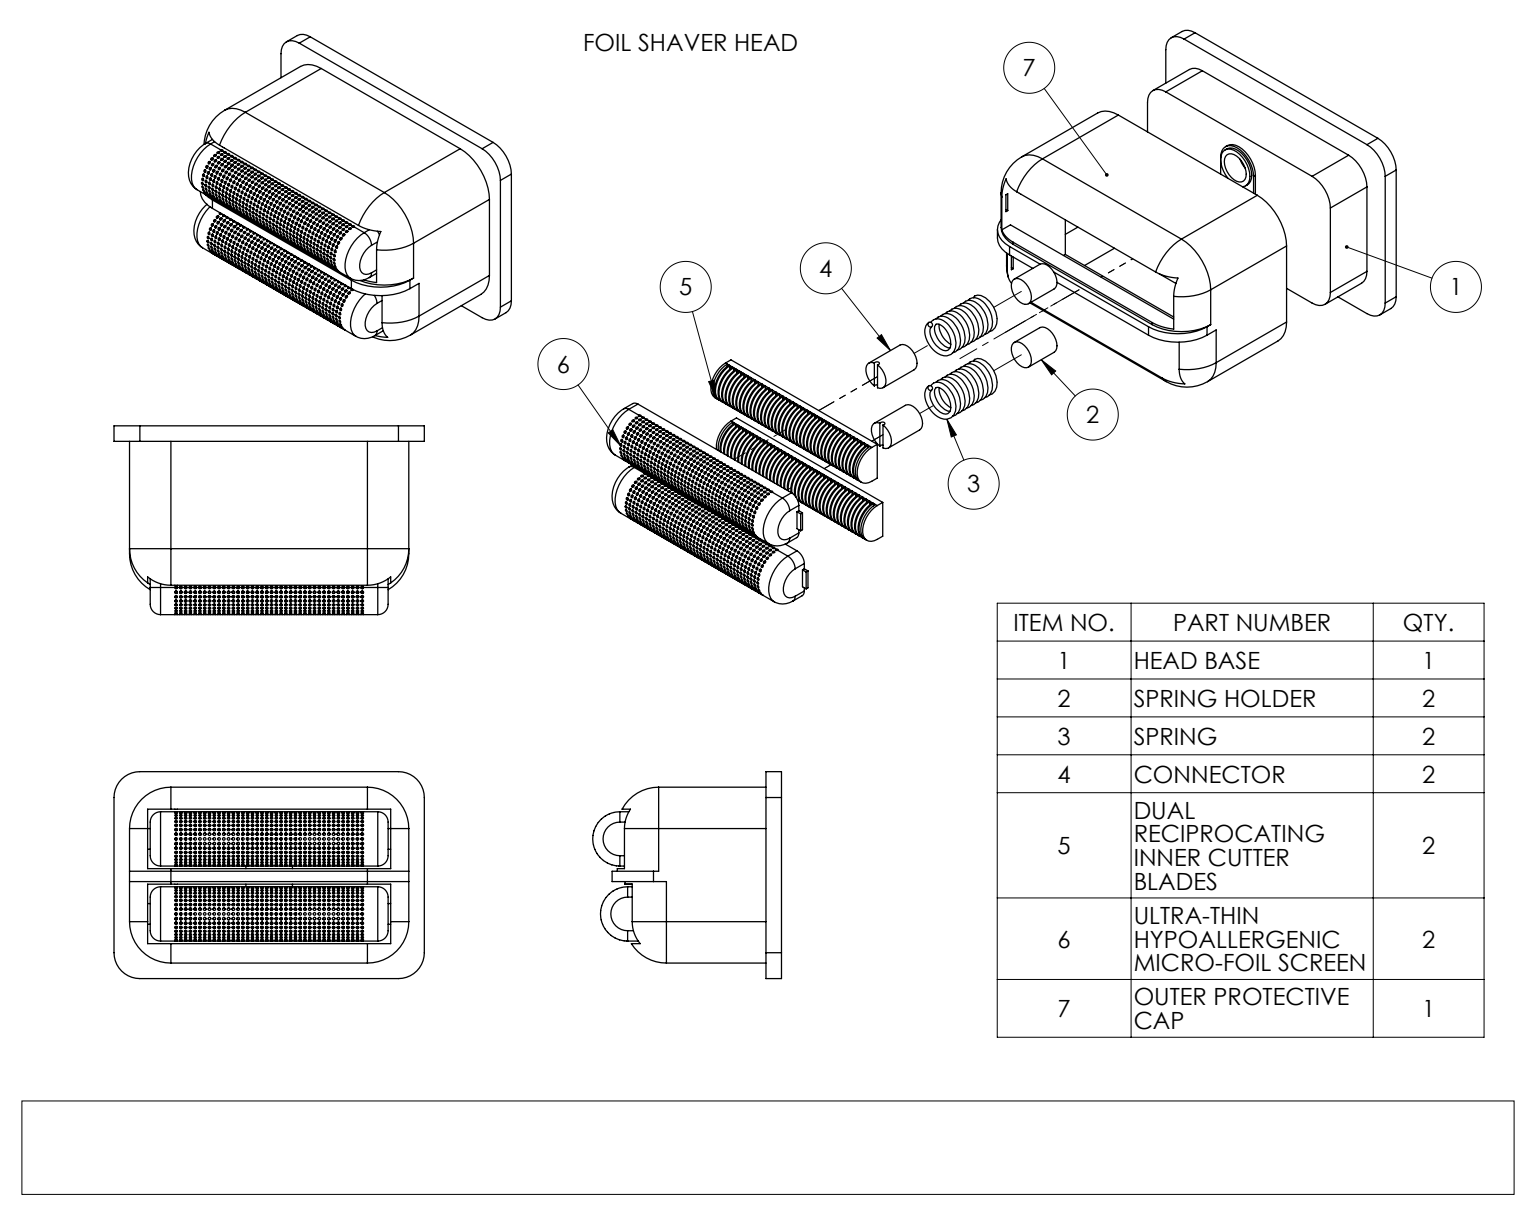
ISO-10303-21;
HEADER;
FILE_DESCRIPTION (('STEP AP214'),
    '1' );
FILE_NAME ('BR-833',
    '2026-10-05T05:16:24',
    ( '' ),
    ( '' ),
    'SwSTEP 2.0',
    'SolidWorks 2026',
    '' );
FILE_SCHEMA (( 'AUTOMOTIVE_DESIGN' ));
ENDSEC;

DATA;
#1 = ORIENTED_EDGE ( 'NONE', *, *, #60678, .F. ) ;
#3 = VERTEX_POINT ( 'NONE', #26210 ) ;
#2 = CARTESIAN_POINT ( 'NONE',  ( 7.173131342990376247, -12.65882529074907126, 30.72640787790839312 ) ) ;
#4 = CARTESIAN_POINT ( 'NONE',  ( -5.143005456283213483, -4.661471528628507777, 34.16647553114621871 ) ) ;
#5 = CARTESIAN_POINT ( 'NONE',  ( -13.13461538461396394, -7.500000000000154543, 35.00000000000007105 ) ) ;
#6 = CARTESIAN_POINT ( 'NONE',  ( 9.561616225640134914, -4.809359713505814149, 33.96456829005828837 ) ) ;
#7 = EDGE_LOOP ( 'NONE', ( #52254, #76310 ) ) ;
#8 = CARTESIAN_POINT ( 'NONE',  ( -3.230769230769352962, -3.643525952248796163, 33.31231777344771672 ) ) ;
#9 = MANIFOLD_SOLID_BREP ( 'Cavity1', #19917 ) ;
#10 = VERTEX_POINT ( 'NONE', #55017 ) ;
#11 = CARTESIAN_POINT ( 'NONE',  ( 8.096099255531889582, -12.68172785388650681, 30.59649109432439218 ) ) ;
#12 = ORIENTED_EDGE ( 'NONE', *, *, #66253, .T. ) ;
#13 = CARTESIAN_POINT ( 'NONE',  ( -14.17690186672535901, -11.93129842949671726, 32.56571108434900452 ) ) ;
#14 = ORIENTED_EDGE ( 'NONE', *, *, #40073, .T. ) ;
#15 = CARTESIAN_POINT ( 'NONE',  ( 1.634669696253701288, -6.567000820036038355, 34.66262288849541306 ) ) ;
#16 = AXIS2_PLACEMENT_3D ( 'NONE', #36065, #63514, #64832 ) ;
#17 = CARTESIAN_POINT ( 'NONE',  ( 12.46153846153846168, -2.292212530054420494, 30.41441678777542634 ) ) ;
#18 = FACE_BOUND ( 'NONE', #68088, .T. ) ;
#19 = CARTESIAN_POINT ( 'NONE',  ( -17.93480601821664777, -2.506253911140446711, 29.99999999999985434 ) ) ;
#20 = CARTESIAN_POINT ( 'NONE',  ( 16.08776377448601735, -3.322132147404559976, 32.92929555188719348 ) ) ;
#21 = CARTESIAN_POINT ( 'NONE',  ( 9.562159722575998444, -2.373036134822904319, 30.88089517874952250 ) ) ;
#22 = CARTESIAN_POINT ( 'NONE',  ( 10.36540787133602493, -10.06842814019191401, 34.32929386961144758 ) ) ;
#23 = CARTESIAN_POINT ( 'NONE',  ( -3.230769230769351186, -3.300289026999228881, 32.46337939537708905 ) ) ;
#24 = CARTESIAN_POINT ( 'NONE',  ( -8.096177070375302876, -9.356822207818506598, 34.66110646841856635 ) ) ;
#25 = DIRECTION ( 'NONE',  ( -0.000000000000000000, 1.000000000000000000, 3.491481338843133355E-15 ) ) ;
#26 = ORIENTED_EDGE ( 'NONE', *, *, #20674, .T. ) ;
#27 = ORIENTED_EDGE ( 'NONE', *, *, #74196, .T. ) ;
#29 = CYLINDRICAL_SURFACE ( 'NONE', #7462, 0.2499999999999994726 ) ;
#28 = CARTESIAN_POINT ( 'NONE',  ( -17.07692307692307665, -9.780366693483667717, 34.19971097300155094 ) ) ;
#30 = FACE_OUTER_BOUND ( 'NONE', #56324, .T. ) ;
#31 = CARTESIAN_POINT ( 'NONE',  ( 3.453548772037640990, -10.81320215134717344, 33.49497208177562868 ) ) ;
#32 = CARTESIAN_POINT ( 'NONE',  ( 9.019230769230707878, -7.565270000091922853, 34.99999999999999289 ) ) ;
#33 = CARTESIAN_POINT ( 'NONE',  ( 11.53846153846153832, -12.09954503811598769, 35.62045528018868623 ) ) ;
#34 = ORIENTED_EDGE ( 'NONE', *, *, #66033, .T. ) ;
#35 = CARTESIAN_POINT ( 'NONE',  ( 2.057669070399343436, -9.271318131107980420, 34.42618302367067429 ) ) ;
#36 = CARTESIAN_POINT ( 'NONE',  ( 3.453548772037639214, -11.41317474335729187, 32.86274602512330034 ) ) ;
#37 = CARTESIAN_POINT ( 'NONE',  ( -14.08491263871424160, -12.47679350104403007, 31.42216943046555855 ) ) ;
#38 = CARTESIAN_POINT ( 'NONE',  ( -7.053224892808619195, -6.809168938359898782, 34.95455904226513866 ) ) ;
#39 = VERTEX_POINT ( 'NONE', #74855 ) ;
#40 = EDGE_LOOP ( 'NONE', ( #88640, #57937, #33954, #2221 ) ) ;
#41 = VECTOR ( 'NONE', #83929, 1000.000000000000000 ) ;
#42 = VECTOR ( 'NONE', #62583, 1000.000000000000114 ) ;
#43 = ORIENTED_EDGE ( 'NONE', *, *, #10350, .F. ) ;
#44 = CARTESIAN_POINT ( 'NONE',  ( -4.153846153846274980, -8.656820664282941280, 34.87096338111179961 ) ) ;
#45 = VERTEX_POINT ( 'NONE', #81605 ) ;
#46 = DIRECTION ( 'NONE',  ( -0.000000000000000000, 1.000000000000000000, 3.491481338843133355E-15 ) ) ;
#47 = CARTESIAN_POINT ( 'NONE',  ( 15.45378207486262667, -4.026326845037962343, 33.68677907613344047 ) ) ;
#48 = CARTESIAN_POINT ( 'NONE',  ( 4.946775867484856093, -6.852621066184267029, 34.70813303252209181 ) ) ;
#49 = CARTESIAN_POINT ( 'NONE',  ( 1.553300858899129944, -11.24999999999998934, 14.70312500000000355 ) ) ;
#50 = CIRCLE ( 'NONE', #37444, 0.2500000000000002220 ) ;
#51 = CIRCLE ( 'NONE', #79120, 0.2500000000000002220 ) ;
#52 = DIRECTION ( 'NONE',  ( 0.000000000000000000, 0.9848077530122072432, 0.1736481776669354937 ) ) ;
#53 = VERTEX_POINT ( 'NONE', #13143 ) ;
#55 = CARTESIAN_POINT ( 'NONE',  ( -15.23076923076922995, -2.486705287966279876, 31.30864560766543647 ) ) ;
#54 = PRESENTATION_LAYER_ASSIGNMENT (  '', '', ( #59002 ) ) ;
#57 = VERTEX_POINT ( 'NONE', #40625 ) ;
#56 = CARTESIAN_POINT ( 'NONE',  ( -0.5276208408985970655, -5.471508081941601986, 34.59228464037088457 ) ) ;
#58 = CARTESIAN_POINT ( 'NONE',  ( -6.923076923076922462, -2.499999999999998668, 29.50000000000001066 ) ) ;
#59 = CYLINDRICAL_SURFACE ( 'NONE', #2416, 0.2500000000000002220 ) ;
#60 = CARTESIAN_POINT ( 'NONE',  ( -13.60754160213153163, -4.887634598454295265, 34.01352882383564946 ) ) ;
#61 = CARTESIAN_POINT ( 'NONE',  ( 11.53846153846153832, -9.905515769479276145, 34.41647553114623292 ) ) ;
#62 = CARTESIAN_POINT ( 'NONE',  ( 2.438482748659261290, -2.494656445102013453, 31.33466734024120015 ) ) ;
#63 = CARTESIAN_POINT ( 'NONE',  ( -10.28846153846153832, -7.500000000000000000, 29.75000000000000355 ) ) ;
#64 = CARTESIAN_POINT ( 'NONE',  ( -3.454254174493178287, -6.760086850603068243, 34.69517049084099369 ) ) ;
#65 = CARTESIAN_POINT ( 'NONE',  ( 1.200186371490529202, -4.775308065498752974, 18.23624329374151642 ) ) ;
#66 = ORIENTED_EDGE ( 'NONE', *, *, #42296, .F. ) ;
#67 = CARTESIAN_POINT ( 'NONE',  ( 15.00784301325308157, -8.239355502252617924, 34.69524867566427417 ) ) ;
#68 = CARTESIAN_POINT ( 'NONE',  ( -14.17716686945866122, -3.625058011473228703, 33.29252011169590020 ) ) ;
#69 = EDGE_CURVE ( 'NONE', #39109, #41438, #13798, .T. ) ;
#70 = CARTESIAN_POINT ( 'NONE',  ( 9.692307692307695177, -10.67929555188718282, 33.92786785259544047 ) ) ;
#71 = ORIENTED_EDGE ( 'NONE', *, *, #84593, .F. ) ;
#72 = ORIENTED_EDGE ( 'NONE', *, *, #88944, .T. ) ;
#73 = CARTESIAN_POINT ( 'NONE',  ( 20.74999999999998224, -2.499999999999999556, 27.25000000000000000 ) ) ;
#74 = CARTESIAN_POINT ( 'NONE',  ( -3.100243529005668019, -6.001044277235011215, 34.52024696741798948 ) ) ;
#75 = CARTESIAN_POINT ( 'NONE',  ( -16.15384615384627409, -3.835265460704628815, 33.15142922262033665 ) ) ;
#76 = CARTESIAN_POINT ( 'NONE',  ( 8.769230769230768274, -1.466349020453238561, 30.81389545987213907 ) ) ;
#77 = CARTESIAN_POINT ( 'NONE',  ( 17.86985203026830504, -2.647304123082329763, 31.75400227202886683 ) ) ;
#78 = ORIENTED_EDGE ( 'NONE', *, *, #41184, .T. ) ;
#79 = DIRECTION ( 'NONE',  ( 0.000000000000000000, 0.000000000000000000, 1.000000000000000000 ) ) ;
#80 = EDGE_CURVE ( 'NONE', #19996, #25471, #12251, .T. ) ;
#81 = CARTESIAN_POINT ( 'NONE',  ( -14.53117725141625094, -2.847400154188067578, 31.58180166144859058 ) ) ;
#82 = LINE ( 'NONE', #529, #19231 ) ;
#84 = ORIENTED_EDGE ( 'NONE', *, *, #75949, .F. ) ;
#83 = AXIS2_PLACEMENT_3D ( 'NONE', #55221, #39954, #48454 ) ;
#85 = CARTESIAN_POINT ( 'NONE',  ( -6.416666666666667851, -7.500000000000000000, 33.75000000000000000 ) ) ;
#86 = EDGE_LOOP ( 'NONE', ( #15345, #5769, #84477, #70207 ) ) ;
#87 = CARTESIAN_POINT ( 'NONE',  ( -16.28453762051371712, -5.582088688514999397, 34.36776431015576350 ) ) ;
#88 = CYLINDRICAL_SURFACE ( 'NONE', #13871, 0.2499999999999997502 ) ;
#89 = ORIENTED_EDGE ( 'NONE', *, *, #31781, .F. ) ;
#90 = B_SPLINE_CURVE_WITH_KNOTS ( 'NONE', 3,
 ( #88183, #40422, #6186, #26896, #54800, #20574, #33653, #54355, #75089, #55682 ),
 .UNSPECIFIED., .F., .F.,
 ( 4, 2, 2, 2, 4 ),
 ( 0.000000000000000000, 0.0001954311564186868202, 0.0003908623128373736404, 0.0005862934692560604335, 0.0007817246256747472808 ),
 .UNSPECIFIED. ) ;
#91 = CARTESIAN_POINT ( 'NONE',  ( 10.74591005361826035, -11.66157788607254098, 32.95092075102925833 ) ) ;
#92 = CYLINDRICAL_SURFACE ( 'NONE', #79519, 0.2499999999999986955 ) ;
#93 = CARTESIAN_POINT ( 'NONE',  ( 1.319344938654610333, -4.481592998940161721, 33.73612834413957984 ) ) ;
#94 = CARTESIAN_POINT ( 'NONE',  ( -8.096177070375304652, -4.931416488878822335, 34.32920672191015399 ) ) ;
#95 = DIRECTION ( 'NONE',  ( -0.000000000000000000, -0.7660444431189791237, -0.6427876096865379196 ) ) ;
#96 = EDGE_CURVE ( 'NONE', #40194, #70315, #60434, .T. ) ;
#97 = ORIENTED_EDGE ( 'NONE', *, *, #11144, .F. ) ;
#98 = AXIS2_PLACEMENT_3D ( 'NONE', #21974, #77793, #7575 ) ;
#99 = FACE_BOUND ( 'NONE', #31817, .T. ) ;
#100 = ORIENTED_EDGE ( 'NONE', *, *, #35787, .T. ) ;
#102 = VECTOR ( 'NONE', #77496, 999.9999999999998863 ) ;
#101 = CYLINDRICAL_SURFACE ( 'NONE', #51513, 0.2499999999999973355 ) ;
#103 = EDGE_CURVE ( 'NONE', #84442, #3259, #72212, .T. ) ;
#104 = VECTOR ( 'NONE', #2101, 1000.000000000000000 ) ;
#105 = EDGE_CURVE ( 'NONE', #4412, #9551, #46022, .T. ) ;
#106 = CARTESIAN_POINT ( 'NONE',  ( 4.853996859406928266, -11.76352882383564769, 32.36236540154569497 ) ) ;
#107 = CARTESIAN_POINT ( 'NONE',  ( 5.999999999999878320, -5.941354392335915335, 34.76329471203413846 ) ) ;
#108 = CARTESIAN_POINT ( 'NONE',  ( 7.145856464345329506, -10.11255958852956027, 34.01340905677048454 ) ) ;
#109 = VECTOR ( 'NONE', #52522, 1000.000000000000227 ) ;
#110 = EDGE_LOOP ( 'NONE', ( #30011, #23876 ) ) ;
#111 = EDGE_LOOP ( 'NONE', ( #30455, #63884, #82521, #35885, #30536 ) ) ;
#112 = EDGE_LOOP ( 'NONE', ( #70272, #77319 ) ) ;
#113 = FACE_OUTER_BOUND ( 'NONE', #58827, .T. ) ;
#114 = ORIENTED_EDGE ( 'NONE', *, *, #66071, .T. ) ;
#115 = CARTESIAN_POINT ( 'NONE',  ( 4.219913487196229163, -9.905515769479277921, 34.41647553114623292 ) ) ;
#116 = B_SPLINE_CURVE_WITH_KNOTS ( 'NONE', 3,
 ( #3209, #77983, #15855, #1446, #43753, #43319, #9097, #77545, #29810, #58146 ),
 .UNSPECIFIED., .F., .F.,
 ( 4, 2, 2, 2, 4 ),
 ( 0.000000000000000000, 0.0001954311564186862239, 0.0003908623128373724478, 0.0005862934692560586988, 0.0007817246256747448956 ),
 .UNSPECIFIED. ) ;
#117 = CARTESIAN_POINT ( 'NONE',  ( -11.76138849736838488, -5.582147617184174848, 34.63737895849758530 ) ) ;
#118 = DIRECTION ( 'NONE',  ( 0.000000000000000000, 0.8660254037844377084, 0.5000000000000015543 ) ) ;
#119 = B_SPLINE_CURVE_WITH_KNOTS ( 'NONE', 3,
 ( #65439, #64982, #64535, #3731, #23563, #51451, #79408, #16806, #85720, #17710 ),
 .UNSPECIFIED., .F., .F.,
 ( 4, 2, 2, 2, 4 ),
 ( 0.000000000000000000, 0.0001954311564186878773, 0.0003908623128373757546, 0.0005862934692560635777, 0.0007817246256747515092 ),
 .UNSPECIFIED. ) ;
#120 = CARTESIAN_POINT ( 'NONE',  ( 3.361294669002876656, -9.503571793651733657, 34.60286762892837942 ) ) ;
#121 = CARTESIAN_POINT ( 'NONE',  ( 2.651650429449539104, -4.848349570550432475, 24.31250000000000000 ) ) ;
#122 = CARTESIAN_POINT ( 'NONE',  ( 5.207448778686637247, -11.46989282347013095, 32.79007818306219946 ) ) ;
#123 = FACE_OUTER_BOUND ( 'NONE', #61461, .T. ) ;
#124 = CARTESIAN_POINT ( 'NONE',  ( 17.29970261819148902, -2.600157965045223563, 30.74683119005207033 ) ) ;
#125 = ORIENTED_EDGE ( 'NONE', *, *, #59924, .F. ) ;
#126 = VERTEX_POINT ( 'NONE', #50456 ) ;
#127 = ORIENTED_EDGE ( 'NONE', *, *, #9186, .F. ) ;
#128 = CARTESIAN_POINT ( 'NONE',  ( -11.76194648218548622, -12.44517049084099725, 30.48991314939691932 ) ) ;
#130 = DIRECTION ( 'NONE',  ( -0.000000000000000000, 1.000000000000000000, -0.000000000000000000 ) ) ;
#129 = DIRECTION ( 'NONE',  ( -0.000000000000000000, -0.1736481776669307198, -0.9848077530122080203 ) ) ;
#131 = VECTOR ( 'NONE', #1295, 1000.000000000000000 ) ;
#132 = CARTESIAN_POINT ( 'NONE',  ( -9.692307692307691624, -13.75783147151868846, 33.36296068462461051 ) ) ;
#133 = FACE_OUTER_BOUND ( 'NONE', #80352, .T. ) ;
#134 = FACE_BOUND ( 'NONE', #49727, .T. ) ;
#135 = CARTESIAN_POINT ( 'NONE',  ( 7.976679547917409963, -11.46989282347013095, 32.79007818306219946 ) ) ;
#136 = ORIENTED_EDGE ( 'NONE', *, *, #30561, .F. ) ;
#137 = LINE ( 'NONE', #38123, #5695 ) ;
#138 = LINE ( 'NONE', #88449, #37538 ) ;
#139 = CARTESIAN_POINT ( 'NONE',  ( -1.515305987725692694, -3.338472653186242756, 32.95098750199972670 ) ) ;
#140 = CIRCLE ( 'NONE', #14540, 4.000000000000000000 ) ;
#141 = EDGE_LOOP ( 'NONE', ( #49067, #42517 ) ) ;
#142 = DIRECTION ( 'NONE',  ( -1.000000000000000000, 0.000000000000000000, 0.000000000000000000 ) ) ;
#143 = ORIENTED_EDGE ( 'NONE', *, *, #6318, .F. ) ;
#144 = FACE_BOUND ( 'NONE', #88806, .T. ) ;
#145 = CARTESIAN_POINT ( 'NONE',  ( -17.14219307747939425, -4.320704448112772766, 33.92786785259540494 ) ) ;
#146 = CARTESIAN_POINT ( 'NONE',  ( -6.249999999999997335, -7.433931650972300353, 34.75000000000000711 ) ) ;
#147 = CARTESIAN_POINT ( 'NONE',  ( -12.46153846153846168, -11.91647553114624181, 32.58852847137148245 ) ) ;
#148 = VERTEX_POINT ( 'NONE', #49138 ) ;
#149 = CARTESIAN_POINT ( 'NONE',  ( -1.384615384615383471, -12.29105614889573062, 35.45975837776705220 ) ) ;
#150 = CARTESIAN_POINT ( 'NONE',  ( 4.153846153846154188, -1.367168528481310208, 33.57946703557072254 ) ) ;
#151 = DIRECTION ( 'NONE',  ( -0.000000000000000000, -0.7660444431189791237, -0.6427876096865379196 ) ) ;
#152 = CYLINDRICAL_SURFACE ( 'NONE', #86329, 0.2499999999999979738 ) ;
#153 = ORIENTED_EDGE ( 'NONE', *, *, #56606, .F. ) ;
#154 = ADVANCED_FACE ( 'NONE', ( #8609 ), #21669, .F. ) ;
#155 = CARTESIAN_POINT ( 'NONE',  ( 17.99999999999987566, -5.219633306517616589, 34.19971097300220464 ) ) ;
#156 = CARTESIAN_POINT ( 'NONE',  ( 0.000000000000000000, -4.000000000000000000, 29.65000000000000213 ) ) ;
#158 = EDGE_LOOP ( 'NONE', ( #23871, #73123 ) ) ;
#157 = CYLINDRICAL_SURFACE ( 'NONE', #25456, 0.2499999999999997502 ) ;
#159 = DIRECTION ( 'NONE',  ( -0.000000000000000000, -0.000000000000000000, -1.000000000000000000 ) ) ;
#160 = CARTESIAN_POINT ( 'NONE',  ( 0.7114838709165050012, -10.92531984108285670, 33.72920026020278073 ) ) ;
#161 = CARTESIAN_POINT ( 'NONE',  ( -4.946397375159514276, -8.586989748646452369, 34.63063291749215011 ) ) ;
#162 = CARTESIAN_POINT ( 'NONE',  ( -13.16183584334697265, -3.755027918224367323, 33.06320215134714857 ) ) ;
#163 = LINE ( 'NONE', #28079, #50987 ) ;
#165 = CARTESIAN_POINT ( 'NONE',  ( 6.923076923076802558, -6.026961402154118908, 34.52809138561165270 ) ) ;
#164 = CARTESIAN_POINT ( 'NONE',  ( 9.019230769230768274, -2.249999999999998668, 29.75000000000000355 ) ) ;
#166 = B_SPLINE_CURVE_WITH_KNOTS ( 'NONE', 3,
 ( #17891, #45348, #37256, #46689, #46249, #54325, #5263, #80940, #74167, #26867 ),
 .UNSPECIFIED., .F., .F.,
 ( 4, 2, 2, 2, 4 ),
 ( 0.0007817359430256306564, 0.0009771253907249969738, 0.001172514838424363291, 0.001367904286123729826, 0.001563293733823096143 ),
 .UNSPECIFIED. ) ;
#167 = CARTESIAN_POINT ( 'NONE',  ( 7.976945653978636308, -4.118422570099831148, 33.43335022499816489 ) ) ;
#168 = CARTESIAN_POINT ( 'NONE',  ( -2.749999999999998224, -7.500000000000015987, 20.09375000000000000 ) ) ;
#169 = ORIENTED_EDGE ( 'NONE', *, *, #57936, .F. ) ;
#170 = B_SPLINE_CURVE_WITH_KNOTS ( 'NONE', 3,
 ( #23736, #63848, #16993, #84585, #2145, #85454, #30936, #70611, #58864, #78697 ),
 .UNSPECIFIED., .F., .F.,
 ( 4, 2, 2, 2, 4 ),
 ( 0.000000000000000000, 0.0001954339857564080165, 0.0003908679715128160329, 0.0005863019572692240765, 0.0007817359430256320659 ),
 .UNSPECIFIED. ) ;
#171 = CARTESIAN_POINT ( 'NONE',  ( -17.86947429823644029, -9.417988943895561960, 34.36773134775778260 ) ) ;
#172 = ORIENTED_EDGE ( 'NONE', *, *, #13053, .F. ) ;
#173 = AXIS2_PLACEMENT_3D ( 'NONE', #50512, #36570, #71672 ) ;
#174 = EDGE_CURVE ( 'NONE', #81993, #52360, #48073, .T. ) ;
#175 = ORIENTED_EDGE ( 'NONE', *, *, #79367, .F. ) ;
#176 = DIRECTION ( 'NONE',  ( -1.000000000000000000, 1.799314243699348838E-16, 0.000000000000000000 ) ) ;
#177 = VERTEX_POINT ( 'NONE', #56344 ) ;
#178 = CARTESIAN_POINT ( 'NONE',  ( -5.326946301144536378, -11.56360843649121861, 33.07473185843129926 ) ) ;
#179 = CARTESIAN_POINT ( 'NONE',  ( 2.750000000000001776, -7.499999999999984013, 18.21875000000000000 ) ) ;
#180 = CARTESIAN_POINT ( 'NONE',  ( 14.37376065869474751, -11.16473453929635440, 33.15142922261926373 ) ) ;
#181 = ADVANCED_FACE ( 'NONE', ( #62640 ), #1839, .F. ) ;
#182 = CARTESIAN_POINT ( 'NONE',  ( 16.15384615384603251, -12.46129190930018460, 30.37095296980731973 ) ) ;
#183 = CYLINDRICAL_SURFACE ( 'NONE', #47613, 0.2499999999999986955 ) ;
#184 = AXIS2_PLACEMENT_3D ( 'NONE', #19967, #48769, #88028 ) ;
#185 = DIRECTION ( 'NONE',  ( -0.000000000000000000, 0.1736481776669307198, -0.9848077530122080203 ) ) ;
#186 = CARTESIAN_POINT ( 'NONE',  ( -1.384615384615383471, -4.098570777380720287, 33.41473453929634729 ) ) ;
#187 = DIRECTION ( 'NONE',  ( -1.000000000000000000, -0.000000000000000000, -0.000000000000000000 ) ) ;
#188 = CARTESIAN_POINT ( 'NONE',  ( -2.651650429449565305, -4.848349570550461785, 26.50000000000000355 ) ) ;
#189 = CARTESIAN_POINT ( 'NONE',  ( 10.55011416942384272, -2.625532179533445198, 30.86335684631481513 ) ) ;
#190 = CARTESIAN_POINT ( 'NONE',  ( -16.94613263595612906, -10.70102852606553157, 33.91149625220312913 ) ) ;
#191 = EDGE_CURVE ( 'NONE', #15565, #57014, #22554, .T. ) ;
#192 = FACE_OUTER_BOUND ( 'NONE', #7478, .T. ) ;
#193 = CARTESIAN_POINT ( 'NONE',  ( 11.53846153846141753, -5.219633306517616589, 34.19971097300220464 ) ) ;
#194 = EDGE_CURVE ( 'NONE', #29769, #50046, #28803, .T. ) ;
#195 = ORIENTED_EDGE ( 'NONE', *, *, #5496, .T. ) ;
#196 = ORIENTED_EDGE ( 'NONE', *, *, #14784, .T. ) ;
#197 = CARTESIAN_POINT ( 'NONE',  ( -7.173076923076921574, -2.249999999999998668, 29.75000000000000355 ) ) ;
#198 = CARTESIAN_POINT ( 'NONE',  ( 1.515140822849032176, -3.625058011473228259, 33.29252011169590020 ) ) ;
#199 = CARTESIAN_POINT ( 'NONE',  ( -6.792286482109973988, -11.93129842949671726, 32.56571108434900452 ) ) ;
#200 = CARTESIAN_POINT ( 'NONE',  ( 0.3954560821783253965, -9.905515769479277921, 34.41647553114623292 ) ) ;
#201 = EDGE_CURVE ( 'NONE', #75095, #37056, #56777, .T. ) ;
#202 = CARTESIAN_POINT ( 'NONE',  ( 9.823098133274644539, -11.37503395064541678, 33.29242100308974273 ) ) ;
#203 = FACE_OUTER_BOUND ( 'NONE', #61905, .T. ) ;
#204 = AXIS2_PLACEMENT_3D ( 'NONE', #81774, #26380, #5659 ) ;
#205 = CARTESIAN_POINT ( 'NONE',  ( -12.46153846153858247, -10.90142922262034020, 33.41473453929536674 ) ) ;
#206 = B_SPLINE_CURVE_WITH_KNOTS ( 'NONE', 3,
 ( #5381, #32848, #40069, #18451, #4487, #53554, #45461, #67081, #59870, #45907 ),
 .UNSPECIFIED., .F., .F.,
 ( 4, 2, 2, 2, 4 ),
 ( 0.000000000000000000, 0.0001954311564186865763, 0.0003908623128373731525, 0.0005862934692560596746, 0.0007817246256747463051 ),
 .UNSPECIFIED. ) ;
#207 = EDGE_CURVE ( 'NONE', #60261, #51867, #35183, .T. ) ;
#208 = ORIENTED_EDGE ( 'NONE', *, *, #85819, .F. ) ;
#209 = FACE_OUTER_BOUND ( 'NONE', #38454, .T. ) ;
#210 = EDGE_CURVE ( 'NONE', #70883, #82406, #15810, .T. ) ;
#211 = ORIENTED_EDGE ( 'NONE', *, *, #69069, .F. ) ;
#212 = CARTESIAN_POINT ( 'NONE',  ( 16.15384615384603251, -9.528491918059723176, 34.59228464037033035 ) ) ;
#213 = CARTESIAN_POINT ( 'NONE',  ( 8.769230769230645706, -9.528491918059723176, 34.59228464037033035 ) ) ;
#214 = EDGE_CURVE ( 'NONE', #41163, #3816, #38532, .T. ) ;
#215 = CARTESIAN_POINT ( 'NONE',  ( 14.05771557674995442, -4.943428324936578910, 34.04746400365624481 ) ) ;
#216 = EDGE_CURVE ( 'NONE', #29227, #38893, #56032, .T. ) ;
#217 = CARTESIAN_POINT ( 'NONE',  ( 16.15384615384615330, -13.63283147151868846, 33.57946703557072254 ) ) ;
#218 = CYLINDRICAL_SURFACE ( 'NONE', #17781, 4.999999999999997335 ) ;
#219 = VERTEX_POINT ( 'NONE', #73411 ) ;
#220 = ORIENTED_EDGE ( 'NONE', *, *, #40538, .F. ) ;
#221 = VERTEX_POINT ( 'NONE', #52233 ) ;
#222 = ORIENTED_EDGE ( 'NONE', *, *, #80830, .F. ) ;
#223 = CARTESIAN_POINT ( 'NONE',  ( -10.68065461594093257, -12.51329471203370325, 31.30864560766548976 ) ) ;
#224 = CARTESIAN_POINT ( 'NONE',  ( 7.596130608860882205, -3.711651800289232916, 33.01384336483936011 ) ) ;
#225 = CARTESIAN_POINT ( 'NONE',  ( 4.153846153846030731, -12.16647553114689728, 32.15551576947799362 ) ) ;
#226 = AXIS2_PLACEMENT_3D ( 'NONE', #60512, #52858, #32161 ) ;
#227 = DIRECTION ( 'NONE',  ( 1.000000000000000000, 0.000000000000000000, 0.000000000000000000 ) ) ;
#228 = CARTESIAN_POINT ( 'NONE',  ( -7.846153846153844924, -4.786620604624113540, 33.94971097300155094 ) ) ;
#229 = CARTESIAN_POINT ( 'NONE',  ( -15.23076923076922995, -2.486705287966279876, 31.30864560766543647 ) ) ;
#230 = ORIENTED_EDGE ( 'NONE', *, *, #73529, .T. ) ;
#231 = ORIENTED_EDGE ( 'NONE', *, *, #20585, .T. ) ;
#232 = AXIS2_PLACEMENT_3D ( 'NONE', #57713, #64451, #65352 ) ;
#233 = ORIENTED_EDGE ( 'NONE', *, *, #46432, .F. ) ;
#235 = VERTEX_POINT ( 'NONE', #52679 ) ;
#234 = CARTESIAN_POINT ( 'NONE',  ( 8.769230769230647482, -9.442884908241554243, 34.35708131394783038 ) ) ;
#236 = CARTESIAN_POINT ( 'NONE',  ( 17.29970274590113632, -10.97394488606063589, 33.68653795673696294 ) ) ;
#237 = CARTESIAN_POINT ( 'NONE',  ( -5.010854725920638408, -11.16473453929635440, 33.15142922261926373 ) ) ;
#238 = EDGE_CURVE ( 'NONE', #50121, #11896, #56698, .T. ) ;
#239 = CARTESIAN_POINT ( 'NONE',  ( -2.651650429449535551, -10.15165042944956753, 18.68750000000000000 ) ) ;
#240 = ORIENTED_EDGE ( 'NONE', *, *, #48332, .T. ) ;
#241 = EDGE_CURVE ( 'NONE', #37535, #9541, #20178, .T. ) ;
#242 = ORIENTED_EDGE ( 'NONE', *, *, #19023, .F. ) ;
#243 = ADVANCED_FACE ( 'NONE', ( #11714 ), #66194, .F. ) ;
#244 = CARTESIAN_POINT ( 'NONE',  ( 7.846153846153846700, -12.10708131394839349, 31.69288490824020244 ) ) ;
#245 = FACE_BOUND ( 'NONE', #29215, .T. ) ;
#246 = CARTESIAN_POINT ( 'NONE',  ( 5.076923076922953193, -5.094484230521993062, 34.41647553114689373 ) ) ;
#247 = EDGE_CURVE ( 'NONE', #52855, #6141, #63243, .T. ) ;
#248 = CARTESIAN_POINT ( 'NONE',  ( -4.376773112753002515, -10.01117774369187252, 34.36070679894347535 ) ) ;
#249 = ORIENTED_EDGE ( 'NONE', *, *, #43935, .F. ) ;
#250 = CARTESIAN_POINT ( 'NONE',  ( 8.769230769230768274, -11.91647553114624181, 32.58852847137148245 ) ) ;
#251 = CARTESIAN_POINT ( 'NONE',  ( 6.923076923076800782, -12.16647553114689728, 32.15551576947799362 ) ) ;
#252 = CARTESIAN_POINT ( 'NONE',  ( 16.37685750545900376, -2.554770724473668597, 30.48948780036025852 ) ) ;
#253 = CARTESIAN_POINT ( 'NONE',  ( 1.384615384615386802, -10.51840700105979565, 33.73612834413961536 ) ) ;
#254 = ORIENTED_EDGE ( 'NONE', *, *, #43401, .T. ) ;
#255 = EDGE_CURVE ( 'NONE', #87291, #13888, #15871, .T. ) ;
#256 = VECTOR ( 'NONE', #26612, 1000.000000000000227 ) ;
#257 = CARTESIAN_POINT ( 'NONE',  ( -0.5268613770306369570, -7.749976743299138882, 34.99404534957040624 ) ) ;
#258 = CARTESIAN_POINT ( 'NONE',  ( 1.634560902963528184, -8.433404298154336232, 34.66254593164985920 ) ) ;
#259 = CARTESIAN_POINT ( 'NONE',  ( -12.68446467905460473, -12.15238873228292071, 31.58232369045353849 ) ) ;
#260 = CARTESIAN_POINT ( 'NONE',  ( -2.557715544985271094, -10.76384336483936011, 33.53834819971076087 ) ) ;
#261 = LINE ( 'NONE', #27723, #60185 ) ;
#262 = FACE_BOUND ( 'NONE', #7058, .T. ) ;
#264 = CARTESIAN_POINT ( 'NONE',  ( 16.82694633287448838, -2.920706130388546651, 32.31842814019191223 ) ) ;
#263 = CARTESIAN_POINT ( 'NONE',  ( 17.07692307692295586, -3.835265460704628815, 33.15142922262033665 ) ) ;
#265 = CARTESIAN_POINT ( 'NONE',  ( 5.326868486301119532, -9.357781135181031829, 34.66075350412533851 ) ) ;
#267 = CARTESIAN_POINT ( 'NONE',  ( -11.47239420511146513, -10.67929555188718282, 33.92786785259544757 ) ) ;
#266 = DIRECTION ( 'NONE',  ( 0.000000000000000000, 0.9848077530122072432, 0.1736481776669354937 ) ) ;
#268 = AXIS2_PLACEMENT_3D ( 'NONE', #2934, #72732, #79505 ) ;
#269 = CARTESIAN_POINT ( 'NONE',  ( -10.86540783960607115, -6.652501968072648708, 34.93155406624980941 ) ) ;
#270 = CARTESIAN_POINT ( 'NONE',  ( -1.987747218494660295, -5.598659921968651254, 17.49813170625848713 ) ) ;
#271 = ORIENTED_EDGE ( 'NONE', *, *, #6399, .T. ) ;
#272 = DIRECTION ( 'NONE',  ( -0.000000000000000000, -0.7660444431189791237, -0.6427876096865379196 ) ) ;
#273 = VERTEX_POINT ( 'NONE', #30632 ) ;
#274 = CARTESIAN_POINT ( 'NONE',  ( 0.5915836243732391919, -2.504778602574659896, 29.97347330155780298 ) ) ;
#275 = VERTEX_POINT ( 'NONE', #24313 ) ;
#276 = CARTESIAN_POINT ( 'NONE',  ( -11.28840722682322451, -2.779044189368095275, 31.39831045268885745 ) ) ;
#277 = CARTESIAN_POINT ( 'NONE',  ( -7.846153846153844924, -9.780366693483667717, 34.19971097300155094 ) ) ;
#279 = EDGE_LOOP ( 'NONE', ( #7724, #29052, #33264, #45854 ) ) ;
#278 = CARTESIAN_POINT ( 'NONE',  ( 5.999999999999878320, -8.656820664282941280, 34.87096338111179961 ) ) ;
#280 = CARTESIAN_POINT ( 'NONE',  ( 5.299935921016470708, -11.98016756924215009, 32.48728574198911190 ) ) ;
#281 = CARTESIAN_POINT ( 'NONE',  ( 1.200186371490561621, -10.22469193450123193, 19.45125670625849068 ) ) ;
#282 = EDGE_CURVE ( 'NONE', #18719, #16151, #10625, .T. ) ;
#283 = CARTESIAN_POINT ( 'NONE',  ( 3.903822916553188804, -9.271318131107980420, 34.42618302367067429 ) ) ;
#284 = CARTESIAN_POINT ( 'NONE',  ( -19.50000000000000000, -3.499999999999999556, 29.75000000000000355 ) ) ;
#285 = CARTESIAN_POINT ( 'NONE',  ( 12.21156173059611127, -2.779195860258146578, 31.39871582349836032 ) ) ;
#286 = CARTESIAN_POINT ( 'NONE',  ( 20.00000000000000000, -4.000000000000000000, 29.75000000000000355 ) ) ;
#287 = CARTESIAN_POINT ( 'NONE',  ( -0.2114841499001467451, -4.235687564193446164, 33.53795663066793509 ) ) ;
#288 = CARTESIAN_POINT ( 'NONE',  ( 11.60452988946397745, -3.513871655860379306, 32.76840700105978499 ) ) ;
#289 = CARTESIAN_POINT ( 'NONE',  ( 1.492201783934598236, -11.27530806549875031, 21.20499329374151998 ) ) ;
#290 = DIRECTION ( 'NONE',  ( 0.000000000000000000, 0.9396926207859126468, 0.3420201433256571111 ) ) ;
#291 = CARTESIAN_POINT ( 'NONE',  ( -1.384615384615383471, -12.78798330534102945, 29.74999999999997868 ) ) ;
#292 = VERTEX_POINT ( 'NONE', #79277 ) ;
#293 = DIRECTION ( 'NONE',  ( 0.000000000000000000, 0.000000000000000000, -1.000000000000000000 ) ) ;
#294 = CARTESIAN_POINT ( 'NONE',  ( 2.608446859217924629, -10.19485399968118422, 24.87686829374151642 ) ) ;
#295 = AXIS2_PLACEMENT_3D ( 'NONE', #58758, #37145, #86253 ) ;
#296 = LINE ( 'NONE', #12484, #72000 ) ;
#297 = CARTESIAN_POINT ( 'NONE',  ( -8.769230769230892619, -3.643525952248795718, 33.31231777344771672 ) ) ;
#298 = VECTOR ( 'NONE', #58906, 1000.000000000000000 ) ;
#299 = ORIENTED_EDGE ( 'NONE', *, *, #31219, .F. ) ;
#300 = CARTESIAN_POINT ( 'NONE',  ( 17.07692307692307665, -12.78798330534102767, 29.49999999999997868 ) ) ;
#301 = CARTESIAN_POINT ( 'NONE',  ( 16.15384615384603251, -2.657715359629662544, 31.77849191805970364 ) ) ;
#303 = ORIENTED_EDGE ( 'NONE', *, *, #59543, .T. ) ;
#302 = CARTESIAN_POINT ( 'NONE',  ( 4.023698184114458343, -9.504002272028875709, 34.60269587691767867 ) ) ;
#304 = CYLINDRICAL_SURFACE ( 'NONE', #8160, 0.2500000000000009437 ) ;
#305 = CARTESIAN_POINT ( 'NONE',  ( -11.53846153846153655, -2.517432740324522911, 35.29906147534542527 ) ) ;
#306 = VECTOR ( 'NONE', #74624, 1000.000000000000000 ) ;
#307 = MANIFOLD_SOLID_BREP ( 'Mirror3', #61571 ) ;
#308 = CARTESIAN_POINT ( 'NONE',  ( 7.053867364043872712, -11.93129842949671726, 32.56571108434900452 ) ) ;
#309 = CARTESIAN_POINT ( 'NONE',  ( -11.53846153846153655, -9.905515769479276145, 34.41647553114623292 ) ) ;
#310 = CARTESIAN_POINT ( 'NONE',  ( -13.38461538461550582, -11.94971097300221174, 32.03036669348237098 ) ) ;
#311 = ADVANCED_FACE ( 'NONE', ( #54905 ), #17579, .F. ) ;
#312 = EDGE_CURVE ( 'NONE', #18504, #32170, #73011, .T. ) ;
#313 = VERTEX_POINT ( 'NONE', #40952 ) ;
#314 = VERTEX_POINT ( 'NONE', #12156 ) ;
#315 = EDGE_CURVE ( 'NONE', #65909, #14846, #33750, .T. ) ;
#316 = ORIENTED_EDGE ( 'NONE', *, *, #59548, .F. ) ;
#317 = CARTESIAN_POINT ( 'NONE',  ( -16.40382289789474513, -3.436278759898155677, 33.07459398097509506 ) ) ;
#318 = CARTESIAN_POINT ( 'NONE',  ( 6.673100192134572950, -2.779195860258147022, 31.39871582349836743 ) ) ;
#319 = ADVANCED_FACE ( 'NONE', ( #87382 ), #67987, .F. ) ;
#320 = CARTESIAN_POINT ( 'NONE',  ( -16.15384615384615330, -11.11383981884818262, 36.00935417666054406 ) ) ;
#321 = CARTESIAN_POINT ( 'NONE',  ( -17.29980259366066520, -7.630690623152299956, 34.99857592706774057 ) ) ;
#322 = ORIENTED_EDGE ( 'NONE', *, *, #43206, .F. ) ;
#323 = ADVANCED_FACE ( 'NONE', ( #5837 ), #60772, .F. ) ;
#324 = CARTESIAN_POINT ( 'NONE',  ( -18.13047670811646483, -7.276988635370451597, 34.74523720219453793 ) ) ;
#325 = VECTOR ( 'NONE', #40257, 1000.000000000000000 ) ;
#326 = ORIENTED_EDGE ( 'NONE', *, *, #40277, .T. ) ;
#327 = VERTEX_POINT ( 'NONE', #68417 ) ;
#328 = VERTEX_POINT ( 'NONE', #87839 ) ;
#330 = ORIENTED_EDGE ( 'NONE', *, *, #1788, .T. ) ;
#329 = DIRECTION ( 'NONE',  ( 0.000000000000000000, 0.9396926207859126468, -0.3420201433256571111 ) ) ;
#331 = CARTESIAN_POINT ( 'NONE',  ( 4.403900465484468008, -5.728107161865375829, 34.42597550085002922 ) ) ;
#332 = VECTOR ( 'NONE', #25563, 1000.000000000000000 ) ;
#333 = ADVANCED_FACE ( 'NONE', ( #53570 ), #13914, .F. ) ;
#334 = B_SPLINE_CURVE_WITH_KNOTS ( 'NONE', 3,
 ( #64908, #72563, #59048, #79330, #31581, #86548, #17176, #4555, #18076, #87001 ),
 .UNSPECIFIED., .F., .F.,
 ( 4, 2, 2, 2, 4 ),
 ( 0.000000000000000000, 0.0001954339857564099680, 0.0003908679715128199361, 0.0005863019572692299312, 0.0007817359430256398721 ),
 .UNSPECIFIED. ) ;
#335 = B_SPLINE_CURVE_WITH_KNOTS ( 'NONE', 3,
 ( #13254, #76272, #55557, #69520, #33961, #81720, #26766, #20005, #48800, #61867 ),
 .UNSPECIFIED., .F., .F.,
 ( 4, 2, 2, 2, 4 ),
 ( 0.0007817246256747453293, 0.0009771112852218889842, 0.001172497944769032531, 0.001367884604316176294, 0.001563271263863319840 ),
 .UNSPECIFIED. ) ;
#336 = LINE ( 'NONE', #27798, #62504 ) ;
#337 = ADVANCED_FACE ( 'NONE', ( #33314 ), #46817, .F. ) ;
#338 = CARTESIAN_POINT ( 'NONE',  ( -12.39628289026243557, -12.27809138561124591, 31.22303859784720359 ) ) ;
#339 = CARTESIAN_POINT ( 'NONE',  ( 1.653273178848927064E-15, -7.500000000000000000, 0.000000000000000000 ) ) ;
#340 = ORIENTED_EDGE ( 'NONE', *, *, #84982, .F. ) ;
#341 = EDGE_LOOP ( 'NONE', ( #3510, #61163, #15292, #57174 ) ) ;
#342 = ORIENTED_EDGE ( 'NONE', *, *, #84967, .F. ) ;
#343 = CARTESIAN_POINT ( 'NONE',  ( -2.242437168179467477, -3.643525952247864463, 33.31231777344670064 ) ) ;
#345 = VERTEX_POINT ( 'NONE', #74747 ) ;
#344 = DIRECTION ( 'NONE',  ( -0.000000000000000000, -0.000000000000000000, -1.000000000000000000 ) ) ;
#346 = CARTESIAN_POINT ( 'NONE',  ( 6.792385456409367528, -6.413092428213692742, 34.63065189839063152 ) ) ;
#347 = ADVANCED_FACE ( 'NONE', ( #13036 ), #40520, .F. ) ;
#348 = DIRECTION ( 'NONE',  ( -0.000000000000000000, 0.9848077530122085754, -0.1736481776669273613 ) ) ;
#349 = EDGE_LOOP ( 'NONE', ( #49195, #32576, #79895, #88984 ) ) ;
#350 = DIRECTION ( 'NONE',  ( -0.000000000000000000, -0.000000000000000000, -1.000000000000000000 ) ) ;
#351 = DIRECTION ( 'NONE',  ( -1.000000000000000000, -0.000000000000000000, -0.000000000000000000 ) ) ;
#352 = ORIENTED_EDGE ( 'NONE', *, *, #65664, .F. ) ;
#353 = FACE_BOUND ( 'NONE', #30448, .T. ) ;
#354 = EDGE_CURVE ( 'NONE', #24770, #59241, #83681, .T. ) ;
#355 = CARTESIAN_POINT ( 'NONE',  ( -19.00000000000000355, 12.75000000000000888, 23.75000000000000000 ) ) ;
#356 = CARTESIAN_POINT ( 'NONE',  ( 16.02369818411445834, -2.647304123082329763, 31.75400227202886683 ) ) ;
#357 = FACE_OUTER_BOUND ( 'NONE', #7317, .T. ) ;
#359 = CARTESIAN_POINT ( 'NONE',  ( -0.4615384615384611200, -3.050289026998446396, 32.03036669348365706 ) ) ;
#358 = CARTESIAN_POINT ( 'NONE',  ( 7.912221179503920787, -10.67929555188718282, 33.92786785259544757 ) ) ;
#360 = AXIS2_PLACEMENT_3D ( 'NONE', #65343, #45520, #72546 ) ;
#361 = FACE_OUTER_BOUND ( 'NONE', #8504, .T. ) ;
#362 = CARTESIAN_POINT ( 'NONE',  ( 5.198717948717946236, -4.000000000000000000, 29.75000000000000355 ) ) ;
#363 = VERTEX_POINT ( 'NONE', #29220 ) ;
#364 = CARTESIAN_POINT ( 'NONE',  ( 11.53846153846153832, -5.415277668671390821, 36.20867863119892149 ) ) ;
#365 = CARTESIAN_POINT ( 'NONE',  ( -19.99999999999996803, 12.00000000000000711, 13.00000000000000178 ) ) ;
#366 = EDGE_LOOP ( 'NONE', ( #41568, #20899 ) ) ;
#367 = AXIS2_PLACEMENT_3D ( 'NONE', #88511, #80411, #5626 ) ;
#368 = B_SPLINE_CURVE_WITH_KNOTS ( 'NONE', 3,
 ( #9005, #62598, #77017, #71569, #35588, #35137, #64363, #36035, #36472, #2659 ),
 .UNSPECIFIED., .F., .F.,
 ( 4, 2, 2, 2, 4 ),
 ( 0.0007817246256747503166, 0.0009771112852218944052, 0.001172497944769038602, 0.001367884604316182799, 0.001563271263863326996 ),
 .UNSPECIFIED. ) ;
#369 = EDGE_CURVE ( 'NONE', #87698, #17125, #35522, .T. ) ;
#370 = CARTESIAN_POINT ( 'NONE',  ( -14.30769230769242917, -9.528491918059723176, 34.59228464037033035 ) ) ;
#371 = CARTESIAN_POINT ( 'NONE',  ( 9.692307692307695177, -2.721908614388771852, 31.22303859784724978 ) ) ;
#373 = VERTEX_POINT ( 'NONE', #845 ) ;
#372 = B_SPLINE_CURVE_WITH_KNOTS ( 'NONE', 3,
 ( #22654, #8712, #16776, #20977, #9578, #2369, #77603, #30301, #37488, #70855 ),
 .UNSPECIFIED., .F., .F.,
 ( 4, 2, 2, 2, 4 ),
 ( 0.0007817246336856289524, 0.0009771112958940101571, 0.001172497958102391253, 0.001367884620310772350, 0.001563271282519153446 ),
 .UNSPECIFIED. ) ;
#374 = CARTESIAN_POINT ( 'NONE',  ( -16.15384615384615330, -11.16473453929635440, 33.15142922261926373 ) ) ;
#375 = CYLINDRICAL_SURFACE ( 'NONE', #76000, 0.2499999999999998890 ) ;
#376 = FACE_BOUND ( 'NONE', #11299, .T. ) ;
#377 = ADVANCED_FACE ( 'NONE', ( #29653 ), #76057, .T. ) ;
#379 = CARTESIAN_POINT ( 'NONE',  ( -4.087777802843714170, -8.120952969808772792, 34.71129190929999453 ) ) ;
#378 = CYLINDRICAL_SURFACE ( 'NONE', #27428, 0.2500000000000002220 ) ;
#380 = CARTESIAN_POINT ( 'NONE',  ( 7.912222197156284054, -8.973038597847271092, 34.52809138561121216 ) ) ;
#381 = CARTESIAN_POINT ( 'NONE',  ( 1.450682717965462443, -12.62096338111211757, 30.90682066428152908 ) ) ;
#382 = CARTESIAN_POINT ( 'NONE',  ( 0.2386122440223126528, -5.667676309546436642, 34.40238873228292249 ) ) ;
#383 = FACE_OUTER_BOUND ( 'NONE', #27024, .T. ) ;
#384 = CARTESIAN_POINT ( 'NONE',  ( -1.614399933863656544, -3.775308065498769405, 16.32625670625849068 ) ) ;
#385 = ORIENTED_EDGE ( 'NONE', *, *, #9056, .F. ) ;
#386 = ORIENTED_EDGE ( 'NONE', *, *, #4189, .F. ) ;
#387 = CARTESIAN_POINT ( 'NONE',  ( -9.757577692864012775, -2.379036618887870436, 30.90682066428147934 ) ) ;
#388 = CARTESIAN_POINT ( 'NONE',  ( 14.37294744720514572, -12.70778746994558439, 30.41441678777536595 ) ) ;
#389 = CARTESIAN_POINT ( 'NONE',  ( -12.46153846153846168, -1.466349020453238561, 30.81389545987213907 ) ) ;
#390 = CARTESIAN_POINT ( 'NONE',  ( -9.019207513279361876, -8.347322224742351082, 34.93158281831414058 ) ) ;
#391 = CARTESIAN_POINT ( 'NONE',  ( 2.980745993476266342, -11.37209801155882971, 32.91403422569032955 ) ) ;
#392 = CARTESIAN_POINT ( 'NONE',  ( -2.608446859217889546, -10.19485399968121264, 18.43563170625848713 ) ) ;
#393 = EDGE_CURVE ( 'NONE', #23382, #20924, #8053, .T. ) ;
#394 = CARTESIAN_POINT ( 'NONE',  ( -11.78846153846154010, -7.566082377512564960, 35.00000000000000711 ) ) ;
#395 = CARTESIAN_POINT ( 'NONE',  ( -3.480769230769229061, -7.500000000000001776, 34.75000000000000000 ) ) ;
#396 = EDGE_CURVE ( 'NONE', #70653, #65231, #6317, .T. ) ;
#397 = CARTESIAN_POINT ( 'NONE',  ( 16.15384615384603251, -2.379036618888197729, 30.90682066428292885 ) ) ;
#398 = CARTESIAN_POINT ( 'NONE',  ( 4.403846153847589484, -7.500000000000155431, 34.75000000000007105 ) ) ;
#399 = CARTESIAN_POINT ( 'NONE',  ( -15.00798968950082291, -11.41317474335729543, 32.86274602512330034 ) ) ;
#400 = CARTESIAN_POINT ( 'NONE',  ( -5.076923076923199218, -6.835583212225970762, 34.95778746994575670 ) ) ;
#401 = CARTESIAN_POINT ( 'NONE',  ( 5.933916589044121004, -12.10708131394839349, 31.69288490824020244 ) ) ;
#402 = CARTESIAN_POINT ( 'NONE',  ( 14.53047184896071897, -11.89424750095246175, 32.13594075562310337 ) ) ;
#403 = LINE ( 'NONE', #13907, #87417 ) ;
#404 = ORIENTED_EDGE ( 'NONE', *, *, #80528, .F. ) ;
#405 = CARTESIAN_POINT ( 'NONE',  ( -0.2387589202700510504, -3.755027918224367767, 33.06320215134714857 ) ) ;
#406 = CARTESIAN_POINT ( 'NONE',  ( 7.622668921589514923, -4.988325925672468131, 34.36044203135681130 ) ) ;
#407 = CARTESIAN_POINT ( 'NONE',  ( -2.724691934501246582, -6.299813628509474128, 20.42374329374152353 ) ) ;
#408 = LINE ( 'NONE', #82831, #54785 ) ;
#409 = DIRECTION ( 'NONE',  ( -0.000000000000000000, -0.3420201433256694901, -0.9396926207859082059 ) ) ;
#410 = ORIENTED_EDGE ( 'NONE', *, *, #80404, .T. ) ;
#411 = DIRECTION ( 'NONE',  ( -0.000000000000000000, 1.000000000000000000, 3.491481338843133355E-15 ) ) ;
#413 = ORIENTED_EDGE ( 'NONE', *, *, #39036, .T. ) ;
#412 = DIRECTION ( 'NONE',  ( 1.000000000000000000, 0.000000000000000000, 0.000000000000000000 ) ) ;
#414 = CARTESIAN_POINT ( 'NONE',  ( 13.38461538461538680, -13.20930481340135110, 34.54067556320372745 ) ) ;
#415 = DIRECTION ( 'NONE',  ( 0.000000000000000000, 0.000000000000000000, 1.000000000000000000 ) ) ;
#416 = ORIENTED_EDGE ( 'NONE', *, *, #77856, .F. ) ;
#417 = DIRECTION ( 'NONE',  ( 1.000000000000000000, 0.000000000000000000, 0.000000000000000000 ) ) ;
#418 = CARTESIAN_POINT ( 'NONE',  ( -16.81410256410256565, -11.50000000000000000, 29.75000000000000355 ) ) ;
#419 = ORIENTED_EDGE ( 'NONE', *, *, #191, .T. ) ;
#420 = CARTESIAN_POINT ( 'NONE',  ( 16.94677586748485609, -11.47017969459903952, 32.78971311882035167 ) ) ;
#421 = CARTESIAN_POINT ( 'NONE',  ( 8.096153846155281997, -7.500000000000155431, 34.75000000000007105 ) ) ;
#422 = CARTESIAN_POINT ( 'NONE',  ( -15.09997742294444478, -12.38066358083363738, 30.83685684665853444 ) ) ;
#423 = VERTEX_POINT ( 'NONE', #22006 ) ;
#424 = ORIENTED_EDGE ( 'NONE', *, *, #87981, .T. ) ;
#425 = CARTESIAN_POINT ( 'NONE',  ( -10.36533019547115941, -2.318338780012835443, 30.59689888758630261 ) ) ;
#426 = COLOUR_RGB ( '', 0.72549020, 0.75294118, 0.79215686) ;
#427 = VERTEX_POINT ( 'NONE', #8497 ) ;
#428 = CARTESIAN_POINT ( 'NONE',  ( -14.98071481085577972, -4.074993327901527351, 33.72946981652012255 ) ) ;
#429 = CARTESIAN_POINT ( 'NONE',  ( -1.161604033002534786, -2.554770724473667709, 30.48948780036025852 ) ) ;
#430 = CARTESIAN_POINT ( 'NONE',  ( -1.384615384615506484, -11.67786785259630911, 32.92929555188603530 ) ) ;
#431 = EDGE_CURVE ( 'NONE', #11896, #58120, #76950, .T. ) ;
#432 = CARTESIAN_POINT ( 'NONE',  ( 0.4615384615384611200, -9.819645486525091727, 36.12317359536749706 ) ) ;
#433 = CARTESIAN_POINT ( 'NONE',  ( -0.4615384615385840772, -5.941354392335915335, 34.76329471203413846 ) ) ;
#434 = FACE_OUTER_BOUND ( 'NONE', #71808, .T. ) ;
#435 = VECTOR ( 'NONE', #75425, 1000.000000000000000 ) ;
#436 = EDGE_CURVE ( 'NONE', #46513, #56514, #28312, .T. ) ;
#437 = CARTESIAN_POINT ( 'NONE',  ( 15.90382292962469180, -12.68155406624981119, 30.59749803192733708 ) ) ;
#438 = ORIENTED_EDGE ( 'NONE', *, *, #56597, .F. ) ;
#439 = ORIENTED_EDGE ( 'NONE', *, *, #3601, .F. ) ;
#441 = VERTEX_POINT ( 'NONE', #70189 ) ;
#440 = CARTESIAN_POINT ( 'NONE',  ( -0.3954701105360236002, -12.10708131394839704, 31.69288490824020954 ) ) ;
#442 = EDGE_CURVE ( 'NONE', #68729, #70011, #35447, .T. ) ;
#443 = CARTESIAN_POINT ( 'NONE',  ( -5.142193077479396912, -5.094484230520674117, 34.41647553114621161 ) ) ;
#444 = ORIENTED_EDGE ( 'NONE', *, *, #26257, .F. ) ;
#445 = CARTESIAN_POINT ( 'NONE',  ( 11.66925197942849302, -3.338503747796866872, 32.95102852606553512 ) ) ;
#446 = CARTESIAN_POINT ( 'NONE',  ( 5.076923076922954969, -3.835265460704628371, 33.15142922262033665 ) ) ;
#447 = ORIENTED_EDGE ( 'NONE', *, *, #84542, .F. ) ;
#448 = DIRECTION ( 'NONE',  ( 0.000000000000000000, 0.000000000000000000, 1.000000000000000000 ) ) ;
#449 = EDGE_CURVE ( 'NONE', #49542, #26693, #14245, .T. ) ;
#450 = AXIS2_PLACEMENT_3D ( 'NONE', #84938, #2938, #44359 ) ;
#451 = ORIENTED_EDGE ( 'NONE', *, *, #81392, .T. ) ;
#452 = CARTESIAN_POINT ( 'NONE',  ( 7.846153846153723244, -12.70778746994576025, 30.41441678777401236 ) ) ;
#453 = ORIENTED_EDGE ( 'NONE', *, *, #29446, .F. ) ;
#454 = CIRCLE ( 'NONE', #72316, 0.4999999999999994449 ) ;
#455 = LINE ( 'NONE', #48625, #11505 ) ;
#456 = VERTEX_POINT ( 'NONE', #21105 ) ;
#457 = CARTESIAN_POINT ( 'NONE',  ( 18.00000000000000000, -6.343179335718451384, 34.87096338111211935 ) ) ;
#458 = CARTESIAN_POINT ( 'NONE',  ( -4.284536756956461190, -6.369640206132550553, 34.87707690430378449 ) ) ;
#459 = B_SPLINE_CURVE_WITH_KNOTS ( 'NONE', 3,
 ( #38721, #52670, #86941, #51764, #3145, #31061, #37374, #10807, #11251, #64844 ),
 .UNSPECIFIED., .F., .F.,
 ( 4, 2, 2, 2, 4 ),
 ( 0.000000000000000000, 0.0001954339857564073659, 0.0003908679715128147319, 0.0005863019572692221250, 0.0007817359430256294638 ),
 .UNSPECIFIED. ) ;
#460 = FACE_BOUND ( 'NONE', #10409, .T. ) ;
#461 = EDGE_CURVE ( 'NONE', #35423, #73834, #49030, .T. ) ;
#462 = CARTESIAN_POINT ( 'NONE',  ( 5.749976775778542937, -2.341070481393820124, 30.72580821765574299 ) ) ;
#463 = CYLINDRICAL_SURFACE ( 'NONE', #51418, 0.2500000000000004996 ) ;
#464 = CARTESIAN_POINT ( 'NONE',  ( 9.442330948259105128, -11.47974371597207899, 33.17467449705390692 ) ) ;
#465 = CARTESIAN_POINT ( 'NONE',  ( -17.07692307692307665, -12.34228464037088635, 31.77849191805839268 ) ) ;
#466 = CARTESIAN_POINT ( 'NONE',  ( -17.32689982097166492, -8.347322224742351082, 34.93158281831414058 ) ) ;
#467 = CARTESIAN_POINT ( 'NONE',  ( -4.219116599806928214, -11.48612834413959582, 32.76840700105983473 ) ) ;
#468 = EDGE_CURVE ( 'NONE', #6055, #84853, #21558, .T. ) ;
#469 = CARTESIAN_POINT ( 'NONE',  ( 8.102564102564102200, -11.00000000000000000, 29.75000000000000355 ) ) ;
#470 = EDGE_LOOP ( 'NONE', ( #48935, #2508, #11631, #61677 ) ) ;
#471 = ORIENTED_EDGE ( 'NONE', *, *, #28570, .F. ) ;
#473 = CARTESIAN_POINT ( 'NONE',  ( 15.00728428704528561, -12.24155766932282496, 31.33739205006857986 ) ) ;
#472 = CARTESIAN_POINT ( 'NONE',  ( -19.99999999999996447, -15.00000000000000533, 13.00000000000000178 ) ) ;
#474 = CARTESIAN_POINT ( 'NONE',  ( -11.66915300512909859, -11.71456829005830080, 32.44064028649416542 ) ) ;
#475 = DIRECTION ( 'NONE',  ( -0.000000000000000000, 0.5000000000000011102, -0.8660254037844380415 ) ) ;
#476 = CARTESIAN_POINT ( 'NONE',  ( -14.30769230769230660, -3.513871655860378418, 32.76840700105978499 ) ) ;
#477 = CYLINDRICAL_SURFACE ( 'NONE', #63424, 0.2499999999999997502 ) ;
#478 = EDGE_LOOP ( 'NONE', ( #50034, #54764 ) ) ;
#479 = CARTESIAN_POINT ( 'NONE',  ( 13.31853197365950692, -4.786620604624113540, 33.94971097300155805 ) ) ;
#480 = EDGE_CURVE ( 'NONE', #74721, #66781, #42289, .T. ) ;
#481 = LINE ( 'NONE', #56306, #79055 ) ;
#482 = DIRECTION ( 'NONE',  ( 0.000000000000000000, 0.000000000000000000, 1.000000000000000000 ) ) ;
#483 = DIRECTION ( 'NONE',  ( -1.845450506358306311E-16, 1.000000000000000000, -5.102127870520021228E-17 ) ) ;
#484 = EDGE_LOOP ( 'NONE', ( #60123, #67289, #74118, #28070 ) ) ;
#485 = VERTEX_POINT ( 'NONE', #68858 ) ;
#486 = AXIS2_PLACEMENT_3D ( 'NONE', #32374, #72456, #59839 ) ;
#487 = EDGE_LOOP ( 'NONE', ( #82911, #37209, #13825, #34035 ) ) ;
#488 = CARTESIAN_POINT ( 'NONE',  ( -9.442362173959550020, -12.43552623307873972, 30.55307653245132826 ) ) ;
#489 = ORIENTED_EDGE ( 'NONE', *, *, #55931, .T. ) ;
#490 = CARTESIAN_POINT ( 'NONE',  ( -9.561517251340744039, -9.929761469519743144, 34.40412654351204225 ) ) ;
#491 = CYLINDRICAL_SURFACE ( 'NONE', #21511, 0.2500000000000009437 ) ;
#492 = CARTESIAN_POINT ( 'NONE',  ( 14.30769230769231015, -5.180354513474913603, 36.12317359536750416 ) ) ;
#493 = CARTESIAN_POINT ( 'NONE',  ( 1.553300858899087311, -3.749999999999992006, 14.23437500000000355 ) ) ;
#494 = ADVANCED_FACE ( 'NONE', ( #69745 ), #7164, .F. ) ;
#495 = CYLINDRICAL_SURFACE ( 'NONE', #2877, 0.2499999999999986955 ) ;
#496 = VERTEX_POINT ( 'NONE', #69311 ) ;
#497 = CARTESIAN_POINT ( 'NONE',  ( 4.403791672194295792, -4.336752205174647656, 33.62275283266504289 ) ) ;
#499 = EDGE_LOOP ( 'NONE', ( #8065, #69891, #54153, #58268 ) ) ;
#498 = FACE_OUTER_BOUND ( 'NONE', #59189, .T. ) ;
#500 = CARTESIAN_POINT ( 'NONE',  ( -9.561781990544126586, -4.459921816937791661, 33.71989282347011851 ) ) ;
#501 = CARTESIAN_POINT ( 'NONE',  ( -8.992110285968356820, -7.630690623152299956, 34.99857592706774057 ) ) ;
#503 = B_SPLINE_CURVE_WITH_KNOTS ( 'NONE', 3,
 ( #55324, #55765, #21540, #35953, #49893, #76935, #63408, #77371, #42272, #34617 ),
 .UNSPECIFIED., .F., .F.,
 ( 4, 2, 2, 2, 4 ),
 ( 0.0007817359527651090859, 0.0009771254036996478414, 0.001172514854634186489, 0.001367904305568725136, 0.001563293756503263783 ),
 .UNSPECIFIED. ) ;
#502 = CYLINDRICAL_SURFACE ( 'NONE', #24257, 0.2500000000000002220 ) ;
#504 = EDGE_CURVE ( 'NONE', #73834, #24183, #58251, .T. ) ;
#505 = ADVANCED_FACE ( 'NONE', ( #65191 ), #59330, .F. ) ;
#506 = CARTESIAN_POINT ( 'NONE',  ( 9.822833394071261992, -10.88167719472716399, 33.43325721877153711 ) ) ;
#507 = CARTESIAN_POINT ( 'NONE',  ( -9.822455662039391910, -12.50552854090298993, 31.33409797877408920 ) ) ;
#508 = CARTESIAN_POINT ( 'NONE',  ( 17.32692307692451195, -7.500000000000155431, 34.75000000000007105 ) ) ;
#509 = B_SPLINE_CURVE_WITH_KNOTS ( 'NONE', 3,
 ( #53464, #32756, #11153, #32322, #19251, #59784, #88619, #20134, #12059, #47600 ),
 .UNSPECIFIED., .F., .F.,
 ( 4, 2, 2, 2, 4 ),
 ( 0.000000000000000000, 0.0001954311584214071026, 0.0003908623168428142051, 0.0005862934752642213077, 0.0007817246336856284103 ),
 .UNSPECIFIED. ) ;
#510 = CARTESIAN_POINT ( 'NONE',  ( -3.296852641725110722, -6.386643153685125363, 34.62446782046654903 ) ) ;
#511 = CARTESIAN_POINT ( 'NONE',  ( 1.901340078031373171, -9.487747218494639867, 23.62686829374151287 ) ) ;
#512 = ORIENTED_EDGE ( 'NONE', *, *, #29886, .T. ) ;
#513 = B_SPLINE_CURVE_WITH_KNOTS ( 'NONE', 3,
 ( #47860, #40679, #88875, #68140, #13632, #69020, #14520, #28035, #82556, #69465 ),
 .UNSPECIFIED., .F., .F.,
 ( 4, 2, 2, 2, 4 ),
 ( 0.000000000000000000, 0.0001954339857564093175, 0.0003908679715128186350, 0.0005863019572692279796, 0.0007817359430256372700 ),
 .UNSPECIFIED. ) ;
#514 = EDGE_CURVE ( 'NONE', #25678, #10982, #60501, .T. ) ;
#515 = CARTESIAN_POINT ( 'NONE',  ( -16.94613126909828793, -10.54018710029568595, 33.71981072465678864 ) ) ;
#516 = FACE_OUTER_BOUND ( 'NONE', #38907, .T. ) ;
#517 = CARTESIAN_POINT ( 'NONE',  ( 8.899756207464411872, -11.04252011169590020, 33.62494198852677130 ) ) ;
#518 = PRESENTATION_STYLE_ASSIGNMENT (( #82052 ) ) ;
#519 = VERTEX_POINT ( 'NONE', #78265 ) ;
#520 = CARTESIAN_POINT ( 'NONE',  ( -4.153846153846152411, -4.661471528628507777, 34.16647553114623292 ) ) ;
#521 = CARTESIAN_POINT ( 'NONE',  ( 11.28848479441295005, -4.075325502946081535, 33.72974371597206300 ) ) ;
#522 = CARTESIAN_POINT ( 'NONE',  ( 1.161689167099238862, -9.086856451489515152, 34.49173150075333183 ) ) ;
#523 = VECTOR ( 'NONE', #26290, 1000.000000000000000 ) ;
#524 = CARTESIAN_POINT ( 'NONE',  ( -6.000000000000119904, -6.879047030192662504, 34.71129190930017927 ) ) ;
#525 = AXIS2_PLACEMENT_3D ( 'NONE', #7311, #6858, #76199 ) ;
#526 = ORIENTED_EDGE ( 'NONE', *, *, #76556, .F. ) ;
#527 = CARTESIAN_POINT ( 'NONE',  ( 16.94623161025551639, -3.062553014421049991, 32.05460306192773601 ) ) ;
#528 = CARTESIAN_POINT ( 'NONE',  ( -3.262820512820514107, -7.500000000000000000, 29.75000000000000355 ) ) ;
#529 = CARTESIAN_POINT ( 'NONE',  ( 12.46153846153846168, -1.629998284177014645, 34.34916445242399163 ) ) ;
#530 = VERTEX_POINT ( 'NONE', #79611 ) ;
#531 = CARTESIAN_POINT ( 'NONE',  ( -2.557692307692305267, -7.500000000000001776, 34.75000000000000000 ) ) ;
#532 = ORIENTED_EDGE ( 'NONE', *, *, #45439, .F. ) ;
#533 = CARTESIAN_POINT ( 'NONE',  ( -2.373775718648186928, -12.10708131394839349, 31.69288490824020244 ) ) ;
#534 = CARTESIAN_POINT ( 'NONE',  ( 1.653273178848927064E-15, -7.500000000000000000, 11.00000000000000178 ) ) ;
#535 = VERTEX_POINT ( 'NONE', #30960 ) ;
#536 = DIRECTION ( 'NONE',  ( 0.000000000000000000, 0.4999999999999960032, -0.8660254037844410391 ) ) ;
#537 = LINE ( 'NONE', #63557, #72302 ) ;
#538 = CARTESIAN_POINT ( 'NONE',  ( -11.78843826940389583, -6.567427716900048118, 34.66269422305636283 ) ) ;
#539 = B_SPLINE_CURVE_WITH_KNOTS ( 'NONE', 3,
 ( #46049, #67220, #52352, #73535, #39310, #24434, #66766, #5067, #60006, #5518 ),
 .UNSPECIFIED., .F., .F.,
 ( 4, 2, 2, 2, 4 ),
 ( 0.0007817359430256372700, 0.0009771253907250054306, 0.001172514838424373483, 0.001367904286123741535, 0.001563293733823109804 ),
 .UNSPECIFIED. ) ;
#540 = B_SPLINE_CURVE_WITH_KNOTS ( 'NONE', 3,
 ( #44835, #25469, #38544, #3854, #5198, #87634, #25913, #52038, #30880, #10621 ),
 .UNSPECIFIED., .F., .F.,
 ( 4, 2, 2, 2, 4 ),
 ( 0.0007817359430256392216, 0.0009771253907250073822, 0.001172514838424375651, 0.001367904286123743920, 0.001563293733823112189 ),
 .UNSPECIFIED. ) ;
#541 = CARTESIAN_POINT ( 'NONE',  ( -0.7115384615384606759, -7.500000000000001776, 35.04278698407183867 ) ) ;
#542 = CARTESIAN_POINT ( 'NONE',  ( -6.923076923076922462, -1.367168528481310208, 33.57946703557072254 ) ) ;
#543 = B_SPLINE_CURVE_WITH_KNOTS ( 'NONE', 3,
 ( #64384, #38707, #65281, #4016, #4480, #31504, #58970, #2684, #57642, #86473 ),
 .UNSPECIFIED., .F., .F.,
 ( 4, 2, 2, 2, 4 ),
 ( 0.000000000000000000, 0.0001954311564186865221, 0.0003908623128373730441, 0.0005862934692560595662, 0.0007817246256747460882 ),
 .UNSPECIFIED. ) ;
#544 = CIRCLE ( 'NONE', #45150, 4.000000000000000000 ) ;
#545 = VERTEX_POINT ( 'NONE', #25105 ) ;
#546 = FACE_BOUND ( 'NONE', #34527, .T. ) ;
#547 = ORIENTED_EDGE ( 'NONE', *, *, #30603, .T. ) ;
#548 = DIRECTION ( 'NONE',  ( -0.000000000000000000, 1.000000000000000000, -0.000000000000000000 ) ) ;
#549 = VECTOR ( 'NONE', #26235, 1000.000000000000227 ) ;
#550 = VECTOR ( 'NONE', #21356, 1000.000000000000000 ) ;
#551 = CARTESIAN_POINT ( 'NONE',  ( 4.826899839630111266, -11.86270091957321249, 32.19358267280087915 ) ) ;
#552 = DIRECTION ( 'NONE',  ( -0.000000000000000000, -0.8660254037844397068, -0.4999999999999978906 ) ) ;
#553 = CARTESIAN_POINT ( 'NONE',  ( 14.37375964104238513, -8.164416787775445883, 34.95778746994558617 ) ) ;
#554 = ORIENTED_EDGE ( 'NONE', *, *, #61196, .F. ) ;
#555 = ORIENTED_EDGE ( 'NONE', *, *, #60770, .T. ) ;
#556 = ORIENTED_EDGE ( 'NONE', *, *, #27457, .T. ) ;
#557 = DIRECTION ( 'NONE',  ( -0.000000000000000000, -0.000000000000000000, 1.000000000000000000 ) ) ;
#558 = VERTEX_POINT ( 'NONE', #38171 ) ;
#559 = CARTESIAN_POINT ( 'NONE',  ( 4.403900573759606196, -10.06805714834173848, 34.32951233291982618 ) ) ;
#560 = CARTESIAN_POINT ( 'NONE',  ( -16.82692307692307665, -2.499999999999998668, 29.75000000000000355 ) ) ;
#561 = CARTESIAN_POINT ( 'NONE',  ( -18.06527000055631760, -6.835583212224500826, 34.95778746994557906 ) ) ;
#563 = ADVANCED_FACE ( 'NONE', ( #72839 ), #85923, .F. ) ;
#562 = CARTESIAN_POINT ( 'NONE',  ( -5.076923076923197442, -10.90142922262034020, 33.41473453929536674 ) ) ;
#564 = B_SPLINE_CURVE_WITH_KNOTS ( 'NONE', 3,
 ( #69872, #41076, #87, #61323, #27112, #74871, #49153, #76634, #75736, #54575 ),
 .UNSPECIFIED., .F., .F.,
 ( 4, 2, 2, 2, 4 ),
 ( 0.000000000000000000, 0.0001954339857564075015, 0.0003908679715128150029, 0.0005863019572692224502, 0.0007817359430256300059 ),
 .UNSPECIFIED. ) ;
#565 = CARTESIAN_POINT ( 'NONE',  ( 17.07692307692295586, -4.481592998941358097, 33.73612834414048933 ) ) ;
#566 = CARTESIAN_POINT ( 'NONE',  ( 15.36156103859402222, -8.999086150933475636, 34.52020707165672775 ) ) ;
#567 = FACE_OUTER_BOUND ( 'NONE', #79244, .T. ) ;
#569 = CARTESIAN_POINT ( 'NONE',  ( -8.769230769230768274, -2.833524468853757305, 32.15551576947925838 ) ) ;
#568 = B_SPLINE_CURVE_WITH_KNOTS ( 'NONE', 3,
 ( #50304, #64261, #58842, #19201, #52528, #86350, #31835, #17873, #30920, #12009 ),
 .UNSPECIFIED., .F., .F.,
 ( 4, 2, 2, 2, 4 ),
 ( 0.0007817246256747451124, 0.0009771112852218881168, 0.001172497944769031230, 0.001367884604316174126, 0.001563271263863317238 ),
 .UNSPECIFIED. ) ;
#570 = ORIENTED_EDGE ( 'NONE', *, *, #5698, .T. ) ;
#571 = EDGE_LOOP ( 'NONE', ( #21663, #30842, #13535, #23130 ) ) ;
#572 = VERTEX_POINT ( 'NONE', #44919 ) ;
#573 = CARTESIAN_POINT ( 'NONE',  ( 20.00000000000000000, -4.000000000000000000, 29.75000000000000355 ) ) ;
#574 = VECTOR ( 'NONE', #40145, 1000.000000000000114 ) ;
#576 = CARTESIAN_POINT ( 'NONE',  ( 10.61538461538461675, -13.63283147151868846, 33.57946703557072254 ) ) ;
#575 = DIRECTION ( 'NONE',  ( 0.000000000000000000, 0.000000000000000000, 1.000000000000000000 ) ) ;
#577 = CARTESIAN_POINT ( 'NONE',  ( 1.515405825582335497, -12.35292014791297710, 31.75344720912887198 ) ) ;
#578 = CARTESIAN_POINT ( 'NONE',  ( -6.673022611438608642, -3.627508038966690496, 32.91356715214248396 ) ) ;
#579 = FACE_BOUND ( 'NONE', #10836, .T. ) ;
#580 = CARTESIAN_POINT ( 'NONE',  ( 16.15384615384615330, -3.050289026998446396, 32.03036669348365706 ) ) ;
#581 = ORIENTED_EDGE ( 'NONE', *, *, #27829, .T. ) ;
#582 = LINE ( 'NONE', #53856, #58701 ) ;
#583 = EDGE_CURVE ( 'NONE', #87491, #41440, #57996, .T. ) ;
#584 = DIRECTION ( 'NONE',  ( -1.000000000000000000, -0.000000000000000000, 0.000000000000000000 ) ) ;
#585 = CARTESIAN_POINT ( 'NONE',  ( 16.82689983963011926, -6.695914987888146541, 34.68535235679833306 ) ) ;
#586 = CARTESIAN_POINT ( 'NONE',  ( 7.146089767170319185, -9.172514111537584114, 34.72667873470787470 ) ) ;
#587 = ORIENTED_EDGE ( 'NONE', *, *, #4080, .T. ) ;
#588 = CARTESIAN_POINT ( 'NONE',  ( 18.22301135161285046, -12.39991518177334129, 30.74647679643404530 ) ) ;
#589 = EDGE_LOOP ( 'NONE', ( #40662, #68267, #42370, #16279 ) ) ;
#590 = FACE_BOUND ( 'NONE', #13874, .T. ) ;
#591 = CARTESIAN_POINT ( 'NONE',  ( -17.07692307692319744, -4.320704448113951379, 33.92786785259630022 ) ) ;
#592 = CARTESIAN_POINT ( 'NONE',  ( -12.33101275977490197, -8.586989748646452369, 34.63063291749215011 ) ) ;
#593 = CARTESIAN_POINT ( 'NONE',  ( -0.4615384615384611200, -9.584722331328613620, 36.20867863119891439 ) ) ;
#594 = ORIENTED_EDGE ( 'NONE', *, *, #40606, .F. ) ;
#595 = CARTESIAN_POINT ( 'NONE',  ( 0.2386122440223146512, -10.61292498521070549, 33.66303323003028680 ) ) ;
#596 = CARTESIAN_POINT ( 'NONE',  ( 5.326923076924511946, -7.500000000000155431, 34.75000000000007105 ) ) ;
#597 = CARTESIAN_POINT ( 'NONE',  ( 18.13052543823364360, -11.04252011169589842, 33.62494198852677840 ) ) ;
#598 = DIRECTION ( 'NONE',  ( 0.000000000000000000, -0.000000000000000000, 1.000000000000000000 ) ) ;
#599 = ORIENTED_EDGE ( 'NONE', *, *, #70850, .F. ) ;
#600 = CARTESIAN_POINT ( 'NONE',  ( 16.28463796167093847, -10.54018710029568595, 33.71981072465678864 ) ) ;
#601 = ORIENTED_EDGE ( 'NONE', *, *, #47247, .T. ) ;
#603 = VERTEX_POINT ( 'NONE', #44032 ) ;
#602 = CARTESIAN_POINT ( 'NONE',  ( -39.05038313613820122, -12.50000000000000000, 29.75000000000000355 ) ) ;
#604 = CARTESIAN_POINT ( 'NONE',  ( 15.93036122928181975, -4.225889041578354544, 33.85425143139329407 ) ) ;
#605 = CARTESIAN_POINT ( 'NONE',  ( -6.792551221313358312, -11.93748526763465279, 32.05452791011430946 ) ) ;
#606 = CARTESIAN_POINT ( 'NONE',  ( 13.13463865367303463, -9.148715823498378086, 34.47080413974185120 ) ) ;
#607 = CARTESIAN_POINT ( 'NONE',  ( 14.08476609017615644, -9.086856451489515152, 34.49173150075333183 ) ) ;
#608 = ADVANCED_FACE ( 'NONE', ( #4389 ), #80051, .F. ) ;
#609 = EDGE_CURVE ( 'NONE', #36550, #75687, #65629, .T. ) ;
#610 = CARTESIAN_POINT ( 'NONE',  ( -39.05038313613820122, -2.499999999999999556, 29.75000000000000355 ) ) ;
#612 = LINE ( 'NONE', #14123, #34562 ) ;
#611 = CARTESIAN_POINT ( 'NONE',  ( -15.23076923076935252, -3.083524468854526912, 32.58852847137268327 ) ) ;
#613 = CARTESIAN_POINT ( 'NONE',  ( 8.096208157792162297, -4.235687564193446164, 33.53795663066793509 ) ) ;
#614 = B_SPLINE_CURVE_WITH_KNOTS ( 'NONE', 3,
 ( #6623, #34090, #7516, #89062, #34972, #75520, #19692, #54356, #26007, #33654 ),
 .UNSPECIFIED., .F., .F.,
 ( 4, 2, 2, 2, 4 ),
 ( 0.000000000000000000, 0.0001954339857564085315, 0.0003908679715128170629, 0.0005863019572692255944, 0.0007817359430256341259 ),
 .UNSPECIFIED. ) ;
#615 = CARTESIAN_POINT ( 'NONE',  ( 1.139087296526029469, -10.24999999999999467, 19.70312500000000355 ) ) ;
#616 = ORIENTED_EDGE ( 'NONE', *, *, #51029, .F. ) ;
#617 = AXIS2_PLACEMENT_3D ( 'NONE', #45736, #44381, #25020 ) ;
#618 = FACE_OUTER_BOUND ( 'NONE', #12115, .T. ) ;
#619 = ORIENTED_EDGE ( 'NONE', *, *, #51470, .F. ) ;
#620 = VECTOR ( 'NONE', #80304, 1000.000000000000000 ) ;
#621 = ADVANCED_FACE ( 'NONE', ( #23757 ), #78718, .F. ) ;
#622 = VERTEX_POINT ( 'NONE', #17015 ) ;
#623 = CARTESIAN_POINT ( 'NONE',  ( 3.164685819813350509, -4.786620604624113540, 33.94971097300155805 ) ) ;
#624 = EDGE_LOOP ( 'NONE', ( #77449, #46209, #13975, #53295 ) ) ;
#625 = CARTESIAN_POINT ( 'NONE',  ( -15.23076923076922995, -2.721908614388771852, 31.22303859784724978 ) ) ;
#626 = CARTESIAN_POINT ( 'NONE',  ( -8.069080805060693251, -8.282780595021769443, 34.94152052738834158 ) ) ;
#627 = FACE_OUTER_BOUND ( 'NONE', #35004, .T. ) ;
#628 = FACE_OUTER_BOUND ( 'NONE', #50378, .T. ) ;
#629 = CARTESIAN_POINT ( 'NONE',  ( 10.83816428436268176, -6.717445702608402236, 34.94155399931962336 ) ) ;
#630 = CARTESIAN_POINT ( 'NONE',  ( -8.769230769230892619, -2.657715359629662544, 31.77849191805970364 ) ) ;
#631 = DIRECTION ( 'NONE',  ( -0.000000000000000000, 0.6427876096865404731, -0.7660444431189771253 ) ) ;
#632 = CARTESIAN_POINT ( 'NONE',  ( 6.857806922520603976, -10.33852847137145048, 34.16647553114627556 ) ) ;
#633 = CARTESIAN_POINT ( 'NONE',  ( -2.176901866725353241, -2.845873456487966635, 32.17976146951972538 ) ) ;
#634 = DIRECTION ( 'NONE',  ( 1.000000000000000000, 0.000000000000000000, 0.000000000000000000 ) ) ;
#635 = LINE ( 'NONE', #42076, #15392 ) ;
#636 = B_SPLINE_CURVE_WITH_KNOTS ( 'NONE', 3,
 ( #21746, #28510, #84351, #50094, #8244, #29406, #50962, #1034, #2345, #42918 ),
 .UNSPECIFIED., .F., .F.,
 ( 4, 2, 2, 2, 4 ),
 ( 0.0007817359430256317406, 0.0009771253907249982749, 0.001172514838424365026, 0.001367904286123731560, 0.001563293733823098094 ),
 .UNSPECIFIED. ) ;
#637 = EDGE_LOOP ( 'NONE', ( #36007, #70907 ) ) ;
#638 = ORIENTED_EDGE ( 'NONE', *, *, #72178, .F. ) ;
#639 = CARTESIAN_POINT ( 'NONE',  ( 12.46153846153833911, -2.657715359629662544, 31.77849191805970364 ) ) ;
#640 = CARTESIAN_POINT ( 'NONE',  ( 0.7114838709165033359, -12.07971442181321997, 32.31769673815850297 ) ) ;
#641 = CARTESIAN_POINT ( 'NONE',  ( 20.00000000000000000, -4.000000000000000000, 29.75000000000000355 ) ) ;
#642 = LINE ( 'NONE', #55575, #34057 ) ;
#643 = CARTESIAN_POINT ( 'NONE',  ( -16.08777882049607655, -8.164416787775445883, 34.95778746994558617 ) ) ;
#644 = CARTESIAN_POINT ( 'NONE',  ( -6.130691466667557599, -8.147922237126337563, 34.70805685702651999 ) ) ;
#645 = AXIS2_PLACEMENT_3D ( 'NONE', #22951, #25062, #80914 ) ;
#646 = DIRECTION ( 'NONE',  ( 0.000000000000000000, 0.000000000000000000, 1.000000000000000000 ) ) ;
#647 = ORIENTED_EDGE ( 'NONE', *, *, #5980, .F. ) ;
#648 = CARTESIAN_POINT ( 'NONE',  ( 6.923076923076924238, -4.945431358278436385, 36.03766855953609394 ) ) ;
#649 = ORIENTED_EDGE ( 'NONE', *, *, #54191, .F. ) ;
#650 = CYLINDRICAL_SURFACE ( 'NONE', #59244, 0.2500000000000002220 ) ;
#651 = LINE ( 'NONE', #55589, #47066 ) ;
#652 = CARTESIAN_POINT ( 'NONE',  ( -0.3307466537136748430, -6.413143153341451352, 34.63066358083362672 ) ) ;
#653 = DIRECTION ( 'NONE',  ( -0.000000000000000000, -0.5000000000000009992, -0.8660254037844380415 ) ) ;
#654 = CARTESIAN_POINT ( 'NONE',  ( 5.869852790561782996, -2.882441371585227063, 31.66841991370171527 ) ) ;
#655 = EDGE_CURVE ( 'NONE', #29143, #16341, #58885, .T. ) ;
#656 = EDGE_LOOP ( 'NONE', ( #72252, #17241 ) ) ;
#657 = EDGE_LOOP ( 'NONE', ( #24562, #75991 ) ) ;
#658 = EDGE_CURVE ( 'NONE', #7553, #4867, #48697, .T. ) ;
#659 = ORIENTED_EDGE ( 'NONE', *, *, #57921, .F. ) ;
#660 = ORIENTED_EDGE ( 'NONE', *, *, #52723, .T. ) ;
#661 = CARTESIAN_POINT ( 'NONE',  ( -5.999999999999998224, -1.629998284177014645, 34.34916445242399163 ) ) ;
#662 = CARTESIAN_POINT ( 'NONE',  ( -12.71151520558705350, -12.65889640711025521, 30.72598325615533454 ) ) ;
#663 = CARTESIAN_POINT ( 'NONE',  ( 4.403900573759607084, -12.01375889529407281, 32.43194544308182969 ) ) ;
#664 = VECTOR ( 'NONE', #76082, 1000.000000000000114 ) ;
#665 = VECTOR ( 'NONE', #5935, 1000.000000000000000 ) ;
#667 = EDGE_CURVE ( 'NONE', #82157, #47301, #84125, .T. ) ;
#666 = CARTESIAN_POINT ( 'NONE',  ( 14.37283708841194318, -7.750023224968867197, 34.99404313364389907 ) ) ;
#668 = CARTESIAN_POINT ( 'NONE',  ( 17.77651507543566822, -3.019605429927187501, 32.48692288466676814 ) ) ;
#669 = DIRECTION ( 'NONE',  ( -0.000000000000000000, -0.9848077530122085754, -0.1736481776669273613 ) ) ;
#670 = ORIENTED_EDGE ( 'NONE', *, *, #69279, .T. ) ;
#671 = EDGE_CURVE ( 'NONE', #32456, #13048, #12924, .T. ) ;
#672 = ORIENTED_EDGE ( 'NONE', *, *, #46655, .T. ) ;
#673 = VERTEX_POINT ( 'NONE', #5723 ) ;
#675 = ORIENTED_EDGE ( 'NONE', *, *, #8517, .T. ) ;
#674 = CARTESIAN_POINT ( 'NONE',  ( 4.023698944407934519, -2.882441371585227063, 31.66841991370171527 ) ) ;
#676 = CARTESIAN_POINT ( 'NONE',  ( 10.39245839786846837, -12.39988816332205701, 30.74660775122750778 ) ) ;
#677 = DIRECTION ( 'NONE',  ( 0.000000000000000000, 1.000000000000000000, 0.000000000000000000 ) ) ;
#678 = CARTESIAN_POINT ( 'NONE',  ( -3.749999999999997335, -7.500000000000021316, 22.59375000000000355 ) ) ;
#679 = ORIENTED_EDGE ( 'NONE', *, *, #61599, .T. ) ;
#680 = EDGE_CURVE ( 'NONE', #18725, #44707, #22528, .T. ) ;
#681 = ORIENTED_EDGE ( 'NONE', *, *, #24672, .T. ) ;
#682 = CARTESIAN_POINT ( 'NONE',  ( 5.142067857642707018, -7.750023224968867197, 34.99404313364389907 ) ) ;
#683 = VERTEX_POINT ( 'NONE', #12485 ) ;
#684 = FACE_BOUND ( 'NONE', #47971, .T. ) ;
#685 = CARTESIAN_POINT ( 'NONE',  ( 3.230769230769108269, -2.657715359629662544, 31.77849191805970364 ) ) ;
#686 = DIRECTION ( 'NONE',  ( -0.000000000000000000, 1.000000000000000000, -0.000000000000000000 ) ) ;
#687 = ORIENTED_EDGE ( 'NONE', *, *, #60462, .T. ) ;
#688 = CARTESIAN_POINT ( 'NONE',  ( -6.700297381808512753, -5.114059244376869984, 34.14424750095245287 ) ) ;
#689 = CARTESIAN_POINT ( 'NONE',  ( -16.02332071561251325, -12.70449254468099198, 30.44128974285582956 ) ) ;
#690 = CARTESIAN_POINT ( 'NONE',  ( 8.899756207464417201, -8.630441415882550871, 34.87705825610312615 ) ) ;
#691 = PLANE ( 'NONE',  #60122 ) ;
#692 = CARTESIAN_POINT ( 'NONE',  ( -3.453696189676080053, -9.172386477786396597, 34.72672124145550043 ) ) ;
#693 = ORIENTED_EDGE ( 'NONE', *, *, #28396, .T. ) ;
#694 = B_SPLINE_CURVE_WITH_KNOTS ( 'NONE', 3,
 ( #37095, #16831, #71325, #9629, #64555, #46532, #25818, #73575, #37996, #12301 ),
 .UNSPECIFIED., .F., .F.,
 ( 4, 2, 2, 2, 4 ),
 ( 0.000000000000000000, 0.0001954311564186864949, 0.0003908623128373729899, 0.0005862934692560594577, 0.0007817246256747459798 ),
 .UNSPECIFIED. ) ;
#695 = VECTOR ( 'NONE', #44680, 1000.000000000000000 ) ;
#696 = CARTESIAN_POINT ( 'NONE',  ( 15.90384615384615330, -7.500000000000001776, 34.75000000000000000 ) ) ;
#697 = CARTESIAN_POINT ( 'NONE',  ( -5.933932666649925025, -3.937682226553329556, 33.60647404775216529 ) ) ;
#698 = CARTESIAN_POINT ( 'NONE',  ( 0.2115617305961062233, -11.79746400365624659, 32.30657167506340954 ) ) ;
#699 = CYLINDRICAL_SURFACE ( 'NONE', #86069, 0.2499999999999979738 ) ;
#700 = FACE_OUTER_BOUND ( 'NONE', #21142, .T. ) ;
#701 = EDGE_CURVE ( 'NONE', #47506, #74563, #43282, .T. ) ;
#702 = FACE_BOUND ( 'NONE', #7070, .T. ) ;
#704 = CARTESIAN_POINT ( 'NONE',  ( 16.40384615384757439, -7.500000000000154543, 35.00000000000007105 ) ) ;
#703 = CARTESIAN_POINT ( 'NONE',  ( 8.769230769230768274, -1.629998284177014645, 34.34916445242399163 ) ) ;
#705 = CARTESIAN_POINT ( 'NONE',  ( 5.326977496836529546, -9.233818618650603938, 34.70587769442853698 ) ) ;
#707 = CARTESIAN_POINT ( 'NONE',  ( -6.222926217516146608, -4.887634598454295265, 34.01352882383564946 ) ) ;
#706 = CARTESIAN_POINT ( 'NONE',  ( 3.512820512820510555, -3.499999999999999556, 29.75000000000000355 ) ) ;
#708 = ADVANCED_FACE ( 'NONE', ( #88171 ), #40412, .F. ) ;
#709 = LINE ( 'NONE', #20095, #66392 ) ;
#710 = CARTESIAN_POINT ( 'NONE',  ( -1.901340078031346525, -9.487747218494661183, 19.68563170625849068 ) ) ;
#711 = EDGE_LOOP ( 'NONE', ( #17027, #50438 ) ) ;
#712 = CARTESIAN_POINT ( 'NONE',  ( 1.254468175177162914, -12.27039167877662251, 31.24851455888617835 ) ) ;
#713 = EDGE_LOOP ( 'NONE', ( #36866, #45226, #35384, #85177 ) ) ;
#714 = CARTESIAN_POINT ( 'NONE',  ( -13.25408994638174320, -11.04252011169590020, 33.62494198852677130 ) ) ;
#715 = EDGE_CURVE ( 'NONE', #45738, #29450, #27327, .T. ) ;
#716 = ORIENTED_EDGE ( 'NONE', *, *, #29790, .F. ) ;
#717 = ADVANCED_FACE ( 'NONE', ( #61106 ), #88613, .F. ) ;
#718 = CARTESIAN_POINT ( 'NONE',  ( -11.28851612908349722, -6.653508905675592722, 34.93172785388651391 ) ) ;
#719 = LINE ( 'NONE', #86139, #25829 ) ;
#720 = VERTEX_POINT ( 'NONE', #73297 ) ;
#721 = CARTESIAN_POINT ( 'NONE',  ( -15.45425417449318317, -5.113361153441934093, 34.14387501736622710 ) ) ;
#722 = CARTESIAN_POINT ( 'NONE',  ( 1.987747218494664292, -9.401340078031346081, 19.37313170625848713 ) ) ;
#723 = DIRECTION ( 'NONE',  ( 1.000000000000000000, 0.000000000000000000, 0.000000000000000000 ) ) ;
#724 = DIRECTION ( 'NONE',  ( -0.000000000000000000, 0.5000000000000011102, -0.8660254037844381525 ) ) ;
#725 = CARTESIAN_POINT ( 'NONE',  ( 12.46153846153846168, -2.721908614388771852, 31.22303859784724978 ) ) ;
#726 = LINE ( 'NONE', #39956, #60282 ) ;
#727 = DIRECTION ( 'NONE',  ( -0.000000000000000000, -0.9848077530122085754, -0.1736481776669273613 ) ) ;
#728 = DIRECTION ( 'NONE',  ( -1.000000000000000000, -0.000000000000000000, -0.000000000000000000 ) ) ;
#729 = CARTESIAN_POINT ( 'NONE',  ( -0.06109907496450878162, -11.25000000000000000, 23.78311829374151998 ) ) ;
#730 = AXIS2_PLACEMENT_3D ( 'NONE', #16205, #11228, #78786 ) ;
#731 = CARTESIAN_POINT ( 'NONE',  ( -9.822454901745913958, -3.817052484675422797, 33.13202310037935661 ) ) ;
#732 = CARTESIAN_POINT ( 'NONE',  ( -14.30769230769230660, -12.48256725967547354, 35.29906147534542527 ) ) ;
#733 = EDGE_LOOP ( 'NONE', ( #34474, #45884, #50430, #8739 ) ) ;
#734 = CARTESIAN_POINT ( 'NONE',  ( -18.00000000000012079, -6.879047030192663392, 34.71129190930017927 ) ) ;
#735 = CARTESIAN_POINT ( 'NONE',  ( 2.694853999681185108, -4.891553140782077591, 23.31436829374150932 ) ) ;
#736 = AXIS2_PLACEMENT_3D ( 'NONE', #62957, #67314, #32632 ) ;
#738 = CARTESIAN_POINT ( 'NONE',  ( -16.15384615384627409, -12.51329471203414379, 31.30864560766407578 ) ) ;
#737 = B_SPLINE_CURVE_WITH_KNOTS ( 'NONE', 3,
 ( #7790, #54628, #21744, #13218, #6896, #62715 ),
 .UNSPECIFIED., .F., .F.,
 ( 4, 2, 4 ),
 ( 0.0003909569690057828153, 0.0005862646681846093912, 0.0007815723673634359129 ),
 .UNSPECIFIED. ) ;
#739 = CARTESIAN_POINT ( 'NONE',  ( -15.23076923076922995, -1.367168528481310208, 33.57946703557072254 ) ) ;
#740 = ORIENTED_EDGE ( 'NONE', *, *, #36232, .T. ) ;
#741 = CARTESIAN_POINT ( 'NONE',  ( 14.30769230769231015, -2.538708090699994813, 30.37095296980875503 ) ) ;
#742 = CARTESIAN_POINT ( 'NONE',  ( 16.40379156322419973, -2.589246495874658827, 31.60778113518102828 ) ) ;
#744 = ORIENTED_EDGE ( 'NONE', *, *, #2317, .F. ) ;
#743 = CARTESIAN_POINT ( 'NONE',  ( 4.023155550735845409, -9.084618155246140248, 34.75535874321725771 ) ) ;
#745 = CARTESIAN_POINT ( 'NONE',  ( -39.05038313613820122, -12.75000000000000178, 29.75000000000000355 ) ) ;
#746 = AXIS2_PLACEMENT_3D ( 'NONE', #34224, #7204, #34678 ) ;
#747 = CARTESIAN_POINT ( 'NONE',  ( 13.51540719244017374, -2.541949514083464479, 30.39797389878540557 ) ) ;
#748 = FACE_OUTER_BOUND ( 'NONE', #30218, .T. ) ;
#749 = CARTESIAN_POINT ( 'NONE',  ( 4.946231610255519051, -4.118384482072085184, 33.43331474514187107 ) ) ;
#750 = EDGE_CURVE ( 'NONE', #66274, #83278, #76626, .T. ) ;
#751 = CARTESIAN_POINT ( 'NONE',  ( 10.36540788444226102, -3.627789207965226748, 32.91389620160131102 ) ) ;
#752 = ORIENTED_EDGE ( 'NONE', *, *, #194, .T. ) ;
#753 = ORIENTED_EDGE ( 'NONE', *, *, #12775, .F. ) ;
#754 = ORIENTED_EDGE ( 'NONE', *, *, #69554, .T. ) ;
#755 = CARTESIAN_POINT ( 'NONE',  ( -9.561781990544128362, -3.285477652293413264, 32.44071101563363158 ) ) ;
#756 = LINE ( 'NONE', #28222, #84616 ) ;
#757 = CARTESIAN_POINT ( 'NONE',  ( -2.307692307692428724, -6.835583212225970762, 34.95778746994575670 ) ) ;
#758 = CARTESIAN_POINT ( 'NONE',  ( -6.923076923076922462, -10.51840700105979565, 33.73612834413961536 ) ) ;
#759 = EDGE_CURVE ( 'NONE', #21493, #48689, #46710, .T. ) ;
#760 = EDGE_CURVE ( 'NONE', #41806, #15172, #56192, .T. ) ;
#761 = ORIENTED_EDGE ( 'NONE', *, *, #66448, .F. ) ;
#762 = CARTESIAN_POINT ( 'NONE',  ( -17.20707028636129721, -4.460286881179643004, 33.72017969459903242 ) ) ;
#763 = VERTEX_POINT ( 'NONE', #78492 ) ;
#764 = ORIENTED_EDGE ( 'NONE', *, *, #17336, .F. ) ;
#765 = VERTEX_POINT ( 'NONE', #50578 ) ;
#767 = EDGE_LOOP ( 'NONE', ( #7918, #41144, #11280, #63000 ) ) ;
#766 = LINE ( 'NONE', #35889, #12781 ) ;
#768 = B_SPLINE_CURVE_WITH_KNOTS ( 'NONE', 3,
 ( #36697, #64149, #2452, #84894, #23180, #71354, #17764, #72247, #80360, #18658 ),
 .UNSPECIFIED., .F., .F.,
 ( 4, 2, 2, 2, 4 ),
 ( 0.000000000000000000, 0.0001954311564186861426, 0.0003908623128373722852, 0.0005862934692560583735, 0.0007817246256747445703 ),
 .UNSPECIFIED. ) ;
#769 = LINE ( 'NONE', #20160, #80481 ) ;
#770 = CARTESIAN_POINT ( 'NONE',  ( 6.065255139512839122, -2.657715359629131857, 31.77849191805844242 ) ) ;
#771 = EDGE_CURVE ( 'NONE', #85264, #19690, #69198, .T. ) ;
#772 = CARTESIAN_POINT ( 'NONE',  ( -3.230769230769351186, -4.481592998941358097, 33.73612834414048933 ) ) ;
#773 = FACE_OUTER_BOUND ( 'NONE', #14188, .T. ) ;
#774 = ORIENTED_EDGE ( 'NONE', *, *, #775, .F. ) ;
#775 = EDGE_CURVE ( 'NONE', #46484, #84195, #71288, .T. ) ;
#776 = ORIENTED_EDGE ( 'NONE', *, *, #15608, .T. ) ;
#777 = ORIENTED_EDGE ( 'NONE', *, *, #70790, .T. ) ;
#778 = CARTESIAN_POINT ( 'NONE',  ( -6.673022503163469565, -2.920487667080175154, 32.31805714834170828 ) ) ;
#780 = ORIENTED_EDGE ( 'NONE', *, *, #80659, .F. ) ;
#779 = CARTESIAN_POINT ( 'NONE',  ( -2.307692307692427391, -2.892918686052166066, 31.69288490824153470 ) ) ;
#781 = DIRECTION ( 'NONE',  ( -0.000000000000000000, -0.8660254037844397068, -0.4999999999999978906 ) ) ;
#782 = VECTOR ( 'NONE', #87590, 1000.000000000000114 ) ;
#783 = CARTESIAN_POINT ( 'NONE',  ( -2.307692307692305711, -4.945431358278436385, 36.03766855953609394 ) ) ;
#784 = ORIENTED_EDGE ( 'NONE', *, *, #41224, .F. ) ;
#785 = EDGE_CURVE ( 'NONE', #34790, #49709, #15373, .T. ) ;
#786 = CARTESIAN_POINT ( 'NONE',  ( -18.00000000000012079, -5.941354392335914447, 34.76329471203413846 ) ) ;
#787 = CARTESIAN_POINT ( 'NONE',  ( -39.05038313613820122, -2.249999999999998668, 29.75000000000000355 ) ) ;
#788 = ORIENTED_EDGE ( 'NONE', *, *, #10295, .T. ) ;
#789 = FACE_BOUND ( 'NONE', #47609, .T. ) ;
#791 = B_SPLINE_CURVE_WITH_KNOTS ( 'NONE', 3,
 ( #20855, #88459, #592, #54189, #81685, #19966, #34810, #40701, #68163, #62277 ),
 .UNSPECIFIED., .F., .F.,
 ( 4, 2, 2, 2, 4 ),
 ( 0.0007817359430256315238, 0.0009771253907249980580, 0.001172514838424364592, 0.001367904286123730910, 0.001563293733823097444 ),
 .UNSPECIFIED. ) ;
#790 = CARTESIAN_POINT ( 'NONE',  ( -11.78843828251013015, -11.47974371597208076, 33.17467449705390692 ) ) ;
#792 = CARTESIAN_POINT ( 'NONE',  ( -18.75000000000000000, -4.000000000000000000, 29.75000000000000355 ) ) ;
#793 = CARTESIAN_POINT ( 'NONE',  ( -9.692307692307691624, -10.67929555188718282, 33.92786785259544047 ) ) ;
#795 = CARTESIAN_POINT ( 'NONE',  ( 4.853996859406926490, -9.886141570436013382, 34.14413921362392301 ) ) ;
#794 = DIRECTION ( 'NONE',  ( -0.000000000000000000, 0.6427876096865404731, -0.7660444431189770143 ) ) ;
#796 = CARTESIAN_POINT ( 'NONE',  ( -3.165514091256391271, -3.643525952247864463, 33.31231777344670064 ) ) ;
#797 = CARTESIAN_POINT ( 'NONE',  ( -4.219928533206287469, -10.67929555188718460, 33.92786785259543336 ) ) ;
#798 = VERTEX_POINT ( 'NONE', #3277 ) ;
#799 = CARTESIAN_POINT ( 'NONE',  ( 14.53047184896071542, -12.44528174975671853, 30.48912976160716681 ) ) ;
#800 = VECTOR ( 'NONE', #28708, 1000.000000000000114 ) ;
#801 = DIRECTION ( 'NONE',  ( -0.000000000000000000, -0.000000000000000000, -1.000000000000000000 ) ) ;
#802 = ORIENTED_EDGE ( 'NONE', *, *, #42651, .F. ) ;
#803 = CYLINDRICAL_SURFACE ( 'NONE', #41598, 0.2499999999999994726 ) ;
#804 = CARTESIAN_POINT ( 'NONE',  ( -7.623374177175779032, -2.353885683473779800, 30.79025554430704403 ) ) ;
#805 = EDGE_LOOP ( 'NONE', ( #48407, #3484, #58265, #43843 ) ) ;
#806 = CYLINDRICAL_SURFACE ( 'NONE', #26995, 0.2499999999999994726 ) ;
#807 = CARTESIAN_POINT ( 'NONE',  ( -10.61538461538461320, -1.790695186598648903, 34.54067556320373455 ) ) ;
#808 = ADVANCED_FACE ( 'NONE', ( #44245 ), #41733, .F. ) ;
#809 = FACE_BOUND ( 'NONE', #1125, .T. ) ;
#811 = DIRECTION ( 'NONE',  ( 1.000000000000000000, 0.000000000000000000, 0.000000000000000000 ) ) ;
#810 = CYLINDRICAL_SURFACE ( 'NONE', #50418, 0.2500000000000009437 ) ;
#812 = CARTESIAN_POINT ( 'NONE',  ( 3.480714749117371998, -8.433404298154334455, 34.66254593164985920 ) ) ;
#813 = CARTESIAN_POINT ( 'NONE',  ( -16.15384615384627409, -2.625532179533778709, 30.86335684631627174 ) ) ;
#815 = CARTESIAN_POINT ( 'NONE',  ( 6.989145274079363368, -12.37446782046654192, 30.86335684631486842 ) ) ;
#814 = CARTESIAN_POINT ( 'NONE',  ( 0.000000000000000000, 14.50000000000000533, 1.499999999999997780 ) ) ;
#816 = CARTESIAN_POINT ( 'NONE',  ( -2.307692307692305711, -2.538708090699994813, 30.37095296980875503 ) ) ;
#817 = CARTESIAN_POINT ( 'NONE',  ( -3.749999999999996447, -7.561099074964554134, 17.34188170625849068 ) ) ;
#818 = EDGE_LOOP ( 'NONE', ( #13516, #54259, #65486, #44692 ) ) ;
#819 = EDGE_CURVE ( 'NONE', #85855, #5133, #61991, .T. ) ;
#820 = VERTEX_POINT ( 'NONE', #30316 ) ;
#821 = CARTESIAN_POINT ( 'NONE',  ( -9.692307692307691624, -2.292212530054420494, 30.41441678777542634 ) ) ;
#822 = VECTOR ( 'NONE', #47003, 1000.000000000000000 ) ;
#823 = EDGE_CURVE ( 'NONE', #22055, #5633, #71733, .T. ) ;
#824 = CARTESIAN_POINT ( 'NONE',  ( 14.55774672760575861, -12.65882529074907126, 30.72640787790839312 ) ) ;
#825 = CARTESIAN_POINT ( 'NONE',  ( 14.55763771707035303, -9.357781135181031829, 34.66075350412533851 ) ) ;
#826 = CARTESIAN_POINT ( 'NONE',  ( 8.519230769230768274, -2.249999999999998668, 29.75000000000000355 ) ) ;
#827 = CARTESIAN_POINT ( 'NONE',  ( -13.31936024510254590, -2.657715359629131857, 31.77849191805844242 ) ) ;
#828 = CARTESIAN_POINT ( 'NONE',  ( 0.06109907496455496689, -11.24999999999999822, 15.77938170625848890 ) ) ;
#829 = CARTESIAN_POINT ( 'NONE',  ( 6.856994543716785628, -2.292212530054419606, 30.41441678777542634 ) ) ;
#830 = CYLINDRICAL_SURFACE ( 'NONE', #73375, 0.2499999999999973355 ) ;
#831 = VECTOR ( 'NONE', #8380, 999.9999999999998863 ) ;
#832 = CARTESIAN_POINT ( 'NONE',  ( 16.81410256410256565, -3.499999999999999556, 29.75000000000000355 ) ) ;
#833 = CARTESIAN_POINT ( 'NONE',  ( -0.4615384615384611200, -10.51840700105979565, 33.73612834413961536 ) ) ;
#834 = DIRECTION ( 'NONE',  ( 0.000000000000000000, -1.000000000000000000, -0.000000000000000000 ) ) ;
#835 = LINE ( 'NONE', #62090, #39737 ) ;
#836 = CARTESIAN_POINT ( 'NONE',  ( -9.757577692864012775, -12.70778746994557551, 30.41441678777548319 ) ) ;
#837 = CARTESIAN_POINT ( 'NONE',  ( -14.05774678934416499, -3.202959910592335646, 32.30730279482227019 ) ) ;
#838 = CARTESIAN_POINT ( 'NONE',  ( -17.78205128205128105, -3.499999999999999556, 29.75000000000000355 ) ) ;
#839 = EDGE_CURVE ( 'NONE', #4529, #49069, #7942, .T. ) ;
#840 = ORIENTED_EDGE ( 'NONE', *, *, #396, .T. ) ;
#841 = LINE ( 'NONE', #21553, #59983 ) ;
#842 = CARTESIAN_POINT ( 'NONE',  ( -0.4615384615384611200, -3.886160181151819604, 36.00935417666054406 ) ) ;
#843 = CARTESIAN_POINT ( 'NONE',  ( -2.749999999999999112, -7.438900925035484057, 22.84561829374151642 ) ) ;
#844 = CARTESIAN_POINT ( 'NONE',  ( -5.749945580086545327, -12.41089969410671223, 31.60739465890703670 ) ) ;
#845 = CARTESIAN_POINT ( 'NONE',  ( -11.53846153846165912, -4.481592998941358097, 33.73612834414048933 ) ) ;
#846 = ORIENTED_EDGE ( 'NONE', *, *, #33882, .T. ) ;
#847 = EDGE_CURVE ( 'NONE', #31771, #32696, #72861, .T. ) ;
#848 = CARTESIAN_POINT ( 'NONE',  ( 10.61538461538492406, -2.506253911140615021, 30.00000000000323297 ) ) ;
#850 = ORIENTED_EDGE ( 'NONE', *, *, #41234, .F. ) ;
#849 = CARTESIAN_POINT ( 'NONE',  ( -1.161835843346973984, -4.387253974876678342, 33.66317474335728832 ) ) ;
#851 = CARTESIAN_POINT ( 'NONE',  ( 20.00000000000000000, -3.499999999999999556, 29.75000000000000355 ) ) ;
#852 = CARTESIAN_POINT ( 'NONE',  ( -9.442362282929648742, -5.766571408460171355, 34.70601412856602508 ) ) ;
#853 = ORIENTED_EDGE ( 'NONE', *, *, #48241, .F. ) ;
#854 = CARTESIAN_POINT ( 'NONE',  ( -13.25408968285182176, -2.619367082507849442, 30.83698974864643461 ) ) ;
#855 = FACE_OUTER_BOUND ( 'NONE', #52842, .T. ) ;
#856 = VERTEX_POINT ( 'NONE', #42182 ) ;
#857 = LINE ( 'NONE', #49041, #17570 ) ;
#858 = EDGE_CURVE ( 'NONE', #40515, #5216, #48469, .T. ) ;
#859 = LINE ( 'NONE', #33327, #83953 ) ;
#860 = LINE ( 'NONE', #69327, #48492 ) ;
#861 = VERTEX_POINT ( 'NONE', #2824 ) ;
#862 = ORIENTED_EDGE ( 'NONE', *, *, #13935, .F. ) ;
#863 = CARTESIAN_POINT ( 'NONE',  ( -6.673131513698878692, -8.476813868363244353, 34.90874843262270133 ) ) ;
#864 = EDGE_CURVE ( 'NONE', #87613, #38306, #6742, .T. ) ;
#865 = ORIENTED_EDGE ( 'NONE', *, *, #66693, .F. ) ;
#866 = EDGE_CURVE ( 'NONE', #87922, #72293, #29882, .T. ) ;
#867 = CARTESIAN_POINT ( 'NONE',  ( 4.153846153846032507, -6.879047030192662504, 34.71129190930017927 ) ) ;
#868 = CARTESIAN_POINT ( 'NONE',  ( -7.173100147298380413, -2.341070481393820124, 30.72580821765574299 ) ) ;
#869 = CARTESIAN_POINT ( 'NONE',  ( -5.869209559033048862, -5.496552790871117367, 34.60292014791297532 ) ) ;
#870 = DIRECTION ( 'NONE',  ( -0.000000000000000000, -0.1736481776669307198, -0.9848077530122080203 ) ) ;
#871 = CARTESIAN_POINT ( 'NONE',  ( 8.769230769230768274, -13.75783147151868846, 33.36296068462461051 ) ) ;
#872 = B_SPLINE_CURVE_WITH_KNOTS ( 'NONE', 3,
 ( #45408, #38215, #52164, #73342, #87320, #11646, #25597, #32799, #79654, #17954 ),
 .UNSPECIFIED., .F., .F.,
 ( 4, 2, 2, 2, 4 ),
 ( 0.0007817246256747469556, 0.0009771112852218896347, 0.001172497944769032531, 0.001367884604316175427, 0.001563271263863318106 ),
 .UNSPECIFIED. ) ;
#873 = CARTESIAN_POINT ( 'NONE',  ( 0.6845015958051353655, -7.369474539155827841, 34.99858011523955525 ) ) ;
#874 = EDGE_CURVE ( 'NONE', #18726, #10877, #86197, .T. ) ;
#875 = CARTESIAN_POINT ( 'NONE',  ( 3.165499230212911019, -10.33852847137145048, 34.16647553114627556 ) ) ;
#876 = ORIENTED_EDGE ( 'NONE', *, *, #18715, .F. ) ;
#877 = ORIENTED_EDGE ( 'NONE', *, *, #70211, .T. ) ;
#879 = VERTEX_POINT ( 'NONE', #51895 ) ;
#878 = CARTESIAN_POINT ( 'NONE',  ( 4.153846153846154188, -8.164416787775445883, 34.95778746994557906 ) ) ;
#880 = CARTESIAN_POINT ( 'NONE',  ( 7.780071466793709867, -2.486705287966279432, 31.30864560766542937 ) ) ;
#881 = ORIENTED_EDGE ( 'NONE', *, *, #4862, .F. ) ;
#882 = VECTOR ( 'NONE', #7598, 1000.000000000000000 ) ;
#883 = CARTESIAN_POINT ( 'NONE',  ( -4.153846153846152411, -7.500000000000001776, 35.04278698407183867 ) ) ;
#884 = CARTESIAN_POINT ( 'NONE',  ( 6.700149964170072359, -9.172386477786396597, 34.72672124145550043 ) ) ;
#885 = ORIENTED_EDGE ( 'NONE', *, *, #13025, .T. ) ;
#886 = EDGE_CURVE ( 'NONE', #67642, #25620, #63682, .T. ) ;
#887 = DIRECTION ( 'NONE',  ( 0.000000000000000000, 0.3420201433256641055, -0.9396926207859100932 ) ) ;
#888 = VECTOR ( 'NONE', #63429, 1000.000000000000000 ) ;
#889 = ORIENTED_EDGE ( 'NONE', *, *, #12602, .F. ) ;
#891 = ORIENTED_EDGE ( 'NONE', *, *, #87975, .T. ) ;
#890 = CARTESIAN_POINT ( 'NONE',  ( -16.40386939113911779, -3.711651800289232916, 33.01384336483936011 ) ) ;
#892 = DIRECTION ( 'NONE',  ( 0.000000000000000000, -6.938893903907222067E-15, 1.000000000000000000 ) ) ;
#893 = EDGE_LOOP ( 'NONE', ( #12164, #44683, #39104, #42360 ) ) ;
#894 = CARTESIAN_POINT ( 'NONE',  ( 14.98074600654777377, -2.341070481393819236, 30.72580821765574299 ) ) ;
#895 = CARTESIAN_POINT ( 'NONE',  ( -4.403869378067608586, -6.652501968072646932, 34.93155406624980941 ) ) ;
#896 = FACE_BOUND ( 'NONE', #56374, .T. ) ;
#897 = B_SPLINE_CURVE_WITH_KNOTS ( 'NONE', 3,
 ( #11961, #39439, #33563, #60574, #74102, #68664, #12395, #60128, #5634, #88091 ),
 .UNSPECIFIED., .F., .F.,
 ( 4, 2, 2, 2, 4 ),
 ( 0.0007817359430256319575, 0.0009771253907249984917, 0.001172514838424365026, 0.001367904286123731343, 0.001563293733823097878 ),
 .UNSPECIFIED. ) ;
#898 = CYLINDRICAL_SURFACE ( 'NONE', #57135, 0.2499999999999993616 ) ;
#899 = DIRECTION ( 'NONE',  ( -0.000000000000000000, -0.8660254037844399289, -0.4999999999999980016 ) ) ;
#900 = CARTESIAN_POINT ( 'NONE',  ( 4.153846153846032507, -12.46129190930018460, 30.37095296980731973 ) ) ;
#901 = B_SPLINE_CURVE_WITH_KNOTS ( 'NONE', 3,
 ( #47578, #67414, #60646, #88158, #38609, #59318, #86825, #25091, #49794, #1167 ),
 .UNSPECIFIED., .F., .F.,
 ( 4, 2, 2, 2, 4 ),
 ( 0.0007817359430256390048, 0.0009771253907250075990, 0.001172514838424376085, 0.001367904286123744571, 0.001563293733823113056 ),
 .UNSPECIFIED. ) ;
#902 = CARTESIAN_POINT ( 'NONE',  ( 0.7115384615384748868, -2.249999999999999112, 29.81603969181031033 ) ) ;
#903 = CARTESIAN_POINT ( 'NONE',  ( -17.14300545628321260, -8.164416787775445883, 34.95778746994557906 ) ) ;
#904 = DIRECTION ( 'NONE',  ( -0.000000000000000000, 0.5000000000000011102, -0.8660254037844380415 ) ) ;
#905 = EDGE_LOOP ( 'NONE', ( #32769, #30107, #48312, #37232 ) ) ;
#906 = CARTESIAN_POINT ( 'NONE',  ( -14.17716660592874334, -3.816742781228458004, 33.13167719472716044 ) ) ;
#907 = ORIENTED_EDGE ( 'NONE', *, *, #15104, .T. ) ;
#908 = ORIENTED_EDGE ( 'NONE', *, *, #77155, .T. ) ;
#910 = DIRECTION ( 'NONE',  ( 0.000000000000000000, 0.4999999999999960032, -0.8660254037844410391 ) ) ;
#909 = CARTESIAN_POINT ( 'NONE',  ( -5.198717948717948012, -7.500000000000000000, 33.75000000000000000 ) ) ;
#911 = LINE ( 'NONE', #28379, #24043 ) ;
#912 = CARTESIAN_POINT ( 'NONE',  ( -16.94613263595612906, -9.929761469519743144, 34.40412654351204225 ) ) ;
#913 = CARTESIAN_POINT ( 'NONE',  ( 19.99999999999997513, -14.99999999999999467, 3.000000000000000888 ) ) ;
#914 = CARTESIAN_POINT ( 'NONE',  ( -12.21148404162500967, -4.818054556918156983, 34.26375889529406749 ) ) ;
#915 = ORIENTED_EDGE ( 'NONE', *, *, #33523, .T. ) ;
#916 = AXIS2_PLACEMENT_3D ( 'NONE', #41610, #74963, #69079 ) ;
#917 = CYLINDRICAL_SURFACE ( 'NONE', #15586, 0.2500000000000002220 ) ;
#918 = CARTESIAN_POINT ( 'NONE',  ( 3.230769230769231726, -11.16473453929635440, 33.15142922261926373 ) ) ;
#919 = CARTESIAN_POINT ( 'NONE',  ( 16.82689985270161870, -4.175268141568689195, 33.81360843649122216 ) ) ;
#920 = DIRECTION ( 'NONE',  ( -0.000000000000000000, 0.6427876096865404731, -0.7660444431189770143 ) ) ;
#921 = DIRECTION ( 'NONE',  ( 0.000000000000000000, 0.3420201433256641055, -0.9396926207859100932 ) ) ;
#922 = VERTEX_POINT ( 'NONE', #31648 ) ;
#923 = ADVANCED_BREP_SHAPE_REPRESENTATION ( '', ( #28293, #83448 ), #70522 ) ;
#924 = ORIENTED_EDGE ( 'NONE', *, *, #46404, .T. ) ;
#925 = EDGE_CURVE ( 'NONE', #39506, #47746, #87062, .T. ) ;
#926 = ORIENTED_EDGE ( 'NONE', *, *, #25814, .T. ) ;
#927 = CARTESIAN_POINT ( 'NONE',  ( -6.989160334032802346, -8.120952969808774569, 34.71129190930000163 ) ) ;
#929 = ORIENTED_EDGE ( 'NONE', *, *, #6810, .F. ) ;
#928 = ADVANCED_FACE ( 'NONE', ( #44697 ), #65861, .F. ) ;
#930 = CARTESIAN_POINT ( 'NONE',  ( -6.923076923076922462, -4.786620604624113540, 33.94971097300155094 ) ) ;
#931 = CARTESIAN_POINT ( 'NONE',  ( -11.53846153846153655, -2.249999999999998668, 29.75000000000001776 ) ) ;
#932 = DIRECTION ( 'NONE',  ( -0.000000000000000000, 0.9396926207859093161, -0.3420201433256662704 ) ) ;
#933 = CARTESIAN_POINT ( 'NONE',  ( -2.651650429449565305, -4.848349570550461785, 14.00000000000000000 ) ) ;
#934 = CARTESIAN_POINT ( 'NONE',  ( 9.823099500132483897, -5.582136614379148654, 34.36778462344220486 ) ) ;
#935 = ORIENTED_EDGE ( 'NONE', *, *, #44196, .T. ) ;
#936 = EDGE_CURVE ( 'NONE', #4757, #82729, #32582, .T. ) ;
#937 = CARTESIAN_POINT ( 'NONE',  ( 4.377221639618572802, -2.251407671071270489, 29.88021292934942252 ) ) ;
#939 = ORIENTED_EDGE ( 'NONE', *, *, #22476, .F. ) ;
#938 = DIRECTION ( 'NONE',  ( 0.000000000000000000, 0.000000000000000000, -1.000000000000000000 ) ) ;
#940 = CYLINDRICAL_SURFACE ( 'NONE', #5295, 4.000000000000000000 ) ;
#941 = CARTESIAN_POINT ( 'NONE',  ( 3.100077764101673239, -12.38065189839062263, 30.83690757178629482 ) ) ;
#942 = CARTESIAN_POINT ( 'NONE',  ( 16.82689983963011926, -3.711651800289232916, 33.01384336483936011 ) ) ;
#943 = CARTESIAN_POINT ( 'NONE',  ( -2.557715531913763218, -12.68155406624981119, 30.59749803192733708 ) ) ;
#944 = CARTESIAN_POINT ( 'NONE',  ( -9.692307692307691624, -12.34228464037088635, 31.77849191805839268 ) ) ;
#945 = CARTESIAN_POINT ( 'NONE',  ( -3.453696189676077832, -10.77366814457252175, 33.85459836347579454 ) ) ;
#946 = FACE_OUTER_BOUND ( 'NONE', #27174, .T. ) ;
#947 = ADVANCED_FACE ( 'NONE', ( #86160 ), #59111, .F. ) ;
#948 = CARTESIAN_POINT ( 'NONE',  ( 1.492201783934598236, -11.27530806549875031, 14.95499329374151642 ) ) ;
#949 = VERTEX_POINT ( 'NONE', #24881 ) ;
#950 = CARTESIAN_POINT ( 'NONE',  ( -4.826923076923015365, -7.434744860731433924, 35.00000000000000711 ) ) ;
#951 = CARTESIAN_POINT ( 'NONE',  ( -1.319360245102545681, -3.643525952247864463, 33.31231777344670064 ) ) ;
#952 = CARTESIAN_POINT ( 'NONE',  ( 8.096099364501988305, -2.587454068350147907, 30.68340429815432202 ) ) ;
#954 = CARTESIAN_POINT ( 'NONE',  ( -7.780898706641007578, -3.083524468853784839, 32.58852847137153930 ) ) ;
#953 = VECTOR ( 'NONE', #29326, 1000.000000000000114 ) ;
#955 = VERTEX_POINT ( 'NONE', #59557 ) ;
#956 = CARTESIAN_POINT ( 'NONE',  ( 1.799775606325937360E-14, -10.25000000000000000, 14.78125000000000178 ) ) ;
#957 = CARTESIAN_POINT ( 'NONE',  ( -3.230769230769229949, -10.51840700105979565, 33.73612834413961536 ) ) ;
#958 = B_SPLINE_CURVE_WITH_KNOTS ( 'NONE', 3,
 ( #11696, #32846, #18003, #72041, #52661, #10351, #45458, #65284, #31508, #26090 ),
 .UNSPECIFIED., .F., .F.,
 ( 4, 2, 2, 2, 4 ),
 ( 0.000000000000000000, 0.0001954339857564078809, 0.0003908679715128157619, 0.0005863019572692236428, 0.0007817359430256315238 ),
 .UNSPECIFIED. ) ;
#959 = AXIS2_PLACEMENT_3D ( 'NONE', #1082, #49271, #73543 ) ;
#960 = CARTESIAN_POINT ( 'NONE',  ( 8.769230769230768274, -13.37000171582298513, 34.34916445242398453 ) ) ;
#961 = DIRECTION ( 'NONE',  ( 0.000000000000000000, 0.9396926207859126468, -0.3420201433256571111 ) ) ;
#962 = ORIENTED_EDGE ( 'NONE', *, *, #41239, .F. ) ;
#963 = PRODUCT ( 'Ultra-Thin Hypoallergenic Micro-Foil Screen', 'Ultra-Thin Hypoallergenic Micro-Foil Screen', '', ( #87462 ) ) ;
#964 = DIRECTION ( 'NONE',  ( -0.000000000000000000, 1.000000000000000000, 3.491481338843133355E-15 ) ) ;
#965 = VECTOR ( 'NONE', #65719, 1000.000000000000000 ) ;
#966 = CARTESIAN_POINT ( 'NONE',  ( 7.846153846153725020, -6.026961402154118019, 34.52809138561165270 ) ) ;
#967 = LINE ( 'NONE', #54571, #72315 ) ;
#968 = ORIENTED_EDGE ( 'NONE', *, *, #4573, .F. ) ;
#969 = CARTESIAN_POINT ( 'NONE',  ( -6.673022503163470454, -6.523592122091591783, 34.90882529074906415 ) ) ;
#970 = EDGE_CURVE ( 'NONE', #1945, #59177, #85244, .T. ) ;
#971 = EDGE_LOOP ( 'NONE', ( #65571, #72867 ) ) ;
#972 = DIRECTION ( 'NONE',  ( -0.000000000000000000, 1.000000000000000000, -0.000000000000000000 ) ) ;
#973 = CARTESIAN_POINT ( 'NONE',  ( -3.930883250284669117, -7.369474270740069777, 34.74850911626239736 ) ) ;
#974 = ORIENTED_EDGE ( 'NONE', *, *, #27473, .F. ) ;
#975 = CARTESIAN_POINT ( 'NONE',  ( -17.77722033102192967, -10.23759521482555535, 34.22997729860117033 ) ) ;
#976 = CARTESIAN_POINT ( 'NONE',  ( -24.00000000000000000, 5.000000000000023093, 29.24999999999999645 ) ) ;
#977 = CARTESIAN_POINT ( 'NONE',  ( -11.66860874789976066, -6.852621066184266141, 34.70813303252209181 ) ) ;
#978 = ADVANCED_FACE ( 'NONE', ( #52797 ), #80287, .F. ) ;
#979 = B_SPLINE_CURVE_WITH_KNOTS ( 'NONE', 3,
 ( #36155, #56847, #63605, #84343, #22618, #70821, #15880, #43342, #64040, #2337 ),
 .UNSPECIFIED., .F., .F.,
 ( 4, 2, 2, 2, 4 ),
 ( 0.0007817359430256369448, 0.0009771253907250049969, 0.001172514838424373049, 0.001367904286123741101, 0.001563293733823109153 ),
 .UNSPECIFIED. ) ;
#980 = DIRECTION ( 'NONE',  ( -0.000000000000000000, 0.6427876096865404731, -0.7660444431189770143 ) ) ;
#981 = CARTESIAN_POINT ( 'NONE',  ( -10.03846153846153832, -4.000000000000000000, 29.25000000000000000 ) ) ;
#982 = B_SPLINE_CURVE_WITH_KNOTS ( 'NONE', 3,
 ( #17469, #52571, #25998, #19248, #5727, #12489, #26450, #59334, #38175, #3935 ),
 .UNSPECIFIED., .F., .F.,
 ( 4, 2, 2, 2, 4 ),
 ( 0.0007817246256747445703, 0.0009771112852218872494, 0.001172497944769030145, 0.001367884604316172825, 0.001563271263863315504 ),
 .UNSPECIFIED. ) ;
#983 = VECTOR ( 'NONE', #76955, 1000.000000000000114 ) ;
#984 = EDGE_CURVE ( 'NONE', #16925, #51011, #66763, .T. ) ;
#985 = ORIENTED_EDGE ( 'NONE', *, *, #59724, .T. ) ;
#987 = EDGE_LOOP ( 'NONE', ( #37352, #22515, #57564, #42926 ) ) ;
#986 = EDGE_CURVE ( 'NONE', #67360, #34311, #25781, .T. ) ;
#988 = FACE_BOUND ( 'NONE', #42867, .T. ) ;
#989 = EDGE_LOOP ( 'NONE', ( #83458, #29915 ) ) ;
#990 = DIRECTION ( 'NONE',  ( -0.000000000000000000, 0.8660254037844397068, -0.4999999999999978906 ) ) ;
#991 = CARTESIAN_POINT ( 'NONE',  ( 4.403791672194296680, -11.86320923018887541, 32.19269448109604781 ) ) ;
#992 = VECTOR ( 'NONE', #4402, 1000.000000000000000 ) ;
#993 = FACE_OUTER_BOUND ( 'NONE', #69056, .T. ) ;
#994 = CARTESIAN_POINT ( 'NONE',  ( -16.15384615384615330, -2.708943851104267164, 35.45975837776705220 ) ) ;
#995 = EDGE_CURVE ( 'NONE', #22351, #45196, #30345, .T. ) ;
#996 = ORIENTED_EDGE ( 'NONE', *, *, #82380, .F. ) ;
#997 = EDGE_LOOP ( 'NONE', ( #81985, #73221, #79489, #65801 ) ) ;
#998 = VERTEX_POINT ( 'NONE', #41961 ) ;
#999 = CYLINDRICAL_SURFACE ( 'NONE', #7439, 0.2499999999999998890 ) ;
#1000 = ADVANCED_FACE ( 'NONE', ( #68534 ), #20790, .F. ) ;
#1002 = VERTEX_POINT ( 'NONE', #13154 ) ;
#1001 = EDGE_CURVE ( 'NONE', #61364, #13048, #34667, .T. ) ;
#1003 = DIRECTION ( 'NONE',  ( -0.000000000000000000, 0.3420201433256694901, -0.9396926207859082059 ) ) ;
#1004 = CARTESIAN_POINT ( 'NONE',  ( -11.78848476268299628, -5.765609946408404518, 34.70566812827425451 ) ) ;
#1005 = EDGE_CURVE ( 'NONE', #29769, #31113, #19901, .T. ) ;
#1006 = CARTESIAN_POINT ( 'NONE',  ( -4.480769230769229061, -4.000000000000000000, 29.75000000000000355 ) ) ;
#1007 = DIRECTION ( 'NONE',  ( -0.000000000000000000, 0.8660254037844399289, -0.4999999999999980016 ) ) ;
#1008 = CARTESIAN_POINT ( 'NONE',  ( -15.23076923076935252, -3.643525952248795718, 33.31231777344771672 ) ) ;
#1009 = CARTESIAN_POINT ( 'NONE',  ( 2.307692307692309264, -2.249999999999998668, 29.75000000000001776 ) ) ;
#1010 = CARTESIAN_POINT ( 'NONE',  ( 11.66925334628632527, -8.147973898785416225, 34.70805048591653730 ) ) ;
#1011 = ORIENTED_EDGE ( 'NONE', *, *, #79161, .T. ) ;
#1012 = VERTEX_POINT ( 'NONE', #48701 ) ;
#1013 = EDGE_LOOP ( 'NONE', ( #6290, #11618, #80010, #73134 ) ) ;
#1014 = DIRECTION ( 'NONE',  ( -0.000000000000000000, -0.1736481776669307198, -0.9848077530122080203 ) ) ;
#1016 = CARTESIAN_POINT ( 'NONE',  ( 10.68064018666064285, -6.879047030191282275, 34.71129190930002295 ) ) ;
#1015 = CARTESIAN_POINT ( 'NONE',  ( -3.007989561791163613, -10.23759521482555357, 34.22997729860117033 ) ) ;
#1017 = CARTESIAN_POINT ( 'NONE',  ( -18.00000000000000000, -5.471508081941599322, 34.59228464037088457 ) ) ;
#1018 = CARTESIAN_POINT ( 'NONE',  ( -3.360916440207448286, -11.47017969459903952, 32.78971311882034456 ) ) ;
#1019 = FACE_BOUND ( 'NONE', #24352, .T. ) ;
#1020 = CARTESIAN_POINT ( 'NONE',  ( 8.545745844666436497, -10.97335522853832579, 33.68706563782419749 ) ) ;
#1021 = ORIENTED_EDGE ( 'NONE', *, *, #63505, .T. ) ;
#1022 = CARTESIAN_POINT ( 'NONE',  ( 17.07692307692295586, -10.90142922262034020, 33.41473453929536674 ) ) ;
#1023 = CIRCLE ( 'NONE', #35556, 4.755951259987792668 ) ;
#1024 = DIRECTION ( 'NONE',  ( -0.000000000000000000, -0.000000000000000000, -1.000000000000000000 ) ) ;
#1025 = LINE ( 'NONE', #61828, #73513 ) ;
#1026 = CARTESIAN_POINT ( 'NONE',  ( 3.361559671736183752, -11.37503395064541678, 33.29242100308974983 ) ) ;
#1027 = ORIENTED_EDGE ( 'NONE', *, *, #76304, .F. ) ;
#1028 = CARTESIAN_POINT ( 'NONE',  ( 6.223012844093395834, -10.77377354290276301, 33.85451476688484718 ) ) ;
#1029 = ORIENTED_EDGE ( 'NONE', *, *, #8831, .T. ) ;
#1030 = FACE_BOUND ( 'NONE', #47160, .T. ) ;
#1031 = ADVANCED_FACE ( 'NONE', ( #5959 ), #53690, .T. ) ;
#1032 = DIRECTION ( 'NONE',  ( -0.000000000000000000, -0.7660444431189791237, -0.6427876096865379196 ) ) ;
#1033 = DIRECTION ( 'NONE',  ( -0.000000000000000000, -0.1736481776669307198, -0.9848077530122080203 ) ) ;
#1034 = CARTESIAN_POINT ( 'NONE',  ( -3.099977422944443894, -8.147973898785416225, 34.70805048591653730 ) ) ;
#1035 = ORIENTED_EDGE ( 'NONE', *, *, #39496, .T. ) ;
#1036 = DIRECTION ( 'NONE',  ( 0.000000000000000000, 0.000000000000000000, -1.000000000000000000 ) ) ;
#1037 = CARTESIAN_POINT ( 'NONE',  ( -5.749945580086545327, -9.233818618650603938, 34.70587769442853698 ) ) ;
#1038 = CARTESIAN_POINT ( 'NONE',  ( -9.692307692307691624, -3.050289026998446396, 32.03036669348365706 ) ) ;
#1039 = CARTESIAN_POINT ( 'NONE',  ( -4.826977667545033768, -5.766571408460171355, 34.70601412856602508 ) ) ;
#1040 = EDGE_LOOP ( 'NONE', ( #39631, #21106 ) ) ;
#1041 = B_SPLINE_CURVE_WITH_KNOTS ( 'NONE', 3,
 ( #44749, #72230, #85313, #10539, #65477, #59160, #51950, #86215, #86667, #24931 ),
 .UNSPECIFIED., .F., .F.,
 ( 4, 2, 2, 2, 4 ),
 ( 0.000000000000000000, 0.0001954311564186863323, 0.0003908623128373726646, 0.0005862934692560590241, 0.0007817246256747453293 ),
 .UNSPECIFIED. ) ;
#1042 = CARTESIAN_POINT ( 'NONE',  ( 16.40379167219429490, -10.76462480002816413, 33.53768742498949962 ) ) ;
#1043 = ORIENTED_EDGE ( 'NONE', *, *, #60668, .F. ) ;
#1044 = ADVANCED_FACE ( 'NONE', ( #6406 ), #74411, .F. ) ;
#1046 = VERTEX_POINT ( 'NONE', #41070 ) ;
#1045 = CARTESIAN_POINT ( 'NONE',  ( -7.846153846153844924, -13.20930481340135110, 34.54067556320372745 ) ) ;
#1047 = CARTESIAN_POINT ( 'NONE',  ( 7.715462379486291766, -10.54014554554150607, 33.71984207302941883 ) ) ;
#1048 = CARTESIAN_POINT ( 'NONE',  ( -6.700297381808511865, -11.89424750095246175, 32.13594075562311758 ) ) ;
#1049 = DIRECTION ( 'NONE',  ( -0.000000000000000000, 1.000000000000000000, 3.491481338843133355E-15 ) ) ;
#1050 = CARTESIAN_POINT ( 'NONE',  ( 23.49999999999999645, 1.250000000000003775, 28.00000000000000000 ) ) ;
#1051 = VECTOR ( 'NONE', #75352, 1000.000000000000000 ) ;
#1052 = CARTESIAN_POINT ( 'NONE',  ( 9.692307692307572609, -9.442884908241554243, 34.35708131394783038 ) ) ;
#1054 = CARTESIAN_POINT ( 'NONE',  ( 16.40390046548447245, -5.728107161865375829, 34.42597550085002922 ) ) ;
#1053 = CARTESIAN_POINT ( 'NONE',  ( -5.869209559033047974, -6.369690395747422684, 34.87708834333098196 ) ) ;
#1055 = CARTESIAN_POINT ( 'NONE',  ( 14.08476609017615644, -3.586966769969701208, 32.86292498521069660 ) ) ;
#1056 = CARTESIAN_POINT ( 'NONE',  ( 2.749999999999995115, -6.360912703473971419, 21.89062500000000355 ) ) ;
#1057 = EDGE_LOOP ( 'NONE', ( #1568, #37917, #18646, #65919 ) ) ;
#1058 = CARTESIAN_POINT ( 'NONE',  ( 14.55769230769231015, -2.499999999999998668, 29.75000000000000355 ) ) ;
#1059 = ORIENTED_EDGE ( 'NONE', *, *, #26331, .T. ) ;
#1060 = ORIENTED_EDGE ( 'NONE', *, *, #64186, .T. ) ;
#1061 = DIRECTION ( 'NONE',  ( 1.000000000000000000, -0.000000000000000000, -0.000000000000000000 ) ) ;
#1063 = ORIENTED_EDGE ( 'NONE', *, *, #7601, .F. ) ;
#1062 = VECTOR ( 'NONE', #67531, 1000.000000000000000 ) ;
#1064 = DIRECTION ( 'NONE',  ( -0.000000000000000000, 0.9848077530122085754, -0.1736481776669273613 ) ) ;
#1065 = LINE ( 'NONE', #41612, #19384 ) ;
#1066 = DIRECTION ( 'NONE',  ( -0.000000000000000000, 0.5000000000000011102, -0.8660254037844381525 ) ) ;
#1067 = CARTESIAN_POINT ( 'NONE',  ( -7.146561847641254239, -9.417330523894424488, 34.63758898049880486 ) ) ;
#1068 = CYLINDRICAL_SURFACE ( 'NONE', #27243, 0.2499999999999995559 ) ;
#1070 = EDGE_CURVE ( 'NONE', #51469, #4867, #82066, .T. ) ;
#1069 = CARTESIAN_POINT ( 'NONE',  ( -16.37733109757010652, -3.236172620538810385, 32.36188796281389557 ) ) ;
#1071 = CARTESIAN_POINT ( 'NONE',  ( 15.90382291655318880, -11.86270091957321071, 32.19358267280088626 ) ) ;
#1072 = CARTESIAN_POINT ( 'NONE',  ( 3.749999999999992006, -5.946699141100872943, 24.39062500000000000 ) ) ;
#1073 = DIRECTION ( 'NONE',  ( 0.000000000000000000, 0.9848077530122072432, -0.1736481776669354937 ) ) ;
#1074 = LINE ( 'NONE', #83501, #7513 ) ;
#1075 = CARTESIAN_POINT ( 'NONE',  ( 14.37288628947566593, -2.506253911140448043, 29.99999999999988631 ) ) ;
#1076 = DIRECTION ( 'NONE',  ( -0.000000000000000000, 0.6427876096865404731, -0.7660444431189771253 ) ) ;
#1077 = ORIENTED_EDGE ( 'NONE', *, *, #57096, .F. ) ;
#1078 = EDGE_LOOP ( 'NONE', ( #31275, #76014, #59362, #29560 ) ) ;
#1079 = AXIS2_PLACEMENT_3D ( 'NONE', #20945, #39913, #48415 ) ;
#1080 = CARTESIAN_POINT ( 'NONE',  ( -15.00798968950081758, -8.496831190052096971, 34.64984203495476578 ) ) ;
#1081 = CARTESIAN_POINT ( 'NONE',  ( -15.90384615384615330, -2.249999999999998668, 29.75000000000000355 ) ) ;
#1082 = CARTESIAN_POINT ( 'NONE',  ( -16.81410256410256565, -7.500000000000000000, 29.75000000000000355 ) ) ;
#1083 = CARTESIAN_POINT ( 'NONE',  ( 9.942253101685738059, -12.07971442181322352, 32.31769673815850297 ) ) ;
#1084 = ORIENTED_EDGE ( 'NONE', *, *, #14407, .T. ) ;
#1085 = ADVANCED_FACE ( 'NONE', ( #26664 ), #48258, .F. ) ;
#1086 = EDGE_CURVE ( 'NONE', #31481, #54731, #6721, .T. ) ;
#1087 = CARTESIAN_POINT ( 'NONE',  ( 9.915087361285756629, -11.60474049983371003, 33.02348890104160262 ) ) ;
#1088 = DIRECTION ( 'NONE',  ( -0.000000000000000000, 0.8660254037844399289, -0.4999999999999980016 ) ) ;
#1089 = CARTESIAN_POINT ( 'NONE',  ( -3.230769230769351186, -12.27809138561165270, 31.22303859784587132 ) ) ;
#1090 = EDGE_CURVE ( 'NONE', #14619, #43616, #79819, .T. ) ;
#1091 = AXIS2_PLACEMENT_3D ( 'NONE', #46818, #39638, #67988 ) ;
#1092 = ORIENTED_EDGE ( 'NONE', *, *, #823, .F. ) ;
#1093 = CARTESIAN_POINT ( 'NONE',  ( -13.38461538461550582, -10.21337939537710326, 33.94971097300076224 ) ) ;
#1094 = ORIENTED_EDGE ( 'NONE', *, *, #49611, .F. ) ;
#1095 = CARTESIAN_POINT ( 'NONE',  ( 0.4615384615384611200, -10.51840700105979565, 33.73612834413961536 ) ) ;
#1096 = CARTESIAN_POINT ( 'NONE',  ( -18.00000000000000711, -12.74702886152665471, 29.99985851721553587 ) ) ;
#1097 = CARTESIAN_POINT ( 'NONE',  ( 12.33139125210024112, -8.587444163452046197, 34.63053765926554206 ) ) ;
#1098 = DIRECTION ( 'NONE',  ( 0.000000000000000000, -1.084202172485503448E-16, 1.000000000000000000 ) ) ;
#1099 = FACE_OUTER_BOUND ( 'NONE', #19965, .T. ) ;
#1100 = EDGE_LOOP ( 'NONE', ( #57674, #76067 ) ) ;
#1101 = ORIENTED_EDGE ( 'NONE', *, *, #72965, .F. ) ;
#1102 = AXIS2_PLACEMENT_3D ( 'NONE', #32167, #59628, #87129 ) ;
#1103 = EDGE_CURVE ( 'NONE', #81224, #48029, #68558, .T. ) ;
#1104 = VERTEX_POINT ( 'NONE', #49597 ) ;
#1105 = ORIENTED_EDGE ( 'NONE', *, *, #51314, .T. ) ;
#1106 = CARTESIAN_POINT ( 'NONE',  ( 13.38461538461526601, -3.300289026999228881, 32.46337939537708905 ) ) ;
#1107 = CARTESIAN_POINT ( 'NONE',  ( -2.557669051740897537, -10.06842814019191401, 34.32929386961144758 ) ) ;
#1108 = VECTOR ( 'NONE', #67592, 1000.000000000000000 ) ;
#1109 = B_SPLINE_CURVE_WITH_KNOTS ( 'NONE', 3,
 ( #52985, #73735, #66520, #39503, #66964, #69615, #42162, #89028, #47567, #20105 ),
 .UNSPECIFIED., .F., .F.,
 ( 4, 2, 2, 2, 4 ),
 ( 0.0007817359430256326080, 0.0009771253907250047801, 0.001172514838424369796, 0.001367904286123735030, 0.001563293733823100263 ),
 .UNSPECIFIED. ) ;
#1110 = CARTESIAN_POINT ( 'NONE',  ( -4.376773112753000738, -12.38737895849757820, 31.66785238281580206 ) ) ;
#1111 = CARTESIAN_POINT ( 'NONE',  ( -2.084679463598911209, -11.43677907613345113, 33.22367315496201456 ) ) ;
#1112 = CARTESIAN_POINT ( 'NONE',  ( -7.596208436775802930, -4.176053281294515251, 33.81426240980091791 ) ) ;
#1113 = CARTESIAN_POINT ( 'NONE',  ( 6.923076923076924238, -10.67929555188718282, 33.92786785259544047 ) ) ;
#1114 = AXIS2_PLACEMENT_3D ( 'NONE', #36527, #65751, #65313 ) ;
#1115 = EDGE_LOOP ( 'NONE', ( #10565, #19181, #33919, #82141 ) ) ;
#1116 = ORIENTED_EDGE ( 'NONE', *, *, #74661, .T. ) ;
#1117 = ORIENTED_EDGE ( 'NONE', *, *, #87020, .T. ) ;
#1119 = ORIENTED_EDGE ( 'NONE', *, *, #83593, .T. ) ;
#1118 = CARTESIAN_POINT ( 'NONE',  ( 3.930919936330007136, -2.758268499246657957, 31.33685645148949561 ) ) ;
#1121 = CARTESIAN_POINT ( 'NONE',  ( 13.63466980452883881, -4.074993327901527351, 33.72946981652012255 ) ) ;
#1120 = CARTESIAN_POINT ( 'NONE',  ( -17.01085472592063752, -8.973038597847269315, 34.52809138561122637 ) ) ;
#1122 = CARTESIAN_POINT ( 'NONE',  ( -17.07692307692307665, -12.37446782046654192, 30.86335684631486131 ) ) ;
#1123 = CARTESIAN_POINT ( 'NONE',  ( 13.45068373561782593, -8.120952969808772792, 34.71129190929999453 ) ) ;
#1124 = ORIENTED_EDGE ( 'NONE', *, *, #12894, .T. ) ;
#1125 = EDGE_LOOP ( 'NONE', ( #67403, #51145 ) ) ;
#1126 = DIRECTION ( 'NONE',  ( -0.000000000000000000, 1.000000000000000000, 3.491481338843133355E-15 ) ) ;
#1127 = EDGE_LOOP ( 'NONE', ( #66624, #58900 ) ) ;
#1128 = FACE_BOUND ( 'NONE', #14400, .T. ) ;
#1129 = CARTESIAN_POINT ( 'NONE',  ( -1.384615384615076605, -2.506253911140615021, 30.00000000000323297 ) ) ;
#1130 = AXIS2_PLACEMENT_3D ( 'NONE', #6250, #89121, #33712 ) ;
#1131 = CARTESIAN_POINT ( 'NONE',  ( 7.846153846153723244, -5.941354392335915335, 34.76329471203413846 ) ) ;
#1132 = ORIENTED_EDGE ( 'NONE', *, *, #59762, .F. ) ;
#1133 = DIRECTION ( 'NONE',  ( 0.000000000000000000, 0.000000000000000000, 1.000000000000000000 ) ) ;
#1134 = DIRECTION ( 'NONE',  ( -0.000000000000000000, 1.000000000000000000, 3.491481338843133355E-15 ) ) ;
#1135 = LINE ( 'NONE', #35819, #16238 ) ;
#1136 = CARTESIAN_POINT ( 'NONE',  ( 4.153846153846154188, -11.16473453929635440, 33.15142922261926373 ) ) ;
#1137 = CARTESIAN_POINT ( 'NONE',  ( 4.284371855609720114, -3.285477652293412820, 32.44071101563363158 ) ) ;
#1138 = ORIENTED_EDGE ( 'NONE', *, *, #84705, .T. ) ;
#1139 = VECTOR ( 'NONE', #24290, 1000.000000000000000 ) ;
#1140 = CARTESIAN_POINT ( 'NONE',  ( 6.130525701763564150, -8.586989748646452369, 34.63063291749215011 ) ) ;
#1141 = CARTESIAN_POINT ( 'NONE',  ( -6.923076923076922462, -9.780366693483667717, 34.19971097300155094 ) ) ;
#1142 = CARTESIAN_POINT ( 'NONE',  ( -0.4615384615384611200, -1.790695186598648903, 34.54067556320373455 ) ) ;
#1143 = CARTESIAN_POINT ( 'NONE',  ( -0.7115152055870532788, -4.818429247618089661, 34.26397095200675125 ) ) ;
#1144 = CARTESIAN_POINT ( 'NONE',  ( -15.23076923076935074, -11.94971097300221174, 32.03036669348237098 ) ) ;
#1145 = FACE_BOUND ( 'NONE', #3062, .T. ) ;
#1147 = CARTESIAN_POINT ( 'NONE',  ( 17.07692307692295586, -3.083524468854526912, 32.58852847137268327 ) ) ;
#1146 = CARTESIAN_POINT ( 'NONE',  ( 13.25392391794783009, -11.71456829005830080, 32.44064028649416542 ) ) ;
#1148 = VECTOR ( 'NONE', #38524, 1000.000000000000000 ) ;
#1149 = CARTESIAN_POINT ( 'NONE',  ( -7.173100160369889622, -12.22074536777954989, 31.39888409691088356 ) ) ;
#1151 = CARTESIAN_POINT ( 'NONE',  ( -18.22348492456433178, -3.019605429927188833, 32.48692288466676104 ) ) ;
#1150 = CARTESIAN_POINT ( 'NONE',  ( -11.28840722682322628, -11.28795663066794575, 33.01431243580653785 ) ) ;
#1152 = CARTESIAN_POINT ( 'NONE',  ( -18.22292621751614305, -9.886141570436018711, 34.14413921362392301 ) ) ;
#1153 = CARTESIAN_POINT ( 'NONE',  ( -0.06109907496454585613, -4.750000000000000000, 23.90438170625849068 ) ) ;
#1154 = ORIENTED_EDGE ( 'NONE', *, *, #4618, .F. ) ;
#1155 = CARTESIAN_POINT ( 'NONE',  ( 12.46153846153846168, -2.538708090699994813, 30.37095296980875503 ) ) ;
#1156 = ORIENTED_EDGE ( 'NONE', *, *, #36963, .F. ) ;
#1157 = CARTESIAN_POINT ( 'NONE',  ( 8.769230769230647482, -6.026961402154118019, 34.52809138561165270 ) ) ;
#1158 = VERTEX_POINT ( 'NONE', #56355 ) ;
#1159 = CARTESIAN_POINT ( 'NONE',  ( -11.47239318745909920, -2.721908614388772296, 31.22303859784725333 ) ) ;
#1160 = CARTESIAN_POINT ( 'NONE',  ( -18.22292621751614305, -2.554751324335734264, 30.48935550225260727 ) ) ;
#1161 = VERTEX_POINT ( 'NONE', #83844 ) ;
#1162 = CARTESIAN_POINT ( 'NONE',  ( -15.36146069743678844, -4.809359713505814149, 33.96456829005828837 ) ) ;
#1163 = CARTESIAN_POINT ( 'NONE',  ( -1.077988221561460236, -10.27530806549876452, 19.60750670625849068 ) ) ;
#1164 = CARTESIAN_POINT ( 'NONE',  ( 2.307692307692186251, -5.941354392335915335, 34.76329471203413846 ) ) ;
#1165 = CARTESIAN_POINT ( 'NONE',  ( -15.23076923076935252, -9.528491918059723176, 34.59228464037033035 ) ) ;
#1166 = CARTESIAN_POINT ( 'NONE',  ( 16.02369818411445834, -8.630895178749536711, 34.87696386517710323 ) ) ;
#1167 = CARTESIAN_POINT ( 'NONE',  ( 7.846153846153846700, -11.69971097300155272, 32.46337939537588113 ) ) ;
#1168 = CARTESIAN_POINT ( 'NONE',  ( 11.31497659473759398, -2.847400154188068022, 31.58180166144859058 ) ) ;
#1169 = DIRECTION ( 'NONE',  ( -0.000000000000000000, 0.3420201433256694901, -0.9396926207859082059 ) ) ;
#1170 = CARTESIAN_POINT ( 'NONE',  ( -2.694853999681181556, -10.10844685921792241, 22.68936829374151287 ) ) ;
#1171 = CARTESIAN_POINT ( 'NONE',  ( -3.230769230769229949, -9.819645486525091727, 36.12317359536749706 ) ) ;
#1172 = CARTESIAN_POINT ( 'NONE',  ( -11.53846153846165912, -11.94971097300221174, 32.03036669348237098 ) ) ;
#1173 = LINE ( 'NONE', #61539, #40183 ) ;
#1174 = CARTESIAN_POINT ( 'NONE',  ( 3.724691934501251023, -9.114399933863618131, 23.54874329374151642 ) ) ;
#1175 = EDGE_CURVE ( 'NONE', #60227, #41430, #46471, .T. ) ;
#1176 = CARTESIAN_POINT ( 'NONE',  ( -20.00000000000000355, 10.00000000000000711, 0.000000000000000000 ) ) ;
#1177 = ORIENTED_EDGE ( 'NONE', *, *, #22871, .T. ) ;
#1178 = CARTESIAN_POINT ( 'NONE',  ( 14.53047184896071897, -2.600157965045224895, 30.74683119005207743 ) ) ;
#1179 = CARTESIAN_POINT ( 'NONE',  ( 16.21910129335899597, -2.657715359629131857, 31.77849191805844242 ) ) ;
#1180 = CARTESIAN_POINT ( 'NONE',  ( -16.85396017336159247, -7.369474270740072441, 34.74850911626239736 ) ) ;
#1181 = DIRECTION ( 'NONE',  ( 0.000000000000000000, 0.4999999999999960032, -0.8660254037844410391 ) ) ;
#1182 = EDGE_CURVE ( 'NONE', #21592, #31771, #29736, .T. ) ;
#1183 = CARTESIAN_POINT ( 'NONE',  ( -16.37677237136229991, -10.61292498521070549, 33.66303323003028680 ) ) ;
#1184 = CARTESIAN_POINT ( 'NONE',  ( 6.989144256427000990, -11.91647553114624358, 32.58852847137148245 ) ) ;
#1185 = FACE_OUTER_BOUND ( 'NONE', #27868, .T. ) ;
#1186 = CARTESIAN_POINT ( 'NONE',  ( 2.307692307692309264, -3.886160181151819604, 36.00935417666054406 ) ) ;
#1187 = EDGE_CURVE ( 'NONE', #82311, #58008, #62561, .T. ) ;
#1188 = ORIENTED_EDGE ( 'NONE', *, *, #40388, .F. ) ;
#1189 = ORIENTED_EDGE ( 'NONE', *, *, #2614, .F. ) ;
#1190 = ORIENTED_EDGE ( 'NONE', *, *, #44498, .T. ) ;
#1191 = CARTESIAN_POINT ( 'NONE',  ( -16.15384615384627409, -3.643525952248796163, 33.31231777344771672 ) ) ;
#1192 = CARTESIAN_POINT ( 'NONE',  ( -4.153846153846152411, -13.87047571288749737, 32.06866353760679544 ) ) ;
#1193 = LINE ( 'NONE', #21916, #2914 ) ;
#1194 = CARTESIAN_POINT ( 'NONE',  ( -13.13456107297707121, -12.17597550085003633, 31.52189283813461884 ) ) ;
#1195 = CARTESIAN_POINT ( 'NONE',  ( 18.00000000000000000, -9.058645607665452459, 34.76329471203371924 ) ) ;
#1196 = VECTOR ( 'NONE', #82084, 1000.000000000000114 ) ;
#1197 = EDGE_LOOP ( 'NONE', ( #72989, #17926 ) ) ;
#1198 = CARTESIAN_POINT ( 'NONE',  ( 23.49999999999998934, 12.75000000000000711, 13.00000000000000178 ) ) ;
#1199 = ORIENTED_EDGE ( 'NONE', *, *, #32116, .T. ) ;
#1200 = ADVANCED_FACE ( 'NONE', ( #42410 ), #83395, .F. ) ;
#1201 = EDGE_LOOP ( 'NONE', ( #63869, #3784 ) ) ;
#1202 = AXIS2_PLACEMENT_3D ( 'NONE', #5534, #46941, #53707 ) ;
#1203 = EDGE_LOOP ( 'NONE', ( #39780, #41369 ) ) ;
#1206 = ORIENTED_EDGE ( 'NONE', *, *, #30331, .F. ) ;
#1205 = EDGE_CURVE ( 'NONE', #18616, #63332, #75754, .T. ) ;
#1204 = CARTESIAN_POINT ( 'NONE',  ( 13.25392478150507891, -4.684245665217972032, 34.18127051446801090 ) ) ;
#1207 = LINE ( 'NONE', #62023, #64637 ) ;
#1208 = EDGE_CURVE ( 'NONE', #76314, #62928, #62650, .T. ) ;
#1209 = CARTESIAN_POINT ( 'NONE',  ( -3.453696189676077832, -11.98009711892699691, 32.48740034544075428 ) ) ;
#1210 = EDGE_CURVE ( 'NONE', #41958, #22384, #59220, .T. ) ;
#1211 = CARTESIAN_POINT ( 'NONE',  ( -9.915233909823838232, -8.239355502252617924, 34.69524867566427417 ) ) ;
#1212 = CARTESIAN_POINT ( 'NONE',  ( 14.53065544195898440, -7.369474539155828730, 34.99858011523957657 ) ) ;
#1213 = EDGE_LOOP ( 'NONE', ( #27297, #63065, #59456, #32063, #63736, #10968 ) ) ;
#1214 = ORIENTED_EDGE ( 'NONE', *, *, #71167, .T. ) ;
#1215 = ORIENTED_EDGE ( 'NONE', *, *, #66533, .F. ) ;
#1216 = CARTESIAN_POINT ( 'NONE',  ( -6.792551484843280640, -3.068774925481847937, 32.56582465632704526 ) ) ;
#1218 = ORIENTED_EDGE ( 'NONE', *, *, #85820, .T. ) ;
#1217 = CARTESIAN_POINT ( 'NONE',  ( 4.376857505459002873, -11.24521262558773671, 33.06293181088029343 ) ) ;
#1219 = LINE ( 'NONE', #77325, #70914 ) ;
#1220 = CARTESIAN_POINT ( 'NONE',  ( -2.084680956079457026, -8.239487800360276282, 34.69522927552633718 ) ) ;
#1221 = CARTESIAN_POINT ( 'NONE',  ( -0.2114840416250089172, -9.233818618650603938, 34.70587769442853698 ) ) ;
#1222 = EDGE_LOOP ( 'NONE', ( #64618, #77801, #78282, #649 ) ) ;
#1223 = FACE_OUTER_BOUND ( 'NONE', #27080, .T. ) ;
#1224 = CARTESIAN_POINT ( 'NONE',  ( -1.384615384615383471, -2.708943851104267164, 35.45975837776705220 ) ) ;
#1225 = B_SPLINE_CURVE_WITH_KNOTS ( 'NONE', 3,
 ( #80204, #18943, #39223, #58138, #58578, #86985, #25252, #72547, #31565, #52714 ),
 .UNSPECIFIED., .F., .F.,
 ( 4, 2, 2, 2, 4 ),
 ( 0.000000000000000000, 0.0001954311564186862510, 0.0003908623128373725020, 0.0005862934692560588072, 0.0007817246256747450040 ),
 .UNSPECIFIED. ) ;
#1226 = AXIS2_PLACEMENT_3D ( 'NONE', #35034, #1696, #8462 ) ;
#1227 = ORIENTED_EDGE ( 'NONE', *, *, #63659, .T. ) ;
#1228 = FACE_BOUND ( 'NONE', #18967, .T. ) ;
#1229 = CARTESIAN_POINT ( 'NONE',  ( -11.66860950819323328, -11.66186481527757302, 32.95055677023626117 ) ) ;
#1230 = CARTESIAN_POINT ( 'NONE',  ( 20.00000000000000711, -9.999999999999994671, 13.00000000000000178 ) ) ;
#1231 = DIRECTION ( 'NONE',  ( 0.000000000000000000, 0.000000000000000000, -1.000000000000000000 ) ) ;
#1233 = CARTESIAN_POINT ( 'NONE',  ( 13.38461538461538680, -4.945431358278436385, 36.03766855953609394 ) ) ;
#1232 = CARTESIAN_POINT ( 'NONE',  ( 18.13079044096695469, -2.845873456487966635, 32.17976146951972538 ) ) ;
#1234 = CARTESIAN_POINT ( 'NONE',  ( -30.00000000000000000, -15.00000000000000000, 0.000000000000000000 ) ) ;
#1235 = CARTESIAN_POINT ( 'NONE',  ( 18.06525557127602610, -2.892918686051626498, 31.69288490824026638 ) ) ;
#1236 = ORIENTED_EDGE ( 'NONE', *, *, #29058, .T. ) ;
#1237 = CARTESIAN_POINT ( 'NONE',  ( -2.307692307692428724, -4.320704448113951379, 33.92786785259630022 ) ) ;
#1238 = CARTESIAN_POINT ( 'NONE',  ( -6.065270000556319374, -11.67786785259541027, 32.92929555188721480 ) ) ;
#1239 = ORIENTED_EDGE ( 'NONE', *, *, #43935, .T. ) ;
#1240 = CARTESIAN_POINT ( 'NONE',  ( 8.519254038288416098, -3.137211980971221781, 32.19342716148376837 ) ) ;
#1241 = CARTESIAN_POINT ( 'NONE',  ( 9.469381474791543241, -2.758268499246657068, 31.33685645148948140 ) ) ;
#1242 = ORIENTED_EDGE ( 'NONE', *, *, #61678, .F. ) ;
#1243 = EDGE_CURVE ( 'NONE', #12426, #74753, #36094, .T. ) ;
#1244 = CARTESIAN_POINT ( 'NONE',  ( -13.16183571563731647, -11.60474049983371003, 33.02348890104160262 ) ) ;
#1245 = CARTESIAN_POINT ( 'NONE',  ( 4.403900465484469784, -9.943054286541403997, 34.11300777759954883 ) ) ;
#1246 = FACE_BOUND ( 'NONE', #48721, .T. ) ;
#1248 = CARTESIAN_POINT ( 'NONE',  ( 3.930919194939304973, -12.38737895849757820, 31.66785238281580206 ) ) ;
#1247 = CARTESIAN_POINT ( 'NONE',  ( 8.769230769230768274, -13.53365097954675988, 30.81389545987213552 ) ) ;
#1249 = LINE ( 'NONE', #48104, #79871 ) ;
#1251 = CARTESIAN_POINT ( 'NONE',  ( -14.05769230769088729, -7.500000000000154543, 35.00000000000007105 ) ) ;
#1250 = CARTESIAN_POINT ( 'NONE',  ( 20.00000000000000000, -4.000000000000000000, 29.75000000000000355 ) ) ;
#1252 = LINE ( 'NONE', #22415, #73550 ) ;
#1253 = CARTESIAN_POINT ( 'NONE',  ( -1.929879867024197893E-14, -3.750000000000000000, 25.40625000000000000 ) ) ;
#1254 = ORIENTED_EDGE ( 'NONE', *, *, #37154, .F. ) ;
#1255 = EDGE_LOOP ( 'NONE', ( #1876, #5321, #78832, #65229 ) ) ;
#1256 = VECTOR ( 'NONE', #85243, 1000.000000000000227 ) ;
#1257 = CARTESIAN_POINT ( 'NONE',  ( 16.15384615384615330, -9.058645607665452459, 34.76329471203371924 ) ) ;
#1258 = CARTESIAN_POINT ( 'NONE',  ( -15.23076923076922995, -5.471508081941601098, 34.59228464037088457 ) ) ;
#1259 = CARTESIAN_POINT ( 'NONE',  ( 5.999999999999880096, -10.21337939537710326, 33.94971097300076224 ) ) ;
#1260 = FACE_OUTER_BOUND ( 'NONE', #59587, .T. ) ;
#1261 = CARTESIAN_POINT ( 'NONE',  ( -13.16160254052199008, -2.523321265292115534, 31.42251411153756990 ) ) ;
#1262 = CARTESIAN_POINT ( 'NONE',  ( 3.775308065498768517, -8.992201783934554271, 15.54500670625849246 ) ) ;
#1263 = EDGE_CURVE ( 'NONE', #72081, #77897, #57141, .T. ) ;
#1264 = DIRECTION ( 'NONE',  ( 0.000000000000000000, 8.131516293641283255E-17, 1.000000000000000000 ) ) ;
#1265 = CARTESIAN_POINT ( 'NONE',  ( 3.903869409797562806, -12.01397095200673881, 32.43157075238190146 ) ) ;
#1266 = CARTESIAN_POINT ( 'NONE',  ( -17.07692307692319744, -5.219633306517616589, 34.19971097300220464 ) ) ;
#1267 = CARTESIAN_POINT ( 'NONE',  ( 17.93474900983875386, -2.506253911140460477, 30.00000000000013856 ) ) ;
#1268 = CARTESIAN_POINT ( 'NONE',  ( 6.416666666666664298, -11.50000000000000000, 29.75000000000000355 ) ) ;
#1269 = CARTESIAN_POINT ( 'NONE',  ( 16.15384615384603251, -5.219633306517616589, 34.19971097300220464 ) ) ;
#1270 = VECTOR ( 'NONE', #7494, 999.9999999999998863 ) ;
#1271 = CARTESIAN_POINT ( 'NONE',  ( 9.942362003946008997, -11.28795663066794575, 33.01431243580653785 ) ) ;
#1272 = DIRECTION ( 'NONE',  ( -0.000000000000000000, -0.3420201433256694901, -0.9396926207859082059 ) ) ;
#1273 = VECTOR ( 'NONE', #84236, 1000.000000000000000 ) ;
#1274 = B_SPLINE_CURVE_WITH_KNOTS ( 'NONE', 3,
 ( #40226, #60926, #54158, #26259, #53728, #67694, #88428, #6869, #54601, #40673 ),
 .UNSPECIFIED., .F., .F.,
 ( 4, 2, 2, 2, 4 ),
 ( 0.000000000000000000, 0.0001954311564186858715, 0.0003908623128373717431, 0.0005862934692560576146, 0.0007817246256747434861 ),
 .UNSPECIFIED. ) ;
#1275 = FACE_OUTER_BOUND ( 'NONE', #59675, .T. ) ;
#1276 = ORIENTED_EDGE ( 'NONE', *, *, #29973, .F. ) ;
#1277 = CARTESIAN_POINT ( 'NONE',  ( 4.153846153846154188, -4.786620604624113540, 33.94971097300155094 ) ) ;
#1278 = CARTESIAN_POINT ( 'NONE',  ( 7.715463243043537034, -4.684245665217972032, 34.18127051446801090 ) ) ;
#1279 = CARTESIAN_POINT ( 'NONE',  ( 2.724691934501250135, -8.700186371490531201, 22.29874329374151642 ) ) ;
#1280 = B_SPLINE_CURVE_WITH_KNOTS ( 'NONE', 3,
 ( #37925, #51399, #4125, #65388, #32058, #17201, #78020, #44657, #72143, #2787 ),
 .UNSPECIFIED., .F., .F.,
 ( 4, 2, 2, 2, 4 ),
 ( 0.000000000000000000, 0.0001954339857564082062, 0.0003908679715128164124, 0.0005863019572692246186, 0.0007817359430256328248 ),
 .UNSPECIFIED. ) ;
#1281 = EDGE_CURVE ( 'NONE', #88074, #55385, #19492, .T. ) ;
#1282 = DIRECTION ( 'NONE',  ( 0.000000000000000000, 0.3420201433256641055, -0.9396926207859100932 ) ) ;
#1283 = CARTESIAN_POINT ( 'NONE',  ( 16.85399611801622655, -11.43668979543635089, 33.22377378376089752 ) ) ;
#1284 = ORIENTED_EDGE ( 'NONE', *, *, #40773, .F. ) ;
#1285 = CARTESIAN_POINT ( 'NONE',  ( 10.36538461538461320, -2.499999999999999556, 29.81609845454691765 ) ) ;
#1287 = VERTEX_POINT ( 'NONE', #66661 ) ;
#1286 = CARTESIAN_POINT ( 'NONE',  ( -14.43783951713053249, -12.27039167877662251, 31.24851455888617835 ) ) ;
#1288 = CARTESIAN_POINT ( 'NONE',  ( 6.988332494352950341, -3.835265460703683349, 33.15142922261929925 ) ) ;
#1289 = CARTESIAN_POINT ( 'NONE',  ( -2.557669051740896649, -10.82459398097509684, 33.81372124010185587 ) ) ;
#1290 = EDGE_CURVE ( 'NONE', #40661, #65909, #31310, .T. ) ;
#1291 = ORIENTED_EDGE ( 'NONE', *, *, #48742, .T. ) ;
#1292 = CARTESIAN_POINT ( 'NONE',  ( -5.326946314216042033, -11.37209801155882971, 32.91403422569032955 ) ) ;
#1293 = CARTESIAN_POINT ( 'NONE',  ( 13.13459216039392885, -9.356822207818506598, 34.66110646841856635 ) ) ;
#1294 = ORIENTED_EDGE ( 'NONE', *, *, #33309, .T. ) ;
#1295 = DIRECTION ( 'NONE',  ( -0.000000000000000000, 1.000000000000000000, 3.491481338843133355E-15 ) ) ;
#1296 = CARTESIAN_POINT ( 'NONE',  ( -11.78843828251013015, -12.41104346484419452, 31.60698883733904196 ) ) ;
#1297 = CARTESIAN_POINT ( 'NONE',  ( -9.627113710524334067, -2.506253911140448487, 29.99999999999988631 ) ) ;
#1298 = EDGE_CURVE ( 'NONE', #29793, #8757, #25230, .T. ) ;
#1299 = ORIENTED_EDGE ( 'NONE', *, *, #42085, .F. ) ;
#1300 = ORIENTED_EDGE ( 'NONE', *, *, #66318, .F. ) ;
#1301 = CARTESIAN_POINT ( 'NONE',  ( -10.39237177129122003, -2.308499170217967134, 30.53291367094873721 ) ) ;
#1302 = ORIENTED_EDGE ( 'NONE', *, *, #36299, .T. ) ;
#1303 = EDGE_CURVE ( 'NONE', #18982, #31195, #9931, .T. ) ;
#1304 = CARTESIAN_POINT ( 'NONE',  ( -1.134561072977069651, -2.564540009722895419, 30.55348353981670684 ) ) ;
#1305 = DIRECTION ( 'NONE',  ( 0.000000000000000000, -1.835858764360062270E-15, -1.000000000000000000 ) ) ;
#1306 = EDGE_CURVE ( 'NONE', #63487, #26549, #52692, .T. ) ;
#1307 = CARTESIAN_POINT ( 'NONE',  ( -4.153846153846273204, -6.879047030192662504, 34.71129190930017927 ) ) ;
#1308 = CARTESIAN_POINT ( 'NONE',  ( -3.903791733932699515, -12.65882529074907126, 30.72640787790839312 ) ) ;
#1309 = B_SPLINE_CURVE_WITH_KNOTS ( 'NONE', 3,
 ( #63041, #54975, #49548, #7681, #21180, #1353, #28842, #15322, #82899, #34706 ),
 .UNSPECIFIED., .F., .F.,
 ( 4, 2, 2, 2, 4 ),
 ( 0.0007817359430256390048, 0.0009771253907250078159, 0.001172514838424376735, 0.001367904286123745655, 0.001563293733823114574 ),
 .UNSPECIFIED. ) ;
#1310 = CARTESIAN_POINT ( 'NONE',  ( 3.100078627658922947, -9.929715669179220328, 34.40415004197138416 ) ) ;
#1311 = B_SPLINE_CURVE_WITH_KNOTS ( 'NONE', 3,
 ( #45122, #64944, #30722, #31161, #58188, #29416, #56865, #51406, #78912, #58634 ),
 .UNSPECIFIED., .F., .F.,
 ( 4, 2, 2, 2, 4 ),
 ( 0.000000000000000000, 0.0001954339857564055499, 0.0003908679715128110998, 0.0005863019572692165955, 0.0007817359430256221996 ),
 .UNSPECIFIED. ) ;
#1312 = EDGE_CURVE ( 'NONE', #74314, #10085, #59898, .T. ) ;
#1313 = ORIENTED_EDGE ( 'NONE', *, *, #22945, .T. ) ;
#1314 = ORIENTED_EDGE ( 'NONE', *, *, #41131, .F. ) ;
#1316 = VERTEX_POINT ( 'NONE', #37852 ) ;
#1315 = CARTESIAN_POINT ( 'NONE',  ( 9.561616225640136690, -4.118384482072086072, 33.43331474514187107 ) ) ;
#1317 = CARTESIAN_POINT ( 'NONE',  ( -5.300408001487407539, -4.988325925672468131, 34.36044203135681130 ) ) ;
#1318 = EDGE_LOOP ( 'NONE', ( #8769, #9636 ) ) ;
#1319 = AXIS2_PLACEMENT_3D ( 'NONE', #27859, #8927, #49896 ) ;
#1320 = CIRCLE ( 'NONE', #45869, 0.2500000000000002220 ) ;
#1321 = ADVANCED_FACE ( 'NONE', ( #85598 ), #37400, .F. ) ;
#1322 = EDGE_CURVE ( 'NONE', #60496, #33135, #52828, .T. ) ;
#1323 = DIRECTION ( 'NONE',  ( -0.000000000000000000, -0.000000000000000000, -1.000000000000000000 ) ) ;
#1324 = CARTESIAN_POINT ( 'NONE',  ( 6.699591998512593349, -9.417330523894424488, 34.63758898049880486 ) ) ;
#1325 = ORIENTED_EDGE ( 'NONE', *, *, #58150, .T. ) ;
#1326 = CARTESIAN_POINT ( 'NONE',  ( -12.21148414990014786, -5.728107161865378494, 34.42597550085002922 ) ) ;
#1327 = AXIS2_PLACEMENT_3D ( 'NONE', #67691, #28352, #40223 ) ;
#1328 = EDGE_LOOP ( 'NONE', ( #27351, #18473, #24324, #5513 ) ) ;
#1330 = EDGE_LOOP ( 'NONE', ( #65690, #41436, #43338, #58463 ) ) ;
#1329 = CARTESIAN_POINT ( 'NONE',  ( -6.923076923076922462, -11.16473453929635440, 33.15142922261926373 ) ) ;
#1331 = AXIS2_PLACEMENT_3D ( 'NONE', #28757, #51198, #49466 ) ;
#1332 = DIRECTION ( 'NONE',  ( 0.000000000000000000, 1.000000000000000000, 0.000000000000000000 ) ) ;
#1333 = VERTEX_POINT ( 'NONE', #30644 ) ;
#1334 = CARTESIAN_POINT ( 'NONE',  ( 16.15384615384615330, -12.37446782046654192, 30.86335684631486131 ) ) ;
#1335 = CARTESIAN_POINT ( 'NONE',  ( -15.23076923076922995, -2.900454961884010974, 35.62045528018868623 ) ) ;
#1336 = FACE_BOUND ( 'NONE', #67379, .T. ) ;
#1337 = CARTESIAN_POINT ( 'NONE',  ( -11.60373198442231413, -2.625532179533444754, 30.86335684631481513 ) ) ;
#1338 = CARTESIAN_POINT ( 'NONE',  ( -17.86947429823643674, -12.27024696741798770, 31.24895572276497901 ) ) ;
#1339 = CARTESIAN_POINT ( 'NONE',  ( -16.15384615384627409, -5.094484230521993062, 34.41647553114689373 ) ) ;
#1340 = CARTESIAN_POINT ( 'NONE',  ( 3.230769230769231726, -4.661471528628507777, 34.16647553114623292 ) ) ;
#1341 = EDGE_CURVE ( 'NONE', #39, #63016, #10830, .T. ) ;
#1342 = DIRECTION ( 'NONE',  ( -0.000000000000000000, 0.3420201433256694901, -0.9396926207859082059 ) ) ;
#1343 = CARTESIAN_POINT ( 'NONE',  ( 10.48469401227430886, -10.70098750199973203, 33.91152734681376302 ) ) ;
#1344 = VERTEX_POINT ( 'NONE', #38745 ) ;
#1345 = CARTESIAN_POINT ( 'NONE',  ( -5.999999999999690914, -2.506253911140614576, 30.00000000000323297 ) ) ;
#1346 = ORIENTED_EDGE ( 'NONE', *, *, #76373, .F. ) ;
#1347 = ORIENTED_EDGE ( 'NONE', *, *, #86412, .F. ) ;
#1349 = CARTESIAN_POINT ( 'NONE',  ( 15.00784301325307979, -12.15238873228292071, 31.58232369045353849 ) ) ;
#1348 = CARTESIAN_POINT ( 'NONE',  ( -8.769230769230768274, -13.75783147151868846, 33.36296068462461051 ) ) ;
#1350 = CARTESIAN_POINT ( 'NONE',  ( -11.78848477575450282, -11.86270091957321249, 32.19358267280087915 ) ) ;
#1351 = DIRECTION ( 'NONE',  ( 1.000000000000000000, 0.000000000000000000, -0.000000000000000000 ) ) ;
#1352 = CARTESIAN_POINT ( 'NONE',  ( -12.33101302330482341, -2.647132371071621471, 31.75357179365171589 ) ) ;
#1353 = CARTESIAN_POINT ( 'NONE',  ( 9.942362003946010773, -2.564540009722896752, 30.55348353981670684 ) ) ;
#1354 = ORIENTED_EDGE ( 'NONE', *, *, #69690, .F. ) ;
#1355 = ADVANCED_FACE ( 'NONE', ( #66208 ), #78831, .F. ) ;
#1356 = CARTESIAN_POINT ( 'NONE',  ( 13.31934493865461278, -5.219633306516282545, 34.19971097300152962 ) ) ;
#1357 = CARTESIAN_POINT ( 'NONE',  ( -6.223484943723947893, -6.760086850603068243, 34.69517049084099369 ) ) ;
#1358 = CARTESIAN_POINT ( 'NONE',  ( -10.39237326377176451, -9.886259254753566594, 34.14407573483972413 ) ) ;
#1359 = CARTESIAN_POINT ( 'NONE',  ( -3.230769230769352962, -3.083524468854526912, 32.58852847137268327 ) ) ;
#1360 = CYLINDRICAL_SURFACE ( 'NONE', #50617, 0.2500000000000012212 ) ;
#1361 = ORIENTED_EDGE ( 'NONE', *, *, #87825, .F. ) ;
#1362 = AXIS2_PLACEMENT_3D ( 'NONE', #81252, #32171, #38483 ) ;
#1363 = EDGE_CURVE ( 'NONE', #62783, #21910, #30186, .T. ) ;
#1364 = CARTESIAN_POINT ( 'NONE',  ( -0.7115616857599191825, -2.341070481393820124, 30.72580821765574299 ) ) ;
#1365 = ORIENTED_EDGE ( 'NONE', *, *, #57441, .T. ) ;
#1367 = ADVANCED_FACE ( 'NONE', ( #32877 ), #46389, .F. ) ;
#1366 = ORIENTED_EDGE ( 'NONE', *, *, #74010, .T. ) ;
#1368 = CARTESIAN_POINT ( 'NONE',  ( -6.065270000556318486, -4.320704448112771878, 33.92786785259540494 ) ) ;
#1369 = VERTEX_POINT ( 'NONE', #40966 ) ;
#1370 = DIRECTION ( 'NONE',  ( -8.673617379884044347E-16, 1.000000000000000000, -5.102127870520020612E-17 ) ) ;
#1371 = CARTESIAN_POINT ( 'NONE',  ( 17.07692307692307665, -13.75783147151868846, 33.36296068462461051 ) ) ;
#1372 = CARTESIAN_POINT ( 'NONE',  ( 14.30769230769231015, -9.905515769479276145, 34.41647553114623292 ) ) ;
#1373 = CARTESIAN_POINT ( 'NONE',  ( 2.557746727605761272, -10.06805714834173848, 34.32951233291982618 ) ) ;
#1374 = FACE_OUTER_BOUND ( 'NONE', #33214, .T. ) ;
#1375 = ADVANCED_FACE ( 'NONE', ( #33764 ), #13928, .F. ) ;
#1376 = CYLINDRICAL_SURFACE ( 'NONE', #15842, 0.2499999999999979738 ) ;
#1377 = ORIENTED_EDGE ( 'NONE', *, *, #68097, .T. ) ;
#1378 = CARTESIAN_POINT ( 'NONE',  ( 4.403900465484468008, -4.235687564193446164, 33.53795663066793509 ) ) ;
#1380 = ORIENTED_EDGE ( 'NONE', *, *, #80549, .T. ) ;
#1379 = CARTESIAN_POINT ( 'NONE',  ( -0.4615384615384611200, -5.471508081941601098, 34.59228464037088457 ) ) ;
#1381 = CARTESIAN_POINT ( 'NONE',  ( -9.442362173959551797, -4.336752205174649433, 33.62275283266504289 ) ) ;
#1382 = FACE_OUTER_BOUND ( 'NONE', #53496, .T. ) ;
#1383 = CARTESIAN_POINT ( 'NONE',  ( -0.7115152055870537229, -4.075325502946086864, 33.72974371597207721 ) ) ;
#1384 = CARTESIAN_POINT ( 'NONE',  ( -3.454254174493178731, -5.113361153441932316, 34.14387501736621999 ) ) ;
#1385 = CARTESIAN_POINT ( 'NONE',  ( -2.177166869458661669, -2.372941743896878286, 30.88044141588254377 ) ) ;
#1386 = PLANE ( 'NONE',  #17654 ) ;
#1387 = DIRECTION ( 'NONE',  ( -0.000000000000000000, -0.1736481776669307198, -0.9848077530122080203 ) ) ;
#1388 = CARTESIAN_POINT ( 'NONE',  ( 1.200186371490529202, -4.775308065498752974, 23.23624329374151642 ) ) ;
#1389 = ORIENTED_EDGE ( 'NONE', *, *, #33394, .T. ) ;
#1390 = CARTESIAN_POINT ( 'NONE',  ( -1.384615384615383471, -11.16473453929635440, 33.15142922261926373 ) ) ;
#1391 = CARTESIAN_POINT ( 'NONE',  ( -1.384615384615383471, -3.322132147404559976, 32.92929555188717927 ) ) ;
#1392 = VECTOR ( 'NONE', #70371, 1000.000000000000114 ) ;
#1393 = AXIS2_PLACEMENT_3D ( 'NONE', #18730, #59256, #59702 ) ;
#1394 = CARTESIAN_POINT ( 'NONE',  ( 9.692307692307695177, -12.29105614889573062, 35.45975837776705220 ) ) ;
#1395 = DIRECTION ( 'NONE',  ( 1.000000000000000000, 0.000000000000000000, 0.000000000000000000 ) ) ;
#1396 = ORIENTED_EDGE ( 'NONE', *, *, #48193, .T. ) ;
#1397 = DIRECTION ( 'NONE',  ( -1.000000000000000000, -0.000000000000000000, 0.000000000000000000 ) ) ;
#1398 = CARTESIAN_POINT ( 'NONE',  ( -16.08777780284372128, -12.10708131394839882, 31.69288490824020954 ) ) ;
#1399 = ADVANCED_FACE ( 'NONE', ( #5854 ), #67554, .F. ) ;
#1400 = AXIS2_PLACEMENT_3D ( 'NONE', #83248, #42268, #48554 ) ;
#1401 = VECTOR ( 'NONE', #24481, 1000.000000000000000 ) ;
#1402 = CARTESIAN_POINT ( 'NONE',  ( 1.134592147322421418, -9.271318131107980420, 34.42618302367067429 ) ) ;
#1403 = ADVANCED_FACE ( 'NONE', ( #73870 ), #3864, .F. ) ;
#1404 = CARTESIAN_POINT ( 'NONE',  ( -0.5276208408985972875, -10.67929555188718460, 33.92786785259543336 ) ) ;
#1405 = AXIS2_PLACEMENT_3D ( 'NONE', #11950, #31322, #53361 ) ;
#1406 = ORIENTED_EDGE ( 'NONE', *, *, #78616, .F. ) ;
#1407 = CARTESIAN_POINT ( 'NONE',  ( -15.48074596171158213, -2.779195860258146578, 31.39871582349836032 ) ) ;
#1408 = CARTESIAN_POINT ( 'NONE',  ( -17.14300545628321260, -2.292212530054420050, 30.41441678777542634 ) ) ;
#1409 = CARTESIAN_POINT ( 'NONE',  ( 1.653273178848927064E-15, -7.500000000000000000, 10.00000000000000178 ) ) ;
#1410 = FACE_OUTER_BOUND ( 'NONE', #39229, .T. ) ;
#1411 = ORIENTED_EDGE ( 'NONE', *, *, #7656, .F. ) ;
#1412 = CARTESIAN_POINT ( 'NONE',  ( -6.923076923076922462, -6.343179335718451384, 34.87096338111211935 ) ) ;
#1413 = B_SPLINE_CURVE_WITH_KNOTS ( 'NONE', 3,
 ( #19596, #45281, #74107, #4306, #66900, #39442, #88095, #86750, #59247, #52486 ),
 .UNSPECIFIED., .F., .F.,
 ( 4, 2, 2, 2, 4 ),
 ( 0.0007817246256747505334, 0.0009771112852218954894, 0.001172497944769040554, 0.001367884604316185618, 0.001563271263863330682 ),
 .UNSPECIFIED. ) ;
#1414 = ORIENTED_EDGE ( 'NONE', *, *, #59284, .T. ) ;
#1415 = CARTESIAN_POINT ( 'NONE',  ( -0.6089743589743593644, -3.499999999999999556, 29.75000000000000355 ) ) ;
#1416 = CYLINDRICAL_SURFACE ( 'NONE', #3843, 0.2499999999999995559 ) ;
#1417 = ORIENTED_EDGE ( 'NONE', *, *, #17439, .T. ) ;
#1418 = FACE_OUTER_BOUND ( 'NONE', #24802, .T. ) ;
#1419 = CARTESIAN_POINT ( 'NONE',  ( 4.153846153846154188, -9.058645607665452459, 34.76329471203371924 ) ) ;
#1420 = CARTESIAN_POINT ( 'NONE',  ( 0.2386122440223140684, -4.186968288167447483, 33.49512374952580984 ) ) ;
#1421 = CARTESIAN_POINT ( 'NONE',  ( 13.38461538461526423, -12.16647553114689728, 32.15551576947799362 ) ) ;
#1422 = CARTESIAN_POINT ( 'NONE',  ( -18.22292621751614305, -4.186968288167451036, 33.49512374952581695 ) ) ;
#1423 = EDGE_CURVE ( 'NONE', #25798, #52031, #74311, .T. ) ;
#1425 = ORIENTED_EDGE ( 'NONE', *, *, #59426, .F. ) ;
#1424 = EDGE_CURVE ( 'NONE', #81511, #81196, #74355, .T. ) ;
#1426 = EDGE_LOOP ( 'NONE', ( #11958, #3521 ) ) ;
#1427 = FACE_BOUND ( 'NONE', #5912, .T. ) ;
#1428 = ORIENTED_EDGE ( 'NONE', *, *, #57736, .F. ) ;
#1429 = CARTESIAN_POINT ( 'NONE',  ( -7.912236225513979981, -5.471508081941602875, 34.59228464037088457 ) ) ;
#1430 = VECTOR ( 'NONE', #86578, 1000.000000000000000 ) ;
#1431 = B_SPLINE_CURVE_WITH_KNOTS ( 'NONE', 3,
 ( #54758, #26411, #82245, #81362, #55201, #12887, #13773, #41258, #48890, #43025 ),
 .UNSPECIFIED., .F., .F.,
 ( 4, 2, 2, 2, 4 ),
 ( 0.000000000000000000, 0.0001954339881912774070, 0.0003908679763825548140, 0.0005863019645738322752, 0.0007817359527651096280 ),
 .UNSPECIFIED. ) ;
#1432 = EDGE_CURVE ( 'NONE', #22613, #47954, #51688, .T. ) ;
#1433 = CARTESIAN_POINT ( 'NONE',  ( -14.08491263871423982, -11.60474049983371003, 33.02348890104160262 ) ) ;
#1434 = EDGE_CURVE ( 'NONE', #50542, #83291, #88729, .T. ) ;
#1435 = CARTESIAN_POINT ( 'NONE',  ( 9.442284455014730682, -12.22074536777954989, 31.39888409691088356 ) ) ;
#1436 = CARTESIAN_POINT ( 'NONE',  ( 0.7114838709165044461, -12.68172785388650681, 30.59649109432439573 ) ) ;
#1437 = VERTEX_POINT ( 'NONE', #81079 ) ;
#1439 = EDGE_CURVE ( 'NONE', #28677, #64411, #73254, .T. ) ;
#1438 = ORIENTED_EDGE ( 'NONE', *, *, #64153, .T. ) ;
#1440 = ORIENTED_EDGE ( 'NONE', *, *, #81732, .T. ) ;
#1441 = CARTESIAN_POINT ( 'NONE',  ( 13.25400502499085675, -7.722926236386453702, 34.74524107206102030 ) ) ;
#1442 = ORIENTED_EDGE ( 'NONE', *, *, #71141, .T. ) ;
#1443 = VECTOR ( 'NONE', #79777, 999.9999999999998863 ) ;
#1444 = CARTESIAN_POINT ( 'NONE',  ( 19.00000000000000000, 1.250000000000002220, 23.75000000000000000 ) ) ;
#1445 = EDGE_CURVE ( 'NONE', #17692, #1987, #20253, .T. ) ;
#1446 = CARTESIAN_POINT ( 'NONE',  ( 14.08476534878545827, -11.98009711892699514, 32.48740034544076138 ) ) ;
#1447 = CARTESIAN_POINT ( 'NONE',  ( 13.60739505359345181, -11.60474049983371003, 33.02348890104160262 ) ) ;
#1448 = ORIENTED_EDGE ( 'NONE', *, *, #31385, .F. ) ;
#1449 = CARTESIAN_POINT ( 'NONE',  ( -8.703975629717932705, -4.320704448112861584, 33.92786785259548310 ) ) ;
#1450 = AXIS2_PLACEMENT_3D ( 'NONE', #52880, #24518, #79482 ) ;
#1451 = DIRECTION ( 'NONE',  ( -0.000000000000000000, 0.1736481776669307198, -0.9848077530122080203 ) ) ;
#1452 = EDGE_CURVE ( 'NONE', #74112, #56593, #80776, .T. ) ;
#1453 = CARTESIAN_POINT ( 'NONE',  ( -18.00000000000000000, -3.679149656540967150, 35.86790692298802696 ) ) ;
#1454 = CARTESIAN_POINT ( 'NONE',  ( -11.53846153846165912, -3.300289026999228881, 32.46337939537708905 ) ) ;
#1455 = ORIENTED_EDGE ( 'NONE', *, *, #59844, .F. ) ;
#1456 = ORIENTED_EDGE ( 'NONE', *, *, #88867, .T. ) ;
#1457 = VECTOR ( 'NONE', #23969, 1000.000000000000000 ) ;
#1458 = ORIENTED_EDGE ( 'NONE', *, *, #42077, .F. ) ;
#1459 = VECTOR ( 'NONE', #50275, 1000.000000000000227 ) ;
#1460 = CARTESIAN_POINT ( 'NONE',  ( 3.454195629684017277, -7.630147987733843173, 34.99859428049665411 ) ) ;
#1462 = CARTESIAN_POINT ( 'NONE',  ( 1.450682717965462887, -11.35647404775217595, 33.31231777344667222 ) ) ;
#1461 = CARTESIAN_POINT ( 'NONE',  ( -8.069080063669991532, -6.503392248772476236, 34.64988816332204635 ) ) ;
#1463 = VECTOR ( 'NONE', #18706, 1000.000000000000227 ) ;
#1464 = CARTESIAN_POINT ( 'NONE',  ( -17.74994558008654622, -5.642605341092954419, 34.66089969410670335 ) ) ;
#1465 = CARTESIAN_POINT ( 'NONE',  ( 12.46153846153846168, -12.62096338111211580, 30.90682066428153263 ) ) ;
#1466 = FACE_BOUND ( 'NONE', #28995, .T. ) ;
#1467 = CARTESIAN_POINT ( 'NONE',  ( 8.639082799499069765, -11.04286588640298561, 33.62463336215343901 ) ) ;
#1468 = EDGE_LOOP ( 'NONE', ( #13731, #4681 ) ) ;
#1469 = CARTESIAN_POINT ( 'NONE',  ( 17.32686859527121470, -10.76462480002816413, 33.53768742498949962 ) ) ;
#1470 = CARTESIAN_POINT ( 'NONE',  ( 9.562159722576005549, -12.15440758774515473, 32.17923288041532004 ) ) ;
#1471 = CARTESIAN_POINT ( 'NONE',  ( 11.40798483034507527, -7.276988635370452485, 34.74523720219453793 ) ) ;
#1472 = CARTESIAN_POINT ( 'NONE',  ( 7.053602361310569613, -9.503571793651733657, 34.60286762892837942 ) ) ;
#1473 = ORIENTED_EDGE ( 'NONE', *, *, #63442, .F. ) ;
#1474 = CARTESIAN_POINT ( 'NONE',  ( -18.06527044596078113, -8.613356846314824011, 34.62446782046655613 ) ) ;
#1475 = EDGE_CURVE ( 'NONE', #48420, #40198, #13133, .T. ) ;
#1476 = ORIENTED_EDGE ( 'NONE', *, *, #76162, .F. ) ;
#1477 = FACE_BOUND ( 'NONE', #64109, .T. ) ;
#1478 = CARTESIAN_POINT ( 'NONE',  ( 6.000000000000001776, -12.62096338111211580, 30.90682066428153263 ) ) ;
#1479 = DIRECTION ( 'NONE',  ( 0.000000000000000000, 0.3420201433256610524, 0.9396926207859113145 ) ) ;
#1480 = CARTESIAN_POINT ( 'NONE',  ( -17.76215049426127024, 12.75000000000001599, 30.81664701255127881 ) ) ;
#1481 = ORIENTED_EDGE ( 'NONE', *, *, #32747, .T. ) ;
#1482 = CARTESIAN_POINT ( 'NONE',  ( 0.3313912521002408962, -10.88202310037936194, 33.43294751532457099 ) ) ;
#1483 = CARTESIAN_POINT ( 'NONE',  ( -3.453696189676078276, -2.308479472611653094, 30.53278059502174457 ) ) ;
#1484 = CARTESIAN_POINT ( 'NONE',  ( 8.769230769230768274, -8.164416787775445883, 34.95778746994557906 ) ) ;
#1485 = CARTESIAN_POINT ( 'NONE',  ( -16.15384615384615330, -6.435427911321262684, 35.78748833219616898 ) ) ;
#1486 = VERTEX_POINT ( 'NONE', #30102 ) ;
#1487 = B_SPLINE_CURVE_WITH_KNOTS ( 'NONE', 3,
 ( #50518, #16738, #43334, #70812, #72125, #30265, #71680, #3223, #30697, #9115 ),
 .UNSPECIFIED., .F., .F.,
 ( 4, 2, 2, 2, 4 ),
 ( 0.000000000000000000, 0.0001954339857564074202, 0.0003908679715128148403, 0.0005863019572692222334, 0.0007817359430256296806 ),
 .UNSPECIFIED. ) ;
#1488 = B_SPLINE_CURVE_WITH_KNOTS ( 'NONE', 3,
 ( #57728, #2327, #83891, #16736, #37447, #71678 ),
 .UNSPECIFIED., .F., .F.,
 ( 4, 2, 4 ),
 ( 0.4999999999999957812, 0.7499999999999978906, 1.000000000000000000 ),
 .UNSPECIFIED. ) ;
#1489 = EDGE_CURVE ( 'NONE', #37467, #53160, #71084, .T. ) ;
#1490 = CARTESIAN_POINT ( 'NONE',  ( -18.03205128205128105, -3.499999999999999556, 29.75000000000000355 ) ) ;
#1491 = EDGE_LOOP ( 'NONE', ( #25827, #67846, #4888, #4081 ) ) ;
#1493 = VERTEX_POINT ( 'NONE', #21123 ) ;
#1492 = CARTESIAN_POINT ( 'NONE',  ( 4.219913487196228274, -2.833524468853757750, 32.15551576947925838 ) ) ;
#1494 = CARTESIAN_POINT ( 'NONE',  ( 11.66898724022510159, -6.852161475712352789, 34.70806712695775786 ) ) ;
#1495 = DIRECTION ( 'NONE',  ( -1.000000000000000000, -0.000000000000000000, -0.000000000000000000 ) ) ;
#1496 = LINE ( 'NONE', #28982, #40056 ) ;
#1497 = B_SPLINE_CURVE_WITH_KNOTS ( 'NONE', 3,
 ( #50986, #61969, #64501, #9157, #34506, #2809, #57326, #84822, #64956, #278 ),
 .UNSPECIFIED., .F., .F.,
 ( 4, 2, 2, 2, 4 ),
 ( 0.000000000000000000, 0.0001954311564186872810, 0.0003908623128373745620, 0.0005862934692560618430, 0.0007817246256747491240 ),
 .UNSPECIFIED. ) ;
#1498 = CARTESIAN_POINT ( 'NONE',  ( -12.68502338610279345, -10.97335522853832579, 33.68706563782419749 ) ) ;
#1500 = CARTESIAN_POINT ( 'NONE',  ( 8.639082799499073317, -4.299443229763728169, 33.91186481527756058 ) ) ;
#1499 = CARTESIAN_POINT ( 'NONE',  ( -5.869474561766354626, -6.808710257144159783, 34.95449254468098843 ) ) ;
#1501 = ADVANCED_FACE ( 'NONE', ( #63440 ), #77841, .F. ) ;
#1502 = CARTESIAN_POINT ( 'NONE',  ( 8.068933387422255521, -4.387253974876678342, 33.66317474335728832 ) ) ;
#1503 = VECTOR ( 'NONE', #30513, 1000.000000000000000 ) ;
#1504 = CARTESIAN_POINT ( 'NONE',  ( -2.749999999999991562, -8.639087296526025028, 26.26562500000000000 ) ) ;
#1505 = ORIENTED_EDGE ( 'NONE', *, *, #84173, .T. ) ;
#1506 = FACE_OUTER_BOUND ( 'NONE', #62728, .T. ) ;
#1507 = ORIENTED_EDGE ( 'NONE', *, *, #80002, .T. ) ;
#1508 = ORIENTED_EDGE ( 'NONE', *, *, #431, .F. ) ;
#1509 = CARTESIAN_POINT ( 'NONE',  ( 4.153846153846154188, -12.34228464037088635, 31.77849191805839268 ) ) ;
#1510 = VERTEX_POINT ( 'NONE', #22020 ) ;
#1511 = CARTESIAN_POINT ( 'NONE',  ( 16.94623161025552704, -4.809359713505814149, 33.96456829005828837 ) ) ;
#1512 = EDGE_CURVE ( 'NONE', #50046, #70330, #62546, .T. ) ;
#1513 = CARTESIAN_POINT ( 'NONE',  ( -5.076923076923075762, -12.62096338111211580, 30.90682066428153263 ) ) ;
#1514 = CARTESIAN_POINT ( 'NONE',  ( 18.00000000000031264, -2.255955759149395501, 30.00000000000324363 ) ) ;
#1515 = LINE ( 'NONE', #29000, #34445 ) ;
#1516 = CARTESIAN_POINT ( 'NONE',  ( 12.46153846153833911, -10.90142922262034020, 33.41473453929536674 ) ) ;
#1517 = EDGE_CURVE ( 'NONE', #55049, #67618, #860, .T. ) ;
#1518 = CARTESIAN_POINT ( 'NONE',  ( 16.15384615384615330, -11.69971097300155272, 32.46337939537588113 ) ) ;
#1519 = CARTESIAN_POINT ( 'NONE',  ( -15.16551409125639260, -8.656820664281605460, 34.87096338111211224 ) ) ;
#1520 = EDGE_CURVE ( 'NONE', #50046, #29769, #88292, .T. ) ;
#1521 = CARTESIAN_POINT ( 'NONE',  ( -18.00000000000012079, -8.613356846316285953, 34.62446782046622218 ) ) ;
#1522 = CARTESIAN_POINT ( 'NONE',  ( -2.307692307692305711, -2.833524468853757305, 32.15551576947925838 ) ) ;
#1523 = DIRECTION ( 'NONE',  ( -1.000000000000000000, 5.997714145664496128E-17, -5.202187765341190574E-33 ) ) ;
#1524 = CARTESIAN_POINT ( 'NONE',  ( 7.846153846153846700, -2.292212530054420494, 30.41441678777542634 ) ) ;
#1525 = AXIS2_PLACEMENT_3D ( 'NONE', #68477, #60388, #68918 ) ;
#1526 = ORIENTED_EDGE ( 'NONE', *, *, #34553, .F. ) ;
#1527 = ORIENTED_EDGE ( 'NONE', *, *, #47274, .F. ) ;
#1528 = CARTESIAN_POINT ( 'NONE',  ( 12.52679360105129724, -2.657715359629132301, 31.77849191805844242 ) ) ;
#1529 = CARTESIAN_POINT ( 'NONE',  ( 3.480823650682683734, -10.82426656108011720, 33.81400080652039009 ) ) ;
#1530 = CARTESIAN_POINT ( 'NONE',  ( -2.373449110206616641, -7.249945686854185389, 34.74374336980224598 ) ) ;
#1531 = VERTEX_POINT ( 'NONE', #22460 ) ;
#1532 = VECTOR ( 'NONE', #28097, 1000.000000000000000 ) ;
#1533 = CARTESIAN_POINT ( 'NONE',  ( 12.21151522424549896, -9.271318131107980420, 34.42618302367067429 ) ) ;
#1534 = AXIS2_PLACEMENT_3D ( 'NONE', #68702, #89001, #40360 ) ;
#1535 = CARTESIAN_POINT ( 'NONE',  ( -10.61538461538473577, -12.70778746994576025, 30.41441678777401236 ) ) ;
#1536 = AXIS2_PLACEMENT_3D ( 'NONE', #48543, #26525, #89128 ) ;
#1537 = CARTESIAN_POINT ( 'NONE',  ( -12.23875892027004753, -10.81320215134717344, 33.49497208177562868 ) ) ;
#1538 = VERTEX_POINT ( 'NONE', #49922 ) ;
#1539 = CYLINDRICAL_SURFACE ( 'NONE', #87522, 0.2499999999999993616 ) ;
#1540 = EDGE_LOOP ( 'NONE', ( #24940, #19961, #33858, #62612 ) ) ;
#1541 = CARTESIAN_POINT ( 'NONE',  ( 10.83816415665302380, -8.496831190052093419, 34.64984203495476578 ) ) ;
#1542 = CARTESIAN_POINT ( 'NONE',  ( 8.900021210197715860, -9.084667340241226796, 34.75534355489798344 ) ) ;
#1543 = CYLINDRICAL_SURFACE ( 'NONE', #7052, 0.2500000000000012212 ) ;
#1544 = CARTESIAN_POINT ( 'NONE',  ( -9.822455662039388358, -8.630895178749533159, 34.87696386517710323 ) ) ;
#1545 = CARTESIAN_POINT ( 'NONE',  ( -17.86947456176635640, -12.50538340440932394, 31.33453814440721885 ) ) ;
#1546 = ORIENTED_EDGE ( 'NONE', *, *, #44070, .T. ) ;
#1547 = EDGE_CURVE ( 'NONE', #76633, #31437, #38415, .T. ) ;
#1548 = ORIENTED_EDGE ( 'NONE', *, *, #24604, .T. ) ;
#1549 = ORIENTED_EDGE ( 'NONE', *, *, #14770, .F. ) ;
#1550 = CARTESIAN_POINT ( 'NONE',  ( 13.38461538461538680, -3.050289026998446396, 32.03036669348365706 ) ) ;
#1551 = CARTESIAN_POINT ( 'NONE',  ( 13.60762673622823726, -9.886259254753566594, 34.14407573483972413 ) ) ;
#1552 = CIRCLE ( 'NONE', #4433, 0.2500000000000002220 ) ;
#1553 = EDGE_CURVE ( 'NONE', #78266, #17849, #49497, .T. ) ;
#1554 = DIRECTION ( 'NONE',  ( 0.000000000000000000, 0.8660254037844377084, 0.5000000000000015543 ) ) ;
#1555 = CARTESIAN_POINT ( 'NONE',  ( 0.3954560821783242308, -12.34228464037088280, 31.77849191805838558 ) ) ;
#1556 = CARTESIAN_POINT ( 'NONE',  ( -7.846153846153844924, -3.937682226553329556, 33.60647404775216529 ) ) ;
#1557 = LINE ( 'NONE', #29045, #38017 ) ;
#1558 = EDGE_LOOP ( 'NONE', ( #33756, #39218 ) ) ;
#1559 = ORIENTED_EDGE ( 'NONE', *, *, #71272, .T. ) ;
#1560 = ORIENTED_EDGE ( 'NONE', *, *, #74064, .F. ) ;
#1561 = EDGE_CURVE ( 'NONE', #27440, #31586, #35624, .T. ) ;
#1563 = ORIENTED_EDGE ( 'NONE', *, *, #50794, .F. ) ;
#1562 = LINE ( 'NONE', #56940, #28726 ) ;
#1565 = DIRECTION ( 'NONE',  ( 0.000000000000000000, 0.000000000000000000, -1.000000000000000000 ) ) ;
#1564 = CARTESIAN_POINT ( 'NONE',  ( -9.822999158975250111, -8.999036380462717588, 34.52022231692819076 ) ) ;
#1566 = CARTESIAN_POINT ( 'NONE',  ( -10.61538461538461320, -5.180354513474913603, 36.12317359536750416 ) ) ;
#1567 = CARTESIAN_POINT ( 'NONE',  ( -10.83886955910856464, -11.89387501736622710, 32.13663884655806413 ) ) ;
#1568 = ORIENTED_EDGE ( 'NONE', *, *, #54155, .F. ) ;
#1569 = VECTOR ( 'NONE', #41135, 1000.000000000000000 ) ;
#1570 = EDGE_LOOP ( 'NONE', ( #71156, #18996, #23444, #80993 ) ) ;
#1571 = CARTESIAN_POINT ( 'NONE',  ( 13.63456079399343146, -10.92531984108285670, 33.72920026020278073 ) ) ;
#1572 = EDGE_CURVE ( 'NONE', #20924, #27696, #5306, .T. ) ;
#1573 = ORIENTED_EDGE ( 'NONE', *, *, #85018, .T. ) ;
#1574 = FACE_BOUND ( 'NONE', #53527, .T. ) ;
#1576 = VECTOR ( 'NONE', #71122, 1000.000000000000000 ) ;
#1575 = CARTESIAN_POINT ( 'NONE',  ( 6.700150705560777631, -4.186968288167446595, 33.49512374952580274 ) ) ;
#1577 = VECTOR ( 'NONE', #24271, 1000.000000000000114 ) ;
#1578 = CARTESIAN_POINT ( 'NONE',  ( -4.284536756956462966, -9.929715669179216775, 34.40415004197138416 ) ) ;
#1579 = ORIENTED_EDGE ( 'NONE', *, *, #36750, .F. ) ;
#1580 = CARTESIAN_POINT ( 'NONE',  ( -14.24162497434223162, -8.164416787775445883, 34.95778746994558617 ) ) ;
#1581 = ADVANCED_FACE ( 'NONE', ( #36425 ), #42744, .F. ) ;
#1582 = DIRECTION ( 'NONE',  ( -1.000000000000000000, -0.000000000000000000, -0.000000000000000000 ) ) ;
#1583 = DIRECTION ( 'NONE',  ( 0.000000000000000000, 0.000000000000000000, -1.000000000000000000 ) ) ;
#1584 = DIRECTION ( 'NONE',  ( -0.000000000000000000, 0.000000000000000000, 1.000000000000000000 ) ) ;
#1585 = CARTESIAN_POINT ( 'NONE',  ( -17.07692307692319744, -2.625532179533778709, 30.86335684631627174 ) ) ;
#1586 = VERTEX_POINT ( 'NONE', #29669 ) ;
#1587 = VECTOR ( 'NONE', #24500, 1000.000000000000000 ) ;
#1588 = CARTESIAN_POINT ( 'NONE',  ( 16.37680905740764103, -7.369474270740072441, 34.74850911626239736 ) ) ;
#1589 = CARTESIAN_POINT ( 'NONE',  ( -8.069638770718174925, -12.11044203135681840, 32.26167407432752299 ) ) ;
#1590 = DIRECTION ( 'NONE',  ( -0.000000000000000000, -0.7660444431189791237, -0.6427876096865379196 ) ) ;
#1591 = CARTESIAN_POINT ( 'NONE',  ( 13.51540582558233794, -2.295524264805589354, 30.44142389570982488 ) ) ;
#1592 = CARTESIAN_POINT ( 'NONE',  ( -15.00798968950081758, -11.89424750095246175, 32.13594075562311758 ) ) ;
#1593 = CARTESIAN_POINT ( 'NONE',  ( 8.992010438208833278, -4.226511098958373402, 33.85474049983370293 ) ) ;
#1595 = CARTESIAN_POINT ( 'NONE',  ( 11.40798635338582123, -7.276987145209184327, 34.99546412871779211 ) ) ;
#1594 = CARTESIAN_POINT ( 'NONE',  ( 5.076923076922954969, -11.48612834414049644, 32.76840700105863391 ) ) ;
#1596 = EDGE_CURVE ( 'NONE', #3333, #49885, #76447, .T. ) ;
#1597 = CARTESIAN_POINT ( 'NONE',  ( -0.4615384615384611200, -2.900454961884010974, 35.62045528018868623 ) ) ;
#1599 = CARTESIAN_POINT ( 'NONE',  ( 2.307692307692186251, -6.835583212225970762, 34.95778746994575670 ) ) ;
#1598 = DIRECTION ( 'NONE',  ( -0.000000000000000000, -0.1736481776669307198, -0.9848077530122080203 ) ) ;
#1600 = CARTESIAN_POINT ( 'NONE',  ( -2.307692307692428724, -5.941354392335915335, 34.76329471203413846 ) ) ;
#1601 = CARTESIAN_POINT ( 'NONE',  ( 2.775308065498768517, -8.577988221561467341, 20.54500670625849068 ) ) ;
#1602 = VERTEX_POINT ( 'NONE', #72854 ) ;
#1603 = B_SPLINE_CURVE_WITH_KNOTS ( 'NONE', 3,
 ( #75818, #21762, #54650, #49240, #6915, #63185, #1937, #48342, #76714, #68621 ),
 .UNSPECIFIED., .F., .F.,
 ( 4, 2, 2, 2, 4 ),
 ( 0.000000000000000000, 0.0001954339857564054144, 0.0003908679715128108288, 0.0005863019572692162703, 0.0007817359430256216575 ),
 .UNSPECIFIED. ) ;
#1604 = CARTESIAN_POINT ( 'NONE',  ( 12.68431800280687050, -2.600157965045224895, 30.74683119005207743 ) ) ;
#1605 = ORIENTED_EDGE ( 'NONE', *, *, #8664, .F. ) ;
#1606 = CARTESIAN_POINT ( 'NONE',  ( -13.38461538461538325, -9.058645607665452459, 34.76329471203371924 ) ) ;
#1607 = ORIENTED_EDGE ( 'NONE', *, *, #49753, .T. ) ;
#1608 = CARTESIAN_POINT ( 'NONE',  ( -13.16160254052199008, -2.308499170217967134, 30.53291367094873721 ) ) ;
#1609 = CARTESIAN_POINT ( 'NONE',  ( 6.000000000000001776, -2.900454961884010974, 35.62045528018868623 ) ) ;
#1610 = ORIENTED_EDGE ( 'NONE', *, *, #74543, .F. ) ;
#1611 = CARTESIAN_POINT ( 'NONE',  ( -7.976301055592065481, -6.001485441113819874, 34.52039167877662607 ) ) ;
#1612 = CARTESIAN_POINT ( 'NONE',  ( -0.06109907496454585613, -4.750000000000000000, 25.15438170625849068 ) ) ;
#1613 = FACE_OUTER_BOUND ( 'NONE', #38638, .T. ) ;
#1614 = EDGE_CURVE ( 'NONE', #32479, #19139, #52139, .T. ) ;
#1615 = CARTESIAN_POINT ( 'NONE',  ( -4.153846153845837108, -2.255955759149395501, 30.00000000000324363 ) ) ;
#1616 = CARTESIAN_POINT ( 'NONE',  ( 17.07692307692295586, -9.528491918059723176, 34.59228464037033035 ) ) ;
#1617 = CARTESIAN_POINT ( 'NONE',  ( 16.94623161025552704, -12.38065189839062263, 30.83690757178629482 ) ) ;
#1618 = CARTESIAN_POINT ( 'NONE',  ( 15.16544521796492262, -7.749976730030849303, 34.74374725381503737 ) ) ;
#1619 = CARTESIAN_POINT ( 'NONE',  ( -39.05038313613820122, -2.499999999999999556, 29.75000000000000355 ) ) ;
#1620 = AXIS2_PLACEMENT_3D ( 'NONE', #26129, #39662, #54032 ) ;
#1621 = CARTESIAN_POINT ( 'NONE',  ( -1.553300858899125059, -3.750000000000009326, 15.32812500000000355 ) ) ;
#1622 = EDGE_CURVE ( 'NONE', #5191, #15410, #45829, .T. ) ;
#1623 = EDGE_CURVE ( 'NONE', #39944, #28593, #65207, .T. ) ;
#1624 = B_SPLINE_CURVE_WITH_KNOTS ( 'NONE', 3,
 ( #85308, #86659, #71329, #78096, #3319, #51482, #79879, #58707, #17284, #57825 ),
 .UNSPECIFIED., .F., .F.,
 ( 4, 2, 2, 2, 4 ),
 ( 0.000000000000000000, 0.0001954339857564097512, 0.0003908679715128195024, 0.0005863019572692292807, 0.0007817359430256390048 ),
 .UNSPECIFIED. ) ;
#1625 = CARTESIAN_POINT ( 'NONE',  ( 11.31497661389721010, -5.827078755546623690, 34.72654668319379567 ) ) ;
#1626 = CARTESIAN_POINT ( 'NONE',  ( 14.53047184896071897, -10.81320215134717344, 33.49497208177562868 ) ) ;
#1627 = VECTOR ( 'NONE', #61858, 1000.000000000000000 ) ;
#1628 = EDGE_CURVE ( 'NONE', #21791, #14730, #87164, .T. ) ;
#1629 = DIRECTION ( 'NONE',  ( 0.000000000000000000, 0.8660254037844377084, -0.5000000000000015543 ) ) ;
#1630 = CARTESIAN_POINT ( 'NONE',  ( -2.651650429449535551, -10.15165042944956753, 17.43750000000000000 ) ) ;
#1631 = EDGE_CURVE ( 'NONE', #69859, #18936, #78279, .T. ) ;
#1632 = B_SPLINE_CURVE_WITH_KNOTS ( 'NONE', 3,
 ( #47902, #83029, #21761, #48787, #6485, #47452, #41155, #68620, #34387, #21313 ),
 .UNSPECIFIED., .F., .F.,
 ( 4, 2, 2, 2, 4 ),
 ( 0.0007817246256747434861, 0.0009771112852218859484, 0.001172497944769028411, 0.001367884604316171090, 0.001563271263863313552 ),
 .UNSPECIFIED. ) ;
#1633 = LINE ( 'NONE', #43054, #36096 ) ;
#1634 = ORIENTED_EDGE ( 'NONE', *, *, #88902, .T. ) ;
#1635 = FACE_OUTER_BOUND ( 'NONE', #22221, .T. ) ;
#1636 = CARTESIAN_POINT ( 'NONE',  ( 16.15384615384603251, -12.27809138561165270, 31.22303859784587132 ) ) ;
#1637 = CARTESIAN_POINT ( 'NONE',  ( -8.899922235898330314, -11.18331474514187995, 33.13161551792790505 ) ) ;
#1638 = CARTESIAN_POINT ( 'NONE',  ( 8.769230769230645706, -5.941354392335915335, 34.76329471203413846 ) ) ;
#1639 = CARTESIAN_POINT ( 'NONE',  ( -16.40386939113911779, -10.76384336483936011, 33.53834819971076087 ) ) ;
#1640 = CARTESIAN_POINT ( 'NONE',  ( -3.164701897419154975, -5.471508081941601098, 34.59228464037088457 ) ) ;
#1641 = CYLINDRICAL_SURFACE ( 'NONE', #77982, 0.2499999999999995559 ) ;
#1642 = VECTOR ( 'NONE', #82692, 1000.000000000000114 ) ;
#1643 = ORIENTED_EDGE ( 'NONE', *, *, #71969, .F. ) ;
#1644 = ORIENTED_EDGE ( 'NONE', *, *, #35630, .T. ) ;
#1645 = VERTEX_POINT ( 'NONE', #64756 ) ;
#1646 = VECTOR ( 'NONE', #7114, 1000.000000000000227 ) ;
#1647 = DIRECTION ( 'NONE',  ( -0.000000000000000000, -0.6427876096865404731, -0.7660444431189770143 ) ) ;
#1648 = DIRECTION ( 'NONE',  ( 0.000000000000000000, 0.3420201433256610524, 0.9396926207859113145 ) ) ;
#1649 = CARTESIAN_POINT ( 'NONE',  ( 6.699591998512590685, -3.019605429927184836, 32.48692288466676814 ) ) ;
#1650 = DIRECTION ( 'NONE',  ( -0.000000000000000000, 0.3420201433256694901, -0.9396926207859082059 ) ) ;
#1651 = CARTESIAN_POINT ( 'NONE',  ( 17.86930939688969033, -9.084618155246140248, 34.75535874321725771 ) ) ;
#1652 = VERTEX_POINT ( 'NONE', #78732 ) ;
#1653 = DIRECTION ( 'NONE',  ( -0.000000000000000000, -0.6427876096865404731, -0.7660444431189771253 ) ) ;
#1654 = ORIENTED_EDGE ( 'NONE', *, *, #27147, .T. ) ;
#1655 = ORIENTED_EDGE ( 'NONE', *, *, #17163, .F. ) ;
#1656 = ORIENTED_EDGE ( 'NONE', *, *, #23547, .T. ) ;
#1658 = ORIENTED_EDGE ( 'NONE', *, *, #86170, .F. ) ;
#1657 = CARTESIAN_POINT ( 'NONE',  ( 8.703148389870630552, -12.34228464037088280, 31.77849191805838558 ) ) ;
#1659 = DIRECTION ( 'NONE',  ( -0.000000000000000000, -0.9848077530122085754, -0.1736481776669273613 ) ) ;
#1660 = CARTESIAN_POINT ( 'NONE',  ( -10.61538461538461320, -4.786620604624113540, 33.94971097300155094 ) ) ;
#1661 = CARTESIAN_POINT ( 'NONE',  ( -9.915792636031639518, -8.496056993536548418, 34.65000542017679663 ) ) ;
#1662 = ORIENTED_EDGE ( 'NONE', *, *, #56806, .T. ) ;
#1663 = EDGE_LOOP ( 'NONE', ( #25110, #61996, #65349, #45435 ) ) ;
#1664 = ORIENTED_EDGE ( 'NONE', *, *, #70919, .F. ) ;
#1665 = CARTESIAN_POINT ( 'NONE',  ( -14.08426534583073675, -7.630147231320743018, 34.74852402298682819 ) ) ;
#1667 = ORIENTED_EDGE ( 'NONE', *, *, #53635, .T. ) ;
#1666 = DIRECTION ( 'NONE',  ( -0.000000000000000000, 0.6427876096865404731, -0.7660444431189770143 ) ) ;
#1668 = CARTESIAN_POINT ( 'NONE',  ( -0.4615384615384611200, -1.367168528481310208, 33.57946703557072254 ) ) ;
#1669 = DIRECTION ( 'NONE',  ( 1.000000000000000000, 0.000000000000000000, 0.000000000000000000 ) ) ;
#1670 = CARTESIAN_POINT ( 'NONE',  ( -2.980714919130914353, -9.943054286541407549, 34.11300777759954883 ) ) ;
#1671 = EDGE_LOOP ( 'NONE', ( #37476, #13300, #1227, #9317 ) ) ;
#1672 = VECTOR ( 'NONE', #82272, 999.9999999999998863 ) ;
#1673 = CARTESIAN_POINT ( 'NONE',  ( -11.40793583669797684, -5.195472089885680766, 34.18748526763464923 ) ) ;
#1674 = CARTESIAN_POINT ( 'NONE',  ( -5.999999999999998224, -2.833524468853757305, 32.15551576947925838 ) ) ;
#1675 = VERTEX_POINT ( 'NONE', #16580 ) ;
#1676 = FACE_BOUND ( 'NONE', #75859, .T. ) ;
#1677 = CARTESIAN_POINT ( 'NONE',  ( -10.74553258511630993, -5.070767119584671079, 34.40440758774516183 ) ) ;
#1678 = CARTESIAN_POINT ( 'NONE',  ( -17.07692307692307665, -3.050289026998446396, 32.03036669348365706 ) ) ;
#1679 = EDGE_CURVE ( 'NONE', #34673, #24943, #58899, .T. ) ;
#1680 = CYLINDRICAL_SURFACE ( 'NONE', #72480, 0.2500000000000008882 ) ;
#1681 = B_SPLINE_CURVE_WITH_KNOTS ( 'NONE', 3,
 ( #73432, #31089, #24332, #45942, #18042, #11278, #45499, #87402, #66668, #38752 ),
 .UNSPECIFIED., .F., .F.,
 ( 4, 2, 2, 2, 4 ),
 ( 0.000000000000000000, 0.0001954311564186867931, 0.0003908623128373735862, 0.0005862934692560603251, 0.0007817246256747471724 ),
 .UNSPECIFIED. ) ;
#1683 = CARTESIAN_POINT ( 'NONE',  ( 14.98076923076923173, -2.249999999999998668, 29.75000000000000355 ) ) ;
#1682 = CARTESIAN_POINT ( 'NONE',  ( -2.294871794871794712, -11.00000000000000000, 29.75000000000000355 ) ) ;
#1684 = CARTESIAN_POINT ( 'NONE',  ( 6.923076923076924238, -2.249999999999998668, 29.50000000000001421 ) ) ;
#1685 = CARTESIAN_POINT ( 'NONE',  ( 18.13052570176355971, -2.882268652242222728, 31.66798894389554064 ) ) ;
#1686 = VERTEX_POINT ( 'NONE', #44482 ) ;
#1687 = CARTESIAN_POINT ( 'NONE',  ( -11.28851602011339494, -12.22109172314383052, 31.39792113162168263 ) ) ;
#1688 = DIRECTION ( 'NONE',  ( 0.000000000000000000, 0.4999999999999960032, -0.8660254037844410391 ) ) ;
#1689 = B_SPLINE_CURVE_WITH_KNOTS ( 'NONE', 3,
 ( #61294, #52771, #87937, #88811, #46902, #80261, #18558, #12240, #54544, #47797 ),
 .UNSPECIFIED., .F., .F.,
 ( 4, 2, 2, 2, 4 ),
 ( 0.0007817246256747455461, 0.0009771112852218883336, 0.001172497944769031230, 0.001367884604316174126, 0.001563271263863317022 ),
 .UNSPECIFIED. ) ;
#1690 = VERTEX_POINT ( 'NONE', #11615 ) ;
#1691 = CARTESIAN_POINT ( 'NONE',  ( -16.28399412357785536, -12.70455904226513866, 30.44083106164009322 ) ) ;
#1692 = CARTESIAN_POINT ( 'NONE',  ( -14.17690186672535901, -9.084667340241226796, 34.75534355489798344 ) ) ;
#1693 = CARTESIAN_POINT ( 'NONE',  ( 2.980769230769232614, -7.433931650972300353, 34.75000000000000711 ) ) ;
#1694 = CARTESIAN_POINT ( 'NONE',  ( 2.177001704582000485, -5.496505350115500121, 34.60290016733514307 ) ) ;
#1695 = CARTESIAN_POINT ( 'NONE',  ( -0.2385271099256124072, -12.39991518177334129, 30.74647679643404530 ) ) ;
#1696 = DIRECTION ( 'NONE',  ( -0.000000000000000000, 1.000000000000000000, 3.491481338843133355E-15 ) ) ;
#1697 = FACE_BOUND ( 'NONE', #74741, .T. ) ;
#1699 = CARTESIAN_POINT ( 'NONE',  ( 15.36129493253279499, -12.27024696741798770, 31.24895572276497546 ) ) ;
#1698 = CARTESIAN_POINT ( 'NONE',  ( 13.25392478150507891, -2.295517848115769421, 30.44137282052137294 ) ) ;
#1700 = EDGE_CURVE ( 'NONE', #10997, #441, #68954, .T. ) ;
#1701 = CARTESIAN_POINT ( 'NONE',  ( -16.15384615384615330, -2.538708090699994813, 30.37095296980875503 ) ) ;
#1703 = CARTESIAN_POINT ( 'NONE',  ( -12.68446467905460828, -4.186968288167449259, 33.49512374952580274 ) ) ;
#1702 = CARTESIAN_POINT ( 'NONE',  ( -6.700064078983529292, -10.77377354290276301, 33.85451476688484718 ) ) ;
#1704 = FACE_OUTER_BOUND ( 'NONE', #66995, .T. ) ;
#1705 = CARTESIAN_POINT ( 'NONE',  ( 0.06109907496455496689, -11.24999999999999822, 22.02938170625849068 ) ) ;
#1706 = VERTEX_POINT ( 'NONE', #4864 ) ;
#1707 = VECTOR ( 'NONE', #20948, 1000.000000000000114 ) ;
#1708 = ORIENTED_EDGE ( 'NONE', *, *, #14428, .T. ) ;
#1709 = CARTESIAN_POINT ( 'NONE',  ( -9.692307692307812417, -11.94971097300221174, 32.03036669348237098 ) ) ;
#1710 = CARTESIAN_POINT ( 'NONE',  ( -0.4615384615385826339, -2.892918686052166066, 31.69288490824153470 ) ) ;
#1711 = CARTESIAN_POINT ( 'NONE',  ( -9.442362173959551797, -9.272278438253398036, 34.42582936511637115 ) ) ;
#1712 = LINE ( 'NONE', #82812, #61063 ) ;
#1713 = CARTESIAN_POINT ( 'NONE',  ( -17.07692307692307665, -6.386643153685126251, 34.62446782046654192 ) ) ;
#1714 = CARTESIAN_POINT ( 'NONE',  ( 1.614399933863660985, -11.22469193450123193, 20.70125670625849423 ) ) ;
#1715 = VECTOR ( 'NONE', #28103, 1000.000000000000227 ) ;
#1716 = CARTESIAN_POINT ( 'NONE',  ( 0.5276057948885357618, -3.937682226553329556, 33.60647404775216529 ) ) ;
#1717 = CARTESIAN_POINT ( 'NONE',  ( 3.930919194939304973, -11.98009711892699691, 32.48740034544075428 ) ) ;
#1718 = CARTESIAN_POINT ( 'NONE',  ( 15.48071474911737333, -11.86320923018887719, 32.19269448109604070 ) ) ;
#1719 = CARTESIAN_POINT ( 'NONE',  ( 17.86930939688969033, -8.191372820521381826, 34.95448215188423546 ) ) ;
#1720 = CARTESIAN_POINT ( 'NONE',  ( -3.361459833879539616, -3.957541250942359756, 33.62499894934981626 ) ) ;
#1721 = DIRECTION ( 'NONE',  ( -0.000000000000000000, -0.9848077530122086864, -0.1736481776669273613 ) ) ;
#1722 = ADVANCED_FACE ( 'NONE', ( #66096 ), #85492, .F. ) ;
#1723 = ADVANCED_FACE ( 'NONE', ( #71972 ), #59347, .F. ) ;
#1724 = CARTESIAN_POINT ( 'NONE',  ( 12.59206389977210705, -2.372941743896879174, 30.88044141588253666 ) ) ;
#1725 = DIRECTION ( 'NONE',  ( 0.000000000000000000, 0.000000000000000000, 1.000000000000000000 ) ) ;
#1726 = VERTEX_POINT ( 'NONE', #86402 ) ;
#1727 = CARTESIAN_POINT ( 'NONE',  ( 2.177544337960614751, -3.625366637846545448, 33.29286588640298561 ) ) ;
#1728 = CARTESIAN_POINT ( 'NONE',  ( 10.68145194873469173, -5.471508081941601098, 34.59228464037088457 ) ) ;
#1729 = CARTESIAN_POINT ( 'NONE',  ( 1.200186371490529202, -4.775308065498752974, 21.98624329374151642 ) ) ;
#1730 = CARTESIAN_POINT ( 'NONE',  ( 4.023698184114456566, -5.070767119584671079, 34.40440758774516183 ) ) ;
#1731 = CARTESIAN_POINT ( 'NONE',  ( 14.16025641025641235, -3.499999999999999556, 29.75000000000000355 ) ) ;
#1732 = EDGE_LOOP ( 'NONE', ( #67383, #34344 ) ) ;
#1733 = DIRECTION ( 'NONE',  ( 0.000000000000000000, 0.000000000000000000, -1.000000000000000000 ) ) ;
#1735 = ORIENTED_EDGE ( 'NONE', *, *, #61774, .F. ) ;
#1734 = FACE_OUTER_BOUND ( 'NONE', #71110, .T. ) ;
#1736 = DIRECTION ( 'NONE',  ( 0.000000000000000000, 0.6427876096865368094, 0.7660444431189802339 ) ) ;
#1737 = CARTESIAN_POINT ( 'NONE',  ( -2.307692307692305711, -2.499999999999998668, 29.50000000000001066 ) ) ;
#1738 = ADVANCED_FACE ( 'NONE', ( #45379 ), #86854, .F. ) ;
#1739 = ORIENTED_EDGE ( 'NONE', *, *, #13994, .F. ) ;
#1740 = DIRECTION ( 'NONE',  ( 0.000000000000000000, 0.6427876096865373645, -0.7660444431189797898 ) ) ;
#1741 = DIRECTION ( 'NONE',  ( -0.000000000000000000, -0.9396926207859092051, -0.3420201433256662704 ) ) ;
#1742 = ORIENTED_EDGE ( 'NONE', *, *, #3228, .T. ) ;
#1743 = VECTOR ( 'NONE', #59624, 1000.000000000000000 ) ;
#1744 = CARTESIAN_POINT ( 'NONE',  ( 9.019176178608812933, -2.341251567377310217, 30.72681386836322659 ) ) ;
#1745 = CARTESIAN_POINT ( 'NONE',  ( -11.60454391782167605, -12.34228464037088280, 31.77849191805838558 ) ) ;
#1746 = CARTESIAN_POINT ( 'NONE',  ( -15.16470087976679437, -12.37446782046654192, 30.86335684631486842 ) ) ;
#1747 = ORIENTED_EDGE ( 'NONE', *, *, #24136, .F. ) ;
#1749 = ORIENTED_EDGE ( 'NONE', *, *, #53727, .T. ) ;
#1748 = VECTOR ( 'NONE', #2612, 1000.000000000000227 ) ;
#1750 = VERTEX_POINT ( 'NONE', #88187 ) ;
#1751 = CARTESIAN_POINT ( 'NONE',  ( 15.29602437028206907, -12.70778746994558439, 30.41441678777536595 ) ) ;
#1752 = PLANE ( 'NONE',  #35748 ) ;
#1753 = CARTESIAN_POINT ( 'NONE',  ( -3.100243792535585907, -8.630441415882550871, 34.87705825610312615 ) ) ;
#1754 = CARTESIAN_POINT ( 'NONE',  ( -17.29984929443922681, -6.503392248772476236, 34.64988816332204635 ) ) ;
#1755 = ORIENTED_EDGE ( 'NONE', *, *, #16817, .F. ) ;
#1756 = EDGE_LOOP ( 'NONE', ( #66255, #3639 ) ) ;
#1758 = EDGE_LOOP ( 'NONE', ( #66722, #50817 ) ) ;
#1757 = CARTESIAN_POINT ( 'NONE',  ( -2.557692307692305711, -7.433932668274255029, 35.00000000000000711 ) ) ;
#1759 = CARTESIAN_POINT ( 'NONE',  ( 18.75000000000000000, -4.000000000000000000, 29.75000000000000355 ) ) ;
#1760 = AXIS2_PLACEMENT_3D ( 'NONE', #26968, #48544, #74267 ) ;
#1761 = ORIENTED_EDGE ( 'NONE', *, *, #17169, .F. ) ;
#1762 = AXIS2_PLACEMENT_3D ( 'NONE', #5424, #67570, #87866 ) ;
#1763 = CYLINDRICAL_SURFACE ( 'NONE', #47856, 0.2499999999999994726 ) ;
#1764 = CARTESIAN_POINT ( 'NONE',  ( 6.923076923076924238, -9.058645607665452459, 34.76329471203371924 ) ) ;
#1765 = ORIENTED_EDGE ( 'NONE', *, *, #75906, .T. ) ;
#1766 = CARTESIAN_POINT ( 'NONE',  ( 7.976945653978629203, -8.147973898785416225, 34.70805048591653730 ) ) ;
#1767 = VECTOR ( 'NONE', #11156, 1000.000000000000114 ) ;
#1768 = EDGE_CURVE ( 'NONE', #63242, #45204, #39547, .T. ) ;
#1769 = ORIENTED_EDGE ( 'NONE', *, *, #79116, .T. ) ;
#1771 = VERTEX_POINT ( 'NONE', #19696 ) ;
#1770 = FACE_OUTER_BOUND ( 'NONE', #23896, .T. ) ;
#1772 = CARTESIAN_POINT ( 'NONE',  ( -5.776988648387149539, -8.239487800360276282, 34.69522927552633718 ) ) ;
#1773 = B_SPLINE_CURVE_WITH_KNOTS ( 'NONE', 3,
 ( #52051, #9740, #86313, #17843, #71431, #85852, #37206, #58357, #24135, #31801 ),
 .UNSPECIFIED., .F., .F.,
 ( 4, 2, 2, 2, 4 ),
 ( 0.000000000000000000, 0.0001954311564186862781, 0.0003908623128373725562, 0.0005862934692560588072, 0.0007817246256747451124 ),
 .UNSPECIFIED. ) ;
#1774 = PLANE ( 'NONE',  #72639 ) ;
#1775 = ORIENTED_EDGE ( 'NONE', *, *, #3712, .T. ) ;
#1776 = CARTESIAN_POINT ( 'NONE',  ( 15.48082354240754555, -3.136992222400443175, 32.19305428654138979 ) ) ;
#1777 = CARTESIAN_POINT ( 'NONE',  ( 6.673100179028331524, -5.643011162660950042, 34.66104346484419096 ) ) ;
#1778 = FACE_BOUND ( 'NONE', #27909, .T. ) ;
#1779 = CARTESIAN_POINT ( 'NONE',  ( -9.626240358957616650, -3.937682226553329556, 33.60647404775216529 ) ) ;
#1780 = FACE_OUTER_BOUND ( 'NONE', #5751, .T. ) ;
#1781 = EDGE_CURVE ( 'NONE', #18284, #20058, #26459, .T. ) ;
#1782 = CARTESIAN_POINT ( 'NONE',  ( 15.36129466900287177, -2.647132371071621471, 31.75357179365171589 ) ) ;
#1783 = DIRECTION ( 'NONE',  ( -0.000000000000000000, -0.9396926207859093161, -0.3420201433256663259 ) ) ;
#1784 = CARTESIAN_POINT ( 'NONE',  ( -11.47320596718551045, -3.300289026998473041, 32.46337939537591666 ) ) ;
#1785 = CARTESIAN_POINT ( 'NONE',  ( 10.36540787133602670, -10.82459398097509329, 33.81372124010185587 ) ) ;
#1786 = ORIENTED_EDGE ( 'NONE', *, *, #69158, .F. ) ;
#1787 = CARTESIAN_POINT ( 'NONE',  ( 14.43848274865925774, -6.369690395747422684, 34.87708834333098196 ) ) ;
#1788 = EDGE_CURVE ( 'NONE', #86079, #14268, #87289, .T. ) ;
#1789 = EDGE_LOOP ( 'NONE', ( #33863, #68262, #3065, #56633 ) ) ;
#1790 = VERTEX_POINT ( 'NONE', #25566 ) ;
#1792 = CYLINDRICAL_SURFACE ( 'NONE', #37614, 0.2500000000000008882 ) ;
#1791 = CARTESIAN_POINT ( 'NONE',  ( 7.780070435197965928, -6.386643153685125363, 34.62446782046654903 ) ) ;
#1793 = VECTOR ( 'NONE', #32508, 1000.000000000000114 ) ;
#1794 = CARTESIAN_POINT ( 'NONE',  ( -11.78843826940389405, -11.79746400365624659, 32.30657167506340954 ) ) ;
#1795 = CARTESIAN_POINT ( 'NONE',  ( 8.068933515131911705, -3.563462043263030399, 33.22394488606062879 ) ) ;
#1796 = CARTESIAN_POINT ( 'NONE',  ( -13.38461538461538325, -7.500000000000001776, 35.04278698407183867 ) ) ;
#1797 = CARTESIAN_POINT ( 'NONE',  ( -0.3962828902624368488, -11.94971097300157403, 32.03036669348361443 ) ) ;
#1798 = EDGE_LOOP ( 'NONE', ( #62360, #54900, #10023, #7450 ) ) ;
#1799 = DIRECTION ( 'NONE',  ( -0.000000000000000000, 1.000000000000000000, 3.491481338843133355E-15 ) ) ;
#1800 = CARTESIAN_POINT ( 'NONE',  ( -6.222926217516143055, -6.503392248772476236, 34.64988816332204635 ) ) ;
#1801 = CARTESIAN_POINT ( 'NONE',  ( -10.55012904410859242, -10.21337939537593620, 33.94971097300152252 ) ) ;
#1802 = EDGE_CURVE ( 'NONE', #18545, #32170, #34092, .T. ) ;
#1803 = CYLINDRICAL_SURFACE ( 'NONE', #35245, 0.2499999999999979738 ) ;
#1804 = CARTESIAN_POINT ( 'NONE',  ( 13.44987052412822237, -5.941354392334607049, 34.76329471203374055 ) ) ;
#1805 = CARTESIAN_POINT ( 'NONE',  ( -3.749999999999997335, -7.500000000000021316, 15.09375000000000000 ) ) ;
#1806 = ORIENTED_EDGE ( 'NONE', *, *, #680, .T. ) ;
#1808 = EDGE_CURVE ( 'NONE', #85122, #71718, #29245, .T. ) ;
#1807 = ORIENTED_EDGE ( 'NONE', *, *, #77572, .T. ) ;
#1809 = CARTESIAN_POINT ( 'NONE',  ( -9.627052121031665521, -12.46129190930001052, 30.37095296980870174 ) ) ;
#1810 = ORIENTED_EDGE ( 'NONE', *, *, #17759, .T. ) ;
#1811 = CARTESIAN_POINT ( 'NONE',  ( -9.758391103263571509, -12.37446782046654192, 30.86335684631486487 ) ) ;
#1812 = CARTESIAN_POINT ( 'NONE',  ( -1.254089946381739651, -10.31582465632705237, 34.18122507451815295 ) ) ;
#1813 = DIRECTION ( 'NONE',  ( -0.000000000000000000, 1.000000000000000000, -0.000000000000000000 ) ) ;
#1814 = CARTESIAN_POINT ( 'NONE',  ( 2.530705151785703322, -10.01129605718032778, 34.36064277460058491 ) ) ;
#1815 = CARTESIAN_POINT ( 'NONE',  ( 2.651650429449569302, -10.15165042944953733, 14.62500000000000000 ) ) ;
#1816 = B_SPLINE_CURVE_WITH_KNOTS ( 'NONE', 3,
 ( #35621, #78701, #71487, #16997, #57977, #63069 ),
 .UNSPECIFIED., .F., .F.,
 ( 4, 2, 4 ),
 ( 0.000000000000000000, 0.0001954784845028921395, 0.0003909569690057842790 ),
 .UNSPECIFIED. ) ;
#1817 = CYLINDRICAL_SURFACE ( 'NONE', #60375, 0.2499999999999973355 ) ;
#1818 = EDGE_LOOP ( 'NONE', ( #71715, #13718 ) ) ;
#1819 = CARTESIAN_POINT ( 'NONE',  ( -12.52680890749923570, -10.90142922261923886, 33.41473453929638993 ) ) ;
#1821 = ORIENTED_EDGE ( 'NONE', *, *, #64204, .F. ) ;
#1820 = CARTESIAN_POINT ( 'NONE',  ( -16.37733109757010297, -11.89387501736623420, 32.13663884655804992 ) ) ;
#1822 = DIRECTION ( 'NONE',  ( -0.000000000000000000, 0.9396926207859092051, -0.3420201433256662704 ) ) ;
#1823 = CARTESIAN_POINT ( 'NONE',  ( -0.7115616857599181833, -4.175268141568689195, 33.81360843649122216 ) ) ;
#1824 = B_SPLINE_CURVE_WITH_KNOTS ( 'NONE', 3,
 ( #47501, #47943, #63232, #48832, #20481, #76760, #40763, #42097, #76306, #14612 ),
 .UNSPECIFIED., .F., .F.,
 ( 4, 2, 2, 2, 4 ),
 ( 0.0007817246256747434861, 0.0009771112852218861652, 0.001172497944769028844, 0.001367884604316171740, 0.001563271263863314419 ),
 .UNSPECIFIED. ) ;
#1825 = CARTESIAN_POINT ( 'NONE',  ( -17.86947429823643674, -11.93748526763465279, 32.05452791011430946 ) ) ;
#1826 = CARTESIAN_POINT ( 'NONE',  ( -16.15384615384615330, -2.292212530054420494, 30.41441678777542634 ) ) ;
#1827 = EDGE_CURVE ( 'NONE', #50611, #13813, #56027, .T. ) ;
#1828 = FACE_OUTER_BOUND ( 'NONE', #30091, .T. ) ;
#1829 = EDGE_CURVE ( 'NONE', #64127, #48416, #12500, .T. ) ;
#1830 = CARTESIAN_POINT ( 'NONE',  ( -1.492201783934593573, -3.724691934501250135, 13.07999329374151642 ) ) ;
#1831 = VERTEX_POINT ( 'NONE', #6188 ) ;
#1832 = DIRECTION ( 'NONE',  ( -1.000000000000000000, -0.000000000000000000, -0.000000000000000000 ) ) ;
#1833 = DIRECTION ( 'NONE',  ( -0.000000000000000000, 1.000000000000000000, 3.491481338843133355E-15 ) ) ;
#1834 = CARTESIAN_POINT ( 'NONE',  ( 2.749999999999995115, -6.360912703473971419, 18.14062500000000711 ) ) ;
#1835 =( GEOMETRIC_REPRESENTATION_CONTEXT ( 3 ) GLOBAL_UNCERTAINTY_ASSIGNED_CONTEXT ( ( #35290 ) ) GLOBAL_UNIT_ASSIGNED_CONTEXT ( ( #39286, #45578, #18562 ) ) REPRESENTATION_CONTEXT ( 'NONE', 'WORKASPACE' ) );
#1836 = AXIS2_PLACEMENT_3D ( 'NONE', #49620, #77094, #64004 ) ;
#1837 = EDGE_CURVE ( 'NONE', #20157, #51126, #54917, .T. ) ;
#1838 = CARTESIAN_POINT ( 'NONE',  ( -13.51476259405360203, -12.45813303252208648, 30.39737893381572675 ) ) ;
#1839 = PLANE ( 'NONE',  #51896 ) ;
#1840 = EDGE_CURVE ( 'NONE', #36102, #52068, #59942, .T. ) ;
#1841 = ORIENTED_EDGE ( 'NONE', *, *, #10731, .F. ) ;
#1842 = CARTESIAN_POINT ( 'NONE',  ( 2.749999999999995115, -6.360912703473971419, 14.39062500000000000 ) ) ;
#1843 = CARTESIAN_POINT ( 'NONE',  ( -16.15384615384615330, -4.945431358278436385, 36.03766855953609394 ) ) ;
#1844 = AXIS2_PLACEMENT_3D ( 'NONE', #65328, #85609, #43296 ) ;
#1845 = ORIENTED_EDGE ( 'NONE', *, *, #82568, .T. ) ;
#1846 = CARTESIAN_POINT ( 'NONE',  ( 6.923076923076924238, -2.499999999999998668, 29.50000000000001066 ) ) ;
#1847 = FACE_OUTER_BOUND ( 'NONE', #20720, .T. ) ;
#1848 = ORIENTED_EDGE ( 'NONE', *, *, #4862, .T. ) ;
#1849 = DIRECTION ( 'NONE',  ( 0.000000000000000000, 0.9848077530122072432, 0.1736481776669354937 ) ) ;
#1850 = CARTESIAN_POINT ( 'NONE',  ( -5.869954837165220596, -2.504778602574660340, 29.97347330155780298 ) ) ;
#1851 = CARTESIAN_POINT ( 'NONE',  ( -12.59222906464877134, -9.929715669179220328, 34.40415004197138416 ) ) ;
#1852 = CARTESIAN_POINT ( 'NONE',  ( -13.25382494364843389, -12.62708834333097663, 30.88030960425257021 ) ) ;
#1853 = ORIENTED_EDGE ( 'NONE', *, *, #14845, .F. ) ;
#1854 = CARTESIAN_POINT ( 'NONE',  ( -8.899790682844132661, -2.254533558242299396, 29.97296025877828285 ) ) ;
#1855 = EDGE_LOOP ( 'NONE', ( #17903, #9416, #24823, #13466 ) ) ;
#1856 = LINE ( 'NONE', #63987, #27063 ) ;
#1857 = CARTESIAN_POINT ( 'NONE',  ( -10.68065506134539078, -2.892918686051582977, 31.69288490824015980 ) ) ;
#1858 = ORIENTED_EDGE ( 'NONE', *, *, #32430, .F. ) ;
#1859 = B_SPLINE_CURVE_WITH_KNOTS ( 'NONE', 3,
 ( #73875, #12173, #32884, #87859, #26125, #81084, #12618, #73265, #65162, #79134 ),
 .UNSPECIFIED., .F., .F.,
 ( 4, 2, 2, 2, 4 ),
 ( 0.000000000000000000, 0.0001954339857564081249, 0.0003908679715128162498, 0.0005863019572692244018, 0.0007817359430256324996 ),
 .UNSPECIFIED. ) ;
#1860 = CARTESIAN_POINT ( 'NONE',  ( -6.066082379360134169, -10.67929555188718460, 33.92786785259543336 ) ) ;
#1861 = DIRECTION ( 'NONE',  ( -0.000000000000000000, 1.000000000000000000, -0.000000000000000000 ) ) ;
#1862 = CARTESIAN_POINT ( 'NONE',  ( 0.2115152242454955700, -4.335965774309649134, 33.62209801155880484 ) ) ;
#1863 = VECTOR ( 'NONE', #23258, 1000.000000000000000 ) ;
#1864 = DIRECTION ( 'NONE',  ( 0.000000000000000000, 0.7660444431189807890, 0.6427876096865361433 ) ) ;
#1865 = CARTESIAN_POINT ( 'NONE',  ( -13.91025641025641058, -11.50000000000000000, 29.75000000000000355 ) ) ;
#1866 = ADVANCED_FACE ( 'NONE', ( #31277 ), #73617, .F. ) ;
#1867 = VERTEX_POINT ( 'NONE', #4701 ) ;
#1868 = VERTEX_POINT ( 'NONE', #59188 ) ;
#1869 = FACE_BOUND ( 'NONE', #86958, .T. ) ;
#1870 = VERTEX_POINT ( 'NONE', #3351 ) ;
#1871 = CARTESIAN_POINT ( 'NONE',  ( 8.703147358274884837, -3.513871655860377086, 32.76840700105978499 ) ) ;
#1872 = EDGE_CURVE ( 'NONE', #31746, #72998, #36661, .T. ) ;
#1873 = CARTESIAN_POINT ( 'NONE',  ( 17.07692307692295586, -12.51329471203414379, 31.30864560766407578 ) ) ;
#1874 = CARTESIAN_POINT ( 'NONE',  ( 6.250054419913455561, -2.920487667080175154, 32.31805714834170828 ) ) ;
#1875 = CARTESIAN_POINT ( 'NONE',  ( -14.08468095607945614, -9.086983370893049639, 34.49168942202179267 ) ) ;
#1876 = ORIENTED_EDGE ( 'NONE', *, *, #17283, .T. ) ;
#1877 = ADVANCED_FACE ( 'NONE', ( #25410 ), #51976, .F. ) ;
#1878 = VERTEX_POINT ( 'NONE', #66841 ) ;
#1879 = VERTEX_POINT ( 'NONE', #4247 ) ;
#1880 = CARTESIAN_POINT ( 'NONE',  ( -9.692307692307691624, -12.09954503811598769, 35.62045528018868623 ) ) ;
#1881 = ORIENTED_EDGE ( 'NONE', *, *, #87497, .T. ) ;
#1882 = CARTESIAN_POINT ( 'NONE',  ( 13.31934493865461278, -2.892918686051582533, 31.69288490824015980 ) ) ;
#1883 = CARTESIAN_POINT ( 'NONE',  ( -2.307692307692305711, -12.34228464037088635, 31.77849191805839268 ) ) ;
#1884 = B_SPLINE_CURVE_WITH_KNOTS ( 'NONE', 3,
 ( #85158, #23443, #50897, #30646, #36533, #84289, #9933, #36095, #30217, #23008 ),
 .UNSPECIFIED., .F., .F.,
 ( 4, 2, 2, 2, 4 ),
 ( 0.0007817246256747453293, 0.0009771112852218889842, 0.001172497944769032531, 0.001367884604316176294, 0.001563271263863319840 ),
 .UNSPECIFIED. ) ;
#1885 = CARTESIAN_POINT ( 'NONE',  ( -17.07692307692319744, -3.083524468854526912, 32.58852847137268327 ) ) ;
#1886 = ORIENTED_EDGE ( 'NONE', *, *, #25312, .F. ) ;
#1887 = CARTESIAN_POINT ( 'NONE',  ( -8.769230769230768274, -3.937682226553329556, 33.60647404775216529 ) ) ;
#1888 = MECHANICAL_DESIGN_GEOMETRIC_PRESENTATION_REPRESENTATION (  '', ( #79567 ), #65141 ) ;
#1889 = EDGE_CURVE ( 'NONE', #12525, #14877, #53795, .T. ) ;
#1890 = CARTESIAN_POINT ( 'NONE',  ( 2.557692307692308376, -2.499999999999998668, 29.75000000000000355 ) ) ;
#1891 = CARTESIAN_POINT ( 'NONE',  ( -17.75000000000000355, -7.500000000000000000, 35.00000000000000000 ) ) ;
#1892 = DIRECTION ( 'NONE',  ( -1.000000000000000000, 0.000000000000000000, -0.000000000000000000 ) ) ;
#1893 = EDGE_LOOP ( 'NONE', ( #21618, #11266 ) ) ;
#1894 = EDGE_CURVE ( 'NONE', #16582, #12053, #65499, .T. ) ;
#1895 = EDGE_LOOP ( 'NONE', ( #86192, #47505, #21474, #23869 ) ) ;
#1896 = ORIENTED_EDGE ( 'NONE', *, *, #35482, .F. ) ;
#1897 = CARTESIAN_POINT ( 'NONE',  ( -3.903791842207835483, -9.943054286541407549, 34.11300777759954883 ) ) ;
#1899 = CARTESIAN_POINT ( 'NONE',  ( 10.36536139116315880, -2.341070481393819236, 30.72580821765574299 ) ) ;
#1898 = CARTESIAN_POINT ( 'NONE',  ( -3.262820512820514107, -7.500000000000000000, 33.75000000000000000 ) ) ;
#1900 = DIRECTION ( 'NONE',  ( -0.000000000000000000, -0.3420201433256694901, -0.9396926207859082059 ) ) ;
#1901 = CARTESIAN_POINT ( 'NONE',  ( -2.241624974342231624, -2.486705287966280320, 31.30864560766543647 ) ) ;
#1902 = FACE_BOUND ( 'NONE', #3198, .T. ) ;
#1903 = CARTESIAN_POINT ( 'NONE',  ( 16.21910172512217585, -3.300289026998473929, 32.46337939537591666 ) ) ;
#1904 = EDGE_LOOP ( 'NONE', ( #76502, #22251 ) ) ;
#1905 = CARTESIAN_POINT ( 'NONE',  ( -18.00000000000012079, -12.46129190930018460, 30.37095296980731973 ) ) ;
#1906 = CYLINDRICAL_SURFACE ( 'NONE', #2779, 0.2499999999999997502 ) ;
#1907 = DIRECTION ( 'NONE',  ( -0.000000000000000000, -0.3420201433256694346, -0.9396926207859080948 ) ) ;
#1908 = ADVANCED_FACE ( 'NONE', ( #60074 ), #86239, .F. ) ;
#1909 = CARTESIAN_POINT ( 'NONE',  ( 3.230769230769231726, -11.35647404775217417, 33.31231777344666511 ) ) ;
#1910 = ORIENTED_EDGE ( 'NONE', *, *, #27758, .F. ) ;
#1911 = CARTESIAN_POINT ( 'NONE',  ( 6.130525438233645374, -11.04252011169590020, 33.62494198852677130 ) ) ;
#1912 = B_SPLINE_CURVE_WITH_KNOTS ( 'NONE', 3,
 ( #25401, #38926, #65032, #3343, #72245, #18656, #10556, #24949, #32163, #79902 ),
 .UNSPECIFIED., .F., .F.,
 ( 4, 2, 2, 2, 4 ),
 ( 0.000000000000000000, 0.0001954339857564086670, 0.0003908679715128173340, 0.0005863019572692260281, 0.0007817359430256346680 ),
 .UNSPECIFIED. ) ;
#1913 = VERTEX_POINT ( 'NONE', #65040 ) ;
#1914 = FACE_BOUND ( 'NONE', #68021, .T. ) ;
#1915 = CARTESIAN_POINT ( 'NONE',  ( 4.853438133199126980, -5.912607949931405038, 34.49155766932282319 ) ) ;
#1916 = B_SPLINE_CURVE_WITH_KNOTS ( 'NONE', 3,
 ( #48411, #55613, #75019, #13747, #33586, #61924, #53848, #81335, #237, #76332 ),
 .UNSPECIFIED., .F., .F.,
 ( 4, 2, 2, 2, 4 ),
 ( 0.0007817359430256257775, 0.0009771253907249911191, 0.001172514838424356352, 0.001367904286123721586, 0.001563293733823086819 ),
 .UNSPECIFIED. ) ;
#1917 = CARTESIAN_POINT ( 'NONE',  ( 4.376858997939548246, -2.523321265292115090, 31.42251411153756280 ) ) ;
#1918 = CARTESIAN_POINT ( 'NONE',  ( 14.17700084102475699, -11.71456829005830080, 32.44064028649416542 ) ) ;
#1919 = ORIENTED_EDGE ( 'NONE', *, *, #26185, .T. ) ;
#1920 = FACE_OUTER_BOUND ( 'NONE', #21485, .T. ) ;
#1921 = CARTESIAN_POINT ( 'NONE',  ( -18.00000000000012079, -2.892918686052166066, 31.69288490824153470 ) ) ;
#1922 = LINE ( 'NONE', #43789, #4961 ) ;
#1923 = CARTESIAN_POINT ( 'NONE',  ( -5.011667937410237528, -5.941354392334606160, 34.76329471203374055 ) ) ;
#1924 = ORIENTED_EDGE ( 'NONE', *, *, #49393, .T. ) ;
#1925 = CARTESIAN_POINT ( 'NONE',  ( -7.846153846153965716, -10.90142922262034020, 33.41473453929536674 ) ) ;
#1927 = ORIENTED_EDGE ( 'NONE', *, *, #17655, .T. ) ;
#1926 = VECTOR ( 'NONE', #72975, 1000.000000000000000 ) ;
#1928 = B_SPLINE_CURVE_WITH_KNOTS ( 'NONE', 3,
 ( #77028, #48655, #42807, #84242, #29291, #56747, #9016, #36484, #76131, #63937 ),
 .UNSPECIFIED., .F., .F.,
 ( 4, 2, 2, 2, 4 ),
 ( 0.0007817246256747524850, 0.0009771112852218972241, 0.001172497944769042072, 0.001367884604316186702, 0.001563271263863331550 ),
 .UNSPECIFIED. ) ;
#1931 = EDGE_LOOP ( 'NONE', ( #9396, #65765, #83074, #80289 ) ) ;
#1930 = VECTOR ( 'NONE', #5639, 999.9999999999998863 ) ;
#1929 = CARTESIAN_POINT ( 'NONE',  ( 13.51514108637895184, -12.27024696741798770, 31.24895572276497546 ) ) ;
#1932 = CARTESIAN_POINT ( 'NONE',  ( 7.623227628637700093, -10.61292498521070549, 33.66303323003028680 ) ) ;
#1933 = CARTESIAN_POINT ( 'NONE',  ( -10.61538461538473399, -12.46129190930018460, 30.37095296980731973 ) ) ;
#1934 = B_SPLINE_CURVE_WITH_KNOTS ( 'NONE', 3,
 ( #45267, #12385, #24556, #39866, #66885, #31774, #11501, #5182, #72298, #72739 ),
 .UNSPECIFIED., .F., .F.,
 ( 4, 2, 2, 2, 4 ),
 ( 0.0007817246256747521597, 0.0009771112852218961399, 0.001172497944769040337, 0.001367884604316184534, 0.001563271263863328514 ),
 .UNSPECIFIED. ) ;
#1935 = CARTESIAN_POINT ( 'NONE',  ( 4.153846153846154188, -11.11383981884818262, 36.00935417666054406 ) ) ;
#1936 = CARTESIAN_POINT ( 'NONE',  ( -12.23852710992561477, -2.758310577978207778, 31.33698337089302299 ) ) ;
#1938 = CARTESIAN_POINT ( 'NONE',  ( -11.60454391782167427, -9.058645607665454236, 34.76329471203372634 ) ) ;
#1937 = CARTESIAN_POINT ( 'NONE',  ( -8.069638789877792817, -10.81261337010820256, 33.49550067578627477 ) ) ;
#1939 = ADVANCED_FACE ( 'NONE', ( #85784 ), #24958, .F. ) ;
#1940 = DIRECTION ( 'NONE',  ( -0.000000000000000000, 0.9396926207859092051, -0.3420201433256662704 ) ) ;
#1941 = CARTESIAN_POINT ( 'NONE',  ( -2.749999999999998224, -7.500000000000015987, 23.84375000000000000 ) ) ;
#1942 = EDGE_LOOP ( 'NONE', ( #7971, #37007, #50893, #53738 ) ) ;
#1943 = FACE_OUTER_BOUND ( 'NONE', #30824, .T. ) ;
#1944 = DIRECTION ( 'NONE',  ( -1.000000000000000000, 0.000000000000000000, -0.000000000000000000 ) ) ;
#1945 = VERTEX_POINT ( 'NONE', #79016 ) ;
#1946 = EDGE_CURVE ( 'NONE', #68769, #43616, #52426, .T. ) ;
#1947 = VERTEX_POINT ( 'NONE', #17771 ) ;
#1948 = EDGE_CURVE ( 'NONE', #49139, #78712, #8756, .T. ) ;
#1949 = ORIENTED_EDGE ( 'NONE', *, *, #22741, .T. ) ;
#1950 = CARTESIAN_POINT ( 'NONE',  ( 10.74591005361826390, -8.630441415882550871, 34.87705825610312615 ) ) ;
#1951 = CARTESIAN_POINT ( 'NONE',  ( -17.14300648787895653, -8.973038597847269315, 34.52809138561120506 ) ) ;
#1952 = LINE ( 'NONE', #29437, #39934 ) ;
#1953 = CARTESIAN_POINT ( 'NONE',  ( -5.076923076923197442, -3.835265460704628371, 33.15142922262033665 ) ) ;
#1954 = CARTESIAN_POINT ( 'NONE',  ( -8.899378738962468560, -2.647304123082328875, 31.75400227202885972 ) ) ;
#1955 = CARTESIAN_POINT ( 'NONE',  ( -8.899921372341079717, -2.845849958028613624, 32.17971566917920967 ) ) ;
#1956 = FACE_OUTER_BOUND ( 'NONE', #49288, .T. ) ;
#1957 = CARTESIAN_POINT ( 'NONE',  ( 7.384615384615385025, -3.499999999999999556, 29.75000000000000355 ) ) ;
#1958 = DIRECTION ( 'NONE',  ( 0.000000000000000000, 0.1736481776669267785, -0.9848077530122087975 ) ) ;
#1959 = B_SPLINE_CURVE_WITH_KNOTS ( 'NONE', 3,
 ( #14843, #15279, #8522, #1754, #29244, #56697, #63889, #52146, #66104, #30114 ),
 .UNSPECIFIED., .F., .F.,
 ( 4, 2, 2, 2, 4 ),
 ( 0.000000000000000000, 0.0001954339857564075286, 0.0003908679715128150572, 0.0005863019572692225586, 0.0007817359430256301143 ),
 .UNSPECIFIED. ) ;
#1960 = VECTOR ( 'NONE', #27474, 1000.000000000000000 ) ;
#1961 = EDGE_CURVE ( 'NONE', #20256, #73637, #73203, .T. ) ;
#1962 = CARTESIAN_POINT ( 'NONE',  ( 7.846153846153725020, -2.892918686052165622, 31.69288490824153470 ) ) ;
#1963 = CARTESIAN_POINT ( 'NONE',  ( -5.076923076923075762, -1.422936976036506707, 30.56769352161908415 ) ) ;
#1964 = CIRCLE ( 'NONE', #52285, 4.000000000000000000 ) ;
#1965 = VECTOR ( 'NONE', #10753, 1000.000000000000000 ) ;
#1966 = ORIENTED_EDGE ( 'NONE', *, *, #12521, .T. ) ;
#1967 = CARTESIAN_POINT ( 'NONE',  ( -17.07692307692307665, -2.486705287966279876, 31.30864560766543647 ) ) ;
#1968 = CARTESIAN_POINT ( 'NONE',  ( 1.384615384615386802, -3.322132147404559976, 32.92929555188717927 ) ) ;
#1969 = CARTESIAN_POINT ( 'NONE',  ( 3.361294669002873992, -11.04252011169590020, 33.62494198852677130 ) ) ;
#1970 = EDGE_CURVE ( 'NONE', #30104, #87793, #20865, .T. ) ;
#1971 = CYLINDRICAL_SURFACE ( 'NONE', #11049, 0.2499999999999994726 ) ;
#1972 = EDGE_LOOP ( 'NONE', ( #51803, #60788, #41402, #7362 ) ) ;
#1973 = CARTESIAN_POINT ( 'NONE',  ( 12.23861224402230974, -9.086856451489515152, 34.49173150075333183 ) ) ;
#1974 = DIRECTION ( 'NONE',  ( 0.000000000000000000, 1.000000000000000000, 0.000000000000000000 ) ) ;
#1975 = CARTESIAN_POINT ( 'NONE',  ( -3.007989689500819352, -12.24180327182771855, 31.33663988360758168 ) ) ;
#1976 = EDGE_CURVE ( 'NONE', #30954, #40782, #4423, .T. ) ;
#1977 = ORIENTED_EDGE ( 'NONE', *, *, #13682, .T. ) ;
#1978 = CARTESIAN_POINT ( 'NONE',  ( 0.6845498131513104711, -5.667800583137508674, 34.40243808032445827 ) ) ;
#1979 = ORIENTED_EDGE ( 'NONE', *, *, #72545, .F. ) ;
#1980 = EDGE_CURVE ( 'NONE', #55785, #38648, #82590, .T. ) ;
#1981 = CARTESIAN_POINT ( 'NONE',  ( 9.692307692307695177, -11.69971097300155272, 32.46337939537588113 ) ) ;
#1982 = DIRECTION ( 'NONE',  ( -0.000000000000000000, 0.3420201433256694346, -0.9396926207859080948 ) ) ;
#1983 = CARTESIAN_POINT ( 'NONE',  ( -6.249976730942354841, -2.564618984488975961, 30.55390908950641915 ) ) ;
#1984 = B_SPLINE_CURVE_WITH_KNOTS ( 'NONE', 3,
 ( #56943, #77218, #15085, #14636, #42121, #8328, #29488, #76331, #77659, #15529 ),
 .UNSPECIFIED., .F., .F.,
 ( 4, 2, 2, 2, 4 ),
 ( 0.0007817246256747484735, 0.0009771112852218931041, 0.001172497944769037735, 0.001367884604316182365, 0.001563271263863326996 ),
 .UNSPECIFIED. ) ;
#1985 = CARTESIAN_POINT ( 'NONE',  ( 12.46153846153846168, -1.466349020453238561, 30.81389545987213907 ) ) ;
#1986 = DIRECTION ( 'NONE',  ( -0.000000000000000000, 0.9848077530122086864, -0.1736481776669273891 ) ) ;
#1987 = VERTEX_POINT ( 'NONE', #88912 ) ;
#1988 = EDGE_CURVE ( 'NONE', #62210, #30670, #7364, .T. ) ;
#1989 = B_SPLINE_CURVE_WITH_KNOTS ( 'NONE', 3,
 ( #85951, #58027, #73326, #78743, #17045, #37755 ),
 .UNSPECIFIED., .F., .F.,
 ( 4, 2, 4 ),
 ( 0.0003909512603273880690, 0.0005862562993132132720, 0.0007815613382990384750 ),
 .UNSPECIFIED. ) ;
#1990 = VECTOR ( 'NONE', #41020, 1000.000000000000227 ) ;
#1991 = ORIENTED_EDGE ( 'NONE', *, *, #54747, .T. ) ;
#1992 = ORIENTED_EDGE ( 'NONE', *, *, #87731, .T. ) ;
#1993 = EDGE_CURVE ( 'NONE', #27467, #75394, #77501, .T. ) ;
#1994 = DIRECTION ( 'NONE',  ( -0.000000000000000000, 0.3420201433256694901, -0.9396926207859082059 ) ) ;
#1995 = CYLINDRICAL_SURFACE ( 'NONE', #44502, 0.2499999999999994726 ) ;
#1996 = CARTESIAN_POINT ( 'NONE',  ( 0.5267936010512989098, -6.835583212224609184, 34.95778746994559327 ) ) ;
#1997 = CARTESIAN_POINT ( 'NONE',  ( -2.057746898314263273, -11.56426240980093567, 33.07394671870546432 ) ) ;
#1998 = CARTESIAN_POINT ( 'NONE',  ( 7.623325748518968936, -7.369209533119140509, 34.99857337881830688 ) ) ;
#1999 = CARTESIAN_POINT ( 'NONE',  ( -6.923076923077045919, -10.33852847137269571, 34.16647553114546554 ) ) ;
#2000 = ORIENTED_EDGE ( 'NONE', *, *, #23568, .F. ) ;
#2001 = EDGE_CURVE ( 'NONE', #45061, #56939, #12783, .T. ) ;
#2002 = EDGE_LOOP ( 'NONE', ( #69498, #76017 ) ) ;
#2003 = ORIENTED_EDGE ( 'NONE', *, *, #18087, .F. ) ;
#2005 = VERTEX_POINT ( 'NONE', #81253 ) ;
#2004 = CARTESIAN_POINT ( 'NONE',  ( -16.15384615384627409, -6.026961402154118908, 34.52809138561165270 ) ) ;
#2006 = EDGE_CURVE ( 'NONE', #35616, #13977, #81696, .T. ) ;
#2008 = CARTESIAN_POINT ( 'NONE',  ( -8.519176457592454454, -11.28795663066794575, 33.01431243580653785 ) ) ;
#2007 = CARTESIAN_POINT ( 'NONE',  ( 8.834486340506792601, -8.613356846314928816, 34.62446782046653482 ) ) ;
#2009 = CARTESIAN_POINT ( 'NONE',  ( -1.553300858899125059, -3.750000000000009326, 25.32812500000000355 ) ) ;
#2010 = ORIENTED_EDGE ( 'NONE', *, *, #58469, .F. ) ;
#2011 = ORIENTED_EDGE ( 'NONE', *, *, #85768, .T. ) ;
#2012 = CARTESIAN_POINT ( 'NONE',  ( 5.011600161430901146, -7.749976743299137993, 34.99404534957040624 ) ) ;
#2013 = VECTOR ( 'NONE', #80302, 1000.000000000000114 ) ;
#2014 = ORIENTED_EDGE ( 'NONE', *, *, #10859, .F. ) ;
#2015 = FACE_BOUND ( 'NONE', #70340, .T. ) ;
#2016 = CARTESIAN_POINT ( 'NONE',  ( 3.480714640147272831, -2.589246495874657938, 31.60778113518102828 ) ) ;
#2017 = CARTESIAN_POINT ( 'NONE',  ( -14.55769230769230660, -7.500000000000001776, 35.00000000000000000 ) ) ;
#2018 = ORIENTED_EDGE ( 'NONE', *, *, #45523, .F. ) ;
#2019 = CARTESIAN_POINT ( 'NONE',  ( 2.177000841024750777, -8.147922237126337563, 34.70805685702651999 ) ) ;
#2020 = CARTESIAN_POINT ( 'NONE',  ( 3.480714749117372886, -3.202959910592335202, 32.30730279482227019 ) ) ;
#2021 = CARTESIAN_POINT ( 'NONE',  ( -8.769230769230768274, -2.721908614388771852, 31.22303859784724978 ) ) ;
#2022 = CARTESIAN_POINT ( 'NONE',  ( -11.60454494941741999, -5.557115091759785130, 34.35708131394839171 ) ) ;
#2023 = CARTESIAN_POINT ( 'NONE',  ( -1.384615384615383471, -2.499999999999998668, 29.50000000000001066 ) ) ;
#2024 = CARTESIAN_POINT ( 'NONE',  ( -7.053768389744480949, -11.18331474514187995, 33.13161551792790505 ) ) ;
#2025 = CARTESIAN_POINT ( 'NONE',  ( -1.384615384615506484, -2.379036618888197285, 30.90682066428292885 ) ) ;
#2026 = CARTESIAN_POINT ( 'NONE',  ( 0.3308469948709038544, -11.71456829005830080, 32.44064028649416542 ) ) ;
#2027 = CARTESIAN_POINT ( 'NONE',  ( -5.198717948717948012, -7.500000000000000000, 33.75000000000000000 ) ) ;
#2028 = DIRECTION ( 'NONE',  ( -0.000000000000000000, -0.7660444431189791237, -0.6427876096865379196 ) ) ;
#2029 = FACE_OUTER_BOUND ( 'NONE', #23695, .T. ) ;
#2031 = CARTESIAN_POINT ( 'NONE',  ( 11.66925334628632882, -4.118422570099828484, 33.43335022499816489 ) ) ;
#2030 = DIRECTION ( 'NONE',  ( 0.000000000000000000, 0.1736481776669267785, -0.9848077530122087975 ) ) ;
#2032 = CARTESIAN_POINT ( 'NONE',  ( -1.318548051265308274, -9.058645607665452459, 34.76329471203371924 ) ) ;
#2034 = CARTESIAN_POINT ( 'NONE',  ( 2.372947447205147053, -6.835583212224609184, 34.95778746994559327 ) ) ;
#2033 = CARTESIAN_POINT ( 'NONE',  ( 12.46153846153846168, -12.37446782046654192, 30.86335684631486131 ) ) ;
#2035 = CARTESIAN_POINT ( 'NONE',  ( 13.25400572941130584, -7.722926974430166069, 34.99546784045485737 ) ) ;
#2036 = CARTESIAN_POINT ( 'NONE',  ( -1.200186371490556958, -4.775308065498765409, 21.32625670625849423 ) ) ;
#2037 = ORIENTED_EDGE ( 'NONE', *, *, #32084, .T. ) ;
#2038 = B_SPLINE_CURVE_WITH_KNOTS ( 'NONE', 3,
 ( #28665, #37177, #63764, #16032, #57006, #70975, #84499, #78171, #76851, #57894 ),
 .UNSPECIFIED., .F., .F.,
 ( 4, 2, 2, 2, 4 ),
 ( 0.000000000000000000, 0.0001954311564186870913, 0.0003908623128373741825, 0.0005862934692560613009, 0.0007817246256747483650 ),
 .UNSPECIFIED. ) ;
#2039 = CARTESIAN_POINT ( 'NONE',  ( 3.155571303690441365, -7.975156536449540035, 14.00000000000001066 ) ) ;
#2040 = ORIENTED_EDGE ( 'NONE', *, *, #30730, .T. ) ;
#2041 = ADVANCED_FACE ( 'NONE', ( #14114 ), #67291, .F. ) ;
#2042 = CARTESIAN_POINT ( 'NONE',  ( -2.557669051740897537, -2.920706130388546651, 32.31842814019191223 ) ) ;
#2043 = ORIENTED_EDGE ( 'NONE', *, *, #39798, .T. ) ;
#2044 = CARTESIAN_POINT ( 'NONE',  ( -10.61538461538461320, -10.89733346790207413, 36.13435417666054406 ) ) ;
#2045 = EDGE_CURVE ( 'NONE', #23088, #78524, #40872, .T. ) ;
#2046 = CARTESIAN_POINT ( 'NONE',  ( 14.30769230769231015, -2.292212530054420494, 30.41441678777542634 ) ) ;
#2047 = ORIENTED_EDGE ( 'NONE', *, *, #16725, .F. ) ;
#2048 = CARTESIAN_POINT ( 'NONE',  ( -6.222926217516144831, -11.76352882383564769, 32.36236540154569497 ) ) ;
#2049 = CARTESIAN_POINT ( 'NONE',  ( -1.077988221561460236, -10.27530806549876452, 22.10750670625849068 ) ) ;
#2050 = CARTESIAN_POINT ( 'NONE',  ( -17.93474486048716088, -9.528491918058456633, 34.59228464037085615 ) ) ;
#2051 = CARTESIAN_POINT ( 'NONE',  ( -5.869474298236434961, -9.417988943895561960, 34.36773134775778260 ) ) ;
#2052 = CARTESIAN_POINT ( 'NONE',  ( 15.90382292962469535, -8.475808217655753651, 34.90892951860618609 ) ) ;
#2053 = AXIS2_PLACEMENT_3D ( 'NONE', #11556, #43662, #73710 ) ;
#2054 = CARTESIAN_POINT ( 'NONE',  ( 15.23076923076910916, -8.656820664282941280, 34.87096338111179961 ) ) ;
#2055 = CARTESIAN_POINT ( 'NONE',  ( -7.846153846153844924, -4.098570777380720287, 33.41473453929634729 ) ) ;
#2056 = LINE ( 'NONE', #43928, #71280 ) ;
#2057 = EDGE_CURVE ( 'NONE', #10922, #33240, #61362, .T. ) ;
#2058 = CARTESIAN_POINT ( 'NONE',  ( 1.553300858899087311, -3.749999999999992006, 15.48437500000000178 ) ) ;
#2059 = CARTESIAN_POINT ( 'NONE',  ( -9.942330929600656120, -3.711651800289232028, 33.01384336483936011 ) ) ;
#2060 = DIRECTION ( 'NONE',  ( 0.000000000000000000, 0.9396926207859126468, 0.3420201433256571111 ) ) ;
#2061 = EDGE_CURVE ( 'NONE', #39874, #45094, #39182, .T. ) ;
#2062 = CARTESIAN_POINT ( 'NONE',  ( 14.43821800945587341, -3.285477652293413264, 32.44071101563363158 ) ) ;
#2063 = CARTESIAN_POINT ( 'NONE',  ( -3.749999999999997335, -7.500000000000021316, 15.09375000000000000 ) ) ;
#2064 = CARTESIAN_POINT ( 'NONE',  ( -13.38461538461538325, -2.499999999999998668, 29.75000000000001421 ) ) ;
#2065 = ORIENTED_EDGE ( 'NONE', *, *, #24111, .T. ) ;
#2066 = CARTESIAN_POINT ( 'NONE',  ( -17.75005448165185484, -2.824170634883621744, 31.52227843825337317 ) ) ;
#2067 = CARTESIAN_POINT ( 'NONE',  ( 11.76147289007438701, -5.667800583137506010, 34.40243808032445827 ) ) ;
#2068 = CARTESIAN_POINT ( 'NONE',  ( 1.254468175177166689, -12.45813303252208648, 30.39737893381572675 ) ) ;
#2069 = CARTESIAN_POINT ( 'NONE',  ( 5.299702618191483694, -2.847695495035524882, 31.58253572463339509 ) ) ;
#2070 = CARTESIAN_POINT ( 'NONE',  ( -19.50000000000000000, -3.499999999999999556, 29.75000000000000355 ) ) ;
#2071 = CARTESIAN_POINT ( 'NONE',  ( -9.019254006523732770, -8.432397168068783699, 34.66272746175022945 ) ) ;
#2072 = DIRECTION ( 'NONE',  ( -0.000000000000000000, -0.8660254037844397068, -0.4999999999999978906 ) ) ;
#2073 = VERTEX_POINT ( 'NONE', #45913 ) ;
#2074 = EDGE_LOOP ( 'NONE', ( #21777, #5506, #55375, #74626, #78628, #49482, #5060, #5658 ) ) ;
#2075 = EDGE_CURVE ( 'NONE', #42909, #68446, #37764, .T. ) ;
#2076 = ORIENTED_EDGE ( 'NONE', *, *, #48961, .T. ) ;
#2077 = CARTESIAN_POINT ( 'NONE',  ( 6.250000000000063949, -7.434744429011176159, 34.75000000000000711 ) ) ;
#2078 = CARTESIAN_POINT ( 'NONE',  ( 6.856993512121045242, -2.721908614388772740, 31.22303859784724622 ) ) ;
#2079 = CARTESIAN_POINT ( 'NONE',  ( 16.15384615384603251, -2.892918686052165622, 31.69288490824153470 ) ) ;
#2080 = CARTESIAN_POINT ( 'NONE',  ( 2.057669070399342992, -5.851115903089112003, 34.47074536777953568 ) ) ;
#2081 = CARTESIAN_POINT ( 'NONE',  ( 17.93472955403921887, -9.442884908240170461, 34.35708131394840592 ) ) ;
#2082 = ORIENTED_EDGE ( 'NONE', *, *, #21168, .T. ) ;
#2083 = EDGE_CURVE ( 'NONE', #7867, #68565, #82969, .T. ) ;
#2084 = CARTESIAN_POINT ( 'NONE',  ( -17.86916158198723181, -7.277220443632451463, 34.74524770363009196 ) ) ;
#2085 = VERTEX_POINT ( 'NONE', #74740 ) ;
#2086 = ORIENTED_EDGE ( 'NONE', *, *, #40449, .T. ) ;
#2087 = EDGE_CURVE ( 'NONE', #19865, #25459, #46367, .T. ) ;
#2088 = EDGE_CURVE ( 'NONE', #25490, #52597, #69994, .T. ) ;
#2090 = VERTEX_POINT ( 'NONE', #18014 ) ;
#2089 = CARTESIAN_POINT ( 'NONE',  ( -15.48074596171158213, -12.17611988154120972, 31.52148481390971213 ) ) ;
#2091 = CARTESIAN_POINT ( 'NONE',  ( 8.519254038288416098, -2.779195860258146578, 31.39871582349836032 ) ) ;
#2092 = CARTESIAN_POINT ( 'NONE',  ( -19.00000000000000000, -7.500000000000000000, 29.75000000000000355 ) ) ;
#2093 = FACE_OUTER_BOUND ( 'NONE', #61524, .T. ) ;
#2094 = DIRECTION ( 'NONE',  ( 0.000000000000000000, 0.6427876096865373645, -0.7660444431189797898 ) ) ;
#2095 = ORIENTED_EDGE ( 'NONE', *, *, #39042, .F. ) ;
#2096 = EDGE_CURVE ( 'NONE', #52736, #41563, #78509, .T. ) ;
#2097 = VERTEX_POINT ( 'NONE', #18899 ) ;
#2098 = CARTESIAN_POINT ( 'NONE',  ( -1.553300858899081538, -11.25000000000000711, 19.85937500000000355 ) ) ;
#2099 = AXIS2_PLACEMENT_3D ( 'NONE', #8921, #49011, #22424 ) ;
#2100 = EDGE_LOOP ( 'NONE', ( #46921, #81866 ) ) ;
#2101 = DIRECTION ( 'NONE',  ( -1.000000000000000000, -0.000000000000000000, 0.000000000000000000 ) ) ;
#2103 = EDGE_LOOP ( 'NONE', ( #22284, #27746, #22039, #53223 ) ) ;
#2102 = FACE_OUTER_BOUND ( 'NONE', #80839, .T. ) ;
#2104 = CARTESIAN_POINT ( 'NONE',  ( 11.47319109250076430, -6.879047030191174805, 34.71129190930000163 ) ) ;
#2105 = CARTESIAN_POINT ( 'NONE',  ( 13.38461538461569411, -2.506253911140615021, 30.00000000000323297 ) ) ;
#2106 = EDGE_CURVE ( 'NONE', #22650, #19302, #52763, .T. ) ;
#2107 = EDGE_CURVE ( 'NONE', #51215, #32941, #66641, .T. ) ;
#2108 = CARTESIAN_POINT ( 'NONE',  ( -0.4615384615385840772, -9.528491918059723176, 34.59228464037033035 ) ) ;
#2109 = ORIENTED_EDGE ( 'NONE', *, *, #5296, .T. ) ;
#2110 = FACE_OUTER_BOUND ( 'NONE', #73589, .T. ) ;
#2111 = CARTESIAN_POINT ( 'NONE',  ( 15.00728430620489995, -2.612411019501189369, 31.66733052389439962 ) ) ;
#2112 = VERTEX_POINT ( 'NONE', #62960 ) ;
#2113 = FACE_BOUND ( 'NONE', #58635, .T. ) ;
#2114 = EDGE_CURVE ( 'NONE', #20560, #13624, #16245, .T. ) ;
#2115 = CARTESIAN_POINT ( 'NONE',  ( -11.76138849736838488, -11.43668979543635089, 33.22377378376089752 ) ) ;
#2116 = CARTESIAN_POINT ( 'NONE',  ( 0.3589743589743582541, -7.500000000000000000, 29.75000000000000355 ) ) ;
#2117 = CARTESIAN_POINT ( 'NONE',  ( -15.00775638667583678, -2.889357225399414197, 32.26129605718031002 ) ) ;
#2119 = CARTESIAN_POINT ( 'NONE',  ( 4.853438133199126980, -3.236172620538810385, 32.36188796281390267 ) ) ;
#2118 = CARTESIAN_POINT ( 'NONE',  ( 8.069166690247241647, -10.77377354290276124, 33.85451476688484718 ) ) ;
#2120 = CARTESIAN_POINT ( 'NONE',  ( 8.546304551714618114, -5.667676309546437530, 34.40238873228292249 ) ) ;
#2121 = CARTESIAN_POINT ( 'NONE',  ( 20.00000000000000000, -4.000000000000000000, 29.75000000000000355 ) ) ;
#2122 = VERTEX_POINT ( 'NONE', #76944 ) ;
#2123 = CARTESIAN_POINT ( 'NONE',  ( 10.61538461538461675, -1.790695186598648903, 34.54067556320373455 ) ) ;
#2124 = CARTESIAN_POINT ( 'NONE',  ( -16.82697766754503377, -6.653508905675593610, 34.93172785388651391 ) ) ;
#2125 = ORIENTED_EDGE ( 'NONE', *, *, #16712, .F. ) ;
#2126 = CARTESIAN_POINT ( 'NONE',  ( -12.21159305216042057, -3.520799739797214389, 33.17531984108286025 ) ) ;
#2127 = CARTESIAN_POINT ( 'NONE',  ( 15.45378058238208219, -4.187068189119697692, 33.49521262558774026 ) ) ;
#2128 = CARTESIAN_POINT ( 'NONE',  ( 3.165012428254921240, -7.249945686854185389, 34.74374336980224598 ) ) ;
#2129 = CARTESIAN_POINT ( 'NONE',  ( 16.82692307692307665, -7.500000000000001776, 35.00000000000000000 ) ) ;
#2130 = DIRECTION ( 'NONE',  ( -0.000000000000000000, -0.7660444431189791237, -0.6427876096865379196 ) ) ;
#2131 = FACE_OUTER_BOUND ( 'NONE', #32724, .T. ) ;
#2132 = FACE_BOUND ( 'NONE', #17620, .T. ) ;
#2134 = CARTESIAN_POINT ( 'NONE',  ( 1.515141086378949398, -2.619367082507848998, 30.83698974864644171 ) ) ;
#2133 = CARTESIAN_POINT ( 'NONE',  ( -1.608100309179714804, -6.716662450894490100, 34.94144148231605840 ) ) ;
#2135 = CARTESIAN_POINT ( 'NONE',  ( -18.00000000000000000, -8.164416787775447659, 34.95778746994557906 ) ) ;
#2137 = CARTESIAN_POINT ( 'NONE',  ( 7.596153846153846700, -2.499999999999998668, 29.75000000000000355 ) ) ;
#2136 = CARTESIAN_POINT ( 'NONE',  ( -7.596208436775802930, -12.68172785388650681, 30.59649109432439218 ) ) ;
#2138 = CYLINDRICAL_SURFACE ( 'NONE', #50494, 0.2499999999999994726 ) ;
#2139 = CARTESIAN_POINT ( 'NONE',  ( 3.749999999999999556, -7.438900925035446754, 19.21688170625848358 ) ) ;
#2140 = EDGE_LOOP ( 'NONE', ( #72686, #39670, #86380, #88421 ) ) ;
#2141 = ADVANCED_FACE ( 'NONE', ( #28304 ), #7155, .F. ) ;
#2142 = ORIENTED_EDGE ( 'NONE', *, *, #37566, .T. ) ;
#2143 = AXIS2_PLACEMENT_3D ( 'NONE', #55120, #69080, #48357 ) ;
#2144 = FACE_OUTER_BOUND ( 'NONE', #19220, .T. ) ;
#2145 = CARTESIAN_POINT ( 'NONE',  ( -4.403822884788507253, -3.137211980971221781, 32.19342716148376837 ) ) ;
#2146 = FACE_OUTER_BOUND ( 'NONE', #5200, .T. ) ;
#2147 = B_SPLINE_CURVE_WITH_KNOTS ( 'NONE', 3,
 ( #73769, #12064, #39543, #60229, #87734, #26006 ),
 .UNSPECIFIED., .F., .F.,
 ( 4, 2, 4 ),
 ( 0.0003909512603273878522, 0.0005862562993132138141, 0.0007815613382990396676 ),
 .UNSPECIFIED. ) ;
#2149 = VECTOR ( 'NONE', #54384, 1000.000000000000114 ) ;
#2148 = CARTESIAN_POINT ( 'NONE',  ( -0.7115616857599186273, -2.985938066672154445, 32.43141759479405550 ) ) ;
#2150 = CARTESIAN_POINT ( 'NONE',  ( -16.15384615384627409, -12.27809138561165270, 31.22303859784587132 ) ) ;
#2151 = CARTESIAN_POINT ( 'NONE',  ( -2.608446859217889546, -10.19485399968121264, 23.43563170625848713 ) ) ;
#2152 = CARTESIAN_POINT ( 'NONE',  ( -1.253777054128622614, -7.277220318596959281, 34.99547417642776992 ) ) ;
#2153 = DIRECTION ( 'NONE',  ( -0.000000000000000000, -0.8660254037844397068, -0.4999999999999978906 ) ) ;
#2154 = CARTESIAN_POINT ( 'NONE',  ( -8.096177070375302876, -2.985938066672154445, 32.43141759479405550 ) ) ;
#2155 = CARTESIAN_POINT ( 'NONE',  ( -1.449885830576159496, -12.46129190929999986, 30.37095296980880832 ) ) ;
#2156 = CARTESIAN_POINT ( 'NONE',  ( -3.454254155333561727, -4.225889041578354544, 33.85425143139329407 ) ) ;
#2157 = DIRECTION ( 'NONE',  ( 0.000000000000000000, 0.6427876096865373645, -0.7660444431189797898 ) ) ;
#2158 = CARTESIAN_POINT ( 'NONE',  ( 14.37376065869474751, -11.69971097300155272, 32.46337939537588113 ) ) ;
#2159 = DIRECTION ( 'NONE',  ( -0.000000000000000000, 0.3420201433256694901, -0.9396926207859082059 ) ) ;
#2160 = ORIENTED_EDGE ( 'NONE', *, *, #26803, .T. ) ;
#2161 = CARTESIAN_POINT ( 'NONE',  ( 15.00784227186238162, -11.43668979543634734, 33.22377378376089752 ) ) ;
#2162 = CARTESIAN_POINT ( 'NONE',  ( -17.20761454359063691, -2.729777683071817229, 31.24903638046269450 ) ) ;
#2163 = CARTESIAN_POINT ( 'NONE',  ( 1.492201783934598236, -11.27530806549875031, 13.70499329374151287 ) ) ;
#2164 = CARTESIAN_POINT ( 'NONE',  ( 0.5923289025054120360, -3.338503747796865984, 32.95102852606553512 ) ) ;
#2165 = CARTESIAN_POINT ( 'NONE',  ( 24.00000000000000000, 9.000000000000024869, 28.74999999999999645 ) ) ;
#2166 = VERTEX_POINT ( 'NONE', #13465 ) ;
#2167 = CARTESIAN_POINT ( 'NONE',  ( 10.55013362522337239, -2.506253911140460922, 30.00000000000013856 ) ) ;
#2169 = VERTEX_POINT ( 'NONE', #27429 ) ;
#2168 = DIRECTION ( 'NONE',  ( -0.000000000000000000, -0.3420201433256694346, -0.9396926207859080948 ) ) ;
#2170 = CARTESIAN_POINT ( 'NONE',  ( 7.976679547917411739, -3.816742781228458892, 33.13167719472716044 ) ) ;
#2171 = DIRECTION ( 'NONE',  ( 0.000000000000000000, 0.8660254037844377084, -0.5000000000000015543 ) ) ;
#2172 = EDGE_LOOP ( 'NONE', ( #70945, #66750, #87537, #2367 ) ) ;
#2173 = CARTESIAN_POINT ( 'NONE',  ( -5.143006487878955646, -11.16473453929635440, 33.15142922261925662 ) ) ;
#2174 = VECTOR ( 'NONE', #49018, 1000.000000000000000 ) ;
#2176 = EDGE_CURVE ( 'NONE', #63712, #74006, #46292, .T. ) ;
#2175 = CARTESIAN_POINT ( 'NONE',  ( 8.992242120843618736, -4.887748414852792322, 34.01359900205216746 ) ) ;
#2177 = ORIENTED_EDGE ( 'NONE', *, *, #59364, .T. ) ;
#2178 = CARTESIAN_POINT ( 'NONE',  ( -12.52762084089859940, -2.292212530054419606, 30.41441678777542634 ) ) ;
#2179 = FILL_AREA_STYLE ('',( #15712 ) ) ;
#2180 = DIRECTION ( 'NONE',  ( 0.000000000000000000, 0.9848077530122072432, 0.1736481776669354937 ) ) ;
#2181 = ORIENTED_EDGE ( 'NONE', *, *, #84922, .T. ) ;
#2182 = VERTEX_POINT ( 'NONE', #7603 ) ;
#2183 = ORIENTED_EDGE ( 'NONE', *, *, #14015, .F. ) ;
#2184 = CARTESIAN_POINT ( 'NONE',  ( 3.230769230769108269, -2.379036618888197285, 30.90682066428292885 ) ) ;
#2185 = CARTESIAN_POINT ( 'NONE',  ( 2.530471976670372936, -11.60474049983370648, 33.02348890104160262 ) ) ;
#2186 = EDGE_CURVE ( 'NONE', #10414, #5178, #33471, .T. ) ;
#2187 = CARTESIAN_POINT ( 'NONE',  ( -8.096153846153844924, -7.500000000000001776, 34.75000000000000000 ) ) ;
#2188 = CARTESIAN_POINT ( 'NONE',  ( 2.980746006547774218, -10.18141759479407327, 34.26406193332782379 ) ) ;
#2189 = VECTOR ( 'NONE', #24278, 1000.000000000000114 ) ;
#2190 = ORIENTED_EDGE ( 'NONE', *, *, #70727, .F. ) ;
#2191 = ADVANCED_FACE ( 'NONE', ( #48569 ), #76050, .F. ) ;
#2192 = VERTEX_POINT ( 'NONE', #15248 ) ;
#2194 = ORIENTED_EDGE ( 'NONE', *, *, #21005, .T. ) ;
#2193 = CARTESIAN_POINT ( 'NONE',  ( 9.692307692307572609, -4.481592998941358097, 33.73612834414048933 ) ) ;
#2195 = CARTESIAN_POINT ( 'NONE',  ( 17.07692307692295586, -5.219633306517616589, 34.19971097300220464 ) ) ;
#2196 = VERTEX_POINT ( 'NONE', #35514 ) ;
#2197 = DIRECTION ( 'NONE',  ( -0.000000000000000000, 0.3420201433256694901, -0.9396926207859082059 ) ) ;
#2198 = CARTESIAN_POINT ( 'NONE',  ( -8.519176349317316266, -12.65882529074907126, 30.72640787790839312 ) ) ;
#2199 = AXIS2_PLACEMENT_3D ( 'NONE', #14959, #44167, #77095 ) ;
#2200 = ORIENTED_EDGE ( 'NONE', *, *, #64434, .F. ) ;
#2201 = ORIENTED_EDGE ( 'NONE', *, *, #69425, .F. ) ;
#2203 = ORIENTED_EDGE ( 'NONE', *, *, #24683, .F. ) ;
#2202 = DIRECTION ( 'NONE',  ( -1.000000000000000000, 0.000000000000000000, 0.000000000000000000 ) ) ;
#2204 = CARTESIAN_POINT ( 'NONE',  ( 4.403900465484468008, -4.943051570960392382, 34.04725096376909477 ) ) ;
#2205 = ADVANCED_FACE ( 'NONE', ( #1275 ), #42721, .F. ) ;
#2206 = CARTESIAN_POINT ( 'NONE',  ( 14.08476534878545827, -5.582147617184174848, 34.63737895849758530 ) ) ;
#2207 = EDGE_LOOP ( 'NONE', ( #10098, #41399 ) ) ;
#2208 = CARTESIAN_POINT ( 'NONE',  ( 15.45378058238208041, -3.105924265160262543, 32.13625925475356127 ) ) ;
#2209 = LINE ( 'NONE', #65680, #52288 ) ;
#2210 = CARTESIAN_POINT ( 'NONE',  ( 17.93391762063986050, -12.34228464037088280, 31.77849191805838558 ) ) ;
#2211 = FACE_BOUND ( 'NONE', #10306, .T. ) ;
#2212 = CARTESIAN_POINT ( 'NONE',  ( -18.75000000000000000, -11.50000000000000000, 29.75000000000000355 ) ) ;
#2213 = CARTESIAN_POINT ( 'NONE',  ( -11.53846153846166089, -6.835583212225970762, 34.95778746994575670 ) ) ;
#2214 = CARTESIAN_POINT ( 'NONE',  ( -13.38461538461538325, -1.509761064869970415, 31.06009739812519044 ) ) ;
#2216 = CARTESIAN_POINT ( 'NONE',  ( -16.02332071561251681, -3.068774925481847937, 32.56582465632704526 ) ) ;
#2215 = CARTESIAN_POINT ( 'NONE',  ( 0.5915835174582330103, -2.254550872974306674, 29.97347326024527447 ) ) ;
#2217 = CARTESIAN_POINT ( 'NONE',  ( -7.976301055592065481, -3.285722584762969856, 32.44110544564090759 ) ) ;
#2218 = CARTESIAN_POINT ( 'NONE',  ( -9.942307692307691624, -2.249999999999998668, 29.75000000000000355 ) ) ;
#2219 = ORIENTED_EDGE ( 'NONE', *, *, #22671, .F. ) ;
#2220 = CARTESIAN_POINT ( 'NONE',  ( -15.90379173393269596, -3.435999193479609026, 33.07426656108011542 ) ) ;
#2221 = ORIENTED_EDGE ( 'NONE', *, *, #54401, .F. ) ;
#2222 = ORIENTED_EDGE ( 'NONE', *, *, #70191, .T. ) ;
#2223 = VECTOR ( 'NONE', #1169, 999.9999999999998863 ) ;
#2225 = LINE ( 'NONE', #55849, #67827 ) ;
#2224 = CARTESIAN_POINT ( 'NONE',  ( -3.230769230769229949, -3.886160181151819604, 36.00935417666054406 ) ) ;
#2226 = DIRECTION ( 'NONE',  ( -0.000000000000000000, -0.1736481776669307198, -0.9848077530122080203 ) ) ;
#2227 = DIRECTION ( 'NONE',  ( -0.000000000000000000, 0.9396926207859093161, -0.3420201433256663259 ) ) ;
#2228 = CARTESIAN_POINT ( 'NONE',  ( -10.39237177129122003, -12.38742843783360748, 31.66772728687926985 ) ) ;
#2229 = CARTESIAN_POINT ( 'NONE',  ( -0.2385271099256119354, -11.76359900205217457, 32.36225158514719880 ) ) ;
#2230 = ORIENTED_EDGE ( 'NONE', *, *, #43221, .T. ) ;
#2231 = CYLINDRICAL_SURFACE ( 'NONE', #37096, 0.2499999999999998890 ) ;
#2232 = CARTESIAN_POINT ( 'NONE',  ( 14.17700170458200581, -12.62707690430377383, 30.88035979386743435 ) ) ;
#2233 = CARTESIAN_POINT ( 'NONE',  ( -2.057692307690886846, -7.500000000000154543, 35.00000000000007105 ) ) ;
#2234 = FACE_OUTER_BOUND ( 'NONE', #22715, .T. ) ;
#2235 = CARTESIAN_POINT ( 'NONE',  ( 20.00000000000000000, -4.000000000000000000, 29.75000000000000355 ) ) ;
#2236 = CARTESIAN_POINT ( 'NONE',  ( 2.320192649118979489E-14, -11.25000000000000000, 16.03125000000000000 ) ) ;
#2237 = EDGE_LOOP ( 'NONE', ( #84036, #26205, #82453, #32891, #73664 ) ) ;
#2238 = ORIENTED_EDGE ( 'NONE', *, *, #56649, .F. ) ;
#2239 = CARTESIAN_POINT ( 'NONE',  ( -7.596099426240391139, -12.01375889529407281, 32.43194544308182969 ) ) ;
#2240 = ORIENTED_EDGE ( 'NONE', *, *, #29973, .T. ) ;
#2241 = CYLINDRICAL_SURFACE ( 'NONE', #25393, 0.2500000000000012212 ) ;
#2242 = CARTESIAN_POINT ( 'NONE',  ( 17.99999999999987566, -6.026961402154118908, 34.52809138561165270 ) ) ;
#2243 = CARTESIAN_POINT ( 'NONE',  ( -6.923076923076922462, -1.242168528481310874, 33.36296068462461051 ) ) ;
#2244 = CARTESIAN_POINT ( 'NONE',  ( -5.010855743573002563, -3.322132147404559976, 32.92929555188717927 ) ) ;
#2245 = CARTESIAN_POINT ( 'NONE',  ( -2.651650429449565305, -4.848349570550461785, 16.50000000000000000 ) ) ;
#2246 = CARTESIAN_POINT ( 'NONE',  ( 8.519254038288414321, -6.567427716900048118, 34.66269422305636283 ) ) ;
#2247 = ORIENTED_EDGE ( 'NONE', *, *, #64813, .T. ) ;
#2249 = B_SPLINE_CURVE_WITH_KNOTS ( 'NONE', 3,
 ( #65012, #3320, #11419, #3766, #31697, #59155, #30792, #86661, #38904, #13631 ),
 .UNSPECIFIED., .F., .F.,
 ( 4, 2, 2, 2, 4 ),
 ( 0.0007817359430256322827, 0.0009771253907249989254, 0.001172514838424365460, 0.001367904286123731994, 0.001563293733823098745 ),
 .UNSPECIFIED. ) ;
#2248 = CARTESIAN_POINT ( 'NONE',  ( 1.326923076923075762, -11.00000000000000000, 29.75000000000000355 ) ) ;
#2251 = VERTEX_POINT ( 'NONE', #62523 ) ;
#2250 = CARTESIAN_POINT ( 'NONE',  ( -2.241623956689869246, -10.51840700105979565, 33.73612834413962247 ) ) ;
#2252 = CARTESIAN_POINT ( 'NONE',  ( 3.100078627658924280, -12.35290016733513951, 31.75349464988449455 ) ) ;
#2253 = CARTESIAN_POINT ( 'NONE',  ( -0.5276208408985965104, -3.937682226553329556, 33.60647404775217240 ) ) ;
#2254 = CARTESIAN_POINT ( 'NONE',  ( -3.361460697436789324, -4.809359713505814149, 33.96456829005828837 ) ) ;
#2256 = AXIS2_PLACEMENT_3D ( 'NONE', #9773, #56636, #71466 ) ;
#2255 = CARTESIAN_POINT ( 'NONE',  ( -12.46153846153846168, -9.780366693483667717, 34.19971097300155094 ) ) ;
#2257 = CARTESIAN_POINT ( 'NONE',  ( 1.384615384615386802, -4.098570777380720287, 33.41473453929634729 ) ) ;
#2258 = FACE_OUTER_BOUND ( 'NONE', #13603, .T. ) ;
#2259 = CARTESIAN_POINT ( 'NONE',  ( -0.06109907496450878162, -11.25000000000000000, 15.03311829374151287 ) ) ;
#2260 = ORIENTED_EDGE ( 'NONE', *, *, #66486, .F. ) ;
#2261 = CARTESIAN_POINT ( 'NONE',  ( -17.01166750564705055, -10.90142922261932057, 33.41473453929631887 ) ) ;
#2262 = DIRECTION ( 'NONE',  ( 0.000000000000000000, 0.7660444431189822323, -0.6427876096865344779 ) ) ;
#2263 = CARTESIAN_POINT ( 'NONE',  ( -2.749999999999991562, -8.639087296526025028, 23.76562499999999645 ) ) ;
#2264 = CARTESIAN_POINT ( 'NONE',  ( -15.93083330975275658, -11.43677907613345113, 33.22367315496201456 ) ) ;
#2265 = CARTESIAN_POINT ( 'NONE',  ( 2.307692307692186251, -12.16647553114689728, 32.15551576947799362 ) ) ;
#2266 = VERTEX_POINT ( 'NONE', #82381 ) ;
#2267 = CARTESIAN_POINT ( 'NONE',  ( -1.139087296525992388, -10.25000000000000711, 16.10937500000000355 ) ) ;
#2268 = CYLINDRICAL_SURFACE ( 'NONE', #74318, 0.2500000000000012212 ) ;
#2269 = CIRCLE ( 'NONE', #6595, 4.000000000000000000 ) ;
#2270 = ORIENTED_EDGE ( 'NONE', *, *, #86880, .F. ) ;
#2271 = DIRECTION ( 'NONE',  ( -0.000000000000000000, 0.7660444431189791237, -0.6427876096865379196 ) ) ;
#2272 = UNCERTAINTY_MEASURE_WITH_UNIT (LENGTH_MEASURE( 1.000000000000000082E-05 ), #31200, 'distance_accuracy_value', 'NONE');
#2273 = EDGE_CURVE ( 'NONE', #37486, #51137, #75601, .T. ) ;
#2274 = EDGE_LOOP ( 'NONE', ( #42968, #75217 ) ) ;
#2275 = CARTESIAN_POINT ( 'NONE',  ( 17.77651505627605033, -6.760086850603066466, 34.69517049084099369 ) ) ;
#2276 = CARTESIAN_POINT ( 'NONE',  ( -17.20707104665477161, -2.373036134822905208, 30.88089517874952250 ) ) ;
#2277 = DIRECTION ( 'NONE',  ( -0.000000000000000000, -0.9848077530122085754, -0.1736481776669273613 ) ) ;
#2278 = CARTESIAN_POINT ( 'NONE',  ( -16.15384615384615330, -5.415277668671390821, 36.20867863119892149 ) ) ;
#2279 = ORIENTED_EDGE ( 'NONE', *, *, #42735, .T. ) ;
#2280 = DIRECTION ( 'NONE',  ( -0.000000000000000000, -5.102127870520021228E-17, -1.000000000000000000 ) ) ;
#2281 = EDGE_CURVE ( 'NONE', #62668, #32981, #403, .T. ) ;
#2282 = EDGE_LOOP ( 'NONE', ( #39969, #10820 ) ) ;
#2283 = CARTESIAN_POINT ( 'NONE',  ( -6.673076923076923350, -2.499999999999998668, 29.75000000000000355 ) ) ;
#2284 = DIRECTION ( 'NONE',  ( -0.000000000000000000, 0.7660444431189791237, -0.6427876096865379196 ) ) ;
#2285 = AXIS2_PLACEMENT_3D ( 'NONE', #3586, #86481, #24753 ) ;
#2286 = ORIENTED_EDGE ( 'NONE', *, *, #77754, .T. ) ;
#2287 = EDGE_CURVE ( 'NONE', #23070, #235, #14045, .T. ) ;
#2288 = CARTESIAN_POINT ( 'NONE',  ( 11.78851595837499211, -12.65882529074907126, 30.72640787790839312 ) ) ;
#2289 = DIRECTION ( 'NONE',  ( 0.000000000000000000, 0.9848077530122072432, 0.1736481776669354937 ) ) ;
#2290 = CARTESIAN_POINT ( 'NONE',  ( 0.4615384615383396616, -4.481592998941358097, 33.73612834414048933 ) ) ;
#2291 = VECTOR ( 'NONE', #33549, 1000.000000000000000 ) ;
#2292 = CARTESIAN_POINT ( 'NONE',  ( 27.00000000000000000, 1.250000000000004663, 31.75000000000000000 ) ) ;
#2293 = LINE ( 'NONE', #22141, #25357 ) ;
#2294 = B_SPLINE_CURVE_WITH_KNOTS ( 'NONE', 3,
 ( #3009, #2564, #65154, #23721, #16979, #22844, #44428, #43561, #58390, #50747 ),
 .UNSPECIFIED., .F., .F.,
 ( 4, 2, 2, 2, 4 ),
 ( 0.0007817246336856293861, 0.0009771112958940108076, 0.001172497958102392121, 0.001367884620310773434, 0.001563271282519154747 ),
 .UNSPECIFIED. ) ;
#2295 = VERTEX_POINT ( 'NONE', #6278 ) ;
#2296 = ORIENTED_EDGE ( 'NONE', *, *, #49343, .F. ) ;
#2297 = EDGE_CURVE ( 'NONE', #69664, #33072, #42283, .T. ) ;
#2298 = FACE_BOUND ( 'NONE', #32128, .T. ) ;
#2299 = ORIENTED_EDGE ( 'NONE', *, *, #85061, .F. ) ;
#2300 = CARTESIAN_POINT ( 'NONE',  ( 8.769230769230768274, -3.513871655860378418, 32.76840700105978499 ) ) ;
#2301 = CARTESIAN_POINT ( 'NONE',  ( -18.06527000055631760, -11.06231777344663136, 33.60647404775220082 ) ) ;
#2302 = CARTESIAN_POINT ( 'NONE',  ( 19.00000000000000000, 17.00000000000000000, 2.999999999999999112 ) ) ;
#2303 = CARTESIAN_POINT ( 'NONE',  ( 5.299934428535925335, -4.187068189119697692, 33.49521262558774026 ) ) ;
#2304 = VERTEX_POINT ( 'NONE', #33743 ) ;
#2305 = EDGE_LOOP ( 'NONE', ( #53271, #45181 ) ) ;
#2306 = CARTESIAN_POINT ( 'NONE',  ( 8.769230769230768274, -4.945431358278436385, 36.03766855953609394 ) ) ;
#2307 = ORIENTED_EDGE ( 'NONE', *, *, #76762, .T. ) ;
#2308 = CARTESIAN_POINT ( 'NONE',  ( -10.68065461594093435, -8.656820664281498878, 34.87096338111211935 ) ) ;
#2309 = AXIS2_PLACEMENT_3D ( 'NONE', #9147, #50105, #76708 ) ;
#2310 = EDGE_CURVE ( 'NONE', #42810, #46099, #9751, .T. ) ;
#2311 = DIRECTION ( 'NONE',  ( -0.000000000000000000, 1.000000000000000000, -0.000000000000000000 ) ) ;
#2312 = EDGE_CURVE ( 'NONE', #74382, #19612, #71948, .T. ) ;
#2313 = CARTESIAN_POINT ( 'NONE',  ( 12.46153846153846168, -2.538708090699994813, 30.37095296980875503 ) ) ;
#2314 = CARTESIAN_POINT ( 'NONE',  ( -18.24997673094235751, -11.28823185664189310, 33.01397839955799896 ) ) ;
#2315 = VERTEX_POINT ( 'NONE', #64292 ) ;
#2316 = CARTESIAN_POINT ( 'NONE',  ( 16.40390057375960708, -2.318338780012835443, 30.59689888758630616 ) ) ;
#2317 = EDGE_CURVE ( 'NONE', #37303, #13779, #85916, .T. ) ;
#2318 = CARTESIAN_POINT ( 'NONE',  ( -6.223484924564330001, -6.716662450894490100, 34.94144148231605840 ) ) ;
#2319 = ADVANCED_FACE ( 'NONE', ( #77380 ), #23751, .F. ) ;
#2320 = CARTESIAN_POINT ( 'NONE',  ( -7.846153846153844924, -1.466349020453238561, 30.81389545987213907 ) ) ;
#2321 = CARTESIAN_POINT ( 'NONE',  ( 8.992243613324164997, -6.460100341425560444, 34.89618726649961644 ) ) ;
#2322 = ORIENTED_EDGE ( 'NONE', *, *, #44361, .F. ) ;
#2323 = VECTOR ( 'NONE', #15206, 1000.000000000000114 ) ;
#2324 = PRODUCT_DEFINITION_CONTEXT ( 'detailed design', #14719, 'design' ) ;
#2325 = ORIENTED_EDGE ( 'NONE', *, *, #62800, .F. ) ;
#2326 = EDGE_LOOP ( 'NONE', ( #24112, #73313, #27769, #48180 ) ) ;
#2328 = CARTESIAN_POINT ( 'NONE',  ( -9.469528023329624844, -8.540255544307065350, 34.89611431652622286 ) ) ;
#2327 = CARTESIAN_POINT ( 'NONE',  ( -18.06870381900330713, -2.255952184585098053, 29.99992509483742609 ) ) ;
#2329 = CARTESIAN_POINT ( 'NONE',  ( -18.00000000000000000, -2.249999999999989786, 29.74999999999998579 ) ) ;
#2330 = CARTESIAN_POINT ( 'NONE',  ( -2.084912638714241595, -2.612705202774697533, 31.66806509827799943 ) ) ;
#2331 = LINE ( 'NONE', #21733, #24220 ) ;
#2332 = DIRECTION ( 'NONE',  ( -0.000000000000000000, -0.6427876096865404731, -0.7660444431189771253 ) ) ;
#2333 = ORIENTED_EDGE ( 'NONE', *, *, #66591, .F. ) ;
#2334 = CARTESIAN_POINT ( 'NONE',  ( -3.230769230769351186, -2.625532179533779154, 30.86335684631627174 ) ) ;
#2335 = CARTESIAN_POINT ( 'NONE',  ( 9.692307692307570832, -12.16647553114689728, 32.15551576947799362 ) ) ;
#2336 = CARTESIAN_POINT ( 'NONE',  ( -9.692307692307691624, -9.819645486525091727, 36.12317359536749706 ) ) ;
#2337 = CARTESIAN_POINT ( 'NONE',  ( -11.53846153846153655, -3.513871655860378418, 32.76840700105978499 ) ) ;
#2338 = ORIENTED_EDGE ( 'NONE', *, *, #31520, .F. ) ;
#2339 = CARTESIAN_POINT ( 'NONE',  ( 14.43848411551709887, -8.999086150933475636, 34.52020707165672775 ) ) ;
#2340 = ORIENTED_EDGE ( 'NONE', *, *, #76448, .T. ) ;
#2341 = FACE_BOUND ( 'NONE', #44611, .T. ) ;
#2342 = B_SPLINE_CURVE_WITH_KNOTS ( 'NONE', 3,
 ( #50353, #70644, #854, #42738, #55791, #15262, #22014, #84615, #77397, #22452 ),
 .UNSPECIFIED., .F., .F.,
 ( 4, 2, 2, 2, 4 ),
 ( 0.0007817359430256392216, 0.0009771253907250080327, 0.001172514838424376952, 0.001367904286123745872, 0.001563293733823114791 ),
 .UNSPECIFIED. ) ;
#2343 = CARTESIAN_POINT ( 'NONE',  ( -0.4615384615384611200, -13.75783147151868846, 33.36296068462461051 ) ) ;
#2344 = DIRECTION ( 'NONE',  ( -0.000000000000000000, -0.8660254037844399289, -0.4999999999999980016 ) ) ;
#2345 = CARTESIAN_POINT ( 'NONE',  ( -3.164700879766791708, -8.120952969808772792, 34.71129190929999453 ) ) ;
#2346 = VERTEX_POINT ( 'NONE', #79155 ) ;
#2347 = CARTESIAN_POINT ( 'NONE',  ( -14.53061852520844965, -12.39988816332205701, 30.74660775122750778 ) ) ;
#2348 = CARTESIAN_POINT ( 'NONE',  ( 15.29602437028206907, -2.379036618887895305, 30.90682066428158592 ) ) ;
#2349 = CARTESIAN_POINT ( 'NONE',  ( 8.703148389870634105, -8.164416787775445883, 34.95778746994557906 ) ) ;
#2350 = CARTESIAN_POINT ( 'NONE',  ( -18.00000000000012079, -3.835265460704626150, 33.15142922262032954 ) ) ;
#2351 = EDGE_LOOP ( 'NONE', ( #79932, #72056, #42009, #57754 ) ) ;
#2352 = AXIS2_PLACEMENT_3D ( 'NONE', #51446, #87512, #17246 ) ;
#2353 = CARTESIAN_POINT ( 'NONE',  ( 14.30769230769218581, -5.094484230521993062, 34.41647553114689373 ) ) ;
#2354 = ORIENTED_EDGE ( 'NONE', *, *, #15042, .F. ) ;
#2356 = ORIENTED_EDGE ( 'NONE', *, *, #33390, .F. ) ;
#2355 = CARTESIAN_POINT ( 'NONE',  ( 13.44987052412822237, -8.656820664281605460, 34.87096338111211224 ) ) ;
#2357 = CARTESIAN_POINT ( 'NONE',  ( 9.626224281351809964, -3.513871655860377086, 32.76840700105978499 ) ) ;
#2358 = CARTESIAN_POINT ( 'NONE',  ( -1.634638608836841644, -12.45566812827425096, 31.48439005359158926 ) ) ;
#2359 = CARTESIAN_POINT ( 'NONE',  ( 7.623226887246994821, -10.01117774369187252, 34.36070679894347535 ) ) ;
#2360 = EDGE_CURVE ( 'NONE', #29827, #86419, #51204, .T. ) ;
#2361 = CARTESIAN_POINT ( 'NONE',  ( -15.36137888597331091, -7.722926974430166069, 34.99546784045485737 ) ) ;
#2363 = CARTESIAN_POINT ( 'NONE',  ( 8.546303810323918171, -4.026226216239094491, 33.68668979543634379 ) ) ;
#2362 = CYLINDRICAL_SURFACE ( 'NONE', #36184, 4.000000000000000000 ) ;
#2364 = VECTOR ( 'NONE', #29528, 1000.000000000000114 ) ;
#2365 = CARTESIAN_POINT ( 'NONE',  ( -9.822998295417995962, -11.93127051446799847, 32.56575433478202797 ) ) ;
#2366 = CARTESIAN_POINT ( 'NONE',  ( -2.749999999999998224, -7.500000000000015987, 25.09374999999999645 ) ) ;
#2367 = ORIENTED_EDGE ( 'NONE', *, *, #77511, .F. ) ;
#2368 = CARTESIAN_POINT ( 'NONE',  ( -0.4615384615385826339, -6.026961402154118908, 34.52809138561165270 ) ) ;
#2369 = CARTESIAN_POINT ( 'NONE',  ( 13.31886195630205805, -7.249945578846651806, 34.99404164642496795 ) ) ;
#2370 = ORIENTED_EDGE ( 'NONE', *, *, #26120, .T. ) ;
#2371 = EDGE_LOOP ( 'NONE', ( #8849, #30221, #25616, #7528 ) ) ;
#2372 = EDGE_LOOP ( 'NONE', ( #81677, #11518 ) ) ;
#2373 = CARTESIAN_POINT ( 'NONE',  ( 4.087762742890273415, -12.10708131394839349, 31.69288490824020244 ) ) ;
#2374 = CARTESIAN_POINT ( 'NONE',  ( -19.99999999999996803, 15.00000000000000711, 3.000000000000000000 ) ) ;
#2375 = CARTESIAN_POINT ( 'NONE',  ( -17.32689980786543060, -9.148715823498378086, 34.47080413974185120 ) ) ;
#2376 = EDGE_CURVE ( 'NONE', #63608, #72717, #64359, .T. ) ;
#2377 = LINE ( 'NONE', #22225, #38519 ) ;
#2378 = DIRECTION ( 'NONE',  ( -1.000000000000000000, -0.000000000000000000, -0.000000000000000000 ) ) ;
#2379 = CARTESIAN_POINT ( 'NONE',  ( 7.053602624840487501, -11.46989282347013095, 32.79007818306219946 ) ) ;
#2380 = CARTESIAN_POINT ( 'NONE',  ( 5.750000000000003553, -7.566082377512563184, 35.00000000000000711 ) ) ;
#2381 = VERTEX_POINT ( 'NONE', #36404 ) ;
#2382 = CIRCLE ( 'NONE', #15324, 4.000000000000000000 ) ;
#2383 = CARTESIAN_POINT ( 'NONE',  ( -6.923076923076922462, -5.415277668671390821, 36.20867863119892149 ) ) ;
#2384 = CARTESIAN_POINT ( 'NONE',  ( -5.076923076923075762, -8.973038597847269315, 34.52809138561121927 ) ) ;
#2385 = CARTESIAN_POINT ( 'NONE',  ( -9.626239341305254271, -11.16473453929635440, 33.15142922261926373 ) ) ;
#2386 = CARTESIAN_POINT ( 'NONE',  ( 5.076923076922954969, -3.300289026999228881, 32.46337939537708905 ) ) ;
#2387 = B_SPLINE_CURVE_WITH_KNOTS ( 'NONE', 3,
 ( #46987, #80356, #39372, #87568, #33493, #54187, #26284, #60952, #88457, #60063 ),
 .UNSPECIFIED., .F., .F.,
 ( 4, 2, 2, 2, 4 ),
 ( 0.0007817359430256285964, 0.0009771253907249948054, 0.001172514838424360906, 0.001367904286123727223, 0.001563293733823093324 ),
 .UNSPECIFIED. ) ;
#2388 = ORIENTED_EDGE ( 'NONE', *, *, #75261, .T. ) ;
#2389 = DIRECTION ( 'NONE',  ( 0.000000000000000000, 0.7660444431189822323, -0.6427876096865344779 ) ) ;
#2390 = B_SPLINE_CURVE_WITH_KNOTS ( 'NONE', 3,
 ( #30173, #57201, #79696, #71587, #77910, #9457, #64382, #23403, #9896, #37358 ),
 .UNSPECIFIED., .F., .F.,
 ( 4, 2, 2, 2, 4 ),
 ( 0.000000000000000000, 0.0001954339857564099951, 0.0003908679715128199903, 0.0005863019572692300396, 0.0007817359430256399806 ),
 .UNSPECIFIED. ) ;
#2391 = EDGE_CURVE ( 'NONE', #59690, #29899, #8490, .T. ) ;
#2392 = VERTEX_POINT ( 'NONE', #78711 ) ;
#2393 = CARTESIAN_POINT ( 'NONE',  ( 12.33084785842815378, -9.084618155246140248, 34.75535874321725771 ) ) ;
#2394 = CARTESIAN_POINT ( 'NONE',  ( -15.90384615384614264, -2.249999999999999112, 29.81603969181033165 ) ) ;
#2395 = CARTESIAN_POINT ( 'NONE',  ( 3.296836564119306701, -10.67929555188718282, 33.92786785259544757 ) ) ;
#2396 = CARTESIAN_POINT ( 'NONE',  ( -14.30769230769230660, -11.11383981884818262, 36.00935417666054406 ) ) ;
#2397 = ORIENTED_EDGE ( 'NONE', *, *, #22673, .F. ) ;
#2398 = VECTOR ( 'NONE', #12052, 1000.000000000000114 ) ;
#2399 = ADVANCED_FACE ( 'NONE', ( #9805 ), #30953, .F. ) ;
#2400 = CARTESIAN_POINT ( 'NONE',  ( 12.71148387091650278, -10.92531984108285670, 33.72920026020278073 ) ) ;
#2401 = CARTESIAN_POINT ( 'NONE',  ( -13.38461538461550759, -11.06231777344772027, 33.60647404775119895 ) ) ;
#2402 = CARTESIAN_POINT ( 'NONE',  ( 8.992010310499175318, -4.387253974876679230, 33.66317474335728832 ) ) ;
#2403 = EDGE_LOOP ( 'NONE', ( #48266, #24806, #24783, #35003 ) ) ;
#2404 = EDGE_CURVE ( 'NONE', #30706, #45661, #63862, .T. ) ;
#2405 = CARTESIAN_POINT ( 'NONE',  ( 7.780071466793708979, -11.35647404775217595, 33.31231777344666511 ) ) ;
#2406 = VERTEX_POINT ( 'NONE', #17007 ) ;
#2407 = CARTESIAN_POINT ( 'NONE',  ( 9.757563263583715951, -11.94971097300157403, 32.03036669348361443 ) ) ;
#2408 = EDGE_CURVE ( 'NONE', #292, #19083, #84998, .T. ) ;
#2409 = CARTESIAN_POINT ( 'NONE',  ( 6.923076923076924238, -2.833524468853757305, 32.15551576947925838 ) ) ;
#2410 = CIRCLE ( 'NONE', #57062, 0.2500000000000002220 ) ;
#2411 = CARTESIAN_POINT ( 'NONE',  ( -7.976301815885547875, -2.647304123082328875, 31.75400227202885972 ) ) ;
#2412 = EDGE_CURVE ( 'NONE', #54986, #54522, #37667, .T. ) ;
#2413 = CARTESIAN_POINT ( 'NONE',  ( -14.24243673641628227, -10.21337939537593620, 33.94971097300152252 ) ) ;
#2414 = CARTESIAN_POINT ( 'NONE',  ( 18.25005441991345378, -8.346898887586322147, 34.93166121998716278 ) ) ;
#2415 = B_SPLINE_CURVE_WITH_KNOTS ( 'NONE', 3,
 ( #75033, #24728, #11670, #66612, #4913, #54743 ),
 .UNSPECIFIED., .F., .F.,
 ( 4, 2, 4 ),
 ( 3.252606517456513302E-19, 0.0001954784845028939284, 0.0003909569690057875316 ),
 .UNSPECIFIED. ) ;
#2416 = AXIS2_PLACEMENT_3D ( 'NONE', #22539, #75706, #54998 ) ;
#2417 = ORIENTED_EDGE ( 'NONE', *, *, #41255, .T. ) ;
#2418 = ORIENTED_EDGE ( 'NONE', *, *, #24350, .F. ) ;
#2419 = VERTEX_POINT ( 'NONE', #3038 ) ;
#2420 = EDGE_CURVE ( 'NONE', #38559, #21246, #24756, .T. ) ;
#2421 = VECTOR ( 'NONE', #3040, 1000.000000000000000 ) ;
#2422 = CARTESIAN_POINT ( 'NONE',  ( 8.769230769230768274, -2.900454961884010974, 35.62045528018868623 ) ) ;
#2423 = CARTESIAN_POINT ( 'NONE',  ( -17.01085472592063397, -3.513871655860379306, 32.76840700105978499 ) ) ;
#2424 = CARTESIAN_POINT ( 'NONE',  ( 14.30769230769231015, -2.486705287966279876, 31.30864560766543647 ) ) ;
#2425 = EDGE_CURVE ( 'NONE', #48052, #5633, #24651, .T. ) ;
#2426 = FACE_OUTER_BOUND ( 'NONE', #52785, .T. ) ;
#2427 = CARTESIAN_POINT ( 'NONE',  ( 11.53846153846153832, -1.129524287112498415, 32.06866353760679544 ) ) ;
#2428 = EDGE_CURVE ( 'NONE', #80371, #39612, #58183, .T. ) ;
#2429 = CARTESIAN_POINT ( 'NONE',  ( 5.326977388561390470, -9.943054286541403997, 34.11300777759954883 ) ) ;
#2430 = EDGE_LOOP ( 'NONE', ( #58554, #86194, #30591, #25383 ) ) ;
#2431 = ORIENTED_EDGE ( 'NONE', *, *, #77572, .F. ) ;
#2432 = ORIENTED_EDGE ( 'NONE', *, *, #24288, .T. ) ;
#2434 = ORIENTED_EDGE ( 'NONE', *, *, #22837, .T. ) ;
#2433 = CARTESIAN_POINT ( 'NONE',  ( 4.153846153846154188, -3.937682226553329556, 33.60647404775216529 ) ) ;
#2436 = CARTESIAN_POINT ( 'NONE',  ( -5.142193077479396024, -12.70778746994557551, 30.41441678777548319 ) ) ;
#2435 = CARTESIAN_POINT ( 'NONE',  ( 0.5920641633020248262, -8.586989748646450593, 34.63063291749215011 ) ) ;
#2437 = VECTOR ( 'NONE', #87966, 1000.000000000000000 ) ;
#2438 = CARTESIAN_POINT ( 'NONE',  ( -3.750000000000007550, -5.946699141100917352, 25.17187500000000000 ) ) ;
#2439 = VERTEX_POINT ( 'NONE', #11138 ) ;
#2440 = ADVANCED_FACE ( 'NONE', ( #25986 ), #31865, .F. ) ;
#2441 = ORIENTED_EDGE ( 'NONE', *, *, #7391, .T. ) ;
#2442 = CARTESIAN_POINT ( 'NONE',  ( 5.326923076923011813, -7.565270000091922853, 34.99999999999999289 ) ) ;
#2443 = ORIENTED_EDGE ( 'NONE', *, *, #1263, .T. ) ;
#2444 = FACE_BOUND ( 'NONE', #1100, .T. ) ;
#2445 = CARTESIAN_POINT ( 'NONE',  ( 3.480823650682684622, -2.544122305571458575, 31.48381861865057729 ) ) ;
#2446 = CYLINDRICAL_SURFACE ( 'NONE', #13219, 0.2499999999999994726 ) ;
#2447 = ORIENTED_EDGE ( 'NONE', *, *, #6766, .T. ) ;
#2448 = EDGE_CURVE ( 'NONE', #6548, #11602, #73751, .T. ) ;
#2449 = CARTESIAN_POINT ( 'NONE',  ( 16.15384615384615330, -11.16473453929635440, 33.15142922261926373 ) ) ;
#2450 = CARTESIAN_POINT ( 'NONE',  ( -10.61538461538461320, -3.886160181151819604, 36.00935417666054406 ) ) ;
#2451 = AXIS2_PLACEMENT_3D ( 'NONE', #65757, #79734, #87396 ) ;
#2452 = CARTESIAN_POINT ( 'NONE',  ( 1.253924781505077801, -3.338472653186242756, 32.95098750199972670 ) ) ;
#2453 = CARTESIAN_POINT ( 'NONE',  ( -11.60373198442231590, -6.026961402152685388, 34.52809138561120506 ) ) ;
#2454 = CYLINDRICAL_SURFACE ( 'NONE', #75419, 0.2500000000000004996 ) ;
#2455 = CARTESIAN_POINT ( 'NONE',  ( 7.846153846153723244, -11.67786785259630911, 32.92929555188603530 ) ) ;
#2456 = FACE_OUTER_BOUND ( 'NONE', #34698, .T. ) ;
#2457 = CARTESIAN_POINT ( 'NONE',  ( -7.976301815885538105, -12.15440758774515473, 32.17923288041532004 ) ) ;
#2458 = CARTESIAN_POINT ( 'NONE',  ( -6.222926217516146608, -5.667676309546437530, 34.40238873228292249 ) ) ;
#2459 = CARTESIAN_POINT ( 'NONE',  ( 16.15384615384615330, -10.67929555188718282, 33.92786785259544047 ) ) ;
#2460 = CYLINDRICAL_SURFACE ( 'NONE', #84762, 0.2499999999999995559 ) ;
#2461 = ADVANCED_FACE ( 'NONE', ( #39519 ), #3924, .F. ) ;
#2462 = CARTESIAN_POINT ( 'NONE',  ( -13.31854805126531005, -12.34228464037088813, 31.77849191805839268 ) ) ;
#2464 = CARTESIAN_POINT ( 'NONE',  ( 2.372947878968333146, -10.21337939537593797, 33.94971097300152252 ) ) ;
#2463 = CARTESIAN_POINT ( 'NONE',  ( 5.011652630962300847, -12.46129190929999986, 30.37095296980880832 ) ) ;
#2465 = CARTESIAN_POINT ( 'NONE',  ( -0.4615384615384611200, -8.164416787775445883, 34.95778746994557906 ) ) ;
#2467 = DIRECTION ( 'NONE',  ( 1.000000000000000000, 0.000000000000000000, 0.000000000000000000 ) ) ;
#2466 = CARTESIAN_POINT ( 'NONE',  ( 12.46153846153846168, -12.29105614889573062, 35.45975837776705220 ) ) ;
#2468 = CARTESIAN_POINT ( 'NONE',  ( -5.749945688361683516, -12.41262288849542017, 30.68299917996395010 ) ) ;
#2469 = CARTESIAN_POINT ( 'NONE',  ( 2.750000000000001332, -7.438900925035452083, 24.21688170625849068 ) ) ;
#2471 = EDGE_CURVE ( 'NONE', #11784, #5488, #12045, .T. ) ;
#2470 = ORIENTED_EDGE ( 'NONE', *, *, #2001, .T. ) ;
#2472 = LINE ( 'NONE', #65061, #49003 ) ;
#2473 = ORIENTED_EDGE ( 'NONE', *, *, #80206, .T. ) ;
#2474 = EDGE_CURVE ( 'NONE', #45845, #16480, #75885, .T. ) ;
#2475 = LINE ( 'NONE', #80266, #50704 ) ;
#2476 = CIRCLE ( 'NONE', #28394, 7.066647012551277918 ) ;
#2477 = VERTEX_POINT ( 'NONE', #33190 ) ;
#2478 = CYLINDRICAL_SURFACE ( 'NONE', #28280, 0.2499999999999994726 ) ;
#2479 = VERTEX_POINT ( 'NONE', #79605 ) ;
#2480 = CARTESIAN_POINT ( 'NONE',  ( -6.130691466667556710, -11.71456829005830080, 32.44064028649416542 ) ) ;
#2481 = CARTESIAN_POINT ( 'NONE',  ( 1.901340078031349856, -5.512252781505337929, 22.81063170625848713 ) ) ;
#2483 = B_SPLINE_CURVE_WITH_KNOTS ( 'NONE', 3,
 ( #28884, #36517, #35634, #23425, #36940, #77059, #63966, #15805, #56341, #43270 ),
 .UNSPECIFIED., .F., .F.,
 ( 4, 2, 2, 2, 4 ),
 ( 0.000000000000000000, 0.0001954339857564058210, 0.0003908679715128116419, 0.0005863019572692174629, 0.0007817359430256232838 ),
 .UNSPECIFIED. ) ;
#2482 = CARTESIAN_POINT ( 'NONE',  ( 6.065255139512838234, -6.835583212224609184, 34.95778746994559327 ) ) ;
#2484 = CARTESIAN_POINT ( 'NONE',  ( -5.777220458731589403, -9.332535724633407526, 34.40230450496446224 ) ) ;
#2485 = CARTESIAN_POINT ( 'NONE',  ( -11.53846153846122391, -2.255955759149395501, 30.00000000000324363 ) ) ;
#2486 = EDGE_CURVE ( 'NONE', #7349, #76616, #3305, .T. ) ;
#2487 = CARTESIAN_POINT ( 'NONE',  ( -17.07692307692307665, -12.62096338111211580, 30.90682066428153263 ) ) ;
#2488 = CARTESIAN_POINT ( 'NONE',  ( -13.51530598772569292, -8.191372820521381826, 34.95448215188424967 ) ) ;
#2489 = CARTESIAN_POINT ( 'NONE',  ( -13.38461538461550759, -12.16647553114689728, 32.15551576947799362 ) ) ;
#2490 = CARTESIAN_POINT ( 'NONE',  ( 2.320192649118979489E-14, -11.25000000000000000, 17.28125000000000000 ) ) ;
#2491 = FACE_OUTER_BOUND ( 'NONE', #51838, .T. ) ;
#2492 = CARTESIAN_POINT ( 'NONE',  ( -15.23076923076935074, -2.625532179533778709, 30.86335684631627174 ) ) ;
#2493 = VECTOR ( 'NONE', #28205, 1000.000000000000000 ) ;
#2494 = CARTESIAN_POINT ( 'NONE',  ( 14.55774661933062397, -3.136992222400443175, 32.19305428654138979 ) ) ;
#2495 = CARTESIAN_POINT ( 'NONE',  ( 1.553300858899129944, -11.24999999999998934, 15.95312500000000000 ) ) ;
#2496 = CARTESIAN_POINT ( 'NONE',  ( -10.48459417441766206, -5.496552790871120031, 34.60292014791297532 ) ) ;
#2497 = VERTEX_POINT ( 'NONE', #32307 ) ;
#2498 = CARTESIAN_POINT ( 'NONE',  ( 17.32697738856139225, -12.17597550085003633, 31.52189283813461884 ) ) ;
#2499 = CARTESIAN_POINT ( 'NONE',  ( 11.66925334628632882, -5.582136614379148654, 34.36778462344220486 ) ) ;
#2500 = CARTESIAN_POINT ( 'NONE',  ( 9.942253210655836781, -6.696923467548660192, 34.68552623307873972 ) ) ;
#2501 = CARTESIAN_POINT ( 'NONE',  ( 5.326868595271218254, -2.824170634883622188, 31.52227843825338738 ) ) ;
#2502 = EDGE_CURVE ( 'NONE', #24740, #74652, #52560, .T. ) ;
#2503 = CARTESIAN_POINT ( 'NONE',  ( 4.087763774486019130, -3.322132147404559976, 32.92929555188719348 ) ) ;
#2504 = CARTESIAN_POINT ( 'NONE',  ( 9.561616225640134914, -11.18331474514187995, 33.13161551792790505 ) ) ;
#2505 = CARTESIAN_POINT ( 'NONE',  ( 8.519254038288414321, -10.66389620160130036, 33.62221079203477103 ) ) ;
#2506 = EDGE_LOOP ( 'NONE', ( #86542, #44118, #22143, #15946, #48903, #37980, #41332, #20143 ) ) ;
#2507 = CARTESIAN_POINT ( 'NONE',  ( 17.86930853333243974, -12.38065189839062263, 30.83690757178629482 ) ) ;
#2508 = ORIENTED_EDGE ( 'NONE', *, *, #42310, .T. ) ;
#2509 = VECTOR ( 'NONE', #35018, 1000.000000000000000 ) ;
#2510 = ORIENTED_EDGE ( 'NONE', *, *, #84358, .T. ) ;
#2511 = CARTESIAN_POINT ( 'NONE',  ( -6.130690603110307890, -12.62707690430377383, 30.88035979386743435 ) ) ;
#2512 = CARTESIAN_POINT ( 'NONE',  ( -13.91025641025641058, -3.499999999999999556, 29.75000000000000355 ) ) ;
#2513 = AXIS2_PLACEMENT_3D ( 'NONE', #838, #35064, #62095 ) ;
#2514 = CYLINDRICAL_SURFACE ( 'NONE', #76706, 0.2499999999999995559 ) ;
#2515 = CYLINDRICAL_SURFACE ( 'NONE', #82657, 0.2500000000000002220 ) ;
#2516 = ORIENTED_EDGE ( 'NONE', *, *, #79009, .T. ) ;
#2517 = CARTESIAN_POINT ( 'NONE',  ( 27.00000000000000355, -1.749999999999999778, 30.25000000000000000 ) ) ;
#2518 = ORIENTED_EDGE ( 'NONE', *, *, #19738, .F. ) ;
#2519 = ORIENTED_EDGE ( 'NONE', *, *, #20527, .F. ) ;
#2520 = EDGE_CURVE ( 'NONE', #84646, #4955, #55947, .T. ) ;
#2521 = CYLINDRICAL_SURFACE ( 'NONE', #58800, 0.2500000000000008882 ) ;
#2522 = FACE_OUTER_BOUND ( 'NONE', #16135, .T. ) ;
#2523 = CARTESIAN_POINT ( 'NONE',  ( -2.307692307692305711, -1.117168528481311540, 33.14645433367849847 ) ) ;
#2524 = EDGE_CURVE ( 'NONE', #37993, #5737, #83944, .T. ) ;
#2525 = AXIS2_PLACEMENT_3D ( 'NONE', #15439, #15882, #9127 ) ;
#2526 = CARTESIAN_POINT ( 'NONE',  ( 6.923076923076924238, -13.37000171582298513, 34.34916445242398453 ) ) ;
#2527 = EDGE_CURVE ( 'NONE', #88852, #39806, #37607, .T. ) ;
#2528 = DIRECTION ( 'NONE',  ( 0.000000000000000000, 0.000000000000000000, 1.000000000000000000 ) ) ;
#2529 = VERTEX_POINT ( 'NONE', #21338 ) ;
#2530 = ORIENTED_EDGE ( 'NONE', *, *, #33972, .F. ) ;
#2531 = CARTESIAN_POINT ( 'NONE',  ( -3.749999999999988454, -9.053300858899127945, 20.01562500000000355 ) ) ;
#2532 = ORIENTED_EDGE ( 'NONE', *, *, #18031, .T. ) ;
#2533 = AXIS2_PLACEMENT_3D ( 'NONE', #32136, #10977, #59152 ) ;
#2535 = EDGE_LOOP ( 'NONE', ( #71781, #25472 ) ) ;
#2534 = CARTESIAN_POINT ( 'NONE',  ( 24.99999999999999645, -19.99999999999999645, 3.000000000000000000 ) ) ;
#2536 = EDGE_CURVE ( 'NONE', #74452, #36240, #19433, .T. ) ;
#2537 = CARTESIAN_POINT ( 'NONE',  ( 1.449870955891410906, -9.442884908240271713, 34.35708131394835618 ) ) ;
#2538 = CARTESIAN_POINT ( 'NONE',  ( -19.50000000000000000, -11.50000000000000000, 29.75000000000000355 ) ) ;
#2539 = B_SPLINE_CURVE_WITH_KNOTS ( 'NONE', 3,
 ( #38395, #73068, #58654, #65416, #59102, #86149, #11366, #31183, #79835, #24420 ),
 .UNSPECIFIED., .F., .F.,
 ( 4, 2, 2, 2, 4 ),
 ( 0.0007817246256747450040, 0.0009771112852218872494, 0.001172497944769029278, 0.001367884604316171523, 0.001563271263863313769 ),
 .UNSPECIFIED. ) ;
#2540 = CARTESIAN_POINT ( 'NONE',  ( 7.146088274689773812, -11.76359900205217457, 32.36225158514719880 ) ) ;
#2541 = VERTEX_POINT ( 'NONE', #15034 ) ;
#2542 = AXIS2_PLACEMENT_3D ( 'NONE', #17138, #23447, #84293 ) ;
#2543 = EDGE_CURVE ( 'NONE', #3325, #1645, #76278, .T. ) ;
#2544 = CARTESIAN_POINT ( 'NONE',  ( -14.98082382139119062, -12.45601412856602686, 31.48342859153981621 ) ) ;
#2545 = ORIENTED_EDGE ( 'NONE', *, *, #27219, .F. ) ;
#2546 = FACE_BOUND ( 'NONE', #81293, .T. ) ;
#2547 = CARTESIAN_POINT ( 'NONE',  ( 15.36129466900287532, -11.66157788607254098, 32.95092075102925833 ) ) ;
#2548 = CARTESIAN_POINT ( 'NONE',  ( 10.68145296638705410, -8.973038597847271092, 34.52809138561121216 ) ) ;
#2549 = B_SPLINE_CURVE_WITH_KNOTS ( 'NONE', 3,
 ( #33079, #31756, #88493, #59213, #67756, #88062, #4271, #81279, #19562, #52451 ),
 .UNSPECIFIED., .F., .F.,
 ( 4, 2, 2, 2, 4 ),
 ( 0.000000000000000000, 0.0001954339857564080707, 0.0003908679715128161414, 0.0005863019572692241849, 0.0007817359430256322827 ),
 .UNSPECIFIED. ) ;
#2550 = DIRECTION ( 'NONE',  ( 0.000000000000000000, 0.6427876096865368094, 0.7660444431189802339 ) ) ;
#2552 = DIRECTION ( 'NONE',  ( 0.000000000000000000, 0.8660254037844377084, 0.5000000000000015543 ) ) ;
#2551 = CYLINDRICAL_SURFACE ( 'NONE', #79179, 0.2499999999999973355 ) ;
#2553 = CARTESIAN_POINT ( 'NONE',  ( -1.384615384615506484, -8.656820664282941280, 34.87096338111179961 ) ) ;
#2554 = CARTESIAN_POINT ( 'NONE',  ( -10.68146802634049486, -10.51840700105979387, 33.73612834413961536 ) ) ;
#2555 = EDGE_LOOP ( 'NONE', ( #62347, #89031 ) ) ;
#2556 = CARTESIAN_POINT ( 'NONE',  ( -11.40766973063675316, -4.118422570099827595, 33.43335022499816489 ) ) ;
#2557 = CYLINDRICAL_SURFACE ( 'NONE', #47928, 0.2500000000000004996 ) ;
#2558 = VERTEX_POINT ( 'NONE', #42950 ) ;
#2559 = CARTESIAN_POINT ( 'NONE',  ( -12.39628332202562433, -3.643525952247864463, 33.31231777344670064 ) ) ;
#2560 = CARTESIAN_POINT ( 'NONE',  ( 15.23076923076911093, -4.481592998941358097, 33.73612834414048933 ) ) ;
#2561 = CARTESIAN_POINT ( 'NONE',  ( -2.939152317953646711E-15, 7.500000000000000000, 14.00000000000000178 ) ) ;
#2562 = CARTESIAN_POINT ( 'NONE',  ( -7.715363405186894674, -10.70102852606553157, 33.91149625220312913 ) ) ;
#2563 = DIRECTION ( 'NONE',  ( 0.000000000000000000, 0.6427876096865373645, -0.7660444431189797898 ) ) ;
#2564 = CARTESIAN_POINT ( 'NONE',  ( -7.596153846153782752, -7.434744860731433924, 35.00000000000000711 ) ) ;
#2565 = FACE_BOUND ( 'NONE', #84441, .T. ) ;
#2567 = CYLINDRICAL_SURFACE ( 'NONE', #24453, 0.2499999999999995559 ) ;
#2566 = CARTESIAN_POINT ( 'NONE',  ( 12.39626801557768587, -3.300289026998414865, 32.46337939537583139 ) ) ;
#2568 = CARTESIAN_POINT ( 'NONE',  ( 15.90386942290380290, -3.137211980971220893, 32.19342716148376837 ) ) ;
#2570 = CARTESIAN_POINT ( 'NONE',  ( -12.46153846153858247, -4.481592998941358097, 33.73612834414048933 ) ) ;
#2569 = CARTESIAN_POINT ( 'NONE',  ( -7.780086512803769949, -12.62096338111211757, 30.90682066428152908 ) ) ;
#2571 = LINE ( 'NONE', #30063, #7312 ) ;
#2572 = CARTESIAN_POINT ( 'NONE',  ( -2.694853999681210865, -4.891553140782108677, 22.49813170625848713 ) ) ;
#2573 = EDGE_CURVE ( 'NONE', #6905, #67687, #74625, .T. ) ;
#2574 = VERTEX_POINT ( 'NONE', #14584 ) ;
#2575 = CYLINDRICAL_SURFACE ( 'NONE', #69438, 0.2500000000000002220 ) ;
#2576 = ADVANCED_FACE ( 'NONE', ( #36202 ), #69525, .F. ) ;
#2577 = AXIS2_PLACEMENT_3D ( 'NONE', #76, #55458, #42841 ) ;
#2578 = CYLINDRICAL_SURFACE ( 'NONE', #19672, 0.2499999999999997502 ) ;
#2579 = CARTESIAN_POINT ( 'NONE',  ( 12.94230769230769340, -3.499999999999999556, 29.75000000000000355 ) ) ;
#2580 = CARTESIAN_POINT ( 'NONE',  ( 16.85399611801622655, -8.282780595021769443, 34.94152052738834868 ) ) ;
#2581 = CARTESIAN_POINT ( 'NONE',  ( 10.68145296638705588, -12.10708131394839704, 31.69288490824020954 ) ) ;
#2582 = CARTESIAN_POINT ( 'NONE',  ( 1.492201783934554493, -3.724691934501233703, 22.73250670625849068 ) ) ;
#2583 = CARTESIAN_POINT ( 'NONE',  ( -11.53846153846153655, -3.513871655860378418, 32.76840700105978499 ) ) ;
#2585 = LINE ( 'NONE', #16552, #25870 ) ;
#2584 = B_SPLINE_CURVE_WITH_KNOTS ( 'NONE', 3,
 ( #49743, #63700, #1564, #56509, #43873, #16847, #70912, #78991, #29487, #22279 ),
 .UNSPECIFIED., .F., .F.,
 ( 4, 2, 2, 2, 4 ),
 ( 0.000000000000000000, 0.0001954339857564073659, 0.0003908679715128147319, 0.0005863019572692221250, 0.0007817359430256294638 ),
 .UNSPECIFIED. ) ;
#2586 = EDGE_CURVE ( 'NONE', #40289, #76427, #56889, .T. ) ;
#2587 = CARTESIAN_POINT ( 'NONE',  ( 3.453548899747297618, -4.226511098958374291, 33.85474049983370293 ) ) ;
#2588 = CARTESIAN_POINT ( 'NONE',  ( -3.007756386675836335, -11.98016756924214832, 32.48728574198911190 ) ) ;
#2589 = CARTESIAN_POINT ( 'NONE',  ( -16.82686865700962286, -4.818054556918155207, 34.26375889529406749 ) ) ;
#2590 = CARTESIAN_POINT ( 'NONE',  ( 12.33139049180676672, -12.70455904226513866, 30.44083106164009322 ) ) ;
#2591 = B_SPLINE_CURVE_WITH_KNOTS ( 'NONE', 3,
 ( #39787, #81215, #40675, #19500, #60927, #81656, #49633, #84766, #36566, #562 ),
 .UNSPECIFIED., .F., .F.,
 ( 4, 2, 2, 2, 4 ),
 ( 0.000000000000000000, 0.0001954339857564053873, 0.0003908679715128107746, 0.0005863019572692161618, 0.0007817359430256215491 ),
 .UNSPECIFIED. ) ;
#2592 = CARTESIAN_POINT ( 'NONE',  ( -14.30769230769230660, -3.886160181151819604, 36.00935417666054406 ) ) ;
#2593 = ADVANCED_FACE ( 'NONE', ( #36631 ), #40405, .F. ) ;
#2594 = CARTESIAN_POINT ( 'NONE',  ( 17.32697749683652688, -2.544122305571458575, 31.48381861865057729 ) ) ;
#2595 = EDGE_LOOP ( 'NONE', ( #64131, #30840, #58349, #12862 ) ) ;
#2596 = CARTESIAN_POINT ( 'NONE',  ( 3.480714640147273720, -12.45601412856602686, 31.48342859153981621 ) ) ;
#2597 = DIRECTION ( 'NONE',  ( -0.000000000000000000, 0.9396926207859093161, -0.3420201433256663259 ) ) ;
#2598 = CARTESIAN_POINT ( 'NONE',  ( -2.694853999681181556, -10.10844685921792241, 15.18936829374151465 ) ) ;
#2599 = CARTESIAN_POINT ( 'NONE',  ( 8.769230769231075584, -2.506253911140615021, 30.00000000000323297 ) ) ;
#2601 = CARTESIAN_POINT ( 'NONE',  ( -17.07692307692307665, -5.471508081941601098, 34.59228464037088457 ) ) ;
#2600 = VECTOR ( 'NONE', #70934, 1000.000000000000114 ) ;
#2602 = VERTEX_POINT ( 'NONE', #35297 ) ;
#2603 = CARTESIAN_POINT ( 'NONE',  ( -16.21911615440247090, -4.320704448112772766, 33.92786785259540494 ) ) ;
#2605 = ORIENTED_EDGE ( 'NONE', *, *, #45005, .F. ) ;
#2604 = CARTESIAN_POINT ( 'NONE',  ( 12.39626801557768587, -6.026961402152685388, 34.52809138561120506 ) ) ;
#2606 = CARTESIAN_POINT ( 'NONE',  ( 11.76124120743959978, -4.989023458446560255, 34.36081565061822118 ) ) ;
#2607 = CARTESIAN_POINT ( 'NONE',  ( -13.31854703361294590, -9.780366693483667717, 34.19971097300155805 ) ) ;
#2608 = EDGE_CURVE ( 'NONE', #80662, #81634, #61100, .T. ) ;
#2609 = DIRECTION ( 'NONE',  ( -0.000000000000000000, -0.3420201433256694346, -0.9396926207859080948 ) ) ;
#2610 = CARTESIAN_POINT ( 'NONE',  ( -0.4615384615384611200, -2.538708090699994813, 30.37095296980875503 ) ) ;
#2611 = ORIENTED_EDGE ( 'NONE', *, *, #6377, .T. ) ;
#2612 = DIRECTION ( 'NONE',  ( -0.000000000000000000, 0.6427876096865404731, -0.7660444431189771253 ) ) ;
#2613 = EDGE_CURVE ( 'NONE', #74655, #67341, #23714, .T. ) ;
#2614 = EDGE_CURVE ( 'NONE', #84921, #11924, #49411, .T. ) ;
#2615 = DIRECTION ( 'NONE',  ( -0.000000000000000000, 0.9848077530122085754, -0.1736481776669273613 ) ) ;
#2616 = CIRCLE ( 'NONE', #27123, 4.000000000000000000 ) ;
#2617 = CARTESIAN_POINT ( 'NONE',  ( 12.46153846153833911, -12.16647553114689728, 32.15551576947799362 ) ) ;
#2618 = VERTEX_POINT ( 'NONE', #78050 ) ;
#2619 = ORIENTED_EDGE ( 'NONE', *, *, #44342, .T. ) ;
#2620 = ADVANCED_FACE ( 'NONE', ( #9587 ), #58213, .F. ) ;
#2621 = EDGE_LOOP ( 'NONE', ( #26570, #72888 ) ) ;
#2622 = FACE_OUTER_BOUND ( 'NONE', #85958, .T. ) ;
#2623 = FACE_OUTER_BOUND ( 'NONE', #72608, .T. ) ;
#2624 = CARTESIAN_POINT ( 'NONE',  ( -7.976630554270308870, -7.276988635370452485, 34.74523720219453793 ) ) ;
#2625 = CARTESIAN_POINT ( 'NONE',  ( -19.99999999999996447, -15.00000000000000533, 3.000000000000000000 ) ) ;
#2626 = EDGE_LOOP ( 'NONE', ( #14256, #1573, #31480, #28064 ) ) ;
#2627 = ORIENTED_EDGE ( 'NONE', *, *, #66914, .T. ) ;
#2629 = EDGE_LOOP ( 'NONE', ( #45771, #11641, #56818, #22527 ) ) ;
#2628 = CARTESIAN_POINT ( 'NONE',  ( 9.469381474791545017, -4.186968288167450147, 33.49512374952580274 ) ) ;
#2630 = CIRCLE ( 'NONE', #81807, 4.999999999999997335 ) ;
#2631 = EDGE_CURVE ( 'NONE', #35283, #64127, #30743, .T. ) ;
#2632 = CARTESIAN_POINT ( 'NONE',  ( -15.23076923076922995, -3.050289026998446396, 32.03036669348365706 ) ) ;
#2633 = CARTESIAN_POINT ( 'NONE',  ( 15.23076923076923173, -1.129524287112498415, 32.06866353760679544 ) ) ;
#2634 = CARTESIAN_POINT ( 'NONE',  ( -8.546217925137375104, -12.64618726649961289, 30.78989965857442712 ) ) ;
#2635 = ORIENTED_EDGE ( 'NONE', *, *, #88523, .T. ) ;
#2636 = EDGE_LOOP ( 'NONE', ( #55609, #79230, #54953, #31412 ) ) ;
#2638 = ORIENTED_EDGE ( 'NONE', *, *, #61565, .F. ) ;
#2637 = CARTESIAN_POINT ( 'NONE',  ( -8.769230769230890843, -8.613356846316285953, 34.62446782046622218 ) ) ;
#2639 = EDGE_CURVE ( 'NONE', #38598, #75373, #12873, .T. ) ;
#2640 = CARTESIAN_POINT ( 'NONE',  ( -5.999999999999998224, -8.120952969808772792, 34.71129190930000163 ) ) ;
#2641 = CARTESIAN_POINT ( 'NONE',  ( -10.68065461594093435, -9.528491918058357157, 34.59228464037090589 ) ) ;
#2642 = ORIENTED_EDGE ( 'NONE', *, *, #72584, .F. ) ;
#2643 = CARTESIAN_POINT ( 'NONE',  ( -6.700297254098856570, -4.989023458446560255, 34.36081565061822118 ) ) ;
#2644 = CARTESIAN_POINT ( 'NONE',  ( 5.326977388561388693, -11.28795663066794219, 33.01431243580653785 ) ) ;
#2645 = EDGE_CURVE ( 'NONE', #63578, #81582, #76378, .T. ) ;
#2646 = CARTESIAN_POINT ( 'NONE',  ( 17.77651507543566112, -12.47654668319379567, 31.42292124445336654 ) ) ;
#2647 = FACE_BOUND ( 'NONE', #52747, .T. ) ;
#2648 = CARTESIAN_POINT ( 'NONE',  ( -8.519176349317316266, -2.318338780012835443, 30.59689888758630261 ) ) ;
#2649 = CARTESIAN_POINT ( 'NONE',  ( 4.023155550735845409, -2.295517848115769421, 30.44137282052136939 ) ) ;
#2650 = CARTESIAN_POINT ( 'NONE',  ( -12.46153846153846168, -4.661471528628507777, 34.16647553114623292 ) ) ;
#2652 = FACE_OUTER_BOUND ( 'NONE', #80909, .T. ) ;
#2651 = LINE ( 'NONE', #79222, #14432 ) ;
#2653 = DIRECTION ( 'NONE',  ( 0.000000000000000000, 1.000000000000000000, 0.000000000000000000 ) ) ;
#2654 = CARTESIAN_POINT ( 'NONE',  ( -16.15384615384615330, -8.564572088678739092, 35.78748833219616898 ) ) ;
#2655 = ORIENTED_EDGE ( 'NONE', *, *, #11058, .F. ) ;
#2656 = CARTESIAN_POINT ( 'NONE',  ( 14.05769230769230838, -7.566083408709835645, 34.74999999999999289 ) ) ;
#2657 = ORIENTED_EDGE ( 'NONE', *, *, #2937, .T. ) ;
#2658 = ORIENTED_EDGE ( 'NONE', *, *, #76196, .T. ) ;
#2660 = CARTESIAN_POINT ( 'NONE',  ( 10.74617505635156789, -12.62708834333097663, 30.88030960425257021 ) ) ;
#2659 = CARTESIAN_POINT ( 'NONE',  ( -1.384615384615383471, -4.661471528628507777, 34.16647553114623292 ) ) ;
#2661 = ADVANCED_FACE ( 'NONE', ( #24423 ), #30310, .F. ) ;
#2662 = AXIS2_PLACEMENT_3D ( 'NONE', #67394, #47108, #27293 ) ;
#2663 = CARTESIAN_POINT ( 'NONE',  ( 13.31934538405906565, -11.67786785259540849, 32.92929555188721480 ) ) ;
#2664 = FACE_OUTER_BOUND ( 'NONE', #68760, .T. ) ;
#2665 = CARTESIAN_POINT ( 'NONE',  ( 2.307692307692309264, -2.292212530054420494, 30.41441678777542634 ) ) ;
#2666 = CARTESIAN_POINT ( 'NONE',  ( -3.930833309752757021, -3.395485233115139057, 33.02377354290275946 ) ) ;
#2667 = ORIENTED_EDGE ( 'NONE', *, *, #61590, .F. ) ;
#2668 = DIRECTION ( 'NONE',  ( 0.000000000000000000, 1.000000000000000000, 0.000000000000000000 ) ) ;
#2669 = DIRECTION ( 'NONE',  ( -0.000000000000000000, -0.5000000000000009992, -0.8660254037844380415 ) ) ;
#2670 = CARTESIAN_POINT ( 'NONE',  ( 17.14217864819909920, -6.879047030191284051, 34.71129190930002295 ) ) ;
#2671 = CARTESIAN_POINT ( 'NONE',  ( 12.46153846153846168, -10.89733346790207413, 36.13435417666054406 ) ) ;
#2672 = LINE ( 'NONE', #2235, #40622 ) ;
#2673 = B_SPLINE_CURVE_WITH_KNOTS ( 'NONE', 3,
 ( #54549, #5499, #81161, #61300, #5939, #55005, #33411, #81600, #48238, #13573 ),
 .UNSPECIFIED., .F., .F.,
 ( 4, 2, 2, 2, 4 ),
 ( 0.0007817359430256253438, 0.0009771253907249898181, 0.001172514838424354401, 0.001367904286123718983, 0.001563293733823083566 ),
 .UNSPECIFIED. ) ;
#2674 = CARTESIAN_POINT ( 'NONE',  ( 2.651650429449569302, -10.15165042944953733, 15.87500000000000000 ) ) ;
#2675 = ORIENTED_EDGE ( 'NONE', *, *, #66910, .T. ) ;
#2676 = ADVANCED_FACE ( 'NONE', ( #72621 ), #10929, .F. ) ;
#2677 = B_SPLINE_CURVE_WITH_KNOTS ( 'NONE', 3,
 ( #60763, #27425, #19783, #53108, #53560, #54898, #20230, #89148, #41386, #26098 ),
 .UNSPECIFIED., .F., .F.,
 ( 4, 2, 2, 2, 4 ),
 ( 0.0007817246256747444619, 0.0009771112852218868158, 0.001172497944769029061, 0.001367884604316171523, 0.001563271263863313769 ),
 .UNSPECIFIED. ) ;
#2678 = ORIENTED_EDGE ( 'NONE', *, *, #36115, .T. ) ;
#2679 = CARTESIAN_POINT ( 'NONE',  ( 14.30769230769231015, -12.34228464037088635, 31.77849191805839268 ) ) ;
#2680 = EDGE_CURVE ( 'NONE', #74021, #13621, #37497, .T. ) ;
#2681 = ORIENTED_EDGE ( 'NONE', *, *, #20197, .T. ) ;
#2682 = CARTESIAN_POINT ( 'NONE',  ( -18.24999999999999645, -7.566083408709835645, 34.74999999999999289 ) ) ;
#2683 = FACE_OUTER_BOUND ( 'NONE', #70992, .T. ) ;
#2684 = CARTESIAN_POINT ( 'NONE',  ( 4.023698184114455678, -11.04286588640298561, 33.62463336215343901 ) ) ;
#2685 = CARTESIAN_POINT ( 'NONE',  ( 17.32692307692449418, -7.500000000000154543, 35.00000000000007105 ) ) ;
#2686 = CARTESIAN_POINT ( 'NONE',  ( 2.651650429449539104, -4.848349570550432475, 16.81250000000000000 ) ) ;
#2687 = FACE_OUTER_BOUND ( 'NONE', #22273, .T. ) ;
#2688 = ORIENTED_EDGE ( 'NONE', *, *, #11664, .T. ) ;
#2689 = DIRECTION ( 'NONE',  ( -0.000000000000000000, -0.3420201433256694346, -0.9396926207859080948 ) ) ;
#2691 = ORIENTED_EDGE ( 'NONE', *, *, #69342, .T. ) ;
#2690 = CYLINDRICAL_SURFACE ( 'NONE', #46803, 0.2500000000000012212 ) ;
#2692 = CARTESIAN_POINT ( 'NONE',  ( 7.846153846153846700, -12.78798330534102767, 29.49999999999997868 ) ) ;
#2693 = CYLINDRICAL_SURFACE ( 'NONE', #8473, 0.2499999999999995559 ) ;
#2694 = CARTESIAN_POINT ( 'NONE',  ( 11.28848480751918437, -4.236021600441997492, 33.53823185664189310 ) ) ;
#2695 = CARTESIAN_POINT ( 'NONE',  ( 13.38461538461526423, -5.094484230521993062, 34.41647553114689373 ) ) ;
#2696 = EDGE_CURVE ( 'NONE', #75758, #57723, #22604, .T. ) ;
#2697 = CARTESIAN_POINT ( 'NONE',  ( -12.46153846153858247, -12.46129190930018460, 30.37095296980731973 ) ) ;
#2698 = CARTESIAN_POINT ( 'NONE',  ( -8.096130577096200653, -12.41269422305637171, 30.68257228309993323 ) ) ;
#2699 = CARTESIAN_POINT ( 'NONE',  ( 3.775308065498752086, -6.007798216065404873, 19.64249329374151642 ) ) ;
#2700 = ORIENTED_EDGE ( 'NONE', *, *, #82394, .F. ) ;
#2701 = CARTESIAN_POINT ( 'NONE',  ( 1.254468175177166245, -6.001485441113818986, 34.52039167877662607 ) ) ;
#2702 = CARTESIAN_POINT ( 'NONE',  ( -13.45069879557126136, -8.973038597847271092, 34.52809138561120506 ) ) ;
#2703 = CARTESIAN_POINT ( 'NONE',  ( 1.799775606325937360E-14, -10.25000000000000000, 24.78125000000000000 ) ) ;
#2704 = CARTESIAN_POINT ( 'NONE',  ( -3.480745961711583902, -9.148715823498378086, 34.47080413974185120 ) ) ;
#2705 = CARTESIAN_POINT ( 'NONE',  ( -0.4615384615384611200, -8.810774026931790459, 35.74407628777942847 ) ) ;
#2706 = ORIENTED_EDGE ( 'NONE', *, *, #48885, .F. ) ;
#2707 = CARTESIAN_POINT ( 'NONE',  ( 7.846153846153846700, -11.91647553114624181, 32.58852847137148245 ) ) ;
#2708 = CARTESIAN_POINT ( 'NONE',  ( -1.384615384615505151, -10.21337939537710326, 33.94971097300076224 ) ) ;
#2709 = EDGE_CURVE ( 'NONE', #24126, #59899, #50573, .T. ) ;
#2710 = EDGE_LOOP ( 'NONE', ( #44549, #61475 ) ) ;
#2711 = CARTESIAN_POINT ( 'NONE',  ( -4.087778820496077437, -2.486705287966279876, 31.30864560766543647 ) ) ;
#2712 = ORIENTED_EDGE ( 'NONE', *, *, #58714, .F. ) ;
#2713 = B_SPLINE_CURVE_WITH_KNOTS ( 'NONE', 3,
 ( #5377, #47686, #39172, #75171, #40937, #21088, #84151, #28754, #41378, #14796 ),
 .UNSPECIFIED., .F., .F.,
 ( 4, 2, 2, 2, 4 ),
 ( 0.000000000000000000, 0.0001954311564186866305, 0.0003908623128373732609, 0.0005862934692560598914, 0.0007817246256747465219 ),
 .UNSPECIFIED. ) ;
#2714 = CARTESIAN_POINT ( 'NONE',  ( 14.53047184896071720, -12.24180327182771855, 31.33663988360758879 ) ) ;
#2715 = ADVANCED_FACE ( 'NONE', ( #59551 ), #68098, .F. ) ;
#2716 = EDGE_CURVE ( 'NONE', #53841, #77088, #5511, .T. ) ;
#2717 = CARTESIAN_POINT ( 'NONE',  ( 3.903822916553188360, -3.711651800289232028, 33.01384336483936011 ) ) ;
#2718 = CARTESIAN_POINT ( 'NONE',  ( -6.923076923076922462, -3.669653830205710676, 35.88435417666054406 ) ) ;
#2719 = CARTESIAN_POINT ( 'NONE',  ( -4.403869378067612139, -11.56360843649121861, 33.07473185843129926 ) ) ;
#2720 = ORIENTED_EDGE ( 'NONE', *, *, #37888, .T. ) ;
#2721 = DIRECTION ( 'NONE',  ( 0.000000000000000000, 0.1736481776669275834, 0.9848077530122086864 ) ) ;
#2722 = B_SPLINE_CURVE_WITH_KNOTS ( 'NONE', 3,
 ( #41589, #47448, #6910, #88916, #46571, #60968, #34383, #54645, #88041, #39825 ),
 .UNSPECIFIED., .F., .F.,
 ( 4, 2, 2, 2, 4 ),
 ( 0.000000000000000000, 0.0001954339857564099951, 0.0003908679715128199903, 0.0005863019572692300396, 0.0007817359430256399806 ),
 .UNSPECIFIED. ) ;
#2723 = B_SPLINE_CURVE_WITH_KNOTS ( 'NONE', 3,
 ( #81048, #47241, #13021, #74735, #12582, #61193, #54442, #67082, #72942, #11699 ),
 .UNSPECIFIED., .F., .F.,
 ( 4, 2, 2, 2, 4 ),
 ( 0.0007817359430256294638, 0.0009771253907249941549, 0.001172514838424358954, 0.001367904286123723754, 0.001563293733823095492 ),
 .UNSPECIFIED. ) ;
#2724 = ORIENTED_EDGE ( 'NONE', *, *, #51536, .T. ) ;
#2725 = VECTOR ( 'NONE', #47467, 1000.000000000000000 ) ;
#2726 = FACE_OUTER_BOUND ( 'NONE', #35318, .T. ) ;
#2727 = CARTESIAN_POINT ( 'NONE',  ( -10.61538461538461320, -2.721908614388771852, 31.22303859784724978 ) ) ;
#2728 = ORIENTED_EDGE ( 'NONE', *, *, #2297, .T. ) ;
#2729 = CARTESIAN_POINT ( 'NONE',  ( 11.76147438255493149, -12.64618726649961289, 30.78989965857442712 ) ) ;
#2730 = LINE ( 'NONE', #51339, #60800 ) ;
#2731 = CARTESIAN_POINT ( 'NONE',  ( -11.76138849736838488, -2.889293201056495786, 32.26117774369186009 ) ) ;
#2732 = DIRECTION ( 'NONE',  ( -1.000000000000000000, 5.997714145664496128E-17, 0.000000000000000000 ) ) ;
#2733 = CARTESIAN_POINT ( 'NONE',  ( -39.05038313613820122, -2.499999999999999556, 29.75000000000000355 ) ) ;
#2734 = AXIS2_PLACEMENT_3D ( 'NONE', #8121, #83342, #7234 ) ;
#2735 = EDGE_LOOP ( 'NONE', ( #63554, #63257 ) ) ;
#2736 = ORIENTED_EDGE ( 'NONE', *, *, #87918, .T. ) ;
#2737 = FACE_BOUND ( 'NONE', #6199, .T. ) ;
#2738 = VERTEX_POINT ( 'NONE', #87056 ) ;
#2739 = CARTESIAN_POINT ( 'NONE',  ( -8.638438961405979555, -4.118422570099831148, 33.43335022499816489 ) ) ;
#2740 = FACE_OUTER_BOUND ( 'NONE', #35708, .T. ) ;
#2741 = CARTESIAN_POINT ( 'NONE',  ( -14.30769230769230660, -8.973038597847269315, 34.52809138561121927 ) ) ;
#2742 = ORIENTED_EDGE ( 'NONE', *, *, #79560, .T. ) ;
#2743 = ORIENTED_EDGE ( 'NONE', *, *, #84313, .T. ) ;
#2744 = B_SPLINE_CURVE_WITH_KNOTS ( 'NONE', 3,
 ( #66752, #80732, #11363, #17683, #38393, #31638, #4150, #18573, #59546, #52338 ),
 .UNSPECIFIED., .F., .F.,
 ( 4, 2, 2, 2, 4 ),
 ( 0.000000000000000000, 0.0001954311564186862781, 0.0003908623128373725562, 0.0005862934692560588072, 0.0007817246256747451124 ),
 .UNSPECIFIED. ) ;
#2745 = ORIENTED_EDGE ( 'NONE', *, *, #43114, .T. ) ;
#2746 = CARTESIAN_POINT ( 'NONE',  ( 0.3308478584281538404, -8.191372820521381826, 34.95448215188423546 ) ) ;
#2747 = EDGE_LOOP ( 'NONE', ( #44824, #22707 ) ) ;
#2748 = B_SPLINE_CURVE_WITH_KNOTS ( 'NONE', 3,
 ( #48164, #34661, #62131, #35551, #27903, #62995, #14386, #47730, #54932, #54034 ),
 .UNSPECIFIED., .F., .F.,
 ( 4, 2, 2, 2, 4 ),
 ( 0.000000000000000000, 0.0001954311564186878773, 0.0003908623128373757546, 0.0005862934692560635777, 0.0007817246256747515092 ),
 .UNSPECIFIED. ) ;
#2749 = CARTESIAN_POINT ( 'NONE',  ( -10.61538461538473577, -8.656820664282941280, 34.87096338111179961 ) ) ;
#2750 = B_SPLINE_CURVE_WITH_KNOTS ( 'NONE', 3,
 ( #76419, #34979, #21015, #29130, #70095, #14721, #69655, #68331, #54812, #75971 ),
 .UNSPECIFIED., .F., .F.,
 ( 4, 2, 2, 2, 4 ),
 ( 0.000000000000000000, 0.0001954339857564092362, 0.0003908679715128184724, 0.0005863019572692276544, 0.0007817359430256369448 ),
 .UNSPECIFIED. ) ;
#2751 = CARTESIAN_POINT ( 'NONE',  ( 2.980745993476266342, -2.823816976329320827, 31.52131813110797154 ) ) ;
#2752 = VECTOR ( 'NONE', #29953, 1000.000000000000114 ) ;
#2753 = CARTESIAN_POINT ( 'NONE',  ( 17.01165307636676260, -3.643525952247789856, 33.31231777344662959 ) ) ;
#2754 = FACE_BOUND ( 'NONE', #11158, .T. ) ;
#2755 = ORIENTED_EDGE ( 'NONE', *, *, #33766, .F. ) ;
#2756 = CARTESIAN_POINT ( 'NONE',  ( 13.38461538461538680, -10.67929555188718282, 33.92786785259544047 ) ) ;
#2757 = CARTESIAN_POINT ( 'NONE',  ( -15.00775638667583500, -3.395485233115139057, 33.02377354290275946 ) ) ;
#2758 = DIRECTION ( 'NONE',  ( 0.000000000000000000, 0.9396926207859126468, -0.3420201433256571111 ) ) ;
#2759 = CARTESIAN_POINT ( 'NONE',  ( 8.769230769230768274, -6.343179335718451384, 34.87096338111211935 ) ) ;
#2760 = ORIENTED_EDGE ( 'NONE', *, *, #10928, .T. ) ;
#2761 = EDGE_LOOP ( 'NONE', ( #60057, #78188, #11316, #9953 ) ) ;
#2762 = ORIENTED_EDGE ( 'NONE', *, *, #79178, .F. ) ;
#2764 = CARTESIAN_POINT ( 'NONE',  ( 6.923076923076924238, -5.180354513474913603, 36.12317359536750416 ) ) ;
#2763 = DIRECTION ( 'NONE',  ( -1.000000000000000000, -0.000000000000000000, -0.000000000000000000 ) ) ;
#2765 = CARTESIAN_POINT ( 'NONE',  ( -8.769230769230768274, -12.34228464037088635, 31.77849191805839268 ) ) ;
#2766 = CARTESIAN_POINT ( 'NONE',  ( -13.38461538461550759, -3.083524468854526912, 32.58852847137268327 ) ) ;
#2767 = CARTESIAN_POINT ( 'NONE',  ( 7.846153846153725020, -12.46129190930018460, 30.37095296980731973 ) ) ;
#2768 = CARTESIAN_POINT ( 'NONE',  ( -6.988346923633241836, -3.643525952247789412, 33.31231777344662959 ) ) ;
#2769 = ORIENTED_EDGE ( 'NONE', *, *, #52930, .T. ) ;
#2770 = DIRECTION ( 'NONE',  ( 1.000000000000000000, 0.000000000000000000, 0.000000000000000000 ) ) ;
#2771 = CARTESIAN_POINT ( 'NONE',  ( -4.153846153846152411, -8.164416787775445883, 34.95778746994557906 ) ) ;
#2772 = DIRECTION ( 'NONE',  ( -0.000000000000000000, -0.7660444431189791237, -0.6427876096865379196 ) ) ;
#2773 = CARTESIAN_POINT ( 'NONE',  ( -3.930834802233303282, -3.587049720035815792, 32.86302985866382897 ) ) ;
#2774 = EDGE_LOOP ( 'NONE', ( #81169, #56402, #25840, #28505 ) ) ;
#2775 = ORIENTED_EDGE ( 'NONE', *, *, #6683, .F. ) ;
#2776 = FACE_BOUND ( 'NONE', #49924, .T. ) ;
#2777 = ADVANCED_FACE ( 'NONE', ( #66757 ), #33425, .F. ) ;
#2778 = B_SPLINE_CURVE_WITH_KNOTS ( 'NONE', 3,
 ( #40848, #42622, #21899, #7945, #2066, #48030, #69637, #48471, #7506, #41735 ),
 .UNSPECIFIED., .F., .F.,
 ( 4, 2, 2, 2, 4 ),
 ( 0.0007817359430256319575, 0.0009771253907250002264, 0.001172514838424368495, 0.001367904286123736764, 0.001563293733823097878 ),
 .UNSPECIFIED. ) ;
#2779 = AXIS2_PLACEMENT_3D ( 'NONE', #42906, #41565, #69038 ) ;
#2780 = B_SPLINE_CURVE_WITH_KNOTS ( 'NONE', 3,
 ( #55747, #35937, #84134, #22410, #43132, #84573, #64266, #27841, #76475, #14777 ),
 .UNSPECIFIED., .F., .F.,
 ( 4, 2, 2, 2, 4 ),
 ( 0.000000000000000000, 0.0001954339857564076641, 0.0003908679715128153282, 0.0005863019572692229923, 0.0007817359430256306564 ),
 .UNSPECIFIED. ) ;
#2781 = VECTOR ( 'NONE', #43857, 1000.000000000000000 ) ;
#2782 = CARTESIAN_POINT ( 'NONE',  ( -7.146561847641254239, -10.23692288466677880, 34.23039457007281072 ) ) ;
#2783 = CARTESIAN_POINT ( 'NONE',  ( 12.39626801557768943, -12.27809138561121394, 31.22303859784730307 ) ) ;
#2784 = B_SPLINE_CURVE_WITH_KNOTS ( 'NONE', 3,
 ( #65951, #37427, #70791, #37882, #36981, #43748, #64010, #51814, #23468, #58583 ),
 .UNSPECIFIED., .F., .F.,
 ( 4, 2, 2, 2, 4 ),
 ( 0.000000000000000000, 0.0001954339857564078538, 0.0003908679715128157077, 0.0005863019572692235344, 0.0007817359430256314154 ),
 .UNSPECIFIED. ) ;
#2785 = ORIENTED_EDGE ( 'NONE', *, *, #6461, .T. ) ;
#2787 = CARTESIAN_POINT ( 'NONE',  ( -3.230769230769351186, -12.46129190930018460, 30.37095296980731973 ) ) ;
#2786 = B_SPLINE_CURVE_WITH_KNOTS ( 'NONE', 3,
 ( #61848, #46132, #40718, #11912, #39388, #40273, #66845, #39826, #33512, #5589 ),
 .UNSPECIFIED., .F., .F.,
 ( 4, 2, 2, 2, 4 ),
 ( 0.000000000000000000, 0.0001954311564186861697, 0.0003908623128373723394, 0.0005862934692560584820, 0.0007817246256747446788 ),
 .UNSPECIFIED. ) ;
#2788 = CARTESIAN_POINT ( 'NONE',  ( 6.856993512121043466, -10.51840700105979387, 33.73612834413961536 ) ) ;
#2789 = CARTESIAN_POINT ( 'NONE',  ( 8.545745844666436497, -2.353723527008296568, 30.78948104536958752 ) ) ;
#2790 = DIRECTION ( 'NONE',  ( 0.000000000000000000, 0.9848077530122072432, 0.1736481776669354937 ) ) ;
#2791 = VERTEX_POINT ( 'NONE', #87496 ) ;
#2792 = VECTOR ( 'NONE', #5260, 1000.000000000000000 ) ;
#2793 = AXIS2_PLACEMENT_3D ( 'NONE', #16606, #50821, #77431 ) ;
#2794 = CARTESIAN_POINT ( 'NONE',  ( -7.596208327805704208, -10.76462480002816235, 33.53768742498949962 ) ) ;
#2795 = ORIENTED_EDGE ( 'NONE', *, *, #80548, .T. ) ;
#2796 = AXIS2_PLACEMENT_3D ( 'NONE', #85379, #21900, #44364 ) ;
#2798 = ORIENTED_EDGE ( 'NONE', *, *, #32188, .F. ) ;
#2797 = CARTESIAN_POINT ( 'NONE',  ( -19.99999999999996803, 15.00000000000000711, 13.00000000000000178 ) ) ;
#2799 = CARTESIAN_POINT ( 'NONE',  ( -8.519230769230832223, -7.565270445406050648, 34.75000000000000000 ) ) ;
#2800 = CARTESIAN_POINT ( 'NONE',  ( 15.10062202133100939, -2.882441371585227508, 31.66841991370172238 ) ) ;
#2801 = FACE_OUTER_BOUND ( 'NONE', #26415, .T. ) ;
#2802 = CARTESIAN_POINT ( 'NONE',  ( -14.30769230769230660, -1.790695186598648903, 34.54067556320373455 ) ) ;
#2803 = LINE ( 'NONE', #58194, #86523 ) ;
#2804 = EDGE_CURVE ( 'NONE', #84823, #52632, #35549, .T. ) ;
#2805 = CARTESIAN_POINT ( 'NONE',  ( 6.250054311638318261, -2.779044189368096163, 31.39831045268886456 ) ) ;
#2806 = CARTESIAN_POINT ( 'NONE',  ( -1.901340078031369618, -5.512252781505359245, 13.00186829374151465 ) ) ;
#2807 = ORIENTED_EDGE ( 'NONE', *, *, #6581, .T. ) ;
#2808 = CARTESIAN_POINT ( 'NONE',  ( 13.38461538461538680, -12.62096338111211580, 30.90682066428153263 ) ) ;
#2809 = CARTESIAN_POINT ( 'NONE',  ( 5.749976775778544713, -8.475808217655753651, 34.90892951860618609 ) ) ;
#2810 = VERTEX_POINT ( 'NONE', #18579 ) ;
#2811 = ORIENTED_EDGE ( 'NONE', *, *, #67110, .F. ) ;
#2812 = ORIENTED_EDGE ( 'NONE', *, *, #12957, .F. ) ;
#2813 = CARTESIAN_POINT ( 'NONE',  ( 5.076923076923075762, -13.88283147151868846, 33.14645433367849847 ) ) ;
#2814 = CARTESIAN_POINT ( 'NONE',  ( 12.46153846153833911, -4.320704448113951379, 33.92786785259630022 ) ) ;
#2815 = CARTESIAN_POINT ( 'NONE',  ( -1.384615384615505151, -9.442884908241554243, 34.35708131394783038 ) ) ;
#2816 = CARTESIAN_POINT ( 'NONE',  ( 9.469381474791545017, -12.39988816332205701, 30.74660775122750778 ) ) ;
#2817 = CYLINDRICAL_SURFACE ( 'NONE', #76173, 0.2499999999999998890 ) ;
#2818 = CARTESIAN_POINT ( 'NONE',  ( -8.899922235898328537, -11.71456829005830080, 32.44064028649416542 ) ) ;
#2819 = ORIENTED_EDGE ( 'NONE', *, *, #30073, .F. ) ;
#2820 = CARTESIAN_POINT ( 'NONE',  ( -12.46153846153846168, -1.044019251281081972, 31.83374038241031911 ) ) ;
#2822 = EDGE_CURVE ( 'NONE', #23412, #71441, #83887, .T. ) ;
#2821 = CARTESIAN_POINT ( 'NONE',  ( -0.3962828902624374594, -8.613356846314930593, 34.62446782046653482 ) ) ;
#2823 = B_SPLINE_CURVE_WITH_KNOTS ( 'NONE', 3,
 ( #67906, #41318, #34994, #49404, #7974, #35441, #61133, #81871, #34559, #68345 ),
 .UNSPECIFIED., .F., .F.,
 ( 4, 2, 2, 2, 4 ),
 ( 0.0007817246256747519429, 0.0009771112852218970073, 0.001172497944769042288, 0.001367884604316187353, 0.001563271263863332417 ),
 .UNSPECIFIED. ) ;
#2824 = CARTESIAN_POINT ( 'NONE',  ( 9.019230769230768274, -2.499999999999998668, 29.75000000000000355 ) ) ;
#2825 = B_SPLINE_CURVE_WITH_KNOTS ( 'NONE', 3,
 ( #73146, #11445, #4694, #32165, #59626, #87126, #40703, #60516, #39813, #49107 ),
 .UNSPECIFIED., .F., .F.,
 ( 4, 2, 2, 2, 4 ),
 ( 0.000000000000000000, 0.0001954311584214072923, 0.0003908623168428145846, 0.0005862934752642218498, 0.0007817246336856291692 ),
 .UNSPECIFIED. ) ;
#2826 = CARTESIAN_POINT ( 'NONE',  ( 7.911409417429871027, -2.892918686051624722, 31.69288490824025928 ) ) ;
#2828 = ORIENTED_EDGE ( 'NONE', *, *, #53808, .F. ) ;
#2827 = VECTOR ( 'NONE', #8252, 1000.000000000000000 ) ;
#2829 = CARTESIAN_POINT ( 'NONE',  ( 9.692307692307695177, -13.04860791097971706, 34.73218667398347037 ) ) ;
#2831 = EDGE_CURVE ( 'NONE', #67219, #84018, #82059, .T. ) ;
#2830 = ORIENTED_EDGE ( 'NONE', *, *, #48090, .T. ) ;
#2832 = CARTESIAN_POINT ( 'NONE',  ( 12.23805353697413167, -9.417330523894424488, 34.63758898049880486 ) ) ;
#2833 = DIRECTION ( 'NONE',  ( -0.000000000000000000, 0.9396926207859092051, -0.3420201433256662704 ) ) ;
#2834 = CARTESIAN_POINT ( 'NONE',  ( 6.130790440966952026, -12.62708834333097663, 30.88030960425257021 ) ) ;
#2835 = VERTEX_POINT ( 'NONE', #88385 ) ;
#2836 = LINE ( 'NONE', #37071, #56430 ) ;
#2837 = LINE ( 'NONE', #57795, #85406 ) ;
#2838 = CYLINDRICAL_SURFACE ( 'NONE', #21101, 0.2499999999999997502 ) ;
#2839 = CARTESIAN_POINT ( 'NONE',  ( -12.21148414990014786, -10.66356715214248396, 33.62249196103329751 ) ) ;
#2840 = ORIENTED_EDGE ( 'NONE', *, *, #874, .F. ) ;
#2841 = AXIS2_PLACEMENT_3D ( 'NONE', #69835, #8142, #63062 ) ;
#2842 = CARTESIAN_POINT ( 'NONE',  ( -0.5276218724943421146, -8.120952969808774569, 34.71129190930000163 ) ) ;
#2843 = VERTEX_POINT ( 'NONE', #20356 ) ;
#2844 = DIRECTION ( 'NONE',  ( -0.000000000000000000, 0.3420201433256694346, -0.9396926207859080948 ) ) ;
#2845 = B_SPLINE_CURVE_WITH_KNOTS ( 'NONE', 3,
 ( #70032, #43451, #71800, #30816, #16423, #44310, #29502, #78120, #10104, #84451 ),
 .UNSPECIFIED., .F., .F.,
 ( 4, 2, 2, 2, 4 ),
 ( 0.0007817359430256314154, 0.0009771253907249980580, 0.001172514838424364592, 0.001367904286123731127, 0.001563293733823097661 ),
 .UNSPECIFIED. ) ;
#2846 = AXIS2_PLACEMENT_3D ( 'NONE', #87239, #18319, #88136 ) ;
#2847 = AXIS2_PLACEMENT_3D ( 'NONE', #8327, #35803, #63258 ) ;
#2848 = CARTESIAN_POINT ( 'NONE',  ( -16.82697766754503377, -3.520799739797214389, 33.17531984108286025 ) ) ;
#2849 = CARTESIAN_POINT ( 'NONE',  ( -1.450697763975518972, -9.058645607665454236, 34.76329471203372634 ) ) ;
#2850 = CARTESIAN_POINT ( 'NONE',  ( -9.942330916529147800, -8.475808217655753651, 34.90892951860618609 ) ) ;
#2851 = CARTESIAN_POINT ( 'NONE',  ( 15.10007776410167679, -11.71456829005830080, 32.44064028649416542 ) ) ;
#2852 = VECTOR ( 'NONE', #1832, 1000.000000000000000 ) ;
#2853 = CIRCLE ( 'NONE', #11558, 4.000000000000000000 ) ;
#2854 = VERTEX_POINT ( 'NONE', #54118 ) ;
#2855 = ORIENTED_EDGE ( 'NONE', *, *, #6324, .T. ) ;
#2856 = VERTEX_POINT ( 'NONE', #75296 ) ;
#2857 = CARTESIAN_POINT ( 'NONE',  ( -10.48459280755982981, -8.147973898785416225, 34.70805048591653730 ) ) ;
#2858 = CARTESIAN_POINT ( 'NONE',  ( 16.15384615384615330, -5.471508081941601098, 34.59228464037088457 ) ) ;
#2859 = CARTESIAN_POINT ( 'NONE',  ( -4.023320715612507925, -6.808710257144159783, 34.95449254468098843 ) ) ;
#2860 = CARTESIAN_POINT ( 'NONE',  ( -0.4615384615385840772, -4.320704448113951379, 33.92786785259630022 ) ) ;
#2861 = CARTESIAN_POINT ( 'NONE',  ( 7.846153846153846700, -12.62096338111211580, 30.90682066428153263 ) ) ;
#2862 = CARTESIAN_POINT ( 'NONE',  ( 11.47319109250076608, -12.27809138561121394, 31.22303859784730307 ) ) ;
#2863 = CARTESIAN_POINT ( 'NONE',  ( -8.769230769230768274, -2.499999999999998668, 29.75000000000001421 ) ) ;
#2864 = CARTESIAN_POINT ( 'NONE',  ( -4.087777802843715946, -10.51840700105979565, 33.73612834413962247 ) ) ;
#2865 = ORIENTED_EDGE ( 'NONE', *, *, #67406, .F. ) ;
#2866 = ORIENTED_EDGE ( 'NONE', *, *, #19475, .T. ) ;
#2867 = EDGE_CURVE ( 'NONE', #38648, #58158, #59998, .T. ) ;
#2868 = ORIENTED_EDGE ( 'NONE', *, *, #61951, .T. ) ;
#2870 = ORIENTED_EDGE ( 'NONE', *, *, #10012, .F. ) ;
#2869 = CARTESIAN_POINT ( 'NONE',  ( 17.78205128205128105, -3.499999999999999556, 29.75000000000000355 ) ) ;
#2872 = CARTESIAN_POINT ( 'NONE',  ( 10.39189967166066708, -9.331801661448606566, 34.40259984581193464 ) ) ;
#2871 = CARTESIAN_POINT ( 'NONE',  ( -11.53846153846153655, -3.937682226553329556, 33.60647404775216529 ) ) ;
#2873 = CARTESIAN_POINT ( 'NONE',  ( 1.634669804528839476, -4.818054556918156983, 34.26375889529406749 ) ) ;
#2874 = CARTESIAN_POINT ( 'NONE',  ( -1.553300858899081760, -11.25000000000000888, 23.60937500000000711 ) ) ;
#2875 = VERTEX_POINT ( 'NONE', #53684 ) ;
#2876 = B_SPLINE_CURVE_WITH_KNOTS ( 'NONE', 3,
 ( #34488, #62826, #8801, #20962, #69165, #7470, #28169, #36272, #63284, #1594 ),
 .UNSPECIFIED., .F., .F.,
 ( 4, 2, 2, 2, 4 ),
 ( 0.000000000000000000, 0.0001954339857564064444, 0.0003908679715128128888, 0.0005863019572692193060, 0.0007817359430256257775 ),
 .UNSPECIFIED. ) ;
#2877 = AXIS2_PLACEMENT_3D ( 'NONE', #82482, #82034, #13124 ) ;
#2878 = ORIENTED_EDGE ( 'NONE', *, *, #4475, .T. ) ;
#2879 = CARTESIAN_POINT ( 'NONE',  ( -11.60373153901785948, -12.16647553114622049, 32.15551576947930812 ) ) ;
#2880 = ORIENTED_EDGE ( 'NONE', *, *, #32246, .T. ) ;
#2881 = FACE_BOUND ( 'NONE', #12925, .T. ) ;
#2882 = CARTESIAN_POINT ( 'NONE',  ( 3.453782074862625784, -2.523321265292116422, 31.42251411153756990 ) ) ;
#2883 = ADVANCED_FACE ( 'NONE', ( #25775 ), #11824, .F. ) ;
#2884 = CARTESIAN_POINT ( 'NONE',  ( 8.769230769230645706, -8.656820664282941280, 34.87096338111179961 ) ) ;
#2885 = VERTEX_POINT ( 'NONE', #13586 ) ;
#2886 = CARTESIAN_POINT ( 'NONE',  ( 16.40390046548447245, -11.28795663066794575, 33.01431243580653785 ) ) ;
#2887 = DIRECTION ( 'NONE',  ( -0.000000000000000000, 0.1736481776669307198, -0.9848077530122080203 ) ) ;
#2888 = LINE ( 'NONE', #77675, #65136 ) ;
#2889 = ORIENTED_EDGE ( 'NONE', *, *, #40562, .T. ) ;
#2890 = EDGE_CURVE ( 'NONE', #10355, #2843, #41066, .T. ) ;
#2891 = CARTESIAN_POINT ( 'NONE',  ( 17.74999999999999645, -7.566082377512564960, 35.00000000000000711 ) ) ;
#2892 = LINE ( 'NONE', #35821, #25065 ) ;
#2893 = VERTEX_POINT ( 'NONE', #80737 ) ;
#2894 = CARTESIAN_POINT ( 'NONE',  ( 3.453780582382080411, -8.239487800360276282, 34.69522927552633718 ) ) ;
#2895 = DIRECTION ( 'NONE',  ( -0.000000000000000000, 1.000000000000000000, 3.491481338843133355E-15 ) ) ;
#2896 = CYLINDRICAL_SURFACE ( 'NONE', #31059, 0.2500000000000002220 ) ;
#2897 = CARTESIAN_POINT ( 'NONE',  ( -2.437839517130525824, -2.619462340734462380, 30.83744416345203021 ) ) ;
#2898 = CARTESIAN_POINT ( 'NONE',  ( 5.869852790561781219, -5.195881422630167279, 34.18770438780618548 ) ) ;
#2899 = DIRECTION ( 'NONE',  ( 0.000000000000000000, -6.938893903907222067E-15, 1.000000000000000000 ) ) ;
#2900 = CARTESIAN_POINT ( 'NONE',  ( 8.096099255531889582, -2.986452184633680673, 32.43230066228895225 ) ) ;
#2902 = DIRECTION ( 'NONE',  ( -0.000000000000000000, 0.6427876096865404731, -0.7660444431189770143 ) ) ;
#2901 = CARTESIAN_POINT ( 'NONE',  ( 4.219101725122178514, -12.27809138561124591, 31.22303859784720359 ) ) ;
#2903 = AXIS2_PLACEMENT_3D ( 'NONE', #6235, #19298, #81009 ) ;
#2904 = EDGE_CURVE ( 'NONE', #35531, #86970, #68527, .T. ) ;
#2905 = CARTESIAN_POINT ( 'NONE',  ( 18.00000000000000000, -1.629998284177014645, 34.34916445242399163 ) ) ;
#2907 = DIRECTION ( 'NONE',  ( 0.000000000000000000, 0.000000000000000000, 1.000000000000000000 ) ) ;
#2906 = CARTESIAN_POINT ( 'NONE',  ( 12.21153846153846168, -7.500000000000001776, 35.00000000000000000 ) ) ;
#2908 = DIRECTION ( 'NONE',  ( 0.000000000000000000, 0.000000000000000000, -1.000000000000000000 ) ) ;
#2909 = CARTESIAN_POINT ( 'NONE',  ( 2.775308065498768517, -8.577988221561467341, 21.79500670625849068 ) ) ;
#2910 = ORIENTED_EDGE ( 'NONE', *, *, #31657, .T. ) ;
#2911 = DIRECTION ( 'NONE',  ( -0.000000000000000000, -0.3420201433256694346, -0.9396926207859080948 ) ) ;
#2912 = ORIENTED_EDGE ( 'NONE', *, *, #70528, .T. ) ;
#2913 = VECTOR ( 'NONE', #79043, 1000.000000000000000 ) ;
#2914 = VECTOR ( 'NONE', #77739, 1000.000000000000114 ) ;
#2915 = ADVANCED_FACE ( 'NONE', ( #46489 ), #73967, .F. ) ;
#2916 = CARTESIAN_POINT ( 'NONE',  ( 9.627037246346919375, -6.879047030191174805, 34.71129190930000163 ) ) ;
#2917 = VERTEX_POINT ( 'NONE', #60440 ) ;
#2918 = CARTESIAN_POINT ( 'NONE',  ( 17.86985279056177589, -12.27039167877662251, 31.24851455888617835 ) ) ;
#2919 = B_SPLINE_CURVE_WITH_KNOTS ( 'NONE', 3,
 ( #59947, #75248, #40143, #33810, #61264, #39250, #80231, #19409, #46876, #27498 ),
 .UNSPECIFIED., .F., .F.,
 ( 4, 2, 2, 2, 4 ),
 ( 0.0007817359430256219828, 0.0009771253907249863487, 0.001172514838424350498, 0.001367904286123714647, 0.001563293733823079013 ),
 .UNSPECIFIED. ) ;
#2920 = EDGE_LOOP ( 'NONE', ( #70504, #51298, #18508, #75672 ) ) ;
#2921 = CARTESIAN_POINT ( 'NONE',  ( -8.069080063669989755, -5.667676309546437530, 34.40238873228292249 ) ) ;
#2922 = CARTESIAN_POINT ( 'NONE',  ( -2.724691934501232371, -8.700186371490559623, 23.51375670625848713 ) ) ;
#2923 = CARTESIAN_POINT ( 'NONE',  ( 7.780883845597525550, -8.656820664281498878, 34.87096338111211935 ) ) ;
#2924 = VECTOR ( 'NONE', #62953, 1000.000000000000227 ) ;
#2925 = CARTESIAN_POINT ( 'NONE',  ( 6.699591979352976345, -11.41268669641500466, 32.86336882939237825 ) ) ;
#2926 = CARTESIAN_POINT ( 'NONE',  ( 7.145856592054988354, -10.23759521482555357, 34.22997729860117033 ) ) ;
#2927 = CARTESIAN_POINT ( 'NONE',  ( -8.769230769230768274, -3.886160181151819604, 36.00935417666054406 ) ) ;
#2928 = AXIS2_PLACEMENT_3D ( 'NONE', #34029, #20950, #48421 ) ;
#2929 = B_SPLINE_CURVE_WITH_KNOTS ( 'NONE', 3,
 ( #55591, #83080, #16380, #15948, #9197, #57364, #8753, #1097, #49284, #50151 ),
 .UNSPECIFIED., .F., .F.,
 ( 4, 2, 2, 2, 4 ),
 ( 0.000000000000000000, 0.0001954339857564079623, 0.0003908679715128159245, 0.0005863019572692238597, 0.0007817359430256318490 ),
 .UNSPECIFIED. ) ;
#2930 = CARTESIAN_POINT ( 'NONE',  ( 15.16468685140909578, -8.164416787775445883, 34.95778746994557906 ) ) ;
#2931 = CARTESIAN_POINT ( 'NONE',  ( -13.38461538461550759, -8.656820664282941280, 34.87096338111179961 ) ) ;
#2932 = CARTESIAN_POINT ( 'NONE',  ( -2.307692307692427391, -5.219633306517616589, 34.19971097300220464 ) ) ;
#2933 = CARTESIAN_POINT ( 'NONE',  ( -1.929879867024197893E-14, -3.750000000000000000, 16.65625000000000000 ) ) ;
#2934 = CARTESIAN_POINT ( 'NONE',  ( -16.15384615384615330, -13.87047571288749737, 32.06866353760679544 ) ) ;
#2936 = EDGE_CURVE ( 'NONE', #32904, #66010, #47339, .T. ) ;
#2935 = DIRECTION ( 'NONE',  ( -0.000000000000000000, 0.9848077530122086864, -0.1736481776669273891 ) ) ;
#2937 = EDGE_CURVE ( 'NONE', #62741, #43377, #7279, .T. ) ;
#2938 = DIRECTION ( 'NONE',  ( -0.000000000000000000, -0.9396926207859093161, -0.3420201433256663259 ) ) ;
#2939 = CARTESIAN_POINT ( 'NONE',  ( 1.553300858899129944, -11.24999999999998934, 17.20312500000000000 ) ) ;
#2940 = ORIENTED_EDGE ( 'NONE', *, *, #74648, .T. ) ;
#2941 = EDGE_CURVE ( 'NONE', #9090, #7426, #31222, .T. ) ;
#2942 = CARTESIAN_POINT ( 'NONE',  ( -13.51530598772569469, -6.369640206132551441, 34.87707690430378449 ) ) ;
#2943 = FACE_OUTER_BOUND ( 'NONE', #39032, .T. ) ;
#2944 = CARTESIAN_POINT ( 'NONE',  ( 1.253924781505078689, -5.496505350115500121, 34.60290016733514307 ) ) ;
#2945 = CARTESIAN_POINT ( 'NONE',  ( 18.22301135161285046, -10.61302985866384141, 33.66295027996417843 ) ) ;
#2946 = ADVANCED_FACE ( 'NONE', ( #1847 ), #63540, .F. ) ;
#2947 = CARTESIAN_POINT ( 'NONE',  ( 15.48076923077066702, -7.500000000000155431, 34.75000000000007105 ) ) ;
#2948 = CARTESIAN_POINT ( 'NONE',  ( -8.835314180186648159, -8.120952969808774569, 34.71129190930000163 ) ) ;
#2949 = ORIENTED_EDGE ( 'NONE', *, *, #30482, .T. ) ;
#2950 = CYLINDRICAL_SURFACE ( 'NONE', #55857, 0.2500000000000004996 ) ;
#2951 = VERTEX_POINT ( 'NONE', #524 ) ;
#2952 = B_SPLINE_CURVE_WITH_KNOTS ( 'NONE', 3,
 ( #22080, #49551, #15328, #7238, #36044, #34709, #22518, #41916, #56745, #29289 ),
 .UNSPECIFIED., .F., .F.,
 ( 4, 2, 2, 2, 4 ),
 ( 0.0007817359430256232838, 0.0009771253907249928539, 0.001172514838424355485, 0.001367904286123718116, 0.001563293733823080747 ),
 .UNSPECIFIED. ) ;
#2953 = VECTOR ( 'NONE', #7163, 1000.000000000000000 ) ;
#2954 = ORIENTED_EDGE ( 'NONE', *, *, #25673, .F. ) ;
#2955 = CARTESIAN_POINT ( 'NONE',  ( -8.769230769230768274, -1.242168528481310874, 33.36296068462461051 ) ) ;
#2956 = CARTESIAN_POINT ( 'NONE',  ( -16.15384615384627409, -12.51329471203414379, 31.30864560766407578 ) ) ;
#2957 = CARTESIAN_POINT ( 'NONE',  ( -8.992157728137616601, -2.308479472611653094, 30.53278059502174457 ) ) ;
#2958 = B_SPLINE_CURVE_WITH_KNOTS ( 'NONE', 3,
 ( #18821, #38643, #80073, #87294, #39989, #60238, #46287, #88632, #6194, #53479 ),
 .UNSPECIFIED., .F., .F.,
 ( 4, 2, 2, 2, 4 ),
 ( 0.000000000000000000, 0.0001954339857564080165, 0.0003908679715128160329, 0.0005863019572692240765, 0.0007817359430256320659 ),
 .UNSPECIFIED. ) ;
#2959 = CARTESIAN_POINT ( 'NONE',  ( -6.000000000000119904, -3.300289026999228881, 32.46337939537708905 ) ) ;
#2960 = LINE ( 'NONE', #30443, #61035 ) ;
#2961 = ORIENTED_EDGE ( 'NONE', *, *, #9294, .F. ) ;
#2962 = CARTESIAN_POINT ( 'NONE',  ( -5.999999999999998224, -5.180354513474913603, 36.12317359536750416 ) ) ;
#2963 = VERTEX_POINT ( 'NONE', #28432 ) ;
#2964 = ADVANCED_FACE ( 'NONE', ( #83390 ), #15371, .F. ) ;
#2965 = ORIENTED_EDGE ( 'NONE', *, *, #31612, .F. ) ;
#2966 = VECTOR ( 'NONE', #38248, 1000.000000000000000 ) ;
#2967 = CARTESIAN_POINT ( 'NONE',  ( -6.988346923633243613, -12.16647553114622049, 32.15551576947930812 ) ) ;
#2968 = CARTESIAN_POINT ( 'NONE',  ( -4.153846153846152411, -7.500000000000001776, 35.04278698407183867 ) ) ;
#2969 = EDGE_CURVE ( 'NONE', #38795, #49416, #67773, .T. ) ;
#2970 = FACE_OUTER_BOUND ( 'NONE', #88818, .T. ) ;
#2971 = AXIS2_PLACEMENT_3D ( 'NONE', #88227, #19741, #47202 ) ;
#2972 = AXIS2_PLACEMENT_3D ( 'NONE', #41805, #26956, #54413 ) ;
#2973 = EDGE_CURVE ( 'NONE', #71975, #46832, #35641, .T. ) ;
#2974 = CARTESIAN_POINT ( 'NONE',  ( -11.76138849736838488, -8.282780595021769443, 34.94152052738834158 ) ) ;
#2975 = CARTESIAN_POINT ( 'NONE',  ( -12.46153846153858424, -5.941354392335915335, 34.76329471203413846 ) ) ;
#2976 = VERTEX_POINT ( 'NONE', #76172 ) ;
#2977 = EDGE_LOOP ( 'NONE', ( #77447, #33383 ) ) ;
#2978 = CARTESIAN_POINT ( 'NONE',  ( -1.553300858899081538, -11.25000000000000711, 23.60937500000000711 ) ) ;
#2979 = VECTOR ( 'NONE', #40702, 1000.000000000000000 ) ;
#2980 = EDGE_CURVE ( 'NONE', #66580, #66677, #10823, .T. ) ;
#2981 = EDGE_LOOP ( 'NONE', ( #73358, #79094, #78240, #84210 ) ) ;
#2983 = VERTEX_POINT ( 'NONE', #41956 ) ;
#2982 = CARTESIAN_POINT ( 'NONE',  ( 15.23076923076910916, -10.33852847137269571, 34.16647553114546554 ) ) ;
#2984 = PRODUCT_DEFINITION_FORMATION_WITH_SPECIFIED_SOURCE ( 'ANY', '', #6674, .NOT_KNOWN. ) ;
#2985 = DIRECTION ( 'NONE',  ( -0.000000000000000000, -0.000000000000000000, -1.000000000000000000 ) ) ;
#2986 = DIRECTION ( 'NONE',  ( -0.000000000000000000, 0.6427876096865404731, -0.7660444431189771253 ) ) ;
#2987 = DIRECTION ( 'NONE',  ( -0.000000000000000000, -0.000000000000000000, -1.000000000000000000 ) ) ;
#2988 = ORIENTED_EDGE ( 'NONE', *, *, #38854, .T. ) ;
#2989 = CARTESIAN_POINT ( 'NONE',  ( 10.61538461538449418, -2.379036618888197729, 30.90682066428292885 ) ) ;
#2990 = ORIENTED_EDGE ( 'NONE', *, *, #9445, .F. ) ;
#2991 = CARTESIAN_POINT ( 'NONE',  ( -3.230769230769229949, -1.367168528481310208, 33.57946703557072254 ) ) ;
#2992 = CARTESIAN_POINT ( 'NONE',  ( 6.923076923076924238, -5.471508081941601098, 34.59228464037088457 ) ) ;
#2993 = DIRECTION ( 'NONE',  ( -0.000000000000000000, -0.9848077530122085754, -0.1736481776669273613 ) ) ;
#2995 = CARTESIAN_POINT ( 'NONE',  ( 5.076923076922954969, -3.300289026999228881, 32.46337939537708905 ) ) ;
#2994 = CARTESIAN_POINT ( 'NONE',  ( 14.98076923076923173, -7.500000000000001776, 34.75000000000000000 ) ) ;
#2996 = CARTESIAN_POINT ( 'NONE',  ( -0.6850233861027943405, -12.47654668319379567, 31.42292124445336654 ) ) ;
#2997 = DIRECTION ( 'NONE',  ( -0.000000000000000000, -0.000000000000000000, -1.000000000000000000 ) ) ;
#2998 = ORIENTED_EDGE ( 'NONE', *, *, #80490, .F. ) ;
#2999 = CARTESIAN_POINT ( 'NONE',  ( -11.53846153846165912, -12.27809138561165270, 31.22303859784587132 ) ) ;
#3000 = LINE ( 'NONE', #16972, #69460 ) ;
#3001 = B_SPLINE_CURVE_WITH_KNOTS ( 'NONE', 3,
 ( #20656, #75593, #13898, #34618, #62514, #27858 ),
 .UNSPECIFIED., .F., .F.,
 ( 4, 2, 4 ),
 ( 4.220987180333913997E-17, 0.0001954756301637161793, 0.0003909512603273901832 ),
 .UNSPECIFIED. ) ;
#3002 = ADVANCED_FACE ( 'NONE', ( #20785 ), #48253, .F. ) ;
#3003 = EDGE_LOOP ( 'NONE', ( #83634, #75850, #22090, #9340 ) ) ;
#3004 = CARTESIAN_POINT ( 'NONE',  ( 5.448717948717947124, -7.500000000000000000, 29.75000000000000355 ) ) ;
#3005 = CARTESIAN_POINT ( 'NONE',  ( 10.54930120442873687, -6.386643153685125363, 34.62446782046654903 ) ) ;
#3006 = CARTESIAN_POINT ( 'NONE',  ( -15.90390063549801347, -10.76462480002816413, 33.53768742498949962 ) ) ;
#3007 = CARTESIAN_POINT ( 'NONE',  ( 2.307692307692186251, -5.941354392335915335, 34.76329471203413846 ) ) ;
#3008 = DIRECTION ( 'NONE',  ( -0.000000000000000000, 0.9848077530122085754, -0.1736481776669273613 ) ) ;
#3009 = CARTESIAN_POINT ( 'NONE',  ( -7.596153846152425615, -7.500000000000154543, 35.00000000000007105 ) ) ;
#3010 = FACE_BOUND ( 'NONE', #2372, .T. ) ;
#3012 = CARTESIAN_POINT ( 'NONE',  ( 18.00000000000000000, -10.67929555188718282, 33.92786785259544047 ) ) ;
#3011 = CARTESIAN_POINT ( 'NONE',  ( 5.076923076923075762, -5.471508081941601098, 34.59228464037088457 ) ) ;
#3013 = CARTESIAN_POINT ( 'NONE',  ( 4.153846153846154188, -13.53365097954675988, 30.81389545987213552 ) ) ;
#3015 = CARTESIAN_POINT ( 'NONE',  ( 14.17700170458200581, -10.70098750199973203, 33.91152734681376302 ) ) ;
#3014 = CARTESIAN_POINT ( 'NONE',  ( -6.857009589726848375, -10.67929555188718282, 33.92786785259544757 ) ) ;
#3016 = CIRCLE ( 'NONE', #41878, 8.000000000000000000 ) ;
#3017 = CARTESIAN_POINT ( 'NONE',  ( 8.769230769230647482, -10.90142922262034020, 33.41473453929536674 ) ) ;
#3018 = CARTESIAN_POINT ( 'NONE',  ( -3.724691934501229262, -9.114399933863657211, 18.51375670625849068 ) ) ;
#3019 = EDGE_LOOP ( 'NONE', ( #83513, #66737 ) ) ;
#3020 = DIRECTION ( 'NONE',  ( 0.000000000000000000, 0.1736481776669275834, 0.9848077530122086864 ) ) ;
#3021 = CARTESIAN_POINT ( 'NONE',  ( -5.076923076923197442, -3.300289026999228881, 32.46337939537708905 ) ) ;
#3022 = CARTESIAN_POINT ( 'NONE',  ( -18.00000000000012079, -9.442884908241554243, 34.35708131394783038 ) ) ;
#3023 = DIRECTION ( 'NONE',  ( -0.000000000000000000, 0.5000000000000011102, -0.8660254037844380415 ) ) ;
#3024 = CARTESIAN_POINT ( 'NONE',  ( 10.83839596699746721, -12.15243808032445827, 31.58219941686247978 ) ) ;
#3025 = LINE ( 'NONE', #76147, #16719 ) ;
#3026 = CARTESIAN_POINT ( 'NONE',  ( -3.749999999999996447, -7.561099074964554134, 22.34188170625849068 ) ) ;
#3027 = CARTESIAN_POINT ( 'NONE',  ( -8.638438961405986660, -2.729792928343269587, 31.24908615093345077 ) ) ;
#3028 = DIRECTION ( 'NONE',  ( 1.000000000000000000, 0.000000000000000000, 0.000000000000000000 ) ) ;
#3029 = CARTESIAN_POINT ( 'NONE',  ( 18.03205128205128105, -11.00000000000000000, 29.75000000000000355 ) ) ;
#3031 = B_SPLINE_CURVE_WITH_KNOTS ( 'NONE', 3,
 ( #18980, #66721, #87458, #60398, #75686, #87916, #82468, #68059, #75257, #54526 ),
 .UNSPECIFIED., .F., .F.,
 ( 4, 2, 2, 2, 4 ),
 ( 0.0007817246256747480398, 0.0009771112852218900684, 0.001172497944769032314, 0.001367884604316174559, 0.001563271263863316588 ),
 .UNSPECIFIED. ) ;
#3030 = CARTESIAN_POINT ( 'NONE',  ( 17.86943940825807076, -2.504760397472873823, 29.97295953869789997 ) ) ;
#3032 = CARTESIAN_POINT ( 'NONE',  ( -17.07692307692319744, -5.094484230521993062, 34.41647553114689373 ) ) ;
#3033 = CARTESIAN_POINT ( 'NONE',  ( 10.74542977821939260, -2.504778602574659896, 29.97347330155780654 ) ) ;
#3034 = B_SPLINE_CURVE_WITH_KNOTS ( 'NONE', 3,
 ( #76400, #88617, #55676, #34530, #61110, #83167, #82728, #26889, #48927, #61995 ),
 .UNSPECIFIED., .F., .F.,
 ( 4, 2, 2, 2, 4 ),
 ( 0.000000000000000000, 0.0001954339857564126514, 0.0003908679715128183098, 0.0005863019572692239681, 0.0007817359430256294638 ),
 .UNSPECIFIED. ) ;
#3036 = EDGE_CURVE ( 'NONE', #82729, #4757, #74139, .T. ) ;
#3035 = CYLINDRICAL_SURFACE ( 'NONE', #60594, 2.000000000000001776 ) ;
#3037 = ADVANCED_FACE ( 'NONE', ( #17126 ), #59001, .F. ) ;
#3038 = CARTESIAN_POINT ( 'NONE',  ( -4.153846153846152411, -3.513871655860378418, 32.76840700105978499 ) ) ;
#3039 = ORIENTED_EDGE ( 'NONE', *, *, #49867, .T. ) ;
#3040 = DIRECTION ( 'NONE',  ( -1.000000000000000000, -0.000000000000000000, -0.000000000000000000 ) ) ;
#3041 = CARTESIAN_POINT ( 'NONE',  ( 7.053602624840485724, -5.195472089885680766, 34.18748526763464923 ) ) ;
#3042 = CARTESIAN_POINT ( 'NONE',  ( 1.987747218494642309, -5.598659921968629050, 24.56436829374151287 ) ) ;
#3043 = EDGE_CURVE ( 'NONE', #43765, #49073, #43042, .T. ) ;
#3044 = VECTOR ( 'NONE', #84328, 1000.000000000000000 ) ;
#3045 = DIRECTION ( 'NONE',  ( -0.000000000000000000, -0.7660444431189791237, -0.6427876096865379196 ) ) ;
#3046 = CARTESIAN_POINT ( 'NONE',  ( -16.94613263595612551, -5.496552790871120031, 34.60292014791297532 ) ) ;
#3047 = ORIENTED_EDGE ( 'NONE', *, *, #34476, .F. ) ;
#3048 = DIRECTION ( 'NONE',  ( 1.000000000000000000, 0.000000000000000000, 0.000000000000000000 ) ) ;
#3050 = EDGE_LOOP ( 'NONE', ( #74419, #33768, #65001, #74676 ) ) ;
#3049 = FACE_OUTER_BOUND ( 'NONE', #71413, .T. ) ;
#3051 = CARTESIAN_POINT ( 'NONE',  ( -11.47326755667818077, -2.506253911140448487, 29.99999999999988631 ) ) ;
#3052 = CARTESIAN_POINT ( 'NONE',  ( 17.20697051217352680, -7.723484941389743952, 34.99544897038808955 ) ) ;
#3053 = EDGE_CURVE ( 'NONE', #22156, #16798, #60255, .T. ) ;
#3054 = CARTESIAN_POINT ( 'NONE',  ( -6.923076923076922462, -4.945431358278436385, 36.03766855953609394 ) ) ;
#3055 = VECTOR ( 'NONE', #65184, 999.9999999999998863 ) ;
#3056 = FACE_OUTER_BOUND ( 'NONE', #7180, .T. ) ;
#3057 = VERTEX_POINT ( 'NONE', #58111 ) ;
#3059 = CARTESIAN_POINT ( 'NONE',  ( -13.38461538461538325, -12.29105614889573062, 35.45975837776705220 ) ) ;
#3058 = B_SPLINE_CURVE_WITH_KNOTS ( 'NONE', 3,
 ( #66267, #85218, #44647, #51387, #38358, #23498, #31141, #9545, #50954, #78444 ),
 .UNSPECIFIED., .F., .F.,
 ( 4, 2, 2, 2, 4 ),
 ( 0.000000000000000000, 0.0001954311564186862510, 0.0003908623128373725020, 0.0005862934692560588072, 0.0007817246256747450040 ),
 .UNSPECIFIED. ) ;
#3060 = CARTESIAN_POINT ( 'NONE',  ( -19.50000000000000000, -3.499999999999999556, 29.75000000000000355 ) ) ;
#3061 = CARTESIAN_POINT ( 'NONE',  ( 4.023154687178593925, -9.804603061927743113, 34.18744698557895845 ) ) ;
#3062 = EDGE_LOOP ( 'NONE', ( #62395, #37464 ) ) ;
#3063 = VERTEX_POINT ( 'NONE', #51324 ) ;
#3064 = EDGE_CURVE ( 'NONE', #65231, #2602, #79730, .T. ) ;
#3065 = ORIENTED_EDGE ( 'NONE', *, *, #78363, .F. ) ;
#3066 = CARTESIAN_POINT ( 'NONE',  ( -18.06527044596078113, -3.835265460703606522, 33.15142922261924241 ) ) ;
#3067 = CARTESIAN_POINT ( 'NONE',  ( -3.164701897419154530, -2.833524468853757750, 32.15551576947925838 ) ) ;
#3068 = EDGE_CURVE ( 'NONE', #78512, #17646, #30111, .T. ) ;
#3069 = FACE_OUTER_BOUND ( 'NONE', #47658, .T. ) ;
#3070 = CARTESIAN_POINT ( 'NONE',  ( -17.75000000000000000, -7.500000000000001776, 35.00000000000000000 ) ) ;
#3071 = VECTOR ( 'NONE', #44190, 1000.000000000000114 ) ;
#3072 = ADVANCED_FACE ( 'NONE', ( #64412 ), #51781, .F. ) ;
#3073 = ORIENTED_EDGE ( 'NONE', *, *, #9713, .T. ) ;
#3074 = ORIENTED_EDGE ( 'NONE', *, *, #10327, .F. ) ;
#3076 = ORIENTED_EDGE ( 'NONE', *, *, #247, .T. ) ;
#3075 = CARTESIAN_POINT ( 'NONE',  ( 15.23076923076911093, -5.219633306517616589, 34.19971097300220464 ) ) ;
#3077 = AXIS2_PLACEMENT_3D ( 'NONE', #88927, #42055, #49246 ) ;
#3078 = ADVANCED_FACE ( 'NONE', ( #71181 ), #23000, .F. ) ;
#3079 = DIRECTION ( 'NONE',  ( 0.000000000000000000, 0.1736481776669275834, 0.9848077530122086864 ) ) ;
#3080 = CARTESIAN_POINT ( 'NONE',  ( 2.372947878968333146, -3.835265460703683349, 33.15142922261929925 ) ) ;
#3081 = DIRECTION ( 'NONE',  ( 0.000000000000000000, 0.000000000000000000, -1.000000000000000000 ) ) ;
#3082 = ORIENTED_EDGE ( 'NONE', *, *, #34856, .T. ) ;
#3083 = B_SPLINE_CURVE_WITH_KNOTS ( 'NONE', 3,
 ( #77215, #42992, #62361, #7879, #77656, #70910, #9215, #48853, #36680, #2433 ),
 .UNSPECIFIED., .F., .F.,
 ( 4, 2, 2, 2, 4 ),
 ( 0.0007817246256747473893, 0.0009771112852218905021, 0.001172497944769033615, 0.001367884604316176944, 0.001563271263863320057 ),
 .UNSPECIFIED. ) ;
#3084 = EDGE_CURVE ( 'NONE', #22055, #74851, #83095, .T. ) ;
#3085 = B_SPLINE_CURVE_WITH_KNOTS ( 'NONE', 3,
 ( #84963, #70107, #21479, #75982, #2089, #8418, #48950, #14281, #70997, #29577 ),
 .UNSPECIFIED., .F., .F.,
 ( 4, 2, 2, 2, 4 ),
 ( 0.000000000000000000, 0.0001954339857564083417, 0.0003908679715128166835, 0.0005863019572692250523, 0.0007817359430256333669 ),
 .UNSPECIFIED. ) ;
#3086 = ORIENTED_EDGE ( 'NONE', *, *, #86630, .F. ) ;
#3088 = ORIENTED_EDGE ( 'NONE', *, *, #36649, .F. ) ;
#3087 = CARTESIAN_POINT ( 'NONE',  ( -6.923076923077044142, -11.48612834414049644, 32.76840700105863391 ) ) ;
#3089 = CARTESIAN_POINT ( 'NONE',  ( -10.03846153846153832, -3.499999999999999556, 29.75000000000000355 ) ) ;
#3090 = DIRECTION ( 'NONE',  ( -0.000000000000000000, 1.000000000000000000, -0.000000000000000000 ) ) ;
#3091 = ORIENTED_EDGE ( 'NONE', *, *, #14653, .T. ) ;
#3092 = EDGE_CURVE ( 'NONE', #55585, #60558, #72966, .T. ) ;
#3093 = CARTESIAN_POINT ( 'NONE',  ( -8.102564102564102200, -7.500000000000000000, 29.75000000000000355 ) ) ;
#3094 = CARTESIAN_POINT ( 'NONE',  ( -14.08467946359890988, -12.64618726649961289, 30.78989965857442712 ) ) ;
#3095 = CARTESIAN_POINT ( 'NONE',  ( 16.09615384615384670, -3.499999999999999556, 29.75000000000000355 ) ) ;
#3096 = FACE_BOUND ( 'NONE', #78501, .T. ) ;
#3097 = CARTESIAN_POINT ( 'NONE',  ( -11.53846153846153655, -2.538708090699994813, 30.37095296980875503 ) ) ;
#3098 = CARTESIAN_POINT ( 'NONE',  ( -6.857009589726848375, -9.058645607665452459, 34.76329471203371924 ) ) ;
#3099 = VECTOR ( 'NONE', #55182, 1000.000000000000000 ) ;
#3100 = CARTESIAN_POINT ( 'NONE',  ( -10.61538461538461320, -6.435427911321262684, 35.78748833219616898 ) ) ;
#3102 = LINE ( 'NONE', #10760, #1576 ) ;
#3101 = CARTESIAN_POINT ( 'NONE',  ( 3.230769230769231726, -3.322132147404559976, 32.92929555188717927 ) ) ;
#3103 = CARTESIAN_POINT ( 'NONE',  ( -1.384615384615383471, -2.499999999999998668, 29.75000000000001421 ) ) ;
#3104 = CARTESIAN_POINT ( 'NONE',  ( 5.326868595271218254, -2.587454068350147462, 30.68340429815432202 ) ) ;
#3105 = ORIENTED_EDGE ( 'NONE', *, *, #72228, .F. ) ;
#3106 = CARTESIAN_POINT ( 'NONE',  ( -5.869474298236434073, -11.93748526763465279, 32.05452791011430946 ) ) ;
#3107 = ORIENTED_EDGE ( 'NONE', *, *, #61059, .F. ) ;
#3108 = EDGE_CURVE ( 'NONE', #83058, #40235, #5404, .T. ) ;
#3109 = ORIENTED_EDGE ( 'NONE', *, *, #59134, .F. ) ;
#3111 = CARTESIAN_POINT ( 'NONE',  ( 1.449870524128225258, -5.941354392334606160, 34.76329471203374055 ) ) ;
#3110 = LINE ( 'NONE', #10770, #87836 ) ;
#3112 = EDGE_CURVE ( 'NONE', #44980, #72129, #11267, .T. ) ;
#3113 = CARTESIAN_POINT ( 'NONE',  ( 2.438484115517094875, -2.541949514083463590, 30.39797389878540557 ) ) ;
#3114 = DIRECTION ( 'NONE',  ( -0.000000000000000000, 0.9848077530122086864, -0.1736481776669273891 ) ) ;
#3115 = DIRECTION ( 'NONE',  ( 0.000000000000000000, 0.7660444431189807890, 0.6427876096865361433 ) ) ;
#3116 = CARTESIAN_POINT ( 'NONE',  ( 14.55774672760576394, -11.47946981652013498, 33.17500667209847620 ) ) ;
#3117 = ORIENTED_EDGE ( 'NONE', *, *, #10410, .F. ) ;
#3118 = CARTESIAN_POINT ( 'NONE',  ( -11.97435897435897267, -7.500000000000000000, 29.75000000000000355 ) ) ;
#3119 = CARTESIAN_POINT ( 'NONE',  ( 0.4615384615384611200, -12.62096338111211580, 30.90682066428153263 ) ) ;
#3120 = CARTESIAN_POINT ( 'NONE',  ( -12.46153846153858247, -5.219633306517616589, 34.19971097300220464 ) ) ;
#3121 = CARTESIAN_POINT ( 'NONE',  ( 14.30769230769218581, -3.643525952248795718, 33.31231777344771672 ) ) ;
#3122 = DIRECTION ( 'NONE',  ( 0.000000000000000000, 0.000000000000000000, -1.000000000000000000 ) ) ;
#3123 = B_SPLINE_CURVE_WITH_KNOTS ( 'NONE', 3,
 ( #31922, #38668, #66131, #4435, #59383, #40465, #27380, #81449, #7552, #6229 ),
 .UNSPECIFIED., .F., .F.,
 ( 4, 2, 2, 2, 4 ),
 ( 0.0007817359430256294638, 0.0009771253907249974075, 0.001172514838424365460, 0.001367904286123733295, 0.001563293733823094191 ),
 .UNSPECIFIED. ) ;
#3124 = CARTESIAN_POINT ( 'NONE',  ( -3.749999999999997335, -7.500000000000021316, 18.84375000000000000 ) ) ;
#3125 = ORIENTED_EDGE ( 'NONE', *, *, #60449, .T. ) ;
#3126 = ORIENTED_EDGE ( 'NONE', *, *, #24364, .T. ) ;
#3127 = DIRECTION ( 'NONE',  ( -0.000000000000000000, 0.6427876096865404731, -0.7660444431189771253 ) ) ;
#3128 = ORIENTED_EDGE ( 'NONE', *, *, #73177, .F. ) ;
#3129 = CARTESIAN_POINT ( 'NONE',  ( 17.29970274590113632, -4.226511098958373402, 33.85474049983370293 ) ) ;
#3130 = CARTESIAN_POINT ( 'NONE',  ( 18.13052570176355971, -6.001044277235009439, 34.52024696741798948 ) ) ;
#3131 = CYLINDRICAL_SURFACE ( 'NONE', #63952, 0.2500000000000009437 ) ;
#3132 = LINE ( 'NONE', #58081, #1139 ) ;
#3133 = CARTESIAN_POINT ( 'NONE',  ( 3.749999999999992006, -5.946699141100872943, 18.14062500000000711 ) ) ;
#3134 = CARTESIAN_POINT ( 'NONE',  ( 14.24160992833217065, -6.343179335718451384, 34.87096338111212646 ) ) ;
#3135 = ORIENTED_EDGE ( 'NONE', *, *, #46165, .F. ) ;
#3136 = FACE_OUTER_BOUND ( 'NONE', #20499, .T. ) ;
#3138 = ORIENTED_EDGE ( 'NONE', *, *, #86303, .T. ) ;
#3137 = CARTESIAN_POINT ( 'NONE',  ( -1.161604033002533454, -9.086983370893047862, 34.49168942202179267 ) ) ;
#3139 = DIRECTION ( 'NONE',  ( -0.000000000000000000, 1.000000000000000000, -0.000000000000000000 ) ) ;
#3140 = CARTESIAN_POINT ( 'NONE',  ( 3.480714749117372442, -2.824170634883621744, 31.52227843825338738 ) ) ;
#3141 = AXIS2_PLACEMENT_3D ( 'NONE', #53306, #32596, #73605 ) ;
#3142 = CARTESIAN_POINT ( 'NONE',  ( 2.242421861731533017, -3.300289026998414865, 32.46337939537583139 ) ) ;
#3143 = CARTESIAN_POINT ( 'NONE',  ( -8.769230769230768274, -2.249999999999998668, 29.75000000000001776 ) ) ;
#3144 = FACE_OUTER_BOUND ( 'NONE', #55607, .T. ) ;
#3145 = CARTESIAN_POINT ( 'NONE',  ( -4.403822884788507253, -9.148715823498378086, 34.47080413974185120 ) ) ;
#3146 = CARTESIAN_POINT ( 'NONE',  ( -7.173053654019278191, -4.943428324936578910, 34.04746400365624481 ) ) ;
#3147 = VECTOR ( 'NONE', #77172, 1000.000000000000114 ) ;
#3148 = CARTESIAN_POINT ( 'NONE',  ( 2.608446859217924629, -10.19485399968118422, 16.12686829374151287 ) ) ;
#3149 = EDGE_LOOP ( 'NONE', ( #52160, #54596, #79589, #55688 ) ) ;
#3150 = CARTESIAN_POINT ( 'NONE',  ( -16.15384615384615330, -9.058645607665452459, 34.76329471203371924 ) ) ;
#3151 = CARTESIAN_POINT ( 'NONE',  ( -13.38461538461550759, -10.33852847137269571, 34.16647553114546554 ) ) ;
#3152 = FACE_OUTER_BOUND ( 'NONE', #73334, .T. ) ;
#3153 = CARTESIAN_POINT ( 'NONE',  ( 1.139087296525997273, -4.749999999999992895, 22.98437500000000000 ) ) ;
#3154 = EDGE_CURVE ( 'NONE', #43102, #76951, #87849, .T. ) ;
#3155 = CARTESIAN_POINT ( 'NONE',  ( -6.923076923076922462, -1.117168528481311540, 33.14645433367849847 ) ) ;
#3156 = CARTESIAN_POINT ( 'NONE',  ( 15.90386940979756858, -4.818429247618089661, 34.26397095200675125 ) ) ;
#3157 = ORIENTED_EDGE ( 'NONE', *, *, #17944, .F. ) ;
#3158 = CARTESIAN_POINT ( 'NONE',  ( -1.944543648263014957, -5.555456351737005249, 19.00000000000000000 ) ) ;
#3159 = CARTESIAN_POINT ( 'NONE',  ( -1.384615384615506484, -12.51329471203414379, 31.30864560766407578 ) ) ;
#3160 = EDGE_CURVE ( 'NONE', #47174, #67701, #53718, .T. ) ;
#3161 = EDGE_LOOP ( 'NONE', ( #12682, #65661, #23637, #63398 ) ) ;
#3162 = CARTESIAN_POINT ( 'NONE',  ( -4.283994123577847368, -8.630895178749536711, 34.87696386517710323 ) ) ;
#3163 = EDGE_CURVE ( 'NONE', #58504, #53160, #9512, .T. ) ;
#3164 = VERTEX_POINT ( 'NONE', #88289 ) ;
#3165 = CARTESIAN_POINT ( 'NONE',  ( 6.923076923076924238, -3.937682226553329556, 33.60647404775216529 ) ) ;
#3166 = CARTESIAN_POINT ( 'NONE',  ( 4.023154687178593036, -3.530157926970578508, 32.79014554554150607 ) ) ;
#3167 = B_SPLINE_CURVE_WITH_KNOTS ( 'NONE', 3,
 ( #65046, #31733, #87139, #25415, #16874, #38040, #65504, #31282, #10118, #44323 ),
 .UNSPECIFIED., .F., .F.,
 ( 4, 2, 2, 2, 4 ),
 ( 0.0007817359527651089775, 0.0009771254036996502267, 0.001172514854634191693, 0.001367904305568727955, 0.001563293756503264216 ),
 .UNSPECIFIED. ) ;
#3168 = CARTESIAN_POINT ( 'NONE',  ( 16.82694633287449193, -6.524016743844656574, 34.90889640711025521 ) ) ;
#3169 = ORIENTED_EDGE ( 'NONE', *, *, #12308, .F. ) ;
#3170 = CARTESIAN_POINT ( 'NONE',  ( -14.55769230769230660, -7.500000000000001776, 35.00000000000000000 ) ) ;
#3171 = B_SPLINE_CURVE_WITH_KNOTS ( 'NONE', 3,
 ( #20875, #36185, #63634, #22212, #41600, #49679, #84369, #69508, #7815, #7377 ),
 .UNSPECIFIED., .F., .F.,
 ( 4, 2, 2, 2, 4 ),
 ( 0.000000000000000000, 0.0001954339881912775425, 0.0003908679763825550850, 0.0005863019645738326005, 0.0007817359527651101701 ),
 .UNSPECIFIED. ) ;
#3172 = ORIENTED_EDGE ( 'NONE', *, *, #77886, .F. ) ;
#3173 = EDGE_CURVE ( 'NONE', #29450, #36333, #27884, .T. ) ;
#3174 = CARTESIAN_POINT ( 'NONE',  ( -5.749945580086545327, -2.318338780012835443, 30.59689888758630261 ) ) ;
#3175 = B_SPLINE_CURVE_WITH_KNOTS ( 'NONE', 3,
 ( #72834, #58423, #16562, #2161, #85918, #31414, #57992, #37721, #45360, #85037 ),
 .UNSPECIFIED., .F., .F.,
 ( 4, 2, 2, 2, 4 ),
 ( 0.000000000000000000, 0.0001954311564186865763, 0.0003908623128373731525, 0.0005862934692560596746, 0.0007817246256747463051 ),
 .UNSPECIFIED. ) ;
#3176 = AXIS2_PLACEMENT_3D ( 'NONE', #38592, #66048, #79133 ) ;
#3177 = ORIENTED_EDGE ( 'NONE', *, *, #74398, .F. ) ;
#3179 = CARTESIAN_POINT ( 'NONE',  ( -18.00000000000000000, -11.91647553114624358, 32.58852847137147535 ) ) ;
#3178 = VECTOR ( 'NONE', #42643, 1000.000000000000000 ) ;
#3180 = CARTESIAN_POINT ( 'NONE',  ( 12.59206416330202849, -12.27024696741798770, 31.24895572276497546 ) ) ;
#3181 = ORIENTED_EDGE ( 'NONE', *, *, #60176, .T. ) ;
#3182 = CARTESIAN_POINT ( 'NONE',  ( 8.519207545009313876, -4.931416488878822335, 34.32920672191015399 ) ) ;
#3183 = CARTESIAN_POINT ( 'NONE',  ( -12.68502340526241312, -5.912607949931405926, 34.49155766932282319 ) ) ;
#3184 = CARTESIAN_POINT ( 'NONE',  ( -4.000000000000002665, 7.500000000000000000, 14.00000000000000178 ) ) ;
#3185 = CIRCLE ( 'NONE', #19071, 4.000000000000000000 ) ;
#3186 = ADVANCED_FACE ( 'NONE', ( #80175 ), #39196, .F. ) ;
#3187 = CARTESIAN_POINT ( 'NONE',  ( -14.17690186672535901, -9.929761469519743144, 34.40412654351204225 ) ) ;
#3188 = LINE ( 'NONE', #65770, #78107 ) ;
#3189 = EDGE_LOOP ( 'NONE', ( #70282, #29367 ) ) ;
#3190 = ORIENTED_EDGE ( 'NONE', *, *, #858, .T. ) ;
#3191 = VERTEX_POINT ( 'NONE', #18475 ) ;
#3193 = ORIENTED_EDGE ( 'NONE', *, *, #45330, .F. ) ;
#3192 = CARTESIAN_POINT ( 'NONE',  ( -7.911423846710166075, -5.941354392334499579, 34.76329471203369792 ) ) ;
#3194 = EDGE_CURVE ( 'NONE', #16561, #39467, #55788, .T. ) ;
#3195 = ADVANCED_FACE ( 'NONE', ( #14824 ), #68425, .F. ) ;
#3196 = CARTESIAN_POINT ( 'NONE',  ( 13.38461538461538680, -10.51840700105979565, 33.73612834413961536 ) ) ;
#3197 = CARTESIAN_POINT ( 'NONE',  ( -14.05763799605399278, -9.148310452688876993, 34.47095581063188519 ) ) ;
#3198 = EDGE_LOOP ( 'NONE', ( #48782, #56070 ) ) ;
#3199 = ORIENTED_EDGE ( 'NONE', *, *, #33265, .T. ) ;
#3200 = ORIENTED_EDGE ( 'NONE', *, *, #34878, .F. ) ;
#3201 = DIRECTION ( 'NONE',  ( -0.000000000000000000, -0.3420201433256694346, -0.9396926207859080948 ) ) ;
#3202 = ORIENTED_EDGE ( 'NONE', *, *, #59874, .F. ) ;
#3203 = VECTOR ( 'NONE', #28287, 1000.000000000000227 ) ;
#3204 = B_SPLINE_CURVE_WITH_KNOTS ( 'NONE', 3,
 ( #84488, #85369, #63754, #84051, #71392, #28651, #22763, #36730, #64184, #2489 ),
 .UNSPECIFIED., .F., .F.,
 ( 4, 2, 2, 2, 4 ),
 ( 0.000000000000000000, 0.0001954311564186861968, 0.0003908623128373723936, 0.0005862934692560585904, 0.0007817246256747447872 ),
 .UNSPECIFIED. ) ;
#3205 = CARTESIAN_POINT ( 'NONE',  ( 11.76147289007438701, -11.24521262558773493, 33.06293181088029343 ) ) ;
#3206 = EDGE_CURVE ( 'NONE', #79207, #29486, #51450, .T. ) ;
#3207 = CARTESIAN_POINT ( 'NONE',  ( 4.153846153846030731, -12.70778746994576025, 30.41441678777401236 ) ) ;
#3208 = VECTOR ( 'NONE', #88293, 1000.000000000000000 ) ;
#3209 = CARTESIAN_POINT ( 'NONE',  ( 14.30769230769231015, -11.91647553114624181, 32.58852847137148245 ) ) ;
#3210 = FACE_BOUND ( 'NONE', #54456, .T. ) ;
#3211 = EDGE_LOOP ( 'NONE', ( #80246, #65990, #20775, #64687 ) ) ;
#3212 = CARTESIAN_POINT ( 'NONE',  ( -11.25641025641025550, -3.499999999999999556, 29.75000000000000355 ) ) ;
#3213 = FACE_OUTER_BOUND ( 'NONE', #51443, .T. ) ;
#3214 = CARTESIAN_POINT ( 'NONE',  ( 9.019285080869083870, -3.136992222400443175, 32.19305428654138979 ) ) ;
#3215 = CARTESIAN_POINT ( 'NONE',  ( -19.50000000000000000, -3.499999999999999556, 29.75000000000000355 ) ) ;
#3216 = ORIENTED_EDGE ( 'NONE', *, *, #65232, .F. ) ;
#3217 = CARTESIAN_POINT ( 'NONE',  ( 2.307692307692187583, -10.90142922262034020, 33.41473453929536674 ) ) ;
#3218 = ORIENTED_EDGE ( 'NONE', *, *, #514, .F. ) ;
#3219 = EDGE_CURVE ( 'NONE', #20214, #18112, #50351, .T. ) ;
#3220 = ORIENTED_EDGE ( 'NONE', *, *, #87400, .T. ) ;
#3222 = DIRECTION ( 'NONE',  ( -0.000000000000000000, 1.000000000000000000, 3.491481338843133355E-15 ) ) ;
#3221 = CARTESIAN_POINT ( 'NONE',  ( 8.769230769230768274, -13.87047571288749737, 32.06866353760679544 ) ) ;
#3223 = CARTESIAN_POINT ( 'NONE',  ( 16.02369894440793630, -6.001485441113818986, 34.52039167877662607 ) ) ;
#3224 = CARTESIAN_POINT ( 'NONE',  ( -6.923076923077045919, -4.320704448113951379, 33.92786785259630022 ) ) ;
#3225 = EDGE_CURVE ( 'NONE', #25408, #21841, #34246, .T. ) ;
#3226 = CARTESIAN_POINT ( 'NONE',  ( -18.06608237936013950, -5.471508081941600210, 34.59228464037088457 ) ) ;
#3227 = CARTESIAN_POINT ( 'NONE',  ( -12.46153846153858247, -4.481592998941358097, 33.73612834414048933 ) ) ;
#3228 = EDGE_CURVE ( 'NONE', #61593, #37663, #89166, .T. ) ;
#3229 = ORIENTED_EDGE ( 'NONE', *, *, #65466, .F. ) ;
#3230 = CARTESIAN_POINT ( 'NONE',  ( -5.326899820971668476, -6.524016743844655686, 34.90889640711025521 ) ) ;
#3231 = CARTESIAN_POINT ( 'NONE',  ( -11.66860874789975888, -10.19110544564092002, 33.96427741523702792 ) ) ;
#3232 = CARTESIAN_POINT ( 'NONE',  ( 11.66929995647430118, -7.277220443632450575, 34.74524770363009196 ) ) ;
#3233 = CARTESIAN_POINT ( 'NONE',  ( -23.50000000000000000, 9.000000000000024869, 28.74999999999999645 ) ) ;
#3234 = ORIENTED_EDGE ( 'NONE', *, *, #86325, .T. ) ;
#3235 = ADVANCED_FACE ( 'NONE', ( #56246 ), #62541, .F. ) ;
#3236 = ORIENTED_EDGE ( 'NONE', *, *, #16268, .T. ) ;
#3237 = FACE_BOUND ( 'NONE', #74474, .T. ) ;
#3238 = VECTOR ( 'NONE', #34391, 1000.000000000000000 ) ;
#3239 = ORIENTED_EDGE ( 'NONE', *, *, #89142, .T. ) ;
#3240 = CARTESIAN_POINT ( 'NONE',  ( 18.00000000000000000, -12.62096338111211580, 30.90682066428153263 ) ) ;
#3241 = CARTESIAN_POINT ( 'NONE',  ( -1.134669975237340367, -2.341251567377310217, 30.72681386836322659 ) ) ;
#3242 = EDGE_LOOP ( 'NONE', ( #68213, #74958 ) ) ;
#3243 = DIRECTION ( 'NONE',  ( -0.000000000000000000, 0.5000000000000011102, -0.8660254037844381525 ) ) ;
#3244 = CARTESIAN_POINT ( 'NONE',  ( -2.057637996053991447, -4.235687564193446164, 33.53795663066793509 ) ) ;
#3245 = CARTESIAN_POINT ( 'NONE',  ( -8.638705067467205012, -6.852161475712352789, 34.70806712695775786 ) ) ;
#3246 = DIRECTION ( 'NONE',  ( 0.000000000000000000, 0.4999999999999960032, -0.8660254037844410391 ) ) ;
#3247 = ORIENTED_EDGE ( 'NONE', *, *, #45459, .T. ) ;
#3248 = DIRECTION ( 'NONE',  ( -0.000000000000000000, 0.6427876096865404731, -0.7660444431189770143 ) ) ;
#3249 = ORIENTED_EDGE ( 'NONE', *, *, #67110, .T. ) ;
#3251 = ORIENTED_EDGE ( 'NONE', *, *, #79029, .T. ) ;
#3250 = CARTESIAN_POINT ( 'NONE',  ( 10.61538461538461675, -4.661471528628507777, 34.16647553114623292 ) ) ;
#3252 = CARTESIAN_POINT ( 'NONE',  ( -7.715628144390283438, -9.417988943895561960, 34.36773134775777550 ) ) ;
#3253 = CARTESIAN_POINT ( 'NONE',  ( -12.71156168575991785, -2.985938066672154445, 32.43141759479405550 ) ) ;
#3254 = DIRECTION ( 'NONE',  ( -0.000000000000000000, 0.7660444431189791237, -0.6427876096865379196 ) ) ;
#3255 = CARTESIAN_POINT ( 'NONE',  ( 5.750000000000002665, -7.500000000000001776, 35.00000000000000000 ) ) ;
#3256 = CARTESIAN_POINT ( 'NONE',  ( 17.07692307692307665, -2.900454961884010974, 35.62045528018868623 ) ) ;
#3257 = CARTESIAN_POINT ( 'NONE',  ( 5.142178648199100977, -12.46129190930001052, 30.37095296980870174 ) ) ;
#3258 = CARTESIAN_POINT ( 'NONE',  ( -2.749999999999999112, -7.438900925035484057, 15.34561829374151465 ) ) ;
#3259 = VERTEX_POINT ( 'NONE', #7619 ) ;
#3260 = CARTESIAN_POINT ( 'NONE',  ( 13.63456079399343146, -12.68172785388650681, 30.59649109432439218 ) ) ;
#3261 = CARTESIAN_POINT ( 'NONE',  ( 6.065193981783355781, -2.506253911140448487, 29.99999999999988631 ) ) ;
#3262 = VERTEX_POINT ( 'NONE', #418 ) ;
#3263 = EDGE_LOOP ( 'NONE', ( #12497, #81130 ) ) ;
#3264 = CARTESIAN_POINT ( 'NONE',  ( 9.942253101685738059, -3.520799739797214389, 33.17531984108286025 ) ) ;
#3265 = CARTESIAN_POINT ( 'NONE',  ( -14.05774689831426727, -2.589246495874658383, 31.60778113518102828 ) ) ;
#3266 = B_SPLINE_CURVE_WITH_KNOTS ( 'NONE', 3,
 ( #51594, #79095, #20501, #81331, #34012, #74566, #61043, #41225, #46645, #33583 ),
 .UNSPECIFIED., .F., .F.,
 ( 4, 2, 2, 2, 4 ),
 ( 0.0007817359430256388964, 0.0009771253907250075990, 0.001172514838424376085, 0.001367904286123744571, 0.001563293733823113273 ),
 .UNSPECIFIED. ) ;
#3267 = CARTESIAN_POINT ( 'NONE',  ( -5.076923076923199218, -12.70778746994576025, 30.41441678777401236 ) ) ;
#3268 = DIRECTION ( 'NONE',  ( -1.000000000000000000, 0.000000000000000000, 0.000000000000000000 ) ) ;
#3269 = CARTESIAN_POINT ( 'NONE',  ( 13.16168842570853492, -2.889293201056495786, 32.26117774369186009 ) ) ;
#3270 = AXIS2_PLACEMENT_3D ( 'NONE', #14250, #42179, #1629 ) ;
#3271 = CARTESIAN_POINT ( 'NONE',  ( 16.28437159207980045, -3.625058011473227815, 33.29252011169590020 ) ) ;
#3272 = VECTOR ( 'NONE', #61182, 1000.000000000000227 ) ;
#3273 = CARTESIAN_POINT ( 'NONE',  ( -6.923076923077044142, -11.94971097300221174, 32.03036669348237098 ) ) ;
#3274 = EDGE_LOOP ( 'NONE', ( #55570, #68131 ) ) ;
#3275 = DIRECTION ( 'NONE',  ( 0.000000000000000000, 0.000000000000000000, -1.000000000000000000 ) ) ;
#3276 = CARTESIAN_POINT ( 'NONE',  ( -17.32689980786543060, -12.17611988154120795, 31.52148481390971213 ) ) ;
#3277 = CARTESIAN_POINT ( 'NONE',  ( 13.38461538461538680, -12.37446782046654192, 30.86335684631486131 ) ) ;
#3278 = CARTESIAN_POINT ( 'NONE',  ( 2.242421861731532573, -3.835265460703609186, 33.15142922261924241 ) ) ;
#3279 = EDGE_LOOP ( 'NONE', ( #82038, #71886 ) ) ;
#3280 = CARTESIAN_POINT ( 'NONE',  ( -17.32692307692307665, -2.249999999999998668, 29.75000000000000355 ) ) ;
#3281 = VERTEX_POINT ( 'NONE', #42299 ) ;
#3282 = CARTESIAN_POINT ( 'NONE',  ( 8.834485908743600291, -3.083524468853784839, 32.58852847137153930 ) ) ;
#3283 = CARTESIAN_POINT ( 'NONE',  ( -1.514762594053604916, -9.418419913701741919, 34.36755862841477693 ) ) ;
#3284 = CARTESIAN_POINT ( 'NONE',  ( -2.057692307692242650, -7.434744429011176159, 34.75000000000000711 ) ) ;
#3285 = ORIENTED_EDGE ( 'NONE', *, *, #46933, .T. ) ;
#3286 = CARTESIAN_POINT ( 'NONE',  ( 7.846153846153846700, -5.415277668671390821, 36.20867863119892149 ) ) ;
#3287 = CARTESIAN_POINT ( 'NONE',  ( 10.55011416942384272, -3.835265460703609186, 33.15142922261924241 ) ) ;
#3288 = CARTESIAN_POINT ( 'NONE',  ( -17.30040802064702987, -3.754499324213721234, 33.06261337010820256 ) ) ;
#3289 = ADVANCED_FACE ( 'NONE', ( #855 ), #21118, .F. ) ;
#3290 = CARTESIAN_POINT ( 'NONE',  ( 8.899278375486456838, -7.723484964179501588, 34.74522123443823318 ) ) ;
#3291 = CARTESIAN_POINT ( 'NONE',  ( -4.854143407945009869, -8.540255544307065350, 34.89611431652622286 ) ) ;
#3292 = VERTEX_POINT ( 'NONE', #27887 ) ;
#3293 = CARTESIAN_POINT ( 'NONE',  ( 7.846153846153723244, -11.67786785259630911, 32.92929555188603530 ) ) ;
#3294 = ORIENTED_EDGE ( 'NONE', *, *, #55497, .F. ) ;
#3295 = B_SPLINE_CURVE_WITH_KNOTS ( 'NONE', 3,
 ( #45530, #4089, #26154, #72110, #72556, #60376, #37890, #53623, #32461, #87887 ),
 .UNSPECIFIED., .F., .F.,
 ( 4, 2, 2, 2, 4 ),
 ( 0.0007817246256747481482, 0.0009771112852218911526, 0.001172497944769034265, 0.001367884604316177161, 0.001563271263863320274 ),
 .UNSPECIFIED. ) ;
#3296 = CIRCLE ( 'NONE', #66576, 4.000000000000000000 ) ;
#3297 = SPHERICAL_SURFACE ( 'NONE', #10520, 8.000000000000000000 ) ;
#3298 = VECTOR ( 'NONE', #9210, 1000.000000000000000 ) ;
#3299 = CARTESIAN_POINT ( 'NONE',  ( -3.230769230769229949, -12.10708131394839349, 31.69288490824020244 ) ) ;
#3300 = B_SPLINE_CURVE_WITH_KNOTS ( 'NONE', 3,
 ( #24187, #29633, #16546, #64722, #31397, #44013, #85020, #77367, #84586, #3470 ),
 .UNSPECIFIED., .F., .F.,
 ( 4, 2, 2, 2, 4 ),
 ( 0.000000000000000000, 0.0001954311564186860884, 0.0003908623128373721767, 0.0005862934692560582651, 0.0007817246256747443535 ),
 .UNSPECIFIED. ) ;
#3301 = CARTESIAN_POINT ( 'NONE',  ( 9.942362112221147186, -2.544122305571458575, 31.48381861865057729 ) ) ;
#3302 = EDGE_CURVE ( 'NONE', #5633, #496, #34222, .T. ) ;
#3303 = FACE_OUTER_BOUND ( 'NONE', #83869, .T. ) ;
#3304 = CARTESIAN_POINT ( 'NONE',  ( 12.71159277317677549, -9.943054286541403997, 34.11300777759954883 ) ) ;
#3305 = B_SPLINE_CURVE_WITH_KNOTS ( 'NONE', 3,
 ( #60210, #52117, #53450, #73291, #58879, #87716, #26440, #72387, #12479, #80953 ),
 .UNSPECIFIED., .F., .F.,
 ( 4, 2, 2, 2, 4 ),
 ( 0.0007817246256747455461, 0.0009771112852218885505, 0.001172497944769031663, 0.001367884604316174559, 0.001563271263863317672 ),
 .UNSPECIFIED. ) ;
#3306 = AXIS2_PLACEMENT_3D ( 'NONE', #72090, #58565, #59017 ) ;
#3307 = ORIENTED_EDGE ( 'NONE', *, *, #7182, .T. ) ;
#3308 = VERTEX_POINT ( 'NONE', #84178 ) ;
#3309 = VERTEX_POINT ( 'NONE', #82399 ) ;
#3310 = EDGE_LOOP ( 'NONE', ( #83643, #82972, #52409, #33244, #73566 ) ) ;
#3311 = EDGE_CURVE ( 'NONE', #27279, #61816, #47711, .T. ) ;
#3312 = CARTESIAN_POINT ( 'NONE',  ( 12.52760681254089903, -11.69971097300155272, 32.46337939537588113 ) ) ;
#3313 = CYLINDRICAL_SURFACE ( 'NONE', #79056, 0.2499999999999998890 ) ;
#3314 = CARTESIAN_POINT ( 'NONE',  ( -3.931066484868086075, -6.717445702608402236, 34.94155399931962336 ) ) ;
#3315 = CARTESIAN_POINT ( 'NONE',  ( -12.46153846153846168, -12.34228464037088635, 31.77849191805839268 ) ) ;
#3316 = B_SPLINE_CURVE_WITH_KNOTS ( 'NONE', 3,
 ( #20890, #40296, #41174, #5613, #19129, #47029, #82621, #46600, #53348, #27651 ),
 .UNSPECIFIED., .F., .F.,
 ( 4, 2, 2, 2, 4 ),
 ( 0.000000000000000000, 0.0001954311564186871184, 0.0003908623128373742367, 0.0005862934692560614093, 0.0007817246256747484735 ),
 .UNSPECIFIED. ) ;
#3317 = CARTESIAN_POINT ( 'NONE',  ( -13.25382357679059986, -5.582136614379148654, 34.36778462344220486 ) ) ;
#3318 = CARTESIAN_POINT ( 'NONE',  ( 8.639083559792549494, -9.418419913701741919, 34.36755862841477693 ) ) ;
#3319 = CARTESIAN_POINT ( 'NONE',  ( 5.750023269057646935, -11.79746400365624659, 32.30657167506340954 ) ) ;
#3320 = CARTESIAN_POINT ( 'NONE',  ( -7.780898274877821486, -3.300289026998474817, 32.46337939537591666 ) ) ;
#3321 = EDGE_LOOP ( 'NONE', ( #51330, #45872, #49558, #18736 ) ) ;
#3322 = VERTEX_POINT ( 'NONE', #13485 ) ;
#3323 = ORIENTED_EDGE ( 'NONE', *, *, #83178, .F. ) ;
#3325 = VERTEX_POINT ( 'NONE', #40962 ) ;
#3324 = DIRECTION ( 'NONE',  ( 0.000000000000000000, 0.3420201433256641055, -0.9396926207859100932 ) ) ;
#3326 = AXIS2_PLACEMENT_3D ( 'NONE', #84353, #69491, #7797 ) ;
#3328 = CARTESIAN_POINT ( 'NONE',  ( 10.39245839786846659, -9.086856451489515152, 34.49173150075333183 ) ) ;
#3327 = CARTESIAN_POINT ( 'NONE',  ( 16.37662569511456567, -11.89424750095246175, 32.13594075562311758 ) ) ;
#3329 = CARTESIAN_POINT ( 'NONE',  ( 8.519230769230768274, -7.500000000000001776, 34.75000000000000000 ) ) ;
#3330 = ADVANCED_FACE ( 'NONE', ( #3056 ), #23767, .F. ) ;
#3331 = DIRECTION ( 'NONE',  ( -0.000000000000000000, 0.7660444431189791237, -0.6427876096865379196 ) ) ;
#3332 = EDGE_CURVE ( 'NONE', #37853, #58001, #85933, .T. ) ;
#3333 = VERTEX_POINT ( 'NONE', #8948 ) ;
#3334 = B_SPLINE_CURVE_WITH_KNOTS ( 'NONE', 3,
 ( #21528, #29625, #57526, #8909, #62939, #7580, #76922, #36380, #815, #43567 ),
 .UNSPECIFIED., .F., .F.,
 ( 4, 2, 2, 2, 4 ),
 ( 0.0007817359430256322827, 0.0009771253907249989254, 0.001172514838424365676, 0.001367904286123732428, 0.001563293733823098962 ),
 .UNSPECIFIED. ) ;
#3335 = VERTEX_POINT ( 'NONE', #36848 ) ;
#3336 = CARTESIAN_POINT ( 'NONE',  ( -6.923076923077045919, -6.835583212225970762, 34.95778746994575670 ) ) ;
#3337 = B_SPLINE_CURVE_WITH_KNOTS ( 'NONE', 3,
 ( #83491, #74961, #74506, #14574, #75393, #48352, #42059, #41607, #27643, #12802 ),
 .UNSPECIFIED., .F., .F.,
 ( 4, 2, 2, 2, 4 ),
 ( 0.0007817246256747474977, 0.0009771112852218911526, 0.001172497944769034699, 0.001367884604316178462, 0.001563271263863322009 ),
 .UNSPECIFIED. ) ;
#3338 = EDGE_LOOP ( 'NONE', ( #76233, #47912 ) ) ;
#3339 = FACE_BOUND ( 'NONE', #711, .T. ) ;
#3340 = DIRECTION ( 'NONE',  ( 0.000000000000000000, 0.000000000000000000, 1.000000000000000000 ) ) ;
#3341 = CARTESIAN_POINT ( 'NONE',  ( -14.30769230769230660, -6.343179335718451384, 34.87096338111211935 ) ) ;
#3342 = ORIENTED_EDGE ( 'NONE', *, *, #24027, .F. ) ;
#3343 = CARTESIAN_POINT ( 'NONE',  ( 17.77707378248385339, -2.758268499246657068, 31.33685645148948851 ) ) ;
#3344 = CARTESIAN_POINT ( 'NONE',  ( 9.692307692307695177, -2.900454961884010974, 35.62045528018868623 ) ) ;
#3345 = CARTESIAN_POINT ( 'NONE',  ( 2.242422307135989001, -11.67786785259541027, 32.92929555188721480 ) ) ;
#3346 = ORIENTED_EDGE ( 'NONE', *, *, #27533, .F. ) ;
#3347 = CARTESIAN_POINT ( 'NONE',  ( -11.76194646302587010, -4.988325925672468131, 34.36044203135681130 ) ) ;
#3348 = CARTESIAN_POINT ( 'NONE',  ( -18.24997673094235751, -4.943428324936578910, 34.04746400365624481 ) ) ;
#3349 = VERTEX_POINT ( 'NONE', #31430 ) ;
#3350 = CARTESIAN_POINT ( 'NONE',  ( 6.250000000001421085, -7.500000000000154543, 35.00000000000007105 ) ) ;
#3351 = CARTESIAN_POINT ( 'NONE',  ( -9.692307692307814193, -2.379036618888197729, 30.90682066428292885 ) ) ;
#3352 = ORIENTED_EDGE ( 'NONE', *, *, #71775, .T. ) ;
#3353 = CARTESIAN_POINT ( 'NONE',  ( 8.519207545009310323, -11.56360843649121861, 33.07473185843129926 ) ) ;
#3354 = CARTESIAN_POINT ( 'NONE',  ( 13.31853197365950514, -2.538708090699994813, 30.37095296980875148 ) ) ;
#3355 = CARTESIAN_POINT ( 'NONE',  ( -8.769230769230890843, -12.46129190930018460, 30.37095296980731973 ) ) ;
#3356 = CARTESIAN_POINT ( 'NONE',  ( 9.070512820512819374, -3.499999999999999556, 29.75000000000000355 ) ) ;
#3357 = CARTESIAN_POINT ( 'NONE',  ( 9.442330948259103351, -12.41104346484419452, 31.60698883733904196 ) ) ;
#3358 = FACE_BOUND ( 'NONE', #81878, .T. ) ;
#3360 = CARTESIAN_POINT ( 'NONE',  ( 7.173131234715237170, -3.136992222400443175, 32.19305428654138979 ) ) ;
#3359 = CARTESIAN_POINT ( 'NONE',  ( 27.00000000000000000, 8.999999999999996447, 23.75000000000000000 ) ) ;
#3361 = DIRECTION ( 'NONE',  ( -0.000000000000000000, -0.7660444431189791237, -0.6427876096865379196 ) ) ;
#3363 = CARTESIAN_POINT ( 'NONE',  ( 12.21156171748986985, -4.818429247618089661, 34.26397095200675125 ) ) ;
#3362 = CARTESIAN_POINT ( 'NONE',  ( 3.007902967706132191, -2.251424796025575770, 29.88072029997477586 ) ) ;
#3364 = CARTESIAN_POINT ( 'NONE',  ( -5.999999999999998224, -12.37446782046654192, 30.86335684631486131 ) ) ;
#3365 = CARTESIAN_POINT ( 'NONE',  ( 2.750000000000008438, -8.639087296525996607, 14.54687500000000178 ) ) ;
#3366 = VERTEX_POINT ( 'NONE', #22890 ) ;
#3367 = CARTESIAN_POINT ( 'NONE',  ( -15.23076923076922995, -12.34228464037088635, 31.77849191805839268 ) ) ;
#3368 = VERTEX_POINT ( 'NONE', #78728 ) ;
#3369 = AXIS2_PLACEMENT_3D ( 'NONE', #86885, #65241, #17512 ) ;
#3370 = CARTESIAN_POINT ( 'NONE',  ( 11.53846153846153832, -11.11383981884818262, 36.00935417666054406 ) ) ;
#3371 = ORIENTED_EDGE ( 'NONE', *, *, #83505, .T. ) ;
#3372 = LINE ( 'NONE', #72275, #49878 ) ;
#3373 = ORIENTED_EDGE ( 'NONE', *, *, #78418, .F. ) ;
#3374 = CARTESIAN_POINT ( 'NONE',  ( -6.000000000000119904, -11.94971097300221174, 32.03036669348237098 ) ) ;
#3375 = CARTESIAN_POINT ( 'NONE',  ( 2.750000000000001332, -7.438900925035452083, 24.21688170625849068 ) ) ;
#3376 = CARTESIAN_POINT ( 'NONE',  ( -17.86920819217521483, -5.582136614379148654, 34.36778462344220486 ) ) ;
#3377 = CARTESIAN_POINT ( 'NONE',  ( -5.750054590621957118, -11.56426240980093745, 33.07394671870546432 ) ) ;
#3378 = CARTESIAN_POINT ( 'NONE',  ( 13.38461538461526423, -3.083524468854526912, 32.58852847137268327 ) ) ;
#3380 = CARTESIAN_POINT ( 'NONE',  ( -6.066082379360134169, -2.486705287966279432, 31.30864560766542937 ) ) ;
#3379 = B_SPLINE_CURVE_WITH_KNOTS ( 'NONE', 3,
 ( #3999, #60732, #86906, #11672, #31487, #19309, #25619, #52191, #46781, #88240 ),
 .UNSPECIFIED., .F., .F.,
 ( 4, 2, 2, 2, 4 ),
 ( 0.0007817359527651104954, 0.0009771254036996493593, 0.001172514854634188440, 0.001367904305568727304, 0.001563293756503266168 ),
 .UNSPECIFIED. ) ;
#3381 = CARTESIAN_POINT ( 'NONE',  ( 15.10007862765892739, -8.191372820521381826, 34.95448215188423546 ) ) ;
#3382 = CARTESIAN_POINT ( 'NONE',  ( -7.623374304885436104, -2.847695495035523994, 31.58253572463339509 ) ) ;
#3383 = CARTESIAN_POINT ( 'NONE',  ( 14.98076923076923173, -7.500000000000001776, 35.00000000000000000 ) ) ;
#3384 = B_SPLINE_CURVE_WITH_KNOTS ( 'NONE', 3,
 ( #19609, #61917, #88981, #54270, #13739, #67803, #60591, #82207, #20496, #33579 ),
 .UNSPECIFIED., .F., .F.,
 ( 4, 2, 2, 2, 4 ),
 ( 0.000000000000000000, 0.0001954311564186860071, 0.0003908623128373720141, 0.0005862934692560580483, 0.0007817246256747440282 ),
 .UNSPECIFIED. ) ;
#3385 = CARTESIAN_POINT ( 'NONE',  ( 1.553300858899129944, -11.24999999999998934, 14.70312500000000355 ) ) ;
#3386 = CARTESIAN_POINT ( 'NONE',  ( 1.384615384615265343, -3.300289026999228881, 32.46337939537708905 ) ) ;
#3387 = DIRECTION ( 'NONE',  ( 0.000000000000000000, -2.546383084002652634E-16, -1.000000000000000000 ) ) ;
#3388 = CYLINDRICAL_SURFACE ( 'NONE', #33506, 0.2500000000000009437 ) ;
#3389 = CARTESIAN_POINT ( 'NONE',  ( -3.750000000000008438, -5.946699141100917352, 15.17187500000000000 ) ) ;
#3390 = VERTEX_POINT ( 'NONE', #43606 ) ;
#3391 = CARTESIAN_POINT ( 'NONE',  ( -13.60810030917971858, -6.716662450894489211, 34.94144148231605840 ) ) ;
#3392 = CARTESIAN_POINT ( 'NONE',  ( 17.07692307692307665, -1.242168528481310874, 33.36296068462461051 ) ) ;
#3393 = LINE ( 'NONE', #38526, #85756 ) ;
#3394 = CARTESIAN_POINT ( 'NONE',  ( 18.06606835100243558, -10.51840700105979565, 33.73612834413962247 ) ) ;
#3395 = CARTESIAN_POINT ( 'NONE',  ( 17.20771351789002424, -12.35292014791297710, 31.75344720912887198 ) ) ;
#3396 = ADVANCED_FACE ( 'NONE', ( #64310 ), #10716, .F. ) ;
#3397 = CARTESIAN_POINT ( 'NONE',  ( -3.230769230769229949, -11.35647404775217417, 33.31231777344666511 ) ) ;
#3398 = EDGE_CURVE ( 'NONE', #3876, #58816, #16576, .T. ) ;
#3399 = ORIENTED_EDGE ( 'NONE', *, *, #32573, .T. ) ;
#3400 = CARTESIAN_POINT ( 'NONE',  ( 7.846153846153723244, -3.083524468854526912, 32.58852847137268327 ) ) ;
#3401 = VERTEX_POINT ( 'NONE', #57124 ) ;
#3402 = ORIENTED_EDGE ( 'NONE', *, *, #51805, .F. ) ;
#3403 = CARTESIAN_POINT ( 'NONE',  ( 10.61538461538461675, -1.044019251281081972, 31.83374038241031911 ) ) ;
#3404 = EDGE_CURVE ( 'NONE', #23906, #22078, #46057, .T. ) ;
#3405 = CARTESIAN_POINT ( 'NONE',  ( 3.361294932532794100, -6.001044277235011215, 34.52024696741798948 ) ) ;
#3406 = CARTESIAN_POINT ( 'NONE',  ( -0.2385753272717870410, -7.369474539155827841, 34.99858011523955525 ) ) ;
#3407 = EDGE_CURVE ( 'NONE', #87412, #1287, #86928, .T. ) ;
#3408 = CARTESIAN_POINT ( 'NONE',  ( -13.38461538461538325, -8.973038597847269315, 34.52809138561121927 ) ) ;
#3409 = CARTESIAN_POINT ( 'NONE',  ( -5.076923076923075762, -8.164416787775445883, 34.95778746994557906 ) ) ;
#3410 = VERTEX_POINT ( 'NONE', #2610 ) ;
#3411 = EDGE_LOOP ( 'NONE', ( #7730, #87088 ) ) ;
#3413 = VERTEX_POINT ( 'NONE', #30098 ) ;
#3412 = AXIS2_PLACEMENT_3D ( 'NONE', #23863, #24768, #31979 ) ;
#3414 = VECTOR ( 'NONE', #68678, 1000.000000000000000 ) ;
#3415 = EDGE_CURVE ( 'NONE', #14630, #80116, #66472, .T. ) ;
#3416 = CARTESIAN_POINT ( 'NONE',  ( 1.319344938654611887, -11.48612834413959582, 32.76840700105983473 ) ) ;
#3417 = CARTESIAN_POINT ( 'NONE',  ( 16.28463796167094557, -12.38066358083363738, 30.83685684665853444 ) ) ;
#3418 = DIRECTION ( 'NONE',  ( -0.000000000000000000, -0.8660254037844397068, -0.4999999999999980016 ) ) ;
#3419 = COLOUR_RGB ( '', 0.09019608, 0.27058824, 0.51372549) ;
#3420 = VECTOR ( 'NONE', #31207, 1000.000000000000000 ) ;
#3421 = CARTESIAN_POINT ( 'NONE',  ( -15.23076923076935074, -3.300289026999228881, 32.46337939537708905 ) ) ;
#3422 = CARTESIAN_POINT ( 'NONE',  ( -4.153846153846152411, -8.120952969808772792, 34.71129190930000163 ) ) ;
#3423 = CARTESIAN_POINT ( 'NONE',  ( 17.86985279056177944, -8.587444163452046197, 34.63053765926554206 ) ) ;
#3424 = ORIENTED_EDGE ( 'NONE', *, *, #26826, .T. ) ;
#3425 = ORIENTED_EDGE ( 'NONE', *, *, #17387, .F. ) ;
#3426 = B_SPLINE_CURVE_WITH_KNOTS ( 'NONE', 3,
 ( #16830, #72211, #84865, #3757, #36668, #59146, #65896, #85302, #24469, #44279 ),
 .UNSPECIFIED., .F., .F.,
 ( 4, 2, 2, 2, 4 ),
 ( 0.0007817359430256324996, 0.0009771253907249991422, 0.001172514838424365676, 0.001367904286123732428, 0.001563293733823098962 ),
 .UNSPECIFIED. ) ;
#3427 = CARTESIAN_POINT ( 'NONE',  ( 2.651650429449539104, -4.848349570550432475, 20.56250000000000000 ) ) ;
#3428 = ORIENTED_EDGE ( 'NONE', *, *, #51871, .F. ) ;
#3430 = ORIENTED_EDGE ( 'NONE', *, *, #69548, .T. ) ;
#3429 = CARTESIAN_POINT ( 'NONE',  ( -5.869208192175213945, -3.062576670634119758, 32.05464942895959979 ) ) ;
#3431 = CARTESIAN_POINT ( 'NONE',  ( -10.39260494640654464, -4.226511098958373402, 33.85474049983370293 ) ) ;
#3432 = CARTESIAN_POINT ( 'NONE',  ( 6.250054311638314708, -12.41262288849542017, 30.68299917996395010 ) ) ;
#3433 = CARTESIAN_POINT ( 'NONE',  ( 3.749999999999992006, -5.946699141100872943, 15.64062500000000178 ) ) ;
#3434 = ADVANCED_FACE ( 'NONE', ( #50788 ), #10275, .F. ) ;
#3435 = ORIENTED_EDGE ( 'NONE', *, *, #19569, .F. ) ;
#3436 = EDGE_CURVE ( 'NONE', #53046, #51788, #42874, .T. ) ;
#3437 = CARTESIAN_POINT ( 'NONE',  ( -14.30769230769230660, -12.34228464037088635, 31.77849191805839268 ) ) ;
#3438 = ORIENTED_EDGE ( 'NONE', *, *, #30030, .T. ) ;
#3439 = CARTESIAN_POINT ( 'NONE',  ( -8.992715693795101828, -4.988325925672468131, 34.36044203135681130 ) ) ;
#3440 = CARTESIAN_POINT ( 'NONE',  ( 17.07692307692307665, -13.88283147151868846, 33.14645433367849847 ) ) ;
#3441 = CARTESIAN_POINT ( 'NONE',  ( 2.177001704582003150, -12.35290016733513951, 31.75349464988449455 ) ) ;
#3443 = LINE ( 'NONE', #37677, #56986 ) ;
#3442 = CARTESIAN_POINT ( 'NONE',  ( 5.750023255951411727, -12.41104346484419452, 31.60698883733904196 ) ) ;
#3444 = EDGE_CURVE ( 'NONE', #50148, #24402, #75102, .T. ) ;
#3445 = CARTESIAN_POINT ( 'NONE',  ( 8.519254038288416098, -5.728515186090277211, 34.42611988154120439 ) ) ;
#3446 = LINE ( 'NONE', #58380, #53455 ) ;
#3447 = EDGE_LOOP ( 'NONE', ( #37992, #2627, #21349, #15975 ) ) ;
#3448 = EDGE_CURVE ( 'NONE', #76927, #73366, #25114, .T. ) ;
#3449 = CYLINDRICAL_SURFACE ( 'NONE', #56164, 0.2499999999999998890 ) ;
#3450 = DIRECTION ( 'NONE',  ( -0.000000000000000000, 1.000000000000000000, -0.000000000000000000 ) ) ;
#3451 = ORIENTED_EDGE ( 'NONE', *, *, #5763, .F. ) ;
#3452 = DIRECTION ( 'NONE',  ( 0.000000000000000000, 0.4999999999999960032, -0.8660254037844410391 ) ) ;
#3453 = CARTESIAN_POINT ( 'NONE',  ( -4.826977558574935045, -5.852078868378311149, 34.47109172314383585 ) ) ;
#3454 = CARTESIAN_POINT ( 'NONE',  ( 10.48469401227430886, -8.191372820521381826, 34.95448215188423546 ) ) ;
#3455 = FACE_OUTER_BOUND ( 'NONE', #34753, .T. ) ;
#3456 = CARTESIAN_POINT ( 'NONE',  ( -24.99999999999999645, 20.00000000000000355, 3.000000000000000000 ) ) ;
#3457 = FACE_BOUND ( 'NONE', #21369, .T. ) ;
#3459 = CARTESIAN_POINT ( 'NONE',  ( 1.607626736228235487, -2.554770724473667709, 30.48948780036025852 ) ) ;
#3458 = CARTESIAN_POINT ( 'NONE',  ( 12.39545608217832395, -9.905515769479276145, 34.41647553114623292 ) ) ;
#3460 = CYLINDRICAL_SURFACE ( 'NONE', #20960, 0.2499999999999993616 ) ;
#3462 = CARTESIAN_POINT ( 'NONE',  ( 9.915319043920545639, -4.187068189119697692, 33.49521262558774026 ) ) ;
#3461 = CARTESIAN_POINT ( 'NONE',  ( 3.007284287045282500, -4.386631170607603991, 33.66268669641500111 ) ) ;
#3463 = CYLINDRICAL_SURFACE ( 'NONE', #48393, 0.2500000000000004996 ) ;
#3464 = CARTESIAN_POINT ( 'NONE',  ( 17.07692307692307665, -1.509761064869970415, 31.06009739812519044 ) ) ;
#3465 = CARTESIAN_POINT ( 'NONE',  ( -2.608446859217889546, -10.19485399968121264, 20.93563170625849068 ) ) ;
#3466 = EDGE_LOOP ( 'NONE', ( #67477, #25046, #38237, #39668, #79080, #56446 ) ) ;
#3467 = CARTESIAN_POINT ( 'NONE',  ( -9.692307692307814193, -3.083524468854526912, 32.58852847137268327 ) ) ;
#3468 = B_SPLINE_CURVE_WITH_KNOTS ( 'NONE', 3,
 ( #40600, #25300, #6797, #27073, #81146, #13120, #87468, #33827, #61285, #39718 ),
 .UNSPECIFIED., .F., .F.,
 ( 4, 2, 2, 2, 4 ),
 ( 0.000000000000000000, 0.0001954339857564073659, 0.0003908679715128147319, 0.0005863019572692221250, 0.0007817359430256294638 ),
 .UNSPECIFIED. ) ;
#3469 = CARTESIAN_POINT ( 'NONE',  ( -14.43838377435986864, -6.413092428213692742, 34.63065189839063152 ) ) ;
#3470 = CARTESIAN_POINT ( 'NONE',  ( -0.4615384615385840772, -3.643525952248795718, 33.31231777344771672 ) ) ;
#3471 = CARTESIAN_POINT ( 'NONE',  ( 2.557692307692308376, -2.249999999999998668, 29.75000000000000355 ) ) ;
#3472 = CARTESIAN_POINT ( 'NONE',  ( 6.792928953345226617, -12.70455904226513866, 30.44083106164009322 ) ) ;
#3473 = DIRECTION ( 'NONE',  ( -0.000000000000000000, 0.5000000000000011102, -0.8660254037844381525 ) ) ;
#3474 = CARTESIAN_POINT ( 'NONE',  ( 0.06109907496455496689, -11.24999999999999822, 22.02938170625849068 ) ) ;
#3475 = CARTESIAN_POINT ( 'NONE',  ( -1.134615384613964384, -7.500000000000154543, 35.00000000000007105 ) ) ;
#3476 = CARTESIAN_POINT ( 'NONE',  ( 0.4615384615384611200, -3.513871655860378418, 32.76840700105978499 ) ) ;
#3477 = CARTESIAN_POINT ( 'NONE',  ( 11.28846153846154188, -7.566082377512564960, 35.00000000000000711 ) ) ;
#3478 = DIRECTION ( 'NONE',  ( 0.000000000000000000, -6.938893903907222067E-15, 1.000000000000000000 ) ) ;
#3479 = CARTESIAN_POINT ( 'NONE',  ( 0.3962680155776860391, -11.48612834413959582, 32.76840700105983473 ) ) ;
#3480 = CARTESIAN_POINT ( 'NONE',  ( 15.23076923076923173, -11.11383981884818262, 36.00935417666054406 ) ) ;
#3481 = EDGE_CURVE ( 'NONE', #46107, #77857, #82617, .T. ) ;
#3482 = FACE_OUTER_BOUND ( 'NONE', #38746, .T. ) ;
#3483 = CARTESIAN_POINT ( 'NONE',  ( 17.07692307692295586, -2.657715359629662544, 31.77849191805970364 ) ) ;
#3484 = ORIENTED_EDGE ( 'NONE', *, *, #73546, .F. ) ;
#3485 = CARTESIAN_POINT ( 'NONE',  ( 3.230769230769108269, -12.51329471203414379, 31.30864560766407578 ) ) ;
#3486 = CARTESIAN_POINT ( 'NONE',  ( 3.230769230769231726, -13.87047571288749737, 32.06866353760679544 ) ) ;
#3487 = CARTESIAN_POINT ( 'NONE',  ( 2.608446859217924629, -10.19485399968118422, 16.12686829374151287 ) ) ;
#3488 = AXIS2_PLACEMENT_3D ( 'NONE', #63887, #16156, #15722 ) ;
#3489 = VECTOR ( 'NONE', #65292, 1000.000000000000000 ) ;
#3490 = CARTESIAN_POINT ( 'NONE',  ( 2.084766090176161324, -4.186968288167446595, 33.49512374952580274 ) ) ;
#3491 = CARTESIAN_POINT ( 'NONE',  ( -16.82686865700962642, -5.642605341092955307, 34.66089969410670335 ) ) ;
#3492 = ORIENTED_EDGE ( 'NONE', *, *, #69496, .F. ) ;
#3493 = CARTESIAN_POINT ( 'NONE',  ( -18.13014720943822056, -9.418419913701741919, 34.36755862841476272 ) ) ;
#3494 = CARTESIAN_POINT ( 'NONE',  ( 2.307692307692309264, -10.67929555188718282, 33.92786785259544047 ) ) ;
#3496 = EDGE_LOOP ( 'NONE', ( #69343, #672 ) ) ;
#3495 = DIRECTION ( 'NONE',  ( 0.000000000000000000, 0.000000000000000000, -1.000000000000000000 ) ) ;
#3497 = CARTESIAN_POINT ( 'NONE',  ( -3.262820512820514107, -7.500000000000000000, 29.75000000000000355 ) ) ;
#3498 = CARTESIAN_POINT ( 'NONE',  ( -17.07692307692307665, -2.486705287966279876, 31.30864560766543647 ) ) ;
#3499 = DIRECTION ( 'NONE',  ( -0.000000000000000000, 0.7660444431189791237, -0.6427876096865379196 ) ) ;
#3500 = EDGE_CURVE ( 'NONE', #62030, #70013, #60673, .T. ) ;
#3501 = CARTESIAN_POINT ( 'NONE',  ( -14.08491276642389955, -11.41317474335729543, 32.86274602512330034 ) ) ;
#3502 = ORIENTED_EDGE ( 'NONE', *, *, #75844, .T. ) ;
#3503 = CARTESIAN_POINT ( 'NONE',  ( 3.230769230769231726, -2.486705287966279876, 31.30864560766543647 ) ) ;
#3504 =( NAMED_UNIT ( * ) SI_UNIT ( $, .STERADIAN. ) SOLID_ANGLE_UNIT ( ) );
#3505 = B_SPLINE_CURVE_WITH_KNOTS ( 'NONE', 3,
 ( #72936, #4481, #11238, #31958, #59422, #78797, #64386, #3578, #79253, #86929 ),
 .UNSPECIFIED., .F., .F.,
 ( 4, 2, 2, 2, 4 ),
 ( 0.0007817359527651096280, 0.0009771254036996484919, 0.001172514854634187573, 0.001367904305568726653, 0.001563293756503265517 ),
 .UNSPECIFIED. ) ;
#3506 = CARTESIAN_POINT ( 'NONE',  ( 15.10062126103753499, -10.31621877034669588, 34.18098118002070152 ) ) ;
#3507 = ORIENTED_EDGE ( 'NONE', *, *, #68893, .T. ) ;
#3508 = ORIENTED_EDGE ( 'NONE', *, *, #3043, .T. ) ;
#3509 = B_SPLINE_CURVE_WITH_KNOTS ( 'NONE', 3,
 ( #87434, #11761, #67149, #59936, #53173, #36027 ),
 .UNSPECIFIED., .F., .F.,
 ( 4, 2, 4 ),
 ( 0.000000000000000000, 0.0001954784845028934947, 0.0003909569690057869895 ),
 .UNSPECIFIED. ) ;
#3510 = ORIENTED_EDGE ( 'NONE', *, *, #50763, .T. ) ;
#3511 = ADVANCED_FACE ( 'NONE', ( #87732 ), #12495, .F. ) ;
#3512 = DIRECTION ( 'NONE',  ( 0.000000000000000000, 0.9848077530122072432, -0.1736481776669354937 ) ) ;
#3513 = CARTESIAN_POINT ( 'NONE',  ( -7.846153846153844924, -13.75783147151868846, 33.36296068462461051 ) ) ;
#3514 = EDGE_CURVE ( 'NONE', #7867, #87048, #88180, .T. ) ;
#3515 = CARTESIAN_POINT ( 'NONE',  ( 13.25392391794782654, -11.18331474514187995, 33.13161551792790505 ) ) ;
#3516 = CARTESIAN_POINT ( 'NONE',  ( 7.846153846153846700, -8.120952969808772792, 34.71129190930000163 ) ) ;
#3517 = VERTEX_POINT ( 'NONE', #47153 ) ;
#3519 = ORIENTED_EDGE ( 'NONE', *, *, #19505, .T. ) ;
#3518 = EDGE_CURVE ( 'NONE', #44526, #16365, #12061, .T. ) ;
#3521 = ORIENTED_EDGE ( 'NONE', *, *, #76748, .T. ) ;
#3520 = CARTESIAN_POINT ( 'NONE',  ( -11.53846153846153655, -2.538708090699994813, 30.37095296980875503 ) ) ;
#3522 = LINE ( 'NONE', #64334, #19383 ) ;
#3523 = EDGE_CURVE ( 'NONE', #59454, #38026, #68704, .T. ) ;
#3524 = CARTESIAN_POINT ( 'NONE',  ( 10.48523740594639442, -11.47017969459903952, 32.78971311882035167 ) ) ;
#3525 = FACE_OUTER_BOUND ( 'NONE', #75446, .T. ) ;
#3526 = EDGE_CURVE ( 'NONE', #60787, #58112, #6351, .T. ) ;
#3527 = EDGE_LOOP ( 'NONE', ( #70212, #78672 ) ) ;
#3528 = ORIENTED_EDGE ( 'NONE', *, *, #25050, .F. ) ;
#3529 = VERTEX_POINT ( 'NONE', #52133 ) ;
#3531 = ORIENTED_EDGE ( 'NONE', *, *, #8095, .F. ) ;
#3530 = CARTESIAN_POINT ( 'NONE',  ( 9.019176287578909879, -2.587454068350148351, 30.68340429815432202 ) ) ;
#3532 = CARTESIAN_POINT ( 'NONE',  ( -0.5916856709766812328, -10.88202310037936194, 33.43294751532457099 ) ) ;
#3533 = B_SPLINE_CURVE_WITH_KNOTS ( 'NONE', 3,
 ( #1379, #56, #20764, #62626, #6803, #83816, #69401, #54995, #40608, #7708 ),
 .UNSPECIFIED., .F., .F.,
 ( 4, 2, 2, 2, 4 ),
 ( 0.000000000000000000, 0.0001954311564186865221, 0.0003908623128373730441, 0.0005862934692560595662, 0.0007817246256747460882 ),
 .UNSPECIFIED. ) ;
#3534 = VECTOR ( 'NONE', #27048, 1000.000000000000227 ) ;
#3535 = CARTESIAN_POINT ( 'NONE',  ( -10.86536135943320502, -9.234221910056348293, 34.70572697212741531 ) ) ;
#3537 = ORIENTED_EDGE ( 'NONE', *, *, #16422, .T. ) ;
#3536 = EDGE_CURVE ( 'NONE', #87771, #4656, #47150, .T. ) ;
#3538 = CARTESIAN_POINT ( 'NONE',  ( 6.923076923077231548, -2.506253911140614576, 30.00000000000323297 ) ) ;
#3539 = CARTESIAN_POINT ( 'NONE',  ( -17.07692307692307665, -4.786620604624113540, 33.94971097300155094 ) ) ;
#3540 = CARTESIAN_POINT ( 'NONE',  ( -5.750054590621955342, -3.520799739797213501, 33.17531984108286025 ) ) ;
#3541 = FACE_BOUND ( 'NONE', #33905, .T. ) ;
#3542 = AXIS2_PLACEMENT_3D ( 'NONE', #21368, #42537, #23139 ) ;
#3543 = CARTESIAN_POINT ( 'NONE',  ( 15.16549878480845770, -6.026961402152685388, 34.52809138561120506 ) ) ;
#3545 = EDGE_CURVE ( 'NONE', #148, #38452, #20572, .T. ) ;
#3544 = CARTESIAN_POINT ( 'NONE',  ( 11.28848480751918437, -8.303909089506435137, 34.68538101551103381 ) ) ;
#3546 = VECTOR ( 'NONE', #50538, 1000.000000000000114 ) ;
#3547 = DIRECTION ( 'NONE',  ( 0.000000000000000000, 0.9848077530122072432, -0.1736481776669354937 ) ) ;
#3549 = CARTESIAN_POINT ( 'NONE',  ( -5.999999999999998224, -10.51840700105979565, 33.73612834413961536 ) ) ;
#3548 = CARTESIAN_POINT ( 'NONE',  ( -12.46153846153858247, -4.481592998941358097, 33.73612834414048933 ) ) ;
#3550 = CARTESIAN_POINT ( 'NONE',  ( -7.911424292114620727, -3.300289026998414865, 32.46337939537583139 ) ) ;
#3551 = CARTESIAN_POINT ( 'NONE',  ( 1.449870524128225036, -2.379036618887895305, 30.90682066428159303 ) ) ;
#3552 = ORIENTED_EDGE ( 'NONE', *, *, #82172, .F. ) ;
#3553 = EDGE_CURVE ( 'NONE', #81210, #35763, #61114, .T. ) ;
#3554 = CARTESIAN_POINT ( 'NONE',  ( 10.39189967166066708, -10.81261337010820256, 33.49550067578627477 ) ) ;
#3555 = EDGE_LOOP ( 'NONE', ( #25277, #67546, #29792, #69570 ) ) ;
#3556 = EDGE_LOOP ( 'NONE', ( #16356, #50702, #32472, #87338 ) ) ;
#3558 = CARTESIAN_POINT ( 'NONE',  ( 1.161689167099240194, -10.61292498521070549, 33.66303323003028680 ) ) ;
#3557 = CARTESIAN_POINT ( 'NONE',  ( -6.857821351800899023, -8.613356846314928816, 34.62446782046653482 ) ) ;
#3559 = CARTESIAN_POINT ( 'NONE',  ( 11.31497661389720832, -8.539481045369596401, 34.89627647299170832 ) ) ;
#3560 = CYLINDRICAL_SURFACE ( 'NONE', #84747, 0.2499999999999998890 ) ;
#3561 = CARTESIAN_POINT ( 'NONE',  ( -2.530619266599154038, -11.43668979543635089, 33.22377378376089752 ) ) ;
#3562 = ORIENTED_EDGE ( 'NONE', *, *, #35933, .T. ) ;
#3563 = DIRECTION ( 'NONE',  ( 0.000000000000000000, 0.000000000000000000, -1.000000000000000000 ) ) ;
#3564 = CARTESIAN_POINT ( 'NONE',  ( 6.856993512121043466, -3.513871655860377086, 32.76840700105978499 ) ) ;
#3565 = CARTESIAN_POINT ( 'NONE',  ( -12.59168567097668401, -5.195881422630166391, 34.18770438780619259 ) ) ;
#3566 = CARTESIAN_POINT ( 'NONE',  ( 5.076923076923075762, -2.499999999999998668, 29.75000000000001421 ) ) ;
#3567 = CARTESIAN_POINT ( 'NONE',  ( 4.153846153846154188, -13.87047571288749737, 32.06866353760679544 ) ) ;
#3568 = ADVANCED_FACE ( 'NONE', ( #56134 ), #48931, .F. ) ;
#3569 = CARTESIAN_POINT ( 'NONE',  ( 3.749999999999992006, -5.946699141100872943, 14.39062500000000178 ) ) ;
#3570 = ORIENTED_EDGE ( 'NONE', *, *, #76304, .T. ) ;
#3571 = ORIENTED_EDGE ( 'NONE', *, *, #23831, .F. ) ;
#3572 = CARTESIAN_POINT ( 'NONE',  ( -5.076923076923075762, -2.499999999999998668, 29.75000000000001421 ) ) ;
#3573 = EDGE_CURVE ( 'NONE', #32448, #64799, #80532, .T. ) ;
#3574 = ORIENTED_EDGE ( 'NONE', *, *, #36519, .T. ) ;
#3575 = CARTESIAN_POINT ( 'NONE',  ( -0.4615384615385840772, -12.16647553114689728, 32.15551576947799362 ) ) ;
#3576 = CARTESIAN_POINT ( 'NONE',  ( -12.39628289026243557, -10.21337939537593620, 33.94971097300152252 ) ) ;
#3577 = LINE ( 'NONE', #17552, #29459 ) ;
#3578 = CARTESIAN_POINT ( 'NONE',  ( 2.084865615213304491, -7.369208160676173236, 34.74850200257122879 ) ) ;
#3579 = CARTESIAN_POINT ( 'NONE',  ( 3.750000000000009770, -9.053300858899081760, 17.04687500000000000 ) ) ;
#3580 = DIRECTION ( 'NONE',  ( -0.000000000000000000, 0.9396926207859093161, -0.3420201433256663259 ) ) ;
#3582 = EDGE_LOOP ( 'NONE', ( #8943, #44814, #13659, #18476 ) ) ;
#3581 = AXIS2_PLACEMENT_3D ( 'NONE', #55321, #76932, #63404 ) ;
#3583 = CARTESIAN_POINT ( 'NONE',  ( -1.384615384615383471, -1.129524287112498415, 32.06866353760679544 ) ) ;
#3585 = EDGE_LOOP ( 'NONE', ( #22965, #230 ) ) ;
#3584 = CARTESIAN_POINT ( 'NONE',  ( -1.384615384615383471, -8.973038597847269315, 34.52809138561121927 ) ) ;
#3586 = CARTESIAN_POINT ( 'NONE',  ( 8.769230769230768274, -13.75783147151868846, 33.36296068462461051 ) ) ;
#3587 = CARTESIAN_POINT ( 'NONE',  ( 18.00000000000000000, -13.04860791097971706, 34.73218667398347037 ) ) ;
#3588 = CARTESIAN_POINT ( 'NONE',  ( -12.59222906464877134, -8.191372820521381826, 34.95448215188424967 ) ) ;
#3589 = EDGE_CURVE ( 'NONE', #88590, #78118, #24681, .T. ) ;
#3590 = CYLINDRICAL_SURFACE ( 'NONE', #6993, 0.2500000000000009437 ) ;
#3591 = LINE ( 'NONE', #17566, #8917 ) ;
#3592 = DIRECTION ( 'NONE',  ( 0.000000000000000000, 0.9848077530122072432, 0.1736481776669354937 ) ) ;
#3593 = DIRECTION ( 'NONE',  ( 0.000000000000000000, 0.000000000000000000, 1.000000000000000000 ) ) ;
#3594 = CARTESIAN_POINT ( 'NONE',  ( 0.06109907496451268821, -3.749999999999999556, 16.90811829374151287 ) ) ;
#3595 = ORIENTED_EDGE ( 'NONE', *, *, #77455, .T. ) ;
#3596 = CARTESIAN_POINT ( 'NONE',  ( -4.376772371362299907, -4.887634598454295265, 34.01352882383564946 ) ) ;
#3597 = ADVANCED_FACE ( 'NONE', ( #41300 ), #13373, .F. ) ;
#3598 = CARTESIAN_POINT ( 'NONE',  ( -13.25382494364843389, -9.929761469519743144, 34.40412654351204225 ) ) ;
#3599 = LINE ( 'NONE', #72503, #8832 ) ;
#3600 = CARTESIAN_POINT ( 'NONE',  ( 1.799775606325937360E-14, -10.25000000000000000, 26.03125000000000000 ) ) ;
#3601 = EDGE_CURVE ( 'NONE', #21923, #31481, #62869, .T. ) ;
#3602 = CARTESIAN_POINT ( 'NONE',  ( -3.361460697436788436, -8.999036380462717588, 34.52022231692819076 ) ) ;
#3603 = CARTESIAN_POINT ( 'NONE',  ( -17.30040802064702987, -2.599994579823202923, 30.74605699353653776 ) ) ;
#3605 = ORIENTED_EDGE ( 'NONE', *, *, #64105, .F. ) ;
#3604 = CARTESIAN_POINT ( 'NONE',  ( 8.519207531937805555, -11.37209801155882793, 32.91403422569033665 ) ) ;
#3606 = CARTESIAN_POINT ( 'NONE',  ( 1.944543648262996083, -5.555456351736983045, 19.31250000000000000 ) ) ;
#3607 = CARTESIAN_POINT ( 'NONE',  ( -1.514762594053607581, -10.19110544564091825, 33.96427741523702792 ) ) ;
#3608 = EDGE_LOOP ( 'NONE', ( #22359, #1291, #31792, #24930 ) ) ;
#3609 = EDGE_CURVE ( 'NONE', #12402, #39715, #52591, .T. ) ;
#3610 = CARTESIAN_POINT ( 'NONE',  ( -4.023055712879203938, -2.494656445102013453, 31.33466734024120015 ) ) ;
#3611 = ORIENTED_EDGE ( 'NONE', *, *, #82733, .T. ) ;
#3612 = CARTESIAN_POINT ( 'NONE',  ( 14.53070365930516061, -12.15243808032445827, 31.58219941686247978 ) ) ;
#3613 = CARTESIAN_POINT ( 'NONE',  ( -7.846153846153844924, -11.69971097300155272, 32.46337939537588113 ) ) ;
#3614 = VECTOR ( 'NONE', #80699, 1000.000000000000000 ) ;
#3615 = CARTESIAN_POINT ( 'NONE',  ( -1.634638621908348632, -4.335965774309649134, 33.62209801155881905 ) ) ;
#3616 = VERTEX_POINT ( 'NONE', #62431 ) ;
#3617 = CARTESIAN_POINT ( 'NONE',  ( 0.2380535369741292595, -4.988325925672468131, 34.36044203135681130 ) ) ;
#3618 = ORIENTED_EDGE ( 'NONE', *, *, #4431, .F. ) ;
#3619 = DIRECTION ( 'NONE',  ( -0.000000000000000000, 0.7660444431189791237, -0.6427876096865379196 ) ) ;
#3620 = EDGE_LOOP ( 'NONE', ( #78325, #40008 ) ) ;
#3621 = CARTESIAN_POINT ( 'NONE',  ( -6.673076923076920686, -2.499999999999999112, 29.81604066197450109 ) ) ;
#3622 = CARTESIAN_POINT ( 'NONE',  ( 12.46153846153833911, -12.27809138561165270, 31.22303859784587132 ) ) ;
#3623 = ORIENTED_EDGE ( 'NONE', *, *, #22161, .T. ) ;
#3624 = VECTOR ( 'NONE', #69672, 1000.000000000000000 ) ;
#3625 = CARTESIAN_POINT ( 'NONE',  ( -5.750054481651856619, -11.37275283266503756, 32.91324779482534524 ) ) ;
#3627 = ADVANCED_FACE ( 'NONE', ( #748 ), #14710, .F. ) ;
#3626 = CARTESIAN_POINT ( 'NONE',  ( -12.46153846153846168, -5.557115091759785130, 34.35708131394839171 ) ) ;
#3628 = CARTESIAN_POINT ( 'NONE',  ( 11.97435897435897623, -11.50000000000000000, 29.75000000000000355 ) ) ;
#3629 = CARTESIAN_POINT ( 'NONE',  ( 20.00000000000000000, -4.000000000000000000, 29.75000000000000355 ) ) ;
#3630 = CARTESIAN_POINT ( 'NONE',  ( -13.31936024510254590, -12.16647553114626490, 32.15551576947920864 ) ) ;
#3631 = ORIENTED_EDGE ( 'NONE', *, *, #64025, .F. ) ;
#3632 = ORIENTED_EDGE ( 'NONE', *, *, #85186, .T. ) ;
#3633 = VERTEX_POINT ( 'NONE', #7952 ) ;
#3635 = ORIENTED_EDGE ( 'NONE', *, *, #64166, .F. ) ;
#3634 = CARTESIAN_POINT ( 'NONE',  ( -19.50000000000000000, -7.500000000000000000, 33.75000000000000000 ) ) ;
#3636 = CARTESIAN_POINT ( 'NONE',  ( -8.992156986746914882, -9.886141570436013382, 34.14413921362392301 ) ) ;
#3637 = CARTESIAN_POINT ( 'NONE',  ( 1.449870955891410906, -2.892918686051626498, 31.69288490824025928 ) ) ;
#3638 = ORIENTED_EDGE ( 'NONE', *, *, #21291, .T. ) ;
#3639 = ORIENTED_EDGE ( 'NONE', *, *, #30452, .T. ) ;
#3640 = EDGE_LOOP ( 'NONE', ( #61494, #14865 ) ) ;
#3641 = CARTESIAN_POINT ( 'NONE',  ( -18.00000000000000000, -11.91647553114624358, 32.58852847137147535 ) ) ;
#3642 = VERTEX_POINT ( 'NONE', #83173 ) ;
#3643 = CARTESIAN_POINT ( 'NONE',  ( 2.557746619330623528, -4.235687564193446164, 33.53795663066793509 ) ) ;
#3644 = FACE_OUTER_BOUND ( 'NONE', #80112, .T. ) ;
#3645 = CARTESIAN_POINT ( 'NONE',  ( -9.822782877383410494, -7.276987145209185215, 34.99546412871779211 ) ) ;
#3646 = FACE_BOUND ( 'NONE', #42577, .T. ) ;
#3647 = EDGE_LOOP ( 'NONE', ( #62792, #87525, #25905, #75128, #60301 ) ) ;
#3648 = CARTESIAN_POINT ( 'NONE',  ( 2.177081948067780104, -7.722926236386453702, 34.74524107206102030 ) ) ;
#3650 = ADVANCED_FACE ( 'NONE', ( #20136 ), #6621, .F. ) ;
#3649 = CARTESIAN_POINT ( 'NONE',  ( 12.52760681254089903, -5.557115091759786019, 34.35708131394839882 ) ) ;
#3651 = DIRECTION ( 'NONE',  ( 0.000000000000000000, 0.9848077530122072432, 0.1736481776669354937 ) ) ;
#3652 = CARTESIAN_POINT ( 'NONE',  ( 8.992242120843616959, -3.105924265160262543, 32.13625925475356127 ) ) ;
#3653 = CARTESIAN_POINT ( 'NONE',  ( 17.20771488474786892, -8.999086150933472084, 34.52020707165672064 ) ) ;
#3654 = EDGE_LOOP ( 'NONE', ( #47561, #62986, #5738, #74868 ) ) ;
#3655 = EDGE_CURVE ( 'NONE', #32155, #88566, #56903, .T. ) ;
#3656 = CARTESIAN_POINT ( 'NONE',  ( -7.053768389744480949, -6.413092428213692742, 34.63065189839063152 ) ) ;
#3657 = VERTEX_POINT ( 'NONE', #9712 ) ;
#3658 = ORIENTED_EDGE ( 'NONE', *, *, #34878, .T. ) ;
#3660 = CARTESIAN_POINT ( 'NONE',  ( -9.626240358957616650, -8.164416787775445883, 34.95778746994558617 ) ) ;
#3659 = CARTESIAN_POINT ( 'NONE',  ( 2.307692307692309264, -6.681629849574314051, 35.83090037661290239 ) ) ;
#3661 = EDGE_CURVE ( 'NONE', #68446, #72207, #77728, .T. ) ;
#3662 = CARTESIAN_POINT ( 'NONE',  ( -10.74553182482283908, -12.27039167877662251, 31.24851455888617835 ) ) ;
#3663 = CARTESIAN_POINT ( 'NONE',  ( 12.46153846153846168, -13.75783147151868846, 33.36296068462461051 ) ) ;
#3664 = CARTESIAN_POINT ( 'NONE',  ( -1.326923076923076872, -3.499999999999999556, 29.75000000000000355 ) ) ;
#3665 = FACE_OUTER_BOUND ( 'NONE', #20317, .T. ) ;
#3666 = ORIENTED_EDGE ( 'NONE', *, *, #70394, .T. ) ;
#3667 = B_SPLINE_CURVE_WITH_KNOTS ( 'NONE', 3,
 ( #35911, #63366, #1673, #70128, #29595, #29161, #64239, #15197, #28252, #84105 ),
 .UNSPECIFIED., .F., .F.,
 ( 4, 2, 2, 2, 4 ),
 ( 0.0007817359430256287049, 0.0009771253907249945886, 0.001172514838424360255, 0.001367904286123725922, 0.001563293733823091806 ),
 .UNSPECIFIED. ) ;
#3668 = VECTOR ( 'NONE', #4082, 1000.000000000000000 ) ;
#3669 = CARTESIAN_POINT ( 'NONE',  ( 6.857806922520603976, -2.657715359629089225, 31.77849191805834295 ) ) ;
#3670 = CARTESIAN_POINT ( 'NONE',  ( -5.999999999999998224, -2.249999999999998668, 29.75000000000001776 ) ) ;
#3671 = CARTESIAN_POINT ( 'NONE',  ( 4.153846153846468603, -2.255955759149395501, 30.00000000000324363 ) ) ;
#3672 = CARTESIAN_POINT ( 'NONE',  ( -3.903791842207838148, -3.627508038966689607, 32.91356715214248396 ) ) ;
#3673 = VERTEX_POINT ( 'NONE', #50244 ) ;
#3674 = EDGE_CURVE ( 'NONE', #63787, #17157, #7458, .T. ) ;
#3675 = VERTEX_POINT ( 'NONE', #70536 ) ;
#3676 = FACE_BOUND ( 'NONE', #83568, .T. ) ;
#3677 = ORIENTED_EDGE ( 'NONE', *, *, #71444, .F. ) ;
#3678 = CARTESIAN_POINT ( 'NONE',  ( 11.60371667797437922, -12.51329471203373345, 31.30864560766537963 ) ) ;
#3679 = DIRECTION ( 'NONE',  ( -0.000000000000000000, -0.3420201433256694346, -0.9396926207859080948 ) ) ;
#3680 = VERTEX_POINT ( 'NONE', #37182 ) ;
#3681 = AXIS2_PLACEMENT_3D ( 'NONE', #35574, #49529, #56280 ) ;
#3682 = CARTESIAN_POINT ( 'NONE',  ( -16.37677311275299985, -11.43668979543635089, 33.22377378376089752 ) ) ;
#3683 = CARTESIAN_POINT ( 'NONE',  ( -10.74553182482283198, -6.852621066184266141, 34.70813303252209181 ) ) ;
#3684 = CARTESIAN_POINT ( 'NONE',  ( 16.08857570788537572, -8.613356846314824011, 34.62446782046655613 ) ) ;
#3685 = CARTESIAN_POINT ( 'NONE',  ( -6.792285115252136407, -3.062576670634119758, 32.05464942895959979 ) ) ;
#3686 = EDGE_LOOP ( 'NONE', ( #46969, #18682, #79831, #72227, #6479, #3837 ) ) ;
#3687 = CARTESIAN_POINT ( 'NONE',  ( -3.903791842207838148, -6.567000820036038355, 34.66262288849541306 ) ) ;
#3688 = VERTEX_POINT ( 'NONE', #56578 ) ;
#3690 = VERTEX_POINT ( 'NONE', #3397 ) ;
#3689 = DIRECTION ( 'NONE',  ( 1.000000000000000000, 0.000000000000000000, 0.000000000000000000 ) ) ;
#3691 = DIRECTION ( 'NONE',  ( 0.000000000000000000, 0.9396926207859126468, -0.3420201433256571111 ) ) ;
#3692 = DIRECTION ( 'NONE',  ( 0.000000000000000000, 0.000000000000000000, -1.000000000000000000 ) ) ;
#3693 = DIRECTION ( 'NONE',  ( -0.000000000000000000, -0.8660254037844397068, -0.4999999999999978906 ) ) ;
#3694 = CARTESIAN_POINT ( 'NONE',  ( 15.29683758177167086, -12.37446782046654192, 30.86335684631486842 ) ) ;
#3695 = CARTESIAN_POINT ( 'NONE',  ( -14.37377468705243899, -8.164416787775445883, 34.95778746994557906 ) ) ;
#3696 = DIRECTION ( 'NONE',  ( -0.000000000000000000, -0.9848077530122086864, -0.1736481776669273613 ) ) ;
#3697 = CARTESIAN_POINT ( 'NONE',  ( -2.749999999999999112, -7.438900925035484057, 14.09561829374151642 ) ) ;
#3698 = ORIENTED_EDGE ( 'NONE', *, *, #27739, .F. ) ;
#3699 = EDGE_CURVE ( 'NONE', #62418, #41186, #32201, .T. ) ;
#3700 = CARTESIAN_POINT ( 'NONE',  ( 4.946232473812769648, -11.93127051446800024, 32.56575433478200665 ) ) ;
#3701 = CARTESIAN_POINT ( 'NONE',  ( 8.102564102564102200, -7.500000000000000000, 29.75000000000000355 ) ) ;
#3702 = CARTESIAN_POINT ( 'NONE',  ( 7.846153846153846700, -2.249999999999998668, 29.50000000000001421 ) ) ;
#3704 = EDGE_LOOP ( 'NONE', ( #35032, #33615, #14508, #211 ) ) ;
#3703 = VECTOR ( 'NONE', #30517, 1000.000000000000114 ) ;
#3705 = ORIENTED_EDGE ( 'NONE', *, *, #12894, .F. ) ;
#3706 = CARTESIAN_POINT ( 'NONE',  ( -1.449866374776626055, -2.506253911140460922, 30.00000000000013856 ) ) ;
#3707 = CARTESIAN_POINT ( 'NONE',  ( -7.715628407920200438, -5.915461855592780260, 34.75538340440931506 ) ) ;
#3708 = CARTESIAN_POINT ( 'NONE',  ( -0.6850233861027920090, -9.417330523894424488, 34.63758898049880486 ) ) ;
#3709 = B_SPLINE_CURVE_WITH_KNOTS ( 'NONE', 3,
 ( #45821, #3051, #4395, #17471, #36845, #44925 ),
 .UNSPECIFIED., .F., .F.,
 ( 4, 2, 4 ),
 ( 0.0003909569690057817311, 0.0005862646681846062470, 0.0007815723673634307088 ),
 .UNSPECIFIED. ) ;
#3710 = CARTESIAN_POINT ( 'NONE',  ( 10.48523740594639619, -6.001485441113819874, 34.52039167877662607 ) ) ;
#3711 = CARTESIAN_POINT ( 'NONE',  ( 16.08776377448601735, -9.905515769479276145, 34.41647553114623292 ) ) ;
#3712 = EDGE_CURVE ( 'NONE', #48041, #62888, #16477, .T. ) ;
#3713 = CARTESIAN_POINT ( 'NONE',  ( -8.834501215191545853, -11.94971097300153140, 32.03036669348370680 ) ) ;
#3714 = B_SPLINE_CURVE_WITH_KNOTS ( 'NONE', 3,
 ( #70659, #71090, #1753, #77850, #8965, #71979, #22031, #36864, #85066, #29677 ),
 .UNSPECIFIED., .F., .F.,
 ( 4, 2, 2, 2, 4 ),
 ( 0.0007817246256747494492, 0.0009771112852218935378, 0.001172497944769037518, 0.001367884604316181498, 0.001563271263863325695 ),
 .UNSPECIFIED. ) ;
#3715 = DIRECTION ( 'NONE',  ( 0.000000000000000000, 0.6427876096865368094, 0.7660444431189802339 ) ) ;
#3716 = EDGE_LOOP ( 'NONE', ( #58715, #36906, #26630, #962 ) ) ;
#3717 = B_SPLINE_CURVE_WITH_KNOTS ( 'NONE', 3,
 ( #3763, #59153, #23590, #10531, #51941, #51481, #38902, #66360, #65903, #18626 ),
 .UNSPECIFIED., .F., .F.,
 ( 4, 2, 2, 2, 4 ),
 ( 0.000000000000000000, 0.0001954311564186882568, 0.0003908623128373765136, 0.0005862934692560647703, 0.0007817246256747530271 ),
 .UNSPECIFIED. ) ;
#3718 = B_SPLINE_CURVE_WITH_KNOTS ( 'NONE', 3,
 ( #73044, #85672, #17663, #23949, #72593, #10901, #59524, #11340, #59078, #87028 ),
 .UNSPECIFIED., .F., .F.,
 ( 4, 2, 2, 2, 4 ),
 ( 0.000000000000000000, 0.0001954339857564126514, 0.0003908679715128183098, 0.0005863019572692239681, 0.0007817359430256294638 ),
 .UNSPECIFIED. ) ;
#3719 = CARTESIAN_POINT ( 'NONE',  ( 6.066068351002440018, -10.51840700105979565, 33.73612834413962247 ) ) ;
#3720 = CARTESIAN_POINT ( 'NONE',  ( 16.15384615384615330, -1.466349020453238561, 30.81389545987213907 ) ) ;
#3721 = EDGE_CURVE ( 'NONE', #10587, #59888, #23562, .T. ) ;
#3722 = CARTESIAN_POINT ( 'NONE',  ( 6.923076923076924238, -6.343179335718451384, 34.87096338111211935 ) ) ;
#3723 = CARTESIAN_POINT ( 'NONE',  ( 9.561617089197389063, -2.494641256782728966, 31.33461815524612959 ) ) ;
#3724 = ORIENTED_EDGE ( 'NONE', *, *, #22949, .T. ) ;
#3725 = CARTESIAN_POINT ( 'NONE',  ( 13.63466969625370062, -6.567000820036036579, 34.66262288849541306 ) ) ;
#3726 = VERTEX_POINT ( 'NONE', #29556 ) ;
#3727 = CARTESIAN_POINT ( 'NONE',  ( 12.46153846153833911, -9.528491918059723176, 34.59228464037033035 ) ) ;
#3728 = CARTESIAN_POINT ( 'NONE',  ( 10.36536139116316058, -3.520140089381495585, 33.17453946501458262 ) ) ;
#3729 = FACE_OUTER_BOUND ( 'NONE', #37395, .T. ) ;
#3730 = VERTEX_POINT ( 'NONE', #57456 ) ;
#3732 = EDGE_CURVE ( 'NONE', #68579, #66377, #30432, .T. ) ;
#3731 = CARTESIAN_POINT ( 'NONE',  ( -1.607542343522232686, -12.64616026154729411, 30.79003144601913533 ) ) ;
#3733 = DIRECTION ( 'NONE',  ( 0.000000000000000000, 0.1736481776669267785, -0.9848077530122087975 ) ) ;
#3734 = CARTESIAN_POINT ( 'NONE',  ( 9.019230769232203571, -7.500000000000155431, 34.75000000000007105 ) ) ;
#3735 = CARTESIAN_POINT ( 'NONE',  ( -4.826868657009623753, -10.82426656108011720, 33.81400080652039009 ) ) ;
#3736 = EDGE_CURVE ( 'NONE', #88905, #54183, #64385, .T. ) ;
#3737 = EDGE_CURVE ( 'NONE', #52906, #5237, #35362, .T. ) ;
#3738 = VECTOR ( 'NONE', #79914, 1000.000000000000114 ) ;
#3739 = ORIENTED_EDGE ( 'NONE', *, *, #70719, .T. ) ;
#3740 = PLANE ( 'NONE',  #67370 ) ;
#3741 = ORIENTED_EDGE ( 'NONE', *, *, #1512, .T. ) ;
#3742 = CARTESIAN_POINT ( 'NONE',  ( -2.557715531913765439, -2.588893531581426544, 31.60682220781847818 ) ) ;
#3743 = ADVANCED_FACE ( 'NONE', ( #52912 ), #38077, .F. ) ;
#3744 = CARTESIAN_POINT ( 'NONE',  ( 4.853438133199126092, -12.24155766932282496, 31.33739205006857986 ) ) ;
#3745 = B_SPLINE_CURVE_WITH_KNOTS ( 'NONE', 3,
 ( #75209, #68876, #27459, #6306, #82413, #47276, #34206, #83292, #75630, #35091 ),
 .UNSPECIFIED., .F., .F.,
 ( 4, 2, 2, 2, 4 ),
 ( 0.000000000000000000, 0.0001954311564186866034, 0.0003908623128373732067, 0.0005862934692560597830, 0.0007817246256747464135 ),
 .UNSPECIFIED. ) ;
#3746 = CARTESIAN_POINT ( 'NONE',  ( -3.480769230769229061, -7.566083408709834757, 34.74999999999999289 ) ) ;
#3747 = CARTESIAN_POINT ( 'NONE',  ( 7.846153846153846700, -13.20930481340135110, 34.54067556320372745 ) ) ;
#3748 = B_SPLINE_CURVE_WITH_KNOTS ( 'NONE', 3,
 ( #26844, #81353, #34038, #61502, #20956, #40807, #67385, #27720, #33155, #19638 ),
 .UNSPECIFIED., .F., .F.,
 ( 4, 2, 2, 2, 4 ),
 ( 0.0007817359430256252354, 0.0009771253907249898181, 0.001172514838424354618, 0.001367904286123719200, 0.001563293733823083783 ),
 .UNSPECIFIED. ) ;
#3749 = AXIS2_PLACEMENT_3D ( 'NONE', #5078, #73991, #18600 ) ;
#3750 = LINE ( 'NONE', #73105, #68099 ) ;
#3751 = CARTESIAN_POINT ( 'NONE',  ( 14.98074599347626368, -11.86270091957321249, 32.19358267280087915 ) ) ;
#3752 = EDGE_LOOP ( 'NONE', ( #12490, #71544, #35024, #451, #52192 ) ) ;
#3753 = ORIENTED_EDGE ( 'NONE', *, *, #10731, .T. ) ;
#3754 = ORIENTED_EDGE ( 'NONE', *, *, #50268, .T. ) ;
#3755 = ORIENTED_EDGE ( 'NONE', *, *, #62683, .T. ) ;
#3756 = VERTEX_POINT ( 'NONE', #79520 ) ;
#3757 = CARTESIAN_POINT ( 'NONE',  ( -1.161835843346973096, -3.236590943229498585, 32.36255958852954251 ) ) ;
#3758 = CARTESIAN_POINT ( 'NONE',  ( -1.253823576790598304, -12.38066358083363738, 30.83685684665853444 ) ) ;
#3759 = CARTESIAN_POINT ( 'NONE',  ( -6.988327913238165934, -2.506253911140460477, 30.00000000000013856 ) ) ;
#3760 = DIRECTION ( 'NONE',  ( 0.000000000000000000, 0.1736481776669267785, -0.9848077530122087975 ) ) ;
#3761 = CARTESIAN_POINT ( 'NONE',  ( -13.63459212866397685, -3.436278759898153901, 33.07459398097509506 ) ) ;
#3762 = EDGE_CURVE ( 'NONE', #14846, #32458, #14960, .T. ) ;
#3763 = CARTESIAN_POINT ( 'NONE',  ( -12.46153846153846168, -12.34228464037088635, 31.77849191805839268 ) ) ;
#3764 = VECTOR ( 'NONE', #64961, 1000.000000000000000 ) ;
#3765 = CARTESIAN_POINT ( 'NONE',  ( -24.00000000000000000, -9.499999999999982236, 27.74999999999999645 ) ) ;
#3766 = CARTESIAN_POINT ( 'NONE',  ( -7.623374304885432551, -3.236590943229497253, 32.36255958852954251 ) ) ;
#3767 = CARTESIAN_POINT ( 'NONE',  ( -4.376772371362299907, -9.886141570436013382, 34.14413921362392301 ) ) ;
#3768 = EDGE_LOOP ( 'NONE', ( #32033, #51337, #64941, #21875 ) ) ;
#3769 = ORIENTED_EDGE ( 'NONE', *, *, #42615, .T. ) ;
#3770 = EDGE_CURVE ( 'NONE', #2392, #2085, #58787, .T. ) ;
#3771 = AXIS2_PLACEMENT_3D ( 'NONE', #57117, #30530, #3495 ) ;
#3772 = EDGE_LOOP ( 'NONE', ( #75303, #84039, #61919, #19823 ) ) ;
#3774 = EDGE_LOOP ( 'NONE', ( #10199, #84548, #42447, #64543 ) ) ;
#3773 = DIRECTION ( 'NONE',  ( -0.000000000000000000, 1.000000000000000000, -0.000000000000000000 ) ) ;
#3776 = CARTESIAN_POINT ( 'NONE',  ( 10.48523740594639619, -9.418419913701741919, 34.36755862841477693 ) ) ;
#3775 = CARTESIAN_POINT ( 'NONE',  ( 6.673053698855464511, -11.56360843649121861, 33.07473185843129926 ) ) ;
#3777 = ADVANCED_FACE ( 'NONE', ( #65986 ), #45270, .F. ) ;
#3778 = DIRECTION ( 'NONE',  ( 1.000000000000000000, 0.000000000000000000, 0.000000000000000000 ) ) ;
#3779 = CARTESIAN_POINT ( 'NONE',  ( -14.43838377435986864, -9.804603061927743113, 34.18744698557895845 ) ) ;
#3780 = ORIENTED_EDGE ( 'NONE', *, *, #63579, .F. ) ;
#3781 = ORIENTED_EDGE ( 'NONE', *, *, #80505, .F. ) ;
#3782 = ADVANCED_FACE ( 'NONE', ( #25457 ), #46177, .F. ) ;
#3783 = CARTESIAN_POINT ( 'NONE',  ( -2.372962753653082402, -12.46129190929999986, 30.37095296980880832 ) ) ;
#3784 = ORIENTED_EDGE ( 'NONE', *, *, #20149, .T. ) ;
#3785 = FACE_BOUND ( 'NONE', #28868, .T. ) ;
#3786 = CARTESIAN_POINT ( 'NONE',  ( 15.00784301325308157, -9.886141570436013382, 34.14413921362392301 ) ) ;
#3787 = CARTESIAN_POINT ( 'NONE',  ( -3.930834802233303282, -11.76359900205217457, 32.36225158514719880 ) ) ;
#3788 = ORIENTED_EDGE ( 'NONE', *, *, #26692, .T. ) ;
#3789 = CARTESIAN_POINT ( 'NONE',  ( 0.000000000000000000, -11.00000000000000000, 29.75000000000000355 ) ) ;
#3790 = CARTESIAN_POINT ( 'NONE',  ( -6.923076923076922462, -2.292212530054420494, 30.41441678777542634 ) ) ;
#3791 = CARTESIAN_POINT ( 'NONE',  ( 2.177544337960611642, -11.66186481527757479, 32.95055677023626117 ) ) ;
#3792 = VERTEX_POINT ( 'NONE', #72743 ) ;
#3793 = LINE ( 'NONE', #59183, #35643 ) ;
#3794 = DIRECTION ( 'NONE',  ( 0.000000000000000000, -6.938893903907222067E-15, 1.000000000000000000 ) ) ;
#3795 = ORIENTED_EDGE ( 'NONE', *, *, #26653, .T. ) ;
#3796 = ADVANCED_FACE ( 'NONE', ( #5187 ), #52027, .F. ) ;
#3797 = CARTESIAN_POINT ( 'NONE',  ( -5.076923076923075762, -13.75783147151868846, 33.36296068462461051 ) ) ;
#3798 = DIRECTION ( 'NONE',  ( 0.000000000000000000, 0.000000000000000000, -1.000000000000000000 ) ) ;
#3799 = ORIENTED_EDGE ( 'NONE', *, *, #51457, .F. ) ;
#3800 = CARTESIAN_POINT ( 'NONE',  ( 7.146089767170318297, -2.523321265292115090, 31.42251411153756280 ) ) ;
#3801 = CARTESIAN_POINT ( 'NONE',  ( -12.39547011053602432, -2.538708090699994813, 30.37095296980875503 ) ) ;
#3802 = CYLINDRICAL_SURFACE ( 'NONE', #28339, 0.2499999999999979738 ) ;
#3803 = CARTESIAN_POINT ( 'NONE',  ( -8.519285250882628446, -9.272278438253398036, 34.42582936511637115 ) ) ;
#3804 = CARTESIAN_POINT ( 'NONE',  ( -18.25002323729296450, -6.695914987888146541, 34.68535235679833306 ) ) ;
#3805 = VECTOR ( 'NONE', #55218, 1000.000000000000000 ) ;
#3806 = CARTESIAN_POINT ( 'NONE',  ( -0.2115384615384616196, -2.249999999999998668, 29.75000000000000355 ) ) ;
#3808 = CARTESIAN_POINT ( 'NONE',  ( 9.915087361285756629, -4.989023458446560255, 34.36081565061822118 ) ) ;
#3807 = CARTESIAN_POINT ( 'NONE',  ( -1.384615384615505151, -2.892918686052166066, 31.69288490824153470 ) ) ;
#3809 = DIRECTION ( 'NONE',  ( 0.000000000000000000, 0.9848077530122072432, 0.1736481776669354937 ) ) ;
#3811 = CARTESIAN_POINT ( 'NONE',  ( -5.076923076923199218, -2.657715359629662988, 31.77849191805970364 ) ) ;
#3810 = CARTESIAN_POINT ( 'NONE',  ( 2.980769230769232170, -2.249999999999998668, 29.75000000000000355 ) ) ;
#3812 = CARTESIAN_POINT ( 'NONE',  ( 1.139087296525997273, -4.749999999999992895, 15.48437500000000178 ) ) ;
#3813 = ORIENTED_EDGE ( 'NONE', *, *, #74543, .T. ) ;
#3814 = CARTESIAN_POINT ( 'NONE',  ( 0.3308469948709023556, -12.38065189839062263, 30.83690757178629482 ) ) ;
#3815 = ORIENTED_EDGE ( 'NONE', *, *, #58445, .F. ) ;
#3816 = VERTEX_POINT ( 'NONE', #4293 ) ;
#3817 = EDGE_CURVE ( 'NONE', #44275, #69035, #53547, .T. ) ;
#3818 = FACE_OUTER_BOUND ( 'NONE', #11087, .T. ) ;
#3820 = ORIENTED_EDGE ( 'NONE', *, *, #78843, .F. ) ;
#3819 = VECTOR ( 'NONE', #9595, 1000.000000000000000 ) ;
#3821 = CARTESIAN_POINT ( 'NONE',  ( 3.453548772037639214, -10.11255958852955850, 34.01340905677048454 ) ) ;
#3822 = CARTESIAN_POINT ( 'NONE',  ( 1.944543648263018731, -9.444543648262994751, 17.12500000000000000 ) ) ;
#3823 = CARTESIAN_POINT ( 'NONE',  ( -11.53846153846153655, -1.242168528481310874, 33.36296068462461051 ) ) ;
#3824 = EDGE_CURVE ( 'NONE', #48826, #63003, #39538, .T. ) ;
#3825 = CARTESIAN_POINT ( 'NONE',  ( -4.826868765284761942, -2.779044189368096163, 31.39831045268886456 ) ) ;
#3826 = CARTESIAN_POINT ( 'NONE',  ( -3.512820512820513663, -3.499999999999999556, 29.75000000000000355 ) ) ;
#3827 = CARTESIAN_POINT ( 'NONE',  ( 17.93472999944368240, -2.379036618887870436, 30.90682066428148644 ) ) ;
#3828 = CARTESIAN_POINT ( 'NONE',  ( -8.638705067467206788, -5.195472089885680766, 34.18748526763464923 ) ) ;
#3829 = DIRECTION ( 'NONE',  ( 0.000000000000000000, 0.7660444431189807890, 0.6427876096865361433 ) ) ;
#3830 = CARTESIAN_POINT ( 'NONE',  ( -7.846153846153844924, -12.10708131394839349, 31.69288490824020244 ) ) ;
#3831 = CARTESIAN_POINT ( 'NONE',  ( -1.553300858899081538, -11.25000000000000711, 19.85937500000000355 ) ) ;
#3832 = CARTESIAN_POINT ( 'NONE',  ( 1.607394925883797177, -3.236590943229498585, 32.36255958852954251 ) ) ;
#3833 = CARTESIAN_POINT ( 'NONE',  ( 13.13459216039393240, -3.520140089381495585, 33.17453946501458262 ) ) ;
#3834 = EDGE_CURVE ( 'NONE', #29630, #74179, #48822, .T. ) ;
#3835 = CARTESIAN_POINT ( 'NONE',  ( 14.43848411551709177, -3.062576670634119758, 32.05464942895959979 ) ) ;
#3836 = ORIENTED_EDGE ( 'NONE', *, *, #73095, .T. ) ;
#3837 = ORIENTED_EDGE ( 'NONE', *, *, #29448, .T. ) ;
#3838 = CARTESIAN_POINT ( 'NONE',  ( -6.673076923076923350, -7.500000000000001776, 35.04278698407183867 ) ) ;
#3839 = LINE ( 'NONE', #12384, #43124 ) ;
#3840 = CARTESIAN_POINT ( 'NONE',  ( -17.07692307692307665, -8.810774026931790459, 35.74407628777942847 ) ) ;
#3841 = FACE_OUTER_BOUND ( 'NONE', #46348, .T. ) ;
#3842 = CARTESIAN_POINT ( 'NONE',  ( 14.08476534878545827, -3.395401636524185474, 33.02366814457250399 ) ) ;
#3843 = AXIS2_PLACEMENT_3D ( 'NONE', #83402, #21684, #28908 ) ;
#3844 = CARTESIAN_POINT ( 'NONE',  ( -16.15384615384615330, -8.973038597847269315, 34.52809138561121927 ) ) ;
#3845 = EDGE_CURVE ( 'NONE', #12325, #44606, #81486, .T. ) ;
#3846 = ORIENTED_EDGE ( 'NONE', *, *, #42171, .F. ) ;
#3847 = CARTESIAN_POINT ( 'NONE',  ( -1.384615384615383471, -9.780366693483667717, 34.19971097300155094 ) ) ;
#3848 = EDGE_LOOP ( 'NONE', ( #9958, #53180 ) ) ;
#3849 = ORIENTED_EDGE ( 'NONE', *, *, #73890, .F. ) ;
#3850 = CARTESIAN_POINT ( 'NONE',  ( -5.776988648387149539, -5.667800583137508674, 34.40243808032445827 ) ) ;
#3851 = CARTESIAN_POINT ( 'NONE',  ( 12.46153846153846168, -2.249999999999998668, 29.50000000000001421 ) ) ;
#3852 = CARTESIAN_POINT ( 'NONE',  ( -4.219116154402472674, -12.70778746994557551, 30.41441678777548319 ) ) ;
#3853 = LINE ( 'NONE', #67347, #86829 ) ;
#3854 = CARTESIAN_POINT ( 'NONE',  ( -2.084912766423895558, -11.89424750095246175, 32.13594075562311758 ) ) ;
#3855 = ORIENTED_EDGE ( 'NONE', *, *, #77944, .T. ) ;
#3856 = VERTEX_POINT ( 'NONE', #13713 ) ;
#3857 = ORIENTED_EDGE ( 'NONE', *, *, #30161, .T. ) ;
#3858 = CARTESIAN_POINT ( 'NONE',  ( -6.923076923077045919, -12.16647553114689728, 32.15551576947799362 ) ) ;
#3859 = CARTESIAN_POINT ( 'NONE',  ( -6.000000000000121680, -9.528491918059723176, 34.59228464037033035 ) ) ;
#3860 = DIRECTION ( 'NONE',  ( 0.000000000000000000, -8.673617379884028076E-17, -1.000000000000000000 ) ) ;
#3861 = CARTESIAN_POINT ( 'NONE',  ( 10.36540787133602493, -4.818429247618089661, 34.26397095200675125 ) ) ;
#3862 = CARTESIAN_POINT ( 'NONE',  ( -4.377331097570101193, -8.496056993536548418, 34.65000542017679663 ) ) ;
#3863 = CARTESIAN_POINT ( 'NONE',  ( -15.90390063549801347, -2.824170634883621744, 31.52227843825337317 ) ) ;
#3864 = TOROIDAL_SURFACE ( 'NONE', #28319, 3.000000000000000888, 2.000000000000000000 ) ;
#3865 = ORIENTED_EDGE ( 'NONE', *, *, #23777, .F. ) ;
#3866 = ORIENTED_EDGE ( 'NONE', *, *, #468, .T. ) ;
#3867 = CARTESIAN_POINT ( 'NONE',  ( -3.750000000000008438, -5.946699141100917352, 22.67187500000000355 ) ) ;
#3868 = B_SPLINE_CURVE_WITH_KNOTS ( 'NONE', 3,
 ( #46035, #73066, #37491, #44684, #52787, #11819, #38845, #58207, #5053, #32517 ),
 .UNSPECIFIED., .F., .F.,
 ( 4, 2, 2, 2, 4 ),
 ( 0.000000000000000000, 0.0001954339857564054144, 0.0003908679715128108288, 0.0005863019572692162703, 0.0007817359430256216575 ),
 .UNSPECIFIED. ) ;
#3869 = ORIENTED_EDGE ( 'NONE', *, *, #38115, .F. ) ;
#3871 = EDGE_LOOP ( 'NONE', ( #60480, #5811, #3957, #27026 ) ) ;
#3870 = CARTESIAN_POINT ( 'NONE',  ( 15.48071474911737333, -5.852078868378309373, 34.47109172314383585 ) ) ;
#3872 = CARTESIAN_POINT ( 'NONE',  ( 7.911409417429871027, -12.46129190930001052, 30.37095296980870174 ) ) ;
#3873 = DIRECTION ( 'NONE',  ( 0.000000000000000000, 0.6427876096865368094, 0.7660444431189802339 ) ) ;
#3874 = B_SPLINE_CURVE_WITH_KNOTS ( 'NONE', 3,
 ( #3299, #22691, #83973, #15947, #72201, #77194, #64545, #70447, #10516, #29904 ),
 .UNSPECIFIED., .F., .F.,
 ( 4, 2, 2, 2, 4 ),
 ( 0.000000000000000000, 0.0001954339857564083146, 0.0003908679715128166293, 0.0005863019572692249439, 0.0007817359430256332585 ),
 .UNSPECIFIED. ) ;
#3875 = CARTESIAN_POINT ( 'NONE',  ( 1.553300858899086867, -3.749999999999992006, 16.73437500000000000 ) ) ;
#3876 = VERTEX_POINT ( 'NONE', #42087 ) ;
#3877 = CARTESIAN_POINT ( 'NONE',  ( -1.254089946381741871, -2.647132371071621471, 31.75357179365173010 ) ) ;
#3878 = ORIENTED_EDGE ( 'NONE', *, *, #69519, .F. ) ;
#3879 = DIRECTION ( 'NONE',  ( 0.000000000000000000, 0.1736481776669275834, 0.9848077530122086864 ) ) ;
#3880 = CYLINDRICAL_SURFACE ( 'NONE', #68751, 0.2500000000000009437 ) ;
#3881 = FACE_BOUND ( 'NONE', #28778, .T. ) ;
#3883 = DIRECTION ( 'NONE',  ( -0.000000000000000000, -0.5000000000000009992, -0.8660254037844380415 ) ) ;
#3882 = CARTESIAN_POINT ( 'NONE',  ( -16.15384615384615330, -12.29105614889573062, 35.45975837776705220 ) ) ;
#3884 = AXIS2_PLACEMENT_3D ( 'NONE', #41339, #8443, #62915 ) ;
#3885 = CARTESIAN_POINT ( 'NONE',  ( -13.19230769230769162, -11.50000000000000000, 29.75000000000000355 ) ) ;
#3886 = PLANE ( 'NONE',  #83698 ) ;
#3887 = ORIENTED_EDGE ( 'NONE', *, *, #79981, .F. ) ;
#3888 = FACE_OUTER_BOUND ( 'NONE', #46997, .T. ) ;
#3889 = CARTESIAN_POINT ( 'NONE',  ( 1.269044939587668397, -4.511073634464840332, 13.80223852175840626 ) ) ;
#3890 = ORIENTED_EDGE ( 'NONE', *, *, #17597, .F. ) ;
#3891 = CARTESIAN_POINT ( 'NONE',  ( -8.638705330997124676, -3.625058011473228703, 33.29252011169590020 ) ) ;
#3892 = CARTESIAN_POINT ( 'NONE',  ( -5.011667505647053211, -6.026961402152789304, 34.52809138561124769 ) ) ;
#3893 = CARTESIAN_POINT ( 'NONE',  ( 10.36536139116316235, -8.475808217655753651, 34.90892951860618609 ) ) ;
#3894 = DIRECTION ( 'NONE',  ( 1.000000000000000000, 0.000000000000000000, 0.000000000000000000 ) ) ;
#3895 = CARTESIAN_POINT ( 'NONE',  ( -22.75000000000000000, -10.50000000000000000, 29.75000000000000355 ) ) ;
#3896 = FACE_BOUND ( 'NONE', #17016, .T. ) ;
#3898 = DIRECTION ( 'NONE',  ( -1.000000000000000000, -0.000000000000000000, -0.000000000000000000 ) ) ;
#3897 = CARTESIAN_POINT ( 'NONE',  ( -2.557692307692305267, -2.499999999999998668, 29.75000000000000355 ) ) ;
#3899 = AXIS2_PLACEMENT_3D ( 'NONE', #7605, #49903, #68854 ) ;
#3900 = CYLINDRICAL_SURFACE ( 'NONE', #75550, 0.2499999999999997502 ) ;
#3902 = CARTESIAN_POINT ( 'NONE',  ( 0.5923289025054107038, -2.845873456487965747, 32.17976146951972538 ) ) ;
#3901 = CARTESIAN_POINT ( 'NONE',  ( 18.00000000000000000, -11.16473453929635440, 33.15142922261926373 ) ) ;
#3903 = CARTESIAN_POINT ( 'NONE',  ( -4.153846153846274980, -11.06231777344772027, 33.60647404775119895 ) ) ;
#3904 = CARTESIAN_POINT ( 'NONE',  ( 8.834486340506792601, -10.90142922261932057, 33.41473453929631887 ) ) ;
#3905 = CARTESIAN_POINT ( 'NONE',  ( -2.608446859217889546, -10.19485399968121264, 23.43563170625848713 ) ) ;
#3906 = ORIENTED_EDGE ( 'NONE', *, *, #40114, .T. ) ;
#3907 = EDGE_CURVE ( 'NONE', #77663, #76807, #19095, .T. ) ;
#3908 = B_SPLINE_CURVE_WITH_KNOTS ( 'NONE', 3,
 ( #9131, #10779, #66155, #66618, #58956, #59409, #84348, #42916, #4920, #32385 ),
 .UNSPECIFIED., .F., .F.,
 ( 4, 2, 2, 2, 4 ),
 ( 0.0007817359430256374869, 0.0009771253907250054306, 0.001172514838424373266, 0.001367904286123741101, 0.001563293733823109153 ),
 .UNSPECIFIED. ) ;
#3909 = CARTESIAN_POINT ( 'NONE',  ( -8.096130577096200653, -11.28823185664190376, 33.01397839955799896 ) ) ;
#3910 = CARTESIAN_POINT ( 'NONE',  ( 5.076923076923075762, -13.20930481340135110, 34.54067556320372745 ) ) ;
#3911 = CARTESIAN_POINT ( 'NONE',  ( 5.869309396889694774, -5.496505350115500121, 34.60290016733514307 ) ) ;
#3912 = CARTESIAN_POINT ( 'NONE',  ( 0.4769952865663710795, -10.20868217879685425, 29.42381992869616880 ) ) ;
#3913 = CARTESIAN_POINT ( 'NONE',  ( 2.307692307692309264, -13.87047571288749737, 32.06866353760679544 ) ) ;
#3914 = CARTESIAN_POINT ( 'NONE',  ( -12.46153846153858424, -6.835583212225970762, 34.95778746994575670 ) ) ;
#3915 = CARTESIAN_POINT ( 'NONE',  ( -2.694853999681210865, -4.891553140782108677, 23.74813170625849068 ) ) ;
#3916 = CARTESIAN_POINT ( 'NONE',  ( -15.29685161012936767, -12.62096338111211580, 30.90682066428152908 ) ) ;
#3917 = DIRECTION ( 'NONE',  ( 0.000000000000000000, 0.6427876096865368094, 0.7660444431189802339 ) ) ;
#3918 = CARTESIAN_POINT ( 'NONE',  ( -7.715363405186896451, -9.929761469519743144, 34.40412654351204225 ) ) ;
#3919 = FACE_OUTER_BOUND ( 'NONE', #55815, .T. ) ;
#3920 = CARTESIAN_POINT ( 'NONE',  ( -6.989160334032802346, -4.098570777380720287, 33.41473453929634729 ) ) ;
#3921 = CARTESIAN_POINT ( 'NONE',  ( 5.207713517890025123, -8.191423895709842640, 34.95447573519442130 ) ) ;
#3922 = LINE ( 'NONE', #72385, #16048 ) ;
#3923 = ADVANCED_FACE ( 'NONE', ( #47936 ), #28113, .F. ) ;
#3924 = CYLINDRICAL_SURFACE ( 'NONE', #78726, 0.2499999999999994726 ) ;
#3925 = ORIENTED_EDGE ( 'NONE', *, *, #49061, .T. ) ;
#3926 = DIRECTION ( 'NONE',  ( -0.000000000000000000, 0.7660444431189791237, -0.6427876096865379196 ) ) ;
#3927 = CARTESIAN_POINT ( 'NONE',  ( -5.750054590621957118, -2.589246495874657938, 31.60778113518102828 ) ) ;
#3928 = VECTOR ( 'NONE', #10062, 1000.000000000000000 ) ;
#3929 = CARTESIAN_POINT ( 'NONE',  ( -2.749999999999999112, -7.438900925035484057, 25.34561829374151642 ) ) ;
#3930 = CARTESIAN_POINT ( 'NONE',  ( -10.86536135943320502, -2.544273027872575366, 31.48422191005632342 ) ) ;
#3931 = CARTESIAN_POINT ( 'NONE',  ( -39.05038313613820122, -2.249999999999998668, 29.75000000000000355 ) ) ;
#3932 = ORIENTED_EDGE ( 'NONE', *, *, #27797, .T. ) ;
#3933 = CARTESIAN_POINT ( 'NONE',  ( 10.61538461538461675, -6.386643153685126251, 34.62446782046654192 ) ) ;
#3934 = CYLINDRICAL_SURFACE ( 'NONE', #28728, 0.2500000000000012212 ) ;
#3936 = VERTEX_POINT ( 'NONE', #68220 ) ;
#3935 = CARTESIAN_POINT ( 'NONE',  ( 8.769230769230768274, -2.486705287966279876, 31.30864560766543647 ) ) ;
#3937 = CARTESIAN_POINT ( 'NONE',  ( -13.63459212866397685, -10.06842814019191401, 34.32929386961144758 ) ) ;
#3938 = CARTESIAN_POINT ( 'NONE',  ( 15.23076923076923173, -6.435427911321262684, 35.78748833219616898 ) ) ;
#3939 = VECTOR ( 'NONE', #25329, 1000.000000000000000 ) ;
#3940 = DIRECTION ( 'NONE',  ( -0.000000000000000000, -0.3420201433256694346, -0.9396926207859080948 ) ) ;
#3941 = CARTESIAN_POINT ( 'NONE',  ( -13.38461538461538325, -3.050289026998446396, 32.03036669348365706 ) ) ;
#3942 = EDGE_LOOP ( 'NONE', ( #35822, #28676, #75035, #62032 ) ) ;
#3943 = DIRECTION ( 'NONE',  ( -0.000000000000000000, 0.3420201433256694346, -0.9396926207859080948 ) ) ;
#3944 = DIRECTION ( 'NONE',  ( -1.000000000000000000, -0.000000000000000000, -0.000000000000000000 ) ) ;
#3945 = EDGE_CURVE ( 'NONE', #34461, #49704, #58502, .T. ) ;
#3946 = DIRECTION ( 'NONE',  ( -0.000000000000000000, 0.8660254037844397068, -0.4999999999999978906 ) ) ;
#3947 = ORIENTED_EDGE ( 'NONE', *, *, #60976, .F. ) ;
#3948 = ORIENTED_EDGE ( 'NONE', *, *, #34547, .F. ) ;
#3949 = EDGE_CURVE ( 'NONE', #43000, #60966, #41755, .T. ) ;
#3950 = ORIENTED_EDGE ( 'NONE', *, *, #9686, .T. ) ;
#3951 = ADVANCED_FACE ( 'NONE', ( #203 ), #83069, .F. ) ;
#3952 = VECTOR ( 'NONE', #74260, 1000.000000000000000 ) ;
#3953 = FACE_OUTER_BOUND ( 'NONE', #65208, .T. ) ;
#3954 = CARTESIAN_POINT ( 'NONE',  ( 6.130525438233648039, -2.372941743896878286, 30.88044141588254377 ) ) ;
#3955 = CARTESIAN_POINT ( 'NONE',  ( -9.469294848214296678, -12.64618726649961289, 30.78989965857442712 ) ) ;
#3956 = FACE_OUTER_BOUND ( 'NONE', #54120, .T. ) ;
#3957 = ORIENTED_EDGE ( 'NONE', *, *, #5157, .T. ) ;
#3958 = AXIS2_PLACEMENT_3D ( 'NONE', #26557, #26996, #54011 ) ;
#3959 = ORIENTED_EDGE ( 'NONE', *, *, #37262, .T. ) ;
#3961 = VERTEX_POINT ( 'NONE', #6522 ) ;
#3960 = CARTESIAN_POINT ( 'NONE',  ( 15.36129493253279499, -5.195472089885680766, 34.18748526763464923 ) ) ;
#3962 = CARTESIAN_POINT ( 'NONE',  ( -5.207613680033381875, -2.494641256782728966, 31.33461815524612959 ) ) ;
#3963 = B_SPLINE_CURVE_WITH_KNOTS ( 'NONE', 3,
 ( #63054, #77471, #69392, #63944, #83354, #21639, #22089, #69829, #1368, #8136 ),
 .UNSPECIFIED., .F., .F.,
 ( 4, 2, 2, 2, 4 ),
 ( 0.000000000000000000, 0.0001954311564186868473, 0.0003908623128373736946, 0.0005862934692560605419, 0.0007817246256747473893 ),
 .UNSPECIFIED. ) ;
#3964 = CARTESIAN_POINT ( 'NONE',  ( 12.46153846153846168, -11.35647404775217417, 33.31231777344666511 ) ) ;
#3965 = CARTESIAN_POINT ( 'NONE',  ( 2.530703659305158393, -3.587049720035815348, 32.86302985866382897 ) ) ;
#3966 = CARTESIAN_POINT ( 'NONE',  ( -1.134669975237340367, -12.68172785388650681, 30.59649109432439573 ) ) ;
#3967 = ORIENTED_EDGE ( 'NONE', *, *, #75764, .F. ) ;
#3968 = ORIENTED_EDGE ( 'NONE', *, *, #34909, .F. ) ;
#3969 = ORIENTED_EDGE ( 'NONE', *, *, #48301, .F. ) ;
#3971 = ORIENTED_EDGE ( 'NONE', *, *, #76726, .T. ) ;
#3970 = CARTESIAN_POINT ( 'NONE',  ( 5.326977388561390470, -4.943051570960391494, 34.04725096376909477 ) ) ;
#3972 = DIRECTION ( 'NONE',  ( 0.000000000000000000, 0.000000000000000000, -1.000000000000000000 ) ) ;
#3973 = ADVANCED_FACE ( 'NONE', ( #67775 ), #83519, .F. ) ;
#3974 = VECTOR ( 'NONE', #64826, 1000.000000000000000 ) ;
#3975 = CARTESIAN_POINT ( 'NONE',  ( -13.51530685128294351, -6.413092428213692742, 34.63065189839063152 ) ) ;
#3976 = ORIENTED_EDGE ( 'NONE', *, *, #4874, .T. ) ;
#3977 = CARTESIAN_POINT ( 'NONE',  ( 12.46153846153833911, -6.835583212225970762, 34.95778746994575670 ) ) ;
#3978 = CARTESIAN_POINT ( 'NONE',  ( -2.307692307692305711, -12.29105614889573062, 35.45975837776705220 ) ) ;
#3979 = DIRECTION ( 'NONE',  ( 1.000000000000000000, 0.000000000000000000, 0.000000000000000000 ) ) ;
#3980 = VECTOR ( 'NONE', #70242, 1000.000000000000000 ) ;
#3981 = FACE_BOUND ( 'NONE', #25485, .T. ) ;
#3982 = CARTESIAN_POINT ( 'NONE',  ( -0.6844646790546080606, -4.186968288167446595, 33.49512374952580274 ) ) ;
#3983 = CARTESIAN_POINT ( 'NONE',  ( 9.469480999828689960, -7.369208160676172348, 34.74850200257122879 ) ) ;
#3984 = LINE ( 'NONE', #2214, #62440 ) ;
#3986 = CARTESIAN_POINT ( 'NONE',  ( -5.869474298236436738, -2.882268652242224505, 31.66798894389554064 ) ) ;
#3985 = DIRECTION ( 'NONE',  ( -0.000000000000000000, 0.6427876096865404731, -0.7660444431189770143 ) ) ;
#3987 = CARTESIAN_POINT ( 'NONE',  ( -11.47239318745910097, -3.050289026998446840, 32.03036669348366416 ) ) ;
#3988 = CARTESIAN_POINT ( 'NONE',  ( 2.294871794871793380, -7.500000000000000000, 29.75000000000000355 ) ) ;
#3989 = ORIENTED_EDGE ( 'NONE', *, *, #57321, .T. ) ;
#3990 = CARTESIAN_POINT ( 'NONE',  ( -16.15384615384627409, -3.643525952248796163, 33.31231777344771672 ) ) ;
#3991 = CARTESIAN_POINT ( 'NONE',  ( -7.596208327805703320, -2.587454068350147462, 30.68340429815432202 ) ) ;
#3992 = ORIENTED_EDGE ( 'NONE', *, *, #52615, .T. ) ;
#3993 = ORIENTED_EDGE ( 'NONE', *, *, #44371, .F. ) ;
#3994 = EDGE_CURVE ( 'NONE', #78946, #64675, #15916, .T. ) ;
#3996 = CARTESIAN_POINT ( 'NONE',  ( -5.869208192175212169, -12.11778462344220841, 31.66786338562085135 ) ) ;
#3995 = CARTESIAN_POINT ( 'NONE',  ( -11.60454391782167605, -12.62096338111211580, 30.90682066428152908 ) ) ;
#3997 = CARTESIAN_POINT ( 'NONE',  ( -6.857821351800898135, -6.879047030191282275, 34.71129190930002295 ) ) ;
#3998 = CARTESIAN_POINT ( 'NONE',  ( -5.198717948717948012, -7.500000000000000000, 29.75000000000000355 ) ) ;
#3999 = CARTESIAN_POINT ( 'NONE',  ( -14.98076923076779465, -7.500000000000155431, 34.75000000000007105 ) ) ;
#4000 = EDGE_LOOP ( 'NONE', ( #72568, #88952 ) ) ;
#4001 = CARTESIAN_POINT ( 'NONE',  ( 5.326923076923075762, -7.500000000000001776, 35.04278698407183867 ) ) ;
#4002 = CARTESIAN_POINT ( 'NONE',  ( -1.384615384615506484, -12.16647553114689728, 32.15551576947799362 ) ) ;
#4004 = CYLINDRICAL_SURFACE ( 'NONE', #61751, 0.2499999999999998890 ) ;
#4003 = CARTESIAN_POINT ( 'NONE',  ( 19.99999999999996803, 15.00000000000000711, 3.000000000000000000 ) ) ;
#4005 = CARTESIAN_POINT ( 'NONE',  ( -1.634638608836840756, -10.18141759479407327, 34.26406193332782379 ) ) ;
#4006 = CARTESIAN_POINT ( 'NONE',  ( 0.2115152373170040290, -3.520140089381497361, 33.17453946501458262 ) ) ;
#4007 = CARTESIAN_POINT ( 'NONE',  ( -17.01166793741023042, -2.657715359629131857, 31.77849191805844242 ) ) ;
#4008 = CARTESIAN_POINT ( 'NONE',  ( 2.651650429449569302, -10.15165042944953733, 23.37500000000000000 ) ) ;
#4009 = ORIENTED_EDGE ( 'NONE', *, *, #36789, .T. ) ;
#4010 = VERTEX_POINT ( 'NONE', #57796 ) ;
#4011 = EDGE_CURVE ( 'NONE', #64127, #17254, #64104, .T. ) ;
#4012 = AXIS2_PLACEMENT_3D ( 'NONE', #47900, #19109, #88476 ) ;
#4013 = LINE ( 'NONE', #31954, #31966 ) ;
#4014 = CARTESIAN_POINT ( 'NONE',  ( 17.07692307692295586, -4.320704448113951379, 33.92786785259630022 ) ) ;
#4015 = DIRECTION ( 'NONE',  ( -0.000000000000000000, -0.5000000000000009992, -0.8660254037844380415 ) ) ;
#4016 = CARTESIAN_POINT ( 'NONE',  ( 3.930919194939304973, -10.77366814457252175, 33.85459836347579454 ) ) ;
#4017 = EDGE_CURVE ( 'NONE', #65065, #26721, #85722, .T. ) ;
#4018 = CYLINDRICAL_SURFACE ( 'NONE', #57208, 0.2500000000000008882 ) ;
#4019 = CARTESIAN_POINT ( 'NONE',  ( -3.749999999999997335, -7.500000000000021316, 17.59375000000000000 ) ) ;
#4020 = CARTESIAN_POINT ( 'NONE',  ( -11.76194646302586655, -9.417330523894424488, 34.63758898049880486 ) ) ;
#4021 = LINE ( 'NONE', #32402, #50337 ) ;
#4022 = CIRCLE ( 'NONE', #22682, 4.000000000000000000 ) ;
#4023 = CYLINDRICAL_SURFACE ( 'NONE', #44457, 0.2500000000000009437 ) ;
#4024 = DIRECTION ( 'NONE',  ( -0.000000000000000000, -0.7660444431189791237, -0.6427876096865379196 ) ) ;
#4025 = CARTESIAN_POINT ( 'NONE',  ( -24.00000000000000000, 5.000000000000023093, 28.74999999999999645 ) ) ;
#4026 = CARTESIAN_POINT ( 'NONE',  ( 3.361294932532794100, -2.882268652242222284, 31.66798894389554064 ) ) ;
#4027 = CARTESIAN_POINT ( 'NONE',  ( -18.00000000000000000, -5.184797716151534175, 36.11096599634342397 ) ) ;
#4028 = CARTESIAN_POINT ( 'NONE',  ( 17.32692307692307665, -2.499999999999998668, 29.75000000000000355 ) ) ;
#4029 = CARTESIAN_POINT ( 'NONE',  ( 10.83839596699746366, -2.758310577978208666, 31.33698337089302299 ) ) ;
#4030 = ADVANCED_FACE ( 'NONE', ( #35772 ), #2838, .F. ) ;
#4031 = CARTESIAN_POINT ( 'NONE',  ( 7.780071466793711643, -3.322132147404559532, 32.92929555188719348 ) ) ;
#4032 = CARTESIAN_POINT ( 'NONE',  ( -15.23076923076935074, -3.300289026999228881, 32.46337939537708905 ) ) ;
#4033 = ORIENTED_EDGE ( 'NONE', *, *, #88681, .F. ) ;
#4034 = FACE_OUTER_BOUND ( 'NONE', #28136, .T. ) ;
#4035 = CARTESIAN_POINT ( 'NONE',  ( -5.326923076923075762, -7.500000000000001776, 35.00000000000000000 ) ) ;
#4036 = DIRECTION ( 'NONE',  ( -1.000000000000000000, -0.000000000000000000, -0.000000000000000000 ) ) ;
#4037 = CARTESIAN_POINT ( 'NONE',  ( 1.944543648262996083, -5.555456351736983045, 25.56250000000000355 ) ) ;
#4038 = EDGE_CURVE ( 'NONE', #56240, #51377, #5212, .T. ) ;
#4039 = CARTESIAN_POINT ( 'NONE',  ( -14.24162395668986747, -4.786620604624113540, 33.94971097300155805 ) ) ;
#4040 = CARTESIAN_POINT ( 'NONE',  ( 2.530705151785703322, -11.98016756924214832, 32.48728574198911190 ) ) ;
#4042 = ORIENTED_EDGE ( 'NONE', *, *, #13960, .T. ) ;
#4041 = CARTESIAN_POINT ( 'NONE',  ( 10.39255651774974076, -7.369209533119137845, 34.99857337881830688 ) ) ;
#4043 = CARTESIAN_POINT ( 'NONE',  ( -2.749999999999998224, -7.500000000000015987, 18.84375000000000000 ) ) ;
#4044 = DIRECTION ( 'NONE',  ( -0.000000000000000000, 0.5000000000000011102, -0.8660254037844381525 ) ) ;
#4045 = EDGE_CURVE ( 'NONE', #41861, #52419, #8406, .T. ) ;
#4046 = B_SPLINE_CURVE_WITH_KNOTS ( 'NONE', 3,
 ( #60153, #38564, #66018, #73236, #25492, #66479 ),
 .UNSPECIFIED., .F., .F.,
 ( 4, 2, 4 ),
 ( 4.220987180333913997E-17, 0.0001954756301637156914, 0.0003909512603273892074 ),
 .UNSPECIFIED. ) ;
#4047 = VERTEX_POINT ( 'NONE', #8743 ) ;
#4048 = CARTESIAN_POINT ( 'NONE',  ( 6.673053698855467175, -6.652501968072646932, 34.93155406624980941 ) ) ;
#4049 = EDGE_LOOP ( 'NONE', ( #71534, #10954, #36982, #59686 ) ) ;
#4050 = CARTESIAN_POINT ( 'NONE',  ( 3.230769230769231726, -1.466349020453238561, 30.81389545987213907 ) ) ;
#4051 = CARTESIAN_POINT ( 'NONE',  ( -1.515305987725691361, -11.93127051446800024, 32.56575433478200665 ) ) ;
#4052 = EDGE_CURVE ( 'NONE', #15474, #19611, #80362, .T. ) ;
#4053 = CARTESIAN_POINT ( 'NONE',  ( 17.07692307692295586, -6.835583212225970762, 34.95778746994575670 ) ) ;
#4054 = VERTEX_POINT ( 'NONE', #37520 ) ;
#4055 = CARTESIAN_POINT ( 'NONE',  ( -10.48459280755982981, -12.38066358083363738, 30.83685684665853444 ) ) ;
#4056 = ORIENTED_EDGE ( 'NONE', *, *, #50291, .T. ) ;
#4057 = CARTESIAN_POINT ( 'NONE',  ( -6.000000000000121680, -2.379036618888197729, 30.90682066428292885 ) ) ;
#4058 = AXIS2_PLACEMENT_3D ( 'NONE', #29828, #76228, #28497 ) ;
#4059 = EDGE_LOOP ( 'NONE', ( #64446, #17971, #7795, #35113 ) ) ;
#4060 = CARTESIAN_POINT ( 'NONE',  ( -0.4615384615385826339, -3.300289026999228881, 32.46337939537708905 ) ) ;
#4061 = FACE_OUTER_BOUND ( 'NONE', #78141, .T. ) ;
#4062 = EDGE_CURVE ( 'NONE', #63180, #2976, #24504, .T. ) ;
#4063 = EDGE_LOOP ( 'NONE', ( #83005, #56493, #12614, #77672 ) ) ;
#4064 = EDGE_CURVE ( 'NONE', #85264, #74870, #71429, .T. ) ;
#4065 = LINE ( 'NONE', #45945, #46226 ) ;
#4066 = CARTESIAN_POINT ( 'NONE',  ( 10.61538461538461675, -12.78798330534103123, 29.99999999999997868 ) ) ;
#4067 = DIRECTION ( 'NONE',  ( -0.000000000000000000, -0.1736481776669307198, -0.9848077530122080203 ) ) ;
#4068 = DIRECTION ( 'NONE',  ( 0.000000000000000000, 0.4999999999999985567, 0.8660254037844395958 ) ) ;
#4069 = CARTESIAN_POINT ( 'NONE',  ( -18.00000000000000000, -5.557115091759784242, 34.35708131394839171 ) ) ;
#4070 = ORIENTED_EDGE ( 'NONE', *, *, #77427, .T. ) ;
#4071 = ORIENTED_EDGE ( 'NONE', *, *, #18028, .T. ) ;
#4072 = EDGE_LOOP ( 'NONE', ( #78909, #62436, #43868, #71226 ) ) ;
#4074 = ORIENTED_EDGE ( 'NONE', *, *, #75691, .T. ) ;
#4073 = CARTESIAN_POINT ( 'NONE',  ( 15.23076923076923173, -2.538708090699994813, 30.37095296980875503 ) ) ;
#4075 = B_SPLINE_CURVE_WITH_KNOTS ( 'NONE', 3,
 ( #75609, #1285, #14358, #22882, #2167, #848 ),
 .UNSPECIFIED., .F., .F.,
 ( 4, 2, 4 ),
 ( 0.000000000000000000, 0.0001954784845028902692, 0.0003909569690057805385 ),
 .UNSPECIFIED. ) ;
#4076 = CARTESIAN_POINT ( 'NONE',  ( -6.923076923076922462, -8.120952969808772792, 34.71129190930000163 ) ) ;
#4077 = CARTESIAN_POINT ( 'NONE',  ( 6.250054419913455561, -10.06805714834173848, 34.32951233291982618 ) ) ;
#4078 = B_SPLINE_CURVE_WITH_KNOTS ( 'NONE', 3,
 ( #30981, #31440, #36859, #30548, #64321, #24225, #57576, #79632, #79185, #17486 ),
 .UNSPECIFIED., .F., .F.,
 ( 4, 2, 2, 2, 4 ),
 ( 0.000000000000000000, 0.0001954339857564090194, 0.0003908679715128180387, 0.0005863019572692270039, 0.0007817359430256360774 ),
 .UNSPECIFIED. ) ;
#4079 = ORIENTED_EDGE ( 'NONE', *, *, #62537, .T. ) ;
#4080 = EDGE_CURVE ( 'NONE', #62746, #27408, #42707, .T. ) ;
#4081 = ORIENTED_EDGE ( 'NONE', *, *, #16703, .F. ) ;
#4082 = DIRECTION ( 'NONE',  ( -0.000000000000000000, -0.5000000000000009992, -0.8660254037844380415 ) ) ;
#4083 = ORIENTED_EDGE ( 'NONE', *, *, #3436, .F. ) ;
#4084 = VECTOR ( 'NONE', #85447, 1000.000000000000000 ) ;
#4085 = CARTESIAN_POINT ( 'NONE',  ( 11.60452988946397745, -11.16473453929635440, 33.15142922261926373 ) ) ;
#4086 = ADVANCED_FACE ( 'NONE', ( #88735 ), #67121, .F. ) ;
#4087 = CARTESIAN_POINT ( 'NONE',  ( 17.01084069756293715, -12.34228464037088280, 31.77849191805838558 ) ) ;
#4088 = ADVANCED_FACE ( 'NONE', ( #19368 ), #12174, .F. ) ;
#4089 = CARTESIAN_POINT ( 'NONE',  ( -16.08859101433330707, -11.06231777344670775, 33.60647404775212266 ) ) ;
#4090 = ADVANCED_FACE ( 'NONE', ( #12619 ), #59906, .F. ) ;
#4091 = FACE_BOUND ( 'NONE', #82233, .T. ) ;
#4092 = EDGE_LOOP ( 'NONE', ( #69559, #18044 ) ) ;
#4093 = CARTESIAN_POINT ( 'NONE',  ( -7.846153846153844924, -2.499999999999998668, 29.75000000000001421 ) ) ;
#4094 = DIRECTION ( 'NONE',  ( 0.000000000000000000, 0.7660444431189807890, 0.6427876096865361433 ) ) ;
#4095 = EDGE_CURVE ( 'NONE', #56825, #33571, #11733, .T. ) ;
#4096 = CARTESIAN_POINT ( 'NONE',  ( -13.38461538461538325, -12.62096338111211580, 30.90682066428153263 ) ) ;
#4097 = CARTESIAN_POINT ( 'NONE',  ( -14.37296275365308418, -9.442884908240170461, 34.35708131394840592 ) ) ;
#4098 = CARTESIAN_POINT ( 'NONE',  ( 19.00000000000000000, -13.24999999999999822, 22.25000000000000000 ) ) ;
#4099 = ORIENTED_EDGE ( 'NONE', *, *, #75056, .F. ) ;
#4100 = CARTESIAN_POINT ( 'NONE',  ( -7.146561866800870355, -6.760086850603068243, 34.69517049084099369 ) ) ;
#4101 = ORIENTED_EDGE ( 'NONE', *, *, #50813, .F. ) ;
#4102 = ORIENTED_EDGE ( 'NONE', *, *, #37745, .F. ) ;
#4103 = EDGE_CURVE ( 'NONE', #9873, #48052, #5861, .T. ) ;
#4105 = CARTESIAN_POINT ( 'NONE',  ( -1.449885385171703289, -5.941354392334500467, 34.76329471203369792 ) ) ;
#4104 = CARTESIAN_POINT ( 'NONE',  ( -7.146561847641255127, -4.225889041578354544, 33.85425143139329407 ) ) ;
#4106 = CARTESIAN_POINT ( 'NONE',  ( -8.519285359852727169, -12.45601412856602686, 31.48342859153981621 ) ) ;
#4107 = LINE ( 'NONE', #51381, #45120 ) ;
#4108 = CARTESIAN_POINT ( 'NONE',  ( 1.515407192440173301, -9.804649428959606894, 34.18742332936588468 ) ) ;
#4109 = CARTESIAN_POINT ( 'NONE',  ( -11.60454391782167427, -2.292212530054419606, 30.41441678777542634 ) ) ;
#4110 = ORIENTED_EDGE ( 'NONE', *, *, #23019, .T. ) ;
#4111 = CARTESIAN_POINT ( 'NONE',  ( 6.699591998512590685, -2.612411019501189813, 31.66733052389439962 ) ) ;
#4112 = DIRECTION ( 'NONE',  ( -0.000000000000000000, -0.5000000000000009992, -0.8660254037844380415 ) ) ;
#4113 = CARTESIAN_POINT ( 'NONE',  ( 2.307692307692186251, -12.70778746994576025, 30.41441678777401236 ) ) ;
#4114 = CARTESIAN_POINT ( 'NONE',  ( 10.86533013373275836, -11.86320923018887719, 32.19269448109604070 ) ) ;
#4115 = VERTEX_POINT ( 'NONE', #13058 ) ;
#4116 = VECTOR ( 'NONE', #46671, 1000.000000000000000 ) ;
#4117 = B_SPLINE_CURVE_WITH_KNOTS ( 'NONE', 3,
 ( #88072, #25892, #81291, #74522, #12817, #73651 ),
 .UNSPECIFIED., .F., .F.,
 ( 4, 2, 4 ),
 ( 0.0003909569690057827069, 0.0005862646681846092828, 0.0007815723673634358045 ),
 .UNSPECIFIED. ) ;
#4118 = ORIENTED_EDGE ( 'NONE', *, *, #24235, .F. ) ;
#4119 = FACE_BOUND ( 'NONE', #73231, .T. ) ;
#4120 = CONTEXT_DEPENDENT_SHAPE_REPRESENTATION ( #63636, #72208 ) ;
#4121 = VERTEX_POINT ( 'NONE', #20260 ) ;
#4122 = CARTESIAN_POINT ( 'NONE',  ( 18.24994540937804643, -12.68172785388650681, 30.59649109432439573 ) ) ;
#4123 = CARTESIAN_POINT ( 'NONE',  ( 6.923076923076924238, -12.10708131394839349, 31.69288490824020244 ) ) ;
#4124 = ORIENTED_EDGE ( 'NONE', *, *, #20014, .T. ) ;
#4125 = CARTESIAN_POINT ( 'NONE',  ( -3.361460697436789324, -12.38065189839062263, 30.83690757178629482 ) ) ;
#4126 = FACE_OUTER_BOUND ( 'NONE', #733, .T. ) ;
#4127 = CYLINDRICAL_SURFACE ( 'NONE', #16458, 0.2499999999999997502 ) ;
#4128 = EDGE_CURVE ( 'NONE', #31550, #87883, #51453, .T. ) ;
#4129 = CARTESIAN_POINT ( 'NONE',  ( -1.384615384615383471, -3.937682226553329556, 33.60647404775216529 ) ) ;
#4130 = EDGE_CURVE ( 'NONE', #20820, #6804, #87878, .T. ) ;
#4131 = CARTESIAN_POINT ( 'NONE',  ( -0.4615384615384611200, -1.629998284177014645, 34.34916445242399163 ) ) ;
#4132 = ORIENTED_EDGE ( 'NONE', *, *, #13927, .T. ) ;
#4134 = ORIENTED_EDGE ( 'NONE', *, *, #49668, .F. ) ;
#4133 = CARTESIAN_POINT ( 'NONE',  ( -15.10024379253558635, -2.372941743896879174, 30.88044141588253666 ) ) ;
#4135 = CARTESIAN_POINT ( 'NONE',  ( -16.15384615384615330, -2.499999999999998668, 29.75000000000001421 ) ) ;
#4136 = CARTESIAN_POINT ( 'NONE',  ( 15.23076923076910916, -5.094484230521993062, 34.41647553114689373 ) ) ;
#4137 = LINE ( 'NONE', #37479, #81837 ) ;
#4138 = CARTESIAN_POINT ( 'NONE',  ( 18.25005431163831204, -8.303483539816726378, 34.68545999027711702 ) ) ;
#4139 = CARTESIAN_POINT ( 'NONE',  ( -5.999999999999683808, -2.255955759149395501, 30.00000000000324363 ) ) ;
#4140 = CARTESIAN_POINT ( 'NONE',  ( 5.326977388561390470, -12.41262288849542017, 30.68299917996395010 ) ) ;
#4141 = CARTESIAN_POINT ( 'NONE',  ( -2.724691934501246582, -6.299813628509474128, 14.17374329374151287 ) ) ;
#4142 = ORIENTED_EDGE ( 'NONE', *, *, #16662, .F. ) ;
#4143 = DIRECTION ( 'NONE',  ( -0.000000000000000000, 0.3420201433256694346, -0.9396926207859080948 ) ) ;
#4144 = LINE ( 'NONE', #39735, #21807 ) ;
#4145 = FACE_OUTER_BOUND ( 'NONE', #47836, .T. ) ;
#4146 = B_SPLINE_CURVE_WITH_KNOTS ( 'NONE', 3,
 ( #59943, #75244, #13974, #77013, #69805, #83779, #63485, #48199, #56293, #41904 ),
 .UNSPECIFIED., .F., .F.,
 ( 4, 2, 2, 2, 4 ),
 ( 0.000000000000000000, 0.0001954339857564091007, 0.0003908679715128182013, 0.0005863019572692273291, 0.0007817359430256364027 ),
 .UNSPECIFIED. ) ;
#4147 = AXIS2_PLACEMENT_3D ( 'NONE', #88267, #13459, #32850 ) ;
#4148 = ORIENTED_EDGE ( 'NONE', *, *, #48127, .F. ) ;
#4149 = VERTEX_POINT ( 'NONE', #66670 ) ;
#4150 = CARTESIAN_POINT ( 'NONE',  ( -8.992715693795100051, -5.827078755546623690, 34.72654668319379567 ) ) ;
#4151 = CARTESIAN_POINT ( 'NONE',  ( -7.846153846153967493, -5.941354392335915335, 34.76329471203413846 ) ) ;
#4152 = CARTESIAN_POINT ( 'NONE',  ( -0.7115152055870527237, -9.234221910056348293, 34.70572697212741531 ) ) ;
#4153 = B_SPLINE_CURVE_WITH_KNOTS ( 'NONE', 3,
 ( #81455, #75138, #87783, #26500, #19740, #26056, #53963, #27386, #87331, #74693 ),
 .UNSPECIFIED., .F., .F.,
 ( 4, 2, 2, 2, 4 ),
 ( 0.000000000000000000, 0.0001954311564186868202, 0.0003908623128373735320, 0.0005862934692560603251, 0.0007817246256747470640 ),
 .UNSPECIFIED. ) ;
#4154 = VECTOR ( 'NONE', #80200, 1000.000000000000000 ) ;
#4155 = CARTESIAN_POINT ( 'NONE',  ( 13.31853300525525086, -2.833524468853757305, 32.15551576947924417 ) ) ;
#4156 = B_SPLINE_CURVE_WITH_KNOTS ( 'NONE', 3,
 ( #32813, #81457, #74696, #12986, #28718, #7562, #62052, #70138, #8449, #35921 ),
 .UNSPECIFIED., .F., .F.,
 ( 4, 2, 2, 2, 4 ),
 ( 0.0007817359430256215491, 0.0009771253907249856981, 0.001172514838424349847, 0.001367904286123713779, 0.001563293733823077928 ),
 .UNSPECIFIED. ) ;
#4157 = DIRECTION ( 'NONE',  ( -0.000000000000000000, 1.000000000000000000, -0.000000000000000000 ) ) ;
#4158 = AXIS2_PLACEMENT_3D ( 'NONE', #66634, #18450, #74282 ) ;
#4159 = CARTESIAN_POINT ( 'NONE',  ( -7.146003140593069958, -11.76352882383564769, 32.36236540154569497 ) ) ;
#4160 = B_SPLINE_CURVE_WITH_KNOTS ( 'NONE', 3,
 ( #55784, #82835, #22009, #75610, #35075, #14359, #76953, #20676, #40523, #7167 ),
 .UNSPECIFIED., .F., .F.,
 ( 4, 2, 2, 2, 4 ),
 ( 0.000000000000000000, 0.0001954311584214072923, 0.0003908623168428145846, 0.0005862934752642218498, 0.0007817246336856291692 ),
 .UNSPECIFIED. ) ;
#4161 = ORIENTED_EDGE ( 'NONE', *, *, #42753, .F. ) ;
#4162 = CARTESIAN_POINT ( 'NONE',  ( -3.230769230769352962, -12.70778746994576025, 30.41441678777401236 ) ) ;
#4163 = DIRECTION ( 'NONE',  ( -1.000000000000000000, -1.734723475976813504E-16, 0.000000000000000000 ) ) ;
#4164 = EDGE_CURVE ( 'NONE', #22486, #11909, #49253, .T. ) ;
#4165 = VECTOR ( 'NONE', #4349, 1000.000000000000000 ) ;
#4166 = EDGE_CURVE ( 'NONE', #40441, #40827, #64213, .T. ) ;
#4167 = CARTESIAN_POINT ( 'NONE',  ( 7.053602361310569613, -6.808710257144159783, 34.95449254468098843 ) ) ;
#4168 = CARTESIAN_POINT ( 'NONE',  ( 17.07692307692339284, -2.255955759149395501, 30.00000000000324363 ) ) ;
#4169 = ORIENTED_EDGE ( 'NONE', *, *, #50814, .F. ) ;
#4170 = CARTESIAN_POINT ( 'NONE',  ( 23.49999999999998934, -9.499999999999982236, 32.75000000000000000 ) ) ;
#4171 = ADVANCED_FACE ( 'NONE', ( #18928 ), #46397, .F. ) ;
#4172 = EDGE_LOOP ( 'NONE', ( #11667, #17271 ) ) ;
#4173 = CARTESIAN_POINT ( 'NONE',  ( 1.634615384615450084, -7.434744429011176159, 34.75000000000000711 ) ) ;
#4174 =( LENGTH_UNIT ( ) NAMED_UNIT ( * ) SI_UNIT ( .MILLI., .METRE. ) );
#4175 = CARTESIAN_POINT ( 'NONE',  ( 16.40384615384617462, -2.249999999999997780, 29.81603969181029257 ) ) ;
#4176 = CARTESIAN_POINT ( 'NONE',  ( -0.4615384615384611200, -4.661471528628507777, 34.16647553114623292 ) ) ;
#4177 = ORIENTED_EDGE ( 'NONE', *, *, #5225, .F. ) ;
#4178 = ADVANCED_FACE ( 'NONE', ( #8518 ), #7634, .F. ) ;
#4179 = DIRECTION ( 'NONE',  ( 0.000000000000000000, 0.000000000000000000, -1.000000000000000000 ) ) ;
#4180 = CARTESIAN_POINT ( 'NONE',  ( 5.869308533332442401, -9.804603061927743113, 34.18744698557895845 ) ) ;
#4181 = CARTESIAN_POINT ( 'NONE',  ( -6.792551484843277976, -12.50538340440932217, 31.33453814440721885 ) ) ;
#4182 = EDGE_CURVE ( 'NONE', #29819, #65895, #7294, .T. ) ;
#4183 = LINE ( 'NONE', #79854, #35127 ) ;
#4184 = CARTESIAN_POINT ( 'NONE',  ( -11.00641025641025550, -11.00000000000000000, 29.75000000000000355 ) ) ;
#4185 = ORIENTED_EDGE ( 'NONE', *, *, #52252, .F. ) ;
#4186 = CARTESIAN_POINT ( 'NONE',  ( 7.596177102105255763, -11.47974371597207899, 33.17467449705390692 ) ) ;
#4187 = ORIENTED_EDGE ( 'NONE', *, *, #69668, .F. ) ;
#4189 = EDGE_CURVE ( 'NONE', #4777, #84330, #21330, .T. ) ;
#4188 = CARTESIAN_POINT ( 'NONE',  ( 5.207713517890026900, -11.37503395064541678, 33.29242100308974983 ) ) ;
#4190 = AXIS2_PLACEMENT_3D ( 'NONE', #16875, #79022, #17322 ) ;
#4191 = FACE_OUTER_BOUND ( 'NONE', #38214, .T. ) ;
#4192 = CARTESIAN_POINT ( 'NONE',  ( -0.3310130233048198534, -2.647132371071621915, 31.75357179365173010 ) ) ;
#4193 = CARTESIAN_POINT ( 'NONE',  ( 7.715463243043540587, -12.35290016733513951, 31.75349464988449455 ) ) ;
#4194 = EDGE_CURVE ( 'NONE', #25778, #5919, #83546, .T. ) ;
#4195 = CARTESIAN_POINT ( 'NONE',  ( -5.999999999999998224, -4.098570777380720287, 33.41473453929634729 ) ) ;
#4196 = CARTESIAN_POINT ( 'NONE',  ( -2.294871794871794712, -7.500000000000000000, 29.75000000000000355 ) ) ;
#4197 = ORIENTED_EDGE ( 'NONE', *, *, #16463, .T. ) ;
#4198 = VERTEX_POINT ( 'NONE', #22027 ) ;
#4199 = ORIENTED_EDGE ( 'NONE', *, *, #46404, .F. ) ;
#4200 = B_SPLINE_CURVE_WITH_KNOTS ( 'NONE', 3,
 ( #62067, #60294, #81917, #74265, #89126, #14327, #6255, #34601, #21073, #53533 ),
 .UNSPECIFIED., .F., .F.,
 ( 4, 2, 2, 2, 4 ),
 ( 0.000000000000000000, 0.0001954339857564074473, 0.0003908679715128148945, 0.0005863019572692223418, 0.0007817359430256297891 ),
 .UNSPECIFIED. ) ;
#4201 = ORIENTED_EDGE ( 'NONE', *, *, #73939, .T. ) ;
#4203 = VERTEX_POINT ( 'NONE', #28333 ) ;
#4202 = EDGE_CURVE ( 'NONE', #79454, #65351, #52420, .T. ) ;
#4204 = DIRECTION ( 'NONE',  ( -1.000000000000000000, -2.602085213965214586E-16, 0.000000000000000000 ) ) ;
#4205 = CYLINDRICAL_SURFACE ( 'NONE', #54603, 0.2500000000000004996 ) ;
#4206 = CARTESIAN_POINT ( 'NONE',  ( -10.39260494640654819, -4.989023458446560255, 34.36081565061822118 ) ) ;
#4207 = EDGE_CURVE ( 'NONE', #80539, #64011, #78272, .T. ) ;
#4208 = CARTESIAN_POINT ( 'NONE',  ( -7.053768389744483613, -3.062553014421049546, 32.05460306192773601 ) ) ;
#4209 = CARTESIAN_POINT ( 'NONE',  ( 13.31853197365950692, -8.120952969808774569, 34.71129190930000163 ) ) ;
#4210 = CARTESIAN_POINT ( 'NONE',  ( 0.6843180028068696075, -5.114059244376869984, 34.14424750095245287 ) ) ;
#4211 = VECTOR ( 'NONE', #14778, 1000.000000000000000 ) ;
#4212 = DIRECTION ( 'NONE',  ( 1.000000000000000000, -0.000000000000000000, -0.000000000000000000 ) ) ;
#4213 = LINE ( 'NONE', #71778, #7812 ) ;
#4214 = LINE ( 'NONE', #66811, #56233 ) ;
#4215 = EDGE_LOOP ( 'NONE', ( #60600, #50026 ) ) ;
#4216 = ORIENTED_EDGE ( 'NONE', *, *, #61033, .F. ) ;
#4217 = B_SPLINE_CURVE_WITH_KNOTS ( 'NONE', 3,
 ( #69911, #49198, #56403, #14977, #20837, #83890, #82562, #7772, #76677, #28486 ),
 .UNSPECIFIED., .F., .F.,
 ( 4, 2, 2, 2, 4 ),
 ( 0.000000000000000000, 0.0001954311564186862239, 0.0003908623128373724478, 0.0005862934692560586988, 0.0007817246256747448956 ),
 .UNSPECIFIED. ) ;
#4218 = EDGE_LOOP ( 'NONE', ( #49024, #33790, #37115, #25724 ) ) ;
#4219 = CIRCLE ( 'NONE', #9944, 2.000000000000001776 ) ;
#4222 = ORIENTED_EDGE ( 'NONE', *, *, #28490, .T. ) ;
#4221 = EDGE_CURVE ( 'NONE', #65186, #28534, #36325, .T. ) ;
#4220 = CARTESIAN_POINT ( 'NONE',  ( 0.3962684609821406356, -12.16647553114622049, 32.15551576947930812 ) ) ;
#4224 = CARTESIAN_POINT ( 'NONE',  ( -0.4615384615384611200, -1.215029322943914858, 32.30358669280327177 ) ) ;
#4223 = CARTESIAN_POINT ( 'NONE',  ( -16.15384615384627409, -6.879047030192662504, 34.71129190930017927 ) ) ;
#4225 = DIRECTION ( 'NONE',  ( -0.000000000000000000, 0.3420201433256694346, -0.9396926207859080948 ) ) ;
#4226 = CARTESIAN_POINT ( 'NONE',  ( -10.61538461538473399, -11.94971097300221174, 32.03036669348237098 ) ) ;
#4227 = FACE_BOUND ( 'NONE', #25106, .T. ) ;
#4228 = ORIENTED_EDGE ( 'NONE', *, *, #72896, .T. ) ;
#4229 = EDGE_CURVE ( 'NONE', #18188, #20537, #68544, .T. ) ;
#4230 = ORIENTED_EDGE ( 'NONE', *, *, #52347, .T. ) ;
#4231 = CARTESIAN_POINT ( 'NONE',  ( -6.923076923077045919, -5.094484230521993062, 34.41647553114689373 ) ) ;
#4232 = ORIENTED_EDGE ( 'NONE', *, *, #30406, .F. ) ;
#4233 = FACE_BOUND ( 'NONE', #70260, .T. ) ;
#4234 = CARTESIAN_POINT ( 'NONE',  ( -9.561517251340744039, -2.295524264805589354, 30.44142389570982488 ) ) ;
#4235 = FACE_OUTER_BOUND ( 'NONE', #14357, .T. ) ;
#4236 = ORIENTED_EDGE ( 'NONE', *, *, #43509, .T. ) ;
#4237 = LINE ( 'NONE', #11443, #1743 ) ;
#4238 = CYLINDRICAL_SURFACE ( 'NONE', #82165, 0.2500000000000004996 ) ;
#4239 = CARTESIAN_POINT ( 'NONE',  ( 2.307692307692309264, -11.35647404775217417, 33.31231777344666511 ) ) ;
#4240 = EDGE_LOOP ( 'NONE', ( #29342, #74023, #19363, #82436 ) ) ;
#4241 = CARTESIAN_POINT ( 'NONE',  ( 12.39545505058258179, -4.786620604624113540, 33.94971097300155805 ) ) ;
#4242 = CARTESIAN_POINT ( 'NONE',  ( 3.165498784808456367, -12.27809138561121394, 31.22303859784730307 ) ) ;
#4243 = EDGE_CURVE ( 'NONE', #40235, #83058, #10484, .T. ) ;
#4244 = ORIENTED_EDGE ( 'NONE', *, *, #41762, .T. ) ;
#4245 = ADVANCED_FACE ( 'NONE', ( #30108 ), #10283, .F. ) ;
#4246 = FACE_OUTER_BOUND ( 'NONE', #51472, .T. ) ;
#4247 = CARTESIAN_POINT ( 'NONE',  ( 13.38461538461538680, -9.780366693483667717, 34.19971097300155094 ) ) ;
#4248 = ORIENTED_EDGE ( 'NONE', *, *, #80438, .T. ) ;
#4249 = CARTESIAN_POINT ( 'NONE',  ( -12.59168643127016196, -5.915902021225889484, 34.75552854090298638 ) ) ;
#4250 = CARTESIAN_POINT ( 'NONE',  ( -12.21148414990014963, -2.564540009722895419, 30.55348353981670684 ) ) ;
#4251 = CARTESIAN_POINT ( 'NONE',  ( -15.90390063549801347, -8.433404298154332679, 34.66254593164985920 ) ) ;
#4252 = CARTESIAN_POINT ( 'NONE',  ( -10.39260507411620260, -5.913360116392397892, 34.49180327182771322 ) ) ;
#4253 = CARTESIAN_POINT ( 'NONE',  ( 0.2115617174898712927, -2.544273027872575366, 31.48422191005632342 ) ) ;
#4254 = DIRECTION ( 'NONE',  ( 0.000000000000000000, 0.000000000000000000, 1.000000000000000000 ) ) ;
#4256 = DIRECTION ( 'NONE',  ( -0.000000000000000000, -0.1736481776669307198, -0.9848077530122080203 ) ) ;
#4255 = CARTESIAN_POINT ( 'NONE',  ( -13.45069776397551564, -3.937682226553330445, 33.60647404775217240 ) ) ;
#4257 = CARTESIAN_POINT ( 'NONE',  ( 10.83816428436268176, -9.418065098278013636, 34.63729479722530158 ) ) ;
#4259 = CARTESIAN_POINT ( 'NONE',  ( -6.673076923075486278, -7.500000000000155431, 34.75000000000007105 ) ) ;
#4258 = CARTESIAN_POINT ( 'NONE',  ( 12.23865894480087846, -7.630690623152299956, 34.99857592706774057 ) ) ;
#4260 = VECTOR ( 'NONE', #42806, 1000.000000000000000 ) ;
#4261 = CARTESIAN_POINT ( 'NONE',  ( 2.749999999999995115, -6.360912703473971419, 15.64062500000000178 ) ) ;
#4262 = VERTEX_POINT ( 'NONE', #77847 ) ;
#4263 = CARTESIAN_POINT ( 'NONE',  ( -4.023055712879203938, -5.496552790871117367, 34.60292014791297532 ) ) ;
#4264 = ORIENTED_EDGE ( 'NONE', *, *, #18566, .F. ) ;
#4265 = ORIENTED_EDGE ( 'NONE', *, *, #77504, .F. ) ;
#4266 = CARTESIAN_POINT ( 'NONE',  ( -7.623141002060450866, -2.523321265292116422, 31.42251411153756990 ) ) ;
#4267 = VERTEX_POINT ( 'NONE', #44048 ) ;
#4268 = CARTESIAN_POINT ( 'NONE',  ( -39.05038313613820122, -2.499999999999999556, 29.75000000000000355 ) ) ;
#4269 = CARTESIAN_POINT ( 'NONE',  ( 1.139087296526029469, -10.24999999999999467, 17.20312500000000000 ) ) ;
#4270 = CARTESIAN_POINT ( 'NONE',  ( -13.31854805126531005, -5.471508081941601098, 34.59228464037088457 ) ) ;
#4271 = CARTESIAN_POINT ( 'NONE',  ( -8.992715712954719720, -3.236172620538810385, 32.36188796281390267 ) ) ;
#4272 = CARTESIAN_POINT ( 'NONE',  ( 19.00000000000000000, -9.000000000000001776, 3.000000000000000444 ) ) ;
#4273 = DIRECTION ( 'NONE',  ( -0.000000000000000000, -0.5000000000000009992, -0.8660254037844380415 ) ) ;
#4274 = CARTESIAN_POINT ( 'NONE',  ( -4.853910232829681703, -2.523321265292115090, 31.42251411153756280 ) ) ;
#4275 = CYLINDRICAL_SURFACE ( 'NONE', #87637, 0.2499999999999973355 ) ;
#4276 = CARTESIAN_POINT ( 'NONE',  ( 5.749976762707035505, -4.335965774309649134, 33.62209801155881905 ) ) ;
#4277 = CARTESIAN_POINT ( 'NONE',  ( -3.749999999999988454, -9.053300858899127945, 21.26562500000000000 ) ) ;
#4278 = CARTESIAN_POINT ( 'NONE',  ( 1.450683735617824821, -3.050289026998446840, 32.03036669348366416 ) ) ;
#4279 = DIRECTION ( 'NONE',  ( 0.000000000000000000, 0.8660254037844377084, -0.5000000000000015543 ) ) ;
#4280 = VECTOR ( 'NONE', #42004, 1000.000000000000227 ) ;
#4281 = FACE_OUTER_BOUND ( 'NONE', #57087, .T. ) ;
#4282 = AXIS2_PLACEMENT_3D ( 'NONE', #37203, #1659, #70557 ) ;
#4283 = ORIENTED_EDGE ( 'NONE', *, *, #55584, .T. ) ;
#4284 = EDGE_LOOP ( 'NONE', ( #69640, #81347 ) ) ;
#4285 = CARTESIAN_POINT ( 'NONE',  ( 0.000000000000000000, -11.00000000000000000, 29.75000000000000355 ) ) ;
#4286 = CARTESIAN_POINT ( 'NONE',  ( -17.07692307692319744, -8.613356846316285953, 34.62446782046622218 ) ) ;
#4287 = DIRECTION ( 'NONE',  ( 0.000000000000000000, 0.000000000000000000, 1.000000000000000000 ) ) ;
#4288 = CARTESIAN_POINT ( 'NONE',  ( -6.988346923633241836, -5.941354392334500467, 34.76329471203369792 ) ) ;
#4289 = ADVANCED_FACE ( 'NONE', ( #24679 ), #51228, .F. ) ;
#4290 = AXIS2_PLACEMENT_3D ( 'NONE', #16216, #30174, #45001 ) ;
#4291 = LINE ( 'NONE', #65088, #73741 ) ;
#4292 = AXIS2_PLACEMENT_3D ( 'NONE', #78754, #24243, #36017 ) ;
#4293 = CARTESIAN_POINT ( 'NONE',  ( 2.307692307692309264, -11.91647553114624181, 32.58852847137148245 ) ) ;
#4294 = ADVANCED_FACE ( 'NONE', ( #3953 ), #71088, .F. ) ;
#4295 = AXIS2_PLACEMENT_3D ( 'NONE', #3392, #60117, #86737 ) ;
#4296 = B_SPLINE_CURVE_WITH_KNOTS ( 'NONE', 3,
 ( #57961, #85441, #62932, #1244, #56197, #21971, #32275, #86797, #58843, #4351 ),
 .UNSPECIFIED., .F., .F.,
 ( 4, 2, 2, 2, 4 ),
 ( 0.0007817246256747463051, 0.0009771112852218896347, 0.001172497944769032747, 0.001367884604316176077, 0.001563271263863319407 ),
 .UNSPECIFIED. ) ;
#4297 = ORIENTED_EDGE ( 'NONE', *, *, #15295, .F. ) ;
#4298 = CARTESIAN_POINT ( 'NONE',  ( 7.596177102105254875, -2.920706130388546651, 32.31842814019191223 ) ) ;
#4299 = VERTEX_POINT ( 'NONE', #9833 ) ;
#4300 = B_SPLINE_CURVE_WITH_KNOTS ( 'NONE', 3,
 ( #47224, #75580, #68387, #88690, #82360, #46791, #81919, #27405, #26077, #61624 ),
 .UNSPECIFIED., .F., .F.,
 ( 4, 2, 2, 2, 4 ),
 ( 0.000000000000000000, 0.0001954311564186864949, 0.0003908623128373729899, 0.0005862934692560594577, 0.0007817246256747459798 ),
 .UNSPECIFIED. ) ;
#4301 = ADVANCED_FACE ( 'NONE', ( #2622 ), #51682, .F. ) ;
#4302 = VERTEX_POINT ( 'NONE', #9399 ) ;
#4303 = CARTESIAN_POINT ( 'NONE',  ( -9.561782254074051579, -3.068774925481847493, 32.56582465632704526 ) ) ;
#4304 = CARTESIAN_POINT ( 'NONE',  ( 5.869523291883536054, -7.276988635370452485, 34.74523720219453793 ) ) ;
#4305 = CARTESIAN_POINT ( 'NONE',  ( -0.5272918898517936492, -7.249945578846653582, 34.99404164642496795 ) ) ;
#4306 = CARTESIAN_POINT ( 'NONE',  ( 11.76124120743960333, -2.353885683473779800, 30.79025554430704403 ) ) ;
#4307 = PLANE ( 'NONE',  #4987 ) ;
#4309 = EDGE_CURVE ( 'NONE', #6804, #20820, #4078, .T. ) ;
#4308 = ORIENTED_EDGE ( 'NONE', *, *, #85512, .F. ) ;
#4310 = VERTEX_POINT ( 'NONE', #44938 ) ;
#4311 = ORIENTED_EDGE ( 'NONE', *, *, #31894, .F. ) ;
#4312 = CARTESIAN_POINT ( 'NONE',  ( -4.023320715612509701, -12.15418822224088657, 32.17964115625579069 ) ) ;
#4313 = CARTESIAN_POINT ( 'NONE',  ( -1.384615384615506484, -5.094484230521993062, 34.41647553114689373 ) ) ;
#4314 = EDGE_CURVE ( 'NONE', #81411, #2917, #72416, .T. ) ;
#4315 = DIRECTION ( 'NONE',  ( 0.000000000000000000, 0.4999999999999985567, 0.8660254037844395958 ) ) ;
#4316 = CARTESIAN_POINT ( 'NONE',  ( 2.307692307692309264, -11.16473453929635440, 33.15142922261926373 ) ) ;
#4317 = CARTESIAN_POINT ( 'NONE',  ( -11.66860950819323328, -8.630895178749533159, 34.87696386517710323 ) ) ;
#4318 = EDGE_CURVE ( 'NONE', #1947, #21625, #27695, .T. ) ;
#4319 = CARTESIAN_POINT ( 'NONE',  ( 9.692307692307695177, -8.564572088678739092, 35.78748833219616898 ) ) ;
#4320 = ORIENTED_EDGE ( 'NONE', *, *, #28448, .F. ) ;
#4321 = ORIENTED_EDGE ( 'NONE', *, *, #25774, .F. ) ;
#4322 = DIRECTION ( 'NONE',  ( 0.000000000000000000, 0.9396926207859126468, 0.3420201433256571111 ) ) ;
#4323 = EDGE_LOOP ( 'NONE', ( #39501, #2728, #18523, #49780 ) ) ;
#4325 = VERTEX_POINT ( 'NONE', #12504 ) ;
#4324 = CARTESIAN_POINT ( 'NONE',  ( -5.749945688361685292, -3.136992222400443175, 32.19305428654138979 ) ) ;
#4326 = CARTESIAN_POINT ( 'NONE',  ( -10.54931728203453822, -3.937682226553329556, 33.60647404775216529 ) ) ;
#4327 = CARTESIAN_POINT ( 'NONE',  ( 8.096153846153846700, -2.499999999999998668, 29.75000000000000355 ) ) ;
#4328 = CARTESIAN_POINT ( 'NONE',  ( -2.651650429449565305, -4.848349570550461785, 16.50000000000000000 ) ) ;
#4329 = ORIENTED_EDGE ( 'NONE', *, *, #31031, .T. ) ;
#4330 = EDGE_CURVE ( 'NONE', #31749, #31146, #2958, .T. ) ;
#4331 = AXIS2_PLACEMENT_3D ( 'NONE', #67044, #88667, #26947 ) ;
#4332 = CARTESIAN_POINT ( 'NONE',  ( -13.60810032833933292, -12.24155766932282496, 31.33739205006857986 ) ) ;
#4333 = VERTEX_POINT ( 'NONE', #46730 ) ;
#4334 = CARTESIAN_POINT ( 'NONE',  ( 11.53846153846141753, -2.892918686052165622, 31.69288490824153470 ) ) ;
#4335 = CARTESIAN_POINT ( 'NONE',  ( 14.43821774592595197, -12.50538340440932394, 31.33453814440721885 ) ) ;
#4336 = FACE_BOUND ( 'NONE', #39804, .T. ) ;
#4338 = DIRECTION ( 'NONE',  ( -0.000000000000000000, 0.1736481776669307198, -0.9848077530122080203 ) ) ;
#4337 = CARTESIAN_POINT ( 'NONE',  ( -6.923076923076922462, -5.471508081941601098, 34.59228464037088457 ) ) ;
#4339 = VECTOR ( 'NONE', #88764, 1000.000000000000000 ) ;
#4340 = CARTESIAN_POINT ( 'NONE',  ( -1.514763354347077540, -3.625366637846545448, 33.29286588640298561 ) ) ;
#4341 = FACE_OUTER_BOUND ( 'NONE', #61544, .T. ) ;
#4342 = EDGE_LOOP ( 'NONE', ( #33568, #63033 ) ) ;
#4343 = CYLINDRICAL_SURFACE ( 'NONE', #67685, 0.2500000000000004996 ) ;
#4344 = CARTESIAN_POINT ( 'NONE',  ( 15.00728428704528561, -4.386631170607603991, 33.66268669641500111 ) ) ;
#4346 = VERTEX_POINT ( 'NONE', #32334 ) ;
#4345 = ADVANCED_FACE ( 'NONE', ( #19702 ), #67450, .F. ) ;
#4347 = AXIS2_PLACEMENT_3D ( 'NONE', #14329, #5805, #46790 ) ;
#4348 = CARTESIAN_POINT ( 'NONE',  ( -8.638440328263817136, -3.338503747796866872, 32.95102852606553512 ) ) ;
#4349 = DIRECTION ( 'NONE',  ( -1.000000000000000000, -0.000000000000000000, -0.000000000000000000 ) ) ;
#4350 = CARTESIAN_POINT ( 'NONE',  ( 14.53047197667037516, -10.23759521482555357, 34.22997729860117033 ) ) ;
#4351 = CARTESIAN_POINT ( 'NONE',  ( -13.38461538461538325, -11.35647404775217417, 33.31231777344666511 ) ) ;
#4352 = ADVANCED_FACE ( 'NONE', ( #59352 ), #18375, .F. ) ;
#4354 = EDGE_CURVE ( 'NONE', #21191, #52651, #15398, .T. ) ;
#4353 = CARTESIAN_POINT ( 'NONE',  ( 12.46153846153833911, -4.320704448113951379, 33.92786785259630022 ) ) ;
#4355 = FACE_BOUND ( 'NONE', #88030, .T. ) ;
#4357 = DIRECTION ( 'NONE',  ( -1.000000000000000000, -0.000000000000000000, 0.000000000000000000 ) ) ;
#4356 = DIRECTION ( 'NONE',  ( -1.000000000000000000, 0.000000000000000000, 0.000000000000000000 ) ) ;
#4358 = LINE ( 'NONE', #59296, #82768 ) ;
#4360 = CARTESIAN_POINT ( 'NONE',  ( 9.822833394071258439, -4.459921816937791661, 33.71989282347011851 ) ) ;
#4359 = CARTESIAN_POINT ( 'NONE',  ( 18.25005431163831204, -11.28795663066794575, 33.01431243580653785 ) ) ;
#4361 = DIRECTION ( 'NONE',  ( -0.000000000000000000, -0.8660254037844399289, -0.4999999999999980016 ) ) ;
#4362 = EDGE_CURVE ( 'NONE', #33850, #61846, #12719, .T. ) ;
#4363 = CARTESIAN_POINT ( 'NONE',  ( 0.000000000000000000, -11.00000000000000000, 29.75000000000000355 ) ) ;
#4364 = CARTESIAN_POINT ( 'NONE',  ( 3.775308065498768517, -8.992201783934554271, 23.04500670625849068 ) ) ;
#4365 = EDGE_CURVE ( 'NONE', #82116, #24019, #22274, .T. ) ;
#4366 = CARTESIAN_POINT ( 'NONE',  ( -12.71153846153846168, -7.500000000000001776, 35.00000000000000000 ) ) ;
#4367 = EDGE_LOOP ( 'NONE', ( #49499, #6334, #67461, #28804 ) ) ;
#4368 = CARTESIAN_POINT ( 'NONE',  ( -4.219929564802034072, -11.69971097300155272, 32.46337939537587403 ) ) ;
#4369 = CARTESIAN_POINT ( 'NONE',  ( -3.230769230769229949, -1.242168528481310874, 33.36296068462461051 ) ) ;
#4370 = CARTESIAN_POINT ( 'NONE',  ( -1.161835843346973762, -10.81320215134717344, 33.49497208177562868 ) ) ;
#4371 = CARTESIAN_POINT ( 'NONE',  ( -9.822999158975248335, -10.54014554554150607, 33.71984207302941883 ) ) ;
#4372 = CARTESIAN_POINT ( 'NONE',  ( 6.673100179028333301, -12.65889640711025521, 30.72598325615533454 ) ) ;
#4373 = CARTESIAN_POINT ( 'NONE',  ( -10.61538461538461320, -1.129524287112498415, 32.06866353760679544 ) ) ;
#4374 = CARTESIAN_POINT ( 'NONE',  ( -0.06109907496455085213, -3.750000000000000888, 23.90438170625849068 ) ) ;
#4375 = DIRECTION ( 'NONE',  ( -0.000000000000000000, 0.9396926207859093161, -0.3420201433256663259 ) ) ;
#4376 = LINE ( 'NONE', #17895, #8707 ) ;
#4377 = CARTESIAN_POINT ( 'NONE',  ( -0.1741240272142571821, -4.754468449490619086, 28.77324492963870028 ) ) ;
#4378 = CARTESIAN_POINT ( 'NONE',  ( 8.769230769230768274, -12.78798330534102945, 29.74999999999997868 ) ) ;
#4379 = CARTESIAN_POINT ( 'NONE',  ( 14.30769230769218581, -3.083524468854526912, 32.58852847137268327 ) ) ;
#4380 = CARTESIAN_POINT ( 'NONE',  ( 1.515405825582336163, -9.929761469519744921, 34.40412654351204225 ) ) ;
#4381 = CARTESIAN_POINT ( 'NONE',  ( -12.46153846153846168, -12.29105614889573062, 35.45975837776705220 ) ) ;
#4382 = CARTESIAN_POINT ( 'NONE',  ( 0.3589743589743582541, -3.499999999999999556, 29.75000000000000355 ) ) ;
#4383 = ORIENTED_EDGE ( 'NONE', *, *, #85167, .F. ) ;
#4384 = AXIS2_PLACEMENT_3D ( 'NONE', #83254, #31858, #78704 ) ;
#4385 = CARTESIAN_POINT ( 'NONE',  ( 16.21991348719623360, -4.661471528628508665, 34.16647553114624003 ) ) ;
#4386 = CARTESIAN_POINT ( 'NONE',  ( -12.46153846153846168, -1.242168528481310874, 33.36296068462461051 ) ) ;
#4387 = CARTESIAN_POINT ( 'NONE',  ( 2.694853999681185108, -4.891553140782077591, 19.56436829374151287 ) ) ;
#4388 = DIRECTION ( 'NONE',  ( -0.000000000000000000, 0.9848077530122085754, -0.1736481776669273613 ) ) ;
#4389 = FACE_OUTER_BOUND ( 'NONE', #33317, .T. ) ;
#4390 = VERTEX_POINT ( 'NONE', #12073 ) ;
#4391 = CARTESIAN_POINT ( 'NONE',  ( 1.384615384615386802, -4.098570777380720287, 33.41473453929634729 ) ) ;
#4392 = CARTESIAN_POINT ( 'NONE',  ( -17.07692307692319744, -9.528491918059723176, 34.59228464037033035 ) ) ;
#4394 = ORIENTED_EDGE ( 'NONE', *, *, #86524, .T. ) ;
#4393 = CARTESIAN_POINT ( 'NONE',  ( 4.826946332874485712, -12.41104346484419452, 31.60698883733904196 ) ) ;
#4395 = CARTESIAN_POINT ( 'NONE',  ( -11.40841637562676070, -2.504778602574660340, 29.97347330155780654 ) ) ;
#4396 = CARTESIAN_POINT ( 'NONE',  ( -3.007989689500820241, -3.755027918224367767, 33.06320215134714857 ) ) ;
#4397 = CARTESIAN_POINT ( 'NONE',  ( -12.46153846153846168, -8.564572088678739092, 35.78748833219616898 ) ) ;
#4398 = CARTESIAN_POINT ( 'NONE',  ( -11.66860950819324039, -2.647304123082328875, 31.75400227202885972 ) ) ;
#4399 = ORIENTED_EDGE ( 'NONE', *, *, #46738, .F. ) ;
#4400 = CARTESIAN_POINT ( 'NONE',  ( -11.53846153846153655, -8.120952969808772792, 34.71129190930000163 ) ) ;
#4401 = LINE ( 'NONE', #25117, #46585 ) ;
#4402 = DIRECTION ( 'NONE',  ( -1.000000000000000000, -0.000000000000000000, 0.000000000000000000 ) ) ;
#4403 = ORIENTED_EDGE ( 'NONE', *, *, #35968, .F. ) ;
#4404 = EDGE_LOOP ( 'NONE', ( #84042, #53048, #56399, #85782 ) ) ;
#4405 = ORIENTED_EDGE ( 'NONE', *, *, #53561, .T. ) ;
#4406 = AXIS2_PLACEMENT_3D ( 'NONE', #15425, #30695, #58160 ) ;
#4407 = DIRECTION ( 'NONE',  ( -0.000000000000000000, 0.7660444431189791237, -0.6427876096865379196 ) ) ;
#4408 = FACE_OUTER_BOUND ( 'NONE', #79355, .T. ) ;
#4409 = CARTESIAN_POINT ( 'NONE',  ( 2.530703659305158837, -5.667800583137508674, 34.40243808032445827 ) ) ;
#4410 = EDGE_CURVE ( 'NONE', #13301, #6878, #35382, .T. ) ;
#4411 = LINE ( 'NONE', #64770, #26209 ) ;
#4412 = VERTEX_POINT ( 'NONE', #39551 ) ;
#4413 = ORIENTED_EDGE ( 'NONE', *, *, #43709, .T. ) ;
#4415 = ORIENTED_EDGE ( 'NONE', *, *, #43726, .F. ) ;
#4414 = DIRECTION ( 'NONE',  ( -0.000000000000000000, 1.000000000000000000, -0.000000000000000000 ) ) ;
#4416 = CARTESIAN_POINT ( 'NONE',  ( -6.673131513698878692, -4.176053281294514363, 33.81426240980091791 ) ) ;
#4417 = B_SPLINE_CURVE_WITH_KNOTS ( 'NONE', 3,
 ( #62459, #70114, #14739, #65005, #42218, #7979, #58257, #57819, #17279, #42655 ),
 .UNSPECIFIED., .F., .F.,
 ( 4, 2, 2, 2, 4 ),
 ( 0.0007817359527651090859, 0.0009771254036996478414, 0.001172514854634186489, 0.001367904305568725136, 0.001563293756503263783 ),
 .UNSPECIFIED. ) ;
#4418 = CARTESIAN_POINT ( 'NONE',  ( 15.23076923076911093, -3.300289026999228881, 32.46337939537708905 ) ) ;
#4419 = EDGE_CURVE ( 'NONE', #52360, #49441, #4868, .T. ) ;
#4420 = CARTESIAN_POINT ( 'NONE',  ( 6.000000000000001776, -3.937682226553329556, 33.60647404775216529 ) ) ;
#4421 = CARTESIAN_POINT ( 'NONE',  ( -1.318548051265307830, -12.62096338111211757, 30.90682066428152908 ) ) ;
#4422 = EDGE_LOOP ( 'NONE', ( #14875, #83873, #69204, #25680 ) ) ;
#4423 = B_SPLINE_CURVE_WITH_KNOTS ( 'NONE', 3,
 ( #74052, #48334, #33056, #88038, #41585, #82139, #13233, #6477, #27626, #19978 ),
 .UNSPECIFIED., .F., .F.,
 ( 4, 2, 2, 2, 4 ),
 ( 0.000000000000000000, 0.0001954311564186865221, 0.0003908623128373730441, 0.0005862934692560595662, 0.0007817246256747460882 ),
 .UNSPECIFIED. ) ;
#4424 = ORIENTED_EDGE ( 'NONE', *, *, #31815, .F. ) ;
#4425 = VERTEX_POINT ( 'NONE', #40434 ) ;
#4427 = EDGE_LOOP ( 'NONE', ( #53587, #66227 ) ) ;
#4426 = CARTESIAN_POINT ( 'NONE',  ( 9.692307692307572609, -11.94971097300221174, 32.03036669348237098 ) ) ;
#4428 = CARTESIAN_POINT ( 'NONE',  ( 16.82689985270161870, -5.765609946408405406, 34.70566812827424741 ) ) ;
#4429 = CARTESIAN_POINT ( 'NONE',  ( -0.2115930521604186265, -4.932303261841488151, 34.32971442181322885 ) ) ;
#4430 = VERTEX_POINT ( 'NONE', #52588 ) ;
#4431 = EDGE_CURVE ( 'NONE', #59397, #30893, #54491, .T. ) ;
#4432 = DIRECTION ( 'NONE',  ( 1.000000000000000000, 0.000000000000000000, 0.000000000000000000 ) ) ;
#4433 = AXIS2_PLACEMENT_3D ( 'NONE', #2064, #84060, #29548 ) ;
#4434 = DIRECTION ( 'NONE',  ( 0.000000000000000000, 0.000000000000000000, -1.000000000000000000 ) ) ;
#4435 = CARTESIAN_POINT ( 'NONE',  ( 4.376625695114563008, -2.847695495035524882, 31.58253572463339509 ) ) ;
#4436 = FACE_BOUND ( 'NONE', #41964, .T. ) ;
#4437 = B_SPLINE_CURVE_WITH_KNOTS ( 'NONE', 3,
 ( #45803, #65181, #72382, #73285, #58415, #66530, #59766, #87261, #25541, #52994 ),
 .UNSPECIFIED., .F., .F.,
 ( 4, 2, 2, 2, 4 ),
 ( 0.000000000000000000, 0.0001954311564186868202, 0.0003908623128373736404, 0.0005862934692560604335, 0.0007817246256747472808 ),
 .UNSPECIFIED. ) ;
#4438 = CARTESIAN_POINT ( 'NONE',  ( -0.7115151924808161832, -4.236021600441998380, 33.53823185664189310 ) ) ;
#4439 = CARTESIAN_POINT ( 'NONE',  ( 11.53846153846141753, -8.613356846316285953, 34.62446782046622218 ) ) ;
#4440 = DIRECTION ( 'NONE',  ( 0.000000000000000000, 0.7660444431189822323, -0.6427876096865344779 ) ) ;
#4442 = CARTESIAN_POINT ( 'NONE',  ( 6.792928953345223064, -11.04286588640298561, 33.62463336215343901 ) ) ;
#4441 = CARTESIAN_POINT ( 'NONE',  ( 16.94677510719138169, -9.504002272028873932, 34.60269587691767867 ) ) ;
#4443 = CARTESIAN_POINT ( 'NONE',  ( 5.076923076923075762, -13.53365097954675988, 30.81389545987213552 ) ) ;
#4444 = CARTESIAN_POINT ( 'NONE',  ( 1.607628228708780638, -2.308499170217967134, 30.53291367094873721 ) ) ;
#4445 = EDGE_LOOP ( 'NONE', ( #50104, #31752 ) ) ;
#4446 = CARTESIAN_POINT ( 'NONE',  ( -15.90384615384471800, -7.500000000000155431, 34.75000000000007105 ) ) ;
#4447 = CYLINDRICAL_SURFACE ( 'NONE', #11997, 0.2499999999999995559 ) ;
#4448 = ORIENTED_EDGE ( 'NONE', *, *, #36636, .F. ) ;
#4449 = EDGE_LOOP ( 'NONE', ( #5427, #34764, #48947, #61517 ) ) ;
#4451 = CARTESIAN_POINT ( 'NONE',  ( 0.4615384615383382183, -8.656820664282941280, 34.87096338111179961 ) ) ;
#4450 = CARTESIAN_POINT ( 'NONE',  ( 16.15384615384615330, -2.708943851104267164, 35.45975837776705220 ) ) ;
#4452 = CARTESIAN_POINT ( 'NONE',  ( 16.21991450484859953, -2.538708090699994813, 30.37095296980875503 ) ) ;
#4453 = CARTESIAN_POINT ( 'NONE',  ( 2.530471976670374268, -2.353885683473778023, 30.79025554430704759 ) ) ;
#4454 = DIRECTION ( 'NONE',  ( -0.000000000000000000, -0.3420201433256694346, -0.9396926207859080948 ) ) ;
#4455 = ORIENTED_EDGE ( 'NONE', *, *, #14588, .F. ) ;
#4457 = EDGE_CURVE ( 'NONE', #28781, #69896, #74933, .T. ) ;
#4456 = PLANE ( 'NONE',  #9739 ) ;
#4458 = EDGE_CURVE ( 'NONE', #63745, #58726, #7071, .T. ) ;
#4459 = CARTESIAN_POINT ( 'NONE',  ( 18.22301284409340028, -2.523321265292116866, 31.42251411153756990 ) ) ;
#4460 = B_SPLINE_CURVE_WITH_KNOTS ( 'NONE', 3,
 ( #75589, #76037, #7590, #41376, #55322, #391, #35051, #63851, #22859, #15236 ),
 .UNSPECIFIED., .F., .F.,
 ( 4, 2, 2, 2, 4 ),
 ( 0.000000000000000000, 0.0001954339857564065528, 0.0003908679715128131056, 0.0005863019572692196313, 0.0007817359430256262112 ),
 .UNSPECIFIED. ) ;
#4462 = DIRECTION ( 'NONE',  ( -0.000000000000000000, -0.6427876096865404731, -0.7660444431189770143 ) ) ;
#4461 = CARTESIAN_POINT ( 'NONE',  ( 11.53846153846141576, -3.083524468854526912, 32.58852847137268327 ) ) ;
#4464 = CARTESIAN_POINT ( 'NONE',  ( 7.846153846153725020, -6.026961402154118019, 34.52809138561165270 ) ) ;
#4463 = B_SPLINE_CURVE_WITH_KNOTS ( 'NONE', 3,
 ( #8683, #35709, #55081, #22620, #48319, #43346, #22189, #69042, #1474, #36158 ),
 .UNSPECIFIED., .F., .F.,
 ( 4, 2, 2, 2, 4 ),
 ( 0.000000000000000000, 0.0001954339857564082062, 0.0003908679715128164124, 0.0005863019572692246186, 0.0007817359430256328248 ),
 .UNSPECIFIED. ) ;
#4465 = VECTOR ( 'NONE', #62632, 1000.000000000000000 ) ;
#4466 = CARTESIAN_POINT ( 'NONE',  ( -1.384615384615383471, -13.04860791097971706, 34.73218667398347037 ) ) ;
#4467 = CARTESIAN_POINT ( 'NONE',  ( -15.16551409125639260, -11.06231777344671130, 33.60647404775212976 ) ) ;
#4468 = B_SPLINE_CURVE_WITH_KNOTS ( 'NONE', 3,
 ( #1131, #21403, #84448, #34473, #21846, #8339, #14649, #63269, #7453, #42132 ),
 .UNSPECIFIED., .F., .F.,
 ( 4, 2, 2, 2, 4 ),
 ( 0.0007817246256747453293, 0.0009771112852218885505, 0.001172497944769031663, 0.001367884604316174993, 0.001563271263863318106 ),
 .UNSPECIFIED. ) ;
#4469 = CARTESIAN_POINT ( 'NONE',  ( -3.749999999999997335, -7.500000000000021316, 20.09375000000000000 ) ) ;
#4470 = EDGE_LOOP ( 'NONE', ( #55949, #42737, #52267, #78416 ) ) ;
#4471 = B_SPLINE_CURVE_WITH_KNOTS ( 'NONE', 3,
 ( #14900, #22529, #28859, #75695, #35609, #56318, #20755, #69831, #49561, #77037 ),
 .UNSPECIFIED., .F., .F.,
 ( 4, 2, 2, 2, 4 ),
 ( 0.0007817359430256318490, 0.0009771253907249984917, 0.001172514838424365026, 0.001367904286123731560, 0.001563293733823098311 ),
 .UNSPECIFIED. ) ;
#4472 = VECTOR ( 'NONE', #37440, 1000.000000000000227 ) ;
#4473 = VECTOR ( 'NONE', #74483, 1000.000000000000000 ) ;
#4474 = ORIENTED_EDGE ( 'NONE', *, *, #28725, .T. ) ;
#4475 = EDGE_CURVE ( 'NONE', #85765, #3642, #49820, .T. ) ;
#4476 = CARTESIAN_POINT ( 'NONE',  ( 19.50000000000000000, -3.499999999999999556, 28.25000000000000000 ) ) ;
#4477 = CYLINDRICAL_SURFACE ( 'NONE', #29701, 0.2500000000000008882 ) ;
#4478 = CARTESIAN_POINT ( 'NONE',  ( 4.403846153846153300, -2.499999999999998668, 29.75000000000000355 ) ) ;
#4479 = EDGE_CURVE ( 'NONE', #80242, #45697, #48490, .T. ) ;
#4480 = CARTESIAN_POINT ( 'NONE',  ( 3.903869409797563250, -10.82459398097509684, 33.81372124010185587 ) ) ;
#4481 = CARTESIAN_POINT ( 'NONE',  ( 2.557692307692372768, -7.434744429011176159, 34.75000000000000711 ) ) ;
#4482 = CARTESIAN_POINT ( 'NONE',  ( 1.553300858899129944, -11.24999999999998934, 23.45312500000000000 ) ) ;
#4483 = AXIS2_PLACEMENT_3D ( 'NONE', #46990, #40258, #13658 ) ;
#4484 = CARTESIAN_POINT ( 'NONE',  ( 13.38461538461538680, -1.629998284177014645, 34.34916445242399163 ) ) ;
#4485 = CARTESIAN_POINT ( 'NONE',  ( -13.38461538461538325, -12.10708131394839349, 31.69288490824020244 ) ) ;
#4486 = CARTESIAN_POINT ( 'NONE',  ( -8.899378738962466784, -12.70455904226513866, 30.44083106164009322 ) ) ;
#4487 = CARTESIAN_POINT ( 'NONE',  ( 12.21156171748987163, -11.47974371597207899, 33.17467449705390692 ) ) ;
#4488 = DIRECTION ( 'NONE',  ( 1.000000000000000000, 0.000000000000000000, 0.000000000000000000 ) ) ;
#4489 = CARTESIAN_POINT ( 'NONE',  ( 14.17754509825408604, -12.27039167877662251, 31.24851455888617835 ) ) ;
#4490 = CYLINDRICAL_SURFACE ( 'NONE', #81182, 0.2500000000000012212 ) ;
#4491 = CARTESIAN_POINT ( 'NONE',  ( 8.069166690247241647, -8.282913670948747864, 34.94150082978203642 ) ) ;
#4492 = CARTESIAN_POINT ( 'NONE',  ( -5.869209559033049750, -4.684288915650984819, 34.18129842949671371 ) ) ;
#4493 = CARTESIAN_POINT ( 'NONE',  ( 9.627037691751372250, -5.094484230520674117, 34.41647553114621161 ) ) ;
#4494 = CARTESIAN_POINT ( 'NONE',  ( -15.45369544828537656, -8.239355502252617924, 34.69524867566427417 ) ) ;
#4495 = ORIENTED_EDGE ( 'NONE', *, *, #45969, .T. ) ;
#4496 = CARTESIAN_POINT ( 'NONE',  ( -16.40382289789473802, -9.234221910056350069, 34.70572697212741531 ) ) ;
#4497 = CARTESIAN_POINT ( 'NONE',  ( 1.318531973659506029, -5.557115091759785130, 34.35708131394839171 ) ) ;
#4498 = CARTESIAN_POINT ( 'NONE',  ( -4.376773112752999850, -5.582147617184174848, 34.63737895849758530 ) ) ;
#4499 = CARTESIAN_POINT ( 'NONE',  ( -2.775308065498752086, -8.577988221561495763, 17.76749329374151287 ) ) ;
#4500 = CARTESIAN_POINT ( 'NONE',  ( 17.07692307692307665, -6.386643153685126251, 34.62446782046654192 ) ) ;
#4501 = DIRECTION ( 'NONE',  ( 0.000000000000000000, 1.000000000000000000, 0.000000000000000000 ) ) ;
#4503 = ORIENTED_EDGE ( 'NONE', *, *, #19598, .F. ) ;
#4502 = CARTESIAN_POINT ( 'NONE',  ( 10.86538461538603606, -7.500000000000154543, 35.00000000000007105 ) ) ;
#4504 = CARTESIAN_POINT ( 'NONE',  ( 1.944543648263018731, -9.444543648262994751, 18.37500000000000355 ) ) ;
#4505 = CARTESIAN_POINT ( 'NONE',  ( -1.515306851282943734, -9.804603061927743113, 34.18744698557895845 ) ) ;
#4506 = ORIENTED_EDGE ( 'NONE', *, *, #64092, .F. ) ;
#4507 = B_SPLINE_CURVE_WITH_KNOTS ( 'NONE', 3,
 ( #69380, #83791, #22077, #42801, #55853, #83343, #33814, #76578, #54521, #82014 ),
 .UNSPECIFIED., .F., .F.,
 ( 4, 2, 2, 2, 4 ),
 ( 0.0007817359430256253438, 0.0009771253907249898181, 0.001172514838424354401, 0.001367904286123718983, 0.001563293733823083566 ),
 .UNSPECIFIED. ) ;
#4508 = CARTESIAN_POINT ( 'NONE',  ( -17.77722045873158763, -3.755027918224366879, 33.06320215134716278 ) ) ;
#4509 = ORIENTED_EDGE ( 'NONE', *, *, #16269, .T. ) ;
#4510 = AXIS2_PLACEMENT_3D ( 'NONE', #432, #6736, #14838 ) ;
#4511 = B_SPLINE_CURVE_WITH_KNOTS ( 'NONE', 3,
 ( #50003, #77918, #15347, #23844, #31053, #37366, #43689, #9465, #64835, #78802 ),
 .UNSPECIFIED., .F., .F.,
 ( 4, 2, 2, 2, 4 ),
 ( 0.0007817246256747511840, 0.0009771112852218952725, 0.001172497944769039470, 0.001367884604316183667, 0.001563271263863327864 ),
 .UNSPECIFIED. ) ;
#4512 = CYLINDRICAL_SURFACE ( 'NONE', #46369, 0.2499999999999998890 ) ;
#4513 = LINE ( 'NONE', #87394, #83999 ) ;
#4514 = CARTESIAN_POINT ( 'NONE',  ( -18.00000000000000000, -12.75000000000001066, 29.99999999999997868 ) ) ;
#4515 = ORIENTED_EDGE ( 'NONE', *, *, #36042, .T. ) ;
#4516 = CARTESIAN_POINT ( 'NONE',  ( -10.61538461538473399, -12.46129190930018460, 30.37095296980731973 ) ) ;
#4518 = ORIENTED_EDGE ( 'NONE', *, *, #29798, .F. ) ;
#4517 = AXIS2_PLACEMENT_3D ( 'NONE', #59989, #80272, #32967 ) ;
#4519 = CARTESIAN_POINT ( 'NONE',  ( -5.933932666649922361, -2.292212530054420494, 30.41441678777542990 ) ) ;
#4520 = EDGE_LOOP ( 'NONE', ( #13365, #70301 ) ) ;
#4521 = CARTESIAN_POINT ( 'NONE',  ( 11.53846153846153832, -3.937682226553329556, 33.60647404775216529 ) ) ;
#4522 = CARTESIAN_POINT ( 'NONE',  ( -16.15384615384627409, -9.528491918059723176, 34.59228464037033035 ) ) ;
#4523 = CARTESIAN_POINT ( 'NONE',  ( -10.83886953994894320, -12.11044203135681840, 32.26167407432752299 ) ) ;
#4524 = CARTESIAN_POINT ( 'NONE',  ( -3.165514091256391715, -5.094484230520773593, 34.41647553114626845 ) ) ;
#4525 = CARTESIAN_POINT ( 'NONE',  ( 11.47319109250076075, -11.94971097300153140, 32.03036669348370680 ) ) ;
#4526 = EDGE_CURVE ( 'NONE', #64401, #65515, #8403, .T. ) ;
#4527 = CARTESIAN_POINT ( 'NONE',  ( 13.38461538461538680, -13.75783147151868846, 33.36296068462461051 ) ) ;
#4528 = ORIENTED_EDGE ( 'NONE', *, *, #82243, .F. ) ;
#4529 = VERTEX_POINT ( 'NONE', #27346 ) ;
#4530 = ORIENTED_EDGE ( 'NONE', *, *, #87060, .T. ) ;
#4532 = VERTEX_POINT ( 'NONE', #83183 ) ;
#4531 = CARTESIAN_POINT ( 'NONE',  ( 3.361294669002873547, -12.70449254468099198, 30.44128974285582956 ) ) ;
#4533 = VECTOR ( 'NONE', #81786, 1000.000000000000000 ) ;
#4534 = ADVANCED_FACE ( 'NONE', ( #48939 ), #35878, .F. ) ;
#4535 = CARTESIAN_POINT ( 'NONE',  ( 4.153846153846154188, -8.810774026931790459, 35.74407628777942847 ) ) ;
#4536 = CARTESIAN_POINT ( 'NONE',  ( -10.86540785267757947, -9.271318131107980420, 34.42618302367067429 ) ) ;
#4538 = EDGE_LOOP ( 'NONE', ( #25366, #23644 ) ) ;
#4537 = EDGE_CURVE ( 'NONE', #54993, #2251, #2750, .T. ) ;
#4539 = CARTESIAN_POINT ( 'NONE',  ( -17.07692307692307665, -8.318370150425687726, 35.83090037661290239 ) ) ;
#4540 = VECTOR ( 'NONE', #9373, 1000.000000000000000 ) ;
#4541 = ORIENTED_EDGE ( 'NONE', *, *, #79517, .T. ) ;
#4542 = CARTESIAN_POINT ( 'NONE',  ( -10.68065506134539078, -3.300289026998414865, 32.46337939537583139 ) ) ;
#4543 = VERTEX_POINT ( 'NONE', #82299 ) ;
#4544 = CARTESIAN_POINT ( 'NONE',  ( -12.71153846153846168, -7.500000000000001776, 35.00000000000000000 ) ) ;
#4545 = EDGE_CURVE ( 'NONE', #83475, #66483, #49905, .T. ) ;
#4546 = LINE ( 'NONE', #59487, #5762 ) ;
#4547 = DIRECTION ( 'NONE',  ( -0.000000000000000000, -1.000000000000000000, -0.000000000000000000 ) ) ;
#4548 = FACE_BOUND ( 'NONE', #49176, .T. ) ;
#4549 = DIRECTION ( 'NONE',  ( -1.000000000000000000, 0.000000000000000000, 0.000000000000000000 ) ) ;
#4550 = CARTESIAN_POINT ( 'NONE',  ( 12.59206416330202671, -6.001044277235009439, 34.52024696741798948 ) ) ;
#4551 = EDGE_CURVE ( 'NONE', #87881, #31043, #62441, .T. ) ;
#4552 = CARTESIAN_POINT ( 'NONE',  ( 13.63456079399342791, -4.932303261841489928, 34.32971442181322885 ) ) ;
#4553 = LINE ( 'NONE', #44629, #17255 ) ;
#4554 = LINE ( 'NONE', #24818, #45205 ) ;
#4555 = CARTESIAN_POINT ( 'NONE',  ( -1.514762594053604250, -2.619462340734462380, 30.83744416345203021 ) ) ;
#4556 = ORIENTED_EDGE ( 'NONE', *, *, #80069, .T. ) ;
#4557 = CARTESIAN_POINT ( 'NONE',  ( 8.769230769230768274, -1.466349020453238561, 30.81389545987213907 ) ) ;
#4558 = B_SPLINE_CURVE_WITH_KNOTS ( 'NONE', 3,
 ( #59667, #54232, #25445, #52901, #32639, #45709, #79946, #26332, #53798, #18247 ),
 .UNSPECIFIED., .F., .F.,
 ( 4, 2, 2, 2, 4 ),
 ( 0.0007817246256747447872, 0.0009771112852218874663, 0.001172497944769030362, 0.001367884604316173258, 0.001563271263863315937 ),
 .UNSPECIFIED. ) ;
#4559 = ORIENTED_EDGE ( 'NONE', *, *, #44696, .T. ) ;
#4560 = B_SPLINE_CURVE_WITH_KNOTS ( 'NONE', 3,
 ( #53511, #25158, #40469, #26055, #73350, #58936, #81008, #88225, #25606, #40026 ),
 .UNSPECIFIED., .F., .F.,
 ( 4, 2, 2, 2, 4 ),
 ( 0.0007817246256747453293, 0.0009771112852218889842, 0.001172497944769032531, 0.001367884604316176294, 0.001563271263863319840 ),
 .UNSPECIFIED. ) ;
#4561 = ORIENTED_EDGE ( 'NONE', *, *, #201, .F. ) ;
#4563 = CYLINDRICAL_SURFACE ( 'NONE', #50593, 0.2499999999999986955 ) ;
#4562 = CARTESIAN_POINT ( 'NONE',  ( 5.999999999999878320, -12.16647553114689728, 32.15551576947799362 ) ) ;
#4564 = CARTESIAN_POINT ( 'NONE',  ( 16.37662582282421653, -11.60474049983370648, 33.02348890104160262 ) ) ;
#4565 = CARTESIAN_POINT ( 'NONE',  ( -4.153846153846273204, -4.481592998941358097, 33.73612834414048933 ) ) ;
#4566 = FACE_OUTER_BOUND ( 'NONE', #29098, .T. ) ;
#4567 = CARTESIAN_POINT ( 'NONE',  ( -15.36146069743679199, -3.530157926970578952, 32.79014554554150607 ) ) ;
#4568 = ORIENTED_EDGE ( 'NONE', *, *, #76269, .T. ) ;
#4569 = ADVANCED_FACE ( 'NONE', ( #28679 ), #7961, .F. ) ;
#4570 = CARTESIAN_POINT ( 'NONE',  ( 16.85343813319912698, -5.912607949931405038, 34.49155766932282319 ) ) ;
#4571 = CARTESIAN_POINT ( 'NONE',  ( -11.78843826940389583, -9.943427161483782584, 34.11278801902876978 ) ) ;
#4572 = CARTESIAN_POINT ( 'NONE',  ( 2.557746727605760384, -12.65882529074907126, 30.72640787790839312 ) ) ;
#4573 = EDGE_CURVE ( 'NONE', #31319, #26024, #65127, .T. ) ;
#4574 = CARTESIAN_POINT ( 'NONE',  ( 4.946312717298547490, -7.722926236386453702, 34.74524107206102030 ) ) ;
#4575 = VECTOR ( 'NONE', #84387, 1000.000000000000000 ) ;
#4576 = VERTEX_POINT ( 'NONE', #84953 ) ;
#4577 = ORIENTED_EDGE ( 'NONE', *, *, #61961, .T. ) ;
#4578 = SHAPE_DEFINITION_REPRESENTATION ( #68530, #14956 ) ;
#4579 = VERTEX_POINT ( 'NONE', #36753 ) ;
#4580 = EDGE_CURVE ( 'NONE', #48470, #58457, #30440, .T. ) ;
#4581 = CARTESIAN_POINT ( 'NONE',  ( 17.93424319748568507, -7.249945686854186278, 34.74374336980224598 ) ) ;
#4583 = EDGE_CURVE ( 'NONE', #36979, #84371, #55411, .T. ) ;
#4582 = CARTESIAN_POINT ( 'NONE',  ( -7.780085495151405794, -4.786620604624114428, 33.94971097300155805 ) ) ;
#4584 = VERTEX_POINT ( 'NONE', #70544 ) ;
#4585 = CARTESIAN_POINT ( 'NONE',  ( 8.769230769230768274, -2.721908614388771852, 31.22303859784724978 ) ) ;
#4586 = CARTESIAN_POINT ( 'NONE',  ( 6.065255139512839122, -11.67786785259547777, 32.92929555188713664 ) ) ;
#4587 = CARTESIAN_POINT ( 'NONE',  ( 0.4615384615384611200, -12.10708131394839349, 31.69288490824020244 ) ) ;
#4588 = CARTESIAN_POINT ( 'NONE',  ( 14.08486561521330493, -7.369208160676172348, 34.74850200257122879 ) ) ;
#4589 = CARTESIAN_POINT ( 'NONE',  ( -2.307692307692305711, -1.129524287112498415, 32.06866353760679544 ) ) ;
#4590 = ORIENTED_EDGE ( 'NONE', *, *, #50857, .T. ) ;
#4592 = EDGE_LOOP ( 'NONE', ( #10183, #18232, #36716, #50559 ) ) ;
#4591 = CARTESIAN_POINT ( 'NONE',  ( -15.23076923076935252, -12.16647553114689728, 32.15551576947799362 ) ) ;
#4593 = DIRECTION ( 'NONE',  ( 0.000000000000000000, 0.8660254037844377084, -0.5000000000000015543 ) ) ;
#4594 = LINE ( 'NONE', #78915, #51129 ) ;
#4595 = CARTESIAN_POINT ( 'NONE',  ( -7.846153846153967493, -3.643525952248795718, 33.31231777344771672 ) ) ;
#4596 = CARTESIAN_POINT ( 'NONE',  ( -4.087777802843713282, -12.37446782046654192, 30.86335684631486842 ) ) ;
#4597 = CARTESIAN_POINT ( 'NONE',  ( 13.25446741488368829, -4.299443229763728169, 33.91186481527756058 ) ) ;
#4598 = CARTESIAN_POINT ( 'NONE',  ( 18.00000000000000000, -2.538708090699994813, 30.37095296980875503 ) ) ;
#4599 = CARTESIAN_POINT ( 'NONE',  ( -2.775308065498752086, -8.577988221561495763, 17.76749329374151287 ) ) ;
#4600 = ORIENTED_EDGE ( 'NONE', *, *, #85508, .T. ) ;
#4601 = B_SPLINE_CURVE_WITH_KNOTS ( 'NONE', 3,
 ( #4195, #79863, #31220, #58691, #18164, #80317, #72203, #25808, #18613, #11401 ),
 .UNSPECIFIED., .F., .F.,
 ( 4, 2, 2, 2, 4 ),
 ( 0.000000000000000000, 0.0001954339857564075828, 0.0003908679715128151656, 0.0005863019572692227755, 0.0007817359430256303312 ),
 .UNSPECIFIED. ) ;
#4602 = CARTESIAN_POINT ( 'NONE',  ( 17.20744851515671670, -3.068774925481847937, 32.56582465632704526 ) ) ;
#4603 = FACE_OUTER_BOUND ( 'NONE', #4716, .T. ) ;
#4604 = CARTESIAN_POINT ( 'NONE',  ( 1.653273178848927064E-15, -7.500000000000000000, 14.00000000000000178 ) ) ;
#4605 = B_SPLINE_CURVE_WITH_KNOTS ( 'NONE', 3,
 ( #36420, #14364, #35080, #7618, #63434, #23329, #76959, #70198, #83279, #35532 ),
 .UNSPECIFIED., .F., .F.,
 ( 4, 2, 2, 2, 4 ),
 ( 0.000000000000000000, 0.0001954339857564081520, 0.0003908679715128163040, 0.0005863019572692244018, 0.0007817359430256326080 ),
 .UNSPECIFIED. ) ;
#4606 = AXIS2_PLACEMENT_3D ( 'NONE', #9450, #30166, #63938 ) ;
#4607 = VECTOR ( 'NONE', #22252, 1000.000000000000000 ) ;
#4608 = ORIENTED_EDGE ( 'NONE', *, *, #75949, .T. ) ;
#4609 = VERTEX_POINT ( 'NONE', #78624 ) ;
#4610 = CARTESIAN_POINT ( 'NONE',  ( 8.769230769230768274, -8.564572088678739092, 35.78748833219616898 ) ) ;
#4611 = CARTESIAN_POINT ( 'NONE',  ( 12.59232890250541281, -3.957578996910242619, 33.62503395064540257 ) ) ;
#4612 = CARTESIAN_POINT ( 'NONE',  ( -4.153846153846273204, -9.442884908241554243, 34.35708131394783038 ) ) ;
#4613 = AXIS2_PLACEMENT_3D ( 'NONE', #74305, #4163, #7172 ) ;
#4614 = CARTESIAN_POINT ( 'NONE',  ( 9.019230769230768274, -2.249999999999998668, 29.75000000000000355 ) ) ;
#4615 = CARTESIAN_POINT ( 'NONE',  ( -8.992156986746916658, -11.76352882383564769, 32.36236540154569497 ) ) ;
#4616 = CARTESIAN_POINT ( 'NONE',  ( -15.23076923076922995, -8.164416787775445883, 34.95778746994557906 ) ) ;
#4617 = EDGE_LOOP ( 'NONE', ( #3754, #23959, #69110, #80274 ) ) ;
#4618 = EDGE_CURVE ( 'NONE', #24436, #80960, #53352, .T. ) ;
#4619 = CARTESIAN_POINT ( 'NONE',  ( -3.165514091256391271, -12.70778746994558439, 30.41441678777536595 ) ) ;
#4620 = CARTESIAN_POINT ( 'NONE',  ( -2.084680956079456582, -9.886259254753566594, 34.14407573483972413 ) ) ;
#4621 = CARTESIAN_POINT ( 'NONE',  ( 9.442284468086237226, -2.588893531581426988, 31.60682220781847818 ) ) ;
#4622 = ORIENTED_EDGE ( 'NONE', *, *, #23777, .T. ) ;
#4623 = CARTESIAN_POINT ( 'NONE',  ( 10.36540787133602670, -9.234221910056348293, 34.70572697212741531 ) ) ;
#4624 = EDGE_LOOP ( 'NONE', ( #41223, #51347, #56237, #68123 ) ) ;
#4625 = CARTESIAN_POINT ( 'NONE',  ( 1.318858582101077204, -7.249945686854186278, 34.74374336980224598 ) ) ;
#4626 = CARTESIAN_POINT ( 'NONE',  ( 6.923076923076924238, -5.557115091759785130, 34.35708131394839171 ) ) ;
#4627 = CARTESIAN_POINT ( 'NONE',  ( 3.100078627658922503, -2.845849958028613624, 32.17971566917920967 ) ) ;
#4628 = EDGE_LOOP ( 'NONE', ( #32446, #19660, #65413, #36113 ) ) ;
#4629 = FACE_OUTER_BOUND ( 'NONE', #4063, .T. ) ;
#4631 = EDGE_CURVE ( 'NONE', #11542, #66197, #56532, .T. ) ;
#4630 = CARTESIAN_POINT ( 'NONE',  ( 17.07692307692307665, -9.819645486525091727, 36.12317359536749706 ) ) ;
#4632 = DIRECTION ( 'NONE',  ( -0.000000000000000000, -0.6427876096865404731, -0.7660444431189771253 ) ) ;
#4633 = ADVANCED_FACE ( 'NONE', ( #24569 ), #63778, .T. ) ;
#4634 = AXIS2_PLACEMENT_3D ( 'NONE', #3572, #52653, #31042 ) ;
#4635 = CARTESIAN_POINT ( 'NONE',  ( -7.846153846153967493, -5.094484230521993062, 34.41647553114689373 ) ) ;
#4636 = CARTESIAN_POINT ( 'NONE',  ( -2.057637887778853703, -10.82426656108011720, 33.81400080652039009 ) ) ;
#4637 = ORIENTED_EDGE ( 'NONE', *, *, #32326, .T. ) ;
#4638 = B_SPLINE_CURVE_WITH_KNOTS ( 'NONE', 3,
 ( #29740, #33942, #27186, #84253, #54644, #1373, #1814, #57204, #29304, #49117 ),
 .UNSPECIFIED., .F., .F.,
 ( 4, 2, 2, 2, 4 ),
 ( 0.0007817246256747461966, 0.0009771112852218892010, 0.001172497944769032314, 0.001367884604316175427, 0.001563271263863318323 ),
 .UNSPECIFIED. ) ;
#4639 = CYLINDRICAL_SURFACE ( 'NONE', #78865, 0.2500000000000008882 ) ;
#4640 = ORIENTED_EDGE ( 'NONE', *, *, #9256, .T. ) ;
#4641 = AXIS2_PLACEMENT_3D ( 'NONE', #83628, #62870, #29558 ) ;
#4642 = CARTESIAN_POINT ( 'NONE',  ( 7.596153846153846700, -2.499999999999998668, 29.75000000000000355 ) ) ;
#4643 = B_SPLINE_CURVE_WITH_KNOTS ( 'NONE', 3,
 ( #67973, #401, #67084, #54897, #89147, #48126, #26544, #82821, #47692, #60315 ),
 .UNSPECIFIED., .F., .F.,
 ( 4, 2, 2, 2, 4 ),
 ( 0.000000000000000000, 0.0001954339857564081520, 0.0003908679715128163040, 0.0005863019572692244018, 0.0007817359430256326080 ),
 .UNSPECIFIED. ) ;
#4644 = CARTESIAN_POINT ( 'NONE',  ( -9.469528151039279251, -12.24180327182772388, 31.33663988360758168 ) ) ;
#4646 = EDGE_CURVE ( 'NONE', #69108, #65429, #73780, .T. ) ;
#4645 = CARTESIAN_POINT ( 'NONE',  ( -0.3962833220256236078, -2.657715359629131857, 31.77849191805844242 ) ) ;
#4647 = DIRECTION ( 'NONE',  ( 1.000000000000000000, 0.000000000000000000, 0.000000000000000000 ) ) ;
#4648 = CARTESIAN_POINT ( 'NONE',  ( 9.019285080869083870, -3.627508038966690496, 32.91356715214248396 ) ) ;
#4649 = LINE ( 'NONE', #53267, #36451 ) ;
#4650 = CARTESIAN_POINT ( 'NONE',  ( 16.02315555073584008, -11.93127051446800380, 32.56575433478200665 ) ) ;
#4651 = EDGE_CURVE ( 'NONE', #28571, #16403, #9297, .T. ) ;
#4652 = ORIENTED_EDGE ( 'NONE', *, *, #30004, .F. ) ;
#4653 = ORIENTED_EDGE ( 'NONE', *, *, #14276, .F. ) ;
#4654 = VERTEX_POINT ( 'NONE', #2956 ) ;
#4655 = EDGE_LOOP ( 'NONE', ( #57573, #71400 ) ) ;
#4656 = VERTEX_POINT ( 'NONE', #3851 ) ;
#4657 = CARTESIAN_POINT ( 'NONE',  ( -4.403846153846151523, -2.499999999999998668, 29.75000000000000355 ) ) ;
#4658 = EDGE_CURVE ( 'NONE', #13650, #84346, #86728, .T. ) ;
#4659 = CARTESIAN_POINT ( 'NONE',  ( -2.084680956079457914, -3.105924265160262543, 32.13625925475356127 ) ) ;
#4660 = LINE ( 'NONE', #52834, #76990 ) ;
#4661 = CARTESIAN_POINT ( 'NONE',  ( -6.923076923077044142, -3.300289026999228881, 32.46337939537708905 ) ) ;
#4662 = CARTESIAN_POINT ( 'NONE',  ( 7.622668921589514923, -12.69144148231606017, 30.53333754910549303 ) ) ;
#4663 = AXIS2_PLACEMENT_3D ( 'NONE', #31170, #84818, #58196 ) ;
#4664 = CARTESIAN_POINT ( 'NONE',  ( 3.164685819813350509, -5.557115091759785130, 34.35708131394839171 ) ) ;
#4665 = DIRECTION ( 'NONE',  ( 1.000000000000000000, 0.000000000000000000, 0.000000000000000000 ) ) ;
#4666 = CARTESIAN_POINT ( 'NONE',  ( 17.07692307692295586, -6.835583212225970762, 34.95778746994575670 ) ) ;
#4667 = CARTESIAN_POINT ( 'NONE',  ( 8.069166690247241647, -4.762714258010882773, 34.23016756924214832 ) ) ;
#4668 = VERTEX_POINT ( 'NONE', #39440 ) ;
#4669 = ORIENTED_EDGE ( 'NONE', *, *, #82770, .F. ) ;
#4670 = AXIS2_PLACEMENT_3D ( 'NONE', #7512, #21903, #77287 ) ;
#4671 = B_SPLINE_CURVE_WITH_KNOTS ( 'NONE', 3,
 ( #45430, #3995, #52184, #59399, #25169, #78775, #72908, #11214, #39146, #86901 ),
 .UNSPECIFIED., .F., .F.,
 ( 4, 2, 2, 2, 4 ),
 ( 0.000000000000000000, 0.0001954311564186876876, 0.0003908623128373753751, 0.0005862934692560630356, 0.0007817246256747507503 ),
 .UNSPECIFIED. ) ;
#4672 = VERTEX_POINT ( 'NONE', #46186 ) ;
#4674 = ORIENTED_EDGE ( 'NONE', *, *, #55465, .T. ) ;
#4673 = CARTESIAN_POINT ( 'NONE',  ( 0.3308478584281537849, -11.93127051446800024, 32.56575433478200665 ) ) ;
#4676 = CARTESIAN_POINT ( 'NONE',  ( -17.93474486048716088, -11.67786785259547777, 32.92929555188713664 ) ) ;
#4675 = DIRECTION ( 'NONE',  ( 0.000000000000000000, 1.000000000000000000, 0.000000000000000000 ) ) ;
#4677 = B_SPLINE_CURVE_WITH_KNOTS ( 'NONE', 3,
 ( #42764, #63458, #71099, #70224, #8528, #30557 ),
 .UNSPECIFIED., .F., .F.,
 ( 4, 2, 4 ),
 ( 0.0003909569690057827069, 0.0005862646681846092828, 0.0007815723673634358045 ),
 .UNSPECIFIED. ) ;
#4678 = CYLINDRICAL_SURFACE ( 'NONE', #34147, 0.2500000000000012212 ) ;
#4679 = CARTESIAN_POINT ( 'NONE',  ( -14.53117725141625627, -10.11188796281391511, 34.01382737946119050 ) ) ;
#4680 = FACE_BOUND ( 'NONE', #38021, .T. ) ;
#4681 = ORIENTED_EDGE ( 'NONE', *, *, #42842, .T. ) ;
#4682 = EDGE_CURVE ( 'NONE', #20422, #68899, #44713, .T. ) ;
#4683 = ORIENTED_EDGE ( 'NONE', *, *, #5175, .T. ) ;
#4684 = CARTESIAN_POINT ( 'NONE',  ( -11.53846153846153655, -11.91647553114624181, 32.58852847137148245 ) ) ;
#4686 = ADVANCED_FACE ( 'NONE', ( #25910 ), #17827, .F. ) ;
#4685 = EDGE_LOOP ( 'NONE', ( #33890, #60463 ) ) ;
#4687 = FACE_BOUND ( 'NONE', #32223, .T. ) ;
#4688 = CARTESIAN_POINT ( 'NONE',  ( -9.692307692307814193, -2.379036618888197729, 30.90682066428292885 ) ) ;
#4689 = FACE_OUTER_BOUND ( 'NONE', #67138, .T. ) ;
#4690 = VERTEX_POINT ( 'NONE', #66897 ) ;
#4691 = CARTESIAN_POINT ( 'NONE',  ( 12.46153846153846168, -9.780366693483667717, 34.19971097300155094 ) ) ;
#4693 = ADVANCED_FACE ( 'NONE', ( #18268 ), #12836, .F. ) ;
#4692 = CARTESIAN_POINT ( 'NONE',  ( -1.514763354347078872, -8.630895178749536711, 34.87696386517710323 ) ) ;
#4694 = CARTESIAN_POINT ( 'NONE',  ( -5.299802593660662531, -7.630690623152302621, 34.99857592706774057 ) ) ;
#4695 = VERTEX_POINT ( 'NONE', #59692 ) ;
#4696 = FACE_OUTER_BOUND ( 'NONE', #16049, .T. ) ;
#4697 = CARTESIAN_POINT ( 'NONE',  ( 3.230769230769231726, -12.10708131394839349, 31.69288490824020244 ) ) ;
#4698 = CARTESIAN_POINT ( 'NONE',  ( -0.4615384615384611200, -2.517432740324522911, 35.29906147534542527 ) ) ;
#4699 = VERTEX_POINT ( 'NONE', #5194 ) ;
#4700 = CARTESIAN_POINT ( 'NONE',  ( -1.608100328339332030, -5.912607949931405038, 34.49155766932282319 ) ) ;
#4701 = CARTESIAN_POINT ( 'NONE',  ( -9.692307692307691624, -11.35647404775217417, 33.31231777344666511 ) ) ;
#4703 = ORIENTED_EDGE ( 'NONE', *, *, #12062, .T. ) ;
#4702 = CIRCLE ( 'NONE', #86692, 0.2500000000000002220 ) ;
#4704 = FACE_OUTER_BOUND ( 'NONE', #40079, .T. ) ;
#4705 = CARTESIAN_POINT ( 'NONE',  ( -10.61538461538473399, -5.219633306517616589, 34.19971097300220464 ) ) ;
#4706 = CARTESIAN_POINT ( 'NONE',  ( 21.00000000000000355, -7.500000000000000000, 29.75000000000000355 ) ) ;
#4707 = DIRECTION ( 'NONE',  ( 1.000000000000000000, 0.000000000000000000, 0.000000000000000000 ) ) ;
#4708 = CYLINDRICAL_SURFACE ( 'NONE', #51604, 0.2500000000000002220 ) ;
#4709 = CARTESIAN_POINT ( 'NONE',  ( 17.29970274590113632, -4.989023458446561143, 34.36081565061822118 ) ) ;
#4711 = CARTESIAN_POINT ( 'NONE',  ( -17.01166750564705055, -8.613356846314930593, 34.62446782046653482 ) ) ;
#4710 = DIRECTION ( 'NONE',  ( -0.000000000000000000, 0.6427876096865404731, -0.7660444431189770143 ) ) ;
#4712 = CARTESIAN_POINT ( 'NONE',  ( 10.74617505635156789, -9.084667340241226796, 34.75534355489798344 ) ) ;
#4713 = LINE ( 'NONE', #41159, #37759 ) ;
#4714 = EDGE_CURVE ( 'NONE', #50483, #65254, #57654, .T. ) ;
#4715 = CARTESIAN_POINT ( 'NONE',  ( -1.139087296526025916, -4.750000000000006217, 14.07812500000000178 ) ) ;
#4716 = EDGE_LOOP ( 'NONE', ( #63443, #14466, #29500, #67780 ) ) ;
#4717 = DIRECTION ( 'NONE',  ( -1.000000000000000000, 0.000000000000000000, -0.000000000000000000 ) ) ;
#4718 = EDGE_LOOP ( 'NONE', ( #4907, #42635, #22946, #57955 ) ) ;
#4719 = B_SPLINE_CURVE_WITH_KNOTS ( 'NONE', 3,
 ( #74987, #12831, #53815, #88517, #59687, #73663, #87184, #80415, #12392, #5190 ),
 .UNSPECIFIED., .F., .F.,
 ( 4, 2, 2, 2, 4 ),
 ( 0.0007817359430256322827, 0.0009771253907249989254, 0.001172514838424365676, 0.001367904286123732428, 0.001563293733823098962 ),
 .UNSPECIFIED. ) ;
#4720 = EDGE_CURVE ( 'NONE', #43004, #66583, #25016, .T. ) ;
#4721 = EDGE_LOOP ( 'NONE', ( #4265, #20171, #85178, #4177 ) ) ;
#4722 = DIRECTION ( 'NONE',  ( -0.000000000000000000, -0.9848077530122085754, -0.1736481776669273613 ) ) ;
#4723 = ORIENTED_EDGE ( 'NONE', *, *, #24111, .F. ) ;
#4724 = CARTESIAN_POINT ( 'NONE',  ( 11.53846153846141576, -2.657715359629662544, 31.77849191805970364 ) ) ;
#4725 = CARTESIAN_POINT ( 'NONE',  ( 1.987747218494664292, -9.401340078031346081, 26.87313170625849423 ) ) ;
#4726 = CARTESIAN_POINT ( 'NONE',  ( 2.307692307692309264, -4.661471528628507777, 34.16647553114623292 ) ) ;
#4727 = CARTESIAN_POINT ( 'NONE',  ( -15.45425415533356528, -12.47654668319379567, 31.42292124445336654 ) ) ;
#4728 = CARTESIAN_POINT ( 'NONE',  ( -0.3307466537136744544, -5.582136614379148654, 34.36778462344220486 ) ) ;
#4729 = CARTESIAN_POINT ( 'NONE',  ( -14.43838291080261449, -10.70098750199973203, 33.91152734681376302 ) ) ;
#4730 = CARTESIAN_POINT ( 'NONE',  ( -10.61538461538461320, -3.322132147404559976, 32.92929555188717927 ) ) ;
#4731 = CARTESIAN_POINT ( 'NONE',  ( -10.74607608205217346, -4.118384482072085184, 33.43331474514187107 ) ) ;
#4732 = FACE_OUTER_BOUND ( 'NONE', #13536, .T. ) ;
#4733 = CARTESIAN_POINT ( 'NONE',  ( -1.929879867024197893E-14, -3.750000000000000000, 21.65625000000000355 ) ) ;
#4734 = B_SPLINE_CURVE_WITH_KNOTS ( 'NONE', 3,
 ( #42398, #76613, #60877, #19890, #27540, #6394, #62638, #75288, #14920, #33849 ),
 .UNSPECIFIED., .F., .F.,
 ( 4, 2, 2, 2, 4 ),
 ( 0.0007817246256747484735, 0.0009771112852218931041, 0.001172497944769037735, 0.001367884604316182365, 0.001563271263863326996 ),
 .UNSPECIFIED. ) ;
#4735 = EDGE_CURVE ( 'NONE', #88166, #19996, #32622, .T. ) ;
#4736 = CARTESIAN_POINT ( 'NONE',  ( -7.173053667125516064, -4.818429247618089661, 34.26397095200675125 ) ) ;
#4737 = DIRECTION ( 'NONE',  ( 0.000000000000000000, 0.000000000000000000, 1.000000000000000000 ) ) ;
#4738 = CARTESIAN_POINT ( 'NONE',  ( 5.869852030268307708, -3.625366637846544560, 33.29286588640298561 ) ) ;
#4739 = EDGE_CURVE ( 'NONE', #87539, #46286, #32931, .T. ) ;
#4740 = AXIS2_PLACEMENT_3D ( 'NONE', #57764, #43803, #31628 ) ;
#4741 = EDGE_CURVE ( 'NONE', #22687, #56815, #74542, .T. ) ;
#4742 = CIRCLE ( 'NONE', #88146, 0.2500000000000002220 ) ;
#4743 = VERTEX_POINT ( 'NONE', #33564 ) ;
#4744 = ORIENTED_EDGE ( 'NONE', *, *, #27598, .T. ) ;
#4745 = CARTESIAN_POINT ( 'NONE',  ( 6.673100192134568509, -2.564618984488975961, 30.55390908950641915 ) ) ;
#4746 = CARTESIAN_POINT ( 'NONE',  ( -14.05774678934416499, -8.433404298154334455, 34.66254593164985920 ) ) ;
#4747 = LINE ( 'NONE', #53362, #31095 ) ;
#4748 = CARTESIAN_POINT ( 'NONE',  ( 2.307692307692309264, -2.292212530054420494, 30.41441678777542634 ) ) ;
#4749 = CARTESIAN_POINT ( 'NONE',  ( -0.3589743589743593088, -7.500000000000000000, 33.75000000000000000 ) ) ;
#4750 = VECTOR ( 'NONE', #41521, 1000.000000000000114 ) ;
#4751 = CARTESIAN_POINT ( 'NONE',  ( -16.28453762051371712, -8.999036380462719364, 34.52022231692819076 ) ) ;
#4752 = ADVANCED_FACE ( 'NONE', ( #52035 ), #72752, .F. ) ;
#4753 = EDGE_CURVE ( 'NONE', #70987, #76146, #41643, .T. ) ;
#4754 = ORIENTED_EDGE ( 'NONE', *, *, #35336, .F. ) ;
#4755 = LINE ( 'NONE', #19150, #73167 ) ;
#4756 = ORIENTED_EDGE ( 'NONE', *, *, #14798, .F. ) ;
#4757 = VERTEX_POINT ( 'NONE', #62340 ) ;
#4758 = CARTESIAN_POINT ( 'NONE',  ( 7.716005876422148191, -11.04286588640298561, 33.62463336215343901 ) ) ;
#4759 = CARTESIAN_POINT ( 'NONE',  ( -2.307692307692428724, -9.528491918059723176, 34.59228464037033035 ) ) ;
#4760 = CARTESIAN_POINT ( 'NONE',  ( -4.153846153846152411, -12.62096338111211580, 30.90682066428153263 ) ) ;
#4761 = CARTESIAN_POINT ( 'NONE',  ( -4.153846153846152411, -6.435427911321262684, 35.78748833219616898 ) ) ;
#4762 = CARTESIAN_POINT ( 'NONE',  ( 13.31934538405906565, -5.941354392334499579, 34.76329471203369792 ) ) ;
#4763 = ADVANCED_FACE ( 'NONE', ( #15060 ), #42533, .F. ) ;
#4764 = ORIENTED_EDGE ( 'NONE', *, *, #40650, .T. ) ;
#4765 = CIRCLE ( 'NONE', #76641, 3.249999999999999556 ) ;
#4766 = AXIS2_PLACEMENT_3D ( 'NONE', #70291, #8598, #63525 ) ;
#4767 = EDGE_LOOP ( 'NONE', ( #78259, #70125, #69660, #69925 ) ) ;
#4768 = VERTEX_POINT ( 'NONE', #21364 ) ;
#4769 = CARTESIAN_POINT ( 'NONE',  ( 17.07692307692307665, -2.499999999999998668, 29.75000000000001421 ) ) ;
#4770 = CARTESIAN_POINT ( 'NONE',  ( -0.2387587925603949501, -10.23759521482555357, 34.22997729860117033 ) ) ;
#4771 = B_SPLINE_CURVE_WITH_KNOTS ( 'NONE', 3,
 ( #42664, #2537, #57489, #56612, #70122, #43097, #84978, #8430, #50720, #22380 ),
 .UNSPECIFIED., .F., .F.,
 ( 4, 2, 2, 2, 4 ),
 ( 0.0007817359430256293554, 0.0009771253907249950223, 0.001172514838424360906, 0.001367904286123726790, 0.001563293733823092457 ),
 .UNSPECIFIED. ) ;
#4772 = DIRECTION ( 'NONE',  ( 0.000000000000000000, 0.7660444431189822323, -0.6427876096865344779 ) ) ;
#4773 = DIRECTION ( 'NONE',  ( 0.000000000000000000, 0.8660254037844377084, -0.5000000000000015543 ) ) ;
#4774 = CARTESIAN_POINT ( 'NONE',  ( -4.283993363284373856, -8.587444163452046197, 34.63053765926554206 ) ) ;
#4775 = CARTESIAN_POINT ( 'NONE',  ( 5.999999999999880096, -12.46129190930018460, 30.37095296980731973 ) ) ;
#4776 = EDGE_LOOP ( 'NONE', ( #22085, #4916 ) ) ;
#4777 = VERTEX_POINT ( 'NONE', #54254 ) ;
#4778 = CARTESIAN_POINT ( 'NONE',  ( 0.5267940328144856688, -11.94971097300157403, 32.03036669348361443 ) ) ;
#4780 = EDGE_LOOP ( 'NONE', ( #63878, #80858, #78523, #73454 ) ) ;
#4779 = CARTESIAN_POINT ( 'NONE',  ( -5.999999999999998224, -3.050289026998446396, 32.03036669348365706 ) ) ;
#4781 = CARTESIAN_POINT ( 'NONE',  ( -39.05038313613820122, -2.249999999999998668, 29.75000000000000355 ) ) ;
#4782 = CARTESIAN_POINT ( 'NONE',  ( -9.758391103263571509, -11.69971097300155272, 32.46337939537587403 ) ) ;
#4783 = CARTESIAN_POINT ( 'NONE',  ( -3.749999999999997335, -7.500000000000021316, 16.34375000000000000 ) ) ;
#4784 = VERTEX_POINT ( 'NONE', #28120 ) ;
#4785 = DIRECTION ( 'NONE',  ( 1.000000000000000000, 0.000000000000000000, 0.000000000000000000 ) ) ;
#4786 = ORIENTED_EDGE ( 'NONE', *, *, #34339, .T. ) ;
#4787 = FACE_OUTER_BOUND ( 'NONE', #88658, .T. ) ;
#4788 = CARTESIAN_POINT ( 'NONE',  ( -5.076923076923075762, -6.386643153685126251, 34.62446782046654192 ) ) ;
#4789 =( GEOMETRIC_REPRESENTATION_CONTEXT ( 3 ) GLOBAL_UNCERTAINTY_ASSIGNED_CONTEXT ( ( #48799 ) ) GLOBAL_UNIT_ASSIGNED_CONTEXT ( ( #88673, #50737, #78670 ) ) REPRESENTATION_CONTEXT ( 'NONE', 'WORKASPACE' ) );
#4790 = ADVANCED_FACE ( 'NONE', ( #6966 ), #69112, .F. ) ;
#4791 = FACE_BOUND ( 'NONE', #4092, .T. ) ;
#4793 = CARTESIAN_POINT ( 'NONE',  ( 7.976944287120795174, -2.295524264805589354, 30.44142389570982488 ) ) ;
#4792 = CARTESIAN_POINT ( 'NONE',  ( 11.53846153846153832, -12.29105614889573062, 35.45975837776705220 ) ) ;
#4794 = CIRCLE ( 'NONE', #86786, 0.2500000000000002220 ) ;
#4795 = DIRECTION ( 'NONE',  ( -0.000000000000000000, 0.5000000000000011102, -0.8660254037844381525 ) ) ;
#4796 = EDGE_LOOP ( 'NONE', ( #59463, #14742 ) ) ;
#4798 = EDGE_CURVE ( 'NONE', #59654, #76676, #651, .T. ) ;
#4797 = CARTESIAN_POINT ( 'NONE',  ( -11.53846153846166089, -8.656820664282941280, 34.87096338111179961 ) ) ;
#4799 = CARTESIAN_POINT ( 'NONE',  ( 11.53846153846185274, -2.255955759149395501, 30.00000000000324363 ) ) ;
#4800 = CARTESIAN_POINT ( 'NONE',  ( 16.15384615384603251, -5.941354392335915335, 34.76329471203413846 ) ) ;
#4801 = VERTEX_POINT ( 'NONE', #35780 ) ;
#4802 = EDGE_CURVE ( 'NONE', #12672, #87474, #1824, .T. ) ;
#4803 = B_SPLINE_CURVE_WITH_KNOTS ( 'NONE', 3,
 ( #3378, #57880, #24538, #29974, #10146, #23650, #56991, #8820, #84484, #43485 ),
 .UNSPECIFIED., .F., .F.,
 ( 4, 2, 2, 2, 4 ),
 ( 0.0007817246256747440282, 0.0009771112852218863821, 0.001172497944769028844, 0.001367884604316171307, 0.001563271263863313769 ),
 .UNSPECIFIED. ) ;
#4804 = LINE ( 'NONE', #18761, #54503 ) ;
#4805 = CARTESIAN_POINT ( 'NONE',  ( -8.769230769230892619, -3.083524468854526912, 32.58852847137268327 ) ) ;
#4806 = CARTESIAN_POINT ( 'NONE',  ( -16.21992853320628925, -11.91647553114624181, 32.58852847137148245 ) ) ;
#4807 = CARTESIAN_POINT ( 'NONE',  ( 7.976679547917411739, -3.285477652293412820, 32.44071101563363158 ) ) ;
#4808 = FACE_BOUND ( 'NONE', #13389, .T. ) ;
#4810 = DIRECTION ( 'NONE',  ( -0.000000000000000000, 0.8660254037844397068, -0.4999999999999978906 ) ) ;
#4809 = DIRECTION ( 'NONE',  ( 1.000000000000000000, 2.891205793294679312E-16, -0.000000000000000000 ) ) ;
#4811 = CARTESIAN_POINT ( 'NONE',  ( 4.153846153846032507, -2.892918686052165622, 31.69288490824153470 ) ) ;
#4812 = CARTESIAN_POINT ( 'NONE',  ( 17.99999999999987566, -11.48612834414049644, 32.76840700105863391 ) ) ;
#4813 = CARTESIAN_POINT ( 'NONE',  ( -4.087778820496076548, -10.67929555188718282, 33.92786785259544757 ) ) ;
#4814 = EDGE_CURVE ( 'NONE', #33014, #88650, #15467, .T. ) ;
#4815 = CARTESIAN_POINT ( 'NONE',  ( 13.38461538461526423, -2.657715359629662544, 31.77849191805970364 ) ) ;
#4816 = CARTESIAN_POINT ( 'NONE',  ( 2.608446859217893099, -4.805146000318787358, 26.56063170625849068 ) ) ;
#4817 = B_SPLINE_CURVE_WITH_KNOTS ( 'NONE', 3,
 ( #54102, #81596, #19883, #47349, #74845, #943, #77051, #23415, #35626, #69847 ),
 .UNSPECIFIED., .F., .F.,
 ( 4, 2, 2, 2, 4 ),
 ( 0.000000000000000000, 0.0001954311564186877960, 0.0003908623128373755920, 0.0005862934692560633609, 0.0007817246256747511840 ),
 .UNSPECIFIED. ) ;
#4818 = DIRECTION ( 'NONE',  ( -0.000000000000000000, -0.7660444431189791237, -0.6427876096865379196 ) ) ;
#4819 = ORIENTED_EDGE ( 'NONE', *, *, #6488, .F. ) ;
#4820 = CARTESIAN_POINT ( 'NONE',  ( -4.153846153846273204, -11.94971097300221174, 32.03036669348237098 ) ) ;
#4821 = CARTESIAN_POINT ( 'NONE',  ( 2.057669083470851756, -2.341070481393819236, 30.72580821765574299 ) ) ;
#4822 = CARTESIAN_POINT ( 'NONE',  ( -1.134561072977068985, -10.66356715214248396, 33.62249196103329751 ) ) ;
#4823 = DIRECTION ( 'NONE',  ( 0.000000000000000000, 0.4999999999999960032, -0.8660254037844410391 ) ) ;
#4824 = CARTESIAN_POINT ( 'NONE',  ( -10.48485917715097315, -12.15418822224088835, 32.17964115625579069 ) ) ;
#4825 = CARTESIAN_POINT ( 'NONE',  ( -12.59222906464877134, -6.369640206132551441, 34.87707690430378449 ) ) ;
#4826 = CARTESIAN_POINT ( 'NONE',  ( -1.614399933863656544, -3.775308065498769405, 26.32625670625849068 ) ) ;
#4827 = CARTESIAN_POINT ( 'NONE',  ( 14.17754509825408960, -10.88202310037935661, 33.43294751532457099 ) ) ;
#4828 = LINE ( 'NONE', #46253, #87807 ) ;
#4829 = VECTOR ( 'NONE', #63096, 1000.000000000000227 ) ;
#4830 = CARTESIAN_POINT ( 'NONE',  ( -4.946132635956128176, -11.93129842949671726, 32.56571108434900452 ) ) ;
#4831 = CARTESIAN_POINT ( 'NONE',  ( 9.442284468086237226, -4.175268141568685643, 33.81360843649122216 ) ) ;
#4832 = LINE ( 'NONE', #31406, #62664 ) ;
#4833 = DIRECTION ( 'NONE',  ( -0.000000000000000000, 0.3420201433256694346, -0.9396926207859080948 ) ) ;
#4834 = CARTESIAN_POINT ( 'NONE',  ( 14.17754509825408960, -6.001485441113819874, 34.52039167877662607 ) ) ;
#4835 = CARTESIAN_POINT ( 'NONE',  ( -11.40793583669797506, -10.88167719472716399, 33.43325721877153711 ) ) ;
#4836 = ORIENTED_EDGE ( 'NONE', *, *, #71660, .T. ) ;
#4837 = CARTESIAN_POINT ( 'NONE',  ( 17.07692307692307665, -2.721908614388771852, 31.22303859784724978 ) ) ;
#4838 = FACE_OUTER_BOUND ( 'NONE', #34839, .T. ) ;
#4839 = CARTESIAN_POINT ( 'NONE',  ( -3.724691934501248802, -5.885600066136383646, 17.92374329374151287 ) ) ;
#4840 = EDGE_CURVE ( 'NONE', #28639, #43192, #82192, .T. ) ;
#4841 = LINE ( 'NONE', #60215, #74920 ) ;
#4842 = CARTESIAN_POINT ( 'NONE',  ( 5.076923076922953193, -6.835583212225970762, 34.95778746994575670 ) ) ;
#4843 = ORIENTED_EDGE ( 'NONE', *, *, #1547, .F. ) ;
#4844 = CARTESIAN_POINT ( 'NONE',  ( 6.923076923076924238, -8.120952969808772792, 34.71129190930000163 ) ) ;
#4845 = CARTESIAN_POINT ( 'NONE',  ( 5.999999999999880096, -11.48612834414049644, 32.76840700105863391 ) ) ;
#4847 = ORIENTED_EDGE ( 'NONE', *, *, #6096, .T. ) ;
#4846 = CARTESIAN_POINT ( 'NONE',  ( 11.78846153846154010, -2.249999999999998668, 29.75000000000000355 ) ) ;
#4848 = CARTESIAN_POINT ( 'NONE',  ( 11.78851585009985570, -4.943051570960394159, 34.04725096376909477 ) ) ;
#4849 = CARTESIAN_POINT ( 'NONE',  ( -3.230769230769351186, -3.835265460704628371, 33.15142922262033665 ) ) ;
#4850 = DIRECTION ( 'NONE',  ( 0.000000000000000000, 0.8660254037844377084, 0.5000000000000015543 ) ) ;
#4851 = B_SPLINE_CURVE_WITH_KNOTS ( 'NONE', 3,
 ( #3280, #64527, #23552, #35761, #83951, #51005 ),
 .UNSPECIFIED., .F., .F.,
 ( 4, 2, 4 ),
 ( 1.769077770938648657E-17, 0.0001954756301636913782, 0.0003909512603273650297 ),
 .UNSPECIFIED. ) ;
#4852 = CARTESIAN_POINT ( 'NONE',  ( -16.37667425148103106, -7.369209533119136069, 34.99857337881830688 ) ) ;
#4853 = EDGE_CURVE ( 'NONE', #5644, #53642, #69989, .T. ) ;
#4854 = ORIENTED_EDGE ( 'NONE', *, *, #36509, .F. ) ;
#4855 = B_SPLINE_CURVE_WITH_KNOTS ( 'NONE', 3,
 ( #69659, #7965, #35428, #56146, #70100, #8409, #35882, #72757, #32231, #86301 ),
 .UNSPECIFIED., .F., .F.,
 ( 4, 2, 2, 2, 4 ),
 ( 0.000000000000000000, 0.0001954311564186870913, 0.0003908623128373741825, 0.0005862934692560613009, 0.0007817246256747483650 ),
 .UNSPECIFIED. ) ;
#4856 = CYLINDRICAL_SURFACE ( 'NONE', #61980, 0.2499999999999986955 ) ;
#4857 = B_SPLINE_CURVE_WITH_KNOTS ( 'NONE', 3,
 ( #64845, #31062, #44125, #58529, #3146, #10364, #9472, #65735, #63962, #71166 ),
 .UNSPECIFIED., .F., .F.,
 ( 4, 2, 2, 2, 4 ),
 ( 0.000000000000000000, 0.0001954339857564070678, 0.0003908679715128141356, 0.0005863019572692211492, 0.0007817359430256282712 ),
 .UNSPECIFIED. ) ;
#4858 = B_SPLINE_CURVE_WITH_KNOTS ( 'NONE', 3,
 ( #73499, #86576, #38822, #32496, #10459, #44213, #66282, #25301, #37927, #4587 ),
 .UNSPECIFIED., .F., .F.,
 ( 4, 2, 2, 2, 4 ),
 ( 0.0007817359430256235007, 0.0009771253907249932875, 0.001172514838424355919, 0.001367904286123718983, 0.001563293733823081615 ),
 .UNSPECIFIED. ) ;
#4859 = LINE ( 'NONE', #32329, #22149 ) ;
#4860 = PRESENTATION_LAYER_ASSIGNMENT (  '', '', ( #29349 ) ) ;
#4861 = VECTOR ( 'NONE', #24583, 1000.000000000000000 ) ;
#4862 = EDGE_CURVE ( 'NONE', #10877, #18726, #8205, .T. ) ;
#4863 = EDGE_CURVE ( 'NONE', #63786, #29793, #64013, .T. ) ;
#4864 = CARTESIAN_POINT ( 'NONE',  ( -15.23076923076922995, -6.343179335718451384, 34.87096338111211935 ) ) ;
#4865 = VERTEX_POINT ( 'NONE', #34437 ) ;
#4866 = ORIENTED_EDGE ( 'NONE', *, *, #51633, .F. ) ;
#4867 = VERTEX_POINT ( 'NONE', #61900 ) ;
#4868 = LINE ( 'NONE', #67009, #23991 ) ;
#4869 = FACE_OUTER_BOUND ( 'NONE', #47292, .T. ) ;
#4870 = CARTESIAN_POINT ( 'NONE',  ( -9.692307692307691624, -5.180354513474913603, 36.12317359536750416 ) ) ;
#4871 = EDGE_CURVE ( 'NONE', #64358, #47735, #18894, .T. ) ;
#4872 = CARTESIAN_POINT ( 'NONE',  ( -18.12834546406995528, -7.274827144381421640, 34.99539338292708379 ) ) ;
#4873 = EDGE_LOOP ( 'NONE', ( #21431, #65058, #63052, #41099 ) ) ;
#4874 = EDGE_CURVE ( 'NONE', #11165, #85470, #9196, .T. ) ;
#4875 = ADVANCED_FACE ( 'NONE', ( #49720 ), #77637, .F. ) ;
#4876 = ORIENTED_EDGE ( 'NONE', *, *, #85167, .T. ) ;
#4877 = ORIENTED_EDGE ( 'NONE', *, *, #6370, .F. ) ;
#4879 = ORIENTED_EDGE ( 'NONE', *, *, #17863, .T. ) ;
#4878 = CARTESIAN_POINT ( 'NONE',  ( 11.66925197942848946, -11.37503395064541678, 33.29242100308974273 ) ) ;
#4880 = DIRECTION ( 'NONE',  ( -0.000000000000000000, -0.9848077530122085754, -0.1736481776669273891 ) ) ;
#4881 = EDGE_CURVE ( 'NONE', #64027, #72207, #3874, .T. ) ;
#4882 = CARTESIAN_POINT ( 'NONE',  ( -3.480792454990687457, -4.931416488878823223, 34.32920672191015399 ) ) ;
#4883 = B_SPLINE_CURVE_WITH_KNOTS ( 'NONE', 3,
 ( #44825, #44373, #2507, #79071, #25010, #72306, #79523, #38536, #52478, #79962 ),
 .UNSPECIFIED., .F., .F.,
 ( 4, 2, 2, 2, 4 ),
 ( 0.000000000000000000, 0.0001954339857564080978, 0.0003908679715128161956, 0.0005863019572692242934, 0.0007817359430256323911 ),
 .UNSPECIFIED. ) ;
#4884 = CARTESIAN_POINT ( 'NONE',  ( 10.55011416942384095, -11.48612834413959582, 32.76840700105983473 ) ) ;
#4885 = CARTESIAN_POINT ( 'NONE',  ( -1.134560964701931463, -12.65882529074907126, 30.72640787790839312 ) ) ;
#4886 = EDGE_LOOP ( 'NONE', ( #16594, #13139, #67745, #50693, #20912, #63814, #12403, #82588, #60363, #32892 ) ) ;
#4887 = B_SPLINE_CURVE_WITH_KNOTS ( 'NONE', 3,
 ( #38941, #23626, #24513, #79915, #45229, #71362, #66398, #2897, #59638, #65942 ),
 .UNSPECIFIED., .F., .F.,
 ( 4, 2, 2, 2, 4 ),
 ( 0.000000000000000000, 0.0001954339857564100222, 0.0003908679715128200445, 0.0005863019572692300396, 0.0007817359430256400890 ),
 .UNSPECIFIED. ) ;
#4888 = ORIENTED_EDGE ( 'NONE', *, *, #15569, .T. ) ;
#4889 = ORIENTED_EDGE ( 'NONE', *, *, #36115, .F. ) ;
#4890 = CARTESIAN_POINT ( 'NONE',  ( 14.30769230769231015, -10.67929555188718282, 33.92786785259544047 ) ) ;
#4892 = ORIENTED_EDGE ( 'NONE', *, *, #701, .T. ) ;
#4891 = CARTESIAN_POINT ( 'NONE',  ( 14.16025641025641235, -11.50000000000000000, 29.75000000000000355 ) ) ;
#4893 = CARTESIAN_POINT ( 'NONE',  ( 3.007843013253083786, -11.76352882383564769, 32.36236540154569497 ) ) ;
#4894 = CARTESIAN_POINT ( 'NONE',  ( -13.38461538461538325, -6.386643153685126251, 34.62446782046654192 ) ) ;
#4895 = CARTESIAN_POINT ( 'NONE',  ( 12.68431813051652846, -6.717445702608402236, 34.94155399931962336 ) ) ;
#4896 = CARTESIAN_POINT ( 'NONE',  ( -1.384615384615383471, -8.120952969808772792, 34.71129190930000163 ) ) ;
#4897 = CARTESIAN_POINT ( 'NONE',  ( -2.176900499867519212, -11.18335022499818621, 33.13157742990016885 ) ) ;
#4898 = FACE_BOUND ( 'NONE', #84623, .T. ) ;
#4899 = CARTESIAN_POINT ( 'NONE',  ( 18.00000000000000000, -11.91647553114624181, 32.58852847137148245 ) ) ;
#4900 = CARTESIAN_POINT ( 'NONE',  ( 10.61538461538461675, -1.367168528481310208, 33.57946703557072254 ) ) ;
#4901 = EDGE_CURVE ( 'NONE', #20256, #69595, #8752, .T. ) ;
#4902 = CARTESIAN_POINT ( 'NONE',  ( -8.992156986746914882, -4.186968288167449259, 33.49512374952580274 ) ) ;
#4904 = CARTESIAN_POINT ( 'NONE',  ( 6.856994543716785628, -10.67929555188718460, 33.92786785259543336 ) ) ;
#4903 = CARTESIAN_POINT ( 'NONE',  ( 9.561616225640133138, -3.062553014421049546, 32.05460306192773601 ) ) ;
#4905 = CARTESIAN_POINT ( 'NONE',  ( 0.2115152242454951537, -12.22074536777954989, 31.39888409691088356 ) ) ;
#4906 = CARTESIAN_POINT ( 'NONE',  ( 7.846153846153725020, -11.48612834414049644, 32.76840700105863391 ) ) ;
#4907 = ORIENTED_EDGE ( 'NONE', *, *, #2075, .T. ) ;
#4908 = DIRECTION ( 'NONE',  ( -0.000000000000000000, -0.6427876096865404731, -0.7660444431189770143 ) ) ;
#4909 = CARTESIAN_POINT ( 'NONE',  ( 12.46153846153846168, -3.322132147404559976, 32.92929555188717927 ) ) ;
#4910 = ORIENTED_EDGE ( 'NONE', *, *, #42355, .F. ) ;
#4911 = EDGE_LOOP ( 'NONE', ( #28871, #3047 ) ) ;
#4912 = CARTESIAN_POINT ( 'NONE',  ( 8.769230769230645706, -11.67786785259630911, 32.92929555188603530 ) ) ;
#4913 = CARTESIAN_POINT ( 'NONE',  ( -0.5267894516997033705, -2.506253911140460922, 30.00000000000013856 ) ) ;
#4914 = DIRECTION ( 'NONE',  ( -0.000000000000000000, 0.5000000000000011102, -0.8660254037844380415 ) ) ;
#4915 = CARTESIAN_POINT ( 'NONE',  ( 12.21156171748987163, -10.82459398097509329, 33.81372124010185587 ) ) ;
#4916 = ORIENTED_EDGE ( 'NONE', *, *, #4362, .T. ) ;
#4917 = CARTESIAN_POINT ( 'NONE',  ( 14.53047184896071542, -9.332535724633409302, 34.40230450496446934 ) ) ;
#4918 = CARTESIAN_POINT ( 'NONE',  ( -4.376773112753001627, -9.172386477786396597, 34.72672124145550043 ) ) ;
#4919 = AXIS2_PLACEMENT_3D ( 'NONE', #2320, #10872, #23048 ) ;
#4921 = CARTESIAN_POINT ( 'NONE',  ( 5.777073041093150785, -6.459968553980839800, 34.89616026154728701 ) ) ;
#4920 = CARTESIAN_POINT ( 'NONE',  ( 18.06606835100244268, -3.513871655860379306, 32.76840700105978499 ) ) ;
#4922 = CARTESIAN_POINT ( 'NONE',  ( 9.692307692307695177, -1.367168528481310208, 33.57946703557072254 ) ) ;
#4923 = CARTESIAN_POINT ( 'NONE',  ( -5.076923076923075762, -8.973038597847269315, 34.52809138561121927 ) ) ;
#4924 = CARTESIAN_POINT ( 'NONE',  ( -19.50000000000000000, -7.500000000000000000, 29.75000000000000355 ) ) ;
#4925 = B_SPLINE_CURVE_WITH_KNOTS ( 'NONE', 3,
 ( #32040, #23932, #64919, #51843, #37907, #18086, #79339, #80233, #17184, #2766 ),
 .UNSPECIFIED., .F., .F.,
 ( 4, 2, 2, 2, 4 ),
 ( 0.000000000000000000, 0.0001954311564186860613, 0.0003908623128373721225, 0.0005862934692560581567, 0.0007817246256747442451 ),
 .UNSPECIFIED. ) ;
#4926 = CARTESIAN_POINT ( 'NONE',  ( 2.651650429449569302, -10.15165042944953733, 19.62500000000000000 ) ) ;
#4927 = EDGE_LOOP ( 'NONE', ( #16053, #57932, #79017, #52065 ) ) ;
#4928 = AXIS2_PLACEMENT_3D ( 'NONE', #12936, #39980, #20576 ) ;
#4929 = EDGE_LOOP ( 'NONE', ( #67408, #77553 ) ) ;
#4930 = LINE ( 'NONE', #53991, #75177 ) ;
#4931 = CARTESIAN_POINT ( 'NONE',  ( 12.39578165902414852, -7.249945686854186278, 34.74374336980224598 ) ) ;
#4932 = CARTESIAN_POINT ( 'NONE',  ( -19.50000000000000000, -3.499999999999999556, 29.75000000000000355 ) ) ;
#4933 = CARTESIAN_POINT ( 'NONE',  ( 20.99999999999998934, -2.249999999999998668, 29.75000000000000355 ) ) ;
#4934 = DIRECTION ( 'NONE',  ( -0.000000000000000000, 0.7660444431189791237, -0.6427876096865379196 ) ) ;
#4935 = CARTESIAN_POINT ( 'NONE',  ( 2.320192649118979489E-14, -11.25000000000000000, 23.53125000000000000 ) ) ;
#4936 = DIRECTION ( 'NONE',  ( -0.000000000000000000, 1.000000000000000000, -0.000000000000000000 ) ) ;
#4937 = CARTESIAN_POINT ( 'NONE',  ( -12.46153846153846168, -6.386643153685126251, 34.62446782046654192 ) ) ;
#4938 = EDGE_CURVE ( 'NONE', #39482, #83084, #36126, .T. ) ;
#4939 = CARTESIAN_POINT ( 'NONE',  ( 17.01083966596719321, -12.10708131394839349, 31.69288490824020244 ) ) ;
#4940 = CARTESIAN_POINT ( 'NONE',  ( 6.000000000000001776, -9.905515769479276145, 34.41647553114623292 ) ) ;
#4941 = CARTESIAN_POINT ( 'NONE',  ( 4.153846153846154188, -13.78497067705608181, 32.30358669280327177 ) ) ;
#4942 = CARTESIAN_POINT ( 'NONE',  ( 8.545745825506822158, -12.24155766932282496, 31.33739205006857986 ) ) ;
#4943 = CARTESIAN_POINT ( 'NONE',  ( 2.952004793765244717, -6.965521097154411478, 14.00000000000000178 ) ) ;
#4944 = CARTESIAN_POINT ( 'NONE',  ( 3.903822916553188804, -12.43535235679832596, 30.55408501211184813 ) ) ;
#4945 = CARTESIAN_POINT ( 'NONE',  ( 10.68064018666064285, -2.892918686051625166, 31.69288490824026638 ) ) ;
#4946 = CARTESIAN_POINT ( 'NONE',  ( 8.519230769230768274, -7.500000000000001776, 35.04278698407183867 ) ) ;
#4947 = ORIENTED_EDGE ( 'NONE', *, *, #68117, .F. ) ;
#4948 = CARTESIAN_POINT ( 'NONE',  ( -1.384615384615383471, -2.538708090699994813, 30.37095296980875503 ) ) ;
#4949 = DIRECTION ( 'NONE',  ( -0.000000000000000000, -0.3420201433256694901, -0.9396926207859082059 ) ) ;
#4950 = DIRECTION ( 'NONE',  ( 0.000000000000000000, 0.3420201433256641055, -0.9396926207859100932 ) ) ;
#4951 = CARTESIAN_POINT ( 'NONE',  ( 1.987747218494642309, -5.598659921968629050, 15.81436829374151465 ) ) ;
#4952 = CARTESIAN_POINT ( 'NONE',  ( 5.326868486301119532, -10.18230066228895758, 34.26354781536631577 ) ) ;
#4953 = CARTESIAN_POINT ( 'NONE',  ( -0.4615384615384611200, -6.189225973068211317, 35.74407628777942847 ) ) ;
#4955 = VERTEX_POINT ( 'NONE', #23136 ) ;
#4954 = CARTESIAN_POINT ( 'NONE',  ( 11.53846153846153832, -2.249999999999998668, 29.75000000000001776 ) ) ;
#4956 = CARTESIAN_POINT ( 'NONE',  ( 1.944543648262996083, -5.555456351736983045, 16.81250000000000000 ) ) ;
#4957 = EDGE_CURVE ( 'NONE', #27791, #58249, #60838, .T. ) ;
#4958 = CYLINDRICAL_SURFACE ( 'NONE', #44058, 4.000000000000000000 ) ;
#4959 = EDGE_CURVE ( 'NONE', #88786, #21236, #50603, .T. ) ;
#4960 = VERTEX_POINT ( 'NONE', #85290 ) ;
#4961 = VECTOR ( 'NONE', #42035, 1000.000000000000227 ) ;
#4962 = CARTESIAN_POINT ( 'NONE',  ( 18.22301135161285046, -9.086983370893049639, 34.49168942202179267 ) ) ;
#4963 = ORIENTED_EDGE ( 'NONE', *, *, #16281, .T. ) ;
#4964 = CARTESIAN_POINT ( 'NONE',  ( -7.596099426240392027, -6.523592122091590895, 34.90882529074906415 ) ) ;
#4965 = CARTESIAN_POINT ( 'NONE',  ( 13.25392391794783187, -9.804603061927743113, 34.18744698557895845 ) ) ;
#4966 = EDGE_CURVE ( 'NONE', #49902, #86068, #51022, .T. ) ;
#4967 = CARTESIAN_POINT ( 'NONE',  ( -1.384615384615505151, -4.481592998941358097, 33.73612834414048933 ) ) ;
#4968 = EDGE_LOOP ( 'NONE', ( #31152, #88726 ) ) ;
#4969 = CARTESIAN_POINT ( 'NONE',  ( -10.39237326377176451, -12.39991518177334129, 30.74647679643404530 ) ) ;
#4970 = EDGE_LOOP ( 'NONE', ( #62096, #9225, #36111, #48053 ) ) ;
#4971 = ORIENTED_EDGE ( 'NONE', *, *, #63299, .F. ) ;
#4972 = CARTESIAN_POINT ( 'NONE',  ( 19.00000000000000000, 0.7500000000000051070, 32.75000000000000000 ) ) ;
#4973 = CARTESIAN_POINT ( 'NONE',  ( -0.4615384615385826339, -10.90142922262034020, 33.41473453929536674 ) ) ;
#4974 = CARTESIAN_POINT ( 'NONE',  ( -10.54931626438217585, -6.386643153685127139, 34.62446782046654192 ) ) ;
#4975 = CARTESIAN_POINT ( 'NONE',  ( 9.561616225640136690, -8.999036380462717588, 34.52022231692819076 ) ) ;
#4976 = CARTESIAN_POINT ( 'NONE',  ( -3.100243792535585907, -5.070358843744209310, 34.40418822224088302 ) ) ;
#4977 = LINE ( 'NONE', #45947, #71069 ) ;
#4978 = DIRECTION ( 'NONE',  ( 0.000000000000000000, 0.000000000000000000, 1.000000000000000000 ) ) ;
#4979 = B_SPLINE_CURVE_WITH_KNOTS ( 'NONE', 3,
 ( #75592, #829, #8925, #28294, #7146, #21989, #43147, #56657, #83253, #49462 ),
 .UNSPECIFIED., .F., .F.,
 ( 4, 2, 2, 2, 4 ),
 ( 0.000000000000000000, 0.0001954311564186879044, 0.0003908623128373758088, 0.0005862934692560636861, 0.0007817246256747516176 ),
 .UNSPECIFIED. ) ;
#4980 = EDGE_CURVE ( 'NONE', #31594, #15866, #17937, .T. ) ;
#4981 = VECTOR ( 'NONE', #68913, 1000.000000000000000 ) ;
#4982 = ORIENTED_EDGE ( 'NONE', *, *, #6426, .F. ) ;
#4983 = VERTEX_POINT ( 'NONE', #72649 ) ;
#4984 = VERTEX_POINT ( 'NONE', #73998 ) ;
#4986 = VERTEX_POINT ( 'NONE', #65885 ) ;
#4985 = DIRECTION ( 'NONE',  ( -1.000000000000000000, 0.000000000000000000, 0.000000000000000000 ) ) ;
#4987 = AXIS2_PLACEMENT_3D ( 'NONE', #31788, #79533, #38092 ) ;
#4988 = B_SPLINE_CURVE_WITH_KNOTS ( 'NONE', 3,
 ( #76045, #68848, #75598, #41383, #9803, #79153, #17454, #3921, #71494, #23311 ),
 .UNSPECIFIED., .F., .F.,
 ( 4, 2, 2, 2, 4 ),
 ( 0.0007817246256747491240, 0.0009771112852218931041, 0.001172497944769036867, 0.001367884604316180631, 0.001563271263863324611 ),
 .UNSPECIFIED. ) ;
#4989 = VECTOR ( 'NONE', #41050, 1000.000000000000114 ) ;
#4990 = CARTESIAN_POINT ( 'NONE',  ( -8.769230769230768274, -9.780366693483667717, 34.19971097300155094 ) ) ;
#4991 = CARTESIAN_POINT ( 'NONE',  ( -10.86536134632696715, -9.148715823498378086, 34.47080413974185120 ) ) ;
#4992 = ORIENTED_EDGE ( 'NONE', *, *, #58669, .T. ) ;
#4993 = DIRECTION ( 'NONE',  ( 0.000000000000000000, 0.000000000000000000, -1.000000000000000000 ) ) ;
#4994 = VERTEX_POINT ( 'NONE', #52817 ) ;
#4995 = CARTESIAN_POINT ( 'NONE',  ( 16.15384615384615330, -13.37000171582298513, 34.34916445242398453 ) ) ;
#4996 = ORIENTED_EDGE ( 'NONE', *, *, #28211, .F. ) ;
#4997 = CARTESIAN_POINT ( 'NONE',  ( -18.06608237936013595, -9.058645607665454236, 34.76329471203372634 ) ) ;
#4998 = CARTESIAN_POINT ( 'NONE',  ( -11.60454494941741999, -3.513871655860377086, 32.76840700105978499 ) ) ;
#4999 = CARTESIAN_POINT ( 'NONE',  ( -11.28851612908349722, -12.07971442181322175, 32.31769673815850297 ) ) ;
#5000 = FACE_BOUND ( 'NONE', #16448, .T. ) ;
#5001 = CARTESIAN_POINT ( 'NONE',  ( 17.07692307692307665, -6.343179335718451384, 34.87096338111211935 ) ) ;
#5002 = DIRECTION ( 'NONE',  ( 0.000000000000000000, 0.8660254037844377084, 0.5000000000000015543 ) ) ;
#5003 = CARTESIAN_POINT ( 'NONE',  ( 13.60739505359345181, -4.989023458446560255, 34.36081565061822118 ) ) ;
#5004 = FACE_OUTER_BOUND ( 'NONE', #51269, .T. ) ;
#5005 = DIRECTION ( 'NONE',  ( -1.000000000000000000, -0.000000000000000000, -0.000000000000000000 ) ) ;
#5006 = CARTESIAN_POINT ( 'NONE',  ( 2.307692307692309264, -1.790695186598648903, 34.54067556320373455 ) ) ;
#5007 = ORIENTED_EDGE ( 'NONE', *, *, #83665, .F. ) ;
#5008 = CARTESIAN_POINT ( 'NONE',  ( 2.307692307692309264, -12.48256725967547354, 35.29906147534542527 ) ) ;
#5009 = ORIENTED_EDGE ( 'NONE', *, *, #64284, .T. ) ;
#5010 = VERTEX_POINT ( 'NONE', #5538 ) ;
#5012 = CARTESIAN_POINT ( 'NONE',  ( -14.17690049986752143, -12.38066358083363738, 30.83685684665853444 ) ) ;
#5011 = CARTESIAN_POINT ( 'NONE',  ( -6.923076923076922462, -3.937682226553329556, 33.60647404775216529 ) ) ;
#5013 = DIRECTION ( 'NONE',  ( -0.000000000000000000, -0.3420201433256694901, -0.9396926207859082059 ) ) ;
#5014 = CARTESIAN_POINT ( 'NONE',  ( -14.55766905174089665, -12.01397095200674059, 32.43157075238190146 ) ) ;
#5015 = LINE ( 'NONE', #75251, #25653 ) ;
#5016 = CARTESIAN_POINT ( 'NONE',  ( 4.480769230769229061, -7.500000000000000000, 33.75000000000000000 ) ) ;
#5017 = ORIENTED_EDGE ( 'NONE', *, *, #40433, .T. ) ;
#5018 = LINE ( 'NONE', #32481, #8385 ) ;
#5019 = DIRECTION ( 'NONE',  ( 0.000000000000000000, 0.000000000000000000, 1.000000000000000000 ) ) ;
#5020 = CARTESIAN_POINT ( 'NONE',  ( 10.36536137809165403, -3.202444869320336451, 32.30641848906366675 ) ) ;
#5021 = CARTESIAN_POINT ( 'NONE',  ( -3.296851610129365451, -12.62096338111211580, 30.90682066428152197 ) ) ;
#5022 = ORIENTED_EDGE ( 'NONE', *, *, #32219, .F. ) ;
#5023 = ORIENTED_EDGE ( 'NONE', *, *, #80249, .T. ) ;
#5024 = VERTEX_POINT ( 'NONE', #24905 ) ;
#5025 = CARTESIAN_POINT ( 'NONE',  ( 0.000000000000000000, -11.00000000000000000, 29.75000000000000355 ) ) ;
#5026 = CARTESIAN_POINT ( 'NONE',  ( 4.826946332874483936, -2.920706130388546651, 32.31842814019191223 ) ) ;
#5027 = ORIENTED_EDGE ( 'NONE', *, *, #61538, .T. ) ;
#5028 = CARTESIAN_POINT ( 'NONE',  ( 3.007842271862382066, -12.64616026154729411, 30.79003144601913533 ) ) ;
#5029 = DIRECTION ( 'NONE',  ( 0.000000000000000000, 0.000000000000000000, 1.000000000000000000 ) ) ;
#5030 = CARTESIAN_POINT ( 'NONE',  ( -7.911424292114622503, -11.94971097300153140, 32.03036669348370680 ) ) ;
#5031 = LINE ( 'NONE', #5485, #21571 ) ;
#5032 = CARTESIAN_POINT ( 'NONE',  ( -11.53846153846165912, -9.442884908241554243, 34.35708131394783038 ) ) ;
#5033 = EDGE_LOOP ( 'NONE', ( #80228, #50565 ) ) ;
#5035 = VERTEX_POINT ( 'NONE', #53264 ) ;
#5034 = CARTESIAN_POINT ( 'NONE',  ( -15.23076923076922995, -2.292212530054420494, 30.41441678777542634 ) ) ;
#5036 = CARTESIAN_POINT ( 'NONE',  ( -11.97435897435897267, -3.499999999999999556, 29.75000000000000355 ) ) ;
#5037 = CARTESIAN_POINT ( 'NONE',  ( 8.519230769230768274, -2.499999999999998668, 29.75000000000000355 ) ) ;
#5038 = CARTESIAN_POINT ( 'NONE',  ( -11.78843828251013015, -10.82459398097509329, 33.81372124010185587 ) ) ;
#5039 = LINE ( 'NONE', #10471, #48112 ) ;
#5041 = VECTOR ( 'NONE', #66159, 1000.000000000000000 ) ;
#5040 = CARTESIAN_POINT ( 'NONE',  ( -3.903900744468109529, -4.932303261841489039, 34.32971442181322885 ) ) ;
#5042 = CARTESIAN_POINT ( 'NONE',  ( 5.076923076923075762, -8.564572088678739092, 35.78748833219616898 ) ) ;
#5043 = CARTESIAN_POINT ( 'NONE',  ( 1.200186371490529202, -4.775308065498752974, 15.73624329374151998 ) ) ;
#5044 = ORIENTED_EDGE ( 'NONE', *, *, #6399, .F. ) ;
#5045 = CARTESIAN_POINT ( 'NONE',  ( 11.66898724022509981, -2.882268652242222284, 31.66798894389554064 ) ) ;
#5046 = LINE ( 'NONE', #19450, #64928 ) ;
#5047 = CARTESIAN_POINT ( 'NONE',  ( -8.769230769230768274, -9.819645486525091727, 36.12317359536749706 ) ) ;
#5048 = VECTOR ( 'NONE', #59966, 1000.000000000000227 ) ;
#5049 = EDGE_CURVE ( 'NONE', #87441, #39364, #15710, .T. ) ;
#5050 = B_SPLINE_CURVE_WITH_KNOTS ( 'NONE', 3,
 ( #73704, #60163, #81785, #20075, #68260, #87667, #53406, #19190, #46660, #74133 ),
 .UNSPECIFIED., .F., .F.,
 ( 4, 2, 2, 2, 4 ),
 ( 0.0007817359430256326080, 0.0009771253907250047801, 0.001172514838424369796, 0.001367904286123735030, 0.001563293733823100046 ),
 .UNSPECIFIED. ) ;
#5051 = ORIENTED_EDGE ( 'NONE', *, *, #3404, .F. ) ;
#5052 = EDGE_LOOP ( 'NONE', ( #56781, #1021, #42484, #31637 ) ) ;
#5053 = CARTESIAN_POINT ( 'NONE',  ( -11.60373198442231590, -10.90142922261923886, 33.41473453929638993 ) ) ;
#5054 = CYLINDRICAL_SURFACE ( 'NONE', #54110, 0.2500000000000002220 ) ;
#5055 = ADVANCED_FACE ( 'NONE', ( #46072 ), #86638, .T. ) ;
#5056 = FACE_OUTER_BOUND ( 'NONE', #64063, .T. ) ;
#5057 = CARTESIAN_POINT ( 'NONE',  ( 10.61538461538449418, -5.094484230521993062, 34.41647553114689373 ) ) ;
#5058 = DIRECTION ( 'NONE',  ( -1.000000000000000000, -0.000000000000000000, -0.000000000000000000 ) ) ;
#5059 = CARTESIAN_POINT ( 'NONE',  ( -7.173053654019277303, -11.79746400365624659, 32.30657167506340954 ) ) ;
#5060 = ORIENTED_EDGE ( 'NONE', *, *, #65557, .F. ) ;
#5061 = B_SPLINE_CURVE_WITH_KNOTS ( 'NONE', 3,
 ( #76614, #8159, #517, #55891, #83380, #83830, #28886, #7722, #5167, #46158 ),
 .UNSPECIFIED., .F., .F.,
 ( 4, 2, 2, 2, 4 ),
 ( 0.0007817246256747451124, 0.0009771112852218885505, 0.001172497944769032097, 0.001367884604316175427, 0.001563271263863318973 ),
 .UNSPECIFIED. ) ;
#5062 = CYLINDRICAL_SURFACE ( 'NONE', #86565, 0.2500000000000009437 ) ;
#5063 = EDGE_CURVE ( 'NONE', #33483, #66604, #75842, .T. ) ;
#5064 = CARTESIAN_POINT ( 'NONE',  ( -2.176900499867519212, -9.804649428959608670, 34.18742332936588468 ) ) ;
#5065 = LINE ( 'NONE', #60004, #57982 ) ;
#5066 = ORIENTED_EDGE ( 'NONE', *, *, #12826, .F. ) ;
#5067 = CARTESIAN_POINT ( 'NONE',  ( 12.59233026936324684, -3.530189275343204702, 32.79018710029569661 ) ) ;
#5068 = VERTEX_POINT ( 'NONE', #11857 ) ;
#5069 = CARTESIAN_POINT ( 'NONE',  ( -0.3307466537136773965, -2.729792928343270031, 31.24908615093345432 ) ) ;
#5070 = CARTESIAN_POINT ( 'NONE',  ( -13.63461538461538147, -7.566082377512564960, 35.00000000000000711 ) ) ;
#5071 = CYLINDRICAL_SURFACE ( 'NONE', #62838, 0.2500000000000012212 ) ;
#5072 = ORIENTED_EDGE ( 'NONE', *, *, #52468, .T. ) ;
#5073 = CARTESIAN_POINT ( 'NONE',  ( -13.25382494364843389, -4.684288915650983043, 34.18129842949671371 ) ) ;
#5074 = CARTESIAN_POINT ( 'NONE',  ( -11.47320596718551045, -12.46129190930001052, 30.37095296980870174 ) ) ;
#5075 = CARTESIAN_POINT ( 'NONE',  ( 19.00000000000000000, -7.500000000000000000, 33.75000000000000000 ) ) ;
#5076 = AXIS2_PLACEMENT_3D ( 'NONE', #22433, #43585, #29209 ) ;
#5077 = CARTESIAN_POINT ( 'NONE',  ( 11.78846153846154010, -2.249999999999998668, 29.75000000000000355 ) ) ;
#5078 = CARTESIAN_POINT ( 'NONE',  ( -0.4615384615384611200, -13.87047571288749737, 32.06866353760679544 ) ) ;
#5079 = ADVANCED_FACE ( 'NONE', ( #38882 ), #32117, .F. ) ;
#5080 = B_SPLINE_CURVE_WITH_KNOTS ( 'NONE', 3,
 ( #74966, #53789, #41169, #74510, #40292, #6932, #25017, #45280, #11066, #44832 ),
 .UNSPECIFIED., .F., .F.,
 ( 4, 2, 2, 2, 4 ),
 ( 0.0007817246256747442451, 0.0009771112852218865989, 0.001172497944769029061, 0.001367884604316171523, 0.001563271263863313986 ),
 .UNSPECIFIED. ) ;
#5081 = ORIENTED_EDGE ( 'NONE', *, *, #82787, .F. ) ;
#5082 = LINE ( 'NONE', #73098, #30014 ) ;
#5083 = ADVANCED_FACE ( 'NONE', ( #11398 ), #59580, .F. ) ;
#5084 = VERTEX_POINT ( 'NONE', #66788 ) ;
#5085 = CARTESIAN_POINT ( 'NONE',  ( 5.326977496836529546, -11.47946981652013498, 33.17500667209846910 ) ) ;
#5086 = B_SPLINE_CURVE_WITH_KNOTS ( 'NONE', 3,
 ( #30918, #2559, #58386, #17422, #2126, #43125, #30050, #85881, #50302, #70592 ),
 .UNSPECIFIED., .F., .F.,
 ( 4, 2, 2, 2, 4 ),
 ( 0.0007817246256747434861, 0.0009771112852218859484, 0.001172497944769028411, 0.001367884604316171090, 0.001563271263863313552 ),
 .UNSPECIFIED. ) ;
#5087 = DIRECTION ( 'NONE',  ( 0.000000000000000000, 0.000000000000000000, -1.000000000000000000 ) ) ;
#5088 = CARTESIAN_POINT ( 'NONE',  ( -3.480769230769229061, -7.500000000000001776, 34.75000000000000000 ) ) ;
#5089 = EDGE_CURVE ( 'NONE', #10170, #67262, #80155, .T. ) ;
#5090 = CARTESIAN_POINT ( 'NONE',  ( 11.53846153846153832, -4.786620604624113540, 33.94971097300155094 ) ) ;
#5091 = ADVANCED_FACE ( 'NONE', ( #2258 ), #37827, .F. ) ;
#5092 = CARTESIAN_POINT ( 'NONE',  ( -14.30769230769230660, -12.10708131394839349, 31.69288490824020244 ) ) ;
#5093 = CARTESIAN_POINT ( 'NONE',  ( 3.230769230769231726, -13.04860791097971706, 34.73218667398347037 ) ) ;
#5094 = DIRECTION ( 'NONE',  ( 0.000000000000000000, 0.000000000000000000, -1.000000000000000000 ) ) ;
#5095 = ORIENTED_EDGE ( 'NONE', *, *, #63450, .T. ) ;
#5096 = ORIENTED_EDGE ( 'NONE', *, *, #14503, .F. ) ;
#5097 = EDGE_LOOP ( 'NONE', ( #57875, #7750 ) ) ;
#5098 = EDGE_LOOP ( 'NONE', ( #10810, #53051, #45393, #64566 ) ) ;
#5099 = AXIS2_PLACEMENT_3D ( 'NONE', #24175, #65159, #36810 ) ;
#5100 = CARTESIAN_POINT ( 'NONE',  ( -5.207613680033385428, -3.957541250942359756, 33.62499894934981626 ) ) ;
#5101 = LINE ( 'NONE', #66801, #28717 ) ;
#5102 = CARTESIAN_POINT ( 'NONE',  ( -2.557692307692304823, -7.566083408709834757, 34.74999999999999289 ) ) ;
#5103 = CARTESIAN_POINT ( 'NONE',  ( 6.250054311638317373, -12.17597550085003633, 31.52189283813461884 ) ) ;
#5104 = CARTESIAN_POINT ( 'NONE',  ( 11.31497659473759043, -2.599994579823202923, 30.74605699353653776 ) ) ;
#5105 = B_SPLINE_CURVE_WITH_KNOTS ( 'NONE', 3,
 ( #40801, #13757, #69151, #28613, #68263, #27713, #41240, #7456, #61495, #21849 ),
 .UNSPECIFIED., .F., .F.,
 ( 4, 2, 2, 2, 4 ),
 ( 0.000000000000000000, 0.0001954311564186871184, 0.0003908623128373742367, 0.0005862934692560614093, 0.0007817246256747484735 ),
 .UNSPECIFIED. ) ;
#5106 = DIRECTION ( 'NONE',  ( -0.000000000000000000, 0.9396926207859092051, -0.3420201433256662704 ) ) ;
#5107 = CARTESIAN_POINT ( 'NONE',  ( -4.854143535654664277, -4.387253974876676565, 33.66317474335728832 ) ) ;
#5108 = CARTESIAN_POINT ( 'NONE',  ( 10.61538461538461675, -13.88283147151868846, 33.14645433367849847 ) ) ;
#5109 = ORIENTED_EDGE ( 'NONE', *, *, #21698, .F. ) ;
#5110 = VECTOR ( 'NONE', #83323, 1000.000000000000000 ) ;
#5111 = ORIENTED_EDGE ( 'NONE', *, *, #65230, .T. ) ;
#5112 = ORIENTED_EDGE ( 'NONE', *, *, #11291, .F. ) ;
#5114 = EDGE_LOOP ( 'NONE', ( #51373, #19888, #35046, #71300 ) ) ;
#5113 = CARTESIAN_POINT ( 'NONE',  ( 5.076923076923075762, -6.681629849574314051, 35.83090037661290239 ) ) ;
#5116 = CARTESIAN_POINT ( 'NONE',  ( 17.07692307692307665, -11.33034616979429110, 35.88435417666054406 ) ) ;
#5115 = CARTESIAN_POINT ( 'NONE',  ( -16.15384615384615330, -6.386643153685126251, 34.62446782046654192 ) ) ;
#5117 = EDGE_CURVE ( 'NONE', #52597, #25490, #61948, .T. ) ;
#5118 = CARTESIAN_POINT ( 'NONE',  ( -0.2115930521604179326, -2.341251567377309772, 30.72681386836322659 ) ) ;
#5119 = CARTESIAN_POINT ( 'NONE',  ( 4.219914504848593317, -2.538708090699994813, 30.37095296980875503 ) ) ;
#5120 = FACE_BOUND ( 'NONE', #37417, .T. ) ;
#5121 = EDGE_LOOP ( 'NONE', ( #8371, #25842 ) ) ;
#5122 = ORIENTED_EDGE ( 'NONE', *, *, #80185, .F. ) ;
#5123 = CARTESIAN_POINT ( 'NONE',  ( 4.946775107191380805, -2.373036134822904319, 30.88089517874952250 ) ) ;
#5124 = ORIENTED_EDGE ( 'NONE', *, *, #84379, .F. ) ;
#5125 = FACE_BOUND ( 'NONE', #4342, .T. ) ;
#5126 = LINE ( 'NONE', #38472, #13082 ) ;
#5127 = LINE ( 'NONE', #73142, #82204 ) ;
#5128 = ORIENTED_EDGE ( 'NONE', *, *, #26771, .T. ) ;
#5129 = AXIS2_PLACEMENT_3D ( 'NONE', #50549, #10909, #38379 ) ;
#5130 = CARTESIAN_POINT ( 'NONE',  ( 10.61538461538461675, -11.69971097300155272, 32.46337939537588113 ) ) ;
#5131 = CARTESIAN_POINT ( 'NONE',  ( -15.23076923076922995, -2.249999999999998668, 29.50000000000001421 ) ) ;
#5132 = CARTESIAN_POINT ( 'NONE',  ( -18.24997674404858827, -4.075325502946086864, 33.72974371597207721 ) ) ;
#5133 = VERTEX_POINT ( 'NONE', #4032 ) ;
#5134 = LINE ( 'NONE', #33500, #19821 ) ;
#5135 = CARTESIAN_POINT ( 'NONE',  ( -18.22348494372394967, -5.113361153441933205, 34.14387501736621999 ) ) ;
#5136 = CARTESIAN_POINT ( 'NONE',  ( -9.442362173959550020, -2.587454068350147018, 30.68340429815432202 ) ) ;
#5137 = ORIENTED_EDGE ( 'NONE', *, *, #13606, .F. ) ;
#5138 = EDGE_CURVE ( 'NONE', #2097, #33427, #59718, .T. ) ;
#5139 = VECTOR ( 'NONE', #74516, 1000.000000000000000 ) ;
#5140 = CARTESIAN_POINT ( 'NONE',  ( -1.449885830576159274, -6.026961402152685388, 34.52809138561120506 ) ) ;
#5141 = CARTESIAN_POINT ( 'NONE',  ( 12.46153846153846168, -1.367168528481310208, 33.57946703557072254 ) ) ;
#5142 = ORIENTED_EDGE ( 'NONE', *, *, #78791, .F. ) ;
#5143 = CARTESIAN_POINT ( 'NONE',  ( 0.3962680155776848734, -9.442884908240170461, 34.35708131394840592 ) ) ;
#5144 = LINE ( 'NONE', #10116, #39705 ) ;
#5145 = CARTESIAN_POINT ( 'NONE',  ( -7.976844449264153702, -12.35290016733513951, 31.75349464988449455 ) ) ;
#5146 = CARTESIAN_POINT ( 'NONE',  ( -0.4615384615385826339, -9.442884908241554243, 34.35708131394783038 ) ) ;
#5147 = CARTESIAN_POINT ( 'NONE',  ( -9.692307692307691624, -6.386643153685126251, 34.62446782046654192 ) ) ;
#5148 = FACE_OUTER_BOUND ( 'NONE', #54609, .T. ) ;
#5150 = CARTESIAN_POINT ( 'NONE',  ( -15.36091644020745051, -12.45813303252208648, 30.39737893381572675 ) ) ;
#5149 = CARTESIAN_POINT ( 'NONE',  ( 14.08482688548867223, -2.501496062324912284, 29.88072118266895671 ) ) ;
#5151 = DIRECTION ( 'NONE',  ( 1.000000000000000000, 0.000000000000000000, 0.000000000000000000 ) ) ;
#5152 = CARTESIAN_POINT ( 'NONE',  ( 0.6089743589743582541, -3.499999999999999556, 29.75000000000000355 ) ) ;
#5153 = CARTESIAN_POINT ( 'NONE',  ( 2.750000000000001332, -7.438900925035452083, 25.46688170625849423 ) ) ;
#5154 = VERTEX_POINT ( 'NONE', #15800 ) ;
#5155 = DIRECTION ( 'NONE',  ( 0.000000000000000000, 0.000000000000000000, -1.000000000000000000 ) ) ;
#5156 = ORIENTED_EDGE ( 'NONE', *, *, #26506, .T. ) ;
#5157 = EDGE_CURVE ( 'NONE', #24285, #64772, #13965, .T. ) ;
#5158 = ORIENTED_EDGE ( 'NONE', *, *, #49477, .F. ) ;
#5159 = CARTESIAN_POINT ( 'NONE',  ( -7.780898706641008467, -2.657715359629131857, 31.77849191805844242 ) ) ;
#5160 = EDGE_LOOP ( 'NONE', ( #49037, #87439, #51459, #27698 ) ) ;
#5161 = CARTESIAN_POINT ( 'NONE',  ( 3.296837581771670411, -9.780366693483667717, 34.19971097300155805 ) ) ;
#5162 = CARTESIAN_POINT ( 'NONE',  ( 1.077988221561464899, -4.724691934501233703, 26.48250670625848713 ) ) ;
#5163 = CARTESIAN_POINT ( 'NONE',  ( -13.13456096470193124, -5.642605341092957971, 34.66089969410670335 ) ) ;
#5164 = EDGE_CURVE ( 'NONE', #62928, #27137, #4857, .T. ) ;
#5165 = CARTESIAN_POINT ( 'NONE',  ( -15.48079245499068612, -12.45566812827425451, 31.48439005359158926 ) ) ;
#5166 = CARTESIAN_POINT ( 'NONE',  ( -9.942307692307691624, -7.500000000000001776, 35.04278698407183867 ) ) ;
#5167 = CARTESIAN_POINT ( 'NONE',  ( 8.835298102580845025, -10.67929555188718282, 33.92786785259544757 ) ) ;
#5168 = CARTESIAN_POINT ( 'NONE',  ( -8.703162418228330921, -4.786620604624113540, 33.94971097300155805 ) ) ;
#5169 = DIRECTION ( 'NONE',  ( -0.000000000000000000, 0.8660254037844397068, -0.4999999999999978906 ) ) ;
#5170 = CARTESIAN_POINT ( 'NONE',  ( -7.623374304885432551, -12.24180327182771855, 31.33663988360758168 ) ) ;
#5171 = CARTESIAN_POINT ( 'NONE',  ( 3.750000000000009770, -9.053300858899081760, 22.04687500000000000 ) ) ;
#5172 = VECTOR ( 'NONE', #59290, 1000.000000000000000 ) ;
#5173 = DIRECTION ( 'NONE',  ( -0.000000000000000000, 0.1736481776669307198, -0.9848077530122080203 ) ) ;
#5174 = CARTESIAN_POINT ( 'NONE',  ( -13.31935981333935537, -6.879047030191282275, 34.71129190930002295 ) ) ;
#5175 = EDGE_CURVE ( 'NONE', #46048, #75057, #45020, .T. ) ;
#5176 = CARTESIAN_POINT ( 'NONE',  ( -2.557715544985271094, -4.335965774309649134, 33.62209801155881905 ) ) ;
#5177 = EDGE_CURVE ( 'NONE', #79680, #87031, #5977, .T. ) ;
#5178 = VERTEX_POINT ( 'NONE', #16231 ) ;
#5179 = ORIENTED_EDGE ( 'NONE', *, *, #24235, .T. ) ;
#5180 = CARTESIAN_POINT ( 'NONE',  ( 14.05771556364371655, -8.347322224742351082, 34.93158281831414769 ) ) ;
#5181 = CARTESIAN_POINT ( 'NONE',  ( 6.000000000000001776, -4.945431358278436385, 36.03766855953609394 ) ) ;
#5182 = CARTESIAN_POINT ( 'NONE',  ( 16.28463659481310444, -12.35292014791297710, 31.75344720912887198 ) ) ;
#5183 = CARTESIAN_POINT ( 'NONE',  ( -16.15384615384627409, -12.46129190930018460, 30.37095296980731973 ) ) ;
#5184 = ADVANCED_FACE ( 'NONE', ( #85139 ), #50448, .F. ) ;
#5185 = CIRCLE ( 'NONE', #64636, 4.000000000000000000 ) ;
#5186 = CARTESIAN_POINT ( 'NONE',  ( 8.519207531937803779, -4.335965774309649134, 33.62209801155881905 ) ) ;
#5187 = FACE_OUTER_BOUND ( 'NONE', #24799, .T. ) ;
#5188 = ADVANCED_FACE ( 'NONE', ( #85579 ), #50878, .F. ) ;
#5189 = EDGE_LOOP ( 'NONE', ( #37507, #59341 ) ) ;
#5190 = CARTESIAN_POINT ( 'NONE',  ( -5.076923076923075762, -12.37446782046654192, 30.86335684631486131 ) ) ;
#5191 = VERTEX_POINT ( 'NONE', #40995 ) ;
#5192 = ORIENTED_EDGE ( 'NONE', *, *, #53688, .T. ) ;
#5193 = CARTESIAN_POINT ( 'NONE',  ( -14.55769230769230660, -7.500000000000001776, 34.75000000000000000 ) ) ;
#5194 = CARTESIAN_POINT ( 'NONE',  ( -7.846153846153965716, -10.90142922262034020, 33.41473453929536674 ) ) ;
#5195 = CARTESIAN_POINT ( 'NONE',  ( -9.692307692307691624, -6.386643153685126251, 34.62446782046654192 ) ) ;
#5196 = EDGE_CURVE ( 'NONE', #8026, #57991, #12349, .T. ) ;
#5197 = DIRECTION ( 'NONE',  ( -0.000000000000000000, -0.000000000000000000, 1.000000000000000000 ) ) ;
#5198 = CARTESIAN_POINT ( 'NONE',  ( -2.057746789344163219, -11.86320923018887719, 32.19269448109604781 ) ) ;
#5199 = VECTOR ( 'NONE', #60118, 1000.000000000000000 ) ;
#5200 = EDGE_LOOP ( 'NONE', ( #9204, #61459, #36948, #14172 ) ) ;
#5201 = VERTEX_POINT ( 'NONE', #76549 ) ;
#5202 = VERTEX_POINT ( 'NONE', #8 ) ;
#5203 = DIRECTION ( 'NONE',  ( -0.000000000000000000, 1.000000000000000000, -0.000000000000000000 ) ) ;
#5204 = CARTESIAN_POINT ( 'NONE',  ( 10.39245765647776842, -11.43668979543634734, 33.22377378376089752 ) ) ;
#5205 = EDGE_CURVE ( 'NONE', #81424, #20877, #55827, .T. ) ;
#5206 = CARTESIAN_POINT ( 'NONE',  ( 16.37662582282421653, -5.827830569534415694, 34.72679350104403539 ) ) ;
#5207 = CARTESIAN_POINT ( 'NONE',  ( -8.519285359852727169, -10.18230066228895758, 34.26354781536631577 ) ) ;
#5208 = EDGE_CURVE ( 'NONE', #41231, #30159, #28813, .T. ) ;
#5209 = CARTESIAN_POINT ( 'NONE',  ( 17.77707378248385339, -4.887634598454295265, 34.01352882383564946 ) ) ;
#5210 = DIRECTION ( 'NONE',  ( 0.000000000000000000, 0.9848077530122072432, 0.1736481776669354937 ) ) ;
#5211 = ORIENTED_EDGE ( 'NONE', *, *, #73596, .T. ) ;
#5212 = B_SPLINE_CURVE_WITH_KNOTS ( 'NONE', 3,
 ( #8296, #9610, #23566, #30330, #9188, #22244 ),
 .UNSPECIFIED., .F., .F.,
 ( 4, 2, 4 ),
 ( 0.000000000000000000, 0.0001954784845028914076, 0.0003909569690057828153 ),
 .UNSPECIFIED. ) ;
#5213 = EDGE_LOOP ( 'NONE', ( #2736, #63189, #16064, #60573 ) ) ;
#5214 = CARTESIAN_POINT ( 'NONE',  ( 3.750000000000000888, -7.499999999999978684, 25.71875000000000000 ) ) ;
#5216 = VERTEX_POINT ( 'NONE', #27478 ) ;
#5215 = CARTESIAN_POINT ( 'NONE',  ( -11.53846153846153655, -13.20930481340135110, 34.54067556320372745 ) ) ;
#5217 = CARTESIAN_POINT ( 'NONE',  ( 1.384615384615386802, -3.886160181151819604, 36.00935417666054406 ) ) ;
#5218 = CARTESIAN_POINT ( 'NONE',  ( 12.71159288145191013, -8.346898887586323923, 34.93166121998716278 ) ) ;
#5219 = ADVANCED_FACE ( 'NONE', ( #76095 ), #23689, .F. ) ;
#5220 = AXIS2_PLACEMENT_3D ( 'NONE', #4373, #26427, #59760 ) ;
#5221 = CARTESIAN_POINT ( 'NONE',  ( 13.13461538461538680, -7.500000000000001776, 35.04278698407183867 ) ) ;
#5222 = ORIENTED_EDGE ( 'NONE', *, *, #18541, .T. ) ;
#5223 = CARTESIAN_POINT ( 'NONE',  ( 23.00000000000000000, -2.249999999999999556, 27.25000000000000000 ) ) ;
#5224 = VERTEX_POINT ( 'NONE', #29257 ) ;
#5225 = EDGE_CURVE ( 'NONE', #15004, #25632, #67234, .T. ) ;
#5226 = DIRECTION ( 'NONE',  ( -0.000000000000000000, 1.000000000000000000, -0.000000000000000000 ) ) ;
#5227 = PLANE ( 'NONE',  #65899 ) ;
#5228 = DIRECTION ( 'NONE',  ( 1.000000000000000000, 0.000000000000000000, 0.000000000000000000 ) ) ;
#5230 = CARTESIAN_POINT ( 'NONE',  ( 8.096099255531889582, -2.341251567377310217, 30.72681386836322659 ) ) ;
#5229 = CARTESIAN_POINT ( 'NONE',  ( -7.173053654019278191, -3.627789207965226748, 32.91389620160131102 ) ) ;
#5231 = ADVANCED_FACE ( 'NONE', ( #28350 ), #15293, .F. ) ;
#5232 = DIRECTION ( 'NONE',  ( 0.000000000000000000, 0.000000000000000000, 1.000000000000000000 ) ) ;
#5233 = EDGE_LOOP ( 'NONE', ( #25318, #57800, #17857, #64875 ) ) ;
#5234 = CARTESIAN_POINT ( 'NONE',  ( -11.40793610022789650, -8.630441415882550871, 34.87705825610312615 ) ) ;
#5235 = CARTESIAN_POINT ( 'NONE',  ( 8.900022577055556994, -6.413143153341454017, 34.63066358083362672 ) ) ;
#5236 = CARTESIAN_POINT ( 'NONE',  ( -14.17716660592874867, -2.882268652242222284, 31.66798894389554064 ) ) ;
#5237 = VERTEX_POINT ( 'NONE', #42769 ) ;
#5238 = ADVANCED_FACE ( 'NONE', ( #62144 ), #82434, .F. ) ;
#5239 = CARTESIAN_POINT ( 'NONE',  ( -9.627052552794857831, -5.094484230520773593, 34.41647553114626845 ) ) ;
#5240 = DIRECTION ( 'NONE',  ( 0.000000000000000000, 0.8660254037844377084, 0.5000000000000015543 ) ) ;
#5241 = DIRECTION ( 'NONE',  ( -0.000000000000000000, 0.6427876096865404731, -0.7660444431189771253 ) ) ;
#5242 = CARTESIAN_POINT ( 'NONE',  ( 4.153846153846030731, -8.656820664282941280, 34.87096338111179961 ) ) ;
#5243 = DIRECTION ( 'NONE',  ( -0.000000000000000000, 0.5000000000000011102, -0.8660254037844381525 ) ) ;
#5244 = FACE_BOUND ( 'NONE', #86644, .T. ) ;
#5246 = CARTESIAN_POINT ( 'NONE',  ( -20.00000000000000355, -10.00000000000000533, 3.000000000000000000 ) ) ;
#5245 = DIRECTION ( 'NONE',  ( -1.000000000000000000, 0.000000000000000000, -0.000000000000000000 ) ) ;
#5247 = DIRECTION ( 'NONE',  ( -0.000000000000000000, -0.8660254037844397068, -0.4999999999999978906 ) ) ;
#5249 = CARTESIAN_POINT ( 'NONE',  ( 14.30769230769231015, -1.466349020453238561, 30.81389545987213907 ) ) ;
#5248 = CARTESIAN_POINT ( 'NONE',  ( -17.93393164899756087, -11.16473453929635440, 33.15142922261927083 ) ) ;
#5250 = B_SPLINE_CURVE_WITH_KNOTS ( 'NONE', 3,
 ( #81707, #20443, #69951, #1055, #83930, #48344, #55993, #14124, #29426, #55548 ),
 .UNSPECIFIED., .F., .F.,
 ( 4, 2, 2, 2, 4 ),
 ( 0.000000000000000000, 0.0001954339857564093175, 0.0003908679715128186350, 0.0005863019572692279796, 0.0007817359430256372700 ),
 .UNSPECIFIED. ) ;
#5251 = DIRECTION ( 'NONE',  ( -0.000000000000000000, -0.8660254037844397068, -0.4999999999999978906 ) ) ;
#5252 = CARTESIAN_POINT ( 'NONE',  ( -1.987747218494660295, -5.598659921968651254, 14.99813170625848713 ) ) ;
#5253 = ORIENTED_EDGE ( 'NONE', *, *, #61708, .F. ) ;
#5254 = DIRECTION ( 'NONE',  ( -0.000000000000000000, 0.000000000000000000, 1.000000000000000000 ) ) ;
#5255 = ORIENTED_EDGE ( 'NONE', *, *, #39907, .F. ) ;
#5256 = DIRECTION ( 'NONE',  ( 1.000000000000000000, 0.000000000000000000, 0.000000000000000000 ) ) ;
#5257 = VECTOR ( 'NONE', #18911, 1000.000000000000000 ) ;
#5258 = EDGE_LOOP ( 'NONE', ( #63900, #27367 ) ) ;
#5259 = CARTESIAN_POINT ( 'NONE',  ( 7.622668902429897919, -9.331801661448606566, 34.40259984581193464 ) ) ;
#5260 = DIRECTION ( 'NONE',  ( -1.000000000000000000, -0.000000000000000000, -0.000000000000000000 ) ) ;
#5262 = ORIENTED_EDGE ( 'NONE', *, *, #42796, .T. ) ;
#5261 = FACE_OUTER_BOUND ( 'NONE', #1972, .T. ) ;
#5263 = CARTESIAN_POINT ( 'NONE',  ( 3.453780582382080855, -6.503523203565942268, 34.64991518177335195 ) ) ;
#5264 = CARTESIAN_POINT ( 'NONE',  ( 6.000000000000001776, -3.322132147404559976, 32.92929555188717927 ) ) ;
#5265 = CARTESIAN_POINT ( 'NONE',  ( 1.614399933863660985, -11.22469193450123193, 24.45125670625849423 ) ) ;
#5266 = EDGE_CURVE ( 'NONE', #54936, #19690, #64296, .T. ) ;
#5267 = CARTESIAN_POINT ( 'NONE',  ( 4.153846153846032507, -10.90142922262034020, 33.41473453929536674 ) ) ;
#5268 = CARTESIAN_POINT ( 'NONE',  ( -14.55766905174089665, -11.47974371597208076, 33.17467449705390692 ) ) ;
#5269 = AXIS2_PLACEMENT_3D ( 'NONE', #43724, #49154, #42417 ) ;
#5270 = DIRECTION ( 'NONE',  ( -0.000000000000000000, -0.8660254037844397068, -0.4999999999999978906 ) ) ;
#5271 = DIRECTION ( 'NONE',  ( 0.000000000000000000, 0.000000000000000000, 1.000000000000000000 ) ) ;
#5272 = CARTESIAN_POINT ( 'NONE',  ( 0.3313912521002431166, -11.47017969459903952, 32.78971311882034456 ) ) ;
#5273 = CARTESIAN_POINT ( 'NONE',  ( 1.515140822849031066, -10.31582465632705237, 34.18122507451815295 ) ) ;
#5274 = CARTESIAN_POINT ( 'NONE',  ( -1.614399933863613468, -11.22469193450124969, 20.11124329374151642 ) ) ;
#5275 = DIRECTION ( 'NONE',  ( 0.000000000000000000, 0.1736481776669267785, -0.9848077530122087975 ) ) ;
#5276 = CARTESIAN_POINT ( 'NONE',  ( 3.230769230769231726, -11.11383981884818262, 36.00935417666054406 ) ) ;
#5277 = ORIENTED_EDGE ( 'NONE', *, *, #44723, .F. ) ;
#5278 = CARTESIAN_POINT ( 'NONE',  ( 6.000000000000001776, -12.29105614889573062, 35.45975837776705220 ) ) ;
#5279 = LINE ( 'NONE', #52563, #73335 ) ;
#5280 = CARTESIAN_POINT ( 'NONE',  ( 3.724691934501251023, -9.114399933863618131, 18.54874329374151642 ) ) ;
#5281 = CARTESIAN_POINT ( 'NONE',  ( 2.177545098254088707, -4.460286881179643004, 33.72017969459903242 ) ) ;
#5282 = DIRECTION ( 'NONE',  ( 0.000000000000000000, 1.000000000000000000, 0.000000000000000000 ) ) ;
#5283 = VERTEX_POINT ( 'NONE', #84207 ) ;
#5284 = CARTESIAN_POINT ( 'NONE',  ( -2.307692307692305711, -6.435427911321262684, 35.78748833219616898 ) ) ;
#5285 = CARTESIAN_POINT ( 'NONE',  ( -6.923076923077045919, -12.16647553114689728, 32.15551576947799362 ) ) ;
#5287 = ORIENTED_EDGE ( 'NONE', *, *, #60360, .F. ) ;
#5286 = CARTESIAN_POINT ( 'NONE',  ( 11.47237915910140771, -2.833524468853757305, 32.15551576947924417 ) ) ;
#5288 = LINE ( 'NONE', #32755, #48480 ) ;
#5289 = CARTESIAN_POINT ( 'NONE',  ( -8.769230769230768274, -2.833524468853757305, 32.15551576947925838 ) ) ;
#5290 = B_SPLINE_CURVE_WITH_KNOTS ( 'NONE', 3,
 ( #56758, #35159, #76141, #77041, #62622, #29305, #47790, #84254, #68500, #41039 ),
 .UNSPECIFIED., .F., .F.,
 ( 4, 2, 2, 2, 4 ),
 ( 0.0007817359430256283796, 0.0009771253907249943717, 0.001172514838424360255, 0.001367904286123726356, 0.001563293733823092240 ),
 .UNSPECIFIED. ) ;
#5291 = CYLINDRICAL_SURFACE ( 'NONE', #36316, 0.2499999999999995559 ) ;
#5292 = CARTESIAN_POINT ( 'NONE',  ( -16.40384615384615330, -7.433932668274255917, 35.00000000000000711 ) ) ;
#5293 = ORIENTED_EDGE ( 'NONE', *, *, #80713, .T. ) ;
#5294 = CARTESIAN_POINT ( 'NONE',  ( 1.326923076923076206, -11.50000000000000000, 29.75000000000000355 ) ) ;
#5295 = AXIS2_PLACEMENT_3D ( 'NONE', #28407, #24190, #22101 ) ;
#5296 = EDGE_CURVE ( 'NONE', #36772, #54237, #51141, .T. ) ;
#5297 = CARTESIAN_POINT ( 'NONE',  ( 1.134638640566794754, -2.920706130388546651, 32.31842814019191223 ) ) ;
#5298 = VERTEX_POINT ( 'NONE', #20714 ) ;
#5299 = VERTEX_POINT ( 'NONE', #41434 ) ;
#5300 = AXIS2_PLACEMENT_3D ( 'NONE', #20580, #48046, #41307 ) ;
#5301 = EDGE_CURVE ( 'NONE', #29766, #27440, #22075, .T. ) ;
#5302 = ORIENTED_EDGE ( 'NONE', *, *, #41534, .T. ) ;
#5303 = DIRECTION ( 'NONE',  ( -0.000000000000000000, 0.6427876096865404731, -0.7660444431189771253 ) ) ;
#5304 = CARTESIAN_POINT ( 'NONE',  ( -6.923076923077044142, -4.481592998941358097, 33.73612834414048933 ) ) ;
#5305 = ADVANCED_FACE ( 'NONE', ( #11977 ), #32244, .F. ) ;
#5306 = CIRCLE ( 'NONE', #35530, 4.000000000000000000 ) ;
#5307 = CARTESIAN_POINT ( 'NONE',  ( 9.692307692307695177, -12.78798330534103123, 29.99999999999997868 ) ) ;
#5308 = EDGE_CURVE ( 'NONE', #12209, #19490, #62887, .T. ) ;
#5309 = CARTESIAN_POINT ( 'NONE',  ( -17.77451305701315221, -7.371803252071508439, 34.99865873832523278 ) ) ;
#5310 = VERTEX_POINT ( 'NONE', #18733 ) ;
#5311 = ORIENTED_EDGE ( 'NONE', *, *, #4739, .T. ) ;
#5312 = VERTEX_POINT ( 'NONE', #32674 ) ;
#5314 = ORIENTED_EDGE ( 'NONE', *, *, #30408, .T. ) ;
#5313 = CARTESIAN_POINT ( 'NONE',  ( -7.846153846153844924, -4.786620604624113540, 33.94971097300155094 ) ) ;
#5315 = CARTESIAN_POINT ( 'NONE',  ( -6.792286482109971324, -3.957578996910242619, 33.62503395064540257 ) ) ;
#5316 = EDGE_CURVE ( 'NONE', #76174, #11728, #59705, .T. ) ;
#5317 = CYLINDRICAL_SURFACE ( 'NONE', #52279, 0.2500000000000009437 ) ;
#5318 = AXIS2_PLACEMENT_3D ( 'NONE', #11306, #25715, #26156 ) ;
#5319 = CARTESIAN_POINT ( 'NONE',  ( 5.750023255951409951, -4.075325502946086864, 33.72974371597207721 ) ) ;
#5320 = CARTESIAN_POINT ( 'NONE',  ( 3.230769230769110045, -8.613356846316285953, 34.62446782046622218 ) ) ;
#5321 = ORIENTED_EDGE ( 'NONE', *, *, #10065, .T. ) ;
#5322 = ORIENTED_EDGE ( 'NONE', *, *, #38640, .F. ) ;
#5323 = AXIS2_PLACEMENT_3D ( 'NONE', #16986, #44435, #10238 ) ;
#5324 = VERTEX_POINT ( 'NONE', #79543 ) ;
#5325 = CARTESIAN_POINT ( 'NONE',  ( 10.68145296638705410, -10.51840700105979565, 33.73612834413962247 ) ) ;
#5327 = ORIENTED_EDGE ( 'NONE', *, *, #62910, .T. ) ;
#5326 = CARTESIAN_POINT ( 'NONE',  ( 8.992242120843616959, -2.554770724473668153, 30.48948780036025852 ) ) ;
#5328 = B_SPLINE_CURVE_WITH_KNOTS ( 'NONE', 3,
 ( #48654, #46885, #68487, #60845, #75685, #919, #54525, #82903, #69384, #74368 ),
 .UNSPECIFIED., .F., .F.,
 ( 4, 2, 2, 2, 4 ),
 ( 0.000000000000000000, 0.0001954311564186869015, 0.0003908623128373738030, 0.0005862934692560607588, 0.0007817246256747476061 ),
 .UNSPECIFIED. ) ;
#5329 = CARTESIAN_POINT ( 'NONE',  ( 17.01165307636676260, -5.941354392334501355, 34.76329471203369792 ) ) ;
#5330 = FACE_OUTER_BOUND ( 'NONE', #68814, .T. ) ;
#5331 = AXIS2_PLACEMENT_3D ( 'NONE', #20450, #41165, #176 ) ;
#5332 = CARTESIAN_POINT ( 'NONE',  ( 16.28463796167094557, -8.147973898785416225, 34.70805048591653730 ) ) ;
#5333 = CARTESIAN_POINT ( 'NONE',  ( -24.00000000000000000, -9.499999999999982236, 27.74999999999999645 ) ) ;
#5334 = CARTESIAN_POINT ( 'NONE',  ( 8.835299120233207404, -5.557115091759786019, 34.35708131394839882 ) ) ;
#5335 = FACE_BOUND ( 'NONE', #64145, .T. ) ;
#5336 = EDGE_CURVE ( 'NONE', #88472, #5216, #57472, .T. ) ;
#5337 = CARTESIAN_POINT ( 'NONE',  ( -0.5268089074992376997, -4.481592998940161721, 33.73612834413957984 ) ) ;
#5338 = DIRECTION ( 'NONE',  ( -0.000000000000000000, -1.000000000000000000, 3.491481338843133355E-15 ) ) ;
#5339 = CARTESIAN_POINT ( 'NONE',  ( 11.78851585009985214, -12.41262288849542017, 30.68299917996395010 ) ) ;
#5341 = CARTESIAN_POINT ( 'NONE',  ( -5.143006487878955646, -3.050289026998445951, 32.03036669348365706 ) ) ;
#5340 = CARTESIAN_POINT ( 'NONE',  ( 9.468822748583747284, -3.236172620538810385, 32.36188796281390267 ) ) ;
#5342 = ADVANCED_FACE ( 'NONE', ( #24133 ), #71881, .F. ) ;
#5343 = CARTESIAN_POINT ( 'NONE',  ( 0.3954550505825807361, -12.10708131394839349, 31.69288490824020244 ) ) ;
#5344 = CARTESIAN_POINT ( 'NONE',  ( 12.71159288145191368, -2.920487667080175598, 32.31805714834170828 ) ) ;
#5345 = ORIENTED_EDGE ( 'NONE', *, *, #64657, .T. ) ;
#5346 = CARTESIAN_POINT ( 'NONE',  ( -17.14300545628320904, -5.471508081941601986, 34.59228464037088457 ) ) ;
#5347 = DIRECTION ( 'NONE',  ( 0.000000000000000000, 0.9848077530122072432, -0.1736481776669354937 ) ) ;
#5348 = ORIENTED_EDGE ( 'NONE', *, *, #54458, .T. ) ;
#5349 = ORIENTED_EDGE ( 'NONE', *, *, #61432, .F. ) ;
#5350 = CARTESIAN_POINT ( 'NONE',  ( -17.20707028636130076, -11.47017969459903952, 32.78971311882035167 ) ) ;
#5351 = EDGE_CURVE ( 'NONE', #68924, #33447, #33877, .T. ) ;
#5352 = CARTESIAN_POINT ( 'NONE',  ( 15.90382291655318880, -3.711651800289232916, 33.01384336483936011 ) ) ;
#5353 = CARTESIAN_POINT ( 'NONE',  ( 20.00000000000000000, -4.000000000000000000, 29.75000000000000355 ) ) ;
#5354 = VERTEX_POINT ( 'NONE', #25922 ) ;
#5355 = AXIS2_PLACEMENT_3D ( 'NONE', #78495, #22233, #16796 ) ;
#5356 = CARTESIAN_POINT ( 'NONE',  ( -2.544871794871794268, -3.499999999999999556, 29.75000000000000355 ) ) ;
#5357 = DIRECTION ( 'NONE',  ( -1.000000000000000000, 0.000000000000000000, 0.000000000000000000 ) ) ;
#5358 = EDGE_CURVE ( 'NONE', #5133, #31652, #73624, .T. ) ;
#5360 = CARTESIAN_POINT ( 'NONE',  ( -16.85354759115065448, -2.251407671071268712, 29.88021292934942963 ) ) ;
#5359 = CARTESIAN_POINT ( 'NONE',  ( -14.37296230824862775, -4.320704448112771878, 33.92786785259540494 ) ) ;
#5361 = DIRECTION ( 'NONE',  ( 0.000000000000000000, 0.000000000000000000, 1.000000000000000000 ) ) ;
#5362 = CARTESIAN_POINT ( 'NONE',  ( -8.102564102564102200, -7.500000000000000000, 29.75000000000000355 ) ) ;
#5364 = CARTESIAN_POINT ( 'NONE',  ( -10.48485917715097138, -11.66157788607254098, 32.95092075102925833 ) ) ;
#5363 =( NAMED_UNIT ( * ) SI_UNIT ( $, .STERADIAN. ) SOLID_ANGLE_UNIT ( ) );
#5365 = AXIS2_PLACEMENT_3D ( 'NONE', #34227, #21152, #887 ) ;
#5366 = CARTESIAN_POINT ( 'NONE',  ( -1.929879867024197893E-14, -3.750000000000000000, 20.40625000000000000 ) ) ;
#5367 = ORIENTED_EDGE ( 'NONE', *, *, #53165, .F. ) ;
#5368 = ORIENTED_EDGE ( 'NONE', *, *, #25211, .F. ) ;
#5369 = CARTESIAN_POINT ( 'NONE',  ( -9.757577692864012775, -2.657715359629089225, 31.77849191805832874 ) ) ;
#5370 = VECTOR ( 'NONE', #81390, 1000.000000000000000 ) ;
#5371 = FACE_OUTER_BOUND ( 'NONE', #47563, .T. ) ;
#5372 = DIRECTION ( 'NONE',  ( -0.000000000000000000, 0.3420201433256694346, -0.9396926207859080948 ) ) ;
#5373 = CARTESIAN_POINT ( 'NONE',  ( -0.2385755579769766321, -7.369474270740072441, 34.74850911626239736 ) ) ;
#5374 = CARTESIAN_POINT ( 'NONE',  ( -3.296039676730006196, -6.026961402152685388, 34.52809138561120506 ) ) ;
#5375 = CARTESIAN_POINT ( 'NONE',  ( -3.749999999999988454, -9.053300858899127945, 25.01562500000000000 ) ) ;
#5376 = EDGE_CURVE ( 'NONE', #23382, #4960, #58809, .T. ) ;
#5377 = CARTESIAN_POINT ( 'NONE',  ( -12.46153846153846168, -3.937682226553329556, 33.60647404775216529 ) ) ;
#5378 = DIRECTION ( 'NONE',  ( 0.000000000000000000, 0.3420201433256641055, -0.9396926207859100932 ) ) ;
#5379 = EDGE_CURVE ( 'NONE', #12293, #81839, #14586, .T. ) ;
#5380 = CARTESIAN_POINT ( 'NONE',  ( -13.13461538461394973, -7.500000000000155431, 34.75000000000007105 ) ) ;
#5381 = CARTESIAN_POINT ( 'NONE',  ( 12.46153846153846168, -11.35647404775217417, 33.31231777344666511 ) ) ;
#5382 = CYLINDRICAL_SURFACE ( 'NONE', #79967, 0.2499999999999986955 ) ;
#5383 = CYLINDRICAL_SURFACE ( 'NONE', #4147, 0.2500000000000008882 ) ;
#5384 = EDGE_CURVE ( 'NONE', #38268, #62375, #61914, .T. ) ;
#5385 = EDGE_CURVE ( 'NONE', #82638, #50277, #85920, .T. ) ;
#5386 = CARTESIAN_POINT ( 'NONE',  ( 7.053867364043878929, -3.338503747796866872, 32.95102852606553512 ) ) ;
#5387 = CARTESIAN_POINT ( 'NONE',  ( 3.930361210122206295, -12.44517049084099725, 30.48991314939691932 ) ) ;
#5388 = CARTESIAN_POINT ( 'NONE',  ( -8.703975629717932705, -11.67786785259547777, 32.92929555188713664 ) ) ;
#5389 = CARTESIAN_POINT ( 'NONE',  ( -7.623142494540996239, -12.39991518177334129, 30.74647679643404530 ) ) ;
#5390 = ORIENTED_EDGE ( 'NONE', *, *, #72138, .F. ) ;
#5391 = EDGE_CURVE ( 'NONE', #41035, #83912, #24127, .T. ) ;
#5392 = CARTESIAN_POINT ( 'NONE',  ( -4.853911725310226188, -11.76359900205217457, 32.36225158514719880 ) ) ;
#5393 = CARTESIAN_POINT ( 'NONE',  ( -17.14219307747939425, -6.835583212224499938, 34.95778746994557906 ) ) ;
#5394 = CARTESIAN_POINT ( 'NONE',  ( 5.750023255951412615, -2.544273027872574922, 31.48422191005632342 ) ) ;
#5395 = CARTESIAN_POINT ( 'NONE',  ( 1.901340078031373171, -9.487747218494639867, 18.62686829374151642 ) ) ;
#5396 = CARTESIAN_POINT ( 'NONE',  ( -17.99999999999969447, -2.506253911140613244, 30.00000000000320455 ) ) ;
#5398 = DIRECTION ( 'NONE',  ( 0.000000000000000000, 0.9848077530122072432, -0.1736481776669354937 ) ) ;
#5397 = CIRCLE ( 'NONE', #65743, 0.2500000000000002220 ) ;
#5399 = CARTESIAN_POINT ( 'NONE',  ( -11.31568186948346977, -4.989023458446560255, 34.36081565061822118 ) ) ;
#5401 = ORIENTED_EDGE ( 'NONE', *, *, #72516, .T. ) ;
#5400 = CYLINDRICAL_SURFACE ( 'NONE', #55474, 0.2499999999999994726 ) ;
#5402 = CARTESIAN_POINT ( 'NONE',  ( -1.139087296525992388, -10.25000000000000711, 24.85937500000000711 ) ) ;
#5403 = CARTESIAN_POINT ( 'NONE',  ( -14.43838291080261627, -5.496505350115501010, 34.60290016733514307 ) ) ;
#5404 = B_SPLINE_CURVE_WITH_KNOTS ( 'NONE', 3,
 ( #60333, #66657, #40092, #4508, #54019, #32872, #20248, #19358, #46825, #66203 ),
 .UNSPECIFIED., .F., .F.,
 ( 4, 2, 2, 2, 4 ),
 ( 0.0007817359430256385711, 0.0009771253907250075990, 0.001172514838424376735, 0.001367904286123745872, 0.001563293733823115008 ),
 .UNSPECIFIED. ) ;
#5405 = VERTEX_POINT ( 'NONE', #33124 ) ;
#5406 = CARTESIAN_POINT ( 'NONE',  ( 0.2386122440223136243, -2.758268499246656180, 31.33685645148946719 ) ) ;
#5407 = ORIENTED_EDGE ( 'NONE', *, *, #42903, .T. ) ;
#5408 = CARTESIAN_POINT ( 'NONE',  ( 3.165499230212912352, -5.094484230520674117, 34.41647553114621161 ) ) ;
#5409 = CARTESIAN_POINT ( 'NONE',  ( -9.442362173959551797, -2.824170634883621744, 31.52227843825338738 ) ) ;
#5410 = VECTOR ( 'NONE', #25554, 1000.000000000000000 ) ;
#5411 = CARTESIAN_POINT ( 'NONE',  ( -7.912237257109728361, -3.513871655860377086, 32.76840700105978499 ) ) ;
#5412 = ORIENTED_EDGE ( 'NONE', *, *, #51691, .T. ) ;
#5413 = EDGE_LOOP ( 'NONE', ( #8614, #19727 ) ) ;
#5414 = B_SPLINE_CURVE_WITH_KNOTS ( 'NONE', 3,
 ( #55897, #28893, #58430, #522, #77067, #1402, #24209, #57999, #14474, #41506 ),
 .UNSPECIFIED., .F., .F.,
 ( 4, 2, 2, 2, 4 ),
 ( 0.000000000000000000, 0.0001954339857564073388, 0.0003908679715128146777, 0.0005863019572692220165, 0.0007817359430256293554 ),
 .UNSPECIFIED. ) ;
#5415 = EDGE_LOOP ( 'NONE', ( #81856, #81074 ) ) ;
#5416 = CARTESIAN_POINT ( 'NONE',  ( -16.08777882049607655, -2.292212530054420494, 30.41441678777542990 ) ) ;
#5417 = CARTESIAN_POINT ( 'NONE',  ( -2.307692307692427391, -9.442884908241554243, 34.35708131394783038 ) ) ;
#5418 = CARTESIAN_POINT ( 'NONE',  ( -9.469528151039281028, -10.11255958852956027, 34.01340905677048454 ) ) ;
#5419 = CARTESIAN_POINT ( 'NONE',  ( 0.6089743589743582541, -11.00000000000000000, 29.75000000000000355 ) ) ;
#5420 = CARTESIAN_POINT ( 'NONE',  ( 9.442284455014730682, -9.271318131107980420, 34.42618302367067429 ) ) ;
#5421 = CARTESIAN_POINT ( 'NONE',  ( 24.00000000000000000, -5.499999999999981348, 27.75000000000000000 ) ) ;
#5422 = CARTESIAN_POINT ( 'NONE',  ( -12.46153846153846168, -4.098570777380720287, 33.41473453929634729 ) ) ;
#5423 = EDGE_CURVE ( 'NONE', #13394, #88674, #27691, .T. ) ;
#5424 = CARTESIAN_POINT ( 'NONE',  ( -17.07692307692307665, -7.500000000000001776, 35.04278698407183867 ) ) ;
#5425 = CIRCLE ( 'NONE', #47060, 4.000000000000000000 ) ;
#5426 = EDGE_LOOP ( 'NONE', ( #41313, #37789, #11722, #54633 ) ) ;
#5427 = ORIENTED_EDGE ( 'NONE', *, *, #55798, .F. ) ;
#5428 = VERTEX_POINT ( 'NONE', #13297 ) ;
#5430 = ORIENTED_EDGE ( 'NONE', *, *, #82470, .F. ) ;
#5429 = CARTESIAN_POINT ( 'NONE',  ( -4.087778820496076548, -8.164416787775445883, 34.95778746994558617 ) ) ;
#5431 = EDGE_CURVE ( 'NONE', #22911, #17317, #28456, .T. ) ;
#5432 = CIRCLE ( 'NONE', #45730, 2.000000000000001776 ) ;
#5433 = B_SPLINE_CURVE_WITH_KNOTS ( 'NONE', 3,
 ( #33074, #38054, #87153, #59653, #26318, #17794, #45246, #18685, #79933, #87598 ),
 .UNSPECIFIED., .F., .F.,
 ( 4, 2, 2, 2, 4 ),
 ( 0.0007817246256747480398, 0.0009771112852218900684, 0.001172497944769032314, 0.001367884604316174559, 0.001563271263863316588 ),
 .UNSPECIFIED. ) ;
#5434 = AXIS2_PLACEMENT_3D ( 'NONE', #17025, #44040, #84617 ) ;
#5435 = CARTESIAN_POINT ( 'NONE',  ( 10.36538461538461675, -2.249999999999998668, 29.75000000000000355 ) ) ;
#5436 = CARTESIAN_POINT ( 'NONE',  ( 12.52679403281448600, -3.300289026998473041, 32.46337939537591666 ) ) ;
#5437 = ORIENTED_EDGE ( 'NONE', *, *, #61784, .F. ) ;
#5438 = LINE ( 'NONE', #32901, #44408 ) ;
#5439 = EDGE_CURVE ( 'NONE', #54976, #84095, #85398, .T. ) ;
#5440 = ORIENTED_EDGE ( 'NONE', *, *, #72392, .F. ) ;
#5441 = CARTESIAN_POINT ( 'NONE',  ( 0.4615384615384611200, -5.180354513474913603, 36.12317359536750416 ) ) ;
#5442 = ORIENTED_EDGE ( 'NONE', *, *, #56930, .T. ) ;
#5443 = CARTESIAN_POINT ( 'NONE',  ( -12.21153846153704237, -7.500000000000154543, 35.00000000000007105 ) ) ;
#5444 = CARTESIAN_POINT ( 'NONE',  ( -2.307692307692305711, -11.33034616979429110, 35.88435417666054406 ) ) ;
#5445 = CARTESIAN_POINT ( 'NONE',  ( -14.30769230769242917, -12.16647553114689728, 32.15551576947799362 ) ) ;
#5446 = FACE_BOUND ( 'NONE', #34330, .T. ) ;
#5447 = ADVANCED_FACE ( 'NONE', ( #41659 ), #33577, .F. ) ;
#5448 = CARTESIAN_POINT ( 'NONE',  ( 2.057692307692309708, -7.500000000000001776, 34.75000000000000000 ) ) ;
#5449 = CARTESIAN_POINT ( 'NONE',  ( 12.46153846153846168, -8.564572088678739092, 35.78748833219616898 ) ) ;
#5450 = FACE_OUTER_BOUND ( 'NONE', #47522, .T. ) ;
#5451 = CARTESIAN_POINT ( 'NONE',  ( 3.230769230769108269, -5.094484230521993062, 34.41647553114689373 ) ) ;
#5452 = AXIS2_PLACEMENT_3D ( 'NONE', #47666, #75151, #34596 ) ;
#5453 = DIRECTION ( 'NONE',  ( 0.000000000000000000, 0.9848077530122072432, 0.1736481776669354937 ) ) ;
#5454 = CARTESIAN_POINT ( 'NONE',  ( 16.08857570788537572, -4.481592998940161721, 33.73612834413957984 ) ) ;
#5455 = VERTEX_POINT ( 'NONE', #82659 ) ;
#5456 = EDGE_CURVE ( 'NONE', #86258, #65223, #56371, .T. ) ;
#5457 = DIRECTION ( 'NONE',  ( 0.000000000000000000, 0.3420201433256641055, -0.9396926207859100932 ) ) ;
#5458 = VERTEX_POINT ( 'NONE', #47514 ) ;
#5459 = B_SPLINE_CURVE_WITH_KNOTS ( 'NONE', 3,
 ( #19752, #40480, #12995, #804, #27836, #61613, #7124, #33710, #28272, #55299 ),
 .UNSPECIFIED., .F., .F.,
 ( 4, 2, 2, 2, 4 ),
 ( 0.0007817246256747504250, 0.0009771112852218954894, 0.001172497944769040554, 0.001367884604316185401, 0.001563271263863330466 ),
 .UNSPECIFIED. ) ;
#5460 = ORIENTED_EDGE ( 'NONE', *, *, #83293, .T. ) ;
#5461 = VECTOR ( 'NONE', #79594, 1000.000000000000000 ) ;
#5463 = DIRECTION ( 'NONE',  ( -0.000000000000000000, 0.1736481776669307198, -0.9848077530122080203 ) ) ;
#5462 = CYLINDRICAL_SURFACE ( 'NONE', #73408, 0.2499999999999994726 ) ;
#5464 = B_SPLINE_CURVE_WITH_KNOTS ( 'NONE', 3,
 ( #81217, #53282, #47859, #5107, #25825, #74450, #19067, #33468, #60930, #12747 ),
 .UNSPECIFIED., .F., .F.,
 ( 4, 2, 2, 2, 4 ),
 ( 0.0007817359430256303312, 0.0009771253907249965402, 0.001172514838424362641, 0.001367904286123728958, 0.001563293733823095059 ),
 .UNSPECIFIED. ) ;
#5465 = B_SPLINE_CURVE_WITH_KNOTS ( 'NONE', 3,
 ( #55769, #26541, #54000, #13456, #27422, #40940, #83258, #81492, #47689, #68847 ),
 .UNSPECIFIED., .F., .F.,
 ( 4, 2, 2, 2, 4 ),
 ( 0.0007817246256747434861, 0.0009771112852218861652, 0.001172497944769028844, 0.001367884604316171740, 0.001563271263863314419 ),
 .UNSPECIFIED. ) ;
#5466 = FACE_OUTER_BOUND ( 'NONE', #6093, .T. ) ;
#5467 = CARTESIAN_POINT ( 'NONE',  ( 3.453780582382079523, -10.61302985866383963, 33.66295027996417843 ) ) ;
#5468 = DIRECTION ( 'NONE',  ( -1.000000000000000000, -0.000000000000000000, 0.000000000000000000 ) ) ;
#5469 = DIRECTION ( 'NONE',  ( -0.000000000000000000, 0.9396926207859092051, -0.3420201433256662704 ) ) ;
#5470 = ORIENTED_EDGE ( 'NONE', *, *, #48090, .F. ) ;
#5471 = CARTESIAN_POINT ( 'NONE',  ( 2.177000841024750777, -8.999036380462717588, 34.52022231692819076 ) ) ;
#5472 = EDGE_CURVE ( 'NONE', #69315, #83335, #44535, .T. ) ;
#5473 = CARTESIAN_POINT ( 'NONE',  ( 15.16549923021291058, -4.320704448112771878, 33.92786785259540494 ) ) ;
#5474 = DIRECTION ( 'NONE',  ( 0.000000000000000000, 0.000000000000000000, -1.000000000000000000 ) ) ;
#5475 = CARTESIAN_POINT ( 'NONE',  ( -3.230769230769351186, -11.94971097300221174, 32.03036669348237098 ) ) ;
#5476 = ORIENTED_EDGE ( 'NONE', *, *, #60288, .F. ) ;
#5477 = VERTEX_POINT ( 'NONE', #62789 ) ;
#5478 = ORIENTED_EDGE ( 'NONE', *, *, #67436, .F. ) ;
#5479 = FACE_OUTER_BOUND ( 'NONE', #37572, .T. ) ;
#5480 = CARTESIAN_POINT ( 'NONE',  ( 1.653273178848927064E-15, -7.500000000000000000, 29.50000000000000355 ) ) ;
#5481 = EDGE_LOOP ( 'NONE', ( #44732, #24211 ) ) ;
#5482 = CARTESIAN_POINT ( 'NONE',  ( 9.692307692307695177, -2.833524468853757305, 32.15551576947925838 ) ) ;
#5483 = CARTESIAN_POINT ( 'NONE',  ( 14.37375964104238335, -5.471508081941601098, 34.59228464037088457 ) ) ;
#5484 = CARTESIAN_POINT ( 'NONE',  ( 6.416666666666664298, -3.499999999999999556, 29.75000000000000355 ) ) ;
#5485 = CARTESIAN_POINT ( 'NONE',  ( 17.07692307692307665, -1.951392089020283160, 34.73218667398347748 ) ) ;
#5486 = EDGE_CURVE ( 'NONE', #30238, #88839, #84428, .T. ) ;
#5487 = CARTESIAN_POINT ( 'NONE',  ( -0.5268089074992364784, -11.48612834413959582, 32.76840700105983473 ) ) ;
#5488 = VERTEX_POINT ( 'NONE', #55604 ) ;
#5490 = EDGE_LOOP ( 'NONE', ( #68024, #52183, #40695, #29887, #49586 ) ) ;
#5489 = CARTESIAN_POINT ( 'NONE',  ( -5.076923076923075762, -2.833524468853757305, 32.15551576947925838 ) ) ;
#5491 = CARTESIAN_POINT ( 'NONE',  ( 20.00000000000000000, -4.000000000000000000, 29.75000000000000355 ) ) ;
#5492 = FACE_OUTER_BOUND ( 'NONE', #50613, .T. ) ;
#5493 = CARTESIAN_POINT ( 'NONE',  ( 11.53846153846153832, -9.905515769479276145, 34.41647553114623292 ) ) ;
#5494 = AXIS2_PLACEMENT_3D ( 'NONE', #62378, #63274, #16425 ) ;
#5495 = EDGE_CURVE ( 'NONE', #74234, #82533, #8041, .T. ) ;
#5496 = EDGE_CURVE ( 'NONE', #18616, #70011, #21378, .T. ) ;
#5497 = CARTESIAN_POINT ( 'NONE',  ( 15.48071474911737333, -12.43552623307873972, 30.55307653245132826 ) ) ;
#5498 = CARTESIAN_POINT ( 'NONE',  ( 2.530471976670372936, -2.612705202774697533, 31.66806509827799943 ) ) ;
#5499 = CARTESIAN_POINT ( 'NONE',  ( 12.52679403281448245, -11.48612834413965977, 32.76840700105972815 ) ) ;
#5500 = CARTESIAN_POINT ( 'NONE',  ( 1.901340078031373171, -9.487747218494639867, 21.12686829374151287 ) ) ;
#5501 = VERTEX_POINT ( 'NONE', #42546 ) ;
#5502 = CARTESIAN_POINT ( 'NONE',  ( -6.923076923076922462, -10.67929555188718282, 33.92786785259544047 ) ) ;
#5503 = CARTESIAN_POINT ( 'NONE',  ( 2.373759641042384239, -3.937682226553329556, 33.60647404775216529 ) ) ;
#5504 = DIRECTION ( 'NONE',  ( -1.000000000000000000, -0.000000000000000000, -0.000000000000000000 ) ) ;
#5506 = ORIENTED_EDGE ( 'NONE', *, *, #58155, .F. ) ;
#5505 = VECTOR ( 'NONE', #27782, 1000.000000000000114 ) ;
#5507 = CARTESIAN_POINT ( 'NONE',  ( 2.438530638179069232, -7.277220318596959281, 34.99547417642776992 ) ) ;
#5508 = CARTESIAN_POINT ( 'NONE',  ( -12.59168567097668401, -3.285722584762969856, 32.44110544564090759 ) ) ;
#5509 = CARTESIAN_POINT ( 'NONE',  ( -0.5922290646487698984, -9.084618155246140248, 34.75535874321725771 ) ) ;
#5510 = DIRECTION ( 'NONE',  ( -0.000000000000000000, 0.1736481776669307198, -0.9848077530122080203 ) ) ;
#5511 = LINE ( 'NONE', #52791, #60013 ) ;
#5512 = CARTESIAN_POINT ( 'NONE',  ( -14.43838291080261627, -2.845849958028613624, 32.17971566917920967 ) ) ;
#5513 = ORIENTED_EDGE ( 'NONE', *, *, #26133, .F. ) ;
#5514 = CARTESIAN_POINT ( 'NONE',  ( -3.007989561791164945, -12.69155399931963046, 30.53255429739157734 ) ) ;
#5515 = CARTESIAN_POINT ( 'NONE',  ( -2.307692307692427391, -10.21337939537710326, 33.94971097300076224 ) ) ;
#5516 = DIRECTION ( 'NONE',  ( -0.000000000000000000, 0.5000000000000011102, -0.8660254037844380415 ) ) ;
#5517 = ORIENTED_EDGE ( 'NONE', *, *, #21257, .T. ) ;
#5518 = CARTESIAN_POINT ( 'NONE',  ( 12.46153846153846168, -3.513871655860378418, 32.76840700105978499 ) ) ;
#5519 = ORIENTED_EDGE ( 'NONE', *, *, #46958, .F. ) ;
#5520 = VECTOR ( 'NONE', #87585, 1000.000000000000227 ) ;
#5521 = DIRECTION ( 'NONE',  ( 0.000000000000000000, 0.000000000000000000, -1.000000000000000000 ) ) ;
#5522 = FILL_AREA_STYLE ('',( #67224 ) ) ;
#5523 = CARTESIAN_POINT ( 'NONE',  ( 5.750000000000002665, -7.500000000000001776, 34.75000000000000000 ) ) ;
#5524 = ORIENTED_EDGE ( 'NONE', *, *, #8488, .T. ) ;
#5525 = B_SPLINE_CURVE_WITH_KNOTS ( 'NONE', 3,
 ( #68102, #27103, #527, #21228, #74863, #6404, #75729, #13152, #28434, #48699 ),
 .UNSPECIFIED., .F., .F.,
 ( 4, 2, 2, 2, 4 ),
 ( 0.000000000000000000, 0.0001954339857564079352, 0.0003908679715128158703, 0.0005863019572692237513, 0.0007817359430256317406 ),
 .UNSPECIFIED. ) ;
#5526 = CARTESIAN_POINT ( 'NONE',  ( -13.13466997523734214, -4.932303261841489928, 34.32971442181322885 ) ) ;
#5527 = CARTESIAN_POINT ( 'NONE',  ( 5.776515056276053883, -10.11188796281391511, 34.01382737946119050 ) ) ;
#5528 = B_SPLINE_CURVE_WITH_KNOTS ( 'NONE', 3,
 ( #62786, #8314, #49293, #15512, #15958, #55601, #42982, #70002, #9205, #48399 ),
 .UNSPECIFIED., .F., .F.,
 ( 4, 2, 2, 2, 4 ),
 ( 0.000000000000000000, 0.0001954339857564064444, 0.0003908679715128128888, 0.0005863019572692193060, 0.0007817359430256257775 ),
 .UNSPECIFIED. ) ;
#5529 = DIRECTION ( 'NONE',  ( 0.000000000000000000, 0.4999999999999960032, -0.8660254037844410391 ) ) ;
#5530 = CARTESIAN_POINT ( 'NONE',  ( 6.989144256427000990, -12.34228464037088813, 31.77849191805839268 ) ) ;
#5531 = CARTESIAN_POINT ( 'NONE',  ( 16.15384615384615330, -4.098570777380720287, 33.41473453929634729 ) ) ;
#5532 = AXIS2_PLACEMENT_3D ( 'NONE', #3664, #37452, #37909 ) ;
#5533 = ORIENTED_EDGE ( 'NONE', *, *, #41239, .T. ) ;
#5534 = CARTESIAN_POINT ( 'NONE',  ( 4.153846153846154188, -1.790695186598648903, 34.54067556320373455 ) ) ;
#5535 = VERTEX_POINT ( 'NONE', #14627 ) ;
#5536 = CARTESIAN_POINT ( 'NONE',  ( 8.769230769230768274, -12.37446782046654192, 30.86335684631486131 ) ) ;
#5537 = FACE_OUTER_BOUND ( 'NONE', #88731, .T. ) ;
#5538 = CARTESIAN_POINT ( 'NONE',  ( 2.307692307692187583, -4.481592998941358097, 33.73612834414048933 ) ) ;
#5539 = DIRECTION ( 'NONE',  ( -0.000000000000000000, -0.6427876096865404731, -0.7660444431189770143 ) ) ;
#5540 = CARTESIAN_POINT ( 'NONE',  ( -14.24243673641627872, -12.27809138561124591, 31.22303859784720359 ) ) ;
#5541 = CARTESIAN_POINT ( 'NONE',  ( -10.61538461538473399, -9.442884908241554243, 34.35708131394783038 ) ) ;
#5542 = ORIENTED_EDGE ( 'NONE', *, *, #42232, .F. ) ;
#5543 = ORIENTED_EDGE ( 'NONE', *, *, #50372, .T. ) ;
#5544 = EDGE_LOOP ( 'NONE', ( #73729, #82208, #42243, #74709 ) ) ;
#5545 = ORIENTED_EDGE ( 'NONE', *, *, #12553, .F. ) ;
#5546 = CARTESIAN_POINT ( 'NONE',  ( 2.084207363968360038, -5.113361153441932316, 34.14387501736621999 ) ) ;
#5547 = CARTESIAN_POINT ( 'NONE',  ( 4.403791563224197070, -10.18230066228895758, 34.26354781536631577 ) ) ;
#5548 = CARTESIAN_POINT ( 'NONE',  ( -2.530570990120954100, -7.630691491037286056, 34.74850469731152458 ) ) ;
#5549 = LINE ( 'NONE', #80333, #86014 ) ;
#5551 = EDGE_CURVE ( 'NONE', #30008, #45585, #26382, .T. ) ;
#5550 = LINE ( 'NONE', #61804, #70093 ) ;
#5552 = CARTESIAN_POINT ( 'NONE',  ( 5.076923076923075762, -2.499999999999998668, 29.75000000000001421 ) ) ;
#5553 = CARTESIAN_POINT ( 'NONE',  ( -2.307692307692427391, -3.835265460704628371, 33.15142922262033665 ) ) ;
#5554 = PLANE ( 'NONE',  #79245 ) ;
#5555 = VERTEX_POINT ( 'NONE', #56931 ) ;
#5556 = EDGE_LOOP ( 'NONE', ( #38375, #63616, #22591, #39013 ) ) ;
#5557 = EDGE_LOOP ( 'NONE', ( #670, #43528, #17289, #50294 ) ) ;
#5559 = ORIENTED_EDGE ( 'NONE', *, *, #55685, .F. ) ;
#5558 = CARTESIAN_POINT ( 'NONE',  ( 2.084766090176160436, -2.554751324335734264, 30.48935550225260727 ) ) ;
#5561 = CARTESIAN_POINT ( 'NONE',  ( -7.912237257109724808, -4.098570777380719399, 33.41473453929634729 ) ) ;
#5560 = CARTESIAN_POINT ( 'NONE',  ( 16.15384615384615330, -11.69971097300155272, 32.46337939537588113 ) ) ;
#5562 = CARTESIAN_POINT ( 'NONE',  ( 16.37727311570772670, -7.630147231320743018, 34.74852402298682819 ) ) ;
#5563 = CARTESIAN_POINT ( 'NONE',  ( -9.942284423250047354, -6.567427716900048118, 34.66269422305636283 ) ) ;
#5564 = FACE_BOUND ( 'NONE', #6462, .T. ) ;
#5565 = VERTEX_POINT ( 'NONE', #69565 ) ;
#5566 = EDGE_CURVE ( 'NONE', #3333, #58130, #35793, .T. ) ;
#5567 = EDGE_LOOP ( 'NONE', ( #82605, #51474, #60399, #9534 ) ) ;
#5568 = CARTESIAN_POINT ( 'NONE',  ( -1.384615384615383471, -11.91647553114624181, 32.58852847137148245 ) ) ;
#5569 = ORIENTED_EDGE ( 'NONE', *, *, #18028, .F. ) ;
#5570 = FACE_BOUND ( 'NONE', #38233, .T. ) ;
#5571 = CARTESIAN_POINT ( 'NONE',  ( 9.915320536401090123, -5.582272713120729257, 34.63742843783360570 ) ) ;
#5572 = VECTOR ( 'NONE', #63305, 1000.000000000000227 ) ;
#5573 = CARTESIAN_POINT ( 'NONE',  ( 15.10062126103753855, -6.809168938359901446, 34.95455904226513866 ) ) ;
#5574 = VERTEX_POINT ( 'NONE', #23152 ) ;
#5575 = CARTESIAN_POINT ( 'NONE',  ( -5.933830859037342975, -7.250054483168843156, 34.74374881642865631 ) ) ;
#5576 = CARTESIAN_POINT ( 'NONE',  ( 4.153846153846154188, -1.242168528481310874, 33.36296068462461051 ) ) ;
#5577 = CARTESIAN_POINT ( 'NONE',  ( 17.07692307692307665, -12.29105614889573062, 35.45975837776705220 ) ) ;
#5578 = ORIENTED_EDGE ( 'NONE', *, *, #84632, .F. ) ;
#5579 = CYLINDRICAL_SURFACE ( 'NONE', #74461, 0.2500000000000008882 ) ;
#5580 = CARTESIAN_POINT ( 'NONE',  ( 6.700150705560775855, -12.39988816332205701, 30.74660775122750778 ) ) ;
#5581 = CARTESIAN_POINT ( 'NONE',  ( -39.05038313613820122, -2.249999999999999556, 27.25000000000000000 ) ) ;
#5582 = ORIENTED_EDGE ( 'NONE', *, *, #86968, .T. ) ;
#5583 = CARTESIAN_POINT ( 'NONE',  ( 18.00000000000000000, -10.51840700105979565, 33.73612834413961536 ) ) ;
#5584 = CARTESIAN_POINT ( 'NONE',  ( 2.557746727605761272, -3.435999193479609470, 33.07426656108011542 ) ) ;
#5585 = AXIS2_PLACEMENT_3D ( 'NONE', #3143, #58092, #36073 ) ;
#5586 = ORIENTED_EDGE ( 'NONE', *, *, #25752, .T. ) ;
#5587 = CARTESIAN_POINT ( 'NONE',  ( 3.480823650682684178, -6.523592122091589118, 34.90882529074906415 ) ) ;
#5588 = DIRECTION ( 'NONE',  ( -0.000000000000000000, 1.000000000000000000, -0.000000000000000000 ) ) ;
#5589 = CARTESIAN_POINT ( 'NONE',  ( -14.30769230769242917, -2.657715359629662544, 31.77849191805970364 ) ) ;
#5590 = CARTESIAN_POINT ( 'NONE',  ( -11.66860874789975888, -8.587444163452046197, 34.63053765926554206 ) ) ;
#5591 = CARTESIAN_POINT ( 'NONE',  ( 0.4615384615383382183, -2.657715359629662544, 31.77849191805970364 ) ) ;
#5592 = EDGE_CURVE ( 'NONE', #29939, #63009, #13460, .T. ) ;
#5593 = ADVANCED_FACE ( 'NONE', ( #2426 ), #29919, .F. ) ;
#5594 = CARTESIAN_POINT ( 'NONE',  ( 17.14217821643591932, -5.094484230520771817, 34.41647553114626845 ) ) ;
#5596 = CARTESIAN_POINT ( 'NONE',  ( -15.29603967673000575, -12.46129190929999986, 30.37095296980880832 ) ) ;
#5595 = CARTESIAN_POINT ( 'NONE',  ( 14.05769230769230838, -2.499999999999998668, 29.75000000000000355 ) ) ;
#5597 = CARTESIAN_POINT ( 'NONE',  ( -3.230769230769351186, -2.625532179533779154, 30.86335684631627174 ) ) ;
#5598 = CARTESIAN_POINT ( 'NONE',  ( -6.673022611438607754, -2.779044189368096163, 31.39831045268886456 ) ) ;
#5599 = CARTESIAN_POINT ( 'NONE',  ( 2.749999999999995115, -6.360912703473971419, 19.39062500000000711 ) ) ;
#5600 = EDGE_LOOP ( 'NONE', ( #35797, #28180, #48878, #80964 ) ) ;
#5601 = CARTESIAN_POINT ( 'NONE',  ( 6.923076923076924238, -7.500000000000001776, 35.04278698407183867 ) ) ;
#5602 = ORIENTED_EDGE ( 'NONE', *, *, #20892, .T. ) ;
#5603 = ADVANCED_FACE ( 'NONE', ( #43862 ), #71328, .F. ) ;
#5604 = ORIENTED_EDGE ( 'NONE', *, *, #60963, .T. ) ;
#5605 = CARTESIAN_POINT ( 'NONE',  ( 11.53846153846153832, -4.661471528628507777, 34.16647553114623292 ) ) ;
#5606 = VERTEX_POINT ( 'NONE', #58261 ) ;
#5607 = CARTESIAN_POINT ( 'NONE',  ( -5.933932666649923249, -9.905515769479277921, 34.41647553114623292 ) ) ;
#5608 = CARTESIAN_POINT ( 'NONE',  ( -1.077988221561460236, -10.27530806549876452, 27.10750670625849423 ) ) ;
#5609 = CARTESIAN_POINT ( 'NONE',  ( 14.53047184896071542, -11.41317474335729543, 32.86274602512330034 ) ) ;
#5610 = CARTESIAN_POINT ( 'NONE',  ( -18.00000000000000000, -11.91647553114624358, 32.58852847137147535 ) ) ;
#5611 = CARTESIAN_POINT ( 'NONE',  ( -7.780898274877820597, -6.026961402152789304, 34.52809138561124769 ) ) ;
#5612 = CARTESIAN_POINT ( 'NONE',  ( -12.46153846153846168, -11.91647553114624181, 32.58852847137148245 ) ) ;
#5613 = CARTESIAN_POINT ( 'NONE',  ( -15.45369618967607828, -4.762599654559228846, 34.23009711892697737 ) ) ;
#5614 = CARTESIAN_POINT ( 'NONE',  ( 2.057715576749954867, -9.943427161483782584, 34.11278801902876978 ) ) ;
#5615 = CARTESIAN_POINT ( 'NONE',  ( 2.320192649118979489E-14, -11.25000000000000000, 23.53125000000000000 ) ) ;
#5616 = CARTESIAN_POINT ( 'NONE',  ( -7.146003881983771677, -4.762599654559228846, 34.23009711892697737 ) ) ;
#5617 = CARTESIAN_POINT ( 'NONE',  ( -17.77722033102193322, -2.353885683473780244, 30.79025554430704759 ) ) ;
#5618 = CYLINDRICAL_SURFACE ( 'NONE', #6183, 0.2500000000000009437 ) ;
#5619 = VECTOR ( 'NONE', #37011, 1000.000000000000000 ) ;
#5620 = EDGE_LOOP ( 'NONE', ( #14694, #50528 ) ) ;
#5621 = ORIENTED_EDGE ( 'NONE', *, *, #87981, .F. ) ;
#5622 = CYLINDRICAL_SURFACE ( 'NONE', #42882, 0.2500000000000009437 ) ;
#5623 = CARTESIAN_POINT ( 'NONE',  ( -3.230769230769229949, -13.75783147151868846, 33.36296068462461051 ) ) ;
#5624 = CARTESIAN_POINT ( 'NONE',  ( 2.307692307692309264, -12.78798330534102945, 29.74999999999997868 ) ) ;
#5625 = CARTESIAN_POINT ( 'NONE',  ( -7.146561847641253351, -5.827078755546623690, 34.72654668319379567 ) ) ;
#5626 = DIRECTION ( 'NONE',  ( 0.000000000000000000, 0.1736481776669275834, 0.9848077530122086864 ) ) ;
#5627 = B_SPLINE_CURVE_WITH_KNOTS ( 'NONE', 3,
 ( #25405, #4241, #71356, #66388, #58736, #72250, #11007, #58287, #24061, #51971 ),
 .UNSPECIFIED., .F., .F.,
 ( 4, 2, 2, 2, 4 ),
 ( 0.000000000000000000, 0.0001954339857564072033, 0.0003908679715128144066, 0.0005863019572692215828, 0.0007817359430256288133 ),
 .UNSPECIFIED. ) ;
#5628 = CARTESIAN_POINT ( 'NONE',  ( -0.5276218724943421146, -6.386643153685125363, 34.62446782046654903 ) ) ;
#5629 = B_SPLINE_CURVE_WITH_KNOTS ( 'NONE', 3,
 ( #23363, #36882, #78756, #17058, #3535, #71109, #22927, #30567, #2641, #31006 ),
 .UNSPECIFIED., .F., .F.,
 ( 4, 2, 2, 2, 4 ),
 ( 0.000000000000000000, 0.0001954311564186865221, 0.0003908623128373730441, 0.0005862934692560595662, 0.0007817246256747460882 ),
 .UNSPECIFIED. ) ;
#5630 = ORIENTED_EDGE ( 'NONE', *, *, #51166, .F. ) ;
#5631 = LINE ( 'NONE', #25460, #9828 ) ;
#5632 = VERTEX_POINT ( 'NONE', #32137 ) ;
#5633 = VERTEX_POINT ( 'NONE', #65469 ) ;
#5634 = CARTESIAN_POINT ( 'NONE',  ( 5.142991427925513115, -8.120952969808772792, 34.71129190929999453 ) ) ;
#5635 = AXIS2_PLACEMENT_3D ( 'NONE', #15136, #20553, #7493 ) ;
#5636 = VECTOR ( 'NONE', #83417, 1000.000000000000000 ) ;
#5637 = CARTESIAN_POINT ( 'NONE',  ( -2.372962308248625085, -9.528491918058357157, 34.59228464037090589 ) ) ;
#5638 = CARTESIAN_POINT ( 'NONE',  ( -4.283993363284373856, -4.460286881179643004, 33.72017969459903242 ) ) ;
#5639 = DIRECTION ( 'NONE',  ( -0.000000000000000000, 0.3420201433256694901, -0.9396926207859082059 ) ) ;
#5640 = CARTESIAN_POINT ( 'NONE',  ( -13.51476335434708709, -2.647304123082328875, 31.75400227202885972 ) ) ;
#5641 = EDGE_CURVE ( 'NONE', #66197, #11542, #66093, .T. ) ;
#5642 = VERTEX_POINT ( 'NONE', #24030 ) ;
#5643 = VECTOR ( 'NONE', #45009, 1000.000000000000000 ) ;
#5644 = VERTEX_POINT ( 'NONE', #44740 ) ;
#5645 = ORIENTED_EDGE ( 'NONE', *, *, #3053, .F. ) ;
#5646 = VERTEX_POINT ( 'NONE', #59598 ) ;
#5647 = DIRECTION ( 'NONE',  ( 0.000000000000000000, 0.7660444431189822323, -0.6427876096865344779 ) ) ;
#5648 = CARTESIAN_POINT ( 'NONE',  ( 10.48523664565292002, -11.66186481527757302, 32.95055677023626117 ) ) ;
#5649 = LINE ( 'NONE', #12849, #3414 ) ;
#5651 = EDGE_CURVE ( 'NONE', #18982, #558, #3717, .T. ) ;
#5650 = CARTESIAN_POINT ( 'NONE',  ( -15.36146069743678844, -11.18331474514187995, 33.13161551792790505 ) ) ;
#5652 = CARTESIAN_POINT ( 'NONE',  ( 17.75002326905764605, -4.943428324936578910, 34.04746400365624481 ) ) ;
#5653 = CARTESIAN_POINT ( 'NONE',  ( -10.36543909703647337, -12.22109172314383052, 31.39792113162168263 ) ) ;
#5654 = VERTEX_POINT ( 'NONE', #85307 ) ;
#5655 = EDGE_CURVE ( 'NONE', #21025, #26289, #71520, .T. ) ;
#5656 = ORIENTED_EDGE ( 'NONE', *, *, #11400, .T. ) ;
#5658 = ORIENTED_EDGE ( 'NONE', *, *, #36655, .F. ) ;
#5657 = CARTESIAN_POINT ( 'NONE',  ( 17.14217864819910275, -12.46129190930001052, 30.37095296980869819 ) ) ;
#5659 = DIRECTION ( 'NONE',  ( 0.000000000000000000, 0.000000000000000000, 1.000000000000000000 ) ) ;
#5660 = CARTESIAN_POINT ( 'NONE',  ( 12.71148387091650278, -8.476813868363244353, 34.90874843262270133 ) ) ;
#5661 = CARTESIAN_POINT ( 'NONE',  ( 3.750000000000009770, -9.053300858899081760, 19.54687500000000000 ) ) ;
#5662 = VERTEX_POINT ( 'NONE', #11872 ) ;
#5663 = EDGE_CURVE ( 'NONE', #86404, #60435, #24924, .T. ) ;
#5664 = CARTESIAN_POINT ( 'NONE',  ( -1.134669975237341921, -2.589246495874657938, 31.60778113518102828 ) ) ;
#5665 = ORIENTED_EDGE ( 'NONE', *, *, #4431, .T. ) ;
#5666 = CARTESIAN_POINT ( 'NONE',  ( -5.999999999999998224, -12.29105614889573062, 35.45975837776705220 ) ) ;
#5667 = DIRECTION ( 'NONE',  ( 1.000000000000000000, 0.000000000000000000, 0.000000000000000000 ) ) ;
#5668 = CARTESIAN_POINT ( 'NONE',  ( -19.50000000000000000, -3.499999999999999556, 29.75000000000000355 ) ) ;
#5669 = CARTESIAN_POINT ( 'NONE',  ( -5.934744860487159990, -3.083524468853784839, 32.58852847137153930 ) ) ;
#5670 = EDGE_CURVE ( 'NONE', #32572, #67440, #61781, .T. ) ;
#5671 = CARTESIAN_POINT ( 'NONE',  ( 8.519254038288414321, -4.943428324936578910, 34.04746400365624481 ) ) ;
#5672 = ORIENTED_EDGE ( 'NONE', *, *, #5914, .T. ) ;
#5673 = DIRECTION ( 'NONE',  ( 0.000000000000000000, 0.3420201433256610524, 0.9396926207859113145 ) ) ;
#5674 =( NAMED_UNIT ( * ) PLANE_ANGLE_UNIT ( ) SI_UNIT ( $, .RADIAN. ) );
#5675 = CARTESIAN_POINT ( 'NONE',  ( -14.08468095607945969, -2.758310577978207778, 31.33698337089302299 ) ) ;
#5676 = ORIENTED_EDGE ( 'NONE', *, *, #60848, .F. ) ;
#5677 = CARTESIAN_POINT ( 'NONE',  ( -9.442253272394237840, -4.818054556918156983, 34.26375889529406749 ) ) ;
#5678 = CARTESIAN_POINT ( 'NONE',  ( -4.023320715612507925, -10.31582465632705237, 34.18122507451815295 ) ) ;
#5679 = CARTESIAN_POINT ( 'NONE',  ( -16.40384615384616041, -2.250000000000000000, 29.81609741502490607 ) ) ;
#5680 = CARTESIAN_POINT ( 'NONE',  ( -9.692307692307691624, -1.790695186598648903, 34.54067556320373455 ) ) ;
#5681 = CARTESIAN_POINT ( 'NONE',  ( 8.899756207464413649, -10.31582465632705237, 34.18122507451815295 ) ) ;
#5682 = EDGE_CURVE ( 'NONE', #13118, #48938, #51040, .T. ) ;
#5683 = FACE_BOUND ( 'NONE', #62574, .T. ) ;
#5685 = DIRECTION ( 'NONE',  ( -1.000000000000000000, -0.000000000000000000, -0.000000000000000000 ) ) ;
#5684 = CARTESIAN_POINT ( 'NONE',  ( 1.319292469123210854, -7.749976743299137993, 34.99404534957040624 ) ) ;
#5686 = CARTESIAN_POINT ( 'NONE',  ( 2.084765348785458272, -10.01117774369187252, 34.36070679894347535 ) ) ;
#5688 = CARTESIAN_POINT ( 'NONE',  ( -2.057692307692306599, -2.499999999999998668, 29.75000000000000355 ) ) ;
#5687 = CARTESIAN_POINT ( 'NONE',  ( -7.134615384615385025, -7.500000000000000000, 33.75000000000000000 ) ) ;
#5689 = EDGE_CURVE ( 'NONE', #66615, #50015, #42509, .T. ) ;
#5690 = CARTESIAN_POINT ( 'NONE',  ( 6.130790440966950250, -4.684288915650984819, 34.18129842949671371 ) ) ;
#5691 = CARTESIAN_POINT ( 'NONE',  ( 0.06109907496455496689, -11.24999999999999822, 23.27938170625849068 ) ) ;
#5692 = ORIENTED_EDGE ( 'NONE', *, *, #3407, .T. ) ;
#5693 = CARTESIAN_POINT ( 'NONE',  ( 10.48523664565292357, -12.15440758774515473, 32.17923288041532004 ) ) ;
#5694 = ORIENTED_EDGE ( 'NONE', *, *, #18098, .T. ) ;
#5695 = VECTOR ( 'NONE', #68592, 1000.000000000000000 ) ;
#5696 = VECTOR ( 'NONE', #83649, 1000.000000000000000 ) ;
#5697 = DIRECTION ( 'NONE',  ( 0.000000000000000000, 0.3420201433256641055, -0.9396926207859100932 ) ) ;
#5698 = EDGE_CURVE ( 'NONE', #72772, #12820, #25263, .T. ) ;
#5699 = ORIENTED_EDGE ( 'NONE', *, *, #76759, .F. ) ;
#5700 = ADVANCED_FACE ( 'NONE', ( #74902 ), #54160, .F. ) ;
#5701 = CARTESIAN_POINT ( 'NONE',  ( 7.846153846153725020, -9.442884908241554243, 34.35708131394783038 ) ) ;
#5702 = DIRECTION ( 'NONE',  ( -1.000000000000000000, 0.000000000000000000, -0.000000000000000000 ) ) ;
#5704 = ORIENTED_EDGE ( 'NONE', *, *, #42159, .T. ) ;
#5703 = CARTESIAN_POINT ( 'NONE',  ( -10.68065461594093435, -11.67786785259540849, 32.92929555188721480 ) ) ;
#5705 = CARTESIAN_POINT ( 'NONE',  ( 7.846153846153725020, -9.442884908241554243, 34.35708131394783038 ) ) ;
#5706 = DIRECTION ( 'NONE',  ( -0.000000000000000000, 0.9396926207859092051, -0.3420201433256662704 ) ) ;
#5707 = CARTESIAN_POINT ( 'NONE',  ( -2.608446859217889546, -10.19485399968121264, 25.93563170625849423 ) ) ;
#5708 = CARTESIAN_POINT ( 'NONE',  ( 4.219101725122178514, -10.90142922261932057, 33.41473453929631887 ) ) ;
#5709 = CARTESIAN_POINT ( 'NONE',  ( 8.639082799499067988, -2.647304123082328875, 31.75400227202885972 ) ) ;
#5710 = CARTESIAN_POINT ( 'NONE',  ( -0.4998584449498338911, -4.795810369898659609, 29.16127627612525330 ) ) ;
#5711 = CARTESIAN_POINT ( 'NONE',  ( 4.023698944407932743, -11.93770438780619259, 32.05411857736982029 ) ) ;
#5712 = CARTESIAN_POINT ( 'NONE',  ( -1.134560964701931018, -6.523592122091591783, 34.90882529074906415 ) ) ;
#5713 = CARTESIAN_POINT ( 'NONE',  ( 1.450682717965462221, -9.905515769479277921, 34.41647553114623292 ) ) ;
#5714 = VECTOR ( 'NONE', #63324, 1000.000000000000000 ) ;
#5715 = CARTESIAN_POINT ( 'NONE',  ( 2.608446859217924629, -10.19485399968118422, 17.37686829374151287 ) ) ;
#5716 = CARTESIAN_POINT ( 'NONE',  ( -4.219928533206289245, -2.833524468853757305, 32.15551576947924417 ) ) ;
#5717 = CARTESIAN_POINT ( 'NONE',  ( -11.53846153846165912, -10.90142922262034020, 33.41473453929536674 ) ) ;
#5718 = EDGE_LOOP ( 'NONE', ( #35076, #3105 ) ) ;
#5719 = DIRECTION ( 'NONE',  ( 1.000000000000000000, 0.000000000000000000, 0.000000000000000000 ) ) ;
#5720 = DIRECTION ( 'NONE',  ( 0.000000000000000000, 0.4999999999999960032, -0.8660254037844410391 ) ) ;
#5721 = CARTESIAN_POINT ( 'NONE',  ( 0.06109907496451268821, -3.749999999999999556, 18.15811829374151642 ) ) ;
#5722 = CARTESIAN_POINT ( 'NONE',  ( 2.177544337960612086, -5.070767119584671967, 34.40440758774516183 ) ) ;
#5723 = CARTESIAN_POINT ( 'NONE',  ( 6.923076923077231548, -2.506253911140614576, 30.00000000000323297 ) ) ;
#5724 = ORIENTED_EDGE ( 'NONE', *, *, #78900, .T. ) ;
#5725 = DIRECTION ( 'NONE',  ( -0.000000000000000000, -0.1736481776669307198, -0.9848077530122080203 ) ) ;
#5726 = DIRECTION ( 'NONE',  ( -0.000000000000000000, -0.3420201433256694346, -0.9396926207859080948 ) ) ;
#5728 = ORIENTED_EDGE ( 'NONE', *, *, #44247, .F. ) ;
#5727 = CARTESIAN_POINT ( 'NONE',  ( 9.019176178608811156, -2.589246495874658383, 31.60778113518102828 ) ) ;
#5729 = FACE_OUTER_BOUND ( 'NONE', #80632, .T. ) ;
#5730 = CARTESIAN_POINT ( 'NONE',  ( -15.00775638667583678, -11.98016756924215009, 32.48728574198911190 ) ) ;
#5731 = CARTESIAN_POINT ( 'NONE',  ( -23.50000000000000000, -4.999999999999999112, 28.00000000000000000 ) ) ;
#5732 = ORIENTED_EDGE ( 'NONE', *, *, #5813, .F. ) ;
#5733 = CARTESIAN_POINT ( 'NONE',  ( 5.011652630962299959, -4.481592998940161721, 33.73612834413957984 ) ) ;
#5734 = EDGE_CURVE ( 'NONE', #31351, #1868, #5550, .T. ) ;
#5735 = CARTESIAN_POINT ( 'NONE',  ( 19.00000000000000000, -8.999999999999996447, 22.25000000000000000 ) ) ;
#5736 = CARTESIAN_POINT ( 'NONE',  ( 1.384615384615386802, -2.833524468853757305, 32.15551576947925838 ) ) ;
#5737 = VERTEX_POINT ( 'NONE', #46535 ) ;
#5738 = ORIENTED_EDGE ( 'NONE', *, *, #4753, .T. ) ;
#5739 = ORIENTED_EDGE ( 'NONE', *, *, #57543, .F. ) ;
#5740 = EDGE_CURVE ( 'NONE', #72102, #87523, #45511, .T. ) ;
#5741 = VECTOR ( 'NONE', #58632, 1000.000000000000114 ) ;
#5742 = ORIENTED_EDGE ( 'NONE', *, *, #88799, .T. ) ;
#5743 = ADVANCED_FACE ( 'NONE', ( #53280 ), #68572, .F. ) ;
#5744 = CARTESIAN_POINT ( 'NONE',  ( 5.326868595271218254, -12.22109172314383052, 31.39792113162168263 ) ) ;
#5745 = CARTESIAN_POINT ( 'NONE',  ( -2.307692307692427391, -6.026961402154118908, 34.52809138561165270 ) ) ;
#5746 = DIRECTION ( 'NONE',  ( -0.000000000000000000, 1.000000000000000000, -0.000000000000000000 ) ) ;
#5747 = FACE_OUTER_BOUND ( 'NONE', #42025, .T. ) ;
#5748 = EDGE_CURVE ( 'NONE', #18634, #26348, #21908, .T. ) ;
#5749 = DIRECTION ( 'NONE',  ( -1.000000000000000000, -0.000000000000000000, -0.000000000000000000 ) ) ;
#5750 = ORIENTED_EDGE ( 'NONE', *, *, #34917, .F. ) ;
#5751 = EDGE_LOOP ( 'NONE', ( #41470, #31607, #88440, #45608 ) ) ;
#5752 = B_SPLINE_CURVE_WITH_KNOTS ( 'NONE', 3,
 ( #47989, #5679, #26845, #60618, #61503, #34484 ),
 .UNSPECIFIED., .F., .F.,
 ( 4, 2, 4 ),
 ( 1.769077770938648657E-17, 0.0001954756301636913782, 0.0003909512603273650297 ),
 .UNSPECIFIED. ) ;
#5753 = VECTOR ( 'NONE', #41479, 1000.000000000000000 ) ;
#5754 = ORIENTED_EDGE ( 'NONE', *, *, #21698, .T. ) ;
#5756 = ORIENTED_EDGE ( 'NONE', *, *, #71480, .F. ) ;
#5755 = CARTESIAN_POINT ( 'NONE',  ( -2.980769230769230393, -2.499999999999998668, 29.75000000000000355 ) ) ;
#5757 = CARTESIAN_POINT ( 'NONE',  ( -16.37677311275299985, -12.38737895849757820, 31.66785238281580206 ) ) ;
#5758 = B_SPLINE_CURVE_WITH_KNOTS ( 'NONE', 3,
 ( #46772, #39590, #33702, #33263, #34587, #12111, #88670, #75142, #53966, #13425 ),
 .UNSPECIFIED., .F., .F.,
 ( 4, 2, 2, 2, 4 ),
 ( 0.000000000000000000, 0.0001954339857564092904, 0.0003908679715128185808, 0.0005863019572692278712, 0.0007817359430256371616 ),
 .UNSPECIFIED. ) ;
#5759 = B_SPLINE_CURVE_WITH_KNOTS ( 'NONE', 3,
 ( #59495, #39690, #25717, #88332, #46867, #47308, #74800, #13091, #73470, #86998 ),
 .UNSPECIFIED., .F., .F.,
 ( 4, 2, 2, 2, 4 ),
 ( 0.000000000000000000, 0.0001954311564186878773, 0.0003908623128373757546, 0.0005862934692560635777, 0.0007817246256747515092 ),
 .UNSPECIFIED. ) ;
#5760 = DIRECTION ( 'NONE',  ( 0.000000000000000000, 0.7660444431189807890, 0.6427876096865361433 ) ) ;
#5761 = VECTOR ( 'NONE', #25421, 1000.000000000000000 ) ;
#5762 = VECTOR ( 'NONE', #80214, 1000.000000000000227 ) ;
#5763 = EDGE_CURVE ( 'NONE', #10580, #58351, #13290, .T. ) ;
#5764 = CARTESIAN_POINT ( 'NONE',  ( 13.19230769230769340, -4.000000000000000000, 29.75000000000000355 ) ) ;
#5765 = CARTESIAN_POINT ( 'NONE',  ( 4.000000000000001776, -7.499999999999999112, 14.00000000000000178 ) ) ;
#5766 = VERTEX_POINT ( 'NONE', #88001 ) ;
#5767 = ADVANCED_FACE ( 'NONE', ( #60039 ), #87546, .F. ) ;
#5768 = ORIENTED_EDGE ( 'NONE', *, *, #63089, .F. ) ;
#5769 = ORIENTED_EDGE ( 'NONE', *, *, #39546, .T. ) ;
#5770 = CARTESIAN_POINT ( 'NONE',  ( 10.68064018666063930, -10.90142922261932057, 33.41473453929631887 ) ) ;
#5772 = EDGE_LOOP ( 'NONE', ( #62273, #26038, #23597, #37806 ) ) ;
#5771 = CYLINDRICAL_SURFACE ( 'NONE', #61688, 0.2499999999999995559 ) ;
#5773 = DIRECTION ( 'NONE',  ( -0.000000000000000000, -0.3420201433256694901, -0.9396926207859082059 ) ) ;
#5774 = DIRECTION ( 'NONE',  ( -1.000000000000000000, -0.000000000000000000, 0.000000000000000000 ) ) ;
#5775 = ORIENTED_EDGE ( 'NONE', *, *, #9846, .T. ) ;
#5776 = FACE_OUTER_BOUND ( 'NONE', #2140, .T. ) ;
#5777 = DIRECTION ( 'NONE',  ( -1.000000000000000000, 0.000000000000000000, 0.000000000000000000 ) ) ;
#5778 = FACE_OUTER_BOUND ( 'NONE', #8619, .T. ) ;
#5779 = FACE_BOUND ( 'NONE', #66797, .T. ) ;
#5780 = CARTESIAN_POINT ( 'NONE',  ( -15.23076923076935252, -8.656820664282941280, 34.87096338111179961 ) ) ;
#5781 = CARTESIAN_POINT ( 'NONE',  ( -1.318547033612944563, -11.69971097300155272, 32.46337939537588113 ) ) ;
#5782 = DIRECTION ( 'NONE',  ( -0.000000000000000000, -0.3420201433256694901, -0.9396926207859082059 ) ) ;
#5784 = CARTESIAN_POINT ( 'NONE',  ( 15.36155967173618286, -9.929761469519743144, 34.40412654351204225 ) ) ;
#5783 = DIRECTION ( 'NONE',  ( -0.000000000000000000, -0.1736481776669307198, -0.9848077530122080203 ) ) ;
#5785 = CYLINDRICAL_SURFACE ( 'NONE', #50979, 0.2499999999999995559 ) ;
#5786 = CARTESIAN_POINT ( 'NONE',  ( 12.46153846153833911, -3.083524468854526912, 32.58852847137268327 ) ) ;
#5787 = ORIENTED_EDGE ( 'NONE', *, *, #83805, .T. ) ;
#5788 = CARTESIAN_POINT ( 'NONE',  ( -17.20761368003338276, -5.496505350115500121, 34.60290016733514307 ) ) ;
#5789 = CARTESIAN_POINT ( 'NONE',  ( 10.61538461538449596, -3.835265460704628371, 33.15142922262033665 ) ) ;
#5790 = ORIENTED_EDGE ( 'NONE', *, *, #37887, .F. ) ;
#5791 = ORIENTED_EDGE ( 'NONE', *, *, #1572, .T. ) ;
#5792 = CARTESIAN_POINT ( 'NONE',  ( -17.14219352288385423, -11.48612834413959582, 32.76840700105983473 ) ) ;
#5793 = CARTESIAN_POINT ( 'NONE',  ( -15.45425417449317784, -2.599994579823203367, 30.74605699353653776 ) ) ;
#5794 = CARTESIAN_POINT ( 'NONE',  ( -11.76194646302586655, -10.23692288466677880, 34.23039457007281072 ) ) ;
#5795 = ORIENTED_EDGE ( 'NONE', *, *, #43074, .F. ) ;
#5796 = CARTESIAN_POINT ( 'NONE',  ( -16.15384615384627409, -11.48612834414049644, 32.76840700105863391 ) ) ;
#5797 = CARTESIAN_POINT ( 'NONE',  ( -4.284536756956460302, -9.084618155246140248, 34.75535874321725771 ) ) ;
#5798 = EDGE_CURVE ( 'NONE', #42433, #17811, #2591, .T. ) ;
#5799 = EDGE_CURVE ( 'NONE', #60703, #10963, #14405, .T. ) ;
#5800 = FACE_BOUND ( 'NONE', #9323, .T. ) ;
#5802 = CARTESIAN_POINT ( 'NONE',  ( -9.915792636031639518, -4.386631170607603991, 33.66268669641500111 ) ) ;
#5801 = DIRECTION ( 'NONE',  ( -0.000000000000000000, 0.9848077530122085754, -0.1736481776669273613 ) ) ;
#5803 = CARTESIAN_POINT ( 'NONE',  ( -13.51530598772569292, -2.295517848115769421, 30.44137282052137294 ) ) ;
#5804 = DIRECTION ( 'NONE',  ( -1.000000000000000000, -0.000000000000000000, -0.000000000000000000 ) ) ;
#5806 = DIRECTION ( 'NONE',  ( -0.000000000000000000, -0.7660444431189791237, -0.6427876096865379196 ) ) ;
#5805 = DIRECTION ( 'NONE',  ( 0.000000000000000000, 0.000000000000000000, 1.000000000000000000 ) ) ;
#5807 = AXIS2_PLACEMENT_3D ( 'NONE', #14922, #54557, #75716 ) ;
#5808 = CARTESIAN_POINT ( 'NONE',  ( -3.750000000000008438, -5.946699141100917352, 21.42187500000000000 ) ) ;
#5809 = VERTEX_POINT ( 'NONE', #76667 ) ;
#5810 = ADVANCED_FACE ( 'NONE', ( #9102 ), #50508, .F. ) ;
#5811 = ORIENTED_EDGE ( 'NONE', *, *, #30990, .T. ) ;
#5812 = CARTESIAN_POINT ( 'NONE',  ( -12.39547112818838670, -5.471508081941601098, 34.59228464037088457 ) ) ;
#5813 = EDGE_CURVE ( 'NONE', #50015, #66615, #59554, .T. ) ;
#5814 = CARTESIAN_POINT ( 'NONE',  ( -4.153846153846273204, -12.46129190930018460, 30.37095296980731973 ) ) ;
#5815 = CARTESIAN_POINT ( 'NONE',  ( -10.61538461538461320, -2.292212530054420494, 30.41441678777542634 ) ) ;
#5816 = DIRECTION ( 'NONE',  ( -1.000000000000000000, -0.000000000000000000, 0.000000000000000000 ) ) ;
#5817 = CARTESIAN_POINT ( 'NONE',  ( -7.716108790234073034, -2.254550872974305342, 29.97347326024527447 ) ) ;
#5818 = CARTESIAN_POINT ( 'NONE',  ( 3.749999999999992006, -5.946699141100872943, 23.14062500000000000 ) ) ;
#5819 = CARTESIAN_POINT ( 'NONE',  ( -8.899378738962465007, -10.31621877034669588, 34.18098118002070152 ) ) ;
#5820 = CARTESIAN_POINT ( 'NONE',  ( 5.869309396889694774, -2.845849958028613624, 32.17971566917920967 ) ) ;
#5821 = CARTESIAN_POINT ( 'NONE',  ( 23.49999999999998934, 1.674711738930281374E-15, 32.75000000000000000 ) ) ;
#5822 = CARTESIAN_POINT ( 'NONE',  ( 13.25392478150507891, -9.929715669179220328, 34.40415004197138416 ) ) ;
#5823 = DIRECTION ( 'NONE',  ( -0.000000000000000000, -0.3420201433256694901, -0.9396926207859082059 ) ) ;
#5824 = CARTESIAN_POINT ( 'NONE',  ( 13.31853197365950514, -4.098570777380720287, 33.41473453929634729 ) ) ;
#5825 = DIRECTION ( 'NONE',  ( -0.000000000000000000, -0.000000000000000000, -1.000000000000000000 ) ) ;
#5826 = CARTESIAN_POINT ( 'NONE',  ( 12.94230769230769340, -4.000000000000000000, 29.75000000000000355 ) ) ;
#5827 = AXIS2_PLACEMENT_3D ( 'NONE', #12108, #39134, #39587 ) ;
#5828 = CARTESIAN_POINT ( 'NONE',  ( -15.23076923076935074, -10.21337939537710326, 33.94971097300076224 ) ) ;
#5829 = ADVANCED_FACE ( 'NONE', ( #69902 ), #56826, .F. ) ;
#5830 = VERTEX_POINT ( 'NONE', #42887 ) ;
#5831 = CARTESIAN_POINT ( 'NONE',  ( -7.846153846153844924, -12.78798330534102767, 29.49999999999997868 ) ) ;
#5832 = CARTESIAN_POINT ( 'NONE',  ( 18.22301284409339672, -4.762714258010882773, 34.23016756924214832 ) ) ;
#5833 = CARTESIAN_POINT ( 'NONE',  ( -1.200186371490524317, -10.22469193450124791, 15.11124329374151287 ) ) ;
#5834 = AXIS2_PLACEMENT_3D ( 'NONE', #56873, #84368, #72487 ) ;
#5835 = AXIS2_PLACEMENT_3D ( 'NONE', #84338, #84781, #85215 ) ;
#5836 = CARTESIAN_POINT ( 'NONE',  ( -18.25000000000000000, -2.499999999999999556, 29.75000000000000355 ) ) ;
#5837 = FACE_OUTER_BOUND ( 'NONE', #87459, .T. ) ;
#5838 = EDGE_CURVE ( 'NONE', #23792, #13144, #35689, .T. ) ;
#5839 = CARTESIAN_POINT ( 'NONE',  ( -1.384615384615383471, -13.88283147151868846, 33.14645433367849847 ) ) ;
#5841 = ORIENTED_EDGE ( 'NONE', *, *, #66428, .T. ) ;
#5840 = CARTESIAN_POINT ( 'NONE',  ( 10.68155122197626028, -7.250054591869670162, 34.99404684341514127 ) ) ;
#5842 = CARTESIAN_POINT ( 'NONE',  ( -1.139087296526025250, -4.750000000000006217, 22.82812500000000355 ) ) ;
#5843 = CARTESIAN_POINT ( 'NONE',  ( 17.07692307692307665, -8.810774026931790459, 35.74407628777942847 ) ) ;
#5844 = CIRCLE ( 'NONE', #71980, 0.2500000000000002220 ) ;
#5845 = EDGE_LOOP ( 'NONE', ( #59574, #30913, #65334, #72865 ) ) ;
#5846 = CARTESIAN_POINT ( 'NONE',  ( -5.076923076923197442, -11.94971097300221174, 32.03036669348237098 ) ) ;
#5847 = AXIS2_PLACEMENT_3D ( 'NONE', #71910, #10220, #36364 ) ;
#5848 = CARTESIAN_POINT ( 'NONE',  ( 18.13079180782478872, -8.999086150933472084, 34.52020707165672064 ) ) ;
#5849 = AXIS2_PLACEMENT_3D ( 'NONE', #41814, #68386, #62069 ) ;
#5850 = ORIENTED_EDGE ( 'NONE', *, *, #87416, .F. ) ;
#5851 = CARTESIAN_POINT ( 'NONE',  ( 3.007842271862381622, -4.762599654559228846, 34.23009711892697737 ) ) ;
#5852 = EDGE_CURVE ( 'NONE', #8365, #47121, #67056, .T. ) ;
#5853 = CARTESIAN_POINT ( 'NONE',  ( -16.21917016665046418, -7.749976730030849303, 34.74374725381503737 ) ) ;
#5854 = FACE_OUTER_BOUND ( 'NONE', #63365, .T. ) ;
#5855 = ORIENTED_EDGE ( 'NONE', *, *, #84982, .T. ) ;
#5856 = VERTEX_POINT ( 'NONE', #56394 ) ;
#5857 = EDGE_CURVE ( 'NONE', #42328, #65392, #69119, .T. ) ;
#5858 = ORIENTED_EDGE ( 'NONE', *, *, #46650, .T. ) ;
#5859 = DIRECTION ( 'NONE',  ( -0.000000000000000000, 0.8660254037844399289, -0.4999999999999980016 ) ) ;
#5860 = CARTESIAN_POINT ( 'NONE',  ( 15.90384615384615330, -2.499999999999998668, 29.75000000000000355 ) ) ;
#5861 = LINE ( 'NONE', #25683, #8194 ) ;
#5862 = CARTESIAN_POINT ( 'NONE',  ( -15.45369618967607828, -2.308479472611653094, 30.53278059502174457 ) ) ;
#5863 = DIRECTION ( 'NONE',  ( 1.000000000000000000, 0.000000000000000000, 0.000000000000000000 ) ) ;
#5864 = LINE ( 'NONE', #38758, #24848 ) ;
#5865 = CARTESIAN_POINT ( 'NONE',  ( 12.46153846153833911, -5.219633306517616589, 34.19971097300220464 ) ) ;
#5866 = EDGE_CURVE ( 'NONE', #314, #32867, #23022, .T. ) ;
#5867 = CARTESIAN_POINT ( 'NONE',  ( 16.02315555073584363, -12.62707690430377383, 30.88035979386743435 ) ) ;
#5868 = ORIENTED_EDGE ( 'NONE', *, *, #48932, .T. ) ;
#5870 = EDGE_CURVE ( 'NONE', #40595, #7366, #10870, .T. ) ;
#5869 = EDGE_LOOP ( 'NONE', ( #49224, #63503 ) ) ;
#5871 = VERTEX_POINT ( 'NONE', #44180 ) ;
#5873 = ORIENTED_EDGE ( 'NONE', *, *, #22145, .T. ) ;
#5872 = DIRECTION ( 'NONE',  ( 0.000000000000000000, 1.000000000000000000, 0.000000000000000000 ) ) ;
#5874 = AXIS2_PLACEMENT_3D ( 'NONE', #8938, #3045, #70634 ) ;
#5875 = DIRECTION ( 'NONE',  ( 0.000000000000000000, -6.938893903907222067E-15, 1.000000000000000000 ) ) ;
#5876 = CARTESIAN_POINT ( 'NONE',  ( 11.78840705680967993, -12.22109172314383052, 31.39792113162168263 ) ) ;
#5877 = VERTEX_POINT ( 'NONE', #18072 ) ;
#5878 = EDGE_CURVE ( 'NONE', #70194, #48033, #55245, .T. ) ;
#5879 = CARTESIAN_POINT ( 'NONE',  ( -12.46153846153858424, -11.67786785259630911, 32.92929555188603530 ) ) ;
#5880 = ADVANCED_FACE ( 'NONE', ( #86997 ), #85640, .F. ) ;
#5881 = ORIENTED_EDGE ( 'NONE', *, *, #69342, .F. ) ;
#5882 = CARTESIAN_POINT ( 'NONE',  ( 16.94623161025551639, -9.804603061927743113, 34.18744698557895845 ) ) ;
#5883 = EDGE_LOOP ( 'NONE', ( #61223, #1848, #48991, #19306 ) ) ;
#5884 = LINE ( 'NONE', #67141, #17206 ) ;
#5885 = CARTESIAN_POINT ( 'NONE',  ( 1.607626736228236819, -6.503523203565942268, 34.64991518177335195 ) ) ;
#5886 = CARTESIAN_POINT ( 'NONE',  ( 16.94677586748486320, -2.882441371585227508, 31.66841991370172238 ) ) ;
#5887 = B_SPLINE_CURVE_WITH_KNOTS ( 'NONE', 3,
 ( #65572, #31358, #65125, #3431, #58819, #52507, #44402, #11536, #4326, #86322 ),
 .UNSPECIFIED., .F., .F.,
 ( 4, 2, 2, 2, 4 ),
 ( 0.0007817246256747465219, 0.0009771112852218900684, 0.001172497944769033615, 0.001367884604316177378, 0.001563271263863320925 ),
 .UNSPECIFIED. ) ;
#5888 = FACE_BOUND ( 'NONE', #82907, .T. ) ;
#5889 = CARTESIAN_POINT ( 'NONE',  ( -14.43784027742400156, -9.504002272028875709, 34.60269587691767867 ) ) ;
#5890 = CARTESIAN_POINT ( 'NONE',  ( 8.769230769230645706, -5.941354392335915335, 34.76329471203413846 ) ) ;
#5891 = VECTOR ( 'NONE', #53283, 1000.000000000000227 ) ;
#5892 = VECTOR ( 'NONE', #53076, 1000.000000000000000 ) ;
#5893 = DIRECTION ( 'NONE',  ( 1.000000000000000000, 0.000000000000000000, 0.000000000000000000 ) ) ;
#5894 = CARTESIAN_POINT ( 'NONE',  ( 0.000000000000000000, -11.00000000000000000, 29.75000000000000355 ) ) ;
#5895 = CYLINDRICAL_SURFACE ( 'NONE', #36611, 4.000000000000000000 ) ;
#5896 = CYLINDRICAL_SURFACE ( 'NONE', #13159, 0.2500000000000012212 ) ;
#5897 = CYLINDRICAL_SURFACE ( 'NONE', #87767, 0.2499999999999979738 ) ;
#5898 = EDGE_LOOP ( 'NONE', ( #50989, #37839, #11867, #56311 ) ) ;
#5899 = EDGE_LOOP ( 'NONE', ( #67957, #38556 ) ) ;
#5900 = VECTOR ( 'NONE', #55086, 1000.000000000000000 ) ;
#5902 = DIRECTION ( 'NONE',  ( 0.000000000000000000, 0.8660254037844377084, -0.5000000000000015543 ) ) ;
#5901 = CARTESIAN_POINT ( 'NONE',  ( -3.230769230769229949, -2.538708090699994813, 30.37095296980875503 ) ) ;
#5903 = FACE_OUTER_BOUND ( 'NONE', #86304, .T. ) ;
#5904 = CARTESIAN_POINT ( 'NONE',  ( -13.38461538461538325, -13.57706302396349152, 30.56769352161908060 ) ) ;
#5905 = CYLINDRICAL_SURFACE ( 'NONE', #8415, 8.000000000000000000 ) ;
#5906 = CARTESIAN_POINT ( 'NONE',  ( -2.242436736416282717, -2.892918686051626498, 31.69288490824026638 ) ) ;
#5907 = ORIENTED_EDGE ( 'NONE', *, *, #78893, .F. ) ;
#5908 = CARTESIAN_POINT ( 'NONE',  ( -5.076923076923075762, -5.471508081941601098, 34.59228464037088457 ) ) ;
#5909 = CARTESIAN_POINT ( 'NONE',  ( 14.08476609017615644, -11.24512374952581872, 33.06303171183252942 ) ) ;
#5910 = FACE_OUTER_BOUND ( 'NONE', #87078, .T. ) ;
#5911 = CARTESIAN_POINT ( 'NONE',  ( 6.923076923076924238, -2.499999999999998668, 29.75000000000001421 ) ) ;
#5912 = EDGE_LOOP ( 'NONE', ( #17761, #34670 ) ) ;
#5913 = ORIENTED_EDGE ( 'NONE', *, *, #36418, .F. ) ;
#5914 = EDGE_CURVE ( 'NONE', #34591, #52302, #64905, .T. ) ;
#5915 = PRODUCT_CONTEXT ( 'NONE', #31413, 'mechanical' ) ;
#5916 = ORIENTED_EDGE ( 'NONE', *, *, #58604, .T. ) ;
#5917 = CARTESIAN_POINT ( 'NONE',  ( 0.3310617534219970626, -7.276988635370452485, 34.74523720219453793 ) ) ;
#5919 = VERTEX_POINT ( 'NONE', #45533 ) ;
#5918 = ADVANCED_FACE ( 'NONE', ( #52287 ), #85201, .F. ) ;
#5920 = LINE ( 'NONE', #88358, #39585 ) ;
#5921 = CARTESIAN_POINT ( 'NONE',  ( 14.43821774592595553, -5.915461855592780260, 34.75538340440931506 ) ) ;
#5922 = CARTESIAN_POINT ( 'NONE',  ( 3.230769230769108269, -10.33852847137269571, 34.16647553114546554 ) ) ;
#5923 = DIRECTION ( 'NONE',  ( -0.000000000000000000, -0.7660444431189791237, -0.6427876096865379196 ) ) ;
#5924 = CARTESIAN_POINT ( 'NONE',  ( 8.546304551714619890, -6.503392248772476236, 34.64988816332204635 ) ) ;
#5925 = ORIENTED_EDGE ( 'NONE', *, *, #55195, .F. ) ;
#5926 = EDGE_CURVE ( 'NONE', #74684, #52843, #75658, .T. ) ;
#5927 = CARTESIAN_POINT ( 'NONE',  ( -15.00775638667583500, -2.523321265292115534, 31.42251411153756990 ) ) ;
#5929 = VERTEX_POINT ( 'NONE', #52728 ) ;
#5928 = CARTESIAN_POINT ( 'NONE',  ( -15.48079245499068435, -12.07920672191015221, 32.31858351112116168 ) ) ;
#5930 = DIRECTION ( 'NONE',  ( -0.000000000000000000, -0.8660254037844399289, -0.4999999999999980016 ) ) ;
#5931 = CARTESIAN_POINT ( 'NONE',  ( -2.531177251416254936, -9.331801661448606566, 34.40259984581193464 ) ) ;
#5933 = B_SPLINE_CURVE_WITH_KNOTS ( 'NONE', 3,
 ( #5267, #5708, #6155, #12906, #67854, #88156, #19229, #75065, #80491, #60644 ),
 .UNSPECIFIED., .F., .F.,
 ( 4, 2, 2, 2, 4 ),
 ( 0.0007817359430256215491, 0.0009771253907249856981, 0.001172514838424349847, 0.001367904286123713779, 0.001563293733823077928 ),
 .UNSPECIFIED. ) ;
#5932 = CARTESIAN_POINT ( 'NONE',  ( -11.53846153846166089, -11.06231777344772027, 33.60647404775119895 ) ) ;
#5934 = AXIS2_PLACEMENT_3D ( 'NONE', #51338, #37863, #45051 ) ;
#5935 = DIRECTION ( 'NONE',  ( -0.000000000000000000, 1.000000000000000000, 3.491481338843133355E-15 ) ) ;
#5936 = FACE_OUTER_BOUND ( 'NONE', #18233, .T. ) ;
#5937 = CARTESIAN_POINT ( 'NONE',  ( -8.519285359852727169, -9.357781135181031829, 34.66075350412533851 ) ) ;
#5938 = B_SPLINE_CURVE_WITH_KNOTS ( 'NONE', 3,
 ( #12825, #33097, #79956, #40310, #67772, #45268 ),
 .UNSPECIFIED., .F., .F.,
 ( 4, 2, 4 ),
 ( 0.0003909512603273932732, 0.0005862562993132219456, 0.0007815613382990506180 ),
 .UNSPECIFIED. ) ;
#5939 = CARTESIAN_POINT ( 'NONE',  ( 12.71148397988660328, -11.37275283266504111, 32.91324779482534524 ) ) ;
#5940 = AXIS2_PLACEMENT_3D ( 'NONE', #42833, #9476, #2262 ) ;
#5941 = EDGE_CURVE ( 'NONE', #50855, #66461, #31123, .T. ) ;
#5942 = CARTESIAN_POINT ( 'NONE',  ( -2.749999999999999112, -7.438900925035484057, 20.34561829374151287 ) ) ;
#5943 = ORIENTED_EDGE ( 'NONE', *, *, #37165, .F. ) ;
#5944 = B_SPLINE_CURVE_WITH_KNOTS ( 'NONE', 3,
 ( #29509, #76809, #8796, #36267, #84459, #49764, #1589, #2457, #22734, #51076 ),
 .UNSPECIFIED., .F., .F.,
 ( 4, 2, 2, 2, 4 ),
 ( 0.000000000000000000, 0.0001954311564186861968, 0.0003908623128373723936, 0.0005862934692560585904, 0.0007817246256747447872 ),
 .UNSPECIFIED. ) ;
#5945 = CARTESIAN_POINT ( 'NONE',  ( -6.989159302437059296, -10.67929555188718460, 33.92786785259543336 ) ) ;
#5946 = CARTESIAN_POINT ( 'NONE',  ( -1.161835715637316913, -3.563462043263030399, 33.22394488606062879 ) ) ;
#5947 = B_SPLINE_CURVE_WITH_KNOTS ( 'NONE', 3,
 ( #55882, #83369, #15353, #16659, #63072, #8151, #84263, #15796, #71600, #84706 ),
 .UNSPECIFIED., .F., .F.,
 ( 4, 2, 2, 2, 4 ),
 ( 0.0007817246256747440282, 0.0009771112852218863821, 0.001172497944769028844, 0.001367884604316171307, 0.001563271263863313769 ),
 .UNSPECIFIED. ) ;
#5948 = EDGE_CURVE ( 'NONE', #59502, #20820, #9525, .T. ) ;
#5949 = ORIENTED_EDGE ( 'NONE', *, *, #3036, .F. ) ;
#5950 = CARTESIAN_POINT ( 'NONE',  ( -1.384615384615383471, -11.69971097300155272, 32.46337939537588113 ) ) ;
#5951 = CARTESIAN_POINT ( 'NONE',  ( -3.230769230769229949, -5.557115091759785130, 34.35708131394839171 ) ) ;
#5952 = LINE ( 'NONE', #26658, #24339 ) ;
#5953 = EDGE_CURVE ( 'NONE', #8955, #37810, #11217, .T. ) ;
#5954 = CARTESIAN_POINT ( 'NONE',  ( 6.923076923076924238, -5.557115091759785130, 34.35708131394839171 ) ) ;
#5955 = CARTESIAN_POINT ( 'NONE',  ( 17.93391762063986761, -2.486705287966279432, 31.30864560766543647 ) ) ;
#5956 = ORIENTED_EDGE ( 'NONE', *, *, #81788, .F. ) ;
#5957 = CYLINDRICAL_SURFACE ( 'NONE', #64990, 0.2499999999999995559 ) ;
#5958 = AXIS2_PLACEMENT_3D ( 'NONE', #65402, #51413, #65837 ) ;
#5959 = FACE_OUTER_BOUND ( 'NONE', #2351, .T. ) ;
#5960 = CARTESIAN_POINT ( 'NONE',  ( 18.13079044096694759, -12.35292014791297710, 31.75344720912887198 ) ) ;
#5961 = VERTEX_POINT ( 'NONE', #72560 ) ;
#5962 = CARTESIAN_POINT ( 'NONE',  ( -17.01166793741023042, -12.16647553114626490, 32.15551576947920864 ) ) ;
#5963 = EDGE_CURVE ( 'NONE', #44313, #87990, #31577, .T. ) ;
#5964 = ORIENTED_EDGE ( 'NONE', *, *, #13142, .T. ) ;
#5965 = CARTESIAN_POINT ( 'NONE',  ( 13.60762673622823549, -3.587049720035815348, 32.86302985866382897 ) ) ;
#5966 = CARTESIAN_POINT ( 'NONE',  ( 15.23076923076923173, -1.790695186598648903, 34.54067556320373455 ) ) ;
#5967 = VERTEX_POINT ( 'NONE', #75239 ) ;
#5968 = ADVANCED_FACE ( 'NONE', ( #39238 ), #46424, .F. ) ;
#5969 = DIRECTION ( 'NONE',  ( -1.000000000000000000, 0.000000000000000000, 0.000000000000000000 ) ) ;
#5970 = CARTESIAN_POINT ( 'NONE',  ( -6.130147969731694069, -2.373036134822904319, 30.88089517874952250 ) ) ;
#5971 = CARTESIAN_POINT ( 'NONE',  ( -9.942284423250045577, -2.564618984488975073, 30.55390908950641915 ) ) ;
#5972 = VECTOR ( 'NONE', #50658, 1000.000000000000000 ) ;
#5973 = B_SPLINE_CURVE_WITH_KNOTS ( 'NONE', 3,
 ( #69316, #1288, #63873, #63431, #57119, #8058, #84172, #15259, #71077, #76512 ),
 .UNSPECIFIED., .F., .F.,
 ( 4, 2, 2, 2, 4 ),
 ( 0.0007817359430256372700, 0.0009771253907250052138, 0.001172514838424373266, 0.001367904286123741101, 0.001563293733823109153 ),
 .UNSPECIFIED. ) ;
#5974 = B_SPLINE_CURVE_WITH_KNOTS ( 'NONE', 3,
 ( #6335, #61697, #54054, #75235, #61250, #47303, #26152, #60820, #74793, #34686 ),
 .UNSPECIFIED., .F., .F.,
 ( 4, 2, 2, 2, 4 ),
 ( 0.0007817246256747453293, 0.0009771112852218889842, 0.001172497944769032531, 0.001367884604316176294, 0.001563271263863319840 ),
 .UNSPECIFIED. ) ;
#5975 = CARTESIAN_POINT ( 'NONE',  ( -14.30769230769230660, -4.786620604624113540, 33.94971097300155094 ) ) ;
#5976 = CARTESIAN_POINT ( 'NONE',  ( -1.514763354347082647, -11.04286588640298561, 33.62463336215343901 ) ) ;
#5977 = B_SPLINE_CURVE_WITH_KNOTS ( 'NONE', 3,
 ( #86025, #72499, #58095, #78812, #70739, #57220, #10808, #17112, #44567, #56769 ),
 .UNSPECIFIED., .F., .F.,
 ( 4, 2, 2, 2, 4 ),
 ( 0.0007817359430256253438, 0.0009771253907249898181, 0.001172514838424354401, 0.001367904286123718983, 0.001563293733823083566 ),
 .UNSPECIFIED. ) ;
#5978 = EDGE_CURVE ( 'NONE', #67015, #76205, #39689, .T. ) ;
#5979 = ORIENTED_EDGE ( 'NONE', *, *, #25373, .F. ) ;
#5980 = EDGE_CURVE ( 'NONE', #81438, #38465, #26157, .T. ) ;
#5981 = FACE_BOUND ( 'NONE', #40325, .T. ) ;
#5982 = ORIENTED_EDGE ( 'NONE', *, *, #36049, .T. ) ;
#5983 = CARTESIAN_POINT ( 'NONE',  ( -9.692307692307691624, -2.499999999999998668, 29.75000000000001421 ) ) ;
#5984 = DIRECTION ( 'NONE',  ( 0.000000000000000000, 0.000000000000000000, 1.000000000000000000 ) ) ;
#5985 = CARTESIAN_POINT ( 'NONE',  ( -13.38461538461538325, -13.88283147151868846, 33.14645433367849847 ) ) ;
#5986 = LINE ( 'NONE', #40217, #62207 ) ;
#5987 = CARTESIAN_POINT ( 'NONE',  ( -11.28851602011339672, -2.587454068350147018, 30.68340429815432202 ) ) ;
#5988 = EDGE_CURVE ( 'NONE', #68238, #35285, #74469, .T. ) ;
#5989 = ORIENTED_EDGE ( 'NONE', *, *, #22457, .T. ) ;
#5990 = VERTEX_POINT ( 'NONE', #18959 ) ;
#5991 = VERTEX_POINT ( 'NONE', #87433 ) ;
#5992 = VECTOR ( 'NONE', #26273, 1000.000000000000227 ) ;
#5993 = EDGE_CURVE ( 'NONE', #88630, #88864, #8984, .T. ) ;
#5995 = EDGE_LOOP ( 'NONE', ( #73917, #38811 ) ) ;
#5994 = EDGE_CURVE ( 'NONE', #11924, #84921, #61611, .T. ) ;
#5996 = CARTESIAN_POINT ( 'NONE',  ( 2.241608896736428047, -4.786620604624113540, 33.94971097300155805 ) ) ;
#5997 = CARTESIAN_POINT ( 'NONE',  ( -6.130147209438218781, -12.45813303252208648, 30.39737893381572675 ) ) ;
#5998 = VECTOR ( 'NONE', #76844, 1000.000000000000000 ) ;
#5999 = CARTESIAN_POINT ( 'NONE',  ( 15.23076923076911093, -5.219633306517616589, 34.19971097300220464 ) ) ;
#6000 = ADVANCED_FACE ( 'NONE', ( #18517 ), #40133, .F. ) ;
#6001 = CARTESIAN_POINT ( 'NONE',  ( 6.222779541268411485, -12.24180327182771855, 31.33663988360758168 ) ) ;
#6002 = CARTESIAN_POINT ( 'NONE',  ( 1.384615384615386802, -8.564572088678739092, 35.78748833219616898 ) ) ;
#6003 = CYLINDRICAL_SURFACE ( 'NONE', #69535, 0.2499999999999997502 ) ;
#6004 = CYLINDRICAL_SURFACE ( 'NONE', #72537, 0.2499999999999979738 ) ;
#6005 = CARTESIAN_POINT ( 'NONE',  ( -4.854143407945010757, -11.60474049983371003, 33.02348890104160262 ) ) ;
#6006 = ORIENTED_EDGE ( 'NONE', *, *, #69682, .T. ) ;
#6007 = VERTEX_POINT ( 'NONE', #5890 ) ;
#6008 = EDGE_LOOP ( 'NONE', ( #11268, #77406 ) ) ;
#6010 = VERTEX_POINT ( 'NONE', #26600 ) ;
#6009 = CARTESIAN_POINT ( 'NONE',  ( -11.78848477575450282, -12.43535235679832596, 30.55408501211184813 ) ) ;
#6012 = CARTESIAN_POINT ( 'NONE',  ( -5.776988648387149539, -3.587049720035815348, 32.86302985866382897 ) ) ;
#6011 = CARTESIAN_POINT ( 'NONE',  ( -3.100243792535585907, -10.31582465632705237, 34.18122507451815295 ) ) ;
#6013 = CARTESIAN_POINT ( 'NONE',  ( -13.38461538461550582, -8.613356846316285953, 34.62446782046622218 ) ) ;
#6014 = CARTESIAN_POINT ( 'NONE',  ( 27.00000000000000000, -1.249999999999999112, 32.75000000000000000 ) ) ;
#6015 = FACE_BOUND ( 'NONE', #82561, .T. ) ;
#6016 = VERTEX_POINT ( 'NONE', #41007 ) ;
#6017 = CYLINDRICAL_SURFACE ( 'NONE', #63395, 0.2500000000000009437 ) ;
#6018 = CARTESIAN_POINT ( 'NONE',  ( -3.296039231325550212, -3.643525952247789412, 33.31231777344662959 ) ) ;
#6019 = EDGE_LOOP ( 'NONE', ( #27780, #74664, #15185, #9682 ) ) ;
#6020 = CARTESIAN_POINT ( 'NONE',  ( 17.32697749683652688, -5.642605341092955307, 34.66089969410670335 ) ) ;
#6021 = ORIENTED_EDGE ( 'NONE', *, *, #44175, .T. ) ;
#6022 = FACE_BOUND ( 'NONE', #13822, .T. ) ;
#6024 = VECTOR ( 'NONE', #83112, 1000.000000000000000 ) ;
#6023 = CARTESIAN_POINT ( 'NONE',  ( -10.61538461538461320, -2.833524468853757305, 32.15551576947925838 ) ) ;
#6025 = CARTESIAN_POINT ( 'NONE',  ( -24.00000000000000000, 9.000000000000024869, 29.25000000000000000 ) ) ;
#6026 = EDGE_LOOP ( 'NONE', ( #81850, #78827 ) ) ;
#6027 = LINE ( 'NONE', #61835, #57855 ) ;
#6028 = CARTESIAN_POINT ( 'NONE',  ( -12.52762084089859584, -11.91647553114624181, 32.58852847137148245 ) ) ;
#6029 = CYLINDRICAL_SURFACE ( 'NONE', #52230, 0.2500000000000008882 ) ;
#6030 = ORIENTED_EDGE ( 'NONE', *, *, #46375, .T. ) ;
#6031 = CARTESIAN_POINT ( 'NONE',  ( 6.673100192134570285, -9.943427161483782584, 34.11278801902876978 ) ) ;
#6032 = CARTESIAN_POINT ( 'NONE',  ( -7.715363405186894674, -8.191423895709840863, 34.95447573519442130 ) ) ;
#6033 = CARTESIAN_POINT ( 'NONE',  ( 12.59233026936325039, -6.413143153341454017, 34.63066358083362672 ) ) ;
#6034 = CARTESIAN_POINT ( 'NONE',  ( -8.096130577096197101, -2.779195860258146578, 31.39871582349836032 ) ) ;
#6035 = ORIENTED_EDGE ( 'NONE', *, *, #74689, .T. ) ;
#6036 = AXIS2_PLACEMENT_3D ( 'NONE', #16575, #79619, #58435 ) ;
#6037 = CARTESIAN_POINT ( 'NONE',  ( 4.826923076923076650, -7.500000000000001776, 35.04278698407183867 ) ) ;
#6038 = CARTESIAN_POINT ( 'NONE',  ( 5.076923076923075762, -1.242168528481310874, 33.36296068462461051 ) ) ;
#6039 = EDGE_LOOP ( 'NONE', ( #23897, #26384, #32819, #20124, #6320 ) ) ;
#6040 = CARTESIAN_POINT ( 'NONE',  ( 18.24994551834813805, -6.696923467548659303, 34.68552623307873972 ) ) ;
#6041 = CARTESIAN_POINT ( 'NONE',  ( 22.00000000000000711, 9.999999999999971578, 10.00000000000000178 ) ) ;
#6042 = CARTESIAN_POINT ( 'NONE',  ( 0.5267936010512995759, -11.06231777344671130, 33.60647404775212976 ) ) ;
#6043 = FACE_OUTER_BOUND ( 'NONE', #22470, .T. ) ;
#6044 = CARTESIAN_POINT ( 'NONE',  ( -15.90390063549801347, -4.336752205174650321, 33.62275283266504289 ) ) ;
#6045 = CARTESIAN_POINT ( 'NONE',  ( 15.10007862765892206, -5.496505350115501010, 34.60290016733514307 ) ) ;
#6047 = CARTESIAN_POINT ( 'NONE',  ( -2.307692307691999289, -2.506253911140615021, 30.00000000000323297 ) ) ;
#6046 = CARTESIAN_POINT ( 'NONE',  ( 0.7114838709165038910, -11.56426240980093567, 33.07394671870546432 ) ) ;
#6048 = CARTESIAN_POINT ( 'NONE',  ( 27.00000000000000000, -9.000000000000001776, 2.291744775602387568E-15 ) ) ;
#6049 = CARTESIAN_POINT ( 'NONE',  ( 1.944543648263018731, -9.444543648262994751, 20.87500000000000000 ) ) ;
#6050 = VERTEX_POINT ( 'NONE', #81556 ) ;
#6051 = CARTESIAN_POINT ( 'NONE',  ( 4.853996118016224770, -6.459968553980839800, 34.89616026154728701 ) ) ;
#6052 = VERTEX_POINT ( 'NONE', #13088 ) ;
#6053 = ORIENTED_EDGE ( 'NONE', *, *, #22052, .F. ) ;
#6054 = CARTESIAN_POINT ( 'NONE',  ( 3.230769230769231726, -2.708943851104267164, 35.45975837776705220 ) ) ;
#6055 = VERTEX_POINT ( 'NONE', #19842 ) ;
#6056 = CARTESIAN_POINT ( 'NONE',  ( -1.384615384615506484, -2.657715359629662544, 31.77849191805970364 ) ) ;
#6057 = CARTESIAN_POINT ( 'NONE',  ( 1.139087296525997273, -4.749999999999992895, 19.23437500000000355 ) ) ;
#6058 = CARTESIAN_POINT ( 'NONE',  ( -7.384615384615385025, -3.499999999999999556, 29.75000000000000355 ) ) ;
#6059 = CARTESIAN_POINT ( 'NONE',  ( 5.869308533332445066, -11.18331474514187995, 33.13161551792790505 ) ) ;
#6060 = CARTESIAN_POINT ( 'NONE',  ( -3.099977422944443006, -8.999086150933472084, 34.52020707165672064 ) ) ;
#6061 = DIRECTION ( 'NONE',  ( -0.000000000000000000, -0.6427876096865404731, -0.7660444431189770143 ) ) ;
#6062 = LINE ( 'NONE', #88065, #81908 ) ;
#6064 = ADVANCED_FACE ( 'NONE', ( #45974 ), #47307, .T. ) ;
#6063 = CARTESIAN_POINT ( 'NONE',  ( -11.60454494941741999, -4.786620604624113540, 33.94971097300155805 ) ) ;
#6065 = CIRCLE ( 'NONE', #33378, 5.000000000000000888 ) ;
#6066 = CARTESIAN_POINT ( 'NONE',  ( -1.553300858899125059, -3.750000000000009326, 24.07812500000000355 ) ) ;
#6067 = LINE ( 'NONE', #68207, #37670 ) ;
#6068 = LINE ( 'NONE', #88069, #1715 ) ;
#6069 = CIRCLE ( 'NONE', #42074, 8.000000000000000000 ) ;
#6070 = CARTESIAN_POINT ( 'NONE',  ( 5.933917620639865831, -3.322132147404559976, 32.92929555188719348 ) ) ;
#6071 = ORIENTED_EDGE ( 'NONE', *, *, #67894, .T. ) ;
#6072 = VERTEX_POINT ( 'NONE', #13526 ) ;
#6073 = CARTESIAN_POINT ( 'NONE',  ( -9.692307692307691624, -3.513871655860378418, 32.76840700105978499 ) ) ;
#6074 = CARTESIAN_POINT ( 'NONE',  ( 15.29602437028206907, -12.16647553114626490, 32.15551576947920864 ) ) ;
#6075 = CARTESIAN_POINT ( 'NONE',  ( -6.792551484843279752, -12.15418822224088657, 32.17964115625579069 ) ) ;
#6076 = CARTESIAN_POINT ( 'NONE',  ( -15.90379184220783948, -12.41262288849542017, 30.68299917996395010 ) ) ;
#6077 = ADVANCED_FACE ( 'NONE', ( #32464 ), #25716, .F. ) ;
#6078 = CARTESIAN_POINT ( 'NONE',  ( -24.00000000000000000, -5.499999999999981348, 27.25000000000000000 ) ) ;
#6079 = CARTESIAN_POINT ( 'NONE',  ( 24.00000000000000000, -9.499999999999982236, 27.74999999999999645 ) ) ;
#6080 = DIRECTION ( 'NONE',  ( 1.000000000000000000, 0.000000000000000000, 0.000000000000000000 ) ) ;
#6081 = ADVANCED_FACE ( 'NONE', ( #82000 ), #20293, .F. ) ;
#6082 = ORIENTED_EDGE ( 'NONE', *, *, #88861, .F. ) ;
#6083 = CARTESIAN_POINT ( 'NONE',  ( 17.07692307692295586, -3.835265460704628815, 33.15142922262033665 ) ) ;
#6084 = ORIENTED_EDGE ( 'NONE', *, *, #66703, .T. ) ;
#6085 = ORIENTED_EDGE ( 'NONE', *, *, #46754, .F. ) ;
#6086 = AXIS2_PLACEMENT_3D ( 'NONE', #32389, #59414, #73374 ) ;
#6087 = CARTESIAN_POINT ( 'NONE',  ( 7.846153846153846700, -13.57706302396349152, 30.56769352161908060 ) ) ;
#6088 = DIRECTION ( 'NONE',  ( -0.000000000000000000, 0.6427876096865404731, -0.7660444431189771253 ) ) ;
#6089 = CARTESIAN_POINT ( 'NONE',  ( 11.66925334628632527, -10.54018710029568595, 33.71981072465678864 ) ) ;
#6090 = CARTESIAN_POINT ( 'NONE',  ( 4.087763774486018242, -6.343179335718451384, 34.87096338111212646 ) ) ;
#6091 = CARTESIAN_POINT ( 'NONE',  ( 11.53846153846153832, -13.75783147151868846, 33.36296068462461051 ) ) ;
#6092 = AXIS2_PLACEMENT_3D ( 'NONE', #84847, #51012, #50589 ) ;
#6093 = EDGE_LOOP ( 'NONE', ( #1858, #68731, #53604, #13435 ) ) ;
#6094 = EDGE_LOOP ( 'NONE', ( #72840, #31198 ) ) ;
#6095 = B_SPLINE_CURVE_WITH_KNOTS ( 'NONE', 3,
 ( #40375, #19209, #39047, #80018, #33161, #52091, #45333, #53875, #32710, #67391 ),
 .UNSPECIFIED., .F., .F.,
 ( 4, 2, 2, 2, 4 ),
 ( 0.0007817246256747517261, 0.0009771112852218961399, 0.001172497944769040771, 0.001367884604316185401, 0.001563271263863329815 ),
 .UNSPECIFIED. ) ;
#6096 = EDGE_CURVE ( 'NONE', #12296, #43958, #55397, .T. ) ;
#6097 = EDGE_CURVE ( 'NONE', #58471, #7620, #5432, .T. ) ;
#6098 = ORIENTED_EDGE ( 'NONE', *, *, #39397, .F. ) ;
#6099 = ORIENTED_EDGE ( 'NONE', *, *, #77450, .T. ) ;
#6100 = LINE ( 'NONE', #26809, #6987 ) ;
#6101 = CARTESIAN_POINT ( 'NONE',  ( -17.06410256410256565, -7.500000000000000000, 33.75000000000000000 ) ) ;
#6102 = CARTESIAN_POINT ( 'NONE',  ( 14.24242230713598723, -2.657715359629088780, 31.77849191805832874 ) ) ;
#6103 = CARTESIAN_POINT ( 'NONE',  ( 16.28437185560971656, -10.19071101563364401, 33.96452234770658407 ) ) ;
#6104 = CARTESIAN_POINT ( 'NONE',  ( -16.15384615384615330, -3.322132147404559976, 32.92929555188717927 ) ) ;
#6105 = CARTESIAN_POINT ( 'NONE',  ( 14.30769230769231015, -12.37446782046654192, 30.86335684631486131 ) ) ;
#6106 = ORIENTED_EDGE ( 'NONE', *, *, #20185, .T. ) ;
#6107 = ORIENTED_EDGE ( 'NONE', *, *, #34999, .F. ) ;
#6108 = EDGE_LOOP ( 'NONE', ( #82918, #3739, #85509, #73785 ) ) ;
#6110 = EDGE_LOOP ( 'NONE', ( #57144, #47599, #41354, #18356 ) ) ;
#6109 = CARTESIAN_POINT ( 'NONE',  ( 17.14299142792551578, -12.37446782046654192, 30.86335684631486842 ) ) ;
#6111 = DIRECTION ( 'NONE',  ( 0.000000000000000000, 0.8660254037844377084, 0.5000000000000015543 ) ) ;
#6112 = PLANE ( 'NONE',  #43188 ) ;
#6113 = AXIS2_PLACEMENT_3D ( 'NONE', #20540, #35840, #75932 ) ;
#6114 = CARTESIAN_POINT ( 'NONE',  ( 3.750000000000000888, -7.499999999999978684, 21.96875000000000355 ) ) ;
#6115 = VERTEX_POINT ( 'NONE', #8550 ) ;
#6116 = CARTESIAN_POINT ( 'NONE',  ( -2.980823712421087901, -12.43552623307873972, 30.55307653245132826 ) ) ;
#6117 = ORIENTED_EDGE ( 'NONE', *, *, #74086, .F. ) ;
#6118 = CYLINDRICAL_SURFACE ( 'NONE', #41320, 0.2499999999999973355 ) ;
#6119 = FACE_BOUND ( 'NONE', #67032, .T. ) ;
#6120 = CYLINDRICAL_SURFACE ( 'NONE', #66181, 0.2499999999999979738 ) ;
#6121 = CARTESIAN_POINT ( 'NONE',  ( 6.416666666666664298, -7.500000000000000000, 33.75000000000000000 ) ) ;
#6122 = EDGE_LOOP ( 'NONE', ( #15540, #30793, #86613, #83352 ) ) ;
#6123 = CARTESIAN_POINT ( 'NONE',  ( 5.076923076923075762, -13.75783147151868846, 33.36296068462461051 ) ) ;
#6124 = B_SPLINE_CURVE_WITH_KNOTS ( 'NONE', 3,
 ( #4451, #26510, #66609, #53524, #67500, #28156, #59400, #86902, #48872, #53973 ),
 .UNSPECIFIED., .F., .F.,
 ( 4, 2, 2, 2, 4 ),
 ( 0.0007817246256747495577, 0.0009771112852218935378, 0.001172497944769037518, 0.001367884604316181715, 0.001563271263863325695 ),
 .UNSPECIFIED. ) ;
#6125 = CARTESIAN_POINT ( 'NONE',  ( 15.23076923076923173, -6.343179335718451384, 34.87096338111211935 ) ) ;
#6126 = EDGE_LOOP ( 'NONE', ( #69156, #87071, #7183, #82131 ) ) ;
#6127 = B_SPLINE_CURVE_WITH_KNOTS ( 'NONE', 3,
 ( #67250, #31691, #58256, #65464, #38443, #79433, #74011, #32132, #59594, #53276 ),
 .UNSPECIFIED., .F., .F.,
 ( 4, 2, 2, 2, 4 ),
 ( 0.000000000000000000, 0.0001954311564186867389, 0.0003908623128373734778, 0.0005862934692560602167, 0.0007817246256747469556 ),
 .UNSPECIFIED. ) ;
#6128 = LINE ( 'NONE', #73713, #57389 ) ;
#6129 = CARTESIAN_POINT ( 'NONE',  ( 1.384615384615386802, -8.120952969808772792, 34.71129190930000163 ) ) ;
#6130 = CARTESIAN_POINT ( 'NONE',  ( -6.923076923076922462, -6.343179335718451384, 34.87096338111211935 ) ) ;
#6131 = DIRECTION ( 'NONE',  ( -0.000000000000000000, -0.7660444431189791237, -0.6427876096865379196 ) ) ;
#6132 = DIRECTION ( 'NONE',  ( -0.000000000000000000, -0.5000000000000009992, -0.8660254037844380415 ) ) ;
#6133 = FACE_BOUND ( 'NONE', #13512, .T. ) ;
#6135 = LINE ( 'NONE', #66044, #12959 ) ;
#6134 = CARTESIAN_POINT ( 'NONE',  ( -10.03846153846153832, -1.926643599941765039, 29.65000000000000213 ) ) ;
#6136 = DIRECTION ( 'NONE',  ( -0.000000000000000000, -0.5000000000000009992, -0.8660254037844380415 ) ) ;
#6138 = CARTESIAN_POINT ( 'NONE',  ( -2.176901866725356349, -8.191423895709840863, 34.95447573519442130 ) ) ;
#6137 = CARTESIAN_POINT ( 'NONE',  ( -5.999999999999998224, -9.780366693483667717, 34.19971097300155094 ) ) ;
#6139 = CARTESIAN_POINT ( 'NONE',  ( 9.019176178608812933, -12.68172785388650681, 30.59649109432439218 ) ) ;
#6140 = CARTESIAN_POINT ( 'NONE',  ( 1.200186371490561621, -10.22469193450123193, 16.95125670625848713 ) ) ;
#6141 = VERTEX_POINT ( 'NONE', #77440 ) ;
#6142 = AXIS2_PLACEMENT_3D ( 'NONE', #69408, #49129, #28415 ) ;
#6143 = CARTESIAN_POINT ( 'NONE',  ( -8.519176457592452678, -5.728107161865378494, 34.42597550085002922 ) ) ;
#6144 = ORIENTED_EDGE ( 'NONE', *, *, #74043, .F. ) ;
#6145 = VECTOR ( 'NONE', #64443, 1000.000000000000227 ) ;
#6146 = CARTESIAN_POINT ( 'NONE',  ( 1.319364394454144440, -2.506253911140460922, 30.00000000000013856 ) ) ;
#6147 = ORIENTED_EDGE ( 'NONE', *, *, #52746, .T. ) ;
#6148 = CARTESIAN_POINT ( 'NONE',  ( 11.97435897435897267, -3.499999999999999556, 29.75000000000000355 ) ) ;
#6149 = CARTESIAN_POINT ( 'NONE',  ( -2.057692307692306599, -7.500000000000001776, 35.04278698407183867 ) ) ;
#6151 = ORIENTED_EDGE ( 'NONE', *, *, #64435, .T. ) ;
#6150 = CARTESIAN_POINT ( 'NONE',  ( -9.692307692307691624, -12.37446782046654192, 30.86335684631486131 ) ) ;
#6152 = CARTESIAN_POINT ( 'NONE',  ( -11.53846153846153655, -2.721908614388771852, 31.22303859784724978 ) ) ;
#6153 = CARTESIAN_POINT ( 'NONE',  ( 0.4615384615384611200, -12.62096338111211580, 30.90682066428153263 ) ) ;
#6154 = CARTESIAN_POINT ( 'NONE',  ( -2.775308065498764964, -6.422011778438537988, 16.17000670625848713 ) ) ;
#6155 = CARTESIAN_POINT ( 'NONE',  ( 4.284371855609718338, -10.88167719472716399, 33.43325721877153711 ) ) ;
#6156 = CARTESIAN_POINT ( 'NONE',  ( 4.946231610255517275, -4.809359713505814149, 33.96456829005828837 ) ) ;
#6157 = CARTESIAN_POINT ( 'NONE',  ( 2.307692307692309264, -2.486705287966279876, 31.30864560766543647 ) ) ;
#6158 = CARTESIAN_POINT ( 'NONE',  ( 1.253924781505077801, -4.684245665217972032, 34.18127051446801090 ) ) ;
#6159 = CYLINDRICAL_SURFACE ( 'NONE', #38239, 0.2500000000000008882 ) ;
#6160 = ADVANCED_FACE ( 'NONE', ( #14412 ), #463, .F. ) ;
#6161 = CARTESIAN_POINT ( 'NONE',  ( 9.561617089197383734, -3.338472653186243644, 32.95098750199972670 ) ) ;
#6162 = EDGE_CURVE ( 'NONE', #59859, #33344, #50909, .T. ) ;
#6163 = CARTESIAN_POINT ( 'NONE',  ( 3.775308065498752086, -6.007798216065404873, 23.39249329374151642 ) ) ;
#6164 = CARTESIAN_POINT ( 'NONE',  ( 9.442307692307693401, -7.566083408709835645, 34.74999999999999289 ) ) ;
#6165 = DIRECTION ( 'NONE',  ( 0.000000000000000000, 0.8660254037844377084, 0.5000000000000015543 ) ) ;
#6166 = ORIENTED_EDGE ( 'NONE', *, *, #15177, .T. ) ;
#6167 = CARTESIAN_POINT ( 'NONE',  ( 7.146503321991712454, -7.630147987733840509, 34.99859428049665411 ) ) ;
#6168 = CARTESIAN_POINT ( 'NONE',  ( -2.608446859217920633, -4.805146000318815780, 19.25186829374151287 ) ) ;
#6169 = ADVANCED_FACE ( 'NONE', ( #43213 ), #36026, .T. ) ;
#6170 = B_SPLINE_CURVE_WITH_KNOTS ( 'NONE', 3,
 ( #16570, #44034, #71074, #10267, #58887, #9382, #71507, #64302, #2603, #51212 ),
 .UNSPECIFIED., .F., .F.,
 ( 4, 2, 2, 2, 4 ),
 ( 0.000000000000000000, 0.0001954311564186870099, 0.0003908623128373740199, 0.0005862934692560609756, 0.0007817246256747480398 ),
 .UNSPECIFIED. ) ;
#6171 = DIRECTION ( 'NONE',  ( -0.000000000000000000, -0.1736481776669307198, -0.9848077530122080203 ) ) ;
#6172 = CARTESIAN_POINT ( 'NONE',  ( 17.29993442853592711, -11.76359900205217457, 32.36225158514719880 ) ) ;
#6173 = VERTEX_POINT ( 'NONE', #84220 ) ;
#6174 = CYLINDRICAL_SURFACE ( 'NONE', #85949, 0.2500000000000002220 ) ;
#6175 = CARTESIAN_POINT ( 'NONE',  ( -17.01085574357299990, -9.058645607665452459, 34.76329471203371924 ) ) ;
#6177 = EDGE_LOOP ( 'NONE', ( #79473, #64330 ) ) ;
#6176 = CARTESIAN_POINT ( 'NONE',  ( 10.36538461538461675, -7.500000000000001776, 35.00000000000000000 ) ) ;
#6178 = FACE_OUTER_BOUND ( 'NONE', #49006, .T. ) ;
#6179 = ADVANCED_FACE ( 'NONE', ( #62587 ), #35578, .F. ) ;
#6180 = B_SPLINE_CURVE_WITH_KNOTS ( 'NONE', 3,
 ( #2727, #84738, #83850, #63553, #23014, #62658, #35654, #8629, #1857, #29341 ),
 .UNSPECIFIED., .F., .F.,
 ( 4, 2, 2, 2, 4 ),
 ( 0.000000000000000000, 0.0001954339857564073388, 0.0003908679715128146777, 0.0005863019572692220165, 0.0007817359430256293554 ),
 .UNSPECIFIED. ) ;
#6181 = CARTESIAN_POINT ( 'NONE',  ( 5.011169648609741678, -7.249945578846651806, 34.99404164642496795 ) ) ;
#6182 = CARTESIAN_POINT ( 'NONE',  ( -12.68502338610279523, -4.988325925672468131, 34.36044203135681130 ) ) ;
#6183 = AXIS2_PLACEMENT_3D ( 'NONE', #60113, #46168, #80856 ) ;
#6184 = ORIENTED_EDGE ( 'NONE', *, *, #63808, .T. ) ;
#6185 = VECTOR ( 'NONE', #83185, 1000.000000000000000 ) ;
#6186 = CARTESIAN_POINT ( 'NONE',  ( 2.177001704581999153, -3.957541250942359756, 33.62499894934981626 ) ) ;
#6187 = CARTESIAN_POINT ( 'NONE',  ( -13.38461538461538325, -11.69971097300155272, 32.46337939537588113 ) ) ;
#6188 = CARTESIAN_POINT ( 'NONE',  ( 2.307692307692309264, -8.164416787775445883, 34.95778746994557906 ) ) ;
#6189 = ADVANCED_FACE ( 'NONE', ( #1780 ), #55837, .F. ) ;
#6190 = EDGE_LOOP ( 'NONE', ( #65881, #37152 ) ) ;
#6191 = ORIENTED_EDGE ( 'NONE', *, *, #10250, .F. ) ;
#6192 = ORIENTED_EDGE ( 'NONE', *, *, #17038, .F. ) ;
#6193 = ORIENTED_EDGE ( 'NONE', *, *, #59556, .F. ) ;
#6194 = CARTESIAN_POINT ( 'NONE',  ( 0.3962680155776852065, -8.613356846314824011, 34.62446782046655613 ) ) ;
#6195 = CARTESIAN_POINT ( 'NONE',  ( 14.24160889673642849, -4.098570777380720287, 33.41473453929634729 ) ) ;
#6196 = CARTESIAN_POINT ( 'NONE',  ( -16.37733107841048508, -3.019605429927187501, 32.48692288466676814 ) ) ;
#6197 = CARTESIAN_POINT ( 'NONE',  ( -19.50000000000000000, -4.000000000000000000, 28.25000000000000000 ) ) ;
#6198 = CARTESIAN_POINT ( 'NONE',  ( -18.25000000000000355, -7.500000000000000000, 35.00000000000000000 ) ) ;
#6199 = EDGE_LOOP ( 'NONE', ( #31704, #58187 ) ) ;
#6200 = EDGE_CURVE ( 'NONE', #3325, #1602, #52997, .T. ) ;
#6201 = EDGE_LOOP ( 'NONE', ( #68130, #39645, #7697, #46448 ) ) ;
#6202 = B_SPLINE_CURVE_WITH_KNOTS ( 'NONE', 3,
 ( #60314, #47243, #20228, #67971, #81049, #39626, #4942, #67083, #40072, #26094 ),
 .UNSPECIFIED., .F., .F.,
 ( 4, 2, 2, 2, 4 ),
 ( 0.000000000000000000, 0.0001954339857564083688, 0.0003908679715128167377, 0.0005863019572692250523, 0.0007817359430256334753 ),
 .UNSPECIFIED. ) ;
#6203 = ORIENTED_EDGE ( 'NONE', *, *, #53113, .F. ) ;
#6206 = ORIENTED_EDGE ( 'NONE', *, *, #22249, .T. ) ;
#6205 = EDGE_CURVE ( 'NONE', #30718, #38938, #16478, .T. ) ;
#6204 = CYLINDRICAL_SURFACE ( 'NONE', #19976, 0.2500000000000008882 ) ;
#6207 = B_SPLINE_CURVE_WITH_KNOTS ( 'NONE', 3,
 ( #68958, #35628, #35175, #945, #34284, #62633, #55443, #82928, #21659, #7266 ),
 .UNSPECIFIED., .F., .F.,
 ( 4, 2, 2, 2, 4 ),
 ( 0.000000000000000000, 0.0001954311564186864949, 0.0003908623128373729899, 0.0005862934692560594577, 0.0007817246256747459798 ),
 .UNSPECIFIED. ) ;
#6208 = CARTESIAN_POINT ( 'NONE',  ( 4.219914504848592429, -5.557115091759786019, 34.35708131394839882 ) ) ;
#6209 = B_SPLINE_CURVE_WITH_KNOTS ( 'NONE', 3,
 ( #28248, #14297, #21492, #6225, #27376, #55280, #54842, #82769, #21044, #53953 ),
 .UNSPECIFIED., .F., .F.,
 ( 4, 2, 2, 2, 4 ),
 ( 0.000000000000000000, 0.0001954311564186867660, 0.0003908623128373735320, 0.0005862934692560603251, 0.0007817246256747470640 ),
 .UNSPECIFIED. ) ;
#6210 = DIRECTION ( 'NONE',  ( 0.000000000000000000, 1.000000000000000000, 0.000000000000000000 ) ) ;
#6211 = AXIS2_PLACEMENT_3D ( 'NONE', #29179, #84561, #8007 ) ;
#6212 = VECTOR ( 'NONE', #16061, 1000.000000000000000 ) ;
#6213 = EDGE_CURVE ( 'NONE', #7402, #39647, #18727, .T. ) ;
#6214 = EDGE_CURVE ( 'NONE', #7653, #37364, #52042, .T. ) ;
#6215 = DIRECTION ( 'NONE',  ( 1.000000000000000000, 0.000000000000000000, 0.000000000000000000 ) ) ;
#6216 = CARTESIAN_POINT ( 'NONE',  ( 0.000000000000000000, -11.00000000000000000, 29.75000000000000355 ) ) ;
#6217 = ORIENTED_EDGE ( 'NONE', *, *, #7602, .T. ) ;
#6218 = VECTOR ( 'NONE', #33444, 1000.000000000000000 ) ;
#6219 = ORIENTED_EDGE ( 'NONE', *, *, #31118, .F. ) ;
#6220 = ORIENTED_EDGE ( 'NONE', *, *, #1802, .T. ) ;
#6221 = LINE ( 'NONE', #25594, #20237 ) ;
#6223 = ORIENTED_EDGE ( 'NONE', *, *, #72660, .F. ) ;
#6222 = DIRECTION ( 'NONE',  ( -0.000000000000000000, 0.8660254037844399289, -0.4999999999999980016 ) ) ;
#6224 = CARTESIAN_POINT ( 'NONE',  ( 9.627037246346915822, -11.94971097300153140, 32.03036669348370680 ) ) ;
#6225 = CARTESIAN_POINT ( 'NONE',  ( -0.6844654204453101132, -6.459968553980839800, 34.89616026154728701 ) ) ;
#6226 = ORIENTED_EDGE ( 'NONE', *, *, #64141, .F. ) ;
#6227 = CYLINDRICAL_SURFACE ( 'NONE', #79111, 0.2499999999999995559 ) ;
#6228 = CARTESIAN_POINT ( 'NONE',  ( 16.40390046548447245, -3.627508038966690496, 32.91356715214248396 ) ) ;
#6229 = CARTESIAN_POINT ( 'NONE',  ( 4.153846153846154188, -2.721908614388771852, 31.22303859784724978 ) ) ;
#6230 = FACE_BOUND ( 'NONE', #4445, .T. ) ;
#6232 = B_SPLINE_CURVE_WITH_KNOTS ( 'NONE', 3,
 ( #63713, #28612, #56075, #83569, #76802, #42571, #56521, #70031, #43009, #8341 ),
 .UNSPECIFIED., .F., .F.,
 ( 4, 2, 2, 2, 4 ),
 ( 0.0007817246336856289524, 0.0009771112958940101571, 0.001172497958102391253, 0.001367884620310772350, 0.001563271282519153446 ),
 .UNSPECIFIED. ) ;
#6231 = CARTESIAN_POINT ( 'NONE',  ( -17.74994568836168440, -8.303483539816726378, 34.68545999027711702 ) ) ;
#6233 = CARTESIAN_POINT ( 'NONE',  ( -1.161604033002534120, -11.76359900205217457, 32.36225158514719880 ) ) ;
#6234 = CARTESIAN_POINT ( 'NONE',  ( 12.23861150263161157, -6.459968553980841577, 34.89616026154728701 ) ) ;
#6236 = CARTESIAN_POINT ( 'NONE',  ( -0.5922299282060162762, -12.11776431015575994, 31.66791131148498906 ) ) ;
#6235 = CARTESIAN_POINT ( 'NONE',  ( -23.00000000000000000, -7.500000000000000000, 29.75000000000000355 ) ) ;
#6237 = CARTESIAN_POINT ( 'NONE',  ( 7.384615384615385025, -11.50000000000000000, 29.75000000000000355 ) ) ;
#6238 = CARTESIAN_POINT ( 'NONE',  ( -4.153846153846274980, -11.67786785259630911, 32.92929555188603530 ) ) ;
#6239 = EDGE_LOOP ( 'NONE', ( #53272, #79400, #16735, #4877 ) ) ;
#6240 = CARTESIAN_POINT ( 'NONE',  ( 2.307692307692187583, -6.879047030192662504, 34.71129190930017927 ) ) ;
#6241 = CARTESIAN_POINT ( 'NONE',  ( -7.846153846153537614, -2.506253911140614576, 30.00000000000323297 ) ) ;
#6242 = ORIENTED_EDGE ( 'NONE', *, *, #72877, .F. ) ;
#6243 = CARTESIAN_POINT ( 'NONE',  ( -6.792285115252136407, -4.809403383903225304, 33.96459661697924304 ) ) ;
#6244 = VECTOR ( 'NONE', #37854, 1000.000000000000000 ) ;
#6245 = VECTOR ( 'NONE', #1098, 1000.000000000000000 ) ;
#6246 = CARTESIAN_POINT ( 'NONE',  ( -13.63463860883683942, -4.931416488878822335, 34.32920672191015399 ) ) ;
#6247 = DIRECTION ( 'NONE',  ( 0.000000000000000000, 0.3420201433256641055, -0.9396926207859100932 ) ) ;
#6248 = VERTEX_POINT ( 'NONE', #57168 ) ;
#6249 = ADVANCED_FACE ( 'NONE', ( #57608 ), #72895, .F. ) ;
#6250 = CARTESIAN_POINT ( 'NONE',  ( -11.53846153846153655, -12.29105614889573062, 35.45975837776705220 ) ) ;
#6251 = CARTESIAN_POINT ( 'NONE',  ( 6.923076923076800782, -8.656820664282941280, 34.87096338111179961 ) ) ;
#6252 = FACE_BOUND ( 'NONE', #38843, .T. ) ;
#6254 = CARTESIAN_POINT ( 'NONE',  ( -16.82692307692307665, -2.249999999999998668, 29.75000000000000355 ) ) ;
#6253 = CARTESIAN_POINT ( 'NONE',  ( 11.53846153846184563, -2.506253911140615021, 30.00000000000323297 ) ) ;
#6255 = CARTESIAN_POINT ( 'NONE',  ( -8.992715712954719720, -6.760086850603066466, 34.69517049084099369 ) ) ;
#6256 = CARTESIAN_POINT ( 'NONE',  ( -5.143006487878955646, -8.973038597847269315, 34.52809138561120506 ) ) ;
#6258 = CARTESIAN_POINT ( 'NONE',  ( -8.546219417617917813, -12.15243808032446005, 31.58219941686247978 ) ) ;
#6257 = DIRECTION ( 'NONE',  ( 0.000000000000000000, 0.000000000000000000, 1.000000000000000000 ) ) ;
#6259 = CARTESIAN_POINT ( 'NONE',  ( -3.749999999999996447, -7.561099074964554134, 16.09188170625848713 ) ) ;
#6260 = ORIENTED_EDGE ( 'NONE', *, *, #59532, .F. ) ;
#6261 = ORIENTED_EDGE ( 'NONE', *, *, #30593, .T. ) ;
#6262 = CARTESIAN_POINT ( 'NONE',  ( 25.00000000000000711, -9.999999999999957367, 3.000000000000000000 ) ) ;
#6263 = CARTESIAN_POINT ( 'NONE',  ( -4.219116599806928214, -12.46129190929999986, 30.37095296980880832 ) ) ;
#6264 = CARTESIAN_POINT ( 'NONE',  ( 16.40379156322419973, -2.986452184633680229, 32.43230066228895225 ) ) ;
#6265 = CARTESIAN_POINT ( 'NONE',  ( -0.5272952640527707180, -7.249945686854186278, 34.74374336980224598 ) ) ;
#6266 = CARTESIAN_POINT ( 'NONE',  ( -3.360916440207450506, -6.001485441113818986, 34.52039167877662607 ) ) ;
#6267 = CARTESIAN_POINT ( 'NONE',  ( -1.553300858899081538, -11.25000000000000711, 21.10937500000000711 ) ) ;
#6268 = EDGE_CURVE ( 'NONE', #28219, #23488, #34828, .T. ) ;
#6269 = CARTESIAN_POINT ( 'NONE',  ( 16.81410256410256565, -4.000000000000000000, 29.75000000000000355 ) ) ;
#6270 = CARTESIAN_POINT ( 'NONE',  ( 8.769230769230768274, -2.833524468853757305, 32.15551576947925838 ) ) ;
#6271 = CARTESIAN_POINT ( 'NONE',  ( 17.93391762063986405, -3.937682226553330445, 33.60647404775217240 ) ) ;
#6272 = CARTESIAN_POINT ( 'NONE',  ( -15.09997742294444301, -11.18335022499818621, 33.13157742990016885 ) ) ;
#6273 = DIRECTION ( 'NONE',  ( -0.000000000000000000, 0.9396926207859092051, -0.3420201433256662704 ) ) ;
#6274 = CARTESIAN_POINT ( 'NONE',  ( 13.38461538461526601, -4.481592998941358097, 33.73612834414048933 ) ) ;
#6275 = LINE ( 'NONE', #54445, #45213 ) ;
#6276 = B_SPLINE_CURVE_WITH_KNOTS ( 'NONE', 3,
 ( #80980, #39556, #88196, #53933, #74662, #12948, #40440, #13388, #67898, #48051 ),
 .UNSPECIFIED., .F., .F.,
 ( 4, 2, 2, 2, 4 ),
 ( 0.0007817359430256282712, 0.0009771253907249941549, 0.001172514838424359822, 0.001367904286123725489, 0.001563293733823091372 ),
 .UNSPECIFIED. ) ;
#6277 = CARTESIAN_POINT ( 'NONE',  ( -8.769230769230768274, -13.95598074871891292, 31.83374038241031911 ) ) ;
#6278 = CARTESIAN_POINT ( 'NONE',  ( 4.403846153846153300, -2.249999999999998668, 29.75000000000000355 ) ) ;
#6279 = ORIENTED_EDGE ( 'NONE', *, *, #33882, .F. ) ;
#6280 = CARTESIAN_POINT ( 'NONE',  ( 1.134592147322422084, -2.587272538249755449, 30.68239716806877837 ) ) ;
#6281 = LINE ( 'NONE', #81501, #58998 ) ;
#6282 = CARTESIAN_POINT ( 'NONE',  ( 0.06109907496451789238, -4.749999999999998224, 16.90811829374151287 ) ) ;
#6283 = AXIS2_PLACEMENT_3D ( 'NONE', #19019, #46491, #86154 ) ;
#6284 = VECTOR ( 'NONE', #36456, 1000.000000000000000 ) ;
#6285 = EDGE_CURVE ( 'NONE', #9213, #27850, #87501, .T. ) ;
#6286 = CARTESIAN_POINT ( 'NONE',  ( 3.930361229281821966, -4.988325925672468131, 34.36044203135681130 ) ) ;
#6287 = CARTESIAN_POINT ( 'NONE',  ( -12.46153846153846168, -11.11383981884818262, 36.00935417666054406 ) ) ;
#6288 = CYLINDRICAL_SURFACE ( 'NONE', #3958, 0.2500000000000008882 ) ;
#6290 = ORIENTED_EDGE ( 'NONE', *, *, #82822, .T. ) ;
#6289 = CARTESIAN_POINT ( 'NONE',  ( -1.134669866267242311, -4.336752205174647656, 33.62275283266504289 ) ) ;
#6291 = CARTESIAN_POINT ( 'NONE',  ( 1.799775606325937360E-14, -10.25000000000000000, 22.28125000000000355 ) ) ;
#6292 = CARTESIAN_POINT ( 'NONE',  ( -1.384615384615383471, -9.819645486525091727, 36.12317359536749706 ) ) ;
#6293 = EDGE_CURVE ( 'NONE', #66691, #54559, #26222, .T. ) ;
#6294 = ORIENTED_EDGE ( 'NONE', *, *, #81115, .T. ) ;
#6295 = CARTESIAN_POINT ( 'NONE',  ( -15.90379184220783948, -9.943054286541403997, 34.11300777759954883 ) ) ;
#6296 = CARTESIAN_POINT ( 'NONE',  ( -2.307692307692427391, -2.625532179533779154, 30.86335684631627174 ) ) ;
#6297 = ORIENTED_EDGE ( 'NONE', *, *, #14711, .T. ) ;
#6298 = CARTESIAN_POINT ( 'NONE',  ( 7.715462379486291766, -4.118384482072085184, 33.43331474514187107 ) ) ;
#6299 = CARTESIAN_POINT ( 'NONE',  ( -15.09993090028246954, -7.277220318596961057, 34.99547417642776992 ) ) ;
#6300 = CARTESIAN_POINT ( 'NONE',  ( -8.069638789877796370, -3.754499324213721234, 33.06261337010820256 ) ) ;
#6301 = EDGE_CURVE ( 'NONE', #19438, #79333, #46632, .T. ) ;
#6302 = ORIENTED_EDGE ( 'NONE', *, *, #68492, .T. ) ;
#6303 = VERTEX_POINT ( 'NONE', #24712 ) ;
#6304 = ORIENTED_EDGE ( 'NONE', *, *, #81061, .F. ) ;
#6305 = EDGE_CURVE ( 'NONE', #56065, #57354, #11655, .T. ) ;
#6306 = CARTESIAN_POINT ( 'NONE',  ( 7.623226887246995709, -9.172386477786396597, 34.72672124145550043 ) ) ;
#6307 = CARTESIAN_POINT ( 'NONE',  ( 7.145856592054987466, -11.60474049983371003, 33.02348890104160262 ) ) ;
#6308 = CARTESIAN_POINT ( 'NONE',  ( 0.4615384615384611200, -13.87047571288749737, 32.06866353760679544 ) ) ;
#6309 = CARTESIAN_POINT ( 'NONE',  ( -12.46153846153858247, -3.300289026999228881, 32.46337939537708905 ) ) ;
#6310 = ADVANCED_FACE ( 'NONE', ( #25156 ), #67486, .F. ) ;
#6311 = CARTESIAN_POINT ( 'NONE',  ( -2.307692307692305711, -4.098570777380720287, 33.41473453929634729 ) ) ;
#6312 = CYLINDRICAL_SURFACE ( 'NONE', #16247, 0.2499999999999973355 ) ;
#6313 = CARTESIAN_POINT ( 'NONE',  ( 13.38461538461526601, -3.300289026999228881, 32.46337939537708905 ) ) ;
#6314 = B_SPLINE_CURVE_WITH_KNOTS ( 'NONE', 3,
 ( #19825, #26137, #53606, #68885, #81096, #19381, #46849, #7199, #74780, #68020 ),
 .UNSPECIFIED., .F., .F.,
 ( 4, 2, 2, 2, 4 ),
 ( 0.0007817246256747484735, 0.0009771112852218915863, 0.001172497944769034916, 0.001367884604316178029, 0.001563271263863321141 ),
 .UNSPECIFIED. ) ;
#6315 = VECTOR ( 'NONE', #34704, 999.9999999999998863 ) ;
#6316 = CARTESIAN_POINT ( 'NONE',  ( -0.3310130233048143023, -12.50538340440932217, 31.33453814440721885 ) ) ;
#6317 = B_SPLINE_CURVE_WITH_KNOTS ( 'NONE', 3,
 ( #50343, #14814, #41844, #1283, #28771, #76507, #56236, #83721, #34635, #22880 ),
 .UNSPECIFIED., .F., .F.,
 ( 4, 2, 2, 2, 4 ),
 ( 0.000000000000000000, 0.0001954311564186872268, 0.0003908623128373744536, 0.0005862934692560616261, 0.0007817246256747489071 ),
 .UNSPECIFIED. ) ;
#6318 = EDGE_CURVE ( 'NONE', #7411, #38055, #78846, .T. ) ;
#6319 = ORIENTED_EDGE ( 'NONE', *, *, #18918, .F. ) ;
#6320 = ORIENTED_EDGE ( 'NONE', *, *, #17694, .F. ) ;
#6322 = VERTEX_POINT ( 'NONE', #33697 ) ;
#6321 = CARTESIAN_POINT ( 'NONE',  ( -1.634615384615383027, -7.500000000000001776, 34.75000000000000000 ) ) ;
#6323 = ADVANCED_FACE ( 'NONE', ( #53961 ), #81453, .T. ) ;
#6324 = EDGE_CURVE ( 'NONE', #79249, #2843, #60269, .T. ) ;
#6325 = LINE ( 'NONE', #68891, #21959 ) ;
#6326 = CARTESIAN_POINT ( 'NONE',  ( 11.60452988946398101, -12.10708131394839704, 31.69288490824020954 ) ) ;
#6327 = ORIENTED_EDGE ( 'NONE', *, *, #64020, .T. ) ;
#6328 = CARTESIAN_POINT ( 'NONE',  ( 15.29683656411930848, -9.058645607665452459, 34.76329471203371924 ) ) ;
#6329 = ORIENTED_EDGE ( 'NONE', *, *, #46955, .F. ) ;
#6330 = CARTESIAN_POINT ( 'NONE',  ( 17.20744851515672025, -9.503571793651730104, 34.60286762892837942 ) ) ;
#6331 = ORIENTED_EDGE ( 'NONE', *, *, #74672, .F. ) ;
#6332 = CARTESIAN_POINT ( 'NONE',  ( -6.923076923076922462, -2.833524468853757305, 32.15551576947925838 ) ) ;
#6333 = AXIS2_PLACEMENT_3D ( 'NONE', #9309, #16941, #16058 ) ;
#6334 = ORIENTED_EDGE ( 'NONE', *, *, #66448, .T. ) ;
#6335 = CARTESIAN_POINT ( 'NONE',  ( -12.46153846153858424, -10.33852847137269571, 34.16647553114546554 ) ) ;
#6336 = EDGE_CURVE ( 'NONE', #43656, #27369, #8316, .T. ) ;
#6337 = B_SPLINE_CURVE_WITH_KNOTS ( 'NONE', 3,
 ( #16180, #43645, #57605, #23368, #50826, #78311, #16611, #32361, #10754, #17961 ),
 .UNSPECIFIED., .F., .F.,
 ( 4, 2, 2, 2, 4 ),
 ( 0.0007817359430256372700, 0.0009771253907250054306, 0.001172514838424373483, 0.001367904286123741535, 0.001563293733823109804 ),
 .UNSPECIFIED. ) ;
#6338 = CARTESIAN_POINT ( 'NONE',  ( 12.23805353697412812, -2.353723527008296568, 30.78948104536958752 ) ) ;
#6339 = FACE_BOUND ( 'NONE', #60342, .T. ) ;
#6340 = B_SPLINE_CURVE_WITH_KNOTS ( 'NONE', 3,
 ( #31969, #16663, #51763, #58981, #44565, #59433, #24759, #10806, #52221, #80158 ),
 .UNSPECIFIED., .F., .F.,
 ( 4, 2, 2, 2, 4 ),
 ( 0.0007817359430256257775, 0.0009771253907249906855, 0.001172514838424355485, 0.001367904286123720285, 0.001563293733823085301 ),
 .UNSPECIFIED. ) ;
#6341 = VECTOR ( 'NONE', #57691, 1000.000000000000000 ) ;
#6342 = CARTESIAN_POINT ( 'NONE',  ( 5.869309396889694774, -2.295517848115769421, 30.44137282052136939 ) ) ;
#6343 = DIRECTION ( 'NONE',  ( -0.000000000000000000, -0.6427876096865404731, -0.7660444431189771253 ) ) ;
#6344 = AXIS2_PLACEMENT_3D ( 'NONE', #18151, #51914, #51455 ) ;
#6345 = DIRECTION ( 'NONE',  ( -1.000000000000000000, -0.000000000000000000, -0.000000000000000000 ) ) ;
#6346 = CARTESIAN_POINT ( 'NONE',  ( 10.48523664565292179, -10.31621877034669588, 34.18098118002070152 ) ) ;
#6347 = EDGE_CURVE ( 'NONE', #68662, #84581, #66924, .T. ) ;
#6348 = DIRECTION ( 'NONE',  ( -0.000000000000000000, 0.1736481776669307198, -0.9848077530122080203 ) ) ;
#6349 = CARTESIAN_POINT ( 'NONE',  ( -9.070512820512819374, -7.500000000000000000, 29.75000000000000355 ) ) ;
#6350 = CARTESIAN_POINT ( 'NONE',  ( -11.76138849736838488, -3.395401636524185474, 33.02366814457250399 ) ) ;
#6351 = B_SPLINE_CURVE_WITH_KNOTS ( 'NONE', 3,
 ( #32325, #53917, #40420, #81405, #19688, #67880, #6182, #24668, #33651, #86396 ),
 .UNSPECIFIED., .F., .F.,
 ( 4, 2, 2, 2, 4 ),
 ( 0.000000000000000000, 0.0001954311564186871184, 0.0003908623128373742367, 0.0005862934692560614093, 0.0007817246256747484735 ),
 .UNSPECIFIED. ) ;
#6352 = VERTEX_POINT ( 'NONE', #52622 ) ;
#6353 = EDGE_LOOP ( 'NONE', ( #24009, #63196, #2003, #1314 ) ) ;
#6355 = CARTESIAN_POINT ( 'NONE',  ( 10.61538461538461675, -5.557115091759785130, 34.35708131394839171 ) ) ;
#6354 = CARTESIAN_POINT ( 'NONE',  ( -17.01085472592063397, -9.780366693483667717, 34.19971097300155805 ) ) ;
#6356 = CARTESIAN_POINT ( 'NONE',  ( 16.40390057375960708, -11.47946981652013498, 33.17500667209846910 ) ) ;
#6357 = CARTESIAN_POINT ( 'NONE',  ( -3.931066484868084299, -9.418065098278011860, 34.63729479722530158 ) ) ;
#6358 = CARTESIAN_POINT ( 'NONE',  ( -17.32689982097166492, -12.41104346484419452, 31.60698883733904196 ) ) ;
#6359 = CARTESIAN_POINT ( 'NONE',  ( -12.22435897435897267, -11.50000000000000000, 29.75000000000000355 ) ) ;
#6360 = EDGE_LOOP ( 'NONE', ( #254, #44849, #64413, #29279 ) ) ;
#6361 = EDGE_CURVE ( 'NONE', #45648, #53485, #81895, .T. ) ;
#6362 = CARTESIAN_POINT ( 'NONE',  ( -5.777220331021931443, -8.540255544307065350, 34.89611431652622286 ) ) ;
#6363 = CARTESIAN_POINT ( 'NONE',  ( 14.05766907039934210, -11.37209801155882793, 32.91403422569033665 ) ) ;
#6364 = CARTESIAN_POINT ( 'NONE',  ( -3.480745974817820887, -11.47974371597207899, 33.17467449705390692 ) ) ;
#6365 = FACE_OUTER_BOUND ( 'NONE', #50860, .T. ) ;
#6366 = EDGE_LOOP ( 'NONE', ( #3618, #3428 ) ) ;
#6367 = EDGE_CURVE ( 'NONE', #76991, #72654, #40025, .T. ) ;
#6368 = ORIENTED_EDGE ( 'NONE', *, *, #17546, .T. ) ;
#6370 = EDGE_CURVE ( 'NONE', #50376, #23593, #19296, .T. ) ;
#6369 = ORIENTED_EDGE ( 'NONE', *, *, #27784, .F. ) ;
#6371 = CARTESIAN_POINT ( 'NONE',  ( 10.61538461538449418, -4.320704448113951379, 33.92786785259630022 ) ) ;
#6372 = ORIENTED_EDGE ( 'NONE', *, *, #31261, .T. ) ;
#6373 = CARTESIAN_POINT ( 'NONE',  ( 17.07692307692307665, -12.78798330534102945, 29.74999999999997868 ) ) ;
#6374 = CARTESIAN_POINT ( 'NONE',  ( -6.923076923077044142, -2.625532179533778709, 30.86335684631627174 ) ) ;
#6375 = CARTESIAN_POINT ( 'NONE',  ( 3.453782074862625784, -5.582272713120728369, 34.63742843783360570 ) ) ;
#6376 = CARTESIAN_POINT ( 'NONE',  ( 20.00000000000000000, -4.000000000000000000, 29.75000000000000355 ) ) ;
#6377 = EDGE_CURVE ( 'NONE', #219, #62136, #15408, .T. ) ;
#6378 = CARTESIAN_POINT ( 'NONE',  ( -11.40766973063675316, -6.413143153341454017, 34.63066358083362672 ) ) ;
#6380 = VERTEX_POINT ( 'NONE', #73805 ) ;
#6379 = VECTOR ( 'NONE', #1813, 1000.000000000000000 ) ;
#6381 = CARTESIAN_POINT ( 'NONE',  ( -11.66893672353726075, -7.276987145209185215, 34.99546412871779211 ) ) ;
#6383 = EDGE_LOOP ( 'NONE', ( #48624, #12280 ) ) ;
#6382 = CARTESIAN_POINT ( 'NONE',  ( -12.46153846153846168, -11.69971097300155272, 32.46337939537588113 ) ) ;
#6384 = CARTESIAN_POINT ( 'NONE',  ( 17.06410256410256565, -7.500000000000000000, 29.75000000000000355 ) ) ;
#6385 = DIRECTION ( 'NONE',  ( -0.000000000000000000, -0.9848077530122086864, -0.1736481776669273613 ) ) ;
#6386 = FACE_OUTER_BOUND ( 'NONE', #28320, .T. ) ;
#6387 = CARTESIAN_POINT ( 'NONE',  ( 11.60371667797437567, -10.33852847137154107, 34.16647553114620450 ) ) ;
#6388 = CARTESIAN_POINT ( 'NONE',  ( -9.692307692307814193, -12.51329471203414379, 31.30864560766407578 ) ) ;
#6389 = B_SPLINE_CURVE_WITH_KNOTS ( 'NONE', 3,
 ( #72494, #72943, #4026, #17107, #3140, #30185, #30617, #65291, #51300, #86019 ),
 .UNSPECIFIED., .F., .F.,
 ( 4, 2, 2, 2, 4 ),
 ( 0.0007817359430256294638, 0.0009771253907249937212, 0.001172514838424358087, 0.001367904286123722453, 0.001563293733823093758 ),
 .UNSPECIFIED. ) ;
#6390 = DIRECTION ( 'NONE',  ( 0.000000000000000000, 0.000000000000000000, 1.000000000000000000 ) ) ;
#6391 = CARTESIAN_POINT ( 'NONE',  ( -0.06109907496451398579, -10.25000000000000178, 22.53311829374151642 ) ) ;
#6392 = ORIENTED_EDGE ( 'NONE', *, *, #62889, .T. ) ;
#6393 = CARTESIAN_POINT ( 'NONE',  ( -16.40384615384615330, -7.500000000000001776, 35.04278698407183867 ) ) ;
#6394 = CARTESIAN_POINT ( 'NONE',  ( 12.71159288145191368, -4.818054556918156983, 34.26375889529406749 ) ) ;
#6395 = SURFACE_STYLE_FILL_AREA ( #48245 ) ;
#6396 = ORIENTED_EDGE ( 'NONE', *, *, #28478, .F. ) ;
#6397 = CARTESIAN_POINT ( 'NONE',  ( 2.557692307693728129, -7.500000000000154543, 35.00000000000007105 ) ) ;
#6398 = CARTESIAN_POINT ( 'NONE',  ( -5.143006487878956534, -6.386643153685125363, 34.62446782046654903 ) ) ;
#6399 = EDGE_CURVE ( 'NONE', #81961, #24104, #53033, .T. ) ;
#6400 = CARTESIAN_POINT ( 'NONE',  ( -10.61538461538461320, -2.292212530054420494, 30.41441678777542634 ) ) ;
#6401 = CARTESIAN_POINT ( 'NONE',  ( -4.853547136224893421, -2.501478030877322567, 29.88021232661720816 ) ) ;
#6402 = DIRECTION ( 'NONE',  ( -0.000000000000000000, 1.000000000000000000, -0.000000000000000000 ) ) ;
#6403 = ORIENTED_EDGE ( 'NONE', *, *, #25235, .F. ) ;
#6404 = CARTESIAN_POINT ( 'NONE',  ( 16.82689983963010860, -3.202444869320336451, 32.30641848906366675 ) ) ;
#6405 = VECTOR ( 'NONE', #55502, 1000.000000000000000 ) ;
#6406 = FACE_OUTER_BOUND ( 'NONE', #65035, .T. ) ;
#6407 = CARTESIAN_POINT ( 'NONE',  ( 18.24994540937804643, -12.45601412856602686, 31.48342859153981621 ) ) ;
#6408 = ORIENTED_EDGE ( 'NONE', *, *, #25530, .F. ) ;
#6409 = CARTESIAN_POINT ( 'NONE',  ( -16.82686865700962286, -12.01375889529407992, 32.43194544308182969 ) ) ;
#6410 = VECTOR ( 'NONE', #82418, 1000.000000000000227 ) ;
#6411 = EDGE_LOOP ( 'NONE', ( #81329, #29247 ) ) ;
#6412 = DIRECTION ( 'NONE',  ( 0.000000000000000000, 0.000000000000000000, -1.000000000000000000 ) ) ;
#6413 = FACE_OUTER_BOUND ( 'NONE', #58921, .T. ) ;
#6414 = ORIENTED_EDGE ( 'NONE', *, *, #17597, .T. ) ;
#6415 = CARTESIAN_POINT ( 'NONE',  ( 12.46153846153846168, -3.513871655860378418, 32.76840700105978499 ) ) ;
#6416 = CARTESIAN_POINT ( 'NONE',  ( 5.869852790561781219, -10.19110544564092002, 33.96427741523702792 ) ) ;
#6417 = CARTESIAN_POINT ( 'NONE',  ( -11.76138775597768138, -6.503392248772476236, 34.64988816332204635 ) ) ;
#6418 = CARTESIAN_POINT ( 'NONE',  ( 2.307692307692309264, -3.050289026998446396, 32.03036669348365706 ) ) ;
#6419 = DIRECTION ( 'NONE',  ( -1.000000000000000000, 0.000000000000000000, 0.000000000000000000 ) ) ;
#6421 = VERTEX_POINT ( 'NONE', #14757 ) ;
#6420 = EDGE_CURVE ( 'NONE', #80799, #72564, #49855, .T. ) ;
#6422 = FACE_OUTER_BOUND ( 'NONE', #7079, .T. ) ;
#6423 = EDGE_LOOP ( 'NONE', ( #70553, #59602, #31130, #64987 ) ) ;
#6424 = CARTESIAN_POINT ( 'NONE',  ( 5.999999999999880096, -2.892918686052165622, 31.69288490824153470 ) ) ;
#6425 = DIRECTION ( 'NONE',  ( -1.000000000000000000, -0.000000000000000000, -0.000000000000000000 ) ) ;
#6426 = EDGE_CURVE ( 'NONE', #14948, #87491, #22893, .T. ) ;
#6427 = CARTESIAN_POINT ( 'NONE',  ( 18.25005431163831915, -12.17597550085003633, 31.52189283813461884 ) ) ;
#6428 = EDGE_CURVE ( 'NONE', #1675, #87698, #55728, .T. ) ;
#6429 = LINE ( 'NONE', #33453, #7561 ) ;
#6430 = CARTESIAN_POINT ( 'NONE',  ( 7.053868730901709405, -9.804649428959608670, 34.18742332936588468 ) ) ;
#6431 = ORIENTED_EDGE ( 'NONE', *, *, #81941, .F. ) ;
#6433 = ADVANCED_FACE ( 'NONE', ( #43109 ), #82334, .T. ) ;
#6432 = VERTEX_POINT ( 'NONE', #1678 ) ;
#6434 = VERTEX_POINT ( 'NONE', #61601 ) ;
#6435 = VERTEX_POINT ( 'NONE', #34132 ) ;
#6436 = CARTESIAN_POINT ( 'NONE',  ( -5.076923076923197442, -5.219633306517616589, 34.19971097300220464 ) ) ;
#6437 = EDGE_CURVE ( 'NONE', #26337, #67575, #82779, .T. ) ;
#6438 = CARTESIAN_POINT ( 'NONE',  ( -9.626138551345036376, -7.250054483168843156, 34.74374881642865631 ) ) ;
#6439 = LINE ( 'NONE', #13194, #81723 ) ;
#6440 = ORIENTED_EDGE ( 'NONE', *, *, #67406, .T. ) ;
#6441 = CARTESIAN_POINT ( 'NONE',  ( 11.31553532094538994, -2.554751324335735152, 30.48935550225260727 ) ) ;
#6442 = CARTESIAN_POINT ( 'NONE',  ( -2.438383774359865974, -4.809359713505814149, 33.96456829005828837 ) ) ;
#6443 = CARTESIAN_POINT ( 'NONE',  ( -2.242436736416281384, -3.835265460703683349, 33.15142922261929925 ) ) ;
#6444 = CARTESIAN_POINT ( 'NONE',  ( -4.946397638689434828, -11.66157788607254275, 32.95092075102925833 ) ) ;
#6445 = VERTEX_POINT ( 'NONE', #22391 ) ;
#6446 = ORIENTED_EDGE ( 'NONE', *, *, #86777, .F. ) ;
#6447 = ORIENTED_EDGE ( 'NONE', *, *, #468, .F. ) ;
#6448 = DIRECTION ( 'NONE',  ( -0.000000000000000000, 0.1736481776669307198, -0.9848077530122080203 ) ) ;
#6450 = CARTESIAN_POINT ( 'NONE',  ( -7.715628407920200438, -9.503571793651731880, 34.60286762892837942 ) ) ;
#6449 = CARTESIAN_POINT ( 'NONE',  ( 1.634669696253701288, -5.728107161865378494, 34.42597550085002922 ) ) ;
#6451 = B_SPLINE_CURVE_WITH_KNOTS ( 'NONE', 3,
 ( #47325, #27952, #34710, #37, #21186, #81133, #76129, #40589, #54980, #14431 ),
 .UNSPECIFIED., .F., .F.,
 ( 4, 2, 2, 2, 4 ),
 ( 0.0007817246256747530271, 0.0009771112852218978746, 0.001172497944769042939, 0.001367884604316188003, 0.001563271263863332851 ),
 .UNSPECIFIED. ) ;
#6452 = LINE ( 'NONE', #33911, #78709 ) ;
#6453 = CARTESIAN_POINT ( 'NONE',  ( -10.83831083290076158, -3.586966769969701208, 32.86292498521069660 ) ) ;
#6454 = FACE_BOUND ( 'NONE', #70472, .T. ) ;
#6455 = ORIENTED_EDGE ( 'NONE', *, *, #11182, .T. ) ;
#6456 = VECTOR ( 'NONE', #40249, 1000.000000000000227 ) ;
#6457 = CARTESIAN_POINT ( 'NONE',  ( -1.253823576790599637, -2.729792928343270031, 31.24908615093345432 ) ) ;
#6458 = CARTESIAN_POINT ( 'NONE',  ( 3.100077764101675459, -10.54014554554150607, 33.71984207302941883 ) ) ;
#6459 = ORIENTED_EDGE ( 'NONE', *, *, #78541, .F. ) ;
#6460 = CARTESIAN_POINT ( 'NONE',  ( 5.076923076923075762, -2.292212530054420494, 30.41441678777542634 ) ) ;
#6461 = EDGE_CURVE ( 'NONE', #24326, #60483, #18351, .T. ) ;
#6462 = EDGE_LOOP ( 'NONE', ( #32561, #67551 ) ) ;
#6463 = FACE_BOUND ( 'NONE', #34588, .T. ) ;
#6464 = CARTESIAN_POINT ( 'NONE',  ( -6.166666666666667851, -11.50000000000000000, 29.75000000000000355 ) ) ;
#6465 = ORIENTED_EDGE ( 'NONE', *, *, #8401, .F. ) ;
#6466 = CARTESIAN_POINT ( 'NONE',  ( -2.307692307692305711, -2.249999999999998668, 29.50000000000001421 ) ) ;
#6467 = DIRECTION ( 'NONE',  ( 1.000000000000000000, 0.000000000000000000, 0.000000000000000000 ) ) ;
#6468 = CARTESIAN_POINT ( 'NONE',  ( 1.384615384615386802, -3.050289026998446396, 32.03036669348365706 ) ) ;
#6469 = ORIENTED_EDGE ( 'NONE', *, *, #81443, .F. ) ;
#6470 = CARTESIAN_POINT ( 'NONE',  ( 6.856993512121041690, -9.780366693483667717, 34.19971097300155805 ) ) ;
#6471 = CARTESIAN_POINT ( 'NONE',  ( 14.55774672760576394, -3.435999193479609914, 33.07426656108010832 ) ) ;
#6472 = CARTESIAN_POINT ( 'NONE',  ( -16.28453762051371356, -12.38065189839062263, 30.83690757178629482 ) ) ;
#6473 = CYLINDRICAL_SURFACE ( 'NONE', #21700, 0.2499999999999995559 ) ;
#6474 = ORIENTED_EDGE ( 'NONE', *, *, #52098, .F. ) ;
#6475 = EDGE_CURVE ( 'NONE', #6435, #2497, #9963, .T. ) ;
#6476 = CARTESIAN_POINT ( 'NONE',  ( -12.23875892027004930, -3.236590943229499029, 32.36255958852954251 ) ) ;
#6477 = CARTESIAN_POINT ( 'NONE',  ( 4.023698184114458343, -10.31621877034669588, 34.18098118002070152 ) ) ;
#6479 = ORIENTED_EDGE ( 'NONE', *, *, #71103, .T. ) ;
#6478 = CARTESIAN_POINT ( 'NONE',  ( 1.515405825582336607, -2.845873456487965747, 32.17976146951972538 ) ) ;
#6480 = CARTESIAN_POINT ( 'NONE',  ( -8.769230769230890843, -10.90142922262034020, 33.41473453929536674 ) ) ;
#6481 = CARTESIAN_POINT ( 'NONE',  ( 0.3589743589743582541, -3.499999999999999556, 29.75000000000000355 ) ) ;
#6482 = CARTESIAN_POINT ( 'NONE',  ( -13.16160403300253279, -4.887748414852792322, 34.01359900205216746 ) ) ;
#6483 = CYLINDRICAL_SURFACE ( 'NONE', #4012, 4.755951259987790891 ) ;
#6484 = CARTESIAN_POINT ( 'NONE',  ( -10.36533030374629938, -2.564540009722895419, 30.55348353981670684 ) ) ;
#6485 = CARTESIAN_POINT ( 'NONE',  ( -13.13466997523734037, -3.520799739797214389, 33.17531984108286025 ) ) ;
#6487 = CARTESIAN_POINT ( 'NONE',  ( -5.198717948717948012, -7.500000000000000000, 29.75000000000000355 ) ) ;
#6486 = PLANE ( 'NONE',  #23167 ) ;
#6488 = EDGE_CURVE ( 'NONE', #62563, #80983, #41793, .T. ) ;
#6489 = CARTESIAN_POINT ( 'NONE',  ( -12.33101275977490197, -11.46989282347013095, 32.79007818306219946 ) ) ;
#6490 = CARTESIAN_POINT ( 'NONE',  ( -2.749999999999991562, -8.639087296526025028, 18.76562500000000000 ) ) ;
#6491 = ORIENTED_EDGE ( 'NONE', *, *, #46945, .F. ) ;
#6492 = CARTESIAN_POINT ( 'NONE',  ( 14.30769230769231015, -1.790695186598648903, 34.54067556320373455 ) ) ;
#6493 = EDGE_LOOP ( 'NONE', ( #87279, #33703, #64868, #42133 ) ) ;
#6494 = ORIENTED_EDGE ( 'NONE', *, *, #2391, .F. ) ;
#6495 = PLANE ( 'NONE',  #5331 ) ;
#6496 = VERTEX_POINT ( 'NONE', #792 ) ;
#6497 = CARTESIAN_POINT ( 'NONE',  ( 14.16025641025641235, -7.500000000000000000, 29.75000000000000355 ) ) ;
#6498 = CARTESIAN_POINT ( 'NONE',  ( -1.409462824231155764E-14, -4.749999999999999112, 17.90625000000000000 ) ) ;
#6499 = CARTESIAN_POINT ( 'NONE',  ( 17.93472999944368240, -5.094484230520675894, 34.41647553114621161 ) ) ;
#6500 = ADVANCED_FACE ( 'NONE', ( #28257 ), #83217, .F. ) ;
#6501 = DIRECTION ( 'NONE',  ( 0.000000000000000000, 0.000000000000000000, -1.000000000000000000 ) ) ;
#6502 = CARTESIAN_POINT ( 'NONE',  ( -1.384615384615383471, -9.819645486525091727, 36.12317359536749706 ) ) ;
#6503 = CIRCLE ( 'NONE', #79853, 8.000000000000000000 ) ;
#6504 = CARTESIAN_POINT ( 'NONE',  ( 13.38461538461538680, -2.499999999999998668, 29.75000000000001421 ) ) ;
#6505 = CYLINDRICAL_SURFACE ( 'NONE', #73288, 0.2499999999999998890 ) ;
#6506 = CARTESIAN_POINT ( 'NONE',  ( 10.61538461538461675, -2.517432740324522911, 35.29906147534542527 ) ) ;
#6507 = CARTESIAN_POINT ( 'NONE',  ( 2.651650429449539104, -4.848349570550432475, 24.31250000000000000 ) ) ;
#6508 = EDGE_CURVE ( 'NONE', #54081, #56507, #21954, .T. ) ;
#6509 = EDGE_CURVE ( 'NONE', #13749, #83195, #15203, .T. ) ;
#6510 = CARTESIAN_POINT ( 'NONE',  ( -7.053224892808620083, -5.070767119584671079, 34.40440758774516183 ) ) ;
#6511 = CARTESIAN_POINT ( 'NONE',  ( -13.13456107297706943, -6.567000820036036579, 34.66262288849541306 ) ) ;
#6512 = CARTESIAN_POINT ( 'NONE',  ( 5.934729999443681514, -11.67786785259541027, 32.92929555188721480 ) ) ;
#6513 = B_SPLINE_CURVE_WITH_KNOTS ( 'NONE', 3,
 ( #46302, #73789, #19721, #47179, #74674, #12963, #37097, #10077, #30351, #78528 ),
 .UNSPECIFIED., .F., .F.,
 ( 4, 2, 2, 2, 4 ),
 ( 0.0007817359430256294638, 0.0009771253907249948054, 0.001172514838424360255, 0.001367904286123725489, 0.001563293733823090939 ),
 .UNSPECIFIED. ) ;
#6514 = ADVANCED_FACE ( 'NONE', ( #43982 ), #3880, .F. ) ;
#6515 = ORIENTED_EDGE ( 'NONE', *, *, #7975, .T. ) ;
#6516 = EDGE_LOOP ( 'NONE', ( #55360, #30269, #63798, #1254 ) ) ;
#6517 = CARTESIAN_POINT ( 'NONE',  ( 2.980792486720641232, -10.82459398097509684, 33.81372124010185587 ) ) ;
#6518 = CARTESIAN_POINT ( 'NONE',  ( 0.4615384615383382183, -12.16647553114689728, 32.15551576947799362 ) ) ;
#6519 = CARTESIAN_POINT ( 'NONE',  ( 10.61538461538461675, -1.509761064869970415, 31.06009739812519044 ) ) ;
#6520 = CARTESIAN_POINT ( 'NONE',  ( 9.823098133274644539, -11.93129842949671726, 32.56571108434900452 ) ) ;
#6521 = CARTESIAN_POINT ( 'NONE',  ( 6.250054311638316484, -4.943051570960391494, 34.04725096376909477 ) ) ;
#6522 = CARTESIAN_POINT ( 'NONE',  ( -3.230769230769352962, -11.67786785259630911, 32.92929555188603530 ) ) ;
#6523 = CARTESIAN_POINT ( 'NONE',  ( 19.99999999999999289, -11.99999999999999467, 0.000000000000000000 ) ) ;
#6524 = AXIS2_PLACEMENT_3D ( 'NONE', #26178, #27510, #32484 ) ;
#6525 = ORIENTED_EDGE ( 'NONE', *, *, #27829, .F. ) ;
#6526 = DIRECTION ( 'NONE',  ( -0.000000000000000000, -0.5000000000000009992, -0.8660254037844380415 ) ) ;
#6527 = ORIENTED_EDGE ( 'NONE', *, *, #34266, .T. ) ;
#6528 = B_SPLINE_CURVE_WITH_KNOTS ( 'NONE', 3,
 ( #73069, #11367, #20784, #48251, #67209, #32977, #33423, #68096, #34297, #53682 ),
 .UNSPECIFIED., .F., .F.,
 ( 4, 2, 2, 2, 4 ),
 ( 0.000000000000000000, 0.0001954311564186863323, 0.0003908623128373726646, 0.0005862934692560590241, 0.0007817246256747453293 ),
 .UNSPECIFIED. ) ;
#6529 = EDGE_CURVE ( 'NONE', #52479, #73448, #71629, .T. ) ;
#6530 = CARTESIAN_POINT ( 'NONE',  ( -8.703975629717932705, -5.094484230520773593, 34.41647553114626845 ) ) ;
#6531 = DIRECTION ( 'NONE',  ( 0.000000000000000000, 0.000000000000000000, -1.000000000000000000 ) ) ;
#6532 = CARTESIAN_POINT ( 'NONE',  ( -7.145956439814507455, -7.630690623152302621, 34.99857592706774057 ) ) ;
#6533 = AXIS2_PLACEMENT_3D ( 'NONE', #20167, #67910, #34116 ) ;
#6534 = CARTESIAN_POINT ( 'NONE',  ( 2.980746006547773774, -8.475808217655753651, 34.90892951860618609 ) ) ;
#6535 = DIRECTION ( 'NONE',  ( -0.000000000000000000, 0.8660254037844399289, -0.4999999999999980016 ) ) ;
#6536 = ORIENTED_EDGE ( 'NONE', *, *, #69796, .T. ) ;
#6537 = EDGE_CURVE ( 'NONE', #2738, #76676, #26095, .T. ) ;
#6538 = ORIENTED_EDGE ( 'NONE', *, *, #41649, .T. ) ;
#6539 = EDGE_LOOP ( 'NONE', ( #20938, #55997, #49401, #4683, #29417, #46971 ) ) ;
#6540 = ORIENTED_EDGE ( 'NONE', *, *, #53299, .F. ) ;
#6541 = CARTESIAN_POINT ( 'NONE',  ( -6.130147969731695845, -5.070767119584671079, 34.40440758774516183 ) ) ;
#6542 = CARTESIAN_POINT ( 'NONE',  ( 4.826899839630110378, -10.76384336483936011, 33.53834819971076087 ) ) ;
#6543 = EDGE_CURVE ( 'NONE', #79083, #69664, #46508, .T. ) ;
#6544 = CARTESIAN_POINT ( 'NONE',  ( 16.02328624023278891, -2.254533558242299396, 29.97296025877828640 ) ) ;
#6545 = CARTESIAN_POINT ( 'NONE',  ( 14.55769230769224798, -7.565270000091922853, 34.99999999999999289 ) ) ;
#6546 = DIRECTION ( 'NONE',  ( -0.000000000000000000, 1.000000000000000000, -0.000000000000000000 ) ) ;
#6547 = CARTESIAN_POINT ( 'NONE',  ( 1.576923076923075762, -11.00000000000000000, 29.75000000000000355 ) ) ;
#6548 = VERTEX_POINT ( 'NONE', #10212 ) ;
#6549 = EDGE_LOOP ( 'NONE', ( #29578, #77211 ) ) ;
#6550 = EDGE_LOOP ( 'NONE', ( #71703, #86951, #74443, #40159 ) ) ;
#6551 = ADVANCED_FACE ( 'NONE', ( #65135 ), #51159, .F. ) ;
#6553 = ORIENTED_EDGE ( 'NONE', *, *, #1976, .T. ) ;
#6552 = DIRECTION ( 'NONE',  ( 0.000000000000000000, 0.7660444431189807890, 0.6427876096865361433 ) ) ;
#6554 = CARTESIAN_POINT ( 'NONE',  ( 8.769230769230768274, -9.819645486525091727, 36.12317359536749706 ) ) ;
#6555 = CARTESIAN_POINT ( 'NONE',  ( 6.923076923076924238, -11.11383981884818262, 36.00935417666054406 ) ) ;
#6556 = CARTESIAN_POINT ( 'NONE',  ( -1.553300858899081760, -11.25000000000000888, 22.35937500000000355 ) ) ;
#6557 = ORIENTED_EDGE ( 'NONE', *, *, #36159, .F. ) ;
#6558 = CARTESIAN_POINT ( 'NONE',  ( -5.999999999999998224, -9.058645607665452459, 34.76329471203371924 ) ) ;
#6559 = ORIENTED_EDGE ( 'NONE', *, *, #18862, .T. ) ;
#6560 = CARTESIAN_POINT ( 'NONE',  ( 2.057669070399342992, -6.695914987888143877, 34.68535235679833306 ) ) ;
#6561 = FACE_BOUND ( 'NONE', #5620, .T. ) ;
#6562 = CARTESIAN_POINT ( 'NONE',  ( 14.87820512820512953, -3.499999999999999556, 29.75000000000000355 ) ) ;
#6563 = CARTESIAN_POINT ( 'NONE',  ( 5.999999999999878320, -3.083524468854526912, 32.58852847137268327 ) ) ;
#6564 = VERTEX_POINT ( 'NONE', #2992 ) ;
#6565 = EDGE_CURVE ( 'NONE', #37401, #85779, #78661, .T. ) ;
#6566 = FACE_OUTER_BOUND ( 'NONE', #15968, .T. ) ;
#6567 = CARTESIAN_POINT ( 'NONE',  ( 8.992243613324164997, -8.282913670948747864, 34.94150082978203642 ) ) ;
#6568 = CARTESIAN_POINT ( 'NONE',  ( 16.21910172512217585, -2.625532179533470512, 30.86335684631491105 ) ) ;
#6569 = LINE ( 'NONE', #21410, #7852 ) ;
#6570 = ORIENTED_EDGE ( 'NONE', *, *, #88271, .T. ) ;
#6571 = CARTESIAN_POINT ( 'NONE',  ( 11.60371710973756620, -3.300289026998473041, 32.46337939537591666 ) ) ;
#6572 = CARTESIAN_POINT ( 'NONE',  ( -6.000000000000121680, -4.320704448113951379, 33.92786785259630022 ) ) ;
#6573 = CARTESIAN_POINT ( 'NONE',  ( 17.29970261819148192, -10.11255958852955672, 34.01340905677048454 ) ) ;
#6574 = LINE ( 'NONE', #33605, #21325 ) ;
#6575 = CARTESIAN_POINT ( 'NONE',  ( -13.38461538461550582, -10.90142922262034020, 33.41473453929536674 ) ) ;
#6576 = AXIS2_PLACEMENT_3D ( 'NONE', #65152, #37235, #15656 ) ;
#6577 = FACE_BOUND ( 'NONE', #2305, .T. ) ;
#6579 = CARTESIAN_POINT ( 'NONE',  ( 11.28843830116857383, -12.43535235679832596, 30.55408501211184813 ) ) ;
#6578 = CARTESIAN_POINT ( 'NONE',  ( -3.230769230769229949, -11.91647553114624181, 32.58852847137148245 ) ) ;
#6580 = EDGE_CURVE ( 'NONE', #54838, #3756, #72342, .T. ) ;
#6581 = EDGE_CURVE ( 'NONE', #49750, #47506, #30472, .T. ) ;
#6582 = DIRECTION ( 'NONE',  ( 0.000000000000000000, 0.4999999999999960032, -0.8660254037844410391 ) ) ;
#6584 = CARTESIAN_POINT ( 'NONE',  ( -2.084912638714241595, -12.47679350104403007, 31.42216943046555855 ) ) ;
#6583 = CARTESIAN_POINT ( 'NONE',  ( -8.638705067467203236, -11.93748526763465279, 32.05452791011430946 ) ) ;
#6585 = CARTESIAN_POINT ( 'NONE',  ( -5.326946301144534601, -12.45566812827425096, 31.48439005359158926 ) ) ;
#6586 = CARTESIAN_POINT ( 'NONE',  ( 0.06109907496454976272, -10.25000000000000000, 18.27938170625849068 ) ) ;
#6587 = ORIENTED_EDGE ( 'NONE', *, *, #63531, .F. ) ;
#6588 = CARTESIAN_POINT ( 'NONE',  ( -8.519230769230704325, -7.434744429011176159, 34.75000000000000711 ) ) ;
#6589 = ORIENTED_EDGE ( 'NONE', *, *, #17057, .F. ) ;
#6590 = CARTESIAN_POINT ( 'NONE',  ( -18.13014796973169851, -3.625366637846541007, 33.29286588640297850 ) ) ;
#6591 = ORIENTED_EDGE ( 'NONE', *, *, #9553, .F. ) ;
#6592 = DIRECTION ( 'NONE',  ( 0.000000000000000000, 1.000000000000000000, 0.000000000000000000 ) ) ;
#6593 = CARTESIAN_POINT ( 'NONE',  ( -16.02332071561251325, -12.15418822224088657, 32.17964115625579069 ) ) ;
#6596 = ORIENTED_EDGE ( 'NONE', *, *, #50969, .T. ) ;
#6595 = AXIS2_PLACEMENT_3D ( 'NONE', #54505, #33360, #41893 ) ;
#6594 = DIRECTION ( 'NONE',  ( -0.000000000000000000, -0.5000000000000009992, -0.8660254037844380415 ) ) ;
#6597 = CARTESIAN_POINT ( 'NONE',  ( -15.29603967673000575, -5.219633306516282545, 34.19971097300152962 ) ) ;
#6598 = CARTESIAN_POINT ( 'NONE',  ( -1.901340078031346525, -9.487747218494661183, 17.18563170625848713 ) ) ;
#6599 = DIRECTION ( 'NONE',  ( 0.000000000000000000, 1.000000000000000000, 0.000000000000000000 ) ) ;
#6600 = DIRECTION ( 'NONE',  ( -0.000000000000000000, -0.000000000000000000, 1.000000000000000000 ) ) ;
#6601 = CARTESIAN_POINT ( 'NONE',  ( -9.692307692307812417, -10.90142922262034020, 33.41473453929536674 ) ) ;
#6602 = LINE ( 'NONE', #12909, #78993 ) ;
#6603 = FACE_OUTER_BOUND ( 'NONE', #73604, .T. ) ;
#6604 = CARTESIAN_POINT ( 'NONE',  ( -2.121320343559653487, -5.378679656440369605, 14.00000000000000178 ) ) ;
#6605 = CARTESIAN_POINT ( 'NONE',  ( -2.608446859217920633, -4.805146000318815780, 24.25186829374150932 ) ) ;
#6606 = EDGE_CURVE ( 'NONE', #20850, #78839, #85868, .T. ) ;
#6607 = CARTESIAN_POINT ( 'NONE',  ( 3.100294045693512857, -7.276987145209184327, 34.99546412871779211 ) ) ;
#6608 = ORIENTED_EDGE ( 'NONE', *, *, #10778, .T. ) ;
#6609 = DIRECTION ( 'NONE',  ( 1.000000000000000000, 0.000000000000000000, 0.000000000000000000 ) ) ;
#6610 = CARTESIAN_POINT ( 'NONE',  ( -3.749999999999997780, -7.438900925035489387, 25.34561829374151642 ) ) ;
#6611 = CARTESIAN_POINT ( 'NONE',  ( 14.16025641025641235, -3.499999999999999556, 29.75000000000000355 ) ) ;
#6612 = CARTESIAN_POINT ( 'NONE',  ( -20.99999999999999645, -12.75000000000000178, 27.25000000000000000 ) ) ;
#6613 = ORIENTED_EDGE ( 'NONE', *, *, #18377, .T. ) ;
#6614 = CARTESIAN_POINT ( 'NONE',  ( 6.673076923076925127, -7.500000000000001776, 35.04278698407183867 ) ) ;
#6615 = CARTESIAN_POINT ( 'NONE',  ( -0.3310127597748996342, -10.19071101563364401, 33.96452234770657697 ) ) ;
#6617 = ORIENTED_EDGE ( 'NONE', *, *, #72018, .F. ) ;
#6616 = CARTESIAN_POINT ( 'NONE',  ( -20.74999999999999645, -10.50000000000000000, 27.25000000000000000 ) ) ;
#6618 = CARTESIAN_POINT ( 'NONE',  ( 0.4615384615384611200, -1.129524287112498415, 32.06866353760679544 ) ) ;
#6619 = CARTESIAN_POINT ( 'NONE',  ( -16.82692307692165556, -7.500000000000154543, 35.00000000000007105 ) ) ;
#6620 = VECTOR ( 'NONE', #30863, 1000.000000000000000 ) ;
#6621 = CYLINDRICAL_SURFACE ( 'NONE', #35656, 0.2500000000000002220 ) ;
#6622 = CARTESIAN_POINT ( 'NONE',  ( 3.165499230212911463, -2.657715359629089225, 31.77849191805834295 ) ) ;
#6623 = CARTESIAN_POINT ( 'NONE',  ( -18.00000000000000000, -12.10708131394839349, 31.69288490824020244 ) ) ;
#6624 = DIRECTION ( 'NONE',  ( 0.000000000000000000, 0.000000000000000000, 1.000000000000000000 ) ) ;
#6625 = ORIENTED_EDGE ( 'NONE', *, *, #70339, .F. ) ;
#6626 = EDGE_LOOP ( 'NONE', ( #78773, #26281, #23100, #22709 ) ) ;
#6627 = ORIENTED_EDGE ( 'NONE', *, *, #42062, .F. ) ;
#6628 = VERTEX_POINT ( 'NONE', #52070 ) ;
#6629 = CARTESIAN_POINT ( 'NONE',  ( 0.4615384615384611755, -11.33034616979429110, 35.88435417666054406 ) ) ;
#6630 = CARTESIAN_POINT ( 'NONE',  ( 14.05771557674995442, -4.236021600441997492, 33.53823185664189310 ) ) ;
#6631 = B_SPLINE_CURVE_WITH_KNOTS ( 'NONE', 3,
 ( #36530, #23439, #56786, #16686, #36951, #9060, #22562, #43283, #78829, #3165 ),
 .UNSPECIFIED., .F., .F.,
 ( 4, 2, 2, 2, 4 ),
 ( 0.0007817246256747473893, 0.0009771112852218905021, 0.001172497944769033615, 0.001367884604316176944, 0.001563271263863320057 ),
 .UNSPECIFIED. ) ;
#6632 = CARTESIAN_POINT ( 'NONE',  ( -25.00000000000000355, 9.999999999999971578, 3.000000000000000000 ) ) ;
#6633 = CARTESIAN_POINT ( 'NONE',  ( -17.20753273212715939, -7.722926974430166069, 34.99546784045485737 ) ) ;
#6634 = B_SPLINE_CURVE_WITH_KNOTS ( 'NONE', 3,
 ( #35439, #62891, #1204, #30449, #17384, #65559, #32238, #44841, #37648, #78194 ),
 .UNSPECIFIED., .F., .F.,
 ( 4, 2, 2, 2, 4 ),
 ( 0.000000000000000000, 0.0001954311564186871184, 0.0003908623128373742367, 0.0005862934692560614093, 0.0007817246256747484735 ),
 .UNSPECIFIED. ) ;
#6635 = CARTESIAN_POINT ( 'NONE',  ( 17.99999999999987566, -11.94971097300221174, 32.03036669348237098 ) ) ;
#6636 = ORIENTED_EDGE ( 'NONE', *, *, #33792, .T. ) ;
#6637 = VECTOR ( 'NONE', #33943, 1000.000000000000000 ) ;
#6638 = ORIENTED_EDGE ( 'NONE', *, *, #46515, .F. ) ;
#6639 = ORIENTED_EDGE ( 'NONE', *, *, #30742, .F. ) ;
#6641 = ORIENTED_EDGE ( 'NONE', *, *, #16725, .T. ) ;
#6640 = CARTESIAN_POINT ( 'NONE',  ( -6.923076923077045919, -8.656820664282941280, 34.87096338111179961 ) ) ;
#6642 = CARTESIAN_POINT ( 'NONE',  ( -0.7115151924808164052, -4.943428324936578910, 34.04746400365624481 ) ) ;
#6643 = CARTESIAN_POINT ( 'NONE',  ( 5.749976775778542937, -12.68155406624981119, 30.59749803192733708 ) ) ;
#6644 = DIRECTION ( 'NONE',  ( -0.000000000000000000, 0.5000000000000011102, -0.8660254037844380415 ) ) ;
#6645 = CARTESIAN_POINT ( 'NONE',  ( 10.03846153846153832, -1.926643599941765039, 29.65000000000000213 ) ) ;
#6646 = AXIS2_PLACEMENT_3D ( 'NONE', #7560, #21054, #48982 ) ;
#6647 = ORIENTED_EDGE ( 'NONE', *, *, #51633, .T. ) ;
#6648 = VERTEX_POINT ( 'NONE', #24603 ) ;
#6649 = ORIENTED_EDGE ( 'NONE', *, *, #86961, .F. ) ;
#6650 = CARTESIAN_POINT ( 'NONE',  ( -5.142247089727384868, -7.749976730030849303, 34.74374725381503737 ) ) ;
#6652 = ORIENTED_EDGE ( 'NONE', *, *, #18647, .T. ) ;
#6651 = CARTESIAN_POINT ( 'NONE',  ( -10.39237177129122003, -2.523321265292115534, 31.42251411153756990 ) ) ;
#6653 = CARTESIAN_POINT ( 'NONE',  ( -11.53846153846153655, -12.62096338111211580, 30.90682066428153263 ) ) ;
#6654 = CYLINDRICAL_SURFACE ( 'NONE', #14858, 0.2500000000000014988 ) ;
#6655 = ORIENTED_EDGE ( 'NONE', *, *, #65346, .F. ) ;
#6656 = CARTESIAN_POINT ( 'NONE',  ( 16.37662569511456567, -3.755027918224367767, 33.06320215134714857 ) ) ;
#6657 = DIRECTION ( 'NONE',  ( -0.000000000000000000, 0.5000000000000011102, -0.8660254037844381525 ) ) ;
#6658 = FACE_BOUND ( 'NONE', #30601, .T. ) ;
#6659 = CARTESIAN_POINT ( 'NONE',  ( 10.83816415665302380, -10.11255958852956027, 34.01340905677048454 ) ) ;
#6660 = CARTESIAN_POINT ( 'NONE',  ( 13.63456079399342791, -6.653508905675592722, 34.93172785388651391 ) ) ;
#6661 = EDGE_CURVE ( 'NONE', #72951, #35434, #9331, .T. ) ;
#6662 = CARTESIAN_POINT ( 'NONE',  ( 15.23076923076923173, -8.318370150425687726, 35.83090037661290239 ) ) ;
#6664 = CARTESIAN_POINT ( 'NONE',  ( -0.5268089074992368115, -12.27809138561121394, 31.22303859784730307 ) ) ;
#6663 = CARTESIAN_POINT ( 'NONE',  ( -10.61538461538461320, -9.584722331328613620, 36.20867863119891439 ) ) ;
#6665 = CIRCLE ( 'NONE', #57004, 5.000000000000000888 ) ;
#6666 = CARTESIAN_POINT ( 'NONE',  ( -4.087777802843714170, -2.721908614388772296, 31.22303859784725333 ) ) ;
#6667 = CARTESIAN_POINT ( 'NONE',  ( -3.903900744468110418, -11.56426240980093745, 33.07394671870546432 ) ) ;
#6668 = ORIENTED_EDGE ( 'NONE', *, *, #86809, .F. ) ;
#6669 = CARTESIAN_POINT ( 'NONE',  ( -7.976844449264153702, -6.369640206132551441, 34.87707690430378449 ) ) ;
#6670 = CARTESIAN_POINT ( 'NONE',  ( -7.976714437895769727, -2.504760397472875155, 29.97295953869789997 ) ) ;
#6671 = VERTEX_POINT ( 'NONE', #17411 ) ;
#6672 = AXIS2_PLACEMENT_3D ( 'NONE', #53142, #80646, #46836 ) ;
#6673 = LINE ( 'NONE', #18864, #41528 ) ;
#6674 = PRODUCT ( 'connector', 'connector', '', ( #46889 ) ) ;
#6675 = CARTESIAN_POINT ( 'NONE',  ( -4.376773112753001627, -3.395401636524186362, 33.02366814457250399 ) ) ;
#6676 = EDGE_LOOP ( 'NONE', ( #15043, #40540 ) ) ;
#6677 = DIRECTION ( 'NONE',  ( 0.000000000000000000, 0.8660254037844377084, -0.5000000000000015543 ) ) ;
#6678 = DIRECTION ( 'NONE',  ( 0.000000000000000000, -6.938893903907222067E-15, 1.000000000000000000 ) ) ;
#6679 = FACE_BOUND ( 'NONE', #80386, .T. ) ;
#6681 = CARTESIAN_POINT ( 'NONE',  ( 15.45354877203763877, -12.24180327182771855, 31.33663988360758879 ) ) ;
#6680 = FACE_OUTER_BOUND ( 'NONE', #20603, .T. ) ;
#6682 = CARTESIAN_POINT ( 'NONE',  ( 7.976679547917409963, -9.417988943895561960, 34.36773134775777550 ) ) ;
#6683 = EDGE_CURVE ( 'NONE', #9491, #40013, #42206, .T. ) ;
#6684 = VECTOR ( 'NONE', #54321, 1000.000000000000000 ) ;
#6685 = CARTESIAN_POINT ( 'NONE',  ( 2.372947878968333590, -5.219633306516380244, 34.19971097300157936 ) ) ;
#6687 = CARTESIAN_POINT ( 'NONE',  ( -0.4615384615384611200, -1.951392089020283160, 34.73218667398347748 ) ) ;
#6686 = CARTESIAN_POINT ( 'NONE',  ( 0.000000000000000000, 0.000000000000000000, 0.000000000000000000 ) ) ;
#6688 = CARTESIAN_POINT ( 'NONE',  ( -1.553300858899081538, -11.25000000000000711, 24.85937500000001421 ) ) ;
#6689 = ORIENTED_EDGE ( 'NONE', *, *, #58662, .T. ) ;
#6690 = ORIENTED_EDGE ( 'NONE', *, *, #44095, .T. ) ;
#6691 = CARTESIAN_POINT ( 'NONE',  ( -15.23076923076922995, -11.69971097300155272, 32.46337939537588113 ) ) ;
#6692 = CARTESIAN_POINT ( 'NONE',  ( -10.36533019547115941, -8.346898887586323923, 34.93166121998716278 ) ) ;
#6693 = DIRECTION ( 'NONE',  ( -0.000000000000000000, -0.6427876096865404731, -0.7660444431189770143 ) ) ;
#6694 = CARTESIAN_POINT ( 'NONE',  ( 6.857806477116148436, -12.27809138561121394, 31.22303859784730307 ) ) ;
#6695 = CARTESIAN_POINT ( 'NONE',  ( 5.207713517890028676, -3.338503747796866872, 32.95102852606553512 ) ) ;
#6696 = CARTESIAN_POINT ( 'NONE',  ( 3.749999999999999556, -7.438900925035446754, 17.96688170625848713 ) ) ;
#6697 = CARTESIAN_POINT ( 'NONE',  ( 0.5915860677941437995, -7.723484964179500700, 34.74522123443823318 ) ) ;
#6698 = CARTESIAN_POINT ( 'NONE',  ( 1.161130460051056357, -10.23692288466677880, 34.23039457007281072 ) ) ;
#6699 = CARTESIAN_POINT ( 'NONE',  ( 17.75002325595140817, -4.075325502946085976, 33.72974371597207721 ) ) ;
#6700 = DIRECTION ( 'NONE',  ( -1.000000000000000000, -0.000000000000000000, -0.000000000000000000 ) ) ;
#6701 = CARTESIAN_POINT ( 'NONE',  ( 18.25005431163831204, -9.943054286541403997, 34.11300777759954883 ) ) ;
#6702 = CARTESIAN_POINT ( 'NONE',  ( 6.250054419913455561, -6.523592122091591783, 34.90882529074906415 ) ) ;
#6703 = CARTESIAN_POINT ( 'NONE',  ( 6.988332062589760696, -3.643525952247864463, 33.31231777344670064 ) ) ;
#6704 = ADVANCED_FACE ( 'NONE', ( #57058 ), #32690, .F. ) ;
#6705 = DIRECTION ( 'NONE',  ( 0.000000000000000000, 0.3420201433256610524, 0.9396926207859113145 ) ) ;
#6706 = CARTESIAN_POINT ( 'NONE',  ( -12.59209905328038026, -2.504760397472875155, 29.97295953869789997 ) ) ;
#6707 = ORIENTED_EDGE ( 'NONE', *, *, #44492, .T. ) ;
#6708 = B_SPLINE_CURVE_WITH_KNOTS ( 'NONE', 3,
 ( #16728, #44184, #28481, #83437, #21720, #69905, #49191, #8215, #63139, #1454 ),
 .UNSPECIFIED., .F., .F.,
 ( 4, 2, 2, 2, 4 ),
 ( 0.000000000000000000, 0.0001954339857564080707, 0.0003908679715128161414, 0.0005863019572692241849, 0.0007817359430256322827 ),
 .UNSPECIFIED. ) ;
#6709 = CARTESIAN_POINT ( 'NONE',  ( 0.4615384615384611200, -8.564572088678739092, 35.78748833219616898 ) ) ;
#6710 = CARTESIAN_POINT ( 'NONE',  ( -17.30040800148741198, -6.716662450894490100, 34.94144148231605840 ) ) ;
#6711 = CARTESIAN_POINT ( 'NONE',  ( -2.724691934501246582, -6.299813628509474128, 21.67374329374151287 ) ) ;
#6712 = ADVANCED_FACE ( 'NONE', ( #66489 ), #86781, .F. ) ;
#6713 = EDGE_CURVE ( 'NONE', #84305, #59182, #63722, .T. ) ;
#6714 = LINE ( 'NONE', #48575, #2953 ) ;
#6715 = DIRECTION ( 'NONE',  ( 0.000000000000000000, 0.9396926207859126468, 0.3420201433256571111 ) ) ;
#6716 = CARTESIAN_POINT ( 'NONE',  ( -11.53846153846153655, -4.661471528628507777, 34.16647553114623292 ) ) ;
#6718 = EDGE_LOOP ( 'NONE', ( #71439, #24664, #38934, #23582 ) ) ;
#6717 = DIRECTION ( 'NONE',  ( -0.000000000000000000, -0.9848077530122086864, -0.1736481776669273613 ) ) ;
#6719 = CARTESIAN_POINT ( 'NONE',  ( 1.944543648262996083, -5.555456351736983045, 25.56250000000000355 ) ) ;
#6720 = CARTESIAN_POINT ( 'NONE',  ( -14.30769230769242917, -5.941354392335915335, 34.76329471203413846 ) ) ;
#6721 = CIRCLE ( 'NONE', #57038, 7.066647012551277918 ) ;
#6722 = VERTEX_POINT ( 'NONE', #4788 ) ;
#6723 = CARTESIAN_POINT ( 'NONE',  ( 11.66925197942848769, -9.084667340241226796, 34.75534355489798344 ) ) ;
#6724 = CARTESIAN_POINT ( 'NONE',  ( 10.83839745947800992, -10.77377354290276124, 33.85451476688484718 ) ) ;
#6725 = ORIENTED_EDGE ( 'NONE', *, *, #29681, .T. ) ;
#6726 = CARTESIAN_POINT ( 'NONE',  ( 16.82689983963011215, -11.37209801155882793, 32.91403422569033665 ) ) ;
#6727 = LINE ( 'NONE', #34200, #7691 ) ;
#6728 = CARTESIAN_POINT ( 'NONE',  ( 2.177001704582001818, -12.62707690430377383, 30.88035979386743435 ) ) ;
#6729 = EDGE_LOOP ( 'NONE', ( #27355, #62874 ) ) ;
#6730 = VERTEX_POINT ( 'NONE', #32263 ) ;
#6731 = CARTESIAN_POINT ( 'NONE',  ( 15.45378207486262667, -4.762714258010881885, 34.23016756924214832 ) ) ;
#6732 = EDGE_LOOP ( 'NONE', ( #22007, #12714, #55571, #82893, #84727, #32780, #29589, #11892, #20486, #69305, #45069, #41570, #8770, #19516, #76424, #88197, #86066, #77163, #13618, #60068, #66458, #56708, #17357, #40141, #77014, #86223, #6974, #14962, #58072, #65817, #48595, #69662, #76166, #49047, #7948, #45831, #8960, #29724, #48770, #78647, #11151, #80574, #43607, #4541, #80061, #17587, #65323, #24272, #34896, #23065, #26972, #74702, #84230, #24839, #30342, #61277, #20497, #29129, #47612, #44170, #50715, #77781, #14043, #14906, #39795, #47545, #49913, #87314, #87688, #88531, #22922, #85957, #1526, #18470, #10522, #19414, #23812, #10562, #89167, #28977, #73570, #4132, #86573, #37817, #8363, #6647 ) ) ;
#6733 = CARTESIAN_POINT ( 'NONE',  ( 3.296836564119306701, -11.91647553114624358, 32.58852847137148245 ) ) ;
#6734 = CARTESIAN_POINT ( 'NONE',  ( -9.469296340694841163, -9.886259254753566594, 34.14407573483972413 ) ) ;
#6735 = CARTESIAN_POINT ( 'NONE',  ( 9.692307692307695177, -9.058645607665452459, 34.76329471203371924 ) ) ;
#6736 = DIRECTION ( 'NONE',  ( -0.000000000000000000, 0.3420201433256694346, -0.9396926207859080948 ) ) ;
#6737 = CARTESIAN_POINT ( 'NONE',  ( 1.384615384615265343, -4.481592998941358097, 33.73612834414048933 ) ) ;
#6738 = CARTESIAN_POINT ( 'NONE',  ( -2.438252221305670542, -2.254533558242299396, 29.97296025877828285 ) ) ;
#6739 = AXIS2_PLACEMENT_3D ( 'NONE', #13130, #82040, #54100 ) ;
#6740 = B_SPLINE_CURVE_WITH_KNOTS ( 'NONE', 3,
 ( #22564, #1408, #57240, #29333, #36531, #63978, #15376, #2276, #64416, #56787 ),
 .UNSPECIFIED., .F., .F.,
 ( 4, 2, 2, 2, 4 ),
 ( 0.000000000000000000, 0.0001954311564186882026, 0.0003908623128373764051, 0.0005862934692560646619, 0.0007817246256747528103 ),
 .UNSPECIFIED. ) ;
#6741 = CARTESIAN_POINT ( 'NONE',  ( -12.68502340526241312, -6.760086850603066466, 34.69517049084099369 ) ) ;
#6742 = B_SPLINE_CURVE_WITH_KNOTS ( 'NONE', 3,
 ( #35407, #23115, #57784, #16359, #83163, #21454, #48923, #85267, #2385, #23548 ),
 .UNSPECIFIED., .F., .F.,
 ( 4, 2, 2, 2, 4 ),
 ( 0.0007817359430256252354, 0.0009771253907249898181, 0.001172514838424354401, 0.001367904286123718983, 0.001563293733823083566 ),
 .UNSPECIFIED. ) ;
#6743 = ADVANCED_FACE ( 'NONE', ( #18299 ), #66025, .F. ) ;
#6744 = ORIENTED_EDGE ( 'NONE', *, *, #63330, .T. ) ;
#6745 = ORIENTED_EDGE ( 'NONE', *, *, #14433, .F. ) ;
#6747 = ORIENTED_EDGE ( 'NONE', *, *, #86116, .T. ) ;
#6746 = CARTESIAN_POINT ( 'NONE',  ( 6.988332062589761584, -12.70778746994558439, 30.41441678777537305 ) ) ;
#6748 = CARTESIAN_POINT ( 'NONE',  ( 2.307692307692309264, -13.37000171582298513, 34.34916445242398453 ) ) ;
#6749 = CARTESIAN_POINT ( 'NONE',  ( -13.63461538461538503, -7.433932668274256805, 35.00000000000000711 ) ) ;
#6750 = CARTESIAN_POINT ( 'NONE',  ( 11.66925334628632704, -12.11778462344221019, 31.66786338562085135 ) ) ;
#6751 = VERTEX_POINT ( 'NONE', #69037 ) ;
#6752 = CARTESIAN_POINT ( 'NONE',  ( -12.46153846153846168, -5.557115091759785130, 34.35708131394839171 ) ) ;
#6753 = ADVANCED_FACE ( 'NONE', ( #34799 ), #62267, .F. ) ;
#6754 = ORIENTED_EDGE ( 'NONE', *, *, #75629, .T. ) ;
#6755 = CARTESIAN_POINT ( 'NONE',  ( -9.692307692307691624, -7.500000000000001776, 35.04278698407183867 ) ) ;
#6756 = ORIENTED_EDGE ( 'NONE', *, *, #4583, .F. ) ;
#6757 = LINE ( 'NONE', #7210, #21513 ) ;
#6758 = VECTOR ( 'NONE', #42515, 1000.000000000000000 ) ;
#6759 = ORIENTED_EDGE ( 'NONE', *, *, #22364, .T. ) ;
#6760 = CARTESIAN_POINT ( 'NONE',  ( 12.46153846153833911, -2.379036618888197729, 30.90682066428292885 ) ) ;
#6761 = CARTESIAN_POINT ( 'NONE',  ( 3.230769230769231726, -2.292212530054420494, 30.41441678777542634 ) ) ;
#6762 = FACE_BOUND ( 'NONE', #39766, .T. ) ;
#6763 = CARTESIAN_POINT ( 'NONE',  ( 14.30769230769231015, -1.129524287112498415, 32.06866353760679544 ) ) ;
#6764 = CARTESIAN_POINT ( 'NONE',  ( 12.22435897435897267, -7.500000000000000000, 29.75000000000000355 ) ) ;
#6765 = B_SPLINE_CURVE_WITH_KNOTS ( 'NONE', 3,
 ( #2560, #44425, #51620, #58387, #51172, #8898, #2127, #23717, #30051, #50743 ),
 .UNSPECIFIED., .F., .F.,
 ( 4, 2, 2, 2, 4 ),
 ( 0.0007817359430256315238, 0.0009771253907249976244, 0.001172514838424363508, 0.001367904286123729392, 0.001563293733823095492 ),
 .UNSPECIFIED. ) ;
#6766 = EDGE_CURVE ( 'NONE', #50121, #70789, #582, .T. ) ;
#6767 = CARTESIAN_POINT ( 'NONE',  ( -24.00000000000000000, -5.499999999999981348, 27.25000000000000000 ) ) ;
#6768 = CARTESIAN_POINT ( 'NONE',  ( 4.403900465484468896, -8.303483539816728154, 34.68545999027711702 ) ) ;
#6769 = CARTESIAN_POINT ( 'NONE',  ( -4.946397638689432164, -4.299079248970732792, 33.91157788607253565 ) ) ;
#6770 = FACE_OUTER_BOUND ( 'NONE', #47897, .T. ) ;
#6771 = AXIS2_PLACEMENT_3D ( 'NONE', #16870, #44319, #3798 ) ;
#6772 = CARTESIAN_POINT ( 'NONE',  ( 14.37294744720514572, -6.835583212224610072, 34.95778746994559327 ) ) ;
#6773 = EDGE_CURVE ( 'NONE', #48865, #4543, #11996, .T. ) ;
#6774 = EDGE_LOOP ( 'NONE', ( #17258, #68046, #58584, #42297, #2432 ) ) ;
#6775 = VERTEX_POINT ( 'NONE', #55516 ) ;
#6777 = DIRECTION ( 'NONE',  ( -0.000000000000000000, -0.9848077530122085754, -0.1736481776669273613 ) ) ;
#6776 = CARTESIAN_POINT ( 'NONE',  ( -16.94613126909828793, -9.804649428959608670, 34.18742332936588468 ) ) ;
#6778 = CARTESIAN_POINT ( 'NONE',  ( -9.692307692307814193, -12.51329471203414379, 31.30864560766407578 ) ) ;
#6779 = CARTESIAN_POINT ( 'NONE',  ( -14.30769230769230660, -11.91647553114624181, 32.58852847137148245 ) ) ;
#6780 = CARTESIAN_POINT ( 'NONE',  ( -17.20707104665477516, -12.50552854090298638, 31.33409797877408920 ) ) ;
#6781 = CARTESIAN_POINT ( 'NONE',  ( -12.21159305216042057, -4.932303261841489928, 34.32971442181322885 ) ) ;
#6782 = EDGE_LOOP ( 'NONE', ( #51489, #20979, #54498, #61337 ) ) ;
#6783 = DIRECTION ( 'NONE',  ( -0.000000000000000000, 1.000000000000000000, -0.000000000000000000 ) ) ;
#6784 = CARTESIAN_POINT ( 'NONE',  ( 14.16025641025641235, -11.50000000000000000, 29.75000000000000355 ) ) ;
#6785 = CARTESIAN_POINT ( 'NONE',  ( -3.296851610129365895, -11.35647404775217595, 33.31231777344666511 ) ) ;
#6786 = EDGE_CURVE ( 'NONE', #70777, #48900, #73243, .T. ) ;
#6787 = DIRECTION ( 'NONE',  ( 1.000000000000000000, 0.000000000000000000, 0.000000000000000000 ) ) ;
#6788 = VERTEX_POINT ( 'NONE', #75786 ) ;
#6789 = ORIENTED_EDGE ( 'NONE', *, *, #30004, .T. ) ;
#6791 = EDGE_CURVE ( 'NONE', #84846, #34142, #44404, .T. ) ;
#6790 = ORIENTED_EDGE ( 'NONE', *, *, #8197, .F. ) ;
#6792 = VECTOR ( 'NONE', #55177, 1000.000000000000000 ) ;
#6793 = FACE_OUTER_BOUND ( 'NONE', #60416, .T. ) ;
#6794 = ORIENTED_EDGE ( 'NONE', *, *, #62694, .T. ) ;
#6795 = ADVANCED_FACE ( 'NONE', ( #39027, #31822 ), #5227, .F. ) ;
#6796 = DIRECTION ( 'NONE',  ( 0.000000000000000000, -6.938893903907222067E-15, 1.000000000000000000 ) ) ;
#6797 = CARTESIAN_POINT ( 'NONE',  ( 15.10007776410167679, -8.999036380462717588, 34.52022231692819076 ) ) ;
#6798 = CARTESIAN_POINT ( 'NONE',  ( 18.00000000000000000, -8.120952969808772792, 34.71129190930000163 ) ) ;
#6799 = CARTESIAN_POINT ( 'NONE',  ( -17.20707104665477161, -9.504002272028873932, 34.60269587691767867 ) ) ;
#6800 = CARTESIAN_POINT ( 'NONE',  ( 9.915319043920545639, -5.667800583137506010, 34.40243808032445827 ) ) ;
#6801 = VERTEX_POINT ( 'NONE', #60161 ) ;
#6802 = CARTESIAN_POINT ( 'NONE',  ( -15.16470189741915320, -2.486705287966280320, 31.30864560766543647 ) ) ;
#6804 = VERTEX_POINT ( 'NONE', #26388 ) ;
#6803 = CARTESIAN_POINT ( 'NONE',  ( -0.7115152055870527237, -5.643011162660950042, 34.66104346484419096 ) ) ;
#6805 = CYLINDRICAL_SURFACE ( 'NONE', #18222, 0.2499999999999986955 ) ;
#6806 = CARTESIAN_POINT ( 'NONE',  ( -3.230769230769229949, -2.708943851104267164, 35.45975837776705220 ) ) ;
#6807 = DIRECTION ( 'NONE',  ( -1.000000000000000000, 0.000000000000000000, 0.000000000000000000 ) ) ;
#6808 = DIRECTION ( 'NONE',  ( -1.000000000000000000, 0.000000000000000000, 0.000000000000000000 ) ) ;
#6809 = CARTESIAN_POINT ( 'NONE',  ( 6.000000000000001776, -1.242168528481310874, 33.36296068462461051 ) ) ;
#6810 = EDGE_CURVE ( 'NONE', #49750, #33268, #48732, .T. ) ;
#6811 = LINE ( 'NONE', #41941, #40674 ) ;
#6812 = CARTESIAN_POINT ( 'NONE',  ( -11.00641025641025550, -3.499999999999999556, 29.75000000000000355 ) ) ;
#6813 = CARTESIAN_POINT ( 'NONE',  ( -2.749999999999999112, -7.438900925035484057, 22.84561829374151642 ) ) ;
#6814 = ORIENTED_EDGE ( 'NONE', *, *, #74797, .T. ) ;
#6815 = PLANE ( 'NONE',  #64702 ) ;
#6816 = CARTESIAN_POINT ( 'NONE',  ( 0.6845498131513094719, -3.105924265160262543, 32.13625925475356127 ) ) ;
#6817 = EDGE_CURVE ( 'NONE', #60898, #30751, #77567, .T. ) ;
#6818 = CARTESIAN_POINT ( 'NONE',  ( 9.758375025657770152, -10.67929555188718282, 33.92786785259544757 ) ) ;
#6819 = ORIENTED_EDGE ( 'NONE', *, *, #82316, .T. ) ;
#6820 = EDGE_CURVE ( 'NONE', #41209, #57354, #76657, .T. ) ;
#6821 = ORIENTED_EDGE ( 'NONE', *, *, #43391, .F. ) ;
#6822 = CARTESIAN_POINT ( 'NONE',  ( -5.869208192175211281, -2.541949514083464479, 30.39797389878540557 ) ) ;
#6823 = CARTESIAN_POINT ( 'NONE',  ( -3.230769230769352962, -5.094484230521993062, 34.41647553114689373 ) ) ;
#6824 = CARTESIAN_POINT ( 'NONE',  ( 10.74591005361826035, -5.070358843744210198, 34.40418822224088302 ) ) ;
#6825 = CARTESIAN_POINT ( 'NONE',  ( 6.989145274079363368, -5.557115091759786019, 34.35708131394839882 ) ) ;
#6826 = CARTESIAN_POINT ( 'NONE',  ( 18.00000000000000000, -2.486705287966279876, 31.30864560766543647 ) ) ;
#6827 = ORIENTED_EDGE ( 'NONE', *, *, #32526, .F. ) ;
#6828 = AXIS2_PLACEMENT_3D ( 'NONE', #2329, #59056, #86556 ) ;
#6829 = CARTESIAN_POINT ( 'NONE',  ( 6.250054311638314708, -5.728107161865375829, 34.42597550085002922 ) ) ;
#6830 = CARTESIAN_POINT ( 'NONE',  ( 3.296024802045256052, -12.27809138561124591, 31.22303859784720359 ) ) ;
#6831 = CARTESIAN_POINT ( 'NONE',  ( 5.142178216435913107, -12.51329471203373700, 31.30864560766537963 ) ) ;
#6832 = ORIENTED_EDGE ( 'NONE', *, *, #62487, .T. ) ;
#6833 = CARTESIAN_POINT ( 'NONE',  ( 7.846153846153846700, -1.790695186598648903, 34.54067556320373455 ) ) ;
#6834 = B_SPLINE_CURVE_WITH_KNOTS ( 'NONE', 3,
 ( #88968, #49285, #67788, #68233, #76763, #6534, #27238, #48834, #54704, #14615 ),
 .UNSPECIFIED., .F., .F.,
 ( 4, 2, 2, 2, 4 ),
 ( 0.000000000000000000, 0.0001954311564186873623, 0.0003908623128373747246, 0.0005862934692560620598, 0.0007817246256747494492 ),
 .UNSPECIFIED. ) ;
#6835 = VECTOR ( 'NONE', #62575, 1000.000000000000227 ) ;
#6836 = ORIENTED_EDGE ( 'NONE', *, *, #71965, .F. ) ;
#6837 = CARTESIAN_POINT ( 'NONE',  ( 1.161788692136382695, -7.369208160676172348, 34.74850200257122879 ) ) ;
#6838 = CARTESIAN_POINT ( 'NONE',  ( 11.28843831424007860, -2.588893531581426988, 31.60682220781847818 ) ) ;
#6839 = EDGE_LOOP ( 'NONE', ( #60946, #27921, #43809, #23205 ) ) ;
#6840 = VECTOR ( 'NONE', #49258, 1000.000000000000000 ) ;
#6841 = CARTESIAN_POINT ( 'NONE',  ( -17.77698715590660328, -10.01129605718032956, 34.36064277460058491 ) ) ;
#6842 = CARTESIAN_POINT ( 'NONE',  ( 4.376625822824220080, -9.418065098278011860, 34.63729479722530158 ) ) ;
#6843 = FACE_OUTER_BOUND ( 'NONE', #15745, .T. ) ;
#6844 = CARTESIAN_POINT ( 'NONE',  ( 11.53846153846141576, -12.51329471203414379, 31.30864560766407578 ) ) ;
#6845 = CARTESIAN_POINT ( 'NONE',  ( 3.480714749117373330, -12.43552623307873972, 30.55307653245132826 ) ) ;
#6846 = EDGE_CURVE ( 'NONE', #66812, #61417, #24180, .T. ) ;
#6847 = ORIENTED_EDGE ( 'NONE', *, *, #22304, .T. ) ;
#6848 = FACE_BOUND ( 'NONE', #17152, .T. ) ;
#6849 = ORIENTED_EDGE ( 'NONE', *, *, #59724, .F. ) ;
#6850 = DIRECTION ( 'NONE',  ( -0.000000000000000000, -0.9848077530122086864, -0.1736481776669273613 ) ) ;
#6851 = EDGE_CURVE ( 'NONE', #7007, #31488, #34702, .T. ) ;
#6852 = EDGE_CURVE ( 'NONE', #11900, #77704, #83899, .T. ) ;
#6853 = AXIS2_PLACEMENT_3D ( 'NONE', #39637, #81949, #32864 ) ;
#6854 = EDGE_CURVE ( 'NONE', #79445, #81564, #36932, .T. ) ;
#6855 = VECTOR ( 'NONE', #3008, 1000.000000000000114 ) ;
#6856 = FACE_OUTER_BOUND ( 'NONE', #79271, .T. ) ;
#6857 = CARTESIAN_POINT ( 'NONE',  ( 2.980746006547773330, -11.56360843649121861, 33.07473185843129926 ) ) ;
#6858 = DIRECTION ( 'NONE',  ( 1.000000000000000000, 0.000000000000000000, 0.000000000000000000 ) ) ;
#6859 = ORIENTED_EDGE ( 'NONE', *, *, #50072, .F. ) ;
#6860 = EDGE_CURVE ( 'NONE', #61382, #66664, #9543, .T. ) ;
#6861 = VECTOR ( 'NONE', #36062, 1000.000000000000000 ) ;
#6862 = ORIENTED_EDGE ( 'NONE', *, *, #1298, .F. ) ;
#6863 = ORIENTED_EDGE ( 'NONE', *, *, #79994, .F. ) ;
#6864 = CARTESIAN_POINT ( 'NONE',  ( -3.007989561791164945, -11.60474049983370648, 33.02348890104160262 ) ) ;
#6865 = EDGE_LOOP ( 'NONE', ( #18169, #87912 ) ) ;
#6866 = VECTOR ( 'NONE', #88282, 1000.000000000000227 ) ;
#6867 = CARTESIAN_POINT ( 'NONE',  ( 15.10007862765892206, -3.338472653186243644, 32.95098750199972670 ) ) ;
#6868 = DIRECTION ( 'NONE',  ( -0.000000000000000000, 0.3420201433256694346, -0.9396926207859080948 ) ) ;
#6869 = CARTESIAN_POINT ( 'NONE',  ( -7.976301815885543434, -3.625366637846544116, 33.29286588640298561 ) ) ;
#6870 = CARTESIAN_POINT ( 'NONE',  ( 3.903846153846154632, -2.499999999999998668, 29.75000000000000355 ) ) ;
#6871 = CARTESIAN_POINT ( 'NONE',  ( 3.750000000000000888, -7.499999999999978684, 24.46875000000000000 ) ) ;
#6872 = CARTESIAN_POINT ( 'NONE',  ( -2.531177251416254936, -5.113361153441932316, 34.14387501736621999 ) ) ;
#6873 = CARTESIAN_POINT ( 'NONE',  ( -6.923076923076922462, -12.29105614889573062, 35.45975837776705220 ) ) ;
#6874 = CARTESIAN_POINT ( 'NONE',  ( -8.519285359852727169, -2.986452184633680229, 32.43230066228895225 ) ) ;
#6875 = VERTEX_POINT ( 'NONE', #1905 ) ;
#6876 = ADVANCED_FACE ( 'NONE', ( #16310 ), #57290, .F. ) ;
#6877 = ORIENTED_EDGE ( 'NONE', *, *, #35665, .T. ) ;
#6878 = VERTEX_POINT ( 'NONE', #23066 ) ;
#6879 = CARTESIAN_POINT ( 'NONE',  ( -11.53846153846165912, -12.46129190930018460, 30.37095296980731973 ) ) ;
#6881 = CARTESIAN_POINT ( 'NONE',  ( -0.4615384615385840772, -8.656820664282941280, 34.87096338111179961 ) ) ;
#6880 = CARTESIAN_POINT ( 'NONE',  ( 1.515407192440173745, -5.582136614379148654, 34.36778462344220486 ) ) ;
#6882 = CARTESIAN_POINT ( 'NONE',  ( 11.53846153846153832, -2.292212530054420494, 30.41441678777542634 ) ) ;
#6883 = AXIS2_PLACEMENT_3D ( 'NONE', #86575, #24845, #18107 ) ;
#6884 = CARTESIAN_POINT ( 'NONE',  ( -10.86540785267757947, -3.711651800289232028, 33.01384336483936011 ) ) ;
#6885 = FACE_BOUND ( 'NONE', #9734, .T. ) ;
#6886 = CARTESIAN_POINT ( 'NONE',  ( -7.173100147298380413, -3.520140089381497361, 33.17453946501458262 ) ) ;
#6887 = VERTEX_POINT ( 'NONE', #50523 ) ;
#6888 = CARTESIAN_POINT ( 'NONE',  ( 7.911408985666682270, -2.379036618887895305, 30.90682066428158592 ) ) ;
#6889 = CARTESIAN_POINT ( 'NONE',  ( -1.254089682851821541, -2.882268652242222728, 31.66798894389554064 ) ) ;
#6890 = CARTESIAN_POINT ( 'NONE',  ( -17.07692307692307665, -3.886160181151819604, 36.00935417666054406 ) ) ;
#6891 = ORIENTED_EDGE ( 'NONE', *, *, #29407, .T. ) ;
#6892 = CARTESIAN_POINT ( 'NONE',  ( -13.38461538461538325, -4.786620604624113540, 33.94971097300155094 ) ) ;
#6893 = VECTOR ( 'NONE', #6343, 1000.000000000000227 ) ;
#6894 = ORIENTED_EDGE ( 'NONE', *, *, #65779, .T. ) ;
#6895 = FACE_BOUND ( 'NONE', #41773, .T. ) ;
#6896 = CARTESIAN_POINT ( 'NONE',  ( -15.90384615384615330, -2.499999999999999112, 29.81604066197449754 ) ) ;
#6897 = CARTESIAN_POINT ( 'NONE',  ( 15.23076923076923173, -13.49023893513002648, 31.06009739812518688 ) ) ;
#6898 = DIRECTION ( 'NONE',  ( 0.000000000000000000, 1.000000000000000000, 0.000000000000000000 ) ) ;
#6899 = VECTOR ( 'NONE', #1741, 1000.000000000000114 ) ;
#6900 = ORIENTED_EDGE ( 'NONE', *, *, #80438, .F. ) ;
#6901 = DIRECTION ( 'NONE',  ( -0.000000000000000000, 0.9396926207859093161, -0.3420201433256663259 ) ) ;
#6902 = LINE ( 'NONE', #66836, #8310 ) ;
#6903 = CARTESIAN_POINT ( 'NONE',  ( 12.46153846153846168, -6.386643153685126251, 34.62446782046654192 ) ) ;
#6904 = CARTESIAN_POINT ( 'NONE',  ( 1.384615384615265343, -6.879047030192662504, 34.71129190930017927 ) ) ;
#6905 = VERTEX_POINT ( 'NONE', #78005 ) ;
#6906 = DIRECTION ( 'NONE',  ( 1.734723475976812518E-16, -1.000000000000000000, 0.000000000000000000 ) ) ;
#6907 = CARTESIAN_POINT ( 'NONE',  ( -16.08859101433330707, -10.33852847137154107, 34.16647553114620450 ) ) ;
#6909 = ORIENTED_EDGE ( 'NONE', *, *, #29491, .T. ) ;
#6908 = DIRECTION ( 'NONE',  ( 0.000000000000000000, 0.000000000000000000, -1.000000000000000000 ) ) ;
#6910 = CARTESIAN_POINT ( 'NONE',  ( -4.284537620513712675, -2.541943142973490666, 30.39792223712631980 ) ) ;
#6911 = CARTESIAN_POINT ( 'NONE',  ( 16.81410256410256565, -3.499999999999999556, 29.75000000000000355 ) ) ;
#6912 = DIRECTION ( 'NONE',  ( -1.000000000000000000, -0.000000000000000000, -0.000000000000000000 ) ) ;
#6913 = CARTESIAN_POINT ( 'NONE',  ( 14.17700084102475522, -8.999036380462717588, 34.52022231692819076 ) ) ;
#6914 = CARTESIAN_POINT ( 'NONE',  ( 18.75000000000000000, -7.500000000000000000, 33.75000000000000000 ) ) ;
#6916 = CARTESIAN_POINT ( 'NONE',  ( 10.03846153846153832, -1.926643599941765039, 29.65000000000000213 ) ) ;
#6915 = CARTESIAN_POINT ( 'NONE',  ( -8.096130577096200653, -10.66389620160130036, 33.62221079203477103 ) ) ;
#6917 = EDGE_CURVE ( 'NONE', #68189, #15487, #37008, .T. ) ;
#6918 = ADVANCED_FACE ( 'NONE', ( #30270 ), #57738, .T. ) ;
#6919 = CARTESIAN_POINT ( 'NONE',  ( 9.692307692307695177, -8.973038597847269315, 34.52809138561121927 ) ) ;
#6920 = CARTESIAN_POINT ( 'NONE',  ( -2.749999999999991562, -8.639087296526025028, 17.51562500000000000 ) ) ;
#6921 = ORIENTED_EDGE ( 'NONE', *, *, #29572, .F. ) ;
#6922 = DIRECTION ( 'NONE',  ( -0.000000000000000000, -0.9848077530122086864, -0.1736481776669273613 ) ) ;
#6923 = ORIENTED_EDGE ( 'NONE', *, *, #13682, .F. ) ;
#6924 = EDGE_CURVE ( 'NONE', #20735, #50090, #31595, .T. ) ;
#6925 = AXIS2_PLACEMENT_3D ( 'NONE', #59193, #4707, #79478 ) ;
#6926 = ORIENTED_EDGE ( 'NONE', *, *, #47745, .T. ) ;
#6927 = CARTESIAN_POINT ( 'NONE',  ( 20.00000000000000355, 10.00000000000000533, 13.00000000000000178 ) ) ;
#6928 = EDGE_CURVE ( 'NONE', #85149, #35421, #44646, .T. ) ;
#6929 = ORIENTED_EDGE ( 'NONE', *, *, #2543, .F. ) ;
#6930 = CARTESIAN_POINT ( 'NONE',  ( -12.46153846153846168, -4.102666532097928531, 36.13435417666054406 ) ) ;
#6931 = CARTESIAN_POINT ( 'NONE',  ( -2.749999999999991562, -8.639087296526025028, 22.51562500000000000 ) ) ;
#6932 = CARTESIAN_POINT ( 'NONE',  ( -14.05763788777885637, -2.920487667080175598, 32.31805714834170828 ) ) ;
#6933 = DIRECTION ( 'NONE',  ( -0.000000000000000000, 0.3420201433256694901, -0.9396926207859082059 ) ) ;
#6934 = DIRECTION ( 'NONE',  ( 0.000000000000000000, 0.9396926207859126468, 0.3420201433256571111 ) ) ;
#6936 = CARTESIAN_POINT ( 'NONE',  ( -6.988346923633242724, -9.528491918058357157, 34.59228464037090589 ) ) ;
#6935 = AXIS2_PLACEMENT_3D ( 'NONE', #14383, #15274, #16154 ) ;
#6937 = CARTESIAN_POINT ( 'NONE',  ( 16.09615384615384670, -7.500000000000000000, 33.75000000000000000 ) ) ;
#6938 = DIRECTION ( 'NONE',  ( 0.000000000000000000, -6.938893903907222067E-15, 1.000000000000000000 ) ) ;
#6939 = ADVANCED_FACE ( 'NONE', ( #86561 ), #59062, .F. ) ;
#6940 = DIRECTION ( 'NONE',  ( -0.000000000000000000, -0.9848077530122086864, -0.1736481776669273613 ) ) ;
#6941 = CARTESIAN_POINT ( 'NONE',  ( 6.673100179028332413, -10.06842814019191401, 34.32929386961144758 ) ) ;
#6942 = CARTESIAN_POINT ( 'NONE',  ( 15.23076923076910916, -9.528491918059723176, 34.59228464037033035 ) ) ;
#6943 = AXIS2_PLACEMENT_3D ( 'NONE', #84942, #24554, #52021 ) ;
#6944 = EDGE_CURVE ( 'NONE', #4960, #30751, #85658, .T. ) ;
#6945 = DIRECTION ( 'NONE',  ( -0.000000000000000000, -0.3420201433256694901, -0.9396926207859082059 ) ) ;
#6946 = CARTESIAN_POINT ( 'NONE',  ( -9.942330916529147800, -3.520140089381495585, 33.17453946501458262 ) ) ;
#6947 = B_SPLINE_CURVE_WITH_KNOTS ( 'NONE', 3,
 ( #23232, #18263, #52030, #64207, #72747, #8074, #16921, #38082, #71862, #78619 ),
 .UNSPECIFIED., .F., .F.,
 ( 4, 2, 2, 2, 4 ),
 ( 0.000000000000000000, 0.0001954311584214072923, 0.0003908623168428145846, 0.0005862934752642218498, 0.0007817246336856291692 ),
 .UNSPECIFIED. ) ;
#6948 = ORIENTED_EDGE ( 'NONE', *, *, #25515, .T. ) ;
#6949 = EDGE_LOOP ( 'NONE', ( #61040, #37601, #63641, #78757, #20835, #88190, #51917, #53034, #28989, #28438 ) ) ;
#6950 = LINE ( 'NONE', #44704, #68720 ) ;
#6951 = CARTESIAN_POINT ( 'NONE',  ( 5.299934428535925335, -9.086983370893049639, 34.49168942202179267 ) ) ;
#6952 = CARTESIAN_POINT ( 'NONE',  ( -0.4615384615384611200, -6.681629849574314051, 35.83090037661290239 ) ) ;
#6953 = ADVANCED_FACE ( 'NONE', ( #78890 ), #16743, .F. ) ;
#6954 = CARTESIAN_POINT ( 'NONE',  ( 9.942362112221147186, -12.01375889529407281, 32.43194544308182969 ) ) ;
#6955 = B_SPLINE_CURVE_WITH_KNOTS ( 'NONE', 3,
 ( #4705, #32175, #86695, #18218, #25861, #79019, #31731, #59191, #10567, #45228 ),
 .UNSPECIFIED., .F., .F.,
 ( 4, 2, 2, 2, 4 ),
 ( 0.0007817359430256287049, 0.0009771253907249945886, 0.001172514838424360255, 0.001367904286123725922, 0.001563293733823091806 ),
 .UNSPECIFIED. ) ;
#6956 = CARTESIAN_POINT ( 'NONE',  ( 9.692307692307570832, -11.67786785259630911, 32.92929555188603530 ) ) ;
#6957 = CARTESIAN_POINT ( 'NONE',  ( -10.03846153846153832, -7.500000000000000000, 29.75000000000000355 ) ) ;
#6958 = CARTESIAN_POINT ( 'NONE',  ( 20.00000000000000000, -4.000000000000000000, 29.75000000000000355 ) ) ;
#6959 = ADVANCED_FACE ( 'NONE', ( #73486 ), #17188, .F. ) ;
#6960 = ORIENTED_EDGE ( 'NONE', *, *, #37205, .F. ) ;
#6961 = CARTESIAN_POINT ( 'NONE',  ( -14.53117723225664015, -12.69144148231606017, 30.53333754910549303 ) ) ;
#6962 = ORIENTED_EDGE ( 'NONE', *, *, #55480, .F. ) ;
#6963 = VECTOR ( 'NONE', #16964, 1000.000000000000000 ) ;
#6964 = EDGE_CURVE ( 'NONE', #64638, #27377, #31513, .T. ) ;
#6965 = CARTESIAN_POINT ( 'NONE',  ( 0.4615384615383382183, -5.094484230521993062, 34.41647553114689373 ) ) ;
#6966 = FACE_OUTER_BOUND ( 'NONE', #25400, .T. ) ;
#6967 = CARTESIAN_POINT ( 'NONE',  ( -7.173076923076921574, -7.500000000000001776, 35.00000000000000000 ) ) ;
#6968 = CARTESIAN_POINT ( 'NONE',  ( -15.48079246806219267, -3.202444869320336451, 32.30641848906366675 ) ) ;
#6969 = DIRECTION ( 'NONE',  ( -1.000000000000000000, -0.000000000000000000, -0.000000000000000000 ) ) ;
#6970 = VERTEX_POINT ( 'NONE', #11778 ) ;
#6971 = ADVANCED_FACE ( 'NONE', ( #79343 ), #86105, .F. ) ;
#6972 = ORIENTED_EDGE ( 'NONE', *, *, #63381, .F. ) ;
#6973 = EDGE_LOOP ( 'NONE', ( #85060, #43370 ) ) ;
#6974 = ORIENTED_EDGE ( 'NONE', *, *, #88867, .F. ) ;
#6975 = EDGE_CURVE ( 'NONE', #45215, #47964, #47624, .T. ) ;
#6976 = CARTESIAN_POINT ( 'NONE',  ( 17.07692307692307665, -9.905515769479276145, 34.41647553114623292 ) ) ;
#6977 = CARTESIAN_POINT ( 'NONE',  ( -12.52762084089859584, -12.62096338111211580, 30.90682066428152908 ) ) ;
#6978 = CARTESIAN_POINT ( 'NONE',  ( -3.480745961711584346, -9.943427161483782584, 34.11278801902876978 ) ) ;
#6979 = CARTESIAN_POINT ( 'NONE',  ( 16.28463796167094202, -9.804649428959608670, 34.18742332936588468 ) ) ;
#6980 = VECTOR ( 'NONE', #12241, 1000.000000000000227 ) ;
#6981 = CARTESIAN_POINT ( 'NONE',  ( -7.715363405186896451, -3.957578996910242619, 33.62503395064540257 ) ) ;
#6982 = CARTESIAN_POINT ( 'NONE',  ( -10.48485891362104816, -12.27024696741798948, 31.24895572276497546 ) ) ;
#6983 = ORIENTED_EDGE ( 'NONE', *, *, #23229, .T. ) ;
#6984 = EDGE_CURVE ( 'NONE', #13048, #61364, #51916, .T. ) ;
#6985 = EDGE_LOOP ( 'NONE', ( #87739, #6986, #36817, #66625 ) ) ;
#6986 = ORIENTED_EDGE ( 'NONE', *, *, #52585, .F. ) ;
#6987 = VECTOR ( 'NONE', #73678, 1000.000000000000227 ) ;
#6989 = ORIENTED_EDGE ( 'NONE', *, *, #785, .F. ) ;
#6988 = CARTESIAN_POINT ( 'NONE',  ( 9.692307692307570832, -6.835583212225970762, 34.95778746994575670 ) ) ;
#6990 = EDGE_CURVE ( 'NONE', #1652, #27448, #5018, .T. ) ;
#6991 = CARTESIAN_POINT ( 'NONE',  ( 17.14299041027315695, -10.67929555188718282, 33.92786785259544757 ) ) ;
#6992 = CARTESIAN_POINT ( 'NONE',  ( -12.39547112818838492, -11.91647553114624358, 32.58852847137148245 ) ) ;
#6993 = AXIS2_PLACEMENT_3D ( 'NONE', #58525, #42828, #86021 ) ;
#6994 = CARTESIAN_POINT ( 'NONE',  ( 1.553300858899129722, -11.24999999999999112, 18.45312499999999645 ) ) ;
#6995 = ORIENTED_EDGE ( 'NONE', *, *, #82028, .F. ) ;
#6996 = VECTOR ( 'NONE', #75423, 1000.000000000000000 ) ;
#6997 = ORIENTED_EDGE ( 'NONE', *, *, #38899, .T. ) ;
#6998 = CARTESIAN_POINT ( 'NONE',  ( 10.03846153846153832, -3.499999999999999556, 29.75000000000000355 ) ) ;
#6999 = FACE_BOUND ( 'NONE', #66921, .T. ) ;
#7000 = CARTESIAN_POINT ( 'NONE',  ( 4.826946332874483936, -4.818429247618089661, 34.26397095200675125 ) ) ;
#7001 = CARTESIAN_POINT ( 'NONE',  ( 4.153846153846154188, -2.249999999999998668, 29.50000000000001421 ) ) ;
#7002 = ORIENTED_EDGE ( 'NONE', *, *, #60808, .F. ) ;
#7003 = CARTESIAN_POINT ( 'NONE',  ( 3.230769230769231726, -12.78798330534102767, 29.49999999999997868 ) ) ;
#7004 = CARTESIAN_POINT ( 'NONE',  ( 6.673053698855464511, -12.07920672191015221, 32.31858351112116168 ) ) ;
#7005 = DIRECTION ( 'NONE',  ( -0.000000000000000000, -0.9848077530122085754, -0.1736481776669273613 ) ) ;
#7006 = LINE ( 'NONE', #69594, #82636 ) ;
#7007 = VERTEX_POINT ( 'NONE', #67165 ) ;
#7008 = CARTESIAN_POINT ( 'NONE',  ( 6.065255571276024327, -8.613356846314928816, 34.62446782046653482 ) ) ;
#7009 = CARTESIAN_POINT ( 'NONE',  ( -4.088591014333315066, -10.33852847137154107, 34.16647553114620450 ) ) ;
#7010 = LINE ( 'NONE', #12441, #31149 ) ;
#7011 = DIRECTION ( 'NONE',  ( -0.000000000000000000, 0.5000000000000011102, -0.8660254037844381525 ) ) ;
#7012 = DIRECTION ( 'NONE',  ( 0.000000000000000000, 1.000000000000000000, 0.000000000000000000 ) ) ;
#7013 = FACE_BOUND ( 'NONE', #15182, .T. ) ;
#7015 = CARTESIAN_POINT ( 'NONE',  ( -17.20707104665477516, -11.04286588640298561, 33.62463336215343901 ) ) ;
#7014 = CARTESIAN_POINT ( 'NONE',  ( -9.019230769230768274, -2.499999999999998668, 29.75000000000000355 ) ) ;
#7016 = FACE_OUTER_BOUND ( 'NONE', #84005, .T. ) ;
#7018 = CARTESIAN_POINT ( 'NONE',  ( 15.48071474911737333, -10.05730279482229683, 34.04704008940765902 ) ) ;
#7017 = CARTESIAN_POINT ( 'NONE',  ( -18.24997674404858827, -2.318417181685855422, 30.59732222474233865 ) ) ;
#7019 = CARTESIAN_POINT ( 'NONE',  ( -1.384615384615383471, -13.53365097954675988, 30.81389545987213552 ) ) ;
#7020 = CIRCLE ( 'NONE', #47273, 4.000000000000000000 ) ;
#7021 = CARTESIAN_POINT ( 'NONE',  ( -2.724691934501232371, -8.700186371490559623, 17.26375670625849068 ) ) ;
#7022 = ORIENTED_EDGE ( 'NONE', *, *, #8986, .F. ) ;
#7023 = CARTESIAN_POINT ( 'NONE',  ( -5.869474561766357290, -11.04252011169590020, 33.62494198852677130 ) ) ;
#7024 = ORIENTED_EDGE ( 'NONE', *, *, #49260, .T. ) ;
#7025 = DIRECTION ( 'NONE',  ( -0.000000000000000000, 0.6427876096865404731, -0.7660444431189771253 ) ) ;
#7026 = ORIENTED_EDGE ( 'NONE', *, *, #15358, .F. ) ;
#7027 = DIRECTION ( 'NONE',  ( 0.000000000000000000, 0.000000000000000000, 1.000000000000000000 ) ) ;
#7028 = ADVANCED_FACE ( 'NONE', ( #25732 ), #19859, .F. ) ;
#7029 = LINE ( 'NONE', #88592, #15737 ) ;
#7031 = ORIENTED_EDGE ( 'NONE', *, *, #38234, .T. ) ;
#7030 = CARTESIAN_POINT ( 'NONE',  ( -9.561782254074051579, -11.66157788607254098, 32.95092075102925833 ) ) ;
#7032 = CARTESIAN_POINT ( 'NONE',  ( 17.77717190236512224, -7.369209533119136069, 34.99857337881830688 ) ) ;
#7033 = CARTESIAN_POINT ( 'NONE',  ( -1.200186371490556958, -4.775308065498765409, 18.82625670625848713 ) ) ;
#7034 = DIRECTION ( 'NONE',  ( -0.000000000000000000, -0.6427876096865404731, -0.7660444431189770143 ) ) ;
#7035 = FACE_OUTER_BOUND ( 'NONE', #25856, .T. ) ;
#7036 = DIRECTION ( 'NONE',  ( 1.000000000000000000, 0.000000000000000000, 0.000000000000000000 ) ) ;
#7037 = CARTESIAN_POINT ( 'NONE',  ( 19.00000000000000000, -7.500000000000000000, 29.75000000000000355 ) ) ;
#7038 = CARTESIAN_POINT ( 'NONE',  ( 6.923076923076924238, -4.098570777380720287, 33.41473453929634729 ) ) ;
#7039 = CARTESIAN_POINT ( 'NONE',  ( 7.846153846153846700, -6.343179335718451384, 34.87096338111211935 ) ) ;
#7040 = EDGE_CURVE ( 'NONE', #42225, #2251, #81131, .T. ) ;
#7041 = B_SPLINE_CURVE_WITH_KNOTS ( 'NONE', 3,
 ( #34169, #13453, #87364, #80604, #32845, #18888, #53551, #19334, #46356, #25196 ),
 .UNSPECIFIED., .F., .F.,
 ( 4, 2, 2, 2, 4 ),
 ( 0.0007817359430256315238, 0.0009771253907249980580, 0.001172514838424364592, 0.001367904286123730910, 0.001563293733823097444 ),
 .UNSPECIFIED. ) ;
#7042 = CARTESIAN_POINT ( 'NONE',  ( 3.724691934501251023, -9.114399933863618131, 24.79874329374151998 ) ) ;
#7043 = CARTESIAN_POINT ( 'NONE',  ( -18.00000000000012079, -11.67786785259630733, 32.92929555188604240 ) ) ;
#7044 = DIRECTION ( 'NONE',  ( -0.000000000000000000, 1.000000000000000000, -0.000000000000000000 ) ) ;
#7045 = B_SPLINE_CURVE_WITH_KNOTS ( 'NONE', 3,
 ( #42625, #68761, #7059, #28209, #83169, #21460, #13370, #21004, #56575, #13814 ),
 .UNSPECIFIED., .F., .F.,
 ( 4, 2, 2, 2, 4 ),
 ( 0.000000000000000000, 0.0001954339881912763499, 0.0003908679763825526998, 0.0005863019645738316247, 0.0007817359527651106038 ),
 .UNSPECIFIED. ) ;
#7046 = EDGE_LOOP ( 'NONE', ( #36217, #44593, #5072, #64822, #89091, #69780 ) ) ;
#7047 = EDGE_CURVE ( 'NONE', #535, #10551, #71215, .T. ) ;
#7048 = CARTESIAN_POINT ( 'NONE',  ( 9.019176287578908102, -10.05730279482229683, 34.04704008940765902 ) ) ;
#7049 = B_SPLINE_CURVE_WITH_KNOTS ( 'NONE', 3,
 ( #62821, #56529, #37134, #23625, #70932, #8350, #43017, #84021, #9242, #85339 ),
 .UNSPECIFIED., .F., .F.,
 ( 4, 2, 2, 2, 4 ),
 ( 0.0007817359430256304396, 0.0009771253907249963233, 0.001172514838424362424, 0.001367904286123728524, 0.001563293733823094408 ),
 .UNSPECIFIED. ) ;
#7050 = CARTESIAN_POINT ( 'NONE',  ( 3.775308065498752086, -6.007798216065404873, 23.39249329374151642 ) ) ;
#7051 = CARTESIAN_POINT ( 'NONE',  ( 2.307692307692309264, -4.661471528628507777, 34.16647553114623292 ) ) ;
#7053 = CARTESIAN_POINT ( 'NONE',  ( 4.088523238353977796, -7.749976743299137993, 34.99404534957040624 ) ) ;
#7052 = AXIS2_PLACEMENT_3D ( 'NONE', #49722, #56486, #85291 ) ;
#7054 = EDGE_LOOP ( 'NONE', ( #33026, #20969, #20577, #49044 ) ) ;
#7055 = CARTESIAN_POINT ( 'NONE',  ( -4.153846153846274980, -2.657715359629662988, 31.77849191805970364 ) ) ;
#7056 = CARTESIAN_POINT ( 'NONE',  ( -14.53061852520844965, -11.24512374952581872, 33.06303171183252942 ) ) ;
#7058 = EDGE_LOOP ( 'NONE', ( #32320, #9191 ) ) ;
#7057 = CARTESIAN_POINT ( 'NONE',  ( 8.769230769230768274, -1.215029322943914858, 32.30358669280327177 ) ) ;
#7059 = CARTESIAN_POINT ( 'NONE',  ( -8.069032528582491537, -7.630691491037285168, 34.74850469731151748 ) ) ;
#7060 = CARTESIAN_POINT ( 'NONE',  ( -17.14267650523641251, -7.249945578846654470, 34.99404164642496795 ) ) ;
#7061 = VECTOR ( 'NONE', #54276, 1000.000000000000227 ) ;
#7063 = ADVANCED_FACE ( 'NONE', ( #75683 ), #88348, .F. ) ;
#7062 = CARTESIAN_POINT ( 'NONE',  ( -10.54931728203453822, -9.058645607665452459, 34.76329471203371924 ) ) ;
#7064 = VECTOR ( 'NONE', #82267, 1000.000000000000227 ) ;
#7065 = CARTESIAN_POINT ( 'NONE',  ( 5.010839665967194989, -4.098570777380720287, 33.41473453929634729 ) ) ;
#7066 = CARTESIAN_POINT ( 'NONE',  ( -13.51476259405360203, -11.93770438780619259, 32.05411857736982029 ) ) ;
#7067 = ORIENTED_EDGE ( 'NONE', *, *, #36613, .F. ) ;
#7068 = ORIENTED_EDGE ( 'NONE', *, *, #75334, .T. ) ;
#7069 = EDGE_CURVE ( 'NONE', #75335, #83859, #64663, .T. ) ;
#7070 = EDGE_LOOP ( 'NONE', ( #54166, #66474 ) ) ;
#7071 = LINE ( 'NONE', #89070, #77224 ) ;
#7072 = PLANE ( 'NONE',  #81771 ) ;
#7073 = EDGE_CURVE ( 'NONE', #11434, #5312, #13171, .T. ) ;
#7074 = DIRECTION ( 'NONE',  ( -0.000000000000000000, 1.000000000000000000, -0.000000000000000000 ) ) ;
#7075 = CARTESIAN_POINT ( 'NONE',  ( -17.32692307692308020, -7.566082377512564960, 35.00000000000000711 ) ) ;
#7076 = CARTESIAN_POINT ( 'NONE',  ( 17.20744851515671670, -11.66157788607254275, 32.95092075102925833 ) ) ;
#7077 = B_SPLINE_CURVE_WITH_KNOTS ( 'NONE', 3,
 ( #86059, #50906, #84299, #2731, #22576, #37865, #57253, #10398, #30227, #24337 ),
 .UNSPECIFIED., .F., .F.,
 ( 4, 2, 2, 2, 4 ),
 ( 0.000000000000000000, 0.0001954311564186860613, 0.0003908623128373721225, 0.0005862934692560581567, 0.0007817246256747442451 ),
 .UNSPECIFIED. ) ;
#7078 = ORIENTED_EDGE ( 'NONE', *, *, #4318, .F. ) ;
#7079 = EDGE_LOOP ( 'NONE', ( #35890, #9296, #56081, #20142 ) ) ;
#7080 = EDGE_CURVE ( 'NONE', #29264, #39978, #24963, .T. ) ;
#7081 = ORIENTED_EDGE ( 'NONE', *, *, #44105, .T. ) ;
#7083 = VERTEX_POINT ( 'NONE', #74366 ) ;
#7082 = CARTESIAN_POINT ( 'NONE',  ( -7.146561847641254239, -8.539481045369598178, 34.89627647299170832 ) ) ;
#7084 = CARTESIAN_POINT ( 'NONE',  ( -14.30769230769230660, -8.810774026931790459, 35.74407628777942847 ) ) ;
#7085 = VECTOR ( 'NONE', #67739, 1000.000000000000114 ) ;
#7086 = CARTESIAN_POINT ( 'NONE',  ( -2.307692307692305711, -2.486705287966279876, 31.30864560766543647 ) ) ;
#7087 = CARTESIAN_POINT ( 'NONE',  ( 6.988332062589761584, -5.094484230520773593, 34.41647553114626845 ) ) ;
#7088 = DIRECTION ( 'NONE',  ( -0.000000000000000000, 0.8660254037844397068, -0.4999999999999978906 ) ) ;
#7089 = ORIENTED_EDGE ( 'NONE', *, *, #10205, .T. ) ;
#7090 = EDGE_CURVE ( 'NONE', #4584, #45693, #57182, .T. ) ;
#7091 = ORIENTED_EDGE ( 'NONE', *, *, #28640, .F. ) ;
#7092 = ORIENTED_EDGE ( 'NONE', *, *, #85130, .T. ) ;
#7093 = DIRECTION ( 'NONE',  ( -0.000000000000000000, 1.000000000000000000, -0.000000000000000000 ) ) ;
#7095 = ORIENTED_EDGE ( 'NONE', *, *, #38218, .F. ) ;
#7094 = LINE ( 'NONE', #12527, #34376 ) ;
#7096 = CARTESIAN_POINT ( 'NONE',  ( -11.31544869436814338, -12.64618726649961289, 30.78989965857442712 ) ) ;
#7097 = ADVANCED_FACE ( 'NONE', ( #70261 ), #917, .F. ) ;
#7098 = EDGE_CURVE ( 'NONE', #7083, #44733, #55416, .T. ) ;
#7099 = FACE_OUTER_BOUND ( 'NONE', #54374, .T. ) ;
#7100 = VERTEX_POINT ( 'NONE', #28844 ) ;
#7101 = CARTESIAN_POINT ( 'NONE',  ( 16.28437185560972011, -3.816742781228458448, 33.13167719472716044 ) ) ;
#7102 = CARTESIAN_POINT ( 'NONE',  ( 12.52760579488853665, -9.058645607665452459, 34.76329471203371924 ) ) ;
#7103 = ORIENTED_EDGE ( 'NONE', *, *, #44196, .F. ) ;
#7104 = FACE_BOUND ( 'NONE', #40317, .T. ) ;
#7105 = EDGE_CURVE ( 'NONE', #35739, #24943, #82901, .T. ) ;
#7106 = DIRECTION ( 'NONE',  ( -0.000000000000000000, 1.000000000000000000, 3.491481338843133355E-15 ) ) ;
#7107 = CARTESIAN_POINT ( 'NONE',  ( 13.63466980452883881, -6.523592122091592671, 34.90882529074906415 ) ) ;
#7108 = CYLINDRICAL_SURFACE ( 'NONE', #27931, 0.2499999999999994726 ) ;
#7111 = CARTESIAN_POINT ( 'NONE',  ( 4.826899839630108602, -10.05641848906368097, 34.04755513067966177 ) ) ;
#7110 = VECTOR ( 'NONE', #52517, 1000.000000000000114 ) ;
#7109 = CARTESIAN_POINT ( 'NONE',  ( 18.06606733335007675, -2.833524468853757750, 32.15551576947925838 ) ) ;
#7112 = VECTOR ( 'NONE', #45288, 1000.000000000000000 ) ;
#7113 = CYLINDRICAL_SURFACE ( 'NONE', #29474, 0.2500000000000002220 ) ;
#7114 = DIRECTION ( 'NONE',  ( -0.000000000000000000, 0.6427876096865404731, -0.7660444431189771253 ) ) ;
#7115 = EDGE_LOOP ( 'NONE', ( #80553, #1662 ) ) ;
#7116 = CARTESIAN_POINT ( 'NONE',  ( 14.55774661933062042, -12.41262288849542017, 30.68299917996395010 ) ) ;
#7117 = CARTESIAN_POINT ( 'NONE',  ( -15.84615384615384670, -3.499999999999999556, 29.75000000000000355 ) ) ;
#7118 = B_SPLINE_CURVE_WITH_KNOTS ( 'NONE', 3,
 ( #33060, #12788, #5145, #60527, #53770, #60969, #26744, #54204, #32610, #81257 ),
 .UNSPECIFIED., .F., .F.,
 ( 4, 2, 2, 2, 4 ),
 ( 0.000000000000000000, 0.0001954311564186879044, 0.0003908623128373758088, 0.0005862934692560636861, 0.0007817246256747516176 ),
 .UNSPECIFIED. ) ;
#7119 = AXIS2_PLACEMENT_3D ( 'NONE', #389, #13449, #55760 ) ;
#7120 = EDGE_LOOP ( 'NONE', ( #75564, #24034 ) ) ;
#7121 = CIRCLE ( 'NONE', #43123, 0.2500000000000002220 ) ;
#7122 = VECTOR ( 'NONE', #46272, 1000.000000000000000 ) ;
#7123 = LINE ( 'NONE', #35477, #25711 ) ;
#7124 = CARTESIAN_POINT ( 'NONE',  ( -7.623141002060451754, -2.308499170217967134, 30.53291367094873721 ) ) ;
#7125 = B_SPLINE_CURVE_WITH_KNOTS ( 'NONE', 3,
 ( #26719, #54179, #54622, #41566, #60944, #585, #55078, #20412, #47424, #61377 ),
 .UNSPECIFIED., .F., .F.,
 ( 4, 2, 2, 2, 4 ),
 ( 0.000000000000000000, 0.0001954339857564075286, 0.0003908679715128150572, 0.0005863019572692225586, 0.0007817359430256301143 ),
 .UNSPECIFIED. ) ;
#7126 = ORIENTED_EDGE ( 'NONE', *, *, #1679, .T. ) ;
#7127 = CARTESIAN_POINT ( 'NONE',  ( -19.99999999999996803, 15.00000000000000711, 13.00000000000000178 ) ) ;
#7128 = CARTESIAN_POINT ( 'NONE',  ( -9.019254006523732770, -5.851115903089112003, 34.47074536777953568 ) ) ;
#7129 = FACE_BOUND ( 'NONE', #24342, .T. ) ;
#7131 = CARTESIAN_POINT ( 'NONE',  ( 15.29683758177167441, -12.10708131394839704, 31.69288490824020954 ) ) ;
#7130 = CARTESIAN_POINT ( 'NONE',  ( -18.00000000000012079, -3.300289026999231545, 32.46337939537709616 ) ) ;
#7132 = CARTESIAN_POINT ( 'NONE',  ( -13.51476335434707821, -2.373036134822904319, 30.88089517874952250 ) ) ;
#7133 = CARTESIAN_POINT ( 'NONE',  ( 1.449870524128224814, -12.70778746994558439, 30.41441678777537305 ) ) ;
#7135 = CARTESIAN_POINT ( 'NONE',  ( 2.307692307692187583, -3.300289026999228881, 32.46337939537708905 ) ) ;
#7134 = CARTESIAN_POINT ( 'NONE',  ( 0.000000000000000000, 0.000000000000000000, 0.000000000000000000 ) ) ;
#7136 = DIRECTION ( 'NONE',  ( 0.000000000000000000, 1.000000000000000000, 8.673617379884033500E-16 ) ) ;
#7137 = CARTESIAN_POINT ( 'NONE',  ( 2.694853999681214862, -10.10844685921789043, 15.62313170625848890 ) ) ;
#7138 = ORIENTED_EDGE ( 'NONE', *, *, #64704, .F. ) ;
#7139 = VERTEX_POINT ( 'NONE', #16202 ) ;
#7140 = CARTESIAN_POINT ( 'NONE',  ( 5.142991427925513115, -6.386643153685127139, 34.62446782046654192 ) ) ;
#7141 = CARTESIAN_POINT ( 'NONE',  ( -15.48079245499068612, -5.765609946408404518, 34.70566812827425451 ) ) ;
#7142 = CARTESIAN_POINT ( 'NONE',  ( 16.21991348719623360, -2.833524468853757750, 32.15551576947925838 ) ) ;
#7143 = CARTESIAN_POINT ( 'NONE',  ( -8.835313148590902443, -8.164416787775445883, 34.95778746994557906 ) ) ;
#7144 = CARTESIAN_POINT ( 'NONE',  ( -16.37733109757011007, -12.24155766932282496, 31.33739205006857986 ) ) ;
#7145 = CARTESIAN_POINT ( 'NONE',  ( 3.775308065498768517, -8.992201783934554271, 16.79500670625849068 ) ) ;
#7146 = CARTESIAN_POINT ( 'NONE',  ( 6.673100179028331524, -2.318417181685854978, 30.59732222474233865 ) ) ;
#7147 = DIRECTION ( 'NONE',  ( 0.000000000000000000, -0.000000000000000000, 1.000000000000000000 ) ) ;
#7148 = CARTESIAN_POINT ( 'NONE',  ( 3.230769230769108269, -4.320704448113951379, 33.92786785259630022 ) ) ;
#7149 = CARTESIAN_POINT ( 'NONE',  ( 1.384615384615386802, -5.557115091759785130, 34.35708131394839171 ) ) ;
#7150 = CARTESIAN_POINT ( 'NONE',  ( -15.16551365949320562, -11.48612834413965977, 32.76840700105972815 ) ) ;
#7151 = CARTESIAN_POINT ( 'NONE',  ( 16.15384615384615330, -4.786620604624113540, 33.94971097300155094 ) ) ;
#7152 = CARTESIAN_POINT ( 'NONE',  ( -3.480792454990687013, -10.18141759479407327, 34.26406193332782379 ) ) ;
#7153 = B_SPLINE_CURVE_WITH_KNOTS ( 'NONE', 3,
 ( #67679, #60913, #26688, #61343, #54145, #88858, #38203, #77093, #2301, #36116 ),
 .UNSPECIFIED., .F., .F.,
 ( 4, 2, 2, 2, 4 ),
 ( 0.000000000000000000, 0.0001954311564186854107, 0.0003908623128373708215, 0.0005862934692560562051, 0.0007817246256747416430 ),
 .UNSPECIFIED. ) ;
#7154 = LINE ( 'NONE', #80613, #57776 ) ;
#7155 = CYLINDRICAL_SURFACE ( 'NONE', #52862, 0.2500000000000008882 ) ;
#7156 = B_SPLINE_CURVE_WITH_KNOTS ( 'NONE', 3,
 ( #11825, #39303, #12259, #4159, #5059, #32523, #65423, #23980, #31644, #3273 ),
 .UNSPECIFIED., .F., .F.,
 ( 4, 2, 2, 2, 4 ),
 ( 0.000000000000000000, 0.0001954339857564097512, 0.0003908679715128195024, 0.0005863019572692292807, 0.0007817359430256390048 ),
 .UNSPECIFIED. ) ;
#7157 = ORIENTED_EDGE ( 'NONE', *, *, #86706, .T. ) ;
#7158 = AXIS2_PLACEMENT_3D ( 'NONE', #11010, #72700, #33055 ) ;
#7160 = CARTESIAN_POINT ( 'NONE',  ( -0.3310127597748955264, -3.816742781228458448, 33.13167719472716044 ) ) ;
#7159 = B_SPLINE_CURVE_WITH_KNOTS ( 'NONE', 3,
 ( #10991, #66820, #85320, #10546, #73132, #18643, #65482, #51495, #23602, #58719 ),
 .UNSPECIFIED., .F., .F.,
 ( 4, 2, 2, 2, 4 ),
 ( 0.0007817246256747460882, 0.0009771112852218900684, 0.001172497944769033832, 0.001367884604316177595, 0.001563271263863321575 ),
 .UNSPECIFIED. ) ;
#7161 = CARTESIAN_POINT ( 'NONE',  ( 7.623226887246995709, -4.762599654559228846, 34.23009711892697737 ) ) ;
#7162 = CARTESIAN_POINT ( 'NONE',  ( -1.987747218494638313, -9.401340078031370950, 23.93936829374151642 ) ) ;
#7163 = DIRECTION ( 'NONE',  ( -0.000000000000000000, -5.102127870520021228E-17, -1.000000000000000000 ) ) ;
#7164 = CYLINDRICAL_SURFACE ( 'NONE', #80075, 0.2499999999999986955 ) ;
#7165 = VERTEX_POINT ( 'NONE', #55856 ) ;
#7166 = CARTESIAN_POINT ( 'NONE',  ( -9.692307692307691624, -5.471508081941601098, 34.59228464037088457 ) ) ;
#7168 = ORIENTED_EDGE ( 'NONE', *, *, #86757, .T. ) ;
#7167 = CARTESIAN_POINT ( 'NONE',  ( -5.749999999998578915, -7.500000000000154543, 35.00000000000007105 ) ) ;
#7169 = CARTESIAN_POINT ( 'NONE',  ( -2.749999999999991562, -8.639087296526026805, 22.51562500000000000 ) ) ;
#7170 = CARTESIAN_POINT ( 'NONE',  ( -5.011667505647053211, -10.21337939537593620, 33.94971097300152252 ) ) ;
#7171 = VERTEX_POINT ( 'NONE', #49550 ) ;
#7172 = DIRECTION ( 'NONE',  ( 1.734723475976813504E-16, -1.000000000000000000, 0.000000000000000000 ) ) ;
#7173 = DIRECTION ( 'NONE',  ( -0.000000000000000000, -0.000000000000000000, 1.000000000000000000 ) ) ;
#7174 = ORIENTED_EDGE ( 'NONE', *, *, #88331, .T. ) ;
#7175 = CARTESIAN_POINT ( 'NONE',  ( 6.923076923076924238, -1.951392089020283160, 34.73218667398347748 ) ) ;
#7176 = CARTESIAN_POINT ( 'NONE',  ( 2.530705151785704210, -8.282913670948747864, 34.94150082978203642 ) ) ;
#7178 = CARTESIAN_POINT ( 'NONE',  ( 2.057715563643717882, -12.65889640711025521, 30.72598325615533454 ) ) ;
#7177 = AXIS2_PLACEMENT_3D ( 'NONE', #70355, #36135, #63587 ) ;
#7179 = ORIENTED_EDGE ( 'NONE', *, *, #39305, .T. ) ;
#7180 = EDGE_LOOP ( 'NONE', ( #43433, #77292, #3193, #88759 ) ) ;
#7181 = CARTESIAN_POINT ( 'NONE',  ( -6.857009589726848375, -8.164416787775445883, 34.95778746994558617 ) ) ;
#7182 = EDGE_CURVE ( 'NONE', #68002, #14815, #50414, .T. ) ;
#7183 = ORIENTED_EDGE ( 'NONE', *, *, #62280, .T. ) ;
#7184 = CIRCLE ( 'NONE', #40303, 5.000000000000000888 ) ;
#7185 = AXIS2_PLACEMENT_3D ( 'NONE', #85524, #86436, #17959 ) ;
#7186 = DIRECTION ( 'NONE',  ( -0.000000000000000000, 0.6427876096865404731, -0.7660444431189771253 ) ) ;
#7187 = CARTESIAN_POINT ( 'NONE',  ( 12.52679403281448600, -9.442884908240273489, 34.35708131394835618 ) ) ;
#7188 = CARTESIAN_POINT ( 'NONE',  ( -1.607542343522232464, -11.43668979543635089, 33.22377378376089752 ) ) ;
#7189 = LINE ( 'NONE', #27018, #85069 ) ;
#7190 = FACE_OUTER_BOUND ( 'NONE', #50073, .T. ) ;
#7191 = CARTESIAN_POINT ( 'NONE',  ( -2.307692307691991296, -2.255955759149395501, 30.00000000000324363 ) ) ;
#7192 = VECTOR ( 'NONE', #52780, 1000.000000000000227 ) ;
#7193 = VECTOR ( 'NONE', #16509, 1000.000000000000000 ) ;
#7194 = AXIS2_PLACEMENT_3D ( 'NONE', #5623, #12823, #20901 ) ;
#7195 = CARTESIAN_POINT ( 'NONE',  ( 10.39245839786846659, -12.15238873228292071, 31.58232369045353849 ) ) ;
#7196 = ORIENTED_EDGE ( 'NONE', *, *, #12757, .F. ) ;
#7197 = EDGE_CURVE ( 'NONE', #49278, #78341, #42361, .T. ) ;
#7198 = VERTEX_POINT ( 'NONE', #29726 ) ;
#7200 = ORIENTED_EDGE ( 'NONE', *, *, #8617, .F. ) ;
#7199 = CARTESIAN_POINT ( 'NONE',  ( 18.13079044096694759, -9.084667340241228572, 34.75534355489798344 ) ) ;
#7201 = CARTESIAN_POINT ( 'NONE',  ( -5.076923076923075762, -4.661471528628507777, 34.16647553114623292 ) ) ;
#7202 = ORIENTED_EDGE ( 'NONE', *, *, #15942, .T. ) ;
#7203 = CARTESIAN_POINT ( 'NONE',  ( -13.25377705412862106, -7.277220318596961057, 34.99547417642776992 ) ) ;
#7204 = DIRECTION ( 'NONE',  ( -0.000000000000000000, 0.8660254037844399289, -0.4999999999999980016 ) ) ;
#7205 = ORIENTED_EDGE ( 'NONE', *, *, #69818, .T. ) ;
#7206 = CARTESIAN_POINT ( 'NONE',  ( -9.942307692307691624, -2.499999999999998668, 29.75000000000000355 ) ) ;
#7207 = ORIENTED_EDGE ( 'NONE', *, *, #80705, .T. ) ;
#7208 = CARTESIAN_POINT ( 'NONE',  ( -16.08859101433330707, -5.941354392334603496, 34.76329471203374055 ) ) ;
#7209 = EDGE_LOOP ( 'NONE', ( #36281, #17636, #10798, #64824 ) ) ;
#7210 = CARTESIAN_POINT ( 'NONE',  ( -22.75000000000000000, -2.249999999999999556, 27.25000000000000000 ) ) ;
#7211 = B_SPLINE_CURVE_WITH_KNOTS ( 'NONE', 3,
 ( #3012, #85009, #10233, #15663, #57965, #30925, #23290, #23725, #58393, #85889 ),
 .UNSPECIFIED., .F., .F.,
 ( 4, 2, 2, 2, 4 ),
 ( 0.000000000000000000, 0.0001954311564186871455, 0.0003908623128373742909, 0.0005862934692560614093, 0.0007817246256747485819 ),
 .UNSPECIFIED. ) ;
#7212 = EDGE_CURVE ( 'NONE', #18418, #51867, #48565, .T. ) ;
#7213 = EDGE_CURVE ( 'NONE', #60134, #54717, #27036, .T. ) ;
#7214 = ORIENTED_EDGE ( 'NONE', *, *, #52463, .T. ) ;
#7215 = CARTESIAN_POINT ( 'NONE',  ( -6.857821783564084228, -5.094484230520773593, 34.41647553114626845 ) ) ;
#7216 = B_SPLINE_CURVE_WITH_KNOTS ( 'NONE', 3,
 ( #18766, #20090, #75044, #88577, #12883, #13770, #40374, #89014, #67390, #33160 ),
 .UNSPECIFIED., .F., .F.,
 ( 4, 2, 2, 2, 4 ),
 ( 0.000000000000000000, 0.0001954311564186875792, 0.0003908623128373751583, 0.0005862934692560627103, 0.0007817246256747503166 ),
 .UNSPECIFIED. ) ;
#7217 = VECTOR ( 'NONE', #57206, 1000.000000000000000 ) ;
#7218 = CARTESIAN_POINT ( 'NONE',  ( 16.85399685940693004, -2.758268499246657068, 31.33685645148948851 ) ) ;
#7219 = FACE_BOUND ( 'NONE', #83397, .T. ) ;
#7220 = CARTESIAN_POINT ( 'NONE',  ( -3.230769230769229949, -7.500000000000001776, 35.04278698407183867 ) ) ;
#7221 = DIRECTION ( 'NONE',  ( 0.000000000000000000, 0.8660254037844377084, -0.5000000000000015543 ) ) ;
#7222 = CARTESIAN_POINT ( 'NONE',  ( -15.93106648486808119, -4.989023458446560255, 34.36081565061822118 ) ) ;
#7224 = EDGE_CURVE ( 'NONE', #48794, #53001, #68992, .T. ) ;
#7223 = CARTESIAN_POINT ( 'NONE',  ( 10.61538461538461675, -9.905515769479276145, 34.41647553114623292 ) ) ;
#7225 = CARTESIAN_POINT ( 'NONE',  ( 18.00000000000000000, -6.386643153685126251, 34.62446782046654192 ) ) ;
#7226 = FACE_OUTER_BOUND ( 'NONE', #77540, .T. ) ;
#7227 = CYLINDRICAL_SURFACE ( 'NONE', #74890, 0.2499999999999997502 ) ;
#7228 = ORIENTED_EDGE ( 'NONE', *, *, #72529, .T. ) ;
#7229 = ORIENTED_EDGE ( 'NONE', *, *, #44604, .T. ) ;
#7231 = DIRECTION ( 'NONE',  ( -0.000000000000000000, 1.000000000000000000, -0.000000000000000000 ) ) ;
#7230 = CARTESIAN_POINT ( 'NONE',  ( -17.07692307692319744, -10.21337939537710326, 33.94971097300076224 ) ) ;
#7232 = CARTESIAN_POINT ( 'NONE',  ( -11.60454494941741999, -11.69971097300155272, 32.46337939537587403 ) ) ;
#7233 = FACE_OUTER_BOUND ( 'NONE', #4059, .T. ) ;
#7234 = DIRECTION ( 'NONE',  ( 0.000000000000000000, 0.9396926207859126468, -0.3420201433256571111 ) ) ;
#7235 = LINE ( 'NONE', #14885, #30321 ) ;
#7236 = EDGE_LOOP ( 'NONE', ( #23234, #40364, #3451, #87851 ) ) ;
#7237 = CARTESIAN_POINT ( 'NONE',  ( -5.300408001487404874, -5.827078755546623690, 34.72654668319379567 ) ) ;
#7238 = CARTESIAN_POINT ( 'NONE',  ( 1.607394925883796510, -12.24180327182771855, 31.33663988360758168 ) ) ;
#7239 = CARTESIAN_POINT ( 'NONE',  ( -8.834501215191544077, -12.27809138561121394, 31.22303859784730307 ) ) ;
#7240 = VECTOR ( 'NONE', #63373, 1000.000000000000114 ) ;
#7241 = CARTESIAN_POINT ( 'NONE',  ( 3.100622021331011169, -3.285722584762969856, 32.44110544564090759 ) ) ;
#7242 = VERTEX_POINT ( 'NONE', #9013 ) ;
#7243 = ORIENTED_EDGE ( 'NONE', *, *, #4840, .T. ) ;
#7244 = CIRCLE ( 'NONE', #57574, 4.000000000000000000 ) ;
#7245 = VERTEX_POINT ( 'NONE', #49980 ) ;
#7246 = CARTESIAN_POINT ( 'NONE',  ( -9.692307692307691624, -12.37446782046654192, 30.86335684631486131 ) ) ;
#7247 = ORIENTED_EDGE ( 'NONE', *, *, #50545, .T. ) ;
#7248 = B_SPLINE_CURVE_WITH_KNOTS ( 'NONE', 3,
 ( #26167, #33375, #66712, #25726, #60835, #81567, #18529, #5012, #74360, #18971 ),
 .UNSPECIFIED., .F., .F.,
 ( 4, 2, 2, 2, 4 ),
 ( 0.0007817359430256326080, 0.0009771253907249993591, 0.001172514838424366327, 0.001367904286123733078, 0.001563293733823099829 ),
 .UNSPECIFIED. ) ;
#7249 = CARTESIAN_POINT ( 'NONE',  ( -9.822999158975250111, -12.38065189839062263, 30.83690757178629482 ) ) ;
#7250 = CARTESIAN_POINT ( 'NONE',  ( 15.36155967173618286, -3.957578996910242619, 33.62503395064540257 ) ) ;
#7251 = DIRECTION ( 'NONE',  ( -0.000000000000000000, -0.9848077530122085754, -0.1736481776669273613 ) ) ;
#7252 = CARTESIAN_POINT ( 'NONE',  ( 3.750000000000000888, -7.499999999999978684, 14.46875000000000000 ) ) ;
#7253 = VECTOR ( 'NONE', #38968, 1000.000000000000000 ) ;
#7254 = VECTOR ( 'NONE', #55735, 1000.000000000000227 ) ;
#7255 = CARTESIAN_POINT ( 'NONE',  ( 9.692307692307695177, -5.557115091759785130, 34.35708131394839171 ) ) ;
#7256 = ORIENTED_EDGE ( 'NONE', *, *, #66349, .F. ) ;
#7258 = CARTESIAN_POINT ( 'NONE',  ( 4.283891209765926966, -2.254550872974306674, 29.97347326024527447 ) ) ;
#7257 = AXIS2_PLACEMENT_3D ( 'NONE', #54875, #54423, #69277 ) ;
#7260 = ORIENTED_EDGE ( 'NONE', *, *, #27981, .F. ) ;
#7259 = CARTESIAN_POINT ( 'NONE',  ( -11.53846153846166089, -11.67786785259630911, 32.92929555188603530 ) ) ;
#7261 = CARTESIAN_POINT ( 'NONE',  ( -17.01085574357300345, -8.164416787775445883, 34.95778746994558617 ) ) ;
#7262 = CYLINDRICAL_SURFACE ( 'NONE', #9622, 0.2499999999999995559 ) ;
#7263 = DIRECTION ( 'NONE',  ( 0.000000000000000000, 0.000000000000000000, -1.000000000000000000 ) ) ;
#7264 = CARTESIAN_POINT ( 'NONE',  ( -6.923076923076922462, -12.78798330534102767, 29.49999999999997868 ) ) ;
#7265 = CARTESIAN_POINT ( 'NONE',  ( 2.307692307692309264, -2.486705287966279876, 31.30864560766543647 ) ) ;
#7266 = CARTESIAN_POINT ( 'NONE',  ( -3.230769230769352962, -11.06231777344772027, 33.60647404775119895 ) ) ;
#7267 = CARTESIAN_POINT ( 'NONE',  ( -0.6850233861027952287, -2.612411019501189369, 31.66733052389439962 ) ) ;
#7268 = CARTESIAN_POINT ( 'NONE',  ( -1.901340078031369618, -5.512252781505359245, 19.25186829374151287 ) ) ;
#7269 = ORIENTED_EDGE ( 'NONE', *, *, #54079, .F. ) ;
#7270 = CARTESIAN_POINT ( 'NONE',  ( -3.164701897419154975, -6.343179335718452272, 34.87096338111212646 ) ) ;
#7271 = DIRECTION ( 'NONE',  ( 0.000000000000000000, 0.000000000000000000, 1.000000000000000000 ) ) ;
#7272 = CARTESIAN_POINT ( 'NONE',  ( 8.068933387422251968, -2.600157965045225783, 30.74683119005207743 ) ) ;
#7273 = CARTESIAN_POINT ( 'NONE',  ( -13.31854703361294767, -8.120952969808772792, 34.71129190929999453 ) ) ;
#7274 = ORIENTED_EDGE ( 'NONE', *, *, #45958, .F. ) ;
#7275 = CARTESIAN_POINT ( 'NONE',  ( 2.373858914283949240, -7.250054591869667497, 34.99404684341514127 ) ) ;
#7276 = CARTESIAN_POINT ( 'NONE',  ( 11.47237915910140771, -3.937682226553330445, 33.60647404775217240 ) ) ;
#7277 = ADVANCED_FACE ( 'NONE', ( #15768 ), #62172, .F. ) ;
#7278 = CARTESIAN_POINT ( 'NONE',  ( -1.161604033002533454, -6.503523203565942268, 34.64991518177335195 ) ) ;
#7279 = LINE ( 'NONE', #49143, #84516 ) ;
#7280 = CARTESIAN_POINT ( 'NONE',  ( -14.30769230769230660, -2.833524468853757305, 32.15551576947925838 ) ) ;
#7281 = ORIENTED_EDGE ( 'NONE', *, *, #39271, .F. ) ;
#7282 = CARTESIAN_POINT ( 'NONE',  ( -12.23852710992561121, -9.086983370893049639, 34.49168942202179267 ) ) ;
#7283 = CARTESIAN_POINT ( 'NONE',  ( 3.361561038594018669, -12.11778462344221019, 31.66786338562085135 ) ) ;
#7284 = CYLINDRICAL_SURFACE ( 'NONE', #30659, 0.2499999999999994726 ) ;
#7286 = EDGE_LOOP ( 'NONE', ( #59348, #15601, #28024, #83746 ) ) ;
#7285 = AXIS2_PLACEMENT_3D ( 'NONE', #284, #32733, #25978 ) ;
#7287 = LINE ( 'NONE', #13158, #2437 ) ;
#7288 = ADVANCED_FACE ( 'NONE', ( #63934 ), #2231, .F. ) ;
#7289 = ORIENTED_EDGE ( 'NONE', *, *, #38087, .T. ) ;
#7290 = B_SPLINE_CURVE_WITH_KNOTS ( 'NONE', 3,
 ( #67759, #80396, #39414, #18693, #60106, #88064, #4274, #86724, #40295, #17802 ),
 .UNSPECIFIED., .F., .F.,
 ( 4, 2, 2, 2, 4 ),
 ( 0.0007817246256747457630, 0.0009771112852218887673, 0.001172497944769031880, 0.001367884604316174993, 0.001563271263863318106 ),
 .UNSPECIFIED. ) ;
#7291 = CARTESIAN_POINT ( 'NONE',  ( -2.307692307692305711, -12.10708131394839349, 31.69288490824020244 ) ) ;
#7292 = CARTESIAN_POINT ( 'NONE',  ( 11.60371667797437567, -6.835583212224610072, 34.95778746994559327 ) ) ;
#7293 = VERTEX_POINT ( 'NONE', #31032 ) ;
#7294 = B_SPLINE_CURVE_WITH_KNOTS ( 'NONE', 3,
 ( #55805, #1751, #13936, #42751, #41865, #15720, #83294, #28794, #69333, #87907 ),
 .UNSPECIFIED., .F., .F.,
 ( 4, 2, 2, 2, 4 ),
 ( 0.0007817246256747507503, 0.0009771112852218959231, 0.001172497944769040987, 0.001367884604316186052, 0.001563271263863331116 ),
 .UNSPECIFIED. ) ;
#7295 = ADVANCED_FACE ( 'NONE', ( #85549 ), #58955, .F. ) ;
#7296 = CARTESIAN_POINT ( 'NONE',  ( 7.622668902429896143, -12.24155766932282496, 31.33739205006857986 ) ) ;
#7297 = CARTESIAN_POINT ( 'NONE',  ( 4.403791563224197070, -9.357781135181031829, 34.66075350412533851 ) ) ;
#7298 = CARTESIAN_POINT ( 'NONE',  ( 13.31853197365950692, -6.386643153685125363, 34.62446782046654903 ) ) ;
#7299 = CARTESIAN_POINT ( 'NONE',  ( 4.826923076923076650, -2.499999999999998668, 29.75000000000000355 ) ) ;
#7300 = CARTESIAN_POINT ( 'NONE',  ( 3.361561038594017781, -12.38066358083363738, 30.83685684665853444 ) ) ;
#7301 = EDGE_LOOP ( 'NONE', ( #88865, #12964, #41411, #27718 ) ) ;
#7302 = VECTOR ( 'NONE', #32279, 1000.000000000000000 ) ;
#7303 = EDGE_CURVE ( 'NONE', #16925, #38200, #58064, .T. ) ;
#7304 = FACE_BOUND ( 'NONE', #4685, .T. ) ;
#7305 = ORIENTED_EDGE ( 'NONE', *, *, #41393, .T. ) ;
#7306 = CARTESIAN_POINT ( 'NONE',  ( -8.769230769230768274, -12.34228464037088635, 31.77849191805839268 ) ) ;
#7307 = VECTOR ( 'NONE', #27504, 1000.000000000000227 ) ;
#7308 = EDGE_CURVE ( 'NONE', #53380, #12502, #85104, .T. ) ;
#7309 = CARTESIAN_POINT ( 'NONE',  ( 18.22301135161285046, -12.15243808032446005, 31.58219941686247978 ) ) ;
#7310 = LINE ( 'NONE', #41987, #10453 ) ;
#7311 = CARTESIAN_POINT ( 'NONE',  ( -7.134615384615385025, -7.500000000000000000, 29.75000000000000355 ) ) ;
#7312 = VECTOR ( 'NONE', #71477, 1000.000000000000000 ) ;
#7313 = ORIENTED_EDGE ( 'NONE', *, *, #17589, .F. ) ;
#7314 = ORIENTED_EDGE ( 'NONE', *, *, #4130, .F. ) ;
#7315 = VERTEX_POINT ( 'NONE', #9882 ) ;
#7316 = CARTESIAN_POINT ( 'NONE',  ( -10.83886953994894675, -8.539481045369596401, 34.89627647299170832 ) ) ;
#7317 = EDGE_LOOP ( 'NONE', ( #51929, #19614, #55066, #88928 ) ) ;
#7318 = EDGE_CURVE ( 'NONE', #64772, #24285, #29985, .T. ) ;
#7319 = B_SPLINE_CURVE_WITH_KNOTS ( 'NONE', 3,
 ( #17342, #53342, #46154, #52450, #31302, #39410, #65070, #3376, #86266, #11035 ),
 .UNSPECIFIED., .F., .F.,
 ( 4, 2, 2, 2, 4 ),
 ( 0.0007817359430256278375, 0.0009771253907249935044, 0.001172514838424359171, 0.001367904286123724838, 0.001563293733823090505 ),
 .UNSPECIFIED. ) ;
#7320 = CARTESIAN_POINT ( 'NONE',  ( 15.23076923076923173, -3.322132147404559976, 32.92929555188717927 ) ) ;
#7321 = EDGE_CURVE ( 'NONE', #76030, #46479, #65704, .T. ) ;
#7322 = CARTESIAN_POINT ( 'NONE',  ( -6.857883934782265989, -2.255955759149235629, 29.99999999999988631 ) ) ;
#7323 = CARTESIAN_POINT ( 'NONE',  ( -1.384615384615383471, -9.905515769479276145, 34.41647553114623292 ) ) ;
#7324 = CARTESIAN_POINT ( 'NONE',  ( 16.37685899793955357, -2.308499170217968022, 30.53291367094874076 ) ) ;
#7325 = ADVANCED_FACE ( 'NONE', ( #51277 ), #24275, .F. ) ;
#7326 = CARTESIAN_POINT ( 'NONE',  ( 2.320192649118979489E-14, -11.25000000000000000, 24.78125000000000000 ) ) ;
#7327 = CARTESIAN_POINT ( 'NONE',  ( -14.17716686945866655, -12.70449254468099198, 30.44128974285582956 ) ) ;
#7328 = EDGE_CURVE ( 'NONE', #63430, #31770, #67882, .T. ) ;
#7329 = CARTESIAN_POINT ( 'NONE',  ( 4.023698184114453014, -2.647304123082328875, 31.75400227202885262 ) ) ;
#7330 = CARTESIAN_POINT ( 'NONE',  ( 17.29993442853592711, -2.554770724473668597, 30.48948780036025852 ) ) ;
#7331 = ORIENTED_EDGE ( 'NONE', *, *, #54372, .F. ) ;
#7332 = B_SPLINE_CURVE_WITH_KNOTS ( 'NONE', 3,
 ( #67523, #74731, #88263, #12579, #33298, #13454, #53998, #48121, #40065, #54437 ),
 .UNSPECIFIED., .F., .F.,
 ( 4, 2, 2, 2, 4 ),
 ( 0.000000000000000000, 0.0001954311564186872810, 0.0003908623128373745620, 0.0005862934692560618430, 0.0007817246256747491240 ),
 .UNSPECIFIED. ) ;
#7333 = ORIENTED_EDGE ( 'NONE', *, *, #49393, .F. ) ;
#7334 = ORIENTED_EDGE ( 'NONE', *, *, #88402, .F. ) ;
#7335 = CYLINDRICAL_SURFACE ( 'NONE', #56041, 0.2499999999999997502 ) ;
#7337 = CARTESIAN_POINT ( 'NONE',  ( -13.44988583057615905, -6.026961402152685388, 34.52809138561120506 ) ) ;
#7336 = LINE ( 'NONE', #82108, #69095 ) ;
#7338 = AXIS2_PLACEMENT_3D ( 'NONE', #12274, #12720, #39759 ) ;
#7339 = FACE_OUTER_BOUND ( 'NONE', #40458, .T. ) ;
#7340 = DIRECTION ( 'NONE',  ( -0.000000000000000000, -0.9396926207859092051, -0.3420201433256662704 ) ) ;
#7341 = LINE ( 'NONE', #70814, #81779 ) ;
#7342 = LINE ( 'NONE', #82115, #24528 ) ;
#7343 = EDGE_LOOP ( 'NONE', ( #69651, #78962, #11450, #67844 ) ) ;
#7344 = DIRECTION ( 'NONE',  ( 0.000000000000000000, 0.6427876096865373645, -0.7660444431189797898 ) ) ;
#7345 = CARTESIAN_POINT ( 'NONE',  ( -15.84615384615384670, -3.499999999999999556, 29.75000000000000355 ) ) ;
#7346 = FACE_OUTER_BOUND ( 'NONE', #50999, .T. ) ;
#7347 = CARTESIAN_POINT ( 'NONE',  ( -3.230769230769352962, -3.643525952248796163, 33.31231777344771672 ) ) ;
#7348 = VECTOR ( 'NONE', #75930, 1000.000000000000000 ) ;
#7349 = VERTEX_POINT ( 'NONE', #4002 ) ;
#7350 = CARTESIAN_POINT ( 'NONE',  ( 18.13052570176356326, -12.45806712695776319, 30.39783852428763566 ) ) ;
#7351 = ORIENTED_EDGE ( 'NONE', *, *, #10327, .T. ) ;
#7352 = FACE_BOUND ( 'NONE', #45153, .T. ) ;
#7353 = CARTESIAN_POINT ( 'NONE',  ( 20.00000000000000000, -4.000000000000000000, 29.75000000000000355 ) ) ;
#7354 = B_SPLINE_CURVE_WITH_KNOTS ( 'NONE', 3,
 ( #1122, #35805, #85646, #52293, #23925, #57724, #51835, #71674, #18078, #79782 ),
 .UNSPECIFIED., .F., .F.,
 ( 4, 2, 2, 2, 4 ),
 ( 0.000000000000000000, 0.0001954339857564082062, 0.0003908679715128164124, 0.0005863019572692246186, 0.0007817359430256328248 ),
 .UNSPECIFIED. ) ;
#7355 = LINE ( 'NONE', #55085, #14659 ) ;
#7356 = CARTESIAN_POINT ( 'NONE',  ( 17.01165307636676260, -12.16647553114622049, 32.15551576947930812 ) ) ;
#7357 = ORIENTED_EDGE ( 'NONE', *, *, #63784, .T. ) ;
#7358 = CARTESIAN_POINT ( 'NONE',  ( 13.91025641025641235, -7.500000000000000000, 29.75000000000000355 ) ) ;
#7359 = CARTESIAN_POINT ( 'NONE',  ( -17.86947456176635640, -4.299079248970731904, 33.91157788607253565 ) ) ;
#7360 = CARTESIAN_POINT ( 'NONE',  ( 6.792385456409367528, -12.38065189839062263, 30.83690757178629482 ) ) ;
#7361 = CYLINDRICAL_SURFACE ( 'NONE', #67614, 0.2499999999999998890 ) ;
#7362 = ORIENTED_EDGE ( 'NONE', *, *, #45497, .T. ) ;
#7363 = CARTESIAN_POINT ( 'NONE',  ( -12.33074665371367651, -3.062576670634119758, 32.05464942895959979 ) ) ;
#7364 = LINE ( 'NONE', #34822, #54220 ) ;
#7366 = VERTEX_POINT ( 'NONE', #72023 ) ;
#7365 = DIRECTION ( 'NONE',  ( 0.000000000000000000, 0.6427876096865368094, 0.7660444431189802339 ) ) ;
#7367 = CARTESIAN_POINT ( 'NONE',  ( -6.166666666666667851, -3.499999999999999556, 29.75000000000000355 ) ) ;
#7368 = DIRECTION ( 'NONE',  ( 0.000000000000000000, 0.4999999999999985567, 0.8660254037844395958 ) ) ;
#7369 = B_SPLINE_CURVE_WITH_KNOTS ( 'NONE', 3,
 ( #76060, #88719, #42292, #83274, #62973, #75190, #69748, #21108, #13478, #8056 ),
 .UNSPECIFIED., .F., .F.,
 ( 4, 2, 2, 2, 4 ),
 ( 0.0007817359430256287049, 0.0009771253907249945886, 0.001172514838424360255, 0.001367904286123725922, 0.001563293733823091806 ),
 .UNSPECIFIED. ) ;
#7370 = CARTESIAN_POINT ( 'NONE',  ( 4.826899852701616034, -2.588893531581426544, 31.60682220781847818 ) ) ;
#7371 = CARTESIAN_POINT ( 'NONE',  ( -13.13456107297707121, -3.627508038966690496, 32.91356715214248396 ) ) ;
#7372 = EDGE_CURVE ( 'NONE', #7245, #45245, #17538, .T. ) ;
#7373 = CARTESIAN_POINT ( 'NONE',  ( 16.85399611801622655, -4.762599654559227069, 34.23009711892697737 ) ) ;
#7375 = CARTESIAN_POINT ( 'NONE',  ( -16.82686876528476105, -8.303483539816726378, 34.68545999027711702 ) ) ;
#7374 = CARTESIAN_POINT ( 'NONE',  ( -2.980714810855777053, -4.074993327901525575, 33.72946981652012255 ) ) ;
#7376 = CIRCLE ( 'NONE', #5585, 0.2500000000000002220 ) ;
#7377 = CARTESIAN_POINT ( 'NONE',  ( 12.71153846153989697, -7.500000000000155431, 34.75000000000007105 ) ) ;
#7378 = CARTESIAN_POINT ( 'NONE',  ( -1.944543648262992530, -9.444543648263016067, 18.68750000000000000 ) ) ;
#7379 = ORIENTED_EDGE ( 'NONE', *, *, #13473, .F. ) ;
#7380 = CARTESIAN_POINT ( 'NONE',  ( 17.99999999999987566, -4.481592998941358097, 33.73612834414048933 ) ) ;
#7381 = ORIENTED_EDGE ( 'NONE', *, *, #62694, .F. ) ;
#7382 = VECTOR ( 'NONE', #7670, 1000.000000000000000 ) ;
#7383 = ORIENTED_EDGE ( 'NONE', *, *, #11988, .T. ) ;
#7384 = DIRECTION ( 'NONE',  ( -0.000000000000000000, -0.6427876096865404731, -0.7660444431189770143 ) ) ;
#7385 = ORIENTED_EDGE ( 'NONE', *, *, #61279, .T. ) ;
#7386 = CARTESIAN_POINT ( 'NONE',  ( -5.142193077479396912, -11.67786785259541027, 32.92929555188721480 ) ) ;
#7387 = EDGE_CURVE ( 'NONE', #86865, #75988, #59253, .T. ) ;
#7388 = LINE ( 'NONE', #13692, #55380 ) ;
#7389 = CARTESIAN_POINT ( 'NONE',  ( 6.066068351002440906, -3.050289026998446840, 32.03036669348366416 ) ) ;
#7390 = AXIS2_PLACEMENT_3D ( 'NONE', #57083, #16540, #50754 ) ;
#7391 = EDGE_CURVE ( 'NONE', #83716, #50957, #37799, .T. ) ;
#7392 = CYLINDRICAL_SURFACE ( 'NONE', #55968, 0.2499999999999998890 ) ;
#7393 = LINE ( 'NONE', #20459, #83318 ) ;
#7394 = CARTESIAN_POINT ( 'NONE',  ( 1.384615384615386802, -8.564572088678739092, 35.78748833219616898 ) ) ;
#7395 = CARTESIAN_POINT ( 'NONE',  ( -1.553300858899125059, -3.750000000000009326, 25.32812500000000711 ) ) ;
#7396 = CARTESIAN_POINT ( 'NONE',  ( -12.46153846153846168, -6.435427911321262684, 35.78748833219616898 ) ) ;
#7397 = CARTESIAN_POINT ( 'NONE',  ( 15.16468685140909400, -9.058645607665454236, 34.76329471203372634 ) ) ;
#7398 = CARTESIAN_POINT ( 'NONE',  ( 5.326868486301119532, -10.92531984108285670, 33.72920026020278073 ) ) ;
#7399 = CARTESIAN_POINT ( 'NONE',  ( -7.976301055592065481, -8.587444163452046197, 34.63053765926554206 ) ) ;
#7401 = EDGE_LOOP ( 'NONE', ( #39382, #63078 ) ) ;
#7400 = EDGE_CURVE ( 'NONE', #67446, #54682, #11330, .T. ) ;
#7402 = VERTEX_POINT ( 'NONE', #40044 ) ;
#7403 = CARTESIAN_POINT ( 'NONE',  ( -15.09997742294444478, -8.147973898785416225, 34.70805048591653730 ) ) ;
#7404 = CARTESIAN_POINT ( 'NONE',  ( 5.326977388561390470, -9.148310452688871663, 34.47095581063188519 ) ) ;
#7405 = LINE ( 'NONE', #40751, #88621 ) ;
#7406 = CARTESIAN_POINT ( 'NONE',  ( 9.692307692307695177, -11.91647553114624181, 32.58852847137148245 ) ) ;
#7407 = EDGE_CURVE ( 'NONE', #43255, #47148, #73308, .T. ) ;
#7408 = CARTESIAN_POINT ( 'NONE',  ( -8.102564102564102200, -3.499999999999999556, 29.75000000000000355 ) ) ;
#7409 = CARTESIAN_POINT ( 'NONE',  ( 11.78840694783958298, -4.176053281294518804, 33.81426240980091791 ) ) ;
#7410 = LINE ( 'NONE', #13273, #39455 ) ;
#7411 = VERTEX_POINT ( 'NONE', #53079 ) ;
#7412 = ADVANCED_FACE ( 'NONE', ( #89122 ), #53529, .F. ) ;
#7413 = DIRECTION ( 'NONE',  ( -0.000000000000000000, -0.3420201433256694346, -0.9396926207859080948 ) ) ;
#7414 = ORIENTED_EDGE ( 'NONE', *, *, #86184, .F. ) ;
#7415 = AXIS2_PLACEMENT_3D ( 'NONE', #77933, #71171, #77493 ) ;
#7416 = CARTESIAN_POINT ( 'NONE',  ( 13.31934538405906565, -12.51329471203370325, 31.30864560766548976 ) ) ;
#7417 = CARTESIAN_POINT ( 'NONE',  ( 1.653273178848927064E-15, -7.500000000000000000, 29.50000000000000355 ) ) ;
#7418 = DIRECTION ( 'NONE',  ( -1.000000000000000000, 0.000000000000000000, 0.000000000000000000 ) ) ;
#7419 = B_SPLINE_CURVE_WITH_KNOTS ( 'NONE', 3,
 ( #36964, #16697, #63991, #31092, #36540, #2288, #2729, #50041, #56799, #30655 ),
 .UNSPECIFIED., .F., .F.,
 ( 4, 2, 2, 2, 4 ),
 ( 0.0007817246256747507503, 0.0009771112852218959231, 0.001172497944769040987, 0.001367884604316186052, 0.001563271263863331116 ),
 .UNSPECIFIED. ) ;
#7420 = CARTESIAN_POINT ( 'NONE',  ( -15.29603967673000575, -3.300289026998414865, 32.46337939537583139 ) ) ;
#7421 = CARTESIAN_POINT ( 'NONE',  ( -18.00000000000012079, -12.51329471203414379, 31.30864560766407578 ) ) ;
#7422 = VERTEX_POINT ( 'NONE', #19314 ) ;
#7423 = EDGE_LOOP ( 'NONE', ( #42089, #34458, #9044, #97 ) ) ;
#7424 = PRODUCT ( 'Outer Protective Cap', 'Outer Protective Cap', '', ( #53651 ) ) ;
#7425 = ORIENTED_EDGE ( 'NONE', *, *, #74183, .T. ) ;
#7426 = VERTEX_POINT ( 'NONE', #80585 ) ;
#7427 = EDGE_CURVE ( 'NONE', #33889, #53025, #20202, .T. ) ;
#7428 = CARTESIAN_POINT ( 'NONE',  ( -10.86540783960607115, -12.45566812827425451, 31.48439005359158926 ) ) ;
#7429 = CARTESIAN_POINT ( 'NONE',  ( -12.46153846153846168, -12.62096338111211580, 30.90682066428153263 ) ) ;
#7430 = CARTESIAN_POINT ( 'NONE',  ( 14.05771556364371833, -2.544273027872575366, 31.48422191005632342 ) ) ;
#7431 = ADVANCED_FACE ( 'NONE', ( #87347 ), #68380, .F. ) ;
#7432 = CIRCLE ( 'NONE', #54881, 0.2500000000000002220 ) ;
#7433 = DIRECTION ( 'NONE',  ( 0.000000000000000000, 0.6427876096865368094, 0.7660444431189802339 ) ) ;
#7434 = CARTESIAN_POINT ( 'NONE',  ( 4.403900465484468008, -6.567000820036038355, 34.66262288849541306 ) ) ;
#7435 = EDGE_CURVE ( 'NONE', #79431, #62505, #2630, .T. ) ;
#7436 = CYLINDRICAL_SURFACE ( 'NONE', #55248, 0.2499999999999995559 ) ;
#7437 = EDGE_LOOP ( 'NONE', ( #68832, #81407, #41481, #25142 ) ) ;
#7438 = VERTEX_POINT ( 'NONE', #33276 ) ;
#7439 = AXIS2_PLACEMENT_3D ( 'NONE', #27581, #76658, #13623 ) ;
#7440 = EDGE_LOOP ( 'NONE', ( #71409, #11511, #30035, #24478 ) ) ;
#7442 = ORIENTED_EDGE ( 'NONE', *, *, #18711, .F. ) ;
#7441 = CARTESIAN_POINT ( 'NONE',  ( 12.68431800280687050, -8.496831190052093419, 34.64984203495476578 ) ) ;
#7443 = CARTESIAN_POINT ( 'NONE',  ( 10.54930120442873331, -12.37446782046654192, 30.86335684631486487 ) ) ;
#7444 = CARTESIAN_POINT ( 'NONE',  ( -12.46153846153858424, -12.16647553114689728, 32.15551576947799362 ) ) ;
#7445 = CARTESIAN_POINT ( 'NONE',  ( 2.320192649118979489E-14, -11.25000000000000000, 21.03125000000000000 ) ) ;
#7446 = VERTEX_POINT ( 'NONE', #60736 ) ;
#7447 = EDGE_CURVE ( 'NONE', #36450, #81317, #61484, .T. ) ;
#7448 = EDGE_LOOP ( 'NONE', ( #31981, #7843, #8982, #37425 ) ) ;
#7449 = CYLINDRICAL_SURFACE ( 'NONE', #49990, 0.2500000000000004996 ) ;
#7450 = ORIENTED_EDGE ( 'NONE', *, *, #32378, .F. ) ;
#7451 = FACE_BOUND ( 'NONE', #42332, .T. ) ;
#7452 = CARTESIAN_POINT ( 'NONE',  ( -2.057637887778852814, -4.818054556918156983, 34.26375889529406749 ) ) ;
#7453 = CARTESIAN_POINT ( 'NONE',  ( 7.912221179503920787, -5.471508081941601098, 34.59228464037088457 ) ) ;
#7454 = EDGE_LOOP ( 'NONE', ( #21254, #47428, #8860, #67117 ) ) ;
#7455 = EDGE_CURVE ( 'NONE', #86041, #59263, #37884, .T. ) ;
#7456 = CARTESIAN_POINT ( 'NONE',  ( -9.822455662039388358, -5.070767119584671079, 34.40440758774516183 ) ) ;
#7457 = CARTESIAN_POINT ( 'NONE',  ( 8.769230769230645706, -8.656820664282941280, 34.87096338111179961 ) ) ;
#7458 = B_SPLINE_CURVE_WITH_KNOTS ( 'NONE', 3,
 ( #44369, #35871, #71859, #51122, #71407, #49812, #57012, #16918, #65090, #36746 ),
 .UNSPECIFIED., .F., .F.,
 ( 4, 2, 2, 2, 4 ),
 ( 0.000000000000000000, 0.0001954339857564083146, 0.0003908679715128166293, 0.0005863019572692249439, 0.0007817359430256332585 ),
 .UNSPECIFIED. ) ;
#7459 = CARTESIAN_POINT ( 'NONE',  ( 0.5920641633020244932, -6.852161475712352789, 34.70806712695775786 ) ) ;
#7460 = CARTESIAN_POINT ( 'NONE',  ( 15.36129466900287532, -6.808710257144161559, 34.95449254468098843 ) ) ;
#7461 = EDGE_LOOP ( 'NONE', ( #39097, #38410 ) ) ;
#7462 = AXIS2_PLACEMENT_3D ( 'NONE', #11772, #73480, #45985 ) ;
#7463 = CARTESIAN_POINT ( 'NONE',  ( -0.7115384615384606759, -7.566082377512564960, 35.00000000000000711 ) ) ;
#7464 = CARTESIAN_POINT ( 'NONE',  ( -5.777220331021931443, -4.226511098958374291, 33.85474049983370293 ) ) ;
#7465 = DIRECTION ( 'NONE',  ( 1.000000000000000000, 0.000000000000000000, 0.000000000000000000 ) ) ;
#7466 = FACE_OUTER_BOUND ( 'NONE', #80389, .T. ) ;
#7467 = CYLINDRICAL_SURFACE ( 'NONE', #87543, 0.2499999999999995559 ) ;
#7468 = EDGE_CURVE ( 'NONE', #41734, #62713, #86244, .T. ) ;
#7469 = FACE_BOUND ( 'NONE', #14445, .T. ) ;
#7471 = CARTESIAN_POINT ( 'NONE',  ( 11.31497659473759043, -12.44517049084099725, 30.48991314939691932 ) ) ;
#7470 = CARTESIAN_POINT ( 'NONE',  ( 4.826899839630110378, -11.37209801155882971, 32.91403422569032955 ) ) ;
#7472 = CARTESIAN_POINT ( 'NONE',  ( -6.923076923076922462, -12.10708131394839349, 31.69288490824020244 ) ) ;
#7474 = CARTESIAN_POINT ( 'NONE',  ( 2.307692307692309264, -6.343179335718451384, 34.87096338111211935 ) ) ;
#7473 = CARTESIAN_POINT ( 'NONE',  ( -18.00000000000012079, -2.379036618888197285, 30.90682066428292885 ) ) ;
#7475 = AXIS2_PLACEMENT_3D ( 'NONE', #56460, #55566, #68642 ) ;
#7476 = CARTESIAN_POINT ( 'NONE',  ( -18.25002323729296450, -10.05641848906368629, 34.04755513067964756 ) ) ;
#7477 = CARTESIAN_POINT ( 'NONE',  ( -1.200186371490556958, -4.775308065498765409, 17.57625670625849068 ) ) ;
#7479 = EDGE_CURVE ( 'NONE', #62888, #53841, #84714, .T. ) ;
#7478 = EDGE_LOOP ( 'NONE', ( #42084, #46511, #70092, #34398 ) ) ;
#7480 = CARTESIAN_POINT ( 'NONE',  ( 1.134638653673032627, -12.17611988154120972, 31.52148481390971213 ) ) ;
#7481 = ORIENTED_EDGE ( 'NONE', *, *, #3154, .T. ) ;
#7482 = ADVANCED_FACE ( 'NONE', ( #41808 ), #375, .F. ) ;
#7483 = CYLINDRICAL_SURFACE ( 'NONE', #6113, 0.2500000000000002220 ) ;
#7484 = ORIENTED_EDGE ( 'NONE', *, *, #42372, .T. ) ;
#7485 = DIRECTION ( 'NONE',  ( 1.000000000000000000, 0.000000000000000000, -0.000000000000000000 ) ) ;
#7486 = CARTESIAN_POINT ( 'NONE',  ( 14.05771556364371833, -4.075325502946081535, 33.72974371597206300 ) ) ;
#7487 = ORIENTED_EDGE ( 'NONE', *, *, #5385, .F. ) ;
#7488 = DIRECTION ( 'NONE',  ( 0.000000000000000000, 0.1736481776669267785, -0.9848077530122087975 ) ) ;
#7489 = CARTESIAN_POINT ( 'NONE',  ( 1.077988221561464899, -4.724691934501233703, 16.48250670625849423 ) ) ;
#7490 = CARTESIAN_POINT ( 'NONE',  ( 4.153846153846154188, -8.973038597847269315, 34.52809138561121927 ) ) ;
#7491 = CARTESIAN_POINT ( 'NONE',  ( 16.02315555073584363, -8.191372820521381826, 34.95448215188423546 ) ) ;
#7492 = EDGE_CURVE ( 'NONE', #27260, #78559, #83996, .T. ) ;
#7493 = DIRECTION ( 'NONE',  ( 0.000000000000000000, 0.7660444431189807890, 0.6427876096865361433 ) ) ;
#7494 = DIRECTION ( 'NONE',  ( -0.000000000000000000, 0.3420201433256694901, -0.9396926207859082059 ) ) ;
#7495 = CARTESIAN_POINT ( 'NONE',  ( 2.557746619330623972, -2.779044189368095719, 31.39831045268885745 ) ) ;
#7496 = CARTESIAN_POINT ( 'NONE',  ( -23.50000000000000000, 12.75000000000000533, 32.75000000000000000 ) ) ;
#7497 = CARTESIAN_POINT ( 'NONE',  ( -1.614399933863613468, -11.22469193450124969, 21.36124329374151642 ) ) ;
#7498 = DIRECTION ( 'NONE',  ( -0.000000000000000000, -0.6427876096865404731, -0.7660444431189771253 ) ) ;
#7499 = CARTESIAN_POINT ( 'NONE',  ( -14.30769230769230660, -9.819645486525091727, 36.12317359536749706 ) ) ;
#7500 = ORIENTED_EDGE ( 'NONE', *, *, #77421, .T. ) ;
#7501 = DIRECTION ( 'NONE',  ( -0.000000000000000000, 1.000000000000000000, -0.000000000000000000 ) ) ;
#7502 = CARTESIAN_POINT ( 'NONE',  ( -2.694853999681181556, -10.10844685921792241, 22.68936829374151287 ) ) ;
#7503 = CARTESIAN_POINT ( 'NONE',  ( 2.241609928332172874, -4.661471528628506888, 34.16647553114621871 ) ) ;
#7504 = DIRECTION ( 'NONE',  ( 1.000000000000000000, 0.000000000000000000, 0.000000000000000000 ) ) ;
#7505 = EDGE_LOOP ( 'NONE', ( #32192, #50257 ) ) ;
#7506 = CARTESIAN_POINT ( 'NONE',  ( -17.93393164899756442, -2.721908614388772296, 31.22303859784725333 ) ) ;
#7507 = CARTESIAN_POINT ( 'NONE',  ( -0.4615384615385826339, -10.21337939537710326, 33.94971097300076224 ) ) ;
#7509 = ORIENTED_EDGE ( 'NONE', *, *, #30019, .T. ) ;
#7508 = PLANE ( 'NONE',  #35416 ) ;
#7510 = CARTESIAN_POINT ( 'NONE',  ( 8.638540166120458608, -5.496505350115501010, 34.60290016733514307 ) ) ;
#7511 = EDGE_CURVE ( 'NONE', #45323, #52135, #77615, .T. ) ;
#7512 = CARTESIAN_POINT ( 'NONE',  ( 1.653273178848927064E-15, -7.500000000000000000, 21.00000000000000000 ) ) ;
#7513 = VECTOR ( 'NONE', #20895, 1000.000000000000114 ) ;
#7514 = CARTESIAN_POINT ( 'NONE',  ( -10.36543920600657209, -9.357781135181031829, 34.66075350412533851 ) ) ;
#7515 = CARTESIAN_POINT ( 'NONE',  ( -9.561517251340742263, -2.494656445102012565, 31.33466734024120015 ) ) ;
#7516 = CARTESIAN_POINT ( 'NONE',  ( -18.13069146666756382, -12.11776431015576172, 31.66791131148498906 ) ) ;
#7517 = ORIENTED_EDGE ( 'NONE', *, *, #54217, .T. ) ;
#7518 = ORIENTED_EDGE ( 'NONE', *, *, #67285, .T. ) ;
#7519 = EDGE_LOOP ( 'NONE', ( #24928, #18571 ) ) ;
#7520 = DIRECTION ( 'NONE',  ( 0.000000000000000000, 0.7660444431189822323, -0.6427876096865344779 ) ) ;
#7521 = FACE_OUTER_BOUND ( 'NONE', #13956, .T. ) ;
#7522 = CARTESIAN_POINT ( 'NONE',  ( -13.13466986626724164, -12.22109172314383052, 31.39792113162168263 ) ) ;
#7523 = CARTESIAN_POINT ( 'NONE',  ( -5.076923076923075762, -13.75783147151868846, 33.36296068462461051 ) ) ;
#7524 = ORIENTED_EDGE ( 'NONE', *, *, #69729, .F. ) ;
#7525 = B_SPLINE_CURVE_WITH_KNOTS ( 'NONE', 3,
 ( #43652, #24258, #45422, #84664, #57613, #72900, #85535, #51264, #71562, #10761 ),
 .UNSPECIFIED., .F., .F.,
 ( 4, 2, 2, 2, 4 ),
 ( 0.000000000000000000, 0.0001954311564186864949, 0.0003908623128373729899, 0.0005862934692560594577, 0.0007817246256747459798 ),
 .UNSPECIFIED. ) ;
#7526 = CARTESIAN_POINT ( 'NONE',  ( -17.06410256410256565, -4.000000000000000000, 29.75000000000000355 ) ) ;
#7527 = AXIS2_PLACEMENT_3D ( 'NONE', #33271, #18421, #46333 ) ;
#7528 = ORIENTED_EDGE ( 'NONE', *, *, #37619, .F. ) ;
#7529 = ORIENTED_EDGE ( 'NONE', *, *, #11272, .F. ) ;
#7530 = ORIENTED_EDGE ( 'NONE', *, *, #67351, .F. ) ;
#7532 = ORIENTED_EDGE ( 'NONE', *, *, #56827, .T. ) ;
#7531 = DIRECTION ( 'NONE',  ( -0.000000000000000000, -0.8660254037844397068, -0.4999999999999978906 ) ) ;
#7533 = CARTESIAN_POINT ( 'NONE',  ( -0.5916856709766811218, -5.195881422630166391, 34.18770438780619259 ) ) ;
#7534 = CIRCLE ( 'NONE', #53563, 4.000000000000000000 ) ;
#7535 = CARTESIAN_POINT ( 'NONE',  ( -3.296039231325550656, -12.16647553114622049, 32.15551576947930812 ) ) ;
#7536 = ADVANCED_FACE ( 'NONE', ( #76473 ), #68823, .F. ) ;
#7537 = CARTESIAN_POINT ( 'NONE',  ( -3.100243529005666687, -4.459921816937789885, 33.71989282347011851 ) ) ;
#7538 = CARTESIAN_POINT ( 'NONE',  ( 8.769230769230647482, -2.625532179533778709, 30.86335684631627174 ) ) ;
#7539 = ADVANCED_FACE ( 'NONE', ( #29619 ), #77353, .F. ) ;
#7540 = ORIENTED_EDGE ( 'NONE', *, *, #86846, .F. ) ;
#7541 = ORIENTED_EDGE ( 'NONE', *, *, #82198, .F. ) ;
#7542 = ORIENTED_EDGE ( 'NONE', *, *, #63795, .T. ) ;
#7543 = DIRECTION ( 'NONE',  ( -1.000000000000000000, -0.000000000000000000, -0.000000000000000000 ) ) ;
#7545 = ORIENTED_EDGE ( 'NONE', *, *, #22235, .F. ) ;
#7544 = DIRECTION ( 'NONE',  ( 0.000000000000000000, 0.4999999999999985567, 0.8660254037844395958 ) ) ;
#7546 = EDGE_CURVE ( 'NONE', #441, #10997, #41086, .T. ) ;
#7547 = CARTESIAN_POINT ( 'NONE',  ( -2.084912766423896446, -8.496831190052096971, 34.64984203495476578 ) ) ;
#7548 = CARTESIAN_POINT ( 'NONE',  ( 7.846153846153846700, -8.564572088678739092, 35.78748833219616898 ) ) ;
#7549 = EDGE_LOOP ( 'NONE', ( #59106, #80811 ) ) ;
#7550 = CARTESIAN_POINT ( 'NONE',  ( -4.153846153846152411, -4.786620604624113540, 33.94971097300155094 ) ) ;
#7551 = EDGE_CURVE ( 'NONE', #86305, #34265, #49873, .T. ) ;
#7552 = CARTESIAN_POINT ( 'NONE',  ( 4.219914504848593317, -2.721908614388772296, 31.22303859784725333 ) ) ;
#7553 = VERTEX_POINT ( 'NONE', #63836 ) ;
#7554 = FACE_BOUND ( 'NONE', #3848, .T. ) ;
#7555 = DIRECTION ( 'NONE',  ( -1.000000000000000000, -9.819216796286635314E-16, -2.454804199071659026E-15 ) ) ;
#7556 = DIRECTION ( 'NONE',  ( 1.000000000000000000, 0.000000000000000000, 0.000000000000000000 ) ) ;
#7557 = AXIS2_PLACEMENT_3D ( 'NONE', #73630, #19549, #39396 ) ;
#7558 = CARTESIAN_POINT ( 'NONE',  ( -19.50000000000000000, -3.499999999999999556, 29.75000000000000355 ) ) ;
#7560 = CARTESIAN_POINT ( 'NONE',  ( -5.076923076923075762, -12.29105614889573062, 35.45975837776705220 ) ) ;
#7559 = CARTESIAN_POINT ( 'NONE',  ( -6.673076923075486278, -7.500000000000155431, 34.75000000000007105 ) ) ;
#7561 = VECTOR ( 'NONE', #20381, 1000.000000000000114 ) ;
#7562 = CARTESIAN_POINT ( 'NONE',  ( -4.826868765284761942, -10.66356715214248396, 33.62249196103329751 ) ) ;
#7563 = CARTESIAN_POINT ( 'NONE',  ( -2.557669038634660996, -3.627789207965226748, 32.91389620160131102 ) ) ;
#7564 = ORIENTED_EDGE ( 'NONE', *, *, #9056, .T. ) ;
#7565 = CARTESIAN_POINT ( 'NONE',  ( -7.846153846153844924, -6.343179335718451384, 34.87096338111211935 ) ) ;
#7566 = CARTESIAN_POINT ( 'NONE',  ( 13.13461538461538680, -7.433931650972300353, 34.75000000000000711 ) ) ;
#7567 = ORIENTED_EDGE ( 'NONE', *, *, #63726, .T. ) ;
#7568 = AXIS2_PLACEMENT_3D ( 'NONE', #37517, #16371, #65873 ) ;
#7569 = CARTESIAN_POINT ( 'NONE',  ( 8.769230769230768274, -3.050289026998446396, 32.03036669348365706 ) ) ;
#7570 = CARTESIAN_POINT ( 'NONE',  ( 9.468822748583749060, -2.847400154188068022, 31.58180166144859058 ) ) ;
#7571 = EDGE_LOOP ( 'NONE', ( #65774, #12763, #56591, #14116 ) ) ;
#7572 = CARTESIAN_POINT ( 'NONE',  ( 17.75002326905764960, -5.728515186090277211, 34.42611988154120439 ) ) ;
#7573 = CARTESIAN_POINT ( 'NONE',  ( -4.376773112752999850, -2.308479472611653094, 30.53278059502174457 ) ) ;
#7574 = FACE_BOUND ( 'NONE', #72500, .T. ) ;
#7576 = LINE ( 'NONE', #35038, #34435 ) ;
#7575 = DIRECTION ( 'NONE',  ( 0.000000000000000000, 0.6427876096865373645, -0.7660444431189797898 ) ) ;
#7577 = CARTESIAN_POINT ( 'NONE',  ( 10.55011416942384095, -8.613356846314824011, 34.62446782046655613 ) ) ;
#7578 = CARTESIAN_POINT ( 'NONE',  ( -15.48074596171158213, -9.148715823498378086, 34.47080413974185120 ) ) ;
#7580 = CARTESIAN_POINT ( 'NONE',  ( 7.173131234715237170, -12.41262288849542017, 30.68299917996395010 ) ) ;
#7579 = PRESENTATION_STYLE_ASSIGNMENT (( #34156 ) ) ;
#7581 = CARTESIAN_POINT ( 'NONE',  ( -2.939152317953646711E-15, 7.500000000000000000, 10.00000000000000178 ) ) ;
#7582 = CARTESIAN_POINT ( 'NONE',  ( -3.724691934501229262, -9.114399933863657211, 17.26375670625849068 ) ) ;
#7583 = ORIENTED_EDGE ( 'NONE', *, *, #52444, .F. ) ;
#7584 = EDGE_CURVE ( 'NONE', #21400, #53945, #48537, .T. ) ;
#7585 = EDGE_LOOP ( 'NONE', ( #10787, #24479, #49614, #27170 ) ) ;
#7586 = CARTESIAN_POINT ( 'NONE',  ( 8.102564102564102200, -7.500000000000000000, 29.75000000000000355 ) ) ;
#7587 = CARTESIAN_POINT ( 'NONE',  ( -24.00000000000000000, -9.499999999999982236, 27.74999999999999645 ) ) ;
#7588 = CARTESIAN_POINT ( 'NONE',  ( 6.792601738001206257, -7.276987145209185215, 34.99546412871779211 ) ) ;
#7589 = FACE_OUTER_BOUND ( 'NONE', #54038, .T. ) ;
#7590 = CARTESIAN_POINT ( 'NONE',  ( 3.100077764101674127, -11.18331474514187995, 33.13161551792790505 ) ) ;
#7591 = CARTESIAN_POINT ( 'NONE',  ( 1.492201783934554493, -3.724691934501233703, 15.23250670625848713 ) ) ;
#7592 = PLANE ( 'NONE',  #58990 ) ;
#7593 = DIRECTION ( 'NONE',  ( -0.000000000000000000, 0.7660444431189791237, -0.6427876096865379196 ) ) ;
#7594 = ADVANCED_FACE ( 'NONE', ( #2131 ), #76019, .F. ) ;
#7595 = CARTESIAN_POINT ( 'NONE',  ( -3.230769230769351186, -6.026961402154118908, 34.52809138561165270 ) ) ;
#7596 = CARTESIAN_POINT ( 'NONE',  ( -5.076923076923075762, -2.292212530054420494, 30.41441678777542634 ) ) ;
#7597 = CARTESIAN_POINT ( 'NONE',  ( 4.153846153846154188, -1.117168528481311540, 33.14645433367849847 ) ) ;
#7598 = DIRECTION ( 'NONE',  ( -1.000000000000000000, -0.000000000000000000, 0.000000000000000000 ) ) ;
#7599 = CARTESIAN_POINT ( 'NONE',  ( -4.826977558574936822, -2.824170634883622188, 31.52227843825338738 ) ) ;
#7601 = EDGE_CURVE ( 'NONE', #47075, #28663, #36761, .T. ) ;
#7600 = CARTESIAN_POINT ( 'NONE',  ( 14.30769230769218758, -11.94971097300221174, 32.03036669348237098 ) ) ;
#7602 = EDGE_CURVE ( 'NONE', #31488, #7007, #2294, .T. ) ;
#7603 = CARTESIAN_POINT ( 'NONE',  ( -13.38461538461550759, -6.835583212225970762, 34.95778746994575670 ) ) ;
#7604 = ORIENTED_EDGE ( 'NONE', *, *, #48463, .T. ) ;
#7605 = CARTESIAN_POINT ( 'NONE',  ( 8.769230769230768274, -6.435427911321262684, 35.78748833219616898 ) ) ;
#7606 = CARTESIAN_POINT ( 'NONE',  ( 0.4615384615384611200, -2.538708090699994813, 30.37095296980875503 ) ) ;
#7607 = CARTESIAN_POINT ( 'NONE',  ( 1.987747218494642309, -5.598659921968629050, 20.81436829374151287 ) ) ;
#7608 = CARTESIAN_POINT ( 'NONE',  ( -5.869474561766353737, -12.50538340440932217, 31.33453814440721885 ) ) ;
#7609 = CARTESIAN_POINT ( 'NONE',  ( -15.93083330975275658, -2.523321265292116866, 31.42251411153756990 ) ) ;
#7610 = ORIENTED_EDGE ( 'NONE', *, *, #62332, .T. ) ;
#7611 = CARTESIAN_POINT ( 'NONE',  ( -9.692307692307814193, -5.941354392335915335, 34.76329471203413846 ) ) ;
#7613 = EDGE_LOOP ( 'NONE', ( #85569, #33522, #7981, #87550 ) ) ;
#7612 = LINE ( 'NONE', #20242, #18059 ) ;
#7614 = CARTESIAN_POINT ( 'NONE',  ( -1.944543648263015179, -5.555456351737005249, 26.50000000000000355 ) ) ;
#7615 = DIRECTION ( 'NONE',  ( -0.000000000000000000, 0.9848077530122085754, -0.1736481776669273613 ) ) ;
#7616 = EDGE_CURVE ( 'NONE', #10070, #62944, #49697, .T. ) ;
#7617 = EDGE_LOOP ( 'NONE', ( #1667, #5858, #26804, #65192 ) ) ;
#7618 = CARTESIAN_POINT ( 'NONE',  ( -5.299849294439222369, -12.15238873228292071, 31.58232369045353849 ) ) ;
#7619 = CARTESIAN_POINT ( 'NONE',  ( 14.87820512820512953, -7.500000000000000000, 33.75000000000000000 ) ) ;
#7620 = VERTEX_POINT ( 'NONE', #3895 ) ;
#7621 = CARTESIAN_POINT ( 'NONE',  ( -10.68065461594093435, -4.320704448112771878, 33.92786785259540494 ) ) ;
#7622 = EDGE_CURVE ( 'NONE', #57991, #8026, #31342, .T. ) ;
#7623 = EDGE_CURVE ( 'NONE', #64470, #19590, #58845, .T. ) ;
#7624 = CARTESIAN_POINT ( 'NONE',  ( -15.16460262417758820, -7.250054591869670162, 34.99404684341514127 ) ) ;
#7625 = CARTESIAN_POINT ( 'NONE',  ( 9.692307692307695177, -6.681629849574314051, 35.83090037661290239 ) ) ;
#7626 = VERTEX_POINT ( 'NONE', #72360 ) ;
#7627 = ORIENTED_EDGE ( 'NONE', *, *, #67473, .T. ) ;
#7628 = CARTESIAN_POINT ( 'NONE',  ( 15.29683758177167086, -10.51840700105979565, 33.73612834413962247 ) ) ;
#7629 = ADVANCED_FACE ( 'NONE', ( #30490 ), #35778, .T. ) ;
#7630 = B_SPLINE_CURVE_WITH_KNOTS ( 'NONE', 3,
 ( #37973, #36645, #51911, #64103, #2400, #23126, #85280, #31205, #24001, #10048 ),
 .UNSPECIFIED., .F., .F.,
 ( 4, 2, 2, 2, 4 ),
 ( 0.0007817246256747451124, 0.0009771112852218885505, 0.001172497944769032097, 0.001367884604316175427, 0.001563271263863318973 ),
 .UNSPECIFIED. ) ;
#7631 = PRESENTATION_LAYER_ASSIGNMENT (  '', '', ( #49347 ) ) ;
#7632 = EDGE_LOOP ( 'NONE', ( #65336, #75891, #43852, #62695 ) ) ;
#7633 = CARTESIAN_POINT ( 'NONE',  ( 3.361559671736180199, -11.93129842949671726, 32.56571108434900452 ) ) ;
#7634 = CYLINDRICAL_SURFACE ( 'NONE', #62807, 0.2499999999999997502 ) ;
#7635 = CARTESIAN_POINT ( 'NONE',  ( 13.51540582558234149, -3.338503747796866872, 32.95102852606553512 ) ) ;
#7636 = CARTESIAN_POINT ( 'NONE',  ( -6.792286482109970436, -11.37503395064541678, 33.29242100308974983 ) ) ;
#7637 = FACE_OUTER_BOUND ( 'NONE', #54344, .T. ) ;
#7638 = CARTESIAN_POINT ( 'NONE',  ( -2.530558570755406134, -2.251424796025575770, 29.88072029997477586 ) ) ;
#7639 = VECTOR ( 'NONE', #65098, 1000.000000000000000 ) ;
#7640 = CYLINDRICAL_SURFACE ( 'NONE', #27614, 0.2500000000000008882 ) ;
#7641 = ORIENTED_EDGE ( 'NONE', *, *, #13372, .F. ) ;
#7642 = ORIENTED_EDGE ( 'NONE', *, *, #32646, .T. ) ;
#7644 = VERTEX_POINT ( 'NONE', #9347 ) ;
#7643 = CARTESIAN_POINT ( 'NONE',  ( -0.3307466537136750095, -12.11778462344221019, 31.66786338562085135 ) ) ;
#7645 = EDGE_CURVE ( 'NONE', #69999, #32213, #86111, .T. ) ;
#7646 = CARTESIAN_POINT ( 'NONE',  ( 16.94623247381277054, -2.295517848115769421, 30.44137282052136939 ) ) ;
#7647 = EDGE_LOOP ( 'NONE', ( #51745, #86403, #38735, #36858 ) ) ;
#7648 = CARTESIAN_POINT ( 'NONE',  ( -24.00000000000000000, 9.000000000000024869, 28.74999999999999645 ) ) ;
#7649 = CARTESIAN_POINT ( 'NONE',  ( -8.069080805060693251, -10.01117774369187252, 34.36070679894347535 ) ) ;
#7650 = ORIENTED_EDGE ( 'NONE', *, *, #80851, .T. ) ;
#7651 = CARTESIAN_POINT ( 'NONE',  ( -15.23076923076922995, -1.951392089020283160, 34.73218667398347748 ) ) ;
#7652 = CIRCLE ( 'NONE', #63699, 4.000000000000000000 ) ;
#7653 = VERTEX_POINT ( 'NONE', #16531 ) ;
#7655 = ORIENTED_EDGE ( 'NONE', *, *, #63111, .T. ) ;
#7654 = CARTESIAN_POINT ( 'NONE',  ( -16.28453762051371712, -3.530157926970578508, 32.79014554554150607 ) ) ;
#7656 = EDGE_CURVE ( 'NONE', #85495, #74960, #38137, .T. ) ;
#7657 = AXIS2_PLACEMENT_3D ( 'NONE', #55885, #36510, #63961 ) ;
#7658 = CARTESIAN_POINT ( 'NONE',  ( 17.99999999999987566, -9.528491918059723176, 34.59228464037033035 ) ) ;
#7659 = VERTEX_POINT ( 'NONE', #9777 ) ;
#7660 = B_SPLINE_CURVE_WITH_KNOTS ( 'NONE', 3,
 ( #67409, #81378, #4824, #52988, #18333, #11581, #67851, #18782, #26426, #33178 ),
 .UNSPECIFIED., .F., .F.,
 ( 4, 2, 2, 2, 4 ),
 ( 0.0007817246256747447872, 0.0009771112852218876831, 0.001172497944769030579, 0.001367884604316173475, 0.001563271263863316371 ),
 .UNSPECIFIED. ) ;
#7661 = CARTESIAN_POINT ( 'NONE',  ( 17.77651505627605033, -10.81261337010820256, 33.49550067578627477 ) ) ;
#7662 = CARTESIAN_POINT ( 'NONE',  ( -8.992715712954716167, -2.847400154188067578, 31.58180166144859058 ) ) ;
#7663 = FACE_BOUND ( 'NONE', #21652, .T. ) ;
#7664 = B_SPLINE_CURVE_WITH_KNOTS ( 'NONE', 3,
 ( #60986, #33528, #82612, #88932, #62306, #7823, #27203, #55115, #19999, #75828 ),
 .UNSPECIFIED., .F., .F.,
 ( 4, 2, 2, 2, 4 ),
 ( 0.0007817246256747504250, 0.0009771112852218954894, 0.001172497944769040554, 0.001367884604316185401, 0.001563271263863330466 ),
 .UNSPECIFIED. ) ;
#7665 = CARTESIAN_POINT ( 'NONE',  ( -14.30769230769230660, -9.058645607665452459, 34.76329471203371924 ) ) ;
#7666 = DIRECTION ( 'NONE',  ( 0.000000000000000000, 0.000000000000000000, 1.000000000000000000 ) ) ;
#7667 = CARTESIAN_POINT ( 'NONE',  ( 4.153846153846154188, -12.37446782046654192, 30.86335684631486131 ) ) ;
#7668 = DIRECTION ( 'NONE',  ( -1.000000000000000000, -0.000000000000000000, -0.000000000000000000 ) ) ;
#7669 = CARTESIAN_POINT ( 'NONE',  ( 5.142178648199100088, -10.90142922261932057, 33.41473453929631887 ) ) ;
#7670 = DIRECTION ( 'NONE',  ( 1.000000000000000000, 0.000000000000000000, 0.000000000000000000 ) ) ;
#7671 = EDGE_LOOP ( 'NONE', ( #19042, #25972 ) ) ;
#7672 = CARTESIAN_POINT ( 'NONE',  ( -14.05774678934416499, -3.712312575010499049, 33.01462480002815170 ) ) ;
#7673 = EDGE_LOOP ( 'NONE', ( #59250, #10074 ) ) ;
#7674 = EDGE_LOOP ( 'NONE', ( #8253, #50348 ) ) ;
#7676 = DIRECTION ( 'NONE',  ( -0.000000000000000000, -0.8660254037844399289, -0.4999999999999980016 ) ) ;
#7675 = CARTESIAN_POINT ( 'NONE',  ( 2.242421861731532573, -10.90142922261923886, 33.41473453929638993 ) ) ;
#7677 = EDGE_CURVE ( 'NONE', #63997, #5154, #37238, .T. ) ;
#7678 = CARTESIAN_POINT ( 'NONE',  ( -12.59222992820602194, -2.541943142973491554, 30.39792223712631980 ) ) ;
#7679 = CARTESIAN_POINT ( 'NONE',  ( -16.85414340794500276, -10.23759521482555357, 34.22997729860117033 ) ) ;
#7680 = CYLINDRICAL_SURFACE ( 'NONE', #14195, 0.2499999999999998890 ) ;
#7681 = CARTESIAN_POINT ( 'NONE',  ( 9.915087233576102221, -2.600157965045224895, 30.74683119005207743 ) ) ;
#7682 = ORIENTED_EDGE ( 'NONE', *, *, #1322, .F. ) ;
#7683 = CARTESIAN_POINT ( 'NONE',  ( 11.53846153846153832, -3.322132147404559976, 32.92929555188717927 ) ) ;
#7684 = VECTOR ( 'NONE', #15729, 1000.000000000000114 ) ;
#7685 = CARTESIAN_POINT ( 'NONE',  ( -14.53061926659915315, -10.01117774369187252, 34.36070679894347535 ) ) ;
#7686 = CARTESIAN_POINT ( 'NONE',  ( -3.230769230769229949, -11.35647404775217417, 33.31231777344666511 ) ) ;
#7687 = CARTESIAN_POINT ( 'NONE',  ( -13.91025641025641058, -3.499999999999999556, 29.75000000000000355 ) ) ;
#7688 = CARTESIAN_POINT ( 'NONE',  ( -13.60754160213152808, -10.61292498521070549, 33.66303323003028680 ) ) ;
#7689 = VERTEX_POINT ( 'NONE', #4353 ) ;
#7690 = ORIENTED_EDGE ( 'NONE', *, *, #64805, .F. ) ;
#7691 = VECTOR ( 'NONE', #54919, 1000.000000000000227 ) ;
#7692 = ITEM_DEFINED_TRANSFORMATION ( 'NONE', 'NONE', #56169,  #83448 ) ;
#7693 = ORIENTED_EDGE ( 'NONE', *, *, #16052, .F. ) ;
#7694 = AXIS2_PLACEMENT_3D ( 'NONE', #60929, #88430, #53730 ) ;
#7695 = LINE ( 'NONE', #42371, #86626 ) ;
#7696 = ADVANCED_FACE ( 'NONE', ( #85442 ), #65595, .F. ) ;
#7697 = ORIENTED_EDGE ( 'NONE', *, *, #17808, .T. ) ;
#7698 = CARTESIAN_POINT ( 'NONE',  ( -9.469528023329623068, -10.23759521482555357, 34.22997729860117033 ) ) ;
#7699 = CARTESIAN_POINT ( 'NONE',  ( -12.46153846153858247, -6.879047030192662504, 34.71129190930017927 ) ) ;
#7700 = CYLINDRICAL_SURFACE ( 'NONE', #72569, 0.2500000000000004996 ) ;
#7701 = CARTESIAN_POINT ( 'NONE',  ( -2.651650429449565305, -4.848349570550461785, 15.25000000000000000 ) ) ;
#7702 = ADVANCED_FACE ( 'NONE', ( #31837 ), #59292, .F. ) ;
#7703 = B_SPLINE_CURVE_WITH_KNOTS ( 'NONE', 3,
 ( #21734, #22182, #77122, #41124, #68588, #6886, #34354, #61825, #2768, #44644 ),
 .UNSPECIFIED., .F., .F.,
 ( 4, 2, 2, 2, 4 ),
 ( 0.000000000000000000, 0.0001954311564186861155, 0.0003908623128373722310, 0.0005862934692560583735, 0.0007817246256747444619 ),
 .UNSPECIFIED. ) ;
#7704 = CARTESIAN_POINT ( 'NONE',  ( 12.39626801557768587, -10.21337939537584383, 33.94971097300158647 ) ) ;
#7705 = ORIENTED_EDGE ( 'NONE', *, *, #84527, .F. ) ;
#7707 = B_SPLINE_CURVE_WITH_KNOTS ( 'NONE', 3,
 ( #24476, #87100, #25376, #9635, #86208, #66362, #23592, #78984, #18181, #37103 ),
 .UNSPECIFIED., .F., .F.,
 ( 4, 2, 2, 2, 4 ),
 ( 0.000000000000000000, 0.0001954311564186863052, 0.0003908623128373726104, 0.0005862934692560589156, 0.0007817246256747452209 ),
 .UNSPECIFIED. ) ;
#7706 = CARTESIAN_POINT ( 'NONE',  ( 8.519230769230768274, -2.249999999999998668, 29.75000000000000355 ) ) ;
#7709 = ORIENTED_EDGE ( 'NONE', *, *, #17869, .F. ) ;
#7708 = CARTESIAN_POINT ( 'NONE',  ( -0.4615384615385840772, -5.941354392335915335, 34.76329471203413846 ) ) ;
#7710 = CARTESIAN_POINT ( 'NONE',  ( -3.361329822511150311, -2.504760397472875155, 29.97295953869789997 ) ) ;
#7711 = CARTESIAN_POINT ( 'NONE',  ( 3.230769230769231726, -12.37446782046654192, 30.86335684631486131 ) ) ;
#7712 = CARTESIAN_POINT ( 'NONE',  ( 17.20771488474786892, -11.18335022499818621, 33.13157742990016885 ) ) ;
#7713 = LINE ( 'NONE', #13569, #4989 ) ;
#7714 = CARTESIAN_POINT ( 'NONE',  ( -17.93474486048716088, -11.06231777344670952, 33.60647404775212266 ) ) ;
#7715 = EDGE_CURVE ( 'NONE', #81881, #26475, #7020, .T. ) ;
#7716 = FACE_OUTER_BOUND ( 'NONE', #35899, .T. ) ;
#7717 = CARTESIAN_POINT ( 'NONE',  ( 6.923076923076800782, -11.67786785259630911, 32.92929555188603530 ) ) ;
#7718 = CARTESIAN_POINT ( 'NONE',  ( 2.608446859217924629, -10.19485399968118422, 14.87686829374151465 ) ) ;
#7719 = ORIENTED_EDGE ( 'NONE', *, *, #15620, .T. ) ;
#7720 = CARTESIAN_POINT ( 'NONE',  ( -4.826923076921656452, -7.500000000000154543, 35.00000000000007105 ) ) ;
#7721 = CARTESIAN_POINT ( 'NONE',  ( -14.05774689831426372, -3.520799739797214389, 33.17531984108286025 ) ) ;
#7722 = CARTESIAN_POINT ( 'NONE',  ( 8.900021210197715860, -10.70102852606553157, 33.91149625220312913 ) ) ;
#7723 = CARTESIAN_POINT ( 'NONE',  ( 9.692307692307570832, -6.835583212225970762, 34.95778746994575670 ) ) ;
#7724 = ORIENTED_EDGE ( 'NONE', *, *, #4901, .F. ) ;
#7725 = CARTESIAN_POINT ( 'NONE',  ( -1.139087296525992388, -10.25000000000000711, 14.85937500000000355 ) ) ;
#7726 = CARTESIAN_POINT ( 'NONE',  ( 23.49999999999998934, -9.499999999999982236, 27.24999999999999645 ) ) ;
#7727 = CARTESIAN_POINT ( 'NONE',  ( -1.318547033612945452, -6.386643153685127139, 34.62446782046654192 ) ) ;
#7728 = VECTOR ( 'NONE', #23716, 1000.000000000000000 ) ;
#7729 = CARTESIAN_POINT ( 'NONE',  ( 14.17754509825408960, -3.285722584762969856, 32.44110544564090759 ) ) ;
#7730 = ORIENTED_EDGE ( 'NONE', *, *, #30780, .T. ) ;
#7731 = CARTESIAN_POINT ( 'NONE',  ( 15.23076923076911093, -4.481592998941358097, 33.73612834414048933 ) ) ;
#7732 = EDGE_CURVE ( 'NONE', #31209, #65326, #52875, .T. ) ;
#7733 = CARTESIAN_POINT ( 'NONE',  ( -0.5268084620947813823, -10.33852847137145048, 34.16647553114627556 ) ) ;
#7734 = CARTESIAN_POINT ( 'NONE',  ( -14.08472917342563591, -7.369474539155828730, 34.99858011523957657 ) ) ;
#7735 = VERTEX_POINT ( 'NONE', #87236 ) ;
#7736 = DIRECTION ( 'NONE',  ( -0.000000000000000000, 0.3420201433256694346, -0.9396926207859080948 ) ) ;
#7737 = ORIENTED_EDGE ( 'NONE', *, *, #51029, .T. ) ;
#7738 = CARTESIAN_POINT ( 'NONE',  ( -2.530618525208453651, -12.15238873228292071, 31.58232369045353849 ) ) ;
#7739 = CARTESIAN_POINT ( 'NONE',  ( 4.853438152358745761, -5.827078755546623690, 34.72654668319379567 ) ) ;
#7740 = EDGE_LOOP ( 'NONE', ( #55686, #47275, #8190, #46826, #38658, #51031, #61137, #86767 ) ) ;
#7741 = DIRECTION ( 'NONE',  ( -0.000000000000000000, -0.8660254037844399289, -0.4999999999999980016 ) ) ;
#7742 = CARTESIAN_POINT ( 'NONE',  ( 7.846153846153846700, -3.886160181151819604, 36.00935417666054406 ) ) ;
#7743 = CARTESIAN_POINT ( 'NONE',  ( 10.61538461538461675, -1.422936976036506707, 30.56769352161908415 ) ) ;
#7744 = CARTESIAN_POINT ( 'NONE',  ( -11.47320639894870276, -5.941354392334607049, 34.76329471203374055 ) ) ;
#7745 = CARTESIAN_POINT ( 'NONE',  ( -0.4615384615384611200, -1.466349020453238561, 30.81389545987213907 ) ) ;
#7746 = AXIS2_PLACEMENT_3D ( 'NONE', #88977, #53834, #14625 ) ;
#7747 = ORIENTED_EDGE ( 'NONE', *, *, #79413, .F. ) ;
#7748 = EDGE_LOOP ( 'NONE', ( #57149, #6414 ) ) ;
#7749 = FACE_BOUND ( 'NONE', #69583, .T. ) ;
#7750 = ORIENTED_EDGE ( 'NONE', *, *, #4229, .F. ) ;
#7751 = CARTESIAN_POINT ( 'NONE',  ( -5.076923076923075762, -8.318370150425687726, 35.83090037661290239 ) ) ;
#7752 = VECTOR ( 'NONE', #80972, 1000.000000000000000 ) ;
#7753 = PLANE ( 'NONE',  #58862 ) ;
#7754 = CARTESIAN_POINT ( 'NONE',  ( 6.222779668978068557, -5.827830569534416583, 34.72679350104403539 ) ) ;
#7755 = CARTESIAN_POINT ( 'NONE',  ( 14.53070515178570332, -8.282913670948747864, 34.94150082978203642 ) ) ;
#7756 = B_SPLINE_CURVE_WITH_KNOTS ( 'NONE', 3,
 ( #27655, #29004, #15037, #28551, #54672, #82170, #61874, #8281, #189, #76281 ),
 .UNSPECIFIED., .F., .F.,
 ( 4, 2, 2, 2, 4 ),
 ( 0.000000000000000000, 0.0001954339857564097512, 0.0003908679715128195024, 0.0005863019572692292807, 0.0007817359430256390048 ),
 .UNSPECIFIED. ) ;
#7757 = ORIENTED_EDGE ( 'NONE', *, *, #56503, .T. ) ;
#7758 = ORIENTED_EDGE ( 'NONE', *, *, #70785, .F. ) ;
#7759 = VERTEX_POINT ( 'NONE', #12012 ) ;
#7760 = FACE_OUTER_BOUND ( 'NONE', #35788, .T. ) ;
#7761 = EDGE_LOOP ( 'NONE', ( #59539, #13844 ) ) ;
#7762 = DIRECTION ( 'NONE',  ( 5.997714145664496128E-17, 1.000000000000000000, -5.102127870520021228E-17 ) ) ;
#7763 = CARTESIAN_POINT ( 'NONE',  ( -11.66860950819323328, -5.915902021225889484, 34.75552854090298638 ) ) ;
#7764 = CARTESIAN_POINT ( 'NONE',  ( -18.06527044596078113, -11.48612834413959405, 32.76840700105983473 ) ) ;
#7765 = CARTESIAN_POINT ( 'NONE',  ( -1.253776966602621057, -7.277220443632450575, 34.74524770363009196 ) ) ;
#7766 = DIRECTION ( 'NONE',  ( 0.000000000000000000, 0.000000000000000000, 1.000000000000000000 ) ) ;
#7767 = CARTESIAN_POINT ( 'NONE',  ( -17.75000000000000711, -12.75000000000000178, 29.75000000000000355 ) ) ;
#7768 = CARTESIAN_POINT ( 'NONE',  ( 17.20771488474786537, -2.541949514083464479, 30.39797389878540557 ) ) ;
#7769 = ORIENTED_EDGE ( 'NONE', *, *, #8010, .F. ) ;
#7770 = ORIENTED_EDGE ( 'NONE', *, *, #28128, .F. ) ;
#7771 = ORIENTED_EDGE ( 'NONE', *, *, #62359, .F. ) ;
#7772 = CARTESIAN_POINT ( 'NONE',  ( 4.023698184114455678, -3.069018819979302926, 32.56621877034667278 ) ) ;
#7773 = VECTOR ( 'NONE', #48648, 1000.000000000000114 ) ;
#7775 = CARTESIAN_POINT ( 'NONE',  ( -13.60810032833933469, -5.912607949931405926, 34.49155766932282319 ) ) ;
#7774 = PLANE ( 'NONE',  #14439 ) ;
#7776 = CARTESIAN_POINT ( 'NONE',  ( 11.40777093535123221, -2.295517848115769421, 30.44137282052137294 ) ) ;
#7777 = DIRECTION ( 'NONE',  ( -0.000000000000000000, 0.3420201433256694901, -0.9396926207859082059 ) ) ;
#7778 = FACE_BOUND ( 'NONE', #23111, .T. ) ;
#7779 = DIRECTION ( 'NONE',  ( -0.000000000000000000, -0.3420201433256694901, -0.9396926207859082059 ) ) ;
#7780 = ORIENTED_EDGE ( 'NONE', *, *, #7492, .F. ) ;
#7781 = CARTESIAN_POINT ( 'NONE',  ( 17.32697749683652688, -12.01375889529407992, 32.43194544308182969 ) ) ;
#7782 = LINE ( 'NONE', #36153, #1392 ) ;
#7783 = CARTESIAN_POINT ( 'NONE',  ( -10.61538461538473577, -3.083524468854526912, 32.58852847137268327 ) ) ;
#7784 = DIRECTION ( 'NONE',  ( 0.000000000000000000, 0.000000000000000000, -1.000000000000000000 ) ) ;
#7785 = VERTEX_POINT ( 'NONE', #52530 ) ;
#7786 = CARTESIAN_POINT ( 'NONE',  ( 8.769230769230768274, -12.62096338111211580, 30.90682066428153263 ) ) ;
#7787 = ORIENTED_EDGE ( 'NONE', *, *, #8596, .F. ) ;
#7788 = FACE_BOUND ( 'NONE', #30256, .T. ) ;
#7789 = B_SPLINE_CURVE_WITH_KNOTS ( 'NONE', 3,
 ( #6619, #82289, #13815, #74193, #68763, #7060, #53014, #12494, #39976, #82732 ),
 .UNSPECIFIED., .F., .F.,
 ( 4, 2, 2, 2, 4 ),
 ( 0.0007817246336856291692, 0.0009771112958940103739, 0.001172497958102391470, 0.001367884620310772566, 0.001563271282519153663 ),
 .UNSPECIFIED. ) ;
#7790 = CARTESIAN_POINT ( 'NONE',  ( -16.15384615384584777, -2.506253911140615021, 30.00000000000323297 ) ) ;
#7791 = EDGE_CURVE ( 'NONE', #6141, #52855, #71059, .T. ) ;
#7792 = B_SPLINE_CURVE_WITH_KNOTS ( 'NONE', 3,
 ( #18991, #12232, #5921, #88359, #54091, #67180, #81584, #19872, #5483, #82031 ),
 .UNSPECIFIED., .F., .F.,
 ( 4, 2, 2, 2, 4 ),
 ( 0.0007817246256747450040, 0.0009771112852218881168, 0.001172497944769031230, 0.001367884604316174342, 0.001563271263863317455 ),
 .UNSPECIFIED. ) ;
#7793 = CARTESIAN_POINT ( 'NONE',  ( 17.01083966596718611, -11.69971097300155272, 32.46337939537587403 ) ) ;
#7794 = CARTESIAN_POINT ( 'NONE',  ( 0.000000000000000000, -11.00000000000000000, 29.75000000000000355 ) ) ;
#7795 = ORIENTED_EDGE ( 'NONE', *, *, #37270, .T. ) ;
#7796 = EDGE_CURVE ( 'NONE', #16308, #1913, #82875, .T. ) ;
#7797 = DIRECTION ( 'NONE',  ( 0.000000000000000000, 0.7660444431189807890, 0.6427876096865361433 ) ) ;
#7798 = CARTESIAN_POINT ( 'NONE',  ( -5.776987155906603277, -9.172514111537584114, 34.72667873470787470 ) ) ;
#7799 = CARTESIAN_POINT ( 'NONE',  ( 8.703960768674447124, -8.656820664281498878, 34.87096338111211935 ) ) ;
#7800 = CARTESIAN_POINT ( 'NONE',  ( 6.222779541268413261, -3.755027918224367767, 33.06320215134714857 ) ) ;
#7801 = ORIENTED_EDGE ( 'NONE', *, *, #60754, .F. ) ;
#7802 = CARTESIAN_POINT ( 'NONE',  ( 16.40390046548447245, -10.66356715214248574, 33.62249196103329751 ) ) ;
#7803 = VERTEX_POINT ( 'NONE', #60175 ) ;
#7805 = ORIENTED_EDGE ( 'NONE', *, *, #54149, .F. ) ;
#7804 = CARTESIAN_POINT ( 'NONE',  ( 4.284636594813106214, -2.845873456487966635, 32.17976146951972538 ) ) ;
#7806 = CARTESIAN_POINT ( 'NONE',  ( 7.596130608860880429, -10.76384336483936011, 33.53834819971076087 ) ) ;
#7807 = CARTESIAN_POINT ( 'NONE',  ( -4.377331097570098528, -2.847400154188068022, 31.58180166144859058 ) ) ;
#7808 = LINE ( 'NONE', #62734, #78854 ) ;
#7809 = LINE ( 'NONE', #35275, #28633 ) ;
#7810 = CARTESIAN_POINT ( 'NONE',  ( -8.769230769230768274, -12.78798330534102767, 29.49999999999997868 ) ) ;
#7813 = CARTESIAN_POINT ( 'NONE',  ( 16.28437185560972011, -6.001044277235009439, 34.52024696741798948 ) ) ;
#7812 = VECTOR ( 'NONE', #44744, 1000.000000000000000 ) ;
#7811 = CARTESIAN_POINT ( 'NONE',  ( -3.230769230769352962, -4.320704448113951379, 33.92786785259630022 ) ) ;
#7814 = EDGE_CURVE ( 'NONE', #78459, #28559, #40810, .T. ) ;
#7815 = CARTESIAN_POINT ( 'NONE',  ( 12.71153846153839950, -7.565270445406050648, 34.75000000000000000 ) ) ;
#7816 = CARTESIAN_POINT ( 'NONE',  ( 1.944543648263018731, -9.444543648262994751, 23.37500000000000000 ) ) ;
#7817 = VERTEX_POINT ( 'NONE', #53418 ) ;
#7818 = CIRCLE ( 'NONE', #38020, 0.2500000000000002220 ) ;
#7819 = CARTESIAN_POINT ( 'NONE',  ( 5.076923076923075762, -1.422936976036506707, 30.56769352161908415 ) ) ;
#7820 = VERTEX_POINT ( 'NONE', #81356 ) ;
#7821 = VECTOR ( 'NONE', #46135, 1000.000000000000227 ) ;
#7822 = ORIENTED_EDGE ( 'NONE', *, *, #9348, .F. ) ;
#7823 = CARTESIAN_POINT ( 'NONE',  ( -11.28840711854808632, -2.318338780012835443, 30.59689888758630261 ) ) ;
#7824 = ORIENTED_EDGE ( 'NONE', *, *, #55980, .F. ) ;
#7825 = CARTESIAN_POINT ( 'NONE',  ( 4.088575707885377497, -12.27809138561121394, 31.22303859784730307 ) ) ;
#7826 = CARTESIAN_POINT ( 'NONE',  ( -7.976301815885541657, -8.630895178749533159, 34.87696386517710323 ) ) ;
#7827 = CYLINDRICAL_SURFACE ( 'NONE', #33218, 0.2499999999999994726 ) ;
#7828 = CARTESIAN_POINT ( 'NONE',  ( 1.161688425708538031, -2.523278758544489353, 31.42238647778637528 ) ) ;
#7829 = CARTESIAN_POINT ( 'NONE',  ( 10.83839745947800992, -6.460100341425560444, 34.89618726649961644 ) ) ;
#7830 = CARTESIAN_POINT ( 'NONE',  ( 12.39626801557768587, -10.90142922261923886, 33.41473453929638993 ) ) ;
#7831 = CARTESIAN_POINT ( 'NONE',  ( 17.07692307692307665, -8.164416787775445883, 34.95778746994557906 ) ) ;
#7832 = CARTESIAN_POINT ( 'NONE',  ( 2.651650429449569302, -10.15165042944953733, 25.87500000000000355 ) ) ;
#7833 = CYLINDRICAL_SURFACE ( 'NONE', #7475, 0.2500000000000009437 ) ;
#7835 = EDGE_CURVE ( 'NONE', #88017, #89081, #47101, .T. ) ;
#7834 = CARTESIAN_POINT ( 'NONE',  ( 18.00000000000000000, -11.69971097300155272, 32.46337939537588113 ) ) ;
#7836 = EDGE_CURVE ( 'NONE', #16729, #66445, #19205, .T. ) ;
#7837 = LINE ( 'NONE', #63208, #86753 ) ;
#7838 = B_SPLINE_CURVE_WITH_KNOTS ( 'NONE', 3,
 ( #72453, #31931, #23811, #24720, #3104, #78770, #17071, #17970, #30579, #52178 ),
 .UNSPECIFIED., .F., .F.,
 ( 4, 2, 2, 2, 4 ),
 ( 0.0007817359430256399806, 0.0009771253907250089001, 0.001172514838424378036, 0.001367904286123746956, 0.001563293733823115875 ),
 .UNSPECIFIED. ) ;
#7839 = CARTESIAN_POINT ( 'NONE',  ( 11.66925334628632882, -4.809403383903225304, 33.96459661697924304 ) ) ;
#7841 = EDGE_CURVE ( 'NONE', #67170, #38356, #73195, .T. ) ;
#7840 = B_SPLINE_CURVE_WITH_KNOTS ( 'NONE', 3,
 ( #46597, #24986, #87158, #53790, #59659, #25436, #53343, #19126, #80844, #74076 ),
 .UNSPECIFIED., .F., .F.,
 ( 4, 2, 2, 2, 4 ),
 ( 0.0007817246256747445703, 0.0009771112852218872494, 0.001172497944769030145, 0.001367884604316172825, 0.001563271263863315504 ),
 .UNSPECIFIED. ) ;
#7842 = EDGE_LOOP ( 'NONE', ( #76539, #32485, #86213, #29033 ) ) ;
#7844 = EDGE_CURVE ( 'NONE', #72978, #82350, #39043, .T. ) ;
#7843 = ORIENTED_EDGE ( 'NONE', *, *, #8207, .T. ) ;
#7845 = DIRECTION ( 'NONE',  ( 1.000000000000000000, 0.000000000000000000, 0.000000000000000000 ) ) ;
#7846 = LINE ( 'NONE', #15046, #20121 ) ;
#7847 = CARTESIAN_POINT ( 'NONE',  ( 3.230769230769231726, -10.67929555188718282, 33.92786785259544047 ) ) ;
#7848 = DIRECTION ( 'NONE',  ( -0.000000000000000000, 0.6427876096865404731, -0.7660444431189771253 ) ) ;
#7849 = EDGE_LOOP ( 'NONE', ( #58330, #72961, #23904, #18650 ) ) ;
#7850 = DIRECTION ( 'NONE',  ( 0.000000000000000000, 0.000000000000000000, -1.000000000000000000 ) ) ;
#7851 = CARTESIAN_POINT ( 'NONE',  ( 11.53846153846141576, -4.320704448113951379, 33.92786785259630022 ) ) ;
#7852 = VECTOR ( 'NONE', #74586, 1000.000000000000227 ) ;
#7853 = FACE_OUTER_BOUND ( 'NONE', #1895, .T. ) ;
#7854 = ORIENTED_EDGE ( 'NONE', *, *, #6336, .F. ) ;
#7855 = CARTESIAN_POINT ( 'NONE',  ( -14.53061926659915315, -12.64616026154729411, 30.79003144601914244 ) ) ;
#7856 = ORIENTED_EDGE ( 'NONE', *, *, #23569, .T. ) ;
#7857 = CARTESIAN_POINT ( 'NONE',  ( -8.769230769230768274, -7.500000000000001776, 35.04278698407183867 ) ) ;
#7858 = CARTESIAN_POINT ( 'NONE',  ( 4.403846153847572609, -7.500000000000154543, 35.00000000000007105 ) ) ;
#7859 = CARTESIAN_POINT ( 'NONE',  ( -1.608100309179714360, -9.417330523894424488, 34.63758898049880486 ) ) ;
#7860 = CARTESIAN_POINT ( 'NONE',  ( -2.307692307692305711, -11.69971097300155272, 32.46337939537588113 ) ) ;
#7861 = CARTESIAN_POINT ( 'NONE',  ( -2.980769230767811084, -7.500000000000154543, 35.00000000000007105 ) ) ;
#7862 = ORIENTED_EDGE ( 'NONE', *, *, #85061, .T. ) ;
#7863 = VERTEX_POINT ( 'NONE', #6575 ) ;
#7864 = B_SPLINE_CURVE_WITH_KNOTS ( 'NONE', 3,
 ( #47120, #67407, #47570, #32727, #34061, #19223, #68291, #12029, #87697, #40391 ),
 .UNSPECIFIED., .F., .F.,
 ( 4, 2, 2, 2, 4 ),
 ( 0.0007817246256747472808, 0.0009771112852218907189, 0.001172497944769034265, 0.001367884604316177595, 0.001563271263863321141 ),
 .UNSPECIFIED. ) ;
#7865 = EDGE_CURVE ( 'NONE', #43710, #77653, #86062, .T. ) ;
#7866 = ORIENTED_EDGE ( 'NONE', *, *, #13576, .F. ) ;
#7867 = VERTEX_POINT ( 'NONE', #13767 ) ;
#7868 = CARTESIAN_POINT ( 'NONE',  ( 13.16168916709923664, -3.105860786376062332, 32.13614157043599562 ) ) ;
#7869 = CARTESIAN_POINT ( 'NONE',  ( -12.71156168575991785, -12.68155406624981119, 30.59749803192733708 ) ) ;
#7870 = CARTESIAN_POINT ( 'NONE',  ( -4.219116154402471786, -12.51329471203370325, 31.30864560766548976 ) ) ;
#7871 = AXIS2_PLACEMENT_3D ( 'NONE', #9847, #64776, #3079 ) ;
#7872 = CARTESIAN_POINT ( 'NONE',  ( 16.85399611801622299, -10.01117774369187252, 34.36070679894347535 ) ) ;
#7873 = FACE_OUTER_BOUND ( 'NONE', #28467, .T. ) ;
#7874 = CARTESIAN_POINT ( 'NONE',  ( 14.43821800945587341, -10.19071101563364756, 33.96452234770658407 ) ) ;
#7875 = VERTEX_POINT ( 'NONE', #7906 ) ;
#7876 = ORIENTED_EDGE ( 'NONE', *, *, #34261, .F. ) ;
#7877 = ADVANCED_FACE ( 'NONE', ( #69163 ), #7467, .F. ) ;
#7878 = EDGE_LOOP ( 'NONE', ( #31110, #78542, #65387, #46441 ) ) ;
#7880 = VERTEX_POINT ( 'NONE', #20526 ) ;
#7879 = CARTESIAN_POINT ( 'NONE',  ( 4.376625822824220080, -4.226511098958374291, 33.85474049983370293 ) ) ;
#7882 = CARTESIAN_POINT ( 'NONE',  ( 13.44987052412822237, -4.320704448112861584, 33.92786785259548310 ) ) ;
#7881 = CARTESIAN_POINT ( 'NONE',  ( -16.94639737515951339, -9.417988943895561960, 34.36773134775778260 ) ) ;
#7883 = CARTESIAN_POINT ( 'NONE',  ( 0.000000000000000000, -11.00000000000000000, 29.75000000000000355 ) ) ;
#7884 = CARTESIAN_POINT ( 'NONE',  ( 13.51514108637895006, -8.586989748646452369, 34.63063291749215011 ) ) ;
#7885 = ORIENTED_EDGE ( 'NONE', *, *, #34867, .T. ) ;
#7886 = ORIENTED_EDGE ( 'NONE', *, *, #75416, .T. ) ;
#7887 = CARTESIAN_POINT ( 'NONE',  ( 3.930919194939302308, -4.026226216239095379, 33.68668979543632958 ) ) ;
#7888 = ORIENTED_EDGE ( 'NONE', *, *, #59827, .T. ) ;
#7889 = FACE_BOUND ( 'NONE', #48450, .T. ) ;
#7890 = CARTESIAN_POINT ( 'NONE',  ( 6.673053685783957967, -4.335965774309649134, 33.62209801155881905 ) ) ;
#7891 = ADVANCED_FACE ( 'NONE', ( #700 ), #69601, .F. ) ;
#7892 = LINE ( 'NONE', #83567, #34752 ) ;
#7893 = ORIENTED_EDGE ( 'NONE', *, *, #21803, .F. ) ;
#7894 = DIRECTION ( 'NONE',  ( -1.000000000000000000, -0.000000000000000000, -0.000000000000000000 ) ) ;
#7895 = CARTESIAN_POINT ( 'NONE',  ( -16.15384615384615330, -12.62096338111211580, 30.90682066428153263 ) ) ;
#7896 = DIRECTION ( 'NONE',  ( 0.000000000000000000, 1.000000000000000000, 0.000000000000000000 ) ) ;
#7897 = EDGE_CURVE ( 'NONE', #80982, #4310, #15110, .T. ) ;
#7898 = CARTESIAN_POINT ( 'NONE',  ( 0.5276068125408991394, -6.386643153685127139, 34.62446782046654192 ) ) ;
#7899 = CARTESIAN_POINT ( 'NONE',  ( 15.48071464014727283, -6.653508905675592722, 34.93172785388651391 ) ) ;
#7900 = ORIENTED_EDGE ( 'NONE', *, *, #4457, .F. ) ;
#7901 = AXIS2_PLACEMENT_3D ( 'NONE', #17225, #51880, #38842 ) ;
#7902 = CARTESIAN_POINT ( 'NONE',  ( -11.28851612908349722, -12.45601412856602686, 31.48342859153981621 ) ) ;
#7903 = LINE ( 'NONE', #83577, #12377 ) ;
#7904 = DIRECTION ( 'NONE',  ( -0.000000000000000000, 0.000000000000000000, 1.000000000000000000 ) ) ;
#7905 = CARTESIAN_POINT ( 'NONE',  ( 6.000000000000001776, -4.786620604624113540, 33.94971097300155094 ) ) ;
#7906 = CARTESIAN_POINT ( 'NONE',  ( -8.769230769230890843, -2.625532179533778709, 30.86335684631627174 ) ) ;
#7907 = FACE_BOUND ( 'NONE', #19903, .T. ) ;
#7909 = DIRECTION ( 'NONE',  ( -1.000000000000000000, 0.000000000000000000, 0.000000000000000000 ) ) ;
#7908 = CARTESIAN_POINT ( 'NONE',  ( -6.923076923076922462, -12.62096338111211580, 30.90682066428153263 ) ) ;
#7910 = EDGE_CURVE ( 'NONE', #16403, #59207, #12742, .T. ) ;
#7911 = CARTESIAN_POINT ( 'NONE',  ( -14.43838291080261627, -3.338472653186243644, 32.95098750199972670 ) ) ;
#7913 = CARTESIAN_POINT ( 'NONE',  ( 5.999999999999880096, -10.90142922262034020, 33.41473453929536674 ) ) ;
#7912 = CARTESIAN_POINT ( 'NONE',  ( -11.31545018684868964, -11.24521262558773493, 33.06293181088029343 ) ) ;
#7914 = DIRECTION ( 'NONE',  ( 0.000000000000000000, 0.8660254037844377084, -0.5000000000000015543 ) ) ;
#7915 = CARTESIAN_POINT ( 'NONE',  ( -2.749999999999997780, -7.561099074964547917, 18.59188170625849068 ) ) ;
#7916 = ORIENTED_EDGE ( 'NONE', *, *, #5049, .T. ) ;
#7917 = CARTESIAN_POINT ( 'NONE',  ( -8.899707477347234885, -7.276988635370452485, 34.74523720219453793 ) ) ;
#7918 = ORIENTED_EDGE ( 'NONE', *, *, #58239, .F. ) ;
#7919 = ADVANCED_FACE ( 'NONE', ( #49335 ), #61949, .F. ) ;
#7920 = CARTESIAN_POINT ( 'NONE',  ( -18.00000000000000000, -6.386643153685127139, 34.62446782046654192 ) ) ;
#7921 = ORIENTED_EDGE ( 'NONE', *, *, #14548, .T. ) ;
#7922 = CARTESIAN_POINT ( 'NONE',  ( -11.28840711854808632, -6.523592122091592671, 34.90882529074906415 ) ) ;
#7924 = EDGE_CURVE ( 'NONE', #27570, #17114, #11885, .T. ) ;
#7923 = CARTESIAN_POINT ( 'NONE',  ( 14.05766908347084865, -4.175268141568685643, 33.81360843649122216 ) ) ;
#7925 = VERTEX_POINT ( 'NONE', #34922 ) ;
#7926 = CARTESIAN_POINT ( 'NONE',  ( -9.942307692307691624, -7.566083408709835645, 34.74999999999999289 ) ) ;
#7927 = CARTESIAN_POINT ( 'NONE',  ( -1.901340078031346525, -9.487747218494661183, 18.43563170625848713 ) ) ;
#7928 = CARTESIAN_POINT ( 'NONE',  ( -10.36533019547115941, -12.65882529074907126, 30.72640787790839312 ) ) ;
#7929 = CARTESIAN_POINT ( 'NONE',  ( 6.989145274079363368, -8.973038597847269315, 34.52809138561122637 ) ) ;
#7930 = CARTESIAN_POINT ( 'NONE',  ( 5.076923076922954969, -6.879047030192662504, 34.71129190930017927 ) ) ;
#7931 = DIRECTION ( 'NONE',  ( -1.000000000000000000, 0.000000000000000000, 0.000000000000000000 ) ) ;
#7932 = LINE ( 'NONE', #14689, #79909 ) ;
#7933 = CARTESIAN_POINT ( 'NONE',  ( -6.000000000000119904, -10.90142922262034020, 33.41473453929536674 ) ) ;
#7934 = CARTESIAN_POINT ( 'NONE',  ( 2.608446859217924629, -10.19485399968118422, 23.62686829374151287 ) ) ;
#7935 = VECTOR ( 'NONE', #43237, 1000.000000000000114 ) ;
#7936 = DIRECTION ( 'NONE',  ( -0.000000000000000000, 0.7660444431189791237, -0.6427876096865379196 ) ) ;
#7938 = EDGE_CURVE ( 'NONE', #14112, #37020, #18542, .T. ) ;
#7937 = CARTESIAN_POINT ( 'NONE',  ( 10.86533013373275658, -11.37275283266504111, 32.91324779482534524 ) ) ;
#7939 = DIRECTION ( 'NONE',  ( -1.000000000000000000, -0.000000000000000000, -0.000000000000000000 ) ) ;
#7940 = CARTESIAN_POINT ( 'NONE',  ( -3.749999999999997780, -7.438900925035489387, 21.59561829374151287 ) ) ;
#7941 = CARTESIAN_POINT ( 'NONE',  ( -17.32692307692307665, -7.500000000000001776, 34.75000000000000000 ) ) ;
#7942 = LINE ( 'NONE', #75956, #39776 ) ;
#7943 = ORIENTED_EDGE ( 'NONE', *, *, #17262, .T. ) ;
#7944 = ADVANCED_FACE ( 'NONE', ( #42582 ), #34486, .F. ) ;
#7945 = CARTESIAN_POINT ( 'NONE',  ( -17.77722045873158763, -2.847695495035523106, 31.58253572463339154 ) ) ;
#7946 = CARTESIAN_POINT ( 'NONE',  ( 16.21991348719623360, -2.486705287966280320, 31.30864560766543647 ) ) ;
#7948 = ORIENTED_EDGE ( 'NONE', *, *, #77177, .F. ) ;
#7947 = CARTESIAN_POINT ( 'NONE',  ( -0.4615384615384611200, -4.102666532097928531, 36.13435417666054406 ) ) ;
#7949 = CARTESIAN_POINT ( 'NONE',  ( -14.53061852520845498, -11.76352882383564769, 32.36236540154569497 ) ) ;
#7950 = EDGE_CURVE ( 'NONE', #62974, #19083, #28166, .T. ) ;
#7951 = CARTESIAN_POINT ( 'NONE',  ( -1.449885830576159940, -10.90142922261923886, 33.41473453929638993 ) ) ;
#7952 = CARTESIAN_POINT ( 'NONE',  ( -12.94230769230769162, -7.500000000000000000, 33.75000000000000000 ) ) ;
#7953 = CARTESIAN_POINT ( 'NONE',  ( -39.05038313613820122, -2.499999999999999556, 29.75000000000000355 ) ) ;
#7954 = CARTESIAN_POINT ( 'NONE',  ( -10.39260507411620260, -10.81320215134717344, 33.49497208177562868 ) ) ;
#7955 = ORIENTED_EDGE ( 'NONE', *, *, #88303, .T. ) ;
#7956 = CARTESIAN_POINT ( 'NONE',  ( 7.053602361310566948, -11.66157788607254275, 32.95092075102925833 ) ) ;
#7957 = VERTEX_POINT ( 'NONE', #8799 ) ;
#7958 = B_SPLINE_CURVE_WITH_KNOTS ( 'NONE', 3,
 ( #45510, #37869, #65332, #74208, #12507, #58568, #86061, #24341, #60685, #81419 ),
 .UNSPECIFIED., .F., .F.,
 ( 4, 2, 2, 2, 4 ),
 ( 0.000000000000000000, 0.0001954311564186877418, 0.0003908623128373754836, 0.0005862934692560632524, 0.0007817246256747509671 ),
 .UNSPECIFIED. ) ;
#7960 = EDGE_LOOP ( 'NONE', ( #80731, #3323 ) ) ;
#7959 = B_SPLINE_CURVE_WITH_KNOTS ( 'NONE', 3,
 ( #7834, #69970, #77173, #54673, #48808, #20464, #83054, #22231, #70424, #56013 ),
 .UNSPECIFIED., .F., .F.,
 ( 4, 2, 2, 2, 4 ),
 ( 0.000000000000000000, 0.0001954339857564096699, 0.0003908679715128193398, 0.0005863019572692289554, 0.0007817359430256386795 ),
 .UNSPECIFIED. ) ;
#7961 = CYLINDRICAL_SURFACE ( 'NONE', #34096, 0.2499999999999979738 ) ;
#7962 = CARTESIAN_POINT ( 'NONE',  ( 6.857806477116149324, -2.892918686051582089, 31.69288490824015270 ) ) ;
#7963 = EDGE_CURVE ( 'NONE', #23024, #87173, #261, .T. ) ;
#7964 = CARTESIAN_POINT ( 'NONE',  ( 9.942362003946010773, -4.943051570960394159, 34.04725096376909477 ) ) ;
#7965 = CARTESIAN_POINT ( 'NONE',  ( 13.31853300525524908, -8.164416787775445883, 34.95778746994557906 ) ) ;
#7966 = ORIENTED_EDGE ( 'NONE', *, *, #14932, .F. ) ;
#7967 = CARTESIAN_POINT ( 'NONE',  ( -17.29984929443921970, -4.186968288167451036, 33.49512374952580274 ) ) ;
#7968 = EDGE_LOOP ( 'NONE', ( #38906, #47783, #15264, #4169 ) ) ;
#7969 = ADVANCED_FACE ( 'NONE', ( #70042 ), #48431, .T. ) ;
#7970 = EDGE_LOOP ( 'NONE', ( #62182, #86002, #35987, #14720 ) ) ;
#7971 = ORIENTED_EDGE ( 'NONE', *, *, #65140, .T. ) ;
#7973 = VERTEX_POINT ( 'NONE', #15551 ) ;
#7972 = DIRECTION ( 'NONE',  ( -1.000000000000000000, -0.000000000000000000, 0.000000000000000000 ) ) ;
#7974 = CARTESIAN_POINT ( 'NONE',  ( -4.826977667545032880, -12.45601412856602863, 31.48342859153981621 ) ) ;
#7975 = EDGE_CURVE ( 'NONE', #42322, #16211, #70491, .T. ) ;
#7976 = CARTESIAN_POINT ( 'NONE',  ( -3.230769230769352962, -12.16647553114689728, 32.15551576947799362 ) ) ;
#7977 = ADVANCED_FACE ( 'NONE', ( #41690 ), #77683, .F. ) ;
#7978 = DIRECTION ( 'NONE',  ( 0.000000000000000000, 0.9396926207859126468, -0.3420201433256571111 ) ) ;
#7979 = CARTESIAN_POINT ( 'NONE',  ( -5.142679879437387136, -7.249945686854186278, 34.74374336980224598 ) ) ;
#7980 = ORIENTED_EDGE ( 'NONE', *, *, #74850, .T. ) ;
#7981 = ORIENTED_EDGE ( 'NONE', *, *, #62093, .T. ) ;
#7982 = EDGE_CURVE ( 'NONE', #41734, #74112, #44324, .T. ) ;
#7983 = ORIENTED_EDGE ( 'NONE', *, *, #56884, .F. ) ;
#7984 = CARTESIAN_POINT ( 'NONE',  ( -2.084679463598910765, -3.395485233115138168, 33.02377354290276656 ) ) ;
#7986 = ORIENTED_EDGE ( 'NONE', *, *, #61460, .T. ) ;
#7985 = CARTESIAN_POINT ( 'NONE',  ( 4.403900465484468008, -11.28795663066794219, 33.01431243580653785 ) ) ;
#7987 = LINE ( 'NONE', #1668, #19163 ) ;
#7988 = DIRECTION ( 'NONE',  ( -1.000000000000000000, 1.681660752236433198E-16, 0.000000000000000000 ) ) ;
#7989 = B_SPLINE_CURVE_WITH_KNOTS ( 'NONE', 3,
 ( #42711, #394, #70617, #43580, #37710, #58411, #85024, #71053, #37259, #10251 ),
 .UNSPECIFIED., .F., .F.,
 ( 4, 2, 2, 2, 4 ),
 ( 0.000000000000000000, 0.0001954311584214072923, 0.0003908623168428145846, 0.0005862934752642218498, 0.0007817246336856291692 ),
 .UNSPECIFIED. ) ;
#7990 = VECTOR ( 'NONE', #5151, 1000.000000000000000 ) ;
#7991 = CARTESIAN_POINT ( 'NONE',  ( -0.3307480205715107036, -9.084667340241226796, 34.75534355489798344 ) ) ;
#7992 = ORIENTED_EDGE ( 'NONE', *, *, #61695, .F. ) ;
#7993 = DIRECTION ( 'NONE',  ( 0.000000000000000000, 0.6427876096865368094, 0.7660444431189802339 ) ) ;
#7994 = CARTESIAN_POINT ( 'NONE',  ( 15.16468685140909400, -2.486705287966279432, 31.30864560766542937 ) ) ;
#7995 = VERTEX_POINT ( 'NONE', #43901 ) ;
#7996 = FACE_BOUND ( 'NONE', #11816, .T. ) ;
#7997 = CARTESIAN_POINT ( 'NONE',  ( -18.00000000000000000, -12.50000000000000000, 29.74999999999997868 ) ) ;
#7998 = CARTESIAN_POINT ( 'NONE',  ( 13.38461538461526423, -6.835583212225970762, 34.95778746994575670 ) ) ;
#7999 = B_SPLINE_CURVE_WITH_KNOTS ( 'NONE', 3,
 ( #49676, #77152, #71262, #85245, #64495, #43365, #70847, #64950, #15461, #76713 ),
 .UNSPECIFIED., .F., .F.,
 ( 4, 2, 2, 2, 4 ),
 ( 0.0007817359430256315238, 0.0009771253907249976244, 0.001172514838424363508, 0.001367904286123729392, 0.001563293733823095492 ),
 .UNSPECIFIED. ) ;
#8000 = CYLINDRICAL_SURFACE ( 'NONE', #52354, 2.000000000000001776 ) ;
#8002 = CARTESIAN_POINT ( 'NONE',  ( 18.22301135161285046, -4.187068189119696804, 33.49521262558774026 ) ) ;
#8001 = DIRECTION ( 'NONE',  ( -0.000000000000000000, -0.000000000000000000, -1.000000000000000000 ) ) ;
#8003 = CARTESIAN_POINT ( 'NONE',  ( -11.53846153846166089, -10.33852847137269571, 34.16647553114546554 ) ) ;
#8004 = CARTESIAN_POINT ( 'NONE',  ( -2.372962753653082402, -3.835265460703609186, 33.15142922261924241 ) ) ;
#8005 = EDGE_LOOP ( 'NONE', ( #10524, #88073, #64116, #46392 ) ) ;
#8006 = DIRECTION ( 'NONE',  ( 0.000000000000000000, 0.6427876096865368094, 0.7660444431189802339 ) ) ;
#8007 = DIRECTION ( 'NONE',  ( 0.000000000000000000, 0.3420201433256610524, 0.9396926207859113145 ) ) ;
#8008 = EDGE_CURVE ( 'NONE', #17545, #64477, #74256, .T. ) ;
#8009 = ORIENTED_EDGE ( 'NONE', *, *, #19204, .T. ) ;
#8010 = EDGE_CURVE ( 'NONE', #5191, #47721, #52706, .T. ) ;
#8011 = DIRECTION ( 'NONE',  ( 0.000000000000000000, -1.000000000000000000, 0.000000000000000000 ) ) ;
#8012 = CARTESIAN_POINT ( 'NONE',  ( 9.562160482869474620, -2.882441371585227508, 31.66841991370172238 ) ) ;
#8013 = VERTEX_POINT ( 'NONE', #57860 ) ;
#8014 = CARTESIAN_POINT ( 'NONE',  ( -0.2387589202700529378, -12.44528174975671853, 30.48912976160716681 ) ) ;
#8015 = DIRECTION ( 'NONE',  ( -0.000000000000000000, -0.7660444431189791237, -0.6427876096865379196 ) ) ;
#8016 = FACE_BOUND ( 'NONE', #31257, .T. ) ;
#8018 = CARTESIAN_POINT ( 'NONE',  ( 15.23076923076923173, -12.10708131394839349, 31.69288490824020244 ) ) ;
#8017 = CARTESIAN_POINT ( 'NONE',  ( -5.076923076923197442, -2.892918686052165622, 31.69288490824153470 ) ) ;
#8019 = CARTESIAN_POINT ( 'NONE',  ( 5.198717948717946236, -7.500000000000000000, 29.75000000000000355 ) ) ;
#8020 = CARTESIAN_POINT ( 'NONE',  ( 12.21156171748987163, -12.41104346484419452, 31.60698883733904196 ) ) ;
#8022 = CARTESIAN_POINT ( 'NONE',  ( 7.780902855992604117, -2.506253911140460922, 30.00000000000013856 ) ) ;
#8021 = CARTESIAN_POINT ( 'NONE',  ( -3.099977422944444783, -11.71459661697925903, 32.44059661609676937 ) ) ;
#8023 = CARTESIAN_POINT ( 'NONE',  ( -14.17690186672535901, -5.496552790871120031, 34.60292014791297532 ) ) ;
#8024 = CARTESIAN_POINT ( 'NONE',  ( 2.320192649118979489E-14, -11.25000000000000000, 26.03125000000000000 ) ) ;
#8025 = ORIENTED_EDGE ( 'NONE', *, *, #44155, .F. ) ;
#8026 = VERTEX_POINT ( 'NONE', #58299 ) ;
#8027 = PLANE ( 'NONE',  #52136 ) ;
#8028 = VECTOR ( 'NONE', #69628, 1000.000000000000227 ) ;
#8029 = CARTESIAN_POINT ( 'NONE',  ( -10.48485917715096782, -8.630441415882550871, 34.87705825610312615 ) ) ;
#8030 = CARTESIAN_POINT ( 'NONE',  ( 1.607395053593452694, -9.418065098278011860, 34.63729479722530158 ) ) ;
#8031 = CARTESIAN_POINT ( 'NONE',  ( -0.4615384615385840772, -3.083524468854526912, 32.58852847137268327 ) ) ;
#8032 = CARTESIAN_POINT ( 'NONE',  ( -13.38461538461550759, -2.657715359629662544, 31.77849191805970364 ) ) ;
#8033 = CARTESIAN_POINT ( 'NONE',  ( -1.929879867024197893E-14, -3.750000000000000000, 25.40625000000000000 ) ) ;
#8034 = CARTESIAN_POINT ( 'NONE',  ( -19.00000000000000000, -1.249999999999997558, 22.25000000000000000 ) ) ;
#8035 = DIRECTION ( 'NONE',  ( -1.000000000000000000, 0.000000000000000000, 0.000000000000000000 ) ) ;
#8036 = VECTOR ( 'NONE', #60996, 1000.000000000000000 ) ;
#8037 = CYLINDRICAL_SURFACE ( 'NONE', #1319, 0.2499999999999997502 ) ;
#8038 = CARTESIAN_POINT ( 'NONE',  ( 7.623226887246997485, -5.582147617184174848, 34.63737895849758530 ) ) ;
#8039 = DIRECTION ( 'NONE',  ( -0.000000000000000000, 1.000000000000000000, 3.491481338843133355E-15 ) ) ;
#8040 = CARTESIAN_POINT ( 'NONE',  ( -17.07692307692307665, -2.249999999999998668, 29.75000000000001776 ) ) ;
#8041 = B_SPLINE_CURVE_WITH_KNOTS ( 'NONE', 3,
 ( #28589, #70461, #43429, #83092, #1997, #77207, #1111, #42985, #70005, #22703 ),
 .UNSPECIFIED., .F., .F.,
 ( 4, 2, 2, 2, 4 ),
 ( 0.0007817246256747478229, 0.0009771112852218913694, 0.001172497944769034916, 0.001367884604316178679, 0.001563271263863322226 ),
 .UNSPECIFIED. ) ;
#8042 = CARTESIAN_POINT ( 'NONE',  ( -9.692307692307814193, -12.70778746994576025, 30.41441678777401236 ) ) ;
#8044 = ADVANCED_FACE ( 'NONE', ( #45231 ), #64158, .F. ) ;
#8043 = DIRECTION ( 'NONE',  ( -0.000000000000000000, 0.9396926207859092051, -0.3420201433256662704 ) ) ;
#8045 = ADVANCED_FACE ( 'NONE', ( #65505 ), #43461, .F. ) ;
#8046 = CARTESIAN_POINT ( 'NONE',  ( -12.71153846153846168, -2.499999999999998668, 29.75000000000000355 ) ) ;
#8047 = EDGE_LOOP ( 'NONE', ( #555, #12318, #44257, #88757 ) ) ;
#8048 = CARTESIAN_POINT ( 'NONE',  ( -14.37377571864818293, -3.513871655860377086, 32.76840700105978499 ) ) ;
#8049 = CARTESIAN_POINT ( 'NONE',  ( 7.846153846153846700, -4.661471528628507777, 34.16647553114623292 ) ) ;
#8050 = CARTESIAN_POINT ( 'NONE',  ( 0.06109907496451789238, -4.749999999999998224, 20.65811829374151287 ) ) ;
#8051 = ADVANCED_FACE ( 'NONE', ( #72260 ), #2460, .F. ) ;
#8052 = DIRECTION ( 'NONE',  ( -0.000000000000000000, 0.7660444431189791237, -0.6427876096865379196 ) ) ;
#8053 = LINE ( 'NONE', #1731, #26952 ) ;
#8054 = ORIENTED_EDGE ( 'NONE', *, *, #54675, .F. ) ;
#8055 = CARTESIAN_POINT ( 'NONE',  ( -9.758390071667825794, -5.471508081941602875, 34.59228464037088457 ) ) ;
#8057 = VERTEX_POINT ( 'NONE', #57410 ) ;
#8056 = CARTESIAN_POINT ( 'NONE',  ( -9.692307692307691624, -4.786620604624113540, 33.94971097300155094 ) ) ;
#8058 = CARTESIAN_POINT ( 'NONE',  ( 7.173131234715237170, -3.627508038966690496, 32.91356715214248396 ) ) ;
#8059 = CARTESIAN_POINT ( 'NONE',  ( -2.438382910802613157, -10.70098750199973203, 33.91152734681376302 ) ) ;
#8060 = EDGE_CURVE ( 'NONE', #24465, #37632, #85790, .T. ) ;
#8061 = EDGE_LOOP ( 'NONE', ( #80915, #38701, #80256, #24488 ) ) ;
#8062 = DIRECTION ( 'NONE',  ( 0.000000000000000000, -1.000000000000000000, 0.000000000000000000 ) ) ;
#8063 = CARTESIAN_POINT ( 'NONE',  ( 13.38461538461538680, -9.058645607665452459, 34.76329471203371924 ) ) ;
#8064 = EDGE_CURVE ( 'NONE', #23956, #32626, #76075, .T. ) ;
#8065 = ORIENTED_EDGE ( 'NONE', *, *, #33339, .F. ) ;
#8066 = CARTESIAN_POINT ( 'NONE',  ( 17.01165263096230262, -11.48612834413959582, 32.76840700105983473 ) ) ;
#8067 = DIRECTION ( 'NONE',  ( 1.000000000000000000, 0.000000000000000000, 0.000000000000000000 ) ) ;
#8068 = DIRECTION ( 'NONE',  ( -0.000000000000000000, 1.000000000000000000, -0.000000000000000000 ) ) ;
#8069 = VERTEX_POINT ( 'NONE', #72707 ) ;
#8070 = EDGE_LOOP ( 'NONE', ( #71863, #42234 ) ) ;
#8071 = ADVANCED_FACE ( 'NONE', ( #10570 ), #37137, .F. ) ;
#8072 = CARTESIAN_POINT ( 'NONE',  ( -10.55012947587177941, -2.379036618887895305, 30.90682066428158592 ) ) ;
#8073 = ORIENTED_EDGE ( 'NONE', *, *, #79413, .T. ) ;
#8074 = CARTESIAN_POINT ( 'NONE',  ( -10.55023983466498017, -7.750023224968867197, 34.99404313364389907 ) ) ;
#8075 = CARTESIAN_POINT ( 'NONE',  ( 5.326977496836529546, -4.818054556918156095, 34.26375889529406749 ) ) ;
#8076 = CARTESIAN_POINT ( 'NONE',  ( -14.37377571864818293, -3.050289026998445951, 32.03036669348365706 ) ) ;
#8077 = ADVANCED_FACE ( 'NONE', ( #23628 ), #78572, .F. ) ;
#8078 = AXIS2_PLACEMENT_3D ( 'NONE', #21958, #42676, #88668 ) ;
#8079 = CARTESIAN_POINT ( 'NONE',  ( -5.076923076923197442, -12.27809138561165270, 31.22303859784587132 ) ) ;
#8080 = CARTESIAN_POINT ( 'NONE',  ( 11.53846153846153832, -1.629998284177014645, 34.34916445242399163 ) ) ;
#8081 = CARTESIAN_POINT ( 'NONE',  ( 15.48076923076923705, -2.499999999999999556, 29.81604066197449754 ) ) ;
#8082 = ORIENTED_EDGE ( 'NONE', *, *, #10857, .F. ) ;
#8083 = ORIENTED_EDGE ( 'NONE', *, *, #30057, .F. ) ;
#8085 = ORIENTED_EDGE ( 'NONE', *, *, #65230, .F. ) ;
#8084 = DIRECTION ( 'NONE',  ( -0.000000000000000000, 0.5000000000000011102, -0.8660254037844381525 ) ) ;
#8086 = EDGE_CURVE ( 'NONE', #8684, #60639, #53111, .T. ) ;
#8087 = CARTESIAN_POINT ( 'NONE',  ( 7.622668921589513147, -2.612411019501189369, 31.66733052389439962 ) ) ;
#8088 = ORIENTED_EDGE ( 'NONE', *, *, #59355, .F. ) ;
#8089 = AXIS2_PLACEMENT_3D ( 'NONE', #20353, #54114, #80733 ) ;
#8090 = CARTESIAN_POINT ( 'NONE',  ( 9.692307692307695177, -12.48256725967547354, 35.29906147534542527 ) ) ;
#8091 = CARTESIAN_POINT ( 'NONE',  ( 8.096208157792160520, -4.943051570960394159, 34.04725096376909477 ) ) ;
#8092 = ORIENTED_EDGE ( 'NONE', *, *, #86036, .F. ) ;
#8093 = CARTESIAN_POINT ( 'NONE',  ( -12.46153846153858247, -6.026961402154118019, 34.52809138561165270 ) ) ;
#8094 = AXIS2_PLACEMENT_3D ( 'NONE', #49374, #78611, #70084 ) ;
#8095 = EDGE_CURVE ( 'NONE', #62614, #4262, #87196, .T. ) ;
#8096 = ORIENTED_EDGE ( 'NONE', *, *, #45232, .F. ) ;
#8098 = ORIENTED_EDGE ( 'NONE', *, *, #38884, .T. ) ;
#8097 = CARTESIAN_POINT ( 'NONE',  ( -8.546451227962359454, -8.496831190052096971, 34.64984203495476578 ) ) ;
#8099 = CARTESIAN_POINT ( 'NONE',  ( -14.24243716817946925, -12.16647553114626490, 32.15551576947920864 ) ) ;
#8100 = VERTEX_POINT ( 'NONE', #26746 ) ;
#8101 = EDGE_CURVE ( 'NONE', #45738, #41484, #66759, .T. ) ;
#8102 = CARTESIAN_POINT ( 'NONE',  ( 14.30769230769231015, -2.499999999999998668, 29.75000000000001421 ) ) ;
#8103 = CARTESIAN_POINT ( 'NONE',  ( 17.93472999944368240, -12.51329471203370325, 31.30864560766548976 ) ) ;
#8104 = FACE_BOUND ( 'NONE', #85866, .T. ) ;
#8105 = CARTESIAN_POINT ( 'NONE',  ( 1.634560902963529072, -12.43552623307873972, 30.55307653245132826 ) ) ;
#8106 = CARTESIAN_POINT ( 'NONE',  ( -18.00000000000000000, -12.10708131394839349, 31.69288490824020244 ) ) ;
#8107 = CARTESIAN_POINT ( 'NONE',  ( 9.469380733400843297, -11.43668979543634734, 33.22377378376089752 ) ) ;
#8108 = CARTESIAN_POINT ( 'NONE',  ( 12.39626846098214230, -3.643525952247789412, 33.31231777344662959 ) ) ;
#8109 = CARTESIAN_POINT ( 'NONE',  ( 6.000000000000001776, -12.37446782046654192, 30.86335684631486131 ) ) ;
#8110 = CARTESIAN_POINT ( 'NONE',  ( -16.28453762051371356, -8.147922237126337563, 34.70805685702651999 ) ) ;
#8111 = ORIENTED_EDGE ( 'NONE', *, *, #69050, .T. ) ;
#8112 = CYLINDRICAL_SURFACE ( 'NONE', #33152, 0.2500000000000002220 ) ;
#8113 = ORIENTED_EDGE ( 'NONE', *, *, #2474, .T. ) ;
#8114 = EDGE_CURVE ( 'NONE', #32882, #3366, #81702, .T. ) ;
#8115 = ORIENTED_EDGE ( 'NONE', *, *, #42048, .T. ) ;
#8117 = DIRECTION ( 'NONE',  ( 0.000000000000000000, 0.3420201433256610524, 0.9396926207859113145 ) ) ;
#8116 = CARTESIAN_POINT ( 'NONE',  ( 9.692307692308007816, -2.255955759149395501, 30.00000000000324363 ) ) ;
#8118 = EDGE_CURVE ( 'NONE', #21774, #75150, #12350, .T. ) ;
#8119 = DIRECTION ( 'NONE',  ( -0.000000000000000000, -0.8660254037844399289, -0.4999999999999980016 ) ) ;
#8120 = CARTESIAN_POINT ( 'NONE',  ( -16.82697766754503377, -10.18230066228895758, 34.26354781536631577 ) ) ;
#8121 = CARTESIAN_POINT ( 'NONE',  ( 5.076923076923075762, -5.180354513474913603, 36.12317359536750416 ) ) ;
#8122 = CARTESIAN_POINT ( 'NONE',  ( -12.39547112818838492, -4.661471528628508665, 34.16647553114624003 ) ) ;
#8123 = ADVANCED_FACE ( 'NONE', ( #60080 ), #4708, .F. ) ;
#8124 = EDGE_LOOP ( 'NONE', ( #72308, #87766, #31778, #65672 ) ) ;
#8125 = VECTOR ( 'NONE', #1064, 1000.000000000000114 ) ;
#8126 = CARTESIAN_POINT ( 'NONE',  ( 11.53846153846141576, -3.643525952248795718, 33.31231777344771672 ) ) ;
#8127 = CARTESIAN_POINT ( 'NONE',  ( -6.065270445960775803, -6.879047030191174805, 34.71129190930000163 ) ) ;
#8128 = LINE ( 'NONE', #8570, #54588 ) ;
#8129 = CARTESIAN_POINT ( 'NONE',  ( 10.61538461538461675, -8.120952969808772792, 34.71129190930000163 ) ) ;
#8130 = CARTESIAN_POINT ( 'NONE',  ( 2.372947447205147942, -5.941354392334606160, 34.76329471203374055 ) ) ;
#8131 = VERTEX_POINT ( 'NONE', #53322 ) ;
#8132 = CARTESIAN_POINT ( 'NONE',  ( -0.5276208408985981757, -2.292212530054419606, 30.41441678777542634 ) ) ;
#8133 = VERTEX_POINT ( 'NONE', #5147 ) ;
#8134 = ITEM_DEFINED_TRANSFORMATION ( 'NONE', 'NONE', #15870,  #83448 ) ;
#8135 = ORIENTED_EDGE ( 'NONE', *, *, #69016, .T. ) ;
#8136 = CARTESIAN_POINT ( 'NONE',  ( -6.000000000000121680, -4.320704448113951379, 33.92786785259630022 ) ) ;
#8137 = EDGE_LOOP ( 'NONE', ( #55390, #48515 ) ) ;
#8138 = PLANE ( 'NONE',  #17965 ) ;
#8139 = CARTESIAN_POINT ( 'NONE',  ( -8.352564102564102200, -7.500000000000000000, 29.75000000000000355 ) ) ;
#8140 = CARTESIAN_POINT ( 'NONE',  ( -17.76215049426128445, -1.749999999999992450, 28.00000000000000000 ) ) ;
#8141 = CARTESIAN_POINT ( 'NONE',  ( -17.14219307747939069, -12.70778746994557551, 30.41441678777548319 ) ) ;
#8142 = DIRECTION ( 'NONE',  ( -0.000000000000000000, 1.000000000000000000, 3.491481338843133355E-15 ) ) ;
#8143 = CARTESIAN_POINT ( 'NONE',  ( 8.703960323269994248, -6.879047030191174805, 34.71129190930000163 ) ) ;
#8144 = EDGE_LOOP ( 'NONE', ( #16860, #78803, #52814, #32722 ) ) ;
#8145 = CARTESIAN_POINT ( 'NONE',  ( -11.40762320797477614, -7.277220318596961057, 34.99547417642776992 ) ) ;
#8147 = ORIENTED_EDGE ( 'NONE', *, *, #57036, .T. ) ;
#8146 = CARTESIAN_POINT ( 'NONE',  ( -17.07692307692319744, -4.481592998941358097, 33.73612834414048933 ) ) ;
#8148 = CARTESIAN_POINT ( 'NONE',  ( -6.000000000000121680, -3.643525952248796163, 33.31231777344771672 ) ) ;
#8149 = LINE ( 'NONE', #63070, #71463 ) ;
#8150 = CARTESIAN_POINT ( 'NONE',  ( -17.32689982097166492, -12.01397095200673881, 32.43157075238190146 ) ) ;
#8151 = CARTESIAN_POINT ( 'NONE',  ( 15.48082365068267841, -2.920487667080175598, 32.31805714834170828 ) ) ;
#8152 = CARTESIAN_POINT ( 'NONE',  ( -9.915234651214539952, -12.38737895849757820, 31.66785238281580206 ) ) ;
#8153 = FACE_OUTER_BOUND ( 'NONE', #15511, .T. ) ;
#8154 = DIRECTION ( 'NONE',  ( 0.000000000000000000, 0.6427876096865368094, 0.7660444431189802339 ) ) ;
#8155 = CARTESIAN_POINT ( 'NONE',  ( -1.614399933863613468, -11.22469193450124969, 13.86124329374151820 ) ) ;
#8156 = ORIENTED_EDGE ( 'NONE', *, *, #39642, .T. ) ;
#8157 = CARTESIAN_POINT ( 'NONE',  ( -16.94639737515951339, -10.88167719472716399, 33.43325721877153711 ) ) ;
#8158 = CARTESIAN_POINT ( 'NONE',  ( -13.51476259405360203, -9.418419913701741919, 34.36755862841477693 ) ) ;
#8159 = CARTESIAN_POINT ( 'NONE',  ( 8.834485908743605620, -11.06231777344671130, 33.60647404775212976 ) ) ;
#8161 = CARTESIAN_POINT ( 'NONE',  ( 9.626225312947559232, -6.343179335718451384, 34.87096338111212646 ) ) ;
#8160 = AXIS2_PLACEMENT_3D ( 'NONE', #14261, #48475, #70085 ) ;
#8162 = EDGE_LOOP ( 'NONE', ( #5322, #67100 ) ) ;
#8163 = DIRECTION ( 'NONE',  ( -0.000000000000000000, 0.9848077530122085754, -0.1736481776669273613 ) ) ;
#8164 = CARTESIAN_POINT ( 'NONE',  ( -15.90379184220783948, -12.17597550085003633, 31.52189283813461884 ) ) ;
#8165 = AXIS2_PLACEMENT_3D ( 'NONE', #19814, #47277, #40542 ) ;
#8166 = CARTESIAN_POINT ( 'NONE',  ( 14.05769230769230838, -2.249999999999998668, 29.75000000000000355 ) ) ;
#8167 = DIRECTION ( 'NONE',  ( -0.000000000000000000, -0.3420201433256694901, -0.9396926207859082059 ) ) ;
#8168 = EDGE_CURVE ( 'NONE', #15450, #38452, #9915, .T. ) ;
#8169 = VERTEX_POINT ( 'NONE', #45682 ) ;
#8170 = B_SPLINE_CURVE_WITH_KNOTS ( 'NONE', 3,
 ( #11241, #36182, #72938, #2363, #49241, #42934, #79703, #1500, #70403, #29425 ),
 .UNSPECIFIED., .F., .F.,
 ( 4, 2, 2, 2, 4 ),
 ( 0.000000000000000000, 0.0001954311564186866034, 0.0003908623128373732067, 0.0005862934692560597830, 0.0007817246256747464135 ),
 .UNSPECIFIED. ) ;
#8171 = CARTESIAN_POINT ( 'NONE',  ( -12.21148414990014963, -9.148310452688876993, 34.47095581063188519 ) ) ;
#8172 = B_SPLINE_CURVE_WITH_KNOTS ( 'NONE', 3,
 ( #12413, #41219, #88106, #34007, #32245, #75443, #54269, #88538, #33578, #11978 ),
 .UNSPECIFIED., .F., .F.,
 ( 4, 2, 2, 2, 4 ),
 ( 0.0007817246256747460882, 0.0009771112852218900684, 0.001172497944769033832, 0.001367884604316177595, 0.001563271263863321575 ),
 .UNSPECIFIED. ) ;
#8173 = AXIS2_PLACEMENT_3D ( 'NONE', #81816, #21432, #76372 ) ;
#8174 = CARTESIAN_POINT ( 'NONE',  ( -0.6850233861027921201, -10.23692288466677880, 34.23039457007281072 ) ) ;
#8175 = CARTESIAN_POINT ( 'NONE',  ( -13.25408994638174320, -12.70449254468099198, 30.44128974285582956 ) ) ;
#8176 = VERTEX_POINT ( 'NONE', #88044 ) ;
#8177 = ADVANCED_FACE ( 'NONE', ( #59194 ), #47451, .F. ) ;
#8178 = CARTESIAN_POINT ( 'NONE',  ( 9.692307692307695177, -12.09954503811598769, 35.62045528018868623 ) ) ;
#8179 = VERTEX_POINT ( 'NONE', #32178 ) ;
#8180 = CARTESIAN_POINT ( 'NONE',  ( -2.531177251416256713, -12.24155766932282496, 31.33739205006857986 ) ) ;
#8181 = CARTESIAN_POINT ( 'NONE',  ( 6.223426961861570739, -7.630147231320743018, 34.74852402298682819 ) ) ;
#8182 = ORIENTED_EDGE ( 'NONE', *, *, #44950, .F. ) ;
#8183 = CARTESIAN_POINT ( 'NONE',  ( -19.50000000000000000, -11.50000000000000000, 29.75000000000000355 ) ) ;
#8184 = CARTESIAN_POINT ( 'NONE',  ( -8.992715712954716167, -2.599994579823203367, 30.74605699353653776 ) ) ;
#8185 = CARTESIAN_POINT ( 'NONE',  ( 1.161130440891438687, -4.386631170607604879, 33.66268669641500111 ) ) ;
#8186 = EDGE_CURVE ( 'NONE', #57379, #66205, #17295, .T. ) ;
#8187 = DIRECTION ( 'NONE',  ( -0.000000000000000000, -0.9848077530122085754, -0.1736481776669273613 ) ) ;
#8188 = FACE_OUTER_BOUND ( 'NONE', #73969, .T. ) ;
#8189 = ORIENTED_EDGE ( 'NONE', *, *, #22291, .F. ) ;
#8190 = ORIENTED_EDGE ( 'NONE', *, *, #7435, .F. ) ;
#8191 = FACE_BOUND ( 'NONE', #53229, .T. ) ;
#8192 = ORIENTED_EDGE ( 'NONE', *, *, #73661, .T. ) ;
#8193 = DIRECTION ( 'NONE',  ( 0.000000000000000000, 0.000000000000000000, 1.000000000000000000 ) ) ;
#8194 = VECTOR ( 'NONE', #53595, 1000.000000000000000 ) ;
#8195 = ADVANCED_FACE ( 'NONE', ( #59640 ), #87140, .F. ) ;
#8196 = CARTESIAN_POINT ( 'NONE',  ( 23.49999999999999645, -4.999999999999999112, 28.00000000000000000 ) ) ;
#8197 = EDGE_CURVE ( 'NONE', #28285, #14918, #42045, .T. ) ;
#8198 = CYLINDRICAL_SURFACE ( 'NONE', #73733, 0.2500000000000004996 ) ;
#8199 = CARTESIAN_POINT ( 'NONE',  ( -13.91025641025641058, -3.499999999999999556, 29.75000000000000355 ) ) ;
#8200 = VERTEX_POINT ( 'NONE', #83479 ) ;
#8201 = B_SPLINE_CURVE_WITH_KNOTS ( 'NONE', 3,
 ( #65850, #10482, #65414, #72616, #3706, #59098 ),
 .UNSPECIFIED., .F., .F.,
 ( 4, 2, 4 ),
 ( 0.000000000000000000, 0.0001954784845028911366, 0.0003909569690057822732 ),
 .UNSPECIFIED. ) ;
#8202 = ORIENTED_EDGE ( 'NONE', *, *, #70714, .F. ) ;
#8203 = ORIENTED_EDGE ( 'NONE', *, *, #34977, .F. ) ;
#8204 = CARTESIAN_POINT ( 'NONE',  ( -0.2385271099256131566, -3.105924265160262543, 32.13625925475356127 ) ) ;
#8205 = B_SPLINE_CURVE_WITH_KNOTS ( 'NONE', 3,
 ( #7858, #81749, #35320, #62776, #28577, #13726, #74993, #41200, #13281, #33991 ),
 .UNSPECIFIED., .F., .F.,
 ( 4, 2, 2, 2, 4 ),
 ( 0.0007817246336856291692, 0.0009771112958940103739, 0.001172497958102391470, 0.001367884620310772566, 0.001563271282519153879 ),
 .UNSPECIFIED. ) ;
#8206 = VERTEX_POINT ( 'NONE', #27190 ) ;
#8207 = EDGE_CURVE ( 'NONE', #42366, #55800, #54648, .T. ) ;
#8208 = CARTESIAN_POINT ( 'NONE',  ( -14.30769230769242739, -3.300289026999228881, 32.46337939537708905 ) ) ;
#8209 = CARTESIAN_POINT ( 'NONE',  ( 1.384615384615264011, -6.835583212225970762, 34.95778746994575670 ) ) ;
#8210 = CARTESIAN_POINT ( 'NONE',  ( 13.38461538461538680, -11.35647404775217417, 33.31231777344666511 ) ) ;
#8211 = DIRECTION ( 'NONE',  ( 0.000000000000000000, 0.4999999999999960032, -0.8660254037844410391 ) ) ;
#8212 = CARTESIAN_POINT ( 'NONE',  ( -6.130690603110307002, -6.369640206132550553, 34.87707690430378449 ) ) ;
#8213 = AXIS2_PLACEMENT_3D ( 'NONE', #11952, #39867, #60563 ) ;
#8214 = LINE ( 'NONE', #28942, #15016 ) ;
#8215 = CARTESIAN_POINT ( 'NONE',  ( -11.66860874789975888, -3.285722584762969856, 32.44110544564090759 ) ) ;
#8216 = ORIENTED_EDGE ( 'NONE', *, *, #51280, .F. ) ;
#8217 = ORIENTED_EDGE ( 'NONE', *, *, #86095, .F. ) ;
#8218 = EDGE_CURVE ( 'NONE', #36898, #60372, #20437, .T. ) ;
#8219 = VERTEX_POINT ( 'NONE', #1050 ) ;
#8220 = CARTESIAN_POINT ( 'NONE',  ( -4.023320452082591814, -10.19071101563364756, 33.96452234770658407 ) ) ;
#8222 = CARTESIAN_POINT ( 'NONE',  ( 10.36540787133602670, -2.318417181685855422, 30.59732222474233865 ) ) ;
#8221 = DIRECTION ( 'NONE',  ( -1.000000000000000000, -0.000000000000000000, -0.000000000000000000 ) ) ;
#8223 = CARTESIAN_POINT ( 'NONE',  ( 1.607628228708780860, -12.38742843783360748, 31.66772728687926985 ) ) ;
#8224 = CARTESIAN_POINT ( 'NONE',  ( 12.46153846153833911, -12.70778746994576025, 30.41441678777401236 ) ) ;
#8225 = ADVANCED_FACE ( 'NONE', ( #55102 ), #68618, .F. ) ;
#8226 = FACE_BOUND ( 'NONE', #38844, .T. ) ;
#8227 = CARTESIAN_POINT ( 'NONE',  ( 7.912222197156282277, -11.16473453929635440, 33.15142922261926373 ) ) ;
#8228 = EDGE_CURVE ( 'NONE', #2251, #54993, #60207, .T. ) ;
#8229 = VERTEX_POINT ( 'NONE', #48786 ) ;
#8230 = DIRECTION ( 'NONE',  ( -0.000000000000000000, 1.000000000000000000, -0.000000000000000000 ) ) ;
#8231 = VECTOR ( 'NONE', #32857, 1000.000000000000227 ) ;
#8232 = DIRECTION ( 'NONE',  ( 0.000000000000000000, 0.000000000000000000, -1.000000000000000000 ) ) ;
#8233 = CARTESIAN_POINT ( 'NONE',  ( -17.29984929443922681, -11.76352882383564769, 32.36236540154569497 ) ) ;
#8234 = CYLINDRICAL_SURFACE ( 'NONE', #28050, 0.2499999999999995559 ) ;
#8235 = VERTEX_POINT ( 'NONE', #76711 ) ;
#8236 = CARTESIAN_POINT ( 'NONE',  ( 2.530471848960718084, -11.89424750095246175, 32.13594075562311758 ) ) ;
#8237 = EDGE_CURVE ( 'NONE', #81196, #16341, #66022, .T. ) ;
#8238 = ORIENTED_EDGE ( 'NONE', *, *, #52947, .F. ) ;
#8239 = FACE_BOUND ( 'NONE', #70342, .T. ) ;
#8240 = CARTESIAN_POINT ( 'NONE',  ( 24.00000000000000000, 5.000000000000023093, 29.24999999999999645 ) ) ;
#8241 = B_SPLINE_CURVE_WITH_KNOTS ( 'NONE', 3,
 ( #35410, #62863, #28664, #61993, #76398, #56129, #55236, #77282, #70531, #83165 ),
 .UNSPECIFIED., .F., .F.,
 ( 4, 2, 2, 2, 4 ),
 ( 0.000000000000000000, 0.0001954339881912772715, 0.0003908679763825545429, 0.0005863019645738318415, 0.0007817359527651090859 ),
 .UNSPECIFIED. ) ;
#8242 = B_SPLINE_CURVE_WITH_KNOTS ( 'NONE', 3,
 ( #83127, #48433, #1146, #21860, #75919, #29082, #22306, #56970, #84464, #50200 ),
 .UNSPECIFIED., .F., .F.,
 ( 4, 2, 2, 2, 4 ),
 ( 0.000000000000000000, 0.0001954339857564097241, 0.0003908679715128194482, 0.0005863019572692291723, 0.0007817359430256388964 ),
 .UNSPECIFIED. ) ;
#8243 = CARTESIAN_POINT ( 'NONE',  ( 4.219101293358989757, -2.657715359629131857, 31.77849191805844242 ) ) ;
#8244 = CARTESIAN_POINT ( 'NONE',  ( -2.980823712421088789, -8.433404298154334455, 34.66254593164985920 ) ) ;
#8245 = B_SPLINE_CURVE_WITH_KNOTS ( 'NONE', 3,
 ( #11022, #88048, #46580, #4257, #53327, #32618, #18226, #4712, #38949, #60086 ),
 .UNSPECIFIED., .F., .F.,
 ( 4, 2, 2, 2, 4 ),
 ( 0.0007817246256747459798, 0.0009771112852218896347, 0.001172497944769033398, 0.001367884604316177161, 0.001563271263863320708 ),
 .UNSPECIFIED. ) ;
#8246 = EDGE_LOOP ( 'NONE', ( #16076, #72558 ) ) ;
#8247 = CARTESIAN_POINT ( 'NONE',  ( 0.3308469948709041319, -10.54014554554150607, 33.71984207302941883 ) ) ;
#8248 = CARTESIAN_POINT ( 'NONE',  ( -18.00000000000012079, -4.320704448113953156, 33.92786785259630022 ) ) ;
#8249 = CARTESIAN_POINT ( 'NONE',  ( 8.639082799499073317, -2.373036134822904319, 30.88089517874952250 ) ) ;
#8250 = CARTESIAN_POINT ( 'NONE',  ( -6.923076923077044142, -10.90142922262034020, 33.41473453929536674 ) ) ;
#8251 = ORIENTED_EDGE ( 'NONE', *, *, #43621, .T. ) ;
#8252 = DIRECTION ( 'NONE',  ( -0.000000000000000000, 1.000000000000000000, -0.000000000000000000 ) ) ;
#8253 = ORIENTED_EDGE ( 'NONE', *, *, #42719, .T. ) ;
#8255 = VERTEX_POINT ( 'NONE', #47901 ) ;
#8254 = CARTESIAN_POINT ( 'NONE',  ( -8.835314180186649935, -3.513871655860377086, 32.76840700105978499 ) ) ;
#8256 = CARTESIAN_POINT ( 'NONE',  ( -8.519230769229334754, -7.500000000000155431, 34.75000000000007105 ) ) ;
#8257 = LINE ( 'NONE', #82594, #66991 ) ;
#8258 = CARTESIAN_POINT ( 'NONE',  ( 7.716005876422150855, -10.31621877034669588, 34.18098118002070152 ) ) ;
#8259 = B_SPLINE_CURVE_WITH_KNOTS ( 'NONE', 3,
 ( #52005, #24539, #79500, #44803, #24988, #17801, #30850, #79940, #37610, #58321 ),
 .UNSPECIFIED., .F., .F.,
 ( 4, 2, 2, 2, 4 ),
 ( 0.0007817246256747465219, 0.0009771112852218900684, 0.001172497944769033615, 0.001367884604316177378, 0.001563271263863320925 ),
 .UNSPECIFIED. ) ;
#8260 = VECTOR ( 'NONE', #9877, 1000.000000000000000 ) ;
#8261 = CARTESIAN_POINT ( 'NONE',  ( -12.21159294319032362, -2.824170634883621744, 31.52227843825338738 ) ) ;
#8263 = CARTESIAN_POINT ( 'NONE',  ( 2.307692307692309264, -10.05456864172156806, 36.03766855953608683 ) ) ;
#8262 = CARTESIAN_POINT ( 'NONE',  ( 8.834423757525421195, -2.255955759149236073, 29.99999999999988631 ) ) ;
#8264 = CARTESIAN_POINT ( 'NONE',  ( 7.846153846153725020, -4.481592998941358097, 33.73612834414048933 ) ) ;
#8265 = CARTESIAN_POINT ( 'NONE',  ( -1.139087296526025916, -4.750000000000006217, 24.07812500000000355 ) ) ;
#8266 = ORIENTED_EDGE ( 'NONE', *, *, #26687, .F. ) ;
#8267 = VECTOR ( 'NONE', #45746, 1000.000000000000000 ) ;
#8268 = CARTESIAN_POINT ( 'NONE',  ( -16.40386937806761125, -4.931416488878823223, 34.32920672191015399 ) ) ;
#8269 = ORIENTED_EDGE ( 'NONE', *, *, #79918, .F. ) ;
#8270 = ORIENTED_EDGE ( 'NONE', *, *, #15736, .T. ) ;
#8271 = CARTESIAN_POINT ( 'NONE',  ( -15.93083330975275658, -6.460100341425561332, 34.89618726649961644 ) ) ;
#8273 = ORIENTED_EDGE ( 'NONE', *, *, #29370, .T. ) ;
#8272 = VECTOR ( 'NONE', #71064, 1000.000000000000114 ) ;
#8274 = CARTESIAN_POINT ( 'NONE',  ( 10.83816428436267820, -8.540255544307065350, 34.89611431652622286 ) ) ;
#8275 = CARTESIAN_POINT ( 'NONE',  ( 2.980792499826876440, -8.303909089506435137, 34.68538101551103381 ) ) ;
#8276 = CARTESIAN_POINT ( 'NONE',  ( -11.76194648218548267, -11.41268669641500466, 32.86336882939237825 ) ) ;
#8277 = LINE ( 'NONE', #56887, #35872 ) ;
#8278 = CARTESIAN_POINT ( 'NONE',  ( 13.38461538461526423, -2.657715359629662544, 31.77849191805970364 ) ) ;
#8279 = CARTESIAN_POINT ( 'NONE',  ( 6.988332494352946789, -11.48612834413965977, 32.76840700105972815 ) ) ;
#8280 = CARTESIAN_POINT ( 'NONE',  ( 13.38461538461538680, -8.318370150425687726, 35.83090037661290239 ) ) ;
#8281 = CARTESIAN_POINT ( 'NONE',  ( 10.48523740594639442, -2.619462340734462380, 30.83744416345203021 ) ) ;
#8282 = CARTESIAN_POINT ( 'NONE',  ( 15.10007862765892206, -9.084618155246140248, 34.75535874321725771 ) ) ;
#8283 = B_SPLINE_CURVE_WITH_KNOTS ( 'NONE', 3,
 ( #7280, #26661, #5512, #47818, #41067, #67654, #68528, #33857, #61315, #61762 ),
 .UNSPECIFIED., .F., .F.,
 ( 4, 2, 2, 2, 4 ),
 ( 0.000000000000000000, 0.0001954311564186860613, 0.0003908623128373721225, 0.0005862934692560581567, 0.0007817246256747442451 ),
 .UNSPECIFIED. ) ;
#8284 = CARTESIAN_POINT ( 'NONE',  ( 14.55769230769231370, -2.499999999999999556, 29.81604066197449754 ) ) ;
#8285 = PLANE ( 'NONE',  #5355 ) ;
#8286 = B_SPLINE_CURVE_WITH_KNOTS ( 'NONE', 3,
 ( #62281, #36597, #21748, #57305, #15000, #50096, #75802, #64055, #42920, #42033 ),
 .UNSPECIFIED., .F., .F.,
 ( 4, 2, 2, 2, 4 ),
 ( 0.0007817359430256320659, 0.0009771253907249987086, 0.001172514838424365460, 0.001367904286123731994, 0.001563293733823098745 ),
 .UNSPECIFIED. ) ;
#8287 = VERTEX_POINT ( 'NONE', #62295 ) ;
#8288 = VERTEX_POINT ( 'NONE', #82596 ) ;
#8289 = VECTOR ( 'NONE', #30906, 1000.000000000000000 ) ;
#8290 = CARTESIAN_POINT ( 'NONE',  ( -15.23076923076935074, -8.613356846316285953, 34.62446782046622218 ) ) ;
#8291 = DIRECTION ( 'NONE',  ( 0.000000000000000000, 1.000000000000000000, 0.000000000000000000 ) ) ;
#8292 = CARTESIAN_POINT ( 'NONE',  ( -2.980823712421089233, -2.824170634883621744, 31.52227843825338738 ) ) ;
#8293 = CARTESIAN_POINT ( 'NONE',  ( 0.2380535369741302587, -10.23692288466677702, 34.23039457007281072 ) ) ;
#8294 = ORIENTED_EDGE ( 'NONE', *, *, #87040, .F. ) ;
#8295 = CARTESIAN_POINT ( 'NONE',  ( 6.000000000000001776, -4.786620604624113540, 33.94971097300155094 ) ) ;
#8296 = CARTESIAN_POINT ( 'NONE',  ( -17.32692307692307665, -2.499999999999998668, 29.75000000000000355 ) ) ;
#8297 = CARTESIAN_POINT ( 'NONE',  ( -3.099977422944442562, -12.11778462344221019, 31.66786338562085135 ) ) ;
#8298 = VECTOR ( 'NONE', #83941, 1000.000000000000000 ) ;
#8299 = ORIENTED_EDGE ( 'NONE', *, *, #49583, .F. ) ;
#8300 = CARTESIAN_POINT ( 'NONE',  ( 18.22277966897806678, -3.563462043263029955, 33.22394488606062879 ) ) ;
#8301 = ORIENTED_EDGE ( 'NONE', *, *, #50058, .F. ) ;
#8302 = DIRECTION ( 'NONE',  ( 0.000000000000000000, 0.000000000000000000, -1.000000000000000000 ) ) ;
#8303 = EDGE_CURVE ( 'NONE', #83509, #60361, #27989, .T. ) ;
#8304 = DIRECTION ( 'NONE',  ( -0.000000000000000000, -0.9848077530122085754, -0.1736481776669273613 ) ) ;
#8305 = CARTESIAN_POINT ( 'NONE',  ( -6.130691466667558487, -2.541943142973490666, 30.39792223712631980 ) ) ;
#8306 = CARTESIAN_POINT ( 'NONE',  ( -14.24162395668986747, -11.69971097300155272, 32.46337939537588113 ) ) ;
#8307 = CARTESIAN_POINT ( 'NONE',  ( 18.13052543823364360, -8.630441415882549094, 34.87705825610312615 ) ) ;
#8308 = ORIENTED_EDGE ( 'NONE', *, *, #46456, .T. ) ;
#8309 = VERTEX_POINT ( 'NONE', #69504 ) ;
#8310 = VECTOR ( 'NONE', #53759, 1000.000000000000000 ) ;
#8311 = ORIENTED_EDGE ( 'NONE', *, *, #27265, .F. ) ;
#8312 = ORIENTED_EDGE ( 'NONE', *, *, #59850, .F. ) ;
#8313 = EDGE_CURVE ( 'NONE', #861, #60596, #7809, .T. ) ;
#8314 = CARTESIAN_POINT ( 'NONE',  ( -6.066083410955878996, -11.16473453929635440, 33.15142922261925662 ) ) ;
#8315 = FACE_OUTER_BOUND ( 'NONE', #87004, .T. ) ;
#8316 = CIRCLE ( 'NONE', #19827, 0.2500000000000002220 ) ;
#8317 = DIRECTION ( 'NONE',  ( -0.000000000000000000, 0.5000000000000011102, -0.8660254037844381525 ) ) ;
#8318 = CARTESIAN_POINT ( 'NONE',  ( 16.94677510719138169, -10.31621877034669588, 34.18098118002070152 ) ) ;
#8319 = CARTESIAN_POINT ( 'NONE',  ( 4.284637961670941131, -6.413143153341454017, 34.63066358083362672 ) ) ;
#8320 = DIRECTION ( 'NONE',  ( -0.000000000000000000, -0.000000000000000000, -1.000000000000000000 ) ) ;
#8321 = AXIS2_PLACEMENT_3D ( 'NONE', #88622, #48477, #42629 ) ;
#8322 = ORIENTED_EDGE ( 'NONE', *, *, #33933, .F. ) ;
#8323 = ORIENTED_EDGE ( 'NONE', *, *, #7372, .F. ) ;
#8324 = VERTEX_POINT ( 'NONE', #25254 ) ;
#8326 = ORIENTED_EDGE ( 'NONE', *, *, #26310, .F. ) ;
#8325 = CARTESIAN_POINT ( 'NONE',  ( -3.007757879156381264, -10.61302985866383963, 33.66295027996417843 ) ) ;
#8328 = CARTESIAN_POINT ( 'NONE',  ( 14.55774672760575861, -4.818054556918156983, 34.26375889529406749 ) ) ;
#8327 = CARTESIAN_POINT ( 'NONE',  ( -13.38461538461538325, -13.75783147151868846, 33.36296068462461051 ) ) ;
#8329 = CYLINDRICAL_SURFACE ( 'NONE', #46013, 0.2499999999999973355 ) ;
#8330 = ADVANCED_FACE ( 'NONE', ( #60368 ), #33352, .T. ) ;
#8331 = CARTESIAN_POINT ( 'NONE',  ( 13.44987095589141113, -8.613356846314928816, 34.62446782046653482 ) ) ;
#8332 = EDGE_CURVE ( 'NONE', #79011, #30706, #44066, .T. ) ;
#8333 = VERTEX_POINT ( 'NONE', #26590 ) ;
#8334 = ORIENTED_EDGE ( 'NONE', *, *, #78010, .F. ) ;
#8335 = CARTESIAN_POINT ( 'NONE',  ( 4.023155550735844521, -3.957541250942359756, 33.62499894934981626 ) ) ;
#8336 = ORIENTED_EDGE ( 'NONE', *, *, #103, .T. ) ;
#8337 = FACE_BOUND ( 'NONE', #40593, .T. ) ;
#8338 = DIRECTION ( 'NONE',  ( 0.000000000000000000, 0.3420201433256610524, 0.9396926207859113145 ) ) ;
#8339 = CARTESIAN_POINT ( 'NONE',  ( 8.096208266067300485, -5.642605341092957971, 34.66089969410670335 ) ) ;
#8340 = ORIENTED_EDGE ( 'NONE', *, *, #46518, .F. ) ;
#8341 = CARTESIAN_POINT ( 'NONE',  ( 14.98076923076923173, -7.500000000000001776, 35.00000000000000000 ) ) ;
#8342 = CARTESIAN_POINT ( 'NONE',  ( 11.31497661389720832, -6.716662450894489211, 34.94144148231605840 ) ) ;
#8343 = DIRECTION ( 'NONE',  ( -0.000000000000000000, -0.5000000000000009992, -0.8660254037844380415 ) ) ;
#8344 = EDGE_CURVE ( 'NONE', #18328, #37947, #19376, .T. ) ;
#8345 = CARTESIAN_POINT ( 'NONE',  ( 0.6845498131513110263, -6.503523203565942268, 34.64991518177335195 ) ) ;
#8346 = DIRECTION ( 'NONE',  ( -1.000000000000000000, -0.000000000000000000, -0.000000000000000000 ) ) ;
#8347 = ORIENTED_EDGE ( 'NONE', *, *, #67920, .F. ) ;
#8348 = VECTOR ( 'NONE', #20433, 1000.000000000000227 ) ;
#8349 = CARTESIAN_POINT ( 'NONE',  ( 11.78851585009985570, -3.136992222400443175, 32.19305428654138979 ) ) ;
#8350 = CARTESIAN_POINT ( 'NONE',  ( 3.480823542407545546, -4.235687564193446164, 33.53795663066793509 ) ) ;
#8351 = CARTESIAN_POINT ( 'NONE',  ( 16.28437185560972011, -9.417988943895561960, 34.36773134775778260 ) ) ;
#8352 = DIRECTION ( 'NONE',  ( -1.000000000000000000, -0.000000000000000000, -0.000000000000000000 ) ) ;
#8353 = CARTESIAN_POINT ( 'NONE',  ( -5.999999999999998224, -1.129524287112498415, 32.06866353760679544 ) ) ;
#8354 = FACE_BOUND ( 'NONE', #52019, .T. ) ;
#8356 = CARTESIAN_POINT ( 'NONE',  ( -8.769230769230892619, -9.528491918059723176, 34.59228464037033035 ) ) ;
#8355 = CARTESIAN_POINT ( 'NONE',  ( -6.673131513698879580, -12.68172785388650681, 30.59649109432439573 ) ) ;
#8357 = AXIS2_PLACEMENT_3D ( 'NONE', #11380, #5521, #60895 ) ;
#8358 = LINE ( 'NONE', #1597, #19494 ) ;
#8360 = CARTESIAN_POINT ( 'NONE',  ( -18.24997674404859183, -2.920706130388549759, 32.31842814019191223 ) ) ;
#8359 = CARTESIAN_POINT ( 'NONE',  ( -3.296039231325550212, -3.083524468853724443, 32.58852847137143272 ) ) ;
#8361 = FACE_OUTER_BOUND ( 'NONE', #59475, .T. ) ;
#8362 = CARTESIAN_POINT ( 'NONE',  ( 2.724691934501235036, -6.299813628509441266, 24.13875670625849068 ) ) ;
#8363 = ORIENTED_EDGE ( 'NONE', *, *, #63023, .F. ) ;
#8364 = CARTESIAN_POINT ( 'NONE',  ( -1.790671178605550695, -4.201618623452029411, 14.00000000000000711 ) ) ;
#8365 = VERTEX_POINT ( 'NONE', #81544 ) ;
#8366 = CARTESIAN_POINT ( 'NONE',  ( -11.53846153846166089, -12.51329471203414379, 31.30864560766407578 ) ) ;
#8367 = ORIENTED_EDGE ( 'NONE', *, *, #5384, .F. ) ;
#8368 = CARTESIAN_POINT ( 'NONE',  ( -11.31545018684869142, -2.758310577978207778, 31.33698337089302299 ) ) ;
#8369 = CARTESIAN_POINT ( 'NONE',  ( -18.25002323729296450, -2.587272538249755005, 30.68239716806877837 ) ) ;
#8370 = B_SPLINE_CURVE_WITH_KNOTS ( 'NONE', 3,
 ( #70701, #9006, #22071, #63491, #29281, #62599, #55407, #36473, #49544, #36036 ),
 .UNSPECIFIED., .F., .F.,
 ( 4, 2, 2, 2, 4 ),
 ( 0.0007817359430256339090, 0.0009771253907250065148, 0.001172514838424371965, 0.001367904286123737632, 0.001563293733823103299 ),
 .UNSPECIFIED. ) ;
#8371 = ORIENTED_EDGE ( 'NONE', *, *, #47317, .F. ) ;
#8372 = CARTESIAN_POINT ( 'NONE',  ( -18.13069146666755671, -12.38065189839062263, 30.83690757178629482 ) ) ;
#8373 = CARTESIAN_POINT ( 'NONE',  ( -1.200186371490556958, -4.775308065498765409, 25.07625670625849423 ) ) ;
#8374 = LINE ( 'NONE', #35847, #5572 ) ;
#8375 = CARTESIAN_POINT ( 'NONE',  ( -15.29603923132555110, -9.528491918058357157, 34.59228464037090589 ) ) ;
#8376 = CARTESIAN_POINT ( 'NONE',  ( 16.15384615384615330, -8.164416787775445883, 34.95778746994557906 ) ) ;
#8377 = B_SPLINE_CURVE_WITH_KNOTS ( 'NONE', 3,
 ( #42321, #56264, #1315, #2628, #16593, #78294, #84636, #62565, #8526, #2193 ),
 .UNSPECIFIED., .F., .F.,
 ( 4, 2, 2, 2, 4 ),
 ( 0.000000000000000000, 0.0001954339857564078809, 0.0003908679715128157619, 0.0005863019572692236428, 0.0007817359430256315238 ),
 .UNSPECIFIED. ) ;
#8378 = CARTESIAN_POINT ( 'NONE',  ( -3.007393744996809115, -2.251407671071270489, 29.88021292934942252 ) ) ;
#8379 = CYLINDRICAL_SURFACE ( 'NONE', #12784, 0.2499999999999993616 ) ;
#8380 = DIRECTION ( 'NONE',  ( -0.000000000000000000, -0.9848077530122086864, -0.1736481776669273613 ) ) ;
#8381 = CARTESIAN_POINT ( 'NONE',  ( 2.320192649118979489E-14, -11.25000000000000000, 14.78125000000000178 ) ) ;
#8382 = CARTESIAN_POINT ( 'NONE',  ( -18.25002322422145440, -11.56360843649121861, 33.07473185843129926 ) ) ;
#8383 = DIRECTION ( 'NONE',  ( 0.000000000000000000, 0.7660444431189807890, 0.6427876096865361433 ) ) ;
#8384 = DIRECTION ( 'NONE',  ( 0.000000000000000000, 0.000000000000000000, -1.000000000000000000 ) ) ;
#8385 = VECTOR ( 'NONE', #6783, 1000.000000000000000 ) ;
#8386 = CARTESIAN_POINT ( 'NONE',  ( 3.775308065498752086, -6.007798216065404873, 22.14249329374151998 ) ) ;
#8387 = CARTESIAN_POINT ( 'NONE',  ( -14.08468095607945791, -10.61302985866383963, 33.66295027996417843 ) ) ;
#8388 = VERTEX_POINT ( 'NONE', #52716 ) ;
#8389 = CYLINDRICAL_SURFACE ( 'NONE', #71603, 0.2499999999999995559 ) ;
#8390 = CARTESIAN_POINT ( 'NONE',  ( 20.00000000000000000, -4.000000000000000000, 29.75000000000000355 ) ) ;
#8391 = CARTESIAN_POINT ( 'NONE',  ( 1.384615384615386802, -12.37446782046654192, 30.86335684631486131 ) ) ;
#8392 = CARTESIAN_POINT ( 'NONE',  ( -5.142193522883852452, -6.026961402152685388, 34.52809138561120506 ) ) ;
#8393 = PLANE ( 'NONE',  #37709 ) ;
#8394 = EDGE_CURVE ( 'NONE', #22482, #72792, #40560, .T. ) ;
#8395 = DIRECTION ( 'NONE',  ( -0.000000000000000000, 1.000000000000000000, 3.491481338843133355E-15 ) ) ;
#8396 = CARTESIAN_POINT ( 'NONE',  ( -5.999999999999998224, -2.499999999999998668, 29.50000000000001066 ) ) ;
#8397 = ORIENTED_EDGE ( 'NONE', *, *, #50545, .F. ) ;
#8398 = ORIENTED_EDGE ( 'NONE', *, *, #41539, .T. ) ;
#8399 = APPLICATION_CONTEXT ( 'automotive_design' ) ;
#8400 = ORIENTED_EDGE ( 'NONE', *, *, #57473, .T. ) ;
#8401 = EDGE_CURVE ( 'NONE', #11121, #17125, #86987, .T. ) ;
#8402 = VECTOR ( 'NONE', #71363, 1000.000000000000000 ) ;
#8403 = LINE ( 'NONE', #61563, #88766 ) ;
#8404 = CARTESIAN_POINT ( 'NONE',  ( -6.792285115252135519, -4.118422570099827595, 33.43335022499816489 ) ) ;
#8405 = CARTESIAN_POINT ( 'NONE',  ( -15.36091720050093024, -11.04286588640298561, 33.62463336215343901 ) ) ;
#8406 = B_SPLINE_CURVE_WITH_KNOTS ( 'NONE', 3,
 ( #43838, #71303, #70881, #56906, #77187, #50591, #43402, #76750, #49711, #64537 ),
 .UNSPECIFIED., .F., .F.,
 ( 4, 2, 2, 2, 4 ),
 ( 0.0007817359527651104954, 0.0009771254036996493593, 0.001172514854634188223, 0.001367904305568727087, 0.001563293756503265951 ),
 .UNSPECIFIED. ) ;
#8407 = EDGE_CURVE ( 'NONE', #52040, #82649, #35476, .T. ) ;
#8408 = DIRECTION ( 'NONE',  ( 1.000000000000000000, 0.000000000000000000, 0.000000000000000000 ) ) ;
#8409 = CARTESIAN_POINT ( 'NONE',  ( 13.13459216039393240, -8.475808217655753651, 34.90892951860618609 ) ) ;
#8410 = VECTOR ( 'NONE', #6850, 999.9999999999998863 ) ;
#8411 = EDGE_LOOP ( 'NONE', ( #70986, #57155, #45065, #52294, #13962 ) ) ;
#8412 = CYLINDRICAL_SURFACE ( 'NONE', #56421, 0.2500000000000004996 ) ;
#8413 = ORIENTED_EDGE ( 'NONE', *, *, #63582, .T. ) ;
#8414 = ORIENTED_EDGE ( 'NONE', *, *, #84070, .T. ) ;
#8415 = AXIS2_PLACEMENT_3D ( 'NONE', #33381, #60839, #33813 ) ;
#8417 = ORIENTED_EDGE ( 'NONE', *, *, #57440, .T. ) ;
#8416 = EDGE_CURVE ( 'NONE', #64954, #4054, #50629, .T. ) ;
#8419 = ORIENTED_EDGE ( 'NONE', *, *, #89077, .T. ) ;
#8418 = CARTESIAN_POINT ( 'NONE',  ( -15.48079246806219800, -12.22074536777954989, 31.39888409691088356 ) ) ;
#8420 = DIRECTION ( 'NONE',  ( -0.000000000000000000, -0.8660254037844397068, -0.4999999999999978906 ) ) ;
#8421 = LINE ( 'NONE', #37651, #65263 ) ;
#8422 = ADVANCED_FACE ( 'NONE', ( #66232 ), #32454, .F. ) ;
#8423 = CARTESIAN_POINT ( 'NONE',  ( -9.942284423250047354, -8.303909089506435137, 34.68538101551103381 ) ) ;
#8424 = VERTEX_POINT ( 'NONE', #12192 ) ;
#8425 = ORIENTED_EDGE ( 'NONE', *, *, #37773, .F. ) ;
#8426 = EDGE_LOOP ( 'NONE', ( #32679, #30335, #71228, #4033 ) ) ;
#8427 = CARTESIAN_POINT ( 'NONE',  ( 14.30769230769231015, -8.810774026931790459, 35.74407628777942847 ) ) ;
#8429 = VERTEX_POINT ( 'NONE', #39677 ) ;
#8428 = CARTESIAN_POINT ( 'NONE',  ( 10.61538461538461675, -1.629998284177014645, 34.34916445242399163 ) ) ;
#8430 = CARTESIAN_POINT ( 'NONE',  ( 1.515407192440174189, -8.999086150933472084, 34.52020707165672064 ) ) ;
#8431 = CARTESIAN_POINT ( 'NONE',  ( 6.923076923076800782, -12.51329471203414379, 31.30864560766407578 ) ) ;
#8432 = CARTESIAN_POINT ( 'NONE',  ( -2.980823712421090121, -10.05730279482229683, 34.04704008940765902 ) ) ;
#8433 = EDGE_CURVE ( 'NONE', #70653, #80357, #5438, .T. ) ;
#8434 = ORIENTED_EDGE ( 'NONE', *, *, #37084, .F. ) ;
#8435 = EDGE_CURVE ( 'NONE', #126, #24282, #23499, .T. ) ;
#8436 = B_SPLINE_CURVE_WITH_KNOTS ( 'NONE', 3,
 ( #87229, #25508, #80461, #30915, #46222, #73709, #58384, #51617, #79117, #17420 ),
 .UNSPECIFIED., .F., .F.,
 ( 4, 2, 2, 2, 4 ),
 ( 0.000000000000000000, 0.0001954311564186866305, 0.0003908623128373732609, 0.0005862934692560598914, 0.0007817246256747465219 ),
 .UNSPECIFIED. ) ;
#8437 = CARTESIAN_POINT ( 'NONE',  ( 14.98079249982687777, -10.66389620160130036, 33.62221079203477103 ) ) ;
#8438 = CYLINDRICAL_SURFACE ( 'NONE', #52605, 0.2499999999999979738 ) ;
#8439 = VECTOR ( 'NONE', #57628, 1000.000000000000114 ) ;
#8440 = ORIENTED_EDGE ( 'NONE', *, *, #32237, .T. ) ;
#8441 = FACE_BOUND ( 'NONE', #74790, .T. ) ;
#8442 = B_SPLINE_CURVE_WITH_KNOTS ( 'NONE', 3,
 ( #86612, #24882, #52798, #11830, #46045, #52350, #80288, #73533, #39308, #66764 ),
 .UNSPECIFIED., .F., .F.,
 ( 4, 2, 2, 2, 4 ),
 ( 0.000000000000000000, 0.0001954311564186872810, 0.0003908623128373745620, 0.0005862934692560618430, 0.0007817246256747491240 ),
 .UNSPECIFIED. ) ;
#8443 = DIRECTION ( 'NONE',  ( -0.000000000000000000, -0.000000000000000000, -1.000000000000000000 ) ) ;
#8444 = CARTESIAN_POINT ( 'NONE',  ( -18.22348492456433178, -12.47654668319379567, 31.42292124445336654 ) ) ;
#8445 = CARTESIAN_POINT ( 'NONE',  ( 9.692307692307695177, -1.466349020453238561, 30.81389545987213907 ) ) ;
#8447 = DIRECTION ( 'NONE',  ( -0.000000000000000000, -0.5000000000000009992, -0.8660254037844380415 ) ) ;
#8446 = CARTESIAN_POINT ( 'NONE',  ( -7.846153846153844924, -10.89733346790207413, 36.13435417666054406 ) ) ;
#8448 = EDGE_CURVE ( 'NONE', #85898, #17034, #44200, .T. ) ;
#8449 = CARTESIAN_POINT ( 'NONE',  ( -5.010854725920639297, -10.51840700105979565, 33.73612834413962247 ) ) ;
#8450 = CARTESIAN_POINT ( 'NONE',  ( -4.219116154402473562, -11.06231777344662781, 33.60647404775220082 ) ) ;
#8451 = ORIENTED_EDGE ( 'NONE', *, *, #49791, .F. ) ;
#8452 = EDGE_CURVE ( 'NONE', #78712, #49139, #81755, .T. ) ;
#8453 = CARTESIAN_POINT ( 'NONE',  ( 14.53070365930516239, -12.39991518177334129, 30.74647679643404530 ) ) ;
#8454 = CARTESIAN_POINT ( 'NONE',  ( -17.07692307692307665, -6.343179335718451384, 34.87096338111211935 ) ) ;
#8455 = B_SPLINE_CURVE_WITH_KNOTS ( 'NONE', 3,
 ( #69731, #9798, #23307, #1717, #1265, #16118, #84592, #28755, #49015, #21990 ),
 .UNSPECIFIED., .F., .F.,
 ( 4, 2, 2, 2, 4 ),
 ( 0.000000000000000000, 0.0001954311564186861697, 0.0003908623128373723394, 0.0005862934692560584820, 0.0007817246256747446788 ),
 .UNSPECIFIED. ) ;
#8456 = EDGE_LOOP ( 'NONE', ( #33582, #63134 ) ) ;
#8457 = FACE_OUTER_BOUND ( 'NONE', #24417, .T. ) ;
#8458 = CARTESIAN_POINT ( 'NONE',  ( -14.08467946359890988, -9.172514111537584114, 34.72667873470787470 ) ) ;
#8459 = CARTESIAN_POINT ( 'NONE',  ( -3.903900635498010807, -2.587454068350147462, 30.68340429815432202 ) ) ;
#8460 = CARTESIAN_POINT ( 'NONE',  ( -5.207614543590634248, -11.71456829005830080, 32.44064028649416542 ) ) ;
#8461 = CARTESIAN_POINT ( 'NONE',  ( 8.068933515131908152, -6.717445702608402236, 34.94155399931962336 ) ) ;
#8462 = DIRECTION ( 'NONE',  ( 0.000000000000000000, -6.938893903907222067E-15, 1.000000000000000000 ) ) ;
#8463 = FACE_BOUND ( 'NONE', #4284, .T. ) ;
#8465 = LINE ( 'NONE', #40919, #66054 ) ;
#8464 = CARTESIAN_POINT ( 'NONE',  ( -1.449885385171703289, -6.835583212224499938, 34.95778746994557906 ) ) ;
#8466 = CYLINDRICAL_SURFACE ( 'NONE', #33842, 0.2500000000000009437 ) ;
#8468 = CARTESIAN_POINT ( 'NONE',  ( -14.30769230769230660, -2.708943851104267164, 35.45975837776705220 ) ) ;
#8467 = LINE ( 'NONE', #1250, #25708 ) ;
#8469 = DIRECTION ( 'NONE',  ( -1.000000000000000000, 0.000000000000000000, 0.000000000000000000 ) ) ;
#8470 = CARTESIAN_POINT ( 'NONE',  ( 3.775308065498768517, -8.992201783934554271, 21.79500670625849068 ) ) ;
#8471 = ORIENTED_EDGE ( 'NONE', *, *, #47507, .T. ) ;
#8472 = EDGE_LOOP ( 'NONE', ( #68867, #48581 ) ) ;
#8473 = AXIS2_PLACEMENT_3D ( 'NONE', #57213, #23847, #44120 ) ;
#8474 = CARTESIAN_POINT ( 'NONE',  ( 5.207714884747862705, -6.413143153341454017, 34.63066358083362672 ) ) ;
#8475 = CARTESIAN_POINT ( 'NONE',  ( -12.23875879256039489, -6.717445702608402236, 34.94155399931962336 ) ) ;
#8476 = CARTESIAN_POINT ( 'NONE',  ( 16.28463659481310799, -2.845873456487966635, 32.17976146951972538 ) ) ;
#8477 = CYLINDRICAL_SURFACE ( 'NONE', #3581, 0.2500000000000009437 ) ;
#8478 = CARTESIAN_POINT ( 'NONE',  ( -16.21911659980693088, -12.27809138561121394, 31.22303859784730307 ) ) ;
#8479 = CARTESIAN_POINT ( 'NONE',  ( -3.724691934501229262, -9.114399933863657211, 17.26375670625849068 ) ) ;
#8480 = B_SPLINE_CURVE_WITH_KNOTS ( 'NONE', 3,
 ( #1008, #77549, #14971, #21718, #23047, #9105, #2757, #63137, #15416, #70802 ),
 .UNSPECIFIED., .F., .F.,
 ( 4, 2, 2, 2, 4 ),
 ( 0.0007817246256747434861, 0.0009771112852218859484, 0.001172497944769028411, 0.001367884604316171090, 0.001563271263863313552 ),
 .UNSPECIFIED. ) ;
#8481 = CARTESIAN_POINT ( 'NONE',  ( 0.5923289025054119250, -3.957578996910242619, 33.62503395064540257 ) ) ;
#8482 = LINE ( 'NONE', #49463, #40282 ) ;
#8483 = AXIS2_PLACEMENT_3D ( 'NONE', #74554, #32670, #53831 ) ;
#8484 = CARTESIAN_POINT ( 'NONE',  ( -17.20707028636129721, -5.195881422630167279, 34.18770438780618548 ) ) ;
#8485 = CARTESIAN_POINT ( 'NONE',  ( -3.164701897419154530, -11.91647553114624358, 32.58852847137148245 ) ) ;
#8486 = LINE ( 'NONE', #23310, #31024 ) ;
#8487 = CARTESIAN_POINT ( 'NONE',  ( -5.011667937410237528, -6.835583212224609184, 34.95778746994559327 ) ) ;
#8488 = EDGE_CURVE ( 'NONE', #36228, #86632, #43341, .T. ) ;
#8489 = CARTESIAN_POINT ( 'NONE',  ( 14.30769230769231015, -11.69971097300155272, 32.46337939537588113 ) ) ;
#8490 = LINE ( 'NONE', #35961, #70098 ) ;
#8491 = ORIENTED_EDGE ( 'NONE', *, *, #40453, .T. ) ;
#8492 = CARTESIAN_POINT ( 'NONE',  ( -4.230769230769230838, -11.00000000000000000, 29.75000000000000355 ) ) ;
#8493 = CARTESIAN_POINT ( 'NONE',  ( 10.68063975489745232, -5.941354392334607049, 34.76329471203374055 ) ) ;
#8494 = CARTESIAN_POINT ( 'NONE',  ( -1.200186371490524317, -10.22469193450124791, 22.61124329374151287 ) ) ;
#8495 = EDGE_CURVE ( 'NONE', #15822, #82638, #9546, .T. ) ;
#8496 = CARTESIAN_POINT ( 'NONE',  ( -2.373774687052441656, -4.661471528628506888, 34.16647553114621871 ) ) ;
#8497 = CARTESIAN_POINT ( 'NONE',  ( -12.22435897435897267, -7.500000000000000000, 33.75000000000000000 ) ) ;
#8498 = ORIENTED_EDGE ( 'NONE', *, *, #86823, .F. ) ;
#8499 = CARTESIAN_POINT ( 'NONE',  ( -9.822998295418001291, -5.496505350115501010, 34.60290016733514307 ) ) ;
#8501 = EDGE_LOOP ( 'NONE', ( #39216, #29158, #58541, #53017 ) ) ;
#8500 = CARTESIAN_POINT ( 'NONE',  ( 3.903822916553187028, -5.851115903089112003, 34.47074536777953568 ) ) ;
#8502 = DIRECTION ( 'NONE',  ( 1.000000000000000000, 0.000000000000000000, 0.000000000000000000 ) ) ;
#8503 = CARTESIAN_POINT ( 'NONE',  ( 17.01084069756293715, -2.486705287966279432, 31.30864560766543647 ) ) ;
#8504 = EDGE_LOOP ( 'NONE', ( #88100, #11085, #12876, #83969 ) ) ;
#8505 = CYLINDRICAL_SURFACE ( 'NONE', #21831, 0.2499999999999998890 ) ;
#8506 = EDGE_CURVE ( 'NONE', #56881, #50988, #8523, .T. ) ;
#8507 = CARTESIAN_POINT ( 'NONE',  ( 10.83816428436268176, -10.97394488606064122, 33.68653795673694873 ) ) ;
#8508 = ORIENTED_EDGE ( 'NONE', *, *, #21935, .T. ) ;
#8509 = DIRECTION ( 'NONE',  ( 0.000000000000000000, 0.9396926207859126468, -0.3420201433256571111 ) ) ;
#8510 = CARTESIAN_POINT ( 'NONE',  ( -11.76194646302587010, -12.47654668319379567, 31.42292124445336654 ) ) ;
#8511 = CARTESIAN_POINT ( 'NONE',  ( 12.46153846153846168, -11.91647553114624181, 32.58852847137148245 ) ) ;
#8512 = ORIENTED_EDGE ( 'NONE', *, *, #14215, .F. ) ;
#8513 = ORIENTED_EDGE ( 'NONE', *, *, #63450, .F. ) ;
#8514 = CARTESIAN_POINT ( 'NONE',  ( 15.29602480204525605, -10.90142922261932057, 33.41473453929631887 ) ) ;
#8515 = VECTOR ( 'NONE', #30273, 1000.000000000000227 ) ;
#8516 = ORIENTED_EDGE ( 'NONE', *, *, #84912, .T. ) ;
#8517 = EDGE_CURVE ( 'NONE', #32626, #65460, #36154, .T. ) ;
#8518 = FACE_OUTER_BOUND ( 'NONE', #75318, .T. ) ;
#8519 = CARTESIAN_POINT ( 'NONE',  ( -15.36091720050093024, -2.373036134822904319, 30.88089517874952250 ) ) ;
#8520 = EDGE_CURVE ( 'NONE', #55273, #7366, #71687, .T. ) ;
#8521 = DIRECTION ( 'NONE',  ( -0.000000000000000000, -0.9848077530122086864, -0.1736481776669273613 ) ) ;
#8522 = CARTESIAN_POINT ( 'NONE',  ( -17.20761454359063691, -6.413092428213692742, 34.63065189839063152 ) ) ;
#8523 = B_SPLINE_CURVE_WITH_KNOTS ( 'NONE', 3,
 ( #69923, #37457, #85219, #29830, #30704, #29397, #57292, #50955, #56846, #64473 ),
 .UNSPECIFIED., .F., .F.,
 ( 4, 2, 2, 2, 4 ),
 ( 0.0007817359430256294638, 0.0009771253907249952391, 0.001172514838424361123, 0.001367904286123726790, 0.001563293733823092673 ),
 .UNSPECIFIED. ) ;
#8524 = EDGE_LOOP ( 'NONE', ( #36740, #25811 ) ) ;
#8525 = EDGE_LOOP ( 'NONE', ( #32011, #9530, #20385, #1505, #19589, #71220 ) ) ;
#8527 = EDGE_LOOP ( 'NONE', ( #38016, #40563 ) ) ;
#8526 = CARTESIAN_POINT ( 'NONE',  ( 9.627037246346919375, -4.481592998940162609, 33.73612834413957984 ) ) ;
#8528 = CARTESIAN_POINT ( 'NONE',  ( 16.40384615384615685, -2.499999999999999556, 29.81604066197449754 ) ) ;
#8529 = VERTEX_POINT ( 'NONE', #84342 ) ;
#8530 = AXIS2_PLACEMENT_3D ( 'NONE', #3670, #57739, #72580 ) ;
#8531 = VECTOR ( 'NONE', #83529, 1000.000000000000000 ) ;
#8532 = DIRECTION ( 'NONE',  ( 0.000000000000000000, 0.8660254037844377084, -0.5000000000000015543 ) ) ;
#8533 = CARTESIAN_POINT ( 'NONE',  ( 7.976945653978634532, -4.809403383903225304, 33.96459661697924304 ) ) ;
#8534 = ORIENTED_EDGE ( 'NONE', *, *, #89064, .T. ) ;
#8535 = DIRECTION ( 'NONE',  ( 0.000000000000000000, 1.000000000000000000, 0.000000000000000000 ) ) ;
#8536 = B_SPLINE_CURVE_WITH_KNOTS ( 'NONE', 3,
 ( #39794, #67261, #60935, #5558, #88438, #33031, #88009, #26270, #53736, #81223 ),
 .UNSPECIFIED., .F., .F.,
 ( 4, 2, 2, 2, 4 ),
 ( 0.000000000000000000, 0.0001954339857564100222, 0.0003908679715128200445, 0.0005863019572692300396, 0.0007817359430256400890 ),
 .UNSPECIFIED. ) ;
#8537 = AXIS2_PLACEMENT_3D ( 'NONE', #23795, #69789, #2202 ) ;
#8538 = B_SPLINE_CURVE_WITH_KNOTS ( 'NONE', 3,
 ( #37299, #85500, #78287, #25125, #52589, #11622, #23779, #44049, #39101, #10284 ),
 .UNSPECIFIED., .F., .F.,
 ( 4, 2, 2, 2, 4 ),
 ( 0.0007817359430256322827, 0.0009771253907249989254, 0.001172514838424365676, 0.001367904286123732428, 0.001563293733823098962 ),
 .UNSPECIFIED. ) ;
#8539 = ORIENTED_EDGE ( 'NONE', *, *, #78866, .F. ) ;
#8541 = VERTEX_POINT ( 'NONE', #23938 ) ;
#8540 = DIRECTION ( 'NONE',  ( 1.000000000000000000, 0.000000000000000000, 0.000000000000000000 ) ) ;
#8542 = CARTESIAN_POINT ( 'NONE',  ( -0.5276218724943410043, -10.51840700105979387, 33.73612834413961536 ) ) ;
#8543 = DIRECTION ( 'NONE',  ( -1.000000000000000000, -0.000000000000000000, -0.000000000000000000 ) ) ;
#8545 = ORIENTED_EDGE ( 'NONE', *, *, #44605, .T. ) ;
#8544 = EDGE_CURVE ( 'NONE', #64424, #47910, #33245, .T. ) ;
#8546 = CARTESIAN_POINT ( 'NONE',  ( 15.16468685140909045, -2.292212530054419606, 30.41441678777542634 ) ) ;
#8547 = CARTESIAN_POINT ( 'NONE',  ( 6.856994543716788293, -5.471508081941601986, 34.59228464037088457 ) ) ;
#8548 = FACE_BOUND ( 'NONE', #77843, .T. ) ;
#8549 = CARTESIAN_POINT ( 'NONE',  ( 1.607394925883794068, -12.44528174975671853, 30.48912976160716681 ) ) ;
#8551 = ADVANCED_FACE ( 'NONE', ( #51388 ), #9123, .F. ) ;
#8550 = CARTESIAN_POINT ( 'NONE',  ( -0.3589743589743593088, -11.00000000000000000, 29.75000000000000355 ) ) ;
#8552 = CARTESIAN_POINT ( 'NONE',  ( 4.376857505459002873, -12.39991518177334129, 30.74647679643404530 ) ) ;
#8553 = CARTESIAN_POINT ( 'NONE',  ( 16.15384615384603251, -4.320704448113951379, 33.92786785259630022 ) ) ;
#8554 = CARTESIAN_POINT ( 'NONE',  ( 14.16025641025641235, -3.499999999999999556, 29.75000000000000355 ) ) ;
#8555 = DIRECTION ( 'NONE',  ( 0.000000000000000000, 0.8660254037844377084, 0.5000000000000015543 ) ) ;
#8556 = ORIENTED_EDGE ( 'NONE', *, *, #33561, .T. ) ;
#8557 = EDGE_CURVE ( 'NONE', #61557, #84346, #84786, .T. ) ;
#8558 = LINE ( 'NONE', #27493, #67628 ) ;
#8559 = ORIENTED_EDGE ( 'NONE', *, *, #41284, .F. ) ;
#8560 = ORIENTED_EDGE ( 'NONE', *, *, #50296, .F. ) ;
#8562 = FACE_OUTER_BOUND ( 'NONE', #3608, .T. ) ;
#8561 = CYLINDRICAL_SURFACE ( 'NONE', #54737, 0.2499999999999994726 ) ;
#8563 = CARTESIAN_POINT ( 'NONE',  ( -9.692307692307691624, -2.833524468853757305, 32.15551576947925838 ) ) ;
#8564 = CARTESIAN_POINT ( 'NONE',  ( 7.846153846153723244, -3.643525952248796163, 33.31231777344771672 ) ) ;
#8565 = CARTESIAN_POINT ( 'NONE',  ( 17.07692307692295586, -10.33852847137269571, 34.16647553114546554 ) ) ;
#8566 = CARTESIAN_POINT ( 'NONE',  ( 14.43848274865926129, -11.37503395064541678, 33.29242100308974273 ) ) ;
#8567 = ORIENTED_EDGE ( 'NONE', *, *, #84000, .T. ) ;
#8568 = CARTESIAN_POINT ( 'NONE',  ( 13.38461538461538680, -4.786620604624113540, 33.94971097300155094 ) ) ;
#8569 = CARTESIAN_POINT ( 'NONE',  ( -6.000000000000119904, -6.879047030192662504, 34.71129190930017927 ) ) ;
#8570 = CARTESIAN_POINT ( 'NONE',  ( 23.49999999999998579, -13.25000000000000000, 32.75000000000000000 ) ) ;
#8571 = CARTESIAN_POINT ( 'NONE',  ( 3.164685819813350509, -3.050289026998445951, 32.03036669348365706 ) ) ;
#8572 = CARTESIAN_POINT ( 'NONE',  ( 2.557746727605761716, -5.642605341092957083, 34.66089969410670335 ) ) ;
#8573 = EDGE_CURVE ( 'NONE', #7973, #76696, #18607, .T. ) ;
#8574 = B_SPLINE_CURVE_WITH_KNOTS ( 'NONE', 3,
 ( #16512, #7994, #56619, #70578, #43979, #9327, #2111, #22823, #15198, #29596 ),
 .UNSPECIFIED., .F., .F.,
 ( 4, 2, 2, 2, 4 ),
 ( 0.000000000000000000, 0.0001954311564186861426, 0.0003908623128373722852, 0.0005862934692560583735, 0.0007817246256747445703 ),
 .UNSPECIFIED. ) ;
#8575 = AXIS2_PLACEMENT_3D ( 'NONE', #78910, #3248, #22634 ) ;
#8576 = CARTESIAN_POINT ( 'NONE',  ( 2.980746006547773774, -12.07920672191015221, 32.31858351112116168 ) ) ;
#8577 = EDGE_LOOP ( 'NONE', ( #42958, #40337 ) ) ;
#8578 = ORIENTED_EDGE ( 'NONE', *, *, #83886, .T. ) ;
#8579 = B_SPLINE_CURVE_WITH_KNOTS ( 'NONE', 3,
 ( #51207, #9808, #45361, #64295, #16127, #65188 ),
 .UNSPECIFIED., .F., .F.,
 ( 4, 2, 4 ),
 ( 4.220987180333913997E-17, 0.0001954756301637146886, 0.0003909512603273872016 ),
 .UNSPECIFIED. ) ;
#8580 = CARTESIAN_POINT ( 'NONE',  ( -19.50000000000000000, -3.499999999999999556, 29.75000000000000355 ) ) ;
#8581 = EDGE_CURVE ( 'NONE', #50385, #67353, #51561, .T. ) ;
#8582 = ORIENTED_EDGE ( 'NONE', *, *, #71164, .F. ) ;
#8583 = DIRECTION ( 'NONE',  ( -0.000000000000000000, 0.9396926207859093161, -0.3420201433256663259 ) ) ;
#8584 = CARTESIAN_POINT ( 'NONE',  ( 3.230769230769231726, -13.63283147151868846, 33.57946703557072254 ) ) ;
#8585 = DIRECTION ( 'NONE',  ( -0.000000000000000000, 0.1736481776669307198, -0.9848077530122080203 ) ) ;
#8586 = LINE ( 'NONE', #88473, #6861 ) ;
#8587 = CARTESIAN_POINT ( 'NONE',  ( -17.07692307692307665, -12.10708131394839349, 31.69288490824020244 ) ) ;
#8588 = FACE_OUTER_BOUND ( 'NONE', #45657, .T. ) ;
#8589 = ORIENTED_EDGE ( 'NONE', *, *, #83067, .F. ) ;
#8590 = DIRECTION ( 'NONE',  ( -1.000000000000000000, 0.000000000000000000, -0.000000000000000000 ) ) ;
#8592 = ORIENTED_EDGE ( 'NONE', *, *, #80126, .F. ) ;
#8591 = CARTESIAN_POINT ( 'NONE',  ( 17.86944008638663206, -2.254533558242299396, 29.97296025877827930 ) ) ;
#8593 = CARTESIAN_POINT ( 'NONE',  ( -10.36543909703647159, -3.712312575010499049, 33.01462480002815170 ) ) ;
#8594 = CARTESIAN_POINT ( 'NONE',  ( -17.30040800148741198, -12.11044203135681840, 32.26167407432752299 ) ) ;
#8595 = CARTESIAN_POINT ( 'NONE',  ( 11.53846153846153832, -4.098570777380720287, 33.41473453929634729 ) ) ;
#8596 = EDGE_CURVE ( 'NONE', #59070, #70481, #15068, .T. ) ;
#8597 = CARTESIAN_POINT ( 'NONE',  ( 0.5923302693632450655, -2.729792928343270031, 31.24908615093345432 ) ) ;
#8598 = DIRECTION ( 'NONE',  ( 0.000000000000000000, -5.102127870520020612E-17, -1.000000000000000000 ) ) ;
#8599 = CARTESIAN_POINT ( 'NONE',  ( -1.077988221561493543, -4.724691934501247914, 23.07999329374151998 ) ) ;
#8600 = ORIENTED_EDGE ( 'NONE', *, *, #89007, .F. ) ;
#8601 = EDGE_CURVE ( 'NONE', #37486, #45648, #89096, .T. ) ;
#8602 = CARTESIAN_POINT ( 'NONE',  ( -15.29603923132555110, -6.835583212224499938, 34.95778746994557906 ) ) ;
#8603 = B_SPLINE_CURVE_WITH_KNOTS ( 'NONE', 3,
 ( #50127, #15919, #43382, #29873, #78048, #59103, #16785, #38396, #31642, #50995 ),
 .UNSPECIFIED., .F., .F.,
 ( 4, 2, 2, 2, 4 ),
 ( 0.0007817246256747463051, 0.0009771112852218896347, 0.001172497944769033181, 0.001367884604316176728, 0.001563271263863320057 ),
 .UNSPECIFIED. ) ;
#8604 = CARTESIAN_POINT ( 'NONE',  ( -17.32694630114453105, -4.931416488878823223, 34.32920672191015399 ) ) ;
#8605 = CARTESIAN_POINT ( 'NONE',  ( -2.750000000000007105, -6.360912703474006946, 21.42187500000000000 ) ) ;
#8606 = CIRCLE ( 'NONE', #58914, 4.500000000000001776 ) ;
#8607 = VECTOR ( 'NONE', #16720, 1000.000000000000227 ) ;
#8608 = DIRECTION ( 'NONE',  ( -0.000000000000000000, -0.8660254037844397068, -0.4999999999999978906 ) ) ;
#8609 = FACE_OUTER_BOUND ( 'NONE', #14018, .T. ) ;
#8610 = ORIENTED_EDGE ( 'NONE', *, *, #19797, .T. ) ;
#8611 = FACE_OUTER_BOUND ( 'NONE', #22313, .T. ) ;
#8612 = CARTESIAN_POINT ( 'NONE',  ( -3.230769230769351186, -10.90142922262034020, 33.41473453929536674 ) ) ;
#8613 = CIRCLE ( 'NONE', #74774, 4.000000000000000000 ) ;
#8614 = ORIENTED_EDGE ( 'NONE', *, *, #76421, .F. ) ;
#8615 = CIRCLE ( 'NONE', #58922, 0.2500000000000002220 ) ;
#8616 = CARTESIAN_POINT ( 'NONE',  ( 0.000000000000000000, -4.000000000000000000, 29.65000000000000213 ) ) ;
#8617 = EDGE_CURVE ( 'NONE', #8229, #63457, #68932, .T. ) ;
#8618 = CARTESIAN_POINT ( 'NONE',  ( 9.561698037103610659, -7.722926974430166069, 34.99546784045485737 ) ) ;
#8619 = EDGE_LOOP ( 'NONE', ( #50496, #73110, #74874, #30023 ) ) ;
#8620 = DIRECTION ( 'NONE',  ( -0.000000000000000000, 1.000000000000000000, -0.000000000000000000 ) ) ;
#8621 = CARTESIAN_POINT ( 'NONE',  ( 2.307692307692309264, -8.564572088678739092, 35.78748833219616898 ) ) ;
#8622 = EDGE_CURVE ( 'NONE', #51137, #53485, #81594, .T. ) ;
#8623 = DIRECTION ( 'NONE',  ( 1.000000000000000000, 0.000000000000000000, 0.000000000000000000 ) ) ;
#8624 = FACE_OUTER_BOUND ( 'NONE', #85714, .T. ) ;
#8625 = ORIENTED_EDGE ( 'NONE', *, *, #81418, .T. ) ;
#8626 = LINE ( 'NONE', #36535, #16851 ) ;
#8627 = ORIENTED_EDGE ( 'NONE', *, *, #8118, .F. ) ;
#8628 = CARTESIAN_POINT ( 'NONE',  ( -17.77698715590659972, -11.98016756924215187, 32.48728574198910479 ) ) ;
#8629 = CARTESIAN_POINT ( 'NONE',  ( -10.74553182482283198, -2.882441371585227508, 31.66841991370172238 ) ) ;
#8630 = ORIENTED_EDGE ( 'NONE', *, *, #49330, .T. ) ;
#8631 = DIRECTION ( 'NONE',  ( 0.000000000000000000, 0.6427876096865373645, -0.7660444431189797898 ) ) ;
#8633 = ADVANCED_FACE ( 'NONE', ( #65813 ), #58615, .T. ) ;
#8632 = CYLINDRICAL_SURFACE ( 'NONE', #42167, 0.2499999999999994726 ) ;
#8634 = CARTESIAN_POINT ( 'NONE',  ( 3.230769230769231726, -8.318370150425687726, 35.83090037661290239 ) ) ;
#8635 = EDGE_CURVE ( 'NONE', #71093, #62448, #11395, .T. ) ;
#8636 = LINE ( 'NONE', #2292, #13220 ) ;
#8637 = CARTESIAN_POINT ( 'NONE',  ( -4.088591014333315066, -4.320704448112861584, 33.92786785259548310 ) ) ;
#8638 = ORIENTED_EDGE ( 'NONE', *, *, #63673, .F. ) ;
#8639 = EDGE_LOOP ( 'NONE', ( #56017, #6297, #72657, #28269 ) ) ;
#8640 = FACE_BOUND ( 'NONE', #8162, .T. ) ;
#8641 = VERTEX_POINT ( 'NONE', #3671 ) ;
#8642 = CARTESIAN_POINT ( 'NONE',  ( 15.48082354240754555, -2.564540009722896752, 30.55348353981670684 ) ) ;
#8643 = CYLINDRICAL_SURFACE ( 'NONE', #78982, 2.000000000000001776 ) ;
#8644 = CARTESIAN_POINT ( 'NONE',  ( 9.469381474791543241, -12.15238873228292071, 31.58232369045353849 ) ) ;
#8645 = CARTESIAN_POINT ( 'NONE',  ( -2.057637887778853703, -10.06805714834173848, 34.32951233291982618 ) ) ;
#8646 = B_SPLINE_CURVE_WITH_KNOTS ( 'NONE', 3,
 ( #45565, #72146, #31616, #64940, #78023, #71700, #10460, #85673, #37928, #4129 ),
 .UNSPECIFIED., .F., .F.,
 ( 4, 2, 2, 2, 4 ),
 ( 0.0007817246256747478229, 0.0009771112852218911526, 0.001172497944769034482, 0.001367884604316177595, 0.001563271263863320925 ),
 .UNSPECIFIED. ) ;
#8647 = EDGE_LOOP ( 'NONE', ( #46101, #6106, #1807, #44948, #17020, #65251 ) ) ;
#8648 = ORIENTED_EDGE ( 'NONE', *, *, #33223, .F. ) ;
#8649 = ORIENTED_EDGE ( 'NONE', *, *, #36816, .F. ) ;
#8650 = CARTESIAN_POINT ( 'NONE',  ( -0.2387589202700509394, -3.236590943229497697, 32.36255958852954251 ) ) ;
#8651 = ORIENTED_EDGE ( 'NONE', *, *, #53689, .T. ) ;
#8652 = FACE_OUTER_BOUND ( 'NONE', #76883, .T. ) ;
#8653 = CARTESIAN_POINT ( 'NONE',  ( -12.21153846153846168, -2.249999999999998668, 29.75000000000000355 ) ) ;
#8654 = CARTESIAN_POINT ( 'NONE',  ( -18.06608341095587633, -11.16473453929635440, 33.15142922261927083 ) ) ;
#8655 = ORIENTED_EDGE ( 'NONE', *, *, #28948, .F. ) ;
#8657 = EDGE_CURVE ( 'NONE', #47954, #22613, #37532, .T. ) ;
#8656 = CARTESIAN_POINT ( 'NONE',  ( 13.31934493865461278, -10.90142922261923886, 33.41473453929638993 ) ) ;
#8658 = VECTOR ( 'NONE', #20222, 1000.000000000000227 ) ;
#8659 = AXIS2_PLACEMENT_3D ( 'NONE', #54172, #81667, #19948 ) ;
#8660 = FACE_OUTER_BOUND ( 'NONE', #64758, .T. ) ;
#8661 = LINE ( 'NONE', #1453, #30804 ) ;
#8662 = CARTESIAN_POINT ( 'NONE',  ( 8.835298102580843249, -6.343179335718452272, 34.87096338111212646 ) ) ;
#8663 = ORIENTED_EDGE ( 'NONE', *, *, #79002, .T. ) ;
#8664 = EDGE_CURVE ( 'NONE', #48302, #1690, #67706, .T. ) ;
#8665 = ORIENTED_EDGE ( 'NONE', *, *, #78746, .T. ) ;
#8666 = ORIENTED_EDGE ( 'NONE', *, *, #24551, .F. ) ;
#8667 = AXIS2_PLACEMENT_3D ( 'NONE', #53950, #5773, #26489 ) ;
#8668 = FACE_OUTER_BOUND ( 'NONE', #77864, .T. ) ;
#8670 = DIRECTION ( 'NONE',  ( 0.000000000000000000, 1.084202172485504434E-16, -1.000000000000000000 ) ) ;
#8669 = FACE_OUTER_BOUND ( 'NONE', #86734, .T. ) ;
#8671 = EDGE_CURVE ( 'NONE', #23103, #60060, #5328, .T. ) ;
#8672 = DIRECTION ( 'NONE',  ( 0.000000000000000000, 0.000000000000000000, 1.000000000000000000 ) ) ;
#8673 = CARTESIAN_POINT ( 'NONE',  ( -8.899378738962466784, -6.809168938359901446, 34.95455904226513866 ) ) ;
#8674 = FACE_BOUND ( 'NONE', #49397, .T. ) ;
#8675 = CARTESIAN_POINT ( 'NONE',  ( 8.096208157792160520, -11.28795663066794575, 33.01431243580653785 ) ) ;
#8676 = VERTEX_POINT ( 'NONE', #27509 ) ;
#8677 = CARTESIAN_POINT ( 'NONE',  ( -3.007757879156381264, -2.554770724473667709, 30.48948780036025852 ) ) ;
#8678 = FACE_OUTER_BOUND ( 'NONE', #33432, .T. ) ;
#8679 = CARTESIAN_POINT ( 'NONE',  ( 11.31563484598253311, -7.369208160676172348, 34.74850200257122879 ) ) ;
#8680 = CARTESIAN_POINT ( 'NONE',  ( 4.153846153846154188, -6.435427911321262684, 35.78748833219616898 ) ) ;
#8681 = ORIENTED_EDGE ( 'NONE', *, *, #19206, .T. ) ;
#8682 = EDGE_CURVE ( 'NONE', #38328, #45741, #22900, .T. ) ;
#8683 = CARTESIAN_POINT ( 'NONE',  ( -18.00000000000000000, -8.120952969808772792, 34.71129190930000163 ) ) ;
#8684 = VERTEX_POINT ( 'NONE', #13111 ) ;
#8685 = FACE_BOUND ( 'NONE', #31543, .T. ) ;
#8686 = CARTESIAN_POINT ( 'NONE',  ( -17.01166750564705055, -4.481592998940251427, 33.73612834413965089 ) ) ;
#8687 = ADVANCED_FACE ( 'NONE', ( #61720 ), #41027, .F. ) ;
#8688 = FACE_OUTER_BOUND ( 'NONE', #49817, .T. ) ;
#8689 = CARTESIAN_POINT ( 'NONE',  ( 12.23861224402230619, -12.15238873228292071, 31.58232369045353849 ) ) ;
#8690 = ORIENTED_EDGE ( 'NONE', *, *, #35351, .F. ) ;
#8691 = DIRECTION ( 'NONE',  ( 0.000000000000000000, 0.000000000000000000, 1.000000000000000000 ) ) ;
#8692 = CARTESIAN_POINT ( 'NONE',  ( -14.43838377435986864, -4.118384482072085184, 33.43331474514187107 ) ) ;
#8693 = LINE ( 'NONE', #63619, #55274 ) ;
#8694 = CARTESIAN_POINT ( 'NONE',  ( -7.053224132515142131, -10.88202310037935661, 33.43294751532457099 ) ) ;
#8695 = ORIENTED_EDGE ( 'NONE', *, *, #70896, .F. ) ;
#8696 = CARTESIAN_POINT ( 'NONE',  ( -9.822455662039393687, -3.069018819979302926, 32.56621877034667278 ) ) ;
#8697 = EDGE_LOOP ( 'NONE', ( #6053, #69356 ) ) ;
#8699 = EDGE_LOOP ( 'NONE', ( #52953, #19507 ) ) ;
#8698 = DIRECTION ( 'NONE',  ( 1.000000000000000000, 0.000000000000000000, 0.000000000000000000 ) ) ;
#8700 = CARTESIAN_POINT ( 'NONE',  ( 11.78851585009985214, -6.567000820036036579, 34.66262288849541306 ) ) ;
#8701 = CARTESIAN_POINT ( 'NONE',  ( -10.86536134632696715, -12.41269422305637171, 30.68257228309993323 ) ) ;
#8702 = CARTESIAN_POINT ( 'NONE',  ( 7.780071466793709867, -9.905515769479276145, 34.41647553114623292 ) ) ;
#8703 = CARTESIAN_POINT ( 'NONE',  ( -3.931066612577741370, -12.44528174975671853, 30.48912976160716681 ) ) ;
#8705 = CYLINDRICAL_SURFACE ( 'NONE', #20163, 0.2499999999999986955 ) ;
#8704 = CARTESIAN_POINT ( 'NONE',  ( -3.164701897419155863, -3.937682226553329556, 33.60647404775216529 ) ) ;
#8706 = LINE ( 'NONE', #49242, #73730 ) ;
#8707 = VECTOR ( 'NONE', #71940, 1000.000000000000000 ) ;
#8708 = CARTESIAN_POINT ( 'NONE',  ( 1.799775606325937360E-14, -10.25000000000000000, 24.78125000000000000 ) ) ;
#8709 = VERTEX_POINT ( 'NONE', #13547 ) ;
#8710 = ADVANCED_FACE ( 'NONE', ( #74818 ), #20745, .F. ) ;
#8711 = FACE_OUTER_BOUND ( 'NONE', #83800, .T. ) ;
#8712 = CARTESIAN_POINT ( 'NONE',  ( 13.63461538461544897, -7.434744860731433924, 35.00000000000000711 ) ) ;
#8713 = ORIENTED_EDGE ( 'NONE', *, *, #9611, .T. ) ;
#8714 = ORIENTED_EDGE ( 'NONE', *, *, #3500, .T. ) ;
#8715 = ORIENTED_EDGE ( 'NONE', *, *, #40494, .F. ) ;
#8716 = CARTESIAN_POINT ( 'NONE',  ( 10.86543903529806876, -8.346898887586323923, 34.93166121998716278 ) ) ;
#8717 = B_SPLINE_CURVE_WITH_KNOTS ( 'NONE', 3,
 ( #77506, #70756, #72073, #30641, #44141, #63977, #2275, #29770, #85595, #57237 ),
 .UNSPECIFIED., .F., .F.,
 ( 4, 2, 2, 2, 4 ),
 ( 0.000000000000000000, 0.0001954339857564075286, 0.0003908679715128150572, 0.0005863019572692225586, 0.0007817359430256301143 ),
 .UNSPECIFIED. ) ;
#8718 = B_SPLINE_CURVE_WITH_KNOTS ( 'NONE', 3,
 ( #2637, #58034, #42331, #8097, #30128, #35568, #49522, #76995, #70232, #43202 ),
 .UNSPECIFIED., .F., .F.,
 ( 4, 2, 2, 2, 4 ),
 ( 0.0007817359430256315238, 0.0009771253907249980580, 0.001172514838424364592, 0.001367904286123730910, 0.001563293733823097444 ),
 .UNSPECIFIED. ) ;
#8719 = DIRECTION ( 'NONE',  ( 0.000000000000000000, 0.000000000000000000, 1.000000000000000000 ) ) ;
#8720 = DIRECTION ( 'NONE',  ( -0.000000000000000000, 1.000000000000000000, 0.000000000000000000 ) ) ;
#8721 = DIRECTION ( 'NONE',  ( 0.000000000000000000, 0.9848077530122072432, 0.1736481776669354937 ) ) ;
#8722 = CARTESIAN_POINT ( 'NONE',  ( 8.639083559792547717, -11.47017969459903952, 32.78971311882035167 ) ) ;
#8723 = EDGE_CURVE ( 'NONE', #21125, #29522, #6451, .T. ) ;
#8724 = CARTESIAN_POINT ( 'NONE',  ( -9.019253993452222673, -2.985938066672154445, 32.43141759479405550 ) ) ;
#8725 = FACE_OUTER_BOUND ( 'NONE', #14849, .T. ) ;
#8726 = CARTESIAN_POINT ( 'NONE',  ( 3.007843013253084230, -6.503392248772476236, 34.64988816332204635 ) ) ;
#8727 = CARTESIAN_POINT ( 'NONE',  ( 14.98079248672064345, -9.234221910056348293, 34.70572697212741531 ) ) ;
#8728 = EDGE_CURVE ( 'NONE', #35073, #12236, #66588, .T. ) ;
#8729 = ADVANCED_FACE ( 'NONE', ( #5910 ), #61273, .F. ) ;
#8730 = VECTOR ( 'NONE', #11999, 1000.000000000000000 ) ;
#8731 = CARTESIAN_POINT ( 'NONE',  ( -1.384615384615069056, -2.255955759149395501, 30.00000000000324363 ) ) ;
#8732 = CARTESIAN_POINT ( 'NONE',  ( 3.230769230769231726, -6.189225973068211317, 35.74407628777942847 ) ) ;
#8733 = VECTOR ( 'NONE', #29711, 1000.000000000000000 ) ;
#8734 = ORIENTED_EDGE ( 'NONE', *, *, #59573, .T. ) ;
#8735 = CARTESIAN_POINT ( 'NONE',  ( 0.6845498131513112483, -9.086983370893047862, 34.49168942202179267 ) ) ;
#8736 = CARTESIAN_POINT ( 'NONE',  ( -15.93047066807373469, -2.251407671071268712, 29.88021292934942963 ) ) ;
#8737 = FACE_OUTER_BOUND ( 'NONE', #12896, .T. ) ;
#8738 = CARTESIAN_POINT ( 'NONE',  ( -2.241523166729649574, -7.250054483168843156, 34.74374881642865631 ) ) ;
#8739 = ORIENTED_EDGE ( 'NONE', *, *, #39774, .F. ) ;
#8740 = VECTOR ( 'NONE', #33630, 999.9999999999998863 ) ;
#8742 = EDGE_CURVE ( 'NONE', #3690, #3961, #20333, .T. ) ;
#8741 = CARTESIAN_POINT ( 'NONE',  ( -15.84615384615384670, -7.500000000000000000, 29.75000000000000355 ) ) ;
#8743 = CARTESIAN_POINT ( 'NONE',  ( 4.153846153846030731, -3.643525952248796163, 33.31231777344771672 ) ) ;
#8744 = CARTESIAN_POINT ( 'NONE',  ( 8.769230769230647482, -4.481592998941358097, 33.73612834414048933 ) ) ;
#8745 = EDGE_CURVE ( 'NONE', #15980, #19105, #75256, .T. ) ;
#8746 = ADVANCED_FACE ( 'NONE', ( #30164 ), #49552, .F. ) ;
#8747 = EDGE_LOOP ( 'NONE', ( #36110, #40984, #75532, #17105 ) ) ;
#8748 = CARTESIAN_POINT ( 'NONE',  ( 4.153846153846154188, -13.88283147151868846, 33.14645433367849847 ) ) ;
#8749 = EDGE_LOOP ( 'NONE', ( #50171, #88542, #74373, #14419 ) ) ;
#8750 = EDGE_CURVE ( 'NONE', #87698, #26806, #49101, .T. ) ;
#8751 = CARTESIAN_POINT ( 'NONE',  ( -14.87820512820512953, -11.50000000000000000, 29.75000000000000355 ) ) ;
#8752 = LINE ( 'NONE', #64993, #88838 ) ;
#8753 = CARTESIAN_POINT ( 'NONE',  ( 12.23805351781451201, -8.496056993536548418, 34.65000542017679663 ) ) ;
#8754 = DIRECTION ( 'NONE',  ( -0.000000000000000000, 0.8660254037844397068, -0.4999999999999978906 ) ) ;
#8755 = CARTESIAN_POINT ( 'NONE',  ( 18.06606733335007675, -8.164416787775445883, 34.95778746994558617 ) ) ;
#8756 = B_SPLINE_CURVE_WITH_KNOTS ( 'NONE', 3,
 ( #73156, #38937, #66394, #59634, #52870, #80369, #18666, #46128, #11907, #39384 ),
 .UNSPECIFIED., .F., .F.,
 ( 4, 2, 2, 2, 4 ),
 ( 0.0007817359430256384627, 0.0009771253907250067317, 0.001172514838424375001, 0.001367904286123743270, 0.001563293733823111539 ),
 .UNSPECIFIED. ) ;
#8757 = VERTEX_POINT ( 'NONE', #71140 ) ;
#8758 = ORIENTED_EDGE ( 'NONE', *, *, #66269, .T. ) ;
#8759 = ORIENTED_EDGE ( 'NONE', *, *, #47438, .T. ) ;
#8760 = CARTESIAN_POINT ( 'NONE',  ( -3.480769230769229061, -2.249999999999998668, 29.75000000000000355 ) ) ;
#8761 = CARTESIAN_POINT ( 'NONE',  ( -12.52680846209478460, -12.70778746994557551, 30.41441678777548319 ) ) ;
#8762 = VECTOR ( 'NONE', #73268, 1000.000000000000000 ) ;
#8763 = CARTESIAN_POINT ( 'NONE',  ( -3.230769230769351186, -10.21337939537710326, 33.94971097300076224 ) ) ;
#8764 = EDGE_CURVE ( 'NONE', #68166, #63712, #36910, .T. ) ;
#8765 = CARTESIAN_POINT ( 'NONE',  ( 0.3308478584281538404, -12.35290016733513951, 31.75349464988449455 ) ) ;
#8766 = DIRECTION ( 'NONE',  ( -0.000000000000000000, -0.8660254037844397068, -0.4999999999999978906 ) ) ;
#8767 = DIRECTION ( 'NONE',  ( 0.000000000000000000, -1.000000000000000000, 0.000000000000000000 ) ) ;
#8768 = ORIENTED_EDGE ( 'NONE', *, *, #80913, .F. ) ;
#8769 = ORIENTED_EDGE ( 'NONE', *, *, #77727, .F. ) ;
#8770 = ORIENTED_EDGE ( 'NONE', *, *, #18098, .F. ) ;
#8772 = ORIENTED_EDGE ( 'NONE', *, *, #56400, .T. ) ;
#8771 = CARTESIAN_POINT ( 'NONE',  ( -3.165513659493205623, -10.90142922261932057, 33.41473453929631887 ) ) ;
#8774 = CARTESIAN_POINT ( 'NONE',  ( 13.63456079399342791, -4.176053281294518804, 33.81426240980091791 ) ) ;
#8773 = CARTESIAN_POINT ( 'NONE',  ( 8.769230769230647482, -8.613356846316285953, 34.62446782046622218 ) ) ;
#8775 = CARTESIAN_POINT ( 'NONE',  ( -2.651650429449565305, -4.848349570550461785, 25.25000000000000000 ) ) ;
#8776 = ORIENTED_EDGE ( 'NONE', *, *, #75153, .F. ) ;
#8777 = B_SPLINE_CURVE_WITH_KNOTS ( 'NONE', 3,
 ( #69581, #50634, #63265, #77666, #76337, #41675, #42128, #15979, #21842, #70918 ),
 .UNSPECIFIED., .F., .F.,
 ( 4, 2, 2, 2, 4 ),
 ( 0.0007817246256747473893, 0.0009771112852218902852, 0.001172497944769033181, 0.001367884604316176294, 0.001563271263863319190 ),
 .UNSPECIFIED. ) ;
#8778 = VECTOR ( 'NONE', #44002, 1000.000000000000114 ) ;
#8779 = ORIENTED_EDGE ( 'NONE', *, *, #29078, .T. ) ;
#8780 = DIRECTION ( 'NONE',  ( -0.000000000000000000, -0.8660254037844399289, -0.4999999999999980016 ) ) ;
#8781 = ORIENTED_EDGE ( 'NONE', *, *, #40063, .F. ) ;
#8782 = FACE_BOUND ( 'NONE', #6865, .T. ) ;
#8784 = AXIS2_PLACEMENT_3D ( 'NONE', #14973, #29817, #43326 ) ;
#8783 = CARTESIAN_POINT ( 'NONE',  ( -5.869474561766359066, -3.068774925481847937, 32.56582465632704526 ) ) ;
#8785 = VECTOR ( 'NONE', #73028, 1000.000000000000000 ) ;
#8786 = DIRECTION ( 'NONE',  ( -0.000000000000000000, 0.5000000000000011102, -0.8660254037844380415 ) ) ;
#8787 = ORIENTED_EDGE ( 'NONE', *, *, #56126, .F. ) ;
#8788 = CARTESIAN_POINT ( 'NONE',  ( -4.284406745588072774, -2.504760397472873823, 29.97295953869789997 ) ) ;
#8789 = CARTESIAN_POINT ( 'NONE',  ( 5.010840697562939816, -8.164416787775445883, 34.95778746994557906 ) ) ;
#8790 = CARTESIAN_POINT ( 'NONE',  ( 9.692307692307695177, -11.69971097300155272, 32.46337939537588113 ) ) ;
#8791 = DIRECTION ( 'NONE',  ( -0.000000000000000000, -1.000000000000000000, -8.673617379884033500E-16 ) ) ;
#8792 = CARTESIAN_POINT ( 'NONE',  ( -13.13466986626723987, -11.86320923018887541, 32.19269448109604781 ) ) ;
#8793 = AXIS2_PLACEMENT_3D ( 'NONE', #28742, #56206, #42260 ) ;
#8794 = EDGE_CURVE ( 'NONE', #51157, #84431, #83839, .T. ) ;
#8795 = DIRECTION ( 'NONE',  ( -0.000000000000000000, -0.6427876096865404731, -0.7660444431189770143 ) ) ;
#8796 = CARTESIAN_POINT ( 'NONE',  ( -7.976844449264150150, -11.93127051446799847, 32.56575433478202797 ) ) ;
#8797 = CARTESIAN_POINT ( 'NONE',  ( -5.076923076923075762, -11.16473453929635440, 33.15142922261926373 ) ) ;
#8798 = CARTESIAN_POINT ( 'NONE',  ( -0.4615384615385840772, -5.094484230521993062, 34.41647553114689373 ) ) ;
#8799 = CARTESIAN_POINT ( 'NONE',  ( -6.923076923076922462, -2.486705287966279876, 31.30864560766543647 ) ) ;
#8800 = CARTESIAN_POINT ( 'NONE',  ( 8.835298102580843249, -3.937682226553329556, 33.60647404775216529 ) ) ;
#8802 = CARTESIAN_POINT ( 'NONE',  ( 2.307692307692187583, -10.21337939537710326, 33.94971097300076224 ) ) ;
#8801 = CARTESIAN_POINT ( 'NONE',  ( 4.946231610255518163, -11.18331474514187995, 33.13161551792790505 ) ) ;
#8803 = CARTESIAN_POINT ( 'NONE',  ( 1.515407192440174189, -11.18335022499818621, 33.13157742990016885 ) ) ;
#8805 = CARTESIAN_POINT ( 'NONE',  ( 8.769230769230647482, -2.892918686052165622, 31.69288490824153470 ) ) ;
#8804 = CARTESIAN_POINT ( 'NONE',  ( 3.903869409797562806, -5.643011162660950042, 34.66104346484419096 ) ) ;
#8806 = CARTESIAN_POINT ( 'NONE',  ( -2.373774687052442545, -5.471508081941601986, 34.59228464037088457 ) ) ;
#8807 = CARTESIAN_POINT ( 'NONE',  ( 1.200186371490561621, -10.22469193450123193, 20.70125670625849423 ) ) ;
#8808 = VERTEX_POINT ( 'NONE', #2233 ) ;
#8809 = CARTESIAN_POINT ( 'NONE',  ( 3.432150206517289082, -7.475741165495100482, 14.00000000000201794 ) ) ;
#8810 = ORIENTED_EDGE ( 'NONE', *, *, #81121, .T. ) ;
#8811 = CARTESIAN_POINT ( 'NONE',  ( 2.294871794871793380, -7.500000000000000000, 29.75000000000000355 ) ) ;
#8812 = VERTEX_POINT ( 'NONE', #16204 ) ;
#8813 = EDGE_CURVE ( 'NONE', #22240, #42959, #9448, .T. ) ;
#8814 = CARTESIAN_POINT ( 'NONE',  ( 0.4615384615384611755, -4.102666532097928531, 36.13435417666054406 ) ) ;
#8815 = CARTESIAN_POINT ( 'NONE',  ( -3.454254174493179619, -3.236172620538810385, 32.36188796281390267 ) ) ;
#8816 = VERTEX_POINT ( 'NONE', #71578 ) ;
#8817 = DIRECTION ( 'NONE',  ( 0.000000000000000000, 0.3420201433256641055, -0.9396926207859100932 ) ) ;
#8818 = CARTESIAN_POINT ( 'NONE',  ( -0.06109907496454585613, -4.750000000000000000, 21.40438170625849068 ) ) ;
#8819 = CARTESIAN_POINT ( 'NONE',  ( 17.14217864819909920, -8.613356846314930593, 34.62446782046653482 ) ) ;
#8820 = CARTESIAN_POINT ( 'NONE',  ( 13.51540582558234149, -2.845873456487966635, 32.17976146951972538 ) ) ;
#8822 = CARTESIAN_POINT ( 'NONE',  ( -5.300408020647024543, -5.113361153441932316, 34.14387501736621999 ) ) ;
#8821 = B_SPLINE_CURVE_WITH_KNOTS ( 'NONE', 3,
 ( #22612, #64033, #37006, #86103, #29826, #43774, #58610, #58166, #51383, #10441 ),
 .UNSPECIFIED., .F., .F.,
 ( 4, 2, 2, 2, 4 ),
 ( 0.000000000000000000, 0.0001954311564186858715, 0.0003908623128373717431, 0.0005862934692560576146, 0.0007817246256747434861 ),
 .UNSPECIFIED. ) ;
#8823 = CARTESIAN_POINT ( 'NONE',  ( -16.28399412357784826, -10.31621877034669588, 34.18098118002070152 ) ) ;
#8824 = LINE ( 'NONE', #21886, #25776 ) ;
#8825 = LINE ( 'NONE', #36297, #831 ) ;
#8826 = B_SPLINE_CURVE_WITH_KNOTS ( 'NONE', 3,
 ( #20052, #61469, #41658, #21377, #6978, #13296, #27250, #34453, #61912, #8763 ),
 .UNSPECIFIED., .F., .F.,
 ( 4, 2, 2, 2, 4 ),
 ( 0.000000000000000000, 0.0001954339857564090465, 0.0003908679715128180929, 0.0005863019572692271123, 0.0007817359430256361858 ),
 .UNSPECIFIED. ) ;
#8827 = AXIS2_PLACEMENT_3D ( 'NONE', #10945, #31660, #42193 ) ;
#8828 = CARTESIAN_POINT ( 'NONE',  ( -2.651650429449565305, -4.848349570550461785, 16.50000000000000000 ) ) ;
#8829 = CARTESIAN_POINT ( 'NONE',  ( 11.53846153846153832, -5.471508081941601098, 34.59228464037088457 ) ) ;
#8830 = DIRECTION ( 'NONE',  ( -0.000000000000000000, 0.3420201433256694346, -0.9396926207859080948 ) ) ;
#8831 = EDGE_CURVE ( 'NONE', #53391, #4984, #50850, .T. ) ;
#8832 = VECTOR ( 'NONE', #10813, 1000.000000000000227 ) ;
#8833 = CARTESIAN_POINT ( 'NONE',  ( -27.00000000000000000, 0.7500000000000059952, 24.75000000000000000 ) ) ;
#8834 = CARTESIAN_POINT ( 'NONE',  ( -2.651650429449535551, -10.15165042944956753, 18.68750000000000000 ) ) ;
#8835 = LINE ( 'NONE', #15588, #61986 ) ;
#8836 = ORIENTED_EDGE ( 'NONE', *, *, #87240, .T. ) ;
#8837 = CARTESIAN_POINT ( 'NONE',  ( 1.607628228708781526, -8.282913670948747864, 34.94150082978203642 ) ) ;
#8838 = CARTESIAN_POINT ( 'NONE',  ( 11.76124107972994537, -5.913360116392397892, 34.49180327182771322 ) ) ;
#8839 = DIRECTION ( 'NONE',  ( 0.000000000000000000, 0.7660444431189822323, -0.6427876096865344779 ) ) ;
#8840 = DIRECTION ( 'NONE',  ( -0.000000000000000000, -0.000000000000000000, -1.000000000000000000 ) ) ;
#8841 = CARTESIAN_POINT ( 'NONE',  ( -16.40382288478850725, -10.66389620160130036, 33.62221079203477103 ) ) ;
#8842 = CARTESIAN_POINT ( 'NONE',  ( 9.562160482869471068, -11.47017969459903952, 32.78971311882035167 ) ) ;
#8843 = CARTESIAN_POINT ( 'NONE',  ( 8.639083559792549494, -10.88202310037935661, 33.43294751532457099 ) ) ;
#8844 = EDGE_CURVE ( 'NONE', #79547, #52311, #8128, .T. ) ;
#8845 = EDGE_CURVE ( 'NONE', #37947, #18328, #69773, .T. ) ;
#8846 = VECTOR ( 'NONE', #54547, 1000.000000000000000 ) ;
#8847 = VERTEX_POINT ( 'NONE', #85113 ) ;
#8848 = VERTEX_POINT ( 'NONE', #83796 ) ;
#8849 = ORIENTED_EDGE ( 'NONE', *, *, #72762, .F. ) ;
#8850 = B_SPLINE_CURVE_WITH_KNOTS ( 'NONE', 3,
 ( #25173, #81909, #87795, #67944, #68376, #80580, #5793, #47213, #26511, #40040 ),
 .UNSPECIFIED., .F., .F.,
 ( 4, 2, 2, 2, 4 ),
 ( 0.000000000000000000, 0.0001954339857564098054, 0.0003908679715128196108, 0.0005863019572692293891, 0.0007817359430256392216 ),
 .UNSPECIFIED. ) ;
#8851 = VECTOR ( 'NONE', #12312, 1000.000000000000000 ) ;
#8852 = CARTESIAN_POINT ( 'NONE',  ( 3.480714749117373330, -5.852078868378310261, 34.47109172314383585 ) ) ;
#8853 = CARTESIAN_POINT ( 'NONE',  ( -6.923076923076922462, -4.098570777380720287, 33.41473453929634729 ) ) ;
#8854 = CARTESIAN_POINT ( 'NONE',  ( 6.923076923076924238, -2.833524468853757305, 32.15551576947925838 ) ) ;
#8855 = CARTESIAN_POINT ( 'NONE',  ( 4.403900465484468008, -3.627508038966689607, 32.91356715214248396 ) ) ;
#8856 = LINE ( 'NONE', #76868, #20795 ) ;
#8857 = VECTOR ( 'NONE', #77251, 1000.000000000000227 ) ;
#8858 = ORIENTED_EDGE ( 'NONE', *, *, #27806, .T. ) ;
#8859 = CARTESIAN_POINT ( 'NONE',  ( -1.384615384615383471, -2.486705287966279876, 31.30864560766543647 ) ) ;
#8860 = ORIENTED_EDGE ( 'NONE', *, *, #5431, .F. ) ;
#8861 = EDGE_LOOP ( 'NONE', ( #71509, #54945, #40186, #29010 ) ) ;
#8863 = ORIENTED_EDGE ( 'NONE', *, *, #8401, .T. ) ;
#8862 = CARTESIAN_POINT ( 'NONE',  ( -30.00000000000000000, -15.00000000000000000, 3.000000000000000000 ) ) ;
#8864 = CARTESIAN_POINT ( 'NONE',  ( 16.40379167219429846, -12.43552623307873972, 30.55307653245132826 ) ) ;
#8865 = DIRECTION ( 'NONE',  ( -1.000000000000000000, -0.000000000000000000, -0.000000000000000000 ) ) ;
#8866 = CARTESIAN_POINT ( 'NONE',  ( 4.153846153846032507, -4.481592998941358097, 33.73612834414048933 ) ) ;
#8867 = CYLINDRICAL_SURFACE ( 'NONE', #38197, 0.2499999999999998890 ) ;
#8868 = EDGE_LOOP ( 'NONE', ( #23998, #58084 ) ) ;
#8869 = B_SPLINE_CURVE_WITH_KNOTS ( 'NONE', 3,
 ( #24546, #58326, #23657, #77716, #29980, #37616, #57438, #65975, #43931, #71395 ),
 .UNSPECIFIED., .F., .F.,
 ( 4, 2, 2, 2, 4 ),
 ( 0.000000000000000000, 0.0001954339857564125972, 0.0003908679715128181471, 0.0005863019572692237513, 0.0007817359430256293554 ),
 .UNSPECIFIED. ) ;
#8870 = EDGE_LOOP ( 'NONE', ( #55065, #59083 ) ) ;
#8871 = CARTESIAN_POINT ( 'NONE',  ( -2.651650429449565305, -4.848349570550461785, 20.25000000000000000 ) ) ;
#8872 = ORIENTED_EDGE ( 'NONE', *, *, #62029, .F. ) ;
#8873 = CARTESIAN_POINT ( 'NONE',  ( -6.792286482109968659, -2.845873456487966635, 32.17976146951972538 ) ) ;
#8875 = ORIENTED_EDGE ( 'NONE', *, *, #54892, .F. ) ;
#8874 = CARTESIAN_POINT ( 'NONE',  ( 8.769230769230768274, -12.29105614889573062, 35.45975837776705220 ) ) ;
#8876 = LINE ( 'NONE', #57047, #1863 ) ;
#8877 = CARTESIAN_POINT ( 'NONE',  ( 4.853438133199125204, -3.754499324213721234, 33.06261337010820256 ) ) ;
#8878 = CYLINDRICAL_SURFACE ( 'NONE', #45056, 0.2499999999999986955 ) ;
#8879 = ORIENTED_EDGE ( 'NONE', *, *, #74087, .F. ) ;
#8880 = VECTOR ( 'NONE', #33968, 1000.000000000000000 ) ;
#8881 = FACE_OUTER_BOUND ( 'NONE', #73444, .T. ) ;
#8882 = CARTESIAN_POINT ( 'NONE',  ( -9.692307692307691624, -4.098570777380720287, 33.41473453929634729 ) ) ;
#8883 = ORIENTED_EDGE ( 'NONE', *, *, #864, .F. ) ;
#8884 = FACE_BOUND ( 'NONE', #52182, .T. ) ;
#8885 = LINE ( 'NONE', #78213, #15417 ) ;
#8886 = CARTESIAN_POINT ( 'NONE',  ( -7.146561866800869467, -2.847400154188068022, 31.58180166144859058 ) ) ;
#8887 = DIRECTION ( 'NONE',  ( 1.000000000000000000, 0.000000000000000000, 0.000000000000000000 ) ) ;
#8889 = CARTESIAN_POINT ( 'NONE',  ( -5.076923076923075762, -11.11383981884818262, 36.00935417666054406 ) ) ;
#8888 = CARTESIAN_POINT ( 'NONE',  ( -6.699649961215353500, -7.630147231320743018, 34.74852402298682819 ) ) ;
#8890 = CARTESIAN_POINT ( 'NONE',  ( 8.703147358274886614, -5.557115091759785130, 34.35708131394839171 ) ) ;
#8891 = CARTESIAN_POINT ( 'NONE',  ( 12.71153846153989697, -7.500000000000155431, 34.75000000000007105 ) ) ;
#8892 = ORIENTED_EDGE ( 'NONE', *, *, #22887, .F. ) ;
#8893 = CARTESIAN_POINT ( 'NONE',  ( -11.31568199719312773, -4.387253974876679230, 33.66317474335728832 ) ) ;
#8894 = ORIENTED_EDGE ( 'NONE', *, *, #59168, .T. ) ;
#8895 = EDGE_CURVE ( 'NONE', #66929, #42644, #29290, .T. ) ;
#8896 = ADVANCED_FACE ( 'NONE', ( #22081 ), #22519, .F. ) ;
#8897 = CARTESIAN_POINT ( 'NONE',  ( 11.28843831424008215, -12.07920672191015221, 32.31858351112116168 ) ) ;
#8898 = CARTESIAN_POINT ( 'NONE',  ( 15.48082354240754555, -4.235687564193448829, 33.53795663066793509 ) ) ;
#8900 = CARTESIAN_POINT ( 'NONE',  ( -16.15384615384615330, -10.51840700105979565, 33.73612834413961536 ) ) ;
#8899 = PRODUCT ( 'BR-833', 'BR-833', '', ( #79801 ) ) ;
#8901 = CARTESIAN_POINT ( 'NONE',  ( 2.241609928332173762, -5.471508081941601986, 34.59228464037088457 ) ) ;
#8902 = CARTESIAN_POINT ( 'NONE',  ( -0.3954701105360228230, -12.37446782046654192, 30.86335684631486842 ) ) ;
#8903 = CARTESIAN_POINT ( 'NONE',  ( 4.284637961670942907, -9.804649428959608670, 34.18742332936588468 ) ) ;
#8904 = FACE_BOUND ( 'NONE', #57727, .T. ) ;
#8906 = CYLINDRICAL_SURFACE ( 'NONE', #48898, 0.2499999999999979738 ) ;
#8905 = CARTESIAN_POINT ( 'NONE',  ( 6.700149964170072359, -4.026226216239095379, 33.68668979543632958 ) ) ;
#8907 = CARTESIAN_POINT ( 'NONE',  ( -15.36146069743679021, -8.999036380462717588, 34.52022231692819076 ) ) ;
#8909 = CARTESIAN_POINT ( 'NONE',  ( 7.145856464345331283, -12.44528174975671853, 30.48912976160716681 ) ) ;
#8908 = CARTESIAN_POINT ( 'NONE',  ( -3.230769230769229949, -11.69971097300155272, 32.46337939537588113 ) ) ;
#8910 = CARTESIAN_POINT ( 'NONE',  ( 8.769230769230768274, -10.51840700105979565, 33.73612834413961536 ) ) ;
#8911 = B_SPLINE_CURVE_WITH_KNOTS ( 'NONE', 3,
 ( #15505, #9619, #85736, #51467, #78968, #42536, #69992, #70892, #8306, #9199 ),
 .UNSPECIFIED., .F., .F.,
 ( 4, 2, 2, 2, 4 ),
 ( 0.0007817359430256388964, 0.0009771253907250075990, 0.001172514838424376085, 0.001367904286123744571, 0.001563293733823113273 ),
 .UNSPECIFIED. ) ;
#8912 = CARTESIAN_POINT ( 'NONE',  ( 1.614399933863660985, -11.22469193450123193, 20.70125670625849423 ) ) ;
#8913 = ORIENTED_EDGE ( 'NONE', *, *, #22016, .F. ) ;
#8914 = AXIS2_PLACEMENT_3D ( 'NONE', #61935, #35357, #70480 ) ;
#8915 = ORIENTED_EDGE ( 'NONE', *, *, #23750, .F. ) ;
#8916 = EDGE_CURVE ( 'NONE', #40550, #10987, #24616, .T. ) ;
#8917 = VECTOR ( 'NONE', #23418, 1000.000000000000114 ) ;
#8918 = DIRECTION ( 'NONE',  ( -0.000000000000000000, -0.9396926207859093161, -0.3420201433256663259 ) ) ;
#8919 = CARTESIAN_POINT ( 'NONE',  ( -14.37296275365308418, -6.879047030191174805, 34.71129190930000163 ) ) ;
#8920 = CARTESIAN_POINT ( 'NONE',  ( -7.715363405186893786, -11.37503395064541678, 33.29242100308974983 ) ) ;
#8921 = CARTESIAN_POINT ( 'NONE',  ( 12.46153846153846168, -1.129524287112498415, 32.06866353760679544 ) ) ;
#8922 = EDGE_CURVE ( 'NONE', #47411, #41231, #54780, .T. ) ;
#8923 = CARTESIAN_POINT ( 'NONE',  ( -13.13456096470192769, -2.544122305571458575, 31.48381861865057729 ) ) ;
#8924 = CARTESIAN_POINT ( 'NONE',  ( 2.694853999681214862, -10.10844685921789043, 19.37313170625848713 ) ) ;
#8925 = CARTESIAN_POINT ( 'NONE',  ( 6.792386319966616348, -2.295517848115769421, 30.44137282052136939 ) ) ;
#8926 = CARTESIAN_POINT ( 'NONE',  ( 3.230769230769231726, -3.513871655860378418, 32.76840700105978499 ) ) ;
#8927 = DIRECTION ( 'NONE',  ( -0.000000000000000000, 0.7660444431189791237, -0.6427876096865379196 ) ) ;
#8928 = CARTESIAN_POINT ( 'NONE',  ( 10.61538461538449418, -6.835583212225970762, 34.95778746994575670 ) ) ;
#8929 = DIRECTION ( 'NONE',  ( 0.000000000000000000, 0.9396926207859126468, 0.3420201433256571111 ) ) ;
#8930 = CARTESIAN_POINT ( 'NONE',  ( 13.63461538461680611, -7.500000000000154543, 35.00000000000007105 ) ) ;
#8931 = CARTESIAN_POINT ( 'NONE',  ( 14.53070365930516061, -11.76359900205217635, 32.36225158514719880 ) ) ;
#8932 = EDGE_CURVE ( 'NONE', #43893, #4302, #73371, .T. ) ;
#8933 = DIRECTION ( 'NONE',  ( -0.000000000000000000, -0.5000000000000009992, -0.8660254037844380415 ) ) ;
#8934 = VERTEX_POINT ( 'NONE', #39606 ) ;
#8935 = DIRECTION ( 'NONE',  ( 0.000000000000000000, 0.000000000000000000, -1.000000000000000000 ) ) ;
#8936 = CARTESIAN_POINT ( 'NONE',  ( -8.769230769230768274, -12.62096338111211580, 30.90682066428153263 ) ) ;
#8937 = CARTESIAN_POINT ( 'NONE',  ( -2.775308065498752086, -8.577988221561495763, 25.26749329374151642 ) ) ;
#8938 = CARTESIAN_POINT ( 'NONE',  ( 7.846153846153846700, -1.790695186598648903, 34.54067556320373455 ) ) ;
#8939 = CARTESIAN_POINT ( 'NONE',  ( -10.61538461538461320, -13.63283147151868846, 33.57946703557072254 ) ) ;
#8940 = EDGE_LOOP ( 'NONE', ( #66011, #64024, #70456, #87506 ) ) ;
#8941 = DIRECTION ( 'NONE',  ( 0.000000000000000000, 0.9396926207859126468, -0.3420201433256571111 ) ) ;
#8943 = ORIENTED_EDGE ( 'NONE', *, *, #54144, .F. ) ;
#8942 = CARTESIAN_POINT ( 'NONE',  ( 7.622668902429898807, -2.599994579823202923, 30.74605699353653776 ) ) ;
#8944 = CARTESIAN_POINT ( 'NONE',  ( 9.469442270104055481, -2.501496062324912284, 29.88072118266895671 ) ) ;
#8945 = CARTESIAN_POINT ( 'NONE',  ( 12.59206389977210705, -5.915461855592780260, 34.75538340440931506 ) ) ;
#8946 = EDGE_LOOP ( 'NONE', ( #34097, #5578, #55629, #61111 ) ) ;
#8947 = DIRECTION ( 'NONE',  ( 0.000000000000000000, 0.6427876096865368094, 0.7660444431189802339 ) ) ;
#8948 = CARTESIAN_POINT ( 'NONE',  ( 15.23076923076923173, -9.905515769479276145, 34.41647553114623292 ) ) ;
#8949 = ORIENTED_EDGE ( 'NONE', *, *, #54889, .T. ) ;
#8950 = DIRECTION ( 'NONE',  ( 0.000000000000000000, 0.1736481776669267785, -0.9848077530122087975 ) ) ;
#8951 = CARTESIAN_POINT ( 'NONE',  ( 5.448717948717947124, -7.500000000000000000, 33.75000000000000000 ) ) ;
#8952 = ADVANCED_FACE ( 'NONE', ( #25181 ), #59411, .F. ) ;
#8953 = B_SPLINE_CURVE_WITH_KNOTS ( 'NONE', 3,
 ( #63477, #78314, #77876, #71116, #30141, #50828, #71557, #84219, #1779, #49959 ),
 .UNSPECIFIED., .F., .F.,
 ( 4, 2, 2, 2, 4 ),
 ( 0.0007817246256747465219, 0.0009771112852218900684, 0.001172497944769033615, 0.001367884604316177378, 0.001563271263863320925 ),
 .UNSPECIFIED. ) ;
#8954 = CARTESIAN_POINT ( 'NONE',  ( -9.468931751609508396, -2.501478030877323455, 29.88021232661721172 ) ) ;
#8955 = VERTEX_POINT ( 'NONE', #31494 ) ;
#8956 = EDGE_CURVE ( 'NONE', #55506, #1287, #65708, .T. ) ;
#8958 = ORIENTED_EDGE ( 'NONE', *, *, #65458, .F. ) ;
#8957 = VECTOR ( 'NONE', #27006, 1000.000000000000000 ) ;
#8959 = B_SPLINE_CURVE_WITH_KNOTS ( 'NONE', 3,
 ( #17564, #87370, #3588, #86020, #58979, #72944, #46363, #25205, #66177, #24300 ),
 .UNSPECIFIED., .F., .F.,
 ( 4, 2, 2, 2, 4 ),
 ( 0.000000000000000000, 0.0001954311564186871184, 0.0003908623128373742367, 0.0005862934692560614093, 0.0007817246256747484735 ),
 .UNSPECIFIED. ) ;
#8960 = ORIENTED_EDGE ( 'NONE', *, *, #26750, .F. ) ;
#8961 = ADVANCED_FACE ( 'NONE', ( #58067 ), #86913, .F. ) ;
#8962 = DIRECTION ( 'NONE',  ( 0.000000000000000000, 0.6427876096865373645, -0.7660444431189797898 ) ) ;
#8963 = CARTESIAN_POINT ( 'NONE',  ( -15.23076923076935252, -2.379036618888197729, 30.90682066428292885 ) ) ;
#8964 = EDGE_CURVE ( 'NONE', #8309, #60949, #86462, .T. ) ;
#8965 = CARTESIAN_POINT ( 'NONE',  ( -2.980823821391187067, -8.476813868363244353, 34.90874843262270133 ) ) ;
#8966 = CARTESIAN_POINT ( 'NONE',  ( 14.30769230769218581, -4.320704448113951379, 33.92786785259630022 ) ) ;
#8967 = ORIENTED_EDGE ( 'NONE', *, *, #73884, .T. ) ;
#8968 = ORIENTED_EDGE ( 'NONE', *, *, #71436, .F. ) ;
#8970 = ORIENTED_EDGE ( 'NONE', *, *, #77003, .T. ) ;
#8969 = CARTESIAN_POINT ( 'NONE',  ( -1.134615384615447420, -7.565270445406050648, 34.75000000000000000 ) ) ;
#8971 = CARTESIAN_POINT ( 'NONE',  ( 12.59206389977210705, -11.66157788607254098, 32.95092075102925833 ) ) ;
#8972 = ORIENTED_EDGE ( 'NONE', *, *, #63331, .T. ) ;
#8973 = AXIS2_PLACEMENT_3D ( 'NONE', #36865, #55811, #28802 ) ;
#8974 = CARTESIAN_POINT ( 'NONE',  ( 11.78846153846154010, -2.499999999999998668, 29.75000000000000355 ) ) ;
#8975 = CARTESIAN_POINT ( 'NONE',  ( 1.653273178848927064E-15, -7.500000000000000000, 11.00000000000000178 ) ) ;
#8976 = ORIENTED_EDGE ( 'NONE', *, *, #84507, .T. ) ;
#8977 = VECTOR ( 'NONE', #55579, 1000.000000000000227 ) ;
#8978 = B_SPLINE_CURVE_WITH_KNOTS ( 'NONE', 3,
 ( #6882, #76680, #7776, #56406, #69915, #55511, #35240, #49203, #77560, #77119 ),
 .UNSPECIFIED., .F., .F.,
 ( 4, 2, 2, 2, 4 ),
 ( 0.000000000000000000, 0.0001954311564186876334, 0.0003908623128373752667, 0.0005862934692560629272, 0.0007817246256747505334 ),
 .UNSPECIFIED. ) ;
#8979 = B_SPLINE_CURVE_WITH_KNOTS ( 'NONE', 3,
 ( #40580, #47765, #75247, #13537, #76120, #46875, #34249, #41017, #7675, #41457 ),
 .UNSPECIFIED., .F., .F.,
 ( 4, 2, 2, 2, 4 ),
 ( 0.000000000000000000, 0.0001954339857564054957, 0.0003908679715128109914, 0.0005863019572692164871, 0.0007817359430256219828 ),
 .UNSPECIFIED. ) ;
#8980 = ORIENTED_EDGE ( 'NONE', *, *, #60693, .F. ) ;
#8982 = ORIENTED_EDGE ( 'NONE', *, *, #56462, .F. ) ;
#8981 = CARTESIAN_POINT ( 'NONE',  ( -12.23875892027004753, -5.114059244376869984, 34.14424750095245287 ) ) ;
#8983 = CARTESIAN_POINT ( 'NONE',  ( 4.219101725122176738, -5.219633306516380244, 34.19971097300157936 ) ) ;
#8984 = B_SPLINE_CURVE_WITH_KNOTS ( 'NONE', 3,
 ( #53626, #54059, #73908, #34239, #73465, #27045, #88330, #66700, #81114, #27488 ),
 .UNSPECIFIED., .F., .F.,
 ( 4, 2, 2, 2, 4 ),
 ( 0.0007817246336856293861, 0.0009771112958940105907, 0.001172497958102391904, 0.001367884620310773217, 0.001563271282519154530 ),
 .UNSPECIFIED. ) ;
#8985 = B_SPLINE_CURVE_WITH_KNOTS ( 'NONE', 3,
 ( #61632, #19331, #5373, #39169, #26535, #6265, #59863, #19772, #74725, #47233 ),
 .UNSPECIFIED., .F., .F.,
 ( 4, 2, 2, 2, 4 ),
 ( 0.0007817359527651099533, 0.0009771254036996487088, 0.001172514854634187573, 0.001367904305568726220, 0.001563293756503265084 ),
 .UNSPECIFIED. ) ;
#8986 = EDGE_CURVE ( 'NONE', #39878, #13065, #79240, .T. ) ;
#8987 = CARTESIAN_POINT ( 'NONE',  ( 14.17700170458200404, -5.496505350115501010, 34.60290016733514307 ) ) ;
#8988 = ORIENTED_EDGE ( 'NONE', *, *, #66143, .F. ) ;
#8989 = CARTESIAN_POINT ( 'NONE',  ( 15.10062126103753855, -2.373036134822904319, 30.88089517874952250 ) ) ;
#8990 = CARTESIAN_POINT ( 'NONE',  ( -14.17690186672535901, -12.62708834333097663, 30.88030960425257021 ) ) ;
#8991 = CARTESIAN_POINT ( 'NONE',  ( 6.923076923076800782, -5.941354392335915335, 34.76329471203413846 ) ) ;
#8992 = FACE_BOUND ( 'NONE', #85133, .T. ) ;
#8993 = CARTESIAN_POINT ( 'NONE',  ( -8.769230769230892619, -2.379036618888197729, 30.90682066428292885 ) ) ;
#8994 = DIRECTION ( 'NONE',  ( 0.000000000000000000, 0.1736481776669275834, 0.9848077530122086864 ) ) ;
#8995 = CARTESIAN_POINT ( 'NONE',  ( 8.519207531937803779, -2.587272538249754117, 30.68239716806877837 ) ) ;
#8997 = CARTESIAN_POINT ( 'NONE',  ( -15.90390074446811042, -2.986452184633680229, 32.43230066228895225 ) ) ;
#8996 = CARTESIAN_POINT ( 'NONE',  ( -5.999999999999998224, -8.164416787775445883, 34.95778746994557906 ) ) ;
#8998 = CARTESIAN_POINT ( 'NONE',  ( -4.826868657009622865, -4.074993327901525575, 33.72946981652012255 ) ) ;
#8999 = FACE_OUTER_BOUND ( 'NONE', #45170, .T. ) ;
#9000 = EDGE_LOOP ( 'NONE', ( #59965, #48043 ) ) ;
#9001 = CARTESIAN_POINT ( 'NONE',  ( 10.36540788444226280, -10.66389620160130036, 33.62221079203477103 ) ) ;
#9002 = ORIENTED_EDGE ( 'NONE', *, *, #86075, .F. ) ;
#9003 = ORIENTED_EDGE ( 'NONE', *, *, #77748, .T. ) ;
#9004 = EDGE_CURVE ( 'NONE', #27408, #18603, #66620, .T. ) ;
#9006 = CARTESIAN_POINT ( 'NONE',  ( 16.21910172512217585, -12.27809138561124591, 31.22303859784720359 ) ) ;
#9005 = CARTESIAN_POINT ( 'NONE',  ( -1.384615384615506484, -5.094484230521993062, 34.41647553114689373 ) ) ;
#9007 = AXIS2_PLACEMENT_3D ( 'NONE', #8811, #84474, #10134 ) ;
#9008 = DIRECTION ( 'NONE',  ( 0.000000000000000000, 0.000000000000000000, -1.000000000000000000 ) ) ;
#9009 = CARTESIAN_POINT ( 'NONE',  ( -11.53846153846153655, -13.87047571288749737, 32.06866353760679544 ) ) ;
#9010 = DIRECTION ( 'NONE',  ( -0.000000000000000000, -0.000000000000000000, -1.000000000000000000 ) ) ;
#9011 = CARTESIAN_POINT ( 'NONE',  ( -2.373774687052441656, -11.35647404775217595, 33.31231777344666511 ) ) ;
#9012 = ORIENTED_EDGE ( 'NONE', *, *, #45343, .T. ) ;
#9013 = CARTESIAN_POINT ( 'NONE',  ( 14.05769230769230838, -2.249999999999998668, 29.75000000000000355 ) ) ;
#9014 = CARTESIAN_POINT ( 'NONE',  ( 14.30769230769231015, -12.62096338111211580, 30.90682066428153263 ) ) ;
#9015 = DIRECTION ( 'NONE',  ( 1.000000000000000000, 0.000000000000000000, 0.000000000000000000 ) ) ;
#9016 = CARTESIAN_POINT ( 'NONE',  ( 15.45378207486262667, -12.38742843783360748, 31.66772728687926985 ) ) ;
#9017 = CARTESIAN_POINT ( 'NONE',  ( 13.60762822870878530, -5.582272713120729257, 34.63742843783360570 ) ) ;
#9018 = CARTESIAN_POINT ( 'NONE',  ( -3.749999999999997335, -7.500000000000021316, 17.59375000000000000 ) ) ;
#9019 = ORIENTED_EDGE ( 'NONE', *, *, #21243, .F. ) ;
#9020 = B_SPLINE_CURVE_WITH_KNOTS ( 'NONE', 3,
 ( #60124, #82189, #80867, #54249, #73210, #74537, #11509, #66446, #38989, #33105 ),
 .UNSPECIFIED., .F., .F.,
 ( 4, 2, 2, 2, 4 ),
 ( 0.000000000000000000, 0.0001954311564186867389, 0.0003908623128373734778, 0.0005862934692560602167, 0.0007817246256747469556 ),
 .UNSPECIFIED. ) ;
#9021 = EDGE_LOOP ( 'NONE', ( #65119, #19753, #26900, #32776 ) ) ;
#9022 = EDGE_CURVE ( 'NONE', #82557, #54935, #41871, .T. ) ;
#9023 = CARTESIAN_POINT ( 'NONE',  ( -7.623374177175780808, -12.11081565061823717, 32.26097654155341843 ) ) ;
#9024 = ORIENTED_EDGE ( 'NONE', *, *, #1298, .T. ) ;
#9025 = CYLINDRICAL_SURFACE ( 'NONE', #11059, 0.2499999999999994726 ) ;
#9026 = CARTESIAN_POINT ( 'NONE',  ( 17.77707304109314634, -11.43668979543635089, 33.22377378376089752 ) ) ;
#9027 = LINE ( 'NONE', #36497, #72514 ) ;
#9028 = ADVANCED_FACE ( 'NONE', ( #85551 ), #23825, .F. ) ;
#9029 = CARTESIAN_POINT ( 'NONE',  ( -0.5276208408985973985, -11.91647553114624181, 32.58852847137148245 ) ) ;
#9030 = CARTESIAN_POINT ( 'NONE',  ( -3.749999999999997335, -7.500000000000021316, 16.34375000000000000 ) ) ;
#9031 = CARTESIAN_POINT ( 'NONE',  ( 14.30769230769231015, -2.708943851104267164, 35.45975837776705220 ) ) ;
#9032 = ORIENTED_EDGE ( 'NONE', *, *, #45241, .F. ) ;
#9033 = CARTESIAN_POINT ( 'NONE',  ( -2.294871794871794712, -3.499999999999999556, 29.75000000000000355 ) ) ;
#9035 = ORIENTED_EDGE ( 'NONE', *, *, #16167, .T. ) ;
#9034 = CARTESIAN_POINT ( 'NONE',  ( 18.00000000000031264, -2.255955759149395501, 30.00000000000324363 ) ) ;
#9036 = CARTESIAN_POINT ( 'NONE',  ( -13.38461538461550582, -11.48612834414049644, 32.76840700105863391 ) ) ;
#9037 = CARTESIAN_POINT ( 'NONE',  ( 20.00000000000000000, -3.499999999999999556, 29.75000000000000355 ) ) ;
#9038 = CARTESIAN_POINT ( 'NONE',  ( 6.000000000000001776, -9.058645607665452459, 34.76329471203371924 ) ) ;
#9039 = CARTESIAN_POINT ( 'NONE',  ( 0.7115927731767757169, -2.779044189368096607, 31.39831045268885035 ) ) ;
#9040 = EDGE_CURVE ( 'NONE', #58008, #82311, #38661, .T. ) ;
#9041 = CARTESIAN_POINT ( 'NONE',  ( -9.692307692307691624, -1.629998284177014645, 34.34916445242399163 ) ) ;
#9042 = CARTESIAN_POINT ( 'NONE',  ( -11.28840711854808632, -2.920487667080175598, 32.31805714834170828 ) ) ;
#9043 = CARTESIAN_POINT ( 'NONE',  ( 0.06109907496451268821, -3.749999999999999556, 13.15811829374151642 ) ) ;
#9044 = ORIENTED_EDGE ( 'NONE', *, *, #36731, .F. ) ;
#9045 = CARTESIAN_POINT ( 'NONE',  ( -17.07692307692319744, -10.90142922262034020, 33.41473453929536674 ) ) ;
#9046 = CARTESIAN_POINT ( 'NONE',  ( 4.153846153846030731, -11.06231777344772027, 33.60647404775119895 ) ) ;
#9047 = CARTESIAN_POINT ( 'NONE',  ( 1.799775606325937360E-14, -10.25000000000000000, 21.03125000000000000 ) ) ;
#9048 = CIRCLE ( 'NONE', #4663, 4.000000000000000000 ) ;
#9049 = ADVANCED_FACE ( 'NONE', ( #26074 ), #20207, .F. ) ;
#9050 = AXIS2_PLACEMENT_3D ( 'NONE', #75325, #14501, #62676 ) ;
#9051 = CARTESIAN_POINT ( 'NONE',  ( -13.38461538461538325, -12.37446782046654192, 30.86335684631486131 ) ) ;
#9052 = DIRECTION ( 'NONE',  ( -0.000000000000000000, 0.9396926207859092051, -0.3420201433256662704 ) ) ;
#9053 = VERTEX_POINT ( 'NONE', #47221 ) ;
#9054 = CARTESIAN_POINT ( 'NONE',  ( 0.000000000000000000, -11.00000000000000000, 29.75000000000000355 ) ) ;
#9055 = CARTESIAN_POINT ( 'NONE',  ( -5.142193522883852452, -6.879047030191174805, 34.71129190930000163 ) ) ;
#9056 = EDGE_CURVE ( 'NONE', #83747, #16683, #9624, .T. ) ;
#9057 = ORIENTED_EDGE ( 'NONE', *, *, #63446, .F. ) ;
#9058 = CARTESIAN_POINT ( 'NONE',  ( -18.24997674404859183, -4.818429247618089661, 34.26397095200675125 ) ) ;
#9059 = ORIENTED_EDGE ( 'NONE', *, *, #6924, .T. ) ;
#9060 = CARTESIAN_POINT ( 'NONE',  ( 7.173131342990376247, -4.074993327901525575, 33.72946981652012255 ) ) ;
#9061 = CARTESIAN_POINT ( 'NONE',  ( -12.46153846153846168, -2.499999999999998668, 29.50000000000001066 ) ) ;
#9062 = EDGE_CURVE ( 'NONE', #61963, #18170, #67952, .T. ) ;
#9063 = DIRECTION ( 'NONE',  ( 0.000000000000000000, 0.000000000000000000, 1.000000000000000000 ) ) ;
#9064 = DIRECTION ( 'NONE',  ( -0.000000000000000000, -0.3420201433256694346, -0.9396926207859080948 ) ) ;
#9065 = EDGE_LOOP ( 'NONE', ( #69141, #36454, #49626, #49654 ) ) ;
#9066 = CARTESIAN_POINT ( 'NONE',  ( -3.007756386675836335, -2.308499170217967134, 30.53291367094873721 ) ) ;
#9067 = EDGE_CURVE ( 'NONE', #10320, #82155, #4200, .T. ) ;
#9068 = ORIENTED_EDGE ( 'NONE', *, *, #46916, .T. ) ;
#9069 = CARTESIAN_POINT ( 'NONE',  ( 12.46153846153833911, -12.16647553114689728, 32.15551576947799362 ) ) ;
#9070 = CARTESIAN_POINT ( 'NONE',  ( 0.5923289025054103707, -9.929761469519744921, 34.40412654351204225 ) ) ;
#9071 = ORIENTED_EDGE ( 'NONE', *, *, #20346, .T. ) ;
#9072 = EDGE_CURVE ( 'NONE', #56712, #56271, #46788, .T. ) ;
#9073 = DIRECTION ( 'NONE',  ( -0.000000000000000000, 0.8660254037844397068, -0.4999999999999978906 ) ) ;
#9074 = FACE_OUTER_BOUND ( 'NONE', #45275, .T. ) ;
#9075 = LINE ( 'NONE', #8634, #10632 ) ;
#9076 = AXIS2_PLACEMENT_3D ( 'NONE', #58222, #44698, #23116 ) ;
#9077 = VECTOR ( 'NONE', #84540, 1000.000000000000227 ) ;
#9078 = DIRECTION ( 'NONE',  ( -0.000000000000000000, 0.9396926207859093161, -0.3420201433256663259 ) ) ;
#9079 = CARTESIAN_POINT ( 'NONE',  ( -3.930833309752757909, -4.026326845037961455, 33.68677907613344047 ) ) ;
#9080 = ORIENTED_EDGE ( 'NONE', *, *, #88924, .T. ) ;
#9081 = ORIENTED_EDGE ( 'NONE', *, *, #61418, .F. ) ;
#9082 = FACE_BOUND ( 'NONE', #50798, .T. ) ;
#9083 = ORIENTED_EDGE ( 'NONE', *, *, #8932, .F. ) ;
#9085 = EDGE_CURVE ( 'NONE', #37091, #14199, #72967, .T. ) ;
#9084 = FACE_OUTER_BOUND ( 'NONE', #84669, .T. ) ;
#9086 = CARTESIAN_POINT ( 'NONE',  ( 0.000000000000000000, -3.499999999999999556, 29.25000000000000000 ) ) ;
#9087 = EDGE_CURVE ( 'NONE', #37061, #67514, #79030, .T. ) ;
#9088 = CYLINDRICAL_SURFACE ( 'NONE', #1836, 0.2500000000000004996 ) ;
#9089 = PLANE ( 'NONE',  #43867 ) ;
#9090 = VERTEX_POINT ( 'NONE', #40049 ) ;
#9091 = EDGE_LOOP ( 'NONE', ( #77364, #9625 ) ) ;
#9092 = DIRECTION ( 'NONE',  ( -0.000000000000000000, -0.3420201433256694346, -0.9396926207859080948 ) ) ;
#9093 = ORIENTED_EDGE ( 'NONE', *, *, #45927, .T. ) ;
#9094 = CYLINDRICAL_SURFACE ( 'NONE', #232, 0.2499999999999986955 ) ;
#9095 = EDGE_CURVE ( 'NONE', #47058, #75513, #55718, .T. ) ;
#9096 = LINE ( 'NONE', #69457, #50235 ) ;
#9097 = CARTESIAN_POINT ( 'NONE',  ( 14.08420738312798015, -12.11044203135681840, 32.26167407432752299 ) ) ;
#9098 = EDGE_CURVE ( 'NONE', #34676, #34885, #45986, .T. ) ;
#9099 = CARTESIAN_POINT ( 'NONE',  ( -18.06608237936013239, -6.343179335718451384, 34.87096338111212646 ) ) ;
#9100 = EDGE_LOOP ( 'NONE', ( #65822, #78103 ) ) ;
#9101 = B_SPLINE_CURVE_WITH_KNOTS ( 'NONE', 3,
 ( #5595, #79920, #5149, #67299, #88921, #60084 ),
 .UNSPECIFIED., .F., .F.,
 ( 4, 2, 4 ),
 ( 0.000000000000000000, 0.0001954784845028915703, 0.0003909569690057831406 ),
 .UNSPECIFIED. ) ;
#9102 = FACE_OUTER_BOUND ( 'NONE', #75969, .T. ) ;
#9103 = ADVANCED_FACE ( 'NONE', ( #42256 ), #21524, .F. ) ;
#9104 = AXIS2_PLACEMENT_3D ( 'NONE', #63794, #35000, #43525 ) ;
#9105 = CARTESIAN_POINT ( 'NONE',  ( -14.98071481085577972, -3.435999193479609914, 33.07426656108010832 ) ) ;
#9106 = CARTESIAN_POINT ( 'NONE',  ( -17.93129618099654010, -7.749508974024934105, 34.99406763069168846 ) ) ;
#9107 = CARTESIAN_POINT ( 'NONE',  ( -9.692307692307691624, -13.37000171582298513, 34.34916445242398453 ) ) ;
#9108 = ORIENTED_EDGE ( 'NONE', *, *, #84957, .T. ) ;
#9109 = EDGE_LOOP ( 'NONE', ( #65669, #69428 ) ) ;
#9110 = VECTOR ( 'NONE', #88413, 999.9999999999998863 ) ;
#9111 = EDGE_LOOP ( 'NONE', ( #71627, #58649 ) ) ;
#9112 = ADVANCED_FACE ( 'NONE', ( #69274 ), #16869, .F. ) ;
#9114 = CARTESIAN_POINT ( 'NONE',  ( 10.86533013373275836, -6.696923467548660192, 34.68552623307873972 ) ) ;
#9113 = CARTESIAN_POINT ( 'NONE',  ( -5.999999999999998224, -2.900454961884010974, 35.62045528018868623 ) ) ;
#9115 = CARTESIAN_POINT ( 'NONE',  ( 16.15384615384603251, -6.026961402154118908, 34.52809138561165270 ) ) ;
#9116 = CARTESIAN_POINT ( 'NONE',  ( -14.30769230769230660, -12.62096338111211580, 30.90682066428153263 ) ) ;
#9117 = FACE_BOUND ( 'NONE', #55522, .T. ) ;
#9118 = CARTESIAN_POINT ( 'NONE',  ( -2.307692307692305711, -9.780366693483667717, 34.19971097300155094 ) ) ;
#9119 = EDGE_LOOP ( 'NONE', ( #51356, #83465, #3967, #15486 ) ) ;
#9120 = CARTESIAN_POINT ( 'NONE',  ( 17.29993442853592711, -10.61302985866384141, 33.66295027996417843 ) ) ;
#9121 = DIRECTION ( 'NONE',  ( -0.000000000000000000, -0.9396926207859093161, -0.3420201433256663259 ) ) ;
#9123 = CYLINDRICAL_SURFACE ( 'NONE', #63130, 0.2499999999999986955 ) ;
#9122 = B_SPLINE_CURVE_WITH_KNOTS ( 'NONE', 3,
 ( #27225, #20903, #54686, #28111, #1083, #6954, #21796, #6520, #48375, #7406 ),
 .UNSPECIFIED., .F., .F.,
 ( 4, 2, 2, 2, 4 ),
 ( 0.0007817246256747448956, 0.0009771112852218876831, 0.001172497944769030579, 0.001367884604316173475, 0.001563271263863316371 ),
 .UNSPECIFIED. ) ;
#9124 = CARTESIAN_POINT ( 'NONE',  ( 10.36538461538461675, -7.500000000000001776, 34.75000000000000000 ) ) ;
#9125 = ORIENTED_EDGE ( 'NONE', *, *, #61260, .F. ) ;
#9126 = B_SPLINE_CURVE_WITH_KNOTS ( 'NONE', 3,
 ( #18839, #5770, #81439, #19725, #82323, #74678, #20604, #61140, #5325, #46750 ),
 .UNSPECIFIED., .F., .F.,
 ( 4, 2, 2, 2, 4 ),
 ( 0.0007817359430256216575, 0.0009771253907249856981, 0.001172514838424349630, 0.001367904286123713779, 0.001563293733823077711 ),
 .UNSPECIFIED. ) ;
#9127 = DIRECTION ( 'NONE',  ( 0.000000000000000000, 0.9396926207859126468, 0.3420201433256571111 ) ) ;
#9128 = EDGE_LOOP ( 'NONE', ( #79849, #16010, #34978, #1077 ) ) ;
#9130 = FACE_BOUND ( 'NONE', #24148, .T. ) ;
#9129 = B_SPLINE_CURVE_WITH_KNOTS ( 'NONE', 3,
 ( #58193, #85684, #49239, #8703, #36180, #32960, #87479, #24858, #4596, #25758 ),
 .UNSPECIFIED., .F., .F.,
 ( 4, 2, 2, 2, 4 ),
 ( 0.0007817359430256322827, 0.0009771253907249989254, 0.001172514838424365676, 0.001367904286123732428, 0.001563293733823098962 ),
 .UNSPECIFIED. ) ;
#9131 = CARTESIAN_POINT ( 'NONE',  ( 17.99999999999987566, -3.835265460704628815, 33.15142922262033665 ) ) ;
#9132 = CARTESIAN_POINT ( 'NONE',  ( -18.00000000000000000, -2.292212530054419606, 30.41441678777542990 ) ) ;
#9133 = CARTESIAN_POINT ( 'NONE',  ( -11.53846153846153655, -8.973038597847269315, 34.52809138561121927 ) ) ;
#9134 = VERTEX_POINT ( 'NONE', #79470 ) ;
#9135 = CARTESIAN_POINT ( 'NONE',  ( 11.76147438255493149, -10.77377354290276124, 33.85451476688484718 ) ) ;
#9136 = CARTESIAN_POINT ( 'NONE',  ( -14.55771554498526932, -4.335965774309648246, 33.62209801155881905 ) ) ;
#9137 = CARTESIAN_POINT ( 'NONE',  ( -9.757578138268467427, -3.300289026998414865, 32.46337939537583139 ) ) ;
#9138 = EDGE_CURVE ( 'NONE', #19850, #81242, #82544, .T. ) ;
#9139 = LINE ( 'NONE', #23083, #74819 ) ;
#9140 = ORIENTED_EDGE ( 'NONE', *, *, #26398, .T. ) ;
#9141 = CARTESIAN_POINT ( 'NONE',  ( -9.757577692864012775, -3.083524468853724443, 32.58852847137143272 ) ) ;
#9143 = ORIENTED_EDGE ( 'NONE', *, *, #25495, .T. ) ;
#9142 = AXIS2_PLACEMENT_3D ( 'NONE', #7358, #43353, #1036 ) ;
#9146 = ORIENTED_EDGE ( 'NONE', *, *, #37247, .T. ) ;
#9145 = VECTOR ( 'NONE', #87989, 1000.000000000000227 ) ;
#9144 = DIRECTION ( 'NONE',  ( 1.000000000000000000, 0.000000000000000000, 0.000000000000000000 ) ) ;
#9147 = CARTESIAN_POINT ( 'NONE',  ( 13.38461538461538680, -9.819645486525091727, 36.12317359536749706 ) ) ;
#9148 = DIRECTION ( 'NONE',  ( -0.000000000000000000, -0.000000000000000000, -1.000000000000000000 ) ) ;
#9149 = CARTESIAN_POINT ( 'NONE',  ( 4.853438152358743096, -2.612411019501189813, 31.66733052389439962 ) ) ;
#9150 = CARTESIAN_POINT ( 'NONE',  ( -15.45364874750681849, -7.630690623152299956, 34.99857592706774057 ) ) ;
#9152 = CARTESIAN_POINT ( 'NONE',  ( 15.23076923076923173, -5.180354513474913603, 36.12317359536750416 ) ) ;
#9151 = DIRECTION ( 'NONE',  ( -1.000000000000000000, -0.000000000000000000, -0.000000000000000000 ) ) ;
#9153 = CARTESIAN_POINT ( 'NONE',  ( 6.130525701763565039, -2.882268652242224505, 31.66798894389554064 ) ) ;
#9154 = CARTESIAN_POINT ( 'NONE',  ( -1.944543648262992530, -9.444543648263016067, 22.43750000000000000 ) ) ;
#9155 = ORIENTED_EDGE ( 'NONE', *, *, #24435, .F. ) ;
#9156 = DIRECTION ( 'NONE',  ( -0.000000000000000000, -0.1736481776669307198, -0.9848077530122080203 ) ) ;
#9157 = CARTESIAN_POINT ( 'NONE',  ( 5.777073041093150785, -8.282780595021769443, 34.94152052738834868 ) ) ;
#9158 = ORIENTED_EDGE ( 'NONE', *, *, #17243, .T. ) ;
#9159 = VERTEX_POINT ( 'NONE', #76477 ) ;
#9160 = ORIENTED_EDGE ( 'NONE', *, *, #10972, .T. ) ;
#9161 = CARTESIAN_POINT ( 'NONE',  ( 4.023154687178592148, -12.11776431015576172, 31.66791131148498906 ) ) ;
#9162 = CARTESIAN_POINT ( 'NONE',  ( -17.07692307692307665, -8.973038597847269315, 34.52809138561121927 ) ) ;
#9163 = B_SPLINE_CURVE_WITH_KNOTS ( 'NONE', 3,
 ( #30219, #85160, #36957, #1854, #14936, #42413 ),
 .UNSPECIFIED., .F., .F.,
 ( 4, 2, 4 ),
 ( 3.879202041849147211E-17, 0.0001954756301637101891, 0.0003909512603273816180 ),
 .UNSPECIFIED. ) ;
#9164 = FACE_OUTER_BOUND ( 'NONE', #78650, .T. ) ;
#9165 = CARTESIAN_POINT ( 'NONE',  ( 6.000000000000001776, -2.538708090699994813, 30.37095296980875503 ) ) ;
#9166 = CARTESIAN_POINT ( 'NONE',  ( -13.38461538461538325, -6.343179335718451384, 34.87096338111211935 ) ) ;
#9167 = DIRECTION ( 'NONE',  ( -0.000000000000000000, -0.7660444431189791237, -0.6427876096865379196 ) ) ;
#9168 = CARTESIAN_POINT ( 'NONE',  ( 0.3962885297643758964, -2.255955759149247619, 30.00000000000013856 ) ) ;
#9169 = ORIENTED_EDGE ( 'NONE', *, *, #63015, .F. ) ;
#9170 = B_SPLINE_CURVE_WITH_KNOTS ( 'NONE', 3,
 ( #80711, #26634, #82032, #46459, #81585, #61286, #6375, #60412, #40601, #67625 ),
 .UNSPECIFIED., .F., .F.,
 ( 4, 2, 2, 2, 4 ),
 ( 0.0007817246256747458714, 0.0009771112852218889842, 0.001172497944769032097, 0.001367884604316175210, 0.001563271263863318323 ),
 .UNSPECIFIED. ) ;
#9171 = CARTESIAN_POINT ( 'NONE',  ( 0.000000000000000000, -11.00000000000000000, 29.75000000000000355 ) ) ;
#9172 = CARTESIAN_POINT ( 'NONE',  ( -16.82692307692164135, -7.500000000000155431, 34.75000000000007105 ) ) ;
#9173 = VECTOR ( 'NONE', #78196, 1000.000000000000000 ) ;
#9174 = ADVANCED_FACE ( 'NONE', ( #28279 ), #58742, .F. ) ;
#9175 = CARTESIAN_POINT ( 'NONE',  ( -3.230769230769229949, -5.180354513474913603, 36.12317359536750416 ) ) ;
#9176 = DIRECTION ( 'NONE',  ( -0.000000000000000000, -0.1736481776669307198, -0.9848077530122080203 ) ) ;
#9177 = CIRCLE ( 'NONE', #20670, 4.000000000000000000 ) ;
#9178 = EDGE_CURVE ( 'NONE', #67715, #56424, #34197, .T. ) ;
#9179 = AXIS2_PLACEMENT_3D ( 'NONE', #72001, #44516, #51254 ) ;
#9180 = EDGE_LOOP ( 'NONE', ( #7202, #7955, #6085, #32079 ) ) ;
#9181 = CARTESIAN_POINT ( 'NONE',  ( -17.29985003582992320, -2.523278758544490685, 31.42238647778638239 ) ) ;
#9182 = PRESENTATION_STYLE_ASSIGNMENT (( #42961 ) ) ;
#9183 = LINE ( 'NONE', #42522, #42685 ) ;
#9184 = CARTESIAN_POINT ( 'NONE',  ( 6.130525438233648927, -12.70449254468099198, 30.44128974285582956 ) ) ;
#9185 = ORIENTED_EDGE ( 'NONE', *, *, #10972, .F. ) ;
#9186 = EDGE_CURVE ( 'NONE', #85950, #4986, #27811, .T. ) ;
#9187 = CARTESIAN_POINT ( 'NONE',  ( -2.372962308248625085, -6.835583212224499938, 34.95778746994557906 ) ) ;
#9188 = CARTESIAN_POINT ( 'NONE',  ( -17.14217406708431923, -2.506253911140460477, 30.00000000000013856 ) ) ;
#9189 = ADVANCED_FACE ( 'NONE', ( #10112 ), #50645, .F. ) ;
#9190 = CARTESIAN_POINT ( 'NONE',  ( 6.923076923076924238, -12.78798330534102767, 29.49999999999997868 ) ) ;
#9191 = ORIENTED_EDGE ( 'NONE', *, *, #54470, .T. ) ;
#9192 = CARTESIAN_POINT ( 'NONE',  ( -0.5268089074992371446, -8.613356846314824011, 34.62446782046655613 ) ) ;
#9193 = ORIENTED_EDGE ( 'NONE', *, *, #4314, .F. ) ;
#9194 = EDGE_CURVE ( 'NONE', #48093, #61557, #19199, .T. ) ;
#9195 = CARTESIAN_POINT ( 'NONE',  ( 13.38461538461538680, -12.34228464037088635, 31.77849191805839268 ) ) ;
#9196 = LINE ( 'NONE', #71314, #3928 ) ;
#9197 = CARTESIAN_POINT ( 'NONE',  ( 12.21156173059610772, -8.303909089506435137, 34.68538101551103381 ) ) ;
#9198 = B_SPLINE_CURVE_WITH_KNOTS ( 'NONE', 3,
 ( #30454, #7208, #29582, #9312, #15622, #84094, #22809, #43089, #70564, #57037 ),
 .UNSPECIFIED., .F., .F.,
 ( 4, 2, 2, 2, 4 ),
 ( 0.0007817246256747470640, 0.0009771112852218896347, 0.001172497944769032314, 0.001367884604316174993, 0.001563271263863317455 ),
 .UNSPECIFIED. ) ;
#9199 = CARTESIAN_POINT ( 'NONE',  ( -14.30769230769230660, -11.69971097300155272, 32.46337939537588113 ) ) ;
#9200 = CARTESIAN_POINT ( 'NONE',  ( -3.361378885973311359, -7.722926974430166069, 34.99546784045485737 ) ) ;
#9201 = EDGE_LOOP ( 'NONE', ( #47443, #43947 ) ) ;
#9202 = VECTOR ( 'NONE', #21280, 1000.000000000000000 ) ;
#9203 = ORIENTED_EDGE ( 'NONE', *, *, #57163, .T. ) ;
#9204 = ORIENTED_EDGE ( 'NONE', *, *, #11183, .T. ) ;
#9205 = CARTESIAN_POINT ( 'NONE',  ( -6.065270445960774914, -11.48612834413959582, 32.76840700105983473 ) ) ;
#9206 = CARTESIAN_POINT ( 'NONE',  ( -16.85391172531022619, -3.587049720035815348, 32.86302985866382897 ) ) ;
#9207 = ADVANCED_FACE ( 'NONE', ( #66840 ), #31727, .F. ) ;
#9208 = CARTESIAN_POINT ( 'NONE',  ( 0.7114838709165038910, -6.653508905675592722, 34.93172785388651391 ) ) ;
#9209 = CARTESIAN_POINT ( 'NONE',  ( 0.2380535369741280383, -12.47654668319379567, 31.42292124445336654 ) ) ;
#9210 = DIRECTION ( 'NONE',  ( -0.000000000000000000, -0.5000000000000009992, -0.8660254037844380415 ) ) ;
#9211 = CARTESIAN_POINT ( 'NONE',  ( -24.99999999999999645, -15.00000000000000000, 3.000000000000000000 ) ) ;
#9212 = ORIENTED_EDGE ( 'NONE', *, *, #34213, .F. ) ;
#9213 = VERTEX_POINT ( 'NONE', #52869 ) ;
#9214 = EDGE_LOOP ( 'NONE', ( #47397, #35475, #51473, #6587 ) ) ;
#9217 = ORIENTED_EDGE ( 'NONE', *, *, #74705, .T. ) ;
#9216 = EDGE_CURVE ( 'NONE', #14730, #21791, #29895, .T. ) ;
#9215 = CARTESIAN_POINT ( 'NONE',  ( 4.376858997939548246, -4.026326845037961455, 33.68677907613344047 ) ) ;
#9219 = CARTESIAN_POINT ( 'NONE',  ( -5.207613680033385428, -12.62707690430377383, 30.88035979386743435 ) ) ;
#9218 = CARTESIAN_POINT ( 'NONE',  ( 9.019176287578908102, -8.433404298154334455, 34.66254593164985920 ) ) ;
#9220 = CARTESIAN_POINT ( 'NONE',  ( -2.651650429449565305, -4.848349570550461785, 26.50000000000000355 ) ) ;
#9221 = ORIENTED_EDGE ( 'NONE', *, *, #34560, .T. ) ;
#9222 = AXIS2_PLACEMENT_3D ( 'NONE', #77108, #49190, #76671 ) ;
#9223 = EDGE_CURVE ( 'NONE', #74234, #26718, #19102, .T. ) ;
#9224 = B_SPLINE_CURVE_WITH_KNOTS ( 'NONE', 3,
 ( #86449, #25614, #53070, #40035, #17528, #39593, #60278, #87791, #51725, #19304 ),
 .UNSPECIFIED., .F., .F.,
 ( 4, 2, 2, 2, 4 ),
 ( 0.0007817246256747465219, 0.0009771112852218900684, 0.001172497944769033615, 0.001367884604316177378, 0.001563271263863320925 ),
 .UNSPECIFIED. ) ;
#9225 = ORIENTED_EDGE ( 'NONE', *, *, #5495, .T. ) ;
#9226 = B_SPLINE_CURVE_WITH_KNOTS ( 'NONE', 3,
 ( #74462, #55072, #25838, #39800, #88015, #48309, #47871, #40244, #81671, #40688 ),
 .UNSPECIFIED., .F., .F.,
 ( 4, 2, 2, 2, 4 ),
 ( 0.000000000000000000, 0.0001954311564186863323, 0.0003908623128373726646, 0.0005862934692560590241, 0.0007817246256747453293 ),
 .UNSPECIFIED. ) ;
#9227 = CARTESIAN_POINT ( 'NONE',  ( -7.846153846153967493, -12.16647553114689728, 32.15551576947799362 ) ) ;
#9228 = AXIS2_PLACEMENT_3D ( 'NONE', #71638, #23453, #50043 ) ;
#9229 = ORIENTED_EDGE ( 'NONE', *, *, #62889, .F. ) ;
#9230 = FACE_BOUND ( 'NONE', #59012, .T. ) ;
#9231 = CARTESIAN_POINT ( 'NONE',  ( 3.361559671736182864, -2.494656445102013453, 31.33466734024120015 ) ) ;
#9232 = VECTOR ( 'NONE', #85093, 1000.000000000000227 ) ;
#9233 = FACE_OUTER_BOUND ( 'NONE', #83023, .T. ) ;
#9234 = VERTEX_POINT ( 'NONE', #79910 ) ;
#9235 = CARTESIAN_POINT ( 'NONE',  ( 16.21991450484859598, -11.16473453929635440, 33.15142922261926373 ) ) ;
#9236 = CARTESIAN_POINT ( 'NONE',  ( 5.076923076923075762, -8.164416787775445883, 34.95778746994557906 ) ) ;
#9237 = CARTESIAN_POINT ( 'NONE',  ( -20.74999999999999645, -4.499999999999999112, 27.25000000000000000 ) ) ;
#9238 = CARTESIAN_POINT ( 'NONE',  ( -24.00000000000000000, 9.000000000000024869, 29.25000000000000000 ) ) ;
#9239 = CARTESIAN_POINT ( 'NONE',  ( 1.450682717965461999, -2.486705287966280320, 31.30864560766543647 ) ) ;
#9240 = ADVANCED_FACE ( 'NONE', ( #74486 ), #88037, .F. ) ;
#9241 = CARTESIAN_POINT ( 'NONE',  ( 8.519254025182180001, -11.47974371597207899, 33.17467449705390692 ) ) ;
#9242 = CARTESIAN_POINT ( 'NONE',  ( 3.296837581771669523, -4.098570777380720287, 33.41473453929635440 ) ) ;
#9243 = CARTESIAN_POINT ( 'NONE',  ( 0.3962680155776844848, -11.94971097300153140, 32.03036669348370680 ) ) ;
#9244 = CARTESIAN_POINT ( 'NONE',  ( 19.50000000000000000, -4.000000000000000000, 28.25000000000000000 ) ) ;
#9245 = ADVANCED_FACE ( 'NONE', ( #4246 ), #32605, .F. ) ;
#9247 = ADVANCED_FACE ( 'NONE', ( #46127 ), #18213, .F. ) ;
#9246 = CARTESIAN_POINT ( 'NONE',  ( -18.24997673094235751, -6.567427716900049006, 34.66269422305636283 ) ) ;
#9248 = CARTESIAN_POINT ( 'NONE',  ( 8.899756207464413649, -4.299079248970732792, 33.91157788607253565 ) ) ;
#9250 = CARTESIAN_POINT ( 'NONE',  ( -7.384615384615385025, -7.500000000000000000, 29.75000000000000355 ) ) ;
#9249 = CARTESIAN_POINT ( 'NONE',  ( 4.284637961670940243, -12.11778462344220841, 31.66786338562085135 ) ) ;
#9251 = CARTESIAN_POINT ( 'NONE',  ( -0.2385256174450666455, -8.282913670948747864, 34.94150082978203642 ) ) ;
#9253 = PLANE ( 'NONE',  #47808 ) ;
#9252 = CARTESIAN_POINT ( 'NONE',  ( -11.40766973063674961, -11.18335022499818621, 33.13157742990016885 ) ) ;
#9254 = CARTESIAN_POINT ( 'NONE',  ( 0.4615384615384611200, -12.37446782046654192, 30.86335684631486131 ) ) ;
#9255 = CARTESIAN_POINT ( 'NONE',  ( 2.724691934501235036, -6.299813628509441266, 20.38875670625849068 ) ) ;
#9256 = EDGE_CURVE ( 'NONE', #10196, #26718, #87993, .T. ) ;
#9257 = ORIENTED_EDGE ( 'NONE', *, *, #51248, .T. ) ;
#9258 = CARTESIAN_POINT ( 'NONE',  ( 3.271582784339720273, -7.991356743646568006, 14.00000000000000533 ) ) ;
#9259 = EDGE_LOOP ( 'NONE', ( #42412, #73949 ) ) ;
#9260 = DIRECTION ( 'NONE',  ( -0.000000000000000000, 0.1736481776669307198, -0.9848077530122080203 ) ) ;
#9261 = ORIENTED_EDGE ( 'NONE', *, *, #58675, .T. ) ;
#9262 = DIRECTION ( 'NONE',  ( -0.000000000000000000, 1.000000000000000000, -0.000000000000000000 ) ) ;
#9263 = ORIENTED_EDGE ( 'NONE', *, *, #8452, .F. ) ;
#9264 = CARTESIAN_POINT ( 'NONE',  ( -16.15384615384615330, -1.367168528481310208, 33.57946703557072254 ) ) ;
#9265 = CARTESIAN_POINT ( 'NONE',  ( 1.987747218494664292, -9.401340078031346081, 25.62313170625849068 ) ) ;
#9266 = CARTESIAN_POINT ( 'NONE',  ( 7.846153846153723244, -8.656820664282941280, 34.87096338111179961 ) ) ;
#9267 = CARTESIAN_POINT ( 'NONE',  ( -3.165514091256390827, -12.51329471203373700, 31.30864560766537963 ) ) ;
#9268 = CARTESIAN_POINT ( 'NONE',  ( 17.74997677577853850, -2.341070481393820124, 30.72580821765574299 ) ) ;
#9269 = VECTOR ( 'NONE', #55187, 1000.000000000000000 ) ;
#9270 = DIRECTION ( 'NONE',  ( -0.000000000000000000, -1.000000000000000000, -8.673617379884033500E-16 ) ) ;
#9271 = CARTESIAN_POINT ( 'NONE',  ( 1.161130460051055024, -4.988325925672468131, 34.36044203135681130 ) ) ;
#9272 = DIRECTION ( 'NONE',  ( 0.000000000000000000, 0.3420201433256610524, 0.9396926207859113145 ) ) ;
#9273 = CARTESIAN_POINT ( 'NONE',  ( -3.749999999999988454, -9.053300858899127945, 16.26562500000000000 ) ) ;
#9274 = CARTESIAN_POINT ( 'NONE',  ( 18.06525513951283202, -11.67786785259547777, 32.92929555188713664 ) ) ;
#9275 = LINE ( 'NONE', #79051, #76492 ) ;
#9276 = CARTESIAN_POINT ( 'NONE',  ( 13.60739492588379562, -4.387253974876679230, 33.66317474335728832 ) ) ;
#9277 = CARTESIAN_POINT ( 'NONE',  ( -1.929879867024197893E-14, -3.750000000000000000, 16.65625000000000000 ) ) ;
#9278 = EDGE_CURVE ( 'NONE', #9598, #57919, #11906, .T. ) ;
#9279 = CARTESIAN_POINT ( 'NONE',  ( -14.05763799605399278, -10.66356715214248396, 33.62249196103329751 ) ) ;
#9280 = ORIENTED_EDGE ( 'NONE', *, *, #43658, .T. ) ;
#9281 = CYLINDRICAL_SURFACE ( 'NONE', #34258, 0.2499999999999995559 ) ;
#9282 = CYLINDRICAL_SURFACE ( 'NONE', #44511, 0.2499999999999986955 ) ;
#9283 = DIRECTION ( 'NONE',  ( -0.000000000000000000, 0.9848077530122086864, -0.1736481776669273891 ) ) ;
#9284 = LINE ( 'NONE', #44819, #15362 ) ;
#9285 = CARTESIAN_POINT ( 'NONE',  ( -1.608100328339332474, -10.81261337010820256, 33.49550067578627477 ) ) ;
#9286 = DIRECTION ( 'NONE',  ( -1.000000000000000000, -0.000000000000000000, -0.000000000000000000 ) ) ;
#9287 = EDGE_CURVE ( 'NONE', #52855, #86735, #59633, .T. ) ;
#9289 = DIRECTION ( 'NONE',  ( -0.000000000000000000, -0.1736481776669307198, -0.9848077530122080203 ) ) ;
#9288 = B_SPLINE_CURVE_WITH_KNOTS ( 'NONE', 3,
 ( #40723, #27635, #55107, #82600, #55991, #6047 ),
 .UNSPECIFIED., .F., .F.,
 ( 4, 2, 4 ),
 ( 4.336808689942017736E-19, 0.0001954784845028939555, 0.0003909569690057874774 ),
 .UNSPECIFIED. ) ;
#9290 = B_SPLINE_CURVE_WITH_KNOTS ( 'NONE', 3,
 ( #50712, #51142, #86763, #2974, #11528, #11079, #72767, #4317, #51587, #30453 ),
 .UNSPECIFIED., .F., .F.,
 ( 4, 2, 2, 2, 4 ),
 ( 0.000000000000000000, 0.0001954311564186871184, 0.0003908623128373742367, 0.0005862934692560614093, 0.0007817246256747484735 ),
 .UNSPECIFIED. ) ;
#9291 = VECTOR ( 'NONE', #89110, 1000.000000000000000 ) ;
#9292 = ORIENTED_EDGE ( 'NONE', *, *, #46342, .T. ) ;
#9293 = EDGE_LOOP ( 'NONE', ( #82227, #30318 ) ) ;
#9294 = EDGE_CURVE ( 'NONE', #63541, #69885, #63221, .T. ) ;
#9295 = AXIS2_PLACEMENT_3D ( 'NONE', #48942, #39993, #61567 ) ;
#9296 = ORIENTED_EDGE ( 'NONE', *, *, #65655, .T. ) ;
#9297 = LINE ( 'NONE', #38088, #67346 ) ;
#9298 = CARTESIAN_POINT ( 'NONE',  ( 16.40384615384759215, -7.500000000000155431, 34.75000000000007105 ) ) ;
#9299 = CARTESIAN_POINT ( 'NONE',  ( 1.515407192440173079, -11.71459661697925903, 32.44059661609676937 ) ) ;
#9300 = CARTESIAN_POINT ( 'NONE',  ( 17.93391762063986050, -9.058645607665454236, 34.76329471203372634 ) ) ;
#9302 = EDGE_CURVE ( 'NONE', #54584, #87771, #71843, .T. ) ;
#9301 = VERTEX_POINT ( 'NONE', #5583 ) ;
#9303 = FACE_OUTER_BOUND ( 'NONE', #22132, .T. ) ;
#9304 = VERTEX_POINT ( 'NONE', #155 ) ;
#9305 = ORIENTED_EDGE ( 'NONE', *, *, #53256, .F. ) ;
#9306 = DIRECTION ( 'NONE',  ( -0.000000000000000000, 0.8660254037844397068, -0.4999999999999978906 ) ) ;
#9307 = CARTESIAN_POINT ( 'NONE',  ( 8.638539302563215116, -2.729777683071817229, 31.24903638046269450 ) ) ;
#9308 = EDGE_CURVE ( 'NONE', #28968, #20065, #73920, .T. ) ;
#9309 = CARTESIAN_POINT ( 'NONE',  ( -14.30769230769230660, -7.500000000000001776, 35.04278698407183867 ) ) ;
#9310 = CARTESIAN_POINT ( 'NONE',  ( -3.165513659493205623, -4.481592998940250538, 33.73612834413965089 ) ) ;
#9311 = ADVANCED_FACE ( 'NONE', ( #75374 ), #69939, .F. ) ;
#9312 = CARTESIAN_POINT ( 'NONE',  ( -15.93106648486808119, -5.827830569534415694, 34.72679350104403539 ) ) ;
#9313 = ORIENTED_EDGE ( 'NONE', *, *, #56372, .F. ) ;
#9314 = ORIENTED_EDGE ( 'NONE', *, *, #48626, .F. ) ;
#9315 = CARTESIAN_POINT ( 'NONE',  ( 3.749999999999992006, -5.946699141100872943, 21.89062500000000355 ) ) ;
#9316 = B_SPLINE_CURVE_WITH_KNOTS ( 'NONE', 3,
 ( #44797, #38056, #80390, #3821, #80840, #18687, #32629, #11930, #5161, #25878 ),
 .UNSPECIFIED., .F., .F.,
 ( 4, 2, 2, 2, 4 ),
 ( 0.0007817359430256361858, 0.0009771253907250041296, 0.001172514838424372182, 0.001367904286123740234, 0.001563293733823108286 ),
 .UNSPECIFIED. ) ;
#9317 = ORIENTED_EDGE ( 'NONE', *, *, #8794, .F. ) ;
#9319 = ORIENTED_EDGE ( 'NONE', *, *, #18067, .F. ) ;
#9318 = CARTESIAN_POINT ( 'NONE',  ( 4.284637961670941131, -11.18335022499818621, 33.13157742990016885 ) ) ;
#9320 = CARTESIAN_POINT ( 'NONE',  ( -7.146561866800870355, -12.44517049084099725, 30.48991314939691932 ) ) ;
#9321 = LINE ( 'NONE', #49845, #66202 ) ;
#9322 = CARTESIAN_POINT ( 'NONE',  ( 7.173022441425066731, -11.86320923018887541, 32.19269448109604781 ) ) ;
#9323 = EDGE_LOOP ( 'NONE', ( #79209, #45554 ) ) ;
#9324 = EDGE_CURVE ( 'NONE', #38200, #69999, #20864, .T. ) ;
#9325 = EDGE_CURVE ( 'NONE', #61773, #20358, #69497, .T. ) ;
#9326 = CARTESIAN_POINT ( 'NONE',  ( 15.23076923076911093, -10.90142922262034020, 33.41473453929536674 ) ) ;
#9327 = CARTESIAN_POINT ( 'NONE',  ( 14.98074600654777200, -2.588893531581426988, 31.60682220781847818 ) ) ;
#9328 = EDGE_LOOP ( 'NONE', ( #60045, #3948, #71017, #78144 ) ) ;
#9329 = FACE_BOUND ( 'NONE', #17510, .T. ) ;
#9330 = CARTESIAN_POINT ( 'NONE',  ( -11.53846153846166089, -11.67786785259630911, 32.92929555188603530 ) ) ;
#9331 = LINE ( 'NONE', #64244, #34289 ) ;
#9332 = CARTESIAN_POINT ( 'NONE',  ( 5.448717948717947124, -7.500000000000000000, 33.75000000000000000 ) ) ;
#9334 = CARTESIAN_POINT ( 'NONE',  ( -1.384615384615505151, -6.026961402154118908, 34.52809138561165270 ) ) ;
#9333 = CARTESIAN_POINT ( 'NONE',  ( -16.09615384615384670, -11.50000000000000000, 29.75000000000000355 ) ) ;
#9335 = CARTESIAN_POINT ( 'NONE',  ( 4.853438133199127869, -2.599994579823202923, 30.74605699353653776 ) ) ;
#9336 = CARTESIAN_POINT ( 'NONE',  ( -15.90379184220783948, -9.148310452688871663, 34.47095581063188519 ) ) ;
#9337 = VERTEX_POINT ( 'NONE', #62286 ) ;
#9338 = CARTESIAN_POINT ( 'NONE',  ( -11.28851602011339672, -4.336752205174649433, 33.62275283266504289 ) ) ;
#9340 = ORIENTED_EDGE ( 'NONE', *, *, #53723, .F. ) ;
#9339 = EDGE_CURVE ( 'NONE', #47459, #60558, #35313, .T. ) ;
#9341 = CARTESIAN_POINT ( 'NONE',  ( 6.988332494352946789, -2.892918686051625166, 31.69288490824025928 ) ) ;
#9342 = CARTESIAN_POINT ( 'NONE',  ( 17.01165307636676260, -11.06231777344662959, 33.60647404775220082 ) ) ;
#9343 = CYLINDRICAL_SURFACE ( 'NONE', #6576, 0.2500000000000002220 ) ;
#9344 = CARTESIAN_POINT ( 'NONE',  ( -7.623141002060451754, -10.77377354290276301, 33.85451476688484718 ) ) ;
#9345 = CARTESIAN_POINT ( 'NONE',  ( 18.00000000000000000, -1.117168528481311540, 33.14645433367849847 ) ) ;
#9346 = EDGE_CURVE ( 'NONE', #5967, #60430, #80464, .T. ) ;
#9348 = EDGE_CURVE ( 'NONE', #80176, #84519, #54597, .T. ) ;
#9347 = CARTESIAN_POINT ( 'NONE',  ( -2.544871794871794268, -7.500000000000000000, 33.75000000000000000 ) ) ;
#9349 = VECTOR ( 'NONE', #27491, 1000.000000000000000 ) ;
#9350 = FACE_BOUND ( 'NONE', #23606, .T. ) ;
#9352 = CYLINDRICAL_SURFACE ( 'NONE', #74764, 0.2499999999999995559 ) ;
#9351 = CARTESIAN_POINT ( 'NONE',  ( -1.607542343522232464, -6.459968553980839800, 34.89616026154728701 ) ) ;
#9353 = CARTESIAN_POINT ( 'NONE',  ( -18.24997674404858827, -8.347322224742352859, 34.93158281831414058 ) ) ;
#9355 = CARTESIAN_POINT ( 'NONE',  ( 20.00000000000000000, -4.000000000000000000, 29.75000000000000355 ) ) ;
#9354 = CARTESIAN_POINT ( 'NONE',  ( -3.230769230769229949, -1.466349020453238561, 30.81389545987213907 ) ) ;
#9356 = CARTESIAN_POINT ( 'NONE',  ( -3.230769230769229949, -11.11383981884818262, 36.00935417666054406 ) ) ;
#9357 = CARTESIAN_POINT ( 'NONE',  ( -2.694853999681210865, -4.891553140782108677, 21.24813170625848713 ) ) ;
#9358 = EDGE_LOOP ( 'NONE', ( #23435, #40477 ) ) ;
#9359 = AXIS2_PLACEMENT_3D ( 'NONE', #6373, #12231, #6796 ) ;
#9360 = CARTESIAN_POINT ( 'NONE',  ( -4.219116599806927326, -11.94971097300153140, 32.03036669348370680 ) ) ;
#9361 = B_SPLINE_CURVE_WITH_KNOTS ( 'NONE', 3,
 ( #75923, #41257, #62828, #56093, #41695, #27292, #42588, #70047, #82694, #21422 ),
 .UNSPECIFIED., .F., .F.,
 ( 4, 2, 2, 2, 4 ),
 ( 0.0007817246256747448956, 0.0009771112852218876831, 0.001172497944769030579, 0.001367884604316173475, 0.001563271263863316371 ),
 .UNSPECIFIED. ) ;
#9362 = CYLINDRICAL_SURFACE ( 'NONE', #45516, 0.2500000000000008882 ) ;
#9363 = CARTESIAN_POINT ( 'NONE',  ( -9.626239341305254271, -8.973038597847271092, 34.52809138561121216 ) ) ;
#9364 = CARTESIAN_POINT ( 'NONE',  ( -0.08744816603778379771, -10.24999508951804650, 28.75002700765198327 ) ) ;
#9365 = CARTESIAN_POINT ( 'NONE',  ( -4.376773112753001627, -4.762599654559228846, 34.23009711892697737 ) ) ;
#9366 = CARTESIAN_POINT ( 'NONE',  ( -3.749999999999996447, -7.561099074964554134, 21.09188170625849068 ) ) ;
#9367 = CARTESIAN_POINT ( 'NONE',  ( -2.307692307692305711, -3.322132147404559976, 32.92929555188717927 ) ) ;
#9368 = CARTESIAN_POINT ( 'NONE',  ( -8.769230769230768274, -6.386643153685126251, 34.62446782046654192 ) ) ;
#9369 = CARTESIAN_POINT ( 'NONE',  ( -16.85414353565466072, -5.913360116392398780, 34.49180327182771322 ) ) ;
#9370 = CARTESIAN_POINT ( 'NONE',  ( -11.53846153846153655, -9.584722331328613620, 36.20867863119891439 ) ) ;
#9371 = CARTESIAN_POINT ( 'NONE',  ( 2.557692307692308376, -2.249999999999998668, 29.75000000000000355 ) ) ;
#9372 = CARTESIAN_POINT ( 'NONE',  ( 4.023698944407932743, -10.88202310037935661, 33.43294751532457099 ) ) ;
#9373 = DIRECTION ( 'NONE',  ( -0.000000000000000000, 1.000000000000000000, -0.000000000000000000 ) ) ;
#9374 = CARTESIAN_POINT ( 'NONE',  ( 8.068933387422251968, -6.760870238392817200, 34.69528174975672385 ) ) ;
#9375 = VERTEX_POINT ( 'NONE', #63176 ) ;
#9376 = CARTESIAN_POINT ( 'NONE',  ( 7.846153846153846700, -13.04860791097971706, 34.73218667398347037 ) ) ;
#9377 = CARTESIAN_POINT ( 'NONE',  ( 7.145856464345331283, -5.114059244376869984, 34.14424750095245287 ) ) ;
#9378 = CARTESIAN_POINT ( 'NONE',  ( 3.750000000000001776, -7.561099074964511502, 14.72061829374151465 ) ) ;
#9379 = CYLINDRICAL_SURFACE ( 'NONE', #70605, 0.2500000000000012212 ) ;
#9380 = DIRECTION ( 'NONE',  ( -0.000000000000000000, 0.3420201433256694346, -0.9396926207859080948 ) ) ;
#9381 = ORIENTED_EDGE ( 'NONE', *, *, #7602, .F. ) ;
#9382 = CARTESIAN_POINT ( 'NONE',  ( -16.40386937806761125, -4.175268141568689195, 33.81360843649122216 ) ) ;
#9384 = EDGE_LOOP ( 'NONE', ( #169, #86856, #59499, #76673 ) ) ;
#9383 = CARTESIAN_POINT ( 'NONE',  ( 7.596177115211490083, -2.564618984488975961, 30.55390908950641915 ) ) ;
#9385 = DIRECTION ( 'NONE',  ( -0.000000000000000000, 0.8660254037844399289, -0.4999999999999980016 ) ) ;
#9386 = CARTESIAN_POINT ( 'NONE',  ( 3.930919936330006248, -8.239355502252617924, 34.69524867566427417 ) ) ;
#9387 = FACE_OUTER_BOUND ( 'NONE', #19600, .T. ) ;
#9388 = AXIS2_PLACEMENT_3D ( 'NONE', #60419, #19437, #26196 ) ;
#9389 = CARTESIAN_POINT ( 'NONE',  ( -15.29601916254331329, -2.255955759149247619, 30.00000000000013856 ) ) ;
#9390 = ORIENTED_EDGE ( 'NONE', *, *, #12535, .F. ) ;
#9391 = LINE ( 'NONE', #44479, #86633 ) ;
#9392 = CARTESIAN_POINT ( 'NONE',  ( 5.142116065217731347, -2.255955759149235629, 29.99999999999988631 ) ) ;
#9393 = B_SPLINE_CURVE_WITH_KNOTS ( 'NONE', 3,
 ( #80842, #10142, #37606, #79041, #52002, #11932, #44799, #58768, #73640, #73182 ),
 .UNSPECIFIED., .F., .F.,
 ( 4, 2, 2, 2, 4 ),
 ( 0.000000000000000000, 0.0001954311564186879044, 0.0003908623128373758088, 0.0005862934692560636861, 0.0007817246256747516176 ),
 .UNSPECIFIED. ) ;
#9394 = CARTESIAN_POINT ( 'NONE',  ( 12.59232890250541281, -11.93129842949671726, 32.56571108434900452 ) ) ;
#9395 = EDGE_LOOP ( 'NONE', ( #75224, #42056, #47172, #55235, #42415 ) ) ;
#9396 = ORIENTED_EDGE ( 'NONE', *, *, #65193, .F. ) ;
#9397 = B_SPLINE_CURVE_WITH_KNOTS ( 'NONE', 3,
 ( #16254, #43719, #56356, #64419, #22128, #2719, #77074, #15379, #10832, #18037 ),
 .UNSPECIFIED., .F., .F.,
 ( 4, 2, 2, 2, 4 ),
 ( 0.000000000000000000, 0.0001954311564186868744, 0.0003908623128373737488, 0.0005862934692560606504, 0.0007817246256747474977 ),
 .UNSPECIFIED. ) ;
#9398 = ORIENTED_EDGE ( 'NONE', *, *, #18684, .T. ) ;
#9399 = CARTESIAN_POINT ( 'NONE',  ( -17.07692307692307665, -8.973038597847269315, 34.52809138561121927 ) ) ;
#9400 = PLANE ( 'NONE',  #74565 ) ;
#9401 = CARTESIAN_POINT ( 'NONE',  ( -7.715315428141081178, -7.277220443632450575, 34.74524770363008486 ) ) ;
#9402 = CARTESIAN_POINT ( 'NONE',  ( 15.48076923076923173, -2.499999999999998668, 29.75000000000000355 ) ) ;
#9403 = AXIS2_PLACEMENT_3D ( 'NONE', #3566, #31035, #25182 ) ;
#9404 = ORIENTED_EDGE ( 'NONE', *, *, #21500, .T. ) ;
#9405 = EDGE_LOOP ( 'NONE', ( #51700, #32936 ) ) ;
#9407 = ORIENTED_EDGE ( 'NONE', *, *, #42263, .T. ) ;
#9406 = CARTESIAN_POINT ( 'NONE',  ( 12.46153846153846168, -1.117168528481311540, 33.14645433367849847 ) ) ;
#9408 = CARTESIAN_POINT ( 'NONE',  ( 17.20744877868664346, -5.195472089885680766, 34.18748526763464923 ) ) ;
#9409 = EDGE_CURVE ( 'NONE', #72081, #86292, #54640, .T. ) ;
#9410 = CARTESIAN_POINT ( 'NONE',  ( -17.77698864838715309, -3.105924265160264319, 32.13625925475356127 ) ) ;
#9411 = CARTESIAN_POINT ( 'NONE',  ( -7.976844449264155479, -9.929715669179220328, 34.40415004197138416 ) ) ;
#9413 = EDGE_LOOP ( 'NONE', ( #37798, #35222, #86346, #41951, #17194 ) ) ;
#9412 = PRODUCT_RELATED_PRODUCT_CATEGORY ( 'part', '', ( #7424 ) ) ;
#9414 = ORIENTED_EDGE ( 'NONE', *, *, #57036, .F. ) ;
#9416 = ORIENTED_EDGE ( 'NONE', *, *, #20713, .T. ) ;
#9415 = CARTESIAN_POINT ( 'NONE',  ( -6.673131404728780858, -11.37275283266503756, 32.91324779482534524 ) ) ;
#9417 = CARTESIAN_POINT ( 'NONE',  ( -0.5922299282060183856, -10.54014554554150607, 33.71984207302941883 ) ) ;
#9418 = CARTESIAN_POINT ( 'NONE',  ( -5.299849294439224145, -9.886141570436013382, 34.14413921362392301 ) ) ;
#9419 = ORIENTED_EDGE ( 'NONE', *, *, #14407, .F. ) ;
#9420 = ADVANCED_FACE ( 'NONE', ( #49231 ), #13668, .F. ) ;
#9421 = CARTESIAN_POINT ( 'NONE',  ( 15.16549923021291058, -2.379036618887870436, 30.90682066428147934 ) ) ;
#9422 = PLANE ( 'NONE',  #46519 ) ;
#9423 = DIRECTION ( 'NONE',  ( -0.000000000000000000, 0.6427876096865404731, -0.7660444431189771253 ) ) ;
#9424 = FACE_BOUND ( 'NONE', #21190, .T. ) ;
#9425 = CARTESIAN_POINT ( 'NONE',  ( 1.384615384615265343, -12.46129190930018460, 30.37095296980731973 ) ) ;
#9426 = CARTESIAN_POINT ( 'NONE',  ( -4.403869391139119571, -12.22074536777954989, 31.39888409691088356 ) ) ;
#9427 = CARTESIAN_POINT ( 'NONE',  ( 8.638539302563209787, -2.541943142973491554, 30.39792223712631980 ) ) ;
#9429 = CARTESIAN_POINT ( 'NONE',  ( -13.91025641025641058, -3.499999999999999556, 29.75000000000000355 ) ) ;
#9428 = CARTESIAN_POINT ( 'NONE',  ( -0.2385256174450665345, -2.889357225399415086, 32.26129605718031712 ) ) ;
#9430 = AXIS2_PLACEMENT_3D ( 'NONE', #14458, #36070, #68952 ) ;
#9431 = DIRECTION ( 'NONE',  ( 1.000000000000000000, 0.000000000000000000, 0.000000000000000000 ) ) ;
#9432 = CARTESIAN_POINT ( 'NONE',  ( -16.28453675695646652, -2.494641256782729855, 31.33461815524612959 ) ) ;
#9433 = VERTEX_POINT ( 'NONE', #10006 ) ;
#9434 = CARTESIAN_POINT ( 'NONE',  ( -16.08777882049607655, -3.322132147404559532, 32.92929555188717927 ) ) ;
#9435 = ORIENTED_EDGE ( 'NONE', *, *, #24038, .F. ) ;
#9436 = ORIENTED_EDGE ( 'NONE', *, *, #71167, .F. ) ;
#9437 = VECTOR ( 'NONE', #74971, 1000.000000000000000 ) ;
#9439 = DIRECTION ( 'NONE',  ( -0.000000000000000000, -0.5000000000000009992, -0.8660254037844380415 ) ) ;
#9438 = DIRECTION ( 'NONE',  ( 0.000000000000000000, 0.000000000000000000, 1.000000000000000000 ) ) ;
#9440 = CARTESIAN_POINT ( 'NONE',  ( 13.16113046005105858, -11.60425143139329940, 33.02411095842164457 ) ) ;
#9441 = CARTESIAN_POINT ( 'NONE',  ( 20.74999999999999645, -10.50000000000000000, 27.25000000000000000 ) ) ;
#9442 = DIRECTION ( 'NONE',  ( -0.000000000000000000, -0.000000000000000000, -1.000000000000000000 ) ) ;
#9443 = CARTESIAN_POINT ( 'NONE',  ( 14.30769230769218581, -11.67786785259630911, 32.92929555188603530 ) ) ;
#9444 = ORIENTED_EDGE ( 'NONE', *, *, #7212, .F. ) ;
#9445 = EDGE_CURVE ( 'NONE', #39542, #17339, #67550, .T. ) ;
#9446 = DIRECTION ( 'NONE',  ( 0.000000000000000000, 0.000000000000000000, 1.000000000000000000 ) ) ;
#9447 = CARTESIAN_POINT ( 'NONE',  ( 6.923076923076924238, -3.513871655860378418, 32.76840700105978499 ) ) ;
#9448 = LINE ( 'NONE', #42363, #40214 ) ;
#9449 = CARTESIAN_POINT ( 'NONE',  ( -17.07692307692307665, -10.51840700105979565, 33.73612834413961536 ) ) ;
#9450 = CARTESIAN_POINT ( 'NONE',  ( 12.46153846153846168, -12.78798330534102945, 29.74999999999997868 ) ) ;
#9451 = CARTESIAN_POINT ( 'NONE',  ( 2.651650429449569302, -10.15165042944953733, 14.62500000000000000 ) ) ;
#9452 = ORIENTED_EDGE ( 'NONE', *, *, #85914, .F. ) ;
#9453 = EDGE_LOOP ( 'NONE', ( #58901, #45691 ) ) ;
#9454 = EDGE_CURVE ( 'NONE', #81222, #85470, #45970, .T. ) ;
#9455 = CARTESIAN_POINT ( 'NONE',  ( 14.08420738312797482, -12.47654668319379567, 31.42292124445336654 ) ) ;
#9456 = EDGE_LOOP ( 'NONE', ( #8894, #28406, #50049, #88518, #36283 ) ) ;
#9457 = CARTESIAN_POINT ( 'NONE',  ( -7.173100160369888734, -2.587272538249754117, 30.68239716806877837 ) ) ;
#9458 = CARTESIAN_POINT ( 'NONE',  ( 18.00000000000000000, -5.557115091759785130, 34.35708131394839171 ) ) ;
#9459 = CARTESIAN_POINT ( 'NONE',  ( 5.198717948717946236, -3.499999999999999556, 29.75000000000000355 ) ) ;
#9460 = CARTESIAN_POINT ( 'NONE',  ( -8.638705067467205012, -10.88167719472716399, 33.43325721877153711 ) ) ;
#9461 = CARTESIAN_POINT ( 'NONE',  ( 2.651650429449539104, -4.848349570550432475, 15.56250000000000000 ) ) ;
#9462 = CARTESIAN_POINT ( 'NONE',  ( 0.7114838709165042241, -9.357781135181031829, 34.66075350412533851 ) ) ;
#9463 = EDGE_LOOP ( 'NONE', ( #83758, #87340, #11262, #51150 ) ) ;
#9464 = CARTESIAN_POINT ( 'NONE',  ( 4.377273115707725815, -7.630147231320743018, 34.74852402298682819 ) ) ;
#9466 = ORIENTED_EDGE ( 'NONE', *, *, #20584, .F. ) ;
#9465 = CARTESIAN_POINT ( 'NONE',  ( -2.176901866725356349, -12.62708834333097663, 30.88030960425257021 ) ) ;
#9467 = DIRECTION ( 'NONE',  ( 0.000000000000000000, 0.000000000000000000, 1.000000000000000000 ) ) ;
#9468 = DIRECTION ( 'NONE',  ( 0.000000000000000000, 0.6427876096865368094, 0.7660444431189802339 ) ) ;
#9469 = CARTESIAN_POINT ( 'NONE',  ( -3.453695448285377001, -4.887634598454295265, 34.01352882383564946 ) ) ;
#9470 = CARTESIAN_POINT ( 'NONE',  ( 11.78840694783958298, -8.476813868363244353, 34.90874843262270133 ) ) ;
#9471 = CARTESIAN_POINT ( 'NONE',  ( -3.361244415844949263, -7.276987145209184327, 34.99546412871779211 ) ) ;
#9472 = CARTESIAN_POINT ( 'NONE',  ( -7.146561866800870355, -5.113361153441932316, 34.14387501736621999 ) ) ;
#9473 = CARTESIAN_POINT ( 'NONE',  ( -1.987747218494638313, -9.401340078031370950, 23.93936829374151642 ) ) ;
#9474 = ORIENTED_EDGE ( 'NONE', *, *, #29009, .T. ) ;
#9475 = CARTESIAN_POINT ( 'NONE',  ( -12.52686247434276900, -7.749976730030849303, 34.74374725381503737 ) ) ;
#9476 = DIRECTION ( 'NONE',  ( -0.000000000000000000, -0.6427876096865404731, -0.7660444431189770143 ) ) ;
#9477 = CARTESIAN_POINT ( 'NONE',  ( -2.749999999999998224, -7.500000000000015987, 26.34375000000000000 ) ) ;
#9478 = CARTESIAN_POINT ( 'NONE',  ( 0.4615384615383396616, -3.835265460704628371, 33.15142922262033665 ) ) ;
#9479 = CARTESIAN_POINT ( 'NONE',  ( 9.692307692307695177, -6.343179335718451384, 34.87096338111211935 ) ) ;
#9480 = EDGE_LOOP ( 'NONE', ( #36003, #61646, #82215, #45761 ) ) ;
#9481 = DIRECTION ( 'NONE',  ( 0.000000000000000000, 0.6427876096865373645, -0.7660444431189797898 ) ) ;
#9482 = CARTESIAN_POINT ( 'NONE',  ( 3.100622021331010725, -9.418419913701741919, 34.36755862841477693 ) ) ;
#9483 = VECTOR ( 'NONE', #20190, 1000.000000000000000 ) ;
#9484 = ORIENTED_EDGE ( 'NONE', *, *, #40138, .F. ) ;
#9485 = CARTESIAN_POINT ( 'NONE',  ( -4.219116154402471786, -8.656820664281497102, 34.87096338111211935 ) ) ;
#9486 = VERTEX_POINT ( 'NONE', #51404 ) ;
#9487 = CARTESIAN_POINT ( 'NONE',  ( -5.198717948717946236, -4.000000000000000000, 29.75000000000000355 ) ) ;
#9488 = CARTESIAN_POINT ( 'NONE',  ( 4.023698944407931855, -3.817052484675422797, 33.13202310037935661 ) ) ;
#9489 = CARTESIAN_POINT ( 'NONE',  ( -12.52762084089859407, -9.905515769479276145, 34.41647553114623292 ) ) ;
#9490 = DIRECTION ( 'NONE',  ( 1.000000000000000000, 0.000000000000000000, 0.000000000000000000 ) ) ;
#9491 = VERTEX_POINT ( 'NONE', #44663 ) ;
#9492 = CARTESIAN_POINT ( 'NONE',  ( -6.857009589726848375, -6.343179335718452272, 34.87096338111212646 ) ) ;
#9493 = ORIENTED_EDGE ( 'NONE', *, *, #84815, .T. ) ;
#9494 = CARTESIAN_POINT ( 'NONE',  ( -1.384615384615506484, -11.67786785259630911, 32.92929555188603530 ) ) ;
#9495 = CARTESIAN_POINT ( 'NONE',  ( -4.219602956360462009, -7.249945686854186278, 34.74374336980224598 ) ) ;
#9496 = EDGE_LOOP ( 'NONE', ( #55832, #16505 ) ) ;
#9497 = CARTESIAN_POINT ( 'NONE',  ( -5.869208192175211281, -11.18335022499818621, 33.13157742990016885 ) ) ;
#9498 = CARTESIAN_POINT ( 'NONE',  ( 10.61538461538461675, -3.050289026998446396, 32.03036669348365706 ) ) ;
#9499 = CARTESIAN_POINT ( 'NONE',  ( -3.903846153846152855, -2.499999999999998668, 29.75000000000000355 ) ) ;
#9500 = ADVANCED_FACE ( 'NONE', ( #30286 ), #29846, .F. ) ;
#9501 = CARTESIAN_POINT ( 'NONE',  ( -11.31544869436814160, -5.582272713120729257, 34.63742843783360570 ) ) ;
#9502 = DIRECTION ( 'NONE',  ( 0.000000000000000000, -6.938893903907222067E-15, 1.000000000000000000 ) ) ;
#9503 = ORIENTED_EDGE ( 'NONE', *, *, #88754, .T. ) ;
#9504 = ORIENTED_EDGE ( 'NONE', *, *, #23915, .T. ) ;
#9505 = FACE_BOUND ( 'NONE', #45109, .T. ) ;
#9506 = ORIENTED_EDGE ( 'NONE', *, *, #18954, .T. ) ;
#9507 = CARTESIAN_POINT ( 'NONE',  ( -7.846153846153844924, -5.471508081941601098, 34.59228464037088457 ) ) ;
#9508 = B_SPLINE_CURVE_WITH_KNOTS ( 'NONE', 3,
 ( #83220, #48085, #6236, #49429, #48525, #21504, #76903, #82782, #6664, #62051 ),
 .UNSPECIFIED., .F., .F.,
 ( 4, 2, 2, 2, 4 ),
 ( 0.000000000000000000, 0.0001954339857564058210, 0.0003908679715128116419, 0.0005863019572692174629, 0.0007817359430256232838 ),
 .UNSPECIFIED. ) ;
#9509 = ADVANCED_FACE ( 'NONE', ( #36172 ), #44216, .F. ) ;
#9510 = CARTESIAN_POINT ( 'NONE',  ( 13.60739492588379385, -10.81320215134717344, 33.49497208177562868 ) ) ;
#9511 = CARTESIAN_POINT ( 'NONE',  ( -14.08491276642389423, -9.332535724633409302, 34.40230450496446934 ) ) ;
#9512 = B_SPLINE_CURVE_WITH_KNOTS ( 'NONE', 3,
 ( #6296, #12163, #73419, #39646, #13045, #73866, #32425, #33323, #74306, #60781 ),
 .UNSPECIFIED., .F., .F.,
 ( 4, 2, 2, 2, 4 ),
 ( 0.0007817359430256400890, 0.0009771253907250091169, 0.001172514838424378253, 0.001367904286123747173, 0.001563293733823116309 ),
 .UNSPECIFIED. ) ;
#9513 = EDGE_CURVE ( 'NONE', #73448, #24740, #68997, .T. ) ;
#9514 = ORIENTED_EDGE ( 'NONE', *, *, #38418, .F. ) ;
#9515 = ORIENTED_EDGE ( 'NONE', *, *, #19062, .T. ) ;
#9516 = CARTESIAN_POINT ( 'NONE',  ( 0.2115152373170033073, -8.475808217655753651, 34.90892951860618609 ) ) ;
#9517 = ORIENTED_EDGE ( 'NONE', *, *, #38313, .F. ) ;
#9518 = CARTESIAN_POINT ( 'NONE',  ( 2.530703659305157949, -4.187068189119697692, 33.49521262558774026 ) ) ;
#9519 = VECTOR ( 'NONE', #81699, 1000.000000000000000 ) ;
#9520 = ADVANCED_FACE ( 'NONE', ( #63624 ), #50970, .F. ) ;
#9521 = CARTESIAN_POINT ( 'NONE',  ( -6.923076923076922462, -1.790695186598648903, 34.54067556320373455 ) ) ;
#9522 = CARTESIAN_POINT ( 'NONE',  ( 16.82689985270161870, -3.520140089381496473, 33.17453946501458262 ) ) ;
#9523 = FACE_BOUND ( 'NONE', #57756, .T. ) ;
#9524 = ORIENTED_EDGE ( 'NONE', *, *, #87657, .T. ) ;
#9525 = LINE ( 'NONE', #36991, #77361 ) ;
#9526 = ADVANCED_FACE ( 'NONE', ( #64060 ), #43793, .F. ) ;
#9527 = DIRECTION ( 'NONE',  ( 0.000000000000000000, 0.000000000000000000, 1.000000000000000000 ) ) ;
#9528 = CARTESIAN_POINT ( 'NONE',  ( 2.084207383127978375, -8.539481045369598178, 34.89627647299170832 ) ) ;
#9529 = FACE_OUTER_BOUND ( 'NONE', #29127, .T. ) ;
#9530 = ORIENTED_EDGE ( 'NONE', *, *, #10202, .F. ) ;
#9531 = VECTOR ( 'NONE', #85157, 1000.000000000000000 ) ;
#9532 = PRODUCT_DEFINITION_CONTEXT ( 'detailed design', #39452, 'design' ) ;
#9533 = VERTEX_POINT ( 'NONE', #37473 ) ;
#9534 = ORIENTED_EDGE ( 'NONE', *, *, #47043, .F. ) ;
#9536 = CARTESIAN_POINT ( 'NONE',  ( 5.749976762707036393, -3.202444869320336451, 32.30641848906366675 ) ) ;
#9535 = CARTESIAN_POINT ( 'NONE',  ( 12.39626801557768943, -6.879047030191174805, 34.71129190930000163 ) ) ;
#9537 = FACE_OUTER_BOUND ( 'NONE', #50183, .T. ) ;
#9538 = DIRECTION ( 'NONE',  ( -0.000000000000000000, -0.6427876096865404731, -0.7660444431189771253 ) ) ;
#9539 = CARTESIAN_POINT ( 'NONE',  ( 7.622668902429898807, -12.44517049084099725, 30.48991314939691932 ) ) ;
#9540 = CARTESIAN_POINT ( 'NONE',  ( -11.53846153846166089, -2.379036618888197729, 30.90682066428292885 ) ) ;
#9541 = VERTEX_POINT ( 'NONE', #2353 ) ;
#9542 = EDGE_CURVE ( 'NONE', #4699, #73779, #85723, .T. ) ;
#9543 = LINE ( 'NONE', #63602, #18485 ) ;
#9544 = B_SPLINE_CURVE_WITH_KNOTS ( 'NONE', 3,
 ( #46573, #68180, #61402, #80824, #60970, #74057, #33945, #41591, #54205, #68617 ),
 .UNSPECIFIED., .F., .F.,
 ( 4, 2, 2, 2, 4 ),
 ( 0.0007817359430256324996, 0.0009771253907249993591, 0.001172514838424366110, 0.001367904286123732861, 0.001563293733823099829 ),
 .UNSPECIFIED. ) ;
#9545 = CARTESIAN_POINT ( 'NONE',  ( 17.86985203026830504, -3.625366637846545448, 33.29286588640298561 ) ) ;
#9546 = LINE ( 'NONE', #63156, #38725 ) ;
#9547 = EDGE_CURVE ( 'NONE', #55800, #68993, #84777, .T. ) ;
#9548 = CARTESIAN_POINT ( 'NONE',  ( 3.296836564119307589, -11.35647404775217595, 33.31231777344667222 ) ) ;
#9549 = EDGE_LOOP ( 'NONE', ( #86115, #45046 ) ) ;
#9550 = CARTESIAN_POINT ( 'NONE',  ( 4.480769230769229061, -3.499999999999999556, 29.75000000000000355 ) ) ;
#9551 = VERTEX_POINT ( 'NONE', #77588 ) ;
#9552 = FACE_BOUND ( 'NONE', #73019, .T. ) ;
#9553 = EDGE_CURVE ( 'NONE', #83933, #73212, #9966, .T. ) ;
#9554 = CARTESIAN_POINT ( 'NONE',  ( -17.07692307692307665, -1.242168528481310874, 33.36296068462461051 ) ) ;
#9556 = EDGE_CURVE ( 'NONE', #18984, #30445, #38374, .T. ) ;
#9555 = CARTESIAN_POINT ( 'NONE',  ( 14.08420736396836226, -11.89387501736622710, 32.13663884655806413 ) ) ;
#9557 = ORIENTED_EDGE ( 'NONE', *, *, #22267, .F. ) ;
#9558 = CARTESIAN_POINT ( 'NONE',  ( -16.15384615384627409, -11.67786785259630911, 32.92929555188603530 ) ) ;
#9559 = CARTESIAN_POINT ( 'NONE',  ( -16.15384615384615330, -12.48256725967547354, 35.29906147534542527 ) ) ;
#9560 = CARTESIAN_POINT ( 'NONE',  ( -11.97435897435897267, -7.500000000000000000, 33.75000000000000000 ) ) ;
#9561 = DIRECTION ( 'NONE',  ( -0.000000000000000000, 0.9848077530122085754, -0.1736481776669273613 ) ) ;
#9562 = ORIENTED_EDGE ( 'NONE', *, *, #69703, .T. ) ;
#9563 = VECTOR ( 'NONE', #86806, 1000.000000000000227 ) ;
#9564 = CARTESIAN_POINT ( 'NONE',  ( -7.715628144390283438, -10.88167719472716399, 33.43325721877153711 ) ) ;
#9565 = VERTEX_POINT ( 'NONE', #66733 ) ;
#9567 = EDGE_LOOP ( 'NONE', ( #84097, #52609, #81694, #30604 ) ) ;
#9566 = CARTESIAN_POINT ( 'NONE',  ( 13.63466969625370595, -12.17597550085003810, 31.52189283813460463 ) ) ;
#9568 = CARTESIAN_POINT ( 'NONE',  ( -18.25000000000000000, -12.75000000000000888, 29.74999999999997868 ) ) ;
#9569 = CARTESIAN_POINT ( 'NONE',  ( -12.46153846153858424, -3.083524468854526912, 32.58852847137268327 ) ) ;
#9570 = DIRECTION ( 'NONE',  ( -0.000000000000000000, -0.7660444431189791237, -0.6427876096865379196 ) ) ;
#9571 = CARTESIAN_POINT ( 'NONE',  ( -15.00734283185444440, -7.630147987733840509, 34.99859428049665411 ) ) ;
#9572 = DIRECTION ( 'NONE',  ( -0.000000000000000000, 1.000000000000000000, 3.491481338843133355E-15 ) ) ;
#9573 = VECTOR ( 'NONE', #51746, 1000.000000000000000 ) ;
#9574 = CARTESIAN_POINT ( 'NONE',  ( 12.23805353697412990, -5.827078755546623690, 34.72654668319379567 ) ) ;
#9575 = CARTESIAN_POINT ( 'NONE',  ( -1.944543648262992530, -9.444543648263016067, 23.68750000000000000 ) ) ;
#9576 = VERTEX_POINT ( 'NONE', #11798 ) ;
#9577 = CARTESIAN_POINT ( 'NONE',  ( 13.44987052412822059, -12.70778746994558439, 30.41441678777536595 ) ) ;
#9578 = CARTESIAN_POINT ( 'NONE',  ( 13.45078199120703033, -7.250054591869670162, 34.99404684341514127 ) ) ;
#9579 = VERTEX_POINT ( 'NONE', #52319 ) ;
#9580 = EDGE_LOOP ( 'NONE', ( #56855, #52321 ) ) ;
#9581 = ORIENTED_EDGE ( 'NONE', *, *, #11760, .T. ) ;
#9582 = CARTESIAN_POINT ( 'NONE',  ( 13.38461538461526423, -11.06231777344772027, 33.60647404775119895 ) ) ;
#9583 = CARTESIAN_POINT ( 'NONE',  ( 11.40831356872984514, -5.070767119584671079, 34.40440758774516183 ) ) ;
#9584 = CARTESIAN_POINT ( 'NONE',  ( -17.14219352288385778, -9.442884908240170461, 34.35708131394840592 ) ) ;
#9585 = CARTESIAN_POINT ( 'NONE',  ( -3.230769230769229949, -7.500000000000001776, 35.04278698407183867 ) ) ;
#9586 = CARTESIAN_POINT ( 'NONE',  ( 8.769230769230768274, -2.292212530054420494, 30.41441678777542634 ) ) ;
#9587 = FACE_OUTER_BOUND ( 'NONE', #10376, .T. ) ;
#9588 = CARTESIAN_POINT ( 'NONE',  ( 5.777120483262417672, -7.630690623152302621, 34.99857592706774057 ) ) ;
#9589 = B_SPLINE_CURVE_WITH_KNOTS ( 'NONE', 3,
 ( #27439, #13916, #41398, #68860, #9383, #71958, #8942, #36414, #30093, #23324 ),
 .UNSPECIFIED., .F., .F.,
 ( 4, 2, 2, 2, 4 ),
 ( 0.000000000000000000, 0.0001954339857564100765, 0.0003908679715128201529, 0.0005863019572692302565, 0.0007817359430256403058 ),
 .UNSPECIFIED. ) ;
#9590 = ORIENTED_EDGE ( 'NONE', *, *, #48894, .F. ) ;
#9591 = EDGE_CURVE ( 'NONE', #68628, #52889, #18084, .T. ) ;
#9592 = AXIS2_PLACEMENT_3D ( 'NONE', #37707, #3473, #44447 ) ;
#9593 = CARTESIAN_POINT ( 'NONE',  ( -4.153846153846152411, -5.557115091759785130, 34.35708131394839171 ) ) ;
#9594 = CARTESIAN_POINT ( 'NONE',  ( -1.384615384615505151, -6.879047030192662504, 34.71129190930017927 ) ) ;
#9595 = DIRECTION ( 'NONE',  ( -1.000000000000000000, -0.000000000000000000, -0.000000000000000000 ) ) ;
#9596 = CARTESIAN_POINT ( 'NONE',  ( 7.912222197156285830, -2.721908614388772740, 31.22303859784725333 ) ) ;
#9597 = ADVANCED_FACE ( 'NONE', ( #32498 ), #24849, .F. ) ;
#9598 = VERTEX_POINT ( 'NONE', #24401 ) ;
#9599 = CARTESIAN_POINT ( 'NONE',  ( 7.622668921589514035, -2.353723527008296124, 30.78948104536958397 ) ) ;
#9600 = EDGE_CURVE ( 'NONE', #23257, #20836, #42825, .T. ) ;
#9601 = EDGE_LOOP ( 'NONE', ( #4474, #3190, #71046, #5881 ) ) ;
#9602 = CARTESIAN_POINT ( 'NONE',  ( -17.75005459062195712, -8.476813868363244353, 34.90874843262270133 ) ) ;
#9603 = DIRECTION ( 'NONE',  ( -0.000000000000000000, 0.7660444431189791237, -0.6427876096865379196 ) ) ;
#9604 = CARTESIAN_POINT ( 'NONE',  ( 11.53846153846153832, -9.780366693483667717, 34.19971097300155094 ) ) ;
#9605 = CARTESIAN_POINT ( 'NONE',  ( 12.46153846153846168, -10.51840700105979565, 33.73612834413961536 ) ) ;
#9606 = ORIENTED_EDGE ( 'NONE', *, *, #32741, .T. ) ;
#9607 = AXIS2_PLACEMENT_3D ( 'NONE', #72077, #31991, #10384 ) ;
#9608 = CARTESIAN_POINT ( 'NONE',  ( 15.23076923076923173, -2.499999999999998668, 29.50000000000001066 ) ) ;
#9609 = DIRECTION ( 'NONE',  ( 0.000000000000000000, 0.8660254037844377084, -0.5000000000000015543 ) ) ;
#9610 = CARTESIAN_POINT ( 'NONE',  ( -17.32692307692308376, -2.499999999999999556, 29.81609845454691765 ) ) ;
#9611 = EDGE_CURVE ( 'NONE', #75299, #63322, #32953, .T. ) ;
#9612 = FACE_OUTER_BOUND ( 'NONE', #818, .T. ) ;
#9613 = EDGE_LOOP ( 'NONE', ( #23989, #1927, #40536, #47332 ) ) ;
#9614 = CARTESIAN_POINT ( 'NONE',  ( 7.622668921589515811, -11.60425143139329940, 33.02411095842164457 ) ) ;
#9615 = ORIENTED_EDGE ( 'NONE', *, *, #83641, .T. ) ;
#9616 = CARTESIAN_POINT ( 'NONE',  ( 12.46153846153846168, -9.819645486525091727, 36.12317359536749706 ) ) ;
#9617 = DIRECTION ( 'NONE',  ( -0.000000000000000000, 0.1736481776669307198, -0.9848077530122080203 ) ) ;
#9618 = CARTESIAN_POINT ( 'NONE',  ( -13.38461538461538325, -10.67929555188718282, 33.92786785259544047 ) ) ;
#9619 = CARTESIAN_POINT ( 'NONE',  ( -14.24243673641628050, -11.94971097300157403, 32.03036669348361443 ) ) ;
#9620 = DIRECTION ( 'NONE',  ( 0.000000000000000000, 0.000000000000000000, 1.000000000000000000 ) ) ;
#9621 = ADVANCED_FACE ( 'NONE', ( #25304 ), #67629, .F. ) ;
#9622 = AXIS2_PLACEMENT_3D ( 'NONE', #35622, #70287, #76148 ) ;
#9623 = VERTEX_POINT ( 'NONE', #26194 ) ;
#9624 = B_SPLINE_CURVE_WITH_KNOTS ( 'NONE', 3,
 ( #87802, #13441, #5803, #13002, #54421, #48541, #32830, #7132, #88247, #20638 ),
 .UNSPECIFIED., .F., .F.,
 ( 4, 2, 2, 2, 4 ),
 ( 0.000000000000000000, 0.0001954311564186876063, 0.0003908623128373752125, 0.0005862934692560628188, 0.0007817246256747504250 ),
 .UNSPECIFIED. ) ;
#9625 = ORIENTED_EDGE ( 'NONE', *, *, #18792, .F. ) ;
#9626 = EDGE_LOOP ( 'NONE', ( #60849, #76752, #77419, #67362 ) ) ;
#9627 = VECTOR ( 'NONE', #25212, 1000.000000000000227 ) ;
#9628 = CARTESIAN_POINT ( 'NONE',  ( -10.39237326377176451, -8.239487800360276282, 34.69522927552633718 ) ) ;
#9629 = CARTESIAN_POINT ( 'NONE',  ( 11.31553457955468645, -9.172386477786396597, 34.72672124145550043 ) ) ;
#9630 = DIRECTION ( 'NONE',  ( -0.000000000000000000, 0.6427876096865404731, -0.7660444431189771253 ) ) ;
#9631 = CARTESIAN_POINT ( 'NONE',  ( -12.21148404162501144, -12.41089969410671223, 31.60739465890703670 ) ) ;
#9632 = CARTESIAN_POINT ( 'NONE',  ( 3.262820512820510999, -7.500000000000000000, 29.75000000000000355 ) ) ;
#9633 = CARTESIAN_POINT ( 'NONE',  ( 11.53846153846153832, -1.466349020453238561, 30.81389545987213907 ) ) ;
#9634 = CYLINDRICAL_SURFACE ( 'NONE', #22026, 0.2500000000000002220 ) ;
#9635 = CARTESIAN_POINT ( 'NONE',  ( 9.469380733400843297, -10.01117774369187252, 34.36070679894347535 ) ) ;
#9636 = ORIENTED_EDGE ( 'NONE', *, *, #54217, .F. ) ;
#9637 = ORIENTED_EDGE ( 'NONE', *, *, #37123, .F. ) ;
#9638 = ORIENTED_EDGE ( 'NONE', *, *, #38910, .T. ) ;
#9640 = EDGE_LOOP ( 'NONE', ( #52202, #50522, #72406, #78322 ) ) ;
#9639 = CARTESIAN_POINT ( 'NONE',  ( 11.66925197942849302, -2.494656445102012565, 31.33466734024120015 ) ) ;
#9642 = CARTESIAN_POINT ( 'NONE',  ( -10.48459417441766561, -6.369690395747422684, 34.87708834333098196 ) ) ;
#9641 = CARTESIAN_POINT ( 'NONE',  ( 0.000000000000000000, -11.00000000000000000, 29.75000000000000355 ) ) ;
#9643 = DIRECTION ( 'NONE',  ( -0.000000000000000000, 1.000000000000000000, -0.000000000000000000 ) ) ;
#9644 = VECTOR ( 'NONE', #27997, 1000.000000000000227 ) ;
#9645 = CARTESIAN_POINT ( 'NONE',  ( -10.68146802634049486, -11.69971097300155272, 32.46337939537587403 ) ) ;
#9646 = ORIENTED_EDGE ( 'NONE', *, *, #76130, .T. ) ;
#9647 = ADVANCED_FACE ( 'NONE', ( #87471 ), #80255, .F. ) ;
#9648 = EDGE_CURVE ( 'NONE', #42418, #70591, #51864, .T. ) ;
#9649 = ORIENTED_EDGE ( 'NONE', *, *, #18162, .F. ) ;
#9650 = CARTESIAN_POINT ( 'NONE',  ( -11.78843828251013015, -12.01397095200674059, 32.43157075238190146 ) ) ;
#9651 = VECTOR ( 'NONE', #77650, 1000.000000000000000 ) ;
#9653 = EDGE_CURVE ( 'NONE', #36678, #33529, #87030, .T. ) ;
#9652 = ORIENTED_EDGE ( 'NONE', *, *, #1001, .T. ) ;
#9654 = FACE_BOUND ( 'NONE', #82022, .T. ) ;
#9655 = FACE_OUTER_BOUND ( 'NONE', #58028, .T. ) ;
#9656 = CARTESIAN_POINT ( 'NONE',  ( 16.08776274289027342, -6.386643153685125363, 34.62446782046654903 ) ) ;
#9657 = ORIENTED_EDGE ( 'NONE', *, *, #80772, .F. ) ;
#9658 = CARTESIAN_POINT ( 'NONE',  ( -14.30769230769230660, -8.164416787775445883, 34.95778746994557906 ) ) ;
#9660 = EDGE_CURVE ( 'NONE', #30359, #38114, #86309, .T. ) ;
#9659 = FACE_OUTER_BOUND ( 'NONE', #60021, .T. ) ;
#9661 = AXIS2_PLACEMENT_3D ( 'NONE', #88828, #27100, #74860 ) ;
#9662 = CARTESIAN_POINT ( 'NONE',  ( -23.00000000000000000, -5.499999999999981348, 27.25000000000000000 ) ) ;
#9663 = ORIENTED_EDGE ( 'NONE', *, *, #41092, .T. ) ;
#9664 = CARTESIAN_POINT ( 'NONE',  ( -11.76138849736838488, -4.762599654559228846, 34.23009711892697737 ) ) ;
#9665 = LINE ( 'NONE', #23618, #33684 ) ;
#9666 = EDGE_LOOP ( 'NONE', ( #89, #41043, #9723, #58789, #79308 ) ) ;
#9667 = CARTESIAN_POINT ( 'NONE',  ( -1.384615384615383471, -13.53365097954675988, 30.81389545987213552 ) ) ;
#9668 = DIRECTION ( 'NONE',  ( 0.000000000000000000, -0.000000000000000000, -1.000000000000000000 ) ) ;
#9669 = CARTESIAN_POINT ( 'NONE',  ( 2.242422307135988557, -12.16647553114622049, 32.15551576947930812 ) ) ;
#9670 = CYLINDRICAL_SURFACE ( 'NONE', #72881, 0.2499999999999998890 ) ;
#9671 = CARTESIAN_POINT ( 'NONE',  ( -0.5916864312701582973, -5.070767119584671967, 34.40440758774516183 ) ) ;
#9672 = CARTESIAN_POINT ( 'NONE',  ( -4.153846153846152411, -8.564572088678739092, 35.78748833219616898 ) ) ;
#9673 = CARTESIAN_POINT ( 'NONE',  ( -13.13466997523734214, -12.45601412856602686, 31.48342859153981621 ) ) ;
#9675 = CARTESIAN_POINT ( 'NONE',  ( 11.78851585009985570, -4.235687564193448829, 33.53795663066793509 ) ) ;
#9674 = CARTESIAN_POINT ( 'NONE',  ( -1.608100328339330254, -2.847400154188068022, 31.58180166144859058 ) ) ;
#9676 = CARTESIAN_POINT ( 'NONE',  ( -1.319360245102545681, -9.528491918058460186, 34.59228464037085615 ) ) ;
#9678 = CARTESIAN_POINT ( 'NONE',  ( -10.61538461538473399, -8.613356846316285953, 34.62446782046622218 ) ) ;
#9677 = CARTESIAN_POINT ( 'NONE',  ( -18.00000000000000000, -2.249999999999990674, 29.49999999999998579 ) ) ;
#9679 = EDGE_CURVE ( 'NONE', #76954, #66225, #76195, .T. ) ;
#9680 = CARTESIAN_POINT ( 'NONE',  ( -0.4615384615384611200, -13.88283147151868846, 33.14645433367849847 ) ) ;
#9681 = CARTESIAN_POINT ( 'NONE',  ( -2.749999999999997780, -7.561099074964547917, 21.09188170625849068 ) ) ;
#9682 = ORIENTED_EDGE ( 'NONE', *, *, #60650, .F. ) ;
#9683 = CARTESIAN_POINT ( 'NONE',  ( 9.692307692307695177, -5.415277668671390821, 36.20867863119892149 ) ) ;
#9684 = ORIENTED_EDGE ( 'NONE', *, *, #25027, .F. ) ;
#9685 = CARTESIAN_POINT ( 'NONE',  ( -9.757578138268467427, -6.026961402152685388, 34.52809138561120506 ) ) ;
#9686 = EDGE_CURVE ( 'NONE', #25656, #50820, #11343, .T. ) ;
#9687 = ORIENTED_EDGE ( 'NONE', *, *, #70774, .F. ) ;
#9688 = CARTESIAN_POINT ( 'NONE',  ( 16.08776274289027342, -11.16473453929635440, 33.15142922261925662 ) ) ;
#9689 = ORIENTED_EDGE ( 'NONE', *, *, #15832, .F. ) ;
#9690 = CARTESIAN_POINT ( 'NONE',  ( -7.976845312821408740, -5.582088688514999397, 34.36776431015576350 ) ) ;
#9691 = CARTESIAN_POINT ( 'NONE',  ( -2.775308065498764964, -6.422011778438537988, 24.92000670625849068 ) ) ;
#9692 = CARTESIAN_POINT ( 'NONE',  ( 17.07692307692295586, -8.613356846316285953, 34.62446782046622218 ) ) ;
#9693 = CARTESIAN_POINT ( 'NONE',  ( 6.792929713638706346, -11.47017969459903952, 32.78971311882034456 ) ) ;
#9694 = CARTESIAN_POINT ( 'NONE',  ( 6.416666666666664298, -3.499999999999999556, 29.75000000000000355 ) ) ;
#9695 = CYLINDRICAL_SURFACE ( 'NONE', #36021, 0.2499999999999994726 ) ;
#9696 = CYLINDRICAL_SURFACE ( 'NONE', #44635, 0.2499999999999993616 ) ;
#9697 = CARTESIAN_POINT ( 'NONE',  ( 11.40777007179398339, -2.729777683071817229, 31.24903638046269450 ) ) ;
#9698 = CARTESIAN_POINT ( 'NONE',  ( -14.30769230769242917, -5.094484230521993062, 34.41647553114689373 ) ) ;
#9699 = CARTESIAN_POINT ( 'NONE',  ( -1.929879867024197893E-14, -3.750000000000000000, 15.40625000000000000 ) ) ;
#9700 = ADVANCED_FACE ( 'NONE', ( #20326 ), #495, .F. ) ;
#9701 = CARTESIAN_POINT ( 'NONE',  ( -11.31544869436814160, -2.523321265292115534, 31.42251411153756990 ) ) ;
#9702 = DIRECTION ( 'NONE',  ( -0.000000000000000000, -0.5000000000000009992, -0.8660254037844380415 ) ) ;
#9703 = CARTESIAN_POINT ( 'NONE',  ( 10.61538461538449418, -5.941354392335915335, 34.76329471203413846 ) ) ;
#9704 = CARTESIAN_POINT ( 'NONE',  ( -2.651650429449535551, -10.15165042944956753, 14.93750000000000000 ) ) ;
#9705 = ADVANCED_FACE ( 'NONE', ( #33400 ), #74835, .F. ) ;
#9706 = ORIENTED_EDGE ( 'NONE', *, *, #20494, .F. ) ;
#9707 = LINE ( 'NONE', #79513, #50062 ) ;
#9708 = FACE_OUTER_BOUND ( 'NONE', #67246, .T. ) ;
#9709 = CARTESIAN_POINT ( 'NONE',  ( -8.835314180186648159, -11.16473453929635440, 33.15142922261925662 ) ) ;
#9710 = CARTESIAN_POINT ( 'NONE',  ( 18.06525557127601900, -10.90142922261932057, 33.41473453929631887 ) ) ;
#9711 = CARTESIAN_POINT ( 'NONE',  ( 15.48076923076929212, -7.434744429011176159, 34.75000000000000711 ) ) ;
#9712 = CARTESIAN_POINT ( 'NONE',  ( -10.61538461538473577, -11.06231777344772027, 33.60647404775119895 ) ) ;
#9713 = EDGE_CURVE ( 'NONE', #57265, #29932, #33084, .T. ) ;
#9714 = AXIS2_PLACEMENT_3D ( 'NONE', #16304, #58163, #17183 ) ;
#9715 = EDGE_CURVE ( 'NONE', #54361, #1645, #13762, .T. ) ;
#9716 = B_SPLINE_CURVE_WITH_KNOTS ( 'NONE', 3,
 ( #77546, #9099, #83431, #49185, #21714, #63133, #36132, #69012, #561, #43320 ),
 .UNSPECIFIED., .F., .F.,
 ( 4, 2, 2, 2, 4 ),
 ( 0.000000000000000000, 0.0001954311564186868473, 0.0003908623128373736946, 0.0005862934692560605419, 0.0007817246256747473893 ),
 .UNSPECIFIED. ) ;
#9717 = B_SPLINE_CURVE_WITH_KNOTS ( 'NONE', 3,
 ( #2459, #84903, #23188, #14663, #69600, #49334, #76811, #58749, #46133, #79021 ),
 .UNSPECIFIED., .F., .F.,
 ( 4, 2, 2, 2, 4 ),
 ( 0.000000000000000000, 0.0001954311564186871455, 0.0003908623128373742909, 0.0005862934692560614093, 0.0007817246256747485819 ),
 .UNSPECIFIED. ) ;
#9718 = ORIENTED_EDGE ( 'NONE', *, *, #10720, .F. ) ;
#9719 = CARTESIAN_POINT ( 'NONE',  ( 20.00000000000000000, -4.000000000000000000, 29.75000000000000355 ) ) ;
#9720 = EDGE_LOOP ( 'NONE', ( #35564, #24836 ) ) ;
#9721 = VECTOR ( 'NONE', #29167, 1000.000000000000000 ) ;
#9722 = B_SPLINE_CURVE_WITH_KNOTS ( 'NONE', 3,
 ( #71380, #57874, #78588, #37157, #77703, #50665, #49784, #16891, #78148, #85359 ),
 .UNSPECIFIED., .F., .F.,
 ( 4, 2, 2, 2, 4 ),
 ( 0.0007817359430256257775, 0.0009771253907249909023, 0.001172514838424356136, 0.001367904286123721369, 0.001563293733823086602 ),
 .UNSPECIFIED. ) ;
#9723 = ORIENTED_EDGE ( 'NONE', *, *, #42881, .F. ) ;
#9724 = CARTESIAN_POINT ( 'NONE',  ( -24.00000000000000000, -9.499999999999982236, 27.25000000000000000 ) ) ;
#9725 = CARTESIAN_POINT ( 'NONE',  ( -6.923076923077045919, -5.941354392335915335, 34.76329471203413846 ) ) ;
#9726 = CARTESIAN_POINT ( 'NONE',  ( 6.856994543716787405, -2.833524468853757305, 32.15551576947924417 ) ) ;
#9727 = AXIS2_PLACEMENT_3D ( 'NONE', #84384, #43385, #42507 ) ;
#9728 = CARTESIAN_POINT ( 'NONE',  ( -8.769230769230768274, -13.04860791097971706, 34.73218667398347037 ) ) ;
#9729 = CARTESIAN_POINT ( 'NONE',  ( 17.75002325595141173, -9.234221910056350069, 34.70572697212741531 ) ) ;
#9730 = ADVANCED_FACE ( 'NONE', ( #75271 ), #40604, .F. ) ;
#9731 = ORIENTED_EDGE ( 'NONE', *, *, #35752, .T. ) ;
#9732 = ADVANCED_FACE ( 'NONE', ( #88805 ), #34721, .F. ) ;
#9733 = CARTESIAN_POINT ( 'NONE',  ( 15.90384615384615330, -7.500000000000001776, 35.04278698407183867 ) ) ;
#9734 = EDGE_LOOP ( 'NONE', ( #55932, #24020 ) ) ;
#9735 = ORIENTED_EDGE ( 'NONE', *, *, #43717, .T. ) ;
#9736 = CARTESIAN_POINT ( 'NONE',  ( 0.4615384615383396616, -11.94971097300221174, 32.03036669348237098 ) ) ;
#9737 = DIRECTION ( 'NONE',  ( -1.000000000000000000, 0.000000000000000000, -0.000000000000000000 ) ) ;
#9738 = CYLINDRICAL_SURFACE ( 'NONE', #50848, 4.000000000000000000 ) ;
#9739 = AXIS2_PLACEMENT_3D ( 'NONE', #80124, #18426, #45886 ) ;
#9740 = CARTESIAN_POINT ( 'NONE',  ( 11.47237915910140416, -10.67929555188718460, 33.92786785259543336 ) ) ;
#9741 = CARTESIAN_POINT ( 'NONE',  ( 8.068933515131908152, -12.69155399931963046, 30.53255429739157734 ) ) ;
#9742 = ORIENTED_EDGE ( 'NONE', *, *, #81166, .F. ) ;
#9743 = ORIENTED_EDGE ( 'NONE', *, *, #68543, .F. ) ;
#9744 = CARTESIAN_POINT ( 'NONE',  ( 2.651650429449569302, -10.15165042944953733, 23.37500000000000000 ) ) ;
#9745 = B_SPLINE_CURVE_WITH_KNOTS ( 'NONE', 3,
 ( #68608, #87576, #61393, #67288, #27178, #88909, #12339, #39818, #25855, #53312 ),
 .UNSPECIFIED., .F., .F.,
 ( 4, 2, 2, 2, 4 ),
 ( 0.0007817246256747446788, 0.0009771112852218872494, 0.001172497944769029929, 0.001367884604316172391, 0.001563271263863315070 ),
 .UNSPECIFIED. ) ;
#9746 = ORIENTED_EDGE ( 'NONE', *, *, #22256, .T. ) ;
#9748 = ORIENTED_EDGE ( 'NONE', *, *, #64096, .T. ) ;
#9747 = CARTESIAN_POINT ( 'NONE',  ( 11.60452887181161508, -5.471508081941601098, 34.59228464037088457 ) ) ;
#9749 = CARTESIAN_POINT ( 'NONE',  ( 3.230769230769108269, -2.379036618888197285, 30.90682066428292885 ) ) ;
#9750 = CARTESIAN_POINT ( 'NONE',  ( 11.53846153846153832, -5.557115091759785130, 34.35708131394839171 ) ) ;
#9751 = B_SPLINE_CURVE_WITH_KNOTS ( 'NONE', 3,
 ( #22437, #65185, #44459, #63417, #15689, #17457, #43155, #56666, #49901, #10259 ),
 .UNSPECIFIED., .F., .F.,
 ( 4, 2, 2, 2, 4 ),
 ( 0.000000000000000000, 0.0001954339857564074473, 0.0003908679715128148945, 0.0005863019572692223418, 0.0007817359430256297891 ),
 .UNSPECIFIED. ) ;
#9752 = B_SPLINE_CURVE_WITH_KNOTS ( 'NONE', 3,
 ( #18789, #3920, #79602, #46696, #73286, #85910, #39514, #80496, #60205, #10695 ),
 .UNSPECIFIED., .F., .F.,
 ( 4, 2, 2, 2, 4 ),
 ( 0.000000000000000000, 0.0001954339857564075828, 0.0003908679715128151656, 0.0005863019572692227755, 0.0007817359430256303312 ),
 .UNSPECIFIED. ) ;
#9753 = CARTESIAN_POINT ( 'NONE',  ( -2.307692307692305711, -1.367168528481310208, 33.57946703557072254 ) ) ;
#9754 = ORIENTED_EDGE ( 'NONE', *, *, #1263, .F. ) ;
#9755 = VECTOR ( 'NONE', #52255, 1000.000000000000227 ) ;
#9756 = CYLINDRICAL_SURFACE ( 'NONE', #33981, 0.2500000000000009437 ) ;
#9757 = ORIENTED_EDGE ( 'NONE', *, *, #30561, .T. ) ;
#9758 = CARTESIAN_POINT ( 'NONE',  ( -10.83831157429146330, -4.762599654559228846, 34.23009711892697737 ) ) ;
#9759 = CARTESIAN_POINT ( 'NONE',  ( -13.38461538461538325, -9.819645486525091727, 36.12317359536749706 ) ) ;
#9760 = DIRECTION ( 'NONE',  ( -0.000000000000000000, -0.000000000000000000, -1.000000000000000000 ) ) ;
#9762 = CARTESIAN_POINT ( 'NONE',  ( -14.30769230769230660, -8.973038597847269315, 34.52809138561121927 ) ) ;
#9761 = CARTESIAN_POINT ( 'NONE',  ( -0.3954711281883854790, -11.35647404775217595, 33.31231777344667222 ) ) ;
#9763 = CARTESIAN_POINT ( 'NONE',  ( -1.134560964701930796, -8.346898887586323923, 34.93166121998716278 ) ) ;
#9764 = CARTESIAN_POINT ( 'NONE',  ( -15.12820512820512953, -11.50000000000000000, 29.75000000000000355 ) ) ;
#9765 = ORIENTED_EDGE ( 'NONE', *, *, #11046, .F. ) ;
#9767 = EDGE_CURVE ( 'NONE', #55252, #52031, #62112, .T. ) ;
#9766 = CARTESIAN_POINT ( 'NONE',  ( -18.06527044596078113, -10.90142922261924063, 33.41473453929638993 ) ) ;
#9768 = CARTESIAN_POINT ( 'NONE',  ( 4.853438152358743984, -4.225889041578354544, 33.85425143139329407 ) ) ;
#9769 = ORIENTED_EDGE ( 'NONE', *, *, #61583, .T. ) ;
#9770 = EDGE_CURVE ( 'NONE', #16297, #61213, #32127, .T. ) ;
#9771 = CARTESIAN_POINT ( 'NONE',  ( -16.37733107841048863, -12.69144148231606017, 30.53333754910549303 ) ) ;
#9772 = CARTESIAN_POINT ( 'NONE',  ( -4.826868765284762830, -5.728107161865375829, 34.42597550085002922 ) ) ;
#9773 = CARTESIAN_POINT ( 'NONE',  ( -19.00000000000000000, -7.500000000000000000, 29.75000000000000355 ) ) ;
#9774 = LINE ( 'NONE', #30488, #20294 ) ;
#9775 = CIRCLE ( 'NONE', #21279, 0.2500000000000002220 ) ;
#9776 = CARTESIAN_POINT ( 'NONE',  ( -10.54931728203453822, -2.833524468853757305, 32.15551576947925838 ) ) ;
#9777 = CARTESIAN_POINT ( 'NONE',  ( -14.30769230769242917, -2.657715359629662544, 31.77849191805970364 ) ) ;
#9778 = FACE_BOUND ( 'NONE', #5899, .T. ) ;
#9780 = DIRECTION ( 'NONE',  ( 0.000000000000000000, 0.9848077530122072432, -0.1736481776669354937 ) ) ;
#9779 = CARTESIAN_POINT ( 'NONE',  ( 12.23861150263161157, -10.01117774369187252, 34.36070679894347535 ) ) ;
#9781 = CARTESIAN_POINT ( 'NONE',  ( 15.93036121012220541, -3.236172620538810385, 32.36188796281390267 ) ) ;
#9783 = CARTESIAN_POINT ( 'NONE',  ( 0.6843181305165246808, -3.020022701398813236, 32.48759521482552515 ) ) ;
#9782 = FACE_OUTER_BOUND ( 'NONE', #46587, .T. ) ;
#9784 = EDGE_CURVE ( 'NONE', #45204, #59880, #57797, .T. ) ;
#9785 = CARTESIAN_POINT ( 'NONE',  ( -6.000000000000119904, -10.90142922262034020, 33.41473453929536674 ) ) ;
#9786 = VECTOR ( 'NONE', #62607, 1000.000000000000000 ) ;
#9787 = CARTESIAN_POINT ( 'NONE',  ( -1.614399933863656544, -3.775308065498769405, 18.82625670625848713 ) ) ;
#9788 = ORIENTED_EDGE ( 'NONE', *, *, #61810, .F. ) ;
#9789 = FACE_OUTER_BOUND ( 'NONE', #21188, .T. ) ;
#9790 = VECTOR ( 'NONE', #9286, 1000.000000000000000 ) ;
#9791 = CARTESIAN_POINT ( 'NONE',  ( 4.153846153846154188, -13.57706302396349152, 30.56769352161908060 ) ) ;
#9792 = CARTESIAN_POINT ( 'NONE',  ( 6.000000000000001776, -5.471508081941601098, 34.59228464037088457 ) ) ;
#9793 = CARTESIAN_POINT ( 'NONE',  ( 0.08713905105068281420, -10.25000490179539980, 28.74997304012405408 ) ) ;
#9794 = LINE ( 'NONE', #24640, #45704 ) ;
#9795 = LINE ( 'NONE', #35168, #32613 ) ;
#9796 = CARTESIAN_POINT ( 'NONE',  ( 3.724691934501232815, -5.885600066136343678, 20.38875670625849068 ) ) ;
#9797 = CARTESIAN_POINT ( 'NONE',  ( -16.28399412357784826, -5.915902021225892149, 34.75552854090298638 ) ) ;
#9798 = CARTESIAN_POINT ( 'NONE',  ( 4.087763774486017354, -11.91647553114624181, 32.58852847137148245 ) ) ;
#9799 = EDGE_CURVE ( 'NONE', #22144, #53138, #69701, .T. ) ;
#9800 = CARTESIAN_POINT ( 'NONE',  ( -7.846153846153967493, -3.083524468854526912, 32.58852847137268327 ) ) ;
#9801 = CARTESIAN_POINT ( 'NONE',  ( 18.00000000000030553, -2.506253911140615021, 30.00000000000323297 ) ) ;
#9802 = CARTESIAN_POINT ( 'NONE',  ( -16.85391023282967993, -4.762714258010882773, 34.23016756924214832 ) ) ;
#9803 = CARTESIAN_POINT ( 'NONE',  ( 5.326868486301119532, -8.476813868363244353, 34.90874843262270133 ) ) ;
#9804 = CARTESIAN_POINT ( 'NONE',  ( -6.249976744048589161, -12.01397095200673881, 32.43157075238190146 ) ) ;
#9805 = FACE_OUTER_BOUND ( 'NONE', #52983, .T. ) ;
#9806 = EDGE_LOOP ( 'NONE', ( #3117, #82029, #13039, #81646 ) ) ;
#9807 = CARTESIAN_POINT ( 'NONE',  ( 17.20771351789002424, -12.62708834333097663, 30.88030960425256310 ) ) ;
#9808 = CARTESIAN_POINT ( 'NONE',  ( -1.634615384615400124, -2.249999999999999112, 29.81609741502488120 ) ) ;
#9809 = CARTESIAN_POINT ( 'NONE',  ( 3.750000000000001776, -7.561099074964511502, 15.97061829374151287 ) ) ;
#9810 = EDGE_CURVE ( 'NONE', #27448, #14834, #37363, .T. ) ;
#9811 = CARTESIAN_POINT ( 'NONE',  ( 7.173131342990376247, -10.82426656108011720, 33.81400080652039009 ) ) ;
#9813 = CARTESIAN_POINT ( 'NONE',  ( -5.299849294439222369, -2.554751324335733820, 30.48935550225260727 ) ) ;
#9812 = CIRCLE ( 'NONE', #41449, 0.2500000000000002220 ) ;
#9814 = ORIENTED_EDGE ( 'NONE', *, *, #81201, .F. ) ;
#9815 = CARTESIAN_POINT ( 'NONE',  ( 1.515407192440173745, -4.118422570099827595, 33.43335022499816489 ) ) ;
#9817 = VERTEX_POINT ( 'NONE', #16221 ) ;
#9816 = CYLINDRICAL_SURFACE ( 'NONE', #81464, 0.2500000000000002220 ) ;
#9818 = CARTESIAN_POINT ( 'NONE',  ( -12.68502338610279168, -9.417330523894424488, 34.63758898049880486 ) ) ;
#9819 = EDGE_CURVE ( 'NONE', #68727, #71459, #36925, .T. ) ;
#9820 = CARTESIAN_POINT ( 'NONE',  ( 17.32692307692301270, -7.565270000091922853, 34.99999999999999289 ) ) ;
#9821 = DIRECTION ( 'NONE',  ( 1.000000000000000000, 0.000000000000000000, 0.000000000000000000 ) ) ;
#9822 = VECTOR ( 'NONE', #30982, 1000.000000000000000 ) ;
#9823 = CARTESIAN_POINT ( 'NONE',  ( -13.51476259405360203, -3.285722584762969856, 32.44110544564090759 ) ) ;
#9824 = ORIENTED_EDGE ( 'NONE', *, *, #81387, .F. ) ;
#9825 = CARTESIAN_POINT ( 'NONE',  ( 8.992010438208831502, -2.353885683473779800, 30.79025554430704403 ) ) ;
#9826 = DIRECTION ( 'NONE',  ( -1.000000000000000000, 0.000000000000000000, -0.000000000000000000 ) ) ;
#9827 = ADVANCED_FACE ( 'NONE', ( #51294 ), #1376, .F. ) ;
#9828 = VECTOR ( 'NONE', #53370, 1000.000000000000000 ) ;
#9829 = CARTESIAN_POINT ( 'NONE',  ( 4.153846153846154188, -9.780366693483667717, 34.19971097300155094 ) ) ;
#9830 = ORIENTED_EDGE ( 'NONE', *, *, #68117, .T. ) ;
#9831 = EDGE_LOOP ( 'NONE', ( #82464, #43035 ) ) ;
#9832 = ORIENTED_EDGE ( 'NONE', *, *, #74425, .T. ) ;
#9833 = CARTESIAN_POINT ( 'NONE',  ( 18.00000000000000000, -2.833524468853757305, 32.15551576947925838 ) ) ;
#9834 = CARTESIAN_POINT ( 'NONE',  ( -7.846153846153844924, -12.62096338111211580, 30.90682066428153263 ) ) ;
#9835 = CARTESIAN_POINT ( 'NONE',  ( -8.068980538632848365, -7.369208160676172348, 34.74850200257123589 ) ) ;
#9836 = EDGE_CURVE ( 'NONE', #21723, #49031, #43686, .T. ) ;
#9837 = CARTESIAN_POINT ( 'NONE',  ( -10.48459280755982981, -3.062576670634119758, 32.05464942895959979 ) ) ;
#9838 = ADVANCED_FACE ( 'NONE', ( #43254 ), #64388, .F. ) ;
#9839 = ADVANCED_FACE ( 'NONE', ( #2687, #15344 ), #42819, .T. ) ;
#9840 = ORIENTED_EDGE ( 'NONE', *, *, #26247, .F. ) ;
#9841 = ORIENTED_EDGE ( 'NONE', *, *, #31867, .F. ) ;
#9843 = ORIENTED_EDGE ( 'NONE', *, *, #82230, .T. ) ;
#9842 = CARTESIAN_POINT ( 'NONE',  ( 3.230769230769110045, -11.48612834414049644, 32.76840700105863391 ) ) ;
#9844 = B_SPLINE_CURVE_WITH_KNOTS ( 'NONE', 3,
 ( #446, #27915, #55383, #82869, #48620, #76093, #14399, #76547, #29692, #63006 ),
 .UNSPECIFIED., .F., .F.,
 ( 4, 2, 2, 2, 4 ),
 ( 0.0007817359430256372700, 0.0009771253907250052138, 0.001172514838424373266, 0.001367904286123741101, 0.001563293733823109153 ),
 .UNSPECIFIED. ) ;
#9845 = AXIS2_PLACEMENT_3D ( 'NONE', #63282, #76356, #61505 ) ;
#9846 = EDGE_CURVE ( 'NONE', #27810, #16174, #17101, .T. ) ;
#9847 = CARTESIAN_POINT ( 'NONE',  ( -10.61538461538461320, -13.53365097954675988, 30.81389545987213552 ) ) ;
#9848 = B_SPLINE_CURVE_WITH_KNOTS ( 'NONE', 3,
 ( #48116, #70169, #63403, #62509, #825, #76488, #14792, #62947, #54885, #20651 ),
 .UNSPECIFIED., .F., .F.,
 ( 4, 2, 2, 2, 4 ),
 ( 0.0007817246256747459798, 0.0009771112852218896347, 0.001172497944769033398, 0.001367884604316177161, 0.001563271263863320708 ),
 .UNSPECIFIED. ) ;
#9849 = CARTESIAN_POINT ( 'NONE',  ( 2.307692307692187583, -3.835265460704628371, 33.15142922262033665 ) ) ;
#9850 = CARTESIAN_POINT ( 'NONE',  ( 13.60739505359345181, -10.23759521482555357, 34.22997729860117033 ) ) ;
#9851 = ORIENTED_EDGE ( 'NONE', *, *, #9715, .F. ) ;
#9852 = ORIENTED_EDGE ( 'NONE', *, *, #87956, .T. ) ;
#9854 = ORIENTED_EDGE ( 'NONE', *, *, #36587, .F. ) ;
#9853 = CYLINDRICAL_SURFACE ( 'NONE', #40189, 0.2499999999999994726 ) ;
#9855 = CYLINDRICAL_SURFACE ( 'NONE', #4292, 0.2499999999999986955 ) ;
#9856 = CARTESIAN_POINT ( 'NONE',  ( -16.02305434602136458, -3.530189275343204702, 32.79018710029569661 ) ) ;
#9857 = ORIENTED_EDGE ( 'NONE', *, *, #655, .F. ) ;
#9858 = CARTESIAN_POINT ( 'NONE',  ( -8.899377978668987055, -10.88202310037935661, 33.43294751532457099 ) ) ;
#9859 = CARTESIAN_POINT ( 'NONE',  ( -2.437839517130527156, -5.195881422630167279, 34.18770438780618548 ) ) ;
#9860 = DIRECTION ( 'NONE',  ( -0.000000000000000000, -0.1736481776669307198, -0.9848077530122080203 ) ) ;
#9861 = FACE_BOUND ( 'NONE', #69453, .T. ) ;
#9862 = CARTESIAN_POINT ( 'NONE',  ( 2.294871794871793380, -7.500000000000000000, 33.75000000000000000 ) ) ;
#9863 = CARTESIAN_POINT ( 'NONE',  ( -4.153846153846273204, -12.27809138561165270, 31.22303859784587132 ) ) ;
#9864 = DIRECTION ( 'NONE',  ( -0.000000000000000000, -0.6427876096865404731, -0.7660444431189770143 ) ) ;
#9866 = CARTESIAN_POINT ( 'NONE',  ( 6.792929713638702793, -11.93770438780619259, 32.05411857736982029 ) ) ;
#9865 = CARTESIAN_POINT ( 'NONE',  ( 3.453548899747298062, -3.563462043263030399, 33.22394488606062879 ) ) ;
#9867 = AXIS2_PLACEMENT_3D ( 'NONE', #56556, #84045, #22325 ) ;
#9868 = CARTESIAN_POINT ( 'NONE',  ( 18.00000000000000000, -6.343179335718451384, 34.87096338111211935 ) ) ;
#9869 = CARTESIAN_POINT ( 'NONE',  ( -16.21911659980693443, -8.613356846314824011, 34.62446782046655613 ) ) ;
#9870 = ORIENTED_EDGE ( 'NONE', *, *, #36108, .T. ) ;
#9871 = FACE_OUTER_BOUND ( 'NONE', #31619, .T. ) ;
#9872 = ORIENTED_EDGE ( 'NONE', *, *, #32996, .F. ) ;
#9873 = VERTEX_POINT ( 'NONE', #71592 ) ;
#9875 = CARTESIAN_POINT ( 'NONE',  ( 1.161130440891438242, -10.81261337010820256, 33.49550067578627477 ) ) ;
#9874 = CARTESIAN_POINT ( 'NONE',  ( 5.934729554039225974, -6.879047030191174805, 34.71129190930000163 ) ) ;
#9876 = AXIS2_PLACEMENT_3D ( 'NONE', #51296, #84699, #85131 ) ;
#9877 = DIRECTION ( 'NONE',  ( -0.000000000000000000, -0.000000000000000000, -1.000000000000000000 ) ) ;
#9878 = CARTESIAN_POINT ( 'NONE',  ( -13.38461538461550759, -11.67786785259630911, 32.92929555188603530 ) ) ;
#9879 = CARTESIAN_POINT ( 'NONE',  ( 14.43773736361208293, -2.254550872974306230, 29.97347326024527092 ) ) ;
#9880 = DIRECTION ( 'NONE',  ( 1.000000000000000000, -0.000000000000000000, -0.000000000000000000 ) ) ;
#9881 = ORIENTED_EDGE ( 'NONE', *, *, #31408, .F. ) ;
#9882 = CARTESIAN_POINT ( 'NONE',  ( -13.63461538461538325, -2.499999999999998668, 29.75000000000000355 ) ) ;
#9883 = VECTOR ( 'NONE', #46227, 1000.000000000000000 ) ;
#9884 = CARTESIAN_POINT ( 'NONE',  ( -15.00798968950081758, -10.11255958852956027, 34.01340905677048454 ) ) ;
#9886 = CARTESIAN_POINT ( 'NONE',  ( -10.36543909703647337, -10.05730279482229683, 34.04704008940765902 ) ) ;
#9885 = B_SPLINE_CURVE_WITH_KNOTS ( 'NONE', 3,
 ( #9425, #43212, #76562, #8549, #8105, #42343, #23370, #36459, #77006, #36889 ),
 .UNSPECIFIED., .F., .F.,
 ( 4, 2, 2, 2, 4 ),
 ( 0.0007817359430256330417, 0.0009771253907250000096, 0.001172514838424367194, 0.001367904286123734162, 0.001563293733823101130 ),
 .UNSPECIFIED. ) ;
#9887 = CARTESIAN_POINT ( 'NONE',  ( 10.61538461538461675, -3.669653830205710676, 35.88435417666054406 ) ) ;
#9888 = CARTESIAN_POINT ( 'NONE',  ( 6.000000000000001776, -13.95598074871891292, 31.83374038241031911 ) ) ;
#9889 = B_SPLINE_CURVE_WITH_KNOTS ( 'NONE', 3,
 ( #41237, #68700, #1578, #248, #29064, #27711, #76799, #28154, #41679, #56519 ),
 .UNSPECIFIED., .F., .F.,
 ( 4, 2, 2, 2, 4 ),
 ( 0.000000000000000000, 0.0001954311564186865221, 0.0003908623128373730441, 0.0005862934692560595662, 0.0007817246256747460882 ),
 .UNSPECIFIED. ) ;
#9890 = CARTESIAN_POINT ( 'NONE',  ( 1.553300858899087311, -3.749999999999992006, 15.48437500000000178 ) ) ;
#9891 = VERTEX_POINT ( 'NONE', #85128 ) ;
#9892 = B_SPLINE_CURVE_WITH_KNOTS ( 'NONE', 3,
 ( #32396, #74272, #46350, #88695, #60304, #59861, #53094, #80597, #18882, #67073 ),
 .UNSPECIFIED., .F., .F.,
 ( 4, 2, 2, 2, 4 ),
 ( 0.0007817359430256326080, 0.0009771253907250047801, 0.001172514838424369796, 0.001367904286123735030, 0.001563293733823100046 ),
 .UNSPECIFIED. ) ;
#9893 = ORIENTED_EDGE ( 'NONE', *, *, #62074, .F. ) ;
#9894 = CARTESIAN_POINT ( 'NONE',  ( -7.976844449264153702, -11.37499894934982692, 33.29245874905763003 ) ) ;
#9895 = EDGE_LOOP ( 'NONE', ( #35199, #80636, #31357, #13832 ) ) ;
#9896 = CARTESIAN_POINT ( 'NONE',  ( -6.988347369037698265, -2.625532179533445198, 30.86335684631481513 ) ) ;
#9897 = CARTESIAN_POINT ( 'NONE',  ( -12.33101275977490197, -10.19071101563364756, 33.96452234770658407 ) ) ;
#9898 = CARTESIAN_POINT ( 'NONE',  ( -16.40382288478850725, -2.779195860258148798, 31.39871582349836743 ) ) ;
#9899 = DIRECTION ( 'NONE',  ( -0.000000000000000000, -0.1736481776669307198, -0.9848077530122080203 ) ) ;
#9900 = CARTESIAN_POINT ( 'NONE',  ( -3.749999999999997335, -7.500000000000021316, 20.09375000000000000 ) ) ;
#9901 = DIRECTION ( 'NONE',  ( -0.000000000000000000, -0.000000000000000000, -1.000000000000000000 ) ) ;
#9902 = EDGE_LOOP ( 'NONE', ( #44486, #12934, #46200, #87148, #46539 ) ) ;
#9903 = CARTESIAN_POINT ( 'NONE',  ( 3.903846153846154632, -7.500000000000001776, 34.75000000000000000 ) ) ;
#9905 = ORIENTED_EDGE ( 'NONE', *, *, #16269, .F. ) ;
#9904 = CARTESIAN_POINT ( 'NONE',  ( -1.161835843346973984, -9.332535724633405749, 34.40230450496446224 ) ) ;
#9906 = CARTESIAN_POINT ( 'NONE',  ( 4.153846153846154188, -13.04860791097971706, 34.73218667398347037 ) ) ;
#9907 = DIRECTION ( 'NONE',  ( -0.000000000000000000, 1.000000000000000000, 3.491481338843133355E-15 ) ) ;
#9908 = CARTESIAN_POINT ( 'NONE',  ( -18.00000000000012079, -6.835583212225971650, 34.95778746994575670 ) ) ;
#9909 = LINE ( 'NONE', #30191, #11679 ) ;
#9910 = CARTESIAN_POINT ( 'NONE',  ( -5.999999999999998224, -9.780366693483667717, 34.19971097300155094 ) ) ;
#9911 = CARTESIAN_POINT ( 'NONE',  ( 11.28843830116857383, -6.695914987888146541, 34.68535235679833306 ) ) ;
#9912 = DIRECTION ( 'NONE',  ( 0.000000000000000000, 0.000000000000000000, -1.000000000000000000 ) ) ;
#9913 = CARTESIAN_POINT ( 'NONE',  ( -0.06109907496450878162, -11.25000000000000000, 20.03311829374151287 ) ) ;
#9914 = ORIENTED_EDGE ( 'NONE', *, *, #12070, .F. ) ;
#9915 = CIRCLE ( 'NONE', #54528, 0.2500000000000002220 ) ;
#9916 = CARTESIAN_POINT ( 'NONE',  ( -9.070512820512819374, -4.000000000000000000, 29.75000000000000355 ) ) ;
#9917 = CARTESIAN_POINT ( 'NONE',  ( 1.384615384615265343, -6.026961402154118908, 34.52809138561165270 ) ) ;
#9918 = CARTESIAN_POINT ( 'NONE',  ( -17.29985003582992320, -4.762599654559227957, 34.23009711892697737 ) ) ;
#9919 = CARTESIAN_POINT ( 'NONE',  ( -0.06109907496451398579, -10.25000000000000178, 13.78311829374151287 ) ) ;
#9920 = CARTESIAN_POINT ( 'NONE',  ( -3.453695448285377445, -9.086856451489515152, 34.49173150075333183 ) ) ;
#9921 = CARTESIAN_POINT ( 'NONE',  ( -17.07692307692319744, -2.625532179533778709, 30.86335684631627174 ) ) ;
#9922 = VERTEX_POINT ( 'NONE', #15788 ) ;
#9923 = CARTESIAN_POINT ( 'NONE',  ( 1.799775606325937360E-14, -10.25000000000000000, 19.78125000000000000 ) ) ;
#9924 = FACE_OUTER_BOUND ( 'NONE', #12091, .T. ) ;
#9925 = EDGE_LOOP ( 'NONE', ( #21512, #56941, #37531, #39255 ) ) ;
#9926 = CARTESIAN_POINT ( 'NONE',  ( -3.903900744468110862, -2.589246495874657938, 31.60778113518102828 ) ) ;
#9927 = EDGE_LOOP ( 'NONE', ( #3857, #18015 ) ) ;
#9928 = CARTESIAN_POINT ( 'NONE',  ( 14.30769230769231015, -12.10708131394839349, 31.69288490824020244 ) ) ;
#9929 = CYLINDRICAL_SURFACE ( 'NONE', #49470, 0.2499999999999995559 ) ;
#9930 = ADVANCED_FACE ( 'NONE', ( #8588 ), #50867, .F. ) ;
#9931 = LINE ( 'NONE', #24780, #71382 ) ;
#9932 = ORIENTED_EDGE ( 'NONE', *, *, #70896, .T. ) ;
#9933 = CARTESIAN_POINT ( 'NONE',  ( -12.23852561744506851, -10.77377354290276124, 33.85451476688484718 ) ) ;
#9934 = VERTEX_POINT ( 'NONE', #69837 ) ;
#9935 = CARTESIAN_POINT ( 'NONE',  ( -2.531177232256634824, -12.11044203135681840, 32.26167407432752299 ) ) ;
#9936 = ORIENTED_EDGE ( 'NONE', *, *, #49343, .T. ) ;
#9937 = VECTOR ( 'NONE', #73104, 999.9999999999998863 ) ;
#9938 = CARTESIAN_POINT ( 'NONE',  ( 12.33139049180676849, -12.15440758774515473, 32.17923288041532004 ) ) ;
#9939 = CARTESIAN_POINT ( 'NONE',  ( -0.4615384615385826339, -4.481592998941358097, 33.73612834414048933 ) ) ;
#9940 = ORIENTED_EDGE ( 'NONE', *, *, #24872, .F. ) ;
#9941 = CARTESIAN_POINT ( 'NONE',  ( -5.933931648997561759, -11.16473453929635440, 33.15142922261926373 ) ) ;
#9942 = CYLINDRICAL_SURFACE ( 'NONE', #66582, 0.2499999999999998890 ) ;
#9943 = CARTESIAN_POINT ( 'NONE',  ( -11.76194648218548267, -2.847400154188067578, 31.58180166144859058 ) ) ;
#9944 = AXIS2_PLACEMENT_3D ( 'NONE', #70571, #83659, #76887 ) ;
#9945 = VECTOR ( 'NONE', #66875, 1000.000000000000000 ) ;
#9946 = CARTESIAN_POINT ( 'NONE',  ( 4.153846153846154188, -2.708943851104267164, 35.45975837776705220 ) ) ;
#9947 = CARTESIAN_POINT ( 'NONE',  ( -13.31854805126531005, -11.91647553114624358, 32.58852847137148245 ) ) ;
#9948 = ADVANCED_FACE ( 'NONE', ( #78352 ), #1817, .F. ) ;
#9949 = EDGE_CURVE ( 'NONE', #11048, #19576, #81529, .T. ) ;
#9950 = ORIENTED_EDGE ( 'NONE', *, *, #67195, .T. ) ;
#9951 = EDGE_LOOP ( 'NONE', ( #59721, #44233, #57671, #86222 ) ) ;
#9952 = FACE_BOUND ( 'NONE', #20310, .T. ) ;
#9953 = ORIENTED_EDGE ( 'NONE', *, *, #19460, .F. ) ;
#9955 = ORIENTED_EDGE ( 'NONE', *, *, #57563, .F. ) ;
#9954 = DIRECTION ( 'NONE',  ( -1.000000000000000000, -0.000000000000000000, -0.000000000000000000 ) ) ;
#9956 = DIRECTION ( 'NONE',  ( -0.000000000000000000, -0.7660444431189791237, -0.6427876096865379196 ) ) ;
#9957 = CARTESIAN_POINT ( 'NONE',  ( 7.846153846153725020, -11.94971097300221174, 32.03036669348237098 ) ) ;
#9958 = ORIENTED_EDGE ( 'NONE', *, *, #57238, .F. ) ;
#9959 = ORIENTED_EDGE ( 'NONE', *, *, #10586, .T. ) ;
#9960 = ORIENTED_EDGE ( 'NONE', *, *, #64405, .F. ) ;
#9961 = CARTESIAN_POINT ( 'NONE',  ( -1.514762594053605360, -11.93770438780619259, 32.05411857736982029 ) ) ;
#9962 = ORIENTED_EDGE ( 'NONE', *, *, #43391, .T. ) ;
#9963 = B_SPLINE_CURVE_WITH_KNOTS ( 'NONE', 3,
 ( #54852, #55288, #13859, #41340, #21051, #68808, #76004, #356, #14305, #28712 ),
 .UNSPECIFIED., .F., .F.,
 ( 4, 2, 2, 2, 4 ),
 ( 0.000000000000000000, 0.0001954311564186867389, 0.0003908623128373734778, 0.0005862934692560602167, 0.0007817246256747469556 ),
 .UNSPECIFIED. ) ;
#9964 = CARTESIAN_POINT ( 'NONE',  ( 2.307692307692309264, -4.098570777380720287, 33.41473453929634729 ) ) ;
#9965 = CARTESIAN_POINT ( 'NONE',  ( 3.930919194939304084, -12.64616026154729411, 30.79003144601913533 ) ) ;
#9966 = CIRCLE ( 'NONE', #86254, 0.2500000000000002220 ) ;
#9967 = CYLINDRICAL_SURFACE ( 'NONE', #41115, 4.000000000000000000 ) ;
#9968 = FACE_BOUND ( 'NONE', #15268, .T. ) ;
#9969 = ORIENTED_EDGE ( 'NONE', *, *, #88741, .F. ) ;
#9970 = CARTESIAN_POINT ( 'NONE',  ( 13.38461538461526601, -9.442884908241554243, 34.35708131394783038 ) ) ;
#9971 = CYLINDRICAL_SURFACE ( 'NONE', #69008, 0.2499999999999994726 ) ;
#9972 = CARTESIAN_POINT ( 'NONE',  ( 6.000000000000001776, -2.538708090699994813, 30.37095296980875503 ) ) ;
#9973 = CARTESIAN_POINT ( 'NONE',  ( 11.60371710973756443, -8.613356846314928816, 34.62446782046653482 ) ) ;
#9974 = ORIENTED_EDGE ( 'NONE', *, *, #65701, .F. ) ;
#9975 = CARTESIAN_POINT ( 'NONE',  ( 10.03846153846153832, -1.926643599941765039, 29.65000000000000213 ) ) ;
#9976 = ORIENTED_EDGE ( 'NONE', *, *, #50449, .F. ) ;
#9977 = B_SPLINE_CURVE_WITH_KNOTS ( 'NONE', 3,
 ( #30830, #29513, #77244, #56969, #29954, #58300, #85792, #15553, #57411, #43021 ),
 .UNSPECIFIED., .F., .F.,
 ( 4, 2, 2, 2, 4 ),
 ( 0.0007817359430256365111, 0.0009771253907250043464, 0.001172514838424372399, 0.001367904286123740234, 0.001563293733823108069 ),
 .UNSPECIFIED. ) ;
#9978 = ORIENTED_EDGE ( 'NONE', *, *, #47230, .T. ) ;
#9980 = CARTESIAN_POINT ( 'NONE',  ( 5.933916589044121004, -3.050289026998445951, 32.03036669348365706 ) ) ;
#9979 = CYLINDRICAL_SURFACE ( 'NONE', #11620, 0.2500000000000008882 ) ;
#9981 = FACE_OUTER_BOUND ( 'NONE', #43949, .T. ) ;
#9982 = FACE_OUTER_BOUND ( 'NONE', #9214, .T. ) ;
#9983 = CARTESIAN_POINT ( 'NONE',  ( 16.82692307692307665, -7.433931650972299465, 34.75000000000000711 ) ) ;
#9984 = CARTESIAN_POINT ( 'NONE',  ( -2.531177251416254936, -10.11188796281391511, 34.01382737946119050 ) ) ;
#9985 = VERTEX_POINT ( 'NONE', #4485 ) ;
#9986 = DIRECTION ( 'NONE',  ( 0.000000000000000000, 0.000000000000000000, 1.000000000000000000 ) ) ;
#9987 = CARTESIAN_POINT ( 'NONE',  ( -0.3310130233048161896, -3.625058011473227815, 33.29252011169590020 ) ) ;
#9988 = CARTESIAN_POINT ( 'NONE',  ( 11.78846153846297362, -7.500000000000155431, 34.75000000000007105 ) ) ;
#9989 = CARTESIAN_POINT ( 'NONE',  ( -13.45069776397551742, -12.62096338111211580, 30.90682066428152908 ) ) ;
#9990 = EDGE_LOOP ( 'NONE', ( #5081, #33228, #44372, #84536, #51679, #5873 ) ) ;
#9991 = ORIENTED_EDGE ( 'NONE', *, *, #43239, .F. ) ;
#9992 = FACE_BOUND ( 'NONE', #46430, .T. ) ;
#9993 = AXIS2_PLACEMENT_3D ( 'NONE', #19318, #53983, #19758 ) ;
#9994 = AXIS2_PLACEMENT_3D ( 'NONE', #56497, #42983, #57818 ) ;
#9995 = EDGE_LOOP ( 'NONE', ( #58558, #84278, #85540, #81521 ) ) ;
#9996 = CARTESIAN_POINT ( 'NONE',  ( -1.384615384615506484, -5.941354392335915335, 34.76329471203413846 ) ) ;
#9997 = CARTESIAN_POINT ( 'NONE',  ( -6.988833725591232060, -7.249945686854186278, 34.74374336980224598 ) ) ;
#9998 = VERTEX_POINT ( 'NONE', #65726 ) ;
#9999 = CARTESIAN_POINT ( 'NONE',  ( -7.623374304885436104, -4.387253974876677454, 33.66317474335728832 ) ) ;
#10000 = CARTESIAN_POINT ( 'NONE',  ( 6.857806477116147548, -10.90142922261923886, 33.41473453929638993 ) ) ;
#10001 = CARTESIAN_POINT ( 'NONE',  ( 1.384615384615265343, -2.625532179533778709, 30.86335684631627174 ) ) ;
#10002 = CARTESIAN_POINT ( 'NONE',  ( 4.153846153846154188, -6.343179335718451384, 34.87096338111211935 ) ) ;
#10003 = ORIENTED_EDGE ( 'NONE', *, *, #60963, .F. ) ;
#10004 = EDGE_CURVE ( 'NONE', #17825, #69315, #86012, .T. ) ;
#10005 = VECTOR ( 'NONE', #3773, 1000.000000000000000 ) ;
#10006 = CARTESIAN_POINT ( 'NONE',  ( 3.262820512820510999, -11.00000000000000000, 29.75000000000000355 ) ) ;
#10007 = EDGE_LOOP ( 'NONE', ( #26592, #30001 ) ) ;
#10008 = AXIS2_PLACEMENT_3D ( 'NONE', #13367, #12927, #82727 ) ;
#10010 = ORIENTED_EDGE ( 'NONE', *, *, #56011, .T. ) ;
#10009 = LINE ( 'NONE', #2797, #85627 ) ;
#10011 = DIRECTION ( 'NONE',  ( 0.000000000000000000, 0.000000000000000000, 1.000000000000000000 ) ) ;
#10012 = EDGE_CURVE ( 'NONE', #74750, #5929, #4021, .T. ) ;
#10013 = CARTESIAN_POINT ( 'NONE',  ( 4.153846153846154188, -6.386643153685126251, 34.62446782046654192 ) ) ;
#10014 = CARTESIAN_POINT ( 'NONE',  ( -12.46153846153858424, -10.33852847137269571, 34.16647553114546554 ) ) ;
#10015 = DIRECTION ( 'NONE',  ( -0.000000000000000000, -0.7660444431189791237, -0.6427876096865379196 ) ) ;
#10016 = DIRECTION ( 'NONE',  ( -0.000000000000000000, 0.3420201433256694346, -0.9396926207859080948 ) ) ;
#10017 = CARTESIAN_POINT ( 'NONE',  ( 12.46153846153833911, -5.941354392335915335, 34.76329471203413846 ) ) ;
#10018 = CARTESIAN_POINT ( 'NONE',  ( 2.724691934501250135, -8.700186371490531201, 16.04874329374151287 ) ) ;
#10019 = VERTEX_POINT ( 'NONE', #37816 ) ;
#10020 = CARTESIAN_POINT ( 'NONE',  ( -14.98071491913091791, -3.627508038966690496, 32.91356715214248396 ) ) ;
#10021 = CARTESIAN_POINT ( 'NONE',  ( -14.30769230769230660, -1.509761064869970415, 31.06009739812519044 ) ) ;
#10022 = ADVANCED_FACE ( 'NONE', ( #18448 ), #53100, .F. ) ;
#10023 = ORIENTED_EDGE ( 'NONE', *, *, #29186, .T. ) ;
#10024 = ORIENTED_EDGE ( 'NONE', *, *, #56308, .F. ) ;
#10025 = CARTESIAN_POINT ( 'NONE',  ( 12.46153846153846168, -12.78798330534102767, 29.49999999999997868 ) ) ;
#10026 = CARTESIAN_POINT ( 'NONE',  ( -14.30769230769242917, -2.657715359629662544, 31.77849191805970364 ) ) ;
#10027 = EDGE_CURVE ( 'NONE', #41438, #39109, #958, .T. ) ;
#10028 = CARTESIAN_POINT ( 'NONE',  ( 3.100622021331010281, -10.19110544564092002, 33.96427741523702792 ) ) ;
#10029 = CARTESIAN_POINT ( 'NONE',  ( 0.4615384615383382183, -5.941354392335915335, 34.76329471203413846 ) ) ;
#10030 = CARTESIAN_POINT ( 'NONE',  ( 13.25392478150507891, -2.845849958028613624, 32.17971566917920967 ) ) ;
#10031 = CARTESIAN_POINT ( 'NONE',  ( 16.15384615384615330, -3.322132147404559976, 32.92929555188717927 ) ) ;
#10032 = FACE_OUTER_BOUND ( 'NONE', #51511, .T. ) ;
#10033 = ORIENTED_EDGE ( 'NONE', *, *, #30398, .T. ) ;
#10034 = CARTESIAN_POINT ( 'NONE',  ( -4.087777802843714170, -5.557115091759786019, 34.35708131394839882 ) ) ;
#10035 = CARTESIAN_POINT ( 'NONE',  ( -16.15384615384615330, -2.249999999999998668, 29.75000000000001776 ) ) ;
#10036 = ADVANCED_FACE ( 'NONE', ( #73843 ), #72939, .F. ) ;
#10037 = CARTESIAN_POINT ( 'NONE',  ( -9.019207513279360100, -11.47974371597208076, 33.17467449705390692 ) ) ;
#10038 = CYLINDRICAL_SURFACE ( 'NONE', #47893, 0.2499999999999994726 ) ;
#10040 = ORIENTED_EDGE ( 'NONE', *, *, #23491, .T. ) ;
#10039 = VECTOR ( 'NONE', #38712, 1000.000000000000114 ) ;
#10041 = CARTESIAN_POINT ( 'NONE',  ( -19.50000000000000000, -3.499999999999999556, 29.75000000000000355 ) ) ;
#10042 = B_SPLINE_CURVE_WITH_KNOTS ( 'NONE', 3,
 ( #39049, #58851, #86357, #31842, #80020, #11570, #66508, #73723, #12017, #39494 ),
 .UNSPECIFIED., .F., .F.,
 ( 4, 2, 2, 2, 4 ),
 ( 0.000000000000000000, 0.0001954311564186878773, 0.0003908623128373757546, 0.0005862934692560635777, 0.0007817246256747515092 ),
 .UNSPECIFIED. ) ;
#10043 = VERTEX_POINT ( 'NONE', #38267 ) ;
#10044 = CARTESIAN_POINT ( 'NONE',  ( -17.86920955903304886, -8.191423895709844416, 34.95447573519442130 ) ) ;
#10045 = CARTESIAN_POINT ( 'NONE',  ( -12.94230769230769340, -4.000000000000000000, 29.75000000000000355 ) ) ;
#10046 = CARTESIAN_POINT ( 'NONE',  ( 12.71148397988660328, -10.76462480002816235, 33.53768742498949962 ) ) ;
#10047 = ORIENTED_EDGE ( 'NONE', *, *, #42146, .T. ) ;
#10048 = CARTESIAN_POINT ( 'NONE',  ( 12.46153846153846168, -10.67929555188718282, 33.92786785259544047 ) ) ;
#10049 = CARTESIAN_POINT ( 'NONE',  ( 10.48523740594639087, -3.817052484675422797, 33.13202310037935661 ) ) ;
#10050 = CARTESIAN_POINT ( 'NONE',  ( -17.14300648787895653, -3.513871655860377086, 32.76840700105978499 ) ) ;
#10051 = DIRECTION ( 'NONE',  ( 0.000000000000000000, 0.000000000000000000, 1.000000000000000000 ) ) ;
#10052 = EDGE_CURVE ( 'NONE', #78478, #17849, #59425, .T. ) ;
#10053 = EDGE_LOOP ( 'NONE', ( #13055, #72477 ) ) ;
#10054 = AXIS2_PLACEMENT_3D ( 'NONE', #69903, #77107, #76212 ) ;
#10055 = CARTESIAN_POINT ( 'NONE',  ( -17.07692307692319744, -2.892918686052165622, 31.69288490824153470 ) ) ;
#10056 = EDGE_CURVE ( 'NONE', #1686, #20644, #58974, .T. ) ;
#10057 = ORIENTED_EDGE ( 'NONE', *, *, #1837, .F. ) ;
#10058 = B_SPLINE_CURVE_WITH_KNOTS ( 'NONE', 3,
 ( #30848, #78594, #62519, #24092, #41833, #1271, #16897, #44349, #24537, #10145 ),
 .UNSPECIFIED., .F., .F.,
 ( 4, 2, 2, 2, 4 ),
 ( 0.0007817359430256253438, 0.0009771253907249898181, 0.001172514838424354401, 0.001367904286123718983, 0.001563293733823083566 ),
 .UNSPECIFIED. ) ;
#10059 = DIRECTION ( 'NONE',  ( 0.000000000000000000, 0.1736481776669267785, -0.9848077530122087975 ) ) ;
#10060 = CIRCLE ( 'NONE', #76211, 0.2500000000000002220 ) ;
#10061 = AXIS2_PLACEMENT_3D ( 'NONE', #79322, #52281, #38332 ) ;
#10062 = DIRECTION ( 'NONE',  ( -0.000000000000000000, 1.000000000000000000, -0.000000000000000000 ) ) ;
#10063 = EDGE_CURVE ( 'NONE', #63601, #20057, #84724, .T. ) ;
#10064 = DIRECTION ( 'NONE',  ( 0.000000000000000000, 0.000000000000000000, 1.000000000000000000 ) ) ;
#10065 = EDGE_CURVE ( 'NONE', #32856, #39715, #51754, .T. ) ;
#10066 = DIRECTION ( 'NONE',  ( -0.000000000000000000, -0.9848077530122085754, -0.1736481776669273613 ) ) ;
#10067 = CARTESIAN_POINT ( 'NONE',  ( 9.468822748583747284, -8.496056993536548418, 34.65000542017679663 ) ) ;
#10068 = VECTOR ( 'NONE', #29097, 1000.000000000000000 ) ;
#10069 = AXIS2_PLACEMENT_3D ( 'NONE', #4557, #60385, #26163 ) ;
#10070 = VERTEX_POINT ( 'NONE', #79257 ) ;
#10071 = EDGE_LOOP ( 'NONE', ( #25690, #61515 ) ) ;
#10072 = AXIS2_PLACEMENT_3D ( 'NONE', #57790, #8291, #51008 ) ;
#10073 = EDGE_LOOP ( 'NONE', ( #1124, #24464, #29061, #70869 ) ) ;
#10074 = ORIENTED_EDGE ( 'NONE', *, *, #43323, .F. ) ;
#10075 = DIRECTION ( 'NONE',  ( -0.000000000000000000, -0.6427876096865404731, -0.7660444431189771253 ) ) ;
#10076 = DIRECTION ( 'NONE',  ( -0.000000000000000000, 0.5000000000000011102, -0.8660254037844381525 ) ) ;
#10077 = CARTESIAN_POINT ( 'NONE',  ( -15.09997742294444301, -8.999086150933475636, 34.52020707165672775 ) ) ;
#10078 = DIRECTION ( 'NONE',  ( -0.000000000000000000, 1.000000000000000000, -0.000000000000000000 ) ) ;
#10079 = CARTESIAN_POINT ( 'NONE',  ( -8.769230769230768274, -3.937682226553329556, 33.60647404775216529 ) ) ;
#10080 = CARTESIAN_POINT ( 'NONE',  ( 0.7114839798866023912, -5.057305518903949526, 34.11320923018887896 ) ) ;
#10081 = DIRECTION ( 'NONE',  ( -0.000000000000000000, 0.5000000000000011102, -0.8660254037844380415 ) ) ;
#10082 = CARTESIAN_POINT ( 'NONE',  ( -18.00000000000000000, -6.386643153685127139, 34.62446782046654192 ) ) ;
#10083 = ORIENTED_EDGE ( 'NONE', *, *, #39056, .F. ) ;
#10084 = VERTEX_POINT ( 'NONE', #66633 ) ;
#10085 = VERTEX_POINT ( 'NONE', #4937 ) ;
#10087 = ORIENTED_EDGE ( 'NONE', *, *, #88235, .F. ) ;
#10086 = FACE_OUTER_BOUND ( 'NONE', #29914, .T. ) ;
#10089 = CARTESIAN_POINT ( 'NONE',  ( -16.37677237136229991, -9.886141570436013382, 34.14413921362392301 ) ) ;
#10088 = CARTESIAN_POINT ( 'NONE',  ( 16.15384615384603251, -11.94971097300221174, 32.03036669348237098 ) ) ;
#10090 = B_SPLINE_CURVE_WITH_KNOTS ( 'NONE', 3,
 ( #1660, #22368, #84092, #77314, #16497, #84528, #71430, #63351, #29145, #63791 ),
 .UNSPECIFIED., .F., .F.,
 ( 4, 2, 2, 2, 4 ),
 ( 0.000000000000000000, 0.0001954339857564071762, 0.0003908679715128143524, 0.0005863019572692215828, 0.0007817359430256287049 ),
 .UNSPECIFIED. ) ;
#10091 = ADVANCED_FACE ( 'NONE', ( #17556 ), #18889, .F. ) ;
#10092 = DIRECTION ( 'NONE',  ( 0.000000000000000000, 0.000000000000000000, -1.000000000000000000 ) ) ;
#10093 = CARTESIAN_POINT ( 'NONE',  ( -16.15384615384615330, -4.098570777380720287, 33.41473453929634729 ) ) ;
#10094 = ORIENTED_EDGE ( 'NONE', *, *, #27779, .F. ) ;
#10095 = VECTOR ( 'NONE', #54775, 1000.000000000000000 ) ;
#10096 = ORIENTED_EDGE ( 'NONE', *, *, #86397, .F. ) ;
#10097 = CARTESIAN_POINT ( 'NONE',  ( -6.923076923076922462, -1.951392089020283160, 34.73218667398347748 ) ) ;
#10098 = ORIENTED_EDGE ( 'NONE', *, *, #11331, .T. ) ;
#10099 = FACE_BOUND ( 'NONE', #86598, .T. ) ;
#10100 = CARTESIAN_POINT ( 'NONE',  ( 3.230769230769231726, -2.486705287966279876, 31.30864560766543647 ) ) ;
#10101 = CARTESIAN_POINT ( 'NONE',  ( 15.90382291655318880, -6.695914987888146541, 34.68535235679833306 ) ) ;
#10102 = EDGE_LOOP ( 'NONE', ( #57749, #17846, #10785, #28814 ) ) ;
#10103 = CARTESIAN_POINT ( 'NONE',  ( -1.161602540521988969, -5.582272713120728369, 34.63742843783360570 ) ) ;
#10104 = CARTESIAN_POINT ( 'NONE',  ( 16.21991450484859598, -4.098570777380720287, 33.41473453929635440 ) ) ;
#10105 = CARTESIAN_POINT ( 'NONE',  ( 5.076923076922954969, -2.625532179533778709, 30.86335684631627174 ) ) ;
#10106 = EDGE_LOOP ( 'NONE', ( #15957, #53429, #62234, #11666 ) ) ;
#10107 = CYLINDRICAL_SURFACE ( 'NONE', #88884, 0.2500000000000002220 ) ;
#10108 = CARTESIAN_POINT ( 'NONE',  ( 1.384615384615264011, -2.657715359629662544, 31.77849191805970364 ) ) ;
#10109 = EDGE_CURVE ( 'NONE', #88311, #16692, #87365, .T. ) ;
#10110 = ORIENTED_EDGE ( 'NONE', *, *, #22267, .T. ) ;
#10111 = ADVANCED_FACE ( 'NONE', ( #33735 ), #61189, .F. ) ;
#10112 = FACE_OUTER_BOUND ( 'NONE', #33230, .T. ) ;
#10113 = DIRECTION ( 'NONE',  ( -0.000000000000000000, -0.8660254037844397068, -0.4999999999999978906 ) ) ;
#10114 = ORIENTED_EDGE ( 'NONE', *, *, #17333, .T. ) ;
#10115 = CYLINDRICAL_SURFACE ( 'NONE', #67444, 0.2500000000000002220 ) ;
#10116 = CARTESIAN_POINT ( 'NONE',  ( -2.307692307692305711, -13.57706302396349152, 30.56769352161908060 ) ) ;
#10117 = DIRECTION ( 'NONE',  ( -0.000000000000000000, 0.9848077530122085754, -0.1736481776669273613 ) ) ;
#10118 = CARTESIAN_POINT ( 'NONE',  ( 7.596153846153847589, -7.433931650972299465, 34.75000000000000000 ) ) ;
#10119 = CARTESIAN_POINT ( 'NONE',  ( -18.00000000000012079, -6.879047030192663392, 34.71129190930017927 ) ) ;
#10120 = CARTESIAN_POINT ( 'NONE',  ( 17.07692307692295586, -5.094484230521993062, 34.41647553114689373 ) ) ;
#10122 = CARTESIAN_POINT ( 'NONE',  ( 2.557746619330623972, -9.943054286541407549, 34.11300777759954883 ) ) ;
#10121 = DIRECTION ( 'NONE',  ( 0.000000000000000000, 0.7660444431189807890, 0.6427876096865361433 ) ) ;
#10123 = VECTOR ( 'NONE', #7668, 1000.000000000000000 ) ;
#10124 = CARTESIAN_POINT ( 'NONE',  ( -15.93106661257773915, -11.89424750095246175, 32.13594075562311758 ) ) ;
#10126 = CARTESIAN_POINT ( 'NONE',  ( -10.83886955910856464, -8.496056993536548418, 34.65000542017679663 ) ) ;
#10125 = CARTESIAN_POINT ( 'NONE',  ( -12.71153846153846168, -2.249999999999998668, 29.75000000000000355 ) ) ;
#10127 = CARTESIAN_POINT ( 'NONE',  ( -5.777220458731586739, -12.44528174975671853, 30.48912976160716681 ) ) ;
#10128 = CARTESIAN_POINT ( 'NONE',  ( 1.901340078031349856, -5.512252781505337929, 20.31063170625848713 ) ) ;
#10129 = ORIENTED_EDGE ( 'NONE', *, *, #18407, .T. ) ;
#10130 = CARTESIAN_POINT ( 'NONE',  ( 18.13079180782478872, -11.71459661697925903, 32.44059661609676937 ) ) ;
#10131 = ORIENTED_EDGE ( 'NONE', *, *, #71669, .T. ) ;
#10132 = VECTOR ( 'NONE', #10795, 1000.000000000000227 ) ;
#10133 = VECTOR ( 'NONE', #50699, 1000.000000000000114 ) ;
#10134 = DIRECTION ( 'NONE',  ( 0.000000000000000000, 0.000000000000000000, -1.000000000000000000 ) ) ;
#10135 = ADVANCED_FACE ( 'NONE', ( #60756 ), #68843, .F. ) ;
#10136 = VERTEX_POINT ( 'NONE', #6270 ) ;
#10137 = B_SPLINE_CURVE_WITH_KNOTS ( 'NONE', 3,
 ( #65941, #51518, #66844, #38038, #18669, #4250, #25413, #17774, #3801, #52873 ),
 .UNSPECIFIED., .F., .F.,
 ( 4, 2, 2, 2, 4 ),
 ( 0.0007817359430256392216, 0.0009771253907250080327, 0.001172514838424376952, 0.001367904286123745872, 0.001563293733823114791 ),
 .UNSPECIFIED. ) ;
#10138 = CARTESIAN_POINT ( 'NONE',  ( 15.93036121012220185, -11.41268669641499756, 32.86336882939238535 ) ) ;
#10139 = ORIENTED_EDGE ( 'NONE', *, *, #53594, .F. ) ;
#10140 = CARTESIAN_POINT ( 'NONE',  ( -7.911424292114620727, -6.026961402152685388, 34.52809138561120506 ) ) ;
#10141 = CARTESIAN_POINT ( 'NONE',  ( -1.901340078031346525, -9.487747218494661183, 25.93563170625849423 ) ) ;
#10142 = CARTESIAN_POINT ( 'NONE',  ( 3.164686851409094004, -2.292212530054419606, 30.41441678777542634 ) ) ;
#10143 = ADVANCED_FACE ( 'NONE', ( #26539 ), #47687, .F. ) ;
#10144 = AXIS2_PLACEMENT_3D ( 'NONE', #24645, #51197, #44021 ) ;
#10145 = CARTESIAN_POINT ( 'NONE',  ( 9.692307692307695177, -11.16473453929635440, 33.15142922261926373 ) ) ;
#10146 = CARTESIAN_POINT ( 'NONE',  ( 13.63456079399342791, -2.986452184633680673, 32.43230066228895225 ) ) ;
#10147 = FACE_OUTER_BOUND ( 'NONE', #88297, .T. ) ;
#10148 = AXIS2_PLACEMENT_3D ( 'NONE', #25944, #53409, #5673 ) ;
#10149 = CARTESIAN_POINT ( 'NONE',  ( 12.46153846153833911, -11.06231777344772027, 33.60647404775119895 ) ) ;
#10150 = DIRECTION ( 'NONE',  ( -0.000000000000000000, 0.7660444431189791237, -0.6427876096865379196 ) ) ;
#10151 = DIRECTION ( 'NONE',  ( -0.000000000000000000, -0.000000000000000000, -1.000000000000000000 ) ) ;
#10152 =( GEOMETRIC_REPRESENTATION_CONTEXT ( 3 ) GLOBAL_UNCERTAINTY_ASSIGNED_CONTEXT ( ( #28487 ) ) GLOBAL_UNIT_ASSIGNED_CONTEXT ( ( #73982, #12270, #74417 ) ) REPRESENTATION_CONTEXT ( 'NONE', 'WORKASPACE' ) );
#10153 = CARTESIAN_POINT ( 'NONE',  ( -2.651650429449535551, -10.15165042944956753, 14.93750000000000000 ) ) ;
#10154 = CARTESIAN_POINT ( 'NONE',  ( -6.416666666666667851, -3.499999999999999556, 29.75000000000000355 ) ) ;
#10155 = DIRECTION ( 'NONE',  ( -0.000000000000000000, -0.1736481776669307198, -0.9848077530122080203 ) ) ;
#10156 = EDGE_CURVE ( 'NONE', #83859, #75335, #7332, .T. ) ;
#10157 = DIRECTION ( 'NONE',  ( 0.000000000000000000, 0.8660254037844377084, 0.5000000000000015543 ) ) ;
#10158 = CARTESIAN_POINT ( 'NONE',  ( 2.651650429449569302, -10.15165042944953733, 18.37500000000000355 ) ) ;
#10159 = ORIENTED_EDGE ( 'NONE', *, *, #74577, .F. ) ;
#10160 = DIRECTION ( 'NONE',  ( -1.000000000000000000, 0.000000000000000000, -0.000000000000000000 ) ) ;
#10161 = CARTESIAN_POINT ( 'NONE',  ( 16.08776274289027342, -12.10708131394839349, 31.69288490824020244 ) ) ;
#10162 = CYLINDRICAL_SURFACE ( 'NONE', #36827, 0.2500000000000009437 ) ;
#10163 = CARTESIAN_POINT ( 'NONE',  ( -3.230769230769229949, -2.249999999999998668, 29.75000000000001776 ) ) ;
#10164 = EDGE_CURVE ( 'NONE', #23513, #26351, #44856, .T. ) ;
#10165 = CARTESIAN_POINT ( 'NONE',  ( 17.14299041027315695, -12.34228464037088813, 31.77849191805839268 ) ) ;
#10166 = CARTESIAN_POINT ( 'NONE',  ( -14.30769230769230660, -3.937682226553329556, 33.60647404775216529 ) ) ;
#10167 = EDGE_CURVE ( 'NONE', #10019, #64009, #11639, .T. ) ;
#10168 = EDGE_LOOP ( 'NONE', ( #46737, #80657 ) ) ;
#10169 = CARTESIAN_POINT ( 'NONE',  ( 7.623226887246995709, -2.889293201056495786, 32.26117774369186009 ) ) ;
#10170 = VERTEX_POINT ( 'NONE', #395 ) ;
#10171 = VECTOR ( 'NONE', #53782, 1000.000000000000227 ) ;
#10172 = EDGE_CURVE ( 'NONE', #13065, #38188, #3001, .T. ) ;
#10173 = ORIENTED_EDGE ( 'NONE', *, *, #52088, .F. ) ;
#10174 = CARTESIAN_POINT ( 'NONE',  ( -9.442253272394237840, -2.920487667080175598, 32.31805714834170828 ) ) ;
#10175 = CARTESIAN_POINT ( 'NONE',  ( -6.923076923076922462, -5.471508081941601098, 34.59228464037088457 ) ) ;
#10176 = CARTESIAN_POINT ( 'NONE',  ( -15.48074597481782178, -10.82459398097509329, 33.81372124010185587 ) ) ;
#10177 = ADVANCED_FACE ( 'NONE', ( #46802 ), #55325, .F. ) ;
#10178 = CARTESIAN_POINT ( 'NONE',  ( 11.53846153846153832, -9.058645607665452459, 34.76329471203371924 ) ) ;
#10179 = CARTESIAN_POINT ( 'NONE',  ( 13.16168842570853492, -5.582147617184174848, 34.63737895849758530 ) ) ;
#10180 = ORIENTED_EDGE ( 'NONE', *, *, #16276, .T. ) ;
#10181 = CARTESIAN_POINT ( 'NONE',  ( -14.05774678934416499, -12.22109172314383052, 31.39792113162168263 ) ) ;
#10182 = ORIENTED_EDGE ( 'NONE', *, *, #6214, .T. ) ;
#10183 = ORIENTED_EDGE ( 'NONE', *, *, #38518, .T. ) ;
#10184 = VECTOR ( 'NONE', #42027, 1000.000000000000000 ) ;
#10185 = CARTESIAN_POINT ( 'NONE',  ( 18.25005441991345378, -2.318338780012835443, 30.59689888758630616 ) ) ;
#10186 = LINE ( 'NONE', #16496, #37308 ) ;
#10187 = ADVANCED_FACE ( 'NONE', ( #76040 ), #830, .F. ) ;
#10188 = B_SPLINE_CURVE_WITH_KNOTS ( 'NONE', 3,
 ( #25042, #3872, #87654, #85861, #11088, #39464, #73235, #25930, #10203, #37664 ),
 .UNSPECIFIED., .F., .F.,
 ( 4, 2, 2, 2, 4 ),
 ( 0.0007817359430256323911, 0.0009771253907249991422, 0.001172514838424365893, 0.001367904286123732861, 0.001563293733823099612 ),
 .UNSPECIFIED. ) ;
#10189 = CARTESIAN_POINT ( 'NONE',  ( -16.21992956480203318, -4.098570777380720287, 33.41473453929634729 ) ) ;
#10190 = VECTOR ( 'NONE', #56637, 1000.000000000000000 ) ;
#10191 = CARTESIAN_POINT ( 'NONE',  ( -24.00000000000000000, -5.499999999999981348, 27.75000000000000000 ) ) ;
#10192 = ADVANCED_FACE ( 'NONE', ( #15681 ), #57095, .F. ) ;
#10193 = CARTESIAN_POINT ( 'NONE',  ( -17.01166750564705410, -3.300289026998475261, 32.46337939537591666 ) ) ;
#10194 = CARTESIAN_POINT ( 'NONE',  ( 17.75002326905764605, -8.303909089506435137, 34.68538101551103381 ) ) ;
#10195 = ORIENTED_EDGE ( 'NONE', *, *, #82259, .T. ) ;
#10196 = VERTEX_POINT ( 'NONE', #36826 ) ;
#10197 = CARTESIAN_POINT ( 'NONE',  ( -3.750000000000008438, -5.946699141100917352, 21.42187500000000000 ) ) ;
#10198 = AXIS2_PLACEMENT_3D ( 'NONE', #51631, #79136, #17437 ) ;
#10199 = ORIENTED_EDGE ( 'NONE', *, *, #54161, .T. ) ;
#10201 = VERTEX_POINT ( 'NONE', #49894 ) ;
#10200 = CARTESIAN_POINT ( 'NONE',  ( -13.63463860883683942, -5.765609946408404518, 34.70566812827425451 ) ) ;
#10202 = EDGE_CURVE ( 'NONE', #64231, #11769, #86291, .T. ) ;
#10203 = CARTESIAN_POINT ( 'NONE',  ( 7.912222197156284054, -12.37446782046654192, 30.86335684631486842 ) ) ;
#10204 = CARTESIAN_POINT ( 'NONE',  ( 6.223011351612852238, -12.39991518177334129, 30.74647679643404530 ) ) ;
#10205 = EDGE_CURVE ( 'NONE', #76909, #21625, #63854, .T. ) ;
#10206 = LINE ( 'NONE', #5221, #68146 ) ;
#10207 = ORIENTED_EDGE ( 'NONE', *, *, #40990, .F. ) ;
#10208 = FACE_OUTER_BOUND ( 'NONE', #83814, .T. ) ;
#10209 = ORIENTED_EDGE ( 'NONE', *, *, #50931, .F. ) ;
#10210 = EDGE_CURVE ( 'NONE', #62470, #26559, #62952, .T. ) ;
#10211 = DIRECTION ( 'NONE',  ( 1.000000000000000000, 0.000000000000000000, 0.000000000000000000 ) ) ;
#10212 = CARTESIAN_POINT ( 'NONE',  ( 19.00000000000000000, -11.50000000000000000, 29.75000000000000355 ) ) ;
#10213 = LINE ( 'NONE', #16081, #45156 ) ;
#10215 = CARTESIAN_POINT ( 'NONE',  ( -14.87820512820512953, -7.500000000000000000, 33.75000000000000000 ) ) ;
#10214 = LINE ( 'NONE', #44868, #15853 ) ;
#10216 = ADVANCED_FACE ( 'NONE', ( #56658 ), #71490, .F. ) ;
#10217 = CARTESIAN_POINT ( 'NONE',  ( 11.25641025641025550, -11.50000000000000000, 29.75000000000000355 ) ) ;
#10218 = CARTESIAN_POINT ( 'NONE',  ( -3.230769230769229949, -8.164416787775445883, 34.95778746994557906 ) ) ;
#10219 = VERTEX_POINT ( 'NONE', #64283 ) ;
#10220 = DIRECTION ( 'NONE',  ( -0.000000000000000000, 0.9396926207859093161, -0.3420201433256663259 ) ) ;
#10221 = CARTESIAN_POINT ( 'NONE',  ( 2.787413173340201222, -6.056457615119054338, 13.93844569653987087 ) ) ;
#10222 = ORIENTED_EDGE ( 'NONE', *, *, #62108, .T. ) ;
#10223 = ADVANCED_FACE ( 'NONE', ( #85025 ), #70174, .F. ) ;
#10224 = CYLINDRICAL_SURFACE ( 'NONE', #32148, 0.2500000000000004996 ) ;
#10225 = VECTOR ( 'NONE', #11385, 1000.000000000000000 ) ;
#10226 = CARTESIAN_POINT ( 'NONE',  ( 17.07692307692307665, -10.67929555188718282, 33.92786785259544047 ) ) ;
#10227 = CARTESIAN_POINT ( 'NONE',  ( 16.02369818411445834, -6.809168938359901446, 34.95455904226513866 ) ) ;
#10228 = CARTESIAN_POINT ( 'NONE',  ( -16.28399412357784826, -12.15440758774515473, 32.17923288041532004 ) ) ;
#10229 = CARTESIAN_POINT ( 'NONE',  ( 7.780883400193070898, -8.613356846314824011, 34.62446782046655613 ) ) ;
#10230 = B_SPLINE_CURVE_WITH_KNOTS ( 'NONE', 3,
 ( #4896, #46313, #38221, #78760, #73801, #31009, #12102, #58474, #85970, #58931 ),
 .UNSPECIFIED., .F., .F.,
 ( 4, 2, 2, 2, 4 ),
 ( 0.000000000000000000, 0.0001954339857564079623, 0.0003908679715128159245, 0.0005863019572692238597, 0.0007817359430256318490 ),
 .UNSPECIFIED. ) ;
#10231 = FACE_BOUND ( 'NONE', #40413, .T. ) ;
#10233 = CARTESIAN_POINT ( 'NONE',  ( 17.86930939688969033, -10.70098750199973203, 33.91152734681376302 ) ) ;
#10232 = CARTESIAN_POINT ( 'NONE',  ( 17.07692307692307665, -13.78497067705608181, 32.30358669280327177 ) ) ;
#10234 = B_SPLINE_CURVE_WITH_KNOTS ( 'NONE', 3,
 ( #83277, #21564, #8059, #35529, #1289, #56242, #83727, #22012, #49488, #76956 ),
 .UNSPECIFIED., .F., .F.,
 ( 4, 2, 2, 2, 4 ),
 ( 0.000000000000000000, 0.0001954311564186864949, 0.0003908623128373729899, 0.0005862934692560594577, 0.0007817246256747459798 ),
 .UNSPECIFIED. ) ;
#10235 = CARTESIAN_POINT ( 'NONE',  ( 15.93091993633000492, -3.105860786376062332, 32.13614157043599562 ) ) ;
#10237 = CARTESIAN_POINT ( 'NONE',  ( -11.28840711854808632, -10.82426656108012075, 33.81400080652039009 ) ) ;
#10236 = CARTESIAN_POINT ( 'NONE',  ( 3.007843013253084230, -4.186968288167446595, 33.49512374952580274 ) ) ;
#10238 = DIRECTION ( 'NONE',  ( 0.000000000000000000, 0.9848077530122072432, 0.1736481776669354937 ) ) ;
#10239 = VECTOR ( 'NONE', #272, 1000.000000000000227 ) ;
#10240 = CARTESIAN_POINT ( 'NONE',  ( 11.53846153846185274, -2.255955759149395501, 30.00000000000324363 ) ) ;
#10241 = CARTESIAN_POINT ( 'NONE',  ( -1.614399933863656544, -3.775308065498769405, 20.07625670625849068 ) ) ;
#10242 = ORIENTED_EDGE ( 'NONE', *, *, #15057, .F. ) ;
#10243 = CARTESIAN_POINT ( 'NONE',  ( -1.384615384615383471, -12.78798330534102945, 29.74999999999997868 ) ) ;
#10244 = CARTESIAN_POINT ( 'NONE',  ( -4.946131269098291483, -3.062576670634119758, 32.05464942895959979 ) ) ;
#10245 = DIRECTION ( 'NONE',  ( -0.000000000000000000, 1.000000000000000000, 3.491481338843133355E-15 ) ) ;
#10246 = CARTESIAN_POINT ( 'NONE',  ( 0.3253212748352863892, -10.23174463298371073, 28.86040964833806299 ) ) ;
#10247 = CARTESIAN_POINT ( 'NONE',  ( -4.284536756956462078, -4.684245665217972032, 34.18127051446801090 ) ) ;
#10248 = CARTESIAN_POINT ( 'NONE',  ( -16.82697766754503377, -8.476813868363244353, 34.90874843262270133 ) ) ;
#10249 = CARTESIAN_POINT ( 'NONE',  ( 3.749999999999999556, -7.438900925035446754, 19.21688170625848358 ) ) ;
#10250 = EDGE_CURVE ( 'NONE', #45495, #38893, #2585, .T. ) ;
#10251 = CARTESIAN_POINT ( 'NONE',  ( -11.28846153846011902, -7.500000000000154543, 35.00000000000007105 ) ) ;
#10252 = CARTESIAN_POINT ( 'NONE',  ( -19.50000000000000000, -3.499999999999999556, 29.75000000000000355 ) ) ;
#10253 = DIRECTION ( 'NONE',  ( 0.000000000000000000, -1.000000000000000000, -8.673617379884033500E-16 ) ) ;
#10254 = CARTESIAN_POINT ( 'NONE',  ( 17.86985203026830504, -8.630895178749536711, 34.87696386517710323 ) ) ;
#10255 = DIRECTION ( 'NONE',  ( -0.000000000000000000, 0.3420201433256694901, -0.9396926207859082059 ) ) ;
#10256 = DIRECTION ( 'NONE',  ( 0.000000000000000000, 0.3420201433256610524, 0.9396926207859113145 ) ) ;
#10257 = CARTESIAN_POINT ( 'NONE',  ( -9.692307692307691624, -1.422936976036506707, 30.56769352161908415 ) ) ;
#10258 = AXIS2_PLACEMENT_3D ( 'NONE', #42148, #35829, #49770 ) ;
#10259 = CARTESIAN_POINT ( 'NONE',  ( 14.30769230769218758, -6.879047030192662504, 34.71129190930017927 ) ) ;
#10260 = VERTEX_POINT ( 'NONE', #22862 ) ;
#10261 = CARTESIAN_POINT ( 'NONE',  ( -11.53846153846153655, -11.11383981884818262, 36.00935417666054406 ) ) ;
#10262 = CARTESIAN_POINT ( 'NONE',  ( -3.230769230769229949, -6.386643153685126251, 34.62446782046654192 ) ) ;
#10263 = CARTESIAN_POINT ( 'NONE',  ( 1.492201783934598236, -11.27530806549875031, 14.95499329374151642 ) ) ;
#10264 = CARTESIAN_POINT ( 'NONE',  ( 6.249945518348143381, -4.336752205174647656, 33.62275283266504289 ) ) ;
#10265 = CARTESIAN_POINT ( 'NONE',  ( 3.361561038594017337, -11.71459661697925903, 32.44059661609676937 ) ) ;
#10266 = ORIENTED_EDGE ( 'NONE', *, *, #29790, .T. ) ;
#10267 = CARTESIAN_POINT ( 'NONE',  ( -16.37677311275300340, -4.026226216239093603, 33.68668979543632958 ) ) ;
#10268 = LINE ( 'NONE', #8616, #50245 ) ;
#10270 = ORIENTED_EDGE ( 'NONE', *, *, #78671, .T. ) ;
#10269 = CARTESIAN_POINT ( 'NONE',  ( 4.023154687178594813, -5.582088688514999397, 34.36776431015576350 ) ) ;
#10271 = CARTESIAN_POINT ( 'NONE',  ( 2.307692307692309264, -13.75783147151868846, 33.36296068462461051 ) ) ;
#10272 = CARTESIAN_POINT ( 'NONE',  ( -13.25408968285182532, -10.19071101563364756, 33.96452234770658407 ) ) ;
#10273 = CYLINDRICAL_SURFACE ( 'NONE', #42101, 0.2499999999999997502 ) ;
#10274 = VECTOR ( 'NONE', #87686, 1000.000000000000000 ) ;
#10275 = CYLINDRICAL_SURFACE ( 'NONE', #80275, 0.2499999999999994726 ) ;
#10276 = EDGE_LOOP ( 'NONE', ( #51440, #38812, #86210, #83993 ) ) ;
#10277 = CARTESIAN_POINT ( 'NONE',  ( -12.46153846153846168, -13.57706302396349152, 30.56769352161908060 ) ) ;
#10278 = CARTESIAN_POINT ( 'NONE',  ( 15.16549923021291058, -10.33852847137145048, 34.16647553114627556 ) ) ;
#10279 = ORIENTED_EDGE ( 'NONE', *, *, #41502, .T. ) ;
#10280 = EDGE_LOOP ( 'NONE', ( #88879, #83982, #85742, #32925, #69482 ) ) ;
#10281 = EDGE_CURVE ( 'NONE', #62019, #35285, #8482, .T. ) ;
#10282 = ORIENTED_EDGE ( 'NONE', *, *, #41002, .T. ) ;
#10283 = CYLINDRICAL_SURFACE ( 'NONE', #32816, 0.2500000000000004996 ) ;
#10284 = CARTESIAN_POINT ( 'NONE',  ( -8.769230769230768274, -3.050289026998446396, 32.03036669348365706 ) ) ;
#10285 = EDGE_CURVE ( 'NONE', #80414, #16715, #8455, .T. ) ;
#10286 = CARTESIAN_POINT ( 'NONE',  ( 0.2115384615384615641, -7.500000000000001776, 35.00000000000000000 ) ) ;
#10287 = EDGE_CURVE ( 'NONE', #16973, #64228, #31712, .T. ) ;
#10288 = CARTESIAN_POINT ( 'NONE',  ( 15.00784301325307979, -3.586966769969701208, 32.86292498521069660 ) ) ;
#10289 = VECTOR ( 'NONE', #83892, 1000.000000000000227 ) ;
#10290 = VERTEX_POINT ( 'NONE', #76936 ) ;
#10291 = ORIENTED_EDGE ( 'NONE', *, *, #78257, .F. ) ;
#10293 = ORIENTED_EDGE ( 'NONE', *, *, #33937, .F. ) ;
#10292 = CARTESIAN_POINT ( 'NONE',  ( 15.29602480204525605, -5.219633306516380244, 34.19971097300157936 ) ) ;
#10294 = VECTOR ( 'NONE', #24865, 1000.000000000000114 ) ;
#10295 = EDGE_CURVE ( 'NONE', #10290, #33013, #41802, .T. ) ;
#10296 = CARTESIAN_POINT ( 'NONE',  ( 17.20771488474786892, -4.809403383903225304, 33.96459661697925014 ) ) ;
#10297 = CARTESIAN_POINT ( 'NONE',  ( -8.546219417617921366, -12.39991518177334129, 30.74647679643404530 ) ) ;
#10298 = CARTESIAN_POINT ( 'NONE',  ( -13.16183584334697443, -12.44528174975671853, 30.48912976160716681 ) ) ;
#10299 = VERTEX_POINT ( 'NONE', #8926 ) ;
#10300 = ORIENTED_EDGE ( 'NONE', *, *, #33109, .F. ) ;
#10301 = ORIENTED_EDGE ( 'NONE', *, *, #42106, .F. ) ;
#10303 = ORIENTED_EDGE ( 'NONE', *, *, #76518, .T. ) ;
#10302 = CARTESIAN_POINT ( 'NONE',  ( 3.230769230769231726, -1.466349020453238561, 30.81389545987213907 ) ) ;
#10304 = CARTESIAN_POINT ( 'NONE',  ( 5.076923076923075762, -5.471508081941601098, 34.59228464037088457 ) ) ;
#10305 = DIRECTION ( 'NONE',  ( 0.000000000000000000, 0.000000000000000000, 1.000000000000000000 ) ) ;
#10306 = EDGE_LOOP ( 'NONE', ( #75024, #34935 ) ) ;
#10307 = CARTESIAN_POINT ( 'NONE',  ( 6.857825932915681655, -2.506253911140460477, 30.00000000000013856 ) ) ;
#10308 = LINE ( 'NONE', #87325, #10585 ) ;
#10309 = FACE_OUTER_BOUND ( 'NONE', #7849, .T. ) ;
#10310 = FACE_BOUND ( 'NONE', #12952, .T. ) ;
#10311 = EDGE_CURVE ( 'NONE', #22055, #54542, #36393, .T. ) ;
#10312 = DIRECTION ( 'NONE',  ( -1.000000000000000000, -0.000000000000000000, 0.000000000000000000 ) ) ;
#10313 = CARTESIAN_POINT ( 'NONE',  ( 9.626550889793387356, -7.249945686854186278, 34.74374336980224598 ) ) ;
#10314 = AXIS2_PLACEMENT_3D ( 'NONE', #47090, #18754, #12870 ) ;
#10315 = CARTESIAN_POINT ( 'NONE',  ( 13.25392478150508069, -12.62707690430377383, 30.88035979386743435 ) ) ;
#10317 = CARTESIAN_POINT ( 'NONE',  ( -16.08777882049607655, -2.833524468853757750, 32.15551576947925838 ) ) ;
#10316 = CARTESIAN_POINT ( 'NONE',  ( 14.55769230769372946, -7.500000000000154543, 35.00000000000007105 ) ) ;
#10318 = CARTESIAN_POINT ( 'NONE',  ( 18.00000000000000000, -13.95598074871891292, 31.83374038241031911 ) ) ;
#10319 = LINE ( 'NONE', #51722, #15983 ) ;
#10320 = VERTEX_POINT ( 'NONE', #9368 ) ;
#10321 = CARTESIAN_POINT ( 'NONE',  ( -5.869208192175213945, -11.71459661697925903, 32.44059661609676937 ) ) ;
#10322 = ORIENTED_EDGE ( 'NONE', *, *, #80431, .F. ) ;
#10323 = ORIENTED_EDGE ( 'NONE', *, *, #86756, .T. ) ;
#10324 = VECTOR ( 'NONE', #69753, 1000.000000000000000 ) ;
#10326 = CARTESIAN_POINT ( 'NONE',  ( -6.000000000000119904, -12.27809138561165270, 31.22303859784587132 ) ) ;
#10325 = CARTESIAN_POINT ( 'NONE',  ( 5.749976762707036393, -6.695914987888143877, 34.68535235679833306 ) ) ;
#10327 = EDGE_CURVE ( 'NONE', #66664, #30312, #50765, .T. ) ;
#10328 = CARTESIAN_POINT ( 'NONE',  ( -6.673131404728780858, -6.696923467548660192, 34.68552623307873972 ) ) ;
#10329 = CARTESIAN_POINT ( 'NONE',  ( 15.23076923076923173, -8.973038597847269315, 34.52809138561121927 ) ) ;
#10330 = CARTESIAN_POINT ( 'NONE',  ( -3.931066484868084299, -3.563462043263029067, 33.22394488606062879 ) ) ;
#10331 = EDGE_LOOP ( 'NONE', ( #21817, #83851 ) ) ;
#10332 = CARTESIAN_POINT ( 'NONE',  ( 4.153846153846030731, -5.094484230521993062, 34.41647553114689373 ) ) ;
#10333 = EDGE_CURVE ( 'NONE', #4609, #68238, #66228, .T. ) ;
#10334 = EDGE_CURVE ( 'NONE', #80428, #33744, #4376, .T. ) ;
#10335 = CARTESIAN_POINT ( 'NONE',  ( -15.16470087976679082, -9.780366693483667717, 34.19971097300155805 ) ) ;
#10336 = DIRECTION ( 'NONE',  ( -0.000000000000000000, 0.1736481776669307198, -0.9848077530122080203 ) ) ;
#10337 = CARTESIAN_POINT ( 'NONE',  ( 0.2380535369741302032, -3.562934362175799841, 33.22335522853832401 ) ) ;
#10338 = DIRECTION ( 'NONE',  ( -0.000000000000000000, -0.1736481776669307198, -0.9848077530122080203 ) ) ;
#10339 = B_SPLINE_CURVE_WITH_KNOTS ( 'NONE', 3,
 ( #60053, #87558, #88885, #53293, #80796, #74027, #28953, #8673, #16305, #55954 ),
 .UNSPECIFIED., .F., .F.,
 ( 4, 2, 2, 2, 4 ),
 ( 0.000000000000000000, 0.0001954311564186868744, 0.0003908623128373737488, 0.0005862934692560606504, 0.0007817246256747474977 ),
 .UNSPECIFIED. ) ;
#10340 = CARTESIAN_POINT ( 'NONE',  ( 1.553300858899087311, -3.749999999999992006, 19.23437500000000355 ) ) ;
#10341 = EDGE_LOOP ( 'NONE', ( #73695, #18486, #19239, #8336 ) ) ;
#10342 = ORIENTED_EDGE ( 'NONE', *, *, #38744, .F. ) ;
#10343 = CARTESIAN_POINT ( 'NONE',  ( -14.55771553191376277, -4.931416488878822335, 34.32920672191015399 ) ) ;
#10344 = ORIENTED_EDGE ( 'NONE', *, *, #30504, .T. ) ;
#10345 = CARTESIAN_POINT ( 'NONE',  ( -19.50000000000000000, -11.50000000000000000, 29.75000000000000355 ) ) ;
#10346 = CARTESIAN_POINT ( 'NONE',  ( -12.46153846153846168, -9.780366693483667717, 34.19971097300155094 ) ) ;
#10347 = DIRECTION ( 'NONE',  ( 0.000000000000000000, 0.3420201433256610524, 0.9396926207859113145 ) ) ;
#10348 = DIRECTION ( 'NONE',  ( 0.000000000000000000, 0.7660444431189807890, 0.6427876096865361433 ) ) ;
#10349 = CARTESIAN_POINT ( 'NONE',  ( -2.651650429449535551, -10.15165042944956753, 17.43750000000000000 ) ) ;
#10350 = EDGE_CURVE ( 'NONE', #21924, #27341, #52109, .T. ) ;
#10351 = CARTESIAN_POINT ( 'NONE',  ( -13.63463862190834952, -8.432397168068783699, 34.66272746175022945 ) ) ;
#10352 = ORIENTED_EDGE ( 'NONE', *, *, #86756, .F. ) ;
#10353 = CARTESIAN_POINT ( 'NONE',  ( 27.00000000000000000, -16.99999999999999289, 30.25000000000000000 ) ) ;
#10355 = VERTEX_POINT ( 'NONE', #32298 ) ;
#10354 = DIRECTION ( 'NONE',  ( -0.000000000000000000, 0.9396926207859092051, -0.3420201433256662704 ) ) ;
#10356 = DIRECTION ( 'NONE',  ( 0.000000000000000000, 0.000000000000000000, -1.000000000000000000 ) ) ;
#10357 = FACE_OUTER_BOUND ( 'NONE', #9626, .T. ) ;
#10358 = EDGE_CURVE ( 'NONE', #18795, #11372, #72879, .T. ) ;
#10359 = EDGE_CURVE ( 'NONE', #24353, #57187, #67471, .T. ) ;
#10360 = CARTESIAN_POINT ( 'NONE',  ( -2.980769230769166445, -7.434744429011176159, 34.75000000000000711 ) ) ;
#10361 = CARTESIAN_POINT ( 'NONE',  ( 11.60452887181161508, -8.164416787775445883, 34.95778746994558617 ) ) ;
#10362 = CARTESIAN_POINT ( 'NONE',  ( -14.30769230769242917, -11.67786785259630911, 32.92929555188603530 ) ) ;
#10363 = DIRECTION ( 'NONE',  ( -0.000000000000000000, -0.000000000000000000, -1.000000000000000000 ) ) ;
#10364 = CARTESIAN_POINT ( 'NONE',  ( -7.173100160369889622, -5.056417327199099532, 34.11270091957320716 ) ) ;
#10365 = VECTOR ( 'NONE', #17806, 1000.000000000000000 ) ;
#10366 = CARTESIAN_POINT ( 'NONE',  ( -0.06109907496450878162, -11.25000000000000000, 16.28311829374151287 ) ) ;
#10367 = EDGE_LOOP ( 'NONE', ( #84539, #15281, #67349, #10969 ) ) ;
#10368 = EDGE_CURVE ( 'NONE', #23052, #81809, #52553, .T. ) ;
#10369 = CARTESIAN_POINT ( 'NONE',  ( -16.08859101433330707, -6.835583212224605631, 34.95778746994559327 ) ) ;
#10370 = CARTESIAN_POINT ( 'NONE',  ( -13.16160254052199008, -10.01129605718032600, 34.36064277460058491 ) ) ;
#10372 = CARTESIAN_POINT ( 'NONE',  ( -4.219928533206288357, -5.471508081941601986, 34.59228464037088457 ) ) ;
#10371 = B_SPLINE_CURVE_WITH_KNOTS ( 'NONE', 3,
 ( #39166, #40497, #60748, #32394, #60302, #67960, #73381, #81925, #53092, #18881 ),
 .UNSPECIFIED., .F., .F.,
 ( 4, 2, 2, 2, 4 ),
 ( 0.000000000000000000, 0.0001954311564186865492, 0.0003908623128373730983, 0.0005862934692560596746, 0.0007817246256747461966 ),
 .UNSPECIFIED. ) ;
#10373 = CARTESIAN_POINT ( 'NONE',  ( -2.749999999999998224, -7.500000000000015987, 25.09374999999999645 ) ) ;
#10374 = CARTESIAN_POINT ( 'NONE',  ( 0.2115152242454959863, -3.711651800289232916, 33.01384336483936011 ) ) ;
#10375 = CARTESIAN_POINT ( 'NONE',  ( 8.519207545009313876, -10.18141759479407327, 34.26406193332782379 ) ) ;
#10376 = EDGE_LOOP ( 'NONE', ( #23159, #28106, #44586, #21061 ) ) ;
#10377 = CARTESIAN_POINT ( 'NONE',  ( 1.799775606325937360E-14, -10.25000000000000000, 17.28125000000000000 ) ) ;
#10378 = CARTESIAN_POINT ( 'NONE',  ( 3.100077764101673239, -8.999036380462717588, 34.52022231692819076 ) ) ;
#10379 = ORIENTED_EDGE ( 'NONE', *, *, #45373, .F. ) ;
#10380 = CARTESIAN_POINT ( 'NONE',  ( -4.153846153846152411, -8.164416787775445883, 34.95778746994557906 ) ) ;
#10381 = ORIENTED_EDGE ( 'NONE', *, *, #60976, .T. ) ;
#10382 = LINE ( 'NONE', #15818, #27584 ) ;
#10383 = CARTESIAN_POINT ( 'NONE',  ( 13.31934493865461278, -10.21337939537584383, 33.94971097300158647 ) ) ;
#10384 = DIRECTION ( 'NONE',  ( 0.000000000000000000, 0.4999999999999985567, 0.8660254037844395958 ) ) ;
#10385 = ORIENTED_EDGE ( 'NONE', *, *, #26761, .F. ) ;
#10386 = DIRECTION ( 'NONE',  ( -0.000000000000000000, -0.7660444431189791237, -0.6427876096865379196 ) ) ;
#10387 = ORIENTED_EDGE ( 'NONE', *, *, #49931, .F. ) ;
#10388 = DIRECTION ( 'NONE',  ( 0.000000000000000000, 0.000000000000000000, -1.000000000000000000 ) ) ;
#10389 = EDGE_CURVE ( 'NONE', #18498, #3281, #49178, .T. ) ;
#10390 = VECTOR ( 'NONE', #82803, 1000.000000000000227 ) ;
#10391 = ORIENTED_EDGE ( 'NONE', *, *, #77994, .F. ) ;
#10393 = CARTESIAN_POINT ( 'NONE',  ( 12.23805353697413167, -12.11044203135681840, 32.26167407432752299 ) ) ;
#10392 = VECTOR ( 'NONE', #38196, 1000.000000000000000 ) ;
#10394 = CARTESIAN_POINT ( 'NONE',  ( -17.07692307692307665, -13.87047571288749737, 32.06866353760679544 ) ) ;
#10395 = ORIENTED_EDGE ( 'NONE', *, *, #5878, .F. ) ;
#10396 = CARTESIAN_POINT ( 'NONE',  ( -6.000000000000119904, -11.48612834414049644, 32.76840700105863391 ) ) ;
#10397 = CARTESIAN_POINT ( 'NONE',  ( -14.53061852520844610, -10.61292498521070549, 33.66303323003028680 ) ) ;
#10398 = CARTESIAN_POINT ( 'NONE',  ( -11.66860950819323861, -3.069018819979302926, 32.56621877034667278 ) ) ;
#10399 = VECTOR ( 'NONE', #22780, 1000.000000000000000 ) ;
#10400 = ADVANCED_FACE ( 'NONE', ( #38158 ), #45801, .F. ) ;
#10401 = DIRECTION ( 'NONE',  ( -0.000000000000000000, 0.6427876096865404731, -0.7660444431189770143 ) ) ;
#10402 = CARTESIAN_POINT ( 'NONE',  ( 18.00000000000000000, -2.292212530054420494, 30.41441678777542634 ) ) ;
#10403 = B_SPLINE_CURVE_WITH_KNOTS ( 'NONE', 3,
 ( #9447, #3564, #44098, #36909, #64814, #64371, #51278, #72024, #72472, #31033 ),
 .UNSPECIFIED., .F., .F.,
 ( 4, 2, 2, 2, 4 ),
 ( 0.000000000000000000, 0.0001954339857564093175, 0.0003908679715128186350, 0.0005863019572692279796, 0.0007817359430256372700 ),
 .UNSPECIFIED. ) ;
#10404 = B_SPLINE_CURVE_WITH_KNOTS ( 'NONE', 3,
 ( #10740, #45399, #78747, #38654, #17049, #51698, #10297, #37761, #65227, #85955 ),
 .UNSPECIFIED., .F., .F.,
 ( 4, 2, 2, 2, 4 ),
 ( 0.0007817359430256326080, 0.0009771253907249993591, 0.001172514838424366327, 0.001367904286123733078, 0.001563293733823099829 ),
 .UNSPECIFIED. ) ;
#10405 = ORIENTED_EDGE ( 'NONE', *, *, #55576, .T. ) ;
#10406 = ORIENTED_EDGE ( 'NONE', *, *, #52347, .F. ) ;
#10407 = ORIENTED_EDGE ( 'NONE', *, *, #32430, .T. ) ;
#10409 = EDGE_LOOP ( 'NONE', ( #39309, #7281 ) ) ;
#10408 = CARTESIAN_POINT ( 'NONE',  ( 2.980792486720639900, -5.643011162660950042, 34.66104346484419096 ) ) ;
#10410 = EDGE_CURVE ( 'NONE', #59263, #78986, #4828, .T. ) ;
#10411 = CARTESIAN_POINT ( 'NONE',  ( 10.39245839786846837, -4.887634598454295265, 34.01352882383564946 ) ) ;
#10412 = CARTESIAN_POINT ( 'NONE',  ( -19.50000000000000000, -11.50000000000000000, 29.75000000000000355 ) ) ;
#10413 = ORIENTED_EDGE ( 'NONE', *, *, #10004, .T. ) ;
#10414 = VERTEX_POINT ( 'NONE', #31403 ) ;
#10415 = ADVANCED_FACE ( 'NONE', ( #86372 ), #66528, .F. ) ;
#10416 = VERTEX_POINT ( 'NONE', #57981 ) ;
#10417 = CARTESIAN_POINT ( 'NONE',  ( 0.3962684609821412463, -8.656820664281497102, 34.87096338111211935 ) ) ;
#10418 = EDGE_LOOP ( 'NONE', ( #44227, #9652 ) ) ;
#10419 = AXIS2_PLACEMENT_3D ( 'NONE', #33289, #87811, #39613 ) ;
#10420 = CARTESIAN_POINT ( 'NONE',  ( -10.36533030374629760, -9.148310452688876993, 34.47095581063188519 ) ) ;
#10421 = CARTESIAN_POINT ( 'NONE',  ( 17.01165307636676260, -12.51329471203370325, 31.30864560766548976 ) ) ;
#10422 = CARTESIAN_POINT ( 'NONE',  ( 12.39626801557768943, -2.625532179533445198, 30.86335684631481513 ) ) ;
#10423 = FACE_BOUND ( 'NONE', #78723, .T. ) ;
#10424 = ORIENTED_EDGE ( 'NONE', *, *, #51993, .F. ) ;
#10425 = CARTESIAN_POINT ( 'NONE',  ( 12.46153846153846168, -6.681629849574314051, 35.83090037661290239 ) ) ;
#10426 = CARTESIAN_POINT ( 'NONE',  ( 1.384615384615386802, -12.62096338111211580, 30.90682066428153263 ) ) ;
#10427 = CARTESIAN_POINT ( 'NONE',  ( 8.835299120233207404, -3.050289026998446840, 32.03036669348366416 ) ) ;
#10428 = CARTESIAN_POINT ( 'NONE',  ( 17.14299142792551578, -8.973038597847269315, 34.52809138561122637 ) ) ;
#10429 = ORIENTED_EDGE ( 'NONE', *, *, #11533, .F. ) ;
#10430 = EDGE_CURVE ( 'NONE', #35664, #22972, #21367, .T. ) ;
#10431 = B_SPLINE_CURVE_WITH_KNOTS ( 'NONE', 3,
 ( #10326, #17077, #79675, #24267, #57180, #36901, #44533, #3996, #71570, #58491 ),
 .UNSPECIFIED., .F., .F.,
 ( 4, 2, 2, 2, 4 ),
 ( 0.0007817359430256326080, 0.0009771253907250047801, 0.001172514838424369796, 0.001367904286123735030, 0.001563293733823100046 ),
 .UNSPECIFIED. ) ;
#10432 = CARTESIAN_POINT ( 'NONE',  ( 9.562160482869472844, -2.619462340734462380, 30.83744416345203021 ) ) ;
#10433 = VERTEX_POINT ( 'NONE', #53442 ) ;
#10434 = ADVANCED_FACE ( 'NONE', ( #20984 ), #88600, .F. ) ;
#10435 = ORIENTED_EDGE ( 'NONE', *, *, #12690, .T. ) ;
#10437 = CARTESIAN_POINT ( 'NONE',  ( -1.634592128663975075, -5.643011162660950042, 34.66104346484419096 ) ) ;
#10436 = CARTESIAN_POINT ( 'NONE',  ( -7.846153846153967493, -5.094484230521993062, 34.41647553114689373 ) ) ;
#10438 = CARTESIAN_POINT ( 'NONE',  ( -10.83831083290076158, -12.15238873228292071, 31.58232369045353849 ) ) ;
#10439 = CARTESIAN_POINT ( 'NONE',  ( -3.903846153844716671, -7.500000000000155431, 34.75000000000007105 ) ) ;
#10440 = CARTESIAN_POINT ( 'NONE',  ( 16.85409638444407321, -7.369208160676171460, 34.74850200257122879 ) ) ;
#10441 = CARTESIAN_POINT ( 'NONE',  ( -15.23076923076935252, -3.643525952248795718, 33.31231777344771672 ) ) ;
#10442 = VERTEX_POINT ( 'NONE', #53895 ) ;
#10443 = DIRECTION ( 'NONE',  ( -0.000000000000000000, 0.3420201433256694346, -0.9396926207859080948 ) ) ;
#10444 = ADVANCED_FACE ( 'NONE', ( #47126 ), #74617, .F. ) ;
#10445 = DIRECTION ( 'NONE',  ( -0.000000000000000000, -0.3420201433256694346, -0.9396926207859080948 ) ) ;
#10446 = CARTESIAN_POINT ( 'NONE',  ( 10.48523664565292002, -3.069018819979302926, 32.56621877034667278 ) ) ;
#10447 = CARTESIAN_POINT ( 'NONE',  ( -13.51530598772569114, -12.62707690430377383, 30.88035979386743435 ) ) ;
#10448 = ORIENTED_EDGE ( 'NONE', *, *, #72403, .F. ) ;
#10449 = ORIENTED_EDGE ( 'NONE', *, *, #76096, .T. ) ;
#10450 = FACE_BOUND ( 'NONE', #44497, .T. ) ;
#10451 = VECTOR ( 'NONE', #52776, 1000.000000000000000 ) ;
#10452 = ORIENTED_EDGE ( 'NONE', *, *, #37766, .F. ) ;
#10453 = VECTOR ( 'NONE', #41095, 1000.000000000000114 ) ;
#10454 = CARTESIAN_POINT ( 'NONE',  ( 18.22301284409339672, -12.64618726649961289, 30.78989965857442712 ) ) ;
#10455 = CARTESIAN_POINT ( 'NONE',  ( -13.38461538461550582, -10.90142922262034020, 33.41473453929536674 ) ) ;
#10456 = ORIENTED_EDGE ( 'NONE', *, *, #27115, .F. ) ;
#10457 = DIRECTION ( 'NONE',  ( 0.000000000000000000, 0.8660254037844377084, 0.5000000000000015543 ) ) ;
#10458 = CARTESIAN_POINT ( 'NONE',  ( 6.000000000000001776, -3.937682226553329556, 33.60647404775216529 ) ) ;
#10459 = CARTESIAN_POINT ( 'NONE',  ( 0.7114839798866031684, -12.22109172314383052, 31.39792113162168263 ) ) ;
#10460 = CARTESIAN_POINT ( 'NONE',  ( -1.161602540521988969, -4.026326845037962343, 33.68677907613344047 ) ) ;
#10461 = ORIENTED_EDGE ( 'NONE', *, *, #62958, .F. ) ;
#10462 = VECTOR ( 'NONE', #73879, 1000.000000000000227 ) ;
#10463 = CARTESIAN_POINT ( 'NONE',  ( -3.931066612577742259, -6.760870238392817200, 34.69528174975672385 ) ) ;
#10464 = EDGE_LOOP ( 'NONE', ( #57468, #25844, #77721, #42103 ) ) ;
#10466 = ORIENTED_EDGE ( 'NONE', *, *, #5175, .F. ) ;
#10465 = CARTESIAN_POINT ( 'NONE',  ( -2.307692307692428724, -9.528491918059723176, 34.59228464037033035 ) ) ;
#10467 = CARTESIAN_POINT ( 'NONE',  ( -8.546451227962359454, -10.11255958852956027, 34.01340905677048454 ) ) ;
#10468 = DIRECTION ( 'NONE',  ( -0.000000000000000000, -0.9848077530122086864, -0.1736481776669273613 ) ) ;
#10469 = CARTESIAN_POINT ( 'NONE',  ( -0.4615384615384611200, -1.117168528481311540, 33.14645433367849847 ) ) ;
#10470 = EDGE_CURVE ( 'NONE', #62031, #62397, #26871, .T. ) ;
#10471 = CARTESIAN_POINT ( 'NONE',  ( 17.07692307692307665, -10.05456864172156806, 36.03766855953608683 ) ) ;
#10472 = CARTESIAN_POINT ( 'NONE',  ( -14.43838291080261449, -8.191372820521381826, 34.95448215188424967 ) ) ;
#10473 = LINE ( 'NONE', #85247, #43497 ) ;
#10474 = CARTESIAN_POINT ( 'NONE',  ( 1.200186371490529202, -4.775308065498752974, 16.98624329374151287 ) ) ;
#10475 = ORIENTED_EDGE ( 'NONE', *, *, #8831, .F. ) ;
#10476 = CARTESIAN_POINT ( 'NONE',  ( 14.17700170458200226, -2.295517848115769421, 30.44137282052137294 ) ) ;
#10477 = DIRECTION ( 'NONE',  ( 0.000000000000000000, 0.000000000000000000, -1.000000000000000000 ) ) ;
#10478 = CARTESIAN_POINT ( 'NONE',  ( -0.3310127597748983574, -5.195472089885679878, 34.18748526763464213 ) ) ;
#10479 = B_SPLINE_CURVE_WITH_KNOTS ( 'NONE', 3,
 ( #83048, #69964, #42066, #41173, #63199, #62311, #8276, #26768, #48802, #54227 ),
 .UNSPECIFIED., .F., .F.,
 ( 4, 2, 2, 2, 4 ),
 ( 0.000000000000000000, 0.0001954339857564063089, 0.0003908679715128126177, 0.0005863019572692189808, 0.0007817359430256252354 ),
 .UNSPECIFIED. ) ;
#10480 = ORIENTED_EDGE ( 'NONE', *, *, #79759, .F. ) ;
#10481 = ORIENTED_EDGE ( 'NONE', *, *, #10532, .T. ) ;
#10482 = CARTESIAN_POINT ( 'NONE',  ( -1.634615384615389466, -2.499999999999999556, 29.81609845454691765 ) ) ;
#10483 = CARTESIAN_POINT ( 'NONE',  ( 11.47319153790521717, -5.094484230520674117, 34.41647553114621161 ) ) ;
#10484 = B_SPLINE_CURVE_WITH_KNOTS ( 'NONE', 3,
 ( #85064, #84627, #78286, #45386, #50368, #37747, #16153, #72859, #3066, #23778 ),
 .UNSPECIFIED., .F., .F.,
 ( 4, 2, 2, 2, 4 ),
 ( 0.000000000000000000, 0.0001954339857564096428, 0.0003908679715128192855, 0.0005863019572692289554, 0.0007817359430256385711 ),
 .UNSPECIFIED. ) ;
#10485 = CARTESIAN_POINT ( 'NONE',  ( -4.946397638689432164, -12.70449254468099198, 30.44128974285582956 ) ) ;
#10486 = DIRECTION ( 'NONE',  ( -0.000000000000000000, -0.9848077530122086864, -0.1736481776669273613 ) ) ;
#10487 = LINE ( 'NONE', #37953, #18641 ) ;
#10488 = AXIS2_PLACEMENT_3D ( 'NONE', #65977, #80403, #87611 ) ;
#10489 = CARTESIAN_POINT ( 'NONE',  ( 16.15384615384603251, -11.94971097300221174, 32.03036669348237098 ) ) ;
#10490 = CARTESIAN_POINT ( 'NONE',  ( -5.076923076923075762, -2.249999999999998668, 29.75000000000001776 ) ) ;
#10491 = ORIENTED_EDGE ( 'NONE', *, *, #59941, .T. ) ;
#10492 = CARTESIAN_POINT ( 'NONE',  ( 3.007284287045283389, -6.760086850603068243, 34.69517049084099369 ) ) ;
#10493 = CARTESIAN_POINT ( 'NONE',  ( -16.82692307692314415, -7.565270445406050648, 34.75000000000000000 ) ) ;
#10494 = CARTESIAN_POINT ( 'NONE',  ( 6.923076923076800782, -6.835583212225970762, 34.95778746994575670 ) ) ;
#10495 = DIRECTION ( 'NONE',  ( -1.000000000000000000, -0.000000000000000000, -0.000000000000000000 ) ) ;
#10496 = ORIENTED_EDGE ( 'NONE', *, *, #84014, .F. ) ;
#10497 = CARTESIAN_POINT ( 'NONE',  ( 10.61538461538461675, -9.058645607665452459, 34.76329471203371924 ) ) ;
#10498 = ORIENTED_EDGE ( 'NONE', *, *, #38163, .T. ) ;
#10499 = CARTESIAN_POINT ( 'NONE',  ( 15.00784301325308157, -11.24512374952581872, 33.06303171183252942 ) ) ;
#10500 =( NAMED_UNIT ( * ) SI_UNIT ( $, .STERADIAN. ) SOLID_ANGLE_UNIT ( ) );
#10501 = PLANE ( 'NONE',  #58464 ) ;
#10502 = DIRECTION ( 'NONE',  ( -0.000000000000000000, -0.5000000000000009992, -0.8660254037844380415 ) ) ;
#10503 = ORIENTED_EDGE ( 'NONE', *, *, #48075, .T. ) ;
#10504 = CARTESIAN_POINT ( 'NONE',  ( -2.557669051740897537, -6.524016743844655686, 34.90889640711025521 ) ) ;
#10505 = CARTESIAN_POINT ( 'NONE',  ( -3.230769230769229949, -1.466349020453238561, 30.81389545987213907 ) ) ;
#10506 = CARTESIAN_POINT ( 'NONE',  ( -3.230769230769229949, -8.810774026931790459, 35.74407628777942847 ) ) ;
#10507 = CARTESIAN_POINT ( 'NONE',  ( 3.453782074862629337, -2.889357225399416862, 32.26129605718031002 ) ) ;
#10508 = VERTEX_POINT ( 'NONE', #20552 ) ;
#10509 = CARTESIAN_POINT ( 'NONE',  ( -0.7115151924808160722, -8.303909089506435137, 34.68538101551103381 ) ) ;
#10510 = ORIENTED_EDGE ( 'NONE', *, *, #79259, .T. ) ;
#10511 = DIRECTION ( 'NONE',  ( -0.000000000000000000, 0.3420201433256694901, -0.9396926207859082059 ) ) ;
#10512 = B_SPLINE_CURVE_WITH_KNOTS ( 'NONE', 3,
 ( #4516, #31993, #65759, #66663, #59900, #11274, #4969, #4055, #52694, #65319 ),
 .UNSPECIFIED., .F., .F.,
 ( 4, 2, 2, 2, 4 ),
 ( 0.0007817359430256326080, 0.0009771253907249993591, 0.001172514838424366327, 0.001367904286123733078, 0.001563293733823099829 ),
 .UNSPECIFIED. ) ;
#10513 = MECHANICAL_DESIGN_GEOMETRIC_PRESENTATION_REPRESENTATION (  '', ( #49347 ), #4789 ) ;
#10514 = CYLINDRICAL_SURFACE ( 'NONE', #75079, 0.2499999999999986955 ) ;
#10515 = AXIS2_PLACEMENT_3D ( 'NONE', #86207, #24925, #71776 ) ;
#10516 = CARTESIAN_POINT ( 'NONE',  ( -3.296039676730005752, -12.27809138561121394, 31.22303859784730307 ) ) ;
#10517 = CARTESIAN_POINT ( 'NONE',  ( -17.07692307692307665, -12.78798330534102767, 29.49999999999997868 ) ) ;
#10518 = CARTESIAN_POINT ( 'NONE',  ( 5.076923076923383071, -2.506253911140614576, 30.00000000000323297 ) ) ;
#10519 = CARTESIAN_POINT ( 'NONE',  ( 16.08857615328984281, -12.16647553114622049, 32.15551576947930812 ) ) ;
#10520 = AXIS2_PLACEMENT_3D ( 'NONE', #59132, #37525, #64991 ) ;
#10521 = ORIENTED_EDGE ( 'NONE', *, *, #67361, .T. ) ;
#10522 = ORIENTED_EDGE ( 'NONE', *, *, #37549, .F. ) ;
#10523 = ORIENTED_EDGE ( 'NONE', *, *, #5117, .T. ) ;
#10524 = ORIENTED_EDGE ( 'NONE', *, *, #54773, .F. ) ;
#10525 = EDGE_LOOP ( 'NONE', ( #66337, #46151 ) ) ;
#10526 = CARTESIAN_POINT ( 'NONE',  ( 7.384615384615385025, -3.499999999999999556, 29.75000000000000355 ) ) ;
#10527 = CARTESIAN_POINT ( 'NONE',  ( -1.319359813339359144, -12.46129190930001052, 30.37095296980870174 ) ) ;
#10528 = DIRECTION ( 'NONE',  ( -0.000000000000000000, 0.5000000000000011102, -0.8660254037844380415 ) ) ;
#10529 = DIRECTION ( 'NONE',  ( -0.000000000000000000, -0.6427876096865404731, -0.7660444431189771253 ) ) ;
#10530 = CYLINDRICAL_SURFACE ( 'NONE', #29894, 0.2500000000000002220 ) ;
#10532 = EDGE_CURVE ( 'NONE', #87552, #63347, #74019, .T. ) ;
#10531 = CARTESIAN_POINT ( 'NONE',  ( -12.68446542044531000, -12.38737895849757820, 31.66785238281580206 ) ) ;
#10533 = FACE_OUTER_BOUND ( 'NONE', #61216, .T. ) ;
#10534 = CARTESIAN_POINT ( 'NONE',  ( -18.00000000000012079, -6.879047030192663392, 34.71129190930017927 ) ) ;
#10535 = CARTESIAN_POINT ( 'NONE',  ( 7.846153846153723244, -2.379036618888197729, 30.90682066428292885 ) ) ;
#10536 = EDGE_LOOP ( 'NONE', ( #38546, #69007, #54151, #33815 ) ) ;
#10537 = EDGE_LOOP ( 'NONE', ( #81268, #81094 ) ) ;
#10538 = EDGE_LOOP ( 'NONE', ( #3855, #29671, #36248, #36547 ) ) ;
#10540 = VERTEX_POINT ( 'NONE', #12907 ) ;
#10539 = CARTESIAN_POINT ( 'NONE',  ( 0.2386115026316112386, -2.889293201056495786, 32.26117774369186009 ) ) ;
#10541 = AXIS2_PLACEMENT_3D ( 'NONE', #64258, #71913, #29614 ) ;
#10543 = CARTESIAN_POINT ( 'NONE',  ( 9.692307692307695177, -12.10708131394839349, 31.69288490824020244 ) ) ;
#10542 = LINE ( 'NONE', #18638, #40304 ) ;
#10544 = AXIS2_PLACEMENT_3D ( 'NONE', #1985, #10066, #23577 ) ;
#10545 = DIRECTION ( 'NONE',  ( -0.000000000000000000, 0.6427876096865404731, -0.7660444431189770143 ) ) ;
#10546 = CARTESIAN_POINT ( 'NONE',  ( -11.31568186948346977, -9.418065098278013636, 34.63729479722530158 ) ) ;
#10547 = ORIENTED_EDGE ( 'NONE', *, *, #11925, .T. ) ;
#10548 = ADVANCED_FACE ( 'NONE', ( #12468 ), #40831, .F. ) ;
#10549 = ORIENTED_EDGE ( 'NONE', *, *, #36299, .F. ) ;
#10550 = CARTESIAN_POINT ( 'NONE',  ( -11.78848476268299628, -12.07920672191015221, 32.31858351112116168 ) ) ;
#10551 = VERTEX_POINT ( 'NONE', #40397 ) ;
#10552 = FACE_BOUND ( 'NONE', #49761, .T. ) ;
#10553 = DIRECTION ( 'NONE',  ( 1.000000000000000000, 0.000000000000000000, 0.000000000000000000 ) ) ;
#10554 = CARTESIAN_POINT ( 'NONE',  ( -14.55766905174090020, -6.524016743844655686, 34.90889640711025521 ) ) ;
#10555 = EDGE_LOOP ( 'NONE', ( #9976, #76996 ) ) ;
#10556 = CARTESIAN_POINT ( 'NONE',  ( 17.77651505627605033, -2.847400154188068910, 31.58180166144859768 ) ) ;
#10557 = DIRECTION ( 'NONE',  ( -0.000000000000000000, 1.000000000000000000, -0.000000000000000000 ) ) ;
#10558 = DIRECTION ( 'NONE',  ( -1.000000000000000000, -0.000000000000000000, -0.000000000000000000 ) ) ;
#10559 = EDGE_LOOP ( 'NONE', ( #51227, #43315 ) ) ;
#10560 = FACE_OUTER_BOUND ( 'NONE', #50269, .T. ) ;
#10561 = CYLINDRICAL_SURFACE ( 'NONE', #45178, 0.2500000000000002220 ) ;
#10562 = ORIENTED_EDGE ( 'NONE', *, *, #775, .T. ) ;
#10563 = CARTESIAN_POINT ( 'NONE',  ( 7.911408985666684046, -11.67786785259547777, 32.92929555188713664 ) ) ;
#10564 = CARTESIAN_POINT ( 'NONE',  ( -9.442362282929646966, -9.357781135181031829, 34.66075350412533851 ) ) ;
#10565 = ORIENTED_EDGE ( 'NONE', *, *, #45999, .T. ) ;
#10566 = FACE_OUTER_BOUND ( 'NONE', #75774, .T. ) ;
#10567 = CARTESIAN_POINT ( 'NONE',  ( -10.54931626438217585, -4.786620604624113540, 33.94971097300155805 ) ) ;
#10568 = DIRECTION ( 'NONE',  ( -1.000000000000000000, -0.000000000000000000, -0.000000000000000000 ) ) ;
#10569 = CARTESIAN_POINT ( 'NONE',  ( -10.39237326377176274, -5.667800583137506010, 34.40243808032445827 ) ) ;
#10570 = FACE_OUTER_BOUND ( 'NONE', #8525, .T. ) ;
#10571 = EDGE_CURVE ( 'NONE', #10700, #31320, #75066, .T. ) ;
#10572 = DIRECTION ( 'NONE',  ( 0.000000000000000000, 0.000000000000000000, 1.000000000000000000 ) ) ;
#10574 = CARTESIAN_POINT ( 'NONE',  ( -15.45369544828537656, -12.39988816332205701, 30.74660775122750778 ) ) ;
#10573 = DIRECTION ( 'NONE',  ( 0.000000000000000000, 0.000000000000000000, -1.000000000000000000 ) ) ;
#10575 = CARTESIAN_POINT ( 'NONE',  ( -7.846153846153844924, -13.87047571288749737, 32.06866353760679544 ) ) ;
#10577 = CARTESIAN_POINT ( 'NONE',  ( -10.86536134632696715, -8.303909089506435137, 34.68538101551103381 ) ) ;
#10576 = CARTESIAN_POINT ( 'NONE',  ( 4.153846153846030731, -5.094484230521993062, 34.41647553114689373 ) ) ;
#10578 = EDGE_CURVE ( 'NONE', #71586, #80366, #89034, .T. ) ;
#10579 = CARTESIAN_POINT ( 'NONE',  ( -1.139087296526025916, -4.750000000000006217, 15.32812500000000355 ) ) ;
#10580 = VERTEX_POINT ( 'NONE', #74171 ) ;
#10581 = EDGE_CURVE ( 'NONE', #88786, #31128, #27312, .T. ) ;
#10582 = VECTOR ( 'NONE', #79390, 1000.000000000000000 ) ;
#10583 = CARTESIAN_POINT ( 'NONE',  ( 3.148534467955792948, -7.948670516411742604, 14.00000000000001066 ) ) ;
#10584 = VERTEX_POINT ( 'NONE', #13792 ) ;
#10585 = VECTOR ( 'NONE', #25600, 1000.000000000000000 ) ;
#10586 = EDGE_CURVE ( 'NONE', #83291, #32479, #67413, .T. ) ;
#10587 = VERTEX_POINT ( 'NONE', #75492 ) ;
#10588 = CARTESIAN_POINT ( 'NONE',  ( -2.176900499867520988, -12.38066358083363738, 30.83685684665853444 ) ) ;
#10589 = VERTEX_POINT ( 'NONE', #68739 ) ;
#10590 = CARTESIAN_POINT ( 'NONE',  ( -5.869209559033048862, -9.929761469519744921, 34.40412654351204225 ) ) ;
#10591 = CARTESIAN_POINT ( 'NONE',  ( 2.750000000000001776, -7.499999999999984013, 16.96875000000000000 ) ) ;
#10592 = CYLINDRICAL_SURFACE ( 'NONE', #21379, 0.2500000000000002220 ) ;
#10593 = CARTESIAN_POINT ( 'NONE',  ( -9.942330916529147800, -12.68155406624981119, 30.59749803192733708 ) ) ;
#10594 = CARTESIAN_POINT ( 'NONE',  ( -0.4615384615385826339, -6.026961402154118908, 34.52809138561165270 ) ) ;
#10595 = CARTESIAN_POINT ( 'NONE',  ( -5.999999999999998224, -2.486705287966279876, 31.30864560766543647 ) ) ;
#10596 = CARTESIAN_POINT ( 'NONE',  ( 20.00000000000000711, -9.999999999999994671, 13.00000000000000178 ) ) ;
#10597 = CARTESIAN_POINT ( 'NONE',  ( -7.596099534515531992, -2.779044189368096163, 31.39831045268886456 ) ) ;
#10598 = CARTESIAN_POINT ( 'NONE',  ( 0.5267936010512987988, -2.657715359629131857, 31.77849191805844242 ) ) ;
#10599 = CARTESIAN_POINT ( 'NONE',  ( -3.750000000000008438, -5.946699141100917352, 20.17187500000000000 ) ) ;
#10600 = DIRECTION ( 'NONE',  ( 0.000000000000000000, -6.938893903907222067E-15, 1.000000000000000000 ) ) ;
#10601 = CARTESIAN_POINT ( 'NONE',  ( 5.076923076922954969, -8.613356846316285953, 34.62446782046622218 ) ) ;
#10602 = CARTESIAN_POINT ( 'NONE',  ( 23.49999999999998934, 12.75000000000000888, 32.75000000000000000 ) ) ;
#10603 = EDGE_LOOP ( 'NONE', ( #41531, #61146, #802, #14183 ) ) ;
#10604 = EDGE_LOOP ( 'NONE', ( #59159, #22755, #2203, #69060 ) ) ;
#10605 = CARTESIAN_POINT ( 'NONE',  ( 14.55763782604044998, -5.057305518903948638, 34.11320923018887896 ) ) ;
#10606 = CARTESIAN_POINT ( 'NONE',  ( -17.32694631421604115, -8.432397168068783699, 34.66272746175022945 ) ) ;
#10607 = DIRECTION ( 'NONE',  ( -1.000000000000000000, -0.000000000000000000, -0.000000000000000000 ) ) ;
#10608 = CARTESIAN_POINT ( 'NONE',  ( 5.142178648199100977, -2.892918686051625166, 31.69288490824025928 ) ) ;
#10609 = CARTESIAN_POINT ( 'NONE',  ( 14.98076923076923173, -7.500000000000001776, 34.75000000000000000 ) ) ;
#10610 = CARTESIAN_POINT ( 'NONE',  ( -16.28399336328437386, -9.418419913701741919, 34.36755862841477693 ) ) ;
#10611 = AXIS2_PLACEMENT_3D ( 'NONE', #73251, #16197, #46224 ) ;
#10612 = ADVANCED_FACE ( 'NONE', ( #7035 ), #34512, .F. ) ;
#10613 = VERTEX_POINT ( 'NONE', #56558 ) ;
#10614 = CARTESIAN_POINT ( 'NONE',  ( 7.596130621932389637, -2.985938066672154445, 32.43141759479405550 ) ) ;
#10615 = ORIENTED_EDGE ( 'NONE', *, *, #15278, .T. ) ;
#10616 = VERTEX_POINT ( 'NONE', #15135 ) ;
#10617 = CARTESIAN_POINT ( 'NONE',  ( -9.626240358957616650, -2.833524468853757305, 32.15551576947925838 ) ) ;
#10618 = CARTESIAN_POINT ( 'NONE',  ( -11.47239420511146157, -11.35647404775217595, 33.31231777344666511 ) ) ;
#10619 = CARTESIAN_POINT ( 'NONE',  ( -13.38461538461550759, -2.657715359629662544, 31.77849191805970364 ) ) ;
#10620 = CARTESIAN_POINT ( 'NONE',  ( 2.242421861731533017, -6.026961402152685388, 34.52809138561120506 ) ) ;
#10621 = CARTESIAN_POINT ( 'NONE',  ( -2.307692307692305711, -11.69971097300155272, 32.46337939537588113 ) ) ;
#10622 = EDGE_CURVE ( 'NONE', #53698, #71149, #35234, .T. ) ;
#10623 = EDGE_LOOP ( 'NONE', ( #18195, #86501, #4042, #44837 ) ) ;
#10624 = ORIENTED_EDGE ( 'NONE', *, *, #49933, .F. ) ;
#10626 = VERTEX_POINT ( 'NONE', #2485 ) ;
#10625 = CIRCLE ( 'NONE', #82529, 4.000000000000000000 ) ;
#10627 = VECTOR ( 'NONE', #66466, 1000.000000000000000 ) ;
#10628 = CARTESIAN_POINT ( 'NONE',  ( 12.71153846153846523, -2.499999999999999556, 29.81604066197449754 ) ) ;
#10629 = CARTESIAN_POINT ( 'NONE',  ( 9.757562831820528970, -2.379036618887895305, 30.90682066428158592 ) ) ;
#10630 = B_SPLINE_CURVE_WITH_KNOTS ( 'NONE', 3,
 ( #75662, #68464, #62152, #54055, #61698, #81552, #7662, #33795, #69362, #27485 ),
 .UNSPECIFIED., .F., .F.,
 ( 4, 2, 2, 2, 4 ),
 ( 0.000000000000000000, 0.0001954339857564073388, 0.0003908679715128146777, 0.0005863019572692220165, 0.0007817359430256293554 ),
 .UNSPECIFIED. ) ;
#10631 = DIRECTION ( 'NONE',  ( -1.000000000000000000, -0.000000000000000000, 0.000000000000000000 ) ) ;
#10632 = VECTOR ( 'NONE', #23018, 1000.000000000000000 ) ;
#10633 = VECTOR ( 'NONE', #34133, 1000.000000000000000 ) ;
#10635 = EDGE_CURVE ( 'NONE', #6496, #36253, #23210, .T. ) ;
#10634 = CARTESIAN_POINT ( 'NONE',  ( -15.16470087976679437, -3.050289026998446840, 32.03036669348366416 ) ) ;
#10636 = CARTESIAN_POINT ( 'NONE',  ( -4.403822884788508141, -8.303909089506435137, 34.68538101551103381 ) ) ;
#10637 = DIRECTION ( 'NONE',  ( 0.000000000000000000, 0.9396926207859126468, 0.3420201433256571111 ) ) ;
#10638 = VERTEX_POINT ( 'NONE', #1616 ) ;
#10639 = EDGE_CURVE ( 'NONE', #22873, #86754, #87927, .T. ) ;
#10640 = ORIENTED_EDGE ( 'NONE', *, *, #54380, .F. ) ;
#10641 = CARTESIAN_POINT ( 'NONE',  ( 1.553300858899087311, -3.749999999999992006, 21.73437500000000000 ) ) ;
#10642 = ORIENTED_EDGE ( 'NONE', *, *, #41663, .F. ) ;
#10644 = ORIENTED_EDGE ( 'NONE', *, *, #68694, .F. ) ;
#10643 = CARTESIAN_POINT ( 'NONE',  ( -12.46153846153858247, -11.48612834414049644, 32.76840700105863391 ) ) ;
#10645 = CARTESIAN_POINT ( 'NONE',  ( 1.134592147322421196, -10.05641848906368452, 34.04755513067966177 ) ) ;
#10646 = CARTESIAN_POINT ( 'NONE',  ( -2.242437168179467033, -4.320704448112861584, 33.92786785259548310 ) ) ;
#10647 = CARTESIAN_POINT ( 'NONE',  ( -1.553300858899125059, -3.750000000000009326, 17.82812500000000000 ) ) ;
#10648 = ORIENTED_EDGE ( 'NONE', *, *, #24978, .F. ) ;
#10649 = ADVANCED_FACE ( 'NONE', ( #69622 ), #22327, .F. ) ;
#10650 = DIRECTION ( 'NONE',  ( -0.000000000000000000, 1.000000000000000000, 3.491481338843133355E-15 ) ) ;
#10651 = ORIENTED_EDGE ( 'NONE', *, *, #12299, .T. ) ;
#10652 = CARTESIAN_POINT ( 'NONE',  ( -4.153846153846152411, -13.53365097954675988, 30.81389545987213552 ) ) ;
#10653 = CARTESIAN_POINT ( 'NONE',  ( -7.053768389744479173, -2.729777683071817229, 31.24903638046268739 ) ) ;
#10654 = FACE_BOUND ( 'NONE', #67921, .T. ) ;
#10656 = DIRECTION ( 'NONE',  ( 0.000000000000000000, 0.000000000000000000, -1.000000000000000000 ) ) ;
#10655 = LINE ( 'NONE', #64246, #57567 ) ;
#10657 = ADVANCED_FACE ( 'NONE', ( #29975 ), #63308, .F. ) ;
#10658 = CARTESIAN_POINT ( 'NONE',  ( 8.703960323269994248, -6.026961402152685388, 34.52809138561120506 ) ) ;
#10659 = CARTESIAN_POINT ( 'NONE',  ( -3.480745974817821331, -8.347322224742351082, 34.93158281831414769 ) ) ;
#10660 = EDGE_LOOP ( 'NONE', ( #80879, #42791, #16990, #56690 ) ) ;
#10661 = PLANE ( 'NONE',  #23127 ) ;
#10662 = EDGE_CURVE ( 'NONE', #69035, #44275, #39570, .T. ) ;
#10663 = FILL_AREA_STYLE ('',( #72353 ) ) ;
#10664 = ORIENTED_EDGE ( 'NONE', *, *, #22912, .F. ) ;
#10665 = VECTOR ( 'NONE', #21643, 1000.000000000000114 ) ;
#10666 = DIRECTION ( 'NONE',  ( 0.000000000000000000, 0.000000000000000000, -1.000000000000000000 ) ) ;
#10667 = CARTESIAN_POINT ( 'NONE',  ( 12.33097786979653776, -2.504760397472875155, 29.97295953869789997 ) ) ;
#10668 = CARTESIAN_POINT ( 'NONE',  ( 0.000000000000000000, -11.00000000000000000, 29.75000000000000355 ) ) ;
#10669 = DIRECTION ( 'NONE',  ( -1.000000000000000000, 0.000000000000000000, 0.000000000000000000 ) ) ;
#10670 = CARTESIAN_POINT ( 'NONE',  ( 20.99999999999999645, -7.500000000000000000, 29.75000000000000355 ) ) ;
#10671 = EDGE_CURVE ( 'NONE', #87581, #36938, #30916, .T. ) ;
#10672 = FACE_BOUND ( 'NONE', #64893, .T. ) ;
#10674 = CARTESIAN_POINT ( 'NONE',  ( -10.36538461538455280, -7.434744860731433924, 35.00000000000000711 ) ) ;
#10673 = CARTESIAN_POINT ( 'NONE',  ( 12.21151523731700550, -10.18141759479407327, 34.26406193332782379 ) ) ;
#10675 = LINE ( 'NONE', #50312, #41052 ) ;
#10677 = CYLINDRICAL_SURFACE ( 'NONE', #44893, 0.2499999999999973355 ) ;
#10676 = CARTESIAN_POINT ( 'NONE',  ( -1.161835843346973318, -12.24180327182771855, 31.33663988360758168 ) ) ;
#10678 = CARTESIAN_POINT ( 'NONE',  ( 6.000000000000001776, -13.78497067705608181, 32.30358669280327177 ) ) ;
#10679 = DIRECTION ( 'NONE',  ( 0.000000000000000000, 0.4999999999999960032, -0.8660254037844410391 ) ) ;
#10680 = CARTESIAN_POINT ( 'NONE',  ( 3.749999999999999556, -7.438900925035446754, 26.71688170625849068 ) ) ;
#10681 = ORIENTED_EDGE ( 'NONE', *, *, #1596, .F. ) ;
#10682 = CARTESIAN_POINT ( 'NONE',  ( 16.08857615328984281, -9.528491918058357157, 34.59228464037090589 ) ) ;
#10683 = EDGE_CURVE ( 'NONE', #18413, #63168, #42754, .T. ) ;
#10684 = EDGE_CURVE ( 'NONE', #67703, #44265, #57881, .T. ) ;
#10685 = CARTESIAN_POINT ( 'NONE',  ( -14.30769230769230660, -1.466349020453238561, 30.81389545987213907 ) ) ;
#10686 = DIRECTION ( 'NONE',  ( 0.000000000000000000, -6.938893903907222067E-15, 1.000000000000000000 ) ) ;
#10687 = CARTESIAN_POINT ( 'NONE',  ( -0.4769917816027518520, -10.20868273765699819, 29.42382599947123722 ) ) ;
#10688 = CARTESIAN_POINT ( 'NONE',  ( 4.230769230769229061, -11.50000000000000000, 29.75000000000000355 ) ) ;
#10689 = CARTESIAN_POINT ( 'NONE',  ( 5.326868486301118644, -12.07971442181322352, 32.31769673815850297 ) ) ;
#10690 = CARTESIAN_POINT ( 'NONE',  ( 3.724691934501232815, -5.885600066136343678, 24.13875670625849068 ) ) ;
#10691 = CARTESIAN_POINT ( 'NONE',  ( -1.134615384615321076, -7.434744860731434812, 35.00000000000000711 ) ) ;
#10692 = CARTESIAN_POINT ( 'NONE',  ( -2.242437168179467033, -6.835583212224609184, 34.95778746994559327 ) ) ;
#10693 = CARTESIAN_POINT ( 'NONE',  ( -7.715628407920200438, -10.31582465632705237, 34.18122507451815295 ) ) ;
#10694 = CARTESIAN_POINT ( 'NONE',  ( 5.076923076922953193, -12.70778746994576025, 30.41441678777401236 ) ) ;
#10695 = CARTESIAN_POINT ( 'NONE',  ( -6.923076923077044142, -4.481592998941358097, 33.73612834414048933 ) ) ;
#10696 = LINE ( 'NONE', #16556, #3703 ) ;
#10697 = VECTOR ( 'NONE', #49299, 1000.000000000000000 ) ;
#10698 = CARTESIAN_POINT ( 'NONE',  ( -18.22292621751615016, -2.758268499246660621, 31.33685645148950272 ) ) ;
#10699 = CARTESIAN_POINT ( 'NONE',  ( 8.096208266067295156, -9.233818618650603938, 34.70587769442853698 ) ) ;
#10700 = VERTEX_POINT ( 'NONE', #85366 ) ;
#10701 = CARTESIAN_POINT ( 'NONE',  ( 3.296024370282069516, -12.51329471203373700, 31.30864560766537963 ) ) ;
#10702 = CARTESIAN_POINT ( 'NONE',  ( 0.4615384615383396616, -10.90142922262034020, 33.41473453929536674 ) ) ;
#10703 = CARTESIAN_POINT ( 'NONE',  ( 2.608446859217924629, -10.19485399968118422, 14.87686829374151465 ) ) ;
#10704 = VECTOR ( 'NONE', #60762, 1000.000000000000000 ) ;
#10705 = DIRECTION ( 'NONE',  ( -0.000000000000000000, 0.9848077530122085754, -0.1736481776669273613 ) ) ;
#10706 = DIRECTION ( 'NONE',  ( -0.000000000000000000, 0.000000000000000000, 1.000000000000000000 ) ) ;
#10707 = ORIENTED_EDGE ( 'NONE', *, *, #53737, .T. ) ;
#10708 = ADVANCED_FACE ( 'NONE', ( #65968 ), #9695, .F. ) ;
#10709 = CARTESIAN_POINT ( 'NONE',  ( -18.22292621751614305, -9.086856451489518705, 34.49173150075333183 ) ) ;
#10710 = FACE_OUTER_BOUND ( 'NONE', #26145, .T. ) ;
#10712 = ORIENTED_EDGE ( 'NONE', *, *, #16924, .T. ) ;
#10711 = CARTESIAN_POINT ( 'NONE',  ( 8.096099255531886030, -2.589246495874658383, 31.60778113518102828 ) ) ;
#10713 = CARTESIAN_POINT ( 'NONE',  ( -13.45069776397551564, -9.905515769479276145, 34.41647553114623292 ) ) ;
#10714 = CARTESIAN_POINT ( 'NONE',  ( 17.14206785764270080, -7.750023224968865421, 34.99404313364389907 ) ) ;
#10715 = CARTESIAN_POINT ( 'NONE',  ( -8.519176457592452678, -2.564540009722895419, 30.55348353981670684 ) ) ;
#10716 = CYLINDRICAL_SURFACE ( 'NONE', #5434, 0.2500000000000008882 ) ;
#10717 = ORIENTED_EDGE ( 'NONE', *, *, #26671, .F. ) ;
#10718 = B_SPLINE_CURVE_WITH_KNOTS ( 'NONE', 3,
 ( #68742, #20987, #75069, #13355, #61531, #89039, #88160, #26435, #61978, #40400 ),
 .UNSPECIFIED., .F., .F.,
 ( 4, 2, 2, 2, 4 ),
 ( 0.0007817246256747484735, 0.0009771112852218928873, 0.001172497944769037084, 0.001367884604316181498, 0.001563271263863325912 ),
 .UNSPECIFIED. ) ;
#10719 = CARTESIAN_POINT ( 'NONE',  ( -6.923076923076922462, -5.180354513474913603, 36.12317359536750416 ) ) ;
#10720 = EDGE_CURVE ( 'NONE', #40851, #20364, #63142, .T. ) ;
#10721 = CARTESIAN_POINT ( 'NONE',  ( 20.00000000000000000, -4.000000000000000000, 29.75000000000000355 ) ) ;
#10722 = CARTESIAN_POINT ( 'NONE',  ( -1.254089682851821763, -6.001044277235011215, 34.52024696741798948 ) ) ;
#10723 = ORIENTED_EDGE ( 'NONE', *, *, #35617, .F. ) ;
#10724 = ORIENTED_EDGE ( 'NONE', *, *, #4479, .F. ) ;
#10725 = EDGE_CURVE ( 'NONE', #17506, #3164, #16849, .T. ) ;
#10726 = VERTEX_POINT ( 'NONE', #58771 ) ;
#10727 = ADVANCED_FACE ( 'NONE', ( #52453 ), #38061, .F. ) ;
#10728 = DIRECTION ( 'NONE',  ( -0.000000000000000000, -0.8660254037844397068, -0.4999999999999978906 ) ) ;
#10729 = CARTESIAN_POINT ( 'NONE',  ( 15.23076923076910916, -11.67786785259630911, 32.92929555188603530 ) ) ;
#10730 = CARTESIAN_POINT ( 'NONE',  ( 2.372947878968333146, -6.026961402152789304, 34.52809138561124769 ) ) ;
#10731 = EDGE_CURVE ( 'NONE', #60841, #82469, #59215, .T. ) ;
#10732 = VECTOR ( 'NONE', #79377, 1000.000000000000000 ) ;
#10733 = CARTESIAN_POINT ( 'NONE',  ( -17.06410256410256565, -11.00000000000000000, 29.75000000000000355 ) ) ;
#10734 = EDGE_LOOP ( 'NONE', ( #6754, #32538, #83656, #41931 ) ) ;
#10735 = ORIENTED_EDGE ( 'NONE', *, *, #38234, .F. ) ;
#10737 = VERTEX_POINT ( 'NONE', #71838 ) ;
#10736 = CARTESIAN_POINT ( 'NONE',  ( 11.60452887181161508, -11.35647404775217595, 33.31231777344666511 ) ) ;
#10738 = CARTESIAN_POINT ( 'NONE',  ( 6.792517009463559852, -2.254533558242299396, 29.97296025877828285 ) ) ;
#10739 = CARTESIAN_POINT ( 'NONE',  ( 15.00784301325307979, -3.105860786376062332, 32.13614157043599562 ) ) ;
#10740 = CARTESIAN_POINT ( 'NONE',  ( -8.769230769230890843, -12.46129190930018460, 30.37095296980731973 ) ) ;
#10741 = CARTESIAN_POINT ( 'NONE',  ( -7.976301815885543434, -10.31621877034669588, 34.18098118002070152 ) ) ;
#10742 = ORIENTED_EDGE ( 'NONE', *, *, #73680, .F. ) ;
#10743 = ADVANCED_FACE ( 'NONE', ( #10147 ), #86721, .F. ) ;
#10744 = ORIENTED_EDGE ( 'NONE', *, *, #36401, .T. ) ;
#10745 = EDGE_CURVE ( 'NONE', #11766, #18984, #8259, .T. ) ;
#10746 = ORIENTED_EDGE ( 'NONE', *, *, #42753, .T. ) ;
#10748 = ORIENTED_EDGE ( 'NONE', *, *, #18434, .T. ) ;
#10747 = CARTESIAN_POINT ( 'NONE',  ( 9.019285080869083870, -2.564540009722896752, 30.55348353981670684 ) ) ;
#10749 = CARTESIAN_POINT ( 'NONE',  ( 3.100077764101675015, -11.71456829005830080, 32.44064028649416542 ) ) ;
#10750 = CARTESIAN_POINT ( 'NONE',  ( 18.22277966897806678, -5.827830569534415694, 34.72679350104403539 ) ) ;
#10751 = VERTEX_POINT ( 'NONE', #18242 ) ;
#10752 = CARTESIAN_POINT ( 'NONE',  ( 9.692307692307695177, -1.790695186598648903, 34.54067556320373455 ) ) ;
#10753 = DIRECTION ( 'NONE',  ( -0.000000000000000000, -0.5000000000000009992, -0.8660254037844380415 ) ) ;
#10754 = CARTESIAN_POINT ( 'NONE',  ( 10.68145296638705410, -3.513871655860379306, 32.76840700105978499 ) ) ;
#10755 = FACE_BOUND ( 'NONE', #31138, .T. ) ;
#10756 = DIRECTION ( 'NONE',  ( 0.000000000000000000, 0.000000000000000000, -1.000000000000000000 ) ) ;
#10757 = CARTESIAN_POINT ( 'NONE',  ( 9.942307692309128697, -7.500000000000155431, 34.75000000000007105 ) ) ;
#10758 = CARTESIAN_POINT ( 'NONE',  ( 1.384615384615386802, -1.242168528481310874, 33.36296068462461051 ) ) ;
#10760 = CARTESIAN_POINT ( 'NONE',  ( 20.00000000000000000, -4.000000000000000000, 29.75000000000000355 ) ) ;
#10759 = CARTESIAN_POINT ( 'NONE',  ( 17.07692307692295586, -9.528491918059723176, 34.59228464037033035 ) ) ;
#10761 = CARTESIAN_POINT ( 'NONE',  ( 8.769230769230645706, -9.528491918059723176, 34.59228464037033035 ) ) ;
#10762 = CARTESIAN_POINT ( 'NONE',  ( -1.326923076923076872, -7.500000000000000000, 29.75000000000000355 ) ) ;
#10763 = EDGE_LOOP ( 'NONE', ( #87595, #1507 ) ) ;
#10764 = CARTESIAN_POINT ( 'NONE',  ( -6.000000000000119904, -11.94971097300221174, 32.03036669348237098 ) ) ;
#10765 = B_SPLINE_CURVE_WITH_KNOTS ( 'NONE', 3,
 ( #63879, #2178, #71968, #76964, #15265, #16144, #36423, #36851, #22455, #17028 ),
 .UNSPECIFIED., .F., .F.,
 ( 4, 2, 2, 2, 4 ),
 ( 0.000000000000000000, 0.0001954311564186876063, 0.0003908623128373752125, 0.0005862934692560628188, 0.0007817246256747504250 ),
 .UNSPECIFIED. ) ;
#10766 = LINE ( 'NONE', #59395, #32190 ) ;
#10767 = VERTEX_POINT ( 'NONE', #45703 ) ;
#10768 = B_SPLINE_CURVE_WITH_KNOTS ( 'NONE', 3,
 ( #19726, #13847, #41327, #62466, #81883, #53499, #6651, #27809, #80996, #46751 ),
 .UNSPECIFIED., .F., .F.,
 ( 4, 2, 2, 2, 4 ),
 ( 0.0007817246256747446788, 0.0009771112852218874663, 0.001172497944769030145, 0.001367884604316172825, 0.001563271263863315720 ),
 .UNSPECIFIED. ) ;
#10769 = ORIENTED_EDGE ( 'NONE', *, *, #47227, .F. ) ;
#10771 = CARTESIAN_POINT ( 'NONE',  ( 1.319344938654610555, -10.90142922261923886, 33.41473453929638993 ) ) ;
#10770 = CARTESIAN_POINT ( 'NONE',  ( 14.30769230769231015, -13.88283147151868846, 33.14645433367849847 ) ) ;
#10772 = CARTESIAN_POINT ( 'NONE',  ( 11.40777093535123399, -8.191372820521381826, 34.95448215188423546 ) ) ;
#10773 = CARTESIAN_POINT ( 'NONE',  ( 0.4615384615383396616, -10.21337939537710326, 33.94971097300076224 ) ) ;
#10774 = CARTESIAN_POINT ( 'NONE',  ( -3.480769230769229061, -2.499999999999998668, 29.75000000000000355 ) ) ;
#10775 = VERTEX_POINT ( 'NONE', #24094 ) ;
#10776 = CARTESIAN_POINT ( 'NONE',  ( 0.000000000000000000, -11.00000000000000000, 29.25000000000000000 ) ) ;
#10777 = EDGE_CURVE ( 'NONE', #27408, #62746, #54501, .T. ) ;
#10778 = EDGE_CURVE ( 'NONE', #67178, #49738, #17983, .T. ) ;
#10780 = CARTESIAN_POINT ( 'NONE',  ( -9.758391103263571509, -4.098570777380719399, 33.41473453929634729 ) ) ;
#10779 = CARTESIAN_POINT ( 'NONE',  ( 18.06525557127602610, -3.835265460703683349, 33.15142922261929925 ) ) ;
#10781 = CARTESIAN_POINT ( 'NONE',  ( -1.514763354347079316, -10.31621877034669588, 34.18098118002070152 ) ) ;
#10782 = LINE ( 'NONE', #30165, #5041 ) ;
#10783 = CARTESIAN_POINT ( 'NONE',  ( -16.82697766754503377, -2.589246495874658827, 31.60778113518102828 ) ) ;
#10784 = CARTESIAN_POINT ( 'NONE',  ( 1.553300858899087311, -3.749999999999992006, 21.73437500000000000 ) ) ;
#10785 = ORIENTED_EDGE ( 'NONE', *, *, #3206, .F. ) ;
#10786 = EDGE_CURVE ( 'NONE', #4262, #49317, #27982, .T. ) ;
#10787 = ORIENTED_EDGE ( 'NONE', *, *, #59543, .F. ) ;
#10788 = CARTESIAN_POINT ( 'NONE',  ( 14.30769230769231015, -10.51840700105979565, 33.73612834413961536 ) ) ;
#10789 = ADVANCED_FACE ( 'NONE', ( #39413 ), #48687, .F. ) ;
#10790 = CARTESIAN_POINT ( 'NONE',  ( -17.86995239374431677, -7.723484964179501588, 34.74522123443823318 ) ) ;
#10791 = CARTESIAN_POINT ( 'NONE',  ( 8.769230769230647482, -12.27809138561165270, 31.22303859784587132 ) ) ;
#10792 = CARTESIAN_POINT ( 'NONE',  ( -14.17690049986752321, -6.413143153341454017, 34.63066358083362672 ) ) ;
#10793 = CARTESIAN_POINT ( 'NONE',  ( -0.5268084620947817154, -12.16647553114622049, 32.15551576947930812 ) ) ;
#10794 = CARTESIAN_POINT ( 'NONE',  ( 1.553300858899129944, -11.24999999999998934, 15.95312500000000000 ) ) ;
#10795 = DIRECTION ( 'NONE',  ( -0.000000000000000000, -0.7660444431189791237, -0.6427876096865379196 ) ) ;
#10796 = CARTESIAN_POINT ( 'NONE',  ( 14.24242230713598900, -6.835583212224499938, 34.95778746994557906 ) ) ;
#10798 = ORIENTED_EDGE ( 'NONE', *, *, #71941, .F. ) ;
#10797 = AXIS2_PLACEMENT_3D ( 'NONE', #70842, #9144, #36604 ) ;
#10799 = ADVANCED_FACE ( 'NONE', ( #55451 ), #76163, .F. ) ;
#10800 = CARTESIAN_POINT ( 'NONE',  ( 17.07692307692295586, -12.27809138561165270, 31.22303859784587132 ) ) ;
#10801 = CARTESIAN_POINT ( 'NONE',  ( -18.24999999999999289, -12.50000000000000000, 29.81604066197449043 ) ) ;
#10802 = DIRECTION ( 'NONE',  ( 1.000000000000000000, 0.000000000000000000, 0.000000000000000000 ) ) ;
#10803 = CARTESIAN_POINT ( 'NONE',  ( -15.23076923076922995, -2.538708090699994813, 30.37095296980875503 ) ) ;
#10804 = CARTESIAN_POINT ( 'NONE',  ( -3.007806327207746211, -7.369474270740069777, 34.74850911626239736 ) ) ;
#10805 = CARTESIAN_POINT ( 'NONE',  ( 6.923076923076924238, -2.292212530054420494, 30.41441678777542634 ) ) ;
#10806 = CARTESIAN_POINT ( 'NONE',  ( -0.3307466537136740103, -11.18335022499818621, 33.13157742990016885 ) ) ;
#10807 = CARTESIAN_POINT ( 'NONE',  ( -4.283993363284374745, -9.418419913701741919, 34.36755862841477693 ) ) ;
#10808 = CARTESIAN_POINT ( 'NONE',  ( 15.45378058238208219, -11.24521262558773493, 33.06293181088029343 ) ) ;
#10809 = EDGE_CURVE ( 'NONE', #79867, #5991, #5061, .T. ) ;
#10810 = ORIENTED_EDGE ( 'NONE', *, *, #7910, .F. ) ;
#10811 = CARTESIAN_POINT ( 'NONE',  ( 8.352564102564102200, -7.500000000000000000, 29.75000000000000355 ) ) ;
#10812 = CARTESIAN_POINT ( 'NONE',  ( 9.019285080869083870, -11.79725096376909654, 32.30694842903959341 ) ) ;
#10813 = DIRECTION ( 'NONE',  ( -0.000000000000000000, 0.6427876096865404731, -0.7660444431189771253 ) ) ;
#10814 = CARTESIAN_POINT ( 'NONE',  ( 1.944543648262996083, -5.555456351736983045, 23.06250000000000000 ) ) ;
#10815 = B_SPLINE_CURVE_WITH_KNOTS ( 'NONE', 3,
 ( #20906, #55139, #62333, #1973, #27669, #1533, #48377, #14156, #41632, #28565 ),
 .UNSPECIFIED., .F., .F.,
 ( 4, 2, 2, 2, 4 ),
 ( 0.000000000000000000, 0.0001954339857564073659, 0.0003908679715128147319, 0.0005863019572692221250, 0.0007817359430256294638 ),
 .UNSPECIFIED. ) ;
#10816 = CARTESIAN_POINT ( 'NONE',  ( 0.3962684609821413573, -5.941354392334500467, 34.76329471203369792 ) ) ;
#10817 = CARTESIAN_POINT ( 'NONE',  ( -17.20761454359064047, -2.541943142973489334, 30.39792223712631980 ) ) ;
#10818 = ADVANCED_FACE ( 'NONE', ( #48244 ), #82935, .F. ) ;
#10820 = ORIENTED_EDGE ( 'NONE', *, *, #74310, .T. ) ;
#10819 = PLANE ( 'NONE',  #74194 ) ;
#10821 = CARTESIAN_POINT ( 'NONE',  ( 2.750000000000008438, -8.639087296525996607, 20.79687500000000000 ) ) ;
#10822 = CARTESIAN_POINT ( 'NONE',  ( -15.48079245499068612, -4.175268141568685643, 33.81360843649122216 ) ) ;
#10823 = B_SPLINE_CURVE_WITH_KNOTS ( 'NONE', 3,
 ( #77503, #1404, #82507, #15816, #55023, #70754, #48694, #14475, #14028, #61760 ),
 .UNSPECIFIED., .F., .F.,
 ( 4, 2, 2, 2, 4 ),
 ( 0.000000000000000000, 0.0001954311564186865221, 0.0003908623128373730441, 0.0005862934692560595662, 0.0007817246256747460882 ),
 .UNSPECIFIED. ) ;
#10824 = ORIENTED_EDGE ( 'NONE', *, *, #6213, .F. ) ;
#10825 = CARTESIAN_POINT ( 'NONE',  ( -4.153846153846274980, -2.657715359629662988, 31.77849191805970364 ) ) ;
#10826 = ORIENTED_EDGE ( 'NONE', *, *, #70670, .F. ) ;
#10827 = CARTESIAN_POINT ( 'NONE',  ( 13.38461538461526601, -12.46129190930018460, 30.37095296980731973 ) ) ;
#10828 = ADVANCED_FACE ( 'NONE', ( #88822 ), #13579, .F. ) ;
#10829 = CARTESIAN_POINT ( 'NONE',  ( -7.715628144390281662, -11.93748526763465279, 32.05452791011430946 ) ) ;
#10830 = LINE ( 'NONE', #80639, #41309 ) ;
#10831 = ORIENTED_EDGE ( 'NONE', *, *, #76048, .F. ) ;
#10832 = CARTESIAN_POINT ( 'NONE',  ( -4.219116154402472674, -11.67786785259541027, 32.92929555188721480 ) ) ;
#10833 = ORIENTED_EDGE ( 'NONE', *, *, #57453, .F. ) ;
#10834 = CARTESIAN_POINT ( 'NONE',  ( 20.00000000000000000, -4.000000000000000000, 29.75000000000000355 ) ) ;
#10835 = EDGE_CURVE ( 'NONE', #22135, #519, #32982, .T. ) ;
#10836 = EDGE_LOOP ( 'NONE', ( #62007, #72139 ) ) ;
#10837 = CYLINDRICAL_SURFACE ( 'NONE', #21261, 0.2500000000000009437 ) ;
#10838 = CARTESIAN_POINT ( 'NONE',  ( 2.438484115517093986, -3.062576670634119758, 32.05464942895959979 ) ) ;
#10839 = ORIENTED_EDGE ( 'NONE', *, *, #16040, .T. ) ;
#10840 = AXIS2_PLACEMENT_3D ( 'NONE', #46090, #18175, #39785 ) ;
#10841 = DIRECTION ( 'NONE',  ( -0.000000000000000000, 0.1736481776669307198, -0.9848077530122080203 ) ) ;
#10842 = CARTESIAN_POINT ( 'NONE',  ( 10.74617642320940369, -3.062576670634119758, 32.05464942895959979 ) ) ;
#10843 = CARTESIAN_POINT ( 'NONE',  ( -1.134669975237339701, -10.92531984108285670, 33.72920026020278073 ) ) ;
#10844 = EDGE_CURVE ( 'NONE', #21562, #58964, #27542, .T. ) ;
#10845 = CARTESIAN_POINT ( 'NONE',  ( -14.30769230769230660, -9.905515769479276145, 34.41647553114623292 ) ) ;
#10846 = CARTESIAN_POINT ( 'NONE',  ( -13.25408994638174320, -12.15418822224088835, 32.17964115625579069 ) ) ;
#10847 = ORIENTED_EDGE ( 'NONE', *, *, #38090, .T. ) ;
#10849 = EDGE_CURVE ( 'NONE', #16242, #10922, #20778, .T. ) ;
#10848 = ORIENTED_EDGE ( 'NONE', *, *, #76712, .F. ) ;
#10850 = VERTEX_POINT ( 'NONE', #70299 ) ;
#10852 = ORIENTED_EDGE ( 'NONE', *, *, #55315, .T. ) ;
#10851 = CARTESIAN_POINT ( 'NONE',  ( 3.007842271862382066, -5.582147617184174848, 34.63737895849758530 ) ) ;
#10853 = B_SPLINE_CURVE_WITH_KNOTS ( 'NONE', 3,
 ( #13783, #41707, #20975, #62401, #22320, #51094, #23204, #2918, #30843, #16011 ),
 .UNSPECIFIED., .F., .F.,
 ( 4, 2, 2, 2, 4 ),
 ( 0.000000000000000000, 0.0001954339857564084773, 0.0003908679715128169545, 0.0005863019572692254860, 0.0007817359430256339090 ),
 .UNSPECIFIED. ) ;
#10854 = CARTESIAN_POINT ( 'NONE',  ( -8.992715712954719720, -10.11188796281391511, 34.01382737946119050 ) ) ;
#10855 = CARTESIAN_POINT ( 'NONE',  ( 9.942307692309128697, -7.500000000000155431, 34.75000000000007105 ) ) ;
#10856 = ORIENTED_EDGE ( 'NONE', *, *, #2391, .T. ) ;
#10857 = EDGE_CURVE ( 'NONE', #83807, #80479, #84505, .T. ) ;
#10858 = AXIS2_PLACEMENT_3D ( 'NONE', #34848, #20460, #67761 ) ;
#10859 = EDGE_CURVE ( 'NONE', #11372, #18795, #25473, .T. ) ;
#10860 = ORIENTED_EDGE ( 'NONE', *, *, #24978, .T. ) ;
#10861 = CARTESIAN_POINT ( 'NONE',  ( 0.4615384615383382183, -8.656820664282941280, 34.87096338111179961 ) ) ;
#10862 = ORIENTED_EDGE ( 'NONE', *, *, #75572, .T. ) ;
#10863 = CARTESIAN_POINT ( 'NONE',  ( 11.60371710973756443, -11.48612834413965977, 32.76840700105972815 ) ) ;
#10864 = EDGE_CURVE ( 'NONE', #5477, #55982, #21156, .T. ) ;
#10865 = CARTESIAN_POINT ( 'NONE',  ( -7.976301055592061928, -2.619462340734462380, 30.83744416345203021 ) ) ;
#10866 = CARTESIAN_POINT ( 'NONE',  ( -9.942307692307691624, -7.500000000000001776, 35.00000000000000000 ) ) ;
#10867 = FACE_BOUND ( 'NONE', #78060, .T. ) ;
#10868 = EDGE_LOOP ( 'NONE', ( #15970, #33705 ) ) ;
#10869 = CYLINDRICAL_SURFACE ( 'NONE', #70112, 0.2499999999999995837 ) ;
#10870 = LINE ( 'NONE', #3212, #71555 ) ;
#10871 = CARTESIAN_POINT ( 'NONE',  ( 4.853996118016225658, -3.395401636524186362, 33.02366814457250399 ) ) ;
#10872 = DIRECTION ( 'NONE',  ( -0.000000000000000000, -0.9848077530122085754, -0.1736481776669273613 ) ) ;
#10873 = CARTESIAN_POINT ( 'NONE',  ( 10.28846153846153832, -11.50000000000000000, 29.75000000000000355 ) ) ;
#10874 = ORIENTED_EDGE ( 'NONE', *, *, #86920, .T. ) ;
#10875 = DIRECTION ( 'NONE',  ( 0.000000000000000000, 0.9396926207859126468, -0.3420201433256571111 ) ) ;
#10876 = ORIENTED_EDGE ( 'NONE', *, *, #68229, .T. ) ;
#10877 = VERTEX_POINT ( 'NONE', #85147 ) ;
#10879 = DIRECTION ( 'NONE',  ( 0.000000000000000000, 0.9396926207859126468, -0.3420201433256571111 ) ) ;
#10878 = CARTESIAN_POINT ( 'NONE',  ( -15.23076923076935252, -3.643525952248795718, 33.31231777344771672 ) ) ;
#10880 = DIRECTION ( 'NONE',  ( -0.000000000000000000, -0.7660444431189791237, -0.6427876096865379196 ) ) ;
#10881 = CARTESIAN_POINT ( 'NONE',  ( 2.307692307692309264, -2.499999999999998668, 29.50000000000001066 ) ) ;
#10882 = CARTESIAN_POINT ( 'NONE',  ( -4.153846153846152411, -2.292212530054420494, 30.41441678777542634 ) ) ;
#10883 = CARTESIAN_POINT ( 'NONE',  ( 14.05771556364371655, -2.920706130388546651, 32.31842814019191223 ) ) ;
#10884 = EDGE_LOOP ( 'NONE', ( #36133, #10921 ) ) ;
#10885 = VECTOR ( 'NONE', #6136, 1000.000000000000000 ) ;
#10886 = CARTESIAN_POINT ( 'NONE',  ( -5.076923076923199218, -6.835583212225970762, 34.95778746994575670 ) ) ;
#10887 = CYLINDRICAL_SURFACE ( 'NONE', #50233, 0.2499999999999994726 ) ;
#10888 = CARTESIAN_POINT ( 'NONE',  ( -1.607541602131532077, -3.586966769969700763, 32.86292498521069660 ) ) ;
#10889 = CARTESIAN_POINT ( 'NONE',  ( 14.43821774592595375, -2.647132371071621471, 31.75357179365171589 ) ) ;
#10890 = ORIENTED_EDGE ( 'NONE', *, *, #35603, .T. ) ;
#10891 = EDGE_LOOP ( 'NONE', ( #39839, #16856 ) ) ;
#10892 = FACE_BOUND ( 'NONE', #25233, .T. ) ;
#10893 = VERTEX_POINT ( 'NONE', #22552 ) ;
#10894 = CARTESIAN_POINT ( 'NONE',  ( -17.74999999976641973, -2.249999999999989786, 29.74999979494859303 ) ) ;
#10895 = CARTESIAN_POINT ( 'NONE',  ( 5.010840697562940704, -2.833524468853757305, 32.15551576947924417 ) ) ;
#10897 = EDGE_LOOP ( 'NONE', ( #60211, #8273, #85221, #79989 ) ) ;
#10896 = EDGE_CURVE ( 'NONE', #80092, #61727, #78108, .T. ) ;
#10898 = AXIS2_PLACEMENT_3D ( 'NONE', #84983, #14753, #50724 ) ;
#10899 = LINE ( 'NONE', #57750, #65410 ) ;
#10900 = CARTESIAN_POINT ( 'NONE',  ( 6.792929713638703682, -10.88202310037935661, 33.43294751532457099 ) ) ;
#10901 = CARTESIAN_POINT ( 'NONE',  ( 4.826899839630108602, -2.823816976329319495, 31.52131813110795733 ) ) ;
#10902 = DIRECTION ( 'NONE',  ( -0.000000000000000000, 0.1736481776669307198, -0.9848077530122080203 ) ) ;
#10903 = CARTESIAN_POINT ( 'NONE',  ( -0.5276218724943415594, -11.16473453929635440, 33.15142922261925662 ) ) ;
#10904 = ORIENTED_EDGE ( 'NONE', *, *, #12821, .F. ) ;
#10905 = EDGE_CURVE ( 'NONE', #23097, #43624, #50885, .T. ) ;
#10907 = ORIENTED_EDGE ( 'NONE', *, *, #77754, .F. ) ;
#10906 = CARTESIAN_POINT ( 'NONE',  ( -14.30769230769199929, -2.506253911140614576, 30.00000000000323297 ) ) ;
#10908 = CARTESIAN_POINT ( 'NONE',  ( -7.623374304885435215, -9.332535724633405749, 34.40230450496446934 ) ) ;
#10909 = DIRECTION ( 'NONE',  ( -0.000000000000000000, -0.6427876096865404731, -0.7660444431189770143 ) ) ;
#10910 = CARTESIAN_POINT ( 'NONE',  ( 12.46153846153846168, -13.20930481340135110, 34.54067556320372745 ) ) ;
#10911 = CARTESIAN_POINT ( 'NONE',  ( 17.99999999999987566, -8.613356846316285953, 34.62446782046622218 ) ) ;
#10912 = LINE ( 'NONE', #70848, #72096 ) ;
#10913 = CARTESIAN_POINT ( 'NONE',  ( 6.000000000000001776, -2.721908614388771852, 31.22303859784724978 ) ) ;
#10914 = EDGE_CURVE ( 'NONE', #45514, #42058, #16240, .T. ) ;
#10915 = CARTESIAN_POINT ( 'NONE',  ( 2.724691934501250135, -8.700186371490531201, 17.29874329374151642 ) ) ;
#10916 = ORIENTED_EDGE ( 'NONE', *, *, #36409, .F. ) ;
#10917 = DIRECTION ( 'NONE',  ( 0.000000000000000000, -0.000000000000000000, -1.000000000000000000 ) ) ;
#10918 = CARTESIAN_POINT ( 'NONE',  ( -9.442362173959551797, -8.433404298154334455, 34.66254593164985920 ) ) ;
#10919 = FACE_OUTER_BOUND ( 'NONE', #62962, .T. ) ;
#10921 = ORIENTED_EDGE ( 'NONE', *, *, #41668, .T. ) ;
#10920 = VECTOR ( 'NONE', #19780, 1000.000000000000114 ) ;
#10922 = VERTEX_POINT ( 'NONE', #43704 ) ;
#10923 = CARTESIAN_POINT ( 'NONE',  ( 9.823098133274648092, -3.338503747796866872, 32.95102852606553512 ) ) ;
#10924 = CARTESIAN_POINT ( 'NONE',  ( 12.71159288145191724, -4.074993327901527351, 33.72946981652012255 ) ) ;
#10925 = LINE ( 'NONE', #65853, #18818 ) ;
#10926 = CARTESIAN_POINT ( 'NONE',  ( 10.39189967166066708, -5.912607949931405926, 34.49155766932282319 ) ) ;
#10927 = CARTESIAN_POINT ( 'NONE',  ( 15.90386940979756503, -10.06842814019191401, 34.32929386961144758 ) ) ;
#10928 = EDGE_CURVE ( 'NONE', #50664, #60409, #64853, .T. ) ;
#10929 = CYLINDRICAL_SURFACE ( 'NONE', #31270, 0.2499999999999995559 ) ;
#10930 = DIRECTION ( 'NONE',  ( -0.000000000000000000, 0.7660444431189791237, -0.6427876096865379196 ) ) ;
#10931 = ORIENTED_EDGE ( 'NONE', *, *, #84971, .F. ) ;
#10932 = CARTESIAN_POINT ( 'NONE',  ( 9.469381474791546793, -10.61292498521070549, 33.66303323003028680 ) ) ;
#10933 = CARTESIAN_POINT ( 'NONE',  ( -0.4615384615384611200, -8.120952969808772792, 34.71129190930000163 ) ) ;
#10934 = CARTESIAN_POINT ( 'NONE',  ( -6.130610359624526495, -7.722926236386453702, 34.74524107206102030 ) ) ;
#10935 = CARTESIAN_POINT ( 'NONE',  ( 17.01165263096229907, -9.442884908240170461, 34.35708131394840592 ) ) ;
#10936 = ORIENTED_EDGE ( 'NONE', *, *, #40498, .F. ) ;
#10937 = CARTESIAN_POINT ( 'NONE',  ( 12.39545608217832218, -2.486705287966279432, 31.30864560766542937 ) ) ;
#10938 = EDGE_CURVE ( 'NONE', #64231, #9817, #58537, .T. ) ;
#10939 = ORIENTED_EDGE ( 'NONE', *, *, #16316, .T. ) ;
#10940 = CARTESIAN_POINT ( 'NONE',  ( 8.769230769230768274, -5.180354513474913603, 36.12317359536750416 ) ) ;
#10941 = CARTESIAN_POINT ( 'NONE',  ( -1.608100328339332252, -9.331801661448606566, 34.40259984581193464 ) ) ;
#10942 = CARTESIAN_POINT ( 'NONE',  ( 15.23076923076923173, -7.500000000000001776, 35.04278698407183867 ) ) ;
#10943 = ORIENTED_EDGE ( 'NONE', *, *, #30776, .F. ) ;
#10944 = EDGE_CURVE ( 'NONE', #11726, #43122, #76999, .T. ) ;
#10945 = CARTESIAN_POINT ( 'NONE',  ( -10.61538461538461320, -1.466349020453238561, 30.81389545987213907 ) ) ;
#10946 = CARTESIAN_POINT ( 'NONE',  ( 5.933916589044118339, -9.780366693483667717, 34.19971097300155805 ) ) ;
#10947 = B_SPLINE_CURVE_WITH_KNOTS ( 'NONE', 3,
 ( #31795, #43960, #79084, #58805, #10628, #30886 ),
 .UNSPECIFIED., .F., .F.,
 ( 4, 2, 4 ),
 ( 0.0003909569690057805385, 0.0005862646681846044039, 0.0007815723673634283235 ),
 .UNSPECIFIED. ) ;
#10948 = CARTESIAN_POINT ( 'NONE',  ( 10.61538461538449418, -12.70778746994576025, 30.41441678777401236 ) ) ;
#10949 = CARTESIAN_POINT ( 'NONE',  ( -3.230769230769229949, -3.669653830205710676, 35.88435417666054406 ) ) ;
#10950 = DIRECTION ( 'NONE',  ( 0.000000000000000000, 0.3420201433256610524, 0.9396926207859113145 ) ) ;
#10951 = EDGE_CURVE ( 'NONE', #57687, #72142, #86948, .T. ) ;
#10952 = ORIENTED_EDGE ( 'NONE', *, *, #36402, .F. ) ;
#10953 = CARTESIAN_POINT ( 'NONE',  ( 5.076923076923075762, -2.833524468853757305, 32.15551576947925838 ) ) ;
#10954 = ORIENTED_EDGE ( 'NONE', *, *, #43118, .F. ) ;
#10955 = CARTESIAN_POINT ( 'NONE',  ( -15.23076923076922995, -6.343179335718451384, 34.87096338111211935 ) ) ;
#10956 = FACE_OUTER_BOUND ( 'NONE', #36844, .T. ) ;
#10957 = CARTESIAN_POINT ( 'NONE',  ( -0.4615384615384611200, -2.486705287966279876, 31.30864560766543647 ) ) ;
#10958 = DIRECTION ( 'NONE',  ( 0.000000000000000000, 0.000000000000000000, 1.000000000000000000 ) ) ;
#10959 = VECTOR ( 'NONE', #60018, 1000.000000000000000 ) ;
#10960 = CARTESIAN_POINT ( 'NONE',  ( 4.854057654719437842, -2.501496062324911840, 29.88072118266895671 ) ) ;
#10961 = CARTESIAN_POINT ( 'NONE',  ( 15.90382292962469535, -12.07920672191015221, 32.31858351112116168 ) ) ;
#10962 = ADVANCED_FACE ( 'NONE', ( #73410 ), #74294, .F. ) ;
#10963 = VERTEX_POINT ( 'NONE', #32417 ) ;
#10964 = ORIENTED_EDGE ( 'NONE', *, *, #54687, .F. ) ;
#10965 = ORIENTED_EDGE ( 'NONE', *, *, #3817, .F. ) ;
#10966 = EDGE_CURVE ( 'NONE', #86663, #72654, #41592, .T. ) ;
#10968 = ORIENTED_EDGE ( 'NONE', *, *, #71445, .F. ) ;
#10967 = EDGE_CURVE ( 'NONE', #70118, #57312, #11430, .T. ) ;
#10969 = ORIENTED_EDGE ( 'NONE', *, *, #82126, .F. ) ;
#10970 = CARTESIAN_POINT ( 'NONE',  ( -10.39260507411620260, -8.496831190052096971, 34.64984203495476578 ) ) ;
#10971 = CARTESIAN_POINT ( 'NONE',  ( -11.78843826940389405, -9.148715823498378086, 34.47080413974185120 ) ) ;
#10972 = EDGE_CURVE ( 'NONE', #37880, #48499, #24767, .T. ) ;
#10973 = B_SPLINE_CURVE_WITH_KNOTS ( 'NONE', 3,
 ( #45400, #79204, #44954, #17501, #3966, #4885, #17050, #31451, #4421, #66579 ),
 .UNSPECIFIED., .F., .F.,
 ( 4, 2, 2, 2, 4 ),
 ( 0.0007817246256747515092, 0.0009771112852218961399, 0.001172497944769040554, 0.001367884604316184968, 0.001563271263863329598 ),
 .UNSPECIFIED. ) ;
#10974 = CARTESIAN_POINT ( 'NONE',  ( -15.36091644020745051, -10.88202310037935661, 33.43294751532457099 ) ) ;
#10975 = ADVANCED_FACE ( 'NONE', ( #46377 ), #46816, .F. ) ;
#10976 = FACE_OUTER_BOUND ( 'NONE', #69430, .T. ) ;
#10977 = DIRECTION ( 'NONE',  ( -0.000000000000000000, -0.8660254037844399289, -0.4999999999999980016 ) ) ;
#10978 = CARTESIAN_POINT ( 'NONE',  ( -6.250023224221454399, -2.985938066672154445, 32.43141759479405550 ) ) ;
#10979 = LINE ( 'NONE', #44285, #3298 ) ;
#10980 = CARTESIAN_POINT ( 'NONE',  ( -4.153846153846273204, -10.90142922262034020, 33.41473453929536674 ) ) ;
#10981 = CARTESIAN_POINT ( 'NONE',  ( 7.911408985666684046, -5.094484230520773593, 34.41647553114626845 ) ) ;
#10982 = VERTEX_POINT ( 'NONE', #45478 ) ;
#10983 = VERTEX_POINT ( 'NONE', #17578 ) ;
#10984 = AXIS2_PLACEMENT_3D ( 'NONE', #10394, #11279, #18488 ) ;
#10985 = EDGE_LOOP ( 'NONE', ( #80655, #15396, #16377, #88338 ) ) ;
#10987 = VERTEX_POINT ( 'NONE', #4500 ) ;
#10986 = CARTESIAN_POINT ( 'NONE',  ( 6.223012844093394946, -12.38742843783360748, 31.66772728687926985 ) ) ;
#10989 = CARTESIAN_POINT ( 'NONE',  ( -17.86947456176635640, -11.66157788607254098, 32.95092075102925833 ) ) ;
#10988 = CARTESIAN_POINT ( 'NONE',  ( 0.3589743589743582541, -3.499999999999999556, 29.75000000000000355 ) ) ;
#10990 = CARTESIAN_POINT ( 'NONE',  ( 1.515405825582335941, -4.684288915650983043, 34.18129842949671371 ) ) ;
#10991 = CARTESIAN_POINT ( 'NONE',  ( -11.53846153846166089, -9.528491918059723176, 34.59228464037033035 ) ) ;
#10992 = FACE_BOUND ( 'NONE', #59052, .T. ) ;
#10993 = EDGE_LOOP ( 'NONE', ( #73196, #31247 ) ) ;
#10994 = VERTEX_POINT ( 'NONE', #25216 ) ;
#10995 = CARTESIAN_POINT ( 'NONE',  ( -12.46153846153846168, -12.62096338111211580, 30.90682066428153263 ) ) ;
#10996 = B_SPLINE_CURVE_WITH_KNOTS ( 'NONE', 3,
 ( #84155, #22432, #49897, #77374, #15684, #63856, #43150, #70620, #2155, #24646 ),
 .UNSPECIFIED., .F., .F.,
 ( 4, 2, 2, 2, 4 ),
 ( 0.000000000000000000, 0.0001954339857564082604, 0.0003908679715128165208, 0.0005863019572692248355, 0.0007817359430256330417 ),
 .UNSPECIFIED. ) ;
#10997 = VERTEX_POINT ( 'NONE', #52678 ) ;
#10998 = FACE_BOUND ( 'NONE', #53242, .T. ) ;
#10999 = CARTESIAN_POINT ( 'NONE',  ( -17.07692307692307665, -12.78798330534103123, 29.99999999999997868 ) ) ;
#11000 = SHAPE_REPRESENTATION ( 'spring', ( #83448 ), #34517 ) ;
#11001 = DIRECTION ( 'NONE',  ( -0.000000000000000000, 0.7660444431189791237, -0.6427876096865379196 ) ) ;
#11002 = ORIENTED_EDGE ( 'NONE', *, *, #55258, .T. ) ;
#11003 = CARTESIAN_POINT ( 'NONE',  ( -1.384615384615506484, -5.941354392335915335, 34.76329471203413846 ) ) ;
#11004 = DIRECTION ( 'NONE',  ( 0.000000000000000000, 0.000000000000000000, -1.000000000000000000 ) ) ;
#11005 = CARTESIAN_POINT ( 'NONE',  ( -18.25002322422145440, -4.175268141568687419, 33.81360843649122216 ) ) ;
#11006 = ORIENTED_EDGE ( 'NONE', *, *, #66327, .T. ) ;
#11007 = CARTESIAN_POINT ( 'NONE',  ( 12.23805351781451201, -5.113361153441934093, 34.14387501736622710 ) ) ;
#11008 = CARTESIAN_POINT ( 'NONE',  ( 7.146089767170319185, -5.582272713120727481, 34.63742843783360570 ) ) ;
#11009 = EDGE_LOOP ( 'NONE', ( #44288, #30691, #10129, #28482 ) ) ;
#11010 = CARTESIAN_POINT ( 'NONE',  ( -8.769230769230768274, -2.708943851104267164, 35.45975837776705220 ) ) ;
#11011 = CARTESIAN_POINT ( 'NONE',  ( 7.173131234715237170, -10.66356715214248396, 33.62249196103329751 ) ) ;
#11012 = ORIENTED_EDGE ( 'NONE', *, *, #26914, .T. ) ;
#11013 = CARTESIAN_POINT ( 'NONE',  ( -12.59222906464877134, -5.496505350115501010, 34.60290016733514307 ) ) ;
#11014 = CARTESIAN_POINT ( 'NONE',  ( 13.16113044089144068, -2.599994579823202923, 30.74605699353653776 ) ) ;
#11015 = CARTESIAN_POINT ( 'NONE',  ( -16.15384615384615330, -8.120952969808772792, 34.71129190930000163 ) ) ;
#11016 = CARTESIAN_POINT ( 'NONE',  ( -10.36543909703647159, -5.852078868378309373, 34.47109172314383585 ) ) ;
#11017 = CARTESIAN_POINT ( 'NONE',  ( 2.307692307692309264, -4.945431358278436385, 36.03766855953609394 ) ) ;
#11018 = VECTOR ( 'NONE', #62308, 1000.000000000000000 ) ;
#11019 = CYLINDRICAL_SURFACE ( 'NONE', #85475, 0.2499999999999995559 ) ;
#11021 = CARTESIAN_POINT ( 'NONE',  ( 9.757562831820530747, -5.094484230520773593, 34.41647553114626845 ) ) ;
#11020 = FACE_OUTER_BOUND ( 'NONE', #22202, .T. ) ;
#11022 = CARTESIAN_POINT ( 'NONE',  ( 10.61538461538449418, -9.528491918059723176, 34.59228464037033035 ) ) ;
#11024 = DIRECTION ( 'NONE',  ( 0.000000000000000000, 0.000000000000000000, 1.000000000000000000 ) ) ;
#11023 = DIRECTION ( 'NONE',  ( 0.000000000000000000, 0.1736481776669275834, 0.9848077530122086864 ) ) ;
#11025 = CARTESIAN_POINT ( 'NONE',  ( 1.944543648262996083, -5.555456351736983045, 15.56250000000000000 ) ) ;
#11026 = ORIENTED_EDGE ( 'NONE', *, *, #86740, .T. ) ;
#11027 = DIRECTION ( 'NONE',  ( -0.000000000000000000, -5.102127870520021228E-17, -1.000000000000000000 ) ) ;
#11028 = ORIENTED_EDGE ( 'NONE', *, *, #20816, .T. ) ;
#11029 = EDGE_LOOP ( 'NONE', ( #55903, #5368 ) ) ;
#11030 = CARTESIAN_POINT ( 'NONE',  ( -7.715363405186893786, -2.494656445102013453, 31.33466734024120015 ) ) ;
#11032 = EDGE_LOOP ( 'NONE', ( #86077, #43231, #74603, #66163 ) ) ;
#11031 = VECTOR ( 'NONE', #53240, 1000.000000000000227 ) ;
#11033 = CARTESIAN_POINT ( 'NONE',  ( -5.750054590621955342, -10.18230066228895758, 34.26354781536631577 ) ) ;
#11034 = CARTESIAN_POINT ( 'NONE',  ( -1.139087296525992166, -10.25000000000000533, 14.85937500000000355 ) ) ;
#11035 = CARTESIAN_POINT ( 'NONE',  ( -18.00000000000000000, -5.557115091759784242, 34.35708131394839171 ) ) ;
#11036 = CARTESIAN_POINT ( 'NONE',  ( -18.13069060311030611, -11.93127051446800024, 32.56575433478201376 ) ) ;
#11037 = DIRECTION ( 'NONE',  ( -0.000000000000000000, -0.8660254037844399289, -0.4999999999999980016 ) ) ;
#11038 = CARTESIAN_POINT ( 'NONE',  ( -6.065270000556317598, -2.657715359629089225, 31.77849191805834295 ) ) ;
#11039 = DIRECTION ( 'NONE',  ( -1.000000000000000000, -0.000000000000000000, -0.000000000000000000 ) ) ;
#11040 = CARTESIAN_POINT ( 'NONE',  ( -10.86536134632696715, -4.236021600441997492, 33.53823185664189310 ) ) ;
#11041 = CARTESIAN_POINT ( 'NONE',  ( 5.933916589044120116, -4.098570777380720287, 33.41473453929634729 ) ) ;
#11042 = CARTESIAN_POINT ( 'NONE',  ( -3.749999999999997335, -7.500000000000021316, 21.34375000000000000 ) ) ;
#11043 = CARTESIAN_POINT ( 'NONE',  ( -11.47320639894870276, -2.657715359629131857, 31.77849191805844242 ) ) ;
#11044 = CARTESIAN_POINT ( 'NONE',  ( -2.241624974342230292, -11.91647553114624358, 32.58852847137148245 ) ) ;
#11045 = CARTESIAN_POINT ( 'NONE',  ( -2.372962753653082846, -4.481592998940161721, 33.73612834413957984 ) ) ;
#11046 = EDGE_CURVE ( 'NONE', #81511, #72329, #25988, .T. ) ;
#11047 = EDGE_LOOP ( 'NONE', ( #69568, #64526, #28938, #58143 ) ) ;
#11048 = VERTEX_POINT ( 'NONE', #81064 ) ;
#11049 = AXIS2_PLACEMENT_3D ( 'NONE', #2396, #77183, #16803 ) ;
#11050 = CARTESIAN_POINT ( 'NONE',  ( -13.45069776397551564, -6.343179335718451384, 34.87096338111212646 ) ) ;
#11051 = CARTESIAN_POINT ( 'NONE',  ( -17.29984929443922681, -8.239355502252617924, 34.69524867566427417 ) ) ;
#11052 = CARTESIAN_POINT ( 'NONE',  ( -1.384615384615383471, -13.87047571288749737, 32.06866353760679544 ) ) ;
#11053 = CARTESIAN_POINT ( 'NONE',  ( -6.250023237292963607, -3.711651800289232916, 33.01384336483936011 ) ) ;
#11054 = CYLINDRICAL_SURFACE ( 'NONE', #24793, 0.2499999999999995559 ) ;
#11055 = B_SPLINE_CURVE_WITH_KNOTS ( 'NONE', 3,
 ( #43227, #72465, #10772, #71571, #50409, #70702, #3559, #30155, #78777, #57623 ),
 .UNSPECIFIED., .F., .F.,
 ( 4, 2, 2, 2, 4 ),
 ( 0.000000000000000000, 0.0001954311564186870913, 0.0003908623128373741825, 0.0005862934692560613009, 0.0007817246256747483650 ),
 .UNSPECIFIED. ) ;
#11056 = VECTOR ( 'NONE', #28002, 1000.000000000000000 ) ;
#11057 = CARTESIAN_POINT ( 'NONE',  ( 11.53846153846153832, -1.466349020453238561, 30.81389545987213907 ) ) ;
#11058 = EDGE_CURVE ( 'NONE', #54717, #60134, #85613, .T. ) ;
#11059 = AXIS2_PLACEMENT_3D ( 'NONE', #44550, #78346, #71150 ) ;
#11060 = ORIENTED_EDGE ( 'NONE', *, *, #82172, .T. ) ;
#11061 = DIRECTION ( 'NONE',  ( -0.000000000000000000, -0.8660254037844399289, -0.4999999999999980016 ) ) ;
#11062 = ORIENTED_EDGE ( 'NONE', *, *, #24489, .F. ) ;
#11063 = ORIENTED_EDGE ( 'NONE', *, *, #31793, .F. ) ;
#11064 = CARTESIAN_POINT ( 'NONE',  ( -5.934744428723973897, -6.026961402152789304, 34.52809138561124769 ) ) ;
#11065 = DIRECTION ( 'NONE',  ( 1.000000000000000000, 0.000000000000000000, 0.000000000000000000 ) ) ;
#11066 = CARTESIAN_POINT ( 'NONE',  ( -14.24162497434223162, -2.833524468853757305, 32.15551576947925838 ) ) ;
#11067 = CARTESIAN_POINT ( 'NONE',  ( 6.222779668978068557, -8.540255544307065350, 34.89611431652622286 ) ) ;
#11068 = CARTESIAN_POINT ( 'NONE',  ( -13.16183584334697443, -3.236590943229499029, 32.36255958852954251 ) ) ;
#11069 = ORIENTED_EDGE ( 'NONE', *, *, #13412, .T. ) ;
#11070 = VERTEX_POINT ( 'NONE', #86493 ) ;
#11071 = AXIS2_PLACEMENT_3D ( 'NONE', #6833, #82517, #35196 ) ;
#11072 = EDGE_CURVE ( 'NONE', #52884, #30224, #70623, .T. ) ;
#11073 = EDGE_CURVE ( 'NONE', #50622, #47174, #26555, .T. ) ;
#11074 = ORIENTED_EDGE ( 'NONE', *, *, #5941, .T. ) ;
#11075 = CARTESIAN_POINT ( 'NONE',  ( 11.53846153846141576, -9.528491918059723176, 34.59228464037033035 ) ) ;
#11076 = LINE ( 'NONE', #73224, #25823 ) ;
#11077 = FACE_OUTER_BOUND ( 'NONE', #19345, .T. ) ;
#11078 = DIRECTION ( 'NONE',  ( -1.000000000000000000, -0.000000000000000000, -0.000000000000000000 ) ) ;
#11079 = CARTESIAN_POINT ( 'NONE',  ( -11.78848476268299628, -8.475808217655753651, 34.90892951860618609 ) ) ;
#11080 = CARTESIAN_POINT ( 'NONE',  ( -15.93106661257774626, -2.847695495035524438, 31.58253572463339154 ) ) ;
#11081 = EDGE_LOOP ( 'NONE', ( #23055, #38895 ) ) ;
#11082 = EDGE_CURVE ( 'NONE', #65772, #45114, #6714, .T. ) ;
#11083 = ORIENTED_EDGE ( 'NONE', *, *, #71200, .T. ) ;
#11084 = CARTESIAN_POINT ( 'NONE',  ( 11.53846153846184563, -2.506253911140615021, 30.00000000000323297 ) ) ;
#11085 = ORIENTED_EDGE ( 'NONE', *, *, #16962, .T. ) ;
#11087 = EDGE_LOOP ( 'NONE', ( #36165, #21532, #76178, #52157 ) ) ;
#11086 = CARTESIAN_POINT ( 'NONE',  ( 2.372947878968333590, -12.46129190930001052, 30.37095296980870174 ) ) ;
#11088 = CARTESIAN_POINT ( 'NONE',  ( 8.096099364501988305, -12.43552623307873972, 30.55307653245132826 ) ) ;
#11089 = CARTESIAN_POINT ( 'NONE',  ( -2.307692307692305711, -3.937682226553329556, 33.60647404775216529 ) ) ;
#11090 = CARTESIAN_POINT ( 'NONE',  ( -3.749999999999988454, -9.053300858899127945, 15.01562500000000178 ) ) ;
#11091 = ORIENTED_EDGE ( 'NONE', *, *, #11555, .T. ) ;
#11092 = CARTESIAN_POINT ( 'NONE',  ( -13.60754160213153163, -12.15238873228292071, 31.58232369045353849 ) ) ;
#11093 = ORIENTED_EDGE ( 'NONE', *, *, #35952, .F. ) ;
#11094 = CARTESIAN_POINT ( 'NONE',  ( 5.869852030268307708, -9.504002272028875709, 34.60269587691767867 ) ) ;
#11095 = CARTESIAN_POINT ( 'NONE',  ( 0.3308478584281527302, -11.37499894934982159, 33.29245874905763003 ) ) ;
#11096 = FACE_BOUND ( 'NONE', #989, .T. ) ;
#11098 = CARTESIAN_POINT ( 'NONE',  ( 23.00000000000000000, -9.499999999999982236, 27.74999999999999645 ) ) ;
#11097 = CARTESIAN_POINT ( 'NONE',  ( -0.2387587925603965044, -11.60474049983370648, 33.02348890104160262 ) ) ;
#11099 = CARTESIAN_POINT ( 'NONE',  ( -1.634592128663976185, -3.436278759898155233, 33.07459398097509506 ) ) ;
#11100 = CARTESIAN_POINT ( 'NONE',  ( 0.6089743589743582541, -7.500000000000000000, 33.75000000000000000 ) ) ;
#11101 = EDGE_LOOP ( 'NONE', ( #7876, #63098, #13245, #14650 ) ) ;
#11102 = FACE_OUTER_BOUND ( 'NONE', #46034, .T. ) ;
#11103 = CARTESIAN_POINT ( 'NONE',  ( 15.10007776410167502, -4.118384482072086072, 33.43331474514187107 ) ) ;
#11104 = EDGE_LOOP ( 'NONE', ( #41554, #62892 ) ) ;
#11105 = B_SPLINE_CURVE_WITH_KNOTS ( 'NONE', 3,
 ( #30040, #84553, #3441, #77336, #15643, #77775, #30908, #43110, #70583, #57499 ),
 .UNSPECIFIED., .F., .F.,
 ( 4, 2, 2, 2, 4 ),
 ( 0.000000000000000000, 0.0001954311564186882026, 0.0003908623128373764051, 0.0005862934692560646619, 0.0007817246256747528103 ),
 .UNSPECIFIED. ) ;
#11106 = CARTESIAN_POINT ( 'NONE',  ( -8.519176349317319819, -3.435999193479609914, 33.07426656108010832 ) ) ;
#11107 = CARTESIAN_POINT ( 'NONE',  ( -9.561782254074051579, -5.070358843744210198, 34.40418822224088302 ) ) ;
#11108 = CARTESIAN_POINT ( 'NONE',  ( -6.249976730942353953, -10.66389620160130036, 33.62221079203477103 ) ) ;
#11109 = LINE ( 'NONE', #46229, #71650 ) ;
#11110 = DIRECTION ( 'NONE',  ( 0.000000000000000000, 0.000000000000000000, 1.000000000000000000 ) ) ;
#11111 = FACE_BOUND ( 'NONE', #53189, .T. ) ;
#11113 = CARTESIAN_POINT ( 'NONE',  ( -2.939152317953646711E-15, 7.500000000000000000, 13.50000000000000178 ) ) ;
#11112 = CARTESIAN_POINT ( 'NONE',  ( 13.38461538461538680, -12.10708131394839349, 31.69288490824020244 ) ) ;
#11114 = AXIS2_PLACEMENT_3D ( 'NONE', #88609, #11596, #86834 ) ;
#11115 = CARTESIAN_POINT ( 'NONE',  ( -6.673131404728780858, -10.76462480002816235, 33.53768742498949962 ) ) ;
#11117 = PLANE ( 'NONE',  #82335 ) ;
#11116 = CARTESIAN_POINT ( 'NONE',  ( 3.165498784808455035, -4.481592998940161721, 33.73612834413957984 ) ) ;
#11118 = CARTESIAN_POINT ( 'NONE',  ( 16.08857570788537572, -10.90142922261923886, 33.41473453929638993 ) ) ;
#11119 = CARTESIAN_POINT ( 'NONE',  ( 6.000000000000001776, -1.367168528481310208, 33.57946703557072254 ) ) ;
#11120 = CARTESIAN_POINT ( 'NONE',  ( -2.694853999681210865, -4.891553140782108677, 23.74813170625849068 ) ) ;
#11121 = VERTEX_POINT ( 'NONE', #55339 ) ;
#11122 = CYLINDRICAL_SURFACE ( 'NONE', #57918, 0.2500000000000002220 ) ;
#11123 = CARTESIAN_POINT ( 'NONE',  ( -15.10072162451355027, -7.723484964179501588, 34.74522123443823318 ) ) ;
#11124 = LINE ( 'NONE', #79592, #57454 ) ;
#11125 = CARTESIAN_POINT ( 'NONE',  ( 17.07692307692295586, -8.656820664282941280, 34.87096338111179961 ) ) ;
#11126 = CARTESIAN_POINT ( 'NONE',  ( -4.403869378067609475, -4.931416488878822335, 34.32920672191015399 ) ) ;
#11127 = CARTESIAN_POINT ( 'NONE',  ( 6.065255139512837346, -3.643525952247864463, 33.31231777344670064 ) ) ;
#11128 = CARTESIAN_POINT ( 'NONE',  ( 2.775308065498768517, -8.577988221561467341, 15.54500670625849246 ) ) ;
#11129 = EDGE_CURVE ( 'NONE', #60966, #43000, #73821, .T. ) ;
#11130 = CARTESIAN_POINT ( 'NONE',  ( -16.37733107841048508, -5.827078755546626354, 34.72654668319379567 ) ) ;
#11131 = CARTESIAN_POINT ( 'NONE',  ( -7.846153846153844924, -2.708943851104267164, 35.45975837776705220 ) ) ;
#11132 = CARTESIAN_POINT ( 'NONE',  ( 3.361294669002876212, -4.299079248970732792, 33.91157788607253565 ) ) ;
#11133 = CARTESIAN_POINT ( 'NONE',  ( 9.626225312947559232, -3.937682226553330445, 33.60647404775217240 ) ) ;
#11134 = CARTESIAN_POINT ( 'NONE',  ( 8.519254038288414321, -9.943427161483782584, 34.11278801902876978 ) ) ;
#11135 = CARTESIAN_POINT ( 'NONE',  ( -8.769230769230768274, -8.973038597847269315, 34.52809138561121927 ) ) ;
#11136 = VECTOR ( 'NONE', #54069, 999.9999999999998863 ) ;
#11137 = LINE ( 'NONE', #37716, #18946 ) ;
#11138 = CARTESIAN_POINT ( 'NONE',  ( 2.307692307692187583, -10.21337939537710326, 33.94971097300076224 ) ) ;
#11139 = ORIENTED_EDGE ( 'NONE', *, *, #5384, .T. ) ;
#11140 = CYLINDRICAL_SURFACE ( 'NONE', #44143, 0.2499999999999994726 ) ;
#11141 = LINE ( 'NONE', #37722, #33099 ) ;
#11142 = AXIS2_PLACEMENT_3D ( 'NONE', #10191, #52495, #66467 ) ;
#11143 = CARTESIAN_POINT ( 'NONE',  ( 1.614399933863618797, -3.775308065498751198, 16.98624329374151287 ) ) ;
#11144 = EDGE_CURVE ( 'NONE', #86745, #19674, #41394, .T. ) ;
#11145 = LINE ( 'NONE', #80506, #53372 ) ;
#11146 = CARTESIAN_POINT ( 'NONE',  ( 4.480769230769229061, -3.499999999999999556, 29.75000000000000355 ) ) ;
#11147 = ORIENTED_EDGE ( 'NONE', *, *, #31665, .T. ) ;
#11148 = CARTESIAN_POINT ( 'NONE',  ( -18.13069146666756382, -8.999036380462717588, 34.52022231692819076 ) ) ;
#11149 = DIRECTION ( 'NONE',  ( 0.000000000000000000, 0.000000000000000000, 1.000000000000000000 ) ) ;
#11151 = ORIENTED_EDGE ( 'NONE', *, *, #22457, .F. ) ;
#11150 = CARTESIAN_POINT ( 'NONE',  ( -7.623374177175780808, -12.47679350104403007, 31.42216943046557276 ) ) ;
#11152 = CARTESIAN_POINT ( 'NONE',  ( 16.15384615384615330, -2.249999999999998668, 29.75000000000001776 ) ) ;
#11153 = CARTESIAN_POINT ( 'NONE',  ( -2.530571824429892036, -7.630690623152302621, 34.99857592706774057 ) ) ;
#11154 = VECTOR ( 'NONE', #19018, 1000.000000000000000 ) ;
#11155 = ADVANCED_FACE ( 'NONE', ( #54452, #62100, #75186, #28311 ), #89157, .F. ) ;
#11156 = DIRECTION ( 'NONE',  ( -0.000000000000000000, 0.9848077530122085754, -0.1736481776669273613 ) ) ;
#11157 = DIRECTION ( 'NONE',  ( -0.000000000000000000, -0.3420201433256694901, -0.9396926207859082059 ) ) ;
#11158 = EDGE_LOOP ( 'NONE', ( #10480, #83018 ) ) ;
#11159 = CARTESIAN_POINT ( 'NONE',  ( -15.23076923076922995, -2.499999999999998668, 29.50000000000001066 ) ) ;
#11160 = FACE_OUTER_BOUND ( 'NONE', #52351, .T. ) ;
#11161 = DIRECTION ( 'NONE',  ( -0.000000000000000000, 0.8660254037844397068, -0.4999999999999978906 ) ) ;
#11162 = EDGE_CURVE ( 'NONE', #55982, #31594, #27875, .T. ) ;
#11163 = ORIENTED_EDGE ( 'NONE', *, *, #46620, .F. ) ;
#11164 = ORIENTED_EDGE ( 'NONE', *, *, #75215, .F. ) ;
#11165 = VERTEX_POINT ( 'NONE', #60771 ) ;
#11166 = EDGE_CURVE ( 'NONE', #77760, #56699, #408, .T. ) ;
#11167 = VECTOR ( 'NONE', #41356, 1000.000000000000227 ) ;
#11168 = CARTESIAN_POINT ( 'NONE',  ( 17.07692307692307665, -6.435427911321262684, 35.78748833219616898 ) ) ;
#11169 = CARTESIAN_POINT ( 'NONE',  ( -3.007756386675832783, -2.889357225399416862, 32.26129605718031002 ) ) ;
#11170 = CARTESIAN_POINT ( 'NONE',  ( -17.07692307692319744, -12.46129190930018460, 30.37095296980731973 ) ) ;
#11171 = VECTOR ( 'NONE', #56824, 1000.000000000000227 ) ;
#11172 = DIRECTION ( 'NONE',  ( -1.000000000000000000, -0.000000000000000000, -0.000000000000000000 ) ) ;
#11173 = EDGE_CURVE ( 'NONE', #66677, #66580, #62003, .T. ) ;
#11174 = EDGE_LOOP ( 'NONE', ( #49943, #70857 ) ) ;
#11175 = ORIENTED_EDGE ( 'NONE', *, *, #28655, .T. ) ;
#11178 = ORIENTED_EDGE ( 'NONE', *, *, #84873, .T. ) ;
#11177 = EDGE_CURVE ( 'NONE', #62136, #219, #74946, .T. ) ;
#11176 = CARTESIAN_POINT ( 'NONE',  ( -1.253823576790597860, -4.809403383903225304, 33.96459661697924304 ) ) ;
#11179 = DIRECTION ( 'NONE',  ( -0.000000000000000000, 0.1736481776669307198, -0.9848077530122080203 ) ) ;
#11180 = B_SPLINE_CURVE_WITH_KNOTS ( 'NONE', 3,
 ( #84098, #42223, #1216, #22376, #55715, #778, #77322, #8873, #48966, #34570 ),
 .UNSPECIFIED., .F., .F.,
 ( 4, 2, 2, 2, 4 ),
 ( 0.0007817246256747447872, 0.0009771112852218874663, 0.001172497944769030362, 0.001367884604316173258, 0.001563271263863315937 ),
 .UNSPECIFIED. ) ;
#11181 = CYLINDRICAL_SURFACE ( 'NONE', #23472, 0.2500000000000002220 ) ;
#11182 = EDGE_CURVE ( 'NONE', #75988, #86865, #37268, .T. ) ;
#11183 = EDGE_CURVE ( 'NONE', #456, #17855, #72679, .T. ) ;
#11184 = CARTESIAN_POINT ( 'NONE',  ( 6.000000000000001776, -9.584722331328613620, 36.20867863119891439 ) ) ;
#11185 = DIRECTION ( 'NONE',  ( 0.000000000000000000, 0.000000000000000000, 1.000000000000000000 ) ) ;
#11186 = ORIENTED_EDGE ( 'NONE', *, *, #26029, .F. ) ;
#11187 = ORIENTED_EDGE ( 'NONE', *, *, #24631, .F. ) ;
#11188 = ORIENTED_EDGE ( 'NONE', *, *, #41617, .T. ) ;
#11190 = ORIENTED_EDGE ( 'NONE', *, *, #69425, .T. ) ;
#11189 = CYLINDRICAL_SURFACE ( 'NONE', #30076, 0.2500000000000008882 ) ;
#11191 = CARTESIAN_POINT ( 'NONE',  ( 16.85399611801622655, -5.582147617184174848, 34.63737895849758530 ) ) ;
#11192 = VECTOR ( 'NONE', #20424, 1000.000000000000227 ) ;
#11193 = CARTESIAN_POINT ( 'NONE',  ( -13.63459211555773720, -6.567427716900048118, 34.66269422305636283 ) ) ;
#11194 = ORIENTED_EDGE ( 'NONE', *, *, #46588, .F. ) ;
#11195 = FACE_OUTER_BOUND ( 'NONE', #49177, .T. ) ;
#11196 = FACE_OUTER_BOUND ( 'NONE', #36285, .T. ) ;
#11197 = CARTESIAN_POINT ( 'NONE',  ( 8.899756470994335089, -6.001044277235009439, 34.52024696741798948 ) ) ;
#11198 = AXIS2_PLACEMENT_3D ( 'NONE', #47756, #49960, #13968 ) ;
#11199 = FACE_BOUND ( 'NONE', #74650, .T. ) ;
#11200 = CARTESIAN_POINT ( 'NONE',  ( 15.10007776410167324, -5.582088688514999397, 34.36776431015576350 ) ) ;
#11201 = CARTESIAN_POINT ( 'NONE',  ( 2.373760658694747061, -8.120952969808772792, 34.71129190929999453 ) ) ;
#11202 = CARTESIAN_POINT ( 'NONE',  ( -7.846153846153965716, -12.27809138561165270, 31.22303859784587132 ) ) ;
#11204 = CARTESIAN_POINT ( 'NONE',  ( 14.30769230769218581, -3.083524468854526912, 32.58852847137268327 ) ) ;
#11203 = CARTESIAN_POINT ( 'NONE',  ( 16.15384615384615330, -3.937682226553329556, 33.60647404775216529 ) ) ;
#11205 = DIRECTION ( 'NONE',  ( 0.000000000000000000, 0.000000000000000000, -1.000000000000000000 ) ) ;
#11206 = CARTESIAN_POINT ( 'NONE',  ( -0.4615384615384611200, -8.973038597847269315, 34.52809138561121927 ) ) ;
#11207 = EDGE_LOOP ( 'NONE', ( #60888, #19930 ) ) ;
#11208 = AXIS2_PLACEMENT_3D ( 'NONE', #17586, #71620, #45036 ) ;
#11209 = CARTESIAN_POINT ( 'NONE',  ( -17.30040800148741198, -5.827078755546626354, 34.72654668319379567 ) ) ;
#11210 = CARTESIAN_POINT ( 'NONE',  ( 12.59232890250541281, -3.338503747796866872, 32.95102852606553512 ) ) ;
#11211 = ORIENTED_EDGE ( 'NONE', *, *, #19148, .F. ) ;
#11212 = EDGE_LOOP ( 'NONE', ( #14437, #11818 ) ) ;
#11213 = B_SPLINE_CURVE_WITH_KNOTS ( 'NONE', 3,
 ( #193, #27660, #66996, #12491, #62759, #4848, #11607, #7839, #74191, #83057 ),
 .UNSPECIFIED., .F., .F.,
 ( 4, 2, 2, 2, 4 ),
 ( 0.0007817359430256288133, 0.0009771253907249948054, 0.001172514838424360689, 0.001367904286123726573, 0.001563293733823092457 ),
 .UNSPECIFIED. ) ;
#11215 = CARTESIAN_POINT ( 'NONE',  ( 1.450682717965462221, -5.471508081941601098, 34.59228464037088457 ) ) ;
#11214 = CARTESIAN_POINT ( 'NONE',  ( -11.66860950819323328, -12.70455904226513866, 30.44083106164009322 ) ) ;
#11216 = CARTESIAN_POINT ( 'NONE',  ( 16.37662569511456567, -2.600157965045223563, 30.74683119005207033 ) ) ;
#11217 = B_SPLINE_CURVE_WITH_KNOTS ( 'NONE', 3,
 ( #2756, #30251, #86088, #45084, #23478, #50935, #78871, #78426, #72113, #24363 ),
 .UNSPECIFIED., .F., .F.,
 ( 4, 2, 2, 2, 4 ),
 ( 0.000000000000000000, 0.0001954311564186862781, 0.0003908623128373725562, 0.0005862934692560588072, 0.0007817246256747451124 ),
 .UNSPECIFIED. ) ;
#11218 = DIRECTION ( 'NONE',  ( -0.000000000000000000, -0.7660444431189791237, -0.6427876096865379196 ) ) ;
#11219 = CARTESIAN_POINT ( 'NONE',  ( -11.53846153846153655, -9.905515769479276145, 34.41647553114623292 ) ) ;
#11221 = ORIENTED_EDGE ( 'NONE', *, *, #65948, .T. ) ;
#11220 = B_SPLINE_CURVE_WITH_KNOTS ( 'NONE', 3,
 ( #41581, #53760, #69054, #39817, #26292, #74482, #12778, #60960, #88465, #15002 ),
 .UNSPECIFIED., .F., .F.,
 ( 4, 2, 2, 2, 4 ),
 ( 0.000000000000000000, 0.0001954339857564126514, 0.0003908679715128183098, 0.0005863019572692239681, 0.0007817359430256294638 ),
 .UNSPECIFIED. ) ;
#11222 = ADVANCED_FACE ( 'NONE', ( #16130 ), #9379, .F. ) ;
#11223 = DIRECTION ( 'NONE',  ( -1.000000000000000000, 0.000000000000000000, -0.000000000000000000 ) ) ;
#11224 = CARTESIAN_POINT ( 'NONE',  ( 4.403791563224197070, -4.932303261841489039, 34.32971442181322885 ) ) ;
#11226 = CARTESIAN_POINT ( 'NONE',  ( -2.298097038856290464, -5.201902961143733961, 26.50000000000000355 ) ) ;
#11225 = CARTESIAN_POINT ( 'NONE',  ( 11.66898697669518192, -3.068774925481848825, 32.56582465632704526 ) ) ;
#11227 = DIRECTION ( 'NONE',  ( -0.000000000000000000, -0.8660254037844397068, -0.4999999999999978906 ) ) ;
#11228 = DIRECTION ( 'NONE',  ( -0.000000000000000000, 1.000000000000000000, -0.000000000000000000 ) ) ;
#11229 = FACE_OUTER_BOUND ( 'NONE', #49290, .T. ) ;
#11230 = CARTESIAN_POINT ( 'NONE',  ( -1.553300858899125059, -3.750000000000009326, 22.82812500000000355 ) ) ;
#11231 = EDGE_LOOP ( 'NONE', ( #53024, #81535 ) ) ;
#11232 = ORIENTED_EDGE ( 'NONE', *, *, #71061, .T. ) ;
#11233 = VECTOR ( 'NONE', #28165, 1000.000000000000000 ) ;
#11234 = LINE ( 'NONE', #58075, #75107 ) ;
#11235 = CARTESIAN_POINT ( 'NONE',  ( -17.86947456176635640, -3.625058011473225150, 33.29252011169590020 ) ) ;
#11236 = LINE ( 'NONE', #80142, #48836 ) ;
#11237 = FACE_OUTER_BOUND ( 'NONE', #10367, .T. ) ;
#11238 = CARTESIAN_POINT ( 'NONE',  ( 2.530655211253793890, -7.369474270740069777, 34.74850911626239736 ) ) ;
#11239 = CARTESIAN_POINT ( 'NONE',  ( 3.750000000000000888, -7.499999999999978684, 24.46875000000000000 ) ) ;
#11240 = ADVANCED_FACE ( 'NONE', ( #22442 ), #62969, .F. ) ;
#11241 = CARTESIAN_POINT ( 'NONE',  ( 8.769230769230768274, -3.937682226553329556, 33.60647404775216529 ) ) ;
#11242 = DIRECTION ( 'NONE',  ( -0.000000000000000000, -0.9848077530122086864, -0.1736481776669273613 ) ) ;
#11243 = VECTOR ( 'NONE', #47390, 1000.000000000000000 ) ;
#11244 = CARTESIAN_POINT ( 'NONE',  ( -9.019253993452226226, -12.68155406624981119, 30.59749803192733708 ) ) ;
#11245 = CARTESIAN_POINT ( 'NONE',  ( 11.53846153846153832, -12.10708131394839349, 31.69288490824020244 ) ) ;
#11246 = CARTESIAN_POINT ( 'NONE',  ( -6.130147209438215228, -2.882441371585227063, 31.66841991370171527 ) ) ;
#11247 = CARTESIAN_POINT ( 'NONE',  ( 14.17700084102474989, -12.11776431015576172, 31.66791131148498906 ) ) ;
#11248 = FACE_OUTER_BOUND ( 'NONE', #40863, .T. ) ;
#11249 = CARTESIAN_POINT ( 'NONE',  ( 7.846153846153723244, -8.656820664282941280, 34.87096338111179961 ) ) ;
#11250 = CARTESIAN_POINT ( 'NONE',  ( 6.000000000000001776, -3.050289026998446396, 32.03036669348365706 ) ) ;
#11251 = CARTESIAN_POINT ( 'NONE',  ( -4.219116599806927326, -9.442884908240170461, 34.35708131394840592 ) ) ;
#11252 = DIRECTION ( 'NONE',  ( -0.000000000000000000, -0.6427876096865404731, -0.7660444431189771253 ) ) ;
#11253 = ORIENTED_EDGE ( 'NONE', *, *, #23861, .F. ) ;
#11254 = DIRECTION ( 'NONE',  ( -0.000000000000000000, -0.000000000000000000, -1.000000000000000000 ) ) ;
#11255 = CARTESIAN_POINT ( 'NONE',  ( 8.835299120233207404, -11.69971097300155272, 32.46337939537588113 ) ) ;
#11256 = LINE ( 'NONE', #59884, #79293 ) ;
#11257 = CARTESIAN_POINT ( 'NONE',  ( 1.944543648263018731, -9.444543648262994751, 23.37500000000000000 ) ) ;
#11258 = EDGE_CURVE ( 'NONE', #72317, #54354, #42727, .T. ) ;
#11259 = CARTESIAN_POINT ( 'NONE',  ( -14.17716660592874689, -5.195472089885680766, 34.18748526763464923 ) ) ;
#11260 = CARTESIAN_POINT ( 'NONE',  ( 2.557746727605762160, -12.01375889529407637, 32.43194544308182969 ) ) ;
#11262 = ORIENTED_EDGE ( 'NONE', *, *, #60230, .T. ) ;
#11261 = DIRECTION ( 'NONE',  ( 0.000000000000000000, 0.8660254037844377084, -0.5000000000000015543 ) ) ;
#11263 = CARTESIAN_POINT ( 'NONE',  ( 2.749999999999995115, -6.360912703473971419, 19.39062500000000355 ) ) ;
#11264 = CARTESIAN_POINT ( 'NONE',  ( 3.230769230769231726, -8.973038597847269315, 34.52809138561121927 ) ) ;
#11265 = EDGE_CURVE ( 'NONE', #86404, #45405, #57695, .T. ) ;
#11266 = ORIENTED_EDGE ( 'NONE', *, *, #21243, .T. ) ;
#11267 = LINE ( 'NONE', #59894, #44232 ) ;
#11268 = ORIENTED_EDGE ( 'NONE', *, *, #35160, .T. ) ;
#11269 = CARTESIAN_POINT ( 'NONE',  ( 9.692307692307695177, -1.790695186598648903, 34.54067556320373455 ) ) ;
#11270 = CARTESIAN_POINT ( 'NONE',  ( 24.00000000000000000, 9.000000000000024869, 29.25000000000000000 ) ) ;
#11271 = CARTESIAN_POINT ( 'NONE',  ( 16.94623247381277054, -6.369640206132551441, 34.87707690430378449 ) ) ;
#11272 = EDGE_CURVE ( 'NONE', #8235, #43627, #36179, .T. ) ;
#11273 = VERTEX_POINT ( 'NONE', #77824 ) ;
#11274 = CARTESIAN_POINT ( 'NONE',  ( -10.36533030374629938, -12.41262288849542017, 30.68299917996395010 ) ) ;
#11275 = ORIENTED_EDGE ( 'NONE', *, *, #75105, .T. ) ;
#11276 = CARTESIAN_POINT ( 'NONE',  ( 11.28843830116857383, -3.711651800289232028, 33.01384336483936011 ) ) ;
#11277 = ORIENTED_EDGE ( 'NONE', *, *, #45726, .T. ) ;
#11278 = CARTESIAN_POINT ( 'NONE',  ( 2.057669083470851756, -9.356822207818506598, 34.66110646841856635 ) ) ;
#11279 = DIRECTION ( 'NONE',  ( -0.000000000000000000, 0.9396926207859093161, -0.3420201433256663259 ) ) ;
#11280 = ORIENTED_EDGE ( 'NONE', *, *, #2831, .T. ) ;
#11281 = CARTESIAN_POINT ( 'NONE',  ( 9.468822748583747284, -9.331801661448606566, 34.40259984581193464 ) ) ;
#11282 = CYLINDRICAL_SURFACE ( 'NONE', #83835, 0.2499999999999973355 ) ;
#11283 = CARTESIAN_POINT ( 'NONE',  ( 12.68454981315131214, -4.887748414852792322, 34.01359900205216746 ) ) ;
#11284 = DIRECTION ( 'NONE',  ( -0.000000000000000000, -0.7660444431189791237, -0.6427876096865379196 ) ) ;
#11285 = EDGE_CURVE ( 'NONE', #16692, #40474, #43288, .T. ) ;
#11286 = ORIENTED_EDGE ( 'NONE', *, *, #85056, .T. ) ;
#11287 = VERTEX_POINT ( 'NONE', #71071 ) ;
#11288 = ORIENTED_EDGE ( 'NONE', *, *, #36750, .T. ) ;
#11290 = ORIENTED_EDGE ( 'NONE', *, *, #25503, .F. ) ;
#11289 = CARTESIAN_POINT ( 'NONE',  ( 3.453548772037640990, -3.755027918224367767, 33.06320215134714857 ) ) ;
#11291 = EDGE_CURVE ( 'NONE', #12426, #861, #81318, .T. ) ;
#11292 = AXIS2_PLACEMENT_3D ( 'NONE', #46361, #68405, #86936 ) ;
#11293 = EDGE_CURVE ( 'NONE', #41920, #32972, #46844, .T. ) ;
#11294 = DIRECTION ( 'NONE',  ( -0.000000000000000000, 0.1736481776669307198, -0.9848077530122080203 ) ) ;
#11295 = CARTESIAN_POINT ( 'NONE',  ( -10.61538461538461320, -6.681629849574314051, 35.83090037661290239 ) ) ;
#11296 = ORIENTED_EDGE ( 'NONE', *, *, #2486, .T. ) ;
#11297 = ORIENTED_EDGE ( 'NONE', *, *, #58686, .F. ) ;
#11298 = CARTESIAN_POINT ( 'NONE',  ( 17.32686848630112308, -9.357781135181033605, 34.66075350412533851 ) ) ;
#11299 = EDGE_LOOP ( 'NONE', ( #36616, #71525 ) ) ;
#11300 = DIRECTION ( 'NONE',  ( -0.000000000000000000, 0.3420201433256694901, -0.9396926207859082059 ) ) ;
#11301 = AXIS2_PLACEMENT_3D ( 'NONE', #83895, #15429, #62703 ) ;
#11302 = CARTESIAN_POINT ( 'NONE',  ( -8.069080063669993308, -2.554751324335734708, 30.48935550225260727 ) ) ;
#11303 = EDGE_CURVE ( 'NONE', #26164, #73448, #32314, .T. ) ;
#11304 = CARTESIAN_POINT ( 'NONE',  ( -11.40767109749459074, -11.93129842949671726, 32.56571108434900452 ) ) ;
#11305 = FACE_BOUND ( 'NONE', #44375, .T. ) ;
#11306 = CARTESIAN_POINT ( 'NONE',  ( 5.076923076923075762, -6.435427911321262684, 35.78748833219616898 ) ) ;
#11307 = DIRECTION ( 'NONE',  ( -0.000000000000000000, -0.7660444431189791237, -0.6427876096865379196 ) ) ;
#11308 = CARTESIAN_POINT ( 'NONE',  ( -4.480769230769230838, -7.500000000000000000, 33.75000000000000000 ) ) ;
#11309 = CARTESIAN_POINT ( 'NONE',  ( -14.30769230769230660, -5.557115091759785130, 34.35708131394839171 ) ) ;
#11310 = EDGE_CURVE ( 'NONE', #65891, #45448, #4841, .T. ) ;
#11311 = CARTESIAN_POINT ( 'NONE',  ( 9.019176287578909879, -3.202959910592335646, 32.30730279482227019 ) ) ;
#11312 = CARTESIAN_POINT ( 'NONE',  ( 7.912222197156284054, -10.51840700105979565, 33.73612834413962247 ) ) ;
#11313 = ORIENTED_EDGE ( 'NONE', *, *, #35473, .T. ) ;
#11314 = CARTESIAN_POINT ( 'NONE',  ( -11.53846153846166089, -3.643525952248795718, 33.31231777344771672 ) ) ;
#11315 = ORIENTED_EDGE ( 'NONE', *, *, #69854, .F. ) ;
#11316 = ORIENTED_EDGE ( 'NONE', *, *, #65950, .T. ) ;
#11318 = CARTESIAN_POINT ( 'NONE',  ( 10.74617642320940369, -5.582136614379148654, 34.36778462344220486 ) ) ;
#11317 = CARTESIAN_POINT ( 'NONE',  ( 10.86533013373275836, -12.43552623307873972, 30.55307653245132826 ) ) ;
#11319 = CARTESIAN_POINT ( 'NONE',  ( 16.37685899793955357, -11.43677907613345113, 33.22367315496201456 ) ) ;
#11320 = CARTESIAN_POINT ( 'NONE',  ( -13.38461538461550759, -12.16647553114689728, 32.15551576947799362 ) ) ;
#11321 = CARTESIAN_POINT ( 'NONE',  ( -19.50000000000000000, -3.499999999999999556, 29.75000000000000355 ) ) ;
#11322 = CARTESIAN_POINT ( 'NONE',  ( -15.23076923076922995, -3.513871655860378418, 32.76840700105978499 ) ) ;
#11323 = VERTEX_POINT ( 'NONE', #24658 ) ;
#11324 = EDGE_CURVE ( 'NONE', #33070, #19283, #85440, .T. ) ;
#11325 = CARTESIAN_POINT ( 'NONE',  ( 16.94623161025551639, -5.582088688514999397, 34.36776431015576350 ) ) ;
#11326 = CARTESIAN_POINT ( 'NONE',  ( 3.007284306204901281, -9.417330523894424488, 34.63758898049880486 ) ) ;
#11327 = CARTESIAN_POINT ( 'NONE',  ( 10.48469314871705649, -3.062553014421049546, 32.05460306192773601 ) ) ;
#11328 = CARTESIAN_POINT ( 'NONE',  ( -4.153846153846152411, -3.513871655860378418, 32.76840700105978499 ) ) ;
#11329 = ORIENTED_EDGE ( 'NONE', *, *, #61789, .T. ) ;
#11330 = CIRCLE ( 'NONE', #45847, 4.000000000000000000 ) ;
#11331 = EDGE_CURVE ( 'NONE', #28697, #5010, #18935, .T. ) ;
#11332 = ORIENTED_EDGE ( 'NONE', *, *, #35351, .T. ) ;
#11333 = APPLICATION_PROTOCOL_DEFINITION ( 'draft international standard', 'automotive_design', 1998, #42340 ) ;
#11334 = EDGE_LOOP ( 'NONE', ( #35981, #75989, #32268, #85677, #58131 ) ) ;
#11335 = CARTESIAN_POINT ( 'NONE',  ( 18.25000000000006395, -7.434744429011175271, 34.75000000000000711 ) ) ;
#11336 = CARTESIAN_POINT ( 'NONE',  ( -13.25408968285182176, -10.88167719472716399, 33.43325721877153711 ) ) ;
#11337 = VERTEX_POINT ( 'NONE', #72838 ) ;
#11338 = DIRECTION ( 'NONE',  ( 0.000000000000000000, 0.6427876096865373645, -0.7660444431189797898 ) ) ;
#11339 = CYLINDRICAL_SURFACE ( 'NONE', #52913, 0.2499999999999994726 ) ;
#11340 = CARTESIAN_POINT ( 'NONE',  ( 4.946775867484856093, -2.882441371585227063, 31.66841991370171527 ) ) ;
#11341 = CARTESIAN_POINT ( 'NONE',  ( 14.55769230769374367, -7.500000000000155431, 34.75000000000007105 ) ) ;
#11342 = EDGE_CURVE ( 'NONE', #68109, #88418, #65628, .T. ) ;
#11343 = LINE ( 'NONE', #31159, #5741 ) ;
#11344 = EDGE_LOOP ( 'NONE', ( #27919, #79427, #71422, #16865 ) ) ;
#11346 = VERTEX_POINT ( 'NONE', #25551 ) ;
#11345 = CYLINDRICAL_SURFACE ( 'NONE', #9388, 0.2500000000000014988 ) ;
#11347 = CARTESIAN_POINT ( 'NONE',  ( -8.546219417617919589, -9.886259254753566594, 34.14407573483972413 ) ) ;
#11348 = DIRECTION ( 'NONE',  ( -1.000000000000000000, -0.000000000000000000, -0.000000000000000000 ) ) ;
#11349 = DIRECTION ( 'NONE',  ( 0.000000000000000000, 0.6427876096865368094, 0.7660444431189802339 ) ) ;
#11350 = CARTESIAN_POINT ( 'NONE',  ( -10.68065461594093435, -3.643525952247789412, 33.31231777344662959 ) ) ;
#11351 = CARTESIAN_POINT ( 'NONE',  ( 13.38461538461538680, -3.937682226553329556, 33.60647404775216529 ) ) ;
#11352 = EDGE_CURVE ( 'NONE', #29059, #62900, #79068, .T. ) ;
#11353 = CARTESIAN_POINT ( 'NONE',  ( 18.13052570176356681, -2.619367082507847666, 30.83698974864643461 ) ) ;
#11354 = CARTESIAN_POINT ( 'NONE',  ( -1.200186371490524317, -10.22469193450124791, 17.61124329374151642 ) ) ;
#11355 = ORIENTED_EDGE ( 'NONE', *, *, #76532, .T. ) ;
#11356 = DIRECTION ( 'NONE',  ( 0.000000000000000000, 0.9396926207859126468, 0.3420201433256571111 ) ) ;
#11357 = DIRECTION ( 'NONE',  ( -0.000000000000000000, -0.6427876096865404731, -0.7660444431189771253 ) ) ;
#11358 = PLANE ( 'NONE',  #7901 ) ;
#11359 = B_SPLINE_CURVE_WITH_KNOTS ( 'NONE', 3,
 ( #11135, #80948, #19235, #72827, #80497, #25094, #67417, #52557, #18790, #80043 ),
 .UNSPECIFIED., .F., .F.,
 ( 4, 2, 2, 2, 4 ),
 ( 0.000000000000000000, 0.0001954339857564073659, 0.0003908679715128147319, 0.0005863019572692221250, 0.0007817359430256294638 ),
 .UNSPECIFIED. ) ;
#11360 = AXIS2_PLACEMENT_3D ( 'NONE', #32553, #4647, #85733 ) ;
#11361 = ORIENTED_EDGE ( 'NONE', *, *, #22386, .T. ) ;
#11362 = VERTEX_POINT ( 'NONE', #80050 ) ;
#11363 = CARTESIAN_POINT ( 'NONE',  ( -8.899921372341079717, -5.496505350115501010, 34.60290016733514307 ) ) ;
#11364 = CARTESIAN_POINT ( 'NONE',  ( -7.623141002060451754, -5.582272713120728369, 34.63742843783360570 ) ) ;
#11365 = EDGE_CURVE ( 'NONE', #69312, #62369, #11145, .T. ) ;
#11366 = CARTESIAN_POINT ( 'NONE',  ( 17.29993592101647693, -3.395485233115139501, 33.02377354290276656 ) ) ;
#11367 = CARTESIAN_POINT ( 'NONE',  ( -8.835313148590902443, -10.67929555188718460, 33.92786785259543336 ) ) ;
#11368 = EDGE_CURVE ( 'NONE', #11539, #73925, #28491, .T. ) ;
#11369 = CARTESIAN_POINT ( 'NONE',  ( 16.21910129335899597, -3.643525952247864019, 33.31231777344670064 ) ) ;
#11370 = AXIS2_PLACEMENT_3D ( 'NONE', #85909, #51649, #13354 ) ;
#11371 = CARTESIAN_POINT ( 'NONE',  ( -15.00775638667583678, -8.282913670948747864, 34.94150082978203642 ) ) ;
#11372 = VERTEX_POINT ( 'NONE', #45813 ) ;
#11373 = CARTESIAN_POINT ( 'NONE',  ( 5.749976762707037281, -3.711651800289232916, 33.01384336483936011 ) ) ;
#11374 = VECTOR ( 'NONE', #80465, 1000.000000000000114 ) ;
#11375 = CARTESIAN_POINT ( 'NONE',  ( 16.15384615384615330, -1.242168528481310874, 33.36296068462461051 ) ) ;
#11376 = CARTESIAN_POINT ( 'NONE',  ( 16.85343813319912698, -9.331801661448606566, 34.40259984581193464 ) ) ;
#11377 = EDGE_LOOP ( 'NONE', ( #87127, #27031, #23662, #63551 ) ) ;
#11378 = CARTESIAN_POINT ( 'NONE',  ( 10.39189969082028497, -9.417330523894424488, 34.63758898049880486 ) ) ;
#11379 = ORIENTED_EDGE ( 'NONE', *, *, #84483, .T. ) ;
#11380 = CARTESIAN_POINT ( 'NONE',  ( -19.50000000000000000, -3.499999999999999556, 29.75000000000000355 ) ) ;
#11381 =( NAMED_UNIT ( * ) SI_UNIT ( $, .STERADIAN. ) SOLID_ANGLE_UNIT ( ) );
#11382 = FACE_OUTER_BOUND ( 'NONE', #15092, .T. ) ;
#11383 = CARTESIAN_POINT ( 'NONE',  ( 17.99999999999987566, -10.33852847137269571, 34.16647553114546554 ) ) ;
#11384 = ORIENTED_EDGE ( 'NONE', *, *, #11817, .F. ) ;
#11385 = DIRECTION ( 'NONE',  ( 1.000000000000000000, 0.000000000000000000, 0.000000000000000000 ) ) ;
#11386 = LINE ( 'NONE', #88404, #36367 ) ;
#11387 = DIRECTION ( 'NONE',  ( -0.000000000000000000, -0.8660254037844399289, -0.4999999999999980016 ) ) ;
#11388 = B_SPLINE_CURVE_WITH_KNOTS ( 'NONE', 3,
 ( #46957, #75336, #75763, #41105, #5547, #559, #26256, #82977, #115, #74445 ),
 .UNSPECIFIED., .F., .F.,
 ( 4, 2, 2, 2, 4 ),
 ( 0.0007817246256747460882, 0.0009771112852218892010, 0.001172497944769032314, 0.001367884604316175210, 0.001563271263863318323 ),
 .UNSPECIFIED. ) ;
#11389 = CARTESIAN_POINT ( 'NONE',  ( -6.130147969731695845, -5.915902021225892149, 34.75552854090298638 ) ) ;
#11390 = CARTESIAN_POINT ( 'NONE',  ( -3.007757879156381264, -12.39991518177334129, 30.74647679643404530 ) ) ;
#11391 = EDGE_LOOP ( 'NONE', ( #42646, #6891, #60136, #64086 ) ) ;
#11392 = DIRECTION ( 'NONE',  ( 0.000000000000000000, -6.938893903907222067E-15, 1.000000000000000000 ) ) ;
#11393 = EDGE_LOOP ( 'NONE', ( #42293, #4283, #64855, #33209 ) ) ;
#11394 = DIRECTION ( 'NONE',  ( -1.000000000000000000, 0.000000000000000000, 0.000000000000000000 ) ) ;
#11395 = CIRCLE ( 'NONE', #30105, 4.000000000000000000 ) ;
#11396 = CARTESIAN_POINT ( 'NONE',  ( 4.946775867484852540, -12.27039167877662251, 31.24851455888617835 ) ) ;
#11397 = EDGE_CURVE ( 'NONE', #1287, #21191, #86585, .T. ) ;
#11398 = FACE_OUTER_BOUND ( 'NONE', #23203, .T. ) ;
#11399 = CARTESIAN_POINT ( 'NONE',  ( -8.769230769230768274, -13.57706302396349152, 30.56769352161908060 ) ) ;
#11400 = EDGE_CURVE ( 'NONE', #79802, #12929, #67714, .T. ) ;
#11401 = CARTESIAN_POINT ( 'NONE',  ( -6.000000000000119904, -4.481592998941358097, 33.73612834414048933 ) ) ;
#11402 = CARTESIAN_POINT ( 'NONE',  ( 9.692307692307572609, -8.613356846316285953, 34.62446782046622218 ) ) ;
#11403 = ORIENTED_EDGE ( 'NONE', *, *, #67902, .T. ) ;
#11405 = EDGE_CURVE ( 'NONE', #20924, #30751, #33642, .T. ) ;
#11404 = ORIENTED_EDGE ( 'NONE', *, *, #33774, .T. ) ;
#11406 = ORIENTED_EDGE ( 'NONE', *, *, #29559, .T. ) ;
#11407 = ORIENTED_EDGE ( 'NONE', *, *, #73136, .T. ) ;
#11408 = EDGE_LOOP ( 'NONE', ( #59627, #46853, #17136, #1841 ) ) ;
#11409 = CARTESIAN_POINT ( 'NONE',  ( -16.21911659980693443, -3.835265460703609186, 33.15142922261924241 ) ) ;
#11410 = CARTESIAN_POINT ( 'NONE',  ( -11.76138775597768671, -9.086856451489515152, 34.49173150075333183 ) ) ;
#11411 = EDGE_CURVE ( 'NONE', #6875, #38908, #41422, .T. ) ;
#11412 = CARTESIAN_POINT ( 'NONE',  ( -4.153846153846273204, -9.442884908241554243, 34.35708131394783038 ) ) ;
#11413 = CARTESIAN_POINT ( 'NONE',  ( -7.146561866800870355, -3.236172620538810385, 32.36188796281390267 ) ) ;
#11414 = CARTESIAN_POINT ( 'NONE',  ( -13.45069776397551564, -3.322132147404559532, 32.92929555188719348 ) ) ;
#11415 = DIRECTION ( 'NONE',  ( -0.000000000000000000, -0.9848077530122085754, -0.1736481776669273613 ) ) ;
#11416 = VECTOR ( 'NONE', #32266, 1000.000000000000000 ) ;
#11417 = VECTOR ( 'NONE', #35791, 1000.000000000000000 ) ;
#11418 = CARTESIAN_POINT ( 'NONE',  ( -5.299849294439221481, -8.239355502252617924, 34.69524867566427417 ) ) ;
#11419 = CARTESIAN_POINT ( 'NONE',  ( -7.715628144390278997, -3.285477652293413264, 32.44071101563363158 ) ) ;
#11421 = DIRECTION ( 'NONE',  ( -1.000000000000000000, 0.000000000000000000, -0.000000000000000000 ) ) ;
#11420 = B_SPLINE_CURVE_WITH_KNOTS ( 'NONE', 3,
 ( #80019, #12016, #12886, #5686, #40376, #53876, #66953, #47556, #53422, #39048 ),
 .UNSPECIFIED., .F., .F.,
 ( 4, 2, 2, 2, 4 ),
 ( 0.000000000000000000, 0.0001954311564186865492, 0.0003908623128373730983, 0.0005862934692560596746, 0.0007817246256747461966 ),
 .UNSPECIFIED. ) ;
#11422 = ORIENTED_EDGE ( 'NONE', *, *, #80030, .T. ) ;
#11423 = ORIENTED_EDGE ( 'NONE', *, *, #66872, .T. ) ;
#11424 = AXIS2_PLACEMENT_3D ( 'NONE', #52103, #59310, #5702 ) ;
#11425 = ORIENTED_EDGE ( 'NONE', *, *, #10683, .T. ) ;
#11427 = VERTEX_POINT ( 'NONE', #68754 ) ;
#11426 = FACE_OUTER_BOUND ( 'NONE', #17052, .T. ) ;
#11429 = FACE_OUTER_BOUND ( 'NONE', #18079, .T. ) ;
#11428 = CYLINDRICAL_SURFACE ( 'NONE', #38881, 0.2500000000000008882 ) ;
#11430 = B_SPLINE_CURVE_WITH_KNOTS ( 'NONE', 3,
 ( #72506, #65742, #11259, #87380, #79276, #80624, #11713, #72958, #4039, #18022 ),
 .UNSPECIFIED., .F., .F.,
 ( 4, 2, 2, 2, 4 ),
 ( 0.0007817359430256287049, 0.0009771253907249945886, 0.001172514838424360255, 0.001367904286123725922, 0.001563293733823091806 ),
 .UNSPECIFIED. ) ;
#11431 = CARTESIAN_POINT ( 'NONE',  ( -1.634638608836841200, -4.931416488878823223, 34.32920672191015399 ) ) ;
#11432 = CARTESIAN_POINT ( 'NONE',  ( 7.053602624840487501, -2.619367082507848554, 30.83698974864644171 ) ) ;
#11433 = FACE_BOUND ( 'NONE', #62326, .T. ) ;
#11434 = VERTEX_POINT ( 'NONE', #61542 ) ;
#11435 = EDGE_LOOP ( 'NONE', ( #46390, #9398, #11904, #10496 ) ) ;
#11436 = DIRECTION ( 'NONE',  ( 1.000000000000000000, 0.000000000000000000, 0.000000000000000000 ) ) ;
#11437 = EDGE_CURVE ( 'NONE', #78559, #27260, #35031, .T. ) ;
#11438 = ORIENTED_EDGE ( 'NONE', *, *, #37757, .F. ) ;
#11439 = FACE_BOUND ( 'NONE', #56805, .T. ) ;
#11440 = CARTESIAN_POINT ( 'NONE',  ( 23.49999999999998934, -9.499999999999982236, 27.74999999999999645 ) ) ;
#11441 = CARTESIAN_POINT ( 'NONE',  ( -13.51530685128294351, -10.54014554554150607, 33.71984207302941883 ) ) ;
#11442 = ORIENTED_EDGE ( 'NONE', *, *, #36567, .T. ) ;
#11443 = CARTESIAN_POINT ( 'NONE',  ( -18.00000000000000000, -11.32085034345903729, 35.86790692298802696 ) ) ;
#11444 = CARTESIAN_POINT ( 'NONE',  ( -1.607542343522232686, -8.282780595021769443, 34.94152052738834868 ) ) ;
#11445 = CARTESIAN_POINT ( 'NONE',  ( -5.326923076923075762, -7.566082377512563184, 35.00000000000000711 ) ) ;
#11446 = ORIENTED_EDGE ( 'NONE', *, *, #12302, .F. ) ;
#11447 = DIRECTION ( 'NONE',  ( -0.000000000000000000, 0.8660254037844399289, -0.4999999999999980016 ) ) ;
#11448 = CARTESIAN_POINT ( 'NONE',  ( 6.923076923076800782, -5.941354392335915335, 34.76329471203413846 ) ) ;
#11449 = CARTESIAN_POINT ( 'NONE',  ( -5.299849294439221481, -11.76352882383564769, 32.36236540154569497 ) ) ;
#11450 = ORIENTED_EDGE ( 'NONE', *, *, #35770, .F. ) ;
#11451 = EDGE_CURVE ( 'NONE', #71975, #29766, #77798, .T. ) ;
#11452 = CARTESIAN_POINT ( 'NONE',  ( -2.307692307692427391, -11.48612834414049644, 32.76840700105863391 ) ) ;
#11453 = CARTESIAN_POINT ( 'NONE',  ( 6.989145274079362480, -10.51840700105979565, 33.73612834413962247 ) ) ;
#11454 = EDGE_LOOP ( 'NONE', ( #11878, #46848 ) ) ;
#11455 = CARTESIAN_POINT ( 'NONE',  ( -17.14300545628321260, -12.62096338111211580, 30.90682066428152908 ) ) ;
#11456 = CARTESIAN_POINT ( 'NONE',  ( -5.076923076923075762, -9.905515769479276145, 34.41647553114623292 ) ) ;
#11457 = CARTESIAN_POINT ( 'NONE',  ( 15.90386940979756503, -2.920706130388546651, 32.31842814019191223 ) ) ;
#11458 = CARTESIAN_POINT ( 'NONE',  ( -11.53846153846165912, -3.300289026999228881, 32.46337939537708905 ) ) ;
#11459 = CARTESIAN_POINT ( 'NONE',  ( -16.02305434602136103, -4.118422570099827595, 33.43335022499816489 ) ) ;
#11460 = CARTESIAN_POINT ( 'NONE',  ( 17.07692307692295586, -6.026961402154118908, 34.52809138561165270 ) ) ;
#11462 = CARTESIAN_POINT ( 'NONE',  ( -15.29685264172511161, -12.37446782046654192, 30.86335684631486487 ) ) ;
#11461 = CARTESIAN_POINT ( 'NONE',  ( -1.607541602131531633, -4.887634598454295265, 34.01352882383564946 ) ) ;
#11463 = ADVANCED_FACE ( 'NONE', ( #47142 ), #34525, .F. ) ;
#11464 = EDGE_CURVE ( 'NONE', #1706, #66304, #296, .T. ) ;
#11465 = CARTESIAN_POINT ( 'NONE',  ( 18.03205128205128105, -3.499999999999999556, 29.75000000000000355 ) ) ;
#11467 = CARTESIAN_POINT ( 'NONE',  ( 12.23805353697412812, -4.988325925672468131, 34.36044203135681130 ) ) ;
#11466 = CARTESIAN_POINT ( 'NONE',  ( -15.00798956179116317, -2.612705202774698421, 31.66806509827799943 ) ) ;
#11468 = B_SPLINE_CURVE_WITH_KNOTS ( 'NONE', 3,
 ( #82623, #26772, #20893, #69085, #34849, #62314, #28101, #83945, #76731, #50131 ),
 .UNSPECIFIED., .F., .F.,
 ( 4, 2, 2, 2, 4 ),
 ( 0.000000000000000000, 0.0001954339857564093175, 0.0003908679715128186350, 0.0005863019572692279796, 0.0007817359430256372700 ),
 .UNSPECIFIED. ) ;
#11469 = AXIS2_PLACEMENT_3D ( 'NONE', #46341, #11678, #66157 ) ;
#11470 = CARTESIAN_POINT ( 'NONE',  ( 2.750000000000001776, -7.499999999999984013, 15.71875000000000000 ) ) ;
#11471 = ORIENTED_EDGE ( 'NONE', *, *, #21667, .T. ) ;
#11472 = LINE ( 'NONE', #79929, #40463 ) ;
#11473 = VERTEX_POINT ( 'NONE', #74630 ) ;
#11474 = ORIENTED_EDGE ( 'NONE', *, *, #34582, .T. ) ;
#11475 = CARTESIAN_POINT ( 'NONE',  ( -2.241623956689867470, -12.37446782046654192, 30.86335684631486842 ) ) ;
#11476 = ORIENTED_EDGE ( 'NONE', *, *, #37138, .F. ) ;
#11477 = CARTESIAN_POINT ( 'NONE',  ( -14.98071491913091791, -5.728107161865378494, 34.42597550085002922 ) ) ;
#11478 = CARTESIAN_POINT ( 'NONE',  ( -2.749999999999991562, -8.639087296526025028, 17.51562500000000000 ) ) ;
#11479 = CARTESIAN_POINT ( 'NONE',  ( -23.50000000000000000, 1.250000000000005329, 32.75000000000000000 ) ) ;
#11480 = EDGE_CURVE ( 'NONE', #40124, #63956, #54342, .T. ) ;
#11481 = CARTESIAN_POINT ( 'NONE',  ( 12.46153846153846168, -2.292212530054420494, 30.41441678777542634 ) ) ;
#11482 = CARTESIAN_POINT ( 'NONE',  ( 9.942362112221147186, -9.233818618650603938, 34.70587769442853698 ) ) ;
#11483 = CARTESIAN_POINT ( 'NONE',  ( 9.822833130541335223, -3.068774925481848825, 32.56582465632704526 ) ) ;
#11484 = CARTESIAN_POINT ( 'NONE',  ( -10.54931728203453822, -3.322132147404559976, 32.92929555188717927 ) ) ;
#11485 = FACE_OUTER_BOUND ( 'NONE', #32353, .T. ) ;
#11486 = CARTESIAN_POINT ( 'NONE',  ( 0.4615384615383382183, -11.06231777344772027, 33.60647404775119895 ) ) ;
#11487 = CARTESIAN_POINT ( 'NONE',  ( 2.320192649118979489E-14, -11.25000000000000000, 21.03125000000000000 ) ) ;
#11488 = EDGE_CURVE ( 'NONE', #3191, #81167, #27763, .T. ) ;
#11489 = EDGE_CURVE ( 'NONE', #48658, #5961, #140, .T. ) ;
#11490 = CARTESIAN_POINT ( 'NONE',  ( 17.29993592101647693, -2.308499170217968022, 30.53291367094874076 ) ) ;
#11491 = LINE ( 'NONE', #74084, #83706 ) ;
#11492 = VECTOR ( 'NONE', #49536, 1000.000000000000000 ) ;
#11493 = LINE ( 'NONE', #52017, #52187 ) ;
#11494 = EDGE_CURVE ( 'NONE', #4654, #70883, #60709, .T. ) ;
#11495 = CIRCLE ( 'NONE', #53199, 1.999999999999998224 ) ;
#11496 = AXIS2_PLACEMENT_3D ( 'NONE', #73128, #4675, #46545 ) ;
#11497 = EDGE_LOOP ( 'NONE', ( #77654, #61795, #2760, #45957 ) ) ;
#11498 = VERTEX_POINT ( 'NONE', #83162 ) ;
#11499 = CARTESIAN_POINT ( 'NONE',  ( 6.856993512121041690, -2.538708090699994813, 30.37095296980875148 ) ) ;
#11500 = PLANE ( 'NONE',  #50301 ) ;
#11501 = CARTESIAN_POINT ( 'NONE',  ( 16.37685899793954292, -12.38742843783360748, 31.66772728687926985 ) ) ;
#11502 = CARTESIAN_POINT ( 'NONE',  ( -7.053767526187231240, -5.496505350115500121, 34.60290016733514307 ) ) ;
#11503 = VECTOR ( 'NONE', #69412, 1000.000000000000114 ) ;
#11504 = CARTESIAN_POINT ( 'NONE',  ( 8.769230769230647482, -11.94971097300221174, 32.03036669348237098 ) ) ;
#11505 = VECTOR ( 'NONE', #21155, 1000.000000000000000 ) ;
#11506 = DIRECTION ( 'NONE',  ( -0.000000000000000000, 1.000000000000000000, -0.000000000000000000 ) ) ;
#11507 = MECHANICAL_DESIGN_GEOMETRIC_PRESENTATION_REPRESENTATION (  '', ( #14389 ), #21585 ) ;
#11508 = ORIENTED_EDGE ( 'NONE', *, *, #70839, .F. ) ;
#11509 = CARTESIAN_POINT ( 'NONE',  ( 3.007284306204901281, -6.716662450894490100, 34.94144148231605840 ) ) ;
#11510 = VERTEX_POINT ( 'NONE', #21453 ) ;
#11512 = ADVANCED_FACE ( 'NONE', ( #74184 ), #16029, .F. ) ;
#11511 = ORIENTED_EDGE ( 'NONE', *, *, #61274, .T. ) ;
#11513 = DIRECTION ( 'NONE',  ( 1.000000000000000000, 0.000000000000000000, 0.000000000000000000 ) ) ;
#11514 = CARTESIAN_POINT ( 'NONE',  ( 5.934243197485690402, -7.249945686854186278, 34.74374336980224598 ) ) ;
#11515 = CARTESIAN_POINT ( 'NONE',  ( -9.469528151039281028, -6.760870238392817200, 34.69528174975672385 ) ) ;
#11516 = CARTESIAN_POINT ( 'NONE',  ( 6.130525438233648039, -8.630441415882550871, 34.87705825610312615 ) ) ;
#11517 = CARTESIAN_POINT ( 'NONE',  ( 17.07692307692307665, -9.780366693483667717, 34.19971097300155094 ) ) ;
#11518 = ORIENTED_EDGE ( 'NONE', *, *, #56904, .T. ) ;
#11519 = ORIENTED_EDGE ( 'NONE', *, *, #2936, .F. ) ;
#11520 = B_SPLINE_CURVE_WITH_KNOTS ( 'NONE', 3,
 ( #28278, #42255, #1699, #6681, #61620, #62066, #48102, #35938, #7131, #8018 ),
 .UNSPECIFIED., .F., .F.,
 ( 4, 2, 2, 2, 4 ),
 ( 0.0007817359430256334753, 0.0009771253907250058643, 0.001172514838424371098, 0.001367904286123736764, 0.001563293733823101998 ),
 .UNSPECIFIED. ) ;
#11521 = ORIENTED_EDGE ( 'NONE', *, *, #40172, .T. ) ;
#11522 = DIRECTION ( 'NONE',  ( -0.000000000000000000, 1.000000000000000000, -0.000000000000000000 ) ) ;
#11523 = CARTESIAN_POINT ( 'NONE',  ( 10.36540787133602670, -11.47974371597207899, 33.17467449705390692 ) ) ;
#11524 = AXIS2_PLACEMENT_3D ( 'NONE', #31050, #3580, #80148 ) ;
#11525 = CARTESIAN_POINT ( 'NONE',  ( 0.000000000000000000, -11.00000000000000000, 29.75000000000000355 ) ) ;
#11526 = CARTESIAN_POINT ( 'NONE',  ( -4.153846153846152411, -3.886160181151819604, 36.00935417666054406 ) ) ;
#11527 = SHAPE_REPRESENTATION ( 'spring holder', ( #83448 ), #56118 ) ;
#11528 = CARTESIAN_POINT ( 'NONE',  ( -11.78843828251013015, -8.347322224742351082, 34.93158281831414058 ) ) ;
#11529 = DIRECTION ( 'NONE',  ( -0.000000000000000000, -0.6427876096865404731, -0.7660444431189770143 ) ) ;
#11530 = ORIENTED_EDGE ( 'NONE', *, *, #16207, .F. ) ;
#11531 = ORIENTED_EDGE ( 'NONE', *, *, #68224, .F. ) ;
#11532 = CARTESIAN_POINT ( 'NONE',  ( -3.230769230769351186, -3.835265460704628371, 33.15142922262033665 ) ) ;
#11533 = EDGE_CURVE ( 'NONE', #68350, #38200, #11650, .T. ) ;
#11535 = VERTEX_POINT ( 'NONE', #7941 ) ;
#11534 = CARTESIAN_POINT ( 'NONE',  ( 15.36129493253280032, -6.001044277235009439, 34.52024696741798948 ) ) ;
#11536 = CARTESIAN_POINT ( 'NONE',  ( -10.48459417441766206, -3.957578996910242619, 33.62503395064540257 ) ) ;
#11537 = CARTESIAN_POINT ( 'NONE',  ( -9.692307692307812417, -11.94971097300221174, 32.03036669348237098 ) ) ;
#11538 = CARTESIAN_POINT ( 'NONE',  ( 3.750000000000009770, -9.053300858899081760, 14.54687500000000000 ) ) ;
#11539 = VERTEX_POINT ( 'NONE', #62860 ) ;
#11540 = AXIS2_PLACEMENT_3D ( 'NONE', #47977, #55621, #76797 ) ;
#11541 = CARTESIAN_POINT ( 'NONE',  ( 10.68145194873469173, -2.292212530054420494, 30.41441678777542990 ) ) ;
#11542 = VERTEX_POINT ( 'NONE', #70972 ) ;
#11543 = CARTESIAN_POINT ( 'NONE',  ( 5.869309396889694774, -9.084618155246140248, 34.75535874321725771 ) ) ;
#11544 = CARTESIAN_POINT ( 'NONE',  ( 27.00000000000000000, 17.00000000000000000, 2.999999999999999112 ) ) ;
#11545 = CARTESIAN_POINT ( 'NONE',  ( -17.07692307692307665, -11.91647553114624181, 32.58852847137148245 ) ) ;
#11547 = CARTESIAN_POINT ( 'NONE',  ( -15.00739329007105027, -2.501478030877323455, 29.88021232661721172 ) ) ;
#11546 = CARTESIAN_POINT ( 'NONE',  ( -7.146003140593069958, -3.586966769969700763, 32.86292498521069660 ) ) ;
#11548 = VECTOR ( 'NONE', #40017, 1000.000000000000000 ) ;
#11549 = CARTESIAN_POINT ( 'NONE',  ( 18.25005431163831560, -2.779044189368097051, 31.39831045268885745 ) ) ;
#11550 = ORIENTED_EDGE ( 'NONE', *, *, #3160, .F. ) ;
#11551 = ADVANCED_FACE ( 'NONE', ( #77720 ), #29114, .F. ) ;
#11552 = CARTESIAN_POINT ( 'NONE',  ( 12.46153846153833911, -6.879047030192662504, 34.71129190930017927 ) ) ;
#11553 = B_SPLINE_CURVE_WITH_KNOTS ( 'NONE', 3,
 ( #82109, #5561, #13639, #27597, #19949, #47416, #60939, #19512, #39797, #55069 ),
 .UNSPECIFIED., .F., .F.,
 ( 4, 2, 2, 2, 4 ),
 ( 0.000000000000000000, 0.0001954339857564078267, 0.0003908679715128156535, 0.0005863019572692235344, 0.0007817359430256313069 ),
 .UNSPECIFIED. ) ;
#11554 = DIRECTION ( 'NONE',  ( 0.000000000000000000, 0.000000000000000000, -1.000000000000000000 ) ) ;
#11555 = EDGE_CURVE ( 'NONE', #77416, #83736, #8835, .T. ) ;
#11556 = CARTESIAN_POINT ( 'NONE',  ( 5.076923076923075762, -12.29105614889573062, 35.45975837776705220 ) ) ;
#11557 = ORIENTED_EDGE ( 'NONE', *, *, #81387, .T. ) ;
#11558 = AXIS2_PLACEMENT_3D ( 'NONE', #84979, #49418, #21942 ) ;
#11559 = B_SPLINE_CURVE_WITH_KNOTS ( 'NONE', 3,
 ( #58315, #39845, #72277, #81276, #68198, #81717, #47022, #88934, #27205, #75831 ),
 .UNSPECIFIED., .F., .F.,
 ( 4, 2, 2, 2, 4 ),
 ( 0.0007817246256747455461, 0.0009771112852218885505, 0.001172497944769031663, 0.001367884604316174559, 0.001563271263863317672 ),
 .UNSPECIFIED. ) ;
#11560 = PRESENTATION_LAYER_ASSIGNMENT (  '', '', ( #79192 ) ) ;
#11561 = CARTESIAN_POINT ( 'NONE',  ( 8.352564102564102200, -7.500000000000000000, 33.75000000000000000 ) ) ;
#11562 = CARTESIAN_POINT ( 'NONE',  ( -6.222926217516144831, -10.61292498521070549, 33.66303323003028680 ) ) ;
#11563 = CARTESIAN_POINT ( 'NONE',  ( 11.40777007179397984, -5.582088688514999397, 34.36776431015576350 ) ) ;
#11564 = CARTESIAN_POINT ( 'NONE',  ( 7.846153846153725020, -3.300289026999228881, 32.46337939537708905 ) ) ;
#11565 = FACE_BOUND ( 'NONE', #15272, .T. ) ;
#11567 = DIRECTION ( 'NONE',  ( 0.000000000000000000, 0.000000000000000000, 1.000000000000000000 ) ) ;
#11566 = CARTESIAN_POINT ( 'NONE',  ( 12.46153846153833911, -10.33852847137269571, 34.16647553114546554 ) ) ;
#11568 = EDGE_CURVE ( 'NONE', #62713, #56593, #48922, .T. ) ;
#11569 = DIRECTION ( 'NONE',  ( -0.000000000000000000, 0.5000000000000011102, -0.8660254037844380415 ) ) ;
#11571 = DIRECTION ( 'NONE',  ( -0.000000000000000000, -0.6427876096865404731, -0.7660444431189771253 ) ) ;
#11570 = CARTESIAN_POINT ( 'NONE',  ( 1.134592160393928628, -12.68155406624981119, 30.59749803192733708 ) ) ;
#11572 = CARTESIAN_POINT ( 'NONE',  ( 16.02315468717859304, -10.54014554554151140, 33.71984207302941883 ) ) ;
#11573 = CARTESIAN_POINT ( 'NONE',  ( -8.638705067467203236, -3.816742781228458004, 33.13167719472716044 ) ) ;
#11574 = CARTESIAN_POINT ( 'NONE',  ( -3.724691934501229262, -9.114399933863657211, 23.51375670625848713 ) ) ;
#11575 = CARTESIAN_POINT ( 'NONE',  ( -8.519285250882626670, -5.852078868378309373, 34.47109172314383585 ) ) ;
#11576 = EDGE_LOOP ( 'NONE', ( #31568, #31942, #15757, #65307 ) ) ;
#11577 = DIRECTION ( 'NONE',  ( -0.000000000000000000, 0.8660254037844399289, -0.4999999999999980016 ) ) ;
#11578 = DIRECTION ( 'NONE',  ( -0.000000000000000000, 1.000000000000000000, -0.000000000000000000 ) ) ;
#11579 = FACE_OUTER_BOUND ( 'NONE', #57814, .T. ) ;
#11580 = DIRECTION ( 'NONE',  ( 1.000000000000000000, -0.000000000000000000, -0.000000000000000000 ) ) ;
#11581 = CARTESIAN_POINT ( 'NONE',  ( -10.36533019547116119, -12.01375889529407281, 32.43194544308182969 ) ) ;
#11582 = CARTESIAN_POINT ( 'NONE',  ( 1.318533005255250412, -11.91647553114624181, 32.58852847137148245 ) ) ;
#11583 = CARTESIAN_POINT ( 'NONE',  ( 1.614399933863660985, -11.22469193450123193, 26.95125670625849068 ) ) ;
#11584 = CARTESIAN_POINT ( 'NONE',  ( 2.307692307692309264, -11.69971097300155272, 32.46337939537588113 ) ) ;
#11585 = DIRECTION ( 'NONE',  ( -0.000000000000000000, 0.7660444431189791237, -0.6427876096865379196 ) ) ;
#11586 = CARTESIAN_POINT ( 'NONE',  ( -5.076923076923199218, -12.16647553114689728, 32.15551576947799362 ) ) ;
#11587 = CARTESIAN_POINT ( 'NONE',  ( -0.7115616857599187384, -8.475808217655753651, 34.90892951860618609 ) ) ;
#11588 = CARTESIAN_POINT ( 'NONE',  ( 14.37376065869474751, -5.557115091759786019, 34.35708131394839882 ) ) ;
#11589 = CARTESIAN_POINT ( 'NONE',  ( 9.627037691751374027, -3.643525952247789412, 33.31231777344662959 ) ) ;
#11590 = EDGE_CURVE ( 'NONE', #70275, #12547, #87713, .T. ) ;
#11591 = CYLINDRICAL_SURFACE ( 'NONE', #53466, 0.2500000000000008882 ) ;
#11592 = CARTESIAN_POINT ( 'NONE',  ( -11.47239318745910275, -10.51840700105979565, 33.73612834413962247 ) ) ;
#11593 = ORIENTED_EDGE ( 'NONE', *, *, #34870, .T. ) ;
#11594 = B_SPLINE_CURVE_WITH_KNOTS ( 'NONE', 3,
 ( #29348, #49162, #64433, #1422, #36968, #22578, #50908, #83858, #69881, #36544 ),
 .UNSPECIFIED., .F., .F.,
 ( 4, 2, 2, 2, 4 ),
 ( 0.000000000000000000, 0.0001954339857564082062, 0.0003908679715128164124, 0.0005863019572692246186, 0.0007817359430256328248 ),
 .UNSPECIFIED. ) ;
#11595 = AXIS2_PLACEMENT_3D ( 'NONE', #83148, #724, #43044 ) ;
#11596 = DIRECTION ( 'NONE',  ( -0.000000000000000000, 0.9848077530122086864, -0.1736481776669273891 ) ) ;
#11597 = CARTESIAN_POINT ( 'NONE',  ( 15.48071464014727283, -10.92531984108285670, 33.72920026020278073 ) ) ;
#11598 = CARTESIAN_POINT ( 'NONE',  ( -3.775308065498748977, -8.992201783934593351, 19.01749329374151287 ) ) ;
#11599 = B_SPLINE_CURVE_WITH_KNOTS ( 'NONE', 3,
 ( #38063, #17348, #3828, #33535, #45705, #87605, #39851, #19128, #5168, #88496 ),
 .UNSPECIFIED., .F., .F.,
 ( 4, 2, 2, 2, 4 ),
 ( 0.0007817359430256287049, 0.0009771253907249945886, 0.001172514838424360255, 0.001367904286123725922, 0.001563293733823091806 ),
 .UNSPECIFIED. ) ;
#11600 = CARTESIAN_POINT ( 'NONE',  ( -10.68065461594093435, -10.33852847137145048, 34.16647553114627556 ) ) ;
#11601 = DIRECTION ( 'NONE',  ( -0.000000000000000000, -0.5000000000000009992, -0.8660254037844380415 ) ) ;
#11602 = VERTEX_POINT ( 'NONE', #63761 ) ;
#11603 = CARTESIAN_POINT ( 'NONE',  ( 0.4615384615383382183, -3.083524468854526912, 32.58852847137268327 ) ) ;
#11604 = DIRECTION ( 'NONE',  ( -0.000000000000000000, -0.000000000000000000, -1.000000000000000000 ) ) ;
#11606 = ORIENTED_EDGE ( 'NONE', *, *, #8764, .T. ) ;
#11605 = CARTESIAN_POINT ( 'NONE',  ( 4.826899852701617810, -12.45566812827425096, 31.48439005359158926 ) ) ;
#11607 = CARTESIAN_POINT ( 'NONE',  ( 11.76147289007438701, -4.887748414852792322, 34.01359900205216746 ) ) ;
#11608 = DIRECTION ( 'NONE',  ( -0.000000000000000000, -0.1736481776669307198, -0.9848077530122080203 ) ) ;
#11609 = DIRECTION ( 'NONE',  ( -0.000000000000000000, 0.5000000000000011102, -0.8660254037844381525 ) ) ;
#11610 = DIRECTION ( 'NONE',  ( 0.000000000000000000, 1.000000000000000000, -8.673617379884035472E-17 ) ) ;
#11611 = VERTEX_POINT ( 'NONE', #56569 ) ;
#11612 = DIRECTION ( 'NONE',  ( -0.000000000000000000, 0.7660444431189791237, -0.6427876096865379196 ) ) ;
#11613 = LINE ( 'NONE', #39094, #39401 ) ;
#11615 = CARTESIAN_POINT ( 'NONE',  ( -14.30769230769242739, -8.613356846316285953, 34.62446782046622218 ) ) ;
#11614 = VECTOR ( 'NONE', #12329, 1000.000000000000000 ) ;
#11616 = ORIENTED_EDGE ( 'NONE', *, *, #13906, .T. ) ;
#11617 = ORIENTED_EDGE ( 'NONE', *, *, #58091, .F. ) ;
#11618 = ORIENTED_EDGE ( 'NONE', *, *, #88423, .T. ) ;
#11619 = VECTOR ( 'NONE', #39120, 1000.000000000000227 ) ;
#11620 = AXIS2_PLACEMENT_3D ( 'NONE', #3221, #14979, #56404 ) ;
#11621 = CARTESIAN_POINT ( 'NONE',  ( -9.942284423250045577, -2.779195860258146578, 31.39871582349836032 ) ) ;
#11622 = CARTESIAN_POINT ( 'NONE',  ( -8.519176457592452678, -3.136992222400443175, 32.19305428654138979 ) ) ;
#11623 = CARTESIAN_POINT ( 'NONE',  ( 13.13459214732242408, -11.37209801155882793, 32.91403422569033665 ) ) ;
#11624 = AXIS2_PLACEMENT_3D ( 'NONE', #44976, #63923, #50836 ) ;
#11625 = PRODUCT_DEFINITION_FORMATION_WITH_SPECIFIED_SOURCE ( 'ANY', '', #7424, .NOT_KNOWN. ) ;
#11626 = CARTESIAN_POINT ( 'NONE',  ( 14.98079249982687955, -3.627789207965226748, 32.91389620160131102 ) ) ;
#11627 = VERTEX_POINT ( 'NONE', #35861 ) ;
#11628 = B_SPLINE_CURVE_WITH_KNOTS ( 'NONE', 3,
 ( #4760, #52922, #25911, #80421, #19156, #73215, #74104, #12398, #3852, #32229 ),
 .UNSPECIFIED., .F., .F.,
 ( 4, 2, 2, 2, 4 ),
 ( 0.000000000000000000, 0.0001954311564186879315, 0.0003908623128373758630, 0.0005862934692560637946, 0.0007817246256747517261 ),
 .UNSPECIFIED. ) ;
#11629 = EDGE_LOOP ( 'NONE', ( #49623, #62547, #46773, #80321 ) ) ;
#11631 = ORIENTED_EDGE ( 'NONE', *, *, #88013, .F. ) ;
#11630 = CARTESIAN_POINT ( 'NONE',  ( 4.403900573759606196, -5.642605341092957083, 34.66089969410670335 ) ) ;
#11632 = B_SPLINE_CURVE_WITH_KNOTS ( 'NONE', 3,
 ( #26507, #43120, #29611, #49864, #2124, #57067, #49434, #64254, #16088, #8454 ),
 .UNSPECIFIED., .F., .F.,
 ( 4, 2, 2, 2, 4 ),
 ( 0.0007817246256747481482, 0.0009771112852218909357, 0.001172497944769033832, 0.001367884604316176728, 0.001563271263863319407 ),
 .UNSPECIFIED. ) ;
#11633 = CARTESIAN_POINT ( 'NONE',  ( -6.792551484843277976, -4.299079248970732792, 33.91157788607253565 ) ) ;
#11634 = B_SPLINE_CURVE_WITH_KNOTS ( 'NONE', 3,
 ( #42616, #56124, #13804, #68750, #7048, #34522, #61987, #49367, #27760, #83614 ),
 .UNSPECIFIED., .F., .F.,
 ( 4, 2, 2, 2, 4 ),
 ( 0.0007817359430256364027, 0.0009771253907250043464, 0.001172514838424372399, 0.001367904286123740234, 0.001563293733823108286 ),
 .UNSPECIFIED. ) ;
#11635 = FACE_OUTER_BOUND ( 'NONE', #36575, .T. ) ;
#11636 = CARTESIAN_POINT ( 'NONE',  ( 1.449870955891410906, -10.90142922261932057, 33.41473453929631887 ) ) ;
#11637 = CARTESIAN_POINT ( 'NONE',  ( -7.846153846153967493, -10.33852847137269571, 34.16647553114546554 ) ) ;
#11638 = ORIENTED_EDGE ( 'NONE', *, *, #5379, .T. ) ;
#11639 = B_SPLINE_CURVE_WITH_KNOTS ( 'NONE', 3,
 ( #47237, #75172, #67967, #40938, #82372, #68400, #6698, #69295, #34170, #61636 ),
 .UNSPECIFIED., .F., .F.,
 ( 4, 2, 2, 2, 4 ),
 ( 0.000000000000000000, 0.0001954311564186864407, 0.0003908623128373728815, 0.0005862934692560593493, 0.0007817246256747457630 ),
 .UNSPECIFIED. ) ;
#11640 = ORIENTED_EDGE ( 'NONE', *, *, #58514, .F. ) ;
#11641 = ORIENTED_EDGE ( 'NONE', *, *, #80830, .T. ) ;
#11642 = LINE ( 'NONE', #80556, #11619 ) ;
#11644 = ORIENTED_EDGE ( 'NONE', *, *, #59706, .T. ) ;
#11643 = CARTESIAN_POINT ( 'NONE',  ( 5.076923076922954969, -5.219633306517616589, 34.19971097300220464 ) ) ;
#11645 = EDGE_CURVE ( 'NONE', #68166, #78927, #1552, .T. ) ;
#11646 = CARTESIAN_POINT ( 'NONE',  ( 18.25005441991345734, -12.01375889529407992, 32.43194544308182969 ) ) ;
#11647 = CIRCLE ( 'NONE', #66291, 4.000000000000000000 ) ;
#11648 = CARTESIAN_POINT ( 'NONE',  ( 12.39626801557768765, -11.48612834413959582, 32.76840700105983473 ) ) ;
#11649 = CARTESIAN_POINT ( 'NONE',  ( -13.51530685128294529, -4.118384482072085184, 33.43331474514187107 ) ) ;
#11650 = CIRCLE ( 'NONE', #83538, 2.000000000000001776 ) ;
#11651 = CARTESIAN_POINT ( 'NONE',  ( -13.51517597635730539, -2.504760397472875155, 29.97295953869789997 ) ) ;
#11652 = CARTESIAN_POINT ( 'NONE',  ( 8.992242120843620512, -5.667800583137506010, 34.40243808032445827 ) ) ;
#11653 = FACE_BOUND ( 'NONE', #12992, .T. ) ;
#11654 = CARTESIAN_POINT ( 'NONE',  ( -0.4615384615384611200, -4.098570777380720287, 33.41473453929634729 ) ) ;
#11655 = LINE ( 'NONE', #45865, #27027 ) ;
#11656 = EDGE_CURVE ( 'NONE', #16922, #72102, #76395, .T. ) ;
#11657 = CARTESIAN_POINT ( 'NONE',  ( -8.899377978668990608, -4.460286881179643004, 33.72017969459903242 ) ) ;
#11659 = CARTESIAN_POINT ( 'NONE',  ( -5.933931648997560870, -2.721908614388772296, 31.22303859784725333 ) ) ;
#11658 = LINE ( 'NONE', #88226, #23038 ) ;
#11660 = CARTESIAN_POINT ( 'NONE',  ( -3.903846153844733102, -7.500000000000154543, 35.00000000000007105 ) ) ;
#11661 = DIRECTION ( 'NONE',  ( 0.000000000000000000, -1.000000000000000000, 4.336808689942017736E-16 ) ) ;
#11662 = ORIENTED_EDGE ( 'NONE', *, *, #49111, .T. ) ;
#11663 = CARTESIAN_POINT ( 'NONE',  ( 11.40777007179397984, -3.062553014421049546, 32.05460306192773601 ) ) ;
#11664 = EDGE_CURVE ( 'NONE', #70063, #8324, #1633, .T. ) ;
#11665 = CARTESIAN_POINT ( 'NONE',  ( 12.52679360105129547, -3.643525952247864463, 33.31231777344670064 ) ) ;
#11666 = ORIENTED_EDGE ( 'NONE', *, *, #60481, .F. ) ;
#11667 = ORIENTED_EDGE ( 'NONE', *, *, #52951, .T. ) ;
#11669 = CARTESIAN_POINT ( 'NONE',  ( 2.307692307692615685, -2.506253911140615021, 30.00000000000323297 ) ) ;
#11668 = CARTESIAN_POINT ( 'NONE',  ( -6.673131404728781746, -8.433404298154334455, 34.66254593164985920 ) ) ;
#11670 = CARTESIAN_POINT ( 'NONE',  ( -0.6844038837421002608, -2.501496062324912284, 29.88072118266895671 ) ) ;
#11671 = CARTESIAN_POINT ( 'NONE',  ( -13.51476335434707821, -5.070767119584671079, 34.40440758774516183 ) ) ;
#11672 = CARTESIAN_POINT ( 'NONE',  ( -15.09993081275646176, -7.277220443632450575, 34.74524770363009196 ) ) ;
#11673 = ORIENTED_EDGE ( 'NONE', *, *, #63094, .F. ) ;
#11674 = CARTESIAN_POINT ( 'NONE',  ( -13.38461538461550759, -12.51329471203414379, 31.30864560766407578 ) ) ;
#11675 = DIRECTION ( 'NONE',  ( -0.000000000000000000, 0.9848077530122086864, -0.1736481776669273891 ) ) ;
#11677 = FACE_OUTER_BOUND ( 'NONE', #77589, .T. ) ;
#11676 = CARTESIAN_POINT ( 'NONE',  ( 11.76147438255493682, -2.889357225399416418, 32.26129605718031002 ) ) ;
#11678 = DIRECTION ( 'NONE',  ( -0.000000000000000000, 0.5000000000000011102, -0.8660254037844381525 ) ) ;
#11679 = VECTOR ( 'NONE', #37824, 1000.000000000000114 ) ;
#11680 = EDGE_CURVE ( 'NONE', #50951, #13993, #45724, .T. ) ;
#11681 = CARTESIAN_POINT ( 'NONE',  ( -3.512820512820514995, -4.000000000000000000, 29.75000000000000355 ) ) ;
#11682 = CARTESIAN_POINT ( 'NONE',  ( -15.23076923076935252, -11.06231777344772027, 33.60647404775119895 ) ) ;
#11683 = CARTESIAN_POINT ( 'NONE',  ( 3.750000000000000888, -7.499999999999978684, 23.21875000000000000 ) ) ;
#11684 = ORIENTED_EDGE ( 'NONE', *, *, #44990, .F. ) ;
#11685 = AXIS2_PLACEMENT_3D ( 'NONE', #62592, #77011, #8555 ) ;
#11686 = AXIS2_PLACEMENT_3D ( 'NONE', #19099, #12779, #13665 ) ;
#11687 = VERTEX_POINT ( 'NONE', #49370 ) ;
#11688 = CARTESIAN_POINT ( 'NONE',  ( 5.207448778686639024, -6.852161475712352789, 34.70806712695775786 ) ) ;
#11689 = CARTESIAN_POINT ( 'NONE',  ( 12.71153846153852385, -7.434744429011176159, 34.75000000000000711 ) ) ;
#11690 = CYLINDRICAL_SURFACE ( 'NONE', #27240, 0.2499999999999993616 ) ;
#11691 = CARTESIAN_POINT ( 'NONE',  ( -16.37677237136229991, -4.887634598454295265, 34.01352882383564946 ) ) ;
#11692 = CYLINDRICAL_SURFACE ( 'NONE', #34195, 0.2499999999999997502 ) ;
#11693 = CARTESIAN_POINT ( 'NONE',  ( 2.651650429449569302, -10.15165042944953733, 22.12500000000000000 ) ) ;
#11694 = AXIS2_PLACEMENT_3D ( 'NONE', #75800, #6467, #61836 ) ;
#11695 = CARTESIAN_POINT ( 'NONE',  ( 8.769230769230768274, -8.810774026931790459, 35.74407628777942847 ) ) ;
#11696 = CARTESIAN_POINT ( 'NONE',  ( -13.38461538461538325, -8.120952969808772792, 34.71129190930000163 ) ) ;
#11697 = CARTESIAN_POINT ( 'NONE',  ( -5.999999999999998224, -1.044019251281081972, 31.83374038241031911 ) ) ;
#11698 = PLANE ( 'NONE',  #22298 ) ;
#11699 = CARTESIAN_POINT ( 'NONE',  ( 9.692307692307695177, -2.721908614388771852, 31.22303859784724978 ) ) ;
#11700 = CARTESIAN_POINT ( 'NONE',  ( 14.98079248672064345, -12.41104346484419452, 31.60698883733904196 ) ) ;
#11701 = CARTESIAN_POINT ( 'NONE',  ( 15.23076923076923173, -2.249999999999998668, 29.75000000000001776 ) ) ;
#11702 = DIRECTION ( 'NONE',  ( -0.000000000000000000, 1.000000000000000000, -0.000000000000000000 ) ) ;
#11703 = EDGE_CURVE ( 'NONE', #32213, #60372, #13648, .T. ) ;
#11704 = CARTESIAN_POINT ( 'NONE',  ( -5.933932666649923249, -4.661471528628508665, 34.16647553114624003 ) ) ;
#11705 = CARTESIAN_POINT ( 'NONE',  ( -17.01085574357300345, -2.833524468853757750, 32.15551576947925838 ) ) ;
#11706 = ADVANCED_FACE ( 'NONE', ( #28499 ), #6017, .F. ) ;
#11707 = ORIENTED_EDGE ( 'NONE', *, *, #59609, .T. ) ;
#11708 = CARTESIAN_POINT ( 'NONE',  ( 8.992243613324164997, -4.762714258010881885, 34.23016756924214832 ) ) ;
#11709 = CARTESIAN_POINT ( 'NONE',  ( -3.361460697436791545, -3.530157926970578508, 32.79014554554150607 ) ) ;
#11710 = CARTESIAN_POINT ( 'NONE',  ( 13.38461538461538680, -6.343179335718451384, 34.87096338111211935 ) ) ;
#11711 = CARTESIAN_POINT ( 'NONE',  ( -2.749999999999999112, -7.438900925035484057, 14.09561829374151642 ) ) ;
#11712 = ADVANCED_FACE ( 'NONE', ( #82574 ), #14095, .F. ) ;
#11713 = CARTESIAN_POINT ( 'NONE',  ( -14.08468095607945791, -4.887748414852792322, 34.01359900205216746 ) ) ;
#11714 = FACE_OUTER_BOUND ( 'NONE', #41414, .T. ) ;
#11715 = EDGE_CURVE ( 'NONE', #10987, #40550, #7125, .T. ) ;
#11717 = ORIENTED_EDGE ( 'NONE', *, *, #75820, .T. ) ;
#11716 = FACE_OUTER_BOUND ( 'NONE', #64439, .T. ) ;
#11718 = CARTESIAN_POINT ( 'NONE',  ( -1.139087296525992388, -10.25000000000000711, 18.60937500000000355 ) ) ;
#11719 = CARTESIAN_POINT ( 'NONE',  ( -3.230769230769352962, -12.70778746994576025, 30.41441678777401236 ) ) ;
#11720 = VERTEX_POINT ( 'NONE', #13211 ) ;
#11721 = CARTESIAN_POINT ( 'NONE',  ( 0.3308469948709040209, -2.729777683071817229, 31.24903638046269450 ) ) ;
#11722 = ORIENTED_EDGE ( 'NONE', *, *, #27918, .T. ) ;
#11723 = DIRECTION ( 'NONE',  ( -0.000000000000000000, 0.9848077530122086864, -0.1736481776669273891 ) ) ;
#11724 = CARTESIAN_POINT ( 'NONE',  ( -15.29603923132555288, -3.083524468853724443, 32.58852847137143272 ) ) ;
#11725 = CARTESIAN_POINT ( 'NONE',  ( 15.36156103859401867, -2.729792928343269587, 31.24908615093345077 ) ) ;
#11726 = VERTEX_POINT ( 'NONE', #20846 ) ;
#11727 = CARTESIAN_POINT ( 'NONE',  ( 0.2115152373170037237, -4.931416488878823223, 34.32920672191015399 ) ) ;
#11728 = VERTEX_POINT ( 'NONE', #55960 ) ;
#11729 = CARTESIAN_POINT ( 'NONE',  ( -5.999999999999998224, -2.292212530054420494, 30.41441678777542634 ) ) ;
#11730 = ORIENTED_EDGE ( 'NONE', *, *, #77999, .T. ) ;
#11731 = CARTESIAN_POINT ( 'NONE',  ( 13.63466969625370417, -11.79725096376909654, 32.30694842903959341 ) ) ;
#11732 = CARTESIAN_POINT ( 'NONE',  ( 12.71148397988660150, -12.22109172314383052, 31.39792113162168263 ) ) ;
#11733 = LINE ( 'NONE', #87404, #39837 ) ;
#11734 = B_SPLINE_CURVE_WITH_KNOTS ( 'NONE', 3,
 ( #40787, #7443, #34897, #676, #62363, #53396, #74123, #12420, #20061, #47523 ),
 .UNSPECIFIED., .F., .F.,
 ( 4, 2, 2, 2, 4 ),
 ( 0.000000000000000000, 0.0001954339857564081249, 0.0003908679715128162498, 0.0005863019572692244018, 0.0007817359430256324996 ),
 .UNSPECIFIED. ) ;
#11735 = LINE ( 'NONE', #39211, #36145 ) ;
#11736 = CARTESIAN_POINT ( 'NONE',  ( -17.07692307692307665, -9.819645486525091727, 36.12317359536749706 ) ) ;
#11737 = CARTESIAN_POINT ( 'NONE',  ( -1.318548051265308052, -10.67929555188718282, 33.92786785259544757 ) ) ;
#11738 = CARTESIAN_POINT ( 'NONE',  ( 5.076923076922954969, -9.442884908241554243, 34.35708131394783038 ) ) ;
#11739 = EDGE_CURVE ( 'NONE', #83736, #30367, #47877, .T. ) ;
#11740 = EDGE_LOOP ( 'NONE', ( #87564, #58835 ) ) ;
#11741 = ORIENTED_EDGE ( 'NONE', *, *, #32681, .F. ) ;
#11742 = EDGE_LOOP ( 'NONE', ( #50390, #67308, #27814, #11211 ) ) ;
#11744 = EDGE_LOOP ( 'NONE', ( #37988, #51134, #20401, #31272, #45517 ) ) ;
#11743 = CARTESIAN_POINT ( 'NONE',  ( 3.480714749117372886, -3.712312575010499938, 33.01462480002815170 ) ) ;
#11745 = CARTESIAN_POINT ( 'NONE',  ( -14.08491263871423982, -10.97394488606064122, 33.68653795673694873 ) ) ;
#11746 = CARTESIAN_POINT ( 'NONE',  ( -10.68146802634049486, -8.973038597847271092, 34.52809138561120506 ) ) ;
#11747 = ORIENTED_EDGE ( 'NONE', *, *, #78758, .T. ) ;
#11748 = CARTESIAN_POINT ( 'NONE',  ( -12.33074802057151409, -11.37503395064541678, 33.29242100308974273 ) ) ;
#11749 = EDGE_CURVE ( 'NONE', #3675, #40454, #1025, .T. ) ;
#11750 = ORIENTED_EDGE ( 'NONE', *, *, #84771, .F. ) ;
#11751 = LINE ( 'NONE', #25259, #32480 ) ;
#11752 = VERTEX_POINT ( 'NONE', #7783 ) ;
#11753 = CARTESIAN_POINT ( 'NONE',  ( -9.468932206535269458, -2.251407671071268712, 29.88021292934943318 ) ) ;
#11754 = CARTESIAN_POINT ( 'NONE',  ( -2.307692307692305711, -13.87047571288749737, 32.06866353760679544 ) ) ;
#11755 = CARTESIAN_POINT ( 'NONE',  ( 3.930979890783055097, -2.251424796025575770, 29.88072029997477586 ) ) ;
#11756 = FACE_BOUND ( 'NONE', #19867, .T. ) ;
#11757 = B_SPLINE_CURVE_WITH_KNOTS ( 'NONE', 3,
 ( #46841, #4524, #4976, #47281, #59908, #53145, #46400, #67567, #39663, #74772 ),
 .UNSPECIFIED., .F., .F.,
 ( 4, 2, 2, 2, 4 ),
 ( 0.0007817246256747499913, 0.0009771112852218944052, 0.001172497944769038819, 0.001367884604316183016, 0.001563271263863327430 ),
 .UNSPECIFIED. ) ;
#11758 = CARTESIAN_POINT ( 'NONE',  ( -7.846153846153844924, -10.05456864172156806, 36.03766855953608683 ) ) ;
#11759 = DIRECTION ( 'NONE',  ( 0.000000000000000000, 0.000000000000000000, -1.000000000000000000 ) ) ;
#11760 = EDGE_CURVE ( 'NONE', #45538, #16403, #138, .T. ) ;
#11761 = CARTESIAN_POINT ( 'NONE',  ( 5.749999999999988454, -2.499999999999999556, 29.81609845454692120 ) ) ;
#11762 = B_SPLINE_CURVE_WITH_KNOTS ( 'NONE', 3,
 ( #76612, #42397, #69855, #63528, #29319, #56340, #15359, #84716, #48685, #1390 ),
 .UNSPECIFIED., .F., .F.,
 ( 4, 2, 2, 2, 4 ),
 ( 0.0007817359430256258859, 0.0009771253907249909023, 0.001172514838424355919, 0.001367904286123720935, 0.001563293733823085951 ),
 .UNSPECIFIED. ) ;
#11763 = CARTESIAN_POINT ( 'NONE',  ( -13.38461538461538325, -5.180354513474913603, 36.12317359536750416 ) ) ;
#11764 = LINE ( 'NONE', #59938, #75436 ) ;
#11765 = CARTESIAN_POINT ( 'NONE',  ( 17.07692307692307665, -8.973038597847269315, 34.52809138561121927 ) ) ;
#11766 = VERTEX_POINT ( 'NONE', #48315 ) ;
#11767 = CARTESIAN_POINT ( 'NONE',  ( -10.39260507411620260, -4.387253974876679230, 33.66317474335728832 ) ) ;
#11768 = EDGE_CURVE ( 'NONE', #59129, #17957, #87943, .T. ) ;
#11769 = VERTEX_POINT ( 'NONE', #81675 ) ;
#11770 = ORIENTED_EDGE ( 'NONE', *, *, #12521, .F. ) ;
#11772 = CARTESIAN_POINT ( 'NONE',  ( -5.076923076923075762, -3.886160181151819604, 36.00935417666054406 ) ) ;
#11771 = CARTESIAN_POINT ( 'NONE',  ( -0.6844646790546091708, -9.086856451489515152, 34.49173150075333183 ) ) ;
#11773 = CARTESIAN_POINT ( 'NONE',  ( 3.230769230769231726, -3.322132147404559976, 32.92929555188717927 ) ) ;
#11774 = CARTESIAN_POINT ( 'NONE',  ( -11.53846153846153655, -1.129524287112498415, 32.06866353760679544 ) ) ;
#11775 = CARTESIAN_POINT ( 'NONE',  ( 16.82689983963011926, -8.432397168068783699, 34.66272746175022945 ) ) ;
#11776 = CARTESIAN_POINT ( 'NONE',  ( -15.36091644020745584, -3.817052484675422797, 33.13202310037935661 ) ) ;
#11777 = ORIENTED_EDGE ( 'NONE', *, *, #68590, .T. ) ;
#11778 = CARTESIAN_POINT ( 'NONE',  ( -6.166666666666667851, -4.000000000000000000, 29.75000000000000355 ) ) ;
#11779 = CARTESIAN_POINT ( 'NONE',  ( -4.946131269098290595, -2.541949514083464479, 30.39797389878540557 ) ) ;
#11780 = CARTESIAN_POINT ( 'NONE',  ( 10.61538461538461675, -3.050289026998446396, 32.03036669348365706 ) ) ;
#11781 = ADVANCED_FACE ( 'NONE', ( #7346 ), #41127, .F. ) ;
#11782 = CARTESIAN_POINT ( 'NONE',  ( 8.769230769230647482, -11.94971097300221174, 32.03036669348237098 ) ) ;
#11783 = VECTOR ( 'NONE', #40299, 1000.000000000000000 ) ;
#11784 = VERTEX_POINT ( 'NONE', #74918 ) ;
#11785 = B_SPLINE_CURVE_WITH_KNOTS ( 'NONE', 3,
 ( #25328, #3711, #24874, #11823, #10927, #87054, #65419, #31185, #51430, #24422 ),
 .UNSPECIFIED., .F., .F.,
 ( 4, 2, 2, 2, 4 ),
 ( 0.000000000000000000, 0.0001954311564186867660, 0.0003908623128373735320, 0.0005862934692560603251, 0.0007817246256747470640 ),
 .UNSPECIFIED. ) ;
#11786 = EDGE_LOOP ( 'NONE', ( #81747, #58600, #21146, #2279, #78024, #81684, #26917, #22752, #44699, #28036, #1092, #54484, #46566, #85352, #75983, #46149, #40359, #76800, #30647, #15158, #85073, #84949, #37862, #86317, #10406, #11139, #40252, #25292, #61926, #2434, #53309, #35326, #58106, #67871, #83489, #18129, #75727, #53301, #36157, #50719, #79728, #63123, #17530, #86073, #41626, #30701, #30650, #78169, #21478, #1992, #30205, #57152, #32586, #42760, #45603, #38976, #44053, #77305, #59553, #75258, #47396, #45939, #35971, #33373, #3993, #80361, #53610, #46528, #26508, #35802, #12841, #35703, #15423, #60400, #39197, #74072, #73796, #86199, #3492, #35711, #69423, #45285, #59915, #61486, #74999, #50583 ) ) ;
#11787 = CONTEXT_DEPENDENT_SHAPE_REPRESENTATION ( #11833, #54300 ) ;
#11789 = EDGE_CURVE ( 'NONE', #16668, #41132, #38216, .T. ) ;
#11788 = ORIENTED_EDGE ( 'NONE', *, *, #32787, .T. ) ;
#11790 = CARTESIAN_POINT ( 'NONE',  ( -1.384615384615505151, -2.892918686052166066, 31.69288490824153470 ) ) ;
#11791 = CARTESIAN_POINT ( 'NONE',  ( -5.869161669513237811, -7.277220318596959281, 34.99547417642776992 ) ) ;
#11792 = ORIENTED_EDGE ( 'NONE', *, *, #72403, .T. ) ;
#11793 = ADVANCED_FACE ( 'NONE', ( #76231 ), #14538, .F. ) ;
#11794 = DIRECTION ( 'NONE',  ( -1.000000000000000000, -0.000000000000000000, -0.000000000000000000 ) ) ;
#11795 = CARTESIAN_POINT ( 'NONE',  ( -5.207614543590633360, -2.729777683071817229, 31.24903638046268739 ) ) ;
#11796 = CARTESIAN_POINT ( 'NONE',  ( 15.93091993633000847, -8.239355502252617924, 34.69524867566427417 ) ) ;
#11797 = CARTESIAN_POINT ( 'NONE',  ( 8.992243613324164997, -3.395485233115139057, 33.02377354290275946 ) ) ;
#11798 = CARTESIAN_POINT ( 'NONE',  ( 18.00000000000000000, -2.538708090699994813, 30.37095296980875503 ) ) ;
#11799 = ORIENTED_EDGE ( 'NONE', *, *, #62043, .F. ) ;
#11801 = ORIENTED_EDGE ( 'NONE', *, *, #55924, .T. ) ;
#11800 = CARTESIAN_POINT ( 'NONE',  ( -15.16551409125639260, -2.379036618887895305, 30.90682066428158592 ) ) ;
#11802 = CARTESIAN_POINT ( 'NONE',  ( -8.519285250882630223, -10.05730279482229683, 34.04704008940765902 ) ) ;
#11803 = CARTESIAN_POINT ( 'NONE',  ( -2.373775718648186484, -8.973038597847271092, 34.52809138561120506 ) ) ;
#11804 = CARTESIAN_POINT ( 'NONE',  ( -13.51476259405360203, -5.195881422630166391, 34.18770438780619259 ) ) ;
#11805 = CARTESIAN_POINT ( 'NONE',  ( 15.36156103859401867, -12.38066358083363738, 30.83685684665853444 ) ) ;
#11806 = CARTESIAN_POINT ( 'NONE',  ( -4.088591014333314178, -5.094484230520773593, 34.41647553114626845 ) ) ;
#11807 = ADVANCED_FACE ( 'NONE', ( #40248 ), #67712, .F. ) ;
#11808 = FACE_OUTER_BOUND ( 'NONE', #77762, .T. ) ;
#11809 = CARTESIAN_POINT ( 'NONE',  ( 9.562160482869472844, -6.852621066184266141, 34.70813303252209181 ) ) ;
#11810 = CARTESIAN_POINT ( 'NONE',  ( 2.775308065498755195, -6.422011778438505125, 13.39249329374151642 ) ) ;
#11811 = ORIENTED_EDGE ( 'NONE', *, *, #83550, .T. ) ;
#11812 = B_SPLINE_CURVE_WITH_KNOTS ( 'NONE', 3,
 ( #3150, #63195, #23857, #66186, #4496, #78368, #16669, #65737, #24763, #58986 ),
 .UNSPECIFIED., .F., .F.,
 ( 4, 2, 2, 2, 4 ),
 ( 0.000000000000000000, 0.0001954311564186870371, 0.0003908623128373740741, 0.0005862934692560610840, 0.0007817246256747481482 ),
 .UNSPECIFIED. ) ;
#11813 = DIRECTION ( 'NONE',  ( -0.000000000000000000, 0.9848077530122085754, -0.1736481776669273613 ) ) ;
#11814 = CARTESIAN_POINT ( 'NONE',  ( -9.561515884482908234, -8.147973898785416225, 34.70805048591653730 ) ) ;
#11815 = DIRECTION ( 'NONE',  ( 0.000000000000000000, -1.734723475976807094E-15, 1.000000000000000000 ) ) ;
#11816 = EDGE_LOOP ( 'NONE', ( #70466, #9381 ) ) ;
#11817 = EDGE_CURVE ( 'NONE', #40406, #11287, #88143, .T. ) ;
#11818 = ORIENTED_EDGE ( 'NONE', *, *, #7924, .T. ) ;
#11819 = CARTESIAN_POINT ( 'NONE',  ( -11.78848477575450282, -10.76384336483936011, 33.53834819971076087 ) ) ;
#11820 = CARTESIAN_POINT ( 'NONE',  ( 0.000000000000000000, -11.00000000000000000, 29.75000000000000355 ) ) ;
#11821 = LINE ( 'NONE', #17685, #38956 ) ;
#11822 = VECTOR ( 'NONE', #48917, 1000.000000000000000 ) ;
#11823 = CARTESIAN_POINT ( 'NONE',  ( 15.93091919493929964, -10.01117774369187252, 34.36070679894347535 ) ) ;
#11824 = CYLINDRICAL_SURFACE ( 'NONE', #88844, 0.2500000000000009437 ) ;
#11825 = CARTESIAN_POINT ( 'NONE',  ( -6.923076923076922462, -11.69971097300155272, 32.46337939537588113 ) ) ;
#11826 = ORIENTED_EDGE ( 'NONE', *, *, #63941, .T. ) ;
#11827 = DIRECTION ( 'NONE',  ( -0.000000000000000000, -0.1736481776669307198, -0.9848077530122080203 ) ) ;
#11828 = CARTESIAN_POINT ( 'NONE',  ( 4.153846153846154188, -13.53365097954675988, 30.81389545987213552 ) ) ;
#11829 = EDGE_CURVE ( 'NONE', #28663, #47075, #66126, .T. ) ;
#11830 = CARTESIAN_POINT ( 'NONE',  ( 3.930919194939304973, -8.282780595021769443, 34.94152052738834868 ) ) ;
#11831 = ORIENTED_EDGE ( 'NONE', *, *, #82010, .F. ) ;
#11832 = CARTESIAN_POINT ( 'NONE',  ( 12.46153846153833911, -2.657715359629662544, 31.77849191805970364 ) ) ;
#11833 =( REPRESENTATION_RELATIONSHIP ('NONE','NONE', #51743, #85713 ) REPRESENTATION_RELATIONSHIP_WITH_TRANSFORMATION ( #73492 )SHAPE_REPRESENTATION_RELATIONSHIP( ) );
#11834 = ORIENTED_EDGE ( 'NONE', *, *, #49289, .T. ) ;
#11835 = DIRECTION ( 'NONE',  ( 1.000000000000000000, 0.000000000000000000, 0.000000000000000000 ) ) ;
#11836 = FILL_AREA_STYLE ('',( #72187 ) ) ;
#11837 = DIRECTION ( 'NONE',  ( 0.000000000000000000, 0.000000000000000000, -1.000000000000000000 ) ) ;
#11838 = EDGE_CURVE ( 'NONE', #83826, #76411, #86811, .T. ) ;
#11839 = CARTESIAN_POINT ( 'NONE',  ( 15.36129466900287532, -5.070358843744210198, 34.40418822224088302 ) ) ;
#11840 = EDGE_LOOP ( 'NONE', ( #46590, #53298 ) ) ;
#11841 = CARTESIAN_POINT ( 'NONE',  ( 0.5920641633020244932, -4.459921816937788996, 33.71989282347011851 ) ) ;
#11842 = CARTESIAN_POINT ( 'NONE',  ( 15.23076923076923173, -9.819645486525091727, 36.12317359536749706 ) ) ;
#11843 = DIRECTION ( 'NONE',  ( -1.000000000000000000, -0.000000000000000000, -0.000000000000000000 ) ) ;
#11844 = B_SPLINE_CURVE_WITH_KNOTS ( 'NONE', 3,
 ( #65797, #30689, #23482, #45087, #72562, #85643, #9528, #52290, #79778, #64907 ),
 .UNSPECIFIED., .F., .F.,
 ( 4, 2, 2, 2, 4 ),
 ( 0.000000000000000000, 0.0001954311564186873623, 0.0003908623128373747246, 0.0005862934692560620598, 0.0007817246256747494492 ),
 .UNSPECIFIED. ) ;
#11845 = AXIS2_PLACEMENT_3D ( 'NONE', #51062, #7894, #1133 ) ;
#11846 = CARTESIAN_POINT ( 'NONE',  ( -7.780898706641007578, -5.094484230520773593, 34.41647553114626845 ) ) ;
#11847 = CARTESIAN_POINT ( 'NONE',  ( -5.076923076923075762, -10.67929555188718282, 33.92786785259544047 ) ) ;
#11848 = B_SPLINE_CURVE_WITH_KNOTS ( 'NONE', 3,
 ( #48458, #27316, #53898, #81385, #20119, #287, #34950, #54778, #67858, #19668 ),
 .UNSPECIFIED., .F., .F.,
 ( 4, 2, 2, 2, 4 ),
 ( 0.0007817359430256302227, 0.0009771253907249963233, 0.001172514838424362424, 0.001367904286123728524, 0.001563293733823094625 ),
 .UNSPECIFIED. ) ;
#11849 = ADVANCED_FACE ( 'NONE', ( #25079 ), #40820, .F. ) ;
#11850 = ORIENTED_EDGE ( 'NONE', *, *, #38124, .T. ) ;
#11851 = FACE_BOUND ( 'NONE', #71276, .T. ) ;
#11852 = ORIENTED_EDGE ( 'NONE', *, *, #64696, .F. ) ;
#11853 = CARTESIAN_POINT ( 'NONE',  ( 8.703960323269994248, -12.46129190929999986, 30.37095296980880832 ) ) ;
#11854 = EDGE_CURVE ( 'NONE', #56424, #67715, #70454, .T. ) ;
#11855 = DIRECTION ( 'NONE',  ( 0.000000000000000000, 0.6427876096865373645, -0.7660444431189797898 ) ) ;
#11856 = ADVANCED_FACE ( 'NONE', ( #25527 ), #39500, .T. ) ;
#11857 = CARTESIAN_POINT ( 'NONE',  ( 3.512820512820510555, -3.499999999999999556, 29.75000000000000355 ) ) ;
#11858 = CARTESIAN_POINT ( 'NONE',  ( -3.230769230769229949, -4.098570777380720287, 33.41473453929634729 ) ) ;
#11859 = CARTESIAN_POINT ( 'NONE',  ( -14.30769230769242739, -12.27809138561165270, 31.22303859784587132 ) ) ;
#11860 = CARTESIAN_POINT ( 'NONE',  ( -9.442362282929648742, -6.653508905675592722, 34.93172785388651391 ) ) ;
#11861 = CARTESIAN_POINT ( 'NONE',  ( 9.561616225640134914, -8.147922237126337563, 34.70805685702651999 ) ) ;
#11862 = ORIENTED_EDGE ( 'NONE', *, *, #39023, .F. ) ;
#11863 = EDGE_CURVE ( 'NONE', #74976, #27257, #13505, .T. ) ;
#11864 = VERTEX_POINT ( 'NONE', #19652 ) ;
#11865 = ORIENTED_EDGE ( 'NONE', *, *, #33322, .T. ) ;
#11866 = ORIENTED_EDGE ( 'NONE', *, *, #46432, .T. ) ;
#11867 = ORIENTED_EDGE ( 'NONE', *, *, #37717, .F. ) ;
#11868 = CARTESIAN_POINT ( 'NONE',  ( -5.076923076923199218, -4.320704448113951379, 33.92786785259630022 ) ) ;
#11869 = CARTESIAN_POINT ( 'NONE',  ( -11.66860874789975888, -9.418419913701741919, 34.36755862841477693 ) ) ;
#11870 = CARTESIAN_POINT ( 'NONE',  ( -10.48485917715097138, -5.070358843744210198, 34.40418822224088302 ) ) ;
#11871 = CARTESIAN_POINT ( 'NONE',  ( 4.853438152358744873, -11.60425143139329940, 33.02411095842164457 ) ) ;
#11872 = CARTESIAN_POINT ( 'NONE',  ( 14.55769230769374367, -7.500000000000155431, 34.75000000000007105 ) ) ;
#11873 = FACE_OUTER_BOUND ( 'NONE', #4970, .T. ) ;
#11874 = CARTESIAN_POINT ( 'NONE',  ( 17.93391658904411656, -2.538708090699995257, 30.37095296980875148 ) ) ;
#11875 = CARTESIAN_POINT ( 'NONE',  ( 0.3954550505825804030, -3.050289026998445951, 32.03036669348365706 ) ) ;
#11876 = EDGE_LOOP ( 'NONE', ( #56262, #29776 ) ) ;
#11877 = EDGE_CURVE ( 'NONE', #70675, #61992, #82271, .T. ) ;
#11878 = ORIENTED_EDGE ( 'NONE', *, *, #11715, .T. ) ;
#11879 = AXIS2_PLACEMENT_3D ( 'NONE', #15050, #29019, #56474 ) ;
#11880 = VERTEX_POINT ( 'NONE', #12892 ) ;
#11882 = ORIENTED_EDGE ( 'NONE', *, *, #32747, .F. ) ;
#11881 = CARTESIAN_POINT ( 'NONE',  ( -1.384615384615505151, -11.48612834414049644, 32.76840700105863391 ) ) ;
#11884 = CARTESIAN_POINT ( 'NONE',  ( 10.61538461538461675, -8.973038597847269315, 34.52809138561121927 ) ) ;
#11883 = CARTESIAN_POINT ( 'NONE',  ( 6.923076923076800782, -11.67786785259630911, 32.92929555188603530 ) ) ;
#11885 = B_SPLINE_CURVE_WITH_KNOTS ( 'NONE', 3,
 ( #1144, #62824, #41251, #1592, #29079, #49767, #14664, #83125, #68715, #76812 ),
 .UNSPECIFIED., .F., .F.,
 ( 4, 2, 2, 2, 4 ),
 ( 0.0007817359430256388964, 0.0009771253907250075990, 0.001172514838424376085, 0.001367904286123744571, 0.001563293733823113273 ),
 .UNSPECIFIED. ) ;
#11886 = CARTESIAN_POINT ( 'NONE',  ( 15.90384615384615330, -7.500000000000001776, 34.75000000000000000 ) ) ;
#11887 = CARTESIAN_POINT ( 'NONE',  ( 4.284637961670941131, -2.541949514083464479, 30.39797389878540557 ) ) ;
#11888 = FACE_BOUND ( 'NONE', #13848, .T. ) ;
#11889 = ORIENTED_EDGE ( 'NONE', *, *, #9660, .T. ) ;
#11890 = ORIENTED_EDGE ( 'NONE', *, *, #76838, .T. ) ;
#11891 = CARTESIAN_POINT ( 'NONE',  ( 1.384615384615701439, -2.255955759149395501, 30.00000000000324363 ) ) ;
#11892 = ORIENTED_EDGE ( 'NONE', *, *, #20072, .T. ) ;
#11893 = FACE_BOUND ( 'NONE', #29847, .T. ) ;
#11894 = CARTESIAN_POINT ( 'NONE',  ( 7.846153846153725020, -11.94971097300221174, 32.03036669348237098 ) ) ;
#11895 = CARTESIAN_POINT ( 'NONE',  ( -13.44988583057615905, -10.90142922261923886, 33.41473453929638993 ) ) ;
#11896 = VERTEX_POINT ( 'NONE', #31848 ) ;
#11897 = CARTESIAN_POINT ( 'NONE',  ( -15.23076923076922995, -12.10708131394839349, 31.69288490824020244 ) ) ;
#11898 = CARTESIAN_POINT ( 'NONE',  ( -24.00000000000000000, -5.499999999999981348, 27.25000000000000000 ) ) ;
#11899 = CARTESIAN_POINT ( 'NONE',  ( 2.177001704582000929, -11.37499894934982514, 33.29245874905763003 ) ) ;
#11900 = VERTEX_POINT ( 'NONE', #40383 ) ;
#11901 = DIRECTION ( 'NONE',  ( 0.000000000000000000, 0.9848077530122072432, 0.1736481776669354937 ) ) ;
#11902 = CARTESIAN_POINT ( 'NONE',  ( -14.37296275365308418, -6.026961402152685388, 34.52809138561120506 ) ) ;
#11903 = CARTESIAN_POINT ( 'NONE',  ( -1.384615384615383471, -11.11383981884818262, 36.00935417666054406 ) ) ;
#11904 = ORIENTED_EDGE ( 'NONE', *, *, #19419, .F. ) ;
#11905 = B_SPLINE_CURVE_WITH_KNOTS ( 'NONE', 3,
 ( #71009, #16506, #83205, #49842, #21489, #77323, #43972, #71440, #57044, #84976 ),
 .UNSPECIFIED., .F., .F.,
 ( 4, 2, 2, 2, 4 ),
 ( 0.0007817246256747504250, 0.0009771112852218954894, 0.001172497944769040554, 0.001367884604316185401, 0.001563271263863330466 ),
 .UNSPECIFIED. ) ;
#11906 = LINE ( 'NONE', #6037, #34467 ) ;
#11907 = CARTESIAN_POINT ( 'NONE',  ( -17.01085472592063397, -11.69971097300155272, 32.46337939537588113 ) ) ;
#11909 = VERTEX_POINT ( 'NONE', #67843 ) ;
#11908 = AXIS2_PLACEMENT_3D ( 'NONE', #5042, #9260, #80724 ) ;
#11910 = CARTESIAN_POINT ( 'NONE',  ( -12.46153846153846168, -5.471508081941601098, 34.59228464037088457 ) ) ;
#11911 = CARTESIAN_POINT ( 'NONE',  ( -5.076923076923075762, -1.790695186598648903, 34.54067556320373455 ) ) ;
#11912 = CARTESIAN_POINT ( 'NONE',  ( -14.53061926659915315, -2.523278758544489797, 31.42238647778637528 ) ) ;
#11913 = CARTESIAN_POINT ( 'NONE',  ( -8.546219417617917813, -9.086983370893049639, 34.49168942202179267 ) ) ;
#11914 = CARTESIAN_POINT ( 'NONE',  ( 1.384615384615386802, -8.810774026931790459, 35.74407628777942847 ) ) ;
#11915 = DIRECTION ( 'NONE',  ( -0.000000000000000000, -0.9848077530122086864, -0.1736481776669273613 ) ) ;
#11917 = DIRECTION ( 'NONE',  ( 0.000000000000000000, -0.000000000000000000, -1.000000000000000000 ) ) ;
#11916 = CARTESIAN_POINT ( 'NONE',  ( 6.065255571276024327, -11.94971097300157403, 32.03036669348361443 ) ) ;
#11918 = EDGE_CURVE ( 'NONE', #59335, #13064, #61821, .T. ) ;
#11919 = LINE ( 'NONE', #45236, #782 ) ;
#11920 = DIRECTION ( 'NONE',  ( 0.000000000000000000, 0.000000000000000000, -1.000000000000000000 ) ) ;
#11921 = CARTESIAN_POINT ( 'NONE',  ( -1.944543648263014957, -5.555456351737005249, 16.50000000000000000 ) ) ;
#11922 = EDGE_LOOP ( 'NONE', ( #1924, #60635 ) ) ;
#11923 = CARTESIAN_POINT ( 'NONE',  ( -7.846153846153844924, -2.249999999999998668, 29.75000000000001776 ) ) ;
#11924 = VERTEX_POINT ( 'NONE', #63294 ) ;
#11925 = EDGE_CURVE ( 'NONE', #57743, #76336, #37089, .T. ) ;
#11926 = EDGE_LOOP ( 'NONE', ( #52166, #34725, #25260, #37870 ) ) ;
#11927 = CARTESIAN_POINT ( 'NONE',  ( -7.846153846153844924, -3.886160181151819604, 36.00935417666054406 ) ) ;
#11928 = EDGE_CURVE ( 'NONE', #43735, #71459, #84035, .T. ) ;
#11929 = ORIENTED_EDGE ( 'NONE', *, *, #88659, .F. ) ;
#11930 = CARTESIAN_POINT ( 'NONE',  ( 3.361561038594018225, -9.804649428959608670, 34.18742332936588468 ) ) ;
#11931 = CARTESIAN_POINT ( 'NONE',  ( 2.750000000000001776, -7.499999999999984013, 14.46875000000000000 ) ) ;
#11932 = CARTESIAN_POINT ( 'NONE',  ( 2.980746006547774218, -2.341070481393819236, 30.72580821765574299 ) ) ;
#11933 = CARTESIAN_POINT ( 'NONE',  ( 11.53846153846141576, -11.06231777344772027, 33.60647404775119895 ) ) ;
#11934 = CARTESIAN_POINT ( 'NONE',  ( -7.623142494540996239, -5.667800583137508674, 34.40243808032445827 ) ) ;
#11935 = CARTESIAN_POINT ( 'NONE',  ( 7.846153846153846700, -2.538708090699994813, 30.37095296980875503 ) ) ;
#11936 = CARTESIAN_POINT ( 'NONE',  ( -5.142193077479396024, -3.643525952247789412, 33.31231777344662959 ) ) ;
#11937 = CARTESIAN_POINT ( 'NONE',  ( -7.623142494540997127, -2.758310577978208222, 31.33698337089303010 ) ) ;
#11938 = CARTESIAN_POINT ( 'NONE',  ( 5.869308533332445066, -4.118384482072085184, 33.43331474514187107 ) ) ;
#11939 = EDGE_CURVE ( 'NONE', #18184, #19674, #32800, .T. ) ;
#11940 = CARTESIAN_POINT ( 'NONE',  ( 1.553300858899087311, -3.749999999999992006, 19.23437500000000355 ) ) ;
#11941 = CARTESIAN_POINT ( 'NONE',  ( -7.173100147298380413, -4.931416488878822335, 34.32920672191015399 ) ) ;
#11942 = CARTESIAN_POINT ( 'NONE',  ( -17.93474486048716088, -2.379036618887894416, 30.90682066428159303 ) ) ;
#11943 = EDGE_CURVE ( 'NONE', #86110, #40731, #68222, .T. ) ;
#11944 = LINE ( 'NONE', #66880, #79535 ) ;
#11945 = AXIS2_PLACEMENT_3D ( 'NONE', #69700, #82790, #60727 ) ;
#11946 = VECTOR ( 'NONE', #83093, 1000.000000000000227 ) ;
#11947 = ORIENTED_EDGE ( 'NONE', *, *, #75227, .F. ) ;
#11948 = ORIENTED_EDGE ( 'NONE', *, *, #37842, .T. ) ;
#11949 = CARTESIAN_POINT ( 'NONE',  ( -9.692307692307812417, -3.835265460704628371, 33.15142922262033665 ) ) ;
#11950 = CARTESIAN_POINT ( 'NONE',  ( -19.50000000000000000, -3.499999999999999556, 29.75000000000000355 ) ) ;
#11951 = CARTESIAN_POINT ( 'NONE',  ( 12.46153846153846168, -11.35647404775217417, 33.31231777344666511 ) ) ;
#11952 = CARTESIAN_POINT ( 'NONE',  ( 9.692307692307695177, -1.466349020453238561, 30.81389545987213907 ) ) ;
#11953 = CARTESIAN_POINT ( 'NONE',  ( 14.05766908347085575, -3.520140089381495585, 33.17453946501458262 ) ) ;
#11954 = AXIS2_PLACEMENT_3D ( 'NONE', #68443, #41868, #14839 ) ;
#11955 = CARTESIAN_POINT ( 'NONE',  ( -4.826868657009622865, -2.920487667080175154, 32.31805714834170828 ) ) ;
#11956 = ORIENTED_EDGE ( 'NONE', *, *, #73989, .F. ) ;
#11957 = CARTESIAN_POINT ( 'NONE',  ( -6.673131404728783522, -10.05730279482229683, 34.04704008940765902 ) ) ;
#11958 = ORIENTED_EDGE ( 'NONE', *, *, #44810, .T. ) ;
#11959 = EDGE_CURVE ( 'NONE', #66553, #84339, #62835, .T. ) ;
#11960 = ORIENTED_EDGE ( 'NONE', *, *, #56342, .F. ) ;
#11961 = CARTESIAN_POINT ( 'NONE',  ( 5.076923076922954969, -8.613356846316285953, 34.62446782046622218 ) ) ;
#11962 = CARTESIAN_POINT ( 'NONE',  ( -2.557715531913763218, -9.356822207818506598, 34.66110646841856635 ) ) ;
#11963 = EDGE_CURVE ( 'NONE', #5202, #83400, #55208, .T. ) ;
#11964 = CARTESIAN_POINT ( 'NONE',  ( 9.942362003946010773, -12.17597550085003810, 31.52189283813460463 ) ) ;
#11965 = CARTESIAN_POINT ( 'NONE',  ( 23.00000000000000000, -5.499999999999981348, 27.75000000000000000 ) ) ;
#11966 = CARTESIAN_POINT ( 'NONE',  ( -13.16160403300253634, -3.105924265160262543, 32.13625925475356127 ) ) ;
#11967 = EDGE_LOOP ( 'NONE', ( #82432, #5179 ) ) ;
#11968 = EDGE_CURVE ( 'NONE', #58506, #69466, #3016, .T. ) ;
#11969 = VECTOR ( 'NONE', #61877, 1000.000000000000227 ) ;
#11970 = AXIS2_PLACEMENT_3D ( 'NONE', #40436, #48049, #8408 ) ;
#11971 = EDGE_LOOP ( 'NONE', ( #37426, #23692 ) ) ;
#11972 = ORIENTED_EDGE ( 'NONE', *, *, #40878, .T. ) ;
#11973 = EDGE_CURVE ( 'NONE', #25338, #61929, #82093, .T. ) ;
#11974 = CARTESIAN_POINT ( 'NONE',  ( 3.230769230769110045, -12.46129190930018460, 30.37095296980731973 ) ) ;
#11975 = CARTESIAN_POINT ( 'NONE',  ( 9.758375025657770152, -2.292212530054420494, 30.41441678777542990 ) ) ;
#11976 = DIRECTION ( 'NONE',  ( 1.000000000000000000, 0.000000000000000000, 0.000000000000000000 ) ) ;
#11977 = FACE_OUTER_BOUND ( 'NONE', #85062, .T. ) ;
#11978 = CARTESIAN_POINT ( 'NONE',  ( -15.23076923076922995, -9.058645607665452459, 34.76329471203371924 ) ) ;
#11979 = CARTESIAN_POINT ( 'NONE',  ( 3.230769230769108269, -2.657715359629662544, 31.77849191805970364 ) ) ;
#11980 = ORIENTED_EDGE ( 'NONE', *, *, #43333, .T. ) ;
#11981 = EDGE_CURVE ( 'NONE', #35784, #57265, #51531, .T. ) ;
#11982 = VERTEX_POINT ( 'NONE', #23638 ) ;
#11983 = CARTESIAN_POINT ( 'NONE',  ( 4.826946332874483936, -10.06842814019191401, 34.32929386961144758 ) ) ;
#11985 = ORIENTED_EDGE ( 'NONE', *, *, #11405, .T. ) ;
#11984 = CARTESIAN_POINT ( 'NONE',  ( 2.373760658694747505, -12.37446782046654192, 30.86335684631486842 ) ) ;
#11986 = FACE_OUTER_BOUND ( 'NONE', #5557, .T. ) ;
#11987 = DIRECTION ( 'NONE',  ( 0.000000000000000000, 0.000000000000000000, -1.000000000000000000 ) ) ;
#11988 = EDGE_CURVE ( 'NONE', #58055, #74098, #29461, .T. ) ;
#11989 = EDGE_CURVE ( 'NONE', #34824, #77581, #2472, .T. ) ;
#11990 = CARTESIAN_POINT ( 'NONE',  ( -1.553300858899125059, -3.750000000000009326, 14.07812500000000178 ) ) ;
#11991 = ORIENTED_EDGE ( 'NONE', *, *, #58006, .F. ) ;
#11992 = CARTESIAN_POINT ( 'NONE',  ( -1.384615384615383471, -11.35647404775217417, 33.31231777344666511 ) ) ;
#11993 = VERTEX_POINT ( 'NONE', #3367 ) ;
#11994 = EDGE_CURVE ( 'NONE', #53679, #14267, #42389, .T. ) ;
#11995 = CARTESIAN_POINT ( 'NONE',  ( -8.992157728137618378, -4.762599654559228846, 34.23009711892697737 ) ) ;
#11996 = LINE ( 'NONE', #45766, #47195 ) ;
#11997 = AXIS2_PLACEMENT_3D ( 'NONE', #45874, #66144, #5347 ) ;
#11998 = CARTESIAN_POINT ( 'NONE',  ( 7.715463243043537034, -3.957541250942359756, 33.62499894934981626 ) ) ;
#12000 = DIRECTION ( 'NONE',  ( 0.000000000000000000, -6.938893903907222067E-15, 1.000000000000000000 ) ) ;
#11999 = DIRECTION ( 'NONE',  ( 1.000000000000000000, 0.000000000000000000, 0.000000000000000000 ) ) ;
#12001 = VECTOR ( 'NONE', #6546, 1000.000000000000000 ) ;
#12002 = LINE ( 'NONE', #46661, #62075 ) ;
#12003 = ORIENTED_EDGE ( 'NONE', *, *, #58507, .F. ) ;
#12004 = CARTESIAN_POINT ( 'NONE',  ( 6.923076923076802558, -8.613356846316285953, 34.62446782046622218 ) ) ;
#12005 = CARTESIAN_POINT ( 'NONE',  ( 8.992010310499175318, -6.760870238392817200, 34.69528174975672385 ) ) ;
#12006 = LINE ( 'NONE', #80462, #65312 ) ;
#12007 = EDGE_LOOP ( 'NONE', ( #20243, #33580, #51334, #48177 ) ) ;
#12008 = DIRECTION ( 'NONE',  ( -0.000000000000000000, -0.6427876096865404731, -0.7660444431189771253 ) ) ;
#12009 = CARTESIAN_POINT ( 'NONE',  ( -15.23076923076922995, -5.471508081941601098, 34.59228464037088457 ) ) ;
#12010 = B_SPLINE_CURVE_WITH_KNOTS ( 'NONE', 3,
 ( #29310, #50441, #57210, #56762, #84258, #22537, #36503, #63955, #2250, #29746 ),
 .UNSPECIFIED., .F., .F.,
 ( 4, 2, 2, 2, 4 ),
 ( 0.0007817359430256219828, 0.0009771253907249863487, 0.001172514838424350498, 0.001367904286123714647, 0.001563293733823079013 ),
 .UNSPECIFIED. ) ;
#12011 = CARTESIAN_POINT ( 'NONE',  ( -16.40382289789474157, -12.01397095200673881, 32.43157075238190146 ) ) ;
#12012 = CARTESIAN_POINT ( 'NONE',  ( 9.692307692307572609, -4.481592998941358097, 33.73612834414048933 ) ) ;
#12013 = FACE_BOUND ( 'NONE', #32426, .T. ) ;
#12015 = CARTESIAN_POINT ( 'NONE',  ( -2.980769230769230393, -2.499999999999998668, 29.75000000000000355 ) ) ;
#12014 = CARTESIAN_POINT ( 'NONE',  ( 13.38461538461526423, -12.51329471203414379, 31.30864560766407578 ) ) ;
#12016 = CARTESIAN_POINT ( 'NONE',  ( 2.241609928332172874, -9.905515769479276145, 34.41647553114623292 ) ) ;
#12018 = CARTESIAN_POINT ( 'NONE',  ( -2.242437168179467477, -8.656820664281605460, 34.87096338111211224 ) ) ;
#12017 = CARTESIAN_POINT ( 'NONE',  ( 1.319345384059067428, -12.70778746994557551, 30.41441678777548319 ) ) ;
#12019 = CARTESIAN_POINT ( 'NONE',  ( 1.607395053593450029, -3.020022701398814124, 32.48759521482552515 ) ) ;
#12020 = CARTESIAN_POINT ( 'NONE',  ( 6.066067333350078528, -4.661471528628508665, 34.16647553114624003 ) ) ;
#12021 = CARTESIAN_POINT ( 'NONE',  ( -2.694853999681210865, -4.891553140782108677, 27.49813170625849068 ) ) ;
#12022 = ORIENTED_EDGE ( 'NONE', *, *, #12273, .F. ) ;
#12023 = EDGE_CURVE ( 'NONE', #45139, #59816, #83208, .T. ) ;
#12024 = CARTESIAN_POINT ( 'NONE',  ( -9.692307692307691624, -4.102666532097928531, 36.13435417666054406 ) ) ;
#12025 = ORIENTED_EDGE ( 'NONE', *, *, #4840, .F. ) ;
#12026 = DIRECTION ( 'NONE',  ( 0.000000000000000000, 0.000000000000000000, -1.000000000000000000 ) ) ;
#12027 = CARTESIAN_POINT ( 'NONE',  ( 7.846153846153846700, -8.973038597847269315, 34.52809138561121927 ) ) ;
#12028 = DIRECTION ( 'NONE',  ( -0.000000000000000000, -0.000000000000000000, -1.000000000000000000 ) ) ;
#12030 = ORIENTED_EDGE ( 'NONE', *, *, #65948, .F. ) ;
#12029 = CARTESIAN_POINT ( 'NONE',  ( -4.946132635956126400, -9.084667340241226796, 34.75534355489798344 ) ) ;
#12031 = DIRECTION ( 'NONE',  ( -0.000000000000000000, -0.6427876096865404731, -0.7660444431189771253 ) ) ;
#12032 = CARTESIAN_POINT ( 'NONE',  ( 6.249945409378045547, -3.520799739797213501, 33.17531984108286025 ) ) ;
#12033 = CARTESIAN_POINT ( 'NONE',  ( 2.608446859217893099, -4.805146000318787358, 25.31063170625848713 ) ) ;
#12034 = CARTESIAN_POINT ( 'NONE',  ( 15.00728430620490350, -12.11044203135681840, 32.26167407432752299 ) ) ;
#12035 = CARTESIAN_POINT ( 'NONE',  ( 8.519207545009310323, -2.588893531581426988, 31.60682220781847818 ) ) ;
#12036 = VECTOR ( 'NONE', #17871, 1000.000000000000000 ) ;
#12037 = LINE ( 'NONE', #66975, #47543 ) ;
#12038 = CARTESIAN_POINT ( 'NONE',  ( -12.46153846153858247, -8.613356846316285953, 34.62446782046622218 ) ) ;
#12039 = CARTESIAN_POINT ( 'NONE',  ( 0.2115617305961066397, -11.28823185664190376, 33.01397839955799896 ) ) ;
#12040 = CYLINDRICAL_SURFACE ( 'NONE', #26728, 0.2499999999999973355 ) ;
#12041 = EDGE_CURVE ( 'NONE', #67890, #28697, #74501, .T. ) ;
#12042 = VECTOR ( 'NONE', #1650, 999.9999999999998863 ) ;
#12043 = CARTESIAN_POINT ( 'NONE',  ( -2.608446859217920633, -4.805146000318815780, 15.50186829374151287 ) ) ;
#12044 = CARTESIAN_POINT ( 'NONE',  ( 14.05766907039934210, -5.851115903089112003, 34.47074536777953568 ) ) ;
#12045 = LINE ( 'NONE', #66982, #85931 ) ;
#12046 = ORIENTED_EDGE ( 'NONE', *, *, #54849, .F. ) ;
#12047 = ADVANCED_FACE ( 'NONE', ( #33524 ), #72716, .F. ) ;
#12048 = CARTESIAN_POINT ( 'NONE',  ( 6.857754007584749623, -7.749976743299137993, 34.99404534957040624 ) ) ;
#12049 = CARTESIAN_POINT ( 'NONE',  ( -19.50000000000000000, -3.499999999999999556, 29.75000000000000355 ) ) ;
#12050 = CARTESIAN_POINT ( 'NONE',  ( -1.614399933863613468, -11.22469193450124969, 17.61124329374151642 ) ) ;
#12051 = CARTESIAN_POINT ( 'NONE',  ( -15.00739374499680778, -2.251407671071270489, 29.88021292934942963 ) ) ;
#12052 = DIRECTION ( 'NONE',  ( -0.000000000000000000, -0.3420201433256694346, -0.9396926207859080948 ) ) ;
#12053 = VERTEX_POINT ( 'NONE', #86710 ) ;
#12054 = FACE_OUTER_BOUND ( 'NONE', #72107, .T. ) ;
#12055 = CARTESIAN_POINT ( 'NONE',  ( -12.21159305216042057, -12.68172785388650681, 30.59649109432439218 ) ) ;
#12057 = EDGE_LOOP ( 'NONE', ( #70026, #88451 ) ) ;
#12056 = CARTESIAN_POINT ( 'NONE',  ( 8.069166690247243423, -2.523321265292118198, 31.42251411153756990 ) ) ;
#12058 = CARTESIAN_POINT ( 'NONE',  ( -9.915792616872023402, -11.60425143139329940, 33.02411095842164457 ) ) ;
#12059 = CARTESIAN_POINT ( 'NONE',  ( -2.057692307692368772, -7.565270000091922853, 34.99999999999999289 ) ) ;
#12060 = CARTESIAN_POINT ( 'NONE',  ( 15.29683656411930848, -5.471508081941601098, 34.59228464037088457 ) ) ;
#12062 = EDGE_CURVE ( 'NONE', #64228, #6730, #37620, .T. ) ;
#12061 = LINE ( 'NONE', #5731, #21237 ) ;
#12063 = EDGE_LOOP ( 'NONE', ( #64275, #79826, #50427, #42765 ) ) ;
#12064 = CARTESIAN_POINT ( 'NONE',  ( 6.988269911371578047, -2.255955759149235629, 29.99999999999988631 ) ) ;
#12065 = CARTESIAN_POINT ( 'NONE',  ( -15.36145983387954139, -11.37499894934982692, 33.29245874905763003 ) ) ;
#12066 = AXIS2_PLACEMENT_3D ( 'NONE', #71879, #59704, #4315 ) ;
#12067 = CARTESIAN_POINT ( 'NONE',  ( 1.253924781505076913, -2.845849958028613624, 32.17971566917920967 ) ) ;
#12068 = ORIENTED_EDGE ( 'NONE', *, *, #72018, .T. ) ;
#12069 = ORIENTED_EDGE ( 'NONE', *, *, #42323, .T. ) ;
#12070 = EDGE_CURVE ( 'NONE', #64945, #68629, #11472, .T. ) ;
#12071 = EDGE_LOOP ( 'NONE', ( #19629, #61689, #89120, #56208, #13405 ) ) ;
#12072 = CIRCLE ( 'NONE', #79631, 0.2500000000000002220 ) ;
#12073 = CARTESIAN_POINT ( 'NONE',  ( -13.38461538461538325, -12.34228464037088635, 31.77849191805839268 ) ) ;
#12074 = DIRECTION ( 'NONE',  ( 0.000000000000000000, 0.9848077530122072432, 0.1736481776669354937 ) ) ;
#12075 = EDGE_CURVE ( 'NONE', #83278, #66274, #52085, .T. ) ;
#12076 = CARTESIAN_POINT ( 'NONE',  ( -12.52680890749923748, -3.835265460703609186, 33.15142922261924241 ) ) ;
#12077 = B_SPLINE_CURVE_WITH_KNOTS ( 'NONE', 3,
 ( #61031, #61466, #87199, #67354, #88975, #46194, #54710, #39450, #47956, #6976 ),
 .UNSPECIFIED., .F., .F.,
 ( 4, 2, 2, 2, 4 ),
 ( 0.0007817246256747470640, 0.0009771112852218898515, 0.001172497944769032747, 0.001367884604316175643, 0.001563271263863318539 ),
 .UNSPECIFIED. ) ;
#12078 = CARTESIAN_POINT ( 'NONE',  ( -16.82686876528476105, -4.943051570960395047, 34.04725096376909477 ) ) ;
#12079 = EDGE_LOOP ( 'NONE', ( #72673, #84952 ) ) ;
#12080 = ORIENTED_EDGE ( 'NONE', *, *, #48877, .F. ) ;
#12081 = ADVANCED_FACE ( 'NONE', ( #87149 ), #66860, .F. ) ;
#12082 = EDGE_LOOP ( 'NONE', ( #11831, #48186 ) ) ;
#12084 = VERTEX_POINT ( 'NONE', #38499 ) ;
#12083 = DIRECTION ( 'NONE',  ( -0.000000000000000000, 0.7660444431189792347, -0.6427876096865379196 ) ) ;
#12085 = CARTESIAN_POINT ( 'NONE',  ( -5.076923076923075762, -2.486705287966279876, 31.30864560766543647 ) ) ;
#12086 = CARTESIAN_POINT ( 'NONE',  ( 15.10062202133100939, -3.285722584762969856, 32.44110544564090759 ) ) ;
#12087 = CARTESIAN_POINT ( 'NONE',  ( -1.384615384615383471, -2.249999999999998668, 29.75000000000001776 ) ) ;
#12088 = CARTESIAN_POINT ( 'NONE',  ( 14.30769230769231015, -13.63283147151868846, 33.57946703557072254 ) ) ;
#12089 = ORIENTED_EDGE ( 'NONE', *, *, #79684, .T. ) ;
#12090 = ADVANCED_FACE ( 'NONE', ( #38954 ), #32623, .F. ) ;
#12091 = EDGE_LOOP ( 'NONE', ( #9390, #73108, #41023, #25285 ) ) ;
#12092 = VECTOR ( 'NONE', #49094, 1000.000000000000114 ) ;
#12093 = EDGE_LOOP ( 'NONE', ( #35540, #62139, #69676, #3635 ) ) ;
#12094 = CARTESIAN_POINT ( 'NONE',  ( -10.86540783960607293, -10.92453946501458795, 33.72985991061850086 ) ) ;
#12096 = ORIENTED_EDGE ( 'NONE', *, *, #13938, .T. ) ;
#12095 = CARTESIAN_POINT ( 'NONE',  ( -13.31942239632073210, -2.255955759149234741, 29.99999999999988631 ) ) ;
#12097 = CARTESIAN_POINT ( 'NONE',  ( 5.076923076922954969, -4.481592998941358097, 33.73612834414048933 ) ) ;
#12098 = ADVANCED_FACE ( 'NONE', ( #46145 ), #73633, .F. ) ;
#12099 = EDGE_CURVE ( 'NONE', #19612, #87599, #78883, .T. ) ;
#12100 = CARTESIAN_POINT ( 'NONE',  ( 12.33084699487090319, -11.18331474514187995, 33.13161551792790505 ) ) ;
#12101 = CARTESIAN_POINT ( 'NONE',  ( -11.28851612908349544, -4.176053281294518804, 33.81426240980091791 ) ) ;
#12102 = CARTESIAN_POINT ( 'NONE',  ( -1.608100328339332696, -8.496056993536548418, 34.65000542017679663 ) ) ;
#12103 = CARTESIAN_POINT ( 'NONE',  ( -2.084680956079457470, -11.24521262558773671, 33.06293181088029343 ) ) ;
#12104 = FACE_BOUND ( 'NONE', #68075, .T. ) ;
#12105 = CARTESIAN_POINT ( 'NONE',  ( -15.23076923076922995, -10.67929555188718282, 33.92786785259544047 ) ) ;
#12106 = CARTESIAN_POINT ( 'NONE',  ( -18.00000000000000000, -12.34228464037088635, 31.77849191805839268 ) ) ;
#12107 = CARTESIAN_POINT ( 'NONE',  ( 12.46153846153846168, -5.180354513474913603, 36.12317359536750416 ) ) ;
#12109 = CARTESIAN_POINT ( 'NONE',  ( 15.23076923076923173, -9.905515769479276145, 34.41647553114623292 ) ) ;
#12108 = CARTESIAN_POINT ( 'NONE',  ( 0.4615384615384611200, -1.466349020453238561, 30.81389545987213907 ) ) ;
#12110 = CARTESIAN_POINT ( 'NONE',  ( -16.15384615384615330, -6.435427911321262684, 35.78748833219616898 ) ) ;
#12111 = CARTESIAN_POINT ( 'NONE',  ( -0.7115616988314261704, -3.711651800289232028, 33.01384336483936011 ) ) ;
#12112 = ORIENTED_EDGE ( 'NONE', *, *, #40665, .T. ) ;
#12113 = CARTESIAN_POINT ( 'NONE',  ( -15.93088325028466734, -7.369474270740072441, 34.74850911626239736 ) ) ;
#12114 = FACE_OUTER_BOUND ( 'NONE', #39569, .T. ) ;
#12115 = EDGE_LOOP ( 'NONE', ( #40087, #31030, #65202, #7900 ) ) ;
#12116 = ORIENTED_EDGE ( 'NONE', *, *, #43323, .T. ) ;
#12117 = FACE_OUTER_BOUND ( 'NONE', #57303, .T. ) ;
#12118 = CARTESIAN_POINT ( 'NONE',  ( 27.00000000000000000, 16.99999999999999289, 31.75000000000000000 ) ) ;
#12119 = CARTESIAN_POINT ( 'NONE',  ( -11.76138849736838488, -10.01117774369187252, 34.36070679894347535 ) ) ;
#12120 = EDGE_LOOP ( 'NONE', ( #67307, #45407, #22975, #20992 ) ) ;
#12121 = FACE_OUTER_BOUND ( 'NONE', #27381, .T. ) ;
#12122 = CARTESIAN_POINT ( 'NONE',  ( -4.403869378067609475, -9.356822207818506598, 34.66110646841856635 ) ) ;
#12123 = AXIS2_PLACEMENT_3D ( 'NONE', #70905, #669, #83094 ) ;
#12125 = CARTESIAN_POINT ( 'NONE',  ( 5.999999999999878320, -6.835583212225970762, 34.95778746994575670 ) ) ;
#12124 = CARTESIAN_POINT ( 'NONE',  ( -14.37377468705243722, -3.937682226553330445, 33.60647404775217240 ) ) ;
#12126 = CARTESIAN_POINT ( 'NONE',  ( -12.52680890749923570, -5.219633306516282545, 34.19971097300152962 ) ) ;
#12127 = CARTESIAN_POINT ( 'NONE',  ( 0.7115928814519140166, -4.818054556918156983, 34.26375889529406749 ) ) ;
#12128 = LINE ( 'NONE', #39609, #65008 ) ;
#12129 = CARTESIAN_POINT ( 'NONE',  ( 3.749999999999992006, -5.946699141100872943, 21.89062500000000355 ) ) ;
#12130 = ORIENTED_EDGE ( 'NONE', *, *, #69022, .F. ) ;
#12131 = B_SPLINE_CURVE_WITH_KNOTS ( 'NONE', 3,
 ( #19778, #6271, #35058, #62088, #6699, #67968, #34171, #88702, #54440, #81934 ),
 .UNSPECIFIED., .F., .F.,
 ( 4, 2, 2, 2, 4 ),
 ( 0.000000000000000000, 0.0001954311564186869015, 0.0003908623128373738030, 0.0005862934692560607588, 0.0007817246256747476061 ),
 .UNSPECIFIED. ) ;
#12132 = EDGE_LOOP ( 'NONE', ( #40428, #59501, #85620, #21590 ) ) ;
#12133 = AXIS2_PLACEMENT_3D ( 'NONE', #47495, #34430, #34866 ) ;
#12134 = CYLINDRICAL_SURFACE ( 'NONE', #10419, 0.2500000000000009437 ) ;
#12135 = CARTESIAN_POINT ( 'NONE',  ( -4.284537620513710010, -12.38065189839062263, 30.83690757178629482 ) ) ;
#12136 = FACE_OUTER_BOUND ( 'NONE', #74962, .T. ) ;
#12137 = DIRECTION ( 'NONE',  ( -0.000000000000000000, 0.8660254037844399289, -0.4999999999999980016 ) ) ;
#12138 = DIRECTION ( 'NONE',  ( -0.000000000000000000, -0.3420201433256694901, -0.9396926207859082059 ) ) ;
#12139 = CARTESIAN_POINT ( 'NONE',  ( -3.749999999999997335, -7.500000000000021316, 23.84375000000000000 ) ) ;
#12140 = CARTESIAN_POINT ( 'NONE',  ( -8.992157728137618378, -10.01117774369187252, 34.36070679894347535 ) ) ;
#12141 = CARTESIAN_POINT ( 'NONE',  ( -0.4330127018922180770, -4.750000000000000000, 29.50000000000000355 ) ) ;
#12142 = CARTESIAN_POINT ( 'NONE',  ( 16.85399685940691938, -12.15238873228291716, 31.58232369045353849 ) ) ;
#12143 = CARTESIAN_POINT ( 'NONE',  ( 5.749976775778544713, -10.18141759479407327, 34.26406193332782379 ) ) ;
#12144 = CARTESIAN_POINT ( 'NONE',  ( 18.06525557127602610, -10.21337939537593797, 33.94971097300152252 ) ) ;
#12145 = DIRECTION ( 'NONE',  ( 0.000000000000000000, 0.000000000000000000, 1.000000000000000000 ) ) ;
#12146 = CARTESIAN_POINT ( 'NONE',  ( -0.2387587925603950056, -4.226511098958374291, 33.85474049983370293 ) ) ;
#12147 = FACE_OUTER_BOUND ( 'NONE', #78149, .T. ) ;
#12148 = CARTESIAN_POINT ( 'NONE',  ( 13.38461538461538680, -2.292212530054420494, 30.41441678777542634 ) ) ;
#12149 = CARTESIAN_POINT ( 'NONE',  ( -3.230769230769229949, -12.34228464037088635, 31.77849191805839268 ) ) ;
#12150 = VERTEX_POINT ( 'NONE', #52442 ) ;
#12151 = DIRECTION ( 'NONE',  ( -0.000000000000000000, 1.000000000000000000, 3.491481338843133355E-15 ) ) ;
#12152 = CYLINDRICAL_SURFACE ( 'NONE', #83440, 0.2500000000000002220 ) ;
#12153 = CARTESIAN_POINT ( 'NONE',  ( 0.4615384615383382183, -8.656820664282941280, 34.87096338111179961 ) ) ;
#12154 = CARTESIAN_POINT ( 'NONE',  ( 2.724691934501250135, -8.700186371490531201, 18.54874329374151642 ) ) ;
#12155 = CARTESIAN_POINT ( 'NONE',  ( 13.63466969625370417, -4.943051570960394159, 34.04725096376909477 ) ) ;
#12156 = CARTESIAN_POINT ( 'NONE',  ( -1.134615384613947953, -7.500000000000155431, 34.75000000000007105 ) ) ;
#12158 = ORIENTED_EDGE ( 'NONE', *, *, #19215, .T. ) ;
#12157 = CARTESIAN_POINT ( 'NONE',  ( -15.12820512820512953, -7.500000000000000000, 29.75000000000000355 ) ) ;
#12159 = CARTESIAN_POINT ( 'NONE',  ( -1.139087296525992388, -10.25000000000000711, 22.35937500000000355 ) ) ;
#12160 = FACE_OUTER_BOUND ( 'NONE', #64616, .T. ) ;
#12161 = ORIENTED_EDGE ( 'NONE', *, *, #17333, .F. ) ;
#12162 = VECTOR ( 'NONE', #53311, 1000.000000000000000 ) ;
#12163 = CARTESIAN_POINT ( 'NONE',  ( -2.242436736416281828, -2.625532179533470512, 30.86335684631491105 ) ) ;
#12164 = ORIENTED_EDGE ( 'NONE', *, *, #22696, .T. ) ;
#12165 = CARTESIAN_POINT ( 'NONE',  ( -18.13014720943822056, -11.93770438780619259, 32.05411857736982029 ) ) ;
#12166 = CARTESIAN_POINT ( 'NONE',  ( -9.692307692307812417, -2.892918686052166066, 31.69288490824153470 ) ) ;
#12167 = CARTESIAN_POINT ( 'NONE',  ( 2.177544337960611198, -12.70455904226513866, 30.44083106164009322 ) ) ;
#12168 = ORIENTED_EDGE ( 'NONE', *, *, #3302, .T. ) ;
#12169 = ORIENTED_EDGE ( 'NONE', *, *, #49174, .T. ) ;
#12170 = EDGE_CURVE ( 'NONE', #71930, #54393, #14460, .T. ) ;
#12171 = EDGE_LOOP ( 'NONE', ( #63462, #16522, #44316, #74552 ) ) ;
#12172 = CARTESIAN_POINT ( 'NONE',  ( -15.90390074446811042, -2.341251567377310217, 30.72681386836322659 ) ) ;
#12173 = CARTESIAN_POINT ( 'NONE',  ( 12.39545505058258001, -12.37446782046654192, 30.86335684631486487 ) ) ;
#12174 = CYLINDRICAL_SURFACE ( 'NONE', #31197, 0.2500000000000008882 ) ;
#12175 = CARTESIAN_POINT ( 'NONE',  ( -17.29984929443921970, -5.667676309546437530, 34.40238873228292249 ) ) ;
#12176 = CARTESIAN_POINT ( 'NONE',  ( -19.50000000000000000, -3.499999999999999556, 29.75000000000000355 ) ) ;
#12177 = DIRECTION ( 'NONE',  ( -0.000000000000000000, 0.9396926207859092051, -0.3420201433256662704 ) ) ;
#12178 = CARTESIAN_POINT ( 'NONE',  ( 11.28848480751918437, -11.79746400365624659, 32.30657167506340954 ) ) ;
#12179 = CARTESIAN_POINT ( 'NONE',  ( -12.71156169883143150, -6.695914987888146541, 34.68535235679833306 ) ) ;
#12180 = CIRCLE ( 'NONE', #20789, 7.999999999999998224 ) ;
#12181 = ORIENTED_EDGE ( 'NONE', *, *, #67653, .F. ) ;
#12182 = ORIENTED_EDGE ( 'NONE', *, *, #70162, .F. ) ;
#12183 = ADVANCED_FACE ( 'NONE', ( #68627 ), #20878, .F. ) ;
#12184 = EDGE_LOOP ( 'NONE', ( #16271, #35220, #29818, #51877 ) ) ;
#12186 = EDGE_LOOP ( 'NONE', ( #63254, #26285, #73699, #63562 ) ) ;
#12185 = CARTESIAN_POINT ( 'NONE',  ( 3.453782074862625784, -12.64618726649961289, 30.78989965857442712 ) ) ;
#12187 = AXIS2_PLACEMENT_3D ( 'NONE', #19276, #67466, #5760 ) ;
#12188 = VECTOR ( 'NONE', #46473, 1000.000000000000000 ) ;
#12189 = CARTESIAN_POINT ( 'NONE',  ( 3.230769230769538147, -2.506253911140615021, 30.00000000000323297 ) ) ;
#12190 = LINE ( 'NONE', #85624, #29554 ) ;
#12191 = ORIENTED_EDGE ( 'NONE', *, *, #39771, .T. ) ;
#12192 = CARTESIAN_POINT ( 'NONE',  ( -0.4615384615385840772, -12.70778746994576025, 30.41441678777401236 ) ) ;
#12193 = ORIENTED_EDGE ( 'NONE', *, *, #34538, .T. ) ;
#12194 = FACE_OUTER_BOUND ( 'NONE', #55388, .T. ) ;
#12195 = ORIENTED_EDGE ( 'NONE', *, *, #72553, .T. ) ;
#12196 = CARTESIAN_POINT ( 'NONE',  ( 9.692307692307572609, -8.613356846316285953, 34.62446782046622218 ) ) ;
#12197 = ADVANCED_FACE ( 'NONE', ( #40727 ), #68192, .F. ) ;
#12198 = ADVANCED_FACE ( 'NONE', ( #55551 ), #69511, .F. ) ;
#12199 = CARTESIAN_POINT ( 'NONE',  ( -8.899377978668987055, -5.195881422630166391, 34.18770438780619259 ) ) ;
#12200 = CARTESIAN_POINT ( 'NONE',  ( -11.47320639894870276, -12.16647553114626490, 32.15551576947920864 ) ) ;
#12201 = FACE_BOUND ( 'NONE', #26513, .T. ) ;
#12202 = CARTESIAN_POINT ( 'NONE',  ( -6.000000000000121680, -8.656820664282941280, 34.87096338111179961 ) ) ;
#12203 = CARTESIAN_POINT ( 'NONE',  ( 16.02369818411445834, -3.625366637846545448, 33.29286588640298561 ) ) ;
#12204 = DIRECTION ( 'NONE',  ( -1.000000000000000000, -0.000000000000000000, -0.000000000000000000 ) ) ;
#12205 = ADVANCED_FACE ( 'NONE', ( #618 ), #21322, .F. ) ;
#12206 = CARTESIAN_POINT ( 'NONE',  ( -3.230769230769351186, -4.481592998941358097, 33.73612834414048933 ) ) ;
#12207 = DIRECTION ( 'NONE',  ( 0.000000000000000000, 0.7660444431189807890, 0.6427876096865361433 ) ) ;
#12208 = LINE ( 'NONE', #82889, #14571 ) ;
#12209 = VERTEX_POINT ( 'NONE', #28990 ) ;
#12210 = CARTESIAN_POINT ( 'NONE',  ( 1.607990870387806526, -2.251407671071270489, 29.88021292934942252 ) ) ;
#12211 = ORIENTED_EDGE ( 'NONE', *, *, #31318, .T. ) ;
#12212 = ORIENTED_EDGE ( 'NONE', *, *, #50083, .F. ) ;
#12213 = AXIS2_PLACEMENT_3D ( 'NONE', #40826, #74610, #4823 ) ;
#12215 = LINE ( 'NONE', #67159, #87994 ) ;
#12214 = CARTESIAN_POINT ( 'NONE',  ( -6.988346923633241836, -4.320704448112771878, 33.92786785259540494 ) ) ;
#12216 = CARTESIAN_POINT ( 'NONE',  ( -4.403846153846151523, -7.566082377512563184, 35.00000000000000711 ) ) ;
#12217 = CYLINDRICAL_SURFACE ( 'NONE', #49436, 0.2500000000000012212 ) ;
#12218 = CARTESIAN_POINT ( 'NONE',  ( 9.019230769232187583, -7.500000000000154543, 35.00000000000007105 ) ) ;
#12219 = CARTESIAN_POINT ( 'NONE',  ( -12.33074665371366940, -4.118422570099831148, 33.43335022499816489 ) ) ;
#12220 = ORIENTED_EDGE ( 'NONE', *, *, #71941, .T. ) ;
#12221 = CARTESIAN_POINT ( 'NONE',  ( -11.66860874789976243, -12.27039167877662251, 31.24851455888617835 ) ) ;
#12222 = CARTESIAN_POINT ( 'NONE',  ( 14.08420736396836048, -11.41268669641499756, 32.86336882939238535 ) ) ;
#12223 = DIRECTION ( 'NONE',  ( 0.000000000000000000, 1.000000000000000000, 0.000000000000000000 ) ) ;
#12224 = CYLINDRICAL_SURFACE ( 'NONE', #88515, 0.2499999999999986955 ) ;
#12225 = EDGE_LOOP ( 'NONE', ( #32835, #26253, #70312, #74313 ) ) ;
#12226 = ORIENTED_EDGE ( 'NONE', *, *, #32924, .T. ) ;
#12227 = ORIENTED_EDGE ( 'NONE', *, *, #75849, .F. ) ;
#12228 = CARTESIAN_POINT ( 'NONE',  ( 10.61538461538461675, -3.937682226553329556, 33.60647404775216529 ) ) ;
#12229 = DIRECTION ( 'NONE',  ( -0.000000000000000000, 0.3420201433256694901, -0.9396926207859082059 ) ) ;
#12230 = VERTEX_POINT ( 'NONE', #33953 ) ;
#12231 = DIRECTION ( 'NONE',  ( -0.000000000000000000, 1.000000000000000000, 3.491481338843133355E-15 ) ) ;
#12232 = CARTESIAN_POINT ( 'NONE',  ( 14.37294744720514572, -5.941354392334607049, 34.76329471203374055 ) ) ;
#12233 = DIRECTION ( 'NONE',  ( -0.000000000000000000, 1.000000000000000000, -0.000000000000000000 ) ) ;
#12234 = CARTESIAN_POINT ( 'NONE',  ( 1.384615384615386802, -3.050289026998446396, 32.03036669348365706 ) ) ;
#12235 = CARTESIAN_POINT ( 'NONE',  ( -0.7115151924808155171, -11.28823185664190376, 33.01397839955799896 ) ) ;
#12236 = VERTEX_POINT ( 'NONE', #61416 ) ;
#12238 = ORIENTED_EDGE ( 'NONE', *, *, #25267, .F. ) ;
#12237 = CARTESIAN_POINT ( 'NONE',  ( 0.2386122440223122920, -9.886141570436013382, 34.14413921362392301 ) ) ;
#12239 = CARTESIAN_POINT ( 'NONE',  ( 4.153846153846154188, -13.63283147151868846, 33.57946703557072254 ) ) ;
#12240 = CARTESIAN_POINT ( 'NONE',  ( -3.099978789802278811, -2.494656445102013453, 31.33466734024120015 ) ) ;
#12241 = DIRECTION ( 'NONE',  ( -0.000000000000000000, 0.6427876096865404731, -0.7660444431189771253 ) ) ;
#12242 = CARTESIAN_POINT ( 'NONE',  ( 18.22301135161285046, -8.239487800360276282, 34.69522927552633718 ) ) ;
#12244 = VECTOR ( 'NONE', #58500, 999.9999999999998863 ) ;
#12243 = CARTESIAN_POINT ( 'NONE',  ( 13.25392478150507891, -3.957541250942358424, 33.62499894934981626 ) ) ;
#12245 = CARTESIAN_POINT ( 'NONE',  ( -5.076923076923075762, -10.67929555188718282, 33.92786785259544047 ) ) ;
#12246 = CARTESIAN_POINT ( 'NONE',  ( -3.480745961711583902, -6.567427716900047230, 34.66269422305636283 ) ) ;
#12247 = CARTESIAN_POINT ( 'NONE',  ( 1.987747218494642309, -5.598659921968629050, 20.81436829374151287 ) ) ;
#12248 = ORIENTED_EDGE ( 'NONE', *, *, #255, .T. ) ;
#12249 = DIRECTION ( 'NONE',  ( -1.000000000000000000, 0.000000000000000000, -0.000000000000000000 ) ) ;
#12250 = CARTESIAN_POINT ( 'NONE',  ( 2.530471976670375156, -4.226511098958374291, 33.85474049983370293 ) ) ;
#12251 = LINE ( 'NONE', #67204, #69275 ) ;
#12252 = EDGE_LOOP ( 'NONE', ( #48815, #65931 ) ) ;
#12253 = CARTESIAN_POINT ( 'NONE',  ( -5.750054481651856619, -2.587454068350147462, 30.68340429815432202 ) ) ;
#12254 = CARTESIAN_POINT ( 'NONE',  ( -3.164700879766791708, -5.557115091759786019, 34.35708131394839882 ) ) ;
#12255 = CARTESIAN_POINT ( 'NONE',  ( 13.38461538461526601, -3.835265460704628371, 33.15142922262033665 ) ) ;
#12256 = ADVANCED_FACE ( 'NONE', ( #1506 ), #48793, .T. ) ;
#12257 = CARTESIAN_POINT ( 'NONE',  ( -9.692307692307691624, -8.810774026931790459, 35.74407628777942847 ) ) ;
#12258 = CARTESIAN_POINT ( 'NONE',  ( -19.50000000000000000, -3.499999999999999556, 29.75000000000000355 ) ) ;
#12259 = CARTESIAN_POINT ( 'NONE',  ( -7.053768389744480949, -11.71456829005830080, 32.44064028649416542 ) ) ;
#12260 = ORIENTED_EDGE ( 'NONE', *, *, #16557, .F. ) ;
#12261 = CARTESIAN_POINT ( 'NONE',  ( -2.307692307692305711, -6.435427911321262684, 35.78748833219616898 ) ) ;
#12262 = CARTESIAN_POINT ( 'NONE',  ( -5.750000000000061284, -7.565270445406050648, 34.75000000000000000 ) ) ;
#12263 = CARTESIAN_POINT ( 'NONE',  ( 17.07692307692295586, -9.442884908241554243, 34.35708131394783038 ) ) ;
#12264 = EDGE_LOOP ( 'NONE', ( #72433, #35155 ) ) ;
#12265 = CARTESIAN_POINT ( 'NONE',  ( -9.320512820512821150, -4.000000000000000000, 29.65000000000000213 ) ) ;
#12266 = B_SPLINE_CURVE_WITH_KNOTS ( 'NONE', 3,
 ( #14672, #34495, #62393, #1152, #27732, #7476, #28632, #83133, #69171, #26854 ),
 .UNSPECIFIED., .F., .F.,
 ( 4, 2, 2, 2, 4 ),
 ( 0.000000000000000000, 0.0001954339857564094801, 0.0003908679715128189603, 0.0005863019572692284133, 0.0007817359430256379206 ),
 .UNSPECIFIED. ) ;
#12267 = EDGE_CURVE ( 'NONE', #66483, #40963, #13683, .T. ) ;
#12268 = ORIENTED_EDGE ( 'NONE', *, *, #73075, .T. ) ;
#12269 = DIRECTION ( 'NONE',  ( -0.000000000000000000, -0.6427876096865404731, -0.7660444431189771253 ) ) ;
#12270 =( NAMED_UNIT ( * ) PLANE_ANGLE_UNIT ( ) SI_UNIT ( $, .RADIAN. ) );
#12271 = CARTESIAN_POINT ( 'NONE',  ( 5.750000000000002665, -2.499999999999998668, 29.75000000000000355 ) ) ;
#12272 = ORIENTED_EDGE ( 'NONE', *, *, #64648, .F. ) ;
#12273 = EDGE_CURVE ( 'NONE', #57, #17236, #27199, .T. ) ;
#12274 = CARTESIAN_POINT ( 'NONE',  ( -0.4615384615384611200, -1.129524287112498415, 32.06866353760679544 ) ) ;
#12275 = CARTESIAN_POINT ( 'NONE',  ( -6.130690603110307890, -2.295517848115769421, 30.44137282052136939 ) ) ;
#12276 = FACE_OUTER_BOUND ( 'NONE', #58063, .T. ) ;
#12277 = VECTOR ( 'NONE', #5774, 1000.000000000000000 ) ;
#12278 = CARTESIAN_POINT ( 'NONE',  ( 8.638620409606241779, -7.722926236386453702, 34.74524107206102030 ) ) ;
#12279 = CARTESIAN_POINT ( 'NONE',  ( 3.230769230769231726, -9.819645486525091727, 36.12317359536749706 ) ) ;
#12280 = ORIENTED_EDGE ( 'NONE', *, *, #69232, .T. ) ;
#12281 = EDGE_CURVE ( 'NONE', #61882, #11602, #54656, .T. ) ;
#12282 = LINE ( 'NONE', #32111, #14145 ) ;
#12283 = ORIENTED_EDGE ( 'NONE', *, *, #4064, .T. ) ;
#12284 = FACE_OUTER_BOUND ( 'NONE', #27778, .T. ) ;
#12285 = B_SPLINE_CURVE_WITH_KNOTS ( 'NONE', 3,
 ( #4812, #72365, #46236, #87242, #85893, #4359, #65600, #52537, #52093, #3901 ),
 .UNSPECIFIED., .F., .F.,
 ( 4, 2, 2, 2, 4 ),
 ( 0.0007817359430256252354, 0.0009771253907249902518, 0.001172514838424355051, 0.001367904286123720068, 0.001563293733823085084 ),
 .UNSPECIFIED. ) ;
#12286 = CARTESIAN_POINT ( 'NONE',  ( -10.36533019547115941, -10.06805714834173493, 34.32951233291982618 ) ) ;
#12287 = EDGE_CURVE ( 'NONE', #40972, #67271, #21943, .T. ) ;
#12288 = DIRECTION ( 'NONE',  ( 0.000000000000000000, 0.4999999999999985567, 0.8660254037844395958 ) ) ;
#12289 = CARTESIAN_POINT ( 'NONE',  ( 6.249945518348142492, -9.272278438253401589, 34.42582936511637826 ) ) ;
#12290 = CARTESIAN_POINT ( 'NONE',  ( -6.700297381808513641, -5.913360116392398780, 34.49180327182771322 ) ) ;
#12291 = CARTESIAN_POINT ( 'NONE',  ( -9.442253272394237840, -6.523592122091592671, 34.90882529074906415 ) ) ;
#12292 = CARTESIAN_POINT ( 'NONE',  ( -5.207613680033387205, -4.684245665217972032, 34.18127051446801090 ) ) ;
#12293 = VERTEX_POINT ( 'NONE', #41603 ) ;
#12294 = ORIENTED_EDGE ( 'NONE', *, *, #1423, .F. ) ;
#12295 = VERTEX_POINT ( 'NONE', #62303 ) ;
#12296 = VERTEX_POINT ( 'NONE', #1058 ) ;
#12297 = B_SPLINE_CURVE_WITH_KNOTS ( 'NONE', 3,
 ( #88961, #55583, #47937, #53813, #81742, #83070, #61013, #69544, #69107, #41634 ),
 .UNSPECIFIED., .F., .F.,
 ( 4, 2, 2, 2, 4 ),
 ( 0.000000000000000000, 0.0001954311564186873623, 0.0003908623128373747246, 0.0005862934692560620598, 0.0007817246256747494492 ),
 .UNSPECIFIED. ) ;
#12298 = VECTOR ( 'NONE', #59644, 1000.000000000000000 ) ;
#12299 = EDGE_CURVE ( 'NONE', #80991, #58896, #74592, .T. ) ;
#12300 = CARTESIAN_POINT ( 'NONE',  ( -10.39237326377176451, -11.24521262558773493, 33.06293181088029343 ) ) ;
#12301 = CARTESIAN_POINT ( 'NONE',  ( 11.53846153846141576, -9.528491918059723176, 34.59228464037033035 ) ) ;
#12302 = EDGE_CURVE ( 'NONE', #20877, #63575, #27375, .T. ) ;
#12303 = B_SPLINE_CURVE_WITH_KNOTS ( 'NONE', 3,
 ( #12985, #31473, #58938, #86444, #24717, #52176, #79666, #17968, #73339, #13406 ),
 .UNSPECIFIED., .F., .F.,
 ( 4, 2, 2, 2, 4 ),
 ( 0.0007817246256747447872, 0.0009771112852218876831, 0.001172497944769030579, 0.001367884604316173475, 0.001563271263863316371 ),
 .UNSPECIFIED. ) ;
#12304 = CARTESIAN_POINT ( 'NONE',  ( -10.61538461538473577, -5.094484230521993062, 34.41647553114689373 ) ) ;
#12305 = CARTESIAN_POINT ( 'NONE',  ( 4.023154687178594813, -3.062553014421049546, 32.05460306192773601 ) ) ;
#12306 = B_SPLINE_CURVE_WITH_KNOTS ( 'NONE', 3,
 ( #42932, #70401, #9150, #2361, #30727, #84816, #29855, #9571, #23524, #78467 ),
 .UNSPECIFIED., .F., .F.,
 ( 4, 2, 2, 2, 4 ),
 ( 0.000000000000000000, 0.0001954311584214072923, 0.0003908623168428145846, 0.0005862934752642218498, 0.0007817246336856291692 ),
 .UNSPECIFIED. ) ;
#12307 = DIRECTION ( 'NONE',  ( 0.000000000000000000, 0.9848077530122072432, 0.1736481776669354937 ) ) ;
#12308 = EDGE_CURVE ( 'NONE', #86632, #1486, #43491, .T. ) ;
#12309 = DIRECTION ( 'NONE',  ( -0.000000000000000000, -0.1736481776669307198, -0.9848077530122080203 ) ) ;
#12310 = ADVANCED_FACE ( 'NONE', ( #1943 ), #70408, .F. ) ;
#12311 = DIRECTION ( 'NONE',  ( -0.000000000000000000, 0.7660444431189791237, -0.6427876096865379196 ) ) ;
#12312 = DIRECTION ( 'NONE',  ( -1.000000000000000000, 0.000000000000000000, -0.000000000000000000 ) ) ;
#12313 = ORIENTED_EDGE ( 'NONE', *, *, #7677, .F. ) ;
#12314 = AXIS2_PLACEMENT_3D ( 'NONE', #32564, #53277, #53726 ) ;
#12315 = VERTEX_POINT ( 'NONE', #78039 ) ;
#12316 = ORIENTED_EDGE ( 'NONE', *, *, #13114, .T. ) ;
#12318 = ORIENTED_EDGE ( 'NONE', *, *, #2317, .T. ) ;
#12317 = CARTESIAN_POINT ( 'NONE',  ( -1.607541602131530967, -11.24512374952581872, 33.06303171183252942 ) ) ;
#12320 = CARTESIAN_POINT ( 'NONE',  ( 11.25641025641025550, -7.500000000000000000, 33.75000000000000000 ) ) ;
#12319 = CYLINDRICAL_SURFACE ( 'NONE', #63296, 0.2500000000000008882 ) ;
#12321 = DIRECTION ( 'NONE',  ( 1.000000000000000000, 0.000000000000000000, -0.000000000000000000 ) ) ;
#12322 = CARTESIAN_POINT ( 'NONE',  ( -15.23076923076922995, -6.386643153685126251, 34.62446782046654192 ) ) ;
#12323 = FACE_BOUND ( 'NONE', #67648, .T. ) ;
#12324 = ORIENTED_EDGE ( 'NONE', *, *, #71663, .F. ) ;
#12325 = VERTEX_POINT ( 'NONE', #43372 ) ;
#12326 = DIRECTION ( 'NONE',  ( -0.000000000000000000, 1.000000000000000000, 3.491481338843133355E-15 ) ) ;
#12327 = VERTEX_POINT ( 'NONE', #64500 ) ;
#12328 = FACE_BOUND ( 'NONE', #78904, .T. ) ;
#12329 = DIRECTION ( 'NONE',  ( -0.000000000000000000, 1.000000000000000000, -0.000000000000000000 ) ) ;
#12330 = CYLINDRICAL_SURFACE ( 'NONE', #77879, 0.2500000000000012212 ) ;
#12331 = ORIENTED_EDGE ( 'NONE', *, *, #73572, .F. ) ;
#12332 = VECTOR ( 'NONE', #58522, 1000.000000000000000 ) ;
#12333 = CARTESIAN_POINT ( 'NONE',  ( 10.61538461538461675, -5.415277668671390821, 36.20867863119892149 ) ) ;
#12334 = CARTESIAN_POINT ( 'NONE',  ( -7.846153846153844924, -12.37446782046654192, 30.86335684631486131 ) ) ;
#12335 = CARTESIAN_POINT ( 'NONE',  ( 1.553300858899087311, -3.749999999999992006, 14.23437500000000355 ) ) ;
#12336 = EDGE_LOOP ( 'NONE', ( #26241, #74454 ) ) ;
#12337 = CARTESIAN_POINT ( 'NONE',  ( 14.30769230769218581, -11.67786785259630911, 32.92929555188603530 ) ) ;
#12338 = CARTESIAN_POINT ( 'NONE',  ( -3.230769230769229949, -1.044019251281081972, 31.83374038241031911 ) ) ;
#12339 = CARTESIAN_POINT ( 'NONE',  ( 2.530705151785706430, -2.889357225399416862, 32.26129605718031002 ) ) ;
#12340 = ORIENTED_EDGE ( 'NONE', *, *, #78372, .F. ) ;
#12341 = AXIS2_PLACEMENT_3D ( 'NONE', #80947, #39070, #65182 ) ;
#12342 = DIRECTION ( 'NONE',  ( -0.000000000000000000, 0.7660444431189791237, -0.6427876096865379196 ) ) ;
#12343 = CARTESIAN_POINT ( 'NONE',  ( -15.90390074446811042, -10.18230066228895758, 34.26354781536631577 ) ) ;
#12344 = ORIENTED_EDGE ( 'NONE', *, *, #46004, .F. ) ;
#12345 = CARTESIAN_POINT ( 'NONE',  ( 8.703960768674447124, -11.67786785259540849, 32.92929555188721480 ) ) ;
#12346 = CARTESIAN_POINT ( 'NONE',  ( -5.999999999999998224, -12.48256725967547354, 35.29906147534542527 ) ) ;
#12347 = CARTESIAN_POINT ( 'NONE',  ( 0.5920638997721030528, -11.04252011169590020, 33.62494198852677130 ) ) ;
#12348 = CARTESIAN_POINT ( 'NONE',  ( 20.00000000000000000, -4.000000000000000000, 29.75000000000000355 ) ) ;
#12349 = B_SPLINE_CURVE_WITH_KNOTS ( 'NONE', 3,
 ( #75652, #63008, #36013, #63463, #56709, #34680, #61687, #1766, #35111, #48178 ),
 .UNSPECIFIED., .F., .F.,
 ( 4, 2, 2, 2, 4 ),
 ( 0.0007817359430256319575, 0.0009771253907249987086, 0.001172514838424365460, 0.001367904286123732428, 0.001563293733823099179 ),
 .UNSPECIFIED. ) ;
#12350 = LINE ( 'NONE', #11914, #14225 ) ;
#12351 = B_SPLINE_CURVE_WITH_KNOTS ( 'NONE', 3,
 ( #1038, #22631, #77584, #85231, #28515, #70835, #23511, #84801, #9137, #36599 ),
 .UNSPECIFIED., .F., .F.,
 ( 4, 2, 2, 2, 4 ),
 ( 0.000000000000000000, 0.0001954339857564080707, 0.0003908679715128161414, 0.0005863019572692241849, 0.0007817359430256322827 ),
 .UNSPECIFIED. ) ;
#12352 = EDGE_CURVE ( 'NONE', #37303, #72857, #36000, .T. ) ;
#12353 = CARTESIAN_POINT ( 'NONE',  ( -0.4615384615381466493, -2.255955759149395501, 30.00000000000324363 ) ) ;
#12355 = CARTESIAN_POINT ( 'NONE',  ( 8.769230769230768274, -2.833524468853757305, 32.15551576947925838 ) ) ;
#12354 = PLANE ( 'NONE',  #13153 ) ;
#12356 = CARTESIAN_POINT ( 'NONE',  ( 9.019176287578909879, -12.22109172314383052, 31.39792113162168263 ) ) ;
#12357 = FACE_OUTER_BOUND ( 'NONE', #79621, .T. ) ;
#12358 = ADVANCED_FACE ( 'NONE', ( #8711 ), #85691, .F. ) ;
#12359 = CARTESIAN_POINT ( 'NONE',  ( 1.139087296525997273, -4.749999999999992895, 17.98437500000000000 ) ) ;
#12360 = ORIENTED_EDGE ( 'NONE', *, *, #1452, .F. ) ;
#12361 = CARTESIAN_POINT ( 'NONE',  ( -19.50000000000000000, -3.499999999999999556, 29.75000000000000355 ) ) ;
#12362 = ORIENTED_EDGE ( 'NONE', *, *, #53585, .T. ) ;
#12363 = ADVANCED_FACE ( 'NONE', ( #17224 ), #56877, .F. ) ;
#12364 = EDGE_LOOP ( 'NONE', ( #36639, #57683 ) ) ;
#12365 = CARTESIAN_POINT ( 'NONE',  ( -7.715628407920203990, -2.647132371071621471, 31.75357179365171589 ) ) ;
#12366 = ORIENTED_EDGE ( 'NONE', *, *, #36409, .T. ) ;
#12367 = CARTESIAN_POINT ( 'NONE',  ( 18.22342696186156985, -7.630147231320743018, 34.74852402298682819 ) ) ;
#12368 = CARTESIAN_POINT ( 'NONE',  ( 1.799775606325937360E-14, -10.25000000000000000, 16.03125000000000000 ) ) ;
#12369 = LINE ( 'NONE', #6058, #27235 ) ;
#12370 = CARTESIAN_POINT ( 'NONE',  ( -18.24997674404858827, -12.01397095200674769, 32.43157075238189435 ) ) ;
#12371 = FACE_OUTER_BOUND ( 'NONE', #48443, .T. ) ;
#12372 = EDGE_CURVE ( 'NONE', #1831, #37364, #36188, .T. ) ;
#12373 = FACE_OUTER_BOUND ( 'NONE', #16410, .T. ) ;
#12374 = CARTESIAN_POINT ( 'NONE',  ( -13.38461538461550582, -2.625532179533778709, 30.86335684631627174 ) ) ;
#12375 = CARTESIAN_POINT ( 'NONE',  ( 2.557746619330623528, -11.28795663066794219, 33.01431243580653785 ) ) ;
#12376 = CARTESIAN_POINT ( 'NONE',  ( -1.929879867024197893E-14, -3.750000000000000000, 22.90625000000000355 ) ) ;
#12377 = VECTOR ( 'NONE', #21855, 1000.000000000000227 ) ;
#12378 = CARTESIAN_POINT ( 'NONE',  ( 17.20771351789003489, -2.295524264805589354, 30.44142389570982488 ) ) ;
#12379 = CARTESIAN_POINT ( 'NONE',  ( -4.376773112752998962, -11.98009711892699691, 32.48740034544075428 ) ) ;
#12380 = CARTESIAN_POINT ( 'NONE',  ( 0.000000000000000000, -11.00000000000000000, 28.75000000000000000 ) ) ;
#12381 = ORIENTED_EDGE ( 'NONE', *, *, #17169, .T. ) ;
#12382 = EDGE_LOOP ( 'NONE', ( #64328, #29253 ) ) ;
#12383 = CARTESIAN_POINT ( 'NONE',  ( 6.923076923076924238, -2.538708090699994813, 30.37095296980875503 ) ) ;
#12384 = CARTESIAN_POINT ( 'NONE',  ( -2.294871794871794712, -3.499999999999999556, 29.75000000000000355 ) ) ;
#12385 = CARTESIAN_POINT ( 'NONE',  ( 16.21910129335899597, -12.51329471203373345, 31.30864560766537963 ) ) ;
#12386 = CYLINDRICAL_SURFACE ( 'NONE', #8213, 0.2500000000000008882 ) ;
#12387 = AXIS2_PLACEMENT_3D ( 'NONE', #80450, #51602, #18745 ) ;
#12388 = ADVANCED_FACE ( 'NONE', ( #77602 ), #15910, .F. ) ;
#12389 = CARTESIAN_POINT ( 'NONE',  ( 9.320512820512821150, -7.500000000000000000, 29.75000000000000355 ) ) ;
#12390 = DIRECTION ( 'NONE',  ( 0.000000000000000000, -1.000000000000000000, 0.000000000000000000 ) ) ;
#12391 = VERTEX_POINT ( 'NONE', #71716 ) ;
#12392 = CARTESIAN_POINT ( 'NONE',  ( -5.010854725920637520, -12.37446782046654192, 30.86335684631486842 ) ) ;
#12393 = ORIENTED_EDGE ( 'NONE', *, *, #81414, .F. ) ;
#12394 = VERTEX_POINT ( 'NONE', #30733 ) ;
#12395 = CARTESIAN_POINT ( 'NONE',  ( 5.299934428535925335, -8.239487800360276282, 34.69522927552633718 ) ) ;
#12396 = CARTESIAN_POINT ( 'NONE',  ( -14.08467946359891165, -6.460100341425560444, 34.89618726649961644 ) ) ;
#12397 = VECTOR ( 'NONE', #25543, 1000.000000000000000 ) ;
#12398 = CARTESIAN_POINT ( 'NONE',  ( -4.283994123577849145, -12.70455904226513866, 30.44083106164009322 ) ) ;
#12399 = CARTESIAN_POINT ( 'NONE',  ( 4.153846153846154188, -2.833524468853757305, 32.15551576947925838 ) ) ;
#12400 = DIRECTION ( 'NONE',  ( -0.000000000000000000, -5.102127870520021228E-17, -1.000000000000000000 ) ) ;
#12401 = ORIENTED_EDGE ( 'NONE', *, *, #27038, .F. ) ;
#12402 = VERTEX_POINT ( 'NONE', #70854 ) ;
#12403 = ORIENTED_EDGE ( 'NONE', *, *, #79194, .F. ) ;
#12404 = ORIENTED_EDGE ( 'NONE', *, *, #32652, .F. ) ;
#12405 = EDGE_CURVE ( 'NONE', #80094, #22635, #30423, .T. ) ;
#12406 = EDGE_CURVE ( 'NONE', #30720, #17545, #37945, .T. ) ;
#12407 = CARTESIAN_POINT ( 'NONE',  ( 5.750023269057646047, -2.564618984488975961, 30.55390908950641915 ) ) ;
#12408 = B_SPLINE_CURVE_WITH_KNOTS ( 'NONE', 3,
 ( #76967, #9392, #64313, #22458, #35537, #50791 ),
 .UNSPECIFIED., .F., .F.,
 ( 4, 2, 4 ),
 ( 0.0003909512603273906169, 0.0005862562993132179340, 0.0007815613382990451970 ),
 .UNSPECIFIED. ) ;
#12409 = DIRECTION ( 'NONE',  ( -0.000000000000000000, -0.5000000000000009992, -0.8660254037844380415 ) ) ;
#12410 = LINE ( 'NONE', #11525, #55174 ) ;
#12411 = EDGE_CURVE ( 'NONE', #8100, #14985, #25131, .T. ) ;
#12412 = CARTESIAN_POINT ( 'NONE',  ( -16.40386937806761125, -2.341070481393820124, 30.72580821765574299 ) ) ;
#12413 = CARTESIAN_POINT ( 'NONE',  ( -15.23076923076935252, -9.528491918059723176, 34.59228464037033035 ) ) ;
#12414 = EDGE_CURVE ( 'NONE', #73086, #27850, #18124, .T. ) ;
#12415 = CARTESIAN_POINT ( 'NONE',  ( -10.55012904410858710, -12.27809138561124591, 31.22303859784720359 ) ) ;
#12416 = ORIENTED_EDGE ( 'NONE', *, *, #22159, .F. ) ;
#12417 = ORIENTED_EDGE ( 'NONE', *, *, #84563, .T. ) ;
#12419 = ORIENTED_EDGE ( 'NONE', *, *, #60821, .T. ) ;
#12418 = DIRECTION ( 'NONE',  ( -0.000000000000000000, 0.7660444431189791237, -0.6427876096865379196 ) ) ;
#12420 = CARTESIAN_POINT ( 'NONE',  ( 10.48523740594639619, -12.45813303252208648, 30.39737893381572675 ) ) ;
#12421 = CARTESIAN_POINT ( 'NONE',  ( -3.230769230769229949, -4.945431358278436385, 36.03766855953609394 ) ) ;
#12422 = CARTESIAN_POINT ( 'NONE',  ( -1.929879867024197893E-14, -3.750000000000000000, 21.65625000000000355 ) ) ;
#12423 = VERTEX_POINT ( 'NONE', #24414 ) ;
#12424 = EDGE_CURVE ( 'NONE', #77096, #38831, #5046, .T. ) ;
#12425 = DIRECTION ( 'NONE',  ( 0.000000000000000000, 0.9848077530122072432, -0.1736481776669354937 ) ) ;
#12426 = VERTEX_POINT ( 'NONE', #31632 ) ;
#12427 = CARTESIAN_POINT ( 'NONE',  ( 19.00000000000000000, -17.00000000000000000, 2.999999999999999112 ) ) ;
#12428 = CARTESIAN_POINT ( 'NONE',  ( 0.2380535369741297036, -11.60425143139329762, 33.02411095842163746 ) ) ;
#12429 = FACE_BOUND ( 'NONE', #74053, .T. ) ;
#12430 = CARTESIAN_POINT ( 'NONE',  ( -6.000000000000121680, -3.083524468854526912, 32.58852847137268327 ) ) ;
#12431 = CARTESIAN_POINT ( 'NONE',  ( 8.769230769230768274, -4.786620604624113540, 33.94971097300155094 ) ) ;
#12432 = EDGE_LOOP ( 'NONE', ( #71291, #20200 ) ) ;
#12433 = EDGE_CURVE ( 'NONE', #37311, #20057, #4144, .T. ) ;
#12434 = LINE ( 'NONE', #39478, #109 ) ;
#12435 = VECTOR ( 'NONE', #14255, 1000.000000000000227 ) ;
#12436 = CARTESIAN_POINT ( 'NONE',  ( -24.99999999999999645, 20.00000000000000355, 3.000000000000000000 ) ) ;
#12437 = CARTESIAN_POINT ( 'NONE',  ( -39.05038313613820122, -2.499999999999999556, 29.75000000000000355 ) ) ;
#12438 = ORIENTED_EDGE ( 'NONE', *, *, #7213, .F. ) ;
#12439 = CARTESIAN_POINT ( 'NONE',  ( -39.05038313613820122, -2.249999999999998668, 29.75000000000000355 ) ) ;
#12440 = DIRECTION ( 'NONE',  ( -0.000000000000000000, 1.000000000000000000, -0.000000000000000000 ) ) ;
#12441 = CARTESIAN_POINT ( 'NONE',  ( 9.320512820512821150, -3.499999999999999556, 29.75000000000000355 ) ) ;
#12442 = CARTESIAN_POINT ( 'NONE',  ( -2.307692307692305711, -9.058645607665452459, 34.76329471203371924 ) ) ;
#12443 = CARTESIAN_POINT ( 'NONE',  ( -0.5268624743427701151, -7.749976730030849303, 34.74374725381503737 ) ) ;
#12444 = EDGE_CURVE ( 'NONE', #33663, #6421, #67108, .T. ) ;
#12445 = FACE_BOUND ( 'NONE', #26271, .T. ) ;
#12447 = DIRECTION ( 'NONE',  ( 0.000000000000000000, 0.000000000000000000, -1.000000000000000000 ) ) ;
#12446 = DIRECTION ( 'NONE',  ( 0.000000000000000000, 0.000000000000000000, 1.000000000000000000 ) ) ;
#12448 = CARTESIAN_POINT ( 'NONE',  ( -15.16551409125639260, -5.094484230520773593, 34.41647553114626845 ) ) ;
#12450 = CARTESIAN_POINT ( 'NONE',  ( -9.442362173959551797, -10.76462480002816235, 33.53768742498949962 ) ) ;
#12449 = FACE_OUTER_BOUND ( 'NONE', #70636, .T. ) ;
#12451 = DIRECTION ( 'NONE',  ( -0.000000000000000000, -0.3420201433256694346, -0.9396926207859080948 ) ) ;
#12452 = CARTESIAN_POINT ( 'NONE',  ( -3.749999999999996447, -7.561099074964554134, 24.84188170625848713 ) ) ;
#12454 = EDGE_CURVE ( 'NONE', #57330, #67890, #45544, .T. ) ;
#12453 = ORIENTED_EDGE ( 'NONE', *, *, #29609, .T. ) ;
#12455 = CARTESIAN_POINT ( 'NONE',  ( -7.173100160369890510, -9.271318131107980420, 34.42618302367067429 ) ) ;
#12456 = ORIENTED_EDGE ( 'NONE', *, *, #21815, .T. ) ;
#12457 = CARTESIAN_POINT ( 'NONE',  ( 1.254054792873465995, -2.504760397472875155, 29.97295953869789997 ) ) ;
#12458 = VECTOR ( 'NONE', #19686, 1000.000000000000000 ) ;
#12459 = VERTEX_POINT ( 'NONE', #74397 ) ;
#12460 = CARTESIAN_POINT ( 'NONE',  ( 7.846153846153846700, -9.905515769479276145, 34.41647553114623292 ) ) ;
#12461 = CARTESIAN_POINT ( 'NONE',  ( -13.63461538461538325, -2.249999999999998668, 29.75000000000000355 ) ) ;
#12463 = VERTEX_POINT ( 'NONE', #66300 ) ;
#12462 = CARTESIAN_POINT ( 'NONE',  ( 3.230769230769231726, -2.833524468853757305, 32.15551576947925838 ) ) ;
#12464 = CARTESIAN_POINT ( 'NONE',  ( -16.94613263595612551, -2.295524264805590686, 30.44142389570982488 ) ) ;
#12465 = CARTESIAN_POINT ( 'NONE',  ( 1.254467414883694065, -12.15440758774515473, 32.17923288041532004 ) ) ;
#12466 = CARTESIAN_POINT ( 'NONE',  ( 2.694853999681214862, -10.10844685921789043, 26.87313170625849423 ) ) ;
#12467 = CARTESIAN_POINT ( 'NONE',  ( 14.98074600654777377, -12.07920672191015221, 32.31858351112116168 ) ) ;
#12468 = FACE_OUTER_BOUND ( 'NONE', #17754, .T. ) ;
#12469 = ADVANCED_FACE ( 'NONE', ( #4603 ), #45136, .T. ) ;
#12470 = LINE ( 'NONE', #54330, #71773 ) ;
#12471 = CARTESIAN_POINT ( 'NONE',  ( 3.930919936330006248, -11.76352882383564769, 32.36236540154569497 ) ) ;
#12472 = CARTESIAN_POINT ( 'NONE',  ( -13.38461538461538325, -6.386643153685126251, 34.62446782046654192 ) ) ;
#12473 = CARTESIAN_POINT ( 'NONE',  ( 1.634669804528838810, -10.06805714834173848, 34.32951233291982618 ) ) ;
#12474 = B_SPLINE_CURVE_WITH_KNOTS ( 'NONE', 3,
 ( #87589, #11021, #25867, #3808, #53325, #80828, #18225, #19113, #46578, #74061 ),
 .UNSPECIFIED., .F., .F.,
 ( 4, 2, 2, 2, 4 ),
 ( 0.0007817246256747484735, 0.0009771112852218931041, 0.001172497944769037735, 0.001367884604316182365, 0.001563271263863326996 ),
 .UNSPECIFIED. ) ;
#12475 = CARTESIAN_POINT ( 'NONE',  ( -3.724691934501248802, -5.885600066136383646, 16.67374329374151998 ) ) ;
#12476 = CARTESIAN_POINT ( 'NONE',  ( 9.942307692309128697, -7.500000000000155431, 34.75000000000007105 ) ) ;
#12477 = ADVANCED_FACE ( 'NONE', ( #52782 ), #87487, .F. ) ;
#12478 = AXIS2_PLACEMENT_3D ( 'NONE', #7587, #47680, #14337 ) ;
#12479 = CARTESIAN_POINT ( 'NONE',  ( -1.318548051265307830, -11.91647553114624358, 32.58852847137148245 ) ) ;
#12480 = ORIENTED_EDGE ( 'NONE', *, *, #57321, .F. ) ;
#12481 = CARTESIAN_POINT ( 'NONE',  ( 7.173076923078343548, -7.500000000000154543, 35.00000000000007105 ) ) ;
#12482 = CARTESIAN_POINT ( 'NONE',  ( 15.23076923076923173, -10.67929555188718282, 33.92786785259544047 ) ) ;
#12483 = CARTESIAN_POINT ( 'NONE',  ( -2.694853999681181556, -10.10844685921792241, 17.68936829374151287 ) ) ;
#12484 = CARTESIAN_POINT ( 'NONE',  ( -15.23076923076922995, -6.189225973068211317, 35.74407628777942847 ) ) ;
#12485 = CARTESIAN_POINT ( 'NONE',  ( 14.30769230769231015, -12.10708131394839349, 31.69288490824020244 ) ) ;
#12486 = ORIENTED_EDGE ( 'NONE', *, *, #25503, .T. ) ;
#12487 = CARTESIAN_POINT ( 'NONE',  ( -11.53846153846153655, -13.75783147151868846, 33.36296068462461051 ) ) ;
#12488 = DIRECTION ( 'NONE',  ( 0.000000000000000000, 0.000000000000000000, -1.000000000000000000 ) ) ;
#12490 = ORIENTED_EDGE ( 'NONE', *, *, #75862, .F. ) ;
#12489 = CARTESIAN_POINT ( 'NONE',  ( 9.019285189144223835, -2.544122305571458575, 31.48381861865057729 ) ) ;
#12491 = CARTESIAN_POINT ( 'NONE',  ( 11.76124107972994359, -5.114059244376869984, 34.14424750095245287 ) ) ;
#12492 = CARTESIAN_POINT ( 'NONE',  ( 8.769230769230768274, -4.102666532097928531, 36.13435417666054406 ) ) ;
#12493 = EDGE_CURVE ( 'NONE', #30065, #87319, #60432, .T. ) ;
#12494 = CARTESIAN_POINT ( 'NONE',  ( -17.29975117455795441, -7.369209533119136069, 34.99857337881830688 ) ) ;
#12495 = CYLINDRICAL_SURFACE ( 'NONE', #88903, 0.2499999999999986955 ) ;
#12496 = ADVANCED_FACE ( 'NONE', ( #31174 ), #59541, .F. ) ;
#12497 = ORIENTED_EDGE ( 'NONE', *, *, #72458, .T. ) ;
#12498 = CARTESIAN_POINT ( 'NONE',  ( -9.692307692307814193, -2.657715359629662544, 31.77849191805970364 ) ) ;
#12499 = CARTESIAN_POINT ( 'NONE',  ( -9.070512820512819374, -7.500000000000000000, 33.75000000000000000 ) ) ;
#12500 = LINE ( 'NONE', #47607, #21112 ) ;
#12501 = ORIENTED_EDGE ( 'NONE', *, *, #72612, .F. ) ;
#12502 = VERTEX_POINT ( 'NONE', #87045 ) ;
#12503 = ORIENTED_EDGE ( 'NONE', *, *, #3736, .F. ) ;
#12504 = CARTESIAN_POINT ( 'NONE',  ( 2.750000000000001776, -7.500000000000000000, 11.00000000000000178 ) ) ;
#12505 = CARTESIAN_POINT ( 'NONE',  ( 14.08420736396836226, -4.386631170607603991, 33.66268669641500111 ) ) ;
#12506 = VECTOR ( 'NONE', #11161, 1000.000000000000227 ) ;
#12507 = CARTESIAN_POINT ( 'NONE',  ( -8.096130590202436750, -12.65889640711025521, 30.72598325615533454 ) ) ;
#12508 = CYLINDRICAL_SURFACE ( 'NONE', #79760, 0.2499999999999986955 ) ;
#12509 = CARTESIAN_POINT ( 'NONE',  ( 16.02369894440793630, -5.195881422630167279, 34.18770438780618548 ) ) ;
#12510 = ORIENTED_EDGE ( 'NONE', *, *, #23861, .T. ) ;
#12511 = B_SPLINE_CURVE_WITH_KNOTS ( 'NONE', 3,
 ( #40363, #20520, #47985, #692, #48425, #75910, #28160, #55628, #54296, #81792 ),
 .UNSPECIFIED., .F., .F.,
 ( 4, 2, 2, 2, 4 ),
 ( 0.000000000000000000, 0.0001954311564186867931, 0.0003908623128373735862, 0.0005862934692560603251, 0.0007817246256747471724 ),
 .UNSPECIFIED. ) ;
#12512 = EDGE_LOOP ( 'NONE', ( #31176, #12169, #57461, #52733 ) ) ;
#12513 = ORIENTED_EDGE ( 'NONE', *, *, #5663, .T. ) ;
#12515 = ORIENTED_EDGE ( 'NONE', *, *, #81933, .T. ) ;
#12514 = CARTESIAN_POINT ( 'NONE',  ( -7.912237257109724808, -4.786620604624113540, 33.94971097300155805 ) ) ;
#12516 = CARTESIAN_POINT ( 'NONE',  ( 11.00641025641025550, -3.499999999999999556, 29.75000000000000355 ) ) ;
#12517 = CARTESIAN_POINT ( 'NONE',  ( -3.230769230769352962, -5.094484230521993062, 34.41647553114689373 ) ) ;
#12518 = EDGE_CURVE ( 'NONE', #62711, #69942, #87538, .T. ) ;
#12519 = DIRECTION ( 'NONE',  ( -0.000000000000000000, -0.9396926207859094271, -0.3420201433256663814 ) ) ;
#12520 = LINE ( 'NONE', #6216, #81312 ) ;
#12521 = EDGE_CURVE ( 'NONE', #64358, #50015, #82050, .T. ) ;
#12522 = ORIENTED_EDGE ( 'NONE', *, *, #8008, .F. ) ;
#12523 = VERTEX_POINT ( 'NONE', #14468 ) ;
#12524 = AXIS2_PLACEMENT_3D ( 'NONE', #34826, #41590, #7368 ) ;
#12525 = VERTEX_POINT ( 'NONE', #41058 ) ;
#12526 = CARTESIAN_POINT ( 'NONE',  ( -4.826923076923139710, -7.565270445406050648, 34.75000000000000000 ) ) ;
#12528 = ORIENTED_EDGE ( 'NONE', *, *, #57921, .T. ) ;
#12527 = CARTESIAN_POINT ( 'NONE',  ( -15.23076923076922995, -13.04860791097971706, 34.73218667398347037 ) ) ;
#12529 = EDGE_CURVE ( 'NONE', #43877, #88176, #27980, .T. ) ;
#12530 = CARTESIAN_POINT ( 'NONE',  ( 2.177544337960608534, -2.647304123082328875, 31.75400227202885262 ) ) ;
#12531 = CARTESIAN_POINT ( 'NONE',  ( 20.00000000000000000, -4.000000000000000000, 29.75000000000000355 ) ) ;
#12532 = ORIENTED_EDGE ( 'NONE', *, *, #80413, .F. ) ;
#12533 = CARTESIAN_POINT ( 'NONE',  ( 16.40390046548447245, -8.303483539816726378, 34.68545999027711702 ) ) ;
#12534 = CARTESIAN_POINT ( 'NONE',  ( 8.899756470994333313, -12.45806712695776319, 30.39783852428763922 ) ) ;
#12535 = EDGE_CURVE ( 'NONE', #31022, #56583, #72080, .T. ) ;
#12536 = FACE_OUTER_BOUND ( 'NONE', #16400, .T. ) ;
#12537 = FACE_BOUND ( 'NONE', #63563, .T. ) ;
#12538 = FACE_OUTER_BOUND ( 'NONE', #86129, .T. ) ;
#12539 = CARTESIAN_POINT ( 'NONE',  ( -12.52680890749923570, -9.442884908240170461, 34.35708131394840592 ) ) ;
#12540 = CARTESIAN_POINT ( 'NONE',  ( -7.911424292114618950, -12.27809138561121394, 31.22303859784730307 ) ) ;
#12542 = CARTESIAN_POINT ( 'NONE',  ( 15.45354889974729673, -10.23759521482555357, 34.22997729860117033 ) ) ;
#12541 = CARTESIAN_POINT ( 'NONE',  ( 8.769230769230768274, -12.78798330534102767, 29.49999999999997868 ) ) ;
#12543 = B_SPLINE_CURVE_WITH_KNOTS ( 'NONE', 3,
 ( #263, #77685, #56536, #69603, #42585, #70045, #48887, #21419, #63728, #22739 ),
 .UNSPECIFIED., .F., .F.,
 ( 4, 2, 2, 2, 4 ),
 ( 0.0007817359430256374869, 0.0009771253907250054306, 0.001172514838424373266, 0.001367904286123741101, 0.001563293733823109153 ),
 .UNSPECIFIED. ) ;
#12544 = EDGE_CURVE ( 'NONE', #49278, #57134, #15582, .T. ) ;
#12545 = CARTESIAN_POINT ( 'NONE',  ( -24.99999999999999645, -19.99999999999999645, 0.000000000000000000 ) ) ;
#12546 = DIRECTION ( 'NONE',  ( -0.000000000000000000, 0.5000000000000011102, -0.8660254037844381525 ) ) ;
#12547 = VERTEX_POINT ( 'NONE', #34291 ) ;
#12548 = CARTESIAN_POINT ( 'NONE',  ( -16.28432286196261458, -7.276988635370451597, 34.74523720219453793 ) ) ;
#12549 = CARTESIAN_POINT ( 'NONE',  ( -7.780898274877818821, -2.625532179533470512, 30.86335684631491105 ) ) ;
#12550 = ORIENTED_EDGE ( 'NONE', *, *, #33141, .T. ) ;
#12551 = VERTEX_POINT ( 'NONE', #20777 ) ;
#12552 = CARTESIAN_POINT ( 'NONE',  ( -6.792551221313360088, -5.195472089885680766, 34.18748526763464923 ) ) ;
#12553 = EDGE_CURVE ( 'NONE', #79092, #78459, #4734, .T. ) ;
#12554 = CARTESIAN_POINT ( 'NONE',  ( 16.15384615384603251, -3.835265460704628815, 33.15142922262033665 ) ) ;
#12555 = LINE ( 'NONE', #72467, #26017 ) ;
#12556 = EDGE_LOOP ( 'NONE', ( #28243, #59158 ) ) ;
#12557 = LINE ( 'NONE', #5356, #12650 ) ;
#12558 = CARTESIAN_POINT ( 'NONE',  ( -4.219116154402471786, -9.528491918058357157, 34.59228464037090589 ) ) ;
#12559 = FACE_BOUND ( 'NONE', #68328, .T. ) ;
#12561 = DIRECTION ( 'NONE',  ( -0.7057856980126717694, -0.7057856980126787638, -0.06109907496453172160 ) ) ;
#12560 = CARTESIAN_POINT ( 'NONE',  ( -18.06608341095587988, -3.050289026998447284, 32.03036669348365706 ) ) ;
#12562 = CARTESIAN_POINT ( 'NONE',  ( 7.911409417429871027, -9.442884908240271713, 34.35708131394835618 ) ) ;
#12563 = CYLINDRICAL_SURFACE ( 'NONE', #25229, 0.2499999999999973355 ) ;
#12565 = CARTESIAN_POINT ( 'NONE',  ( 0.4615384615384611200, -5.557115091759785130, 34.35708131394839171 ) ) ;
#12564 = CARTESIAN_POINT ( 'NONE',  ( 0.000000000000000000, 0.000000000000000000, 0.000000000000000000 ) ) ;
#12566 = CARTESIAN_POINT ( 'NONE',  ( 2.651650429449539104, -4.848349570550432475, 24.31250000000000000 ) ) ;
#12567 = ORIENTED_EDGE ( 'NONE', *, *, #37856, .F. ) ;
#12568 = ADVANCED_FACE ( 'NONE', ( #516 ), #81604, .F. ) ;
#12569 = EDGE_LOOP ( 'NONE', ( #43117, #77644 ) ) ;
#12570 = CARTESIAN_POINT ( 'NONE',  ( -9.070512820512819374, -7.500000000000000000, 29.75000000000000355 ) ) ;
#12571 = EDGE_CURVE ( 'NONE', #14333, #24897, #76843, .T. ) ;
#12572 = AXIS2_PLACEMENT_3D ( 'NONE', #5276, #39961, #66535 ) ;
#12573 = DIRECTION ( 'NONE',  ( -0.000000000000000000, 0.9848077530122086864, -0.1736481776669273891 ) ) ;
#12574 = CARTESIAN_POINT ( 'NONE',  ( -17.75000000000000355, -7.500000000000000000, 35.00000000000000000 ) ) ;
#12575 = DIRECTION ( 'NONE',  ( 0.000000000000000000, 0.4999999999999985567, 0.8660254037844395958 ) ) ;
#12576 = DIRECTION ( 'NONE',  ( 0.000000000000000000, 0.3420201433256641055, -0.9396926207859100932 ) ) ;
#12577 = CARTESIAN_POINT ( 'NONE',  ( -1.929879867024197893E-14, -3.750000000000000000, 22.90625000000000355 ) ) ;
#12578 = CARTESIAN_POINT ( 'NONE',  ( 0.6849654234000311925, -7.630147231320743018, 34.74852402298682819 ) ) ;
#12579 = CARTESIAN_POINT ( 'NONE',  ( -6.222926958906846551, -8.282780595021769443, 34.94152052738834868 ) ) ;
#12580 = CARTESIAN_POINT ( 'NONE',  ( 14.30769230769231015, -13.75783147151868846, 33.36296068462461051 ) ) ;
#12581 = DIRECTION ( 'NONE',  ( 0.000000000000000000, 0.3420201433256641055, -0.9396926207859100932 ) ) ;
#12582 = CARTESIAN_POINT ( 'NONE',  ( 9.942253210655838558, -2.824170634883621744, 31.52227843825338738 ) ) ;
#12583 = DIRECTION ( 'NONE',  ( 0.000000000000000000, 0.000000000000000000, 1.000000000000000000 ) ) ;
#12584 = CARTESIAN_POINT ( 'NONE',  ( 7.146089767170320073, -3.395485233115139057, 33.02377354290275946 ) ) ;
#12586 = EDGE_CURVE ( 'NONE', #44505, #54542, #55449, .T. ) ;
#12585 = DIRECTION ( 'NONE',  ( -0.000000000000000000, 1.000000000000000000, -0.000000000000000000 ) ) ;
#12587 = EDGE_CURVE ( 'NONE', #17248, #58442, #84334, .T. ) ;
#12588 = CARTESIAN_POINT ( 'NONE',  ( -15.45425417449318317, -8.496056993536548418, 34.65000542017679663 ) ) ;
#12589 = B_SPLINE_CURVE_WITH_KNOTS ( 'NONE', 3,
 ( #30311, #2380, #9588, #64518, #70422, #29875, #37055, #43819, #29441, #28550 ),
 .UNSPECIFIED., .F., .F.,
 ( 4, 2, 2, 2, 4 ),
 ( 0.000000000000000000, 0.0001954311584214072923, 0.0003908623168428145846, 0.0005862934752642218498, 0.0007817246336856291692 ),
 .UNSPECIFIED. ) ;
#12590 = EDGE_LOOP ( 'NONE', ( #12238, #38535, #82048, #8883 ) ) ;
#12591 = CARTESIAN_POINT ( 'NONE',  ( -5.076923076923197442, -11.94971097300221174, 32.03036669348237098 ) ) ;
#12592 = DIRECTION ( 'NONE',  ( -1.000000000000000000, 0.000000000000000000, 0.000000000000000000 ) ) ;
#12593 = CARTESIAN_POINT ( 'NONE',  ( -2.749999999999999112, -7.438900925035484057, 16.59561829374151287 ) ) ;
#12594 = CARTESIAN_POINT ( 'NONE',  ( -18.06525099016123548, -2.506253911140459145, 30.00000000000011369 ) ) ;
#12596 = DIRECTION ( 'NONE',  ( 0.000000000000000000, 0.3420201433256610524, 0.9396926207859113145 ) ) ;
#12595 = VECTOR ( 'NONE', #25604, 1000.000000000000000 ) ;
#12597 = CARTESIAN_POINT ( 'NONE',  ( 10.54930120442873687, -5.557115091759785130, 34.35708131394839171 ) ) ;
#12599 = ORIENTED_EDGE ( 'NONE', *, *, #64216, .T. ) ;
#12598 = CARTESIAN_POINT ( 'NONE',  ( 5.207448515156721136, -4.299079248970732792, 33.91157788607253565 ) ) ;
#12600 = CARTESIAN_POINT ( 'NONE',  ( 1.944543648263018731, -9.444543648262994751, 22.12500000000000000 ) ) ;
#12601 = CARTESIAN_POINT ( 'NONE',  ( 17.77707378248384629, -3.586966769969702540, 32.86292498521069660 ) ) ;
#12602 = EDGE_CURVE ( 'NONE', #81210, #80449, #73320, .T. ) ;
#12603 = EDGE_LOOP ( 'NONE', ( #58369, #9978, #54127, #1739 ) ) ;
#12604 = CARTESIAN_POINT ( 'NONE',  ( 8.545745825506822158, -8.496056993536548418, 34.65000542017679663 ) ) ;
#12605 = CARTESIAN_POINT ( 'NONE',  ( 0.2380535178145145869, -2.847400154188068022, 31.58180166144859058 ) ) ;
#12606 = EDGE_LOOP ( 'NONE', ( #18866, #81302, #1313, #69869 ) ) ;
#12607 = DIRECTION ( 'NONE',  ( -0.000000000000000000, 0.9396926207859092051, -0.3420201433256662704 ) ) ;
#12608 = ADVANCED_FACE ( 'NONE', ( #3152 ), #16671, .F. ) ;
#12609 = ADVANCED_FACE ( 'NONE', ( #84717 ), #22988, .F. ) ;
#12610 = CARTESIAN_POINT ( 'NONE',  ( 2.372947447205147942, -8.656820664281605460, 34.87096338111211224 ) ) ;
#12611 = AXIS2_PLACEMENT_3D ( 'NONE', #81066, #82389, #48139 ) ;
#12612 = CARTESIAN_POINT ( 'NONE',  ( 14.30769230769231015, -2.517432740324522911, 35.29906147534542527 ) ) ;
#12613 = ORIENTED_EDGE ( 'NONE', *, *, #30019, .F. ) ;
#12614 = ORIENTED_EDGE ( 'NONE', *, *, #23910, .F. ) ;
#12615 = ADVANCED_FACE ( 'NONE', ( #85145 ), #83828, .F. ) ;
#12616 = ORIENTED_EDGE ( 'NONE', *, *, #1070, .F. ) ;
#12617 = FACE_OUTER_BOUND ( 'NONE', #63975, .T. ) ;
#12618 = CARTESIAN_POINT ( 'NONE',  ( 12.23805351781451201, -12.44517049084099725, 30.48991314939691932 ) ) ;
#12619 = FACE_OUTER_BOUND ( 'NONE', #55973, .T. ) ;
#12620 = CARTESIAN_POINT ( 'NONE',  ( -1.326923076923076872, -7.500000000000000000, 33.75000000000000000 ) ) ;
#12621 = CARTESIAN_POINT ( 'NONE',  ( -10.68065461594093435, -12.16647553114622049, 32.15551576947930812 ) ) ;
#12622 = LINE ( 'NONE', #40546, #65089 ) ;
#12623 = CARTESIAN_POINT ( 'NONE',  ( -1.384615384615506484, -11.06231777344772027, 33.60647404775119895 ) ) ;
#12624 = B_SPLINE_CURVE_WITH_KNOTS ( 'NONE', 3,
 ( #82358, #7133, #62068, #42696, #70155, #62937, #28739, #27403, #381, #42257 ),
 .UNSPECIFIED., .F., .F.,
 ( 4, 2, 2, 2, 4 ),
 ( 0.0007817246256747515092, 0.0009771112852218961399, 0.001172497944769040554, 0.001367884604316184968, 0.001563271263863329598 ),
 .UNSPECIFIED. ) ;
#12625 = CARTESIAN_POINT ( 'NONE',  ( -0.2114840416250085564, -12.41089969410671223, 31.60739465890703670 ) ) ;
#12626 = AXIS2_PLACEMENT_3D ( 'NONE', #73149, #11447, #17767 ) ;
#12627 = ORIENTED_EDGE ( 'NONE', *, *, #7427, .F. ) ;
#12628 = ORIENTED_EDGE ( 'NONE', *, *, #42372, .F. ) ;
#12629 = ORIENTED_EDGE ( 'NONE', *, *, #63136, .T. ) ;
#12631 = ORIENTED_EDGE ( 'NONE', *, *, #28904, .F. ) ;
#12630 = PLANE ( 'NONE',  #77521 ) ;
#12632 = VECTOR ( 'NONE', #43172, 1000.000000000000000 ) ;
#12633 = CARTESIAN_POINT ( 'NONE',  ( 14.05769230769230838, -2.499999999999998668, 29.75000000000000355 ) ) ;
#12634 = CARTESIAN_POINT ( 'NONE',  ( 9.627037246346917598, -5.219633306516282545, 34.19971097300152962 ) ) ;
#12635 = ORIENTED_EDGE ( 'NONE', *, *, #71311, .T. ) ;
#12636 = CARTESIAN_POINT ( 'NONE',  ( -12.21148404162501144, -11.47946981652013498, 33.17500667209847620 ) ) ;
#12637 = ORIENTED_EDGE ( 'NONE', *, *, #59833, .F. ) ;
#12638 = CARTESIAN_POINT ( 'NONE',  ( -9.692307692307691624, -3.937682226553329556, 33.60647404775216529 ) ) ;
#12639 = ORIENTED_EDGE ( 'NONE', *, *, #23910, .T. ) ;
#12640 = CARTESIAN_POINT ( 'NONE',  ( -12.59214811674254442, -7.722926974430166069, 34.99546784045485737 ) ) ;
#12641 = B_SPLINE_CURVE_WITH_KNOTS ( 'NONE', 3,
 ( #40487, #26964, #81916, #5360, #67951, #6254 ),
 .UNSPECIFIED., .F., .F.,
 ( 4, 2, 4 ),
 ( 0.0003909512603273650297, 0.0005862562993131907206, 0.0007815613382990164656 ),
 .UNSPECIFIED. ) ;
#12642 = B_SPLINE_CURVE_WITH_KNOTS ( 'NONE', 3,
 ( #71206, #44166, #36118, #9510, #71651, #29360, #64891, #22588, #57705, #3196 ),
 .UNSPECIFIED., .F., .F.,
 ( 4, 2, 2, 2, 4 ),
 ( 0.0007817359430256216575, 0.0009771253907249856981, 0.001172514838424349630, 0.001367904286123713779, 0.001563293733823077711 ),
 .UNSPECIFIED. ) ;
#12643 = CARTESIAN_POINT ( 'NONE',  ( -8.769230769230890843, -5.219633306517616589, 34.19971097300220464 ) ) ;
#12644 = CARTESIAN_POINT ( 'NONE',  ( 10.68064018666064108, -5.219633306516380244, 34.19971097300157936 ) ) ;
#12645 = FACE_BOUND ( 'NONE', #42008, .T. ) ;
#12646 = LINE ( 'NONE', #21164, #24085 ) ;
#12647 = CARTESIAN_POINT ( 'NONE',  ( 18.00000000000000000, -2.249999999999998668, 29.75000000000001776 ) ) ;
#12648 = DIRECTION ( 'NONE',  ( -0.000000000000000000, 0.000000000000000000, 1.000000000000000000 ) ) ;
#12649 = CARTESIAN_POINT ( 'NONE',  ( 4.153846153846154188, -8.120952969808772792, 34.71129190930000163 ) ) ;
#12650 = VECTOR ( 'NONE', #38246, 1000.000000000000000 ) ;
#12651 = DIRECTION ( 'NONE',  ( -0.000000000000000000, 1.000000000000000000, -0.000000000000000000 ) ) ;
#12652 = DIRECTION ( 'NONE',  ( -0.000000000000000000, -0.9396926207859093161, -0.3420201433256663259 ) ) ;
#12653 = DIRECTION ( 'NONE',  ( -0.000000000000000000, -0.6427876096865404731, -0.7660444431189770143 ) ) ;
#12654 = ORIENTED_EDGE ( 'NONE', *, *, #30958, .T. ) ;
#12655 = EDGE_LOOP ( 'NONE', ( #66353, #3218 ) ) ;
#12657 = DIRECTION ( 'NONE',  ( -0.000000000000000000, -0.5000000000000009992, -0.8660254037844380415 ) ) ;
#12656 = CARTESIAN_POINT ( 'NONE',  ( 2.177001704581999597, -2.845849958028613624, 32.17971566917920967 ) ) ;
#12658 = EDGE_CURVE ( 'NONE', #45245, #720, #2483, .T. ) ;
#12659 = CARTESIAN_POINT ( 'NONE',  ( 15.48082365068268018, -8.346898887586323923, 34.93166121998716278 ) ) ;
#12660 = LINE ( 'NONE', #5904, #574 ) ;
#12661 = DIRECTION ( 'NONE',  ( -0.000000000000000000, 0.1736481776669307198, -0.9848077530122080203 ) ) ;
#12662 = CARTESIAN_POINT ( 'NONE',  ( -1.384615384615383471, -10.89733346790207413, 36.13435417666054406 ) ) ;
#12663 = ORIENTED_EDGE ( 'NONE', *, *, #71119, .F. ) ;
#12664 = CARTESIAN_POINT ( 'NONE',  ( -5.749945580086545327, -8.346898887586323923, 34.93166121998716278 ) ) ;
#12665 = VECTOR ( 'NONE', #12269, 1000.000000000000227 ) ;
#12666 = CARTESIAN_POINT ( 'NONE',  ( 15.00728430620490172, -4.225889041578353655, 33.85425143139329407 ) ) ;
#12667 = DIRECTION ( 'NONE',  ( -0.000000000000000000, 1.000000000000000000, -0.000000000000000000 ) ) ;
#12668 = DIRECTION ( 'NONE',  ( 0.000000000000000000, 0.000000000000000000, 1.000000000000000000 ) ) ;
#12669 = ORIENTED_EDGE ( 'NONE', *, *, #47027, .F. ) ;
#12670 = ORIENTED_EDGE ( 'NONE', *, *, #28655, .F. ) ;
#12671 = APPLICATION_PROTOCOL_DEFINITION ( 'draft international standard', 'automotive_design', 1998, #14719 ) ;
#12672 = VERTEX_POINT ( 'NONE', #69856 ) ;
#12673 = CARTESIAN_POINT ( 'NONE',  ( 0.7115384615398965273, -7.500000000000155431, 34.75000000000007105 ) ) ;
#12674 = EDGE_CURVE ( 'NONE', #58928, #56507, #64674, .T. ) ;
#12675 = ORIENTED_EDGE ( 'NONE', *, *, #52809, .F. ) ;
#12676 = DIRECTION ( 'NONE',  ( 0.000000000000000000, 0.000000000000000000, -1.000000000000000000 ) ) ;
#12677 = CARTESIAN_POINT ( 'NONE',  ( -6.249976744048591826, -9.234221910056348293, 34.70572697212741531 ) ) ;
#12678 = CARTESIAN_POINT ( 'NONE',  ( 5.011652630962299959, -6.879047030191174805, 34.71129190930000163 ) ) ;
#12679 = CARTESIAN_POINT ( 'NONE',  ( -2.437839517130528044, -8.587444163452046197, 34.63053765926554206 ) ) ;
#12680 = B_SPLINE_CURVE_WITH_KNOTS ( 'NONE', 3,
 ( #28704, #13409, #35008, #55719, #19728, #40459, #83207, #67918, #6224, #21491 ),
 .UNSPECIFIED., .F., .F.,
 ( 4, 2, 2, 2, 4 ),
 ( 0.000000000000000000, 0.0001954339857564097241, 0.0003908679715128194482, 0.0005863019572692291723, 0.0007817359430256388964 ),
 .UNSPECIFIED. ) ;
#12681 = CARTESIAN_POINT ( 'NONE',  ( -11.28851602011339672, -9.272278438253398036, 34.42582936511637115 ) ) ;
#12682 = ORIENTED_EDGE ( 'NONE', *, *, #70891, .T. ) ;
#12684 = ORIENTED_EDGE ( 'NONE', *, *, #60417, .F. ) ;
#12683 = CARTESIAN_POINT ( 'NONE',  ( -15.36145983387953606, -11.93127051446799847, 32.56575433478202797 ) ) ;
#12685 = DIRECTION ( 'NONE',  ( -0.000000000000000000, 0.3420201433256694901, -0.9396926207859082059 ) ) ;
#12686 = FACE_OUTER_BOUND ( 'NONE', #3871, .T. ) ;
#12687 = LINE ( 'NONE', #19001, #78925 ) ;
#12688 = CARTESIAN_POINT ( 'NONE',  ( 11.76124120743960333, -10.23759521482555357, 34.22997729860117033 ) ) ;
#12689 = CARTESIAN_POINT ( 'NONE',  ( -5.776624514227577833, -2.251407671071270489, 29.88021292934942252 ) ) ;
#12690 = EDGE_CURVE ( 'NONE', #43255, #48795, #30628, .T. ) ;
#12691 = DIRECTION ( 'NONE',  ( -0.000000000000000000, 0.3420201433256694346, -0.9396926207859080948 ) ) ;
#12692 = CARTESIAN_POINT ( 'NONE',  ( -3.453695448285377445, -6.503392248772476236, 34.64988816332204635 ) ) ;
#12693 = CARTESIAN_POINT ( 'NONE',  ( 1.901340078031373171, -9.487747218494639867, 19.87686829374151287 ) ) ;
#12694 = ORIENTED_EDGE ( 'NONE', *, *, #19711, .T. ) ;
#12695 = AXIS2_PLACEMENT_3D ( 'NONE', #28051, #73701, #66931 ) ;
#12696 = CARTESIAN_POINT ( 'NONE',  ( 11.60371710973756620, -2.892918686051625166, 31.69288490824026638 ) ) ;
#12697 = DIRECTION ( 'NONE',  ( 0.000000000000000000, 0.4999999999999985567, 0.8660254037844395958 ) ) ;
#12698 = ORIENTED_EDGE ( 'NONE', *, *, #63673, .T. ) ;
#12700 = EDGE_LOOP ( 'NONE', ( #88862, #16958 ) ) ;
#12699 = VECTOR ( 'NONE', #58234, 1000.000000000000000 ) ;
#12701 = CARTESIAN_POINT ( 'NONE',  ( -4.153846153846152411, -4.786620604624113540, 33.94971097300155094 ) ) ;
#12702 = CARTESIAN_POINT ( 'NONE',  ( 11.53846153846153832, -12.62096338111211580, 30.90682066428153263 ) ) ;
#12703 = CARTESIAN_POINT ( 'NONE',  ( -10.83831157429146330, -2.308479472611653094, 30.53278059502174457 ) ) ;
#12704 = CARTESIAN_POINT ( 'NONE',  ( -9.320512820512821150, -4.000000000000000000, 29.25000000000000000 ) ) ;
#12705 = CARTESIAN_POINT ( 'NONE',  ( 0.6843181305165273454, -2.353885683473779800, 30.79025554430704759 ) ) ;
#12706 = EDGE_LOOP ( 'NONE', ( #32954, #14510, #35927, #85228 ) ) ;
#12708 = EDGE_CURVE ( 'NONE', #10084, #63192, #37900, .T. ) ;
#12707 = CYLINDRICAL_SURFACE ( 'NONE', #13192, 0.2500000000000002220 ) ;
#12709 = EDGE_CURVE ( 'NONE', #59816, #45139, #74437, .T. ) ;
#12710 = CARTESIAN_POINT ( 'NONE',  ( -14.30769230769242739, -2.892918686052166066, 31.69288490824153470 ) ) ;
#12711 = CARTESIAN_POINT ( 'NONE',  ( -3.480792468062194889, -11.86270091957321249, 32.19358267280087915 ) ) ;
#12712 = ORIENTED_EDGE ( 'NONE', *, *, #44209, .F. ) ;
#12713 = DIRECTION ( 'NONE',  ( -0.000000000000000000, 0.9848077530122086864, -0.1736481776669273891 ) ) ;
#12714 = ORIENTED_EDGE ( 'NONE', *, *, #12768, .F. ) ;
#12715 = B_SPLINE_CURVE_WITH_KNOTS ( 'NONE', 3,
 ( #37556, #71342, #84880, #16406, #43875, #78994, #18191, #85319, #79890, #3329 ),
 .UNSPECIFIED., .F., .F.,
 ( 4, 2, 2, 2, 4 ),
 ( 0.0007817359527651101701, 0.0009771254036996489256, 0.001172514854634187790, 0.001367904305568726653, 0.001563293756503265517 ),
 .UNSPECIFIED. ) ;
#12716 = CYLINDRICAL_SURFACE ( 'NONE', #18458, 0.2499999999999995559 ) ;
#12717 = CARTESIAN_POINT ( 'NONE',  ( 11.31497661389720477, -2.612411019501189369, 31.66733052389439962 ) ) ;
#12718 = ORIENTED_EDGE ( 'NONE', *, *, #62653, .F. ) ;
#12719 = B_SPLINE_CURVE_WITH_KNOTS ( 'NONE', 3,
 ( #87744, #73775, #81861, #47615, #5744, #88192, #67892, #31892, #59797, #47164 ),
 .UNSPECIFIED., .F., .F.,
 ( 4, 2, 2, 2, 4 ),
 ( 0.0007817359430256326080, 0.0009771253907250047801, 0.001172514838424369796, 0.001367904286123735030, 0.001563293733823100046 ),
 .UNSPECIFIED. ) ;
#12720 = DIRECTION ( 'NONE',  ( -0.000000000000000000, -0.9396926207859093161, -0.3420201433256663259 ) ) ;
#12721 = CARTESIAN_POINT ( 'NONE',  ( -5.999999999999998224, -2.292212530054420494, 30.41441678777542634 ) ) ;
#12722 = CARTESIAN_POINT ( 'NONE',  ( -9.915792636031637741, -2.599994579823203367, 30.74605699353653776 ) ) ;
#12723 = VECTOR ( 'NONE', #47839, 1000.000000000000227 ) ;
#12724 = VECTOR ( 'NONE', #79923, 999.9999999999998863 ) ;
#12725 = CARTESIAN_POINT ( 'NONE',  ( -4.153846153846152411, -13.63283147151868846, 33.57946703557072254 ) ) ;
#12726 = CARTESIAN_POINT ( 'NONE',  ( -1.515305987725690917, -10.70098750199973203, 33.91152734681376302 ) ) ;
#12727 = AXIS2_PLACEMENT_3D ( 'NONE', #45274, #84950, #50694 ) ;
#12728 = VERTEX_POINT ( 'NONE', #37832 ) ;
#12729 = FACE_BOUND ( 'NONE', #56879, .T. ) ;
#12730 = VERTEX_POINT ( 'NONE', #18464 ) ;
#12731 = CARTESIAN_POINT ( 'NONE',  ( -8.769230769230892619, -12.51329471203414379, 31.30864560766407578 ) ) ;
#12732 = CARTESIAN_POINT ( 'NONE',  ( -12.21148404162501144, -2.920487667080175598, 32.31805714834170828 ) ) ;
#12733 = CARTESIAN_POINT ( 'NONE',  ( 6.065255571276024327, -9.442884908240271713, 34.35708131394835618 ) ) ;
#12734 = CYLINDRICAL_SURFACE ( 'NONE', #9050, 4.000000000000000000 ) ;
#12735 = FACE_OUTER_BOUND ( 'NONE', #62179, .T. ) ;
#12736 = ORIENTED_EDGE ( 'NONE', *, *, #18080, .T. ) ;
#12737 = ORIENTED_EDGE ( 'NONE', *, *, #80670, .F. ) ;
#12738 = ORIENTED_EDGE ( 'NONE', *, *, #24444, .F. ) ;
#12739 = ORIENTED_EDGE ( 'NONE', *, *, #30189, .T. ) ;
#12740 = CARTESIAN_POINT ( 'NONE',  ( -5.142193077479396024, -4.320704448112771878, 33.92786785259540494 ) ) ;
#12741 = CARTESIAN_POINT ( 'NONE',  ( 15.10062126103753499, -3.625366637846545892, 33.29286588640298561 ) ) ;
#12742 = CIRCLE ( 'NONE', #48684, 2.000000000000001776 ) ;
#12743 = CARTESIAN_POINT ( 'NONE',  ( -2.242546528360342073, -7.750023238201980469, 34.74374492549440419 ) ) ;
#12744 = CARTESIAN_POINT ( 'NONE',  ( 6.065255571276026103, -12.27809138561124591, 31.22303859784720359 ) ) ;
#12745 = DIRECTION ( 'NONE',  ( -0.000000000000000000, 0.000000000000000000, 1.000000000000000000 ) ) ;
#12746 = LINE ( 'NONE', #46094, #83955 ) ;
#12747 = CARTESIAN_POINT ( 'NONE',  ( -5.076923076923075762, -4.098570777380720287, 33.41473453929634729 ) ) ;
#12748 = CYLINDRICAL_SURFACE ( 'NONE', #76418, 0.2499999999999986955 ) ;
#12749 = ORIENTED_EDGE ( 'NONE', *, *, #60356, .T. ) ;
#12750 = ORIENTED_EDGE ( 'NONE', *, *, #76965, .T. ) ;
#12751 = ORIENTED_EDGE ( 'NONE', *, *, #79177, .T. ) ;
#12753 = ORIENTED_EDGE ( 'NONE', *, *, #69657, .T. ) ;
#12752 = LINE ( 'NONE', #39356, #61817 ) ;
#12755 = LINE ( 'NONE', #54173, #46291 ) ;
#12754 = CARTESIAN_POINT ( 'NONE',  ( -1.384615384615383471, -2.486705287966279876, 31.30864560766543647 ) ) ;
#12756 = EDGE_CURVE ( 'NONE', #34882, #66105, #72955, .T. ) ;
#12757 = EDGE_CURVE ( 'NONE', #68985, #33215, #11256, .T. ) ;
#12758 = DIRECTION ( 'NONE',  ( -1.000000000000000000, -0.000000000000000000, -0.000000000000000000 ) ) ;
#12759 = DIRECTION ( 'NONE',  ( 0.000000000000000000, 0.7660444431189822323, -0.6427876096865344779 ) ) ;
#12760 = FACE_BOUND ( 'NONE', #33115, .T. ) ;
#12761 = ORIENTED_EDGE ( 'NONE', *, *, #34356, .T. ) ;
#12762 = CARTESIAN_POINT ( 'NONE',  ( -3.480745974817822663, -3.436278759898155233, 33.07459398097509506 ) ) ;
#12763 = ORIENTED_EDGE ( 'NONE', *, *, #33980, .T. ) ;
#12764 = CARTESIAN_POINT ( 'NONE',  ( 17.07692307692295586, -5.941354392335915335, 34.76329471203413846 ) ) ;
#12765 = VERTEX_POINT ( 'NONE', #32415 ) ;
#12766 = FACE_BOUND ( 'NONE', #10168, .T. ) ;
#12767 = CARTESIAN_POINT ( 'NONE',  ( -1.384615384615506484, -11.06231777344772027, 33.60647404775119895 ) ) ;
#12768 = EDGE_CURVE ( 'NONE', #80730, #82878, #25214, .T. ) ;
#12769 = CARTESIAN_POINT ( 'NONE',  ( 15.23076923076910916, -6.835583212225970762, 34.95778746994575670 ) ) ;
#12770 = ORIENTED_EDGE ( 'NONE', *, *, #81609, .F. ) ;
#12771 = DIRECTION ( 'NONE',  ( 0.000000000000000000, -1.000000000000000000, 0.000000000000000000 ) ) ;
#12772 = CARTESIAN_POINT ( 'NONE',  ( -12.21153846153846168, -7.500000000000001776, 35.04278698407183867 ) ) ;
#12773 = CARTESIAN_POINT ( 'NONE',  ( -0.6844654204453102242, -2.308479472611653094, 30.53278059502174457 ) ) ;
#12774 = ORIENTED_EDGE ( 'NONE', *, *, #61801, .T. ) ;
#12775 = EDGE_CURVE ( 'NONE', #13977, #73914, #87377, .T. ) ;
#12776 = DIRECTION ( 'NONE',  ( -0.000000000000000000, -0.7660444431189791237, -0.6427876096865379196 ) ) ;
#12777 = CARTESIAN_POINT ( 'NONE',  ( 14.05771556364371833, -11.47974371597207899, 33.17467449705390692 ) ) ;
#12778 = CARTESIAN_POINT ( 'NONE',  ( -3.454254174493176954, -2.847400154188067578, 31.58180166144859768 ) ) ;
#12779 = DIRECTION ( 'NONE',  ( -0.000000000000000000, -0.6427876096865404731, -0.7660444431189770143 ) ) ;
#12780 = VERTEX_POINT ( 'NONE', #12153 ) ;
#12781 = VECTOR ( 'NONE', #83647, 1000.000000000000227 ) ;
#12782 = CARTESIAN_POINT ( 'NONE',  ( -1.384615384615505151, -6.026961402154118908, 34.52809138561165270 ) ) ;
#12783 = LINE ( 'NONE', #55095, #15401 ) ;
#12784 = AXIS2_PLACEMENT_3D ( 'NONE', #50225, #15579, #7931 ) ;
#12785 = VERTEX_POINT ( 'NONE', #79274 ) ;
#12786 = CARTESIAN_POINT ( 'NONE',  ( -12.71151520558705172, -5.643011162660950042, 34.66104346484419096 ) ) ;
#12787 = CARTESIAN_POINT ( 'NONE',  ( 9.758474298899335153, -7.250054591869670162, 34.99404684341514127 ) ) ;
#12788 = CARTESIAN_POINT ( 'NONE',  ( -7.912236225513981758, -12.34228464037088280, 31.77849191805838558 ) ) ;
#12789 = DIRECTION ( 'NONE',  ( -0.000000000000000000, 0.8660254037844397068, -0.4999999999999978906 ) ) ;
#12790 = CARTESIAN_POINT ( 'NONE',  ( 0.3954560821783256186, -2.486705287966280320, 31.30864560766544002 ) ) ;
#12791 = CARTESIAN_POINT ( 'NONE',  ( 17.01165307636676260, -5.094484230520675894, 34.41647553114621161 ) ) ;
#12793 = CARTESIAN_POINT ( 'NONE',  ( 16.21991450484859598, -5.557115091759786019, 34.35708131394839882 ) ) ;
#12792 = DIRECTION ( 'NONE',  ( 0.000000000000000000, 0.7660444431189807890, 0.6427876096865361433 ) ) ;
#12794 = AXIS2_PLACEMENT_3D ( 'NONE', #3998, #65258, #64808 ) ;
#12795 = EDGE_CURVE ( 'NONE', #87491, #14948, #81955, .T. ) ;
#12796 = CARTESIAN_POINT ( 'NONE',  ( 18.00000000000000000, -1.790695186598648903, 34.54067556320373455 ) ) ;
#12797 = CARTESIAN_POINT ( 'NONE',  ( 2.750000000000008438, -8.639087296525996607, 17.04687500000000000 ) ) ;
#12798 = ORIENTED_EDGE ( 'NONE', *, *, #62528, .T. ) ;
#12799 = CARTESIAN_POINT ( 'NONE',  ( 17.74997676270703550, -4.335965774309648246, 33.62209801155881905 ) ) ;
#12800 = ORIENTED_EDGE ( 'NONE', *, *, #83946, .T. ) ;
#12801 = EDGE_LOOP ( 'NONE', ( #75487, #7024 ) ) ;
#12802 = CARTESIAN_POINT ( 'NONE',  ( -8.769230769230768274, -6.343179335718451384, 34.87096338111211935 ) ) ;
#12803 = EDGE_LOOP ( 'NONE', ( #19364, #86743, #38988, #9081 ) ) ;
#12804 = CARTESIAN_POINT ( 'NONE',  ( -4.403869378067613027, -2.588893531581426544, 31.60682220781847818 ) ) ;
#12805 = CARTESIAN_POINT ( 'NONE',  ( 2.750000000000008438, -8.639087296525996607, 19.54687499999999645 ) ) ;
#12806 = CARTESIAN_POINT ( 'NONE',  ( 12.33106327646274103, -7.276987145209184327, 34.99546412871779211 ) ) ;
#12807 = CARTESIAN_POINT ( 'NONE',  ( -13.38461538461538325, -11.91647553114624181, 32.58852847137148245 ) ) ;
#12808 = CARTESIAN_POINT ( 'NONE',  ( -4.153846153846273204, -3.835265460704628371, 33.15142922262033665 ) ) ;
#12809 = DIRECTION ( 'NONE',  ( -0.000000000000000000, 1.000000000000000000, -0.000000000000000000 ) ) ;
#12810 = CARTESIAN_POINT ( 'NONE',  ( 14.30769230769231015, -11.35647404775217417, 33.31231777344666511 ) ) ;
#12811 = CARTESIAN_POINT ( 'NONE',  ( 2.557637826040450868, -11.37275283266503756, 32.91324779482534524 ) ) ;
#12812 = CARTESIAN_POINT ( 'NONE',  ( -1.553300858899081538, -11.25000000000000711, 24.85937500000001421 ) ) ;
#12813 = CARTESIAN_POINT ( 'NONE',  ( 10.86543903529806876, -12.41089969410671223, 31.60739465890703670 ) ) ;
#12815 = ADVANCED_FACE ( 'NONE', ( #24310 ), #65739, .F. ) ;
#12814 = CARTESIAN_POINT ( 'NONE',  ( -4.219928533206287469, -11.91647553114624181, 32.58852847137148245 ) ) ;
#12816 = EDGE_CURVE ( 'NONE', #42788, #45049, #3599, .T. ) ;
#12817 = CARTESIAN_POINT ( 'NONE',  ( 18.25000000000000000, -2.499999999999999556, 29.81604066197449754 ) ) ;
#12818 = VECTOR ( 'NONE', #1907, 1000.000000000000114 ) ;
#12819 = ORIENTED_EDGE ( 'NONE', *, *, #81031, .T. ) ;
#12821 = EDGE_CURVE ( 'NONE', #73573, #17458, #17488, .T. ) ;
#12820 = VERTEX_POINT ( 'NONE', #86491 ) ;
#12822 = CARTESIAN_POINT ( 'NONE',  ( 6.923076923076802558, -2.625532179533778709, 30.86335684631627174 ) ) ;
#12823 = DIRECTION ( 'NONE',  ( -0.000000000000000000, 0.8660254037844399289, -0.4999999999999980016 ) ) ;
#12824 = DIRECTION ( 'NONE',  ( 1.000000000000000000, 0.000000000000000000, 0.000000000000000000 ) ) ;
#12825 = CARTESIAN_POINT ( 'NONE',  ( 6.000000000000317080, -2.255955759149395501, 30.00000000000324363 ) ) ;
#12826 = EDGE_CURVE ( 'NONE', #7659, #45196, #46373, .T. ) ;
#12827 = LINE ( 'NONE', #4749, #86665 ) ;
#12828 = CARTESIAN_POINT ( 'NONE',  ( -5.999999999999998224, -8.120952969808772792, 34.71129190930000163 ) ) ;
#12829 = FACE_OUTER_BOUND ( 'NONE', #50735, .T. ) ;
#12830 = ORIENTED_EDGE ( 'NONE', *, *, #84164, .F. ) ;
#12831 = CARTESIAN_POINT ( 'NONE',  ( -5.011667505647053211, -12.46129190930001052, 30.37095296980870174 ) ) ;
#12832 = ORIENTED_EDGE ( 'NONE', *, *, #60564, .T. ) ;
#12833 = ORIENTED_EDGE ( 'NONE', *, *, #82525, .T. ) ;
#12834 = CARTESIAN_POINT ( 'NONE',  ( 17.93391658904412012, -3.050289026998445951, 32.03036669348365706 ) ) ;
#12835 = CIRCLE ( 'NONE', #9993, 4.000000000000000000 ) ;
#12836 = PLANE ( 'NONE',  #51485 ) ;
#12837 = CARTESIAN_POINT ( 'NONE',  ( 14.17754509825408960, -5.195881422630166391, 34.18770438780619259 ) ) ;
#12838 = CARTESIAN_POINT ( 'NONE',  ( 5.999999999999878320, -8.656820664282941280, 34.87096338111179961 ) ) ;
#12839 = CARTESIAN_POINT ( 'NONE',  ( -13.38461538461550759, -2.657715359629662544, 31.77849191805970364 ) ) ;
#12840 = AXIS2_PLACEMENT_3D ( 'NONE', #42772, #37314, #36877 ) ;
#12841 = ORIENTED_EDGE ( 'NONE', *, *, #79709, .F. ) ;
#12842 = VECTOR ( 'NONE', #26217, 1000.000000000000227 ) ;
#12843 = ORIENTED_EDGE ( 'NONE', *, *, #60235, .T. ) ;
#12844 = EDGE_CURVE ( 'NONE', #86258, #54572, #89042, .T. ) ;
#12845 = EDGE_LOOP ( 'NONE', ( #9955, #50916, #35208, #49349, #12025, #62804 ) ) ;
#12846 = EDGE_LOOP ( 'NONE', ( #36419, #48731, #84634, #87750 ) ) ;
#12847 = CARTESIAN_POINT ( 'NONE',  ( -17.14300648787895653, -10.51840700105979565, 33.73612834413961536 ) ) ;
#12848 = CARTESIAN_POINT ( 'NONE',  ( 5.010839665967196765, -10.51840700105979387, 33.73612834413961536 ) ) ;
#12849 = CARTESIAN_POINT ( 'NONE',  ( 20.00000000000000000, -4.000000000000000000, 29.75000000000000355 ) ) ;
#12850 = CARTESIAN_POINT ( 'NONE',  ( -16.40382289789473802, -2.318417181685854978, 30.59732222474233865 ) ) ;
#12851 = LINE ( 'NONE', #46640, #16292 ) ;
#12852 = CYLINDRICAL_SURFACE ( 'NONE', #35117, 0.2499999999999997502 ) ;
#12853 = EDGE_LOOP ( 'NONE', ( #55817, #53038, #84820, #32332 ) ) ;
#12854 = ORIENTED_EDGE ( 'NONE', *, *, #42597, .T. ) ;
#12855 = EDGE_CURVE ( 'NONE', #57187, #53046, #44572, .T. ) ;
#12856 = VERTEX_POINT ( 'NONE', #62853 ) ;
#12858 = ORIENTED_EDGE ( 'NONE', *, *, #26788, .T. ) ;
#12857 = CARTESIAN_POINT ( 'NONE',  ( -0.4615384615384611200, -9.819645486525091727, 36.12317359536749706 ) ) ;
#12859 = CARTESIAN_POINT ( 'NONE',  ( 9.692307692307695177, -8.164416787775445883, 34.95778746994557906 ) ) ;
#12860 = CARTESIAN_POINT ( 'NONE',  ( 6.857320120562612864, -7.249945686854186278, 34.74374336980224598 ) ) ;
#12861 = CARTESIAN_POINT ( 'NONE',  ( 1.553300858899086867, -3.749999999999992006, 19.23437500000000000 ) ) ;
#12862 = ORIENTED_EDGE ( 'NONE', *, *, #36567, .F. ) ;
#12863 = CYLINDRICAL_SURFACE ( 'NONE', #55505, 0.2499999999999995559 ) ;
#12864 = AXIS2_PLACEMENT_3D ( 'NONE', #64942, #50543, #37026 ) ;
#12865 = ORIENTED_EDGE ( 'NONE', *, *, #86142, .T. ) ;
#12866 = DIRECTION ( 'NONE',  ( -0.000000000000000000, -0.3420201433256694346, -0.9396926207859080948 ) ) ;
#12867 = FACE_BOUND ( 'NONE', #30426, .T. ) ;
#12868 = CYLINDRICAL_SURFACE ( 'NONE', #74881, 0.2499999999999973355 ) ;
#12869 = ADVANCED_FACE ( 'NONE', ( #83611 ), #15141, .T. ) ;
#12870 = DIRECTION ( 'NONE',  ( 0.000000000000000000, 0.8660254037844377084, 0.5000000000000015543 ) ) ;
#12871 = ORIENTED_EDGE ( 'NONE', *, *, #36613, .T. ) ;
#12872 = DIRECTION ( 'NONE',  ( -0.000000000000000000, 0.7660444431189792347, -0.6427876096865379196 ) ) ;
#12873 = B_SPLINE_CURVE_WITH_KNOTS ( 'NONE', 3,
 ( #16786, #37954, #79389, #65422, #85704, #17234, #84831, #44690, #43818, #58657 ),
 .UNSPECIFIED., .F., .F.,
 ( 4, 2, 2, 2, 4 ),
 ( 0.0007817246256747489071, 0.0009771112852218920199, 0.001172497944769035133, 0.001367884604316178246, 0.001563271263863321358 ),
 .UNSPECIFIED. ) ;
#12874 = ADVANCED_FACE ( 'NONE', ( #56998 ), #35401, .F. ) ;
#12875 = CARTESIAN_POINT ( 'NONE',  ( 5.076923076923075762, -1.509761064869970415, 31.06009739812519044 ) ) ;
#12876 = ORIENTED_EDGE ( 'NONE', *, *, #66341, .F. ) ;
#12877 = CARTESIAN_POINT ( 'NONE',  ( -9.442362282929648742, -4.932303261841489928, 34.32971442181322885 ) ) ;
#12878 = CARTESIAN_POINT ( 'NONE',  ( 1.253924781505077579, -3.957541250942359756, 33.62499894934981626 ) ) ;
#12879 = CARTESIAN_POINT ( 'NONE',  ( -3.930833309752758797, -2.308499170217967134, 30.53291367094873721 ) ) ;
#12880 = DIRECTION ( 'NONE',  ( 0.000000000000000000, 0.8660254037844377084, 0.5000000000000015543 ) ) ;
#12881 = DIRECTION ( 'NONE',  ( -0.000000000000000000, 0.8660254037844397068, -0.4999999999999978906 ) ) ;
#12882 = FACE_BOUND ( 'NONE', #29180, .T. ) ;
#12884 = CARTESIAN_POINT ( 'NONE',  ( -7.846153846153967493, -11.06231777344772027, 33.60647404775119895 ) ) ;
#12883 = CARTESIAN_POINT ( 'NONE',  ( 5.750023255951409951, -4.818429247618089661, 34.26397095200675125 ) ) ;
#12885 = EDGE_CURVE ( 'NONE', #17603, #28930, #83065, .T. ) ;
#12886 = CARTESIAN_POINT ( 'NONE',  ( 2.177001704581999597, -9.929715669179220328, 34.40415004197138416 ) ) ;
#12888 = CARTESIAN_POINT ( 'NONE',  ( -9.626239341305252495, -10.51840700105979565, 33.73612834413962247 ) ) ;
#12887 = CARTESIAN_POINT ( 'NONE',  ( 3.295915010101195364, -7.750023238201980469, 34.74374492549440419 ) ) ;
#12889 = CARTESIAN_POINT ( 'NONE',  ( -8.703975197954742171, -3.835265460703683349, 33.15142922261929925 ) ) ;
#12890 = CARTESIAN_POINT ( 'NONE',  ( -0.06109907496454585613, -4.750000000000000000, 20.15438170625849068 ) ) ;
#12891 = EDGE_LOOP ( 'NONE', ( #55595, #13985, #3249, #84377 ) ) ;
#12892 = CARTESIAN_POINT ( 'NONE',  ( 8.102564102564102200, -4.000000000000000000, 29.75000000000000355 ) ) ;
#12893 = ORIENTED_EDGE ( 'NONE', *, *, #82910, .F. ) ;
#12894 = EDGE_CURVE ( 'NONE', #32391, #79032, #50802, .T. ) ;
#12895 = CARTESIAN_POINT ( 'NONE',  ( -18.00000000000012079, -3.643525952248793498, 33.31231777344770961 ) ) ;
#12896 = EDGE_LOOP ( 'NONE', ( #30436, #24948, #25039, #4556 ) ) ;
#12897 = CARTESIAN_POINT ( 'NONE',  ( 7.780070435197966816, -8.973038597847269315, 34.52809138561120506 ) ) ;
#12899 = EDGE_CURVE ( 'NONE', #38093, #25274, #21798, .T. ) ;
#12898 = DIRECTION ( 'NONE',  ( -0.000000000000000000, -0.1736481776669307198, -0.9848077530122080203 ) ) ;
#12901 = EDGE_LOOP ( 'NONE', ( #50495, #69490, #6948, #7314 ) ) ;
#12900 = CARTESIAN_POINT ( 'NONE',  ( 15.10020863902730959, -2.504760397472875155, 29.97295953869789997 ) ) ;
#12902 = CARTESIAN_POINT ( 'NONE',  ( -11.53846153846153655, -2.249999999999998668, 29.75000000000001776 ) ) ;
#12903 = CARTESIAN_POINT ( 'NONE',  ( 18.13083833048675686, -7.277220318596959281, 34.99547417642776992 ) ) ;
#12904 = CARTESIAN_POINT ( 'NONE',  ( 2.775308065498768517, -8.577988221561467341, 19.29500670625849068 ) ) ;
#12905 = AXIS2_PLACEMENT_3D ( 'NONE', #25639, #53545, #20217 ) ;
#12906 = CARTESIAN_POINT ( 'NONE',  ( 4.376625695114562120, -10.81320215134717344, 33.49497208177562868 ) ) ;
#12907 = CARTESIAN_POINT ( 'NONE',  ( 10.61538461538449418, -9.528491918059723176, 34.59228464037033035 ) ) ;
#12908 = CARTESIAN_POINT ( 'NONE',  ( -4.853910232829680815, -11.98016756924215009, 32.48728574198911190 ) ) ;
#12909 = CARTESIAN_POINT ( 'NONE',  ( 0.000000000000000000, -11.00000000000000000, 29.75000000000000355 ) ) ;
#12910 = DIRECTION ( 'NONE',  ( 0.000000000000000000, 0.7660444431189807890, 0.6427876096865361433 ) ) ;
#12911 = CARTESIAN_POINT ( 'NONE',  ( -11.28851602011339672, -10.05730279482229683, 34.04704008940765902 ) ) ;
#12912 = AXIS2_PLACEMENT_3D ( 'NONE', #69965, #50571, #63200 ) ;
#12913 = CARTESIAN_POINT ( 'NONE',  ( 3.775308065498752086, -6.007798216065404873, 15.89249329374151820 ) ) ;
#12915 = EDGE_CURVE ( 'NONE', #26314, #27369, #27756, .T. ) ;
#12914 = CARTESIAN_POINT ( 'NONE',  ( 3.480769230769293898, -7.434744860731434812, 35.00000000000000711 ) ) ;
#12916 = B_SPLINE_CURVE_WITH_KNOTS ( 'NONE', 3,
 ( #23627, #73623, #85789, #30389, #3803, #86697, #11913, #32177, #66399, #51078 ),
 .UNSPECIFIED., .F., .F.,
 ( 4, 2, 2, 2, 4 ),
 ( 0.0007817359430256294638, 0.0009771253907249948054, 0.001172514838424360255, 0.001367904286123725489, 0.001563293733823090939 ),
 .UNSPECIFIED. ) ;
#12917 = CARTESIAN_POINT ( 'NONE',  ( 6.989145274079363368, -11.16473453929635440, 33.15142922261926373 ) ) ;
#12918 = VERTEX_POINT ( 'NONE', #75950 ) ;
#12919 = CARTESIAN_POINT ( 'NONE',  ( 8.769230769230645706, -9.528491918059723176, 34.59228464037033035 ) ) ;
#12920 = DIRECTION ( 'NONE',  ( -0.000000000000000000, 1.000000000000000000, -0.000000000000000000 ) ) ;
#12921 = CARTESIAN_POINT ( 'NONE',  ( 2.608446859217924629, -10.19485399968118422, 17.37686829374151287 ) ) ;
#12922 = EDGE_CURVE ( 'NONE', #19281, #39535, #55228, .T. ) ;
#12923 = CARTESIAN_POINT ( 'NONE',  ( -17.93474442872397034, -12.46129190930001052, 30.37095296980869819 ) ) ;
#12924 = LINE ( 'NONE', #53006, #2398 ) ;
#12925 = EDGE_LOOP ( 'NONE', ( #63115, #42892 ) ) ;
#12926 = FACE_OUTER_BOUND ( 'NONE', #49168, .T. ) ;
#12927 = DIRECTION ( 'NONE',  ( 1.000000000000000000, 0.000000000000000000, 0.000000000000000000 ) ) ;
#12929 = VERTEX_POINT ( 'NONE', #41726 ) ;
#12928 = DIRECTION ( 'NONE',  ( 0.000000000000000000, 0.9396926207859126468, 0.3420201433256571111 ) ) ;
#12930 = CARTESIAN_POINT ( 'NONE',  ( 12.71148397988660150, -12.43552623307873972, 30.55307653245132826 ) ) ;
#12931 = EDGE_CURVE ( 'NONE', #5154, #46042, #49365, .T. ) ;
#12932 = CARTESIAN_POINT ( 'NONE',  ( 5.326923076923138822, -7.434744860731433924, 35.00000000000000711 ) ) ;
#12933 = CARTESIAN_POINT ( 'NONE',  ( -11.53846153846153655, -2.486705287966279876, 31.30864560766543647 ) ) ;
#12934 = ORIENTED_EDGE ( 'NONE', *, *, #44903, .T. ) ;
#12935 = CARTESIAN_POINT ( 'NONE',  ( -11.53846153846166089, -4.320704448113951379, 33.92786785259630022 ) ) ;
#12936 = CARTESIAN_POINT ( 'NONE',  ( -24.99999999999999645, 15.00000000000000355, 3.000000000000000000 ) ) ;
#12937 = DIRECTION ( 'NONE',  ( -1.000000000000000000, -0.000000000000000000, 0.000000000000000000 ) ) ;
#12938 = EDGE_LOOP ( 'NONE', ( #81441, #2082, #37092, #74916 ) ) ;
#12939 = ORIENTED_EDGE ( 'NONE', *, *, #73718, .T. ) ;
#12940 = EDGE_CURVE ( 'NONE', #79735, #58351, #29543, .T. ) ;
#12941 = ORIENTED_EDGE ( 'NONE', *, *, #69620, .T. ) ;
#12942 = EDGE_LOOP ( 'NONE', ( #64362, #55957, #60394, #54027 ) ) ;
#12943 = CARTESIAN_POINT ( 'NONE',  ( 12.52760579488853665, -9.905515769479276145, 34.41647553114623292 ) ) ;
#12944 = FACE_OUTER_BOUND ( 'NONE', #69698, .T. ) ;
#12945 = EDGE_CURVE ( 'NONE', #27787, #31685, #48584, .T. ) ;
#12946 = CARTESIAN_POINT ( 'NONE',  ( 13.38461538461538680, -3.050289026998446396, 32.03036669348365706 ) ) ;
#12947 = CARTESIAN_POINT ( 'NONE',  ( -16.85349667800829465, -7.630147987733843173, 34.99859428049665411 ) ) ;
#12948 = CARTESIAN_POINT ( 'NONE',  ( 5.326977388561388693, -5.728107161865375829, 34.42597550085002922 ) ) ;
#12949 = ORIENTED_EDGE ( 'NONE', *, *, #4551, .F. ) ;
#12950 = B_SPLINE_CURVE_WITH_KNOTS ( 'NONE', 3,
 ( #34408, #6063, #61872, #26328, #82622, #14141, #69084, #88498, #25885, #80848 ),
 .UNSPECIFIED., .F., .F.,
 ( 4, 2, 2, 2, 4 ),
 ( 0.000000000000000000, 0.0001954339857564071762, 0.0003908679715128143524, 0.0005863019572692215828, 0.0007817359430256287049 ),
 .UNSPECIFIED. ) ;
#12951 = EDGE_CURVE ( 'NONE', #74505, #57294, #36734, .T. ) ;
#12952 = EDGE_LOOP ( 'NONE', ( #1361, #5542 ) ) ;
#12953 = EDGE_LOOP ( 'NONE', ( #40090, #63762 ) ) ;
#12955 = ORIENTED_EDGE ( 'NONE', *, *, #63416, .T. ) ;
#12954 = CARTESIAN_POINT ( 'NONE',  ( -7.146003881983771677, -8.282780595021769443, 34.94152052738834868 ) ) ;
#12956 = CARTESIAN_POINT ( 'NONE',  ( 15.12820512820512953, -3.499999999999999556, 29.75000000000000355 ) ) ;
#12957 = EDGE_CURVE ( 'NONE', #19489, #83181, #55138, .T. ) ;
#12958 = CARTESIAN_POINT ( 'NONE',  ( -10.55023883605264956, -7.750023238201979581, 34.74374492549440419 ) ) ;
#12959 = VECTOR ( 'NONE', #4357, 1000.000000000000000 ) ;
#12960 = VECTOR ( 'NONE', #28041, 999.9999999999998863 ) ;
#12961 = EDGE_CURVE ( 'NONE', #47159, #43004, #52013, .T. ) ;
#12962 = CARTESIAN_POINT ( 'NONE',  ( 5.999999999999878320, -4.320704448113951379, 33.92786785259630022 ) ) ;
#12963 = CARTESIAN_POINT ( 'NONE',  ( -14.98071491913091791, -9.148310452688876993, 34.47095581063188519 ) ) ;
#12964 = ORIENTED_EDGE ( 'NONE', *, *, #67670, .T. ) ;
#12965 = VECTOR ( 'NONE', #76504, 1000.000000000000114 ) ;
#12966 = ORIENTED_EDGE ( 'NONE', *, *, #70824, .T. ) ;
#12967 = AXIS2_PLACEMENT_3D ( 'NONE', #30029, #37665, #76891 ) ;
#12968 = ADVANCED_FACE ( 'NONE', ( #43492 ), #30855, .F. ) ;
#12969 = ORIENTED_EDGE ( 'NONE', *, *, #63442, .T. ) ;
#12970 = CARTESIAN_POINT ( 'NONE',  ( -10.61538461538473577, -11.06231777344772027, 33.60647404775119895 ) ) ;
#12972 = ORIENTED_EDGE ( 'NONE', *, *, #71227, .F. ) ;
#12971 = DIRECTION ( 'NONE',  ( 0.000000000000000000, 0.9848077530122072432, -0.1736481776669354937 ) ) ;
#12973 =( GEOMETRIC_REPRESENTATION_CONTEXT ( 3 ) GLOBAL_UNCERTAINTY_ASSIGNED_CONTEXT ( ( #69912 ) ) GLOBAL_UNIT_ASSIGNED_CONTEXT ( ( #73083, #38862, #32535 ) ) REPRESENTATION_CONTEXT ( 'NONE', 'WORKASPACE' ) );
#12974 = CARTESIAN_POINT ( 'NONE',  ( -11.53846153846166089, -12.70778746994576025, 30.41441678777401236 ) ) ;
#12975 = CARTESIAN_POINT ( 'NONE',  ( -14.43783951713052716, -2.619462340734462380, 30.83744416345203021 ) ) ;
#12976 = ORIENTED_EDGE ( 'NONE', *, *, #81263, .F. ) ;
#12977 = CARTESIAN_POINT ( 'NONE',  ( -17.07692307692319744, -9.442884908241554243, 34.35708131394783038 ) ) ;
#12978 = CARTESIAN_POINT ( 'NONE',  ( 8.834486340506792601, -12.46129190930001052, 30.37095296980870174 ) ) ;
#12979 = CARTESIAN_POINT ( 'NONE',  ( -14.87820512820512953, -7.500000000000000000, 29.75000000000000355 ) ) ;
#12980 = FACE_BOUND ( 'NONE', #27114, .T. ) ;
#12981 = CARTESIAN_POINT ( 'NONE',  ( -17.07692307692307665, -1.509761064869970415, 31.06009739812519044 ) ) ;
#12982 = CARTESIAN_POINT ( 'NONE',  ( -15.23076923076922995, -9.584722331328613620, 36.20867863119891439 ) ) ;
#12983 = CARTESIAN_POINT ( 'NONE',  ( -3.230769230769229949, -8.164416787775445883, 34.95778746994557906 ) ) ;
#12985 = CARTESIAN_POINT ( 'NONE',  ( -8.769230769230892619, -12.16647553114689728, 32.15551576947799362 ) ) ;
#12984 = CARTESIAN_POINT ( 'NONE',  ( -2.307692307692305711, -8.120952969808772792, 34.71129190930000163 ) ) ;
#12986 = CARTESIAN_POINT ( 'NONE',  ( -4.854143535654665165, -10.81320215134717344, 33.49497208177562868 ) ) ;
#12987 = CARTESIAN_POINT ( 'NONE',  ( 12.68455130563185840, -2.889357225399416418, 32.26129605718031002 ) ) ;
#12988 = ORIENTED_EDGE ( 'NONE', *, *, #28431, .F. ) ;
#12989 = CARTESIAN_POINT ( 'NONE',  ( -17.29985003582992320, -5.582147617184174848, 34.63737895849758530 ) ) ;
#12990 = DIRECTION ( 'NONE',  ( -0.000000000000000000, 0.000000000000000000, 1.000000000000000000 ) ) ;
#12991 = ADVANCED_FACE ( 'NONE', ( #2491 ), #64631, .F. ) ;
#12992 = EDGE_LOOP ( 'NONE', ( #38295, #71646 ) ) ;
#12993 = CARTESIAN_POINT ( 'NONE',  ( -6.673022611438607754, -4.943051570960391494, 34.04725096376909477 ) ) ;
#12994 = CARTESIAN_POINT ( 'NONE',  ( -14.55771554498526932, -5.056417327199099532, 34.11270091957321426 ) ) ;
#12995 = CARTESIAN_POINT ( 'NONE',  ( -7.715628407920204879, -2.372941743896878286, 30.88044141588253666 ) ) ;
#12996 = ORIENTED_EDGE ( 'NONE', *, *, #57907, .T. ) ;
#12997 = FACE_OUTER_BOUND ( 'NONE', #9895, .T. ) ;
#12998 = CARTESIAN_POINT ( 'NONE',  ( 6.792386319966617236, -8.191372820521381826, 34.95448215188423546 ) ) ;
#12999 = FACE_BOUND ( 'NONE', #75713, .T. ) ;
#13001 = DIRECTION ( 'NONE',  ( 0.000000000000000000, 0.6427876096865368094, 0.7660444431189802339 ) ) ;
#13000 = DIRECTION ( 'NONE',  ( -0.000000000000000000, -0.8660254037844397068, -0.4999999999999978906 ) ) ;
#13002 = CARTESIAN_POINT ( 'NONE',  ( -13.60754234352223335, -2.308479472611653094, 30.53278059502174457 ) ) ;
#13003 = CARTESIAN_POINT ( 'NONE',  ( -16.15384615384615330, -5.180354513474913603, 36.12317359536750416 ) ) ;
#13005 = CARTESIAN_POINT ( 'NONE',  ( -10.54931728203453822, -11.35647404775217595, 33.31231777344666511 ) ) ;
#13004 = DIRECTION ( 'NONE',  ( 0.000000000000000000, 0.000000000000000000, 1.000000000000000000 ) ) ;
#13006 = VECTOR ( 'NONE', #6600, 1000.000000000000000 ) ;
#13007 = APPLICATION_CONTEXT ( 'automotive_design' ) ;
#13008 = CARTESIAN_POINT ( 'NONE',  ( -2.651650429449535551, -10.15165042944956753, 26.18750000000000355 ) ) ;
#13009 = ORIENTED_EDGE ( 'NONE', *, *, #77213, .T. ) ;
#13010 = ORIENTED_EDGE ( 'NONE', *, *, #82942, .T. ) ;
#13011 = DIRECTION ( 'NONE',  ( -0.000000000000000000, 0.6427876096865404731, -0.7660444431189771253 ) ) ;
#13012 = CARTESIAN_POINT ( 'NONE',  ( 12.21153846153846168, -7.500000000000001776, 34.75000000000000000 ) ) ;
#13013 = CARTESIAN_POINT ( 'NONE',  ( 16.21910129335899242, -3.083524468853783951, 32.58852847137153930 ) ) ;
#13014 = CARTESIAN_POINT ( 'NONE',  ( 10.83816428436267820, -3.020022701398814569, 32.48759521482552515 ) ) ;
#13015 = CARTESIAN_POINT ( 'NONE',  ( 5.142990410273151625, -3.322132147404559976, 32.92929555188717927 ) ) ;
#13016 = CARTESIAN_POINT ( 'NONE',  ( -2.651650429449565305, -4.848349570550461785, 24.00000000000000000 ) ) ;
#13017 = CARTESIAN_POINT ( 'NONE',  ( -1.608100309179715470, -4.225889041578353655, 33.85425143139329407 ) ) ;
#13018 = CARTESIAN_POINT ( 'NONE',  ( 5.934729999443682402, -3.083524468853724443, 32.58852847137143272 ) ) ;
#13019 = CYLINDRICAL_SURFACE ( 'NONE', #50176, 0.2500000000000002220 ) ;
#13020 = CARTESIAN_POINT ( 'NONE',  ( -1.634615384615382805, -7.566082377512563184, 35.00000000000000711 ) ) ;
#13021 = CARTESIAN_POINT ( 'NONE',  ( 9.822833394071254887, -2.882268652242222284, 31.66798894389554064 ) ) ;
#13022 = CARTESIAN_POINT ( 'NONE',  ( 13.25446817517716447, -4.460286881179643004, 33.72017969459903242 ) ) ;
#13023 = CARTESIAN_POINT ( 'NONE',  ( 6.923076923076924238, -11.16473453929635440, 33.15142922261926373 ) ) ;
#13024 = CARTESIAN_POINT ( 'NONE',  ( 10.61538461538461675, -2.538708090699994813, 30.37095296980875503 ) ) ;
#13025 = EDGE_CURVE ( 'NONE', #32479, #80662, #65078, .T. ) ;
#13026 = VECTOR ( 'NONE', #8001, 1000.000000000000000 ) ;
#13027 = CARTESIAN_POINT ( 'NONE',  ( -16.85414340794500987, -3.020022701398814569, 32.48759521482552515 ) ) ;
#13028 = ORIENTED_EDGE ( 'NONE', *, *, #69781, .F. ) ;
#13029 = CARTESIAN_POINT ( 'NONE',  ( 1.318531973659504697, -2.538708090699994813, 30.37095296980875148 ) ) ;
#13030 = FACE_OUTER_BOUND ( 'NONE', #48326, .T. ) ;
#13031 = CARTESIAN_POINT ( 'NONE',  ( -1.200186371490524317, -10.22469193450124791, 17.61124329374151642 ) ) ;
#13032 = EDGE_CURVE ( 'NONE', #81366, #38816, #8869, .T. ) ;
#13033 = CIRCLE ( 'NONE', #31674, 0.2500000000000002220 ) ;
#13034 = CIRCLE ( 'NONE', #79184, 2.750000000000000000 ) ;
#13035 = DIRECTION ( 'NONE',  ( -0.000000000000000000, 0.3420201433256694901, -0.9396926207859082059 ) ) ;
#13036 = FACE_OUTER_BOUND ( 'NONE', #56502, .T. ) ;
#13037 = CARTESIAN_POINT ( 'NONE',  ( -11.28840711854808632, -4.818054556918156983, 34.26375889529406749 ) ) ;
#13039 = ORIENTED_EDGE ( 'NONE', *, *, #28306, .T. ) ;
#13038 = DIRECTION ( 'NONE',  ( -0.000000000000000000, -0.5000000000000009992, -0.8660254037844380415 ) ) ;
#13040 = CARTESIAN_POINT ( 'NONE',  ( -2.750000000000006217, -6.360912703474006946, 25.17187500000000000 ) ) ;
#13041 = CARTESIAN_POINT ( 'NONE',  ( 3.361559671736180643, -8.191423895709840863, 34.95447573519442130 ) ) ;
#13042 = EDGE_CURVE ( 'NONE', #77857, #46107, #66940, .T. ) ;
#13043 = ORIENTED_EDGE ( 'NONE', *, *, #59532, .T. ) ;
#13044 = PLANE ( 'NONE',  #66457 ) ;
#13045 = CARTESIAN_POINT ( 'NONE',  ( -2.057746789344163663, -2.587454068350147907, 30.68340429815432202 ) ) ;
#13046 = EDGE_CURVE ( 'NONE', #33447, #28242, #51110, .T. ) ;
#13047 =( GEOMETRIC_REPRESENTATION_CONTEXT ( 3 ) GLOBAL_UNCERTAINTY_ASSIGNED_CONTEXT ( ( #36572 ) ) GLOBAL_UNIT_ASSIGNED_CONTEXT ( ( #18432, #17991, #38698 ) ) REPRESENTATION_CONTEXT ( 'NONE', 'WORKASPACE' ) );
#13048 = VERTEX_POINT ( 'NONE', #51549 ) ;
#13049 = CARTESIAN_POINT ( 'NONE',  ( 10.86538461538461675, -2.249999999999998668, 29.75000000000000355 ) ) ;
#13050 = CARTESIAN_POINT ( 'NONE',  ( 8.519207545009313876, -6.652501968072648708, 34.93155406624980941 ) ) ;
#13051 = VERTEX_POINT ( 'NONE', #84490 ) ;
#13052 = EDGE_LOOP ( 'NONE', ( #72517, #69997 ) ) ;
#13053 = EDGE_CURVE ( 'NONE', #3349, #11323, #62620, .T. ) ;
#13054 = B_SPLINE_CURVE_WITH_KNOTS ( 'NONE', 3,
 ( #64199, #29121, #27772, #48476, #21006, #76855, #9285, #35415, #7951, #75964 ),
 .UNSPECIFIED., .F., .F.,
 ( 4, 2, 2, 2, 4 ),
 ( 0.000000000000000000, 0.0001954339857564054686, 0.0003908679715128109372, 0.0005863019572692163787, 0.0007817359430256218744 ),
 .UNSPECIFIED. ) ;
#13055 = ORIENTED_EDGE ( 'NONE', *, *, #70274, .F. ) ;
#13056 = CARTESIAN_POINT ( 'NONE',  ( -15.00775638667583500, -4.026326845037962343, 33.68677907613344047 ) ) ;
#13057 = FACE_OUTER_BOUND ( 'NONE', #46542, .T. ) ;
#13058 = CARTESIAN_POINT ( 'NONE',  ( -17.75000000000000711, -12.75000000000000178, 29.75000000000000355 ) ) ;
#13059 = CARTESIAN_POINT ( 'NONE',  ( -1.515305987725692249, -11.37499894934982514, 33.29245874905763003 ) ) ;
#13060 = LINE ( 'NONE', #88737, #54840 ) ;
#13061 = LINE ( 'NONE', #80649, #10462 ) ;
#13062 = DIRECTION ( 'NONE',  ( -0.000000000000000000, 1.000000000000000000, -0.000000000000000000 ) ) ;
#13063 = DIRECTION ( 'NONE',  ( -0.000000000000000000, -0.5000000000000009992, -0.8660254037844380415 ) ) ;
#13064 = VERTEX_POINT ( 'NONE', #67763 ) ;
#13065 = VERTEX_POINT ( 'NONE', #18697 ) ;
#13067 = ORIENTED_EDGE ( 'NONE', *, *, #20037, .F. ) ;
#13066 = CARTESIAN_POINT ( 'NONE',  ( -8.352564102564102200, -7.500000000000000000, 33.75000000000000000 ) ) ;
#13068 = VECTOR ( 'NONE', #82723, 1000.000000000000227 ) ;
#13069 = EDGE_CURVE ( 'NONE', #67310, #36896, #46605, .T. ) ;
#13070 = B_SPLINE_CURVE_WITH_KNOTS ( 'NONE', 3,
 ( #88159, #40834, #53897, #61530, #75068, #83150, #55224, #20554, #20986, #82713 ),
 .UNSPECIFIED., .F., .F.,
 ( 4, 2, 2, 2, 4 ),
 ( 0.000000000000000000, 0.0001954311564186861426, 0.0003908623128373722852, 0.0005862934692560583735, 0.0007817246256747445703 ),
 .UNSPECIFIED. ) ;
#13071 = CARTESIAN_POINT ( 'NONE',  ( -13.31844877802374327, -7.250054591869670162, 34.99404684341514127 ) ) ;
#13072 = LINE ( 'NONE', #75650, #45347 ) ;
#13073 = ORIENTED_EDGE ( 'NONE', *, *, #22371, .T. ) ;
#13074 = CARTESIAN_POINT ( 'NONE',  ( -12.23852561744506495, -11.43677907613344757, 33.22367315496202167 ) ) ;
#13075 = EDGE_CURVE ( 'NONE', #11627, #26195, #78738, .T. ) ;
#13076 = ORIENTED_EDGE ( 'NONE', *, *, #39541, .F. ) ;
#13077 = CARTESIAN_POINT ( 'NONE',  ( 17.07692307692295586, -9.528491918059723176, 34.59228464037033035 ) ) ;
#13078 = ORIENTED_EDGE ( 'NONE', *, *, #28818, .T. ) ;
#13079 = CARTESIAN_POINT ( 'NONE',  ( 9.942253210655836781, -8.433404298154334455, 34.66254593164985920 ) ) ;
#13080 = ORIENTED_EDGE ( 'NONE', *, *, #79676, .F. ) ;
#13081 = EDGE_CURVE ( 'NONE', #4198, #77888, #61497, .T. ) ;
#13082 = VECTOR ( 'NONE', #65924, 1000.000000000000000 ) ;
#13083 = CARTESIAN_POINT ( 'NONE',  ( -8.769230769230768274, -4.786620604624113540, 33.94971097300155094 ) ) ;
#13084 = CARTESIAN_POINT ( 'NONE',  ( 10.74617642320940369, -4.809403383903225304, 33.96459661697924304 ) ) ;
#13085 = FACE_BOUND ( 'NONE', #80664, .T. ) ;
#13086 = B_SPLINE_CURVE_WITH_KNOTS ( 'NONE', 3,
 ( #13998, #1811, #7249, #48221, #29301, #84250, #82477, #54987, #15783, #43248 ),
 .UNSPECIFIED., .F., .F.,
 ( 4, 2, 2, 2, 4 ),
 ( 0.000000000000000000, 0.0001954339857564081520, 0.0003908679715128163040, 0.0005863019572692244018, 0.0007817359430256326080 ),
 .UNSPECIFIED. ) ;
#13087 = CARTESIAN_POINT ( 'NONE',  ( -17.75000000000000355, -2.499999999999999556, 29.81604066197449043 ) ) ;
#13088 = CARTESIAN_POINT ( 'NONE',  ( 1.134615384615387246, -2.249999999999998668, 29.75000000000000355 ) ) ;
#13089 = AXIS2_PLACEMENT_3D ( 'NONE', #53513, #73808, #19299 ) ;
#13090 = AXIS2_PLACEMENT_3D ( 'NONE', #62060, #35478, #6247 ) ;
#13091 = CARTESIAN_POINT ( 'NONE',  ( -1.514763354347080870, -2.373036134822905208, 30.88089517874951540 ) ) ;
#13092 = CARTESIAN_POINT ( 'NONE',  ( 4.219914504848592429, -8.120952969808772792, 34.71129190929999453 ) ) ;
#13093 = CARTESIAN_POINT ( 'NONE',  ( 14.30769230769231015, -2.499999999999998668, 29.50000000000001066 ) ) ;
#13094 = DIRECTION ( 'NONE',  ( -1.000000000000000000, -0.000000000000000000, -0.000000000000000000 ) ) ;
#13095 = CARTESIAN_POINT ( 'NONE',  ( -10.61538461538461320, -4.098570777380720287, 33.41473453929634729 ) ) ;
#13096 = EDGE_LOOP ( 'NONE', ( #21272, #54152, #38084, #89027 ) ) ;
#13097 = EDGE_CURVE ( 'NONE', #76314, #76451, #24984, .T. ) ;
#13098 = VERTEX_POINT ( 'NONE', #86729 ) ;
#13099 = AXIS2_PLACEMENT_3D ( 'NONE', #35259, #6898, #88901 ) ;
#13101 = CARTESIAN_POINT ( 'NONE',  ( -18.06608237936013239, -9.905515769479279697, 34.41647553114623292 ) ) ;
#13100 = DIRECTION ( 'NONE',  ( -0.000000000000000000, 1.000000000000000000, -0.000000000000000000 ) ) ;
#13102 = CARTESIAN_POINT ( 'NONE',  ( 16.21991348719623360, -11.35647404775217595, 33.31231777344667222 ) ) ;
#13103 = CARTESIAN_POINT ( 'NONE',  ( -3.903791733932699515, -9.233818618650603938, 34.70587769442853698 ) ) ;
#13104 = EDGE_CURVE ( 'NONE', #63264, #45061, #4558, .T. ) ;
#13105 = CARTESIAN_POINT ( 'NONE',  ( 5.076923076923075762, -2.249999999999998668, 29.75000000000001776 ) ) ;
#13106 = CARTESIAN_POINT ( 'NONE',  ( -13.31935981333936603, -2.892918686051626498, 31.69288490824026638 ) ) ;
#13107 = ADVANCED_FACE ( 'NONE', ( #47032 ), #19571, .F. ) ;
#13108 = ORIENTED_EDGE ( 'NONE', *, *, #11162, .F. ) ;
#13109 = CARTESIAN_POINT ( 'NONE',  ( -5.934744860487159102, -8.656820664281605460, 34.87096338111211224 ) ) ;
#13110 = DIRECTION ( 'NONE',  ( 0.000000000000000000, 1.000000000000000000, 0.000000000000000000 ) ) ;
#13111 = CARTESIAN_POINT ( 'NONE',  ( 24.99999999999999645, -19.99999999999999645, 0.000000000000000000 ) ) ;
#13112 = CARTESIAN_POINT ( 'NONE',  ( -3.230769230769352962, -12.70778746994576025, 30.41441678777401236 ) ) ;
#13113 = ORIENTED_EDGE ( 'NONE', *, *, #47017, .T. ) ;
#13114 = EDGE_CURVE ( 'NONE', #37535, #8529, #73190, .T. ) ;
#13115 = ORIENTED_EDGE ( 'NONE', *, *, #76428, .F. ) ;
#13116 = ORIENTED_EDGE ( 'NONE', *, *, #9302, .F. ) ;
#13117 = DIRECTION ( 'NONE',  ( -0.000000000000000000, -0.9396926207859093161, -0.3420201433256663259 ) ) ;
#13118 = VERTEX_POINT ( 'NONE', #39419 ) ;
#13119 = CARTESIAN_POINT ( 'NONE',  ( 2.980746006547773330, -12.68155406624981119, 30.59749803192733708 ) ) ;
#13120 = CARTESIAN_POINT ( 'NONE',  ( 14.98074599347626368, -9.271318131107980420, 34.42618302367067429 ) ) ;
#13121 = CARTESIAN_POINT ( 'NONE',  ( -5.142193522883852452, -4.481592998940161721, 33.73612834413957984 ) ) ;
#13122 = CARTESIAN_POINT ( 'NONE',  ( 8.899756207464417201, -3.625058011473228703, 33.29252011169590020 ) ) ;
#13123 = B_SPLINE_CURVE_WITH_KNOTS ( 'NONE', 3,
 ( #9118, #44194, #15875, #43337, #71683, #78887, #9984, #70815, #64921, #36582 ),
 .UNSPECIFIED., .F., .F.,
 ( 4, 2, 2, 2, 4 ),
 ( 0.000000000000000000, 0.0001954339857564090465, 0.0003908679715128180929, 0.0005863019572692271123, 0.0007817359430256361858 ),
 .UNSPECIFIED. ) ;
#13124 = DIRECTION ( 'NONE',  ( 0.000000000000000000, 0.9396926207859126468, -0.3420201433256571111 ) ) ;
#13125 = ORIENTED_EDGE ( 'NONE', *, *, #20823, .F. ) ;
#13126 = CARTESIAN_POINT ( 'NONE',  ( 15.23076923076923173, -11.16473453929635440, 33.15142922261926373 ) ) ;
#13128 = ORIENTED_EDGE ( 'NONE', *, *, #73089, .T. ) ;
#13127 = DIRECTION ( 'NONE',  ( -0.000000000000000000, 0.7660444431189791237, -0.6427876096865379196 ) ) ;
#13129 = CARTESIAN_POINT ( 'NONE',  ( -19.99999999999996803, 15.00000000000000711, 13.00000000000000178 ) ) ;
#13130 = CARTESIAN_POINT ( 'NONE',  ( -4.153846153846152411, -13.20930481340135110, 34.54067556320372745 ) ) ;
#13131 = CARTESIAN_POINT ( 'NONE',  ( 1.514662990871069592, -7.723484964179500700, 34.74522123443823318 ) ) ;
#13133 = B_SPLINE_CURVE_WITH_KNOTS ( 'NONE', 3,
 ( #2617, #29233, #57130, #84622, #48594, #76968, #56688, #9394, #84183, #8511 ),
 .UNSPECIFIED., .F., .F.,
 ( 4, 2, 2, 2, 4 ),
 ( 0.0007817246256747448956, 0.0009771112852218876831, 0.001172497944769030579, 0.001367884604316173475, 0.001563271263863316371 ),
 .UNSPECIFIED. ) ;
#13132 = VECTOR ( 'NONE', #82955, 1000.000000000000000 ) ;
#13134 = CARTESIAN_POINT ( 'NONE',  ( 8.992243613324164997, -11.98016756924215009, 32.48728574198911190 ) ) ;
#13135 = DIRECTION ( 'NONE',  ( 0.000000000000000000, 1.000000000000000000, 0.000000000000000000 ) ) ;
#13136 = CARTESIAN_POINT ( 'NONE',  ( 18.25005431163831204, -2.564540009722896752, 30.55348353981672105 ) ) ;
#13137 = CARTESIAN_POINT ( 'NONE',  ( -9.692307692307812417, -6.026961402154118019, 34.52809138561165270 ) ) ;
#13138 = CARTESIAN_POINT ( 'NONE',  ( 2.750000000000002665, -7.561099074964516831, 22.22061829374151287 ) ) ;
#13139 = ORIENTED_EDGE ( 'NONE', *, *, #87746, .T. ) ;
#13140 = CARTESIAN_POINT ( 'NONE',  ( 11.78851585009985214, -2.779044189368095719, 31.39831045268885745 ) ) ;
#13141 = DIRECTION ( 'NONE',  ( 1.000000000000000000, 0.000000000000000000, 0.000000000000000000 ) ) ;
#13142 = EDGE_CURVE ( 'NONE', #19996, #17369, #6067, .T. ) ;
#13143 = CARTESIAN_POINT ( 'NONE',  ( -6.923076923076922462, -3.322132147404559976, 32.92929555188717927 ) ) ;
#13144 = VERTEX_POINT ( 'NONE', #33539 ) ;
#13145 = CARTESIAN_POINT ( 'NONE',  ( -5.777220458731590291, -2.600157965045225339, 30.74683119005207743 ) ) ;
#13146 = CARTESIAN_POINT ( 'NONE',  ( -12.71156169883143150, -3.202444869320336451, 32.30641848906366675 ) ) ;
#13147 = CARTESIAN_POINT ( 'NONE',  ( -7.053768389744482725, -5.582088688514999397, 34.36776431015576350 ) ) ;
#13148 = CARTESIAN_POINT ( 'NONE',  ( -4.946877914088298134, -2.504778602574660340, 29.97347330155780298 ) ) ;
#13149 = EDGE_CURVE ( 'NONE', #3410, #9565, #16370, .T. ) ;
#13150 = CARTESIAN_POINT ( 'NONE',  ( -15.23076923076935252, -8.656820664282941280, 34.87096338111179961 ) ) ;
#13151 = EDGE_LOOP ( 'NONE', ( #19153, #17053, #34750, #13184 ) ) ;
#13152 = CARTESIAN_POINT ( 'NONE',  ( 16.94677586748485965, -3.285722584762969856, 32.44110544564090759 ) ) ;
#13153 = AXIS2_PLACEMENT_3D ( 'NONE', #59642, #53774, #87142 ) ;
#13154 = CARTESIAN_POINT ( 'NONE',  ( 9.692307692307572609, -3.835265460704628371, 33.15142922262033665 ) ) ;
#13155 = CARTESIAN_POINT ( 'NONE',  ( -14.05769230769088729, -7.500000000000154543, 35.00000000000007105 ) ) ;
#13156 = VERTEX_POINT ( 'NONE', #1521 ) ;
#13157 = ADVANCED_FACE ( 'NONE', ( #20894 ), #7833, .F. ) ;
#13158 = CARTESIAN_POINT ( 'NONE',  ( 20.00000000000000000, -4.000000000000000000, 29.75000000000000355 ) ) ;
#13159 = AXIS2_PLACEMENT_3D ( 'NONE', #20298, #12652, #40137 ) ;
#13160 = VERTEX_POINT ( 'NONE', #27215 ) ;
#13161 = DIRECTION ( 'NONE',  ( 0.000000000000000000, 0.1736481776669275834, 0.9848077530122086864 ) ) ;
#13162 = DIRECTION ( 'NONE',  ( 0.000000000000000000, 0.000000000000000000, 1.000000000000000000 ) ) ;
#13163 = ORIENTED_EDGE ( 'NONE', *, *, #20905, .F. ) ;
#13164 = DIRECTION ( 'NONE',  ( 0.000000000000000000, 0.000000000000000000, 1.000000000000000000 ) ) ;
#13165 = DIRECTION ( 'NONE',  ( -0.000000000000000000, 0.9396926207859092051, -0.3420201433256662704 ) ) ;
#13166 = CARTESIAN_POINT ( 'NONE',  ( -6.792286482109973988, -12.35292014791297710, 31.75344720912887198 ) ) ;
#13167 = VECTOR ( 'NONE', #12585, 1000.000000000000000 ) ;
#13168 = EDGE_CURVE ( 'NONE', #53882, #83423, #7756, .T. ) ;
#13169 = CARTESIAN_POINT ( 'NONE',  ( 9.692307692307572609, -6.026961402154118019, 34.52809138561165270 ) ) ;
#13170 = LINE ( 'NONE', #542, #28183 ) ;
#13171 = B_SPLINE_CURVE_WITH_KNOTS ( 'NONE', 3,
 ( #87913, #47775, #88788, #33816, #61271, #73927, #40149, #12221, #27062, #54523 ),
 .UNSPECIFIED., .F., .F.,
 ( 4, 2, 2, 2, 4 ),
 ( 0.000000000000000000, 0.0001954339857564083417, 0.0003908679715128166835, 0.0005863019572692250523, 0.0007817359430256333669 ),
 .UNSPECIFIED. ) ;
#13172 = VERTEX_POINT ( 'NONE', #14143 ) ;
#13173 = DIRECTION ( 'NONE',  ( 0.000000000000000000, 0.000000000000000000, 1.000000000000000000 ) ) ;
#13174 = VERTEX_POINT ( 'NONE', #75406 ) ;
#13175 = CARTESIAN_POINT ( 'NONE',  ( -8.769230769230890843, -4.481592998941358097, 33.73612834414048933 ) ) ;
#13176 = CARTESIAN_POINT ( 'NONE',  ( -12.39547112818838492, -2.833524468853757305, 32.15551576947925838 ) ) ;
#13177 = CARTESIAN_POINT ( 'NONE',  ( 4.853438133199127869, -11.89387501736622710, 32.13663884655806413 ) ) ;
#13178 = ADVANCED_FACE ( 'NONE', ( #63204 ), #83947, .F. ) ;
#13179 = CARTESIAN_POINT ( 'NONE',  ( 6.065255139512838234, -5.941354392334606160, 34.76329471203374055 ) ) ;
#13180 = CARTESIAN_POINT ( 'NONE',  ( -7.384615384615385025, -4.000000000000000000, 29.75000000000000355 ) ) ;
#13181 = ADVANCED_FACE ( 'NONE', ( #88945 ), #55126, .T. ) ;
#13182 = B_SPLINE_CURVE_WITH_KNOTS ( 'NONE', 3,
 ( #80826, #73626, #18673, #19111, #46575, #38491, #86247, #58752, #65506, #32180 ),
 .UNSPECIFIED., .F., .F.,
 ( 4, 2, 2, 2, 4 ),
 ( 0.000000000000000000, 0.0001954339857564073659, 0.0003908679715128147319, 0.0005863019572692221250, 0.0007817359430256294638 ),
 .UNSPECIFIED. ) ;
#13183 = VERTEX_POINT ( 'NONE', #69527 ) ;
#13184 = ORIENTED_EDGE ( 'NONE', *, *, #48131, .F. ) ;
#13185 = ORIENTED_EDGE ( 'NONE', *, *, #57147, .F. ) ;
#13186 = VECTOR ( 'NONE', #25835, 1000.000000000000114 ) ;
#13187 = EDGE_LOOP ( 'NONE', ( #35600, #68783 ) ) ;
#13188 = ADVANCED_FACE ( 'NONE', ( #41179 ), #22230, .F. ) ;
#13189 = CARTESIAN_POINT ( 'NONE',  ( 2.057715576749953978, -4.943428324936578910, 34.04746400365624481 ) ) ;
#13190 = ADVANCED_FACE ( 'NONE', ( #41619 ), #61434, .F. ) ;
#13191 = CARTESIAN_POINT ( 'NONE',  ( 16.15384615384615330, -10.67929555188718282, 33.92786785259544047 ) ) ;
#13192 = AXIS2_PLACEMENT_3D ( 'NONE', #25332, #88388, #52345 ) ;
#13193 = DIRECTION ( 'NONE',  ( 1.000000000000000000, 0.000000000000000000, 0.000000000000000000 ) ) ;
#13194 = CARTESIAN_POINT ( 'NONE',  ( -12.46153846153846168, -11.33034616979429110, 35.88435417666054406 ) ) ;
#13195 = ORIENTED_EDGE ( 'NONE', *, *, #42470, .T. ) ;
#13196 = CARTESIAN_POINT ( 'NONE',  ( 3.480714640147274164, -9.357781135181031829, 34.66075350412533851 ) ) ;
#13197 = CARTESIAN_POINT ( 'NONE',  ( -2.307692307692305711, -4.786620604624113540, 33.94971097300155094 ) ) ;
#13198 = CARTESIAN_POINT ( 'NONE',  ( 17.99999999999987566, -2.625532179533778709, 30.86335684631627174 ) ) ;
#13199 = CARTESIAN_POINT ( 'NONE',  ( 2.307692307692186251, -9.528491918059723176, 34.59228464037033035 ) ) ;
#13200 = EDGE_LOOP ( 'NONE', ( #49302, #84788, #47595, #16160 ) ) ;
#13201 = ORIENTED_EDGE ( 'NONE', *, *, #58690, .T. ) ;
#13202 = EDGE_LOOP ( 'NONE', ( #5124, #37956, #67610, #59324, #4652 ) ) ;
#13203 = DIRECTION ( 'NONE',  ( 0.000000000000000000, 0.8660254037844377084, 0.5000000000000015543 ) ) ;
#13205 = CARTESIAN_POINT ( 'NONE',  ( -9.915792616872023402, -4.225889041578353655, 33.85425143139329407 ) ) ;
#13204 = CARTESIAN_POINT ( 'NONE',  ( -2.980823821391186623, -10.18230066228895758, 34.26354781536631577 ) ) ;
#13206 = LINE ( 'NONE', #74460, #75874 ) ;
#13207 = DIRECTION ( 'NONE',  ( 0.000000000000000000, 0.9848077530122072432, -0.1736481776669354937 ) ) ;
#13208 = EDGE_CURVE ( 'NONE', #62266, #48201, #59450, .T. ) ;
#13209 = FACE_BOUND ( 'NONE', #85961, .T. ) ;
#13210 = EDGE_LOOP ( 'NONE', ( #17041, #44560, #75203, #61413 ) ) ;
#13211 = CARTESIAN_POINT ( 'NONE',  ( 20.00000000000000000, -3.499999999999999556, 28.25000000000000000 ) ) ;
#13212 = CARTESIAN_POINT ( 'NONE',  ( -3.099977422944443006, -6.413143153341454017, 34.63066358083362672 ) ) ;
#13213 = EDGE_LOOP ( 'NONE', ( #8009, #27095 ) ) ;
#13215 = B_SPLINE_CURVE_WITH_KNOTS ( 'NONE', 3,
 ( #20483, #47946, #75429, #41203, #35323, #6968, #68667, #75868, #7420, #34879 ),
 .UNSPECIFIED., .F., .F.,
 ( 4, 2, 2, 2, 4 ),
 ( 0.000000000000000000, 0.0001954339857564080707, 0.0003908679715128161414, 0.0005863019572692241849, 0.0007817359430256322827 ),
 .UNSPECIFIED. ) ;
#13214 = CARTESIAN_POINT ( 'NONE',  ( 17.07692307692307665, -5.471508081941601098, 34.59228464037088457 ) ) ;
#13216 = EDGE_LOOP ( 'NONE', ( #56546, #47262 ) ) ;
#13217 = FACE_BOUND ( 'NONE', #33620, .T. ) ;
#13219 = AXIS2_PLACEMENT_3D ( 'NONE', #86229, #57845, #51965 ) ;
#13218 = CARTESIAN_POINT ( 'NONE',  ( -15.93047021314797007, -2.501478030877323011, 29.88021232661721172 ) ) ;
#13220 = VECTOR ( 'NONE', #2732, 1000.000000000000000 ) ;
#13221 = ORIENTED_EDGE ( 'NONE', *, *, #10311, .F. ) ;
#13222 = DIRECTION ( 'NONE',  ( 0.000000000000000000, 0.4999999999999985567, 0.8660254037844395958 ) ) ;
#13223 = LINE ( 'NONE', #12772, #26021 ) ;
#13224 = CARTESIAN_POINT ( 'NONE',  ( -19.50000000000000000, -3.499999999999999556, 29.75000000000000355 ) ) ;
#13225 = ORIENTED_EDGE ( 'NONE', *, *, #51944, .F. ) ;
#13226 = LINE ( 'NONE', #20423, #13431 ) ;
#13227 = CARTESIAN_POINT ( 'NONE',  ( 14.17700170458200581, -11.37499894934982692, 33.29245874905763003 ) ) ;
#13228 = CARTESIAN_POINT ( 'NONE',  ( 15.23076923076923173, -11.91647553114624181, 32.58852847137148245 ) ) ;
#13229 = CARTESIAN_POINT ( 'NONE',  ( -9.627052121031661969, -2.625532179533470512, 30.86335684631491105 ) ) ;
#13230 = ORIENTED_EDGE ( 'NONE', *, *, #8435, .F. ) ;
#13231 = VECTOR ( 'NONE', #19133, 1000.000000000000000 ) ;
#13232 = CARTESIAN_POINT ( 'NONE',  ( -12.39628289026243380, -3.300289026998473041, 32.46337939537591666 ) ) ;
#13233 = CARTESIAN_POINT ( 'NONE',  ( 3.930361229281822855, -10.23692288466677880, 34.23039457007281072 ) ) ;
#13234 = ORIENTED_EDGE ( 'NONE', *, *, #2287, .F. ) ;
#13235 = LINE ( 'NONE', #81698, #24142 ) ;
#13236 = CARTESIAN_POINT ( 'NONE',  ( 9.823146022794453813, -7.277220318596961057, 34.99547417642776992 ) ) ;
#13237 = CARTESIAN_POINT ( 'NONE',  ( 5.934729554039226862, -9.442884908240170461, 34.35708131394840592 ) ) ;
#13238 = CARTESIAN_POINT ( 'NONE',  ( -5.076923076923197442, -8.613356846316285953, 34.62446782046622218 ) ) ;
#13239 = CARTESIAN_POINT ( 'NONE',  ( -10.61538461538461320, -2.538708090699994813, 30.37095296980875503 ) ) ;
#13240 = DIRECTION ( 'NONE',  ( -0.000000000000000000, 0.6427876096865404731, -0.7660444431189771253 ) ) ;
#13242 = CARTESIAN_POINT ( 'NONE',  ( -16.15384615384615330, -8.164416787775445883, 34.95778746994557906 ) ) ;
#13241 = CARTESIAN_POINT ( 'NONE',  ( -1.384615384615383471, -4.786620604624113540, 33.94971097300155094 ) ) ;
#13243 = CARTESIAN_POINT ( 'NONE',  ( -9.692307692307691624, -6.681629849574314051, 35.83090037661290239 ) ) ;
#13244 = CARTESIAN_POINT ( 'NONE',  ( -2.749999999999998224, -7.500000000000015987, 17.59375000000000000 ) ) ;
#13245 = ORIENTED_EDGE ( 'NONE', *, *, #13501, .T. ) ;
#13246 = DIRECTION ( 'NONE',  ( 0.000000000000000000, 0.000000000000000000, -1.000000000000000000 ) ) ;
#13247 = ORIENTED_EDGE ( 'NONE', *, *, #65779, .F. ) ;
#13248 = ORIENTED_EDGE ( 'NONE', *, *, #37353, .F. ) ;
#13249 = DIRECTION ( 'NONE',  ( -0.000000000000000000, 0.9848077530122086864, -0.1736481776669273891 ) ) ;
#13250 = ORIENTED_EDGE ( 'NONE', *, *, #81810, .T. ) ;
#13251 = CARTESIAN_POINT ( 'NONE',  ( -5.143005456283213483, -11.35647404775217595, 33.31231777344666511 ) ) ;
#13252 = CARTESIAN_POINT ( 'NONE',  ( 1.944543648263018731, -9.444543648262994751, 20.87500000000000000 ) ) ;
#13253 = CARTESIAN_POINT ( 'NONE',  ( 14.30769230769218758, -11.48612834414049644, 32.76840700105863391 ) ) ;
#13254 = CARTESIAN_POINT ( 'NONE',  ( -11.53846153846166089, -10.33852847137269571, 34.16647553114546554 ) ) ;
#13255 = CARTESIAN_POINT ( 'NONE',  ( -2.307692307692305711, -6.386643153685126251, 34.62446782046654192 ) ) ;
#13256 = DIRECTION ( 'NONE',  ( -0.000000000000000000, -0.8660254037844399289, -0.4999999999999980016 ) ) ;
#13257 = CARTESIAN_POINT ( 'NONE',  ( -13.63459211555773720, -2.564618984488975073, 30.55390908950641915 ) ) ;
#13258 = LINE ( 'NONE', #81726, #8036 ) ;
#13259 = VECTOR ( 'NONE', #78017, 1000.000000000000000 ) ;
#13260 = CARTESIAN_POINT ( 'NONE',  ( -16.15384615384615330, -8.564572088678739092, 35.78748833219616898 ) ) ;
#13261 = CARTESIAN_POINT ( 'NONE',  ( -6.988346923633242724, -5.094484230520674117, 34.41647553114621161 ) ) ;
#13262 = DIRECTION ( 'NONE',  ( -1.000000000000000000, -0.000000000000000000, -0.000000000000000000 ) ) ;
#13263 = B_SPLINE_CURVE_WITH_KNOTS ( 'NONE', 3,
 ( #62383, #43459, #2026, #16431, #698, #28164, #76354, #76810, #9243, #42143 ),
 .UNSPECIFIED., .F., .F.,
 ( 4, 2, 2, 2, 4 ),
 ( 0.000000000000000000, 0.0001954339857564098596, 0.0003908679715128197192, 0.0005863019572692296059, 0.0007817359430256394385 ),
 .UNSPECIFIED. ) ;
#13264 = CARTESIAN_POINT ( 'NONE',  ( 5.776515075435670887, -11.60425143139329940, 33.02411095842164457 ) ) ;
#13265 = ORIENTED_EDGE ( 'NONE', *, *, #45343, .F. ) ;
#13266 = ORIENTED_EDGE ( 'NONE', *, *, #26362, .T. ) ;
#13267 = CARTESIAN_POINT ( 'NONE',  ( -11.40793583669797506, -6.001044277235009439, 34.52024696741798948 ) ) ;
#13268 = DIRECTION ( 'NONE',  ( -0.000000000000000000, -0.5000000000000009992, -0.8660254037844380415 ) ) ;
#13269 = DIRECTION ( 'NONE',  ( -0.000000000000000000, -0.9848077530122086864, -0.1736481776669273613 ) ) ;
#13270 = CARTESIAN_POINT ( 'NONE',  ( 5.869308533332442401, -5.582088688514999397, 34.36776431015576350 ) ) ;
#13271 = CARTESIAN_POINT ( 'NONE',  ( 24.99999999999999645, -19.99999999999999645, 3.000000000000000000 ) ) ;
#13272 = DIRECTION ( 'NONE',  ( 0.000000000000000000, 0.000000000000000000, -1.000000000000000000 ) ) ;
#13273 = CARTESIAN_POINT ( 'NONE',  ( -39.05038313613820122, -2.499999999999999556, 29.75000000000000355 ) ) ;
#13274 = EDGE_LOOP ( 'NONE', ( #71321, #36383, #30231, #80298 ) ) ;
#13275 = FACE_OUTER_BOUND ( 'NONE', #30377, .T. ) ;
#13276 = ORIENTED_EDGE ( 'NONE', *, *, #31567, .F. ) ;
#13277 = VERTEX_POINT ( 'NONE', #69969 ) ;
#13278 = AXIS2_PLACEMENT_3D ( 'NONE', #44543, #3122, #24280 ) ;
#13279 = CARTESIAN_POINT ( 'NONE',  ( 17.77651505627605033, -3.236172620538810385, 32.36188796281390267 ) ) ;
#13280 = EDGE_CURVE ( 'NONE', #27014, #54976, #42953, .T. ) ;
#13281 = CARTESIAN_POINT ( 'NONE',  ( 3.903846153846155520, -7.433932668274256805, 35.00000000000000711 ) ) ;
#13282 = CARTESIAN_POINT ( 'NONE',  ( -4.403869391139117795, -4.335965774309649134, 33.62209801155881905 ) ) ;
#13283 = CARTESIAN_POINT ( 'NONE',  ( -1.384615384615505151, -6.879047030192662504, 34.71129190930017927 ) ) ;
#13284 = CARTESIAN_POINT ( 'NONE',  ( 5.776515056276056548, -2.847400154188068022, 31.58180166144859058 ) ) ;
#13285 = AXIS2_PLACEMENT_3D ( 'NONE', #73659, #75417, #13711 ) ;
#13286 = B_SPLINE_CURVE_WITH_KNOTS ( 'NONE', 3,
 ( #59054, #67158, #17640, #17181, #51378, #87445, #66258, #51840, #45984, #4562 ),
 .UNSPECIFIED., .F., .F.,
 ( 4, 2, 2, 2, 4 ),
 ( 0.000000000000000000, 0.0001954311564186861697, 0.0003908623128373723394, 0.0005862934692560584820, 0.0007817246256747446788 ),
 .UNSPECIFIED. ) ;
#13287 = ORIENTED_EDGE ( 'NONE', *, *, #25012, .T. ) ;
#13288 = B_SPLINE_CURVE_WITH_KNOTS ( 'NONE', 3,
 ( #52375, #72204, #72653, #79426, #17267, #3304, #80318, #51468, #18165, #46077 ),
 .UNSPECIFIED., .F., .F.,
 ( 4, 2, 2, 2, 4 ),
 ( 0.0007817359430256364027, 0.0009771253907250043464, 0.001172514838424372399, 0.001367904286123740234, 0.001563293733823108286 ),
 .UNSPECIFIED. ) ;
#13289 = ORIENTED_EDGE ( 'NONE', *, *, #53178, .T. ) ;
#13290 = B_SPLINE_CURVE_WITH_KNOTS ( 'NONE', 3,
 ( #53729, #47855, #80784, #6441, #41547, #54602, #5104, #67695, #33899, #13628 ),
 .UNSPECIFIED., .F., .F.,
 ( 4, 2, 2, 2, 4 ),
 ( 0.000000000000000000, 0.0001954339857564097512, 0.0003908679715128195024, 0.0005863019572692292807, 0.0007817359430256390048 ),
 .UNSPECIFIED. ) ;
#13291 = ORIENTED_EDGE ( 'NONE', *, *, #51202, .T. ) ;
#13292 = ORIENTED_EDGE ( 'NONE', *, *, #81649, .T. ) ;
#13293 = EDGE_CURVE ( 'NONE', #70102, #33999, #15482, .T. ) ;
#13294 = CARTESIAN_POINT ( 'NONE',  ( 18.06606733335007675, -2.292212530054420050, 30.41441678777542990 ) ) ;
#13295 = CARTESIAN_POINT ( 'NONE',  ( 4.946231610255519051, -10.54014554554150607, 33.71984207302941883 ) ) ;
#13296 = CARTESIAN_POINT ( 'NONE',  ( -3.480792468062195333, -10.05641848906368097, 34.04755513067966177 ) ) ;
#13297 = CARTESIAN_POINT ( 'NONE',  ( 17.99999999999987566, -5.941354392335915335, 34.76329471203413846 ) ) ;
#13298 = CARTESIAN_POINT ( 'NONE',  ( -17.07692307692307665, -6.435427911321262684, 35.78748833219616898 ) ) ;
#13299 = ORIENTED_EDGE ( 'NONE', *, *, #23539, .F. ) ;
#13300 = ORIENTED_EDGE ( 'NONE', *, *, #57086, .T. ) ;
#13301 = VERTEX_POINT ( 'NONE', #86156 ) ;
#13303 = ORIENTED_EDGE ( 'NONE', *, *, #32323, .T. ) ;
#13302 = CARTESIAN_POINT ( 'NONE',  ( -4.153846153846152411, -12.48256725967547354, 35.29906147534542527 ) ) ;
#13304 = CARTESIAN_POINT ( 'NONE',  ( 17.20771351789002424, -10.70102852606553157, 33.91149625220312913 ) ) ;
#13305 = CARTESIAN_POINT ( 'NONE',  ( 7.173076923078359535, -7.500000000000155431, 34.75000000000007105 ) ) ;
#13306 = VECTOR ( 'NONE', #44896, 1000.000000000000227 ) ;
#13307 = CARTESIAN_POINT ( 'NONE',  ( -3.749999999999988454, -9.053300858899127945, 21.26562500000000000 ) ) ;
#13308 = EDGE_CURVE ( 'NONE', #622, #6303, #18443, .T. ) ;
#13309 = ORIENTED_EDGE ( 'NONE', *, *, #53086, .F. ) ;
#13310 = CARTESIAN_POINT ( 'NONE',  ( -1.134560964701929464, -2.544122305571458575, 31.48381861865057729 ) ) ;
#13311 = ORIENTED_EDGE ( 'NONE', *, *, #83911, .T. ) ;
#13312 = LINE ( 'NONE', #19622, #84476 ) ;
#13313 = ADVANCED_FACE ( 'NONE', ( #24428 ), #45148, .F. ) ;
#13314 = FACE_BOUND ( 'NONE', #79606, .T. ) ;
#13315 = DIRECTION ( 'NONE',  ( 0.000000000000000000, 0.7660444431189807890, 0.6427876096865361433 ) ) ;
#13316 = EDGE_CURVE ( 'NONE', #53642, #45062, #57803, .T. ) ;
#13317 = CARTESIAN_POINT ( 'NONE',  ( 8.769230769230647482, -5.219633306517616589, 34.19971097300220464 ) ) ;
#13318 = EDGE_LOOP ( 'NONE', ( #68055, #11750, #35082, #44569 ) ) ;
#13319 = LINE ( 'NONE', #61938, #34645 ) ;
#13320 = CARTESIAN_POINT ( 'NONE',  ( 6.792386319966616348, -11.93127051446800024, 32.56575433478200665 ) ) ;
#13321 = CARTESIAN_POINT ( 'NONE',  ( -13.31946960528342139, -7.750023238201979581, 34.74374492549440419 ) ) ;
#13322 = CARTESIAN_POINT ( 'NONE',  ( 0.7115927731767756059, -12.41262288849542017, 30.68299917996395010 ) ) ;
#13323 = ORIENTED_EDGE ( 'NONE', *, *, #86586, .T. ) ;
#13324 = CARTESIAN_POINT ( 'NONE',  ( -0.2381120626236742921, -7.630147987733843173, 34.99859428049665411 ) ) ;
#13325 = DIRECTION ( 'NONE',  ( -0.000000000000000000, 0.5000000000000011102, -0.8660254037844381525 ) ) ;
#13326 = CARTESIAN_POINT ( 'NONE',  ( 4.403900573759606196, -11.47946981652013498, 33.17500667209846910 ) ) ;
#13327 = CARTESIAN_POINT ( 'NONE',  ( 7.846153846153846700, -13.95598074871891292, 31.83374038241031911 ) ) ;
#13328 = DIRECTION ( 'NONE',  ( 1.000000000000000000, 0.000000000000000000, 0.000000000000000000 ) ) ;
#13329 = FACE_BOUND ( 'NONE', #85216, .T. ) ;
#13331 = CARTESIAN_POINT ( 'NONE',  ( -5.999999999999998224, -9.905515769479276145, 34.41647553114623292 ) ) ;
#13330 = CARTESIAN_POINT ( 'NONE',  ( -6.989159302437059296, -12.34228464037088280, 31.77849191805838558 ) ) ;
#13332 = CARTESIAN_POINT ( 'NONE',  ( -9.442362282929648742, -12.07971442181322175, 32.31769673815850297 ) ) ;
#13334 = CARTESIAN_POINT ( 'NONE',  ( -9.627052121031667298, -10.90142922261932057, 33.41473453929631887 ) ) ;
#13333 = DIRECTION ( 'NONE',  ( 0.000000000000000000, 0.9848077530122072432, -0.1736481776669354937 ) ) ;
#13335 = CARTESIAN_POINT ( 'NONE',  ( -5.076923076923199218, -12.51329471203414379, 31.30864560766407578 ) ) ;
#13336 = CARTESIAN_POINT ( 'NONE',  ( 1.200186371490561621, -10.22469193450123193, 19.45125670625849068 ) ) ;
#13337 = EDGE_LOOP ( 'NONE', ( #81958, #25707 ) ) ;
#13338 = AXIS2_PLACEMENT_3D ( 'NONE', #365, #61609, #40908 ) ;
#13339 = CARTESIAN_POINT ( 'NONE',  ( -12.21153846153704237, -7.500000000000154543, 35.00000000000007105 ) ) ;
#13340 = ORIENTED_EDGE ( 'NONE', *, *, #38918, .F. ) ;
#13341 = VECTOR ( 'NONE', #2197, 999.9999999999998863 ) ;
#13342 = DIRECTION ( 'NONE',  ( -0.000000000000000000, 0.3420201433256694901, -0.9396926207859082059 ) ) ;
#13343 = ORIENTED_EDGE ( 'NONE', *, *, #64136, .F. ) ;
#13344 = CYLINDRICAL_SURFACE ( 'NONE', #75730, 0.2500000000000009437 ) ;
#13345 = DIRECTION ( 'NONE',  ( -0.000000000000000000, -0.7660444431189791237, -0.6427876096865379196 ) ) ;
#13347 = ORIENTED_EDGE ( 'NONE', *, *, #64791, .F. ) ;
#13346 = DIRECTION ( 'NONE',  ( -0.000000000000000000, 0.1736481776669307198, -0.9848077530122080203 ) ) ;
#13348 = CARTESIAN_POINT ( 'NONE',  ( -15.29685264172511161, -4.786620604624113540, 33.94971097300155805 ) ) ;
#13349 = CARTESIAN_POINT ( 'NONE',  ( 2.775308065498768517, -8.577988221561467341, 18.04500670625848713 ) ) ;
#13350 = AXIS2_PLACEMENT_3D ( 'NONE', #83853, #48268, #75740 ) ;
#13351 = CARTESIAN_POINT ( 'NONE',  ( -18.00000000000000000, -2.721908614388771852, 31.22303859784724978 ) ) ;
#13352 = CARTESIAN_POINT ( 'NONE',  ( -6.923076923076922462, -12.62096338111211580, 30.90682066428153263 ) ) ;
#13353 = CARTESIAN_POINT ( 'NONE',  ( -5.142193522883852452, -12.46129190929999986, 30.37095296980880832 ) ) ;
#13354 = DIRECTION ( 'NONE',  ( -1.000000000000000000, 0.000000000000000000, 0.000000000000000000 ) ) ;
#13355 = CARTESIAN_POINT ( 'NONE',  ( -12.23875879256039489, -8.540255544307065350, 34.89611431652622286 ) ) ;
#13356 = CARTESIAN_POINT ( 'NONE',  ( -5.776988648387150427, -10.61302985866383963, 33.66295027996417843 ) ) ;
#13357 = CARTESIAN_POINT ( 'NONE',  ( -1.492201783934593573, -3.724691934501250135, 23.07999329374151998 ) ) ;
#13358 = EDGE_CURVE ( 'NONE', #75410, #63745, #29443, .T. ) ;
#13359 = CARTESIAN_POINT ( 'NONE',  ( 5.207448515156718472, -2.647132371071621471, 31.75357179365173010 ) ) ;
#13360 = VERTEX_POINT ( 'NONE', #30746 ) ;
#13361 = DIRECTION ( 'NONE',  ( -0.000000000000000000, 0.3420201433256694901, -0.9396926207859082059 ) ) ;
#13362 = CARTESIAN_POINT ( 'NONE',  ( -2.694853999681181556, -10.10844685921792241, 25.18936829374151642 ) ) ;
#13363 = CARTESIAN_POINT ( 'NONE',  ( -5.999999999999998224, -13.37000171582298513, 34.34916445242398453 ) ) ;
#13364 = CARTESIAN_POINT ( 'NONE',  ( 5.299935921016470708, -6.460100341425561332, 34.89618726649961644 ) ) ;
#13365 = ORIENTED_EDGE ( 'NONE', *, *, #8664, .T. ) ;
#13366 = CARTESIAN_POINT ( 'NONE',  ( -0.7115384615384606759, -7.500000000000001776, 34.75000000000000000 ) ) ;
#13367 = CARTESIAN_POINT ( 'NONE',  ( 13.19230769230769340, -7.500000000000000000, 29.75000000000000355 ) ) ;
#13369 = ORIENTED_EDGE ( 'NONE', *, *, #49974, .F. ) ;
#13368 = CARTESIAN_POINT ( 'NONE',  ( -23.00000000000000000, -10.75000000000000000, 29.75000000000000355 ) ) ;
#13370 = CARTESIAN_POINT ( 'NONE',  ( -7.716106239898160801, -7.723484964179499812, 34.74522123443822608 ) ) ;
#13371 = DIRECTION ( 'NONE',  ( 0.000000000000000000, 0.9848077530122072432, 0.1736481776669354937 ) ) ;
#13372 = EDGE_CURVE ( 'NONE', #36979, #25874, #85707, .T. ) ;
#13373 = CYLINDRICAL_SURFACE ( 'NONE', #61550, 0.2500000000000004996 ) ;
#13374 = AXIS2_PLACEMENT_3D ( 'NONE', #62320, #634, #61437 ) ;
#13375 = CARTESIAN_POINT ( 'NONE',  ( -17.01166750564705410, -2.892918686051626054, 31.69288490824025928 ) ) ;
#13376 = LINE ( 'NONE', #81853, #7752 ) ;
#13377 = CARTESIAN_POINT ( 'NONE',  ( -13.38461538461538325, -8.164416787775445883, 34.95778746994557906 ) ) ;
#13378 = ORIENTED_EDGE ( 'NONE', *, *, #70926, .F. ) ;
#13379 = VERTEX_POINT ( 'NONE', #51434 ) ;
#13380 = ORIENTED_EDGE ( 'NONE', *, *, #53594, .T. ) ;
#13381 = ORIENTED_EDGE ( 'NONE', *, *, #51107, .T. ) ;
#13382 = EDGE_CURVE ( 'NONE', #17730, #34333, #85265, .T. ) ;
#13383 = CARTESIAN_POINT ( 'NONE',  ( -9.627052121031665521, -3.300289026998473041, 32.46337939537591666 ) ) ;
#13384 = CARTESIAN_POINT ( 'NONE',  ( 14.30769230769231015, -4.098570777380720287, 33.41473453929634729 ) ) ;
#13385 = EDGE_CURVE ( 'NONE', #38776, #33822, #36634, .T. ) ;
#13386 = CARTESIAN_POINT ( 'NONE',  ( -13.38461538461550582, -12.27809138561165270, 31.22303859784587132 ) ) ;
#13387 = CYLINDRICAL_SURFACE ( 'NONE', #35124, 0.2500000000000009437 ) ;
#13388 = CARTESIAN_POINT ( 'NONE',  ( 5.207714884747862705, -5.582136614379148654, 34.36778462344220486 ) ) ;
#13389 = EDGE_LOOP ( 'NONE', ( #42349, #73873 ) ) ;
#13390 = ORIENTED_EDGE ( 'NONE', *, *, #69998, .F. ) ;
#13392 = VERTEX_POINT ( 'NONE', #63651 ) ;
#13391 = EDGE_CURVE ( 'NONE', #36002, #67813, #88337, .T. ) ;
#13394 = VERTEX_POINT ( 'NONE', #1957 ) ;
#13393 = CARTESIAN_POINT ( 'NONE',  ( -7.173100147298381302, -8.475808217655753651, 34.90892951860618609 ) ) ;
#13395 = CARTESIAN_POINT ( 'NONE',  ( -1.634592128663975741, -2.920706130388546651, 32.31842814019191223 ) ) ;
#13396 = CARTESIAN_POINT ( 'NONE',  ( -10.74599497500914325, -7.722926236386453702, 34.74524107206102030 ) ) ;
#13397 = EDGE_CURVE ( 'NONE', #64660, #14886, #58216, .T. ) ;
#13398 = AXIS2_PLACEMENT_3D ( 'NONE', #23250, #79545, #25034 ) ;
#13399 = CARTESIAN_POINT ( 'NONE',  ( 7.053602361310566948, -5.070358843744210198, 34.40418822224088302 ) ) ;
#13400 = LINE ( 'NONE', #41322, #30939 ) ;
#13401 = EDGE_CURVE ( 'NONE', #87539, #86167, #78054, .T. ) ;
#13402 = ORIENTED_EDGE ( 'NONE', *, *, #29009, .F. ) ;
#13403 = AXIS2_PLACEMENT_3D ( 'NONE', #50907, #9078, #63560 ) ;
#13404 = ORIENTED_EDGE ( 'NONE', *, *, #68033, .T. ) ;
#13405 = ORIENTED_EDGE ( 'NONE', *, *, #32911, .T. ) ;
#13406 = CARTESIAN_POINT ( 'NONE',  ( -8.769230769230768274, -11.91647553114624181, 32.58852847137148245 ) ) ;
#13408 = ORIENTED_EDGE ( 'NONE', *, *, #7732, .T. ) ;
#13407 = CARTESIAN_POINT ( 'NONE',  ( 3.262820512820510999, -7.500000000000000000, 33.75000000000000000 ) ) ;
#13409 = CARTESIAN_POINT ( 'NONE',  ( 9.626224281351811740, -11.69971097300155272, 32.46337939537587403 ) ) ;
#13410 = B_SPLINE_CURVE_WITH_KNOTS ( 'NONE', 3,
 ( #11584, #54328, #39953, #60201, #53894, #18336, #80943, #39066, #66063, #52991 ),
 .UNSPECIFIED., .F., .F.,
 ( 4, 2, 2, 2, 4 ),
 ( 0.000000000000000000, 0.0001954339857564098054, 0.0003908679715128196108, 0.0005863019572692293891, 0.0007817359430256392216 ),
 .UNSPECIFIED. ) ;
#13411 = CARTESIAN_POINT ( 'NONE',  ( -2.294871794871794712, -7.500000000000000000, 29.75000000000000355 ) ) ;
#13412 = EDGE_CURVE ( 'NONE', #14506, #85420, #40932, .T. ) ;
#13413 = ORIENTED_EDGE ( 'NONE', *, *, #29791, .T. ) ;
#13414 = CARTESIAN_POINT ( 'NONE',  ( -4.023320452082589149, -5.195472089885680766, 34.18748526763464923 ) ) ;
#13415 = DIRECTION ( 'NONE',  ( 0.000000000000000000, -6.938893903907222067E-15, 1.000000000000000000 ) ) ;
#13416 = B_SPLINE_CURVE_WITH_KNOTS ( 'NONE', 3,
 ( #21309, #14559, #1047, #1932, #15900, #7806, #83476, #50548, #64492, #70844 ),
 .UNSPECIFIED., .F., .F.,
 ( 4, 2, 2, 2, 4 ),
 ( 0.000000000000000000, 0.0001954339857564054144, 0.0003908679715128108288, 0.0005863019572692162703, 0.0007817359430256216575 ),
 .UNSPECIFIED. ) ;
#13417 = FACE_BOUND ( 'NONE', #37156, .T. ) ;
#13418 = CARTESIAN_POINT ( 'NONE',  ( -0.5916856709766825650, -10.19110544564092002, 33.96427741523702792 ) ) ;
#13419 = CARTESIAN_POINT ( 'NONE',  ( -39.05038313613820122, 12.25000000000000711, 28.74999999999999645 ) ) ;
#13420 = CARTESIAN_POINT ( 'NONE',  ( 12.39626846098214230, -6.835583212224499938, 34.95778746994557906 ) ) ;
#13422 = DIRECTION ( 'NONE',  ( 0.000000000000000000, -1.000000000000000000, 0.000000000000000000 ) ) ;
#13421 = CARTESIAN_POINT ( 'NONE',  ( -17.77440776823446100, -12.74866226681162296, 29.87809195722894628 ) ) ;
#13423 = EDGE_CURVE ( 'NONE', #2558, #7803, #64520, .T. ) ;
#13424 = CYLINDRICAL_SURFACE ( 'NONE', #71108, 0.2500000000000004996 ) ;
#13425 = CARTESIAN_POINT ( 'NONE',  ( -0.4615384615385826339, -3.835265460704628371, 33.15142922262033665 ) ) ;
#13426 = ORIENTED_EDGE ( 'NONE', *, *, #17456, .T. ) ;
#13427 = EDGE_CURVE ( 'NONE', #64802, #80981, #51748, .T. ) ;
#13428 = CARTESIAN_POINT ( 'NONE',  ( -2.437840277424002444, -4.299443229763728169, 33.91186481527756058 ) ) ;
#13429 = PLANE ( 'NONE',  #13338 ) ;
#13430 = ORIENTED_EDGE ( 'NONE', *, *, #23135, .T. ) ;
#13431 = VECTOR ( 'NONE', #12776, 1000.000000000000227 ) ;
#13432 = AXIS2_PLACEMENT_3D ( 'NONE', #40766, #48391, #55592 ) ;
#13433 = CARTESIAN_POINT ( 'NONE',  ( -14.55766903863466055, -4.943428324936578910, 34.04746400365624481 ) ) ;
#13434 = CARTESIAN_POINT ( 'NONE',  ( -4.153846153846274980, -3.643525952248796163, 33.31231777344771672 ) ) ;
#13435 = ORIENTED_EDGE ( 'NONE', *, *, #69105, .F. ) ;
#13436 = DIRECTION ( 'NONE',  ( -0.000000000000000000, 0.9848077530122086864, -0.1736481776669273891 ) ) ;
#13437 = CARTESIAN_POINT ( 'NONE',  ( -15.09997878980228059, -12.62708834333097663, 30.88030960425257021 ) ) ;
#13438 = FACE_BOUND ( 'NONE', #2747, .T. ) ;
#13440 = CARTESIAN_POINT ( 'NONE',  ( -16.85414353565466428, -12.44528174975671853, 30.48912976160715615 ) ) ;
#13439 = CARTESIAN_POINT ( 'NONE',  ( -15.45369544828538011, -5.667676309546437530, 34.40238873228292249 ) ) ;
#13441 = CARTESIAN_POINT ( 'NONE',  ( -13.45069776397551742, -2.292212530054419606, 30.41441678777542634 ) ) ;
#13442 = LINE ( 'NONE', #47673, #49649 ) ;
#13443 = CARTESIAN_POINT ( 'NONE',  ( -8.703975197954742171, -12.27809138561124591, 31.22303859784720359 ) ) ;
#13444 = CARTESIAN_POINT ( 'NONE',  ( 2.320192649118979489E-14, -11.25000000000000000, 24.78125000000000000 ) ) ;
#13445 = ORIENTED_EDGE ( 'NONE', *, *, #74326, .F. ) ;
#13446 = EDGE_LOOP ( 'NONE', ( #86883, #59901, #76602, #31099 ) ) ;
#13447 = CARTESIAN_POINT ( 'NONE',  ( -5.076923076923075762, -13.04860791097971706, 34.73218667398347037 ) ) ;
#13448 = PLANE ( 'NONE',  #12478 ) ;
#13449 = DIRECTION ( 'NONE',  ( -0.000000000000000000, -0.9848077530122085754, -0.1736481776669273613 ) ) ;
#13450 = DIRECTION ( 'NONE',  ( 0.000000000000000000, 0.7660444431189807890, 0.6427876096865361433 ) ) ;
#13451 = CARTESIAN_POINT ( 'NONE',  ( -7.846153846153530509, -2.255955759149395501, 30.00000000000324363 ) ) ;
#13452 = CARTESIAN_POINT ( 'NONE',  ( -2.694853999681210865, -4.891553140782108677, 14.99813170625848713 ) ) ;
#13453 = CARTESIAN_POINT ( 'NONE',  ( -7.780898274877820597, -8.613356846314928816, 34.62446782046653482 ) ) ;
#13454 = CARTESIAN_POINT ( 'NONE',  ( -6.250023224221455287, -8.475808217655753651, 34.90892951860618609 ) ) ;
#13455 = CARTESIAN_POINT ( 'NONE',  ( -4.826868657009623753, -2.318338780012835443, 30.59689888758630261 ) ) ;
#13456 = CARTESIAN_POINT ( 'NONE',  ( 10.83816428436267820, -3.563462043263030399, 33.22394488606062879 ) ) ;
#13457 = CARTESIAN_POINT ( 'NONE',  ( -4.946397638689432164, -6.808710257144159783, 34.95449254468098843 ) ) ;
#13458 = B_SPLINE_CURVE_WITH_KNOTS ( 'NONE', 3,
 ( #45837, #30983, #66103, #31895, #39102, #59800, #87298, #25575, #12076, #39553 ),
 .UNSPECIFIED., .F., .F.,
 ( 4, 2, 2, 2, 4 ),
 ( 0.000000000000000000, 0.0001954339857564092362, 0.0003908679715128184724, 0.0005863019572692276544, 0.0007817359430256369448 ),
 .UNSPECIFIED. ) ;
#13459 = DIRECTION ( 'NONE',  ( -0.000000000000000000, 0.9396926207859093161, -0.3420201433256663259 ) ) ;
#13460 = B_SPLINE_CURVE_WITH_KNOTS ( 'NONE', 3,
 ( #63250, #1555, #8765, #29042, #56499, #70903, #9209, #36234, #50618, #36672 ),
 .UNSPECIFIED., .F., .F.,
 ( 4, 2, 2, 2, 4 ),
 ( 0.000000000000000000, 0.0001954311564186880670, 0.0003908623128373761341, 0.0005862934692560642282, 0.0007817246256747522682 ),
 .UNSPECIFIED. ) ;
#13461 = CARTESIAN_POINT ( 'NONE',  ( 17.32692307692307665, -2.249999999999998668, 29.75000000000000355 ) ) ;
#13462 = EDGE_CURVE ( 'NONE', #19422, #27220, #66774, .T. ) ;
#13463 = VECTOR ( 'NONE', #75430, 1000.000000000000114 ) ;
#13464 = CARTESIAN_POINT ( 'NONE',  ( -3.453695448285377445, -8.239355502252617924, 34.69524867566427417 ) ) ;
#13465 = CARTESIAN_POINT ( 'NONE',  ( 6.000000000000001776, -5.557115091759785130, 34.35708131394839171 ) ) ;
#13466 = ORIENTED_EDGE ( 'NONE', *, *, #15508, .F. ) ;
#13467 = ADVANCED_FACE ( 'NONE', ( #67656 ), #5062, .F. ) ;
#13468 = CARTESIAN_POINT ( 'NONE',  ( -5.010854725920637520, -11.69971097300155272, 32.46337939537588113 ) ) ;
#13469 = ADVANCED_FACE ( 'NONE', ( #73971 ), #12707, .F. ) ;
#13470 = CARTESIAN_POINT ( 'NONE',  ( -3.454254174493179619, -3.754499324213721234, 33.06261337010820256 ) ) ;
#13471 = CARTESIAN_POINT ( 'NONE',  ( 0.06109907496451789238, -4.749999999999998224, 19.40811829374151287 ) ) ;
#13472 = AXIS2_PLACEMENT_3D ( 'NONE', #74758, #27007, #74309 ) ;
#13473 = EDGE_CURVE ( 'NONE', #66098, #34205, #33330, .T. ) ;
#13474 = CIRCLE ( 'NONE', #7694, 0.2500000000000002220 ) ;
#13475 = CARTESIAN_POINT ( 'NONE',  ( -16.15384615384615330, -13.04860791097971706, 34.73218667398347037 ) ) ;
#13476 = CARTESIAN_POINT ( 'NONE',  ( -17.77698864838715309, -10.61302985866384141, 33.66295027996417843 ) ) ;
#13477 = CARTESIAN_POINT ( 'NONE',  ( -11.47239420511146513, -4.661471528628508665, 34.16647553114624003 ) ) ;
#13479 = ORIENTED_EDGE ( 'NONE', *, *, #75333, .T. ) ;
#13478 = CARTESIAN_POINT ( 'NONE',  ( -9.626239341305252495, -4.786620604624113540, 33.94971097300155805 ) ) ;
#13480 = CARTESIAN_POINT ( 'NONE',  ( 2.750000000000001776, -7.499999999999984013, 23.21875000000000000 ) ) ;
#13481 = DIRECTION ( 'NONE',  ( -0.000000000000000000, 0.1736481776669307198, -0.9848077530122080203 ) ) ;
#13482 = ORIENTED_EDGE ( 'NONE', *, *, #59609, .F. ) ;
#13483 = FACE_OUTER_BOUND ( 'NONE', #9413, .T. ) ;
#13484 = ADVANCED_FACE ( 'NONE', ( #79840 ), #5957, .F. ) ;
#13485 = CARTESIAN_POINT ( 'NONE',  ( 4.153846153846154188, -6.343179335718451384, 34.87096338111211935 ) ) ;
#13486 = ORIENTED_EDGE ( 'NONE', *, *, #15552, .T. ) ;
#13487 = CARTESIAN_POINT ( 'NONE',  ( -10.86536135943320502, -4.075325502946081535, 33.72974371597206300 ) ) ;
#13488 = CARTESIAN_POINT ( 'NONE',  ( 27.00000000000000000, 0.7500000000000052180, 31.75000000000000000 ) ) ;
#13489 = CARTESIAN_POINT ( 'NONE',  ( 15.29683758177167086, -2.721908614388771852, 31.22303859784725333 ) ) ;
#13490 = ORIENTED_EDGE ( 'NONE', *, *, #64503, .T. ) ;
#13491 = ORIENTED_EDGE ( 'NONE', *, *, #34818, .T. ) ;
#13492 = CARTESIAN_POINT ( 'NONE',  ( 17.93391762063986405, -9.905515769479276145, 34.41647553114623292 ) ) ;
#13493 = ORIENTED_EDGE ( 'NONE', *, *, #9556, .F. ) ;
#13494 = B_SPLINE_CURVE_WITH_KNOTS ( 'NONE', 3,
 ( #69765, #31779, #65988, #10169, #4298, #10614, #29998, #37633, #65095, #3400 ),
 .UNSPECIFIED., .F., .F.,
 ( 4, 2, 2, 2, 4 ),
 ( 0.000000000000000000, 0.0001954311564186859800, 0.0003908623128373719599, 0.0005862934692560579399, 0.0007817246256747439198 ),
 .UNSPECIFIED. ) ;
#13495 = CARTESIAN_POINT ( 'NONE',  ( -17.86920955903305597, -4.684288915650983043, 34.18129842949671371 ) ) ;
#13496 = CARTESIAN_POINT ( 'NONE',  ( -9.442253380669374252, -9.943054286541403997, 34.11300777759954883 ) ) ;
#13497 = CARTESIAN_POINT ( 'NONE',  ( -17.30040802064702987, -5.912607949931405038, 34.49155766932282319 ) ) ;
#13498 = B_SPLINE_CURVE_WITH_KNOTS ( 'NONE', 3,
 ( #452, #40997, #30021, #9741, #11, #27480, #77317, #20716, #41437, #57481 ),
 .UNSPECIFIED., .F., .F.,
 ( 4, 2, 2, 2, 4 ),
 ( 0.0007817246256747506419, 0.0009771112852218957062, 0.001172497944769040771, 0.001367884604316185835, 0.001563271263863330899 ),
 .UNSPECIFIED. ) ;
#13499 = CARTESIAN_POINT ( 'NONE',  ( 3.230769230769231726, -6.435427911321262684, 35.78748833219616898 ) ) ;
#13501 = EDGE_CURVE ( 'NONE', #36898, #71705, #47720, .T. ) ;
#13500 = CARTESIAN_POINT ( 'NONE',  ( 15.00784301325308157, -6.503392248772476236, 34.64988816332204635 ) ) ;
#13502 = CARTESIAN_POINT ( 'NONE',  ( 13.51514108637895006, -3.285477652293413264, 32.44071101563363158 ) ) ;
#13503 = VECTOR ( 'NONE', #36038, 1000.000000000000000 ) ;
#13504 = DIRECTION ( 'NONE',  ( -0.000000000000000000, -0.000000000000000000, -1.000000000000000000 ) ) ;
#13505 = B_SPLINE_CURVE_WITH_KNOTS ( 'NONE', 3,
 ( #46681, #81368, #39941, #66960, #52982, #80478, #75053, #5693, #60188, #52542 ),
 .UNSPECIFIED., .F., .F.,
 ( 4, 2, 2, 2, 4 ),
 ( 0.000000000000000000, 0.0001954311564186862239, 0.0003908623128373724478, 0.0005862934692560586988, 0.0007817246256747448956 ),
 .UNSPECIFIED. ) ;
#13506 = ORIENTED_EDGE ( 'NONE', *, *, #32299, .T. ) ;
#13507 = ORIENTED_EDGE ( 'NONE', *, *, #48820, .T. ) ;
#13509 = VERTEX_POINT ( 'NONE', #53687 ) ;
#13508 = CYLINDRICAL_SURFACE ( 'NONE', #78931, 0.2500000000000002220 ) ;
#13510 = CARTESIAN_POINT ( 'NONE',  ( -39.05038313613820122, -2.249999999999998668, 29.75000000000000355 ) ) ;
#13511 = CARTESIAN_POINT ( 'NONE',  ( 9.692307692307572609, -5.219633306517616589, 34.19971097300220464 ) ) ;
#13512 = EDGE_LOOP ( 'NONE', ( #45247, #49213 ) ) ;
#13513 = CARTESIAN_POINT ( 'NONE',  ( 15.45378207486262667, -9.172514111537584114, 34.72667873470787470 ) ) ;
#13514 = EDGE_LOOP ( 'NONE', ( #599, #37743, #68344, #84511 ) ) ;
#13515 = DIRECTION ( 'NONE',  ( -1.000000000000000000, -0.000000000000000000, -0.000000000000000000 ) ) ;
#13516 = ORIENTED_EDGE ( 'NONE', *, *, #36717, .F. ) ;
#13517 = FACE_OUTER_BOUND ( 'NONE', #80501, .T. ) ;
#13518 = VECTOR ( 'NONE', #17839, 1000.000000000000227 ) ;
#13520 = ORIENTED_EDGE ( 'NONE', *, *, #87265, .T. ) ;
#13519 = EDGE_CURVE ( 'NONE', #74089, #88595, #74274, .T. ) ;
#13521 = EDGE_CURVE ( 'NONE', #27705, #67440, #52795, .T. ) ;
#13522 = CARTESIAN_POINT ( 'NONE',  ( -4.219928533206287469, -3.937682226553329556, 33.60647404775217240 ) ) ;
#13523 = CARTESIAN_POINT ( 'NONE',  ( 5.448717948717947124, -3.499999999999999556, 29.75000000000000355 ) ) ;
#13524 = FACE_BOUND ( 'NONE', #366, .T. ) ;
#13525 = DIRECTION ( 'NONE',  ( -0.000000000000000000, 0.3420201433256694346, -0.9396926207859080948 ) ) ;
#13527 = EDGE_CURVE ( 'NONE', #42531, #60579, #26663, .T. ) ;
#13526 = CARTESIAN_POINT ( 'NONE',  ( -18.25000000000000355, -7.500000000000000000, 35.00000000000000000 ) ) ;
#13528 = VECTOR ( 'NONE', #71559, 1000.000000000000000 ) ;
#13529 = CARTESIAN_POINT ( 'NONE',  ( 3.230769230769231726, -12.78798330534102945, 29.74999999999997868 ) ) ;
#13530 = CARTESIAN_POINT ( 'NONE',  ( 1.318533005255249746, -12.34228464037088280, 31.77849191805838558 ) ) ;
#13531 = CARTESIAN_POINT ( 'NONE',  ( -9.692307692307812417, -8.613356846316285953, 34.62446782046622218 ) ) ;
#13532 = CARTESIAN_POINT ( 'NONE',  ( -10.03846153846153832, -11.00000000000000000, 29.65000000000000213 ) ) ;
#13533 = EDGE_CURVE ( 'NONE', #52054, #57554, #47468, .T. ) ;
#13534 = CARTESIAN_POINT ( 'NONE',  ( -14.08468095607945969, -3.587049720035815348, 32.86302985866382897 ) ) ;
#13535 = ORIENTED_EDGE ( 'NONE', *, *, #81115, .F. ) ;
#13536 = EDGE_LOOP ( 'NONE', ( #29023, #28902, #26791, #68341 ) ) ;
#13538 = CARTESIAN_POINT ( 'NONE',  ( 9.320512820512821150, -7.500000000000000000, 33.75000000000000000 ) ) ;
#13537 = CARTESIAN_POINT ( 'NONE',  ( 2.084766090176162212, -10.61292498521070549, 33.66303323003028680 ) ) ;
#13539 = EDGE_CURVE ( 'NONE', #48169, #54584, #22728, .T. ) ;
#13540 = CARTESIAN_POINT ( 'NONE',  ( 7.146088274689773812, -6.503523203565942268, 34.64991518177335195 ) ) ;
#13541 = CARTESIAN_POINT ( 'NONE',  ( -3.230769230769229949, -5.557115091759785130, 34.35708131394839171 ) ) ;
#13542 = DIRECTION ( 'NONE',  ( 0.000000000000000000, 0.000000000000000000, -1.000000000000000000 ) ) ;
#13543 = CARTESIAN_POINT ( 'NONE',  ( 9.692307692307695177, -13.49023893513002648, 31.06009739812518688 ) ) ;
#13544 = ORIENTED_EDGE ( 'NONE', *, *, #60808, .T. ) ;
#13545 = CARTESIAN_POINT ( 'NONE',  ( 17.20771488474786182, -3.062576670634119758, 32.05464942895959979 ) ) ;
#13546 = CARTESIAN_POINT ( 'NONE',  ( 15.23076923076923173, -3.937682226553329556, 33.60647404775216529 ) ) ;
#13547 = CARTESIAN_POINT ( 'NONE',  ( 5.999999999999880096, -12.27809138561165270, 31.22303859784587132 ) ) ;
#13548 = CARTESIAN_POINT ( 'NONE',  ( -2.307692307692305711, -4.102666532097928531, 36.13435417666054406 ) ) ;
#13549 = EDGE_LOOP ( 'NONE', ( #32447, #55705, #63906, #42308 ) ) ;
#13550 = EDGE_CURVE ( 'NONE', #54586, #13301, #41069, .T. ) ;
#13551 = ORIENTED_EDGE ( 'NONE', *, *, #33119, .T. ) ;
#13552 = ORIENTED_EDGE ( 'NONE', *, *, #74581, .F. ) ;
#13553 = CARTESIAN_POINT ( 'NONE',  ( 15.23076923076911093, -6.879047030192662504, 34.71129190930017927 ) ) ;
#13554 = EDGE_CURVE ( 'NONE', #39978, #29264, #5525, .T. ) ;
#13555 = VERTEX_POINT ( 'NONE', #34746 ) ;
#13556 = CARTESIAN_POINT ( 'NONE',  ( 3.007284306204899504, -12.69144148231606017, 30.53333754910549303 ) ) ;
#13557 = CARTESIAN_POINT ( 'NONE',  ( -9.692307692307812417, -11.94971097300221174, 32.03036669348237098 ) ) ;
#13558 = CARTESIAN_POINT ( 'NONE',  ( -5.326899807865431491, -4.236021600441998380, 33.53823185664189310 ) ) ;
#13559 = CARTESIAN_POINT ( 'NONE',  ( -17.07692307692307665, -9.058645607665452459, 34.76329471203371924 ) ) ;
#13560 = CARTESIAN_POINT ( 'NONE',  ( 14.37376065869474751, -4.098570777380720287, 33.41473453929635440 ) ) ;
#13562 = ORIENTED_EDGE ( 'NONE', *, *, #17908, .T. ) ;
#13561 = AXIS2_PLACEMENT_3D ( 'NONE', #47095, #61061, #88564 ) ;
#13563 = LINE ( 'NONE', #41044, #24217 ) ;
#13565 = ORIENTED_EDGE ( 'NONE', *, *, #10172, .F. ) ;
#13564 = CARTESIAN_POINT ( 'NONE',  ( -16.28453762051371712, -11.71456829005830080, 32.44064028649416542 ) ) ;
#13566 = CARTESIAN_POINT ( 'NONE',  ( 0.4615384615383396616, -6.026961402154118908, 34.52809138561165270 ) ) ;
#13567 = CYLINDRICAL_SURFACE ( 'NONE', #48265, 0.5000000000000004441 ) ;
#13568 = CARTESIAN_POINT ( 'NONE',  ( 1.319291371811078362, -7.749976730030849303, 34.74374725381503737 ) ) ;
#13569 = CARTESIAN_POINT ( 'NONE',  ( -4.153846153846152411, -1.044019251281081972, 31.83374038241031911 ) ) ;
#13570 = EDGE_CURVE ( 'NONE', #57920, #48838, #48256, .T. ) ;
#13571 = CARTESIAN_POINT ( 'NONE',  ( -12.52762187249434156, -2.721908614388770964, 31.22303859784723912 ) ) ;
#13572 = DIRECTION ( 'NONE',  ( -0.000000000000000000, -0.7660444431189791237, -0.6427876096865379196 ) ) ;
#13573 = CARTESIAN_POINT ( 'NONE',  ( 12.46153846153846168, -11.16473453929635440, 33.15142922261926373 ) ) ;
#13574 = CARTESIAN_POINT ( 'NONE',  ( 2.775308065498755195, -6.422011778438505125, 22.14249329374151998 ) ) ;
#13575 = ORIENTED_EDGE ( 'NONE', *, *, #43956, .F. ) ;
#13576 = EDGE_CURVE ( 'NONE', #84581, #68662, #53842, .T. ) ;
#13577 = CARTESIAN_POINT ( 'NONE',  ( 14.98074599347626368, -8.432397168068783699, 34.66272746175022945 ) ) ;
#13578 = DIRECTION ( 'NONE',  ( 0.000000000000000000, 0.3420201433256641055, -0.9396926207859100932 ) ) ;
#13579 = CYLINDRICAL_SURFACE ( 'NONE', #5807, 0.2500000000000009437 ) ;
#13580 = CARTESIAN_POINT ( 'NONE',  ( -13.13456107297706588, -8.303483539816728154, 34.68545999027711702 ) ) ;
#13581 = VERTEX_POINT ( 'NONE', #7731 ) ;
#13582 = CARTESIAN_POINT ( 'NONE',  ( 23.49999999999998934, 4.710477821889702467E-15, 29.24999999999999289 ) ) ;
#13583 = CARTESIAN_POINT ( 'NONE',  ( 11.31497661389720832, -12.69144148231606017, 30.53333754910549303 ) ) ;
#13584 = CARTESIAN_POINT ( 'NONE',  ( 2.557637717070352590, -10.92531984108285670, 33.72920026020278073 ) ) ;
#13585 = EDGE_CURVE ( 'NONE', #28571, #2346, #82945, .T. ) ;
#13586 = CARTESIAN_POINT ( 'NONE',  ( -19.00000000000000000, 17.00000000000000000, 2.999999999999999112 ) ) ;
#13587 = CARTESIAN_POINT ( 'NONE',  ( 16.15384615384615330, -3.886160181151819604, 36.00935417666054406 ) ) ;
#13588 = VERTEX_POINT ( 'NONE', #55460 ) ;
#13589 = B_SPLINE_CURVE_WITH_KNOTS ( 'NONE', 3,
 ( #46801, #33297, #60755, #61635, #26538, #52660, #13017, #73842, #87818, #80147 ),
 .UNSPECIFIED., .F., .F.,
 ( 4, 2, 2, 2, 4 ),
 ( 0.000000000000000000, 0.0001954311564186869557, 0.0003908623128373739115, 0.0005862934692560608672, 0.0007817246256747478229 ),
 .UNSPECIFIED. ) ;
#13590 = CARTESIAN_POINT ( 'NONE',  ( -16.37733107841048508, -6.716662450894490100, 34.94144148231605840 ) ) ;
#13591 = B_SPLINE_CURVE_WITH_KNOTS ( 'NONE', 3,
 ( #42326, #56269, #85076, #35108, #29691, #42766, #9410, #57150, #43631, #62571 ),
 .UNSPECIFIED., .F., .F.,
 ( 4, 2, 2, 2, 4 ),
 ( 0.0007817359430256324996, 0.0009771253907249991422, 0.001172514838424365676, 0.001367904286123732428, 0.001563293733823098962 ),
 .UNSPECIFIED. ) ;
#13592 = EDGE_CURVE ( 'NONE', #65829, #2166, #69961, .T. ) ;
#13593 = DIRECTION ( 'NONE',  ( -0.000000000000000000, -0.7660444431189791237, -0.6427876096865379196 ) ) ;
#13594 = CARTESIAN_POINT ( 'NONE',  ( -14.53052040532718614, -7.369209533119140509, 34.99857337881830688 ) ) ;
#13595 = ORIENTED_EDGE ( 'NONE', *, *, #70142, .F. ) ;
#13596 = CARTESIAN_POINT ( 'NONE',  ( -5.999999999999998224, -13.04860791097971706, 34.73218667398347037 ) ) ;
#13597 = VECTOR ( 'NONE', #8521, 999.9999999999998863 ) ;
#13598 = B_SPLINE_CURVE_WITH_KNOTS ( 'NONE', 3,
 ( #40170, #27082, #67189, #47347, #20332, #67635, #73507, #73951, #25309, #19440 ),
 .UNSPECIFIED., .F., .F.,
 ( 4, 2, 2, 2, 4 ),
 ( 0.0007817246256747524850, 0.0009771112852218972241, 0.001172497944769042072, 0.001367884604316186702, 0.001563271263863331550 ),
 .UNSPECIFIED. ) ;
#13599 = CIRCLE ( 'NONE', #68243, 4.000000000000000000 ) ;
#13600 = ORIENTED_EDGE ( 'NONE', *, *, #81007, .T. ) ;
#13601 = DIRECTION ( 'NONE',  ( -1.000000000000000000, 0.000000000000000000, -0.000000000000000000 ) ) ;
#13602 = PLANE ( 'NONE',  #46970 ) ;
#13603 = EDGE_LOOP ( 'NONE', ( #73712, #25816, #33241, #63253 ) ) ;
#13604 = CARTESIAN_POINT ( 'NONE',  ( 7.596177115211492747, -12.17611988154120972, 31.52148481390971213 ) ) ;
#13606 = EDGE_CURVE ( 'NONE', #37663, #71986, #86072, .T. ) ;
#13605 = CARTESIAN_POINT ( 'NONE',  ( -14.37296230824862775, -2.379036618887870436, 30.90682066428147934 ) ) ;
#13607 = CARTESIAN_POINT ( 'NONE',  ( -10.61538461538461320, -5.557115091759785130, 34.35708131394839171 ) ) ;
#13608 = ADVANCED_FACE ( 'NONE', ( #47369 ), #40634, .F. ) ;
#13609 = CARTESIAN_POINT ( 'NONE',  ( 6.988332062589760696, -12.51329471203373700, 31.30864560766537963 ) ) ;
#13610 = CARTESIAN_POINT ( 'NONE',  ( -0.4615384615384611200, -11.35647404775217417, 33.31231777344666511 ) ) ;
#13611 = ORIENTED_EDGE ( 'NONE', *, *, #29112, .F. ) ;
#13612 = FACE_BOUND ( 'NONE', #75017, .T. ) ;
#13613 = EDGE_LOOP ( 'NONE', ( #62150, #17032, #28522, #14523 ) ) ;
#13614 = CARTESIAN_POINT ( 'NONE',  ( 11.53846153846153832, -2.292212530054420494, 30.41441678777542634 ) ) ;
#13615 = DIRECTION ( 'NONE',  ( 0.000000000000000000, 0.000000000000000000, 1.000000000000000000 ) ) ;
#13616 = CARTESIAN_POINT ( 'NONE',  ( 3.165499230212911019, -11.67786785259541027, 32.92929555188721480 ) ) ;
#13617 = DIRECTION ( 'NONE',  ( -0.000000000000000000, 1.000000000000000000, -0.000000000000000000 ) ) ;
#13618 = ORIENTED_EDGE ( 'NONE', *, *, #41041, .F. ) ;
#13619 = B_SPLINE_CURVE_WITH_KNOTS ( 'NONE', 3,
 ( #52890, #59210, #65962, #32198, #31753, #85808, #66419, #12367, #87155, #39408 ),
 .UNSPECIFIED., .F., .F.,
 ( 4, 2, 2, 2, 4 ),
 ( 0.000000000000000000, 0.0001954339881912783286, 0.0003908679763825566571, 0.0005863019645738349857, 0.0007817359527651133143 ),
 .UNSPECIFIED. ) ;
#13620 = VECTOR ( 'NONE', #53994, 1000.000000000000000 ) ;
#13621 = VERTEX_POINT ( 'NONE', #9487 ) ;
#13622 = EDGE_LOOP ( 'NONE', ( #26211, #46992, #78375, #45198 ) ) ;
#13623 = DIRECTION ( 'NONE',  ( 0.000000000000000000, 0.6427876096865373645, -0.7660444431189797898 ) ) ;
#13624 = VERTEX_POINT ( 'NONE', #64862 ) ;
#13625 = CARTESIAN_POINT ( 'NONE',  ( -3.230769230769229949, -8.973038597847269315, 34.52809138561121927 ) ) ;
#13626 = LINE ( 'NONE', #82097, #71249 ) ;
#13627 = CARTESIAN_POINT ( 'NONE',  ( 4.853996118016225658, -11.43668979543635089, 33.22377378376089752 ) ) ;
#13628 = CARTESIAN_POINT ( 'NONE',  ( 11.53846153846141753, -2.625532179533778709, 30.86335684631627174 ) ) ;
#13629 = FACE_OUTER_BOUND ( 'NONE', #80211, .T. ) ;
#13630 = CARTESIAN_POINT ( 'NONE',  ( -3.230769230769229949, -1.509761064869970415, 31.06009739812519044 ) ) ;
#13631 = CARTESIAN_POINT ( 'NONE',  ( -7.846153846153844924, -3.050289026998446396, 32.03036669348365706 ) ) ;
#13632 = CARTESIAN_POINT ( 'NONE',  ( -5.326899807865431491, -3.627789207965226748, 32.91389620160131102 ) ) ;
#13633 = EDGE_LOOP ( 'NONE', ( #65998, #29434, #46146, #13287 ) ) ;
#13634 = EDGE_CURVE ( 'NONE', #51834, #30410, #85155, .T. ) ;
#13635 = VERTEX_POINT ( 'NONE', #50030 ) ;
#13636 = EDGE_LOOP ( 'NONE', ( #16690, #17624, #66023, #1755 ) ) ;
#13637 = CARTESIAN_POINT ( 'NONE',  ( -11.66915300512910214, -12.38065189839062263, 30.83690757178629482 ) ) ;
#13639 = CARTESIAN_POINT ( 'NONE',  ( -7.976845312821407852, -4.118384482072085184, 33.43331474514187107 ) ) ;
#13638 = CARTESIAN_POINT ( 'NONE',  ( 30.00000000000000000, 15.00000000000000355, 0.000000000000000000 ) ) ;
#13640 = EDGE_CURVE ( 'NONE', #59182, #26485, #10382, .T. ) ;
#13641 = DIRECTION ( 'NONE',  ( 1.000000000000000000, 0.000000000000000000, 0.000000000000000000 ) ) ;
#13642 = CARTESIAN_POINT ( 'NONE',  ( -9.822999158975251888, -6.413092428213692742, 34.63065189839063152 ) ) ;
#13643 = FACE_BOUND ( 'NONE', #85297, .T. ) ;
#13644 = DIRECTION ( 'NONE',  ( -0.000000000000000000, -0.6427876096865404731, -0.7660444431189771253 ) ) ;
#13645 = ORIENTED_EDGE ( 'NONE', *, *, #13702, .T. ) ;
#13646 = AXIS2_PLACEMENT_3D ( 'NONE', #80003, #19958, #59280 ) ;
#13647 = CARTESIAN_POINT ( 'NONE',  ( 18.75000000000000000, -7.500000000000000000, 29.75000000000000355 ) ) ;
#13648 = LINE ( 'NONE', #75789, #23148 ) ;
#13649 = CARTESIAN_POINT ( 'NONE',  ( 3.165498784808455923, -10.90142922261923886, 33.41473453929638993 ) ) ;
#13650 = VERTEX_POINT ( 'NONE', #17128 ) ;
#13651 = EDGE_CURVE ( 'NONE', #25023, #32515, #50464, .T. ) ;
#13652 = CARTESIAN_POINT ( 'NONE',  ( 17.29970274590113632, -5.827830569534415694, 34.72679350104403539 ) ) ;
#13653 = EDGE_LOOP ( 'NONE', ( #33878, #73585, #81815, #39014 ) ) ;
#13654 = FACE_BOUND ( 'NONE', #86055, .T. ) ;
#13655 = CARTESIAN_POINT ( 'NONE',  ( -4.153846153846273204, -11.48612834414049644, 32.76840700105863391 ) ) ;
#13656 = B_SPLINE_CURVE_WITH_KNOTS ( 'NONE', 3,
 ( #24421, #12597, #26106, #79387, #33315, #47256, #10926, #3710, #40953, #61208 ),
 .UNSPECIFIED., .F., .F.,
 ( 4, 2, 2, 2, 4 ),
 ( 0.000000000000000000, 0.0001954339857564074473, 0.0003908679715128148945, 0.0005863019572692223418, 0.0007817359430256297891 ),
 .UNSPECIFIED. ) ;
#13657 = LINE ( 'NONE', #41137, #46362 ) ;
#13658 = DIRECTION ( 'NONE',  ( 0.000000000000000000, 0.8660254037844377084, 0.5000000000000015543 ) ) ;
#13659 = ORIENTED_EDGE ( 'NONE', *, *, #39986, .T. ) ;
#13660 = VECTOR ( 'NONE', #26036, 1000.000000000000000 ) ;
#13662 = CARTESIAN_POINT ( 'NONE',  ( 25.00000000000000355, 9.999999999999971578, 13.00000000000000178 ) ) ;
#13661 = B_SPLINE_CURVE_WITH_KNOTS ( 'NONE', 3,
 ( #38753, #86972, #31549, #37860, #17602, #16694, #25238, #59014, #45943, #65325 ),
 .UNSPECIFIED., .F., .F.,
 ( 4, 2, 2, 2, 4 ),
 ( 0.0007817359430256261028, 0.0009771253907249911191, 0.001172514838424356136, 0.001367904286123721152, 0.001563293733823086168 ),
 .UNSPECIFIED. ) ;
#13663 = CARTESIAN_POINT ( 'NONE',  ( 3.000000000000001776, -7.500000000000000000, 0.000000000000000000 ) ) ;
#13664 = CARTESIAN_POINT ( 'NONE',  ( -16.21911659980693443, -12.46129190929999986, 30.37095296980880832 ) ) ;
#13665 = DIRECTION ( 'NONE',  ( 0.000000000000000000, 0.7660444431189822323, -0.6427876096865344779 ) ) ;
#13666 = VERTEX_POINT ( 'NONE', #58550 ) ;
#13667 = EDGE_CURVE ( 'NONE', #22635, #51776, #84285, .T. ) ;
#13668 = CYLINDRICAL_SURFACE ( 'NONE', #51680, 0.2499999999999994726 ) ;
#13669 = CARTESIAN_POINT ( 'NONE',  ( -15.23076923076935074, -4.481592998941358097, 33.73612834414048933 ) ) ;
#13671 = VERTEX_POINT ( 'NONE', #22125 ) ;
#13670 = CARTESIAN_POINT ( 'NONE',  ( 16.15384615384615330, -3.513871655860378418, 32.76840700105978499 ) ) ;
#13672 = CARTESIAN_POINT ( 'NONE',  ( 16.08857615328984281, -4.320704448112772766, 33.92786785259540494 ) ) ;
#13673 = CARTESIAN_POINT ( 'NONE',  ( 5.776515056276054771, -9.331801661448606566, 34.40259984581193464 ) ) ;
#13674 = CARTESIAN_POINT ( 'NONE',  ( -11.76138775597768138, -8.239355502252617924, 34.69524867566427417 ) ) ;
#13675 = CARTESIAN_POINT ( 'NONE',  ( -10.54931626438217585, -2.538708090699994813, 30.37095296980875503 ) ) ;
#13676 = CARTESIAN_POINT ( 'NONE',  ( 16.15384615384645883, -2.506253911140615021, 30.00000000000323297 ) ) ;
#13678 = CARTESIAN_POINT ( 'NONE',  ( -16.40386937806761125, -8.475808217655753651, 34.90892951860618609 ) ) ;
#13677 = LINE ( 'NONE', #41156, #24650 ) ;
#13679 = DIRECTION ( 'NONE',  ( -0.000000000000000000, 0.8660254037844399289, -0.4999999999999980016 ) ) ;
#13680 = CARTESIAN_POINT ( 'NONE',  ( -1.139087296525992166, -10.25000000000000533, 21.10937500000000711 ) ) ;
#13681 = ORIENTED_EDGE ( 'NONE', *, *, #43828, .T. ) ;
#13682 = EDGE_CURVE ( 'NONE', #12459, #31749, #37850, .T. ) ;
#13683 = LINE ( 'NONE', #34836, #83613 ) ;
#13684 = EDGE_LOOP ( 'NONE', ( #76119, #29988, #14149, #17158 ) ) ;
#13685 = ORIENTED_EDGE ( 'NONE', *, *, #18414, .F. ) ;
#13686 = EDGE_CURVE ( 'NONE', #40474, #88311, #34853, .T. ) ;
#13687 = CARTESIAN_POINT ( 'NONE',  ( -18.25000000000000000, -12.75000000000000888, 29.74999999999997868 ) ) ;
#13688 = ORIENTED_EDGE ( 'NONE', *, *, #41493, .F. ) ;
#13689 = CARTESIAN_POINT ( 'NONE',  ( 14.30769230769231015, -8.120952969808772792, 34.71129190930000163 ) ) ;
#13690 = CARTESIAN_POINT ( 'NONE',  ( 1.799775606325937360E-14, -10.25000000000000000, 22.28125000000000355 ) ) ;
#13691 = CARTESIAN_POINT ( 'NONE',  ( 17.99999999999987566, -5.094484230521993062, 34.41647553114689373 ) ) ;
#13692 = CARTESIAN_POINT ( 'NONE',  ( 0.000000000000000000, -11.00000000000000000, 29.75000000000000355 ) ) ;
#13693 = CARTESIAN_POINT ( 'NONE',  ( -16.15384615384615330, -5.557115091759785130, 34.35708131394839171 ) ) ;
#13694 = VECTOR ( 'NONE', #6700, 1000.000000000000000 ) ;
#13695 = DIRECTION ( 'NONE',  ( 0.000000000000000000, 0.6427876096865373645, -0.7660444431189797898 ) ) ;
#13696 = CYLINDRICAL_SURFACE ( 'NONE', #22925, 0.2500000000000012212 ) ;
#13697 = CARTESIAN_POINT ( 'NONE',  ( 2.177545098254087375, -10.19110544564092002, 33.96427741523702792 ) ) ;
#13698 = CARTESIAN_POINT ( 'NONE',  ( -2.651650429449535551, -10.15165042944956753, 26.18750000000000355 ) ) ;
#13699 = CARTESIAN_POINT ( 'NONE',  ( 6.700149964170072359, -10.01117774369187252, 34.36070679894347535 ) ) ;
#13700 = DIRECTION ( 'NONE',  ( 0.000000000000000000, 0.9396926207859126468, -0.3420201433256571111 ) ) ;
#13701 = B_SPLINE_CURVE_WITH_KNOTS ( 'NONE', 3,
 ( #41644, #14168, #27237, #88967, #20038, #13282, #19595, #5638, #75428, #88094 ),
 .UNSPECIFIED., .F., .F.,
 ( 4, 2, 2, 2, 4 ),
 ( 0.000000000000000000, 0.0001954339857564075828, 0.0003908679715128151656, 0.0005863019572692227755, 0.0007817359430256303312 ),
 .UNSPECIFIED. ) ;
#13702 = EDGE_CURVE ( 'NONE', #530, #72319, #6631, .T. ) ;
#13703 = B_SPLINE_CURVE_WITH_KNOTS ( 'NONE', 3,
 ( #33426, #67211, #68100, #12705, #81174, #60887, #88386, #14029, #20357, #19458 ),
 .UNSPECIFIED., .F., .F.,
 ( 4, 2, 2, 2, 4 ),
 ( 0.0007817246256747514008, 0.0009771112852218961399, 0.001172497944769040771, 0.001367884604316185401, 0.001563271263863330032 ),
 .UNSPECIFIED. ) ;
#13704 = CARTESIAN_POINT ( 'NONE',  ( 5.326977496836529546, -10.82426656108011720, 33.81400080652039009 ) ) ;
#13705 = ORIENTED_EDGE ( 'NONE', *, *, #48185, .F. ) ;
#13706 = VERTEX_POINT ( 'NONE', #44587 ) ;
#13707 = CARTESIAN_POINT ( 'NONE',  ( 12.46153846153846168, -2.486705287966279876, 31.30864560766543647 ) ) ;
#13708 = CARTESIAN_POINT ( 'NONE',  ( 0.6843181305165253470, -12.11081565061823717, 32.26097654155341843 ) ) ;
#13709 = DIRECTION ( 'NONE',  ( 0.000000000000000000, 0.7660444431189807890, 0.6427876096865361433 ) ) ;
#13710 = CARTESIAN_POINT ( 'NONE',  ( 5.934729554039225974, -6.026961402152685388, 34.52809138561120506 ) ) ;
#13712 = EDGE_CURVE ( 'NONE', #33744, #34857, #8717, .T. ) ;
#13711 = DIRECTION ( 'NONE',  ( 1.000000000000000000, 0.000000000000000000, 0.000000000000000000 ) ) ;
#13713 = CARTESIAN_POINT ( 'NONE',  ( 15.84615384615384670, -7.500000000000000000, 33.75000000000000000 ) ) ;
#13714 = CARTESIAN_POINT ( 'NONE',  ( 27.00000000000000000, 0.000000000000000000, 23.75000000000000000 ) ) ;
#13715 = EDGE_CURVE ( 'NONE', #74633, #39901, #65315, .T. ) ;
#13716 = EDGE_CURVE ( 'NONE', #62266, #83312, #23005, .T. ) ;
#13717 = AXIS2_PLACEMENT_3D ( 'NONE', #77901, #72027, #85114 ) ;
#13718 = ORIENTED_EDGE ( 'NONE', *, *, #19717, .F. ) ;
#13719 = DIRECTION ( 'NONE',  ( -0.000000000000000000, 0.8660254037844397068, -0.4999999999999978906 ) ) ;
#13720 = EDGE_LOOP ( 'NONE', ( #29034, #51704 ) ) ;
#13721 = EDGE_CURVE ( 'NONE', #60694, #683, #14135, .T. ) ;
#13722 = ADVANCED_FACE ( 'NONE', ( #53580 ), #79287, .F. ) ;
#13723 = B_SPLINE_CURVE_WITH_KNOTS ( 'NONE', 3,
 ( #71799, #51505, #17308, #44765, #65491, #31267, #58732, #86231, #24499, #51967 ),
 .UNSPECIFIED., .F., .F.,
 ( 4, 2, 2, 2, 4 ),
 ( 0.000000000000000000, 0.0001954339857564073659, 0.0003908679715128147319, 0.0005863019572692221250, 0.0007817359430256294638 ),
 .UNSPECIFIED. ) ;
#13724 = CARTESIAN_POINT ( 'NONE',  ( -14.43816901580877143, -7.276988635370452485, 34.74523720219453793 ) ) ;
#13725 = B_SPLINE_CURVE_WITH_KNOTS ( 'NONE', 3,
 ( #43222, #65252, #30149, #50404, #9001, #79228, #3554, #71566, #77887, #58942 ),
 .UNSPECIFIED., .F., .F.,
 ( 4, 2, 2, 2, 4 ),
 ( 0.000000000000000000, 0.0001954339857564054144, 0.0003908679715128108288, 0.0005863019572692162703, 0.0007817359430256216575 ),
 .UNSPECIFIED. ) ;
#13726 = CARTESIAN_POINT ( 'NONE',  ( 4.088092725532820992, -7.249945578846651806, 34.99404164642496795 ) ) ;
#13727 = FACE_OUTER_BOUND ( 'NONE', #54515, .T. ) ;
#13728 = FACE_OUTER_BOUND ( 'NONE', #35569, .T. ) ;
#13729 = CARTESIAN_POINT ( 'NONE',  ( 17.99999999999987566, -3.083524468854526912, 32.58852847137268327 ) ) ;
#13730 = VERTEX_POINT ( 'NONE', #38742 ) ;
#13731 = ORIENTED_EDGE ( 'NONE', *, *, #80505, .T. ) ;
#13732 = ORIENTED_EDGE ( 'NONE', *, *, #22754, .T. ) ;
#13733 = ORIENTED_EDGE ( 'NONE', *, *, #78326, .T. ) ;
#13734 = DIRECTION ( 'NONE',  ( 0.000000000000000000, 0.4999999999999960032, -0.8660254037844410391 ) ) ;
#13735 = CARTESIAN_POINT ( 'NONE',  ( 7.622668902429896143, -3.754499324213721234, 33.06261337010820256 ) ) ;
#13736 = DIRECTION ( 'NONE',  ( -1.000000000000000000, 0.000000000000000000, -0.000000000000000000 ) ) ;
#13737 = CARTESIAN_POINT ( 'NONE',  ( 16.37662569511456212, -10.11255958852955672, 34.01340905677048454 ) ) ;
#13738 = CARTESIAN_POINT ( 'NONE',  ( -17.01085472592063752, -3.050289026998446840, 32.03036669348366416 ) ) ;
#13739 = CARTESIAN_POINT ( 'NONE',  ( 12.21156171748986985, -2.920706130388546651, 32.31842814019191223 ) ) ;
#13740 = ORIENTED_EDGE ( 'NONE', *, *, #13894, .F. ) ;
#13741 = ORIENTED_EDGE ( 'NONE', *, *, #18584, .F. ) ;
#13742 = AXIS2_PLACEMENT_3D ( 'NONE', #55661, #61094, #47580 ) ;
#13743 = ORIENTED_EDGE ( 'NONE', *, *, #46376, .T. ) ;
#13745 = ORIENTED_EDGE ( 'NONE', *, *, #77768, .T. ) ;
#13744 = CARTESIAN_POINT ( 'NONE',  ( -3.453696189676078276, -2.523278758544489353, 31.42238647778637528 ) ) ;
#13746 = DIRECTION ( 'NONE',  ( -0.000000000000000000, 0.9848077530122086864, -0.1736481776669273891 ) ) ;
#13747 = CARTESIAN_POINT ( 'NONE',  ( -4.854143535654667829, -11.41317474335729187, 32.86274602512330034 ) ) ;
#13748 = CARTESIAN_POINT ( 'NONE',  ( 2.320192649118979489E-14, -11.25000000000000000, 18.53125000000000000 ) ) ;
#13749 = VERTEX_POINT ( 'NONE', #51783 ) ;
#13750 = CARTESIAN_POINT ( 'NONE',  ( -14.98076923076922995, -2.249999999999998668, 29.75000000000000355 ) ) ;
#13751 = EDGE_LOOP ( 'NONE', ( #67052, #7780 ) ) ;
#13752 = LINE ( 'NONE', #53403, #13995 ) ;
#13753 = FACE_BOUND ( 'NONE', #59476, .T. ) ;
#13754 = CARTESIAN_POINT ( 'NONE',  ( 6.923076923076924238, -4.098570777380720287, 33.41473453929634729 ) ) ;
#13755 = DIRECTION ( 'NONE',  ( 0.000000000000000000, 0.000000000000000000, 1.000000000000000000 ) ) ;
#13756 = ORIENTED_EDGE ( 'NONE', *, *, #34973, .F. ) ;
#13757 = CARTESIAN_POINT ( 'NONE',  ( -9.758390071667825794, -4.661471528628507777, 34.16647553114621871 ) ) ;
#13758 = CARTESIAN_POINT ( 'NONE',  ( 6.673100179028334189, -12.01397095200673881, 32.43157075238190146 ) ) ;
#13759 = LINE ( 'NONE', #54295, #81614 ) ;
#13760 = CARTESIAN_POINT ( 'NONE',  ( 14.08476534878545827, -9.172386477786396597, 34.72672124145550043 ) ) ;
#13761 = VERTEX_POINT ( 'NONE', #39648 ) ;
#13762 = B_SPLINE_CURVE_WITH_KNOTS ( 'NONE', 3,
 ( #61288, #83361, #14451, #48225, #82917, #68945, #62188, #6378, #76142, #47791 ),
 .UNSPECIFIED., .F., .F.,
 ( 4, 2, 2, 2, 4 ),
 ( 0.0007817359430256297891, 0.0009771253907249958896, 0.001172514838424361990, 0.001367904286123728091, 0.001563293733823094191 ),
 .UNSPECIFIED. ) ;
#13763 = CARTESIAN_POINT ( 'NONE',  ( 11.78840705680968171, -3.202959910592335646, 32.30730279482227019 ) ) ;
#13764 = CARTESIAN_POINT ( 'NONE',  ( 1.634669696253701732, -8.303483539816728154, 34.68545999027711702 ) ) ;
#13765 = CARTESIAN_POINT ( 'NONE',  ( 4.376858997939548246, -11.43677907613344757, 33.22367315496201456 ) ) ;
#13766 = CARTESIAN_POINT ( 'NONE',  ( -2.084912638714238931, -9.418065098278011860, 34.63729479722530158 ) ) ;
#13767 = CARTESIAN_POINT ( 'NONE',  ( 8.096153846153846700, -2.249999999999998668, 29.75000000000000355 ) ) ;
#13768 = CIRCLE ( 'NONE', #87166, 3.000000000000000444 ) ;
#13769 = FACE_BOUND ( 'NONE', #22628, .T. ) ;
#13771 = CYLINDRICAL_SURFACE ( 'NONE', #64693, 0.2499999999999994726 ) ;
#13770 = CARTESIAN_POINT ( 'NONE',  ( 5.749976775778542937, -4.931416488878822335, 34.32920672191015399 ) ) ;
#13772 = CARTESIAN_POINT ( 'NONE',  ( -14.43784027742400156, -3.625366637846544116, 33.29286588640298561 ) ) ;
#13774 = CARTESIAN_POINT ( 'NONE',  ( -2.057637887778852814, -8.346898887586323923, 34.93166121998716278 ) ) ;
#13773 = CARTESIAN_POINT ( 'NONE',  ( 3.360816837024914960, -7.723484964179500700, 34.74522123443823318 ) ) ;
#13775 = DIRECTION ( 'NONE',  ( 0.000000000000000000, 0.1736481776669275834, 0.9848077530122086864 ) ) ;
#13776 = CARTESIAN_POINT ( 'NONE',  ( 1.987747218494664292, -9.401340078031346081, 18.12313170625849068 ) ) ;
#13777 = ORIENTED_EDGE ( 'NONE', *, *, #54258, .F. ) ;
#13778 = CARTESIAN_POINT ( 'NONE',  ( 12.46153846153833911, -2.625532179533778709, 30.86335684631627174 ) ) ;
#13779 = VERTEX_POINT ( 'NONE', #10827 ) ;
#13780 = EDGE_CURVE ( 'NONE', #3936, #67310, #59262, .T. ) ;
#13781 = CARTESIAN_POINT ( 'NONE',  ( -13.25408994638174320, -9.503571793651731880, 34.60286762892837942 ) ) ;
#13782 = ORIENTED_EDGE ( 'NONE', *, *, #52361, .F. ) ;
#13783 = CARTESIAN_POINT ( 'NONE',  ( 18.00000000000000000, -12.10708131394839349, 31.69288490824020244 ) ) ;
#13784 = CARTESIAN_POINT ( 'NONE',  ( -16.08777882049607655, -11.91647553114624358, 32.58852847137148245 ) ) ;
#13785 = B_SPLINE_CURVE_WITH_KNOTS ( 'NONE', 3,
 ( #77018, #21620, #27942, #28838, #15762, #14880, #54970, #56299, #83784, #43226 ),
 .UNSPECIFIED., .F., .F.,
 ( 4, 2, 2, 2, 4 ),
 ( 0.0007817359430256365111, 0.0009771253907250045632, 0.001172514838424372615, 0.001367904286123740668, 0.001563293733823108720 ),
 .UNSPECIFIED. ) ;
#13788 = ORIENTED_EDGE ( 'NONE', *, *, #16391, .F. ) ;
#13787 = VECTOR ( 'NONE', #72892, 1000.000000000000114 ) ;
#13786 = DIRECTION ( 'NONE',  ( -0.000000000000000000, -0.8660254037844397068, -0.4999999999999978906 ) ) ;
#13789 = CARTESIAN_POINT ( 'NONE',  ( -15.48079246806219267, -5.056417327199099532, 34.11270091957321426 ) ) ;
#13790 = CARTESIAN_POINT ( 'NONE',  ( 0.06109907496454976272, -10.25000000000000000, 17.02938170625848713 ) ) ;
#13791 = CARTESIAN_POINT ( 'NONE',  ( 3.930919936330004472, -9.086856451489516928, 34.49173150075333183 ) ) ;
#13792 = CARTESIAN_POINT ( 'NONE',  ( -14.05769230769230660, -2.499999999999998668, 29.75000000000000355 ) ) ;
#13793 = B_SPLINE_CURVE_WITH_KNOTS ( 'NONE', 3,
 ( #84524, #55703, #29142, #56598, #76430, #84088, #22365, #57030, #49830, #15616 ),
 .UNSPECIFIED., .F., .F.,
 ( 4, 2, 2, 2, 4 ),
 ( 0.0007817246256747518345, 0.0009771112852218970073, 0.001172497944769042072, 0.001367884604316187136, 0.001563271263863332200 ),
 .UNSPECIFIED. ) ;
#13794 = DIRECTION ( 'NONE',  ( -0.000000000000000000, 0.7660444431189791237, -0.6427876096865379196 ) ) ;
#13795 = CARTESIAN_POINT ( 'NONE',  ( 3.930361210122205406, -11.89387501736622710, 32.13663884655806413 ) ) ;
#13796 = CARTESIAN_POINT ( 'NONE',  ( 2.557637826040450424, -2.824170634883621744, 31.52227843825338738 ) ) ;
#13797 = DIRECTION ( 'NONE',  ( 0.000000000000000000, 0.4999999999999960032, -0.8660254037844410391 ) ) ;
#13798 = B_SPLINE_CURVE_WITH_KNOTS ( 'NONE', 3,
 ( #73961, #19011, #47810, #19451, #75290, #13580, #82501, #41501, #7273, #46482 ),
 .UNSPECIFIED., .F., .F.,
 ( 4, 2, 2, 2, 4 ),
 ( 0.0007817359430256315238, 0.0009771253907249980580, 0.001172514838424364592, 0.001367904286123730910, 0.001563293733823097444 ),
 .UNSPECIFIED. ) ;
#13799 = CARTESIAN_POINT ( 'NONE',  ( 1.614399933863618797, -3.775308065498751198, 20.73624329374151287 ) ) ;
#13800 = CARTESIAN_POINT ( 'NONE',  ( -18.22348492456433178, -11.60425143139329940, 33.02411095842164457 ) ) ;
#13801 = CARTESIAN_POINT ( 'NONE',  ( 10.61538461538461675, -11.16473453929635440, 33.15142922261926373 ) ) ;
#13802 = ADVANCED_FACE ( 'NONE', ( #38299 ), #24777, .F. ) ;
#13803 = ORIENTED_EDGE ( 'NONE', *, *, #27140, .F. ) ;
#13804 = CARTESIAN_POINT ( 'NONE',  ( 8.899756470994329760, -10.19071101563364756, 33.96452234770658407 ) ) ;
#13805 = CARTESIAN_POINT ( 'NONE',  ( 0.06109907496451268821, -3.749999999999999556, 24.40811829374151642 ) ) ;
#13806 = CARTESIAN_POINT ( 'NONE',  ( 2.307692307692186251, -5.094484230521993062, 34.41647553114689373 ) ) ;
#13807 = CARTESIAN_POINT ( 'NONE',  ( -8.769230769230892619, -11.67786785259630911, 32.92929555188603530 ) ) ;
#13808 = ORIENTED_EDGE ( 'NONE', *, *, #64688, .T. ) ;
#13809 = VECTOR ( 'NONE', #30184, 1000.000000000000000 ) ;
#13810 = CARTESIAN_POINT ( 'NONE',  ( 15.84615384615384670, -11.00000000000000000, 29.75000000000000355 ) ) ;
#13811 = CARTESIAN_POINT ( 'NONE',  ( -0.2385271099256117411, -9.886259254753566594, 34.14407573483973124 ) ) ;
#13813 = VERTEX_POINT ( 'NONE', #18033 ) ;
#13812 = CARTESIAN_POINT ( 'NONE',  ( 3.930919194939303196, -9.172386477786396597, 34.72672124145550043 ) ) ;
#13814 = CARTESIAN_POINT ( 'NONE',  ( -7.596153846152408740, -7.500000000000155431, 34.75000000000007105 ) ) ;
#13815 = CARTESIAN_POINT ( 'NONE',  ( -16.85395994265639885, -7.369474539155830506, 34.99858011523957657 ) ) ;
#13816 = AXIS2_PLACEMENT_3D ( 'NONE', #47147, #20568, #12928 ) ;
#13817 = CARTESIAN_POINT ( 'NONE',  ( 0.4615384615384611200, -1.242168528481310874, 33.36296068462461051 ) ) ;
#13818 = CARTESIAN_POINT ( 'NONE',  ( 3.100621261037531440, -2.647304123082328875, 31.75400227202885262 ) ) ;
#13819 = CARTESIAN_POINT ( 'NONE',  ( 6.856993512121044354, -4.786620604624113540, 33.94971097300155805 ) ) ;
#13820 = EDGE_CURVE ( 'NONE', #38892, #11165, #6069, .T. ) ;
#13821 = EDGE_CURVE ( 'NONE', #42909, #64027, #65754, .T. ) ;
#13822 = EDGE_LOOP ( 'NONE', ( #64736, #14150 ) ) ;
#13823 = EDGE_LOOP ( 'NONE', ( #43885, #45123, #86981, #59265 ) ) ;
#13824 = B_SPLINE_CURVE_WITH_KNOTS ( 'NONE', 3,
 ( #23702, #58371, #31363, #11092, #79101, #39024, #4332, #86778, #17408, #25048 ),
 .UNSPECIFIED., .F., .F.,
 ( 4, 2, 2, 2, 4 ),
 ( 0.000000000000000000, 0.0001954339857564083417, 0.0003908679715128166835, 0.0005863019572692250523, 0.0007817359430256333669 ),
 .UNSPECIFIED. ) ;
#13825 = ORIENTED_EDGE ( 'NONE', *, *, #80658, .F. ) ;
#13826 = ADVANCED_FACE ( 'NONE', ( #66659 ), #45489, .F. ) ;
#13827 = DIRECTION ( 'NONE',  ( -1.000000000000000000, -0.000000000000000000, -0.000000000000000000 ) ) ;
#13828 = CARTESIAN_POINT ( 'NONE',  ( -2.176900499867519212, -5.582136614379148654, 34.36778462344220486 ) ) ;
#13829 = DIRECTION ( 'NONE',  ( -0.000000000000000000, 1.000000000000000000, 3.491481338843133355E-15 ) ) ;
#13830 = CARTESIAN_POINT ( 'NONE',  ( -8.069080805060693251, -10.77366814457252175, 33.85459836347579454 ) ) ;
#13831 = CARTESIAN_POINT ( 'NONE',  ( 16.08857570788537572, -5.219633306516282545, 34.19971097300152252 ) ) ;
#13832 = ORIENTED_EDGE ( 'NONE', *, *, #26692, .F. ) ;
#13833 = VECTOR ( 'NONE', #51868, 1000.000000000000114 ) ;
#13834 = ORIENTED_EDGE ( 'NONE', *, *, #10905, .F. ) ;
#13835 = ORIENTED_EDGE ( 'NONE', *, *, #38226, .T. ) ;
#13837 = EDGE_LOOP ( 'NONE', ( #35288, #73676 ) ) ;
#13836 = CARTESIAN_POINT ( 'NONE',  ( -21.00000000000000355, -12.75000000000000178, 27.25000000000000000 ) ) ;
#13838 = DIRECTION ( 'NONE',  ( -1.000000000000000000, 0.000000000000000000, -0.000000000000000000 ) ) ;
#13839 = B_SPLINE_CURVE_WITH_KNOTS ( 'NONE', 3,
 ( #51117, #16914, #50686, #22342, #77283, #43502, #15591, #15149, #57450, #35865 ),
 .UNSPECIFIED., .F., .F.,
 ( 4, 2, 2, 2, 4 ),
 ( 0.0007817359430256314154, 0.0009771253907249978412, 0.001172514838424364375, 0.001367904286123730693, 0.001563293733823097227 ),
 .UNSPECIFIED. ) ;
#13840 = CARTESIAN_POINT ( 'NONE',  ( -3.296851610129365895, -11.91647553114624181, 32.58852847137148245 ) ) ;
#13841 = CARTESIAN_POINT ( 'NONE',  ( -4.230769230769230838, -11.50000000000000000, 29.75000000000000355 ) ) ;
#13842 = LINE ( 'NONE', #74224, #2149 ) ;
#13843 = ORIENTED_EDGE ( 'NONE', *, *, #11489, .T. ) ;
#13844 = ORIENTED_EDGE ( 'NONE', *, *, #15956, .F. ) ;
#13845 = VERTEX_POINT ( 'NONE', #72970 ) ;
#13846 = CARTESIAN_POINT ( 'NONE',  ( -13.38461538461538325, -3.937682226553329556, 33.60647404775216529 ) ) ;
#13848 = EDGE_LOOP ( 'NONE', ( #15522, #46621 ) ) ;
#13847 = CARTESIAN_POINT ( 'NONE',  ( -10.55012947587177763, -2.657715359629131857, 31.77849191805844242 ) ) ;
#13849 = DIRECTION ( 'NONE',  ( -0.000000000000000000, -0.1736481776669307198, -0.9848077530122080203 ) ) ;
#13850 = CARTESIAN_POINT ( 'NONE',  ( -2.307692307692305711, -2.517432740324522911, 35.29906147534542527 ) ) ;
#13851 = EDGE_LOOP ( 'NONE', ( #47724, #69389 ) ) ;
#13852 = B_SPLINE_CURVE_WITH_KNOTS ( 'NONE', 3,
 ( #13238, #67296, #161, #40719, #82595, #67738, #48339, #25863, #53321, #33061 ),
 .UNSPECIFIED., .F., .F.,
 ( 4, 2, 2, 2, 4 ),
 ( 0.0007817359430256319575, 0.0009771253907249984917, 0.001172514838424365026, 0.001367904286123731343, 0.001563293733823097878 ),
 .UNSPECIFIED. ) ;
#13853 = B_SPLINE_CURVE_WITH_KNOTS ( 'NONE', 3,
 ( #42590, #48891, #21865, #76819, #8360, #62830, #1151, #15559, #35833, #64165 ),
 .UNSPECIFIED., .F., .F.,
 ( 4, 2, 2, 2, 4 ),
 ( 0.000000000000000000, 0.0001954311564186868473, 0.0003908623128373736946, 0.0005862934692560605419, 0.0007817246256747473893 ),
 .UNSPECIFIED. ) ;
#13854 = CARTESIAN_POINT ( 'NONE',  ( 9.019176287578909879, -12.43552623307873972, 30.55307653245132826 ) ) ;
#13855 = DIRECTION ( 'NONE',  ( -1.000000000000000000, -0.000000000000000000, -0.000000000000000000 ) ) ;
#13856 = ORIENTED_EDGE ( 'NONE', *, *, #70714, .T. ) ;
#13857 = FACE_BOUND ( 'NONE', #65122, .T. ) ;
#13858 = CARTESIAN_POINT ( 'NONE',  ( 10.83839596699746721, -9.886259254753566594, 34.14407573483972413 ) ) ;
#13859 = CARTESIAN_POINT ( 'NONE',  ( 16.02315555073584008, -2.494641256782728966, 31.33461815524612959 ) ) ;
#13860 = CARTESIAN_POINT ( 'NONE',  ( 3.480714749117372442, -9.272278438253398036, 34.42582936511637826 ) ) ;
#13862 = CARTESIAN_POINT ( 'NONE',  ( 18.13079180782478872, -4.118422570099827595, 33.43335022499816489 ) ) ;
#13861 = CARTESIAN_POINT ( 'NONE',  ( 18.06525513951284267, -3.083524468853783951, 32.58852847137153930 ) ) ;
#13863 = AXIS2_PLACEMENT_3D ( 'NONE', #70196, #42734, #415 ) ;
#13864 = CARTESIAN_POINT ( 'NONE',  ( -4.153846153846273204, -2.625532179533778709, 30.86335684631627174 ) ) ;
#13865 = CARTESIAN_POINT ( 'NONE',  ( -4.023055712879200385, -11.37503395064541678, 33.29242100308974983 ) ) ;
#13866 = ORIENTED_EDGE ( 'NONE', *, *, #72574, .T. ) ;
#13867 = CARTESIAN_POINT ( 'NONE',  ( -18.25002323729296450, -10.76384336483936011, 33.53834819971076087 ) ) ;
#13868 = FILL_AREA_STYLE_COLOUR ( '', #426 ) ;
#13869 = ORIENTED_EDGE ( 'NONE', *, *, #52559, .F. ) ;
#13870 = ADVANCED_FACE ( 'NONE', ( #67552 ), #4512, .F. ) ;
#13871 = AXIS2_PLACEMENT_3D ( 'NONE', #60454, #74418, #60897 ) ;
#13872 = FACE_OUTER_BOUND ( 'NONE', #52695, .T. ) ;
#13873 = CARTESIAN_POINT ( 'NONE',  ( -4.219116154402471786, -3.643525952247789412, 33.31231777344662959 ) ) ;
#13874 = EDGE_LOOP ( 'NONE', ( #30779, #78990 ) ) ;
#13875 = CARTESIAN_POINT ( 'NONE',  ( -15.93083480223330817, -11.24521262558773493, 33.06293181088029343 ) ) ;
#13876 = CARTESIAN_POINT ( 'NONE',  ( -9.019207500173124004, -5.728515186090277211, 34.42611988154120439 ) ) ;
#13877 = FACE_BOUND ( 'NONE', #53500, .T. ) ;
#13879 = CARTESIAN_POINT ( 'NONE',  ( -17.07692307692319744, -3.083524468854526912, 32.58852847137268327 ) ) ;
#13878 = CARTESIAN_POINT ( 'NONE',  ( -15.36091644020745051, -6.001485441113819874, 34.52039167877662607 ) ) ;
#13880 = CARTESIAN_POINT ( 'NONE',  ( 2.307692307692186251, -6.835583212225970762, 34.95778746994575670 ) ) ;
#13881 = AXIS2_PLACEMENT_3D ( 'NONE', #88057, #86261, #58764 ) ;
#13882 = CARTESIAN_POINT ( 'NONE',  ( -5.076923076922761346, -2.255955759149395501, 30.00000000000324363 ) ) ;
#13884 = CARTESIAN_POINT ( 'NONE',  ( -8.546451227962361230, -12.24180327182772388, 31.33663988360758168 ) ) ;
#13883 = SURFACE_STYLE_FILL_AREA ( #48105 ) ;
#13885 = CARTESIAN_POINT ( 'NONE',  ( -5.999999999999998224, -13.63283147151868846, 33.57946703557072254 ) ) ;
#13886 = CARTESIAN_POINT ( 'NONE',  ( -3.749999999999988454, -9.053300858899127945, 25.01562500000000000 ) ) ;
#13887 = ORIENTED_EDGE ( 'NONE', *, *, #68228, .T. ) ;
#13888 = VERTEX_POINT ( 'NONE', #25672 ) ;
#13889 = EDGE_CURVE ( 'NONE', #33135, #40550, #31989, .T. ) ;
#13890 = CARTESIAN_POINT ( 'NONE',  ( 5.299702618191483694, -6.760870238392817200, 34.69528174975672385 ) ) ;
#13891 = CARTESIAN_POINT ( 'NONE',  ( -0.5916856709766799005, -2.882441371585227952, 31.66841991370172948 ) ) ;
#13892 = DIRECTION ( 'NONE',  ( -0.000000000000000000, 0.7660444431189791237, -0.6427876096865379196 ) ) ;
#13893 = CARTESIAN_POINT ( 'NONE',  ( -1.384615384615383471, -3.050289026998446396, 32.03036669348365706 ) ) ;
#13894 = EDGE_CURVE ( 'NONE', #32821, #69536, #38867, .T. ) ;
#13895 = CARTESIAN_POINT ( 'NONE',  ( -16.94639737515951339, -6.852161475712351013, 34.70806712695775786 ) ) ;
#13896 = CARTESIAN_POINT ( 'NONE',  ( -2.651650429449565305, -4.848349570550461785, 26.50000000000000355 ) ) ;
#13897 = CARTESIAN_POINT ( 'NONE',  ( -24.00000000000000000, -5.499999999999981348, 27.75000000000000000 ) ) ;
#13898 = CARTESIAN_POINT ( 'NONE',  ( 2.084826044629209729, -2.251424796025575770, 29.88072029997477586 ) ) ;
#13899 = CARTESIAN_POINT ( 'NONE',  ( 9.469380733400843297, -10.77366814457252175, 33.85459836347579454 ) ) ;
#13900 = CARTESIAN_POINT ( 'NONE',  ( 7.846153846153723244, -5.941354392335915335, 34.76329471203413846 ) ) ;
#13901 = LINE ( 'NONE', #88265, #13694 ) ;
#13902 = CARTESIAN_POINT ( 'NONE',  ( 16.21991450484859598, -4.786620604624113540, 33.94971097300155805 ) ) ;
#13903 = CARTESIAN_POINT ( 'NONE',  ( -0.2114840416250090560, -4.074993327901525575, 33.72946981652012255 ) ) ;
#13904 = VECTOR ( 'NONE', #19226, 1000.000000000000114 ) ;
#13905 = CARTESIAN_POINT ( 'NONE',  ( -3.230769230769229949, -13.87047571288749737, 32.06866353760679544 ) ) ;
#13906 = EDGE_CURVE ( 'NONE', #79258, #77968, #35674, .T. ) ;
#13907 = CARTESIAN_POINT ( 'NONE',  ( -2.307692307692305711, -13.95598074871891292, 31.83374038241031911 ) ) ;
#13908 = VERTEX_POINT ( 'NONE', #13049 ) ;
#13909 = CARTESIAN_POINT ( 'NONE',  ( 12.21156171748987163, -4.075325502946081535, 33.72974371597206300 ) ) ;
#13910 = CARTESIAN_POINT ( 'NONE',  ( 0.5920641633020234940, -2.619367082507848998, 30.83698974864644171 ) ) ;
#13911 = CARTESIAN_POINT ( 'NONE',  ( -2.749999999999999112, -7.438900925035484057, 20.34561829374151287 ) ) ;
#13912 = EDGE_CURVE ( 'NONE', #38831, #45094, #74105, .T. ) ;
#13913 = CARTESIAN_POINT ( 'NONE',  ( 18.00000000000000000, -10.05456864172156806, 36.03766855953608683 ) ) ;
#13914 = CYLINDRICAL_SURFACE ( 'NONE', #25359, 0.2500000000000012212 ) ;
#13915 = FACE_OUTER_BOUND ( 'NONE', #4592, .T. ) ;
#13917 = EDGE_LOOP ( 'NONE', ( #66683, #44661 ) ) ;
#13916 = CARTESIAN_POINT ( 'NONE',  ( 7.780070435197965040, -2.538708090699994813, 30.37095296980875148 ) ) ;
#13918 = CARTESIAN_POINT ( 'NONE',  ( -1.944543648262992530, -9.444543648263016067, 26.18750000000000355 ) ) ;
#13919 = CARTESIAN_POINT ( 'NONE',  ( 13.38461538461538680, -12.34228464037088635, 31.77849191805839268 ) ) ;
#13920 = AXIS2_PLACEMENT_3D ( 'NONE', #60216, #26885, #54343 ) ;
#13921 = ORIENTED_EDGE ( 'NONE', *, *, #80490, .T. ) ;
#13922 = CARTESIAN_POINT ( 'NONE',  ( 11.76124120743960333, -9.418065098278013636, 34.63729479722530158 ) ) ;
#13923 = CARTESIAN_POINT ( 'NONE',  ( 10.86543903529806876, -10.82426656108012075, 33.81400080652039009 ) ) ;
#13924 = EDGE_LOOP ( 'NONE', ( #15978, #71675 ) ) ;
#13925 = CARTESIAN_POINT ( 'NONE',  ( 14.30769230769218758, -2.625532179533778709, 30.86335684631627174 ) ) ;
#13926 = CARTESIAN_POINT ( 'NONE',  ( 2.438217745925952862, -8.630441415882550871, 34.87705825610312615 ) ) ;
#13927 = EDGE_CURVE ( 'NONE', #61963, #53841, #75198, .T. ) ;
#13928 = CYLINDRICAL_SURFACE ( 'NONE', #68631, 0.2499999999999986955 ) ;
#13929 = VERTEX_POINT ( 'NONE', #68427 ) ;
#13930 = EDGE_CURVE ( 'NONE', #10, #47709, #34199, .T. ) ;
#13931 = ORIENTED_EDGE ( 'NONE', *, *, #27924, .F. ) ;
#13932 = CARTESIAN_POINT ( 'NONE',  ( 15.45378058238208041, -10.61302985866384141, 33.66295027996417843 ) ) ;
#13933 = VERTEX_POINT ( 'NONE', #75620 ) ;
#13934 = CARTESIAN_POINT ( 'NONE',  ( -7.911423846710166075, -2.379036618887870436, 30.90682066428147934 ) ) ;
#13935 = EDGE_CURVE ( 'NONE', #80357, #2602, #31180, .T. ) ;
#13936 = CARTESIAN_POINT ( 'NONE',  ( 15.36129466900287532, -12.70449254468099198, 30.44128974285582956 ) ) ;
#13937 = CARTESIAN_POINT ( 'NONE',  ( -17.07692307692307665, -5.557115091759785130, 34.35708131394839171 ) ) ;
#13938 = EDGE_CURVE ( 'NONE', #11611, #5488, #87051, .T. ) ;
#13939 = FACE_OUTER_BOUND ( 'NONE', #5567, .T. ) ;
#13940 = CARTESIAN_POINT ( 'NONE',  ( 12.46153846153846168, -13.57706302396349152, 30.56769352161908060 ) ) ;
#13941 = CARTESIAN_POINT ( 'NONE',  ( 16.09615384615384670, -7.500000000000000000, 29.75000000000000355 ) ) ;
#13942 = AXIS2_PLACEMENT_3D ( 'NONE', #71160, #3139, #9467 ) ;
#13943 = FACE_OUTER_BOUND ( 'NONE', #73554, .T. ) ;
#13944 = ORIENTED_EDGE ( 'NONE', *, *, #69513, .F. ) ;
#13945 = VERTEX_POINT ( 'NONE', #33761 ) ;
#13947 = ORIENTED_EDGE ( 'NONE', *, *, #45451, .F. ) ;
#13946 = CARTESIAN_POINT ( 'NONE',  ( -4.480769230769230838, -11.00000000000000000, 29.75000000000000355 ) ) ;
#13948 = CARTESIAN_POINT ( 'NONE',  ( -5.076923076923199218, -5.094484230521993062, 34.41647553114689373 ) ) ;
#13949 = EDGE_LOOP ( 'NONE', ( #28584, #17270 ) ) ;
#13950 = CARTESIAN_POINT ( 'NONE',  ( -8.638705330997128229, -11.04252011169590020, 33.62494198852677130 ) ) ;
#13951 = FACE_OUTER_BOUND ( 'NONE', #62045, .T. ) ;
#13952 = B_SPLINE_CURVE_WITH_KNOTS ( 'NONE', 3,
 ( #59120, #76857, #70537, #49382, #2505, #36747, #57458, #8843, #86173, #24441 ),
 .UNSPECIFIED., .F., .F.,
 ( 4, 2, 2, 2, 4 ),
 ( 0.000000000000000000, 0.0001954339857564054144, 0.0003908679715128108288, 0.0005863019572692162703, 0.0007817359430256216575 ),
 .UNSPECIFIED. ) ;
#13953 = EDGE_LOOP ( 'NONE', ( #74141, #45424, #51358, #23711 ) ) ;
#13954 = CARTESIAN_POINT ( 'NONE',  ( -12.33074665371367651, -5.582136614379148654, 34.36778462344220486 ) ) ;
#13955 = B_SPLINE_CURVE_WITH_KNOTS ( 'NONE', 3,
 ( #4544, #52278, #81548, #12640, #87884, #79769, #40126, #18064, #18950, #5443 ),
 .UNSPECIFIED., .F., .F.,
 ( 4, 2, 2, 2, 4 ),
 ( 0.000000000000000000, 0.0001954311584214072923, 0.0003908623168428145846, 0.0005862934752642218498, 0.0007817246336856291692 ),
 .UNSPECIFIED. ) ;
#13956 = EDGE_LOOP ( 'NONE', ( #89150, #50924, #49613, #9057 ) ) ;
#13957 = CARTESIAN_POINT ( 'NONE',  ( 14.16025641025641235, -7.500000000000000000, 33.75000000000000000 ) ) ;
#13958 = ORIENTED_EDGE ( 'NONE', *, *, #60991, .T. ) ;
#13959 = FACE_OUTER_BOUND ( 'NONE', #83885, .T. ) ;
#13960 = EDGE_CURVE ( 'NONE', #43735, #3876, #83282, .T. ) ;
#13961 = VECTOR ( 'NONE', #24212, 1000.000000000000227 ) ;
#13962 = ORIENTED_EDGE ( 'NONE', *, *, #50612, .T. ) ;
#13963 = CARTESIAN_POINT ( 'NONE',  ( -13.38461538461550582, -12.46129190930018460, 30.37095296980731973 ) ) ;
#13964 = CARTESIAN_POINT ( 'NONE',  ( -4.377331078410484189, -6.716662450894490100, 34.94144148231605840 ) ) ;
#13965 = CIRCLE ( 'NONE', #26970, 0.5000000000000004441 ) ;
#13966 = FACE_BOUND ( 'NONE', #77871, .T. ) ;
#13967 = DIRECTION ( 'NONE',  ( -1.000000000000000000, 0.000000000000000000, 0.000000000000000000 ) ) ;
#13968 = DIRECTION ( 'NONE',  ( 0.000000000000000000, 0.7660444431189822323, -0.6427876096865344779 ) ) ;
#13969 = CARTESIAN_POINT ( 'NONE',  ( 9.626225312947561008, -11.35647404775217595, 33.31231777344666511 ) ) ;
#13970 = CARTESIAN_POINT ( 'NONE',  ( -3.453695448285377001, -4.186968288167446595, 33.49512374952580274 ) ) ;
#13971 = CARTESIAN_POINT ( 'NONE',  ( 5.076923076923391065, -2.255955759149395501, 30.00000000000324363 ) ) ;
#13972 = CARTESIAN_POINT ( 'NONE',  ( 16.08776274289027342, -4.098570777380720287, 33.41473453929634729 ) ) ;
#13973 = VECTOR ( 'NONE', #65644, 1000.000000000000000 ) ;
#13974 = CARTESIAN_POINT ( 'NONE',  ( 10.48469314871706004, -9.804603061927743113, 34.18744698557895845 ) ) ;
#13975 = ORIENTED_EDGE ( 'NONE', *, *, #30391, .F. ) ;
#13976 = EDGE_CURVE ( 'NONE', #62924, #87005, #59100, .T. ) ;
#13977 = VERTEX_POINT ( 'NONE', #62544 ) ;
#13978 = EDGE_CURVE ( 'NONE', #13635, #44538, #857, .T. ) ;
#13980 = CARTESIAN_POINT ( 'NONE',  ( -3.296039231325549324, -5.941354392334500467, 34.76329471203369792 ) ) ;
#13979 = CARTESIAN_POINT ( 'NONE',  ( 11.97435897435897267, -3.499999999999999556, 29.75000000000000355 ) ) ;
#13981 = CARTESIAN_POINT ( 'NONE',  ( 18.00000000000000000, -12.78798330534102945, 29.74999999999997868 ) ) ;
#13982 = DIRECTION ( 'NONE',  ( -0.000000000000000000, 0.9396926207859093161, -0.3420201433256663259 ) ) ;
#13983 = DIRECTION ( 'NONE',  ( -1.000000000000000000, 0.000000000000000000, 0.000000000000000000 ) ) ;
#13984 = LINE ( 'NONE', #13543, #77823 ) ;
#13985 = ORIENTED_EDGE ( 'NONE', *, *, #4164, .T. ) ;
#13986 = CARTESIAN_POINT ( 'NONE',  ( -5.869209559033047974, -8.191423895709842640, 34.95447573519442130 ) ) ;
#13987 = DIRECTION ( 'NONE',  ( 1.000000000000000000, 0.000000000000000000, 0.000000000000000000 ) ) ;
#13988 = DIRECTION ( 'NONE',  ( -0.000000000000000000, 0.6427876096865404731, -0.7660444431189770143 ) ) ;
#13989 = CYLINDRICAL_SURFACE ( 'NONE', #59742, 0.2499999999999973355 ) ;
#13990 = VERTEX_POINT ( 'NONE', #69757 ) ;
#13991 = B_SPLINE_CURVE_WITH_KNOTS ( 'NONE', 3,
 ( #62685, #7322, #21713, #28029, #42440, #49184 ),
 .UNSPECIFIED., .F., .F.,
 ( 4, 2, 4 ),
 ( 0.0003909512603273892074, 0.0005862562993132157656, 0.0007815613382990422697 ),
 .UNSPECIFIED. ) ;
#13992 = VERTEX_POINT ( 'NONE', #26566 ) ;
#13993 = VERTEX_POINT ( 'NONE', #81515 ) ;
#13994 = EDGE_CURVE ( 'NONE', #11726, #80537, #19804, .T. ) ;
#13995 = VECTOR ( 'NONE', #20073, 1000.000000000000000 ) ;
#13996 = DIRECTION ( 'NONE',  ( -1.000000000000000000, -0.000000000000000000, -0.000000000000000000 ) ) ;
#13997 = EDGE_LOOP ( 'NONE', ( #16494, #51032 ) ) ;
#13998 = CARTESIAN_POINT ( 'NONE',  ( -9.692307692307691624, -12.37446782046654192, 30.86335684631486131 ) ) ;
#13999 = DIRECTION ( 'NONE',  ( -0.000000000000000000, 0.8660254037844399289, -0.4999999999999980016 ) ) ;
#14000 = CARTESIAN_POINT ( 'NONE',  ( -5.999999999999998224, -1.466349020453238561, 30.81389545987213907 ) ) ;
#14001 = EDGE_CURVE ( 'NONE', #18284, #88230, #78395, .T. ) ;
#14002 = CARTESIAN_POINT ( 'NONE',  ( -1.553300858899081538, -11.25000000000000711, 14.85937500000000355 ) ) ;
#14003 = DIRECTION ( 'NONE',  ( -1.000000000000000000, 0.000000000000000000, -0.000000000000000000 ) ) ;
#14004 = EDGE_LOOP ( 'NONE', ( #71643, #12068, #46541, #38993 ) ) ;
#14005 = DIRECTION ( 'NONE',  ( 1.000000000000000000, 0.000000000000000000, 0.000000000000000000 ) ) ;
#14007 = EDGE_LOOP ( 'NONE', ( #84562, #18506, #12522, #55415 ) ) ;
#14006 = CARTESIAN_POINT ( 'NONE',  ( -12.21159294319032007, -11.86320923018887541, 32.19269448109604781 ) ) ;
#14008 = CARTESIAN_POINT ( 'NONE',  ( -5.326946301144534601, -2.341070481393820124, 30.72580821765574299 ) ) ;
#14009 = PLANE ( 'NONE',  #9430 ) ;
#14010 = CARTESIAN_POINT ( 'NONE',  ( 18.00000000000000000, -7.500000000000001776, 35.04278698407183867 ) ) ;
#14011 = CARTESIAN_POINT ( 'NONE',  ( 9.757563263583717728, -10.90142922261932057, 33.41473453929631887 ) ) ;
#14012 = CARTESIAN_POINT ( 'NONE',  ( -17.86947456176635640, -11.04252011169590197, 33.62494198852677840 ) ) ;
#14013 = VECTOR ( 'NONE', #70082, 1000.000000000000114 ) ;
#14014 = CARTESIAN_POINT ( 'NONE',  ( 16.82692307692308376, -7.566083408709835645, 34.74999999999999289 ) ) ;
#14015 = EDGE_CURVE ( 'NONE', #51615, #78324, #30538, .T. ) ;
#14016 = CARTESIAN_POINT ( 'NONE',  ( -2.980769230767811084, -7.500000000000154543, 35.00000000000007105 ) ) ;
#14017 = CARTESIAN_POINT ( 'NONE',  ( -0.06109907496451398579, -10.25000000000000178, 18.78311829374151287 ) ) ;
#14018 = EDGE_LOOP ( 'NONE', ( #82282, #55132, #26037, #46834 ) ) ;
#14019 = CARTESIAN_POINT ( 'NONE',  ( -3.099978789802281032, -6.369690395747422684, 34.87708834333098196 ) ) ;
#14020 = B_SPLINE_CURVE_WITH_KNOTS ( 'NONE', 3,
 ( #41955, #83389, #42404, #70305, #14027, #65195, #7278, #36087, #7727, #62645 ),
 .UNSPECIFIED., .F., .F.,
 ( 4, 2, 2, 2, 4 ),
 ( 0.0007817359430256307648, 0.0009771253907249971907, 0.001172514838424363508, 0.001367904286123729826, 0.001563293733823096143 ),
 .UNSPECIFIED. ) ;
#14021 = CARTESIAN_POINT ( 'NONE',  ( 8.769230769230768274, -10.05456864172156806, 36.03766855953608683 ) ) ;
#14022 = CARTESIAN_POINT ( 'NONE',  ( 8.352564102564102200, -3.499999999999999556, 29.75000000000000355 ) ) ;
#14023 = EDGE_LOOP ( 'NONE', ( #52709, #14495, #1276, #55645 ) ) ;
#14024 = ORIENTED_EDGE ( 'NONE', *, *, #40538, .T. ) ;
#14025 = CARTESIAN_POINT ( 'NONE',  ( 2.557692307692372324, -7.434744860731434812, 35.00000000000000711 ) ) ;
#14026 = CARTESIAN_POINT ( 'NONE',  ( 16.15384615384615330, -3.050289026998446396, 32.03036669348365706 ) ) ;
#14027 = CARTESIAN_POINT ( 'NONE',  ( -1.134669866267241645, -6.696923467548660192, 34.68552623307873972 ) ) ;
#14028 = CARTESIAN_POINT ( 'NONE',  ( -0.5268084620947816044, -11.06231777344662781, 33.60647404775220082 ) ) ;
#14029 = CARTESIAN_POINT ( 'NONE',  ( 0.5923289025054093715, -2.295524264805589354, 30.44142389570982488 ) ) ;
#14030 = VERTEX_POINT ( 'NONE', #22018 ) ;
#14031 = AXIS2_PLACEMENT_3D ( 'NONE', #66713, #5013, #87908 ) ;
#14032 = CARTESIAN_POINT ( 'NONE',  ( 6.000000000000001776, -5.557115091759785130, 34.35708131394839171 ) ) ;
#14033 = EDGE_CURVE ( 'NONE', #53401, #77030, #9391, .T. ) ;
#14034 = B_SPLINE_CURVE_WITH_KNOTS ( 'NONE', 3,
 ( #53596, #39659, #87861, #82415, #19369, #20261, #47727, #48160, #19816, #40976 ),
 .UNSPECIFIED., .F., .F.,
 ( 4, 2, 2, 2, 4 ),
 ( 0.000000000000000000, 0.0001954339857564098054, 0.0003908679715128196108, 0.0005863019572692293891, 0.0007817359430256392216 ),
 .UNSPECIFIED. ) ;
#14035 = CARTESIAN_POINT ( 'NONE',  ( 3.361294932532796320, -12.27024696741798770, 31.24895572276497546 ) ) ;
#14036 = CARTESIAN_POINT ( 'NONE',  ( 17.99999999999987566, -12.51329471203414379, 31.30864560766407578 ) ) ;
#14037 = ORIENTED_EDGE ( 'NONE', *, *, #70283, .F. ) ;
#14038 = CARTESIAN_POINT ( 'NONE',  ( -17.07692307692307665, -11.91647553114624181, 32.58852847137148245 ) ) ;
#14039 = EDGE_CURVE ( 'NONE', #25666, #76945, #10765, .T. ) ;
#14040 = ORIENTED_EDGE ( 'NONE', *, *, #47555, .T. ) ;
#14041 = FACE_OUTER_BOUND ( 'NONE', #70911, .T. ) ;
#14042 = CARTESIAN_POINT ( 'NONE',  ( 10.61538461538449418, -2.379036618888197729, 30.90682066428292885 ) ) ;
#14043 = ORIENTED_EDGE ( 'NONE', *, *, #26033, .F. ) ;
#14044 = EDGE_CURVE ( 'NONE', #60933, #373, #39815, .T. ) ;
#14045 = CIRCLE ( 'NONE', #15473, 4.000000000000000000 ) ;
#14046 = CARTESIAN_POINT ( 'NONE',  ( 7.780070435197965928, -12.10708131394839349, 31.69288490824020244 ) ) ;
#14047 = DIRECTION ( 'NONE',  ( -0.000000000000000000, -0.5000000000000009992, -0.8660254037844380415 ) ) ;
#14048 = CARTESIAN_POINT ( 'NONE',  ( -13.38461538461538325, -9.819645486525091727, 36.12317359536749706 ) ) ;
#14049 = CARTESIAN_POINT ( 'NONE',  ( -7.911423846710166075, -5.094484230520674117, 34.41647553114621161 ) ) ;
#14050 = CARTESIAN_POINT ( 'NONE',  ( 3.296024802045255164, -12.46129190930001052, 30.37095296980870174 ) ) ;
#14051 = ORIENTED_EDGE ( 'NONE', *, *, #5980, .T. ) ;
#14052 = FACE_BOUND ( 'NONE', #8699, .T. ) ;
#14053 = ORIENTED_EDGE ( 'NONE', *, *, #55304, .F. ) ;
#14055 = EDGE_CURVE ( 'NONE', #78946, #1158, #70201, .T. ) ;
#14054 = CARTESIAN_POINT ( 'NONE',  ( -9.019253993452224449, -12.45566812827425451, 31.48439005359158926 ) ) ;
#14056 = AXIS2_PLACEMENT_3D ( 'NONE', #86224, #11436, #24048 ) ;
#14057 = CARTESIAN_POINT ( 'NONE',  ( 18.00000000000000000, -12.10708131394839349, 31.69288490824020244 ) ) ;
#14058 = ADVANCED_FACE ( 'NONE', ( #84619 ), #35535, .F. ) ;
#14059 = DIRECTION ( 'NONE',  ( -0.000000000000000000, 0.3420201433256694346, -0.9396926207859080948 ) ) ;
#14060 = CARTESIAN_POINT ( 'NONE',  ( 14.43848274865925774, -8.191423895709840863, 34.95447573519442130 ) ) ;
#14061 = ORIENTED_EDGE ( 'NONE', *, *, #36088, .F. ) ;
#14062 = VECTOR ( 'NONE', #63512, 1000.000000000000114 ) ;
#14063 = ORIENTED_EDGE ( 'NONE', *, *, #34417, .F. ) ;
#14064 = EDGE_LOOP ( 'NONE', ( #31521, #13311, #88795, #68143 ) ) ;
#14065 = B_SPLINE_CURVE_WITH_KNOTS ( 'NONE', 3,
 ( #4940, #31510, #32404, #19337, #59428, #12143, #52215, #18006, #39624, #72491 ),
 .UNSPECIFIED., .F., .F.,
 ( 4, 2, 2, 2, 4 ),
 ( 0.000000000000000000, 0.0001954311564186865221, 0.0003908623128373730441, 0.0005862934692560595662, 0.0007817246256747460882 ),
 .UNSPECIFIED. ) ;
#14066 = CARTESIAN_POINT ( 'NONE',  ( 13.63461538461532285, -7.565270445406050648, 34.75000000000000000 ) ) ;
#14067 = ORIENTED_EDGE ( 'NONE', *, *, #64670, .T. ) ;
#14068 = ADVANCED_FACE ( 'NONE', ( #30100 ), #71519, .F. ) ;
#14069 = FACE_OUTER_BOUND ( 'NONE', #88530, .T. ) ;
#14070 = CARTESIAN_POINT ( 'NONE',  ( -9.561469274294926990, -7.277220443632450575, 34.74524770363009196 ) ) ;
#14071 = EDGE_CURVE ( 'NONE', #78927, #84142, #37288, .T. ) ;
#14072 = CARTESIAN_POINT ( 'NONE',  ( 3.230769230769108269, -8.656820664282941280, 34.87096338111179961 ) ) ;
#14073 = CARTESIAN_POINT ( 'NONE',  ( 3.230769230769231726, -9.058645607665452459, 34.76329471203371924 ) ) ;
#14074 = EDGE_CURVE ( 'NONE', #4690, #42018, #7534, .T. ) ;
#14075 = CARTESIAN_POINT ( 'NONE',  ( 5.076923076923075762, -9.905515769479276145, 34.41647553114623292 ) ) ;
#14076 = CARTESIAN_POINT ( 'NONE',  ( 15.45378058238208219, -9.086983370893049639, 34.49168942202179267 ) ) ;
#14077 = DIRECTION ( 'NONE',  ( -0.000000000000000000, 0.8660254037844397068, -0.4999999999999978906 ) ) ;
#14078 = CARTESIAN_POINT ( 'NONE',  ( 11.28843830116857383, -10.05641848906368097, 34.04755513067966177 ) ) ;
#14079 = EDGE_LOOP ( 'NONE', ( #86488, #40350, #23639, #52871 ) ) ;
#14080 = ORIENTED_EDGE ( 'NONE', *, *, #62198, .F. ) ;
#14081 = ORIENTED_EDGE ( 'NONE', *, *, #54258, .T. ) ;
#14083 = EDGE_CURVE ( 'NONE', #60639, #81205, #64753, .T. ) ;
#14082 = CARTESIAN_POINT ( 'NONE',  ( 4.153846153846154188, -2.538708090699994813, 30.37095296980875503 ) ) ;
#14085 = CARTESIAN_POINT ( 'NONE',  ( -5.933931648997561759, -3.513871655860379306, 32.76840700105978499 ) ) ;
#14084 = CARTESIAN_POINT ( 'NONE',  ( -3.099978789802281032, -9.929761469519744921, 34.40412654351204225 ) ) ;
#14086 = CARTESIAN_POINT ( 'NONE',  ( 1.515140822849027957, -12.50538340440932394, 31.33453814440721885 ) ) ;
#14087 = AXIS2_PLACEMENT_3D ( 'NONE', #33931, #88907, #41141 ) ;
#14088 = LINE ( 'NONE', #47421, #65233 ) ;
#14089 = FACE_BOUND ( 'NONE', #29530, .T. ) ;
#14090 = CARTESIAN_POINT ( 'NONE',  ( 9.822833394071260216, -3.816742781228458448, 33.13167719472716044 ) ) ;
#14091 = ORIENTED_EDGE ( 'NONE', *, *, #17401, .T. ) ;
#14092 = CARTESIAN_POINT ( 'NONE',  ( 14.53070515178570332, -12.38742843783360748, 31.66772728687926985 ) ) ;
#14093 = ADVANCED_FACE ( 'NONE', ( #50356 ), #42742, .F. ) ;
#14094 = CARTESIAN_POINT ( 'NONE',  ( -0.2115929431903201818, -9.272278438253398036, 34.42582936511637826 ) ) ;
#14095 = CYLINDRICAL_SURFACE ( 'NONE', #26049, 0.2499999999999973355 ) ;
#14096 = CARTESIAN_POINT ( 'NONE',  ( 6.000000000000001776, -11.11383981884818262, 36.00935417666054406 ) ) ;
#14097 = VERTEX_POINT ( 'NONE', #4400 ) ;
#14098 = CARTESIAN_POINT ( 'NONE',  ( 2.530703659305157949, -11.76359900205217457, 32.36225158514719880 ) ) ;
#14099 = AXIS2_PLACEMENT_3D ( 'NONE', #2116, #31366, #64690 ) ;
#14100 = ORIENTED_EDGE ( 'NONE', *, *, #49815, .F. ) ;
#14101 = FACE_BOUND ( 'NONE', #29318, .T. ) ;
#14102 = CARTESIAN_POINT ( 'NONE',  ( -17.30040800148741198, -4.225889041578354544, 33.85425143139329407 ) ) ;
#14103 = CARTESIAN_POINT ( 'NONE',  ( 18.00000000000000000, -8.810774026931790459, 35.74407628777942847 ) ) ;
#14104 = LINE ( 'NONE', #14547, #57645 ) ;
#14105 = VECTOR ( 'NONE', #45825, 1000.000000000000227 ) ;
#14106 = EDGE_LOOP ( 'NONE', ( #6995, #85630 ) ) ;
#14107 = CARTESIAN_POINT ( 'NONE',  ( -14.55771554498526932, -12.43535235679832596, 30.55408501211184813 ) ) ;
#14108 = CARTESIAN_POINT ( 'NONE',  ( -5.869474561766354626, -9.503571793651733657, 34.60286762892837942 ) ) ;
#14109 = DIRECTION ( 'NONE',  ( -0.000000000000000000, -0.9396926207859092051, -0.3420201433256662704 ) ) ;
#14110 = EDGE_CURVE ( 'NONE', #58603, #49729, #11647, .T. ) ;
#14111 = CARTESIAN_POINT ( 'NONE',  ( 4.153846153846154188, -2.708943851104267164, 35.45975837776705220 ) ) ;
#14112 = VERTEX_POINT ( 'NONE', #11159 ) ;
#14113 = CARTESIAN_POINT ( 'NONE',  ( 13.25392391794782654, -5.582088688514999397, 34.36776431015576350 ) ) ;
#14114 = FACE_OUTER_BOUND ( 'NONE', #15899, .T. ) ;
#14116 = ORIENTED_EDGE ( 'NONE', *, *, #71737, .F. ) ;
#14115 = CARTESIAN_POINT ( 'NONE',  ( 3.903846153846154632, -2.499999999999998668, 29.75000000000000355 ) ) ;
#14117 = CARTESIAN_POINT ( 'NONE',  ( 16.02315555073584008, -3.957541250942358424, 33.62499894934981626 ) ) ;
#14118 = DIRECTION ( 'NONE',  ( -1.000000000000000000, 0.000000000000000000, 0.000000000000000000 ) ) ;
#14119 = CARTESIAN_POINT ( 'NONE',  ( 16.40390057375961064, -12.01375889529407992, 32.43194544308182969 ) ) ;
#14120 = CARTESIAN_POINT ( 'NONE',  ( -13.38461538461550582, -3.835265460704628371, 33.15142922262033665 ) ) ;
#14121 = CARTESIAN_POINT ( 'NONE',  ( 11.53846153846141576, -8.656820664282941280, 34.87096338111179961 ) ) ;
#14123 = CARTESIAN_POINT ( 'NONE',  ( -1.944543648263014957, -5.555456351737005249, 14.00000000000000178 ) ) ;
#14122 = CARTESIAN_POINT ( 'NONE',  ( -6.000000000000121680, -6.835583212225970762, 34.95778746994575670 ) ) ;
#14124 = CARTESIAN_POINT ( 'NONE',  ( 14.17754509825408604, -3.817052484675422797, 33.13202310037935661 ) ) ;
#14125 = CARTESIAN_POINT ( 'NONE',  ( 1.139087296525997273, -4.749999999999992895, 16.73437500000000000 ) ) ;
#14126 = EDGE_LOOP ( 'NONE', ( #30032, #47464, #76118, #83266 ) ) ;
#14127 = CARTESIAN_POINT ( 'NONE',  ( -17.93393164899756087, -8.973038597847269315, 34.52809138561122637 ) ) ;
#14128 = ORIENTED_EDGE ( 'NONE', *, *, #74646, .T. ) ;
#14129 = VECTOR ( 'NONE', #72259, 1000.000000000000000 ) ;
#14130 = ORIENTED_EDGE ( 'NONE', *, *, #88659, .T. ) ;
#14131 = CYLINDRICAL_SURFACE ( 'NONE', #67196, 0.2499999999999979738 ) ;
#14132 = VERTEX_POINT ( 'NONE', #5294 ) ;
#14133 = CYLINDRICAL_SURFACE ( 'NONE', #916, 0.2499999999999995559 ) ;
#14134 = CARTESIAN_POINT ( 'NONE',  ( -1.139087296525992166, -10.25000000000000533, 18.60937500000000355 ) ) ;
#14135 = B_SPLINE_CURVE_WITH_KNOTS ( 'NONE', 3,
 ( #58113, #31081, #78382, #2714, #50894, #71623, #3612, #51326, #49593, #9928 ),
 .UNSPECIFIED., .F., .F.,
 ( 4, 2, 2, 2, 4 ),
 ( 0.0007817359430256334753, 0.0009771253907250058643, 0.001172514838424371098, 0.001367904286123736764, 0.001563293733823101998 ),
 .UNSPECIFIED. ) ;
#14136 = FACE_OUTER_BOUND ( 'NONE', #51806, .T. ) ;
#14137 = CARTESIAN_POINT ( 'NONE',  ( 2.980745993476266786, -8.432397168068783699, 34.66272746175022945 ) ) ;
#14139 = CARTESIAN_POINT ( 'NONE',  ( -7.146003881983771677, -9.172386477786396597, 34.72672124145550043 ) ) ;
#14138 = VECTOR ( 'NONE', #44163, 1000.000000000000000 ) ;
#14140 = CARTESIAN_POINT ( 'NONE',  ( 9.942253101685738059, -12.45601412856602686, 31.48342859153981621 ) ) ;
#14141 = CARTESIAN_POINT ( 'NONE',  ( -11.78848477575450282, -5.056417327199099532, 34.11270091957321426 ) ) ;
#14142 = CARTESIAN_POINT ( 'NONE',  ( 2.320192649118979489E-14, -11.25000000000000000, 24.78125000000000000 ) ) ;
#14143 = CARTESIAN_POINT ( 'NONE',  ( -7.846153846153844924, -11.69971097300155272, 32.46337939537588113 ) ) ;
#14144 = CARTESIAN_POINT ( 'NONE',  ( 15.00784227186238162, -9.172386477786396597, 34.72672124145550043 ) ) ;
#14145 = VECTOR ( 'NONE', #39767, 1000.000000000000114 ) ;
#14146 = FACE_OUTER_BOUND ( 'NONE', #24820, .T. ) ;
#14147 = CARTESIAN_POINT ( 'NONE',  ( -13.38461538461550582, -11.48612834414049644, 32.76840700105863391 ) ) ;
#14148 = ADVANCED_FACE ( 'NONE', ( #80062 ), #31885, .F. ) ;
#14149 = ORIENTED_EDGE ( 'NONE', *, *, #39338, .T. ) ;
#14150 = ORIENTED_EDGE ( 'NONE', *, *, #66195, .T. ) ;
#14151 = CARTESIAN_POINT ( 'NONE',  ( -39.05038313613820122, -2.249999999999998668, 29.75000000000000355 ) ) ;
#14152 = DIRECTION ( 'NONE',  ( -0.000000000000000000, 0.6427876096865404731, -0.7660444431189771253 ) ) ;
#14153 = CARTESIAN_POINT ( 'NONE',  ( -16.15384615384615330, -11.33034616979429110, 35.88435417666054406 ) ) ;
#14154 = CARTESIAN_POINT ( 'NONE',  ( -11.78846153846154010, -7.433931650972299465, 34.75000000000000711 ) ) ;
#14155 = ADVANCED_FACE ( 'NONE', ( #86851 ), #4856, .F. ) ;
#14156 = CARTESIAN_POINT ( 'NONE',  ( 12.33139125210024112, -9.418419913701741919, 34.36755862841477693 ) ) ;
#14157 = CARTESIAN_POINT ( 'NONE',  ( -9.822455662039388358, -6.809168938359901446, 34.95455904226513866 ) ) ;
#14158 = EDGE_CURVE ( 'NONE', #62900, #27787, #79622, .T. ) ;
#14159 = CYLINDRICAL_SURFACE ( 'NONE', #50858, 0.2499999999999986955 ) ;
#14160 = ORIENTED_EDGE ( 'NONE', *, *, #84483, .F. ) ;
#14161 = CARTESIAN_POINT ( 'NONE',  ( 15.93036121012220541, -2.847400154188068910, 31.58180166144859768 ) ) ;
#14162 = VERTEX_POINT ( 'NONE', #79175 ) ;
#14163 = EDGE_CURVE ( 'NONE', #5477, #15866, #30973, .T. ) ;
#14164 = AXIS2_PLACEMENT_3D ( 'NONE', #36806, #11110, #86352 ) ;
#14165 = B_SPLINE_CURVE_WITH_KNOTS ( 'NONE', 3,
 ( #59338, #66550, #37285, #65639, #64750, #10715, #32324, #59785, #45372, #73305 ),
 .UNSPECIFIED., .F., .F.,
 ( 4, 2, 2, 2, 4 ),
 ( 0.0007817359430256392216, 0.0009771253907250080327, 0.001172514838424376952, 0.001367904286123745872, 0.001563293733823114791 ),
 .UNSPECIFIED. ) ;
#14166 = CARTESIAN_POINT ( 'NONE',  ( 9.822833394071260216, -11.93748526763465279, 32.05452791011430946 ) ) ;
#14167 = CARTESIAN_POINT ( 'NONE',  ( 18.00000000000000000, -12.78798330534103123, 29.99999999999997868 ) ) ;
#14168 = CARTESIAN_POINT ( 'NONE',  ( -4.219929564802033184, -4.098570777380720287, 33.41473453929634729 ) ) ;
#14169 = CARTESIAN_POINT ( 'NONE',  ( 3.930919194939304973, -6.459968553980839800, 34.89616026154728701 ) ) ;
#14170 = CARTESIAN_POINT ( 'NONE',  ( -20.00000000000000355, -10.00000000000000533, 13.00000000000000178 ) ) ;
#14171 = EDGE_LOOP ( 'NONE', ( #33173, #59631, #23338, #31666 ) ) ;
#14172 = ORIENTED_EDGE ( 'NONE', *, *, #35105, .F. ) ;
#14173 = ORIENTED_EDGE ( 'NONE', *, *, #41024, .T. ) ;
#14174 = VERTEX_POINT ( 'NONE', #58897 ) ;
#14175 = DIRECTION ( 'NONE',  ( -0.000000000000000000, 0.9848077530122085754, -0.1736481776669273613 ) ) ;
#14176 = CARTESIAN_POINT ( 'NONE',  ( 7.780070435197965928, -3.513871655860377086, 32.76840700105978499 ) ) ;
#14177 = ADVANCED_FACE ( 'NONE', ( #44931 ), #18367, .F. ) ;
#14178 = PLANE ( 'NONE',  #53775 ) ;
#14179 = CARTESIAN_POINT ( 'NONE',  ( -15.29685264172511161, -11.16473453929635440, 33.15142922261925662 ) ) ;
#14180 = AXIS2_PLACEMENT_3D ( 'NONE', #27083, #68509, #6807 ) ;
#14181 = CARTESIAN_POINT ( 'NONE',  ( 7.780400417840515281, -7.249945578846652694, 34.99404164642496795 ) ) ;
#14182 = LINE ( 'NONE', #75884, #62434 ) ;
#14183 = ORIENTED_EDGE ( 'NONE', *, *, #8895, .F. ) ;
#14184 = ORIENTED_EDGE ( 'NONE', *, *, #58544, .F. ) ;
#14185 = ORIENTED_EDGE ( 'NONE', *, *, #58318, .F. ) ;
#14188 = EDGE_LOOP ( 'NONE', ( #44401, #48071, #38739, #85769 ) ) ;
#14187 = EDGE_CURVE ( 'NONE', #17157, #63787, #73148, .T. ) ;
#14186 = LINE ( 'NONE', #41666, #77641 ) ;
#14189 = CARTESIAN_POINT ( 'NONE',  ( 9.442330948259101575, -8.347322224742351082, 34.93158281831414769 ) ) ;
#14190 = CARTESIAN_POINT ( 'NONE',  ( -12.33074802057151409, -11.93129842949671726, 32.56571108434900452 ) ) ;
#14191 = AXIS2_PLACEMENT_3D ( 'NONE', #30496, #49448, #49001 ) ;
#14192 = CARTESIAN_POINT ( 'NONE',  ( 3.749999999999992006, -5.946699141100872943, 21.89062500000000355 ) ) ;
#14193 = VERTEX_POINT ( 'NONE', #46281 ) ;
#14194 = EDGE_CURVE ( 'NONE', #85648, #21721, #66555, .T. ) ;
#14195 = AXIS2_PLACEMENT_3D ( 'NONE', #36476, #76577, #36039 ) ;
#14196 = ADVANCED_FACE ( 'NONE', ( #72851 ), #32763, .F. ) ;
#14197 = B_SPLINE_CURVE_WITH_KNOTS ( 'NONE', 3,
 ( #38446, #4209, #18177, #45642, #73117, #38901, #25371, #59597, #87097, #46092 ),
 .UNSPECIFIED., .F., .F.,
 ( 4, 2, 2, 2, 4 ),
 ( 0.000000000000000000, 0.0001954339857564079623, 0.0003908679715128159245, 0.0005863019572692238597, 0.0007817359430256318490 ),
 .UNSPECIFIED. ) ;
#14198 = B_SPLINE_CURVE_WITH_KNOTS ( 'NONE', 3,
 ( #3097, #69797, #35577, #22059, #56283, #30573, #29707, #83772, #1337, #49532 ),
 .UNSPECIFIED., .F., .F.,
 ( 4, 2, 2, 2, 4 ),
 ( 0.000000000000000000, 0.0001954339857564098054, 0.0003908679715128196108, 0.0005863019572692293891, 0.0007817359430256392216 ),
 .UNSPECIFIED. ) ;
#14199 = VERTEX_POINT ( 'NONE', #46722 ) ;
#14200 = CARTESIAN_POINT ( 'NONE',  ( 13.38461538461538680, -10.67929555188718282, 33.92786785259544047 ) ) ;
#14201 = EDGE_LOOP ( 'NONE', ( #9940, #23972 ) ) ;
#14202 = FACE_BOUND ( 'NONE', #55167, .T. ) ;
#14203 = DIRECTION ( 'NONE',  ( -0.000000000000000000, 0.9396926207859093161, -0.3420201433256663259 ) ) ;
#14204 = DIRECTION ( 'NONE',  ( -0.000000000000000000, -0.000000000000000000, -1.000000000000000000 ) ) ;
#14205 = VERTEX_POINT ( 'NONE', #59789 ) ;
#14206 = DIRECTION ( 'NONE',  ( -0.000000000000000000, 1.000000000000000000, 3.491481338843133355E-15 ) ) ;
#14207 = DIRECTION ( 'NONE',  ( -0.000000000000000000, -0.5000000000000011102, -0.8660254037844381525 ) ) ;
#14208 = CARTESIAN_POINT ( 'NONE',  ( -13.38461538461550759, -4.320704448113951379, 33.92786785259630022 ) ) ;
#14210 = EDGE_LOOP ( 'NONE', ( #82121, #65484, #54720, #28127 ) ) ;
#14209 = EDGE_CURVE ( 'NONE', #73790, #26695, #31433, .T. ) ;
#14211 = CARTESIAN_POINT ( 'NONE',  ( -12.39547112818838492, -2.292212530054420494, 30.41441678777542990 ) ) ;
#14212 = CARTESIAN_POINT ( 'NONE',  ( -4.023055712879203938, -9.929761469519744921, 34.40412654351204225 ) ) ;
#14213 = CARTESIAN_POINT ( 'NONE',  ( 4.284371592079796010, -11.66157788607254275, 32.95092075102925833 ) ) ;
#14214 = CARTESIAN_POINT ( 'NONE',  ( -2.057746898314262829, -9.357781135181031829, 34.66075350412533851 ) ) ;
#14215 = EDGE_CURVE ( 'NONE', #23399, #9486, #2147, .T. ) ;
#14217 = EDGE_CURVE ( 'NONE', #85803, #69402, #53470, .T. ) ;
#14216 = DIRECTION ( 'NONE',  ( -0.000000000000000000, 0.5000000000000011102, -0.8660254037844380415 ) ) ;
#14218 = FACE_BOUND ( 'NONE', #56292, .T. ) ;
#14220 = CARTESIAN_POINT ( 'NONE',  ( -6.065270000556318486, -10.33852847137145048, 34.16647553114627556 ) ) ;
#14219 = CARTESIAN_POINT ( 'NONE',  ( -6.700064078983528404, -12.64618726649961289, 30.78989965857442712 ) ) ;
#14221 = CARTESIAN_POINT ( 'NONE',  ( -7.146003140593069958, -12.15238873228292071, 31.58232369045353849 ) ) ;
#14223 = CARTESIAN_POINT ( 'NONE',  ( 2.438482748659258625, -6.369690395747422684, 34.87708834333098196 ) ) ;
#14222 = CARTESIAN_POINT ( 'NONE',  ( -5.777220458731591179, -10.11255958852956027, 34.01340905677048454 ) ) ;
#14224 = CARTESIAN_POINT ( 'NONE',  ( -7.911423846710166075, -4.320704448112771878, 33.92786785259540494 ) ) ;
#14225 = VECTOR ( 'NONE', #38943, 1000.000000000000000 ) ;
#14226 = CARTESIAN_POINT ( 'NONE',  ( -2.749999999999997780, -7.561099074964547917, 17.34188170625849068 ) ) ;
#14227 = EDGE_CURVE ( 'NONE', #35007, #32782, #79531, .T. ) ;
#14228 = VERTEX_POINT ( 'NONE', #81852 ) ;
#14229 = CARTESIAN_POINT ( 'NONE',  ( 1.134592147322421196, -12.22074536777954989, 31.39888409691088356 ) ) ;
#14230 = ORIENTED_EDGE ( 'NONE', *, *, #58489, .T. ) ;
#14231 = CARTESIAN_POINT ( 'NONE',  ( -13.31854805126531005, -10.67929555188718282, 33.92786785259544757 ) ) ;
#14232 = ORIENTED_EDGE ( 'NONE', *, *, #54818, .T. ) ;
#14233 = CARTESIAN_POINT ( 'NONE',  ( -11.53846153846166089, -6.835583212225970762, 34.95778746994575670 ) ) ;
#14234 = CARTESIAN_POINT ( 'NONE',  ( 14.17754433796061875, -4.299443229763728169, 33.91186481527756058 ) ) ;
#14235 = EDGE_LOOP ( 'NONE', ( #41700, #89092, #67946, #46715 ) ) ;
#14236 = CARTESIAN_POINT ( 'NONE',  ( 2.307692307692309264, -8.120952969808772792, 34.71129190930000163 ) ) ;
#14237 = CARTESIAN_POINT ( 'NONE',  ( 0.06109907496454976272, -10.25000000000000000, 18.27938170625849068 ) ) ;
#14238 = CARTESIAN_POINT ( 'NONE',  ( 3.930361210122205406, -9.331801661448606566, 34.40259984581193464 ) ) ;
#14240 = CARTESIAN_POINT ( 'NONE',  ( 5.010839665967195877, -4.786620604624113540, 33.94971097300155805 ) ) ;
#14239 = B_SPLINE_CURVE_WITH_KNOTS ( 'NONE', 3,
 ( #83783, #1791, #50407, #23383, #28377, #55848, #69809, #14879, #43659, #49972 ),
 .UNSPECIFIED., .F., .F.,
 ( 4, 2, 2, 2, 4 ),
 ( 0.000000000000000000, 0.0001954339857564076912, 0.0003908679715128153824, 0.0005863019572692231007, 0.0007817359430256307648 ),
 .UNSPECIFIED. ) ;
#14241 = CARTESIAN_POINT ( 'NONE',  ( -3.100724174849458059, -2.254550872974306674, 29.97347326024527447 ) ) ;
#14242 = DIRECTION ( 'NONE',  ( 0.000000000000000000, -1.000000000000000000, 0.000000000000000000 ) ) ;
#14243 = CARTESIAN_POINT ( 'NONE',  ( 2.373760658694747061, -2.721908614388771852, 31.22303859784725333 ) ) ;
#14244 = CARTESIAN_POINT ( 'NONE',  ( -5.749945688361683516, -10.66356715214248396, 33.62249196103329751 ) ) ;
#14245 = B_SPLINE_CURVE_WITH_KNOTS ( 'NONE', 3,
 ( #27876, #63426, #84167, #63868, #22443, #49909, #7609, #14356, #77387, #43162 ),
 .UNSPECIFIED., .F., .F.,
 ( 4, 2, 2, 2, 4 ),
 ( 0.0007817246256747469556, 0.0009771112852218892010, 0.001172497944769031230, 0.001367884604316173258, 0.001563271263863315504 ),
 .UNSPECIFIED. ) ;
#14246 = CARTESIAN_POINT ( 'NONE',  ( 0.06109907496451268821, -3.749999999999999556, 24.40811829374151642 ) ) ;
#14247 = CARTESIAN_POINT ( 'NONE',  ( -18.13069060311031677, -11.37499894934982514, 33.29245874905763003 ) ) ;
#14248 = CARTESIAN_POINT ( 'NONE',  ( 10.61538461538449596, -11.48612834414049644, 32.76840700105863391 ) ) ;
#14249 = VERTEX_POINT ( 'NONE', #20137 ) ;
#14250 = CARTESIAN_POINT ( 'NONE',  ( 17.07692307692307665, -3.886160181151819604, 36.00935417666054406 ) ) ;
#14251 = CARTESIAN_POINT ( 'NONE',  ( 2.651650429449569302, -10.15165042944953733, 14.62500000000000000 ) ) ;
#14252 = EDGE_CURVE ( 'NONE', #76909, #41676, #54796, .T. ) ;
#14253 = CARTESIAN_POINT ( 'NONE',  ( -15.93106648486808119, -12.47679350104403007, 31.42216943046555855 ) ) ;
#14255 = DIRECTION ( 'NONE',  ( -0.000000000000000000, -0.8660254037844397068, -0.4999999999999978906 ) ) ;
#14254 = AXIS2_PLACEMENT_3D ( 'NONE', #27796, #48058, #13838 ) ;
#14256 = ORIENTED_EDGE ( 'NONE', *, *, #62567, .T. ) ;
#14257 = CARTESIAN_POINT ( 'NONE',  ( 14.37376065869474751, -2.538708090699994813, 30.37095296980875503 ) ) ;
#14258 = CARTESIAN_POINT ( 'NONE',  ( -14.55771554498527287, -11.37209801155882971, 32.91403422569032955 ) ) ;
#14260 = ORIENTED_EDGE ( 'NONE', *, *, #27613, .F. ) ;
#14259 = CARTESIAN_POINT ( 'NONE',  ( -2.749999999999998224, -7.500000000000000000, 11.00000000000000178 ) ) ;
#14261 = CARTESIAN_POINT ( 'NONE',  ( 14.30769230769231015, -13.53365097954675988, 30.81389545987213552 ) ) ;
#14262 = CARTESIAN_POINT ( 'NONE',  ( 13.51514108637895184, -2.619367082507849442, 30.83698974864643461 ) ) ;
#14263 = AXIS2_PLACEMENT_3D ( 'NONE', #82665, #61479, #6552 ) ;
#14264 = CARTESIAN_POINT ( 'NONE',  ( 16.15384615384615330, -8.973038597847269315, 34.52809138561121927 ) ) ;
#14265 = CARTESIAN_POINT ( 'NONE',  ( -17.07692307692307665, -2.721908614388771852, 31.22303859784724978 ) ) ;
#14266 = CARTESIAN_POINT ( 'NONE',  ( 6.699591979352975457, -5.113361153441932316, 34.14387501736621999 ) ) ;
#14267 = VERTEX_POINT ( 'NONE', #69209 ) ;
#14268 = VERTEX_POINT ( 'NONE', #68321 ) ;
#14269 = ORIENTED_EDGE ( 'NONE', *, *, #84507, .F. ) ;
#14270 = B_SPLINE_CURVE_WITH_KNOTS ( 'NONE', 3,
 ( #7569, #20629, #69266, #76469, #1240, #42248, #42687, #22404, #89118, #21515 ),
 .UNSPECIFIED., .F., .F.,
 ( 4, 2, 2, 2, 4 ),
 ( 0.000000000000000000, 0.0001954339857564080707, 0.0003908679715128161414, 0.0005863019572692241849, 0.0007817359430256322827 ),
 .UNSPECIFIED. ) ;
#14271 = CARTESIAN_POINT ( 'NONE',  ( 14.87820512820512953, -3.499999999999999556, 29.75000000000000355 ) ) ;
#14272 = LINE ( 'NONE', #35426, #60149 ) ;
#14273 = CYLINDRICAL_SURFACE ( 'NONE', #37794, 0.2499999999999994726 ) ;
#14274 = CARTESIAN_POINT ( 'NONE',  ( -6.923076923076922462, -3.937682226553329556, 33.60647404775216529 ) ) ;
#14276 = EDGE_CURVE ( 'NONE', #23267, #50940, #36626, .T. ) ;
#14275 = ORIENTED_EDGE ( 'NONE', *, *, #29640, .T. ) ;
#14277 = CARTESIAN_POINT ( 'NONE',  ( 17.14217821643591577, -11.67786785259547777, 32.92929555188713664 ) ) ;
#14278 = VERTEX_POINT ( 'NONE', #12935 ) ;
#14279 = ORIENTED_EDGE ( 'NONE', *, *, #35933, .F. ) ;
#14280 = ORIENTED_EDGE ( 'NONE', *, *, #67022, .T. ) ;
#14282 = VERTEX_POINT ( 'NONE', #309 ) ;
#14281 = CARTESIAN_POINT ( 'NONE',  ( -15.36091644020745584, -12.27039167877662251, 31.24851455888617835 ) ) ;
#14283 = CARTESIAN_POINT ( 'NONE',  ( -0.7115616988314262814, -5.056417327199099532, 34.11270091957321426 ) ) ;
#14284 = AXIS2_PLACEMENT_3D ( 'NONE', #71255, #72148, #36602 ) ;
#14285 = CARTESIAN_POINT ( 'NONE',  ( 5.869852030268304155, -12.70455904226513866, 30.44083106164009322 ) ) ;
#14286 = CARTESIAN_POINT ( 'NONE',  ( -10.61538461538461320, -6.343179335718451384, 34.87096338111211935 ) ) ;
#14287 = EDGE_CURVE ( 'NONE', #67890, #57330, #90, .T. ) ;
#14288 = CARTESIAN_POINT ( 'NONE',  ( -6.923076923076922462, -8.564572088678739092, 35.78748833219616898 ) ) ;
#14289 = ORIENTED_EDGE ( 'NONE', *, *, #49496, .F. ) ;
#14290 = EDGE_CURVE ( 'NONE', #2529, #29364, #41301, .T. ) ;
#14291 = ORIENTED_EDGE ( 'NONE', *, *, #26863, .F. ) ;
#14292 = ORIENTED_EDGE ( 'NONE', *, *, #66998, .F. ) ;
#14293 = CARTESIAN_POINT ( 'NONE',  ( -2.307692307692305711, -3.322132147404559976, 32.92929555188717927 ) ) ;
#14295 = ORIENTED_EDGE ( 'NONE', *, *, #2645, .T. ) ;
#14294 = FACE_OUTER_BOUND ( 'NONE', #9328, .T. ) ;
#14296 = LINE ( 'NONE', #75126, #15867 ) ;
#14297 = CARTESIAN_POINT ( 'NONE',  ( -0.5276208408985970655, -6.343179335718451384, 34.87096338111212646 ) ) ;
#14298 = ORIENTED_EDGE ( 'NONE', *, *, #61408, .T. ) ;
#14299 = EDGE_CURVE ( 'NONE', #45063, #56304, #35500, .T. ) ;
#14300 = CYLINDRICAL_SURFACE ( 'NONE', #23554, 0.2500000000000002220 ) ;
#14301 = DIRECTION ( 'NONE',  ( 0.000000000000000000, 0.000000000000000000, 1.000000000000000000 ) ) ;
#14302 = ORIENTED_EDGE ( 'NONE', *, *, #12281, .F. ) ;
#14303 = FACE_BOUND ( 'NONE', #27001, .T. ) ;
#14304 = CARTESIAN_POINT ( 'NONE',  ( -0.4615384615385826339, -10.21337939537710326, 33.94971097300076224 ) ) ;
#14305 = CARTESIAN_POINT ( 'NONE',  ( 16.08857615328984281, -2.657715359629089669, 31.77849191805833584 ) ) ;
#14306 = CARTESIAN_POINT ( 'NONE',  ( 12.21156171748986985, -6.524016743844655686, 34.90889640711025521 ) ) ;
#14309 = CARTESIAN_POINT ( 'NONE',  ( -9.692307692307812417, -2.892918686052166066, 31.69288490824153470 ) ) ;
#14308 = AXIS2_PLACEMENT_3D ( 'NONE', #87349, #32829, #66619 ) ;
#14307 = CARTESIAN_POINT ( 'NONE',  ( 18.13052543823364360, -3.068774925481847937, 32.56582465632704526 ) ) ;
#14310 = DIRECTION ( 'NONE',  ( 0.000000000000000000, 0.6427876096865373645, -0.7660444431189797898 ) ) ;
#14311 = CARTESIAN_POINT ( 'NONE',  ( -2.307692307692427391, -3.835265460704628371, 33.15142922262033665 ) ) ;
#14312 = ORIENTED_EDGE ( 'NONE', *, *, #64096, .F. ) ;
#14313 = DIRECTION ( 'NONE',  ( -0.000000000000000000, -0.3420201433256694346, -0.9396926207859080948 ) ) ;
#14314 = CARTESIAN_POINT ( 'NONE',  ( 13.60757828817687276, -7.369474270740069777, 34.74850911626239736 ) ) ;
#14315 = VERTEX_POINT ( 'NONE', #21464 ) ;
#14316 = VECTOR ( 'NONE', #70235, 1000.000000000000114 ) ;
#14317 = VECTOR ( 'NONE', #82505, 1000.000000000000000 ) ;
#14318 = CARTESIAN_POINT ( 'NONE',  ( 27.00000000000000000, 0.7500000000000061062, 23.75000000000000000 ) ) ;
#14319 = CARTESIAN_POINT ( 'NONE',  ( 16.81410256410256565, -7.500000000000000000, 33.75000000000000000 ) ) ;
#14320 = ORIENTED_EDGE ( 'NONE', *, *, #70443, .F. ) ;
#14321 = CARTESIAN_POINT ( 'NONE',  ( 18.00000000000000000, -5.557115091759785130, 34.35708131394839171 ) ) ;
#14322 = ADVANCED_FACE ( 'NONE', ( #74198 ), #39979, .F. ) ;
#14323 = DIRECTION ( 'NONE',  ( 0.000000000000000000, 0.6427876096865373645, -0.7660444431189797898 ) ) ;
#14324 = FACE_BOUND ( 'NONE', #72014, .T. ) ;
#14326 = CARTESIAN_POINT ( 'NONE',  ( 4.088576153289833925, -12.51329471203370325, 31.30864560766548976 ) ) ;
#14325 = CARTESIAN_POINT ( 'NONE',  ( 6.673053698855467175, -4.175268141568689195, 33.81360843649122216 ) ) ;
#14327 = CARTESIAN_POINT ( 'NONE',  ( -9.019254006523732770, -6.695914987888146541, 34.68535235679833306 ) ) ;
#14328 = CARTESIAN_POINT ( 'NONE',  ( -15.29685264172511161, -8.973038597847271092, 34.52809138561120506 ) ) ;
#14330 = CARTESIAN_POINT ( 'NONE',  ( 0.2115152242454954590, -5.851115903089113779, 34.47074536777953568 ) ) ;
#14329 = CARTESIAN_POINT ( 'NONE',  ( 0.000000000000000000, 0.000000000000000000, 0.000000000000000000 ) ) ;
#14331 = CARTESIAN_POINT ( 'NONE',  ( -17.86920819217521483, -4.809403383903224416, 33.96459661697924304 ) ) ;
#14332 = CARTESIAN_POINT ( 'NONE',  ( 0.06109907496455496689, -11.24999999999999822, 17.02938170625848713 ) ) ;
#14333 = VERTEX_POINT ( 'NONE', #72636 ) ;
#14334 = B_SPLINE_CURVE_WITH_KNOTS ( 'NONE', 3,
 ( #42178, #35402, #63316, #1626, #29109, #36302, #38517, #77717, #51550, #30422 ),
 .UNSPECIFIED., .F., .F.,
 ( 4, 2, 2, 2, 4 ),
 ( 0.0007817359430256216575, 0.0009771253907249856981, 0.001172514838424349630, 0.001367904286123713779, 0.001563293733823077711 ),
 .UNSPECIFIED. ) ;
#14335 = ORIENTED_EDGE ( 'NONE', *, *, #64595, .T. ) ;
#14336 = CARTESIAN_POINT ( 'NONE',  ( -9.758390071667831123, -2.292212530054419606, 30.41441678777542634 ) ) ;
#14337 = DIRECTION ( 'NONE',  ( 0.000000000000000000, 0.000000000000000000, -1.000000000000000000 ) ) ;
#14338 = CARTESIAN_POINT ( 'NONE',  ( 1.515140822849031732, -9.503571793651733657, 34.60286762892837942 ) ) ;
#14339 = CARTESIAN_POINT ( 'NONE',  ( -8.899378738962466784, -8.630895178749533159, 34.87696386517710323 ) ) ;
#14340 = CARTESIAN_POINT ( 'NONE',  ( -16.28399336328438096, -12.27039167877662251, 31.24851455888617835 ) ) ;
#14341 = CARTESIAN_POINT ( 'NONE',  ( 1.492201783934554493, -3.724691934501233703, 17.73250670625848713 ) ) ;
#14342 = CYLINDRICAL_SURFACE ( 'NONE', #18751, 0.2500000000000008882 ) ;
#14343 = CARTESIAN_POINT ( 'NONE',  ( 5.750023255951409951, -2.920706130388546651, 32.31842814019191223 ) ) ;
#14344 = CARTESIAN_POINT ( 'NONE',  ( 6.065255139512838234, -4.320704448112861584, 33.92786785259548310 ) ) ;
#14345 = DIRECTION ( 'NONE',  ( 0.000000000000000000, 0.000000000000000000, 1.000000000000000000 ) ) ;
#14346 = CARTESIAN_POINT ( 'NONE',  ( -15.10024352900566846, -11.46989282347013095, 32.79007818306219946 ) ) ;
#14347 = CARTESIAN_POINT ( 'NONE',  ( 18.24994551834813805, -10.05730279482229683, 34.04704008940765902 ) ) ;
#14348 = CARTESIAN_POINT ( 'NONE',  ( -9.692307692307691624, -12.62096338111211580, 30.90682066428153263 ) ) ;
#14349 = FACE_OUTER_BOUND ( 'NONE', #29933, .T. ) ;
#14350 = CARTESIAN_POINT ( 'NONE',  ( 2.980745993476267675, -2.587272538249755449, 30.68239716806877837 ) ) ;
#14351 = EDGE_LOOP ( 'NONE', ( #71419, #35741, #18136, #34396 ) ) ;
#14352 = CARTESIAN_POINT ( 'NONE',  ( 2.084765348785459160, -3.395401636524185474, 33.02366814457250399 ) ) ;
#14353 = LINE ( 'NONE', #62526, #21583 ) ;
#14354 = CARTESIAN_POINT ( 'NONE',  ( -2.775308065498752086, -8.577988221561495763, 21.51749329374151998 ) ) ;
#14355 = CARTESIAN_POINT ( 'NONE',  ( -0.3307480205715112032, -10.70102852606553157, 33.91149625220312913 ) ) ;
#14356 = CARTESIAN_POINT ( 'NONE',  ( -16.02305571287920216, -2.494656445102014342, 31.33466734024120015 ) ) ;
#14357 = EDGE_LOOP ( 'NONE', ( #11384, #59528, #83362, #32793 ) ) ;
#14358 = CARTESIAN_POINT ( 'NONE',  ( 10.39251919318097883, -2.501496062324912284, 29.88072118266895671 ) ) ;
#14360 = ORIENTED_EDGE ( 'NONE', *, *, #57133, .F. ) ;
#14359 = CARTESIAN_POINT ( 'NONE',  ( -5.934855219280366967, -7.750023224968867197, 34.99404313364389907 ) ) ;
#14361 = CARTESIAN_POINT ( 'NONE',  ( -22.00000000000000711, 9.999999999999971578, 0.000000000000000000 ) ) ;
#14362 = CARTESIAN_POINT ( 'NONE',  ( -9.626240358957616650, -5.471508081941601098, 34.59228464037088457 ) ) ;
#14363 = VERTEX_POINT ( 'NONE', #8396 ) ;
#14364 = CARTESIAN_POINT ( 'NONE',  ( -5.143006487878956534, -12.10708131394839349, 31.69288490824020244 ) ) ;
#14365 = CARTESIAN_POINT ( 'NONE',  ( 7.976201452409529047, -7.723484964179499812, 34.74522123443822608 ) ) ;
#14366 = ORIENTED_EDGE ( 'NONE', *, *, #75165, .T. ) ;
#14367 = B_SPLINE_CURVE_WITH_KNOTS ( 'NONE', 3,
 ( #28095, #35292, #14579, #27649, #8275, #14137, #61428, #82619, #55558, #83494 ),
 .UNSPECIFIED., .F., .F.,
 ( 4, 2, 2, 2, 4 ),
 ( 0.000000000000000000, 0.0001954339857564079352, 0.0003908679715128158703, 0.0005863019572692237513, 0.0007817359430256317406 ),
 .UNSPECIFIED. ) ;
#14368 = CARTESIAN_POINT ( 'NONE',  ( -10.83886953994894675, -4.225889041578353655, 33.85425143139329407 ) ) ;
#14369 = CARTESIAN_POINT ( 'NONE',  ( -16.02379854759047006, -7.723484964179501588, 34.74522123443823318 ) ) ;
#14370 = B_SPLINE_CURVE_WITH_KNOTS ( 'NONE', 3,
 ( #49272, #200, #76294, #21353, #40752, #27667, #8293, #26784, #34862, #83064 ),
 .UNSPECIFIED., .F., .F.,
 ( 4, 2, 2, 2, 4 ),
 ( 0.000000000000000000, 0.0001954311564186865763, 0.0003908623128373730441, 0.0005862934692560595662, 0.0007817246256747460882 ),
 .UNSPECIFIED. ) ;
#14372 = CARTESIAN_POINT ( 'NONE',  ( 9.692307692307570832, -6.835583212225970762, 34.95778746994575670 ) ) ;
#14371 = AXIS2_PLACEMENT_3D ( 'NONE', #11763, #45535, #17174 ) ;
#14373 = ORIENTED_EDGE ( 'NONE', *, *, #59451, .F. ) ;
#14374 = ORIENTED_EDGE ( 'NONE', *, *, #65155, .T. ) ;
#14375 = CARTESIAN_POINT ( 'NONE',  ( -6.923076923076922462, -8.164416787775445883, 34.95778746994557906 ) ) ;
#14376 = B_SPLINE_CURVE_WITH_KNOTS ( 'NONE', 3,
 ( #17739, #10981, #86662, #66363, #22815, #51484, #4667, #78985, #34343, #55503 ),
 .UNSPECIFIED., .F., .F.,
 ( 4, 2, 2, 2, 4 ),
 ( 0.0007817246256747494492, 0.0009771112852218941883, 0.001172497944769039036, 0.001367884604316183883, 0.001563271263863328731 ),
 .UNSPECIFIED. ) ;
#14377 = B_SPLINE_CURVE_WITH_KNOTS ( 'NONE', 3,
 ( #39179, #10360, #10804, #85575, #38273, #45016, #32407, #51301, #31514, #66638 ),
 .UNSPECIFIED., .F., .F.,
 ( 4, 2, 2, 2, 4 ),
 ( 0.0007817359527651096280, 0.0009771254036996484919, 0.001172514854634187573, 0.001367904305568726653, 0.001563293756503265517 ),
 .UNSPECIFIED. ) ;
#14378 = ORIENTED_EDGE ( 'NONE', *, *, #86712, .F. ) ;
#14379 = CIRCLE ( 'NONE', #50288, 4.999999999999997335 ) ;
#14380 = VECTOR ( 'NONE', #80793, 1000.000000000000114 ) ;
#14381 = CARTESIAN_POINT ( 'NONE',  ( -17.93393266664992325, -4.661471528628506888, 34.16647553114624003 ) ) ;
#14382 = CARTESIAN_POINT ( 'NONE',  ( -6.988346923633241836, -2.379036618887870436, 30.90682066428147934 ) ) ;
#14383 = CARTESIAN_POINT ( 'NONE',  ( 3.230769230769231726, -8.564572088678739092, 35.78748833219616898 ) ) ;
#14384 = CARTESIAN_POINT ( 'NONE',  ( 12.46153846153846168, -8.318370150425687726, 35.83090037661290239 ) ) ;
#14385 = CARTESIAN_POINT ( 'NONE',  ( -0.2115930521604186265, -5.766571408460171355, 34.70601412856602508 ) ) ;
#14386 = CARTESIAN_POINT ( 'NONE',  ( 1.161130460051056135, -2.353723527008297012, 30.78948104536958397 ) ) ;
#14387 = AXIS2_PLACEMENT_3D ( 'NONE', #30198, #50882, #38727 ) ;
#14388 = AXIS2_PLACEMENT_3D ( 'NONE', #1566, #28601, #10875 ) ;
#14389 = STYLED_ITEM ( 'NONE', ( #9182 ), #73996 ) ;
#14390 = FACE_OUTER_BOUND ( 'NONE', #83957, .T. ) ;
#14391 = ORIENTED_EDGE ( 'NONE', *, *, #40180, .F. ) ;
#14392 = EDGE_LOOP ( 'NONE', ( #40033, #5672, #51796, #6921 ) ) ;
#14394 = ORIENTED_EDGE ( 'NONE', *, *, #79644, .F. ) ;
#14393 = CARTESIAN_POINT ( 'NONE',  ( -0.3962828902624367933, -12.27809138561124591, 31.22303859784720359 ) ) ;
#14395 = LINE ( 'NONE', #25809, #85529 ) ;
#14396 = ADVANCED_FACE ( 'NONE', ( #1185 ), #22782, .F. ) ;
#14397 = ORIENTED_EDGE ( 'NONE', *, *, #51107, .F. ) ;
#14398 = DIRECTION ( 'NONE',  ( -0.000000000000000000, 1.000000000000000000, 3.491481338843133355E-15 ) ) ;
#14399 = CARTESIAN_POINT ( 'NONE',  ( 5.299934428535925335, -3.587049720035815348, 32.86302985866382897 ) ) ;
#14400 = EDGE_LOOP ( 'NONE', ( #31361, #42561 ) ) ;
#14401 = CARTESIAN_POINT ( 'NONE',  ( -9.942307692307695177, -2.499999999999999556, 29.81609845454691765 ) ) ;
#14402 = ORIENTED_EDGE ( 'NONE', *, *, #88083, .F. ) ;
#14403 = ORIENTED_EDGE ( 'NONE', *, *, #82442, .T. ) ;
#14404 = CARTESIAN_POINT ( 'NONE',  ( -10.48454619737184679, -7.277220443632450575, 34.74524770363009196 ) ) ;
#14405 = B_SPLINE_CURVE_WITH_KNOTS ( 'NONE', 3,
 ( #28477, #21266, #55940, #77106, #70354, #49187, #14970, #50067, #8656, #77548 ),
 .UNSPECIFIED., .F., .F.,
 ( 4, 2, 2, 2, 4 ),
 ( 0.000000000000000000, 0.0001954339857564054144, 0.0003908679715128108288, 0.0005863019572692162703, 0.0007817359430256216575 ),
 .UNSPECIFIED. ) ;
#14406 = ORIENTED_EDGE ( 'NONE', *, *, #79507, .F. ) ;
#14407 = EDGE_CURVE ( 'NONE', #76825, #55297, #36278, .T. ) ;
#14408 = CARTESIAN_POINT ( 'NONE',  ( 17.77707378248384629, -10.61292498521070549, 33.66303323003028680 ) ) ;
#14409 = CARTESIAN_POINT ( 'NONE',  ( 17.07692307692307665, -2.721908614388771852, 31.22303859784724978 ) ) ;
#14410 = FACE_BOUND ( 'NONE', #13720, .T. ) ;
#14411 = DIRECTION ( 'NONE',  ( -0.000000000000000000, 0.9848077530122085754, -0.1736481776669273613 ) ) ;
#14412 = FACE_OUTER_BOUND ( 'NONE', #12225, .T. ) ;
#14413 = CARTESIAN_POINT ( 'NONE',  ( 4.403900465484468008, -12.41262288849542017, 30.68299917996395010 ) ) ;
#14414 = CARTESIAN_POINT ( 'NONE',  ( 3.480823650682683734, -4.818054556918156983, 34.26375889529406749 ) ) ;
#14415 = CARTESIAN_POINT ( 'NONE',  ( 5.076923076923075762, -10.51840700105979565, 33.73612834413961536 ) ) ;
#14416 = CARTESIAN_POINT ( 'NONE',  ( -9.822867605921057788, -2.254533558242300284, 29.97296025877828285 ) ) ;
#14417 = ORIENTED_EDGE ( 'NONE', *, *, #67038, .F. ) ;
#14418 = CARTESIAN_POINT ( 'NONE',  ( 14.53070515178570332, -6.460100341425560444, 34.89618726649961644 ) ) ;
#14419 = ORIENTED_EDGE ( 'NONE', *, *, #1622, .F. ) ;
#14420 = ORIENTED_EDGE ( 'NONE', *, *, #4802, .T. ) ;
#14422 = CYLINDRICAL_SURFACE ( 'NONE', #33325, 0.2500000000000004996 ) ;
#14421 = FACE_OUTER_BOUND ( 'NONE', #44277, .T. ) ;
#14423 = CARTESIAN_POINT ( 'NONE',  ( -9.561517251340744039, -12.35292014791297710, 31.75344720912887198 ) ) ;
#14424 = LINE ( 'NONE', #41460, #7773 ) ;
#14425 = CARTESIAN_POINT ( 'NONE',  ( 1.607628228708781082, -10.77377354290276301, 33.85451476688484718 ) ) ;
#14426 = DIRECTION ( 'NONE',  ( -0.000000000000000000, 0.1736481776669307198, -0.9848077530122080203 ) ) ;
#14427 = VERTEX_POINT ( 'NONE', #45162 ) ;
#14428 = EDGE_CURVE ( 'NONE', #17730, #34055, #49813, .T. ) ;
#14429 = DIRECTION ( 'NONE',  ( -0.000000000000000000, 0.7660444431189791237, -0.6427876096865379196 ) ) ;
#14430 = CARTESIAN_POINT ( 'NONE',  ( -14.55771553191376277, -10.18141759479407327, 34.26406193332782379 ) ) ;
#14431 = CARTESIAN_POINT ( 'NONE',  ( -14.30769230769230660, -12.34228464037088635, 31.77849191805839268 ) ) ;
#14432 = VECTOR ( 'NONE', #60271, 1000.000000000000000 ) ;
#14433 = EDGE_CURVE ( 'NONE', #74452, #21962, #86623, .T. ) ;
#14434 = CYLINDRICAL_SURFACE ( 'NONE', #22333, 0.2500000000000002220 ) ;
#14435 = CARTESIAN_POINT ( 'NONE',  ( 14.30769230769231015, -8.120952969808772792, 34.71129190930000163 ) ) ;
#14436 = ORIENTED_EDGE ( 'NONE', *, *, #70283, .T. ) ;
#14437 = ORIENTED_EDGE ( 'NONE', *, *, #86872, .T. ) ;
#14438 = ADVANCED_FACE ( 'NONE', ( #63329 ), #77290, .T. ) ;
#14439 = AXIS2_PLACEMENT_3D ( 'NONE', #62698, #76678, #28949 ) ;
#14440 = ORIENTED_EDGE ( 'NONE', *, *, #51673, .T. ) ;
#14441 = ADVANCED_FACE ( 'NONE', ( #84504 ), #1641, .F. ) ;
#14442 = DIRECTION ( 'NONE',  ( -0.000000000000000000, 0.5000000000000011102, -0.8660254037844380415 ) ) ;
#14443 = ADVANCED_FACE ( 'NONE', ( #29125 ), #70088, .F. ) ;
#14444 = B_SPLINE_CURVE_WITH_KNOTS ( 'NONE', 3,
 ( #64946, #86582, #3252, #10908, #65832, #59084, #52324, #66288, #58190, #32066 ),
 .UNSPECIFIED., .F., .F.,
 ( 4, 2, 2, 2, 4 ),
 ( 0.0007817359430256294638, 0.0009771253907249948054, 0.001172514838424360255, 0.001367904286123725706, 0.001563293733823091156 ),
 .UNSPECIFIED. ) ;
#14445 = EDGE_LOOP ( 'NONE', ( #87627, #52521 ) ) ;
#14446 = DIRECTION ( 'NONE',  ( -0.000000000000000000, 0.5000000000000011102, -0.8660254037844381525 ) ) ;
#14447 = DIRECTION ( 'NONE',  ( 1.000000000000000000, 0.000000000000000000, 0.000000000000000000 ) ) ;
#14448 = CARTESIAN_POINT ( 'NONE',  ( 14.24242230713598900, -10.33852847137145048, 34.16647553114627556 ) ) ;
#14449 = CARTESIAN_POINT ( 'NONE',  ( -17.32694630114453105, -9.356822207818511927, 34.66110646841856635 ) ) ;
#14450 = CIRCLE ( 'NONE', #63356, 0.2500000000000002220 ) ;
#14451 = CARTESIAN_POINT ( 'NONE',  ( -11.40793583669797506, -6.852161475712352789, 34.70806712695775786 ) ) ;
#14452 = VERTEX_POINT ( 'NONE', #56581 ) ;
#14454 = CARTESIAN_POINT ( 'NONE',  ( -11.28846153846011902, -7.500000000000154543, 35.00000000000007105 ) ) ;
#14453 =( GEOMETRIC_REPRESENTATION_CONTEXT ( 3 ) GLOBAL_UNCERTAINTY_ASSIGNED_CONTEXT ( ( #83445 ) ) GLOBAL_UNIT_ASSIGNED_CONTEXT ( ( #81033, #52199, #58960 ) ) REPRESENTATION_CONTEXT ( 'NONE', 'WORKASPACE' ) );
#14456 = ORIENTED_EDGE ( 'NONE', *, *, #23340, .F. ) ;
#14455 = DIRECTION ( 'NONE',  ( -0.000000000000000000, -0.9396926207859092051, -0.3420201433256662704 ) ) ;
#14457 = DIRECTION ( 'NONE',  ( -0.000000000000000000, 0.9848077530122085754, -0.1736481776669273613 ) ) ;
#14458 = CARTESIAN_POINT ( 'NONE',  ( -7.134615384615385025, -7.500000000000000000, 29.75000000000000355 ) ) ;
#14459 = CARTESIAN_POINT ( 'NONE',  ( 17.29993442853592711, -11.24521262558773493, 33.06293181088029343 ) ) ;
#14460 = B_SPLINE_CURVE_WITH_KNOTS ( 'NONE', 3,
 ( #18681, #18231, #19553, #88053, #47015, #12799, #45692, #69073, #76264, #7380 ),
 .UNSPECIFIED., .F., .F.,
 ( 4, 2, 2, 2, 4 ),
 ( 0.000000000000000000, 0.0001954339857564078538, 0.0003908679715128157077, 0.0005863019572692235344, 0.0007817359430256314154 ),
 .UNSPECIFIED. ) ;
#14461 = CARTESIAN_POINT ( 'NONE',  ( -16.40384615384615330, -7.500000000000001776, 35.00000000000000000 ) ) ;
#14462 = CARTESIAN_POINT ( 'NONE',  ( -18.00000000000012079, -11.06231777344772027, 33.60647404775119895 ) ) ;
#14463 = CARTESIAN_POINT ( 'NONE',  ( 9.627037246346917598, -10.21337939537584383, 33.94971097300158647 ) ) ;
#14464 = CARTESIAN_POINT ( 'NONE',  ( -12.52762187249434156, -12.37446782046654192, 30.86335684631486487 ) ) ;
#14465 = CARTESIAN_POINT ( 'NONE',  ( 2.694853999681185108, -4.891553140782077591, 14.56436829374151287 ) ) ;
#14466 = ORIENTED_EDGE ( 'NONE', *, *, #8495, .T. ) ;
#14467 = LINE ( 'NONE', #41946, #11503 ) ;
#14468 = CARTESIAN_POINT ( 'NONE',  ( -16.15384615384615330, -5.471508081941601098, 34.59228464037088457 ) ) ;
#14469 = CARTESIAN_POINT ( 'NONE',  ( 7.912222197156284054, -2.538708090699994813, 30.37095296980875503 ) ) ;
#14470 = DIRECTION ( 'NONE',  ( -0.000000000000000000, 1.000000000000000000, -0.000000000000000000 ) ) ;
#14471 = EDGE_LOOP ( 'NONE', ( #75584, #20703, #21404, #58134 ) ) ;
#14472 = CARTESIAN_POINT ( 'NONE',  ( 18.00000000000000000, -3.886160181151819604, 36.00935417666054406 ) ) ;
#14473 = CARTESIAN_POINT ( 'NONE',  ( 10.61538461538461675, -1.129524287112498415, 32.06866353760679544 ) ) ;
#14474 = CARTESIAN_POINT ( 'NONE',  ( 1.319344938654610777, -9.442884908240170461, 34.35708131394840592 ) ) ;
#14475 = CARTESIAN_POINT ( 'NONE',  ( -0.5916864312701604067, -11.04286588640298561, 33.62463336215343901 ) ) ;
#14476 = ORIENTED_EDGE ( 'NONE', *, *, #9004, .T. ) ;
#14477 = ADVANCED_FACE ( 'NONE', ( #38416 ), #84069, .F. ) ;
#14478 = CARTESIAN_POINT ( 'NONE',  ( -12.21159294319032362, -9.272278438253398036, 34.42582936511637115 ) ) ;
#14479 = CARTESIAN_POINT ( 'NONE',  ( -14.55766903863466055, -2.779195860258146578, 31.39871582349836032 ) ) ;
#14480 = CARTESIAN_POINT ( 'NONE',  ( 7.596177115211492747, -9.943427161483782584, 34.11278801902876978 ) ) ;
#14481 = EDGE_LOOP ( 'NONE', ( #13248, #43194, #49056, #48719 ) ) ;
#14482 = CARTESIAN_POINT ( 'NONE',  ( -2.307692307692305711, -12.29105614889573062, 35.45975837776705220 ) ) ;
#14483 = ORIENTED_EDGE ( 'NONE', *, *, #30452, .F. ) ;
#14484 = CYLINDRICAL_SURFACE ( 'NONE', #70204, 0.2500000000000009437 ) ;
#14485 = CARTESIAN_POINT ( 'NONE',  ( 5.010840697562940704, -5.471508081941601986, 34.59228464037088457 ) ) ;
#14486 = ORIENTED_EDGE ( 'NONE', *, *, #19290, .T. ) ;
#14487 = CARTESIAN_POINT ( 'NONE',  ( -17.93474486048716088, -10.33852847137154463, 34.16647553114620450 ) ) ;
#14488 = CARTESIAN_POINT ( 'NONE',  ( 17.07692307692307665, -10.67929555188718282, 33.92786785259544047 ) ) ;
#14489 = CARTESIAN_POINT ( 'NONE',  ( -11.78846153846153832, -7.500000000000001776, 34.75000000000000000 ) ) ;
#14490 = EDGE_CURVE ( 'NONE', #62484, #43877, #22349, .T. ) ;
#14491 = CARTESIAN_POINT ( 'NONE',  ( 18.00000000000000000, -12.34228464037088635, 31.77849191805839268 ) ) ;
#14492 = DIRECTION ( 'NONE',  ( 1.000000000000000000, 0.000000000000000000, 0.000000000000000000 ) ) ;
#14493 = EDGE_LOOP ( 'NONE', ( #70951, #75931, #37434, #43302 ) ) ;
#14494 = FACE_BOUND ( 'NONE', #41863, .T. ) ;
#14495 = ORIENTED_EDGE ( 'NONE', *, *, #14290, .T. ) ;
#14496 = CARTESIAN_POINT ( 'NONE',  ( -11.53846153846153655, -13.04860791097971706, 34.73218667398347037 ) ) ;
#14497 = VECTOR ( 'NONE', #24927, 1000.000000000000227 ) ;
#14498 = VECTOR ( 'NONE', #5469, 1000.000000000000114 ) ;
#14499 = EDGE_CURVE ( 'NONE', #86398, #50071, #16039, .T. ) ;
#14500 = CARTESIAN_POINT ( 'NONE',  ( 4.153846153846154188, -11.69971097300155272, 32.46337939537588113 ) ) ;
#14501 = DIRECTION ( 'NONE',  ( -1.000000000000000000, -0.000000000000000000, -0.000000000000000000 ) ) ;
#14502 = CARTESIAN_POINT ( 'NONE',  ( 7.173022441425064066, -10.05730279482229683, 34.04704008940765902 ) ) ;
#14503 = EDGE_CURVE ( 'NONE', #328, #10043, #13952, .T. ) ;
#14504 = VECTOR ( 'NONE', #69280, 1000.000000000000227 ) ;
#14505 = VERTEX_POINT ( 'NONE', #51910 ) ;
#14506 = VERTEX_POINT ( 'NONE', #79407 ) ;
#14507 = CARTESIAN_POINT ( 'NONE',  ( -5.999999999999998224, -13.95598074871891292, 31.83374038241031911 ) ) ;
#14508 = ORIENTED_EDGE ( 'NONE', *, *, #62276, .F. ) ;
#14509 = LINE ( 'NONE', #69455, #57708 ) ;
#14510 = ORIENTED_EDGE ( 'NONE', *, *, #29458, .T. ) ;
#14511 = ADVANCED_FACE ( 'NONE', ( #76406 ), #15155, .F. ) ;
#14512 = CARTESIAN_POINT ( 'NONE',  ( 15.23076923076910916, -3.643525952248795718, 33.31231777344771672 ) ) ;
#14513 = CARTESIAN_POINT ( 'NONE',  ( 1.449870955891411795, -3.835265460703683349, 33.15142922261929925 ) ) ;
#14514 = CARTESIAN_POINT ( 'NONE',  ( 13.38461538461526423, -11.67786785259630911, 32.92929555188603530 ) ) ;
#14515 = B_SPLINE_CURVE_WITH_KNOTS ( 'NONE', 3,
 ( #70290, #51302, #78808, #56767, #30619, #9039, #43694, #8597, #50010, #85576 ),
 .UNSPECIFIED., .F., .F.,
 ( 4, 2, 2, 2, 4 ),
 ( 0.0007817359430256295722, 0.0009771253907249976244, 0.001172514838424365460, 0.001367904286123733729, 0.001563293733823094625 ),
 .UNSPECIFIED. ) ;
#14516 = CARTESIAN_POINT ( 'NONE',  ( -1.134615384615320410, -7.434744429011176159, 34.75000000000000711 ) ) ;
#14517 = EDGE_CURVE ( 'NONE', #83778, #20800, #69644, .T. ) ;
#14518 = DIRECTION ( 'NONE',  ( -0.000000000000000000, -0.6427876096865404731, -0.7660444431189770143 ) ) ;
#14519 = CARTESIAN_POINT ( 'NONE',  ( -6.923076923076922462, -12.10708131394839349, 31.69288490824020244 ) ) ;
#14520 = CARTESIAN_POINT ( 'NONE',  ( -5.300408020647027207, -3.754499324213721234, 33.06261337010820256 ) ) ;
#14521 = ORIENTED_EDGE ( 'NONE', *, *, #30993, .T. ) ;
#14522 = EDGE_CURVE ( 'NONE', #9579, #67514, #46503, .T. ) ;
#14523 = ORIENTED_EDGE ( 'NONE', *, *, #48667, .F. ) ;
#14524 = ORIENTED_EDGE ( 'NONE', *, *, #5651, .T. ) ;
#14525 = CARTESIAN_POINT ( 'NONE',  ( -3.903900635498012139, -10.05730279482229506, 34.04704008940765902 ) ) ;
#14527 = CARTESIAN_POINT ( 'NONE',  ( 1.515405825582338828, -11.37503395064541678, 33.29242100308974983 ) ) ;
#14526 = CARTESIAN_POINT ( 'NONE',  ( 1.450683735617824821, -5.557115091759786019, 34.35708131394839882 ) ) ;
#14528 = B_SPLINE_CURVE_WITH_KNOTS ( 'NONE', 3,
 ( #49359, #55220, #68295, #41275, #69621, #7928, #42607, #21438, #48453, #48908 ),
 .UNSPECIFIED., .F., .F.,
 ( 4, 2, 2, 2, 4 ),
 ( 0.0007817246256747507503, 0.0009771112852218957062, 0.001172497944769040771, 0.001367884604316185835, 0.001563271263863330682 ),
 .UNSPECIFIED. ) ;
#14529 = AXIS2_PLACEMENT_3D ( 'NONE', #57013, #77730, #56135 ) ;
#14530 = CARTESIAN_POINT ( 'NONE',  ( -11.53846153846165912, -2.625532179533778709, 30.86335684631627174 ) ) ;
#14531 = CARTESIAN_POINT ( 'NONE',  ( -6.700297381808511865, -3.755027918224367767, 33.06320215134714857 ) ) ;
#14532 = FACE_BOUND ( 'NONE', #45594, .T. ) ;
#14533 = LINE ( 'NONE', #27602, #48956 ) ;
#14534 = ORIENTED_EDGE ( 'NONE', *, *, #83665, .T. ) ;
#14535 = EDGE_CURVE ( 'NONE', #4865, #49069, #44085, .T. ) ;
#14536 = CARTESIAN_POINT ( 'NONE',  ( 17.14299142792551578, -10.51840700105979565, 33.73612834413962247 ) ) ;
#14537 = DIRECTION ( 'NONE',  ( 0.000000000000000000, 0.3420201433256641055, -0.9396926207859100932 ) ) ;
#14538 = CYLINDRICAL_SURFACE ( 'NONE', #59090, 0.2500000000000009437 ) ;
#14539 = DIRECTION ( 'NONE',  ( -0.000000000000000000, -0.5000000000000009992, -0.8660254037844380415 ) ) ;
#14540 = AXIS2_PLACEMENT_3D ( 'NONE', #39967, #20996, #75955 ) ;
#14541 = ORIENTED_EDGE ( 'NONE', *, *, #69225, .T. ) ;
#14542 = CARTESIAN_POINT ( 'NONE',  ( 6.250054419913455561, -10.82426656108011720, 33.81400080652039009 ) ) ;
#14543 = ORIENTED_EDGE ( 'NONE', *, *, #58469, .T. ) ;
#14544 = FACE_BOUND ( 'NONE', #44483, .T. ) ;
#14545 = CARTESIAN_POINT ( 'NONE',  ( 9.692307692307572609, -6.026961402154118019, 34.52809138561165270 ) ) ;
#14546 = CARTESIAN_POINT ( 'NONE',  ( 15.12820512820512953, -11.50000000000000000, 29.75000000000000355 ) ) ;
#14548 = EDGE_CURVE ( 'NONE', #955, #88209, #74875, .T. ) ;
#14547 = CARTESIAN_POINT ( 'NONE',  ( 0.000000000000000000, -11.00000000000000000, 29.75000000000000355 ) ) ;
#14549 = VERTEX_POINT ( 'NONE', #46058 ) ;
#14550 = CARTESIAN_POINT ( 'NONE',  ( 11.60452887181161508, -10.67929555188718282, 33.92786785259544757 ) ) ;
#14551 = CARTESIAN_POINT ( 'NONE',  ( -5.750054590621955342, -9.357781135181031829, 34.66075350412533851 ) ) ;
#14552 = CARTESIAN_POINT ( 'NONE',  ( 8.703960768674447124, -2.379036618887870436, 30.90682066428147934 ) ) ;
#14553 = CARTESIAN_POINT ( 'NONE',  ( -5.076923076923075762, -5.471508081941601098, 34.59228464037088457 ) ) ;
#14554 = EDGE_LOOP ( 'NONE', ( #5949, #58963 ) ) ;
#14555 = CARTESIAN_POINT ( 'NONE',  ( 13.13459214732242408, -5.851115903089112003, 34.47074536777953568 ) ) ;
#14556 = VERTEX_POINT ( 'NONE', #25344 ) ;
#14558 = ORIENTED_EDGE ( 'NONE', *, *, #49505, .T. ) ;
#14557 = CARTESIAN_POINT ( 'NONE',  ( 16.22001276043779328, -7.250054591869668386, 34.99404684341514127 ) ) ;
#14559 = CARTESIAN_POINT ( 'NONE',  ( 7.780070435197965040, -10.51840700105979387, 33.73612834413961536 ) ) ;
#14560 = CARTESIAN_POINT ( 'NONE',  ( -4.403822884788506364, -2.779195860258147022, 31.39871582349836743 ) ) ;
#14561 = CARTESIAN_POINT ( 'NONE',  ( 11.53846153846153832, -2.900454961884010974, 35.62045528018868623 ) ) ;
#14562 = CARTESIAN_POINT ( 'NONE',  ( 12.46153846153846168, -6.435427911321262684, 35.78748833219616898 ) ) ;
#14563 = LINE ( 'NONE', #42049, #40928 ) ;
#14565 = CARTESIAN_POINT ( 'NONE',  ( 16.15384615384603251, -6.026961402154118908, 34.52809138561165270 ) ) ;
#14564 = CARTESIAN_POINT ( 'NONE',  ( 13.60762673622823726, -5.667800583137506010, 34.40243808032445827 ) ) ;
#14566 = DIRECTION ( 'NONE',  ( 0.000000000000000000, 0.9396926207859126468, -0.3420201433256571111 ) ) ;
#14567 = CARTESIAN_POINT ( 'NONE',  ( -2.749999999999991562, -8.639087296526025028, 25.01562500000000000 ) ) ;
#14568 = ORIENTED_EDGE ( 'NONE', *, *, #53864, .T. ) ;
#14569 = DIRECTION ( 'NONE',  ( 0.000000000000000000, 0.4999999999999960032, -0.8660254037844410391 ) ) ;
#14570 = EDGE_LOOP ( 'NONE', ( #18554, #1138, #14825, #61797 ) ) ;
#14571 = VECTOR ( 'NONE', #13094, 1000.000000000000000 ) ;
#14572 = ADVANCED_FACE ( 'NONE', ( #4629 ), #53249, .F. ) ;
#14573 = EDGE_LOOP ( 'NONE', ( #48585, #21832, #32728, #52759 ) ) ;
#14574 = CARTESIAN_POINT ( 'NONE',  ( -8.546451100252703270, -6.717445702608402236, 34.94155399931962336 ) ) ;
#14575 = ORIENTED_EDGE ( 'NONE', *, *, #28153, .F. ) ;
#14576 = CARTESIAN_POINT ( 'NONE',  ( -13.38461538461538325, -1.466349020453238561, 30.81389545987213907 ) ) ;
#14577 = UNCERTAINTY_MEASURE_WITH_UNIT (LENGTH_MEASURE( 1.000000000000000082E-05 ), #80064, 'distance_accuracy_value', 'NONE');
#14578 = CARTESIAN_POINT ( 'NONE',  ( -8.069638770718176701, -8.539481045369596401, 34.89627647299170832 ) ) ;
#14579 = CARTESIAN_POINT ( 'NONE',  ( 3.100077764101672795, -8.147922237126337563, 34.70805685702651999 ) ) ;
#14580 = VECTOR ( 'NONE', #70943, 1000.000000000000227 ) ;
#14581 = CYLINDRICAL_SURFACE ( 'NONE', #81650, 0.2500000000000004996 ) ;
#14582 = LINE ( 'NONE', #69523, #57457 ) ;
#14583 = CARTESIAN_POINT ( 'NONE',  ( 12.33139125210024112, -10.88202310037935661, 33.43294751532457099 ) ) ;
#14584 = CARTESIAN_POINT ( 'NONE',  ( -7.846153846153844924, -2.292212530054420494, 30.41441678777542634 ) ) ;
#14585 = CARTESIAN_POINT ( 'NONE',  ( 3.749999999999992006, -5.946699141100872943, 25.64062500000000000 ) ) ;
#14586 = B_SPLINE_CURVE_WITH_KNOTS ( 'NONE', 3,
 ( #4316, #31800, #59258, #18280, #67357, #54268, #68244, #62354, #20493, #20929 ),
 .UNSPECIFIED., .F., .F.,
 ( 4, 2, 2, 2, 4 ),
 ( 0.000000000000000000, 0.0001954339857564065528, 0.0003908679715128131056, 0.0005863019572692196313, 0.0007817359430256262112 ),
 .UNSPECIFIED. ) ;
#14587 = B_SPLINE_CURVE_WITH_KNOTS ( 'NONE', 3,
 ( #20081, #47544, #35364, #88127, #75034, #13322, #26399, #75463, #28616, #77237 ),
 .UNSPECIFIED., .F., .F.,
 ( 4, 2, 2, 2, 4 ),
 ( 0.0007817359430256327164, 0.0009771253907249995759, 0.001172514838424366327, 0.001367904286123733078, 0.001563293733823099829 ),
 .UNSPECIFIED. ) ;
#14588 = EDGE_CURVE ( 'NONE', #9053, #68539, #64509, .T. ) ;
#14589 = DIRECTION ( 'NONE',  ( 0.000000000000000000, 0.1736481776669267785, -0.9848077530122087975 ) ) ;
#14590 = CARTESIAN_POINT ( 'NONE',  ( -17.01166793741023042, -11.06231777344670775, 33.60647404775212266 ) ) ;
#14591 = CARTESIAN_POINT ( 'NONE',  ( 24.00000000000000000, 0.000000000000000000, 0.000000000000000000 ) ) ;
#14592 = CARTESIAN_POINT ( 'NONE',  ( -13.51476335434707821, -10.31621877034669588, 34.18098118002070152 ) ) ;
#14593 = EDGE_CURVE ( 'NONE', #31453, #46051, #28004, .T. ) ;
#14594 = EDGE_CURVE ( 'NONE', #28534, #86900, #33438, .T. ) ;
#14595 = ORIENTED_EDGE ( 'NONE', *, *, #3553, .F. ) ;
#14596 = EDGE_LOOP ( 'NONE', ( #28698, #46000 ) ) ;
#14597 = LINE ( 'NONE', #14151, #32779 ) ;
#14598 = CARTESIAN_POINT ( 'NONE',  ( 0.5920638997721040520, -12.15418822224088657, 32.17964115625579069 ) ) ;
#14599 = DIRECTION ( 'NONE',  ( 0.000000000000000000, 0.9848077530122072432, -0.1736481776669354937 ) ) ;
#14600 = CARTESIAN_POINT ( 'NONE',  ( -11.31549863490005237, -7.369474270740069777, 34.74850911626239736 ) ) ;
#14601 = ORIENTED_EDGE ( 'NONE', *, *, #42355, .T. ) ;
#14602 = CARTESIAN_POINT ( 'NONE',  ( -0.4615384615384611200, -13.57706302396349152, 30.56769352161908060 ) ) ;
#14603 = CARTESIAN_POINT ( 'NONE',  ( 10.61538461538461675, -13.75783147151868846, 33.36296068462461051 ) ) ;
#14604 = EDGE_CURVE ( 'NONE', #51011, #17681, #57730, .T. ) ;
#14605 = AXIS2_PLACEMENT_3D ( 'NONE', #19178, #60597, #54723 ) ;
#14606 = LINE ( 'NONE', #13714, #16418 ) ;
#14607 = VERTEX_POINT ( 'NONE', #19035 ) ;
#14608 = CARTESIAN_POINT ( 'NONE',  ( -25.00000000000000355, 9.999999999999971578, 3.000000000000000000 ) ) ;
#14609 = ORIENTED_EDGE ( 'NONE', *, *, #47267, .T. ) ;
#14610 = CARTESIAN_POINT ( 'NONE',  ( 9.823099500132483897, -11.71459661697925903, 32.44059661609676937 ) ) ;
#14611 = B_SPLINE_CURVE_WITH_KNOTS ( 'NONE', 3,
 ( #33716, #12124, #68382, #20205, #48101, #47219, #60738, #73827, #5359, #75155 ),
 .UNSPECIFIED., .F., .F.,
 ( 4, 2, 2, 2, 4 ),
 ( 0.000000000000000000, 0.0001954311564186866305, 0.0003908623128373732609, 0.0005862934692560598914, 0.0007817246256747465219 ),
 .UNSPECIFIED. ) ;
#14612 = CARTESIAN_POINT ( 'NONE',  ( 15.23076923076923173, -3.322132147404559976, 32.92929555188717927 ) ) ;
#14613 = CARTESIAN_POINT ( 'NONE',  ( -18.00000000000001421, 17.49999999999802824, 32.75000000000000000 ) ) ;
#14614 = B_SPLINE_CURVE_WITH_KNOTS ( 'NONE', 3,
 ( #75046, #12448, #52536, #81803, #74598, #18321, #81361, #60625, #80472, #73722 ),
 .UNSPECIFIED., .F., .F.,
 ( 4, 2, 2, 2, 4 ),
 ( 0.0007817246256747484735, 0.0009771112852218922368, 0.001172497944769036217, 0.001367884604316180197, 0.001563271263863323960 ),
 .UNSPECIFIED. ) ;
#14615 = CARTESIAN_POINT ( 'NONE',  ( 3.230769230769108269, -8.656820664282941280, 34.87096338111179961 ) ) ;
#14616 = B_SPLINE_CURVE_WITH_KNOTS ( 'NONE', 3,
 ( #62293, #55542, #48784, #76251, #14560, #69502, #7807, #62733, #24856, #57760 ),
 .UNSPECIFIED., .F., .F.,
 ( 4, 2, 2, 2, 4 ),
 ( 0.000000000000000000, 0.0001954339857564126514, 0.0003908679715128183098, 0.0005863019572692239681, 0.0007817359430256294638 ),
 .UNSPECIFIED. ) ;
#14617 = CARTESIAN_POINT ( 'NONE',  ( 10.61538461538461675, -5.180354513474913603, 36.12317359536750416 ) ) ;
#14618 = ADVANCED_FACE ( 'NONE', ( #74420 ), #68113, .F. ) ;
#14619 = VERTEX_POINT ( 'NONE', #60899 ) ;
#14620 = ORIENTED_EDGE ( 'NONE', *, *, #1872, .T. ) ;
#14621 = EDGE_LOOP ( 'NONE', ( #8892, #26121, #83182, #81793 ) ) ;
#14622 = ORIENTED_EDGE ( 'NONE', *, *, #87665, .T. ) ;
#14623 = CARTESIAN_POINT ( 'NONE',  ( -10.83831157429145975, -12.38737895849757820, 31.66785238281580206 ) ) ;
#14624 = CARTESIAN_POINT ( 'NONE',  ( -15.93083330975275658, -9.172514111537580561, 34.72667873470787470 ) ) ;
#14625 = DIRECTION ( 'NONE',  ( 1.000000000000000000, 0.000000000000000000, -0.000000000000000000 ) ) ;
#14626 = VECTOR ( 'NONE', #52961, 1000.000000000000000 ) ;
#14627 = CARTESIAN_POINT ( 'NONE',  ( 6.923076923076802558, -2.892918686052165622, 31.69288490824153470 ) ) ;
#14628 = DIRECTION ( 'NONE',  ( 0.000000000000000000, 0.000000000000000000, 1.000000000000000000 ) ) ;
#14629 = CARTESIAN_POINT ( 'NONE',  ( -2.307692307692427391, -12.27809138561165270, 31.22303859784587132 ) ) ;
#14630 = VERTEX_POINT ( 'NONE', #88403 ) ;
#14631 = EDGE_LOOP ( 'NONE', ( #27880, #7567, #75202, #15760 ) ) ;
#14632 = ORIENTED_EDGE ( 'NONE', *, *, #62582, .F. ) ;
#14634 = ORIENTED_EDGE ( 'NONE', *, *, #7601, .T. ) ;
#14633 = CYLINDRICAL_SURFACE ( 'NONE', #48837, 0.2499999999999997502 ) ;
#14636 = CARTESIAN_POINT ( 'NONE',  ( 14.53047197667037516, -4.989023458446560255, 34.36081565061822118 ) ) ;
#14635 = CARTESIAN_POINT ( 'NONE',  ( -16.82686876528476105, -9.148310452688871663, 34.47095581063188519 ) ) ;
#14637 = CARTESIAN_POINT ( 'NONE',  ( -10.03846153846153832, -7.500000000000000000, 29.75000000000000355 ) ) ;
#14638 = CARTESIAN_POINT ( 'NONE',  ( -3.749999999999988454, -9.053300858899127945, 23.76562500000000000 ) ) ;
#14639 = EDGE_LOOP ( 'NONE', ( #22944, #891 ) ) ;
#14640 = EDGE_CURVE ( 'NONE', #72902, #70346, #62038, .T. ) ;
#14641 = B_SPLINE_CURVE_WITH_KNOTS ( 'NONE', 3,
 ( #67553, #41408, #21570, #20687, #68869, #13050, #61218, #20251, #55354, #76069 ),
 .UNSPECIFIED., .F., .F.,
 ( 4, 2, 2, 2, 4 ),
 ( 0.000000000000000000, 0.0001954311564186868473, 0.0003908623128373736946, 0.0005862934692560605419, 0.0007817246256747473893 ),
 .UNSPECIFIED. ) ;
#14642 = EDGE_LOOP ( 'NONE', ( #18236, #31004, #48621, #74126 ) ) ;
#14643 = B_SPLINE_CURVE_WITH_KNOTS ( 'NONE', 3,
 ( #75353, #68151, #60941, #6453, #46548, #6884, #33912, #34352, #19953, #41560 ),
 .UNSPECIFIED., .F., .F.,
 ( 4, 2, 2, 2, 4 ),
 ( 0.000000000000000000, 0.0001954339857564092362, 0.0003908679715128184724, 0.0005863019572692276544, 0.0007817359430256369448 ),
 .UNSPECIFIED. ) ;
#14644 = CARTESIAN_POINT ( 'NONE',  ( -6.923076923076922462, -4.661471528628507777, 34.16647553114623292 ) ) ;
#14646 = EDGE_CURVE ( 'NONE', #36124, #11535, #52362, .T. ) ;
#14645 = VERTEX_POINT ( 'NONE', #24891 ) ;
#14647 = FACE_BOUND ( 'NONE', #76795, .T. ) ;
#14648 = CARTESIAN_POINT ( 'NONE',  ( 4.946232473812766983, -4.684245665217972032, 34.18127051446801090 ) ) ;
#14649 = CARTESIAN_POINT ( 'NONE',  ( 8.069166690247241647, -5.582272713120729257, 34.63742843783360570 ) ) ;
#14650 = ORIENTED_EDGE ( 'NONE', *, *, #20454, .T. ) ;
#14651 = CARTESIAN_POINT ( 'NONE',  ( 1.384615384615386802, -5.471508081941601098, 34.59228464037088457 ) ) ;
#14653 = EDGE_CURVE ( 'NONE', #78266, #64241, #48267, .T. ) ;
#14652 = CARTESIAN_POINT ( 'NONE',  ( 8.703960768674448900, -12.16647553114622049, 32.15551576947930812 ) ) ;
#14654 = CARTESIAN_POINT ( 'NONE',  ( 10.36540788444226635, -2.779195860258146578, 31.39871582349836032 ) ) ;
#14655 = CARTESIAN_POINT ( 'NONE',  ( 0.7115927731767752729, -6.567000820036038355, 34.66262288849541306 ) ) ;
#14656 = CARTESIAN_POINT ( 'NONE',  ( -27.00000000000000000, -1.250000000000000000, 22.25000000000000000 ) ) ;
#14657 = ORIENTED_EDGE ( 'NONE', *, *, #51565, .F. ) ;
#14658 = ADVANCED_FACE ( 'NONE', ( #1418 ), #21238, .F. ) ;
#14659 = VECTOR ( 'NONE', #81243, 1000.000000000000227 ) ;
#14660 = CARTESIAN_POINT ( 'NONE',  ( -11.53846153846153655, -12.34228464037088635, 31.77849191805839268 ) ) ;
#14661 = CARTESIAN_POINT ( 'NONE',  ( 1.450683735617824599, -8.120952969808772792, 34.71129190929999453 ) ) ;
#14662 = CARTESIAN_POINT ( 'NONE',  ( 16.28463796167094557, -8.999086150933472084, 34.52020707165672064 ) ) ;
#14663 = CARTESIAN_POINT ( 'NONE',  ( 15.93091919493930675, -10.77366814457252175, 33.85459836347580875 ) ) ;
#14664 = CARTESIAN_POINT ( 'NONE',  ( -15.00775787915638126, -11.76359900205217457, 32.36225158514719880 ) ) ;
#14665 = FACE_BOUND ( 'NONE', #45855, .T. ) ;
#14667 = CARTESIAN_POINT ( 'NONE',  ( 11.28848480751918437, -12.41269422305637171, 30.68257228309993323 ) ) ;
#14666 = CARTESIAN_POINT ( 'NONE',  ( -8.992096191434411523, -2.501496062324912284, 29.88072118266895671 ) ) ;
#14668 = CARTESIAN_POINT ( 'NONE',  ( 5.207448515156721136, -2.372941743896878286, 30.88044141588254377 ) ) ;
#14670 = CARTESIAN_POINT ( 'NONE',  ( 9.692307692307570832, -3.083524468854526912, 32.58852847137268327 ) ) ;
#14669 = DIRECTION ( 'NONE',  ( -0.000000000000000000, -0.9848077530122085754, -0.1736481776669273613 ) ) ;
#14671 = EDGE_CURVE ( 'NONE', #34671, #68238, #69434, .T. ) ;
#14672 = CARTESIAN_POINT ( 'NONE',  ( -18.00000000000000000, -9.780366693483671270, 34.19971097300155094 ) ) ;
#14673 = CARTESIAN_POINT ( 'NONE',  ( -2.775308065498764964, -6.422011778438537988, 16.17000670625848713 ) ) ;
#14674 = EDGE_LOOP ( 'NONE', ( #12248, #9950 ) ) ;
#14675 = CARTESIAN_POINT ( 'NONE',  ( -5.869209559033048862, -10.70102852606553157, 33.91149625220312913 ) ) ;
#14676 = ORIENTED_EDGE ( 'NONE', *, *, #76201, .F. ) ;
#14677 = CARTESIAN_POINT ( 'NONE',  ( -14.98071491913091613, -4.235687564193445276, 33.53795663066793509 ) ) ;
#14678 = EDGE_CURVE ( 'NONE', #21592, #19635, #77081, .T. ) ;
#14679 = EDGE_LOOP ( 'NONE', ( #20146, #39263 ) ) ;
#14680 = CARTESIAN_POINT ( 'NONE',  ( -11.53846153846165912, -2.892918686052166066, 31.69288490824153470 ) ) ;
#14681 = DIRECTION ( 'NONE',  ( -0.000000000000000000, -0.3420201433256694901, -0.9396926207859082059 ) ) ;
#14682 = ORIENTED_EDGE ( 'NONE', *, *, #2696, .F. ) ;
#14683 = CARTESIAN_POINT ( 'NONE',  ( -9.942307692307691624, -7.500000000000001776, 34.75000000000000000 ) ) ;
#14684 = CARTESIAN_POINT ( 'NONE',  ( -2.724691934501232371, -8.700186371490559623, 21.01375670625849068 ) ) ;
#14685 = DIRECTION ( 'NONE',  ( -0.000000000000000000, 1.000000000000000000, 3.491481338843133355E-15 ) ) ;
#14686 = CARTESIAN_POINT ( 'NONE',  ( -5.142193522883853340, -5.219633306516282545, 34.19971097300152252 ) ) ;
#14687 = CARTESIAN_POINT ( 'NONE',  ( -5.207614543590634248, -12.38065189839062263, 30.83690757178629482 ) ) ;
#14688 = CARTESIAN_POINT ( 'NONE',  ( 15.45419619263079802, -7.630147231320743018, 34.74852402298682819 ) ) ;
#14689 = CARTESIAN_POINT ( 'NONE',  ( -19.50000000000000000, -3.499999999999999556, 29.75000000000000355 ) ) ;
#14690 = CARTESIAN_POINT ( 'NONE',  ( -17.07692307692307665, -1.629998284177014645, 34.34916445242399163 ) ) ;
#14691 = CARTESIAN_POINT ( 'NONE',  ( -3.749999999999997780, -7.438900925035489387, 25.34561829374151642 ) ) ;
#14692 = CARTESIAN_POINT ( 'NONE',  ( -9.822999158975251888, -3.530157926970578952, 32.79014554554150607 ) ) ;
#14693 = CARTESIAN_POINT ( 'NONE',  ( 10.74617642320940369, -11.18335022499818621, 33.13157742990016885 ) ) ;
#14694 = ORIENTED_EDGE ( 'NONE', *, *, #30761, .T. ) ;
#14695 = LINE ( 'NONE', #76846, #14799 ) ;
#14696 = CARTESIAN_POINT ( 'NONE',  ( 1.614399933863618797, -3.775308065498751198, 21.98624329374151642 ) ) ;
#14697 = ADVANCED_FACE ( 'NONE', ( #62661 ), #63106, .F. ) ;
#14698 = CARTESIAN_POINT ( 'NONE',  ( -14.24243673641628050, -10.90142922261932057, 33.41473453929631887 ) ) ;
#14699 = CARTESIAN_POINT ( 'NONE',  ( 9.692307692307695177, -13.75783147151868846, 33.36296068462461051 ) ) ;
#14700 = VECTOR ( 'NONE', #11284, 1000.000000000000227 ) ;
#14701 = VERTEX_POINT ( 'NONE', #54578 ) ;
#14702 = ADVANCED_FACE ( 'NONE', ( #34757 ), #41080, .F. ) ;
#14703 = CARTESIAN_POINT ( 'NONE',  ( 14.55763782604045176, -2.587454068350148351, 30.68340429815432202 ) ) ;
#14704 = CARTESIAN_POINT ( 'NONE',  ( 16.40390057375960708, -2.544122305571458575, 31.48381861865057729 ) ) ;
#14706 = ORIENTED_EDGE ( 'NONE', *, *, #53045, .F. ) ;
#14705 = CARTESIAN_POINT ( 'NONE',  ( 12.46153846153846168, -2.900454961884010974, 35.62045528018868623 ) ) ;
#14707 = CARTESIAN_POINT ( 'NONE',  ( 8.703960768674447124, -5.941354392334499579, 34.76329471203369792 ) ) ;
#14708 = DIRECTION ( 'NONE',  ( -0.000000000000000000, -0.000000000000000000, -1.000000000000000000 ) ) ;
#14709 = VECTOR ( 'NONE', #32653, 1000.000000000000227 ) ;
#14710 = CYLINDRICAL_SURFACE ( 'NONE', #18415, 0.2500000000000009437 ) ;
#14711 = EDGE_CURVE ( 'NONE', #70329, #30760, #88006, .T. ) ;
#14712 = DIRECTION ( 'NONE',  ( 0.000000000000000000, 0.9848077530122072432, -0.1736481776669354937 ) ) ;
#14713 = CARTESIAN_POINT ( 'NONE',  ( 10.36536139116315880, -12.68155406624981119, 30.59749803192733708 ) ) ;
#14714 = B_SPLINE_CURVE_WITH_KNOTS ( 'NONE', 3,
 ( #66113, #11636, #38207, #52603, #30558, #79203, #79646, #59812, #87311, #65667 ),
 .UNSPECIFIED., .F., .F.,
 ( 4, 2, 2, 2, 4 ),
 ( 0.0007817359430256218744, 0.0009771253907249861318, 0.001172514838424350498, 0.001367904286123714864, 0.001563293733823079229 ),
 .UNSPECIFIED. ) ;
#14715 = ADVANCED_FACE ( 'NONE', ( #28446 ), #42858, .F. ) ;
#14716 = EDGE_LOOP ( 'NONE', ( #43267, #46097, #3399, #57529 ) ) ;
#14717 = CARTESIAN_POINT ( 'NONE',  ( -0.2385271099256124627, -10.61302985866383963, 33.66295027996417843 ) ) ;
#14718 = ORIENTED_EDGE ( 'NONE', *, *, #75899, .T. ) ;
#14719 = APPLICATION_CONTEXT ( 'automotive_design' ) ;
#14720 = ORIENTED_EDGE ( 'NONE', *, *, #64191, .F. ) ;
#14721 = CARTESIAN_POINT ( 'NONE',  ( -13.63463862190834952, -3.711651800289232028, 33.01384336483936011 ) ) ;
#14722 = DIRECTION ( 'NONE',  ( -0.000000000000000000, 0.6427876096865404731, -0.7660444431189771253 ) ) ;
#14723 = LINE ( 'NONE', #41310, #56580 ) ;
#14724 = CARTESIAN_POINT ( 'NONE',  ( 14.87820512820512953, -4.000000000000000000, 29.75000000000000355 ) ) ;
#14725 = EDGE_CURVE ( 'NONE', #8176, #47629, #49376, .T. ) ;
#14726 = EDGE_LOOP ( 'NONE', ( #27511, #15472, #70161, #82127 ) ) ;
#14727 = EDGE_CURVE ( 'NONE', #45168, #54472, #35657, .T. ) ;
#14728 = LINE ( 'NONE', #43078, #42029 ) ;
#14729 = AXIS2_PLACEMENT_3D ( 'NONE', #52544, #25081, #5697 ) ;
#14730 = VERTEX_POINT ( 'NONE', #82075 ) ;
#14731 = EDGE_CURVE ( 'NONE', #54551, #79352, #61161, .T. ) ;
#14732 = ORIENTED_EDGE ( 'NONE', *, *, #85858, .T. ) ;
#14733 = ORIENTED_EDGE ( 'NONE', *, *, #62181, .T. ) ;
#14735 = ORIENTED_EDGE ( 'NONE', *, *, #28365, .T. ) ;
#14734 = CARTESIAN_POINT ( 'NONE',  ( -16.15384615384615330, -1.466349020453238561, 30.81389545987213907 ) ) ;
#14736 = CARTESIAN_POINT ( 'NONE',  ( -0.4615384615385826339, -5.219633306517616589, 34.19971097300220464 ) ) ;
#14737 = CARTESIAN_POINT ( 'NONE',  ( 6.250054419913457338, -2.544122305571457687, 31.48381861865059150 ) ) ;
#14738 = CARTESIAN_POINT ( 'NONE',  ( -3.099977422944443450, -4.118422570099827595, 33.43335022499816489 ) ) ;
#14739 = CARTESIAN_POINT ( 'NONE',  ( -4.853960173361592467, -7.369474270740069777, 34.74850911626239736 ) ) ;
#14740 = B_SPLINE_CURVE_WITH_KNOTS ( 'NONE', 3,
 ( #28378, #77892, #44089, #58058, #44982, #38686, #85989, #2660, #51272, #65256 ),
 .UNSPECIFIED., .F., .F.,
 ( 4, 2, 2, 2, 4 ),
 ( 0.0007817246256747507503, 0.0009771112852218959231, 0.001172497944769040987, 0.001367884604316186052, 0.001563271263863331116 ),
 .UNSPECIFIED. ) ;
#14741 = VERTEX_POINT ( 'NONE', #79300 ) ;
#14742 = ORIENTED_EDGE ( 'NONE', *, *, #52006, .T. ) ;
#14743 = B_SPLINE_CURVE_WITH_KNOTS ( 'NONE', 3,
 ( #61971, #13348, #1162, #68293, #48904, #13789, #721, #54771, #6597, #28185 ),
 .UNSPECIFIED., .F., .F.,
 ( 4, 2, 2, 2, 4 ),
 ( 0.000000000000000000, 0.0001954339857564071762, 0.0003908679715128143524, 0.0005863019572692215828, 0.0007817359430256287049 ),
 .UNSPECIFIED. ) ;
#14744 = ORIENTED_EDGE ( 'NONE', *, *, #70435, .T. ) ;
#14745 = CARTESIAN_POINT ( 'NONE',  ( -2.176901866725355461, -3.338503747796865984, 32.95102852606552801 ) ) ;
#14747 = EDGE_LOOP ( 'NONE', ( #8582, #41860, #80788, #56384 ) ) ;
#14746 = CARTESIAN_POINT ( 'NONE',  ( -2.531177251416252272, -2.847400154188067578, 31.58180166144859768 ) ) ;
#14748 = CYLINDRICAL_SURFACE ( 'NONE', #85318, 0.2500000000000002220 ) ;
#14749 = CARTESIAN_POINT ( 'NONE',  ( 13.31936439445414422, -2.506253911140460922, 30.00000000000013856 ) ) ;
#14750 = CARTESIAN_POINT ( 'NONE',  ( 5.999999999999880096, -6.026961402154118908, 34.52809138561165270 ) ) ;
#14751 = ORIENTED_EDGE ( 'NONE', *, *, #25311, .F. ) ;
#14752 = DIRECTION ( 'NONE',  ( -0.000000000000000000, -0.3420201433256694901, -0.9396926207859082059 ) ) ;
#14753 = DIRECTION ( 'NONE',  ( -0.000000000000000000, -0.7660444431189791237, -0.6427876096865379196 ) ) ;
#14754 = ORIENTED_EDGE ( 'NONE', *, *, #61565, .T. ) ;
#14755 = FACE_BOUND ( 'NONE', #60244, .T. ) ;
#14756 = CARTESIAN_POINT ( 'NONE',  ( 23.49999999999998934, 5.000000000000023093, 28.74999999999999645 ) ) ;
#14757 = CARTESIAN_POINT ( 'NONE',  ( -9.692307692307691624, -8.120952969808772792, 34.71129190930000163 ) ) ;
#14758 = VECTOR ( 'NONE', #16339, 1000.000000000000000 ) ;
#14759 = DIRECTION ( 'NONE',  ( -1.000000000000000000, 0.000000000000000000, -0.000000000000000000 ) ) ;
#14761 = CYLINDRICAL_SURFACE ( 'NONE', #6646, 0.2499999999999973355 ) ;
#14760 = CARTESIAN_POINT ( 'NONE',  ( 18.22277966897806323, -3.020022701398814569, 32.48759521482552515 ) ) ;
#14762 = AXIS2_PLACEMENT_3D ( 'NONE', #25358, #36759, #78630 ) ;
#14763 = CARTESIAN_POINT ( 'NONE',  ( -17.07692307692307665, -12.78798330534102945, 29.74999999999997868 ) ) ;
#14764 = CARTESIAN_POINT ( 'NONE',  ( 14.37375964104238513, -2.292212530054420494, 30.41441678777542990 ) ) ;
#14765 = ORIENTED_EDGE ( 'NONE', *, *, #62702, .T. ) ;
#14766 = CARTESIAN_POINT ( 'NONE',  ( -9.692307692307691624, -12.29105614889573062, 35.45975837776705220 ) ) ;
#14767 = PLANE ( 'NONE',  #29169 ) ;
#14768 = VERTEX_POINT ( 'NONE', #58124 ) ;
#14769 = AXIS2_PLACEMENT_3D ( 'NONE', #11842, #32540, #74421 ) ;
#14770 = EDGE_CURVE ( 'NONE', #43224, #29911, #44599, .T. ) ;
#14771 = CARTESIAN_POINT ( 'NONE',  ( -9.692307692307691624, -1.242168528481310874, 33.36296068462461051 ) ) ;
#14772 = FACE_OUTER_BOUND ( 'NONE', #79976, .T. ) ;
#14773 = ORIENTED_EDGE ( 'NONE', *, *, #59345, .F. ) ;
#14774 = CARTESIAN_POINT ( 'NONE',  ( 2.307692307692186251, -8.656820664282941280, 34.87096338111179961 ) ) ;
#14775 = CARTESIAN_POINT ( 'NONE',  ( 2.438217745925953750, -5.070358843744209310, 34.40418822224088302 ) ) ;
#14776 = FACE_BOUND ( 'NONE', #56808, .T. ) ;
#14778 = DIRECTION ( 'NONE',  ( 1.000000000000000000, 0.000000000000000000, 0.000000000000000000 ) ) ;
#14777 = CARTESIAN_POINT ( 'NONE',  ( -2.307692307692427391, -6.879047030192662504, 34.71129190930017927 ) ) ;
#14779 = CARTESIAN_POINT ( 'NONE',  ( -6.673131404728782634, -9.272278438253401589, 34.42582936511637826 ) ) ;
#14780 = CARTESIAN_POINT ( 'NONE',  ( -15.48079246806219267, -9.271318131107980420, 34.42618302367067429 ) ) ;
#14782 = DIRECTION ( 'NONE',  ( -0.000000000000000000, 1.000000000000000000, -0.000000000000000000 ) ) ;
#14781 = CARTESIAN_POINT ( 'NONE',  ( -12.46153846153858247, -3.835265460704628371, 33.15142922262033665 ) ) ;
#14783 = B_SPLINE_CURVE_WITH_KNOTS ( 'NONE', 3,
 ( #28385, #30594, #85112, #9884, #78336, #58066, #79239, #36481, #10335, #63935 ),
 .UNSPECIFIED., .F., .F.,
 ( 4, 2, 2, 2, 4 ),
 ( 0.0007817359430256360774, 0.0009771253907250041296, 0.001172514838424371965, 0.001367904286123740017, 0.001563293733823108069 ),
 .UNSPECIFIED. ) ;
#14784 = EDGE_CURVE ( 'NONE', #54531, #64679, #7419, .T. ) ;
#14785 = CARTESIAN_POINT ( 'NONE',  ( -14.30769230769242917, -5.941354392335915335, 34.76329471203413846 ) ) ;
#14786 = CARTESIAN_POINT ( 'NONE',  ( -1.553300858899125059, -3.750000000000009326, 25.32812500000000711 ) ) ;
#14787 = ORIENTED_EDGE ( 'NONE', *, *, #52743, .F. ) ;
#14788 = ORIENTED_EDGE ( 'NONE', *, *, #73192, .T. ) ;
#14789 = B_SPLINE_CURVE_WITH_KNOTS ( 'NONE', 3,
 ( #47883, #61384, #34808, #75797, #76693, #27168, #82125, #28507, #28060, #14545 ),
 .UNSPECIFIED., .F., .F.,
 ( 4, 2, 2, 2, 4 ),
 ( 0.000000000000000000, 0.0001954339857564074473, 0.0003908679715128148945, 0.0005863019572692223418, 0.0007817359430256297891 ),
 .UNSPECIFIED. ) ;
#14790 = CARTESIAN_POINT ( 'NONE',  ( -0.3589743589743593088, -7.500000000000000000, 29.75000000000000355 ) ) ;
#14791 = CARTESIAN_POINT ( 'NONE',  ( -10.48459417441766561, -8.191423895709840863, 34.95447573519442130 ) ) ;
#14792 = CARTESIAN_POINT ( 'NONE',  ( 14.53070515178570332, -9.172514111537584114, 34.72667873470787470 ) ) ;
#14793 = CARTESIAN_POINT ( 'NONE',  ( -1.450698795571264021, -3.050289026998445951, 32.03036669348365706 ) ) ;
#14794 = CARTESIAN_POINT ( 'NONE',  ( -3.903900744468109973, -2.986452184633680229, 32.43230066228895225 ) ) ;
#14795 = CARTESIAN_POINT ( 'NONE',  ( -1.614399933863656544, -3.775308065498769405, 15.07625670625849068 ) ) ;
#14796 = CARTESIAN_POINT ( 'NONE',  ( -12.46153846153858424, -4.320704448113951379, 33.92786785259630022 ) ) ;
#14797 = DIRECTION ( 'NONE',  ( 0.000000000000000000, 0.4999999999999960032, -0.8660254037844410391 ) ) ;
#14798 = EDGE_CURVE ( 'NONE', #40731, #86110, #40765, .T. ) ;
#14799 = VECTOR ( 'NONE', #78164, 1000.000000000000000 ) ;
#14800 = CARTESIAN_POINT ( 'NONE',  ( 6.066067333350076751, -3.937682226553329556, 33.60647404775216529 ) ) ;
#14801 = CARTESIAN_POINT ( 'NONE',  ( 14.30769230769231015, -2.249999999999998668, 29.75000000000001776 ) ) ;
#14802 = CARTESIAN_POINT ( 'NONE',  ( -15.23076923076922995, -11.16473453929635440, 33.15142922261926373 ) ) ;
#14803 = LINE ( 'NONE', #20227, #15232 ) ;
#14804 = CIRCLE ( 'NONE', #56511, 4.000000000000000000 ) ;
#14805 = CARTESIAN_POINT ( 'NONE',  ( -5.869474561766359066, -11.66157788607254275, 32.95092075102925833 ) ) ;
#14806 = CARTESIAN_POINT ( 'NONE',  ( 12.59232890250541281, -2.295524264805589354, 30.44142389570982488 ) ) ;
#14807 = CARTESIAN_POINT ( 'NONE',  ( 12.68454981315130858, -2.758310577978208666, 31.33698337089302299 ) ) ;
#14808 = ORIENTED_EDGE ( 'NONE', *, *, #48958, .T. ) ;
#14809 = CARTESIAN_POINT ( 'NONE',  ( -14.53117725141625627, -3.754499324213721234, 33.06261337010820256 ) ) ;
#14810 = CARTESIAN_POINT ( 'NONE',  ( 5.999999999999878320, -12.16647553114689728, 32.15551576947799362 ) ) ;
#14811 = CARTESIAN_POINT ( 'NONE',  ( -1.077988221561493543, -4.724691934501247914, 20.57999329374151998 ) ) ;
#14812 = EDGE_CURVE ( 'NONE', #20155, #55155, #26705, .T. ) ;
#14813 = CARTESIAN_POINT ( 'NONE',  ( -5.934744860487159102, -12.51329471203373700, 31.30864560766537963 ) ) ;
#14814 = CARTESIAN_POINT ( 'NONE',  ( 17.01084069756293715, -11.35647404775217595, 33.31231777344666511 ) ) ;
#14815 = VERTEX_POINT ( 'NONE', #23450 ) ;
#14816 = CARTESIAN_POINT ( 'NONE',  ( -6.923076923077045919, -3.083524468854526912, 32.58852847137268327 ) ) ;
#14818 = ORIENTED_EDGE ( 'NONE', *, *, #44361, .T. ) ;
#14817 = CARTESIAN_POINT ( 'NONE',  ( -14.55771554498526932, -12.22074536777954989, 31.39888409691088356 ) ) ;
#14819 = CARTESIAN_POINT ( 'NONE',  ( 7.912222197156284054, -3.513871655860379306, 32.76840700105978499 ) ) ;
#14820 = ADVANCED_FACE ( 'NONE', ( #71636 ), #57689, .T. ) ;
#14821 = DIRECTION ( 'NONE',  ( -0.000000000000000000, -0.9848077530122085754, -0.1736481776669273613 ) ) ;
#14822 = ORIENTED_EDGE ( 'NONE', *, *, #56224, .F. ) ;
#14823 = LINE ( 'NONE', #21566, #69291 ) ;
#14824 = FACE_OUTER_BOUND ( 'NONE', #80704, .T. ) ;
#14825 = ORIENTED_EDGE ( 'NONE', *, *, #47187, .F. ) ;
#14826 = DIRECTION ( 'NONE',  ( -1.000000000000000000, -0.000000000000000000, -0.000000000000000000 ) ) ;
#14827 = LINE ( 'NONE', #57566, #27873 ) ;
#14828 = EDGE_CURVE ( 'NONE', #64401, #74021, #58564, .T. ) ;
#14829 = CARTESIAN_POINT ( 'NONE',  ( 9.823098133274644539, -6.369690395747422684, 34.87708834333098196 ) ) ;
#14830 = ORIENTED_EDGE ( 'NONE', *, *, #41284, .T. ) ;
#14831 = VERTEX_POINT ( 'NONE', #23016 ) ;
#14832 = CARTESIAN_POINT ( 'NONE',  ( -6.673022503163470454, -8.346898887586323923, 34.93166121998716278 ) ) ;
#14833 = VECTOR ( 'NONE', #29068, 1000.000000000000114 ) ;
#14834 = VERTEX_POINT ( 'NONE', #78397 ) ;
#14835 = CARTESIAN_POINT ( 'NONE',  ( -7.912236225513983534, -2.292212530054419606, 30.41441678777542634 ) ) ;
#14836 = CARTESIAN_POINT ( 'NONE',  ( -1.384615384615505151, -2.625532179533778709, 30.86335684631627174 ) ) ;
#14837 = CARTESIAN_POINT ( 'NONE',  ( -14.43783951713053249, -3.285722584762969856, 32.44110544564090759 ) ) ;
#14838 = DIRECTION ( 'NONE',  ( 0.000000000000000000, 0.9396926207859126468, 0.3420201433256571111 ) ) ;
#14839 = DIRECTION ( 'NONE',  ( 0.000000000000000000, 0.7660444431189807890, 0.6427876096865361433 ) ) ;
#14840 = CARTESIAN_POINT ( 'NONE',  ( 0.3957850332251287018, -7.249945578846653582, 34.99404164642496795 ) ) ;
#14841 = EDGE_CURVE ( 'NONE', #14278, #373, #51798, .T. ) ;
#14842 = AXIS2_PLACEMENT_3D ( 'NONE', #69439, #43300, #55914 ) ;
#14843 = CARTESIAN_POINT ( 'NONE',  ( -17.07692307692307665, -6.386643153685126251, 34.62446782046654192 ) ) ;
#14844 = EDGE_CURVE ( 'NONE', #81167, #64959, #39660, .T. ) ;
#14845 = EDGE_CURVE ( 'NONE', #37064, #45937, #57251, .T. ) ;
#14846 = VERTEX_POINT ( 'NONE', #84740 ) ;
#14847 = ORIENTED_EDGE ( 'NONE', *, *, #31312, .T. ) ;
#14849 = EDGE_LOOP ( 'NONE', ( #33617, #5704, #67007, #60878 ) ) ;
#14848 = CARTESIAN_POINT ( 'NONE',  ( -2.307692307692428724, -2.379036618888197285, 30.90682066428292885 ) ) ;
#14850 = EDGE_CURVE ( 'NONE', #82495, #71093, #43727, .T. ) ;
#14851 = DIRECTION ( 'NONE',  ( 0.000000000000000000, -1.000000000000000000, 0.000000000000000000 ) ) ;
#14852 = ORIENTED_EDGE ( 'NONE', *, *, #72931, .T. ) ;
#14853 = B_SPLINE_CURVE_WITH_KNOTS ( 'NONE', 3,
 ( #7565, #20194, #6669, #42681, #21509, #21059, #48091, #48986, #68815, #35025 ),
 .UNSPECIFIED., .F., .F.,
 ( 4, 2, 2, 2, 4 ),
 ( 0.000000000000000000, 0.0001954311564186868744, 0.0003908623128373737488, 0.0005862934692560606504, 0.0007817246256747474977 ),
 .UNSPECIFIED. ) ;
#14854 = LINE ( 'NONE', #49517, #13341 ) ;
#14855 = CARTESIAN_POINT ( 'NONE',  ( -8.769230769230892619, -12.70778746994576025, 30.41441678777401236 ) ) ;
#14856 = ORIENTED_EDGE ( 'NONE', *, *, #29572, .T. ) ;
#14857 = CARTESIAN_POINT ( 'NONE',  ( 14.30769230769231015, -13.87047571288749737, 32.06866353760679544 ) ) ;
#14858 = AXIS2_PLACEMENT_3D ( 'NONE', #47189, #34124, #40894 ) ;
#14859 = ORIENTED_EDGE ( 'NONE', *, *, #54658, .T. ) ;
#14860 = B_SPLINE_CURVE_WITH_KNOTS ( 'NONE', 3,
 ( #27388, #796, #20621, #55732, #83221, #21506, #48087, #75562, #48983, #76463 ),
 .UNSPECIFIED., .F., .F.,
 ( 4, 2, 2, 2, 4 ),
 ( 0.0007817246256747442451, 0.0009771112852218870326, 0.001172497944769029929, 0.001367884604316172825, 0.001563271263863315504 ),
 .UNSPECIFIED. ) ;
#14862 = ORIENTED_EDGE ( 'NONE', *, *, #65778, .F. ) ;
#14861 = CYLINDRICAL_SURFACE ( 'NONE', #12840, 0.2500000000000009437 ) ;
#14863 = VECTOR ( 'NONE', #76609, 1000.000000000000227 ) ;
#14864 = LINE ( 'NONE', #20285, #51703 ) ;
#14865 = ORIENTED_EDGE ( 'NONE', *, *, #37749, .F. ) ;
#14866 = CARTESIAN_POINT ( 'NONE',  ( 5.326923076924511946, -7.500000000000155431, 34.75000000000007105 ) ) ;
#14867 = CARTESIAN_POINT ( 'NONE',  ( -8.899378738962463231, -12.15440758774515473, 32.17923288041532004 ) ) ;
#14868 = FACE_BOUND ( 'NONE', #35978, .T. ) ;
#14869 = DIRECTION ( 'NONE',  ( 0.000000000000000000, 0.000000000000000000, -1.000000000000000000 ) ) ;
#14870 = CARTESIAN_POINT ( 'NONE',  ( -17.93393164899756442, -12.10708131394839882, 31.69288490824020954 ) ) ;
#14871 = CARTESIAN_POINT ( 'NONE',  ( 9.692307692307695177, -11.35647404775217417, 33.31231777344666511 ) ) ;
#14872 = LINE ( 'NONE', #42346, #10123 ) ;
#14873 = CARTESIAN_POINT ( 'NONE',  ( -17.20707104665477161, -8.630895178749536711, 34.87696386517710323 ) ) ;
#14874 = CARTESIAN_POINT ( 'NONE',  ( -16.21992956480203318, -8.120952969808774569, 34.71129190930000163 ) ) ;
#14875 = ORIENTED_EDGE ( 'NONE', *, *, #88572, .T. ) ;
#14876 = DIRECTION ( 'NONE',  ( -0.000000000000000000, -0.1736481776669307198, -0.9848077530122080203 ) ) ;
#14877 = VERTEX_POINT ( 'NONE', #53598 ) ;
#14878 = ORIENTED_EDGE ( 'NONE', *, *, #78056, .F. ) ;
#14880 = CARTESIAN_POINT ( 'NONE',  ( 8.096208157792160520, -9.943054286541403997, 34.11300777759954883 ) ) ;
#14879 = CARTESIAN_POINT ( 'NONE',  ( 7.716006636715624367, -6.852621066184267029, 34.70813303252209181 ) ) ;
#14881 = FACE_OUTER_BOUND ( 'NONE', #29484, .T. ) ;
#14882 = B_SPLINE_CURVE_WITH_KNOTS ( 'NONE', 3,
 ( #3119, #45441, #50416, #77899, #78784, #65266, #52196, #57189, #22956, #23392 ),
 .UNSPECIFIED., .F., .F.,
 ( 4, 2, 2, 2, 4 ),
 ( 0.000000000000000000, 0.0001954311564186878502, 0.0003908623128373757004, 0.0005862934692560635777, 0.0007817246256747514008 ),
 .UNSPECIFIED. ) ;
#14883 = FACE_OUTER_BOUND ( 'NONE', #78494, .T. ) ;
#14884 = CARTESIAN_POINT ( 'NONE',  ( -12.39628332202562788, -2.657715359629131857, 31.77849191805844242 ) ) ;
#14885 = CARTESIAN_POINT ( 'NONE',  ( -19.50000000000000000, -3.499999999999999556, 29.75000000000000355 ) ) ;
#14886 = VERTEX_POINT ( 'NONE', #47280 ) ;
#14887 = CARTESIAN_POINT ( 'NONE',  ( 11.40831356872984514, -3.625366637846545892, 33.29286588640298561 ) ) ;
#14888 = AXIS2_PLACEMENT_3D ( 'NONE', #87757, #25138, #17945 ) ;
#14889 = CARTESIAN_POINT ( 'NONE',  ( -13.38461538461538325, -13.20930481340135110, 34.54067556320372745 ) ) ;
#14890 = DIRECTION ( 'NONE',  ( 0.000000000000000000, 0.000000000000000000, -1.000000000000000000 ) ) ;
#14891 = CARTESIAN_POINT ( 'NONE',  ( -8.519285359852730721, -2.589246495874658383, 31.60778113518102828 ) ) ;
#14892 = CARTESIAN_POINT ( 'NONE',  ( 13.51514082284903040, -5.915461855592780260, 34.75538340440931506 ) ) ;
#14893 = ORIENTED_EDGE ( 'NONE', *, *, #58929, .F. ) ;
#14894 = CARTESIAN_POINT ( 'NONE',  ( 1.161130440891438020, -3.236172620538810385, 32.36188796281390267 ) ) ;
#14895 = EDGE_LOOP ( 'NONE', ( #58995, #51491, #45157, #58694 ) ) ;
#14896 = VECTOR ( 'NONE', #71728, 1000.000000000000000 ) ;
#14897 = ORIENTED_EDGE ( 'NONE', *, *, #88519, .T. ) ;
#14898 = CARTESIAN_POINT ( 'NONE',  ( -7.053224132515142131, -8.587444163452046197, 34.63053765926554206 ) ) ;
#14899 = ORIENTED_EDGE ( 'NONE', *, *, #24855, .T. ) ;
#14900 = CARTESIAN_POINT ( 'NONE',  ( -1.384615384615505151, -8.613356846316285953, 34.62446782046622218 ) ) ;
#14901 = CARTESIAN_POINT ( 'NONE',  ( -12.33101275977490019, -6.852161475712352789, 34.70806712695775786 ) ) ;
#14902 = CARTESIAN_POINT ( 'NONE',  ( -13.38461538461538325, -13.04860791097971706, 34.73218667398347037 ) ) ;
#14903 = CARTESIAN_POINT ( 'NONE',  ( -17.30040800148741553, -12.69144148231606017, 30.53333754910549303 ) ) ;
#14904 = CARTESIAN_POINT ( 'NONE',  ( -17.14300545628321260, -9.058645607665454236, 34.76329471203372634 ) ) ;
#14905 = CARTESIAN_POINT ( 'NONE',  ( 12.23805351781451201, -10.11188796281391511, 34.01382737946119050 ) ) ;
#14906 = ORIENTED_EDGE ( 'NONE', *, *, #47763, .T. ) ;
#14907 = DIRECTION ( 'NONE',  ( -0.000000000000000000, -0.7660444431189791237, -0.6427876096865379196 ) ) ;
#14909 = ORIENTED_EDGE ( 'NONE', *, *, #37512, .T. ) ;
#14908 = DIRECTION ( 'NONE',  ( -1.000000000000000000, 0.000000000000000000, 0.000000000000000000 ) ) ;
#14910 = CARTESIAN_POINT ( 'NONE',  ( -3.453634652972869201, -2.501496062324912284, 29.88072118266895671 ) ) ;
#14911 = CARTESIAN_POINT ( 'NONE',  ( -8.704085988511138794, -7.750023224968867197, 34.99404313364389907 ) ) ;
#14912 = CARTESIAN_POINT ( 'NONE',  ( 17.07692307692307665, -11.16473453929635440, 33.15142922261926373 ) ) ;
#14913 = CARTESIAN_POINT ( 'NONE',  ( -18.00000000000012079, -11.94971097300221352, 32.03036669348236387 ) ) ;
#14914 = CARTESIAN_POINT ( 'NONE',  ( -2.307692307692428724, -2.379036618888197285, 30.90682066428292885 ) ) ;
#14915 = CARTESIAN_POINT ( 'NONE',  ( 9.692307692307572609, -10.21337939537710326, 33.94971097300076224 ) ) ;
#14916 = CARTESIAN_POINT ( 'NONE',  ( -3.296522659082562257, -7.249945578846654470, 34.99404164642496795 ) ) ;
#14917 = CARTESIAN_POINT ( 'NONE',  ( -1.901340078031369618, -5.512252781505359245, 25.50186829374151287 ) ) ;
#14918 = VERTEX_POINT ( 'NONE', #66671 ) ;
#14919 = LINE ( 'NONE', #84271, #50298 ) ;
#14920 = CARTESIAN_POINT ( 'NONE',  ( 12.52760579488853665, -4.661471528628508665, 34.16647553114624003 ) ) ;
#14921 = ADVANCED_FACE ( 'NONE', ( #74771 ), #87405, .F. ) ;
#14922 = CARTESIAN_POINT ( 'NONE',  ( 6.923076923076924238, -13.75783147151868846, 33.36296068462461051 ) ) ;
#14923 = CARTESIAN_POINT ( 'NONE',  ( -3.007756386675836335, -10.77377354290276301, 33.85451476688484718 ) ) ;
#14924 = ORIENTED_EDGE ( 'NONE', *, *, #23135, .F. ) ;
#14925 = LINE ( 'NONE', #76617, #44158 ) ;
#14926 = CARTESIAN_POINT ( 'NONE',  ( -5.076923076923075762, -8.810774026931790459, 35.74407628777942847 ) ) ;
#14927 = LINE ( 'NONE', #68972, #70395 ) ;
#14928 = B_SPLINE_CURVE_WITH_KNOTS ( 'NONE', 3,
 ( #79310, #38768, #4531, #86980, #86067, #18939, #12185, #24801, #72992, #52270 ),
 .UNSPECIFIED., .F., .F.,
 ( 4, 2, 2, 2, 4 ),
 ( 0.0007817246256747511840, 0.0009771112852218952725, 0.001172497944769039470, 0.001367884604316183667, 0.001563271263863327864 ),
 .UNSPECIFIED. ) ;
#14929 = CARTESIAN_POINT ( 'NONE',  ( 14.30769230769218758, -3.300289026999228881, 32.46337939537708905 ) ) ;
#14930 = ORIENTED_EDGE ( 'NONE', *, *, #46203, .T. ) ;
#14931 = CARTESIAN_POINT ( 'NONE',  ( -15.36146069743678844, -2.729777683071817229, 31.24903638046269450 ) ) ;
#14932 = EDGE_CURVE ( 'NONE', #27837, #6801, #23508, .T. ) ;
#14933 = CARTESIAN_POINT ( 'NONE',  ( -8.638440328263817136, -5.496552790871120031, 34.60292014791297532 ) ) ;
#14934 = CARTESIAN_POINT ( 'NONE',  ( -6.923076923076922462, -6.681629849574314051, 35.83090037661290239 ) ) ;
#14935 = EDGE_LOOP ( 'NONE', ( #81151, #74893, #53573, #21298 ) ) ;
#14936 = CARTESIAN_POINT ( 'NONE',  ( -8.834480701004853387, -2.255955759149247619, 30.00000000000013856 ) ) ;
#14937 = ORIENTED_EDGE ( 'NONE', *, *, #40107, .F. ) ;
#14938 = CARTESIAN_POINT ( 'NONE',  ( 12.71148387091650278, -12.45601412856602686, 31.48342859153981621 ) ) ;
#14939 = CARTESIAN_POINT ( 'NONE',  ( -4.087677012883497163, -7.250054483168843156, 34.74374881642865631 ) ) ;
#14940 = ORIENTED_EDGE ( 'NONE', *, *, #42281, .T. ) ;
#14941 = CARTESIAN_POINT ( 'NONE',  ( -17.74994558008654622, -10.06805714834173848, 34.32951233291982618 ) ) ;
#14942 = CARTESIAN_POINT ( 'NONE',  ( -8.992156986746916658, -2.554751324335734708, 30.48935550225260727 ) ) ;
#14943 = CARTESIAN_POINT ( 'NONE',  ( -10.86540785267757947, -5.851115903089112003, 34.47074536777953568 ) ) ;
#14944 = CARTESIAN_POINT ( 'NONE',  ( -11.28840711854808632, -5.642605341092957971, 34.66089969410670335 ) ) ;
#14945 = DIRECTION ( 'NONE',  ( -1.000000000000000000, 0.000000000000000000, -0.000000000000000000 ) ) ;
#14946 = EDGE_CURVE ( 'NONE', #36760, #15767, #25240, .T. ) ;
#14947 = EDGE_CURVE ( 'NONE', #76455, #47929, #4065, .T. ) ;
#14948 = VERTEX_POINT ( 'NONE', #33337 ) ;
#14949 = ORIENTED_EDGE ( 'NONE', *, *, #39053, .T. ) ;
#14950 = FACE_BOUND ( 'NONE', #70822, .T. ) ;
#14951 = ORIENTED_EDGE ( 'NONE', *, *, #11749, .T. ) ;
#14952 = CARTESIAN_POINT ( 'NONE',  ( 8.769230769230647482, -3.835265460704628371, 33.15142922262033665 ) ) ;
#14953 = B_SPLINE_CURVE_WITH_KNOTS ( 'NONE', 3,
 ( #65294, #4945, #23851, #32409, #86939, #24302, #4029, #25207, #79713, #65733 ),
 .UNSPECIFIED., .F., .F.,
 ( 4, 2, 2, 2, 4 ),
 ( 0.0007817359430256294638, 0.0009771253907249941549, 0.001172514838424358954, 0.001367904286123723754, 0.001563293733823095492 ),
 .UNSPECIFIED. ) ;
#14954 = VECTOR ( 'NONE', #4632, 1000.000000000000227 ) ;
#14955 = AXIS2_PLACEMENT_3D ( 'NONE', #38872, #87076, #78958 ) ;
#14956 = SHAPE_REPRESENTATION ( 'connector', ( #83448 ), #41778 ) ;
#14957 = CARTESIAN_POINT ( 'NONE',  ( 4.219101725122177626, -11.94971097300157403, 32.03036669348361443 ) ) ;
#14958 = CARTESIAN_POINT ( 'NONE',  ( 17.99999999999987566, -5.941354392335915335, 34.76329471203413846 ) ) ;
#14959 = CARTESIAN_POINT ( 'NONE',  ( 18.03205128205128105, -7.500000000000000000, 29.75000000000000355 ) ) ;
#14960 = B_SPLINE_CURVE_WITH_KNOTS ( 'NONE', 3,
 ( #60121, #5628, #66443, #17821, #88081, #33102, #31326, #18713, #74095, #38984 ),
 .UNSPECIFIED., .F., .F.,
 ( 4, 2, 2, 2, 4 ),
 ( 0.000000000000000000, 0.0001954339857564077183, 0.0003908679715128154366, 0.0005863019572692231007, 0.0007817359430256308733 ),
 .UNSPECIFIED. ) ;
#14961 = ORIENTED_EDGE ( 'NONE', *, *, #68822, .T. ) ;
#14962 = ORIENTED_EDGE ( 'NONE', *, *, #45241, .T. ) ;
#14963 = ORIENTED_EDGE ( 'NONE', *, *, #14194, .F. ) ;
#14964 = DIRECTION ( 'NONE',  ( -0.000000000000000000, 1.000000000000000000, -0.000000000000000000 ) ) ;
#14965 = ORIENTED_EDGE ( 'NONE', *, *, #28232, .T. ) ;
#14966 = CARTESIAN_POINT ( 'NONE',  ( -4.946131269098290595, -4.809403383903225304, 33.96459661697924304 ) ) ;
#14967 = FACE_OUTER_BOUND ( 'NONE', #11744, .T. ) ;
#14968 = CYLINDRICAL_SURFACE ( 'NONE', #58740, 0.2500000000000012212 ) ;
#14969 = ORIENTED_EDGE ( 'NONE', *, *, #56579, .T. ) ;
#14970 = CARTESIAN_POINT ( 'NONE',  ( 13.16113044089144068, -10.81261337010820256, 33.49550067578627477 ) ) ;
#14971 = CARTESIAN_POINT ( 'NONE',  ( -15.10024379253558635, -3.625058011473228703, 33.29252011169590020 ) ) ;
#14972 = CARTESIAN_POINT ( 'NONE',  ( 14.43821800945587519, -6.852161475712352789, 34.70806712695775786 ) ) ;
#14973 = CARTESIAN_POINT ( 'NONE',  ( 1.653273178848927064E-15, -7.500000000000000000, 14.00000000000000178 ) ) ;
#14974 = VERTEX_POINT ( 'NONE', #38757 ) ;
#14975 = VERTEX_POINT ( 'NONE', #31551 ) ;
#14976 = ORIENTED_EDGE ( 'NONE', *, *, #54694, .T. ) ;
#14977 = CARTESIAN_POINT ( 'NONE',  ( 3.930919194939304084, -2.889293201056495786, 32.26117774369186009 ) ) ;
#14978 = UNCERTAINTY_MEASURE_WITH_UNIT (LENGTH_MEASURE( 1.000000000000000082E-05 ), #26230, 'distance_accuracy_value', 'NONE');
#14980 = CARTESIAN_POINT ( 'NONE',  ( 10.39245765647776309, -2.308479472611653094, 30.53278059502174457 ) ) ;
#14979 = DIRECTION ( 'NONE',  ( -0.000000000000000000, 0.9396926207859093161, -0.3420201433256663259 ) ) ;
#14981 = CARTESIAN_POINT ( 'NONE',  ( 1.634560793993430128, -12.45601412856602686, 31.48342859153981621 ) ) ;
#14982 = CARTESIAN_POINT ( 'NONE',  ( -3.454254174493177842, -11.41268669641500466, 32.86336882939237825 ) ) ;
#14983 = FACE_BOUND ( 'NONE', #7505, .T. ) ;
#14984 = FACE_OUTER_BOUND ( 'NONE', #31157, .T. ) ;
#14985 = VERTEX_POINT ( 'NONE', #53144 ) ;
#14986 = CARTESIAN_POINT ( 'NONE',  ( -2.980714919130916130, -2.564540009722895419, 30.55348353981670684 ) ) ;
#14987 = B_SPLINE_CURVE_WITH_KNOTS ( 'NONE', 3,
 ( #87938, #75279, #60423, #53669, #13568, #74842, #13131, #88812, #60869, #81156 ),
 .UNSPECIFIED., .F., .F.,
 ( 4, 2, 2, 2, 4 ),
 ( 0.000000000000000000, 0.0001954339881912774612, 0.0003908679763825549224, 0.0005863019645738323836, 0.0007817359527651098448 ),
 .UNSPECIFIED. ) ;
#14988 = CARTESIAN_POINT ( 'NONE',  ( -0.2387589202700517999, -9.332535724633405749, 34.40230450496446224 ) ) ;
#14989 = DIRECTION ( 'NONE',  ( -0.000000000000000000, -0.000000000000000000, -1.000000000000000000 ) ) ;
#14990 = CARTESIAN_POINT ( 'NONE',  ( 7.173022332454967120, -9.357781135181031829, 34.66075350412533851 ) ) ;
#14991 = B_SPLINE_CURVE_WITH_KNOTS ( 'NONE', 3,
 ( #58642, #23966, #2365, #23526, #86136, #78919, #50555, #29858, #30296, #78035 ),
 .UNSPECIFIED., .F., .F.,
 ( 4, 2, 2, 2, 4 ),
 ( 0.000000000000000000, 0.0001954311564186861968, 0.0003908623128373723936, 0.0005862934692560585904, 0.0007817246256747447872 ),
 .UNSPECIFIED. ) ;
#14992 = EDGE_LOOP ( 'NONE', ( #79168, #62362, #7758, #75762 ) ) ;
#14993 = CARTESIAN_POINT ( 'NONE',  ( 4.946775107191379028, -12.70455904226513866, 30.44083106164009322 ) ) ;
#14994 = ORIENTED_EDGE ( 'NONE', *, *, #87105, .T. ) ;
#14995 = FACE_BOUND ( 'NONE', #2207, .T. ) ;
#14996 = DIRECTION ( 'NONE',  ( -1.000000000000000000, -0.000000000000000000, -0.000000000000000000 ) ) ;
#14997 = CARTESIAN_POINT ( 'NONE',  ( 17.01165263096229907, -11.94971097300153140, 32.03036669348370680 ) ) ;
#14998 = CARTESIAN_POINT ( 'NONE',  ( 14.08476609017615644, -11.76352882383564769, 32.36236540154569497 ) ) ;
#14999 = ORIENTED_EDGE ( 'NONE', *, *, #56784, .T. ) ;
#15000 = CARTESIAN_POINT ( 'NONE',  ( 5.326868595271218254, -3.202959910592335202, 32.30730279482227019 ) ) ;
#15001 = CARTESIAN_POINT ( 'NONE',  ( -3.296851610129365451, -2.292212530054419606, 30.41441678777542634 ) ) ;
#15002 = CARTESIAN_POINT ( 'NONE',  ( -3.230769230769351186, -2.892918686052166066, 31.69288490824153470 ) ) ;
#15003 = CARTESIAN_POINT ( 'NONE',  ( -6.989160334032800570, -10.51840700105979387, 33.73612834413961536 ) ) ;
#15004 = VERTEX_POINT ( 'NONE', #88307 ) ;
#15005 = ADVANCED_FACE ( 'NONE', ( #32887 ), #79747, .F. ) ;
#15006 = CARTESIAN_POINT ( 'NONE',  ( 12.68491394731088029, -2.251407671071270489, 29.88021292934942963 ) ) ;
#15007 = EDGE_LOOP ( 'NONE', ( #41503, #21897 ) ) ;
#15009 = EDGE_LOOP ( 'NONE', ( #2370, #38166, #11519, #34566 ) ) ;
#15008 = CARTESIAN_POINT ( 'NONE',  ( 10.03846153846153832, -7.500000000000000000, 29.75000000000000355 ) ) ;
#15010 = CARTESIAN_POINT ( 'NONE',  ( 9.562160482869471068, -3.817052484675422797, 33.13202310037935661 ) ) ;
#15011 = CARTESIAN_POINT ( 'NONE',  ( -8.769230769230768274, -11.11383981884818262, 36.00935417666054406 ) ) ;
#15012 = CARTESIAN_POINT ( 'NONE',  ( -18.00000000000012079, -4.320704448113953156, 33.92786785259630022 ) ) ;
#15013 = CARTESIAN_POINT ( 'NONE',  ( -20.74999999999999645, -4.499999999999999112, 29.75000000000000355 ) ) ;
#15014 = CARTESIAN_POINT ( 'NONE',  ( -12.71151520558705172, -10.82459398097509329, 33.81372124010185587 ) ) ;
#15017 = LINE ( 'NONE', #4484, #10132 ) ;
#15016 = VECTOR ( 'NONE', #14077, 1000.000000000000227 ) ;
#15015 = CARTESIAN_POINT ( 'NONE',  ( -12.46153846153858424, -12.70778746994576025, 30.41441678777401236 ) ) ;
#15018 = CYLINDRICAL_SURFACE ( 'NONE', #32051, 0.2499999999999986955 ) ;
#15019 = CARTESIAN_POINT ( 'NONE',  ( 1.944543648262996083, -5.555456351736983045, 23.06250000000000000 ) ) ;
#15020 = ORIENTED_EDGE ( 'NONE', *, *, #3404, .T. ) ;
#15021 = CARTESIAN_POINT ( 'NONE',  ( -16.37677311275300340, -4.762599654559227957, 34.23009711892697737 ) ) ;
#15022 = EDGE_LOOP ( 'NONE', ( #17666, #24776 ) ) ;
#15023 = ADVANCED_FACE ( 'NONE', ( #72982 ), #46840, .F. ) ;
#15024 = ORIENTED_EDGE ( 'NONE', *, *, #88565, .F. ) ;
#15025 = CARTESIAN_POINT ( 'NONE',  ( 11.78851585009985570, -11.79725096376909654, 32.30694842903959341 ) ) ;
#15026 = ORIENTED_EDGE ( 'NONE', *, *, #26087, .T. ) ;
#15027 = LINE ( 'NONE', #2813, #38330 ) ;
#15028 = EDGE_CURVE ( 'NONE', #6548, #6628, #46399, .T. ) ;
#15029 = CARTESIAN_POINT ( 'NONE',  ( 7.623287583090747610, -2.251424796025575770, 29.88072029997477586 ) ) ;
#15030 = B_SPLINE_CURVE_WITH_KNOTS ( 'NONE', 3,
 ( #38673, #38228, #31472, #17967, #31015, #50831, #66137, #4441, #58937, #10759 ),
 .UNSPECIFIED., .F., .F.,
 ( 4, 2, 2, 2, 4 ),
 ( 0.000000000000000000, 0.0001954311564186871184, 0.0003908623128373742367, 0.0005862934692560614093, 0.0007817246256747484735 ),
 .UNSPECIFIED. ) ;
#15031 = CYLINDRICAL_SURFACE ( 'NONE', #28659, 0.2499999999999973355 ) ;
#15032 = FACE_OUTER_BOUND ( 'NONE', #43571, .T. ) ;
#15033 = CARTESIAN_POINT ( 'NONE',  ( 8.769230769230647482, -11.48612834414049644, 32.76840700105863391 ) ) ;
#15034 = CARTESIAN_POINT ( 'NONE',  ( -16.15384615384627409, -5.219633306517616589, 34.19971097300220464 ) ) ;
#15035 = DIRECTION ( 'NONE',  ( 0.000000000000000000, 0.9848077530122072432, -0.1736481776669354937 ) ) ;
#15036 = B_SPLINE_CURVE_WITH_KNOTS ( 'NONE', 3,
 ( #83609, #35398, #56561, #77713, #76383, #43489, #57436, #22331, #49796, #77271 ),
 .UNSPECIFIED., .F., .F.,
 ( 4, 2, 2, 2, 4 ),
 ( 0.000000000000000000, 0.0001954339857564079894, 0.0003908679715128159787, 0.0005863019572692239681, 0.0007817359430256319575 ),
 .UNSPECIFIED. ) ;
#15037 = CARTESIAN_POINT ( 'NONE',  ( 10.48469314871705826, -2.541943142973491554, 30.39792223712631980 ) ) ;
#15038 = CARTESIAN_POINT ( 'NONE',  ( 15.16549923021291058, -9.528491918058357157, 34.59228464037090589 ) ) ;
#15039 = EDGE_CURVE ( 'NONE', #74721, #44439, #55736, .T. ) ;
#15040 = CARTESIAN_POINT ( 'NONE',  ( 5.749976775778542049, -11.56360843649121861, 33.07473185843129926 ) ) ;
#15041 = CARTESIAN_POINT ( 'NONE',  ( 7.716005876422148191, -2.373036134822904319, 30.88089517874951540 ) ) ;
#15042 = EDGE_CURVE ( 'NONE', #44439, #82483, #19817, .T. ) ;
#15043 = ORIENTED_EDGE ( 'NONE', *, *, #31470, .T. ) ;
#15044 = EDGE_LOOP ( 'NONE', ( #69875, #29148, #27198, #55212 ) ) ;
#15045 = CARTESIAN_POINT ( 'NONE',  ( 12.71148387091650278, -2.589246495874658383, 31.60778113518102828 ) ) ;
#15046 = CARTESIAN_POINT ( 'NONE',  ( 1.384615384615386802, -13.04860791097971706, 34.73218667398347037 ) ) ;
#15047 = LINE ( 'NONE', #22676, #68525 ) ;
#15048 = LINE ( 'NONE', #42523, #19719 ) ;
#15049 = ORIENTED_EDGE ( 'NONE', *, *, #78326, .F. ) ;
#15050 = CARTESIAN_POINT ( 'NONE',  ( 13.38461538461538680, -13.20930481340135110, 34.54067556320372745 ) ) ;
#15051 = CARTESIAN_POINT ( 'NONE',  ( -10.83831157429145975, -12.64616026154729411, 30.79003144601914244 ) ) ;
#15052 = AXIS2_PLACEMENT_3D ( 'NONE', #80938, #59757, #87253 ) ;
#15053 = CARTESIAN_POINT ( 'NONE',  ( -12.33074665371367651, -10.54018710029568595, 33.71981072465678864 ) ) ;
#15054 = ADVANCED_FACE ( 'NONE', ( #86973 ), #67566, .F. ) ;
#15055 = ORIENTED_EDGE ( 'NONE', *, *, #40666, .T. ) ;
#15056 = DIRECTION ( 'NONE',  ( -0.000000000000000000, -0.000000000000000000, -1.000000000000000000 ) ) ;
#15057 = EDGE_CURVE ( 'NONE', #47954, #39557, #11735, .T. ) ;
#15058 = EDGE_LOOP ( 'NONE', ( #66437, #50891 ) ) ;
#15059 = CARTESIAN_POINT ( 'NONE',  ( 10.61538461538449418, -2.657715359629662544, 31.77849191805970364 ) ) ;
#15060 = FACE_OUTER_BOUND ( 'NONE', #85986, .T. ) ;
#15061 = ADVANCED_FACE ( 'NONE', ( #69336 ), #82416, .F. ) ;
#15062 = DIRECTION ( 'NONE',  ( 0.000000000000000000, 0.000000000000000000, 1.000000000000000000 ) ) ;
#15063 = ADVANCED_FACE ( 'NONE', ( #13939 ), #61673, .F. ) ;
#15064 = CARTESIAN_POINT ( 'NONE',  ( 14.30769230769231015, -8.564572088678739092, 35.78748833219616898 ) ) ;
#15065 = CARTESIAN_POINT ( 'NONE',  ( -17.74994558008654622, -12.41089969410671046, 31.60739465890703670 ) ) ;
#15066 = ORIENTED_EDGE ( 'NONE', *, *, #60476, .F. ) ;
#15067 = EDGE_LOOP ( 'NONE', ( #30794, #47678 ) ) ;
#15068 = B_SPLINE_CURVE_WITH_KNOTS ( 'NONE', 3,
 ( #59064, #73032, #72581, #87457, #59956, #25289 ),
 .UNSPECIFIED., .F., .F.,
 ( 4, 2, 4 ),
 ( 0.0003909512603273637287, 0.0005862562993131885522, 0.0007815613382990133215 ),
 .UNSPECIFIED. ) ;
#15069 = VERTEX_POINT ( 'NONE', #28335 ) ;
#15070 = ORIENTED_EDGE ( 'NONE', *, *, #69016, .F. ) ;
#15071 = CARTESIAN_POINT ( 'NONE',  ( 13.25392391794782654, -3.062553014421049546, 32.05460306192773601 ) ) ;
#15072 = CARTESIAN_POINT ( 'NONE',  ( 8.096153846153846700, -7.500000000000001776, 35.04278698407183867 ) ) ;
#15073 = CYLINDRICAL_SURFACE ( 'NONE', #35062, 0.2499999999999994726 ) ;
#15074 = AXIS2_PLACEMENT_3D ( 'NONE', #6091, #6535, #33567 ) ;
#15075 = CIRCLE ( 'NONE', #61104, 0.2500000000000002220 ) ;
#15076 = DIRECTION ( 'NONE',  ( 1.000000000000000000, -0.000000000000000000, -0.000000000000000000 ) ) ;
#15077 = CARTESIAN_POINT ( 'NONE',  ( 5.076923076922953193, -12.51329471203414379, 31.30864560766407578 ) ) ;
#15078 = CARTESIAN_POINT ( 'NONE',  ( 14.53070365930516061, -9.886259254753566594, 34.14407573483972413 ) ) ;
#15079 = ORIENTED_EDGE ( 'NONE', *, *, #33984, .T. ) ;
#15080 = VERTEX_POINT ( 'NONE', #6311 ) ;
#15081 = VERTEX_POINT ( 'NONE', #55808 ) ;
#15083 = EDGE_LOOP ( 'NONE', ( #77363, #12966, #32102, #67008 ) ) ;
#15082 = CARTESIAN_POINT ( 'NONE',  ( 12.46153846153846168, -8.120952969808772792, 34.71129190930000163 ) ) ;
#15085 = CARTESIAN_POINT ( 'NONE',  ( 14.43821774592595197, -5.070358843744210198, 34.40418822224088302 ) ) ;
#15084 = CARTESIAN_POINT ( 'NONE',  ( -16.94613126909829148, -8.999086150933472084, 34.52020707165672064 ) ) ;
#15086 = PLANE ( 'NONE',  #25902 ) ;
#15087 = EDGE_CURVE ( 'NONE', #43722, #17581, #20698, .T. ) ;
#15088 = CARTESIAN_POINT ( 'NONE',  ( -10.86540785267757947, -11.86270091957321249, 32.19358267280087915 ) ) ;
#15089 = ORIENTED_EDGE ( 'NONE', *, *, #21148, .T. ) ;
#15090 = ORIENTED_EDGE ( 'NONE', *, *, #51389, .T. ) ;
#15091 = DIRECTION ( 'NONE',  ( 0.000000000000000000, 0.4999999999999960032, -0.8660254037844410391 ) ) ;
#15092 = EDGE_LOOP ( 'NONE', ( #24598, #73476, #63875, #42129 ) ) ;
#15093 = FACE_BOUND ( 'NONE', #33832, .T. ) ;
#15094 = CARTESIAN_POINT ( 'NONE',  ( -1.134615384615383915, -2.499999999999998668, 29.75000000000000355 ) ) ;
#15095 = EDGE_CURVE ( 'NONE', #39467, #16561, #56856, .T. ) ;
#15096 = CARTESIAN_POINT ( 'NONE',  ( -3.230769230769352962, -2.379036618888197285, 30.90682066428292885 ) ) ;
#15097 = ORIENTED_EDGE ( 'NONE', *, *, #88574, .T. ) ;
#15098 = CARTESIAN_POINT ( 'NONE',  ( 20.00000000000000000, -4.000000000000000000, 28.25000000000000000 ) ) ;
#15099 = CARTESIAN_POINT ( 'NONE',  ( 3.296837581771669523, -3.050289026998446840, 32.03036669348366416 ) ) ;
#15100 = PLANE ( 'NONE',  #34933 ) ;
#15101 = CARTESIAN_POINT ( 'NONE',  ( -15.36091644020745051, -6.852621066184266141, 34.70813303252209181 ) ) ;
#15102 = CARTESIAN_POINT ( 'NONE',  ( -7.846153846153844924, -9.905515769479276145, 34.41647553114623292 ) ) ;
#15103 = ORIENTED_EDGE ( 'NONE', *, *, #77646, .T. ) ;
#15104 = EDGE_CURVE ( 'NONE', #69549, #32791, #30997, .T. ) ;
#15105 = VECTOR ( 'NONE', #70409, 1000.000000000000000 ) ;
#15106 = CARTESIAN_POINT ( 'NONE',  ( -12.23852561744506851, -2.308499170217967134, 30.53291367094873721 ) ) ;
#15107 = CARTESIAN_POINT ( 'NONE',  ( -7.715362038329057981, -6.413143153341454017, 34.63066358083362672 ) ) ;
#15108 = CARTESIAN_POINT ( 'NONE',  ( 16.15384615384603251, -9.442884908241554243, 34.35708131394783038 ) ) ;
#15109 = CARTESIAN_POINT ( 'NONE',  ( -0.6850233861027930082, -4.988325925672468131, 34.36044203135681130 ) ) ;
#15110 = LINE ( 'NONE', #84024, #57361 ) ;
#15111 = FACE_BOUND ( 'NONE', #75161, .T. ) ;
#15113 = DIRECTION ( 'NONE',  ( 0.000000000000000000, 0.000000000000000000, -1.000000000000000000 ) ) ;
#15112 = FACE_OUTER_BOUND ( 'NONE', #20416, .T. ) ;
#15114 = CARTESIAN_POINT ( 'NONE',  ( 5.142990410273153401, -2.292212530054420494, 30.41441678777542990 ) ) ;
#15116 = DIRECTION ( 'NONE',  ( 0.000000000000000000, 0.000000000000000000, -1.000000000000000000 ) ) ;
#15115 = CARTESIAN_POINT ( 'NONE',  ( -3.361459833879539172, -2.845849958028613624, 32.17971566917920967 ) ) ;
#15117 = CARTESIAN_POINT ( 'NONE',  ( -5.142193077479396912, -12.51329471203370325, 31.30864560766548976 ) ) ;
#15118 = B_SPLINE_CURVE_WITH_KNOTS ( 'NONE', 3,
 ( #39347, #46533, #25369, #32134, #58702, #52385, #79874, #86202, #74012, #5999 ),
 .UNSPECIFIED., .F., .F.,
 ( 4, 2, 2, 2, 4 ),
 ( 0.000000000000000000, 0.0001954339857564072033, 0.0003908679715128144066, 0.0005863019572692215828, 0.0007817359430256288133 ),
 .UNSPECIFIED. ) ;
#15119 = CARTESIAN_POINT ( 'NONE',  ( -2.724691934501232371, -8.700186371490559623, 22.26375670625849068 ) ) ;
#15120 = ORIENTED_EDGE ( 'NONE', *, *, #53473, .F. ) ;
#15121 = CARTESIAN_POINT ( 'NONE',  ( -3.230769230769229949, -1.951392089020283160, 34.73218667398347748 ) ) ;
#15122 = ORIENTED_EDGE ( 'NONE', *, *, #86699, .F. ) ;
#15123 = CARTESIAN_POINT ( 'NONE',  ( -18.00000000000012079, -5.094484230521992174, 34.41647553114689373 ) ) ;
#15124 = ADVANCED_FACE ( 'NONE', ( #42315 ), #41867, .F. ) ;
#15125 = B_SPLINE_CURVE_WITH_KNOTS ( 'NONE', 3,
 ( #17443, #38151, #15676, #43575, #58865, #70612, #22423, #8920, #36387, #39946 ),
 .UNSPECIFIED., .F., .F.,
 ( 4, 2, 2, 2, 4 ),
 ( 0.0007817246256747463051, 0.0009771112852218898515, 0.001172497944769033181, 0.001367884604316176728, 0.001563271263863320274 ),
 .UNSPECIFIED. ) ;
#15126 = ORIENTED_EDGE ( 'NONE', *, *, #18055, .F. ) ;
#15127 = DIRECTION ( 'NONE',  ( -0.000000000000000000, -0.9396926207859092051, -0.3420201433256662704 ) ) ;
#15128 = CARTESIAN_POINT ( 'NONE',  ( -18.00000000000000000, -2.538708090699994813, 30.37095296980875858 ) ) ;
#15129 = ORIENTED_EDGE ( 'NONE', *, *, #27888, .F. ) ;
#15130 = DIRECTION ( 'NONE',  ( -1.000000000000000000, -0.000000000000000000, -0.000000000000000000 ) ) ;
#15131 = CARTESIAN_POINT ( 'NONE',  ( -2.775308065498764964, -6.422011778438537988, 23.67000670625849779 ) ) ;
#15132 = LINE ( 'NONE', #15575, #76032 ) ;
#15133 = EDGE_CURVE ( 'NONE', #25570, #3292, #13060, .T. ) ;
#15134 = CARTESIAN_POINT ( 'NONE',  ( 4.088575707885377497, -9.442884908240170461, 34.35708131394840592 ) ) ;
#15135 = CARTESIAN_POINT ( 'NONE',  ( 4.153846153846030731, -4.320704448113951379, 33.92786785259630022 ) ) ;
#15136 = CARTESIAN_POINT ( 'NONE',  ( -14.30769230769230660, -12.29105614889573062, 35.45975837776705220 ) ) ;
#15137 = FACE_OUTER_BOUND ( 'NONE', #84143, .T. ) ;
#15138 = CARTESIAN_POINT ( 'NONE',  ( -9.692307692307691624, -3.050289026998446396, 32.03036669348365706 ) ) ;
#15139 = CARTESIAN_POINT ( 'NONE',  ( 3.750000000000000888, -7.499999999999978684, 14.46875000000000000 ) ) ;
#15140 = VECTOR ( 'NONE', #55419, 1000.000000000000000 ) ;
#15141 = PLANE ( 'NONE',  #76525 ) ;
#15142 = CYLINDRICAL_SURFACE ( 'NONE', #29048, 0.2499999999999986955 ) ;
#15143 = DIRECTION ( 'NONE',  ( -0.000000000000000000, -0.8660254037844397068, -0.4999999999999978906 ) ) ;
#15144 = CARTESIAN_POINT ( 'NONE',  ( 2.694853999681185108, -4.891553140782077591, 24.56436829374151287 ) ) ;
#15145 = B_SPLINE_CURVE_WITH_KNOTS ( 'NONE', 3,
 ( #88497, #26769, #20009, #61871, #14140, #47920, #47472, #88941, #82167, #74970 ),
 .UNSPECIFIED., .F., .F.,
 ( 4, 2, 2, 2, 4 ),
 ( 0.0007817246256747524850, 0.0009771112852218972241, 0.001172497944769042072, 0.001367884604316186702, 0.001563271263863331550 ),
 .UNSPECIFIED. ) ;
#15146 = DIRECTION ( 'NONE',  ( 0.000000000000000000, 0.000000000000000000, 1.000000000000000000 ) ) ;
#15147 = EDGE_LOOP ( 'NONE', ( #32677, #75757 ) ) ;
#15148 = LINE ( 'NONE', #82283, #14013 ) ;
#15149 = CARTESIAN_POINT ( 'NONE',  ( -11.40766973063675493, -8.147973898785416225, 34.70805048591653730 ) ) ;
#15150 = CARTESIAN_POINT ( 'NONE',  ( 9.915087233576103998, -6.760870238392817200, 34.69528174975672385 ) ) ;
#15151 = CARTESIAN_POINT ( 'NONE',  ( 8.546303810323914618, -5.582147617184174848, 34.63737895849758530 ) ) ;
#15152 = VECTOR ( 'NONE', #86071, 1000.000000000000114 ) ;
#15153 = CARTESIAN_POINT ( 'NONE',  ( -3.165513659493206067, -5.219633306516380244, 34.19971097300157936 ) ) ;
#15154 = CARTESIAN_POINT ( 'NONE',  ( -18.00000000000000000, -13.72934399251292170, 33.34651343095209342 ) ) ;
#15155 = CYLINDRICAL_SURFACE ( 'NONE', #8827, 0.2500000000000008882 ) ;
#15156 = EDGE_CURVE ( 'NONE', #3726, #58506, #7189, .T. ) ;
#15157 = ORIENTED_EDGE ( 'NONE', *, *, #40029, .T. ) ;
#15158 = ORIENTED_EDGE ( 'NONE', *, *, #25373, .T. ) ;
#15159 = B_SPLINE_CURVE_WITH_KNOTS ( 'NONE', 3,
 ( #29730, #56748, #57192, #28388, #29292, #56310 ),
 .UNSPECIFIED., .F., .F.,
 ( 4, 2, 4 ),
 ( 0.000000000000000000, 0.0001954784845028895374, 0.0003909569690057790748 ),
 .UNSPECIFIED. ) ;
#15160 = EDGE_CURVE ( 'NONE', #43765, #83533, #81977, .T. ) ;
#15161 = ORIENTED_EDGE ( 'NONE', *, *, #3228, .F. ) ;
#15162 = CARTESIAN_POINT ( 'NONE',  ( 5.326977388561390470, -11.79725096376909299, 32.30694842903960762 ) ) ;
#15163 = CARTESIAN_POINT ( 'NONE',  ( 3.230769230769231726, -8.164416787775445883, 34.95778746994557906 ) ) ;
#15164 = CARTESIAN_POINT ( 'NONE',  ( -17.07692307692307665, -13.20930481340135110, 34.54067556320372745 ) ) ;
#15165 = EDGE_CURVE ( 'NONE', #82297, #11287, #84798, .T. ) ;
#15166 = DIRECTION ( 'NONE',  ( 0.000000000000000000, 0.9848077530122072432, 0.1736481776669354937 ) ) ;
#15167 = DIRECTION ( 'NONE',  ( -0.000000000000000000, 0.1736481776669307198, -0.9848077530122080203 ) ) ;
#15168 = VECTOR ( 'NONE', #4024, 1000.000000000000227 ) ;
#15169 = ORIENTED_EDGE ( 'NONE', *, *, #79709, .T. ) ;
#15170 = LINE ( 'NONE', #34986, #3178 ) ;
#15171 = ORIENTED_EDGE ( 'NONE', *, *, #62116, .T. ) ;
#15172 = VERTEX_POINT ( 'NONE', #61482 ) ;
#15173 = ORIENTED_EDGE ( 'NONE', *, *, #85750, .F. ) ;
#15175 = ORIENTED_EDGE ( 'NONE', *, *, #86295, .T. ) ;
#15174 = CARTESIAN_POINT ( 'NONE',  ( 8.703960768674448900, -12.51329471203370325, 31.30864560766548976 ) ) ;
#15176 = CARTESIAN_POINT ( 'NONE',  ( 4.284637961670941131, -5.582136614379148654, 34.36778462344220486 ) ) ;
#15177 = EDGE_CURVE ( 'NONE', #4656, #48169, #39038, .T. ) ;
#15178 = CARTESIAN_POINT ( 'NONE',  ( 10.61538461538461675, -12.78798330534102945, 29.74999999999997868 ) ) ;
#15179 = EDGE_CURVE ( 'NONE', #44047, #56065, #48249, .T. ) ;
#15180 = DIRECTION ( 'NONE',  ( -0.000000000000000000, 0.7660444431189791237, -0.6427876096865379196 ) ) ;
#15181 = CARTESIAN_POINT ( 'NONE',  ( -7.173076923076929567, -2.499999999999999556, 29.81609845454692120 ) ) ;
#15182 = EDGE_LOOP ( 'NONE', ( #87064, #6690 ) ) ;
#15183 = ORIENTED_EDGE ( 'NONE', *, *, #41889, .T. ) ;
#15184 = B_SPLINE_CURVE_WITH_KNOTS ( 'NONE', 3,
 ( #23821, #16199, #37343, #85108, #36905, #15766, #50412, #64368, #85992, #29723 ),
 .UNSPECIFIED., .F., .F.,
 ( 4, 2, 2, 2, 4 ),
 ( 0.000000000000000000, 0.0001954339857564097783, 0.0003908679715128195566, 0.0005863019572692293891, 0.0007817359430256391132 ),
 .UNSPECIFIED. ) ;
#15185 = ORIENTED_EDGE ( 'NONE', *, *, #61798, .F. ) ;
#15186 = DIRECTION ( 'NONE',  ( 0.000000000000000000, 0.000000000000000000, 1.000000000000000000 ) ) ;
#15188 = ORIENTED_EDGE ( 'NONE', *, *, #83244, .T. ) ;
#15187 = DIRECTION ( 'NONE',  ( -0.000000000000000000, -0.000000000000000000, -1.000000000000000000 ) ) ;
#15189 = B_SPLINE_CURVE_WITH_KNOTS ( 'NONE', 3,
 ( #58708, #32141, #59600, #31240, #78535, #24033 ),
 .UNSPECIFIED., .F., .F.,
 ( 4, 2, 4 ),
 ( 4.220987180333913997E-17, 0.0001954756301637163962, 0.0003909512603273906169 ),
 .UNSPECIFIED. ) ;
#15190 = CARTESIAN_POINT ( 'NONE',  ( 4.480769230769229061, -3.499999999999999556, 29.75000000000000355 ) ) ;
#15191 = CARTESIAN_POINT ( 'NONE',  ( -13.38461538461538325, -8.164416787775445883, 34.95778746994557906 ) ) ;
#15192 = B_SPLINE_CURVE_WITH_KNOTS ( 'NONE', 3,
 ( #3032, #77375, #16555, #71057, #84596, #2589, #9802, #77812, #23747, #22866 ),
 .UNSPECIFIED., .F., .F.,
 ( 4, 2, 2, 2, 4 ),
 ( 0.0007817246256747514008, 0.0009771112852218952725, 0.001172497944769039253, 0.001367884604316183233, 0.001563271263863327213 ),
 .UNSPECIFIED. ) ;
#15193 = ADVANCED_FACE ( 'NONE', ( #67809 ), #53847, .F. ) ;
#15194 = VECTOR ( 'NONE', #9092, 1000.000000000000114 ) ;
#15195 = CARTESIAN_POINT ( 'NONE',  ( -3.100243529005668019, -10.19071101563364401, 33.96452234770658407 ) ) ;
#15196 = ORIENTED_EDGE ( 'NONE', *, *, #31049, .T. ) ;
#15197 = CARTESIAN_POINT ( 'NONE',  ( -11.40766973063674961, -4.809403383903225304, 33.96459661697924304 ) ) ;
#15198 = CARTESIAN_POINT ( 'NONE',  ( 15.16549923021291235, -2.657715359629088780, 31.77849191805832874 ) ) ;
#15199 = VERTEX_POINT ( 'NONE', #75892 ) ;
#15200 = FACE_BOUND ( 'NONE', #40681, .T. ) ;
#15201 = ADVANCED_FACE ( 'NONE', ( #19615 ), #40343, .F. ) ;
#15202 = LINE ( 'NONE', #23268, #29815 ) ;
#15203 = LINE ( 'NONE', #63371, #9721 ) ;
#15204 = DIRECTION ( 'NONE',  ( 0.000000000000000000, 0.000000000000000000, -1.000000000000000000 ) ) ;
#15206 = DIRECTION ( 'NONE',  ( -0.000000000000000000, -0.3420201433256694346, -0.9396926207859080948 ) ) ;
#15205 = LINE ( 'NONE', #42239, #46064 ) ;
#15207 = CARTESIAN_POINT ( 'NONE',  ( -4.153846153846152411, -2.721908614388771852, 31.22303859784724978 ) ) ;
#15208 = LINE ( 'NONE', #76010, #41967 ) ;
#15209 = ORIENTED_EDGE ( 'NONE', *, *, #5551, .F. ) ;
#15210 = LINE ( 'NONE', #62485, #7254 ) ;
#15211 = AXIS2_PLACEMENT_3D ( 'NONE', #54846, #81003, #19293 ) ;
#15212 = CARTESIAN_POINT ( 'NONE',  ( 4.826899852701619587, -4.175268141568689195, 33.81360843649122216 ) ) ;
#15213 = ORIENTED_EDGE ( 'NONE', *, *, #13397, .T. ) ;
#15214 = ADVANCED_FACE ( 'NONE', ( #27701 ), #68689, .F. ) ;
#15215 = CARTESIAN_POINT ( 'NONE',  ( 19.00000000000000000, 0.000000000000000000, 24.75000000000000000 ) ) ;
#15216 = CARTESIAN_POINT ( 'NONE',  ( -3.903791842207838592, -2.564540009722896752, 30.55348353981670684 ) ) ;
#15217 = LINE ( 'NONE', #70148, #37510 ) ;
#15218 = CARTESIAN_POINT ( 'NONE',  ( 17.74997676270703550, -5.851115903089112003, 34.47074536777953568 ) ) ;
#15219 = CARTESIAN_POINT ( 'NONE',  ( 4.376857505459002873, -9.886259254753566594, 34.14407573483972413 ) ) ;
#15220 = FACE_BOUND ( 'NONE', #56434, .T. ) ;
#15221 = ADVANCED_FACE ( 'NONE', ( #82216 ), #69135, .F. ) ;
#15223 = CARTESIAN_POINT ( 'NONE',  ( 17.07692307692295586, -9.442884908241554243, 34.35708131394783038 ) ) ;
#15222 = CARTESIAN_POINT ( 'NONE',  ( 13.31853300525524908, -2.292212530054419606, 30.41441678777542634 ) ) ;
#15224 = CARTESIAN_POINT ( 'NONE',  ( 12.46153846153833911, -12.51329471203414379, 31.30864560766407578 ) ) ;
#15226 = CARTESIAN_POINT ( 'NONE',  ( -14.08426590877751927, -7.630147987733840509, 34.99859428049665411 ) ) ;
#15225 = CARTESIAN_POINT ( 'NONE',  ( -4.826977667545033768, -10.18230066228895758, 34.26354781536631577 ) ) ;
#15227 = CARTESIAN_POINT ( 'NONE',  ( -18.00000000000000000, -4.786620604624112651, 33.94971097300155094 ) ) ;
#15228 = CARTESIAN_POINT ( 'NONE',  ( 3.749999999999999556, -7.438900925035446754, 20.46688170625848713 ) ) ;
#15229 = ORIENTED_EDGE ( 'NONE', *, *, #69846, .T. ) ;
#15230 = ORIENTED_EDGE ( 'NONE', *, *, #39982, .F. ) ;
#15231 = CARTESIAN_POINT ( 'NONE',  ( 15.93091919493930320, -9.172386477786394821, 34.72672124145550043 ) ) ;
#15232 = VECTOR ( 'NONE', #47690, 1000.000000000000114 ) ;
#15233 = CARTESIAN_POINT ( 'NONE',  ( -0.5268089074992367005, -2.892918686051582977, 31.69288490824016691 ) ) ;
#15234 = CARTESIAN_POINT ( 'NONE',  ( -9.627052121031665521, -9.442884908240273489, 34.35708131394835618 ) ) ;
#15235 = DIRECTION ( 'NONE',  ( 0.000000000000000000, 0.000000000000000000, -1.000000000000000000 ) ) ;
#15236 = CARTESIAN_POINT ( 'NONE',  ( 3.230769230769110045, -11.48612834414049644, 32.76840700105863391 ) ) ;
#15237 = CARTESIAN_POINT ( 'NONE',  ( -2.608446859217889546, -10.19485399968121264, 17.18563170625848713 ) ) ;
#15238 = EDGE_CURVE ( 'NONE', #20998, #1316, #22399, .T. ) ;
#15239 = CARTESIAN_POINT ( 'NONE',  ( 10.61538461538461675, -9.905515769479276145, 34.41647553114623292 ) ) ;
#15240 = DIRECTION ( 'NONE',  ( 0.000000000000000000, 0.000000000000000000, 1.000000000000000000 ) ) ;
#15241 = VECTOR ( 'NONE', #20891, 1000.000000000000227 ) ;
#15242 = EDGE_CURVE ( 'NONE', #2963, #22454, #11734, .T. ) ;
#15243 = CARTESIAN_POINT ( 'NONE',  ( -17.29984929443922681, -4.887634598454295265, 34.01352882383564946 ) ) ;
#15244 = CARTESIAN_POINT ( 'NONE',  ( -3.100243792535587684, -12.15418822224088657, 32.17964115625579069 ) ) ;
#15245 = CARTESIAN_POINT ( 'NONE',  ( 5.206968239757855166, -2.504778602574660340, 29.97347330155780298 ) ) ;
#15246 = LINE ( 'NONE', #21093, #85751 ) ;
#15247 = CYLINDRICAL_SURFACE ( 'NONE', #80754, 0.2499999999999986955 ) ;
#15248 = CARTESIAN_POINT ( 'NONE',  ( 19.99999999999996803, 12.00000000000000711, 10.00000000000000178 ) ) ;
#15249 = ORIENTED_EDGE ( 'NONE', *, *, #80652, .T. ) ;
#15250 = CARTESIAN_POINT ( 'NONE',  ( 12.23805353697412812, -4.225889041578353655, 33.85425143139329407 ) ) ;
#15251 = CYLINDRICAL_SURFACE ( 'NONE', #86345, 0.2499999999999994726 ) ;
#15252 = CARTESIAN_POINT ( 'NONE',  ( -1.901340078031369618, -5.512252781505359245, 20.50186829374151287 ) ) ;
#15253 = DIRECTION ( 'NONE',  ( 1.000000000000000000, 0.000000000000000000, 0.000000000000000000 ) ) ;
#15254 = CARTESIAN_POINT ( 'NONE',  ( 1.384615384615386802, -2.900454961884010974, 35.62045528018868623 ) ) ;
#15255 = ORIENTED_EDGE ( 'NONE', *, *, #83797, .F. ) ;
#15256 = CARTESIAN_POINT ( 'NONE',  ( -1.326923076923076872, -7.500000000000000000, 29.75000000000000355 ) ) ;
#15258 = ORIENTED_EDGE ( 'NONE', *, *, #8557, .T. ) ;
#15257 = PLANE ( 'NONE',  #3771 ) ;
#15259 = CARTESIAN_POINT ( 'NONE',  ( 7.053868730901711182, -3.530189275343204702, 32.79018710029569661 ) ) ;
#15260 = CARTESIAN_POINT ( 'NONE',  ( -5.010854725920637520, -9.780366693483667717, 34.19971097300155805 ) ) ;
#15261 = ORIENTED_EDGE ( 'NONE', *, *, #241, .F. ) ;
#15262 = CARTESIAN_POINT ( 'NONE',  ( -13.13456107297707121, -2.564540009722895419, 30.55348353981670684 ) ) ;
#15263 = CARTESIAN_POINT ( 'NONE',  ( 13.25446741488369362, -9.504002272028875709, 34.60269587691767867 ) ) ;
#15264 = ORIENTED_EDGE ( 'NONE', *, *, #73825, .F. ) ;
#15265 = CARTESIAN_POINT ( 'NONE',  ( -12.71151520558705172, -2.318417181685855422, 30.59732222474233865 ) ) ;
#15266 = LINE ( 'NONE', #49921, #39454 ) ;
#15267 = DIRECTION ( 'NONE',  ( 0.000000000000000000, 0.000000000000000000, -1.000000000000000000 ) ) ;
#15268 = EDGE_LOOP ( 'NONE', ( #39437, #61320 ) ) ;
#15269 = EDGE_LOOP ( 'NONE', ( #11929, #547, #67051, #45816 ) ) ;
#15270 = CARTESIAN_POINT ( 'NONE',  ( 3.007284306204898172, -3.019605429927184836, 32.48692288466676814 ) ) ;
#15271 = EDGE_CURVE ( 'NONE', #14174, #38958, #54916, .T. ) ;
#15272 = EDGE_LOOP ( 'NONE', ( #77203, #57840 ) ) ;
#15273 = CARTESIAN_POINT ( 'NONE',  ( -13.38461538461538325, -13.20930481340135110, 34.54067556320372745 ) ) ;
#15274 = DIRECTION ( 'NONE',  ( -0.000000000000000000, 0.1736481776669307198, -0.9848077530122080203 ) ) ;
#15275 = EDGE_CURVE ( 'NONE', #8288, #34216, #63234, .T. ) ;
#15276 = AXIS2_PLACEMENT_3D ( 'NONE', #75743, #6419, #82079 ) ;
#15277 = CARTESIAN_POINT ( 'NONE',  ( -3.903846153846152855, -2.499999999999998668, 29.75000000000000355 ) ) ;
#15278 = EDGE_CURVE ( 'NONE', #58032, #59229, #38528, .T. ) ;
#15279 = CARTESIAN_POINT ( 'NONE',  ( -17.14300648787895298, -6.386643153685125363, 34.62446782046654903 ) ) ;
#15280 = ORIENTED_EDGE ( 'NONE', *, *, #32219, .T. ) ;
#15281 = ORIENTED_EDGE ( 'NONE', *, *, #46868, .T. ) ;
#15283 = ORIENTED_EDGE ( 'NONE', *, *, #32794, .T. ) ;
#15282 = CARTESIAN_POINT ( 'NONE',  ( -1.161188422753813176, -7.630147231320743018, 34.74852402298682819 ) ) ;
#15284 = EDGE_CURVE ( 'NONE', #9541, #37535, #1984, .T. ) ;
#15285 = B_SPLINE_CURVE_WITH_KNOTS ( 'NONE', 3,
 ( #51810, #11746, #79314, #45068, #4991, #4536, #53156, #79763, #59030, #17619 ),
 .UNSPECIFIED., .F., .F.,
 ( 4, 2, 2, 2, 4 ),
 ( 0.000000000000000000, 0.0001954339857564073659, 0.0003908679715128147319, 0.0005863019572692221250, 0.0007817359430256294638 ),
 .UNSPECIFIED. ) ;
#15286 = B_SPLINE_CURVE_WITH_KNOTS ( 'NONE', 3,
 ( #24429, #51893, #77617, #15925, #3276, #78055, #51435, #86157, #43822, #30747 ),
 .UNSPECIFIED., .F., .F.,
 ( 4, 2, 2, 2, 4 ),
 ( 0.000000000000000000, 0.0001954339857564084502, 0.0003908679715128169003, 0.0005863019572692253776, 0.0007817359430256338006 ),
 .UNSPECIFIED. ) ;
#15287 = CARTESIAN_POINT ( 'NONE',  ( 24.00000000000000000, -9.499999999999982236, 27.74999999999999645 ) ) ;
#15288 = VERTEX_POINT ( 'NONE', #57384 ) ;
#15289 = EDGE_CURVE ( 'NONE', #77161, #37000, #37546, .T. ) ;
#15290 = CARTESIAN_POINT ( 'NONE',  ( 7.780883845597525550, -12.16647553114622049, 32.15551576947930812 ) ) ;
#15291 = CARTESIAN_POINT ( 'NONE',  ( 6.856994543716788293, -9.058645607665454236, 34.76329471203372634 ) ) ;
#15292 = ORIENTED_EDGE ( 'NONE', *, *, #30780, .F. ) ;
#15293 = CYLINDRICAL_SURFACE ( 'NONE', #5365, 0.2500000000000012212 ) ;
#15294 = AXIS2_PLACEMENT_3D ( 'NONE', #16473, #42624, #8839 ) ;
#15295 = EDGE_CURVE ( 'NONE', #33331, #80197, #15973, .T. ) ;
#15296 = ORIENTED_EDGE ( 'NONE', *, *, #14593, .F. ) ;
#15298 = EDGE_LOOP ( 'NONE', ( #72685, #86643, #75432, #58886, #49251 ) ) ;
#15297 = CARTESIAN_POINT ( 'NONE',  ( 9.758375025657770152, -8.164416787775445883, 34.95778746994558617 ) ) ;
#15299 = CARTESIAN_POINT ( 'NONE',  ( -12.46153846153858424, -3.643525952248795718, 33.31231777344771672 ) ) ;
#15300 = CARTESIAN_POINT ( 'NONE',  ( 14.30769230769218581, -5.941354392335915335, 34.76329471203413846 ) ) ;
#15301 = ORIENTED_EDGE ( 'NONE', *, *, #19197, .T. ) ;
#15302 = CARTESIAN_POINT ( 'NONE',  ( 16.15384615384603251, -12.46129190930018460, 30.37095296980731973 ) ) ;
#15303 = LINE ( 'NONE', #1335, #81376 ) ;
#15304 = FACE_BOUND ( 'NONE', #1758, .T. ) ;
#15305 = EDGE_CURVE ( 'NONE', #66929, #27245, #45050, .T. ) ;
#15306 = DIRECTION ( 'NONE',  ( 1.000000000000000000, 0.000000000000000000, 0.000000000000000000 ) ) ;
#15307 = CARTESIAN_POINT ( 'NONE',  ( -6.857821783564084228, -9.528491918058460186, 34.59228464037085615 ) ) ;
#15308 = CARTESIAN_POINT ( 'NONE',  ( 9.442284468086237226, -2.341070481393819236, 30.72580821765574299 ) ) ;
#15309 = CARTESIAN_POINT ( 'NONE',  ( -0.3307480205715113142, -2.845873456487964859, 32.17976146951973249 ) ) ;
#15310 = CARTESIAN_POINT ( 'NONE',  ( -17.07692307692307665, -8.164416787775445883, 34.95778746994557906 ) ) ;
#15311 = CYLINDRICAL_SURFACE ( 'NONE', #85040, 0.2499999999999997502 ) ;
#15312 = ORIENTED_EDGE ( 'NONE', *, *, #29870, .T. ) ;
#15313 = ADVANCED_FACE ( 'NONE', ( #28142 ), #55612, .T. ) ;
#15314 = FACE_OUTER_BOUND ( 'NONE', #14210, .T. ) ;
#15315 = ORIENTED_EDGE ( 'NONE', *, *, #70455, .F. ) ;
#15316 = VERTEX_POINT ( 'NONE', #29928 ) ;
#15318 = CARTESIAN_POINT ( 'NONE',  ( -3.230769230769229949, -5.471508081941601098, 34.59228464037088457 ) ) ;
#15317 = CARTESIAN_POINT ( 'NONE',  ( 14.37376065869474751, -3.513871655860379306, 32.76840700105978499 ) ) ;
#15319 = CARTESIAN_POINT ( 'NONE',  ( 11.53846153846141576, -12.16647553114689728, 32.15551576947799362 ) ) ;
#15320 = CARTESIAN_POINT ( 'NONE',  ( 7.911408985666682270, -3.643525952247864463, 33.31231777344670064 ) ) ;
#15321 = CARTESIAN_POINT ( 'NONE',  ( -12.33074802057151409, -2.494656445102012565, 31.33466734024120015 ) ) ;
#15322 = CARTESIAN_POINT ( 'NONE',  ( 9.823099500132480344, -2.541949514083464479, 30.39797389878540557 ) ) ;
#15323 = ORIENTED_EDGE ( 'NONE', *, *, #2980, .T. ) ;
#15324 = AXIS2_PLACEMENT_3D ( 'NONE', #6497, #61424, #55556 ) ;
#15325 = CARTESIAN_POINT ( 'NONE',  ( 13.16168916709923664, -4.887634598454295265, 34.01352882383564946 ) ) ;
#15326 = ADVANCED_FACE ( 'NONE', ( #29054 ), #22280, .F. ) ;
#15327 = ADVANCED_FACE ( 'NONE', ( #30799 ), #30364, .F. ) ;
#15328 = CARTESIAN_POINT ( 'NONE',  ( 1.515141086378952062, -12.27024696741798770, 31.24895572276497546 ) ) ;
#15329 = CARTESIAN_POINT ( 'NONE',  ( 24.00000000000000000, 14.50000000000000533, 1.499999999999997780 ) ) ;
#15330 = DIRECTION ( 'NONE',  ( -0.000000000000000000, 1.000000000000000000, 3.491481338843133355E-15 ) ) ;
#15331 = CARTESIAN_POINT ( 'NONE',  ( -11.78846153846153832, -2.499999999999998668, 29.75000000000000355 ) ) ;
#15332 = B_SPLINE_CURVE_WITH_KNOTS ( 'NONE', 3,
 ( #61360, #75773, #27149, #35231, #54607, #14078, #74451, #62254, #82103, #41113 ),
 .UNSPECIFIED., .F., .F.,
 ( 4, 2, 2, 2, 4 ),
 ( 0.000000000000000000, 0.0001954339857564091007, 0.0003908679715128182013, 0.0005863019572692273291, 0.0007817359430256364027 ),
 .UNSPECIFIED. ) ;
#15333 = CARTESIAN_POINT ( 'NONE',  ( 3.100078627658924280, -11.93127051446800024, 32.56575433478200665 ) ) ;
#15334 = ORIENTED_EDGE ( 'NONE', *, *, #28251, .T. ) ;
#15335 = EDGE_LOOP ( 'NONE', ( #61115, #66119 ) ) ;
#15336 = FACE_OUTER_BOUND ( 'NONE', #56504, .T. ) ;
#15337 = ORIENTED_EDGE ( 'NONE', *, *, #22899, .F. ) ;
#15338 = CYLINDRICAL_SURFACE ( 'NONE', #63985, 0.2500000000000008882 ) ;
#15339 = CARTESIAN_POINT ( 'NONE',  ( 15.29683656411930848, -3.937682226553329556, 33.60647404775216529 ) ) ;
#15340 = CARTESIAN_POINT ( 'NONE',  ( -14.24243673641627872, -6.879047030191282275, 34.71129190930002295 ) ) ;
#15341 = DIRECTION ( 'NONE',  ( 0.000000000000000000, 0.000000000000000000, -1.000000000000000000 ) ) ;
#15342 = CARTESIAN_POINT ( 'NONE',  ( 12.22435897435897267, -3.499999999999999556, 29.75000000000000355 ) ) ;
#15343 = EDGE_CURVE ( 'NONE', #43192, #4609, #24458, .T. ) ;
#15344 = FACE_BOUND ( 'NONE', #68935, .T. ) ;
#15345 = ORIENTED_EDGE ( 'NONE', *, *, #10662, .T. ) ;
#15346 = CARTESIAN_POINT ( 'NONE',  ( 3.930967471417507131, -7.630691491037286056, 34.74850469731152458 ) ) ;
#15348 = ORIENTED_EDGE ( 'NONE', *, *, #15509, .F. ) ;
#15347 = CARTESIAN_POINT ( 'NONE',  ( -2.177166869458663889, -12.70449254468099198, 30.44128974285582956 ) ) ;
#15349 = CARTESIAN_POINT ( 'NONE',  ( 3.165498784808455479, -12.46129190929999986, 30.37095296980880832 ) ) ;
#15350 = CARTESIAN_POINT ( 'NONE',  ( -17.20761368003338987, -11.93127051446800380, 32.56575433478200665 ) ) ;
#15351 = EDGE_CURVE ( 'NONE', #76215, #87554, #62128, .T. ) ;
#15352 = ADVANCED_FACE ( 'NONE', ( #11429 ), #66371, .F. ) ;
#15353 = CARTESIAN_POINT ( 'NONE',  ( 15.36129466900287177, -3.068774925481848825, 32.56582465632704526 ) ) ;
#15354 = CARTESIAN_POINT ( 'NONE',  ( -9.758390071667831123, -12.34228464037088280, 31.77849191805838558 ) ) ;
#15355 = CARTESIAN_POINT ( 'NONE',  ( -12.68502340526241312, -12.44517049084099725, 30.48991314939691932 ) ) ;
#15356 = CARTESIAN_POINT ( 'NONE',  ( 2.750000000000002665, -7.561099074964516831, 23.47061829374151642 ) ) ;
#15357 = ORIENTED_EDGE ( 'NONE', *, *, #39036, .F. ) ;
#15358 = EDGE_CURVE ( 'NONE', #88209, #81743, #87110, .T. ) ;
#15359 = CARTESIAN_POINT ( 'NONE',  ( -1.161604033002534342, -11.24521262558773671, 33.06293181088029343 ) ) ;
#15360 = CARTESIAN_POINT ( 'NONE',  ( -13.44988583057615905, -9.442884908240170461, 34.35708131394840592 ) ) ;
#15361 = CARTESIAN_POINT ( 'NONE',  ( -3.296852641725108946, -8.973038597847271092, 34.52809138561120506 ) ) ;
#15363 = CARTESIAN_POINT ( 'NONE',  ( -3.007989561791164945, -10.97394488606064122, 33.68653795673694873 ) ) ;
#15362 = VECTOR ( 'NONE', #17362, 1000.000000000000114 ) ;
#15364 = ORIENTED_EDGE ( 'NONE', *, *, #83244, .F. ) ;
#15365 = DIRECTION ( 'NONE',  ( -0.000000000000000000, -0.7660444431189791237, -0.6427876096865379196 ) ) ;
#15366 = CARTESIAN_POINT ( 'NONE',  ( 11.31497661389720477, -4.225889041578353655, 33.85425143139329407 ) ) ;
#15367 = ORIENTED_EDGE ( 'NONE', *, *, #6860, .F. ) ;
#15368 = B_SPLINE_CURVE_WITH_KNOTS ( 'NONE', 3,
 ( #37450, #64918, #57731, #65805, #4106, #17642, #44191, #29823, #84778, #2765 ),
 .UNSPECIFIED., .F., .F.,
 ( 4, 2, 2, 2, 4 ),
 ( 0.0007817246256747530271, 0.0009771112852218978746, 0.001172497944769042939, 0.001367884604316188003, 0.001563271263863332851 ),
 .UNSPECIFIED. ) ;
#15369 = CIRCLE ( 'NONE', #65671, 4.000000000000000000 ) ;
#15370 = DIRECTION ( 'NONE',  ( -0.000000000000000000, 0.1736481776669307198, -0.9848077530122080203 ) ) ;
#15371 = CYLINDRICAL_SURFACE ( 'NONE', #2577, 0.2500000000000008882 ) ;
#15372 = VERTEX_POINT ( 'NONE', #72233 ) ;
#15373 = B_SPLINE_CURVE_WITH_KNOTS ( 'NONE', 3,
 ( #37059, #20564, #34961, #16792, #10037, #51002, #78058, #62422, #43824, #13807 ),
 .UNSPECIFIED., .F., .F.,
 ( 4, 2, 2, 2, 4 ),
 ( 0.000000000000000000, 0.0001954311564186865763, 0.0003908623128373731525, 0.0005862934692560596746, 0.0007817246256747463051 ),
 .UNSPECIFIED. ) ;
#15374 = B_SPLINE_CURVE_WITH_KNOTS ( 'NONE', 3,
 ( #58470, #79211, #44961, #10750, #65676, #31462, #58927, #24704, #84810, #16763 ),
 .UNSPECIFIED., .F., .F.,
 ( 4, 2, 2, 2, 4 ),
 ( 0.0007817246256747473893, 0.0009771112852218900684, 0.001172497944769032747, 0.001367884604316175643, 0.001563271263863318323 ),
 .UNSPECIFIED. ) ;
#15375 = CARTESIAN_POINT ( 'NONE',  ( 0.4615384615384611200, -8.318370150425687726, 35.83090037661290239 ) ) ;
#15376 = CARTESIAN_POINT ( 'NONE',  ( -17.30040800148741198, -2.353723527008297012, 30.78948104536958752 ) ) ;
#15377 = AXIS2_PLACEMENT_3D ( 'NONE', #36820, #85019, #77366 ) ;
#15378 = CARTESIAN_POINT ( 'NONE',  ( 8.096208157792160520, -5.728107161865378494, 34.42597550085002922 ) ) ;
#15379 = CARTESIAN_POINT ( 'NONE',  ( -4.283994123577849145, -11.66186481527757479, 32.95055677023626117 ) ) ;
#15380 = ORIENTED_EDGE ( 'NONE', *, *, #12931, .F. ) ;
#15381 = CARTESIAN_POINT ( 'NONE',  ( -13.38461538461550759, -3.083524468854526912, 32.58852847137268327 ) ) ;
#15382 = EDGE_CURVE ( 'NONE', #28930, #17603, #49194, .T. ) ;
#15383 = ORIENTED_EDGE ( 'NONE', *, *, #72295, .T. ) ;
#15384 = CARTESIAN_POINT ( 'NONE',  ( -6.857882941293567569, -2.506253911140448487, 29.99999999999988631 ) ) ;
#15385 = CARTESIAN_POINT ( 'NONE',  ( 0.6845513056318554002, -10.01129605718032778, 34.36064277460058491 ) ) ;
#15386 = ORIENTED_EDGE ( 'NONE', *, *, #84475, .F. ) ;
#15387 = CARTESIAN_POINT ( 'NONE',  ( -17.86920955903305597, -9.929761469519744921, 34.40412654351204225 ) ) ;
#15388 = CARTESIAN_POINT ( 'NONE',  ( 16.15384615384615330, -13.78497067705608181, 32.30358669280327177 ) ) ;
#15389 = CARTESIAN_POINT ( 'NONE',  ( -3.930470213147969183, -2.501478030877322567, 29.88021232661720816 ) ) ;
#15390 = CYLINDRICAL_SURFACE ( 'NONE', #23298, 0.2499999999999973355 ) ;
#15391 = PLANE ( 'NONE',  #65588 ) ;
#15392 = VECTOR ( 'NONE', #28556, 1000.000000000000000 ) ;
#15393 = ORIENTED_EDGE ( 'NONE', *, *, #19484, .F. ) ;
#15394 = EDGE_LOOP ( 'NONE', ( #27022, #12830, #647, #52526 ) ) ;
#15395 = FACE_BOUND ( 'NONE', #49828, .T. ) ;
#15396 = ORIENTED_EDGE ( 'NONE', *, *, #73469, .T. ) ;
#15397 = CARTESIAN_POINT ( 'NONE',  ( 15.45354877203763877, -2.600157965045224895, 30.74683119005207743 ) ) ;
#15398 = CIRCLE ( 'NONE', #65711, 0.2500000000000002220 ) ;
#15399 = B_SPLINE_CURVE_WITH_KNOTS ( 'NONE', 3,
 ( #70593, #34144, #21063, #55739, #61612, #48533, #76015, #38134, #30919, #44879 ),
 .UNSPECIFIED., .F., .F.,
 ( 4, 2, 2, 2, 4 ),
 ( 0.000000000000000000, 0.0001954339857564091007, 0.0003908679715128182013, 0.0005863019572692273291, 0.0007817359430256364027 ),
 .UNSPECIFIED. ) ;
#15400 = CARTESIAN_POINT ( 'NONE',  ( 13.13461538461538680, -7.500000000000001776, 34.75000000000000000 ) ) ;
#15401 = VECTOR ( 'NONE', #19539, 1000.000000000000227 ) ;
#15402 = CARTESIAN_POINT ( 'NONE',  ( 17.93391762063986761, -5.471508081941601986, 34.59228464037088457 ) ) ;
#15403 = CARTESIAN_POINT ( 'NONE',  ( -14.05774678934416499, -9.272278438253398036, 34.42582936511637115 ) ) ;
#15404 = ORIENTED_EDGE ( 'NONE', *, *, #47334, .T. ) ;
#15405 = EDGE_CURVE ( 'NONE', #76676, #2738, #23343, .T. ) ;
#15406 = ORIENTED_EDGE ( 'NONE', *, *, #32140, .T. ) ;
#15407 = VERTEX_POINT ( 'NONE', #51493 ) ;
#15408 = B_SPLINE_CURVE_WITH_KNOTS ( 'NONE', 3,
 ( #20187, #68362, #47652, #40468, #75135, #74240, #73349, #31925, #39131, #80105 ),
 .UNSPECIFIED., .F., .F.,
 ( 4, 2, 2, 2, 4 ),
 ( 0.000000000000000000, 0.0001954311564186879857, 0.0003908623128373759715, 0.0005862934692560640114, 0.0007817246256747519429 ),
 .UNSPECIFIED. ) ;
#15409 = CARTESIAN_POINT ( 'NONE',  ( -10.83831157429145975, -8.282780595021769443, 34.94152052738834158 ) ) ;
#15410 = VERTEX_POINT ( 'NONE', #10543 ) ;
#15411 = CARTESIAN_POINT ( 'NONE',  ( 13.25392391794783542, -2.729777683071817229, 31.24903638046269450 ) ) ;
#15412 = CARTESIAN_POINT ( 'NONE',  ( -12.23816297576603951, -2.251407671071268712, 29.88021292934943318 ) ) ;
#15413 = CARTESIAN_POINT ( 'NONE',  ( -17.32694630114453105, -2.985938066672154445, 32.43141759479405550 ) ) ;
#15414 = VERTEX_POINT ( 'NONE', #38010 ) ;
#15415 = CARTESIAN_POINT ( 'NONE',  ( 8.900022577055558770, -8.999086150933475636, 34.52020707165672775 ) ) ;
#15416 = CARTESIAN_POINT ( 'NONE',  ( -15.16470189741915320, -3.322132147404559976, 32.92929555188717927 ) ) ;
#15417 = VECTOR ( 'NONE', #71019, 1000.000000000000000 ) ;
#15418 = CARTESIAN_POINT ( 'NONE',  ( 14.55763782604045176, -6.696923467548660192, 34.68552623307873972 ) ) ;
#15419 = FACE_BOUND ( 'NONE', #79429, .T. ) ;
#15420 = VERTEX_POINT ( 'NONE', #58717 ) ;
#15421 = ADVANCED_FACE ( 'NONE', ( #86218 ), #45200, .F. ) ;
#15422 = EDGE_LOOP ( 'NONE', ( #20487, #79612 ) ) ;
#15423 = ORIENTED_EDGE ( 'NONE', *, *, #11405, .F. ) ;
#15424 = DIRECTION ( 'NONE',  ( 0.000000000000000000, 1.000000000000000000, 0.000000000000000000 ) ) ;
#15426 = CARTESIAN_POINT ( 'NONE',  ( -13.60754160213153163, -5.667676309546437530, 34.40238873228292249 ) ) ;
#15425 = CARTESIAN_POINT ( 'NONE',  ( 24.99999999999999645, 15.00000000000000355, 0.000000000000000000 ) ) ;
#15427 = FACE_OUTER_BOUND ( 'NONE', #59893, .T. ) ;
#15428 = CARTESIAN_POINT ( 'NONE',  ( -2.176901866725354573, -2.494656445102013453, 31.33466734024120015 ) ) ;
#15429 = DIRECTION ( 'NONE',  ( 1.000000000000000000, 0.000000000000000000, 0.000000000000000000 ) ) ;
#15430 = CARTESIAN_POINT ( 'NONE',  ( 7.976945653978634532, -11.18335022499818621, 33.13157742990016885 ) ) ;
#15431 = EDGE_LOOP ( 'NONE', ( #76132, #66816 ) ) ;
#15432 = CARTESIAN_POINT ( 'NONE',  ( -7.716106410903393886, -7.723484941389745728, 34.99544897038809665 ) ) ;
#15433 = EDGE_CURVE ( 'NONE', #87441, #88485, #32150, .T. ) ;
#15434 = CIRCLE ( 'NONE', #45577, 4.000000000000000000 ) ;
#15435 = CYLINDRICAL_SURFACE ( 'NONE', #41641, 0.2500000000000012212 ) ;
#15436 = CARTESIAN_POINT ( 'NONE',  ( -17.32689980786543060, -11.79746400365624659, 32.30657167506340954 ) ) ;
#15437 = FACE_OUTER_BOUND ( 'NONE', #64332, .T. ) ;
#15438 = VERTEX_POINT ( 'NONE', #12320 ) ;
#15439 = CARTESIAN_POINT ( 'NONE',  ( 6.000000000000001776, -9.819645486525091727, 36.12317359536749706 ) ) ;
#15440 = ORIENTED_EDGE ( 'NONE', *, *, #58698, .T. ) ;
#15441 = FACE_BOUND ( 'NONE', #8527, .T. ) ;
#15442 = CARTESIAN_POINT ( 'NONE',  ( -17.07692307692319744, -4.481592998941358097, 33.73612834414048933 ) ) ;
#15443 = DIRECTION ( 'NONE',  ( -1.000000000000000000, 0.000000000000000000, 0.000000000000000000 ) ) ;
#15444 = CARTESIAN_POINT ( 'NONE',  ( -16.15384615384615330, -8.973038597847269315, 34.52809138561121927 ) ) ;
#15445 = EDGE_LOOP ( 'NONE', ( #11792, #68946, #5676, #23822 ) ) ;
#15446 = DIRECTION ( 'NONE',  ( -1.000000000000000000, -0.000000000000000000, -0.000000000000000000 ) ) ;
#15447 = CARTESIAN_POINT ( 'NONE',  ( -5.869209559033047974, -9.084667340241226796, 34.75534355489798344 ) ) ;
#15448 = CARTESIAN_POINT ( 'NONE',  ( 8.545745844666436497, -8.539481045369596401, 34.89627647299170832 ) ) ;
#15449 = CARTESIAN_POINT ( 'NONE',  ( -5.010855743573000787, -5.471508081941601098, 34.59228464037088457 ) ) ;
#15450 = VERTEX_POINT ( 'NONE', #41120 ) ;
#15451 = CARTESIAN_POINT ( 'NONE',  ( -4.087777802843714170, -6.386643153685127139, 34.62446782046654192 ) ) ;
#15452 = ORIENTED_EDGE ( 'NONE', *, *, #12273, .T. ) ;
#15454 = ORIENTED_EDGE ( 'NONE', *, *, #71377, .T. ) ;
#15453 = CARTESIAN_POINT ( 'NONE',  ( 16.28468448433291016, -7.277220318596959281, 34.99547417642776992 ) ) ;
#15455 = CARTESIAN_POINT ( 'NONE',  ( 9.469381474791543241, -3.586966769969701208, 32.86292498521069660 ) ) ;
#15456 = CARTESIAN_POINT ( 'NONE',  ( -10.61538461538461320, -12.37446782046654192, 30.86335684631486131 ) ) ;
#15457 = CARTESIAN_POINT ( 'NONE',  ( 13.38461538461526601, -9.442884908241554243, 34.35708131394783038 ) ) ;
#15458 = AXIS2_PLACEMENT_3D ( 'NONE', #81669, #20405, #25387 ) ;
#15459 = EDGE_CURVE ( 'NONE', #49638, #83085, #81227, .T. ) ;
#15460 = EDGE_CURVE ( 'NONE', #78324, #63745, #12755, .T. ) ;
#15461 = CARTESIAN_POINT ( 'NONE',  ( 12.52760681254089725, -4.098570777380720287, 33.41473453929635440 ) ) ;
#15463 = CARTESIAN_POINT ( 'NONE',  ( -11.76138849736838488, -9.172386477786396597, 34.72672124145550043 ) ) ;
#15462 = CARTESIAN_POINT ( 'NONE',  ( -3.007989561791163169, -4.226511098958374291, 33.85474049983370293 ) ) ;
#15464 = CARTESIAN_POINT ( 'NONE',  ( 8.069165197766697162, -4.187068189119699468, 33.49521262558774026 ) ) ;
#15465 = CARTESIAN_POINT ( 'NONE',  ( 2.750000000000008438, -8.639087296525996607, 22.04687500000000000 ) ) ;
#15466 = ORIENTED_EDGE ( 'NONE', *, *, #56002, .T. ) ;
#15467 = CIRCLE ( 'NONE', #29797, 2.750000000000000000 ) ;
#15468 = DIRECTION ( 'NONE',  ( 0.000000000000000000, 0.4999999999999960032, -0.8660254037844410391 ) ) ;
#15469 = CARTESIAN_POINT ( 'NONE',  ( -9.692307692307691624, -11.35647404775217417, 33.31231777344666511 ) ) ;
#15470 = EDGE_LOOP ( 'NONE', ( #70549, #75362, #14298, #32666 ) ) ;
#15471 = B_SPLINE_CURVE_WITH_KNOTS ( 'NONE', 3,
 ( #48567, #21096, #76049, #62520, #837, #28303, #55772, #21549, #71497, #38164 ),
 .UNSPECIFIED., .F., .F.,
 ( 4, 2, 2, 2, 4 ),
 ( 0.0007817359430256322827, 0.0009771253907249989254, 0.001172514838424365676, 0.001367904286123732428, 0.001563293733823098962 ),
 .UNSPECIFIED. ) ;
#15472 = ORIENTED_EDGE ( 'NONE', *, *, #71880, .T. ) ;
#15474 = VERTEX_POINT ( 'NONE', #88012 ) ;
#15473 = AXIS2_PLACEMENT_3D ( 'NONE', #28764, #55773, #40945 ) ;
#15475 = CARTESIAN_POINT ( 'NONE',  ( 10.68145194873469173, -8.164416787775445883, 34.95778746994558617 ) ) ;
#15476 = CARTESIAN_POINT ( 'NONE',  ( -24.99999999999999645, -15.00000000000000000, 0.000000000000000000 ) ) ;
#15477 = CYLINDRICAL_SURFACE ( 'NONE', #70126, 0.2500000000000008882 ) ;
#15478 = DIRECTION ( 'NONE',  ( -0.000000000000000000, -0.3420201433256694346, -0.9396926207859080948 ) ) ;
#15479 = CARTESIAN_POINT ( 'NONE',  ( -16.21911659980693443, -3.300289026998414865, 32.46337939537583850 ) ) ;
#15480 = CARTESIAN_POINT ( 'NONE',  ( -8.769230769230768274, -2.833524468853757305, 32.15551576947925838 ) ) ;
#15481 = CARTESIAN_POINT ( 'NONE',  ( 13.51466044053515958, -2.254550872974306674, 29.97347326024527092 ) ) ;
#15482 = LINE ( 'NONE', #70423, #8880 ) ;
#15483 = CARTESIAN_POINT ( 'NONE',  ( 11.28843830116857383, -10.76384336483936011, 33.53834819971076087 ) ) ;
#15484 = CARTESIAN_POINT ( 'NONE',  ( 12.23861224402230974, -11.76352882383564769, 32.36236540154569497 ) ) ;
#15485 = CARTESIAN_POINT ( 'NONE',  ( -6.923076923076922462, -2.708943851104267164, 35.45975837776705220 ) ) ;
#15486 = ORIENTED_EDGE ( 'NONE', *, *, #82733, .F. ) ;
#15487 = VERTEX_POINT ( 'NONE', #53741 ) ;
#15488 = VECTOR ( 'NONE', #45208, 1000.000000000000227 ) ;
#15489 = CARTESIAN_POINT ( 'NONE',  ( -17.77713457779637807, -12.49850393767509260, 29.88072118266894250 ) ) ;
#15490 = SHAPE_REPRESENTATION_RELATIONSHIP ( 'NONE' , 'NONE' ,  #85713, #73996 ) ;
#15491 = DIRECTION ( 'NONE',  ( 0.000000000000000000, 0.000000000000000000, -1.000000000000000000 ) ) ;
#15492 = CARTESIAN_POINT ( 'NONE',  ( -14.30769230769230660, -9.780366693483667717, 34.19971097300155094 ) ) ;
#15493 = ORIENTED_EDGE ( 'NONE', *, *, #47371, .F. ) ;
#15494 = DIRECTION ( 'NONE',  ( -0.000000000000000000, 1.000000000000000000, -0.000000000000000000 ) ) ;
#15495 = CARTESIAN_POINT ( 'NONE',  ( -10.61538461538461320, -12.62096338111211580, 30.90682066428153263 ) ) ;
#15496 = CARTESIAN_POINT ( 'NONE',  ( 1.653273178848927064E-15, -7.500000000000000000, 10.00000000000000178 ) ) ;
#15497 = VECTOR ( 'NONE', #80961, 1000.000000000000227 ) ;
#15498 = ORIENTED_EDGE ( 'NONE', *, *, #17958, .T. ) ;
#15499 = B_SPLINE_CURVE_WITH_KNOTS ( 'NONE', 3,
 ( #74145, #34039, #14213, #54302, #68712, #13326, #13765, #75468, #33156, #40808 ),
 .UNSPECIFIED., .F., .F.,
 ( 4, 2, 2, 2, 4 ),
 ( 0.0007817246256747477145, 0.0009771112852218911526, 0.001172497944769034699, 0.001367884604316178246, 0.001563271263863321792 ),
 .UNSPECIFIED. ) ;
#15500 = CARTESIAN_POINT ( 'NONE',  ( -13.60754160213153163, -9.886141570436013382, 34.14413921362392301 ) ) ;
#15501 = VERTEX_POINT ( 'NONE', #60051 ) ;
#15502 = CARTESIAN_POINT ( 'NONE',  ( 13.25446741488368829, -12.50552854090298638, 31.33409797877408920 ) ) ;
#15503 = CARTESIAN_POINT ( 'NONE',  ( 6.988332062589762472, -3.083524468853784839, 32.58852847137153930 ) ) ;
#15504 = CARTESIAN_POINT ( 'NONE',  ( 6.923076923076802558, -8.613356846316285953, 34.62446782046622218 ) ) ;
#15505 = CARTESIAN_POINT ( 'NONE',  ( -14.30769230769242739, -11.94971097300221174, 32.03036669348237098 ) ) ;
#15506 = CARTESIAN_POINT ( 'NONE',  ( 18.00000000000000000, -8.164416787775445883, 34.95778746994557906 ) ) ;
#15507 = ORIENTED_EDGE ( 'NONE', *, *, #70785, .T. ) ;
#15508 = EDGE_CURVE ( 'NONE', #86943, #36959, #77111, .T. ) ;
#15509 = EDGE_CURVE ( 'NONE', #26228, #29264, #33910, .T. ) ;
#15510 = ORIENTED_EDGE ( 'NONE', *, *, #10167, .T. ) ;
#15511 = EDGE_LOOP ( 'NONE', ( #84473, #6540, #51977, #21323, #16006 ) ) ;
#15512 = CARTESIAN_POINT ( 'NONE',  ( -6.222926217516143055, -11.24512374952581872, 33.06303171183252942 ) ) ;
#15513 = CARTESIAN_POINT ( 'NONE',  ( 5.076923076923075762, -11.11383981884818262, 36.00935417666054406 ) ) ;
#15514 = CARTESIAN_POINT ( 'NONE',  ( 17.20744877868664346, -4.459921816937789885, 33.71989282347011851 ) ) ;
#15516 = ADVANCED_FACE ( 'NONE', ( #46546 ), #81668, .F. ) ;
#15515 = CARTESIAN_POINT ( 'NONE',  ( 16.85343815235874132, -10.23692288466677880, 34.23039457007281072 ) ) ;
#15517 = CARTESIAN_POINT ( 'NONE',  ( -17.93474442872397034, -4.481592998940253203, 33.73612834413965089 ) ) ;
#15518 = LINE ( 'NONE', #76322, #10697 ) ;
#15519 = AXIS2_PLACEMENT_3D ( 'NONE', #42739, #34646, #20683 ) ;
#15520 = ORIENTED_EDGE ( 'NONE', *, *, #67891, .F. ) ;
#15521 = EDGE_CURVE ( 'NONE', #87868, #59899, #11553, .T. ) ;
#15522 = ORIENTED_EDGE ( 'NONE', *, *, #53764, .F. ) ;
#15523 = B_SPLINE_CURVE_WITH_KNOTS ( 'NONE', 3,
 ( #73976, #86614, #59560, #39754, #24884, #87065, #25336, #86165, #52800, #18588 ),
 .UNSPECIFIED., .F., .F.,
 ( 4, 2, 2, 2, 4 ),
 ( 0.000000000000000000, 0.0001954311564186880399, 0.0003908623128373760799, 0.0005862934692560641198, 0.0007817246256747521597 ),
 .UNSPECIFIED. ) ;
#15524 = B_SPLINE_CURVE_WITH_KNOTS ( 'NONE', 3,
 ( #63146, #64915, #16301, #1461, #84775, #77997, #22177, #50075, #77117, #50516 ),
 .UNSPECIFIED., .F., .F.,
 ( 4, 2, 2, 2, 4 ),
 ( 0.000000000000000000, 0.0001954339857564074473, 0.0003908679715128148945, 0.0005863019572692223418, 0.0007817359430256297891 ),
 .UNSPECIFIED. ) ;
#15525 = ORIENTED_EDGE ( 'NONE', *, *, #88323, .F. ) ;
#15527 = ORIENTED_EDGE ( 'NONE', *, *, #17696, .F. ) ;
#15526 = CARTESIAN_POINT ( 'NONE',  ( 4.023154687178595701, -2.729777683071817229, 31.24903638046268739 ) ) ;
#15529 = CARTESIAN_POINT ( 'NONE',  ( 14.30769230769231015, -4.661471528628507777, 34.16647553114623292 ) ) ;
#15528 = CARTESIAN_POINT ( 'NONE',  ( 9.019285080869085647, -8.303483539816731707, 34.68545999027711702 ) ) ;
#15530 = CARTESIAN_POINT ( 'NONE',  ( 3.749999999999992006, -5.946699141100872943, 23.14062499999999645 ) ) ;
#15531 = ORIENTED_EDGE ( 'NONE', *, *, #66560, .T. ) ;
#15532 = EDGE_CURVE ( 'NONE', #35909, #79975, #88957, .T. ) ;
#15533 = ORIENTED_EDGE ( 'NONE', *, *, #52025, .F. ) ;
#15534 = CARTESIAN_POINT ( 'NONE',  ( 13.63461538461538680, -2.499999999999998668, 29.75000000000000355 ) ) ;
#15535 = ORIENTED_EDGE ( 'NONE', *, *, #30073, .T. ) ;
#15536 = FACE_BOUND ( 'NONE', #31659, .T. ) ;
#15537 = CARTESIAN_POINT ( 'NONE',  ( 4.853996118016225658, -4.762599654559228846, 34.23009711892697737 ) ) ;
#15538 = AXIS2_PLACEMENT_3D ( 'NONE', #20958, #41689, #54752 ) ;
#15539 = CARTESIAN_POINT ( 'NONE',  ( -8.769230769230768274, -1.215029322943914858, 32.30358669280327177 ) ) ;
#15540 = ORIENTED_EDGE ( 'NONE', *, *, #43863, .T. ) ;
#15541 = CARTESIAN_POINT ( 'NONE',  ( -14.08467946359890988, -8.282913670948747864, 34.94150082978203642 ) ) ;
#15542 = DIRECTION ( 'NONE',  ( -1.799314243699348838E-16, -1.000000000000000000, 5.102127870520021228E-17 ) ) ;
#15543 = DIRECTION ( 'NONE',  ( 1.000000000000000000, 0.000000000000000000, 0.000000000000000000 ) ) ;
#15544 = CARTESIAN_POINT ( 'NONE',  ( -15.45369544828537656, -6.503392248772476236, 34.64988816332204635 ) ) ;
#15545 = DIRECTION ( 'NONE',  ( -0.000000000000000000, -0.9848077530122085754, -0.1736481776669273613 ) ) ;
#15546 = ORIENTED_EDGE ( 'NONE', *, *, #21182, .T. ) ;
#15547 = CARTESIAN_POINT ( 'NONE',  ( -7.173053654019277303, -11.28823185664190376, 33.01397839955799896 ) ) ;
#15548 = DIRECTION ( 'NONE',  ( 1.000000000000000000, 0.000000000000000000, 0.000000000000000000 ) ) ;
#15549 = CARTESIAN_POINT ( 'NONE',  ( -19.50000000000000000, -3.499999999999999556, 29.75000000000000355 ) ) ;
#15550 = DIRECTION ( 'NONE',  ( 0.000000000000000000, -0.000000000000000000, 1.000000000000000000 ) ) ;
#15551 = CARTESIAN_POINT ( 'NONE',  ( 15.12820512820512953, -7.500000000000000000, 33.75000000000000000 ) ) ;
#15552 = EDGE_CURVE ( 'NONE', #26886, #68329, #21271, .T. ) ;
#15553 = CARTESIAN_POINT ( 'NONE',  ( 6.130791807824789608, -9.804649428959608670, 34.18742332936588468 ) ) ;
#15555 = CARTESIAN_POINT ( 'NONE',  ( -7.846153846153844924, -12.29105614889573062, 35.45975837776705220 ) ) ;
#15554 = CARTESIAN_POINT ( 'NONE',  ( 5.198717948717946236, -3.499999999999999556, 29.75000000000000355 ) ) ;
#15556 = AXIS2_PLACEMENT_3D ( 'NONE', #57893, #17359, #70974 ) ;
#15557 = CARTESIAN_POINT ( 'NONE',  ( 8.703979779069525691, -2.506253911140460922, 30.00000000000013856 ) ) ;
#15559 = CARTESIAN_POINT ( 'NONE',  ( -18.13014796973169851, -3.069018819979306034, 32.56621877034668699 ) ) ;
#15558 = CARTESIAN_POINT ( 'NONE',  ( -3.453696189676079609, -2.889293201056495786, 32.26117774369186009 ) ) ;
#15560 = EDGE_CURVE ( 'NONE', #45585, #32628, #68584, .T. ) ;
#15561 = CARTESIAN_POINT ( 'NONE',  ( -2.307692307692305711, -5.471508081941601098, 34.59228464037088457 ) ) ;
#15562 = CARTESIAN_POINT ( 'NONE',  ( -2.775308065498764964, -6.422011778438537988, 21.17000670625848713 ) ) ;
#15563 = ORIENTED_EDGE ( 'NONE', *, *, #59556, .T. ) ;
#15564 = CARTESIAN_POINT ( 'NONE',  ( 0.07543784382008528189, -3.752057646953216530, 13.99999999999965894 ) ) ;
#15565 = VERTEX_POINT ( 'NONE', #6881 ) ;
#15566 = CARTESIAN_POINT ( 'NONE',  ( 0.5267324433218166790, -2.506253911140448043, 29.99999999999988631 ) ) ;
#15567 = EDGE_CURVE ( 'NONE', #74976, #16308, #53290, .T. ) ;
#15568 = ORIENTED_EDGE ( 'NONE', *, *, #63439, .T. ) ;
#15569 = EDGE_CURVE ( 'NONE', #48285, #87573, #76221, .T. ) ;
#15570 = CARTESIAN_POINT ( 'NONE',  ( -13.25382494364843389, -2.295524264805589354, 30.44142389570982488 ) ) ;
#15571 = CARTESIAN_POINT ( 'NONE',  ( 17.29993592101647693, -2.889357225399416418, 32.26129605718031002 ) ) ;
#15572 = EDGE_LOOP ( 'NONE', ( #21637, #21797, #67792, #46496 ) ) ;
#15573 = CARTESIAN_POINT ( 'NONE',  ( -18.06527044596078113, -12.46129190929999986, 30.37095296980880832 ) ) ;
#15574 = CARTESIAN_POINT ( 'NONE',  ( -2.724691934501232371, -8.700186371490559623, 22.26375670625849068 ) ) ;
#15575 = CARTESIAN_POINT ( 'NONE',  ( 7.846153846153846700, -1.509761064869970415, 31.06009739812519044 ) ) ;
#15576 = CARTESIAN_POINT ( 'NONE',  ( -3.230769230769352962, -12.51329471203414379, 31.30864560766407578 ) ) ;
#15577 = CARTESIAN_POINT ( 'NONE',  ( 7.173131234715239835, -9.148310452688871663, 34.47095581063188519 ) ) ;
#15578 = CARTESIAN_POINT ( 'NONE',  ( 8.769230769230768274, -3.513871655860378418, 32.76840700105978499 ) ) ;
#15579 = DIRECTION ( 'NONE',  ( -0.000000000000000000, -0.000000000000000000, -1.000000000000000000 ) ) ;
#15580 = CARTESIAN_POINT ( 'NONE',  ( 1.384615384615386802, -2.292212530054420494, 30.41441678777542634 ) ) ;
#15581 = CARTESIAN_POINT ( 'NONE',  ( -2.651650429449565305, -4.848349570550461785, 15.25000000000000000 ) ) ;
#15582 = B_SPLINE_CURVE_WITH_KNOTS ( 'NONE', 3,
 ( #40621, #41948, #49135, #33416, #20348, #35181, #88820, #68091, #55012, #41498 ),
 .UNSPECIFIED., .F., .F.,
 ( 4, 2, 2, 2, 4 ),
 ( 0.000000000000000000, 0.0001954311564186867931, 0.0003908623128373735862, 0.0005862934692560603251, 0.0007817246256747471724 ),
 .UNSPECIFIED. ) ;
#15583 = CARTESIAN_POINT ( 'NONE',  ( 11.47237915910140771, -5.471508081941602875, 34.59228464037088457 ) ) ;
#15584 = CYLINDRICAL_SURFACE ( 'NONE', #40561, 0.2499999999999979738 ) ;
#15585 = DIRECTION ( 'NONE',  ( -0.000000000000000000, -5.102127870520021228E-17, -1.000000000000000000 ) ) ;
#15586 = AXIS2_PLACEMENT_3D ( 'NONE', #83794, #1799, #84679 ) ;
#15587 = CARTESIAN_POINT ( 'NONE',  ( 2.320192649118979489E-14, -11.25000000000000000, 18.53125000000000000 ) ) ;
#15588 = CARTESIAN_POINT ( 'NONE',  ( 20.00000000000000000, -4.000000000000000000, 28.25000000000000000 ) ) ;
#15589 = ORIENTED_EDGE ( 'NONE', *, *, #34738, .T. ) ;
#15590 = CARTESIAN_POINT ( 'NONE',  ( 14.43848411551709709, -2.541949514083464479, 30.39797389878540557 ) ) ;
#15591 = CARTESIAN_POINT ( 'NONE',  ( -11.31545018684868964, -8.239487800360276282, 34.69522927552633718 ) ) ;
#15592 = CARTESIAN_POINT ( 'NONE',  ( 1.384615384615265343, -12.46129190930018460, 30.37095296980731973 ) ) ;
#15593 = CARTESIAN_POINT ( 'NONE',  ( 16.37727255276093530, -7.630147987733843173, 34.99859428049665411 ) ) ;
#15594 = CARTESIAN_POINT ( 'NONE',  ( -2.980823712421089233, -5.057305518903949526, 34.11320923018887896 ) ) ;
#15595 = CARTESIAN_POINT ( 'NONE',  ( -8.992715712954719720, -8.496056993536548418, 34.65000542017679663 ) ) ;
#15596 = CARTESIAN_POINT ( 'NONE',  ( -24.00000000000000000, -9.499999999999982236, 27.74999999999999645 ) ) ;
#15597 = EDGE_CURVE ( 'NONE', #62488, #64833, #36578, .T. ) ;
#15598 = ORIENTED_EDGE ( 'NONE', *, *, #51644, .F. ) ;
#15599 = B_SPLINE_CURVE_WITH_KNOTS ( 'NONE', 3,
 ( #83283, #75200, #40095, #27452, #5853, #67999, #14369, #88294, #27891, #19805 ),
 .UNSPECIFIED., .F., .F.,
 ( 4, 2, 2, 2, 4 ),
 ( 0.000000000000000000, 0.0001954339881912783015, 0.0003908679763825566029, 0.0005863019645738348773, 0.0007817359527651132059 ),
 .UNSPECIFIED. ) ;
#15600 = ORIENTED_EDGE ( 'NONE', *, *, #86325, .F. ) ;
#15601 = ORIENTED_EDGE ( 'NONE', *, *, #84957, .F. ) ;
#15602 = VECTOR ( 'NONE', #45126, 999.9999999999998863 ) ;
#15603 = CARTESIAN_POINT ( 'NONE',  ( 3.296024802045255164, -6.026961402152789304, 34.52809138561124769 ) ) ;
#15604 = CARTESIAN_POINT ( 'NONE',  ( 6.699591979352978122, -2.847400154188068022, 31.58180166144859058 ) ) ;
#15605 = CYLINDRICAL_SURFACE ( 'NONE', #23046, 0.2500000000000009437 ) ;
#15606 = CARTESIAN_POINT ( 'NONE',  ( 1.384615384615265343, -11.94971097300221174, 32.03036669348237098 ) ) ;
#15607 = CARTESIAN_POINT ( 'NONE',  ( 17.77651505627605033, -9.331801661448606566, 34.40259984581193464 ) ) ;
#15608 = EDGE_CURVE ( 'NONE', #74921, #47774, #82558, .T. ) ;
#15609 = VECTOR ( 'NONE', #26684, 1000.000000000000000 ) ;
#15610 = ORIENTED_EDGE ( 'NONE', *, *, #36512, .F. ) ;
#15611 = CARTESIAN_POINT ( 'NONE',  ( -7.846153846153844924, -2.708943851104267164, 35.45975837776705220 ) ) ;
#15612 = AXIS2_PLACEMENT_3D ( 'NONE', #40377, #61511, #13333 ) ;
#15613 = ORIENTED_EDGE ( 'NONE', *, *, #26758, .T. ) ;
#15614 = EDGE_LOOP ( 'NONE', ( #63496, #38183, #28176, #27077 ) ) ;
#15615 = AXIS2_PLACEMENT_3D ( 'NONE', #18717, #6526, #68226 ) ;
#15617 = ORIENTED_EDGE ( 'NONE', *, *, #12915, .T. ) ;
#15616 = CARTESIAN_POINT ( 'NONE',  ( 4.153846153846154188, -12.34228464037088635, 31.77849191805839268 ) ) ;
#15618 = CARTESIAN_POINT ( 'NONE',  ( 16.37662569511456212, -12.44528174975671853, 30.48912976160715615 ) ) ;
#15619 = CARTESIAN_POINT ( 'NONE',  ( -16.40386939113911779, -4.335965774309648246, 33.62209801155881905 ) ) ;
#15620 = EDGE_CURVE ( 'NONE', #80339, #39978, #56837, .T. ) ;
#15621 = DIRECTION ( 'NONE',  ( 0.000000000000000000, 0.000000000000000000, 1.000000000000000000 ) ) ;
#15622 = CARTESIAN_POINT ( 'NONE',  ( -15.90390074446811042, -5.766571408460170467, 34.70601412856602508 ) ) ;
#15623 = ORIENTED_EDGE ( 'NONE', *, *, #20312, .T. ) ;
#15624 = EDGE_CURVE ( 'NONE', #44546, #9922, #69323, .T. ) ;
#15625 = ORIENTED_EDGE ( 'NONE', *, *, #57544, .F. ) ;
#15626 = VERTEX_POINT ( 'NONE', #42013 ) ;
#15627 = CARTESIAN_POINT ( 'NONE',  ( -9.469528151039279251, -5.913360116392397892, 34.49180327182771322 ) ) ;
#15629 = VERTEX_POINT ( 'NONE', #70811 ) ;
#15628 = CARTESIAN_POINT ( 'NONE',  ( 1.318531973659506251, -8.120952969808774569, 34.71129190930000163 ) ) ;
#15630 = LINE ( 'NONE', #15190, #21995 ) ;
#15631 = CARTESIAN_POINT ( 'NONE',  ( 6.130525701763564150, -12.45806712695776319, 30.39783852428763922 ) ) ;
#15632 = LINE ( 'NONE', #78655, #83919 ) ;
#15633 = ORIENTED_EDGE ( 'NONE', *, *, #23028, .F. ) ;
#15634 = EDGE_CURVE ( 'NONE', #86086, #86521, #20168, .T. ) ;
#15635 = CARTESIAN_POINT ( 'NONE',  ( -10.61538461538461320, -1.509761064869970415, 31.06009739812519044 ) ) ;
#15636 = DIRECTION ( 'NONE',  ( -0.000000000000000000, 1.000000000000000000, -0.000000000000000000 ) ) ;
#15637 = VECTOR ( 'NONE', #45329, 1000.000000000000000 ) ;
#15638 = ORIENTED_EDGE ( 'NONE', *, *, #83550, .F. ) ;
#15639 = FACE_BOUND ( 'NONE', #73541, .T. ) ;
#15640 = CARTESIAN_POINT ( 'NONE',  ( 11.28848480751918437, -4.943428324936578910, 34.04746400365624481 ) ) ;
#15641 = DIRECTION ( 'NONE',  ( 0.000000000000000000, 0.000000000000000000, 1.000000000000000000 ) ) ;
#15642 = B_SPLINE_CURVE_WITH_KNOTS ( 'NONE', 3,
 ( #59536, #11806, #80264, #66742, #5040, #32961, #25759, #26645, #53220, #19443 ),
 .UNSPECIFIED., .F., .F.,
 ( 4, 2, 2, 2, 4 ),
 ( 0.0007817246256747503166, 0.0009771112852218946220, 0.001172497944769039036, 0.001367884604316183450, 0.001563271263863327864 ),
 .UNSPECIFIED. ) ;
#15643 = CARTESIAN_POINT ( 'NONE',  ( 2.057715563643718326, -12.41104346484419452, 31.60698883733904196 ) ) ;
#15645 = CARTESIAN_POINT ( 'NONE',  ( -10.86536135943320502, -5.643011162660950042, 34.66104346484419096 ) ) ;
#15644 = CARTESIAN_POINT ( 'NONE',  ( 8.096099255531889582, -10.92531984108285670, 33.72920026020278073 ) ) ;
#15646 = EDGE_CURVE ( 'NONE', #27448, #34293, #48752, .T. ) ;
#15647 = CARTESIAN_POINT ( 'NONE',  ( 15.90382291655318880, -2.587272538249754117, 30.68239716806877837 ) ) ;
#15648 = CARTESIAN_POINT ( 'NONE',  ( -2.438383774359867751, -3.530157926970578508, 32.79014554554150607 ) ) ;
#15649 = VERTEX_POINT ( 'NONE', #21728 ) ;
#15650 = CYLINDRICAL_SURFACE ( 'NONE', #5847, 0.2500000000000008882 ) ;
#15651 = EDGE_CURVE ( 'NONE', #59172, #43517, #25589, .T. ) ;
#15652 = CARTESIAN_POINT ( 'NONE',  ( 5.076923076923075762, -3.937682226553329556, 33.60647404775216529 ) ) ;
#15653 = ORIENTED_EDGE ( 'NONE', *, *, #54841, .F. ) ;
#15654 = CARTESIAN_POINT ( 'NONE',  ( 23.49999999999998579, -8.999999999999996447, 28.86437827766148345 ) ) ;
#15655 = LINE ( 'NONE', #83682, #51581 ) ;
#15656 = DIRECTION ( 'NONE',  ( 0.000000000000000000, -6.938893903907222067E-15, 1.000000000000000000 ) ) ;
#15657 = CARTESIAN_POINT ( 'NONE',  ( 6.923076923076924238, -6.343179335718451384, 34.87096338111211935 ) ) ;
#15658 = CARTESIAN_POINT ( 'NONE',  ( 7.912221179503920787, -6.343179335718452272, 34.87096338111212646 ) ) ;
#15659 = CARTESIAN_POINT ( 'NONE',  ( -4.283994123577848256, -2.373036134822904319, 30.88089517874952250 ) ) ;
#15660 = EDGE_CURVE ( 'NONE', #80250, #71551, #29908, .T. ) ;
#15661 = FACE_BOUND ( 'NONE', #40342, .T. ) ;
#15663 = CARTESIAN_POINT ( 'NONE',  ( 17.77707304109314279, -10.77366814457252175, 33.85459836347580875 ) ) ;
#15662 = CARTESIAN_POINT ( 'NONE',  ( 6.699591998512592461, -4.225889041578354544, 33.85425143139329407 ) ) ;
#15664 = CARTESIAN_POINT ( 'NONE',  ( -15.23076923076935074, -9.442884908241554243, 34.35708131394783038 ) ) ;
#15666 = CARTESIAN_POINT ( 'NONE',  ( -12.71156169883143150, -4.335965774309648246, 33.62209801155881905 ) ) ;
#15665 = CARTESIAN_POINT ( 'NONE',  ( -17.75005448165186195, -11.37275283266504111, 32.91324779482534524 ) ) ;
#15667 = LINE ( 'NONE', #43137, #86476 ) ;
#15668 = CARTESIAN_POINT ( 'NONE',  ( -0.06109907496455085213, -3.750000000000000888, 22.65438170625849068 ) ) ;
#15669 = ORIENTED_EDGE ( 'NONE', *, *, #21776, .F. ) ;
#15670 = EDGE_CURVE ( 'NONE', #68060, #12150, #50297, .T. ) ;
#15671 = B_SPLINE_CURVE_WITH_KNOTS ( 'NONE', 3,
 ( #73846, #12144, #39625, #62956, #14347, #6701, #54896, #55770, #21994, #83712 ),
 .UNSPECIFIED., .F., .F.,
 ( 4, 2, 2, 2, 4 ),
 ( 0.0007817359430256365111, 0.0009771253907250045632, 0.001172514838424372399, 0.001367904286123740451, 0.001563293733823108503 ),
 .UNSPECIFIED. ) ;
#15672 = VERTEX_POINT ( 'NONE', #30264 ) ;
#15673 = CARTESIAN_POINT ( 'NONE',  ( -9.442253380669377805, -11.79725096376909299, 32.30694842903960762 ) ) ;
#15674 = EDGE_CURVE ( 'NONE', #16624, #40595, #57729, .T. ) ;
#15675 = CARTESIAN_POINT ( 'NONE',  ( -4.854143535654665165, -3.236590943229499029, 32.36255958852954251 ) ) ;
#15676 = CARTESIAN_POINT ( 'NONE',  ( -7.715628407920203102, -11.66157788607254098, 32.95092075102925833 ) ) ;
#15677 = CARTESIAN_POINT ( 'NONE',  ( -16.94613126909829148, -11.18335022499818621, 33.13157742990016885 ) ) ;
#15678 = CARTESIAN_POINT ( 'NONE',  ( -4.087778820496077437, -2.833524468853757750, 32.15551576947925838 ) ) ;
#15679 = CARTESIAN_POINT ( 'NONE',  ( 2.608446859217893099, -4.805146000318787358, 19.06063170625849068 ) ) ;
#15680 = CARTESIAN_POINT ( 'NONE',  ( -5.448717948717948012, -7.500000000000000000, 29.75000000000000355 ) ) ;
#15681 = FACE_OUTER_BOUND ( 'NONE', #18815, .T. ) ;
#15682 = AXIS2_PLACEMENT_3D ( 'NONE', #45518, #17153, #18053 ) ;
#15683 = CARTESIAN_POINT ( 'NONE',  ( 15.29602480204525605, -11.94971097300157403, 32.03036669348361443 ) ) ;
#15684 = CARTESIAN_POINT ( 'NONE',  ( -1.634592115557738090, -12.41269422305637171, 30.68257228309993323 ) ) ;
#15685 = DIRECTION ( 'NONE',  ( -0.000000000000000000, 1.000000000000000000, -0.000000000000000000 ) ) ;
#15686 = CARTESIAN_POINT ( 'NONE',  ( 12.23861150263161157, -12.64616026154729411, 30.79003144601914244 ) ) ;
#15687 = CARTESIAN_POINT ( 'NONE',  ( 14.37294787896832915, -11.94971097300157403, 32.03036669348361443 ) ) ;
#15688 = VECTOR ( 'NONE', #17318, 1000.000000000000000 ) ;
#15689 = CARTESIAN_POINT ( 'NONE',  ( 14.05771557674995442, -6.567427716900048118, 34.66269422305636283 ) ) ;
#15690 = EDGE_CURVE ( 'NONE', #17646, #21818, #51841, .T. ) ;
#15691 = EDGE_LOOP ( 'NONE', ( #45875, #58275, #3088, #16051 ) ) ;
#15692 = DIRECTION ( 'NONE',  ( 1.000000000000000000, 0.000000000000000000, 0.000000000000000000 ) ) ;
#15693 = CARTESIAN_POINT ( 'NONE',  ( 7.780883845597524662, -5.094484230520674117, 34.41647553114621161 ) ) ;
#15694 = CARTESIAN_POINT ( 'NONE',  ( 2.694853999681185108, -4.891553140782077591, 14.56436829374151287 ) ) ;
#15695 = CARTESIAN_POINT ( 'NONE',  ( 4.088576153289833037, -5.094484230520674117, 34.41647553114621161 ) ) ;
#15696 = DIRECTION ( 'NONE',  ( 0.000000000000000000, 0.000000000000000000, 1.000000000000000000 ) ) ;
#15697 = ORIENTED_EDGE ( 'NONE', *, *, #34909, .T. ) ;
#15698 = EDGE_CURVE ( 'NONE', #57142, #17177, #59891, .T. ) ;
#15699 = DIRECTION ( 'NONE',  ( -0.000000000000000000, -0.3420201433256694901, -0.9396926207859082059 ) ) ;
#15701 = ORIENTED_EDGE ( 'NONE', *, *, #40386, .T. ) ;
#15700 = CARTESIAN_POINT ( 'NONE',  ( 12.46153846153846168, -5.557115091759785130, 34.35708131394839171 ) ) ;
#15702 = DIRECTION ( 'NONE',  ( 0.000000000000000000, 0.000000000000000000, -1.000000000000000000 ) ) ;
#15703 = CARTESIAN_POINT ( 'NONE',  ( 17.01165307636676260, -2.657715359629089669, 31.77849191805833584 ) ) ;
#15704 = VERTEX_POINT ( 'NONE', #31133 ) ;
#15705 = CYLINDRICAL_SURFACE ( 'NONE', #46332, 0.2499999999999997502 ) ;
#15706 = B_SPLINE_CURVE_WITH_KNOTS ( 'NONE', 3,
 ( #1334, #42338, #36885, #49954, #36020, #77872, #16178, #76105, #63474, #15302 ),
 .UNSPECIFIED., .F., .F.,
 ( 4, 2, 2, 2, 4 ),
 ( 0.000000000000000000, 0.0001954339857564080978, 0.0003908679715128161956, 0.0005863019572692242934, 0.0007817359430256323911 ),
 .UNSPECIFIED. ) ;
#15707 = DIRECTION ( 'NONE',  ( 0.000000000000000000, 0.1736481776669275834, 0.9848077530122086864 ) ) ;
#15708 = ORIENTED_EDGE ( 'NONE', *, *, #75218, .T. ) ;
#15709 = DIRECTION ( 'NONE',  ( -0.000000000000000000, -0.9848077530122085754, -0.1736481776669273613 ) ) ;
#15710 = B_SPLINE_CURVE_WITH_KNOTS ( 'NONE', 3,
 ( #51924, #4645, #4192, #86187, #80313, #18610, #58688, #80763, #59133, #10957 ),
 .UNSPECIFIED., .F., .F.,
 ( 4, 2, 2, 2, 4 ),
 ( 0.0007817246256747455461, 0.0009771112852218881168, 0.001172497944769030796, 0.001367884604316173475, 0.001563271263863316154 ),
 .UNSPECIFIED. ) ;
#15711 = EDGE_CURVE ( 'NONE', #72244, #45222, #72571, .T. ) ;
#15712 = FILL_AREA_STYLE_COLOUR ( '', #3419 ) ;
#15713 = CARTESIAN_POINT ( 'NONE',  ( -9.442307692307691624, -2.499999999999998668, 29.75000000000000355 ) ) ;
#15714 = VERTEX_POINT ( 'NONE', #23490 ) ;
#15715 = ORIENTED_EDGE ( 'NONE', *, *, #43407, .T. ) ;
#15716 = AXIS2_PLACEMENT_3D ( 'NONE', #25864, #73163, #52432 ) ;
#15717 = EDGE_CURVE ( 'NONE', #34093, #59880, #86099, .T. ) ;
#15718 = ORIENTED_EDGE ( 'NONE', *, *, #79367, .T. ) ;
#15719 = ADVANCED_FACE ( 'NONE', ( #85650 ), #16737, .F. ) ;
#15720 = CARTESIAN_POINT ( 'NONE',  ( 15.48082365068268018, -12.65882529074907126, 30.72640787790839312 ) ) ;
#15721 = CARTESIAN_POINT ( 'NONE',  ( -14.53117725141625627, -3.236172620538810385, 32.36188796281390267 ) ) ;
#15722 = DIRECTION ( 'NONE',  ( 0.000000000000000000, 0.000000000000000000, -1.000000000000000000 ) ) ;
#15723 = EDGE_CURVE ( 'NONE', #75481, #51727, #78882, .T. ) ;
#15724 = CYLINDRICAL_SURFACE ( 'NONE', #40623, 0.2499999999999986955 ) ;
#15725 = ORIENTED_EDGE ( 'NONE', *, *, #48854, .F. ) ;
#15726 = EDGE_LOOP ( 'NONE', ( #11770, #46242, #72549, #5732 ) ) ;
#15728 = ORIENTED_EDGE ( 'NONE', *, *, #17567, .T. ) ;
#15727 = CARTESIAN_POINT ( 'NONE',  ( -2.373445736005638462, -7.249945578846654470, 34.99404164642496795 ) ) ;
#15729 = DIRECTION ( 'NONE',  ( -0.000000000000000000, 0.9848077530122085754, -0.1736481776669273613 ) ) ;
#15730 = ORIENTED_EDGE ( 'NONE', *, *, #41973, .F. ) ;
#15731 = VECTOR ( 'NONE', #69713, 1000.000000000000114 ) ;
#15732 = VECTOR ( 'NONE', #28236, 1000.000000000000000 ) ;
#15733 = DIRECTION ( 'NONE',  ( 0.000000000000000000, 0.000000000000000000, 1.000000000000000000 ) ) ;
#15734 = CARTESIAN_POINT ( 'NONE',  ( 8.096099364501986528, -5.057305518903948638, 34.11320923018887896 ) ) ;
#15735 = ORIENTED_EDGE ( 'NONE', *, *, #80063, .F. ) ;
#15736 = EDGE_CURVE ( 'NONE', #61262, #16685, #84630, .T. ) ;
#15737 = VECTOR ( 'NONE', #13345, 1000.000000000000227 ) ;
#15738 = AXIS2_PLACEMENT_3D ( 'NONE', #8874, #1666, #42662 ) ;
#15739 = EDGE_LOOP ( 'NONE', ( #84316, #30961, #67274, #16814 ) ) ;
#15741 = ORIENTED_EDGE ( 'NONE', *, *, #20905, .T. ) ;
#15740 = CARTESIAN_POINT ( 'NONE',  ( 9.692307692307695177, -8.164416787775445883, 34.95778746994557906 ) ) ;
#15742 = AXIS2_PLACEMENT_3D ( 'NONE', #40190, #74859, #54117 ) ;
#15743 = CARTESIAN_POINT ( 'NONE',  ( -0.7115616988314267255, -10.76384336483936011, 33.53834819971076087 ) ) ;
#15744 = CARTESIAN_POINT ( 'NONE',  ( -6.923076923077044142, -3.835265460704628371, 33.15142922262033665 ) ) ;
#15745 = EDGE_LOOP ( 'NONE', ( #23281, #6368, #23815, #84360 ) ) ;
#15746 = CARTESIAN_POINT ( 'NONE',  ( 15.23076923076910916, -2.379036618888197729, 30.90682066428292885 ) ) ;
#15747 = CARTESIAN_POINT ( 'NONE',  ( -2.557715544985270206, -5.056417327199099532, 34.11270091957320716 ) ) ;
#15748 = CARTESIAN_POINT ( 'NONE',  ( 6.857806922520604864, -5.941354392334500467, 34.76329471203369792 ) ) ;
#15749 = FACE_BOUND ( 'NONE', #52914, .T. ) ;
#15750 = DIRECTION ( 'NONE',  ( -0.000000000000000000, -0.1736481776669307198, -0.9848077530122080203 ) ) ;
#15751 = CARTESIAN_POINT ( 'NONE',  ( -6.923076923076922462, -12.10708131394839349, 31.69288490824020244 ) ) ;
#15752 = CARTESIAN_POINT ( 'NONE',  ( -15.23076923076922995, -5.471508081941601098, 34.59228464037088457 ) ) ;
#15754 = CARTESIAN_POINT ( 'NONE',  ( 4.403900573759605308, -2.318338780012835443, 30.59689888758630261 ) ) ;
#15753 = DIRECTION ( 'NONE',  ( -0.000000000000000000, 0.9848077530122085754, -0.1736481776669273613 ) ) ;
#15755 = CARTESIAN_POINT ( 'NONE',  ( -2.980714919130916574, -3.136992222400443175, 32.19305428654138979 ) ) ;
#15756 = LINE ( 'NONE', #57614, #46197 ) ;
#15757 = ORIENTED_EDGE ( 'NONE', *, *, #24031, .F. ) ;
#15758 = DIRECTION ( 'NONE',  ( 0.000000000000000000, 0.8660254037844377084, -0.5000000000000015543 ) ) ;
#15759 = ORIENTED_EDGE ( 'NONE', *, *, #70436, .F. ) ;
#15760 = ORIENTED_EDGE ( 'NONE', *, *, #24182, .F. ) ;
#15762 = CARTESIAN_POINT ( 'NONE',  ( 8.096099364501986528, -10.05730279482229683, 34.04704008940765902 ) ) ;
#15761 = DIRECTION ( 'NONE',  ( 1.000000000000000000, 0.000000000000000000, 0.000000000000000000 ) ) ;
#15763 = CARTESIAN_POINT ( 'NONE',  ( -5.869208192175211281, -6.413143153341454017, 34.63066358083362672 ) ) ;
#15764 = FACE_OUTER_BOUND ( 'NONE', #22505, .T. ) ;
#15765 = CARTESIAN_POINT ( 'NONE',  ( -10.48485917715096960, -12.50538340440932394, 31.33453814440721885 ) ) ;
#15766 = CARTESIAN_POINT ( 'NONE',  ( 1.134592147322421862, -11.86270091957321249, 32.19358267280087915 ) ) ;
#15767 = VERTEX_POINT ( 'NONE', #24373 ) ;
#15768 = FACE_OUTER_BOUND ( 'NONE', #78452, .T. ) ;
#15769 = ADVANCED_FACE ( 'NONE', ( #17641 ), #4563, .F. ) ;
#15770 = CARTESIAN_POINT ( 'NONE',  ( -14.55766905174090020, -10.06842814019191401, 34.32929386961144758 ) ) ;
#15771 = CARTESIAN_POINT ( 'NONE',  ( 24.00000000000000000, 9.000000000000024869, 29.25000000000000000 ) ) ;
#15772 = CARTESIAN_POINT ( 'NONE',  ( -18.00000000000000000, -8.164416787775447659, 34.95778746994557906 ) ) ;
#15774 = FACE_OUTER_BOUND ( 'NONE', #39099, .T. ) ;
#15773 = B_SPLINE_CURVE_WITH_KNOTS ( 'NONE', 3,
 ( #54632, #8132, #60956, #12773, #35601, #1364, #60067, #40259, #56312, #83801 ),
 .UNSPECIFIED., .F., .F.,
 ( 4, 2, 2, 2, 4 ),
 ( 0.000000000000000000, 0.0001954311564186879315, 0.0003908623128373758630, 0.0005862934692560637946, 0.0007817246256747517261 ),
 .UNSPECIFIED. ) ;
#15775 = AXIS2_PLACEMENT_3D ( 'NONE', #84683, #49984, #43235 ) ;
#15776 = CARTESIAN_POINT ( 'NONE',  ( -3.749999999999997335, -7.500000000000021316, 16.34375000000000000 ) ) ;
#15777 = ORIENTED_EDGE ( 'NONE', *, *, #86886, .F. ) ;
#15778 = EDGE_CURVE ( 'NONE', #16542, #37672, #53494, .T. ) ;
#15779 = ORIENTED_EDGE ( 'NONE', *, *, #4938, .T. ) ;
#15780 = CARTESIAN_POINT ( 'NONE',  ( 3.480769230769230838, -2.499999999999998668, 29.75000000000000355 ) ) ;
#15782 = ORIENTED_EDGE ( 'NONE', *, *, #18060, .F. ) ;
#15781 = ADVANCED_FACE ( 'NONE', ( #32474 ), #29, .F. ) ;
#15783 = CARTESIAN_POINT ( 'NONE',  ( -9.757578138268467427, -12.46129190929999986, 30.37095296980880832 ) ) ;
#15784 = CARTESIAN_POINT ( 'NONE',  ( -12.46153846153846168, -6.386643153685126251, 34.62446782046654192 ) ) ;
#15785 = CARTESIAN_POINT ( 'NONE',  ( 14.30769230769218581, -10.33852847137269571, 34.16647553114546554 ) ) ;
#15786 = LINE ( 'NONE', #76596, #60105 ) ;
#15787 = CARTESIAN_POINT ( 'NONE',  ( -1.553300858899125059, -3.750000000000009326, 15.32812500000000355 ) ) ;
#15788 = CARTESIAN_POINT ( 'NONE',  ( 27.00000000000000000, 0.7500000000000059952, 24.75000000000000000 ) ) ;
#15789 = ORIENTED_EDGE ( 'NONE', *, *, #23423, .T. ) ;
#15790 = EDGE_CURVE ( 'NONE', #51461, #65658, #2919, .T. ) ;
#15791 = CARTESIAN_POINT ( 'NONE',  ( 16.15384615384615330, -12.78798330534103123, 29.99999999999997868 ) ) ;
#15793 = VERTEX_POINT ( 'NONE', #53183 ) ;
#15792 = CARTESIAN_POINT ( 'NONE',  ( 17.75000000000000000, -2.249999999999998668, 29.75000000000000355 ) ) ;
#15794 = CARTESIAN_POINT ( 'NONE',  ( -10.48485891362104816, -3.816742781228458004, 33.13167719472716044 ) ) ;
#15795 = CARTESIAN_POINT ( 'NONE',  ( 16.94677586748485965, -3.817052484675422797, 33.13202310037935661 ) ) ;
#15796 = CARTESIAN_POINT ( 'NONE',  ( 15.36155967173618642, -2.845873456487966635, 32.17976146951972538 ) ) ;
#15797 = CARTESIAN_POINT ( 'NONE',  ( -2.057637887778853703, -2.318338780012835443, 30.59689888758630261 ) ) ;
#15798 = AXIS2_PLACEMENT_3D ( 'NONE', #1485, #55091, #41582 ) ;
#15799 = DIRECTION ( 'NONE',  ( 1.000000000000000000, 0.000000000000000000, 0.000000000000000000 ) ) ;
#15800 = CARTESIAN_POINT ( 'NONE',  ( -9.320512820512821150, -4.000000000000000000, 29.75000000000000355 ) ) ;
#15801 = EDGE_CURVE ( 'NONE', #5654, #13172, #80688, .T. ) ;
#15802 = CARTESIAN_POINT ( 'NONE',  ( -3.775308065498748977, -8.992201783934593351, 14.01749329374151642 ) ) ;
#15803 = ORIENTED_EDGE ( 'NONE', *, *, #39418, .F. ) ;
#15804 = CARTESIAN_POINT ( 'NONE',  ( -15.36145983387953962, -6.369640206132551441, 34.87707690430378449 ) ) ;
#15805 = CARTESIAN_POINT ( 'NONE',  ( -1.514762594053607803, -12.27039167877662251, 31.24851455888617835 ) ) ;
#15806 = CARTESIAN_POINT ( 'NONE',  ( -1.139087296526025916, -4.750000000000006217, 21.57812500000000355 ) ) ;
#15807 = B_SPLINE_CURVE_WITH_KNOTS ( 'NONE', 3,
 ( #9236, #8789, #64588, #22726, #84893, #23614, #15987, #23179, #51064, #71353 ),
 .UNSPECIFIED., .F., .F.,
 ( 4, 2, 2, 2, 4 ),
 ( 0.000000000000000000, 0.0001954311564186872810, 0.0003908623128373745620, 0.0005862934692560618430, 0.0007817246256747491240 ),
 .UNSPECIFIED. ) ;
#15808 = AXIS2_PLACEMENT_3D ( 'NONE', #76207, #34779, #69010 ) ;
#15809 = CARTESIAN_POINT ( 'NONE',  ( -13.51530685128294529, -12.38065189839062263, 30.83690757178629482 ) ) ;
#15810 = LINE ( 'NONE', #70747, #50421 ) ;
#15811 = ORIENTED_EDGE ( 'NONE', *, *, #11368, .T. ) ;
#15812 = CARTESIAN_POINT ( 'NONE',  ( -1.409462824231155764E-14, -4.749999999999999112, 15.40625000000000000 ) ) ;
#15813 = CARTESIAN_POINT ( 'NONE',  ( 11.53846153846153832, -3.937682226553329556, 33.60647404775216529 ) ) ;
#15814 = EDGE_LOOP ( 'NONE', ( #33935, #61292, #28085, #44794 ) ) ;
#15815 = AXIS2_PLACEMENT_3D ( 'NONE', #62149, #21601, #56277 ) ;
#15816 = CARTESIAN_POINT ( 'NONE',  ( -0.6844654204453101132, -10.77366814457252175, 33.85459836347579454 ) ) ;
#15817 = ORIENTED_EDGE ( 'NONE', *, *, #86135, .T. ) ;
#15818 = CARTESIAN_POINT ( 'NONE',  ( 0.4615384615384611755, -13.37000171582298513, 34.34916445242398453 ) ) ;
#15819 = CARTESIAN_POINT ( 'NONE',  ( 16.82692307692308020, -2.499999999999999556, 29.81609845454690699 ) ) ;
#15820 = CARTESIAN_POINT ( 'NONE',  ( 7.846153846153846700, -5.557115091759785130, 34.35708131394839171 ) ) ;
#15821 = PLANE ( 'NONE',  #52263 ) ;
#15822 = VERTEX_POINT ( 'NONE', #87446 ) ;
#15823 = CARTESIAN_POINT ( 'NONE',  ( -6.923076923077045919, -6.835583212225970762, 34.95778746994575670 ) ) ;
#15824 = EDGE_CURVE ( 'NONE', #7139, #77956, #54068, .T. ) ;
#15825 = ORIENTED_EDGE ( 'NONE', *, *, #45812, .F. ) ;
#15826 = CARTESIAN_POINT ( 'NONE',  ( -17.86920955903304886, -11.93129842949672437, 32.56571108434900452 ) ) ;
#15827 = CARTESIAN_POINT ( 'NONE',  ( 8.769230769230647482, -3.300289026999228881, 32.46337939537708905 ) ) ;
#15828 = ORIENTED_EDGE ( 'NONE', *, *, #62605, .T. ) ;
#15829 = CARTESIAN_POINT ( 'NONE',  ( 8.546303810323914618, -4.762599654559228846, 34.23009711892697737 ) ) ;
#15830 = FACE_OUTER_BOUND ( 'NONE', #53816, .T. ) ;
#15831 = CARTESIAN_POINT ( 'NONE',  ( 11.53846153846153832, -1.129524287112498415, 32.06866353760679544 ) ) ;
#15832 = EDGE_CURVE ( 'NONE', #55623, #17845, #7248, .T. ) ;
#15833 = CARTESIAN_POINT ( 'NONE',  ( 1.161130460051055913, -6.716662450894490100, 34.94144148231605840 ) ) ;
#15834 = CARTESIAN_POINT ( 'NONE',  ( -4.023320715612507925, -4.299079248970732792, 33.91157788607253565 ) ) ;
#15835 = B_SPLINE_CURVE_WITH_KNOTS ( 'NONE', 3,
 ( #70337, #43744, #16709, #8644, #36553, #1435, #57262, #42431, #69888, #77974 ),
 .UNSPECIFIED., .F., .F.,
 ( 4, 2, 2, 2, 4 ),
 ( 0.000000000000000000, 0.0001954339857564083688, 0.0003908679715128167377, 0.0005863019572692250523, 0.0007817359430256334753 ),
 .UNSPECIFIED. ) ;
#15836 = EDGE_LOOP ( 'NONE', ( #75234, #68112, #3425, #52812 ) ) ;
#15838 = ADVANCED_FACE ( 'NONE', ( #46436 ), #81125, .F. ) ;
#15837 = VERTEX_POINT ( 'NONE', #39699 ) ;
#15839 = FACE_BOUND ( 'NONE', #86560, .T. ) ;
#15840 = ORIENTED_EDGE ( 'NONE', *, *, #34592, .T. ) ;
#15841 = CARTESIAN_POINT ( 'NONE',  ( 8.546304551714618114, -3.586966769969701208, 32.86292498521069660 ) ) ;
#15842 = AXIS2_PLACEMENT_3D ( 'NONE', #9031, #22096, #28867 ) ;
#15843 = DIRECTION ( 'NONE',  ( -0.000000000000000000, 0.1736481776669307198, -0.9848077530122080203 ) ) ;
#15844 = CARTESIAN_POINT ( 'NONE',  ( 6.000000000000001776, -2.833524468853757305, 32.15551576947925838 ) ) ;
#15845 = DIRECTION ( 'NONE',  ( -0.000000000000000000, 0.6427876096865404731, -0.7660444431189771253 ) ) ;
#15846 = EDGE_CURVE ( 'NONE', #83859, #77663, #12215, .T. ) ;
#15847 = EDGE_LOOP ( 'NONE', ( #86532, #74720 ) ) ;
#15848 = ORIENTED_EDGE ( 'NONE', *, *, #57127, .T. ) ;
#15849 = VERTEX_POINT ( 'NONE', #32928 ) ;
#15850 = CARTESIAN_POINT ( 'NONE',  ( 2.557637826040450424, -4.336752205174647656, 33.62275283266504289 ) ) ;
#15851 = ADVANCED_FACE ( 'NONE', ( #61712 ), #67603, .F. ) ;
#15852 = ADVANCED_FACE ( 'NONE', ( #34250 ), #87905, .F. ) ;
#15853 = VECTOR ( 'NONE', #36793, 1000.000000000000227 ) ;
#15854 = DIRECTION ( 'NONE',  ( -0.000000000000000000, -0.7660444431189791237, -0.6427876096865379196 ) ) ;
#15855 = CARTESIAN_POINT ( 'NONE',  ( 14.17700170458200759, -11.93127051446799847, 32.56575433478202797 ) ) ;
#15856 = EDGE_CURVE ( 'NONE', #30760, #70329, #28797, .T. ) ;
#15857 = DIRECTION ( 'NONE',  ( 0.000000000000000000, 0.3420201433256641055, -0.9396926207859100932 ) ) ;
#15858 = EDGE_LOOP ( 'NONE', ( #752, #3741, #15527, #23603 ) ) ;
#15859 = CARTESIAN_POINT ( 'NONE',  ( 8.899756470994333313, -9.417988943895561960, 34.36773134775777550 ) ) ;
#15860 = CARTESIAN_POINT ( 'NONE',  ( -6.000000000000121680, -6.835583212225970762, 34.95778746994575670 ) ) ;
#15861 = CARTESIAN_POINT ( 'NONE',  ( 4.153846153846154188, -10.51840700105979565, 33.73612834413961536 ) ) ;
#15862 = CARTESIAN_POINT ( 'NONE',  ( 11.76147289007438523, -8.239487800360276282, 34.69522927552633718 ) ) ;
#15863 = VERTEX_POINT ( 'NONE', #22508 ) ;
#15864 = VERTEX_POINT ( 'NONE', #49092 ) ;
#15865 = CIRCLE ( 'NONE', #27310, 0.2500000000000002220 ) ;
#15866 = VERTEX_POINT ( 'NONE', #42354 ) ;
#15867 = VECTOR ( 'NONE', #781, 1000.000000000000227 ) ;
#15869 = CARTESIAN_POINT ( 'NONE',  ( -9.561782254074046250, -8.630441415882550871, 34.87705825610312615 ) ) ;
#15868 = CARTESIAN_POINT ( 'NONE',  ( 12.21156173059610772, -6.567427716900048118, 34.66269422305636283 ) ) ;
#15870 = AXIS2_PLACEMENT_3D ( 'NONE', #34603, #13004, #47223 ) ;
#15871 = B_SPLINE_CURVE_WITH_KNOTS ( 'NONE', 3,
 ( #30204, #86949, #10817, #58539, #44134, #59444, #3603, #16676, #71615, #9921 ),
 .UNSPECIFIED., .F., .F.,
 ( 4, 2, 2, 2, 4 ),
 ( 0.000000000000000000, 0.0001954339857564098867, 0.0003908679715128197734, 0.0005863019572692296059, 0.0007817359430256395469 ),
 .UNSPECIFIED. ) ;
#15872 = DIRECTION ( 'NONE',  ( 0.000000000000000000, 0.9396926207859126468, -0.3420201433256571111 ) ) ;
#15873 = CARTESIAN_POINT ( 'NONE',  ( -10.61538461538473399, -10.90142922262034020, 33.41473453929536674 ) ) ;
#15874 = FACE_BOUND ( 'NONE', #30583, .T. ) ;
#15875 = CARTESIAN_POINT ( 'NONE',  ( -2.438383774359865086, -9.804603061927743113, 34.18744698557895845 ) ) ;
#15876 = VERTEX_POINT ( 'NONE', #35138 ) ;
#15877 = DIRECTION ( 'NONE',  ( 1.000000000000000000, 0.000000000000000000, 0.000000000000000000 ) ) ;
#15878 = CARTESIAN_POINT ( 'NONE',  ( 9.692307692307695177, -11.91647553114624181, 32.58852847137148245 ) ) ;
#15879 = CARTESIAN_POINT ( 'NONE',  ( -17.14300648787895653, -11.69971097300155272, 32.46337939537587403 ) ) ;
#15880 = CARTESIAN_POINT ( 'NONE',  ( -11.31545018684868964, -3.587049720035815348, 32.86302985866382897 ) ) ;
#15881 = ORIENTED_EDGE ( 'NONE', *, *, #8313, .F. ) ;
#15882 = DIRECTION ( 'NONE',  ( -0.000000000000000000, 0.3420201433256694346, -0.9396926207859080948 ) ) ;
#15883 = ORIENTED_EDGE ( 'NONE', *, *, #47708, .F. ) ;
#15884 = FACE_BOUND ( 'NONE', #20880, .T. ) ;
#15885 = ADVANCED_FACE ( 'NONE', ( #48646 ), #68919, .F. ) ;
#15886 = CARTESIAN_POINT ( 'NONE',  ( -16.82686876528476105, -4.235687564193445276, 33.53795663066793509 ) ) ;
#15887 = CARTESIAN_POINT ( 'NONE',  ( 12.46153846153833911, -3.083524468854526912, 32.58852847137268327 ) ) ;
#15888 = CARTESIAN_POINT ( 'NONE',  ( 12.23805351781451378, -12.24155766932282496, 31.33739205006857986 ) ) ;
#15889 = ORIENTED_EDGE ( 'NONE', *, *, #54236, .T. ) ;
#15890 = CARTESIAN_POINT ( 'NONE',  ( -12.68502340526241312, -10.11188796281391511, 34.01382737946119050 ) ) ;
#15891 = CARTESIAN_POINT ( 'NONE',  ( 5.011166274408766164, -7.249945686854186278, 34.74374336980224598 ) ) ;
#15892 = CARTESIAN_POINT ( 'NONE',  ( 8.546303810323914618, -2.308479472611653094, 30.53278059502174457 ) ) ;
#15893 = DIRECTION ( 'NONE',  ( -0.000000000000000000, -0.5000000000000009992, -0.8660254037844380415 ) ) ;
#15894 = ORIENTED_EDGE ( 'NONE', *, *, #71839, .F. ) ;
#15895 = DIRECTION ( 'NONE',  ( -0.000000000000000000, 0.5000000000000011102, -0.8660254037844381525 ) ) ;
#15896 = ORIENTED_EDGE ( 'NONE', *, *, #41010, .T. ) ;
#15897 = ADVANCED_FACE ( 'NONE', ( #8562 ), #1792, .F. ) ;
#15899 = EDGE_LOOP ( 'NONE', ( #67247, #65547, #2470, #54107 ) ) ;
#15898 = DIRECTION ( 'NONE',  ( 0.000000000000000000, 0.000000000000000000, -1.000000000000000000 ) ) ;
#15900 = CARTESIAN_POINT ( 'NONE',  ( 7.596177115211490971, -10.66389620160130036, 33.62221079203477103 ) ) ;
#15901 = CARTESIAN_POINT ( 'NONE',  ( -1.634592128663974853, -12.41104346484419452, 31.60698883733904196 ) ) ;
#15902 = LINE ( 'NONE', #78032, #25635 ) ;
#15903 = CARTESIAN_POINT ( 'NONE',  ( -12.39628289026243912, -2.892918686051626498, 31.69288490824026638 ) ) ;
#15905 = CARTESIAN_POINT ( 'NONE',  ( -11.78848476268299628, -9.356822207818506598, 34.66110646841856635 ) ) ;
#15904 = CARTESIAN_POINT ( 'NONE',  ( 13.45068373561782593, -5.557115091759786019, 34.35708131394839882 ) ) ;
#15906 = CARTESIAN_POINT ( 'NONE',  ( -0.4615384615384611200, -1.509761064869970415, 31.06009739812519044 ) ) ;
#15907 = EDGE_CURVE ( 'NONE', #81743, #5154, #2225, .T. ) ;
#15908 = CARTESIAN_POINT ( 'NONE',  ( 2.750000000000008438, -8.639087296525996607, 24.54687500000000000 ) ) ;
#15909 = ORIENTED_EDGE ( 'NONE', *, *, #61449, .F. ) ;
#15910 = CYLINDRICAL_SURFACE ( 'NONE', #49131, 0.2499999999999994726 ) ;
#15911 = CARTESIAN_POINT ( 'NONE',  ( 15.23076923076923173, -12.78798330534102767, 29.49999999999997868 ) ) ;
#15912 = ORIENTED_EDGE ( 'NONE', *, *, #4038, .F. ) ;
#15913 = ORIENTED_EDGE ( 'NONE', *, *, #69996, .T. ) ;
#15914 = ORIENTED_EDGE ( 'NONE', *, *, #28018, .T. ) ;
#15915 = CARTESIAN_POINT ( 'NONE',  ( 17.07692307692295586, -5.219633306517616589, 34.19971097300220464 ) ) ;
#15916 = B_SPLINE_CURVE_WITH_KNOTS ( 'NONE', 3,
 ( #41633, #33554, #26786, #54245, #81741, #20025, #16808, #69981, #42526, #2401 ),
 .UNSPECIFIED., .F., .F.,
 ( 4, 2, 2, 2, 4 ),
 ( 0.000000000000000000, 0.0001954311564186863323, 0.0003908623128373726646, 0.0005862934692560590241, 0.0007817246256747453293 ),
 .UNSPECIFIED. ) ;
#15917 = CARTESIAN_POINT ( 'NONE',  ( 6.223011351612852238, -11.24521262558773671, 33.06293181088029343 ) ) ;
#15918 = CYLINDRICAL_SURFACE ( 'NONE', #24101, 0.2499999999999993616 ) ;
#15919 = CARTESIAN_POINT ( 'NONE',  ( 8.834485908743605620, -11.67786785259547777, 32.92929555188713664 ) ) ;
#15921 = EDGE_CURVE ( 'NONE', #38438, #22548, #80315, .T. ) ;
#15920 = CARTESIAN_POINT ( 'NONE',  ( -13.16183571563731647, -6.717445702608402236, 34.94155399931962336 ) ) ;
#15922 = CARTESIAN_POINT ( 'NONE',  ( 18.00000000000000000, -1.951392089020283160, 34.73218667398347748 ) ) ;
#15923 = CARTESIAN_POINT ( 'NONE',  ( -20.74999999999999645, -7.500000000000000000, 29.75000000000000355 ) ) ;
#15924 = CARTESIAN_POINT ( 'NONE',  ( -3.903900635498010807, -5.852078868378310261, 34.47109172314383585 ) ) ;
#15925 = CARTESIAN_POINT ( 'NONE',  ( -17.29984929443921970, -12.15238873228291716, 31.58232369045353849 ) ) ;
#15926 = CIRCLE ( 'NONE', #49022, 0.2500000000000002220 ) ;
#15927 = CARTESIAN_POINT ( 'NONE',  ( 2.057715576749953978, -3.627789207965226748, 32.91389620160131102 ) ) ;
#15928 = CARTESIAN_POINT ( 'NONE',  ( 15.23076923076923173, -12.10708131394839349, 31.69288490824020244 ) ) ;
#15929 = EDGE_CURVE ( 'NONE', #56147, #50666, #13785, .T. ) ;
#15930 = ORIENTED_EDGE ( 'NONE', *, *, #85067, .F. ) ;
#15931 = CARTESIAN_POINT ( 'NONE',  ( 15.00728428704528561, -11.41268669641499756, 32.86336882939238535 ) ) ;
#15932 = LINE ( 'NONE', #69539, #59842 ) ;
#15933 = CARTESIAN_POINT ( 'NONE',  ( 12.46153846153846168, -2.833524468853757305, 32.15551576947925838 ) ) ;
#15934 = ORIENTED_EDGE ( 'NONE', *, *, #68888, .F. ) ;
#15935 = EDGE_CURVE ( 'NONE', #20644, #80080, #8370, .T. ) ;
#15936 = CARTESIAN_POINT ( 'NONE',  ( -2.307692307692428724, -6.835583212225970762, 34.95778746994575670 ) ) ;
#15937 = AXIS2_PLACEMENT_3D ( 'NONE', #77674, #56956, #30379 ) ;
#15938 = CARTESIAN_POINT ( 'NONE',  ( 9.442284468086239002, -2.985938066672154445, 32.43141759479405550 ) ) ;
#15939 = PRODUCT_DEFINITION_FORMATION_WITH_SPECIFIED_SOURCE ( 'ANY', '', #963, .NOT_KNOWN. ) ;
#15940 = CARTESIAN_POINT ( 'NONE',  ( -8.834500769787091201, -9.528491918058357157, 34.59228464037090589 ) ) ;
#15941 = B_SPLINE_CURVE_WITH_KNOTS ( 'NONE', 3,
 ( #88492, #68200, #61865, #60546, #88061, #54664, #40734, #81719, #6499, #13691 ),
 .UNSPECIFIED., .F., .F.,
 ( 4, 2, 2, 2, 4 ),
 ( 0.000000000000000000, 0.0001954311564186878502, 0.0003908623128373757004, 0.0005862934692560635777, 0.0007817246256747514008 ),
 .UNSPECIFIED. ) ;
#15942 = EDGE_CURVE ( 'NONE', #54183, #88905, #83515, .T. ) ;
#15943 = VERTEX_POINT ( 'NONE', #21176 ) ;
#15945 = ADVANCED_FACE ( 'NONE', ( #76121 ), #14422, .F. ) ;
#15944 = CARTESIAN_POINT ( 'NONE',  ( -1.384615384615383471, -3.513871655860378418, 32.76840700105978499 ) ) ;
#15946 = ORIENTED_EDGE ( 'NONE', *, *, #29149, .T. ) ;
#15947 = CARTESIAN_POINT ( 'NONE',  ( -3.453695448285377445, -12.15238873228292071, 31.58232369045353849 ) ) ;
#15948 = CARTESIAN_POINT ( 'NONE',  ( 12.23861224402231151, -8.239355502252617924, 34.69524867566427417 ) ) ;
#15949 = CARTESIAN_POINT ( 'NONE',  ( 1.319345384059067428, -8.656820664281497102, 34.87096338111211935 ) ) ;
#15950 = CYLINDRICAL_SURFACE ( 'NONE', #30873, 0.2499999999999986955 ) ;
#15951 = EDGE_CURVE ( 'NONE', #55459, #25295, #14740, .T. ) ;
#15952 = ORIENTED_EDGE ( 'NONE', *, *, #21224, .T. ) ;
#15953 = VECTOR ( 'NONE', #78730, 1000.000000000000000 ) ;
#15954 = EDGE_CURVE ( 'NONE', #67048, #56388, #63057, .T. ) ;
#15956 = EDGE_CURVE ( 'NONE', #27257, #74976, #30932, .T. ) ;
#15955 = VERTEX_POINT ( 'NONE', #64364 ) ;
#15957 = ORIENTED_EDGE ( 'NONE', *, *, #49266, .F. ) ;
#15958 = CARTESIAN_POINT ( 'NONE',  ( -6.249976730942353065, -11.28823185664190376, 33.01397839955799896 ) ) ;
#15959 = CARTESIAN_POINT ( 'NONE',  ( -13.38461538461538325, -1.790695186598648903, 34.54067556320373455 ) ) ;
#15960 = VECTOR ( 'NONE', #77279, 1000.000000000000000 ) ;
#15961 = CARTESIAN_POINT ( 'NONE',  ( -4.153846153846274980, -12.51329471203414379, 31.30864560766407578 ) ) ;
#15962 = CARTESIAN_POINT ( 'NONE',  ( 15.23076923076923173, -10.89733346790207413, 36.13435417666054406 ) ) ;
#15963 = CARTESIAN_POINT ( 'NONE',  ( -17.77698864838715309, -4.187068189119697692, 33.49521262558774026 ) ) ;
#15964 = LINE ( 'NONE', #56935, #29424 ) ;
#15965 = EDGE_LOOP ( 'NONE', ( #11741, #80183 ) ) ;
#15966 = ORIENTED_EDGE ( 'NONE', *, *, #58338, .F. ) ;
#15967 = B_SPLINE_CURVE_WITH_KNOTS ( 'NONE', 3,
 ( #76007, #13861, #14307, #14760, #21053, #76461, #21957, #1232, #7109, #21502 ),
 .UNSPECIFIED., .F., .F.,
 ( 4, 2, 2, 2, 4 ),
 ( 0.0007817246256747550871, 0.0009771112852218989588, 0.001172497944769042939, 0.001367884604316186702, 0.001563271263863330682 ),
 .UNSPECIFIED. ) ;
#15968 = EDGE_LOOP ( 'NONE', ( #4528, #58804, #26338, #7351 ) ) ;
#15970 = ORIENTED_EDGE ( 'NONE', *, *, #76926, .F. ) ;
#15969 = CARTESIAN_POINT ( 'NONE',  ( -2.980823712421088345, -10.76462480002816235, 33.53768742498949962 ) ) ;
#15971 = B_SPLINE_CURVE_WITH_KNOTS ( 'NONE', 3,
 ( #2553, #43115, #23709, #30911, #37678, #9763, #49860, #16968, #43548, #22832 ),
 .UNSPECIFIED., .F., .F.,
 ( 4, 2, 2, 2, 4 ),
 ( 0.0007817246256747497745, 0.0009771112852218937547, 0.001172497944769037518, 0.001367884604316181498, 0.001563271263863325478 ),
 .UNSPECIFIED. ) ;
#15973 = LINE ( 'NONE', #84879, #27580 ) ;
#15972 = DIRECTION ( 'NONE',  ( -0.000000000000000000, 0.5000000000000011102, -0.8660254037844380415 ) ) ;
#15974 = CARTESIAN_POINT ( 'NONE',  ( 13.38461538461526601, -8.613356846316285953, 34.62446782046622218 ) ) ;
#15975 = ORIENTED_EDGE ( 'NONE', *, *, #50866, .F. ) ;
#15976 = VECTOR ( 'NONE', #53324, 1000.000000000000000 ) ;
#15977 = VECTOR ( 'NONE', #55452, 1000.000000000000000 ) ;
#15978 = ORIENTED_EDGE ( 'NONE', *, *, #45472, .F. ) ;
#15979 = CARTESIAN_POINT ( 'NONE',  ( -17.86920955903304886, -2.845873456487967079, 32.17976146951973959 ) ) ;
#15980 = VERTEX_POINT ( 'NONE', #66148 ) ;
#15981 = FACE_BOUND ( 'NONE', #67365, .T. ) ;
#15983 = VECTOR ( 'NONE', #65250, 1000.000000000000000 ) ;
#15982 = CARTESIAN_POINT ( 'NONE',  ( 8.769230769230768274, -3.669653830205710676, 35.88435417666054406 ) ) ;
#15984 = CARTESIAN_POINT ( 'NONE',  ( 15.93091993633000847, -6.503392248772476236, 34.64988816332204635 ) ) ;
#15985 = EDGE_LOOP ( 'NONE', ( #23359, #38033, #42032, #3200 ) ) ;
#15986 = CARTESIAN_POINT ( 'NONE',  ( 16.40379167219429846, -11.37275283266504111, 32.91324779482534524 ) ) ;
#15987 = CARTESIAN_POINT ( 'NONE',  ( 4.853438152358744873, -8.539481045369598178, 34.89627647299170832 ) ) ;
#15988 = CARTESIAN_POINT ( 'NONE',  ( 2.307692307692309264, -4.098570777380720287, 33.41473453929634729 ) ) ;
#15989 = LINE ( 'NONE', #9238, #57236 ) ;
#15990 = CARTESIAN_POINT ( 'NONE',  ( 1.515140822849028179, -2.647132371071621471, 31.75357179365173010 ) ) ;
#15991 = AXIS2_PLACEMENT_3D ( 'NONE', #81244, #27172, #33927 ) ;
#15992 = CARTESIAN_POINT ( 'NONE',  ( 8.769230769230768274, -11.35647404775217417, 33.31231777344666511 ) ) ;
#15993 = CARTESIAN_POINT ( 'NONE',  ( 6.416666666666664298, -7.500000000000000000, 29.75000000000000355 ) ) ;
#15994 = CARTESIAN_POINT ( 'NONE',  ( -7.846153846153844924, -13.20930481340135110, 34.54067556320372745 ) ) ;
#15995 = LINE ( 'NONE', #35826, #2600 ) ;
#15996 = CARTESIAN_POINT ( 'NONE',  ( -18.13069146666755671, -6.413092428213692742, 34.63065189839063152 ) ) ;
#15997 = FACE_BOUND ( 'NONE', #50868, .T. ) ;
#15998 = B_SPLINE_CURVE_WITH_KNOTS ( 'NONE', 3,
 ( #40981, #40549, #5867, #62132, #53602, #437, #27465, #54036, #33778, #82420 ),
 .UNSPECIFIED., .F., .F.,
 ( 4, 2, 2, 2, 4 ),
 ( 0.000000000000000000, 0.0001954311564186879857, 0.0003908623128373759715, 0.0005862934692560640114, 0.0007817246256747519429 ),
 .UNSPECIFIED. ) ;
#16000 = CARTESIAN_POINT ( 'NONE',  ( -15.23076923076922995, -4.098570777380720287, 33.41473453929634729 ) ) ;
#15999 = DIRECTION ( 'NONE',  ( 0.000000000000000000, -1.000000000000000000, 4.336808689942017736E-16 ) ) ;
#16001 = DIRECTION ( 'NONE',  ( 0.000000000000000000, 0.9396926207859126468, 0.3420201433256571111 ) ) ;
#16003 = DIRECTION ( 'NONE',  ( 0.000000000000000000, 0.000000000000000000, -1.000000000000000000 ) ) ;
#16002 = CARTESIAN_POINT ( 'NONE',  ( -6.923076923076922462, -1.466349020453238561, 30.81389545987213907 ) ) ;
#16004 = CARTESIAN_POINT ( 'NONE',  ( 8.769230769230647482, -11.48612834414049644, 32.76840700105863391 ) ) ;
#16005 = CARTESIAN_POINT ( 'NONE',  ( -1.077988221561460236, -10.27530806549876452, 24.60750670625849779 ) ) ;
#16006 = ORIENTED_EDGE ( 'NONE', *, *, #52712, .F. ) ;
#16007 = CARTESIAN_POINT ( 'NONE',  ( 3.181675156714246278, -8.024245293229201437, 13.99999999999999289 ) ) ;
#16008 = VERTEX_POINT ( 'NONE', #29719 ) ;
#16009 = CYLINDRICAL_SURFACE ( 'NONE', #20505, 0.2499999999999994726 ) ;
#16010 = ORIENTED_EDGE ( 'NONE', *, *, #62187, .T. ) ;
#16011 = CARTESIAN_POINT ( 'NONE',  ( 17.99999999999987566, -12.27809138561165270, 31.22303859784587132 ) ) ;
#16012 = ORIENTED_EDGE ( 'NONE', *, *, #20299, .F. ) ;
#16013 = DIRECTION ( 'NONE',  ( -0.000000000000000000, -0.9396926207859093161, -0.3420201433256663259 ) ) ;
#16014 = CARTESIAN_POINT ( 'NONE',  ( -1.987747218494660295, -5.598659921968651254, 21.24813170625848713 ) ) ;
#16015 = CARTESIAN_POINT ( 'NONE',  ( 17.20744877868664346, -8.586989748646450593, 34.63063291749215011 ) ) ;
#16016 = CARTESIAN_POINT ( 'NONE',  ( 6.988332062589762472, -10.33852847137154107, 34.16647553114620450 ) ) ;
#16017 = CARTESIAN_POINT ( 'NONE',  ( 20.00000000000000000, -4.000000000000000000, 29.75000000000000355 ) ) ;
#16018 = CARTESIAN_POINT ( 'NONE',  ( -3.903846153846152855, -7.500000000000001776, 35.04278698407183867 ) ) ;
#16019 = CARTESIAN_POINT ( 'NONE',  ( -19.50000000000000000, -3.499999999999999556, 29.75000000000000355 ) ) ;
#16020 = CARTESIAN_POINT ( 'NONE',  ( 6.923076923076924238, -13.87047571288749737, 32.06866353760679544 ) ) ;
#16021 = AXIS2_PLACEMENT_3D ( 'NONE', #13499, #870, #41418 ) ;
#16022 = CARTESIAN_POINT ( 'NONE',  ( 1.553300858899087311, -3.749999999999992006, 16.73437500000000000 ) ) ;
#16023 = CARTESIAN_POINT ( 'NONE',  ( -10.54931626438217407, -2.721908614388772296, 31.22303859784725333 ) ) ;
#16024 = CARTESIAN_POINT ( 'NONE',  ( -2.307692307692305711, -11.91647553114624181, 32.58852847137148245 ) ) ;
#16025 = VECTOR ( 'NONE', #67645, 1000.000000000000114 ) ;
#16026 = CARTESIAN_POINT ( 'NONE',  ( -2.438383774359863310, -4.118384482072085184, 33.43331474514187107 ) ) ;
#16027 = CARTESIAN_POINT ( 'NONE',  ( -3.749999999999997335, -7.500000000000021316, 17.59375000000000000 ) ) ;
#16028 = EDGE_CURVE ( 'NONE', #49403, #70118, #43660, .T. ) ;
#16029 = PLANE ( 'NONE',  #20272 ) ;
#16030 = ORIENTED_EDGE ( 'NONE', *, *, #9542, .T. ) ;
#16031 = CARTESIAN_POINT ( 'NONE',  ( -13.63459212866397685, -6.524016743844655686, 34.90889640711025521 ) ) ;
#16032 = CARTESIAN_POINT ( 'NONE',  ( 12.23861150263161335, -8.282780595021769443, 34.94152052738834868 ) ) ;
#16033 = CARTESIAN_POINT ( 'NONE',  ( 9.692307692307572609, -6.879047030192662504, 34.71129190930017927 ) ) ;
#16034 = CARTESIAN_POINT ( 'NONE',  ( 14.98076923076922995, -7.566082377512564960, 35.00000000000000711 ) ) ;
#16035 = B_SPLINE_CURVE_WITH_KNOTS ( 'NONE', 3,
 ( #40238, #47414, #13637, #46543, #19946, #6009, #128, #46100, #67702, #6879 ),
 .UNSPECIFIED., .F., .F.,
 ( 4, 2, 2, 2, 4 ),
 ( 0.000000000000000000, 0.0001954339857564081520, 0.0003908679715128163040, 0.0005863019572692244018, 0.0007817359430256326080 ),
 .UNSPECIFIED. ) ;
#16036 = CARTESIAN_POINT ( 'NONE',  ( -3.230769230769229949, -2.499999999999998668, 29.75000000000001421 ) ) ;
#16037 = CARTESIAN_POINT ( 'NONE',  ( -14.05763788777885281, -4.074993327901527351, 33.72946981652012255 ) ) ;
#16038 = B_SPLINE_CURVE_WITH_KNOTS ( 'NONE', 3,
 ( #57701, #84752, #50489, #85182, #23462, #49618 ),
 .UNSPECIFIED., .F., .F.,
 ( 4, 2, 4 ),
 ( 0.0003909512603273906169, 0.0005862562993132179340, 0.0007815613382990451970 ),
 .UNSPECIFIED. ) ;
#16039 = LINE ( 'NONE', #21907, #72072 ) ;
#16040 = EDGE_CURVE ( 'NONE', #29682, #81991, #10431, .T. ) ;
#16041 = ORIENTED_EDGE ( 'NONE', *, *, #22123, .T. ) ;
#16042 = ORIENTED_EDGE ( 'NONE', *, *, #771, .T. ) ;
#16043 = ORIENTED_EDGE ( 'NONE', *, *, #41663, .T. ) ;
#16044 = CARTESIAN_POINT ( 'NONE',  ( 3.453780582382080855, -5.667800583137508674, 34.40243808032445827 ) ) ;
#16045 = FACE_OUTER_BOUND ( 'NONE', #10603, .T. ) ;
#16046 = CARTESIAN_POINT ( 'NONE',  ( -13.31854703361294767, -8.973038597847271092, 34.52809138561121216 ) ) ;
#16047 = CARTESIAN_POINT ( 'NONE',  ( 10.74591005361826213, -10.31582465632705237, 34.18122507451815295 ) ) ;
#16048 = VECTOR ( 'NONE', #17006, 1000.000000000000227 ) ;
#16049 = EDGE_LOOP ( 'NONE', ( #30560, #79792, #19359, #35726 ) ) ;
#16050 = FACE_OUTER_BOUND ( 'NONE', #46467, .T. ) ;
#16051 = ORIENTED_EDGE ( 'NONE', *, *, #50996, .F. ) ;
#16052 = EDGE_CURVE ( 'NONE', #85070, #40219, #22241, .T. ) ;
#16053 = ORIENTED_EDGE ( 'NONE', *, *, #42392, .F. ) ;
#16054 = CARTESIAN_POINT ( 'NONE',  ( -7.846153846153965716, -5.219633306517616589, 34.19971097300220464 ) ) ;
#16055 = CARTESIAN_POINT ( 'NONE',  ( -11.53846153846153655, -11.16473453929635440, 33.15142922261926373 ) ) ;
#16056 = EDGE_CURVE ( 'NONE', #48397, #30065, #78166, .T. ) ;
#16057 = B_SPLINE_CURVE_WITH_KNOTS ( 'NONE', 3,
 ( #86747, #45732, #30875, #73213, #85838, #44830, #79074, #80418, #17373, #24117 ),
 .UNSPECIFIED., .F., .F.,
 ( 4, 2, 2, 2, 4 ),
 ( 0.0007817246256747522682, 0.0009771112852218972241, 0.001172497944769042288, 0.001367884604316187353, 0.001563271263863332417 ),
 .UNSPECIFIED. ) ;
#16058 = DIRECTION ( 'NONE',  ( -1.000000000000000000, 0.000000000000000000, 0.000000000000000000 ) ) ;
#16059 = ADVANCED_FACE ( 'NONE', ( #32822 ), #45879, .F. ) ;
#16060 = B_SPLINE_CURVE_WITH_KNOTS ( 'NONE', 3,
 ( #17905, #38168, #72835, #32745, #39076, #59773, #88168, #87719, #39523, #45810 ),
 .UNSPECIFIED., .F., .F.,
 ( 4, 2, 2, 2, 4 ),
 ( 0.0007817359430256253438, 0.0009771253907249898181, 0.001172514838424354401, 0.001367904286123718983, 0.001563293733823083566 ),
 .UNSPECIFIED. ) ;
#16061 = DIRECTION ( 'NONE',  ( -0.000000000000000000, -0.000000000000000000, -1.000000000000000000 ) ) ;
#16062 = FACE_OUTER_BOUND ( 'NONE', #42556, .T. ) ;
#16063 = ORIENTED_EDGE ( 'NONE', *, *, #42110, .F. ) ;
#16064 = ORIENTED_EDGE ( 'NONE', *, *, #10027, .F. ) ;
#16065 = CARTESIAN_POINT ( 'NONE',  ( 3.749999999999992006, -5.946699141100872943, 20.64062500000000000 ) ) ;
#16066 = ORIENTED_EDGE ( 'NONE', *, *, #34838, .F. ) ;
#16068 = EDGE_LOOP ( 'NONE', ( #5327, #48167 ) ) ;
#16067 = CARTESIAN_POINT ( 'NONE',  ( -11.53846153846166089, -12.70778746994576025, 30.41441678777401236 ) ) ;
#16069 = CARTESIAN_POINT ( 'NONE',  ( 18.00000000000000000, -6.435427911321262684, 35.78748833219616898 ) ) ;
#16070 = DIRECTION ( 'NONE',  ( -0.000000000000000000, -0.000000000000000000, -1.000000000000000000 ) ) ;
#16071 = CARTESIAN_POINT ( 'NONE',  ( 6.988332494352947677, -11.94971097300157403, 32.03036669348361443 ) ) ;
#16072 = ORIENTED_EDGE ( 'NONE', *, *, #26942, .F. ) ;
#16073 = VECTOR ( 'NONE', #18583, 1000.000000000000000 ) ;
#16074 = LINE ( 'NONE', #43537, #72415 ) ;
#16075 = PLANE ( 'NONE',  #64053 ) ;
#16076 = ORIENTED_EDGE ( 'NONE', *, *, #17879, .F. ) ;
#16077 = FACE_BOUND ( 'NONE', #64318, .T. ) ;
#16078 = B_SPLINE_CURVE_WITH_KNOTS ( 'NONE', 3,
 ( #89052, #41295, #20567, #7056, #48031, #14258, #40415, #83166, #81400, #34964 ),
 .UNSPECIFIED., .F., .F.,
 ( 4, 2, 2, 2, 4 ),
 ( 0.000000000000000000, 0.0001954339857564063089, 0.0003908679715128126177, 0.0005863019572692189808, 0.0007817359430256252354 ),
 .UNSPECIFIED. ) ;
#16079 = CARTESIAN_POINT ( 'NONE',  ( 11.31553532094539172, -4.887634598454295265, 34.01352882383564946 ) ) ;
#16080 = CARTESIAN_POINT ( 'NONE',  ( -17.07692307692307665, -12.48256725967547354, 35.29906147534542527 ) ) ;
#16081 = CARTESIAN_POINT ( 'NONE',  ( -39.05038313613820122, -12.50000000000000000, 27.25000000000000000 ) ) ;
#16083 = CARTESIAN_POINT ( 'NONE',  ( 5.011652630962299959, -3.300289026998414865, 32.46337939537583139 ) ) ;
#16082 = LINE ( 'NONE', #17413, #60465 ) ;
#16084 = CARTESIAN_POINT ( 'NONE',  ( 4.946231610255516387, -2.541943142973490666, 30.39792223712631980 ) ) ;
#16085 = CARTESIAN_POINT ( 'NONE',  ( 14.30769230769218581, -2.379036618888197729, 30.90682066428292885 ) ) ;
#16086 = EDGE_LOOP ( 'NONE', ( #33866, #10498 ) ) ;
#16087 = CARTESIAN_POINT ( 'NONE',  ( -10.86540785267757947, -10.05641848906368097, 34.04755513067966177 ) ) ;
#16088 = CARTESIAN_POINT ( 'NONE',  ( -17.01085574357299990, -6.343179335718451384, 34.87096338111212646 ) ) ;
#16089 = ORIENTED_EDGE ( 'NONE', *, *, #34225, .F. ) ;
#16090 = CARTESIAN_POINT ( 'NONE',  ( -5.448717948717948012, -11.50000000000000000, 29.75000000000000355 ) ) ;
#16091 = CARTESIAN_POINT ( 'NONE',  ( 16.94623247381277054, -10.70098750199973203, 33.91152734681376302 ) ) ;
#16092 = DIRECTION ( 'NONE',  ( 0.000000000000000000, 0.000000000000000000, 1.000000000000000000 ) ) ;
#16093 = CARTESIAN_POINT ( 'NONE',  ( 2.084207383127978819, -5.827078755546623690, 34.72654668319379567 ) ) ;
#16094 = CARTESIAN_POINT ( 'NONE',  ( -0.4615384615385826339, -12.46129190930018460, 30.37095296980731973 ) ) ;
#16095 = CARTESIAN_POINT ( 'NONE',  ( 12.46153846153846168, -4.098570777380720287, 33.41473453929634729 ) ) ;
#16096 = FACE_BOUND ( 'NONE', #16068, .T. ) ;
#16098 = CARTESIAN_POINT ( 'NONE',  ( 1.634669696253701288, -2.564540009722895419, 30.55348353981670684 ) ) ;
#16097 = DIRECTION ( 'NONE',  ( 0.000000000000000000, 0.9848077530122072432, 0.1736481776669354937 ) ) ;
#16099 = B_SPLINE_CURVE_WITH_KNOTS ( 'NONE', 3,
 ( #16094, #37237, #64709, #8014, #84130, #29185, #1695, #49442, #8902, #50746 ),
 .UNSPECIFIED., .F., .F.,
 ( 4, 2, 2, 2, 4 ),
 ( 0.0007817359430256330417, 0.0009771253907250000096, 0.001172514838424367194, 0.001367904286123734162, 0.001563293733823101130 ),
 .UNSPECIFIED. ) ;
#16100 = FACE_OUTER_BOUND ( 'NONE', #58359, .T. ) ;
#16102 = CARTESIAN_POINT ( 'NONE',  ( 27.00000000000000000, 0.000000000000000000, 22.25000000000000000 ) ) ;
#16101 = CARTESIAN_POINT ( 'NONE',  ( -7.846153846153844924, -12.62096338111211580, 30.90682066428153263 ) ) ;
#16103 = B_SPLINE_CURVE_WITH_KNOTS ( 'NONE', 3,
 ( #1599, #2034, #29086, #56540, #69169, #84030, #77250, #14223, #36277, #7474 ),
 .UNSPECIFIED., .F., .F.,
 ( 4, 2, 2, 2, 4 ),
 ( 0.0007817246256747469556, 0.0009771112852218902852, 0.001172497944769033615, 0.001367884604316176728, 0.001563271263863320057 ),
 .UNSPECIFIED. ) ;
#16104 = LINE ( 'NONE', #3464, #46159 ) ;
#16105 = CARTESIAN_POINT ( 'NONE',  ( 3.775308065498768517, -8.992201783934554271, 20.54500670625849068 ) ) ;
#16106 = VECTOR ( 'NONE', #37349, 1000.000000000000114 ) ;
#16107 = ORIENTED_EDGE ( 'NONE', *, *, #47261, .T. ) ;
#16108 = VECTOR ( 'NONE', #32997, 1000.000000000000227 ) ;
#16109 = DIRECTION ( 'NONE',  ( 0.000000000000000000, -6.938893903907222067E-15, 1.000000000000000000 ) ) ;
#16110 = FACE_OUTER_BOUND ( 'NONE', #82328, .T. ) ;
#16111 = CARTESIAN_POINT ( 'NONE',  ( -9.469296340694841163, -9.086983370893049639, 34.49168942202179267 ) ) ;
#16112 = CARTESIAN_POINT ( 'NONE',  ( 3.230769230769231726, -13.37000171582298513, 34.34916445242398453 ) ) ;
#16113 = CARTESIAN_POINT ( 'NONE',  ( -4.219928533206289245, -4.661471528628507777, 34.16647553114621871 ) ) ;
#16114 = CARTESIAN_POINT ( 'NONE',  ( -0.06109907496455085213, -3.750000000000000888, 22.65438170625849068 ) ) ;
#16115 = AXIS2_PLACEMENT_3D ( 'NONE', #64521, #36635, #64089 ) ;
#16116 = EDGE_CURVE ( 'NONE', #56516, #69466, #81019, .T. ) ;
#16117 = FACE_OUTER_BOUND ( 'NONE', #85547, .T. ) ;
#16118 = CARTESIAN_POINT ( 'NONE',  ( 3.903822929624694904, -12.07920672191015221, 32.31858351112116168 ) ) ;
#16119 = CARTESIAN_POINT ( 'NONE',  ( 3.361559671736181976, -3.957578996910244395, 33.62503395064540257 ) ) ;
#16120 = CARTESIAN_POINT ( 'NONE',  ( 10.55011461482829738, -6.835583212224499938, 34.95778746994557906 ) ) ;
#16121 = CARTESIAN_POINT ( 'NONE',  ( 2.557692307692323475, -2.249999999999999112, 29.81603969181031033 ) ) ;
#16122 = CARTESIAN_POINT ( 'NONE',  ( 12.46153846153846168, -12.62096338111211580, 30.90682066428153263 ) ) ;
#16123 = CARTESIAN_POINT ( 'NONE',  ( 14.55774661933062575, -11.79725096376909654, 32.30694842903959341 ) ) ;
#16124 = CARTESIAN_POINT ( 'NONE',  ( -14.30769230769230660, -12.78798330534102945, 29.74999999999997868 ) ) ;
#16125 = ORIENTED_EDGE ( 'NONE', *, *, #49514, .F. ) ;
#16126 = CARTESIAN_POINT ( 'NONE',  ( 3.262820512820510999, -3.499999999999999556, 29.75000000000000355 ) ) ;
#16127 = CARTESIAN_POINT ( 'NONE',  ( -1.449865316389469028, -2.255955759149247619, 30.00000000000013856 ) ) ;
#16128 = CARTESIAN_POINT ( 'NONE',  ( -0.06109907496450878162, -11.25000000000000000, 13.78311829374151287 ) ) ;
#16129 = ADVANCED_FACE ( 'NONE', ( #40038 ), #60730, .F. ) ;
#16130 = FACE_OUTER_BOUND ( 'NONE', #5052, .T. ) ;
#16131 = CARTESIAN_POINT ( 'NONE',  ( -4.153846153846152411, -13.37000171582298513, 34.34916445242398453 ) ) ;
#16132 = VERTEX_POINT ( 'NONE', #11669 ) ;
#16133 = CARTESIAN_POINT ( 'NONE',  ( -14.30769230769242917, -9.528491918059723176, 34.59228464037033035 ) ) ;
#16135 = EDGE_LOOP ( 'NONE', ( #9305, #74564, #79348, #72255 ) ) ;
#16134 = CARTESIAN_POINT ( 'NONE',  ( -7.780898706641007578, -12.51329471203373700, 31.30864560766537963 ) ) ;
#16136 = CARTESIAN_POINT ( 'NONE',  ( -15.23076923076922995, -12.09954503811598769, 35.62045528018868623 ) ) ;
#16137 = CARTESIAN_POINT ( 'NONE',  ( 4.023154687178594813, -8.147922237126337563, 34.70805685702651999 ) ) ;
#16138 = EDGE_CURVE ( 'NONE', #88830, #56373, #73362, .T. ) ;
#16139 = B_SPLINE_CURVE_WITH_KNOTS ( 'NONE', 3,
 ( #82587, #75805, #50099, #7800, #69055, #84356, #56428, #83470, #76700, #83916 ),
 .UNSPECIFIED., .F., .F.,
 ( 4, 2, 2, 2, 4 ),
 ( 0.0007817359430256372700, 0.0009771253907250052138, 0.001172514838424373266, 0.001367904286123741101, 0.001563293733823109153 ),
 .UNSPECIFIED. ) ;
#16140 = DIRECTION ( 'NONE',  ( -0.000000000000000000, -0.3420201433256694346, -0.9396926207859080948 ) ) ;
#16141 = CARTESIAN_POINT ( 'NONE',  ( 8.769230769230768274, -4.786620604624113540, 33.94971097300155094 ) ) ;
#16142 = VERTEX_POINT ( 'NONE', #26065 ) ;
#16143 = B_SPLINE_CURVE_WITH_KNOTS ( 'NONE', 3,
 ( #62313, #67319, #40739, #41616, #5614, #88942, #75403, #13697, #27213, #68640 ),
 .UNSPECIFIED., .F., .F.,
 ( 4, 2, 2, 2, 4 ),
 ( 0.000000000000000000, 0.0001954339857564090465, 0.0003908679715128180929, 0.0005863019572692271123, 0.0007817359430256361858 ),
 .UNSPECIFIED. ) ;
#16144 = CARTESIAN_POINT ( 'NONE',  ( -12.71156168575991785, -2.341070481393819236, 30.72580821765574299 ) ) ;
#16145 = CARTESIAN_POINT ( 'NONE',  ( -15.90379184220783948, -3.136992222400443175, 32.19305428654138979 ) ) ;
#16146 = DIRECTION ( 'NONE',  ( 1.000000000000000000, 0.000000000000000000, 0.000000000000000000 ) ) ;
#16147 = EDGE_CURVE ( 'NONE', #12780, #12459, #6124, .T. ) ;
#16148 = VERTEX_POINT ( 'NONE', #4912 ) ;
#16150 = ORIENTED_EDGE ( 'NONE', *, *, #36183, .T. ) ;
#16149 = AXIS2_PLACEMENT_3D ( 'NONE', #4050, #26117, #59896 ) ;
#16151 = VERTEX_POINT ( 'NONE', #67943 ) ;
#16152 = EDGE_CURVE ( 'NONE', #62016, #45177, #86810, .T. ) ;
#16153 = CARTESIAN_POINT ( 'NONE',  ( -18.22348494372394612, -3.754499324213722122, 33.06261337010820256 ) ) ;
#16154 = DIRECTION ( 'NONE',  ( 0.000000000000000000, 0.9848077530122072432, 0.1736481776669354937 ) ) ;
#16155 = EDGE_CURVE ( 'NONE', #78547, #44728, #87341, .T. ) ;
#16156 = DIRECTION ( 'NONE',  ( 1.000000000000000000, 0.000000000000000000, 0.000000000000000000 ) ) ;
#16157 = FACE_OUTER_BOUND ( 'NONE', #3716, .T. ) ;
#16158 = ADVANCED_FACE ( 'NONE', ( #73816 ), #80118, .T. ) ;
#16159 = EDGE_LOOP ( 'NONE', ( #77472, #74219, #42494, #22963 ) ) ;
#16160 = ORIENTED_EDGE ( 'NONE', *, *, #29541, .F. ) ;
#16163 = ADVANCED_FACE ( 'NONE', ( #12117 ), #61164, .F. ) ;
#16162 = ORIENTED_EDGE ( 'NONE', *, *, #54939, .F. ) ;
#16161 = CARTESIAN_POINT ( 'NONE',  ( -1.319469605283419389, -7.750023238201980469, 34.74374492549440419 ) ) ;
#16164 = CARTESIAN_POINT ( 'NONE',  ( 16.28463659481310799, -8.191423895709842640, 34.95447573519442130 ) ) ;
#16165 = COLOUR_RGB ( '', 0.40784314, 0.44705882, 0.49803922) ;
#16166 = VECTOR ( 'NONE', #23782, 1000.000000000000227 ) ;
#16167 = EDGE_CURVE ( 'NONE', #27137, #62928, #21217, .T. ) ;
#16168 = EDGE_CURVE ( 'NONE', #88199, #44873, #17932, .T. ) ;
#16169 = LINE ( 'NONE', #36010, #32054 ) ;
#16170 = DIRECTION ( 'NONE',  ( 0.000000000000000000, 0.000000000000000000, 1.000000000000000000 ) ) ;
#16171 = ORIENTED_EDGE ( 'NONE', *, *, #57988, .F. ) ;
#16172 = ORIENTED_EDGE ( 'NONE', *, *, #8520, .T. ) ;
#16174 = VERTEX_POINT ( 'NONE', #22725 ) ;
#16173 = LINE ( 'NONE', #43636, #27241 ) ;
#16175 = DIRECTION ( 'NONE',  ( -0.000000000000000000, -0.8660254037844399289, -0.4999999999999980016 ) ) ;
#16176 = CARTESIAN_POINT ( 'NONE',  ( -15.90379184220783948, -3.627508038966690496, 32.91356715214248396 ) ) ;
#16177 = ORIENTED_EDGE ( 'NONE', *, *, #14770, .T. ) ;
#16178 = CARTESIAN_POINT ( 'NONE',  ( 15.93036121012220541, -12.44517049084099725, 30.48991314939691932 ) ) ;
#16179 = CARTESIAN_POINT ( 'NONE',  ( -2.372962753653081958, -5.219633306516282545, 34.19971097300152252 ) ) ;
#16180 = CARTESIAN_POINT ( 'NONE',  ( 10.61538461538449596, -3.835265460704628371, 33.15142922262033665 ) ) ;
#16181 = FACE_BOUND ( 'NONE', #37295, .T. ) ;
#16182 = CARTESIAN_POINT ( 'NONE',  ( 14.30769230769231015, -5.557115091759785130, 34.35708131394839171 ) ) ;
#16183 = CARTESIAN_POINT ( 'NONE',  ( 11.31553532094539172, -8.239355502252617924, 34.69524867566427417 ) ) ;
#16184 = CARTESIAN_POINT ( 'NONE',  ( -15.16551365949320740, -10.90142922261932057, 33.41473453929631887 ) ) ;
#16186 = CARTESIAN_POINT ( 'NONE',  ( 6.673053685783957967, -11.86270091957321249, 32.19358267280087915 ) ) ;
#16185 = CARTESIAN_POINT ( 'NONE',  ( -16.85391023282967993, -12.38742843783360748, 31.66772728687926985 ) ) ;
#16187 = DIRECTION ( 'NONE',  ( 0.000000000000000000, 0.000000000000000000, 1.000000000000000000 ) ) ;
#16188 = CARTESIAN_POINT ( 'NONE',  ( -9.915173955370791603, -2.251424796025575326, 29.88072029997477586 ) ) ;
#16189 = EDGE_LOOP ( 'NONE', ( #29685, #66395 ) ) ;
#16190 = DIRECTION ( 'NONE',  ( -0.000000000000000000, -0.000000000000000000, -1.000000000000000000 ) ) ;
#16191 = VERTEX_POINT ( 'NONE', #78556 ) ;
#16192 = B_SPLINE_CURVE_WITH_KNOTS ( 'NONE', 3,
 ( #22048, #77429, #49948, #57594, #50386, #22923, #85081, #71546, #15297, #15740 ),
 .UNSPECIFIED., .F., .F.,
 ( 4, 2, 2, 2, 4 ),
 ( 0.0007817246256747483650, 0.0009771112852218926705, 0.001172497944769037084, 0.001367884604316181498, 0.001563271263863325695 ),
 .UNSPECIFIED. ) ;
#16193 = ORIENTED_EDGE ( 'NONE', *, *, #70436, .T. ) ;
#16195 = CARTESIAN_POINT ( 'NONE',  ( 1.318531973659507139, -10.51840700105979387, 33.73612834413961536 ) ) ;
#16194 = CARTESIAN_POINT ( 'NONE',  ( 1.653273178848927064E-15, -7.500000000000000000, 11.00000000000000178 ) ) ;
#16196 = CARTESIAN_POINT ( 'NONE',  ( 2.438218009455871638, -2.619367082507848998, 30.83698974864644171 ) ) ;
#16197 = DIRECTION ( 'NONE',  ( 0.000000000000000000, 0.000000000000000000, 1.000000000000000000 ) ) ;
#16198 = CARTESIAN_POINT ( 'NONE',  ( 2.307692307692186251, -2.379036618888197285, 30.90682066428292885 ) ) ;
#16199 = CARTESIAN_POINT ( 'NONE',  ( 1.318531973659505363, -11.69971097300155272, 32.46337939537587403 ) ) ;
#16200 = ORIENTED_EDGE ( 'NONE', *, *, #65887, .T. ) ;
#16201 = EDGE_CURVE ( 'NONE', #49352, #23024, #58858, .T. ) ;
#16202 = CARTESIAN_POINT ( 'NONE',  ( 9.320512820512821150, -7.500000000000000000, 33.75000000000000000 ) ) ;
#16203 = CARTESIAN_POINT ( 'NONE',  ( 15.10007862765892739, -10.70098750199973203, 33.91152734681376302 ) ) ;
#16204 = CARTESIAN_POINT ( 'NONE',  ( -18.25000000000000711, -2.249999999999998668, 29.75000000000000355 ) ) ;
#16205 = CARTESIAN_POINT ( 'NONE',  ( -6.923076923076922462, -2.249999999999998668, 29.75000000000001776 ) ) ;
#16206 = CARTESIAN_POINT ( 'NONE',  ( 15.23076923076923173, -1.129524287112498415, 32.06866353760679544 ) ) ;
#16207 = EDGE_CURVE ( 'NONE', #20943, #35516, #74990, .T. ) ;
#16208 = EDGE_CURVE ( 'NONE', #88347, #57345, #70482, .T. ) ;
#16209 = CARTESIAN_POINT ( 'NONE',  ( -3.750000000000008438, -5.946699141100917352, 16.42187500000000000 ) ) ;
#16210 = ORIENTED_EDGE ( 'NONE', *, *, #15567, .F. ) ;
#16212 = EDGE_CURVE ( 'NONE', #69974, #46007, #38344, .T. ) ;
#16211 = VERTEX_POINT ( 'NONE', #36695 ) ;
#16213 = CARTESIAN_POINT ( 'NONE',  ( -15.23076923076922995, -8.564572088678739092, 35.78748833219616898 ) ) ;
#16214 = ORIENTED_EDGE ( 'NONE', *, *, #53478, .F. ) ;
#16215 = CARTESIAN_POINT ( 'NONE',  ( 17.20744851515672025, -4.299079248970731015, 33.91157788607253565 ) ) ;
#16216 = CARTESIAN_POINT ( 'NONE',  ( -1.384615384615383471, -5.180354513474913603, 36.12317359536750416 ) ) ;
#16217 = FACE_OUTER_BOUND ( 'NONE', #87561, .T. ) ;
#16218 = CARTESIAN_POINT ( 'NONE',  ( -8.703162418228330921, -10.51840700105979565, 33.73612834413962247 ) ) ;
#16219 = CARTESIAN_POINT ( 'NONE',  ( 1.553300858899087311, -3.749999999999992006, 15.48437500000000178 ) ) ;
#16220 = EDGE_CURVE ( 'NONE', #30874, #58158, #30378, .T. ) ;
#16221 = CARTESIAN_POINT ( 'NONE',  ( -8.096153846153844924, -2.499999999999998668, 29.75000000000000355 ) ) ;
#16222 = ORIENTED_EDGE ( 'NONE', *, *, #62521, .F. ) ;
#16223 = DIRECTION ( 'NONE',  ( -0.000000000000000000, 0.7660444431189791237, -0.6427876096865379196 ) ) ;
#16225 = EDGE_LOOP ( 'NONE', ( #25828, #32559 ) ) ;
#16224 = CARTESIAN_POINT ( 'NONE',  ( -10.61538461538461320, -10.67929555188718282, 33.92786785259544047 ) ) ;
#16226 = CARTESIAN_POINT ( 'NONE',  ( -12.46153846153846168, -5.471508081941601098, 34.59228464037088457 ) ) ;
#16227 = CARTESIAN_POINT ( 'NONE',  ( -9.822999158975251888, -12.11776431015576172, 31.66791131148498906 ) ) ;
#16228 = CYLINDRICAL_SURFACE ( 'NONE', #78316, 0.2499999999999997502 ) ;
#16229 = CARTESIAN_POINT ( 'NONE',  ( 11.76124120743959978, -8.540255544307065350, 34.89611431652622286 ) ) ;
#16230 = CYLINDRICAL_SURFACE ( 'NONE', #7657, 0.2499999999999986955 ) ;
#16231 = CARTESIAN_POINT ( 'NONE',  ( 3.230769230769110045, -2.625532179533779154, 30.86335684631627174 ) ) ;
#16232 = CARTESIAN_POINT ( 'NONE',  ( -3.775308065498748977, -8.992201783934593351, 15.26749329374151465 ) ) ;
#16233 = ORIENTED_EDGE ( 'NONE', *, *, #49145, .T. ) ;
#16234 = B_SPLINE_CURVE_WITH_KNOTS ( 'NONE', 3,
 ( #37539, #75987, #2859, #3314, #35445, #82760, #37997, #64556, #30786, #65465 ),
 .UNSPECIFIED., .F., .F.,
 ( 4, 2, 2, 2, 4 ),
 ( 0.0007817246256747484735, 0.0009771112852218920199, 0.001172497944769035566, 0.001367884604316179113, 0.001563271263863322659 ),
 .UNSPECIFIED. ) ;
#16235 = CARTESIAN_POINT ( 'NONE',  ( -5.142676505236408069, -7.249945578846651806, 34.99404164642496795 ) ) ;
#16236 = CARTESIAN_POINT ( 'NONE',  ( 0.4615384615384611200, -12.78798330534102945, 29.74999999999997868 ) ) ;
#16237 = CARTESIAN_POINT ( 'NONE',  ( -2.750000000000007105, -6.360912703474006946, 25.17187500000000000 ) ) ;
#16238 = VECTOR ( 'NONE', #37126, 1000.000000000000114 ) ;
#16239 = AXIS2_PLACEMENT_3D ( 'NONE', #61239, #14398, #5875 ) ;
#16240 = LINE ( 'NONE', #43272, #86381 ) ;
#16241 = CARTESIAN_POINT ( 'NONE',  ( 2.530471976670373380, -12.11081565061823717, 32.26097654155341843 ) ) ;
#16242 = VERTEX_POINT ( 'NONE', #57399 ) ;
#16243 = CYLINDRICAL_SURFACE ( 'NONE', #26898, 0.2499999999999998890 ) ;
#16244 = CARTESIAN_POINT ( 'NONE',  ( -15.45425415533356350, -4.225889041578353655, 33.85425143139329407 ) ) ;
#16245 = B_SPLINE_CURVE_WITH_KNOTS ( 'NONE', 3,
 ( #61198, #41836, #48129, #68409, #75180, #21097, #14807, #81942, #68852, #82824 ),
 .UNSPECIFIED., .F., .F.,
 ( 4, 2, 2, 2, 4 ),
 ( 0.0007817359430256294638, 0.0009771253907249941549, 0.001172514838424358954, 0.001367904286123723754, 0.001563293733823095492 ),
 .UNSPECIFIED. ) ;
#16246 = ADVANCED_FACE ( 'NONE', ( #84892 ), #29066, .T. ) ;
#16247 = AXIS2_PLACEMENT_3D ( 'NONE', #20264, #20699, #69337 ) ;
#16248 = ORIENTED_EDGE ( 'NONE', *, *, #35443, .F. ) ;
#16249 = CARTESIAN_POINT ( 'NONE',  ( 6.792928953345228393, -6.809168938359898782, 34.95455904226513866 ) ) ;
#16250 = EDGE_LOOP ( 'NONE', ( #78204, #1775, #48519, #50498 ) ) ;
#16251 = DIRECTION ( 'NONE',  ( -0.000000000000000000, 0.1736481776669307198, -0.9848077530122080203 ) ) ;
#16252 = CARTESIAN_POINT ( 'NONE',  ( 3.007842271862381622, -4.026226216239095379, 33.68668979543632958 ) ) ;
#16253 = CARTESIAN_POINT ( 'NONE',  ( -12.46153846153858424, -10.33852847137269571, 34.16647553114546554 ) ) ;
#16254 = CARTESIAN_POINT ( 'NONE',  ( -4.153846153846152411, -11.35647404775217417, 33.31231777344666511 ) ) ;
#16255 = EDGE_LOOP ( 'NONE', ( #61322, #80747 ) ) ;
#16256 = CARTESIAN_POINT ( 'NONE',  ( -2.437840277423998891, -12.15440758774515473, 32.17923288041532004 ) ) ;
#16257 = B_SPLINE_CURVE_WITH_KNOTS ( 'NONE', 3,
 ( #84050, #56560, #9697, #57883, #35852, #62849, #1168, #85368, #63753, #29537 ),
 .UNSPECIFIED., .F., .F.,
 ( 4, 2, 2, 2, 4 ),
 ( 0.000000000000000000, 0.0001954339857564073659, 0.0003908679715128147319, 0.0005863019572692221250, 0.0007817359430256294638 ),
 .UNSPECIFIED. ) ;
#16258 = ORIENTED_EDGE ( 'NONE', *, *, #81015, .F. ) ;
#16259 = CARTESIAN_POINT ( 'NONE',  ( -6.699700982378739234, -2.501478030877322567, 29.88021232661720816 ) ) ;
#16260 = CYLINDRICAL_SURFACE ( 'NONE', #5269, 0.2499999999999994726 ) ;
#16261 = ORIENTED_EDGE ( 'NONE', *, *, #38599, .F. ) ;
#16262 = CARTESIAN_POINT ( 'NONE',  ( 8.769230769230645706, -5.094484230521993062, 34.41647553114689373 ) ) ;
#16263 = CARTESIAN_POINT ( 'NONE',  ( -12.59168567097668401, -6.001485441113819874, 34.52039167877662607 ) ) ;
#16264 = DIRECTION ( 'NONE',  ( 0.000000000000000000, 0.3420201433256641055, -0.9396926207859100932 ) ) ;
#16265 = AXIS2_PLACEMENT_3D ( 'NONE', #5217, #87212, #79097 ) ;
#16266 = CARTESIAN_POINT ( 'NONE',  ( 1.318533005255250856, -6.343179335718451384, 34.87096338111212646 ) ) ;
#16267 = FACE_OUTER_BOUND ( 'NONE', #44988, .T. ) ;
#16268 = EDGE_CURVE ( 'NONE', #88393, #70106, #6232, .T. ) ;
#16270 = ORIENTED_EDGE ( 'NONE', *, *, #26498, .T. ) ;
#16269 = EDGE_CURVE ( 'NONE', #37364, #7653, #22338, .T. ) ;
#16271 = ORIENTED_EDGE ( 'NONE', *, *, #43978, .T. ) ;
#16272 = FACE_BOUND ( 'NONE', #73041, .T. ) ;
#16273 = EDGE_LOOP ( 'NONE', ( #23432, #74376 ) ) ;
#16274 = DIRECTION ( 'NONE',  ( -0.000000000000000000, -0.1736481776669307198, -0.9848077530122080203 ) ) ;
#16275 = EDGE_CURVE ( 'NONE', #72596, #27372, #1912, .T. ) ;
#16276 = EDGE_CURVE ( 'NONE', #16685, #61262, #54460, .T. ) ;
#16277 = DIRECTION ( 'NONE',  ( 0.000000000000000000, 0.4999999999999960032, -0.8660254037844410391 ) ) ;
#16278 = CYLINDRICAL_SURFACE ( 'NONE', #2199, 4.000000000000000000 ) ;
#16279 = ORIENTED_EDGE ( 'NONE', *, *, #41385, .F. ) ;
#16281 = EDGE_CURVE ( 'NONE', #66547, #37408, #70667, .T. ) ;
#16280 = ORIENTED_EDGE ( 'NONE', *, *, #82877, .F. ) ;
#16282 = CARTESIAN_POINT ( 'NONE',  ( 0.2386115026316120158, -8.282780595021769443, 34.94152052738834868 ) ) ;
#16283 = ORIENTED_EDGE ( 'NONE', *, *, #61363, .T. ) ;
#16284 = CARTESIAN_POINT ( 'NONE',  ( 2.057692307692309708, -7.500000000000001776, 35.00000000000000000 ) ) ;
#16285 = DIRECTION ( 'NONE',  ( 0.000000000000000000, 0.6427876096865373645, -0.7660444431189797898 ) ) ;
#16286 = EDGE_CURVE ( 'NONE', #70329, #485, #4237, .T. ) ;
#16287 = CARTESIAN_POINT ( 'NONE',  ( -12.39634547324380520, -2.255955759149235629, 29.99999999999988987 ) ) ;
#16288 = FACE_BOUND ( 'NONE', #22417, .T. ) ;
#16289 = ORIENTED_EDGE ( 'NONE', *, *, #30331, .T. ) ;
#16290 = VECTOR ( 'NONE', #47094, 1000.000000000000227 ) ;
#16291 = CARTESIAN_POINT ( 'NONE',  ( -8.519176349317316266, -4.074993327901527351, 33.72946981652012255 ) ) ;
#16292 = VECTOR ( 'NONE', #67358, 999.9999999999998863 ) ;
#16293 = FACE_OUTER_BOUND ( 'NONE', #56155, .T. ) ;
#16294 = EDGE_CURVE ( 'NONE', #74652, #24285, #66832, .T. ) ;
#16295 = CARTESIAN_POINT ( 'NONE',  ( -14.53117725141625627, -9.331801661448606566, 34.40259984581193464 ) ) ;
#16296 = CARTESIAN_POINT ( 'NONE',  ( 20.00000000000000000, -4.000000000000000000, 29.75000000000000355 ) ) ;
#16297 = VERTEX_POINT ( 'NONE', #4691 ) ;
#16298 = ORIENTED_EDGE ( 'NONE', *, *, #81831, .F. ) ;
#16299 = B_SPLINE_CURVE_WITH_KNOTS ( 'NONE', 3,
 ( #63170, #20860, #14108, #28970, #14551, #1037, #7798, #15447, #83914, #28514 ),
 .UNSPECIFIED., .F., .F.,
 ( 4, 2, 2, 2, 4 ),
 ( 0.0007817246256747472808, 0.0009771112852218907189, 0.001172497944769034265, 0.001367884604316177595, 0.001563271263863321141 ),
 .UNSPECIFIED. ) ;
#16300 = ORIENTED_EDGE ( 'NONE', *, *, #66974, .F. ) ;
#16302 = CARTESIAN_POINT ( 'NONE',  ( 10.68145296638705410, -5.557115091759786019, 34.35708131394839882 ) ) ;
#16301 = CARTESIAN_POINT ( 'NONE',  ( -7.976845312821407852, -6.413092428213692742, 34.63065189839063152 ) ) ;
#16303 = B_SPLINE_CURVE_WITH_KNOTS ( 'NONE', 3,
 ( #45932, #31082, #4051, #46388, #65316, #58551, #73869, #24778, #59458, #52246 ),
 .UNSPECIFIED., .F., .F.,
 ( 4, 2, 2, 2, 4 ),
 ( 0.000000000000000000, 0.0001954311564186863865, 0.0003908623128373727731, 0.0005862934692560591325, 0.0007817246256747455461 ),
 .UNSPECIFIED. ) ;
#16304 = CARTESIAN_POINT ( 'NONE',  ( -5.076923076923075762, -5.180354513474913603, 36.12317359536750416 ) ) ;
#16305 = CARTESIAN_POINT ( 'NONE',  ( -8.834500769787091201, -6.835583212224499938, 34.95778746994557906 ) ) ;
#16306 = FACE_BOUND ( 'NONE', #12655, .T. ) ;
#16307 = CARTESIAN_POINT ( 'NONE',  ( -11.78843828251013015, -2.318417181685855422, 30.59732222474233865 ) ) ;
#16308 = VERTEX_POINT ( 'NONE', #5130 ) ;
#16309 = ADVANCED_FACE ( 'NONE', ( #80358 ), #44309, .F. ) ;
#16310 = FACE_OUTER_BOUND ( 'NONE', #42104, .T. ) ;
#16311 = CARTESIAN_POINT ( 'NONE',  ( 9.692307692307570832, -11.06231777344772027, 33.60647404775119895 ) ) ;
#16312 = CARTESIAN_POINT ( 'NONE',  ( -17.30040802064702632, -11.89387501736623420, 32.13663884655804992 ) ) ;
#16313 = DIRECTION ( 'NONE',  ( -0.000000000000000000, -0.6427876096865404731, -0.7660444431189770143 ) ) ;
#16314 = ORIENTED_EDGE ( 'NONE', *, *, #52590, .F. ) ;
#16315 = DIRECTION ( 'NONE',  ( -0.000000000000000000, 0.1736481776669307198, -0.9848077530122080203 ) ) ;
#16316 = EDGE_CURVE ( 'NONE', #19193, #13671, #13723, .T. ) ;
#16317 = VERTEX_POINT ( 'NONE', #17762 ) ;
#16318 = FACE_BOUND ( 'NONE', #32688, .T. ) ;
#16319 = CARTESIAN_POINT ( 'NONE',  ( 4.284636594813102661, -2.494656445102013453, 31.33466734024120015 ) ) ;
#16320 = CARTESIAN_POINT ( 'NONE',  ( 12.33139125210024112, -12.27039167877662251, 31.24851455888617835 ) ) ;
#16321 = EDGE_LOOP ( 'NONE', ( #56359, #34421 ) ) ;
#16322 = CARTESIAN_POINT ( 'NONE',  ( 4.153846153846154188, -11.35647404775217417, 33.31231777344666511 ) ) ;
#16323 = CARTESIAN_POINT ( 'NONE',  ( -2.242436736416281384, -4.481592998940250538, 33.73612834413965089 ) ) ;
#16324 = CARTESIAN_POINT ( 'NONE',  ( 22.00000000000000711, 9.999999999999991118, 10.00000000000000178 ) ) ;
#16325 = LINE ( 'NONE', #37024, #28785 ) ;
#16326 = EDGE_LOOP ( 'NONE', ( #11730, #54376 ) ) ;
#16327 = ADVANCED_FACE ( 'NONE', ( #45216 ), #31720, .T. ) ;
#16328 = DIRECTION ( 'NONE',  ( 0.000000000000000000, 0.000000000000000000, -1.000000000000000000 ) ) ;
#16329 = VERTEX_POINT ( 'NONE', #6466 ) ;
#16332 = EDGE_LOOP ( 'NONE', ( #11175, #80174, #67997, #43532, #57382 ) ) ;
#16331 = CIRCLE ( 'NONE', #52264, 4.000000000000000000 ) ;
#16330 = CYLINDRICAL_SURFACE ( 'NONE', #69808, 2.000000000000001776 ) ;
#16333 = CARTESIAN_POINT ( 'NONE',  ( -8.834554782035079157, -7.749976730030849303, 34.74374725381503737 ) ) ;
#16334 = CARTESIAN_POINT ( 'NONE',  ( 15.10007776410167857, -2.729777683071817229, 31.24903638046269450 ) ) ;
#16335 = CARTESIAN_POINT ( 'NONE',  ( -15.23076923076935252, -11.06231777344772027, 33.60647404775119895 ) ) ;
#16336 = FACE_OUTER_BOUND ( 'NONE', #37901, .T. ) ;
#16337 = DIRECTION ( 'NONE',  ( -0.000000000000000000, 0.000000000000000000, 1.000000000000000000 ) ) ;
#16338 = EDGE_CURVE ( 'NONE', #12423, #28595, #74475, .T. ) ;
#16339 = DIRECTION ( 'NONE',  ( -0.000000000000000000, 0.1736481776669307198, -0.9848077530122080203 ) ) ;
#16340 = CARTESIAN_POINT ( 'NONE',  ( -1.409462824231155764E-14, -4.749999999999999112, 21.65625000000000355 ) ) ;
#16341 = VERTEX_POINT ( 'NONE', #54630 ) ;
#16342 = CARTESIAN_POINT ( 'NONE',  ( -14.98082371242109012, -3.712312575010499049, 33.01462480002815170 ) ) ;
#16343 = CARTESIAN_POINT ( 'NONE',  ( 5.076923076923075762, -9.584722331328613620, 36.20867863119891439 ) ) ;
#16344 = EDGE_LOOP ( 'NONE', ( #693, #59782 ) ) ;
#16345 = EDGE_LOOP ( 'NONE', ( #49884, #75544, #54084, #55053 ) ) ;
#16346 = EDGE_LOOP ( 'NONE', ( #88747, #13043, #68580, #14632 ) ) ;
#16347 = CARTESIAN_POINT ( 'NONE',  ( -10.68065506134539078, -11.48612834413959582, 32.76840700105983473 ) ) ;
#16348 = CARTESIAN_POINT ( 'NONE',  ( 6.000000000000001776, -12.29105614889573062, 35.45975837776705220 ) ) ;
#16349 = EDGE_CURVE ( 'NONE', #65895, #19974, #53754, .T. ) ;
#16350 = CARTESIAN_POINT ( 'NONE',  ( 6.222779541268408821, -11.41317474335729187, 32.86274602512330034 ) ) ;
#16351 = FACE_OUTER_BOUND ( 'NONE', #7286, .T. ) ;
#16352 = CARTESIAN_POINT ( 'NONE',  ( 5.999999999999880096, -2.625532179533778709, 30.86335684631627174 ) ) ;
#16353 = EDGE_CURVE ( 'NONE', #38648, #3292, #6027, .T. ) ;
#16354 = CARTESIAN_POINT ( 'NONE',  ( 16.37685899793955357, -3.395485233115139501, 33.02377354290276656 ) ) ;
#16355 = CARTESIAN_POINT ( 'NONE',  ( 13.63461538461538680, -2.249999999999998668, 29.75000000000000355 ) ) ;
#16356 = ORIENTED_EDGE ( 'NONE', *, *, #65444, .T. ) ;
#16357 = CARTESIAN_POINT ( 'NONE',  ( -3.903791842207838148, -5.728107161865378494, 34.42597550085002922 ) ) ;
#16358 = CARTESIAN_POINT ( 'NONE',  ( -1.634638621908349077, -6.695914987888143877, 34.68535235679833306 ) ) ;
#16359 = CARTESIAN_POINT ( 'NONE',  ( -9.469528151039282804, -11.41317474335729543, 32.86274602512330034 ) ) ;
#16360 = CARTESIAN_POINT ( 'NONE',  ( 12.23805351781451201, -11.89387501736622710, 32.13663884655806413 ) ) ;
#16361 = ORIENTED_EDGE ( 'NONE', *, *, #38894, .F. ) ;
#16362 = CARTESIAN_POINT ( 'NONE',  ( 18.75000000000000000, -7.500000000000000000, 29.75000000000000355 ) ) ;
#16363 = VECTOR ( 'NONE', #39747, 1000.000000000000114 ) ;
#16364 = AXIS2_PLACEMENT_3D ( 'NONE', #28114, #62770, #26346 ) ;
#16365 = VERTEX_POINT ( 'NONE', #33495 ) ;
#16366 = CARTESIAN_POINT ( 'NONE',  ( -17.32694630114453460, -2.588893531581426544, 31.60682220781847818 ) ) ;
#16367 = CYLINDRICAL_SURFACE ( 'NONE', #959, 4.000000000000000000 ) ;
#16368 = CARTESIAN_POINT ( 'NONE',  ( 9.692307692307695177, -2.499999999999998668, 29.50000000000001066 ) ) ;
#16369 = ORIENTED_EDGE ( 'NONE', *, *, #81297, .F. ) ;
#16370 = B_SPLINE_CURVE_WITH_KNOTS ( 'NONE', 3,
 ( #80853, #61000, #59223, #83053, #56012, #34850, #47925, #42072, #20463, #35300 ),
 .UNSPECIFIED., .F., .F.,
 ( 4, 2, 2, 2, 4 ),
 ( 0.000000000000000000, 0.0001954339857564100493, 0.0003908679715128200987, 0.0005863019572692301480, 0.0007817359430256401974 ),
 .UNSPECIFIED. ) ;
#16371 = DIRECTION ( 'NONE',  ( 0.7057856980126718804, 0.7057856980126787638, 0.06109907496453181874 ) ) ;
#16372 = FACE_OUTER_BOUND ( 'NONE', #86552, .T. ) ;
#16373 = CARTESIAN_POINT ( 'NONE',  ( 9.468822767743361624, -3.019605429927184392, 32.48692288466676814 ) ) ;
#16374 = CARTESIAN_POINT ( 'NONE',  ( -9.019253993452224449, -9.356822207818506598, 34.66110646841856635 ) ) ;
#16375 = ORIENTED_EDGE ( 'NONE', *, *, #41533, .F. ) ;
#16376 = CARTESIAN_POINT ( 'NONE',  ( -0.4615384615385826339, -8.613356846316285953, 34.62446782046622218 ) ) ;
#16377 = ORIENTED_EDGE ( 'NONE', *, *, #88796, .F. ) ;
#16378 = CARTESIAN_POINT ( 'NONE',  ( -8.769230769230768274, -1.466349020453238561, 30.81389545987213907 ) ) ;
#16379 = CARTESIAN_POINT ( 'NONE',  ( -16.15384615384615330, -8.810774026931790459, 35.74407628777942847 ) ) ;
#16380 = CARTESIAN_POINT ( 'NONE',  ( 12.33084699487090319, -8.147922237126337563, 34.70805685702651999 ) ) ;
#16381 = EDGE_CURVE ( 'NONE', #52756, #16542, #34367, .T. ) ;
#16382 = CARTESIAN_POINT ( 'NONE',  ( 15.23076923076911093, -10.90142922262034020, 33.41473453929536674 ) ) ;
#16383 = CYLINDRICAL_SURFACE ( 'NONE', #3542, 0.2500000000000008882 ) ;
#16384 = ORIENTED_EDGE ( 'NONE', *, *, #71516, .T. ) ;
#16385 = AXIS2_PLACEMENT_3D ( 'NONE', #54175, #68586, #13207 ) ;
#16386 = EDGE_CURVE ( 'NONE', #20537, #10414, #39811, .T. ) ;
#16387 = ORIENTED_EDGE ( 'NONE', *, *, #3589, .F. ) ;
#16388 = ORIENTED_EDGE ( 'NONE', *, *, #84313, .F. ) ;
#16389 = PLANE ( 'NONE',  #38761 ) ;
#16390 = CARTESIAN_POINT ( 'NONE',  ( -6.416666666666667851, -3.499999999999999556, 29.75000000000000355 ) ) ;
#16391 = EDGE_CURVE ( 'NONE', #75823, #68357, #27171, .T. ) ;
#16392 = B_SPLINE_CURVE_WITH_KNOTS ( 'NONE', 3,
 ( #37986, #45175, #86189, #108, #14502, #60916, #41988, #6430, #34771, #69451 ),
 .UNSPECIFIED., .F., .F.,
 ( 4, 2, 2, 2, 4 ),
 ( 0.0007817359430256365111, 0.0009771253907250043464, 0.001172514838424372399, 0.001367904286123740234, 0.001563293733823108069 ),
 .UNSPECIFIED. ) ;
#16393 = CARTESIAN_POINT ( 'NONE',  ( 17.07692307692307665, -4.098570777380720287, 33.41473453929634729 ) ) ;
#16394 = CARTESIAN_POINT ( 'NONE',  ( -16.15384615384627409, -2.625532179533778709, 30.86335684631627174 ) ) ;
#16395 = CARTESIAN_POINT ( 'NONE',  ( 11.28848480751918437, -12.17611988154120972, 31.52148481390971213 ) ) ;
#16396 = FACE_OUTER_BOUND ( 'NONE', #893, .T. ) ;
#16397 = LINE ( 'NONE', #34891, #42336 ) ;
#16398 = EDGE_LOOP ( 'NONE', ( #43805, #41552 ) ) ;
#16399 = ORIENTED_EDGE ( 'NONE', *, *, #78408, .F. ) ;
#16400 = EDGE_LOOP ( 'NONE', ( #23675, #75701, #69456, #78793, #71797, #53091 ) ) ;
#16401 = EDGE_CURVE ( 'NONE', #6730, #36558, #47051, .T. ) ;
#16403 = VERTEX_POINT ( 'NONE', #60514 ) ;
#16402 = CARTESIAN_POINT ( 'NONE',  ( 11.78851595837499566, -2.544122305571458575, 31.48381861865057729 ) ) ;
#16405 = CARTESIAN_POINT ( 'NONE',  ( -8.638705067467208565, -11.46989282347013095, 32.79007818306219946 ) ) ;
#16404 = LINE ( 'NONE', #29053, #27361 ) ;
#16406 = CARTESIAN_POINT ( 'NONE',  ( 8.900069187243529356, -7.277220443632450575, 34.74524770363009196 ) ) ;
#16407 = CARTESIAN_POINT ( 'NONE',  ( -2.651650429449535551, -10.15165042944956753, 24.93750000000000000 ) ) ;
#16408 = ORIENTED_EDGE ( 'NONE', *, *, #65534, .T. ) ;
#16409 = VECTOR ( 'NONE', #80786, 1000.000000000000114 ) ;
#16410 = EDGE_LOOP ( 'NONE', ( #18360, #58582, #56743, #19452 ) ) ;
#16411 =( REPRESENTATION_RELATIONSHIP ('NONE','NONE', #51743, #11000 ) REPRESENTATION_RELATIONSHIP_WITH_TRANSFORMATION ( #66724 )SHAPE_REPRESENTATION_RELATIONSHIP( ) );
#16412 = CARTESIAN_POINT ( 'NONE',  ( -11.60454391782167605, -11.91647553114624181, 32.58852847137148245 ) ) ;
#16413 = EDGE_CURVE ( 'NONE', #25620, #67642, #63161, .T. ) ;
#16414 = B_SPLINE_CURVE_WITH_KNOTS ( 'NONE', 3,
 ( #14454, #82484, #20763, #8145, #56325, #41482, #6381, #40607, #74837, #41932 ),
 .UNSPECIFIED., .F., .F.,
 ( 4, 2, 2, 2, 4 ),
 ( 0.0007817246336856291692, 0.0009771112958940105907, 0.001172497958102391904, 0.001367884620310773434, 0.001563271282519154747 ),
 .UNSPECIFIED. ) ;
#16415 = EDGE_LOOP ( 'NONE', ( #48474, #84559, #55470, #30025 ) ) ;
#16416 = FACE_BOUND ( 'NONE', #73107, .T. ) ;
#16417 = CARTESIAN_POINT ( 'NONE',  ( -6.222926217516146608, -9.086856451489516928, 34.49173150075333183 ) ) ;
#16418 = VECTOR ( 'NONE', #41194, 1000.000000000000000 ) ;
#16419 = CARTESIAN_POINT ( 'NONE',  ( 9.692307692307695177, -4.786620604624113540, 33.94971097300155094 ) ) ;
#16420 = ORIENTED_EDGE ( 'NONE', *, *, #74834, .F. ) ;
#16421 = CARTESIAN_POINT ( 'NONE',  ( -15.00798968950081758, -5.114059244376869984, 34.14424750095245287 ) ) ;
#16422 = EDGE_CURVE ( 'NONE', #10508, #63945, #7355, .T. ) ;
#16423 = CARTESIAN_POINT ( 'NONE',  ( 16.40379167219429490, -4.336752205174650321, 33.62275283266504289 ) ) ;
#16424 = FACE_OUTER_BOUND ( 'NONE', #13202, .T. ) ;
#16425 = DIRECTION ( 'NONE',  ( 0.000000000000000000, 0.000000000000000000, -1.000000000000000000 ) ) ;
#16426 = CARTESIAN_POINT ( 'NONE',  ( 1.384615384615386802, -2.486705287966279876, 31.30864560766543647 ) ) ;
#16427 = EDGE_LOOP ( 'NONE', ( #45138, #48937, #69979, #35694 ) ) ;
#16428 = CARTESIAN_POINT ( 'NONE',  ( 10.61538461538449596, -8.613356846316285953, 34.62446782046622218 ) ) ;
#16429 = FACE_OUTER_BOUND ( 'NONE', #77318, .T. ) ;
#16430 = CARTESIAN_POINT ( 'NONE',  ( 2.084207383127980595, -12.11044203135681840, 32.26167407432752299 ) ) ;
#16431 = CARTESIAN_POINT ( 'NONE',  ( 0.2386122440223129304, -11.76352882383564769, 32.36236540154569497 ) ) ;
#16432 = PLANE ( 'NONE',  #54429 ) ;
#16433 = CARTESIAN_POINT ( 'NONE',  ( -18.00000000000000000, -8.563426751879235965, 35.78099280442780383 ) ) ;
#16434 = CARTESIAN_POINT ( 'NONE',  ( -13.13456096470193302, -12.41089969410671223, 31.60739465890703670 ) ) ;
#16436 = CARTESIAN_POINT ( 'NONE',  ( 2.438484115517095763, -9.804649428959608670, 34.18742332936588468 ) ) ;
#16435 = DIRECTION ( 'NONE',  ( 1.000000000000000000, 0.000000000000000000, 0.000000000000000000 ) ) ;
#16437 = EDGE_CURVE ( 'NONE', #40122, #87461, #13657, .T. ) ;
#16438 = LINE ( 'NONE', #43907, #32432 ) ;
#16440 = LINE ( 'NONE', #23634, #36356 ) ;
#16439 = CYLINDRICAL_SURFACE ( 'NONE', #27120, 0.2500000000000008882 ) ;
#16441 = CARTESIAN_POINT ( 'NONE',  ( 13.31929246912321396, -7.749976743299138882, 34.99404534957040624 ) ) ;
#16442 = B_SPLINE_CURVE_WITH_KNOTS ( 'NONE', 3,
 ( #2218, #76114, #16188, #14416, #28831, #76567 ),
 .UNSPECIFIED., .F., .F.,
 ( 4, 2, 4 ),
 ( 3.508529156471553821E-17, 0.0001954756301637064486, 0.0003909512603273778233 ),
 .UNSPECIFIED. ) ;
#16443 = CARTESIAN_POINT ( 'NONE',  ( -0.06109907496454585613, -4.750000000000000000, 25.15438170625849068 ) ) ;
#16444 = ORIENTED_EDGE ( 'NONE', *, *, #41996, .F. ) ;
#16445 = CARTESIAN_POINT ( 'NONE',  ( 3.174020486757124004, -8.011881170783730965, 14.00000000000000888 ) ) ;
#16446 = ORIENTED_EDGE ( 'NONE', *, *, #27668, .F. ) ;
#16447 = CARTESIAN_POINT ( 'NONE',  ( -2.307692307692305711, -2.833524468853757305, 32.15551576947925838 ) ) ;
#16448 = EDGE_LOOP ( 'NONE', ( #35587, #24721 ) ) ;
#16449 = CARTESIAN_POINT ( 'NONE',  ( -15.23076923076922995, -3.513871655860378418, 32.76840700105978499 ) ) ;
#16450 = ORIENTED_EDGE ( 'NONE', *, *, #50493, .F. ) ;
#16451 = CARTESIAN_POINT ( 'NONE',  ( -6.249976730942353953, -11.79746400365624659, 32.30657167506340954 ) ) ;
#16452 = CARTESIAN_POINT ( 'NONE',  ( 2.775308065498768517, -8.577988221561467341, 24.29500670625849423 ) ) ;
#16453 = CARTESIAN_POINT ( 'NONE',  ( 7.596177102105253987, -8.347322224742351082, 34.93158281831414769 ) ) ;
#16454 = ADVANCED_FACE ( 'NONE', ( #74929 ), #60954, .F. ) ;
#16455 = CARTESIAN_POINT ( 'NONE',  ( 6.700150705560775855, -11.24512374952581872, 33.06303171183252942 ) ) ;
#16456 = CARTESIAN_POINT ( 'NONE',  ( -2.980823821391187511, -12.45601412856602686, 31.48342859153981621 ) ) ;
#16457 = CARTESIAN_POINT ( 'NONE',  ( 15.93036122928182330, -8.539481045369598178, 34.89627647299170832 ) ) ;
#16458 = AXIS2_PLACEMENT_3D ( 'NONE', #31615, #87469, #51401 ) ;
#16459 = CARTESIAN_POINT ( 'NONE',  ( -17.87219494718144119, -2.249999999999999556, 29.52383875849255546 ) ) ;
#16460 = CARTESIAN_POINT ( 'NONE',  ( 1.384615384615264011, -5.094484230521993062, 34.41647553114689373 ) ) ;
#16461 = CARTESIAN_POINT ( 'NONE',  ( -14.08491263871423982, -4.989023458446560255, 34.36081565061822118 ) ) ;
#16462 = CARTESIAN_POINT ( 'NONE',  ( -1.553300858899081538, -11.25000000000000711, 16.10937500000000355 ) ) ;
#16463 = EDGE_CURVE ( 'NONE', #87599, #19612, #791, .T. ) ;
#16464 = EDGE_CURVE ( 'NONE', #56650, #33104, #51230, .T. ) ;
#16465 = DIRECTION ( 'NONE',  ( -0.000000000000000000, 1.000000000000000000, -0.000000000000000000 ) ) ;
#16466 = CARTESIAN_POINT ( 'NONE',  ( 17.07692307692307665, -2.486705287966279876, 31.30864560766543647 ) ) ;
#16467 = CARTESIAN_POINT ( 'NONE',  ( 7.134615384615385025, -3.499999999999999556, 29.75000000000000355 ) ) ;
#16468 = CARTESIAN_POINT ( 'NONE',  ( -1.553300858899125059, -3.750000000000009326, 15.32812500000000355 ) ) ;
#16469 = ADVANCED_FACE ( 'NONE', ( #21745 ), #36163, .F. ) ;
#16470 = ORIENTED_EDGE ( 'NONE', *, *, #4354, .T. ) ;
#16471 = CARTESIAN_POINT ( 'NONE',  ( 17.14217864819909920, -12.27809138561124591, 31.22303859784720359 ) ) ;
#16472 = CARTESIAN_POINT ( 'NONE',  ( 11.78840705680968171, -5.852078868378309373, 34.47109172314383585 ) ) ;
#16473 = CARTESIAN_POINT ( 'NONE',  ( 6.923076923076924238, -2.708943851104267164, 35.45975837776705220 ) ) ;
#16474 = CARTESIAN_POINT ( 'NONE',  ( 15.45419562968402261, -7.630147987733840509, 34.99859428049665411 ) ) ;
#16475 = CARTESIAN_POINT ( 'NONE',  ( 3.930361229281823743, -3.562934362175799841, 33.22335522853832401 ) ) ;
#16476 = B_SPLINE_CURVE_WITH_KNOTS ( 'NONE', 3,
 ( #40582, #12216, #54518, #80232, #81568, #47318, #53185, #66260, #68051, #33811 ),
 .UNSPECIFIED., .F., .F.,
 ( 4, 2, 2, 2, 4 ),
 ( 0.000000000000000000, 0.0001954311584214072652, 0.0003908623168428145304, 0.0005862934752642217414, 0.0007817246336856290608 ),
 .UNSPECIFIED. ) ;
#16477 = LINE ( 'NONE', #70979, #9790 ) ;
#16478 = B_SPLINE_CURVE_WITH_KNOTS ( 'NONE', 3,
 ( #29708, #21608, #1338, #49080, #82447, #48192, #75665, #27930, #14870, #8106 ),
 .UNSPECIFIED., .F., .F.,
 ( 4, 2, 2, 2, 4 ),
 ( 0.0007817359430256341259, 0.0009771253907250067317, 0.001172514838424372399, 0.001367904286123738065, 0.001563293733823103732 ),
 .UNSPECIFIED. ) ;
#16479 = AXIS2_PLACEMENT_3D ( 'NONE', #63920, #86445, #37331 ) ;
#16480 = VERTEX_POINT ( 'NONE', #83909 ) ;
#16481 = CARTESIAN_POINT ( 'NONE',  ( 1.326923076923075762, -3.499999999999999556, 29.75000000000000355 ) ) ;
#16482 = EDGE_LOOP ( 'NONE', ( #58013, #40567 ) ) ;
#16483 = AXIS2_PLACEMENT_3D ( 'NONE', #58452, #17489, #73321 ) ;
#16484 = ORIENTED_EDGE ( 'NONE', *, *, #79684, .F. ) ;
#16485 = CARTESIAN_POINT ( 'NONE',  ( -0.2385256174450663957, -5.582272713120728369, 34.63742843783360570 ) ) ;
#16486 = VECTOR ( 'NONE', #81157, 1000.000000000000114 ) ;
#16487 = DIRECTION ( 'NONE',  ( -0.000000000000000000, -0.000000000000000000, -1.000000000000000000 ) ) ;
#16488 = DIRECTION ( 'NONE',  ( -1.000000000000000000, -0.000000000000000000, -0.000000000000000000 ) ) ;
#16489 = CARTESIAN_POINT ( 'NONE',  ( -6.250023237292964495, -3.202444869320336451, 32.30641848906366675 ) ) ;
#16490 = CARTESIAN_POINT ( 'NONE',  ( -3.903846153844733102, -7.500000000000154543, 35.00000000000007105 ) ) ;
#16491 = ORIENTED_EDGE ( 'NONE', *, *, #69732, .T. ) ;
#16492 = FACE_OUTER_BOUND ( 'NONE', #72236, .T. ) ;
#16493 = ORIENTED_EDGE ( 'NONE', *, *, #58312, .F. ) ;
#16494 = ORIENTED_EDGE ( 'NONE', *, *, #12411, .F. ) ;
#16495 = CARTESIAN_POINT ( 'NONE',  ( 1.384615384615386802, -11.16473453929635440, 33.15142922261926373 ) ) ;
#16496 = CARTESIAN_POINT ( 'NONE',  ( 0.4615384615384611200, -1.117168528481311540, 33.14645433367849847 ) ) ;
#16497 = CARTESIAN_POINT ( 'NONE',  ( -10.86536134632696715, -4.943428324936578910, 34.04746400365624481 ) ) ;
#16498 = B_SPLINE_CURVE_WITH_KNOTS ( 'NONE', 3,
 ( #87011, #25283, #80234, #66715, #54520, #11775, #74363, #54071, #46879, #87910 ),
 .UNSPECIFIED., .F., .F.,
 ( 4, 2, 2, 2, 4 ),
 ( 0.000000000000000000, 0.0001954339857564080165, 0.0003908679715128160329, 0.0005863019572692240765, 0.0007817359430256320659 ),
 .UNSPECIFIED. ) ;
#16499 = CARTESIAN_POINT ( 'NONE',  ( -17.07692307692319744, -3.300289026999228437, 32.46337939537709616 ) ) ;
#16500 = DIRECTION ( 'NONE',  ( 0.000000000000000000, -1.000000000000000000, -8.673617379884033500E-16 ) ) ;
#16501 = EDGE_LOOP ( 'NONE', ( #66558, #67766, #80578, #83136 ) ) ;
#16502 = EDGE_LOOP ( 'NONE', ( #86771, #49639, #9484, #5022 ) ) ;
#16503 = CARTESIAN_POINT ( 'NONE',  ( 1.553300858899129944, -11.24999999999998934, 22.20312500000000000 ) ) ;
#16504 = VECTOR ( 'NONE', #50118, 999.9999999999998863 ) ;
#16505 = ORIENTED_EDGE ( 'NONE', *, *, #22369, .T. ) ;
#16507 = ORIENTED_EDGE ( 'NONE', *, *, #31530, .T. ) ;
#16506 = CARTESIAN_POINT ( 'NONE',  ( -14.24243716817946925, -2.379036618887895305, 30.90682066428158592 ) ) ;
#16508 = FACE_OUTER_BOUND ( 'NONE', #14895, .T. ) ;
#16509 = DIRECTION ( 'NONE',  ( 1.000000000000000000, 0.000000000000000000, 0.000000000000000000 ) ) ;
#16510 = LINE ( 'NONE', #28705, #42247 ) ;
#16511 = VERTEX_POINT ( 'NONE', #9132 ) ;
#16512 = CARTESIAN_POINT ( 'NONE',  ( 15.23076923076923173, -2.486705287966279876, 31.30864560766543647 ) ) ;
#16513 = EDGE_LOOP ( 'NONE', ( #46297, #55250 ) ) ;
#16514 = CARTESIAN_POINT ( 'NONE',  ( 15.36155967173617931, -11.37503395064541678, 33.29242100308974273 ) ) ;
#16515 = CARTESIAN_POINT ( 'NONE',  ( 10.74617642320940725, -8.999086150933475636, 34.52020707165672775 ) ) ;
#16516 = EDGE_CURVE ( 'NONE', #81813, #33011, #18983, .T. ) ;
#16517 = CARTESIAN_POINT ( 'NONE',  ( -17.77698715590659972, -2.523321265292116866, 31.42251411153756990 ) ) ;
#16519 = CARTESIAN_POINT ( 'NONE',  ( -10.83886953994894498, -5.827078755546623690, 34.72654668319379567 ) ) ;
#16518 = CARTESIAN_POINT ( 'NONE',  ( 10.36538461538461675, -7.500000000000001776, 34.75000000000000000 ) ) ;
#16520 = CARTESIAN_POINT ( 'NONE',  ( 4.853996859406926490, -2.554751324335733820, 30.48935550225260727 ) ) ;
#16521 = CARTESIAN_POINT ( 'NONE',  ( -0.2114840416250090838, -12.65882529074907126, 30.72640787790839312 ) ) ;
#16522 = ORIENTED_EDGE ( 'NONE', *, *, #11989, .T. ) ;
#16523 = CARTESIAN_POINT ( 'NONE',  ( -11.47239318745910275, -4.098570777380720287, 33.41473453929635440 ) ) ;
#16524 = CARTESIAN_POINT ( 'NONE',  ( -6.222926958906846551, -11.43668979543635089, 33.22377378376089752 ) ) ;
#16525 = ORIENTED_EDGE ( 'NONE', *, *, #38209, .T. ) ;
#16526 = CARTESIAN_POINT ( 'NONE',  ( -16.40386937806761836, -12.68155406624981119, 30.59749803192733708 ) ) ;
#16527 = CARTESIAN_POINT ( 'NONE',  ( -4.853911725310227077, -5.667800583137508674, 34.40243808032445827 ) ) ;
#16528 = DIRECTION ( 'NONE',  ( 1.000000000000000000, 0.000000000000000000, 0.000000000000000000 ) ) ;
#16529 = CARTESIAN_POINT ( 'NONE',  ( -5.207070286361298095, -11.93770438780619259, 32.05411857736982029 ) ) ;
#16530 = CARTESIAN_POINT ( 'NONE',  ( -10.61538461538461320, -2.833524468853757305, 32.15551576947925838 ) ) ;
#16531 = CARTESIAN_POINT ( 'NONE',  ( 2.307692307692187583, -8.613356846316285953, 34.62446782046622218 ) ) ;
#16532 = CIRCLE ( 'NONE', #730, 0.2500000000000002220 ) ;
#16533 = FACE_BOUND ( 'NONE', #14596, .T. ) ;
#16535 = CARTESIAN_POINT ( 'NONE',  ( -10.74585980046033562, -7.276987145209185215, 34.99546412871779211 ) ) ;
#16534 = CARTESIAN_POINT ( 'NONE',  ( 12.33139049180676672, -10.31621877034669588, 34.18098118002070152 ) ) ;
#16536 = ADVANCED_FACE ( 'NONE', ( #64479 ), #22193, .F. ) ;
#16537 = CARTESIAN_POINT ( 'NONE',  ( -12.21153846153846168, -2.249999999999998668, 29.75000000000000355 ) ) ;
#16539 = CARTESIAN_POINT ( 'NONE',  ( 9.692307692307572609, -4.481592998941358097, 33.73612834414048933 ) ) ;
#16538 = CARTESIAN_POINT ( 'NONE',  ( -4.946132635956127288, -9.929761469519744921, 34.40412654351204225 ) ) ;
#16540 = DIRECTION ( 'NONE',  ( -1.000000000000000000, -0.000000000000000000, -0.000000000000000000 ) ) ;
#16541 = CARTESIAN_POINT ( 'NONE',  ( 2.694853999681214862, -10.10844685921789043, 18.12313170625849068 ) ) ;
#16542 = VERTEX_POINT ( 'NONE', #29405 ) ;
#16543 = AXIS2_PLACEMENT_3D ( 'NONE', #68040, #45975, #45534 ) ;
#16544 = LINE ( 'NONE', #44010, #67972 ) ;
#16545 = CARTESIAN_POINT ( 'NONE',  ( -4.826868765284762830, -3.136992222400443175, 32.19305428654138979 ) ) ;
#16546 = CARTESIAN_POINT ( 'NONE',  ( -0.5922290646487706756, -3.338472653186242756, 32.95098750199972670 ) ) ;
#16547 = CARTESIAN_POINT ( 'NONE',  ( 14.30769230769231015, -11.33034616979429110, 35.88435417666054406 ) ) ;
#16548 = CARTESIAN_POINT ( 'NONE',  ( 6.792386319966616348, -12.62707690430377383, 30.88035979386743435 ) ) ;
#16549 = CARTESIAN_POINT ( 'NONE',  ( -9.561515884482904681, -4.118422570099831148, 33.43335022499816489 ) ) ;
#16550 = CARTESIAN_POINT ( 'NONE',  ( 3.749999999999999556, -7.438900925035446754, 21.71688170625848713 ) ) ;
#16551 = CARTESIAN_POINT ( 'NONE',  ( -16.37677311275299985, -5.582147617184174848, 34.63737895849758530 ) ) ;
#16552 = CARTESIAN_POINT ( 'NONE',  ( -39.05038313613820122, -2.499999999999999556, 29.75000000000000355 ) ) ;
#16553 = CARTESIAN_POINT ( 'NONE',  ( -17.07692307692307665, -5.557115091759785130, 34.35708131394839171 ) ) ;
#16554 = DIRECTION ( 'NONE',  ( -0.000000000000000000, 0.3420201433256694901, -0.9396926207859082059 ) ) ;
#16555 = CARTESIAN_POINT ( 'NONE',  ( -16.94639763868943660, -5.070358843744209310, 34.40418822224088302 ) ) ;
#16556 = CARTESIAN_POINT ( 'NONE',  ( 4.153846153846154188, -4.945431358278436385, 36.03766855953609394 ) ) ;
#16557 = EDGE_CURVE ( 'NONE', #32412, #19193, #83011, .T. ) ;
#16558 = EDGE_CURVE ( 'NONE', #74563, #47506, #55498, .T. ) ;
#16559 = DIRECTION ( 'NONE',  ( 0.000000000000000000, 0.7660444431189807890, 0.6427876096865361433 ) ) ;
#16560 = CARTESIAN_POINT ( 'NONE',  ( 17.32686848630112308, -2.589246495874658827, 31.60778113518102828 ) ) ;
#16561 = VERTEX_POINT ( 'NONE', #84350 ) ;
#16562 = CARTESIAN_POINT ( 'NONE',  ( 15.10007862765892739, -11.37499894934982692, 33.29245874905763003 ) ) ;
#16563 = CARTESIAN_POINT ( 'NONE',  ( -17.20707028636129365, -2.882441371585227508, 31.66841991370172238 ) ) ;
#16564 = CARTESIAN_POINT ( 'NONE',  ( -1.492201783934593573, -3.724691934501250135, 15.57999329374151110 ) ) ;
#16565 = B_SPLINE_CURVE_WITH_KNOTS ( 'NONE', 3,
 ( #33741, #5388, #47246, #88708, #81054, #20663, #68851, #54004, #40512, #34625 ),
 .UNSPECIFIED., .F., .F.,
 ( 4, 2, 2, 2, 4 ),
 ( 0.0007817246256747463051, 0.0009771112852218896347, 0.001172497944769032747, 0.001367884604316176077, 0.001563271263863319407 ),
 .UNSPECIFIED. ) ;
#16566 = ADVANCED_FACE ( 'NONE', ( #49659 ), #77135, .F. ) ;
#16567 = CARTESIAN_POINT ( 'NONE',  ( 7.053602361310566948, -11.04252011169590020, 33.62494198852677130 ) ) ;
#16568 = CARTESIAN_POINT ( 'NONE',  ( 3.296024802045256941, -11.94971097300157403, 32.03036669348361443 ) ) ;
#16569 = ORIENTED_EDGE ( 'NONE', *, *, #67934, .F. ) ;
#16570 = CARTESIAN_POINT ( 'NONE',  ( -16.15384615384615330, -3.937682226553329556, 33.60647404775216529 ) ) ;
#16572 = ORIENTED_EDGE ( 'NONE', *, *, #54053, .F. ) ;
#16571 = CARTESIAN_POINT ( 'NONE',  ( 17.07692307692307665, -11.35647404775217417, 33.31231777344666511 ) ) ;
#16573 = CARTESIAN_POINT ( 'NONE',  ( 6.673053685783957967, -3.202444869320336451, 32.30641848906366675 ) ) ;
#16574 = DIRECTION ( 'NONE',  ( -0.000000000000000000, -0.8660254037844397068, -0.4999999999999978906 ) ) ;
#16575 = CARTESIAN_POINT ( 'NONE',  ( -15.84615384615384670, -7.500000000000000000, 29.75000000000000355 ) ) ;
#16576 = LINE ( 'NONE', #17476, #85982 ) ;
#16577 = ORIENTED_EDGE ( 'NONE', *, *, #36764, .T. ) ;
#16578 = DIRECTION ( 'NONE',  ( 0.000000000000000000, 0.000000000000000000, -1.000000000000000000 ) ) ;
#16579 = CARTESIAN_POINT ( 'NONE',  ( -14.30769230769230660, -12.34228464037088635, 31.77849191805839268 ) ) ;
#16580 = CARTESIAN_POINT ( 'NONE',  ( 24.00000000000000000, 5.000000000000023093, 28.74999999999999645 ) ) ;
#16581 = EDGE_LOOP ( 'NONE', ( #3677, #30869 ) ) ;
#16582 = VERTEX_POINT ( 'NONE', #15887 ) ;
#16583 = ORIENTED_EDGE ( 'NONE', *, *, #36300, .T. ) ;
#16584 = DIRECTION ( 'NONE',  ( 0.000000000000000000, 0.4999999999999960032, -0.8660254037844410391 ) ) ;
#16585 = CARTESIAN_POINT ( 'NONE',  ( 5.999999999999878320, -2.379036618888197729, 30.90682066428292885 ) ) ;
#16586 = CARTESIAN_POINT ( 'NONE',  ( -8.096153846153848477, -7.433931650972301242, 34.75000000000000711 ) ) ;
#16587 = CARTESIAN_POINT ( 'NONE',  ( 15.10062202133101295, -3.817052484675422797, 33.13202310037935661 ) ) ;
#16588 = B_SPLINE_CURVE_WITH_KNOTS ( 'NONE', 3,
 ( #28591, #15517, #82660, #42112, #70007, #22704, #15963, #56053, #20931, #84429 ),
 .UNSPECIFIED., .F., .F.,
 ( 4, 2, 2, 2, 4 ),
 ( 0.0007817359430256328248, 0.0009771253907249995759, 0.001172514838424366327, 0.001367904286123732861, 0.001563293733823099612 ),
 .UNSPECIFIED. ) ;
#16589 = AXIS2_PLACEMENT_3D ( 'NONE', #6755, #55389, #68898 ) ;
#16590 = ORIENTED_EDGE ( 'NONE', *, *, #80160, .T. ) ;
#16591 = B_SPLINE_CURVE_WITH_KNOTS ( 'NONE', 3,
 ( #27770, #55240, #75514, #41298, #61997, #48929, #82730, #76853, #8392, #55678 ),
 .UNSPECIFIED., .F., .F.,
 ( 4, 2, 2, 2, 4 ),
 ( 0.000000000000000000, 0.0001954339857564070678, 0.0003908679715128141356, 0.0005863019572692211492, 0.0007817359430256282712 ),
 .UNSPECIFIED. ) ;
#16592 = ORIENTED_EDGE ( 'NONE', *, *, #9799, .F. ) ;
#16594 = ORIENTED_EDGE ( 'NONE', *, *, #64615, .T. ) ;
#16593 = CARTESIAN_POINT ( 'NONE',  ( 9.442330961365339448, -4.236021600441997492, 33.53823185664189310 ) ) ;
#16595 = B_SPLINE_CURVE_WITH_KNOTS ( 'NONE', 3,
 ( #40721, #74494, #28527, #7373, #68182, #83480, #69065, #27192, #12791, #34830 ),
 .UNSPECIFIED., .F., .F.,
 ( 4, 2, 2, 2, 4 ),
 ( 0.000000000000000000, 0.0001954311564186878502, 0.0003908623128373757004, 0.0005862934692560635777, 0.0007817246256747514008 ),
 .UNSPECIFIED. ) ;
#16596 = CARTESIAN_POINT ( 'NONE',  ( 9.823099500132483897, -12.38066358083363738, 30.83685684665853444 ) ) ;
#16597 = CARTESIAN_POINT ( 'NONE',  ( 15.48076923076924949, -2.249999999999997780, 29.81603969181029257 ) ) ;
#16598 = CARTESIAN_POINT ( 'NONE',  ( -7.912236225513983534, -9.905515769479276145, 34.41647553114623292 ) ) ;
#16599 = VECTOR ( 'NONE', #76896, 1000.000000000000227 ) ;
#16600 = ORIENTED_EDGE ( 'NONE', *, *, #30986, .T. ) ;
#16601 = EDGE_CURVE ( 'NONE', #76696, #42959, #43350, .T. ) ;
#16602 = ORIENTED_EDGE ( 'NONE', *, *, #53839, .T. ) ;
#16604 = ORIENTED_EDGE ( 'NONE', *, *, #60883, .F. ) ;
#16603 = CARTESIAN_POINT ( 'NONE',  ( -10.61538461538461320, -11.16473453929635440, 33.15142922261926373 ) ) ;
#16605 = ADVANCED_FACE ( 'NONE', ( #8688 ), #70830, .F. ) ;
#16606 = CARTESIAN_POINT ( 'NONE',  ( 12.46153846153846168, -1.466349020453238561, 30.81389545987213907 ) ) ;
#16607 = CARTESIAN_POINT ( 'NONE',  ( -16.15384615384627409, -3.835265460704628815, 33.15142922262033665 ) ) ;
#16608 = ORIENTED_EDGE ( 'NONE', *, *, #21707, .T. ) ;
#16609 = CARTESIAN_POINT ( 'NONE',  ( 12.71148387091650278, -6.653508905675592722, 34.93172785388651391 ) ) ;
#16610 = CARTESIAN_POINT ( 'NONE',  ( 15.23076923076923173, -8.973038597847269315, 34.52809138561121927 ) ) ;
#16611 = CARTESIAN_POINT ( 'NONE',  ( 10.83839596699746544, -3.587049720035815348, 32.86302985866382897 ) ) ;
#16612 = FACE_BOUND ( 'NONE', #66658, .T. ) ;
#16613 = CARTESIAN_POINT ( 'NONE',  ( 8.096099255531889582, -12.45601412856602863, 31.48342859153981621 ) ) ;
#16614 = CARTESIAN_POINT ( 'NONE',  ( -6.673131513698878692, -9.357781135181031829, 34.66075350412533851 ) ) ;
#16615 = EDGE_CURVE ( 'NONE', #5809, #34461, #29837, .T. ) ;
#16616 = CARTESIAN_POINT ( 'NONE',  ( -14.98071491913091791, -10.66356715214248396, 33.62249196103329751 ) ) ;
#16618 = CARTESIAN_POINT ( 'NONE',  ( -2.294871794871794712, -3.499999999999999556, 29.75000000000000355 ) ) ;
#16617 = CARTESIAN_POINT ( 'NONE',  ( 17.20696823975784895, -2.504778602574659896, 29.97347330155780654 ) ) ;
#16619 = CARTESIAN_POINT ( 'NONE',  ( 11.47319109250076430, -11.48612834413959582, 32.76840700105983473 ) ) ;
#16620 = CARTESIAN_POINT ( 'NONE',  ( -16.28399336328437386, -8.587444163452046197, 34.63053765926554206 ) ) ;
#16621 = ORIENTED_EDGE ( 'NONE', *, *, #13539, .F. ) ;
#16622 = CARTESIAN_POINT ( 'NONE',  ( 9.942307692307695177, -2.249999999999998668, 29.75000000000000355 ) ) ;
#16623 = EDGE_CURVE ( 'NONE', #69664, #79083, #33971, .T. ) ;
#16624 = VERTEX_POINT ( 'NONE', #46005 ) ;
#16625 = ORIENTED_EDGE ( 'NONE', *, *, #24338, .F. ) ;
#16626 = B_SPLINE_CURVE_WITH_KNOTS ( 'NONE', 3,
 ( #29702, #43643, #64346, #14408, #28820, #69361, #7661, #69793, #56279, #83768 ),
 .UNSPECIFIED., .F., .F.,
 ( 4, 2, 2, 2, 4 ),
 ( 0.000000000000000000, 0.0001954339857564055499, 0.0003908679715128110998, 0.0005863019572692165955, 0.0007817359430256221996 ),
 .UNSPECIFIED. ) ;
#16627 = AXIS2_PLACEMENT_3D ( 'NONE', #7394, #61431, #74080 ) ;
#16629 = CARTESIAN_POINT ( 'NONE',  ( 1.634669804528840142, -5.642605341092957083, 34.66089969410670335 ) ) ;
#16628 = DIRECTION ( 'NONE',  ( -0.000000000000000000, -0.5000000000000009992, -0.8660254037844380415 ) ) ;
#16630 = B_SPLINE_CURVE_WITH_KNOTS ( 'NONE', 3,
 ( #46627, #54705, #75870, #62343, #82195, #80877, #53824, #5640, #47948, #12839 ),
 .UNSPECIFIED., .F., .F.,
 ( 4, 2, 2, 2, 4 ),
 ( 0.000000000000000000, 0.0001954311564186861697, 0.0003908623128373723394, 0.0005862934692560584820, 0.0007817246256747446788 ),
 .UNSPECIFIED. ) ;
#16631 = CARTESIAN_POINT ( 'NONE',  ( 13.38461538461526423, -11.67786785259630911, 32.92929555188603530 ) ) ;
#16632 = CARTESIAN_POINT ( 'NONE',  ( 14.43848274865926129, -3.957578996910242619, 33.62503395064540257 ) ) ;
#16633 = CARTESIAN_POINT ( 'NONE',  ( 1.161689167099239084, -6.503392248772476236, 34.64988816332204635 ) ) ;
#16634 = CARTESIAN_POINT ( 'NONE',  ( -10.61538461538461320, -8.120952969808772792, 34.71129190930000163 ) ) ;
#16635 = ORIENTED_EDGE ( 'NONE', *, *, #37876, .F. ) ;
#16636 = CARTESIAN_POINT ( 'NONE',  ( 18.06606733335007320, -3.937682226553329556, 33.60647404775216529 ) ) ;
#16637 = CARTESIAN_POINT ( 'NONE',  ( -0.4615384615385840772, -10.33852847137269571, 34.16647553114546554 ) ) ;
#16638 = CARTESIAN_POINT ( 'NONE',  ( 17.32686859527121470, -6.696923467548659303, 34.68552623307873972 ) ) ;
#16639 = ADVANCED_FACE ( 'NONE', ( #51395 ), #78901, .F. ) ;
#16640 = CARTESIAN_POINT ( 'NONE',  ( 0.4615384615384611200, -10.89733346790207413, 36.13435417666054406 ) ) ;
#16641 = DIRECTION ( 'NONE',  ( 0.000000000000000000, 0.000000000000000000, 1.000000000000000000 ) ) ;
#16642 = CARTESIAN_POINT ( 'NONE',  ( -2.651650429449535551, -10.15165042944956753, 18.68750000000000000 ) ) ;
#16643 = EDGE_LOOP ( 'NONE', ( #58592, #44065, #15533, #50218 ) ) ;
#16644 = ORIENTED_EDGE ( 'NONE', *, *, #45439, .T. ) ;
#16645 = PLANE ( 'NONE',  #63576 ) ;
#16646 = ORIENTED_EDGE ( 'NONE', *, *, #30477, .F. ) ;
#16647 = LINE ( 'NONE', #10345, #9573 ) ;
#16648 = CARTESIAN_POINT ( 'NONE',  ( 17.75002325595141173, -11.47974371597207899, 33.17467449705390692 ) ) ;
#16649 = CARTESIAN_POINT ( 'NONE',  ( -16.28399336328437386, -2.882441371585227508, 31.66841991370172238 ) ) ;
#16650 = DIRECTION ( 'NONE',  ( -0.000000000000000000, 0.6427876096865404731, -0.7660444431189770143 ) ) ;
#16651 = CARTESIAN_POINT ( 'NONE',  ( -1.929879867024197893E-14, -3.750000000000000000, 17.90625000000000000 ) ) ;
#16652 = DIRECTION ( 'NONE',  ( 0.000000000000000000, 0.7660444431189807890, 0.6427876096865361433 ) ) ;
#16653 = ORIENTED_EDGE ( 'NONE', *, *, #19415, .T. ) ;
#16654 = CARTESIAN_POINT ( 'NONE',  ( 13.38461538461538680, -2.486705287966279876, 31.30864560766543647 ) ) ;
#16656 = VERTEX_POINT ( 'NONE', #17198 ) ;
#16655 = CARTESIAN_POINT ( 'NONE',  ( -16.21911659980693443, -11.94971097300153140, 32.03036669348370680 ) ) ;
#16657 = CARTESIAN_POINT ( 'NONE',  ( -13.51530685128294351, -11.18331474514187995, 33.13161551792790505 ) ) ;
#16658 = CARTESIAN_POINT ( 'NONE',  ( 14.24160889673642849, -12.10708131394839349, 31.69288490824020244 ) ) ;
#16659 = CARTESIAN_POINT ( 'NONE',  ( 15.45354889974729318, -3.020022701398814569, 32.48759521482552515 ) ) ;
#16661 = AXIS2_PLACEMENT_3D ( 'NONE', #60526, #80822, #68615 ) ;
#16660 = CARTESIAN_POINT ( 'NONE',  ( 11.60371667797437567, -8.656820664281605460, 34.87096338111211224 ) ) ;
#16662 = EDGE_CURVE ( 'NONE', #77586, #57769, #42594, .T. ) ;
#16663 = CARTESIAN_POINT ( 'NONE',  ( -0.3962828902624371263, -11.48612834413965977, 32.76840700105972815 ) ) ;
#16664 = CARTESIAN_POINT ( 'NONE',  ( 11.40777007179398161, -6.413092428213692742, 34.63065189839063152 ) ) ;
#16665 = CARTESIAN_POINT ( 'NONE',  ( -7.912237257109724808, -12.37446782046654192, 30.86335684631486487 ) ) ;
#16666 = EDGE_CURVE ( 'NONE', #42722, #76991, #65224, .T. ) ;
#16667 = CARTESIAN_POINT ( 'NONE',  ( -3.749999999999997780, -7.438900925035489387, 17.84561829374150932 ) ) ;
#16668 = VERTEX_POINT ( 'NONE', #11790 ) ;
#16669 = CARTESIAN_POINT ( 'NONE',  ( -16.37733107841048508, -9.417330523894424488, 34.63758898049880486 ) ) ;
#16670 = CARTESIAN_POINT ( 'NONE',  ( 8.992242120843618736, -11.76359900205217635, 32.36225158514719880 ) ) ;
#16671 = CYLINDRICAL_SURFACE ( 'NONE', #5940, 0.2499999999999979738 ) ;
#16672 = CARTESIAN_POINT ( 'NONE',  ( -1.944543648263014957, -5.555456351737005249, 25.25000000000000000 ) ) ;
#16673 = B_SPLINE_CURVE_WITH_KNOTS ( 'NONE', 3,
 ( #68540, #21234, #47378, #61771, #14938, #83401, #35653, #40641, #21683, #55032 ),
 .UNSPECIFIED., .F., .F.,
 ( 4, 2, 2, 2, 4 ),
 ( 0.0007817246256747524850, 0.0009771112852218972241, 0.001172497944769042072, 0.001367884604316186702, 0.001563271263863331550 ),
 .UNSPECIFIED. ) ;
#16674 = ADVANCED_FACE ( 'NONE', ( #52312 ), #79803, .F. ) ;
#16675 = DIRECTION ( 'NONE',  ( -0.000000000000000000, 0.1736481776669307198, -0.9848077530122080203 ) ) ;
#16676 = CARTESIAN_POINT ( 'NONE',  ( -17.20707028636129721, -2.619462340734462380, 30.83744416345203021 ) ) ;
#16677 = EDGE_CURVE ( 'NONE', #26012, #17825, #71610, .T. ) ;
#16678 = B_SPLINE_CURVE_WITH_KNOTS ( 'NONE', 3,
 ( #43526, #22372, #34682, #84532, #62147, #47747 ),
 .UNSPECIFIED., .F., .F.,
 ( 4, 2, 4 ),
 ( 0.0003909569690057804843, 0.0005862646681846042955, 0.0007815723673634281067 ),
 .UNSPECIFIED. ) ;
#16679 = ORIENTED_EDGE ( 'NONE', *, *, #70850, .T. ) ;
#16680 = CARTESIAN_POINT ( 'NONE',  ( 1.799775606325937360E-14, -10.25000000000000000, 18.53125000000000000 ) ) ;
#16681 = CARTESIAN_POINT ( 'NONE',  ( -15.29685161012936412, -3.937682226553330445, 33.60647404775217240 ) ) ;
#16682 = VECTOR ( 'NONE', #14945, 1000.000000000000000 ) ;
#16683 = VERTEX_POINT ( 'NONE', #51856 ) ;
#16684 = DIRECTION ( 'NONE',  ( 0.000000000000000000, 0.1736481776669275834, 0.9848077530122086864 ) ) ;
#16685 = VERTEX_POINT ( 'NONE', #9996 ) ;
#16686 = CARTESIAN_POINT ( 'NONE',  ( 7.145856592054988354, -4.226511098958374291, 33.85474049983370293 ) ) ;
#16687 = CARTESIAN_POINT ( 'NONE',  ( 3.165499230212911908, -4.320704448112771878, 33.92786785259540494 ) ) ;
#16688 = CARTESIAN_POINT ( 'NONE',  ( -12.71151520558705528, -10.06842814019191401, 34.32929386961144758 ) ) ;
#16689 = DIRECTION ( 'NONE',  ( -0.000000000000000000, 0.7660444431189791237, -0.6427876096865379196 ) ) ;
#16690 = ORIENTED_EDGE ( 'NONE', *, *, #3112, .F. ) ;
#16691 = DIRECTION ( 'NONE',  ( 0.000000000000000000, 0.3420201433256641055, -0.9396926207859100932 ) ) ;
#16692 = VERTEX_POINT ( 'NONE', #79353 ) ;
#16693 = CARTESIAN_POINT ( 'NONE',  ( -17.86947456176635640, -12.15418822224088835, 32.17964115625579069 ) ) ;
#16694 = CARTESIAN_POINT ( 'NONE',  ( 0.7115927731767747177, -11.28795663066794219, 33.01431243580653785 ) ) ;
#16695 = VECTOR ( 'NONE', #35399, 1000.000000000000000 ) ;
#16696 = ORIENTED_EDGE ( 'NONE', *, *, #82783, .F. ) ;
#16697 = CARTESIAN_POINT ( 'NONE',  ( 11.60371667797437567, -12.70778746994558439, 30.41441678777536595 ) ) ;
#16698 = CARTESIAN_POINT ( 'NONE',  ( -14.43783951713053249, -10.88202310037935661, 33.43294751532457099 ) ) ;
#16699 = CARTESIAN_POINT ( 'NONE',  ( -11.76138775597768316, -2.758268499246657068, 31.33685645148948140 ) ) ;
#16700 = AXIS2_PLACEMENT_3D ( 'NONE', #11052, #17816, #46613 ) ;
#16701 = DIRECTION ( 'NONE',  ( 0.000000000000000000, 0.7660444431189822323, -0.6427876096865344779 ) ) ;
#16702 = CARTESIAN_POINT ( 'NONE',  ( -16.37677311275300340, -2.889293201056495786, 32.26117774369186009 ) ) ;
#16703 = EDGE_CURVE ( 'NONE', #20844, #87573, #22163, .T. ) ;
#16704 = ORIENTED_EDGE ( 'NONE', *, *, #5651, .F. ) ;
#16705 = ORIENTED_EDGE ( 'NONE', *, *, #63030, .F. ) ;
#16706 = FACE_BOUND ( 'NONE', #88777, .T. ) ;
#16707 = VERTEX_POINT ( 'NONE', #52757 ) ;
#16708 = CARTESIAN_POINT ( 'NONE',  ( -8.096177070375304652, -5.765609946408404518, 34.70566812827425451 ) ) ;
#16709 = CARTESIAN_POINT ( 'NONE',  ( 9.561616225640133138, -12.11776431015576172, 31.66791131148498906 ) ) ;
#16710 = CARTESIAN_POINT ( 'NONE',  ( 0.5923289025054110368, -12.62708834333097663, 30.88030960425257021 ) ) ;
#16711 = ORIENTED_EDGE ( 'NONE', *, *, #55538, .T. ) ;
#16712 = EDGE_CURVE ( 'NONE', #13174, #27068, #80247, .T. ) ;
#16713 = VERTEX_POINT ( 'NONE', #18546 ) ;
#16714 = EDGE_CURVE ( 'NONE', #37962, #42538, #81367, .T. ) ;
#16715 = VERTEX_POINT ( 'NONE', #39713 ) ;
#16716 = CARTESIAN_POINT ( 'NONE',  ( -1.450698795571264688, -11.69971097300155272, 32.46337939537587403 ) ) ;
#16717 = ORIENTED_EDGE ( 'NONE', *, *, #63505, .F. ) ;
#16718 = CYLINDRICAL_SURFACE ( 'NONE', #43380, 0.2500000000000008882 ) ;
#16719 = VECTOR ( 'NONE', #14457, 1000.000000000000114 ) ;
#16720 = DIRECTION ( 'NONE',  ( -0.000000000000000000, 0.8660254037844397068, -0.4999999999999978906 ) ) ;
#16721 = CARTESIAN_POINT ( 'NONE',  ( -2.438382910802612713, -12.35290016733513951, 31.75349464988449455 ) ) ;
#16722 = FACE_BOUND ( 'NONE', #31884, .T. ) ;
#16723 = ORIENTED_EDGE ( 'NONE', *, *, #17473, .T. ) ;
#16724 = CARTESIAN_POINT ( 'NONE',  ( -1.515092092731847861, -7.276988635370452485, 34.74523720219453793 ) ) ;
#16725 = EDGE_CURVE ( 'NONE', #31293, #17102, #6065, .T. ) ;
#16726 = DIRECTION ( 'NONE',  ( 0.000000000000000000, 0.9848077530122072432, -0.1736481776669354937 ) ) ;
#16727 = CARTESIAN_POINT ( 'NONE',  ( 14.30769230769231015, -6.681629849574314051, 35.83090037661290239 ) ) ;
#16728 = CARTESIAN_POINT ( 'NONE',  ( -11.53846153846153655, -3.050289026998446396, 32.03036669348365706 ) ) ;
#16729 = VERTEX_POINT ( 'NONE', #61280 ) ;
#16730 = VECTOR ( 'NONE', #34080, 1000.000000000000000 ) ;
#16731 = UNCERTAINTY_MEASURE_WITH_UNIT (LENGTH_MEASURE( 1.000000000000000082E-05 ), #73373, 'distance_accuracy_value', 'NONE');
#16732 = DIRECTION ( 'NONE',  ( 0.000000000000000000, 0.000000000000000000, 1.000000000000000000 ) ) ;
#16733 = ADVANCED_FACE ( 'NONE', ( #5479 ), #20752, .F. ) ;
#16734 = EDGE_LOOP ( 'NONE', ( #72780, #65253 ) ) ;
#16735 = ORIENTED_EDGE ( 'NONE', *, *, #35123, .F. ) ;
#16737 = CYLINDRICAL_SURFACE ( 'NONE', #26116, 0.2500000000000002220 ) ;
#16736 = CARTESIAN_POINT ( 'NONE',  ( -18.22559223176554966, -2.251337733188375267, 29.87809195722895339 ) ) ;
#16738 = CARTESIAN_POINT ( 'NONE',  ( 16.08776274289027342, -5.557115091759785130, 34.35708131394839171 ) ) ;
#16739 = CARTESIAN_POINT ( 'NONE',  ( -4.023054346021365468, -4.118422570099827595, 33.43335022499816489 ) ) ;
#16740 = CARTESIAN_POINT ( 'NONE',  ( 13.38461538461538680, -1.509761064869970415, 31.06009739812519044 ) ) ;
#16741 = DIRECTION ( 'NONE',  ( 0.000000000000000000, 0.7660444431189807890, 0.6427876096865361433 ) ) ;
#16742 = ORIENTED_EDGE ( 'NONE', *, *, #7047, .T. ) ;
#16743 = CYLINDRICAL_SURFACE ( 'NONE', #86051, 0.2499999999999986955 ) ;
#16744 = CARTESIAN_POINT ( 'NONE',  ( 10.61538461538461675, -4.945431358278436385, 36.03766855953609394 ) ) ;
#16745 = DIRECTION ( 'NONE',  ( -1.000000000000000000, -0.000000000000000000, -0.000000000000000000 ) ) ;
#16746 = EDGE_CURVE ( 'NONE', #42102, #56815, #24386, .T. ) ;
#16747 = CARTESIAN_POINT ( 'NONE',  ( 15.48076923077066702, -7.500000000000155431, 34.75000000000007105 ) ) ;
#16748 = ORIENTED_EDGE ( 'NONE', *, *, #29442, .T. ) ;
#16749 = ORIENTED_EDGE ( 'NONE', *, *, #83334, .F. ) ;
#16750 = FACE_BOUND ( 'NONE', #2002, .T. ) ;
#16751 = VECTOR ( 'NONE', #13481, 1000.000000000000000 ) ;
#16752 = CARTESIAN_POINT ( 'NONE',  ( 11.60452887181161508, -12.34228464037088813, 31.77849191805839268 ) ) ;
#16753 = CARTESIAN_POINT ( 'NONE',  ( -6.700114019515439168, -7.369474270740069777, 34.74850911626239736 ) ) ;
#16754 = ORIENTED_EDGE ( 'NONE', *, *, #13423, .F. ) ;
#16755 = CARTESIAN_POINT ( 'NONE',  ( 3.930919194939304084, -11.43668979543635089, 33.22377378376089752 ) ) ;
#16756 = CARTESIAN_POINT ( 'NONE',  ( 6.700150705560777631, -10.61292498521070549, 33.66303323003028680 ) ) ;
#16757 = CARTESIAN_POINT ( 'NONE',  ( 15.93036121012220541, -8.496056993536548418, 34.65000542017679663 ) ) ;
#16758 = CARTESIAN_POINT ( 'NONE',  ( 27.00000000000000000, 0.000000000000000000, 0.000000000000000000 ) ) ;
#16759 = ORIENTED_EDGE ( 'NONE', *, *, #22544, .T. ) ;
#16760 = CIRCLE ( 'NONE', #52704, 8.000000000000000000 ) ;
#16761 = CARTESIAN_POINT ( 'NONE',  ( -7.623142494540996239, -10.61302985866384141, 33.66295027996417843 ) ) ;
#16762 = EDGE_LOOP ( 'NONE', ( #50973, #8967 ) ) ;
#16764 = ORIENTED_EDGE ( 'NONE', *, *, #64435, .F. ) ;
#16763 = CARTESIAN_POINT ( 'NONE',  ( 18.00000000000000000, -5.471508081941601098, 34.59228464037088457 ) ) ;
#16765 = LINE ( 'NONE', #46020, #68484 ) ;
#16766 = LINE ( 'NONE', #79368, #20930 ) ;
#16768 = B_SPLINE_CURVE_WITH_KNOTS ( 'NONE', 3,
 ( #8802, #2464, #64604, #30832, #44328, #10122, #58302, #16436, #72263, #43464 ),
 .UNSPECIFIED., .F., .F.,
 ( 4, 2, 2, 2, 4 ),
 ( 0.0007817359430256361858, 0.0009771253907250041296, 0.001172514838424372182, 0.001367904286123740234, 0.001563293733823108286 ),
 .UNSPECIFIED. ) ;
#16767 = CYLINDRICAL_SURFACE ( 'NONE', #73081, 0.2500000000000009437 ) ;
#16769 = CARTESIAN_POINT ( 'NONE',  ( -12.52762084089859584, -10.67929555188718460, 33.92786785259543336 ) ) ;
#16770 = CARTESIAN_POINT ( 'NONE',  ( -14.55771553191376277, -8.475808217655753651, 34.90892951860618609 ) ) ;
#16771 = EDGE_CURVE ( 'NONE', #35211, #14267, #47784, .T. ) ;
#16772 = CARTESIAN_POINT ( 'NONE',  ( 6.222779541268410597, -2.847695495035524882, 31.58253572463339509 ) ) ;
#16773 = CARTESIAN_POINT ( 'NONE',  ( -2.775308065498752086, -8.577988221561495763, 16.51749329374151642 ) ) ;
#16774 = ORIENTED_EDGE ( 'NONE', *, *, #14499, .T. ) ;
#16775 = DIRECTION ( 'NONE',  ( 0.000000000000000000, 0.8660254037844377084, -0.5000000000000015543 ) ) ;
#16776 = CARTESIAN_POINT ( 'NONE',  ( 13.60757851888206105, -7.369474539155828730, 34.99858011523957657 ) ) ;
#16777 = EDGE_CURVE ( 'NONE', #52397, #85757, #70502, .T. ) ;
#16778 = ORIENTED_EDGE ( 'NONE', *, *, #74903, .F. ) ;
#16779 = EDGE_CURVE ( 'NONE', #33955, #2392, #33393, .T. ) ;
#16780 = ORIENTED_EDGE ( 'NONE', *, *, #36781, .F. ) ;
#16781 = CARTESIAN_POINT ( 'NONE',  ( -10.61538461538461320, -11.16473453929635440, 33.15142922261926373 ) ) ;
#16782 = DIRECTION ( 'NONE',  ( 1.000000000000000000, 0.000000000000000000, 0.000000000000000000 ) ) ;
#16783 = DIRECTION ( 'NONE',  ( -1.000000000000000000, 0.000000000000000000, 0.000000000000000000 ) ) ;
#16784 = CARTESIAN_POINT ( 'NONE',  ( -5.076923076923075762, -2.499999999999998668, 29.50000000000001066 ) ) ;
#16785 = CARTESIAN_POINT ( 'NONE',  ( 8.992243613324164997, -11.43677907613344757, 33.22367315496202167 ) ) ;
#16786 = CARTESIAN_POINT ( 'NONE',  ( -17.07692307692319744, -11.67786785259630911, 32.92929555188603530 ) ) ;
#16787 = DIRECTION ( 'NONE',  ( -0.000000000000000000, -0.9848077530122086864, -0.1736481776669273613 ) ) ;
#16788 = ORIENTED_EDGE ( 'NONE', *, *, #41453, .T. ) ;
#16789 = AXIS2_PLACEMENT_3D ( 'NONE', #414, #55346, #1736 ) ;
#16790 = DIRECTION ( 'NONE',  ( -1.000000000000000000, -0.000000000000000000, 0.000000000000000000 ) ) ;
#16791 = LINE ( 'NONE', #41403, #49159 ) ;
#16792 = CARTESIAN_POINT ( 'NONE',  ( -8.992157728137614825, -11.43668979543635089, 33.22377378376089752 ) ) ;
#16793 = EDGE_CURVE ( 'NONE', #87653, #42680, #86635, .T. ) ;
#16794 = CARTESIAN_POINT ( 'NONE',  ( 7.497142682080633102E-17, 1.250000000000003553, 28.00000000000000000 ) ) ;
#16795 = ORIENTED_EDGE ( 'NONE', *, *, #53839, .F. ) ;
#16796 = DIRECTION ( 'NONE',  ( 0.000000000000000000, 0.000000000000000000, -1.000000000000000000 ) ) ;
#16797 = VECTOR ( 'NONE', #6088, 1000.000000000000227 ) ;
#16798 = VERTEX_POINT ( 'NONE', #44 ) ;
#16799 = CARTESIAN_POINT ( 'NONE',  ( -18.00000000000012079, -8.656820664282943056, 34.87096338111179961 ) ) ;
#16800 = PRESENTATION_STYLE_ASSIGNMENT (( #37969 ) ) ;
#16801 = CARTESIAN_POINT ( 'NONE',  ( 10.54930223602447903, -3.322132147404559532, 32.92929555188719348 ) ) ;
#16802 = ADVANCED_FACE ( 'NONE', ( #26629 ), #54086, .F. ) ;
#16803 = DIRECTION ( 'NONE',  ( 0.000000000000000000, 0.8660254037844377084, 0.5000000000000015543 ) ) ;
#16804 = ORIENTED_EDGE ( 'NONE', *, *, #62280, .F. ) ;
#16805 = VECTOR ( 'NONE', #67005, 1000.000000000000000 ) ;
#16806 = CARTESIAN_POINT ( 'NONE',  ( -1.514763354347081092, -12.70455904226513866, 30.44083106164009322 ) ) ;
#16807 = CARTESIAN_POINT ( 'NONE',  ( 10.48469314871705826, -3.530157926970578952, 32.79014554554150607 ) ) ;
#16808 = CARTESIAN_POINT ( 'NONE',  ( -13.60810030917971680, -10.97335522853832579, 33.68706563782419749 ) ) ;
#16809 = CARTESIAN_POINT ( 'NONE',  ( -9.692307692307691624, -3.322132147404559976, 32.92929555188717927 ) ) ;
#16810 = B_SPLINE_CURVE_WITH_KNOTS ( 'NONE', 3,
 ( #4565, #59506, #87010, #30698, #37004, #45988, #78439, #16739, #44192, #71681 ),
 .UNSPECIFIED., .F., .F.,
 ( 4, 2, 2, 2, 4 ),
 ( 0.0007817359430256303312, 0.0009771253907249965402, 0.001172514838424362641, 0.001367904286123728958, 0.001563293733823095059 ),
 .UNSPECIFIED. ) ;
#16811 = ADVANCED_FACE ( 'NONE', ( #6793 ), #74827, .F. ) ;
#16812 = ORIENTED_EDGE ( 'NONE', *, *, #7105, .T. ) ;
#16813 = CARTESIAN_POINT ( 'NONE',  ( 7.715463243043538810, -11.37499894934982514, 33.29245874905763003 ) ) ;
#16814 = ORIENTED_EDGE ( 'NONE', *, *, #38096, .T. ) ;
#16815 = EDGE_CURVE ( 'NONE', #33014, #76058, #27958, .T. ) ;
#16816 = CARTESIAN_POINT ( 'NONE',  ( -9.627052121031661969, -12.27809138561124591, 31.22303859784720359 ) ) ;
#16817 = EDGE_CURVE ( 'NONE', #72129, #68389, #74822, .T. ) ;
#16818 = CARTESIAN_POINT ( 'NONE',  ( -16.21992956480203318, -11.16473453929635440, 33.15142922261925662 ) ) ;
#16819 = AXIS2_PLACEMENT_3D ( 'NONE', #54473, #54924, #75627 ) ;
#16820 = CARTESIAN_POINT ( 'NONE',  ( 7.596130621932389637, -12.45566812827425096, 31.48439005359158926 ) ) ;
#16821 = DIRECTION ( 'NONE',  ( -0.000000000000000000, -0.7660444431189791237, -0.6427876096865379196 ) ) ;
#16822 = CARTESIAN_POINT ( 'NONE',  ( 9.626224281351815293, -8.120952969808774569, 34.71129190930000163 ) ) ;
#16823 = VECTOR ( 'NONE', #23413, 1000.000000000000000 ) ;
#16824 = ORIENTED_EDGE ( 'NONE', *, *, #18960, .F. ) ;
#16825 = EDGE_CURVE ( 'NONE', #58630, #58791, #87756, .T. ) ;
#16826 = ORIENTED_EDGE ( 'NONE', *, *, #1445, .F. ) ;
#16827 = ORIENTED_EDGE ( 'NONE', *, *, #37390, .T. ) ;
#16828 = ORIENTED_EDGE ( 'NONE', *, *, #30781, .F. ) ;
#16829 = VECTOR ( 'NONE', #30955, 1000.000000000000114 ) ;
#16830 = CARTESIAN_POINT ( 'NONE',  ( -1.384615384615505151, -3.300289026999228881, 32.46337939537708905 ) ) ;
#16831 = CARTESIAN_POINT ( 'NONE',  ( 11.47237915910140771, -9.058645607665454236, 34.76329471203372634 ) ) ;
#16832 = CYLINDRICAL_SURFACE ( 'NONE', #68371, 0.2499999999999995559 ) ;
#16833 = CARTESIAN_POINT ( 'NONE',  ( 17.14299142792551578, -4.098570777380720287, 33.41473453929635440 ) ) ;
#16834 = CARTESIAN_POINT ( 'NONE',  ( -13.25408968285182176, -6.001044277235009439, 34.52024696741798948 ) ) ;
#16835 = CARTESIAN_POINT ( 'NONE',  ( 2.980745993476265898, -5.851115903089112003, 34.47074536777953568 ) ) ;
#16836 = B_SPLINE_CURVE_WITH_KNOTS ( 'NONE', 3,
 ( #8290, #68214, #88953, #1080, #27222, #35764, #34859, #7403, #28561, #82630 ),
 .UNSPECIFIED., .F., .F.,
 ( 4, 2, 2, 2, 4 ),
 ( 0.0007817359430256314154, 0.0009771253907249978412, 0.001172514838424364375, 0.001367904286123730693, 0.001563293733823097227 ),
 .UNSPECIFIED. ) ;
#16837 = CARTESIAN_POINT ( 'NONE',  ( -18.00000000000012079, -10.21337939537710504, 33.94971097300076224 ) ) ;
#16838 = CARTESIAN_POINT ( 'NONE',  ( 17.01167314514899331, -2.255955759149247619, 30.00000000000014566 ) ) ;
#16839 = B_SPLINE_CURVE_WITH_KNOTS ( 'NONE', 3,
 ( #72266, #51084, #56972, #36275, #15557, #64605 ),
 .UNSPECIFIED., .F., .F.,
 ( 4, 2, 4 ),
 ( 0.000000000000000000, 0.0001954784845028888327, 0.0003909569690057776653 ),
 .UNSPECIFIED. ) ;
#16840 = ORIENTED_EDGE ( 'NONE', *, *, #20438, .F. ) ;
#16841 = B_SPLINE_CURVE_WITH_KNOTS ( 'NONE', 3,
 ( #37514, #79404, #45159, #64979, #72633, #38863, #10941, #3283, #31656, #32100 ),
 .UNSPECIFIED., .F., .F.,
 ( 4, 2, 2, 2, 4 ),
 ( 0.000000000000000000, 0.0001954339857564073388, 0.0003908679715128146777, 0.0005863019572692220165, 0.0007817359430256293554 ),
 .UNSPECIFIED. ) ;
#16842 = EDGE_CURVE ( 'NONE', #29464, #54551, #7695, .T. ) ;
#16843 = ORIENTED_EDGE ( 'NONE', *, *, #18400, .T. ) ;
#16844 = ORIENTED_EDGE ( 'NONE', *, *, #49109, .T. ) ;
#16846 = ORIENTED_EDGE ( 'NONE', *, *, #35105, .T. ) ;
#16845 = LINE ( 'NONE', #44291, #63238 ) ;
#16848 = CARTESIAN_POINT ( 'NONE',  ( -17.86920955903304886, -11.37503395064541678, 33.29242100308974983 ) ) ;
#16847 = CARTESIAN_POINT ( 'NONE',  ( -9.942330929600657896, -9.271318131107980420, 34.42618302367067429 ) ) ;
#16849 = B_SPLINE_CURVE_WITH_KNOTS ( 'NONE', 3,
 ( #59661, #65525, #4729, #85814, #87160, #30416, #51102, #32204, #51543, #38966 ),
 .UNSPECIFIED., .F., .F.,
 ( 4, 2, 2, 2, 4 ),
 ( 0.000000000000000000, 0.0001954311564186863323, 0.0003908623128373726646, 0.0005862934692560590241, 0.0007817246256747453293 ),
 .UNSPECIFIED. ) ;
#16850 = CARTESIAN_POINT ( 'NONE',  ( -0.4615384615385840772, -3.643525952248795718, 33.31231777344771672 ) ) ;
#16851 = VECTOR ( 'NONE', #2280, 1000.000000000000000 ) ;
#16852 = CARTESIAN_POINT ( 'NONE',  ( 4.403900465484467119, -2.564540009722896752, 30.55348353981670684 ) ) ;
#16853 = ORIENTED_EDGE ( 'NONE', *, *, #47781, .T. ) ;
#16854 = ORIENTED_EDGE ( 'NONE', *, *, #68012, .T. ) ;
#16855 = CARTESIAN_POINT ( 'NONE',  ( -13.38461538461538325, -2.833524468853757305, 32.15551576947925838 ) ) ;
#16856 = ORIENTED_EDGE ( 'NONE', *, *, #78621, .T. ) ;
#16857 = FACE_BOUND ( 'NONE', #7115, .T. ) ;
#16858 = CARTESIAN_POINT ( 'NONE',  ( 8.769230769230768274, -12.34228464037088635, 31.77849191805839268 ) ) ;
#16859 = CARTESIAN_POINT ( 'NONE',  ( -4.087777802843713282, -11.69971097300155272, 32.46337939537588113 ) ) ;
#16860 = ORIENTED_EDGE ( 'NONE', *, *, #37599, .F. ) ;
#16861 = CARTESIAN_POINT ( 'NONE',  ( -4.153846153845845102, -2.506253911140614576, 30.00000000000323297 ) ) ;
#16862 = CARTESIAN_POINT ( 'NONE',  ( 11.40777093535123043, -6.369640206132551441, 34.87707690430378449 ) ) ;
#16863 = AXIS2_PLACEMENT_3D ( 'NONE', #46811, #39630, #32411 ) ;
#16864 = CARTESIAN_POINT ( 'NONE',  ( -5.076923076923075762, -12.78798330534102945, 29.74999999999997868 ) ) ;
#16865 = ORIENTED_EDGE ( 'NONE', *, *, #78573, .F. ) ;
#16866 = CARTESIAN_POINT ( 'NONE',  ( -18.00000000000000000, -9.580279128651994824, 36.19647103217484130 ) ) ;
#16867 = CARTESIAN_POINT ( 'NONE',  ( -13.25382357679059986, -11.71459661697925903, 32.44059661609676937 ) ) ;
#16868 = EDGE_LOOP ( 'NONE', ( #10964, #2510, #78224, #14360 ) ) ;
#16869 = CYLINDRICAL_SURFACE ( 'NONE', #27267, 0.2499999999999997502 ) ;
#16870 = CARTESIAN_POINT ( 'NONE',  ( 11.00641025641025550, -7.500000000000000000, 29.75000000000000355 ) ) ;
#16871 = CARTESIAN_POINT ( 'NONE',  ( 8.703148389870634105, -11.35647404775217595, 33.31231777344666511 ) ) ;
#16872 = CARTESIAN_POINT ( 'NONE',  ( 13.38461538461526601, -2.625532179533778709, 30.86335684631627174 ) ) ;
#16873 = CARTESIAN_POINT ( 'NONE',  ( 13.38461538461538680, -1.790695186598648903, 34.54067556320373455 ) ) ;
#16874 = CARTESIAN_POINT ( 'NONE',  ( 7.912322987116502837, -7.250054483168843156, 34.74374881642865631 ) ) ;
#16875 = CARTESIAN_POINT ( 'NONE',  ( -10.61538461538461320, -2.708943851104267164, 35.45975837776705220 ) ) ;
#16876 = LINE ( 'NONE', #44326, #79761 ) ;
#16878 = DIRECTION ( 'NONE',  ( -0.000000000000000000, 0.1736481776669307198, -0.9848077530122080203 ) ) ;
#16877 = DIRECTION ( 'NONE',  ( -0.000000000000000000, 0.6427876096865404731, -0.7660444431189770143 ) ) ;
#16879 = CARTESIAN_POINT ( 'NONE',  ( 1.450683735617824821, -11.16473453929635440, 33.15142922261926373 ) ) ;
#16881 = CARTESIAN_POINT ( 'NONE',  ( -0.4615384615384611200, -4.786620604624113540, 33.94971097300155094 ) ) ;
#16880 = CARTESIAN_POINT ( 'NONE',  ( 3.480769230769234834, -2.499999999999999556, 29.81604066197450109 ) ) ;
#16882 = DIRECTION ( 'NONE',  ( 0.000000000000000000, 0.4999999999999985567, 0.8660254037844395958 ) ) ;
#16883 = CARTESIAN_POINT ( 'NONE',  ( -2.724691934501232371, -8.700186371490559623, 23.51375670625848713 ) ) ;
#16884 = ORIENTED_EDGE ( 'NONE', *, *, #12690, .F. ) ;
#16885 = CARTESIAN_POINT ( 'NONE',  ( 3.064640908609403969, -5.597845033694389016, 14.00000000000009059 ) ) ;
#16886 = EDGE_LOOP ( 'NONE', ( #83392, #38682 ) ) ;
#16887 = EDGE_CURVE ( 'NONE', #22384, #53843, #76136, .T. ) ;
#16888 = CARTESIAN_POINT ( 'NONE',  ( -9.692307692307691624, -5.557115091759785130, 34.35708131394839171 ) ) ;
#16889 = VECTOR ( 'NONE', #87328, 1000.000000000000000 ) ;
#16890 = VERTEX_POINT ( 'NONE', #83806 ) ;
#16891 = CARTESIAN_POINT ( 'NONE',  ( -4.023054346021365468, -11.18335022499818621, 33.13157742990016885 ) ) ;
#16892 = EDGE_CURVE ( 'NONE', #17395, #84497, #3963, .T. ) ;
#16893 = ORIENTED_EDGE ( 'NONE', *, *, #27145, .T. ) ;
#16894 = CYLINDRICAL_SURFACE ( 'NONE', #64221, 0.2500000000000012212 ) ;
#16895 = CARTESIAN_POINT ( 'NONE',  ( 1.077988221561464899, -4.724691934501233703, 21.48250670625849068 ) ) ;
#16896 = CARTESIAN_POINT ( 'NONE',  ( 17.07692307692307665, -9.058645607665452459, 34.76329471203371924 ) ) ;
#16897 = CARTESIAN_POINT ( 'NONE',  ( 9.915319043920545639, -11.24521262558773493, 33.06293181088029343 ) ) ;
#16898 = CARTESIAN_POINT ( 'NONE',  ( -3.100243792535588128, -12.50538340440932217, 31.33453814440721885 ) ) ;
#16899 = CARTESIAN_POINT ( 'NONE',  ( -6.222926958906846551, -2.523278758544489797, 31.42238647778637528 ) ) ;
#16900 = DIRECTION ( 'NONE',  ( 1.000000000000000000, 0.000000000000000000, 0.000000000000000000 ) ) ;
#16901 = CARTESIAN_POINT ( 'NONE',  ( -7.596208327805705096, -2.824170634883622633, 31.52227843825338738 ) ) ;
#16902 = CARTESIAN_POINT ( 'NONE',  ( -7.846153846153965716, -12.27809138561165270, 31.22303859784587132 ) ) ;
#16903 = ADVANCED_FACE ( 'NONE', ( #28857 ), #35606, .F. ) ;
#16904 = CARTESIAN_POINT ( 'NONE',  ( 3.749999999999992006, -5.946699141100872943, 16.89062500000000000 ) ) ;
#16905 = CARTESIAN_POINT ( 'NONE',  ( 1.634669696253700621, -3.136992222400443175, 32.19305428654138979 ) ) ;
#16906 = CYLINDRICAL_SURFACE ( 'NONE', #27624, 8.000000000000000000 ) ;
#16907 = VECTOR ( 'NONE', #72172, 1000.000000000000114 ) ;
#16908 = ADVANCED_FACE ( 'NONE', ( #15336 ), #70273, .F. ) ;
#16909 = DIRECTION ( 'NONE',  ( 0.000000000000000000, 0.4999999999999985567, 0.8660254037844395958 ) ) ;
#16910 = CARTESIAN_POINT ( 'NONE',  ( -1.929879867024197893E-14, -3.750000000000000000, 15.40625000000000000 ) ) ;
#16911 = B_SPLINE_CURVE_WITH_KNOTS ( 'NONE', 3,
 ( #79463, #39375, #17763, #11444, #53307, #38927, #66385, #4692, #66833, #32164 ),
 .UNSPECIFIED., .F., .F.,
 ( 4, 2, 2, 2, 4 ),
 ( 0.000000000000000000, 0.0001954311564186874436, 0.0003908623128373748873, 0.0005862934692560622767, 0.0007817246256747497745 ),
 .UNSPECIFIED. ) ;
#16912 = ORIENTED_EDGE ( 'NONE', *, *, #87067, .T. ) ;
#16913 = PLANE ( 'NONE',  #51458 ) ;
#16914 = CARTESIAN_POINT ( 'NONE',  ( -11.47320596718551045, -8.613356846314928816, 34.62446782046653482 ) ) ;
#16915 = CARTESIAN_POINT ( 'NONE',  ( 1.161130460051056579, -5.827078755546626354, 34.72654668319379567 ) ) ;
#16916 = DIRECTION ( 'NONE',  ( -1.000000000000000000, -0.000000000000000000, -0.000000000000000000 ) ) ;
#16917 = CARTESIAN_POINT ( 'NONE',  ( 14.24160992833217065, -3.322132147404559532, 32.92929555188719348 ) ) ;
#16918 = CARTESIAN_POINT ( 'NONE',  ( 2.177545098254085154, -12.27039167877662251, 31.24851455888617835 ) ) ;
#16919 = AXIS2_PLACEMENT_3D ( 'NONE', #53292, #18642, #81228 ) ;
#16920 = ORIENTED_EDGE ( 'NONE', *, *, #85141, .F. ) ;
#16921 = CARTESIAN_POINT ( 'NONE',  ( -10.48533718013415950, -7.723484941389743952, 34.99544897038808955 ) ) ;
#16922 = VERTEX_POINT ( 'NONE', #15780 ) ;
#16923 = AXIS2_PLACEMENT_3D ( 'NONE', #69798, #83326, #7221 ) ;
#16924 = EDGE_CURVE ( 'NONE', #76326, #5654, #38284, .T. ) ;
#16925 = VERTEX_POINT ( 'NONE', #23400 ) ;
#16926 = CARTESIAN_POINT ( 'NONE',  ( -15.23076923076922995, -12.37446782046654192, 30.86335684631486131 ) ) ;
#16927 = CARTESIAN_POINT ( 'NONE',  ( 5.076923076923075762, -11.69971097300155272, 32.46337939537588113 ) ) ;
#16928 = CARTESIAN_POINT ( 'NONE',  ( 6.700149964170072359, -2.889293201056495786, 32.26117774369186009 ) ) ;
#16929 = VECTOR ( 'NONE', #66090, 1000.000000000000000 ) ;
#16930 = CARTESIAN_POINT ( 'NONE',  ( -13.31935981333936425, -9.442884908240273489, 34.35708131394835618 ) ) ;
#16931 = FACE_OUTER_BOUND ( 'NONE', #9395, .T. ) ;
#16932 = VERTEX_POINT ( 'NONE', #17548 ) ;
#16933 = ADVANCED_FACE ( 'NONE', ( #72930 ), #16645, .F. ) ;
#16934 = CARTESIAN_POINT ( 'NONE',  ( 8.769230769230647482, -3.835265460704628371, 33.15142922262033665 ) ) ;
#16935 = VERTEX_POINT ( 'NONE', #23832 ) ;
#16936 = VERTEX_POINT ( 'NONE', #78344 ) ;
#16937 = EDGE_CURVE ( 'NONE', #70729, #77416, #24742, .T. ) ;
#16938 = EDGE_CURVE ( 'NONE', #73980, #35887, #67327, .T. ) ;
#16939 = CARTESIAN_POINT ( 'NONE',  ( 18.22277966897806678, -2.353885683473779800, 30.79025554430704759 ) ) ;
#16940 = CARTESIAN_POINT ( 'NONE',  ( 16.28437185560971656, -12.45806712695776319, 30.39783852428763566 ) ) ;
#16941 = DIRECTION ( 'NONE',  ( -0.000000000000000000, -0.000000000000000000, -1.000000000000000000 ) ) ;
#16942 = CARTESIAN_POINT ( 'NONE',  ( 10.48469401227430708, -4.684245665217972032, 34.18127051446801090 ) ) ;
#16943 = CARTESIAN_POINT ( 'NONE',  ( -4.376724836274800801, -7.630691491037286056, 34.74850469731152458 ) ) ;
#16944 = CARTESIAN_POINT ( 'NONE',  ( 16.15384615384615330, -1.044019251281081972, 31.83374038241031911 ) ) ;
#16945 = ORIENTED_EDGE ( 'NONE', *, *, #51918, .T. ) ;
#16946 = EDGE_CURVE ( 'NONE', #34142, #84846, #83430, .T. ) ;
#16947 = ORIENTED_EDGE ( 'NONE', *, *, #19034, .F. ) ;
#16948 = CARTESIAN_POINT ( 'NONE',  ( -3.750000000000008438, -5.946699141100917352, 20.17187500000000000 ) ) ;
#16949 = ORIENTED_EDGE ( 'NONE', *, *, #15238, .F. ) ;
#16950 = CIRCLE ( 'NONE', #50001, 0.2500000000000002220 ) ;
#16952 = ORIENTED_EDGE ( 'NONE', *, *, #56076, .F. ) ;
#16951 = CARTESIAN_POINT ( 'NONE',  ( 15.45354877203763877, -5.913360116392397892, 34.49180327182771322 ) ) ;
#16953 = CARTESIAN_POINT ( 'NONE',  ( -9.942330916529147800, -10.18141759479407327, 34.26406193332782379 ) ) ;
#16954 = CARTESIAN_POINT ( 'NONE',  ( 5.999999999999880096, -12.46129190930018460, 30.37095296980731973 ) ) ;
#16955 = EDGE_CURVE ( 'NONE', #72548, #35799, #11234, .T. ) ;
#16956 = EDGE_CURVE ( 'NONE', #65236, #34858, #4013, .T. ) ;
#16957 = CARTESIAN_POINT ( 'NONE',  ( -0.3310130233048164672, -9.503571793651733657, 34.60286762892837942 ) ) ;
#16958 = ORIENTED_EDGE ( 'NONE', *, *, #48163, .T. ) ;
#16959 = AXIS2_PLACEMENT_3D ( 'NONE', #33435, #19469, #87068 ) ;
#16960 = CYLINDRICAL_SURFACE ( 'NONE', #62692, 0.2500000000000008882 ) ;
#16961 = ORIENTED_EDGE ( 'NONE', *, *, #1623, .T. ) ;
#16962 = EDGE_CURVE ( 'NONE', #12394, #67447, #38704, .T. ) ;
#16963 = CARTESIAN_POINT ( 'NONE',  ( 2.307692307692187583, -9.442884908241554243, 34.35708131394783038 ) ) ;
#16964 = DIRECTION ( 'NONE',  ( -1.000000000000000000, -0.000000000000000000, -0.000000000000000000 ) ) ;
#16965 = CARTESIAN_POINT ( 'NONE',  ( -17.86920955903304886, -2.494656445102014342, 31.33466734024120015 ) ) ;
#16967 = CARTESIAN_POINT ( 'NONE',  ( 1.384615384615264011, -8.656820664282941280, 34.87096338111179961 ) ) ;
#16966 = CARTESIAN_POINT ( 'NONE',  ( 5.869309396889695662, -12.35290016733513951, 31.75349464988449455 ) ) ;
#16968 = CARTESIAN_POINT ( 'NONE',  ( -1.253824943648433887, -8.191423895709840863, 34.95447573519442130 ) ) ;
#16969 = FACE_OUTER_BOUND ( 'NONE', #42880, .T. ) ;
#16970 = ORIENTED_EDGE ( 'NONE', *, *, #10864, .F. ) ;
#16971 = CARTESIAN_POINT ( 'NONE',  ( -11.40793583669797151, -12.27024696741798948, 31.24895572276497546 ) ) ;
#16972 = CARTESIAN_POINT ( 'NONE',  ( 6.923076923076924238, -8.318370150425687726, 35.83090037661290239 ) ) ;
#16973 = VERTEX_POINT ( 'NONE', #44999 ) ;
#16974 = CARTESIAN_POINT ( 'NONE',  ( 6.923076923076924238, -2.721908614388771852, 31.22303859784724978 ) ) ;
#16975 = CARTESIAN_POINT ( 'NONE',  ( 10.61538461538449596, -6.879047030192662504, 34.71129190930017927 ) ) ;
#16976 = CARTESIAN_POINT ( 'NONE',  ( 15.93091919493930320, -6.459968553980840689, 34.89616026154728701 ) ) ;
#16977 = AXIS2_PLACEMENT_3D ( 'NONE', #931, #70723, #62184 ) ;
#16978 = CARTESIAN_POINT ( 'NONE',  ( -16.37733107841048508, -12.11044203135681840, 32.26167407432752299 ) ) ;
#16979 = CARTESIAN_POINT ( 'NONE',  ( -7.779987239562206724, -7.250054591869668386, 34.99404684341514127 ) ) ;
#16980 = FACE_BOUND ( 'NONE', #6094, .T. ) ;
#16982 = CARTESIAN_POINT ( 'NONE',  ( -15.23076923076922995, -5.180354513474913603, 36.12317359536750416 ) ) ;
#16981 = LINE ( 'NONE', #10232, #8778 ) ;
#16983 = DIRECTION ( 'NONE',  ( -1.000000000000000000, -0.000000000000000000, 0.000000000000000000 ) ) ;
#16985 = CYLINDRICAL_SURFACE ( 'NONE', #3176, 0.2499999999999986955 ) ;
#16984 = CARTESIAN_POINT ( 'NONE',  ( -1.161604033002533898, -12.15243808032445827, 31.58219941686247978 ) ) ;
#16986 = CARTESIAN_POINT ( 'NONE',  ( -10.61538461538461320, -8.564572088678739092, 35.78748833219616898 ) ) ;
#16987 = DIRECTION ( 'NONE',  ( -0.000000000000000000, -0.8660254037844399289, -0.4999999999999980016 ) ) ;
#16988 = CARTESIAN_POINT ( 'NONE',  ( 2.608446859217893099, -4.805146000318787358, 17.81063170625849068 ) ) ;
#16989 = EDGE_CURVE ( 'NONE', #33332, #49403, #80243, .T. ) ;
#16990 = ORIENTED_EDGE ( 'NONE', *, *, #671, .T. ) ;
#16991 = CARTESIAN_POINT ( 'NONE',  ( 16.15384615384603251, -9.528491918059723176, 34.59228464037033035 ) ) ;
#16992 = AXIS2_PLACEMENT_3D ( 'NONE', #55253, #1647, #40867 ) ;
#16993 = CARTESIAN_POINT ( 'NONE',  ( -4.284537620513712675, -3.062553014421049546, 32.05460306192773601 ) ) ;
#16994 = CARTESIAN_POINT ( 'NONE',  ( 5.749976775778542937, -5.765609946408404518, 34.70566812827425451 ) ) ;
#16995 = LINE ( 'NONE', #58406, #58235 ) ;
#16996 = CARTESIAN_POINT ( 'NONE',  ( 7.715462379486287325, -4.809359713505815925, 33.96456829005828837 ) ) ;
#16997 = CARTESIAN_POINT ( 'NONE',  ( -5.207483668664997012, -2.504760397472873823, 29.97295953869789997 ) ) ;
#16998 = CARTESIAN_POINT ( 'NONE',  ( -1.614399933863656544, -3.775308065498769405, 20.07625670625849068 ) ) ;
#16999 = CARTESIAN_POINT ( 'NONE',  ( -1.634615384615383027, -7.500000000000001776, 35.00000000000000000 ) ) ;
#17000 = CARTESIAN_POINT ( 'NONE',  ( 0.6843180028068712728, -3.755027918224367767, 33.06320215134714857 ) ) ;
#17001 = CARTESIAN_POINT ( 'NONE',  ( -7.846153846153967493, -10.33852847137269571, 34.16647553114546554 ) ) ;
#17002 = LINE ( 'NONE', #9370, #34380 ) ;
#17003 = LINE ( 'NONE', #71944, #42553 ) ;
#17004 = DIRECTION ( 'NONE',  ( -0.000000000000000000, 0.9396926207859093161, -0.3420201433256663259 ) ) ;
#17005 = EDGE_CURVE ( 'NONE', #52632, #43220, #43456, .T. ) ;
#17006 = DIRECTION ( 'NONE',  ( -0.000000000000000000, 0.7660444431189791237, -0.6427876096865379196 ) ) ;
#17007 = CARTESIAN_POINT ( 'NONE',  ( -17.07692307692307665, -5.557115091759785130, 34.35708131394839171 ) ) ;
#17008 = ORIENTED_EDGE ( 'NONE', *, *, #73824, .F. ) ;
#17009 = B_SPLINE_CURVE_WITH_KNOTS ( 'NONE', 3,
 ( #86177, #32108, #87077, #79412, #65877, #52811, #10507, #25796, #24446, #51456 ),
 .UNSPECIFIED., .F., .F.,
 ( 4, 2, 2, 2, 4 ),
 ( 0.0007817246256747446788, 0.0009771112852218872494, 0.001172497944769029929, 0.001367884604316172391, 0.001563271263863315070 ),
 .UNSPECIFIED. ) ;
#17010 = FACE_OUTER_BOUND ( 'NONE', #72206, .T. ) ;
#17011 = CYLINDRICAL_SURFACE ( 'NONE', #74833, 0.2500000000000008882 ) ;
#17012 = CARTESIAN_POINT ( 'NONE',  ( 1.614399933863618797, -3.775308065498751198, 15.73624329374151998 ) ) ;
#17013 = CARTESIAN_POINT ( 'NONE',  ( 6.673100179028331524, -4.818429247618089661, 34.26397095200675125 ) ) ;
#17015 = CARTESIAN_POINT ( 'NONE',  ( 5.999999999999880096, -10.90142922262034020, 33.41473453929536674 ) ) ;
#17014 = VECTOR ( 'NONE', #12789, 1000.000000000000227 ) ;
#17016 = EDGE_LOOP ( 'NONE', ( #56794, #27153 ) ) ;
#17017 = CARTESIAN_POINT ( 'NONE',  ( -18.25002323729296450, -9.271318131107980420, 34.42618302367067429 ) ) ;
#17018 = CARTESIAN_POINT ( 'NONE',  ( -6.923076923076922462, -2.499999999999998668, 29.75000000000001421 ) ) ;
#17020 = ORIENTED_EDGE ( 'NONE', *, *, #29687, .F. ) ;
#17019 = CARTESIAN_POINT ( 'NONE',  ( -15.23076923076922995, -4.102666532097928531, 36.13435417666054406 ) ) ;
#17021 = CARTESIAN_POINT ( 'NONE',  ( -12.71156168575991785, -9.356822207818506598, 34.66110646841856635 ) ) ;
#17022 = FACE_OUTER_BOUND ( 'NONE', #81463, .T. ) ;
#17023 = CARTESIAN_POINT ( 'NONE',  ( 4.153846153846154188, -13.49023893513002648, 31.06009739812518688 ) ) ;
#17024 = AXIS2_PLACEMENT_3D ( 'NONE', #27017, #27461, #76351 ) ;
#17026 = ADVANCED_FACE ( 'NONE', ( #58508 ), #24284, .T. ) ;
#17025 = CARTESIAN_POINT ( 'NONE',  ( 1.384615384615386802, -13.87047571288749737, 32.06866353760679544 ) ) ;
#17027 = ORIENTED_EDGE ( 'NONE', *, *, #61851, .T. ) ;
#17028 = CARTESIAN_POINT ( 'NONE',  ( -12.46153846153858424, -2.379036618888197729, 30.90682066428292885 ) ) ;
#17029 = VECTOR ( 'NONE', #20029, 1000.000000000000114 ) ;
#17030 = CARTESIAN_POINT ( 'NONE',  ( -1.384615384615383471, -5.557115091759785130, 34.35708131394839171 ) ) ;
#17031 = VERTEX_POINT ( 'NONE', #72481 ) ;
#17032 = ORIENTED_EDGE ( 'NONE', *, *, #36849, .T. ) ;
#17033 = ADVANCED_BREP_SHAPE_REPRESENTATION ( '', ( #28008, #83448 ), #41778 ) ;
#17034 = VERTEX_POINT ( 'NONE', #10788 ) ;
#17035 = CARTESIAN_POINT ( 'NONE',  ( -19.50000000000000000, -3.499999999999999556, 29.75000000000000355 ) ) ;
#17036 = DIRECTION ( 'NONE',  ( -0.000000000000000000, -0.8660254037844399289, -0.4999999999999980016 ) ) ;
#17037 = ADVANCED_FACE ( 'NONE', ( #71148 ), #36917, .T. ) ;
#17038 = EDGE_CURVE ( 'NONE', #70094, #42102, #4930, .T. ) ;
#17039 = CARTESIAN_POINT ( 'NONE',  ( -5.999999999999998224, -7.500000000000001776, 35.04278698407183867 ) ) ;
#17040 = CARTESIAN_POINT ( 'NONE',  ( -10.61538461538473399, -3.300289026999228881, 32.46337939537708905 ) ) ;
#17041 = ORIENTED_EDGE ( 'NONE', *, *, #71531, .T. ) ;
#17042 = B_SPLINE_CURVE_WITH_KNOTS ( 'NONE', 3,
 ( #36506, #63958, #15350, #76605, #8150, #42826, #8594, #70288, #62630, #35623 ),
 .UNSPECIFIED., .F., .F.,
 ( 4, 2, 2, 2, 4 ),
 ( 0.000000000000000000, 0.0001954311564186867660, 0.0003908623128373735320, 0.0005862934692560603251, 0.0007817246256747470640 ),
 .UNSPECIFIED. ) ;
#17043 = EDGE_CURVE ( 'NONE', #78354, #56712, #10371, .T. ) ;
#17044 = ORIENTED_EDGE ( 'NONE', *, *, #56551, .F. ) ;
#17046 = EDGE_LOOP ( 'NONE', ( #68780, #7916, #76599, #68817 ) ) ;
#17045 = CARTESIAN_POINT ( 'NONE',  ( 10.86538461538463274, -2.249999999999999112, 29.81603969181029967 ) ) ;
#17047 = B_SPLINE_CURVE_WITH_KNOTS ( 'NONE', 3,
 ( #86344, #71911, #52079, #12005, #60168, #65147, #38580, #5235, #53410, #66035 ),
 .UNSPECIFIED., .F., .F.,
 ( 4, 2, 2, 2, 4 ),
 ( 0.0007817359430256297891, 0.0009771253907249958896, 0.001172514838424361990, 0.001367904286123728091, 0.001563293733823094191 ),
 .UNSPECIFIED. ) ;
#17048 = CARTESIAN_POINT ( 'NONE',  ( 9.692307692307572609, -12.27809138561165270, 31.22303859784587132 ) ) ;
#17049 = CARTESIAN_POINT ( 'NONE',  ( -8.519285250882628446, -12.43552623307873972, 30.55307653245132826 ) ) ;
#17050 = CARTESIAN_POINT ( 'NONE',  ( -1.161602540521988525, -12.64618726649961289, 30.78989965857442712 ) ) ;
#17051 = VERTEX_POINT ( 'NONE', #34162 ) ;
#17052 = EDGE_LOOP ( 'NONE', ( #36620, #11379, #48144, #22619 ) ) ;
#17053 = ORIENTED_EDGE ( 'NONE', *, *, #73902, .T. ) ;
#17055 = ORIENTED_EDGE ( 'NONE', *, *, #66336, .T. ) ;
#17054 = CARTESIAN_POINT ( 'NONE',  ( 8.900022577055555217, -2.541949514083464479, 30.39797389878540557 ) ) ;
#17056 = CARTESIAN_POINT ( 'NONE',  ( 15.23076923076923173, -13.57706302396349152, 30.56769352161908060 ) ) ;
#17057 = EDGE_CURVE ( 'NONE', #88830, #13977, #32839, .T. ) ;
#17058 = CARTESIAN_POINT ( 'NONE',  ( -10.83831157429146330, -9.172386477786396597, 34.72672124145550043 ) ) ;
#17059 = ORIENTED_EDGE ( 'NONE', *, *, #48961, .F. ) ;
#17060 = CARTESIAN_POINT ( 'NONE',  ( -13.45069879557126669, -4.098570777380719399, 33.41473453929634729 ) ) ;
#17061 = DIRECTION ( 'NONE',  ( 0.000000000000000000, 1.000000000000000000, 8.673617379884034486E-16 ) ) ;
#17062 = LINE ( 'NONE', #18848, #20918 ) ;
#17063 = FACE_BOUND ( 'NONE', #2621, .T. ) ;
#17064 = CARTESIAN_POINT ( 'NONE',  ( 15.00728428704528561, -5.912607949931405926, 34.49155766932282319 ) ) ;
#17065 = CARTESIAN_POINT ( 'NONE',  ( 9.915270595869179360, -7.369474270740069777, 34.74850911626239736 ) ) ;
#17066 = CARTESIAN_POINT ( 'NONE',  ( 13.31853300525524908, -12.62096338111211580, 30.90682066428152908 ) ) ;
#17067 = B_SPLINE_CURVE_WITH_KNOTS ( 'NONE', 3,
 ( #79991, #25043, #80447, #45305, #5660, #5218, #38111, #72336, #79554, #19179 ),
 .UNSPECIFIED., .F., .F.,
 ( 4, 2, 2, 2, 4 ),
 ( 0.0007817246256747483650, 0.0009771112852218926705, 0.001172497944769037084, 0.001367884604316181498, 0.001563271263863325695 ),
 .UNSPECIFIED. ) ;
#17069 = DIRECTION ( 'NONE',  ( -0.000000000000000000, 1.000000000000000000, -0.000000000000000000 ) ) ;
#17068 = CARTESIAN_POINT ( 'NONE',  ( 3.453782074862626228, -3.395485233115138168, 33.02377354290276656 ) ) ;
#17070 = CARTESIAN_POINT ( 'NONE',  ( 17.93391762063986761, -6.343179335718451384, 34.87096338111212646 ) ) ;
#17071 = CARTESIAN_POINT ( 'NONE',  ( 5.299934428535924447, -2.554770724473668153, 30.48948780036025852 ) ) ;
#17072 = ORIENTED_EDGE ( 'NONE', *, *, #15824, .T. ) ;
#17073 = CYLINDRICAL_SURFACE ( 'NONE', #11624, 0.2500000000000012212 ) ;
#17074 = ORIENTED_EDGE ( 'NONE', *, *, #58271, .F. ) ;
#17075 = ORIENTED_EDGE ( 'NONE', *, *, #56121, .F. ) ;
#17077 = CARTESIAN_POINT ( 'NONE',  ( -5.934744428723974785, -12.27809138561124591, 31.22303859784720359 ) ) ;
#17076 = CARTESIAN_POINT ( 'NONE',  ( -6.792285115252135519, -8.147973898785416225, 34.70805048591653730 ) ) ;
#17078 = B_SPLINE_CURVE_WITH_KNOTS ( 'NONE', 3,
 ( #78218, #77339, #57949, #57505, #71906, #15647, #79112, #71457, #43986, #50733 ),
 .UNSPECIFIED., .F., .F.,
 ( 4, 2, 2, 2, 4 ),
 ( 0.000000000000000000, 0.0001954339857564098054, 0.0003908679715128196108, 0.0005863019572692293891, 0.0007817359430256392216 ),
 .UNSPECIFIED. ) ;
#17079 = AXIS2_PLACEMENT_3D ( 'NONE', #39180, #31968, #73849 ) ;
#17080 = B_SPLINE_CURVE_WITH_KNOTS ( 'NONE', 3,
 ( #62533, #28315, #61653, #849, #6289, #48140, #33752, #26997, #34189, #89159 ),
 .UNSPECIFIED., .F., .F.,
 ( 4, 2, 2, 2, 4 ),
 ( 0.0007817359430256302227, 0.0009771253907249963233, 0.001172514838424362424, 0.001367904286123728524, 0.001563293733823094625 ),
 .UNSPECIFIED. ) ;
#17081 = LINE ( 'NONE', #56739, #8260 ) ;
#17082 = CARTESIAN_POINT ( 'NONE',  ( 15.23076923076910916, -5.094484230521993062, 34.41647553114689373 ) ) ;
#17083 = CARTESIAN_POINT ( 'NONE',  ( 14.55763771707034948, -11.56426240980093745, 33.07394671870546432 ) ) ;
#17084 = ORIENTED_EDGE ( 'NONE', *, *, #78565, .F. ) ;
#17085 = CARTESIAN_POINT ( 'NONE',  ( 18.22277966897806678, -2.612705202774696200, 31.66806509827799943 ) ) ;
#17086 = AXIS2_PLACEMENT_3D ( 'NONE', #12118, #83229, #54863 ) ;
#17087 = LINE ( 'NONE', #58498, #40229 ) ;
#17088 = CARTESIAN_POINT ( 'NONE',  ( -1.608100309179714582, -10.23692288466677880, 34.23039457007281072 ) ) ;
#17089 = CARTESIAN_POINT ( 'NONE',  ( 10.61538461538449596, -8.613356846316285953, 34.62446782046622218 ) ) ;
#17090 = CARTESIAN_POINT ( 'NONE',  ( -15.23076923076922995, -10.67929555188718282, 33.92786785259544047 ) ) ;
#17091 = CARTESIAN_POINT ( 'NONE',  ( -1.929879867024197893E-14, -3.750000000000000000, 19.15625000000000000 ) ) ;
#17092 = EDGE_LOOP ( 'NONE', ( #35816, #67688 ) ) ;
#17093 = EDGE_LOOP ( 'NONE', ( #83307, #21231, #88931, #17741 ) ) ;
#17094 = DIRECTION ( 'NONE',  ( -0.000000000000000000, -0.7660444431189791237, -0.6427876096865379196 ) ) ;
#17095 = ORIENTED_EDGE ( 'NONE', *, *, #4045, .F. ) ;
#17096 = CARTESIAN_POINT ( 'NONE',  ( 17.20771351789003489, -3.957578996910245284, 33.62503395064540257 ) ) ;
#17097 = CARTESIAN_POINT ( 'NONE',  ( -12.46153846153858247, -10.21337939537710326, 33.94971097300076224 ) ) ;
#17098 = CARTESIAN_POINT ( 'NONE',  ( -16.40382288478850725, -4.943428324936578910, 34.04746400365624481 ) ) ;
#17099 = CARTESIAN_POINT ( 'NONE',  ( -15.00798968950081935, -2.847695495035523550, 31.58253572463339154 ) ) ;
#17100 = CARTESIAN_POINT ( 'NONE',  ( 2.320192649118979489E-14, -11.25000000000000000, 16.03125000000000000 ) ) ;
#17101 = LINE ( 'NONE', #22534, #56066 ) ;
#17102 = VERTEX_POINT ( 'NONE', #6262 ) ;
#17103 = CARTESIAN_POINT ( 'NONE',  ( 4.023235794221623252, -7.722926236386453702, 34.74524107206102030 ) ) ;
#17105 = ORIENTED_EDGE ( 'NONE', *, *, #88396, .T. ) ;
#17104 = FACE_OUTER_BOUND ( 'NONE', #77996, .T. ) ;
#17106 = CARTESIAN_POINT ( 'NONE',  ( 3.007284306204899060, -12.47654668319379567, 31.42292124445336654 ) ) ;
#17107 = CARTESIAN_POINT ( 'NONE',  ( 3.453548772037639658, -2.847695495035523550, 31.58253572463339154 ) ) ;
#17108 = DIRECTION ( 'NONE',  ( 0.000000000000000000, 0.4999999999999960032, -0.8660254037844410391 ) ) ;
#17109 = CARTESIAN_POINT ( 'NONE',  ( 6.792928953345230170, -3.625366637846544560, 33.29286588640298561 ) ) ;
#17110 = CARTESIAN_POINT ( 'NONE',  ( 17.07692307692307665, -4.102666532097928531, 36.13435417666054406 ) ) ;
#17111 = CARTESIAN_POINT ( 'NONE',  ( -30.00000000000000000, 15.00000000000000355, 3.000000000000000000 ) ) ;
#17112 = CARTESIAN_POINT ( 'NONE',  ( 15.36156103859402222, -11.18335022499818621, 33.13157742990016885 ) ) ;
#17113 = CARTESIAN_POINT ( 'NONE',  ( -2.608446859217920633, -4.805146000318815780, 16.75186829374151287 ) ) ;
#17114 = VERTEX_POINT ( 'NONE', #6691 ) ;
#17115 = AXIS2_PLACEMENT_3D ( 'NONE', #65377, #79345, #46444 ) ;
#17116 = CARTESIAN_POINT ( 'NONE',  ( -4.219929564802033184, -4.786620604624113540, 33.94971097300155805 ) ) ;
#17117 = CARTESIAN_POINT ( 'NONE',  ( 8.769230769230768274, -11.69971097300155272, 32.46337939537588113 ) ) ;
#17118 = CARTESIAN_POINT ( 'NONE',  ( 4.219101293358991533, -11.06231777344671130, 33.60647404775212266 ) ) ;
#17119 = CARTESIAN_POINT ( 'NONE',  ( 2.749999999999995115, -6.360912703473971419, 23.14062500000000000 ) ) ;
#17120 = CARTESIAN_POINT ( 'NONE',  ( 0.2380535178145108122, -3.754499324213721234, 33.06261337010820256 ) ) ;
#17121 = CARTESIAN_POINT ( 'NONE',  ( 8.703148389870632329, -9.905515769479276145, 34.41647553114623292 ) ) ;
#17122 = ORIENTED_EDGE ( 'NONE', *, *, #1961, .F. ) ;
#17123 = CARTESIAN_POINT ( 'NONE',  ( 1.139087296525997051, -4.749999999999992895, 20.48437500000000000 ) ) ;
#17124 = CARTESIAN_POINT ( 'NONE',  ( -1.134560964701931240, -12.41089969410671223, 31.60739465890703670 ) ) ;
#17125 = VERTEX_POINT ( 'NONE', #33727 ) ;
#17126 = FACE_OUTER_BOUND ( 'NONE', #12853, .T. ) ;
#17127 = VERTEX_POINT ( 'NONE', #46349 ) ;
#17128 = CARTESIAN_POINT ( 'NONE',  ( 6.250000000001437961, -7.500000000000155431, 34.75000000000007105 ) ) ;
#17129 = CARTESIAN_POINT ( 'NONE',  ( -5.776624059301814107, -2.501478030877322567, 29.88021232661720816 ) ) ;
#17130 = CARTESIAN_POINT ( 'NONE',  ( -0.3310130233048171333, -6.808710257144159783, 34.95449254468098843 ) ) ;
#17131 = EDGE_LOOP ( 'NONE', ( #9506, #70627, #17055, #68156, #39911, #67901, #63783, #41654 ) ) ;
#17132 = LINE ( 'NONE', #44592, #6244 ) ;
#17133 = ORIENTED_EDGE ( 'NONE', *, *, #36151, .F. ) ;
#17134 = CARTESIAN_POINT ( 'NONE',  ( -0.4615384615384611200, -3.669653830205710676, 35.88435417666054406 ) ) ;
#17135 = EDGE_CURVE ( 'NONE', #14030, #75330, #75164, .T. ) ;
#17136 = ORIENTED_EDGE ( 'NONE', *, *, #53932, .F. ) ;
#17137 = VECTOR ( 'NONE', #18161, 1000.000000000000000 ) ;
#17138 = CARTESIAN_POINT ( 'NONE',  ( -15.23076923076922995, -9.819645486525091727, 36.12317359536749706 ) ) ;
#17139 = CARTESIAN_POINT ( 'NONE',  ( 12.68431800280686872, -12.24180327182771855, 31.33663988360758879 ) ) ;
#17140 = ORIENTED_EDGE ( 'NONE', *, *, #47661, .F. ) ;
#17141 = ADVANCED_FACE ( 'NONE', ( #26974 ), #12134, .F. ) ;
#17142 = CARTESIAN_POINT ( 'NONE',  ( -6.250023224221457951, -10.92453946501458439, 33.72985991061850086 ) ) ;
#17143 = FACE_OUTER_BOUND ( 'NONE', #57586, .T. ) ;
#17144 = LINE ( 'NONE', #43729, #59561 ) ;
#17145 = AXIS2_PLACEMENT_3D ( 'NONE', #55277, #344, #82765 ) ;
#17146 = B_SPLINE_CURVE_WITH_KNOTS ( 'NONE', 3,
 ( #83184, #2078, #77297, #43072, #318, #42200, #15604, #70545, #7962, #27783 ),
 .UNSPECIFIED., .F., .F.,
 ( 4, 2, 2, 2, 4 ),
 ( 0.000000000000000000, 0.0001954339857564126514, 0.0003908679715128183098, 0.0005863019572692239681, 0.0007817359430256294638 ),
 .UNSPECIFIED. ) ;
#17147 = CARTESIAN_POINT ( 'NONE',  ( -14.08467946359890988, -10.01129605718032600, 34.36064277460058491 ) ) ;
#17148 = CARTESIAN_POINT ( 'NONE',  ( -16.15384615384627409, -3.083524468854526912, 32.58852847137268327 ) ) ;
#17149 = EDGE_LOOP ( 'NONE', ( #59097, #7381, #58226, #21308, #68307 ) ) ;
#17150 = EDGE_LOOP ( 'NONE', ( #29483, #79524, #57031, #49280 ) ) ;
#17151 = EDGE_CURVE ( 'NONE', #41676, #76909, #79104, .T. ) ;
#17152 = EDGE_LOOP ( 'NONE', ( #26026, #31393 ) ) ;
#17154 = ORIENTED_EDGE ( 'NONE', *, *, #5663, .F. ) ;
#17153 = DIRECTION ( 'NONE',  ( -0.000000000000000000, 0.5000000000000011102, -0.8660254037844381525 ) ) ;
#17155 = CARTESIAN_POINT ( 'NONE',  ( 10.61538461538461675, -4.786620604624113540, 33.94971097300155094 ) ) ;
#17156 = CARTESIAN_POINT ( 'NONE',  ( 5.999999999999878320, -10.33852847137269571, 34.16647553114546554 ) ) ;
#17157 = VERTEX_POINT ( 'NONE', #46795 ) ;
#17158 = ORIENTED_EDGE ( 'NONE', *, *, #34466, .F. ) ;
#17159 = ORIENTED_EDGE ( 'NONE', *, *, #44371, .T. ) ;
#17160 = CARTESIAN_POINT ( 'NONE',  ( -1.607541602131531189, -11.76352882383564769, 32.36236540154569497 ) ) ;
#17161 = ORIENTED_EDGE ( 'NONE', *, *, #64682, .T. ) ;
#17162 = CARTESIAN_POINT ( 'NONE',  ( 16.08857570788537572, -10.21337939537584383, 33.94971097300158647 ) ) ;
#17163 = EDGE_CURVE ( 'NONE', #36033, #72869, #75929, .T. ) ;
#17164 = CARTESIAN_POINT ( 'NONE',  ( 16.82694633287449193, -12.41104346484419452, 31.60698883733904196 ) ) ;
#17165 = ADVANCED_FACE ( 'NONE', ( #19328 ), #74271, .T. ) ;
#17166 = AXIS2_PLACEMENT_3D ( 'NONE', #78785, #10336, #65267 ) ;
#17167 = CARTESIAN_POINT ( 'NONE',  ( 12.21156173059610772, -2.564618984488975517, 30.55390908950641915 ) ) ;
#17168 = FACE_BOUND ( 'NONE', #33765, .T. ) ;
#17170 = ORIENTED_EDGE ( 'NONE', *, *, #16937, .F. ) ;
#17169 = EDGE_CURVE ( 'NONE', #41455, #27570, #54883, .T. ) ;
#17171 = B_SPLINE_CURVE_WITH_KNOTS ( 'NONE', 3,
 ( #3626, #23017, #50477, #77962, #84298, #64877, #3183, #16263, #57690, #17605 ),
 .UNSPECIFIED., .F., .F.,
 ( 4, 2, 2, 2, 4 ),
 ( 0.000000000000000000, 0.0001954339857564074473, 0.0003908679715128148945, 0.0005863019572692223418, 0.0007817359430256297891 ),
 .UNSPECIFIED. ) ;
#17172 = CARTESIAN_POINT ( 'NONE',  ( -1.634615384615383027, -7.433931650972300353, 34.75000000000000711 ) ) ;
#17173 = EDGE_CURVE ( 'NONE', #42667, #82873, #48001, .T. ) ;
#17174 = DIRECTION ( 'NONE',  ( 0.000000000000000000, 0.9396926207859126468, -0.3420201433256571111 ) ) ;
#17175 = FACE_OUTER_BOUND ( 'NONE', #38109, .T. ) ;
#17176 = CARTESIAN_POINT ( 'NONE',  ( -1.608100328339331586, -2.599994579823203367, 30.74605699353653776 ) ) ;
#17177 = VERTEX_POINT ( 'NONE', #35496 ) ;
#17178 = CARTESIAN_POINT ( 'NONE',  ( -5.076923076923199218, -2.379036618888197729, 30.90682066428292885 ) ) ;
#17179 = ORIENTED_EDGE ( 'NONE', *, *, #57485, .T. ) ;
#17180 = ORIENTED_EDGE ( 'NONE', *, *, #43740, .T. ) ;
#17182 = CARTESIAN_POINT ( 'NONE',  ( -1.450697763975519416, -5.471508081941601986, 34.59228464037088457 ) ) ;
#17181 = CARTESIAN_POINT ( 'NONE',  ( 5.777073041093152561, -11.98009711892699691, 32.48740034544075428 ) ) ;
#17183 = DIRECTION ( 'NONE',  ( 0.000000000000000000, 0.9396926207859126468, -0.3420201433256571111 ) ) ;
#17184 = CARTESIAN_POINT ( 'NONE',  ( -13.44988538517170795, -3.083524468853724443, 32.58852847137143272 ) ) ;
#17185 = CARTESIAN_POINT ( 'NONE',  ( 7.596177115211490971, -12.41269422305637171, 30.68257228309993323 ) ) ;
#17186 = CARTESIAN_POINT ( 'NONE',  ( -12.23875892027004753, -4.387253974876679230, 33.66317474335728832 ) ) ;
#17187 = ORIENTED_EDGE ( 'NONE', *, *, #26214, .F. ) ;
#17188 = CYLINDRICAL_SURFACE ( 'NONE', #40021, 0.2499999999999998890 ) ;
#17189 = CARTESIAN_POINT ( 'NONE',  ( 0.4615384615383382183, -9.528491918059723176, 34.59228464037033035 ) ) ;
#17190 = CARTESIAN_POINT ( 'NONE',  ( -1.515306851282945511, -3.530157926970578508, 32.79014554554150607 ) ) ;
#17191 = CARTESIAN_POINT ( 'NONE',  ( 13.31934493865461278, -12.46129190929999986, 30.37095296980880832 ) ) ;
#17192 = ORIENTED_EDGE ( 'NONE', *, *, #51259, .F. ) ;
#17193 = B_SPLINE_CURVE_WITH_KNOTS ( 'NONE', 3,
 ( #5057, #60438, #6824, #59996, #75724, #41065, #87495, #87955, #67651, #40630 ),
 .UNSPECIFIED., .F., .F.,
 ( 4, 2, 2, 2, 4 ),
 ( 0.0007817246256747484735, 0.0009771112852218931041, 0.001172497944769037735, 0.001367884604316182365, 0.001563271263863326996 ),
 .UNSPECIFIED. ) ;
#17194 = ORIENTED_EDGE ( 'NONE', *, *, #55161, .F. ) ;
#17195 = FACE_BOUND ( 'NONE', #77332, .T. ) ;
#17196 = AXIS2_PLACEMENT_3D ( 'NONE', #66156, #4462, #31946 ) ;
#17197 = ORIENTED_EDGE ( 'NONE', *, *, #12041, .T. ) ;
#17198 = CARTESIAN_POINT ( 'NONE',  ( -6.000000000000121680, -5.094484230521993062, 34.41647553114689373 ) ) ;
#17199 = CARTESIAN_POINT ( 'NONE',  ( -1.253824943648435442, -2.295524264805589354, 30.44142389570982488 ) ) ;
#17200 = VERTEX_POINT ( 'NONE', #41371 ) ;
#17201 = CARTESIAN_POINT ( 'NONE',  ( -3.480792468062195333, -12.43535235679832596, 30.55408501211184813 ) ) ;
#17202 = CARTESIAN_POINT ( 'NONE',  ( -10.61538461538473399, -6.879047030192662504, 34.71129190930017927 ) ) ;
#17203 = CARTESIAN_POINT ( 'NONE',  ( 14.30769230769231015, -11.69971097300155272, 32.46337939537588113 ) ) ;
#17204 = CYLINDRICAL_SURFACE ( 'NONE', #53193, 0.2499999999999995559 ) ;
#17205 = EDGE_LOOP ( 'NONE', ( #21140, #33171 ) ) ;
#17206 = VECTOR ( 'NONE', #59928, 1000.000000000000000 ) ;
#17207 = CARTESIAN_POINT ( 'NONE',  ( -7.846153846153844924, -10.51840700105979565, 33.73612834413961536 ) ) ;
#17208 = VERTEX_POINT ( 'NONE', #28747 ) ;
#17209 = VECTOR ( 'NONE', #41615, 1000.000000000000000 ) ;
#17211 = ORIENTED_EDGE ( 'NONE', *, *, #56345, .T. ) ;
#17210 = CARTESIAN_POINT ( 'NONE',  ( 13.38461538461526423, -8.656820664282941280, 34.87096338111179961 ) ) ;
#17212 = DIRECTION ( 'NONE',  ( -0.000000000000000000, -0.1736481776669307198, -0.9848077530122080203 ) ) ;
#17213 = FACE_OUTER_BOUND ( 'NONE', #75434, .T. ) ;
#17214 = LINE ( 'NONE', #10469, #63102 ) ;
#17215 = ADVANCED_FACE ( 'NONE', ( #35946 ), #22420, .F. ) ;
#17216 = CARTESIAN_POINT ( 'NONE',  ( 15.45378058238208396, -12.39991518177334129, 30.74647679643404530 ) ) ;
#17217 = CARTESIAN_POINT ( 'NONE',  ( -14.55766905174089842, -8.347322224742351082, 34.93158281831414058 ) ) ;
#17218 = CARTESIAN_POINT ( 'NONE',  ( 5.076923076923075762, -12.37446782046654192, 30.86335684631486131 ) ) ;
#17219 = B_SPLINE_CURVE_WITH_KNOTS ( 'NONE', 3,
 ( #31843, #24177, #17434, #9783, #51629, #65601, #72366, #3902, #31388, #85448 ),
 .UNSPECIFIED., .F., .F.,
 ( 4, 2, 2, 2, 4 ),
 ( 0.0007817246256747453293, 0.0009771112852218881168, 0.001172497944769030796, 0.001367884604316173475, 0.001563271263863316154 ),
 .UNSPECIFIED. ) ;
#17220 = CARTESIAN_POINT ( 'NONE',  ( -0.06109907496451398579, -10.25000000000000178, 13.78311829374151287 ) ) ;
#17221 = EDGE_LOOP ( 'NONE', ( #64897, #3236, #77100, #67826 ) ) ;
#17222 = B_SPLINE_CURVE_WITH_KNOTS ( 'NONE', 3,
 ( #35964, #63420, #55335, #14352, #70628, #62965, #48132, #1727, #29216, #22439 ),
 .UNSPECIFIED., .F., .F.,
 ( 4, 2, 2, 2, 4 ),
 ( 0.000000000000000000, 0.0001954311564186860613, 0.0003908623128373721225, 0.0005862934692560581567, 0.0007817246256747442451 ),
 .UNSPECIFIED. ) ;
#17223 = CARTESIAN_POINT ( 'NONE',  ( 1.653273178848927064E-15, -7.500000000000000000, 14.00000000000000178 ) ) ;
#17224 = FACE_OUTER_BOUND ( 'NONE', #62307, .T. ) ;
#17225 = CARTESIAN_POINT ( 'NONE',  ( 4.499999999999999112, 7.500000000000002665, 13.50000000000000178 ) ) ;
#17226 = VERTEX_POINT ( 'NONE', #68835 ) ;
#17227 = ORIENTED_EDGE ( 'NONE', *, *, #105, .T. ) ;
#17228 = DIRECTION ( 'NONE',  ( 0.000000000000000000, 0.1736481776669275834, 0.9848077530122086864 ) ) ;
#17229 = DIRECTION ( 'NONE',  ( -1.000000000000000000, 0.000000000000000000, 0.000000000000000000 ) ) ;
#17230 = CARTESIAN_POINT ( 'NONE',  ( 2.980745993476265898, -10.05641848906368097, 34.04755513067966177 ) ) ;
#17231 = EDGE_CURVE ( 'NONE', #68982, #36238, #63401, .T. ) ;
#17232 = CARTESIAN_POINT ( 'NONE',  ( 9.692307692307572609, -12.46129190930018460, 30.37095296980731973 ) ) ;
#17233 = CARTESIAN_POINT ( 'NONE',  ( 10.36536137809165403, -4.335965774309649134, 33.62209801155881905 ) ) ;
#17234 = CARTESIAN_POINT ( 'NONE',  ( -16.82686865700962642, -11.47946981652013498, 33.17500667209846910 ) ) ;
#17235 = DIRECTION ( 'NONE',  ( -0.000000000000000000, 0.5000000000000011102, -0.8660254037844381525 ) ) ;
#17236 = VERTEX_POINT ( 'NONE', #55757 ) ;
#17237 = CARTESIAN_POINT ( 'NONE',  ( 3.100077764101673683, -6.413092428213692742, 34.63065189839063152 ) ) ;
#17238 = CARTESIAN_POINT ( 'NONE',  ( -16.85349611506149969, -7.630147231320743018, 34.74852402298682819 ) ) ;
#17239 = CARTESIAN_POINT ( 'NONE',  ( 4.403846153846090239, -7.565270000091922853, 34.99999999999999289 ) ) ;
#17240 = CARTESIAN_POINT ( 'NONE',  ( 7.846153846153846700, -3.886160181151819604, 36.00935417666054406 ) ) ;
#17241 = ORIENTED_EDGE ( 'NONE', *, *, #57086, .F. ) ;
#17242 = CARTESIAN_POINT ( 'NONE',  ( -7.715628144390278997, -3.816742781228458448, 33.13167719472716044 ) ) ;
#17243 = EDGE_CURVE ( 'NONE', #40454, #74101, #44623, .T. ) ;
#17244 = ORIENTED_EDGE ( 'NONE', *, *, #22877, .T. ) ;
#17245 = CARTESIAN_POINT ( 'NONE',  ( -0.4615384615385826339, -2.892918686052166066, 31.69288490824153470 ) ) ;
#17246 = DIRECTION ( 'NONE',  ( -1.000000000000000000, 0.000000000000000000, 0.000000000000000000 ) ) ;
#17247 = CARTESIAN_POINT ( 'NONE',  ( -2.176853889679542853, -7.277220443632450575, 34.74524770363009196 ) ) ;
#17248 = VERTEX_POINT ( 'NONE', #21534 ) ;
#17249 = EDGE_CURVE ( 'NONE', #69237, #1870, #88713, .T. ) ;
#17250 = CYLINDRICAL_SURFACE ( 'NONE', #6092, 0.2500000000000009437 ) ;
#17251 = LINE ( 'NONE', #51912, #58073 ) ;
#17252 = CYLINDRICAL_SURFACE ( 'NONE', #14955, 0.2500000000000004996 ) ;
#17253 = CARTESIAN_POINT ( 'NONE',  ( 7.846153846153846700, -9.058645607665452459, 34.76329471203371924 ) ) ;
#17254 = VERTEX_POINT ( 'NONE', #27851 ) ;
#17255 = VECTOR ( 'NONE', #24817, 1000.000000000000000 ) ;
#17256 = ADVANCED_FACE ( 'NONE', ( #21081 ), #77365, .F. ) ;
#17257 = CARTESIAN_POINT ( 'NONE',  ( -1.134669866267241423, -3.712312575010499938, 33.01462480002815170 ) ) ;
#17258 = ORIENTED_EDGE ( 'NONE', *, *, #14074, .T. ) ;
#17259 = LINE ( 'NONE', #35879, #77398 ) ;
#17260 = CARTESIAN_POINT ( 'NONE',  ( 5.076923076922954969, -12.27809138561165270, 31.22303859784587132 ) ) ;
#17261 = AXIS2_PLACEMENT_3D ( 'NONE', #49183, #53166, #64901 ) ;
#17262 = EDGE_CURVE ( 'NONE', #60982, #47138, #36385, .T. ) ;
#17263 = CARTESIAN_POINT ( 'NONE',  ( -16.37733109757011007, -11.41268669641499756, 32.86336882939238535 ) ) ;
#17264 = CARTESIAN_POINT ( 'NONE',  ( 8.769230769230647482, -2.892918686052165622, 31.69288490824153470 ) ) ;
#17265 = ADVANCED_FACE ( 'NONE', ( #2144 ), #8027, .F. ) ;
#17266 = DIRECTION ( 'NONE',  ( 0.000000000000000000, 0.000000000000000000, 1.000000000000000000 ) ) ;
#17267 = CARTESIAN_POINT ( 'NONE',  ( 12.71148397988660150, -10.05730279482229683, 34.04704008940765902 ) ) ;
#17268 = AXIS2_PLACEMENT_3D ( 'NONE', #30522, #78714, #79159 ) ;
#17269 = AXIS2_PLACEMENT_3D ( 'NONE', #26381, #75893, #67810 ) ;
#17270 = ORIENTED_EDGE ( 'NONE', *, *, #61896, .T. ) ;
#17271 = ORIENTED_EDGE ( 'NONE', *, *, #71855, .T. ) ;
#17272 = COLOUR_RGB ( '', 0.66274510, 0.83137255, 0.94901961) ;
#17273 = ORIENTED_EDGE ( 'NONE', *, *, #49450, .F. ) ;
#17274 = ORIENTED_EDGE ( 'NONE', *, *, #15856, .T. ) ;
#17275 = ORIENTED_EDGE ( 'NONE', *, *, #39736, .T. ) ;
#17276 = EDGE_CURVE ( 'NONE', #74633, #37657, #53557, .T. ) ;
#17277 = CARTESIAN_POINT ( 'NONE',  ( -12.71153846153846168, -2.249999999999998668, 29.75000000000000355 ) ) ;
#17278 = CARTESIAN_POINT ( 'NONE',  ( -11.76194648218548622, -9.331801661448606566, 34.40259984581193464 ) ) ;
#17279 = CARTESIAN_POINT ( 'NONE',  ( -5.326923076923075762, -7.433931650972300353, 34.75000000000000711 ) ) ;
#17280 = CARTESIAN_POINT ( 'NONE',  ( -0.4615384615385826339, -6.879047030192662504, 34.71129190930017927 ) ) ;
#17281 = CARTESIAN_POINT ( 'NONE',  ( -16.40382288478850725, -2.564618984488975517, 30.55390908950641915 ) ) ;
#17282 = CARTESIAN_POINT ( 'NONE',  ( 3.230769230769110045, -6.026961402154118908, 34.52809138561165270 ) ) ;
#17283 = EDGE_CURVE ( 'NONE', #69537, #32856, #36050, .T. ) ;
#17284 = CARTESIAN_POINT ( 'NONE',  ( 5.934729554039226862, -11.94971097300153140, 32.03036669348370680 ) ) ;
#17285 = EDGE_CURVE ( 'NONE', #6434, #58891, #64276, .T. ) ;
#17286 = CARTESIAN_POINT ( 'NONE',  ( 6.923076923076924238, -11.69971097300155272, 32.46337939537588113 ) ) ;
#17287 = DIRECTION ( 'NONE',  ( 0.000000000000000000, 0.7660444431189822323, -0.6427876096865344779 ) ) ;
#17288 = ORIENTED_EDGE ( 'NONE', *, *, #79170, .F. ) ;
#17289 = ORIENTED_EDGE ( 'NONE', *, *, #68792, .F. ) ;
#17290 = ORIENTED_EDGE ( 'NONE', *, *, #45402, .T. ) ;
#17292 = ORIENTED_EDGE ( 'NONE', *, *, #84190, .T. ) ;
#17291 = DIRECTION ( 'NONE',  ( 0.000000000000000000, 0.4999999999999960032, -0.8660254037844410391 ) ) ;
#17294 = DIRECTION ( 'NONE',  ( 0.000000000000000000, 0.000000000000000000, 1.000000000000000000 ) ) ;
#17293 = FACE_OUTER_BOUND ( 'NONE', #80068, .T. ) ;
#17295 = B_SPLINE_CURVE_WITH_KNOTS ( 'NONE', 3,
 ( #19110, #26305, #65944, #86698, #6044, #24965, #74058, #11459, #81259, #80825 ),
 .UNSPECIFIED., .F., .F.,
 ( 4, 2, 2, 2, 4 ),
 ( 0.0007817359430256315238, 0.0009771253907249980580, 0.001172514838424364592, 0.001367904286123731127, 0.001563293733823097661 ),
 .UNSPECIFIED. ) ;
#17296 = CARTESIAN_POINT ( 'NONE',  ( -1.319422396320729440, -2.255955759149235629, 29.99999999999988631 ) ) ;
#17297 = CARTESIAN_POINT ( 'NONE',  ( 6.923076923076924238, -2.538708090699994813, 30.37095296980875503 ) ) ;
#17298 = ORIENTED_EDGE ( 'NONE', *, *, #85975, .T. ) ;
#17299 = VECTOR ( 'NONE', #36080, 1000.000000000000000 ) ;
#17300 = ORIENTED_EDGE ( 'NONE', *, *, #37296, .T. ) ;
#17301 = CARTESIAN_POINT ( 'NONE',  ( -11.66915214157184089, -11.93127051446799847, 32.56575433478202797 ) ) ;
#17302 = ORIENTED_EDGE ( 'NONE', *, *, #27895, .F. ) ;
#17303 = FACE_BOUND ( 'NONE', #70231, .T. ) ;
#17304 = CARTESIAN_POINT ( 'NONE',  ( 3.361294669002873547, -2.647132371071621471, 31.75357179365173010 ) ) ;
#17305 = CARTESIAN_POINT ( 'NONE',  ( 11.53846153846153832, -9.584722331328613620, 36.20867863119891439 ) ) ;
#17306 = VERTEX_POINT ( 'NONE', #17887 ) ;
#17307 = ADVANCED_FACE ( 'NONE', ( #71931 ), #2575, .F. ) ;
#17308 = CARTESIAN_POINT ( 'NONE',  ( 14.17700084102475699, -2.729777683071817229, 31.24903638046269450 ) ) ;
#17309 = CARTESIAN_POINT ( 'NONE',  ( 8.703477340917435967, -7.249945578846651806, 34.99404164642496795 ) ) ;
#17310 = CARTESIAN_POINT ( 'NONE',  ( -5.076923076923197442, -3.835265460704628371, 33.15142922262033665 ) ) ;
#17311 = ORIENTED_EDGE ( 'NONE', *, *, #33265, .F. ) ;
#17312 = DIRECTION ( 'NONE',  ( -1.000000000000000000, 0.000000000000000000, 0.000000000000000000 ) ) ;
#17313 = CARTESIAN_POINT ( 'NONE',  ( -14.55771554498526932, -5.851115903089112003, 34.47074536777953568 ) ) ;
#17314 = ORIENTED_EDGE ( 'NONE', *, *, #57195, .F. ) ;
#17315 = CARTESIAN_POINT ( 'NONE',  ( 5.869524814924282907, -7.276987145209185215, 34.99546412871779211 ) ) ;
#17316 = CARTESIAN_POINT ( 'NONE',  ( 3.230769230769231726, -13.78497067705608181, 32.30358669280327177 ) ) ;
#17317 = VERTEX_POINT ( 'NONE', #37702 ) ;
#17318 = DIRECTION ( 'NONE',  ( -0.000000000000000000, 0.1736481776669307198, -0.9848077530122080203 ) ) ;
#17319 = CARTESIAN_POINT ( 'NONE',  ( 14.43848411551709177, -8.147973898785416225, 34.70805048591653730 ) ) ;
#17320 = FACE_OUTER_BOUND ( 'NONE', #37785, .T. ) ;
#17321 = DIRECTION ( 'NONE',  ( -0.000000000000000000, 0.5000000000000011102, -0.8660254037844380415 ) ) ;
#17322 = DIRECTION ( 'NONE',  ( 0.000000000000000000, 0.7660444431189822323, -0.6427876096865344779 ) ) ;
#17323 = ADVANCED_FACE ( 'NONE', ( #65166 ), #78242, .F. ) ;
#17324 = DIRECTION ( 'NONE',  ( 0.000000000000000000, 0.000000000000000000, -1.000000000000000000 ) ) ;
#17326 = CARTESIAN_POINT ( 'NONE',  ( 7.053868730901709405, -3.062576670634119758, 32.05464942895959979 ) ) ;
#17325 = CARTESIAN_POINT ( 'NONE',  ( -9.692307692307691624, -5.471508081941601098, 34.59228464037088457 ) ) ;
#17327 = CIRCLE ( 'NONE', #4331, 4.000000000000000000 ) ;
#17328 = CARTESIAN_POINT ( 'NONE',  ( -1.384615384615383471, -9.058645607665452459, 34.76329471203371924 ) ) ;
#17330 = CARTESIAN_POINT ( 'NONE',  ( -8.519230769230754063, -2.249999999999998224, 29.81603969181031033 ) ) ;
#17329 = CARTESIAN_POINT ( 'NONE',  ( 12.52668324225809293, -7.750023224968867197, 34.99404313364389907 ) ) ;
#17331 = CARTESIAN_POINT ( 'NONE',  ( -2.750000000000007105, -6.360912703474006946, 15.17187500000000000 ) ) ;
#17333 = EDGE_CURVE ( 'NONE', #30874, #6322, #51637, .T. ) ;
#17332 = ORIENTED_EDGE ( 'NONE', *, *, #12023, .T. ) ;
#17334 = CARTESIAN_POINT ( 'NONE',  ( 0.2380535178145127273, -12.44517049084099725, 30.48991314939691932 ) ) ;
#17335 = ORIENTED_EDGE ( 'NONE', *, *, #58338, .T. ) ;
#17336 = EDGE_CURVE ( 'NONE', #23503, #31091, #16544, .T. ) ;
#17337 = ORIENTED_EDGE ( 'NONE', *, *, #19916, .T. ) ;
#17338 = CARTESIAN_POINT ( 'NONE',  ( 16.02315468717859659, -11.18331474514187995, 33.13161551792790505 ) ) ;
#17339 = VERTEX_POINT ( 'NONE', #3467 ) ;
#17340 = CARTESIAN_POINT ( 'NONE',  ( -15.16470087976679437, -5.557115091759786019, 34.35708131394839882 ) ) ;
#17341 = CARTESIAN_POINT ( 'NONE',  ( -2.750000000000007105, -6.360912703474006946, 16.42187500000000000 ) ) ;
#17342 = CARTESIAN_POINT ( 'NONE',  ( -18.00000000000012079, -6.026961402154117131, 34.52809138561165270 ) ) ;
#17343 = CARTESIAN_POINT ( 'NONE',  ( -4.946397375159514276, -2.882268652242224505, 31.66798894389554064 ) ) ;
#17344 = CARTESIAN_POINT ( 'NONE',  ( -20.00000000000000355, -10.00000000000000533, 13.00000000000000178 ) ) ;
#17345 = CARTESIAN_POINT ( 'NONE',  ( -6.130147969731699398, -2.647304123082328875, 31.75400227202885262 ) ) ;
#17346 = VECTOR ( 'NONE', #50295, 1000.000000000000114 ) ;
#17347 = EDGE_CURVE ( 'NONE', #34740, #15372, #67145, .T. ) ;
#17348 = CARTESIAN_POINT ( 'NONE',  ( -8.703975197954745724, -5.219633306516380244, 34.19971097300157936 ) ) ;
#17349 = DIRECTION ( 'NONE',  ( -0.000000000000000000, 0.6427876096865404731, -0.7660444431189770143 ) ) ;
#17350 = CARTESIAN_POINT ( 'NONE',  ( -7.596099534515532881, -12.17597550085003633, 31.52189283813461884 ) ) ;
#17351 = AXIS2_PLACEMENT_3D ( 'NONE', #61177, #20640, #60742 ) ;
#17352 = CARTESIAN_POINT ( 'NONE',  ( -1.553300858899081538, -11.25000000000000711, 23.60937500000000711 ) ) ;
#17353 = CARTESIAN_POINT ( 'NONE',  ( 18.22277966897806678, -11.60474049983370648, 33.02348890104160262 ) ) ;
#17354 = CARTESIAN_POINT ( 'NONE',  ( -2.057746898314263717, -12.07971442181321997, 32.31769673815850297 ) ) ;
#17355 = CARTESIAN_POINT ( 'NONE',  ( 11.53846153846153832, -12.62096338111211580, 30.90682066428153263 ) ) ;
#17356 = B_SPLINE_CURVE_WITH_KNOTS ( 'NONE', 3,
 ( #26690, #41096, #54148, #55048, #48728, #81644, #28020, #19929, #34327, #68129 ),
 .UNSPECIFIED., .F., .F.,
 ( 4, 2, 2, 2, 4 ),
 ( 0.000000000000000000, 0.0001954339857564098054, 0.0003908679715128196108, 0.0005863019572692293891, 0.0007817359430256392216 ),
 .UNSPECIFIED. ) ;
#17357 = ORIENTED_EDGE ( 'NONE', *, *, #43153, .F. ) ;
#17358 = ORIENTED_EDGE ( 'NONE', *, *, #71061, .F. ) ;
#17359 = DIRECTION ( 'NONE',  ( -0.000000000000000000, -0.000000000000000000, -1.000000000000000000 ) ) ;
#17360 = DIRECTION ( 'NONE',  ( 0.000000000000000000, 0.000000000000000000, -1.000000000000000000 ) ) ;
#17361 = CARTESIAN_POINT ( 'NONE',  ( -2.557715531913763218, -2.341070481393819236, 30.72580821765574299 ) ) ;
#17362 = DIRECTION ( 'NONE',  ( -0.000000000000000000, -0.9396926207859092051, -0.3420201433256662704 ) ) ;
#17363 = ADVANCED_FACE ( 'NONE', ( #9789 ), #85899, .F. ) ;
#17364 = CARTESIAN_POINT ( 'NONE',  ( 10.61538461538449418, -12.70778746994576025, 30.41441678777401236 ) ) ;
#17365 = CARTESIAN_POINT ( 'NONE',  ( -3.007756386675835003, -5.582272713120728369, 34.63742843783360570 ) ) ;
#17366 = EDGE_CURVE ( 'NONE', #32906, #74101, #24184, .T. ) ;
#17367 = ORIENTED_EDGE ( 'NONE', *, *, #36758, .T. ) ;
#17368 = DIRECTION ( 'NONE',  ( 0.000000000000000000, 0.4999999999999960032, -0.8660254037844410391 ) ) ;
#17369 = VERTEX_POINT ( 'NONE', #79590 ) ;
#17370 = AXIS2_PLACEMENT_3D ( 'NONE', #63321, #42181, #22339 ) ;
#17371 = B_SPLINE_CURVE_WITH_KNOTS ( 'NONE', 3,
 ( #42067, #22662, #21782, #629, #35295, #64082, #7829, #42948, #49256, #63646 ),
 .UNSPECIFIED., .F., .F.,
 ( 4, 2, 2, 2, 4 ),
 ( 0.0007817246256747473893, 0.0009771112852218909357, 0.001172497944769034482, 0.001367884604316178246, 0.001563271263863321792 ),
 .UNSPECIFIED. ) ;
#17372 = ORIENTED_EDGE ( 'NONE', *, *, #85591, .F. ) ;
#17373 = CARTESIAN_POINT ( 'NONE',  ( 0.5276057948885374271, -12.34228464037088813, 31.77849191805839268 ) ) ;
#17374 = CARTESIAN_POINT ( 'NONE',  ( -11.53846153846166089, -11.67786785259630911, 32.92929555188603530 ) ) ;
#17375 = CARTESIAN_POINT ( 'NONE',  ( 14.30769230769218758, -10.90142922262034020, 33.41473453929536674 ) ) ;
#17376 = CARTESIAN_POINT ( 'NONE',  ( 2.084207363968360927, -5.912607949931405038, 34.49155766932282319 ) ) ;
#17377 = CARTESIAN_POINT ( 'NONE',  ( -13.31935981333936070, -3.300289026998473041, 32.46337939537591666 ) ) ;
#17378 = ORIENTED_EDGE ( 'NONE', *, *, #58312, .T. ) ;
#17379 = ORIENTED_EDGE ( 'NONE', *, *, #75404, .T. ) ;
#17380 = ORIENTED_EDGE ( 'NONE', *, *, #30220, .F. ) ;
#17381 = ADVANCED_FACE ( 'NONE', ( #85017 ), #72371, .F. ) ;
#17382 = ADVANCED_FACE ( 'NONE', ( #23299 ), #11122, .F. ) ;
#17383 = VECTOR ( 'NONE', #42693, 1000.000000000000000 ) ;
#17384 = CARTESIAN_POINT ( 'NONE',  ( 13.13463864056679498, -4.818429247618089661, 34.26397095200675125 ) ) ;
#17385 = DIRECTION ( 'NONE',  ( -0.000000000000000000, -0.5000000000000009992, -0.8660254037844380415 ) ) ;
#17386 = DIRECTION ( 'NONE',  ( -0.000000000000000000, -0.6427876096865404731, -0.7660444431189770143 ) ) ;
#17387 = EDGE_CURVE ( 'NONE', #2854, #19448, #21030, .T. ) ;
#17388 = CIRCLE ( 'NONE', #46147, 5.000000000000000888 ) ;
#17389 = VECTOR ( 'NONE', #9880, 1000.000000000000000 ) ;
#17390 = CARTESIAN_POINT ( 'NONE',  ( 1.161689167099237974, -3.586966769969700763, 32.86292498521069660 ) ) ;
#17391 = CARTESIAN_POINT ( 'NONE',  ( -2.307692307692305711, -3.886160181151819604, 36.00935417666054406 ) ) ;
#17392 = ADVANCED_FACE ( 'NONE', ( #74161 ), #80027, .F. ) ;
#17393 = CARTESIAN_POINT ( 'NONE',  ( 17.07692307692307665, -2.708943851104267164, 35.45975837776705220 ) ) ;
#17394 = ORIENTED_EDGE ( 'NONE', *, *, #22436, .T. ) ;
#17395 = VERTEX_POINT ( 'NONE', #32290 ) ;
#17396 = CARTESIAN_POINT ( 'NONE',  ( 2.651650429449569302, -10.15165042944953733, 19.62500000000000000 ) ) ;
#17397 = CIRCLE ( 'NONE', #43313, 4.000000000000000000 ) ;
#17398 = EDGE_LOOP ( 'NONE', ( #18099, #35253, #55555, #82309 ) ) ;
#17400 = VERTEX_POINT ( 'NONE', #39943 ) ;
#17399 = CARTESIAN_POINT ( 'NONE',  ( -13.51530598772569469, -5.496505350115501010, 34.60290016733514307 ) ) ;
#17401 = EDGE_CURVE ( 'NONE', #17400, #57207, #47565, .T. ) ;
#17402 = AXIS2_PLACEMENT_3D ( 'NONE', #53805, #55135, #33548 ) ;
#17403 = CARTESIAN_POINT ( 'NONE',  ( -9.692307692307691624, -9.905515769479276145, 34.41647553114623292 ) ) ;
#17404 = CARTESIAN_POINT ( 'NONE',  ( -9.915792636031639518, -11.89387501736622710, 32.13663884655806413 ) ) ;
#17405 = CARTESIAN_POINT ( 'NONE',  ( -2.651650429449535551, -10.15165042944956753, 17.43750000000000000 ) ) ;
#17406 = ORIENTED_EDGE ( 'NONE', *, *, #85504, .F. ) ;
#17407 = EDGE_CURVE ( 'NONE', #24055, #72513, #4702, .T. ) ;
#17408 = CARTESIAN_POINT ( 'NONE',  ( -13.44988583057615728, -12.27809138561121394, 31.22303859784730307 ) ) ;
#17409 = VERTEX_POINT ( 'NONE', #25529 ) ;
#17410 = DIRECTION ( 'NONE',  ( 0.000000000000000000, 0.000000000000000000, -1.000000000000000000 ) ) ;
#17411 = CARTESIAN_POINT ( 'NONE',  ( 4.153846153846154188, -9.058645607665452459, 34.76329471203371924 ) ) ;
#17412 = CARTESIAN_POINT ( 'NONE',  ( -15.09997878980228059, -2.845873456487965747, 32.17976146951972538 ) ) ;
#17414 = CARTESIAN_POINT ( 'NONE',  ( 4.946775867484856093, -3.285722584762969856, 32.44110544564090759 ) ) ;
#17413 = CARTESIAN_POINT ( 'NONE',  ( 11.53846153846153832, -11.33034616979429110, 35.88435417666054406 ) ) ;
#17415 = CARTESIAN_POINT ( 'NONE',  ( 5.011652630962300847, -2.625532179533445198, 30.86335684631481513 ) ) ;
#17416 = LINE ( 'NONE', #80004, #85092 ) ;
#17417 = EDGE_LOOP ( 'NONE', ( #2260, #85181, #55144, #53399 ) ) ;
#17418 = EDGE_CURVE ( 'NONE', #58891, #27959, #60768, .T. ) ;
#17419 = CARTESIAN_POINT ( 'NONE',  ( -11.53846153846153655, -12.10708131394839349, 31.69288490824020244 ) ) ;
#17420 = CARTESIAN_POINT ( 'NONE',  ( -8.769230769230892619, -4.320704448113951379, 33.92786785259630022 ) ) ;
#17421 = EDGE_LOOP ( 'NONE', ( #51948, #51742 ) ) ;
#17422 = CARTESIAN_POINT ( 'NONE',  ( -12.23875879256039489, -3.563462043263030399, 33.22394488606062879 ) ) ;
#17423 = VECTOR ( 'NONE', #56364, 1000.000000000000000 ) ;
#17424 = CARTESIAN_POINT ( 'NONE',  ( 10.61538461538461675, -6.386643153685126251, 34.62446782046654192 ) ) ;
#17425 = CARTESIAN_POINT ( 'NONE',  ( -6.130691466667555822, -10.54014554554150607, 33.71984207302941883 ) ) ;
#17426 = B_SPLINE_CURVE_WITH_KNOTS ( 'NONE', 3,
 ( #24852, #59974, #52322, #53214, #39723, #66286, #19878, #79814, #67186, #73048 ),
 .UNSPECIFIED., .F., .F.,
 ( 4, 2, 2, 2, 4 ),
 ( 0.0007817359430256360774, 0.0009771253907250039127, 0.001172514838424371965, 0.001367904286123739800, 0.001563293733823107635 ),
 .UNSPECIFIED. ) ;
#17427 = PLANE ( 'NONE',  #54289 ) ;
#17428 = CARTESIAN_POINT ( 'NONE',  ( 12.46153846153833911, -4.481592998941358097, 33.73612834414048933 ) ) ;
#17429 = FACE_BOUND ( 'NONE', #21292, .T. ) ;
#17431 = CARTESIAN_POINT ( 'NONE',  ( -10.86538461538461320, -7.500000000000001776, 35.00000000000000000 ) ) ;
#17430 = CARTESIAN_POINT ( 'NONE',  ( 13.16168842570853492, -2.308479472611653094, 30.53278059502174457 ) ) ;
#17432 = CARTESIAN_POINT ( 'NONE',  ( 0.4615384615383382183, -12.70778746994576025, 30.41441678777401236 ) ) ;
#17434 = CARTESIAN_POINT ( 'NONE',  ( 0.5920638997721023866, -3.068774925481847937, 32.56582465632704526 ) ) ;
#17433 = CARTESIAN_POINT ( 'NONE',  ( -11.47331575912957469, -7.750023238201979581, 34.74374492549440419 ) ) ;
#17435 = CARTESIAN_POINT ( 'NONE',  ( -17.07692307692307665, -1.951392089020283160, 34.73218667398347748 ) ) ;
#17436 = AXIS2_PLACEMENT_3D ( 'NONE', #27640, #13246, #76719 ) ;
#17437 = DIRECTION ( 'NONE',  ( 1.000000000000000000, 0.000000000000000000, 0.000000000000000000 ) ) ;
#17438 = CARTESIAN_POINT ( 'NONE',  ( 0.06109907496455496689, -11.24999999999999822, 25.77938170625848713 ) ) ;
#17439 = EDGE_CURVE ( 'NONE', #23926, #64222, #55337, .T. ) ;
#17440 = ORIENTED_EDGE ( 'NONE', *, *, #75629, .F. ) ;
#17441 = DIRECTION ( 'NONE',  ( 0.000000000000000000, 0.7660444431189822323, -0.6427876096865344779 ) ) ;
#17442 = CARTESIAN_POINT ( 'NONE',  ( 7.846153846153723244, -10.33852847137269571, 34.16647553114546554 ) ) ;
#17443 = CARTESIAN_POINT ( 'NONE',  ( -7.846153846153967493, -11.67786785259630911, 32.92929555188603530 ) ) ;
#17444 = LINE ( 'NONE', #64279, #85568 ) ;
#17445 = CARTESIAN_POINT ( 'NONE',  ( -20.00000000000000000, -3.499999999999999556, 29.75000000000000355 ) ) ;
#17446 = CARTESIAN_POINT ( 'NONE',  ( -16.85391023282967637, -8.282913670948747864, 34.94150082978203642 ) ) ;
#17447 = CARTESIAN_POINT ( 'NONE',  ( 2.694853999681214862, -10.10844685921789043, 23.12313170625848713 ) ) ;
#17448 = DIRECTION ( 'NONE',  ( 0.000000000000000000, 0.9396926207859126468, 0.3420201433256571111 ) ) ;
#17449 = CARTESIAN_POINT ( 'NONE',  ( -2.307692307692305711, -6.343179335718451384, 34.87096338111211935 ) ) ;
#17450 = ADVANCED_FACE ( 'NONE', ( #20103 ), #73734, .F. ) ;
#17451 = CARTESIAN_POINT ( 'NONE',  ( -8.096130590202436750, -2.920706130388546651, 32.31842814019191223 ) ) ;
#17452 = CARTESIAN_POINT ( 'NONE',  ( 9.627037691751372250, -4.320704448112771878, 33.92786785259540494 ) ) ;
#17453 = CARTESIAN_POINT ( 'NONE',  ( 7.146088274689773812, -4.187068189119697692, 33.49521262558774026 ) ) ;
#17454 = CARTESIAN_POINT ( 'NONE',  ( 5.299935921016470708, -8.282913670948747864, 34.94150082978203642 ) ) ;
#17455 = DIRECTION ( 'NONE',  ( -0.000000000000000000, 1.000000000000000000, -0.000000000000000000 ) ) ;
#17456 = EDGE_CURVE ( 'NONE', #81637, #64401, #63649, .T. ) ;
#17457 = CARTESIAN_POINT ( 'NONE',  ( 14.05766907039934210, -6.695914987888146541, 34.68535235679833306 ) ) ;
#17458 = VERTEX_POINT ( 'NONE', #75055 ) ;
#17459 = CARTESIAN_POINT ( 'NONE',  ( -5.076923076923075762, -2.900454961884010974, 35.62045528018868623 ) ) ;
#17460 = CARTESIAN_POINT ( 'NONE',  ( -5.933932666649924137, -2.486705287966279876, 31.30864560766543647 ) ) ;
#17461 = CARTESIAN_POINT ( 'NONE',  ( -1.492201783934593573, -3.724691934501250135, 14.32999329374151465 ) ) ;
#17462 = B_SPLINE_CURVE_WITH_KNOTS ( 'NONE', 3,
 ( #10226, #72357, #16091, #64259, #24619, #64706, #37686, #30486, #9342, #31378 ),
 .UNSPECIFIED., .F., .F.,
 ( 4, 2, 2, 2, 4 ),
 ( 0.000000000000000000, 0.0001954311564186871455, 0.0003908623128373742909, 0.0005862934692560614093, 0.0007817246256747485819 ),
 .UNSPECIFIED. ) ;
#17463 = VECTOR ( 'NONE', #76672, 1000.000000000000227 ) ;
#17464 = CARTESIAN_POINT ( 'NONE',  ( -10.61538461538473577, -10.33852847137269571, 34.16647553114546554 ) ) ;
#17465 = DIRECTION ( 'NONE',  ( 0.000000000000000000, 0.3420201433256610524, 0.9396926207859113145 ) ) ;
#17466 = ORIENTED_EDGE ( 'NONE', *, *, #30653, .F. ) ;
#17467 = CARTESIAN_POINT ( 'NONE',  ( 1.515141086378950508, -4.459921816937788996, 33.71989282347011851 ) ) ;
#17468 = DIRECTION ( 'NONE',  ( 0.000000000000000000, 0.3420201433256641055, -0.9396926207859100932 ) ) ;
#17470 = ORIENTED_EDGE ( 'NONE', *, *, #26580, .F. ) ;
#17469 = CARTESIAN_POINT ( 'NONE',  ( 8.769230769230645706, -2.657715359629662544, 31.77849191805970364 ) ) ;
#17471 = CARTESIAN_POINT ( 'NONE',  ( -11.31508559776335510, -2.501478030877323455, 29.88021232661721172 ) ) ;
#17472 = CARTESIAN_POINT ( 'NONE',  ( 16.82692307692308020, -7.566082377512564960, 35.00000000000000711 ) ) ;
#17473 = EDGE_CURVE ( 'NONE', #28852, #24412, #81814, .T. ) ;
#17474 = LINE ( 'NONE', #305, #70838 ) ;
#17475 = VECTOR ( 'NONE', #86081, 1000.000000000000000 ) ;
#17476 = CARTESIAN_POINT ( 'NONE',  ( 0.000000000000000000, -11.00000000000000000, 29.75000000000000355 ) ) ;
#17477 = EDGE_CURVE ( 'NONE', #83475, #41702, #66962, .T. ) ;
#17478 = EDGE_LOOP ( 'NONE', ( #32249, #21158 ) ) ;
#17479 = CARTESIAN_POINT ( 'NONE',  ( 2.438484115517096207, -12.11778462344221019, 31.66786338562085135 ) ) ;
#17480 = EDGE_CURVE ( 'NONE', #17254, #47272, #88147, .T. ) ;
#17481 = LINE ( 'NONE', #10721, #29356 ) ;
#17482 = DIRECTION ( 'NONE',  ( -0.000000000000000000, -0.000000000000000000, -1.000000000000000000 ) ) ;
#17483 = ORIENTED_EDGE ( 'NONE', *, *, #80515, .T. ) ;
#17484 = VERTEX_POINT ( 'NONE', #25967 ) ;
#17485 = ORIENTED_EDGE ( 'NONE', *, *, #68792, .T. ) ;
#17486 = CARTESIAN_POINT ( 'NONE',  ( -9.692307692307812417, -10.21337939537710326, 33.94971097300076224 ) ) ;
#17487 = CYLINDRICAL_SURFACE ( 'NONE', #25645, 0.2500000000000004996 ) ;
#17488 = B_SPLINE_CURVE_WITH_KNOTS ( 'NONE', 3,
 ( #67093, #24765, #80619, #79720, #5394, #25660, #61535, #53115, #18019, #18903 ),
 .UNSPECIFIED., .F., .F.,
 ( 4, 2, 2, 2, 4 ),
 ( 0.000000000000000000, 0.0001954311564186864407, 0.0003908623128373728815, 0.0005862934692560593493, 0.0007817246256747457630 ),
 .UNSPECIFIED. ) ;
#17489 = DIRECTION ( 'NONE',  ( -0.000000000000000000, 1.000000000000000000, 3.491481338843133355E-15 ) ) ;
#17490 = B_SPLINE_CURVE_WITH_KNOTS ( 'NONE', 3,
 ( #39473, #67375, #79999, #73702, #33142, #18300, #81344, #39028, #46658, #44867 ),
 .UNSPECIFIED., .F., .F.,
 ( 4, 2, 2, 2, 4 ),
 ( 0.0007817359430256326080, 0.0009771253907249993591, 0.001172514838424366327, 0.001367904286123733078, 0.001563293733823099829 ),
 .UNSPECIFIED. ) ;
#17491 = LINE ( 'NONE', #3070, #36309 ) ;
#17492 = AXIS2_PLACEMENT_3D ( 'NONE', #19853, #6777, #60389 ) ;
#17493 = ORIENTED_EDGE ( 'NONE', *, *, #13382, .F. ) ;
#17494 = EDGE_LOOP ( 'NONE', ( #71547, #40140 ) ) ;
#17496 = EDGE_LOOP ( 'NONE', ( #12344, #12893 ) ) ;
#17495 = CARTESIAN_POINT ( 'NONE',  ( 10.36538461538461675, -7.500000000000001776, 35.04278698407183867 ) ) ;
#17497 = FACE_OUTER_BOUND ( 'NONE', #58545, .T. ) ;
#17498 = VECTOR ( 'NONE', #7936, 1000.000000000000227 ) ;
#17499 = CARTESIAN_POINT ( 'NONE',  ( -18.03205128205128105, -7.500000000000000000, 29.75000000000000355 ) ) ;
#17500 = CARTESIAN_POINT ( 'NONE',  ( 8.352564102564102200, -11.00000000000000000, 29.75000000000000355 ) ) ;
#17501 = CARTESIAN_POINT ( 'NONE',  ( -1.161835715637316913, -12.69155399931963046, 30.53255429739158444 ) ) ;
#17502 = ORIENTED_EDGE ( 'NONE', *, *, #86250, .F. ) ;
#17503 = ORIENTED_EDGE ( 'NONE', *, *, #65348, .T. ) ;
#17504 = VERTEX_POINT ( 'NONE', #26419 ) ;
#17506 = VERTEX_POINT ( 'NONE', #80934 ) ;
#17505 = CARTESIAN_POINT ( 'NONE',  ( -13.38461538461506883, -2.255955759149395501, 30.00000000000324363 ) ) ;
#17507 = EDGE_CURVE ( 'NONE', #10416, #36685, #77984, .T. ) ;
#17508 = DIRECTION ( 'NONE',  ( -0.000000000000000000, -0.1736481776669307198, -0.9848077530122080203 ) ) ;
#17509 = CARTESIAN_POINT ( 'NONE',  ( -7.846153846153844924, -3.050289026998446396, 32.03036669348365706 ) ) ;
#17510 = EDGE_LOOP ( 'NONE', ( #36321, #6639 ) ) ;
#17511 = LINE ( 'NONE', #51712, #25894 ) ;
#17512 = DIRECTION ( 'NONE',  ( 0.000000000000000000, 0.9848077530122072432, -0.1736481776669354937 ) ) ;
#17513 = EDGE_CURVE ( 'NONE', #17369, #17400, #59308, .T. ) ;
#17514 = DIRECTION ( 'NONE',  ( 0.000000000000000000, -6.938893903907222067E-15, 1.000000000000000000 ) ) ;
#17515 = B_SPLINE_CURVE_WITH_KNOTS ( 'NONE', 3,
 ( #32663, #6090, #33566, #14169, #27680, #76308, #69555, #61902, #56038, #28122 ),
 .UNSPECIFIED., .F., .F.,
 ( 4, 2, 2, 2, 4 ),
 ( 0.000000000000000000, 0.0001954311564186871184, 0.0003908623128373742367, 0.0005862934692560614093, 0.0007817246256747484735 ),
 .UNSPECIFIED. ) ;
#17516 = FACE_BOUND ( 'NONE', #82836, .T. ) ;
#17517 = DIRECTION ( 'NONE',  ( 0.000000000000000000, 1.000000000000000000, 0.000000000000000000 ) ) ;
#17518 = CARTESIAN_POINT ( 'NONE',  ( 11.28843830116857383, -8.432397168068783699, 34.66272746175022945 ) ) ;
#17519 = VECTOR ( 'NONE', #71026, 1000.000000000000000 ) ;
#17520 = CARTESIAN_POINT ( 'NONE',  ( -15.00775787915638304, -10.61302985866383963, 33.66295027996417843 ) ) ;
#17522 = CARTESIAN_POINT ( 'NONE',  ( 9.692307692307695177, -3.050289026998446396, 32.03036669348365706 ) ) ;
#17521 = FACE_OUTER_BOUND ( 'NONE', #80523, .T. ) ;
#17523 = AXIS2_PLACEMENT_3D ( 'NONE', #24011, #44721, #23134 ) ;
#17524 = FACE_BOUND ( 'NONE', #79964, .T. ) ;
#17525 = CARTESIAN_POINT ( 'NONE',  ( 1.634669804528839254, -2.318338780012835443, 30.59689888758630261 ) ) ;
#17526 = VERTEX_POINT ( 'NONE', #69613 ) ;
#17527 = CYLINDRICAL_SURFACE ( 'NONE', #37446, 0.2499999999999994726 ) ;
#17528 = CARTESIAN_POINT ( 'NONE',  ( -13.13466997523734392, -4.176053281294518804, 33.81426240980091791 ) ) ;
#17529 = ORIENTED_EDGE ( 'NONE', *, *, #5870, .F. ) ;
#17530 = ORIENTED_EDGE ( 'NONE', *, *, #13715, .F. ) ;
#17532 = CARTESIAN_POINT ( 'NONE',  ( 1.384615384615386802, -10.51840700105979565, 33.73612834413961536 ) ) ;
#17531 = CARTESIAN_POINT ( 'NONE',  ( -13.38461538461538325, -12.78798330534102945, 29.74999999999997868 ) ) ;
#17533 = ADVANCED_FACE ( 'NONE', ( #48445 ), #7483, .F. ) ;
#17534 = CARTESIAN_POINT ( 'NONE',  ( -5.777220458731586739, -6.760870238392817200, 34.69528174975672385 ) ) ;
#17535 = CARTESIAN_POINT ( 'NONE',  ( 1.319344938654611221, -6.879047030191174805, 34.71129190930000163 ) ) ;
#17536 = CARTESIAN_POINT ( 'NONE',  ( -0.4615384615385826339, -11.94971097300221174, 32.03036669348237098 ) ) ;
#17537 = ORIENTED_EDGE ( 'NONE', *, *, #25203, .T. ) ;
#17538 = LINE ( 'NONE', #78335, #8439 ) ;
#17540 = CARTESIAN_POINT ( 'NONE',  ( 15.23076923076910916, -11.06231777344772027, 33.60647404775119895 ) ) ;
#17539 = CARTESIAN_POINT ( 'NONE',  ( 11.60452887181161685, -2.833524468853757750, 32.15551576947925838 ) ) ;
#17541 = CARTESIAN_POINT ( 'NONE',  ( 7.780070435197966816, -5.557115091759785130, 34.35708131394839171 ) ) ;
#17542 = DIRECTION ( 'NONE',  ( -0.000000000000000000, 1.000000000000000000, -0.000000000000000000 ) ) ;
#17543 = CARTESIAN_POINT ( 'NONE',  ( -7.846153846153967493, -9.528491918059723176, 34.59228464037033035 ) ) ;
#17544 = CARTESIAN_POINT ( 'NONE',  ( 3.749999999999992006, -5.946699141100872943, 15.64062500000000178 ) ) ;
#17545 = VERTEX_POINT ( 'NONE', #7920 ) ;
#17546 = EDGE_CURVE ( 'NONE', #54081, #8200, #37150, .T. ) ;
#17547 = EDGE_LOOP ( 'NONE', ( #22784, #4071, #2238, #48260 ) ) ;
#17548 = CARTESIAN_POINT ( 'NONE',  ( -15.23076923076935252, -4.320704448113951379, 33.92786785259630022 ) ) ;
#17549 = EDGE_CURVE ( 'NONE', #71998, #86919, #48953, .T. ) ;
#17550 = DIRECTION ( 'NONE',  ( -0.000000000000000000, -0.9396926207859093161, -0.3420201433256663259 ) ) ;
#17551 = CYLINDRICAL_SURFACE ( 'NONE', #4290, 0.2499999999999986955 ) ;
#17552 = CARTESIAN_POINT ( 'NONE',  ( 4.499999999999999112, 7.500000000000002665, 13.50000000000000178 ) ) ;
#17553 = CARTESIAN_POINT ( 'NONE',  ( 16.85409497928819533, -7.369209533119136069, 34.99857337881830688 ) ) ;
#17554 = CARTESIAN_POINT ( 'NONE',  ( -3.749999999999988454, -9.053300858899127945, 17.51562500000000000 ) ) ;
#17555 = CARTESIAN_POINT ( 'NONE',  ( -12.46153846153846168, -3.513871655860378418, 32.76840700105978499 ) ) ;
#17556 = FACE_OUTER_BOUND ( 'NONE', #78037, .T. ) ;
#17557 = EDGE_LOOP ( 'NONE', ( #34766, #49684 ) ) ;
#17558 = CARTESIAN_POINT ( 'NONE',  ( -8.835313148590902443, -12.62096338111211580, 30.90682066428152908 ) ) ;
#17560 = ORIENTED_EDGE ( 'NONE', *, *, #61348, .T. ) ;
#17559 = CARTESIAN_POINT ( 'NONE',  ( 1.384615384615386802, -1.629998284177014645, 34.34916445242399163 ) ) ;
#17561 = CARTESIAN_POINT ( 'NONE',  ( -9.915187209045276617, -7.630690623152299956, 34.99857592706774057 ) ) ;
#17562 = CARTESIAN_POINT ( 'NONE',  ( -9.757578138268465651, -12.27809138561121394, 31.22303859784730307 ) ) ;
#17563 = AXIS2_PLACEMENT_3D ( 'NONE', #54532, #54985, #88798 ) ;
#17564 = CARTESIAN_POINT ( 'NONE',  ( -12.46153846153846168, -8.164416787775445883, 34.95778746994557906 ) ) ;
#17565 = LINE ( 'NONE', #73395, #78935 ) ;
#17567 = EDGE_CURVE ( 'NONE', #84690, #47265, #55648, .T. ) ;
#17566 = CARTESIAN_POINT ( 'NONE',  ( 11.53846153846153832, -1.044019251281081972, 31.83374038241031911 ) ) ;
#17568 = CARTESIAN_POINT ( 'NONE',  ( 7.623226887246995709, -3.395401636524185474, 33.02366814457250399 ) ) ;
#17569 = CARTESIAN_POINT ( 'NONE',  ( -8.069080063669991532, -12.39988816332205701, 30.74660775122750778 ) ) ;
#17570 = VECTOR ( 'NONE', #14826, 1000.000000000000000 ) ;
#17571 = CARTESIAN_POINT ( 'NONE',  ( 1.492201783934598236, -11.27530806549875031, 19.95499329374151642 ) ) ;
#17572 = ORIENTED_EDGE ( 'NONE', *, *, #3945, .F. ) ;
#17573 = PLANE ( 'NONE',  #22615 ) ;
#17574 = CARTESIAN_POINT ( 'NONE',  ( 8.769230769230647482, -11.94971097300221174, 32.03036669348237098 ) ) ;
#17575 = CARTESIAN_POINT ( 'NONE',  ( 13.25446741488368829, -6.809168938359901446, 34.95455904226513866 ) ) ;
#17576 = CARTESIAN_POINT ( 'NONE',  ( 1.901340078031373171, -9.487747218494639867, 13.62686829374151642 ) ) ;
#17577 = B_SPLINE_CURVE_WITH_KNOTS ( 'NONE', 3,
 ( #63480, #82448, #1782, #56288, #82886, #62589, #83774, #49082, #35128, #29272 ),
 .UNSPECIFIED., .F., .F.,
 ( 4, 2, 2, 2, 4 ),
 ( 0.0007817246256747445703, 0.0009771112852218872494, 0.001172497944769030145, 0.001367884604316172825, 0.001563271263863315504 ),
 .UNSPECIFIED. ) ;
#17578 = CARTESIAN_POINT ( 'NONE',  ( 3.230769230769231726, -3.937682226553329556, 33.60647404775216529 ) ) ;
#17579 = CYLINDRICAL_SURFACE ( 'NONE', #34184, 0.2500000000000009437 ) ;
#17581 = VERTEX_POINT ( 'NONE', #34502 ) ;
#17580 = CARTESIAN_POINT ( 'NONE',  ( -9.019253993452226226, -2.588893531581426988, 31.60682220781847818 ) ) ;
#17582 = CARTESIAN_POINT ( 'NONE',  ( -1.139087296526025250, -4.750000000000006217, 19.07812500000000000 ) ) ;
#17583 = CARTESIAN_POINT ( 'NONE',  ( 19.50000000000000000, -3.499999999999999556, 29.75000000000000355 ) ) ;
#17584 = EDGE_CURVE ( 'NONE', #64675, #78946, #27433, .T. ) ;
#17585 = ORIENTED_EDGE ( 'NONE', *, *, #86026, .F. ) ;
#17586 = CARTESIAN_POINT ( 'NONE',  ( -15.84615384615384670, -7.500000000000000000, 29.75000000000000355 ) ) ;
#17587 = ORIENTED_EDGE ( 'NONE', *, *, #28048, .T. ) ;
#17588 = CARTESIAN_POINT ( 'NONE',  ( -7.846153846153967493, -6.835583212225970762, 34.95778746994575670 ) ) ;
#17589 = EDGE_CURVE ( 'NONE', #43442, #3517, #77257, .T. ) ;
#17590 = EDGE_CURVE ( 'NONE', #9159, #67813, #62837, .T. ) ;
#17591 = FACE_OUTER_BOUND ( 'NONE', #38414, .T. ) ;
#17592 = CARTESIAN_POINT ( 'NONE',  ( 16.85399611801622655, -6.459968553980840689, 34.89616026154728701 ) ) ;
#17593 = ORIENTED_EDGE ( 'NONE', *, *, #14844, .T. ) ;
#17594 = CARTESIAN_POINT ( 'NONE',  ( -19.50000000000000000, -3.499999999999999556, 29.75000000000000355 ) ) ;
#17595 = ORIENTED_EDGE ( 'NONE', *, *, #64595, .F. ) ;
#17596 = CARTESIAN_POINT ( 'NONE',  ( 13.13461538461537437, -2.249999999999998668, 29.81609741502487410 ) ) ;
#17597 = EDGE_CURVE ( 'NONE', #78524, #23088, #39235, .T. ) ;
#17598 = CIRCLE ( 'NONE', #72219, 4.000000000000000000 ) ;
#17599 = VERTEX_POINT ( 'NONE', #1157 ) ;
#17601 = CARTESIAN_POINT ( 'NONE',  ( -15.93106648486808119, -2.353885683473779356, 30.79025554430704759 ) ) ;
#17600 = AXIS2_PLACEMENT_3D ( 'NONE', #51687, #58023, #31896 ) ;
#17602 = CARTESIAN_POINT ( 'NONE',  ( 0.7114839798866035014, -11.37275283266503756, 32.91324779482534524 ) ) ;
#17603 = VERTEX_POINT ( 'NONE', #28638 ) ;
#17604 = CARTESIAN_POINT ( 'NONE',  ( -6.065270000556320262, -11.06231777344662781, 33.60647404775220082 ) ) ;
#17605 = CARTESIAN_POINT ( 'NONE',  ( -12.46153846153858247, -6.026961402154118019, 34.52809138561165270 ) ) ;
#17606 = CARTESIAN_POINT ( 'NONE',  ( 12.71159277317677549, -4.943051570960394159, 34.04725096376909477 ) ) ;
#17607 = AXIS2_PLACEMENT_3D ( 'NONE', #8741, #69542, #7850 ) ;
#17608 = B_SPLINE_CURVE_WITH_KNOTS ( 'NONE', 3,
 ( #24374, #44641, #78000, #10438, #43771, #37906, #72572, #3662, #71232, #79338 ),
 .UNSPECIFIED., .F., .F.,
 ( 4, 2, 2, 2, 4 ),
 ( 0.000000000000000000, 0.0001954339857564083417, 0.0003908679715128166835, 0.0005863019572692250523, 0.0007817359430256333669 ),
 .UNSPECIFIED. ) ;
#17609 = B_SPLINE_CURVE_WITH_KNOTS ( 'NONE', 3,
 ( #35324, #62780, #28580, #56039, #83531, #21813, #79864, #18614, #59138, #24016 ),
 .UNSPECIFIED., .F., .F.,
 ( 4, 2, 2, 2, 4 ),
 ( 0.0007817246256747457630, 0.0009771112852218887673, 0.001172497944769031880, 0.001367884604316174993, 0.001563271263863318106 ),
 .UNSPECIFIED. ) ;
#17610 = DIRECTION ( 'NONE',  ( -1.000000000000000000, -0.000000000000000000, -0.000000000000000000 ) ) ;
#17611 = DIRECTION ( 'NONE',  ( -0.000000000000000000, 0.5000000000000011102, -0.8660254037844380415 ) ) ;
#17612 = ORIENTED_EDGE ( 'NONE', *, *, #63108, .F. ) ;
#17613 = VERTEX_POINT ( 'NONE', #76827 ) ;
#17614 = ORIENTED_EDGE ( 'NONE', *, *, #33771, .F. ) ;
#17616 = EDGE_LOOP ( 'NONE', ( #77075, #3091, #65989, #68506 ) ) ;
#17615 = CARTESIAN_POINT ( 'NONE',  ( -39.05038313613820122, -2.499999999999999556, 29.75000000000000355 ) ) ;
#17617 =( REPRESENTATION_RELATIONSHIP ('NONE','NONE', #51743, #36256 ) REPRESENTATION_RELATIONSHIP_WITH_TRANSFORMATION ( #74372 )SHAPE_REPRESENTATION_RELATIONSHIP( ) );
#17618 = CARTESIAN_POINT ( 'NONE',  ( 4.153846153846154188, -10.05456864172156806, 36.03766855953608683 ) ) ;
#17619 = CARTESIAN_POINT ( 'NONE',  ( -10.61538461538473399, -9.442884908241554243, 34.35708131394783038 ) ) ;
#17620 = EDGE_LOOP ( 'NONE', ( #14634, #40286 ) ) ;
#17621 = ORIENTED_EDGE ( 'NONE', *, *, #62398, .T. ) ;
#17622 = ORIENTED_EDGE ( 'NONE', *, *, #68801, .F. ) ;
#17623 = CARTESIAN_POINT ( 'NONE',  ( -1.634638621908348410, -11.86270091957321249, 32.19358267280087915 ) ) ;
#17624 = ORIENTED_EDGE ( 'NONE', *, *, #30742, .T. ) ;
#17625 = VECTOR ( 'NONE', #28179, 1000.000000000000000 ) ;
#17626 = CARTESIAN_POINT ( 'NONE',  ( -10.48485891362105171, -9.417988943895561960, 34.36773134775777550 ) ) ;
#17627 = CARTESIAN_POINT ( 'NONE',  ( 16.85399611801622655, -12.38737895849757820, 31.66785238281580206 ) ) ;
#17628 = CARTESIAN_POINT ( 'NONE',  ( 0.4330127018922180770, -4.750000000000000000, 29.50000000000000355 ) ) ;
#17629 = FACE_BOUND ( 'NONE', #5481, .T. ) ;
#17630 = ORIENTED_EDGE ( 'NONE', *, *, #46184, .F. ) ;
#17631 = CARTESIAN_POINT ( 'NONE',  ( -7.846153846153967493, -5.941354392335915335, 34.76329471203413846 ) ) ;
#17632 = CARTESIAN_POINT ( 'NONE',  ( 12.68431800280687050, -5.913360116392397892, 34.49180327182771322 ) ) ;
#17633 = DIRECTION ( 'NONE',  ( 0.000000000000000000, 0.1736481776669275834, 0.9848077530122086864 ) ) ;
#17634 = CARTESIAN_POINT ( 'NONE',  ( -14.55771554498526932, -9.271318131107980420, 34.42618302367067429 ) ) ;
#17635 = CARTESIAN_POINT ( 'NONE',  ( 7.976679547917413515, -10.88167719472716399, 33.43325721877153711 ) ) ;
#17636 = ORIENTED_EDGE ( 'NONE', *, *, #56477, .T. ) ;
#17637 = CARTESIAN_POINT ( 'NONE',  ( -9.692307692307691624, -12.29105614889573062, 35.45975837776705220 ) ) ;
#17638 = EDGE_LOOP ( 'NONE', ( #35913, #88483 ) ) ;
#17639 = VERTEX_POINT ( 'NONE', #84037 ) ;
#17641 = FACE_OUTER_BOUND ( 'NONE', #43321, .T. ) ;
#17640 = CARTESIAN_POINT ( 'NONE',  ( 5.869309396889695662, -11.93127051446800024, 32.56575433478200665 ) ) ;
#17642 = CARTESIAN_POINT ( 'NONE',  ( -8.519176349317316266, -12.41089969410671223, 31.60739465890703670 ) ) ;
#17643 = DIRECTION ( 'NONE',  ( 0.000000000000000000, 0.000000000000000000, 1.000000000000000000 ) ) ;
#17644 = CARTESIAN_POINT ( 'NONE',  ( 1.634560902963527962, -10.05730279482229683, 34.04704008940765902 ) ) ;
#17645 = CARTESIAN_POINT ( 'NONE',  ( -11.78848476268299628, -2.341070481393819236, 30.72580821765574299 ) ) ;
#17646 = VERTEX_POINT ( 'NONE', #15123 ) ;
#17647 = DIRECTION ( 'NONE',  ( -1.000000000000000000, -0.000000000000000000, -0.000000000000000000 ) ) ;
#17648 = CARTESIAN_POINT ( 'NONE',  ( 11.53846153846153832, -2.721908614388771852, 31.22303859784724978 ) ) ;
#17649 = CARTESIAN_POINT ( 'NONE',  ( 10.48469401227430708, -2.845849958028613624, 32.17971566917920967 ) ) ;
#17650 = CARTESIAN_POINT ( 'NONE',  ( 10.74591031714818357, -11.93748526763465279, 32.05452791011430946 ) ) ;
#17651 = EDGE_LOOP ( 'NONE', ( #24260, #89023, #3307, #10301 ) ) ;
#17652 = VERTEX_POINT ( 'NONE', #8366 ) ;
#17653 = FACE_BOUND ( 'NONE', #85329, .T. ) ;
#17654 = AXIS2_PLACEMENT_3D ( 'NONE', #63, #82492, #20771 ) ;
#17655 = EDGE_CURVE ( 'NONE', #44478, #19274, #22318, .T. ) ;
#17656 = ORIENTED_EDGE ( 'NONE', *, *, #38096, .F. ) ;
#17657 = VECTOR ( 'NONE', #15733, 1000.000000000000000 ) ;
#17658 = CARTESIAN_POINT ( 'NONE',  ( 18.25000000000143530, -7.500000000000155431, 34.75000000000007105 ) ) ;
#17659 = CARTESIAN_POINT ( 'NONE',  ( -13.31854703361294767, -10.51840700105979565, 33.73612834413962247 ) ) ;
#17660 = ORIENTED_EDGE ( 'NONE', *, *, #86872, .F. ) ;
#17661 = FACE_OUTER_BOUND ( 'NONE', #15814, .T. ) ;
#17662 = CARTESIAN_POINT ( 'NONE',  ( -30.00000000000000000, 15.00000000000000355, 3.000000000000000000 ) ) ;
#17663 = CARTESIAN_POINT ( 'NONE',  ( 4.946231610255517275, -2.729777683071817229, 31.24903638046268739 ) ) ;
#17664 = DIRECTION ( 'NONE',  ( -0.000000000000000000, -0.1736481776669307198, -0.9848077530122080203 ) ) ;
#17665 = DIRECTION ( 'NONE',  ( -0.000000000000000000, 0.000000000000000000, 1.000000000000000000 ) ) ;
#17666 = ORIENTED_EDGE ( 'NONE', *, *, #17813, .T. ) ;
#17668 = ORIENTED_EDGE ( 'NONE', *, *, #84407, .F. ) ;
#17667 = CARTESIAN_POINT ( 'NONE',  ( 13.51540582558233794, -8.191423895709840863, 34.95447573519442130 ) ) ;
#17669 = CARTESIAN_POINT ( 'NONE',  ( -14.30769230769230660, -5.180354513474913603, 36.12317359536750416 ) ) ;
#17670 = CYLINDRICAL_SURFACE ( 'NONE', #5129, 0.2499999999999979738 ) ;
#17671 = DIRECTION ( 'NONE',  ( -0.000000000000000000, 0.9848077530122086864, -0.1736481776669273891 ) ) ;
#17672 = CARTESIAN_POINT ( 'NONE',  ( -10.03846153846153832, -7.500000000000000000, 29.75000000000000355 ) ) ;
#17673 = CARTESIAN_POINT ( 'NONE',  ( 12.46153846153833911, -12.27809138561165270, 31.22303859784587132 ) ) ;
#17674 = EDGE_CURVE ( 'NONE', #21236, #68727, #43034, .T. ) ;
#17675 = CARTESIAN_POINT ( 'NONE',  ( 12.21156171748987163, -5.643011162660950042, 34.66104346484419096 ) ) ;
#17676 = CARTESIAN_POINT ( 'NONE',  ( 1.987747218494642309, -5.598659921968629050, 15.81436829374151465 ) ) ;
#17677 = ORIENTED_EDGE ( 'NONE', *, *, #46727, .F. ) ;
#17678 = CARTESIAN_POINT ( 'NONE',  ( -3.453695448285378333, -3.105860786376062332, 32.13614157043598851 ) ) ;
#17679 = CARTESIAN_POINT ( 'NONE',  ( 7.976201281404299515, -7.723484941389745728, 34.99544897038809665 ) ) ;
#17680 = CARTESIAN_POINT ( 'NONE',  ( 0.000000000000000000, -11.00000000000000000, 29.75000000000000355 ) ) ;
#17681 = VERTEX_POINT ( 'NONE', #65063 ) ;
#17682 = ORIENTED_EDGE ( 'NONE', *, *, #65991, .F. ) ;
#17683 = CARTESIAN_POINT ( 'NONE',  ( -8.992157728137616601, -5.582147617184174848, 34.63737895849758530 ) ) ;
#17684 = CARTESIAN_POINT ( 'NONE',  ( -14.17690186672535901, -2.494656445102012565, 31.33466734024120015 ) ) ;
#17685 = CARTESIAN_POINT ( 'NONE',  ( 1.576923076923075762, -7.500000000000000000, 33.75000000000000000 ) ) ;
#17686 = CARTESIAN_POINT ( 'NONE',  ( -4.153846153846152411, -9.058645607665452459, 34.76329471203371924 ) ) ;
#17687 = DIRECTION ( 'NONE',  ( -0.000000000000000000, -0.3420201433256694346, -0.9396926207859080948 ) ) ;
#17688 = VECTOR ( 'NONE', #34854, 999.9999999999998863 ) ;
#17689 = CARTESIAN_POINT ( 'NONE',  ( -8.835314180186648159, -11.69971097300155272, 32.46337939537587403 ) ) ;
#17690 = VECTOR ( 'NONE', #63076, 1000.000000000000000 ) ;
#17691 = CARTESIAN_POINT ( 'NONE',  ( 18.03205128205128105, -3.499999999999999556, 29.75000000000000355 ) ) ;
#17692 = VERTEX_POINT ( 'NONE', #18563 ) ;
#17694 = EDGE_CURVE ( 'NONE', #75640, #1333, #29139, .T. ) ;
#17693 = CARTESIAN_POINT ( 'NONE',  ( 6.065255571276024327, -10.90142922261932057, 33.41473453929631887 ) ) ;
#17696 = EDGE_CURVE ( 'NONE', #31113, #70330, #43523, .T. ) ;
#17695 = CARTESIAN_POINT ( 'NONE',  ( -17.32692307692307310, -7.566083408709835645, 34.74999999999999289 ) ) ;
#17697 = DIRECTION ( 'NONE',  ( -0.000000000000000000, -0.8660254037844399289, -0.4999999999999980016 ) ) ;
#17698 = CARTESIAN_POINT ( 'NONE',  ( 16.82694634598072270, -9.148715823498378086, 34.47080413974185120 ) ) ;
#17699 = EDGE_LOOP ( 'NONE', ( #70208, #12003 ) ) ;
#17700 = CARTESIAN_POINT ( 'NONE',  ( 10.54930223602447903, -9.058645607665454236, 34.76329471203372634 ) ) ;
#17701 = B_SPLINE_CURVE_WITH_KNOTS ( 'NONE', 3,
 ( #48733, #35221, #35680, #6864, #55052, #70343, #28025, #41102, #21259, #55491 ),
 .UNSPECIFIED., .F., .F.,
 ( 4, 2, 2, 2, 4 ),
 ( 0.0007817246256747478229, 0.0009771112852218913694, 0.001172497944769034916, 0.001367884604316178679, 0.001563271263863322226 ),
 .UNSPECIFIED. ) ;
#17702 = EDGE_LOOP ( 'NONE', ( #81995, #63846, #72656, #26267 ) ) ;
#17703 = DIRECTION ( 'NONE',  ( 0.000000000000000000, 0.4999999999999960032, -0.8660254037844410391 ) ) ;
#17704 =( NAMED_UNIT ( * ) SI_UNIT ( $, .STERADIAN. ) SOLID_ANGLE_UNIT ( ) );
#17705 = CARTESIAN_POINT ( 'NONE',  ( -13.51522503981946599, -7.722926974430166069, 34.99546784045485737 ) ) ;
#17706 = CARTESIAN_POINT ( 'NONE',  ( 6.249945409378044658, -12.07971442181322352, 32.31769673815850297 ) ) ;
#17707 = ORIENTED_EDGE ( 'NONE', *, *, #11303, .T. ) ;
#17708 = EDGE_CURVE ( 'NONE', #72244, #5990, #58310, .T. ) ;
#17709 = DIRECTION ( 'NONE',  ( 0.7057856980126718804, 0.7057856980126787638, 0.06109907496453181874 ) ) ;
#17710 = CARTESIAN_POINT ( 'NONE',  ( -1.384615384615506484, -12.70778746994576025, 30.41441678777401236 ) ) ;
#17711 = CARTESIAN_POINT ( 'NONE',  ( -10.55012904410859242, -10.90142922261932057, 33.41473453929631887 ) ) ;
#17712 = CARTESIAN_POINT ( 'NONE',  ( -7.715363405186896451, -4.684288915650983043, 34.18129842949671371 ) ) ;
#17713 = CYLINDRICAL_SURFACE ( 'NONE', #3749, 0.2500000000000008882 ) ;
#17714 = ORIENTED_EDGE ( 'NONE', *, *, #65335, .T. ) ;
#17715 = CARTESIAN_POINT ( 'NONE',  ( -10.83825003758825467, -2.501496062324912284, 29.88072118266895671 ) ) ;
#17716 = ORIENTED_EDGE ( 'NONE', *, *, #77748, .F. ) ;
#17717 = CARTESIAN_POINT ( 'NONE',  ( -17.07692307692319744, -5.219633306517616589, 34.19971097300220464 ) ) ;
#17718 = VECTOR ( 'NONE', #86233, 1000.000000000000114 ) ;
#17719 = CARTESIAN_POINT ( 'NONE',  ( -9.561515884482904681, -12.11778462344220841, 31.66786338562085135 ) ) ;
#17720 = VECTOR ( 'NONE', #4212, 1000.000000000000000 ) ;
#17721 = CARTESIAN_POINT ( 'NONE',  ( -13.63459211555773720, -2.779195860258146578, 31.39871582349836032 ) ) ;
#17722 = FACE_OUTER_BOUND ( 'NONE', #78041, .T. ) ;
#17723 = CARTESIAN_POINT ( 'NONE',  ( 15.23076923076923173, -1.629998284177014645, 34.34916445242399163 ) ) ;
#17724 = CARTESIAN_POINT ( 'NONE',  ( 16.02369818411445834, -12.15440758774515473, 32.17923288041532004 ) ) ;
#17725 = AXIS2_PLACEMENT_3D ( 'NONE', #85288, #23574, #51020 ) ;
#17726 = ORIENTED_EDGE ( 'NONE', *, *, #82926, .F. ) ;
#17727 = EDGE_LOOP ( 'NONE', ( #78379, #49234, #1473, #21840 ) ) ;
#17728 = ORIENTED_EDGE ( 'NONE', *, *, #29449, .T. ) ;
#17729 = ORIENTED_EDGE ( 'NONE', *, *, #67033, .F. ) ;
#17730 = VERTEX_POINT ( 'NONE', #78145 ) ;
#17731 = CARTESIAN_POINT ( 'NONE',  ( -10.48485891362105171, -8.586989748646452369, 34.63063291749215011 ) ) ;
#17732 = CARTESIAN_POINT ( 'NONE',  ( -21.00000000000000000, -2.249999999999998668, 29.75000000000000355 ) ) ;
#17733 = DIRECTION ( 'NONE',  ( -0.000000000000000000, 0.7660444431189791237, -0.6427876096865379196 ) ) ;
#17734 = DIRECTION ( 'NONE',  ( -0.000000000000000000, -0.9848077530122085754, -0.1736481776669273613 ) ) ;
#17735 = CARTESIAN_POINT ( 'NONE',  ( -13.51530598772569469, -3.338472653186243644, 32.95098750199972670 ) ) ;
#17736 = CARTESIAN_POINT ( 'NONE',  ( 0.4615384615384611200, -4.786620604624113540, 33.94971097300155094 ) ) ;
#17737 = CARTESIAN_POINT ( 'NONE',  ( -0.4615384615384611200, -11.69971097300155272, 32.46337939537588113 ) ) ;
#17738 = CARTESIAN_POINT ( 'NONE',  ( 4.153846153846030731, -3.083524468854526912, 32.58852847137268327 ) ) ;
#17739 = CARTESIAN_POINT ( 'NONE',  ( 7.846153846153723244, -5.094484230521993062, 34.41647553114689373 ) ) ;
#17740 = ORIENTED_EDGE ( 'NONE', *, *, #73680, .T. ) ;
#17741 = ORIENTED_EDGE ( 'NONE', *, *, #21803, .T. ) ;
#17742 = EDGE_CURVE ( 'NONE', #33011, #78633, #73512, .T. ) ;
#17743 = ORIENTED_EDGE ( 'NONE', *, *, #31077, .F. ) ;
#17745 = EDGE_LOOP ( 'NONE', ( #61627, #29844, #43434, #48166 ) ) ;
#17744 = CARTESIAN_POINT ( 'NONE',  ( 0.4615384615384611200, -11.91647553114624181, 32.58852847137148245 ) ) ;
#17746 = AXIS2_PLACEMENT_3D ( 'NONE', #69868, #29335, #43287 ) ;
#17748 = CARTESIAN_POINT ( 'NONE',  ( -18.00000000000000000, -11.35647404775217240, 33.31231777344666511 ) ) ;
#17747 = LINE ( 'NONE', #65479, #14380 ) ;
#17749 = VECTOR ( 'NONE', #52374, 1000.000000000000227 ) ;
#17750 = CARTESIAN_POINT ( 'NONE',  ( -1.449885385171703511, -5.094484230520674117, 34.41647553114621161 ) ) ;
#17751 = CARTESIAN_POINT ( 'NONE',  ( -13.38461538461538325, -1.215029322943914858, 32.30358669280327177 ) ) ;
#17752 = FACE_BOUND ( 'NONE', #56490, .T. ) ;
#17753 = ORIENTED_EDGE ( 'NONE', *, *, #62487, .F. ) ;
#17754 = EDGE_LOOP ( 'NONE', ( #17314, #12854, #40284, #7866 ) ) ;
#17755 = CARTESIAN_POINT ( 'NONE',  ( 17.99999999999987566, -3.835265460704628815, 33.15142922262033665 ) ) ;
#17756 = VERTEX_POINT ( 'NONE', #77701 ) ;
#17757 = FACE_BOUND ( 'NONE', #47181, .T. ) ;
#17758 = CARTESIAN_POINT ( 'NONE',  ( -16.15384615384615330, -3.669653830205710676, 35.88435417666054406 ) ) ;
#17759 = EDGE_CURVE ( 'NONE', #51881, #84238, #29672, .T. ) ;
#17760 = CARTESIAN_POINT ( 'NONE',  ( -14.30769230769230660, -13.20930481340135110, 34.54067556320372745 ) ) ;
#17761 = ORIENTED_EDGE ( 'NONE', *, *, #54725, .F. ) ;
#17762 = CARTESIAN_POINT ( 'NONE',  ( 12.21153846153846168, -7.500000000000001776, 35.00000000000000000 ) ) ;
#17763 = CARTESIAN_POINT ( 'NONE',  ( -1.515305987725691139, -8.191372820521381826, 34.95448215188423546 ) ) ;
#17764 = CARTESIAN_POINT ( 'NONE',  ( 1.161130460051056357, -3.562934362175799841, 33.22335522853832401 ) ) ;
#17765 = EDGE_LOOP ( 'NONE', ( #71763, #38131 ) ) ;
#17766 = ADVANCED_FACE ( 'NONE', ( #25761 ), #16009, .F. ) ;
#17767 = DIRECTION ( 'NONE',  ( 0.000000000000000000, 0.4999999999999985567, 0.8660254037844395958 ) ) ;
#17768 = CARTESIAN_POINT ( 'NONE',  ( -18.22292621751613950, -4.887634598454294377, 34.01352882383564946 ) ) ;
#17769 = ORIENTED_EDGE ( 'NONE', *, *, #65265, .F. ) ;
#17770 = DIRECTION ( 'NONE',  ( -0.000000000000000000, -0.1736481776669307198, -0.9848077530122080203 ) ) ;
#17771 = CARTESIAN_POINT ( 'NONE',  ( -9.692307692307691624, -2.721908614388771852, 31.22303859784724978 ) ) ;
#17772 = ORIENTED_EDGE ( 'NONE', *, *, #32652, .T. ) ;
#17773 = CARTESIAN_POINT ( 'NONE',  ( 18.22277954126840172, -6.760870238392814535, 34.69528174975672385 ) ) ;
#17774 = CARTESIAN_POINT ( 'NONE',  ( -12.33074665371367828, -2.541949514083464479, 30.39797389878540557 ) ) ;
#17775 = CARTESIAN_POINT ( 'NONE',  ( 16.15384615384603251, -3.083524468854526912, 32.58852847137268327 ) ) ;
#17776 = CARTESIAN_POINT ( 'NONE',  ( 15.00784227186237985, -12.64616026154729411, 30.79003144601914244 ) ) ;
#17777 = DIRECTION ( 'NONE',  ( -0.000000000000000000, 0.9848077530122085754, -0.1736481776669273613 ) ) ;
#17778 = B_SPLINE_CURVE_WITH_KNOTS ( 'NONE', 3,
 ( #46010, #64939, #24398, #18551, #32060, #86123, #45117, #38372, #5030, #52317 ),
 .UNSPECIFIED., .F., .F.,
 ( 4, 2, 2, 2, 4 ),
 ( 0.000000000000000000, 0.0001954339857564097241, 0.0003908679715128194482, 0.0005863019572692291723, 0.0007817359430256388964 ),
 .UNSPECIFIED. ) ;
#17779 = DIRECTION ( 'NONE',  ( -1.000000000000000000, -0.000000000000000000, -0.000000000000000000 ) ) ;
#17782 = CARTESIAN_POINT ( 'NONE',  ( -17.07692307692319744, -8.613356846316285953, 34.62446782046622218 ) ) ;
#17781 = AXIS2_PLACEMENT_3D ( 'NONE', #14170, #41646, #69115 ) ;
#17780 = CARTESIAN_POINT ( 'NONE',  ( 5.076923076923075762, -12.37446782046654192, 30.86335684631486131 ) ) ;
#17783 = EDGE_CURVE ( 'NONE', #80137, #38748, #23385, .T. ) ;
#17784 = CARTESIAN_POINT ( 'NONE',  ( -3.296039676730006640, -2.625532179533444754, 30.86335684631481513 ) ) ;
#17786 = FACE_OUTER_BOUND ( 'NONE', #33355, .T. ) ;
#17785 = CARTESIAN_POINT ( 'NONE',  ( 12.39621554604628706, -7.749976743299138882, 34.99404534957040624 ) ) ;
#17787 = CARTESIAN_POINT ( 'NONE',  ( 2.724691934501235036, -6.299813628509441266, 26.63875670625848713 ) ) ;
#17788 = ORIENTED_EDGE ( 'NONE', *, *, #50706, .F. ) ;
#17789 = AXIS2_PLACEMENT_3D ( 'NONE', #38850, #17235, #66312 ) ;
#17790 = CARTESIAN_POINT ( 'NONE',  ( -12.52762187249433978, -8.120952969808774569, 34.71129190930000163 ) ) ;
#17791 = ORIENTED_EDGE ( 'NONE', *, *, #76801, .T. ) ;
#17792 = ADVANCED_FACE ( 'NONE', ( #52777 ), #70950, .F. ) ;
#17793 = ORIENTED_EDGE ( 'NONE', *, *, #11664, .F. ) ;
#17794 = CARTESIAN_POINT ( 'NONE',  ( -16.82686865700962642, -4.074993327901529128, 33.72946981652012255 ) ) ;
#17795 = EDGE_LOOP ( 'NONE', ( #58488, #1284, #15173, #62216, #72136 ) ) ;
#17796 = CARTESIAN_POINT ( 'NONE',  ( -5.869474561766354626, -10.31582465632705237, 34.18122507451815295 ) ) ;
#17797 = CARTESIAN_POINT ( 'NONE',  ( -1.409462824231155764E-14, -4.749999999999999112, 14.15625000000000000 ) ) ;
#17798 = CARTESIAN_POINT ( 'NONE',  ( 17.06410256410256565, -3.499999999999999556, 29.75000000000000355 ) ) ;
#17799 = CARTESIAN_POINT ( 'NONE',  ( -15.36091720050092846, -12.50552854090298993, 31.33409797877408920 ) ) ;
#17800 = LINE ( 'NONE', #45252, #87892 ) ;
#17801 = CARTESIAN_POINT ( 'NONE',  ( -12.21148404162501144, -4.074993327901527351, 33.72946981652012255 ) ) ;
#17802 = CARTESIAN_POINT ( 'NONE',  ( -5.076923076923075762, -2.486705287966279876, 31.30864560766543647 ) ) ;
#17803 = CARTESIAN_POINT ( 'NONE',  ( -10.86540785267757947, -4.335965774309648246, 33.62209801155881905 ) ) ;
#17804 = CARTESIAN_POINT ( 'NONE',  ( 6.000000000000001776, -4.098570777380720287, 33.41473453929634729 ) ) ;
#17805 = CARTESIAN_POINT ( 'NONE',  ( -1.553300858899081538, -11.25000000000000711, 22.35937500000000711 ) ) ;
#17806 = DIRECTION ( 'NONE',  ( -0.000000000000000000, -0.5000000000000009992, -0.8660254037844380415 ) ) ;
#17808 = EDGE_CURVE ( 'NONE', #43520, #75897, #2475, .T. ) ;
#17807 = CARTESIAN_POINT ( 'NONE',  ( -15.09997742294444478, -2.541949514083464479, 30.39797389878540557 ) ) ;
#17809 = EDGE_CURVE ( 'NONE', #75253, #43597, #53221, .T. ) ;
#17810 = DIRECTION ( 'NONE',  ( -0.000000000000000000, 0.7660444431189791237, -0.6427876096865379196 ) ) ;
#17811 = VERTEX_POINT ( 'NONE', #78586 ) ;
#17813 = EDGE_CURVE ( 'NONE', #45, #52162, #65059, .T. ) ;
#17812 = ORIENTED_EDGE ( 'NONE', *, *, #84199, .F. ) ;
#17814 = CARTESIAN_POINT ( 'NONE',  ( 14.55774661933062575, -4.943051570960394159, 34.04725096376909477 ) ) ;
#17815 = CARTESIAN_POINT ( 'NONE',  ( -17.30040802064702987, -8.496056993536548418, 34.65000542017679663 ) ) ;
#17816 = DIRECTION ( 'NONE',  ( -0.000000000000000000, 0.9396926207859093161, -0.3420201433256663259 ) ) ;
#17817 = DIRECTION ( 'NONE',  ( -0.000000000000000000, -5.102127870520021228E-17, -1.000000000000000000 ) ) ;
#17818 = EDGE_CURVE ( 'NONE', #15876, #27342, #28557, .T. ) ;
#17819 = B_SPLINE_CURVE_WITH_KNOTS ( 'NONE', 3,
 ( #67737, #87584, #88917, #81700, #68179, #19983, #6482, #33944, #27188, #63182 ),
 .UNSPECIFIED., .F., .F.,
 ( 4, 2, 2, 2, 4 ),
 ( 0.0007817359430256287049, 0.0009771253907249945886, 0.001172514838424360255, 0.001367904286123725922, 0.001563293733823091806 ),
 .UNSPECIFIED. ) ;
#17820 = CARTESIAN_POINT ( 'NONE',  ( 3.903869409797561030, -3.436278759898155677, 33.07459398097509506 ) ) ;
#17821 = CARTESIAN_POINT ( 'NONE',  ( -0.6844646790546087267, -6.503392248772476236, 34.64988816332204635 ) ) ;
#17822 = ORIENTED_EDGE ( 'NONE', *, *, #58663, .T. ) ;
#17823 = CARTESIAN_POINT ( 'NONE',  ( -1.254089682851822873, -10.19071101563364756, 33.96452234770658407 ) ) ;
#17824 = EDGE_LOOP ( 'NONE', ( #13808, #75219 ) ) ;
#17825 = VERTEX_POINT ( 'NONE', #34285 ) ;
#17826 = CARTESIAN_POINT ( 'NONE',  ( 7.846153846153846700, -10.67929555188718282, 33.92786785259544047 ) ) ;
#17827 = PLANE ( 'NONE',  #28511 ) ;
#17828 = CARTESIAN_POINT ( 'NONE',  ( -0.5920136466141803222, -7.276987145209185215, 34.99546412871779921 ) ) ;
#17829 = CARTESIAN_POINT ( 'NONE',  ( 1.319345384059066317, -11.67786785259541027, 32.92929555188721480 ) ) ;
#17830 = CARTESIAN_POINT ( 'NONE',  ( 0.4615384615383396616, -8.613356846316285953, 34.62446782046622218 ) ) ;
#17831 = ORIENTED_EDGE ( 'NONE', *, *, #35325, .F. ) ;
#17832 = ORIENTED_EDGE ( 'NONE', *, *, #80007, .F. ) ;
#17833 = ADVANCED_FACE ( 'NONE', ( #54105 ), #21213, .F. ) ;
#17834 = EDGE_LOOP ( 'NONE', ( #23905, #34991 ) ) ;
#17835 = AXIS2_PLACEMENT_3D ( 'NONE', #35645, #56354, #64863 ) ;
#17836 = CARTESIAN_POINT ( 'NONE',  ( -7.173053667125512511, -12.01397095200673881, 32.43157075238190146 ) ) ;
#17837 = CARTESIAN_POINT ( 'NONE',  ( 17.07692307692307665, -3.669653830205710676, 35.88435417666054406 ) ) ;
#17838 = B_SPLINE_CURVE_WITH_KNOTS ( 'NONE', 3,
 ( #72682, #79891, #78546, #45655, #38915, #16852, #73593, #11887, #5119, #32584 ),
 .UNSPECIFIED., .F., .F.,
 ( 4, 2, 2, 2, 4 ),
 ( 0.0007817359430256399806, 0.0009771253907250089001, 0.001172514838424378036, 0.001367904286123746956, 0.001563293733823115875 ),
 .UNSPECIFIED. ) ;
#17839 = DIRECTION ( 'NONE',  ( -0.000000000000000000, -0.6427876096865404731, -0.7660444431189771253 ) ) ;
#17840 = EDGE_CURVE ( 'NONE', #15955, #48246, #14804, .T. ) ;
#17841 = AXIS2_PLACEMENT_3D ( 'NONE', #75858, #75420, #68221 ) ;
#17842 = CARTESIAN_POINT ( 'NONE',  ( -8.519176349317316266, -10.06805714834173493, 34.32951233291982618 ) ) ;
#17843 = CARTESIAN_POINT ( 'NONE',  ( 11.31553457955469000, -10.77366814457252175, 33.85459836347579454 ) ) ;
#17844 = FACE_OUTER_BOUND ( 'NONE', #67573, .T. ) ;
#17845 = VERTEX_POINT ( 'NONE', #53673 ) ;
#17846 = ORIENTED_EDGE ( 'NONE', *, *, #79994, .T. ) ;
#17847 = CARTESIAN_POINT ( 'NONE',  ( 2.651650429449539104, -4.848349570550432475, 21.81250000000000000 ) ) ;
#17848 = EDGE_CURVE ( 'NONE', #46179, #64437, #2673, .T. ) ;
#17849 = VERTEX_POINT ( 'NONE', #20341 ) ;
#17851 = EDGE_LOOP ( 'NONE', ( #89160, #47155 ) ) ;
#17850 = CARTESIAN_POINT ( 'NONE',  ( 2.438484115517093986, -12.38066358083363738, 30.83685684665853444 ) ) ;
#17852 = DIRECTION ( 'NONE',  ( -0.000000000000000000, 0.7660444431189791237, -0.6427876096865379196 ) ) ;
#17853 = DIRECTION ( 'NONE',  ( -1.000000000000000000, 0.000000000000000000, -0.000000000000000000 ) ) ;
#17854 = CARTESIAN_POINT ( 'NONE',  ( 1.553300858899086867, -3.749999999999992006, 14.23437500000000178 ) ) ;
#17855 = VERTEX_POINT ( 'NONE', #41054 ) ;
#17856 = LINE ( 'NONE', #37221, #62644 ) ;
#17857 = ORIENTED_EDGE ( 'NONE', *, *, #47817, .T. ) ;
#17858 = CARTESIAN_POINT ( 'NONE',  ( 2.372947878968333146, -9.442884908240271713, 34.35708131394835618 ) ) ;
#17859 = DIRECTION ( 'NONE',  ( 0.000000000000000000, 0.1736481776669275834, 0.9848077530122086864 ) ) ;
#17860 = FACE_BOUND ( 'NONE', #27644, .T. ) ;
#17862 = CARTESIAN_POINT ( 'NONE',  ( -14.98076923076922995, -2.499999999999998668, 29.75000000000000355 ) ) ;
#17861 = CARTESIAN_POINT ( 'NONE',  ( 10.48490790726815547, -7.276988635370452485, 34.74523720219453793 ) ) ;
#17863 = EDGE_CURVE ( 'NONE', #70222, #78622, #19886, .T. ) ;
#17864 = CYLINDRICAL_SURFACE ( 'NONE', #43802, 0.2499999999999994726 ) ;
#17865 = CARTESIAN_POINT ( 'NONE',  ( -0.4615384615384611200, -12.62096338111211580, 30.90682066428153263 ) ) ;
#17866 = ORIENTED_EDGE ( 'NONE', *, *, #41453, .F. ) ;
#17867 = CARTESIAN_POINT ( 'NONE',  ( -11.31544869436814338, -8.282913670948747864, 34.94150082978203642 ) ) ;
#17868 = DIRECTION ( 'NONE',  ( 0.000000000000000000, 0.000000000000000000, 1.000000000000000000 ) ) ;
#17869 = EDGE_CURVE ( 'NONE', #21320, #86419, #19446, .T. ) ;
#17870 = EDGE_LOOP ( 'NONE', ( #36258, #27106 ) ) ;
#17871 = DIRECTION ( 'NONE',  ( -1.000000000000000000, -0.000000000000000000, -0.000000000000000000 ) ) ;
#17872 = CARTESIAN_POINT ( 'NONE',  ( 12.21153846153845812, -2.499999999999999556, 29.81609845454691765 ) ) ;
#17873 = CARTESIAN_POINT ( 'NONE',  ( -15.09997878980228059, -5.496552790871120031, 34.60292014791297532 ) ) ;
#17874 = CARTESIAN_POINT ( 'NONE',  ( 11.53846153846141753, -6.026961402154118019, 34.52809138561165270 ) ) ;
#17875 = DIRECTION ( 'NONE',  ( 0.000000000000000000, 0.4999999999999985567, 0.8660254037844395958 ) ) ;
#17876 = FACE_BOUND ( 'NONE', #34263, .T. ) ;
#17878 = DIRECTION ( 'NONE',  ( 0.000000000000000000, 0.000000000000000000, 1.000000000000000000 ) ) ;
#17877 = CARTESIAN_POINT ( 'NONE',  ( 13.13459216039392885, -2.341070481393819236, 30.72580821765574299 ) ) ;
#17879 = EDGE_CURVE ( 'NONE', #39364, #87441, #19923, .T. ) ;
#17880 = FACE_OUTER_BOUND ( 'NONE', #75447, .T. ) ;
#17882 = CARTESIAN_POINT ( 'NONE',  ( 14.24242230713598723, -11.06231777344662781, 33.60647404775220082 ) ) ;
#17881 = CARTESIAN_POINT ( 'NONE',  ( -11.28846153846010303, -7.500000000000155431, 34.75000000000007105 ) ) ;
#17883 = CARTESIAN_POINT ( 'NONE',  ( 12.46153846153846168, -1.242168528481310874, 33.36296068462461051 ) ) ;
#17884 = CARTESIAN_POINT ( 'NONE',  ( -1.634615384615383027, -7.500000000000001776, 35.00000000000000000 ) ) ;
#17885 = CARTESIAN_POINT ( 'NONE',  ( -3.775308065498766297, -6.007798216065450170, 26.17000670625849068 ) ) ;
#17886 = ORIENTED_EDGE ( 'NONE', *, *, #23348, .T. ) ;
#17887 = CARTESIAN_POINT ( 'NONE',  ( -3.230769230769352962, -9.528491918059723176, 34.59228464037033035 ) ) ;
#17888 = CARTESIAN_POINT ( 'NONE',  ( 16.21991348719623360, -12.62096338111211757, 30.90682066428152908 ) ) ;
#17889 = DIRECTION ( 'NONE',  ( 0.000000000000000000, 0.000000000000000000, -1.000000000000000000 ) ) ;
#17890 = CARTESIAN_POINT ( 'NONE',  ( 17.01165307636676260, -8.656820664281497102, 34.87096338111211935 ) ) ;
#17891 = CARTESIAN_POINT ( 'NONE',  ( 3.230769230769110045, -6.879047030192662504, 34.71129190930017927 ) ) ;
#17892 = FACE_OUTER_BOUND ( 'NONE', #71526, .T. ) ;
#17893 = CARTESIAN_POINT ( 'NONE',  ( 1.077988221561464899, -4.724691934501233703, 15.23250670625848713 ) ) ;
#17894 = CARTESIAN_POINT ( 'NONE',  ( -15.29603923132555110, -12.70778746994557551, 30.41441678777548319 ) ) ;
#17895 = CARTESIAN_POINT ( 'NONE',  ( 18.00000000000000000, -6.189225973068211317, 35.74407628777942847 ) ) ;
#17896 = CARTESIAN_POINT ( 'NONE',  ( -7.976844449264155479, -2.845849958028613624, 32.17971566917920967 ) ) ;
#17897 = CARTESIAN_POINT ( 'NONE',  ( 15.12820512820512953, -7.500000000000000000, 29.75000000000000355 ) ) ;
#17898 = CARTESIAN_POINT ( 'NONE',  ( 14.37294787896832915, -6.026961402152789304, 34.52809138561124769 ) ) ;
#17899 = CARTESIAN_POINT ( 'NONE',  ( 1.607395053593452694, -10.23759521482555357, 34.22997729860117033 ) ) ;
#17901 = EDGE_CURVE ( 'NONE', #42078, #50903, #36975, .T. ) ;
#17900 = CARTESIAN_POINT ( 'NONE',  ( -18.24997673094235751, -2.779195860258149686, 31.39871582349837453 ) ) ;
#17902 = DIRECTION ( 'NONE',  ( -0.000000000000000000, -0.9848077530122086864, -0.1736481776669273613 ) ) ;
#17903 = ORIENTED_EDGE ( 'NONE', *, *, #34316, .F. ) ;
#17904 = CARTESIAN_POINT ( 'NONE',  ( 17.29970274590113632, -12.69155399931963046, 30.53255429739158444 ) ) ;
#17905 = CARTESIAN_POINT ( 'NONE',  ( 8.769230769230647482, -11.48612834414049644, 32.76840700105863391 ) ) ;
#17906 = CARTESIAN_POINT ( 'NONE',  ( -1.492201783934593573, -3.724691934501250135, 16.82999329374151287 ) ) ;
#17907 = AXIS2_PLACEMENT_3D ( 'NONE', #76976, #50370, #58022 ) ;
#17908 = EDGE_CURVE ( 'NONE', #58446, #77667, #25185, .T. ) ;
#17909 = CARTESIAN_POINT ( 'NONE',  ( -10.61538461538473577, -2.657715359629662544, 31.77849191805970364 ) ) ;
#17910 = DIRECTION ( 'NONE',  ( 0.000000000000000000, 0.1736481776669267785, -0.9848077530122087975 ) ) ;
#17911 = EDGE_LOOP ( 'NONE', ( #4199, #61139, #59113, #25461 ) ) ;
#17912 = CARTESIAN_POINT ( 'NONE',  ( -17.86920955903305597, -6.369690395747425349, 34.87708834333098196 ) ) ;
#17913 = CARTESIAN_POINT ( 'NONE',  ( 9.626225312947559232, -12.62096338111211580, 30.90682066428152908 ) ) ;
#17915 = ORIENTED_EDGE ( 'NONE', *, *, #15832, .T. ) ;
#17914 = DIRECTION ( 'NONE',  ( 1.000000000000000000, 0.000000000000000000, 0.000000000000000000 ) ) ;
#17916 = CARTESIAN_POINT ( 'NONE',  ( -12.71151520558705172, -9.234221910056348293, 34.70572697212741531 ) ) ;
#17917 = CARTESIAN_POINT ( 'NONE',  ( -0.4615384615384611200, -13.75783147151868846, 33.36296068462461051 ) ) ;
#17918 = ADVANCED_FACE ( 'NONE', ( #77055 ), #84266, .F. ) ;
#17919 = CYLINDRICAL_SURFACE ( 'NONE', #40629, 0.2499999999999994726 ) ;
#17920 = CARTESIAN_POINT ( 'NONE',  ( 12.46153846153846168, -2.249999999999998668, 29.75000000000001776 ) ) ;
#17921 = ORIENTED_EDGE ( 'NONE', *, *, #39881, .T. ) ;
#17922 = CARTESIAN_POINT ( 'NONE',  ( 2.438218009455874302, -12.27024696741798770, 31.24895572276497546 ) ) ;
#17923 = CARTESIAN_POINT ( 'NONE',  ( -12.52762084089859584, -2.486705287966279432, 31.30864560766542937 ) ) ;
#17924 = CARTESIAN_POINT ( 'NONE',  ( 4.087762742890270751, -9.780366693483667717, 34.19971097300155805 ) ) ;
#17925 = ORIENTED_EDGE ( 'NONE', *, *, #31578, .F. ) ;
#17926 = ORIENTED_EDGE ( 'NONE', *, *, #65348, .F. ) ;
#17927 = ADVANCED_FACE ( 'NONE', ( #946 ), #36074, .F. ) ;
#17928 = ORIENTED_EDGE ( 'NONE', *, *, #54075, .T. ) ;
#17929 = CARTESIAN_POINT ( 'NONE',  ( -16.15384615384615330, -1.117168528481311540, 33.14645433367849847 ) ) ;
#17930 = DIRECTION ( 'NONE',  ( 0.000000000000000000, 1.000000000000000000, 0.000000000000000000 ) ) ;
#17931 = ADVANCED_FACE ( 'NONE', ( #85138 ), #22545, .F. ) ;
#17932 = B_SPLINE_CURVE_WITH_KNOTS ( 'NONE', 3,
 ( #57847, #77673, #78119, #16421, #49756, #21848, #64587, #29501, #23178, #50640 ),
 .UNSPECIFIED., .F., .F.,
 ( 4, 2, 2, 2, 4 ),
 ( 0.0007817359430256287049, 0.0009771253907249945886, 0.001172514838424360255, 0.001367904286123725922, 0.001563293733823091806 ),
 .UNSPECIFIED. ) ;
#17933 = CARTESIAN_POINT ( 'NONE',  ( -9.692307692307814193, -12.70778746994576025, 30.41441678777401236 ) ) ;
#17934 = B_SPLINE_CURVE_WITH_KNOTS ( 'NONE', 3,
 ( #41657, #81760, #47511, #69563, #1107, #82202, #28586, #88534, #54711, #40777 ),
 .UNSPECIFIED., .F., .F.,
 ( 4, 2, 2, 2, 4 ),
 ( 0.000000000000000000, 0.0001954311564186865492, 0.0003908623128373730983, 0.0005862934692560596746, 0.0007817246256747461966 ),
 .UNSPECIFIED. ) ;
#17935 = AXIS2_PLACEMENT_3D ( 'NONE', #18781, #6594, #80033 ) ;
#17936 = LINE ( 'NONE', #85503, #16166 ) ;
#17937 = B_SPLINE_CURVE_WITH_KNOTS ( 'NONE', 3,
 ( #78517, #16818, #37082, #85732, #51465, #78965, #17263, #44722, #25355, #46520 ),
 .UNSPECIFIED., .F., .F.,
 ( 4, 2, 2, 2, 4 ),
 ( 0.000000000000000000, 0.0001954339857564062817, 0.0003908679715128125635, 0.0005863019572692188723, 0.0007817359430256251270 ),
 .UNSPECIFIED. ) ;
#17938 = EDGE_CURVE ( 'NONE', #29227, #43656, #35629, .T. ) ;
#17939 = ORIENTED_EDGE ( 'NONE', *, *, #75008, .T. ) ;
#17940 = ORIENTED_EDGE ( 'NONE', *, *, #52253, .F. ) ;
#17942 = ORIENTED_EDGE ( 'NONE', *, *, #38343, .T. ) ;
#17941 = DIRECTION ( 'NONE',  ( -0.000000000000000000, -0.000000000000000000, -1.000000000000000000 ) ) ;
#17943 = DIRECTION ( 'NONE',  ( -0.000000000000000000, 0.9848077530122085754, -0.1736481776669273613 ) ) ;
#17944 = EDGE_CURVE ( 'NONE', #86388, #38093, #56335, .T. ) ;
#17945 = DIRECTION ( 'NONE',  ( 0.000000000000000000, 0.8660254037844377084, 0.5000000000000015543 ) ) ;
#17946 = CARTESIAN_POINT ( 'NONE',  ( -14.30769230769230660, -2.538708090699994813, 30.37095296980875503 ) ) ;
#17947 = FACE_OUTER_BOUND ( 'NONE', #81139, .T. ) ;
#17948 = ORIENTED_EDGE ( 'NONE', *, *, #62576, .T. ) ;
#17949 = ORIENTED_EDGE ( 'NONE', *, *, #50505, .F. ) ;
#17950 = ADVANCED_FACE ( 'NONE', ( #50012 ), #28417, .F. ) ;
#17951 = EDGE_LOOP ( 'NONE', ( #78749, #10860, #39904, #17311 ) ) ;
#17953 = EDGE_LOOP ( 'NONE', ( #74100, #62548, #41992, #41745 ) ) ;
#17952 = CARTESIAN_POINT ( 'NONE',  ( 8.834486340506796154, -2.625532179533470512, 30.86335684631491105 ) ) ;
#17954 = CARTESIAN_POINT ( 'NONE',  ( 18.00000000000000000, -11.91647553114624181, 32.58852847137148245 ) ) ;
#17955 = AXIS2_PLACEMENT_3D ( 'NONE', #73353, #26058, #53515 ) ;
#17956 = CYLINDRICAL_SURFACE ( 'NONE', #78413, 0.2499999999999997502 ) ;
#17957 = VERTEX_POINT ( 'NONE', #83824 ) ;
#17958 = EDGE_CURVE ( 'NONE', #57194, #75095, #22983, .T. ) ;
#17959 = DIRECTION ( 'NONE',  ( 0.000000000000000000, 0.000000000000000000, 1.000000000000000000 ) ) ;
#17960 = CYLINDRICAL_SURFACE ( 'NONE', #20671, 0.2499999999999993616 ) ;
#17961 = CARTESIAN_POINT ( 'NONE',  ( 10.61538461538461675, -3.513871655860378418, 32.76840700105978499 ) ) ;
#17962 = FACE_BOUND ( 'NONE', #60979, .T. ) ;
#17963 = PLANE ( 'NONE',  #48504 ) ;
#17964 = DIRECTION ( 'NONE',  ( 0.000000000000000000, 0.3420201433256641055, -0.9396926207859100932 ) ) ;
#17965 = AXIS2_PLACEMENT_3D ( 'NONE', #83808, #1370, #42374 ) ;
#17966 = DIRECTION ( 'NONE',  ( -0.000000000000000000, -0.6427876096865404731, -0.7660444431189770143 ) ) ;
#17968 = CARTESIAN_POINT ( 'NONE',  ( -8.638440328263820689, -11.93129842949671726, 32.56571108434900452 ) ) ;
#17967 = CARTESIAN_POINT ( 'NONE',  ( 16.85399611801622655, -9.172386477786394821, 34.72672124145550043 ) ) ;
#17969 = CARTESIAN_POINT ( 'NONE',  ( -7.846153846153965716, -3.300289026999228881, 32.46337939537708905 ) ) ;
#17970 = CARTESIAN_POINT ( 'NONE',  ( 5.207714884747862705, -2.541949514083464479, 30.39797389878540557 ) ) ;
#17971 = ORIENTED_EDGE ( 'NONE', *, *, #70707, .T. ) ;
#17972 = DIRECTION ( 'NONE',  ( -0.000000000000000000, 0.000000000000000000, 1.000000000000000000 ) ) ;
#17973 = DIRECTION ( 'NONE',  ( -0.000000000000000000, -0.9396926207859092051, -0.3420201433256662704 ) ) ;
#17974 = ORIENTED_EDGE ( 'NONE', *, *, #29448, .F. ) ;
#17975 = EDGE_CURVE ( 'NONE', #72564, #61394, #53617, .T. ) ;
#17976 = ORIENTED_EDGE ( 'NONE', *, *, #44356, .F. ) ;
#17978 = CARTESIAN_POINT ( 'NONE',  ( 1.384615384615264011, -5.941354392335915335, 34.76329471203413846 ) ) ;
#17977 = CYLINDRICAL_SURFACE ( 'NONE', #38957, 0.2499999999999979738 ) ;
#17979 = ADVANCED_FACE ( 'NONE', ( #77926 ), #16230, .F. ) ;
#17980 = CARTESIAN_POINT ( 'NONE',  ( 16.37685899793954292, -6.460100341425561332, 34.89618726649961644 ) ) ;
#17981 = CARTESIAN_POINT ( 'NONE',  ( 14.30769230769262279, -2.255955759149395501, 30.00000000000324363 ) ) ;
#17982 = LINE ( 'NONE', #5353, #47614 ) ;
#17983 = B_SPLINE_CURVE_WITH_KNOTS ( 'NONE', 3,
 ( #42399, #49137, #69857, #7272, #952, #28425, #56343, #63083, #14469, #11935 ),
 .UNSPECIFIED., .F., .F.,
 ( 4, 2, 2, 2, 4 ),
 ( 0.0007817359430256403058, 0.0009771253907250093337, 0.001172514838424378470, 0.001367904286123747606, 0.001563293733823116743 ),
 .UNSPECIFIED. ) ;
#17984 = ORIENTED_EDGE ( 'NONE', *, *, #28924, .F. ) ;
#17985 = CARTESIAN_POINT ( 'NONE',  ( 8.519207545009312099, -12.68155406624981119, 30.59749803192733708 ) ) ;
#17986 = DIRECTION ( 'NONE',  ( -0.000000000000000000, -0.7660444431189791237, -0.6427876096865379196 ) ) ;
#17988 = CARTESIAN_POINT ( 'NONE',  ( 14.05771556364371833, -12.65889640711025521, 30.72598325615533454 ) ) ;
#17987 = DIRECTION ( 'NONE',  ( 0.000000000000000000, 0.1736481776669267785, -0.9848077530122087975 ) ) ;
#17989 = CARTESIAN_POINT ( 'NONE',  ( 7.716006636715626144, -6.001485441113818986, 34.52039167877662607 ) ) ;
#17990 = CARTESIAN_POINT ( 'NONE',  ( 0.2386115026316113497, -3.395401636524185474, 33.02366814457250399 ) ) ;
#17992 = CARTESIAN_POINT ( 'NONE',  ( -15.09997878980228059, -10.70102852606553157, 33.91149625220312913 ) ) ;
#17991 =( NAMED_UNIT ( * ) PLANE_ANGLE_UNIT ( ) SI_UNIT ( $, .RADIAN. ) );
#17993 = CARTESIAN_POINT ( 'NONE',  ( 3.750000000000000888, -7.499999999999978684, 21.96875000000000355 ) ) ;
#17994 = ORIENTED_EDGE ( 'NONE', *, *, #30633, .T. ) ;
#17995 = VERTEX_POINT ( 'NONE', #2257 ) ;
#17996 = CARTESIAN_POINT ( 'NONE',  ( -7.976301815885543434, -11.66186481527757302, 32.95055677023626117 ) ) ;
#17997 = CARTESIAN_POINT ( 'NONE',  ( 17.32697749683652688, -4.074993327901525575, 33.72946981652012255 ) ) ;
#17998 = CARTESIAN_POINT ( 'NONE',  ( 10.68064018666064285, -2.625532179533470512, 30.86335684631491105 ) ) ;
#17999 = DIRECTION ( 'NONE',  ( -0.000000000000000000, 0.9396926207859093161, -0.3420201433256663259 ) ) ;
#18000 = DIRECTION ( 'NONE',  ( -0.000000000000000000, 0.9396926207859093161, -0.3420201433256663259 ) ) ;
#18001 = CARTESIAN_POINT ( 'NONE',  ( 2.651650429449539104, -4.848349570550432475, 20.56250000000000000 ) ) ;
#18002 = DIRECTION ( 'NONE',  ( 0.000000000000000000, 0.9396926207859126468, -0.3420201433256571111 ) ) ;
#18003 = CARTESIAN_POINT ( 'NONE',  ( -13.51530685128294351, -8.147922237126337563, 34.70805685702651999 ) ) ;
#18004 = AXIS2_PLACEMENT_3D ( 'NONE', #28405, #82920, #68949 ) ;
#18005 = CARTESIAN_POINT ( 'NONE',  ( -8.899921372341076165, -12.62707690430377383, 30.88035979386743435 ) ) ;
#18006 = CARTESIAN_POINT ( 'NONE',  ( 5.869852030268307708, -10.31621877034669588, 34.18098118002070152 ) ) ;
#18007 = CARTESIAN_POINT ( 'NONE',  ( -13.38461538461538325, -11.16473453929635440, 33.15142922261926373 ) ) ;
#18008 = CARTESIAN_POINT ( 'NONE',  ( -9.822454901745915734, -12.27039167877662251, 31.24851455888617835 ) ) ;
#18009 = CARTESIAN_POINT ( 'NONE',  ( 2.177000841024749445, -3.062553014421049991, 32.05460306192774311 ) ) ;
#18010 = FACE_OUTER_BOUND ( 'NONE', #13653, .T. ) ;
#18011 = B_SPLINE_CURVE_WITH_KNOTS ( 'NONE', 3,
 ( #25202, #45909, #87823, #59872, #80610, #53556, #88705, #25649, #53104, #46807 ),
 .UNSPECIFIED., .F., .F.,
 ( 4, 2, 2, 2, 4 ),
 ( 0.0007817246256747445703, 0.0009771112852218872494, 0.001172497944769030145, 0.001367884604316172825, 0.001563271263863315504 ),
 .UNSPECIFIED. ) ;
#18012 = CARTESIAN_POINT ( 'NONE',  ( -5.749945580086545327, -4.818054556918156095, 34.26375889529406749 ) ) ;
#18013 = CARTESIAN_POINT ( 'NONE',  ( 11.31553532094539172, -6.503392248772476236, 34.64988816332204635 ) ) ;
#18014 = CARTESIAN_POINT ( 'NONE',  ( -1.384615384615383471, -9.780366693483667717, 34.19971097300155094 ) ) ;
#18015 = ORIENTED_EDGE ( 'NONE', *, *, #38708, .T. ) ;
#18017 = CARTESIAN_POINT ( 'NONE',  ( 11.66898724022510159, -11.93748526763465279, 32.05452791011430946 ) ) ;
#18016 = B_SPLINE_CURVE_WITH_KNOTS ( 'NONE', 3,
 ( #65591, #35720, #70833, #48771, #48327, #35262, #15890, #62720, #28969, #49663 ),
 .UNSPECIFIED., .F., .F.,
 ( 4, 2, 2, 2, 4 ),
 ( 0.000000000000000000, 0.0001954339857564090194, 0.0003908679715128180387, 0.0005863019572692270039, 0.0007817359430256360774 ),
 .UNSPECIFIED. ) ;
#18018 = CARTESIAN_POINT ( 'NONE',  ( 7.497142682080631869E-17, 1.250000000000003775, 32.75000000000000000 ) ) ;
#18019 = CARTESIAN_POINT ( 'NONE',  ( 5.934729999443683290, -2.657715359629089225, 31.77849191805834295 ) ) ;
#18020 = CARTESIAN_POINT ( 'NONE',  ( -1.139087296525992166, -10.25000000000000533, 23.60937500000000711 ) ) ;
#18021 = EDGE_CURVE ( 'NONE', #38647, #69402, #22002, .T. ) ;
#18022 = CARTESIAN_POINT ( 'NONE',  ( -14.30769230769230660, -4.786620604624113540, 33.94971097300155094 ) ) ;
#18023 = CARTESIAN_POINT ( 'NONE',  ( 8.769230769230768274, -9.905515769479276145, 34.41647553114623292 ) ) ;
#18025 = VERTEX_POINT ( 'NONE', #7717 ) ;
#18024 = CARTESIAN_POINT ( 'NONE',  ( 17.07692307692307665, -13.20930481340135110, 34.54067556320372745 ) ) ;
#18026 = CARTESIAN_POINT ( 'NONE',  ( -1.944543648262992530, -9.444543648263016067, 21.18750000000000000 ) ) ;
#18027 = CARTESIAN_POINT ( 'NONE',  ( 2.557692307692308376, -7.500000000000001776, 35.04278698407183867 ) ) ;
#18028 = EDGE_CURVE ( 'NONE', #31229, #10290, #62634, .T. ) ;
#18029 = ORIENTED_EDGE ( 'NONE', *, *, #13280, .T. ) ;
#18030 = CARTESIAN_POINT ( 'NONE',  ( 17.07692307692307665, -13.37000171582298513, 34.34916445242398453 ) ) ;
#18031 = EDGE_CURVE ( 'NONE', #7626, #2885, #82439, .T. ) ;
#18032 = ORIENTED_EDGE ( 'NONE', *, *, #45920, .T. ) ;
#18033 = CARTESIAN_POINT ( 'NONE',  ( 1.384615384615264011, -3.083524468854526912, 32.58852847137268327 ) ) ;
#18034 = DIRECTION ( 'NONE',  ( -0.000000000000000000, -0.6427876096865404731, -0.7660444431189771253 ) ) ;
#18035 = CARTESIAN_POINT ( 'NONE',  ( -0.4615384615384611200, -6.343179335718451384, 34.87096338111211935 ) ) ;
#18036 = ORIENTED_EDGE ( 'NONE', *, *, #22131, .F. ) ;
#18037 = CARTESIAN_POINT ( 'NONE',  ( -4.153846153846274980, -11.67786785259630911, 32.92929555188603530 ) ) ;
#18038 = EDGE_LOOP ( 'NONE', ( #21725, #8776 ) ) ;
#18039 = ADVANCED_FACE ( 'NONE', ( #1828 ), #29316, .F. ) ;
#18040 = CARTESIAN_POINT ( 'NONE',  ( 11.53846153846153832, -3.513871655860378418, 32.76840700105978499 ) ) ;
#18041 = EDGE_LOOP ( 'NONE', ( #62256, #20792, #21039, #38391 ) ) ;
#18042 = CARTESIAN_POINT ( 'NONE',  ( 2.057715563643717438, -9.234221910056348293, 34.70572697212741531 ) ) ;
#18043 = CYLINDRICAL_SURFACE ( 'NONE', #61365, 0.2500000000000009437 ) ;
#18044 = ORIENTED_EDGE ( 'NONE', *, *, #86630, .T. ) ;
#18045 = DIRECTION ( 'NONE',  ( 1.000000000000000000, 0.000000000000000000, 0.000000000000000000 ) ) ;
#18046 = DIRECTION ( 'NONE',  ( -1.000000000000000000, -0.000000000000000000, -0.000000000000000000 ) ) ;
#18047 = CARTESIAN_POINT ( 'NONE',  ( -1.161835715637319133, -10.97394488606064122, 33.68653795673694873 ) ) ;
#18048 = CARTESIAN_POINT ( 'NONE',  ( -14.24243716817946925, -10.33852847137154107, 34.16647553114620450 ) ) ;
#18049 = DIRECTION ( 'NONE',  ( -0.7057856980126717694, -0.7057856980126787638, -0.06109907496453172160 ) ) ;
#18050 = VERTEX_POINT ( 'NONE', #72498 ) ;
#18051 = ORIENTED_EDGE ( 'NONE', *, *, #71995, .T. ) ;
#18052 = EDGE_LOOP ( 'NONE', ( #64594, #21372, #31903, #18058 ) ) ;
#18054 = ORIENTED_EDGE ( 'NONE', *, *, #87422, .F. ) ;
#18053 = DIRECTION ( 'NONE',  ( 0.000000000000000000, 0.8660254037844377084, 0.5000000000000015543 ) ) ;
#18055 = EDGE_CURVE ( 'NONE', #48795, #24566, #459, .T. ) ;
#18056 = CARTESIAN_POINT ( 'NONE',  ( 10.61538461538449596, -5.219633306517616589, 34.19971097300220464 ) ) ;
#18057 = CARTESIAN_POINT ( 'NONE',  ( 6.000000000000001776, -3.513871655860378418, 32.76840700105978499 ) ) ;
#18058 = ORIENTED_EDGE ( 'NONE', *, *, #85750, .T. ) ;
#18059 = VECTOR ( 'NONE', #412, 1000.000000000000000 ) ;
#18060 = EDGE_CURVE ( 'NONE', #75689, #89174, #74653, .T. ) ;
#18061 = VERTEX_POINT ( 'NONE', #78811 ) ;
#18062 = LINE ( 'NONE', #2306, #55442 ) ;
#18063 = ORIENTED_EDGE ( 'NONE', *, *, #70043, .F. ) ;
#18064 = CARTESIAN_POINT ( 'NONE',  ( -12.23811206262367435, -7.630147987733840509, 34.99859428049665411 ) ) ;
#18065 = B_SPLINE_CURVE_WITH_KNOTS ( 'NONE', 3,
 ( #43777, #52304, #79795, #45104, #71238, #79344, #11326, #85659, #30703, #58169 ),
 .UNSPECIFIED., .F., .F.,
 ( 4, 2, 2, 2, 4 ),
 ( 0.000000000000000000, 0.0001954311564186867931, 0.0003908623128373735862, 0.0005862934692560603251, 0.0007817246256747471724 ),
 .UNSPECIFIED. ) ;
#18066 = EDGE_CURVE ( 'NONE', #40270, #61417, #25208, .T. ) ;
#18067 = EDGE_CURVE ( 'NONE', #51804, #87399, #62806, .T. ) ;
#18068 = DIRECTION ( 'NONE',  ( 0.000000000000000000, 0.6427876096865373645, -0.7660444431189797898 ) ) ;
#18069 = CARTESIAN_POINT ( 'NONE',  ( 0.3313912521002405076, -5.195881422630166391, 34.18770438780619259 ) ) ;
#18070 = FACE_BOUND ( 'NONE', #24678, .T. ) ;
#18071 = CARTESIAN_POINT ( 'NONE',  ( -17.99999999999969447, -2.506253911140613244, 30.00000000000320455 ) ) ;
#18072 = CARTESIAN_POINT ( 'NONE',  ( -14.30769230769230660, -12.10708131394839349, 31.69288490824020244 ) ) ;
#18073 = CARTESIAN_POINT ( 'NONE',  ( 20.00000000000000000, -4.000000000000000000, 29.75000000000000355 ) ) ;
#18074 = DIRECTION ( 'NONE',  ( -0.000000000000000000, -0.1736481776669307198, -0.9848077530122080203 ) ) ;
#18075 = CARTESIAN_POINT ( 'NONE',  ( 8.992010310499175318, -3.236590943229499029, 32.36255958852954251 ) ) ;
#18076 = CARTESIAN_POINT ( 'NONE',  ( -1.449885830576159940, -2.625532179533444754, 30.86335684631481513 ) ) ;
#18077 = VERTEX_POINT ( 'NONE', #24760 ) ;
#18078 = CARTESIAN_POINT ( 'NONE',  ( -17.14219352288385778, -12.46129190929999986, 30.37095296980880832 ) ) ;
#18079 = EDGE_LOOP ( 'NONE', ( #12736, #27067, #82989, #36945 ) ) ;
#18080 = EDGE_CURVE ( 'NONE', #39225, #61500, #53087, .T. ) ;
#18081 = ORIENTED_EDGE ( 'NONE', *, *, #60861, .F. ) ;
#18083 = CARTESIAN_POINT ( 'NONE',  ( 10.86533013373275836, -5.852078868378309373, 34.47109172314383585 ) ) ;
#18082 = CARTESIAN_POINT ( 'NONE',  ( -6.923076923077044142, -11.94971097300221174, 32.03036669348237098 ) ) ;
#18084 = B_SPLINE_CURVE_WITH_KNOTS ( 'NONE', 3,
 ( #5032, #59080, #66284, #18553, #12681, #86126, #60415, #79812, #73945, #80714 ),
 .UNSPECIFIED., .F., .F.,
 ( 4, 2, 2, 2, 4 ),
 ( 0.0007817359430256294638, 0.0009771253907249948054, 0.001172514838424360255, 0.001367904286123725489, 0.001563293733823090939 ),
 .UNSPECIFIED. ) ;
#18085 = CARTESIAN_POINT ( 'NONE',  ( 2.980746006547774218, -3.520140089381496473, 33.17453946501458262 ) ) ;
#18086 = CARTESIAN_POINT ( 'NONE',  ( -13.63463860883683942, -2.985938066672154445, 32.43141759479405550 ) ) ;
#18087 = EDGE_CURVE ( 'NONE', #19800, #5458, #73536, .T. ) ;
#18088 = CARTESIAN_POINT ( 'NONE',  ( -18.00000000000012079, -5.941354392335914447, 34.76329471203413846 ) ) ;
#18089 = DIRECTION ( 'NONE',  ( -0.000000000000000000, 0.3420201433256694901, -0.9396926207859082059 ) ) ;
#18090 = EDGE_CURVE ( 'NONE', #87089, #81733, #7987, .T. ) ;
#18091 = ORIENTED_EDGE ( 'NONE', *, *, #55576, .F. ) ;
#18092 = AXIS2_PLACEMENT_3D ( 'NONE', #10575, #86251, #44332 ) ;
#18093 = CARTESIAN_POINT ( 'NONE',  ( -5.300408001487407539, -6.716662450894490100, 34.94144148231605840 ) ) ;
#18094 = CARTESIAN_POINT ( 'NONE',  ( -1.576923076923076872, -11.00000000000000000, 29.75000000000000355 ) ) ;
#18095 = CARTESIAN_POINT ( 'NONE',  ( 10.61538461538461675, -2.833524468853757305, 32.15551576947925838 ) ) ;
#18096 = CARTESIAN_POINT ( 'NONE',  ( -13.51476335434707821, -12.70455904226513866, 30.44083106164009322 ) ) ;
#18097 = ORIENTED_EDGE ( 'NONE', *, *, #16937, .T. ) ;
#18098 = EDGE_CURVE ( 'NONE', #76696, #25471, #64680, .T. ) ;
#18099 = ORIENTED_EDGE ( 'NONE', *, *, #19426, .T. ) ;
#18100 = ITEM_DEFINED_TRANSFORMATION ( 'NONE', 'NONE', #84934,  #83448 ) ;
#18101 = ORIENTED_EDGE ( 'NONE', *, *, #29503, .T. ) ;
#18102 = CARTESIAN_POINT ( 'NONE',  ( 11.53846153846153832, -12.34228464037088635, 31.77849191805839268 ) ) ;
#18103 = CARTESIAN_POINT ( 'NONE',  ( -6.065753428313330531, -7.249945578846651806, 34.99404164642496795 ) ) ;
#18104 = ORIENTED_EDGE ( 'NONE', *, *, #84084, .T. ) ;
#18105 = AXIS2_PLACEMENT_3D ( 'NONE', #26051, #55284, #53506 ) ;
#18106 = CARTESIAN_POINT ( 'NONE',  ( -7.846153846153844924, -4.098570777380720287, 33.41473453929634729 ) ) ;
#18107 = DIRECTION ( 'NONE',  ( 0.000000000000000000, 0.1736481776669267785, -0.9848077530122087975 ) ) ;
#18108 = CARTESIAN_POINT ( 'NONE',  ( -8.519285250882628446, -6.696923467548660192, 34.68552623307873972 ) ) ;
#18109 = DIRECTION ( 'NONE',  ( 0.000000000000000000, 0.000000000000000000, 1.000000000000000000 ) ) ;
#18110 = B_SPLINE_CURVE_WITH_KNOTS ( 'NONE', 3,
 ( #37770, #8542, #9417, #65237, #84211, #15743, #22488, #3532, #31005, #29698 ),
 .UNSPECIFIED., .F., .F.,
 ( 4, 2, 2, 2, 4 ),
 ( 0.000000000000000000, 0.0001954339857564054686, 0.0003908679715128109372, 0.0005863019572692163787, 0.0007817359430256218744 ),
 .UNSPECIFIED. ) ;
#18111 = DIRECTION ( 'NONE',  ( 0.000000000000000000, 0.000000000000000000, 1.000000000000000000 ) ) ;
#18112 = VERTEX_POINT ( 'NONE', #30028 ) ;
#18114 = ORIENTED_EDGE ( 'NONE', *, *, #20016, .F. ) ;
#18113 = CARTESIAN_POINT ( 'NONE',  ( -14.98071481085577972, -2.318338780012835443, 30.59689888758630261 ) ) ;
#18115 = CARTESIAN_POINT ( 'NONE',  ( 19.99999999999999289, -11.99999999999999467, 10.00000000000000178 ) ) ;
#18116 = CARTESIAN_POINT ( 'NONE',  ( -12.59168643127016374, -3.069018819979302926, 32.56621877034667278 ) ) ;
#18117 = DIRECTION ( 'NONE',  ( 0.000000000000000000, 0.6427876096865373645, -0.7660444431189797898 ) ) ;
#18118 = CARTESIAN_POINT ( 'NONE',  ( 15.36129493253279499, -12.45806712695776319, 30.39783852428763922 ) ) ;
#18119 = DIRECTION ( 'NONE',  ( 1.000000000000000000, 0.000000000000000000, 0.000000000000000000 ) ) ;
#18120 = SURFACE_SIDE_STYLE ('',( #54548 ) ) ;
#18121 = CARTESIAN_POINT ( 'NONE',  ( 1.901340078031373171, -9.487747218494639867, 17.37686829374151287 ) ) ;
#18122 = ORIENTED_EDGE ( 'NONE', *, *, #14490, .T. ) ;
#18123 = CARTESIAN_POINT ( 'NONE',  ( -20.74999999999999645, -2.499999999999999556, 27.25000000000000000 ) ) ;
#18124 = LINE ( 'NONE', #73960, #10294 ) ;
#18125 = DIRECTION ( 'NONE',  ( 0.000000000000000000, 0.9396926207859126468, 0.3420201433256571111 ) ) ;
#18126 = ADVANCED_FACE ( 'NONE', ( #70573 ), #14748, .F. ) ;
#18128 = ORIENTED_EDGE ( 'NONE', *, *, #28490, .F. ) ;
#18127 = VECTOR ( 'NONE', #728, 1000.000000000000000 ) ;
#18129 = ORIENTED_EDGE ( 'NONE', *, *, #84407, .T. ) ;
#18130 = DIRECTION ( 'NONE',  ( -0.000000000000000000, 1.000000000000000000, 3.491481338843133355E-15 ) ) ;
#18131 = CARTESIAN_POINT ( 'NONE',  ( 11.53846153846153832, -4.661471528628507777, 34.16647553114623292 ) ) ;
#18132 = CARTESIAN_POINT ( 'NONE',  ( -0.7115616857599190714, -9.356822207818506598, 34.66110646841856635 ) ) ;
#18133 = DIRECTION ( 'NONE',  ( -0.000000000000000000, -0.7660444431189791237, -0.6427876096865379196 ) ) ;
#18134 = CARTESIAN_POINT ( 'NONE',  ( -8.992715712954719720, -11.89387501736622710, 32.13663884655806413 ) ) ;
#18135 = CYLINDRICAL_SURFACE ( 'NONE', #19188, 0.2499999999999995559 ) ;
#18136 = ORIENTED_EDGE ( 'NONE', *, *, #68323, .F. ) ;
#18137 = CARTESIAN_POINT ( 'NONE',  ( 9.562160482869472844, -10.88202310037935661, 33.43294751532457099 ) ) ;
#18138 = CARTESIAN_POINT ( 'NONE',  ( -2.242436736416282272, -10.21337939537593797, 33.94971097300152252 ) ) ;
#18139 = CARTESIAN_POINT ( 'NONE',  ( 9.442330948259105128, -2.544273027872575366, 31.48422191005632342 ) ) ;
#18140 = ORIENTED_EDGE ( 'NONE', *, *, #38331, .F. ) ;
#18141 = CARTESIAN_POINT ( 'NONE',  ( -7.623142494540996239, -3.587049720035815348, 32.86302985866382897 ) ) ;
#18142 = ORIENTED_EDGE ( 'NONE', *, *, #25008, .F. ) ;
#18143 = CARTESIAN_POINT ( 'NONE',  ( 13.51514108637895184, -3.816742781228458448, 33.13167719472716044 ) ) ;
#18144 = CARTESIAN_POINT ( 'NONE',  ( -13.13461538461396394, -7.500000000000154543, 35.00000000000007105 ) ) ;
#18145 = LINE ( 'NONE', #87070, #48446 ) ;
#18146 = ORIENTED_EDGE ( 'NONE', *, *, #61909, .F. ) ;
#18147 = CARTESIAN_POINT ( 'NONE',  ( 12.23861224402230619, -3.586966769969701208, 32.86292498521069660 ) ) ;
#18148 = CARTESIAN_POINT ( 'NONE',  ( 9.692307692307570832, -9.528491918059723176, 34.59228464037033035 ) ) ;
#18149 = CARTESIAN_POINT ( 'NONE',  ( 30.00000000000000000, -15.00000000000000000, 3.000000000000000000 ) ) ;
#18150 = EDGE_CURVE ( 'NONE', #36240, #46929, #56170, .T. ) ;
#18151 = CARTESIAN_POINT ( 'NONE',  ( -5.999999999999998224, -1.129524287112498415, 32.06866353760679544 ) ) ;
#18152 = CARTESIAN_POINT ( 'NONE',  ( -5.010855743573000787, -10.67929555188718282, 33.92786785259544757 ) ) ;
#18153 = AXIS2_PLACEMENT_3D ( 'NONE', #4135, #30724, #10011 ) ;
#18154 = ORIENTED_EDGE ( 'NONE', *, *, #88340, .F. ) ;
#18155 = LINE ( 'NONE', #19920, #40076 ) ;
#18156 = ORIENTED_EDGE ( 'NONE', *, *, #54191, .T. ) ;
#18157 = CARTESIAN_POINT ( 'NONE',  ( -15.23076923076935252, -6.835583212225970762, 34.95778746994575670 ) ) ;
#18158 = B_SPLINE_CURVE_WITH_KNOTS ( 'NONE', 3,
 ( #79514, #46612, #32216, #11051, #58332, #10606, #17815, #72738, #65982, #4286 ),
 .UNSPECIFIED., .F., .F.,
 ( 4, 2, 2, 2, 4 ),
 ( 0.000000000000000000, 0.0001954339857564079080, 0.0003908679715128158161, 0.0005863019572692237513, 0.0007817359430256316322 ),
 .UNSPECIFIED. ) ;
#18159 = DIRECTION ( 'NONE',  ( -0.000000000000000000, -0.8660254037844397068, -0.4999999999999978906 ) ) ;
#18160 = DIRECTION ( 'NONE',  ( -0.000000000000000000, -0.8660254037844399289, -0.4999999999999980016 ) ) ;
#18161 = DIRECTION ( 'NONE',  ( -0.000000000000000000, 1.000000000000000000, -0.000000000000000000 ) ) ;
#18162 = EDGE_CURVE ( 'NONE', #60114, #41758, #84217, .T. ) ;
#18163 = VECTOR ( 'NONE', #62233, 1000.000000000000000 ) ;
#18164 = CARTESIAN_POINT ( 'NONE',  ( -6.249976730942353953, -4.236021600441998380, 33.53823185664189310 ) ) ;
#18165 = CARTESIAN_POINT ( 'NONE',  ( 12.52760681254089903, -9.780366693483667717, 34.19971097300155805 ) ) ;
#18166 = VERTEX_POINT ( 'NONE', #77763 ) ;
#18167 = EDGE_LOOP ( 'NONE', ( #45296, #84808, #754, #43166 ) ) ;
#18168 = VERTEX_POINT ( 'NONE', #49417 ) ;
#18169 = ORIENTED_EDGE ( 'NONE', *, *, #8622, .T. ) ;
#18170 = VERTEX_POINT ( 'NONE', #29155 ) ;
#18171 = EDGE_CURVE ( 'NONE', #62161, #54250, #1219, .T. ) ;
#18172 = CARTESIAN_POINT ( 'NONE',  ( 17.07692307692307665, -1.629998284177014645, 34.34916445242399163 ) ) ;
#18173 = CARTESIAN_POINT ( 'NONE',  ( 6.000000000000001776, -6.435427911321262684, 35.78748833219616898 ) ) ;
#18174 = B_SPLINE_CURVE_WITH_KNOTS ( 'NONE', 3,
 ( #8805, #63732, #34928, #62392, #65054, #51528, #71821, #24080, #79028, #71371 ),
 .UNSPECIFIED., .F., .F.,
 ( 4, 2, 2, 2, 4 ),
 ( 0.0007817359430256294638, 0.0009771253907249941549, 0.001172514838424358954, 0.001367904286123723754, 0.001563293733823095492 ),
 .UNSPECIFIED. ) ;
#18175 = DIRECTION ( 'NONE',  ( 1.000000000000000000, 0.000000000000000000, 0.000000000000000000 ) ) ;
#18176 = CARTESIAN_POINT ( 'NONE',  ( -5.750054481651857508, -5.057305518903949526, 34.11320923018887896 ) ) ;
#18177 = CARTESIAN_POINT ( 'NONE',  ( 13.25392391794782654, -8.147922237126337563, 34.70805685702651999 ) ) ;
#18178 = CARTESIAN_POINT ( 'NONE',  ( 8.703147358274888390, -8.973038597847271092, 34.52809138561120506 ) ) ;
#18179 = VECTOR ( 'NONE', #54795, 1000.000000000000114 ) ;
#18180 = CARTESIAN_POINT ( 'NONE',  ( -17.86920819217521483, -9.804649428959613999, 34.18742332936588468 ) ) ;
#18181 = CARTESIAN_POINT ( 'NONE',  ( 9.627037691751374027, -10.33852847137145048, 34.16647553114627556 ) ) ;
#18182 = CARTESIAN_POINT ( 'NONE',  ( 6.923076923076924238, -5.415277668671390821, 36.20867863119892149 ) ) ;
#18183 = VERTEX_POINT ( 'NONE', #36778 ) ;
#18184 = VERTEX_POINT ( 'NONE', #21941 ) ;
#18185 = VECTOR ( 'NONE', #52539, 1000.000000000000000 ) ;
#18186 = ORIENTED_EDGE ( 'NONE', *, *, #10109, .T. ) ;
#18188 = VERTEX_POINT ( 'NONE', #9749 ) ;
#18187 = DIRECTION ( 'NONE',  ( -0.000000000000000000, -0.9396926207859093161, -0.3420201433256663259 ) ) ;
#18190 = CARTESIAN_POINT ( 'NONE',  ( 1.384615384615386802, -5.180354513474913603, 36.12317359536750416 ) ) ;
#18189 = CARTESIAN_POINT ( 'NONE',  ( -15.93083480223330817, -6.503523203565941380, 34.64991518177335195 ) ) ;
#18191 = CARTESIAN_POINT ( 'NONE',  ( 8.638754061114305216, -7.276988635370452485, 34.74523720219453793 ) ) ;
#18192 = DIRECTION ( 'NONE',  ( 0.000000000000000000, 0.000000000000000000, 1.000000000000000000 ) ) ;
#18193 = EDGE_CURVE ( 'NONE', #63742, #81234, #15630, .T. ) ;
#18194 = FACE_BOUND ( 'NONE', #87871, .T. ) ;
#18195 = ORIENTED_EDGE ( 'NONE', *, *, #62417, .F. ) ;
#18196 = VECTOR ( 'NONE', #45793, 1000.000000000000000 ) ;
#18197 = VERTEX_POINT ( 'NONE', #57933 ) ;
#18198 = CARTESIAN_POINT ( 'NONE',  ( -16.15384615384615330, -1.629998284177014645, 34.34916445242399163 ) ) ;
#18199 = ORIENTED_EDGE ( 'NONE', *, *, #33134, .F. ) ;
#18200 = FACE_BOUND ( 'NONE', #11231, .T. ) ;
#18201 = FACE_OUTER_BOUND ( 'NONE', #25510, .T. ) ;
#18202 = CARTESIAN_POINT ( 'NONE',  ( -19.50000000000000000, -11.50000000000000000, 29.75000000000000355 ) ) ;
#18203 = ORIENTED_EDGE ( 'NONE', *, *, #60428, .T. ) ;
#18204 = CARTESIAN_POINT ( 'NONE',  ( -1.319360245102545015, -5.941354392334606160, 34.76329471203374055 ) ) ;
#18205 = CARTESIAN_POINT ( 'NONE',  ( -6.923076923077045919, -2.379036618888197729, 30.90682066428292885 ) ) ;
#18206 = CARTESIAN_POINT ( 'NONE',  ( 14.30769230769218581, -10.33852847137269571, 34.16647553114546554 ) ) ;
#18207 = ORIENTED_EDGE ( 'NONE', *, *, #67920, .T. ) ;
#18208 = LINE ( 'NONE', #71803, #45725 ) ;
#18209 = CARTESIAN_POINT ( 'NONE',  ( 3.230769230769110045, -12.27809138561165270, 31.22303859784587132 ) ) ;
#18210 = DIRECTION ( 'NONE',  ( 0.000000000000000000, 0.9396926207859126468, 0.3420201433256571111 ) ) ;
#18211 = ORIENTED_EDGE ( 'NONE', *, *, #64092, .T. ) ;
#18212 = B_SPLINE_CURVE_WITH_KNOTS ( 'NONE', 3,
 ( #13559, #14904, #75270, #21644, #70280, #14449, #27520, #6799, #76597, #34273 ),
 .UNSPECIFIED., .F., .F.,
 ( 4, 2, 2, 2, 4 ),
 ( 0.000000000000000000, 0.0001954311564186870371, 0.0003908623128373740741, 0.0005862934692560610840, 0.0007817246256747481482 ),
 .UNSPECIFIED. ) ;
#18213 = CYLINDRICAL_SURFACE ( 'NONE', #1362, 0.2500000000000012212 ) ;
#18214 = CARTESIAN_POINT ( 'NONE',  ( -10.61538461538461320, -12.29105614889573062, 35.45975837776705220 ) ) ;
#18215 = B_SPLINE_CURVE_WITH_KNOTS ( 'NONE', 3,
 ( #11660, #87786, #46324, #81901, #31930, #86894, #67491, #20191, #18411, #67046 ),
 .UNSPECIFIED., .F., .F.,
 ( 4, 2, 2, 2, 4 ),
 ( 0.0007817246336856290608, 0.0009771112958940101571, 0.001172497958102391253, 0.001367884620310772350, 0.001563271282519153446 ),
 .UNSPECIFIED. ) ;
#18216 = EDGE_LOOP ( 'NONE', ( #66859, #9203, #974, #39477 ) ) ;
#18217 = CARTESIAN_POINT ( 'NONE',  ( 18.00000000000000000, -6.386643153685126251, 34.62446782046654192 ) ) ;
#18218 = CARTESIAN_POINT ( 'NONE',  ( -10.39260507411620260, -5.114059244376869984, 34.14424750095245287 ) ) ;
#18219 = CARTESIAN_POINT ( 'NONE',  ( -10.61538461538461320, -2.708943851104267164, 35.45975837776705220 ) ) ;
#18220 = CARTESIAN_POINT ( 'NONE',  ( 15.00728430620490172, -12.69144148231606017, 30.53333754910549303 ) ) ;
#18221 = CARTESIAN_POINT ( 'NONE',  ( -7.053552108152643108, -7.276987145209185215, 34.99546412871779211 ) ) ;
#18222 = AXIS2_PLACEMENT_3D ( 'NONE', #34279, #81592, #47346 ) ;
#18223 = DIRECTION ( 'NONE',  ( 1.000000000000000000, 0.000000000000000000, 0.000000000000000000 ) ) ;
#18225 = CARTESIAN_POINT ( 'NONE',  ( 9.915320536401090123, -4.762714258010881885, 34.23016756924214832 ) ) ;
#18224 = CARTESIAN_POINT ( 'NONE',  ( -1.634638621908348410, -5.056417327199099532, 34.11270091957321426 ) ) ;
#18226 = CARTESIAN_POINT ( 'NONE',  ( 10.83839745947800992, -9.172514111537584114, 34.72667873470787470 ) ) ;
#18228 = CARTESIAN_POINT ( 'NONE',  ( 12.33084785842815378, -4.684245665217972032, 34.18127051446801090 ) ) ;
#18227 = CARTESIAN_POINT ( 'NONE',  ( -15.23076923076935252, -2.657715359629662544, 31.77849191805970364 ) ) ;
#18229 = CARTESIAN_POINT ( 'NONE',  ( -1.139087296525992166, -10.25000000000000533, 16.10937500000000355 ) ) ;
#18230 = ORIENTED_EDGE ( 'NONE', *, *, #88361, .F. ) ;
#18231 = CARTESIAN_POINT ( 'NONE',  ( 17.93391658904412012, -4.098570777380720287, 33.41473453929634729 ) ) ;
#18232 = ORIENTED_EDGE ( 'NONE', *, *, #78435, .T. ) ;
#18233 = EDGE_LOOP ( 'NONE', ( #31160, #71104, #85666, #72042 ) ) ;
#18234 = DIRECTION ( 'NONE',  ( 0.000000000000000000, 0.1736481776669267785, -0.9848077530122087975 ) ) ;
#18236 = ORIENTED_EDGE ( 'NONE', *, *, #17480, .F. ) ;
#18235 = AXIS2_PLACEMENT_3D ( 'NONE', #14699, #34526, #64524 ) ;
#18237 = CARTESIAN_POINT ( 'NONE',  ( -5.777220331021931443, -10.23759521482555357, 34.22997729860117033 ) ) ;
#18238 = CARTESIAN_POINT ( 'NONE',  ( -1.944543648262992530, -9.444543648263016067, 14.93750000000000000 ) ) ;
#18239 = DIRECTION ( 'NONE',  ( 0.000000000000000000, 0.4999999999999985567, 0.8660254037844395958 ) ) ;
#18240 = CARTESIAN_POINT ( 'NONE',  ( 6.000000000000001776, -11.16473453929635440, 33.15142922261926373 ) ) ;
#18241 = CARTESIAN_POINT ( 'NONE',  ( -15.23076923076922995, -1.242168528481310874, 33.36296068462461051 ) ) ;
#18242 = CARTESIAN_POINT ( 'NONE',  ( 2.750000000000001776, -7.500000000000000000, 18.00000000000000355 ) ) ;
#18243 = DIRECTION ( 'NONE',  ( -0.000000000000000000, 0.1736481776669307198, -0.9848077530122080203 ) ) ;
#18244 = CARTESIAN_POINT ( 'NONE',  ( 7.846153846153846700, -2.486705287966279876, 31.30864560766543647 ) ) ;
#18245 = CARTESIAN_POINT ( 'NONE',  ( -7.623142494540995351, -12.15243808032446005, 31.58219941686247978 ) ) ;
#18246 = CARTESIAN_POINT ( 'NONE',  ( 3.749999999999992006, -5.946699141100872943, 23.14062500000000000 ) ) ;
#18247 = CARTESIAN_POINT ( 'NONE',  ( 5.076923076923075762, -2.833524468853757305, 32.15551576947925838 ) ) ;
#18248 = CARTESIAN_POINT ( 'NONE',  ( 12.46153846153833911, -5.219633306517616589, 34.19971097300220464 ) ) ;
#18249 = CARTESIAN_POINT ( 'NONE',  ( 5.777073041093149897, -3.395401636524186362, 33.02366814457250399 ) ) ;
#18250 = VERTEX_POINT ( 'NONE', #64234 ) ;
#18251 = ORIENTED_EDGE ( 'NONE', *, *, #77562, .T. ) ;
#18252 = VECTOR ( 'NONE', #42580, 1000.000000000000227 ) ;
#18253 = CARTESIAN_POINT ( 'NONE',  ( 7.846153846153846700, -13.20930481340135110, 34.54067556320372745 ) ) ;
#18254 = CARTESIAN_POINT ( 'NONE',  ( 7.846153846153846700, -11.16473453929635440, 33.15142922261926373 ) ) ;
#18255 = CARTESIAN_POINT ( 'NONE',  ( 1.318533005255250412, -10.67929555188718460, 33.92786785259543336 ) ) ;
#18256 = CARTESIAN_POINT ( 'NONE',  ( -10.61538461538461320, -11.91647553114624181, 32.58852847137148245 ) ) ;
#18257 = CARTESIAN_POINT ( 'NONE',  ( -17.07692307692319744, -9.442884908241554243, 34.35708131394783038 ) ) ;
#18258 = CARTESIAN_POINT ( 'NONE',  ( -9.758390071667825794, -6.343179335718451384, 34.87096338111212646 ) ) ;
#18259 = ADVANCED_FACE ( 'NONE', ( #16508 ), #43974, .F. ) ;
#18260 = PRESENTATION_LAYER_ASSIGNMENT (  '', '', ( #74701 ) ) ;
#18261 = AXIS2_PLACEMENT_3D ( 'NONE', #5278, #53452, #75074 ) ;
#18262 = ORIENTED_EDGE ( 'NONE', *, *, #78997, .T. ) ;
#18263 = CARTESIAN_POINT ( 'NONE',  ( -10.86538461538461497, -7.566082377512564960, 35.00000000000000711 ) ) ;
#18264 = VERTEX_POINT ( 'NONE', #28703 ) ;
#18265 = ORIENTED_EDGE ( 'NONE', *, *, #48482, .F. ) ;
#18266 = CARTESIAN_POINT ( 'NONE',  ( -9.561517251340744039, -2.845873456487965747, 32.17976146951972538 ) ) ;
#18267 = EDGE_CURVE ( 'NONE', #572, #78341, #4771, .T. ) ;
#18268 = FACE_OUTER_BOUND ( 'NONE', #82250, .T. ) ;
#18269 = CARTESIAN_POINT ( 'NONE',  ( 11.66898724022510514, -10.88167719472716399, 33.43325721877153711 ) ) ;
#18270 = EDGE_CURVE ( 'NONE', #6115, #7880, #8876, .T. ) ;
#18271 = FACE_OUTER_BOUND ( 'NONE', #7613, .T. ) ;
#18272 = CARTESIAN_POINT ( 'NONE',  ( 13.25392478150507891, -5.496505350115501010, 34.60290016733514307 ) ) ;
#18273 = VERTEX_POINT ( 'NONE', #22818 ) ;
#18274 = ORIENTED_EDGE ( 'NONE', *, *, #42232, .T. ) ;
#18275 = EDGE_LOOP ( 'NONE', ( #45008, #72644, #62771, #34774, #58454, #9637 ) ) ;
#18276 = EDGE_CURVE ( 'NONE', #12463, #1012, #43533, .T. ) ;
#18277 = CARTESIAN_POINT ( 'NONE',  ( -5.999999999999998224, -8.973038597847269315, 34.52809138561121927 ) ) ;
#18278 = CARTESIAN_POINT ( 'NONE',  ( -14.30769230769230660, -2.499999999999998668, 29.75000000000001421 ) ) ;
#18279 = CARTESIAN_POINT ( 'NONE',  ( 16.21910129335899597, -5.941354392334603496, 34.76329471203374055 ) ) ;
#18280 = CARTESIAN_POINT ( 'NONE',  ( 2.084766090176162212, -11.24512374952581872, 33.06303171183252942 ) ) ;
#18281 = CARTESIAN_POINT ( 'NONE',  ( -4.284456513470680683, -7.722926236386453702, 34.74524107206102030 ) ) ;
#18282 = CARTESIAN_POINT ( 'NONE',  ( 5.776515056276055660, -12.44517049084099725, 30.48991314939691932 ) ) ;
#18283 = VECTOR ( 'NONE', #11252, 1000.000000000000227 ) ;
#18284 = VERTEX_POINT ( 'NONE', #66017 ) ;
#18285 = ORIENTED_EDGE ( 'NONE', *, *, #71275, .F. ) ;
#18286 = CARTESIAN_POINT ( 'NONE',  ( 1.553300858899087311, -3.749999999999992006, 25.48437500000000000 ) ) ;
#18288 = ORIENTED_EDGE ( 'NONE', *, *, #16771, .T. ) ;
#18287 = LINE ( 'NONE', #52942, #45877 ) ;
#18289 = FACE_OUTER_BOUND ( 'NONE', #37199, .T. ) ;
#18290 = CARTESIAN_POINT ( 'NONE',  ( -9.757578138268469203, -11.94971097300153140, 32.03036669348370680 ) ) ;
#18291 = CARTESIAN_POINT ( 'NONE',  ( -3.749999999999997335, -7.500000000000021316, 17.59375000000000000 ) ) ;
#18292 = ADVANCED_FACE ( 'NONE', ( #11986 ), #71892, .F. ) ;
#18293 = ORIENTED_EDGE ( 'NONE', *, *, #27286, .T. ) ;
#18294 = EDGE_CURVE ( 'NONE', #273, #19105, #10188, .T. ) ;
#18295 = LINE ( 'NONE', #44862, #67026 ) ;
#18296 = B_SPLINE_CURVE_WITH_KNOTS ( 'NONE', 3,
 ( #2313, #23914, #51364, #78868, #17167, #35686, #38333, #65790, #10422, #87430 ),
 .UNSPECIFIED., .F., .F.,
 ( 4, 2, 2, 2, 4 ),
 ( 0.000000000000000000, 0.0001954339857564097512, 0.0003908679715128195024, 0.0005863019572692292807, 0.0007817359430256390048 ),
 .UNSPECIFIED. ) ;
#18297 = ORIENTED_EDGE ( 'NONE', *, *, #48877, .T. ) ;
#18298 = CARTESIAN_POINT ( 'NONE',  ( 2.438218009455872970, -9.417988943895561960, 34.36773134775778260 ) ) ;
#18299 = FACE_OUTER_BOUND ( 'NONE', #64209, .T. ) ;
#18300 = CARTESIAN_POINT ( 'NONE',  ( -12.21148414990014963, -12.41262288849542017, 30.68299917996395010 ) ) ;
#18302 = DIRECTION ( 'NONE',  ( 1.000000000000000000, 0.000000000000000000, 0.000000000000000000 ) ) ;
#18301 = DIRECTION ( 'NONE',  ( -0.000000000000000000, -0.6427876096865404731, -0.7660444431189770143 ) ) ;
#18303 = EDGE_CURVE ( 'NONE', #87005, #62924, #5887, .T. ) ;
#18304 = B_SPLINE_CURVE_WITH_KNOTS ( 'NONE', 3,
 ( #74853, #12696, #5045, #19889, #32511, #13140, #75287, #34290, #59988, #67202 ),
 .UNSPECIFIED., .F., .F.,
 ( 4, 2, 2, 2, 4 ),
 ( 0.0007817359430256294638, 0.0009771253907249941549, 0.001172514838424358954, 0.001367904286123723754, 0.001563293733823095492 ),
 .UNSPECIFIED. ) ;
#18305 = AXIS2_PLACEMENT_3D ( 'NONE', #31012, #17517, #72447 ) ;
#18306 = DIRECTION ( 'NONE',  ( 0.000000000000000000, 0.000000000000000000, -1.000000000000000000 ) ) ;
#18307 = ORIENTED_EDGE ( 'NONE', *, *, #24435, .T. ) ;
#18308 = EDGE_CURVE ( 'NONE', #79391, #59502, #42429, .T. ) ;
#18309 = DIRECTION ( 'NONE',  ( -0.000000000000000000, 0.7660444431189791237, -0.6427876096865379196 ) ) ;
#18310 = CARTESIAN_POINT ( 'NONE',  ( 4.153846153846154188, -8.120952969808772792, 34.71129190930000163 ) ) ;
#18311 = CARTESIAN_POINT ( 'NONE',  ( -11.53846153846153655, -13.53365097954675988, 30.81389545987213552 ) ) ;
#18312 = VERTEX_POINT ( 'NONE', #44855 ) ;
#18313 = DIRECTION ( 'NONE',  ( 0.000000000000000000, 0.000000000000000000, 1.000000000000000000 ) ) ;
#18314 = CARTESIAN_POINT ( 'NONE',  ( -13.19230769230769162, -3.499999999999999556, 29.75000000000000355 ) ) ;
#18315 = FACE_OUTER_BOUND ( 'NONE', #48149, .T. ) ;
#18316 = CARTESIAN_POINT ( 'NONE',  ( 10.36540788444226280, -11.79746400365624659, 32.30657167506340954 ) ) ;
#18317 = FACE_BOUND ( 'NONE', #42741, .T. ) ;
#18319 = DIRECTION ( 'NONE',  ( -0.000000000000000000, -0.7660444431189792347, -0.6427876096865379196 ) ) ;
#18318 = CARTESIAN_POINT ( 'NONE',  ( 12.23805351781451201, -3.236172620538810385, 32.36188796281390267 ) ) ;
#18320 = AXIS2_PLACEMENT_3D ( 'NONE', #31184, #34188, #19793 ) ;
#18321 = CARTESIAN_POINT ( 'NONE',  ( -14.98071481085577972, -4.818054556918156983, 34.26375889529406749 ) ) ;
#18323 = CARTESIAN_POINT ( 'NONE',  ( 14.08476534878546360, -10.77366814457252175, 33.85459836347579454 ) ) ;
#18322 = CARTESIAN_POINT ( 'NONE',  ( 3.164685819813350065, -4.098570777380720287, 33.41473453929634729 ) ) ;
#18324 = CARTESIAN_POINT ( 'NONE',  ( 16.08776274289027342, -10.51840700105979565, 33.73612834413961536 ) ) ;
#18325 = CARTESIAN_POINT ( 'NONE',  ( 13.13463864056679853, -2.544273027872575366, 31.48422191005632342 ) ) ;
#18326 = CARTESIAN_POINT ( 'NONE',  ( -1.492201783934549164, -11.27530806549876807, 24.60750670625849779 ) ) ;
#18327 = DIRECTION ( 'NONE',  ( 1.000000000000000000, 0.000000000000000000, 0.000000000000000000 ) ) ;
#18328 = VERTEX_POINT ( 'NONE', #52944 ) ;
#18329 = CARTESIAN_POINT ( 'NONE',  ( 0.3313912521002404521, -6.852621066184267029, 34.70813303252209181 ) ) ;
#18330 = CARTESIAN_POINT ( 'NONE',  ( 16.28463659481310444, -12.62708834333097663, 30.88030960425256310 ) ) ;
#18331 = CARTESIAN_POINT ( 'NONE',  ( -1.134669866267242089, -10.76462480002816235, 33.53768742498949962 ) ) ;
#18332 = CARTESIAN_POINT ( 'NONE',  ( -2.531177251416254936, -11.89387501736622710, 32.13663884655806413 ) ) ;
#18333 = CARTESIAN_POINT ( 'NONE',  ( -10.36543920600657209, -12.07971442181322175, 32.31769673815850297 ) ) ;
#18334 = CARTESIAN_POINT ( 'NONE',  ( 1.134592160393927740, -12.07920672191015221, 32.31858351112116168 ) ) ;
#18335 = CARTESIAN_POINT ( 'NONE',  ( 0.06109907496454976272, -10.25000000000000000, 15.77938170625848890 ) ) ;
#18336 = CARTESIAN_POINT ( 'NONE',  ( 2.057669070399343880, -11.86270091957321249, 32.19358267280087915 ) ) ;
#18337 = CARTESIAN_POINT ( 'NONE',  ( -2.241624974342230736, -6.343179335718452272, 34.87096338111212646 ) ) ;
#18338 = CARTESIAN_POINT ( 'NONE',  ( -12.46153846153858424, -9.528491918059723176, 34.59228464037033035 ) ) ;
#18339 = CARTESIAN_POINT ( 'NONE',  ( 9.442330948259105128, -4.075325502946081535, 33.72974371597206300 ) ) ;
#18340 = CARTESIAN_POINT ( 'NONE',  ( 0.2115152242454953757, -11.37209801155882971, 32.91403422569032955 ) ) ;
#18341 = CARTESIAN_POINT ( 'NONE',  ( -5.076923076923075762, -9.819645486525091727, 36.12317359536749706 ) ) ;
#18342 = ADVANCED_FACE ( 'NONE', ( #18289 ), #66478, .F. ) ;
#18343 = AXIS2_PLACEMENT_3D ( 'NONE', #48308, #50077, #15872 ) ;
#18344 = CARTESIAN_POINT ( 'NONE',  ( -2.084316821919886209, -2.251407671071270489, 29.88021292934942252 ) ) ;
#18345 = B_SPLINE_CURVE_WITH_KNOTS ( 'NONE', 3,
 ( #20525, #39929, #40809, #48430, #47990, #260, #61947, #40370, #34485, #27722 ),
 .UNSPECIFIED., .F., .F.,
 ( 4, 2, 2, 2, 4 ),
 ( 0.000000000000000000, 0.0001954339857564054957, 0.0003908679715128109914, 0.0005863019572692164871, 0.0007817359430256219828 ),
 .UNSPECIFIED. ) ;
#18346 = DIRECTION ( 'NONE',  ( 1.000000000000000000, 0.000000000000000000, 0.000000000000000000 ) ) ;
#18347 = EDGE_LOOP ( 'NONE', ( #63660, #73135, #26880, #83535 ) ) ;
#18348 = B_SPLINE_CURVE_WITH_KNOTS ( 'NONE', 3,
 ( #16539, #85894, #4360, #52094, #57968, #37244, #3462, #44006, #38143, #23728 ),
 .UNSPECIFIED., .F., .F.,
 ( 4, 2, 2, 2, 4 ),
 ( 0.0007817359430256315238, 0.0009771253907249976244, 0.001172514838424363508, 0.001367904286123729392, 0.001563293733823095492 ),
 .UNSPECIFIED. ) ;
#18349 = CARTESIAN_POINT ( 'NONE',  ( 17.32697738856139580, -2.779044189368097051, 31.39831045268885745 ) ) ;
#18350 = LINE ( 'NONE', #80503, #54688 ) ;
#18351 = CIRCLE ( 'NONE', #68676, 5.000000000000000888 ) ;
#18352 = CARTESIAN_POINT ( 'NONE',  ( 0.06109907496451268821, -3.749999999999999556, 20.65811829374151287 ) ) ;
#18353 = B_SPLINE_CURVE_WITH_KNOTS ( 'NONE', 3,
 ( #17442, #44897, #72372, #38150, #65608, #31396, #25082, #53434, #60636, #12460 ),
 .UNSPECIFIED., .F., .F.,
 ( 4, 2, 2, 2, 4 ),
 ( 0.0007817246256747452209, 0.0009771112852218889842, 0.001172497944769032747, 0.001367884604316176294, 0.001563271263863320057 ),
 .UNSPECIFIED. ) ;
#18354 = CARTESIAN_POINT ( 'NONE',  ( -10.68065461594093435, -2.657715359629089225, 31.77849191805832874 ) ) ;
#18355 = CARTESIAN_POINT ( 'NONE',  ( -16.21992853320628925, -10.67929555188718460, 33.92786785259543336 ) ) ;
#18356 = ORIENTED_EDGE ( 'NONE', *, *, #72984, .F. ) ;
#18357 = LINE ( 'NONE', #45817, #15497 ) ;
#18358 = LINE ( 'NONE', #72398, #7122 ) ;
#18360 = ORIENTED_EDGE ( 'NONE', *, *, #67448, .F. ) ;
#18359 = CARTESIAN_POINT ( 'NONE',  ( -23.50000000000000000, 1.674711738930281374E-15, 13.00000000000000178 ) ) ;
#18361 = CARTESIAN_POINT ( 'NONE',  ( -6.166666666666667851, -7.500000000000000000, 29.75000000000000355 ) ) ;
#18362 = CARTESIAN_POINT ( 'NONE',  ( -4.153846153846152411, -11.11383981884818262, 36.00935417666054406 ) ) ;
#18363 = FACE_OUTER_BOUND ( 'NONE', #39711, .T. ) ;
#18364 = ADVANCED_FACE ( 'NONE', ( #25491 ), #39019, .F. ) ;
#18365 = CARTESIAN_POINT ( 'NONE',  ( -11.78848476268299628, -2.588893531581426988, 31.60682220781847818 ) ) ;
#18366 = ORIENTED_EDGE ( 'NONE', *, *, #65892, .T. ) ;
#18367 = CYLINDRICAL_SURFACE ( 'NONE', #73509, 0.2499999999999997502 ) ;
#18368 = CARTESIAN_POINT ( 'NONE',  ( 10.68063975489745232, -4.320704448112861584, 33.92786785259548310 ) ) ;
#18369 = CARTESIAN_POINT ( 'NONE',  ( 9.692307692307695177, -13.63283147151868846, 33.57946703557072254 ) ) ;
#18370 = VERTEX_POINT ( 'NONE', #38563 ) ;
#18371 = ORIENTED_EDGE ( 'NONE', *, *, #22379, .F. ) ;
#18372 = ORIENTED_EDGE ( 'NONE', *, *, #73270, .F. ) ;
#18373 = EDGE_CURVE ( 'NONE', #1790, #31437, #45758, .T. ) ;
#18374 = AXIS2_PLACEMENT_3D ( 'NONE', #78011, #16315, #43781 ) ;
#18375 = CYLINDRICAL_SURFACE ( 'NONE', #51283, 0.2499999999999995559 ) ;
#18376 = CARTESIAN_POINT ( 'NONE',  ( -3.230769230769352962, -3.083524468854526912, 32.58852847137268327 ) ) ;
#18377 = EDGE_CURVE ( 'NONE', #73835, #32057, #56281, .T. ) ;
#18378 = CARTESIAN_POINT ( 'NONE',  ( -18.00000000000000000, -9.905515769479279697, 34.41647553114623292 ) ) ;
#18379 = VECTOR ( 'NONE', #76933, 1000.000000000000000 ) ;
#18380 = LINE ( 'NONE', #2625, #49219 ) ;
#18381 = ORIENTED_EDGE ( 'NONE', *, *, #31288, .F. ) ;
#18383 = EDGE_LOOP ( 'NONE', ( #11438, #75957, #72623, #27246 ) ) ;
#18382 = EDGE_CURVE ( 'NONE', #10219, #51322, #64889, .T. ) ;
#18385 = ORIENTED_EDGE ( 'NONE', *, *, #43998, .T. ) ;
#18384 = CARTESIAN_POINT ( 'NONE',  ( -1.384615384615383471, -4.786620604624113540, 33.94971097300155094 ) ) ;
#18386 = CARTESIAN_POINT ( 'NONE',  ( -5.143005456283209931, -2.486705287966279432, 31.30864560766542937 ) ) ;
#18387 = CARTESIAN_POINT ( 'NONE',  ( -3.230769230769229949, -4.661471528628507777, 34.16647553114623292 ) ) ;
#18388 = EDGE_CURVE ( 'NONE', #81411, #25475, #28360, .T. ) ;
#18389 = CARTESIAN_POINT ( 'NONE',  ( 7.846153846153846700, -2.708943851104267164, 35.45975837776705220 ) ) ;
#18390 = CARTESIAN_POINT ( 'NONE',  ( 13.60762822870878352, -10.01129605718032600, 34.36064277460058491 ) ) ;
#18391 = EDGE_CURVE ( 'NONE', #66561, #62271, #66004, .T. ) ;
#18392 = ORIENTED_EDGE ( 'NONE', *, *, #14932, .T. ) ;
#18393 = EDGE_LOOP ( 'NONE', ( #65656, #87690 ) ) ;
#18394 = ORIENTED_EDGE ( 'NONE', *, *, #79201, .F. ) ;
#18396 = ORIENTED_EDGE ( 'NONE', *, *, #40494, .T. ) ;
#18395 = CARTESIAN_POINT ( 'NONE',  ( 8.835299120233207404, -2.538708090699994813, 30.37095296980875503 ) ) ;
#18397 = CYLINDRICAL_SURFACE ( 'NONE', #8667, 0.2499999999999986955 ) ;
#18398 = VECTOR ( 'NONE', #42575, 1000.000000000000000 ) ;
#18399 = CARTESIAN_POINT ( 'NONE',  ( 12.21156173059610772, -11.28823185664190376, 33.01397839955799896 ) ) ;
#18400 = EDGE_CURVE ( 'NONE', #26040, #72902, #65107, .T. ) ;
#18401 = LINE ( 'NONE', #38666, #41704 ) ;
#18402 = DIRECTION ( 'NONE',  ( 0.000000000000000000, -1.000000000000000000, -0.000000000000000000 ) ) ;
#18403 = CYLINDRICAL_SURFACE ( 'NONE', #55456, 0.2499999999999979738 ) ;
#18404 = FACE_BOUND ( 'NONE', #27345, .T. ) ;
#18405 = CARTESIAN_POINT ( 'NONE',  ( -0.5916856709766815658, -4.460286881179644780, 33.72017969459903242 ) ) ;
#18407 = EDGE_CURVE ( 'NONE', #63342, #84095, #64881, .T. ) ;
#18406 = CARTESIAN_POINT ( 'NONE',  ( -1.134669866267240979, -11.86320923018887719, 32.19269448109604781 ) ) ;
#18408 = CARTESIAN_POINT ( 'NONE',  ( -8.992715712954719720, -4.386631170607603991, 33.66268669641500111 ) ) ;
#18410 = CARTESIAN_POINT ( 'NONE',  ( 15.29602437028207085, -10.33852847137154107, 34.16647553114620450 ) ) ;
#18409 = CARTESIAN_POINT ( 'NONE',  ( 16.37685899793955002, -4.026326845037969449, 33.68677907613345468 ) ) ;
#18411 = CARTESIAN_POINT ( 'NONE',  ( -4.403846153846151523, -7.433932668274256805, 35.00000000000000711 ) ) ;
#18412 = DIRECTION ( 'NONE',  ( 1.000000000000000000, 0.000000000000000000, 0.000000000000000000 ) ) ;
#18413 = VERTEX_POINT ( 'NONE', #10402 ) ;
#18414 = EDGE_CURVE ( 'NONE', #34255, #87211, #3188, .T. ) ;
#18415 = AXIS2_PLACEMENT_3D ( 'NONE', #15154, #28213, #55681 ) ;
#18416 = CARTESIAN_POINT ( 'NONE',  ( 11.47237812750566022, -3.050289026998445951, 32.03036669348365706 ) ) ;
#18417 = CYLINDRICAL_SURFACE ( 'NONE', #486, 0.2499999999999994726 ) ;
#18418 = VERTEX_POINT ( 'NONE', #4069 ) ;
#18419 = ORIENTED_EDGE ( 'NONE', *, *, #81201, .T. ) ;
#18421 = DIRECTION ( 'NONE',  ( 1.000000000000000000, 0.000000000000000000, 0.000000000000000000 ) ) ;
#18420 = CARTESIAN_POINT ( 'NONE',  ( 23.00000000000000000, -9.499999999999982236, 27.74999999999999645 ) ) ;
#18422 = CARTESIAN_POINT ( 'NONE',  ( 18.00000000000000000, -1.466349020453238561, 30.81389545987213907 ) ) ;
#18423 = CARTESIAN_POINT ( 'NONE',  ( 16.02369894440793630, -3.817052484675422797, 33.13202310037935661 ) ) ;
#18424 = CARTESIAN_POINT ( 'NONE',  ( -11.66915214157184622, -9.929715669179220328, 34.40415004197138416 ) ) ;
#18425 = ORIENTED_EDGE ( 'NONE', *, *, #56684, .T. ) ;
#18426 = DIRECTION ( 'NONE',  ( 0.000000000000000000, 0.000000000000000000, -1.000000000000000000 ) ) ;
#18427 = CARTESIAN_POINT ( 'NONE',  ( 4.284636594813102661, -4.684288915650984819, 34.18129842949671371 ) ) ;
#18429 = CARTESIAN_POINT ( 'NONE',  ( 16.15384615384615330, -13.87047571288749737, 32.06866353760679544 ) ) ;
#18428 = PLANE ( 'NONE',  #20231 ) ;
#18430 = CARTESIAN_POINT ( 'NONE',  ( -17.07692307692307665, -9.584722331328613620, 36.20867863119891439 ) ) ;
#18431 = CARTESIAN_POINT ( 'NONE',  ( -5.207070286361298095, -9.418419913701741919, 34.36755862841477693 ) ) ;
#18433 = CARTESIAN_POINT ( 'NONE',  ( -15.00798956179116317, -10.97394488606064122, 33.68653795673694873 ) ) ;
#18432 =( LENGTH_UNIT ( ) NAMED_UNIT ( * ) SI_UNIT ( .MILLI., .METRE. ) );
#18434 = EDGE_CURVE ( 'NONE', #73496, #15649, #31557, .T. ) ;
#18435 = CARTESIAN_POINT ( 'NONE',  ( -1.929879867024197893E-14, -3.750000000000000000, 22.90625000000000355 ) ) ;
#18436 = VERTEX_POINT ( 'NONE', #12946 ) ;
#18437 = EDGE_LOOP ( 'NONE', ( #87484, #68449, #37320, #81369 ) ) ;
#18438 = AXIS2_PLACEMENT_3D ( 'NONE', #85885, #51622, #79126 ) ;
#18439 = DIRECTION ( 'NONE',  ( 0.000000000000000000, 0.000000000000000000, 1.000000000000000000 ) ) ;
#18440 = EDGE_CURVE ( 'NONE', #28286, #58074, #454, .T. ) ;
#18441 = CARTESIAN_POINT ( 'NONE',  ( -2.307692307692305711, -6.681629849574314051, 35.83090037661290239 ) ) ;
#18442 = CARTESIAN_POINT ( 'NONE',  ( 4.377222094544336528, -2.501478030877322567, 29.88021232661720816 ) ) ;
#18443 = B_SPLINE_CURVE_WITH_KNOTS ( 'NONE', 3,
 ( #23983, #17693, #64971, #70870, #30313, #44243, #31191, #78939, #3719, #78489 ),
 .UNSPECIFIED., .F., .F.,
 ( 4, 2, 2, 2, 4 ),
 ( 0.0007817359430256215491, 0.0009771253907249856981, 0.001172514838424349847, 0.001367904286123713779, 0.001563293733823077928 ),
 .UNSPECIFIED. ) ;
#18444 = CARTESIAN_POINT ( 'NONE',  ( -16.40386939113912135, -2.823816976329320827, 31.52131813110797154 ) ) ;
#18445 = CARTESIAN_POINT ( 'NONE',  ( -0.6850233861027902327, -12.11044203135681840, 32.26167407432752299 ) ) ;
#18446 = CARTESIAN_POINT ( 'NONE',  ( -1.553300858899125059, -3.750000000000009326, 21.57812500000000355 ) ) ;
#18447 = CARTESIAN_POINT ( 'NONE',  ( 22.75000000000000000, -4.499999999999999112, 27.25000000000000000 ) ) ;
#18448 = FACE_OUTER_BOUND ( 'NONE', #2403, .T. ) ;
#18449 = AXIS2_PLACEMENT_3D ( 'NONE', #1192, #42637, #1648 ) ;
#18450 = DIRECTION ( 'NONE',  ( -0.000000000000000000, -0.5000000000000009992, -0.8660254037844380415 ) ) ;
#18451 = CARTESIAN_POINT ( 'NONE',  ( 12.23861150263161157, -11.43668979543634734, 33.22377378376089752 ) ) ;
#18452 = CARTESIAN_POINT ( 'NONE',  ( -9.758391103263569732, -11.16473453929635440, 33.15142922261925662 ) ) ;
#18453 = CARTESIAN_POINT ( 'NONE',  ( 13.38461538461538680, -4.098570777380720287, 33.41473453929634729 ) ) ;
#18454 = CARTESIAN_POINT ( 'NONE',  ( -19.50000000000000000, -3.499999999999999556, 29.75000000000000355 ) ) ;
#18455 = EDGE_CURVE ( 'NONE', #47638, #46856, #7958, .T. ) ;
#18456 = DIRECTION ( 'NONE',  ( -0.000000000000000000, 0.9396926207859092051, -0.3420201433256662704 ) ) ;
#18457 = CARTESIAN_POINT ( 'NONE',  ( -6.222926217516146608, -9.886141570436013382, 34.14413921362392301 ) ) ;
#18458 = AXIS2_PLACEMENT_3D ( 'NONE', #52357, #53696, #81184 ) ;
#18459 = CARTESIAN_POINT ( 'NONE',  ( -15.29603967673000575, -8.613356846314824011, 34.62446782046655613 ) ) ;
#18460 = ORIENTED_EDGE ( 'NONE', *, *, #84199, .T. ) ;
#18461 = CARTESIAN_POINT ( 'NONE',  ( 8.834485908743605620, -5.094484230520773593, 34.41647553114626845 ) ) ;
#18462 = ADVANCED_FACE ( 'NONE', ( #19705 ), #51802, .F. ) ;
#18463 = DIRECTION ( 'NONE',  ( 0.000000000000000000, 0.000000000000000000, -1.000000000000000000 ) ) ;
#18464 = CARTESIAN_POINT ( 'NONE',  ( 5.076923076923075762, -2.721908614388771852, 31.22303859784724978 ) ) ;
#18465 = CARTESIAN_POINT ( 'NONE',  ( 1.200186371490529202, -4.775308065498752974, 18.23624329374151642 ) ) ;
#18466 = EDGE_CURVE ( 'NONE', #59616, #19865, #46490, .T. ) ;
#18467 = CARTESIAN_POINT ( 'NONE',  ( 0.3313904918067658856, -5.915902021225892149, 34.75552854090298638 ) ) ;
#18468 = CARTESIAN_POINT ( 'NONE',  ( 14.24160992833217065, -4.661471528628507777, 34.16647553114621871 ) ) ;
#18470 = ORIENTED_EDGE ( 'NONE', *, *, #56793, .T. ) ;
#18469 = CARTESIAN_POINT ( 'NONE',  ( -17.99999999841483955, -2.249999999999995115, 29.50000000010503953 ) ) ;
#18471 = CARTESIAN_POINT ( 'NONE',  ( -1.139087296525992388, -10.25000000000000711, 17.35937499999999645 ) ) ;
#18472 = CARTESIAN_POINT ( 'NONE',  ( 17.93472955403921887, -3.835265460703609186, 33.15142922261924241 ) ) ;
#18473 = ORIENTED_EDGE ( 'NONE', *, *, #7328, .T. ) ;
#18474 = EDGE_CURVE ( 'NONE', #83657, #9985, #24049, .T. ) ;
#18475 = CARTESIAN_POINT ( 'NONE',  ( -6.000000000000121680, -11.67786785259630911, 32.92929555188603530 ) ) ;
#18476 = ORIENTED_EDGE ( 'NONE', *, *, #12287, .F. ) ;
#18477 = CARTESIAN_POINT ( 'NONE',  ( 3.230769230769231726, -4.661471528628507777, 34.16647553114623292 ) ) ;
#18478 = CARTESIAN_POINT ( 'NONE',  ( -15.48079245499068435, -2.985938066672154445, 32.43141759479405550 ) ) ;
#18479 = DIRECTION ( 'NONE',  ( -0.000000000000000000, 1.000000000000000000, 3.491481338843133355E-15 ) ) ;
#18480 = ORIENTED_EDGE ( 'NONE', *, *, #19694, .T. ) ;
#18481 = CYLINDRICAL_SURFACE ( 'NONE', #19161, 0.2500000000000009437 ) ;
#18482 = EDGE_LOOP ( 'NONE', ( #52711, #64929 ) ) ;
#18483 = CARTESIAN_POINT ( 'NONE',  ( 13.16174912155229038, -2.251424796025574881, 29.88072029997477586 ) ) ;
#18484 = B_SPLINE_CURVE_WITH_KNOTS ( 'NONE', 3,
 ( #49173, #37423, #55928, #76653, #83867, #22153, #2303, #57263, #30669, #44614 ),
 .UNSPECIFIED., .F., .F.,
 ( 4, 2, 2, 2, 4 ),
 ( 0.0007817359430256303312, 0.0009771253907249965402, 0.001172514838424362641, 0.001367904286123728958, 0.001563293733823095059 ),
 .UNSPECIFIED. ) ;
#18485 = VECTOR ( 'NONE', #8230, 1000.000000000000000 ) ;
#18486 = ORIENTED_EDGE ( 'NONE', *, *, #76117, .F. ) ;
#18487 = CARTESIAN_POINT ( 'NONE',  ( -0.5268089074992375886, -3.300289026998414865, 32.46337939537583139 ) ) ;
#18488 = DIRECTION ( 'NONE',  ( 0.000000000000000000, 0.3420201433256610524, 0.9396926207859113145 ) ) ;
#18489 = B_SPLINE_CURVE_WITH_KNOTS ( 'NONE', 3,
 ( #24744, #85562, #79251, #77911, #79697, #23835, #43681, #51290, #58512, #44110 ),
 .UNSPECIFIED., .F., .F.,
 ( 4, 2, 2, 2, 4 ),
 ( 0.0007817359430256364027, 0.0009771253907250043464, 0.001172514838424372399, 0.001367904286123740234, 0.001563293733823108286 ),
 .UNSPECIFIED. ) ;
#18490 = CARTESIAN_POINT ( 'NONE',  ( -10.36543909703647159, -6.696923467548660192, 34.68552623307873972 ) ) ;
#18491 = DIRECTION ( 'NONE',  ( -0.000000000000000000, 1.000000000000000000, 3.491481338843133355E-15 ) ) ;
#18493 = ADVANCED_FACE ( 'NONE', ( #76867 ), #41756, .F. ) ;
#18492 = CARTESIAN_POINT ( 'NONE',  ( 15.16468581981335184, -6.386643153685125363, 34.62446782046654903 ) ) ;
#18494 = CARTESIAN_POINT ( 'NONE',  ( 12.52760681254089903, -4.786620604624113540, 33.94971097300155805 ) ) ;
#18495 = CARTESIAN_POINT ( 'NONE',  ( 5.011652630962299959, -9.442884908240170461, 34.35708131394840592 ) ) ;
#18496 = ORIENTED_EDGE ( 'NONE', *, *, #75516, .F. ) ;
#18497 = VERTEX_POINT ( 'NONE', #56145 ) ;
#18498 = VERTEX_POINT ( 'NONE', #757 ) ;
#18500 = VERTEX_POINT ( 'NONE', #42201 ) ;
#18499 = CARTESIAN_POINT ( 'NONE',  ( -14.30769230769230660, -8.120952969808772792, 34.71129190930000163 ) ) ;
#18501 = VECTOR ( 'NONE', #29313, 1000.000000000000000 ) ;
#18502 = FACE_OUTER_BOUND ( 'NONE', #13684, .T. ) ;
#18503 = CARTESIAN_POINT ( 'NONE',  ( 1.607626736228234599, -2.758310577978207334, 31.33698337089302299 ) ) ;
#18504 = VERTEX_POINT ( 'NONE', #61566 ) ;
#18505 = CARTESIAN_POINT ( 'NONE',  ( -14.05763799605399278, -4.235687564193447052, 33.53795663066793509 ) ) ;
#18506 = ORIENTED_EDGE ( 'NONE', *, *, #32487, .T. ) ;
#18507 = CARTESIAN_POINT ( 'NONE',  ( 16.82694634598072270, -9.943427161483782584, 34.11278801902876978 ) ) ;
#18508 = ORIENTED_EDGE ( 'NONE', *, *, #69513, .T. ) ;
#18509 = VECTOR ( 'NONE', #51527, 1000.000000000000227 ) ;
#18510 = DIRECTION ( 'NONE',  ( -0.000000000000000000, 1.000000000000000000, -0.000000000000000000 ) ) ;
#18511 = ADVANCED_FACE ( 'NONE', ( #27785 ), #14273, .F. ) ;
#18512 = FACE_OUTER_BOUND ( 'NONE', #75826, .T. ) ;
#18513 = CARTESIAN_POINT ( 'NONE',  ( 0.2380535178145123110, -5.113361153441934093, 34.14387501736622710 ) ) ;
#18514 = FACE_BOUND ( 'NONE', #86907, .T. ) ;
#18515 = B_SPLINE_CURVE_WITH_KNOTS ( 'NONE', 3,
 ( #39717, #59522, #33396, #5028, #20321, #13119, #13556, #32494, #80251, #25299 ),
 .UNSPECIFIED., .F., .F.,
 ( 4, 2, 2, 2, 4 ),
 ( 0.000000000000000000, 0.0001954311564186877960, 0.0003908623128373755920, 0.0005862934692560633609, 0.0007817246256747511840 ),
 .UNSPECIFIED. ) ;
#18516 = FACE_OUTER_BOUND ( 'NONE', #48200, .T. ) ;
#18518 = EDGE_CURVE ( 'NONE', #88116, #36558, #28224, .T. ) ;
#18517 = FACE_OUTER_BOUND ( 'NONE', #34226, .T. ) ;
#18519 = CARTESIAN_POINT ( 'NONE',  ( -24.00000000000000000, -9.499999999999982236, 27.74999999999999645 ) ) ;
#18520 = CARTESIAN_POINT ( 'NONE',  ( -10.61538461538461320, -6.435427911321262684, 35.78748833219616898 ) ) ;
#18521 = LINE ( 'NONE', #18963, #39449 ) ;
#18522 = CARTESIAN_POINT ( 'NONE',  ( 17.07692307692295586, -9.442884908241554243, 34.35708131394783038 ) ) ;
#18523 = ORIENTED_EDGE ( 'NONE', *, *, #44810, .F. ) ;
#18524 = ADVANCED_FACE ( 'NONE', ( #42640 ), #69218, .F. ) ;
#18525 = CARTESIAN_POINT ( 'NONE',  ( -11.76194646302586655, -3.562934362175800285, 33.22335522853832401 ) ) ;
#18526 = ORIENTED_EDGE ( 'NONE', *, *, #82740, .T. ) ;
#18527 = EDGE_LOOP ( 'NONE', ( #10385, #72015, #18366, #30599 ) ) ;
#18529 = CARTESIAN_POINT ( 'NONE',  ( -14.08468095607945969, -12.39991518177334129, 30.74647679643404530 ) ) ;
#18528 = DIRECTION ( 'NONE',  ( 0.000000000000000000, 0.8660254037844377084, -0.5000000000000015543 ) ) ;
#18530 = EDGE_CURVE ( 'NONE', #22067, #22580, #49391, .T. ) ;
#18531 = DIRECTION ( 'NONE',  ( 0.000000000000000000, 0.4999999999999985567, 0.8660254037844395958 ) ) ;
#18532 = LINE ( 'NONE', #57732, #63829 ) ;
#18533 = CARTESIAN_POINT ( 'NONE',  ( 7.623227628637698317, -12.39988816332205701, 30.74660775122750778 ) ) ;
#18534 = DIRECTION ( 'NONE',  ( -0.000000000000000000, 0.5000000000000011102, -0.8660254037844380415 ) ) ;
#18535 = ORIENTED_EDGE ( 'NONE', *, *, #3573, .F. ) ;
#18536 = CARTESIAN_POINT ( 'NONE',  ( 0.6089743589743582541, -3.499999999999999556, 29.75000000000000355 ) ) ;
#18537 = CARTESIAN_POINT ( 'NONE',  ( -4.826868765284761942, -2.564540009722896752, 30.55348353981670684 ) ) ;
#18538 = CARTESIAN_POINT ( 'NONE',  ( -14.37377571864818293, -8.120952969808774569, 34.71129190930000163 ) ) ;
#18539 = CARTESIAN_POINT ( 'NONE',  ( 13.38461538461538680, -12.37446782046654192, 30.86335684631486131 ) ) ;
#18540 = ORIENTED_EDGE ( 'NONE', *, *, #7308, .T. ) ;
#18541 = EDGE_CURVE ( 'NONE', #18197, #64611, #68773, .T. ) ;
#18542 = CIRCLE ( 'NONE', #38652, 0.2500000000000002220 ) ;
#18543 = EDGE_LOOP ( 'NONE', ( #70576, #74032, #30881, #71271 ) ) ;
#18544 = APPLICATION_PROTOCOL_DEFINITION ( 'draft international standard', 'automotive_design', 1998, #71649 ) ;
#18545 = VERTEX_POINT ( 'NONE', #48941 ) ;
#18546 = CARTESIAN_POINT ( 'NONE',  ( 16.15384615384603251, -6.026961402154118908, 34.52809138561165270 ) ) ;
#18547 = CARTESIAN_POINT ( 'NONE',  ( -1.384615384615506484, -2.379036618888197285, 30.90682066428292885 ) ) ;
#18548 = ORIENTED_EDGE ( 'NONE', *, *, #40990, .T. ) ;
#18549 = CARTESIAN_POINT ( 'NONE',  ( -16.08777780284371772, -4.786620604624113540, 33.94971097300155805 ) ) ;
#18550 = CARTESIAN_POINT ( 'NONE',  ( -6.065270000556318486, -9.528491918058357157, 34.59228464037090589 ) ) ;
#18551 = CARTESIAN_POINT ( 'NONE',  ( -8.069080063669991532, -11.76352882383564769, 32.36236540154569497 ) ) ;
#18552 = CARTESIAN_POINT ( 'NONE',  ( 14.43853072570506946, -7.277220443632450575, 34.74524770363009196 ) ) ;
#18553 = CARTESIAN_POINT ( 'NONE',  ( -11.31568199719312773, -9.332535724633409302, 34.40230450496446934 ) ) ;
#18554 = ORIENTED_EDGE ( 'NONE', *, *, #31098, .T. ) ;
#18556 = EDGE_LOOP ( 'NONE', ( #17726, #80518, #48651, #20684 ) ) ;
#18555 = CARTESIAN_POINT ( 'NONE',  ( -15.29685161012936945, -11.91647553114624181, 32.58852847137148245 ) ) ;
#18557 = CARTESIAN_POINT ( 'NONE',  ( 15.48071474911737333, -8.433404298154334455, 34.66254593164985920 ) ) ;
#18558 = CARTESIAN_POINT ( 'NONE',  ( -3.007756386675835003, -2.523321265292116422, 31.42251411153756990 ) ) ;
#18559 = CARTESIAN_POINT ( 'NONE',  ( -13.63459211555773720, -4.943428324936578910, 34.04746400365624481 ) ) ;
#18560 = DIRECTION ( 'NONE',  ( 0.000000000000000000, 0.000000000000000000, 1.000000000000000000 ) ) ;
#18561 = CARTESIAN_POINT ( 'NONE',  ( -8.546451100252699717, -8.540255544307065350, 34.89611431652622286 ) ) ;
#18562 =( NAMED_UNIT ( * ) SI_UNIT ( $, .STERADIAN. ) SOLID_ANGLE_UNIT ( ) );
#18563 = CARTESIAN_POINT ( 'NONE',  ( 2.307692307692186251, -2.657715359629662544, 31.77849191805970364 ) ) ;
#18564 = CARTESIAN_POINT ( 'NONE',  ( 1.200186371490529202, -4.775308065498752974, 14.48624329374151465 ) ) ;
#18565 = EDGE_LOOP ( 'NONE', ( #44308, #55909 ) ) ;
#18566 = EDGE_CURVE ( 'NONE', #43445, #68660, #21472, .T. ) ;
#18567 = CARTESIAN_POINT ( 'NONE',  ( 5.076923076922953193, -12.16647553114689728, 32.15551576947799362 ) ) ;
#18568 = CARTESIAN_POINT ( 'NONE',  ( -9.627052121031665521, -8.613356846314928816, 34.62446782046653482 ) ) ;
#18569 = DIRECTION ( 'NONE',  ( -0.000000000000000000, 1.000000000000000000, 3.491481338843133355E-15 ) ) ;
#18570 = AXIS2_PLACEMENT_3D ( 'NONE', #52819, #65886, #10958 ) ;
#18571 = ORIENTED_EDGE ( 'NONE', *, *, #79521, .T. ) ;
#18572 = ORIENTED_EDGE ( 'NONE', *, *, #25655, .F. ) ;
#18573 = CARTESIAN_POINT ( 'NONE',  ( -8.899378738962466784, -5.915902021225889484, 34.75552854090298638 ) ) ;
#18574 = CARTESIAN_POINT ( 'NONE',  ( -7.780086512803769949, -5.471508081941601098, 34.59228464037088457 ) ) ;
#18575 = CARTESIAN_POINT ( 'NONE',  ( -0.5268084620947812713, -9.528491918058357157, 34.59228464037090589 ) ) ;
#18576 = VECTOR ( 'NONE', #88214, 1000.000000000000000 ) ;
#18577 = CARTESIAN_POINT ( 'NONE',  ( -20.99999999999999289, -7.500000000000000000, 29.75000000000000355 ) ) ;
#18578 = EDGE_CURVE ( 'NONE', #26148, #48943, #14723, .T. ) ;
#18579 = CARTESIAN_POINT ( 'NONE',  ( -15.48076923076922995, -7.500000000000001776, 35.00000000000000000 ) ) ;
#18580 = AXIS2_PLACEMENT_3D ( 'NONE', #78252, #57984, #29642 ) ;
#18581 = LINE ( 'NONE', #72622, #16363 ) ;
#18582 = EDGE_LOOP ( 'NONE', ( #69344, #44033, #11028, #60832 ) ) ;
#18583 = DIRECTION ( 'NONE',  ( -1.000000000000000000, -0.000000000000000000, 0.000000000000000000 ) ) ;
#18584 = EDGE_CURVE ( 'NONE', #52830, #26637, #61540, .T. ) ;
#18585 = CARTESIAN_POINT ( 'NONE',  ( -6.249999999999996447, -7.566083408709834757, 34.74999999999999289 ) ) ;
#18586 = DIRECTION ( 'NONE',  ( 0.000000000000000000, 0.3420201433256641055, -0.9396926207859100932 ) ) ;
#18587 = ORIENTED_EDGE ( 'NONE', *, *, #78682, .T. ) ;
#18588 = CARTESIAN_POINT ( 'NONE',  ( 16.15384615384603251, -12.51329471203414379, 31.30864560766407578 ) ) ;
#18589 = VERTEX_POINT ( 'NONE', #68334 ) ;
#18590 = CARTESIAN_POINT ( 'NONE',  ( -0.2115929431903180169, -2.824170634883619524, 31.52227843825337317 ) ) ;
#18591 = SURFACE_STYLE_FILL_AREA ( #23995 ) ;
#18592 = CARTESIAN_POINT ( 'NONE',  ( 10.55011461482829738, -3.643525952247789412, 33.31231777344662959 ) ) ;
#18593 = DIRECTION ( 'NONE',  ( -1.000000000000000000, 0.000000000000000000, 0.000000000000000000 ) ) ;
#18594 = ORIENTED_EDGE ( 'NONE', *, *, #80536, .T. ) ;
#18595 = CARTESIAN_POINT ( 'NONE',  ( 0.7115927731767753839, -4.235687564193446164, 33.53795663066793509 ) ) ;
#18597 = EDGE_CURVE ( 'NONE', #4430, #44526, #27348, .T. ) ;
#18596 = CARTESIAN_POINT ( 'NONE',  ( 13.45068271796546178, -9.058645607665452459, 34.76329471203371924 ) ) ;
#18598 = CARTESIAN_POINT ( 'NONE',  ( -9.915233909823841785, -2.554751324335734708, 30.48935550225260727 ) ) ;
#18599 = CARTESIAN_POINT ( 'NONE',  ( 24.00000000000000000, -9.499999999999982236, 27.74999999999999645 ) ) ;
#18600 = DIRECTION ( 'NONE',  ( 0.000000000000000000, 0.3420201433256610524, 0.9396926207859113145 ) ) ;
#18601 = EDGE_CURVE ( 'NONE', #3366, #21486, #26139, .T. ) ;
#18602 = EDGE_CURVE ( 'NONE', #54354, #67169, #63776, .T. ) ;
#18603 = VERTEX_POINT ( 'NONE', #44834 ) ;
#18604 = CYLINDRICAL_SURFACE ( 'NONE', #51525, 0.2500000000000002220 ) ;
#18605 = ORIENTED_EDGE ( 'NONE', *, *, #18862, .F. ) ;
#18606 = CARTESIAN_POINT ( 'NONE',  ( -15.00775638667583678, -6.460100341425560444, 34.89618726649961644 ) ) ;
#18607 = CIRCLE ( 'NONE', #60250, 4.000000000000000000 ) ;
#18608 = EDGE_CURVE ( 'NONE', #54359, #5224, #83089, .T. ) ;
#18609 = CARTESIAN_POINT ( 'NONE',  ( -12.23852561744506851, -2.889357225399414197, 32.26129605718031002 ) ) ;
#18610 = CARTESIAN_POINT ( 'NONE',  ( -0.2114840416250075017, -2.544122305571458575, 31.48381861865057729 ) ) ;
#18611 = DIRECTION ( 'NONE',  ( 1.000000000000000000, 0.000000000000000000, 0.000000000000000000 ) ) ;
#18612 = CARTESIAN_POINT ( 'NONE',  ( -6.700065571464073777, -5.667800583137508674, 34.40243808032445827 ) ) ;
#18613 = CARTESIAN_POINT ( 'NONE',  ( -6.065270445960775803, -4.481592998940161721, 33.73612834413957984 ) ) ;
#18614 = CARTESIAN_POINT ( 'NONE',  ( -6.792286482109971324, -2.494656445102013453, 31.33466734024120015 ) ) ;
#18615 = ORIENTED_EDGE ( 'NONE', *, *, #17407, .F. ) ;
#18616 = VERTEX_POINT ( 'NONE', #57021 ) ;
#18617 = VERTEX_POINT ( 'NONE', #10178 ) ;
#18618 = ORIENTED_EDGE ( 'NONE', *, *, #33220, .T. ) ;
#18619 = ORIENTED_EDGE ( 'NONE', *, *, #38778, .F. ) ;
#18620 = CARTESIAN_POINT ( 'NONE',  ( -5.300408001487407539, -4.225889041578354544, 33.85425143139329407 ) ) ;
#18621 = LINE ( 'NONE', #24470, #51697 ) ;
#18622 = CARTESIAN_POINT ( 'NONE',  ( -3.903791842207837259, -9.148310452688871663, 34.47095581063188519 ) ) ;
#18623 = CARTESIAN_POINT ( 'NONE',  ( 24.00000000000000000, -5.499999999999981348, 27.25000000000000000 ) ) ;
#18624 = CARTESIAN_POINT ( 'NONE',  ( -13.19230769230769162, -7.500000000000000000, 29.75000000000000355 ) ) ;
#18625 = EDGE_CURVE ( 'NONE', #34790, #34216, #84080, .T. ) ;
#18626 = CARTESIAN_POINT ( 'NONE',  ( -12.46153846153858424, -12.51329471203414379, 31.30864560766407578 ) ) ;
#18627 = AXIS2_PLACEMENT_3D ( 'NONE', #20411, #80457, #12000 ) ;
#18628 = CARTESIAN_POINT ( 'NONE',  ( -5.207070286361298095, -8.587444163452046197, 34.63053765926554206 ) ) ;
#18629 = CARTESIAN_POINT ( 'NONE',  ( -4.023320452082588261, -10.88167719472716399, 33.43325721877153711 ) ) ;
#18630 = DIRECTION ( 'NONE',  ( 1.000000000000000000, 0.000000000000000000, 0.000000000000000000 ) ) ;
#18631 = ORIENTED_EDGE ( 'NONE', *, *, #3053, .T. ) ;
#18632 = VERTEX_POINT ( 'NONE', #49824 ) ;
#18633 = CIRCLE ( 'NONE', #30125, 4.000000000000000000 ) ;
#18634 = VERTEX_POINT ( 'NONE', #77300 ) ;
#18635 = AXIS2_PLACEMENT_3D ( 'NONE', #59605, #78989, #17291 ) ;
#18637 = ORIENTED_EDGE ( 'NONE', *, *, #35053, .T. ) ;
#18636 = CARTESIAN_POINT ( 'NONE',  ( -1.449885830576158607, -11.48612834413959582, 32.76840700105983473 ) ) ;
#18639 = DIRECTION ( 'NONE',  ( -0.000000000000000000, -0.5000000000000009992, -0.8660254037844380415 ) ) ;
#18638 = CARTESIAN_POINT ( 'NONE',  ( 14.30769230769231015, -1.422936976036506707, 30.56769352161908415 ) ) ;
#18640 = EDGE_CURVE ( 'NONE', #40157, #70140, #18649, .T. ) ;
#18641 = VECTOR ( 'NONE', #17687, 1000.000000000000114 ) ;
#18642 = DIRECTION ( 'NONE',  ( 1.000000000000000000, 0.000000000000000000, 0.000000000000000000 ) ) ;
#18643 = CARTESIAN_POINT ( 'NONE',  ( -11.28840711854808632, -9.233818618650603938, 34.70587769442853698 ) ) ;
#18644 = FACE_BOUND ( 'NONE', #36870, .T. ) ;
#18645 = EDGE_LOOP ( 'NONE', ( #38326, #38369 ) ) ;
#18646 = ORIENTED_EDGE ( 'NONE', *, *, #84038, .T. ) ;
#18647 = EDGE_CURVE ( 'NONE', #56507, #58928, #71268, .T. ) ;
#18649 = B_SPLINE_CURVE_WITH_KNOTS ( 'NONE', 3,
 ( #78186, #71868, #84517, #24121, #43075, #8855, #43953, #22790, #37193, #36326 ),
 .UNSPECIFIED., .F., .F.,
 ( 4, 2, 2, 2, 4 ),
 ( 0.0007817359430256370532, 0.0009771253907250049969, 0.001172514838424372832, 0.001367904286123740668, 0.001563293733823108503 ),
 .UNSPECIFIED. ) ;
#18648 = CARTESIAN_POINT ( 'NONE',  ( -4.946131269098287930, -6.413143153341454017, 34.63066358083362672 ) ) ;
#18650 = ORIENTED_EDGE ( 'NONE', *, *, #29186, .F. ) ;
#18651 = FACE_BOUND ( 'NONE', #20933, .T. ) ;
#18652 = B_SPLINE_CURVE_WITH_KNOTS ( 'NONE', 3,
 ( #46606, #12814, #52902, #12379, #18698, #39856, #73650, #39420, #67322, #40300 ),
 .UNSPECIFIED., .F., .F.,
 ( 4, 2, 2, 2, 4 ),
 ( 0.000000000000000000, 0.0001954311564186861697, 0.0003908623128373723394, 0.0005862934692560584820, 0.0007817246256747446788 ),
 .UNSPECIFIED. ) ;
#18653 = LINE ( 'NONE', #59620, #76335 ) ;
#18654 = LINE ( 'NONE', #18202, #43428 ) ;
#18655 = VERTEX_POINT ( 'NONE', #43515 ) ;
#18656 = CARTESIAN_POINT ( 'NONE',  ( 17.74997676270703550, -2.823816976329320827, 31.52131813110797154 ) ) ;
#18657 = CARTESIAN_POINT ( 'NONE',  ( -20.00000000000000000, -3.499999999999999556, 28.25000000000000000 ) ) ;
#18658 = CARTESIAN_POINT ( 'NONE',  ( 1.384615384615264011, -3.643525952248795718, 33.31231777344771672 ) ) ;
#18659 = EDGE_LOOP ( 'NONE', ( #36150, #38320, #85864, #19305 ) ) ;
#18660 = DIRECTION ( 'NONE',  ( -0.000000000000000000, -0.9848077530122085754, -0.1736481776669273613 ) ) ;
#18661 = CARTESIAN_POINT ( 'NONE',  ( -18.13069146666755671, -4.809359713505812373, 33.96456829005828837 ) ) ;
#18662 = FACE_OUTER_BOUND ( 'NONE', #27264, .T. ) ;
#18663 = ORIENTED_EDGE ( 'NONE', *, *, #47639, .T. ) ;
#18664 = ADVANCED_FACE ( 'NONE', ( #70990 ), #2514, .F. ) ;
#18665 = CARTESIAN_POINT ( 'NONE',  ( -1.634592115557737646, -5.728515186090277211, 34.42611988154120439 ) ) ;
#18666 = CARTESIAN_POINT ( 'NONE',  ( -16.85391172531022974, -11.76359900205217457, 32.36225158514719880 ) ) ;
#18667 = ORIENTED_EDGE ( 'NONE', *, *, #64760, .F. ) ;
#18668 = CARTESIAN_POINT ( 'NONE',  ( -12.46153846153858424, -5.941354392335915335, 34.76329471203413846 ) ) ;
#18669 = CARTESIAN_POINT ( 'NONE',  ( -12.21159294319032185, -2.587454068350147018, 30.68340429815432202 ) ) ;
#18670 = DIRECTION ( 'NONE',  ( -0.000000000000000000, 1.000000000000000000, -0.000000000000000000 ) ) ;
#18671 = CARTESIAN_POINT ( 'NONE',  ( 15.10007862765892739, -12.62707690430377383, 30.88035979386743435 ) ) ;
#18672 = CARTESIAN_POINT ( 'NONE',  ( -7.173076923076922462, -7.433932668274256805, 35.00000000000000711 ) ) ;
#18673 = CARTESIAN_POINT ( 'NONE',  ( 6.792385456409367528, -8.999036380462719364, 34.52022231692819076 ) ) ;
#18675 = DIRECTION ( 'NONE',  ( -0.000000000000000000, -0.000000000000000000, -1.000000000000000000 ) ) ;
#18674 = FACE_OUTER_BOUND ( 'NONE', #2074, .T. ) ;
#18676 = CARTESIAN_POINT ( 'NONE',  ( -3.361460697436789768, -2.541943142973489778, 30.39792223712631980 ) ) ;
#18677 = CARTESIAN_POINT ( 'NONE',  ( -14.87820512820512953, -3.499999999999999556, 29.75000000000000355 ) ) ;
#18678 = CARTESIAN_POINT ( 'NONE',  ( -1.944543648262992530, -9.444543648263016067, 16.18750000000000000 ) ) ;
#18679 = ORIENTED_EDGE ( 'NONE', *, *, #43900, .F. ) ;
#18680 = EDGE_CURVE ( 'NONE', #52311, #4149, #64658, .T. ) ;
#18681 = CARTESIAN_POINT ( 'NONE',  ( 18.00000000000000000, -4.098570777380720287, 33.41473453929634729 ) ) ;
#18682 = ORIENTED_EDGE ( 'NONE', *, *, #62994, .F. ) ;
#18683 = VERTEX_POINT ( 'NONE', #31787 ) ;
#18684 = EDGE_CURVE ( 'NONE', #88590, #19138, #66455, .T. ) ;
#18685 = CARTESIAN_POINT ( 'NONE',  ( -16.94613263595612551, -3.957578996910245284, 33.62503395064540257 ) ) ;
#18686 = ORIENTED_EDGE ( 'NONE', *, *, #86622, .F. ) ;
#18687 = CARTESIAN_POINT ( 'NONE',  ( 3.480823542407546434, -9.943054286541407549, 34.11300777759954883 ) ) ;
#18688 = CARTESIAN_POINT ( 'NONE',  ( -2.750000000000007105, -6.360912703474006946, 15.17187500000000000 ) ) ;
#18689 = CARTESIAN_POINT ( 'NONE',  ( -13.38461538461538325, -5.471508081941601098, 34.59228464037088457 ) ) ;
#18690 = CARTESIAN_POINT ( 'NONE',  ( -18.13014796973169851, -12.15440758774515650, 32.17923288041532004 ) ) ;
#18691 = CARTESIAN_POINT ( 'NONE',  ( -7.715628144390279886, -6.001044277235009439, 34.52024696741798948 ) ) ;
#18692 = CARTESIAN_POINT ( 'NONE',  ( 9.915087361285756629, -3.020022701398814569, 32.48759521482552515 ) ) ;
#18693 = CARTESIAN_POINT ( 'NONE',  ( -4.854143407945009869, -2.612705202774697533, 31.66806509827799943 ) ) ;
#18694 = CARTESIAN_POINT ( 'NONE',  ( 0.6843181305165266792, -5.827830569534416583, 34.72679350104403539 ) ) ;
#18695 = CARTESIAN_POINT ( 'NONE',  ( 0.6843181305165249029, -2.612705202774697533, 31.66806509827799943 ) ) ;
#18696 = CARTESIAN_POINT ( 'NONE',  ( -2.651650429449565305, -4.848349570550461785, 19.00000000000000000 ) ) ;
#18697 = CARTESIAN_POINT ( 'NONE',  ( 2.057692307692309708, -2.249999999999998668, 29.75000000000000355 ) ) ;
#18698 = CARTESIAN_POINT ( 'NONE',  ( -4.403822897894742461, -12.01397095200673881, 32.43157075238190146 ) ) ;
#18699 = EDGE_CURVE ( 'NONE', #61882, #70729, #3853, .T. ) ;
#18700 = B_SPLINE_CURVE_WITH_KNOTS ( 'NONE', 3,
 ( #70878, #57353, #9184, #36643, #84845, #85277, #64533, #2834, #23560, #78500 ),
 .UNSPECIFIED., .F., .F.,
 ( 4, 2, 2, 2, 4 ),
 ( 0.0007817246256747517261, 0.0009771112852218961399, 0.001172497944769040771, 0.001367884604316185401, 0.001563271263863329815 ),
 .UNSPECIFIED. ) ;
#18701 = DIRECTION ( 'NONE',  ( -0.000000000000000000, -0.6427876096865404731, -0.7660444431189771253 ) ) ;
#18702 = AXIS2_PLACEMENT_3D ( 'NONE', #59643, #4256, #79921 ) ;
#18703 = ORIENTED_EDGE ( 'NONE', *, *, #70642, .F. ) ;
#18704 = ORIENTED_EDGE ( 'NONE', *, *, #37296, .F. ) ;
#18705 = CARTESIAN_POINT ( 'NONE',  ( -8.769230769230890843, -12.46129190930018460, 30.37095296980731973 ) ) ;
#18706 = DIRECTION ( 'NONE',  ( -0.000000000000000000, -0.8660254037844397068, -0.4999999999999978906 ) ) ;
#18707 = CARTESIAN_POINT ( 'NONE',  ( 1.134592160393928406, -10.92453946501458439, 33.72985991061850086 ) ) ;
#18708 = CARTESIAN_POINT ( 'NONE',  ( -6.249976730942354841, -3.627789207965226748, 32.91389620160131102 ) ) ;
#18709 = AXIS2_PLACEMENT_3D ( 'NONE', #63965, #56773, #22549 ) ;
#18711 = EDGE_CURVE ( 'NONE', #39142, #3390, #25019, .T. ) ;
#18710 = FACE_OUTER_BOUND ( 'NONE', #1671, .T. ) ;
#18712 = AXIS2_PLACEMENT_3D ( 'NONE', #82217, #81775, #20940 ) ;
#18713 = CARTESIAN_POINT ( 'NONE',  ( -0.5916856709766818989, -6.852621066184267029, 34.70813303252209181 ) ) ;
#18714 = EDGE_CURVE ( 'NONE', #39878, #84116, #60886, .T. ) ;
#18715 = EDGE_CURVE ( 'NONE', #19020, #34521, #79969, .T. ) ;
#18716 = ORIENTED_EDGE ( 'NONE', *, *, #75834, .T. ) ;
#18717 = CARTESIAN_POINT ( 'NONE',  ( -12.46153846153846168, -3.886160181151819604, 36.00935417666054406 ) ) ;
#18718 = ORIENTED_EDGE ( 'NONE', *, *, #36252, .F. ) ;
#18719 = VERTEX_POINT ( 'NONE', #53378 ) ;
#18720 = CARTESIAN_POINT ( 'NONE',  ( 17.75002326905764960, -3.137211980971220893, 32.19342716148376837 ) ) ;
#18721 = CARTESIAN_POINT ( 'NONE',  ( -14.05774689831426372, -6.653508905675592722, 34.93172785388651391 ) ) ;
#18722 = DIRECTION ( 'NONE',  ( -0.000000000000000000, -0.000000000000000000, -1.000000000000000000 ) ) ;
#18723 = CARTESIAN_POINT ( 'NONE',  ( 1.384615384615264011, -11.67786785259630911, 32.92929555188603530 ) ) ;
#18724 = CARTESIAN_POINT ( 'NONE',  ( 5.933916589044122780, -2.721908614388772740, 31.22303859784724622 ) ) ;
#18725 = VERTEX_POINT ( 'NONE', #24571 ) ;
#18726 = VERTEX_POINT ( 'NONE', #60131 ) ;
#18727 = B_SPLINE_CURVE_WITH_KNOTS ( 'NONE', 3,
 ( #22060, #15307, #42783, #30142, #16614, #79663, #44520, #85091, #3098, #38225 ),
 .UNSPECIFIED., .F., .F.,
 ( 4, 2, 2, 2, 4 ),
 ( 0.0007817246256747472808, 0.0009771112852218907189, 0.001172497944769034265, 0.001367884604316177595, 0.001563271263863321141 ),
 .UNSPECIFIED. ) ;
#18728 = EDGE_LOOP ( 'NONE', ( #30677, #47952 ) ) ;
#18729 = CARTESIAN_POINT ( 'NONE',  ( -6.130690603110308778, -4.684245665217972032, 34.18127051446801090 ) ) ;
#18730 = CARTESIAN_POINT ( 'NONE',  ( -14.87820512820512953, -3.499999999999999556, 29.75000000000000355 ) ) ;
#18731 = AXIS2_PLACEMENT_3D ( 'NONE', #4589, #39721, #59526 ) ;
#18732 = CARTESIAN_POINT ( 'NONE',  ( 9.019285189144223835, -5.642605341092957971, 34.66089969410670335 ) ) ;
#18733 = CARTESIAN_POINT ( 'NONE',  ( -8.769230769230768274, -2.292212530054420494, 30.41441678777542634 ) ) ;
#18734 = FACE_OUTER_BOUND ( 'NONE', #68411, .T. ) ;
#18735 = ORIENTED_EDGE ( 'NONE', *, *, #86420, .F. ) ;
#18736 = ORIENTED_EDGE ( 'NONE', *, *, #28502, .F. ) ;
#18737 = CARTESIAN_POINT ( 'NONE',  ( 5.010840697562940704, -9.905515769479276145, 34.41647553114623292 ) ) ;
#18739 = VERTEX_POINT ( 'NONE', #12399 ) ;
#18738 = CARTESIAN_POINT ( 'NONE',  ( 2.557637826040450868, -12.43552623307873972, 30.55307653245132826 ) ) ;
#18740 = CARTESIAN_POINT ( 'NONE',  ( 1.253923917947826983, -9.804603061927743113, 34.18744698557895845 ) ) ;
#18741 = CARTESIAN_POINT ( 'NONE',  ( 5.076923076923075762, -8.973038597847269315, 34.52809138561121927 ) ) ;
#18742 = CARTESIAN_POINT ( 'NONE',  ( -3.749999999999997335, -7.500000000000021316, 15.09375000000000000 ) ) ;
#18743 = EDGE_LOOP ( 'NONE', ( #70898, #19812, #72185, #70920 ) ) ;
#18744 = AXIS2_PLACEMENT_3D ( 'NONE', #85094, #73351, #52175 ) ;
#18745 = DIRECTION ( 'NONE',  ( 0.000000000000000000, -6.938893903907222067E-15, 1.000000000000000000 ) ) ;
#18746 = EDGE_LOOP ( 'NONE', ( #78750, #22535 ) ) ;
#18747 = CARTESIAN_POINT ( 'NONE',  ( -13.60754234352223158, -11.43668979543635089, 33.22377378376089752 ) ) ;
#18748 = CARTESIAN_POINT ( 'NONE',  ( 3.230769230769231726, -2.708943851104267164, 35.45975837776705220 ) ) ;
#18749 = CARTESIAN_POINT ( 'NONE',  ( 7.780071466793709867, -3.937682226553329556, 33.60647404775217240 ) ) ;
#18752 = FACE_OUTER_BOUND ( 'NONE', #81860, .T. ) ;
#18751 = AXIS2_PLACEMENT_3D ( 'NONE', #20655, #41826, #29204 ) ;
#18750 = DIRECTION ( 'NONE',  ( -1.000000000000000000, 0.000000000000000000, 0.000000000000000000 ) ) ;
#18753 = VECTOR ( 'NONE', #60834, 1000.000000000000227 ) ;
#18754 = DIRECTION ( 'NONE',  ( -0.000000000000000000, 0.5000000000000011102, -0.8660254037844381525 ) ) ;
#18755 = ORIENTED_EDGE ( 'NONE', *, *, #66486, .T. ) ;
#18756 = FACE_OUTER_BOUND ( 'NONE', #75785, .T. ) ;
#18757 = CARTESIAN_POINT ( 'NONE',  ( 15.16468581981334829, -4.098570777380720287, 33.41473453929634729 ) ) ;
#18758 = VECTOR ( 'NONE', #46694, 1000.000000000000000 ) ;
#18759 = FACE_OUTER_BOUND ( 'NONE', #79866, .T. ) ;
#18760 = ORIENTED_EDGE ( 'NONE', *, *, #16623, .T. ) ;
#18761 = CARTESIAN_POINT ( 'NONE',  ( -18.00000000000000000, -10.88783764156682032, 36.11790692298802696 ) ) ;
#18762 = CARTESIAN_POINT ( 'NONE',  ( 10.61538461538461675, -8.164416787775445883, 34.95778746994557906 ) ) ;
#18763 = FACE_OUTER_BOUND ( 'NONE', #31023, .T. ) ;
#18764 = DIRECTION ( 'NONE',  ( 0.000000000000000000, 0.000000000000000000, -1.000000000000000000 ) ) ;
#18765 = FACE_BOUND ( 'NONE', #3411, .T. ) ;
#18767 = DIRECTION ( 'NONE',  ( 0.000000000000000000, 0.7660444431189822323, -0.6427876096865344779 ) ) ;
#18766 = CARTESIAN_POINT ( 'NONE',  ( 6.000000000000001776, -4.661471528628507777, 34.16647553114623292 ) ) ;
#18768 = CARTESIAN_POINT ( 'NONE',  ( -9.627052552794854279, -12.16647553114626490, 32.15551576947920864 ) ) ;
#18770 = CARTESIAN_POINT ( 'NONE',  ( 17.75002326905764605, -11.28823185664190376, 33.01397839955799896 ) ) ;
#18769 = CARTESIAN_POINT ( 'NONE',  ( -1.318547033612946118, -12.10708131394839704, 31.69288490824020954 ) ) ;
#18771 = CARTESIAN_POINT ( 'NONE',  ( -4.088591014333314178, -11.06231777344671130, 33.60647404775212976 ) ) ;
#18772 = CARTESIAN_POINT ( 'NONE',  ( 15.23076923076923173, -5.557115091759785130, 34.35708131394839171 ) ) ;
#18773 = CARTESIAN_POINT ( 'NONE',  ( -2.608446859217889546, -10.19485399968121264, 27.18563170625849068 ) ) ;
#18774 = EDGE_LOOP ( 'NONE', ( #12030, #44343 ) ) ;
#18775 = CARTESIAN_POINT ( 'NONE',  ( -6.923076923077044142, -9.442884908241554243, 34.35708131394783038 ) ) ;
#18776 = ORIENTED_EDGE ( 'NONE', *, *, #34004, .F. ) ;
#18777 = ADVANCED_FACE ( 'NONE', ( #18271 ), #73216, .F. ) ;
#18778 = CARTESIAN_POINT ( 'NONE',  ( 1.134615384615387246, -2.499999999999998668, 29.75000000000000355 ) ) ;
#18779 = CARTESIAN_POINT ( 'NONE',  ( -14.98076923076779465, -7.500000000000155431, 34.75000000000007105 ) ) ;
#18780 = CARTESIAN_POINT ( 'NONE',  ( 12.94230769230769340, -7.500000000000000000, 29.75000000000000355 ) ) ;
#18781 = CARTESIAN_POINT ( 'NONE',  ( -5.999999999999998224, -3.886160181151819604, 36.00935417666054406 ) ) ;
#18782 = CARTESIAN_POINT ( 'NONE',  ( -10.48459417441766561, -11.93129842949671726, 32.56571108434900452 ) ) ;
#18783 = CARTESIAN_POINT ( 'NONE',  ( -11.76138849736838488, -4.026226216239094491, 33.68668979543634379 ) ) ;
#18784 = CARTESIAN_POINT ( 'NONE',  ( 2.608446859217893099, -4.805146000318787358, 24.06063170625849423 ) ) ;
#18785 = CYLINDRICAL_SURFACE ( 'NONE', #69094, 0.2499999999999995559 ) ;
#18786 = CARTESIAN_POINT ( 'NONE',  ( 8.519254025182180001, -2.544273027872575366, 31.48422191005632342 ) ) ;
#18787 = CARTESIAN_POINT ( 'NONE',  ( -8.769230769230768274, -4.786620604624113540, 33.94971097300155094 ) ) ;
#18788 = CARTESIAN_POINT ( 'NONE',  ( 17.75000000000000000, -7.500000000000001776, 34.75000000000000000 ) ) ;
#18789 = CARTESIAN_POINT ( 'NONE',  ( -6.923076923076922462, -4.098570777380720287, 33.41473453929634729 ) ) ;
#18790 = CARTESIAN_POINT ( 'NONE',  ( -8.834501215191545853, -9.442884908240170461, 34.35708131394840592 ) ) ;
#18791 = CARTESIAN_POINT ( 'NONE',  ( -16.40384615384615330, -2.499999999999998668, 29.75000000000000355 ) ) ;
#18792 = EDGE_CURVE ( 'NONE', #79735, #48079, #1413, .T. ) ;
#18793 = CARTESIAN_POINT ( 'NONE',  ( 7.846153846153846700, -9.058645607665452459, 34.76329471203371924 ) ) ;
#18794 = B_SPLINE_CURVE_WITH_KNOTS ( 'NONE', 3,
 ( #25794, #52808, #60016, #18598, #5971, #60901, #12722, #87976, #46060, #19037 ),
 .UNSPECIFIED., .F., .F.,
 ( 4, 2, 2, 2, 4 ),
 ( 0.000000000000000000, 0.0001954339857564098054, 0.0003908679715128196108, 0.0005863019572692293891, 0.0007817359430256392216 ),
 .UNSPECIFIED. ) ;
#18795 = VERTEX_POINT ( 'NONE', #58798 ) ;
#18796 = CARTESIAN_POINT ( 'NONE',  ( 16.21910129335899597, -5.094484230520771817, 34.41647553114626845 ) ) ;
#18797 = DIRECTION ( 'NONE',  ( -0.000000000000000000, 0.1736481776669307198, -0.9848077530122080203 ) ) ;
#18798 = CARTESIAN_POINT ( 'NONE',  ( -1.614399933863613468, -11.22469193450124969, 18.86124329374151287 ) ) ;
#18799 = CARTESIAN_POINT ( 'NONE',  ( 6.130525701763565927, -4.459921816937789885, 33.71989282347011851 ) ) ;
#18800 = CARTESIAN_POINT ( 'NONE',  ( 17.32697738856138869, -11.79725096376909299, 32.30694842903960762 ) ) ;
#18801 = VERTEX_POINT ( 'NONE', #46626 ) ;
#18802 = CARTESIAN_POINT ( 'NONE',  ( 7.173022441425065843, -8.433404298154334455, 34.66254593164985920 ) ) ;
#18803 = CARTESIAN_POINT ( 'NONE',  ( 9.442330948259103351, -12.65889640711025521, 30.72598325615533454 ) ) ;
#18805 = ORIENTED_EDGE ( 'NONE', *, *, #20534, .F. ) ;
#18804 = CARTESIAN_POINT ( 'NONE',  ( 11.31497661389720477, -3.019605429927184392, 32.48692288466676814 ) ) ;
#18806 = CARTESIAN_POINT ( 'NONE',  ( -9.942284436356285227, -3.436278759898153901, 33.07459398097509506 ) ) ;
#18807 = CARTESIAN_POINT ( 'NONE',  ( 12.46153846153833911, -12.46129190930018460, 30.37095296980731973 ) ) ;
#18808 = CARTESIAN_POINT ( 'NONE',  ( 15.23076923076923173, -5.471508081941601098, 34.59228464037088457 ) ) ;
#18809 = CARTESIAN_POINT ( 'NONE',  ( -3.230769230769229949, -2.900454961884010974, 35.62045528018868623 ) ) ;
#18810 = ORIENTED_EDGE ( 'NONE', *, *, #31700, .F. ) ;
#18811 = DIRECTION ( 'NONE',  ( 0.000000000000000000, 0.000000000000000000, -1.000000000000000000 ) ) ;
#18812 = CARTESIAN_POINT ( 'NONE',  ( 10.68145194873469173, -3.937682226553329556, 33.60647404775216529 ) ) ;
#18813 = EDGE_CURVE ( 'NONE', #53579, #70248, #74468, .T. ) ;
#18814 = CARTESIAN_POINT ( 'NONE',  ( 8.703960768674448900, -3.643525952247789412, 33.31231777344662959 ) ) ;
#18815 = EDGE_LOOP ( 'NONE', ( #11866, #40592, #10024, #67725 ) ) ;
#18816 = ORIENTED_EDGE ( 'NONE', *, *, #1679, .F. ) ;
#18817 = ORIENTED_EDGE ( 'NONE', *, *, #85768, .F. ) ;
#18818 = VECTOR ( 'NONE', #50832, 999.9999999999998863 ) ;
#18819 = VECTOR ( 'NONE', #48775, 1000.000000000000000 ) ;
#18820 = EDGE_CURVE ( 'NONE', #47774, #74921, #37943, .T. ) ;
#18821 = CARTESIAN_POINT ( 'NONE',  ( 0.4615384615384611200, -8.120952969808772792, 34.71129190930000163 ) ) ;
#18822 = CARTESIAN_POINT ( 'NONE',  ( 9.692307692307570832, -12.51329471203414379, 31.30864560766407578 ) ) ;
#18823 = CARTESIAN_POINT ( 'NONE',  ( 13.16113044089143891, -11.41268669641499756, 32.86336882939238535 ) ) ;
#18824 = AXIS2_PLACEMENT_3D ( 'NONE', #24950, #58733, #51968 ) ;
#18825 = CARTESIAN_POINT ( 'NONE',  ( 7.846153846153846700, -5.557115091759785130, 34.35708131394839171 ) ) ;
#18826 = VERTEX_POINT ( 'NONE', #19157 ) ;
#18827 = VERTEX_POINT ( 'NONE', #72756 ) ;
#18828 = ORIENTED_EDGE ( 'NONE', *, *, #79161, .F. ) ;
#18830 = ORIENTED_EDGE ( 'NONE', *, *, #42850, .T. ) ;
#18829 = CARTESIAN_POINT ( 'NONE',  ( 15.29683758177167086, -4.786620604624113540, 33.94971097300155805 ) ) ;
#18831 = CARTESIAN_POINT ( 'NONE',  ( -16.40386937806761836, -12.45566812827425096, 31.48439005359158926 ) ) ;
#18832 = FACE_OUTER_BOUND ( 'NONE', #69467, .T. ) ;
#18833 = B_SPLINE_CURVE_WITH_KNOTS ( 'NONE', 3,
 ( #43366, #3695, #10472, #23964, #17217, #16770, #37939, #44224, #71711, #64496 ),
 .UNSPECIFIED., .F., .F.,
 ( 4, 2, 2, 2, 4 ),
 ( 0.000000000000000000, 0.0001954311564186871184, 0.0003908623128373742367, 0.0005862934692560614093, 0.0007817246256747484735 ),
 .UNSPECIFIED. ) ;
#18834 = DIRECTION ( 'NONE',  ( 0.000000000000000000, 0.000000000000000000, 1.000000000000000000 ) ) ;
#18835 = CARTESIAN_POINT ( 'NONE',  ( -5.776988648387149539, -4.187068189119697692, 33.49521262558774026 ) ) ;
#18836 = ORIENTED_EDGE ( 'NONE', *, *, #31917, .T. ) ;
#18837 = EDGE_LOOP ( 'NONE', ( #87842, #52718, #19069, #86457 ) ) ;
#18838 = ORIENTED_EDGE ( 'NONE', *, *, #54231, .F. ) ;
#18839 = CARTESIAN_POINT ( 'NONE',  ( 10.61538461538449596, -10.90142922262034020, 33.41473453929536674 ) ) ;
#18841 = VERTEX_POINT ( 'NONE', #46188 ) ;
#18840 = CARTESIAN_POINT ( 'NONE',  ( 5.076923076923075762, -2.499999999999998668, 29.50000000000001066 ) ) ;
#18842 = CARTESIAN_POINT ( 'NONE',  ( 3.230769230769110045, -11.94971097300221174, 32.03036669348237098 ) ) ;
#18843 = VECTOR ( 'NONE', #18045, 1000.000000000000000 ) ;
#18844 = DIRECTION ( 'NONE',  ( 0.000000000000000000, 0.000000000000000000, 1.000000000000000000 ) ) ;
#18845 = CARTESIAN_POINT ( 'NONE',  ( -5.076923076923075762, -4.102666532097928531, 36.13435417666054406 ) ) ;
#18846 = AXIS2_PLACEMENT_3D ( 'NONE', #69039, #75358, #88890 ) ;
#18847 = CARTESIAN_POINT ( 'NONE',  ( 8.352564102564102200, -7.500000000000000000, 33.75000000000000000 ) ) ;
#18848 = CARTESIAN_POINT ( 'NONE',  ( -39.05038313613820122, -2.249999999999998668, 29.75000000000000355 ) ) ;
#18849 = FACE_BOUND ( 'NONE', #40421, .T. ) ;
#18850 = DIRECTION ( 'NONE',  ( -1.000000000000000000, -0.000000000000000000, -0.000000000000000000 ) ) ;
#18851 = DIRECTION ( 'NONE',  ( -0.000000000000000000, 1.000000000000000000, -0.000000000000000000 ) ) ;
#18852 = CARTESIAN_POINT ( 'NONE',  ( -7.846153846153844924, -12.10708131394839349, 31.69288490824020244 ) ) ;
#18854 = CARTESIAN_POINT ( 'NONE',  ( 6.700149964170072359, -10.77366814457252175, 33.85459836347579454 ) ) ;
#18853 = CARTESIAN_POINT ( 'NONE',  ( -17.93129618099663958, -12.74404781541490372, 29.99992509483736214 ) ) ;
#18855 = PLANE ( 'NONE',  #26581 ) ;
#18856 = CARTESIAN_POINT ( 'NONE',  ( -4.087778820496075660, -11.35647404775217595, 33.31231777344667222 ) ) ;
#18857 = ORIENTED_EDGE ( 'NONE', *, *, #23019, .F. ) ;
#18858 = CARTESIAN_POINT ( 'NONE',  ( 11.40831432902331954, -3.285722584762969856, 32.44110544564090759 ) ) ;
#18859 = CARTESIAN_POINT ( 'NONE',  ( 12.71148387091650278, -3.520799739797214389, 33.17531984108286025 ) ) ;
#18860 = ORIENTED_EDGE ( 'NONE', *, *, #14844, .F. ) ;
#18861 = ORIENTED_EDGE ( 'NONE', *, *, #15433, .T. ) ;
#18862 = EDGE_CURVE ( 'NONE', #2073, #68833, #73672, .T. ) ;
#18863 = CARTESIAN_POINT ( 'NONE',  ( 27.00000000000000000, -17.00000000000000000, 2.999999999999999112 ) ) ;
#18864 = CARTESIAN_POINT ( 'NONE',  ( -5.999999999999998224, -10.89733346790207413, 36.13435417666054406 ) ) ;
#18865 = CARTESIAN_POINT ( 'NONE',  ( 12.33139049180676139, -11.04286588640298561, 33.62463336215343901 ) ) ;
#18866 = ORIENTED_EDGE ( 'NONE', *, *, #66948, .F. ) ;
#18867 = DIRECTION ( 'NONE',  ( -0.000000000000000000, 0.6427876096865404731, -0.7660444431189771253 ) ) ;
#18868 = CARTESIAN_POINT ( 'NONE',  ( -7.173100160369890510, -10.05641848906368097, 34.04755513067966177 ) ) ;
#18870 = CARTESIAN_POINT ( 'NONE',  ( 2.307692307692309264, -12.62096338111211580, 30.90682066428153263 ) ) ;
#18869 = DIRECTION ( 'NONE',  ( 0.000000000000000000, 0.000000000000000000, 1.000000000000000000 ) ) ;
#18871 = DIRECTION ( 'NONE',  ( -0.000000000000000000, 0.3420201433256694901, -0.9396926207859082059 ) ) ;
#18872 = VECTOR ( 'NONE', #22643, 1000.000000000000000 ) ;
#18873 = CARTESIAN_POINT ( 'NONE',  ( 0.6843181305165257911, -4.989023458446561143, 34.36081565061822118 ) ) ;
#18874 = DIRECTION ( 'NONE',  ( 0.000000000000000000, 0.000000000000000000, 1.000000000000000000 ) ) ;
#18875 = CARTESIAN_POINT ( 'NONE',  ( 1.553300858899087311, -3.749999999999992006, 20.48437500000000000 ) ) ;
#18876 = ORIENTED_EDGE ( 'NONE', *, *, #88857, .T. ) ;
#18877 = VECTOR ( 'NONE', #32468, 1000.000000000000000 ) ;
#18878 = CIRCLE ( 'NONE', #35984, 0.2500000000000002220 ) ;
#18879 = ORIENTED_EDGE ( 'NONE', *, *, #21446, .T. ) ;
#18880 = EDGE_CURVE ( 'NONE', #3322, #7083, #17515, .T. ) ;
#18881 = CARTESIAN_POINT ( 'NONE',  ( 5.076923076922953193, -11.06231777344772027, 33.60647404775119895 ) ) ;
#18882 = CARTESIAN_POINT ( 'NONE',  ( 6.989145274079364256, -12.10708131394839882, 31.69288490824020954 ) ) ;
#18883 = LINE ( 'NONE', #60305, #54611 ) ;
#18884 = CARTESIAN_POINT ( 'NONE',  ( 13.38461538461538680, -2.900454961884010974, 35.62045528018868623 ) ) ;
#18885 = ADVANCED_FACE ( 'NONE', ( #13728 ), #41645, .F. ) ;
#18886 = CARTESIAN_POINT ( 'NONE',  ( -7.780960857859191115, -2.255955759149236073, 29.99999999999988631 ) ) ;
#18887 = CARTESIAN_POINT ( 'NONE',  ( 3.750000000000000888, -7.499999999999978684, 23.21875000000000000 ) ) ;
#18888 = CARTESIAN_POINT ( 'NONE',  ( -7.596099534515528440, -8.303483539816728154, 34.68545999027711702 ) ) ;
#18889 = CYLINDRICAL_SURFACE ( 'NONE', #54653, 0.2500000000000009437 ) ;
#18890 = CARTESIAN_POINT ( 'NONE',  ( -17.07692307692307665, -2.538708090699994813, 30.37095296980875503 ) ) ;
#18891 = CARTESIAN_POINT ( 'NONE',  ( 13.38461538461526423, -10.33852847137269571, 34.16647553114546554 ) ) ;
#18892 = CARTESIAN_POINT ( 'NONE',  ( -6.223484943723945229, -2.847400154188068022, 31.58180166144859058 ) ) ;
#18893 = FACE_OUTER_BOUND ( 'NONE', #33671, .T. ) ;
#18894 = B_SPLINE_CURVE_WITH_KNOTS ( 'NONE', 3,
 ( #213, #27678, #82644, #44269, #29466, #30337, #70889, #1542, #42974, #50150 ),
 .UNSPECIFIED., .F., .F.,
 ( 4, 2, 2, 2, 4 ),
 ( 0.0007817246256747459798, 0.0009771112852218896347, 0.001172497944769033398, 0.001367884604316177161, 0.001563271263863320708 ),
 .UNSPECIFIED. ) ;
#18895 = DIRECTION ( 'NONE',  ( 0.000000000000000000, 0.000000000000000000, 1.000000000000000000 ) ) ;
#18896 = CARTESIAN_POINT ( 'NONE',  ( 4.088575707885377497, -12.46129190929999986, 30.37095296980880832 ) ) ;
#18897 = DIRECTION ( 'NONE',  ( -1.000000000000000000, -0.000000000000000000, -0.000000000000000000 ) ) ;
#18898 = ADVANCED_FACE ( 'NONE', ( #26799 ), #82194, .F. ) ;
#18899 = CARTESIAN_POINT ( 'NONE',  ( -11.53846153846166089, -3.083524468854526912, 32.58852847137268327 ) ) ;
#18900 = ORIENTED_EDGE ( 'NONE', *, *, #9346, .T. ) ;
#18901 = CARTESIAN_POINT ( 'NONE',  ( -4.219116599806927326, -5.219633306516282545, 34.19971097300152252 ) ) ;
#18902 = CARTESIAN_POINT ( 'NONE',  ( -15.23076923076935252, -12.70778746994576025, 30.41441678777401236 ) ) ;
#18903 = CARTESIAN_POINT ( 'NONE',  ( 5.999999999999878320, -2.657715359629662988, 31.77849191805970364 ) ) ;
#18904 = CARTESIAN_POINT ( 'NONE',  ( 1.077988221561497539, -10.27530806549875386, 16.20499329374151642 ) ) ;
#18905 = ADVANCED_FACE ( 'NONE', ( #69114 ), #33994, .T. ) ;
#18906 = CARTESIAN_POINT ( 'NONE',  ( -5.999999999999998224, -9.819645486525091727, 36.12317359536749706 ) ) ;
#18907 =( NAMED_UNIT ( * ) SI_UNIT ( $, .STERADIAN. ) SOLID_ANGLE_UNIT ( ) );
#18909 = ORIENTED_EDGE ( 'NONE', *, *, #19215, .F. ) ;
#18908 = CARTESIAN_POINT ( 'NONE',  ( -18.25000000000000711, -2.250000000000000000, 29.68055622560741114 ) ) ;
#18910 = CARTESIAN_POINT ( 'NONE',  ( -2.750000000000006217, -6.360912703474006946, 22.67187499999999645 ) ) ;
#18911 = DIRECTION ( 'NONE',  ( -0.000000000000000000, -0.1736481776669307198, -0.9848077530122080203 ) ) ;
#18912 = ORIENTED_EDGE ( 'NONE', *, *, #56308, .T. ) ;
#18913 = CARTESIAN_POINT ( 'NONE',  ( 0.2115617305961081662, -2.779195860258146578, 31.39871582349836032 ) ) ;
#18914 = ORIENTED_EDGE ( 'NONE', *, *, #54639, .F. ) ;
#18915 = AXIS2_PLACEMENT_3D ( 'NONE', #73919, #88342, #68478 ) ;
#18916 = DIRECTION ( 'NONE',  ( 0.000000000000000000, -6.938893903907222067E-15, 1.000000000000000000 ) ) ;
#18917 = CARTESIAN_POINT ( 'NONE',  ( -7.623142494540994463, -11.76359900205217635, 32.36225158514719169 ) ) ;
#18918 = EDGE_CURVE ( 'NONE', #87461, #6628, #16331, .T. ) ;
#18919 = DIRECTION ( 'NONE',  ( -2.891205793294678326E-16, 1.000000000000000000, -0.000000000000000000 ) ) ;
#18920 = EDGE_LOOP ( 'NONE', ( #49541, #54216 ) ) ;
#18921 = EDGE_CURVE ( 'NONE', #67903, #45764, #21366, .T. ) ;
#18922 = FACE_OUTER_BOUND ( 'NONE', #5600, .T. ) ;
#18923 = ORIENTED_EDGE ( 'NONE', *, *, #11272, .T. ) ;
#18924 = VERTEX_POINT ( 'NONE', #13283 ) ;
#18925 = CARTESIAN_POINT ( 'NONE',  ( -0.5276218724943418925, -3.050289026998445951, 32.03036669348365706 ) ) ;
#18926 = CARTESIAN_POINT ( 'NONE',  ( 7.846153846153846700, -12.09954503811598769, 35.62045528018868623 ) ) ;
#18927 = ADVANCED_FACE ( 'NONE', ( #21812 ), #20041, .F. ) ;
#18928 = FACE_OUTER_BOUND ( 'NONE', #25579, .T. ) ;
#18929 = CARTESIAN_POINT ( 'NONE',  ( 9.692307692307570832, -9.528491918059723176, 34.59228464037033035 ) ) ;
#18930 = EDGE_CURVE ( 'NONE', #47846, #47342, #6834, .T. ) ;
#18931 = DIRECTION ( 'NONE',  ( 0.000000000000000000, 0.6427876096865373645, -0.7660444431189797898 ) ) ;
#18932 = DIRECTION ( 'NONE',  ( -0.000000000000000000, 0.3420201433256694346, -0.9396926207859080948 ) ) ;
#18933 = CARTESIAN_POINT ( 'NONE',  ( 0.2115152373170033351, -2.341070481393820124, 30.72580821765574299 ) ) ;
#18934 = CARTESIAN_POINT ( 'NONE',  ( -0.3307480205715124799, -12.35292014791297710, 31.75344720912887198 ) ) ;
#18935 = B_SPLINE_CURVE_WITH_KNOTS ( 'NONE', 3,
 ( #87721, #52122, #25993, #3490, #85922, #53456, #79610, #5281, #80958, #24204 ),
 .UNSPECIFIED., .F., .F.,
 ( 4, 2, 2, 2, 4 ),
 ( 0.000000000000000000, 0.0001954339857564076099, 0.0003908679715128152198, 0.0005863019572692228839, 0.0007817359430256304396 ),
 .UNSPECIFIED. ) ;
#18936 = VERTEX_POINT ( 'NONE', #7860 ) ;
#18937 = VERTEX_POINT ( 'NONE', #20919 ) ;
#18938 = ORIENTED_EDGE ( 'NONE', *, *, #11854, .F. ) ;
#18940 = EDGE_LOOP ( 'NONE', ( #77451, #12774, #8534, #51812 ) ) ;
#18939 = CARTESIAN_POINT ( 'NONE',  ( 3.480823650682683734, -12.65882529074907126, 30.72640787790839312 ) ) ;
#18941 = AXIS2_PLACEMENT_3D ( 'NONE', #26835, #82226, #88559 ) ;
#18942 = CARTESIAN_POINT ( 'NONE',  ( -14.17716686945866655, -11.04252011169590020, 33.62494198852677130 ) ) ;
#18943 = CARTESIAN_POINT ( 'NONE',  ( 9.626225312947559232, -5.471508081941602875, 34.59228464037088457 ) ) ;
#18944 = VERTEX_POINT ( 'NONE', #42099 ) ;
#18945 = DIRECTION ( 'NONE',  ( -0.000000000000000000, -0.000000000000000000, -1.000000000000000000 ) ) ;
#18946 = VECTOR ( 'NONE', #17455, 1000.000000000000000 ) ;
#18947 = ORIENTED_EDGE ( 'NONE', *, *, #23837, .T. ) ;
#18948 = CARTESIAN_POINT ( 'NONE',  ( 17.07692307692295586, -10.21337939537710326, 33.94971097300076224 ) ) ;
#18949 = EDGE_LOOP ( 'NONE', ( #53486, #40201, #81068, #62648 ) ) ;
#18950 = CARTESIAN_POINT ( 'NONE',  ( -12.21153846153852385, -7.565270000091922853, 34.99999999999999289 ) ) ;
#18951 = EDGE_CURVE ( 'NONE', #31652, #5133, #13215, .T. ) ;
#18952 = B_SPLINE_CURVE_WITH_KNOTS ( 'NONE', 3,
 ( #21811, #2849, #57806, #42098, #69553, #63233, #7859, #35321, #84414, #83974 ),
 .UNSPECIFIED., .F., .F.,
 ( 4, 2, 2, 2, 4 ),
 ( 0.000000000000000000, 0.0001954311564186867931, 0.0003908623128373735862, 0.0005862934692560603251, 0.0007817246256747471724 ),
 .UNSPECIFIED. ) ;
#18953 = CARTESIAN_POINT ( 'NONE',  ( 24.00000000000000000, -9.499999999999982236, 27.25000000000000000 ) ) ;
#18954 = EDGE_CURVE ( 'NONE', #45845, #9922, #34439, .T. ) ;
#18955 = LINE ( 'NONE', #17628, #42535 ) ;
#18956 = B_SPLINE_CURVE_WITH_KNOTS ( 'NONE', 3,
 ( #37557, #86221, #3779, #66374, #59165, #31708, #4679, #32153, #24044, #71789 ),
 .UNSPECIFIED., .F., .F.,
 ( 4, 2, 2, 2, 4 ),
 ( 0.000000000000000000, 0.0001954339857564090194, 0.0003908679715128180387, 0.0005863019572692270039, 0.0007817359430256360774 ),
 .UNSPECIFIED. ) ;
#18957 = FACE_BOUND ( 'NONE', #60681, .T. ) ;
#18958 = CARTESIAN_POINT ( 'NONE',  ( 17.32697749683652688, -6.523592122091590895, 34.90882529074906415 ) ) ;
#18959 = CARTESIAN_POINT ( 'NONE',  ( -10.03846153846153832, -11.00000000000000000, 29.75000000000000355 ) ) ;
#18960 = EDGE_CURVE ( 'NONE', #33835, #74655, #28579, .T. ) ;
#18961 = DIRECTION ( 'NONE',  ( -0.000000000000000000, -0.8660254037844399289, -0.4999999999999980016 ) ) ;
#18962 = CARTESIAN_POINT ( 'NONE',  ( -3.360916440207450062, -4.460286881179643004, 33.72017969459903242 ) ) ;
#18963 = CARTESIAN_POINT ( 'NONE',  ( -17.06410256410256565, -3.499999999999999556, 29.75000000000000355 ) ) ;
#18964 = CARTESIAN_POINT ( 'NONE',  ( 17.20744877868664346, -9.417988943895561960, 34.36773134775778260 ) ) ;
#18965 = ORIENTED_EDGE ( 'NONE', *, *, #80007, .T. ) ;
#18966 = DIRECTION ( 'NONE',  ( -1.000000000000000000, -0.000000000000000000, -0.000000000000000000 ) ) ;
#18967 = EDGE_LOOP ( 'NONE', ( #35135, #6756 ) ) ;
#18968 = EDGE_LOOP ( 'NONE', ( #6863, #8734, #27594, #80406 ) ) ;
#18969 = EDGE_CURVE ( 'NONE', #23968, #25274, #37085, .T. ) ;
#18971 = CARTESIAN_POINT ( 'NONE',  ( -14.30769230769230660, -12.37446782046654192, 30.86335684631486131 ) ) ;
#18970 = LINE ( 'NONE', #87007, #46071 ) ;
#18972 = CARTESIAN_POINT ( 'NONE',  ( 3.007284306204900837, -3.562934362175799841, 33.22335522853832401 ) ) ;
#18973 = DIRECTION ( 'NONE',  ( -0.000000000000000000, 0.8660254037844397068, -0.4999999999999978906 ) ) ;
#18974 = CARTESIAN_POINT ( 'NONE',  ( 8.519230769230768274, -7.500000000000001776, 35.00000000000000000 ) ) ;
#18975 = CARTESIAN_POINT ( 'NONE',  ( -15.23076923076935074, -3.835265460704628371, 33.15142922262033665 ) ) ;
#18976 = VERTEX_POINT ( 'NONE', #30339 ) ;
#18977 = CARTESIAN_POINT ( 'NONE',  ( 17.14217864819909920, -3.300289026998473929, 32.46337939537591666 ) ) ;
#18978 = CARTESIAN_POINT ( 'NONE',  ( 11.76188850032310995, -7.630147231320743018, 34.74852402298682819 ) ) ;
#18979 = CARTESIAN_POINT ( 'NONE',  ( -14.55771554498526932, -8.432397168068783699, 34.66272746175022945 ) ) ;
#18980 = CARTESIAN_POINT ( 'NONE',  ( -16.15384615384627409, -4.320704448113951379, 33.92786785259630022 ) ) ;
#18981 = VECTOR ( 'NONE', #16465, 1000.000000000000000 ) ;
#18982 = VERTEX_POINT ( 'NONE', #24015 ) ;
#18983 = B_SPLINE_CURVE_WITH_KNOTS ( 'NONE', 3,
 ( #64048, #8243, #84795, #76694, #28509, #42917, #1917, #16319, #62717, #43784 ),
 .UNSPECIFIED., .F., .F.,
 ( 4, 2, 2, 2, 4 ),
 ( 0.0007817246256747457630, 0.0009771112852218887673, 0.001172497944769031880, 0.001367884604316174993, 0.001563271263863318106 ),
 .UNSPECIFIED. ) ;
#18984 = VERTEX_POINT ( 'NONE', #63678 ) ;
#18985 = ITEM_DEFINED_TRANSFORMATION ( 'NONE', 'NONE', #54692,  #83448 ) ;
#18986 = ORIENTED_EDGE ( 'NONE', *, *, #19777, .T. ) ;
#18987 = CARTESIAN_POINT ( 'NONE',  ( 10.39189969082028675, -4.225889041578353655, 33.85425143139329407 ) ) ;
#18988 = CARTESIAN_POINT ( 'NONE',  ( -13.31935981333936070, -10.90142922261932057, 33.41473453929631887 ) ) ;
#18989 = ORIENTED_EDGE ( 'NONE', *, *, #4651, .T. ) ;
#18990 = DIRECTION ( 'NONE',  ( -0.000000000000000000, -0.7660444431189791237, -0.6427876096865379196 ) ) ;
#18991 = CARTESIAN_POINT ( 'NONE',  ( 14.30769230769218581, -5.941354392335915335, 34.76329471203413846 ) ) ;
#18992 = CARTESIAN_POINT ( 'NONE',  ( 5.010839665967195877, -6.386643153685125363, 34.62446782046654903 ) ) ;
#18993 = ADVANCED_FACE ( 'NONE', ( #64113 ), #49725, .F. ) ;
#18994 = CARTESIAN_POINT ( 'NONE',  ( -17.01166750564705055, -12.27809138561124591, 31.22303859784720359 ) ) ;
#18995 = DIRECTION ( 'NONE',  ( -0.000000000000000000, -0.9848077530122086864, -0.1736481776669273613 ) ) ;
#18996 = ORIENTED_EDGE ( 'NONE', *, *, #50810, .T. ) ;
#18998 = VERTEX_POINT ( 'NONE', #29468 ) ;
#18997 = CARTESIAN_POINT ( 'NONE',  ( -15.48074597481782178, -12.01397095200674059, 32.43157075238190146 ) ) ;
#18999 = CARTESIAN_POINT ( 'NONE',  ( 18.25000000000000000, -7.500000000000001776, 35.04278698407183867 ) ) ;
#19000 = DIRECTION ( 'NONE',  ( -0.000000000000000000, 0.6427876096865404731, -0.7660444431189770143 ) ) ;
#19001 = CARTESIAN_POINT ( 'NONE',  ( 15.23076923076923173, -1.422936976036506707, 30.56769352161908415 ) ) ;
#19002 = CARTESIAN_POINT ( 'NONE',  ( -10.68146699474474914, -3.322132147404559532, 32.92929555188719348 ) ) ;
#19003 = CARTESIAN_POINT ( 'NONE',  ( -8.769230769230768274, -8.164416787775445883, 34.95778746994557906 ) ) ;
#19004 = CYLINDRICAL_SURFACE ( 'NONE', #26260, 0.2499999999999986955 ) ;
#19005 = CARTESIAN_POINT ( 'NONE',  ( -6.923076923076922462, -6.189225973068211317, 35.74407628777942847 ) ) ;
#19006 = CARTESIAN_POINT ( 'NONE',  ( -2.775308065498752086, -8.577988221561495763, 20.26749329374151998 ) ) ;
#19007 = ORIENTED_EDGE ( 'NONE', *, *, #56503, .F. ) ;
#19008 = FACE_OUTER_BOUND ( 'NONE', #86047, .T. ) ;
#19009 = CARTESIAN_POINT ( 'NONE',  ( 7.911298626873478845, -7.750023224968868085, 34.99404313364389907 ) ) ;
#19010 = VECTOR ( 'NONE', #20586, 1000.000000000000114 ) ;
#19011 = CARTESIAN_POINT ( 'NONE',  ( -13.31935981333936425, -8.613356846314928816, 34.62446782046653482 ) ) ;
#19012 = ORIENTED_EDGE ( 'NONE', *, *, #103, .F. ) ;
#19013 = LINE ( 'NONE', #10025, #84386 ) ;
#19014 = CYLINDRICAL_SURFACE ( 'NONE', #8089, 0.2499999999999998890 ) ;
#19015 = CARTESIAN_POINT ( 'NONE',  ( 13.13459214732242408, -3.711651800289232028, 33.01384336483936011 ) ) ;
#19016 = CIRCLE ( 'NONE', #20428, 0.2500000000000002220 ) ;
#19017 = CARTESIAN_POINT ( 'NONE',  ( -10.68146699474474914, -2.292212530054419606, 30.41441678777542634 ) ) ;
#19018 = DIRECTION ( 'NONE',  ( -0.000000000000000000, 1.000000000000000000, -0.000000000000000000 ) ) ;
#19019 = CARTESIAN_POINT ( 'NONE',  ( -0.3589743589743593088, -7.500000000000000000, 29.75000000000000355 ) ) ;
#19020 = VERTEX_POINT ( 'NONE', #29909 ) ;
#19021 = B_SPLINE_CURVE_WITH_KNOTS ( 'NONE', 3,
 ( #9014, #30163, #2232, #37346, #17988, #57629, #29727, #37800, #84682, #65706 ),
 .UNSPECIFIED., .F., .F.,
 ( 4, 2, 2, 2, 4 ),
 ( 0.000000000000000000, 0.0001954311564186876876, 0.0003908623128373753751, 0.0005862934692560630356, 0.0007817246256747507503 ),
 .UNSPECIFIED. ) ;
#19022 = CARTESIAN_POINT ( 'NONE',  ( 5.777073782483851616, -3.586966769969700763, 32.86292498521069660 ) ) ;
#19023 = EDGE_CURVE ( 'NONE', #33753, #74977, #22933, .T. ) ;
#19024 = EDGE_CURVE ( 'NONE', #12150, #68060, #29338, .T. ) ;
#19025 = DIRECTION ( 'NONE',  ( 0.000000000000000000, 0.1736481776669275834, 0.9848077530122086864 ) ) ;
#19026 = CARTESIAN_POINT ( 'NONE',  ( -3.296852641725111166, -11.69971097300155272, 32.46337939537587403 ) ) ;
#19027 = ORIENTED_EDGE ( 'NONE', *, *, #52524, .F. ) ;
#19028 = CARTESIAN_POINT ( 'NONE',  ( 10.55011461482829738, -9.528491918058357157, 34.59228464037090589 ) ) ;
#19029 = ADVANCED_FACE ( 'NONE', ( #3303 ), #23138, .F. ) ;
#19030 = VERTEX_POINT ( 'NONE', #16382 ) ;
#19031 = CARTESIAN_POINT ( 'NONE',  ( 13.38461538461538680, -3.513871655860378418, 32.76840700105978499 ) ) ;
#19032 = CARTESIAN_POINT ( 'NONE',  ( 11.66925197942848769, -6.369690395747422684, 34.87708834333098196 ) ) ;
#19033 = EDGE_LOOP ( 'NONE', ( #12628, #52204 ) ) ;
#19034 = EDGE_CURVE ( 'NONE', #44514, #21774, #66986, .T. ) ;
#19035 = CARTESIAN_POINT ( 'NONE',  ( -7.846153846153844924, -3.322132147404559976, 32.92929555188717927 ) ) ;
#19036 = CARTESIAN_POINT ( 'NONE',  ( -14.53055857075540658, -2.251424796025575326, 29.88072029997477586 ) ) ;
#19037 = CARTESIAN_POINT ( 'NONE',  ( -9.692307692307812417, -2.625532179533778709, 30.86335684631627174 ) ) ;
#19038 = CARTESIAN_POINT ( 'NONE',  ( 8.519230769230768274, -7.566083408709835645, 34.74999999999999289 ) ) ;
#19039 = CARTESIAN_POINT ( 'NONE',  ( -4.826977667545033768, -8.476813868363244353, 34.90874843262270133 ) ) ;
#19040 = ORIENTED_EDGE ( 'NONE', *, *, #61465, .T. ) ;
#19041 = CARTESIAN_POINT ( 'NONE',  ( -4.088591014333315066, -12.51329471203373700, 31.30864560766537963 ) ) ;
#19042 = ORIENTED_EDGE ( 'NONE', *, *, #22386, .F. ) ;
#19043 = AXIS2_PLACEMENT_3D ( 'NONE', #53129, #11723, #45038 ) ;
#19045 = EDGE_CURVE ( 'NONE', #20445, #65338, #8911, .T. ) ;
#19044 = CARTESIAN_POINT ( 'NONE',  ( -15.09997878980228059, -6.369690395747422684, 34.87708834333098196 ) ) ;
#19046 = CARTESIAN_POINT ( 'NONE',  ( -12.46153846153846168, -2.833524468853757305, 32.15551576947925838 ) ) ;
#19047 = CARTESIAN_POINT ( 'NONE',  ( -3.100721624513547159, -7.723484964179500700, 34.74522123443823318 ) ) ;
#19048 = DIRECTION ( 'NONE',  ( -0.000000000000000000, -0.9396926207859093161, -0.3420201433256663259 ) ) ;
#19049 = EDGE_CURVE ( 'NONE', #63003, #48826, #21822, .T. ) ;
#19050 = CARTESIAN_POINT ( 'NONE',  ( -4.153846153846274980, -10.33852847137269571, 34.16647553114546554 ) ) ;
#19051 = DIRECTION ( 'NONE',  ( 0.000000000000000000, 0.000000000000000000, 1.000000000000000000 ) ) ;
#19052 = DIRECTION ( 'NONE',  ( 1.000000000000000000, 0.000000000000000000, 0.000000000000000000 ) ) ;
#19053 = ORIENTED_EDGE ( 'NONE', *, *, #66481, .T. ) ;
#19054 = B_SPLINE_CURVE_WITH_KNOTS ( 'NONE', 3,
 ( #85458, #79145, #23741, #71937, #10248, #30941, #17446, #68951, #7261, #34726 ),
 .UNSPECIFIED., .F., .F.,
 ( 4, 2, 2, 2, 4 ),
 ( 0.0007817246256747477145, 0.0009771112852218907189, 0.001172497944769033615, 0.001367884604316176511, 0.001563271263863319407 ),
 .UNSPECIFIED. ) ;
#19055 = ORIENTED_EDGE ( 'NONE', *, *, #11365, .T. ) ;
#19056 = ORIENTED_EDGE ( 'NONE', *, *, #26362, .F. ) ;
#19057 = ORIENTED_EDGE ( 'NONE', *, *, #7584, .F. ) ;
#19058 = EDGE_CURVE ( 'NONE', #72244, #28699, #3750, .T. ) ;
#19059 = CARTESIAN_POINT ( 'NONE',  ( -10.36533030374629938, -11.28795663066794575, 33.01431243580653785 ) ) ;
#19060 = CARTESIAN_POINT ( 'NONE',  ( -2.084912766423894670, -3.236590943229497253, 32.36255958852954251 ) ) ;
#19061 = CARTESIAN_POINT ( 'NONE',  ( -15.29685264172511161, -10.51840700105979387, 33.73612834413961536 ) ) ;
#19062 = EDGE_CURVE ( 'NONE', #71506, #28072, #4649, .T. ) ;
#19063 = DIRECTION ( 'NONE',  ( 1.000000000000000000, 0.000000000000000000, 0.000000000000000000 ) ) ;
#19064 = VECTOR ( 'NONE', #3696, 999.9999999999998863 ) ;
#19065 = DIRECTION ( 'NONE',  ( -0.000000000000000000, 0.1736481776669307198, -0.9848077530122080203 ) ) ;
#19066 = DIRECTION ( 'NONE',  ( -0.000000000000000000, -0.8660254037844397068, -0.4999999999999978906 ) ) ;
#19067 = CARTESIAN_POINT ( 'NONE',  ( -4.853911725310227077, -4.187068189119697692, 33.49521262558774026 ) ) ;
#19068 = CARTESIAN_POINT ( 'NONE',  ( -19.50000000000000000, -3.499999999999999556, 29.75000000000000355 ) ) ;
#19069 = ORIENTED_EDGE ( 'NONE', *, *, #29492, .F. ) ;
#19070 = EDGE_LOOP ( 'NONE', ( #66329, #88051 ) ) ;
#19071 = AXIS2_PLACEMENT_3D ( 'NONE', #38179, #9821, #72404 ) ;
#19072 = ORIENTED_EDGE ( 'NONE', *, *, #32911, .F. ) ;
#19075 = ORIENTED_EDGE ( 'NONE', *, *, #10202, .T. ) ;
#19074 = EDGE_CURVE ( 'NONE', #23084, #67515, #24459, .T. ) ;
#19073 = CARTESIAN_POINT ( 'NONE',  ( -13.45069776397551742, -12.34228464037088280, 31.77849191805838558 ) ) ;
#19077 = CARTESIAN_POINT ( 'NONE',  ( -5.999999999999998224, -3.513871655860378418, 32.76840700105978499 ) ) ;
#19076 = CARTESIAN_POINT ( 'NONE',  ( 7.622668902429897919, -3.236172620538810385, 32.36188796281390267 ) ) ;
#19078 = CARTESIAN_POINT ( 'NONE',  ( 16.02323579422162680, -7.722926236386454590, 34.74524107206102030 ) ) ;
#19079 = CYLINDRICAL_SURFACE ( 'NONE', #86876, 0.2499999999999973355 ) ;
#19080 = FACE_BOUND ( 'NONE', #26655, .T. ) ;
#19081 = ORIENTED_EDGE ( 'NONE', *, *, #18308, .F. ) ;
#19082 = EDGE_CURVE ( 'NONE', #57294, #80708, #45414, .T. ) ;
#19083 = VERTEX_POINT ( 'NONE', #87086 ) ;
#19084 = CARTESIAN_POINT ( 'NONE',  ( 17.32686848630112308, -5.766571408460170467, 34.70601412856602508 ) ) ;
#19085 = EDGE_LOOP ( 'NONE', ( #20370, #1239 ) ) ;
#19086 = FACE_BOUND ( 'NONE', #35534, .T. ) ;
#19087 = DIRECTION ( 'NONE',  ( -0.000000000000000000, -0.7660444431189791237, -0.6427876096865379196 ) ) ;
#19088 = B_SPLINE_CURVE_WITH_KNOTS ( 'NONE', 3,
 ( #65631, #23759, #71956, #37728, #38173, #52125, #31875, #37279, #64745, #30092 ),
 .UNSPECIFIED., .F., .F.,
 ( 4, 2, 2, 2, 4 ),
 ( 0.0007817246256747460882, 0.0009771112852218892010, 0.001172497944769032314, 0.001367884604316175210, 0.001563271263863318323 ),
 .UNSPECIFIED. ) ;
#19089 = CARTESIAN_POINT ( 'NONE',  ( 7.976198902073619479, -2.254550872974306674, 29.97347326024527092 ) ) ;
#19090 = EDGE_LOOP ( 'NONE', ( #32436, #51061 ) ) ;
#19091 = CARTESIAN_POINT ( 'NONE',  ( -7.053767526187233905, -9.929715669179216775, 34.40415004197138416 ) ) ;
#19092 = DIRECTION ( 'NONE',  ( -0.000000000000000000, 1.000000000000000000, -0.000000000000000000 ) ) ;
#19093 = CARTESIAN_POINT ( 'NONE',  ( -2.115085314324983479, -5.372444627205700485, 13.85595217397070478 ) ) ;
#19094 = ORIENTED_EDGE ( 'NONE', *, *, #44420, .F. ) ;
#19095 = B_SPLINE_CURVE_WITH_KNOTS ( 'NONE', 3,
 ( #12828, #88512, #644, #69104, #34865, #62334, #47494, #48379, #40313, #61011 ),
 .UNSPECIFIED., .F., .F.,
 ( 4, 2, 2, 2, 4 ),
 ( 0.000000000000000000, 0.0001954339857564079894, 0.0003908679715128159787, 0.0005863019572692239681, 0.0007817359430256319575 ),
 .UNSPECIFIED. ) ;
#19096 = CARTESIAN_POINT ( 'NONE',  ( -7.780898706641007578, -8.656820664281605460, 34.87096338111211224 ) ) ;
#19097 = CARTESIAN_POINT ( 'NONE',  ( -18.00000000000012079, -5.219633306517615701, 34.19971097300220464 ) ) ;
#19098 = EDGE_CURVE ( 'NONE', #5646, #2479, #65452, .T. ) ;
#19099 = CARTESIAN_POINT ( 'NONE',  ( -3.230769230769229949, -2.708943851104267164, 35.45975837776705220 ) ) ;
#19100 = ORIENTED_EDGE ( 'NONE', *, *, #65978, .T. ) ;
#19101 = EDGE_CURVE ( 'NONE', #78927, #7315, #20628, .T. ) ;
#19102 = LINE ( 'NONE', #40268, #67533 ) ;
#19104 = CARTESIAN_POINT ( 'NONE',  ( -15.45425417449318317, -4.386631170607604879, 33.66268669641500111 ) ) ;
#19103 = VECTOR ( 'NONE', #15143, 1000.000000000000227 ) ;
#19105 = VERTEX_POINT ( 'NONE', #74002 ) ;
#19106 = CYLINDRICAL_SURFACE ( 'NONE', #75912, 0.2500000000000008882 ) ;
#19107 = LINE ( 'NONE', #12346, #33967 ) ;
#19108 = CARTESIAN_POINT ( 'NONE',  ( 0.5923289025054110368, -10.70102852606553157, 33.91149625220312913 ) ) ;
#19109 = DIRECTION ( 'NONE',  ( -0.000000000000000000, -5.102127870520021228E-17, -1.000000000000000000 ) ) ;
#19110 = CARTESIAN_POINT ( 'NONE',  ( -16.15384615384627409, -4.481592998941358097, 33.73612834414048933 ) ) ;
#19111 = CARTESIAN_POINT ( 'NONE',  ( 6.700150705560775855, -9.086856451489516928, 34.49173150075333183 ) ) ;
#19113 = CARTESIAN_POINT ( 'NONE',  ( 9.823098133274644539, -4.684288915650983043, 34.18129842949671371 ) ) ;
#19112 = CARTESIAN_POINT ( 'NONE',  ( 6.250054311638313820, -11.79725096376909299, 32.30694842903960762 ) ) ;
#19114 = LINE ( 'NONE', #66407, #12298 ) ;
#19115 = CARTESIAN_POINT ( 'NONE',  ( -6.700297381808512753, -2.847695495035524882, 31.58253572463339509 ) ) ;
#19116 = CARTESIAN_POINT ( 'NONE',  ( 1.200186371490561621, -10.22469193450123193, 26.95125670625849068 ) ) ;
#19117 = ORIENTED_EDGE ( 'NONE', *, *, #70213, .T. ) ;
#19118 = CARTESIAN_POINT ( 'NONE',  ( -4.087778820496076548, -5.471508081941601098, 34.59228464037088457 ) ) ;
#19119 = EDGE_LOOP ( 'NONE', ( #51920, #56415, #17380, #55887 ) ) ;
#19120 = ORIENTED_EDGE ( 'NONE', *, *, #4631, .F. ) ;
#19121 = LINE ( 'NONE', #47019, #58472 ) ;
#19122 = ORIENTED_EDGE ( 'NONE', *, *, #1086, .F. ) ;
#19123 = CARTESIAN_POINT ( 'NONE',  ( -0.4615384615384611200, -13.04860791097971706, 34.73218667398347037 ) ) ;
#19124 = CARTESIAN_POINT ( 'NONE',  ( 2.750000000000008438, -8.639087296525996607, 14.54687500000000178 ) ) ;
#19125 = DIRECTION ( 'NONE',  ( -0.000000000000000000, -5.102127870520021228E-17, -1.000000000000000000 ) ) ;
#19126 = CARTESIAN_POINT ( 'NONE',  ( 10.74617505635156789, -2.494656445102012565, 31.33466734024120015 ) ) ;
#19127 = CARTESIAN_POINT ( 'NONE',  ( 9.822833130541338775, -9.503571793651731880, 34.60286762892837942 ) ) ;
#19128 = CARTESIAN_POINT ( 'NONE',  ( -8.638438961405983108, -4.809403383903225304, 33.96459661697924304 ) ) ;
#19129 = CARTESIAN_POINT ( 'NONE',  ( -15.48074597481782178, -4.818429247618089661, 34.26397095200675125 ) ) ;
#19130 = FACE_OUTER_BOUND ( 'NONE', #56912, .T. ) ;
#19131 = CARTESIAN_POINT ( 'NONE',  ( -1.553300858899125059, -3.750000000000009326, 22.82812500000000355 ) ) ;
#19132 = CARTESIAN_POINT ( 'NONE',  ( 14.30769230769231015, -3.669653830205710676, 35.88435417666054406 ) ) ;
#19133 = DIRECTION ( 'NONE',  ( -0.000000000000000000, -0.000000000000000000, -1.000000000000000000 ) ) ;
#19134 = CARTESIAN_POINT ( 'NONE',  ( 5.750023255951409951, -3.436278759898155677, 33.07459398097509506 ) ) ;
#19135 = VECTOR ( 'NONE', #40802, 1000.000000000000000 ) ;
#19136 = EDGE_CURVE ( 'NONE', #44956, #9090, #59585, .T. ) ;
#19137 = AXIS2_PLACEMENT_3D ( 'NONE', #48848, #76321, #14628 ) ;
#19138 = VERTEX_POINT ( 'NONE', #5541 ) ;
#19139 = VERTEX_POINT ( 'NONE', #66791 ) ;
#19140 = CARTESIAN_POINT ( 'NONE',  ( -11.28851602011339672, -5.852078868378309373, 34.47109172314383585 ) ) ;
#19141 = FACE_OUTER_BOUND ( 'NONE', #78182, .T. ) ;
#19142 = DIRECTION ( 'NONE',  ( -0.000000000000000000, 0.5000000000000011102, -0.8660254037844380415 ) ) ;
#19143 = CARTESIAN_POINT ( 'NONE',  ( -6.130691466667561151, -3.530157926970578508, 32.79014554554150607 ) ) ;
#19144 = ADVANCED_FACE ( 'NONE', ( #79425, #44726 ), #32556, .F. ) ;
#19145 = CARTESIAN_POINT ( 'NONE',  ( 8.703960323269994248, -4.481592998940162609, 33.73612834413957984 ) ) ;
#19146 = AXIS2_PLACEMENT_3D ( 'NONE', #62556, #62993, #48162 ) ;
#19147 = CARTESIAN_POINT ( 'NONE',  ( -16.40382288478850725, -9.148715823498378086, 34.47080413974185120 ) ) ;
#19148 = EDGE_CURVE ( 'NONE', #87474, #23981, #60028, .T. ) ;
#19149 = ORIENTED_EDGE ( 'NONE', *, *, #3036, .T. ) ;
#19150 = CARTESIAN_POINT ( 'NONE',  ( -18.00000000000000000, -1.546599033411489632, 31.05360187035683239 ) ) ;
#19151 = ORIENTED_EDGE ( 'NONE', *, *, #85914, .T. ) ;
#19152 = EDGE_CURVE ( 'NONE', #29922, #78448, #4601, .T. ) ;
#19153 = ORIENTED_EDGE ( 'NONE', *, *, #31105, .T. ) ;
#19154 = CARTESIAN_POINT ( 'NONE',  ( -8.519285359852727169, -4.932303261841489928, 34.32971442181322885 ) ) ;
#19155 = CARTESIAN_POINT ( 'NONE',  ( -14.08491263871423982, -6.717445702608402236, 34.94155399931962336 ) ) ;
#19156 = CARTESIAN_POINT ( 'NONE',  ( -4.403822897894743349, -12.65889640711025521, 30.72598325615533454 ) ) ;
#19157 = CARTESIAN_POINT ( 'NONE',  ( 30.00000000000000000, -15.00000000000000000, 3.000000000000000000 ) ) ;
#19158 = FACE_OUTER_BOUND ( 'NONE', #67542, .T. ) ;
#19160 = EDGE_CURVE ( 'NONE', #26482, #48447, #46076, .T. ) ;
#19159 = ORIENTED_EDGE ( 'NONE', *, *, #449, .T. ) ;
#19161 = AXIS2_PLACEMENT_3D ( 'NONE', #45936, #73428, #87398 ) ;
#19162 = B_SPLINE_CURVE_WITH_KNOTS ( 'NONE', 3,
 ( #18539, #51390, #30705, #30274, #86564, #45997, #58171, #24834, #17191, #44649 ),
 .UNSPECIFIED., .F., .F.,
 ( 4, 2, 2, 2, 4 ),
 ( 0.000000000000000000, 0.0001954339857564081249, 0.0003908679715128162498, 0.0005863019572692244018, 0.0007817359430256324996 ),
 .UNSPECIFIED. ) ;
#19163 = VECTOR ( 'NONE', #71442, 1000.000000000000227 ) ;
#19164 = ORIENTED_EDGE ( 'NONE', *, *, #39305, .F. ) ;
#19165 = EDGE_LOOP ( 'NONE', ( #19081, #29717 ) ) ;
#19166 = CARTESIAN_POINT ( 'NONE',  ( 5.869308533332442401, -2.541943142973490666, 30.39792223712631980 ) ) ;
#19167 = CARTESIAN_POINT ( 'NONE',  ( -0.3962833220256234412, -10.33852847137154107, 34.16647553114620450 ) ) ;
#19168 = ADVANCED_FACE ( 'NONE', ( #67244 ), #66346, .F. ) ;
#19169 = LINE ( 'NONE', #44844, #4861 ) ;
#19170 = CARTESIAN_POINT ( 'NONE',  ( 4.153846153846154188, -13.20930481340135110, 34.54067556320372745 ) ) ;
#19171 = CARTESIAN_POINT ( 'NONE',  ( 17.93391762063986050, -2.833524468853757305, 32.15551576947924417 ) ) ;
#19172 = EDGE_CURVE ( 'NONE', #4579, #83312, #16392, .T. ) ;
#19173 = DIRECTION ( 'NONE',  ( 0.000000000000000000, 0.9848077530122072432, -0.1736481776669354937 ) ) ;
#19174 = VERTEX_POINT ( 'NONE', #27576 ) ;
#19175 = EDGE_LOOP ( 'NONE', ( #34540, #16399, #80837, #56876 ) ) ;
#19177 = ORIENTED_EDGE ( 'NONE', *, *, #75759, .T. ) ;
#19176 = CARTESIAN_POINT ( 'NONE',  ( 17.29970261819148192, -12.44528174975671853, 30.48912976160715615 ) ) ;
#19178 = CARTESIAN_POINT ( 'NONE',  ( -5.999999999999998224, -1.466349020453238561, 30.81389545987213907 ) ) ;
#19179 = CARTESIAN_POINT ( 'NONE',  ( 12.46153846153846168, -8.164416787775445883, 34.95778746994557906 ) ) ;
#19180 = CARTESIAN_POINT ( 'NONE',  ( -2.651650429449565305, -4.848349570550461785, 15.25000000000000000 ) ) ;
#19181 = ORIENTED_EDGE ( 'NONE', *, *, #81536, .T. ) ;
#19182 = AXIS2_PLACEMENT_3D ( 'NONE', #68668, #6969, #47057 ) ;
#19183 = EDGE_CURVE ( 'NONE', #81991, #29682, #48614, .T. ) ;
#19184 = CARTESIAN_POINT ( 'NONE',  ( -1.161835715637318689, -11.60474049983370648, 33.02348890104160262 ) ) ;
#19185 = EDGE_LOOP ( 'NONE', ( #44579, #60243, #81332, #19164 ) ) ;
#19186 = CARTESIAN_POINT ( 'NONE',  ( 13.51514082284902862, -11.04252011169590020, 33.62494198852677130 ) ) ;
#19187 = CARTESIAN_POINT ( 'NONE',  ( 0.2115617174898700992, -11.47974371597208076, 33.17467449705390692 ) ) ;
#19188 = AXIS2_PLACEMENT_3D ( 'NONE', #78936, #53236, #80738 ) ;
#19189 = FACE_BOUND ( 'NONE', #88005, .T. ) ;
#19190 = CARTESIAN_POINT ( 'NONE',  ( -4.946131269098289707, -12.11778462344220841, 31.66786338562085135 ) ) ;
#19191 = VECTOR ( 'NONE', #17061, 1000.000000000000000 ) ;
#19192 = CARTESIAN_POINT ( 'NONE',  ( -14.05769230769230660, -2.499999999999998668, 29.75000000000000355 ) ) ;
#19193 = VERTEX_POINT ( 'NONE', #68560 ) ;
#19194 = CARTESIAN_POINT ( 'NONE',  ( 11.53846153846153832, -11.35647404775217417, 33.31231777344666511 ) ) ;
#19195 = CARTESIAN_POINT ( 'NONE',  ( -1.216139819124259613, -4.489159616049914980, 13.64598852175840626 ) ) ;
#19196 = FACE_OUTER_BOUND ( 'NONE', #41609, .T. ) ;
#19198 = ORIENTED_EDGE ( 'NONE', *, *, #2543, .T. ) ;
#19197 = EDGE_CURVE ( 'NONE', #34055, #78547, #62677, .T. ) ;
#19199 = B_SPLINE_CURVE_WITH_KNOTS ( 'NONE', 3,
 ( #3350, #30822, #58292, #24066, #51514, #79015, #17315, #72253, #51975, #41812 ),
 .UNSPECIFIED., .F., .F.,
 ( 4, 2, 2, 2, 4 ),
 ( 0.0007817246336856291692, 0.0009771112958940103739, 0.001172497958102391470, 0.001367884620310772566, 0.001563271282519153879 ),
 .UNSPECIFIED. ) ;
#19200 = LINE ( 'NONE', #11561, #44388 ) ;
#19201 = CARTESIAN_POINT ( 'NONE',  ( -15.00798956179115962, -5.827830569534417471, 34.72679350104403539 ) ) ;
#19202 = CARTESIAN_POINT ( 'NONE',  ( -12.71156169883142795, -12.22074536777954989, 31.39888409691088356 ) ) ;
#19203 = CARTESIAN_POINT ( 'NONE',  ( -8.769230769230768274, -8.318370150425687726, 35.83090037661290239 ) ) ;
#19204 = EDGE_CURVE ( 'NONE', #75911, #6016, #17356, .T. ) ;
#19206 = EDGE_CURVE ( 'NONE', #8429, #65065, #78604, .T. ) ;
#19205 = LINE ( 'NONE', #80014, #78896 ) ;
#19207 = FACE_BOUND ( 'NONE', #45401, .T. ) ;
#19209 = CARTESIAN_POINT ( 'NONE',  ( 4.219101293358990645, -12.70778746994558439, 30.41441678777537305 ) ) ;
#19208 = LINE ( 'NONE', #73720, #69140 ) ;
#19210 = CARTESIAN_POINT ( 'NONE',  ( -15.23076923076922995, -1.242168528481310874, 33.36296068462461051 ) ) ;
#19212 = FACE_OUTER_BOUND ( 'NONE', #54201, .T. ) ;
#19211 = DIRECTION ( 'NONE',  ( -0.000000000000000000, 0.1736481776669307198, -0.9848077530122080203 ) ) ;
#19213 = CARTESIAN_POINT ( 'NONE',  ( 8.834485908743603844, -12.70778746994558439, 30.41441678777536595 ) ) ;
#19214 = CARTESIAN_POINT ( 'NONE',  ( -3.724691934501229262, -9.114399933863657211, 24.76375670625848713 ) ) ;
#19215 = EDGE_CURVE ( 'NONE', #81105, #57687, #78177, .T. ) ;
#19216 = ORIENTED_EDGE ( 'NONE', *, *, #41094, .T. ) ;
#19217 = CARTESIAN_POINT ( 'NONE',  ( -12.52729188985179221, -7.249945578846652694, 34.99404164642496795 ) ) ;
#19218 = ORIENTED_EDGE ( 'NONE', *, *, #74713, .F. ) ;
#19219 = CARTESIAN_POINT ( 'NONE',  ( -18.00000000000000000, -3.322132147404558200, 32.92929555188717217 ) ) ;
#19220 = EDGE_LOOP ( 'NONE', ( #51755, #45089, #67399, #54125, #87305 ) ) ;
#19221 = CARTESIAN_POINT ( 'NONE',  ( 2.307692307692309264, -2.292212530054420494, 30.41441678777542634 ) ) ;
#19222 = DIRECTION ( 'NONE',  ( 0.000000000000000000, 0.000000000000000000, -1.000000000000000000 ) ) ;
#19224 = EDGE_LOOP ( 'NONE', ( #69815, #10270, #3989, #81479 ) ) ;
#19223 = CARTESIAN_POINT ( 'NONE',  ( -4.826868657009622865, -9.233818618650603938, 34.70587769442853698 ) ) ;
#19225 = CARTESIAN_POINT ( 'NONE',  ( -16.82697766754503377, -2.341251567377310217, 30.72681386836322659 ) ) ;
#19226 = DIRECTION ( 'NONE',  ( -0.000000000000000000, 0.9396926207859092051, -0.3420201433256662704 ) ) ;
#19227 = CARTESIAN_POINT ( 'NONE',  ( -1.614399933863656544, -3.775308065498769405, 25.07625670625849423 ) ) ;
#19228 = B_SPLINE_CURVE_WITH_KNOTS ( 'NONE', 3,
 ( #83319, #28817, #20718, #14404, #40999, #35116, #61248, #33791, #62580, #49524 ),
 .UNSPECIFIED., .F., .F.,
 ( 4, 2, 2, 2, 4 ),
 ( 0.0007817359527651104954, 0.0009771254036996493593, 0.001172514854634188223, 0.001367904305568727087, 0.001563293756503265951 ),
 .UNSPECIFIED. ) ;
#19229 = CARTESIAN_POINT ( 'NONE',  ( 4.376857505459002873, -10.61302985866383963, 33.66295027996417843 ) ) ;
#19230 = CARTESIAN_POINT ( 'NONE',  ( -7.173053667125515176, -12.65889640711025521, 30.72598325615533454 ) ) ;
#19231 = VECTOR ( 'NONE', #27994, 1000.000000000000227 ) ;
#19232 = CARTESIAN_POINT ( 'NONE',  ( -4.854143407945010757, -12.11081565061823717, 32.26097654155341843 ) ) ;
#19233 = CARTESIAN_POINT ( 'NONE',  ( -0.6844654204453100022, -8.282780595021769443, 34.94152052738834868 ) ) ;
#19234 = CARTESIAN_POINT ( 'NONE',  ( 0.2386122440223135410, -11.24512374952581872, 33.06303171183252942 ) ) ;
#19235 = CARTESIAN_POINT ( 'NONE',  ( -8.899922235898328537, -8.999036380462717588, 34.52022231692819076 ) ) ;
#19236 = CARTESIAN_POINT ( 'NONE',  ( -3.749999999999997780, -7.438900925035489387, 19.09561829374150932 ) ) ;
#19237 = CARTESIAN_POINT ( 'NONE',  ( 5.326868486301116867, -2.589246495874657938, 31.60778113518102828 ) ) ;
#19238 = CARTESIAN_POINT ( 'NONE',  ( 8.096099255531889582, -9.357781135181031829, 34.66075350412533851 ) ) ;
#19239 = ORIENTED_EDGE ( 'NONE', *, *, #23278, .T. ) ;
#19240 = CARTESIAN_POINT ( 'NONE',  ( 16.40390057375961064, -4.818054556918155207, 34.26375889529406749 ) ) ;
#19241 = CARTESIAN_POINT ( 'NONE',  ( -15.23076923076922995, -11.11383981884818262, 36.00935417666054406 ) ) ;
#19242 = CARTESIAN_POINT ( 'NONE',  ( 3.750000000000001776, -7.561099074964511502, 18.47061829374151287 ) ) ;
#19243 = CARTESIAN_POINT ( 'NONE',  ( -10.83886953994894853, -2.612411019501189369, 31.66733052389439962 ) ) ;
#19244 = CARTESIAN_POINT ( 'NONE',  ( 5.076923076923075762, -6.343179335718451384, 34.87096338111211935 ) ) ;
#19245 = EDGE_LOOP ( 'NONE', ( #37499, #47780, #64998, #32145 ) ) ;
#19246 = CARTESIAN_POINT ( 'NONE',  ( -3.262820512820514107, -3.499999999999999556, 29.75000000000000355 ) ) ;
#19247 = CARTESIAN_POINT ( 'NONE',  ( -19.50000000000000000, -3.499999999999999556, 29.75000000000000355 ) ) ;
#19249 = ORIENTED_EDGE ( 'NONE', *, *, #44932, .T. ) ;
#19248 = CARTESIAN_POINT ( 'NONE',  ( 8.992010438208827949, -2.612705202774698421, 31.66806509827799943 ) ) ;
#19250 = CARTESIAN_POINT ( 'NONE',  ( -13.44988538517170440, -10.33852847137145048, 34.16647553114627556 ) ) ;
#19251 = CARTESIAN_POINT ( 'NONE',  ( -2.373015223184481215, -7.749976743299137993, 34.99404534957040624 ) ) ;
#19252 = CARTESIAN_POINT ( 'NONE',  ( 2.241608896736428047, -12.37446782046654192, 30.86335684631486487 ) ) ;
#19253 = CARTESIAN_POINT ( 'NONE',  ( 11.76124107972994359, -9.332535724633409302, 34.40230450496446934 ) ) ;
#19254 = VERTEX_POINT ( 'NONE', #13180 ) ;
#19255 = CARTESIAN_POINT ( 'NONE',  ( 6.923076923076924238, -9.819645486525091727, 36.12317359536749706 ) ) ;
#19256 = DIRECTION ( 'NONE',  ( -0.000000000000000000, 1.000000000000000000, -0.000000000000000000 ) ) ;
#19257 = VECTOR ( 'NONE', #70309, 1000.000000000000000 ) ;
#19258 = CARTESIAN_POINT ( 'NONE',  ( -13.38461538461550759, -8.656820664282941280, 34.87096338111179961 ) ) ;
#19259 = ORIENTED_EDGE ( 'NONE', *, *, #79178, .T. ) ;
#19260 = VERTEX_POINT ( 'NONE', #20815 ) ;
#19261 = B_SPLINE_CURVE_WITH_KNOTS ( 'NONE', 3,
 ( #9195, #76758, #69111, #70887, #77193, #34873, #56483, #15502, #7416, #21809 ),
 .UNSPECIFIED., .F., .F.,
 ( 4, 2, 2, 2, 4 ),
 ( 0.000000000000000000, 0.0001954311564186881213, 0.0003908623128373762425, 0.0005862934692560643367, 0.0007817246256747524850 ),
 .UNSPECIFIED. ) ;
#19262 = AXIS2_PLACEMENT_3D ( 'NONE', #10505, #65440, #3733 ) ;
#19263 = ORIENTED_EDGE ( 'NONE', *, *, #49174, .F. ) ;
#19264 = VECTOR ( 'NONE', #45165, 1000.000000000000227 ) ;
#19265 = CARTESIAN_POINT ( 'NONE',  ( -9.942330929600657896, -2.823816976329319051, 31.52131813110795733 ) ) ;
#19266 = CYLINDRICAL_SURFACE ( 'NONE', #45755, 8.000000000000000000 ) ;
#19267 = DIRECTION ( 'NONE',  ( -0.000000000000000000, -0.3420201433256694901, -0.9396926207859082059 ) ) ;
#19268 = ADVANCED_FACE ( 'NONE', ( #12735 ), #48284, .F. ) ;
#19269 = CARTESIAN_POINT ( 'NONE',  ( -7.846153846153844924, -10.67929555188718282, 33.92786785259544047 ) ) ;
#19270 = VERTEX_POINT ( 'NONE', #67682 ) ;
#19271 = ORIENTED_EDGE ( 'NONE', *, *, #17975, .T. ) ;
#19272 = ORIENTED_EDGE ( 'NONE', *, *, #29559, .F. ) ;
#19274 = VERTEX_POINT ( 'NONE', #40659 ) ;
#19273 = DIRECTION ( 'NONE',  ( -0.000000000000000000, -0.9848077530122085754, -0.1736481776669273613 ) ) ;
#19275 = CARTESIAN_POINT ( 'NONE',  ( 3.230769230769546141, -2.255955759149395501, 30.00000000000324363 ) ) ;
#19276 = CARTESIAN_POINT ( 'NONE',  ( -0.4615384615384611200, -12.29105614889573062, 35.45975837776705220 ) ) ;
#19277 = FACE_OUTER_BOUND ( 'NONE', #1663, .T. ) ;
#19278 = EDGE_CURVE ( 'NONE', #39220, #48663, #71097, .T. ) ;
#19279 = LINE ( 'NONE', #6645, #13660 ) ;
#19280 = ORIENTED_EDGE ( 'NONE', *, *, #62108, .F. ) ;
#19281 = VERTEX_POINT ( 'NONE', #84754 ) ;
#19282 = AXIS2_PLACEMENT_3D ( 'NONE', #27944, #22512, #22074 ) ;
#19283 = VERTEX_POINT ( 'NONE', #57706 ) ;
#19284 = CARTESIAN_POINT ( 'NONE',  ( 14.43848274865925774, -10.70102852606553157, 33.91149625220312913 ) ) ;
#19286 = VERTEX_POINT ( 'NONE', #56812 ) ;
#19285 = CARTESIAN_POINT ( 'NONE',  ( -8.769230769230892619, -11.67786785259630911, 32.92929555188603530 ) ) ;
#19287 = CARTESIAN_POINT ( 'NONE',  ( 17.07692307692295586, -5.941354392335915335, 34.76329471203413846 ) ) ;
#19288 = LINE ( 'NONE', #26047, #12277 ) ;
#19289 = VERTEX_POINT ( 'NONE', #77537 ) ;
#19290 = EDGE_CURVE ( 'NONE', #35211, #37367, #29163, .T. ) ;
#19291 = CARTESIAN_POINT ( 'NONE',  ( 16.21991450484859598, -8.120952969808772792, 34.71129190929999453 ) ) ;
#19292 = CARTESIAN_POINT ( 'NONE',  ( -3.903791842207837259, -4.943051570960391494, 34.04725096376909477 ) ) ;
#19293 = DIRECTION ( 'NONE',  ( 0.000000000000000000, 0.000000000000000000, -1.000000000000000000 ) ) ;
#19294 = FACE_BOUND ( 'NONE', #57557, .T. ) ;
#19295 = CARTESIAN_POINT ( 'NONE',  ( -0.5276218724943426697, -9.780366693483667717, 34.19971097300155805 ) ) ;
#19296 = LINE ( 'NONE', #12982, #81679 ) ;
#19297 = CARTESIAN_POINT ( 'NONE',  ( 15.90384615384615330, -7.500000000000001776, 35.00000000000000000 ) ) ;
#19299 = DIRECTION ( 'NONE',  ( 0.000000000000000000, 0.4999999999999960032, -0.8660254037844410391 ) ) ;
#19298 = DIRECTION ( 'NONE',  ( 1.000000000000000000, 0.000000000000000000, 0.000000000000000000 ) ) ;
#19300 = CARTESIAN_POINT ( 'NONE',  ( 16.15384615384603251, -6.835583212225970762, 34.95778746994575670 ) ) ;
#19301 = CARTESIAN_POINT ( 'NONE',  ( 13.38461538461538680, -2.517432740324522911, 35.29906147534542527 ) ) ;
#19302 = VERTEX_POINT ( 'NONE', #63122 ) ;
#19303 = CARTESIAN_POINT ( 'NONE',  ( -17.07692307692307665, -5.471508081941601098, 34.59228464037088457 ) ) ;
#19304 = CARTESIAN_POINT ( 'NONE',  ( -13.38461538461538325, -3.937682226553329556, 33.60647404775216529 ) ) ;
#19305 = ORIENTED_EDGE ( 'NONE', *, *, #33220, .F. ) ;
#19306 = ORIENTED_EDGE ( 'NONE', *, *, #23798, .F. ) ;
#19307 = DIRECTION ( 'NONE',  ( 0.000000000000000000, 1.000000000000000000, 5.102127870520020612E-17 ) ) ;
#19308 = CARTESIAN_POINT ( 'NONE',  ( 15.93091993633000136, -3.586966769969702540, 32.86292498521069660 ) ) ;
#19309 = CARTESIAN_POINT ( 'NONE',  ( -15.29652603328353955, -7.249945686854186278, 34.74374336980224598 ) ) ;
#19310 = EDGE_LOOP ( 'NONE', ( #28637, #73773, #20944, #49197 ) ) ;
#19312 = EDGE_CURVE ( 'NONE', #69245, #77080, #49621, .T. ) ;
#19311 = CARTESIAN_POINT ( 'NONE',  ( 14.53070365930516061, -9.086983370893049639, 34.49168942202179267 ) ) ;
#19313 = ADVANCED_FACE ( 'NONE', ( #36119 ), #16278, .T. ) ;
#19314 = CARTESIAN_POINT ( 'NONE',  ( -13.38461538461550759, -10.33852847137269571, 34.16647553114546554 ) ) ;
#19315 = AXIS2_PLACEMENT_3D ( 'NONE', #55062, #67255, #27590 ) ;
#19316 = FACE_BOUND ( 'NONE', #6549, .T. ) ;
#19318 = CARTESIAN_POINT ( 'NONE',  ( -11.00641025641025550, -7.500000000000000000, 29.75000000000000355 ) ) ;
#19317 = CARTESIAN_POINT ( 'NONE',  ( -39.05038313613820122, -2.249999999999998668, 29.75000000000000355 ) ) ;
#19319 = CARTESIAN_POINT ( 'NONE',  ( 2.307692307692309264, -6.343179335718451384, 34.87096338111211935 ) ) ;
#19320 = CARTESIAN_POINT ( 'NONE',  ( -8.769230769230768274, -9.819645486525091727, 36.12317359536749706 ) ) ;
#19321 = CARTESIAN_POINT ( 'NONE',  ( -8.703162418228332697, -12.10708131394839882, 31.69288490824020954 ) ) ;
#19322 = APPLICATION_CONTEXT ( 'automotive_design' ) ;
#19323 = CARTESIAN_POINT ( 'NONE',  ( -1.929879867024197893E-14, -3.750000000000000000, 21.65625000000000355 ) ) ;
#19324 = EDGE_LOOP ( 'NONE', ( #13265, #78729, #20761, #67941 ) ) ;
#19325 = CIRCLE ( 'NONE', #66825, 4.000000000000000000 ) ;
#19326 = ORIENTED_EDGE ( 'NONE', *, *, #74241, .F. ) ;
#19327 = AXIS2_PLACEMENT_3D ( 'NONE', #4027, #52219, #73848 ) ;
#19328 = FACE_OUTER_BOUND ( 'NONE', #54263, .T. ) ;
#19329 = CARTESIAN_POINT ( 'NONE',  ( 16.28463796167094557, -6.413143153341454017, 34.63066358083362672 ) ) ;
#19330 = FACE_OUTER_BOUND ( 'NONE', #15044, .T. ) ;
#19331 = CARTESIAN_POINT ( 'NONE',  ( -0.2115384615383979761, -7.434744429011175271, 34.75000000000000711 ) ) ;
#19332 = CARTESIAN_POINT ( 'NONE',  ( -15.16470087976679082, -2.721908614388772296, 31.22303859784725333 ) ) ;
#19333 = CARTESIAN_POINT ( 'NONE',  ( 2.651650429449569302, -10.15165042944953733, 20.87500000000000000 ) ) ;
#19334 = CARTESIAN_POINT ( 'NONE',  ( -7.715362038329059757, -8.147973898785416225, 34.70805048591653730 ) ) ;
#19335 = DIRECTION ( 'NONE',  ( 0.000000000000000000, 0.7660444431189807890, 0.6427876096865361433 ) ) ;
#19336 = FACE_BOUND ( 'NONE', #83331, .T. ) ;
#19337 = CARTESIAN_POINT ( 'NONE',  ( 5.777073041093149897, -10.01117774369187252, 34.36070679894347535 ) ) ;
#19338 = CARTESIAN_POINT ( 'NONE',  ( -9.942330929600657896, -11.37209801155882971, 32.91403422569032955 ) ) ;
#19339 = CARTESIAN_POINT ( 'NONE',  ( 13.25392391794783187, -4.118384482072086072, 33.43331474514187107 ) ) ;
#19340 = B_SPLINE_CURVE_WITH_KNOTS ( 'NONE', 3,
 ( #28548, #83050, #62752, #38290, #56007, #3604, #76729, #8722, #50128, #15033 ),
 .UNSPECIFIED., .F., .F.,
 ( 4, 2, 2, 2, 4 ),
 ( 0.000000000000000000, 0.0001954339857564063360, 0.0003908679715128126719, 0.0005863019572692189808, 0.0007817359430256253438 ),
 .UNSPECIFIED. ) ;
#19341 = CARTESIAN_POINT ( 'NONE',  ( -19.50000000000000000, -3.499999999999999556, 29.75000000000000355 ) ) ;
#19342 = CARTESIAN_POINT ( 'NONE',  ( 4.153846153846154188, -12.37446782046654192, 30.86335684631486131 ) ) ;
#19343 = CARTESIAN_POINT ( 'NONE',  ( -3.296852641725108946, -8.120952969808774569, 34.71129190930000163 ) ) ;
#19344 = CARTESIAN_POINT ( 'NONE',  ( -15.36091644020745051, -10.19110544564092002, 33.96427741523702792 ) ) ;
#19345 = EDGE_LOOP ( 'NONE', ( #6192, #22689, #44127, #64651 ) ) ;
#19346 = CARTESIAN_POINT ( 'NONE',  ( 9.019285189144222059, -4.818054556918156983, 34.26375889529406749 ) ) ;
#19347 = DIRECTION ( 'NONE',  ( -0.000000000000000000, -0.1736481776669307198, -0.9848077530122080203 ) ) ;
#19348 = CARTESIAN_POINT ( 'NONE',  ( -0.06109907496451398579, -10.25000000000000178, 17.53311829374151287 ) ) ;
#19349 = DIRECTION ( 'NONE',  ( -0.000000000000000000, 0.3420201433256694346, -0.9396926207859080948 ) ) ;
#19350 = CARTESIAN_POINT ( 'NONE',  ( -11.40767109749459074, -4.684288915650983043, 34.18129842949671371 ) ) ;
#19352 = ORIENTED_EDGE ( 'NONE', *, *, #85635, .F. ) ;
#19351 = CARTESIAN_POINT ( 'NONE',  ( 10.48490943030889788, -7.276987145209184327, 34.99546412871779211 ) ) ;
#19353 = CARTESIAN_POINT ( 'NONE',  ( -1.409462824231155764E-14, -4.749999999999999112, 22.90625000000000355 ) ) ;
#19354 = CARTESIAN_POINT ( 'NONE',  ( 17.07692307692307665, -2.486705287966279876, 31.30864560766543647 ) ) ;
#19355 = ORIENTED_EDGE ( 'NONE', *, *, #86846, .T. ) ;
#19356 = CARTESIAN_POINT ( 'NONE',  ( -11.31508605268911793, -2.251407671071268712, 29.88021292934943318 ) ) ;
#19357 = VECTOR ( 'NONE', #53659, 1000.000000000000000 ) ;
#19358 = CARTESIAN_POINT ( 'NONE',  ( -17.86920819217521483, -3.530189275343200705, 32.79018710029568240 ) ) ;
#19359 = ORIENTED_EDGE ( 'NONE', *, *, #73893, .F. ) ;
#19360 = CARTESIAN_POINT ( 'NONE',  ( -19.00000000000000000, 0.7500000000000041078, 23.75000000000000000 ) ) ;
#19361 = CARTESIAN_POINT ( 'NONE',  ( -15.36091720050093024, -3.069018819979302926, 32.56621877034667278 ) ) ;
#19362 = DIRECTION ( 'NONE',  ( -0.000000000000000000, -0.6427876096865404731, -0.7660444431189771253 ) ) ;
#19363 = ORIENTED_EDGE ( 'NONE', *, *, #64924, .T. ) ;
#19364 = ORIENTED_EDGE ( 'NONE', *, *, #74843, .F. ) ;
#19365 = ORIENTED_EDGE ( 'NONE', *, *, #60821, .F. ) ;
#19366 = CARTESIAN_POINT ( 'NONE',  ( -16.02332071561251325, -2.372941743896878286, 30.88044141588253311 ) ) ;
#19367 = LINE ( 'NONE', #18926, #57011 ) ;
#19368 = FACE_OUTER_BOUND ( 'NONE', #49953, .T. ) ;
#19369 = CARTESIAN_POINT ( 'NONE',  ( -10.86536134632696715, -2.564618984488975073, 30.55390908950641915 ) ) ;
#19370 = CARTESIAN_POINT ( 'NONE',  ( -5.999999999999998224, -1.242168528481310874, 33.36296068462461051 ) ) ;
#19371 = CARTESIAN_POINT ( 'NONE',  ( 15.23076923076923173, -12.29105614889573062, 35.45975837776705220 ) ) ;
#19372 = CARTESIAN_POINT ( 'NONE',  ( 11.47237812750565666, -11.69971097300155272, 32.46337939537587403 ) ) ;
#19373 = EDGE_CURVE ( 'NONE', #68660, #21721, #49580, .T. ) ;
#19374 = DIRECTION ( 'NONE',  ( 0.000000000000000000, 0.8660254037844377084, -0.5000000000000015543 ) ) ;
#19375 = EDGE_CURVE ( 'NONE', #79832, #57707, #66803, .T. ) ;
#19376 = B_SPLINE_CURVE_WITH_KNOTS ( 'NONE', 3,
 ( #5879, #39226, #19389, #47293, #74337, #12636, #13074, #11748, #54048, #88756 ),
 .UNSPECIFIED., .F., .F.,
 ( 4, 2, 2, 2, 4 ),
 ( 0.0007817246256747463051, 0.0009771112852218896347, 0.001172497944769032747, 0.001367884604316176077, 0.001563271263863319407 ),
 .UNSPECIFIED. ) ;
#19377 = VECTOR ( 'NONE', #69259, 1000.000000000000000 ) ;
#19378 = ORIENTED_EDGE ( 'NONE', *, *, #41998, .T. ) ;
#19379 = ORIENTED_EDGE ( 'NONE', *, *, #86886, .T. ) ;
#19380 = ORIENTED_EDGE ( 'NONE', *, *, #33487, .F. ) ;
#19382 = ORIENTED_EDGE ( 'NONE', *, *, #10662, .F. ) ;
#19381 = CARTESIAN_POINT ( 'NONE',  ( 18.25005441991345734, -9.233818618650598609, 34.70587769442853698 ) ) ;
#19383 = VECTOR ( 'NONE', #22913, 1000.000000000000114 ) ;
#19384 = VECTOR ( 'NONE', #54666, 1000.000000000000000 ) ;
#19385 = ADVANCED_FACE ( 'NONE', ( #85184 ), #50923, .F. ) ;
#19386 = CARTESIAN_POINT ( 'NONE',  ( 11.66898697669518725, -3.625058011473228703, 33.29252011169590020 ) ) ;
#19387 = FACE_OUTER_BOUND ( 'NONE', #61654, .T. ) ;
#19388 = VERTEX_POINT ( 'NONE', #71652 ) ;
#19389 = CARTESIAN_POINT ( 'NONE',  ( -12.33101302330481808, -11.66157788607254098, 32.95092075102925833 ) ) ;
#19390 = ORIENTED_EDGE ( 'NONE', *, *, #82314, .F. ) ;
#19391 = DIRECTION ( 'NONE',  ( 1.000000000000000000, 0.000000000000000000, 0.000000000000000000 ) ) ;
#19392 = VERTEX_POINT ( 'NONE', #56381 ) ;
#19393 = CARTESIAN_POINT ( 'NONE',  ( -24.00000000000000000, -5.499999999999981348, 27.75000000000000000 ) ) ;
#19394 = ADVANCED_FACE ( 'NONE', ( #50055 ), #9089, .F. ) ;
#19395 = CARTESIAN_POINT ( 'NONE',  ( -4.153846153846152411, -3.937682226553329556, 33.60647404775216529 ) ) ;
#19396 = CARTESIAN_POINT ( 'NONE',  ( -9.469344558041020932, -7.369474539155828730, 34.99858011523957657 ) ) ;
#19397 = FACE_BOUND ( 'NONE', #66494, .T. ) ;
#19398 = CARTESIAN_POINT ( 'NONE',  ( -6.000000000000119904, -6.026961402154118908, 34.52809138561165270 ) ) ;
#19399 = CARTESIAN_POINT ( 'NONE',  ( 15.93036122928181975, -3.562934362175799841, 33.22335522853832401 ) ) ;
#19400 = FACE_OUTER_BOUND ( 'NONE', #17795, .T. ) ;
#19401 = LINE ( 'NONE', #68469, #89171 ) ;
#19402 = DIRECTION ( 'NONE',  ( 0.000000000000000000, 0.000000000000000000, 1.000000000000000000 ) ) ;
#19403 = CARTESIAN_POINT ( 'NONE',  ( 10.61538461538461675, -10.67929555188718282, 33.92786785259544047 ) ) ;
#19404 = CARTESIAN_POINT ( 'NONE',  ( -13.16123944391720180, -2.501478030877323455, 29.88021232661721172 ) ) ;
#19405 = VERTEX_POINT ( 'NONE', #9957 ) ;
#19406 = ORIENTED_EDGE ( 'NONE', *, *, #45927, .F. ) ;
#19407 = CIRCLE ( 'NONE', #88419, 3.000000000000000000 ) ;
#19409 = CARTESIAN_POINT ( 'NONE',  ( 2.438484115517093986, -10.54018710029568595, 33.71981072465678864 ) ) ;
#19408 = LINE ( 'NONE', #67602, #31748 ) ;
#19410 = DIRECTION ( 'NONE',  ( -0.000000000000000000, 0.8660254037844399289, -0.4999999999999980016 ) ) ;
#19411 = CARTESIAN_POINT ( 'NONE',  ( -14.37296230824862953, -12.16647553114622049, 32.15551576947930812 ) ) ;
#19412 = CARTESIAN_POINT ( 'NONE',  ( -17.32694630114453460, -12.45566812827425096, 31.48439005359158926 ) ) ;
#19413 = LINE ( 'NONE', #67608, #8785 ) ;
#19414 = ORIENTED_EDGE ( 'NONE', *, *, #24899, .T. ) ;
#19415 = EDGE_CURVE ( 'NONE', #50940, #23267, #18484, .T. ) ;
#19416 = CARTESIAN_POINT ( 'NONE',  ( 2.241608896736428491, -8.973038597847271092, 34.52809138561120506 ) ) ;
#19417 = CARTESIAN_POINT ( 'NONE',  ( 14.30769230769231015, -11.16473453929635440, 33.15142922261926373 ) ) ;
#19418 = DIRECTION ( 'NONE',  ( 0.000000000000000000, 0.7660444431189807890, 0.6427876096865361433 ) ) ;
#19419 = EDGE_CURVE ( 'NONE', #65478, #19138, #15285, .T. ) ;
#19420 = CARTESIAN_POINT ( 'NONE',  ( -6.988346923633241836, -6.835583212224499938, 34.95778746994557906 ) ) ;
#19421 = ORIENTED_EDGE ( 'NONE', *, *, #6437, .F. ) ;
#19422 = VERTEX_POINT ( 'NONE', #18057 ) ;
#19423 = B_SPLINE_CURVE_WITH_KNOTS ( 'NONE', 3,
 ( #56133, #69206, #28669, #1183, #8841, #1639, #63327, #36315, #63767, #55680 ),
 .UNSPECIFIED., .F., .F.,
 ( 4, 2, 2, 2, 4 ),
 ( 0.000000000000000000, 0.0001954339857564055499, 0.0003908679715128110998, 0.0005863019572692165955, 0.0007817359430256221996 ),
 .UNSPECIFIED. ) ;
#19424 = APPLICATION_PROTOCOL_DEFINITION ( 'draft international standard', 'automotive_design', 1998, #82604 ) ;
#19425 = ORIENTED_EDGE ( 'NONE', *, *, #40988, .T. ) ;
#19426 = EDGE_CURVE ( 'NONE', #42127, #35784, #1225, .T. ) ;
#19427 = CARTESIAN_POINT ( 'NONE',  ( 10.36536139116316058, -4.175268141568685643, 33.81360843649122216 ) ) ;
#19428 = ADVANCED_FACE ( 'NONE', ( #45521 ), #65344, .F. ) ;
#19429 = VERTEX_POINT ( 'NONE', #38772 ) ;
#19430 = CYLINDRICAL_SURFACE ( 'NONE', #43861, 4.000000000000000000 ) ;
#19431 = CARTESIAN_POINT ( 'NONE',  ( -5.999999999999998224, -9.058645607665452459, 34.76329471203371924 ) ) ;
#19433 = B_SPLINE_CURVE_WITH_KNOTS ( 'NONE', 3,
 ( #15480, #88607, #1955, #83498, #33637, #8724, #70866, #47137, #77613, #77169 ),
 .UNSPECIFIED., .F., .F.,
 ( 4, 2, 2, 2, 4 ),
 ( 0.000000000000000000, 0.0001954311564186860613, 0.0003908623128373721225, 0.0005862934692560581567, 0.0007817246256747442451 ),
 .UNSPECIFIED. ) ;
#19432 = CYLINDRICAL_SURFACE ( 'NONE', #35163, 0.2500000000000008882 ) ;
#19434 = CARTESIAN_POINT ( 'NONE',  ( 14.24193550517800055, -7.249945686854186278, 34.74374336980224598 ) ) ;
#19435 = CARTESIAN_POINT ( 'NONE',  ( -12.46153846153846168, -2.517432740324522911, 35.29906147534542527 ) ) ;
#19436 = ORIENTED_EDGE ( 'NONE', *, *, #85018, .F. ) ;
#19438 = VERTEX_POINT ( 'NONE', #10855 ) ;
#19437 = DIRECTION ( 'NONE',  ( -0.000000000000000000, 0.9396926207859094271, -0.3420201433256663259 ) ) ;
#19439 = DIRECTION ( 'NONE',  ( -1.000000000000000000, -0.000000000000000000, -0.000000000000000000 ) ) ;
#19440 = CARTESIAN_POINT ( 'NONE',  ( 8.769230769230768274, -12.34228464037088635, 31.77849191805839268 ) ) ;
#19441 = LINE ( 'NONE', #88371, #73141 ) ;
#19442 = CARTESIAN_POINT ( 'NONE',  ( -3.230769230769351186, -9.442884908241554243, 34.35708131394783038 ) ) ;
#19444 = VECTOR ( 'NONE', #43670, 1000.000000000000000 ) ;
#19443 = CARTESIAN_POINT ( 'NONE',  ( -4.153846153846152411, -4.661471528628507777, 34.16647553114623292 ) ) ;
#19445 = SURFACE_STYLE_USAGE ( .BOTH. , #18120 ) ;
#19446 = LINE ( 'NONE', #6812, #59402 ) ;
#19447 = CARTESIAN_POINT ( 'NONE',  ( 1.200186371490529202, -4.775308065498752974, 20.73624329374151287 ) ) ;
#19448 = VERTEX_POINT ( 'NONE', #46412 ) ;
#19449 = CARTESIAN_POINT ( 'NONE',  ( 13.38461538461538680, -6.386643153685126251, 34.62446782046654192 ) ) ;
#19450 = CARTESIAN_POINT ( 'NONE',  ( 7.846153846153846700, -2.517432740324522911, 35.29906147534542527 ) ) ;
#19451 = CARTESIAN_POINT ( 'NONE',  ( -13.16183584334697265, -8.496831190052096971, 34.64984203495476578 ) ) ;
#19452 = ORIENTED_EDGE ( 'NONE', *, *, #19415, .F. ) ;
#19453 = CARTESIAN_POINT ( 'NONE',  ( 10.61538461538461675, -3.937682226553329556, 33.60647404775216529 ) ) ;
#19454 = LINE ( 'NONE', #19894, #33992 ) ;
#19455 = VECTOR ( 'NONE', #36873, 1000.000000000000114 ) ;
#19456 = CARTESIAN_POINT ( 'NONE',  ( -6.988347369037697376, -6.026961402152685388, 34.52809138561120506 ) ) ;
#19457 = CARTESIAN_POINT ( 'NONE',  ( 7.053868730901711182, -5.582136614379148654, 34.36778462344220486 ) ) ;
#19458 = CARTESIAN_POINT ( 'NONE',  ( 0.4615384615384611200, -2.292212530054420494, 30.41441678777542634 ) ) ;
#19459 = ORIENTED_EDGE ( 'NONE', *, *, #15179, .F. ) ;
#19460 = EDGE_CURVE ( 'NONE', #38816, #81366, #72214, .T. ) ;
#19461 = CARTESIAN_POINT ( 'NONE',  ( -3.164701897419154530, -12.62096338111211757, 30.90682066428152908 ) ) ;
#19462 = B_SPLINE_CURVE_WITH_KNOTS ( 'NONE', 3,
 ( #8032, #827, #68839, #48557, #35502, #8923, #1261, #62511, #63405, #49012 ),
 .UNSPECIFIED., .F., .F.,
 ( 4, 2, 2, 2, 4 ),
 ( 0.0007817246256747446788, 0.0009771112852218874663, 0.001172497944769030145, 0.001367884604316172825, 0.001563271263863315720 ),
 .UNSPECIFIED. ) ;
#19463 = CARTESIAN_POINT ( 'NONE',  ( 17.20744877868664346, -6.001044277235009439, 34.52024696741798948 ) ) ;
#19464 = CARTESIAN_POINT ( 'NONE',  ( -2.084679463598910765, -5.582272713120728369, 34.63742843783360570 ) ) ;
#19465 = B_SPLINE_CURVE_WITH_KNOTS ( 'NONE', 3,
 ( #15331, #77029, #64374, #83349, #76585, #22959 ),
 .UNSPECIFIED., .F., .F.,
 ( 4, 2, 4 ),
 ( 0.000000000000000000, 0.0001954784845028908655, 0.0003909569690057817311 ),
 .UNSPECIFIED. ) ;
#19466 = ORIENTED_EDGE ( 'NONE', *, *, #81414, .T. ) ;
#19467 = FACE_OUTER_BOUND ( 'NONE', #33929, .T. ) ;
#19468 = ORIENTED_EDGE ( 'NONE', *, *, #23312, .T. ) ;
#19469 = DIRECTION ( 'NONE',  ( -0.000000000000000000, 0.6427876096865404731, -0.7660444431189770143 ) ) ;
#19470 = SURFACE_STYLE_FILL_AREA ( #74872 ) ;
#19471 = ORIENTED_EDGE ( 'NONE', *, *, #22493, .T. ) ;
#19472 = DIRECTION ( 'NONE',  ( -0.000000000000000000, 0.3420201433256694901, -0.9396926207859082059 ) ) ;
#19473 = CARTESIAN_POINT ( 'NONE',  ( -11.31545018684868964, -12.39991518177334129, 30.74647679643404530 ) ) ;
#19474 = DIRECTION ( 'NONE',  ( -0.000000000000000000, -0.000000000000000000, -1.000000000000000000 ) ) ;
#19475 = EDGE_CURVE ( 'NONE', #58032, #40441, #72997, .T. ) ;
#19476 = AXIS2_PLACEMENT_3D ( 'NONE', #78307, #77869, #23799 ) ;
#19477 = CARTESIAN_POINT ( 'NONE',  ( -7.912236225513983534, -4.661471528628507777, 34.16647553114621871 ) ) ;
#19478 = CARTESIAN_POINT ( 'NONE',  ( -0.4615384615385840772, -11.67786785259630911, 32.92929555188603530 ) ) ;
#19479 = ORIENTED_EDGE ( 'NONE', *, *, #22242, .F. ) ;
#19480 = DIRECTION ( 'NONE',  ( -1.000000000000000000, -0.000000000000000000, -0.000000000000000000 ) ) ;
#19481 = ORIENTED_EDGE ( 'NONE', *, *, #67814, .T. ) ;
#19482 = CARTESIAN_POINT ( 'NONE',  ( -5.076923076923199218, -6.835583212225970762, 34.95778746994575670 ) ) ;
#19483 = CARTESIAN_POINT ( 'NONE',  ( -12.21159305216042057, -2.986452184633680229, 32.43230066228895225 ) ) ;
#19484 = EDGE_CURVE ( 'NONE', #66313, #32743, #66686, .T. ) ;
#19485 = CARTESIAN_POINT ( 'NONE',  ( 4.826946345980720920, -11.79746400365624659, 32.30657167506340954 ) ) ;
#19486 = CARTESIAN_POINT ( 'NONE',  ( 3.230769230769231726, -11.35647404775217417, 33.31231777344666511 ) ) ;
#19487 = CARTESIAN_POINT ( 'NONE',  ( 17.06410256410256565, -3.499999999999999556, 29.75000000000000355 ) ) ;
#19488 = EDGE_CURVE ( 'NONE', #1493, #80799, #12190, .T. ) ;
#19489 = VERTEX_POINT ( 'NONE', #25697 ) ;
#19490 = VERTEX_POINT ( 'NONE', #39675 ) ;
#19491 = EDGE_LOOP ( 'NONE', ( #83193, #43775 ) ) ;
#19492 = B_SPLINE_CURVE_WITH_KNOTS ( 'NONE', 3,
 ( #43718, #71186, #36954, #65317, #45933, #3615, #71625, #51329, #25675, #4967 ),
 .UNSPECIFIED., .F., .F.,
 ( 4, 2, 2, 2, 4 ),
 ( 0.000000000000000000, 0.0001954339857564075557, 0.0003908679715128151114, 0.0005863019572692226671, 0.0007817359430256302227 ),
 .UNSPECIFIED. ) ;
#19493 = ORIENTED_EDGE ( 'NONE', *, *, #81941, .T. ) ;
#19494 = VECTOR ( 'NONE', #55639, 1000.000000000000227 ) ;
#19495 = CARTESIAN_POINT ( 'NONE',  ( -5.326899820971668476, -4.075325502946086864, 33.72974371597207721 ) ) ;
#19496 = EDGE_CURVE ( 'NONE', #30224, #28230, #67135, .T. ) ;
#19497 = CARTESIAN_POINT ( 'NONE',  ( 16.28437159207980045, -11.04252011169589842, 33.62494198852677840 ) ) ;
#19498 = CARTESIAN_POINT ( 'NONE',  ( -10.36543920600657209, -4.932303261841489928, 34.32971442181322885 ) ) ;
#19499 = CARTESIAN_POINT ( 'NONE',  ( 5.999999999999880096, -12.27809138561165270, 31.22303859784587132 ) ) ;
#19500 = CARTESIAN_POINT ( 'NONE',  ( -5.299849294439221481, -10.61292498521070549, 33.66303323003028680 ) ) ;
#19501 = CARTESIAN_POINT ( 'NONE',  ( -5.076923076923197442, -8.613356846316285953, 34.62446782046622218 ) ) ;
#19502 = FACE_OUTER_BOUND ( 'NONE', #32125, .T. ) ;
#19503 = FACE_OUTER_BOUND ( 'NONE', #73049, .T. ) ;
#19504 = EDGE_LOOP ( 'NONE', ( #42197, #924, #80542, #85617 ) ) ;
#19505 = EDGE_CURVE ( 'NONE', #20712, #5961, #51353, .T. ) ;
#19506 = AXIS2_PLACEMENT_3D ( 'NONE', #88426, #6868, #81654 ) ;
#19507 = ORIENTED_EDGE ( 'NONE', *, *, #64324, .F. ) ;
#19508 = ORIENTED_EDGE ( 'NONE', *, *, #78903, .F. ) ;
#19510 = ORIENTED_EDGE ( 'NONE', *, *, #9085, .T. ) ;
#19509 = CARTESIAN_POINT ( 'NONE',  ( -10.61538461538430589, -2.506253911140614576, 30.00000000000323297 ) ) ;
#19512 = CARTESIAN_POINT ( 'NONE',  ( -7.976301055592065481, -4.460286881179644780, 33.72017969459903242 ) ) ;
#19511 = DIRECTION ( 'NONE',  ( 0.000000000000000000, 0.3420201433256610524, 0.9396926207859113145 ) ) ;
#19513 = CARTESIAN_POINT ( 'NONE',  ( 1.653273178848927064E-15, -7.500000000000000000, 11.00000000000000178 ) ) ;
#19514 = CYLINDRICAL_SURFACE ( 'NONE', #53739, 0.2499999999999979738 ) ;
#19515 = FACE_BOUND ( 'NONE', #27990, .T. ) ;
#19516 = ORIENTED_EDGE ( 'NONE', *, *, #16601, .T. ) ;
#19517 = EDGE_CURVE ( 'NONE', #12327, #76524, #55009, .T. ) ;
#19518 = CARTESIAN_POINT ( 'NONE',  ( -2.980714919130916130, -6.567000820036038355, 34.66262288849541306 ) ) ;
#19519 = ORIENTED_EDGE ( 'NONE', *, *, #5953, .F. ) ;
#19520 = CYLINDRICAL_SURFACE ( 'NONE', #60095, 0.2499999999999986955 ) ;
#19522 = EDGE_CURVE ( 'NONE', #12053, #7293, #79739, .T. ) ;
#19521 = ORIENTED_EDGE ( 'NONE', *, *, #50008, .F. ) ;
#19523 = FACE_BOUND ( 'NONE', #27479, .T. ) ;
#19524 = CARTESIAN_POINT ( 'NONE',  ( 9.942253101685738059, -5.766571408460171355, 34.70601412856602508 ) ) ;
#19525 = CYLINDRICAL_SURFACE ( 'NONE', #226, 0.2499999999999995837 ) ;
#19526 = VERTEX_POINT ( 'NONE', #47740 ) ;
#19527 = VECTOR ( 'NONE', #1721, 999.9999999999998863 ) ;
#19528 = DIRECTION ( 'NONE',  ( -1.000000000000000000, -0.000000000000000000, -0.000000000000000000 ) ) ;
#19530 = EDGE_CURVE ( 'NONE', #46303, #52843, #13072, .T. ) ;
#19529 = CARTESIAN_POINT ( 'NONE',  ( 17.01084069756293715, -11.91647553114624181, 32.58852847137148245 ) ) ;
#19531 = LINE ( 'NONE', #42809, #36428 ) ;
#19532 = ORIENTED_EDGE ( 'NONE', *, *, #41772, .T. ) ;
#19533 = CARTESIAN_POINT ( 'NONE',  ( 6.792929713638702793, -10.19110544564092002, 33.96427741523702792 ) ) ;
#19534 = CARTESIAN_POINT ( 'NONE',  ( 14.24160992833217421, -11.35647404775217595, 33.31231777344666511 ) ) ;
#19535 = CARTESIAN_POINT ( 'NONE',  ( 6.673053685783957967, -12.43535235679832596, 30.55408501211184813 ) ) ;
#19536 = CARTESIAN_POINT ( 'NONE',  ( -9.626239341305252495, -2.538708090699994813, 30.37095296980875503 ) ) ;
#19537 = VERTEX_POINT ( 'NONE', #67578 ) ;
#19538 = CARTESIAN_POINT ( 'NONE',  ( 12.46153846153877609, -2.255955759149395501, 30.00000000000324363 ) ) ;
#19539 = DIRECTION ( 'NONE',  ( -0.000000000000000000, -0.8660254037844397068, -0.4999999999999978906 ) ) ;
#19540 = ORIENTED_EDGE ( 'NONE', *, *, #13550, .T. ) ;
#19541 = CARTESIAN_POINT ( 'NONE',  ( -5.999999999999998224, -13.87047571288749737, 32.06866353760679544 ) ) ;
#19542 = LINE ( 'NONE', #20434, #9519 ) ;
#19543 = CARTESIAN_POINT ( 'NONE',  ( 0.7115928814519127954, -10.82426656108011720, 33.81400080652039009 ) ) ;
#19544 = CARTESIAN_POINT ( 'NONE',  ( 16.28463659481310444, -11.93129842949672437, 32.56571108434900452 ) ) ;
#19545 = DIRECTION ( 'NONE',  ( -0.000000000000000000, -0.1736481776669307198, -0.9848077530122080203 ) ) ;
#19546 = FACE_OUTER_BOUND ( 'NONE', #5098, .T. ) ;
#19548 = CARTESIAN_POINT ( 'NONE',  ( 8.519207545009310323, -2.985938066672154445, 32.43141759479405550 ) ) ;
#19547 = CARTESIAN_POINT ( 'NONE',  ( 0.6845513056318561773, -11.43677907613345113, 33.22367315496201456 ) ) ;
#19549 = DIRECTION ( 'NONE',  ( -0.000000000000000000, 0.8660254037844399289, -0.4999999999999980016 ) ) ;
#19550 = ADVANCED_FACE ( 'NONE', ( #82431, #19387 ), #26144, .F. ) ;
#19551 = CARTESIAN_POINT ( 'NONE',  ( 2.750000000000008438, -8.639087296525996607, 20.79687500000000000 ) ) ;
#19552 = EDGE_LOOP ( 'NONE', ( #74470, #24138, #46729, #21283 ) ) ;
#19553 = CARTESIAN_POINT ( 'NONE',  ( 17.86930853333243618, -4.118384482072086072, 33.43331474514187107 ) ) ;
#19554 = EDGE_LOOP ( 'NONE', ( #24128, #36190, #33057, #80903 ) ) ;
#19555 = EDGE_CURVE ( 'NONE', #26637, #52830, #69986, .T. ) ;
#19556 = VERTEX_POINT ( 'NONE', #26587 ) ;
#19557 = FACE_OUTER_BOUND ( 'NONE', #67647, .T. ) ;
#19558 = ORIENTED_EDGE ( 'NONE', *, *, #38282, .T. ) ;
#19559 = CYLINDRICAL_SURFACE ( 'NONE', #55565, 0.2500000000000002220 ) ;
#19560 = CARTESIAN_POINT ( 'NONE',  ( -1.409462824231155764E-14, -4.749999999999999112, 20.40625000000000000 ) ) ;
#19561 = CARTESIAN_POINT ( 'NONE',  ( 14.37294787896833270, -11.48612834413965977, 32.76840700105972815 ) ) ;
#19562 = CARTESIAN_POINT ( 'NONE',  ( -8.834501215191545853, -3.300289026998414865, 32.46337939537583139 ) ) ;
#19563 = B_SPLINE_CURVE_WITH_KNOTS ( 'NONE', 3,
 ( #26367, #12847, #35790, #56048, #22264, #42107, #76770, #20926, #83536, #50158 ),
 .UNSPECIFIED., .F., .F.,
 ( 4, 2, 2, 2, 4 ),
 ( 0.000000000000000000, 0.0001954339857564055499, 0.0003908679715128110998, 0.0005863019572692165955, 0.0007817359430256221996 ),
 .UNSPECIFIED. ) ;
#19564 = DIRECTION ( 'NONE',  ( 0.000000000000000000, -5.102127870520020612E-17, -1.000000000000000000 ) ) ;
#19565 = CARTESIAN_POINT ( 'NONE',  ( -5.076923076923199218, -3.643525952248796163, 33.31231777344771672 ) ) ;
#19566 = DIRECTION ( 'NONE',  ( 0.000000000000000000, 0.000000000000000000, -1.000000000000000000 ) ) ;
#19567 = CARTESIAN_POINT ( 'NONE',  ( 2.372947878968333146, -11.48612834413965977, 32.76840700105972815 ) ) ;
#19568 = CARTESIAN_POINT ( 'NONE',  ( 6.673100179028333301, -12.41104346484419452, 31.60698883733904196 ) ) ;
#19569 = EDGE_CURVE ( 'NONE', #83335, #69315, #31391, .T. ) ;
#19570 = VECTOR ( 'NONE', #26198, 1000.000000000000000 ) ;
#19571 = CYLINDRICAL_SURFACE ( 'NONE', #50601, 0.2499999999999995559 ) ;
#19572 = CARTESIAN_POINT ( 'NONE',  ( -18.00000000000012079, -2.379036618888197285, 30.90682066428292885 ) ) ;
#19573 = FACE_OUTER_BOUND ( 'NONE', #84994, .T. ) ;
#19574 = ADVANCED_FACE ( 'NONE', ( #13951 ), #33785, .F. ) ;
#19575 = ADVANCED_FACE ( 'NONE', ( #27030 ), #81988, .F. ) ;
#19576 = VERTEX_POINT ( 'NONE', #62142 ) ;
#19577 = EDGE_LOOP ( 'NONE', ( #79374, #57904, #22484, #77969 ) ) ;
#19578 = CYLINDRICAL_SURFACE ( 'NONE', #67324, 0.2499999999999997502 ) ;
#19579 = LINE ( 'NONE', #69100, #37394 ) ;
#19580 = CARTESIAN_POINT ( 'NONE',  ( 2.307692307692309264, -6.435427911321262684, 35.78748833219616898 ) ) ;
#19581 = CARTESIAN_POINT ( 'NONE',  ( -16.08777780284371417, -12.37446782046654192, 30.86335684631486842 ) ) ;
#19582 = VECTOR ( 'NONE', #27823, 1000.000000000000000 ) ;
#19583 = FACE_OUTER_BOUND ( 'NONE', #63292, .T. ) ;
#19584 = DIRECTION ( 'NONE',  ( -0.000000000000000000, 0.3420201433256694346, -0.9396926207859080948 ) ) ;
#19585 = EDGE_CURVE ( 'NONE', #48512, #5871, #9844, .T. ) ;
#19586 = CARTESIAN_POINT ( 'NONE',  ( -3.230769230769351186, -5.219633306517616589, 34.19971097300220464 ) ) ;
#19587 = ORIENTED_EDGE ( 'NONE', *, *, #33552, .F. ) ;
#19588 = CARTESIAN_POINT ( 'NONE',  ( -6.857821351800898135, -10.21337939537593620, 33.94971097300152252 ) ) ;
#19589 = ORIENTED_EDGE ( 'NONE', *, *, #27515, .T. ) ;
#19590 = VERTEX_POINT ( 'NONE', #36443 ) ;
#19591 = CARTESIAN_POINT ( 'NONE',  ( 10.61538461538461675, -12.29105614889573062, 35.45975837776705220 ) ) ;
#19592 = CARTESIAN_POINT ( 'NONE',  ( -14.24162497434223162, -6.343179335718452272, 34.87096338111212646 ) ) ;
#19593 = B_SPLINE_CURVE_WITH_KNOTS ( 'NONE', 3,
 ( #19431, #54535, #66730, #46894, #12677, #68497, #74378, #73942, #18550, #59967 ),
 .UNSPECIFIED., .F., .F.,
 ( 4, 2, 2, 2, 4 ),
 ( 0.000000000000000000, 0.0001954311564186868202, 0.0003908623128373736404, 0.0005862934692560604335, 0.0007817246256747472808 ),
 .UNSPECIFIED. ) ;
#19594 = VECTOR ( 'NONE', #7615, 1000.000000000000114 ) ;
#19595 = CARTESIAN_POINT ( 'NONE',  ( -4.377331097570101193, -4.386631170607603991, 33.66268669641500111 ) ) ;
#19596 = CARTESIAN_POINT ( 'NONE',  ( 11.53846153846141576, -2.379036618888197729, 30.90682066428292885 ) ) ;
#19597 = CARTESIAN_POINT ( 'NONE',  ( 7.846153846153725020, -3.300289026999228881, 32.46337939537708905 ) ) ;
#19598 = EDGE_CURVE ( 'NONE', #28403, #2875, #84057, .T. ) ;
#19599 = VECTOR ( 'NONE', #13269, 999.9999999999998863 ) ;
#19600 = EDGE_LOOP ( 'NONE', ( #67579, #19681, #1910, #85163 ) ) ;
#19601 = VERTEX_POINT ( 'NONE', #29255 ) ;
#19602 = ORIENTED_EDGE ( 'NONE', *, *, #63165, .T. ) ;
#19603 = ORIENTED_EDGE ( 'NONE', *, *, #4753, .F. ) ;
#19604 = LINE ( 'NONE', #20490, #73153 ) ;
#19605 = CARTESIAN_POINT ( 'NONE',  ( 5.076923076923075762, -10.51840700105979565, 33.73612834413961536 ) ) ;
#19606 = FACE_OUTER_BOUND ( 'NONE', #49192, .T. ) ;
#19607 = CARTESIAN_POINT ( 'NONE',  ( 7.384615384615385025, -3.499999999999999556, 29.75000000000000355 ) ) ;
#19608 = CARTESIAN_POINT ( 'NONE',  ( 17.74997676270703550, -5.056417327199097755, 34.11270091957320716 ) ) ;
#19609 = CARTESIAN_POINT ( 'NONE',  ( 12.46153846153846168, -2.833524468853757305, 32.15551576947925838 ) ) ;
#19610 = VERTEX_POINT ( 'NONE', #28348 ) ;
#19611 = VERTEX_POINT ( 'NONE', #35563 ) ;
#19612 = VERTEX_POINT ( 'NONE', #21594 ) ;
#19614 = ORIENTED_EDGE ( 'NONE', *, *, #2716, .T. ) ;
#19613 = CARTESIAN_POINT ( 'NONE',  ( -4.153846153846273204, -3.300289026999228881, 32.46337939537708905 ) ) ;
#19615 = FACE_OUTER_BOUND ( 'NONE', #32316, .T. ) ;
#19616 = FACE_OUTER_BOUND ( 'NONE', #24553, .T. ) ;
#19617 = CARTESIAN_POINT ( 'NONE',  ( -1.553300858899081760, -11.25000000000000888, 19.85937500000000711 ) ) ;
#19618 = ORIENTED_EDGE ( 'NONE', *, *, #216, .T. ) ;
#19619 = B_SPLINE_CURVE_WITH_KNOTS ( 'NONE', 3,
 ( #84109, #22390, #36354, #2115, #790, #29599, #48978, #1229, #77773, #9330 ),
 .UNSPECIFIED., .F., .F.,
 ( 4, 2, 2, 2, 4 ),
 ( 0.000000000000000000, 0.0001954311564186865763, 0.0003908623128373731525, 0.0005862934692560596746, 0.0007817246256747463051 ),
 .UNSPECIFIED. ) ;
#19620 = CARTESIAN_POINT ( 'NONE',  ( 3.480769230769245937, -2.249999999999999112, 29.81603969181031033 ) ) ;
#19621 = EDGE_LOOP ( 'NONE', ( #30882, #77409, #6725, #85048 ) ) ;
#19622 = CARTESIAN_POINT ( 'NONE',  ( 3.230769230769231726, -4.945431358278436385, 36.03766855953609394 ) ) ;
#19623 = CARTESIAN_POINT ( 'NONE',  ( 14.37294744720514927, -12.51329471203373345, 31.30864560766537963 ) ) ;
#19624 = B_SPLINE_CURVE_WITH_KNOTS ( 'NONE', 3,
 ( #1258, #70168, #48115, #68836, #84146, #7141, #83701, #35048, #34612, #62078 ),
 .UNSPECIFIED., .F., .F.,
 ( 4, 2, 2, 2, 4 ),
 ( 0.000000000000000000, 0.0001954311564186862781, 0.0003908623128373725562, 0.0005862934692560588072, 0.0007817246256747451124 ),
 .UNSPECIFIED. ) ;
#19625 = ADVANCED_FACE ( 'NONE', ( #49518 ), #22043, .T. ) ;
#19626 = FACE_BOUND ( 'NONE', #84086, .T. ) ;
#19627 = DIRECTION ( 'NONE',  ( -0.000000000000000000, -0.000000000000000000, -1.000000000000000000 ) ) ;
#19628 = CARTESIAN_POINT ( 'NONE',  ( 8.639083559792549494, -5.195881422630166391, 34.18770438780619259 ) ) ;
#19629 = ORIENTED_EDGE ( 'NONE', *, *, #33937, .T. ) ;
#19631 = EDGE_CURVE ( 'NONE', #42943, #41914, #40020, .T. ) ;
#19630 = CARTESIAN_POINT ( 'NONE',  ( 6.792385456409365752, -8.147922237126337563, 34.70805685702651999 ) ) ;
#19632 = VECTOR ( 'NONE', #26224, 1000.000000000000000 ) ;
#19633 = LINE ( 'NONE', #81790, #16290 ) ;
#19634 = CARTESIAN_POINT ( 'NONE',  ( 15.45378207486262667, -6.460100341425560444, 34.89618726649961644 ) ) ;
#19635 = VERTEX_POINT ( 'NONE', #42327 ) ;
#19636 = EDGE_CURVE ( 'NONE', #5555, #13671, #70227, .T. ) ;
#19637 = CARTESIAN_POINT ( 'NONE',  ( -9.469294848214296678, -4.762714258010881885, 34.23016756924214832 ) ) ;
#19638 = CARTESIAN_POINT ( 'NONE',  ( -7.846153846153844924, -11.16473453929635440, 33.15142922261926373 ) ) ;
#19639 = CARTESIAN_POINT ( 'NONE',  ( -3.230769230769229949, -13.63283147151868846, 33.57946703557072254 ) ) ;
#19640 = FACE_OUTER_BOUND ( 'NONE', #62773, .T. ) ;
#19641 = CARTESIAN_POINT ( 'NONE',  ( 8.769230769230768274, -9.905515769479276145, 34.41647553114623292 ) ) ;
#19642 = FACE_BOUND ( 'NONE', #69264, .T. ) ;
#19644 = FACE_OUTER_BOUND ( 'NONE', #54386, .T. ) ;
#19643 = CARTESIAN_POINT ( 'NONE',  ( -27.00000000000000000, 8.999999999999996447, 23.75000000000000000 ) ) ;
#19645 = CARTESIAN_POINT ( 'NONE',  ( 17.75000000000000000, -2.249999999999998668, 29.75000000000000355 ) ) ;
#19647 = CARTESIAN_POINT ( 'NONE',  ( -9.442253380669377805, -10.66356715214248396, 33.62249196103329751 ) ) ;
#19646 = CARTESIAN_POINT ( 'NONE',  ( -18.06608237936013595, -2.292212530054419606, 30.41441678777542634 ) ) ;
#19648 = EDGE_CURVE ( 'NONE', #46336, #43624, #80869, .T. ) ;
#19649 = CARTESIAN_POINT ( 'NONE',  ( -8.638438961405983108, -3.530189275343204702, 32.79018710029569661 ) ) ;
#19650 = CARTESIAN_POINT ( 'NONE',  ( 1.987747218494664292, -9.401340078031346081, 16.87313170625849068 ) ) ;
#19651 = ORIENTED_EDGE ( 'NONE', *, *, #87825, .T. ) ;
#19652 = CARTESIAN_POINT ( 'NONE',  ( -13.13461538461538325, -2.249999999999998668, 29.75000000000000355 ) ) ;
#19653 = ORIENTED_EDGE ( 'NONE', *, *, #73060, .F. ) ;
#19654 = CARTESIAN_POINT ( 'NONE',  ( -18.24997674404859183, -3.436278759898155233, 33.07459398097509506 ) ) ;
#19655 = VECTOR ( 'NONE', #7848, 1000.000000000000227 ) ;
#19656 = EDGE_LOOP ( 'NONE', ( #52512, #63672 ) ) ;
#19657 = CARTESIAN_POINT ( 'NONE',  ( 2.307692307692186251, -2.379036618888197285, 30.90682066428292885 ) ) ;
#19658 = CARTESIAN_POINT ( 'NONE',  ( 7.846153846153846700, -2.833524468853757305, 32.15551576947925838 ) ) ;
#19660 = ORIENTED_EDGE ( 'NONE', *, *, #47569, .T. ) ;
#19659 = CARTESIAN_POINT ( 'NONE',  ( -10.74553258511631171, -11.66186481527757302, 32.95055677023626117 ) ) ;
#19661 = DIRECTION ( 'NONE',  ( 0.000000000000000000, 0.000000000000000000, 1.000000000000000000 ) ) ;
#19662 = CARTESIAN_POINT ( 'NONE',  ( -9.562260086052006613, -7.723484964179501588, 34.74522123443823318 ) ) ;
#19663 = CARTESIAN_POINT ( 'NONE',  ( -3.749999999999996447, -7.561099074964554134, 26.09188170625848358 ) ) ;
#19664 = DIRECTION ( 'NONE',  ( 0.000000000000000000, 1.000000000000000000, 0.000000000000000000 ) ) ;
#19665 = DIRECTION ( 'NONE',  ( 0.000000000000000000, 0.9396926207859126468, -0.3420201433256571111 ) ) ;
#19666 = CARTESIAN_POINT ( 'NONE',  ( -0.4330127018922180770, -4.784304877199946127, 29.50000000000000355 ) ) ;
#19667 = CARTESIAN_POINT ( 'NONE',  ( 1.384615384615386802, -4.661471528628507777, 34.16647553114623292 ) ) ;
#19668 = CARTESIAN_POINT ( 'NONE',  ( -0.4615384615384611200, -4.098570777380720287, 33.41473453929634729 ) ) ;
#19669 = CARTESIAN_POINT ( 'NONE',  ( 9.468822767743363400, -3.562934362175799841, 33.22335522853832401 ) ) ;
#19670 = CARTESIAN_POINT ( 'NONE',  ( -1.492201783934593573, -3.724691934501250135, 19.32999329374151642 ) ) ;
#19671 = CARTESIAN_POINT ( 'NONE',  ( 5.207713517890026012, -2.494656445102013453, 31.33466734024120015 ) ) ;
#19672 = AXIS2_PLACEMENT_3D ( 'NONE', #3910, #71483, #24186 ) ;
#19673 = CARTESIAN_POINT ( 'NONE',  ( 6.923076923076802558, -11.48612834414049644, 32.76840700105863391 ) ) ;
#19674 = VERTEX_POINT ( 'NONE', #50816 ) ;
#19675 = CARTESIAN_POINT ( 'NONE',  ( 6.792467267872841497, -7.722926974430166069, 34.99546784045485737 ) ) ;
#19676 = CARTESIAN_POINT ( 'NONE',  ( 17.07692307692307665, -2.499999999999998668, 29.50000000000001066 ) ) ;
#19677 = CARTESIAN_POINT ( 'NONE',  ( -3.749999999999997780, -7.438900925035489387, 20.34561829374151287 ) ) ;
#19678 = ADVANCED_FACE ( 'NONE', ( #57151 ), #77863, .T. ) ;
#19679 = CARTESIAN_POINT ( 'NONE',  ( -16.08859101433330707, -12.51329471203373700, 31.30864560766537963 ) ) ;
#19680 = CARTESIAN_POINT ( 'NONE',  ( -11.53846153846153655, -2.499999999999998668, 29.75000000000001421 ) ) ;
#19681 = ORIENTED_EDGE ( 'NONE', *, *, #12756, .T. ) ;
#19682 = CARTESIAN_POINT ( 'NONE',  ( 4.153846153846154188, -3.937682226553329556, 33.60647404775216529 ) ) ;
#19683 = CARTESIAN_POINT ( 'NONE',  ( 3.100077764101670574, -3.530157926970578508, 32.79014554554150607 ) ) ;
#19685 = ORIENTED_EDGE ( 'NONE', *, *, #9770, .F. ) ;
#19684 = CARTESIAN_POINT ( 'NONE',  ( 4.087763774486018242, -9.058645607665454236, 34.76329471203372634 ) ) ;
#19686 = DIRECTION ( 'NONE',  ( -0.000000000000000000, -0.5000000000000009992, -0.8660254037844380415 ) ) ;
#19687 = CARTESIAN_POINT ( 'NONE',  ( 2.307692307692187583, -12.46129190930018460, 30.37095296980731973 ) ) ;
#19688 = CARTESIAN_POINT ( 'NONE',  ( -12.71151520558705528, -4.818429247618089661, 34.26397095200675125 ) ) ;
#19689 = EDGE_CURVE ( 'NONE', #73212, #71584, #48176, .T. ) ;
#19690 = VERTEX_POINT ( 'NONE', #63461 ) ;
#19691 = CARTESIAN_POINT ( 'NONE',  ( -9.442362282929652295, -2.589246495874658383, 31.60778113518102828 ) ) ;
#19692 = CARTESIAN_POINT ( 'NONE',  ( -18.22348494372395322, -12.24155766932282496, 31.33739205006857986 ) ) ;
#19693 = VECTOR ( 'NONE', #69750, 1000.000000000000227 ) ;
#19694 = EDGE_CURVE ( 'NONE', #67157, #9337, #62473, .T. ) ;
#19695 = ADVANCED_FACE ( 'NONE', ( #17947 ), #65668, .F. ) ;
#19696 = CARTESIAN_POINT ( 'NONE',  ( 7.173076923078359535, -7.500000000000155431, 34.75000000000007105 ) ) ;
#19697 = ORIENTED_EDGE ( 'NONE', *, *, #42274, .F. ) ;
#19698 = ORIENTED_EDGE ( 'NONE', *, *, #71480, .T. ) ;
#19699 = ORIENTED_EDGE ( 'NONE', *, *, #88636, .F. ) ;
#19700 = AXIS2_PLACEMENT_3D ( 'NONE', #6079, #21800, #74533 ) ;
#19701 = ORIENTED_EDGE ( 'NONE', *, *, #1547, .T. ) ;
#19702 = FACE_OUTER_BOUND ( 'NONE', #71212, .T. ) ;
#19703 = CARTESIAN_POINT ( 'NONE',  ( -19.00000000000000000, 0.7500000000000051070, 24.75000000000000000 ) ) ;
#19704 = VECTOR ( 'NONE', #53922, 999.9999999999998863 ) ;
#19705 = FACE_OUTER_BOUND ( 'NONE', #60817, .T. ) ;
#19706 = CARTESIAN_POINT ( 'NONE',  ( -16.15384615384627409, -3.643525952248796163, 33.31231777344771672 ) ) ;
#19707 = EDGE_CURVE ( 'NONE', #52584, #82252, #66899, .T. ) ;
#19708 = DIRECTION ( 'NONE',  ( -0.000000000000000000, 0.6427876096865404731, -0.7660444431189771253 ) ) ;
#19709 = ORIENTED_EDGE ( 'NONE', *, *, #6370, .T. ) ;
#19710 = EDGE_CURVE ( 'NONE', #18801, #17226, #38655, .T. ) ;
#19711 = EDGE_CURVE ( 'NONE', #4695, #17051, #78748, .T. ) ;
#19712 = ORIENTED_EDGE ( 'NONE', *, *, #87956, .F. ) ;
#19713 = ORIENTED_EDGE ( 'NONE', *, *, #47736, .F. ) ;
#19715 = VERTEX_POINT ( 'NONE', #86871 ) ;
#19714 = CARTESIAN_POINT ( 'NONE',  ( -7.146561847641257792, -2.612411019501189813, 31.66733052389439962 ) ) ;
#19716 = CARTESIAN_POINT ( 'NONE',  ( -6.700064078983528404, -4.026326845037961455, 33.68677907613344047 ) ) ;
#19717 = EDGE_CURVE ( 'NONE', #83441, #13051, #10973, .T. ) ;
#19718 = CARTESIAN_POINT ( 'NONE',  ( 6.000000000000001776, -2.486705287966279876, 31.30864560766543647 ) ) ;
#19719 = VECTOR ( 'NONE', #48819, 1000.000000000000000 ) ;
#19720 = CARTESIAN_POINT ( 'NONE',  ( -15.12820512820512953, -7.500000000000000000, 29.75000000000000355 ) ) ;
#19721 = CARTESIAN_POINT ( 'NONE',  ( -15.10024352900566846, -9.417988943895561960, 34.36773134775777550 ) ) ;
#19722 = EDGE_LOOP ( 'NONE', ( #84891, #9140, #23023, #23685 ) ) ;
#19723 = VERTEX_POINT ( 'NONE', #87312 ) ;
#19724 = ORIENTED_EDGE ( 'NONE', *, *, #31584, .F. ) ;
#19725 = CARTESIAN_POINT ( 'NONE',  ( 10.83816415665302202, -10.81320215134717344, 33.49497208177562868 ) ) ;
#19727 = ORIENTED_EDGE ( 'NONE', *, *, #36136, .F. ) ;
#19726 = CARTESIAN_POINT ( 'NONE',  ( -10.61538461538473577, -2.657715359629662544, 31.77849191805970364 ) ) ;
#19728 = CARTESIAN_POINT ( 'NONE',  ( 9.442330961365341224, -11.79746400365624659, 32.30657167506340954 ) ) ;
#19729 = CARTESIAN_POINT ( 'NONE',  ( -14.37377571864818293, -2.538708090699994813, 30.37095296980875148 ) ) ;
#19730 = VERTEX_POINT ( 'NONE', #44504 ) ;
#19731 = VECTOR ( 'NONE', #12151, 1000.000000000000000 ) ;
#19732 = CARTESIAN_POINT ( 'NONE',  ( 17.07692307692307665, -8.564572088678739092, 35.78748833219616898 ) ) ;
#19733 = DIRECTION ( 'NONE',  ( -0.000000000000000000, 1.000000000000000000, 3.491481338843133355E-15 ) ) ;
#19734 = CYLINDRICAL_SURFACE ( 'NONE', #59758, 0.2500000000000002220 ) ;
#19735 = FACE_BOUND ( 'NONE', #54659, .T. ) ;
#19736 = CARTESIAN_POINT ( 'NONE',  ( -0.5268089074992373666, -10.21337939537584383, 33.94971097300158647 ) ) ;
#19737 = DIRECTION ( 'NONE',  ( 1.000000000000000000, 0.000000000000000000, 0.000000000000000000 ) ) ;
#19738 = EDGE_CURVE ( 'NONE', #80479, #83807, #23880, .T. ) ;
#19739 = FACE_OUTER_BOUND ( 'NONE', #2326, .T. ) ;
#19741 = DIRECTION ( 'NONE',  ( -0.000000000000000000, 1.000000000000000000, 3.491481338843133355E-15 ) ) ;
#19740 = CARTESIAN_POINT ( 'NONE',  ( 0.2115617174898692943, -6.524016743844655686, 34.90889640711025521 ) ) ;
#19742 = DIRECTION ( 'NONE',  ( 1.000000000000000000, 0.000000000000000000, 0.000000000000000000 ) ) ;
#19743 = CARTESIAN_POINT ( 'NONE',  ( 11.53846153846153832, -9.780366693483667717, 34.19971097300155094 ) ) ;
#19744 = ORIENTED_EDGE ( 'NONE', *, *, #21658, .F. ) ;
#19745 = CARTESIAN_POINT ( 'NONE',  ( -17.14219307747939425, -5.941354392334501355, 34.76329471203369792 ) ) ;
#19746 = FILL_AREA_STYLE ('',( #13868 ) ) ;
#19747 = EDGE_LOOP ( 'NONE', ( #85755, #66963, #57016, #37753 ) ) ;
#19748 = ORIENTED_EDGE ( 'NONE', *, *, #71535, .F. ) ;
#19749 = CARTESIAN_POINT ( 'NONE',  ( -6.673131404728781746, -5.057305518903949526, 34.11320923018887896 ) ) ;
#19750 = ADVANCED_FACE ( 'NONE', ( #3525 ), #31908, .F. ) ;
#19751 = CARTESIAN_POINT ( 'NONE',  ( 8.769230769230645706, -12.51329471203414379, 31.30864560766407578 ) ) ;
#19752 = CARTESIAN_POINT ( 'NONE',  ( -7.846153846153967493, -2.379036618888197729, 30.90682066428292885 ) ) ;
#19753 = ORIENTED_EDGE ( 'NONE', *, *, #25287, .T. ) ;
#19754 = CARTESIAN_POINT ( 'NONE',  ( -9.692307692307691624, -9.058645607665452459, 34.76329471203371924 ) ) ;
#19755 = CARTESIAN_POINT ( 'NONE',  ( -4.403822897894744237, -9.234221910056348293, 34.70572697212741531 ) ) ;
#19756 = FACE_BOUND ( 'NONE', #50047, .T. ) ;
#19758 = DIRECTION ( 'NONE',  ( 0.000000000000000000, 0.000000000000000000, -1.000000000000000000 ) ) ;
#19757 = CARTESIAN_POINT ( 'NONE',  ( -24.99999999999999645, -19.99999999999999645, 3.000000000000000000 ) ) ;
#19759 = DIRECTION ( 'NONE',  ( 1.000000000000000000, 0.000000000000000000, 0.000000000000000000 ) ) ;
#19760 = CARTESIAN_POINT ( 'NONE',  ( -5.076923076923197442, -9.442884908241554243, 34.35708131394783038 ) ) ;
#19762 = CARTESIAN_POINT ( 'NONE',  ( -8.519285250882626670, -12.22109172314383052, 31.39792113162168263 ) ) ;
#19761 = DIRECTION ( 'NONE',  ( 1.000000000000000000, 0.000000000000000000, 0.000000000000000000 ) ) ;
#19763 = EDGE_CURVE ( 'NONE', #5737, #40194, #40993, .T. ) ;
#19764 = VECTOR ( 'NONE', #58706, 1000.000000000000000 ) ;
#19765 = CARTESIAN_POINT ( 'NONE',  ( 3.750000000000009770, -9.053300858899081760, 20.79687500000000000 ) ) ;
#19766 = ORIENTED_EDGE ( 'NONE', *, *, #9556, .T. ) ;
#19767 = VERTEX_POINT ( 'NONE', #80087 ) ;
#19768 = CARTESIAN_POINT ( 'NONE',  ( -9.915234651214539952, -2.523278758544489797, 31.42238647778637528 ) ) ;
#19769 = VECTOR ( 'NONE', #76730, 1000.000000000000000 ) ;
#19770 = CARTESIAN_POINT ( 'NONE',  ( 12.52770760250111870, -7.250054483168843156, 34.74374881642865631 ) ) ;
#19771 = DIRECTION ( 'NONE',  ( -1.000000000000000000, 0.000000000000000000, 0.000000000000000000 ) ) ;
#19772 = CARTESIAN_POINT ( 'NONE',  ( -0.6843651540174652270, -7.369208160676172348, 34.74850200257122879 ) ) ;
#19773 = CARTESIAN_POINT ( 'NONE',  ( -3.296852641725110722, -5.557115091759785130, 34.35708131394839171 ) ) ;
#19774 = CARTESIAN_POINT ( 'NONE',  ( -1.553300858899125059, -3.750000000000009326, 22.82812500000000355 ) ) ;
#19775 = CARTESIAN_POINT ( 'NONE',  ( -8.992715693795100051, -10.23692288466677880, 34.23039457007281072 ) ) ;
#19776 = CARTESIAN_POINT ( 'NONE',  ( 5.776515075435669111, -3.019605429927184836, 32.48692288466676814 ) ) ;
#19777 = EDGE_CURVE ( 'NONE', #47021, #86793, #88378, .T. ) ;
#19778 = CARTESIAN_POINT ( 'NONE',  ( 18.00000000000000000, -3.937682226553329556, 33.60647404775216529 ) ) ;
#19779 = FACE_OUTER_BOUND ( 'NONE', #62503, .T. ) ;
#19780 = DIRECTION ( 'NONE',  ( -0.000000000000000000, -0.3420201433256694346, -0.9396926207859080948 ) ) ;
#19781 = CARTESIAN_POINT ( 'NONE',  ( 15.10007862765892739, -12.35290016733513951, 31.75349464988449455 ) ) ;
#19782 = CARTESIAN_POINT ( 'NONE',  ( -3.230769230769352962, -10.33852847137269571, 34.16647553114546554 ) ) ;
#19783 = CARTESIAN_POINT ( 'NONE',  ( -6.792551484843277976, -3.625058011473227815, 33.29252011169590020 ) ) ;
#19784 = CARTESIAN_POINT ( 'NONE',  ( -17.07692307692319744, -3.083524468854526912, 32.58852847137268327 ) ) ;
#19785 = ORIENTED_EDGE ( 'NONE', *, *, #86511, .T. ) ;
#19786 = CARTESIAN_POINT ( 'NONE',  ( -4.826977558574933269, -11.86320923018887541, 32.19269448109604781 ) ) ;
#19787 = DIRECTION ( 'NONE',  ( -0.000000000000000000, -0.1736481776669307198, -0.9848077530122080203 ) ) ;
#19788 = CARTESIAN_POINT ( 'NONE',  ( -1.987747218494638313, -9.401340078031370950, 16.43936829374151287 ) ) ;
#19789 = B_SPLINE_CURVE_WITH_KNOTS ( 'NONE', 3,
 ( #11249, #80612, #60316, #38718, #87371, #66178, #4491, #25651, #53107, #87826 ),
 .UNSPECIFIED., .F., .F.,
 ( 4, 2, 2, 2, 4 ),
 ( 0.0007817246256747482566, 0.0009771112852218926705, 0.001172497944769037084, 0.001367884604316181281, 0.001563271263863325695 ),
 .UNSPECIFIED. ) ;
#19790 = CARTESIAN_POINT ( 'NONE',  ( 4.023155550735844521, -4.684245665217972032, 34.18127051446801090 ) ) ;
#19792 = DIRECTION ( 'NONE',  ( -0.000000000000000000, -0.1736481776669307198, -0.9848077530122080203 ) ) ;
#19791 = AXIS2_PLACEMENT_3D ( 'NONE', #59492, #32463, #60378 ) ;
#19793 = DIRECTION ( 'NONE',  ( 0.000000000000000000, -1.000000000000000000, 8.673617379884035472E-17 ) ) ;
#19795 = ORIENTED_EDGE ( 'NONE', *, *, #22921, .T. ) ;
#19794 = CARTESIAN_POINT ( 'NONE',  ( -0.2387589202700528268, -2.600157965045225783, 30.74683119005207743 ) ) ;
#19796 = CARTESIAN_POINT ( 'NONE',  ( 1.139087296525997051, -4.749999999999992895, 24.23437500000000355 ) ) ;
#19797 = EDGE_CURVE ( 'NONE', #19260, #80757, #51790, .T. ) ;
#19798 = CARTESIAN_POINT ( 'NONE',  ( 3.453548899747296730, -8.540255544307065350, 34.89611431652622286 ) ) ;
#19799 = EDGE_CURVE ( 'NONE', #11510, #58008, #32790, .T. ) ;
#19800 = VERTEX_POINT ( 'NONE', #81875 ) ;
#19801 = CARTESIAN_POINT ( 'NONE',  ( 8.769230769230647482, -8.613356846316285953, 34.62446782046622218 ) ) ;
#19802 = CARTESIAN_POINT ( 'NONE',  ( 18.00000000000000000, -8.973038597847269315, 34.52809138561121927 ) ) ;
#19803 = ORIENTED_EDGE ( 'NONE', *, *, #37081, .T. ) ;
#19804 = LINE ( 'NONE', #47266, #77786 ) ;
#19805 = CARTESIAN_POINT ( 'NONE',  ( -15.90384615384471800, -7.500000000000155431, 34.75000000000007105 ) ) ;
#19806 = EDGE_CURVE ( 'NONE', #84840, #24050, #13400, .T. ) ;
#19807 = VECTOR ( 'NONE', #33199, 1000.000000000000114 ) ;
#19808 = B_SPLINE_CURVE_WITH_KNOTS ( 'NONE', 3,
 ( #42963, #3284, #30759, #17247, #8738, #1530, #37068, #70433, #36212, #22677 ),
 .UNSPECIFIED., .F., .F.,
 ( 4, 2, 2, 2, 4 ),
 ( 0.0007817359527651096280, 0.0009771254036996484919, 0.001172514854634187573, 0.001367904305568726653, 0.001563293756503265517 ),
 .UNSPECIFIED. ) ;
#19809 = CARTESIAN_POINT ( 'NONE',  ( -7.846153846153844924, -3.513871655860378418, 32.76840700105978499 ) ) ;
#19810 = ORIENTED_EDGE ( 'NONE', *, *, #30140, .T. ) ;
#19811 = EDGE_LOOP ( 'NONE', ( #62538, #26931, #22655, #35586 ) ) ;
#19812 = ORIENTED_EDGE ( 'NONE', *, *, #73551, .F. ) ;
#19813 = CARTESIAN_POINT ( 'NONE',  ( -15.16551409125639260, -4.320704448112861584, 33.92786785259548310 ) ) ;
#19814 = CARTESIAN_POINT ( 'NONE',  ( 1.653273178848927064E-15, -7.500000000000000000, 11.00000000000000178 ) ) ;
#19815 = CARTESIAN_POINT ( 'NONE',  ( 18.06525513951284267, -10.33852847137154107, 34.16647553114620450 ) ) ;
#19816 = CARTESIAN_POINT ( 'NONE',  ( -10.68065506134538722, -2.625532179533444754, 30.86335684631481513 ) ) ;
#19817 = LINE ( 'NONE', #59016, #60567 ) ;
#19818 = FACE_OUTER_BOUND ( 'NONE', #49568, .T. ) ;
#19819 = DIRECTION ( 'NONE',  ( -0.000000000000000000, -0.5000000000000009992, -0.8660254037844380415 ) ) ;
#19820 = CARTESIAN_POINT ( 'NONE',  ( 10.61538461538461675, -12.10708131394839349, 31.69288490824020244 ) ) ;
#19821 = VECTOR ( 'NONE', #27620, 1000.000000000000000 ) ;
#19822 = EDGE_CURVE ( 'NONE', #4054, #67556, #68790, .T. ) ;
#19823 = ORIENTED_EDGE ( 'NONE', *, *, #19648, .F. ) ;
#19824 = ORIENTED_EDGE ( 'NONE', *, *, #81922, .F. ) ;
#19826 = VERTEX_POINT ( 'NONE', #55270 ) ;
#19825 = CARTESIAN_POINT ( 'NONE',  ( 17.99999999999987566, -9.528491918059723176, 34.59228464037033035 ) ) ;
#19827 = AXIS2_PLACEMENT_3D ( 'NONE', #26945, #47199, #32809 ) ;
#19828 = LINE ( 'NONE', #43198, #24840 ) ;
#19829 = CARTESIAN_POINT ( 'NONE',  ( 11.76124107972994537, -12.24180327182771855, 31.33663988360758879 ) ) ;
#19830 = ORIENTED_EDGE ( 'NONE', *, *, #29370, .F. ) ;
#19831 = CARTESIAN_POINT ( 'NONE',  ( 14.43848274865925774, -11.93129842949671726, 32.56571108434900452 ) ) ;
#19832 = ORIENTED_EDGE ( 'NONE', *, *, #36064, .T. ) ;
#19833 = CARTESIAN_POINT ( 'NONE',  ( 11.78851585009985570, -2.564540009722896752, 30.55348353981670684 ) ) ;
#19834 = ORIENTED_EDGE ( 'NONE', *, *, #51576, .T. ) ;
#19835 = CARTESIAN_POINT ( 'NONE',  ( 9.822833394071260216, -8.586989748646452369, 34.63063291749215011 ) ) ;
#19836 = B_SPLINE_CURVE_WITH_KNOTS ( 'NONE', 3,
 ( #54536, #18992, #20323, #75269, #34272, #26191, #61732, #48, #12678, #54989 ),
 .UNSPECIFIED., .F., .F.,
 ( 4, 2, 2, 2, 4 ),
 ( 0.000000000000000000, 0.0001954339857564077183, 0.0003908679715128154366, 0.0005863019572692231007, 0.0007817359430256308733 ),
 .UNSPECIFIED. ) ;
#19837 = EDGE_LOOP ( 'NONE', ( #75794, #59793 ) ) ;
#19838 = CARTESIAN_POINT ( 'NONE',  ( -16.15384615384627409, -6.879047030192662504, 34.71129190930017927 ) ) ;
#19839 = CARTESIAN_POINT ( 'NONE',  ( 16.82694634598072625, -2.779195860258148798, 31.39871582349836743 ) ) ;
#19840 = FACE_BOUND ( 'NONE', #64460, .T. ) ;
#19841 = CYLINDRICAL_SURFACE ( 'NONE', #31296, 0.2500000000000009437 ) ;
#19842 = CARTESIAN_POINT ( 'NONE',  ( -4.153846153846274980, -11.67786785259630911, 32.92929555188603530 ) ) ;
#19843 = CYLINDRICAL_SURFACE ( 'NONE', #58204, 4.000000000000000000 ) ;
#19844 = CARTESIAN_POINT ( 'NONE',  ( 1.319345384059066983, -12.51329471203370325, 31.30864560766548976 ) ) ;
#19845 = VECTOR ( 'NONE', #63387, 1000.000000000000000 ) ;
#19846 = FACE_OUTER_BOUND ( 'NONE', #73774, .T. ) ;
#19847 = CARTESIAN_POINT ( 'NONE',  ( 15.90382291655318880, -4.335965774309648246, 33.62209801155881905 ) ) ;
#19848 = CARTESIAN_POINT ( 'NONE',  ( 1.449808372910040388, -2.255955759149235629, 29.99999999999988631 ) ) ;
#19849 = VERTEX_POINT ( 'NONE', #80990 ) ;
#19850 = VERTEX_POINT ( 'NONE', #5320 ) ;
#19851 = AXIS2_PLACEMENT_3D ( 'NONE', #3913, #85022, #72375 ) ;
#19853 = CARTESIAN_POINT ( 'NONE',  ( 1.384615384615386802, -1.466349020453238561, 30.81389545987213907 ) ) ;
#19852 = CARTESIAN_POINT ( 'NONE',  ( -5.207613680033384540, -11.93127051446800024, 32.56575433478200665 ) ) ;
#19854 = CARTESIAN_POINT ( 'NONE',  ( 3.100621261037536769, -3.625366637846545448, 33.29286588640298561 ) ) ;
#19855 = DIRECTION ( 'NONE',  ( -1.000000000000000000, -0.000000000000000000, -0.000000000000000000 ) ) ;
#19856 = CARTESIAN_POINT ( 'NONE',  ( 8.519230769230766498, -7.566082377512564960, 35.00000000000000711 ) ) ;
#19857 = CARTESIAN_POINT ( 'NONE',  ( -13.31854703361294412, -2.721908614388772296, 31.22303859784725333 ) ) ;
#19858 = ORIENTED_EDGE ( 'NONE', *, *, #36984, .T. ) ;
#19859 = CYLINDRICAL_SURFACE ( 'NONE', #80270, 0.2499999999999994726 ) ;
#19860 = AXIS2_PLACEMENT_3D ( 'NONE', #68983, #6412, #13601 ) ;
#19861 = CARTESIAN_POINT ( 'NONE',  ( 15.00784227186238162, -4.026226216239094491, 33.68668979543634379 ) ) ;
#19862 = DIRECTION ( 'NONE',  ( -0.000000000000000000, 0.000000000000000000, 1.000000000000000000 ) ) ;
#19863 = CARTESIAN_POINT ( 'NONE',  ( 12.46153846153833911, -6.835583212225970762, 34.95778746994575670 ) ) ;
#19864 = ORIENTED_EDGE ( 'NONE', *, *, #69441, .F. ) ;
#19865 = VERTEX_POINT ( 'NONE', #5765 ) ;
#19866 = B_SPLINE_CURVE_WITH_KNOTS ( 'NONE', 3,
 ( #79297, #66214, #79743, #45047, #86971, #11731, #65763, #32439, #86053, #67562 ),
 .UNSPECIFIED., .F., .F.,
 ( 4, 2, 2, 2, 4 ),
 ( 0.0007817359430256388964, 0.0009771253907250073822, 0.001172514838424375868, 0.001367904286123744571, 0.001563293733823113056 ),
 .UNSPECIFIED. ) ;
#19867 = EDGE_LOOP ( 'NONE', ( #21109, #51852 ) ) ;
#19868 = CARTESIAN_POINT ( 'NONE',  ( 7.384615384615385025, -11.50000000000000000, 29.75000000000000355 ) ) ;
#19869 = B_SPLINE_CURVE_WITH_KNOTS ( 'NONE', 3,
 ( #48880, #54750, #12878, #89009, #27282, #20523, #75038, #54301, #55191, #47988 ),
 .UNSPECIFIED., .F., .F.,
 ( 4, 2, 2, 2, 4 ),
 ( 0.000000000000000000, 0.0001954311564186869557, 0.0003908623128373739115, 0.0005862934692560608672, 0.0007817246256747478229 ),
 .UNSPECIFIED. ) ;
#19870 = VERTEX_POINT ( 'NONE', #26924 ) ;
#19871 = CARTESIAN_POINT ( 'NONE',  ( 12.46153846153846168, -1.951392089020283160, 34.73218667398347748 ) ) ;
#19872 = CARTESIAN_POINT ( 'NONE',  ( 14.43848274865926129, -5.496552790871120031, 34.60292014791297532 ) ) ;
#19873 = CARTESIAN_POINT ( 'NONE',  ( 9.692307692307570832, -2.379036618888197729, 30.90682066428292885 ) ) ;
#19874 = CARTESIAN_POINT ( 'NONE',  ( -4.153846153846273204, -10.21337939537710326, 33.94971097300076224 ) ) ;
#19875 = DIRECTION ( 'NONE',  ( -0.000000000000000000, 0.1736481776669307198, -0.9848077530122080203 ) ) ;
#19876 = EDGE_LOOP ( 'NONE', ( #61121, #47462, #26080, #17133 ) ) ;
#19877 = CARTESIAN_POINT ( 'NONE',  ( 2.980769230769210409, -2.249999999999999112, 29.81609741502488120 ) ) ;
#19879 = ORIENTED_EDGE ( 'NONE', *, *, #16558, .F. ) ;
#19878 = CARTESIAN_POINT ( 'NONE',  ( -7.623142494540996239, -9.886259254753566594, 34.14407573483972413 ) ) ;
#19880 = DIRECTION ( 'NONE',  ( -0.000000000000000000, 0.8660254037844397068, -0.4999999999999978906 ) ) ;
#19881 = LINE ( 'NONE', #88370, #55658 ) ;
#19882 = CYLINDRICAL_SURFACE ( 'NONE', #65925, 0.2499999999999986955 ) ;
#19883 = CARTESIAN_POINT ( 'NONE',  ( -2.438382910802614045, -12.62707690430377383, 30.88035979386743435 ) ) ;
#19884 = CARTESIAN_POINT ( 'NONE',  ( -23.00000000000000000, -10.75000000000000000, 27.25000000000000000 ) ) ;
#19885 = CARTESIAN_POINT ( 'NONE',  ( 18.24994551834813805, -2.587454068350149239, 30.68340429815432557 ) ) ;
#19886 = LINE ( 'NONE', #68086, #36399 ) ;
#19887 = CARTESIAN_POINT ( 'NONE',  ( -2.724691934501246582, -6.299813628509474128, 19.17374329374151642 ) ) ;
#19888 = ORIENTED_EDGE ( 'NONE', *, *, #81653, .T. ) ;
#19889 = CARTESIAN_POINT ( 'NONE',  ( 11.76124107972994892, -2.847695495035523550, 31.58253572463339154 ) ) ;
#19890 = CARTESIAN_POINT ( 'NONE',  ( 12.68431813051652846, -4.989023458446560255, 34.36081565061822118 ) ) ;
#19891 = ADVANCED_FACE ( 'NONE', ( #40885 ), #27363, .F. ) ;
#19892 = ORIENTED_EDGE ( 'NONE', *, *, #42792, .T. ) ;
#19893 = DIRECTION ( 'NONE',  ( 0.000000000000000000, 0.000000000000000000, -1.000000000000000000 ) ) ;
#19894 = CARTESIAN_POINT ( 'NONE',  ( -19.50000000000000000, -3.499999999999999556, 29.75000000000000355 ) ) ;
#19895 = CARTESIAN_POINT ( 'NONE',  ( -7.146003140593070846, -5.667676309546437530, 34.40238873228292249 ) ) ;
#19896 = CARTESIAN_POINT ( 'NONE',  ( -4.826923076923076650, -2.499999999999998668, 29.75000000000000355 ) ) ;
#19897 = DIRECTION ( 'NONE',  ( -0.000000000000000000, -0.5000000000000009992, -0.8660254037844380415 ) ) ;
#19898 = VERTEX_POINT ( 'NONE', #60253 ) ;
#19899 = CARTESIAN_POINT ( 'NONE',  ( -16.28453675695646652, -6.369640206132551441, 34.87707690430378449 ) ) ;
#19900 = EDGE_CURVE ( 'NONE', #10019, #73835, #13842, .T. ) ;
#19901 = LINE ( 'NONE', #47372, #19632 ) ;
#19902 = CARTESIAN_POINT ( 'NONE',  ( 5.076923076922953193, -12.51329471203414379, 31.30864560766407578 ) ) ;
#19903 = EDGE_LOOP ( 'NONE', ( #20388, #64780 ) ) ;
#19904 = CARTESIAN_POINT ( 'NONE',  ( -9.019230769230768274, -7.500000000000001776, 35.00000000000000000 ) ) ;
#19905 = EDGE_LOOP ( 'NONE', ( #77698, #25737, #64977, #69074 ) ) ;
#19906 = CARTESIAN_POINT ( 'NONE',  ( -2.437839517130529821, -12.27039167877662251, 31.24851455888617835 ) ) ;
#19907 = CYLINDRICAL_SURFACE ( 'NONE', #78614, 0.2499999999999998890 ) ;
#19908 = ORIENTED_EDGE ( 'NONE', *, *, #9542, .F. ) ;
#19909 = CARTESIAN_POINT ( 'NONE',  ( 12.39626801557768943, -3.835265460703609186, 33.15142922261924241 ) ) ;
#19910 = DIRECTION ( 'NONE',  ( 0.000000000000000000, 0.9396926207859126468, 0.3420201433256571111 ) ) ;
#19911 = DIRECTION ( 'NONE',  ( 1.000000000000000000, 0.000000000000000000, 0.000000000000000000 ) ) ;
#19912 = AXIS2_PLACEMENT_3D ( 'NONE', #40103, #68878, #55364 ) ;
#19913 = VECTOR ( 'NONE', #82695, 1000.000000000000000 ) ;
#19914 = CYLINDRICAL_SURFACE ( 'NONE', #66452, 0.2500000000000004996 ) ;
#19915 = CARTESIAN_POINT ( 'NONE',  ( -1.607542343522232242, -10.77366814457252175, 33.85459836347579454 ) ) ;
#19917 = CLOSED_SHELL ( 'NONE', ( #28910, #86761, #83372, #11512, #19975, #1738 ) ) ;
#19916 = EDGE_CURVE ( 'NONE', #9623, #34447, #19279, .T. ) ;
#19918 = VECTOR ( 'NONE', #5468, 1000.000000000000000 ) ;
#19919 = ORIENTED_EDGE ( 'NONE', *, *, #9324, .T. ) ;
#19920 = CARTESIAN_POINT ( 'NONE',  ( 8.352564102564102200, -11.50000000000000000, 29.75000000000000355 ) ) ;
#19921 = ORIENTED_EDGE ( 'NONE', *, *, #37247, .F. ) ;
#19922 = CARTESIAN_POINT ( 'NONE',  ( 1.384615384615386802, -12.78798330534103123, 29.99999999999997868 ) ) ;
#19923 = B_SPLINE_CURVE_WITH_KNOTS ( 'NONE', 3,
 ( #67640, #40616, #73956, #88816, #67199, #41492, #7267, #61746, #46907, #62200 ),
 .UNSPECIFIED., .F., .F.,
 ( 4, 2, 2, 2, 4 ),
 ( 0.000000000000000000, 0.0001954311564186863865, 0.0003908623128373727731, 0.0005862934692560591325, 0.0007817246256747455461 ),
 .UNSPECIFIED. ) ;
#19924 = ADVANCED_FACE ( 'NONE', ( #47636 ), #61581, .F. ) ;
#19925 = DIRECTION ( 'NONE',  ( -0.000000000000000000, -0.5000000000000009992, -0.8660254037844380415 ) ) ;
#19926 = EDGE_CURVE ( 'NONE', #43749, #20735, #12520, .T. ) ;
#19927 = CARTESIAN_POINT ( 'NONE',  ( 18.13052570176356326, -12.27024696741798770, 31.24895572276497546 ) ) ;
#19928 = CARTESIAN_POINT ( 'NONE',  ( -1.384615384615383471, -3.322132147404559976, 32.92929555188717927 ) ) ;
#19929 = CARTESIAN_POINT ( 'NONE',  ( 16.94677586748485965, -2.619462340734461048, 30.83744416345203021 ) ) ;
#19930 = ORIENTED_EDGE ( 'NONE', *, *, #50291, .F. ) ;
#19931 = VERTEX_POINT ( 'NONE', #40007 ) ;
#19932 = ORIENTED_EDGE ( 'NONE', *, *, #49703, .F. ) ;
#19933 = ORIENTED_EDGE ( 'NONE', *, *, #68223, .F. ) ;
#19934 = CARTESIAN_POINT ( 'NONE',  ( -4.219116599806928214, -6.026961402152685388, 34.52809138561120506 ) ) ;
#19935 = CARTESIAN_POINT ( 'NONE',  ( 16.21991348719623360, -10.67929555188718282, 33.92786785259544757 ) ) ;
#19936 = VECTOR ( 'NONE', #47217, 1000.000000000000114 ) ;
#19937 = CARTESIAN_POINT ( 'NONE',  ( 2.307692307692186251, -3.643525952248796163, 33.31231777344771672 ) ) ;
#19938 = CARTESIAN_POINT ( 'NONE',  ( -11.53846153846153655, -13.87047571288749737, 32.06866353760679544 ) ) ;
#19939 = CARTESIAN_POINT ( 'NONE',  ( 3.453548899747297618, -9.418065098278011860, 34.63729479722530158 ) ) ;
#19940 = DIRECTION ( 'NONE',  ( 0.000000000000000000, 2.413528314402514090E-16, -1.000000000000000000 ) ) ;
#19941 = CARTESIAN_POINT ( 'NONE',  ( -1.384615384615383471, -6.343179335718451384, 34.87096338111211935 ) ) ;
#19942 = CARTESIAN_POINT ( 'NONE',  ( -4.853910232829680815, -11.43677907613344757, 33.22367315496201456 ) ) ;
#19943 = ORIENTED_EDGE ( 'NONE', *, *, #79510, .T. ) ;
#19944 = ORIENTED_EDGE ( 'NONE', *, *, #62373, .F. ) ;
#19945 = EDGE_LOOP ( 'NONE', ( #78042, #61335 ) ) ;
#19947 = EDGE_LOOP ( 'NONE', ( #76390, #10648 ) ) ;
#19946 = CARTESIAN_POINT ( 'NONE',  ( -11.78843826940389583, -12.41269422305637171, 30.68257228309993323 ) ) ;
#19949 = CARTESIAN_POINT ( 'NONE',  ( -8.096130577096200653, -4.236021600441997492, 33.53823185664189310 ) ) ;
#19948 = DIRECTION ( 'NONE',  ( 0.000000000000000000, 0.8660254037844377084, -0.5000000000000015543 ) ) ;
#19950 = B_SPLINE_CURVE_WITH_KNOTS ( 'NONE', 3,
 ( #63729, #29956, #84908, #49771, #77246, #9675, #43023, #2031, #50654, #56971 ),
 .UNSPECIFIED., .F., .F.,
 ( 4, 2, 2, 2, 4 ),
 ( 0.0007817359430256315238, 0.0009771253907249976244, 0.001172514838424363508, 0.001367904286123729392, 0.001563293733823095492 ),
 .UNSPECIFIED. ) ;
#19951 = EDGE_CURVE ( 'NONE', #78448, #29922, #51603, .T. ) ;
#19952 = CARTESIAN_POINT ( 'NONE',  ( -0.3307480205715128685, -2.295524264805589354, 30.44142389570982488 ) ) ;
#19953 = CARTESIAN_POINT ( 'NONE',  ( -10.68065506134538722, -3.835265460703609186, 33.15142922261924241 ) ) ;
#19954 = FACE_BOUND ( 'NONE', #52568, .T. ) ;
#19955 = ORIENTED_EDGE ( 'NONE', *, *, #32140, .F. ) ;
#19957 = DIRECTION ( 'NONE',  ( -1.000000000000000000, 0.000000000000000000, 0.000000000000000000 ) ) ;
#19956 = B_SPLINE_CURVE_WITH_KNOTS ( 'NONE', 3,
 ( #20782, #6398, #33853, #61311, #88826, #54561, #84280, #63087, #9055, #76168 ),
 .UNSPECIFIED., .F., .F.,
 ( 4, 2, 2, 2, 4 ),
 ( 0.000000000000000000, 0.0001954339857564077183, 0.0003908679715128154366, 0.0005863019572692231007, 0.0007817359430256308733 ),
 .UNSPECIFIED. ) ;
#19958 = DIRECTION ( 'NONE',  ( -0.000000000000000000, -0.000000000000000000, -1.000000000000000000 ) ) ;
#19959 = ORIENTED_EDGE ( 'NONE', *, *, #53627, .F. ) ;
#19960 = CARTESIAN_POINT ( 'NONE',  ( 5.076923076922953193, -2.379036618888197729, 30.90682066428292885 ) ) ;
#19961 = ORIENTED_EDGE ( 'NONE', *, *, #56981, .T. ) ;
#19962 = FACE_BOUND ( 'NONE', #69023, .T. ) ;
#19963 = CARTESIAN_POINT ( 'NONE',  ( -10.74607521849492464, -2.845849958028613624, 32.17971566917920967 ) ) ;
#19964 = DIRECTION ( 'NONE',  ( 1.000000000000000000, 0.000000000000000000, 0.000000000000000000 ) ) ;
#19965 = EDGE_LOOP ( 'NONE', ( #25098, #79934, #11644, #17074 ) ) ;
#19966 = CARTESIAN_POINT ( 'NONE',  ( -12.21148414990014786, -8.303483539816728154, 34.68545999027711702 ) ) ;
#19967 = CARTESIAN_POINT ( 'NONE',  ( -1.384615384615383471, -2.249999999999998668, 29.75000000000001776 ) ) ;
#19968 = CYLINDRICAL_SURFACE ( 'NONE', #86782, 0.2499999999999973355 ) ;
#19969 = EDGE_LOOP ( 'NONE', ( #8592, #57595 ) ) ;
#19970 = CARTESIAN_POINT ( 'NONE',  ( 6.673053685783957967, -5.851115903089112003, 34.47074536777953568 ) ) ;
#19971 = CARTESIAN_POINT ( 'NONE',  ( 14.08420738312797837, -11.60425143139329940, 33.02411095842164457 ) ) ;
#19972 = CARTESIAN_POINT ( 'NONE',  ( 6.857806477116147548, -12.46129190929999986, 30.37095296980880832 ) ) ;
#19973 = CARTESIAN_POINT ( 'NONE',  ( -17.75005459062195712, -12.68172785388650681, 30.59649109432439573 ) ) ;
#19974 = VERTEX_POINT ( 'NONE', #82318 ) ;
#19975 = ADVANCED_FACE ( 'NONE', ( #20598 ), #48062, .T. ) ;
#19976 = AXIS2_PLACEMENT_3D ( 'NONE', #54377, #19273, #75111 ) ;
#19977 = CARTESIAN_POINT ( 'NONE',  ( 9.692307692307695177, -2.708943851104267164, 35.45975837776705220 ) ) ;
#19978 = CARTESIAN_POINT ( 'NONE',  ( 4.153846153846030731, -10.33852847137269571, 34.16647553114546554 ) ) ;
#19979 = CIRCLE ( 'NONE', #1331, 4.000000000000000000 ) ;
#19980 = EDGE_LOOP ( 'NONE', ( #57853, #54740, #87183, #22319 ) ) ;
#19981 = CARTESIAN_POINT ( 'NONE',  ( -8.519285250882630223, -10.76462480002816235, 33.53768742498949962 ) ) ;
#19982 = CARTESIAN_POINT ( 'NONE',  ( -8.519230769230768274, -7.500000000000001776, 35.04278698407183867 ) ) ;
#19983 = CARTESIAN_POINT ( 'NONE',  ( -13.13456107297706588, -4.943051570960394159, 34.04725096376909477 ) ) ;
#19984 = CARTESIAN_POINT ( 'NONE',  ( -11.53846153846153655, -8.120952969808772792, 34.71129190930000163 ) ) ;
#19985 = DIRECTION ( 'NONE',  ( 0.000000000000000000, 0.000000000000000000, 1.000000000000000000 ) ) ;
#19986 = COLOUR_RGB ( '', 0.66274510, 0.83137255, 0.94901961) ;
#19987 = CARTESIAN_POINT ( 'NONE',  ( 9.822833394071260216, -9.417988943895561960, 34.36773134775777550 ) ) ;
#19989 = CARTESIAN_POINT ( 'NONE',  ( -16.21992853320628925, -8.164416787775445883, 34.95778746994557906 ) ) ;
#19988 = DIRECTION ( 'NONE',  ( -0.000000000000000000, 0.000000000000000000, 1.000000000000000000 ) ) ;
#19990 = AXIS2_PLACEMENT_3D ( 'NONE', #15215, #8011, #49438 ) ;
#19991 = CYLINDRICAL_SURFACE ( 'NONE', #7557, 0.2500000000000009437 ) ;
#19992 = CARTESIAN_POINT ( 'NONE',  ( 1.139087296526029469, -10.24999999999999467, 17.20312500000000000 ) ) ;
#19993 = ORIENTED_EDGE ( 'NONE', *, *, #6565, .T. ) ;
#19994 = CARTESIAN_POINT ( 'NONE',  ( -16.15384615384627409, -5.094484230521993062, 34.41647553114689373 ) ) ;
#19996 = VERTEX_POINT ( 'NONE', #81432 ) ;
#19995 = PRODUCT_DEFINITION ( 'UNKNOWN', '', #54748, #85206 ) ;
#19997 = EDGE_CURVE ( 'NONE', #48855, #23593, #6513, .T. ) ;
#19998 = ORIENTED_EDGE ( 'NONE', *, *, #57726, .T. ) ;
#19999 = CARTESIAN_POINT ( 'NONE',  ( -11.47239420511146513, -2.292212530054420494, 30.41441678777542990 ) ) ;
#20000 = EDGE_LOOP ( 'NONE', ( #20399, #7709, #28855, #21385 ) ) ;
#20001 = DIRECTION ( 'NONE',  ( -0.000000000000000000, -0.000000000000000000, -1.000000000000000000 ) ) ;
#20002 = CARTESIAN_POINT ( 'NONE',  ( -1.139087296526025916, -4.750000000000006217, 20.32812500000000000 ) ) ;
#20003 = CARTESIAN_POINT ( 'NONE',  ( 2.294871794871793380, -3.499999999999999556, 29.75000000000000355 ) ) ;
#20004 = ADVANCED_FACE ( 'NONE', ( #773 ), #16832, .F. ) ;
#20005 = CARTESIAN_POINT ( 'NONE',  ( -11.40767109749459074, -9.929761469519743144, 34.40412654351204225 ) ) ;
#20006 = CARTESIAN_POINT ( 'NONE',  ( -2.176900499867519212, -6.413143153341454017, 34.63066358083362672 ) ) ;
#20007 = B_SPLINE_CURVE_WITH_KNOTS ( 'NONE', 3,
 ( #13689, #21329, #33958, #41167, #54662, #33530, #82160, #68633, #20452, #48798 ),
 .UNSPECIFIED., .F., .F.,
 ( 4, 2, 2, 2, 4 ),
 ( 0.000000000000000000, 0.0001954339857564079623, 0.0003908679715128159245, 0.0005863019572692238597, 0.0007817359430256318490 ),
 .UNSPECIFIED. ) ;
#20008 = CARTESIAN_POINT ( 'NONE',  ( 1.253924781505080688, -2.494641256782728966, 31.33461815524612959 ) ) ;
#20009 = CARTESIAN_POINT ( 'NONE',  ( 9.822833130541336999, -12.50538340440932394, 31.33453814440721885 ) ) ;
#20010 = DIRECTION ( 'NONE',  ( -0.000000000000000000, 1.000000000000000000, 3.491481338843133355E-15 ) ) ;
#20011 = CARTESIAN_POINT ( 'NONE',  ( -0.4615384615384611200, -12.48256725967547354, 35.29906147534542527 ) ) ;
#20012 = CARTESIAN_POINT ( 'NONE',  ( 10.83816428436267820, -12.47679350104403007, 31.42216943046555855 ) ) ;
#20013 = CARTESIAN_POINT ( 'NONE',  ( -13.38461538461550582, -6.879047030192662504, 34.71129190930017927 ) ) ;
#20014 = EDGE_CURVE ( 'NONE', #67514, #64117, #47328, .T. ) ;
#20015 = DIRECTION ( 'NONE',  ( -0.000000000000000000, 0.9396926207859093161, -0.3420201433256663259 ) ) ;
#20016 = EDGE_CURVE ( 'NONE', #21487, #37386, #4417, .T. ) ;
#20017 = ORIENTED_EDGE ( 'NONE', *, *, #52186, .T. ) ;
#20018 = ORIENTED_EDGE ( 'NONE', *, *, #85698, .F. ) ;
#20019 = FACE_OUTER_BOUND ( 'NONE', #7970, .T. ) ;
#20020 = CARTESIAN_POINT ( 'NONE',  ( 5.299702618191484582, -9.332535724633407526, 34.40230450496446224 ) ) ;
#20021 = DIRECTION ( 'NONE',  ( 1.000000000000000000, 0.000000000000000000, 0.000000000000000000 ) ) ;
#20022 = LINE ( 'NONE', #47489, #67174 ) ;
#20023 = EDGE_CURVE ( 'NONE', #41920, #31746, #83653, .T. ) ;
#20024 = CARTESIAN_POINT ( 'NONE',  ( 6.249945518348142492, -5.057305518903949526, 34.11320923018887896 ) ) ;
#20025 = CARTESIAN_POINT ( 'NONE',  ( -13.63463860883684475, -10.92453946501458795, 33.72985991061850086 ) ) ;
#20026 = CARTESIAN_POINT ( 'NONE',  ( -1.384615384615505151, -8.613356846316285953, 34.62446782046622218 ) ) ;
#20027 = EDGE_CURVE ( 'NONE', #20780, #13277, #71769, .T. ) ;
#20028 = EDGE_LOOP ( 'NONE', ( #83556, #71691 ) ) ;
#20029 = DIRECTION ( 'NONE',  ( -0.000000000000000000, -0.3420201433256694346, -0.9396926207859080948 ) ) ;
#20030 = ORIENTED_EDGE ( 'NONE', *, *, #30527, .T. ) ;
#20031 = ORIENTED_EDGE ( 'NONE', *, *, #28322, .F. ) ;
#20032 = CARTESIAN_POINT ( 'NONE',  ( -14.05769230769224087, -7.434744429011176159, 34.75000000000000711 ) ) ;
#20033 = AXIS2_PLACEMENT_3D ( 'NONE', #14889, #35146, #84240 ) ;
#20034 = B_SPLINE_CURVE_WITH_KNOTS ( 'NONE', 3,
 ( #47669, #75576, #67507, #13439, #32828, #39604, #46786, #13878, #60291, #34599 ),
 .UNSPECIFIED., .F., .F.,
 ( 4, 2, 2, 2, 4 ),
 ( 0.000000000000000000, 0.0001954339857564074473, 0.0003908679715128148945, 0.0005863019572692223418, 0.0007817359430256297891 ),
 .UNSPECIFIED. ) ;
#20035 = VECTOR ( 'NONE', #86868, 1000.000000000000000 ) ;
#20036 = DIRECTION ( 'NONE',  ( -1.000000000000000000, 0.000000000000000000, -0.000000000000000000 ) ) ;
#20037 = EDGE_CURVE ( 'NONE', #77909, #63742, #31234, .T. ) ;
#20038 = CARTESIAN_POINT ( 'NONE',  ( -4.403822884788508141, -4.236021600441998380, 33.53823185664189310 ) ) ;
#20039 = EDGE_CURVE ( 'NONE', #42366, #37921, #16234, .T. ) ;
#20040 = B_SPLINE_CURVE_WITH_KNOTS ( 'NONE', 3,
 ( #80831, #74062, #25422, #79483, #12356, #79922, #52437, #72711, #39833, #52881 ),
 .UNSPECIFIED., .F., .F.,
 ( 4, 2, 2, 2, 4 ),
 ( 0.0007817359430256334753, 0.0009771253907250058643, 0.001172514838424371098, 0.001367904286123736764, 0.001563293733823101998 ),
 .UNSPECIFIED. ) ;
#20041 = CYLINDRICAL_SURFACE ( 'NONE', #13432, 0.2500000000000012212 ) ;
#20042 = B_SPLINE_CURVE_WITH_KNOTS ( 'NONE', 3,
 ( #83022, #48781, #21755, #15453, #14557, #82140, #69499, #35269, #76705, #20431 ),
 .UNSPECIFIED., .F., .F.,
 ( 4, 2, 2, 2, 4 ),
 ( 0.0007817246336856289524, 0.0009771112958940099402, 0.001172497958102391036, 0.001367884620310772133, 0.001563271282519153229 ),
 .UNSPECIFIED. ) ;
#20043 = CARTESIAN_POINT ( 'NONE',  ( -23.50000000000000000, -13.25000000000000888, 32.75000000000000000 ) ) ;
#20044 = AXIS2_PLACEMENT_3D ( 'NONE', #66354, #60484, #32131 ) ;
#20045 = EDGE_LOOP ( 'NONE', ( #20614, #39280 ) ) ;
#20046 = CIRCLE ( 'NONE', #64647, 0.2500000000000002220 ) ;
#20047 = EDGE_LOOP ( 'NONE', ( #80798, #24731, #21576, #71517 ) ) ;
#20048 = EDGE_LOOP ( 'NONE', ( #63504, #33597 ) ) ;
#20049 = ORIENTED_EDGE ( 'NONE', *, *, #10430, .F. ) ;
#20050 = CARTESIAN_POINT ( 'NONE',  ( -6.222926958906846551, -4.762599654559228846, 34.23009711892697737 ) ) ;
#20051 = LINE ( 'NONE', #75004, #89178 ) ;
#20052 = CARTESIAN_POINT ( 'NONE',  ( -3.230769230769229949, -9.780366693483667717, 34.19971097300155094 ) ) ;
#20053 = CARTESIAN_POINT ( 'NONE',  ( -16.21911615440247090, -2.379036618887870880, 30.90682066428148644 ) ) ;
#20054 = CARTESIAN_POINT ( 'NONE',  ( 18.00000000000000000, -4.786620604624113540, 33.94971097300155094 ) ) ;
#20055 = DIRECTION ( 'NONE',  ( -0.000000000000000000, 1.000000000000000000, -0.000000000000000000 ) ) ;
#20056 = ORIENTED_EDGE ( 'NONE', *, *, #80127, .F. ) ;
#20057 = VERTEX_POINT ( 'NONE', #69236 ) ;
#20058 = VERTEX_POINT ( 'NONE', #7538 ) ;
#20060 = ORIENTED_EDGE ( 'NONE', *, *, #80695, .T. ) ;
#20059 = DIRECTION ( 'NONE',  ( -0.000000000000000000, -0.9396926207859092051, -0.3420201433256662704 ) ) ;
#20061 = CARTESIAN_POINT ( 'NONE',  ( 10.55011416942384095, -12.46129190929999986, 30.37095296980880832 ) ) ;
#20062 = DIRECTION ( 'NONE',  ( 0.000000000000000000, 0.000000000000000000, -1.000000000000000000 ) ) ;
#20063 = ADVANCED_FACE ( 'NONE', ( #85746 ), #21035, .F. ) ;
#20064 = CARTESIAN_POINT ( 'NONE',  ( -1.553300858899125059, -3.750000000000009326, 20.32812500000000711 ) ) ;
#20065 = VERTEX_POINT ( 'NONE', #85304 ) ;
#20066 = B_SPLINE_CURVE_WITH_KNOTS ( 'NONE', 3,
 ( #61021, #88524, #20917, #62341, #26798, #54255, #81750, #652, #47502, #28121 ),
 .UNSPECIFIED., .F., .F.,
 ( 4, 2, 2, 2, 4 ),
 ( 0.0007817359430256308733, 0.0009771253907249974075, 0.001172514838424363725, 0.001367904286123730259, 0.001563293733823096577 ),
 .UNSPECIFIED. ) ;
#20067 = CARTESIAN_POINT ( 'NONE',  ( 7.846153846153846700, -3.937682226553329556, 33.60647404775216529 ) ) ;
#20068 = EDGE_CURVE ( 'NONE', #83912, #41035, #66643, .T. ) ;
#20069 = VECTOR ( 'NONE', #87932, 1000.000000000000227 ) ;
#20070 = EDGE_LOOP ( 'NONE', ( #80384, #58763, #78879, #36969 ) ) ;
#20071 = B_SPLINE_CURVE_WITH_KNOTS ( 'NONE', 3,
 ( #36166, #41579, #8247, #595, #83014, #69933, #21299, #1482, #77582, #76241 ),
 .UNSPECIFIED., .F., .F.,
 ( 4, 2, 2, 2, 4 ),
 ( 0.000000000000000000, 0.0001954339857564054415, 0.0003908679715128108830, 0.0005863019572692163787, 0.0007817359430256217660 ),
 .UNSPECIFIED. ) ;
#20072 = EDGE_CURVE ( 'NONE', #38958, #85779, #76880, .T. ) ;
#20073 = DIRECTION ( 'NONE',  ( -0.000000000000000000, -0.000000000000000000, -1.000000000000000000 ) ) ;
#20074 = FACE_BOUND ( 'NONE', #67686, .T. ) ;
#20075 = CARTESIAN_POINT ( 'NONE',  ( -4.854143535654666053, -12.24180327182771855, 31.33663988360758168 ) ) ;
#20076 = EDGE_CURVE ( 'NONE', #75373, #62016, #4660, .T. ) ;
#20077 = DIRECTION ( 'NONE',  ( -0.000000000000000000, -0.9396926207859092051, -0.3420201433256662704 ) ) ;
#20078 = ORIENTED_EDGE ( 'NONE', *, *, #42106, .T. ) ;
#20079 = CARTESIAN_POINT ( 'NONE',  ( 4.826923076923076650, -2.249999999999998668, 29.75000000000000355 ) ) ;
#20080 = CARTESIAN_POINT ( 'NONE',  ( -13.25456777835970179, -7.723484964179501588, 34.74522123443823318 ) ) ;
#20081 = CARTESIAN_POINT ( 'NONE',  ( 0.4615384615383396616, -12.46129190930018460, 30.37095296980731973 ) ) ;
#20082 = EDGE_LOOP ( 'NONE', ( #61014, #84984 ) ) ;
#20083 = EDGE_CURVE ( 'NONE', #75897, #31900, #15118, .T. ) ;
#20084 = CARTESIAN_POINT ( 'NONE',  ( -3.230769230769229949, -13.87047571288749737, 32.06866353760679544 ) ) ;
#20085 = CARTESIAN_POINT ( 'NONE',  ( 1.607394925883795622, -8.496831190052093419, 34.64984203495476578 ) ) ;
#20086 = LINE ( 'NONE', #54751, #36943 ) ;
#20087 = CARTESIAN_POINT ( 'NONE',  ( -10.61538461538461320, -13.49023893513002648, 31.06009739812518688 ) ) ;
#20088 = CARTESIAN_POINT ( 'NONE',  ( 8.992010438208833278, -10.23759521482555357, 34.22997729860117033 ) ) ;
#20089 = FACE_BOUND ( 'NONE', #11104, .T. ) ;
#20091 = DIRECTION ( 'NONE',  ( -0.000000000000000000, -0.5000000000000009992, -0.8660254037844380415 ) ) ;
#20090 = CARTESIAN_POINT ( 'NONE',  ( 5.933917620639865831, -4.661471528628507777, 34.16647553114621871 ) ) ;
#20092 = LINE ( 'NONE', #52975, #66949 ) ;
#20094 = CARTESIAN_POINT ( 'NONE',  ( 17.74997676270703550, -11.37209801155882793, 32.91403422569033665 ) ) ;
#20093 = CARTESIAN_POINT ( 'NONE',  ( -18.13069060311030967, -2.295517848115768977, 30.44137282052137650 ) ) ;
#20095 = CARTESIAN_POINT ( 'NONE',  ( -3.230769230769229949, -13.49023893513002648, 31.06009739812518688 ) ) ;
#20096 = CARTESIAN_POINT ( 'NONE',  ( -1.200186371490556958, -4.775308065498765409, 16.32625670625849068 ) ) ;
#20097 = VERTEX_POINT ( 'NONE', #40225 ) ;
#20098 = CARTESIAN_POINT ( 'NONE',  ( -8.769230769230890843, -6.026961402154118019, 34.52809138561165270 ) ) ;
#20099 = VERTEX_POINT ( 'NONE', #45185 ) ;
#20100 = B_SPLINE_CURVE_WITH_KNOTS ( 'NONE', 3,
 ( #85331, #78557, #16862, #85777, #49324, #42572, #8342, #63272, #56522, #49757 ),
 .UNSPECIFIED., .F., .F.,
 ( 4, 2, 2, 2, 4 ),
 ( 0.000000000000000000, 0.0001954311564186868473, 0.0003908623128373736946, 0.0005862934692560605419, 0.0007817246256747473893 ),
 .UNSPECIFIED. ) ;
#20101 = AXIS2_PLACEMENT_3D ( 'NONE', #39492, #79582, #66952 ) ;
#20102 = CIRCLE ( 'NONE', #73272, 0.2500000000000002220 ) ;
#20103 = FACE_OUTER_BOUND ( 'NONE', #86447, .T. ) ;
#20104 = ORIENTED_EDGE ( 'NONE', *, *, #76024, .F. ) ;
#20105 = CARTESIAN_POINT ( 'NONE',  ( -4.153846153846152411, -12.10708131394839349, 31.69288490824020244 ) ) ;
#20106 = CARTESIAN_POINT ( 'NONE',  ( 14.17700170458200404, -3.957541250942358424, 33.62499894934981626 ) ) ;
#20108 = ORIENTED_EDGE ( 'NONE', *, *, #461, .F. ) ;
#20107 = LINE ( 'NONE', #75061, #52454 ) ;
#20109 = CARTESIAN_POINT ( 'NONE',  ( -13.38461538461538325, -1.466349020453238561, 30.81389545987213907 ) ) ;
#20110 = CARTESIAN_POINT ( 'NONE',  ( 1.901340078031349856, -5.512252781505337929, 20.31063170625848713 ) ) ;
#20111 = EDGE_CURVE ( 'NONE', #42018, #59060, #88525, .T. ) ;
#20112 = VECTOR ( 'NONE', #67405, 1000.000000000000114 ) ;
#20113 = DIRECTION ( 'NONE',  ( 0.000000000000000000, 0.4999999999999960032, -0.8660254037844410391 ) ) ;
#20114 = CARTESIAN_POINT ( 'NONE',  ( 9.692307692307695177, -2.517432740324522911, 35.29906147534542527 ) ) ;
#20115 = VECTOR ( 'NONE', #33356, 1000.000000000000000 ) ;
#20116 = EDGE_CURVE ( 'NONE', #11864, #84142, #52485, .T. ) ;
#20117 = DIRECTION ( 'NONE',  ( -0.000000000000000000, 1.000000000000000000, 3.491481338843133355E-15 ) ) ;
#20118 = LINE ( 'NONE', #81384, #30081 ) ;
#20119 = CARTESIAN_POINT ( 'NONE',  ( -0.2115929431903197377, -4.336752205174647656, 33.62275283266504289 ) ) ;
#20120 = CARTESIAN_POINT ( 'NONE',  ( 11.66925334628632527, -3.530189275343204702, 32.79018710029569661 ) ) ;
#20121 = VECTOR ( 'NONE', #9603, 1000.000000000000227 ) ;
#20122 = CARTESIAN_POINT ( 'NONE',  ( -3.749999999999997780, -7.438900925035489387, 21.59561829374151287 ) ) ;
#20123 = CARTESIAN_POINT ( 'NONE',  ( 14.24160889673642849, -5.557115091759785130, 34.35708131394839171 ) ) ;
#20124 = ORIENTED_EDGE ( 'NONE', *, *, #78640, .F. ) ;
#20125 = CARTESIAN_POINT ( 'NONE',  ( 17.14217864819910275, -2.892918686051626498, 31.69288490824026638 ) ) ;
#20126 = CARTESIAN_POINT ( 'NONE',  ( 1.492201783934598236, -11.27530806549875031, 24.95499329374151287 ) ) ;
#20127 = CARTESIAN_POINT ( 'NONE',  ( -14.98076923076922107, -2.249999999999999112, 29.81603969181033165 ) ) ;
#20128 = CARTESIAN_POINT ( 'NONE',  ( 5.207448515156721136, -6.808710257144159783, 34.95449254468098843 ) ) ;
#20129 = ORIENTED_EDGE ( 'NONE', *, *, #5682, .T. ) ;
#20130 = LINE ( 'NONE', #6614, #5410 ) ;
#20131 = CARTESIAN_POINT ( 'NONE',  ( -0.4615384615384611200, -9.780366693483667717, 34.19971097300155094 ) ) ;
#20133 = EDGE_LOOP ( 'NONE', ( #40340, #86363 ) ) ;
#20132 = DIRECTION ( 'NONE',  ( 0.000000000000000000, 2.413528314402514090E-16, -1.000000000000000000 ) ) ;
#20134 = CARTESIAN_POINT ( 'NONE',  ( -2.084265908777518828, -7.630147987733843173, 34.99859428049665411 ) ) ;
#20135 = CARTESIAN_POINT ( 'NONE',  ( 2.084766090176161324, -12.39988816332205701, 30.74660775122750778 ) ) ;
#20136 = FACE_OUTER_BOUND ( 'NONE', #68489, .T. ) ;
#20137 = CARTESIAN_POINT ( 'NONE',  ( -4.153846153846152411, -2.538708090699994813, 30.37095296980875503 ) ) ;
#20138 = CARTESIAN_POINT ( 'NONE',  ( -10.28846153846153832, -4.000000000000000000, 29.75000000000000355 ) ) ;
#20139 = EDGE_CURVE ( 'NONE', #45673, #85149, #57054, .T. ) ;
#20140 = EDGE_CURVE ( 'NONE', #38794, #67806, #62321, .T. ) ;
#20141 = CARTESIAN_POINT ( 'NONE',  ( 8.769230769230768274, -1.509761064869970415, 31.06009739812519044 ) ) ;
#20142 = ORIENTED_EDGE ( 'NONE', *, *, #41184, .F. ) ;
#20143 = ORIENTED_EDGE ( 'NONE', *, *, #57350, .T. ) ;
#20144 = ORIENTED_EDGE ( 'NONE', *, *, #15521, .F. ) ;
#20145 = EDGE_CURVE ( 'NONE', #88347, #30358, #61162, .T. ) ;
#20146 = ORIENTED_EDGE ( 'NONE', *, *, #85558, .T. ) ;
#20147 = DIRECTION ( 'NONE',  ( -0.000000000000000000, 1.000000000000000000, -0.000000000000000000 ) ) ;
#20148 = CARTESIAN_POINT ( 'NONE',  ( 0.2115617305961061678, -2.564618984488975961, 30.55390908950641915 ) ) ;
#20149 = EDGE_CURVE ( 'NONE', #24566, #48795, #55937, .T. ) ;
#20150 = CARTESIAN_POINT ( 'NONE',  ( 9.822833394071260216, -5.195472089885680766, 34.18748526763464923 ) ) ;
#20151 = CARTESIAN_POINT ( 'NONE',  ( -8.096177070375302876, -10.92453946501458795, 33.72985991061850086 ) ) ;
#20152 = EDGE_CURVE ( 'NONE', #62404, #275, #38724, .T. ) ;
#20153 = CARTESIAN_POINT ( 'NONE',  ( -2.651650429449565305, -4.848349570550461785, 26.50000000000000355 ) ) ;
#20154 = ORIENTED_EDGE ( 'NONE', *, *, #61409, .F. ) ;
#20155 = VERTEX_POINT ( 'NONE', #47402 ) ;
#20156 = VECTOR ( 'NONE', #70135, 1000.000000000000000 ) ;
#20157 = VERTEX_POINT ( 'NONE', #48738 ) ;
#20159 = EDGE_LOOP ( 'NONE', ( #70286, #75062 ) ) ;
#20158 = DIRECTION ( 'NONE',  ( -0.000000000000000000, -0.1736481776669307198, -0.9848077530122080203 ) ) ;
#20160 = CARTESIAN_POINT ( 'NONE',  ( 10.61538461538461675, -13.49023893513002648, 31.06009739812518688 ) ) ;
#20161 = ADVANCED_FACE ( 'NONE', ( #14967 ), #75765, .T. ) ;
#20162 = CARTESIAN_POINT ( 'NONE',  ( -10.83826329781326159, -7.630691491037285168, 34.74850469731152458 ) ) ;
#20163 = AXIS2_PLACEMENT_3D ( 'NONE', #9152, #79256, #18002 ) ;
#20164 = AXIS2_PLACEMENT_3D ( 'NONE', #82564, #55509, #21276 ) ;
#20165 = EDGE_CURVE ( 'NONE', #24900, #60879, #78420, .T. ) ;
#20166 = CARTESIAN_POINT ( 'NONE',  ( -12.21148414990014963, -12.17597550085003633, 31.52189283813461884 ) ) ;
#20167 = CARTESIAN_POINT ( 'NONE',  ( -9.692307692307691624, -13.53365097954675988, 30.81389545987213552 ) ) ;
#20168 = B_SPLINE_CURVE_WITH_KNOTS ( 'NONE', 3,
 ( #21277, #77118, #42451, #15426, #83447, #23058, #7775, #62699, #7337, #22608 ),
 .UNSPECIFIED., .F., .F.,
 ( 4, 2, 2, 2, 4 ),
 ( 0.000000000000000000, 0.0001954339857564074473, 0.0003908679715128148945, 0.0005863019572692223418, 0.0007817359430256297891 ),
 .UNSPECIFIED. ) ;
#20169 = VERTEX_POINT ( 'NONE', #54600 ) ;
#20170 = B_SPLINE_CURVE_WITH_KNOTS ( 'NONE', 3,
 ( #45759, #10646, #86774, #46649, #85862, #59716, #59269, #66923, #39020, #11089 ),
 .UNSPECIFIED., .F., .F.,
 ( 4, 2, 2, 2, 4 ),
 ( 0.0007817246256747472808, 0.0009771112852218905021, 0.001172497944769033832, 0.001367884604316177161, 0.001563271263863320274 ),
 .UNSPECIFIED. ) ;
#20171 = ORIENTED_EDGE ( 'NONE', *, *, #17163, .T. ) ;
#20172 = AXIS2_PLACEMENT_3D ( 'NONE', #63363, #16070, #85418 ) ;
#20173 = ORIENTED_EDGE ( 'NONE', *, *, #40958, .F. ) ;
#20174 = CARTESIAN_POINT ( 'NONE',  ( -14.87820512820512953, -11.50000000000000000, 29.75000000000000355 ) ) ;
#20176 = ORIENTED_EDGE ( 'NONE', *, *, #9278, .F. ) ;
#20175 = CARTESIAN_POINT ( 'NONE',  ( 10.61538461538461675, -1.466349020453238561, 30.81389545987213907 ) ) ;
#20178 = B_SPLINE_CURVE_WITH_KNOTS ( 'NONE', 3,
 ( #51317, #18468, #31072, #50886, #72507, #39190, #65744, #38733, #58993, #45922 ),
 .UNSPECIFIED., .F., .F.,
 ( 4, 2, 2, 2, 4 ),
 ( 0.000000000000000000, 0.0001954311564186871184, 0.0003908623128373742367, 0.0005862934692560614093, 0.0007817246256747484735 ),
 .UNSPECIFIED. ) ;
#20177 = CARTESIAN_POINT ( 'NONE',  ( 6.699591979352975457, -6.760086850603068243, 34.69517049084099369 ) ) ;
#20179 = EDGE_CURVE ( 'NONE', #5216, #88472, #80701, .T. ) ;
#20180 = CARTESIAN_POINT ( 'NONE',  ( -14.30769230769230660, -2.538708090699994813, 30.37095296980875503 ) ) ;
#20181 = ORIENTED_EDGE ( 'NONE', *, *, #73173, .T. ) ;
#20182 = CARTESIAN_POINT ( 'NONE',  ( 16.28463796167094202, -3.530189275343204702, 32.79018710029569661 ) ) ;
#20183 = CARTESIAN_POINT ( 'NONE',  ( 0.3954560821783251190, -9.058645607665454236, 34.76329471203372634 ) ) ;
#20184 = FACE_BOUND ( 'NONE', #6026, .T. ) ;
#20185 = EDGE_CURVE ( 'NONE', #43220, #6788, #13626, .T. ) ;
#20186 = DIRECTION ( 'NONE',  ( -0.000000000000000000, -0.6427876096865404731, -0.7660444431189770143 ) ) ;
#20187 = CARTESIAN_POINT ( 'NONE',  ( -5.999999999999998224, -12.34228464037088635, 31.77849191805839268 ) ) ;
#20188 = CARTESIAN_POINT ( 'NONE',  ( -5.999999999999690914, -2.506253911140614576, 30.00000000000323297 ) ) ;
#20190 = DIRECTION ( 'NONE',  ( -0.000000000000000000, 1.000000000000000000, -0.000000000000000000 ) ) ;
#20189 = DIRECTION ( 'NONE',  ( 0.000000000000000000, -1.000000000000000000, 0.000000000000000000 ) ) ;
#20191 = CARTESIAN_POINT ( 'NONE',  ( -4.376674251481031064, -7.369209533119140509, 34.99857337881830688 ) ) ;
#20192 = CYLINDRICAL_SURFACE ( 'NONE', #67800, 0.2499999999999994726 ) ;
#20193 = EDGE_LOOP ( 'NONE', ( #52938, #6035 ) ) ;
#20194 = CARTESIAN_POINT ( 'NONE',  ( -7.912236225513979981, -6.343179335718451384, 34.87096338111212646 ) ) ;
#20195 = CARTESIAN_POINT ( 'NONE',  ( 0.3962684609821406356, -11.06231777344662781, 33.60647404775220082 ) ) ;
#20196 = ORIENTED_EDGE ( 'NONE', *, *, #86616, .T. ) ;
#20197 = EDGE_CURVE ( 'NONE', #44046, #75329, #13991, .T. ) ;
#20198 = CARTESIAN_POINT ( 'NONE',  ( -14.53061852520844965, -4.887634598454295265, 34.01352882383564946 ) ) ;
#20199 = DIRECTION ( 'NONE',  ( 0.000000000000000000, -4.336808689942017736E-16, 1.000000000000000000 ) ) ;
#20200 = ORIENTED_EDGE ( 'NONE', *, *, #74581, .T. ) ;
#20201 = CARTESIAN_POINT ( 'NONE',  ( 11.47237915910140771, -9.905515769479276145, 34.41647553114623292 ) ) ;
#20202 = LINE ( 'NONE', #67061, #19936 ) ;
#20203 = FACE_BOUND ( 'NONE', #6383, .T. ) ;
#20204 = EDGE_CURVE ( 'NONE', #51377, #62161, #31213, .T. ) ;
#20206 = CYLINDRICAL_SURFACE ( 'NONE', #17196, 0.2499999999999979738 ) ;
#20205 = CARTESIAN_POINT ( 'NONE',  ( -14.53061926659915315, -4.026226216239094491, 33.68668979543634379 ) ) ;
#20207 = PLANE ( 'NONE',  #22960 ) ;
#20208 = DIRECTION ( 'NONE',  ( -0.000000000000000000, -0.6427876096865404731, -0.7660444431189771253 ) ) ;
#20209 = CARTESIAN_POINT ( 'NONE',  ( -10.61538461538473577, -11.67786785259630911, 32.92929555188603530 ) ) ;
#20210 = B_SPLINE_CURVE_WITH_KNOTS ( 'NONE', 3,
 ( #26830, #60601, #53853, #88117, #47085, #20509, #46653, #74575, #39468, #20067 ),
 .UNSPECIFIED., .F., .F.,
 ( 4, 2, 2, 2, 4 ),
 ( 0.0007817246256747465219, 0.0009771112852218900684, 0.001172497944769033615, 0.001367884604316176944, 0.001563271263863320491 ),
 .UNSPECIFIED. ) ;
#20211 = VECTOR ( 'NONE', #13035, 999.9999999999998863 ) ;
#20212 = CARTESIAN_POINT ( 'NONE',  ( 2.651650429449569302, -10.15165042944953733, 24.62500000000000000 ) ) ;
#20213 = ORIENTED_EDGE ( 'NONE', *, *, #79416, .T. ) ;
#20214 = VERTEX_POINT ( 'NONE', #62247 ) ;
#20215 = CARTESIAN_POINT ( 'NONE',  ( -12.23875879256039312, -5.827830569534417471, 34.72679350104403539 ) ) ;
#20216 = CARTESIAN_POINT ( 'NONE',  ( -18.00000000000012079, -3.643525952248793498, 33.31231777344770961 ) ) ;
#20217 = DIRECTION ( 'NONE',  ( 0.000000000000000000, 0.000000000000000000, -1.000000000000000000 ) ) ;
#20218 = LINE ( 'NONE', #89137, #45254 ) ;
#20219 = CYLINDRICAL_SURFACE ( 'NONE', #87444, 0.2500000000000008882 ) ;
#20220 = CARTESIAN_POINT ( 'NONE',  ( 2.608446859217893099, -4.805146000318787358, 17.81063170625849068 ) ) ;
#20221 = EDGE_CURVE ( 'NONE', #17526, #18050, #77491, .T. ) ;
#20222 = DIRECTION ( 'NONE',  ( -0.000000000000000000, -0.8660254037844397068, -0.4999999999999978906 ) ) ;
#20223 = CARTESIAN_POINT ( 'NONE',  ( 5.749976775778544713, -2.985938066672154445, 32.43141759479405550 ) ) ;
#20224 = ADVANCED_FACE ( 'NONE', ( #28475 ), #68569, .F. ) ;
#20225 = FACE_OUTER_BOUND ( 'NONE', #36055, .T. ) ;
#20226 = CARTESIAN_POINT ( 'NONE',  ( 19.00000000000000000, 8.999999999999996447, 23.75000000000000000 ) ) ;
#20227 = CARTESIAN_POINT ( 'NONE',  ( 3.230769230769231726, -1.215029322943914858, 32.30358669280327177 ) ) ;
#20228 = CARTESIAN_POINT ( 'NONE',  ( 8.638539302563209787, -12.11776431015576172, 31.66791131148498906 ) ) ;
#20229 = FACE_OUTER_BOUND ( 'NONE', #31456, .T. ) ;
#20230 = CARTESIAN_POINT ( 'NONE',  ( -6.700064078983527516, -3.395485233115139057, 33.02377354290275946 ) ) ;
#20231 = AXIS2_PLACEMENT_3D ( 'NONE', #23076, #31492, #44991 ) ;
#20232 = CARTESIAN_POINT ( 'NONE',  ( 10.61538461538461675, -1.117168528481311540, 33.14645433367849847 ) ) ;
#20233 = ORIENTED_EDGE ( 'NONE', *, *, #17975, .F. ) ;
#20234 = DIRECTION ( 'NONE',  ( -0.000000000000000000, 1.000000000000000000, -0.000000000000000000 ) ) ;
#20235 = FACE_OUTER_BOUND ( 'NONE', #34647, .T. ) ;
#20236 = CARTESIAN_POINT ( 'NONE',  ( -2.724691934501246582, -6.299813628509474128, 14.17374329374151287 ) ) ;
#20237 = VECTOR ( 'NONE', #33686, 1000.000000000000114 ) ;
#20238 = CIRCLE ( 'NONE', #4406, 5.000000000000000888 ) ;
#20239 = CARTESIAN_POINT ( 'NONE',  ( 5.076923076923075762, -9.905515769479276145, 34.41647553114623292 ) ) ;
#20240 = CARTESIAN_POINT ( 'NONE',  ( -17.74994568836168440, -10.66356715214248752, 33.62249196103329751 ) ) ;
#20241 = DIRECTION ( 'NONE',  ( -0.000000000000000000, -0.5000000000000009992, -0.8660254037844380415 ) ) ;
#20243 = ORIENTED_EDGE ( 'NONE', *, *, #36663, .F. ) ;
#20242 = CARTESIAN_POINT ( 'NONE',  ( -39.05038313613820122, -2.499999999999999556, 29.75000000000000355 ) ) ;
#20244 = CARTESIAN_POINT ( 'NONE',  ( -2.749999999999998224, -7.500000000000015987, 21.34375000000000000 ) ) ;
#20245 = CARTESIAN_POINT ( 'NONE',  ( -14.55766905174089665, -5.643011162660950042, 34.66104346484419096 ) ) ;
#20246 = ORIENTED_EDGE ( 'NONE', *, *, #60883, .T. ) ;
#20247 = CARTESIAN_POINT ( 'NONE',  ( 11.78851595837499211, -9.233818618650603938, 34.70587769442853698 ) ) ;
#20248 = CARTESIAN_POINT ( 'NONE',  ( -17.77698864838715664, -3.587049720035813127, 32.86302985866382897 ) ) ;
#20249 = EDGE_LOOP ( 'NONE', ( #8879, #85572, #59035, #32547 ) ) ;
#20250 = CARTESIAN_POINT ( 'NONE',  ( 14.30769230769231015, -2.538708090699994813, 30.37095296980875503 ) ) ;
#20251 = CARTESIAN_POINT ( 'NONE',  ( 8.639082799499073317, -6.809168938359901446, 34.95455904226513866 ) ) ;
#20252 = B_SPLINE_CURVE_WITH_KNOTS ( 'NONE', 3,
 ( #81937, #54002, #19781, #75176, #11700, #31965, #39177, #52665, #66637, #80154 ),
 .UNSPECIFIED., .F., .F.,
 ( 4, 2, 2, 2, 4 ),
 ( 0.000000000000000000, 0.0001954311564186881213, 0.0003908623128373762425, 0.0005862934692560643367, 0.0007817246256747524850 ),
 .UNSPECIFIED. ) ;
#20253 = LINE ( 'NONE', #61663, #75829 ) ;
#20254 = ORIENTED_EDGE ( 'NONE', *, *, #33188, .F. ) ;
#20255 = B_SPLINE_CURVE_WITH_KNOTS ( 'NONE', 3,
 ( #47540, #27276, #13320, #47983, #13758, #7004, #68703, #34477, #61939, #251 ),
 .UNSPECIFIED., .F., .F.,
 ( 4, 2, 2, 2, 4 ),
 ( 0.000000000000000000, 0.0001954311564186861697, 0.0003908623128373723394, 0.0005862934692560584820, 0.0007817246256747446788 ),
 .UNSPECIFIED. ) ;
#20256 = VERTEX_POINT ( 'NONE', #19937 ) ;
#20257 = CARTESIAN_POINT ( 'NONE',  ( 15.45354889974729495, -4.989023458446560255, 34.36081565061822118 ) ) ;
#20258 = VERTEX_POINT ( 'NONE', #34336 ) ;
#20259 = CARTESIAN_POINT ( 'NONE',  ( -8.069080805060693251, -2.308479472611653094, 30.53278059502174457 ) ) ;
#20260 = CARTESIAN_POINT ( 'NONE',  ( -13.38461538461538325, -2.538708090699994813, 30.37095296980875503 ) ) ;
#20261 = CARTESIAN_POINT ( 'NONE',  ( -10.86540785267757592, -2.587272538249755893, 30.68239716806877837 ) ) ;
#20262 = ADVANCED_FACE ( 'NONE', ( #61802 ), #27585, .F. ) ;
#20263 = CARTESIAN_POINT ( 'NONE',  ( -4.153846153846152411, -1.215029322943914858, 32.30358669280327177 ) ) ;
#20264 = CARTESIAN_POINT ( 'NONE',  ( 17.07692307692307665, -12.29105614889573062, 35.45975837776705220 ) ) ;
#20265 = CARTESIAN_POINT ( 'NONE',  ( -2.557692307692305267, -2.249999999999998668, 29.75000000000000355 ) ) ;
#20266 = EDGE_CURVE ( 'NONE', #30501, #60387, #43028, .T. ) ;
#20267 = CARTESIAN_POINT ( 'NONE',  ( 10.36536137809165403, -12.22074536777954989, 31.39888409691088356 ) ) ;
#20268 = VERTEX_POINT ( 'NONE', #30248 ) ;
#20269 = ORIENTED_EDGE ( 'NONE', *, *, #36522, .T. ) ;
#20271 = ORIENTED_EDGE ( 'NONE', *, *, #37201, .F. ) ;
#20270 = CARTESIAN_POINT ( 'NONE',  ( -17.14219352288385778, -10.21337939537584383, 33.94971097300158647 ) ) ;
#20272 = AXIS2_PLACEMENT_3D ( 'NONE', #50234, #78168, #70529 ) ;
#20273 = EDGE_CURVE ( 'NONE', #74021, #50542, #57272, .T. ) ;
#20274 = B_SPLINE_CURVE_WITH_KNOTS ( 'NONE', 3,
 ( #19303, #5346, #5788, #12989, #72904, #73812, #11209, #80575, #19745, #38679 ),
 .UNSPECIFIED., .F., .F.,
 ( 4, 2, 2, 2, 4 ),
 ( 0.000000000000000000, 0.0001954311564186867660, 0.0003908623128373735320, 0.0005862934692560603251, 0.0007817246256747470640 ),
 .UNSPECIFIED. ) ;
#20275 = CARTESIAN_POINT ( 'NONE',  ( -8.769230769230768274, -10.67929555188718282, 33.92786785259544047 ) ) ;
#20276 = CARTESIAN_POINT ( 'NONE',  ( 9.626224281351815293, -4.786620604624113540, 33.94971097300155805 ) ) ;
#20277 = VERTEX_POINT ( 'NONE', #70349 ) ;
#20278 = CARTESIAN_POINT ( 'NONE',  ( 14.53047197667037516, -12.11081565061823717, 32.26097654155341843 ) ) ;
#20279 = B_SPLINE_CURVE_WITH_KNOTS ( 'NONE', 3,
 ( #82781, #78216, #58377, #51611, #79108, #38122, #17861, #31824, #59278, #16518 ),
 .UNSPECIFIED., .F., .F.,
 ( 4, 2, 2, 2, 4 ),
 ( 0.0007817359527651101701, 0.0009771254036996489256, 0.001172514854634187790, 0.001367904305568726653, 0.001563293756503265517 ),
 .UNSPECIFIED. ) ;
#20280 = EDGE_CURVE ( 'NONE', #70987, #62668, #88203, .T. ) ;
#20281 = ORIENTED_EDGE ( 'NONE', *, *, #20291, .T. ) ;
#20282 = CARTESIAN_POINT ( 'NONE',  ( -15.23076923076922995, -2.249999999999998668, 29.75000000000001776 ) ) ;
#20283 = B_SPLINE_CURVE_WITH_KNOTS ( 'NONE', 3,
 ( #73931, #5021, #33819, #39261, #46446, #26623, #81135, #74369, #25736, #13112 ),
 .UNSPECIFIED., .F., .F.,
 ( 4, 2, 2, 2, 4 ),
 ( 0.000000000000000000, 0.0001954311564186877960, 0.0003908623128373755920, 0.0005862934692560633609, 0.0007817246256747511840 ),
 .UNSPECIFIED. ) ;
#20284 = ORIENTED_EDGE ( 'NONE', *, *, #71311, .F. ) ;
#20285 = CARTESIAN_POINT ( 'NONE',  ( 24.00000000000000000, 5.000000000000023093, 28.74999999999999645 ) ) ;
#20286 = ORIENTED_EDGE ( 'NONE', *, *, #26687, .T. ) ;
#20287 = VECTOR ( 'NONE', #54186, 1000.000000000000000 ) ;
#20288 = CARTESIAN_POINT ( 'NONE',  ( -8.899922235898330314, -4.809359713505814149, 33.96456829005828837 ) ) ;
#20289 = DIRECTION ( 'NONE',  ( -0.000000000000000000, -0.9396926207859092051, -0.3420201433256662704 ) ) ;
#20290 = FACE_BOUND ( 'NONE', #60932, .T. ) ;
#20291 = EDGE_CURVE ( 'NONE', #45665, #50666, #44622, .T. ) ;
#20292 = CARTESIAN_POINT ( 'NONE',  ( 14.30769230769231015, -13.95598074871891292, 31.83374038241031911 ) ) ;
#20293 = CYLINDRICAL_SURFACE ( 'NONE', #11198, 0.2499999999999979738 ) ;
#20294 = VECTOR ( 'NONE', #35932, 1000.000000000000000 ) ;
#20295 = CARTESIAN_POINT ( 'NONE',  ( -15.93083330975275658, -4.762714258010882773, 34.23016756924214832 ) ) ;
#20296 = CARTESIAN_POINT ( 'NONE',  ( 20.00000000000000000, -4.000000000000000000, 29.75000000000000355 ) ) ;
#20297 = CYLINDRICAL_SURFACE ( 'NONE', #84132, 0.2499999999999995559 ) ;
#20298 = CARTESIAN_POINT ( 'NONE',  ( -1.384615384615383471, -1.129524287112498415, 32.06866353760679544 ) ) ;
#20299 = EDGE_CURVE ( 'NONE', #4054, #64954, #116, .T. ) ;
#20300 = CARTESIAN_POINT ( 'NONE',  ( 9.692307692307695177, -2.292212530054420494, 30.41441678777542634 ) ) ;
#20301 = EDGE_LOOP ( 'NONE', ( #22603, #48660, #43357, #10833 ) ) ;
#20302 = ORIENTED_EDGE ( 'NONE', *, *, #39056, .T. ) ;
#20303 = VECTOR ( 'NONE', #72589, 1000.000000000000114 ) ;
#20305 = CARTESIAN_POINT ( 'NONE',  ( -18.06527000055631405, -10.33852847137145403, 34.16647553114627556 ) ) ;
#20304 = CARTESIAN_POINT ( 'NONE',  ( -16.82697755857493149, -10.05730279482229683, 34.04704008940765902 ) ) ;
#20306 = DIRECTION ( 'NONE',  ( 0.000000000000000000, -6.938893903907222067E-15, 1.000000000000000000 ) ) ;
#20307 = CARTESIAN_POINT ( 'NONE',  ( 3.230769230769231726, -10.51840700105979565, 33.73612834413961536 ) ) ;
#20308 = CARTESIAN_POINT ( 'NONE',  ( 8.638621114026685532, -7.722926974430166069, 34.99546784045485737 ) ) ;
#20309 = DIRECTION ( 'NONE',  ( 1.000000000000000000, 0.000000000000000000, 0.000000000000000000 ) ) ;
#20310 = EDGE_LOOP ( 'NONE', ( #52579, #62113 ) ) ;
#20311 = CARTESIAN_POINT ( 'NONE',  ( 17.20744877868664346, -3.285477652293413264, 32.44071101563363158 ) ) ;
#20312 = EDGE_CURVE ( 'NONE', #72884, #35268, #60249, .T. ) ;
#20313 = CARTESIAN_POINT ( 'NONE',  ( 0.5920641633020228278, -10.19071101563364401, 33.96452234770658407 ) ) ;
#20314 = CARTESIAN_POINT ( 'NONE',  ( -3.296039231325550656, -11.67786785259541027, 32.92929555188721480 ) ) ;
#20315 = CARTESIAN_POINT ( 'NONE',  ( -6.923076923076922462, -6.343179335718451384, 34.87096338111211935 ) ) ;
#20316 = ORIENTED_EDGE ( 'NONE', *, *, #8416, .F. ) ;
#20317 = EDGE_LOOP ( 'NONE', ( #40654, #14951, #63924, #26609 ) ) ;
#20318 = ORIENTED_EDGE ( 'NONE', *, *, #4330, .T. ) ;
#20319 = CARTESIAN_POINT ( 'NONE',  ( 0.5923302693632472860, -10.54018710029568595, 33.71981072465678864 ) ) ;
#20320 = EDGE_LOOP ( 'NONE', ( #82382, #10096 ) ) ;
#20321 = CARTESIAN_POINT ( 'NONE',  ( 2.980792486720640788, -12.65889640711025521, 30.72598325615533454 ) ) ;
#20322 = CARTESIAN_POINT ( 'NONE',  ( -2.749999999999998224, -7.500000000000000000, 29.50000000000000355 ) ) ;
#20323 = CARTESIAN_POINT ( 'NONE',  ( 4.946231610255518163, -6.413092428213692742, 34.63065189839063152 ) ) ;
#20324 = CARTESIAN_POINT ( 'NONE',  ( -2.307692307692305711, -8.120952969808772792, 34.71129190930000163 ) ) ;
#20325 = ADVANCED_FACE ( 'NONE', ( #85197 ), #85636, .F. ) ;
#20326 = FACE_OUTER_BOUND ( 'NONE', #76611, .T. ) ;
#20327 = VERTEX_POINT ( 'NONE', #8209 ) ;
#20328 = LINE ( 'NONE', #61736, #42951 ) ;
#20330 = ORIENTED_EDGE ( 'NONE', *, *, #72873, .T. ) ;
#20329 = CARTESIAN_POINT ( 'NONE',  ( 6.416666666666664298, -7.500000000000000000, 33.75000000000000000 ) ) ;
#20331 = PLANE ( 'NONE',  #36853 ) ;
#20333 = B_SPLINE_CURVE_WITH_KNOTS ( 'NONE', 3,
 ( #7686, #6785, #62609, #68058, #6364, #33818, #88790, #27065, #20314, #47777 ),
 .UNSPECIFIED., .F., .F.,
 ( 4, 2, 2, 2, 4 ),
 ( 0.000000000000000000, 0.0001954311564186869557, 0.0003908623128373739115, 0.0005862934692560608672, 0.0007817246256747478229 ),
 .UNSPECIFIED. ) ;
#20332 = CARTESIAN_POINT ( 'NONE',  ( 9.019176178608812933, -12.45601412856602686, 31.48342859153981621 ) ) ;
#20334 = DIRECTION ( 'NONE',  ( -0.000000000000000000, -0.3420201433256694901, -0.9396926207859082059 ) ) ;
#20335 = VECTOR ( 'NONE', #36103, 1000.000000000000000 ) ;
#20336 = ADVANCED_FACE ( 'NONE', ( #30682 ), #9967, .T. ) ;
#20337 = EDGE_CURVE ( 'NONE', #76336, #57743, #18296, .T. ) ;
#20338 = CARTESIAN_POINT ( 'NONE',  ( 11.76147438255493149, -10.01129605718032600, 34.36064277460058491 ) ) ;
#20339 = CARTESIAN_POINT ( 'NONE',  ( 9.692307692307695177, -13.88283147151868846, 33.14645433367849847 ) ) ;
#20340 = CARTESIAN_POINT ( 'NONE',  ( 17.01159906411876932, -7.749976730030849303, 34.74374725381503737 ) ) ;
#20341 = CARTESIAN_POINT ( 'NONE',  ( 5.448717948717947124, -11.00000000000000000, 29.75000000000000355 ) ) ;
#20342 = AXIS2_PLACEMENT_3D ( 'NONE', #5601, #46586, #26756 ) ;
#20343 = CARTESIAN_POINT ( 'NONE',  ( -1.987747218494638313, -9.401340078031370950, 21.43936829374151642 ) ) ;
#20344 = EDGE_CURVE ( 'NONE', #88650, #2791, #18955, .T. ) ;
#20345 = EDGE_LOOP ( 'NONE', ( #13303, #62890 ) ) ;
#20346 = EDGE_CURVE ( 'NONE', #67440, #32572, #34414, .T. ) ;
#20347 = CARTESIAN_POINT ( 'NONE',  ( 13.38461538461538680, -5.471508081941601098, 34.59228464037088457 ) ) ;
#20348 = CARTESIAN_POINT ( 'NONE',  ( 1.134638640566795420, -9.234221910056348293, 34.70572697212741531 ) ) ;
#20349 = CARTESIAN_POINT ( 'NONE',  ( 9.942362112221147186, -10.82426656108012075, 33.81400080652039009 ) ) ;
#20350 = CARTESIAN_POINT ( 'NONE',  ( 11.97435897435897267, -7.500000000000000000, 29.75000000000000355 ) ) ;
#20351 = ORIENTED_EDGE ( 'NONE', *, *, #60462, .F. ) ;
#20352 = CARTESIAN_POINT ( 'NONE',  ( -5.749945688361683516, -2.564540009722896752, 30.55348353981670684 ) ) ;
#20353 = CARTESIAN_POINT ( 'NONE',  ( -16.15384615384615330, -1.790695186598648903, 34.54067556320373455 ) ) ;
#20354 = CARTESIAN_POINT ( 'NONE',  ( 2.372947447205147942, -11.06231777344671130, 33.60647404775212976 ) ) ;
#20355 = B_SPLINE_CURVE_WITH_KNOTS ( 'NONE', 3,
 ( #18157, #39328, #73100, #79859, #53261, #46067, #18606, #19044, #46514, #10955 ),
 .UNSPECIFIED., .F., .F.,
 ( 4, 2, 2, 2, 4 ),
 ( 0.0007817246256747474977, 0.0009771112852218911526, 0.001172497944769034699, 0.001367884604316178462, 0.001563271263863322009 ),
 .UNSPECIFIED. ) ;
#20356 = CARTESIAN_POINT ( 'NONE',  ( 10.28846153846153832, -4.000000000000000000, 29.75000000000000355 ) ) ;
#20357 = CARTESIAN_POINT ( 'NONE',  ( 0.5276057948885373161, -2.292212530054420494, 30.41441678777542990 ) ) ;
#20358 = VERTEX_POINT ( 'NONE', #45079 ) ;
#20359 = PRODUCT_DEFINITION_SHAPE ( 'NONE', 'NONE',  #35967 ) ;
#20360 = CARTESIAN_POINT ( 'NONE',  ( 12.21153846153846168, -2.249999999999998668, 29.75000000000000355 ) ) ;
#20361 = VECTOR ( 'NONE', #29514, 1000.000000000000227 ) ;
#20362 = DIRECTION ( 'NONE',  ( -0.000000000000000000, -0.5000000000000009992, -0.8660254037844380415 ) ) ;
#20363 = CARTESIAN_POINT ( 'NONE',  ( 5.142990410273153401, -12.34228464037088813, 31.77849191805839268 ) ) ;
#20364 = VERTEX_POINT ( 'NONE', #39234 ) ;
#20365 = CARTESIAN_POINT ( 'NONE',  ( -16.94639763868943660, -12.15418822224088657, 32.17964115625579069 ) ) ;
#20366 = ORIENTED_EDGE ( 'NONE', *, *, #78889, .F. ) ;
#20367 = CARTESIAN_POINT ( 'NONE',  ( -2.557669038634660552, -12.17611988154120972, 31.52148481390971213 ) ) ;
#20368 = SURFACE_SIDE_STYLE ('',( #19470 ) ) ;
#20369 = CARTESIAN_POINT ( 'NONE',  ( -5.934744860487160878, -12.16647553114626490, 32.15551576947920864 ) ) ;
#20370 = ORIENTED_EDGE ( 'NONE', *, *, #12899, .T. ) ;
#20371 = CARTESIAN_POINT ( 'NONE',  ( 18.00000000000000000, -12.78798330534102767, 29.49999999999997868 ) ) ;
#20372 = CARTESIAN_POINT ( 'NONE',  ( 4.219101293358989757, -9.528491918058460186, 34.59228464037085615 ) ) ;
#20373 = CARTESIAN_POINT ( 'NONE',  ( 13.25392391794782654, -6.413092428213692742, 34.63065189839063152 ) ) ;
#20374 = CARTESIAN_POINT ( 'NONE',  ( 25.00000000000000711, -9.999999999999957367, 3.000000000000000000 ) ) ;
#20375 = CARTESIAN_POINT ( 'NONE',  ( 3.230769230769110045, -12.46129190930018460, 30.37095296980731973 ) ) ;
#20376 = ORIENTED_EDGE ( 'NONE', *, *, #60235, .F. ) ;
#20377 = FACE_BOUND ( 'NONE', #49312, .T. ) ;
#20378 = EDGE_LOOP ( 'NONE', ( #22388, #14403, #5255, #87717 ) ) ;
#20379 = CARTESIAN_POINT ( 'NONE',  ( -8.835313148590904220, -12.34228464037088280, 31.77849191805838558 ) ) ;
#20380 = DIRECTION ( 'NONE',  ( 0.000000000000000000, 0.7660444431189822323, -0.6427876096865344779 ) ) ;
#20381 = DIRECTION ( 'NONE',  ( -0.000000000000000000, 0.9848077530122085754, -0.1736481776669273613 ) ) ;
#20382 = CARTESIAN_POINT ( 'NONE',  ( -6.066083410955878108, -12.10708131394839349, 31.69288490824020244 ) ) ;
#20383 = EDGE_LOOP ( 'NONE', ( #2762, #7414 ) ) ;
#20384 = ORIENTED_EDGE ( 'NONE', *, *, #83805, .F. ) ;
#20385 = ORIENTED_EDGE ( 'NONE', *, *, #76620, .F. ) ;
#20386 = AXIS2_PLACEMENT_3D ( 'NONE', #68252, #34015, #56062 ) ;
#20387 = CARTESIAN_POINT ( 'NONE',  ( -0.3962828902624365157, -3.300289026998475705, 32.46337939537591666 ) ) ;
#20388 = ORIENTED_EDGE ( 'NONE', *, *, #35123, .T. ) ;
#20389 = CARTESIAN_POINT ( 'NONE',  ( -17.32689982097166492, -10.06842814019191401, 34.32929386961144758 ) ) ;
#20390 = VECTOR ( 'NONE', #82063, 1000.000000000000000 ) ;
#20391 = CARTESIAN_POINT ( 'NONE',  ( 1.607626736228235931, -3.587049720035815348, 32.86302985866382897 ) ) ;
#20392 = CYLINDRICAL_SURFACE ( 'NONE', #87640, 0.2500000000000002220 ) ;
#20394 = EDGE_CURVE ( 'NONE', #47301, #82157, #3295, .T. ) ;
#20393 = DIRECTION ( 'NONE',  ( 1.000000000000000000, 0.000000000000000000, 0.000000000000000000 ) ) ;
#20395 = CARTESIAN_POINT ( 'NONE',  ( 3.750000000000009770, -9.053300858899081760, 24.54687500000000000 ) ) ;
#20396 = CARTESIAN_POINT ( 'NONE',  ( -4.376712416909251502, -2.251424796025575770, 29.88072029997477586 ) ) ;
#20397 = CARTESIAN_POINT ( 'NONE',  ( 18.00000000000000000, -2.538708090699994813, 30.37095296980875503 ) ) ;
#20398 = FACE_OUTER_BOUND ( 'NONE', #57869, .T. ) ;
#20399 = ORIENTED_EDGE ( 'NONE', *, *, #50439, .F. ) ;
#20400 = VERTEX_POINT ( 'NONE', #31119 ) ;
#20401 = ORIENTED_EDGE ( 'NONE', *, *, #26310, .T. ) ;
#20402 = FACE_OUTER_BOUND ( 'NONE', #87185, .T. ) ;
#20404 = CARTESIAN_POINT ( 'NONE',  ( -5.869474298236433185, -3.816742781228458448, 33.13167719472716044 ) ) ;
#20403 = CARTESIAN_POINT ( 'NONE',  ( -3.007756386675836779, -10.01129605718032778, 34.36064277460058491 ) ) ;
#20405 = DIRECTION ( 'NONE',  ( -0.000000000000000000, -0.9848077530122085754, -0.1736481776669273613 ) ) ;
#20406 = CARTESIAN_POINT ( 'NONE',  ( 3.230769230769108269, -10.33852847137269571, 34.16647553114546554 ) ) ;
#20407 = FACE_BOUND ( 'NONE', #16273, .T. ) ;
#20408 = CARTESIAN_POINT ( 'NONE',  ( 16.40379167219429490, -3.202959910592336090, 32.30730279482227019 ) ) ;
#20409 = ORIENTED_EDGE ( 'NONE', *, *, #54134, .F. ) ;
#20410 = EDGE_CURVE ( 'NONE', #71524, #47112, #72057, .T. ) ;
#20411 = CARTESIAN_POINT ( 'NONE',  ( 15.23076923076923173, -12.78798330534102945, 29.74999999999997868 ) ) ;
#20412 = CARTESIAN_POINT ( 'NONE',  ( 16.94677586748485965, -6.852621066184266141, 34.70813303252209181 ) ) ;
#20413 = DIRECTION ( 'NONE',  ( 0.000000000000000000, 0.000000000000000000, 1.000000000000000000 ) ) ;
#20414 = EDGE_LOOP ( 'NONE', ( #65148, #50364, #89112, #85109 ) ) ;
#20415 = CARTESIAN_POINT ( 'NONE',  ( 4.853996118016226546, -2.308479472611653094, 30.53278059502174457 ) ) ;
#20416 = EDGE_LOOP ( 'NONE', ( #28107, #1845, #75651, #86899 ) ) ;
#20417 = FACE_BOUND ( 'NONE', #31726, .T. ) ;
#20418 = CARTESIAN_POINT ( 'NONE',  ( -18.00000000000000000, -1.652287802724643262, 34.33046132563154629 ) ) ;
#20419 = VECTOR ( 'NONE', #35319, 1000.000000000000000 ) ;
#20420 = DIRECTION ( 'NONE',  ( -0.000000000000000000, -0.3420201433256694346, -0.9396926207859080948 ) ) ;
#20421 = DIRECTION ( 'NONE',  ( 0.000000000000000000, 0.8660254037844377084, -0.5000000000000015543 ) ) ;
#20422 = VERTEX_POINT ( 'NONE', #86084 ) ;
#20423 = CARTESIAN_POINT ( 'NONE',  ( 4.153846153846154188, -1.951392089020283160, 34.73218667398347748 ) ) ;
#20424 = DIRECTION ( 'NONE',  ( -0.000000000000000000, -0.8660254037844397068, -0.4999999999999978906 ) ) ;
#20425 = CARTESIAN_POINT ( 'NONE',  ( 16.15384615384615330, -1.509761064869970415, 31.06009739812519044 ) ) ;
#20426 = CARTESIAN_POINT ( 'NONE',  ( -8.069638789877792817, -2.847400154188067578, 31.58180166144859058 ) ) ;
#20427 = ORIENTED_EDGE ( 'NONE', *, *, #31459, .F. ) ;
#20428 = AXIS2_PLACEMENT_3D ( 'NONE', #10035, #22667, #31192 ) ;
#20429 = DIRECTION ( 'NONE',  ( -0.000000000000000000, 0.5000000000000011102, -0.8660254037844380415 ) ) ;
#20430 = CARTESIAN_POINT ( 'NONE',  ( -15.45369544828537656, -4.186968288167451036, 33.49512374952580274 ) ) ;
#20432 = ORIENTED_EDGE ( 'NONE', *, *, #49208, .F. ) ;
#20431 = CARTESIAN_POINT ( 'NONE',  ( 15.90384615384615330, -7.500000000000001776, 35.00000000000000000 ) ) ;
#20433 = DIRECTION ( 'NONE',  ( -0.000000000000000000, -0.7660444431189791237, -0.6427876096865379196 ) ) ;
#20434 = CARTESIAN_POINT ( 'NONE',  ( -10.03846153846153832, -7.500000000000000000, 33.75000000000000000 ) ) ;
#20435 = CARTESIAN_POINT ( 'NONE',  ( 15.48076923076923173, -7.500000000000001776, 35.04278698407183867 ) ) ;
#20436 = FACE_OUTER_BOUND ( 'NONE', #17417, .T. ) ;
#20437 = LINE ( 'NONE', #40720, #48737 ) ;
#20438 = EDGE_CURVE ( 'NONE', #36014, #42886, #50503, .T. ) ;
#20439 = ADVANCED_FACE ( 'NONE', ( #25265 ), #52725, .F. ) ;
#20440 = CARTESIAN_POINT ( 'NONE',  ( 9.915087233576098669, -9.332535724633409302, 34.40230450496446934 ) ) ;
#20442 = DIRECTION ( 'NONE',  ( 0.000000000000000000, 0.000000000000000000, 1.000000000000000000 ) ) ;
#20441 = CARTESIAN_POINT ( 'NONE',  ( 12.22435897435897267, -7.500000000000000000, 29.75000000000000355 ) ) ;
#20443 = CARTESIAN_POINT ( 'NONE',  ( 14.24160889673642494, -3.513871655860377086, 32.76840700105978499 ) ) ;
#20444 = CARTESIAN_POINT ( 'NONE',  ( -1.944543648262992530, -9.444543648263016067, 17.43750000000000000 ) ) ;
#20445 = VERTEX_POINT ( 'NONE', #45971 ) ;
#20446 = CARTESIAN_POINT ( 'NONE',  ( -10.61538461538461320, -13.20930481340135110, 34.54067556320372745 ) ) ;
#20447 = ORIENTED_EDGE ( 'NONE', *, *, #29128, .T. ) ;
#20448 = EDGE_CURVE ( 'NONE', #19635, #8641, #80525, .T. ) ;
#20449 = VERTEX_POINT ( 'NONE', #5445 ) ;
#20450 = CARTESIAN_POINT ( 'NONE',  ( -3.148799926473854982E-16, -1.749999999999995559, 32.75000000000000000 ) ) ;
#20451 = VERTEX_POINT ( 'NONE', #88326 ) ;
#20452 = CARTESIAN_POINT ( 'NONE',  ( 14.24242186173153435, -8.613356846314824011, 34.62446782046655613 ) ) ;
#20453 = CARTESIAN_POINT ( 'NONE',  ( 2.750000000000001776, -7.499999999999984013, 21.96875000000000355 ) ) ;
#20454 = EDGE_CURVE ( 'NONE', #71705, #22195, #74345, .T. ) ;
#20455 = CARTESIAN_POINT ( 'NONE',  ( 12.21153846153846345, -7.433932668274256805, 35.00000000000000711 ) ) ;
#20456 = CARTESIAN_POINT ( 'NONE',  ( 3.230769230769231726, -1.129524287112498415, 32.06866353760679544 ) ) ;
#20457 = CARTESIAN_POINT ( 'NONE',  ( -2.084912766423896446, -6.760870238392817200, 34.69528174975672385 ) ) ;
#20458 = CARTESIAN_POINT ( 'NONE',  ( 17.07692307692307665, -8.120952969808772792, 34.71129190930000163 ) ) ;
#20459 = CARTESIAN_POINT ( 'NONE',  ( -17.07692307692307665, -13.78497067705608181, 32.30358669280327177 ) ) ;
#20460 = DIRECTION ( 'NONE',  ( 1.000000000000000000, 0.000000000000000000, 0.000000000000000000 ) ) ;
#20461 = VECTOR ( 'NONE', #57747, 1000.000000000000000 ) ;
#20462 = LINE ( 'NONE', #55564, #59491 ) ;
#20463 = CARTESIAN_POINT ( 'NONE',  ( -0.5268089074992378107, -2.625532179533444754, 30.86335684631481513 ) ) ;
#20464 = CARTESIAN_POINT ( 'NONE',  ( 17.74997676270703550, -11.86270091957321071, 32.19358267280088626 ) ) ;
#20465 = VECTOR ( 'NONE', #12607, 1000.000000000000114 ) ;
#20466 = PLANE ( 'NONE',  #27774 ) ;
#20467 = VERTEX_POINT ( 'NONE', #34687 ) ;
#20468 = ORIENTED_EDGE ( 'NONE', *, *, #29865, .T. ) ;
#20469 = CARTESIAN_POINT ( 'NONE',  ( -18.22292695890684655, -2.523278758544489353, 31.42238647778637528 ) ) ;
#20470 = CARTESIAN_POINT ( 'NONE',  ( 12.46153846153846168, -3.886160181151819604, 36.00935417666054406 ) ) ;
#20471 = DIRECTION ( 'NONE',  ( -0.000000000000000000, 0.6427876096865404731, -0.7660444431189770143 ) ) ;
#20472 = CARTESIAN_POINT ( 'NONE',  ( 5.750023269057647823, -5.728515186090277211, 34.42611988154120439 ) ) ;
#20473 = CARTESIAN_POINT ( 'NONE',  ( -14.30769230769242739, -12.46129190930018460, 30.37095296980731973 ) ) ;
#20474 = CARTESIAN_POINT ( 'NONE',  ( 11.66898697669518548, -4.299079248970732792, 33.91157788607253565 ) ) ;
#20475 = CARTESIAN_POINT ( 'NONE',  ( 8.769230769230647482, -10.21337939537710326, 33.94971097300076224 ) ) ;
#20476 = VERTEX_POINT ( 'NONE', #13523 ) ;
#20477 = CARTESIAN_POINT ( 'NONE',  ( 18.13079044096695469, -3.338503747796866872, 32.95102852606552801 ) ) ;
#20478 = ORIENTED_EDGE ( 'NONE', *, *, #7950, .F. ) ;
#20479 = AXIS2_PLACEMENT_3D ( 'NONE', #29959, #86705, #57417 ) ;
#20480 = CARTESIAN_POINT ( 'NONE',  ( -8.519176349317314489, -4.818054556918156983, 34.26375889529406749 ) ) ;
#20481 = CARTESIAN_POINT ( 'NONE',  ( 15.48071464014727283, -3.520799739797214389, 33.17531984108286025 ) ) ;
#20482 = CARTESIAN_POINT ( 'NONE',  ( -20.74999999999999289, -7.500000000000000000, 29.75000000000000355 ) ) ;
#20483 = CARTESIAN_POINT ( 'NONE',  ( -15.23076923076922995, -3.050289026998446396, 32.03036669348365706 ) ) ;
#20484 = FACE_OUTER_BOUND ( 'NONE', #11032, .T. ) ;
#20485 = EDGE_CURVE ( 'NONE', #26693, #23594, #68907, .T. ) ;
#20486 = ORIENTED_EDGE ( 'NONE', *, *, #6565, .F. ) ;
#20487 = ORIENTED_EDGE ( 'NONE', *, *, #44870, .T. ) ;
#20488 = VERTEX_POINT ( 'NONE', #20722 ) ;
#20489 = ORIENTED_EDGE ( 'NONE', *, *, #82946, .F. ) ;
#20490 = CARTESIAN_POINT ( 'NONE',  ( 6.416666666666664298, -3.499999999999999556, 29.75000000000000355 ) ) ;
#20491 = CARTESIAN_POINT ( 'NONE',  ( 5.999999999999878320, -2.379036618888197729, 30.90682066428292885 ) ) ;
#20492 = PLANE ( 'NONE',  #75384 ) ;
#20494 = EDGE_CURVE ( 'NONE', #62209, #80426, #71878, .T. ) ;
#20493 = CARTESIAN_POINT ( 'NONE',  ( 2.242421861731534349, -11.48612834413959582, 32.76840700105983473 ) ) ;
#20495 = CARTESIAN_POINT ( 'NONE',  ( 17.77707304109313924, -2.889293201056495786, 32.26117774369186009 ) ) ;
#20496 = CARTESIAN_POINT ( 'NONE',  ( 12.39626846098214052, -3.083524468853724443, 32.58852847137143272 ) ) ;
#20497 = ORIENTED_EDGE ( 'NONE', *, *, #39765, .F. ) ;
#20498 = EDGE_CURVE ( 'NONE', #28583, #66822, #10630, .T. ) ;
#20499 = EDGE_LOOP ( 'NONE', ( #32129, #9638, #52720, #46190, #72294, #21600 ) ) ;
#20500 = ORIENTED_EDGE ( 'NONE', *, *, #78873, .T. ) ;
#20502 = EDGE_LOOP ( 'NONE', ( #7289, #22695, #82197, #44290 ) ) ;
#20501 = CARTESIAN_POINT ( 'NONE',  ( -10.48485891362104816, -11.93748526763465279, 32.05452791011430946 ) ) ;
#20503 = CARTESIAN_POINT ( 'NONE',  ( 12.46153846153846168, -13.53365097954675988, 30.81389545987213552 ) ) ;
#20504 = DIRECTION ( 'NONE',  ( 0.000000000000000000, 0.8660254037844377084, 0.5000000000000015543 ) ) ;
#20505 = AXIS2_PLACEMENT_3D ( 'NONE', #3370, #66744, #43475 ) ;
#20506 = CARTESIAN_POINT ( 'NONE',  ( 2.651650429449569302, -10.15165042944953733, 18.37500000000000355 ) ) ;
#20507 = ORIENTED_EDGE ( 'NONE', *, *, #59355, .T. ) ;
#20508 = EDGE_CURVE ( 'NONE', #37921, #42366, #24677, .T. ) ;
#20509 = CARTESIAN_POINT ( 'NONE',  ( 8.096208266067295156, -4.074993327901524687, 33.72946981652012255 ) ) ;
#20510 = EDGE_LOOP ( 'NONE', ( #73505, #71159, #70792, #63789 ) ) ;
#20511 = CARTESIAN_POINT ( 'NONE',  ( 8.068933387422253745, -12.24180327182772210, 31.33663988360758168 ) ) ;
#20512 = FACE_BOUND ( 'NONE', #40690, .T. ) ;
#20513 = CYLINDRICAL_SURFACE ( 'NONE', #11540, 0.2499999999999995559 ) ;
#20514 = EDGE_CURVE ( 'NONE', #62121, #75871, #64375, .T. ) ;
#20515 = CARTESIAN_POINT ( 'NONE',  ( -14.05769230769230482, -2.499999999999999556, 29.81604066197449754 ) ) ;
#20516 = EDGE_LOOP ( 'NONE', ( #36213, #55092 ) ) ;
#20517 = LINE ( 'NONE', #88561, #79190 ) ;
#20518 = CARTESIAN_POINT ( 'NONE',  ( 8.769230769230768274, -8.164416787775445883, 34.95778746994557906 ) ) ;
#20519 = CARTESIAN_POINT ( 'NONE',  ( -16.85414340794500276, -12.69155399931963046, 30.53255429739158444 ) ) ;
#20520 = CARTESIAN_POINT ( 'NONE',  ( -3.296851610129365451, -9.058645607665454236, 34.76329471203372634 ) ) ;
#20521 = EDGE_LOOP ( 'NONE', ( #2638, #51726, #34122, #11290 ) ) ;
#20522 = CARTESIAN_POINT ( 'NONE',  ( 15.90384615384615685, -7.433931650972299465, 34.75000000000000711 ) ) ;
#20523 = CARTESIAN_POINT ( 'NONE',  ( 1.134592160393929960, -4.175268141568689195, 33.81360843649122216 ) ) ;
#20524 = CARTESIAN_POINT ( 'NONE',  ( -12.52762187249433978, -12.10708131394839349, 31.69288490824020244 ) ) ;
#20525 = CARTESIAN_POINT ( 'NONE',  ( -2.307692307692305711, -10.51840700105979565, 33.73612834413961536 ) ) ;
#20526 = CARTESIAN_POINT ( 'NONE',  ( -0.6089743589743593644, -11.00000000000000000, 29.75000000000000355 ) ) ;
#20527 = EDGE_CURVE ( 'NONE', #45384, #30104, #2269, .T. ) ;
#20528 = FACE_BOUND ( 'NONE', #4796, .T. ) ;
#20530 = CARTESIAN_POINT ( 'NONE',  ( 11.47237812750565666, -12.37446782046654192, 30.86335684631486487 ) ) ;
#20529 = CARTESIAN_POINT ( 'NONE',  ( -6.923076923077045919, -12.51329471203414379, 31.30864560766407578 ) ) ;
#20531 = CARTESIAN_POINT ( 'NONE',  ( 5.076923076923075762, -9.058645607665452459, 34.76329471203371924 ) ) ;
#20533 = CARTESIAN_POINT ( 'NONE',  ( -2.241624974342229404, -12.34228464037088813, 31.77849191805839268 ) ) ;
#20532 = CARTESIAN_POINT ( 'NONE',  ( -5.869474298236438514, -10.19071101563364756, 33.96452234770658407 ) ) ;
#20534 = EDGE_CURVE ( 'NONE', #28242, #89067, #85940, .T. ) ;
#20535 = CARTESIAN_POINT ( 'NONE',  ( -7.846153846153967493, -4.320704448113951379, 33.92786785259630022 ) ) ;
#20536 = CARTESIAN_POINT ( 'NONE',  ( 2.724691934501235036, -6.299813628509441266, 15.38875670625848890 ) ) ;
#20537 = VERTEX_POINT ( 'NONE', #6761 ) ;
#20538 = CARTESIAN_POINT ( 'NONE',  ( -6.000000000000121680, -11.06231777344772027, 33.60647404775119895 ) ) ;
#20539 = EDGE_LOOP ( 'NONE', ( #57546, #2516, #70000, #41509, #46447, #15912 ) ) ;
#20540 = CARTESIAN_POINT ( 'NONE',  ( 13.38461538461538680, -7.500000000000001776, 35.04278698407183867 ) ) ;
#20541 = EDGE_CURVE ( 'NONE', #16932, #78524, #15303, .T. ) ;
#20542 = B_SPLINE_CURVE_WITH_KNOTS ( 'NONE', 3,
 ( #88150, #38602, #66058, #4370, #18331, #4822, #32292, #59756, #20546, #75060 ),
 .UNSPECIFIED., .F., .F.,
 ( 4, 2, 2, 2, 4 ),
 ( 0.0007817359430256218744, 0.0009771253907249861318, 0.001172514838424350498, 0.001367904286123714864, 0.001563293733823079229 ),
 .UNSPECIFIED. ) ;
#20543 = ORIENTED_EDGE ( 'NONE', *, *, #8601, .F. ) ;
#20544 = ADVANCED_FACE ( 'NONE', ( #21605 ), #57164, .F. ) ;
#20545 = FACE_OUTER_BOUND ( 'NONE', #49969, .T. ) ;
#20546 = CARTESIAN_POINT ( 'NONE',  ( -1.318547033612946340, -10.51840700105979565, 33.73612834413962247 ) ) ;
#20548 = EDGE_LOOP ( 'NONE', ( #38439, #11297 ) ) ;
#20547 = CARTESIAN_POINT ( 'NONE',  ( -5.076923076923075762, -1.117168528481311540, 33.14645433367849847 ) ) ;
#20549 = CARTESIAN_POINT ( 'NONE',  ( -14.30769230769230660, -13.88283147151868846, 33.14645433367849847 ) ) ;
#20550 = CARTESIAN_POINT ( 'NONE',  ( 2.775308065498768517, -8.577988221561467341, 20.54500670625849068 ) ) ;
#20551 = CARTESIAN_POINT ( 'NONE',  ( -13.38461538461538325, -2.708943851104267164, 35.45975837776705220 ) ) ;
#20552 = CARTESIAN_POINT ( 'NONE',  ( -4.153846153846152411, -11.35647404775217417, 33.31231777344666511 ) ) ;
#20553 = DIRECTION ( 'NONE',  ( -0.000000000000000000, 0.6427876096865404731, -0.7660444431189770143 ) ) ;
#20554 = CARTESIAN_POINT ( 'NONE',  ( 10.48523664565291469, -2.647304123082328875, 31.75400227202885972 ) ) ;
#20555 = DIRECTION ( 'NONE',  ( -0.000000000000000000, -0.3420201433256694346, -0.9396926207859080948 ) ) ;
#20556 = CARTESIAN_POINT ( 'NONE',  ( 6.000000000000001776, -2.486705287966279876, 31.30864560766543647 ) ) ;
#20557 = CARTESIAN_POINT ( 'NONE',  ( 2.694853999681185108, -4.891553140782077591, 23.31436829374150932 ) ) ;
#20558 = CARTESIAN_POINT ( 'NONE',  ( 11.47319153790521717, -5.941354392334499579, 34.76329471203369792 ) ) ;
#20559 = CARTESIAN_POINT ( 'NONE',  ( -4.219116154402471786, -3.083524468853724443, 32.58852847137143272 ) ) ;
#20560 = VERTEX_POINT ( 'NONE', #36887 ) ;
#20561 = CARTESIAN_POINT ( 'NONE',  ( 10.61538461538449418, -6.835583212225970762, 34.95778746994575670 ) ) ;
#20562 = CARTESIAN_POINT ( 'NONE',  ( 2.608446859217924629, -10.19485399968118422, 22.37686829374150932 ) ) ;
#20563 = CARTESIAN_POINT ( 'NONE',  ( -17.77698864838715309, -12.39991518177334129, 30.74647679643404530 ) ) ;
#20564 = CARTESIAN_POINT ( 'NONE',  ( -8.835313148590902443, -11.35647404775217595, 33.31231777344666511 ) ) ;
#20565 = ORIENTED_EDGE ( 'NONE', *, *, #61059, .T. ) ;
#20566 = CARTESIAN_POINT ( 'NONE',  ( -12.94230769230769162, -11.00000000000000000, 29.75000000000000355 ) ) ;
#20567 = CARTESIAN_POINT ( 'NONE',  ( -14.43838377435986864, -11.18331474514187995, 33.13161551792790505 ) ) ;
#20569 = ORIENTED_EDGE ( 'NONE', *, *, #61678, .T. ) ;
#20568 = DIRECTION ( 'NONE',  ( -0.000000000000000000, 0.3420201433256694346, -0.9396926207859080948 ) ) ;
#20570 = DIRECTION ( 'NONE',  ( 0.000000000000000000, 0.3420201433256641055, -0.9396926207859100932 ) ) ;
#20571 = CARTESIAN_POINT ( 'NONE',  ( -15.23076923076935252, -12.16647553114689728, 32.15551576947799362 ) ) ;
#20572 = LINE ( 'NONE', #82291, #52923 ) ;
#20573 = VECTOR ( 'NONE', #48681, 1000.000000000000227 ) ;
#20574 = CARTESIAN_POINT ( 'NONE',  ( 2.057669083470853089, -4.175268141568689195, 33.81360843649122216 ) ) ;
#20575 = EDGE_CURVE ( 'NONE', #11048, #42810, #64789, .T. ) ;
#20576 = DIRECTION ( 'NONE',  ( -1.000000000000000000, 0.000000000000000000, 0.000000000000000000 ) ) ;
#20577 = ORIENTED_EDGE ( 'NONE', *, *, #59173, .T. ) ;
#20578 = EDGE_LOOP ( 'NONE', ( #29286, #74540 ) ) ;
#20579 = ORIENTED_EDGE ( 'NONE', *, *, #31751, .T. ) ;
#20580 = CARTESIAN_POINT ( 'NONE',  ( 2.307692307692309264, -2.499999999999998668, 29.75000000000001421 ) ) ;
#20581 = CARTESIAN_POINT ( 'NONE',  ( 0.2115152242454959586, -2.587272538249754117, 30.68239716806877837 ) ) ;
#20582 = CARTESIAN_POINT ( 'NONE',  ( -13.16183584334697088, -12.24180327182772388, 31.33663988360758168 ) ) ;
#20583 = FACE_OUTER_BOUND ( 'NONE', #79381, .T. ) ;
#20584 = EDGE_CURVE ( 'NONE', #79867, #10043, #63019, .T. ) ;
#20585 = EDGE_CURVE ( 'NONE', #57207, #36536, #42779, .T. ) ;
#20586 = DIRECTION ( 'NONE',  ( -0.000000000000000000, -0.9396926207859092051, -0.3420201433256662704 ) ) ;
#20587 = ORIENTED_EDGE ( 'NONE', *, *, #46958, .T. ) ;
#20588 = ORIENTED_EDGE ( 'NONE', *, *, #16771, .F. ) ;
#20589 = ORIENTED_EDGE ( 'NONE', *, *, #60157, .T. ) ;
#20591 = ORIENTED_EDGE ( 'NONE', *, *, #1005, .T. ) ;
#20590 = CARTESIAN_POINT ( 'NONE',  ( 11.53846153846153832, -13.95598074871891292, 31.83374038241031911 ) ) ;
#20592 = CARTESIAN_POINT ( 'NONE',  ( 15.23076923076923173, -8.810774026931790459, 35.74407628777942847 ) ) ;
#20593 = DIRECTION ( 'NONE',  ( -0.000000000000000000, -0.1736481776669307198, -0.9848077530122080203 ) ) ;
#20594 = AXIS2_PLACEMENT_3D ( 'NONE', #56188, #17868, #39480 ) ;
#20595 = CIRCLE ( 'NONE', #83881, 0.2500000000000002220 ) ;
#20596 = EDGE_CURVE ( 'NONE', #5035, #33753, #44074, .T. ) ;
#20597 = CARTESIAN_POINT ( 'NONE',  ( -12.46153846153858247, -12.27809138561165270, 31.22303859784587132 ) ) ;
#20598 = FACE_OUTER_BOUND ( 'NONE', #71824, .T. ) ;
#20599 = ORIENTED_EDGE ( 'NONE', *, *, #63770, .F. ) ;
#20600 = EDGE_CURVE ( 'NONE', #43223, #26530, #45078, .T. ) ;
#20601 = VECTOR ( 'NONE', #54135, 999.9999999999998863 ) ;
#20602 = EDGE_LOOP ( 'NONE', ( #13292, #51155 ) ) ;
#20603 = EDGE_LOOP ( 'NONE', ( #82306, #64041, #11862, #16493 ) ) ;
#20604 = CARTESIAN_POINT ( 'NONE',  ( 10.83839596699746544, -10.61302985866384141, 33.66295027996417843 ) ) ;
#20606 = ORIENTED_EDGE ( 'NONE', *, *, #84883, .F. ) ;
#20605 = DIRECTION ( 'NONE',  ( -0.000000000000000000, -0.1736481776669307198, -0.9848077530122080203 ) ) ;
#20607 = B_SPLINE_CURVE_WITH_KNOTS ( 'NONE', 3,
 ( #80886, #18279, #73226, #5206, #80436, #60139, #46637, #74115, #47067, #54713 ),
 .UNSPECIFIED., .F., .F.,
 ( 4, 2, 2, 2, 4 ),
 ( 0.0007817246256747473893, 0.0009771112852218900684, 0.001172497944769032747, 0.001367884604316175643, 0.001563271263863318323 ),
 .UNSPECIFIED. ) ;
#20608 = CARTESIAN_POINT ( 'NONE',  ( 13.25405479287346466, -2.504760397472875155, 29.97295953869789997 ) ) ;
#20609 = CARTESIAN_POINT ( 'NONE',  ( 15.23076923076923173, -12.62096338111211580, 30.90682066428153263 ) ) ;
#20610 = EDGE_LOOP ( 'NONE', ( #39655, #80348 ) ) ;
#20611 = EDGE_CURVE ( 'NONE', #57426, #82401, #52586, .T. ) ;
#20612 = CARTESIAN_POINT ( 'NONE',  ( -4.088590582570128973, -5.219633306516380244, 34.19971097300157936 ) ) ;
#20613 = CARTESIAN_POINT ( 'NONE',  ( -9.692307692307812417, -10.21337939537710326, 33.94971097300076224 ) ) ;
#20614 = ORIENTED_EDGE ( 'NONE', *, *, #16275, .T. ) ;
#20615 = FACE_BOUND ( 'NONE', #63773, .T. ) ;
#20616 = CARTESIAN_POINT ( 'NONE',  ( -13.38461538461538325, -11.35647404775217417, 33.31231777344666511 ) ) ;
#20617 = CARTESIAN_POINT ( 'NONE',  ( 19.00000000000000000, -3.499999999999999556, 29.75000000000000355 ) ) ;
#20618 = CARTESIAN_POINT ( 'NONE',  ( 12.46153846153846168, -6.343179335718451384, 34.87096338111211935 ) ) ;
#20620 = CYLINDRICAL_SURFACE ( 'NONE', #88649, 0.2500000000000002220 ) ;
#20619 = LINE ( 'NONE', #46769, #64755 ) ;
#20621 = CARTESIAN_POINT ( 'NONE',  ( -3.100243792535585463, -3.625058011473228259, 33.29252011169590020 ) ) ;
#20622 = CARTESIAN_POINT ( 'NONE',  ( 6.988270904860278243, -2.506253911140448487, 29.99999999999988631 ) ) ;
#20623 = ORIENTED_EDGE ( 'NONE', *, *, #12885, .T. ) ;
#20624 = CARTESIAN_POINT ( 'NONE',  ( -14.30769230769242739, -4.481592998941358097, 33.73612834414048933 ) ) ;
#20625 = DIRECTION ( 'NONE',  ( 1.000000000000000000, 0.000000000000000000, 0.000000000000000000 ) ) ;
#20626 = ORIENTED_EDGE ( 'NONE', *, *, #87460, .F. ) ;
#20627 = VECTOR ( 'NONE', #41962, 1000.000000000000000 ) ;
#20628 = CIRCLE ( 'NONE', #33570, 0.2500000000000002220 ) ;
#20629 = CARTESIAN_POINT ( 'NONE',  ( 8.703147358274886614, -3.050289026998445951, 32.03036669348365706 ) ) ;
#20630 = DIRECTION ( 'NONE',  ( -1.000000000000000000, -0.000000000000000000, -0.000000000000000000 ) ) ;
#20631 = ORIENTED_EDGE ( 'NONE', *, *, #87488, .T. ) ;
#20632 = CARTESIAN_POINT ( 'NONE',  ( -9.758390071667825794, -9.058645607665454236, 34.76329471203372634 ) ) ;
#20633 = CARTESIAN_POINT ( 'NONE',  ( -15.16470189741915675, -12.62096338111211757, 30.90682066428152908 ) ) ;
#20634 = EDGE_CURVE ( 'NONE', #6564, #3308, #63263, .T. ) ;
#20635 = FACE_BOUND ( 'NONE', #25918, .T. ) ;
#20637 = CARTESIAN_POINT ( 'NONE',  ( -39.05038313613820122, -2.249999999999998668, 29.75000000000000355 ) ) ;
#20636 = DIRECTION ( 'NONE',  ( -0.000000000000000000, 1.000000000000000000, -0.000000000000000000 ) ) ;
#20638 = CARTESIAN_POINT ( 'NONE',  ( -13.38461538461550759, -2.379036618888197729, 30.90682066428292885 ) ) ;
#20639 = DIRECTION ( 'NONE',  ( -0.000000000000000000, 0.9848077530122086864, -0.1736481776669273891 ) ) ;
#20641 = CARTESIAN_POINT ( 'NONE',  ( -14.17764487244185290, -7.723484941389743952, 34.99544897038808955 ) ) ;
#20640 = DIRECTION ( 'NONE',  ( 0.000000000000000000, 0.000000000000000000, 1.000000000000000000 ) ) ;
#20642 = CARTESIAN_POINT ( 'NONE',  ( -39.05038313613820122, -2.249999999999998668, 29.75000000000000355 ) ) ;
#20643 = CARTESIAN_POINT ( 'NONE',  ( -3.749999999999988454, -9.053300858899127945, 26.26562500000000000 ) ) ;
#20644 = VERTEX_POINT ( 'NONE', #36457 ) ;
#20645 = ADVANCED_FACE ( 'NONE', ( #84653 ), #71554, .F. ) ;
#20646 = B_SPLINE_CURVE_WITH_KNOTS ( 'NONE', 3,
 ( #20740, #35141, #83790, #62603, #48207, #62169, #27946, #41912, #76124, #22513 ),
 .UNSPECIFIED., .F., .F.,
 ( 4, 2, 2, 2, 4 ),
 ( 0.0007817359430256372700, 0.0009771253907250054306, 0.001172514838424373483, 0.001367904286123741535, 0.001563293733823109804 ),
 .UNSPECIFIED. ) ;
#20647 = ORIENTED_EDGE ( 'NONE', *, *, #6975, .F. ) ;
#20648 = DIRECTION ( 'NONE',  ( 0.000000000000000000, 0.1736481776669267785, -0.9848077530122087975 ) ) ;
#20649 = EDGE_CURVE ( 'NONE', #29364, #61122, #6337, .T. ) ;
#20650 = CARTESIAN_POINT ( 'NONE',  ( -17.07692307692319744, -5.094484230521993062, 34.41647553114689373 ) ) ;
#20651 = CARTESIAN_POINT ( 'NONE',  ( 14.30769230769231015, -9.058645607665452459, 34.76329471203371924 ) ) ;
#20652 = CARTESIAN_POINT ( 'NONE',  ( 17.30029856269549526, -2.251407671071269601, 29.88021292934942252 ) ) ;
#20653 = CARTESIAN_POINT ( 'NONE',  ( -7.596153846153831601, -2.249999999999998224, 29.81603969181031033 ) ) ;
#20654 = CARTESIAN_POINT ( 'NONE',  ( 3.750000000000009770, -9.053300858899081760, 25.79687500000000355 ) ) ;
#20655 = CARTESIAN_POINT ( 'NONE',  ( -16.15384615384615330, -1.466349020453238561, 30.81389545987213907 ) ) ;
#20656 = CARTESIAN_POINT ( 'NONE',  ( 2.057692307692309708, -2.249999999999998668, 29.75000000000000355 ) ) ;
#20657 = CARTESIAN_POINT ( 'NONE',  ( 15.23076923076923173, -11.69971097300155272, 32.46337939537588113 ) ) ;
#20658 = FACE_OUTER_BOUND ( 'NONE', #75718, .T. ) ;
#20659 = CARTESIAN_POINT ( 'NONE',  ( -1.161188985700596366, -7.630147987733843173, 34.99859428049665411 ) ) ;
#20660 = DIRECTION ( 'NONE',  ( -0.000000000000000000, 0.5000000000000011102, -0.8660254037844380415 ) ) ;
#20661 = CARTESIAN_POINT ( 'NONE',  ( 7.173131342990377135, -3.435999193479609914, 33.07426656108010832 ) ) ;
#20662 = VECTOR ( 'NONE', #78979, 1000.000000000000000 ) ;
#20663 = CARTESIAN_POINT ( 'NONE',  ( -8.519176349317316266, -11.47946981652013498, 33.17500667209847620 ) ) ;
#20664 = CARTESIAN_POINT ( 'NONE',  ( 3.164685819813349177, -2.538708090699994813, 30.37095296980875148 ) ) ;
#20665 = EDGE_CURVE ( 'NONE', #26718, #10196, #48279, .T. ) ;
#20666 = ORIENTED_EDGE ( 'NONE', *, *, #28746, .F. ) ;
#20667 = CARTESIAN_POINT ( 'NONE',  ( 3.903869422903798458, -4.943428324936578910, 34.04746400365624481 ) ) ;
#20668 = CARTESIAN_POINT ( 'NONE',  ( 17.07692307692307665, -4.661471528628507777, 34.16647553114623292 ) ) ;
#20669 = CARTESIAN_POINT ( 'NONE',  ( -2.749999999999999112, -7.438900925035484057, 21.59561829374151287 ) ) ;
#20670 = AXIS2_PLACEMENT_3D ( 'NONE', #30540, #63880, #22019 ) ;
#20671 = AXIS2_PLACEMENT_3D ( 'NONE', #45412, #350, #5777 ) ;
#20672 = CARTESIAN_POINT ( 'NONE',  ( -0.3310130233048192983, -11.04252011169590020, 33.62494198852677130 ) ) ;
#20673 = SURFACE_SIDE_STYLE ('',( #88281 ) ) ;
#20674 = EDGE_CURVE ( 'NONE', #80960, #10201, #67039, .T. ) ;
#20675 = FACE_OUTER_BOUND ( 'NONE', #58693, .T. ) ;
#20677 = ORIENTED_EDGE ( 'NONE', *, *, #77500, .T. ) ;
#20676 = CARTESIAN_POINT ( 'NONE',  ( -5.776573601085211784, -7.630147987733840509, 34.99859428049665411 ) ) ;
#20678 = CARTESIAN_POINT ( 'NONE',  ( 1.139087296526029469, -10.24999999999999289, 25.95312500000000000 ) ) ;
#20679 = CARTESIAN_POINT ( 'NONE',  ( -9.692307692307814193, -5.941354392335915335, 34.76329471203413846 ) ) ;
#20681 = ORIENTED_EDGE ( 'NONE', *, *, #42602, .T. ) ;
#20680 = B_SPLINE_CURVE_WITH_KNOTS ( 'NONE', 3,
 ( #70690, #57169, #9427, #58479, #51718, #8995, #30143, #85976, #78317, #84222 ),
 .UNSPECIFIED., .F., .F.,
 ( 4, 2, 2, 2, 4 ),
 ( 0.000000000000000000, 0.0001954339857564097512, 0.0003908679715128195024, 0.0005863019572692292807, 0.0007817359430256390048 ),
 .UNSPECIFIED. ) ;
#20682 = CARTESIAN_POINT ( 'NONE',  ( -15.93083480223330817, -9.886259254753566594, 34.14407573483972413 ) ) ;
#20683 = DIRECTION ( 'NONE',  ( -1.000000000000000000, 0.000000000000000000, -0.000000000000000000 ) ) ;
#20684 = ORIENTED_EDGE ( 'NONE', *, *, #53035, .F. ) ;
#20685 = CARTESIAN_POINT ( 'NONE',  ( 14.08476609017615644, -2.554751324335735152, 30.48935550225260727 ) ) ;
#20686 = ADVANCED_FACE ( 'NONE', ( #85971 ), #73346, .F. ) ;
#20687 = CARTESIAN_POINT ( 'NONE',  ( 8.546303810323914618, -6.459968553980841577, 34.89616026154728701 ) ) ;
#20688 = CARTESIAN_POINT ( 'NONE',  ( -15.00798968950081758, -12.44528174975671853, 30.48912976160716681 ) ) ;
#20689 = EDGE_LOOP ( 'NONE', ( #9319, #56701 ) ) ;
#20690 = EDGE_LOOP ( 'NONE', ( #74413, #78202 ) ) ;
#20691 = DIRECTION ( 'NONE',  ( -0.000000000000000000, -0.5000000000000009992, -0.8660254037844380415 ) ) ;
#20692 = EDGE_CURVE ( 'NONE', #17599, #2983, #39684, .T. ) ;
#20693 = VERTEX_POINT ( 'NONE', #39128 ) ;
#20694 = EDGE_CURVE ( 'NONE', #80088, #8812, #17062, .T. ) ;
#20695 = CARTESIAN_POINT ( 'NONE',  ( -8.069638770718176701, -2.353723527008296568, 30.78948104536958752 ) ) ;
#20696 = CARTESIAN_POINT ( 'NONE',  ( -6.923076923077045919, -2.379036618888197729, 30.90682066428292885 ) ) ;
#20697 = CARTESIAN_POINT ( 'NONE',  ( -17.07692307692319744, -6.026961402154118908, 34.52809138561165270 ) ) ;
#20698 = LINE ( 'NONE', #14384, #21730 ) ;
#20699 = DIRECTION ( 'NONE',  ( -0.000000000000000000, 0.6427876096865404731, -0.7660444431189770143 ) ) ;
#20700 = CARTESIAN_POINT ( 'NONE',  ( 13.63456090296352841, -3.202959910592335646, 32.30730279482227019 ) ) ;
#20701 = EDGE_CURVE ( 'NONE', #82664, #34676, #86887, .T. ) ;
#20702 = FACE_OUTER_BOUND ( 'NONE', #2774, .T. ) ;
#20704 = ADVANCED_FACE ( 'NONE', ( #10309 ), #18403, .F. ) ;
#20703 = ORIENTED_EDGE ( 'NONE', *, *, #37397, .T. ) ;
#20705 = ORIENTED_EDGE ( 'NONE', *, *, #76368, .T. ) ;
#20707 = ORIENTED_EDGE ( 'NONE', *, *, #63760, .T. ) ;
#20706 = CARTESIAN_POINT ( 'NONE',  ( -0.2115929431903189328, -12.22109172314383052, 31.39792113162168263 ) ) ;
#20708 = B_SPLINE_CURVE_WITH_KNOTS ( 'NONE', 3,
 ( #49917, #2173, #62978, #29662, #57123, #1292, #36847, #57561, #77834, #43603 ),
 .UNSPECIFIED., .F., .F.,
 ( 4, 2, 2, 2, 4 ),
 ( 0.000000000000000000, 0.0001954339857564064444, 0.0003908679715128128888, 0.0005863019572692193060, 0.0007817359430256257775 ),
 .UNSPECIFIED. ) ;
#20709 = DIRECTION ( 'NONE',  ( -0.000000000000000000, -0.9396926207859093161, -0.3420201433256663259 ) ) ;
#20710 = CARTESIAN_POINT ( 'NONE',  ( 10.55013468361053164, -2.255955759149247619, 30.00000000000013856 ) ) ;
#20711 = CARTESIAN_POINT ( 'NONE',  ( 12.71159277317677549, -3.136992222400443175, 32.19305428654138979 ) ) ;
#20712 = VERTEX_POINT ( 'NONE', #59825 ) ;
#20713 = EDGE_CURVE ( 'NONE', #37130, #38219, #23550, .T. ) ;
#20714 = CARTESIAN_POINT ( 'NONE',  ( -19.50000000000000000, -4.000000000000000000, 29.75000000000000355 ) ) ;
#20715 = ORIENTED_EDGE ( 'NONE', *, *, #39986, .F. ) ;
#20716 = CARTESIAN_POINT ( 'NONE',  ( 7.976944287120795174, -12.62708834333097663, 30.88030960425257021 ) ) ;
#20717 = EDGE_LOOP ( 'NONE', ( #36748, #81756, #16759, #73793 ) ) ;
#20718 = CARTESIAN_POINT ( 'NONE',  ( -10.39242171182312724, -7.369474270740069777, 34.74850911626239736 ) ) ;
#20719 = AXIS2_PLACEMENT_3D ( 'NONE', #60382, #54511, #12207 ) ;
#20720 = EDGE_LOOP ( 'NONE', ( #88962, #55741, #6098, #4297 ) ) ;
#20721 = LINE ( 'NONE', #5444, #71905 ) ;
#20722 = CARTESIAN_POINT ( 'NONE',  ( 13.38461538461526423, -12.16647553114689728, 32.15551576947799362 ) ) ;
#20723 = FACE_BOUND ( 'NONE', #25580, .T. ) ;
#20725 = AXIS2_PLACEMENT_3D ( 'NONE', #15831, #64878, #16264 ) ;
#20724 = B_SPLINE_CURVE_WITH_KNOTS ( 'NONE', 3,
 ( #9903, #49569, #15346, #17103, #71157, #58519, #43256, #9464, #36927, #42821 ),
 .UNSPECIFIED., .F., .F.,
 ( 4, 2, 2, 2, 4 ),
 ( 0.000000000000000000, 0.0001954339881912772715, 0.0003908679763825545429, 0.0005863019645738318415, 0.0007817359527651090859 ),
 .UNSPECIFIED. ) ;
#20726 = DIRECTION ( 'NONE',  ( -0.000000000000000000, -0.6427876096865404731, -0.7660444431189770143 ) ) ;
#20727 = CARTESIAN_POINT ( 'NONE',  ( -11.66860950819323328, -6.809168938359901446, 34.95455904226513866 ) ) ;
#20728 = VECTOR ( 'NONE', #21501, 999.9999999999998863 ) ;
#20729 = CARTESIAN_POINT ( 'NONE',  ( 4.219101725122176738, -12.46129190930001052, 30.37095296980870174 ) ) ;
#20730 = DIRECTION ( 'NONE',  ( -1.000000000000000000, -0.000000000000000000, 0.000000000000000000 ) ) ;
#20731 = CARTESIAN_POINT ( 'NONE',  ( -3.165513659493203846, -3.300289026998474817, 32.46337939537591666 ) ) ;
#20732 = CARTESIAN_POINT ( 'NONE',  ( -4.284537620513710010, -11.18331474514187995, 33.13161551792790505 ) ) ;
#20733 = CARTESIAN_POINT ( 'NONE',  ( -14.17690049986752143, -3.530189275343204702, 32.79018710029569661 ) ) ;
#20734 = ORIENTED_EDGE ( 'NONE', *, *, #41502, .F. ) ;
#20735 = VERTEX_POINT ( 'NONE', #86438 ) ;
#20737 = CARTESIAN_POINT ( 'NONE',  ( -3.361459833879539172, -5.496505350115500121, 34.60290016733514307 ) ) ;
#20736 = CARTESIAN_POINT ( 'NONE',  ( -20.74999999999999289, -7.500000000000000000, 34.75000000000000000 ) ) ;
#20738 = CARTESIAN_POINT ( 'NONE',  ( -9.627052552794854279, -12.51329471203373700, 31.30864560766537963 ) ) ;
#20739 = CARTESIAN_POINT ( 'NONE',  ( -4.153846153846152411, -9.058645607665452459, 34.76329471203371924 ) ) ;
#20740 = CARTESIAN_POINT ( 'NONE',  ( 15.23076923076911093, -3.835265460704628371, 33.15142922262033665 ) ) ;
#20741 = DIRECTION ( 'NONE',  ( -0.000000000000000000, 0.5000000000000011102, -0.8660254037844380415 ) ) ;
#20742 = ORIENTED_EDGE ( 'NONE', *, *, #49835, .T. ) ;
#20743 = CARTESIAN_POINT ( 'NONE',  ( 2.084207363968360482, -9.331801661448606566, 34.40259984581193464 ) ) ;
#20744 = CARTESIAN_POINT ( 'NONE',  ( 3.480823542407545546, -11.28795663066794219, 33.01431243580653785 ) ) ;
#20745 = CYLINDRICAL_SURFACE ( 'NONE', #58826, 0.2500000000000008882 ) ;
#20746 = CARTESIAN_POINT ( 'NONE',  ( -6.923076923077045919, -6.835583212225970762, 34.95778746994575670 ) ) ;
#20747 = EDGE_LOOP ( 'NONE', ( #86283, #39640 ) ) ;
#20748 = B_SPLINE_CURVE_WITH_KNOTS ( 'NONE', 3,
 ( #51372, #44631, #17635, #58599, #59939, #59498, #72116, #73015, #11312, #87438 ),
 .UNSPECIFIED., .F., .F.,
 ( 4, 2, 2, 2, 4 ),
 ( 0.0007817359430256216575, 0.0009771253907249856981, 0.001172514838424349847, 0.001367904286123713779, 0.001563293733823077928 ),
 .UNSPECIFIED. ) ;
#20749 = VERTEX_POINT ( 'NONE', #52170 ) ;
#20750 = EDGE_CURVE ( 'NONE', #63009, #61570, #79659, .T. ) ;
#20751 = EDGE_LOOP ( 'NONE', ( #2619, #3126 ) ) ;
#20752 = CYLINDRICAL_SURFACE ( 'NONE', #17563, 0.2499999999999997502 ) ;
#20754 = ORIENTED_EDGE ( 'NONE', *, *, #61784, .T. ) ;
#20753 = EDGE_CURVE ( 'NONE', #35413, #78633, #3123, .T. ) ;
#20755 = CARTESIAN_POINT ( 'NONE',  ( -1.161604033002534120, -8.239487800360276282, 34.69522927552633718 ) ) ;
#20756 = CARTESIAN_POINT ( 'NONE',  ( -12.39628289026243380, -6.879047030191282275, 34.71129190930002295 ) ) ;
#20757 = CARTESIAN_POINT ( 'NONE',  ( -5.207614543590632472, -4.118384482072085184, 33.43331474514187107 ) ) ;
#20758 = CARTESIAN_POINT ( 'NONE',  ( -1.929879867024197893E-14, -3.750000000000000000, 14.15625000000000000 ) ) ;
#20759 = CARTESIAN_POINT ( 'NONE',  ( 9.942362003946008997, -5.728107161865378494, 34.42597550085002922 ) ) ;
#20761 = ORIENTED_EDGE ( 'NONE', *, *, #50937, .T. ) ;
#20760 = AXIS2_PLACEMENT_3D ( 'NONE', #78123, #15545, #44315 ) ;
#20762 = ADVANCED_FACE ( 'NONE', ( #5778 ), #33254, .F. ) ;
#20763 = CARTESIAN_POINT ( 'NONE',  ( -11.31549840419486586, -7.369474539155828730, 34.99858011523957657 ) ) ;
#20765 = ORIENTED_EDGE ( 'NONE', *, *, #50501, .F. ) ;
#20764 = CARTESIAN_POINT ( 'NONE',  ( -0.5922290646487697874, -5.496505350115500121, 34.60290016733514307 ) ) ;
#20766 = DIRECTION ( 'NONE',  ( 1.000000000000000000, 0.000000000000000000, 0.000000000000000000 ) ) ;
#20767 = CARTESIAN_POINT ( 'NONE',  ( 13.38461538461538680, -12.62096338111211580, 30.90682066428153263 ) ) ;
#20768 = CARTESIAN_POINT ( 'NONE',  ( 17.14299142792551578, -11.16473453929635440, 33.15142922261926373 ) ) ;
#20769 = CARTESIAN_POINT ( 'NONE',  ( -15.90384615384622258, -7.565270000091922853, 34.99999999999999289 ) ) ;
#20770 = CARTESIAN_POINT ( 'NONE',  ( -18.00000000000000000, -10.67929555188718282, 33.92786785259543336 ) ) ;
#20771 = DIRECTION ( 'NONE',  ( 0.000000000000000000, 0.000000000000000000, -1.000000000000000000 ) ) ;
#20772 = CARTESIAN_POINT ( 'NONE',  ( -3.296039676730006196, -6.879047030191174805, 34.71129190930000163 ) ) ;
#20773 = EDGE_CURVE ( 'NONE', #53138, #22144, #26753, .T. ) ;
#20774 = CARTESIAN_POINT ( 'NONE',  ( 0.06109907496451789238, -4.749999999999998224, 18.15811829374151642 ) ) ;
#20775 = ORIENTED_EDGE ( 'NONE', *, *, #64087, .T. ) ;
#20776 = CARTESIAN_POINT ( 'NONE',  ( 8.769230769230768274, -13.95598074871891292, 31.83374038241031911 ) ) ;
#20777 = CARTESIAN_POINT ( 'NONE',  ( -0.3589743589743586982, -11.50000000000000000, 29.75000000000000355 ) ) ;
#20778 = LINE ( 'NONE', #41500, #24490 ) ;
#20779 = FILL_AREA_STYLE_COLOUR ( '', #19986 ) ;
#20780 = VERTEX_POINT ( 'NONE', #34129 ) ;
#20781 = DIRECTION ( 'NONE',  ( -0.000000000000000000, -0.5000000000000009992, -0.8660254037844380415 ) ) ;
#20782 = CARTESIAN_POINT ( 'NONE',  ( -5.076923076923075762, -6.386643153685126251, 34.62446782046654192 ) ) ;
#20783 = B_SPLINE_CURVE_WITH_KNOTS ( 'NONE', 3,
 ( #15823, #56358, #50035, #71628, #35649, #969, #63099, #77512, #9492, #1412 ),
 .UNSPECIFIED., .F., .F.,
 ( 4, 2, 2, 2, 4 ),
 ( 0.0007817246256747484735, 0.0009771112852218920199, 0.001172497944769035783, 0.001367884604316179330, 0.001563271263863322876 ),
 .UNSPECIFIED. ) ;
#20784 = CARTESIAN_POINT ( 'NONE',  ( -8.899921372341079717, -10.70098750199973203, 33.91152734681376302 ) ) ;
#20785 = FACE_OUTER_BOUND ( 'NONE', #15691, .T. ) ;
#20786 = CARTESIAN_POINT ( 'NONE',  ( -2.307692307692305711, -10.51840700105979565, 33.73612834413961536 ) ) ;
#20787 = ORIENTED_EDGE ( 'NONE', *, *, #44725, .T. ) ;
#20788 = CARTESIAN_POINT ( 'NONE',  ( -15.36091644020745051, -2.882441371585227508, 31.66841991370172238 ) ) ;
#20789 = AXIS2_PLACEMENT_3D ( 'NONE', #87333, #26502, #80572 ) ;
#20790 = CYLINDRICAL_SURFACE ( 'NONE', #46947, 0.2499999999999994726 ) ;
#20791 = CARTESIAN_POINT ( 'NONE',  ( 7.622668902429897919, -10.11188796281391511, 34.01382737946119050 ) ) ;
#20792 = ORIENTED_EDGE ( 'NONE', *, *, #39114, .T. ) ;
#20793 = CARTESIAN_POINT ( 'NONE',  ( -8.899705954306490696, -7.276987145209185215, 34.99546412871779211 ) ) ;
#20794 = ADVANCED_FACE ( 'NONE', ( #82330 ), #48078, .T. ) ;
#20795 = VECTOR ( 'NONE', #49825, 1000.000000000000000 ) ;
#20796 = AXIS2_PLACEMENT_3D ( 'NONE', #84366, #30294, #23092 ) ;
#20797 = EDGE_LOOP ( 'NONE', ( #81982, #11187 ) ) ;
#20798 = LINE ( 'NONE', #1415, #80238 ) ;
#20799 = FACE_OUTER_BOUND ( 'NONE', #72355, .T. ) ;
#20800 = VERTEX_POINT ( 'NONE', #41335 ) ;
#20801 = CARTESIAN_POINT ( 'NONE',  ( 7.716006636715621703, -12.27039167877662251, 31.24851455888617835 ) ) ;
#20802 = CYLINDRICAL_SURFACE ( 'NONE', #13350, 0.2500000000000002220 ) ;
#20803 = CARTESIAN_POINT ( 'NONE',  ( -8.769230769230890843, -9.442884908241554243, 34.35708131394783038 ) ) ;
#20804 = EDGE_CURVE ( 'NONE', #85054, #77909, #22400, .T. ) ;
#20805 = CARTESIAN_POINT ( 'NONE',  ( 6.923076923076800782, -12.51329471203414379, 31.30864560766407578 ) ) ;
#20806 = CYLINDRICAL_SURFACE ( 'NONE', #23868, 0.2499999999999995559 ) ;
#20807 = EDGE_CURVE ( 'NONE', #58206, #41132, #46762, .T. ) ;
#20808 = ORIENTED_EDGE ( 'NONE', *, *, #88186, .T. ) ;
#20809 = EDGE_CURVE ( 'NONE', #6970, #80662, #53958, .T. ) ;
#20810 = FACE_BOUND ( 'NONE', #9201, .T. ) ;
#20811 = EDGE_LOOP ( 'NONE', ( #3632, #62338, #36762, #45133 ) ) ;
#20812 = CARTESIAN_POINT ( 'NONE',  ( 6.250000000001421085, -7.500000000000154543, 35.00000000000007105 ) ) ;
#20813 = CARTESIAN_POINT ( 'NONE',  ( 18.13079044096694759, -6.369690395747422684, 34.87708834333098196 ) ) ;
#20814 = CARTESIAN_POINT ( 'NONE',  ( 6.249945409378045547, -5.766571408460171355, 34.70601412856602508 ) ) ;
#20815 = CARTESIAN_POINT ( 'NONE',  ( 16.15384615384615330, -11.35647404775217417, 33.31231777344666511 ) ) ;
#20816 = EDGE_CURVE ( 'NONE', #44546, #61438, #41787, .T. ) ;
#20817 = ORIENTED_EDGE ( 'NONE', *, *, #27451, .F. ) ;
#20818 = VECTOR ( 'NONE', #13786, 1000.000000000000227 ) ;
#20819 = ORIENTED_EDGE ( 'NONE', *, *, #8064, .T. ) ;
#20820 = VERTEX_POINT ( 'NONE', #20613 ) ;
#20821 = DIRECTION ( 'NONE',  ( -0.000000000000000000, 0.1736481776669307198, -0.9848077530122080203 ) ) ;
#20822 = ADVANCED_FACE ( 'NONE', ( #12536 ), #19734, .F. ) ;
#20824 = ORIENTED_EDGE ( 'NONE', *, *, #83040, .T. ) ;
#20823 = EDGE_CURVE ( 'NONE', #5830, #21769, #51439, .T. ) ;
#20825 = CARTESIAN_POINT ( 'NONE',  ( -17.29985003582992320, -10.01117774369187252, 34.36070679894347535 ) ) ;
#20826 = DIRECTION ( 'NONE',  ( 0.000000000000000000, 0.000000000000000000, -1.000000000000000000 ) ) ;
#20827 = EDGE_CURVE ( 'NONE', #48447, #78324, #77065, .T. ) ;
#20828 = DIRECTION ( 'NONE',  ( -0.000000000000000000, 1.000000000000000000, -0.000000000000000000 ) ) ;
#20829 = CARTESIAN_POINT ( 'NONE',  ( 4.153846153846460609, -2.506253911140614576, 30.00000000000323297 ) ) ;
#20830 = CARTESIAN_POINT ( 'NONE',  ( -3.749999999999997335, -7.500000000000021316, 26.34375000000000000 ) ) ;
#20831 = CARTESIAN_POINT ( 'NONE',  ( 15.48071474911737333, -9.272278438253398036, 34.42582936511637115 ) ) ;
#20832 = CARTESIAN_POINT ( 'NONE',  ( 17.07692307692307665, -11.91647553114624181, 32.58852847137148245 ) ) ;
#20833 = CARTESIAN_POINT ( 'NONE',  ( -8.546451100252703270, -3.020022701398813236, 32.48759521482552515 ) ) ;
#20834 = ORIENTED_EDGE ( 'NONE', *, *, #14731, .F. ) ;
#20835 = ORIENTED_EDGE ( 'NONE', *, *, #80670, .T. ) ;
#20836 = VERTEX_POINT ( 'NONE', #67483 ) ;
#20837 = CARTESIAN_POINT ( 'NONE',  ( 3.903869409797562806, -2.920706130388546651, 32.31842814019191223 ) ) ;
#20839 = CARTESIAN_POINT ( 'NONE',  ( -9.822455662039388358, -4.299443229763728169, 33.91186481527756058 ) ) ;
#20838 = CARTESIAN_POINT ( 'NONE',  ( 1.449870955891410462, -6.026961402152789304, 34.52809138561124769 ) ) ;
#20840 = DIRECTION ( 'NONE',  ( 1.000000000000000000, 0.000000000000000000, 0.000000000000000000 ) ) ;
#20841 = DIRECTION ( 'NONE',  ( -0.000000000000000000, 0.6427876096865404731, -0.7660444431189770143 ) ) ;
#20842 = FACE_BOUND ( 'NONE', #55962, .T. ) ;
#20843 = CARTESIAN_POINT ( 'NONE',  ( 16.40390046548446890, -3.136992222400443175, 32.19305428654138979 ) ) ;
#20844 = VERTEX_POINT ( 'NONE', #26494 ) ;
#20845 = CARTESIAN_POINT ( 'NONE',  ( -0.3962828902624371263, -9.442884908240271713, 34.35708131394835618 ) ) ;
#20846 = CARTESIAN_POINT ( 'NONE',  ( 0.4615384615384611200, -5.471508081941601098, 34.59228464037088457 ) ) ;
#20847 = CARTESIAN_POINT ( 'NONE',  ( -3.480792454990687013, -3.520140089381496473, 33.17453946501458262 ) ) ;
#20848 = ORIENTED_EDGE ( 'NONE', *, *, #82111, .T. ) ;
#20849 = DIRECTION ( 'NONE',  ( -1.000000000000000000, 0.000000000000000000, 0.000000000000000000 ) ) ;
#20850 = VERTEX_POINT ( 'NONE', #61149 ) ;
#20851 = FACE_BOUND ( 'NONE', #14679, .T. ) ;
#20852 = EDGE_CURVE ( 'NONE', #41806, #26379, #88662, .T. ) ;
#20853 = LINE ( 'NONE', #20418, #1569 ) ;
#20854 = AXIS2_PLACEMENT_3D ( 'NONE', #81557, #18961, #81116 ) ;
#20855 = CARTESIAN_POINT ( 'NONE',  ( -12.46153846153858247, -8.613356846316285953, 34.62446782046622218 ) ) ;
#20856 = CARTESIAN_POINT ( 'NONE',  ( -15.23076923076922995, -9.780366693483667717, 34.19971097300155094 ) ) ;
#20857 = VERTEX_POINT ( 'NONE', #8882 ) ;
#20858 = AXIS2_PLACEMENT_3D ( 'NONE', #994, #75756, #40218 ) ;
#20859 = CARTESIAN_POINT ( 'NONE',  ( -14.30769230769242739, -12.46129190930018460, 30.37095296980731973 ) ) ;
#20860 = CARTESIAN_POINT ( 'NONE',  ( -5.934744860487159102, -9.528491918058460186, 34.59228464037085615 ) ) ;
#20861 = CARTESIAN_POINT ( 'NONE',  ( -16.21992956480203318, -12.37446782046654192, 30.86335684631486487 ) ) ;
#20862 = DIRECTION ( 'NONE',  ( -0.000000000000000000, -0.7660444431189791237, -0.6427876096865379196 ) ) ;
#20863 = ORIENTED_EDGE ( 'NONE', *, *, #6537, .F. ) ;
#20864 = LINE ( 'NONE', #34378, #48810 ) ;
#20865 = LINE ( 'NONE', #26298, #31204 ) ;
#20867 = ORIENTED_EDGE ( 'NONE', *, *, #34345, .F. ) ;
#20866 = FACE_OUTER_BOUND ( 'NONE', #74122, .T. ) ;
#20868 = CARTESIAN_POINT ( 'NONE',  ( 16.15384615384615330, -3.937682226553329556, 33.60647404775216529 ) ) ;
#20869 = CARTESIAN_POINT ( 'NONE',  ( 16.15384615384603251, -2.625532179533778709, 30.86335684631627174 ) ) ;
#20870 = CARTESIAN_POINT ( 'NONE',  ( -11.60454494941741999, -8.120952969808774569, 34.71129190930000163 ) ) ;
#20871 = CARTESIAN_POINT ( 'NONE',  ( 14.30769230769231015, -8.973038597847269315, 34.52809138561121927 ) ) ;
#20872 = CARTESIAN_POINT ( 'NONE',  ( 9.692307692307695177, -8.973038597847269315, 34.52809138561121927 ) ) ;
#20874 = CYLINDRICAL_SURFACE ( 'NONE', #63352, 0.2500000000000009437 ) ;
#20873 = DIRECTION ( 'NONE',  ( -1.000000000000000000, -0.000000000000000000, -0.000000000000000000 ) ) ;
#20875 = CARTESIAN_POINT ( 'NONE',  ( 12.21153846153846168, -7.500000000000001776, 34.75000000000000000 ) ) ;
#20876 = CARTESIAN_POINT ( 'NONE',  ( -2.750000000000007105, -6.360912703474006946, 21.42187500000000000 ) ) ;
#20877 = VERTEX_POINT ( 'NONE', #57494 ) ;
#20878 = PLANE ( 'NONE',  #17436 ) ;
#20879 = ORIENTED_EDGE ( 'NONE', *, *, #13820, .T. ) ;
#20880 = EDGE_LOOP ( 'NONE', ( #52652, #17921 ) ) ;
#20881 = CARTESIAN_POINT ( 'NONE',  ( 2.980745993476266342, -5.056417327199099532, 34.11270091957320716 ) ) ;
#20882 = VERTEX_POINT ( 'NONE', #62912 ) ;
#20883 = CARTESIAN_POINT ( 'NONE',  ( -4.377331078410485965, -2.612411019501189813, 31.66733052389439962 ) ) ;
#20884 = CARTESIAN_POINT ( 'NONE',  ( -2.749999999999991562, -8.639087296526025028, 18.76562500000000000 ) ) ;
#20885 = CARTESIAN_POINT ( 'NONE',  ( 13.51514108637894473, -2.882268652242222284, 31.66798894389554064 ) ) ;
#20886 = DIRECTION ( 'NONE',  ( 1.000000000000000000, 0.000000000000000000, 0.000000000000000000 ) ) ;
#20887 = CARTESIAN_POINT ( 'NONE',  ( 7.596153846153846700, -2.249999999999998668, 29.75000000000000355 ) ) ;
#20888 = AXIS2_PLACEMENT_3D ( 'NONE', #45409, #67479, #53053 ) ;
#20889 = CARTESIAN_POINT ( 'NONE',  ( 1.384615384615386802, -2.486705287966279876, 31.30864560766543647 ) ) ;
#20890 = CARTESIAN_POINT ( 'NONE',  ( -15.23076923076922995, -4.661471528628507777, 34.16647553114623292 ) ) ;
#20892 = EDGE_CURVE ( 'NONE', #37401, #17730, #23266, .T. ) ;
#20891 = DIRECTION ( 'NONE',  ( -0.000000000000000000, -0.6427876096865404731, -0.7660444431189771253 ) ) ;
#20893 = CARTESIAN_POINT ( 'NONE',  ( -4.284537620513712675, -3.530157926970578508, 32.79014554554150607 ) ) ;
#20894 = FACE_OUTER_BOUND ( 'NONE', #66760, .T. ) ;
#20895 = DIRECTION ( 'NONE',  ( -0.000000000000000000, 0.9848077530122085754, -0.1736481776669273613 ) ) ;
#20896 = CARTESIAN_POINT ( 'NONE',  ( 5.076923076922953193, -11.06231777344772027, 33.60647404775119895 ) ) ;
#20897 = CARTESIAN_POINT ( 'NONE',  ( -9.822998295418001291, -3.338472653186243644, 32.95098750199972670 ) ) ;
#20898 = ORIENTED_EDGE ( 'NONE', *, *, #69220, .F. ) ;
#20899 = ORIENTED_EDGE ( 'NONE', *, *, #76983, .F. ) ;
#20900 = CARTESIAN_POINT ( 'NONE',  ( 3.007842271862382066, -10.77366814457252175, 33.85459836347579454 ) ) ;
#20901 = DIRECTION ( 'NONE',  ( 0.000000000000000000, 0.4999999999999985567, 0.8660254037844395958 ) ) ;
#20902 = CARTESIAN_POINT ( 'NONE',  ( -6.673022503163469565, -12.01375889529407281, 32.43194544308182969 ) ) ;
#20903 = CARTESIAN_POINT ( 'NONE',  ( 9.757562831820528970, -12.16647553114626490, 32.15551576947920864 ) ) ;
#20904 = ADVANCED_FACE ( 'NONE', ( #22387 ), #43105, .F. ) ;
#20905 = EDGE_CURVE ( 'NONE', #13730, #72856, #8574, .T. ) ;
#20906 = CARTESIAN_POINT ( 'NONE',  ( 12.46153846153846168, -8.973038597847269315, 34.52809138561121927 ) ) ;
#20907 = CARTESIAN_POINT ( 'NONE',  ( 11.60452887181161508, -3.937682226553329556, 33.60647404775216529 ) ) ;
#20908 = B_SPLINE_CURVE_WITH_KNOTS ( 'NONE', 3,
 ( #66527, #59763, #74170, #46252, #73742, #12467, #12034, #39510, #66972, #35849 ),
 .UNSPECIFIED., .F., .F.,
 ( 4, 2, 2, 2, 4 ),
 ( 0.000000000000000000, 0.0001954311564186862239, 0.0003908623128373724478, 0.0005862934692560586988, 0.0007817246256747448956 ),
 .UNSPECIFIED. ) ;
#20909 = DIRECTION ( 'NONE',  ( -0.000000000000000000, -1.000000000000000000, 8.673617379884028076E-17 ) ) ;
#20910 = VECTOR ( 'NONE', #50851, 1000.000000000000114 ) ;
#20911 = EDGE_CURVE ( 'NONE', #27559, #11993, #31037, .T. ) ;
#20912 = ORIENTED_EDGE ( 'NONE', *, *, #41392, .T. ) ;
#20913 = CARTESIAN_POINT ( 'NONE',  ( -14.43838291080261271, -12.62707690430377383, 30.88035979386743435 ) ) ;
#20914 = EDGE_LOOP ( 'NONE', ( #18396, #53695, #10707, #8858, #77225 ) ) ;
#20915 = CARTESIAN_POINT ( 'NONE',  ( 10.74591031714818357, -8.586989748646452369, 34.63063291749215011 ) ) ;
#20916 = DIRECTION ( 'NONE',  ( 1.000000000000000000, 0.000000000000000000, 0.000000000000000000 ) ) ;
#20917 = CARTESIAN_POINT ( 'NONE',  ( -0.3310127597748980244, -6.852161475712351901, 34.70806712695776497 ) ) ;
#20918 = VECTOR ( 'NONE', #3979, 1000.000000000000000 ) ;
#20919 = CARTESIAN_POINT ( 'NONE',  ( 10.61538461538461675, -10.51840700105979565, 33.73612834413961536 ) ) ;
#20920 = DIRECTION ( 'NONE',  ( -1.000000000000000000, 0.000000000000000000, -0.000000000000000000 ) ) ;
#20921 = ORIENTED_EDGE ( 'NONE', *, *, #10928, .F. ) ;
#20922 = VERTEX_POINT ( 'NONE', #42669 ) ;
#20923 = EDGE_CURVE ( 'NONE', #87771, #63694, #83667, .T. ) ;
#20924 = VERTEX_POINT ( 'NONE', #69686 ) ;
#20925 = EDGE_LOOP ( 'NONE', ( #58644, #20104 ) ) ;
#20926 = CARTESIAN_POINT ( 'NONE',  ( -17.20707028636129721, -10.88202310037936194, 33.43294751532457099 ) ) ;
#20927 = CARTESIAN_POINT ( 'NONE',  ( 13.38461538461538680, -1.466349020453238561, 30.81389545987213907 ) ) ;
#20928 = FACE_BOUND ( 'NONE', #69239, .T. ) ;
#20929 = CARTESIAN_POINT ( 'NONE',  ( 2.307692307692187583, -11.48612834414049644, 32.76840700105863391 ) ) ;
#20930 = VECTOR ( 'NONE', #58637, 1000.000000000000000 ) ;
#20931 = CARTESIAN_POINT ( 'NONE',  ( -17.93393164899755732, -4.098570777380720287, 33.41473453929635440 ) ) ;
#20932 = CARTESIAN_POINT ( 'NONE',  ( 14.24242186173153435, -12.46129190929999986, 30.37095296980880832 ) ) ;
#20933 = EDGE_LOOP ( 'NONE', ( #68853, #3932 ) ) ;
#20934 = EDGE_LOOP ( 'NONE', ( #32158, #5982, #48395, #74502 ) ) ;
#20935 = VECTOR ( 'NONE', #70621, 1000.000000000000227 ) ;
#20936 = EDGE_LOOP ( 'NONE', ( #19508, #56553 ) ) ;
#20938 = ORIENTED_EDGE ( 'NONE', *, *, #17938, .F. ) ;
#20937 = CYLINDRICAL_SURFACE ( 'NONE', #14263, 0.2499999999999973355 ) ;
#20939 = CARTESIAN_POINT ( 'NONE',  ( -9.942330929600657896, -5.056417327199099532, 34.11270091957321426 ) ) ;
#20940 = DIRECTION ( 'NONE',  ( 0.000000000000000000, 0.6427876096865368094, 0.7660444431189802339 ) ) ;
#20941 = B_SPLINE_CURVE_WITH_KNOTS ( 'NONE', 3,
 ( #72313, #17377, #59697, #11068, #65552, #73673, #11966, #39443, #58799, #65102 ),
 .UNSPECIFIED., .F., .F.,
 ( 4, 2, 2, 2, 4 ),
 ( 0.0007817359430256322827, 0.0009771253907249989254, 0.001172514838424365676, 0.001367904286123732428, 0.001563293733823098962 ),
 .UNSPECIFIED. ) ;
#20942 = CARTESIAN_POINT ( 'NONE',  ( 2.651650429449569302, -10.15165042944953733, 20.87500000000000000 ) ) ;
#20943 = VERTEX_POINT ( 'NONE', #50281 ) ;
#20944 = ORIENTED_EDGE ( 'NONE', *, *, #45127, .T. ) ;
#20945 = CARTESIAN_POINT ( 'NONE',  ( 6.923076923076924238, -3.886160181151819604, 36.00935417666054406 ) ) ;
#20946 = FACE_BOUND ( 'NONE', #25449, .T. ) ;
#20947 = CARTESIAN_POINT ( 'NONE',  ( -15.23076923076922995, -13.87047571288749737, 32.06866353760679544 ) ) ;
#20948 = DIRECTION ( 'NONE',  ( -0.000000000000000000, -0.9396926207859092051, -0.3420201433256662704 ) ) ;
#20949 = ORIENTED_EDGE ( 'NONE', *, *, #27663, .F. ) ;
#20950 = DIRECTION ( 'NONE',  ( -0.000000000000000000, 0.000000000000000000, 1.000000000000000000 ) ) ;
#20951 = CARTESIAN_POINT ( 'NONE',  ( -1.384615384615383471, -6.189225973068211317, 35.74407628777942847 ) ) ;
#20952 = CARTESIAN_POINT ( 'NONE',  ( -16.85391023282967993, -12.64618726649961289, 30.78989965857442712 ) ) ;
#20953 = CARTESIAN_POINT ( 'NONE',  ( 15.45354889974729495, -6.717445702608402236, 34.94155399931962336 ) ) ;
#20954 = VERTEX_POINT ( 'NONE', #77770 ) ;
#20955 = CARTESIAN_POINT ( 'NONE',  ( -11.47239420511146513, -12.34228464037088813, 31.77849191805839268 ) ) ;
#20956 = CARTESIAN_POINT ( 'NONE',  ( -7.596208327805703320, -11.37275283266504111, 32.91324779482534524 ) ) ;
#20957 = CARTESIAN_POINT ( 'NONE',  ( -4.088591014333315066, -2.379036618887895305, 30.90682066428159303 ) ) ;
#20958 = CARTESIAN_POINT ( 'NONE',  ( -1.384615384615383471, -1.242168528481310874, 33.36296068462461051 ) ) ;
#20959 = CARTESIAN_POINT ( 'NONE',  ( -15.23076923076922995, -7.500000000000001776, 35.04278698407183867 ) ) ;
#20960 = AXIS2_PLACEMENT_3D ( 'NONE', #30926, #58394, #85892 ) ;
#20961 = FACE_BOUND ( 'NONE', #61463, .T. ) ;
#20963 = CARTESIAN_POINT ( 'NONE',  ( -6.066082379360133281, -9.905515769479276145, 34.41647553114623292 ) ) ;
#20962 = CARTESIAN_POINT ( 'NONE',  ( 4.853996859406927378, -11.24512374952581872, 33.06303171183252942 ) ) ;
#20964 = CARTESIAN_POINT ( 'NONE',  ( 5.299702745901139878, -2.353885683473779800, 30.79025554430704759 ) ) ;
#20966 = CARTESIAN_POINT ( 'NONE',  ( -9.692307692307384315, -2.506253911140614576, 30.00000000000323297 ) ) ;
#20965 = CARTESIAN_POINT ( 'NONE',  ( -18.22348492456433178, -2.353723527008296568, 30.78948104536958752 ) ) ;
#20967 = LINE ( 'NONE', #42153, #53393 ) ;
#20968 = CARTESIAN_POINT ( 'NONE',  ( -1.987747218494660295, -5.598659921968651254, 18.74813170625849068 ) ) ;
#20969 = ORIENTED_EDGE ( 'NONE', *, *, #21788, .T. ) ;
#20970 = DIRECTION ( 'NONE',  ( 0.000000000000000000, -5.102127870520020612E-17, -1.000000000000000000 ) ) ;
#20971 = ORIENTED_EDGE ( 'NONE', *, *, #5748, .F. ) ;
#20972 = B_SPLINE_CURVE_WITH_KNOTS ( 'NONE', 3,
 ( #84395, #51445, #78063, #37513, #71295, #57789, #8735, #50137, #23557, #51007 ),
 .UNSPECIFIED., .F., .F.,
 ( 4, 2, 2, 2, 4 ),
 ( 0.0007817359430256295722, 0.0009771253907249954559, 0.001172514838424361123, 0.001367904286123726790, 0.001563293733823092673 ),
 .UNSPECIFIED. ) ;
#20973 = CARTESIAN_POINT ( 'NONE',  ( 0.4615384615387678746, -2.506253911140615021, 30.00000000000323297 ) ) ;
#20974 = ORIENTED_EDGE ( 'NONE', *, *, #43963, .F. ) ;
#20975 = CARTESIAN_POINT ( 'NONE',  ( 17.86930853333243618, -12.11776431015576172, 31.66791131148498906 ) ) ;
#20976 = CARTESIAN_POINT ( 'NONE',  ( -7.976845312821407852, -9.804603061927743113, 34.18744698557895845 ) ) ;
#20979 = ORIENTED_EDGE ( 'NONE', *, *, #40498, .T. ) ;
#20978 = VECTOR ( 'NONE', #24895, 1000.000000000000000 ) ;
#20977 = CARTESIAN_POINT ( 'NONE',  ( 13.51545371510214189, -7.277220318596961057, 34.99547417642776992 ) ) ;
#20980 = CARTESIAN_POINT ( 'NONE',  ( 17.93424657168666059, -7.249945578846654470, 34.99404164642496795 ) ) ;
#20981 = CARTESIAN_POINT ( 'NONE',  ( -0.06109907496454585613, -4.750000000000000000, 18.90438170625848713 ) ) ;
#20982 = B_SPLINE_CURVE_WITH_KNOTS ( 'NONE', 3,
 ( #10013, #72600, #45573, #37478, #23522, #57316, #85682, #24406, #51409, #73051 ),
 .UNSPECIFIED., .F., .F.,
 ( 4, 2, 2, 2, 4 ),
 ( 0.000000000000000000, 0.0001954339857564077183, 0.0003908679715128154366, 0.0005863019572692231007, 0.0007817359430256308733 ),
 .UNSPECIFIED. ) ;
#20983 = CARTESIAN_POINT ( 'NONE',  ( -11.53846153846153655, -12.78798330534103123, 29.99999999999997868 ) ) ;
#20984 = FACE_OUTER_BOUND ( 'NONE', #12603, .T. ) ;
#20985 = FACE_OUTER_BOUND ( 'NONE', #77381, .T. ) ;
#20986 = CARTESIAN_POINT ( 'NONE',  ( 10.55011461482829560, -2.657715359629088780, 31.77849191805832874 ) ) ;
#20987 = CARTESIAN_POINT ( 'NONE',  ( -12.39628332202562433, -8.656820664281605460, 34.87096338111211224 ) ) ;
#20988 = CARTESIAN_POINT ( 'NONE',  ( -3.262820512820514107, -3.499999999999999556, 29.75000000000000355 ) ) ;
#20989 = CARTESIAN_POINT ( 'NONE',  ( -2.694853999681181556, -10.10844685921792241, 21.43936829374151642 ) ) ;
#20990 = CARTESIAN_POINT ( 'NONE',  ( -10.36543909703647515, -2.824170634883621744, 31.52227843825338738 ) ) ;
#20991 = CARTESIAN_POINT ( 'NONE',  ( -1.384615384615383471, -2.900454961884010974, 35.62045528018868623 ) ) ;
#20992 = ORIENTED_EDGE ( 'NONE', *, *, #61560, .F. ) ;
#20993 = FACE_OUTER_BOUND ( 'NONE', #13318, .T. ) ;
#20994 = CARTESIAN_POINT ( 'NONE',  ( 1.492201783934598236, -11.27530806549875031, 22.45499329374151287 ) ) ;
#20995 = ADVANCED_FACE ( 'NONE', ( #55724 ), #8438, .F. ) ;
#20996 = DIRECTION ( 'NONE',  ( 1.000000000000000000, 0.000000000000000000, 0.000000000000000000 ) ) ;
#20997 = DIRECTION ( 'NONE',  ( -0.000000000000000000, 1.000000000000000000, -0.000000000000000000 ) ) ;
#20998 = VERTEX_POINT ( 'NONE', #48975 ) ;
#20999 = VECTOR ( 'NONE', #68300, 1000.000000000000000 ) ;
#21000 = CARTESIAN_POINT ( 'NONE',  ( -13.91025641025641058, -7.500000000000000000, 29.75000000000000355 ) ) ;
#21001 = CARTESIAN_POINT ( 'NONE',  ( -16.82686865700962286, -9.233818618650598609, 34.70587769442853698 ) ) ;
#21003 = ORIENTED_EDGE ( 'NONE', *, *, #14163, .T. ) ;
#21002 = DIRECTION ( 'NONE',  ( -0.000000000000000000, -0.5000000000000009992, -0.8660254037844380415 ) ) ;
#21004 = CARTESIAN_POINT ( 'NONE',  ( -7.622726884292275074, -7.630147231320743018, 34.74852402298682819 ) ) ;
#21005 = EDGE_CURVE ( 'NONE', #83848, #50855, #76454, .T. ) ;
#21006 = CARTESIAN_POINT ( 'NONE',  ( -1.634592115557738090, -10.66389620160130036, 33.62221079203477103 ) ) ;
#21007 = VECTOR ( 'NONE', #69639, 1000.000000000000000 ) ;
#21008 = CARTESIAN_POINT ( 'NONE',  ( -10.61538461538461320, -9.058645607665452459, 34.76329471203371924 ) ) ;
#21009 = CARTESIAN_POINT ( 'NONE',  ( 2.980746006547771554, -2.588893531581426544, 31.60682220781847818 ) ) ;
#21010 = CARTESIAN_POINT ( 'NONE',  ( -11.53846153846153655, -13.78497067705608181, 32.30358669280327177 ) ) ;
#21011 = EDGE_CURVE ( 'NONE', #8206, #14619, #42233, .T. ) ;
#21012 = ORIENTED_EDGE ( 'NONE', *, *, #66591, .T. ) ;
#21013 = ORIENTED_EDGE ( 'NONE', *, *, #75153, .T. ) ;
#21014 = ORIENTED_EDGE ( 'NONE', *, *, #39422, .F. ) ;
#21015 = CARTESIAN_POINT ( 'NONE',  ( -13.51530685128294884, -3.530157926970578952, 32.79014554554150607 ) ) ;
#21016 = CARTESIAN_POINT ( 'NONE',  ( -3.903791842207836815, -3.136992222400443175, 32.19305428654139689 ) ) ;
#21017 = DIRECTION ( 'NONE',  ( -0.000000000000000000, -5.102127870520021228E-17, -1.000000000000000000 ) ) ;
#21018 = CARTESIAN_POINT ( 'NONE',  ( -7.911423846710166075, -11.06231777344662781, 33.60647404775220082 ) ) ;
#21019 = ORIENTED_EDGE ( 'NONE', *, *, #89064, .F. ) ;
#21020 = CARTESIAN_POINT ( 'NONE',  ( -17.30040802064702987, -4.386631170607603991, 33.66268669641500111 ) ) ;
#21021 = ORIENTED_EDGE ( 'NONE', *, *, #14828, .F. ) ;
#21022 = VECTOR ( 'NONE', #19880, 1000.000000000000227 ) ;
#21023 = EDGE_CURVE ( 'NONE', #63925, #19030, #64240, .T. ) ;
#21024 = ORIENTED_EDGE ( 'NONE', *, *, #78582, .F. ) ;
#21025 = VERTEX_POINT ( 'NONE', #1674 ) ;
#21028 = EDGE_LOOP ( 'NONE', ( #31715, #28055, #61276, #11403 ) ) ;
#21027 = ADVANCED_FACE ( 'NONE', ( #29162 ), #16075, .F. ) ;
#21026 = LINE ( 'NONE', #20590, #65997 ) ;
#21029 = CARTESIAN_POINT ( 'NONE',  ( 4.219101725122176738, -6.026961402152789304, 34.52809138561124769 ) ) ;
#21030 = B_SPLINE_CURVE_WITH_KNOTS ( 'NONE', 3,
 ( #66056, #4368, #77802, #57972, #43573, #71047, #51188, #78696, #9360, #4820 ),
 .UNSPECIFIED., .F., .F.,
 ( 4, 2, 2, 2, 4 ),
 ( 0.000000000000000000, 0.0001954339857564097512, 0.0003908679715128195024, 0.0005863019572692292807, 0.0007817359430256390048 ),
 .UNSPECIFIED. ) ;
#21031 = CARTESIAN_POINT ( 'NONE',  ( -2.939152317953646711E-15, 7.500000000000000000, 14.00000000000000178 ) ) ;
#21032 = EDGE_CURVE ( 'NONE', #52380, #33767, #89151, .T. ) ;
#21033 = EDGE_CURVE ( 'NONE', #1104, #28433, #17856, .T. ) ;
#21034 = FACE_OUTER_BOUND ( 'NONE', #79897, .T. ) ;
#21035 = CYLINDRICAL_SURFACE ( 'NONE', #65474, 0.2499999999999997502 ) ;
#21036 = VECTOR ( 'NONE', #64300, 1000.000000000000000 ) ;
#21037 = ORIENTED_EDGE ( 'NONE', *, *, #36130, .T. ) ;
#21038 = VERTEX_POINT ( 'NONE', #31818 ) ;
#21039 = ORIENTED_EDGE ( 'NONE', *, *, #85642, .F. ) ;
#21040 = CARTESIAN_POINT ( 'NONE',  ( -11.53846153846153655, -8.318370150425687726, 35.83090037661290239 ) ) ;
#21042 = ORIENTED_EDGE ( 'NONE', *, *, #17418, .F. ) ;
#21041 = CARTESIAN_POINT ( 'NONE',  ( 13.38461538461538680, -13.75783147151868846, 33.36296068462461051 ) ) ;
#21043 = CARTESIAN_POINT ( 'NONE',  ( 6.673053685783957967, -6.695914987888143877, 34.68535235679833306 ) ) ;
#21044 = CARTESIAN_POINT ( 'NONE',  ( -0.5268084620947809382, -6.835583212224499938, 34.95778746994557906 ) ) ;
#21045 = ORIENTED_EDGE ( 'NONE', *, *, #24394, .T. ) ;
#21046 = CARTESIAN_POINT ( 'NONE',  ( -17.86947429823643674, -2.619367082507847222, 30.83698974864643461 ) ) ;
#21047 = CARTESIAN_POINT ( 'NONE',  ( 0.2380535369741303697, -9.417330523894424488, 34.63758898049880486 ) ) ;
#21048 = ORIENTED_EDGE ( 'NONE', *, *, #35681, .F. ) ;
#21049 = FACE_BOUND ( 'NONE', #28218, .T. ) ;
#21050 = CARTESIAN_POINT ( 'NONE',  ( -15.29603923132555110, -8.656820664281498878, 34.87096338111211935 ) ) ;
#21051 = CARTESIAN_POINT ( 'NONE',  ( 15.90386940979756858, -2.544273027872574477, 31.48422191005632698 ) ) ;
#21052 = FACE_OUTER_BOUND ( 'NONE', #21843, .T. ) ;
#21054 = DIRECTION ( 'NONE',  ( -0.000000000000000000, 0.6427876096865404731, -0.7660444431189770143 ) ) ;
#21053 = CARTESIAN_POINT ( 'NONE',  ( 18.24994540937804288, -2.986452184633680229, 32.43230066228895225 ) ) ;
#21055 = VECTOR ( 'NONE', #57230, 1000.000000000000000 ) ;
#21056 = DIRECTION ( 'NONE',  ( -0.000000000000000000, -0.7660444431189791237, -0.6427876096865379196 ) ) ;
#21057 = CARTESIAN_POINT ( 'NONE',  ( -2.557715544985270206, -3.711651800289232916, 33.01384336483936011 ) ) ;
#21058 = ORIENTED_EDGE ( 'NONE', *, *, #56870, .F. ) ;
#21059 = CARTESIAN_POINT ( 'NONE',  ( -8.096177070375304652, -6.652501968072648708, 34.93155406624980941 ) ) ;
#21060 = CARTESIAN_POINT ( 'NONE',  ( -1.944543648263015179, -5.555456351737005249, 26.50000000000000355 ) ) ;
#21061 = ORIENTED_EDGE ( 'NONE', *, *, #79422, .T. ) ;
#21062 = B_SPLINE_CURVE_WITH_KNOTS ( 'NONE', 3,
 ( #38946, #11462, #31737, #10574, #24969, #67300, #45235, #5150, #5596, #38044 ),
 .UNSPECIFIED., .F., .F.,
 ( 4, 2, 2, 2, 4 ),
 ( 0.000000000000000000, 0.0001954339857564081520, 0.0003908679715128163040, 0.0005863019572692244018, 0.0007817359430256326080 ),
 .UNSPECIFIED. ) ;
#21063 = CARTESIAN_POINT ( 'NONE',  ( 14.17700084102475344, -9.804603061927743113, 34.18744698557895845 ) ) ;
#21064 = LINE ( 'NONE', #56195, #82156 ) ;
#21065 = ORIENTED_EDGE ( 'NONE', *, *, #55333, .F. ) ;
#21066 = EDGE_CURVE ( 'NONE', #29522, #21125, #36486, .T. ) ;
#21067 = CYLINDRICAL_SURFACE ( 'NONE', #1130, 0.2499999999999973355 ) ;
#21068 = CARTESIAN_POINT ( 'NONE',  ( 4.219101725122177626, -10.21337939537593797, 33.94971097300152252 ) ) ;
#21069 = B_SPLINE_CURVE_WITH_KNOTS ( 'NONE', 3,
 ( #35338, #76775, #77651, #42548, #1112, #35795, #42986, #6981, #55605, #1556 ),
 .UNSPECIFIED., .F., .F.,
 ( 4, 2, 2, 2, 4 ),
 ( 0.0007817246256747465219, 0.0009771112852218902852, 0.001172497944769034049, 0.001367884604316177595, 0.001563271263863321358 ),
 .UNSPECIFIED. ) ;
#21070 = FACE_BOUND ( 'NONE', #13851, .T. ) ;
#21072 = CARTESIAN_POINT ( 'NONE',  ( 0.4615384615384611200, -10.67929555188718282, 33.92786785259544047 ) ) ;
#21071 = CARTESIAN_POINT ( 'NONE',  ( 6.923076923076800782, -4.320704448113951379, 33.92786785259630022 ) ) ;
#21073 = CARTESIAN_POINT ( 'NONE',  ( -8.834501215191544077, -6.879047030191174805, 34.71129190930000163 ) ) ;
#21074 = CARTESIAN_POINT ( 'NONE',  ( -15.23076923076922995, -8.973038597847269315, 34.52809138561121927 ) ) ;
#21076 = CARTESIAN_POINT ( 'NONE',  ( -14.16025641025641058, -7.500000000000000000, 29.75000000000000355 ) ) ;
#21075 = DIRECTION ( 'NONE',  ( 0.000000000000000000, 0.000000000000000000, 1.000000000000000000 ) ) ;
#21077 = DIRECTION ( 'NONE',  ( 1.000000000000000000, 0.000000000000000000, 0.000000000000000000 ) ) ;
#21078 = CARTESIAN_POINT ( 'NONE',  ( 2.608446859217893099, -4.805146000318787358, 16.56063170625848713 ) ) ;
#21079 = EDGE_LOOP ( 'NONE', ( #64408, #33490, #24578, #79511 ) ) ;
#21080 = ORIENTED_EDGE ( 'NONE', *, *, #18960, .T. ) ;
#21081 = FACE_OUTER_BOUND ( 'NONE', #67571, .T. ) ;
#21082 = LINE ( 'NONE', #89135, #61375 ) ;
#21083 = CARTESIAN_POINT ( 'NONE',  ( -5.999999999999998224, -2.486705287966279876, 31.30864560766543647 ) ) ;
#21084 = CARTESIAN_POINT ( 'NONE',  ( -8.992715693795101828, -8.539481045369596401, 34.89627647299170832 ) ) ;
#21085 = LINE ( 'NONE', #27855, #52896 ) ;
#21086 = CARTESIAN_POINT ( 'NONE',  ( -3.749999999999996447, -7.561099074964554134, 18.59188170625849068 ) ) ;
#21087 = EDGE_CURVE ( 'NONE', #6010, #15849, #25239, .T. ) ;
#21088 = CARTESIAN_POINT ( 'NONE',  ( -12.71156168575991963, -4.175268141568685643, 33.81360843649122216 ) ) ;
#21089 = DIRECTION ( 'NONE',  ( -0.000000000000000000, -0.1736481776669307198, -0.9848077530122080203 ) ) ;
#21090 = CARTESIAN_POINT ( 'NONE',  ( 6.130790440966953803, -3.957578996910242619, 33.62503395064540257 ) ) ;
#21091 = CARTESIAN_POINT ( 'NONE',  ( -5.076923076923075762, -12.78798330534102945, 29.74999999999997868 ) ) ;
#21092 = CARTESIAN_POINT ( 'NONE',  ( -14.98071491913091613, -11.28795663066794575, 33.01431243580653785 ) ) ;
#21093 = CARTESIAN_POINT ( 'NONE',  ( -15.84615384615384670, -3.499999999999999556, 29.75000000000000355 ) ) ;
#21094 = CARTESIAN_POINT ( 'NONE',  ( -0.3954711281883867002, -3.937682226553329556, 33.60647404775216529 ) ) ;
#21095 = AXIS2_PLACEMENT_3D ( 'NONE', #78150, #15130, #23645 ) ;
#21096 = CARTESIAN_POINT ( 'NONE',  ( -14.24243673641628050, -3.300289026998473041, 32.46337939537591666 ) ) ;
#21097 = CARTESIAN_POINT ( 'NONE',  ( 12.71159277317678082, -2.779044189368095719, 31.39831045268885745 ) ) ;
#21098 = ORIENTED_EDGE ( 'NONE', *, *, #54483, .F. ) ;
#21099 = CARTESIAN_POINT ( 'NONE',  ( -0.3307466537136750095, -3.530189275343204702, 32.79018710029569661 ) ) ;
#21100 = CARTESIAN_POINT ( 'NONE',  ( -2.307692307692427391, -12.46129190930018460, 30.37095296980731973 ) ) ;
#21101 = AXIS2_PLACEMENT_3D ( 'NONE', #49275, #22681, #29893 ) ;
#21102 = CARTESIAN_POINT ( 'NONE',  ( -2.775308065498752086, -8.577988221561495763, 20.26749329374151998 ) ) ;
#21103 = EDGE_CURVE ( 'NONE', #27440, #18632, #66021, .T. ) ;
#21104 = CARTESIAN_POINT ( 'NONE',  ( -0.3962833220256226641, -11.06231777344671130, 33.60647404775212976 ) ) ;
#21105 = CARTESIAN_POINT ( 'NONE',  ( -2.307692307692305711, -4.661471528628507777, 34.16647553114623292 ) ) ;
#21106 = ORIENTED_EDGE ( 'NONE', *, *, #71200, .F. ) ;
#21107 = DIRECTION ( 'NONE',  ( -0.000000000000000000, 0.9848077530122086864, -0.1736481776669273891 ) ) ;
#21109 = ORIENTED_EDGE ( 'NONE', *, *, #69265, .F. ) ;
#21108 = CARTESIAN_POINT ( 'NONE',  ( -9.561515884482904681, -4.809403383903225304, 33.96459661697924304 ) ) ;
#21110 = CARTESIAN_POINT ( 'NONE',  ( 8.069165197766695385, -3.587049720035815348, 32.86302985866382897 ) ) ;
#21111 = CARTESIAN_POINT ( 'NONE',  ( 12.59232890250541281, -5.496552790871120031, 34.60292014791297532 ) ) ;
#21112 = VECTOR ( 'NONE', #12937, 1000.000000000000000 ) ;
#21113 = ADVANCED_FACE ( 'NONE', ( #24600 ), #73239, .F. ) ;
#21114 = EDGE_LOOP ( 'NONE', ( #27877, #76289, #51780, #74611 ) ) ;
#21115 = FACE_OUTER_BOUND ( 'NONE', #87965, .T. ) ;
#21116 = B_SPLINE_CURVE_WITH_KNOTS ( 'NONE', 3,
 ( #84480, #37604, #9690, #2921, #70064, #63303, #36723, #1611, #10140, #22323 ),
 .UNSPECIFIED., .F., .F.,
 ( 4, 2, 2, 2, 4 ),
 ( 0.000000000000000000, 0.0001954339857564074473, 0.0003908679715128148945, 0.0005863019572692223418, 0.0007817359430256297891 ),
 .UNSPECIFIED. ) ;
#21117 = B_SPLINE_CURVE_WITH_KNOTS ( 'NONE', 3,
 ( #7429, #6977, #34887, #34450, #662, #7869, #35333, #63247, #8761, #84425 ),
 .UNSPECIFIED., .F., .F.,
 ( 4, 2, 2, 2, 4 ),
 ( 0.000000000000000000, 0.0001954311564186876876, 0.0003908623128373753751, 0.0005862934692560630356, 0.0007817246256747507503 ),
 .UNSPECIFIED. ) ;
#21118 = CYLINDRICAL_SURFACE ( 'NONE', #68762, 3.000000000000000444 ) ;
#21119 = EDGE_LOOP ( 'NONE', ( #51930, #1035, #10381, #72432 ) ) ;
#21120 = CARTESIAN_POINT ( 'NONE',  ( -10.74607521849492464, -3.957541250942358424, 33.62499894934981626 ) ) ;
#21121 = B_SPLINE_CURVE_WITH_KNOTS ( 'NONE', 3,
 ( #65933, #79013, #59184, #86688, #87575, #17313, #24954, #66837, #11902, #66389 ),
 .UNSPECIFIED., .F., .F.,
 ( 4, 2, 2, 2, 4 ),
 ( 0.000000000000000000, 0.0001954339857564074473, 0.0003908679715128148945, 0.0005863019572692223418, 0.0007817359430256297891 ),
 .UNSPECIFIED. ) ;
#21122 = CARTESIAN_POINT ( 'NONE',  ( -6.416666666666667851, -7.500000000000000000, 29.75000000000000355 ) ) ;
#21123 = CARTESIAN_POINT ( 'NONE',  ( 19.00000000000000000, -4.000000000000000000, 29.75000000000000355 ) ) ;
#21124 = ADVANCED_FACE ( 'NONE', ( #37671 ), #9756, .F. ) ;
#21125 = VERTEX_POINT ( 'NONE', #57940 ) ;
#21126 = ORIENTED_EDGE ( 'NONE', *, *, #30433, .F. ) ;
#21127 = CARTESIAN_POINT ( 'NONE',  ( 6.222779541268409709, -6.760870238392817200, 34.69528174975672385 ) ) ;
#21128 = VERTEX_POINT ( 'NONE', #86330 ) ;
#21129 = ADVANCED_FACE ( 'NONE', ( #10208 ), #16960, .F. ) ;
#21130 = FACE_OUTER_BOUND ( 'NONE', #79317, .T. ) ;
#21131 = CARTESIAN_POINT ( 'NONE',  ( -5.299850035829926753, -9.172386477786396597, 34.72672124145550043 ) ) ;
#21132 = CARTESIAN_POINT ( 'NONE',  ( -5.777220331021931443, -5.827830569534416583, 34.72679350104403539 ) ) ;
#21133 = EDGE_CURVE ( 'NONE', #71551, #80250, #38550, .T. ) ;
#21134 = CARTESIAN_POINT ( 'NONE',  ( -2.557669038634660108, -5.728515186090277211, 34.42611988154120439 ) ) ;
#21135 = CARTESIAN_POINT ( 'NONE',  ( -0.3307480205715112032, -5.496552790871119143, 34.60292014791297532 ) ) ;
#21136 = PLANE ( 'NONE',  #46638 ) ;
#21137 = AXIS2_PLACEMENT_3D ( 'NONE', #22639, #9148, #14118 ) ;
#21138 = CARTESIAN_POINT ( 'NONE',  ( 15.29596321255258928, -2.506253911140448043, 29.99999999999988631 ) ) ;
#21139 = EDGE_CURVE ( 'NONE', #9985, #83657, #13824, .T. ) ;
#21140 = ORIENTED_EDGE ( 'NONE', *, *, #49791, .T. ) ;
#21141 = VECTOR ( 'NONE', #20234, 1000.000000000000000 ) ;
#21142 = EDGE_LOOP ( 'NONE', ( #24999, #60234, #19653, #60467 ) ) ;
#21144 = ORIENTED_EDGE ( 'NONE', *, *, #84869, .F. ) ;
#21143 = CARTESIAN_POINT ( 'NONE',  ( -17.07692307692307665, -9.780366693483667717, 34.19971097300155094 ) ) ;
#21145 = CARTESIAN_POINT ( 'NONE',  ( 16.82689985270161870, -2.341070481393820124, 30.72580821765574299 ) ) ;
#21146 = ORIENTED_EDGE ( 'NONE', *, *, #78074, .F. ) ;
#21147 = B_SPLINE_CURVE_WITH_KNOTS ( 'NONE', 3,
 ( #55967, #35255, #48766, #49658, #76237, #35715, #14102, #41572, #145, #591 ),
 .UNSPECIFIED., .F., .F.,
 ( 4, 2, 2, 2, 4 ),
 ( 0.000000000000000000, 0.0001954311564186870099, 0.0003908623128373740199, 0.0005862934692560609756, 0.0007817246256747480398 ),
 .UNSPECIFIED. ) ;
#21148 = EDGE_CURVE ( 'NONE', #70481, #86621, #18295, .T. ) ;
#21149 = FACE_OUTER_BOUND ( 'NONE', #33413, .T. ) ;
#21150 = CARTESIAN_POINT ( 'NONE',  ( 9.442284455014730682, -5.056417327199099532, 34.11270091957321426 ) ) ;
#21151 = EDGE_LOOP ( 'NONE', ( #41117, #88489 ) ) ;
#21152 = DIRECTION ( 'NONE',  ( -0.000000000000000000, -0.9396926207859093161, -0.3420201433256663259 ) ) ;
#21153 = ORIENTED_EDGE ( 'NONE', *, *, #48661, .F. ) ;
#21154 = ORIENTED_EDGE ( 'NONE', *, *, #12372, .F. ) ;
#21155 = DIRECTION ( 'NONE',  ( -0.000000000000000000, 1.000000000000000000, -0.000000000000000000 ) ) ;
#21156 = B_SPLINE_CURVE_WITH_KNOTS ( 'NONE', 3,
 ( #77060, #57665, #36942, #65304, #64406, #77495, #2264, #57226, #22991, #84276 ),
 .UNSPECIFIED., .F., .F.,
 ( 4, 2, 2, 2, 4 ),
 ( 0.0007817246256747489071, 0.0009771112852218920199, 0.001172497944769035133, 0.001367884604316178246, 0.001563271263863321358 ),
 .UNSPECIFIED. ) ;
#21157 = AXIS2_PLACEMENT_3D ( 'NONE', #10271, #9385, #58892 ) ;
#21158 = ORIENTED_EDGE ( 'NONE', *, *, #64593, .T. ) ;
#21159 = CARTESIAN_POINT ( 'NONE',  ( -6.700064078983529292, -4.762714258010880997, 34.23016756924214832 ) ) ;
#21160 = EDGE_CURVE ( 'NONE', #37680, #58206, #46046, .T. ) ;
#21161 = CARTESIAN_POINT ( 'NONE',  ( 12.39626846098214230, -2.379036618887870436, 30.90682066428147934 ) ) ;
#21162 = AXIS2_PLACEMENT_3D ( 'NONE', #83079, #20916, #6531 ) ;
#21163 = FACE_BOUND ( 'NONE', #56620, .T. ) ;
#21164 = CARTESIAN_POINT ( 'NONE',  ( -14.87820512820512953, -3.499999999999999556, 29.75000000000000355 ) ) ;
#21165 = CARTESIAN_POINT ( 'NONE',  ( -11.60454391782167249, -6.343179335718451384, 34.87096338111212646 ) ) ;
#21166 = CARTESIAN_POINT ( 'NONE',  ( -16.02332071561251325, -5.070358843744209310, 34.40418822224088302 ) ) ;
#21167 = CARTESIAN_POINT ( 'NONE',  ( 1.384615384615386802, -1.129524287112498415, 32.06866353760679544 ) ) ;
#21168 = EDGE_CURVE ( 'NONE', #44468, #57842, #39521, .T. ) ;
#21169 = CARTESIAN_POINT ( 'NONE',  ( -17.07692307692319744, -8.656820664282941280, 34.87096338111179961 ) ) ;
#21170 = DIRECTION ( 'NONE',  ( 0.000000000000000000, 0.6427876096865368094, 0.7660444431189802339 ) ) ;
#21171 = VECTOR ( 'NONE', #28100, 1000.000000000000000 ) ;
#21172 = DIRECTION ( 'NONE',  ( -0.000000000000000000, 0.7660444431189791237, -0.6427876096865379196 ) ) ;
#21173 = VERTEX_POINT ( 'NONE', #75454 ) ;
#21174 = ORIENTED_EDGE ( 'NONE', *, *, #21160, .F. ) ;
#21176 = CARTESIAN_POINT ( 'NONE',  ( -19.00000000000000000, -1.249999999999999334, 30.25000000000000000 ) ) ;
#21175 = CARTESIAN_POINT ( 'NONE',  ( -17.01166750564705055, -10.21337939537593797, 33.94971097300152252 ) ) ;
#21177 = CARTESIAN_POINT ( 'NONE',  ( -5.076923076923075762, -1.367168528481310208, 33.57946703557072254 ) ) ;
#21178 = DIRECTION ( 'NONE',  ( 0.000000000000000000, 0.8660254037844377084, 0.5000000000000015543 ) ) ;
#21179 = CARTESIAN_POINT ( 'NONE',  ( -10.36533019547115941, -12.41089969410671223, 31.60739465890703670 ) ) ;
#21180 = CARTESIAN_POINT ( 'NONE',  ( 9.942253210655836781, -2.587454068350148351, 30.68340429815432202 ) ) ;
#21181 = ORIENTED_EDGE ( 'NONE', *, *, #22122, .T. ) ;
#21182 = EDGE_CURVE ( 'NONE', #62448, #83471, #52685, .T. ) ;
#21183 = CARTESIAN_POINT ( 'NONE',  ( 13.13463865367303285, -4.943428324936578910, 34.04746400365624481 ) ) ;
#21184 = B_SPLINE_CURVE_WITH_KNOTS ( 'NONE', 3,
 ( #77921, #31056, #16227, #85135, #51760, #24299, #24754, #18008, #17562, #23414 ),
 .UNSPECIFIED., .F., .F.,
 ( 4, 2, 2, 2, 4 ),
 ( 0.000000000000000000, 0.0001954339857564083417, 0.0003908679715128166835, 0.0005863019572692250523, 0.0007817359430256333669 ),
 .UNSPECIFIED. ) ;
#21185 = FACE_OUTER_BOUND ( 'NONE', #58123, .T. ) ;
#21186 = CARTESIAN_POINT ( 'NONE',  ( -14.05774689831426372, -12.45601412856602686, 31.48342859153981621 ) ) ;
#21187 = CARTESIAN_POINT ( 'NONE',  ( -7.846153846153844924, -11.16473453929635440, 33.15142922261926373 ) ) ;
#21188 = EDGE_LOOP ( 'NONE', ( #56520, #4600, #65234, #32143 ) ) ;
#21189 = EDGE_CURVE ( 'NONE', #39874, #77096, #20210, .T. ) ;
#21190 = EDGE_LOOP ( 'NONE', ( #47966, #74429 ) ) ;
#21192 = EDGE_CURVE ( 'NONE', #79428, #21592, #72833, .T. ) ;
#21191 = VERTEX_POINT ( 'NONE', #13750 ) ;
#21193 = VECTOR ( 'NONE', #44865, 1000.000000000000227 ) ;
#21194 = CARTESIAN_POINT ( 'NONE',  ( -7.173100160369890510, -8.432397168068783699, 34.66272746175022945 ) ) ;
#21195 = EDGE_LOOP ( 'NONE', ( #5111, #57766 ) ) ;
#21196 = FACE_OUTER_BOUND ( 'NONE', #71129, .T. ) ;
#21197 = DIRECTION ( 'NONE',  ( 0.000000000000000000, 0.000000000000000000, -1.000000000000000000 ) ) ;
#21198 = CARTESIAN_POINT ( 'NONE',  ( 13.38461538461526423, -3.083524468854526912, 32.58852847137268327 ) ) ;
#21199 = CARTESIAN_POINT ( 'NONE',  ( -3.750000000000008438, -5.946699141100917352, 15.17187500000000000 ) ) ;
#21200 = ADVANCED_FACE ( 'NONE', ( #40792 ), #12863, .F. ) ;
#21201 = CARTESIAN_POINT ( 'NONE',  ( 12.39545505058258001, -9.780366693483667717, 34.19971097300155805 ) ) ;
#21202 = VERTEX_POINT ( 'NONE', #6558 ) ;
#21203 = DIRECTION ( 'NONE',  ( -0.000000000000000000, -0.9396926207859092051, -0.3420201433256662704 ) ) ;
#21205 = ORIENTED_EDGE ( 'NONE', *, *, #78966, .T. ) ;
#21204 = CYLINDRICAL_SURFACE ( 'NONE', #59712, 0.2500000000000002220 ) ;
#21206 = CARTESIAN_POINT ( 'NONE',  ( -17.07692307692307665, -1.422936976036506707, 30.56769352161908415 ) ) ;
#21207 = CARTESIAN_POINT ( 'NONE',  ( -6.000000000000121680, -12.16647553114689728, 32.15551576947799362 ) ) ;
#21208 = CARTESIAN_POINT ( 'NONE',  ( -0.5916864312701578532, -4.299443229763728169, 33.91186481527756058 ) ) ;
#21209 = CARTESIAN_POINT ( 'NONE',  ( -16.21916906933833147, -7.749976743299138882, 34.99404534957040624 ) ) ;
#21210 = CARTESIAN_POINT ( 'NONE',  ( -12.71151519248081563, -2.779195860258146578, 31.39871582349836032 ) ) ;
#21211 = VECTOR ( 'NONE', #42730, 1000.000000000000114 ) ;
#21212 = CARTESIAN_POINT ( 'NONE',  ( 9.692307692307695177, -9.780366693483667717, 34.19971097300155094 ) ) ;
#21213 = CYLINDRICAL_SURFACE ( 'NONE', #29211, 0.2500000000000008882 ) ;
#21214 = CARTESIAN_POINT ( 'NONE',  ( 3.775308065498752086, -6.007798216065404873, 13.39249329374151642 ) ) ;
#21215 = ORIENTED_EDGE ( 'NONE', *, *, #45850, .F. ) ;
#21216 = CYLINDRICAL_SURFACE ( 'NONE', #18709, 0.2500000000000008882 ) ;
#21218 = CARTESIAN_POINT ( 'NONE',  ( -14.87820512820512953, -3.499999999999999556, 29.75000000000000355 ) ) ;
#21217 = B_SPLINE_CURVE_WITH_KNOTS ( 'NONE', 3,
 ( #67054, #46779, #12552, #688, #19749, #12993, #40478, #6243, #33708, #55624 ),
 .UNSPECIFIED., .F., .F.,
 ( 4, 2, 2, 2, 4 ),
 ( 0.0007817359430256282712, 0.0009771253907249945886, 0.001172514838424360689, 0.001367904286123726790, 0.001563293733823093107 ),
 .UNSPECIFIED. ) ;
#21219 = CARTESIAN_POINT ( 'NONE',  ( 9.692307692307695177, -2.833524468853757305, 32.15551576947925838 ) ) ;
#21220 = CARTESIAN_POINT ( 'NONE',  ( -7.846153846153967493, -3.083524468854526912, 32.58852847137268327 ) ) ;
#21221 = ORIENTED_EDGE ( 'NONE', *, *, #86306, .T. ) ;
#21222 = CARTESIAN_POINT ( 'NONE',  ( 2.750000000000001776, -7.499999999999984013, 14.46875000000000000 ) ) ;
#21223 = CARTESIAN_POINT ( 'NONE',  ( -3.480792468062196221, -10.76384336483936011, 33.53834819971076087 ) ) ;
#21224 = EDGE_CURVE ( 'NONE', #74312, #15069, #34022, .T. ) ;
#21225 = CARTESIAN_POINT ( 'NONE',  ( -0.7115616857599196265, -12.68155406624981119, 30.59749803192733708 ) ) ;
#21226 = CARTESIAN_POINT ( 'NONE',  ( 9.915734091222482505, -7.630147987733840509, 34.99859428049665411 ) ) ;
#21227 = EDGE_LOOP ( 'NONE', ( #34198, #83201 ) ) ;
#21228 = CARTESIAN_POINT ( 'NONE',  ( 16.85399685940691938, -3.105860786376062332, 32.13614157043599562 ) ) ;
#21229 = CARTESIAN_POINT ( 'NONE',  ( 17.07692307692307665, -5.557115091759785130, 34.35708131394839171 ) ) ;
#21230 = DIRECTION ( 'NONE',  ( 0.000000000000000000, 0.8660254037844377084, -0.5000000000000015543 ) ) ;
#21231 = ORIENTED_EDGE ( 'NONE', *, *, #80069, .F. ) ;
#21232 = FACE_OUTER_BOUND ( 'NONE', #82663, .T. ) ;
#21233 = VERTEX_POINT ( 'NONE', #40349 ) ;
#21234 = CARTESIAN_POINT ( 'NONE',  ( 12.52679360105129902, -12.51329471203373345, 31.30864560766537963 ) ) ;
#21235 = CARTESIAN_POINT ( 'NONE',  ( 0.7115928814519132395, -10.06805714834173848, 34.32951233291982618 ) ) ;
#21236 = VERTEX_POINT ( 'NONE', #39910 ) ;
#21237 = VECTOR ( 'NONE', #11610, 1000.000000000000000 ) ;
#21238 = CYLINDRICAL_SURFACE ( 'NONE', #76386, 0.2499999999999998890 ) ;
#21239 = CARTESIAN_POINT ( 'NONE',  ( 7.846153846153725020, -10.21337939537710326, 33.94971097300076224 ) ) ;
#21240 = CARTESIAN_POINT ( 'NONE',  ( 1.384615384615386802, -4.098570777380720287, 33.41473453929634729 ) ) ;
#21241 = CARTESIAN_POINT ( 'NONE',  ( -12.46153846153846168, -10.05456864172156806, 36.03766855953608683 ) ) ;
#21242 = CARTESIAN_POINT ( 'NONE',  ( 7.846153846153846700, -1.629998284177014645, 34.34916445242399163 ) ) ;
#21244 = EDGE_LOOP ( 'NONE', ( #48814, #31911 ) ) ;
#21243 = EDGE_CURVE ( 'NONE', #41980, #71008, #44914, .T. ) ;
#21245 = FACE_BOUND ( 'NONE', #75952, .T. ) ;
#21246 = VERTEX_POINT ( 'NONE', #17253 ) ;
#21247 = LINE ( 'NONE', #60908, #1196 ) ;
#21248 = EDGE_CURVE ( 'NONE', #4672, #50472, #80349, .T. ) ;
#21249 = VECTOR ( 'NONE', #40251, 1000.000000000000227 ) ;
#21250 = CARTESIAN_POINT ( 'NONE',  ( -14.30769230769242917, -11.67786785259630911, 32.92929555188603530 ) ) ;
#21251 = EDGE_CURVE ( 'NONE', #76288, #67886, #28821, .T. ) ;
#21252 = CARTESIAN_POINT ( 'NONE',  ( 3.100078627658922947, -11.37499894934982514, 33.29245874905763003 ) ) ;
#21253 = CARTESIAN_POINT ( 'NONE',  ( -11.53846153846153655, -2.538708090699994813, 30.37095296980875503 ) ) ;
#21254 = ORIENTED_EDGE ( 'NONE', *, *, #29759, .T. ) ;
#21255 = AXIS2_PLACEMENT_3D ( 'NONE', #88260, #12138, #26536 ) ;
#21257 = EDGE_CURVE ( 'NONE', #27164, #68374, #17009, .T. ) ;
#21256 = ORIENTED_EDGE ( 'NONE', *, *, #52473, .T. ) ;
#21258 = ORIENTED_EDGE ( 'NONE', *, *, #6336, .T. ) ;
#21259 = CARTESIAN_POINT ( 'NONE',  ( -3.164701897419154530, -11.35647404775217595, 33.31231777344667222 ) ) ;
#21260 = ORIENTED_EDGE ( 'NONE', *, *, #73728, .T. ) ;
#21261 = AXIS2_PLACEMENT_3D ( 'NONE', #86513, #5859, #26572 ) ;
#21262 = CARTESIAN_POINT ( 'NONE',  ( -5.999999999999998224, -12.37446782046654192, 30.86335684631486131 ) ) ;
#21263 = ADVANCED_FACE ( 'NONE', ( #80305 ), #17713, .F. ) ;
#21264 = CARTESIAN_POINT ( 'NONE',  ( -9.758064494821999446, -7.249945686854186278, 34.74374336980224598 ) ) ;
#21265 = DIRECTION ( 'NONE',  ( -0.000000000000000000, -0.9396926207859093161, -0.3420201433256663259 ) ) ;
#21266 = CARTESIAN_POINT ( 'NONE',  ( 13.31853197365950514, -10.51840700105979387, 33.73612834413961536 ) ) ;
#21267 = CARTESIAN_POINT ( 'NONE',  ( 2.651650429449569302, -10.15165042944953733, 24.62500000000000000 ) ) ;
#21268 = CARTESIAN_POINT ( 'NONE',  ( 14.53070365930516239, -6.503523203565941380, 34.64991518177335195 ) ) ;
#21269 = DIRECTION ( 'NONE',  ( 1.000000000000000000, 0.000000000000000000, 0.000000000000000000 ) ) ;
#21270 = ORIENTED_EDGE ( 'NONE', *, *, #5870, .T. ) ;
#21271 = B_SPLINE_CURVE_WITH_KNOTS ( 'NONE', 3,
 ( #34350, #68148, #6450, #74025, #33034, #67264, #61370, #54615, #75351, #60500 ),
 .UNSPECIFIED., .F., .F.,
 ( 4, 2, 2, 2, 4 ),
 ( 0.0007817246256747460882, 0.0009771112852218900684, 0.001172497944769034049, 0.001367884604316177812, 0.001563271263863321792 ),
 .UNSPECIFIED. ) ;
#21272 = ORIENTED_EDGE ( 'NONE', *, *, #47833, .F. ) ;
#21273 = B_SPLINE_CURVE_WITH_KNOTS ( 'NONE', 3,
 ( #76445, #68355, #34123, #20608, #14749, #2105 ),
 .UNSPECIFIED., .F., .F.,
 ( 4, 2, 4 ),
 ( 0.000000000000000000, 0.0001954784845028888327, 0.0003909569690057776653 ),
 .UNSPECIFIED. ) ;
#21274 = EDGE_LOOP ( 'NONE', ( #71575, #45446, #12613, #48734 ) ) ;
#21275 = CARTESIAN_POINT ( 'NONE',  ( 3.480769230769168665, -7.565270000091922853, 34.99999999999999289 ) ) ;
#21277 = CARTESIAN_POINT ( 'NONE',  ( -13.38461538461538325, -5.557115091759785130, 34.35708131394839171 ) ) ;
#21276 = DIRECTION ( 'NONE',  ( 0.000000000000000000, 0.000000000000000000, 1.000000000000000000 ) ) ;
#21278 = DIRECTION ( 'NONE',  ( 0.000000000000000000, 0.3420201433256641055, -0.9396926207859100932 ) ) ;
#21279 = AXIS2_PLACEMENT_3D ( 'NONE', #47337, #39274, #5029 ) ;
#21280 = DIRECTION ( 'NONE',  ( -1.000000000000000000, -0.000000000000000000, -0.000000000000000000 ) ) ;
#21281 = CYLINDRICAL_SURFACE ( 'NONE', #11301, 5.250000000000000888 ) ;
#21282 = CARTESIAN_POINT ( 'NONE',  ( 16.37685750545900021, -3.105924265160262099, 32.13625925475356127 ) ) ;
#21283 = ORIENTED_EDGE ( 'NONE', *, *, #54470, .F. ) ;
#21284 = CARTESIAN_POINT ( 'NONE',  ( 19.00000000000000000, -7.500000000000000000, 29.75000000000000355 ) ) ;
#21285 = CARTESIAN_POINT ( 'NONE',  ( 9.469380733400843297, -11.98009711892699514, 32.48740034544076138 ) ) ;
#21286 = CARTESIAN_POINT ( 'NONE',  ( -1.161835843346974650, -2.847695495035523106, 31.58253572463339154 ) ) ;
#21287 = CARTESIAN_POINT ( 'NONE',  ( 3.230769230769108269, -11.67786785259630911, 32.92929555188603530 ) ) ;
#21288 = EDGE_LOOP ( 'NONE', ( #61942, #16583, #76401, #44036 ) ) ;
#21289 = CARTESIAN_POINT ( 'NONE',  ( 18.13079180782478872, -12.38066358083363738, 30.83685684665853444 ) ) ;
#21290 = VECTOR ( 'NONE', #2770, 1000.000000000000000 ) ;
#21291 = EDGE_CURVE ( 'NONE', #12551, #24740, #45166, .T. ) ;
#21292 = EDGE_LOOP ( 'NONE', ( #60583, #1481 ) ) ;
#21293 = FACE_BOUND ( 'NONE', #75122, .T. ) ;
#21294 = LINE ( 'NONE', #69486, #73459 ) ;
#21295 = ADVANCED_FACE ( 'NONE', ( #87521 ), #46507, .F. ) ;
#21296 = CARTESIAN_POINT ( 'NONE',  ( -10.03846153846153832, -3.499999999999999556, 29.75000000000000355 ) ) ;
#21297 = FACE_OUTER_BOUND ( 'NONE', #55489, .T. ) ;
#21298 = ORIENTED_EDGE ( 'NONE', *, *, #25571, .F. ) ;
#21299 = CARTESIAN_POINT ( 'NONE',  ( 0.2380535178145125053, -10.81261337010820256, 33.49550067578627477 ) ) ;
#21300 = CARTESIAN_POINT ( 'NONE',  ( 4.854096384444071433, -7.369208160676172348, 34.74850200257122879 ) ) ;
#21301 = CARTESIAN_POINT ( 'NONE',  ( -16.28399336328437386, -12.45813303252208648, 30.39737893381572675 ) ) ;
#21302 = CARTESIAN_POINT ( 'NONE',  ( -4.853910232829682592, -5.582272713120727481, 34.63742843783360570 ) ) ;
#21303 = ORIENTED_EDGE ( 'NONE', *, *, #80623, .F. ) ;
#21304 = ADVANCED_FACE ( 'NONE', ( #72643 ), #59126, .F. ) ;
#21305 = CARTESIAN_POINT ( 'NONE',  ( -4.826868657009623753, -4.818054556918156095, 34.26375889529406749 ) ) ;
#21306 = ORIENTED_EDGE ( 'NONE', *, *, #17696, .T. ) ;
#21308 = ORIENTED_EDGE ( 'NONE', *, *, #64257, .F. ) ;
#21307 = CARTESIAN_POINT ( 'NONE',  ( -9.692307692307812417, -12.46129190930018460, 30.37095296980731973 ) ) ;
#21309 = CARTESIAN_POINT ( 'NONE',  ( 7.846153846153846700, -10.51840700105979565, 33.73612834413961536 ) ) ;
#21310 = CARTESIAN_POINT ( 'NONE',  ( 12.46153846153846168, -2.499999999999998668, 29.50000000000001066 ) ) ;
#21311 = CARTESIAN_POINT ( 'NONE',  ( 7.596130621932389637, -10.18141759479407327, 34.26406193332782379 ) ) ;
#21312 = DIRECTION ( 'NONE',  ( -0.000000000000000000, -0.1736481776669307198, -0.9848077530122080203 ) ) ;
#21313 = CARTESIAN_POINT ( 'NONE',  ( -13.38461538461538325, -3.322132147404559976, 32.92929555188717927 ) ) ;
#21315 = CARTESIAN_POINT ( 'NONE',  ( -17.01085472592063752, -8.120952969808772792, 34.71129190929999453 ) ) ;
#21314 = CARTESIAN_POINT ( 'NONE',  ( 13.60739492588379385, -5.913360116392397892, 34.49180327182771322 ) ) ;
#21316 = EDGE_CURVE ( 'NONE', #16624, #88786, #38421, .T. ) ;
#21317 = CARTESIAN_POINT ( 'NONE',  ( 8.096099364501986528, -4.336752205174647656, 33.62275283266504289 ) ) ;
#21318 = B_SPLINE_CURVE_WITH_KNOTS ( 'NONE', 3,
 ( #13610, #76188, #88850, #68119, #88407, #39763, #47835, #60461, #67233, #19478 ),
 .UNSPECIFIED., .F., .F.,
 ( 4, 2, 2, 2, 4 ),
 ( 0.000000000000000000, 0.0001954311564186869286, 0.0003908623128373738573, 0.0005862934692560607588, 0.0007817246256747477145 ),
 .UNSPECIFIED. ) ;
#21319 = CARTESIAN_POINT ( 'NONE',  ( 2.750000000000008438, -8.639087296525996607, 18.29687500000000000 ) ) ;
#21320 = VERTEX_POINT ( 'NONE', #4184 ) ;
#21321 = B_SPLINE_CURVE_WITH_KNOTS ( 'NONE', 3,
 ( #80312, #40656, #40215, #46069, #19483, #12732, #18609, #39772, #13176, #19046 ),
 .UNSPECIFIED., .F., .F.,
 ( 4, 2, 2, 2, 4 ),
 ( 0.0007817246256747442451, 0.0009771112852218865989, 0.001172497944769029061, 0.001367884604316171523, 0.001563271263863313986 ),
 .UNSPECIFIED. ) ;
#21322 = CYLINDRICAL_SURFACE ( 'NONE', #87998, 0.2500000000000004996 ) ;
#21323 = ORIENTED_EDGE ( 'NONE', *, *, #88510, .F. ) ;
#21324 = B_SPLINE_CURVE_WITH_KNOTS ( 'NONE', 3,
 ( #77373, #15683, #28296, #76938, #1718, #29207, #56659, #41380, #82817, #20657 ),
 .UNSPECIFIED., .F., .F.,
 ( 4, 2, 2, 2, 4 ),
 ( 0.0007817359430256388964, 0.0009771253907250073822, 0.001172514838424375868, 0.001367904286123744571, 0.001563293733823113056 ),
 .UNSPECIFIED. ) ;
#21325 = VECTOR ( 'NONE', #75916, 1000.000000000000000 ) ;
#21326 = ORIENTED_EDGE ( 'NONE', *, *, #80030, .F. ) ;
#21327 = CARTESIAN_POINT ( 'NONE',  ( 3.100077764101672795, -4.809359713505814149, 33.96456829005828837 ) ) ;
#21328 = ORIENTED_EDGE ( 'NONE', *, *, #21670, .T. ) ;
#21329 = CARTESIAN_POINT ( 'NONE',  ( 14.24160889673642849, -8.120952969808774569, 34.71129190930000163 ) ) ;
#21330 = B_SPLINE_CURVE_WITH_KNOTS ( 'NONE', 3,
 ( #70214, #41416, #36431, #27899, #48159, #8075, #27460, #62991, #56256, #82414 ),
 .UNSPECIFIED., .F., .F.,
 ( 4, 2, 2, 2, 4 ),
 ( 0.0007817246256747503166, 0.0009771112852218946220, 0.001172497944769039036, 0.001367884604316183233, 0.001563271263863327647 ),
 .UNSPECIFIED. ) ;
#21331 = EDGE_CURVE ( 'NONE', #14831, #3309, #52405, .T. ) ;
#21332 = CARTESIAN_POINT ( 'NONE',  ( -8.096177070375304652, -8.475808217655753651, 34.90892951860618609 ) ) ;
#21333 = CARTESIAN_POINT ( 'NONE',  ( -14.30769230769230660, -11.35647404775217417, 33.31231777344666511 ) ) ;
#21334 = CARTESIAN_POINT ( 'NONE',  ( 1.134592160393927296, -2.588893531581426544, 31.60682220781847818 ) ) ;
#21335 = CARTESIAN_POINT ( 'NONE',  ( 6.066068351002442682, -2.538708090699994813, 30.37095296980875503 ) ) ;
#21336 = CARTESIAN_POINT ( 'NONE',  ( -16.28453762051371712, -3.062553014421049991, 32.05460306192773601 ) ) ;
#21337 = EDGE_CURVE ( 'NONE', #23467, #47762, #13170, .T. ) ;
#21338 = CARTESIAN_POINT ( 'NONE',  ( 10.61538461538449418, -3.643525952248795718, 33.31231777344771672 ) ) ;
#21339 = CARTESIAN_POINT ( 'NONE',  ( 2.651650429449569302, -10.15165042944953733, 24.62500000000000000 ) ) ;
#21340 = ADVANCED_FACE ( 'NONE', ( #53704 ), #28011, .F. ) ;
#21341 = EDGE_CURVE ( 'NONE', #8541, #55049, #82961, .T. ) ;
#21342 = CARTESIAN_POINT ( 'NONE',  ( -9.692307692307691624, -1.466349020453238561, 30.81389545987213907 ) ) ;
#21343 = CARTESIAN_POINT ( 'NONE',  ( 11.47319109250076430, -10.90142922261923886, 33.41473453929638993 ) ) ;
#21344 = AXIS2_PLACEMENT_3D ( 'NONE', #13105, #40584, #68053 ) ;
#21345 = LINE ( 'NONE', #34413, #11969 ) ;
#21346 = CARTESIAN_POINT ( 'NONE',  ( -9.692307692307691624, -11.35647404775217417, 33.31231777344666511 ) ) ;
#21347 = EDGE_CURVE ( 'NONE', #51804, #44547, #47386, .T. ) ;
#21348 = EDGE_LOOP ( 'NONE', ( #10664, #7379, #17159, #80582 ) ) ;
#21349 = ORIENTED_EDGE ( 'NONE', *, *, #2096, .F. ) ;
#21350 = CARTESIAN_POINT ( 'NONE',  ( -17.75000000000001066, -12.50000000000000000, 29.81609845454690699 ) ) ;
#21351 = CARTESIAN_POINT ( 'NONE',  ( 1.515405825582337718, -3.338503747796865984, 32.95102852606552801 ) ) ;
#21352 = DIRECTION ( 'NONE',  ( 0.000000000000000000, -6.938893903907222067E-15, 1.000000000000000000 ) ) ;
#21353 = CARTESIAN_POINT ( 'NONE',  ( 0.2386115026316106003, -10.01117774369187252, 34.36070679894347535 ) ) ;
#21354 = CARTESIAN_POINT ( 'NONE',  ( -13.38461538461538325, -8.318370150425687726, 35.83090037661290239 ) ) ;
#21355 = CARTESIAN_POINT ( 'NONE',  ( 11.60371667797437567, -4.320704448112861584, 33.92786785259548310 ) ) ;
#21356 = DIRECTION ( 'NONE',  ( -0.000000000000000000, 1.000000000000000000, -0.000000000000000000 ) ) ;
#21357 = B_SPLINE_CURVE_WITH_KNOTS ( 'NONE', 3,
 ( #4595, #52772, #31165, #72154, #79818, #58638, #25310, #43799, #80262, #64494 ),
 .UNSPECIFIED., .F., .F.,
 ( 4, 2, 2, 2, 4 ),
 ( 0.0007817246256747434861, 0.0009771112852218861652, 0.001172497944769028844, 0.001367884604316171523, 0.001563271263863314203 ),
 .UNSPECIFIED. ) ;
#21358 = ORIENTED_EDGE ( 'NONE', *, *, #54212, .T. ) ;
#21359 = CARTESIAN_POINT ( 'NONE',  ( -13.63463862190834952, -10.05641848906368097, 34.04755513067966177 ) ) ;
#21360 = EDGE_LOOP ( 'NONE', ( #38657, #67689, #32720, #88982 ) ) ;
#21361 = B_SPLINE_CURVE_WITH_KNOTS ( 'NONE', 3,
 ( #61512, #53424, #54759, #89018, #7018, #80927, #28173, #43026, #48437, #63289 ),
 .UNSPECIFIED., .F., .F.,
 ( 4, 2, 2, 2, 4 ),
 ( 0.0007817359430256364027, 0.0009771253907250043464, 0.001172514838424372399, 0.001367904286123740234, 0.001563293733823108286 ),
 .UNSPECIFIED. ) ;
#21362 = AXIS2_PLACEMENT_3D ( 'NONE', #25622, #81026, #6678 ) ;
#21363 = CARTESIAN_POINT ( 'NONE',  ( -19.00000000000000355, 12.75000000000004974, 30.81664701255125394 ) ) ;
#21364 = CARTESIAN_POINT ( 'NONE',  ( -18.00000000000000000, -8.120952969808772792, 34.71129190930000163 ) ) ;
#21365 = CARTESIAN_POINT ( 'NONE',  ( -6.923076923076922462, -12.34228464037088635, 31.77849191805839268 ) ) ;
#21366 = LINE ( 'NONE', #74995, #29261 ) ;
#21367 = B_SPLINE_CURVE_WITH_KNOTS ( 'NONE', 3,
 ( #24644, #66064, #52992, #80492, #18786, #12035, #39511, #5709, #67855, #81382 ),
 .UNSPECIFIED., .F., .F.,
 ( 4, 2, 2, 2, 4 ),
 ( 0.000000000000000000, 0.0001954311564186861426, 0.0003908623128373722852, 0.0005862934692560583735, 0.0007817246256747445703 ),
 .UNSPECIFIED. ) ;
#21368 = CARTESIAN_POINT ( 'NONE',  ( -14.30769230769230660, -13.87047571288749737, 32.06866353760679544 ) ) ;
#21369 = EDGE_LOOP ( 'NONE', ( #83897, #73567 ) ) ;
#21370 = EDGE_CURVE ( 'NONE', #60953, #27674, #21318, .T. ) ;
#21371 = ORIENTED_EDGE ( 'NONE', *, *, #8964, .T. ) ;
#21372 = ORIENTED_EDGE ( 'NONE', *, *, #4959, .F. ) ;
#21373 = VERTEX_POINT ( 'NONE', #5531 ) ;
#21374 = DIRECTION ( 'NONE',  ( 0.000000000000000000, 0.7660444431189822323, -0.6427876096865344779 ) ) ;
#21375 = CARTESIAN_POINT ( 'NONE',  ( 4.826946345980720920, -10.66389620160130036, 33.62221079203477103 ) ) ;
#21376 = ADVANCED_FACE ( 'NONE', ( #87980 ), #81633, .F. ) ;
#21377 = CARTESIAN_POINT ( 'NONE',  ( -3.453695448285378333, -9.886141570436013382, 34.14413921362392301 ) ) ;
#21378 = LINE ( 'NONE', #50161, #9651 ) ;
#21379 = AXIS2_PLACEMENT_3D ( 'NONE', #24535, #38508, #87602 ) ;
#21380 = CARTESIAN_POINT ( 'NONE',  ( 8.069116980420522722, -7.369474539155828730, 34.99858011523957657 ) ) ;
#21381 = FACE_OUTER_BOUND ( 'NONE', #42989, .T. ) ;
#21382 = ORIENTED_EDGE ( 'NONE', *, *, #51533, .T. ) ;
#21383 = EDGE_LOOP ( 'NONE', ( #73327, #85358 ) ) ;
#21384 = B_SPLINE_CURVE_WITH_KNOTS ( 'NONE', 3,
 ( #28368, #22062, #77009, #22938, #50399, #77881, #16185, #42785, #70244, #465 ),
 .UNSPECIFIED., .F., .F.,
 ( 4, 2, 2, 2, 4 ),
 ( 0.0007817246256747525934, 0.0009771112852218970073, 0.001172497944769041204, 0.001367884604316185401, 0.001563271263863329815 ),
 .UNSPECIFIED. ) ;
#21385 = ORIENTED_EDGE ( 'NONE', *, *, #15674, .T. ) ;
#21386 = AXIS2_PLACEMENT_3D ( 'NONE', #8862, #56154, #63348 ) ;
#21387 = EDGE_CURVE ( 'NONE', #28560, #84690, #53537, .T. ) ;
#21389 = ORIENTED_EDGE ( 'NONE', *, *, #49109, .F. ) ;
#21388 = CARTESIAN_POINT ( 'NONE',  ( -2.980714919130914797, -10.66356715214248396, 33.62249196103329751 ) ) ;
#21390 = B_SPLINE_CURVE_WITH_KNOTS ( 'NONE', 3,
 ( #65584, #84557, #68594, #47425, #12762, #20847, #48316, #75790, #6018, #7347 ),
 .UNSPECIFIED., .F., .F.,
 ( 4, 2, 2, 2, 4 ),
 ( 0.000000000000000000, 0.0001954311564186860613, 0.0003908623128373721225, 0.0005862934692560581567, 0.0007817246256747442451 ),
 .UNSPECIFIED. ) ;
#21392 = CARTESIAN_POINT ( 'NONE',  ( -10.36543920600657209, -6.653508905675592722, 34.93172785388651391 ) ) ;
#21391 = LINE ( 'NONE', #18845, #11548 ) ;
#21393 = CARTESIAN_POINT ( 'NONE',  ( 6.673076923076925127, -7.433931650972300353, 34.75000000000000711 ) ) ;
#21394 = CARTESIAN_POINT ( 'NONE',  ( -1.553300858899125059, -3.750000000000009326, 24.07812500000000711 ) ) ;
#21395 = ORIENTED_EDGE ( 'NONE', *, *, #3536, .T. ) ;
#21396 = AXIS2_PLACEMENT_3D ( 'NONE', #58949, #79678, #67057 ) ;
#21397 = ORIENTED_EDGE ( 'NONE', *, *, #40247, .T. ) ;
#21398 = CARTESIAN_POINT ( 'NONE',  ( -2.530618525208453207, -12.39988816332205701, 30.74660775122750778 ) ) ;
#21399 = ADVANCED_FACE ( 'NONE', ( #55041 ), #20806, .F. ) ;
#21400 = VERTEX_POINT ( 'NONE', #74879 ) ;
#21401 = FACE_BOUND ( 'NONE', #37106, .T. ) ;
#21402 = CARTESIAN_POINT ( 'NONE',  ( -1.161239443917200242, -2.501478030877322567, 29.88021232661720816 ) ) ;
#21403 = CARTESIAN_POINT ( 'NONE',  ( 7.911408985666682270, -5.941354392334607049, 34.76329471203374055 ) ) ;
#21404 = ORIENTED_EDGE ( 'NONE', *, *, #50367, .F. ) ;
#21405 = DIRECTION ( 'NONE',  ( -0.000000000000000000, -0.000000000000000000, 1.000000000000000000 ) ) ;
#21406 = ADVANCED_FACE ( 'NONE', ( #40649 ), #48274, .F. ) ;
#21407 = CARTESIAN_POINT ( 'NONE',  ( -15.93083330975275658, -12.64618726649961289, 30.78989965857442712 ) ) ;
#21408 = CARTESIAN_POINT ( 'NONE',  ( 17.06410256410256565, -7.500000000000000000, 29.75000000000000355 ) ) ;
#21409 = CARTESIAN_POINT ( 'NONE',  ( 3.903869422903799347, -11.28823185664190376, 33.01397839955799896 ) ) ;
#21410 = CARTESIAN_POINT ( 'NONE',  ( 15.23076923076923173, -1.367168528481310208, 33.57946703557072254 ) ) ;
#21411 = ORIENTED_EDGE ( 'NONE', *, *, #56441, .T. ) ;
#21412 = CARTESIAN_POINT ( 'NONE',  ( 6.130791807824788719, -8.147973898785416225, 34.70805048591653730 ) ) ;
#21413 = PLANE ( 'NONE',  #26773 ) ;
#21414 = CARTESIAN_POINT ( 'NONE',  ( 16.37685750545900376, -9.086983370893049639, 34.49168942202179267 ) ) ;
#21415 = CARTESIAN_POINT ( 'NONE',  ( -0.6844654204453110014, -4.762599654559228846, 34.23009711892697737 ) ) ;
#21416 = CARTESIAN_POINT ( 'NONE',  ( -0.2381114996768911307, -7.630147231320743018, 34.74852402298682819 ) ) ;
#21417 = FACE_BOUND ( 'NONE', #6729, .T. ) ;
#21418 = B_SPLINE_CURVE_WITH_KNOTS ( 'NONE', 3,
 ( #37080, #16816, #73102, #4644, #65449, #30771, #86636, #17719, #31672, #84855 ),
 .UNSPECIFIED., .F., .F.,
 ( 4, 2, 2, 2, 4 ),
 ( 0.0007817359430256333669, 0.0009771253907250056474, 0.001172514838424370881, 0.001367904286123736331, 0.001563293733823101564 ),
 .UNSPECIFIED. ) ;
#21420 = LINE ( 'NONE', #48888, #57502 ) ;
#21419 = CARTESIAN_POINT ( 'NONE',  ( 17.20771488474786537, -3.530189275343204702, 32.79018710029569661 ) ) ;
#21421 = EDGE_CURVE ( 'NONE', #49108, #85857, #84651, .T. ) ;
#21422 = CARTESIAN_POINT ( 'NONE',  ( 11.53846153846153832, -11.91647553114624181, 32.58852847137148245 ) ) ;
#21424 = CARTESIAN_POINT ( 'NONE',  ( -6.249976730942354841, -4.943428324936578910, 34.04746400365624481 ) ) ;
#21423 = DIRECTION ( 'NONE',  ( -0.000000000000000000, 1.000000000000000000, -0.000000000000000000 ) ) ;
#21425 = CARTESIAN_POINT ( 'NONE',  ( -5.299850035829924089, -12.38737895849757820, 31.66785238281580206 ) ) ;
#21426 = CARTESIAN_POINT ( 'NONE',  ( -2.749999999999997780, -7.561099074964547917, 19.84188170625848713 ) ) ;
#21427 = ORIENTED_EDGE ( 'NONE', *, *, #77554, .F. ) ;
#21428 = CARTESIAN_POINT ( 'NONE',  ( -5.749945580086545327, -10.82426656108011720, 33.81400080652039009 ) ) ;
#21429 = ORIENTED_EDGE ( 'NONE', *, *, #27051, .T. ) ;
#21430 = CARTESIAN_POINT ( 'NONE',  ( -13.38461538461550759, -11.06231777344772027, 33.60647404775119895 ) ) ;
#21431 = ORIENTED_EDGE ( 'NONE', *, *, #39883, .F. ) ;
#21432 = DIRECTION ( 'NONE',  ( -0.000000000000000000, 0.1736481776669307198, -0.9848077530122080203 ) ) ;
#21433 = CARTESIAN_POINT ( 'NONE',  ( 14.08420738312797837, -4.225889041578353655, 33.85425143139329407 ) ) ;
#21434 = VERTEX_POINT ( 'NONE', #1865 ) ;
#21435 = DIRECTION ( 'NONE',  ( 0.000000000000000000, 0.8660254037844377084, 0.5000000000000015543 ) ) ;
#21436 = CARTESIAN_POINT ( 'NONE',  ( -2.775308065498764964, -6.422011778438537988, 17.42000670625848713 ) ) ;
#21437 = EDGE_CURVE ( 'NONE', #66225, #79431, #63561, .T. ) ;
#21438 = CARTESIAN_POINT ( 'NONE',  ( -10.48459417441766561, -12.62708834333097663, 30.88030960425257021 ) ) ;
#21439 = CARTESIAN_POINT ( 'NONE',  ( -5.076923076923075762, -4.786620604624113540, 33.94971097300155094 ) ) ;
#21440 = CARTESIAN_POINT ( 'NONE',  ( -5.076923076923075762, -12.37446782046654192, 30.86335684631486131 ) ) ;
#21441 = CARTESIAN_POINT ( 'NONE',  ( 4.153846153846154188, -11.69971097300155272, 32.46337939537588113 ) ) ;
#21442 = CARTESIAN_POINT ( 'NONE',  ( -16.15384615384615330, -12.29105614889573062, 35.45975837776705220 ) ) ;
#21443 = FACE_OUTER_BOUND ( 'NONE', #75094, .T. ) ;
#21444 = CARTESIAN_POINT ( 'NONE',  ( 3.775308065498752086, -6.007798216065404873, 22.14249329374151998 ) ) ;
#21445 = EDGE_CURVE ( 'NONE', #39535, #56699, #11594, .T. ) ;
#21446 = EDGE_CURVE ( 'NONE', #27135, #71888, #76644, .T. ) ;
#21447 = CARTESIAN_POINT ( 'NONE',  ( -10.48459280755982981, -2.729792928343269587, 31.24908615093345077 ) ) ;
#21448 = CARTESIAN_POINT ( 'NONE',  ( 20.00000000000000000, -4.000000000000000000, 29.75000000000000355 ) ) ;
#21449 = EDGE_LOOP ( 'NONE', ( #66608, #9003, #88284, #27893 ) ) ;
#21450 = DIRECTION ( 'NONE',  ( -0.000000000000000000, 0.6427876096865404731, -0.7660444431189771253 ) ) ;
#21451 = CARTESIAN_POINT ( 'NONE',  ( 3.750000000000001776, -7.561099074964511502, 23.47061829374151642 ) ) ;
#21452 = AXIS2_PLACEMENT_3D ( 'NONE', #59216, #18243, #76274 ) ;
#21453 = CARTESIAN_POINT ( 'NONE',  ( 7.846153846153846700, -5.471508081941601098, 34.59228464037088457 ) ) ;
#21454 = CARTESIAN_POINT ( 'NONE',  ( -9.442253380669377805, -11.28795663066794575, 33.01431243580653785 ) ) ;
#21455 = ORIENTED_EDGE ( 'NONE', *, *, #56918, .F. ) ;
#21456 = CARTESIAN_POINT ( 'NONE',  ( 1.515140822849031066, -8.630441415882550871, 34.87705825610312615 ) ) ;
#21457 = CARTESIAN_POINT ( 'NONE',  ( 2.980792499826876440, -3.627789207965226748, 32.91389620160131102 ) ) ;
#21459 = VERTEX_POINT ( 'NONE', #56370 ) ;
#21458 = CARTESIAN_POINT ( 'NONE',  ( 4.153846153846030731, -9.528491918059723176, 34.59228464037033035 ) ) ;
#21460 = CARTESIAN_POINT ( 'NONE',  ( -7.781008066821878622, -7.750023238201979581, 34.74374492549440419 ) ) ;
#21461 = CARTESIAN_POINT ( 'NONE',  ( -3.007989689500821573, -5.114059244376869984, 34.14424750095245287 ) ) ;
#21462 = DIRECTION ( 'NONE',  ( -0.000000000000000000, 1.000000000000000000, 3.491481338843133355E-15 ) ) ;
#21463 = VECTOR ( 'NONE', #5169, 1000.000000000000227 ) ;
#21464 = CARTESIAN_POINT ( 'NONE',  ( -8.769230769230768274, -9.058645607665452459, 34.76329471203371924 ) ) ;
#21465 = CARTESIAN_POINT ( 'NONE',  ( -10.36533030374629760, -10.66356715214248396, 33.62249196103329751 ) ) ;
#21466 = VERTEX_POINT ( 'NONE', #28915 ) ;
#21467 = DIRECTION ( 'NONE',  ( 0.000000000000000000, 0.8660254037844377084, 0.5000000000000015543 ) ) ;
#21468 = ORIENTED_EDGE ( 'NONE', *, *, #15351, .F. ) ;
#21469 = ORIENTED_EDGE ( 'NONE', *, *, #69339, .T. ) ;
#21470 = CARTESIAN_POINT ( 'NONE',  ( -9.692307692307691624, -3.050289026998446396, 32.03036669348365706 ) ) ;
#21471 = CARTESIAN_POINT ( 'NONE',  ( -19.50000000000000000, -3.499999999999999556, 29.75000000000000355 ) ) ;
#21472 = LINE ( 'NONE', #76422, #12042 ) ;
#21473 = PLANE ( 'NONE',  #9295 ) ;
#21474 = ORIENTED_EDGE ( 'NONE', *, *, #10578, .F. ) ;
#21475 = CARTESIAN_POINT ( 'NONE',  ( -27.00000000000000000, 9.000000000000001776, 2.999999999999995559 ) ) ;
#21476 = ORIENTED_EDGE ( 'NONE', *, *, #21906, .F. ) ;
#21477 = ORIENTED_EDGE ( 'NONE', *, *, #13889, .F. ) ;
#21478 = ORIENTED_EDGE ( 'NONE', *, *, #42861, .F. ) ;
#21480 = ORIENTED_EDGE ( 'NONE', *, *, #12951, .T. ) ;
#21479 = CARTESIAN_POINT ( 'NONE',  ( -15.36146069743679199, -12.11776431015576172, 31.66791131148498906 ) ) ;
#21481 = CARTESIAN_POINT ( 'NONE',  ( 4.376625695114562120, -5.913360116392398780, 34.49180327182771322 ) ) ;
#21482 = CARTESIAN_POINT ( 'NONE',  ( 6.222779668978065004, -2.612705202774697533, 31.66806509827799943 ) ) ;
#21483 = CARTESIAN_POINT ( 'NONE',  ( -2.980714919130915685, -4.235687564193446164, 33.53795663066793509 ) ) ;
#21484 = DIRECTION ( 'NONE',  ( 0.000000000000000000, 0.9848077530122072432, 0.1736481776669354937 ) ) ;
#21485 = EDGE_LOOP ( 'NONE', ( #70010, #42937, #14037, #69722 ) ) ;
#21486 = VERTEX_POINT ( 'NONE', #21690 ) ;
#21487 = VERTEX_POINT ( 'NONE', #63996 ) ;
#21488 = CARTESIAN_POINT ( 'NONE',  ( -14.05769230769087130, -7.500000000000155431, 34.75000000000007105 ) ) ;
#21490 = ORIENTED_EDGE ( 'NONE', *, *, #13554, .F. ) ;
#21489 = CARTESIAN_POINT ( 'NONE',  ( -14.05774689831426372, -2.341251567377310217, 30.72681386836322659 ) ) ;
#21491 = CARTESIAN_POINT ( 'NONE',  ( 9.692307692307572609, -11.94971097300221174, 32.03036669348237098 ) ) ;
#21492 = CARTESIAN_POINT ( 'NONE',  ( -0.5922290646487691212, -6.369640206132550553, 34.87707690430378449 ) ) ;
#21493 = VERTEX_POINT ( 'NONE', #77967 ) ;
#21494 = CARTESIAN_POINT ( 'NONE',  ( 15.16468581981335007, -10.51840700105979387, 33.73612834413961536 ) ) ;
#21495 = DIRECTION ( 'NONE',  ( 0.000000000000000000, 0.7660444431189822323, -0.6427876096865344779 ) ) ;
#21496 = EDGE_LOOP ( 'NONE', ( #6021, #17292, #1458, #28541 ) ) ;
#21497 = FACE_BOUND ( 'NONE', #23784, .T. ) ;
#21498 = CARTESIAN_POINT ( 'NONE',  ( 15.23076923076923173, -11.35647404775217417, 33.31231777344666511 ) ) ;
#21499 = CARTESIAN_POINT ( 'NONE',  ( 13.60739505359345181, -6.717445702608402236, 34.94155399931962336 ) ) ;
#21500 = EDGE_CURVE ( 'NONE', #53616, #19601, #2293, .T. ) ;
#21501 = DIRECTION ( 'NONE',  ( -0.000000000000000000, 0.3420201433256694901, -0.9396926207859082059 ) ) ;
#21504 = CARTESIAN_POINT ( 'NONE',  ( -0.7115616988314271696, -12.22074536777954989, 31.39888409691088356 ) ) ;
#21503 = AXIS2_PLACEMENT_3D ( 'NONE', #11226, #12561, #38695 ) ;
#21502 = CARTESIAN_POINT ( 'NONE',  ( 18.00000000000000000, -2.833524468853757305, 32.15551576947925838 ) ) ;
#21505 = AXIS2_PLACEMENT_3D ( 'NONE', #57476, #22367, #65111 ) ;
#21506 = CARTESIAN_POINT ( 'NONE',  ( -2.980714810855777497, -3.435999193479609470, 33.07426656108011542 ) ) ;
#21507 = CARTESIAN_POINT ( 'NONE',  ( 14.43821774592595197, -2.372941743896879174, 30.88044141588253666 ) ) ;
#21508 = ORIENTED_EDGE ( 'NONE', *, *, #49160, .F. ) ;
#21509 = CARTESIAN_POINT ( 'NONE',  ( -8.096130590202436750, -6.524016743844655686, 34.90889640711025521 ) ) ;
#21510 = CARTESIAN_POINT ( 'NONE',  ( -8.069019268357486396, -2.501496062324912284, 29.88072118266895671 ) ) ;
#21511 = AXIS2_PLACEMENT_3D ( 'NONE', #1371, #13999, #70277 ) ;
#21512 = ORIENTED_EDGE ( 'NONE', *, *, #11959, .F. ) ;
#21513 = VECTOR ( 'NONE', #1332, 1000.000000000000000 ) ;
#21514 = AXIS2_PLACEMENT_3D ( 'NONE', #46039, #66310, #23538 ) ;
#21515 = CARTESIAN_POINT ( 'NONE',  ( 8.769230769230647482, -3.300289026999228881, 32.46337939537708905 ) ) ;
#21516 = LINE ( 'NONE', #62930, #39008 ) ;
#21517 = ORIENTED_EDGE ( 'NONE', *, *, #55578, .F. ) ;
#21518 = CARTESIAN_POINT ( 'NONE',  ( -9.822455662039388358, -9.504002272028875709, 34.60269587691767867 ) ) ;
#21519 = CARTESIAN_POINT ( 'NONE',  ( 12.46153846153846168, -1.790695186598648903, 34.54067556320373455 ) ) ;
#21520 = FACE_BOUND ( 'NONE', #41665, .T. ) ;
#21522 = CARTESIAN_POINT ( 'NONE',  ( -16.94613126909828793, -12.38066358083363738, 30.83685684665853444 ) ) ;
#21521 = DIRECTION ( 'NONE',  ( 0.000000000000000000, 0.7660444431189822323, -0.6427876096865344779 ) ) ;
#21524 = CYLINDRICAL_SURFACE ( 'NONE', #38781, 0.2500000000000009437 ) ;
#21523 = B_SPLINE_CURVE_WITH_KNOTS ( 'NONE', 3,
 ( #14321, #27838, #76018, #41807, #7572, #15218, #23720, #70149, #43997, #49872 ),
 .UNSPECIFIED., .F., .F.,
 ( 4, 2, 2, 2, 4 ),
 ( 0.000000000000000000, 0.0001954339857564074202, 0.0003908679715128148403, 0.0005863019572692222334, 0.0007817359430256296806 ),
 .UNSPECIFIED. ) ;
#21525 = ADVANCED_FACE ( 'NONE', ( #55915 ), #30229, .F. ) ;
#21526 = CARTESIAN_POINT ( 'NONE',  ( -19.50000000000000000, -3.499999999999999556, 29.75000000000000355 ) ) ;
#21528 = CARTESIAN_POINT ( 'NONE',  ( 6.923076923076802558, -12.46129190930018460, 30.37095296980731973 ) ) ;
#21527 = CARTESIAN_POINT ( 'NONE',  ( -4.854143407945009869, -10.23759521482555357, 34.22997729860117033 ) ) ;
#21529 = B_SPLINE_CURVE_WITH_KNOTS ( 'NONE', 3,
 ( #2137, #30062, #85012, #70157, #8022, #29193 ),
 .UNSPECIFIED., .F., .F.,
 ( 4, 2, 4 ),
 ( 0.000000000000000000, 0.0001954784845028912450, 0.0003909569690057824900 ),
 .UNSPECIFIED. ) ;
#21530 = LINE ( 'NONE', #20642, #77835 ) ;
#21531 = CARTESIAN_POINT ( 'NONE',  ( -1.614399933863656544, -3.775308065498769405, 17.57625670625849068 ) ) ;
#21532 = ORIENTED_EDGE ( 'NONE', *, *, #65614, .T. ) ;
#21533 = ORIENTED_EDGE ( 'NONE', *, *, #30408, .F. ) ;
#21534 = CARTESIAN_POINT ( 'NONE',  ( -1.384615384615506484, -3.643525952248795718, 33.31231777344771672 ) ) ;
#21535 = CARTESIAN_POINT ( 'NONE',  ( 14.43848274865925774, -12.62708834333097663, 30.88030960425257021 ) ) ;
#21536 = CYLINDRICAL_SURFACE ( 'NONE', #7119, 0.2500000000000008882 ) ;
#21537 = CARTESIAN_POINT ( 'NONE',  ( -1.607541602131531855, -3.105860786376062332, 32.13614157043599562 ) ) ;
#21538 = CARTESIAN_POINT ( 'NONE',  ( -16.85414353565466072, -6.760870238392814535, 34.69528174975672385 ) ) ;
#21539 = CARTESIAN_POINT ( 'NONE',  ( 3.749999999999999556, -7.438900925035446754, 16.71688170625848713 ) ) ;
#21540 = CARTESIAN_POINT ( 'NONE',  ( 4.376809057407638370, -7.369474270740069777, 34.74850911626239736 ) ) ;
#21541 = CARTESIAN_POINT ( 'NONE',  ( 18.22301135161284336, -3.105924265160262099, 32.13625925475356127 ) ) ;
#21542 = CARTESIAN_POINT ( 'NONE',  ( 5.999999999999878320, -4.320704448113951379, 33.92786785259630022 ) ) ;
#21543 = FACE_OUTER_BOUND ( 'NONE', #38839, .T. ) ;
#21544 = LINE ( 'NONE', #82375, #2174 ) ;
#21545 = CARTESIAN_POINT ( 'NONE',  ( 16.37662569511456567, -5.114059244376869096, 34.14424750095245287 ) ) ;
#21546 = DIRECTION ( 'NONE',  ( -0.000000000000000000, -0.5000000000000009992, -0.8660254037844380415 ) ) ;
#21547 = ADVANCED_FACE ( 'NONE', ( #8188 ), #49610, .F. ) ;
#21548 = EDGE_CURVE ( 'NONE', #19601, #51674, #36107, .T. ) ;
#21549 = CARTESIAN_POINT ( 'NONE',  ( -14.17690049986752143, -3.062576670634119758, 32.05464942895959979 ) ) ;
#21550 = DIRECTION ( 'NONE',  ( -0.000000000000000000, 0.9848077530122085754, -0.1736481776669273613 ) ) ;
#21551 = ORIENTED_EDGE ( 'NONE', *, *, #34369, .F. ) ;
#21552 = AXIS2_PLACEMENT_3D ( 'NONE', #74381, #72595, #46464 ) ;
#21553 = CARTESIAN_POINT ( 'NONE',  ( -23.50000000000000000, 4.710477821889702467E-15, 29.24999999999999289 ) ) ;
#21554 = CARTESIAN_POINT ( 'NONE',  ( 7.596177102105254875, -4.818429247618089661, 34.26397095200675125 ) ) ;
#21555 = CARTESIAN_POINT ( 'NONE',  ( 1.077988221561497539, -10.27530806549875386, 23.70499329374151642 ) ) ;
#21556 = ADVANCED_FACE ( 'NONE', ( #35662 ), #15391, .T. ) ;
#21557 = CARTESIAN_POINT ( 'NONE',  ( -5.933932666649922361, -12.34228464037088813, 31.77849191805839268 ) ) ;
#21558 = LINE ( 'NONE', #16131, #47634 ) ;
#21559 = ORIENTED_EDGE ( 'NONE', *, *, #19172, .T. ) ;
#21560 = CARTESIAN_POINT ( 'NONE',  ( -7.146003881983771677, -2.889293201056495786, 32.26117774369186009 ) ) ;
#21562 = VERTEX_POINT ( 'NONE', #42863 ) ;
#21561 = CARTESIAN_POINT ( 'NONE',  ( -18.00000000000000000, -13.60434399251292170, 33.56301978189820545 ) ) ;
#21563 = FACE_OUTER_BOUND ( 'NONE', #25115, .T. ) ;
#21564 = CARTESIAN_POINT ( 'NONE',  ( -2.373774687052440768, -10.67929555188718460, 33.92786785259543336 ) ) ;
#21565 = ORIENTED_EDGE ( 'NONE', *, *, #13539, .T. ) ;
#21566 = CARTESIAN_POINT ( 'NONE',  ( -12.46153846153846168, -4.945431358278436385, 36.03766855953609394 ) ) ;
#21567 = CARTESIAN_POINT ( 'NONE',  ( 13.16168842570853492, -9.172386477786396597, 34.72672124145550043 ) ) ;
#21568 = ORIENTED_EDGE ( 'NONE', *, *, #77856, .T. ) ;
#21569 = CARTESIAN_POINT ( 'NONE',  ( -10.74553258511630993, -4.299443229763728169, 33.91186481527756058 ) ) ;
#21570 = CARTESIAN_POINT ( 'NONE',  ( 8.638540166120458608, -6.369640206132551441, 34.87707690430378449 ) ) ;
#21572 = CARTESIAN_POINT ( 'NONE',  ( 9.942362112221147186, -6.523592122091592671, 34.90882529074906415 ) ) ;
#21571 = VECTOR ( 'NONE', #5923, 1000.000000000000227 ) ;
#21573 = EDGE_LOOP ( 'NONE', ( #37545, #82611 ) ) ;
#21574 = ORIENTED_EDGE ( 'NONE', *, *, #44436, .F. ) ;
#21575 = CARTESIAN_POINT ( 'NONE',  ( 1.384615384615265343, -8.613356846316285953, 34.62446782046622218 ) ) ;
#21576 = ORIENTED_EDGE ( 'NONE', *, *, #64688, .F. ) ;
#21577 = CARTESIAN_POINT ( 'NONE',  ( 3.453782074862625340, -11.98016756924214832, 32.48728574198911190 ) ) ;
#21578 = CARTESIAN_POINT ( 'NONE',  ( 12.46153846153833911, -9.442884908241554243, 34.35708131394783038 ) ) ;
#21579 = CARTESIAN_POINT ( 'NONE',  ( -5.999999999999998224, -5.471508081941601098, 34.59228464037088457 ) ) ;
#21580 = CARTESIAN_POINT ( 'NONE',  ( -6.923076923076922462, -11.35647404775217417, 33.31231777344666511 ) ) ;
#21581 = CARTESIAN_POINT ( 'NONE',  ( -13.38461538461550582, -9.442884908241554243, 34.35708131394783038 ) ) ;
#21582 = CARTESIAN_POINT ( 'NONE',  ( 0.3310632764627420288, -7.276987145209185215, 34.99546412871779921 ) ) ;
#21583 = VECTOR ( 'NONE', #57993, 1000.000000000000000 ) ;
#21584 = VECTOR ( 'NONE', #65573, 1000.000000000000114 ) ;
#21585 =( GEOMETRIC_REPRESENTATION_CONTEXT ( 3 ) GLOBAL_UNCERTAINTY_ASSIGNED_CONTEXT ( ( #23001 ) ) GLOBAL_UNIT_ASSIGNED_CONTEXT ( ( #49270, #56469, #71296 ) ) REPRESENTATION_CONTEXT ( 'NONE', 'WORKASPACE' ) );
#21586 = DIRECTION ( 'NONE',  ( -0.000000000000000000, 0.9848077530122086864, -0.1736481776669273891 ) ) ;
#21587 = ORIENTED_EDGE ( 'NONE', *, *, #5456, .T. ) ;
#21588 = ORIENTED_EDGE ( 'NONE', *, *, #44164, .T. ) ;
#21590 = ORIENTED_EDGE ( 'NONE', *, *, #31636, .F. ) ;
#21589 = CARTESIAN_POINT ( 'NONE',  ( 5.076923076923075762, -11.35647404775217417, 33.31231777344666511 ) ) ;
#21591 = DIRECTION ( 'NONE',  ( -2.602085213965214586E-16, 1.000000000000000000, 0.000000000000000000 ) ) ;
#21592 = VERTEX_POINT ( 'NONE', #70327 ) ;
#21593 = DIRECTION ( 'NONE',  ( -0.000000000000000000, 0.6427876096865404731, -0.7660444431189771253 ) ) ;
#21594 = CARTESIAN_POINT ( 'NONE',  ( -12.46153846153846168, -8.120952969808772792, 34.71129190930000163 ) ) ;
#21595 = EDGE_LOOP ( 'NONE', ( #45629, #70501, #9068, #36082 ) ) ;
#21596 = CARTESIAN_POINT ( 'NONE',  ( -12.39547011053602432, -5.557115091759786019, 34.35708131394839882 ) ) ;
#21597 = EDGE_CURVE ( 'NONE', #65096, #38767, #27689, .T. ) ;
#21598 = ORIENTED_EDGE ( 'NONE', *, *, #30958, .F. ) ;
#21600 = ORIENTED_EDGE ( 'NONE', *, *, #63620, .T. ) ;
#21599 = CARTESIAN_POINT ( 'NONE',  ( 2.242421861731533017, -5.219633306516282545, 34.19971097300152252 ) ) ;
#21601 = DIRECTION ( 'NONE',  ( -0.000000000000000000, -0.1736481776669307198, -0.9848077530122080203 ) ) ;
#21602 = VERTEX_POINT ( 'NONE', #69440 ) ;
#21603 = CARTESIAN_POINT ( 'NONE',  ( -6.792286482109974877, -4.684288915650984819, 34.18129842949671371 ) ) ;
#21604 = AXIS2_PLACEMENT_3D ( 'NONE', #35395, #56113, #35850 ) ;
#21605 = FACE_OUTER_BOUND ( 'NONE', #84525, .T. ) ;
#21606 = FACE_BOUND ( 'NONE', #66861, .T. ) ;
#21607 = CARTESIAN_POINT ( 'NONE',  ( -17.86995483716523125, -2.504778602574659008, 29.97347330155778167 ) ) ;
#21608 = CARTESIAN_POINT ( 'NONE',  ( -17.93474442872397390, -12.27809138561124591, 31.22303859784719648 ) ) ;
#21609 = ADVANCED_FACE ( 'NONE', ( #16267 ), #35207, .F. ) ;
#21610 = CARTESIAN_POINT ( 'NONE',  ( 4.284371855609715674, -12.45806712695776319, 30.39783852428763922 ) ) ;
#21611 = CYLINDRICAL_SURFACE ( 'NONE', #54674, 0.2500000000000012212 ) ;
#21612 = CARTESIAN_POINT ( 'NONE',  ( -17.32694630114453105, -8.475808217655753651, 34.90892951860618609 ) ) ;
#21613 = LINE ( 'NONE', #63921, #43308 ) ;
#21614 = ORIENTED_EDGE ( 'NONE', *, *, #84475, .T. ) ;
#21615 = DIRECTION ( 'NONE',  ( -0.000000000000000000, -0.9396926207859092051, -0.3420201433256662704 ) ) ;
#21616 = EDGE_CURVE ( 'NONE', #53616, #55785, #62667, .T. ) ;
#21617 = ORIENTED_EDGE ( 'NONE', *, *, #80281, .F. ) ;
#21618 = ORIENTED_EDGE ( 'NONE', *, *, #62647, .T. ) ;
#21620 = CARTESIAN_POINT ( 'NONE',  ( 7.911409417429869251, -10.21337939537593620, 33.94971097300152252 ) ) ;
#21619 = CARTESIAN_POINT ( 'NONE',  ( 9.627057760533610065, -2.255955759149247619, 30.00000000000013856 ) ) ;
#21621 = CYLINDRICAL_SURFACE ( 'NONE', #32739, 0.2500000000000002220 ) ;
#21622 = LINE ( 'NONE', #63493, #6315 ) ;
#21623 = CARTESIAN_POINT ( 'NONE',  ( 1.515140822849028845, -11.04252011169590020, 33.62494198852677130 ) ) ;
#21624 = DIRECTION ( 'NONE',  ( 0.000000000000000000, 0.6427876096865368094, 0.7660444431189802339 ) ) ;
#21625 = VERTEX_POINT ( 'NONE', #14309 ) ;
#21626 = CARTESIAN_POINT ( 'NONE',  ( 4.153846153846154188, -6.681629849574314051, 35.83090037661290239 ) ) ;
#21627 = DIRECTION ( 'NONE',  ( 0.000000000000000000, 0.000000000000000000, -1.000000000000000000 ) ) ;
#21628 = CARTESIAN_POINT ( 'NONE',  ( -10.48485891362105349, -10.19071101563364756, 33.96452234770658407 ) ) ;
#21629 = AXIS2_PLACEMENT_3D ( 'NONE', #29171, #794, #68810 ) ;
#21630 = EDGE_CURVE ( 'NONE', #28230, #41653, #49243, .T. ) ;
#21631 = CARTESIAN_POINT ( 'NONE',  ( 3.007843013253082010, -3.105860786376062332, 32.13614157043598851 ) ) ;
#21632 = DIRECTION ( 'NONE',  ( -0.000000000000000000, -0.9396926207859093161, -0.3420201433256663259 ) ) ;
#21633 = ORIENTED_EDGE ( 'NONE', *, *, #87891, .T. ) ;
#21634 = CARTESIAN_POINT ( 'NONE',  ( 3.164686851409094004, -11.91647553114624181, 32.58852847137148245 ) ) ;
#21635 = ORIENTED_EDGE ( 'NONE', *, *, #17005, .F. ) ;
#21636 = VECTOR ( 'NONE', #2763, 1000.000000000000000 ) ;
#21638 = ADVANCED_FACE ( 'NONE', ( #41796 ), #20620, .F. ) ;
#21637 = ORIENTED_EDGE ( 'NONE', *, *, #22169, .T. ) ;
#21639 = CARTESIAN_POINT ( 'NONE',  ( -6.250023224221455287, -4.175268141568689195, 33.81360843649122216 ) ) ;
#21640 = EDGE_LOOP ( 'NONE', ( #82862, #15466, #14173, #10395 ) ) ;
#21641 = DIRECTION ( 'NONE',  ( -0.000000000000000000, 0.8660254037844397068, -0.4999999999999978906 ) ) ;
#21642 = CARTESIAN_POINT ( 'NONE',  ( -12.33074665371367651, -6.413143153341454017, 34.63066358083362672 ) ) ;
#21643 = DIRECTION ( 'NONE',  ( -0.000000000000000000, -0.9396926207859092051, -0.3420201433256662704 ) ) ;
#21644 = CARTESIAN_POINT ( 'NONE',  ( -17.29985003582992320, -9.172386477786394821, 34.72672124145550043 ) ) ;
#21645 = VECTOR ( 'NONE', #35507, 1000.000000000000000 ) ;
#21646 = VECTOR ( 'NONE', #2887, 1000.000000000000000 ) ;
#21647 = CARTESIAN_POINT ( 'NONE',  ( 12.33139125210024112, -10.19110544564092002, 33.96427741523702792 ) ) ;
#21648 = ORIENTED_EDGE ( 'NONE', *, *, #42159, .F. ) ;
#21650 = FACE_OUTER_BOUND ( 'NONE', #66667, .T. ) ;
#21649 = COLOUR_RGB ( '', 0.09019608, 0.27058824, 0.51372549) ;
#21652 = EDGE_LOOP ( 'NONE', ( #77607, #79082 ) ) ;
#21651 = CARTESIAN_POINT ( 'NONE',  ( -12.46153846153846168, -7.500000000000001776, 35.04278698407183867 ) ) ;
#21653 = DIRECTION ( 'NONE',  ( 1.000000000000000000, 0.000000000000000000, 0.000000000000000000 ) ) ;
#21654 = CARTESIAN_POINT ( 'NONE',  ( -8.834553684722942890, -7.749976743299138882, 34.99404534957040624 ) ) ;
#21655 = CARTESIAN_POINT ( 'NONE',  ( 17.29970261819148192, -11.41317474335729543, 32.86274602512330034 ) ) ;
#21656 = CARTESIAN_POINT ( 'NONE',  ( 5.999999999999878320, -9.528491918059723176, 34.59228464037033035 ) ) ;
#21657 = CARTESIAN_POINT ( 'NONE',  ( -17.86920955903305597, -10.70102852606553157, 33.91149625220312913 ) ) ;
#21658 = EDGE_CURVE ( 'NONE', #28072, #14886, #9508, .T. ) ;
#21659 = CARTESIAN_POINT ( 'NONE',  ( -3.296039231325550656, -11.06231777344662781, 33.60647404775220082 ) ) ;
#21660 = DIRECTION ( 'NONE',  ( -0.000000000000000000, 0.8660254037844399289, -0.4999999999999980016 ) ) ;
#21661 = ADVANCED_FACE ( 'NONE', ( #55731 ), #14761, .F. ) ;
#21662 = CARTESIAN_POINT ( 'NONE',  ( 1.077988221561497539, -10.27530806549875386, 23.70499329374151642 ) ) ;
#21663 = ORIENTED_EDGE ( 'NONE', *, *, #44813, .T. ) ;
#21664 = CARTESIAN_POINT ( 'NONE',  ( -15.45425415533356350, -6.716662450894489211, 34.94144148231605840 ) ) ;
#21665 = CARTESIAN_POINT ( 'NONE',  ( -14.30769230769230660, -3.322132147404559976, 32.92929555188717927 ) ) ;
#21666 = B_SPLINE_CURVE_WITH_KNOTS ( 'NONE', 3,
 ( #2947, #9711, #30431, #51559, #59234, #57455, #57897, #79064, #84946, #10609 ),
 .UNSPECIFIED., .F., .F.,
 ( 4, 2, 2, 2, 4 ),
 ( 0.0007817359527651101701, 0.0009771254036996489256, 0.001172514854634187790, 0.001367904305568726653, 0.001563293756503265517 ),
 .UNSPECIFIED. ) ;
#21667 = EDGE_CURVE ( 'NONE', #85035, #2085, #41344, .T. ) ;
#21668 = DIRECTION ( 'NONE',  ( 0.000000000000000000, 0.6427876096865373645, -0.7660444431189797898 ) ) ;
#21669 = CYLINDRICAL_SURFACE ( 'NONE', #63418, 0.2499999999999995559 ) ;
#21670 = EDGE_CURVE ( 'NONE', #54393, #71930, #75096, .T. ) ;
#21671 = ORIENTED_EDGE ( 'NONE', *, *, #79676, .T. ) ;
#21672 = CARTESIAN_POINT ( 'NONE',  ( -2.750000000000006217, -6.360912703474006946, 15.17187500000000000 ) ) ;
#21673 = DIRECTION ( 'NONE',  ( 0.000000000000000000, 0.3420201433256641055, -0.9396926207859100932 ) ) ;
#21674 = CARTESIAN_POINT ( 'NONE',  ( -0.5922290646487693433, -12.62707690430377383, 30.88035979386743435 ) ) ;
#21675 = CARTESIAN_POINT ( 'NONE',  ( -4.283993363284373856, -10.88202310037935661, 33.43294751532457099 ) ) ;
#21676 = ORIENTED_EDGE ( 'NONE', *, *, #86411, .T. ) ;
#21677 = CARTESIAN_POINT ( 'NONE',  ( 6.222779541268408821, -5.913360116392398780, 34.49180327182771322 ) ) ;
#21678 = CARTESIAN_POINT ( 'NONE',  ( -8.546217925137373328, -5.582272713120729257, 34.63742843783360570 ) ) ;
#21679 = CARTESIAN_POINT ( 'NONE',  ( 7.846153846153846700, -9.780366693483667717, 34.19971097300155094 ) ) ;
#21680 = ORIENTED_EDGE ( 'NONE', *, *, #63055, .F. ) ;
#21681 = CARTESIAN_POINT ( 'NONE',  ( 9.692307692307695177, -1.129524287112498415, 32.06866353760679544 ) ) ;
#21682 = ORIENTED_EDGE ( 'NONE', *, *, #15620, .F. ) ;
#21683 = CARTESIAN_POINT ( 'NONE',  ( 12.52760579488853665, -12.34228464037088813, 31.77849191805839268 ) ) ;
#21684 = DIRECTION ( 'NONE',  ( -0.000000000000000000, 0.1736481776669307198, -0.9848077530122080203 ) ) ;
#21685 = ORIENTED_EDGE ( 'NONE', *, *, #9278, .T. ) ;
#21686 = CARTESIAN_POINT ( 'NONE',  ( 10.83816428436268176, -11.60474049983371003, 33.02348890104160262 ) ) ;
#21687 = DIRECTION ( 'NONE',  ( -0.000000000000000000, -0.3420201433256694901, -0.9396926207859082059 ) ) ;
#21688 = CARTESIAN_POINT ( 'NONE',  ( -6.700064078983529292, -12.38742843783360748, 31.66772728687926985 ) ) ;
#21689 = FACE_OUTER_BOUND ( 'NONE', #87118, .T. ) ;
#21690 = CARTESIAN_POINT ( 'NONE',  ( 2.307692307692187583, -6.026961402154118908, 34.52809138561165270 ) ) ;
#21691 = ADVANCED_FACE ( 'NONE', ( #69695 ), #68811, .T. ) ;
#21692 = ORIENTED_EDGE ( 'NONE', *, *, #84869, .T. ) ;
#21693 = VERTEX_POINT ( 'NONE', #359 ) ;
#21694 = AXIS2_PLACEMENT_3D ( 'NONE', #56951, #10553, #51059 ) ;
#21695 = FACE_BOUND ( 'NONE', #22322, .T. ) ;
#21696 = ORIENTED_EDGE ( 'NONE', *, *, #76754, .F. ) ;
#21697 = CARTESIAN_POINT ( 'NONE',  ( 15.29602480204525783, -2.625532179533470512, 30.86335684631491105 ) ) ;
#21698 = EDGE_CURVE ( 'NONE', #41427, #5967, #62920, .T. ) ;
#21699 = AXIS2_PLACEMENT_3D ( 'NONE', #59601, #18630, #51946 ) ;
#21700 = AXIS2_PLACEMENT_3D ( 'NONE', #52867, #73612, #26293 ) ;
#21701 = ADVANCED_FACE ( 'NONE', ( #61156 ), #28716, .T. ) ;
#21702 = DIRECTION ( 'NONE',  ( -1.000000000000000000, -0.000000000000000000, 0.000000000000000000 ) ) ;
#21703 = CARTESIAN_POINT ( 'NONE',  ( 18.00000000000000000, -5.471508081941601098, 34.59228464037088457 ) ) ;
#21704 = CARTESIAN_POINT ( 'NONE',  ( -2.177166869458661225, -10.31582465632705237, 34.18122507451815295 ) ) ;
#21705 = CIRCLE ( 'NONE', #11694, 4.000000000000000000 ) ;
#21706 = ORIENTED_EDGE ( 'NONE', *, *, #64542, .T. ) ;
#21707 = EDGE_CURVE ( 'NONE', #58726, #62375, #54404, .T. ) ;
#21708 = ORIENTED_EDGE ( 'NONE', *, *, #36136, .T. ) ;
#21709 = ORIENTED_EDGE ( 'NONE', *, *, #25703, .F. ) ;
#21710 = CARTESIAN_POINT ( 'NONE',  ( -0.3954701105360233782, -3.050289026998446840, 32.03036669348366416 ) ) ;
#21711 = EDGE_LOOP ( 'NONE', ( #73109, #39823, #84399, #14963 ) ) ;
#21712 = CARTESIAN_POINT ( 'NONE',  ( -5.010854725920637520, -4.786620604624113540, 33.94971097300155805 ) ) ;
#21713 = CARTESIAN_POINT ( 'NONE',  ( -6.793031867157151460, -2.254550872974306674, 29.97347326024527447 ) ) ;
#21714 = CARTESIAN_POINT ( 'NONE',  ( -18.24997674404858827, -6.524016743844656574, 34.90889640711025521 ) ) ;
#21715 = ORIENTED_EDGE ( 'NONE', *, *, #68415, .F. ) ;
#21716 = CARTESIAN_POINT ( 'NONE',  ( 8.769230769230768274, -8.973038597847269315, 34.52809138561121927 ) ) ;
#21717 = EDGE_CURVE ( 'NONE', #56939, #65067, #70781, .T. ) ;
#21718 = CARTESIAN_POINT ( 'NONE',  ( -15.00798956179115962, -3.563462043263030399, 33.22394488606062879 ) ) ;
#21719 = LINE ( 'NONE', #82983, #69646 ) ;
#21720 = CARTESIAN_POINT ( 'NONE',  ( -11.78843826940389050, -3.137211980971221781, 32.19342716148376837 ) ) ;
#21721 = VERTEX_POINT ( 'NONE', #9762 ) ;
#21722 = EDGE_CURVE ( 'NONE', #40455, #78447, #86917, .T. ) ;
#21723 = VERTEX_POINT ( 'NONE', #50731 ) ;
#21724 = B_SPLINE_CURVE_WITH_KNOTS ( 'NONE', 3,
 ( #31593, #59951, #46880, #59059, #60840, #88346, #52301, #45548, #87451, #32042 ),
 .UNSPECIFIED., .F., .F.,
 ( 4, 2, 2, 2, 4 ),
 ( 0.0007817246256747478229, 0.0009771112852218911526, 0.001172497944769034482, 0.001367884604316177595, 0.001563271263863320925 ),
 .UNSPECIFIED. ) ;
#21725 = ORIENTED_EDGE ( 'NONE', *, *, #48735, .F. ) ;
#21726 = CARTESIAN_POINT ( 'NONE',  ( 2.980769230769232614, -7.566082377512563184, 35.00000000000000711 ) ) ;
#21728 = CARTESIAN_POINT ( 'NONE',  ( 2.999999999999997335, 7.500000000000000000, 14.00000000000000178 ) ) ;
#21727 = CARTESIAN_POINT ( 'NONE',  ( 12.21151522424549896, -6.695914987888146541, 34.68535235679833306 ) ) ;
#21729 = B_SPLINE_CURVE_WITH_KNOTS ( 'NONE', 3,
 ( #77949, #15819, #29771, #43284, #30643, #58114 ),
 .UNSPECIFIED., .F., .F.,
 ( 4, 2, 4 ),
 ( 0.000000000000000000, 0.0001954784845028886158, 0.0003909569690057772317 ),
 .UNSPECIFIED. ) ;
#21730 = VECTOR ( 'NONE', #34209, 1000.000000000000000 ) ;
#21731 = CARTESIAN_POINT ( 'NONE',  ( -0.4615384615384611200, -1.790695186598648903, 34.54067556320373455 ) ) ;
#21732 = DIRECTION ( 'NONE',  ( -0.000000000000000000, -0.5000000000000009992, -0.8660254037844380415 ) ) ;
#21733 = CARTESIAN_POINT ( 'NONE',  ( 24.00000000000000000, -9.499999999999982236, 27.74999999999999645 ) ) ;
#21734 = CARTESIAN_POINT ( 'NONE',  ( -6.923076923076922462, -3.322132147404559976, 32.92929555188717927 ) ) ;
#21735 = ORIENTED_EDGE ( 'NONE', *, *, #7400, .T. ) ;
#21736 = CARTESIAN_POINT ( 'NONE',  ( -7.622727447239059373, -7.630147987733840509, 34.99859428049666121 ) ) ;
#21737 = CARTESIAN_POINT ( 'NONE',  ( -25.00000000000000355, 9.999999999999971578, 3.000000000000000000 ) ) ;
#21738 = DIRECTION ( 'NONE',  ( 0.000000000000000000, 0.4999999999999985567, 0.8660254037844395958 ) ) ;
#21739 = FACE_OUTER_BOUND ( 'NONE', #46081, .T. ) ;
#21740 = ORIENTED_EDGE ( 'NONE', *, *, #33504, .F. ) ;
#21741 = CARTESIAN_POINT ( 'NONE',  ( 5.010840697562939816, -12.62096338111211580, 30.90682066428152197 ) ) ;
#21742 = ORIENTED_EDGE ( 'NONE', *, *, #88254, .F. ) ;
#21743 = FACE_BOUND ( 'NONE', #50507, .T. ) ;
#21744 = CARTESIAN_POINT ( 'NONE',  ( -16.02380099101138455, -2.504778602574659896, 29.97347330155780654 ) ) ;
#21745 = FACE_OUTER_BOUND ( 'NONE', #63486, .T. ) ;
#21746 = CARTESIAN_POINT ( 'NONE',  ( -3.230769230769351186, -8.613356846316285953, 34.62446782046622218 ) ) ;
#21747 = ORIENTED_EDGE ( 'NONE', *, *, #65167, .T. ) ;
#21748 = CARTESIAN_POINT ( 'NONE',  ( 5.207448778686640800, -3.285477652293412820, 32.44071101563363158 ) ) ;
#21749 = CARTESIAN_POINT ( 'NONE',  ( -17.74994558008654622, -4.074993327901529128, 33.72946981652012255 ) ) ;
#21750 = LINE ( 'NONE', #30283, #37989 ) ;
#21751 = PLANE ( 'NONE',  #69148 ) ;
#21752 = ORIENTED_EDGE ( 'NONE', *, *, #52245, .T. ) ;
#21753 = CARTESIAN_POINT ( 'NONE',  ( -4.826977667545033768, -4.932303261841489039, 34.32971442181322885 ) ) ;
#21754 = ORIENTED_EDGE ( 'NONE', *, *, #71723, .T. ) ;
#21756 = EDGE_LOOP ( 'NONE', ( #73690, #49923, #2940, #72065 ) ) ;
#21755 = CARTESIAN_POINT ( 'NONE',  ( 16.37680928811283110, -7.369474539155830506, 34.99858011523957657 ) ) ;
#21757 = CARTESIAN_POINT ( 'NONE',  ( 3.361561038594017337, -2.541949514083463590, 30.39797389878540557 ) ) ;
#21758 = CARTESIAN_POINT ( 'NONE',  ( -1.514763354347082425, -12.50552854090298993, 31.33409797877408920 ) ) ;
#21759 = CYLINDRICAL_SURFACE ( 'NONE', #87509, 0.2500000000000012212 ) ;
#21760 = CARTESIAN_POINT ( 'NONE',  ( 14.24160889673643027, -8.973038597847271092, 34.52809138561120506 ) ) ;
#21761 = CARTESIAN_POINT ( 'NONE',  ( -13.25408994638174143, -3.625058011473228703, 33.29252011169590020 ) ) ;
#21763 = DIRECTION ( 'NONE',  ( -1.000000000000000000, -0.000000000000000000, -0.000000000000000000 ) ) ;
#21762 = CARTESIAN_POINT ( 'NONE',  ( -7.912237257109724808, -10.51840700105979387, 33.73612834413961536 ) ) ;
#21764 = EDGE_CURVE ( 'NONE', #13993, #50951, #82602, .T. ) ;
#21765 = ADVANCED_FACE ( 'NONE', ( #77777 ), #85427, .F. ) ;
#21766 = AXIS2_PLACEMENT_3D ( 'NONE', #20441, #36181, #42050 ) ;
#21767 = LINE ( 'NONE', #76716, #57890 ) ;
#21768 = CARTESIAN_POINT ( 'NONE',  ( -2.750000000000007105, -6.360912703474006946, 23.92187500000000355 ) ) ;
#21769 = VERTEX_POINT ( 'NONE', #30042 ) ;
#21770 = CARTESIAN_POINT ( 'NONE',  ( -16.28453675695646652, -4.684245665217972032, 34.18127051446801090 ) ) ;
#21771 = ORIENTED_EDGE ( 'NONE', *, *, #25515, .F. ) ;
#21772 = EDGE_CURVE ( 'NONE', #12525, #58918, #63374, .T. ) ;
#21773 = AXIS2_PLACEMENT_3D ( 'NONE', #38232, #52628, #24259 ) ;
#21774 = VERTEX_POINT ( 'NONE', #16967 ) ;
#21775 = CARTESIAN_POINT ( 'NONE',  ( 4.480769230769229061, -11.00000000000000000, 29.75000000000000355 ) ) ;
#21776 = EDGE_CURVE ( 'NONE', #61500, #52830, #23273, .T. ) ;
#21777 = ORIENTED_EDGE ( 'NONE', *, *, #13501, .F. ) ;
#21778 = CARTESIAN_POINT ( 'NONE',  ( -10.61538461538473399, -11.48612834414049644, 32.76840700105863391 ) ) ;
#21779 = CARTESIAN_POINT ( 'NONE',  ( -2.242436736416282272, -6.879047030191282275, 34.71129190930002295 ) ) ;
#21780 = AXIS2_PLACEMENT_3D ( 'NONE', #28174, #69608, #7914 ) ;
#21781 = CARTESIAN_POINT ( 'NONE',  ( -9.692307692307814193, -11.06231777344772027, 33.60647404775119895 ) ) ;
#21782 = CARTESIAN_POINT ( 'NONE',  ( 10.74591005361826035, -6.808710257144161559, 34.95449254468098843 ) ) ;
#21783 = CARTESIAN_POINT ( 'NONE',  ( -16.21992956480203318, -3.050289026998445951, 32.03036669348365706 ) ) ;
#21784 = CARTESIAN_POINT ( 'NONE',  ( 16.08857570788537572, -11.94971097300153140, 32.03036669348370680 ) ) ;
#21785 = CARTESIAN_POINT ( 'NONE',  ( -0.4615384615384611200, -8.164416787775445883, 34.95778746994557906 ) ) ;
#21786 = DIRECTION ( 'NONE',  ( 0.000000000000000000, -0.000000000000000000, -1.000000000000000000 ) ) ;
#21787 = CYLINDRICAL_SURFACE ( 'NONE', #79386, 0.2499999999999986955 ) ;
#21788 = EDGE_CURVE ( 'NONE', #32252, #24890, #71455, .T. ) ;
#21789 = DIRECTION ( 'NONE',  ( 0.000000000000000000, 0.9396926207859126468, -0.3420201433256571111 ) ) ;
#21790 = CARTESIAN_POINT ( 'NONE',  ( -9.692307692307814193, -3.643525952248795718, 33.31231777344771672 ) ) ;
#21791 = VERTEX_POINT ( 'NONE', #9334 ) ;
#21792 = ORIENTED_EDGE ( 'NONE', *, *, #81451, .F. ) ;
#21793 = CARTESIAN_POINT ( 'NONE',  ( -18.13014796973169851, -2.647304123082328875, 31.75400227202885262 ) ) ;
#21794 = DIRECTION ( 'NONE',  ( 0.000000000000000000, 0.000000000000000000, -1.000000000000000000 ) ) ;
#21795 = EDGE_CURVE ( 'NONE', #73491, #69353, #3443, .T. ) ;
#21796 = CARTESIAN_POINT ( 'NONE',  ( 9.915320536401090123, -11.98016756924215009, 32.48728574198911190 ) ) ;
#21797 = ORIENTED_EDGE ( 'NONE', *, *, #78069, .T. ) ;
#21798 = B_SPLINE_CURVE_WITH_KNOTS ( 'NONE', 3,
 ( #69190, #55664, #14692, #63756, #34954, #2059, #29108, #731, #21890, #56564 ),
 .UNSPECIFIED., .F., .F.,
 ( 4, 2, 2, 2, 4 ),
 ( 0.000000000000000000, 0.0001954339857564092362, 0.0003908679715128184724, 0.0005863019572692276544, 0.0007817359430256369448 ),
 .UNSPECIFIED. ) ;
#21799 = FACE_OUTER_BOUND ( 'NONE', #36722, .T. ) ;
#21800 = DIRECTION ( 'NONE',  ( -0.000000000000000000, 1.000000000000000000, 0.000000000000000000 ) ) ;
#21801 = AXIS2_PLACEMENT_3D ( 'NONE', #39905, #47079, #6111 ) ;
#21802 = CARTESIAN_POINT ( 'NONE',  ( -9.627052552794856055, -3.643525952247864463, 33.31231777344670064 ) ) ;
#21803 = EDGE_CURVE ( 'NONE', #17681, #32213, #23708, .T. ) ;
#21804 = ORIENTED_EDGE ( 'NONE', *, *, #11789, .T. ) ;
#21805 = CARTESIAN_POINT ( 'NONE',  ( -9.692307692307814193, -12.70778746994576025, 30.41441678777401236 ) ) ;
#21806 = ORIENTED_EDGE ( 'NONE', *, *, #34547, .T. ) ;
#21807 = VECTOR ( 'NONE', #79828, 1000.000000000000000 ) ;
#21808 = ADVANCED_FACE ( 'NONE', ( #64247 ), #57503, .F. ) ;
#21809 = CARTESIAN_POINT ( 'NONE',  ( 13.38461538461526423, -12.51329471203414379, 31.30864560766407578 ) ) ;
#21810 = DIRECTION ( 'NONE',  ( 0.000000000000000000, 0.000000000000000000, 1.000000000000000000 ) ) ;
#21811 = CARTESIAN_POINT ( 'NONE',  ( -1.384615384615383471, -9.058645607665452459, 34.76329471203371924 ) ) ;
#21812 = FACE_OUTER_BOUND ( 'NONE', #48640, .T. ) ;
#21813 = CARTESIAN_POINT ( 'NONE',  ( -6.673022503163468677, -2.544122305571457687, 31.48381861865059150 ) ) ;
#21814 = ORIENTED_EDGE ( 'NONE', *, *, #63567, .F. ) ;
#21815 = EDGE_CURVE ( 'NONE', #53903, #57115, #82528, .T. ) ;
#21816 = ORIENTED_EDGE ( 'NONE', *, *, #22364, .F. ) ;
#21817 = ORIENTED_EDGE ( 'NONE', *, *, #47113, .T. ) ;
#21818 = VERTEX_POINT ( 'NONE', #55077 ) ;
#21819 = ADVANCED_FACE ( 'NONE', ( #34357 ), #73705, .F. ) ;
#21820 = FACE_OUTER_BOUND ( 'NONE', #21847, .T. ) ;
#21821 = LINE ( 'NONE', #51035, #11417 ) ;
#21822 = B_SPLINE_CURVE_WITH_KNOTS ( 'NONE', 3,
 ( #35782, #83975, #42976, #36659, #11860, #12291, #80767, #25360, #72652, #45625 ),
 .UNSPECIFIED., .F., .F.,
 ( 4, 2, 2, 2, 4 ),
 ( 0.0007817246256747474977, 0.0009771112852218911526, 0.001172497944769034699, 0.001367884604316178462, 0.001563271263863322009 ),
 .UNSPECIFIED. ) ;
#21823 = CARTESIAN_POINT ( 'NONE',  ( 11.53846153846153832, -5.471508081941601098, 34.59228464037088457 ) ) ;
#21824 = VECTOR ( 'NONE', #56952, 1000.000000000000000 ) ;
#21825 = CARTESIAN_POINT ( 'NONE',  ( 11.53846153846141753, -12.27809138561165270, 31.22303859784587132 ) ) ;
#21826 = CARTESIAN_POINT ( 'NONE',  ( -9.692307692307814193, -10.33852847137269571, 34.16647553114546554 ) ) ;
#21827 = CYLINDRICAL_SURFACE ( 'NONE', #68239, 5.000000000000000888 ) ;
#21828 = ORIENTED_EDGE ( 'NONE', *, *, #87785, .F. ) ;
#21829 = EDGE_CURVE ( 'NONE', #25168, #24368, #30872, .T. ) ;
#21830 = ORIENTED_EDGE ( 'NONE', *, *, #59924, .T. ) ;
#21831 = AXIS2_PLACEMENT_3D ( 'NONE', #49038, #35979, #1740 ) ;
#21832 = ORIENTED_EDGE ( 'NONE', *, *, #78548, .T. ) ;
#21834 = ORIENTED_EDGE ( 'NONE', *, *, #73315, .F. ) ;
#21833 = CARTESIAN_POINT ( 'NONE',  ( 12.71148397988660150, -8.433404298154334455, 34.66254593164985920 ) ) ;
#21835 = EDGE_CURVE ( 'NONE', #55506, #56098, #22362, .T. ) ;
#21837 = CARTESIAN_POINT ( 'NONE',  ( -12.94230769230769162, -7.500000000000000000, 29.75000000000000355 ) ) ;
#21836 = CARTESIAN_POINT ( 'NONE',  ( -11.31544869436814160, -4.026326845037962343, 33.68677907613344047 ) ) ;
#21838 = CARTESIAN_POINT ( 'NONE',  ( -2.241623956689868358, -8.973038597847269315, 34.52809138561122637 ) ) ;
#21839 = CARTESIAN_POINT ( 'NONE',  ( 3.750000000000009770, -9.053300858899081760, 24.54687500000000000 ) ) ;
#21840 = ORIENTED_EDGE ( 'NONE', *, *, #12768, .T. ) ;
#21841 = VERTEX_POINT ( 'NONE', #52959 ) ;
#21842 = CARTESIAN_POINT ( 'NONE',  ( -17.93393266664992680, -2.833524468853757305, 32.15551576947926549 ) ) ;
#21843 = EDGE_LOOP ( 'NONE', ( #8589, #33456, #45894, #57040 ) ) ;
#21844 = FACE_BOUND ( 'NONE', #80535, .T. ) ;
#21845 = CARTESIAN_POINT ( 'NONE',  ( -2.242437168179467033, -5.094484230520773593, 34.41647553114626845 ) ) ;
#21846 = CARTESIAN_POINT ( 'NONE',  ( 8.096099255531887806, -5.766571408460171355, 34.70601412856602508 ) ) ;
#21847 = EDGE_LOOP ( 'NONE', ( #13347, #19159, #56945, #66798 ) ) ;
#21848 = CARTESIAN_POINT ( 'NONE',  ( -14.98071491913091791, -4.943051570960394159, 34.04725096376909477 ) ) ;
#21849 = CARTESIAN_POINT ( 'NONE',  ( -9.692307692307814193, -5.094484230521993062, 34.41647553114689373 ) ) ;
#21850 = CARTESIAN_POINT ( 'NONE',  ( 0.6089743589743582541, -7.500000000000000000, 29.75000000000000355 ) ) ;
#21851 = CARTESIAN_POINT ( 'NONE',  ( -4.153846153846152411, -4.098570777380720287, 33.41473453929634729 ) ) ;
#21852 = CARTESIAN_POINT ( 'NONE',  ( 16.15384615384603251, -8.613356846316285953, 34.62446782046622218 ) ) ;
#21853 = ORIENTED_EDGE ( 'NONE', *, *, #75849, .T. ) ;
#21854 = CARTESIAN_POINT ( 'NONE',  ( 16.02336944572969202, -7.276988635370451597, 34.74523720219453793 ) ) ;
#21855 = DIRECTION ( 'NONE',  ( -0.000000000000000000, -0.6427876096865404731, -0.7660444431189771253 ) ) ;
#21856 = CARTESIAN_POINT ( 'NONE',  ( -13.38461538461507594, -2.506253911140614576, 30.00000000000323297 ) ) ;
#21857 = CARTESIAN_POINT ( 'NONE',  ( -25.00000000000000355, 9.999999999999971578, 13.00000000000000178 ) ) ;
#21858 = DIRECTION ( 'NONE',  ( -1.000000000000000000, 0.000000000000000000, 0.000000000000000000 ) ) ;
#21859 = FACE_BOUND ( 'NONE', #79318, .T. ) ;
#21861 = CARTESIAN_POINT ( 'NONE',  ( -6.249976744048591826, -10.06842814019191401, 34.32929386961144758 ) ) ;
#21860 = CARTESIAN_POINT ( 'NONE',  ( 13.16168916709923487, -11.76352882383564769, 32.36236540154569497 ) ) ;
#21862 = B_SPLINE_CURVE_WITH_KNOTS ( 'NONE', 3,
 ( #82851, #35088, #42748, #21127, #41862, #49500, #69762, #35541, #56254, #83289 ),
 .UNSPECIFIED., .F., .F.,
 ( 4, 2, 2, 2, 4 ),
 ( 0.0007817359430256308733, 0.0009771253907249971907, 0.001172514838424363725, 0.001367904286123730259, 0.001563293733823096577 ),
 .UNSPECIFIED. ) ;
#21863 = DIRECTION ( 'NONE',  ( -0.000000000000000000, -0.8660254037844399289, -0.4999999999999980016 ) ) ;
#21865 = CARTESIAN_POINT ( 'NONE',  ( -18.13069060311030611, -2.845849958028614957, 32.17971566917920256 ) ) ;
#21864 = FACE_OUTER_BOUND ( 'NONE', #26755, .T. ) ;
#21866 = VECTOR ( 'NONE', #65425, 1000.000000000000000 ) ;
#21867 = DIRECTION ( 'NONE',  ( 1.000000000000000000, 0.000000000000000000, 0.000000000000000000 ) ) ;
#21868 = B_SPLINE_CURVE_WITH_KNOTS ( 'NONE', 3,
 ( #67698, #54165, #6444, #6005, #60931, #47409, #19942, #82984, #48299, #88432 ),
 .UNSPECIFIED., .F., .F.,
 ( 4, 2, 2, 2, 4 ),
 ( 0.0007817246256747474977, 0.0009771112852218909357, 0.001172497944769034482, 0.001367884604316178029, 0.001563271263863321575 ),
 .UNSPECIFIED. ) ;
#21869 = CARTESIAN_POINT ( 'NONE',  ( 2.775308065498768517, -8.577988221561467341, 23.04500670625849068 ) ) ;
#21870 = VERTEX_POINT ( 'NONE', #31825 ) ;
#21871 = CARTESIAN_POINT ( 'NONE',  ( 1.318531973659506251, -12.10708131394839349, 31.69288490824020244 ) ) ;
#21872 = ORIENTED_EDGE ( 'NONE', *, *, #58162, .F. ) ;
#21873 = ADVANCED_FACE ( 'NONE', ( #18752 ), #45769, .F. ) ;
#21874 = CARTESIAN_POINT ( 'NONE',  ( -15.23076923076935074, -4.481592998941358097, 33.73612834414048933 ) ) ;
#21875 = ORIENTED_EDGE ( 'NONE', *, *, #41723, .T. ) ;
#21876 = CARTESIAN_POINT ( 'NONE',  ( -11.40767109749459074, -6.369690395747422684, 34.87708834333098196 ) ) ;
#21877 = EDGE_CURVE ( 'NONE', #54838, #56977, #5185, .T. ) ;
#21878 = CYLINDRICAL_SURFACE ( 'NONE', #76169, 0.2499999999999986955 ) ;
#21879 = VERTEX_POINT ( 'NONE', #11098 ) ;
#21880 = CARTESIAN_POINT ( 'NONE',  ( -6.066083410955879884, -11.69971097300155272, 32.46337939537587403 ) ) ;
#21881 = CARTESIAN_POINT ( 'NONE',  ( 2.724691934501235036, -6.299813628509441266, 17.88875670625848713 ) ) ;
#21882 = CARTESIAN_POINT ( 'NONE',  ( 6.000000000000001776, -6.343179335718451384, 34.87096338111211935 ) ) ;
#21883 = CARTESIAN_POINT ( 'NONE',  ( 4.023154687178596589, -8.999036380462719364, 34.52022231692819076 ) ) ;
#21884 = CARTESIAN_POINT ( 'NONE',  ( -5.326946314216041145, -5.056417327199099532, 34.11270091957320716 ) ) ;
#21885 = CARTESIAN_POINT ( 'NONE',  ( 12.33084699487090674, -2.729777683071817229, 31.24903638046269450 ) ) ;
#21886 = CARTESIAN_POINT ( 'NONE',  ( 23.00000000000000000, -5.499999999999981348, 27.75000000000000000 ) ) ;
#21887 = DIRECTION ( 'NONE',  ( -0.000000000000000000, -0.8660254037844397068, -0.4999999999999978906 ) ) ;
#21888 = EDGE_CURVE ( 'NONE', #39225, #26637, #137, .T. ) ;
#21889 = CARTESIAN_POINT ( 'NONE',  ( 3.775308065498752086, -6.007798216065404873, 24.64249329374151642 ) ) ;
#21890 = CARTESIAN_POINT ( 'NONE',  ( -9.757578138268465651, -3.835265460703609186, 33.15142922261924241 ) ) ;
#21891 = FACE_OUTER_BOUND ( 'NONE', #21711, .T. ) ;
#21892 = ADVANCED_FACE ( 'NONE', ( #24607 ), #66492, .F. ) ;
#21893 = CARTESIAN_POINT ( 'NONE',  ( -11.53846153846153655, -1.117168528481311540, 33.14645433367849847 ) ) ;
#21894 = CARTESIAN_POINT ( 'NONE',  ( -1.614399933863613468, -11.22469193450124969, 22.61124329374151287 ) ) ;
#21895 = CARTESIAN_POINT ( 'NONE',  ( -10.54931728203453822, -5.471508081941601098, 34.59228464037088457 ) ) ;
#21896 = VECTOR ( 'NONE', #19708, 1000.000000000000227 ) ;
#21897 = ORIENTED_EDGE ( 'NONE', *, *, #69200, .F. ) ;
#21898 = EDGE_CURVE ( 'NONE', #5201, #17409, #31369, .T. ) ;
#21899 = CARTESIAN_POINT ( 'NONE',  ( -17.86947429823643674, -2.882268652242223173, 31.66798894389554064 ) ) ;
#21900 = DIRECTION ( 'NONE',  ( 1.000000000000000000, 0.000000000000000000, 0.000000000000000000 ) ) ;
#21901 = CARTESIAN_POINT ( 'NONE',  ( 1.319344938654610999, -12.46129190929999986, 30.37095296980880832 ) ) ;
#21902 = CARTESIAN_POINT ( 'NONE',  ( 17.07692307692307665, -11.69971097300155272, 32.46337939537588113 ) ) ;
#21903 = DIRECTION ( 'NONE',  ( 0.000000000000000000, 0.000000000000000000, 1.000000000000000000 ) ) ;
#21904 = VECTOR ( 'NONE', #42086, 1000.000000000000114 ) ;
#21906 = EDGE_CURVE ( 'NONE', #75988, #78555, #82573, .T. ) ;
#21905 = CARTESIAN_POINT ( 'NONE',  ( -10.48459417441766561, -9.084667340241226796, 34.75534355489798344 ) ) ;
#21907 = CARTESIAN_POINT ( 'NONE',  ( -39.05038313613820122, -2.499999999999999556, 29.75000000000000355 ) ) ;
#21908 = B_SPLINE_CURVE_WITH_KNOTS ( 'NONE', 3,
 ( #74448, #82552, #120, #19939, #13196, #74014, #34338, #60489, #48295, #14073 ),
 .UNSPECIFIED., .F., .F.,
 ( 4, 2, 2, 2, 4 ),
 ( 0.0007817246256747471724, 0.0009771112852218905021, 0.001172497944769033615, 0.001367884604316176944, 0.001563271263863320274 ),
 .UNSPECIFIED. ) ;
#21909 = DIRECTION ( 'NONE',  ( 0.000000000000000000, 0.6427876096865368094, 0.7660444431189802339 ) ) ;
#21910 = VERTEX_POINT ( 'NONE', #61376 ) ;
#21911 = EDGE_LOOP ( 'NONE', ( #13402, #74439 ) ) ;
#21912 = ADVANCED_FACE ( 'NONE', ( #75357 ), #80001, .F. ) ;
#21913 = ORIENTED_EDGE ( 'NONE', *, *, #50439, .T. ) ;
#21914 = CARTESIAN_POINT ( 'NONE',  ( 5.207448778686640800, -11.93748526763465279, 32.05452791011430946 ) ) ;
#21915 = DIRECTION ( 'NONE',  ( 0.000000000000000000, 0.000000000000000000, -1.000000000000000000 ) ) ;
#21916 = CARTESIAN_POINT ( 'NONE',  ( 12.46153846153846168, -1.215029322943914858, 32.30358669280327177 ) ) ;
#21917 = EDGE_CURVE ( 'NONE', #11165, #64684, #86338, .T. ) ;
#21918 = DIRECTION ( 'NONE',  ( 0.000000000000000000, 0.9396926207859126468, 0.3420201433256571111 ) ) ;
#21919 = CARTESIAN_POINT ( 'NONE',  ( -5.999999999999998224, -11.33034616979429110, 35.88435417666054406 ) ) ;
#21920 = EDGE_LOOP ( 'NONE', ( #39184, #77222, #62977, #87933 ) ) ;
#21921 = DIRECTION ( 'NONE',  ( 0.000000000000000000, 0.7660444431189822323, -0.6427876096865344779 ) ) ;
#21922 = AXIS2_PLACEMENT_3D ( 'NONE', #12570, #40057, #26532 ) ;
#21923 = VERTEX_POINT ( 'NONE', #73246 ) ;
#21924 = VERTEX_POINT ( 'NONE', #59729 ) ;
#21925 = ADVANCED_FACE ( 'NONE', ( #54621 ), #87223, .F. ) ;
#21926 = ADVANCED_FACE ( 'NONE', ( #66934 ), #15435, .F. ) ;
#21927 = EDGE_LOOP ( 'NONE', ( #26060, #28141 ) ) ;
#21929 = ORIENTED_EDGE ( 'NONE', *, *, #5994, .F. ) ;
#21928 = CARTESIAN_POINT ( 'NONE',  ( 8.546303810323914618, -12.38737895849757820, 31.66785238281580206 ) ) ;
#21930 = DIRECTION ( 'NONE',  ( -0.000000000000000000, 0.1736481776669307198, -0.9848077530122080203 ) ) ;
#21931 = CARTESIAN_POINT ( 'NONE',  ( -16.37733109757010652, -4.386631170607603991, 33.66268669641500111 ) ) ;
#21932 = CARTESIAN_POINT ( 'NONE',  ( -15.90384615384615330, -2.499999999999998668, 29.75000000000000355 ) ) ;
#21933 = CARTESIAN_POINT ( 'NONE',  ( 14.17721712261659128, -7.276987145209184327, 34.99546412871779211 ) ) ;
#21934 = EDGE_LOOP ( 'NONE', ( #25497, #78587, #20144, #33216 ) ) ;
#21935 = EDGE_CURVE ( 'NONE', #42554, #59805, #7782, .T. ) ;
#21936 = ORIENTED_EDGE ( 'NONE', *, *, #86397, .T. ) ;
#21937 = EDGE_LOOP ( 'NONE', ( #32162, #17939 ) ) ;
#21938 = CARTESIAN_POINT ( 'NONE',  ( -2.177166869458660781, -3.625058011473228259, 33.29252011169590020 ) ) ;
#21940 = ORIENTED_EDGE ( 'NONE', *, *, #72031, .F. ) ;
#21939 = CARTESIAN_POINT ( 'NONE',  ( -2.437839517130524047, -2.882441371585227508, 31.66841991370171527 ) ) ;
#21941 = CARTESIAN_POINT ( 'NONE',  ( -8.519230769229334754, -7.500000000000155431, 34.75000000000007105 ) ) ;
#21942 = DIRECTION ( 'NONE',  ( 0.000000000000000000, 0.000000000000000000, -1.000000000000000000 ) ) ;
#21943 = B_SPLINE_CURVE_WITH_KNOTS ( 'NONE', 3,
 ( #82154, #69955, #171, #48348, #35284, #75825, #55111, #62742, #14127, #47460 ),
 .UNSPECIFIED., .F., .F.,
 ( 4, 2, 2, 2, 4 ),
 ( 0.0007817359430256289217, 0.0009771253907249945886, 0.001172514838424360255, 0.001367904286123725922, 0.001563293733823091589 ),
 .UNSPECIFIED. ) ;
#21944 = EDGE_CURVE ( 'NONE', #5455, #38257, #84341, .T. ) ;
#21945 = ADVANCED_FACE ( 'NONE', ( #8678 ), #1906, .F. ) ;
#21946 = CARTESIAN_POINT ( 'NONE',  ( 6.989145274079363368, -11.69971097300155272, 32.46337939537588113 ) ) ;
#21947 = ORIENTED_EDGE ( 'NONE', *, *, #89019, .T. ) ;
#21948 = LINE ( 'NONE', #62911, #60912 ) ;
#21949 = CARTESIAN_POINT ( 'NONE',  ( 15.23076923076923173, -12.48256725967547354, 35.29906147534542527 ) ) ;
#21950 = ORIENTED_EDGE ( 'NONE', *, *, #22509, .F. ) ;
#21951 = FACE_BOUND ( 'NONE', #57377, .T. ) ;
#21952 = EDGE_CURVE ( 'NONE', #57828, #87883, #45940, .T. ) ;
#21953 = CARTESIAN_POINT ( 'NONE',  ( -10.61538461538473577, -5.094484230521993062, 34.41647553114689373 ) ) ;
#21954 = LINE ( 'NONE', #49426, #64349 ) ;
#21955 = VECTOR ( 'NONE', #76259, 1000.000000000000114 ) ;
#21956 = DIRECTION ( 'NONE',  ( -0.000000000000000000, -0.9848077530122086864, -0.1736481776669273613 ) ) ;
#21958 = CARTESIAN_POINT ( 'NONE',  ( 14.16025641025641235, -7.500000000000000000, 29.75000000000000355 ) ) ;
#21957 = CARTESIAN_POINT ( 'NONE',  ( 18.22301284409340028, -2.889357225399416418, 32.26129605718031002 ) ) ;
#21959 = VECTOR ( 'NONE', #33784, 1000.000000000000227 ) ;
#21960 = CARTESIAN_POINT ( 'NONE',  ( -3.930834802233305059, -2.758310577978207778, 31.33698337089303010 ) ) ;
#21961 = CARTESIAN_POINT ( 'NONE',  ( 14.30769230769231015, -2.292212530054420494, 30.41441678777542634 ) ) ;
#21962 = VERTEX_POINT ( 'NONE', #34800 ) ;
#21963 = CARTESIAN_POINT ( 'NONE',  ( -2.438382910802615378, -3.957541250942359756, 33.62499894934981626 ) ) ;
#21964 = FACE_BOUND ( 'NONE', #79199, .T. ) ;
#21965 = ORIENTED_EDGE ( 'NONE', *, *, #31041, .F. ) ;
#21966 = VECTOR ( 'NONE', #61328, 1000.000000000000227 ) ;
#21967 = DIRECTION ( 'NONE',  ( -0.000000000000000000, 0.5000000000000011102, -0.8660254037844381525 ) ) ;
#21968 = CARTESIAN_POINT ( 'NONE',  ( 15.90386940979756858, -6.524016743844656574, 34.90889640711025521 ) ) ;
#21969 = LINE ( 'NONE', #4698, #23174 ) ;
#21970 = ORIENTED_EDGE ( 'NONE', *, *, #29881, .F. ) ;
#21971 = CARTESIAN_POINT ( 'NONE',  ( -13.13456096470193124, -11.47946981652013498, 33.17500667209847620 ) ) ;
#21972 = DIRECTION ( 'NONE',  ( -1.000000000000000000, -0.000000000000000000, -0.000000000000000000 ) ) ;
#21973 = FACE_BOUND ( 'NONE', #24798, .T. ) ;
#21975 = CARTESIAN_POINT ( 'NONE',  ( 3.903822929624694904, -12.45566812827425096, 31.48439005359158926 ) ) ;
#21974 = CARTESIAN_POINT ( 'NONE',  ( -16.15384615384615330, -1.790695186598648903, 34.54067556320373455 ) ) ;
#21976 = CARTESIAN_POINT ( 'NONE',  ( -15.90379184220783948, -2.564540009722896752, 30.55348353981672105 ) ) ;
#21978 = FACE_OUTER_BOUND ( 'NONE', #14726, .T. ) ;
#21977 = CARTESIAN_POINT ( 'NONE',  ( -4.853910232829682592, -10.01129605718032778, 34.36064277460058491 ) ) ;
#21979 = CARTESIAN_POINT ( 'NONE',  ( -17.93474442872397034, -5.219633306516379356, 34.19971097300157936 ) ) ;
#21980 = CARTESIAN_POINT ( 'NONE',  ( 2.651650429449569302, -10.15165042944953733, 25.87500000000000355 ) ) ;
#21981 = EDGE_LOOP ( 'NONE', ( #15889, #28216 ) ) ;
#21982 = ORIENTED_EDGE ( 'NONE', *, *, #88519, .F. ) ;
#21983 = CARTESIAN_POINT ( 'NONE',  ( 5.076923076923075762, -6.386643153685126251, 34.62446782046654192 ) ) ;
#21984 = CARTESIAN_POINT ( 'NONE',  ( 14.37375964104238513, -12.62096338111211757, 30.90682066428152908 ) ) ;
#21985 = CYLINDRICAL_SURFACE ( 'NONE', #28723, 0.2500000000000008882 ) ;
#21986 = CARTESIAN_POINT ( 'NONE',  ( -17.07692307692307665, -11.16473453929635440, 33.15142922261926373 ) ) ;
#21987 = CARTESIAN_POINT ( 'NONE',  ( -16.28453762051371712, -12.11776431015576172, 31.66791131148498906 ) ) ;
#21988 = CARTESIAN_POINT ( 'NONE',  ( 1.614399933863660985, -11.22469193450123193, 16.95125670625848713 ) ) ;
#21989 = CARTESIAN_POINT ( 'NONE',  ( 6.673053698855467175, -2.341070481393820124, 30.72580821765574299 ) ) ;
#21990 = CARTESIAN_POINT ( 'NONE',  ( 4.153846153846030731, -12.16647553114689728, 32.15551576947799362 ) ) ;
#21991 = CARTESIAN_POINT ( 'NONE',  ( -4.153846153846274980, -6.835583212225970762, 34.95778746994575670 ) ) ;
#21992 = CARTESIAN_POINT ( 'NONE',  ( 17.77713457779636386, -2.501496062324911840, 29.88072118266895671 ) ) ;
#21993 = DIRECTION ( 'NONE',  ( -0.000000000000000000, 0.3420201433256694346, -0.9396926207859080948 ) ) ;
#21994 = CARTESIAN_POINT ( 'NONE',  ( 18.06606835100244268, -9.780366693483667717, 34.19971097300155805 ) ) ;
#21995 = VECTOR ( 'NONE', #63804, 1000.000000000000000 ) ;
#21996 = CARTESIAN_POINT ( 'NONE',  ( -5.010854725920639297, -2.721908614388772296, 31.22303859784725333 ) ) ;
#21997 = CARTESIAN_POINT ( 'NONE',  ( 10.55006169989244214, -7.749976743299138882, 34.99404534957040624 ) ) ;
#21998 = CARTESIAN_POINT ( 'NONE',  ( 3.100622021331011169, -2.619462340734462380, 30.83744416345203021 ) ) ;
#21999 = ORIENTED_EDGE ( 'NONE', *, *, #70860, .F. ) ;
#22000 = CARTESIAN_POINT ( 'NONE',  ( 12.21151523731700372, -4.175268141568685643, 33.81360843649122216 ) ) ;
#22001 = CARTESIAN_POINT ( 'NONE',  ( 14.30769230769231015, -12.62096338111211580, 30.90682066428153263 ) ) ;
#22002 = B_SPLINE_CURVE_WITH_KNOTS ( 'NONE', 3,
 ( #71165, #14464, #41942, #36935, #43696, #64398, #15355, #69409, #42829, #2697 ),
 .UNSPECIFIED., .F., .F.,
 ( 4, 2, 2, 2, 4 ),
 ( 0.000000000000000000, 0.0001954339857564081520, 0.0003908679715128163040, 0.0005863019572692244018, 0.0007817359430256326080 ),
 .UNSPECIFIED. ) ;
#22003 = CARTESIAN_POINT ( 'NONE',  ( 2.724691934501250135, -8.700186371490531201, 21.04874329374151642 ) ) ;
#22004 = B_SPLINE_CURVE_WITH_KNOTS ( 'NONE', 3,
 ( #33166, #88140, #26413, #81364, #18325, #45787, #73266, #39054, #66511, #4815 ),
 .UNSPECIFIED., .F., .F.,
 ( 4, 2, 2, 2, 4 ),
 ( 0.000000000000000000, 0.0001954311564186861426, 0.0003908623128373722852, 0.0005862934692560583735, 0.0007817246256747445703 ),
 .UNSPECIFIED. ) ;
#22005 = CARTESIAN_POINT ( 'NONE',  ( 6.856994543716787405, -4.661471528628507777, 34.16647553114621871 ) ) ;
#22006 = CARTESIAN_POINT ( 'NONE',  ( -23.50000000000000000, 9.000000000000024869, 29.25000000000000000 ) ) ;
#22007 = ORIENTED_EDGE ( 'NONE', *, *, #70919, .T. ) ;
#22008 = DIRECTION ( 'NONE',  ( -0.000000000000000000, -0.1736481776669307198, -0.9848077530122080203 ) ) ;
#22010 = ORIENTED_EDGE ( 'NONE', *, *, #69854, .T. ) ;
#22009 = CARTESIAN_POINT ( 'NONE',  ( -6.222879516737585881, -7.630690623152302621, 34.99857592706774057 ) ) ;
#22011 = CARTESIAN_POINT ( 'NONE',  ( 4.153846153846154188, -11.33034616979429110, 35.88435417666054406 ) ) ;
#22012 = CARTESIAN_POINT ( 'NONE',  ( -2.437840277424004665, -11.04286588640298561, 33.62463336215343901 ) ) ;
#22013 = ORIENTED_EDGE ( 'NONE', *, *, #41630, .F. ) ;
#22014 = CARTESIAN_POINT ( 'NONE',  ( -13.16160403300253634, -2.554770724473667265, 30.48948780036025852 ) ) ;
#22016 = EDGE_CURVE ( 'NONE', #62711, #42060, #28052, .T. ) ;
#22015 = CARTESIAN_POINT ( 'NONE',  ( 7.623275163725200088, -7.630691491037286056, 34.74850469731151748 ) ) ;
#22017 = ORIENTED_EDGE ( 'NONE', *, *, #62198, .T. ) ;
#22018 = CARTESIAN_POINT ( 'NONE',  ( -5.076923076923075762, -11.35647404775217417, 33.31231777344666511 ) ) ;
#22019 = DIRECTION ( 'NONE',  ( 0.000000000000000000, 0.000000000000000000, -1.000000000000000000 ) ) ;
#22020 = CARTESIAN_POINT ( 'NONE',  ( 15.23076923076923173, -11.35647404775217417, 33.31231777344666511 ) ) ;
#22021 = ORIENTED_EDGE ( 'NONE', *, *, #15651, .T. ) ;
#22022 = VERTEX_POINT ( 'NONE', #29396 ) ;
#22023 = CARTESIAN_POINT ( 'NONE',  ( 2.980792486720639900, -2.920706130388546651, 32.31842814019191223 ) ) ;
#22024 = VECTOR ( 'NONE', #30817, 1000.000000000000114 ) ;
#22025 = VERTEX_POINT ( 'NONE', #35248 ) ;
#22026 = AXIS2_PLACEMENT_3D ( 'NONE', #50619, #64562, #36673 ) ;
#22027 = CARTESIAN_POINT ( 'NONE',  ( 10.61538461538449418, -12.51329471203414379, 31.30864560766407578 ) ) ;
#22028 = CARTESIAN_POINT ( 'NONE',  ( 2.557746727605762160, -11.47946981652013498, 33.17500667209846910 ) ) ;
#22029 = EDGE_CURVE ( 'NONE', #79431, #33821, #35705, .T. ) ;
#22030 = FACE_OUTER_BOUND ( 'NONE', #83532, .T. ) ;
#22031 = CARTESIAN_POINT ( 'NONE',  ( -3.007756386675835891, -8.282913670948747864, 34.94150082978203642 ) ) ;
#22032 = CARTESIAN_POINT ( 'NONE',  ( 12.46153846153833911, -2.625532179533778709, 30.86335684631627174 ) ) ;
#22033 = B_SPLINE_CURVE_WITH_KNOTS ( 'NONE', 3,
 ( #69248, #20612, #13414, #47192, #46761, #19292, #68802, #26938, #40896, #7550 ),
 .UNSPECIFIED., .F., .F.,
 ( 4, 2, 2, 2, 4 ),
 ( 0.0007817359430256282712, 0.0009771253907249943717, 0.001172514838424360689, 0.001367904286123726790, 0.001563293733823092890 ),
 .UNSPECIFIED. ) ;
#22034 = EDGE_LOOP ( 'NONE', ( #24440, #28316 ) ) ;
#22035 = EDGE_CURVE ( 'NONE', #48826, #8133, #55517, .T. ) ;
#22036 = B_SPLINE_CURVE_WITH_KNOTS ( 'NONE', 3,
 ( #82181, #75414, #14600, #69102, #41191, #75855, #74981, #42083, #14154, #69540 ),
 .UNSPECIFIED., .F., .F.,
 ( 4, 2, 2, 2, 4 ),
 ( 0.0007817359527651104954, 0.0009771254036996493593, 0.001172514854634188440, 0.001367904305568727304, 0.001563293756503266168 ),
 .UNSPECIFIED. ) ;
#22037 = ORIENTED_EDGE ( 'NONE', *, *, #88552, .F. ) ;
#22039 = ORIENTED_EDGE ( 'NONE', *, *, #3907, .F. ) ;
#22038 = LINE ( 'NONE', #9406, #86150 ) ;
#22040 = DIRECTION ( 'NONE',  ( -1.000000000000000000, -2.602085213965214586E-16, 0.000000000000000000 ) ) ;
#22041 = VERTEX_POINT ( 'NONE', #77125 ) ;
#22042 = CARTESIAN_POINT ( 'NONE',  ( 7.715463243043539698, -11.93127051446800024, 32.56575433478200665 ) ) ;
#22043 = CYLINDRICAL_SURFACE ( 'NONE', #85607, 8.000000000000000000 ) ;
#22044 = ORIENTED_EDGE ( 'NONE', *, *, #7511, .F. ) ;
#22045 = DIRECTION ( 'NONE',  ( 0.000000000000000000, 0.000000000000000000, 1.000000000000000000 ) ) ;
#22046 = AXIS2_PLACEMENT_3D ( 'NONE', #27175, #81247, #67726 ) ;
#22047 = VERTEX_POINT ( 'NONE', #63155 ) ;
#22049 = VERTEX_POINT ( 'NONE', #83455 ) ;
#22048 = CARTESIAN_POINT ( 'NONE',  ( 9.692307692307570832, -8.656820664282941280, 34.87096338111179961 ) ) ;
#22050 = VECTOR ( 'NONE', #5197, 1000.000000000000000 ) ;
#22051 = CYLINDRICAL_SURFACE ( 'NONE', #34443, 0.2500000000000002220 ) ;
#22052 = EDGE_CURVE ( 'NONE', #39944, #55341, #42798, .T. ) ;
#22053 = EDGE_CURVE ( 'NONE', #50855, #69909, #76686, .T. ) ;
#22054 = DIRECTION ( 'NONE',  ( 1.000000000000000000, 0.000000000000000000, 0.000000000000000000 ) ) ;
#22055 = VERTEX_POINT ( 'NONE', #7345 ) ;
#22056 = CARTESIAN_POINT ( 'NONE',  ( -6.857009589726848375, -4.661471528628508665, 34.16647553114624003 ) ) ;
#22057 = CARTESIAN_POINT ( 'NONE',  ( 17.86930939688969033, -12.35290016733513951, 31.75349464988449455 ) ) ;
#22058 = FACE_BOUND ( 'NONE', #13751, .T. ) ;
#22059 = CARTESIAN_POINT ( 'NONE',  ( -11.76138775597768138, -2.554751324335734708, 30.48935550225260727 ) ) ;
#22060 = CARTESIAN_POINT ( 'NONE',  ( -6.923076923077045919, -9.528491918059723176, 34.59228464037033035 ) ) ;
#22061 = CARTESIAN_POINT ( 'NONE',  ( 9.442330948259103351, -2.318417181685855422, 30.59732222474233865 ) ) ;
#22062 = CARTESIAN_POINT ( 'NONE',  ( -17.01166793741023042, -12.51329471203373700, 31.30864560766537963 ) ) ;
#22063 = LINE ( 'NONE', #8554, #78306 ) ;
#22064 = CARTESIAN_POINT ( 'NONE',  ( -6.923076923077044142, -6.879047030192662504, 34.71129190930017927 ) ) ;
#22065 = ORIENTED_EDGE ( 'NONE', *, *, #38287, .F. ) ;
#22066 = CARTESIAN_POINT ( 'NONE',  ( 1.384615384615386802, -12.78798330534102945, 29.74999999999997868 ) ) ;
#22067 = VERTEX_POINT ( 'NONE', #21737 ) ;
#22068 = ORIENTED_EDGE ( 'NONE', *, *, #62218, .F. ) ;
#22069 = B_SPLINE_CURVE_WITH_KNOTS ( 'NONE', 3,
 ( #22448, #82837, #2170, #29658, #28776, #35077, #21110, #43167, #14819, #56241 ),
 .UNSPECIFIED., .F., .F.,
 ( 4, 2, 2, 2, 4 ),
 ( 0.0007817359430256372700, 0.0009771253907250054306, 0.001172514838424373700, 0.001367904286123741969, 0.001563293733823110238 ),
 .UNSPECIFIED. ) ;
#22071 = CARTESIAN_POINT ( 'NONE',  ( 16.28437185560971656, -12.27024696741798770, 31.24895572276497546 ) ) ;
#22070 = CARTESIAN_POINT ( 'NONE',  ( -5.142193077479397800, -12.16647553114622049, 32.15551576947930812 ) ) ;
#22072 = B_SPLINE_CURVE_WITH_KNOTS ( 'NONE', 3,
 ( #5865, #67125, #38759, #45505, #87865, #17606, #11283, #53600, #18494, #80650 ),
 .UNSPECIFIED., .F., .F.,
 ( 4, 2, 2, 2, 4 ),
 ( 0.0007817359430256288133, 0.0009771253907249948054, 0.001172514838424360689, 0.001367904286123726573, 0.001563293733823092457 ),
 .UNSPECIFIED. ) ;
#22073 = CARTESIAN_POINT ( 'NONE',  ( 6.988332494352946789, -6.879047030191282275, 34.71129190930002295 ) ) ;
#22075 = B_SPLINE_CURVE_WITH_KNOTS ( 'NONE', 3,
 ( #7206, #14401, #27917, #55387, #82871, #69354 ),
 .UNSPECIFIED., .F., .F.,
 ( 4, 2, 4 ),
 ( 0.000000000000000000, 0.0001954784845028902421, 0.0003909569690057804843 ),
 .UNSPECIFIED. ) ;
#22074 = DIRECTION ( 'NONE',  ( 0.000000000000000000, 0.6427876096865368094, 0.7660444431189802339 ) ) ;
#22076 = CARTESIAN_POINT ( 'NONE',  ( -12.21159305216042235, -2.589246495874658383, 31.60778113518102828 ) ) ;
#22077 = CARTESIAN_POINT ( 'NONE',  ( 13.51514108637895184, -11.46989282347013095, 32.79007818306219946 ) ) ;
#22078 = VERTEX_POINT ( 'NONE', #56412 ) ;
#22079 = DIRECTION ( 'NONE',  ( -0.000000000000000000, 0.3420201433256694901, -0.9396926207859082059 ) ) ;
#22080 = CARTESIAN_POINT ( 'NONE',  ( 1.384615384615265343, -12.27809138561165270, 31.22303859784587132 ) ) ;
#22081 = FACE_OUTER_BOUND ( 'NONE', #1013, .T. ) ;
#22082 = CARTESIAN_POINT ( 'NONE',  ( -0.4615384615385840772, -9.528491918059723176, 34.59228464037033035 ) ) ;
#22083 = DIRECTION ( 'NONE',  ( 1.000000000000000000, 0.000000000000000000, 0.000000000000000000 ) ) ;
#22084 = ORIENTED_EDGE ( 'NONE', *, *, #2287, .T. ) ;
#22085 = ORIENTED_EDGE ( 'NONE', *, *, #56918, .T. ) ;
#22086 = VECTOR ( 'NONE', #32980, 1000.000000000000227 ) ;
#22087 = ORIENTED_EDGE ( 'NONE', *, *, #42683, .F. ) ;
#22088 = AXIS2_PLACEMENT_3D ( 'NONE', #77330, #14752, #57051 ) ;
#22089 = CARTESIAN_POINT ( 'NONE',  ( -6.223484924564330001, -4.225889041578354544, 33.85425143139329407 ) ) ;
#22090 = ORIENTED_EDGE ( 'NONE', *, *, #68149, .F. ) ;
#22091 = CARTESIAN_POINT ( 'NONE',  ( -18.03205128205128105, -7.500000000000000000, 33.75000000000000000 ) ) ;
#22092 = DIRECTION ( 'NONE',  ( 0.000000000000000000, 0.000000000000000000, -1.000000000000000000 ) ) ;
#22093 = CARTESIAN_POINT ( 'NONE',  ( -18.00000000000000000, -13.75143057439168182, 32.29137909377919868 ) ) ;
#22094 = CARTESIAN_POINT ( 'NONE',  ( -8.769230769230768274, -10.51840700105979565, 33.73612834413961536 ) ) ;
#22095 = CARTESIAN_POINT ( 'NONE',  ( -17.01085472592064107, -12.10708131394839882, 31.69288490824020954 ) ) ;
#22096 = DIRECTION ( 'NONE',  ( -0.000000000000000000, -0.6427876096865404731, -0.7660444431189770143 ) ) ;
#22097 = ORIENTED_EDGE ( 'NONE', *, *, #36491, .T. ) ;
#22098 = CARTESIAN_POINT ( 'NONE',  ( 4.153846153846154188, -4.098570777380720287, 33.41473453929634729 ) ) ;
#22100 = ORIENTED_EDGE ( 'NONE', *, *, #39651, .F. ) ;
#22099 = CARTESIAN_POINT ( 'NONE',  ( -13.16160403300253279, -4.187068189119699468, 33.49521262558774026 ) ) ;
#22101 = DIRECTION ( 'NONE',  ( 0.000000000000000000, 0.000000000000000000, 1.000000000000000000 ) ) ;
#22102 = CARTESIAN_POINT ( 'NONE',  ( 2.980745993476265010, -12.43535235679832596, 30.55408501211184813 ) ) ;
#22103 = CARTESIAN_POINT ( 'NONE',  ( -0.4615384615384611200, -3.937682226553329556, 33.60647404775216529 ) ) ;
#22104 = CARTESIAN_POINT ( 'NONE',  ( 6.223012844093396723, -9.172514111537584114, 34.72667873470787470 ) ) ;
#22105 = CYLINDRICAL_SURFACE ( 'NONE', #43304, 0.2499999999999986955 ) ;
#22106 = CARTESIAN_POINT ( 'NONE',  ( 16.85404439449444070, -7.630691491037286056, 34.74850469731152458 ) ) ;
#22107 = CARTESIAN_POINT ( 'NONE',  ( -19.50000000000000000, -11.50000000000000000, 29.75000000000000355 ) ) ;
#22108 = CARTESIAN_POINT ( 'NONE',  ( 2.608446859217924629, -10.19485399968118422, 13.62686829374151642 ) ) ;
#22109 = VERTEX_POINT ( 'NONE', #62268 ) ;
#22110 = CARTESIAN_POINT ( 'NONE',  ( 1.384615384615265343, -6.026961402154118908, 34.52809138561165270 ) ) ;
#22111 = CARTESIAN_POINT ( 'NONE',  ( 4.284371592079796898, -11.04252011169590020, 33.62494198852677840 ) ) ;
#22112 = B_SPLINE_CURVE_WITH_KNOTS ( 'NONE', 3,
 ( #44596, #36537, #30222, #77958, #56795, #71192 ),
 .UNSPECIFIED., .F., .F.,
 ( 4, 2, 4 ),
 ( 0.0003909569690057848211, 0.0005862646681846116680, 0.0007815723673634385150 ),
 .UNSPECIFIED. ) ;
#22113 = CARTESIAN_POINT ( 'NONE',  ( 0.3308478584281526191, -5.496505350115500121, 34.60290016733514307 ) ) ;
#22114 = CARTESIAN_POINT ( 'NONE',  ( 9.627037691751372250, -6.835583212224499938, 34.95778746994557906 ) ) ;
#22115 = ORIENTED_EDGE ( 'NONE', *, *, #14548, .F. ) ;
#22116 = CARTESIAN_POINT ( 'NONE',  ( -1.139087296526025250, -4.750000000000006217, 15.32812500000000178 ) ) ;
#22117 = CARTESIAN_POINT ( 'NONE',  ( 11.28843831424008215, -4.175268141568685643, 33.81360843649122216 ) ) ;
#22118 = VERTEX_POINT ( 'NONE', #83900 ) ;
#22119 = CARTESIAN_POINT ( 'NONE',  ( -0.4615384615384611200, -12.62096338111211580, 30.90682066428153263 ) ) ;
#22120 = VECTOR ( 'NONE', #18973, 1000.000000000000227 ) ;
#22121 = CARTESIAN_POINT ( 'NONE',  ( 14.05771557674995265, -3.137211980971221781, 32.19342716148376837 ) ) ;
#22122 = EDGE_CURVE ( 'NONE', #81634, #18370, #49210, .T. ) ;
#22123 = EDGE_CURVE ( 'NONE', #77581, #25833, #63097, .T. ) ;
#22124 = VERTEX_POINT ( 'NONE', #78006 ) ;
#22125 = CARTESIAN_POINT ( 'NONE',  ( 14.30769230769218758, -2.892918686052165622, 31.69288490824153470 ) ) ;
#22126 = CARTESIAN_POINT ( 'NONE',  ( -5.934806018216642443, -2.506253911140448487, 29.99999999999988631 ) ) ;
#22127 = CARTESIAN_POINT ( 'NONE',  ( -8.519176349317316266, -5.642605341092957971, 34.66089969410670335 ) ) ;
#22128 = CARTESIAN_POINT ( 'NONE',  ( -4.403822897894743349, -11.47974371597207899, 33.17467449705390692 ) ) ;
#22129 = ORIENTED_EDGE ( 'NONE', *, *, #51942, .T. ) ;
#22130 = CARTESIAN_POINT ( 'NONE',  ( -2.307692307692305711, -11.91647553114624181, 32.58852847137148245 ) ) ;
#22131 = EDGE_CURVE ( 'NONE', #63016, #67027, #31596, .T. ) ;
#22132 = EDGE_LOOP ( 'NONE', ( #24283, #43612, #54464, #81921 ) ) ;
#22133 = DIRECTION ( 'NONE',  ( -1.000000000000000000, 0.000000000000000000, -0.000000000000000000 ) ) ;
#22134 = CARTESIAN_POINT ( 'NONE',  ( -3.903846153844716671, -7.500000000000155431, 34.75000000000007105 ) ) ;
#22135 = VERTEX_POINT ( 'NONE', #16311 ) ;
#22136 = EDGE_CURVE ( 'NONE', #42284, #42418, #87872, .T. ) ;
#22137 = CARTESIAN_POINT ( 'NONE',  ( 10.86543903529806698, -11.47946981652013498, 33.17500667209847620 ) ) ;
#22138 = CARTESIAN_POINT ( 'NONE',  ( -14.30769230769242917, -2.379036618888197729, 30.90682066428292885 ) ) ;
#22139 = CARTESIAN_POINT ( 'NONE',  ( 1.134638653673032183, -4.236021600441998380, 33.53823185664189310 ) ) ;
#22140 = CARTESIAN_POINT ( 'NONE',  ( -16.15384615384627409, -4.481592998941358097, 33.73612834414048933 ) ) ;
#22141 = CARTESIAN_POINT ( 'NONE',  ( -10.03846153846153832, -1.926643599941765039, 28.25000000000000000 ) ) ;
#22142 = VECTOR ( 'NONE', #79090, 1000.000000000000227 ) ;
#22143 = ORIENTED_EDGE ( 'NONE', *, *, #19098, .T. ) ;
#22144 = VERTEX_POINT ( 'NONE', #17189 ) ;
#22145 = EDGE_CURVE ( 'NONE', #22188, #35493, #30121, .T. ) ;
#22146 = FACE_BOUND ( 'NONE', #48797, .T. ) ;
#22147 = ORIENTED_EDGE ( 'NONE', *, *, #73999, .F. ) ;
#22148 = CARTESIAN_POINT ( 'NONE',  ( -7.846153846153967493, -5.941354392335915335, 34.76329471203413846 ) ) ;
#22149 = VECTOR ( 'NONE', #59790, 1000.000000000000000 ) ;
#22150 = VECTOR ( 'NONE', #40314, 1000.000000000000114 ) ;
#22151 = CARTESIAN_POINT ( 'NONE',  ( 4.376625695114563008, -11.89424750095246175, 32.13594075562311758 ) ) ;
#22152 = CARTESIAN_POINT ( 'NONE',  ( 0.4615384615384611200, -1.242168528481310874, 33.36296068462461051 ) ) ;
#22153 = CARTESIAN_POINT ( 'NONE',  ( 5.326977388561388693, -4.235687564193446164, 33.53795663066793509 ) ) ;
#22154 = EDGE_LOOP ( 'NONE', ( #84362, #28961 ) ) ;
#22155 = VERTEX_POINT ( 'NONE', #58614 ) ;
#22156 = VERTEX_POINT ( 'NONE', #2771 ) ;
#22157 = CARTESIAN_POINT ( 'NONE',  ( 6.000000000000001776, -8.973038597847269315, 34.52809138561121927 ) ) ;
#22158 = ORIENTED_EDGE ( 'NONE', *, *, #11994, .T. ) ;
#22159 = EDGE_CURVE ( 'NONE', #4801, #40289, #3058, .T. ) ;
#22160 = CYLINDRICAL_SURFACE ( 'NONE', #24389, 0.2500000000000008882 ) ;
#22161 = EDGE_CURVE ( 'NONE', #60044, #37672, #50524, .T. ) ;
#22162 = CARTESIAN_POINT ( 'NONE',  ( 17.07692307692307665, -3.322132147404559976, 32.92929555188717927 ) ) ;
#22163 = B_SPLINE_CURVE_WITH_KNOTS ( 'NONE', 3,
 ( #17658, #11335, #37465, #72588, #38817, #4581, #85226, #32055, #87023, #25296 ),
 .UNSPECIFIED., .F., .F.,
 ( 4, 2, 2, 2, 4 ),
 ( 0.0007817359527651133143, 0.0009771254036996530456, 0.001172514854634192777, 0.001367904305568732291, 0.001563293756503272023 ),
 .UNSPECIFIED. ) ;
#22164 = CARTESIAN_POINT ( 'NONE',  ( 13.45068271796546533, -11.35647404775217595, 33.31231777344666511 ) ) ;
#22165 = ORIENTED_EDGE ( 'NONE', *, *, #17549, .F. ) ;
#22166 = DIRECTION ( 'NONE',  ( -0.000000000000000000, -0.8660254037844399289, -0.4999999999999980016 ) ) ;
#22167 = EDGE_CURVE ( 'NONE', #35719, #70760, #71713, .T. ) ;
#22168 = FACE_OUTER_BOUND ( 'NONE', #44826, .T. ) ;
#22169 = EDGE_CURVE ( 'NONE', #26348, #18634, #18065, .T. ) ;
#22170 = CARTESIAN_POINT ( 'NONE',  ( 4.023155550735848074, -2.494641256782728966, 31.33461815524612959 ) ) ;
#22171 = CARTESIAN_POINT ( 'NONE',  ( -1.384615384615383471, -2.833524468853757305, 32.15551576947925838 ) ) ;
#22172 = ORIENTED_EDGE ( 'NONE', *, *, #81922, .T. ) ;
#22173 = VERTEX_POINT ( 'NONE', #17648 ) ;
#22174 = EDGE_LOOP ( 'NONE', ( #81183, #49059, #74549, #63466 ) ) ;
#22175 = CARTESIAN_POINT ( 'NONE',  ( 0.4615384615384611200, -11.16473453929635440, 33.15142922261926373 ) ) ;
#22176 = VECTOR ( 'NONE', #8585, 1000.000000000000000 ) ;
#22178 = DIRECTION ( 'NONE',  ( -0.000000000000000000, -0.000000000000000000, -1.000000000000000000 ) ) ;
#22177 = CARTESIAN_POINT ( 'NONE',  ( -8.069638789877792817, -6.760086850603066466, 34.69517049084099369 ) ) ;
#22179 = CARTESIAN_POINT ( 'NONE',  ( -17.86947456176635640, -5.915461855592775819, 34.75538340440931506 ) ) ;
#22180 = CARTESIAN_POINT ( 'NONE',  ( -2.177166869458664777, -2.647132371071621471, 31.75357179365173010 ) ) ;
#22181 = DIRECTION ( 'NONE',  ( -0.000000000000000000, -0.5000000000000009992, -0.8660254037844380415 ) ) ;
#22182 = CARTESIAN_POINT ( 'NONE',  ( -6.989159302437057519, -3.322132147404559976, 32.92929555188719348 ) ) ;
#22183 = EDGE_LOOP ( 'NONE', ( #77526, #11521, #60092, #853 ) ) ;
#22184 = CARTESIAN_POINT ( 'NONE',  ( 17.20771351789002424, -11.93129842949672437, 32.56571108434900452 ) ) ;
#22185 = CARTESIAN_POINT ( 'NONE',  ( -0.2114841499001460789, -9.148310452688873440, 34.47095581063188519 ) ) ;
#22186 = CARTESIAN_POINT ( 'NONE',  ( -11.00641025641025550, -3.499999999999999556, 29.75000000000000355 ) ) ;
#22187 = LINE ( 'NONE', #83457, #36733 ) ;
#22188 = VERTEX_POINT ( 'NONE', #45551 ) ;
#22189 = CARTESIAN_POINT ( 'NONE',  ( -18.22348494372394967, -8.496056993536548418, 34.65000542017679663 ) ) ;
#22190 = ORIENTED_EDGE ( 'NONE', *, *, #27955, .F. ) ;
#22191 = FACE_BOUND ( 'NONE', #32289, .T. ) ;
#22192 = DIRECTION ( 'NONE',  ( -1.000000000000000000, -0.000000000000000000, -0.000000000000000000 ) ) ;
#22193 = CYLINDRICAL_SURFACE ( 'NONE', #83732, 0.2499999999999995559 ) ;
#22194 = CARTESIAN_POINT ( 'NONE',  ( 9.692307692307695177, -13.95598074871891292, 31.83374038241031911 ) ) ;
#22195 = VERTEX_POINT ( 'NONE', #23937 ) ;
#22196 = CARTESIAN_POINT ( 'NONE',  ( 11.53846153846153832, -10.67929555188718282, 33.92786785259544047 ) ) ;
#22197 = CARTESIAN_POINT ( 'NONE',  ( 15.45378207486262667, -2.308499170217967134, 30.53291367094873721 ) ) ;
#22198 = CARTESIAN_POINT ( 'NONE',  ( 8.769230769230645706, -2.379036618888197729, 30.90682066428292885 ) ) ;
#22199 = CARTESIAN_POINT ( 'NONE',  ( -17.93393266664992325, -12.62096338111211757, 30.90682066428152908 ) ) ;
#22200 = ORIENTED_EDGE ( 'NONE', *, *, #85493, .T. ) ;
#22201 = DIRECTION ( 'NONE',  ( -0.000000000000000000, -0.1736481776669307198, -0.9848077530122080203 ) ) ;
#22202 = EDGE_LOOP ( 'NONE', ( #45301, #45243, #25848, #5142 ) ) ;
#22204 = ORIENTED_EDGE ( 'NONE', *, *, #13906, .F. ) ;
#22203 = CARTESIAN_POINT ( 'NONE',  ( -23.50000000000000000, 1.250000000000005329, 30.36437827766147279 ) ) ;
#22205 = CARTESIAN_POINT ( 'NONE',  ( -9.019230769230768274, -7.566083408709835645, 34.74999999999999289 ) ) ;
#22206 = DIRECTION ( 'NONE',  ( -1.000000000000000000, -0.000000000000000000, -0.000000000000000000 ) ) ;
#22207 = CARTESIAN_POINT ( 'NONE',  ( 7.622668921589517588, -10.23692288466677880, 34.23039457007281072 ) ) ;
#22208 = ADVANCED_FACE ( 'NONE', ( #86562 ), #10887, .F. ) ;
#22209 = CARTESIAN_POINT ( 'NONE',  ( -12.52680846209478460, -11.06231777344662781, 33.60647404775220082 ) ) ;
#22211 = CARTESIAN_POINT ( 'NONE',  ( -11.66860950819323328, -9.504002272028875709, 34.60269587691767867 ) ) ;
#22210 = DIRECTION ( 'NONE',  ( -0.000000000000000000, -0.6427876096865404731, -0.7660444431189771253 ) ) ;
#22212 = CARTESIAN_POINT ( 'NONE',  ( 12.33092810191393518, -7.722926236386453702, 34.74524107206102030 ) ) ;
#22213 = CARTESIAN_POINT ( 'NONE',  ( 2.750000000000001776, -7.499999999999984013, 23.21875000000000000 ) ) ;
#22214 = APPLICATION_CONTEXT ( 'automotive_design' ) ;
#22215 = ORIENTED_EDGE ( 'NONE', *, *, #77394, .T. ) ;
#22216 = CIRCLE ( 'NONE', #85474, 0.2500000000000002220 ) ;
#22217 = CARTESIAN_POINT ( 'NONE',  ( -0.7115151924808155171, -5.728515186090277211, 34.42611988154120439 ) ) ;
#22218 = VERTEX_POINT ( 'NONE', #18094 ) ;
#22219 = ORIENTED_EDGE ( 'NONE', *, *, #16353, .F. ) ;
#22220 = CARTESIAN_POINT ( 'NONE',  ( 11.53846153846153832, -11.69971097300155272, 32.46337939537588113 ) ) ;
#22221 = EDGE_LOOP ( 'NONE', ( #24917, #50963, #73975, #87218 ) ) ;
#22222 = DIRECTION ( 'NONE',  ( -1.000000000000000000, 0.000000000000000000, 0.000000000000000000 ) ) ;
#22223 = CARTESIAN_POINT ( 'NONE',  ( -12.46153846153846168, -12.09954503811598769, 35.62045528018868623 ) ) ;
#22224 = ADVANCED_FACE ( 'NONE', ( #23067 ), #53645, .T. ) ;
#22225 = CARTESIAN_POINT ( 'NONE',  ( -7.846153846153844924, -1.509761064869970415, 31.06009739812519044 ) ) ;
#22226 = LINE ( 'NONE', #36629, #61761 ) ;
#22227 = CARTESIAN_POINT ( 'NONE',  ( 6.000000000000001776, -8.164416787775445883, 34.95778746994557906 ) ) ;
#22228 = CARTESIAN_POINT ( 'NONE',  ( 7.173131234715237170, -11.28795663066794219, 33.01431243580653785 ) ) ;
#22229 = CARTESIAN_POINT ( 'NONE',  ( 13.38461538461570122, -2.255955759149395501, 30.00000000000324363 ) ) ;
#22230 = CYLINDRICAL_SURFACE ( 'NONE', #29026, 0.2499999999999995559 ) ;
#22231 = CARTESIAN_POINT ( 'NONE',  ( 17.86985279056177944, -11.93770438780619259, 32.05411857736982029 ) ) ;
#22232 = CARTESIAN_POINT ( 'NONE',  ( 8.068933387422255521, -2.847695495035523994, 31.58253572463339509 ) ) ;
#22233 = DIRECTION ( 'NONE',  ( 1.000000000000000000, 0.000000000000000000, 0.000000000000000000 ) ) ;
#22235 = EDGE_CURVE ( 'NONE', #47910, #64424, #55698, .T. ) ;
#22234 = ORIENTED_EDGE ( 'NONE', *, *, #71855, .F. ) ;
#22236 = VERTEX_POINT ( 'NONE', #33817 ) ;
#22237 = CARTESIAN_POINT ( 'NONE',  ( 3.007284306204898172, -10.97335522853832579, 33.68706563782419749 ) ) ;
#22238 = CARTESIAN_POINT ( 'NONE',  ( -3.099977422944445671, -2.729792928343269587, 31.24908615093345077 ) ) ;
#22239 = CARTESIAN_POINT ( 'NONE',  ( 12.68431800280686694, -10.81320215134717344, 33.49497208177562868 ) ) ;
#22240 = VERTEX_POINT ( 'NONE', #6784 ) ;
#22241 = B_SPLINE_CURVE_WITH_KNOTS ( 'NONE', 3,
 ( #51729, #64804, #85103, #30153, #58947, #31484, #85542, #23384, #78328, #37791 ),
 .UNSPECIFIED., .F., .F.,
 ( 4, 2, 2, 2, 4 ),
 ( 0.000000000000000000, 0.0001954311564186860071, 0.0003908623128373720141, 0.0005862934692560580483, 0.0007817246256747440282 ),
 .UNSPECIFIED. ) ;
#22242 = EDGE_CURVE ( 'NONE', #45697, #22109, #66400, .T. ) ;
#22243 = DIRECTION ( 'NONE',  ( -0.000000000000000000, -0.8660254037844397068, -0.4999999999999978906 ) ) ;
#22244 = CARTESIAN_POINT ( 'NONE',  ( -17.07692307692277112, -2.506253911140615021, 30.00000000000323297 ) ) ;
#22245 = B_SPLINE_CURVE_WITH_KNOTS ( 'NONE', 3,
 ( #65068, #42604, #8372, #35845, #29099, #84043, #49788, #77264, #15573, #79494 ),
 .UNSPECIFIED., .F., .F.,
 ( 4, 2, 2, 2, 4 ),
 ( 0.000000000000000000, 0.0001954339857564081520, 0.0003908679715128163040, 0.0005863019572692244018, 0.0007817359430256326080 ),
 .UNSPECIFIED. ) ;
#22246 = VECTOR ( 'NONE', #46352, 1000.000000000000227 ) ;
#22247 = CARTESIAN_POINT ( 'NONE',  ( 25.00000000000000711, -9.999999999999957367, 13.00000000000000178 ) ) ;
#22248 = EDGE_LOOP ( 'NONE', ( #58696, #86216, #22909, #17075 ) ) ;
#22249 = EDGE_CURVE ( 'NONE', #32170, #79550, #81574, .T. ) ;
#22250 = CARTESIAN_POINT ( 'NONE',  ( 0.4615384615384611200, -5.557115091759785130, 34.35708131394839171 ) ) ;
#22251 = ORIENTED_EDGE ( 'NONE', *, *, #64648, .T. ) ;
#22252 = DIRECTION ( 'NONE',  ( -1.000000000000000000, -0.000000000000000000, -0.000000000000000000 ) ) ;
#22253 = EDGE_CURVE ( 'NONE', #72117, #29336, #34175, .T. ) ;
#22254 = CARTESIAN_POINT ( 'NONE',  ( -17.07692307692319744, -3.643525952248796163, 33.31231777344771672 ) ) ;
#22255 = CARTESIAN_POINT ( 'NONE',  ( -13.38461538461538325, -2.499999999999998668, 29.50000000000001066 ) ) ;
#22256 = EDGE_CURVE ( 'NONE', #53989, #79559, #29877, .T. ) ;
#22257 = CARTESIAN_POINT ( 'NONE',  ( 1.134638640566794976, -8.347322224742351082, 34.93158281831414769 ) ) ;
#22258 = CARTESIAN_POINT ( 'NONE',  ( 18.06525513951284267, -8.656820664281605460, 34.87096338111211224 ) ) ;
#22259 = ORIENTED_EDGE ( 'NONE', *, *, #85512, .T. ) ;
#22260 = EDGE_LOOP ( 'NONE', ( #24263, #11826, #58781, #51664 ) ) ;
#22261 = EDGE_LOOP ( 'NONE', ( #42222, #38678, #18372, #21411, #55351, #88422 ) ) ;
#22262 = VECTOR ( 'NONE', #82450, 1000.000000000000000 ) ;
#22263 = ADVANCED_FACE ( 'NONE', ( #32938 ), #60844, .F. ) ;
#22264 = CARTESIAN_POINT ( 'NONE',  ( -17.32689980786543060, -10.66389620160130036, 33.62221079203477103 ) ) ;
#22265 = CARTESIAN_POINT ( 'NONE',  ( 16.08776377448601735, -5.471508081941601986, 34.59228464037088457 ) ) ;
#22266 = FACE_OUTER_BOUND ( 'NONE', #82543, .T. ) ;
#22267 = EDGE_CURVE ( 'NONE', #4867, #7553, #78191, .T. ) ;
#22268 = CARTESIAN_POINT ( 'NONE',  ( 17.01165307636676260, -10.33852847137145048, 34.16647553114627556 ) ) ;
#22269 = B_SPLINE_CURVE_WITH_KNOTS ( 'NONE', 3,
 ( #49255, #75838, #47919, #14139, #69522, #54668, #1067, #56005, #6936, #83495 ),
 .UNSPECIFIED., .F., .F.,
 ( 4, 2, 2, 2, 4 ),
 ( 0.000000000000000000, 0.0001954311564186868202, 0.0003908623128373736404, 0.0005862934692560604335, 0.0007817246256747472808 ),
 .UNSPECIFIED. ) ;
#22270 = CARTESIAN_POINT ( 'NONE',  ( 17.74997677577853850, -2.985938066672154889, 32.43141759479405550 ) ) ;
#22271 = ADVANCED_FACE ( 'NONE', ( #21185 ), #83346, .F. ) ;
#22272 = CARTESIAN_POINT ( 'NONE',  ( 4.153846153846154188, -2.486705287966279876, 31.30864560766543647 ) ) ;
#22273 = EDGE_LOOP ( 'NONE', ( #11062, #19944, #52099, #21950, #16369, #27894, #86581, #74895 ) ) ;
#22274 = B_SPLINE_CURVE_WITH_KNOTS ( 'NONE', 3,
 ( #26468, #66562, #53927, #86860, #25124, #75100, #74656, #81416, #12943, #26018 ),
 .UNSPECIFIED., .F., .F.,
 ( 4, 2, 2, 2, 4 ),
 ( 0.0007817246256747452209, 0.0009771112852218887673, 0.001172497944769032531, 0.001367884604316176294, 0.001563271263863319840 ),
 .UNSPECIFIED. ) ;
#22275 = VERTEX_POINT ( 'NONE', #28845 ) ;
#22276 = ORIENTED_EDGE ( 'NONE', *, *, #73716, .F. ) ;
#22278 = ORIENTED_EDGE ( 'NONE', *, *, #8956, .T. ) ;
#22277 = CARTESIAN_POINT ( 'NONE',  ( 3.903869422903798903, -2.779195860258149686, 31.39871582349837453 ) ) ;
#22280 = PLANE ( 'NONE',  #24685 ) ;
#22279 = CARTESIAN_POINT ( 'NONE',  ( -9.692307692307812417, -9.442884908241554243, 34.35708131394783038 ) ) ;
#22281 = CARTESIAN_POINT ( 'NONE',  ( 2.320192649118979489E-14, -11.25000000000000000, 24.78125000000000000 ) ) ;
#22282 = EDGE_LOOP ( 'NONE', ( #15669, #66769, #77324, #13741 ) ) ;
#22283 = ADVANCED_FACE ( 'NONE', ( #42805 ), #55858, .F. ) ;
#22284 = ORIENTED_EDGE ( 'NONE', *, *, #10156, .T. ) ;
#22285 = CARTESIAN_POINT ( 'NONE',  ( 14.30769230769231015, -1.242168528481310874, 33.36296068462461051 ) ) ;
#22286 = VERTEX_POINT ( 'NONE', #34259 ) ;
#22287 = FACE_BOUND ( 'NONE', #47845, .T. ) ;
#22288 = CARTESIAN_POINT ( 'NONE',  ( 5.011653076366756387, -5.094484230520674117, 34.41647553114621161 ) ) ;
#22289 = CARTESIAN_POINT ( 'NONE',  ( 0.000000000000000000, -11.00000000000000000, 29.75000000000000355 ) ) ;
#22290 = ORIENTED_EDGE ( 'NONE', *, *, #55272, .F. ) ;
#22291 = EDGE_CURVE ( 'NONE', #66107, #2951, #35299, .T. ) ;
#22292 = CARTESIAN_POINT ( 'NONE',  ( 16.37685750545900376, -11.24521262558773493, 33.06293181088029343 ) ) ;
#22293 = CARTESIAN_POINT ( 'NONE',  ( 16.15384615384615330, -8.318370150425687726, 35.83090037661290239 ) ) ;
#22294 = DIRECTION ( 'NONE',  ( -0.000000000000000000, 0.000000000000000000, 1.000000000000000000 ) ) ;
#22295 = DIRECTION ( 'NONE',  ( 1.000000000000000000, 0.000000000000000000, 0.000000000000000000 ) ) ;
#22296 = CARTESIAN_POINT ( 'NONE',  ( 4.403791672194295792, -3.202959910592335202, 32.30730279482227019 ) ) ;
#22297 = ORIENTED_EDGE ( 'NONE', *, *, #6437, .T. ) ;
#22298 = AXIS2_PLACEMENT_3D ( 'NONE', #66635, #34172, #75597 ) ;
#22299 = CARTESIAN_POINT ( 'NONE',  ( -7.173100160369889622, -11.37209801155882971, 32.91403422569032955 ) ) ;
#22300 = CARTESIAN_POINT ( 'NONE',  ( 2.084765348785460937, -11.98009711892699691, 32.48740034544075428 ) ) ;
#22301 = CARTESIAN_POINT ( 'NONE',  ( -17.07692307692307665, -2.517432740324522911, 35.29906147534542527 ) ) ;
#22302 = CARTESIAN_POINT ( 'NONE',  ( 1.384615384615386802, -13.75783147151868846, 33.36296068462461051 ) ) ;
#22303 = DIRECTION ( 'NONE',  ( 0.000000000000000000, 0.3420201433256641055, -0.9396926207859100932 ) ) ;
#22304 = EDGE_CURVE ( 'NONE', #82752, #34884, #481, .T. ) ;
#22305 = CARTESIAN_POINT ( 'NONE',  ( -13.25408994638174498, -12.50538340440932394, 31.33453814440721885 ) ) ;
#22307 = DIRECTION ( 'NONE',  ( 0.000000000000000000, 0.7660444431189807890, 0.6427876096865361433 ) ) ;
#22306 = CARTESIAN_POINT ( 'NONE',  ( 13.16113044089144068, -11.89387501736622710, 32.13663884655806413 ) ) ;
#22308 = CARTESIAN_POINT ( 'NONE',  ( 5.299935921016470708, -9.172514111537584114, 34.72667873470787470 ) ) ;
#22310 = CARTESIAN_POINT ( 'NONE',  ( -6.130147209438219669, -5.195881422630167279, 34.18770438780618548 ) ) ;
#22309 = CARTESIAN_POINT ( 'NONE',  ( 8.769230769230768274, -9.780366693483667717, 34.19971097300155094 ) ) ;
#22311 = CARTESIAN_POINT ( 'NONE',  ( -5.776988648387149539, -12.39991518177334129, 30.74647679643404530 ) ) ;
#22312 = CARTESIAN_POINT ( 'NONE',  ( 1.901340078031349856, -5.512252781505337929, 24.06063170625849423 ) ) ;
#22314 = EDGE_CURVE ( 'NONE', #9486, #67330, #55417, .T. ) ;
#22313 = EDGE_LOOP ( 'NONE', ( #38502, #12865, #1425, #764 ) ) ;
#22315 = CARTESIAN_POINT ( 'NONE',  ( -1.196977438190478971, -3.948374222870081773, 14.00000000000000000 ) ) ;
#22316 = VERTEX_POINT ( 'NONE', #63498 ) ;
#22317 = EDGE_CURVE ( 'NONE', #55756, #5035, #35194, .T. ) ;
#22318 = LINE ( 'NONE', #49781, #42123 ) ;
#22319 = ORIENTED_EDGE ( 'NONE', *, *, #69620, .F. ) ;
#22320 = CARTESIAN_POINT ( 'NONE',  ( 17.75002326905764960, -12.17611988154120795, 31.52148481390971213 ) ) ;
#22321 = CARTESIAN_POINT ( 'NONE',  ( 17.32697749683652688, -2.920487667080175154, 32.31805714834170828 ) ) ;
#22322 = EDGE_LOOP ( 'NONE', ( #45493, #67329 ) ) ;
#22323 = CARTESIAN_POINT ( 'NONE',  ( -7.846153846153965716, -6.026961402154118019, 34.52809138561165270 ) ) ;
#22324 = CARTESIAN_POINT ( 'NONE',  ( 1.901340078031349856, -5.512252781505337929, 25.31063170625848713 ) ) ;
#22325 = DIRECTION ( 'NONE',  ( 0.000000000000000000, 0.9848077530122072432, -0.1736481776669354937 ) ) ;
#22326 = DIRECTION ( 'NONE',  ( -1.000000000000000000, -0.000000000000000000, -0.000000000000000000 ) ) ;
#22327 = CYLINDRICAL_SURFACE ( 'NONE', #21604, 0.2499999999999993616 ) ;
#22328 = EDGE_CURVE ( 'NONE', #13064, #59335, #2952, .T. ) ;
#22329 = CARTESIAN_POINT ( 'NONE',  ( -5.300408020647024543, -12.44517049084099725, 30.48991314939691932 ) ) ;
#22330 = CARTESIAN_POINT ( 'NONE',  ( 15.48076923077066702, -7.500000000000155431, 34.75000000000007105 ) ) ;
#22331 = CARTESIAN_POINT ( 'NONE',  ( 4.946775867484856093, -8.587444163452046197, 34.63053765926554206 ) ) ;
#22332 = CARTESIAN_POINT ( 'NONE',  ( -3.749999999999988454, -9.053300858899127945, 18.76562500000000000 ) ) ;
#22333 = AXIS2_PLACEMENT_3D ( 'NONE', #57191, #15330, #22520 ) ;
#22334 = CARTESIAN_POINT ( 'NONE',  ( 11.40777093535123043, -5.496505350115501010, 34.60290016733514307 ) ) ;
#22335 = CARTESIAN_POINT ( 'NONE',  ( -6.223484924564328225, -3.562934362175799841, 33.22335522853832401 ) ) ;
#22336 = CARTESIAN_POINT ( 'NONE',  ( -7.846153846153844924, -1.117168528481311540, 33.14645433367849847 ) ) ;
#22337 = CARTESIAN_POINT ( 'NONE',  ( 2.651650429449539104, -4.848349570550432475, 18.06250000000000355 ) ) ;
#22338 = B_SPLINE_CURVE_WITH_KNOTS ( 'NONE', 3,
 ( #84012, #77231, #2019, #58283, #52416, #39374, #72693, #80808, #86683, #65928 ),
 .UNSPECIFIED., .F., .F.,
 ( 4, 2, 2, 2, 4 ),
 ( 0.000000000000000000, 0.0001954339857564079352, 0.0003908679715128158703, 0.0005863019572692237513, 0.0007817359430256317406 ),
 .UNSPECIFIED. ) ;
#22339 = DIRECTION ( 'NONE',  ( 0.000000000000000000, 0.7660444431189822323, -0.6427876096865344779 ) ) ;
#22340 = EDGE_LOOP ( 'NONE', ( #16952, #46080 ) ) ;
#22341 = DIRECTION ( 'NONE',  ( -0.000000000000000000, -0.1736481776669307198, -0.9848077530122080203 ) ) ;
#22342 = CARTESIAN_POINT ( 'NONE',  ( -11.31568199719312773, -8.496831190052096971, 34.64984203495476578 ) ) ;
#22343 = CARTESIAN_POINT ( 'NONE',  ( 23.00000000000000000, -4.249999999999998224, 27.25000000000000000 ) ) ;
#22344 = CARTESIAN_POINT ( 'NONE',  ( -14.30769230769242739, -11.94971097300221174, 32.03036669348237098 ) ) ;
#22345 = EDGE_CURVE ( 'NONE', #31805, #59859, #69383, .T. ) ;
#22346 = CARTESIAN_POINT ( 'NONE',  ( -19.50000000000000000, -3.499999999999999556, 29.75000000000000355 ) ) ;
#22347 = DIRECTION ( 'NONE',  ( -0.000000000000000000, 0.9396926207859092051, -0.3420201433256662704 ) ) ;
#22348 = B_SPLINE_CURVE_WITH_KNOTS ( 'NONE', 3,
 ( #20315, #67168, #82021, #60846, #53647, #34262, #61721, #38, #19420, #20746 ),
 .UNSPECIFIED., .F., .F.,
 ( 4, 2, 2, 2, 4 ),
 ( 0.000000000000000000, 0.0001954311564186871184, 0.0003908623128373742367, 0.0005862934692560614093, 0.0007817246256747484735 ),
 .UNSPECIFIED. ) ;
#22349 = LINE ( 'NONE', #15596, #64861 ) ;
#22350 = EDGE_LOOP ( 'NONE', ( #61326, #16653 ) ) ;
#22351 = VERTEX_POINT ( 'NONE', #82466 ) ;
#22352 = ORIENTED_EDGE ( 'NONE', *, *, #11365, .F. ) ;
#22353 = CARTESIAN_POINT ( 'NONE',  ( -9.626239341305252495, -3.050289026998446840, 32.03036669348366416 ) ) ;
#22354 = CARTESIAN_POINT ( 'NONE',  ( -3.903900635498011695, -3.202959910592335202, 32.30730279482228440 ) ) ;
#22355 = CARTESIAN_POINT ( 'NONE',  ( 6.923076923076800782, -3.083524468854526912, 32.58852847137268327 ) ) ;
#22356 = CARTESIAN_POINT ( 'NONE',  ( 1.449870955891410462, -11.94971097300157403, 32.03036669348361443 ) ) ;
#22357 = CARTESIAN_POINT ( 'NONE',  ( -5.076923076923197442, -6.879047030192662504, 34.71129190930017927 ) ) ;
#22358 = VECTOR ( 'NONE', #59218, 1000.000000000000000 ) ;
#22359 = ORIENTED_EDGE ( 'NONE', *, *, #57218, .T. ) ;
#22360 = DIRECTION ( 'NONE',  ( 0.000000000000000000, 0.4999999999999960032, -0.8660254037844410391 ) ) ;
#22361 = ORIENTED_EDGE ( 'NONE', *, *, #55475, .F. ) ;
#22362 = B_SPLINE_CURVE_WITH_KNOTS ( 'NONE', 3,
 ( #27604, #45315, #39030, #11547, #88889, #17862 ),
 .UNSPECIFIED., .F., .F.,
 ( 4, 2, 4 ),
 ( 0.0003909569690057790748, 0.0005862646681846022355, 0.0007815723673634252877 ),
 .UNSPECIFIED. ) ;
#22363 = EDGE_LOOP ( 'NONE', ( #12663, #76235 ) ) ;
#22364 = EDGE_CURVE ( 'NONE', #48597, #67515, #47081, .T. ) ;
#22366 = ORIENTED_EDGE ( 'NONE', *, *, #68440, .T. ) ;
#22365 = CARTESIAN_POINT ( 'NONE',  ( 4.376858997939547358, -12.38742843783360748, 31.66772728687926985 ) ) ;
#22367 = DIRECTION ( 'NONE',  ( -0.000000000000000000, 0.5000000000000011102, -0.8660254037844381525 ) ) ;
#22368 = CARTESIAN_POINT ( 'NONE',  ( -10.68146802634049308, -4.786620604624113540, 33.94971097300155805 ) ) ;
#22369 = EDGE_CURVE ( 'NONE', #41563, #52736, #14783, .T. ) ;
#22370 = DIRECTION ( 'NONE',  ( 0.000000000000000000, 0.000000000000000000, -1.000000000000000000 ) ) ;
#22371 = EDGE_CURVE ( 'NONE', #37367, #35211, #14882, .T. ) ;
#22372 = CARTESIAN_POINT ( 'NONE',  ( -12.39634447975510412, -2.506253911140448487, 29.99999999999988631 ) ) ;
#22373 = ORIENTED_EDGE ( 'NONE', *, *, #31738, .T. ) ;
#22374 = ORIENTED_EDGE ( 'NONE', *, *, #26438, .F. ) ;
#22375 = ORIENTED_EDGE ( 'NONE', *, *, #73003, .T. ) ;
#22376 = CARTESIAN_POINT ( 'NONE',  ( -6.700297254098856570, -3.020022701398814569, 32.48759521482552515 ) ) ;
#22378 = ORIENTED_EDGE ( 'NONE', *, *, #49714, .T. ) ;
#22377 = CARTESIAN_POINT ( 'NONE',  ( 11.78840694783958298, -5.766571408460171355, 34.70601412856602508 ) ) ;
#22379 = EDGE_CURVE ( 'NONE', #72548, #63925, #77087, .T. ) ;
#22380 = CARTESIAN_POINT ( 'NONE',  ( 1.384615384615386802, -8.973038597847269315, 34.52809138561121927 ) ) ;
#22381 = CARTESIAN_POINT ( 'NONE',  ( 4.480769230769229061, -7.500000000000000000, 29.75000000000000355 ) ) ;
#22382 = VECTOR ( 'NONE', #37687, 1000.000000000000227 ) ;
#22383 = CARTESIAN_POINT ( 'NONE',  ( 2.530705151785704654, -9.172514111537584114, 34.72667873470787470 ) ) ;
#22384 = VERTEX_POINT ( 'NONE', #16637 ) ;
#22385 = CARTESIAN_POINT ( 'NONE',  ( -8.769230769230892619, -5.941354392335915335, 34.76329471203413846 ) ) ;
#22386 = EDGE_CURVE ( 'NONE', #41905, #72231, #19021, .T. ) ;
#22387 = FACE_OUTER_BOUND ( 'NONE', #87508, .T. ) ;
#22388 = ORIENTED_EDGE ( 'NONE', *, *, #20221, .T. ) ;
#22389 = FACE_BOUND ( 'NONE', #7673, .T. ) ;
#22390 = CARTESIAN_POINT ( 'NONE',  ( -11.60454391782167249, -11.35647404775217595, 33.31231777344666511 ) ) ;
#22391 = CARTESIAN_POINT ( 'NONE',  ( 2.307692307692309264, -11.35647404775217417, 33.31231777344666511 ) ) ;
#22392 = CARTESIAN_POINT ( 'NONE',  ( 9.692307692307695177, -2.721908614388771852, 31.22303859784724978 ) ) ;
#22394 = CARTESIAN_POINT ( 'NONE',  ( 15.16551929899514484, -2.255955759149247619, 30.00000000000013856 ) ) ;
#22393 = DIRECTION ( 'NONE',  ( 0.000000000000000000, 0.000000000000000000, 1.000000000000000000 ) ) ;
#22395 = FACE_OUTER_BOUND ( 'NONE', #83525, .T. ) ;
#22396 = CARTESIAN_POINT ( 'NONE',  ( -16.02305434602136103, -8.999086150933472084, 34.52020707165672064 ) ) ;
#22397 = ORIENTED_EDGE ( 'NONE', *, *, #35675, .F. ) ;
#22398 = CYLINDRICAL_SURFACE ( 'NONE', #86415, 0.2499999999999995559 ) ;
#22399 = B_SPLINE_CURVE_WITH_KNOTS ( 'NONE', 3,
 ( #12859, #47967, #61045, #75450, #14189, #88547, #55170, #26824, #82668, #75018 ),
 .UNSPECIFIED., .F., .F.,
 ( 4, 2, 2, 2, 4 ),
 ( 0.000000000000000000, 0.0001954311564186870913, 0.0003908623128373741825, 0.0005862934692560613009, 0.0007817246256747483650 ),
 .UNSPECIFIED. ) ;
#22400 = CIRCLE ( 'NONE', #15211, 4.000000000000000000 ) ;
#22401 = PLANE ( 'NONE',  #59441 ) ;
#22402 = ORIENTED_EDGE ( 'NONE', *, *, #25917, .T. ) ;
#22403 = CARTESIAN_POINT ( 'NONE',  ( 7.053602624840485724, -2.882268652242224505, 31.66798894389554064 ) ) ;
#22404 = CARTESIAN_POINT ( 'NONE',  ( 8.639083559792549494, -3.285722584762969856, 32.44110544564090759 ) ) ;
#22405 = LINE ( 'NONE', #83683, #52595 ) ;
#22406 = CARTESIAN_POINT ( 'NONE',  ( -7.596208436775802930, -10.92531984108285670, 33.72920026020278073 ) ) ;
#22407 = FACE_OUTER_BOUND ( 'NONE', #46193, .T. ) ;
#22408 = CARTESIAN_POINT ( 'NONE',  ( 4.284371855609715674, -10.19071101563364401, 33.96452234770658407 ) ) ;
#22409 = FACE_BOUND ( 'NONE', #64098, .T. ) ;
#22411 = CARTESIAN_POINT ( 'NONE',  ( -19.50000000000000000, -3.499999999999999556, 29.75000000000000355 ) ) ;
#22410 = CARTESIAN_POINT ( 'NONE',  ( -2.530618525208451874, -6.503392248772476236, 34.64988816332204635 ) ) ;
#22412 = DIRECTION ( 'NONE',  ( 0.000000000000000000, 0.000000000000000000, -1.000000000000000000 ) ) ;
#22414 = DIRECTION ( 'NONE',  ( -0.000000000000000000, 0.7660444431189791237, -0.6427876096865379196 ) ) ;
#22413 = CYLINDRICAL_SURFACE ( 'NONE', #50130, 0.2500000000000008882 ) ;
#22415 = CARTESIAN_POINT ( 'NONE',  ( -3.230769230769229949, -13.37000171582298513, 34.34916445242398453 ) ) ;
#22416 = CARTESIAN_POINT ( 'NONE',  ( -3.749999999999996447, -7.561099074964554134, 22.34188170625849068 ) ) ;
#22417 = EDGE_LOOP ( 'NONE', ( #69569, #83697 ) ) ;
#22418 = ADVANCED_FACE ( 'NONE', ( #51735 ), #4004, .F. ) ;
#22419 = ORIENTED_EDGE ( 'NONE', *, *, #78418, .T. ) ;
#22420 = CYLINDRICAL_SURFACE ( 'NONE', #88114, 0.2500000000000012212 ) ;
#22421 = VECTOR ( 'NONE', #6273, 1000.000000000000114 ) ;
#22422 = CARTESIAN_POINT ( 'NONE',  ( -12.39547112818838670, -6.343179335718452272, 34.87096338111212646 ) ) ;
#22423 = CARTESIAN_POINT ( 'NONE',  ( -7.623141002060450866, -11.43677907613345113, 33.22367315496201456 ) ) ;
#22424 = DIRECTION ( 'NONE',  ( 0.000000000000000000, 0.3420201433256641055, -0.9396926207859100932 ) ) ;
#22425 = CARTESIAN_POINT ( 'NONE',  ( -17.07692307692319744, -6.879047030192662504, 34.71129190930017927 ) ) ;
#22426 = CARTESIAN_POINT ( 'NONE',  ( -3.775308065498766297, -6.007798216065450170, 19.92000670625849068 ) ) ;
#22427 = CARTESIAN_POINT ( 'NONE',  ( 11.53846153846153832, -2.486705287966279876, 31.30864560766543647 ) ) ;
#22428 = CARTESIAN_POINT ( 'NONE',  ( 18.06525557127601900, -3.300289026998473929, 32.46337939537591666 ) ) ;
#22429 = VECTOR ( 'NONE', #42731, 1000.000000000000227 ) ;
#22430 = EDGE_CURVE ( 'NONE', #83085, #47709, #10403, .T. ) ;
#22431 = CARTESIAN_POINT ( 'NONE',  ( 6.250054419913453785, -4.074993327901525575, 33.72946981652012255 ) ) ;
#22432 = CARTESIAN_POINT ( 'NONE',  ( -1.450698795571264021, -12.37446782046654192, 30.86335684631486487 ) ) ;
#22433 = CARTESIAN_POINT ( 'NONE',  ( -19.50000000000000000, -3.499999999999999556, 29.75000000000000355 ) ) ;
#22434 = CARTESIAN_POINT ( 'NONE',  ( 3.903822916553187028, -10.76384336483936011, 33.53834819971076087 ) ) ;
#22435 = DIRECTION ( 'NONE',  ( -0.000000000000000000, -0.3420201433256694346, -0.9396926207859080948 ) ) ;
#22436 = EDGE_CURVE ( 'NONE', #22716, #59465, #17087, .T. ) ;
#22437 = CARTESIAN_POINT ( 'NONE',  ( 14.30769230769231015, -6.386643153685126251, 34.62446782046654192 ) ) ;
#22438 = ORIENTED_EDGE ( 'NONE', *, *, #8573, .T. ) ;
#22439 = CARTESIAN_POINT ( 'NONE',  ( 2.307692307692186251, -3.643525952248796163, 33.31231777344771672 ) ) ;
#22440 = CARTESIAN_POINT ( 'NONE',  ( 7.716005876422150855, -5.070767119584671079, 34.40440758774516183 ) ) ;
#22441 = CARTESIAN_POINT ( 'NONE',  ( 1.901340078031373171, -9.487747218494639867, 19.87686829374151287 ) ) ;
#22442 = FACE_OUTER_BOUND ( 'NONE', #28458, .T. ) ;
#22443 = CARTESIAN_POINT ( 'NONE',  ( -15.90390074446811042, -2.589246495874658827, 31.60778113518102828 ) ) ;
#22444 = ORIENTED_EDGE ( 'NONE', *, *, #14227, .T. ) ;
#22445 = CARTESIAN_POINT ( 'NONE',  ( -9.942330916529147800, -5.765609946408404518, 34.70566812827425451 ) ) ;
#22447 = ORIENTED_EDGE ( 'NONE', *, *, #20649, .F. ) ;
#22446 = CARTESIAN_POINT ( 'NONE',  ( 12.33139125210024112, -6.001485441113819874, 34.52039167877662607 ) ) ;
#22448 = CARTESIAN_POINT ( 'NONE',  ( 7.846153846153725020, -3.835265460704628371, 33.15142922262033665 ) ) ;
#22449 = CARTESIAN_POINT ( 'NONE',  ( -9.469528023329626620, -5.827830569534417471, 34.72679350104403539 ) ) ;
#22450 = EDGE_CURVE ( 'NONE', #20857, #55599, #43732, .T. ) ;
#22451 = EDGE_LOOP ( 'NONE', ( #36589, #43977, #80326, #72907 ) ) ;
#22452 = CARTESIAN_POINT ( 'NONE',  ( -13.38461538461538325, -2.538708090699994813, 30.37095296980875503 ) ) ;
#22453 = CARTESIAN_POINT ( 'NONE',  ( -13.60754160213153163, -3.105860786376062332, 32.13614157043599562 ) ) ;
#22454 = VERTEX_POINT ( 'NONE', #73828 ) ;
#22455 = CARTESIAN_POINT ( 'NONE',  ( -12.52680846209478460, -2.379036618887870436, 30.90682066428147934 ) ) ;
#22456 = EDGE_CURVE ( 'NONE', #32510, #5283, #63013, .T. ) ;
#22457 = EDGE_CURVE ( 'NONE', #13929, #1333, #72920, .T. ) ;
#22458 = CARTESIAN_POINT ( 'NONE',  ( 5.300298562695495264, -2.251407671071270489, 29.88021292934942252 ) ) ;
#22459 = AXIS2_PLACEMENT_3D ( 'NONE', #11911, #31280, #32609 ) ;
#22460 = CARTESIAN_POINT ( 'NONE',  ( -1.384615384615505151, -12.46129190930018460, 30.37095296980731973 ) ) ;
#22461 = ORIENTED_EDGE ( 'NONE', *, *, #55685, .T. ) ;
#22462 = ORIENTED_EDGE ( 'NONE', *, *, #27265, .T. ) ;
#22463 = EDGE_CURVE ( 'NONE', #75823, #43796, #12835, .T. ) ;
#22464 = ORIENTED_EDGE ( 'NONE', *, *, #77994, .T. ) ;
#22465 = CARTESIAN_POINT ( 'NONE',  ( -1.384615384615383471, -2.538708090699994813, 30.37095296980875503 ) ) ;
#22466 = CARTESIAN_POINT ( 'NONE',  ( -14.30769230769230660, -3.050289026998446396, 32.03036669348365706 ) ) ;
#22467 = AXIS2_PLACEMENT_3D ( 'NONE', #7745, #77525, #77086 ) ;
#22468 = CARTESIAN_POINT ( 'NONE',  ( -4.023055712879202162, -12.62708834333097663, 30.88030960425257021 ) ) ;
#22469 = CARTESIAN_POINT ( 'NONE',  ( 3.100621261037536769, -10.31621877034669588, 34.18098118002070152 ) ) ;
#22470 = EDGE_LOOP ( 'NONE', ( #51425, #18029, #84315, #42993 ) ) ;
#22471 = EDGE_LOOP ( 'NONE', ( #55650, #60746, #81219, #46721 ) ) ;
#22473 = ORIENTED_EDGE ( 'NONE', *, *, #759, .T. ) ;
#22472 = CARTESIAN_POINT ( 'NONE',  ( -2.557692307692305267, -7.500000000000001776, 35.00000000000000000 ) ) ;
#22474 = B_SPLINE_CURVE_WITH_KNOTS ( 'NONE', 3,
 ( #46677, #74154, #88139, #6584, #67838, #33612, #87685, #26853, #20533, #68723 ),
 .UNSPECIFIED., .F., .F.,
 ( 4, 2, 2, 2, 4 ),
 ( 0.0007817246256747528103, 0.0009771112852218980915, 0.001172497944769043156, 0.001367884604316188437, 0.001563271263863333718 ),
 .UNSPECIFIED. ) ;
#22475 = B_SPLINE_CURVE_WITH_KNOTS ( 'NONE', 3,
 ( #1277, #34629, #28767, #54901, #20667, #55775, #83717, #36406, #62097, #89153 ),
 .UNSPECIFIED., .F., .F.,
 ( 4, 2, 2, 2, 4 ),
 ( 0.000000000000000000, 0.0001954339857564070136, 0.0003908679715128140272, 0.0005863019572692210407, 0.0007817359430256280543 ),
 .UNSPECIFIED. ) ;
#22476 = EDGE_CURVE ( 'NONE', #58074, #28286, #60345, .T. ) ;
#22477 = DIRECTION ( 'NONE',  ( 0.000000000000000000, 0.000000000000000000, 1.000000000000000000 ) ) ;
#22478 = ORIENTED_EDGE ( 'NONE', *, *, #38447, .F. ) ;
#22479 = AXIS2_PLACEMENT_3D ( 'NONE', #72067, #4044, #31534 ) ;
#22480 = CARTESIAN_POINT ( 'NONE',  ( 0.4615384615384611200, -6.386643153685126251, 34.62446782046654192 ) ) ;
#22481 = CARTESIAN_POINT ( 'NONE',  ( 6.792386319966616348, -9.084618155246140248, 34.75535874321725771 ) ) ;
#22482 = VERTEX_POINT ( 'NONE', #26520 ) ;
#22483 = AXIS2_PLACEMENT_3D ( 'NONE', #31090, #78838, #58560 ) ;
#22484 = ORIENTED_EDGE ( 'NONE', *, *, #41256, .F. ) ;
#22486 = VERTEX_POINT ( 'NONE', #25626 ) ;
#22485 = CARTESIAN_POINT ( 'NONE',  ( -12.33101275977490197, -5.195472089885680766, 34.18748526763464923 ) ) ;
#22487 = ADVANCED_FACE ( 'NONE', ( #54420 ), #81473, .F. ) ;
#22488 = CARTESIAN_POINT ( 'NONE',  ( -0.6850234052624101233, -10.81261337010820256, 33.49550067578627477 ) ) ;
#22489 = CARTESIAN_POINT ( 'NONE',  ( -5.076923076923197442, -10.21337939537710326, 33.94971097300076224 ) ) ;
#22490 = EDGE_LOOP ( 'NONE', ( #46201, #35875 ) ) ;
#22491 = CARTESIAN_POINT ( 'NONE',  ( 15.29602480204525605, -3.300289026998473041, 32.46337939537591666 ) ) ;
#22492 = CARTESIAN_POINT ( 'NONE',  ( 5.299702618191482806, -11.41317474335729187, 32.86274602512330034 ) ) ;
#22493 = EDGE_CURVE ( 'NONE', #27221, #9934, #12641, .T. ) ;
#22494 = CARTESIAN_POINT ( 'NONE',  ( 6.699591998512595126, -5.827078755546623690, 34.72654668319379567 ) ) ;
#22495 = FACE_BOUND ( 'NONE', #20159, .T. ) ;
#22496 = CARTESIAN_POINT ( 'NONE',  ( 8.068933515131915257, -12.47679350104403007, 31.42216943046555855 ) ) ;
#22497 = DIRECTION ( 'NONE',  ( -0.000000000000000000, 0.9848077530122086864, -0.1736481776669273891 ) ) ;
#22498 = LINE ( 'NONE', #58047, #13528 ) ;
#22500 = CARTESIAN_POINT ( 'NONE',  ( -5.749945688361684404, -2.779044189368096163, 31.39831045268886456 ) ) ;
#22499 = CARTESIAN_POINT ( 'NONE',  ( 12.33084785842815378, -3.338472653186243644, 32.95098750199972670 ) ) ;
#22501 = CARTESIAN_POINT ( 'NONE',  ( -11.28851602011339672, -3.202959910592335646, 32.30730279482227019 ) ) ;
#22502 = CYLINDRICAL_SURFACE ( 'NONE', #87967, 0.2499999999999995559 ) ;
#22503 = EDGE_LOOP ( 'NONE', ( #8972, #56902 ) ) ;
#22504 = CARTESIAN_POINT ( 'NONE',  ( 17.07692307692307665, -7.500000000000001776, 35.04278698407183867 ) ) ;
#22505 = EDGE_LOOP ( 'NONE', ( #69906, #76969, #67721, #26861 ) ) ;
#22506 = VERTEX_POINT ( 'NONE', #53081 ) ;
#22508 = CARTESIAN_POINT ( 'NONE',  ( -6.923076923076922462, -11.91647553114624181, 32.58852847137148245 ) ) ;
#22507 = LINE ( 'NONE', #63926, #63353 ) ;
#22509 = EDGE_CURVE ( 'NONE', #50943, #66812, #86912, .T. ) ;
#22510 = B_SPLINE_CURVE_WITH_KNOTS ( 'NONE', 3,
 ( #47759, #41011, #6769, #34243, #87000, #8998, #56731, #28369, #70693, #34694 ),
 .UNSPECIFIED., .F., .F.,
 ( 4, 2, 2, 2, 4 ),
 ( 0.0007817246256747473893, 0.0009771112852218905021, 0.001172497944769033615, 0.001367884604316176944, 0.001563271263863320057 ),
 .UNSPECIFIED. ) ;
#22511 = CARTESIAN_POINT ( 'NONE',  ( -6.923076923077044142, -6.879047030192662504, 34.71129190930017927 ) ) ;
#22512 = DIRECTION ( 'NONE',  ( -0.000000000000000000, 0.7660444431189792347, -0.6427876096865379196 ) ) ;
#22513 = CARTESIAN_POINT ( 'NONE',  ( 15.23076923076923173, -3.513871655860378418, 32.76840700105978499 ) ) ;
#22514 = CARTESIAN_POINT ( 'NONE',  ( -3.903791733932699515, -3.435999193479609914, 33.07426656108010832 ) ) ;
#22515 = ORIENTED_EDGE ( 'NONE', *, *, #53126, .F. ) ;
#22516 = VECTOR ( 'NONE', #5706, 1000.000000000000114 ) ;
#22517 = CARTESIAN_POINT ( 'NONE',  ( 11.40777093535123043, -3.338472653186243644, 32.95098750199972670 ) ) ;
#22518 = CARTESIAN_POINT ( 'NONE',  ( 1.607626736228236597, -12.15243808032445827, 31.58219941686247978 ) ) ;
#22519 = CYLINDRICAL_SURFACE ( 'NONE', #15775, 0.2499999999999986955 ) ;
#22520 = DIRECTION ( 'NONE',  ( 0.000000000000000000, -6.938893903907222067E-15, 1.000000000000000000 ) ) ;
#22521 = DIRECTION ( 'NONE',  ( -0.000000000000000000, 1.000000000000000000, -0.000000000000000000 ) ) ;
#22522 = CARTESIAN_POINT ( 'NONE',  ( 2.651650429449539104, -4.848349570550432475, 15.56250000000000000 ) ) ;
#22523 = ORIENTED_EDGE ( 'NONE', *, *, #88970, .F. ) ;
#22524 = ORIENTED_EDGE ( 'NONE', *, *, #9216, .F. ) ;
#22525 = CARTESIAN_POINT ( 'NONE',  ( -7.146003140593069958, -8.239355502252617924, 34.69524867566427417 ) ) ;
#22526 = ADVANCED_FACE ( 'NONE', ( #33717 ), #61173, .F. ) ;
#22527 = ORIENTED_EDGE ( 'NONE', *, *, #53597, .F. ) ;
#22528 = CIRCLE ( 'NONE', #67103, 0.2500000000000002220 ) ;
#22529 = CARTESIAN_POINT ( 'NONE',  ( -1.319359813339359588, -8.613356846314930593, 34.62446782046653482 ) ) ;
#22530 = CARTESIAN_POINT ( 'NONE',  ( -1.161602540521989191, -10.01129605718032778, 34.36064277460058491 ) ) ;
#22531 = DIRECTION ( 'NONE',  ( -0.000000000000000000, 1.000000000000000000, 3.491481338843133355E-15 ) ) ;
#22532 = CARTESIAN_POINT ( 'NONE',  ( -4.946397638689431275, -3.625058011473227815, 33.29252011169590020 ) ) ;
#22533 = CARTESIAN_POINT ( 'NONE',  ( 3.750000000000000888, -7.499999999999978684, 15.71875000000000000 ) ) ;
#22534 = CARTESIAN_POINT ( 'NONE',  ( 6.000000000000001776, -3.669653830205710676, 35.88435417666054406 ) ) ;
#22535 = ORIENTED_EDGE ( 'NONE', *, *, #86640, .T. ) ;
#22536 = CARTESIAN_POINT ( 'NONE',  ( 1.384615384615386802, -13.37000171582298513, 34.34916445242398453 ) ) ;
#22538 = ORIENTED_EDGE ( 'NONE', *, *, #71445, .T. ) ;
#22537 = CARTESIAN_POINT ( 'NONE',  ( -2.057637996053991447, -10.66356715214248396, 33.62249196103329751 ) ) ;
#22539 = CARTESIAN_POINT ( 'NONE',  ( -18.00000000000000000, -12.75000000000000888, 29.74999999999997868 ) ) ;
#22540 = FACE_OUTER_BOUND ( 'NONE', #69956, .T. ) ;
#22541 = CARTESIAN_POINT ( 'NONE',  ( 11.31553532094539172, -4.186968288167450147, 33.49512374952580274 ) ) ;
#22542 = CARTESIAN_POINT ( 'NONE',  ( 9.692307692307695177, -8.564572088678739092, 35.78748833219616898 ) ) ;
#22543 = ADVANCED_FACE ( 'NONE', ( #60292 ), #87801, .F. ) ;
#22544 = EDGE_CURVE ( 'NONE', #5084, #30133, #52645, .T. ) ;
#22545 = CYLINDRICAL_SURFACE ( 'NONE', #79536, 0.2500000000000008882 ) ;
#22546 = CARTESIAN_POINT ( 'NONE',  ( -7.976301055592065481, -12.45813303252208648, 30.39737893381572675 ) ) ;
#22547 = CARTESIAN_POINT ( 'NONE',  ( 2.750000000000002665, -7.561099074964516831, 24.72061829374150932 ) ) ;
#22548 = VERTEX_POINT ( 'NONE', #45889 ) ;
#22549 = DIRECTION ( 'NONE',  ( 0.000000000000000000, 0.3420201433256610524, 0.9396926207859113145 ) ) ;
#22550 = DIRECTION ( 'NONE',  ( 0.000000000000000000, -6.938893903907222067E-15, 1.000000000000000000 ) ) ;
#22551 = CARTESIAN_POINT ( 'NONE',  ( -1.139087296526025916, -4.750000000000006217, 19.07812500000000000 ) ) ;
#22552 = CARTESIAN_POINT ( 'NONE',  ( 13.38461538461526601, -6.879047030192662504, 34.71129190930017927 ) ) ;
#22554 = LINE ( 'NONE', #2705, #15977 ) ;
#22553 = AXIS2_PLACEMENT_3D ( 'NONE', #15549, #55632, #36703 ) ;
#22555 = ORIENTED_EDGE ( 'NONE', *, *, #3732, .T. ) ;
#22556 = CARTESIAN_POINT ( 'NONE',  ( 1.799775606325937360E-14, -10.25000000000000000, 16.03125000000000000 ) ) ;
#22557 = FACE_OUTER_BOUND ( 'NONE', #9128, .T. ) ;
#22558 = ORIENTED_EDGE ( 'NONE', *, *, #10639, .T. ) ;
#22559 = AXIS2_PLACEMENT_3D ( 'NONE', #4706, #10568, #80374 ) ;
#22560 = CARTESIAN_POINT ( 'NONE',  ( 14.08420736396836226, -3.236172620538810385, 32.36188796281390267 ) ) ;
#22561 = EDGE_LOOP ( 'NONE', ( #75368, #10279 ) ) ;
#22562 = CARTESIAN_POINT ( 'NONE',  ( 7.146089767170319185, -4.026326845037961455, 33.68677907613344047 ) ) ;
#22563 = ADVANCED_FACE ( 'NONE', ( #11677 ), #20206, .F. ) ;
#22564 = CARTESIAN_POINT ( 'NONE',  ( -17.07692307692307665, -2.292212530054420494, 30.41441678777542634 ) ) ;
#22565 = CARTESIAN_POINT ( 'NONE',  ( -12.68502338610279168, -10.23692288466677880, 34.23039457007281072 ) ) ;
#22566 = CARTESIAN_POINT ( 'NONE',  ( -13.16183571563731647, -12.69155399931963046, 30.53255429739157734 ) ) ;
#22567 = VERTEX_POINT ( 'NONE', #80587 ) ;
#22568 = CARTESIAN_POINT ( 'NONE',  ( -2.373774687052441212, -11.91647553114624181, 32.58852847137148245 ) ) ;
#22569 = ORIENTED_EDGE ( 'NONE', *, *, #87668, .T. ) ;
#22570 = CARTESIAN_POINT ( 'NONE',  ( 12.23861150263161335, -11.98009711892699514, 32.48740034544076138 ) ) ;
#22571 = CARTESIAN_POINT ( 'NONE',  ( -4.376672846325156740, -7.369208160676172348, 34.74850200257122879 ) ) ;
#22572 = ORIENTED_EDGE ( 'NONE', *, *, #12433, .F. ) ;
#22573 = CARTESIAN_POINT ( 'NONE',  ( 8.545745844666436497, -4.988325925672468131, 34.36044203135681130 ) ) ;
#22574 = CARTESIAN_POINT ( 'NONE',  ( -14.43838377435986686, -10.54014554554150607, 33.71984207302941883 ) ) ;
#22575 = B_SPLINE_CURVE_WITH_KNOTS ( 'NONE', 3,
 ( #17505, #12095, #24701, #66586, #65235, #32797 ),
 .UNSPECIFIED., .F., .F.,
 ( 4, 2, 4 ),
 ( 0.0003909512603273676860, 0.0005862562993131928890, 0.0007815613382990180920 ),
 .UNSPECIFIED. ) ;
#22576 = CARTESIAN_POINT ( 'NONE',  ( -11.78843828251013015, -2.920706130388546651, 32.31842814019191223 ) ) ;
#22577 = CARTESIAN_POINT ( 'NONE',  ( 13.44987052412822059, -12.16647553114626490, 32.15551576947920864 ) ) ;
#22578 = CARTESIAN_POINT ( 'NONE',  ( -18.25002323729296450, -4.335965774309649134, 33.62209801155881905 ) ) ;
#22579 = VECTOR ( 'NONE', #84839, 1000.000000000000000 ) ;
#22580 = VERTEX_POINT ( 'NONE', #39157 ) ;
#22581 = EDGE_LOOP ( 'NONE', ( #73209, #82308, #44962, #34975 ) ) ;
#22582 = FACE_BOUND ( 'NONE', #68791, .T. ) ;
#22583 = ORIENTED_EDGE ( 'NONE', *, *, #56395, .T. ) ;
#22584 = CARTESIAN_POINT ( 'NONE',  ( 14.98074599347626368, -12.43535235679832596, 30.55408501211184813 ) ) ;
#22585 = AXIS2_PLACEMENT_3D ( 'NONE', #14603, #1088, #28567 ) ;
#22586 = DIRECTION ( 'NONE',  ( -1.000000000000000000, 0.000000000000000000, 0.000000000000000000 ) ) ;
#22587 = VECTOR ( 'NONE', #89065, 999.9999999999998863 ) ;
#22588 = CARTESIAN_POINT ( 'NONE',  ( 13.51540719244017374, -10.54018710029568595, 33.71981072465678864 ) ) ;
#22589 = CARTESIAN_POINT ( 'NONE',  ( 13.38461538461538680, -11.11383981884818262, 36.00935417666054406 ) ) ;
#22590 = EDGE_LOOP ( 'NONE', ( #26650, #48300, #52477, #84269 ) ) ;
#22591 = ORIENTED_EDGE ( 'NONE', *, *, #87751, .F. ) ;
#22592 = ORIENTED_EDGE ( 'NONE', *, *, #74131, .T. ) ;
#22593 = CARTESIAN_POINT ( 'NONE',  ( -18.03205128205128105, -11.50000000000000000, 29.75000000000000355 ) ) ;
#22594 = DIRECTION ( 'NONE',  ( 0.000000000000000000, 0.3420201433256610524, 0.9396926207859113145 ) ) ;
#22595 = CARTESIAN_POINT ( 'NONE',  ( 11.25641025641025550, -7.500000000000000000, 29.75000000000000355 ) ) ;
#22596 = CARTESIAN_POINT ( 'NONE',  ( 9.320512820512821150, -3.499999999999999556, 29.75000000000000355 ) ) ;
#22597 = ORIENTED_EDGE ( 'NONE', *, *, #41255, .F. ) ;
#22598 = CARTESIAN_POINT ( 'NONE',  ( 16.21910129335899597, -2.379036618887895305, 30.90682066428158592 ) ) ;
#22599 = CARTESIAN_POINT ( 'NONE',  ( -6.065270000556318486, -6.835583212224499938, 34.95778746994557906 ) ) ;
#22600 = VECTOR ( 'NONE', #41006, 1000.000000000000000 ) ;
#22601 = CARTESIAN_POINT ( 'NONE',  ( -18.12796115882773407, -7.725261176542461250, 34.99539040900690168 ) ) ;
#22602 = CARTESIAN_POINT ( 'NONE',  ( -1.161602540521988747, -2.889357225399415086, 32.26129605718031002 ) ) ;
#22603 = ORIENTED_EDGE ( 'NONE', *, *, #32392, .T. ) ;
#22604 = B_SPLINE_CURVE_WITH_KNOTS ( 'NONE', 3,
 ( #31643, #23109, #59104, #66311, #86605, #24875, #45592, #64967, #73071, #38849 ),
 .UNSPECIFIED., .F., .F.,
 ( 4, 2, 2, 2, 4 ),
 ( 0.000000000000000000, 0.0001954311564186867389, 0.0003908623128373734778, 0.0005862934692560602167, 0.0007817246256747469556 ),
 .UNSPECIFIED. ) ;
#22605 = ORIENTED_EDGE ( 'NONE', *, *, #57181, .F. ) ;
#22606 = VERTEX_POINT ( 'NONE', #32386 ) ;
#22608 = CARTESIAN_POINT ( 'NONE',  ( -13.38461538461550582, -6.026961402154118019, 34.52809138561165270 ) ) ;
#22607 = CARTESIAN_POINT ( 'NONE',  ( 12.23861224402231151, -6.503392248772476236, 34.64988816332204635 ) ) ;
#22609 = CYLINDRICAL_SURFACE ( 'NONE', #18343, 0.2499999999999986955 ) ;
#22610 = DIRECTION ( 'NONE',  ( -0.000000000000000000, -0.1736481776669307198, -0.9848077530122080203 ) ) ;
#22611 = FACE_BOUND ( 'NONE', #73477, .T. ) ;
#22612 = CARTESIAN_POINT ( 'NONE',  ( -15.23076923076922995, -3.322132147404559976, 32.92929555188717927 ) ) ;
#22613 = VERTEX_POINT ( 'NONE', #18870 ) ;
#22614 = CARTESIAN_POINT ( 'NONE',  ( 17.29970261819148902, -10.81320215134717166, 33.49497208177562868 ) ) ;
#22615 = AXIS2_PLACEMENT_3D ( 'NONE', #45474, #30626, #72501 ) ;
#22616 = CARTESIAN_POINT ( 'NONE',  ( 9.626225312947559232, -11.91647553114624181, 32.58852847137148245 ) ) ;
#22617 = CARTESIAN_POINT ( 'NONE',  ( 11.28846153846153832, -7.500000000000001776, 34.75000000000000000 ) ) ;
#22618 = CARTESIAN_POINT ( 'NONE',  ( -11.28851602011339494, -3.712312575010499049, 33.01462480002815170 ) ) ;
#22619 = ORIENTED_EDGE ( 'NONE', *, *, #49941, .F. ) ;
#22620 = CARTESIAN_POINT ( 'NONE',  ( -18.22292621751613950, -8.239355502252617924, 34.69524867566427417 ) ) ;
#22621 = B_SPLINE_CURVE_WITH_KNOTS ( 'NONE', 3,
 ( #8166, #27986, #35187, #35640, #83837, #55457 ),
 .UNSPECIFIED., .F., .F.,
 ( 4, 2, 4 ),
 ( 4.934251614402251635E-17, 0.0001954756301637220611, 0.0003909512603273947911 ),
 .UNSPECIFIED. ) ;
#22622 = ORIENTED_EDGE ( 'NONE', *, *, #38351, .T. ) ;
#22623 = FACE_BOUND ( 'NONE', #83301, .T. ) ;
#22624 = CARTESIAN_POINT ( 'NONE',  ( -16.82697755857493505, -4.336752205174650321, 33.62275283266504289 ) ) ;
#22625 = EDGE_CURVE ( 'NONE', #24594, #28775, #71641, .T. ) ;
#22626 = CARTESIAN_POINT ( 'NONE',  ( -14.30769230769230660, -7.500000000000001776, 35.04278698407183867 ) ) ;
#22627 = DIRECTION ( 'NONE',  ( -0.000000000000000000, 0.9396926207859092051, -0.3420201433256662704 ) ) ;
#22628 = EDGE_LOOP ( 'NONE', ( #27889, #64943 ) ) ;
#22629 = CARTESIAN_POINT ( 'NONE',  ( 11.78840694783958476, -10.92531984108285670, 33.72920026020278073 ) ) ;
#22630 = CARTESIAN_POINT ( 'NONE',  ( -14.43783951713053249, -4.460286881179643004, 33.72017969459903242 ) ) ;
#22631 = CARTESIAN_POINT ( 'NONE',  ( -9.758391103263569732, -3.050289026998445951, 32.03036669348365706 ) ) ;
#22632 = CARTESIAN_POINT ( 'NONE',  ( -18.00000000000000000, -12.62096338111211580, 30.90682066428153263 ) ) ;
#22633 = ORIENTED_EDGE ( 'NONE', *, *, #76005, .F. ) ;
#22634 = DIRECTION ( 'NONE',  ( 0.000000000000000000, 0.7660444431189807890, 0.6427876096865361433 ) ) ;
#22635 = VERTEX_POINT ( 'NONE', #68826 ) ;
#22637 = ORIENTED_EDGE ( 'NONE', *, *, #9553, .T. ) ;
#22636 = CARTESIAN_POINT ( 'NONE',  ( 6.923076923076924238, -13.88283147151868846, 33.14645433367849847 ) ) ;
#22638 = CARTESIAN_POINT ( 'NONE',  ( 9.442284455014732458, -3.711651800289232028, 33.01384336483936011 ) ) ;
#22639 = CARTESIAN_POINT ( 'NONE',  ( 2.307692307692309264, -7.500000000000001776, 35.04278698407183867 ) ) ;
#22640 = CARTESIAN_POINT ( 'NONE',  ( -1.326923076923076872, -11.00000000000000000, 29.75000000000000355 ) ) ;
#22641 = AXIS2_PLACEMENT_3D ( 'NONE', #58557, #44594, #72082 ) ;
#22642 = CARTESIAN_POINT ( 'NONE',  ( 8.769230769230768274, -2.499999999999998668, 29.75000000000001421 ) ) ;
#22644 = CARTESIAN_POINT ( 'NONE',  ( -19.50000000000000000, -11.50000000000000000, 29.75000000000000355 ) ) ;
#22643 = DIRECTION ( 'NONE',  ( -0.000000000000000000, 0.1736481776669307198, -0.9848077530122080203 ) ) ;
#22645 = B_SPLINE_CURVE_WITH_KNOTS ( 'NONE', 3,
 ( #86908, #25176, #46783, #4917, #73367, #81025, #19311, #2339, #39152, #66616 ),
 .UNSPECIFIED., .F., .F.,
 ( 4, 2, 2, 2, 4 ),
 ( 0.0007817359430256294638, 0.0009771253907249950223, 0.001172514838424360472, 0.001367904286123725922, 0.001563293733823091372 ),
 .UNSPECIFIED. ) ;
#22646 = EDGE_CURVE ( 'NONE', #79547, #65630, #22914, .T. ) ;
#22647 = CARTESIAN_POINT ( 'NONE',  ( 7.976679547917409963, -4.459921816937791661, 33.71989282347011851 ) ) ;
#22648 = B_SPLINE_CURVE_WITH_KNOTS ( 'NONE', 3,
 ( #68829, #13443, #48106, #13884, #19762, #41365, #6258, #88250, #19321, #75159 ),
 .UNSPECIFIED., .F., .F.,
 ( 4, 2, 2, 2, 4 ),
 ( 0.0007817359430256333669, 0.0009771253907250056474, 0.001172514838424370881, 0.001367904286123736331, 0.001563293733823101564 ),
 .UNSPECIFIED. ) ;
#22649 = CARTESIAN_POINT ( 'NONE',  ( 1.139087296525997273, -4.749999999999992895, 21.73437500000000000 ) ) ;
#22650 = VERTEX_POINT ( 'NONE', #13879 ) ;
#22651 = VECTOR ( 'NONE', #75426, 1000.000000000000000 ) ;
#22652 = B_SPLINE_CURVE_WITH_KNOTS ( 'NONE', 3,
 ( #29968, #9688, #17338, #56984, #29096, #57427, #10138, #84478, #43918, #51535 ),
 .UNSPECIFIED., .F., .F.,
 ( 4, 2, 2, 2, 4 ),
 ( 0.000000000000000000, 0.0001954339857564063089, 0.0003908679715128126177, 0.0005863019572692189808, 0.0007817359430256252354 ),
 .UNSPECIFIED. ) ;
#22653 = CARTESIAN_POINT ( 'NONE',  ( 13.51514082284903040, -12.70449254468099198, 30.44128974285582956 ) ) ;
#22654 = CARTESIAN_POINT ( 'NONE',  ( 13.63461538461680611, -7.500000000000154543, 35.00000000000007105 ) ) ;
#22655 = ORIENTED_EDGE ( 'NONE', *, *, #11715, .F. ) ;
#22656 = ORIENTED_EDGE ( 'NONE', *, *, #24357, .T. ) ;
#22658 = ORIENTED_EDGE ( 'NONE', *, *, #78889, .T. ) ;
#22657 = VECTOR ( 'NONE', #64516, 1000.000000000000000 ) ;
#22659 = CARTESIAN_POINT ( 'NONE',  ( -10.86536134632696715, -11.28823185664190376, 33.01397839955799896 ) ) ;
#22660 = CARTESIAN_POINT ( 'NONE',  ( -14.30769230769242917, -5.941354392335915335, 34.76329471203413846 ) ) ;
#22661 = CARTESIAN_POINT ( 'NONE',  ( -1.384615384615383471, -1.466349020453238561, 30.81389545987213907 ) ) ;
#22662 = CARTESIAN_POINT ( 'NONE',  ( 10.68063975489745232, -6.835583212224610072, 34.95778746994559327 ) ) ;
#22663 = CARTESIAN_POINT ( 'NONE',  ( -16.28399336328437386, -3.285722584762970744, 32.44110544564090048 ) ) ;
#22664 = CARTESIAN_POINT ( 'NONE',  ( 10.61538461538461675, -11.11383981884818262, 36.00935417666054406 ) ) ;
#22665 = DIRECTION ( 'NONE',  ( 0.000000000000000000, 0.000000000000000000, 1.000000000000000000 ) ) ;
#22666 = CARTESIAN_POINT ( 'NONE',  ( -4.153846153846273204, -6.026961402154118908, 34.52809138561165270 ) ) ;
#22668 = EDGE_CURVE ( 'NONE', #11864, #86922, #41360, .T. ) ;
#22667 = DIRECTION ( 'NONE',  ( -0.000000000000000000, 1.000000000000000000, -0.000000000000000000 ) ) ;
#22669 = DIRECTION ( 'NONE',  ( 0.000000000000000000, 0.000000000000000000, 1.000000000000000000 ) ) ;
#22670 = LINE ( 'NONE', #49702, #22579 ) ;
#22671 = EDGE_CURVE ( 'NONE', #22548, #38438, #11520, .T. ) ;
#22673 = EDGE_CURVE ( 'NONE', #4203, #40013, #27842, .T. ) ;
#22672 = VERTEX_POINT ( 'NONE', #15223 ) ;
#22674 = AXIS2_PLACEMENT_3D ( 'NONE', #77352, #43129, #56638 ) ;
#22675 = CARTESIAN_POINT ( 'NONE',  ( 15.23076923076923173, -11.16473453929635440, 33.15142922261926373 ) ) ;
#22676 = CARTESIAN_POINT ( 'NONE',  ( 12.46153846153846168, -11.33034616979429110, 35.88435417666054406 ) ) ;
#22677 = CARTESIAN_POINT ( 'NONE',  ( -2.557692307692305267, -7.500000000000001776, 34.75000000000000000 ) ) ;
#22678 = ORIENTED_EDGE ( 'NONE', *, *, #20072, .F. ) ;
#22679 = CARTESIAN_POINT ( 'NONE',  ( 6.223011351612851350, -4.887748414852792322, 34.01359900205216746 ) ) ;
#22680 = B_SPLINE_CURVE_WITH_KNOTS ( 'NONE', 3,
 ( #88362, #53661, #25749, #60413, #59525, #26635, #26192, #68072, #52764, #61287 ),
 .UNSPECIFIED., .F., .F.,
 ( 4, 2, 2, 2, 4 ),
 ( 0.0007817246256747471724, 0.0009771112852218905021, 0.001172497944769033615, 0.001367884604316176944, 0.001563271263863320274 ),
 .UNSPECIFIED. ) ;
#22681 = DIRECTION ( 'NONE',  ( -0.000000000000000000, 0.7660444431189791237, -0.6427876096865379196 ) ) ;
#22682 = AXIS2_PLACEMENT_3D ( 'NONE', #77040, #71153, #15341 ) ;
#22683 = B_SPLINE_CURVE_WITH_KNOTS ( 'NONE', 3,
 ( #10534, #38002, #24926, #57826, #37544, #52390, #45191, #65471, #44286, #10082 ),
 .UNSPECIFIED., .F., .F.,
 ( 4, 2, 2, 2, 4 ),
 ( 0.0007817359430256300059, 0.0009771253907249963233, 0.001172514838424362424, 0.001367904286123728741, 0.001563293733823095059 ),
 .UNSPECIFIED. ) ;
#22684 = DIRECTION ( 'NONE',  ( 1.000000000000000000, 0.000000000000000000, 0.000000000000000000 ) ) ;
#22685 = B_SPLINE_CURVE_WITH_KNOTS ( 'NONE', 3,
 ( #87709, #72826, #25542, #65619, #11134, #73746, #51650, #38611, #86827, #32302 ),
 .UNSPECIFIED., .F., .F.,
 ( 4, 2, 2, 2, 4 ),
 ( 0.000000000000000000, 0.0001954339857564091007, 0.0003908679715128182013, 0.0005863019572692273291, 0.0007817359430256364027 ),
 .UNSPECIFIED. ) ;
#22686 = AXIS2_PLACEMENT_3D ( 'NONE', #38623, #3048, #66082 ) ;
#22687 = VERTEX_POINT ( 'NONE', #21072 ) ;
#22688 = CARTESIAN_POINT ( 'NONE',  ( 7.846153846153725020, -4.481592998941358097, 33.73612834414048933 ) ) ;
#22689 = ORIENTED_EDGE ( 'NONE', *, *, #72386, .T. ) ;
#22690 = CARTESIAN_POINT ( 'NONE',  ( 10.86543892702293412, -8.303483539816731707, 34.68545999027711702 ) ) ;
#22691 = CARTESIAN_POINT ( 'NONE',  ( -3.296852641725109834, -12.10708131394839349, 31.69288490824020244 ) ) ;
#22692 = CARTESIAN_POINT ( 'NONE',  ( -7.846153846153844924, -2.486705287966279876, 31.30864560766543647 ) ) ;
#22693 = CARTESIAN_POINT ( 'NONE',  ( -14.30769230769242739, -10.21337939537710326, 33.94971097300076224 ) ) ;
#22694 = CARTESIAN_POINT ( 'NONE',  ( 19.99999999999997158, -14.99999999999999467, 3.000000000000000000 ) ) ;
#22695 = ORIENTED_EDGE ( 'NONE', *, *, #27251, .T. ) ;
#22696 = EDGE_CURVE ( 'NONE', #63890, #87106, #36246, .T. ) ;
#22697 = VECTOR ( 'NONE', #68168, 1000.000000000000000 ) ;
#22698 = ORIENTED_EDGE ( 'NONE', *, *, #80702, .F. ) ;
#22699 = ORIENTED_EDGE ( 'NONE', *, *, #67325, .F. ) ;
#22700 = DIRECTION ( 'NONE',  ( -0.000000000000000000, -0.9396926207859093161, -0.3420201433256663259 ) ) ;
#22701 = CARTESIAN_POINT ( 'NONE',  ( -18.00000000000012079, -12.70778746994576025, 30.41441678777401236 ) ) ;
#22702 = CARTESIAN_POINT ( 'NONE',  ( 5.999999999999880096, -8.613356846316285953, 34.62446782046622218 ) ) ;
#22703 = CARTESIAN_POINT ( 'NONE',  ( -2.307692307692305711, -11.35647404775217417, 33.31231777344666511 ) ) ;
#22704 = CARTESIAN_POINT ( 'NONE',  ( -17.74994568836168440, -4.235687564193448829, 33.53795663066793509 ) ) ;
#22705 = CARTESIAN_POINT ( 'NONE',  ( 5.076923076922954969, -10.21337939537710326, 33.94971097300076224 ) ) ;
#22706 = EDGE_LOOP ( 'NONE', ( #27609, #38999 ) ) ;
#22707 = ORIENTED_EDGE ( 'NONE', *, *, #32527, .T. ) ;
#22708 = EDGE_CURVE ( 'NONE', #17208, #82422, #8465, .T. ) ;
#22709 = ORIENTED_EDGE ( 'NONE', *, *, #41762, .F. ) ;
#22711 = EDGE_LOOP ( 'NONE', ( #56278, #11083, #76367, #50484 ) ) ;
#22710 = CARTESIAN_POINT ( 'NONE',  ( 3.930361210122207183, -2.847400154188068466, 31.58180166144859768 ) ) ;
#22713 = CARTESIAN_POINT ( 'NONE',  ( -10.55012947587177941, -6.835583212224610072, 34.95778746994559327 ) ) ;
#22712 = CARTESIAN_POINT ( 'NONE',  ( 9.692307692307572609, -10.90142922262034020, 33.41473453929536674 ) ) ;
#22714 = CARTESIAN_POINT ( 'NONE',  ( 2.651650429449539104, -4.848349570550432475, 25.56250000000000355 ) ) ;
#22715 = EDGE_LOOP ( 'NONE', ( #81588, #36066, #51702, #37198, #34716, #79465 ) ) ;
#22716 = VERTEX_POINT ( 'NONE', #56642 ) ;
#22717 = CARTESIAN_POINT ( 'NONE',  ( -2.438383774359864642, -12.38065189839062263, 30.83690757178629482 ) ) ;
#22718 = ORIENTED_EDGE ( 'NONE', *, *, #71377, .F. ) ;
#22719 = FACE_BOUND ( 'NONE', #52295, .T. ) ;
#22720 = CARTESIAN_POINT ( 'NONE',  ( 15.16468581981334829, -9.780366693483667717, 34.19971097300155805 ) ) ;
#22721 = EDGE_CURVE ( 'NONE', #75758, #74098, #7576, .T. ) ;
#22722 = AXIS2_PLACEMENT_3D ( 'NONE', #27189, #27631, #54647 ) ;
#22723 = CARTESIAN_POINT ( 'NONE',  ( -19.50000000000000000, -3.499999999999999556, 29.75000000000000355 ) ) ;
#22724 = EDGE_LOOP ( 'NONE', ( #37684, #23079, #19352, #16063 ) ) ;
#22725 = CARTESIAN_POINT ( 'NONE',  ( 6.000000000000001776, -4.786620604624113540, 33.94971097300155094 ) ) ;
#22726 = CARTESIAN_POINT ( 'NONE',  ( 4.853996118016224770, -8.282780595021769443, 34.94152052738834868 ) ) ;
#22727 = CARTESIAN_POINT ( 'NONE',  ( -4.153846153846274980, -3.083524468854526912, 32.58852847137268327 ) ) ;
#22728 = B_SPLINE_CURVE_WITH_KNOTS ( 'NONE', 3,
 ( #20360, #76175, #68977, #34302, #33859, #61317 ),
 .UNSPECIFIED., .F., .F.,
 ( 4, 2, 4 ),
 ( 4.563551064100006665E-17, 0.0001954756301637168570, 0.0003909512603273880690 ),
 .UNSPECIFIED. ) ;
#22729 = EDGE_CURVE ( 'NONE', #18077, #57194, #84793, .T. ) ;
#22730 = CARTESIAN_POINT ( 'NONE',  ( 3.930919936330005360, -11.24512374952581872, 33.06303171183252942 ) ) ;
#22731 = CARTESIAN_POINT ( 'NONE',  ( -7.846153846153965716, -8.613356846316285953, 34.62446782046622218 ) ) ;
#22732 = CIRCLE ( 'NONE', #19912, 5.000000000000000888 ) ;
#22733 = CARTESIAN_POINT ( 'NONE',  ( 7.173131342990377135, -2.544122305571457687, 31.48381861865059150 ) ) ;
#22734 = CARTESIAN_POINT ( 'NONE',  ( -7.911423846710166075, -12.16647553114622049, 32.15551576947930812 ) ) ;
#22735 = CYLINDRICAL_SURFACE ( 'NONE', #39863, 0.2499999999999998890 ) ;
#22736 = CARTESIAN_POINT ( 'NONE',  ( 5.869308533332443290, -4.809359713505814149, 33.96456829005828837 ) ) ;
#22737 = CARTESIAN_POINT ( 'NONE',  ( -14.30769230769230660, -13.87047571288749737, 32.06866353760679544 ) ) ;
#22738 = CARTESIAN_POINT ( 'NONE',  ( 7.846153846153723244, -3.083524468854526912, 32.58852847137268327 ) ) ;
#22740 = CARTESIAN_POINT ( 'NONE',  ( 11.66929986894829696, -7.277220318596961057, 34.99547417642776992 ) ) ;
#22739 = CARTESIAN_POINT ( 'NONE',  ( 17.07692307692307665, -3.513871655860378418, 32.76840700105978499 ) ) ;
#22741 = EDGE_CURVE ( 'NONE', #30710, #51792, #56663, .T. ) ;
#22742 = CARTESIAN_POINT ( 'NONE',  ( -16.08859058257012720, -11.94971097300157403, 32.03036669348361443 ) ) ;
#22744 = LINE ( 'NONE', #50204, #56420 ) ;
#22743 = CARTESIAN_POINT ( 'NONE',  ( -3.480792454990687013, -2.985938066672154445, 32.43141759479405550 ) ) ;
#22745 = CARTESIAN_POINT ( 'NONE',  ( -1.576923076923076428, -3.499999999999999556, 29.75000000000000355 ) ) ;
#22746 = CARTESIAN_POINT ( 'NONE',  ( 1.200186371490561621, -10.22469193450123193, 21.95125670625849068 ) ) ;
#22747 = ORIENTED_EDGE ( 'NONE', *, *, #75939, .T. ) ;
#22748 = CARTESIAN_POINT ( 'NONE',  ( 0.2386122440223129304, -12.39988816332205701, 30.74660775122750778 ) ) ;
#22749 = ORIENTED_EDGE ( 'NONE', *, *, #33446, .T. ) ;
#22750 = EDGE_CURVE ( 'NONE', #78293, #50090, #76919, .T. ) ;
#22751 = DIRECTION ( 'NONE',  ( -0.000000000000000000, 1.000000000000000000, -0.000000000000000000 ) ) ;
#22752 = ORIENTED_EDGE ( 'NONE', *, *, #55497, .T. ) ;
#22753 = CARTESIAN_POINT ( 'NONE',  ( -22.75000000000000000, -10.49999999999999822, 27.25000000000000000 ) ) ;
#22754 = EDGE_CURVE ( 'NONE', #59461, #77977, #53469, .T. ) ;
#22755 = ORIENTED_EDGE ( 'NONE', *, *, #68888, .T. ) ;
#22756 = CARTESIAN_POINT ( 'NONE',  ( -5.999999999999998224, -11.69971097300155272, 32.46337939537588113 ) ) ;
#22757 = CARTESIAN_POINT ( 'NONE',  ( 2.750000000000001332, -7.438900925035452083, 25.46688170625849423 ) ) ;
#22758 = CARTESIAN_POINT ( 'NONE',  ( 17.29993442853592711, -8.239487800360276282, 34.69522927552633718 ) ) ;
#22759 = CARTESIAN_POINT ( 'NONE',  ( 6.923076923076924238, -12.37446782046654192, 30.86335684631486131 ) ) ;
#22760 = CARTESIAN_POINT ( 'NONE',  ( 7.145856464345332171, -9.332535724633407526, 34.40230450496446224 ) ) ;
#22761 = CARTESIAN_POINT ( 'NONE',  ( -39.05038313613820122, -2.249999999999998668, 29.75000000000000355 ) ) ;
#22762 = CARTESIAN_POINT ( 'NONE',  ( -13.45069776397551742, -8.164416787775445883, 34.95778746994557906 ) ) ;
#22763 = CARTESIAN_POINT ( 'NONE',  ( -13.60810030917971503, -12.11044203135681840, 32.26167407432752299 ) ) ;
#22764 = CARTESIAN_POINT ( 'NONE',  ( 3.750000000000000888, -7.499999999999978684, 15.71875000000000000 ) ) ;
#22765 = CARTESIAN_POINT ( 'NONE',  ( -11.28840711854808632, -2.544122305571458575, 31.48381861865057729 ) ) ;
#22767 = ADVANCED_FACE ( 'NONE', ( #44003 ), #9352, .F. ) ;
#22766 = DIRECTION ( 'NONE',  ( -0.000000000000000000, 0.6427876096865404731, -0.7660444431189770143 ) ) ;
#22768 = CARTESIAN_POINT ( 'NONE',  ( -2.307692307692305711, -4.098570777380720287, 33.41473453929634729 ) ) ;
#22769 = VECTOR ( 'NONE', #45437, 1000.000000000000000 ) ;
#22770 = CARTESIAN_POINT ( 'NONE',  ( -2.651650429449535551, -10.15165042944956753, 16.18750000000000000 ) ) ;
#22771 = B_SPLINE_CURVE_WITH_KNOTS ( 'NONE', 3,
 ( #30534, #58005, #51218, #30969, #72847, #86395, #24667, #52576, #79172, #58894 ),
 .UNSPECIFIED., .F., .F.,
 ( 4, 2, 2, 2, 4 ),
 ( 0.0007817359430256294638, 0.0009771253907249952391, 0.001172514838424361123, 0.001367904286123726790, 0.001563293733823092673 ),
 .UNSPECIFIED. ) ;
#22772 = CARTESIAN_POINT ( 'NONE',  ( -10.39260494640654642, -5.827830569534417471, 34.72679350104403539 ) ) ;
#22773 = EDGE_LOOP ( 'NONE', ( #2755, #20271 ) ) ;
#22774 = EDGE_CURVE ( 'NONE', #7402, #67715, #64267, .T. ) ;
#22775 = CARTESIAN_POINT ( 'NONE',  ( 14.30769230769218758, -5.219633306517616589, 34.19971097300220464 ) ) ;
#22776 = DIRECTION ( 'NONE',  ( -0.000000000000000000, 0.3420201433256694346, -0.9396926207859080948 ) ) ;
#22777 = CARTESIAN_POINT ( 'NONE',  ( -20.00000000000000000, -11.50000000000000000, 29.75000000000000355 ) ) ;
#22778 = CARTESIAN_POINT ( 'NONE',  ( 16.40384615384608935, -7.565270000091922853, 34.99999999999999289 ) ) ;
#22779 = ADVANCED_FACE ( 'NONE', ( #71472 ), #2567, .F. ) ;
#22780 = DIRECTION ( 'NONE',  ( 1.000000000000000000, 0.000000000000000000, 0.000000000000000000 ) ) ;
#22781 = CARTESIAN_POINT ( 'NONE',  ( 9.442330961365339448, -11.28823185664190376, 33.01397839955799896 ) ) ;
#22782 = CYLINDRICAL_SURFACE ( 'NONE', #29087, 0.2499999999999997502 ) ;
#22783 = AXIS2_PLACEMENT_3D ( 'NONE', #39475, #72788, #61827 ) ;
#22784 = ORIENTED_EDGE ( 'NONE', *, *, #59459, .T. ) ;
#22785 = ORIENTED_EDGE ( 'NONE', *, *, #11739, .F. ) ;
#22786 = ORIENTED_EDGE ( 'NONE', *, *, #58126, .F. ) ;
#22787 = CARTESIAN_POINT ( 'NONE',  ( -6.857009589726848375, -5.471508081941601098, 34.59228464037088457 ) ) ;
#22788 = CARTESIAN_POINT ( 'NONE',  ( 7.134615384615385025, -7.500000000000000000, 29.75000000000000355 ) ) ;
#22789 = CARTESIAN_POINT ( 'NONE',  ( 16.28437185560971301, -2.882268652242222728, 31.66798894389554064 ) ) ;
#22790 = CARTESIAN_POINT ( 'NONE',  ( 4.284637961670941131, -3.530189275343204702, 32.79018710029569661 ) ) ;
#22791 = CARTESIAN_POINT ( 'NONE',  ( 10.61538461538449418, -10.33852847137269571, 34.16647553114546554 ) ) ;
#22792 = EDGE_LOOP ( 'NONE', ( #71729, #55862 ) ) ;
#22793 = CARTESIAN_POINT ( 'NONE',  ( 17.20771351789003489, -11.37503395064541678, 33.29242100308974983 ) ) ;
#22794 = AXIS2_PLACEMENT_3D ( 'NONE', #28404, #76144, #34276 ) ;
#22795 = EDGE_LOOP ( 'NONE', ( #49670, #69749, #63124, #53664, #38911 ) ) ;
#22796 = EDGE_CURVE ( 'NONE', #67575, #15414, #80285, .T. ) ;
#22797 = ORIENTED_EDGE ( 'NONE', *, *, #84672, .F. ) ;
#22798 = VECTOR ( 'NONE', #37185, 1000.000000000000000 ) ;
#22799 = B_SPLINE_CURVE_WITH_KNOTS ( 'NONE', 3,
 ( #70931, #57856, #2024, #84458, #15547, #22299, #49763, #85338, #50193, #36266 ),
 .UNSPECIFIED., .F., .F.,
 ( 4, 2, 2, 2, 4 ),
 ( 0.000000000000000000, 0.0001954339857564064444, 0.0003908679715128128888, 0.0005863019572692193060, 0.0007817359430256257775 ),
 .UNSPECIFIED. ) ;
#22800 = B_SPLINE_CURVE_WITH_KNOTS ( 'NONE', 3,
 ( #42782, #29270, #50396, #22496, #16613, #37326, #57167, #64792, #77439, #64351 ),
 .UNSPECIFIED., .F., .F.,
 ( 4, 2, 2, 2, 4 ),
 ( 0.0007817246256747528103, 0.0009771112852218978746, 0.001172497944769042722, 0.001367884604316187570, 0.001563271263863332634 ),
 .UNSPECIFIED. ) ;
#22801 = LINE ( 'NONE', #50261, #61637 ) ;
#22802 = DIRECTION ( 'NONE',  ( -1.000000000000000000, -0.000000000000000000, -0.000000000000000000 ) ) ;
#22803 = EDGE_CURVE ( 'NONE', #19870, #48154, #7211, .T. ) ;
#22804 = B_SPLINE_CURVE_WITH_KNOTS ( 'NONE', 3,
 ( #39809, #87122, #19089, #81683, #32594, #33045 ),
 .UNSPECIFIED., .F., .F.,
 ( 4, 2, 4 ),
 ( 0.0003909512603273869848, 0.0005862562993132133804, 0.0007815613382990397760 ),
 .UNSPECIFIED. ) ;
#22805 = ADVANCED_FACE ( 'NONE', ( #29622 ), #24174, .F. ) ;
#22806 = CARTESIAN_POINT ( 'NONE',  ( -12.46153846153846168, -1.422936976036506707, 30.56769352161908415 ) ) ;
#22807 = EDGE_CURVE ( 'NONE', #55920, #43958, #10060, .T. ) ;
#22808 = CARTESIAN_POINT ( 'NONE',  ( 25.00000000000000355, 9.999999999999971578, 13.00000000000000178 ) ) ;
#22809 = CARTESIAN_POINT ( 'NONE',  ( -15.93083330975275658, -5.582272713120730145, 34.63742843783360570 ) ) ;
#22810 = ORIENTED_EDGE ( 'NONE', *, *, #23029, .T. ) ;
#22811 = ORIENTED_EDGE ( 'NONE', *, *, #22912, .T. ) ;
#22812 = CARTESIAN_POINT ( 'NONE',  ( -1.553300858899125059, -3.750000000000009326, 19.07812500000000000 ) ) ;
#22813 = ADVANCED_FACE ( 'NONE', ( #78234 ), #64713, .F. ) ;
#22814 = ORIENTED_EDGE ( 'NONE', *, *, #30868, .F. ) ;
#22815 = CARTESIAN_POINT ( 'NONE',  ( 8.096099255531887806, -4.932303261841489039, 34.32971442181322885 ) ) ;
#22817 = ORIENTED_EDGE ( 'NONE', *, *, #11166, .T. ) ;
#22816 = CARTESIAN_POINT ( 'NONE',  ( 4.376625695114562120, -11.41317474335729187, 32.86274602512330034 ) ) ;
#22818 = CARTESIAN_POINT ( 'NONE',  ( 20.99999999999998224, -12.75000000000000178, 27.25000000000000000 ) ) ;
#22819 = CARTESIAN_POINT ( 'NONE',  ( 5.076923076922954969, -3.835265460704628371, 33.15142922262033665 ) ) ;
#22820 = CARTESIAN_POINT ( 'NONE',  ( 1.384615384615386802, -1.044019251281081972, 31.83374038241031911 ) ) ;
#22821 = ORIENTED_EDGE ( 'NONE', *, *, #40388, .T. ) ;
#22822 = CARTESIAN_POINT ( 'NONE',  ( 15.00784301325308157, -10.61292498521070549, 33.66303323003028680 ) ) ;
#22823 = CARTESIAN_POINT ( 'NONE',  ( 15.10062126103753322, -2.647304123082328875, 31.75400227202885972 ) ) ;
#22824 = VECTOR ( 'NONE', #6132, 1000.000000000000000 ) ;
#22825 = ORIENTED_EDGE ( 'NONE', *, *, #11656, .F. ) ;
#22826 = FACE_BOUND ( 'NONE', #28313, .T. ) ;
#22827 = CARTESIAN_POINT ( 'NONE',  ( -10.61538461538461320, -4.661471528628507777, 34.16647553114623292 ) ) ;
#22828 = DIRECTION ( 'NONE',  ( 1.000000000000000000, 0.000000000000000000, 0.000000000000000000 ) ) ;
#22829 = CYLINDRICAL_SURFACE ( 'NONE', #25031, 0.2500000000000008882 ) ;
#22831 = CARTESIAN_POINT ( 'NONE',  ( -6.857008572074483332, -2.538708090699994813, 30.37095296980875503 ) ) ;
#22830 = CYLINDRICAL_SURFACE ( 'NONE', #21629, 0.2499999999999973355 ) ;
#22832 = CARTESIAN_POINT ( 'NONE',  ( -1.384615384615383471, -8.164416787775445883, 34.95778746994557906 ) ) ;
#22833 = CARTESIAN_POINT ( 'NONE',  ( -4.403822897894743349, -10.82459398097509684, 33.81372124010185587 ) ) ;
#22834 = ORIENTED_EDGE ( 'NONE', *, *, #4980, .F. ) ;
#22835 = CARTESIAN_POINT ( 'NONE',  ( -0.4615384615384611200, -13.49023893513002648, 31.06009739812518688 ) ) ;
#22836 = CARTESIAN_POINT ( 'NONE',  ( -6.130690603110307890, -11.37499894934982514, 33.29245874905763003 ) ) ;
#22837 = EDGE_CURVE ( 'NONE', #18370, #80137, #38140, .T. ) ;
#22838 = ORIENTED_EDGE ( 'NONE', *, *, #74155, .F. ) ;
#22839 = CARTESIAN_POINT ( 'NONE',  ( -16.40382289789473802, -12.65889640711025521, 30.72598325615533454 ) ) ;
#22840 = CARTESIAN_POINT ( 'NONE',  ( 10.48523740594639442, -6.852621066184266141, 34.70813303252209181 ) ) ;
#22841 = CARTESIAN_POINT ( 'NONE',  ( -16.15384615384627409, -10.90142922262034020, 33.41473453929536674 ) ) ;
#22842 = DIRECTION ( 'NONE',  ( -0.000000000000000000, -0.6427876096865404731, -0.7660444431189771253 ) ) ;
#22843 = LINE ( 'NONE', #9345, #51444 ) ;
#22844 = CARTESIAN_POINT ( 'NONE',  ( -7.911907274467175455, -7.249945578846651806, 34.99404164642496795 ) ) ;
#22845 = FACE_BOUND ( 'NONE', #49152, .T. ) ;
#22847 = CARTESIAN_POINT ( 'NONE',  ( -10.36538461538319389, -7.500000000000154543, 35.00000000000007105 ) ) ;
#22846 = DIRECTION ( 'NONE',  ( 1.000000000000000000, 0.000000000000000000, 0.000000000000000000 ) ) ;
#22848 = CARTESIAN_POINT ( 'NONE',  ( 16.08857570788537572, -3.300289026998414865, 32.46337939537583139 ) ) ;
#22850 = DIRECTION ( 'NONE',  ( 0.000000000000000000, -1.000000000000000000, 0.000000000000000000 ) ) ;
#22849 = CARTESIAN_POINT ( 'NONE',  ( -6.700297254098858346, -10.97394488606064122, 33.68653795673694873 ) ) ;
#22851 = DIRECTION ( 'NONE',  ( -0.000000000000000000, -0.9848077530122086864, -0.1736481776669273613 ) ) ;
#22852 = CARTESIAN_POINT ( 'NONE',  ( -0.06109907496455085213, -3.750000000000000888, 18.90438170625848713 ) ) ;
#22853 = ORIENTED_EDGE ( 'NONE', *, *, #59801, .F. ) ;
#22854 = ORIENTED_EDGE ( 'NONE', *, *, #20023, .T. ) ;
#22855 = CARTESIAN_POINT ( 'NONE',  ( 16.02369818411445834, -9.504002272028873932, 34.60269587691767867 ) ) ;
#22856 = CARTESIAN_POINT ( 'NONE',  ( -5.011667505647051435, -3.300289026998475705, 32.46337939537591666 ) ) ;
#22857 = DIRECTION ( 'NONE',  ( 1.000000000000000000, 2.602085213965214586E-16, 0.000000000000000000 ) ) ;
#22858 = CARTESIAN_POINT ( 'NONE',  ( -1.384615384615505151, -3.300289026999228881, 32.46337939537708905 ) ) ;
#22859 = CARTESIAN_POINT ( 'NONE',  ( 3.165498784808456811, -11.48612834413959582, 32.76840700105983473 ) ) ;
#22860 = CARTESIAN_POINT ( 'NONE',  ( 1.614399933863660985, -11.22469193450123193, 19.45125670625849068 ) ) ;
#22861 = CARTESIAN_POINT ( 'NONE',  ( -16.15384615384627409, -5.941354392335915335, 34.76329471203413846 ) ) ;
#22862 = CARTESIAN_POINT ( 'NONE',  ( -18.00000000000012079, -11.48612834414049644, 32.76840700105863391 ) ) ;
#22863 = VECTOR ( 'NONE', #15187, 1000.000000000000000 ) ;
#22864 = CARTESIAN_POINT ( 'NONE',  ( 3.480714640147274608, -4.176053281294514363, 33.81426240980091791 ) ) ;
#22865 = CARTESIAN_POINT ( 'NONE',  ( 10.48523664565292002, -6.809168938359901446, 34.95455904226513866 ) ) ;
#22866 = CARTESIAN_POINT ( 'NONE',  ( -17.07692307692307665, -4.661471528628507777, 34.16647553114623292 ) ) ;
#22867 = CARTESIAN_POINT ( 'NONE',  ( 10.68057859716797431, -2.506253911140448043, 29.99999999999988631 ) ) ;
#22868 = VECTOR ( 'NONE', #43584, 1000.000000000000227 ) ;
#22870 = ADVANCED_FACE ( 'NONE', ( #77356 ), #8906, .F. ) ;
#22869 = LINE ( 'NONE', #62092, #75014 ) ;
#22871 = EDGE_CURVE ( 'NONE', #85628, #8309, #8606, .T. ) ;
#22872 = CARTESIAN_POINT ( 'NONE',  ( 7.976945653978634532, -6.413143153341454017, 34.63066358083362672 ) ) ;
#22873 = VERTEX_POINT ( 'NONE', #46233 ) ;
#22874 = CARTESIAN_POINT ( 'NONE',  ( 6.166666666666664298, -11.50000000000000000, 29.75000000000000355 ) ) ;
#22875 = DIRECTION ( 'NONE',  ( -0.000000000000000000, -0.1736481776669307198, -0.9848077530122080203 ) ) ;
#22876 = CARTESIAN_POINT ( 'NONE',  ( -1.077988221561493543, -4.724691934501247914, 24.32999329374151642 ) ) ;
#22877 = EDGE_CURVE ( 'NONE', #33903, #31532, #67835, .T. ) ;
#22878 = B_SPLINE_CURVE_WITH_KNOTS ( 'NONE', 3,
 ( #88239, #81466, #59845, #20198, #13433, #12994, #33709, #61166, #88676, #26955 ),
 .UNSPECIFIED., .F., .F.,
 ( 4, 2, 2, 2, 4 ),
 ( 0.000000000000000000, 0.0001954339857564071762, 0.0003908679715128143524, 0.0005863019572692215828, 0.0007817359430256287049 ),
 .UNSPECIFIED. ) ;
#22879 = CARTESIAN_POINT ( 'NONE',  ( -2.307692307692305711, -4.661471528628507777, 34.16647553114623292 ) ) ;
#22880 = CARTESIAN_POINT ( 'NONE',  ( 17.07692307692295586, -11.67786785259630911, 32.92929555188603530 ) ) ;
#22881 = ORIENTED_EDGE ( 'NONE', *, *, #53620, .F. ) ;
#22882 = CARTESIAN_POINT ( 'NONE',  ( 10.48482402364269639, -2.504760397472875155, 29.97295953869789997 ) ) ;
#22884 = VERTEX_POINT ( 'NONE', #12015 ) ;
#22883 = DIRECTION ( 'NONE',  ( -0.000000000000000000, 1.000000000000000000, -0.000000000000000000 ) ) ;
#22885 = CARTESIAN_POINT ( 'NONE',  ( 9.442307692307691624, -2.499999999999999556, 29.81609845454691765 ) ) ;
#22886 = CARTESIAN_POINT ( 'NONE',  ( 6.923076923076800782, -12.70778746994576025, 30.41441678777401236 ) ) ;
#22887 = EDGE_CURVE ( 'NONE', #33821, #78112, #14379, .T. ) ;
#22888 = VERTEX_POINT ( 'NONE', #73261 ) ;
#22889 = CARTESIAN_POINT ( 'NONE',  ( -10.36538461538461320, -7.500000000000001776, 35.04278698407183867 ) ) ;
#22890 = CARTESIAN_POINT ( 'NONE',  ( 2.307692307692309264, -5.557115091759785130, 34.35708131394839171 ) ) ;
#22891 = ADVANCED_FACE ( 'NONE', ( #19644 ), #25518, .F. ) ;
#22892 = VERTEX_POINT ( 'NONE', #45782 ) ;
#22893 = B_SPLINE_CURVE_WITH_KNOTS ( 'NONE', 3,
 ( #7998, #69692, #84110, #21499, #6660, #7107, #62477, #62916, #27384, #34581 ),
 .UNSPECIFIED., .F., .F.,
 ( 4, 2, 2, 2, 4 ),
 ( 0.0007817246256747473893, 0.0009771112852218909357, 0.001172497944769034482, 0.001367884604316178246, 0.001563271263863321792 ),
 .UNSPECIFIED. ) ;
#22894 = CARTESIAN_POINT ( 'NONE',  ( 30.00000000000000000, -15.00000000000000000, 0.000000000000000000 ) ) ;
#22895 = LINE ( 'NONE', #85057, #27799 ) ;
#22896 = CARTESIAN_POINT ( 'NONE',  ( 15.23076923076923173, -9.905515769479276145, 34.41647553114623292 ) ) ;
#22897 = VERTEX_POINT ( 'NONE', #12884 ) ;
#22898 = ORIENTED_EDGE ( 'NONE', *, *, #59874, .T. ) ;
#22899 = EDGE_CURVE ( 'NONE', #70106, #84245, #26408, .T. ) ;
#22900 = CIRCLE ( 'NONE', #80451, 0.2500000000000002220 ) ;
#22901 = ORIENTED_EDGE ( 'NONE', *, *, #16779, .F. ) ;
#22902 = CARTESIAN_POINT ( 'NONE',  ( 6.923076923076924238, -1.242168528481310874, 33.36296068462461051 ) ) ;
#22903 = CARTESIAN_POINT ( 'NONE',  ( -5.750054590621955342, -5.766571408460171355, 34.70601412856602508 ) ) ;
#22904 = EDGE_CURVE ( 'NONE', #18589, #51403, #6095, .T. ) ;
#22905 = CARTESIAN_POINT ( 'NONE',  ( -4.153846153846274980, -12.70778746994576025, 30.41441678777401236 ) ) ;
#22906 = DIRECTION ( 'NONE',  ( 0.000000000000000000, 0.9396926207859126468, -0.3420201433256571111 ) ) ;
#22907 = EDGE_CURVE ( 'NONE', #59376, #64075, #66505, .T. ) ;
#22908 = ORIENTED_EDGE ( 'NONE', *, *, #72543, .T. ) ;
#22909 = ORIENTED_EDGE ( 'NONE', *, *, #88902, .F. ) ;
#22911 = VERTEX_POINT ( 'NONE', #52974 ) ;
#22910 = CARTESIAN_POINT ( 'NONE',  ( 4.403791563224197070, -8.476813868363244353, 34.90874843262270133 ) ) ;
#22912 = EDGE_CURVE ( 'NONE', #34205, #856, #52534, .T. ) ;
#22913 = DIRECTION ( 'NONE',  ( -0.000000000000000000, -0.9396926207859092051, -0.3420201433256662704 ) ) ;
#22914 = CIRCLE ( 'NONE', #86206, 6.614378277661484340 ) ;
#22915 = CIRCLE ( 'NONE', #34436, 8.000000000000000000 ) ;
#22916 = CARTESIAN_POINT ( 'NONE',  ( 7.716005876422152632, -12.15440758774515473, 32.17923288041532004 ) ) ;
#22917 = CARTESIAN_POINT ( 'NONE',  ( -8.546451100252703270, -12.69155399931963046, 30.53255429739157734 ) ) ;
#22918 = ORIENTED_EDGE ( 'NONE', *, *, #1208, .F. ) ;
#22919 = AXIS2_PLACEMENT_3D ( 'NONE', #27743, #70062, #34060 ) ;
#22920 = AXIS2_PLACEMENT_3D ( 'NONE', #28597, #79446, #57831 ) ;
#22921 = EDGE_CURVE ( 'NONE', #55647, #32571, #39933, .T. ) ;
#22922 = ORIENTED_EDGE ( 'NONE', *, *, #52688, .F. ) ;
#22924 = EDGE_LOOP ( 'NONE', ( #43139, #51251, #512, #6474 ) ) ;
#22923 = CARTESIAN_POINT ( 'NONE',  ( 9.942362112221147186, -8.346898887586323923, 34.93166121998716278 ) ) ;
#22925 = AXIS2_PLACEMENT_3D ( 'NONE', #34847, #33082, #67318 ) ;
#22926 = CARTESIAN_POINT ( 'NONE',  ( 4.219914504848592429, -4.786620604624113540, 33.94971097300155805 ) ) ;
#22927 = CARTESIAN_POINT ( 'NONE',  ( -10.83886953994894498, -9.417330523894424488, 34.63758898049880486 ) ) ;
#22928 = ORIENTED_EDGE ( 'NONE', *, *, #59581, .T. ) ;
#22929 = ADVANCED_FACE ( 'NONE', ( #73721 ), #86355, .F. ) ;
#22930 = DIRECTION ( 'NONE',  ( -0.000000000000000000, 0.8660254037844399289, -0.4999999999999980016 ) ) ;
#22931 = LINE ( 'NONE', #27589, #47978 ) ;
#22932 = DIRECTION ( 'NONE',  ( -0.000000000000000000, 0.9848077530122086864, -0.1736481776669273891 ) ) ;
#22933 = B_SPLINE_CURVE_WITH_KNOTS ( 'NONE', 3,
 ( #22693, #2413, #51025, #84858, #57807, #78084, #64549, #37528, #44271, #50605 ),
 .UNSPECIFIED., .F., .F.,
 ( 4, 2, 2, 2, 4 ),
 ( 0.0007817359430256360774, 0.0009771253907250041296, 0.001172514838424371965, 0.001367904286123740017, 0.001563293733823108069 ),
 .UNSPECIFIED. ) ;
#22934 = FACE_BOUND ( 'NONE', #3242, .T. ) ;
#22935 = CARTESIAN_POINT ( 'NONE',  ( -8.519285359852727169, -2.341251567377310217, 30.72681386836322659 ) ) ;
#22936 = CARTESIAN_POINT ( 'NONE',  ( 2.557637826040450424, -8.433404298154334455, 34.66254593164985920 ) ) ;
#22937 = CARTESIAN_POINT ( 'NONE',  ( 13.13463864056679675, -12.65889640711025521, 30.72598325615533454 ) ) ;
#22939 = CARTESIAN_POINT ( 'NONE',  ( 4.403791563224197070, -2.341251567377310217, 30.72681386836322659 ) ) ;
#22938 = CARTESIAN_POINT ( 'NONE',  ( -16.85414340794500276, -12.47679350104403007, 31.42216943046555855 ) ) ;
#22940 = CARTESIAN_POINT ( 'NONE',  ( 17.77707304109314634, -6.459968553980840689, 34.89616026154728701 ) ) ;
#22941 = CARTESIAN_POINT ( 'NONE',  ( -7.846153846153967493, -2.657715359629662544, 31.77849191805970364 ) ) ;
#22942 = ORIENTED_EDGE ( 'NONE', *, *, #51259, .T. ) ;
#22943 = FACE_OUTER_BOUND ( 'NONE', #81967, .T. ) ;
#22944 = ORIENTED_EDGE ( 'NONE', *, *, #82877, .T. ) ;
#22945 = EDGE_CURVE ( 'NONE', #40194, #40709, #11495, .T. ) ;
#22946 = ORIENTED_EDGE ( 'NONE', *, *, #4881, .F. ) ;
#22948 = CARTESIAN_POINT ( 'NONE',  ( 10.74591005361826035, -12.15418822224088657, 32.17964115625579069 ) ) ;
#22947 = LINE ( 'NONE', #71130, #86408 ) ;
#22949 = EDGE_CURVE ( 'NONE', #19931, #65515, #31604, .T. ) ;
#22950 = CARTESIAN_POINT ( 'NONE',  ( -5.776988648387149539, -6.503523203565942268, 34.64991518177335195 ) ) ;
#22951 = CARTESIAN_POINT ( 'NONE',  ( -0.4615384615384611200, -12.78798330534102945, 29.74999999999997868 ) ) ;
#22952 = CARTESIAN_POINT ( 'NONE',  ( 14.55769230769231015, -2.249999999999998668, 29.75000000000000355 ) ) ;
#22953 = DIRECTION ( 'NONE',  ( -0.000000000000000000, 0.1736481776669307198, -0.9848077530122080203 ) ) ;
#22954 = ORIENTED_EDGE ( 'NONE', *, *, #89117, .T. ) ;
#22955 = CARTESIAN_POINT ( 'NONE',  ( -12.46153846153846168, -1.790695186598648903, 34.54067556320373455 ) ) ;
#22956 = CARTESIAN_POINT ( 'NONE',  ( 0.3962684609821418014, -12.70778746994557551, 30.41441678777548319 ) ) ;
#22957 = CARTESIAN_POINT ( 'NONE',  ( 17.20744877868664346, -6.852161475712351013, 34.70806712695775786 ) ) ;
#22958 = FACE_OUTER_BOUND ( 'NONE', #25298, .T. ) ;
#22959 = CARTESIAN_POINT ( 'NONE',  ( -11.53846153846123102, -2.506253911140614576, 30.00000000000323297 ) ) ;
#22960 = AXIS2_PLACEMENT_3D ( 'NONE', #54873, #19759, #27402 ) ;
#22961 = CARTESIAN_POINT ( 'NONE',  ( -1.553300858899081538, -11.25000000000000711, 14.85937500000000355 ) ) ;
#22962 = ORIENTED_EDGE ( 'NONE', *, *, #89173, .T. ) ;
#22963 = ORIENTED_EDGE ( 'NONE', *, *, #66799, .F. ) ;
#22964 = CARTESIAN_POINT ( 'NONE',  ( -7.780086512803768173, -11.91647553114624358, 32.58852847137148245 ) ) ;
#22965 = ORIENTED_EDGE ( 'NONE', *, *, #36252, .T. ) ;
#22966 = CARTESIAN_POINT ( 'NONE',  ( 17.07692307692307665, -3.937682226553329556, 33.60647404775216529 ) ) ;
#22967 = CARTESIAN_POINT ( 'NONE',  ( 18.06606835100243913, -5.557115091759786019, 34.35708131394839882 ) ) ;
#22968 = CARTESIAN_POINT ( 'NONE',  ( -5.076923076923075762, -8.164416787775445883, 34.95778746994557906 ) ) ;
#22969 = CARTESIAN_POINT ( 'NONE',  ( -8.703975197954745724, -10.90142922261932057, 33.41473453929631887 ) ) ;
#22970 = CARTESIAN_POINT ( 'NONE',  ( 3.750000000000009770, -9.053300858899081760, 19.54687499999999645 ) ) ;
#22971 = CARTESIAN_POINT ( 'NONE',  ( 17.07692307692307665, -7.500000000000001776, 35.04278698407183867 ) ) ;
#22972 = VERTEX_POINT ( 'NONE', #53421 ) ;
#22973 = DIRECTION ( 'NONE',  ( -0.000000000000000000, 0.6427876096865404731, -0.7660444431189771253 ) ) ;
#22975 = ORIENTED_EDGE ( 'NONE', *, *, #45850, .T. ) ;
#22974 = CARTESIAN_POINT ( 'NONE',  ( -9.692307692307691624, -2.292212530054420494, 30.41441678777542634 ) ) ;
#22976 = CARTESIAN_POINT ( 'NONE',  ( -9.692307692307691624, -11.11383981884818262, 36.00935417666054406 ) ) ;
#22978 = B_SPLINE_CURVE_WITH_KNOTS ( 'NONE', 3,
 ( #75836, #68202, #48801, #34845, #76273, #55121, #41613, #75400, #42064, #13693 ),
 .UNSPECIFIED., .F., .F.,
 ( 4, 2, 2, 2, 4 ),
 ( 0.0007817359430256300059, 0.0009771253907249963233, 0.001172514838424362858, 0.001367904286123729392, 0.001563293733823095709 ),
 .UNSPECIFIED. ) ;
#22977 = CARTESIAN_POINT ( 'NONE',  ( -12.33101275977489841, -3.816742781228458004, 33.13167719472716044 ) ) ;
#22979 = CARTESIAN_POINT ( 'NONE',  ( 11.53846153846141753, -4.481592998941358097, 33.73612834414048933 ) ) ;
#22980 = CARTESIAN_POINT ( 'NONE',  ( 6.792386319966615460, -3.338472653186242756, 32.95098750199972670 ) ) ;
#22981 = B_SPLINE_CURVE_WITH_KNOTS ( 'NONE', 3,
 ( #84460, #77681, #64156, #2458, #84901, #23187, #48881, #73008, #52286, #19398 ),
 .UNSPECIFIED., .F., .F.,
 ( 4, 2, 2, 2, 4 ),
 ( 0.000000000000000000, 0.0001954339857564070678, 0.0003908679715128141356, 0.0005863019572692211492, 0.0007817359430256282712 ),
 .UNSPECIFIED. ) ;
#22982 = VECTOR ( 'NONE', #82449, 1000.000000000000114 ) ;
#22983 = LINE ( 'NONE', #22107, #62290 ) ;
#22984 = CARTESIAN_POINT ( 'NONE',  ( -7.846153846153844924, -12.37446782046654192, 30.86335684631486131 ) ) ;
#22985 = CARTESIAN_POINT ( 'NONE',  ( 1.987747218494642309, -5.598659921968629050, 23.31436829374150932 ) ) ;
#22986 = ORIENTED_EDGE ( 'NONE', *, *, #25820, .T. ) ;
#22987 = CARTESIAN_POINT ( 'NONE',  ( -2.980823821391186623, -6.653508905675590945, 34.93172785388651391 ) ) ;
#22988 = CYLINDRICAL_SURFACE ( 'NONE', #59149, 0.2500000000000002220 ) ;
#22989 = CARTESIAN_POINT ( 'NONE',  ( 1.139087296525997273, -4.749999999999992895, 24.23437500000000355 ) ) ;
#22990 = AXIS2_PLACEMENT_3D ( 'NONE', #74151, #81360, #47105 ) ;
#22991 = CARTESIAN_POINT ( 'NONE',  ( -16.08777882049607655, -11.35647404775217595, 33.31231777344667222 ) ) ;
#22992 = DIRECTION ( 'NONE',  ( -0.000000000000000000, -0.000000000000000000, -1.000000000000000000 ) ) ;
#22993 = ORIENTED_EDGE ( 'NONE', *, *, #17473, .F. ) ;
#22994 = CYLINDRICAL_SURFACE ( 'NONE', #83028, 0.2499999999999994726 ) ;
#22995 = CARTESIAN_POINT ( 'NONE',  ( 3.164685819813350509, -8.973038597847271092, 34.52809138561120506 ) ) ;
#22996 = ADVANCED_FACE ( 'NONE', ( #38589 ), #80923, .F. ) ;
#22997 = AXIS2_PLACEMENT_3D ( 'NONE', #4386, #73294, #5720 ) ;
#22998 = ORIENTED_EDGE ( 'NONE', *, *, #61421, .F. ) ;
#22999 = AXIS2_PLACEMENT_3D ( 'NONE', #52062, #11987, #17853 ) ;
#23000 = CYLINDRICAL_SURFACE ( 'NONE', #42857, 0.2500000000000009437 ) ;
#23001 = UNCERTAINTY_MEASURE_WITH_UNIT (LENGTH_MEASURE( 1.000000000000000082E-05 ), #49270, 'distance_accuracy_value', 'NONE');
#23002 = EDGE_CURVE ( 'NONE', #77088, #24805, #6135, .T. ) ;
#23003 =( GEOMETRIC_REPRESENTATION_CONTEXT ( 3 ) GLOBAL_UNCERTAINTY_ASSIGNED_CONTEXT ( ( #2272 ) ) GLOBAL_UNIT_ASSIGNED_CONTEXT ( ( #31200, #65434, #11381 ) ) REPRESENTATION_CONTEXT ( 'NONE', 'WORKASPACE' ) );
#23004 = ORIENTED_EDGE ( 'NONE', *, *, #47817, .F. ) ;
#23005 = LINE ( 'NONE', #43715, #40591 ) ;
#23006 = DIRECTION ( 'NONE',  ( 0.000000000000000000, 0.9848077530122072432, 0.1736481776669354937 ) ) ;
#23007 = CARTESIAN_POINT ( 'NONE',  ( -12.59168643127015841, -10.31621877034669588, 34.18098118002070152 ) ) ;
#23008 = CARTESIAN_POINT ( 'NONE',  ( -12.46153846153846168, -10.67929555188718282, 33.92786785259544047 ) ) ;
#23009 = VERTEX_POINT ( 'NONE', #8356 ) ;
#23010 = EDGE_CURVE ( 'NONE', #41430, #47075, #88578, .T. ) ;
#23011 = CARTESIAN_POINT ( 'NONE',  ( 13.13461538461538680, -2.249999999999998668, 29.75000000000000355 ) ) ;
#23012 = VERTEX_POINT ( 'NONE', #40813 ) ;
#23013 = DIRECTION ( 'NONE',  ( -0.000000000000000000, 0.6427876096865404731, -0.7660444431189771253 ) ) ;
#23014 = CARTESIAN_POINT ( 'NONE',  ( -10.86536134632696715, -2.779195860258146578, 31.39871582349836032 ) ) ;
#23015 = ORIENTED_EDGE ( 'NONE', *, *, #16381, .F. ) ;
#23016 = CARTESIAN_POINT ( 'NONE',  ( -2.307692307692428724, -11.06231777344772027, 33.60647404775119895 ) ) ;
#23017 = CARTESIAN_POINT ( 'NONE',  ( -12.52762187249433978, -5.557115091759785130, 34.35708131394839171 ) ) ;
#23018 = DIRECTION ( 'NONE',  ( -0.000000000000000000, 0.1736481776669307198, -0.9848077530122080203 ) ) ;
#23019 = EDGE_CURVE ( 'NONE', #80339, #26228, #49163, .T. ) ;
#23020 = FACE_OUTER_BOUND ( 'NONE', #69469, .T. ) ;
#23021 = DIRECTION ( 'NONE',  ( 0.000000000000000000, -1.000000000000000000, 0.000000000000000000 ) ) ;
#23022 = B_SPLINE_CURVE_WITH_KNOTS ( 'NONE', 3,
 ( #76210, #14516, #69461, #7765, #38786, #30686, #16724, #71668, #17172, #86544 ),
 .UNSPECIFIED., .F., .F.,
 ( 4, 2, 2, 2, 4 ),
 ( 0.0007817359527651098448, 0.0009771254036996487088, 0.001172514854634187573, 0.001367904305568726220, 0.001563293756503265084 ),
 .UNSPECIFIED. ) ;
#23023 = ORIENTED_EDGE ( 'NONE', *, *, #58587, .F. ) ;
#23024 = VERTEX_POINT ( 'NONE', #62388 ) ;
#23025 = FACE_BOUND ( 'NONE', #88720, .T. ) ;
#23026 = ORIENTED_EDGE ( 'NONE', *, *, #23071, .T. ) ;
#23027 = LINE ( 'NONE', #56809, #14138 ) ;
#23028 = EDGE_CURVE ( 'NONE', #82752, #20850, #28760, .T. ) ;
#23029 = EDGE_CURVE ( 'NONE', #26488, #59736, #44839, .T. ) ;
#23030 = CARTESIAN_POINT ( 'NONE',  ( 17.77707304109314634, -5.582147617184174848, 34.63737895849758530 ) ) ;
#23031 = CARTESIAN_POINT ( 'NONE',  ( 0.4615384615383382183, -12.70778746994576025, 30.41441678777401236 ) ) ;
#23032 = ORIENTED_EDGE ( 'NONE', *, *, #13385, .T. ) ;
#23033 = ORIENTED_EDGE ( 'NONE', *, *, #55059, .F. ) ;
#23034 = DIRECTION ( 'NONE',  ( -0.000000000000000000, -0.6427876096865404731, -0.7660444431189771253 ) ) ;
#23035 = ORIENTED_EDGE ( 'NONE', *, *, #32205, .F. ) ;
#23036 = CARTESIAN_POINT ( 'NONE',  ( -10.55012904410859065, -9.442884908240273489, 34.35708131394835618 ) ) ;
#23037 = ADVANCED_FACE ( 'NONE', ( #42149 ), #13771, .F. ) ;
#23038 = VECTOR ( 'NONE', #53062, 1000.000000000000000 ) ;
#23039 = CARTESIAN_POINT ( 'NONE',  ( 13.31853197365950336, -2.721908614388770964, 31.22303859784723912 ) ) ;
#23040 = CARTESIAN_POINT ( 'NONE',  ( 0.000000000000000000, -11.00000000000000000, 29.75000000000000355 ) ) ;
#23041 = FACE_BOUND ( 'NONE', #81868, .T. ) ;
#23042 = ORIENTED_EDGE ( 'NONE', *, *, #74672, .T. ) ;
#23043 = CARTESIAN_POINT ( 'NONE',  ( 8.834486340506792601, -9.442884908240273489, 34.35708131394835618 ) ) ;
#23044 = B_SPLINE_CURVE_WITH_KNOTS ( 'NONE', 3,
 ( #29888, #3282, #43830, #42960, #86168, #65433, #50584, #70430, #85275, #29451 ),
 .UNSPECIFIED., .F., .F.,
 ( 4, 2, 2, 2, 4 ),
 ( 0.0007817246256747440282, 0.0009771112852218863821, 0.001172497944769028844, 0.001367884604316171307, 0.001563271263863313769 ),
 .UNSPECIFIED. ) ;
#23045 = VECTOR ( 'NONE', #74279, 1000.000000000000227 ) ;
#23046 = AXIS2_PLACEMENT_3D ( 'NONE', #63780, #78185, #78625 ) ;
#23047 = CARTESIAN_POINT ( 'NONE',  ( -14.98082382139119062, -3.520799739797214389, 33.17531984108286025 ) ) ;
#23048 = DIRECTION ( 'NONE',  ( 0.000000000000000000, 0.1736481776669267785, -0.9848077530122087975 ) ) ;
#23049 = CARTESIAN_POINT ( 'NONE',  ( -19.50000000000000000, -3.499999999999999556, 29.75000000000000355 ) ) ;
#23050 = ORIENTED_EDGE ( 'NONE', *, *, #60191, .F. ) ;
#23051 = PRODUCT_DEFINITION_CONTEXT ( 'detailed design', #88395, 'design' ) ;
#23052 = VERTEX_POINT ( 'NONE', #704 ) ;
#23053 = VECTOR ( 'NONE', #13794, 1000.000000000000227 ) ;
#23054 = ADVANCED_FACE ( 'NONE', ( #34925 ), #82693, .F. ) ;
#23055 = ORIENTED_EDGE ( 'NONE', *, *, #41178, .T. ) ;
#23056 = VECTOR ( 'NONE', #37899, 1000.000000000000000 ) ;
#23058 = CARTESIAN_POINT ( 'NONE',  ( -13.63463862190834952, -5.851115903089112003, 34.47074536777953568 ) ) ;
#23057 = DIRECTION ( 'NONE',  ( 0.000000000000000000, 0.7660444431189822323, -0.6427876096865344779 ) ) ;
#23059 = FACE_OUTER_BOUND ( 'NONE', #44159, .T. ) ;
#23060 = CARTESIAN_POINT ( 'NONE',  ( -6.923076923077044142, -3.835265460704628371, 33.15142922262033665 ) ) ;
#23061 = EDGE_CURVE ( 'NONE', #60707, #14975, #24426, .T. ) ;
#23062 = CYLINDRICAL_SURFACE ( 'NONE', #83192, 0.2499999999999994726 ) ;
#23063 = CARTESIAN_POINT ( 'NONE',  ( 14.17700170458200404, -2.845849958028613624, 32.17971566917920967 ) ) ;
#23064 = EDGE_CURVE ( 'NONE', #21870, #49519, #21420, .T. ) ;
#23065 = ORIENTED_EDGE ( 'NONE', *, *, #61590, .T. ) ;
#23066 = CARTESIAN_POINT ( 'NONE',  ( -15.90384615384615330, -2.249999999999998668, 29.75000000000000355 ) ) ;
#23067 = FACE_OUTER_BOUND ( 'NONE', #64989, .T. ) ;
#23068 = CARTESIAN_POINT ( 'NONE',  ( 5.750000000000002665, -7.500000000000001776, 35.04278698407183867 ) ) ;
#23069 = CARTESIAN_POINT ( 'NONE',  ( 6.988332062589762472, -9.528491918058460186, 34.59228464037085615 ) ) ;
#23070 = VERTEX_POINT ( 'NONE', #62827 ) ;
#23071 = EDGE_CURVE ( 'NONE', #7366, #68357, #46001, .T. ) ;
#23072 = CARTESIAN_POINT ( 'NONE',  ( -2.307692307692305711, -1.790695186598648903, 34.54067556320373455 ) ) ;
#23073 = EDGE_CURVE ( 'NONE', #2893, #55087, #68301, .T. ) ;
#23074 = EDGE_LOOP ( 'NONE', ( #2642, #6997, #80684, #48968 ) ) ;
#23075 = FACE_BOUND ( 'NONE', #79868, .T. ) ;
#23076 = CARTESIAN_POINT ( 'NONE',  ( -16.81410256410256565, -3.499999999999999556, 29.75000000000000355 ) ) ;
#23077 = CARTESIAN_POINT ( 'NONE',  ( 18.06525513951284267, -12.70778746994558439, 30.41441678777537305 ) ) ;
#23078 = CARTESIAN_POINT ( 'NONE',  ( 12.21156173059610772, -12.17611988154120972, 31.52148481390971213 ) ) ;
#23079 = ORIENTED_EDGE ( 'NONE', *, *, #27744, .F. ) ;
#23080 = CARTESIAN_POINT ( 'NONE',  ( -16.28453675695646652, -11.37499894934982514, 33.29245874905763003 ) ) ;
#23081 = CARTESIAN_POINT ( 'NONE',  ( 6.923076923076802558, -10.90142922262034020, 33.41473453929536674 ) ) ;
#23082 = CARTESIAN_POINT ( 'NONE',  ( 0.4615384615384611200, -4.786620604624113540, 33.94971097300155094 ) ) ;
#23083 = CARTESIAN_POINT ( 'NONE',  ( 1.384615384615386802, -13.57706302396349152, 30.56769352161908060 ) ) ;
#23084 = VERTEX_POINT ( 'NONE', #36273 ) ;
#23085 = CARTESIAN_POINT ( 'NONE',  ( -9.915234651214539952, -2.889293201056495786, 32.26117774369186009 ) ) ;
#23086 = ORIENTED_EDGE ( 'NONE', *, *, #64949, .T. ) ;
#23088 = VERTEX_POINT ( 'NONE', #16000 ) ;
#23087 = DIRECTION ( 'NONE',  ( -1.000000000000000000, 0.000000000000000000, -0.000000000000000000 ) ) ;
#23089 = CARTESIAN_POINT ( 'NONE',  ( -5.999999999999998224, -1.215029322943914858, 32.30358669280327177 ) ) ;
#23090 = CARTESIAN_POINT ( 'NONE',  ( 15.16549923021291058, -5.094484230520674117, 34.41647553114621161 ) ) ;
#23091 = CARTESIAN_POINT ( 'NONE',  ( 5.076923076923075762, -2.486705287966279876, 31.30864560766543647 ) ) ;
#23092 = DIRECTION ( 'NONE',  ( 0.000000000000000000, 0.6427876096865368094, 0.7660444431189802339 ) ) ;
#23093 = CARTESIAN_POINT ( 'NONE',  ( -7.911424292114620727, -9.442884908240170461, 34.35708131394840592 ) ) ;
#23094 = FACE_OUTER_BOUND ( 'NONE', #29583, .T. ) ;
#23095 = AXIS2_PLACEMENT_3D ( 'NONE', #25438, #86270, #52895 ) ;
#23096 = CARTESIAN_POINT ( 'NONE',  ( -1.139087296526025916, -4.750000000000006217, 25.32812500000000711 ) ) ;
#23097 = VERTEX_POINT ( 'NONE', #57863 ) ;
#23098 = CARTESIAN_POINT ( 'NONE',  ( -0.6844646790546095039, -5.667676309546437530, 34.40238873228292249 ) ) ;
#23099 = CARTESIAN_POINT ( 'NONE',  ( 16.81410256410256565, -3.499999999999999556, 29.75000000000000355 ) ) ;
#23100 = ORIENTED_EDGE ( 'NONE', *, *, #67661, .F. ) ;
#23101 =( BOUNDED_CURVE ( )  B_SPLINE_CURVE ( 2, ( #73250, #19195, #59734, #3889, #45322, #10221, #72795 ),
 .UNSPECIFIED., .F., .F. ) 
 B_SPLINE_CURVE_WITH_KNOTS ( ( 3, 2, 2, 3 ),
 ( 0.000000000000000000, 0.01250000000000000069, 0.02500000000000000139, 0.03447824448891075727 ),
 .UNSPECIFIED. ) 
 CURVE ( )  GEOMETRIC_REPRESENTATION_ITEM ( )  RATIONAL_B_SPLINE_CURVE ( ( 0.5359370743784122038, 0.4951412937321941765, 0.5359370743784122038, 0.4951412937321941765, 0.5359370743784122038, 0.5050032837319460288, 0.5209811780000378478 ) ) 
 REPRESENTATION_ITEM ( '' )  );
#23102 = EDGE_LOOP ( 'NONE', ( #22158, #52142 ) ) ;
#23103 = VERTEX_POINT ( 'NONE', #78576 ) ;
#23104 = CARTESIAN_POINT ( 'NONE',  ( 16.82689983963011926, -5.056417327199097755, 34.11270091957320716 ) ) ;
#23105 = DIRECTION ( 'NONE',  ( -0.000000000000000000, -5.102127870520021228E-17, -1.000000000000000000 ) ) ;
#23106 = CARTESIAN_POINT ( 'NONE',  ( 3.230769230769110045, -10.21337939537710326, 33.94971097300076224 ) ) ;
#23107 = CARTESIAN_POINT ( 'NONE',  ( 9.692307692307695177, -12.37446782046654192, 30.86335684631486131 ) ) ;
#23108 = CARTESIAN_POINT ( 'NONE',  ( 6.222779541268408821, -2.600157965045225339, 30.74683119005207743 ) ) ;
#23109 = CARTESIAN_POINT ( 'NONE',  ( 17.93391762063986050, -11.91647553114624181, 32.58852847137148245 ) ) ;
#23110 = FACE_OUTER_BOUND ( 'NONE', #33455, .T. ) ;
#23111 = EDGE_LOOP ( 'NONE', ( #40234, #30434 ) ) ;
#23112 = CARTESIAN_POINT ( 'NONE',  ( 3.165498784808455923, -6.879047030191174805, 34.71129190930000163 ) ) ;
#23113 = CARTESIAN_POINT ( 'NONE',  ( -19.00000000000000000, -16.99999999999999645, 22.25000000000000355 ) ) ;
#23114 = AXIS2_PLACEMENT_3D ( 'NONE', #6134, #5245, #39491 ) ;
#23115 = CARTESIAN_POINT ( 'NONE',  ( -9.627052121031667298, -11.48612834413965977, 32.76840700105972815 ) ) ;
#23116 = DIRECTION ( 'NONE',  ( 0.000000000000000000, 0.000000000000000000, -1.000000000000000000 ) ) ;
#23117 = ORIENTED_EDGE ( 'NONE', *, *, #59459, .F. ) ;
#23118 = CARTESIAN_POINT ( 'NONE',  ( 7.780071466793708979, -2.292212530054419606, 30.41441678777542634 ) ) ;
#23119 = VECTOR ( 'NONE', #7093, 1000.000000000000000 ) ;
#23120 = ORIENTED_EDGE ( 'NONE', *, *, #74834, .T. ) ;
#23121 = CARTESIAN_POINT ( 'NONE',  ( 12.23861150263161335, -9.172386477786396597, 34.72672124145550043 ) ) ;
#23122 = CYLINDRICAL_SURFACE ( 'NONE', #47418, 0.2500000000000009437 ) ;
#23123 = LINE ( 'NONE', #28562, #87193 ) ;
#23124 = CARTESIAN_POINT ( 'NONE',  ( 12.71159277317677549, -10.66356715214248752, 33.62249196103329751 ) ) ;
#23125 = ORIENTED_EDGE ( 'NONE', *, *, #34917, .T. ) ;
#23126 = CARTESIAN_POINT ( 'NONE',  ( 12.71159288145191013, -10.82426656108012075, 33.81400080652039009 ) ) ;
#23127 = AXIS2_PLACEMENT_3D ( 'NONE', #31374, #24611, #59733 ) ;
#23128 = CARTESIAN_POINT ( 'NONE',  ( 9.442330948259101575, -2.920706130388546651, 32.31842814019191223 ) ) ;
#23129 = CARTESIAN_POINT ( 'NONE',  ( 8.835299120233205628, -4.098570777380720287, 33.41473453929635440 ) ) ;
#23130 = ORIENTED_EDGE ( 'NONE', *, *, #43878, .F. ) ;
#23131 = CARTESIAN_POINT ( 'NONE',  ( -1.253823576790597638, -3.530189275343204702, 32.79018710029569661 ) ) ;
#23132 = ORIENTED_EDGE ( 'NONE', *, *, #39125, .F. ) ;
#23133 = B_SPLINE_CURVE_WITH_KNOTS ( 'NONE', 3,
 ( #28080, #55546, #83030, #21314, #48788, #76255, #14564, #85685, #15904, #57763 ),
 .UNSPECIFIED., .F., .F.,
 ( 4, 2, 2, 2, 4 ),
 ( 0.0007817359430256297891, 0.0009771253907249958896, 0.001172514838424362207, 0.001367904286123728524, 0.001563293733823094625 ),
 .UNSPECIFIED. ) ;
#23134 = DIRECTION ( 'NONE',  ( 0.000000000000000000, 0.3420201433256610524, 0.9396926207859113145 ) ) ;
#23135 = EDGE_CURVE ( 'NONE', #49385, #71780, #81972, .T. ) ;
#23136 = CARTESIAN_POINT ( 'NONE',  ( 17.07692307692307665, -8.164416787775445883, 34.95778746994557906 ) ) ;
#23137 = CARTESIAN_POINT ( 'NONE',  ( -7.912236225513978205, -2.486705287966279432, 31.30864560766542937 ) ) ;
#23138 = PLANE ( 'NONE',  #59471 ) ;
#23139 = DIRECTION ( 'NONE',  ( 0.000000000000000000, 0.3420201433256610524, 0.9396926207859113145 ) ) ;
#23140 = ORIENTED_EDGE ( 'NONE', *, *, #48187, .T. ) ;
#23141 = VECTOR ( 'NONE', #67003, 1000.000000000000114 ) ;
#23142 = ORIENTED_EDGE ( 'NONE', *, *, #15569, .F. ) ;
#23144 = ORIENTED_EDGE ( 'NONE', *, *, #21087, .F. ) ;
#23143 = B_SPLINE_CURVE_WITH_KNOTS ( 'NONE', 3,
 ( #17737, #45190, #60490, #27146, #53281, #38903, #74015, #80785, #52838, #45644 ),
 .UNSPECIFIED., .F., .F.,
 ( 4, 2, 2, 2, 4 ),
 ( 0.000000000000000000, 0.0001954339857564098325, 0.0003908679715128196650, 0.0005863019572692294975, 0.0007817359430256393300 ),
 .UNSPECIFIED. ) ;
#23145 = EDGE_CURVE ( 'NONE', #89080, #39107, #40402, .T. ) ;
#23146 = CARTESIAN_POINT ( 'NONE',  ( -7.173076923076921574, -7.500000000000001776, 34.75000000000000000 ) ) ;
#23147 = CARTESIAN_POINT ( 'NONE',  ( -9.692307692307814193, -4.320704448113951379, 33.92786785259630022 ) ) ;
#23148 = VECTOR ( 'NONE', #33484, 1000.000000000000000 ) ;
#23149 = B_SPLINE_CURVE_WITH_KNOTS ( 'NONE', 3,
 ( #63720, #56084, #29950, #57407, #50194, #43458, #78569, #15107, #56962, #77680 ),
 .UNSPECIFIED., .F., .F.,
 ( 4, 2, 2, 2, 4 ),
 ( 0.0007817359430256297891, 0.0009771253907249958896, 0.001172514838424361990, 0.001367904286123727874, 0.001563293733823093975 ),
 .UNSPECIFIED. ) ;
#23150 = CARTESIAN_POINT ( 'NONE',  ( -12.23852561744506851, -12.38742843783360748, 31.66772728687926985 ) ) ;
#23151 = B_SPLINE_CURVE_WITH_KNOTS ( 'NONE', 3,
 ( #78045, #81828, #26875, #28192, #27317, #55662, #83152, #20120, #288, #82269 ),
 .UNSPECIFIED., .F., .F.,
 ( 4, 2, 2, 2, 4 ),
 ( 0.0007817359430256372700, 0.0009771253907250054306, 0.001172514838424373483, 0.001367904286123741535, 0.001563293733823109804 ),
 .UNSPECIFIED. ) ;
#23152 = CARTESIAN_POINT ( 'NONE',  ( -8.769230769230892619, -6.835583212225970762, 34.95778746994575670 ) ) ;
#23153 = CARTESIAN_POINT ( 'NONE',  ( -6.923076923076922462, -3.513871655860378418, 32.76840700105978499 ) ) ;
#23154 = CARTESIAN_POINT ( 'NONE',  ( 5.142991427925515779, -9.780366693483667717, 34.19971097300155805 ) ) ;
#23155 = ORIENTED_EDGE ( 'NONE', *, *, #51424, .T. ) ;
#23156 = ORIENTED_EDGE ( 'NONE', *, *, #54675, .T. ) ;
#23157 = EDGE_LOOP ( 'NONE', ( #69740, #15255 ) ) ;
#23159 = ORIENTED_EDGE ( 'NONE', *, *, #88924, .F. ) ;
#23158 = CARTESIAN_POINT ( 'NONE',  ( -3.164700879766792596, -10.51840700105979565, 33.73612834413962247 ) ) ;
#23161 = CARTESIAN_POINT ( 'NONE',  ( -24.00000000000000000, 9.000000000000024869, 29.25000000000000000 ) ) ;
#23160 = CARTESIAN_POINT ( 'NONE',  ( 0.6843180028068700516, -8.496831190052093419, 34.64984203495476578 ) ) ;
#23162 = CARTESIAN_POINT ( 'NONE',  ( 1.449870524128225258, -5.094484230520773593, 34.41647553114626845 ) ) ;
#23163 = EDGE_CURVE ( 'NONE', #44514, #65922, #37588, .T. ) ;
#23164 = CARTESIAN_POINT ( 'NONE',  ( 3.750000000000000888, -7.499999999999978684, 24.46875000000000000 ) ) ;
#23165 = EDGE_CURVE ( 'NONE', #2439, #13277, #16768, .T. ) ;
#23166 = ORIENTED_EDGE ( 'NONE', *, *, #75120, .T. ) ;
#23167 = AXIS2_PLACEMENT_3D ( 'NONE', #81705, #19988, #40722 ) ;
#23168 = EDGE_LOOP ( 'NONE', ( #53484, #50403 ) ) ;
#23169 = CYLINDRICAL_SURFACE ( 'NONE', #37065, 0.2500000000000002220 ) ;
#23170 = ORIENTED_EDGE ( 'NONE', *, *, #35681, .T. ) ;
#23171 = FACE_BOUND ( 'NONE', #40640, .T. ) ;
#23173 = AXIS2_PLACEMENT_3D ( 'NONE', #67152, #74803, #21170 ) ;
#23172 = CARTESIAN_POINT ( 'NONE',  ( -6.130147209438219669, -9.418419913701741919, 34.36755862841477693 ) ) ;
#23174 = VECTOR ( 'NONE', #22842, 1000.000000000000227 ) ;
#23175 = EDGE_CURVE ( 'NONE', #78911, #57769, #70938, .T. ) ;
#23176 = DIRECTION ( 'NONE',  ( -0.000000000000000000, 0.3420201433256694346, -0.9396926207859080948 ) ) ;
#23177 = EDGE_LOOP ( 'NONE', ( #8347, #889 ) ) ;
#23178 = CARTESIAN_POINT ( 'NONE',  ( -15.16470087976679615, -4.786620604624113540, 33.94971097300155805 ) ) ;
#23179 = CARTESIAN_POINT ( 'NONE',  ( 4.946775107191381693, -8.630895178749536711, 34.87696386517710323 ) ) ;
#23180 = CARTESIAN_POINT ( 'NONE',  ( 1.134638640566794310, -3.436278759898155233, 33.07459398097509506 ) ) ;
#23181 = LINE ( 'NONE', #50643, #29913 ) ;
#23182 = CARTESIAN_POINT ( 'NONE',  ( 1.607628228708781970, -2.523321265292116422, 31.42251411153756990 ) ) ;
#23183 = B_SPLINE_CURVE_WITH_KNOTS ( 'NONE', 3,
 ( #58588, #44176, #45968, #11302, #45077, #66695, #71662, #10865, #65788, #66239 ),
 .UNSPECIFIED., .F., .F.,
 ( 4, 2, 2, 2, 4 ),
 ( 0.000000000000000000, 0.0001954339857564098054, 0.0003908679715128196108, 0.0005863019572692293891, 0.0007817359430256392216 ),
 .UNSPECIFIED. ) ;
#23184 = CARTESIAN_POINT ( 'NONE',  ( 8.069166690247241647, -11.43677907613344757, 33.22367315496202167 ) ) ;
#23185 = CARTESIAN_POINT ( 'NONE',  ( -14.05769230769087130, -7.500000000000155431, 34.75000000000007105 ) ) ;
#23186 = CARTESIAN_POINT ( 'NONE',  ( 2.307692307692309264, -11.91647553114624181, 32.58852847137148245 ) ) ;
#23187 = CARTESIAN_POINT ( 'NONE',  ( -6.250023237292964495, -5.851115903089112003, 34.47074536777953568 ) ) ;
#23188 = CARTESIAN_POINT ( 'NONE',  ( 16.02315555073584363, -10.70098750199973203, 33.91152734681376302 ) ) ;
#23189 = DIRECTION ( 'NONE',  ( 0.000000000000000000, 0.9848077530122072432, 0.1736481776669354937 ) ) ;
#23190 = B_SPLINE_CURVE_WITH_KNOTS ( 'NONE', 3,
 ( #11448, #45221, #39380, #60070, #73150, #32602, #11008, #80364, #51510, #87130 ),
 .UNSPECIFIED., .F., .F.,
 ( 4, 2, 2, 2, 4 ),
 ( 0.0007817246256747459798, 0.0009771112852218896347, 0.001172497944769033181, 0.001367884604316176728, 0.001563271263863320491 ),
 .UNSPECIFIED. ) ;
#23191 = CARTESIAN_POINT ( 'NONE',  ( -39.05038313613820122, -7.500000000000000000, 29.75000000000000355 ) ) ;
#23193 = DIRECTION ( 'NONE',  ( -1.000000000000000000, -0.000000000000000000, -0.000000000000000000 ) ) ;
#23192 = CARTESIAN_POINT ( 'NONE',  ( -13.44988538517170440, -4.320704448112771878, 33.92786785259540494 ) ) ;
#23194 = CARTESIAN_POINT ( 'NONE',  ( -1.161835715637316913, -9.418065098278011860, 34.63729479722530158 ) ) ;
#23196 = CARTESIAN_POINT ( 'NONE',  ( 12.23861150263161157, -4.762599654559228846, 34.23009711892697737 ) ) ;
#23195 = CARTESIAN_POINT ( 'NONE',  ( 16.15384615384603251, -8.656820664282941280, 34.87096338111179961 ) ) ;
#23197 = CARTESIAN_POINT ( 'NONE',  ( -5.934744428723973897, -12.46129190930001052, 30.37095296980870174 ) ) ;
#23198 = CARTESIAN_POINT ( 'NONE',  ( 2.750000000000001332, -7.438900925035452083, 22.96688170625849068 ) ) ;
#23199 = ORIENTED_EDGE ( 'NONE', *, *, #18820, .F. ) ;
#23200 = CARTESIAN_POINT ( 'NONE',  ( 3.255975518055617357, -8.015373823202054382, 14.00000000000003553 ) ) ;
#23201 = ORIENTED_EDGE ( 'NONE', *, *, #15935, .F. ) ;
#23202 = CARTESIAN_POINT ( 'NONE',  ( -9.942330929600657896, -5.851115903089112003, 34.47074536777953568 ) ) ;
#23203 = EDGE_LOOP ( 'NONE', ( #34193, #87536, #86989, #42875 ) ) ;
#23204 = CARTESIAN_POINT ( 'NONE',  ( 17.77651505627604678, -12.24155766932282496, 31.33739205006857986 ) ) ;
#23205 = ORIENTED_EDGE ( 'NONE', *, *, #35133, .F. ) ;
#23206 = CARTESIAN_POINT ( 'NONE',  ( 10.61538461538461675, -2.833524468853757305, 32.15551576947925838 ) ) ;
#23207 = CARTESIAN_POINT ( 'NONE',  ( 2.724691934501235036, -6.299813628509441266, 22.88875670625849068 ) ) ;
#23208 = CARTESIAN_POINT ( 'NONE',  ( -17.75005459062195712, -9.357781135181033605, 34.66075350412533851 ) ) ;
#23209 = LINE ( 'NONE', #3826, #41768 ) ;
#23210 = LINE ( 'NONE', #16017, #54712 ) ;
#23211 = CARTESIAN_POINT ( 'NONE',  ( -17.99999999841483955, -2.249999999999995115, 29.50000000010503953 ) ) ;
#23212 = CARTESIAN_POINT ( 'NONE',  ( -13.63463860883683942, -8.475808217655753651, 34.90892951860618609 ) ) ;
#23213 = CARTESIAN_POINT ( 'NONE',  ( 16.15384615384603251, -11.48612834414049644, 32.76840700105863391 ) ) ;
#23214 = CARTESIAN_POINT ( 'NONE',  ( -3.749999999999997335, -7.500000000000021316, 17.59375000000000000 ) ) ;
#23215 = CARTESIAN_POINT ( 'NONE',  ( -11.53846153846153655, -2.486705287966279876, 31.30864560766543647 ) ) ;
#23216 = CARTESIAN_POINT ( 'NONE',  ( 9.692307692307695177, -13.53365097954675988, 30.81389545987213552 ) ) ;
#23217 = AXIS2_PLACEMENT_3D ( 'NONE', #81165, #32076, #12697 ) ;
#23218 = CARTESIAN_POINT ( 'NONE',  ( 10.39245765647776309, -5.582147617184174848, 34.63737895849758530 ) ) ;
#23219 = CARTESIAN_POINT ( 'NONE',  ( -3.749999999999997335, -7.500000000000021316, 18.84375000000000000 ) ) ;
#23220 = B_SPLINE_CURVE_WITH_KNOTS ( 'NONE', 3,
 ( #639, #1528, #76743, #27664, #15045, #42520, #47931, #75411, #63213, #13707 ),
 .UNSPECIFIED., .F., .F.,
 ( 4, 2, 2, 2, 4 ),
 ( 0.0007817246256747445703, 0.0009771112852218872494, 0.001172497944769030145, 0.001367884604316172825, 0.001563271263863315504 ),
 .UNSPECIFIED. ) ;
#23221 = CARTESIAN_POINT ( 'NONE',  ( -14.30769230769242739, -10.90142922262034020, 33.41473453929536674 ) ) ;
#23222 = ORIENTED_EDGE ( 'NONE', *, *, #81657, .T. ) ;
#23223 = CARTESIAN_POINT ( 'NONE',  ( -13.63463860883683942, -6.652501968072648708, 34.93155406624980941 ) ) ;
#23224 = CARTESIAN_POINT ( 'NONE',  ( 11.53846153846141753, -6.026961402154118019, 34.52809138561165270 ) ) ;
#23225 = DIRECTION ( 'NONE',  ( 0.000000000000000000, 0.000000000000000000, -1.000000000000000000 ) ) ;
#23226 = CARTESIAN_POINT ( 'NONE',  ( 5.142991427925514891, -2.721908614388772296, 31.22303859784725333 ) ) ;
#23227 = B_SPLINE_CURVE_WITH_KNOTS ( 'NONE', 3,
 ( #71707, #84813, #44670, #51869, #30725, #38833, #78465, #78031, #23090, #4136 ),
 .UNSPECIFIED., .F., .F.,
 ( 4, 2, 2, 2, 4 ),
 ( 0.000000000000000000, 0.0001954311564186871184, 0.0003908623128373742367, 0.0005862934692560614093, 0.0007817246256747484735 ),
 .UNSPECIFIED. ) ;
#23228 = CARTESIAN_POINT ( 'NONE',  ( -19.50000000000000000, -3.499999999999999556, 29.75000000000000355 ) ) ;
#23229 = EDGE_CURVE ( 'NONE', #58726, #63997, #64162, .T. ) ;
#23230 = CARTESIAN_POINT ( 'NONE',  ( -8.769230769230890843, -8.613356846316285953, 34.62446782046622218 ) ) ;
#23231 = ORIENTED_EDGE ( 'NONE', *, *, #54826, .F. ) ;
#23232 = CARTESIAN_POINT ( 'NONE',  ( -10.86538461538461320, -7.500000000000001776, 35.00000000000000000 ) ) ;
#23233 = ORIENTED_EDGE ( 'NONE', *, *, #62958, .T. ) ;
#23234 = ORIENTED_EDGE ( 'NONE', *, *, #39240, .T. ) ;
#23235 = ADVANCED_FACE ( 'NONE', ( #29083 ), #56537, .F. ) ;
#23236 = CARTESIAN_POINT ( 'NONE',  ( -11.28840711854808632, -11.47946981652013498, 33.17500667209847620 ) ) ;
#23237 = CARTESIAN_POINT ( 'NONE',  ( -15.45369618967607828, -10.77366814457252175, 33.85459836347579454 ) ) ;
#23238 = EDGE_CURVE ( 'NONE', #56029, #31297, #19950, .T. ) ;
#23239 = CARTESIAN_POINT ( 'NONE',  ( 1.607394925883796510, -11.89424750095246175, 32.13594075562311758 ) ) ;
#23240 = CARTESIAN_POINT ( 'NONE',  ( 7.846153846153723244, -8.656820664282941280, 34.87096338111179961 ) ) ;
#23241 = ORIENTED_EDGE ( 'NONE', *, *, #55873, .T. ) ;
#23242 = CYLINDRICAL_SURFACE ( 'NONE', #66577, 0.2500000000000008882 ) ;
#23243 = ORIENTED_EDGE ( 'NONE', *, *, #12267, .T. ) ;
#23244 = ORIENTED_EDGE ( 'NONE', *, *, #19689, .F. ) ;
#23245 = ADVANCED_FACE ( 'NONE', ( #78134 ), #37141, .F. ) ;
#23246 = CARTESIAN_POINT ( 'NONE',  ( -12.71153846153846168, -7.500000000000001776, 35.04278698407183867 ) ) ;
#23247 = CARTESIAN_POINT ( 'NONE',  ( 16.15384615384615330, -12.37446782046654192, 30.86335684631486131 ) ) ;
#23248 = CARTESIAN_POINT ( 'NONE',  ( -16.28399336328437386, -4.460286881179643004, 33.72017969459903242 ) ) ;
#23249 = EDGE_CURVE ( 'NONE', #56593, #74112, #21062, .T. ) ;
#23250 = CARTESIAN_POINT ( 'NONE',  ( -9.070512820512819374, -7.500000000000000000, 29.75000000000000355 ) ) ;
#23251 = LINE ( 'NONE', #50266, #88575 ) ;
#23252 = VERTEX_POINT ( 'NONE', #45686 ) ;
#23253 = ORIENTED_EDGE ( 'NONE', *, *, #30612, .F. ) ;
#23254 = CARTESIAN_POINT ( 'NONE',  ( 1.553300858899087311, -3.749999999999992006, 22.98437500000000000 ) ) ;
#23255 = ORIENTED_EDGE ( 'NONE', *, *, #26323, .F. ) ;
#23257 = VERTEX_POINT ( 'NONE', #72710 ) ;
#23256 = CARTESIAN_POINT ( 'NONE',  ( 11.76124120743959978, -5.827830569534417471, 34.72679350104403539 ) ) ;
#23258 = DIRECTION ( 'NONE',  ( -1.000000000000000000, -0.000000000000000000, 0.000000000000000000 ) ) ;
#23259 = CARTESIAN_POINT ( 'NONE',  ( 5.076923076923075762, -3.513871655860378418, 32.76840700105978499 ) ) ;
#23260 = AXIS2_PLACEMENT_3D ( 'NONE', #38913, #51953, #72678 ) ;
#23261 = CARTESIAN_POINT ( 'NONE',  ( -0.3954711281883859786, -9.058645607665452459, 34.76329471203371924 ) ) ;
#23262 = EDGE_CURVE ( 'NONE', #68032, #33581, #80379, .T. ) ;
#23263 = ORIENTED_EDGE ( 'NONE', *, *, #23071, .F. ) ;
#23264 = ADVANCED_FACE ( 'NONE', ( #66851 ), #52435, .F. ) ;
#23265 = AXIS2_PLACEMENT_3D ( 'NONE', #37057, #29878, #3275 ) ;
#23266 = LINE ( 'NONE', #78211, #49724 ) ;
#23267 = VERTEX_POINT ( 'NONE', #33066 ) ;
#23268 = CARTESIAN_POINT ( 'NONE',  ( 12.46153846153846168, -1.509761064869970415, 31.06009739812519044 ) ) ;
#23269 = CARTESIAN_POINT ( 'NONE',  ( -7.053224132515140354, -2.882441371585227063, 31.66841991370171527 ) ) ;
#23270 = CARTESIAN_POINT ( 'NONE',  ( 4.230769230769229061, -7.500000000000000000, 29.75000000000000355 ) ) ;
#23271 = B_SPLINE_CURVE_WITH_KNOTS ( 'NONE', 3,
 ( #147, #6028, #61387, #33496, #53755, #55528, #41576, #47885, #88460, #69489 ),
 .UNSPECIFIED., .F., .F.,
 ( 4, 2, 2, 2, 4 ),
 ( 0.000000000000000000, 0.0001954311564186861968, 0.0003908623128373723936, 0.0005862934692560585904, 0.0007817246256747447872 ),
 .UNSPECIFIED. ) ;
#23273 = LINE ( 'NONE', #71024, #45485 ) ;
#23272 = CARTESIAN_POINT ( 'NONE',  ( 5.999999999999878320, -12.51329471203414379, 31.30864560766407578 ) ) ;
#23274 = EDGE_CURVE ( 'NONE', #79550, #22067, #7184, .T. ) ;
#23275 = CARTESIAN_POINT ( 'NONE',  ( 4.946775867484856093, -2.619462340734462380, 30.83744416345203021 ) ) ;
#23276 = CARTESIAN_POINT ( 'NONE',  ( -10.68065506134539078, -10.90142922261923886, 33.41473453929638993 ) ) ;
#23277 = ORIENTED_EDGE ( 'NONE', *, *, #27358, .T. ) ;
#23278 = EDGE_CURVE ( 'NONE', #79307, #84442, #87143, .T. ) ;
#23279 = CARTESIAN_POINT ( 'NONE',  ( -10.61538461538461320, -9.780366693483667717, 34.19971097300155094 ) ) ;
#23280 = FACE_OUTER_BOUND ( 'NONE', #589, .T. ) ;
#23281 = ORIENTED_EDGE ( 'NONE', *, *, #6508, .F. ) ;
#23282 = DIRECTION ( 'NONE',  ( -1.000000000000000000, -0.000000000000000000, -0.000000000000000000 ) ) ;
#23283 = CARTESIAN_POINT ( 'NONE',  ( -18.22292695890684655, -12.64616026154729411, 30.79003144601914244 ) ) ;
#23284 = CARTESIAN_POINT ( 'NONE',  ( -3.230769230769229949, -3.322132147404559976, 32.92929555188717927 ) ) ;
#23285 = CARTESIAN_POINT ( 'NONE',  ( -5.076923076923075762, -11.69971097300155272, 32.46337939537588113 ) ) ;
#23286 = CARTESIAN_POINT ( 'NONE',  ( 7.976944287120794286, -6.369690395747422684, 34.87708834333098196 ) ) ;
#23287 = CARTESIAN_POINT ( 'NONE',  ( 12.23861224402231151, -4.186968288167450147, 33.49512374952580274 ) ) ;
#23288 = FACE_BOUND ( 'NONE', #28376, .T. ) ;
#23290 = CARTESIAN_POINT ( 'NONE',  ( 17.77651507543566822, -10.97335522853832934, 33.68706563782419749 ) ) ;
#23289 = FACE_OUTER_BOUND ( 'NONE', #7617, .T. ) ;
#23291 = CYLINDRICAL_SURFACE ( 'NONE', #69849, 0.2500000000000009437 ) ;
#23293 = CARTESIAN_POINT ( 'NONE',  ( -15.23076923076922995, -6.386643153685126251, 34.62446782046654192 ) ) ;
#23292 = CARTESIAN_POINT ( 'NONE',  ( -5.076923076923199218, -10.33852847137269571, 34.16647553114546554 ) ) ;
#23294 = CYLINDRICAL_SURFACE ( 'NONE', #7390, 4.000000000000000000 ) ;
#23295 = CARTESIAN_POINT ( 'NONE',  ( 1.614399933863660985, -11.22469193450123193, 21.95125670625849068 ) ) ;
#23296 = AXIS2_PLACEMENT_3D ( 'NONE', #84911, #24521, #11024 ) ;
#23297 = ORIENTED_EDGE ( 'NONE', *, *, #45308, .T. ) ;
#23298 = AXIS2_PLACEMENT_3D ( 'NONE', #71198, #70326, #1864 ) ;
#23299 = FACE_OUTER_BOUND ( 'NONE', #81843, .T. ) ;
#23300 = CARTESIAN_POINT ( 'NONE',  ( -12.46153846153846168, -6.343179335718451384, 34.87096338111211935 ) ) ;
#23301 = CARTESIAN_POINT ( 'NONE',  ( 5.776515075435673552, -5.827078755546623690, 34.72654668319379567 ) ) ;
#23302 = CARTESIAN_POINT ( 'NONE',  ( -10.61538461538461320, -11.35647404775217417, 33.31231777344666511 ) ) ;
#23303 = CARTESIAN_POINT ( 'NONE',  ( 7.780883400193070898, -5.219633306516282545, 34.19971097300152252 ) ) ;
#23304 = CARTESIAN_POINT ( 'NONE',  ( 2.694853999681214862, -10.10844685921789043, 21.87313170625849068 ) ) ;
#23305 = AXIS2_PLACEMENT_3D ( 'NONE', #62539, #8062, #56682 ) ;
#23306 = CARTESIAN_POINT ( 'NONE',  ( -8.519176457592452678, -2.779044189368095275, 31.39831045268885745 ) ) ;
#23307 = CARTESIAN_POINT ( 'NONE',  ( 4.023155550735847186, -11.93127051446800024, 32.56575433478200665 ) ) ;
#23308 = CARTESIAN_POINT ( 'NONE',  ( 11.60360631918116958, -7.750023224968867197, 34.99404313364389907 ) ) ;
#23309 = CARTESIAN_POINT ( 'NONE',  ( 17.74999999999999289, -2.499999999999999556, 29.81609845454691765 ) ) ;
#23310 = CARTESIAN_POINT ( 'NONE',  ( 9.320512820512821150, -3.499999999999999556, 29.75000000000000355 ) ) ;
#23311 = CARTESIAN_POINT ( 'NONE',  ( 5.076923076923075762, -8.164416787775445883, 34.95778746994557906 ) ) ;
#23312 = EDGE_CURVE ( 'NONE', #48689, #86112, #69014, .T. ) ;
#23313 = B_SPLINE_CURVE_WITH_KNOTS ( 'NONE', 3,
 ( #5435, #33349, #26143, #54943, #20710, #88315 ),
 .UNSPECIFIED., .F., .F.,
 ( 4, 2, 4 ),
 ( 4.563551064100006665E-17, 0.0001954756301637168570, 0.0003909512603273880690 ),
 .UNSPECIFIED. ) ;
#23314 = DIRECTION ( 'NONE',  ( -0.000000000000000000, 0.3420201433256694901, -0.9396926207859082059 ) ) ;
#23315 = CARTESIAN_POINT ( 'NONE',  ( 17.20771351789003489, -2.494656445102014342, 31.33466734024120015 ) ) ;
#23316 = ORIENTED_EDGE ( 'NONE', *, *, #48958, .F. ) ;
#23317 = CARTESIAN_POINT ( 'NONE',  ( 17.32686848630112308, -12.68172785388650681, 30.59649109432439573 ) ) ;
#23318 = CARTESIAN_POINT ( 'NONE',  ( -5.934744860487160878, -2.657715359629131857, 31.77849191805844242 ) ) ;
#23319 = CARTESIAN_POINT ( 'NONE',  ( -2.608446859217920633, -4.805146000318815780, 14.25186829374151465 ) ) ;
#23320 = CARTESIAN_POINT ( 'NONE',  ( 6.923076923076800782, -11.06231777344772027, 33.60647404775119895 ) ) ;
#23321 = CARTESIAN_POINT ( 'NONE',  ( -16.85414340794500276, -5.827830569534415694, 34.72679350104403539 ) ) ;
#23322 = ORIENTED_EDGE ( 'NONE', *, *, #71208, .T. ) ;
#23323 = FACE_OUTER_BOUND ( 'NONE', #68027, .T. ) ;
#23325 = ORIENTED_EDGE ( 'NONE', *, *, #81007, .F. ) ;
#23324 = CARTESIAN_POINT ( 'NONE',  ( 7.846153846153725020, -2.625532179533779154, 30.86335684631627174 ) ) ;
#23326 = CARTESIAN_POINT ( 'NONE',  ( 6.700150705560774966, -3.105860786376062332, 32.13614157043599562 ) ) ;
#23327 = CARTESIAN_POINT ( 'NONE',  ( -13.31935981333936070, -10.21337939537593620, 33.94971097300152252 ) ) ;
#23328 = EDGE_CURVE ( 'NONE', #60613, #74633, #65508, .T. ) ;
#23329 = CARTESIAN_POINT ( 'NONE',  ( -5.326946314216044698, -12.22074536777954989, 31.39888409691088356 ) ) ;
#23330 = EDGE_CURVE ( 'NONE', #61500, #39225, #12474, .T. ) ;
#23331 = CARTESIAN_POINT ( 'NONE',  ( -13.51530685128294529, -3.062553014421049546, 32.05460306192773601 ) ) ;
#23332 = ORIENTED_EDGE ( 'NONE', *, *, #16842, .F. ) ;
#23333 = VECTOR ( 'NONE', #64380, 1000.000000000000000 ) ;
#23334 = CARTESIAN_POINT ( 'NONE',  ( 8.992243613324164997, -2.308499170217967134, 30.53291367094873721 ) ) ;
#23335 = CARTESIAN_POINT ( 'NONE',  ( -5.198717948717948012, -7.500000000000000000, 29.75000000000000355 ) ) ;
#23336 = CARTESIAN_POINT ( 'NONE',  ( -1.319359813339359144, -6.026961402152789304, 34.52809138561124769 ) ) ;
#23337 = ORIENTED_EDGE ( 'NONE', *, *, #60697, .T. ) ;
#23338 = ORIENTED_EDGE ( 'NONE', *, *, #59227, .F. ) ;
#23339 = VERTEX_POINT ( 'NONE', #51986 ) ;
#23340 = EDGE_CURVE ( 'NONE', #10136, #2618, #85520, .T. ) ;
#23341 = CARTESIAN_POINT ( 'NONE',  ( 3.230769230769231726, -2.292212530054420494, 30.41441678777542634 ) ) ;
#23342 = DIRECTION ( 'NONE',  ( -0.000000000000000000, 0.8660254037844399289, -0.4999999999999980016 ) ) ;
#23343 = B_SPLINE_CURVE_WITH_KNOTS ( 'NONE', 3,
 ( #11884, #44752, #39360, #3328, #24041, #44294, #2872, #3776, #38459, #71786 ),
 .UNSPECIFIED., .F., .F.,
 ( 4, 2, 2, 2, 4 ),
 ( 0.000000000000000000, 0.0001954339857564073659, 0.0003908679715128147319, 0.0005863019572692221250, 0.0007817359430256294638 ),
 .UNSPECIFIED. ) ;
#23344 = ADVANCED_FACE ( 'NONE', ( #58754 ), #86249, .F. ) ;
#23345 = CARTESIAN_POINT ( 'NONE',  ( -3.903900744468108641, -12.68172785388650681, 30.59649109432439573 ) ) ;
#23346 = CARTESIAN_POINT ( 'NONE',  ( -10.03846153846153832, -7.500000000000000000, 29.75000000000000355 ) ) ;
#23347 = ORIENTED_EDGE ( 'NONE', *, *, #52468, .F. ) ;
#23349 = ORIENTED_EDGE ( 'NONE', *, *, #81845, .F. ) ;
#23348 = EDGE_CURVE ( 'NONE', #58923, #72792, #36091, .T. ) ;
#23351 = ORIENTED_EDGE ( 'NONE', *, *, #71766, .F. ) ;
#23350 = CARTESIAN_POINT ( 'NONE',  ( -2.241525701100665735, -7.250054591869667497, 34.99404684341514127 ) ) ;
#23352 = FACE_OUTER_BOUND ( 'NONE', #7878, .T. ) ;
#23353 = AXIS2_PLACEMENT_3D ( 'NONE', #33068, #26752, #11920 ) ;
#23354 = VECTOR ( 'NONE', #23683, 1000.000000000000000 ) ;
#23355 = CARTESIAN_POINT ( 'NONE',  ( -6.923076923077044142, -8.613356846316285953, 34.62446782046622218 ) ) ;
#23356 = CARTESIAN_POINT ( 'NONE',  ( 8.069165197766697162, -4.887748414852792322, 34.01359900205216746 ) ) ;
#23357 = ORIENTED_EDGE ( 'NONE', *, *, #43401, .F. ) ;
#23358 = VECTOR ( 'NONE', #75856, 1000.000000000000000 ) ;
#23359 = ORIENTED_EDGE ( 'NONE', *, *, #34020, .T. ) ;
#23361 = VERTEX_POINT ( 'NONE', #27194 ) ;
#23360 = FACE_OUTER_BOUND ( 'NONE', #39902, .T. ) ;
#23362 = CYLINDRICAL_SURFACE ( 'NONE', #2793, 0.2500000000000008882 ) ;
#23363 = CARTESIAN_POINT ( 'NONE',  ( -10.61538461538461320, -9.058645607665452459, 34.76329471203371924 ) ) ;
#23365 = ORIENTED_EDGE ( 'NONE', *, *, #5866, .T. ) ;
#23364 = ADVANCED_FACE ( 'NONE', ( #61854 ), #41596, .T. ) ;
#23366 = CARTESIAN_POINT ( 'NONE',  ( 12.68455130563185662, -6.460100341425560444, 34.89618726649961644 ) ) ;
#23367 = CARTESIAN_POINT ( 'NONE',  ( 15.45354877203763522, -9.332535724633409302, 34.40230450496446934 ) ) ;
#23368 = CARTESIAN_POINT ( 'NONE',  ( 10.83816415665302735, -3.755027918224367767, 33.06320215134714857 ) ) ;
#23369 = FACE_BOUND ( 'NONE', #70475, .T. ) ;
#23370 = CARTESIAN_POINT ( 'NONE',  ( 1.607626736228235709, -12.39991518177334129, 30.74647679643404530 ) ) ;
#23372 = ADVANCED_FACE ( 'NONE', ( #62298 ), #20874, .F. ) ;
#23371 = CARTESIAN_POINT ( 'NONE',  ( 3.930919194939304973, -2.308479472611653094, 30.53278059502174457 ) ) ;
#23373 = LINE ( 'NONE', #65685, #9232 ) ;
#23375 = CARTESIAN_POINT ( 'NONE',  ( 4.284371592079798674, -2.372941743896878286, 30.88044141588254377 ) ) ;
#23374 = CARTESIAN_POINT ( 'NONE',  ( 3.230769230769108269, -3.643525952248796163, 33.31231777344771672 ) ) ;
#23376 = CARTESIAN_POINT ( 'NONE',  ( -8.096177083446811196, -3.202444869320336451, 32.30641848906366675 ) ) ;
#23377 = CARTESIAN_POINT ( 'NONE',  ( 10.39245765647776842, -10.77366814457252175, 33.85459836347579454 ) ) ;
#23378 = ORIENTED_EDGE ( 'NONE', *, *, #33376, .T. ) ;
#23379 = EDGE_CURVE ( 'NONE', #83302, #49902, #50108, .T. ) ;
#23380 = CYLINDRICAL_SURFACE ( 'NONE', #50436, 0.2499999999999979738 ) ;
#23381 = EDGE_LOOP ( 'NONE', ( #37069, #7529 ) ) ;
#23382 = VERTEX_POINT ( 'NONE', #55547 ) ;
#23384 = CARTESIAN_POINT ( 'NONE',  ( 15.10062126103753855, -3.069018819979302926, 32.56621877034667278 ) ) ;
#23383 = CARTESIAN_POINT ( 'NONE',  ( 7.623227628637697428, -6.503392248772476236, 34.64988816332204635 ) ) ;
#23385 = CIRCLE ( 'NONE', #70867, 4.000000000000000000 ) ;
#23386 = DIRECTION ( 'NONE',  ( 0.000000000000000000, 0.9848077530122072432, -0.1736481776669354937 ) ) ;
#23387 = CARTESIAN_POINT ( 'NONE',  ( -14.17690049986752321, -2.729792928343269587, 31.24908615093345077 ) ) ;
#23388 = CARTESIAN_POINT ( 'NONE',  ( 1.384615384615265343, -6.879047030192662504, 34.71129190930017927 ) ) ;
#23389 = CARTESIAN_POINT ( 'NONE',  ( -2.437840277424003332, -11.66186481527757479, 32.95055677023626117 ) ) ;
#23390 = VERTEX_POINT ( 'NONE', #33949 ) ;
#23391 = CARTESIAN_POINT ( 'NONE',  ( 18.22301284409340028, -4.026326845037969449, 33.68677907613345468 ) ) ;
#23392 = CARTESIAN_POINT ( 'NONE',  ( 0.4615384615383382183, -12.70778746994576025, 30.41441678777401236 ) ) ;
#23393 = DIRECTION ( 'NONE',  ( -0.000000000000000000, -0.000000000000000000, 1.000000000000000000 ) ) ;
#23394 = CARTESIAN_POINT ( 'NONE',  ( 0.3313904918067667182, -3.625366637846545448, 33.29286588640298561 ) ) ;
#23395 = CYLINDRICAL_SURFACE ( 'NONE', #86655, 0.2499999999999979738 ) ;
#23396 = ADVANCED_FACE ( 'NONE', ( #54651 ), #83031, .F. ) ;
#23397 = CARTESIAN_POINT ( 'NONE',  ( 3.749999999999992006, -5.946699141100872943, 16.89062500000000000 ) ) ;
#23398 = ORIENTED_EDGE ( 'NONE', *, *, #80331, .F. ) ;
#23399 = VERTEX_POINT ( 'NONE', #26749 ) ;
#23400 = CARTESIAN_POINT ( 'NONE',  ( -22.00000000000000711, 9.999999999999971578, 10.00000000000000178 ) ) ;
#23401 = ADVANCED_FACE ( 'NONE', ( #47454 ), #41157, .T. ) ;
#23402 = ORIENTED_EDGE ( 'NONE', *, *, #39221, .T. ) ;
#23403 = CARTESIAN_POINT ( 'NONE',  ( -7.053224132515141243, -2.619462340734462380, 30.83744416345203021 ) ) ;
#23404 = CARTESIAN_POINT ( 'NONE',  ( -12.23875892027004753, -10.11255958852956027, 34.01340905677048454 ) ) ;
#23405 = CARTESIAN_POINT ( 'NONE',  ( -14.24162395668986747, -6.386643153685127139, 34.62446782046654192 ) ) ;
#23406 = CARTESIAN_POINT ( 'NONE',  ( -15.23076923076935074, -2.892918686052166066, 31.69288490824153470 ) ) ;
#23407 = CARTESIAN_POINT ( 'NONE',  ( 1.553300858899087311, -3.749999999999992006, 19.23437500000000355 ) ) ;
#23408 = CARTESIAN_POINT ( 'NONE',  ( 0.5276057948885365390, -9.058645607665452459, 34.76329471203371924 ) ) ;
#23409 = ORIENTED_EDGE ( 'NONE', *, *, #12674, .F. ) ;
#23410 = CARTESIAN_POINT ( 'NONE',  ( -12.46153846153858247, -10.90142922262034020, 33.41473453929536674 ) ) ;
#23412 = VERTEX_POINT ( 'NONE', #165 ) ;
#23411 = CARTESIAN_POINT ( 'NONE',  ( -16.28399336328437386, -11.93770438780619259, 32.05411857736982029 ) ) ;
#23413 = DIRECTION ( 'NONE',  ( 1.000000000000000000, -0.000000000000000000, -0.000000000000000000 ) ) ;
#23414 = CARTESIAN_POINT ( 'NONE',  ( -9.692307692307812417, -12.27809138561165270, 31.22303859784587132 ) ) ;
#23415 = CARTESIAN_POINT ( 'NONE',  ( -2.437840277424004221, -12.70455904226513866, 30.44083106164009322 ) ) ;
#23416 = EDGE_CURVE ( 'NONE', #85301, #47862, #9288, .T. ) ;
#23417 = PLANE ( 'NONE',  #77816 ) ;
#23418 = DIRECTION ( 'NONE',  ( -0.000000000000000000, -0.9396926207859092051, -0.3420201433256662704 ) ) ;
#23419 = CARTESIAN_POINT ( 'NONE',  ( 9.626225312947559232, -4.661471528628507777, 34.16647553114621871 ) ) ;
#23420 = DIRECTION ( 'NONE',  ( 0.000000000000000000, 0.000000000000000000, -1.000000000000000000 ) ) ;
#23421 = CARTESIAN_POINT ( 'NONE',  ( 2.608446859217924629, -10.19485399968118422, 18.62686829374151642 ) ) ;
#23422 = EDGE_LOOP ( 'NONE', ( #54111, #66231, #82080, #33389, #68688, #8217, #22473 ) ) ;
#23423 = EDGE_CURVE ( 'NONE', #48528, #313, #48789, .T. ) ;
#23424 = CARTESIAN_POINT ( 'NONE',  ( 1.384615384615386802, -5.557115091759785130, 34.35708131394839171 ) ) ;
#23425 = CARTESIAN_POINT ( 'NONE',  ( -1.607541602131528968, -12.15238873228291538, 31.58232369045354915 ) ) ;
#23426 = CARTESIAN_POINT ( 'NONE',  ( 2.750000000000008438, -8.639087296525996607, 24.54687500000000000 ) ) ;
#23427 = MECHANICAL_DESIGN_GEOMETRIC_PRESENTATION_REPRESENTATION (  '', ( #63737 ), #55130 ) ;
#23428 = EDGE_CURVE ( 'NONE', #73515, #25338, #612, .T. ) ;
#23429 = AXIS2_PLACEMENT_3D ( 'NONE', #56159, #36768, #15621 ) ;
#23430 = CARTESIAN_POINT ( 'NONE',  ( -3.360916440207450950, -9.418419913701741919, 34.36755862841477693 ) ) ;
#23431 = CARTESIAN_POINT ( 'NONE',  ( 16.08776377448601735, -4.661471528628507777, 34.16647553114621871 ) ) ;
#23432 = ORIENTED_EDGE ( 'NONE', *, *, #31245, .F. ) ;
#23433 = CARTESIAN_POINT ( 'NONE',  ( -1.944543648262992530, -9.444543648263016067, 19.93750000000000000 ) ) ;
#23434 = CARTESIAN_POINT ( 'NONE',  ( -1.607541602131532077, -9.886141570436013382, 34.14413921362392301 ) ) ;
#23435 = ORIENTED_EDGE ( 'NONE', *, *, #70926, .T. ) ;
#23436 = EDGE_CURVE ( 'NONE', #16713, #80197, #88744, .T. ) ;
#23437 = CARTESIAN_POINT ( 'NONE',  ( -18.22292695890684655, -4.762599654559228846, 34.23009711892697737 ) ) ;
#23438 = EDGE_LOOP ( 'NONE', ( #54762, #36441 ) ) ;
#23439 = CARTESIAN_POINT ( 'NONE',  ( 6.988332062589762472, -4.320704448112861584, 33.92786785259548310 ) ) ;
#23440 = CARTESIAN_POINT ( 'NONE',  ( 2.980792486720639456, -4.075325502946086864, 33.72974371597207721 ) ) ;
#23441 = EDGE_CURVE ( 'NONE', #61249, #1771, #31960, .T. ) ;
#23442 = DIRECTION ( 'NONE',  ( 0.000000000000000000, 0.000000000000000000, -1.000000000000000000 ) ) ;
#23443 = CARTESIAN_POINT ( 'NONE',  ( -12.39628332202562255, -11.06231777344671130, 33.60647404775212976 ) ) ;
#23444 = ORIENTED_EDGE ( 'NONE', *, *, #48187, .F. ) ;
#23445 = CARTESIAN_POINT ( 'NONE',  ( -2.307692307692428724, -12.16647553114689728, 32.15551576947799362 ) ) ;
#23446 = EDGE_LOOP ( 'NONE', ( #7334, #4723 ) ) ;
#23447 = DIRECTION ( 'NONE',  ( -0.000000000000000000, 0.3420201433256694346, -0.9396926207859080948 ) ) ;
#23448 = CARTESIAN_POINT ( 'NONE',  ( 9.692307692307570832, -4.320704448113951379, 33.92786785259630022 ) ) ;
#23449 = ORIENTED_EDGE ( 'NONE', *, *, #15295, .T. ) ;
#23450 = CARTESIAN_POINT ( 'NONE',  ( 8.769230769230768274, -11.16473453929635440, 33.15142922261926373 ) ) ;
#23452 = EDGE_CURVE ( 'NONE', #13160, #21459, #64762, .T. ) ;
#23451 = DIRECTION ( 'NONE',  ( -0.000000000000000000, 0.1736481776669307198, -0.9848077530122080203 ) ) ;
#23453 = DIRECTION ( 'NONE',  ( -0.000000000000000000, -0.5000000000000009992, -0.8660254037844380415 ) ) ;
#23454 = AXIS2_PLACEMENT_3D ( 'NONE', #55128, #6945, #21789 ) ;
#23455 = VECTOR ( 'NONE', #32255, 1000.000000000000000 ) ;
#23456 = CARTESIAN_POINT ( 'NONE',  ( 20.99999999999998934, -12.75000000000000178, 29.75000000000000355 ) ) ;
#23457 = CARTESIAN_POINT ( 'NONE',  ( -4.153846153846274980, -4.320704448113951379, 33.92786785259630022 ) ) ;
#23458 = ORIENTED_EDGE ( 'NONE', *, *, #39622, .F. ) ;
#23459 = VERTEX_POINT ( 'NONE', #43367 ) ;
#23460 = FACE_BOUND ( 'NONE', #63153, .T. ) ;
#23461 = ORIENTED_EDGE ( 'NONE', *, *, #24908, .F. ) ;
#23462 = CARTESIAN_POINT ( 'NONE',  ( -4.826923076923062439, -2.249999999999999112, 29.81603969181031033 ) ) ;
#23463 = CARTESIAN_POINT ( 'NONE',  ( 4.153846153846154188, -1.790695186598648903, 34.54067556320373455 ) ) ;
#23464 = CARTESIAN_POINT ( 'NONE',  ( -2.241624974342230736, -9.905515769479277921, 34.41647553114623292 ) ) ;
#23465 = ORIENTED_EDGE ( 'NONE', *, *, #78074, .T. ) ;
#23466 = EDGE_LOOP ( 'NONE', ( #74035, #52269 ) ) ;
#23467 = VERTEX_POINT ( 'NONE', #52212 ) ;
#23468 = CARTESIAN_POINT ( 'NONE',  ( 17.01165263096229907, -4.481592998940161721, 33.73612834413957984 ) ) ;
#23469 = EDGE_LOOP ( 'NONE', ( #43969, #80975, #13611, #42541 ) ) ;
#23470 = CARTESIAN_POINT ( 'NONE',  ( 15.93036121012220541, -10.11188796281391511, 34.01382737946119050 ) ) ;
#23471 = B_SPLINE_CURVE_WITH_KNOTS ( 'NONE', 3,
 ( #66566, #81421, #39996, #75106, #60687, #12078, #27350, #54819, #53031, #25578 ),
 .UNSPECIFIED., .F., .F.,
 ( 4, 2, 2, 2, 4 ),
 ( 0.0007817359430256285964, 0.0009771253907249945886, 0.001172514838424360472, 0.001367904286123726356, 0.001563293733823092457 ),
 .UNSPECIFIED. ) ;
#23472 = AXIS2_PLACEMENT_3D ( 'NONE', #72872, #26032, #66575 ) ;
#23473 = CARTESIAN_POINT ( 'NONE',  ( 13.38461538461526601, -2.892918686052165622, 31.69288490824153470 ) ) ;
#23474 = DIRECTION ( 'NONE',  ( -1.000000000000000000, -0.000000000000000000, 0.000000000000000000 ) ) ;
#23475 = FACE_BOUND ( 'NONE', #48638, .T. ) ;
#23476 = EDGE_LOOP ( 'NONE', ( #39445, #18274, #45586, #33805 ) ) ;
#23477 = VECTOR ( 'NONE', #25166, 999.9999999999998863 ) ;
#23479 = EDGE_CURVE ( 'NONE', #3262, #84195, #57320, .T. ) ;
#23478 = CARTESIAN_POINT ( 'NONE',  ( 13.13463864056679853, -10.82459398097509329, 33.81372124010185587 ) ) ;
#23480 = AXIS2_PLACEMENT_3D ( 'NONE', #54605, #19940, #87547 ) ;
#23481 = DIRECTION ( 'NONE',  ( -0.000000000000000000, -0.1736481776669307198, -0.9848077530122080203 ) ) ;
#23482 = CARTESIAN_POINT ( 'NONE',  ( 2.177001704582002262, -8.191372820521381826, 34.95448215188423546 ) ) ;
#23483 = CARTESIAN_POINT ( 'NONE',  ( 11.60452988946397745, -8.120952969808772792, 34.71129190929999453 ) ) ;
#23484 = ORIENTED_EDGE ( 'NONE', *, *, #37339, .T. ) ;
#23485 = EDGE_CURVE ( 'NONE', #31340, #37534, #47869, .T. ) ;
#23486 = CARTESIAN_POINT ( 'NONE',  ( 9.626224281351809964, -2.538708090699994813, 30.37095296980875148 ) ) ;
#23487 = EDGE_LOOP ( 'NONE', ( #48656, #34798, #26915, #53745 ) ) ;
#23488 = VERTEX_POINT ( 'NONE', #64069 ) ;
#23490 = CARTESIAN_POINT ( 'NONE',  ( 0.6089743589743589203, -4.000000000000000000, 29.75000000000000355 ) ) ;
#23489 = CARTESIAN_POINT ( 'NONE',  ( 4.480769230769229061, -4.000000000000000000, 29.75000000000000355 ) ) ;
#23491 = EDGE_CURVE ( 'NONE', #58342, #8131, #8170, .T. ) ;
#23492 = DIRECTION ( 'NONE',  ( -0.000000000000000000, 1.000000000000000000, -0.000000000000000000 ) ) ;
#23493 = CARTESIAN_POINT ( 'NONE',  ( -2.307692307692427391, -12.27809138561165270, 31.22303859784587132 ) ) ;
#23494 = LINE ( 'NONE', #16740, #80380 ) ;
#23495 = CARTESIAN_POINT ( 'NONE',  ( -5.999999999999998224, -12.10708131394839349, 31.69288490824020244 ) ) ;
#23496 = ORIENTED_EDGE ( 'NONE', *, *, #29613, .T. ) ;
#23497 = DIRECTION ( 'NONE',  ( 1.000000000000000000, 0.000000000000000000, 0.000000000000000000 ) ) ;
#23498 = CARTESIAN_POINT ( 'NONE',  ( 17.74997677577854560, -3.520140089381496473, 33.17453946501458262 ) ) ;
#23499 = LINE ( 'NONE', #50525, #35835 ) ;
#23500 = CARTESIAN_POINT ( 'NONE',  ( 5.206970683178758108, -7.723484964179500700, 34.74522123443823318 ) ) ;
#23501 = ORIENTED_EDGE ( 'NONE', *, *, #50205, .T. ) ;
#23502 = ADVANCED_FACE ( 'NONE', ( #51753 ), #8705, .F. ) ;
#23503 = VERTEX_POINT ( 'NONE', #63633 ) ;
#23504 = FACE_BOUND ( 'NONE', #1732, .T. ) ;
#23505 = CARTESIAN_POINT ( 'NONE',  ( 18.22277966897806678, -12.69155399931963046, 30.53255429739158444 ) ) ;
#23506 = CARTESIAN_POINT ( 'NONE',  ( -11.40793583669797329, -11.93748526763465279, 32.05452791011430946 ) ) ;
#23507 = ORIENTED_EDGE ( 'NONE', *, *, #80603, .F. ) ;
#23508 = B_SPLINE_CURVE_WITH_KNOTS ( 'NONE', 3,
 ( #86516, #52701, #4975, #81087, #38311, #5420, #11281, #59907, #73878, #60797 ),
 .UNSPECIFIED., .F., .F.,
 ( 4, 2, 2, 2, 4 ),
 ( 0.000000000000000000, 0.0001954339857564073659, 0.0003908679715128147319, 0.0005863019572692221250, 0.0007817359430256294638 ),
 .UNSPECIFIED. ) ;
#23509 = CARTESIAN_POINT ( 'NONE',  ( -16.28399412357785181, -11.66186481527757479, 32.95055677023626117 ) ) ;
#23510 = CARTESIAN_POINT ( 'NONE',  ( -10.83886955910856464, -6.760086850603066466, 34.69517049084099369 ) ) ;
#23511 = CARTESIAN_POINT ( 'NONE',  ( -9.915792636031639518, -3.236172620538810385, 32.36188796281390267 ) ) ;
#23512 = CARTESIAN_POINT ( 'NONE',  ( -6.700065571464075553, -3.105924265160262543, 32.13625925475356127 ) ) ;
#23513 = VERTEX_POINT ( 'NONE', #24292 ) ;
#23514 = B_SPLINE_CURVE_WITH_KNOTS ( 'NONE', 3,
 ( #86535, #73899, #24810, #11753, #66692, #25710 ),
 .UNSPECIFIED., .F., .F.,
 ( 4, 2, 4 ),
 ( 0.0003909512603273778233, 0.0005862562993132030805, 0.0007815613382990282835 ),
 .UNSPECIFIED. ) ;
#23515 = B_SPLINE_CURVE_WITH_KNOTS ( 'NONE', 3,
 ( #84513, #62442, #57019, #69656, #22354, #21016, #77738, #83636, #69217, #62879 ),
 .UNSPECIFIED., .F., .F.,
 ( 4, 2, 2, 2, 4 ),
 ( 0.0007817359430256320659, 0.0009771253907249987086, 0.001172514838424365460, 0.001367904286123731994, 0.001563293733823098745 ),
 .UNSPECIFIED. ) ;
#23516 = DIRECTION ( 'NONE',  ( -0.000000000000000000, -0.7660444431189791237, -0.6427876096865379196 ) ) ;
#23518 = ORIENTED_EDGE ( 'NONE', *, *, #58018, .T. ) ;
#23517 = VECTOR ( 'NONE', #45042, 1000.000000000000000 ) ;
#23520 = VERTEX_POINT ( 'NONE', #45006 ) ;
#23519 = CARTESIAN_POINT ( 'NONE',  ( 13.60739505359345181, -8.540255544307065350, 34.89611431652622286 ) ) ;
#23521 = FACE_OUTER_BOUND ( 'NONE', #25080, .T. ) ;
#23522 = CARTESIAN_POINT ( 'NONE',  ( 3.903869422903799347, -6.567427716900047230, 34.66269422305636283 ) ) ;
#23523 = CARTESIAN_POINT ( 'NONE',  ( 23.00000000000000000, -7.500000000000000000, 29.75000000000000355 ) ) ;
#23524 = CARTESIAN_POINT ( 'NONE',  ( -14.98076923076929390, -7.565270000091922853, 34.99999999999999289 ) ) ;
#23525 = CARTESIAN_POINT ( 'NONE',  ( -5.198717948717948012, -3.499999999999999556, 29.75000000000000355 ) ) ;
#23526 = CARTESIAN_POINT ( 'NONE',  ( -9.915234651214536399, -11.98009711892699514, 32.48740034544076138 ) ) ;
#23527 = CARTESIAN_POINT ( 'NONE',  ( 2.750000000000001776, -7.499999999999984013, 24.46875000000000000 ) ) ;
#23528 = VERTEX_POINT ( 'NONE', #17555 ) ;
#23529 = EDGE_CURVE ( 'NONE', #5501, #13929, #33144, .T. ) ;
#23530 = CARTESIAN_POINT ( 'NONE',  ( 10.61538461538461675, -1.242168528481310874, 33.36296068462461051 ) ) ;
#23531 = CARTESIAN_POINT ( 'NONE',  ( 7.846153846153846700, -1.367168528481310208, 33.57946703557072254 ) ) ;
#23532 = ORIENTED_EDGE ( 'NONE', *, *, #69211, .F. ) ;
#23533 = ORIENTED_EDGE ( 'NONE', *, *, #15133, .F. ) ;
#23534 = CARTESIAN_POINT ( 'NONE',  ( 17.07692307692307665, -4.786620604624113540, 33.94971097300155094 ) ) ;
#23535 = CARTESIAN_POINT ( 'NONE',  ( 11.40777093535123043, -4.684245665217972032, 34.18127051446801090 ) ) ;
#23536 = CARTESIAN_POINT ( 'NONE',  ( -17.20761454359064047, -8.999036380462719364, 34.52022231692819076 ) ) ;
#23537 = CARTESIAN_POINT ( 'NONE',  ( 0.3962155460462854495, -7.749976743299137993, 34.99404534957040624 ) ) ;
#23538 = DIRECTION ( 'NONE',  ( 0.000000000000000000, 1.084202172485504434E-16, -1.000000000000000000 ) ) ;
#23539 = EDGE_CURVE ( 'NONE', #65380, #35523, #15017, .T. ) ;
#23540 = CARTESIAN_POINT ( 'NONE',  ( 16.37662582282421653, -3.563462043263029955, 33.22394488606062879 ) ) ;
#23541 = CARTESIAN_POINT ( 'NONE',  ( -7.846153846153844924, -3.886160181151819604, 36.00935417666054406 ) ) ;
#23542 = VERTEX_POINT ( 'NONE', #58973 ) ;
#23543 = CARTESIAN_POINT ( 'NONE',  ( 3.230769230769110045, -6.879047030192662504, 34.71129190930017927 ) ) ;
#23544 = CARTESIAN_POINT ( 'NONE',  ( -0.4615384615385826339, -8.613356846316285953, 34.62446782046622218 ) ) ;
#23545 = AXIS2_PLACEMENT_3D ( 'NONE', #25028, #73681, #79979 ) ;
#23546 = ADVANCED_FACE ( 'NONE', ( #45457 ), #42490, .F. ) ;
#23547 = EDGE_CURVE ( 'NONE', #77538, #31266, #31507, .T. ) ;
#23548 = CARTESIAN_POINT ( 'NONE',  ( -9.692307692307691624, -11.16473453929635440, 33.15142922261926373 ) ) ;
#23549 = DIRECTION ( 'NONE',  ( 0.000000000000000000, 0.000000000000000000, 1.000000000000000000 ) ) ;
#23550 = B_SPLINE_CURVE_WITH_KNOTS ( 'NONE', 3,
 ( #65242, #51714, #79216, #87326, #3540, #25152, #24709, #31466, #25601, #58932 ),
 .UNSPECIFIED., .F., .F.,
 ( 4, 2, 2, 2, 4 ),
 ( 0.0007817246256747444619, 0.0009771112852218868158, 0.001172497944769029061, 0.001367884604316171523, 0.001563271263863313769 ),
 .UNSPECIFIED. ) ;
#23551 = EDGE_LOOP ( 'NONE', ( #37212, #3508, #72425, #28254 ) ) ;
#23552 = CARTESIAN_POINT ( 'NONE',  ( -17.29978933998617663, -2.251424796025575770, 29.88072029997477586 ) ) ;
#23553 = B_SPLINE_CURVE_WITH_KNOTS ( 'NONE', 3,
 ( #433, #76534, #54480, #68880, #14385, #83743, #16485, #21135, #75213, #34660 ),
 .UNSPECIFIED., .F., .F.,
 ( 4, 2, 2, 2, 4 ),
 ( 0.0007817246256747460882, 0.0009771112852218892010, 0.001172497944769032314, 0.001367884604316175427, 0.001563271263863318539 ),
 .UNSPECIFIED. ) ;
#23554 = AXIS2_PLACEMENT_3D ( 'NONE', #53957, #19733, #74686 ) ;
#23555 = ORIENTED_EDGE ( 'NONE', *, *, #57239, .T. ) ;
#23556 = B_SPLINE_CURVE_WITH_KNOTS ( 'NONE', 3,
 ( #72824, #3477, #44907, #65617, #85026, #23308, #85908, #50767, #31404, #85463 ),
 .UNSPECIFIED., .F., .F.,
 ( 4, 2, 2, 2, 4 ),
 ( 0.000000000000000000, 0.0001954311584214072381, 0.0003908623168428144762, 0.0005862934752642217414, 0.0007817246336856289524 ),
 .UNSPECIFIED. ) ;
#23557 = CARTESIAN_POINT ( 'NONE',  ( 0.5276068125408986953, -8.973038597847269315, 34.52809138561122637 ) ) ;
#23558 = CARTESIAN_POINT ( 'NONE',  ( 1.450682717965460666, -3.322132147404559976, 32.92929555188717927 ) ) ;
#23559 = DIRECTION ( 'NONE',  ( -0.000000000000000000, -0.000000000000000000, -1.000000000000000000 ) ) ;
#23560 = CARTESIAN_POINT ( 'NONE',  ( 6.066067333350077639, -12.62096338111211757, 30.90682066428152908 ) ) ;
#23561 = EDGE_LOOP ( 'NONE', ( #36422, #58633 ) ) ;
#23562 = B_SPLINE_CURVE_WITH_KNOTS ( 'NONE', 3,
 ( #64201, #2948, #84947, #63768, #85833, #2071, #15595, #29994, #43063, #23230 ),
 .UNSPECIFIED., .F., .F.,
 ( 4, 2, 2, 2, 4 ),
 ( 0.000000000000000000, 0.0001954339857564078809, 0.0003908679715128157619, 0.0005863019572692236428, 0.0007817359430256315238 ),
 .UNSPECIFIED. ) ;
#23564 = EDGE_CURVE ( 'NONE', #25175, #10551, #38711, .T. ) ;
#23563 = CARTESIAN_POINT ( 'NONE',  ( -1.634592128663974409, -12.65889640711025521, 30.72598325615533454 ) ) ;
#23565 = CARTESIAN_POINT ( 'NONE',  ( 10.54930223602447903, -12.62096338111211580, 30.90682066428152908 ) ) ;
#23566 = CARTESIAN_POINT ( 'NONE',  ( -17.29978849912671635, -2.501496062324912284, 29.88072118266895671 ) ) ;
#23567 = CARTESIAN_POINT ( 'NONE',  ( -9.692307692307814193, -3.643525952248795718, 33.31231777344771672 ) ) ;
#23568 = EDGE_CURVE ( 'NONE', #85757, #52397, #80096, .T. ) ;
#23569 = EDGE_CURVE ( 'NONE', #67226, #9533, #7041, .T. ) ;
#23570 = ORIENTED_EDGE ( 'NONE', *, *, #16281, .F. ) ;
#23571 = CARTESIAN_POINT ( 'NONE',  ( -1.161604033002534342, -3.587049720035815348, 32.86302985866382897 ) ) ;
#23572 = ORIENTED_EDGE ( 'NONE', *, *, #82150, .F. ) ;
#23573 = EDGE_CURVE ( 'NONE', #69827, #63622, #13589, .T. ) ;
#23574 = DIRECTION ( 'NONE',  ( -0.000000000000000000, 1.000000000000000000, -0.000000000000000000 ) ) ;
#23575 = CARTESIAN_POINT ( 'NONE',  ( 6.923076923076800782, -3.083524468854526912, 32.58852847137268327 ) ) ;
#23576 = CARTESIAN_POINT ( 'NONE',  ( -6.130147209438218781, -2.619462340734462380, 30.83744416345203021 ) ) ;
#23577 = DIRECTION ( 'NONE',  ( 0.000000000000000000, 0.1736481776669267785, -0.9848077530122087975 ) ) ;
#23578 = LINE ( 'NONE', #59586, #39324 ) ;
#23579 = ORIENTED_EDGE ( 'NONE', *, *, #62389, .F. ) ;
#23580 = VECTOR ( 'NONE', #475, 1000.000000000000114 ) ;
#23581 = EDGE_LOOP ( 'NONE', ( #30242, #11026 ) ) ;
#23582 = ORIENTED_EDGE ( 'NONE', *, *, #11988, .F. ) ;
#23583 = ORIENTED_EDGE ( 'NONE', *, *, #79497, .F. ) ;
#23584 = CARTESIAN_POINT ( 'NONE',  ( 5.448717948717947124, -3.499999999999999556, 29.75000000000000355 ) ) ;
#23585 = CARTESIAN_POINT ( 'NONE',  ( 16.08857615328984281, -5.941354392334501355, 34.76329471203369792 ) ) ;
#23586 = CARTESIAN_POINT ( 'NONE',  ( 18.03205128205128105, -11.50000000000000000, 29.75000000000000355 ) ) ;
#23587 = CARTESIAN_POINT ( 'NONE',  ( 17.29993442853592711, -4.187068189119696804, 33.49521262558774026 ) ) ;
#23588 = CARTESIAN_POINT ( 'NONE',  ( -23.50000000000000000, -9.499999999999982236, 27.74999999999999645 ) ) ;
#23589 = EDGE_CURVE ( 'NONE', #41513, #5871, #53997, .T. ) ;
#23590 = CARTESIAN_POINT ( 'NONE',  ( -12.59222906464876957, -12.35290016733513951, 31.75349464988449455 ) ) ;
#23591 = CARTESIAN_POINT ( 'NONE',  ( 13.38461538461538680, -10.89733346790207413, 36.13435417666054406 ) ) ;
#23592 = CARTESIAN_POINT ( 'NONE',  ( 9.468822767743363400, -10.23692288466677880, 34.23039457007281072 ) ) ;
#23593 = VERTEX_POINT ( 'NONE', #40064 ) ;
#23594 = VERTEX_POINT ( 'NONE', #60309 ) ;
#23595 = VERTEX_POINT ( 'NONE', #18447 ) ;
#23597 = ORIENTED_EDGE ( 'NONE', *, *, #62647, .F. ) ;
#23596 = LINE ( 'NONE', #2869, #10005 ) ;
#23599 = CARTESIAN_POINT ( 'NONE',  ( -16.21911659980693443, -10.21337939537584383, 33.94971097300158647 ) ) ;
#23598 = LINE ( 'NONE', #84878, #33091 ) ;
#23600 = EDGE_CURVE ( 'NONE', #19490, #12209, #55370, .T. ) ;
#23601 = CARTESIAN_POINT ( 'NONE',  ( -1.608100309179715470, -4.988325925672468131, 34.36044203135681130 ) ) ;
#23602 = CARTESIAN_POINT ( 'NONE',  ( -11.47239420511146513, -9.058645607665452459, 34.76329471203371924 ) ) ;
#23603 = ORIENTED_EDGE ( 'NONE', *, *, #1005, .F. ) ;
#23604 = ORIENTED_EDGE ( 'NONE', *, *, #4207, .T. ) ;
#23605 = LINE ( 'NONE', #26279, #48576 ) ;
#23606 = EDGE_LOOP ( 'NONE', ( #79447, #67059 ) ) ;
#23607 = FACE_BOUND ( 'NONE', #81231, .T. ) ;
#23608 = CARTESIAN_POINT ( 'NONE',  ( 30.00000000000000000, 15.00000000000000355, 3.000000000000000000 ) ) ;
#23609 = CIRCLE ( 'NONE', #17841, 8.000000000000000000 ) ;
#23610 =( BOUNDED_SURFACE ( )  B_SPLINE_SURFACE ( 3, 2, ( 
 ( #25851, #77031, #80810, #12335, #67283, #3569, #30168, #64818, #9451, #79243, #58071, #22961, #29731, #72029, #1805, #84244, #30598, #44102, #49987, #9890, #22522, #17544, #56749, #65271, #2674, #50422, #2236, #77468, #57633, #31038, #15776, #16209, #44545, #36051, #44996, #37351, #43240, #23397, #70716, #86000, #77904, #58503, #50854, #72476, #57193, #24281, #9018, #36487, #43672, #78340, #71144, #85116, #36913, #51740, #63939, #71582, #85555, #64376, #63502, #29293, #16642, #84686, #3124, #23828, #51284, #78788, #17091, #10340, #37805, #39610, #53988, #67513, #4926, #67067, #73376, #81478, #32834, #86918, #4469, #46792, #65712, #58962, #5366, #18875, #24739, #73833, #86465, #19765, #31498, #40053, #66623, #25186, #66162, #52201, #32390, #5808, #79690, #80134, #19323, #10784, #47225, #12129, #17993, #87354, #45445, #60745, #52650, #33285, #25631, #38256, #31951, #88251, #72927, #11230, #18435, #53088, #45893, #59857, #11683, #26527, #4008, #74268, #26078, #38700, #59415, #39161, #80593, #46346, #60298, #87808, #53538, #81035, #12566, #68831, #56207, #62942, #20212, #40924, #13444, #6688, #41817, #13886, #34159, #74719, #89131, #14786, #1253, #67956, #27407, #69719, #83696, #54878, #21980, #75160, #8024, #28743, #13008, #20643, #42261, #82361, #35492 ),
 ( #76029, #83241, #62502, #75582, #40492, #62072, #47675, #41368, #7137, #27848, #48108, #61625, #35044, #55312, #6259, #34608, #68388, #384, #69281, #82805, #21078, #33722, #48547, #61179, #88691, #26971, #14332, #54426, #81920, #7582, #817, #28284, #55754, #21531, #49005, #76482, #16988, #63844, #78694, #85015, #16541, #63397, #50755, #77800, #43570, #3018, #57084, #49883, #71478, #9787, #22852, #35943, #51186, #44438, #2139, #30064, #77362, #36814, #84580, #30931, #70160, #57528, #44008, #50316, #71927, #10241, #64274, #84141, #49452, #70607, #15228, #16105, #58399, #8912, #85897, #78239, #3465, #37698, #71045, #37246, #9357, #76924, #64718, #36382, #43138, #85451, #42700, #8470, #30499, #23295, #1705, #57970, #29195, #56647, #22416, #65164, #2572, #29628, #15668, #23731, #45789, #80929, #38146, #4364, #32719, #24181, #5691, #87246, #3905, #11574, #58856, #74157, #11120, #46679, #39055, #60630, #79588, #53426, #65604, #86361, #66052, #66512, #38596, #18326, #31846, #19214, #12452, #87687, #39498, #51632, #39939, #79137, #59302, #24633, #67398, #72812, #73727, #33167, #17438, #73267, #44892, #72369, #52097, #17885, #25078, #45339, #86808, #66957, #4816, #52541, #10680, #31392, #80024, #32286, #59751, #25526, #18773, #52981, #80477, #46241, #12021 ),
 ( #5252, #60186, #25962, #26414, #34051, #20536, #40818, #82249, #47999, #40381, #55206, #68725, #88584, #67841, #75927, #14673, #82698, #20096, #35380, #61514, #69172, #55643, #81808, #41699, #19650, #6140, #53880, #47111, #81365, #7021, #14226, #68281, #270, #7477, #34930, #89021, #69609, #75478, #33614, #54761, #13776, #41261, #6586, #47560, #48439, #34496, #7915, #27296, #20968, #61959, #61077, #74602, #75051, #88141, #27733, #26855, #54314, #13336, #62394, #83135, #710, #28175, #21426, #48893, #76364, #42154, #12890, #29961, #10128, #9255, #57419, #1601, #49777, #8807, #43911, #64610, #36713, #71373, #9681, #15562, #37147, #2036, #84033, #76821, #70944, #84470, #78581, #2909, #23636, #22746, #42592, #77252, #70052, #15119, #43470, #63291, #43030, #62832, #77694, #56097, #30400, #57868, #23198, #21869, #84914, #51088, #70500, #36280, #85351, #16883, #64168, #44337, #71823, #63734, #1153, #29521, #22312, #8362, #2469, #50208, #28634, #83592, #49345, #16005, #35836, #56976, #29089, #56542, #50659, #78140, #16443, #74065, #52440, #30837, #5153, #32620, #87147, #85800, #32186, #25871, #38497, #31292, #65512, #80383, #59202, #24523, #60088, #87592, #53329, #17787, #80833, #66858, #59646, #19116, #86707, #72269, #24973, #45690, #73171, #46582, #38952 ),
 ( #58759, #4715, #65954, #86255, #37594, #51991, #65057, #3365, #58306, #79486, #24081, #51529, #45239, #79031, #38048, #17331, #44788, #10579, #72714, #3812, #11025, #4261, #11470, #25424, #31743, #66410, #79925, #18229, #18678, #52883, #46143, #73631, #11921, #39398, #88050, #14125, #41601, #54213, #82152, #12797, #88925, #19992, #83033, #33069, #20444, #6920, #13244, #34834, #69071, #27197, #47012, #12359, #33521, #67304, #74955, #21319, #60978, #48791, #41160, #55549, #7378, #6490, #68624, #40725, #39835, #34393, #88482, #26754, #61856, #5599, #60536, #33951, #26313, #615, #74498, #67744, #40283, #81708, #168, #68188, #47458, #53779, #61412, #62301, #28084, #81267, #54654, #19551, #6049, #47906, #75387, #13680, #27638, #55109, #82603, #20876, #48345, #75822, #16340, #22649, #43369, #1056, #77600, #15465, #70406, #29859, #83932, #76717, #9154, #36615, #49680, #62740, #78036, #43804, #28988, #56875, #15019, #63635, #22213, #57765, #7816, #84370, #70852, #77157, #9575, #71266, #1941, #21768, #76261, #8265, #42053, #42936, #85249, #35738, #23527, #15908, #30298, #37038, #8708, #64071, #36186, #14567, #2366, #63188, #69952, #23096, #69509, #35282, #57323, #50115, #28532, #84819, #55994, #83486, #49244, #64498, #29427, #1504, #42493, #56443, #50558 ),
 ( #2806, #24861, #30731, #38385, #85688, #11810, #37941, #73514, #65840, #87483, #17220, #80268, #64953, #23967, #3697, #4141, #65405, #45132, #31171, #18564, #46028, #25317, #66297, #50982, #39289, #78472, #58643, #51416, #66745, #59091, #3258, #52331, #37485, #32509, #71714, #5043, #17676, #86137, #44676, #10018, #72607, #59986, #58197, #24411, #59538, #16773, #44226, #79825, #78920, #31629, #72160, #10474, #51876, #79373, #86590, #10915, #18121, #45580, #73058, #11354, #38838, #4599, #32073, #87042, #52778, #82494, #20774, #65, #41055, #25763, #55006, #53222, #40178, #26204, #14017, #74394, #75285, #68960, #34734, #19887, #7268, #41494, #60429, #81162, #53674, #46908, #82047, #54106, #12693, #80726, #67641, #48239, #62202, #19006, #5942, #75712, #46478, #33412, #73957, #19447, #12247, #39732, #67200, #60874, #5500, #88376, #32964, #61301, #20343, #87944, #27088, #81601, #47354, #68515, #26649, #74849, #47803, #13574, #13138, #40618, #27537, #68087, #6391, #33845, #88817, #54550, #6813, #34287, #61747, #8599, #84268, #1388, #22985, #57221, #15356, #35177, #511, #21662, #55446, #63077, #9473, #49132, #36937, #29317, #43698, #84712, #83825, #56771, #28880, #71168, #22547, #76610, #83374, #36513, #82930, #48682, #50014, #27977, #35631, #50450, #14917 ),
 ( #42395, #1830, #9043, #77489, #56338, #21214, #77056, #62635, #22108, #49578, #42830, #8155, #69852, #15802, #70293, #76156, #36075, #43266, #63526, #41944, #14465, #70741, #69410, #63963, #7718, #948, #2259, #29754, #77929, #16232, #28418, #55886, #12043, #33187, #78813, #57660, #32738, #12913, #39516, #60208, #3148, #51308, #10366, #46699, #67418, #66979, #74176, #12475, #17113, #39959, #3594, #85580, #78366, #73748, #86027, #81388, #5715, #26437, #24305, #44126, #44568, #71606, #16667, #46258, #64846, #72055, #64400, #79270, #85142, #60651, #88162, #25984, #23421, #87712, #53900, #65298, #58096, #30624, #19236, #51766, #37828, #19670, #47133, #74623, #31063, #2699, #30195, #53447, #50879, #17571, #9913, #5274, #80950, #37376, #23855, #58530, #76842, #28193, #61534, #13799, #67860, #75498, #61981, #82270, #34518, #289, #81829, #7497, #20989, #40839, #20122, #55663, #56119, #34953, #89041, #40403, #41282, #21444, #27319, #54334, #48460, #27755, #83610, #48915, #1170, #55227, #47583, #54781, #75071, #13357, #75946, #68302, #20557, #6163, #82716, #33634, #7934, #35400, #729, #88605, #62414, #28652, #68744, #34072, #6605, #83153, #14246, #48020, #62852, #21889, #49364, #7042, #61096, #69629, #76387, #26877, #41725, #69189, #14691, #42176, #50675 ),
 ( #70523, #43048, #36298, #71394, #43490, #63755, #15139, #29539, #44355, #3385, #8381, #56997, #10153, #85818, #84489, #24098, #15581, #1621, #9699, #2058, #77715, #71844, #22764, #37615, #78160, #37169, #29107, #16462, #70963, #9273, #57885, #50227, #8828, #64630, #2933, #16022, #56563, #16904, #65077, #36732, #84935, #64185, #2490, #29979, #51548, #35854, #23214, #30420, #57437, #30854, #58325, #43929, #49797, #42612, #85370, #70074, #23656, #63314, #51106, #84052, #78600, #22332, #77272, #73189, #18696, #52458, #33085, #11940, #65972, #72730, #25887, #44807, #38066, #73648, #87165, #3831, #52900, #65529, #60554, #10599, #39417, #59666, #88067, #31765, #66877, #25444, #31311, #58775, #38515, #79048, #11487, #86275, #24544, #4277, #11042, #74081, #46163, #52011, #4733, #80399, #46604, #59221, #72286, #5171, #26329, #32638, #60109, #17805, #86727, #24992, #87608, #80850, #53351, #19131, #12376, #79944, #39854, #18246, #45708, #79504, #67320, #38972, #5615, #17352, #45258, #66430, #32209, #68206, #60997, #6066, #34409, #54230, #6507, #1072, #68641, #47031, #21339, #48806, #14142, #12812, #48363, #42071, #54671, #47474, #81727, #7395, #75405, #40741, #76279, #14585, #69526, #33966, #7832, #83052, #75841, #35298, #13698, #88499, #41176, #61873, #188 ) ),
 .UNSPECIFIED., .T., .F., .F. ) 
 B_SPLINE_SURFACE_WITH_KNOTS ( ( 4, 3, 4 ),
 ( 3, 2, 2, 2, 2, 2, 2, 2, 2, 2, 2, 2, 2, 2, 2, 2, 2, 2, 2, 2, 2, 2, 2, 2, 2, 2, 2, 2, 2, 2, 2, 2, 2, 2, 2, 2, 2, 2, 2, 2, 2, 2, 2, 2, 2, 2, 2, 2, 2, 2, 2, 2, 2, 2, 2, 2, 2, 2, 2, 2, 2, 2, 2, 2, 2, 2, 2, 2, 2, 2, 2, 2, 2, 2, 2, 2, 2, 2, 2, 2, 3 ),
 ( 0.000000000000000000, 0.5000000000000000000, 1.000000000000000000 ),
 ( 0.000000000000000000, 0.01250000000000000069, 0.02500000000000000139, 0.03749999999999999861, 0.05000000000000000278, 0.06250000000000000000, 0.07499999999999999722, 0.08749999999999999445, 0.1000000000000000056, 0.1125000000000000028, 0.1250000000000000000, 0.1375000000000000111, 0.1499999999999999944, 0.1625000000000000056, 0.1749999999999999889, 0.1875000000000000000, 0.2000000000000000111, 0.2124999999999999944, 0.2250000000000000056, 0.2374999999999999889, 0.2500000000000000000, 0.2625000000000000111, 0.2750000000000000222, 0.2874999999999999778, 0.2999999999999999889, 0.3125000000000000000, 0.3250000000000000111, 0.3375000000000000222, 0.3499999999999999778, 0.3624999999999999889, 0.3750000000000000000, 0.3875000000000000111, 0.4000000000000000222, 0.4124999999999999778, 0.4249999999999999889, 0.4375000000000000000, 0.4500000000000000111, 0.4625000000000000222, 0.4749999999999999778, 0.4874999999999999889, 0.5000000000000000000, 0.5124999999999999556, 0.5250000000000000222, 0.5374999999999999778, 0.5500000000000000444, 0.5625000000000000000, 0.5749999999999999556, 0.5875000000000000222, 0.5999999999999999778, 0.6125000000000000444, 0.6250000000000000000, 0.6374999999999999556, 0.6500000000000000222, 0.6624999999999999778, 0.6750000000000000444, 0.6875000000000000000, 0.6999999999999999556, 0.7125000000000000222, 0.7249999999999999778, 0.7375000000000000444, 0.7500000000000000000, 0.7624999999999999556, 0.7750000000000000222, 0.7874999999999999778, 0.8000000000000000444, 0.8125000000000000000, 0.8249999999999999556, 0.8375000000000000222, 0.8499999999999999778, 0.8625000000000000444, 0.8750000000000000000, 0.8874999999999999556, 0.9000000000000000222, 0.9124999999999999778, 0.9250000000000000444, 0.9375000000000000000, 0.9499999999999999556, 0.9625000000000000222, 0.9749999999999999778, 0.9875000000000000444, 1.000000000000000000 ),
 .UNSPECIFIED. ) 
 GEOMETRIC_REPRESENTATION_ITEM ( )  RATIONAL_B_SPLINE_SURFACE ( (
 ( 1.000000000000000000, 0.9238795325112867385, 1.000000000000000000, 0.9238795325112867385, 1.000000000000000000, 0.9238795325112867385, 1.000000000000000000, 0.9238795325112867385, 1.000000000000000000, 0.9238795325112867385, 1.000000000000000000, 0.9238795325112867385, 1.000000000000000000, 0.9238795325112867385, 1.000000000000000000, 0.9238795325112867385, 1.000000000000000000, 0.9238795325112867385, 1.000000000000000000, 0.9238795325112867385, 1.000000000000000000, 0.9238795325112867385, 1.000000000000000000, 0.9238795325112867385, 1.000000000000000000, 0.9238795325112867385, 1.000000000000000000, 0.9238795325112867385, 1.000000000000000000, 0.9238795325112867385, 1.000000000000000000, 0.9238795325112867385, 1.000000000000000000, 0.9238795325112867385, 1.000000000000000000, 0.9238795325112867385, 1.000000000000000000, 0.9238795325112867385, 1.000000000000000000, 0.9238795325112867385, 1.000000000000000000, 0.9238795325112867385, 1.000000000000000000, 0.9238795325112867385, 1.000000000000000000, 0.9238795325112867385, 1.000000000000000000, 0.9238795325112867385, 1.000000000000000000, 0.9238795325112867385, 1.000000000000000000, 0.9238795325112867385, 1.000000000000000000, 0.9238795325112867385, 1.000000000000000000, 0.9238795325112867385, 1.000000000000000000, 0.9238795325112867385, 1.000000000000000000, 0.9238795325112867385, 1.000000000000000000, 0.9238795325112867385, 1.000000000000000000, 0.9238795325112867385, 1.000000000000000000, 0.9238795325112867385, 1.000000000000000000, 0.9238795325112867385, 1.000000000000000000, 0.9238795325112867385, 1.000000000000000000, 0.9238795325112867385, 1.000000000000000000, 0.9238795325112867385, 1.000000000000000000, 0.9238795325112867385, 1.000000000000000000, 0.9238795325112867385, 1.000000000000000000, 0.9238795325112867385, 1.000000000000000000, 0.9238795325112867385, 1.000000000000000000, 0.9238795325112867385, 1.000000000000000000, 0.9238795325112867385, 1.000000000000000000, 0.9238795325112867385, 1.000000000000000000, 0.9238795325112867385, 1.000000000000000000, 0.9238795325112867385, 1.000000000000000000, 0.9238795325112867385, 1.000000000000000000, 0.9238795325112867385, 1.000000000000000000, 0.9238795325112867385, 1.000000000000000000, 0.9238795325112867385, 1.000000000000000000, 0.9238795325112867385, 1.000000000000000000, 0.9238795325112867385, 1.000000000000000000, 0.9238795325112867385, 1.000000000000000000, 0.9238795325112867385, 1.000000000000000000, 0.9238795325112867385, 1.000000000000000000, 0.9238795325112867385, 1.000000000000000000, 0.9238795325112867385, 1.000000000000000000, 0.9238795325112867385, 1.000000000000000000, 0.9238795325112867385, 1.000000000000000000, 0.9238795325112867385, 1.000000000000000000, 0.9238795325112867385, 1.000000000000000000, 0.9238795325112867385, 1.000000000000000000, 0.9238795325112867385, 1.000000000000000000, 0.9238795325112867385, 1.000000000000000000, 0.9238795325112867385, 1.000000000000000000, 0.9238795325112867385, 1.000000000000000000, 0.9238795325112867385, 1.000000000000000000, 0.9238795325112867385, 1.000000000000000000, 0.9238795325112867385, 1.000000000000000000, 0.9238795325112867385, 1.000000000000000000, 0.9238795325112867385, 1.000000000000000000, 0.9238795325112867385, 1.000000000000000000, 0.9238795325112867385, 1.000000000000000000, 0.9238795325112867385, 1.000000000000000000, 0.9238795325112867385, 1.000000000000000000, 0.9238795325112867385, 1.000000000000000000, 0.9238795325112867385, 1.000000000000000000, 0.9238795325112867385, 1.000000000000000000, 0.9238795325112867385, 1.000000000000000000, 0.9238795325112867385, 1.000000000000000000),
 ( 0.3333333333333333703, 0.3079598441704289313, 0.3333333333333333703, 0.3079598441704289313, 0.3333333333333333703, 0.3079598441704289313, 0.3333333333333333703, 0.3079598441704289313, 0.3333333333333333703, 0.3079598441704289313, 0.3333333333333333703, 0.3079598441704289313, 0.3333333333333333703, 0.3079598441704289313, 0.3333333333333333703, 0.3079598441704289313, 0.3333333333333333703, 0.3079598441704289313, 0.3333333333333333703, 0.3079598441704289313, 0.3333333333333333703, 0.3079598441704289313, 0.3333333333333333703, 0.3079598441704289313, 0.3333333333333333703, 0.3079598441704289313, 0.3333333333333333703, 0.3079598441704289313, 0.3333333333333333703, 0.3079598441704289313, 0.3333333333333333703, 0.3079598441704289313, 0.3333333333333333703, 0.3079598441704289313, 0.3333333333333333703, 0.3079598441704289313, 0.3333333333333333703, 0.3079598441704289313, 0.3333333333333333703, 0.3079598441704289313, 0.3333333333333333703, 0.3079598441704289313, 0.3333333333333333703, 0.3079598441704289313, 0.3333333333333333703, 0.3079598441704289313, 0.3333333333333333703, 0.3079598441704289313, 0.3333333333333333703, 0.3079598441704289313, 0.3333333333333333703, 0.3079598441704289313, 0.3333333333333333703, 0.3079598441704289313, 0.3333333333333333703, 0.3079598441704289313, 0.3333333333333333703, 0.3079598441704289313, 0.3333333333333333703, 0.3079598441704289313, 0.3333333333333333703, 0.3079598441704289313, 0.3333333333333333703, 0.3079598441704289313, 0.3333333333333333703, 0.3079598441704289313, 0.3333333333333333703, 0.3079598441704289313, 0.3333333333333333703, 0.3079598441704289313, 0.3333333333333333703, 0.3079598441704289313, 0.3333333333333333703, 0.3079598441704289313, 0.3333333333333333703, 0.3079598441704289313, 0.3333333333333333703, 0.3079598441704289313, 0.3333333333333333703, 0.3079598441704289313, 0.3333333333333333703, 0.3079598441704289313, 0.3333333333333333703, 0.3079598441704289313, 0.3333333333333333703, 0.3079598441704289313, 0.3333333333333333703, 0.3079598441704289313, 0.3333333333333333703, 0.3079598441704289313, 0.3333333333333333703, 0.3079598441704289313, 0.3333333333333333703, 0.3079598441704289313, 0.3333333333333333703, 0.3079598441704289313, 0.3333333333333333703, 0.3079598441704289313, 0.3333333333333333703, 0.3079598441704289313, 0.3333333333333333703, 0.3079598441704289313, 0.3333333333333333703, 0.3079598441704289313, 0.3333333333333333703, 0.3079598441704289313, 0.3333333333333333703, 0.3079598441704289313, 0.3333333333333333703, 0.3079598441704289313, 0.3333333333333333703, 0.3079598441704289313, 0.3333333333333333703, 0.3079598441704289313, 0.3333333333333333703, 0.3079598441704289313, 0.3333333333333333703, 0.3079598441704289313, 0.3333333333333333703, 0.3079598441704289313, 0.3333333333333333703, 0.3079598441704289313, 0.3333333333333333703, 0.3079598441704289313, 0.3333333333333333703, 0.3079598441704289313, 0.3333333333333333703, 0.3079598441704289313, 0.3333333333333333703, 0.3079598441704289313, 0.3333333333333333703, 0.3079598441704289313, 0.3333333333333333703, 0.3079598441704289313, 0.3333333333333333703, 0.3079598441704289313, 0.3333333333333333703, 0.3079598441704289313, 0.3333333333333333703, 0.3079598441704289313, 0.3333333333333333703, 0.3079598441704289313, 0.3333333333333333703, 0.3079598441704289313, 0.3333333333333333703, 0.3079598441704289313, 0.3333333333333333703, 0.3079598441704289313, 0.3333333333333333703, 0.3079598441704289313, 0.3333333333333333703, 0.3079598441704289313, 0.3333333333333333703, 0.3079598441704289313, 0.3333333333333333703, 0.3079598441704289313, 0.3333333333333333703, 0.3079598441704289313, 0.3333333333333333703, 0.3079598441704289313, 0.3333333333333333703),
 ( 0.3333333333333333703, 0.3079598441704289313, 0.3333333333333333703, 0.3079598441704289313, 0.3333333333333333703, 0.3079598441704289313, 0.3333333333333333703, 0.3079598441704289313, 0.3333333333333333703, 0.3079598441704289313, 0.3333333333333333703, 0.3079598441704289313, 0.3333333333333333703, 0.3079598441704289313, 0.3333333333333333703, 0.3079598441704289313, 0.3333333333333333703, 0.3079598441704289313, 0.3333333333333333703, 0.3079598441704289313, 0.3333333333333333703, 0.3079598441704289313, 0.3333333333333333703, 0.3079598441704289313, 0.3333333333333333703, 0.3079598441704289313, 0.3333333333333333703, 0.3079598441704289313, 0.3333333333333333703, 0.3079598441704289313, 0.3333333333333333703, 0.3079598441704289313, 0.3333333333333333703, 0.3079598441704289313, 0.3333333333333333703, 0.3079598441704289313, 0.3333333333333333703, 0.3079598441704289313, 0.3333333333333333703, 0.3079598441704289313, 0.3333333333333333703, 0.3079598441704289313, 0.3333333333333333703, 0.3079598441704289313, 0.3333333333333333703, 0.3079598441704289313, 0.3333333333333333703, 0.3079598441704289313, 0.3333333333333333703, 0.3079598441704289313, 0.3333333333333333703, 0.3079598441704289313, 0.3333333333333333703, 0.3079598441704289313, 0.3333333333333333703, 0.3079598441704289313, 0.3333333333333333703, 0.3079598441704289313, 0.3333333333333333703, 0.3079598441704289313, 0.3333333333333333703, 0.3079598441704289313, 0.3333333333333333703, 0.3079598441704289313, 0.3333333333333333703, 0.3079598441704289313, 0.3333333333333333703, 0.3079598441704289313, 0.3333333333333333703, 0.3079598441704289313, 0.3333333333333333703, 0.3079598441704289313, 0.3333333333333333703, 0.3079598441704289313, 0.3333333333333333703, 0.3079598441704289313, 0.3333333333333333703, 0.3079598441704289313, 0.3333333333333333703, 0.3079598441704289313, 0.3333333333333333703, 0.3079598441704289313, 0.3333333333333333703, 0.3079598441704289313, 0.3333333333333333703, 0.3079598441704289313, 0.3333333333333333703, 0.3079598441704289313, 0.3333333333333333703, 0.3079598441704289313, 0.3333333333333333703, 0.3079598441704289313, 0.3333333333333333703, 0.3079598441704289313, 0.3333333333333333703, 0.3079598441704289313, 0.3333333333333333703, 0.3079598441704289313, 0.3333333333333333703, 0.3079598441704289313, 0.3333333333333333703, 0.3079598441704289313, 0.3333333333333333703, 0.3079598441704289313, 0.3333333333333333703, 0.3079598441704289313, 0.3333333333333333703, 0.3079598441704289313, 0.3333333333333333703, 0.3079598441704289313, 0.3333333333333333703, 0.3079598441704289313, 0.3333333333333333703, 0.3079598441704289313, 0.3333333333333333703, 0.3079598441704289313, 0.3333333333333333703, 0.3079598441704289313, 0.3333333333333333703, 0.3079598441704289313, 0.3333333333333333703, 0.3079598441704289313, 0.3333333333333333703, 0.3079598441704289313, 0.3333333333333333703, 0.3079598441704289313, 0.3333333333333333703, 0.3079598441704289313, 0.3333333333333333703, 0.3079598441704289313, 0.3333333333333333703, 0.3079598441704289313, 0.3333333333333333703, 0.3079598441704289313, 0.3333333333333333703, 0.3079598441704289313, 0.3333333333333333703, 0.3079598441704289313, 0.3333333333333333703, 0.3079598441704289313, 0.3333333333333333703, 0.3079598441704289313, 0.3333333333333333703, 0.3079598441704289313, 0.3333333333333333703, 0.3079598441704289313, 0.3333333333333333703, 0.3079598441704289313, 0.3333333333333333703, 0.3079598441704289313, 0.3333333333333333703, 0.3079598441704289313, 0.3333333333333333703, 0.3079598441704289313, 0.3333333333333333703, 0.3079598441704289313, 0.3333333333333333703, 0.3079598441704289313, 0.3333333333333333703, 0.3079598441704289313, 0.3333333333333333703),
 ( 1.000000000000000000, 0.9238795325112867385, 1.000000000000000000, 0.9238795325112867385, 1.000000000000000000, 0.9238795325112867385, 1.000000000000000000, 0.9238795325112867385, 1.000000000000000000, 0.9238795325112867385, 1.000000000000000000, 0.9238795325112867385, 1.000000000000000000, 0.9238795325112867385, 1.000000000000000000, 0.9238795325112867385, 1.000000000000000000, 0.9238795325112867385, 1.000000000000000000, 0.9238795325112867385, 1.000000000000000000, 0.9238795325112867385, 1.000000000000000000, 0.9238795325112867385, 1.000000000000000000, 0.9238795325112867385, 1.000000000000000000, 0.9238795325112867385, 1.000000000000000000, 0.9238795325112867385, 1.000000000000000000, 0.9238795325112867385, 1.000000000000000000, 0.9238795325112867385, 1.000000000000000000, 0.9238795325112867385, 1.000000000000000000, 0.9238795325112867385, 1.000000000000000000, 0.9238795325112867385, 1.000000000000000000, 0.9238795325112867385, 1.000000000000000000, 0.9238795325112867385, 1.000000000000000000, 0.9238795325112867385, 1.000000000000000000, 0.9238795325112867385, 1.000000000000000000, 0.9238795325112867385, 1.000000000000000000, 0.9238795325112867385, 1.000000000000000000, 0.9238795325112867385, 1.000000000000000000, 0.9238795325112867385, 1.000000000000000000, 0.9238795325112867385, 1.000000000000000000, 0.9238795325112867385, 1.000000000000000000, 0.9238795325112867385, 1.000000000000000000, 0.9238795325112867385, 1.000000000000000000, 0.9238795325112867385, 1.000000000000000000, 0.9238795325112867385, 1.000000000000000000, 0.9238795325112867385, 1.000000000000000000, 0.9238795325112867385, 1.000000000000000000, 0.9238795325112867385, 1.000000000000000000, 0.9238795325112867385, 1.000000000000000000, 0.9238795325112867385, 1.000000000000000000, 0.9238795325112867385, 1.000000000000000000, 0.9238795325112867385, 1.000000000000000000, 0.9238795325112867385, 1.000000000000000000, 0.9238795325112867385, 1.000000000000000000, 0.9238795325112867385, 1.000000000000000000, 0.9238795325112867385, 1.000000000000000000, 0.9238795325112867385, 1.000000000000000000, 0.9238795325112867385, 1.000000000000000000, 0.9238795325112867385, 1.000000000000000000, 0.9238795325112867385, 1.000000000000000000, 0.9238795325112867385, 1.000000000000000000, 0.9238795325112867385, 1.000000000000000000, 0.9238795325112867385, 1.000000000000000000, 0.9238795325112867385, 1.000000000000000000, 0.9238795325112867385, 1.000000000000000000, 0.9238795325112867385, 1.000000000000000000, 0.9238795325112867385, 1.000000000000000000, 0.9238795325112867385, 1.000000000000000000, 0.9238795325112867385, 1.000000000000000000, 0.9238795325112867385, 1.000000000000000000, 0.9238795325112867385, 1.000000000000000000, 0.9238795325112867385, 1.000000000000000000, 0.9238795325112867385, 1.000000000000000000, 0.9238795325112867385, 1.000000000000000000, 0.9238795325112867385, 1.000000000000000000, 0.9238795325112867385, 1.000000000000000000, 0.9238795325112867385, 1.000000000000000000, 0.9238795325112867385, 1.000000000000000000, 0.9238795325112867385, 1.000000000000000000, 0.9238795325112867385, 1.000000000000000000, 0.9238795325112867385, 1.000000000000000000, 0.9238795325112867385, 1.000000000000000000, 0.9238795325112867385, 1.000000000000000000, 0.9238795325112867385, 1.000000000000000000, 0.9238795325112867385, 1.000000000000000000, 0.9238795325112867385, 1.000000000000000000, 0.9238795325112867385, 1.000000000000000000, 0.9238795325112867385, 1.000000000000000000, 0.9238795325112867385, 1.000000000000000000, 0.9238795325112867385, 1.000000000000000000, 0.9238795325112867385, 1.000000000000000000),
 ( 0.3333333333333333703, 0.3079598441704289313, 0.3333333333333333703, 0.3079598441704289313, 0.3333333333333333703, 0.3079598441704289313, 0.3333333333333333703, 0.3079598441704289313, 0.3333333333333333703, 0.3079598441704289313, 0.3333333333333333703, 0.3079598441704289313, 0.3333333333333333703, 0.3079598441704289313, 0.3333333333333333703, 0.3079598441704289313, 0.3333333333333333703, 0.3079598441704289313, 0.3333333333333333703, 0.3079598441704289313, 0.3333333333333333703, 0.3079598441704289313, 0.3333333333333333703, 0.3079598441704289313, 0.3333333333333333703, 0.3079598441704289313, 0.3333333333333333703, 0.3079598441704289313, 0.3333333333333333703, 0.3079598441704289313, 0.3333333333333333703, 0.3079598441704289313, 0.3333333333333333703, 0.3079598441704289313, 0.3333333333333333703, 0.3079598441704289313, 0.3333333333333333703, 0.3079598441704289313, 0.3333333333333333703, 0.3079598441704289313, 0.3333333333333333703, 0.3079598441704289313, 0.3333333333333333703, 0.3079598441704289313, 0.3333333333333333703, 0.3079598441704289313, 0.3333333333333333703, 0.3079598441704289313, 0.3333333333333333703, 0.3079598441704289313, 0.3333333333333333703, 0.3079598441704289313, 0.3333333333333333703, 0.3079598441704289313, 0.3333333333333333703, 0.3079598441704289313, 0.3333333333333333703, 0.3079598441704289313, 0.3333333333333333703, 0.3079598441704289313, 0.3333333333333333703, 0.3079598441704289313, 0.3333333333333333703, 0.3079598441704289313, 0.3333333333333333703, 0.3079598441704289313, 0.3333333333333333703, 0.3079598441704289313, 0.3333333333333333703, 0.3079598441704289313, 0.3333333333333333703, 0.3079598441704289313, 0.3333333333333333703, 0.3079598441704289313, 0.3333333333333333703, 0.3079598441704289313, 0.3333333333333333703, 0.3079598441704289313, 0.3333333333333333703, 0.3079598441704289313, 0.3333333333333333703, 0.3079598441704289313, 0.3333333333333333703, 0.3079598441704289313, 0.3333333333333333703, 0.3079598441704289313, 0.3333333333333333703, 0.3079598441704289313, 0.3333333333333333703, 0.3079598441704289313, 0.3333333333333333703, 0.3079598441704289313, 0.3333333333333333703, 0.3079598441704289313, 0.3333333333333333703, 0.3079598441704289313, 0.3333333333333333703, 0.3079598441704289313, 0.3333333333333333703, 0.3079598441704289313, 0.3333333333333333703, 0.3079598441704289313, 0.3333333333333333703, 0.3079598441704289313, 0.3333333333333333703, 0.3079598441704289313, 0.3333333333333333703, 0.3079598441704289313, 0.3333333333333333703, 0.3079598441704289313, 0.3333333333333333703, 0.3079598441704289313, 0.3333333333333333703, 0.3079598441704289313, 0.3333333333333333703, 0.3079598441704289313, 0.3333333333333333703, 0.3079598441704289313, 0.3333333333333333703, 0.3079598441704289313, 0.3333333333333333703, 0.3079598441704289313, 0.3333333333333333703, 0.3079598441704289313, 0.3333333333333333703, 0.3079598441704289313, 0.3333333333333333703, 0.3079598441704289313, 0.3333333333333333703, 0.3079598441704289313, 0.3333333333333333703, 0.3079598441704289313, 0.3333333333333333703, 0.3079598441704289313, 0.3333333333333333703, 0.3079598441704289313, 0.3333333333333333703, 0.3079598441704289313, 0.3333333333333333703, 0.3079598441704289313, 0.3333333333333333703, 0.3079598441704289313, 0.3333333333333333703, 0.3079598441704289313, 0.3333333333333333703, 0.3079598441704289313, 0.3333333333333333703, 0.3079598441704289313, 0.3333333333333333703, 0.3079598441704289313, 0.3333333333333333703, 0.3079598441704289313, 0.3333333333333333703, 0.3079598441704289313, 0.3333333333333333703, 0.3079598441704289313, 0.3333333333333333703, 0.3079598441704289313, 0.3333333333333333703, 0.3079598441704289313, 0.3333333333333333703),
 ( 0.3333333333333333703, 0.3079598441704289313, 0.3333333333333333703, 0.3079598441704289313, 0.3333333333333333703, 0.3079598441704289313, 0.3333333333333333703, 0.3079598441704289313, 0.3333333333333333703, 0.3079598441704289313, 0.3333333333333333703, 0.3079598441704289313, 0.3333333333333333703, 0.3079598441704289313, 0.3333333333333333703, 0.3079598441704289313, 0.3333333333333333703, 0.3079598441704289313, 0.3333333333333333703, 0.3079598441704289313, 0.3333333333333333703, 0.3079598441704289313, 0.3333333333333333703, 0.3079598441704289313, 0.3333333333333333703, 0.3079598441704289313, 0.3333333333333333703, 0.3079598441704289313, 0.3333333333333333703, 0.3079598441704289313, 0.3333333333333333703, 0.3079598441704289313, 0.3333333333333333703, 0.3079598441704289313, 0.3333333333333333703, 0.3079598441704289313, 0.3333333333333333703, 0.3079598441704289313, 0.3333333333333333703, 0.3079598441704289313, 0.3333333333333333703, 0.3079598441704289313, 0.3333333333333333703, 0.3079598441704289313, 0.3333333333333333703, 0.3079598441704289313, 0.3333333333333333703, 0.3079598441704289313, 0.3333333333333333703, 0.3079598441704289313, 0.3333333333333333703, 0.3079598441704289313, 0.3333333333333333703, 0.3079598441704289313, 0.3333333333333333703, 0.3079598441704289313, 0.3333333333333333703, 0.3079598441704289313, 0.3333333333333333703, 0.3079598441704289313, 0.3333333333333333703, 0.3079598441704289313, 0.3333333333333333703, 0.3079598441704289313, 0.3333333333333333703, 0.3079598441704289313, 0.3333333333333333703, 0.3079598441704289313, 0.3333333333333333703, 0.3079598441704289313, 0.3333333333333333703, 0.3079598441704289313, 0.3333333333333333703, 0.3079598441704289313, 0.3333333333333333703, 0.3079598441704289313, 0.3333333333333333703, 0.3079598441704289313, 0.3333333333333333703, 0.3079598441704289313, 0.3333333333333333703, 0.3079598441704289313, 0.3333333333333333703, 0.3079598441704289313, 0.3333333333333333703, 0.3079598441704289313, 0.3333333333333333703, 0.3079598441704289313, 0.3333333333333333703, 0.3079598441704289313, 0.3333333333333333703, 0.3079598441704289313, 0.3333333333333333703, 0.3079598441704289313, 0.3333333333333333703, 0.3079598441704289313, 0.3333333333333333703, 0.3079598441704289313, 0.3333333333333333703, 0.3079598441704289313, 0.3333333333333333703, 0.3079598441704289313, 0.3333333333333333703, 0.3079598441704289313, 0.3333333333333333703, 0.3079598441704289313, 0.3333333333333333703, 0.3079598441704289313, 0.3333333333333333703, 0.3079598441704289313, 0.3333333333333333703, 0.3079598441704289313, 0.3333333333333333703, 0.3079598441704289313, 0.3333333333333333703, 0.3079598441704289313, 0.3333333333333333703, 0.3079598441704289313, 0.3333333333333333703, 0.3079598441704289313, 0.3333333333333333703, 0.3079598441704289313, 0.3333333333333333703, 0.3079598441704289313, 0.3333333333333333703, 0.3079598441704289313, 0.3333333333333333703, 0.3079598441704289313, 0.3333333333333333703, 0.3079598441704289313, 0.3333333333333333703, 0.3079598441704289313, 0.3333333333333333703, 0.3079598441704289313, 0.3333333333333333703, 0.3079598441704289313, 0.3333333333333333703, 0.3079598441704289313, 0.3333333333333333703, 0.3079598441704289313, 0.3333333333333333703, 0.3079598441704289313, 0.3333333333333333703, 0.3079598441704289313, 0.3333333333333333703, 0.3079598441704289313, 0.3333333333333333703, 0.3079598441704289313, 0.3333333333333333703, 0.3079598441704289313, 0.3333333333333333703, 0.3079598441704289313, 0.3333333333333333703, 0.3079598441704289313, 0.3333333333333333703, 0.3079598441704289313, 0.3333333333333333703, 0.3079598441704289313, 0.3333333333333333703, 0.3079598441704289313, 0.3333333333333333703),
 ( 1.000000000000000000, 0.9238795325112867385, 1.000000000000000000, 0.9238795325112867385, 1.000000000000000000, 0.9238795325112867385, 1.000000000000000000, 0.9238795325112867385, 1.000000000000000000, 0.9238795325112867385, 1.000000000000000000, 0.9238795325112867385, 1.000000000000000000, 0.9238795325112867385, 1.000000000000000000, 0.9238795325112867385, 1.000000000000000000, 0.9238795325112867385, 1.000000000000000000, 0.9238795325112867385, 1.000000000000000000, 0.9238795325112867385, 1.000000000000000000, 0.9238795325112867385, 1.000000000000000000, 0.9238795325112867385, 1.000000000000000000, 0.9238795325112867385, 1.000000000000000000, 0.9238795325112867385, 1.000000000000000000, 0.9238795325112867385, 1.000000000000000000, 0.9238795325112867385, 1.000000000000000000, 0.9238795325112867385, 1.000000000000000000, 0.9238795325112867385, 1.000000000000000000, 0.9238795325112867385, 1.000000000000000000, 0.9238795325112867385, 1.000000000000000000, 0.9238795325112867385, 1.000000000000000000, 0.9238795325112867385, 1.000000000000000000, 0.9238795325112867385, 1.000000000000000000, 0.9238795325112867385, 1.000000000000000000, 0.9238795325112867385, 1.000000000000000000, 0.9238795325112867385, 1.000000000000000000, 0.9238795325112867385, 1.000000000000000000, 0.9238795325112867385, 1.000000000000000000, 0.9238795325112867385, 1.000000000000000000, 0.9238795325112867385, 1.000000000000000000, 0.9238795325112867385, 1.000000000000000000, 0.9238795325112867385, 1.000000000000000000, 0.9238795325112867385, 1.000000000000000000, 0.9238795325112867385, 1.000000000000000000, 0.9238795325112867385, 1.000000000000000000, 0.9238795325112867385, 1.000000000000000000, 0.9238795325112867385, 1.000000000000000000, 0.9238795325112867385, 1.000000000000000000, 0.9238795325112867385, 1.000000000000000000, 0.9238795325112867385, 1.000000000000000000, 0.9238795325112867385, 1.000000000000000000, 0.9238795325112867385, 1.000000000000000000, 0.9238795325112867385, 1.000000000000000000, 0.9238795325112867385, 1.000000000000000000, 0.9238795325112867385, 1.000000000000000000, 0.9238795325112867385, 1.000000000000000000, 0.9238795325112867385, 1.000000000000000000, 0.9238795325112867385, 1.000000000000000000, 0.9238795325112867385, 1.000000000000000000, 0.9238795325112867385, 1.000000000000000000, 0.9238795325112867385, 1.000000000000000000, 0.9238795325112867385, 1.000000000000000000, 0.9238795325112867385, 1.000000000000000000, 0.9238795325112867385, 1.000000000000000000, 0.9238795325112867385, 1.000000000000000000, 0.9238795325112867385, 1.000000000000000000, 0.9238795325112867385, 1.000000000000000000, 0.9238795325112867385, 1.000000000000000000, 0.9238795325112867385, 1.000000000000000000, 0.9238795325112867385, 1.000000000000000000, 0.9238795325112867385, 1.000000000000000000, 0.9238795325112867385, 1.000000000000000000, 0.9238795325112867385, 1.000000000000000000, 0.9238795325112867385, 1.000000000000000000, 0.9238795325112867385, 1.000000000000000000, 0.9238795325112867385, 1.000000000000000000, 0.9238795325112867385, 1.000000000000000000, 0.9238795325112867385, 1.000000000000000000, 0.9238795325112867385, 1.000000000000000000, 0.9238795325112867385, 1.000000000000000000, 0.9238795325112867385, 1.000000000000000000, 0.9238795325112867385, 1.000000000000000000, 0.9238795325112867385, 1.000000000000000000, 0.9238795325112867385, 1.000000000000000000, 0.9238795325112867385, 1.000000000000000000, 0.9238795325112867385, 1.000000000000000000, 0.9238795325112867385, 1.000000000000000000, 0.9238795325112867385, 1.000000000000000000, 0.9238795325112867385, 1.000000000000000000) ) ) 
 REPRESENTATION_ITEM ( '' )  SURFACE ( )  );
#23611 = CARTESIAN_POINT ( 'NONE',  ( 15.90386942290380290, -6.567427716900048118, 34.66269422305636283 ) ) ;
#23612 = ORIENTED_EDGE ( 'NONE', *, *, #6428, .T. ) ;
#23613 = CARTESIAN_POINT ( 'NONE',  ( -14.08491263871424160, -8.540255544307065350, 34.89611431652622286 ) ) ;
#23614 = CARTESIAN_POINT ( 'NONE',  ( 4.826899852701619587, -8.475808217655753651, 34.90892951860618609 ) ) ;
#23615 = CARTESIAN_POINT ( 'NONE',  ( -9.692307692307812417, -3.300289026999228881, 32.46337939537708905 ) ) ;
#23616 = ORIENTED_EDGE ( 'NONE', *, *, #18601, .T. ) ;
#23617 = FACE_OUTER_BOUND ( 'NONE', #27603, .T. ) ;
#23618 = CARTESIAN_POINT ( 'NONE',  ( -5.198717948717948012, -3.499999999999999556, 29.75000000000000355 ) ) ;
#23619 = VERTEX_POINT ( 'NONE', #6269 ) ;
#23620 = B_SPLINE_CURVE_WITH_KNOTS ( 'NONE', 3,
 ( #73911, #13530, #27490, #75241, #88771, #87435, #27047, #48195, #19844, #47309 ),
 .UNSPECIFIED., .F., .F.,
 ( 4, 2, 2, 2, 4 ),
 ( 0.000000000000000000, 0.0001954311564186882026, 0.0003908623128373764051, 0.0005862934692560646619, 0.0007817246256747528103 ),
 .UNSPECIFIED. ) ;
#23621 = ADVANCED_FACE ( 'NONE', ( #25643 ), #53099, .F. ) ;
#23622 = CARTESIAN_POINT ( 'NONE',  ( 3.361561038594017337, -8.147973898785416225, 34.70805048591653730 ) ) ;
#23623 = B_SPLINE_CURVE_WITH_KNOTS ( 'NONE', 3,
 ( #9868, #17070, #37783, #22940, #36894, #38231, #65249, #64356, #31018, #51721 ),
 .UNSPECIFIED., .F., .F.,
 ( 4, 2, 2, 2, 4 ),
 ( 0.000000000000000000, 0.0001954311564186871726, 0.0003908623128373743452, 0.0005862934692560615177, 0.0007817246256747486903 ),
 .UNSPECIFIED. ) ;
#23624 = DIRECTION ( 'NONE',  ( 0.000000000000000000, -6.938893903907222067E-15, 1.000000000000000000 ) ) ;
#23625 = CARTESIAN_POINT ( 'NONE',  ( 3.453548772037639214, -4.387253974876676565, 33.66317474335728832 ) ) ;
#23626 = CARTESIAN_POINT ( 'NONE',  ( -2.373775718648187816, -2.538708090699994813, 30.37095296980875148 ) ) ;
#23627 = CARTESIAN_POINT ( 'NONE',  ( -8.769230769230890843, -9.442884908241554243, 34.35708131394783038 ) ) ;
#23628 = FACE_OUTER_BOUND ( 'NONE', #29795, .T. ) ;
#23629 = CARTESIAN_POINT ( 'NONE',  ( 7.976944287120800503, -2.845873456487966635, 32.17976146951972538 ) ) ;
#23631 = CARTESIAN_POINT ( 'NONE',  ( 11.28846153846154010, -7.433932668274256805, 35.00000000000000711 ) ) ;
#23630 = CARTESIAN_POINT ( 'NONE',  ( 4.946231610255517275, -12.38065189839062263, 30.83690757178629482 ) ) ;
#23632 = CARTESIAN_POINT ( 'NONE',  ( 1.607394925883794068, -11.41317474335729187, 32.86274602512330034 ) ) ;
#23634 = CARTESIAN_POINT ( 'NONE',  ( 0.4615384615384611755, -12.78798330534102767, 29.49999999999997868 ) ) ;
#23633 = DIRECTION ( 'NONE',  ( -0.000000000000000000, -1.000000000000000000, 3.491481338843133355E-15 ) ) ;
#23635 = CARTESIAN_POINT ( 'NONE',  ( -6.923076923076922462, -13.75783147151868846, 33.36296068462461051 ) ) ;
#23636 = CARTESIAN_POINT ( 'NONE',  ( 1.987747218494664292, -9.401340078031346081, 21.87313170625849068 ) ) ;
#23637 = ORIENTED_EDGE ( 'NONE', *, *, #41649, .F. ) ;
#23638 = CARTESIAN_POINT ( 'NONE',  ( 14.30769230769218758, -5.219633306517616589, 34.19971097300220464 ) ) ;
#23639 = ORIENTED_EDGE ( 'NONE', *, *, #11162, .T. ) ;
#23640 = CARTESIAN_POINT ( 'NONE',  ( -2.530619266599154926, -2.889293201056495786, 32.26117774369186009 ) ) ;
#23641 = EDGE_LOOP ( 'NONE', ( #27885, #42942 ) ) ;
#23642 = EDGE_CURVE ( 'NONE', #6970, #79996, #88700, .T. ) ;
#23643 = CARTESIAN_POINT ( 'NONE',  ( -13.25408994638174320, -2.372941743896879174, 30.88044141588253666 ) ) ;
#23644 = ORIENTED_EDGE ( 'NONE', *, *, #63207, .F. ) ;
#23645 = DIRECTION ( 'NONE',  ( 0.000000000000000000, 0.000000000000000000, 1.000000000000000000 ) ) ;
#23646 = CARTESIAN_POINT ( 'NONE',  ( -2.775308065498764964, -6.422011778438537988, 22.42000670625849068 ) ) ;
#23647 = CARTESIAN_POINT ( 'NONE',  ( 17.07692307692307665, -8.120952969808772792, 34.71129190930000163 ) ) ;
#23648 = EDGE_CURVE ( 'NONE', #74633, #52479, #26981, .T. ) ;
#23649 = CYLINDRICAL_SURFACE ( 'NONE', #84144, 0.2499999999999994726 ) ;
#23650 = CARTESIAN_POINT ( 'NONE',  ( 13.63466980452883703, -2.920487667080175598, 32.31805714834170828 ) ) ;
#23651 = CARTESIAN_POINT ( 'NONE',  ( -6.250023224221458840, -2.588893531581426544, 31.60682220781847818 ) ) ;
#23652 = VECTOR ( 'NONE', #12233, 1000.000000000000000 ) ;
#23653 = DIRECTION ( 'NONE',  ( -1.000000000000000000, 0.000000000000000000, 0.000000000000000000 ) ) ;
#23654 = CARTESIAN_POINT ( 'NONE',  ( 1.254467414883689624, -5.070767119584671967, 34.40440758774516183 ) ) ;
#23655 = CARTESIAN_POINT ( 'NONE',  ( -22.00000000000000355, -10.00000000000000533, 0.000000000000000000 ) ) ;
#23656 = CARTESIAN_POINT ( 'NONE',  ( 2.651650429449569302, -10.15165042944953733, 18.37500000000000355 ) ) ;
#23657 = CARTESIAN_POINT ( 'NONE',  ( 1.253923917947829869, -2.729777683071817229, 31.24903638046269094 ) ) ;
#23658 = CARTESIAN_POINT ( 'NONE',  ( -15.00775787915638304, -2.554770724473667265, 30.48948780036025852 ) ) ;
#23659 = EDGE_CURVE ( 'NONE', #26583, #73759, #39619, .T. ) ;
#23660 = CARTESIAN_POINT ( 'NONE',  ( 15.23076923076923173, -13.75783147151868846, 33.36296068462461051 ) ) ;
#23661 = CARTESIAN_POINT ( 'NONE',  ( -1.553300858899125059, -3.750000000000009326, 17.82812500000000000 ) ) ;
#23662 = ORIENTED_EDGE ( 'NONE', *, *, #37339, .F. ) ;
#23663 = LINE ( 'NONE', #51116, #1148 ) ;
#23664 = CARTESIAN_POINT ( 'NONE',  ( -2.307692307692305711, -1.466349020453238561, 30.81389545987213907 ) ) ;
#23665 = FACE_OUTER_BOUND ( 'NONE', #54923, .T. ) ;
#23666 = CARTESIAN_POINT ( 'NONE',  ( 15.90384615384615330, -7.500000000000001776, 35.00000000000000000 ) ) ;
#23667 = CARTESIAN_POINT ( 'NONE',  ( 4.023698184114459231, -3.625366637846544560, 33.29286588640298561 ) ) ;
#23668 = CARTESIAN_POINT ( 'NONE',  ( 9.692307692307572609, -11.48612834414049644, 32.76840700105863391 ) ) ;
#23669 = EDGE_CURVE ( 'NONE', #39542, #69896, #81931, .T. ) ;
#23670 = VECTOR ( 'NONE', #46771, 999.9999999999998863 ) ;
#23671 = ORIENTED_EDGE ( 'NONE', *, *, #50931, .T. ) ;
#23672 = CYLINDRICAL_SURFACE ( 'NONE', #31435, 0.2499999999999998890 ) ;
#23673 = ORIENTED_EDGE ( 'NONE', *, *, #39597, .F. ) ;
#23674 = CIRCLE ( 'NONE', #40858, 0.2500000000000002220 ) ;
#23675 = ORIENTED_EDGE ( 'NONE', *, *, #43087, .F. ) ;
#23676 = CARTESIAN_POINT ( 'NONE',  ( 27.00000000000000000, -16.99999999999999645, 22.25000000000000355 ) ) ;
#23677 = AXIS2_PLACEMENT_3D ( 'NONE', #22642, #56871, #44223 ) ;
#23678 = CARTESIAN_POINT ( 'NONE',  ( -6.673131513698878692, -5.766571408460171355, 34.70601412856602508 ) ) ;
#23679 = CARTESIAN_POINT ( 'NONE',  ( 6.792386319966615460, -2.845849958028613624, 32.17971566917920967 ) ) ;
#23680 = CARTESIAN_POINT ( 'NONE',  ( -13.16183584334697265, -9.332535724633409302, 34.40230450496446934 ) ) ;
#23681 = CARTESIAN_POINT ( 'NONE',  ( 10.86533002476265963, -10.18230066228895758, 34.26354781536631577 ) ) ;
#23682 = ORIENTED_EDGE ( 'NONE', *, *, #31899, .T. ) ;
#23683 = DIRECTION ( 'NONE',  ( 1.000000000000000000, -1.799314243699348838E-16, 0.000000000000000000 ) ) ;
#23684 = ORIENTED_EDGE ( 'NONE', *, *, #33807, .F. ) ;
#23685 = ORIENTED_EDGE ( 'NONE', *, *, #66802, .F. ) ;
#23686 = CARTESIAN_POINT ( 'NONE',  ( -4.023055712879203938, -11.93129842949671726, 32.56571108434900452 ) ) ;
#23687 = CARTESIAN_POINT ( 'NONE',  ( 3.230769230769231726, -8.810774026931790459, 35.74407628777942847 ) ) ;
#23688 = CARTESIAN_POINT ( 'NONE',  ( -16.15384615384627409, -4.481592998941358097, 33.73612834414048933 ) ) ;
#23689 = CYLINDRICAL_SURFACE ( 'NONE', #54266, 0.5000000000000004441 ) ;
#23690 = CARTESIAN_POINT ( 'NONE',  ( -4.219116599806928214, -8.613356846314824011, 34.62446782046655613 ) ) ;
#23691 = CARTESIAN_POINT ( 'NONE',  ( -16.15384615384615330, -2.721908614388771852, 31.22303859784724978 ) ) ;
#23692 = ORIENTED_EDGE ( 'NONE', *, *, #71060, .F. ) ;
#23693 = ORIENTED_EDGE ( 'NONE', *, *, #81873, .F. ) ;
#23694 = CARTESIAN_POINT ( 'NONE',  ( -1.929879867024197893E-14, -3.750000000000000000, 19.15625000000000000 ) ) ;
#23695 = EDGE_LOOP ( 'NONE', ( #46066, #67480, #5390, #31376, #48255, #32943, #76519, #30634, #51723, #50102, #25768, #75509, #30461, #82905, #47258, #66350, #9493, #72104, #59483, #32147, #44495, #26277, #53719, #15535, #62679, #48289, #11606, #74479, #44768, #60847, #15613, #76579, #29876, #71568, #53358, #84314, #46983, #68454, #68968, #22259, #28892, #39463, #15334, #18548, #33675, #4124, #25022, #35002, #5412, #56466, #59032, #43872, #52587, #46270, #54020, #64034, #42749, #87764, #79845, #77123, #33806, #2340, #84120, #36529, #8976, #87857, #88234, #1548, #32342, #33169, #68351, #40906, #1417, #56705, #424, #30384, #78780, #63942, #21260, #38792, #65097, #64771, #15055, #21480, #74928, #42891, #39611, #6832, #46098, #2142, #5293, #62839, #32499, #36426, #74583, #38107, #39791, #48850, #49229, #51288, #79843, #16042, #11980, #84096, #78583, #63777, #41885, #15229, #68225, #56526, #46583, #84508, #52257, #44160, #54273, #53151, #4847, #73176, #19998, #18879, #78834, #60733, #18203, #60679, #60851, #16774, #37516, #2247 ) ) ;
#23697 = ORIENTED_EDGE ( 'NONE', *, *, #87144, .T. ) ;
#23696 = CARTESIAN_POINT ( 'NONE',  ( -5.776988648387152203, -3.105924265160262543, 32.13625925475356127 ) ) ;
#23698 = DIRECTION ( 'NONE',  ( 1.000000000000000000, 0.000000000000000000, 0.000000000000000000 ) ) ;
#23699 = DIRECTION ( 'NONE',  ( -0.000000000000000000, 0.9396926207859092051, -0.3420201433256662704 ) ) ;
#23700 = CARTESIAN_POINT ( 'NONE',  ( -4.153846153846273204, -10.90142922262034020, 33.41473453929536674 ) ) ;
#23701 = EDGE_LOOP ( 'NONE', ( #61050, #37903 ) ) ;
#23702 = CARTESIAN_POINT ( 'NONE',  ( -13.38461538461538325, -12.10708131394839349, 31.69288490824020244 ) ) ;
#23703 = ORIENTED_EDGE ( 'NONE', *, *, #45447, .F. ) ;
#23704 = CARTESIAN_POINT ( 'NONE',  ( 2.530703659305159725, -9.086983370893047862, 34.49168942202179267 ) ) ;
#23705 = CARTESIAN_POINT ( 'NONE',  ( 10.86533013373275658, -9.272278438253398036, 34.42582936511637115 ) ) ;
#23706 = CARTESIAN_POINT ( 'NONE',  ( -15.16470189741915675, -2.833524468853757305, 32.15551576947925838 ) ) ;
#23708 = LINE ( 'NONE', #36794, #68495 ) ;
#23707 = CARTESIAN_POINT ( 'NONE',  ( -6.792551221313360088, -12.45806712695776319, 30.39783852428763922 ) ) ;
#23709 = CARTESIAN_POINT ( 'NONE',  ( -1.254089946381740095, -8.630441415882550871, 34.87705825610312615 ) ) ;
#23710 = CARTESIAN_POINT ( 'NONE',  ( -10.61538461538461320, -10.51840700105979565, 33.73612834413961536 ) ) ;
#23711 = ORIENTED_EDGE ( 'NONE', *, *, #72858, .F. ) ;
#23712 = FACE_OUTER_BOUND ( 'NONE', #8861, .T. ) ;
#23713 = CARTESIAN_POINT ( 'NONE',  ( -4.153846153846152411, -12.37446782046654192, 30.86335684631486131 ) ) ;
#23714 = B_SPLINE_CURVE_WITH_KNOTS ( 'NONE', 3,
 ( #1518, #62753, #55563, #83051, #29002, #1071, #28549, #56009, #21784, #10489 ),
 .UNSPECIFIED., .F., .F.,
 ( 4, 2, 2, 2, 4 ),
 ( 0.000000000000000000, 0.0001954339857564096699, 0.0003908679715128193398, 0.0005863019572692289554, 0.0007817359430256386795 ),
 .UNSPECIFIED. ) ;
#23715 = ORIENTED_EDGE ( 'NONE', *, *, #18813, .F. ) ;
#23716 = DIRECTION ( 'NONE',  ( -0.000000000000000000, -0.5000000000000009992, -0.8660254037844380415 ) ) ;
#23717 = CARTESIAN_POINT ( 'NONE',  ( 15.36156103859402222, -4.118422570099828484, 33.43335022499816489 ) ) ;
#23718 = CARTESIAN_POINT ( 'NONE',  ( 15.93036122928182330, -6.716662450894490988, 34.94144148231605840 ) ) ;
#23719 = DIRECTION ( 'NONE',  ( -0.000000000000000000, 0.3420201433256694346, -0.9396926207859080948 ) ) ;
#23720 = CARTESIAN_POINT ( 'NONE',  ( 17.77651505627605033, -5.912607949931405038, 34.49155766932282319 ) ) ;
#23721 = CARTESIAN_POINT ( 'NONE',  ( -7.715315515667081847, -7.277220318596959281, 34.99547417642776992 ) ) ;
#23722 = AXIS2_PLACEMENT_3D ( 'NONE', #54874, #49879, #28281 ) ;
#23723 = FACE_BOUND ( 'NONE', #31987, .T. ) ;
#23725 = CARTESIAN_POINT ( 'NONE',  ( 17.86985203026830504, -11.04286588640298916, 33.62463336215343901 ) ) ;
#23724 = CARTESIAN_POINT ( 'NONE',  ( -19.50000000000000000, -3.499999999999999556, 29.75000000000000355 ) ) ;
#23726 = CARTESIAN_POINT ( 'NONE',  ( -6.700065571464074665, -10.61302985866383963, 33.66295027996417843 ) ) ;
#23728 = CARTESIAN_POINT ( 'NONE',  ( 9.692307692307695177, -4.098570777380720287, 33.41473453929634729 ) ) ;
#23727 = CARTESIAN_POINT ( 'NONE',  ( 3.100077764101675015, -4.118384482072085184, 33.43331474514187107 ) ) ;
#23729 = DIRECTION ( 'NONE',  ( 0.000000000000000000, 0.6427876096865368094, 0.7660444431189802339 ) ) ;
#23730 = DIRECTION ( 'NONE',  ( -0.000000000000000000, -0.7660444431189791237, -0.6427876096865379196 ) ) ;
#23731 = CARTESIAN_POINT ( 'NONE',  ( 1.492201783934554493, -3.724691934501233703, 22.73250670625849068 ) ) ;
#23732 = ORIENTED_EDGE ( 'NONE', *, *, #80, .F. ) ;
#23733 = VECTOR ( 'NONE', #34844, 1000.000000000000000 ) ;
#23734 = EDGE_CURVE ( 'NONE', #18984, #11766, #2713, .T. ) ;
#23735 = DIRECTION ( 'NONE',  ( 0.000000000000000000, -1.000000000000000000, 0.000000000000000000 ) ) ;
#23736 = CARTESIAN_POINT ( 'NONE',  ( -4.153846153846152411, -3.050289026998446396, 32.03036669348365706 ) ) ;
#23737 = DIRECTION ( 'NONE',  ( -0.000000000000000000, -0.5000000000000009992, -0.8660254037844380415 ) ) ;
#23738 = CARTESIAN_POINT ( 'NONE',  ( -9.942284423250047354, -10.66389620160130036, 33.62221079203477103 ) ) ;
#23739 = ADVANCED_FACE ( 'NONE', ( #36392 ), #69293, .F. ) ;
#23740 = CARTESIAN_POINT ( 'NONE',  ( 7.716006636715625255, -5.195881422630167279, 34.18770438780618548 ) ) ;
#23741 = CARTESIAN_POINT ( 'NONE',  ( -16.94639763868943660, -8.630441415882549094, 34.87705825610312615 ) ) ;
#23742 = CARTESIAN_POINT ( 'NONE',  ( -1.614399933863656544, -3.775308065498769405, 21.32625670625849423 ) ) ;
#23743 = FACE_OUTER_BOUND ( 'NONE', #73036, .T. ) ;
#23744 = CARTESIAN_POINT ( 'NONE',  ( 0.6845498131513103601, -3.587049720035815348, 32.86302985866382897 ) ) ;
#23745 = LINE ( 'NONE', #58414, #48962 ) ;
#23746 = CARTESIAN_POINT ( 'NONE',  ( -6.923076923076922462, -2.517432740324522911, 35.29906147534542527 ) ) ;
#23747 = CARTESIAN_POINT ( 'NONE',  ( -17.01085574357299990, -4.661471528628508665, 34.16647553114624003 ) ) ;
#23748 = CARTESIAN_POINT ( 'NONE',  ( 10.86538461538461853, -2.499999999999999556, 29.81604066197449754 ) ) ;
#23749 = DIRECTION ( 'NONE',  ( -1.734723475976813504E-16, 1.000000000000000000, 0.000000000000000000 ) ) ;
#23750 = EDGE_CURVE ( 'NONE', #2835, #4529, #25386, .T. ) ;
#23751 = PLANE ( 'NONE',  #65780 ) ;
#23752 = ORIENTED_EDGE ( 'NONE', *, *, #66981, .F. ) ;
#23753 = CARTESIAN_POINT ( 'NONE',  ( 3.296836564119307589, -12.34228464037088813, 31.77849191805839268 ) ) ;
#23754 = CARTESIAN_POINT ( 'NONE',  ( -5.869474561766359066, -2.647132371071621471, 31.75357179365173010 ) ) ;
#23755 = CARTESIAN_POINT ( 'NONE',  ( -0.06109907496450878162, -11.25000000000000000, 16.28311829374151287 ) ) ;
#23756 = CARTESIAN_POINT ( 'NONE',  ( -2.557715531913763218, -4.931416488878823223, 34.32920672191015399 ) ) ;
#23757 = FACE_OUTER_BOUND ( 'NONE', #56804, .T. ) ;
#23758 = EDGE_LOOP ( 'NONE', ( #36916, #32956 ) ) ;
#23759 = CARTESIAN_POINT ( 'NONE',  ( -6.857821783564084228, -10.33852847137154107, 34.16647553114620450 ) ) ;
#23760 = CARTESIAN_POINT ( 'NONE',  ( -11.53846153846153655, -11.69971097300155272, 32.46337939537588113 ) ) ;
#23762 = VERTEX_POINT ( 'NONE', #54890 ) ;
#23761 = DIRECTION ( 'NONE',  ( -1.000000000000000000, -0.000000000000000000, -0.000000000000000000 ) ) ;
#23763 = CARTESIAN_POINT ( 'NONE',  ( 6.792929713638703682, -3.285722584762969856, 32.44110544564090759 ) ) ;
#23764 = LINE ( 'NONE', #36846, #29690 ) ;
#23765 = CARTESIAN_POINT ( 'NONE',  ( 17.07692307692307665, -6.189225973068211317, 35.74407628777942847 ) ) ;
#23766 = CIRCLE ( 'NONE', #65441, 0.2500000000000002220 ) ;
#23767 = CYLINDRICAL_SURFACE ( 'NONE', #25612, 0.2500000000000009437 ) ;
#23768 = VERTEX_POINT ( 'NONE', #22427 ) ;
#23769 = CARTESIAN_POINT ( 'NONE',  ( -11.66915300512910214, -4.118384482072085184, 33.43331474514187107 ) ) ;
#23770 = ADVANCED_FACE ( 'NONE', ( #76493 ), #7592, .T. ) ;
#23771 = DIRECTION ( 'NONE',  ( -0.000000000000000000, 0.9396926207859093161, -0.3420201433256663259 ) ) ;
#23772 = ORIENTED_EDGE ( 'NONE', *, *, #26671, .T. ) ;
#23773 = EDGE_CURVE ( 'NONE', #67027, #15943, #67678, .T. ) ;
#23774 = EDGE_LOOP ( 'NONE', ( #38578, #62793, #29612, #65634 ) ) ;
#23775 = ADVANCED_FACE ( 'NONE', ( #82371 ), #14342, .F. ) ;
#23776 = VERTEX_POINT ( 'NONE', #48120 ) ;
#23777 = EDGE_CURVE ( 'NONE', #11427, #57709, #4979, .T. ) ;
#23778 = CARTESIAN_POINT ( 'NONE',  ( -18.00000000000012079, -3.835265460704626150, 33.15142922262032954 ) ) ;
#23779 = CARTESIAN_POINT ( 'NONE',  ( -8.546219417617921366, -3.105924265160262543, 32.13625925475356127 ) ) ;
#23780 = CARTESIAN_POINT ( 'NONE',  ( -18.00000000000012079, -3.300289026999231545, 32.46337939537709616 ) ) ;
#23781 = B_SPLINE_CURVE_WITH_KNOTS ( 'NONE', 3,
 ( #51588, #39458, #72768, #11080, #3863, #32247, #44395, #71884, #37655, #23691 ),
 .UNSPECIFIED., .F., .F.,
 ( 4, 2, 2, 2, 4 ),
 ( 0.0007817359430256347764, 0.0009771253907250036959, 0.001172514838424372832, 0.001367904286123741969, 0.001563293733823103949 ),
 .UNSPECIFIED. ) ;
#23782 = DIRECTION ( 'NONE',  ( -0.000000000000000000, 0.6427876096865404731, -0.7660444431189771253 ) ) ;
#23783 = CIRCLE ( 'NONE', #30985, 0.2500000000000002220 ) ;
#23784 = EDGE_LOOP ( 'NONE', ( #64007, #29276 ) ) ;
#23785 = ORIENTED_EDGE ( 'NONE', *, *, #62600, .T. ) ;
#23787 = ORIENTED_EDGE ( 'NONE', *, *, #58690, .F. ) ;
#23786 = LINE ( 'NONE', #17495, #40120 ) ;
#23788 = CARTESIAN_POINT ( 'NONE',  ( -15.23076923076922995, -8.810774026931790459, 35.74407628777942847 ) ) ;
#23789 = DIRECTION ( 'NONE',  ( 0.000000000000000000, 0.000000000000000000, 1.000000000000000000 ) ) ;
#23790 = DIRECTION ( 'NONE',  ( -0.000000000000000000, 0.5000000000000011102, -0.8660254037844381525 ) ) ;
#23791 = VECTOR ( 'NONE', #37776, 1000.000000000000114 ) ;
#23792 = VERTEX_POINT ( 'NONE', #15239 ) ;
#23793 = ORIENTED_EDGE ( 'NONE', *, *, #4537, .F. ) ;
#23794 = ORIENTED_EDGE ( 'NONE', *, *, #14217, .F. ) ;
#23796 = ORIENTED_EDGE ( 'NONE', *, *, #9302, .T. ) ;
#23795 = CARTESIAN_POINT ( 'NONE',  ( -2.939152317953646711E-15, 7.500000000000000000, 14.00000000000000178 ) ) ;
#23797 = CARTESIAN_POINT ( 'NONE',  ( -5.869208192175211281, -8.147973898785416225, 34.70805048591653730 ) ) ;
#23798 = EDGE_CURVE ( 'NONE', #87392, #74998, #503, .T. ) ;
#23799 = DIRECTION ( 'NONE',  ( 0.000000000000000000, 0.9396926207859126468, 0.3420201433256571111 ) ) ;
#23800 = ORIENTED_EDGE ( 'NONE', *, *, #7645, .T. ) ;
#23801 = DIRECTION ( 'NONE',  ( 0.000000000000000000, 0.1736481776669275834, 0.9848077530122086864 ) ) ;
#23802 = CARTESIAN_POINT ( 'NONE',  ( 16.15384615384603251, -4.320704448113951379, 33.92786785259630022 ) ) ;
#23803 = CARTESIAN_POINT ( 'NONE',  ( -2.084912766423897779, -11.41317474335729187, 32.86274602512330034 ) ) ;
#23804 = FACE_BOUND ( 'NONE', #58509, .T. ) ;
#23805 = DIRECTION ( 'NONE',  ( 1.000000000000000000, 0.000000000000000000, 0.000000000000000000 ) ) ;
#23806 = CARTESIAN_POINT ( 'NONE',  ( 4.023698184114458343, -2.373036134822904319, 30.88089517874952250 ) ) ;
#23807 = CARTESIAN_POINT ( 'NONE',  ( 13.16113046005105325, -12.69144148231606017, 30.53333754910549303 ) ) ;
#23809 = CARTESIAN_POINT ( 'NONE',  ( -15.93106648486808652, -3.020022701398814569, 32.48759521482552515 ) ) ;
#23808 = CARTESIAN_POINT ( 'NONE',  ( -2.544871794871794268, -7.500000000000000000, 29.75000000000000355 ) ) ;
#23810 = CARTESIAN_POINT ( 'NONE',  ( -8.069080063669989755, -3.105860786376062332, 32.13614157043599562 ) ) ;
#23811 = CARTESIAN_POINT ( 'NONE',  ( 5.207448778686637247, -2.619367082507848554, 30.83698974864644171 ) ) ;
#23812 = ORIENTED_EDGE ( 'NONE', *, *, #66122, .F. ) ;
#23813 = CARTESIAN_POINT ( 'NONE',  ( -15.90390074446811042, -3.520799739797214389, 33.17531984108286025 ) ) ;
#23814 = VERTEX_POINT ( 'NONE', #82815 ) ;
#23815 = ORIENTED_EDGE ( 'NONE', *, *, #78285, .T. ) ;
#23816 = EDGE_CURVE ( 'NONE', #76951, #19931, #24527, .T. ) ;
#23818 = CARTESIAN_POINT ( 'NONE',  ( 1.607628228708781748, -5.582272713120728369, 34.63742843783360570 ) ) ;
#23817 = CARTESIAN_POINT ( 'NONE',  ( 5.869308533332445066, -6.413092428213692742, 34.63065189839063152 ) ) ;
#23819 = FACE_OUTER_BOUND ( 'NONE', #49300, .T. ) ;
#23820 = CARTESIAN_POINT ( 'NONE',  ( 14.55769230769232614, -2.249999999999997780, 29.81603969181030322 ) ) ;
#23821 = CARTESIAN_POINT ( 'NONE',  ( 1.384615384615386802, -11.69971097300155272, 32.46337939537588113 ) ) ;
#23822 = ORIENTED_EDGE ( 'NONE', *, *, #37270, .F. ) ;
#23823 = CARTESIAN_POINT ( 'NONE',  ( 18.22277966897806678, -4.226511098958373402, 33.85474049983370293 ) ) ;
#23824 = CARTESIAN_POINT ( 'NONE',  ( 15.00784227186238162, -10.77366814457252175, 33.85459836347579454 ) ) ;
#23825 = CYLINDRICAL_SURFACE ( 'NONE', #17166, 0.2499999999999995559 ) ;
#23826 = CARTESIAN_POINT ( 'NONE',  ( 10.61538461538449596, -4.481592998941358097, 33.73612834414048933 ) ) ;
#23827 = CYLINDRICAL_SURFACE ( 'NONE', #39132, 0.2499999999999979738 ) ;
#23828 = CARTESIAN_POINT ( 'NONE',  ( -3.750000000000008438, -5.946699141100917352, 18.92187500000000355 ) ) ;
#23829 = EDGE_LOOP ( 'NONE', ( #44069, #40168 ) ) ;
#23830 = EDGE_LOOP ( 'NONE', ( #76973, #25363, #59895, #40704 ) ) ;
#23831 = EDGE_CURVE ( 'NONE', #5084, #1104, #7989, .T. ) ;
#23832 = CARTESIAN_POINT ( 'NONE',  ( 3.230769230769231726, -8.973038597847269315, 34.52809138561121927 ) ) ;
#23833 = EDGE_LOOP ( 'NONE', ( #31611, #62886 ) ) ;
#23834 = CARTESIAN_POINT ( 'NONE',  ( 1.653273178848927064E-15, -7.500000000000000000, 29.50000000000000355 ) ) ;
#23835 = CARTESIAN_POINT ( 'NONE',  ( 9.942362003946010773, -9.943054286541403997, 34.11300777759954883 ) ) ;
#23836 = CARTESIAN_POINT ( 'NONE',  ( 14.55763782604045353, -2.824170634883621744, 31.52227843825338738 ) ) ;
#23837 = EDGE_CURVE ( 'NONE', #88055, #69004, #49935, .T. ) ;
#23838 = CARTESIAN_POINT ( 'NONE',  ( 5.750000000000002665, -2.249999999999998668, 29.75000000000000355 ) ) ;
#23839 = CARTESIAN_POINT ( 'NONE',  ( 3.749999999999992006, -5.946699141100872943, 16.89062500000000000 ) ) ;
#23840 = B_SPLINE_CURVE_WITH_KNOTS ( 'NONE', 3,
 ( #86307, #86758, #4312, #51138, #85847, #24581, #52046, #23686, #79539, #57922 ),
 .UNSPECIFIED., .F., .F.,
 ( 4, 2, 2, 2, 4 ),
 ( 0.0007817246256747446788, 0.0009771112852218879000, 0.001172497944769031013, 0.001367884604316174126, 0.001563271263863317238 ),
 .UNSPECIFIED. ) ;
#23841 = CARTESIAN_POINT ( 'NONE',  ( 14.08476534878545827, -6.459968553980841577, 34.89616026154728701 ) ) ;
#23842 = ORIENTED_EDGE ( 'NONE', *, *, #35053, .F. ) ;
#23843 = CARTESIAN_POINT ( 'NONE',  ( -4.153846153845837108, -2.255955759149395501, 30.00000000000324363 ) ) ;
#23845 = EDGE_LOOP ( 'NONE', ( #26990, #8491, #56703, #39948 ) ) ;
#23844 = CARTESIAN_POINT ( 'NONE',  ( -2.084912638714240707, -12.69155399931963046, 30.53255429739157734 ) ) ;
#23846 = CARTESIAN_POINT ( 'NONE',  ( -13.63459211555773720, -11.28823185664190376, 33.01397839955799896 ) ) ;
#23847 = DIRECTION ( 'NONE',  ( -0.000000000000000000, 0.1736481776669307198, -0.9848077530122080203 ) ) ;
#23848 = CARTESIAN_POINT ( 'NONE',  ( -8.769230769230768274, -1.129524287112498415, 32.06866353760679544 ) ) ;
#23850 = AXIS2_PLACEMENT_3D ( 'NONE', #68507, #5930, #33405 ) ;
#23849 = CARTESIAN_POINT ( 'NONE',  ( 6.857806922520603976, -3.643525952247789412, 33.31231777344662959 ) ) ;
#23851 = CARTESIAN_POINT ( 'NONE',  ( 10.74591031714817824, -2.882268652242222284, 31.66798894389554064 ) ) ;
#23852 = ADVANCED_FACE ( 'NONE', ( #23743 ), #51645, .F. ) ;
#23853 = CARTESIAN_POINT ( 'NONE',  ( 7.622668921589515811, -3.562934362175799841, 33.22335522853832401 ) ) ;
#23854 = CARTESIAN_POINT ( 'NONE',  ( -7.976845312821407852, -12.38065189839062263, 30.83690757178629482 ) ) ;
#23855 = CARTESIAN_POINT ( 'NONE',  ( -3.749999999999997780, -7.438900925035489387, 20.34561829374151287 ) ) ;
#23856 = VERTEX_POINT ( 'NONE', #2583 ) ;
#23857 = CARTESIAN_POINT ( 'NONE',  ( -16.28453675695646652, -9.084618155246140248, 34.75535874321725771 ) ) ;
#23858 = CARTESIAN_POINT ( 'NONE',  ( 1.319344938654611221, -6.026961402152685388, 34.52809138561120506 ) ) ;
#23859 = CARTESIAN_POINT ( 'NONE',  ( -17.20707104665477516, -5.070767119584671079, 34.40440758774516183 ) ) ;
#23860 = CARTESIAN_POINT ( 'NONE',  ( -1.200186371490524317, -10.22469193450124791, 13.86124329374151820 ) ) ;
#23861 = EDGE_CURVE ( 'NONE', #66822, #28583, #33839, .T. ) ;
#23862 = CARTESIAN_POINT ( 'NONE',  ( -13.45069879557126669, -12.37446782046654192, 30.86335684631486487 ) ) ;
#23863 = CARTESIAN_POINT ( 'NONE',  ( -6.923076923076922462, -1.129524287112498415, 32.06866353760679544 ) ) ;
#23864 = EDGE_LOOP ( 'NONE', ( #86431, #26150 ) ) ;
#23865 = CARTESIAN_POINT ( 'NONE',  ( 1.139087296525997051, -4.749999999999992895, 17.98437500000000000 ) ) ;
#23866 = CARTESIAN_POINT ( 'NONE',  ( -1.608100328339333585, -10.11188796281391333, 34.01382737946119050 ) ) ;
#23867 = EDGE_CURVE ( 'NONE', #12523, #23814, #38133, .T. ) ;
#23868 = AXIS2_PLACEMENT_3D ( 'NONE', #61332, #60903, #54582 ) ;
#23869 = ORIENTED_EDGE ( 'NONE', *, *, #82942, .F. ) ;
#23870 = CARTESIAN_POINT ( 'NONE',  ( -4.153846153846152411, -2.486705287966279876, 31.30864560766543647 ) ) ;
#23871 = ORIENTED_EDGE ( 'NONE', *, *, #42973, .F. ) ;
#23872 = DIRECTION ( 'NONE',  ( -0.000000000000000000, 0.7660444431189791237, -0.6427876096865379196 ) ) ;
#23873 = DIRECTION ( 'NONE',  ( 0.000000000000000000, 0.9848077530122072432, -0.1736481776669354937 ) ) ;
#23874 = EDGE_CURVE ( 'NONE', #67070, #53330, #51030, .T. ) ;
#23875 = CARTESIAN_POINT ( 'NONE',  ( 16.82689985270161870, -6.652501968072647820, 34.93155406624980941 ) ) ;
#23876 = ORIENTED_EDGE ( 'NONE', *, *, #69545, .T. ) ;
#23877 = DIRECTION ( 'NONE',  ( 0.000000000000000000, 0.6427876096865368094, 0.7660444431189802339 ) ) ;
#23878 = ORIENTED_EDGE ( 'NONE', *, *, #58802, .T. ) ;
#23879 = DIRECTION ( 'NONE',  ( 1.000000000000000000, 0.000000000000000000, 0.000000000000000000 ) ) ;
#23880 = B_SPLINE_CURVE_WITH_KNOTS ( 'NONE', 3,
 ( #25140, #71989, #86426, #10298, #32346, #30996, #59813, #24697, #80551, #72431 ),
 .UNSPECIFIED., .F., .F.,
 ( 4, 2, 2, 2, 4 ),
 ( 0.0007817359430256326080, 0.0009771253907249993591, 0.001172514838424366327, 0.001367904286123733078, 0.001563293733823099829 ),
 .UNSPECIFIED. ) ;
#23881 = ORIENTED_EDGE ( 'NONE', *, *, #35660, .F. ) ;
#23882 = DIRECTION ( 'NONE',  ( -1.000000000000000000, -0.000000000000000000, -0.000000000000000000 ) ) ;
#23883 = CARTESIAN_POINT ( 'NONE',  ( 5.011653076366756387, -5.941354392334500467, 34.76329471203369792 ) ) ;
#23884 = EDGE_CURVE ( 'NONE', #62713, #41734, #67191, .T. ) ;
#23885 = B_SPLINE_CURVE_WITH_KNOTS ( 'NONE', 3,
 ( #41477, #28399, #76594, #43249, #55870, #48665, #47, #7250, #15339, #27518 ),
 .UNSPECIFIED., .F., .F.,
 ( 4, 2, 2, 2, 4 ),
 ( 0.0007817246256747464135, 0.0009771112852218900684, 0.001172497944769033615, 0.001367884604316177161, 0.001563271263863320925 ),
 .UNSPECIFIED. ) ;
#23886 = AXIS2_PLACEMENT_3D ( 'NONE', #62851, #47581, #13797 ) ;
#23887 = ORIENTED_EDGE ( 'NONE', *, *, #56400, .F. ) ;
#23888 = ADVANCED_FACE ( 'NONE', ( #16117 ), #32297, .F. ) ;
#23889 = CARTESIAN_POINT ( 'NONE',  ( 8.639082799499073317, -5.070767119584671079, 34.40440758774516183 ) ) ;
#23890 = CARTESIAN_POINT ( 'NONE',  ( -14.55771554498526932, -10.76384336483936011, 33.53834819971076087 ) ) ;
#23891 = CARTESIAN_POINT ( 'NONE',  ( -11.53846153846165912, -2.892918686052166066, 31.69288490824153470 ) ) ;
#23892 = VECTOR ( 'NONE', #53806, 1000.000000000000000 ) ;
#23893 = FACE_OUTER_BOUND ( 'NONE', #86429, .T. ) ;
#23894 = DIRECTION ( 'NONE',  ( -0.7071067811865510144, 0.7071067811865440200, 0.000000000000000000 ) ) ;
#23895 = ORIENTED_EDGE ( 'NONE', *, *, #34041, .T. ) ;
#23896 = EDGE_LOOP ( 'NONE', ( #31891, #88365, #42732, #62617 ) ) ;
#23897 = ORIENTED_EDGE ( 'NONE', *, *, #85198, .F. ) ;
#23899 = ORIENTED_EDGE ( 'NONE', *, *, #3589, .T. ) ;
#23898 = CARTESIAN_POINT ( 'NONE',  ( 3.230769230769231726, -5.471508081941601098, 34.59228464037088457 ) ) ;
#23900 =( REPRESENTATION_RELATIONSHIP ('NONE','NONE', #51743, #14956 ) REPRESENTATION_RELATIONSHIP_WITH_TRANSFORMATION ( #8134 )SHAPE_REPRESENTATION_RELATIONSHIP( ) );
#23901 = ADVANCED_FACE ( 'NONE', ( #47125 ), #81822, .F. ) ;
#23902 = CARTESIAN_POINT ( 'NONE',  ( 10.55011416942384095, -5.219633306516282545, 34.19971097300152962 ) ) ;
#23903 = CARTESIAN_POINT ( 'NONE',  ( 5.076923076923075762, -10.89733346790207413, 36.13435417666054406 ) ) ;
#23904 = ORIENTED_EDGE ( 'NONE', *, *, #35714, .F. ) ;
#23905 = ORIENTED_EDGE ( 'NONE', *, *, #26553, .T. ) ;
#23906 = VERTEX_POINT ( 'NONE', #67412 ) ;
#23907 = CARTESIAN_POINT ( 'NONE',  ( 0.3954560821783248969, -8.164416787775445883, 34.95778746994557906 ) ) ;
#23908 = EDGE_LOOP ( 'NONE', ( #27712, #34, #69612, #57039 ) ) ;
#23909 = CARTESIAN_POINT ( 'NONE',  ( -10.39260507411620260, -9.332535724633409302, 34.40230450496446934 ) ) ;
#23910 = EDGE_CURVE ( 'NONE', #18826, #84614, #40396, .T. ) ;
#23911 = VECTOR ( 'NONE', #56452, 999.9999999999998863 ) ;
#23912 = B_SPLINE_CURVE_WITH_KNOTS ( 'NONE', 3,
 ( #45864, #87780, #11200, #65244, #85973, #78764, #17064, #44519, #3543, #31468 ),
 .UNSPECIFIED., .F., .F.,
 ( 4, 2, 2, 2, 4 ),
 ( 0.000000000000000000, 0.0001954339857564074473, 0.0003908679715128148945, 0.0005863019572692223418, 0.0007817359430256297891 ),
 .UNSPECIFIED. ) ;
#23913 = CARTESIAN_POINT ( 'NONE',  ( 3.903822929624696236, -12.68155406624981119, 30.59749803192733708 ) ) ;
#23914 = CARTESIAN_POINT ( 'NONE',  ( 12.39545505058257824, -2.538708090699994813, 30.37095296980875148 ) ) ;
#23915 = EDGE_CURVE ( 'NONE', #35763, #33353, #5933, .T. ) ;
#23916 = FACE_BOUND ( 'NONE', #85719, .T. ) ;
#23917 = ORIENTED_EDGE ( 'NONE', *, *, #33446, .F. ) ;
#23918 = CARTESIAN_POINT ( 'NONE',  ( 13.63466969625370240, -9.148310452688876993, 34.47095581063188519 ) ) ;
#23919 = EDGE_CURVE ( 'NONE', #17034, #78771, #60614, .T. ) ;
#23920 = CARTESIAN_POINT ( 'NONE',  ( 4.853438152358745761, -3.562934362175799841, 33.22335522853832401 ) ) ;
#23921 = CARTESIAN_POINT ( 'NONE',  ( 8.834486340506794377, -3.300289026998473041, 32.46337939537591666 ) ) ;
#23922 = CARTESIAN_POINT ( 'NONE',  ( 17.14217864819909920, -9.442884908240273489, 34.35708131394835618 ) ) ;
#23923 = ORIENTED_EDGE ( 'NONE', *, *, #22509, .T. ) ;
#23924 = VECTOR ( 'NONE', #87504, 1000.000000000000000 ) ;
#23925 = CARTESIAN_POINT ( 'NONE',  ( -17.32689980786543060, -12.41269422305637171, 30.68257228309993323 ) ) ;
#23926 = VERTEX_POINT ( 'NONE', #26870 ) ;
#23927 = ORIENTED_EDGE ( 'NONE', *, *, #13032, .T. ) ;
#23928 = EDGE_CURVE ( 'NONE', #13509, #83846, #13410, .T. ) ;
#23930 = CARTESIAN_POINT ( 'NONE',  ( 5.869852790561781219, -3.285722584762969856, 32.44110544564090759 ) ) ;
#23929 = CARTESIAN_POINT ( 'NONE',  ( -16.15384615384615330, -3.886160181151819604, 36.00935417666054406 ) ) ;
#23931 = LINE ( 'NONE', #50947, #78755 ) ;
#23932 = CARTESIAN_POINT ( 'NONE',  ( -13.45069776397551564, -2.833524468853757305, 32.15551576947924417 ) ) ;
#23933 = CARTESIAN_POINT ( 'NONE',  ( -18.22348492456433178, -5.827078755546625466, 34.72654668319379567 ) ) ;
#23934 = CARTESIAN_POINT ( 'NONE',  ( 6.923076923076924238, -2.517432740324522911, 35.29906147534542527 ) ) ;
#23935 = ORIENTED_EDGE ( 'NONE', *, *, #75572, .F. ) ;
#23936 = CARTESIAN_POINT ( 'NONE',  ( 6.856994543716787405, -2.486705287966279432, 31.30864560766542937 ) ) ;
#23937 = CARTESIAN_POINT ( 'NONE',  ( 22.00000000000001066, -9.999999999999957367, 0.000000000000000000 ) ) ;
#23938 = CARTESIAN_POINT ( 'NONE',  ( 10.03846153846153832, -11.50000000000000000, 29.75000000000000355 ) ) ;
#23939 = CARTESIAN_POINT ( 'NONE',  ( -13.60754234352223335, -12.64616026154729411, 30.79003144601914244 ) ) ;
#23940 = EDGE_LOOP ( 'NONE', ( #63774, #14130, #2000, #68872 ) ) ;
#23941 = ORIENTED_EDGE ( 'NONE', *, *, #50007, .T. ) ;
#23942 = FACE_BOUND ( 'NONE', #21937, .T. ) ;
#23943 = ORIENTED_EDGE ( 'NONE', *, *, #42540, .T. ) ;
#23944 = CARTESIAN_POINT ( 'NONE',  ( 14.30769230769231015, -5.180354513474913603, 36.12317359536750416 ) ) ;
#23945 = CARTESIAN_POINT ( 'NONE',  ( -7.623374304885435215, -5.114059244376869984, 34.14424750095245287 ) ) ;
#23946 = ORIENTED_EDGE ( 'NONE', *, *, #13960, .F. ) ;
#23947 = CARTESIAN_POINT ( 'NONE',  ( 16.40384615384615330, -2.249999999999998668, 29.75000000000000355 ) ) ;
#23948 = CARTESIAN_POINT ( 'NONE',  ( 17.99999999999987566, -3.643525952248796163, 33.31231777344771672 ) ) ;
#23949 = CARTESIAN_POINT ( 'NONE',  ( 4.853996859406929154, -2.758268499246657957, 31.33685645148948140 ) ) ;
#23950 = EDGE_CURVE ( 'NONE', #73783, #60358, #87704, .T. ) ;
#23951 = CARTESIAN_POINT ( 'NONE',  ( -17.07692307692307665, -3.322132147404559976, 32.92929555188717927 ) ) ;
#23952 = EDGE_LOOP ( 'NONE', ( #11889, #71790 ) ) ;
#23953 = VECTOR ( 'NONE', #23559, 1000.000000000000000 ) ;
#23954 = ADVANCED_FACE ( 'NONE', ( #81381 ), #18785, .F. ) ;
#23955 = CARTESIAN_POINT ( 'NONE',  ( -4.023320452082589149, -6.852161475712352789, 34.70806712695775786 ) ) ;
#23956 = VERTEX_POINT ( 'NONE', #46692 ) ;
#23957 = B_SPLINE_CURVE_WITH_KNOTS ( 'NONE', 3,
 ( #53041, #74222, #31905, #10739, #73787, #53940, #80545, #12086, #45398, #4418 ),
 .UNSPECIFIED., .F., .F.,
 ( 4, 2, 2, 2, 4 ),
 ( 0.000000000000000000, 0.0001954339857564080707, 0.0003908679715128161414, 0.0005863019572692241849, 0.0007817359430256322827 ),
 .UNSPECIFIED. ) ;
#23959 = ORIENTED_EDGE ( 'NONE', *, *, #71750, .T. ) ;
#23958 = CARTESIAN_POINT ( 'NONE',  ( 13.44987095589141468, -12.27809138561124591, 31.22303859784720359 ) ) ;
#23960 = CARTESIAN_POINT ( 'NONE',  ( 15.36129493253279499, -8.586989748646452369, 34.63063291749215011 ) ) ;
#23961 = LINE ( 'NONE', #31164, #28133 ) ;
#23962 = DIRECTION ( 'NONE',  ( -0.000000000000000000, -0.9396926207859092051, -0.3420201433256662704 ) ) ;
#23963 = CARTESIAN_POINT ( 'NONE',  ( 15.23076923076923173, -12.37446782046654192, 30.86335684631486131 ) ) ;
#23964 = CARTESIAN_POINT ( 'NONE',  ( -14.53061926659915315, -8.282780595021769443, 34.94152052738834158 ) ) ;
#23965 = AXIS2_PLACEMENT_3D ( 'NONE', #77260, #36720, #43479 ) ;
#23966 = CARTESIAN_POINT ( 'NONE',  ( -9.758390071667825794, -11.91647553114624181, 32.58852847137148245 ) ) ;
#23967 = CARTESIAN_POINT ( 'NONE',  ( -2.775308065498752086, -8.577988221561495763, 14.01749329374151642 ) ) ;
#23968 = VERTEX_POINT ( 'NONE', #45800 ) ;
#23969 = DIRECTION ( 'NONE',  ( -0.000000000000000000, -0.1736481776669307198, -0.9848077530122080203 ) ) ;
#23970 = DIRECTION ( 'NONE',  ( 1.000000000000000000, 0.000000000000000000, 0.000000000000000000 ) ) ;
#23971 = DIRECTION ( 'NONE',  ( 0.000000000000000000, 0.9396926207859126468, 0.3420201433256571111 ) ) ;
#23972 = ORIENTED_EDGE ( 'NONE', *, *, #60809, .F. ) ;
#23973 = ORIENTED_EDGE ( 'NONE', *, *, #66703, .F. ) ;
#23974 = CYLINDRICAL_SURFACE ( 'NONE', #29725, 0.2500000000000009437 ) ;
#23975 = CARTESIAN_POINT ( 'NONE',  ( 12.68431813051652313, -4.226511098958373402, 33.85474049983370293 ) ) ;
#23976 = DIRECTION ( 'NONE',  ( -0.000000000000000000, 0.6427876096865404731, -0.7660444431189771253 ) ) ;
#23977 = CARTESIAN_POINT ( 'NONE',  ( 9.627037246346917598, -12.46129190929999986, 30.37095296980880832 ) ) ;
#23978 = CARTESIAN_POINT ( 'NONE',  ( 13.13463864056679498, -2.920706130388546651, 32.31842814019191223 ) ) ;
#23979 = CARTESIAN_POINT ( 'NONE',  ( -8.769230769230768274, -11.69971097300155272, 32.46337939537588113 ) ) ;
#23980 = CARTESIAN_POINT ( 'NONE',  ( -7.053224132515143907, -11.93770438780619259, 32.05411857736982029 ) ) ;
#23981 = VERTEX_POINT ( 'NONE', #87257 ) ;
#23982 = AXIS2_PLACEMENT_3D ( 'NONE', #21681, #78388, #16691 ) ;
#23983 = CARTESIAN_POINT ( 'NONE',  ( 5.999999999999880096, -10.90142922262034020, 33.41473453929536674 ) ) ;
#23984 = CARTESIAN_POINT ( 'NONE',  ( -17.14224708972738753, -7.749976730030849303, 34.74374725381503737 ) ) ;
#23985 = EDGE_CURVE ( 'NONE', #67360, #30707, #20908, .T. ) ;
#23986 = EDGE_CURVE ( 'NONE', #34679, #10626, #40830, .T. ) ;
#23987 = DIRECTION ( 'NONE',  ( -0.000000000000000000, 0.8660254037844397068, -0.4999999999999978906 ) ) ;
#23988 = CARTESIAN_POINT ( 'NONE',  ( -4.153846153846274980, -4.320704448113951379, 33.92786785259630022 ) ) ;
#23989 = ORIENTED_EDGE ( 'NONE', *, *, #85408, .T. ) ;
#23990 = DIRECTION ( 'NONE',  ( 0.000000000000000000, 0.000000000000000000, 1.000000000000000000 ) ) ;
#23991 = VECTOR ( 'NONE', #5303, 1000.000000000000227 ) ;
#23992 = EDGE_CURVE ( 'NONE', #19611, #15474, #14528, .T. ) ;
#23993 = ORIENTED_EDGE ( 'NONE', *, *, #58698, .F. ) ;
#23994 = CARTESIAN_POINT ( 'NONE',  ( 15.16549878480845592, -11.48612834413959582, 32.76840700105983473 ) ) ;
#23995 = FILL_AREA_STYLE ('',( #85716 ) ) ;
#23996 = FACE_OUTER_BOUND ( 'NONE', #17616, .T. ) ;
#23997 = FACE_OUTER_BOUND ( 'NONE', #55774, .T. ) ;
#23998 = ORIENTED_EDGE ( 'NONE', *, *, #194, .F. ) ;
#23999 = EDGE_CURVE ( 'NONE', #17208, #15714, #62845, .T. ) ;
#24000 = AXIS2_PLACEMENT_3D ( 'NONE', #33328, #55355, #40535 ) ;
#24001 = CARTESIAN_POINT ( 'NONE',  ( 12.52760579488853665, -10.67929555188718282, 33.92786785259544757 ) ) ;
#24002 = DIRECTION ( 'NONE',  ( -1.000000000000000000, 0.000000000000000000, -0.000000000000000000 ) ) ;
#24003 = CARTESIAN_POINT ( 'NONE',  ( -10.61538461538473399, -6.879047030192662504, 34.71129190930017927 ) ) ;
#24004 = ADVANCED_FACE ( 'NONE', ( #41715 ), #49792, .F. ) ;
#24005 = CARTESIAN_POINT ( 'NONE',  ( 8.992657731092338125, -7.630147231320743018, 34.74852402298682819 ) ) ;
#24006 = CARTESIAN_POINT ( 'NONE',  ( -4.826977667545032880, -10.92531984108285670, 33.72920026020278073 ) ) ;
#24007 = ORIENTED_EDGE ( 'NONE', *, *, #27409, .T. ) ;
#24008 = CARTESIAN_POINT ( 'NONE',  ( 16.28463659481310444, -9.929761469519743144, 34.40412654351204225 ) ) ;
#24009 = ORIENTED_EDGE ( 'NONE', *, *, #52535, .T. ) ;
#24010 = EDGE_CURVE ( 'NONE', #50376, #82473, #35906, .T. ) ;
#24011 = CARTESIAN_POINT ( 'NONE',  ( -17.07692307692307665, -13.87047571288749737, 32.06866353760679544 ) ) ;
#24012 = CARTESIAN_POINT ( 'NONE',  ( -11.97435897435897267, -3.499999999999999556, 29.75000000000000355 ) ) ;
#24013 = CYLINDRICAL_SURFACE ( 'NONE', #18570, 4.000000000000000000 ) ;
#24014 = ADVANCED_FACE ( 'NONE', ( #28647 ), #56112, .F. ) ;
#24015 = CARTESIAN_POINT ( 'NONE',  ( -12.46153846153846168, -12.34228464037088635, 31.77849191805839268 ) ) ;
#24016 = CARTESIAN_POINT ( 'NONE',  ( -6.923076923076922462, -2.486705287966279876, 31.30864560766543647 ) ) ;
#24017 = VECTOR ( 'NONE', #66739, 1000.000000000000000 ) ;
#24018 = ORIENTED_EDGE ( 'NONE', *, *, #18373, .F. ) ;
#24019 = VERTEX_POINT ( 'NONE', #75490 ) ;
#24020 = ORIENTED_EDGE ( 'NONE', *, *, #79781, .F. ) ;
#24021 = ORIENTED_EDGE ( 'NONE', *, *, #28518, .F. ) ;
#24022 = ORIENTED_EDGE ( 'NONE', *, *, #6096, .F. ) ;
#24023 = CIRCLE ( 'NONE', #52775, 2.999999999999999112 ) ;
#24024 = DIRECTION ( 'NONE',  ( -0.000000000000000000, -0.7660444431189791237, -0.6427876096865379196 ) ) ;
#24025 = CARTESIAN_POINT ( 'NONE',  ( -1.134561072977069651, -12.41262288849542017, 30.68299917996395010 ) ) ;
#24026 = CARTESIAN_POINT ( 'NONE',  ( -7.173076923076921574, -2.499999999999998668, 29.75000000000000355 ) ) ;
#24027 = EDGE_CURVE ( 'NONE', #18998, #52344, #13033, .T. ) ;
#24028 = CARTESIAN_POINT ( 'NONE',  ( -6.416666666666667851, -11.00000000000000000, 29.75000000000000355 ) ) ;
#24029 = CARTESIAN_POINT ( 'NONE',  ( -16.40386939113911779, -2.587272538249754117, 30.68239716806877837 ) ) ;
#24030 = CARTESIAN_POINT ( 'NONE',  ( 19.99999999999996803, 15.00000000000000711, 13.00000000000000178 ) ) ;
#24031 = EDGE_CURVE ( 'NONE', #50988, #56881, #87621, .T. ) ;
#24032 = CARTESIAN_POINT ( 'NONE',  ( -3.999999999999998224, -7.500000000000000000, 14.00000000000000178 ) ) ;
#24033 = CARTESIAN_POINT ( 'NONE',  ( -5.076923076922761346, -2.255955759149395501, 30.00000000000324363 ) ) ;
#24034 = ORIENTED_EDGE ( 'NONE', *, *, #46945, .T. ) ;
#24035 = VERTEX_POINT ( 'NONE', #70068 ) ;
#24036 = ORIENTED_EDGE ( 'NONE', *, *, #37918, .F. ) ;
#24039 = ORIENTED_EDGE ( 'NONE', *, *, #39883, .T. ) ;
#24038 = EDGE_CURVE ( 'NONE', #46042, #80082, #37436, .T. ) ;
#24037 = CARTESIAN_POINT ( 'NONE',  ( 6.250054419913455561, -12.41089969410671223, 31.60739465890703670 ) ) ;
#24041 = CARTESIAN_POINT ( 'NONE',  ( 10.36540788444226280, -9.148715823498378086, 34.47080413974185120 ) ) ;
#24040 = LINE ( 'NONE', #36682, #50290 ) ;
#24042 = CARTESIAN_POINT ( 'NONE',  ( 1.384615384615386802, -12.29105614889573062, 35.45975837776705220 ) ) ;
#24043 = VECTOR ( 'NONE', #55850, 1000.000000000000114 ) ;
#24044 = CARTESIAN_POINT ( 'NONE',  ( -14.37296275365308418, -10.21337939537584383, 33.94971097300158647 ) ) ;
#24045 = ORIENTED_EDGE ( 'NONE', *, *, #25623, .T. ) ;
#24046 = EDGE_CURVE ( 'NONE', #87173, #38328, #34952, .T. ) ;
#24047 = EDGE_LOOP ( 'NONE', ( #44716, #85606, #35451, #64072 ) ) ;
#24049 = B_SPLINE_CURVE_WITH_KNOTS ( 'NONE', 3,
 ( #13386, #82302, #28682, #20582, #7522, #1194, #34545, #75527, #35881, #54367 ),
 .UNSPECIFIED., .F., .F.,
 ( 4, 2, 2, 2, 4 ),
 ( 0.0007817359430256333669, 0.0009771253907250056474, 0.001172514838424370881, 0.001367904286123736331, 0.001563293733823101564 ),
 .UNSPECIFIED. ) ;
#24048 = DIRECTION ( 'NONE',  ( 0.000000000000000000, 0.000000000000000000, -1.000000000000000000 ) ) ;
#24050 = VERTEX_POINT ( 'NONE', #13351 ) ;
#24051 = FACE_BOUND ( 'NONE', #63355, .T. ) ;
#24052 = B_SPLINE_CURVE_WITH_KNOTS ( 'NONE', 3,
 ( #19572, #11942, #66879, #5617, #61435, #38974, #87610, #60556, #24994, #79947 ),
 .UNSPECIFIED., .F., .F.,
 ( 4, 2, 2, 2, 4 ),
 ( 0.0007817246256747490156, 0.0009771112852218922368, 0.001172497944769035350, 0.001367884604316178462, 0.001563271263863321575 ),
 .UNSPECIFIED. ) ;
#24053 = CARTESIAN_POINT ( 'NONE',  ( 13.51540582558233794, -12.35292014791297710, 31.75344720912887198 ) ) ;
#24054 = CARTESIAN_POINT ( 'NONE',  ( 7.846153846153725020, -3.835265460704628371, 33.15142922262033665 ) ) ;
#24055 = VERTEX_POINT ( 'NONE', #61527 ) ;
#24056 = CARTESIAN_POINT ( 'NONE',  ( -1.384615384615383471, -5.471508081941601098, 34.59228464037088457 ) ) ;
#24057 = CARTESIAN_POINT ( 'NONE',  ( 8.900069099717528687, -7.277220318596961057, 34.99547417642776992 ) ) ;
#24058 = VECTOR ( 'NONE', #31411, 1000.000000000000000 ) ;
#24059 = CYLINDRICAL_SURFACE ( 'NONE', #56544, 0.2499999999999979738 ) ;
#24060 = VERTEX_POINT ( 'NONE', #89035 ) ;
#24061 = CARTESIAN_POINT ( 'NONE',  ( 12.39626801557768587, -5.219633306516282545, 34.19971097300152962 ) ) ;
#24062 = CARTESIAN_POINT ( 'NONE',  ( 2.980745993476265010, -12.22074536777954989, 31.39888409691088356 ) ) ;
#24063 = EDGE_CURVE ( 'NONE', #81272, #48918, #45631, .T. ) ;
#24064 = ORIENTED_EDGE ( 'NONE', *, *, #50890, .T. ) ;
#24065 = EDGE_CURVE ( 'NONE', #36243, #79961, #66190, .T. ) ;
#24066 = CARTESIAN_POINT ( 'NONE',  ( 6.130838330486762189, -7.277220318596959281, 34.99547417642776992 ) ) ;
#24067 = CARTESIAN_POINT ( 'NONE',  ( -9.561517251340744039, -9.084667340241226796, 34.75534355489798344 ) ) ;
#24068 = ORIENTED_EDGE ( 'NONE', *, *, #26034, .F. ) ;
#24069 = CARTESIAN_POINT ( 'NONE',  ( 2.307692307692186251, -3.083524468854526912, 32.58852847137268327 ) ) ;
#24070 = CARTESIAN_POINT ( 'NONE',  ( 14.30769230769218758, -8.613356846316285953, 34.62446782046622218 ) ) ;
#24071 = FACE_OUTER_BOUND ( 'NONE', #470, .T. ) ;
#24072 = CARTESIAN_POINT ( 'NONE',  ( -10.61538461538473399, -6.026961402154118019, 34.52809138561165270 ) ) ;
#24074 = EDGE_CURVE ( 'NONE', #21038, #33780, #7244, .T. ) ;
#24073 = CARTESIAN_POINT ( 'NONE',  ( -14.30769230769230660, -5.415277668671390821, 36.20867863119892149 ) ) ;
#24075 = FACE_BOUND ( 'NONE', #34595, .T. ) ;
#24077 = DIRECTION ( 'NONE',  ( -0.000000000000000000, -0.9396926207859092051, -0.3420201433256662704 ) ) ;
#24076 = CARTESIAN_POINT ( 'NONE',  ( -1.607541602131530967, -2.758268499246656624, 31.33685645148948140 ) ) ;
#24078 = CARTESIAN_POINT ( 'NONE',  ( -1.254089946381738985, -9.503571793651733657, 34.60286762892837942 ) ) ;
#24080 = CARTESIAN_POINT ( 'NONE',  ( 8.900022577055551665, -2.729792928343269587, 31.24908615093345077 ) ) ;
#24079 = LINE ( 'NONE', #52438, #18509 ) ;
#24081 = CARTESIAN_POINT ( 'NONE',  ( 1.799775606325937360E-14, -10.25000000000000000, 14.78125000000000178 ) ) ;
#24082 = VERTEX_POINT ( 'NONE', #22759 ) ;
#24083 = CARTESIAN_POINT ( 'NONE',  ( 18.00000000000000000, -11.69971097300155272, 32.46337939537588113 ) ) ;
#24084 = ORIENTED_EDGE ( 'NONE', *, *, #51580, .F. ) ;
#24085 = VECTOR ( 'NONE', #54958, 1000.000000000000000 ) ;
#24086 = ORIENTED_EDGE ( 'NONE', *, *, #52712, .T. ) ;
#24087 = LINE ( 'NONE', #70952, #88746 ) ;
#24088 = EDGE_LOOP ( 'NONE', ( #79534, #62236, #84433, #46405 ) ) ;
#24089 = CARTESIAN_POINT ( 'NONE',  ( -9.692307692307691624, -8.973038597847269315, 34.52809138561121927 ) ) ;
#24090 = CARTESIAN_POINT ( 'NONE',  ( 2.724691934501235036, -6.299813628509441266, 26.63875670625848713 ) ) ;
#24091 = DIRECTION ( 'NONE',  ( -0.000000000000000000, -0.8660254037844399289, -0.4999999999999980016 ) ) ;
#24092 = CARTESIAN_POINT ( 'NONE',  ( 9.915087233576100445, -11.41317474335729543, 32.86274602512330034 ) ) ;
#24093 = CARTESIAN_POINT ( 'NONE',  ( -12.46153846153858424, -2.657715359629662544, 31.77849191805970364 ) ) ;
#24094 = CARTESIAN_POINT ( 'NONE',  ( 4.153846153846154188, -8.164416787775445883, 34.95778746994557906 ) ) ;
#24095 = CARTESIAN_POINT ( 'NONE',  ( -17.74984401280907775, -2.249999999999999556, 29.68153322838372787 ) ) ;
#24096 = DIRECTION ( 'NONE',  ( -0.000000000000000000, 0.3420201433256694346, -0.9396926207859080948 ) ) ;
#24097 = CARTESIAN_POINT ( 'NONE',  ( -4.403846153846151523, -7.500000000000001776, 35.04278698407183867 ) ) ;
#24098 = CARTESIAN_POINT ( 'NONE',  ( -3.750000000000008438, -5.946699141100917352, 15.17187500000000000 ) ) ;
#24099 = CARTESIAN_POINT ( 'NONE',  ( 10.61538461538461675, -4.102666532097928531, 36.13435417666054406 ) ) ;
#24100 = CARTESIAN_POINT ( 'NONE',  ( 13.13463864056679498, -3.436278759898153901, 33.07459398097509506 ) ) ;
#24101 = AXIS2_PLACEMENT_3D ( 'NONE', #9585, #43381, #3268 ) ;
#24102 = CARTESIAN_POINT ( 'NONE',  ( 13.60762673622823726, -4.187068189119697692, 33.49521262558774026 ) ) ;
#24103 = B_SPLINE_CURVE_WITH_KNOTS ( 'NONE', 3,
 ( #30577, #57171, #50400, #77882, #51262, #16186, #85534, #9866, #37330, #37782 ),
 .UNSPECIFIED., .F., .F.,
 ( 4, 2, 2, 2, 4 ),
 ( 0.000000000000000000, 0.0001954339857564097512, 0.0003908679715128195024, 0.0005863019572692292807, 0.0007817359430256390048 ),
 .UNSPECIFIED. ) ;
#24104 = VERTEX_POINT ( 'NONE', #64625 ) ;
#24105 = CARTESIAN_POINT ( 'NONE',  ( -13.51476335434707821, -6.809168938359901446, 34.95455904226513866 ) ) ;
#24106 = LINE ( 'NONE', #5181, #87772 ) ;
#24107 = CARTESIAN_POINT ( 'NONE',  ( 1.384615384615264011, -11.06231777344772027, 33.60647404775119895 ) ) ;
#24108 = CARTESIAN_POINT ( 'NONE',  ( 1.607991325313570252, -2.501478030877322567, 29.88021232661720816 ) ) ;
#24109 = CARTESIAN_POINT ( 'NONE',  ( -0.4615384615384611200, -6.435427911321262684, 35.78748833219616898 ) ) ;
#24110 = CARTESIAN_POINT ( 'NONE',  ( -2.980823821391187955, -5.766571408460171355, 34.70601412856602508 ) ) ;
#24111 = EDGE_CURVE ( 'NONE', #67703, #53125, #4803, .T. ) ;
#24112 = ORIENTED_EDGE ( 'NONE', *, *, #27955, .T. ) ;
#24113 = FACE_OUTER_BOUND ( 'NONE', #26759, .T. ) ;
#24114 = VERTEX_POINT ( 'NONE', #24093 ) ;
#24115 = EDGE_CURVE ( 'NONE', #48201, #62266, #25225, .T. ) ;
#24116 = EDGE_LOOP ( 'NONE', ( #27136, #75054, #77113, #31889 ) ) ;
#24117 = CARTESIAN_POINT ( 'NONE',  ( 0.4615384615384611200, -12.34228464037088635, 31.77849191805839268 ) ) ;
#24118 = CARTESIAN_POINT ( 'NONE',  ( 3.480823542407545101, -5.728107161865378494, 34.42597550085002922 ) ) ;
#24119 = CARTESIAN_POINT ( 'NONE',  ( 9.692307692307572609, -12.27809138561165270, 31.22303859784587132 ) ) ;
#24120 = VECTOR ( 'NONE', #39977, 1000.000000000000000 ) ;
#24121 = CARTESIAN_POINT ( 'NONE',  ( 4.376625695114563896, -3.755027918224367767, 33.06320215134714857 ) ) ;
#24122 = CARTESIAN_POINT ( 'NONE',  ( -5.142193077479396024, -8.656820664281497102, 34.87096338111211935 ) ) ;
#24124 = EDGE_CURVE ( 'NONE', #68446, #42909, #28410, .T. ) ;
#24123 = EDGE_LOOP ( 'NONE', ( #43820, #16030 ) ) ;
#24125 = B_SPLINE_CURVE_WITH_KNOTS ( 'NONE', 3,
 ( #43420, #70893, #28123, #9200, #55593, #36660, #83082, #48835, #69556, #7861 ),
 .UNSPECIFIED., .F., .F.,
 ( 4, 2, 2, 2, 4 ),
 ( 0.000000000000000000, 0.0001954311584214071026, 0.0003908623168428142051, 0.0005862934752642213077, 0.0007817246336856284103 ),
 .UNSPECIFIED. ) ;
#24126 = VERTEX_POINT ( 'NONE', #70516 ) ;
#24127 = B_SPLINE_CURVE_WITH_KNOTS ( 'NONE', 3,
 ( #54714, #75007, #34889, #47959, #75882, #666, #81763, #74557, #6545, #88978 ),
 .UNSPECIFIED., .F., .F.,
 ( 4, 2, 2, 2, 4 ),
 ( 0.000000000000000000, 0.0001954311584214072381, 0.0003908623168428144762, 0.0005862934752642217414, 0.0007817246336856289524 ),
 .UNSPECIFIED. ) ;
#24128 = ORIENTED_EDGE ( 'NONE', *, *, #78502, .T. ) ;
#24129 = CARTESIAN_POINT ( 'NONE',  ( 1.161689167099239084, -11.24512374952581872, 33.06303171183252942 ) ) ;
#24130 = CARTESIAN_POINT ( 'NONE',  ( 8.703960323269994248, -2.892918686051582533, 31.69288490824015980 ) ) ;
#24131 = EDGE_CURVE ( 'NONE', #35014, #23070, #23209, .T. ) ;
#24132 = CARTESIAN_POINT ( 'NONE',  ( 8.992010438208831502, -5.827830569534417471, 34.72679350104403539 ) ) ;
#24133 = FACE_OUTER_BOUND ( 'NONE', #25365, .T. ) ;
#24134 = VECTOR ( 'NONE', #53528, 1000.000000000000000 ) ;
#24135 = CARTESIAN_POINT ( 'NONE',  ( 11.47319153790521717, -11.06231777344662781, 33.60647404775220082 ) ) ;
#24136 = EDGE_CURVE ( 'NONE', #11498, #35739, #71388, .T. ) ;
#24137 = CYLINDRICAL_SURFACE ( 'NONE', #36546, 0.2499999999999979738 ) ;
#24138 = ORIENTED_EDGE ( 'NONE', *, *, #69009, .T. ) ;
#24139 = ORIENTED_EDGE ( 'NONE', *, *, #1840, .F. ) ;
#24140 = CARTESIAN_POINT ( 'NONE',  ( -2.651650429449565305, -4.848349570550461785, 24.00000000000000000 ) ) ;
#24141 = VERTEX_POINT ( 'NONE', #44350 ) ;
#24142 = VECTOR ( 'NONE', #50434, 1000.000000000000000 ) ;
#24144 = ORIENTED_EDGE ( 'NONE', *, *, #10896, .T. ) ;
#24143 = DIRECTION ( 'NONE',  ( 0.000000000000000000, 0.8660254037844377084, 0.5000000000000015543 ) ) ;
#24145 = CARTESIAN_POINT ( 'NONE',  ( -9.758390071667825794, -9.905515769479276145, 34.41647553114623292 ) ) ;
#24146 = CARTESIAN_POINT ( 'NONE',  ( -9.822454901745912181, -11.93770438780619259, 32.05411857736982029 ) ) ;
#24147 = CARTESIAN_POINT ( 'NONE',  ( -1.929879867024197893E-14, -3.750000000000000000, 16.65625000000000000 ) ) ;
#24148 = EDGE_LOOP ( 'NONE', ( #8625, #16041 ) ) ;
#24149 = ADVANCED_FACE ( 'NONE', ( #37163 ), #30415, .F. ) ;
#24150 = CIRCLE ( 'NONE', #6943, 0.2500000000000002220 ) ;
#24151 = CARTESIAN_POINT ( 'NONE',  ( -14.43784027742400866, -12.50552854090298993, 31.33409797877408920 ) ) ;
#24152 = ORIENTED_EDGE ( 'NONE', *, *, #64333, .T. ) ;
#24153 = CARTESIAN_POINT ( 'NONE',  ( -13.51530598772569292, -11.37499894934982692, 33.29245874905763003 ) ) ;
#24154 = CARTESIAN_POINT ( 'NONE',  ( 10.61538461538449596, -9.442884908241554243, 34.35708131394783038 ) ) ;
#24155 = CARTESIAN_POINT ( 'NONE',  ( -14.98082382139119062, -2.986452184633680229, 32.43230066228895225 ) ) ;
#24157 = DIRECTION ( 'NONE',  ( -0.000000000000000000, 0.5000000000000011102, -0.8660254037844381525 ) ) ;
#24156 = CARTESIAN_POINT ( 'NONE',  ( 5.777073041093150785, -12.38737895849757820, 31.66785238281580206 ) ) ;
#24158 = CARTESIAN_POINT ( 'NONE',  ( -0.6844654204453104462, -12.38737895849757820, 31.66785238281580206 ) ) ;
#24159 = CARTESIAN_POINT ( 'NONE',  ( -3.296851610129365451, -8.164416787775445883, 34.95778746994557906 ) ) ;
#24160 = EDGE_LOOP ( 'NONE', ( #5645, #61221 ) ) ;
#24161 = CARTESIAN_POINT ( 'NONE',  ( -11.31568199719312773, -12.24180327182772388, 31.33663988360758168 ) ) ;
#24162 = CARTESIAN_POINT ( 'NONE',  ( 11.47321160668745677, -2.255955759149247619, 30.00000000000013856 ) ) ;
#24164 = ORIENTED_EDGE ( 'NONE', *, *, #79750, .T. ) ;
#24163 = EDGE_CURVE ( 'NONE', #1486, #86632, #42452, .T. ) ;
#24165 = CARTESIAN_POINT ( 'NONE',  ( 11.28848479441295005, -12.01397095200674059, 32.43157075238190146 ) ) ;
#24166 = CARTESIAN_POINT ( 'NONE',  ( -5.076923076923075762, -5.557115091759785130, 34.35708131394839171 ) ) ;
#24167 = DIRECTION ( 'NONE',  ( -1.000000000000000000, -0.000000000000000000, 0.000000000000000000 ) ) ;
#24168 = CARTESIAN_POINT ( 'NONE',  ( -16.15384615384615330, -11.91647553114624181, 32.58852847137148245 ) ) ;
#24169 = ADVANCED_FACE ( 'NONE', ( #12371 ), #38965, .F. ) ;
#24171 = ADVANCED_FACE ( 'NONE', ( #31757 ), #40294, .F. ) ;
#24170 = CARTESIAN_POINT ( 'NONE',  ( 7.846153846153846700, -8.120952969808772792, 34.71129190930000163 ) ) ;
#24172 = FACE_BOUND ( 'NONE', #19085, .T. ) ;
#24174 = CYLINDRICAL_SURFACE ( 'NONE', #35919, 0.2500000000000002220 ) ;
#24173 = CARTESIAN_POINT ( 'NONE',  ( 5.142178216435913107, -5.941354392334606160, 34.76329471203374055 ) ) ;
#24175 = CARTESIAN_POINT ( 'NONE',  ( 0.4615384615384611200, -13.53365097954675988, 30.81389545987213552 ) ) ;
#24177 = CARTESIAN_POINT ( 'NONE',  ( 0.5267936010512991318, -3.083524468853784839, 32.58852847137153930 ) ) ;
#24176 = CARTESIAN_POINT ( 'NONE',  ( -18.00000000000000000, -11.16473453929635440, 33.15142922261927083 ) ) ;
#24178 = CARTESIAN_POINT ( 'NONE',  ( 1.634560793993429906, -2.986452184633681117, 32.43230066228895225 ) ) ;
#24179 = PLANE ( 'NONE',  #10198 ) ;
#24180 = CIRCLE ( 'NONE', #4058, 5.000000000000000888 ) ;
#24181 = CARTESIAN_POINT ( 'NONE',  ( 1.614399933863660985, -11.22469193450123193, 23.20125670625849068 ) ) ;
#24182 = EDGE_CURVE ( 'NONE', #61727, #80092, #81075, .T. ) ;
#24183 = VERTEX_POINT ( 'NONE', #46598 ) ;
#24184 = LINE ( 'NONE', #57530, #13306 ) ;
#24185 = AXIS2_PLACEMENT_3D ( 'NONE', #11168, #65215, #3512 ) ;
#24186 = DIRECTION ( 'NONE',  ( 0.000000000000000000, 0.6427876096865368094, 0.7660444431189802339 ) ) ;
#24187 = CARTESIAN_POINT ( 'NONE',  ( -0.4615384615384611200, -3.322132147404559976, 32.92929555188717927 ) ) ;
#24188 = DIRECTION ( 'NONE',  ( -0.000000000000000000, -0.000000000000000000, 1.000000000000000000 ) ) ;
#24189 = CARTESIAN_POINT ( 'NONE',  ( 10.86543892702293235, -12.17597550085003810, 31.52189283813460463 ) ) ;
#24190 = DIRECTION ( 'NONE',  ( -1.000000000000000000, -0.000000000000000000, -0.000000000000000000 ) ) ;
#24191 = CARTESIAN_POINT ( 'NONE',  ( -3.724691934501229262, -9.114399933863657211, 21.01375670625849068 ) ) ;
#24192 = CARTESIAN_POINT ( 'NONE',  ( -8.769230769230890843, -2.892918686052166066, 31.69288490824153470 ) ) ;
#24193 = CARTESIAN_POINT ( 'NONE',  ( 0.7114839798866033904, -3.712312575010499938, 33.01462480002815170 ) ) ;
#24194 = CARTESIAN_POINT ( 'NONE',  ( -7.780898706641007578, -10.33852847137154107, 34.16647553114620450 ) ) ;
#24195 = CARTESIAN_POINT ( 'NONE',  ( -0.7115152055870529457, -8.347322224742351082, 34.93158281831414769 ) ) ;
#24196 = CARTESIAN_POINT ( 'NONE',  ( -10.61538461538461320, -12.10708131394839349, 31.69288490824020244 ) ) ;
#24197 = PLANE ( 'NONE',  #45421 ) ;
#24198 = CARTESIAN_POINT ( 'NONE',  ( -18.13014720943821700, -2.882441371585227508, 31.66841991370171527 ) ) ;
#24199 = CARTESIAN_POINT ( 'NONE',  ( 13.38461538461538680, -13.57706302396349152, 30.56769352161908060 ) ) ;
#24200 = ORIENTED_EDGE ( 'NONE', *, *, #10745, .F. ) ;
#24201 = DIRECTION ( 'NONE',  ( -0.000000000000000000, -0.6427876096865404731, -0.7660444431189771253 ) ) ;
#24202 = CARTESIAN_POINT ( 'NONE',  ( -0.3589743589743593088, -3.499999999999999556, 29.75000000000000355 ) ) ;
#24203 = CARTESIAN_POINT ( 'NONE',  ( 0.06109907496451268821, -3.749999999999999556, 13.15811829374151642 ) ) ;
#24204 = CARTESIAN_POINT ( 'NONE',  ( 2.307692307692187583, -4.481592998941358097, 33.73612834414048933 ) ) ;
#24206 = CARTESIAN_POINT ( 'NONE',  ( 3.480714749117374218, -11.86320923018887719, 32.19269448109604781 ) ) ;
#24205 = VECTOR ( 'NONE', #9570, 1000.000000000000227 ) ;
#24207 = ORIENTED_EDGE ( 'NONE', *, *, #51909, .F. ) ;
#24208 = CARTESIAN_POINT ( 'NONE',  ( 12.46153846153846168, -6.343179335718451384, 34.87096338111211935 ) ) ;
#24209 = CARTESIAN_POINT ( 'NONE',  ( 1.161130440891438464, -9.331801661448606566, 34.40259984581193464 ) ) ;
#24211 = ORIENTED_EDGE ( 'NONE', *, *, #54862, .F. ) ;
#24210 = CARTESIAN_POINT ( 'NONE',  ( 15.84615384615384670, -3.499999999999999556, 29.75000000000000355 ) ) ;
#24212 = DIRECTION ( 'NONE',  ( -0.000000000000000000, -0.6427876096865404731, -0.7660444431189771253 ) ) ;
#24213 = FACE_OUTER_BOUND ( 'NONE', #65475, .T. ) ;
#24214 = CARTESIAN_POINT ( 'NONE',  ( 6.000000000000001776, -12.78798330534102945, 29.74999999999997868 ) ) ;
#24215 = CARTESIAN_POINT ( 'NONE',  ( 8.769230769230647482, -5.219633306517616589, 34.19971097300220464 ) ) ;
#24216 = ORIENTED_EDGE ( 'NONE', *, *, #78684, .T. ) ;
#24217 = VECTOR ( 'NONE', #68504, 1000.000000000000000 ) ;
#24218 = DIRECTION ( 'NONE',  ( 0.000000000000000000, 0.9848077530122072432, 0.1736481776669354937 ) ) ;
#24219 = CLOSED_SHELL ( 'NONE', ( #72577, #75317, #79081, #79121, #70166, #48705, #83284, #35996, #52238, #57899, #59276, #59206, #68998, #65103, #23364, #62457, #24985, #31495, #25791, #48204, #65810, #30859, #59576, #46365, #74433, #65543, #377, #66666, #49380, #16246, #78857, #58243, #7969, #84139, #53251, #87559, #71495, #12469, #43103, #58407, #1031, #83320, #83514, #76791, #87832, #74737, #44335, #83469, #55359, #59873, #51357, #50168, #47850, #68474, #35112, #45383, #22283, #68067, #4294, #31820, #4693, #30976, #49508, #76155, #69576, #25257, #5091, #87322, #88743, #44273, #16908, #74082, #59074, #37290, #64487, #10612, #41087, #29905, #26160, #2576, #35233, #79574, #40672, #9730, #4790, #52684, #27427, #15885, #47970, #2915, #75750, #12090, #32253, #77071, #30491, #68929, #29557, #1501, #12183, #56287, #33442, #3195, #79469, #47541, #76769, #69414, #71425, #44464, #26881, #41982, #85890, #43846, #42189, #71240, #75327, #1877, #2319, #68333, #23344, #89002, #12047, #88950, #60919, #84920, #11155, #77346, #73118, #27298, #86193, #79305, #82959, #21912, #86262, #10135, #25137, #41467, #85758, #33557, #37985, #32097, #55916, #6918, #27450, #21819, #75648, #19313, #16327, #37114, #21027, #77201, #36971, #19029, #11807, #73010, #62317, #10743, #71666, #61305, #35247, #86709, #27910, #21701, #60164, #44382, #62443, #6169, #34650, #31125, #51983, #85796, #6064, #54933, #2620, #20336, #38783, #1908, #3235, #25810, #12256, #55822, #16933, #75745, #65353, #21340, #39868, #63933, #47519, #17265, #75273, #68777, #52131, #43572, #59730, #46082, #16158, #16163, #64775, #45885, #77385, #9174, #505, #5055, #32306, #61072, #44669, #31268, #14438, #30649, #56481, #26309, #11856, #25815, #8729, #70671, #43618, #28569, #6939, #84590, #57029, #4763, #181, #62775, #72318, #60456, #45378, #32029, #38985, #69075, #52436, #37503, #65936, #83966, #73478, #82671, #20161, #62705, #79394, #68687, #52066, #70127, #85913, #37102, #45632, #38534, #87427, #74096, #75497, #29507, #49369, #82643, #72755, #63907, #9647, #34974, #51114, #75661, #75415, #25564, #17165, #42686, #5743, #61573, #51375, #28119, #28452, #66480, #21556, #81220, #36995, #79049, #12869, #62455, #55679, #6433, #15313, #39044, #19394, #81271, #63976, #9049, #79710, #20794, #48378, #5184, #28220, #55104, #68989, #30000, #85006, #71420, #8633, #41499, #2191, #85963, #68654, #28421, #84068, #51464, #67549, #23401, #41780, #42659, #85399 ) ) ;
#24220 = VECTOR ( 'NONE', #29825, 1000.000000000000000 ) ;
#24221 = CARTESIAN_POINT ( 'NONE',  ( 3.930361210122205406, -10.11188796281391511, 34.01382737946119050 ) ) ;
#24222 = EDGE_LOOP ( 'NONE', ( #30470, #63427, #24862, #57055 ) ) ;
#24223 = ORIENTED_EDGE ( 'NONE', *, *, #36445, .T. ) ;
#24224 = ORIENTED_EDGE ( 'NONE', *, *, #70292, .F. ) ;
#24225 = CARTESIAN_POINT ( 'NONE',  ( -9.942330929600657896, -10.05641848906368097, 34.04755513067966177 ) ) ;
#24226 = CARTESIAN_POINT ( 'NONE',  ( -2.980823821391187511, -2.986452184633681117, 32.43230066228895225 ) ) ;
#24227 = CARTESIAN_POINT ( 'NONE',  ( -9.561782254074051579, -12.70449254468099198, 30.44128974285582956 ) ) ;
#24228 = CYLINDRICAL_SURFACE ( 'NONE', #17600, 0.2499999999999986955 ) ;
#24229 = ORIENTED_EDGE ( 'NONE', *, *, #58218, .T. ) ;
#24230 = EDGE_LOOP ( 'NONE', ( #21598, #21065 ) ) ;
#24232 = ORIENTED_EDGE ( 'NONE', *, *, #18530, .T. ) ;
#24231 = CARTESIAN_POINT ( 'NONE',  ( 15.23076923076923173, -6.189225973068211317, 35.74407628777942847 ) ) ;
#24233 = DIRECTION ( 'NONE',  ( -0.000000000000000000, -1.000000000000000000, 8.673617379884035472E-17 ) ) ;
#24234 = CARTESIAN_POINT ( 'NONE',  ( 16.15384615384603251, -8.656820664282941280, 34.87096338111179961 ) ) ;
#24235 = EDGE_CURVE ( 'NONE', #51727, #87990, #58548, .T. ) ;
#24236 = CARTESIAN_POINT ( 'NONE',  ( 5.869309396889692110, -3.957541250942359756, 33.62499894934981626 ) ) ;
#24237 = DIRECTION ( 'NONE',  ( 0.000000000000000000, 0.8660254037844377084, 0.5000000000000015543 ) ) ;
#24238 = ORIENTED_EDGE ( 'NONE', *, *, #12922, .T. ) ;
#24239 = ORIENTED_EDGE ( 'NONE', *, *, #38614, .F. ) ;
#24240 = ORIENTED_EDGE ( 'NONE', *, *, #71896, .F. ) ;
#24242 = ORIENTED_EDGE ( 'NONE', *, *, #76813, .F. ) ;
#24241 = CARTESIAN_POINT ( 'NONE',  ( 15.00728428704528561, -2.599994579823202923, 30.74605699353653776 ) ) ;
#24243 = DIRECTION ( 'NONE',  ( -0.000000000000000000, -0.3420201433256694901, -0.9396926207859082059 ) ) ;
#24244 = DIRECTION ( 'NONE',  ( -0.000000000000000000, 0.7660444431189791237, -0.6427876096865379196 ) ) ;
#24245 = EDGE_LOOP ( 'NONE', ( #66485, #84961 ) ) ;
#24246 = EDGE_CURVE ( 'NONE', #47112, #60879, #66870, .T. ) ;
#24247 = CARTESIAN_POINT ( 'NONE',  ( -13.38461538461550582, -4.481592998941358097, 33.73612834414048933 ) ) ;
#24248 = CYLINDRICAL_SURFACE ( 'NONE', #9179, 0.2500000000000012212 ) ;
#24249 = CARTESIAN_POINT ( 'NONE',  ( -2.307692307692305711, -11.16473453929635440, 33.15142922261926373 ) ) ;
#24250 = FACE_BOUND ( 'NONE', #71481, .T. ) ;
#24251 = FACE_OUTER_BOUND ( 'NONE', #8124, .T. ) ;
#24252 = CARTESIAN_POINT ( 'NONE',  ( -4.219929564802032296, -12.10708131394839349, 31.69288490824020244 ) ) ;
#24253 = B_SPLINE_CURVE_WITH_KNOTS ( 'NONE', 3,
 ( #65183, #22867, #3033, #85466, #23748, #71945 ),
 .UNSPECIFIED., .F., .F.,
 ( 4, 2, 4 ),
 ( 0.0003909569690057805385, 0.0005862646681846044039, 0.0007815723673634283235 ),
 .UNSPECIFIED. ) ;
#24254 = CARTESIAN_POINT ( 'NONE',  ( 14.30769230769231015, -7.500000000000001776, 35.04278698407183867 ) ) ;
#24256 = CARTESIAN_POINT ( 'NONE',  ( 4.284636594813102661, -2.295524264805589354, 30.44142389570982488 ) ) ;
#24255 = CARTESIAN_POINT ( 'NONE',  ( -7.846153846153965716, -3.300289026999228881, 32.46337939537708905 ) ) ;
#24257 = AXIS2_PLACEMENT_3D ( 'NONE', #55439, #9907, #37369 ) ;
#24258 = CARTESIAN_POINT ( 'NONE',  ( 8.703148389870632329, -9.058645607665454236, 34.76329471203372634 ) ) ;
#24259 = DIRECTION ( 'NONE',  ( 0.000000000000000000, 0.000000000000000000, 1.000000000000000000 ) ) ;
#24260 = ORIENTED_EDGE ( 'NONE', *, *, #88539, .F. ) ;
#24261 = CARTESIAN_POINT ( 'NONE',  ( 14.08481362526366354, -7.630691491037285168, 34.74850469731152458 ) ) ;
#24262 = FACE_OUTER_BOUND ( 'NONE', #85397, .T. ) ;
#24263 = ORIENTED_EDGE ( 'NONE', *, *, #60300, .F. ) ;
#24264 = ORIENTED_EDGE ( 'NONE', *, *, #5866, .F. ) ;
#24265 = VECTOR ( 'NONE', #14175, 1000.000000000000114 ) ;
#24267 = CARTESIAN_POINT ( 'NONE',  ( -5.777220458731588515, -12.24180327182771855, 31.33663988360758168 ) ) ;
#24266 = CARTESIAN_POINT ( 'NONE',  ( -6.792551221313360088, -8.586989748646452369, 34.63063291749215011 ) ) ;
#24268 = AXIS2_PLACEMENT_3D ( 'NONE', #40939, #76043, #40507 ) ;
#24269 = CARTESIAN_POINT ( 'NONE',  ( -6.923076923076922462, -6.386643153685126251, 34.62446782046654192 ) ) ;
#24270 = CARTESIAN_POINT ( 'NONE',  ( 2.557746727605760384, -2.318338780012835443, 30.59689888758630261 ) ) ;
#24271 = DIRECTION ( 'NONE',  ( -0.000000000000000000, 0.9396926207859092051, -0.3420201433256662704 ) ) ;
#24272 = ORIENTED_EDGE ( 'NONE', *, *, #35449, .T. ) ;
#24273 = EDGE_CURVE ( 'NONE', #56000, #17031, #77852, .T. ) ;
#24274 = EDGE_CURVE ( 'NONE', #56516, #76174, #66244, .T. ) ;
#24275 = CYLINDRICAL_SURFACE ( 'NONE', #54474, 0.2500000000000002220 ) ;
#24276 = CARTESIAN_POINT ( 'NONE',  ( 15.16468685140909578, -10.67929555188718460, 33.92786785259543336 ) ) ;
#24277 = CARTESIAN_POINT ( 'NONE',  ( 7.715462379486287325, -5.582088688514999397, 34.36776431015576350 ) ) ;
#24278 = DIRECTION ( 'NONE',  ( -0.000000000000000000, 0.5000000000000011102, -0.8660254037844380415 ) ) ;
#24280 = DIRECTION ( 'NONE',  ( -1.000000000000000000, 0.000000000000000000, -0.000000000000000000 ) ) ;
#24279 = SURFACE_SIDE_STYLE ('',( #59413 ) ) ;
#24281 = CARTESIAN_POINT ( 'NONE',  ( -3.749999999999988454, -9.053300858899127945, 17.51562500000000000 ) ) ;
#24282 = VERTEX_POINT ( 'NONE', #12808 ) ;
#24283 = ORIENTED_EDGE ( 'NONE', *, *, #56784, .F. ) ;
#24284 = PLANE ( 'NONE',  #54971 ) ;
#24285 = VERTEX_POINT ( 'NONE', #60993 ) ;
#24286 = CARTESIAN_POINT ( 'NONE',  ( -18.25000000000000000, -7.500000000000001776, 34.75000000000000000 ) ) ;
#24287 = CARTESIAN_POINT ( 'NONE',  ( 18.13079180782478872, -5.582136614379148654, 34.36778462344220486 ) ) ;
#24288 = EDGE_CURVE ( 'NONE', #17254, #4690, #59214, .T. ) ;
#24289 = CARTESIAN_POINT ( 'NONE',  ( -16.37677237136229991, -2.758268499246657068, 31.33685645148948851 ) ) ;
#24290 = DIRECTION ( 'NONE',  ( -0.000000000000000000, -0.000000000000000000, -1.000000000000000000 ) ) ;
#24291 = CARTESIAN_POINT ( 'NONE',  ( 1.553300858899129944, -11.24999999999998934, 18.45312500000000355 ) ) ;
#24292 = CARTESIAN_POINT ( 'NONE',  ( 6.000000000000001776, -2.833524468853757305, 32.15551576947925838 ) ) ;
#24293 = CARTESIAN_POINT ( 'NONE',  ( 11.53846153846153832, -13.78497067705608181, 32.30358669280327177 ) ) ;
#24294 = EDGE_LOOP ( 'NONE', ( #19892, #19177, #52080, #77758, #41495, #12694, #86417, #14051 ) ) ;
#24295 = DIRECTION ( 'NONE',  ( -0.000000000000000000, 0.000000000000000000, -1.000000000000000000 ) ) ;
#24297 = ORIENTED_EDGE ( 'NONE', *, *, #83655, .F. ) ;
#24296 = DIRECTION ( 'NONE',  ( -0.000000000000000000, 0.8660254037844397068, -0.4999999999999978906 ) ) ;
#24298 = CARTESIAN_POINT ( 'NONE',  ( 3.230769230769108269, -12.51329471203414379, 31.30864560766407578 ) ) ;
#24299 = CARTESIAN_POINT ( 'NONE',  ( -9.942330929600657896, -12.22074536777954989, 31.39888409691088356 ) ) ;
#24300 = CARTESIAN_POINT ( 'NONE',  ( -12.46153846153858424, -8.656820664282941280, 34.87096338111179961 ) ) ;
#24301 = CARTESIAN_POINT ( 'NONE',  ( 11.78851595837499211, -8.346898887586323923, 34.93166121998716278 ) ) ;
#24302 = CARTESIAN_POINT ( 'NONE',  ( 10.86543892702293412, -2.779044189368095719, 31.39831045268885745 ) ) ;
#24303 = CARTESIAN_POINT ( 'NONE',  ( 7.846153846153723244, -3.643525952248796163, 33.31231777344771672 ) ) ;
#24304 = CARTESIAN_POINT ( 'NONE',  ( -2.980769230769293898, -7.565270445406050648, 34.75000000000000000 ) ) ;
#24305 = CARTESIAN_POINT ( 'NONE',  ( -0.06109907496450878162, -11.25000000000000000, 17.53311829374151287 ) ) ;
#24306 = ORIENTED_EDGE ( 'NONE', *, *, #66481, .F. ) ;
#24307 = AXIS2_PLACEMENT_3D ( 'NONE', #15013, #28526, #42047 ) ;
#24308 = CARTESIAN_POINT ( 'NONE',  ( -4.153846153846152411, -11.16473453929635440, 33.15142922261926373 ) ) ;
#24309 = CARTESIAN_POINT ( 'NONE',  ( -12.21153846153852562, -7.565270445406050648, 34.75000000000000000 ) ) ;
#24310 = FACE_OUTER_BOUND ( 'NONE', #68785, .T. ) ;
#24311 = CARTESIAN_POINT ( 'NONE',  ( -1.944543648263014957, -5.555456351737005249, 26.50000000000000355 ) ) ;
#24312 = DIRECTION ( 'NONE',  ( -0.000000000000000000, 0.3420201433256694901, -0.9396926207859082059 ) ) ;
#24313 = CARTESIAN_POINT ( 'NONE',  ( -15.23076923076935074, -10.90142922262034020, 33.41473453929536674 ) ) ;
#24315 = EDGE_LOOP ( 'NONE', ( #56161, #3795, #76349, #55854 ) ) ;
#24314 = CARTESIAN_POINT ( 'NONE',  ( -13.31854805126531005, -6.343179335718452272, 34.87096338111212646 ) ) ;
#24316 = CARTESIAN_POINT ( 'NONE',  ( -1.944543648263014957, -5.555456351737005249, 20.25000000000000000 ) ) ;
#24317 = CARTESIAN_POINT ( 'NONE',  ( -1.384615384615383471, -12.34228464037088635, 31.77849191805839268 ) ) ;
#24318 = ORIENTED_EDGE ( 'NONE', *, *, #48823, .T. ) ;
#24319 = CARTESIAN_POINT ( 'NONE',  ( -4.023320715612509701, -2.647132371071621471, 31.75357179365173010 ) ) ;
#24320 = EDGE_LOOP ( 'NONE', ( #64579, #23241, #66903, #69500 ) ) ;
#24321 = CARTESIAN_POINT ( 'NONE',  ( -18.22292621751614305, -11.76352882383565301, 32.36236540154568075 ) ) ;
#24322 = CARTESIAN_POINT ( 'NONE',  ( 13.31853197365950514, -9.780366693483667717, 34.19971097300155805 ) ) ;
#24323 = CARTESIAN_POINT ( 'NONE',  ( 17.07692307692307665, -6.343179335718451384, 34.87096338111211935 ) ) ;
#24324 = ORIENTED_EDGE ( 'NONE', *, *, #86961, .T. ) ;
#24325 = CARTESIAN_POINT ( 'NONE',  ( -0.5920983751518260618, -2.254533558242299396, 29.97296025877828285 ) ) ;
#24326 = VERTEX_POINT ( 'NONE', #79499 ) ;
#24327 = LINE ( 'NONE', #72525, #74342 ) ;
#24328 = EDGE_LOOP ( 'NONE', ( #23973, #1563 ) ) ;
#24329 = B_SPLINE_CURVE_WITH_KNOTS ( 'NONE', 3,
 ( #81294, #52469, #33547, #31772, #5180, #60560, #60116, #53360, #74527, #67332 ),
 .UNSPECIFIED., .F., .F.,
 ( 4, 2, 2, 2, 4 ),
 ( 0.000000000000000000, 0.0001954311564186870913, 0.0003908623128373741825, 0.0005862934692560613009, 0.0007817246256747483650 ),
 .UNSPECIFIED. ) ;
#24330 = AXIS2_PLACEMENT_3D ( 'NONE', #18429, #88686, #59852 ) ;
#24331 = VECTOR ( 'NONE', #79862, 1000.000000000000114 ) ;
#24332 = CARTESIAN_POINT ( 'NONE',  ( 2.177001704582000929, -9.084618155246140248, 34.75535874321725771 ) ) ;
#24333 = CARTESIAN_POINT ( 'NONE',  ( 12.52760681254090258, -12.10708131394839704, 31.69288490824020954 ) ) ;
#24334 = ORIENTED_EDGE ( 'NONE', *, *, #19707, .F. ) ;
#24335 = CARTESIAN_POINT ( 'NONE',  ( -5.777220458731590291, -11.41317474335729187, 32.86274602512330034 ) ) ;
#24336 = CARTESIAN_POINT ( 'NONE',  ( 10.61538461538461675, -8.564572088678739092, 35.78748833219616898 ) ) ;
#24337 = CARTESIAN_POINT ( 'NONE',  ( -11.53846153846166089, -3.083524468854526912, 32.58852847137268327 ) ) ;
#24338 = EDGE_CURVE ( 'NONE', #88630, #64217, #17800, .T. ) ;
#24339 = VECTOR ( 'NONE', #60884, 1000.000000000000000 ) ;
#24340 = CARTESIAN_POINT ( 'NONE',  ( -4.153846153846152411, -8.318370150425687726, 35.83090037661290239 ) ) ;
#24341 = CARTESIAN_POINT ( 'NONE',  ( -7.976301815885541657, -12.70455904226513866, 30.44083106164009322 ) ) ;
#24342 = EDGE_LOOP ( 'NONE', ( #33217, #23155 ) ) ;
#24343 = ORIENTED_EDGE ( 'NONE', *, *, #29120, .F. ) ;
#24344 = EDGE_LOOP ( 'NONE', ( #24929, #22898, #21048, #38189 ) ) ;
#24346 = ORIENTED_EDGE ( 'NONE', *, *, #19916, .F. ) ;
#24345 = CARTESIAN_POINT ( 'NONE',  ( -4.088591014333315066, -8.656820664281605460, 34.87096338111211224 ) ) ;
#24347 = EDGE_CURVE ( 'NONE', #17177, #57142, #88567, .T. ) ;
#24348 = CARTESIAN_POINT ( 'NONE',  ( 9.692307692307695177, -1.422936976036506707, 30.56769352161908415 ) ) ;
#24349 = CARTESIAN_POINT ( 'NONE',  ( 6.249945409378045547, -10.18230066228895758, 34.26354781536631577 ) ) ;
#24351 = ORIENTED_EDGE ( 'NONE', *, *, #43589, .T. ) ;
#24350 = EDGE_CURVE ( 'NONE', #81242, #19850, #14367, .T. ) ;
#24352 = EDGE_LOOP ( 'NONE', ( #86525, #44840 ) ) ;
#24353 = VERTEX_POINT ( 'NONE', #21333 ) ;
#24354 = LINE ( 'NONE', #65785, #15194 ) ;
#24355 = ORIENTED_EDGE ( 'NONE', *, *, #12844, .F. ) ;
#24356 = CARTESIAN_POINT ( 'NONE',  ( 2.307692307692187583, -4.481592998941358097, 33.73612834414048933 ) ) ;
#24357 = EDGE_CURVE ( 'NONE', #67330, #76071, #55189, .T. ) ;
#24358 = CARTESIAN_POINT ( 'NONE',  ( 16.94623247381277054, -12.35290016733513951, 31.75349464988449455 ) ) ;
#24359 = CARTESIAN_POINT ( 'NONE',  ( 0.4615384615384611200, -4.786620604624113540, 33.94971097300155094 ) ) ;
#24360 = FACE_BOUND ( 'NONE', #80512, .T. ) ;
#24361 = ORIENTED_EDGE ( 'NONE', *, *, #81649, .F. ) ;
#24362 = CARTESIAN_POINT ( 'NONE',  ( -8.769230769230768274, -8.973038597847269315, 34.52809138561121927 ) ) ;
#24363 = CARTESIAN_POINT ( 'NONE',  ( 13.38461538461526423, -11.06231777344772027, 33.60647404775119895 ) ) ;
#24364 = EDGE_CURVE ( 'NONE', #50087, #20467, #22978, .T. ) ;
#24365 = DIRECTION ( 'NONE',  ( -0.000000000000000000, 0.9848077530122086864, -0.1736481776669273891 ) ) ;
#24366 = LINE ( 'NONE', #86091, #40916 ) ;
#24367 = DIRECTION ( 'NONE',  ( 0.000000000000000000, 0.4999999999999960032, -0.8660254037844410391 ) ) ;
#24368 = VERTEX_POINT ( 'NONE', #69081 ) ;
#24369 = CARTESIAN_POINT ( 'NONE',  ( 9.561616225640133138, -2.541943142973491554, 30.39792223712631980 ) ) ;
#24370 = ORIENTED_EDGE ( 'NONE', *, *, #17808, .F. ) ;
#24371 = ORIENTED_EDGE ( 'NONE', *, *, #26628, .F. ) ;
#24373 = CARTESIAN_POINT ( 'NONE',  ( 17.32692307692451195, -7.500000000000155431, 34.75000000000007105 ) ) ;
#24372 = DIRECTION ( 'NONE',  ( -0.000000000000000000, 0.5000000000000011102, -0.8660254037844380415 ) ) ;
#24374 = CARTESIAN_POINT ( 'NONE',  ( -10.61538461538461320, -12.10708131394839349, 31.69288490824020244 ) ) ;
#24375 = FACE_OUTER_BOUND ( 'NONE', #85854, .T. ) ;
#24376 = CARTESIAN_POINT ( 'NONE',  ( 1.449870955891409352, -10.21337939537593620, 33.94971097300152252 ) ) ;
#24377 = CARTESIAN_POINT ( 'NONE',  ( 14.08476534878545827, -2.889293201056495786, 32.26117774369186009 ) ) ;
#24378 = ORIENTED_EDGE ( 'NONE', *, *, #46579, .T. ) ;
#24379 = ADVANCED_FACE ( 'NONE', ( #68637 ), #183, .F. ) ;
#24380 = CARTESIAN_POINT ( 'NONE',  ( -5.326946301144534601, -6.652501968072646932, 34.93155406624980941 ) ) ;
#24381 = CARTESIAN_POINT ( 'NONE',  ( -11.53846153846165912, -10.21337939537710326, 33.94971097300076224 ) ) ;
#24382 = CARTESIAN_POINT ( 'NONE',  ( 10.61538461538449596, -3.300289026999228881, 32.46337939537708905 ) ) ;
#24383 = ADVANCED_FACE ( 'NONE', ( #627 ), #26767, .F. ) ;
#24384 = CARTESIAN_POINT ( 'NONE',  ( -13.60810030917971858, -12.69144148231606017, 30.53333754910549303 ) ) ;
#24385 = ORIENTED_EDGE ( 'NONE', *, *, #61521, .T. ) ;
#24386 = B_SPLINE_CURVE_WITH_KNOTS ( 'NONE', 3,
 ( #25742, #60406, #40158, #53203, #82027, #87464, #82475, #20319, #32946, #27070 ),
 .UNSPECIFIED., .F., .F.,
 ( 4, 2, 2, 2, 4 ),
 ( 0.0007817359430256217660, 0.0009771253907249859150, 0.001172514838424349847, 0.001367904286123713779, 0.001563293733823077928 ),
 .UNSPECIFIED. ) ;
#24387 = EDGE_LOOP ( 'NONE', ( #61574, #49910 ) ) ;
#24388 = FACE_BOUND ( 'NONE', #83990, .T. ) ;
#24389 = AXIS2_PLACEMENT_3D ( 'NONE', #56821, #84320, #22594 ) ;
#24390 = ORIENTED_EDGE ( 'NONE', *, *, #31781, .T. ) ;
#24391 = ADVANCED_FACE ( 'NONE', ( #42501 ), #7827, .F. ) ;
#24392 = CARTESIAN_POINT ( 'NONE',  ( 11.66925197942848769, -12.35292014791297710, 31.75344720912887198 ) ) ;
#24394 = EDGE_CURVE ( 'NONE', #56760, #19723, #75619, .T. ) ;
#24393 = DIRECTION ( 'NONE',  ( -0.000000000000000000, -0.000000000000000000, -1.000000000000000000 ) ) ;
#24395 = ORIENTED_EDGE ( 'NONE', *, *, #51909, .T. ) ;
#24396 = CARTESIAN_POINT ( 'NONE',  ( -6.673076923075503153, -7.500000000000154543, 35.00000000000007105 ) ) ;
#24397 = DIRECTION ( 'NONE',  ( -0.000000000000000000, -0.9396926207859093161, -0.3420201433256663259 ) ) ;
#24398 = CARTESIAN_POINT ( 'NONE',  ( -7.976845312821404299, -11.71456829005830080, 32.44064028649416542 ) ) ;
#24399 = CARTESIAN_POINT ( 'NONE',  ( -6.857008572074484221, -3.050289026998446840, 32.03036669348366416 ) ) ;
#24400 = AXIS2_PLACEMENT_3D ( 'NONE', #37704, #50323, #44898 ) ;
#24401 = CARTESIAN_POINT ( 'NONE',  ( 4.826923076923076650, -7.500000000000001776, 35.00000000000000000 ) ) ;
#24402 = VERTEX_POINT ( 'NONE', #40736 ) ;
#24404 = ORIENTED_EDGE ( 'NONE', *, *, #1210, .F. ) ;
#24403 = DIRECTION ( 'NONE',  ( -0.000000000000000000, -0.000000000000000000, -1.000000000000000000 ) ) ;
#24405 = DIRECTION ( 'NONE',  ( -0.000000000000000000, 0.9848077530122086864, -0.1736481776669273891 ) ) ;
#24406 = CARTESIAN_POINT ( 'NONE',  ( 4.023698944407932743, -6.852621066184267029, 34.70813303252209181 ) ) ;
#24407 = DIRECTION ( 'NONE',  ( -0.000000000000000000, -0.7660444431189791237, -0.6427876096865379196 ) ) ;
#24408 = CARTESIAN_POINT ( 'NONE',  ( -10.86536135943320502, -3.436278759898153901, 33.07459398097509506 ) ) ;
#24409 = CARTESIAN_POINT ( 'NONE',  ( -8.096177083446809419, -9.271318131107980420, 34.42618302367067429 ) ) ;
#24410 = CARTESIAN_POINT ( 'NONE',  ( 12.46153846153846168, -5.471508081941601098, 34.59228464037088457 ) ) ;
#24411 = CARTESIAN_POINT ( 'NONE',  ( -1.200186371490524317, -10.22469193450124791, 16.36124329374151642 ) ) ;
#24412 = VERTEX_POINT ( 'NONE', #2815 ) ;
#24413 = CARTESIAN_POINT ( 'NONE',  ( 14.08420738312797837, -2.353723527008296568, 30.78948104536958752 ) ) ;
#24414 = CARTESIAN_POINT ( 'NONE',  ( 17.99999999999987566, -8.656820664282941280, 34.87096338111179961 ) ) ;
#24415 = CYLINDRICAL_SURFACE ( 'NONE', #28022, 0.2499999999999986955 ) ;
#24416 = ORIENTED_EDGE ( 'NONE', *, *, #12826, .T. ) ;
#24417 = EDGE_LOOP ( 'NONE', ( #9960, #79627, #50621, #51237 ) ) ;
#24418 = CARTESIAN_POINT ( 'NONE',  ( 9.758375025657770152, -3.322132147404559976, 32.92929555188717927 ) ) ;
#24419 = FACE_OUTER_BOUND ( 'NONE', #40427, .T. ) ;
#24420 = CARTESIAN_POINT ( 'NONE',  ( 17.07692307692307665, -3.322132147404559976, 32.92929555188717927 ) ) ;
#24421 = CARTESIAN_POINT ( 'NONE',  ( 10.61538461538461675, -5.557115091759785130, 34.35708131394839171 ) ) ;
#24422 = CARTESIAN_POINT ( 'NONE',  ( 16.15384615384603251, -10.33852847137269571, 34.16647553114546554 ) ) ;
#24423 = FACE_OUTER_BOUND ( 'NONE', #47398, .T. ) ;
#24424 = CARTESIAN_POINT ( 'NONE',  ( -22.75000000000000000, -4.499999999999999112, 27.25000000000000000 ) ) ;
#24425 = EDGE_LOOP ( 'NONE', ( #63584, #89044, #44340, #14676 ) ) ;
#24426 = B_SPLINE_CURVE_WITH_KNOTS ( 'NONE', 3,
 ( #13331, #20963, #83585, #76359, #21861, #41254, #34489, #75920, #14220, #83128 ),
 .UNSPECIFIED., .F., .F.,
 ( 4, 2, 2, 2, 4 ),
 ( 0.000000000000000000, 0.0001954311564186865221, 0.0003908623128373730441, 0.0005862934692560595662, 0.0007817246256747460882 ),
 .UNSPECIFIED. ) ;
#24427 = EDGE_CURVE ( 'NONE', #44538, #2392, #47534, .T. ) ;
#24428 = FACE_OUTER_BOUND ( 'NONE', #53382, .T. ) ;
#24429 = CARTESIAN_POINT ( 'NONE',  ( -17.07692307692307665, -12.10708131394839349, 31.69288490824020244 ) ) ;
#24430 = CARTESIAN_POINT ( 'NONE',  ( -13.38461538461538325, -5.180354513474913603, 36.12317359536750416 ) ) ;
#24431 = CARTESIAN_POINT ( 'NONE',  ( 9.692307692307695177, -2.486705287966279876, 31.30864560766543647 ) ) ;
#24433 = ORIENTED_EDGE ( 'NONE', *, *, #56043, .F. ) ;
#24432 = AXIS2_PLACEMENT_3D ( 'NONE', #62085, #7593, #41379 ) ;
#24434 = CARTESIAN_POINT ( 'NONE',  ( 12.71159277317677549, -3.627508038966690496, 32.91356715214248396 ) ) ;
#24435 = EDGE_CURVE ( 'NONE', #73490, #32743, #46603, .T. ) ;
#24436 = VERTEX_POINT ( 'NONE', #50568 ) ;
#24437 = CARTESIAN_POINT ( 'NONE',  ( 12.39626846098214230, -9.528491918058357157, 34.59228464037090589 ) ) ;
#24438 = CARTESIAN_POINT ( 'NONE',  ( -13.25456794936493310, -7.723484941389743952, 34.99544897038808955 ) ) ;
#24439 = CARTESIAN_POINT ( 'NONE',  ( 17.75002325595140817, -10.06842814019191401, 34.32929386961144758 ) ) ;
#24440 = ORIENTED_EDGE ( 'NONE', *, *, #40150, .F. ) ;
#24441 = CARTESIAN_POINT ( 'NONE',  ( 8.769230769230647482, -10.90142922262034020, 33.41473453929536674 ) ) ;
#24442 = DIRECTION ( 'NONE',  ( 1.000000000000000000, 0.000000000000000000, 0.000000000000000000 ) ) ;
#24443 = CARTESIAN_POINT ( 'NONE',  ( 10.61538461538461675, -12.62096338111211580, 30.90682066428153263 ) ) ;
#24444 = EDGE_CURVE ( 'NONE', #4302, #55479, #34775, .T. ) ;
#24445 = CARTESIAN_POINT ( 'NONE',  ( -7.623374177175779920, -4.989023458446560255, 34.36081565061822118 ) ) ;
#24446 = CARTESIAN_POINT ( 'NONE',  ( 3.296836564119307145, -2.833524468853757750, 32.15551576947925838 ) ) ;
#24447 = ORIENTED_EDGE ( 'NONE', *, *, #39597, .T. ) ;
#24448 = AXIS2_PLACEMENT_3D ( 'NONE', #18520, #23481, #16726 ) ;
#24449 = CARTESIAN_POINT ( 'NONE',  ( 7.846153846153846700, -11.35647404775217417, 33.31231777344666511 ) ) ;
#24450 = EDGE_LOOP ( 'NONE', ( #31689, #66460 ) ) ;
#24451 = CARTESIAN_POINT ( 'NONE',  ( 5.076923076923075762, -11.35647404775217417, 33.31231777344666511 ) ) ;
#24452 = CARTESIAN_POINT ( 'NONE',  ( -10.55019063360125742, -2.506253911140448487, 29.99999999999988631 ) ) ;
#24453 = AXIS2_PLACEMENT_3D ( 'NONE', #36809, #84574, #9780 ) ;
#24454 = CIRCLE ( 'NONE', #74825, 0.2500000000000002220 ) ;
#24456 = EDGE_CURVE ( 'NONE', #88631, #71689, #31589, .T. ) ;
#24455 = CARTESIAN_POINT ( 'NONE',  ( -13.45069879557126669, -2.721908614388770964, 31.22303859784723912 ) ) ;
#24457 = CYLINDRICAL_SURFACE ( 'NONE', #37249, 0.2499999999999997502 ) ;
#24458 = B_SPLINE_CURVE_WITH_KNOTS ( 'NONE', 3,
 ( #31249, #85317, #45653, #65913, #86670, #46103 ),
 .UNSPECIFIED., .F., .F.,
 ( 4, 2, 4 ),
 ( 0.0003909512603274038984, 0.0005862562993132300771, 0.0007815613382990563643 ),
 .UNSPECIFIED. ) ;
#24459 = LINE ( 'NONE', #5093, #9145 ) ;
#24460 = CARTESIAN_POINT ( 'NONE',  ( 15.00784301325308157, -11.76352882383564769, 32.36236540154569497 ) ) ;
#24461 = EDGE_CURVE ( 'NONE', #63896, #52314, #51428, .T. ) ;
#24462 = VECTOR ( 'NONE', #71501, 1000.000000000000000 ) ;
#24463 = AXIS2_PLACEMENT_3D ( 'NONE', #31359, #51597, #25931 ) ;
#24464 = ORIENTED_EDGE ( 'NONE', *, *, #52052, .T. ) ;
#24465 = VERTEX_POINT ( 'NONE', #22660 ) ;
#24466 = ORIENTED_EDGE ( 'NONE', *, *, #8101, .F. ) ;
#24467 = ORIENTED_EDGE ( 'NONE', *, *, #66590, .F. ) ;
#24468 = ORIENTED_EDGE ( 'NONE', *, *, #11959, .T. ) ;
#24469 = CARTESIAN_POINT ( 'NONE',  ( -1.318547033612945674, -3.050289026998446840, 32.03036669348366416 ) ) ;
#24470 = CARTESIAN_POINT ( 'NONE',  ( 12.46153846153846168, -10.05456864172156806, 36.03766855953608683 ) ) ;
#24471 = DIRECTION ( 'NONE',  ( -0.000000000000000000, 1.000000000000000000, -0.000000000000000000 ) ) ;
#24472 = DIRECTION ( 'NONE',  ( -0.000000000000000000, -0.3420201433256694346, -0.9396926207859080948 ) ) ;
#24473 = CARTESIAN_POINT ( 'NONE',  ( 7.596177102105255763, -12.65889640711025521, 30.72598325615533454 ) ) ;
#24474 = CARTESIAN_POINT ( 'NONE',  ( 3.100622021331010725, -6.001485441113818986, 34.52039167877662607 ) ) ;
#24475 = DIRECTION ( 'NONE',  ( 0.000000000000000000, 0.000000000000000000, 1.000000000000000000 ) ) ;
#24476 = CARTESIAN_POINT ( 'NONE',  ( 9.692307692307695177, -9.905515769479276145, 34.41647553114623292 ) ) ;
#24477 = CARTESIAN_POINT ( 'NONE',  ( 12.46153846153846168, -10.51840700105979565, 33.73612834413961536 ) ) ;
#24478 = ORIENTED_EDGE ( 'NONE', *, *, #7732, .F. ) ;
#24479 = ORIENTED_EDGE ( 'NONE', *, *, #83898, .T. ) ;
#24480 = ORIENTED_EDGE ( 'NONE', *, *, #19197, .F. ) ;
#24482 = EDGE_LOOP ( 'NONE', ( #10033, #41029, #19713, #82106 ) ) ;
#24481 = DIRECTION ( 'NONE',  ( -0.000000000000000000, 1.000000000000000000, -0.000000000000000000 ) ) ;
#24484 = DIRECTION ( 'NONE',  ( -0.000000000000000000, -0.3420201433256694901, -0.9396926207859082059 ) ) ;
#24483 = CARTESIAN_POINT ( 'NONE',  ( 6.857806922520602200, -11.67786785259541027, 32.92929555188721480 ) ) ;
#24485 = CARTESIAN_POINT ( 'NONE',  ( 1.384615384615386802, -4.661471528628507777, 34.16647553114623292 ) ) ;
#24486 = CARTESIAN_POINT ( 'NONE',  ( -25.00000000000000355, 9.999999999999971578, 13.00000000000000178 ) ) ;
#24487 = FACE_BOUND ( 'NONE', #9259, .T. ) ;
#24488 = ORIENTED_EDGE ( 'NONE', *, *, #27145, .F. ) ;
#24489 = EDGE_CURVE ( 'NONE', #34053, #34010, #17388, .T. ) ;
#24490 = VECTOR ( 'NONE', #16675, 1000.000000000000000 ) ;
#24491 = ORIENTED_EDGE ( 'NONE', *, *, #43371, .F. ) ;
#24492 = CARTESIAN_POINT ( 'NONE',  ( -2.939152317953646711E-15, 7.500000000000000000, 14.00000000000000178 ) ) ;
#24494 = ADVANCED_FACE ( 'NONE', ( #78930 ), #44236, .F. ) ;
#24493 = ORIENTED_EDGE ( 'NONE', *, *, #51099, .F. ) ;
#24495 = FACE_BOUND ( 'NONE', #62669, .T. ) ;
#24496 = DIRECTION ( 'NONE',  ( 0.000000000000000000, 0.000000000000000000, -1.000000000000000000 ) ) ;
#24497 = CARTESIAN_POINT ( 'NONE',  ( -14.43784027742400689, -6.809168938359901446, 34.95455904226513866 ) ) ;
#24498 = ORIENTED_EDGE ( 'NONE', *, *, #26771, .F. ) ;
#24499 = CARTESIAN_POINT ( 'NONE',  ( 14.24242186173153435, -2.892918686051582533, 31.69288490824015980 ) ) ;
#24501 = EDGE_CURVE ( 'NONE', #61262, #14730, #43379, .T. ) ;
#24500 = DIRECTION ( 'NONE',  ( -1.000000000000000000, -0.000000000000000000, -0.000000000000000000 ) ) ;
#24502 = FACE_OUTER_BOUND ( 'NONE', #42203, .T. ) ;
#24503 = EDGE_LOOP ( 'NONE', ( #74358, #19748 ) ) ;
#24504 = B_SPLINE_CURVE_WITH_KNOTS ( 'NONE', 3,
 ( #29020, #10050, #64984, #56475, #83965, #57356, #3288, #30764, #70438, #63667 ),
 .UNSPECIFIED., .F., .F.,
 ( 4, 2, 2, 2, 4 ),
 ( 0.000000000000000000, 0.0001954339857564092904, 0.0003908679715128185808, 0.0005863019572692278712, 0.0007817359430256371616 ),
 .UNSPECIFIED. ) ;
#24505 = CARTESIAN_POINT ( 'NONE',  ( -11.66915214157184622, -4.684245665217972032, 34.18127051446801090 ) ) ;
#24506 = CARTESIAN_POINT ( 'NONE',  ( 2.980792499826877773, -12.17611988154120972, 31.52148481390971213 ) ) ;
#24507 = ORIENTED_EDGE ( 'NONE', *, *, #42568, .T. ) ;
#24508 = CARTESIAN_POINT ( 'NONE',  ( 7.846153846153846700, -11.35647404775217417, 33.31231777344666511 ) ) ;
#24509 = CARTESIAN_POINT ( 'NONE',  ( 11.53846153846153832, -13.75783147151868846, 33.36296068462461051 ) ) ;
#24510 = ORIENTED_EDGE ( 'NONE', *, *, #27140, .T. ) ;
#24511 = CARTESIAN_POINT ( 'NONE',  ( 3.230769230769231726, -6.343179335718451384, 34.87096338111211935 ) ) ;
#24512 = CARTESIAN_POINT ( 'NONE',  ( 14.53070365930516061, -8.239487800360276282, 34.69522927552633718 ) ) ;
#24513 = CARTESIAN_POINT ( 'NONE',  ( -2.438383774359866418, -2.541943142973489778, 30.39792223712631980 ) ) ;
#24514 = DIRECTION ( 'NONE',  ( 0.000000000000000000, 0.1736481776669275834, 0.9848077530122086864 ) ) ;
#24515 = DIRECTION ( 'NONE',  ( 0.000000000000000000, 1.000000000000000000, 0.000000000000000000 ) ) ;
#24516 = FACE_OUTER_BOUND ( 'NONE', #10341, .T. ) ;
#24518 = DIRECTION ( 'NONE',  ( 0.000000000000000000, 0.000000000000000000, -1.000000000000000000 ) ) ;
#24517 = CARTESIAN_POINT ( 'NONE',  ( -1.515306851282940404, -2.729777683071817229, 31.24903638046269094 ) ) ;
#24519 = CARTESIAN_POINT ( 'NONE',  ( -0.2387587925603957550, -8.540255544307065350, 34.89611431652622286 ) ) ;
#24521 = DIRECTION ( 'NONE',  ( -0.000000000000000000, 1.000000000000000000, -0.000000000000000000 ) ) ;
#24520 = LINE ( 'NONE', #64606, #81776 ) ;
#24522 = EDGE_CURVE ( 'NONE', #2843, #66098, #37493, .T. ) ;
#24523 = CARTESIAN_POINT ( 'NONE',  ( -1.200186371490556958, -4.775308065498765409, 26.32625670625849068 ) ) ;
#24524 = ORIENTED_EDGE ( 'NONE', *, *, #36667, .F. ) ;
#24525 = CARTESIAN_POINT ( 'NONE',  ( 0.3313912521002411737, -12.45813303252208648, 30.39737893381572675 ) ) ;
#24526 = ORIENTED_EDGE ( 'NONE', *, *, #74410, .F. ) ;
#24527 = CIRCLE ( 'NONE', #40355, 4.000000000000000000 ) ;
#24528 = VECTOR ( 'NONE', #47874, 1000.000000000000000 ) ;
#24529 = EDGE_CURVE ( 'NONE', #27245, #66929, #27280, .T. ) ;
#24530 = ORIENTED_EDGE ( 'NONE', *, *, #59426, .T. ) ;
#24531 = CARTESIAN_POINT ( 'NONE',  ( -2.084912766423897335, -12.44528174975671853, 30.48912976160716681 ) ) ;
#24532 = VERTEX_POINT ( 'NONE', #57333 ) ;
#24533 = DIRECTION ( 'NONE',  ( -1.000000000000000000, -0.000000000000000000, -0.000000000000000000 ) ) ;
#24534 = CARTESIAN_POINT ( 'NONE',  ( -1.987747218494660295, -5.598659921968651254, 26.24813170625849068 ) ) ;
#24535 = CARTESIAN_POINT ( 'NONE',  ( 18.00000000000000000, -12.78798330534102945, 29.74999999999997868 ) ) ;
#24536 = CIRCLE ( 'NONE', #36063, 4.000000000000000000 ) ;
#24537 = CARTESIAN_POINT ( 'NONE',  ( 9.758376043310132530, -11.16473453929635440, 33.15142922261926373 ) ) ;
#24538 = CARTESIAN_POINT ( 'NONE',  ( 13.51514082284902862, -3.068774925481848825, 32.56582465632704526 ) ) ;
#24539 = CARTESIAN_POINT ( 'NONE',  ( -12.39628332202562433, -4.320704448112861584, 33.92786785259548310 ) ) ;
#24540 = CARTESIAN_POINT ( 'NONE',  ( 15.00784227186238162, -8.282780595021769443, 34.94152052738834868 ) ) ;
#24541 = CARTESIAN_POINT ( 'NONE',  ( -10.68065506134538545, -4.481592998940162609, 33.73612834413957984 ) ) ;
#24542 = CARTESIAN_POINT ( 'NONE',  ( 0.7115928814519150158, -2.544122305571458575, 31.48381861865057729 ) ) ;
#24543 =( GEOMETRIC_REPRESENTATION_CONTEXT ( 3 ) GLOBAL_UNCERTAINTY_ASSIGNED_CONTEXT ( ( #43763 ) ) GLOBAL_UNIT_ASSIGNED_CONTEXT ( ( #43396, #78064, #17704 ) ) REPRESENTATION_CONTEXT ( 'NONE', 'WORKASPACE' ) );
#24544 = CARTESIAN_POINT ( 'NONE',  ( -2.651650429449535551, -10.15165042944956753, 21.18750000000000000 ) ) ;
#24545 = EDGE_CURVE ( 'NONE', #50957, #58964, #86601, .T. ) ;
#24546 = CARTESIAN_POINT ( 'NONE',  ( 1.384615384615386802, -2.721908614388771852, 31.22303859784724978 ) ) ;
#24547 = CARTESIAN_POINT ( 'NONE',  ( 13.31934538405906743, -3.643525952247789412, 33.31231777344662959 ) ) ;
#24548 = B_SPLINE_CURVE_WITH_KNOTS ( 'NONE', 3,
 ( #83368, #29749, #82489, #21655, #49126, #76149, #14459, #7712, #20768, #14912 ),
 .UNSPECIFIED., .F., .F.,
 ( 4, 2, 2, 2, 4 ),
 ( 0.0007817359430256252354, 0.0009771253907249902518, 0.001172514838424355051, 0.001367904286123720068, 0.001563293733823085084 ),
 .UNSPECIFIED. ) ;
#24549 = FACE_OUTER_BOUND ( 'NONE', #11009, .T. ) ;
#24550 = B_SPLINE_CURVE_WITH_KNOTS ( 'NONE', 3,
 ( #21679, #88835, #33431, #34304, #14480, #27105, #20791, #28437, #34749, #81617 ),
 .UNSPECIFIED., .F., .F.,
 ( 4, 2, 2, 2, 4 ),
 ( 0.000000000000000000, 0.0001954339857564091278, 0.0003908679715128182556, 0.0005863019572692274375, 0.0007817359430256365111 ),
 .UNSPECIFIED. ) ;
#24551 = EDGE_CURVE ( 'NONE', #5501, #85209, #11821, .T. ) ;
#24552 = ORIENTED_EDGE ( 'NONE', *, *, #43371, .T. ) ;
#24553 = EDGE_LOOP ( 'NONE', ( #51234, #9503, #9974, #75775 ) ) ;
#24554 = DIRECTION ( 'NONE',  ( -0.000000000000000000, 1.000000000000000000, -0.000000000000000000 ) ) ;
#24555 = CARTESIAN_POINT ( 'NONE',  ( -19.50000000000000000, -3.499999999999999556, 29.75000000000000355 ) ) ;
#24556 = CARTESIAN_POINT ( 'NONE',  ( 16.28437159207980045, -12.50538340440932394, 31.33453814440721885 ) ) ;
#24557 = DIRECTION ( 'NONE',  ( 1.000000000000000000, 0.000000000000000000, 0.000000000000000000 ) ) ;
#24558 = CARTESIAN_POINT ( 'NONE',  ( 8.769230769230768274, -11.69971097300155272, 32.46337939537588113 ) ) ;
#24559 = DIRECTION ( 'NONE',  ( 0.000000000000000000, -0.000000000000000000, -1.000000000000000000 ) ) ;
#24560 = EDGE_CURVE ( 'NONE', #2196, #34824, #43403, .T. ) ;
#24561 = EDGE_CURVE ( 'NONE', #60387, #30501, #2539, .T. ) ;
#24562 = ORIENTED_EDGE ( 'NONE', *, *, #61596, .F. ) ;
#24563 = CARTESIAN_POINT ( 'NONE',  ( 12.46153846153833911, -12.51329471203414379, 31.30864560766407578 ) ) ;
#24564 = ORIENTED_EDGE ( 'NONE', *, *, #28128, .T. ) ;
#24565 = VECTOR ( 'NONE', #79162, 1000.000000000000000 ) ;
#24566 = VERTEX_POINT ( 'NONE', #4612 ) ;
#24567 = CARTESIAN_POINT ( 'NONE',  ( 7.596177102105255763, -10.82459398097509506, 33.81372124010185587 ) ) ;
#24568 = B_SPLINE_CURVE_WITH_KNOTS ( 'NONE', 3,
 ( #80683, #87900, #40139, #19404, #54064, #61259 ),
 .UNSPECIFIED., .F., .F.,
 ( 4, 2, 4 ),
 ( 0.0003909569690057804843, 0.0005862646681846042955, 0.0007815723673634281067 ),
 .UNSPECIFIED. ) ;
#24569 = FACE_OUTER_BOUND ( 'NONE', #74667, .T. ) ;
#24570 = CARTESIAN_POINT ( 'NONE',  ( -0.2115384615370421995, -7.500000000000154543, 35.00000000000007105 ) ) ;
#24571 = CARTESIAN_POINT ( 'NONE',  ( -11.28846153846153655, -2.499999999999998668, 29.75000000000000355 ) ) ;
#24572 = CARTESIAN_POINT ( 'NONE',  ( -5.143005456283213483, -8.164416787775445883, 34.95778746994557906 ) ) ;
#24573 = ADVANCED_FACE ( 'NONE', ( #5056 ), #51885, .F. ) ;
#24574 = B_SPLINE_CURVE_WITH_KNOTS ( 'NONE', 3,
 ( #47654, #18853, #74243, #13421, #54854, #73807 ),
 .UNSPECIFIED., .F., .F.,
 ( 4, 2, 4 ),
 ( 0.5000000000000000000, 0.7500000000000000000, 1.000000000000000000 ),
 .UNSPECIFIED. ) ;
#24575 = EDGE_LOOP ( 'NONE', ( #62876, #56751, #64093, #48985 ) ) ;
#24576 = EDGE_CURVE ( 'NONE', #17369, #43749, #32083, .T. ) ;
#24577 = B_SPLINE_CURVE_WITH_KNOTS ( 'NONE', 3,
 ( #54856, #41797, #41345, #82340, #56184, #40904, #21960, #68367, #6666, #15207 ),
 .UNSPECIFIED., .F., .F.,
 ( 4, 2, 2, 2, 4 ),
 ( 0.0007817359430256294638, 0.0009771253907249976244, 0.001172514838424365676, 0.001367904286123733729, 0.001563293733823094625 ),
 .UNSPECIFIED. ) ;
#24578 = ORIENTED_EDGE ( 'NONE', *, *, #85284, .T. ) ;
#24579 = ORIENTED_EDGE ( 'NONE', *, *, #28553, .F. ) ;
#24580 = VECTOR ( 'NONE', #87800, 1000.000000000000000 ) ;
#24581 = CARTESIAN_POINT ( 'NONE',  ( -3.903791733932698182, -12.01375889529407281, 32.43194544308182969 ) ) ;
#24582 = CARTESIAN_POINT ( 'NONE',  ( 9.822833130541338775, -2.372941743896879174, 30.88044141588253666 ) ) ;
#24583 = DIRECTION ( 'NONE',  ( -0.000000000000000000, 1.000000000000000000, 3.491481338843133355E-15 ) ) ;
#24584 = AXIS2_PLACEMENT_3D ( 'NONE', #35452, #7543, #15186 ) ;
#24585 = AXIS2_PLACEMENT_3D ( 'NONE', #32169, #49871, #85439 ) ;
#24586 = CARTESIAN_POINT ( 'NONE',  ( 10.48523664565292002, -5.070767119584671079, 34.40440758774516183 ) ) ;
#24587 = CARTESIAN_POINT ( 'NONE',  ( -4.403869391139117795, -8.432397168068783699, 34.66272746175022945 ) ) ;
#24588 = CARTESIAN_POINT ( 'NONE',  ( -1.634615384615383027, -7.500000000000001776, 34.75000000000000000 ) ) ;
#24589 = EDGE_LOOP ( 'NONE', ( #54681, #3950, #16280, #82852 ) ) ;
#24590 = ORIENTED_EDGE ( 'NONE', *, *, #63489, .F. ) ;
#24591 = CARTESIAN_POINT ( 'NONE',  ( 1.553300858899087311, -3.749999999999992006, 20.48437500000000000 ) ) ;
#24592 = ORIENTED_EDGE ( 'NONE', *, *, #53689, .F. ) ;
#24594 = VERTEX_POINT ( 'NONE', #46038 ) ;
#24593 = CARTESIAN_POINT ( 'NONE',  ( -13.63459212866397685, -5.643011162660950042, 34.66104346484419096 ) ) ;
#24595 = CARTESIAN_POINT ( 'NONE',  ( -9.822998295418001291, -9.929715669179220328, 34.40415004197138416 ) ) ;
#24596 = PLANE ( 'NONE',  #22999 ) ;
#24597 = DIRECTION ( 'NONE',  ( 1.000000000000000000, 0.000000000000000000, 0.000000000000000000 ) ) ;
#24598 = ORIENTED_EDGE ( 'NONE', *, *, #53851, .T. ) ;
#24599 = B_SPLINE_CURVE_WITH_KNOTS ( 'NONE', 3,
 ( #87748, #26023, #53482, #2084, #29573, #27788, #324, #49396, #55696, #29138 ),
 .UNSPECIFIED., .F., .F.,
 ( 4, 2, 2, 2, 4 ),
 ( 0.0007817359527651132059, 0.0009771254036996528287, 0.001172514854634192560, 0.001367904305568732291, 0.001563293756503272023 ),
 .UNSPECIFIED. ) ;
#24600 = FACE_OUTER_BOUND ( 'NONE', #61748, .T. ) ;
#24601 = ORIENTED_EDGE ( 'NONE', *, *, #41493, .T. ) ;
#24602 = CARTESIAN_POINT ( 'NONE',  ( 5.777073041093150785, -9.172386477786396597, 34.72672124145550043 ) ) ;
#24603 = CARTESIAN_POINT ( 'NONE',  ( 4.153846153846154188, -3.322132147404559976, 32.92929555188717927 ) ) ;
#24604 = EDGE_CURVE ( 'NONE', #46048, #38377, #78806, .T. ) ;
#24605 = CARTESIAN_POINT ( 'NONE',  ( 7.596130621932389637, -4.175268141568689195, 33.81360843649122216 ) ) ;
#24607 = FACE_OUTER_BOUND ( 'NONE', #37461, .T. ) ;
#24606 = CARTESIAN_POINT ( 'NONE',  ( -6.923076923077044142, -4.481592998941358097, 33.73612834414048933 ) ) ;
#24608 = LINE ( 'NONE', #34803, #6456 ) ;
#24609 = CARTESIAN_POINT ( 'NONE',  ( -10.61538461538473399, -10.90142922262034020, 33.41473453929536674 ) ) ;
#24610 = ORIENTED_EDGE ( 'NONE', *, *, #41622, .T. ) ;
#24612 = EDGE_CURVE ( 'NONE', #35523, #42119, #42301, .T. ) ;
#24611 = DIRECTION ( 'NONE',  ( 1.000000000000000000, 1.734723475976812518E-16, -0.000000000000000000 ) ) ;
#24613 = CARTESIAN_POINT ( 'NONE',  ( 15.23076923076923173, -4.098570777380720287, 33.41473453929634729 ) ) ;
#24614 = ORIENTED_EDGE ( 'NONE', *, *, #36763, .T. ) ;
#24615 = EDGE_CURVE ( 'NONE', #65392, #85801, #10925, .T. ) ;
#24616 = B_SPLINE_CURVE_WITH_KNOTS ( 'NONE', 3,
 ( #70711, #2670, #22957, #77900, #16638, #44099, #64815, #28386, #52197, #45890 ),
 .UNSPECIFIED., .F., .F.,
 ( 4, 2, 2, 2, 4 ),
 ( 0.0007817359430256301143, 0.0009771253907249963233, 0.001172514838424362641, 0.001367904286123728958, 0.001563293733823095276 ),
 .UNSPECIFIED. ) ;
#24617 = CARTESIAN_POINT ( 'NONE',  ( 6.923076923076924238, -9.780366693483667717, 34.19971097300155094 ) ) ;
#24618 = VECTOR ( 'NONE', #71195, 1000.000000000000227 ) ;
#24619 = CARTESIAN_POINT ( 'NONE',  ( 16.82694633287448838, -10.82459398097509862, 33.81372124010183455 ) ) ;
#24620 = CARTESIAN_POINT ( 'NONE',  ( 10.36540787133602493, -8.347322224742351082, 34.93158281831414769 ) ) ;
#24621 = CARTESIAN_POINT ( 'NONE',  ( -18.03205128205128105, -11.00000000000000000, 29.75000000000000355 ) ) ;
#24622 = CARTESIAN_POINT ( 'NONE',  ( 12.21156173059610772, -4.236021600441997492, 33.53823185664189310 ) ) ;
#24623 = FACE_BOUND ( 'NONE', #47637, .T. ) ;
#24625 = CARTESIAN_POINT ( 'NONE',  ( 20.75000000000000000, -10.50000000000000000, 29.75000000000000355 ) ) ;
#24624 = CARTESIAN_POINT ( 'NONE',  ( 12.33084699487089964, -3.062553014421049546, 32.05460306192773601 ) ) ;
#24626 = CARTESIAN_POINT ( 'NONE',  ( -19.50000000000000000, -3.499999999999999556, 29.75000000000000355 ) ) ;
#24628 = CARTESIAN_POINT ( 'NONE',  ( -10.61538461538473577, -11.67786785259630911, 32.92929555188603530 ) ) ;
#24627 = CARTESIAN_POINT ( 'NONE',  ( -11.31503457659996847, -7.630147231320743018, 34.74852402298682819 ) ) ;
#24629 = CARTESIAN_POINT ( 'NONE',  ( 3.230769230769231726, -13.20930481340135110, 34.54067556320372745 ) ) ;
#24630 = VECTOR ( 'NONE', #69413, 1000.000000000000000 ) ;
#24631 = EDGE_CURVE ( 'NONE', #25475, #81411, #84262, .T. ) ;
#24632 = DIRECTION ( 'NONE',  ( 0.000000000000000000, 0.8660254037844377084, 0.5000000000000015543 ) ) ;
#24633 = CARTESIAN_POINT ( 'NONE',  ( 3.724691934501232815, -5.885600066136343678, 25.38875670625849423 ) ) ;
#24634 = ORIENTED_EDGE ( 'NONE', *, *, #50599, .F. ) ;
#24635 = CARTESIAN_POINT ( 'NONE',  ( -7.911424292114620727, -11.48612834413959582, 32.76840700105983473 ) ) ;
#24636 = EDGE_CURVE ( 'NONE', #58140, #35531, #3102, .T. ) ;
#24637 = DIRECTION ( 'NONE',  ( 0.000000000000000000, 0.4999999999999960032, -0.8660254037844410391 ) ) ;
#24638 = CARTESIAN_POINT ( 'NONE',  ( -24.00000000000000000, -5.499999999999981348, 27.75000000000000000 ) ) ;
#24639 = CARTESIAN_POINT ( 'NONE',  ( 0.3892027609374598685, -10.22267510014235370, 28.92434864502809688 ) ) ;
#24640 = CARTESIAN_POINT ( 'NONE',  ( 4.499999999999999112, 7.500000000000002665, 13.50000000000000178 ) ) ;
#24641 = CARTESIAN_POINT ( 'NONE',  ( 5.207448515156719360, -12.15418822224088657, 32.17964115625579069 ) ) ;
#24642 = CARTESIAN_POINT ( 'NONE',  ( -3.749999999999996447, -7.561099074964554134, 27.34188170625848713 ) ) ;
#24643 = CARTESIAN_POINT ( 'NONE',  ( -2.372962308248625973, -3.643525952247789412, 33.31231777344662959 ) ) ;
#24644 = CARTESIAN_POINT ( 'NONE',  ( 8.769230769230768274, -2.486705287966279876, 31.30864560766543647 ) ) ;
#24645 = CARTESIAN_POINT ( 'NONE',  ( 17.07692307692307665, -1.466349020453238561, 30.81389545987213907 ) ) ;
#24646 = CARTESIAN_POINT ( 'NONE',  ( -1.384615384615505151, -12.46129190930018460, 30.37095296980731973 ) ) ;
#24647 = CARTESIAN_POINT ( 'NONE',  ( 0.2380535178145138098, -11.41268669641500466, 32.86336882939237825 ) ) ;
#24648 = CARTESIAN_POINT ( 'NONE',  ( -11.40766973063674961, -9.804649428959608670, 34.18742332936588468 ) ) ;
#24649 = LINE ( 'NONE', #10257, #3055 ) ;
#24650 = VECTOR ( 'NONE', #22210, 1000.000000000000227 ) ;
#24651 = LINE ( 'NONE', #53902, #61474 ) ;
#24652 = ORIENTED_EDGE ( 'NONE', *, *, #53337, .T. ) ;
#24653 = CARTESIAN_POINT ( 'NONE',  ( 9.070512820512819374, -4.000000000000000000, 29.75000000000000355 ) ) ;
#24654 = FACE_OUTER_BOUND ( 'NONE', #39143, .T. ) ;
#24655 = CARTESIAN_POINT ( 'NONE',  ( -0.06109907496450878162, -11.25000000000000000, 15.03311829374151287 ) ) ;
#24656 = EDGE_CURVE ( 'NONE', #21434, #58816, #36464, .T. ) ;
#24657 = CIRCLE ( 'NONE', #70631, 4.000000000000000000 ) ;
#24658 = CARTESIAN_POINT ( 'NONE',  ( 18.00000000000000000, -11.35647404775217417, 33.31231777344666511 ) ) ;
#24659 = CARTESIAN_POINT ( 'NONE',  ( -22.75000000000000000, -4.499999999999999112, 29.75000000000000355 ) ) ;
#24660 = ORIENTED_EDGE ( 'NONE', *, *, #52361, .T. ) ;
#24661 = CARTESIAN_POINT ( 'NONE',  ( -18.06527044596078113, -9.442884908240170461, 34.35708131394842013 ) ) ;
#24662 = FACE_OUTER_BOUND ( 'NONE', #63547, .T. ) ;
#24664 = ORIENTED_EDGE ( 'NONE', *, *, #50958, .T. ) ;
#24663 = LINE ( 'NONE', #18359, #28212 ) ;
#24665 = CARTESIAN_POINT ( 'NONE',  ( 11.66925197942848769, -4.684288915650983043, 34.18129842949671371 ) ) ;
#24666 = DIRECTION ( 'NONE',  ( -0.000000000000000000, 0.7660444431189791237, -0.6427876096865379196 ) ) ;
#24667 = CARTESIAN_POINT ( 'NONE',  ( -4.853911725310227077, -9.086983370893049639, 34.49168942202179267 ) ) ;
#24668 = CARTESIAN_POINT ( 'NONE',  ( -12.59168643127016196, -5.070767119584671079, 34.40440758774516183 ) ) ;
#24669 = EDGE_LOOP ( 'NONE', ( #41638, #14765 ) ) ;
#24670 = DIRECTION ( 'NONE',  ( 0.000000000000000000, 0.6427876096865368094, 0.7660444431189802339 ) ) ;
#24671 = CARTESIAN_POINT ( 'NONE',  ( -12.71151520558705172, -2.544273027872575366, 31.48422191005632342 ) ) ;
#24672 = EDGE_CURVE ( 'NONE', #29224, #54838, #44972, .T. ) ;
#24673 = EDGE_CURVE ( 'NONE', #54559, #66691, #39112, .T. ) ;
#24674 = CARTESIAN_POINT ( 'NONE',  ( 14.98074600654777377, -10.18141759479407327, 34.26406193332782379 ) ) ;
#24675 = ORIENTED_EDGE ( 'NONE', *, *, #210, .F. ) ;
#24676 = VERTEX_POINT ( 'NONE', #3549 ) ;
#24677 = B_SPLINE_CURVE_WITH_KNOTS ( 'NONE', 3,
 ( #40129, #82444, #458, #88765, #46863, #895, #13964, #55394, #55834, #41442 ),
 .UNSPECIFIED., .F., .F.,
 ( 4, 2, 2, 2, 4 ),
 ( 0.000000000000000000, 0.0001954311564186871184, 0.0003908623128373742367, 0.0005862934692560614093, 0.0007817246256747484735 ),
 .UNSPECIFIED. ) ;
#24678 = EDGE_LOOP ( 'NONE', ( #30302, #49394 ) ) ;
#24679 = FACE_OUTER_BOUND ( 'NONE', #7440, .T. ) ;
#24680 = CARTESIAN_POINT ( 'NONE',  ( 6.130790440966951138, -2.295524264805589354, 30.44142389570982488 ) ) ;
#24681 = B_SPLINE_CURVE_WITH_KNOTS ( 'NONE', 3,
 ( #55243, #26893, #82734, #81848, #7514, #89057, #75518, #21905, #7062, #21008 ),
 .UNSPECIFIED., .F., .F.,
 ( 4, 2, 2, 2, 4 ),
 ( 0.0007817246256747460882, 0.0009771112852218900684, 0.001172497944769033832, 0.001367884604316177595, 0.001563271263863321575 ),
 .UNSPECIFIED. ) ;
#24682 = CARTESIAN_POINT ( 'NONE',  ( -18.00000000000012079, -12.27809138561165270, 31.22303859784587132 ) ) ;
#24683 = EDGE_CURVE ( 'NONE', #33151, #19849, #24103, .T. ) ;
#24684 = CARTESIAN_POINT ( 'NONE',  ( 15.16468581981334651, -3.513871655860377086, 32.76840700105978499 ) ) ;
#24685 = AXIS2_PLACEMENT_3D ( 'NONE', #23161, #25385, #17294 ) ;
#24686 = ADVANCED_FACE ( 'NONE', ( #2652 ), #30145, .F. ) ;
#24687 = EDGE_CURVE ( 'NONE', #18603, #30988, #53136, .T. ) ;
#24688 = EDGE_LOOP ( 'NONE', ( #67699, #34871, #83534, #60631 ) ) ;
#24689 = ORIENTED_EDGE ( 'NONE', *, *, #52116, .T. ) ;
#24691 = ORIENTED_EDGE ( 'NONE', *, *, #18270, .F. ) ;
#24690 = CARTESIAN_POINT ( 'NONE',  ( -1.134669866267242533, -5.057305518903949526, 34.11320923018887896 ) ) ;
#24692 = CARTESIAN_POINT ( 'NONE',  ( -5.142193077479396024, -2.657715359629089225, 31.77849191805834295 ) ) ;
#24693 = VECTOR ( 'NONE', #16790, 1000.000000000000000 ) ;
#24694 = EDGE_CURVE ( 'NONE', #60609, #55169, #55205, .T. ) ;
#24695 = DIRECTION ( 'NONE',  ( 0.000000000000000000, 0.000000000000000000, -1.000000000000000000 ) ) ;
#24696 = CARTESIAN_POINT ( 'NONE',  ( -15.23076923076922995, -2.499999999999998668, 29.75000000000001421 ) ) ;
#24697 = CARTESIAN_POINT ( 'NONE',  ( -13.25382357679060519, -12.38066358083363738, 30.83685684665853444 ) ) ;
#24698 = ORIENTED_EDGE ( 'NONE', *, *, #34747, .T. ) ;
#24699 = ORIENTED_EDGE ( 'NONE', *, *, #49703, .T. ) ;
#24700 = ORIENTED_EDGE ( 'NONE', *, *, #78758, .F. ) ;
#24702 = ORIENTED_EDGE ( 'NONE', *, *, #19024, .T. ) ;
#24701 = CARTESIAN_POINT ( 'NONE',  ( -13.25457032869561402, -2.254550872974305342, 29.97347326024527092 ) ) ;
#24703 = LINE ( 'NONE', #38662, #86347 ) ;
#24704 = CARTESIAN_POINT ( 'NONE',  ( 18.13079044096695469, -5.496552790871120031, 34.60292014791297532 ) ) ;
#24705 = ORIENTED_EDGE ( 'NONE', *, *, #23423, .F. ) ;
#24706 = MECHANICAL_DESIGN_GEOMETRIC_PRESENTATION_REPRESENTATION (  '', ( #29349 ), #72806 ) ;
#24707 = CARTESIAN_POINT ( 'NONE',  ( -8.769230769230890843, -10.90142922262034020, 33.41473453929536674 ) ) ;
#24708 = DIRECTION ( 'NONE',  ( 0.000000000000000000, 0.7660444431189807890, 0.6427876096865361433 ) ) ;
#24709 = CARTESIAN_POINT ( 'NONE',  ( -5.776987155906603277, -3.395485233115139057, 33.02377354290275946 ) ) ;
#24710 = FACE_BOUND ( 'NONE', #78334, .T. ) ;
#24711 = CARTESIAN_POINT ( 'NONE',  ( 25.00000000000000355, 9.999999999999971578, 13.00000000000000178 ) ) ;
#24712 = CARTESIAN_POINT ( 'NONE',  ( 6.000000000000001776, -10.51840700105979565, 33.73612834413961536 ) ) ;
#24713 = EDGE_CURVE ( 'NONE', #49885, #3333, #63813, .T. ) ;
#24714 = VECTOR ( 'NONE', #85773, 999.9999999999998863 ) ;
#24715 = CARTESIAN_POINT ( 'NONE',  ( -6.923076923076922462, -12.78798330534103123, 29.99999999999997868 ) ) ;
#24717 = CARTESIAN_POINT ( 'NONE',  ( -8.519285359852728945, -12.07971442181322175, 32.31769673815850297 ) ) ;
#24716 = CARTESIAN_POINT ( 'NONE',  ( 17.07692307692338218, -2.506253911140615021, 30.00000000000323297 ) ) ;
#24718 = AXIS2_PLACEMENT_3D ( 'NONE', #29903, #75863, #8302 ) ;
#24719 = CARTESIAN_POINT ( 'NONE',  ( 16.15384615384615330, -11.91647553114624181, 32.58852847137148245 ) ) ;
#24720 = CARTESIAN_POINT ( 'NONE',  ( 5.299702618191482806, -2.600157965045225339, 30.74683119005207743 ) ) ;
#24721 = ORIENTED_EDGE ( 'NONE', *, *, #58489, .F. ) ;
#24722 = CARTESIAN_POINT ( 'NONE',  ( 8.769230769230768274, -2.538708090699994813, 30.37095296980875503 ) ) ;
#24723 = CARTESIAN_POINT ( 'NONE',  ( -7.623142494540995351, -2.554770724473668153, 30.48948780036025852 ) ) ;
#24724 = ORIENTED_EDGE ( 'NONE', *, *, #49596, .F. ) ;
#24725 = EDGE_LOOP ( 'NONE', ( #61101, #24468, #39342, #70009 ) ) ;
#24727 = CARTESIAN_POINT ( 'NONE',  ( 1.515405825582336607, -5.496552790871119143, 34.60292014791297532 ) ) ;
#24726 = DIRECTION ( 'NONE',  ( -0.000000000000000000, 1.000000000000000000, 3.491481338843133355E-15 ) ) ;
#24728 = CARTESIAN_POINT ( 'NONE',  ( -0.7115384615384742206, -2.499999999999999556, 29.81609845454692120 ) ) ;
#24729 = CARTESIAN_POINT ( 'NONE',  ( 3.230769230769231726, -9.905515769479276145, 34.41647553114623292 ) ) ;
#24730 = DIRECTION ( 'NONE',  ( 0.000000000000000000, 0.8660254037844377084, 0.5000000000000015543 ) ) ;
#24731 = ORIENTED_EDGE ( 'NONE', *, *, #38013, .T. ) ;
#24732 = DIRECTION ( 'NONE',  ( -0.000000000000000000, 0.9396926207859093161, -0.3420201433256662704 ) ) ;
#24733 = CARTESIAN_POINT ( 'NONE',  ( 18.24994540937804643, -4.176053281294515251, 33.81426240980091791 ) ) ;
#24735 = CARTESIAN_POINT ( 'NONE',  ( -9.942330929600657896, -4.335965774309648246, 33.62209801155881905 ) ) ;
#24734 = CARTESIAN_POINT ( 'NONE',  ( 11.76124120743959978, -3.020022701398814569, 32.48759521482552515 ) ) ;
#24736 = CARTESIAN_POINT ( 'NONE',  ( 7.622668902429897919, -5.912607949931405038, 34.49155766932282319 ) ) ;
#24737 = LINE ( 'NONE', #9887, #19444 ) ;
#24738 = CARTESIAN_POINT ( 'NONE',  ( 2.373759641042384683, -5.471508081941601098, 34.59228464037088457 ) ) ;
#24739 = CARTESIAN_POINT ( 'NONE',  ( 2.651650429449539104, -4.848349570550432475, 20.56250000000000000 ) ) ;
#24740 = VERTEX_POINT ( 'NONE', #25160 ) ;
#24741 = ORIENTED_EDGE ( 'NONE', *, *, #26252, .T. ) ;
#24742 = LINE ( 'NONE', #4476, #23333 ) ;
#24743 = DIRECTION ( 'NONE',  ( 0.000000000000000000, 0.000000000000000000, 1.000000000000000000 ) ) ;
#24744 = CARTESIAN_POINT ( 'NONE',  ( 9.692307692307572609, -10.21337939537710326, 33.94971097300076224 ) ) ;
#24745 = CARTESIAN_POINT ( 'NONE',  ( -16.28453762051371356, -4.809359713505814149, 33.96456829005828837 ) ) ;
#24746 = CARTESIAN_POINT ( 'NONE',  ( -0.4615384615385840772, -12.16647553114689728, 32.15551576947799362 ) ) ;
#24747 = CARTESIAN_POINT ( 'NONE',  ( 1.553300858899087311, -3.749999999999992006, 20.48437500000000000 ) ) ;
#24748 = DIRECTION ( 'NONE',  ( -0.000000000000000000, 0.9396926207859092051, -0.3420201433256662704 ) ) ;
#24749 = CARTESIAN_POINT ( 'NONE',  ( 1.607626736228235709, -4.887748414852792322, 34.01359900205216746 ) ) ;
#24750 = EDGE_CURVE ( 'NONE', #69684, #44956, #41336, .T. ) ;
#24751 = DIRECTION ( 'NONE',  ( 1.000000000000000000, 0.000000000000000000, -0.000000000000000000 ) ) ;
#24752 = CARTESIAN_POINT ( 'NONE',  ( 13.16168842570853492, -10.01117774369187252, 34.36070679894347535 ) ) ;
#24753 = DIRECTION ( 'NONE',  ( 0.000000000000000000, 0.4999999999999985567, 0.8660254037844395958 ) ) ;
#24754 = CARTESIAN_POINT ( 'NONE',  ( -9.915792636031639518, -12.24155766932282496, 31.33739205006857986 ) ) ;
#24756 = B_SPLINE_CURVE_WITH_KNOTS ( 'NONE', 3,
 ( #39073, #59770, #46261, #80500, #19238, #10699, #38165, #45358, #65622, #18793 ),
 .UNSPECIFIED., .F., .F.,
 ( 4, 2, 2, 2, 4 ),
 ( 0.0007817246256747464135, 0.0009771112852218902852, 0.001172497944769034265, 0.001367884604316178029, 0.001563271263863322009 ),
 .UNSPECIFIED. ) ;
#24755 = VECTOR ( 'NONE', #83463, 1000.000000000000114 ) ;
#24757 = FACE_OUTER_BOUND ( 'NONE', #10464, .T. ) ;
#24758 = CARTESIAN_POINT ( 'NONE',  ( -2.307692307692428724, -5.941354392335915335, 34.76329471203413846 ) ) ;
#24759 = CARTESIAN_POINT ( 'NONE',  ( -0.2385271099256120741, -11.24521262558773671, 33.06293181088029343 ) ) ;
#24760 = CARTESIAN_POINT ( 'NONE',  ( 13.19230769230769340, -7.500000000000000000, 33.75000000000000000 ) ) ;
#24761 = CARTESIAN_POINT ( 'NONE',  ( 4.000000000000001776, -7.499999999999999112, 14.00000000000000178 ) ) ;
#24762 = ORIENTED_EDGE ( 'NONE', *, *, #42048, .F. ) ;
#24763 = CARTESIAN_POINT ( 'NONE',  ( -16.21911615440247090, -9.528491918058357157, 34.59228464037090589 ) ) ;
#24764 = CARTESIAN_POINT ( 'NONE',  ( 18.06525513951284267, -5.094484230520771817, 34.41647553114626845 ) ) ;
#24765 = CARTESIAN_POINT ( 'NONE',  ( 5.933917620639864943, -2.486705287966279432, 31.30864560766542937 ) ) ;
#24766 = CARTESIAN_POINT ( 'NONE',  ( 2.750000000000008438, -8.639087296525996607, 25.79687500000000355 ) ) ;
#24767 = LINE ( 'NONE', #58992, #30297 ) ;
#24768 = DIRECTION ( 'NONE',  ( -0.000000000000000000, -0.9396926207859093161, -0.3420201433256663259 ) ) ;
#24770 = VERTEX_POINT ( 'NONE', #39588 ) ;
#24769 = CARTESIAN_POINT ( 'NONE',  ( -0.3307466537136761198, -2.541949514083463590, 30.39797389878540557 ) ) ;
#24771 = CARTESIAN_POINT ( 'NONE',  ( 1.139087296526029469, -10.24999999999999289, 20.95312500000000000 ) ) ;
#24772 = EDGE_CURVE ( 'NONE', #81618, #2005, #59516, .T. ) ;
#24773 = CARTESIAN_POINT ( 'NONE',  ( -1.449885830576159940, -10.21337939537584205, 33.94971097300158647 ) ) ;
#24774 = ORIENTED_EDGE ( 'NONE', *, *, #75793, .T. ) ;
#24775 = CARTESIAN_POINT ( 'NONE',  ( -4.376773112753000738, -8.282780595021769443, 34.94152052738834868 ) ) ;
#24776 = ORIENTED_EDGE ( 'NONE', *, *, #24936, .T. ) ;
#24777 = CYLINDRICAL_SURFACE ( 'NONE', #16149, 0.2500000000000008882 ) ;
#24778 = CARTESIAN_POINT ( 'NONE',  ( -1.514763354347077096, -12.15440758774515473, 32.17923288041532004 ) ) ;
#24779 = EDGE_CURVE ( 'NONE', #32972, #41920, #52018, .T. ) ;
#24780 = CARTESIAN_POINT ( 'NONE',  ( -12.46153846153846168, -13.78497067705608181, 32.30358669280327177 ) ) ;
#24781 = VERTEX_POINT ( 'NONE', #40471 ) ;
#24782 = CARTESIAN_POINT ( 'NONE',  ( 11.40777093535123576, -11.93127051446799847, 32.56575433478202797 ) ) ;
#24783 = ORIENTED_EDGE ( 'NONE', *, *, #44940, .F. ) ;
#24784 = CYLINDRICAL_SURFACE ( 'NONE', #22641, 0.2500000000000009437 ) ;
#24785 = ORIENTED_EDGE ( 'NONE', *, *, #43695, .F. ) ;
#24787 = CARTESIAN_POINT ( 'NONE',  ( 6.923076923076924238, -2.900454961884010974, 35.62045528018868623 ) ) ;
#24786 = AXIS2_PLACEMENT_3D ( 'NONE', #72092, #65331, #52265 ) ;
#24788 = CARTESIAN_POINT ( 'NONE',  ( 5.076923076922953193, -5.941354392335915335, 34.76329471203413846 ) ) ;
#24789 = ORIENTED_EDGE ( 'NONE', *, *, #47247, .F. ) ;
#24790 = CARTESIAN_POINT ( 'NONE',  ( -10.61538461538461320, -11.91647553114624181, 32.58852847137148245 ) ) ;
#24791 = CARTESIAN_POINT ( 'NONE',  ( 7.173131342990376247, -8.346898887586323923, 34.93166121998716278 ) ) ;
#24792 = DIRECTION ( 'NONE',  ( 0.000000000000000000, 0.000000000000000000, 1.000000000000000000 ) ) ;
#24793 = AXIS2_PLACEMENT_3D ( 'NONE', #24109, #37181, #45722 ) ;
#24794 = LINE ( 'NONE', #3629, #31999 ) ;
#24795 = DIRECTION ( 'NONE',  ( -0.000000000000000000, -0.000000000000000000, 1.000000000000000000 ) ) ;
#24796 = ADVANCED_FACE ( 'NONE', ( #53063 ), #46322, .F. ) ;
#24797 = ADVANCED_FACE ( 'NONE', ( #46770 ), #74244, .F. ) ;
#24798 = EDGE_LOOP ( 'NONE', ( #25875, #52427 ) ) ;
#24799 = EDGE_LOOP ( 'NONE', ( #40968, #73316, #3107, #83917, #77388, #4608, #51931 ) ) ;
#24800 = ORIENTED_EDGE ( 'NONE', *, *, #85079, .F. ) ;
#24802 = EDGE_LOOP ( 'NONE', ( #59623, #77401, #46016, #81648 ) ) ;
#24801 = CARTESIAN_POINT ( 'NONE',  ( 3.361559671736181976, -12.62708834333097663, 30.88030960425257021 ) ) ;
#24803 = CARTESIAN_POINT ( 'NONE',  ( 3.262820512820511443, -3.499999999999999556, 29.75000000000000355 ) ) ;
#24804 = DIRECTION ( 'NONE',  ( -0.000000000000000000, 1.000000000000000000, -0.000000000000000000 ) ) ;
#24805 = VERTEX_POINT ( 'NONE', #74694 ) ;
#24806 = ORIENTED_EDGE ( 'NONE', *, *, #36402, .T. ) ;
#24807 = CARTESIAN_POINT ( 'NONE',  ( -10.86536134632696715, -3.137211980971221781, 32.19342716148376837 ) ) ;
#24808 = ORIENTED_EDGE ( 'NONE', *, *, #55789, .T. ) ;
#24809 = AXIS2_PLACEMENT_3D ( 'NONE', #33172, #66519, #12026 ) ;
#24810 = CARTESIAN_POINT ( 'NONE',  ( -9.562262636387920622, -2.254550872974305342, 29.97347326024527092 ) ) ;
#24811 = CARTESIAN_POINT ( 'NONE',  ( 17.07692307692307665, -12.34228464037088635, 31.77849191805839268 ) ) ;
#24812 = CARTESIAN_POINT ( 'NONE',  ( -9.915135789942574718, -7.369209533119140509, 34.99857337881830688 ) ) ;
#24813 = FACE_BOUND ( 'NONE', #62357, .T. ) ;
#24814 = ORIENTED_EDGE ( 'NONE', *, *, #11182, .F. ) ;
#24815 = DIRECTION ( 'NONE',  ( -0.000000000000000000, -0.000000000000000000, -1.000000000000000000 ) ) ;
#24816 = CARTESIAN_POINT ( 'NONE',  ( 13.44987095589141113, -9.442884908240273489, 34.35708131394835618 ) ) ;
#24817 = DIRECTION ( 'NONE',  ( -0.000000000000000000, -0.000000000000000000, -1.000000000000000000 ) ) ;
#24818 = CARTESIAN_POINT ( 'NONE',  ( 0.4615384615384611200, -13.04860791097971706, 34.73218667398347037 ) ) ;
#24819 = DIRECTION ( 'NONE',  ( -0.000000000000000000, -0.7660444431189791237, -0.6427876096865379196 ) ) ;
#24820 = EDGE_LOOP ( 'NONE', ( #38485, #41788, #81221, #71106 ) ) ;
#24821 = LINE ( 'NONE', #58156, #23056 ) ;
#24822 = EDGE_LOOP ( 'NONE', ( #74332, #73632, #47750, #30756 ) ) ;
#24823 = ORIENTED_EDGE ( 'NONE', *, *, #49182, .T. ) ;
#24825 = CARTESIAN_POINT ( 'NONE',  ( -9.561517251340744039, -8.191423895709840863, 34.95447573519442130 ) ) ;
#24824 = CARTESIAN_POINT ( 'NONE',  ( -0.5268089074992374776, -9.442884908240170461, 34.35708131394840592 ) ) ;
#24826 = LINE ( 'NONE', #64030, #70090 ) ;
#24827 = CARTESIAN_POINT ( 'NONE',  ( -1.326923076923076872, -7.500000000000000000, 29.75000000000000355 ) ) ;
#24828 = PLANE ( 'NONE',  #58755 ) ;
#24829 = CARTESIAN_POINT ( 'NONE',  ( -16.15384615384615330, -10.67929555188718282, 33.92786785259544047 ) ) ;
#24830 = ORIENTED_EDGE ( 'NONE', *, *, #87105, .F. ) ;
#24831 = CARTESIAN_POINT ( 'NONE',  ( -10.61538461538461320, -3.669653830205710676, 35.88435417666054406 ) ) ;
#24832 = DIRECTION ( 'NONE',  ( 0.000000000000000000, 0.8660254037844377084, -0.5000000000000015543 ) ) ;
#24833 = CARTESIAN_POINT ( 'NONE',  ( 2.438217745925951530, -12.70449254468099198, 30.44128974285582956 ) ) ;
#24834 = CARTESIAN_POINT ( 'NONE',  ( 13.25446817517716980, -12.45813303252208648, 30.39737893381572675 ) ) ;
#24835 = ORIENTED_EDGE ( 'NONE', *, *, #84389, .T. ) ;
#24836 = ORIENTED_EDGE ( 'NONE', *, *, #71737, .T. ) ;
#24837 = FACE_BOUND ( 'NONE', #37354, .T. ) ;
#24838 = CONTEXT_DEPENDENT_SHAPE_REPRESENTATION ( #59027, #40664 ) ;
#24839 = ORIENTED_EDGE ( 'NONE', *, *, #32593, .T. ) ;
#24840 = VECTOR ( 'NONE', #28347, 1000.000000000000000 ) ;
#24841 = CARTESIAN_POINT ( 'NONE',  ( -17.77479207347706236, -2.251340707108580919, 29.87818027815299615 ) ) ;
#24842 = CARTESIAN_POINT ( 'NONE',  ( -1.161602540521989857, -2.308499170217967134, 30.53291367094873721 ) ) ;
#24843 = ORIENTED_EDGE ( 'NONE', *, *, #21032, .T. ) ;
#24844 = CYLINDRICAL_SURFACE ( 'NONE', #79830, 0.2499999999999994726 ) ;
#24845 = DIRECTION ( 'NONE',  ( -0.000000000000000000, -0.9848077530122085754, -0.1736481776669273613 ) ) ;
#24846 = DIRECTION ( 'NONE',  ( -0.000000000000000000, 0.000000000000000000, 1.000000000000000000 ) ) ;
#24847 = CARTESIAN_POINT ( 'NONE',  ( 4.219913487196228274, -6.343179335718452272, 34.87096338111212646 ) ) ;
#24848 = VECTOR ( 'NONE', #18046, 1000.000000000000000 ) ;
#24849 = CYLINDRICAL_SURFACE ( 'NONE', #18731, 0.2500000000000012212 ) ;
#24850 = ORIENTED_EDGE ( 'NONE', *, *, #69818, .F. ) ;
#24851 = EDGE_CURVE ( 'NONE', #26530, #43223, #12303, .T. ) ;
#24853 = VERTEX_POINT ( 'NONE', #67915 ) ;
#24852 = CARTESIAN_POINT ( 'NONE',  ( -7.846153846153965716, -10.21337939537710326, 33.94971097300076224 ) ) ;
#24854 = CARTESIAN_POINT ( 'NONE',  ( -8.638438961405983108, -9.804649428959608670, 34.18742332936588468 ) ) ;
#24855 = EDGE_CURVE ( 'NONE', #5324, #18937, #9126, .T. ) ;
#24856 = CARTESIAN_POINT ( 'NONE',  ( -4.219116599806929102, -2.892918686051582089, 31.69288490824015270 ) ) ;
#24857 = DIRECTION ( 'NONE',  ( 0.000000000000000000, 0.1736481776669275834, 0.9848077530122086864 ) ) ;
#24858 = CARTESIAN_POINT ( 'NONE',  ( -4.023054346021368133, -12.38066358083363738, 30.83685684665853444 ) ) ;
#24859 = CARTESIAN_POINT ( 'NONE',  ( 13.13463864056679853, -4.075325502946081535, 33.72974371597206300 ) ) ;
#24860 = CARTESIAN_POINT ( 'NONE',  ( -15.23076923076922995, -12.48256725967547354, 35.29906147534542527 ) ) ;
#24861 = CARTESIAN_POINT ( 'NONE',  ( -1.077988221561493543, -4.724691934501247914, 13.07999329374151642 ) ) ;
#24862 = ORIENTED_EDGE ( 'NONE', *, *, #45752, .F. ) ;
#24863 = CARTESIAN_POINT ( 'NONE',  ( -3.296852641725109834, -3.050289026998445951, 32.03036669348365706 ) ) ;
#24864 = B_SPLINE_CURVE_WITH_KNOTS ( 'NONE', 3,
 ( #44908, #79151, #52555, #19233, #24195, #11587, #25092, #74173, #80495, #72825 ),
 .UNSPECIFIED., .F., .F.,
 ( 4, 2, 2, 2, 4 ),
 ( 0.000000000000000000, 0.0001954311564186873352, 0.0003908623128373746704, 0.0005862934692560620598, 0.0007817246256747493408 ),
 .UNSPECIFIED. ) ;
#24865 = DIRECTION ( 'NONE',  ( -0.000000000000000000, 0.9396926207859092051, -0.3420201433256662704 ) ) ;
#24866 = CARTESIAN_POINT ( 'NONE',  ( -0.2115929431903200153, -5.057305518903948638, 34.11320923018887186 ) ) ;
#24867 = EDGE_CURVE ( 'NONE', #66835, #33483, #6221, .T. ) ;
#24868 = ORIENTED_EDGE ( 'NONE', *, *, #20485, .F. ) ;
#24869 = ORIENTED_EDGE ( 'NONE', *, *, #82547, .F. ) ;
#24870 = CARTESIAN_POINT ( 'NONE',  ( 9.757562831820530747, -3.643525952247864463, 33.31231777344670064 ) ) ;
#24871 = CARTESIAN_POINT ( 'NONE',  ( 25.00000000000000355, 9.999999999999971578, 3.000000000000000000 ) ) ;
#24872 = EDGE_CURVE ( 'NONE', #69245, #3657, #79950, .T. ) ;
#24873 = CARTESIAN_POINT ( 'NONE',  ( -0.3314932987036833256, -2.504778602574660340, 29.97347330155780298 ) ) ;
#24874 = CARTESIAN_POINT ( 'NONE',  ( 16.02315555073584008, -9.929715669179216775, 34.40415004197138416 ) ) ;
#24875 = CARTESIAN_POINT ( 'NONE',  ( 17.74997677577853850, -12.07920672191015221, 32.31858351112116168 ) ) ;
#24876 = VECTOR ( 'NONE', #10363, 1000.000000000000000 ) ;
#24877 = CYLINDRICAL_SURFACE ( 'NONE', #68125, 0.2499999999999997502 ) ;
#24878 = ORIENTED_EDGE ( 'NONE', *, *, #16662, .T. ) ;
#24879 = CARTESIAN_POINT ( 'NONE',  ( 9.692307692307695177, -10.51840700105979565, 33.73612834413961536 ) ) ;
#24880 = EDGE_CURVE ( 'NONE', #66904, #39806, #11642, .T. ) ;
#24881 = CARTESIAN_POINT ( 'NONE',  ( -19.00000000000000000, -7.500000000000000000, 33.75000000000000000 ) ) ;
#24882 = CARTESIAN_POINT ( 'NONE',  ( 4.087763774486018242, -8.164416787775445883, 34.95778746994557906 ) ) ;
#24883 = ORIENTED_EDGE ( 'NONE', *, *, #79490, .T. ) ;
#24884 = CARTESIAN_POINT ( 'NONE',  ( 15.90386940979756858, -12.41104346484419452, 31.60698883733904196 ) ) ;
#24885 = B_SPLINE_CURVE_WITH_KNOTS ( 'NONE', 3,
 ( #900, #20729, #21610, #48194, #41447, #14413, #8552, #68911, #55398, #7667 ),
 .UNSPECIFIED., .F., .F.,
 ( 4, 2, 2, 2, 4 ),
 ( 0.0007817359430256322827, 0.0009771253907249989254, 0.001172514838424365676, 0.001367904286123732428, 0.001563293733823098962 ),
 .UNSPECIFIED. ) ;
#24886 = ORIENTED_EDGE ( 'NONE', *, *, #67818, .F. ) ;
#24887 = CARTESIAN_POINT ( 'NONE',  ( -7.846153846153844924, -2.517432740324522911, 35.29906147534542527 ) ) ;
#24888 = CARTESIAN_POINT ( 'NONE',  ( -9.442307692306272315, -7.500000000000154543, 35.00000000000007105 ) ) ;
#24889 = CARTESIAN_POINT ( 'NONE',  ( 17.86985203026830504, -10.31621877034669588, 34.18098118002070152 ) ) ;
#24890 = VERTEX_POINT ( 'NONE', #60259 ) ;
#24891 = CARTESIAN_POINT ( 'NONE',  ( 8.769230769230768274, -12.10708131394839349, 31.69288490824020244 ) ) ;
#24892 = FACE_OUTER_BOUND ( 'NONE', #71462, .T. ) ;
#24893 = CARTESIAN_POINT ( 'NONE',  ( 1.326923076923075762, -7.500000000000000000, 29.75000000000000355 ) ) ;
#24894 = CARTESIAN_POINT ( 'NONE',  ( -12.46153846153846168, -3.050289026998446396, 32.03036669348365706 ) ) ;
#24895 = DIRECTION ( 'NONE',  ( -1.000000000000000000, -0.000000000000000000, 0.000000000000000000 ) ) ;
#24896 = EDGE_CURVE ( 'NONE', #66653, #85898, #77860, .T. ) ;
#24897 = VERTEX_POINT ( 'NONE', #27370 ) ;
#24898 = CARTESIAN_POINT ( 'NONE',  ( -4.153846153846152411, -12.34228464037088635, 31.77849191805839268 ) ) ;
#24899 = EDGE_CURVE ( 'NONE', #56816, #26148, #81882, .T. ) ;
#24900 = VERTEX_POINT ( 'NONE', #33242 ) ;
#24901 = CARTESIAN_POINT ( 'NONE',  ( 8.546304551714619890, -12.39988816332205701, 30.74660775122750778 ) ) ;
#24902 = AXIS2_PLACEMENT_3D ( 'NONE', #12436, #39921, #74585 ) ;
#24903 = CARTESIAN_POINT ( 'NONE',  ( 5.010839665967195877, -12.10708131394839349, 31.69288490824020244 ) ) ;
#24904 = COLOUR_RGB ( '', 0.66274510, 0.83137255, 0.94901961) ;
#24905 = CARTESIAN_POINT ( 'NONE',  ( -7.596153846152408740, -7.500000000000155431, 34.75000000000007105 ) ) ;
#24906 = ADVANCED_FACE ( 'NONE', ( #87769 ), #75123, .F. ) ;
#24907 = LINE ( 'NONE', #60026, #17137 ) ;
#24908 = EDGE_CURVE ( 'NONE', #37386, #21487, #84270, .T. ) ;
#24909 = CARTESIAN_POINT ( 'NONE',  ( 27.00000000000000000, -1.249999999999999112, 32.75000000000000000 ) ) ;
#24910 = CARTESIAN_POINT ( 'NONE',  ( -10.61538461538473577, -12.51329471203414379, 31.30864560766407578 ) ) ;
#24911 = AXIS2_PLACEMENT_3D ( 'NONE', #81199, #52816, #11855 ) ;
#24912 = B_SPLINE_CURVE_WITH_KNOTS ( 'NONE', 3,
 ( #30590, #70259, #72021, #10330, #84237, #22514, #2666, #70705, #57186, #37797 ),
 .UNSPECIFIED., .F., .F.,
 ( 4, 2, 2, 2, 4 ),
 ( 0.0007817246256747444619, 0.0009771112852218868158, 0.001172497944769029061, 0.001367884604316171523, 0.001563271263863313769 ),
 .UNSPECIFIED. ) ;
#24913 = ORIENTED_EDGE ( 'NONE', *, *, #56571, .T. ) ;
#24914 = ORIENTED_EDGE ( 'NONE', *, *, #88415, .T. ) ;
#24915 = EDGE_LOOP ( 'NONE', ( #86979, #74573, #80577, #24869 ) ) ;
#24916 = B_SPLINE_CURVE_WITH_KNOTS ( 'NONE', 3,
 ( #73948, #18555, #12683, #33403, #18997, #5928, #73504, #87934, #38830, #4591 ),
 .UNSPECIFIED., .F., .F.,
 ( 4, 2, 2, 2, 4 ),
 ( 0.000000000000000000, 0.0001954311564186861968, 0.0003908623128373723936, 0.0005862934692560585904, 0.0007817246256747447872 ),
 .UNSPECIFIED. ) ;
#24917 = ORIENTED_EDGE ( 'NONE', *, *, #80070, .T. ) ;
#24918 = EDGE_LOOP ( 'NONE', ( #56585, #86428 ) ) ;
#24919 = CARTESIAN_POINT ( 'NONE',  ( -14.30769230769230660, -2.499999999999998668, 29.50000000000001066 ) ) ;
#24920 = DIRECTION ( 'NONE',  ( -0.000000000000000000, -0.8660254037844399289, -0.4999999999999980016 ) ) ;
#24921 = DIRECTION ( 'NONE',  ( -1.000000000000000000, -0.000000000000000000, -0.000000000000000000 ) ) ;
#24922 = CARTESIAN_POINT ( 'NONE',  ( -5.776988648387149539, -4.887748414852792322, 34.01359900205216746 ) ) ;
#24923 = DIRECTION ( 'NONE',  ( 1.000000000000000000, 0.000000000000000000, 0.000000000000000000 ) ) ;
#24924 = LINE ( 'NONE', #31237, #19764 ) ;
#24925 = DIRECTION ( 'NONE',  ( -0.000000000000000000, 0.5000000000000011102, -0.8660254037844381525 ) ) ;
#24926 = CARTESIAN_POINT ( 'NONE',  ( -17.86947429823644029, -6.852161475712352789, 34.70806712695775786 ) ) ;
#24927 = DIRECTION ( 'NONE',  ( -0.000000000000000000, -0.6427876096865404731, -0.7660444431189771253 ) ) ;
#24928 = ORIENTED_EDGE ( 'NONE', *, *, #70642, .T. ) ;
#24929 = ORIENTED_EDGE ( 'NONE', *, *, #40150, .T. ) ;
#24930 = ORIENTED_EDGE ( 'NONE', *, *, #10004, .F. ) ;
#24932 = VERTEX_POINT ( 'NONE', #67475 ) ;
#24931 = CARTESIAN_POINT ( 'NONE',  ( 0.4615384615383382183, -3.083524468854526912, 32.58852847137268327 ) ) ;
#24934 = CARTESIAN_POINT ( 'NONE',  ( -16.15384615384615330, -9.780366693483667717, 34.19971097300155094 ) ) ;
#24933 = CARTESIAN_POINT ( 'NONE',  ( 7.715462379486287325, -3.062553014421049546, 32.05460306192773601 ) ) ;
#24935 = VECTOR ( 'NONE', #31338, 1000.000000000000000 ) ;
#24936 = EDGE_CURVE ( 'NONE', #52162, #45, #43413, .T. ) ;
#24937 = CARTESIAN_POINT ( 'NONE',  ( 1.607395053593452028, -4.989023458446560255, 34.36081565061822118 ) ) ;
#24938 = CARTESIAN_POINT ( 'NONE',  ( 7.173131234715237170, -2.564540009722896752, 30.55348353981670684 ) ) ;
#24939 = FACE_BOUND ( 'NONE', #39343, .T. ) ;
#24940 = ORIENTED_EDGE ( 'NONE', *, *, #74221, .F. ) ;
#24941 = ORIENTED_EDGE ( 'NONE', *, *, #24489, .T. ) ;
#24942 = CARTESIAN_POINT ( 'NONE',  ( -2.057692307692306599, -2.499999999999998668, 29.75000000000000355 ) ) ;
#24943 = VERTEX_POINT ( 'NONE', #48069 ) ;
#24944 = FACE_BOUND ( 'NONE', #37756, .T. ) ;
#24945 = B_SPLINE_CURVE_WITH_KNOTS ( 'NONE', 3,
 ( #17424, #3005, #43557, #86349, #57071, #36802, #84565, #22840, #50303, #16975 ),
 .UNSPECIFIED., .F., .F.,
 ( 4, 2, 2, 2, 4 ),
 ( 0.000000000000000000, 0.0001954339857564074473, 0.0003908679715128148945, 0.0005863019572692223418, 0.0007817359430256297891 ),
 .UNSPECIFIED. ) ;
#24946 = CARTESIAN_POINT ( 'NONE',  ( -10.68065461594093435, -3.083524468853724443, 32.58852847137143272 ) ) ;
#24947 = DIRECTION ( 'NONE',  ( 1.000000000000000000, 0.000000000000000000, 0.000000000000000000 ) ) ;
#24948 = ORIENTED_EDGE ( 'NONE', *, *, #7303, .F. ) ;
#24949 = CARTESIAN_POINT ( 'NONE',  ( 17.86985279056178300, -2.882441371585227508, 31.66841991370172238 ) ) ;
#24950 = CARTESIAN_POINT ( 'NONE',  ( -20.00000000000000000, -7.500000000000000000, 29.75000000000000355 ) ) ;
#24951 = DIRECTION ( 'NONE',  ( 0.000000000000000000, 0.1736481776669275834, 0.9848077530122086864 ) ) ;
#24952 = ORIENTED_EDGE ( 'NONE', *, *, #72945, .T. ) ;
#24953 = CARTESIAN_POINT ( 'NONE',  ( -11.53846153846153655, -4.661471528628507777, 34.16647553114623292 ) ) ;
#24954 = CARTESIAN_POINT ( 'NONE',  ( -14.53117725141625627, -5.912607949931405926, 34.49155766932282319 ) ) ;
#24955 = ORIENTED_EDGE ( 'NONE', *, *, #2006, .F. ) ;
#24956 = EDGE_CURVE ( 'NONE', #8429, #40093, #82764, .T. ) ;
#24957 = CARTESIAN_POINT ( 'NONE',  ( -2.557669038634660108, -11.28823185664190376, 33.01397839955799896 ) ) ;
#24958 = CYLINDRICAL_SURFACE ( 'NONE', #81561, 0.2500000000000009437 ) ;
#24959 = ORIENTED_EDGE ( 'NONE', *, *, #3407, .F. ) ;
#24960 = CARTESIAN_POINT ( 'NONE',  ( 18.06525557127601900, -6.879047030191284051, 34.71129190930002295 ) ) ;
#24961 = FACE_OUTER_BOUND ( 'NONE', #84643, .T. ) ;
#24963 = B_SPLINE_CURVE_WITH_KNOTS ( 'NONE', 3,
 ( #82016, #18977, #20311, #26175, #41025, #39706, #75254, #13545, #41464, #60395 ),
 .UNSPECIFIED., .F., .F.,
 ( 4, 2, 2, 2, 4 ),
 ( 0.0007817359430256317406, 0.0009771253907249982749, 0.001172514838424365026, 0.001367904286123731560, 0.001563293733823098094 ),
 .UNSPECIFIED. ) ;
#24962 = CARTESIAN_POINT ( 'NONE',  ( 12.46153846153846168, -13.49023893513002648, 31.06009739812518688 ) ) ;
#24964 = DIRECTION ( 'NONE',  ( -0.000000000000000000, -0.3420201433256694346, -0.9396926207859080948 ) ) ;
#24965 = CARTESIAN_POINT ( 'NONE',  ( -15.90379184220783948, -4.235687564193445276, 33.53795663066793509 ) ) ;
#24966 = LINE ( 'NONE', #87587, #43810 ) ;
#24969 = CARTESIAN_POINT ( 'NONE',  ( -15.48074596171158390, -12.41269422305637171, 30.68257228309993323 ) ) ;
#24968 = VECTOR ( 'NONE', #26812, 1000.000000000000114 ) ;
#24967 = CARTESIAN_POINT ( 'NONE',  ( 5.076923076922954969, -12.46129190930018460, 30.37095296980731973 ) ) ;
#24970 = DIRECTION ( 'NONE',  ( -0.000000000000000000, 1.000000000000000000, -0.000000000000000000 ) ) ;
#24972 = DIRECTION ( 'NONE',  ( -0.000000000000000000, -0.8660254037844397068, -0.4999999999999978906 ) ) ;
#24971 = CARTESIAN_POINT ( 'NONE',  ( 6.923076923076924238, -13.53365097954675988, 30.81389545987213552 ) ) ;
#24973 = CARTESIAN_POINT ( 'NONE',  ( -1.901340078031346525, -9.487747218494661183, 27.18563170625849068 ) ) ;
#24974 = ORIENTED_EDGE ( 'NONE', *, *, #61769, .F. ) ;
#24975 = VECTOR ( 'NONE', #82846, 1000.000000000000227 ) ;
#24976 = DIRECTION ( 'NONE',  ( 0.000000000000000000, 0.3420201433256641055, -0.9396926207859100932 ) ) ;
#24977 = ORIENTED_EDGE ( 'NONE', *, *, #43709, .F. ) ;
#24978 = EDGE_CURVE ( 'NONE', #69004, #88055, #28420, .T. ) ;
#24979 = ORIENTED_EDGE ( 'NONE', *, *, #73193, .F. ) ;
#24980 = CARTESIAN_POINT ( 'NONE',  ( -2.307692307692305711, -12.37446782046654192, 30.86335684631486131 ) ) ;
#24981 = EDGE_LOOP ( 'NONE', ( #5017, #10222 ) ) ;
#24982 = CARTESIAN_POINT ( 'NONE',  ( -15.00798968950081758, -5.913360116392397892, 34.49180327182771322 ) ) ;
#24983 = CARTESIAN_POINT ( 'NONE',  ( -2.775308065498764964, -6.422011778438537988, 27.42000670625849068 ) ) ;
#24984 = B_SPLINE_CURVE_WITH_KNOTS ( 'NONE', 3,
 ( #26774, #46166, #39855, #5616, #4736, #11941, #88068, #6510, #13261, #24993 ),
 .UNSPECIFIED., .F., .F.,
 ( 4, 2, 2, 2, 4 ),
 ( 0.000000000000000000, 0.0001954311564186875792, 0.0003908623128373751583, 0.0005862934692560627103, 0.0007817246256747503166 ),
 .UNSPECIFIED. ) ;
#24985 = ADVANCED_FACE ( 'NONE', ( #75992 ), #76441, .T. ) ;
#24986 = CARTESIAN_POINT ( 'NONE',  ( 10.68063975489745410, -2.657715359629132301, 31.77849191805844242 ) ) ;
#24987 = DIRECTION ( 'NONE',  ( -0.000000000000000000, -0.000000000000000000, -1.000000000000000000 ) ) ;
#24988 = CARTESIAN_POINT ( 'NONE',  ( -12.21159305216042057, -4.176053281294518804, 33.81426240980091791 ) ) ;
#24989 = LINE ( 'NONE', #53347, #57580 ) ;
#24990 = DIRECTION ( 'NONE',  ( -0.000000000000000000, 0.6427876096865404731, -0.7660444431189770143 ) ) ;
#24991 = FACE_OUTER_BOUND ( 'NONE', #88723, .T. ) ;
#24992 = CARTESIAN_POINT ( 'NONE',  ( -3.749999999999988454, -9.053300858899127945, 22.51562500000000000 ) ) ;
#24993 = CARTESIAN_POINT ( 'NONE',  ( -6.923076923077045919, -5.094484230521993062, 34.41647553114689373 ) ) ;
#24994 = CARTESIAN_POINT ( 'NONE',  ( -17.93393266664992680, -2.292212530054420050, 30.41441678777543345 ) ) ;
#24995 = EDGE_CURVE ( 'NONE', #42300, #14097, #41775, .T. ) ;
#24996 = DIRECTION ( 'NONE',  ( -0.000000000000000000, -0.9396926207859092051, -0.3420201433256662704 ) ) ;
#24997 = EDGE_CURVE ( 'NONE', #55965, #46285, #83134, .T. ) ;
#24998 = ORIENTED_EDGE ( 'NONE', *, *, #76662, .T. ) ;
#24999 = ORIENTED_EDGE ( 'NONE', *, *, #10720, .T. ) ;
#25000 = CARTESIAN_POINT ( 'NONE',  ( -11.53846153846153655, -5.557115091759785130, 34.35708131394839171 ) ) ;
#25001 = DIRECTION ( 'NONE',  ( 0.000000000000000000, 0.3420201433256641055, -0.9396926207859100932 ) ) ;
#25002 = CARTESIAN_POINT ( 'NONE',  ( 1.134638640566795642, -10.82459398097509684, 33.81372124010185587 ) ) ;
#25003 = CARTESIAN_POINT ( 'NONE',  ( -15.93083480223330817, -12.39991518177334129, 30.74647679643404530 ) ) ;
#25004 = EDGE_CURVE ( 'NONE', #35065, #65093, #70570, .T. ) ;
#25005 = CARTESIAN_POINT ( 'NONE',  ( 17.07692307692295586, -12.51329471203414379, 31.30864560766407578 ) ) ;
#25006 = CARTESIAN_POINT ( 'NONE',  ( -4.853910232829679039, -2.889357225399416862, 32.26129605718031002 ) ) ;
#25007 = VECTOR ( 'NONE', #19855, 1000.000000000000000 ) ;
#25008 = EDGE_CURVE ( 'NONE', #23467, #50664, #11180, .T. ) ;
#25009 = EDGE_LOOP ( 'NONE', ( #67616, #43959 ) ) ;
#25010 = CARTESIAN_POINT ( 'NONE',  ( 17.75002326905764605, -12.41269422305637171, 30.68257228309993323 ) ) ;
#25011 = ORIENTED_EDGE ( 'NONE', *, *, #39153, .T. ) ;
#25012 = EDGE_CURVE ( 'NONE', #58001, #18170, #36342, .T. ) ;
#25014 = ORIENTED_EDGE ( 'NONE', *, *, #42156, .F. ) ;
#25013 = B_SPLINE_CURVE_WITH_KNOTS ( 'NONE', 3,
 ( #2492, #50677, #85373, #79506, #45260, #84937, #23658, #17807, #71846, #78162 ),
 .UNSPECIFIED., .F., .F.,
 ( 4, 2, 2, 2, 4 ),
 ( 0.0007817359430256392216, 0.0009771253907250080327, 0.001172514838424376952, 0.001367904286123745872, 0.001563293733823114791 ),
 .UNSPECIFIED. ) ;
#25015 = CARTESIAN_POINT ( 'NONE',  ( -5.777220458731590291, -5.913360116392398780, 34.49180327182771322 ) ) ;
#25016 = LINE ( 'NONE', #45733, #86056 ) ;
#25017 = CARTESIAN_POINT ( 'NONE',  ( -14.08467946359890988, -2.889357225399414197, 32.26129605718031002 ) ) ;
#25018 = EDGE_CURVE ( 'NONE', #5565, #79802, #27435, .T. ) ;
#25019 = LINE ( 'NONE', #25912, #24935 ) ;
#25020 = DIRECTION ( 'NONE',  ( 1.000000000000000000, 0.000000000000000000, 0.000000000000000000 ) ) ;
#25021 = ORIENTED_EDGE ( 'NONE', *, *, #21337, .T. ) ;
#25022 = ORIENTED_EDGE ( 'NONE', *, *, #44481, .T. ) ;
#25023 = VERTEX_POINT ( 'NONE', #13846 ) ;
#25024 = AXIS2_PLACEMENT_3D ( 'NONE', #39895, #17386, #4772 ) ;
#25025 = CARTESIAN_POINT ( 'NONE',  ( -7.053767526187231240, -11.93127051446800024, 32.56575433478200665 ) ) ;
#25026 = CARTESIAN_POINT ( 'NONE',  ( 9.915087361285756629, -2.353885683473779800, 30.79025554430704403 ) ) ;
#25027 = EDGE_CURVE ( 'NONE', #43796, #21320, #41326, .T. ) ;
#25028 = CARTESIAN_POINT ( 'NONE',  ( 0.4615384615384611200, -12.29105614889573062, 35.45975837776705220 ) ) ;
#25030 = STYLED_ITEM ( 'NONE', ( #71522 ), #29637 ) ;
#25029 = B_SPLINE_CURVE_WITH_KNOTS ( 'NONE', 3,
 ( #57098, #23309, #21992, #3030, #1267, #9801 ),
 .UNSPECIFIED., .F., .F.,
 ( 4, 2, 4 ),
 ( 0.000000000000000000, 0.0001954784845028913534, 0.0003909569690057827069 ),
 .UNSPECIFIED. ) ;
#25031 = AXIS2_PLACEMENT_3D ( 'NONE', #8445, #2993, #37675 ) ;
#25032 = CARTESIAN_POINT ( 'NONE',  ( 1.384615384615386802, -3.513871655860378418, 32.76840700105978499 ) ) ;
#25033 = EDGE_CURVE ( 'NONE', #10616, #54130, #27808, .T. ) ;
#25034 = DIRECTION ( 'NONE',  ( 0.000000000000000000, 0.000000000000000000, 1.000000000000000000 ) ) ;
#25035 = LINE ( 'NONE', #44848, #22142 ) ;
#25036 = ORIENTED_EDGE ( 'NONE', *, *, #26654, .F. ) ;
#25037 = ORIENTED_EDGE ( 'NONE', *, *, #26323, .T. ) ;
#25038 = CARTESIAN_POINT ( 'NONE',  ( -3.749999999999988454, -9.053300858899127945, 26.26562500000000000 ) ) ;
#25039 = ORIENTED_EDGE ( 'NONE', *, *, #984, .T. ) ;
#25041 = ORIENTED_EDGE ( 'NONE', *, *, #48193, .F. ) ;
#25040 = CARTESIAN_POINT ( 'NONE',  ( 15.29602480204525605, -6.026961402152789304, 34.52809138561124769 ) ) ;
#25042 = CARTESIAN_POINT ( 'NONE',  ( 7.846153846153725020, -12.46129190930018460, 30.37095296980731973 ) ) ;
#25043 = CARTESIAN_POINT ( 'NONE',  ( 12.52679360105129547, -8.656820664281605460, 34.87096338111211224 ) ) ;
#25044 = EDGE_CURVE ( 'NONE', #27257, #1913, #32142, .T. ) ;
#25045 = CARTESIAN_POINT ( 'NONE',  ( -2.651650429449535551, -10.15165042944956753, 14.93750000000000000 ) ) ;
#25046 = ORIENTED_EDGE ( 'NONE', *, *, #74844, .F. ) ;
#25047 = B_SPLINE_CURVE_WITH_KNOTS ( 'NONE', 3,
 ( #15992, #16871, #77239, #29508, #9241, #3353, #36701, #74054, #12345, #66843 ),
 .UNSPECIFIED., .F., .F.,
 ( 4, 2, 2, 2, 4 ),
 ( 0.000000000000000000, 0.0001954311564186865763, 0.0003908623128373731525, 0.0005862934692560596746, 0.0007817246256747463051 ),
 .UNSPECIFIED. ) ;
#25048 = CARTESIAN_POINT ( 'NONE',  ( -13.38461538461550582, -12.27809138561165270, 31.22303859784587132 ) ) ;
#25049 = ORIENTED_EDGE ( 'NONE', *, *, #25303, .T. ) ;
#25050 = EDGE_CURVE ( 'NONE', #3308, #23412, #45646, .T. ) ;
#25051 = DIRECTION ( 'NONE',  ( 0.000000000000000000, 0.000000000000000000, -1.000000000000000000 ) ) ;
#25052 = CARTESIAN_POINT ( 'NONE',  ( 0.2386115026316120158, -11.43668979543635267, 33.22377378376090462 ) ) ;
#25053 = CARTESIAN_POINT ( 'NONE',  ( 0.2115384615384616196, -2.499999999999998668, 29.75000000000000355 ) ) ;
#25055 = CARTESIAN_POINT ( 'NONE',  ( 8.769230769230768274, -13.57706302396349152, 30.56769352161908060 ) ) ;
#25054 = CARTESIAN_POINT ( 'NONE',  ( 27.00000000000000000, -8.999999999999996447, 22.25000000000000000 ) ) ;
#25056 = EDGE_CURVE ( 'NONE', #31713, #72564, #38451, .T. ) ;
#25057 = CARTESIAN_POINT ( 'NONE',  ( -3.007989689500821573, -6.760870238392817200, 34.69528174975672385 ) ) ;
#25058 = CARTESIAN_POINT ( 'NONE',  ( -9.692307692307691624, -13.87047571288749737, 32.06866353760679544 ) ) ;
#25059 = ORIENTED_EDGE ( 'NONE', *, *, #7924, .F. ) ;
#25060 = CARTESIAN_POINT ( 'NONE',  ( 6.673100192134569397, -8.303909089506435137, 34.68538101551103381 ) ) ;
#25061 = CARTESIAN_POINT ( 'NONE',  ( -11.28846153846010303, -7.500000000000155431, 34.75000000000007105 ) ) ;
#25062 = DIRECTION ( 'NONE',  ( -0.000000000000000000, 1.000000000000000000, 3.491481338843133355E-15 ) ) ;
#25063 = ORIENTED_EDGE ( 'NONE', *, *, #42900, .T. ) ;
#25064 = EDGE_CURVE ( 'NONE', #50717, #14174, #60540, .T. ) ;
#25065 = VECTOR ( 'NONE', #83573, 1000.000000000000114 ) ;
#25066 = CYLINDRICAL_SURFACE ( 'NONE', #68903, 3.000000000000000000 ) ;
#25067 = DIRECTION ( 'NONE',  ( -0.000000000000000000, 1.000000000000000000, -0.000000000000000000 ) ) ;
#25068 = CARTESIAN_POINT ( 'NONE',  ( -10.61538461538461320, -10.51840700105979565, 33.73612834413961536 ) ) ;
#25069 = CARTESIAN_POINT ( 'NONE',  ( 10.48469314871705826, -11.71456829005830080, 32.44064028649416542 ) ) ;
#25070 = FACE_BOUND ( 'NONE', #55261, .T. ) ;
#25072 = CARTESIAN_POINT ( 'NONE',  ( -16.15384615384615330, -13.88283147151868846, 33.14645433367849847 ) ) ;
#25071 = CARTESIAN_POINT ( 'NONE',  ( 5.299935921016469820, -5.582272713120727481, 34.63742843783360570 ) ) ;
#25073 = CARTESIAN_POINT ( 'NONE',  ( 9.942307692307695177, -2.499999999999998668, 29.75000000000000355 ) ) ;
#25075 = DIRECTION ( 'NONE',  ( 0.000000000000000000, 0.6427876096865368094, 0.7660444431189802339 ) ) ;
#25074 = CARTESIAN_POINT ( 'NONE',  ( -1.319359813339359144, -12.27809138561124591, 31.22303859784720359 ) ) ;
#25076 = CARTESIAN_POINT ( 'NONE',  ( -3.903791733932700847, -10.82426656108011720, 33.81400080652039009 ) ) ;
#25077 = CARTESIAN_POINT ( 'NONE',  ( 6.249945409378045547, -4.932303261841489039, 34.32971442181322885 ) ) ;
#25078 = CARTESIAN_POINT ( 'NONE',  ( -2.694853999681210865, -4.891553140782108677, 26.24813170625849068 ) ) ;
#25079 = FACE_OUTER_BOUND ( 'NONE', #9601, .T. ) ;
#25080 = EDGE_LOOP ( 'NONE', ( #56467, #43330, #38851, #86512 ) ) ;
#25081 = DIRECTION ( 'NONE',  ( -0.000000000000000000, -0.9396926207859093161, -0.3420201433256663259 ) ) ;
#25082 = CARTESIAN_POINT ( 'NONE',  ( 8.069166690247241647, -10.01129605718032600, 34.36064277460058491 ) ) ;
#25083 = LINE ( 'NONE', #73275, #2792 ) ;
#25084 = CARTESIAN_POINT ( 'NONE',  ( -0.4330127018922180770, -10.21569512280005299, 29.50000000000000355 ) ) ;
#25085 = CARTESIAN_POINT ( 'NONE',  ( -16.85414340794500276, -2.353885683473779356, 30.79025554430704759 ) ) ;
#25086 = CARTESIAN_POINT ( 'NONE',  ( -12.52680846209478460, -6.835583212224499938, 34.95778746994557906 ) ) ;
#25087 = CARTESIAN_POINT ( 'NONE',  ( 1.901340078031349856, -5.512252781505337929, 15.31063170625849068 ) ) ;
#25088 = EDGE_CURVE ( 'NONE', #24897, #14333, #37014, .T. ) ;
#25089 = DIRECTION ( 'NONE',  ( -0.000000000000000000, -0.1736481776669307198, -0.9848077530122080203 ) ) ;
#25090 = CARTESIAN_POINT ( 'NONE',  ( -14.43838291080261449, -11.37499894934982692, 33.29245874905763003 ) ) ;
#25091 = CARTESIAN_POINT ( 'NONE',  ( 7.976945653978634532, -11.71459661697925903, 32.44059661609676937 ) ) ;
#25092 = CARTESIAN_POINT ( 'NONE',  ( -0.6850233861027921201, -8.539481045369598178, 34.89627647299170832 ) ) ;
#25093 = LINE ( 'NONE', #32736, #77084 ) ;
#25094 = CARTESIAN_POINT ( 'NONE',  ( -9.019254006523732770, -9.271318131107980420, 34.42618302367067429 ) ) ;
#25095 = B_SPLINE_CURVE_WITH_KNOTS ( 'NONE', 3,
 ( #57533, #44899, #58866, #2580, #65172, #85021, #78699, #85456, #17890, #11125 ),
 .UNSPECIFIED., .F., .F.,
 ( 4, 2, 2, 2, 4 ),
 ( 0.000000000000000000, 0.0001954311564186869015, 0.0003908623128373738030, 0.0005862934692560607588, 0.0007817246256747476061 ),
 .UNSPECIFIED. ) ;
#25096 = CYLINDRICAL_SURFACE ( 'NONE', #73614, 0.2499999999999994726 ) ;
#25097 = CARTESIAN_POINT ( 'NONE',  ( 17.32686848630112308, -8.476813868363244353, 34.90874843262270133 ) ) ;
#25098 = ORIENTED_EDGE ( 'NONE', *, *, #64097, .F. ) ;
#25099 = CARTESIAN_POINT ( 'NONE',  ( 6.988221703796556383, -7.750023224968867197, 34.99404313364389907 ) ) ;
#25100 = CARTESIAN_POINT ( 'NONE',  ( -4.153846153846152411, -2.249999999999998668, 29.75000000000001776 ) ) ;
#25101 = CARTESIAN_POINT ( 'NONE',  ( 1.614399933863618797, -3.775308065498751198, 19.48624329374152353 ) ) ;
#25102 = CIRCLE ( 'NONE', #65340, 5.000000000000000888 ) ;
#25103 = VECTOR ( 'NONE', #48341, 1000.000000000000000 ) ;
#25104 = CARTESIAN_POINT ( 'NONE',  ( 6.223011351612852238, -4.187068189119697692, 33.49521262558774026 ) ) ;
#25105 = CARTESIAN_POINT ( 'NONE',  ( -23.50000000000000000, 12.75000000000000355, 29.19862367942583603 ) ) ;
#25106 = EDGE_LOOP ( 'NONE', ( #45111, #33147 ) ) ;
#25107 = CARTESIAN_POINT ( 'NONE',  ( 1.607394925883795622, -4.387253974876678342, 33.66317474335728832 ) ) ;
#25108 = CARTESIAN_POINT ( 'NONE',  ( -12.46153846153846168, -12.62096338111211580, 30.90682066428153263 ) ) ;
#25110 = ORIENTED_EDGE ( 'NONE', *, *, #87812, .F. ) ;
#25109 = CARTESIAN_POINT ( 'NONE',  ( 11.28848479441294650, -2.920706130388546651, 32.31842814019191223 ) ) ;
#25111 = CARTESIAN_POINT ( 'NONE',  ( 11.66898697669518192, -5.070358843744210198, 34.40418822224088302 ) ) ;
#25112 = CYLINDRICAL_SURFACE ( 'NONE', #84349, 0.2499999999999986955 ) ;
#25113 = FACE_OUTER_BOUND ( 'NONE', #84259, .T. ) ;
#25114 = LINE ( 'NONE', #59339, #16929 ) ;
#25115 = EDGE_LOOP ( 'NONE', ( #79780, #56104, #21752, #77479 ) ) ;
#25116 = CARTESIAN_POINT ( 'NONE',  ( 2.557746619330623528, -12.17597550085003455, 31.52189283813461884 ) ) ;
#25117 = CARTESIAN_POINT ( 'NONE',  ( 1.384615384615386802, -13.78497067705608181, 32.30358669280327177 ) ) ;
#25118 = EDGE_CURVE ( 'NONE', #17226, #83191, #71310, .T. ) ;
#25119 = CARTESIAN_POINT ( 'NONE',  ( 15.00728430620490350, -10.23692288466677880, 34.23039457007281072 ) ) ;
#25120 = ORIENTED_EDGE ( 'NONE', *, *, #64050, .T. ) ;
#25121 = ORIENTED_EDGE ( 'NONE', *, *, #22807, .T. ) ;
#25122 = EDGE_CURVE ( 'NONE', #5856, #30896, #60492, .T. ) ;
#25123 = ORIENTED_EDGE ( 'NONE', *, *, #24636, .T. ) ;
#25124 = CARTESIAN_POINT ( 'NONE',  ( 12.71148387091650278, -10.18230066228895758, 34.26354781536631577 ) ) ;
#25125 = CARTESIAN_POINT ( 'NONE',  ( -8.546451227962359454, -3.236590943229499029, 32.36255958852954251 ) ) ;
#25126 = EDGE_CURVE ( 'NONE', #11427, #42436, #4214, .T. ) ;
#25127 = DIRECTION ( 'NONE',  ( -0.000000000000000000, 0.9396926207859092051, -0.3420201433256662704 ) ) ;
#25128 = VECTOR ( 'NONE', #86367, 1000.000000000000227 ) ;
#25129 = ADVANCED_FACE ( 'NONE', ( #60043 ), #87549, .F. ) ;
#25130 = CARTESIAN_POINT ( 'NONE',  ( -10.55012904410859065, -3.300289026998473041, 32.46337939537591666 ) ) ;
#25131 = B_SPLINE_CURVE_WITH_KNOTS ( 'NONE', 3,
 ( #73062, #25766, #80729, #86140, #53677, #19009, #17679, #32512, #66748, #52334 ),
 .UNSPECIFIED., .F., .F.,
 ( 4, 2, 2, 2, 4 ),
 ( 0.000000000000000000, 0.0001954311584214085934, 0.0003908623168428171867, 0.0005862934752642231509, 0.0007817246336856291692 ),
 .UNSPECIFIED. ) ;
#25132 = ORIENTED_EDGE ( 'NONE', *, *, #27337, .F. ) ;
#25133 = VERTEX_POINT ( 'NONE', #67256 ) ;
#25135 = ORIENTED_EDGE ( 'NONE', *, *, #87534, .T. ) ;
#25134 = DIRECTION ( 'NONE',  ( -1.000000000000000000, 0.000000000000000000, 0.000000000000000000 ) ) ;
#25136 = LINE ( 'NONE', #60248, #54556 ) ;
#25137 = ADVANCED_FACE ( 'NONE', ( #79881 ), #5554, .F. ) ;
#25138 = DIRECTION ( 'NONE',  ( -0.000000000000000000, 0.5000000000000011102, -0.8660254037844381525 ) ) ;
#25139 = CARTESIAN_POINT ( 'NONE',  ( 10.36538461538461675, -2.249999999999998668, 29.75000000000000355 ) ) ;
#25140 = CARTESIAN_POINT ( 'NONE',  ( -13.38461538461550582, -12.46129190930018460, 30.37095296980731973 ) ) ;
#25141 = ORIENTED_EDGE ( 'NONE', *, *, #73207, .F. ) ;
#25142 = ORIENTED_EDGE ( 'NONE', *, *, #8750, .F. ) ;
#25143 = VERTEX_POINT ( 'NONE', #24477 ) ;
#25145 = ORIENTED_EDGE ( 'NONE', *, *, #69846, .F. ) ;
#25144 = CARTESIAN_POINT ( 'NONE',  ( -19.50000000000000000, -3.499999999999999556, 29.75000000000000355 ) ) ;
#25146 = CARTESIAN_POINT ( 'NONE',  ( -10.83825087844771495, -2.251424796025575326, 29.88072029997477941 ) ) ;
#25147 = VECTOR ( 'NONE', #14539, 1000.000000000000000 ) ;
#25148 = DIRECTION ( 'NONE',  ( 0.000000000000000000, 0.6427876096865368094, 0.7660444431189802339 ) ) ;
#25149 = VERTEX_POINT ( 'NONE', #38905 ) ;
#25150 = CARTESIAN_POINT ( 'NONE',  ( -8.992156986746913105, -10.61292498521070549, 33.66303323003028680 ) ) ;
#25151 = CARTESIAN_POINT ( 'NONE',  ( -13.63461538461538325, -2.499999999999998668, 29.75000000000000355 ) ) ;
#25152 = CARTESIAN_POINT ( 'NONE',  ( -5.749945580086545327, -3.435999193479609914, 33.07426656108010832 ) ) ;
#25153 = FACE_BOUND ( 'NONE', #88586, .T. ) ;
#25154 = EDGE_CURVE ( 'NONE', #53616, #30978, #46538, .T. ) ;
#25155 = CYLINDRICAL_SURFACE ( 'NONE', #35605, 4.000000000000000000 ) ;
#25156 = FACE_OUTER_BOUND ( 'NONE', #35988, .T. ) ;
#25157 = VECTOR ( 'NONE', #83261, 1000.000000000000114 ) ;
#25158 = CARTESIAN_POINT ( 'NONE',  ( -10.55012947587177408, -11.06231777344671130, 33.60647404775212976 ) ) ;
#25160 = CARTESIAN_POINT ( 'NONE',  ( 0.3589743589743586982, -11.50000000000000000, 29.75000000000000355 ) ) ;
#25159 = CARTESIAN_POINT ( 'NONE',  ( 17.14211705870643243, -2.506253911140448043, 29.99999999999988631 ) ) ;
#25161 = DIRECTION ( 'NONE',  ( 1.000000000000000000, 0.000000000000000000, 0.000000000000000000 ) ) ;
#25162 = FACE_OUTER_BOUND ( 'NONE', #21348, .T. ) ;
#25163 = EDGE_LOOP ( 'NONE', ( #13803, #8434, #1029, #24913 ) ) ;
#25164 = CARTESIAN_POINT ( 'NONE',  ( -16.02300773583338867, -7.277220443632451463, 34.74524770363009196 ) ) ;
#25165 = AXIS2_PLACEMENT_3D ( 'NONE', #61240, #88753, #41432 ) ;
#25166 = DIRECTION ( 'NONE',  ( -0.000000000000000000, 0.3420201433256694901, -0.9396926207859082059 ) ) ;
#25167 = ORIENTED_EDGE ( 'NONE', *, *, #20165, .T. ) ;
#25168 = VERTEX_POINT ( 'NONE', #10535 ) ;
#25170 = CARTESIAN_POINT ( 'NONE',  ( -17.07692307692307665, -11.16473453929635440, 33.15142922261926373 ) ) ;
#25169 = CARTESIAN_POINT ( 'NONE',  ( -11.78843828251013015, -12.65889640711025521, 30.72598325615533454 ) ) ;
#25171 = EDGE_CURVE ( 'NONE', #65576, #23097, #14376, .T. ) ;
#25172 = CARTESIAN_POINT ( 'NONE',  ( -13.44993939741969413, -7.749976730030849303, 34.74374725381503737 ) ) ;
#25173 = CARTESIAN_POINT ( 'NONE',  ( -15.23076923076922995, -2.538708090699994813, 30.37095296980875503 ) ) ;
#25174 = CARTESIAN_POINT ( 'NONE',  ( -5.198717948717948012, -3.499999999999999556, 29.75000000000000355 ) ) ;
#25175 = VERTEX_POINT ( 'NONE', #13199 ) ;
#25176 = CARTESIAN_POINT ( 'NONE',  ( 14.37294787896833270, -9.442884908240273489, 34.35708131394835618 ) ) ;
#25177 = CARTESIAN_POINT ( 'NONE',  ( 18.06606733335007675, -2.486705287966280320, 31.30864560766543647 ) ) ;
#25178 = EDGE_CURVE ( 'NONE', #68357, #75345, #24657, .T. ) ;
#25180 = CARTESIAN_POINT ( 'NONE',  ( 5.749976775778542937, -6.652501968072646932, 34.93155406624980941 ) ) ;
#25179 = DIRECTION ( 'NONE',  ( -0.000000000000000000, -0.9848077530122086864, -0.1736481776669273613 ) ) ;
#25181 = FACE_OUTER_BOUND ( 'NONE', #21449, .T. ) ;
#25182 = DIRECTION ( 'NONE',  ( 0.000000000000000000, 0.000000000000000000, 1.000000000000000000 ) ) ;
#25184 = CARTESIAN_POINT ( 'NONE',  ( -16.85414340794500276, -2.612705202774696200, 31.66806509827799943 ) ) ;
#25183 = SURFACE_STYLE_USAGE ( .BOTH. , #24279 ) ;
#25185 = B_SPLINE_CURVE_WITH_KNOTS ( 'NONE', 3,
 ( #14016, #34733, #27976, #55444, #82929, #14916, #9471, #70738, #57219, #76154 ),
 .UNSPECIFIED., .F., .F.,
 ( 4, 2, 2, 2, 4 ),
 ( 0.0007817246336856284103, 0.0009771112958940092897, 0.001172497958102390169, 0.001367884620310771265, 0.001563271282519152145 ),
 .UNSPECIFIED. ) ;
#25186 = CARTESIAN_POINT ( 'NONE',  ( -1.553300858899081538, -11.25000000000000711, 21.10937500000000711 ) ) ;
#25187 = ORIENTED_EDGE ( 'NONE', *, *, #18434, .F. ) ;
#25188 = EDGE_LOOP ( 'NONE', ( #58026, #5841, #81680, #65762 ) ) ;
#25189 = CARTESIAN_POINT ( 'NONE',  ( -14.53117723225663838, -4.988325925672468131, 34.36044203135681130 ) ) ;
#25190 = LINE ( 'NONE', #18441, #35487 ) ;
#25191 = CARTESIAN_POINT ( 'NONE',  ( 10.86533013373275836, -2.587454068350148351, 30.68340429815432202 ) ) ;
#25192 = CARTESIAN_POINT ( 'NONE',  ( 2.307692307692309264, -3.513871655860378418, 32.76840700105978499 ) ) ;
#25193 = DIRECTION ( 'NONE',  ( 0.000000000000000000, 0.3420201433256610524, 0.9396926207859113145 ) ) ;
#25194 = CARTESIAN_POINT ( 'NONE',  ( -2.651650429449535551, -10.15165042944956753, 22.43750000000000000 ) ) ;
#25195 = ADVANCED_FACE ( 'NONE', ( #20398 ), #12748, .F. ) ;
#25196 = CARTESIAN_POINT ( 'NONE',  ( -7.846153846153844924, -8.120952969808772792, 34.71129190930000163 ) ) ;
#25197 = CARTESIAN_POINT ( 'NONE',  ( 14.30769230769218581, -6.835583212225970762, 34.95778746994575670 ) ) ;
#25198 = AXIS2_PLACEMENT_3D ( 'NONE', #72597, #15898, #23087 ) ;
#25199 = CARTESIAN_POINT ( 'NONE',  ( 17.07692307692307665, -12.10708131394839349, 31.69288490824020244 ) ) ;
#25200 = CARTESIAN_POINT ( 'NONE',  ( 13.16113046005105680, -10.23692288466677880, 34.23039457007281072 ) ) ;
#25201 = CARTESIAN_POINT ( 'NONE',  ( -10.61538461538461320, -8.164416787775445883, 34.95778746994557906 ) ) ;
#25202 = CARTESIAN_POINT ( 'NONE',  ( 13.38461538461526423, -2.657715359629662544, 31.77849191805970364 ) ) ;
#25203 = EDGE_CURVE ( 'NONE', #47389, #28787, #513, .T. ) ;
#25204 = EDGE_CURVE ( 'NONE', #36240, #74452, #32718, .T. ) ;
#25205 = CARTESIAN_POINT ( 'NONE',  ( -12.59168643127016196, -8.630895178749533159, 34.87696386517710323 ) ) ;
#25206 = CARTESIAN_POINT ( 'NONE',  ( 3.903869422903798458, -12.41269422305637171, 30.68257228309993323 ) ) ;
#25207 = CARTESIAN_POINT ( 'NONE',  ( 10.74617642320939837, -2.729792928343269587, 31.24908615093345077 ) ) ;
#25208 = LINE ( 'NONE', #17111, #24876 ) ;
#25209 = CARTESIAN_POINT ( 'NONE',  ( -15.23076923076922995, -9.780366693483667717, 34.19971097300155094 ) ) ;
#25210 = EDGE_LOOP ( 'NONE', ( #49992, #76417 ) ) ;
#25211 = EDGE_CURVE ( 'NONE', #72338, #14030, #21868, .T. ) ;
#25212 = DIRECTION ( 'NONE',  ( -0.000000000000000000, -0.6427876096865404731, -0.7660444431189771253 ) ) ;
#25213 = CYLINDRICAL_SURFACE ( 'NONE', #43187, 2.000000000000001776 ) ;
#25214 = LINE ( 'NONE', #65302, #57742 ) ;
#25215 = CARTESIAN_POINT ( 'NONE',  ( -1.077988221561493543, -4.724691934501247914, 18.07999329374151287 ) ) ;
#25216 = CARTESIAN_POINT ( 'NONE',  ( -14.30769230769230660, -5.471508081941601098, 34.59228464037088457 ) ) ;
#25217 = CARTESIAN_POINT ( 'NONE',  ( 16.02369818411445479, -5.070767119584671079, 34.40440758774516183 ) ) ;
#25219 = EDGE_LOOP ( 'NONE', ( #26134, #76689 ) ) ;
#25218 = LINE ( 'NONE', #59887, #85700 ) ;
#25220 = CARTESIAN_POINT ( 'NONE',  ( -1.944543648263014957, -5.555456351737005249, 16.50000000000000000 ) ) ;
#25221 = DIRECTION ( 'NONE',  ( -1.000000000000000000, 0.000000000000000000, -0.000000000000000000 ) ) ;
#25222 = EDGE_LOOP ( 'NONE', ( #58087, #33371 ) ) ;
#25223 = CARTESIAN_POINT ( 'NONE',  ( 18.06606835100243913, -8.973038597847269315, 34.52809138561122637 ) ) ;
#25224 = VERTEX_POINT ( 'NONE', #33902 ) ;
#25225 = B_SPLINE_CURVE_WITH_KNOTS ( 'NONE', 3,
 ( #85365, #16016, #70958, #2926, #84929, #77267, #50222, #78595, #71837, #78155 ),
 .UNSPECIFIED., .F., .F.,
 ( 4, 2, 2, 2, 4 ),
 ( 0.0007817246256747460882, 0.0009771112852218892010, 0.001172497944769032314, 0.001367884604316175210, 0.001563271263863318323 ),
 .UNSPECIFIED. ) ;
#25226 = CARTESIAN_POINT ( 'NONE',  ( -18.00000000000012079, -11.94971097300221352, 32.03036669348236387 ) ) ;
#25227 = B_SPLINE_CURVE_WITH_KNOTS ( 'NONE', 3,
 ( #69566, #83987, #43431, #70462, #62355, #7434, #83543, #8319, #49735, #77208 ),
 .UNSPECIFIED., .F., .F.,
 ( 4, 2, 2, 2, 4 ),
 ( 0.0007817359430256308733, 0.0009771253907249971907, 0.001172514838424363725, 0.001367904286123730259, 0.001563293733823096577 ),
 .UNSPECIFIED. ) ;
#25228 = CARTESIAN_POINT ( 'NONE',  ( -15.48076923076922995, -7.500000000000001776, 35.04278698407183867 ) ) ;
#25229 = AXIS2_PLACEMENT_3D ( 'NONE', #81918, #34155, #40050 ) ;
#25230 = LINE ( 'NONE', #4514, #59892 ) ;
#25231 = VERTEX_POINT ( 'NONE', #81661 ) ;
#25232 = CARTESIAN_POINT ( 'NONE',  ( 0.3954560821783248969, -4.661471528628507777, 34.16647553114621871 ) ) ;
#25233 = EDGE_LOOP ( 'NONE', ( #21747, #21676 ) ) ;
#25234 = FACE_OUTER_BOUND ( 'NONE', #59474, .T. ) ;
#25235 = EDGE_CURVE ( 'NONE', #25963, #87033, #15332, .T. ) ;
#25236 = ORIENTED_EDGE ( 'NONE', *, *, #53715, .F. ) ;
#25237 = CARTESIAN_POINT ( 'NONE',  ( -6.923076923076922462, -11.33034616979429110, 35.88435417666054406 ) ) ;
#25238 = CARTESIAN_POINT ( 'NONE',  ( 0.6845498131513102491, -11.24521262558773671, 33.06293181088029343 ) ) ;
#25239 = CIRCLE ( 'NONE', #75566, 8.000000000000000000 ) ;
#25240 = LINE ( 'NONE', #25684, #33247 ) ;
#25241 = DIRECTION ( 'NONE',  ( -0.000000000000000000, 0.6427876096865404731, -0.7660444431189770143 ) ) ;
#25242 = CARTESIAN_POINT ( 'NONE',  ( -1.319360245102545237, -11.06231777344671130, 33.60647404775212976 ) ) ;
#25243 = EDGE_CURVE ( 'NONE', #6016, #75911, #84091, .T. ) ;
#25244 = DIRECTION ( 'NONE',  ( 0.000000000000000000, 0.7660444431189807890, 0.6427876096865361433 ) ) ;
#25245 = ORIENTED_EDGE ( 'NONE', *, *, #36636, .T. ) ;
#25246 = ORIENTED_EDGE ( 'NONE', *, *, #83434, .T. ) ;
#25247 = ORIENTED_EDGE ( 'NONE', *, *, #67025, .T. ) ;
#25249 = EDGE_LOOP ( 'NONE', ( #5066, #37248, #1749, #40663 ) ) ;
#25248 = CARTESIAN_POINT ( 'NONE',  ( 3.361561038594017781, -3.530189275343204702, 32.79018710029569661 ) ) ;
#25250 = ADVANCED_FACE ( 'NONE', ( #19503, #15419 ), #56831, .T. ) ;
#25251 = CARTESIAN_POINT ( 'NONE',  ( -8.899922235898328537, -9.804603061927743113, 34.18744698557895845 ) ) ;
#25252 = CARTESIAN_POINT ( 'NONE',  ( 9.468822767743365176, -5.827078755546623690, 34.72654668319379567 ) ) ;
#25253 = ORIENTED_EDGE ( 'NONE', *, *, #14039, .T. ) ;
#25254 = CARTESIAN_POINT ( 'NONE',  ( 16.15384615384615330, -6.386643153685126251, 34.62446782046654192 ) ) ;
#25255 = B_SPLINE_CURVE_WITH_KNOTS ( 'NONE', 3,
 ( #19395, #13522, #27041, #54504, #82443, #75660, #53621, #68463, #34234, #62151 ),
 .UNSPECIFIED., .F., .F.,
 ( 4, 2, 2, 2, 4 ),
 ( 0.000000000000000000, 0.0001954311564186868473, 0.0003908623128373736946, 0.0005862934692560605419, 0.0007817246256747473893 ),
 .UNSPECIFIED. ) ;
#25256 = AXIS2_PLACEMENT_3D ( 'NONE', #49257, #58540, #28099 ) ;
#25257 = ADVANCED_FACE ( 'NONE', ( #9529 ), #63589, .F. ) ;
#25258 = EDGE_LOOP ( 'NONE', ( #80079, #35342, #59026, #45954 ) ) ;
#25259 = CARTESIAN_POINT ( 'NONE',  ( -9.320512820512821150, -11.00000000000000000, 29.25000000000000000 ) ) ;
#25260 = ORIENTED_EDGE ( 'NONE', *, *, #86823, .T. ) ;
#25261 = B_SPLINE_CURVE_WITH_KNOTS ( 'NONE', 3,
 ( #36327, #84081, #37194, #64659, #78187, #64215, #15607, #84518, #2081, #43076 ),
 .UNSPECIFIED., .F., .F.,
 ( 4, 2, 2, 2, 4 ),
 ( 0.000000000000000000, 0.0001954339857564073388, 0.0003908679715128146777, 0.0005863019572692220165, 0.0007817359430256293554 ),
 .UNSPECIFIED. ) ;
#25262 = LINE ( 'NONE', #80212, #31617 ) ;
#25263 = B_SPLINE_CURVE_WITH_KNOTS ( 'NONE', 3,
 ( #88871, #27144, #82099, #67253, #47405, #68137, #33465, #46961, #32566, #25822 ),
 .UNSPECIFIED., .F., .F.,
 ( 4, 2, 2, 2, 4 ),
 ( 0.000000000000000000, 0.0001954339857564091278, 0.0003908679715128182556, 0.0005863019572692274375, 0.0007817359430256365111 ),
 .UNSPECIFIED. ) ;
#25264 = DIRECTION ( 'NONE',  ( -0.000000000000000000, 0.9396926207859093161, -0.3420201433256663259 ) ) ;
#25265 = FACE_OUTER_BOUND ( 'NONE', #44747, .T. ) ;
#25266 = FACE_BOUND ( 'NONE', #48485, .T. ) ;
#25267 = EDGE_CURVE ( 'NONE', #57235, #87613, #57278, .T. ) ;
#25268 = PLANE ( 'NONE',  #29761 ) ;
#25269 = DIRECTION ( 'NONE',  ( 0.000000000000000000, 0.6427876096865373645, -0.7660444431189797898 ) ) ;
#25270 = FACE_OUTER_BOUND ( 'NONE', #74088, .T. ) ;
#25271 = CARTESIAN_POINT ( 'NONE',  ( -14.17690049986752321, -5.582136614379148654, 34.36778462344220486 ) ) ;
#25272 = SPHERICAL_SURFACE ( 'NONE', #48040, 8.000000000000000000 ) ;
#25273 = CARTESIAN_POINT ( 'NONE',  ( -2.651650429449565305, -4.848349570550461785, 14.00000000000000178 ) ) ;
#25274 = VERTEX_POINT ( 'NONE', #77109 ) ;
#25275 = EDGE_CURVE ( 'NONE', #69909, #18250, #50070, .T. ) ;
#25276 = CARTESIAN_POINT ( 'NONE',  ( 1.514660440535158692, -2.254550872974306674, 29.97347326024527447 ) ) ;
#25277 = ORIENTED_EDGE ( 'NONE', *, *, #37660, .T. ) ;
#25278 = EDGE_LOOP ( 'NONE', ( #61906, #4099 ) ) ;
#25280 = CARTESIAN_POINT ( 'NONE',  ( 10.86543892702292879, -5.728107161865378494, 34.42597550085002922 ) ) ;
#25279 = LINE ( 'NONE', #3659, #59044 ) ;
#25281 = DIRECTION ( 'NONE',  ( 0.000000000000000000, 0.9848077530122072432, 0.1736481776669354937 ) ) ;
#25282 = CYLINDRICAL_SURFACE ( 'NONE', #79650, 0.2500000000000009437 ) ;
#25283 = CARTESIAN_POINT ( 'NONE',  ( 17.01083966596719677, -8.120952969808774569, 34.71129190930000163 ) ) ;
#25284 = CARTESIAN_POINT ( 'NONE',  ( -15.48079246806219444, -3.711651800289232028, 33.01384336483936011 ) ) ;
#25285 = ORIENTED_EDGE ( 'NONE', *, *, #38205, .T. ) ;
#25286 = CARTESIAN_POINT ( 'NONE',  ( 17.01165263096229907, -6.026961402152685388, 34.52809138561120506 ) ) ;
#25287 = EDGE_CURVE ( 'NONE', #70777, #48470, #74523, .T. ) ;
#25288 = CARTESIAN_POINT ( 'NONE',  ( 14.17754509825408604, -11.47017969459903952, 32.78971311882035167 ) ) ;
#25289 = CARTESIAN_POINT ( 'NONE',  ( -14.05769230769230660, -2.249999999999998668, 29.75000000000000355 ) ) ;
#25290 = ADVANCED_FACE ( 'NONE', ( #84769 ), #64459, .F. ) ;
#25291 = CARTESIAN_POINT ( 'NONE',  ( 5.326923076923011813, -7.565270445406050648, 34.75000000000000000 ) ) ;
#25292 = ORIENTED_EDGE ( 'NONE', *, *, #82278, .T. ) ;
#25293 = ORIENTED_EDGE ( 'NONE', *, *, #79634, .T. ) ;
#25294 = APPLICATION_PROTOCOL_DEFINITION ( 'draft international standard', 'automotive_design', 1998, #8399 ) ;
#25295 = VERTEX_POINT ( 'NONE', #49636 ) ;
#25296 = CARTESIAN_POINT ( 'NONE',  ( 17.75000000000000000, -7.500000000000001776, 34.75000000000000000 ) ) ;
#25297 = CARTESIAN_POINT ( 'NONE',  ( -5.749999999998578915, -7.500000000000154543, 35.00000000000007105 ) ) ;
#25298 = EDGE_LOOP ( 'NONE', ( #40154, #1325, #29035, #8083 ) ) ;
#25299 = CARTESIAN_POINT ( 'NONE',  ( 3.230769230769108269, -12.70778746994576025, 30.41441678777401236 ) ) ;
#25300 = CARTESIAN_POINT ( 'NONE',  ( 15.16468581981335007, -8.973038597847271092, 34.52809138561120506 ) ) ;
#25301 = CARTESIAN_POINT ( 'NONE',  ( 0.5923302693632472860, -12.11778462344221019, 31.66786338562085135 ) ) ;
#25302 = CARTESIAN_POINT ( 'NONE',  ( -13.13461538461394973, -7.500000000000155431, 34.75000000000007105 ) ) ;
#25303 = EDGE_CURVE ( 'NONE', #34093, #63242, #49776, .T. ) ;
#25304 = FACE_OUTER_BOUND ( 'NONE', #53633, .T. ) ;
#25305 = ORIENTED_EDGE ( 'NONE', *, *, #87387, .T. ) ;
#25307 = ORIENTED_EDGE ( 'NONE', *, *, #71535, .T. ) ;
#25306 = CARTESIAN_POINT ( 'NONE',  ( -0.4615384615384611200, -11.91647553114624181, 32.58852847137148245 ) ) ;
#25308 = DIRECTION ( 'NONE',  ( -0.000000000000000000, -0.5000000000000009992, -0.8660254037844380415 ) ) ;
#25309 = CARTESIAN_POINT ( 'NONE',  ( 8.835298102580845025, -12.34228464037088813, 31.77849191805839268 ) ) ;
#25310 = CARTESIAN_POINT ( 'NONE',  ( -7.623141002060449090, -3.395485233115139057, 33.02377354290275946 ) ) ;
#25311 = EDGE_CURVE ( 'NONE', #23488, #28219, #61578, .T. ) ;
#25312 = EDGE_CURVE ( 'NONE', #68692, #77497, #6708, .T. ) ;
#25313 = CARTESIAN_POINT ( 'NONE',  ( 10.61538461538461675, -12.34228464037088635, 31.77849191805839268 ) ) ;
#25314 = CARTESIAN_POINT ( 'NONE',  ( 13.16168842570853670, -4.026226216239094491, 33.68668979543634379 ) ) ;
#25315 = CARTESIAN_POINT ( 'NONE',  ( -39.05038313613820122, -2.249999999999998668, 29.75000000000000355 ) ) ;
#25316 = CARTESIAN_POINT ( 'NONE',  ( 9.626224281351815293, -6.386643153685125363, 34.62446782046654903 ) ) ;
#25317 = CARTESIAN_POINT ( 'NONE',  ( 2.775308065498755195, -6.422011778438505125, 14.64249329374151110 ) ) ;
#25318 = ORIENTED_EDGE ( 'NONE', *, *, #43766, .F. ) ;
#25319 = CARTESIAN_POINT ( 'NONE',  ( 4.853996118016227435, -11.98009711892699691, 32.48740034544075428 ) ) ;
#25320 = CARTESIAN_POINT ( 'NONE',  ( -14.30769230769242917, -3.643525952248795718, 33.31231777344771672 ) ) ;
#25321 = CARTESIAN_POINT ( 'NONE',  ( -0.2387589202700527991, -5.114059244376870872, 34.14424750095245997 ) ) ;
#25323 = ORIENTED_EDGE ( 'NONE', *, *, #29362, .F. ) ;
#25322 = VECTOR ( 'NONE', #37368, 1000.000000000000227 ) ;
#25324 = EDGE_LOOP ( 'NONE', ( #47375, #6465, #52543, #36998 ) ) ;
#25325 = DIRECTION ( 'NONE',  ( 0.000000000000000000, 0.9848077530122072432, 0.1736481776669354937 ) ) ;
#25326 = CARTESIAN_POINT ( 'NONE',  ( 7.623226887246997485, -6.459968553980839800, 34.89616026154728701 ) ) ;
#25327 = CARTESIAN_POINT ( 'NONE',  ( 0.000000000000000000, -11.00000000000000000, 29.75000000000000355 ) ) ;
#25328 = CARTESIAN_POINT ( 'NONE',  ( 16.15384615384615330, -9.905515769479276145, 34.41647553114623292 ) ) ;
#25329 = DIRECTION ( 'NONE',  ( 0.000000000000000000, 0.000000000000000000, -1.000000000000000000 ) ) ;
#25330 = LINE ( 'NONE', #59552, #86857 ) ;
#25331 = VERTEX_POINT ( 'NONE', #56398 ) ;
#25332 = CARTESIAN_POINT ( 'NONE',  ( -0.4615384615384611200, -12.78798330534102945, 29.74999999999997868 ) ) ;
#25333 = CARTESIAN_POINT ( 'NONE',  ( -2.057746789344165439, -10.05730279482229683, 34.04704008940765902 ) ) ;
#25334 = CARTESIAN_POINT ( 'NONE',  ( -3.296039676730006640, -11.94971097300153140, 32.03036669348370680 ) ) ;
#25335 = ORIENTED_EDGE ( 'NONE', *, *, #40276, .T. ) ;
#25336 = CARTESIAN_POINT ( 'NONE',  ( 15.93036122928181975, -12.47654668319379567, 31.42292124445336654 ) ) ;
#25337 = B_SPLINE_CURVE_WITH_KNOTS ( 'NONE', 3,
 ( #23060, #43772, #62701, #14531, #42015, #578, #70365, #62263, #56839, #49204 ),
 .UNSPECIFIED., .F., .F.,
 ( 4, 2, 2, 2, 4 ),
 ( 0.0007817359430256372700, 0.0009771253907250052138, 0.001172514838424373266, 0.001367904286123741101, 0.001563293733823109153 ),
 .UNSPECIFIED. ) ;
#25338 = VERTEX_POINT ( 'NONE', #25273 ) ;
#25339 = CARTESIAN_POINT ( 'NONE',  ( 18.00000000000000000, -3.513871655860378418, 32.76840700105978499 ) ) ;
#25340 =( NAMED_UNIT ( * ) PLANE_ANGLE_UNIT ( ) SI_UNIT ( $, .RADIAN. ) );
#25341 = CARTESIAN_POINT ( 'NONE',  ( 3.262820512820511443, -11.50000000000000000, 29.75000000000000355 ) ) ;
#25342 = CARTESIAN_POINT ( 'NONE',  ( 3.164686851409094448, -2.833524468853757305, 32.15551576947924417 ) ) ;
#25343 = ORIENTED_EDGE ( 'NONE', *, *, #47979, .T. ) ;
#25344 = CARTESIAN_POINT ( 'NONE',  ( -11.53846153846153655, -12.37446782046654192, 30.86335684631486131 ) ) ;
#25345 = CARTESIAN_POINT ( 'NONE',  ( -11.53846153846153655, -12.37446782046654192, 30.86335684631486131 ) ) ;
#25346 = CARTESIAN_POINT ( 'NONE',  ( 13.38461538461538680, -12.48256725967547354, 35.29906147534542527 ) ) ;
#25347 = CARTESIAN_POINT ( 'NONE',  ( -6.000000000000119904, -2.892918686052165622, 31.69288490824153470 ) ) ;
#25348 = CARTESIAN_POINT ( 'NONE',  ( -4.826868657009622865, -8.346898887586323923, 34.93166121998716278 ) ) ;
#25349 = AXIS2_PLACEMENT_3D ( 'NONE', #15993, #36702, #64155 ) ;
#25350 = EDGE_LOOP ( 'NONE', ( #55919, #86977 ) ) ;
#25351 = FACE_OUTER_BOUND ( 'NONE', #38874, .T. ) ;
#25352 = EDGE_LOOP ( 'NONE', ( #24789, #31500, #39548, #68317 ) ) ;
#25353 = LINE ( 'NONE', #32548, #48644 ) ;
#25354 = CARTESIAN_POINT ( 'NONE',  ( -10.48485917715096960, -10.31582465632705237, 34.18122507451815295 ) ) ;
#25355 = CARTESIAN_POINT ( 'NONE',  ( -16.21911659980693088, -11.48612834413959582, 32.76840700105983473 ) ) ;
#25356 = DIRECTION ( 'NONE',  ( -0.000000000000000000, 0.7660444431189791237, -0.6427876096865379196 ) ) ;
#25357 = VECTOR ( 'NONE', #23021, 1000.000000000000000 ) ;
#25359 = AXIS2_PLACEMENT_3D ( 'NONE', #41396, #74295, #81065 ) ;
#25358 = CARTESIAN_POINT ( 'NONE',  ( 11.25641025641025550, -7.500000000000000000, 29.75000000000000355 ) ) ;
#25360 = CARTESIAN_POINT ( 'NONE',  ( -9.561517251340744039, -6.369690395747422684, 34.87708834333098196 ) ) ;
#25361 = CARTESIAN_POINT ( 'NONE',  ( -10.86538461538461320, -2.249999999999998668, 29.75000000000000355 ) ) ;
#25362 = ORIENTED_EDGE ( 'NONE', *, *, #67587, .T. ) ;
#25363 = ORIENTED_EDGE ( 'NONE', *, *, #63468, .T. ) ;
#25364 = ORIENTED_EDGE ( 'NONE', *, *, #40334, .F. ) ;
#25365 = EDGE_LOOP ( 'NONE', ( #41088, #41114, #80654, #40729 ) ) ;
#25366 = ORIENTED_EDGE ( 'NONE', *, *, #37207, .F. ) ;
#25367 = CARTESIAN_POINT ( 'NONE',  ( -4.377331097570101193, -5.912607949931405038, 34.49155766932282319 ) ) ;
#25368 = FACE_OUTER_BOUND ( 'NONE', #4218, .T. ) ;
#25369 = CARTESIAN_POINT ( 'NONE',  ( 15.10007776410167324, -4.809359713505814149, 33.96456829005828837 ) ) ;
#25370 = CARTESIAN_POINT ( 'NONE',  ( 0.4615384615383396616, -5.219633306517616589, 34.19971097300220464 ) ) ;
#25371 = CARTESIAN_POINT ( 'NONE',  ( 13.16113044089144068, -8.496056993536548418, 34.65000542017679663 ) ) ;
#25373 = EDGE_CURVE ( 'NONE', #83780, #7366, #86092, .T. ) ;
#25372 = CARTESIAN_POINT ( 'NONE',  ( -5.999999999999998224, -2.833524468853757305, 32.15551576947925838 ) ) ;
#25374 = VECTOR ( 'NONE', #31427, 999.9999999999998863 ) ;
#25375 = CARTESIAN_POINT ( 'NONE',  ( -12.22435897435897267, -7.500000000000000000, 29.75000000000000355 ) ) ;
#25376 = CARTESIAN_POINT ( 'NONE',  ( 9.561617089197383734, -9.929715669179220328, 34.40415004197138416 ) ) ;
#25377 = CARTESIAN_POINT ( 'NONE',  ( 0.4615384615384611200, -3.050289026998446396, 32.03036669348365706 ) ) ;
#25378 = EDGE_LOOP ( 'NONE', ( #81787, #5739, #20196, #41903 ) ) ;
#25379 = PRODUCT_DEFINITION ( 'UNKNOWN', '', #2984, #30258 ) ;
#25380 = ORIENTED_EDGE ( 'NONE', *, *, #369, .T. ) ;
#25381 = ORIENTED_EDGE ( 'NONE', *, *, #85984, .T. ) ;
#25383 = ORIENTED_EDGE ( 'NONE', *, *, #78507, .F. ) ;
#25382 = CARTESIAN_POINT ( 'NONE',  ( 5.999999999999878320, -12.51329471203414379, 31.30864560766407578 ) ) ;
#25385 = DIRECTION ( 'NONE',  ( 0.000000000000000000, 1.000000000000000000, -0.000000000000000000 ) ) ;
#25384 = CARTESIAN_POINT ( 'NONE',  ( 7.846153846153846700, -1.466349020453238561, 30.81389545987213907 ) ) ;
#25386 = B_SPLINE_CURVE_WITH_KNOTS ( 'NONE', 3,
 ( #56216, #89140, #35505, #83707, #27857, #76039, #35054, #8481, #1716, #62951 ),
 .UNSPECIFIED., .F., .F.,
 ( 4, 2, 2, 2, 4 ),
 ( 0.0007817246256747476061, 0.0009771112852218909357, 0.001172497944769034049, 0.001367884604316177161, 0.001563271263863320491 ),
 .UNSPECIFIED. ) ;
#25387 = DIRECTION ( 'NONE',  ( 0.000000000000000000, 0.1736481776669267785, -0.9848077530122087975 ) ) ;
#25388 = CARTESIAN_POINT ( 'NONE',  ( 6.923076923076802558, -2.625532179533778709, 30.86335684631627174 ) ) ;
#25389 = FACE_BOUND ( 'NONE', #61665, .T. ) ;
#25390 = ORIENTED_EDGE ( 'NONE', *, *, #85118, .F. ) ;
#25391 = B_SPLINE_CURVE_WITH_KNOTS ( 'NONE', 3,
 ( #54715, #19171, #82206, #20495, #56500, #22270, #668, #55162, #27692, #63251 ),
 .UNSPECIFIED., .F., .F.,
 ( 4, 2, 2, 2, 4 ),
 ( 0.000000000000000000, 0.0001954311564186887718, 0.0003908623128373775435, 0.0005862934692560662882, 0.0007817246256747550871 ),
 .UNSPECIFIED. ) ;
#25392 = ADVANCED_FACE ( 'NONE', ( #85644 ), #51833, .F. ) ;
#25393 = AXIS2_PLACEMENT_3D ( 'NONE', #30605, #17550, #57640 ) ;
#25394 = EDGE_LOOP ( 'NONE', ( #79036, #16066 ) ) ;
#25395 = CARTESIAN_POINT ( 'NONE',  ( -5.076923076923075762, -6.681629849574314051, 35.83090037661290239 ) ) ;
#25396 = VERTEX_POINT ( 'NONE', #38791 ) ;
#25397 = FACE_BOUND ( 'NONE', #88188, .T. ) ;
#25398 = CARTESIAN_POINT ( 'NONE',  ( -15.23076923076922995, -6.435427911321262684, 35.78748833219616898 ) ) ;
#25399 = CARTESIAN_POINT ( 'NONE',  ( -13.51476259405360203, -10.88202310037935661, 33.43294751532457099 ) ) ;
#25400 = EDGE_LOOP ( 'NONE', ( #42207, #36019, #79628, #46086 ) ) ;
#25401 = CARTESIAN_POINT ( 'NONE',  ( 18.00000000000000000, -2.721908614388771852, 31.22303859784724978 ) ) ;
#25402 = CARTESIAN_POINT ( 'NONE',  ( 8.992193903497444296, -7.369474539155828730, 34.99858011523957657 ) ) ;
#25403 = CARTESIAN_POINT ( 'NONE',  ( -18.13069060311030611, -3.957541250942359756, 33.62499894934981626 ) ) ;
#25404 = VERTEX_POINT ( 'NONE', #78876 ) ;
#25405 = CARTESIAN_POINT ( 'NONE',  ( 12.46153846153846168, -4.786620604624113540, 33.94971097300155094 ) ) ;
#25406 = DIRECTION ( 'NONE',  ( -1.000000000000000000, 0.000000000000000000, 0.000000000000000000 ) ) ;
#25407 = CARTESIAN_POINT ( 'NONE',  ( -9.469296340694842939, -2.554770724473667265, 30.48948780036025852 ) ) ;
#25408 = VERTEX_POINT ( 'NONE', #66706 ) ;
#25409 = CARTESIAN_POINT ( 'NONE',  ( 2.557637717070352146, -12.45601412856602686, 31.48342859153981621 ) ) ;
#25410 = FACE_OUTER_BOUND ( 'NONE', #8747, .T. ) ;
#25411 = EDGE_LOOP ( 'NONE', ( #76537, #42831 ) ) ;
#25412 = CARTESIAN_POINT ( 'NONE',  ( -2.307692307692427391, -2.892918686052166066, 31.69288490824153470 ) ) ;
#25413 = CARTESIAN_POINT ( 'NONE',  ( -12.23852710992561299, -2.554770724473667265, 30.48948780036025852 ) ) ;
#25414 = CARTESIAN_POINT ( 'NONE',  ( 24.00000000000000000, -5.499999999999981348, 27.75000000000000000 ) ) ;
#25415 = CARTESIAN_POINT ( 'NONE',  ( 7.976992264166607782, -7.277220443632449687, 34.74524770363009907 ) ) ;
#25416 = CARTESIAN_POINT ( 'NONE',  ( -6.700113788810249105, -7.369474539155828730, 34.99858011523957657 ) ) ;
#25417 = VECTOR ( 'NONE', #31300, 1000.000000000000000 ) ;
#25418 = EDGE_CURVE ( 'NONE', #64011, #80539, #334, .T. ) ;
#25419 = CYLINDRICAL_SURFACE ( 'NONE', #39527, 2.000000000000001776 ) ;
#25421 = DIRECTION ( 'NONE',  ( -0.000000000000000000, 1.000000000000000000, -0.000000000000000000 ) ) ;
#25420 = FACE_BOUND ( 'NONE', #77321, .T. ) ;
#25422 = CARTESIAN_POINT ( 'NONE',  ( 8.899756470994333313, -12.27024696741798770, 31.24895572276497546 ) ) ;
#25423 = DIRECTION ( 'NONE',  ( 1.000000000000000000, 0.000000000000000000, 0.000000000000000000 ) ) ;
#25424 = CARTESIAN_POINT ( 'NONE',  ( 2.750000000000008438, -8.639087296525996607, 15.79687500000000178 ) ) ;
#25425 = ORIENTED_EDGE ( 'NONE', *, *, #54694, .F. ) ;
#25426 = CARTESIAN_POINT ( 'NONE',  ( -12.68446467905460828, -8.239355502252617924, 34.69524867566427417 ) ) ;
#25427 = EDGE_LOOP ( 'NONE', ( #41604, #36973, #2657, #6557 ) ) ;
#25428 = ADVANCED_FACE ( 'NONE', ( #65798 ), #80681, .F. ) ;
#25429 = ORIENTED_EDGE ( 'NONE', *, *, #35056, .T. ) ;
#25430 = FACE_OUTER_BOUND ( 'NONE', #45180, .T. ) ;
#25432 = ORIENTED_EDGE ( 'NONE', *, *, #2310, .F. ) ;
#25431 = VECTOR ( 'NONE', #55672, 1000.000000000000227 ) ;
#25433 = CARTESIAN_POINT ( 'NONE',  ( -14.98082371242109012, -5.852078868378309373, 34.47109172314383585 ) ) ;
#25434 = CARTESIAN_POINT ( 'NONE',  ( 1.944543648262996083, -5.555456351736983045, 14.31250000000000000 ) ) ;
#25435 = DIRECTION ( 'NONE',  ( 0.000000000000000000, 1.000000000000000000, 0.000000000000000000 ) ) ;
#25436 = CARTESIAN_POINT ( 'NONE',  ( 10.86543903529806876, -2.544122305571458575, 31.48381861865057729 ) ) ;
#25437 = DIRECTION ( 'NONE',  ( 0.000000000000000000, 0.4999999999999960032, -0.8660254037844410391 ) ) ;
#25438 = CARTESIAN_POINT ( 'NONE',  ( 15.84615384615384670, -7.500000000000000000, 29.75000000000000355 ) ) ;
#25439 = B_SPLINE_CURVE_WITH_KNOTS ( 'NONE', 3,
 ( #48674, #49124, #14910, #7710, #85904, #42386 ),
 .UNSPECIFIED., .F., .F.,
 ( 4, 2, 4 ),
 ( 4.336808689942017736E-19, 0.0001954784845028932508, 0.0003909569690057860679 ),
 .UNSPECIFIED. ) ;
#25440 = B_SPLINE_CURVE_WITH_KNOTS ( 'NONE', 3,
 ( #77205, #70459, #44280, #65004, #56927, #83537, #1551, #29476, #36231, #49294 ),
 .UNSPECIFIED., .F., .F.,
 ( 4, 2, 2, 2, 4 ),
 ( 0.0007817359430256364027, 0.0009771253907250043464, 0.001172514838424372399, 0.001367904286123740234, 0.001563293733823108286 ),
 .UNSPECIFIED. ) ;
#25441 = CARTESIAN_POINT ( 'NONE',  ( -5.326946301144532825, -3.520140089381497361, 33.17453946501458262 ) ) ;
#25442 = LINE ( 'NONE', #46161, #21463 ) ;
#25443 = CARTESIAN_POINT ( 'NONE',  ( -7.715362038329057981, -12.11778462344220841, 31.66786338562085135 ) ) ;
#25444 = CARTESIAN_POINT ( 'NONE',  ( 3.749999999999992006, -5.946699141100872943, 20.64062500000000000 ) ) ;
#25445 = CARTESIAN_POINT ( 'NONE',  ( 5.207448515156718472, -3.068774925481847937, 32.56582465632704526 ) ) ;
#25446 = LINE ( 'NONE', #73191, #13231 ) ;
#25447 = CARTESIAN_POINT ( 'NONE',  ( -9.692307692307691624, -2.517432740324522911, 35.29906147534542527 ) ) ;
#25448 = ORIENTED_EDGE ( 'NONE', *, *, #58126, .T. ) ;
#25449 = EDGE_LOOP ( 'NONE', ( #52943, #13479 ) ) ;
#25450 = VECTOR ( 'NONE', #24557, 1000.000000000000000 ) ;
#25451 = CARTESIAN_POINT ( 'NONE',  ( -8.834501215191545853, -12.46129190929999986, 30.37095296980880832 ) ) ;
#25452 = LINE ( 'NONE', #80408, #1463 ) ;
#25453 = CARTESIAN_POINT ( 'NONE',  ( -2.531177232256636156, -2.353723527008296568, 30.78948104536958752 ) ) ;
#25454 = CARTESIAN_POINT ( 'NONE',  ( -16.15384615384615330, -12.37446782046654192, 30.86335684631486131 ) ) ;
#25455 = LINE ( 'NONE', #6078, #85234 ) ;
#25456 = AXIS2_PLACEMENT_3D ( 'NONE', #1045, #49671, #7365 ) ;
#25457 = FACE_OUTER_BOUND ( 'NONE', #64744, .T. ) ;
#25458 = AXIS2_PLACEMENT_3D ( 'NONE', #73754, #67865, #32309 ) ;
#25459 = VERTEX_POINT ( 'NONE', #52732 ) ;
#25460 = CARTESIAN_POINT ( 'NONE',  ( 20.00000000000000000, -4.000000000000000000, 29.75000000000000355 ) ) ;
#25461 = ORIENTED_EDGE ( 'NONE', *, *, #81900, .F. ) ;
#25462 = VERTEX_POINT ( 'NONE', #10873 ) ;
#25463 = CARTESIAN_POINT ( 'NONE',  ( 7.780883845597524662, -11.06231777344662781, 33.60647404775220082 ) ) ;
#25464 = B_SPLINE_CURVE_WITH_KNOTS ( 'NONE', 3,
 ( #42947, #70862, #36628, #64081, #23537, #78484, #57335, #36198, #71281, #63645 ),
 .UNSPECIFIED., .F., .F.,
 ( 4, 2, 2, 2, 4 ),
 ( 0.000000000000000000, 0.0001954311584214072652, 0.0003908623168428145304, 0.0005862934752642217414, 0.0007817246336856290608 ),
 .UNSPECIFIED. ) ;
#25465 = B_SPLINE_CURVE_WITH_KNOTS ( 'NONE', 3,
 ( #67719, #32592, #47430, #52857, #60062, #25846, #74925, #38923, #88455, #11894 ),
 .UNSPECIFIED., .F., .F.,
 ( 4, 2, 2, 2, 4 ),
 ( 0.000000000000000000, 0.0001954339857564097512, 0.0003908679715128195024, 0.0005863019572692292807, 0.0007817359430256390048 ),
 .UNSPECIFIED. ) ;
#25466 = CARTESIAN_POINT ( 'NONE',  ( -14.24243716817946925, -6.835583212224610072, 34.95778746994559327 ) ) ;
#25467 = CARTESIAN_POINT ( 'NONE',  ( 5.076923076922953193, -12.16647553114689728, 32.15551576947799362 ) ) ;
#25468 = CARTESIAN_POINT ( 'NONE',  ( 1.253924781505078689, -11.37499894934982514, 33.29245874905763003 ) ) ;
#25469 = CARTESIAN_POINT ( 'NONE',  ( -2.242436736416280940, -11.94971097300157403, 32.03036669348361443 ) ) ;
#25470 = EDGE_CURVE ( 'NONE', #47330, #67660, #52291, .T. ) ;
#25471 = VERTEX_POINT ( 'NONE', #79779 ) ;
#25472 = ORIENTED_EDGE ( 'NONE', *, *, #81703, .T. ) ;
#25473 = B_SPLINE_CURVE_WITH_KNOTS ( 'NONE', 3,
 ( #44132, #49584, #84719, #78820, #29760, #10374, #17120, #51315, #37837, #9478 ),
 .UNSPECIFIED., .F., .F.,
 ( 4, 2, 2, 2, 4 ),
 ( 0.000000000000000000, 0.0001954339857564093175, 0.0003908679715128186350, 0.0005863019572692279796, 0.0007817359430256372700 ),
 .UNSPECIFIED. ) ;
#25474 = CIRCLE ( 'NONE', #87345, 3.000000000000000444 ) ;
#25475 = VERTEX_POINT ( 'NONE', #45537 ) ;
#25476 = CARTESIAN_POINT ( 'NONE',  ( 18.00000000000000000, -1.242168528481310874, 33.36296068462461051 ) ) ;
#25477 = CARTESIAN_POINT ( 'NONE',  ( 0.000000000000000000, -11.00000000000000000, 29.75000000000000355 ) ) ;
#25478 = VECTOR ( 'NONE', #227, 1000.000000000000000 ) ;
#25479 = CARTESIAN_POINT ( 'NONE',  ( 4.376625822824220080, -3.563462043263029955, 33.22394488606062879 ) ) ;
#25481 = EDGE_CURVE ( 'NONE', #62418, #52040, #38341, .T. ) ;
#25480 = CARTESIAN_POINT ( 'NONE',  ( 1.161130440891436466, -3.754499324213721234, 33.06261337010820256 ) ) ;
#25482 = LINE ( 'NONE', #40335, #70949 ) ;
#25483 = DIRECTION ( 'NONE',  ( -0.000000000000000000, -0.9396926207859092051, -0.3420201433256662704 ) ) ;
#25484 = AXIS2_PLACEMENT_3D ( 'NONE', #47718, #27892, #54469 ) ;
#25485 = EDGE_LOOP ( 'NONE', ( #75435, #29832 ) ) ;
#25486 = EDGE_CURVE ( 'NONE', #34572, #20451, #20748, .T. ) ;
#25487 = EDGE_LOOP ( 'NONE', ( #29664, #38478 ) ) ;
#25488 = CARTESIAN_POINT ( 'NONE',  ( -1.553300858899081538, -11.25000000000000711, 26.10937500000001066 ) ) ;
#25490 = VERTEX_POINT ( 'NONE', #80224 ) ;
#25489 = DIRECTION ( 'NONE',  ( -0.000000000000000000, 1.000000000000000000, 3.491481338843133355E-15 ) ) ;
#25491 = FACE_OUTER_BOUND ( 'NONE', #23476, .T. ) ;
#25492 = CARTESIAN_POINT ( 'NONE',  ( -6.988326854851008463, -2.255955759149247619, 30.00000000000013856 ) ) ;
#25493 = CARTESIAN_POINT ( 'NONE',  ( 2.651650429449569302, -10.15165042944953733, 15.87500000000000000 ) ) ;
#25494 = ORIENTED_EDGE ( 'NONE', *, *, #25171, .F. ) ;
#25495 = EDGE_CURVE ( 'NONE', #87883, #79547, #75006, .T. ) ;
#25496 = DIRECTION ( 'NONE',  ( -0.000000000000000000, -1.000000000000000000, -0.000000000000000000 ) ) ;
#25497 = ORIENTED_EDGE ( 'NONE', *, *, #53582, .T. ) ;
#25498 = CARTESIAN_POINT ( 'NONE',  ( -13.60810030917971680, -11.60425143139329940, 33.02411095842164457 ) ) ;
#25499 = DIRECTION ( 'NONE',  ( -0.000000000000000000, 5.102127870520020612E-17, 1.000000000000000000 ) ) ;
#25500 = DIRECTION ( 'NONE',  ( -0.000000000000000000, -0.9848077530122085754, -0.1736481776669273613 ) ) ;
#25502 = CARTESIAN_POINT ( 'NONE',  ( -0.4615384615384611200, -8.564572088678739092, 35.78748833219616898 ) ) ;
#25501 = CARTESIAN_POINT ( 'NONE',  ( -7.053224132515143907, -3.817052484675422797, 33.13202310037935661 ) ) ;
#25503 = EDGE_CURVE ( 'NONE', #22672, #24781, #35760, .T. ) ;
#25504 = AXIS2_PLACEMENT_3D ( 'NONE', #6763, #88329, #47306 ) ;
#25505 = CARTESIAN_POINT ( 'NONE',  ( -6.000000000000121680, -3.083524468854526912, 32.58852847137268327 ) ) ;
#25506 = VERTEX_POINT ( 'NONE', #39244 ) ;
#25507 = DIRECTION ( 'NONE',  ( 0.000000000000000000, 0.000000000000000000, 1.000000000000000000 ) ) ;
#25508 = CARTESIAN_POINT ( 'NONE',  ( -8.835313148590904220, -3.937682226553330445, 33.60647404775217240 ) ) ;
#25509 = DIRECTION ( 'NONE',  ( 0.000000000000000000, 0.9396926207859126468, 0.3420201433256571111 ) ) ;
#25510 = EDGE_LOOP ( 'NONE', ( #26866, #57050, #638, #61480 ) ) ;
#25511 = CARTESIAN_POINT ( 'NONE',  ( 12.46153846153833911, -3.835265460704628371, 33.15142922262033665 ) ) ;
#25512 = CARTESIAN_POINT ( 'NONE',  ( -6.250023237292963607, -10.76384336483936011, 33.53834819971076087 ) ) ;
#25513 = CARTESIAN_POINT ( 'NONE',  ( 17.06410256410256565, -7.500000000000000000, 29.75000000000000355 ) ) ;
#25514 = CARTESIAN_POINT ( 'NONE',  ( 7.976945653978629203, -3.062576670634119758, 32.05464942895959979 ) ) ;
#25515 = EDGE_CURVE ( 'NONE', #79391, #6804, #46429, .T. ) ;
#25516 = FACE_BOUND ( 'NONE', #18645, .T. ) ;
#25518 = CYLINDRICAL_SURFACE ( 'NONE', #2846, 0.2499999999999998890 ) ;
#25517 = CARTESIAN_POINT ( 'NONE',  ( 1.161735867877800699, -7.630690623152302621, 34.99857592706774057 ) ) ;
#25519 = VECTOR ( 'NONE', #77610, 1000.000000000000000 ) ;
#25520 = CARTESIAN_POINT ( 'NONE',  ( -3.512820512820513663, -11.00000000000000000, 29.75000000000000355 ) ) ;
#25522 = CARTESIAN_POINT ( 'NONE',  ( -5.076923076923199218, -12.70778746994576025, 30.41441678777401236 ) ) ;
#25521 = CARTESIAN_POINT ( 'NONE',  ( 2.980792499826877329, -4.236021600441998380, 33.53823185664189310 ) ) ;
#25523 = CARTESIAN_POINT ( 'NONE',  ( 1.384615384615264011, -3.083524468854526912, 32.58852847137268327 ) ) ;
#25524 = ADVANCED_FACE ( 'NONE', ( #61258 ), #5896, .F. ) ;
#25525 = LINE ( 'NONE', #53879, #37577 ) ;
#25526 = CARTESIAN_POINT ( 'NONE',  ( -1.492201783934549164, -11.27530806549876807, 27.10750670625849423 ) ) ;
#25527 = FACE_OUTER_BOUND ( 'NONE', #20914, .T. ) ;
#25528 = EDGE_LOOP ( 'NONE', ( #85557, #13195, #49667, #10916 ) ) ;
#25529 = CARTESIAN_POINT ( 'NONE',  ( 8.769230769230647482, -12.46129190930018460, 30.37095296980731973 ) ) ;
#25530 = EDGE_CURVE ( 'NONE', #18328, #21233, #41012, .T. ) ;
#25531 = EDGE_CURVE ( 'NONE', #68329, #26886, #79771, .T. ) ;
#25532 = CARTESIAN_POINT ( 'NONE',  ( 2.177001704582001818, -2.295517848115769421, 30.44137282052137294 ) ) ;
#25533 = DIRECTION ( 'NONE',  ( -0.000000000000000000, 0.3420201433256694901, -0.9396926207859082059 ) ) ;
#25534 = CARTESIAN_POINT ( 'NONE',  ( -19.99999999999998934, 12.00000000000000711, 0.000000000000000000 ) ) ;
#25535 = CARTESIAN_POINT ( 'NONE',  ( 16.85399611801622655, -12.64616026154729411, 30.79003144601914244 ) ) ;
#25536 = CARTESIAN_POINT ( 'NONE',  ( 6.130790440966954691, -3.338503747796866872, 32.95102852606553512 ) ) ;
#25537 = CARTESIAN_POINT ( 'NONE',  ( -1.492201783934549164, -11.27530806549876807, 27.10750670625849423 ) ) ;
#25538 = CARTESIAN_POINT ( 'NONE',  ( 14.08476609017616177, -10.61292498521070549, 33.66303323003028680 ) ) ;
#25539 = CARTESIAN_POINT ( 'NONE',  ( -2.057746898314262829, -6.653508905675590945, 34.93172785388651391 ) ) ;
#25540 = CARTESIAN_POINT ( 'NONE',  ( 0.4765651934480724106, -4.791246328801548771, 29.07531184057632601 ) ) ;
#25541 = CARTESIAN_POINT ( 'NONE',  ( 5.011653076366756387, -9.528491918058357157, 34.59228464037090589 ) ) ;
#25542 = CARTESIAN_POINT ( 'NONE',  ( 8.638539302563209787, -9.804603061927743113, 34.18744698557895845 ) ) ;
#25543 = DIRECTION ( 'NONE',  ( -1.000000000000000000, -0.000000000000000000, -0.000000000000000000 ) ) ;
#25544 = CARTESIAN_POINT ( 'NONE',  ( 9.822355298563376635, -7.723484964179501588, 34.74522123443823318 ) ) ;
#25545 = DIRECTION ( 'NONE',  ( 0.000000000000000000, -1.000000000000000000, -1.084202172485503448E-16 ) ) ;
#25546 = ORIENTED_EDGE ( 'NONE', *, *, #1341, .T. ) ;
#25547 = CARTESIAN_POINT ( 'NONE',  ( 11.78846153846297362, -7.500000000000155431, 34.75000000000007105 ) ) ;
#25548 = CARTESIAN_POINT ( 'NONE',  ( 1.384615384615386802, -1.242168528481310874, 33.36296068462461051 ) ) ;
#25549 = AXIS2_PLACEMENT_3D ( 'NONE', #48979, #56179, #83671 ) ;
#25550 = CARTESIAN_POINT ( 'NONE',  ( 3.750000000000001776, -7.561099074964511502, 17.22061829374151287 ) ) ;
#25551 = CARTESIAN_POINT ( 'NONE',  ( 9.320512820512821150, -4.000000000000000000, 29.65000000000000213 ) ) ;
#25552 = CARTESIAN_POINT ( 'NONE',  ( -5.207070286361294542, -2.619462340734462380, 30.83744416345203021 ) ) ;
#25553 = ORIENTED_EDGE ( 'NONE', *, *, #85111, .F. ) ;
#25554 = DIRECTION ( 'NONE',  ( -0.000000000000000000, -0.000000000000000000, -1.000000000000000000 ) ) ;
#25555 = CARTESIAN_POINT ( 'NONE',  ( -12.39547112818838492, -12.62096338111211757, 30.90682066428152908 ) ) ;
#25557 = ORIENTED_EDGE ( 'NONE', *, *, #3415, .F. ) ;
#25556 = CARTESIAN_POINT ( 'NONE',  ( 11.40777093535123043, -2.845849958028613624, 32.17971566917920967 ) ) ;
#25558 = CARTESIAN_POINT ( 'NONE',  ( -7.912237257109724808, -8.120952969808774569, 34.71129190930000163 ) ) ;
#25559 = CARTESIAN_POINT ( 'NONE',  ( -3.007757879156381264, -3.587049720035815348, 32.86302985866382897 ) ) ;
#25560 = CARTESIAN_POINT ( 'NONE',  ( -5.326923076923075762, -7.500000000000001776, 35.04278698407183867 ) ) ;
#25561 = CARTESIAN_POINT ( 'NONE',  ( 11.60452988946397745, -8.973038597847271092, 34.52809138561121216 ) ) ;
#25562 = EDGE_LOOP ( 'NONE', ( #58309, #62904 ) ) ;
#25563 = DIRECTION ( 'NONE',  ( -1.000000000000000000, -0.000000000000000000, -0.000000000000000000 ) ) ;
#25564 = ADVANCED_FACE ( 'NONE', ( #7226 ), #67597, .T. ) ;
#25565 = CARTESIAN_POINT ( 'NONE',  ( -15.23076923076922995, -11.35647404775217417, 33.31231777344666511 ) ) ;
#25566 = CARTESIAN_POINT ( 'NONE',  ( -11.28846153846153655, -2.249999999999998668, 29.75000000000000355 ) ) ;
#25567 = ORIENTED_EDGE ( 'NONE', *, *, #74004, .F. ) ;
#25568 = ORIENTED_EDGE ( 'NONE', *, *, #20448, .F. ) ;
#25569 = EDGE_CURVE ( 'NONE', #21373, #39792, #54082, .T. ) ;
#25570 = VERTEX_POINT ( 'NONE', #13532 ) ;
#25571 = EDGE_CURVE ( 'NONE', #27642, #82422, #47311, .T. ) ;
#25572 = VECTOR ( 'NONE', #83459, 1000.000000000000000 ) ;
#25573 = CARTESIAN_POINT ( 'NONE',  ( -16.21992853320628925, -3.322132147404559976, 32.92929555188719348 ) ) ;
#25574 = FACE_OUTER_BOUND ( 'NONE', #29296, .T. ) ;
#25575 = CARTESIAN_POINT ( 'NONE',  ( -12.59168567097668756, -3.817052484675422797, 33.13202310037935661 ) ) ;
#25576 = ADVANCED_FACE ( 'NONE', ( #6770 ), #88335, .F. ) ;
#25577 = AXIS2_PLACEMENT_3D ( 'NONE', #70614, #31854, #51192 ) ;
#25578 = CARTESIAN_POINT ( 'NONE',  ( -17.07692307692307665, -4.786620604624113540, 33.94971097300155094 ) ) ;
#25579 = EDGE_LOOP ( 'NONE', ( #7885, #81734, #2014, #31600 ) ) ;
#25580 = EDGE_LOOP ( 'NONE', ( #75641, #79164 ) ) ;
#25581 = AXIS2_PLACEMENT_3D ( 'NONE', #48263, #69431, #27560 ) ;
#25582 = EDGE_LOOP ( 'NONE', ( #58487, #58670 ) ) ;
#25584 = ORIENTED_EDGE ( 'NONE', *, *, #59287, .F. ) ;
#25583 = CARTESIAN_POINT ( 'NONE',  ( -1.384615384615505151, -5.219633306517616589, 34.19971097300220464 ) ) ;
#25585 = DIRECTION ( 'NONE',  ( -0.000000000000000000, 0.000000000000000000, 1.000000000000000000 ) ) ;
#25586 = LINE ( 'NONE', #46300, #72409 ) ;
#25587 = CARTESIAN_POINT ( 'NONE',  ( 2.557637826040450868, -3.712312575010499938, 33.01462480002815170 ) ) ;
#25588 = DIRECTION ( 'NONE',  ( 0.000000000000000000, 0.7660444431189822323, -0.6427876096865344779 ) ) ;
#25589 = B_SPLINE_CURVE_WITH_KNOTS ( 'NONE', 3,
 ( #41558, #1016, #34793, #76679, #9114, #49202, #50076, #28950, #28042, #70363 ),
 .UNSPECIFIED., .F., .F.,
 ( 4, 2, 2, 2, 4 ),
 ( 0.0007817359430256297891, 0.0009771253907249958896, 0.001172514838424361990, 0.001367904286123728091, 0.001563293733823094191 ),
 .UNSPECIFIED. ) ;
#25590 = ORIENTED_EDGE ( 'NONE', *, *, #17848, .F. ) ;
#25591 = EDGE_CURVE ( 'NONE', #23520, #76927, #12208, .T. ) ;
#25592 = ORIENTED_EDGE ( 'NONE', *, *, #3108, .F. ) ;
#25593 = EDGE_LOOP ( 'NONE', ( #65987, #40287, #8216, #59914 ) ) ;
#25594 = CARTESIAN_POINT ( 'NONE',  ( -13.38461538461538325, -1.044019251281081972, 31.83374038241031911 ) ) ;
#25596 = ORIENTED_EDGE ( 'NONE', *, *, #1303, .F. ) ;
#25595 = CARTESIAN_POINT ( 'NONE',  ( 5.142991427925514003, -4.786620604624113540, 33.94971097300155805 ) ) ;
#25597 = CARTESIAN_POINT ( 'NONE',  ( 18.22301284409339672, -11.98016756924215187, 32.48728574198911190 ) ) ;
#25598 = CARTESIAN_POINT ( 'NONE',  ( 15.23076923076923173, -13.20930481340135110, 34.54067556320372745 ) ) ;
#25599 = DIRECTION ( 'NONE',  ( 0.000000000000000000, 0.000000000000000000, 1.000000000000000000 ) ) ;
#25600 = DIRECTION ( 'NONE',  ( 1.000000000000000000, 0.000000000000000000, 0.000000000000000000 ) ) ;
#25601 = CARTESIAN_POINT ( 'NONE',  ( -5.933932666649925025, -3.322132147404559976, 32.92929555188717927 ) ) ;
#25602 = VECTOR ( 'NONE', #22828, 1000.000000000000000 ) ;
#25603 = FACE_BOUND ( 'NONE', #13187, .T. ) ;
#25604 = DIRECTION ( 'NONE',  ( -0.000000000000000000, -1.000000000000000000, -0.000000000000000000 ) ) ;
#25605 = CARTESIAN_POINT ( 'NONE',  ( -12.52762187249433801, -8.973038597847271092, 34.52809138561120506 ) ) ;
#25606 = CARTESIAN_POINT ( 'NONE',  ( -10.54931728203453822, -10.67929555188718282, 33.92786785259544757 ) ) ;
#25608 = CARTESIAN_POINT ( 'NONE',  ( -5.299849294439224145, -3.105860786376062332, 32.13614157043599562 ) ) ;
#25607 = CARTESIAN_POINT ( 'NONE',  ( -17.07692307692319744, -12.70778746994576025, 30.41441678777401236 ) ) ;
#25609 = CARTESIAN_POINT ( 'NONE',  ( 0.4615384615383396616, -12.27809138561165270, 31.22303859784587132 ) ) ;
#25610 = CARTESIAN_POINT ( 'NONE',  ( 7.053122085911702754, -2.504778602574660340, 29.97347330155780298 ) ) ;
#25611 = VERTEX_POINT ( 'NONE', #34244 ) ;
#25612 = AXIS2_PLACEMENT_3D ( 'NONE', #70646, #37286, #15707 ) ;
#25613 = CARTESIAN_POINT ( 'NONE',  ( 2.307692307692309264, -6.386643153685126251, 34.62446782046654192 ) ) ;
#25614 = CARTESIAN_POINT ( 'NONE',  ( -13.31936024510254590, -4.320704448112861584, 33.92786785259548310 ) ) ;
#25615 = ORIENTED_EDGE ( 'NONE', *, *, #46223, .F. ) ;
#25616 = ORIENTED_EDGE ( 'NONE', *, *, #32526, .T. ) ;
#25617 = DIRECTION ( 'NONE',  ( -0.000000000000000000, 0.7660444431189791237, -0.6427876096865379196 ) ) ;
#25618 = CARTESIAN_POINT ( 'NONE',  ( 15.90382292962469535, -2.341070481393820124, 30.72580821765574299 ) ) ;
#25619 = CARTESIAN_POINT ( 'NONE',  ( -15.36124593888569478, -7.276988635370452485, 34.74523720219453793 ) ) ;
#25620 = VERTEX_POINT ( 'NONE', #27492 ) ;
#25621 = DIRECTION ( 'NONE',  ( 0.000000000000000000, 0.6427876096865373645, -0.7660444431189797898 ) ) ;
#25622 = CARTESIAN_POINT ( 'NONE',  ( -9.692307692307691624, -12.78798330534102945, 29.74999999999997868 ) ) ;
#25623 = EDGE_CURVE ( 'NONE', #63945, #84853, #29372, .T. ) ;
#25624 = EDGE_CURVE ( 'NONE', #30118, #80116, #60383, .T. ) ;
#25626 = CARTESIAN_POINT ( 'NONE',  ( 17.99999999999987566, -10.33852847137269571, 34.16647553114546554 ) ) ;
#25625 = CARTESIAN_POINT ( 'NONE',  ( 11.78840694783958298, -2.986452184633680673, 32.43230066228895225 ) ) ;
#25627 = CARTESIAN_POINT ( 'NONE',  ( -12.71151519248081740, -4.943428324936578910, 34.04746400365624481 ) ) ;
#25628 = LINE ( 'NONE', #39607, #74097 ) ;
#25630 = DIRECTION ( 'NONE',  ( -1.000000000000000000, 0.000000000000000000, 0.000000000000000000 ) ) ;
#25629 =( NAMED_UNIT ( * ) PLANE_ANGLE_UNIT ( ) SI_UNIT ( $, .RADIAN. ) );
#25631 = CARTESIAN_POINT ( 'NONE',  ( -2.651650429449535551, -10.15165042944956753, 22.43750000000000000 ) ) ;
#25632 = VERTEX_POINT ( 'NONE', #81119 ) ;
#25633 = EDGE_CURVE ( 'NONE', #21841, #25408, #70210, .T. ) ;
#25634 = ORIENTED_EDGE ( 'NONE', *, *, #37033, .T. ) ;
#25635 = VECTOR ( 'NONE', #76710, 1000.000000000000000 ) ;
#25636 = CARTESIAN_POINT ( 'NONE',  ( -9.942330916529147800, -2.588893531581426988, 31.60682220781847818 ) ) ;
#25637 = ADVANCED_FACE ( 'NONE', ( #85097 ), #15311, .F. ) ;
#25638 = CARTESIAN_POINT ( 'NONE',  ( 16.21910172512217585, -6.879047030191284051, 34.71129190930002295 ) ) ;
#25639 = CARTESIAN_POINT ( 'NONE',  ( 9.320512820512821150, -7.500000000000000000, 29.75000000000000355 ) ) ;
#25640 = CARTESIAN_POINT ( 'NONE',  ( -2.544871794871794268, -7.500000000000000000, 29.75000000000000355 ) ) ;
#25641 = CARTESIAN_POINT ( 'NONE',  ( 15.23076923076910916, -5.941354392335915335, 34.76329471203413846 ) ) ;
#25642 = CARTESIAN_POINT ( 'NONE',  ( -3.750000000000008438, -5.946699141100917352, 21.42187500000000000 ) ) ;
#25643 = FACE_OUTER_BOUND ( 'NONE', #49247, .T. ) ;
#25644 = CARTESIAN_POINT ( 'NONE',  ( 14.08420738312797837, -6.716662450894489211, 34.94144148231605840 ) ) ;
#25645 = AXIS2_PLACEMENT_3D ( 'NONE', #45387, #17036, #72860 ) ;
#25646 = CARTESIAN_POINT ( 'NONE',  ( -13.51509209273184986, -7.276988635370452485, 34.74523720219453793 ) ) ;
#25647 = CARTESIAN_POINT ( 'NONE',  ( 13.25446741488369362, -10.31621877034669588, 34.18098118002070152 ) ) ;
#25648 = DIRECTION ( 'NONE',  ( 1.000000000000000000, 0.000000000000000000, 0.000000000000000000 ) ) ;
#25649 = CARTESIAN_POINT ( 'NONE',  ( 13.51540582558234149, -2.494656445102012565, 31.33466734024120015 ) ) ;
#25650 = LINE ( 'NONE', #58524, #3489 ) ;
#25651 = CARTESIAN_POINT ( 'NONE',  ( 7.976944287120795174, -8.191423895709840863, 34.95447573519442130 ) ) ;
#25652 = DIRECTION ( 'NONE',  ( -0.000000000000000000, 0.9396926207859092051, -0.3420201433256662704 ) ) ;
#25653 = VECTOR ( 'NONE', #88784, 1000.000000000000000 ) ;
#25654 = CARTESIAN_POINT ( 'NONE',  ( -3.361459833879537396, -12.35290016733513951, 31.75349464988449455 ) ) ;
#25655 = EDGE_CURVE ( 'NONE', #59185, #37020, #42348, .T. ) ;
#25656 = VERTEX_POINT ( 'NONE', #22941 ) ;
#25657 = DIRECTION ( 'NONE',  ( 0.000000000000000000, 0.9848077530122072432, 0.1736481776669354937 ) ) ;
#25658 = DIRECTION ( 'NONE',  ( 0.000000000000000000, 0.9848077530122072432, -0.1736481776669354937 ) ) ;
#25659 = B_SPLINE_CURVE_WITH_KNOTS ( 'NONE', 3,
 ( #23224, #71852, #78610, #8838, #16472, #36312, #2067, #2499, #29551, #50238 ),
 .UNSPECIFIED., .F., .F.,
 ( 4, 2, 2, 2, 4 ),
 ( 0.0007817359430256297891, 0.0009771253907249958896, 0.001172514838424362207, 0.001367904286123728524, 0.001563293733823094625 ),
 .UNSPECIFIED. ) ;
#25660 = CARTESIAN_POINT ( 'NONE',  ( 5.749976775778542049, -2.588893531581426544, 31.60682220781847818 ) ) ;
#25661 = CARTESIAN_POINT ( 'NONE',  ( 1.200186371490529202, -4.775308065498752974, 14.48624329374151465 ) ) ;
#25662 = CARTESIAN_POINT ( 'NONE',  ( 13.38461538461526601, -5.219633306517616589, 34.19971097300220464 ) ) ;
#25663 = CARTESIAN_POINT ( 'NONE',  ( -17.86947429823644029, -10.88167719472716577, 33.43325721877153711 ) ) ;
#25664 = EDGE_CURVE ( 'NONE', #48838, #18632, #16442, .T. ) ;
#25666 = VERTEX_POINT ( 'NONE', #41902 ) ;
#25665 = CYLINDRICAL_SURFACE ( 'NONE', #84231, 0.2499999999999997502 ) ;
#25667 = CARTESIAN_POINT ( 'NONE',  ( 1.139087296526029469, -10.24999999999999289, 24.70312500000000000 ) ) ;
#25668 = DIRECTION ( 'NONE',  ( 0.000000000000000000, 0.9396926207859126468, 0.3420201433256571111 ) ) ;
#25669 = ORIENTED_EDGE ( 'NONE', *, *, #73989, .T. ) ;
#25670 = CARTESIAN_POINT ( 'NONE',  ( -7.173100147298381302, -11.56360843649121861, 33.07473185843129926 ) ) ;
#25671 = ORIENTED_EDGE ( 'NONE', *, *, #48750, .F. ) ;
#25672 = CARTESIAN_POINT ( 'NONE',  ( -17.07692307692319744, -2.625532179533778709, 30.86335684631627174 ) ) ;
#25673 = EDGE_CURVE ( 'NONE', #9337, #20097, #21613, .T. ) ;
#25674 = CARTESIAN_POINT ( 'NONE',  ( -7.780898274877822374, -11.94971097300157403, 32.03036669348361443 ) ) ;
#25675 = CARTESIAN_POINT ( 'NONE',  ( -1.449885830576160162, -4.481592998940161721, 33.73612834413957984 ) ) ;
#25676 = VERTEX_POINT ( 'NONE', #22064 ) ;
#25677 = CARTESIAN_POINT ( 'NONE',  ( 0.3313904918067641647, -5.070767119584671967, 34.40440758774516183 ) ) ;
#25678 = VERTEX_POINT ( 'NONE', #56291 ) ;
#25679 = ADVANCED_FACE ( 'NONE', ( #8999 ), #49538, .F. ) ;
#25680 = ORIENTED_EDGE ( 'NONE', *, *, #52186, .F. ) ;
#25681 = CARTESIAN_POINT ( 'NONE',  ( 3.230769230769110045, -2.892918686052166066, 31.69288490824153470 ) ) ;
#25682 = DIRECTION ( 'NONE',  ( -0.000000000000000000, -0.1736481776669307198, -0.9848077530122080203 ) ) ;
#25683 = CARTESIAN_POINT ( 'NONE',  ( -16.81410256410256565, -3.499999999999999556, 29.75000000000000355 ) ) ;
#25684 = CARTESIAN_POINT ( 'NONE',  ( 17.32692307692307665, -7.500000000000001776, 35.04278698407183867 ) ) ;
#25685 = CARTESIAN_POINT ( 'NONE',  ( 9.942362112221147186, -10.06805714834173493, 34.32951233291982618 ) ) ;
#25686 = CARTESIAN_POINT ( 'NONE',  ( -24.00000000000000000, 9.000000000000024869, 28.74999999999999645 ) ) ;
#25687 = EDGE_CURVE ( 'NONE', #26693, #49542, #77693, .T. ) ;
#25688 = DIRECTION ( 'NONE',  ( -0.000000000000000000, -0.6427876096865404731, -0.7660444431189770143 ) ) ;
#25689 = EDGE_LOOP ( 'NONE', ( #42599, #83804, #69649, #82322 ) ) ;
#25691 = ADVANCED_FACE ( 'NONE', ( #70694 ), #50402, .F. ) ;
#25690 = ORIENTED_EDGE ( 'NONE', *, *, #21658, .T. ) ;
#25692 = VERTEX_POINT ( 'NONE', #77884 ) ;
#25694 = ORIENTED_EDGE ( 'NONE', *, *, #43640, .F. ) ;
#25693 = DIRECTION ( 'NONE',  ( 0.000000000000000000, -6.938893903907222067E-15, 1.000000000000000000 ) ) ;
#25695 = CIRCLE ( 'NONE', #77444, 0.2500000000000002220 ) ;
#25696 = DIRECTION ( 'NONE',  ( -0.000000000000000000, 0.8660254037844397068, -0.4999999999999978906 ) ) ;
#25697 = CARTESIAN_POINT ( 'NONE',  ( 1.384615384615265343, -3.300289026999228881, 32.46337939537708905 ) ) ;
#25698 = VERTEX_POINT ( 'NONE', #36895 ) ;
#25699 = ADVANCED_FACE ( 'NONE', ( #64357 ), #22502, .F. ) ;
#25700 = CARTESIAN_POINT ( 'NONE',  ( -7.846153846153844924, -7.500000000000001776, 35.04278698407183867 ) ) ;
#25701 = B_SPLINE_CURVE_WITH_KNOTS ( 'NONE', 3,
 ( #35580, #82887, #76112, #77442, #63025, #43650, #9428, #15309, #62157, #28829 ),
 .UNSPECIFIED., .F., .F.,
 ( 4, 2, 2, 2, 4 ),
 ( 0.0007817246256747453293, 0.0009771112852218881168, 0.001172497944769031013, 0.001367884604316173692, 0.001563271263863316371 ),
 .UNSPECIFIED. ) ;
#25702 = AXIS2_PLACEMENT_3D ( 'NONE', #59025, #32010, #25693 ) ;
#25703 = EDGE_CURVE ( 'NONE', #53001, #89000, #15756, .T. ) ;
#25704 = ORIENTED_EDGE ( 'NONE', *, *, #48823, .F. ) ;
#25705 = DIRECTION ( 'NONE',  ( 0.000000000000000000, 0.000000000000000000, -1.000000000000000000 ) ) ;
#25706 = B_SPLINE_CURVE_WITH_KNOTS ( 'NONE', 3,
 ( #43325, #83883, #22170, #48744, #49635, #42889, #69019, #7329, #70356, #36137 ),
 .UNSPECIFIED., .F., .F.,
 ( 4, 2, 2, 2, 4 ),
 ( 0.000000000000000000, 0.0001954311564186864407, 0.0003908623128373728815, 0.0005862934692560593493, 0.0007817246256747457630 ),
 .UNSPECIFIED. ) ;
#25707 = ORIENTED_EDGE ( 'NONE', *, *, #14001, .F. ) ;
#25708 = VECTOR ( 'NONE', #64270, 1000.000000000000000 ) ;
#25709 = B_SPLINE_CURVE_WITH_KNOTS ( 'NONE', 3,
 ( #15700, #64303, #43165, #44035, #78722, #84610, #37730, #22446, #2604, #78268 ),
 .UNSPECIFIED., .F., .F.,
 ( 4, 2, 2, 2, 4 ),
 ( 0.000000000000000000, 0.0001954339857564074473, 0.0003908679715128148945, 0.0005863019572692223418, 0.0007817359430256297891 ),
 .UNSPECIFIED. ) ;
#25710 = CARTESIAN_POINT ( 'NONE',  ( -9.442307692307691624, -2.249999999999998668, 29.75000000000000355 ) ) ;
#25711 = VECTOR ( 'NONE', #84126, 1000.000000000000114 ) ;
#25712 = CARTESIAN_POINT ( 'NONE',  ( 4.023155550735845409, -12.62707690430377383, 30.88035979386743435 ) ) ;
#25713 = CARTESIAN_POINT ( 'NONE',  ( 4.088596222072069075, -2.255955759149247619, 30.00000000000013856 ) ) ;
#25714 = FACE_BOUND ( 'NONE', #49605, .T. ) ;
#25715 = DIRECTION ( 'NONE',  ( -0.000000000000000000, -0.1736481776669307198, -0.9848077530122080203 ) ) ;
#25716 = CYLINDRICAL_SURFACE ( 'NONE', #29861, 0.2500000000000004996 ) ;
#25717 = CARTESIAN_POINT ( 'NONE',  ( -1.515305987725691805, -2.295517848115769421, 30.44137282052137294 ) ) ;
#25718 = LINE ( 'NONE', #20296, #61799 ) ;
#25719 = CARTESIAN_POINT ( 'NONE',  ( 10.39250593295597014, -7.630691491037285168, 34.74850469731152458 ) ) ;
#25720 = DIRECTION ( 'NONE',  ( -0.000000000000000000, -0.8660254037844399289, -0.4999999999999980016 ) ) ;
#25721 = ORIENTED_EDGE ( 'NONE', *, *, #30154, .F. ) ;
#25722 = CARTESIAN_POINT ( 'NONE',  ( -11.78843828251013015, -3.436278759898153901, 33.07459398097509506 ) ) ;
#25723 = ORIENTED_EDGE ( 'NONE', *, *, #32133, .T. ) ;
#25724 = ORIENTED_EDGE ( 'NONE', *, *, #75129, .F. ) ;
#25726 = CARTESIAN_POINT ( 'NONE',  ( -14.08491276642389423, -12.44528174975671853, 30.48912976160716681 ) ) ;
#25725 = CARTESIAN_POINT ( 'NONE',  ( -10.61538461538461320, -1.044019251281081972, 31.83374038241031911 ) ) ;
#25727 = CARTESIAN_POINT ( 'NONE',  ( 15.45378207486262667, -8.282913670948747864, 34.94150082978203642 ) ) ;
#25728 = CARTESIAN_POINT ( 'NONE',  ( 7.384615384615385025, -7.500000000000000000, 29.75000000000000355 ) ) ;
#25729 = CARTESIAN_POINT ( 'NONE',  ( -1.134615384615383915, -2.499999999999998668, 29.75000000000000355 ) ) ;
#25730 = LINE ( 'NONE', #5016, #87893 ) ;
#25731 = ORIENTED_EDGE ( 'NONE', *, *, #34115, .F. ) ;
#25732 = FACE_OUTER_BOUND ( 'NONE', #63445, .T. ) ;
#25733 = B_SPLINE_CURVE_WITH_KNOTS ( 'NONE', 3,
 ( #76643, #7744, #35206, #56802, #56369, #14944, #9501, #42422, #28454, #69880 ),
 .UNSPECIFIED., .F., .F.,
 ( 4, 2, 2, 2, 4 ),
 ( 0.0007817246256747451124, 0.0009771112852218881168, 0.001172497944769031230, 0.001367884604316174126, 0.001563271263863317238 ),
 .UNSPECIFIED. ) ;
#25734 = CARTESIAN_POINT ( 'NONE',  ( 0.5923302693632473970, -9.804649428959606894, 34.18742332936588468 ) ) ;
#25735 = CARTESIAN_POINT ( 'NONE',  ( -14.30769230769230660, -8.120952969808772792, 34.71129190930000163 ) ) ;
#25736 = CARTESIAN_POINT ( 'NONE',  ( -3.296039231325549768, -12.70778746994557551, 30.41441678777548319 ) ) ;
#25737 = ORIENTED_EDGE ( 'NONE', *, *, #77903, .T. ) ;
#25738 = AXIS2_PLACEMENT_3D ( 'NONE', #78892, #12223, #38359 ) ;
#25739 = ORIENTED_EDGE ( 'NONE', *, *, #72524, .T. ) ;
#25740 = CONTEXT_DEPENDENT_SHAPE_REPRESENTATION ( #16411, #31227 ) ;
#25741 = EDGE_LOOP ( 'NONE', ( #79799, #24351 ) ) ;
#25742 = CARTESIAN_POINT ( 'NONE',  ( 0.4615384615383396616, -10.90142922262034020, 33.41473453929536674 ) ) ;
#25743 = CARTESIAN_POINT ( 'NONE',  ( -1.384615384615383471, -2.292212530054420494, 30.41441678777542634 ) ) ;
#25745 = ORIENTED_EDGE ( 'NONE', *, *, #56477, .F. ) ;
#25744 = EDGE_CURVE ( 'NONE', #24853, #86068, #32549, .T. ) ;
#25746 = CARTESIAN_POINT ( 'NONE',  ( -4.153846153846152411, -2.708943851104267164, 35.45975837776705220 ) ) ;
#25747 = CARTESIAN_POINT ( 'NONE',  ( -9.692307692307814193, -5.094484230521993062, 34.41647553114689373 ) ) ;
#25748 = FACE_OUTER_BOUND ( 'NONE', #11435, .T. ) ;
#25749 = CARTESIAN_POINT ( 'NONE',  ( 1.515140822849030844, -6.808710257144161559, 34.95449254468098843 ) ) ;
#25750 = DIRECTION ( 'NONE',  ( -0.000000000000000000, -0.7660444431189791237, -0.6427876096865379196 ) ) ;
#25751 = ORIENTED_EDGE ( 'NONE', *, *, #37573, .T. ) ;
#25752 = EDGE_CURVE ( 'NONE', #26337, #69932, #48657, .T. ) ;
#25754 = ORIENTED_EDGE ( 'NONE', *, *, #52717, .T. ) ;
#25753 = CARTESIAN_POINT ( 'NONE',  ( 0.2115152242454951537, -10.05641848906368097, 34.04755513067966177 ) ) ;
#25755 = DIRECTION ( 'NONE',  ( 0.000000000000000000, -0.000000000000000000, -1.000000000000000000 ) ) ;
#25756 = CARTESIAN_POINT ( 'NONE',  ( -2.307692307692427391, -9.442884908241554243, 34.35708131394783038 ) ) ;
#25757 = CARTESIAN_POINT ( 'NONE',  ( -2.307692307692305711, -12.48256725967547354, 35.29906147534542527 ) ) ;
#25758 = CARTESIAN_POINT ( 'NONE',  ( -4.153846153846152411, -12.37446782046654192, 30.86335684631486131 ) ) ;
#25759 = CARTESIAN_POINT ( 'NONE',  ( -3.930833309752758797, -4.762714258010880997, 34.23016756924214832 ) ) ;
#25760 = CARTESIAN_POINT ( 'NONE',  ( -5.207613680033383652, -10.70098750199973203, 33.91152734681376302 ) ) ;
#25761 = FACE_OUTER_BOUND ( 'NONE', #60918, .T. ) ;
#25762 = EDGE_CURVE ( 'NONE', #28791, #17236, #7838, .T. ) ;
#25763 = CARTESIAN_POINT ( 'NONE',  ( 2.775308065498755195, -6.422011778438505125, 18.39249329374151642 ) ) ;
#25764 = ORIENTED_EDGE ( 'NONE', *, *, #62187, .F. ) ;
#25765 = CARTESIAN_POINT ( 'NONE',  ( 15.16468581981335184, -8.120952969808774569, 34.71129190930000163 ) ) ;
#25766 = CARTESIAN_POINT ( 'NONE',  ( 7.596153846153845812, -7.566082377512564072, 35.00000000000000711 ) ) ;
#25767 = ORIENTED_EDGE ( 'NONE', *, *, #39897, .T. ) ;
#25768 = ORIENTED_EDGE ( 'NONE', *, *, #75516, .T. ) ;
#25769 = CARTESIAN_POINT ( 'NONE',  ( 5.076923076922953193, -9.528491918059723176, 34.59228464037033035 ) ) ;
#25770 = FACE_OUTER_BOUND ( 'NONE', #62987, .T. ) ;
#25771 = B_SPLINE_CURVE_WITH_KNOTS ( 'NONE', 3,
 ( #80791, #52844, #41118, #12317, #60497, #32577, #74022, #73587, #18636, #11881 ),
 .UNSPECIFIED., .F., .F.,
 ( 4, 2, 2, 2, 4 ),
 ( 0.000000000000000000, 0.0001954339857564064715, 0.0003908679715128129430, 0.0005863019572692194144, 0.0007817359430256258859 ),
 .UNSPECIFIED. ) ;
#25772 = DIRECTION ( 'NONE',  ( -0.000000000000000000, 0.8660254037844399289, -0.4999999999999980016 ) ) ;
#25773 = FACE_OUTER_BOUND ( 'NONE', #9806, .T. ) ;
#25774 = EDGE_CURVE ( 'NONE', #40198, #67006, #79668, .T. ) ;
#25775 = FACE_OUTER_BOUND ( 'NONE', #22711, .T. ) ;
#25776 = VECTOR ( 'NONE', #36296, 1000.000000000000000 ) ;
#25777 = CARTESIAN_POINT ( 'NONE',  ( -3.230769230769229949, -1.629998284177014645, 34.34916445242399163 ) ) ;
#25778 = VERTEX_POINT ( 'NONE', #66603 ) ;
#25779 = CARTESIAN_POINT ( 'NONE',  ( 5.934729554039226862, -3.835265460703609186, 33.15142922261924241 ) ) ;
#25780 = AXIS2_PLACEMENT_3D ( 'NONE', #65282, #16650, #71590 ) ;
#25781 = LINE ( 'NONE', #73973, #11031 ) ;
#25782 = CARTESIAN_POINT ( 'NONE',  ( -2.307692307692428724, -5.941354392335915335, 34.76329471203413846 ) ) ;
#25783 = ORIENTED_EDGE ( 'NONE', *, *, #49926, .F. ) ;
#25784 = CARTESIAN_POINT ( 'NONE',  ( 12.21151523731700372, -2.588893531581426988, 31.60682220781847818 ) ) ;
#25785 = ADVANCED_FACE ( 'NONE', ( #58051 ), #37784, .T. ) ;
#25786 = EDGE_LOOP ( 'NONE', ( #79362, #67559, #58179, #29574 ) ) ;
#25787 = CARTESIAN_POINT ( 'NONE',  ( -0.2387589202700525215, -2.847695495035523550, 31.58253572463339509 ) ) ;
#25788 =( LENGTH_UNIT ( ) NAMED_UNIT ( * ) SI_UNIT ( .MILLI., .METRE. ) );
#25789 = CARTESIAN_POINT ( 'NONE',  ( -13.60749490135297179, -7.630690623152299956, 34.99857592706774057 ) ) ;
#25790 = VERTEX_POINT ( 'NONE', #4906 ) ;
#25791 = ADVANCED_FACE ( 'NONE', ( #87334 ), #79226, .T. ) ;
#25792 = CARTESIAN_POINT ( 'NONE',  ( -20.00000000000000355, -10.00000000000000533, 10.00000000000000178 ) ) ;
#25793 = CARTESIAN_POINT ( 'NONE',  ( -11.47239318745910097, -12.37446782046654192, 30.86335684631486842 ) ) ;
#25794 = CARTESIAN_POINT ( 'NONE',  ( -9.692307692307691624, -2.538708090699994813, 30.37095296980875503 ) ) ;
#25795 = CARTESIAN_POINT ( 'NONE',  ( -0.3589743589743586982, -4.000000000000000000, 29.75000000000000355 ) ) ;
#25796 = CARTESIAN_POINT ( 'NONE',  ( 3.361559671736185528, -2.845873456487966635, 32.17976146951972538 ) ) ;
#25797 = EDGE_CURVE ( 'NONE', #21038, #40946, #10319, .T. ) ;
#25798 = VERTEX_POINT ( 'NONE', #85980 ) ;
#25799 = FACE_BOUND ( 'NONE', #44162, .T. ) ;
#25800 = ORIENTED_EDGE ( 'NONE', *, *, #52045, .F. ) ;
#25801 = CARTESIAN_POINT ( 'NONE',  ( -2.438382910802612269, -2.494641256782728966, 31.33461815524612959 ) ) ;
#25802 = AXIS2_PLACEMENT_3D ( 'NONE', #26296, #53765, #26739 ) ;
#25803 = B_SPLINE_CURVE_WITH_KNOTS ( 'NONE', 3,
 ( #72750, #52919, #4303, #58343, #71865, #10174, #37637, #18266, #10617, #31784 ),
 .UNSPECIFIED., .F., .F.,
 ( 4, 2, 2, 2, 4 ),
 ( 0.0007817246256747442451, 0.0009771112852218865989, 0.001172497944769029061, 0.001367884604316171523, 0.001563271263863313986 ),
 .UNSPECIFIED. ) ;
#25804 = CARTESIAN_POINT ( 'NONE',  ( -10.39260494640654464, -10.23759521482555357, 34.22997729860117033 ) ) ;
#25805 = CARTESIAN_POINT ( 'NONE',  ( -3.165623451437267200, -7.750023238201980469, 34.74374492549440419 ) ) ;
#25806 = CARTESIAN_POINT ( 'NONE',  ( 7.846153846153723244, -12.51329471203414379, 31.30864560766407578 ) ) ;
#25807 = CYLINDRICAL_SURFACE ( 'NONE', #14762, 4.000000000000000000 ) ;
#25808 = CARTESIAN_POINT ( 'NONE',  ( -6.130147209438218781, -4.460286881179643004, 33.72017969459903242 ) ) ;
#25809 = CARTESIAN_POINT ( 'NONE',  ( -19.50000000000000000, -3.499999999999999556, 29.75000000000000355 ) ) ;
#25810 = ADVANCED_FACE ( 'NONE', ( #25162 ), #39138, .T. ) ;
#25811 = ORIENTED_EDGE ( 'NONE', *, *, #59251, .T. ) ;
#25812 = ORIENTED_EDGE ( 'NONE', *, *, #55258, .F. ) ;
#25813 = ORIENTED_EDGE ( 'NONE', *, *, #37876, .T. ) ;
#25814 = EDGE_CURVE ( 'NONE', #62595, #66445, #49081, .T. ) ;
#25816 = ORIENTED_EDGE ( 'NONE', *, *, #31768, .F. ) ;
#25815 = ADVANCED_FACE ( 'NONE', ( #80111 ), #65689, .F. ) ;
#25817 = CARTESIAN_POINT ( 'NONE',  ( -10.39260507411620793, -11.41317474335729543, 32.86274602512330034 ) ) ;
#25818 = CARTESIAN_POINT ( 'NONE',  ( 11.31497661389721010, -9.417330523894424488, 34.63758898049880486 ) ) ;
#25819 = CARTESIAN_POINT ( 'NONE',  ( -4.153846153846152411, -8.973038597847269315, 34.52809138561121927 ) ) ;
#25820 = EDGE_CURVE ( 'NONE', #79559, #13581, #31475, .T. ) ;
#25821 = CARTESIAN_POINT ( 'NONE',  ( 5.076923076923075762, -11.35647404775217417, 33.31231777344666511 ) ) ;
#25822 = CARTESIAN_POINT ( 'NONE',  ( 17.99999999999987566, -10.21337939537710326, 33.94971097300076224 ) ) ;
#25823 = VECTOR ( 'NONE', #73679, 1000.000000000000000 ) ;
#25824 = LINE ( 'NONE', #47407, #73859 ) ;
#25825 = CARTESIAN_POINT ( 'NONE',  ( -4.826977558574935045, -4.336752205174647656, 33.62275283266504289 ) ) ;
#25826 = CARTESIAN_POINT ( 'NONE',  ( 0.3962680155776847624, -3.300289026998414865, 32.46337939537583139 ) ) ;
#25827 = ORIENTED_EDGE ( 'NONE', *, *, #37033, .F. ) ;
#25828 = ORIENTED_EDGE ( 'NONE', *, *, #23928, .T. ) ;
#25829 = VECTOR ( 'NONE', #65407, 1000.000000000000114 ) ;
#25830 = ORIENTED_EDGE ( 'NONE', *, *, #37566, .F. ) ;
#25831 = AXIS2_PLACEMENT_3D ( 'NONE', #71107, #16175, #44512 ) ;
#25833 = VERTEX_POINT ( 'NONE', #11206 ) ;
#25832 = CARTESIAN_POINT ( 'NONE',  ( -13.38461538461550759, -12.51329471203414379, 31.30864560766407578 ) ) ;
#25835 = DIRECTION ( 'NONE',  ( -0.000000000000000000, 0.5000000000000011102, -0.8660254037844380415 ) ) ;
#25834 = FACE_OUTER_BOUND ( 'NONE', #27256, .T. ) ;
#25836 = AXIS2_PLACEMENT_3D ( 'NONE', #18577, #51888, #45590 ) ;
#25837 = CARTESIAN_POINT ( 'NONE',  ( -0.4615384615384611200, -2.292212530054420494, 30.41441678777542634 ) ) ;
#25838 = CARTESIAN_POINT ( 'NONE',  ( -15.36145983387954139, -9.929715669179220328, 34.40415004197138416 ) ) ;
#25839 = FACE_BOUND ( 'NONE', #55018, .T. ) ;
#25840 = ORIENTED_EDGE ( 'NONE', *, *, #78873, .F. ) ;
#25841 = B_SPLINE_CURVE_WITH_KNOTS ( 'NONE', 3,
 ( #14514, #42885, #62686, #1447, #36564, #48740, #28937, #70351, #22164, #8210 ),
 .UNSPECIFIED., .F., .F.,
 ( 4, 2, 2, 2, 4 ),
 ( 0.0007817246256747463051, 0.0009771112852218896347, 0.001172497944769033181, 0.001367884604316176728, 0.001563271263863320057 ),
 .UNSPECIFIED. ) ;
#25842 = ORIENTED_EDGE ( 'NONE', *, *, #43478, .F. ) ;
#25843 = CARTESIAN_POINT ( 'NONE',  ( -8.769230769230460965, -2.506253911140614576, 30.00000000000323297 ) ) ;
#25844 = ORIENTED_EDGE ( 'NONE', *, *, #26545, .T. ) ;
#25845 = FACE_BOUND ( 'NONE', #22503, .T. ) ;
#25846 = CARTESIAN_POINT ( 'NONE',  ( 7.596130608860880429, -11.86270091957321249, 32.19358267280087915 ) ) ;
#25847 = CARTESIAN_POINT ( 'NONE',  ( -13.38461538461550582, -10.90142922262034020, 33.41473453929536674 ) ) ;
#25848 = ORIENTED_EDGE ( 'NONE', *, *, #82307, .T. ) ;
#25849 = CARTESIAN_POINT ( 'NONE',  ( -1.161835715637317801, -5.827830569534415694, 34.72679350104403539 ) ) ;
#25850 = DIRECTION ( 'NONE',  ( 0.000000000000000000, 0.4999999999999960032, -0.8660254037844410391 ) ) ;
#25851 = CARTESIAN_POINT ( 'NONE',  ( -2.651650429449565305, -4.848349570550461785, 14.00000000000000000 ) ) ;
#25852 = VERTEX_POINT ( 'NONE', #38677 ) ;
#25853 = CARTESIAN_POINT ( 'NONE',  ( 14.37294744720514572, -3.643525952247864463, 33.31231777344670064 ) ) ;
#25854 = FACE_OUTER_BOUND ( 'NONE', #30554, .T. ) ;
#25855 = CARTESIAN_POINT ( 'NONE',  ( 2.373759641042384683, -2.833524468853757750, 32.15551576947925838 ) ) ;
#25856 = EDGE_LOOP ( 'NONE', ( #40346, #13340, #35079, #35557 ) ) ;
#25857 = DIRECTION ( 'NONE',  ( 0.000000000000000000, 0.9848077530122072432, -0.1736481776669354937 ) ) ;
#25858 = CARTESIAN_POINT ( 'NONE',  ( 2.373759641042383794, -3.322132147404559976, 32.92929555188717927 ) ) ;
#25859 = ORIENTED_EDGE ( 'NONE', *, *, #11082, .T. ) ;
#25860 = CARTESIAN_POINT ( 'NONE',  ( -12.52680846209478460, -5.941354392334499579, 34.76329471203369792 ) ) ;
#25861 = CARTESIAN_POINT ( 'NONE',  ( -10.36543909703647337, -5.057305518903948638, 34.11320923018887896 ) ) ;
#25862 = CARTESIAN_POINT ( 'NONE',  ( -22.75000000000000000, -7.500000000000000000, 32.75000000000000000 ) ) ;
#25863 = CARTESIAN_POINT ( 'NONE',  ( -4.946131269098287930, -8.147973898785416225, 34.70805048591653730 ) ) ;
#25864 = CARTESIAN_POINT ( 'NONE',  ( 8.769230769230768274, -1.129524287112498415, 32.06866353760679544 ) ) ;
#25865 = LINE ( 'NONE', #53323, #29432 ) ;
#25867 = CARTESIAN_POINT ( 'NONE',  ( 9.822833130541336999, -5.070358843744210198, 34.40418822224088302 ) ) ;
#25866 = CARTESIAN_POINT ( 'NONE',  ( 0.5276057948885370941, -11.35647404775217595, 33.31231777344667222 ) ) ;
#25868 = LINE ( 'NONE', #11465, #35315 ) ;
#25869 = DIRECTION ( 'NONE',  ( 0.000000000000000000, 0.000000000000000000, 1.000000000000000000 ) ) ;
#25870 = VECTOR ( 'NONE', #3028, 1000.000000000000000 ) ;
#25871 = CARTESIAN_POINT ( 'NONE',  ( -1.077988221561460236, -10.27530806549876452, 25.85750670625849068 ) ) ;
#25872 = EDGE_LOOP ( 'NONE', ( #50725, #35743, #53285, #50249 ) ) ;
#25873 = CARTESIAN_POINT ( 'NONE',  ( -3.930833309752757909, -5.582272713120727481, 34.63742843783360570 ) ) ;
#25874 = VERTEX_POINT ( 'NONE', #66140 ) ;
#25875 = ORIENTED_EDGE ( 'NONE', *, *, #18162, .T. ) ;
#25876 = CARTESIAN_POINT ( 'NONE',  ( -7.846153846153844924, -2.486705287966279876, 31.30864560766543647 ) ) ;
#25877 = EDGE_LOOP ( 'NONE', ( #21982, #49947 ) ) ;
#25878 = CARTESIAN_POINT ( 'NONE',  ( 3.230769230769231726, -9.780366693483667717, 34.19971097300155094 ) ) ;
#25879 = CARTESIAN_POINT ( 'NONE',  ( 1.944543648262996083, -5.555456351736983045, 15.56250000000000000 ) ) ;
#25880 = CARTESIAN_POINT ( 'NONE',  ( -13.31936024510254768, -5.941354392334607049, 34.76329471203374055 ) ) ;
#25881 = CARTESIAN_POINT ( 'NONE',  ( -15.45369618967607828, -12.38737895849757820, 31.66785238281580206 ) ) ;
#25882 = CARTESIAN_POINT ( 'NONE',  ( -2.980714919130915685, -9.148310452688873440, 34.47095581063188519 ) ) ;
#25883 = CARTESIAN_POINT ( 'NONE',  ( -10.55012947587177941, -3.643525952247864463, 33.31231777344670064 ) ) ;
#25884 = CARTESIAN_POINT ( 'NONE',  ( -13.45069879557126491, -2.538708090699994813, 30.37095296980875148 ) ) ;
#25885 = CARTESIAN_POINT ( 'NONE',  ( -11.60373198442231590, -5.219633306516282545, 34.19971097300152962 ) ) ;
#25886 = B_SPLINE_CURVE_WITH_KNOTS ( 'NONE', 3,
 ( #47408, #74905, #40678, #29379, #57277, #7767 ),
 .UNSPECIFIED., .F., .F.,
 ( 4, 2, 4 ),
 ( 0.2500000000000000000, 0.3750000652700731796, 0.5000001305401463592 ),
 .UNSPECIFIED. ) ;
#25887 = CARTESIAN_POINT ( 'NONE',  ( 3.750000000000000888, -7.499999999999978684, 19.46875000000000000 ) ) ;
#25888 = B_SPLINE_CURVE_WITH_KNOTS ( 'NONE', 3,
 ( #45010, #52663, #73845, #79261, #58976, #39175 ),
 .UNSPECIFIED., .F., .F.,
 ( 4, 2, 4 ),
 ( 4.220987180333913997E-17, 0.0001954756301637163962, 0.0003909512603273906169 ),
 .UNSPECIFIED. ) ;
#25889 = CARTESIAN_POINT ( 'NONE',  ( 18.00000000000000000, -11.35647404775217417, 33.31231777344666511 ) ) ;
#25890 = CARTESIAN_POINT ( 'NONE',  ( 13.38461538461526423, -3.643525952248795718, 33.31231777344771672 ) ) ;
#25891 = AXIS2_PLACEMENT_3D ( 'NONE', #27963, #83360, #56322 ) ;
#25892 = CARTESIAN_POINT ( 'NONE',  ( 18.06519398178335578, -2.506253911140448043, 29.99999999999988631 ) ) ;
#25893 = AXIS2_PLACEMENT_3D ( 'NONE', #9250, #71368, #51524 ) ;
#25894 = VECTOR ( 'NONE', #30569, 1000.000000000000000 ) ;
#25895 = ORIENTED_EDGE ( 'NONE', *, *, #77054, .T. ) ;
#25896 = ORIENTED_EDGE ( 'NONE', *, *, #49450, .T. ) ;
#25897 = CARTESIAN_POINT ( 'NONE',  ( -9.626239341305252495, -3.513871655860379306, 32.76840700105978499 ) ) ;
#25898 = CARTESIAN_POINT ( 'NONE',  ( -14.30769230769242739, -8.613356846316285953, 34.62446782046622218 ) ) ;
#25899 = CARTESIAN_POINT ( 'NONE',  ( 1.161130460051053914, -10.97335522853832579, 33.68706563782419749 ) ) ;
#25900 = CARTESIAN_POINT ( 'NONE',  ( -6.066083410955879884, -3.513871655860377086, 32.76840700105978499 ) ) ;
#25901 = CARTESIAN_POINT ( 'NONE',  ( 2.307692307692309264, -12.78798330534103123, 29.99999999999997868 ) ) ;
#25902 = AXIS2_PLACEMENT_3D ( 'NONE', #9975, #16732, #79332 ) ;
#25903 = DIRECTION ( 'NONE',  ( -0.000000000000000000, 0.3420201433256694346, -0.9396926207859080948 ) ) ;
#25904 = ADVANCED_FACE ( 'NONE', ( #37332 ), #47657, .F. ) ;
#25905 = ORIENTED_EDGE ( 'NONE', *, *, #4458, .F. ) ;
#25906 = CARTESIAN_POINT ( 'NONE',  ( -6.700065571464073777, -9.886259254753566594, 34.14407573483972413 ) ) ;
#25907 = ORIENTED_EDGE ( 'NONE', *, *, #6661, .T. ) ;
#25908 = ORIENTED_EDGE ( 'NONE', *, *, #34843, .T. ) ;
#25909 = CARTESIAN_POINT ( 'NONE',  ( -14.08472940413082242, -7.369474270740069777, 34.74850911626239736 ) ) ;
#25910 = FACE_OUTER_BOUND ( 'NONE', #14126, .T. ) ;
#25911 = CARTESIAN_POINT ( 'NONE',  ( -4.284536756956459413, -12.62707690430377383, 30.88035979386743435 ) ) ;
#25912 = CARTESIAN_POINT ( 'NONE',  ( 12.46153846153846168, -8.810774026931790459, 35.74407628777942847 ) ) ;
#25913 = CARTESIAN_POINT ( 'NONE',  ( -2.084680956079456582, -11.76359900205217457, 32.36225158514719880 ) ) ;
#25914 = ORIENTED_EDGE ( 'NONE', *, *, #8435, .T. ) ;
#25915 = VERTEX_POINT ( 'NONE', #80573 ) ;
#25916 = ADVANCED_FACE ( 'NONE', ( #73810 ), #20192, .F. ) ;
#25917 = EDGE_CURVE ( 'NONE', #74851, #496, #27389, .T. ) ;
#25918 = EDGE_LOOP ( 'NONE', ( #76511, #10110 ) ) ;
#25919 = CARTESIAN_POINT ( 'NONE',  ( 4.153846153846032507, -6.026961402154118908, 34.52809138561165270 ) ) ;
#25920 = CARTESIAN_POINT ( 'NONE',  ( 11.53846153846141576, -2.379036618888197729, 30.90682066428292885 ) ) ;
#25921 = CARTESIAN_POINT ( 'NONE',  ( 4.284636594813107102, -3.338503747796866872, 32.95102852606553512 ) ) ;
#25922 = CARTESIAN_POINT ( 'NONE',  ( 12.46153846153833911, -2.657715359629662544, 31.77849191805970364 ) ) ;
#25923 = CARTESIAN_POINT ( 'NONE',  ( -19.00000000000000000, -3.499999999999999556, 29.75000000000000355 ) ) ;
#25924 = CARTESIAN_POINT ( 'NONE',  ( -15.23076923076935252, -2.657715359629662544, 31.77849191805970364 ) ) ;
#25925 = ORIENTED_EDGE ( 'NONE', *, *, #3398, .F. ) ;
#25926 = ORIENTED_EDGE ( 'NONE', *, *, #86920, .F. ) ;
#25927 = CARTESIAN_POINT ( 'NONE',  ( 4.853996118016224770, -10.01117774369187252, 34.36070679894347535 ) ) ;
#25929 = ORIENTED_EDGE ( 'NONE', *, *, #19636, .T. ) ;
#25928 = CARTESIAN_POINT ( 'NONE',  ( -3.480792454990688789, -2.588893531581426544, 31.60682220781847818 ) ) ;
#25930 = CARTESIAN_POINT ( 'NONE',  ( 7.976945653978634532, -12.38066358083363738, 30.83685684665853444 ) ) ;
#25931 = DIRECTION ( 'NONE',  ( 0.000000000000000000, 0.000000000000000000, -1.000000000000000000 ) ) ;
#25932 = CARTESIAN_POINT ( 'NONE',  ( 3.750000000000000888, -7.499999999999978684, 14.46875000000000000 ) ) ;
#25933 = ORIENTED_EDGE ( 'NONE', *, *, #26926, .F. ) ;
#25934 = AXIS2_PLACEMENT_3D ( 'NONE', #89107, #20189, #53512 ) ;
#25935 = DIRECTION ( 'NONE',  ( -0.000000000000000000, -0.1736481776669307198, -0.9848077530122080203 ) ) ;
#25936 = VERTEX_POINT ( 'NONE', #62053 ) ;
#25937 = CARTESIAN_POINT ( 'NONE',  ( 2.307692307692309264, -6.386643153685126251, 34.62446782046654192 ) ) ;
#25938 = DIRECTION ( 'NONE',  ( 0.000000000000000000, 0.7660444431189822323, -0.6427876096865344779 ) ) ;
#25939 = CARTESIAN_POINT ( 'NONE',  ( 7.780883845597526438, -4.320704448112771878, 33.92786785259540494 ) ) ;
#25941 = VECTOR ( 'NONE', #76715, 1000.000000000000000 ) ;
#25940 = CARTESIAN_POINT ( 'NONE',  ( -6.923076923076922462, -3.513871655860378418, 32.76840700105978499 ) ) ;
#25942 = DIRECTION ( 'NONE',  ( 0.000000000000000000, 0.000000000000000000, 1.000000000000000000 ) ) ;
#25943 = VERTEX_POINT ( 'NONE', #81012 ) ;
#25944 = CARTESIAN_POINT ( 'NONE',  ( -8.769230769230768274, -13.87047571288749737, 32.06866353760679544 ) ) ;
#25945 = PLANE ( 'NONE',  #70946 ) ;
#25946 = CARTESIAN_POINT ( 'NONE',  ( -14.30769230769230660, -2.721908614388771852, 31.22303859784724978 ) ) ;
#25947 = ORIENTED_EDGE ( 'NONE', *, *, #83557, .F. ) ;
#25948 = AXIS2_PLACEMENT_3D ( 'NONE', #14766, #42244, #69699 ) ;
#25949 = MECHANICAL_DESIGN_GEOMETRIC_PRESENTATION_REPRESENTATION (  '', ( #79192 ), #40366 ) ;
#25950 = LINE ( 'NONE', #53866, #4165 ) ;
#25951 = CARTESIAN_POINT ( 'NONE',  ( 14.37294744720514572, -10.33852847137154107, 34.16647553114620450 ) ) ;
#25952 = DIRECTION ( 'NONE',  ( 1.000000000000000000, -0.000000000000000000, -0.000000000000000000 ) ) ;
#25953 = CARTESIAN_POINT ( 'NONE',  ( 9.692307692307572609, -10.21337939537710326, 33.94971097300076224 ) ) ;
#25954 = CARTESIAN_POINT ( 'NONE',  ( 10.61538461538449596, -11.94971097300221174, 32.03036669348237098 ) ) ;
#25955 = FACE_BOUND ( 'NONE', #68483, .T. ) ;
#25957 = DIRECTION ( 'NONE',  ( 1.000000000000000000, 0.000000000000000000, 0.000000000000000000 ) ) ;
#25956 = CARTESIAN_POINT ( 'NONE',  ( 1.254005729411304060, -7.722926974430166069, 34.99546784045485737 ) ) ;
#25958 = CARTESIAN_POINT ( 'NONE',  ( -3.230769230769351186, -10.90142922262034020, 33.41473453929536674 ) ) ;
#25960 = CARTESIAN_POINT ( 'NONE',  ( -2.241624974342230736, -8.164416787775445883, 34.95778746994558617 ) ) ;
#25959 = CARTESIAN_POINT ( 'NONE',  ( -5.776988648387149539, -9.886259254753566594, 34.14407573483972413 ) ) ;
#25961 = CARTESIAN_POINT ( 'NONE',  ( 8.992243613324164997, -12.64618726649961289, 30.78989965857442712 ) ) ;
#25962 = CARTESIAN_POINT ( 'NONE',  ( -0.06109907496454585613, -4.750000000000000000, 15.15438170625848890 ) ) ;
#25963 = VERTEX_POINT ( 'NONE', #19743 ) ;
#25964 = B_SPLINE_CURVE_WITH_KNOTS ( 'NONE', 3,
 ( #36205, #29005, #83948, #62316, #49699, #15483, #55567, #88946, #21343, #42954 ),
 .UNSPECIFIED., .F., .F.,
 ( 4, 2, 2, 2, 4 ),
 ( 0.000000000000000000, 0.0001954339857564054144, 0.0003908679715128108288, 0.0005863019572692162703, 0.0007817359430256216575 ),
 .UNSPECIFIED. ) ;
#25965 = CARTESIAN_POINT ( 'NONE',  ( -12.59201364661418232, -7.276987145209185215, 34.99546412871779211 ) ) ;
#25966 = EDGE_LOOP ( 'NONE', ( #2990, #438 ) ) ;
#25967 = CARTESIAN_POINT ( 'NONE',  ( 8.769230769230768274, -4.098570777380720287, 33.41473453929634729 ) ) ;
#25968 = ORIENTED_EDGE ( 'NONE', *, *, #2524, .F. ) ;
#25969 = CARTESIAN_POINT ( 'NONE',  ( 2.177544337960613863, -2.373036134822904319, 30.88089517874952250 ) ) ;
#25970 = CARTESIAN_POINT ( 'NONE',  ( -19.99999999999996447, -15.00000000000000533, 13.00000000000000178 ) ) ;
#25972 = ORIENTED_EDGE ( 'NONE', *, *, #63206, .F. ) ;
#25971 = CARTESIAN_POINT ( 'NONE',  ( -2.557669038634660996, -11.79746400365624659, 32.30657167506340954 ) ) ;
#25973 = CARTESIAN_POINT ( 'NONE',  ( -16.85391023282967637, -2.308499170217968466, 30.53291367094874076 ) ) ;
#25974 = CARTESIAN_POINT ( 'NONE',  ( -20.99999999999999645, -10.75000000000000000, 29.75000000000000355 ) ) ;
#25975 = CARTESIAN_POINT ( 'NONE',  ( -0.06109907496455085213, -3.750000000000000888, 26.40438170625848713 ) ) ;
#25976 = EDGE_CURVE ( 'NONE', #16582, #75011, #63657, .T. ) ;
#25977 = CARTESIAN_POINT ( 'NONE',  ( 14.30769230769231015, -10.51840700105979565, 33.73612834413961536 ) ) ;
#25978 = DIRECTION ( 'NONE',  ( -1.000000000000000000, 0.000000000000000000, -0.000000000000000000 ) ) ;
#25979 = CARTESIAN_POINT ( 'NONE',  ( -12.33101302330481808, -9.503571793651731880, 34.60286762892837942 ) ) ;
#25980 = CYLINDRICAL_SURFACE ( 'NONE', #11370, 0.2500000000000002220 ) ;
#25981 = CARTESIAN_POINT ( 'NONE',  ( 7.173022441425065843, -4.336752205174647656, 33.62275283266504289 ) ) ;
#25982 = CARTESIAN_POINT ( 'NONE',  ( -11.31545018684868786, -9.886259254753566594, 34.14407573483972413 ) ) ;
#25983 = EDGE_CURVE ( 'NONE', #37000, #33880, #88229, .T. ) ;
#25984 = CARTESIAN_POINT ( 'NONE',  ( 3.724691934501251023, -9.114399933863618131, 18.54874329374151642 ) ) ;
#25985 = CARTESIAN_POINT ( 'NONE',  ( 14.30769230769231015, -5.557115091759785130, 34.35708131394839171 ) ) ;
#25986 = FACE_OUTER_BOUND ( 'NONE', #59922, .T. ) ;
#25987 = ORIENTED_EDGE ( 'NONE', *, *, #41749, .F. ) ;
#25988 = CIRCLE ( 'NONE', #76318, 2.000000000000001776 ) ;
#25989 = CARTESIAN_POINT ( 'NONE',  ( 17.29993442853592711, -2.758310577978207778, 31.33698337089302299 ) ) ;
#25990 = CARTESIAN_POINT ( 'NONE',  ( 15.45354889974729318, -10.97394488606064122, 33.68653795673694873 ) ) ;
#25991 = CARTESIAN_POINT ( 'NONE',  ( 0.06109907496451268821, -3.749999999999999556, 16.90811829374151287 ) ) ;
#25992 = EDGE_CURVE ( 'NONE', #21493, #81662, #79312, .T. ) ;
#25993 = CARTESIAN_POINT ( 'NONE',  ( 2.177000841024752109, -4.118384482072085184, 33.43331474514187107 ) ) ;
#25994 = CARTESIAN_POINT ( 'NONE',  ( 5.142990410273149848, -6.343179335718452272, 34.87096338111212646 ) ) ;
#25995 = ORIENTED_EDGE ( 'NONE', *, *, #64136, .T. ) ;
#25996 = CARTESIAN_POINT ( 'NONE',  ( 7.053868730901711182, -8.147973898785416225, 34.70805048591653730 ) ) ;
#25997 = CARTESIAN_POINT ( 'NONE',  ( -12.33101302330481808, -12.70449254468099198, 30.44128974285582956 ) ) ;
#25999 = ORIENTED_EDGE ( 'NONE', *, *, #13358, .F. ) ;
#25998 = CARTESIAN_POINT ( 'NONE',  ( 8.899756207464410096, -2.647132371071621471, 31.75357179365171589 ) ) ;
#26000 = CARTESIAN_POINT ( 'NONE',  ( -1.384615384615383471, -6.386643153685126251, 34.62446782046654192 ) ) ;
#26001 = CARTESIAN_POINT ( 'NONE',  ( 4.153846153846032507, -8.613356846316285953, 34.62446782046622218 ) ) ;
#26002 = EDGE_CURVE ( 'NONE', #8955, #60703, #54857, .T. ) ;
#26003 = CARTESIAN_POINT ( 'NONE',  ( -15.00798956179116317, -12.11081565061824250, 32.26097654155340422 ) ) ;
#26004 = CARTESIAN_POINT ( 'NONE',  ( -15.90384615384473399, -7.500000000000154543, 35.00000000000007105 ) ) ;
#26005 = EDGE_LOOP ( 'NONE', ( #78744, #22462 ) ) ;
#26006 = CARTESIAN_POINT ( 'NONE',  ( 7.173076923076923350, -2.249999999999998668, 29.75000000000000355 ) ) ;
#26007 = CARTESIAN_POINT ( 'NONE',  ( -18.06527044596078113, -12.27809138561121394, 31.22303859784730307 ) ) ;
#26008 = B_SPLINE_CURVE_WITH_KNOTS ( 'NONE', 3,
 ( #69926, #50088, #70823, #8236, #69483, #28962, #14098, #36590, #56416, #64042 ),
 .UNSPECIFIED., .F., .F.,
 ( 4, 2, 2, 2, 4 ),
 ( 0.0007817359430256392216, 0.0009771253907250073822, 0.001172514838424375651, 0.001367904286123743920, 0.001563293733823112189 ),
 .UNSPECIFIED. ) ;
#26010 = DIRECTION ( 'NONE',  ( -0.000000000000000000, -0.1736481776669307198, -0.9848077530122080203 ) ) ;
#26009 = CIRCLE ( 'NONE', #37504, 8.000000000000000000 ) ;
#26011 = EDGE_CURVE ( 'NONE', #70591, #22567, #5758, .T. ) ;
#26012 = VERTEX_POINT ( 'NONE', #74247 ) ;
#26013 = ORIENTED_EDGE ( 'NONE', *, *, #77736, .T. ) ;
#26014 = B_SPLINE_CURVE_WITH_KNOTS ( 'NONE', 3,
 ( #3341, #72243, #78554, #31718, #10554, #64585, #71350, #24497, #43448, #36693 ),
 .UNSPECIFIED., .F., .F.,
 ( 4, 2, 2, 2, 4 ),
 ( 0.000000000000000000, 0.0001954311564186868744, 0.0003908623128373737488, 0.0005862934692560606504, 0.0007817246256747474977 ),
 .UNSPECIFIED. ) ;
#26015 = ORIENTED_EDGE ( 'NONE', *, *, #23328, .F. ) ;
#26016 = VECTOR ( 'NONE', #17069, 1000.000000000000000 ) ;
#26017 = VECTOR ( 'NONE', #26512, 1000.000000000000227 ) ;
#26018 = CARTESIAN_POINT ( 'NONE',  ( 12.46153846153846168, -9.905515769479276145, 34.41647553114623292 ) ) ;
#26019 = CARTESIAN_POINT ( 'NONE',  ( 6.923076923076802558, -3.835265460704628371, 33.15142922262033665 ) ) ;
#26020 = DIRECTION ( 'NONE',  ( -1.000000000000000000, 0.000000000000000000, 0.000000000000000000 ) ) ;
#26021 = VECTOR ( 'NONE', #60955, 1000.000000000000000 ) ;
#26022 = VECTOR ( 'NONE', #30131, 1000.000000000000114 ) ;
#26023 = CARTESIAN_POINT ( 'NONE',  ( -17.74999999999992895, -7.434744429011174383, 34.75000000000000711 ) ) ;
#26024 = VERTEX_POINT ( 'NONE', #67492 ) ;
#26025 = EDGE_CURVE ( 'NONE', #673, #76455, #70022, .T. ) ;
#26026 = ORIENTED_EDGE ( 'NONE', *, *, #77535, .F. ) ;
#26027 = ORIENTED_EDGE ( 'NONE', *, *, #67301, .F. ) ;
#26030 = ORIENTED_EDGE ( 'NONE', *, *, #76216, .T. ) ;
#26029 = EDGE_CURVE ( 'NONE', #6055, #10508, #78638, .T. ) ;
#26028 = CARTESIAN_POINT ( 'NONE',  ( -7.053767526187231240, -8.191372820521381826, 34.95448215188423546 ) ) ;
#26031 = CARTESIAN_POINT ( 'NONE',  ( -9.692307692307691624, -9.905515769479276145, 34.41647553114623292 ) ) ;
#26032 = DIRECTION ( 'NONE',  ( -0.000000000000000000, 1.000000000000000000, 3.491481338843133355E-15 ) ) ;
#26033 = EDGE_CURVE ( 'NONE', #955, #78324, #68813, .T. ) ;
#26034 = EDGE_CURVE ( 'NONE', #11784, #20954, #85036, .T. ) ;
#26035 = CARTESIAN_POINT ( 'NONE',  ( 6.989144256427000990, -4.661471528628508665, 34.16647553114624003 ) ) ;
#26036 = DIRECTION ( 'NONE',  ( 0.000000000000000000, -1.000000000000000000, 0.000000000000000000 ) ) ;
#26037 = ORIENTED_EDGE ( 'NONE', *, *, #55742, .T. ) ;
#26038 = ORIENTED_EDGE ( 'NONE', *, *, #63665, .T. ) ;
#26039 = B_SPLINE_CURVE_WITH_KNOTS ( 'NONE', 3,
 ( #67163, #13106, #38804, #39254, #80235, #74813, #32934, #46440, #19857, #47321 ),
 .UNSPECIFIED., .F., .F.,
 ( 4, 2, 2, 2, 4 ),
 ( 0.0007817359430256293554, 0.0009771253907249941549, 0.001172514838424358954, 0.001367904286123723537, 0.001563293733823095276 ),
 .UNSPECIFIED. ) ;
#26040 = VERTEX_POINT ( 'NONE', #69260 ) ;
#26041 = CARTESIAN_POINT ( 'NONE',  ( -18.00000000000000000, -9.815202283848471154, 36.11096599634342397 ) ) ;
#26043 = ORIENTED_EDGE ( 'NONE', *, *, #24182, .T. ) ;
#26042 = CARTESIAN_POINT ( 'NONE',  ( 0.6089743589743582541, -3.499999999999999556, 29.75000000000000355 ) ) ;
#26044 = B_SPLINE_CURVE_WITH_KNOTS ( 'NONE', 3,
 ( #42545, #1996, #29477, #70902, #9208, #29040, #29918, #36670, #35334, #49732 ),
 .UNSPECIFIED., .F., .F.,
 ( 4, 2, 2, 2, 4 ),
 ( 0.0007817246256747470640, 0.0009771112852218902852, 0.001172497944769033398, 0.001367884604316176728, 0.001563271263863319840 ),
 .UNSPECIFIED. ) ;
#26045 = CARTESIAN_POINT ( 'NONE',  ( 3.230769230769231726, -11.69971097300155272, 32.46337939537588113 ) ) ;
#26046 = AXIS2_PLACEMENT_3D ( 'NONE', #79850, #5969, #87973 ) ;
#26047 = CARTESIAN_POINT ( 'NONE',  ( 0.000000000000000000, -11.00000000000000000, 29.75000000000000355 ) ) ;
#26048 = CARTESIAN_POINT ( 'NONE',  ( 19.00000000000000000, -3.499999999999999556, 29.75000000000000355 ) ) ;
#26049 = AXIS2_PLACEMENT_3D ( 'NONE', #33917, #82118, #62269 ) ;
#26050 = DIRECTION ( 'NONE',  ( 0.000000000000000000, 0.000000000000000000, -1.000000000000000000 ) ) ;
#26051 = CARTESIAN_POINT ( 'NONE',  ( -8.352564102564102200, -7.500000000000000000, 29.75000000000000355 ) ) ;
#26052 = FACE_BOUND ( 'NONE', #34161, .T. ) ;
#26053 = CARTESIAN_POINT ( 'NONE',  ( -0.7115616988314271696, -10.05641848906368097, 34.04755513067966177 ) ) ;
#26054 = CARTESIAN_POINT ( 'NONE',  ( -1.319359813339359588, -11.94971097300157403, 32.03036669348361443 ) ) ;
#26055 = CARTESIAN_POINT ( 'NONE',  ( -10.39260494640654819, -10.97394488606064122, 33.68653795673694873 ) ) ;
#26057 = CARTESIAN_POINT ( 'NONE',  ( -5.300408020647025431, -3.236172620538810385, 32.36188796281390267 ) ) ;
#26056 = CARTESIAN_POINT ( 'NONE',  ( 0.2115152373170034461, -6.652501968072650484, 34.93155406624983783 ) ) ;
#26058 = DIRECTION ( 'NONE',  ( 1.000000000000000000, 0.000000000000000000, 0.000000000000000000 ) ) ;
#26059 = CARTESIAN_POINT ( 'NONE',  ( 7.173076923076923350, -2.499999999999998668, 29.75000000000000355 ) ) ;
#26060 = ORIENTED_EDGE ( 'NONE', *, *, #85279, .F. ) ;
#26061 = CARTESIAN_POINT ( 'NONE',  ( 11.31553532094538994, -3.105860786376062332, 32.13614157043599562 ) ) ;
#26062 = CARTESIAN_POINT ( 'NONE',  ( -13.63463860883683942, -9.356822207818506598, 34.66110646841856635 ) ) ;
#26063 = ORIENTED_EDGE ( 'NONE', *, *, #12287, .T. ) ;
#26064 = EDGE_LOOP ( 'NONE', ( #83523, #33941, #5602, #1708, #15301 ) ) ;
#26065 = CARTESIAN_POINT ( 'NONE',  ( 5.076923076923075762, -3.937682226553329556, 33.60647404775216529 ) ) ;
#26066 = CARTESIAN_POINT ( 'NONE',  ( -4.153846153846152411, -2.249999999999998668, 29.50000000000001421 ) ) ;
#26067 = CARTESIAN_POINT ( 'NONE',  ( -15.23076923076935252, -9.528491918059723176, 34.59228464037033035 ) ) ;
#26068 = EDGE_LOOP ( 'NONE', ( #5569, #18104, #82319, #79839 ) ) ;
#26069 = EDGE_CURVE ( 'NONE', #5237, #52906, #60297, .T. ) ;
#26070 = PLANE ( 'NONE',  #39988 ) ;
#26071 = CARTESIAN_POINT ( 'NONE',  ( -7.146561866800873020, -10.11188796281391511, 34.01382737946119050 ) ) ;
#26073 = DIRECTION ( 'NONE',  ( 1.000000000000000000, 0.000000000000000000, 0.000000000000000000 ) ) ;
#26072 = CARTESIAN_POINT ( 'NONE',  ( 15.23076923076923173, -2.833524468853757305, 32.15551576947925838 ) ) ;
#26074 = FACE_OUTER_BOUND ( 'NONE', #77771, .T. ) ;
#26075 = VECTOR ( 'NONE', #43801, 1000.000000000000227 ) ;
#26076 = DIRECTION ( 'NONE',  ( -0.000000000000000000, -0.3420201433256694901, -0.9396926207859082059 ) ) ;
#26077 = CARTESIAN_POINT ( 'NONE',  ( 2.242422307135989001, -11.06231777344662781, 33.60647404775220082 ) ) ;
#26078 = CARTESIAN_POINT ( 'NONE',  ( 2.320192649118979489E-14, -11.25000000000000000, 23.53125000000000000 ) ) ;
#26079 = VERTEX_POINT ( 'NONE', #362 ) ;
#26080 = ORIENTED_EDGE ( 'NONE', *, *, #50996, .T. ) ;
#26081 = CARTESIAN_POINT ( 'NONE',  ( -9.822998295417995962, -2.494641256782728966, 31.33461815524612959 ) ) ;
#26082 = CARTESIAN_POINT ( 'NONE',  ( -17.93393266664992325, -3.322132147404559088, 32.92929555188717217 ) ) ;
#26083 = CYLINDRICAL_SURFACE ( 'NONE', #60354, 0.2499999999999986955 ) ;
#26084 = CARTESIAN_POINT ( 'NONE',  ( -17.07692307692319744, -11.48612834414049644, 32.76840700105863391 ) ) ;
#26085 = CYLINDRICAL_SURFACE ( 'NONE', #32774, 0.2500000000000012212 ) ;
#26086 = CARTESIAN_POINT ( 'NONE',  ( -3.750000000000008438, -5.946699141100917352, 22.67187500000000355 ) ) ;
#26087 = EDGE_CURVE ( 'NONE', #26451, #79311, #81859, .T. ) ;
#26088 = EDGE_CURVE ( 'NONE', #59796, #29766, #83222, .T. ) ;
#26089 = CARTESIAN_POINT ( 'NONE',  ( 0.5266842408704249801, -7.750023238201980469, 34.74374492549440419 ) ) ;
#26090 = CARTESIAN_POINT ( 'NONE',  ( -13.38461538461550582, -8.613356846316285953, 34.62446782046622218 ) ) ;
#26091 = CARTESIAN_POINT ( 'NONE',  ( 17.07692307692307665, -13.57706302396349152, 30.56769352161908060 ) ) ;
#26092 = CARTESIAN_POINT ( 'NONE',  ( 16.15384615384603251, -12.70778746994576025, 30.41441678777401236 ) ) ;
#26093 = CYLINDRICAL_SURFACE ( 'NONE', #52626, 4.000000000000000000 ) ;
#26094 = CARTESIAN_POINT ( 'NONE',  ( 8.769230769230647482, -12.27809138561165270, 31.22303859784587132 ) ) ;
#26095 = B_SPLINE_CURVE_WITH_KNOTS ( 'NONE', 3,
 ( #24154, #78214, #58374, #36791, #23705, #29600, #50285, #16515, #2548, #58829 ),
 .UNSPECIFIED., .F., .F.,
 ( 4, 2, 2, 2, 4 ),
 ( 0.0007817359430256294638, 0.0009771253907249950223, 0.001172514838424360472, 0.001367904286123725922, 0.001563293733823091372 ),
 .UNSPECIFIED. ) ;
#26096 = CARTESIAN_POINT ( 'NONE',  ( -12.71153846153846168, -7.500000000000001776, 35.00000000000000000 ) ) ;
#26097 = CARTESIAN_POINT ( 'NONE',  ( 6.923076923076924238, -4.661471528628507777, 34.16647553114623292 ) ) ;
#26098 = CARTESIAN_POINT ( 'NONE',  ( -6.923076923076922462, -3.322132147404559976, 32.92929555188717927 ) ) ;
#26099 = CARTESIAN_POINT ( 'NONE',  ( -16.82697766754503377, -2.986452184633680229, 32.43230066228895225 ) ) ;
#26100 = EDGE_LOOP ( 'NONE', ( #34362, #65670, #52825, #5437 ) ) ;
#26101 = CARTESIAN_POINT ( 'NONE',  ( -16.15384615384627409, -11.94971097300221174, 32.03036669348237098 ) ) ;
#26102 = CARTESIAN_POINT ( 'NONE',  ( -3.230769230769351186, -3.835265460704628371, 33.15142922262033665 ) ) ;
#26103 = CARTESIAN_POINT ( 'NONE',  ( -1.200186371490524317, -10.22469193450124791, 18.86124329374151287 ) ) ;
#26104 = EDGE_CURVE ( 'NONE', #50090, #31043, #50293, .T. ) ;
#26105 = CARTESIAN_POINT ( 'NONE',  ( 5.207448515156721136, -10.31582465632705237, 34.18122507451815295 ) ) ;
#26106 = CARTESIAN_POINT ( 'NONE',  ( 10.48469314871705649, -5.582088688514999397, 34.36776431015576350 ) ) ;
#26108 = ORIENTED_EDGE ( 'NONE', *, *, #18921, .F. ) ;
#26107 = CARTESIAN_POINT ( 'NONE',  ( 5.299935921016470708, -4.026326845037961455, 33.68677907613344047 ) ) ;
#26109 = CARTESIAN_POINT ( 'NONE',  ( -2.749999999999998224, -7.500000000000015987, 22.59375000000000355 ) ) ;
#26110 = CARTESIAN_POINT ( 'NONE',  ( 18.00000000000000000, -11.69971097300155272, 32.46337939537588113 ) ) ;
#26111 = ADVANCED_FACE ( 'NONE', ( #28719 ), #29605, .F. ) ;
#26112 = EDGE_LOOP ( 'NONE', ( #21517, #6217, #52275, #23253 ) ) ;
#26113 = CARTESIAN_POINT ( 'NONE',  ( 8.639083559792549494, -8.587444163452046197, 34.63053765926554206 ) ) ;
#26114 = DIRECTION ( 'NONE',  ( -0.000000000000000000, 1.000000000000000000, -0.000000000000000000 ) ) ;
#26115 = VERTEX_POINT ( 'NONE', #8891 ) ;
#26116 = AXIS2_PLACEMENT_3D ( 'NONE', #64465, #3222, #79336 ) ;
#26117 = DIRECTION ( 'NONE',  ( -0.000000000000000000, -0.9848077530122085754, -0.1736481776669273613 ) ) ;
#26118 = CARTESIAN_POINT ( 'NONE',  ( -9.692307692307691624, -2.721908614388771852, 31.22303859784724978 ) ) ;
#26119 = CARTESIAN_POINT ( 'NONE',  ( -7.911424292114618950, -3.835265460703609186, 33.15142922261924241 ) ) ;
#26120 = EDGE_CURVE ( 'NONE', #41328, #4532, #36687, .T. ) ;
#26121 = ORIENTED_EDGE ( 'NONE', *, *, #22029, .F. ) ;
#26122 = EDGE_LOOP ( 'NONE', ( #22558, #86043, #35527, #36031 ) ) ;
#26123 = EDGE_LOOP ( 'NONE', ( #27495, #52754, #1656, #22234 ) ) ;
#26124 = CARTESIAN_POINT ( 'NONE',  ( 3.512820512820510555, -3.499999999999999556, 29.75000000000000355 ) ) ;
#26125 = CARTESIAN_POINT ( 'NONE',  ( 12.21156173059610772, -12.41269422305637171, 30.68257228309993323 ) ) ;
#26126 = CARTESIAN_POINT ( 'NONE',  ( -9.627052121031669074, -10.21337939537593620, 33.94971097300152252 ) ) ;
#26127 = CARTESIAN_POINT ( 'NONE',  ( -8.096153846153844924, -7.500000000000001776, 35.04278698407183867 ) ) ;
#26128 = EDGE_CURVE ( 'NONE', #61830, #75640, #15208, .T. ) ;
#26129 = CARTESIAN_POINT ( 'NONE',  ( -15.23076923076922995, -12.29105614889573062, 35.45975837776705220 ) ) ;
#26130 = CARTESIAN_POINT ( 'NONE',  ( 9.692307692307695177, -9.905515769479276145, 34.41647553114623292 ) ) ;
#26131 = CARTESIAN_POINT ( 'NONE',  ( 11.31553532094538994, -11.76352882383564769, 32.36236540154569497 ) ) ;
#26132 = CARTESIAN_POINT ( 'NONE',  ( -7.134615384615385025, -11.50000000000000000, 29.75000000000000355 ) ) ;
#26133 = EDGE_CURVE ( 'NONE', #27372, #72596, #33520, .T. ) ;
#26134 = ORIENTED_EDGE ( 'NONE', *, *, #62462, .F. ) ;
#26135 = EDGE_LOOP ( 'NONE', ( #24144, #26043 ) ) ;
#26136 = ORIENTED_EDGE ( 'NONE', *, *, #25154, .T. ) ;
#26138 = EDGE_LOOP ( 'NONE', ( #47296, #38650 ) ) ;
#26137 = CARTESIAN_POINT ( 'NONE',  ( 18.06525513951284267, -9.528491918058456633, 34.59228464037085615 ) ) ;
#26139 = B_SPLINE_CURVE_WITH_KNOTS ( 'NONE', 3,
 ( #54815, #48493, #62881, #72312, #29133, #2080, #17376, #56589, #10620, #78626 ),
 .UNSPECIFIED., .F., .F.,
 ( 4, 2, 2, 2, 4 ),
 ( 0.000000000000000000, 0.0001954339857564070949, 0.0003908679715128141898, 0.0005863019572692212576, 0.0007817359430256283796 ),
 .UNSPECIFIED. ) ;
#26140 = ADVANCED_FACE ( 'NONE', ( #16969 ), #86788, .F. ) ;
#26141 = AXIS2_PLACEMENT_3D ( 'NONE', #66493, #4795, #59731 ) ;
#26142 = EDGE_CURVE ( 'NONE', #7620, #63664, #3446, .T. ) ;
#26143 = CARTESIAN_POINT ( 'NONE',  ( 10.39251835232151677, -2.251424796025574881, 29.88072029997477230 ) ) ;
#26144 = PLANE ( 'NONE',  #35261 ) ;
#26145 = EDGE_LOOP ( 'NONE', ( #31601, #18861, #50000, #8322 ) ) ;
#26146 = CARTESIAN_POINT ( 'NONE',  ( -14.17716660592874689, -4.459921816937791661, 33.71989282347011851 ) ) ;
#26147 = CIRCLE ( 'NONE', #62145, 0.2500000000000002220 ) ;
#26148 = VERTEX_POINT ( 'NONE', #9764 ) ;
#26149 = CARTESIAN_POINT ( 'NONE',  ( -10.86540785267757947, -3.202444869320336451, 32.30641848906366675 ) ) ;
#26150 = ORIENTED_EDGE ( 'NONE', *, *, #19206, .F. ) ;
#26151 = LINE ( 'NONE', #19393, #41647 ) ;
#26152 = CARTESIAN_POINT ( 'NONE',  ( -12.23852561744506851, -10.01129605718032600, 34.36064277460058491 ) ) ;
#26153 = ADVANCED_FACE ( 'NONE', ( #30912 ), #52075, .F. ) ;
#26154 = CARTESIAN_POINT ( 'NONE',  ( -16.02332071561251325, -11.04252011169590020, 33.62494198852677840 ) ) ;
#26155 = FACE_BOUND ( 'NONE', #20320, .T. ) ;
#26156 = DIRECTION ( 'NONE',  ( 0.000000000000000000, 0.9848077530122072432, -0.1736481776669354937 ) ) ;
#26157 = LINE ( 'NONE', #60379, #1108 ) ;
#26158 = CYLINDRICAL_SURFACE ( 'NONE', #16543, 0.2499999999999986955 ) ;
#26159 = CARTESIAN_POINT ( 'NONE',  ( -11.97435897435897267, -3.499999999999999556, 29.75000000000000355 ) ) ;
#26160 = ADVANCED_FACE ( 'NONE', ( #37229 ), #3886, .F. ) ;
#26161 = CARTESIAN_POINT ( 'NONE',  ( -4.153846153846152411, -8.564572088678739092, 35.78748833219616898 ) ) ;
#26162 = CARTESIAN_POINT ( 'NONE',  ( -7.976301815885543434, -9.504002272028875709, 34.60269587691767867 ) ) ;
#26163 = DIRECTION ( 'NONE',  ( 0.000000000000000000, 0.1736481776669267785, -0.9848077530122087975 ) ) ;
#26164 = VERTEX_POINT ( 'NONE', #11100 ) ;
#26165 = ORIENTED_EDGE ( 'NONE', *, *, #42475, .F. ) ;
#26167 = CARTESIAN_POINT ( 'NONE',  ( -14.30769230769242739, -12.46129190930018460, 30.37095296980731973 ) ) ;
#26166 = CYLINDRICAL_SURFACE ( 'NONE', #51829, 0.2499999999999994726 ) ;
#26168 = AXIS2_PLACEMENT_3D ( 'NONE', #8580, #36057, #63506 ) ;
#26169 = CYLINDRICAL_SURFACE ( 'NONE', #41355, 0.2500000000000009437 ) ;
#26170 = CARTESIAN_POINT ( 'NONE',  ( -0.4615384615384611200, -10.67929555188718282, 33.92786785259544047 ) ) ;
#26171 = CARTESIAN_POINT ( 'NONE',  ( -17.07692307692319744, -12.51329471203414379, 31.30864560766407578 ) ) ;
#26172 = LINE ( 'NONE', #40585, #14498 ) ;
#26173 = ORIENTED_EDGE ( 'NONE', *, *, #34213, .T. ) ;
#26174 = EDGE_CURVE ( 'NONE', #44526, #68629, #17416, .T. ) ;
#26175 = CARTESIAN_POINT ( 'NONE',  ( 17.29970261819148902, -3.236590943229497697, 32.36255958852954251 ) ) ;
#26176 = CARTESIAN_POINT ( 'NONE',  ( -19.00000000000000000, -16.99999999999999289, 22.25000000000000000 ) ) ;
#26177 = CARTESIAN_POINT ( 'NONE',  ( -14.43783951713053249, -8.587444163452046197, 34.63053765926554206 ) ) ;
#26178 = CARTESIAN_POINT ( 'NONE',  ( -13.38461538461538325, -13.87047571288749737, 32.06866353760679544 ) ) ;
#26179 = VECTOR ( 'NONE', #64415, 1000.000000000000227 ) ;
#26180 = ORIENTED_EDGE ( 'NONE', *, *, #53256, .T. ) ;
#26181 = EDGE_CURVE ( 'NONE', #77080, #66348, #66857, .T. ) ;
#26182 = ORIENTED_EDGE ( 'NONE', *, *, #57342, .F. ) ;
#26183 = SHAPE_DEFINITION_REPRESENTATION ( #20359, #60984 ) ;
#26185 = EDGE_CURVE ( 'NONE', #8424, #6380, #76414, .T. ) ;
#26184 = ORIENTED_EDGE ( 'NONE', *, *, #69232, .F. ) ;
#26186 = CARTESIAN_POINT ( 'NONE',  ( 0.2115384615384615918, -7.433931650972300353, 34.75000000000000711 ) ) ;
#26187 = PLANE ( 'NONE',  #51913 ) ;
#26188 = ORIENTED_EDGE ( 'NONE', *, *, #3817, .T. ) ;
#26189 = DIRECTION ( 'NONE',  ( 1.000000000000000000, 0.000000000000000000, 0.000000000000000000 ) ) ;
#26190 = CARTESIAN_POINT ( 'NONE',  ( -5.076923076923075762, -1.951392089020283160, 34.73218667398347748 ) ) ;
#26191 = CARTESIAN_POINT ( 'NONE',  ( 4.826899839630109490, -6.695914987888143877, 34.68535235679833306 ) ) ;
#26192 = CARTESIAN_POINT ( 'NONE',  ( 1.607628228708781748, -6.460100341425561332, 34.89618726649961644 ) ) ;
#26193 = ADVANCED_FACE ( 'NONE', ( #4341 ), #45318, .F. ) ;
#26194 = CARTESIAN_POINT ( 'NONE',  ( 10.03846153846153832, -4.000000000000000000, 29.65000000000000213 ) ) ;
#26195 = VERTEX_POINT ( 'NONE', #78667 ) ;
#26197 = EDGE_LOOP ( 'NONE', ( #63824, #49549, #72030, #26483 ) ) ;
#26196 = DIRECTION ( 'NONE',  ( 0.000000000000000000, 0.3420201433256671586, 0.9396926207859089830 ) ) ;
#26198 = DIRECTION ( 'NONE',  ( -0.000000000000000000, -0.000000000000000000, -1.000000000000000000 ) ) ;
#26199 = DIRECTION ( 'NONE',  ( 0.000000000000000000, 0.7660444431189807890, 0.6427876096865361433 ) ) ;
#26200 = CARTESIAN_POINT ( 'NONE',  ( 17.07692307692307665, -5.180354513474913603, 36.12317359536750416 ) ) ;
#26201 = CARTESIAN_POINT ( 'NONE',  ( 11.66925197942848769, -9.929761469519743144, 34.40412654351204225 ) ) ;
#26202 = CARTESIAN_POINT ( 'NONE',  ( -5.934807011705343527, -2.255955759149235629, 29.99999999999988631 ) ) ;
#26203 = CARTESIAN_POINT ( 'NONE',  ( -0.4615384615384611200, -12.37446782046654192, 30.86335684631486131 ) ) ;
#26204 = CARTESIAN_POINT ( 'NONE',  ( 1.077988221561497539, -10.27530806549875386, 18.70499329374151287 ) ) ;
#26205 = ORIENTED_EDGE ( 'NONE', *, *, #87714, .T. ) ;
#26206 = CARTESIAN_POINT ( 'NONE',  ( -6.923076923077045919, -11.06231777344772027, 33.60647404775119895 ) ) ;
#26207 = CARTESIAN_POINT ( 'NONE',  ( 2.438217745925953750, -4.299079248970732792, 33.91157788607253565 ) ) ;
#26208 = AXIS2_PLACEMENT_3D ( 'NONE', #77467, #22083, #42808 ) ;
#26209 = VECTOR ( 'NONE', #86416, 1000.000000000000227 ) ;
#26210 = CARTESIAN_POINT ( 'NONE',  ( 6.923076923076802558, -6.879047030192662504, 34.71129190930017927 ) ) ;
#26211 = ORIENTED_EDGE ( 'NONE', *, *, #38397, .F. ) ;
#26212 = CARTESIAN_POINT ( 'NONE',  ( 8.069166690247241647, -11.98016756924214832, 32.48728574198911190 ) ) ;
#26213 = CARTESIAN_POINT ( 'NONE',  ( 11.40831356872984514, -12.70455904226513866, 30.44083106164009322 ) ) ;
#26214 = EDGE_CURVE ( 'NONE', #60841, #49648, #58223, .T. ) ;
#26215 = VECTOR ( 'NONE', #53364, 1000.000000000000000 ) ;
#26216 = B_SPLINE_CURVE_WITH_KNOTS ( 'NONE', 3,
 ( #67707, #88444, #39361, #26715, #5118, #54617, #39799, #19952, #32583, #25837 ),
 .UNSPECIFIED., .F., .F.,
 ( 4, 2, 2, 2, 4 ),
 ( 0.0007817246256747517261, 0.0009771112852218963567, 0.001172497944769040987, 0.001367884604316185618, 0.001563271263863330249 ),
 .UNSPECIFIED. ) ;
#26217 = DIRECTION ( 'NONE',  ( -0.000000000000000000, 0.6427876096865404731, -0.7660444431189771253 ) ) ;
#26218 = CARTESIAN_POINT ( 'NONE',  ( -6.923076923076922462, -13.75783147151868846, 33.36296068462461051 ) ) ;
#26219 = B_SPLINE_CURVE_WITH_KNOTS ( 'NONE', 3,
 ( #51928, #52823, #2851, #24460, #37529, #3751, #64997, #78969, #65889, #31221 ),
 .UNSPECIFIED., .F., .F.,
 ( 4, 2, 2, 2, 4 ),
 ( 0.000000000000000000, 0.0001954339857564097241, 0.0003908679715128194482, 0.0005863019572692291723, 0.0007817359430256388964 ),
 .UNSPECIFIED. ) ;
#26220 = DIRECTION ( 'NONE',  ( 0.000000000000000000, 0.8660254037844377084, -0.5000000000000015543 ) ) ;
#26221 = ORIENTED_EDGE ( 'NONE', *, *, #34619, .F. ) ;
#26222 = B_SPLINE_CURVE_WITH_KNOTS ( 'NONE', 3,
 ( #64352, #37327, #2649, #23371, #78315, #64793, #85531, #23806, #51258, #58935 ),
 .UNSPECIFIED., .F., .F.,
 ( 4, 2, 2, 2, 4 ),
 ( 0.000000000000000000, 0.0001954311564186879044, 0.0003908623128373758088, 0.0005862934692560636861, 0.0007817246256747516176 ),
 .UNSPECIFIED. ) ;
#26223 = CARTESIAN_POINT ( 'NONE',  ( 9.626224281351813516, -10.51840700105979387, 33.73612834413961536 ) ) ;
#26224 = DIRECTION ( 'NONE',  ( -0.000000000000000000, -0.1736481776669307198, -0.9848077530122080203 ) ) ;
#26225 = CARTESIAN_POINT ( 'NONE',  ( -3.361460697436787992, -11.71456829005830080, 32.44064028649416542 ) ) ;
#26226 = ORIENTED_EDGE ( 'NONE', *, *, #83157, .F. ) ;
#26227 = DIRECTION ( 'NONE',  ( 0.000000000000000000, 0.000000000000000000, -1.000000000000000000 ) ) ;
#26228 = VERTEX_POINT ( 'NONE', #60165 ) ;
#26229 = DIRECTION ( 'NONE',  ( 0.000000000000000000, 0.9396926207859126468, -0.3420201433256571111 ) ) ;
#26230 =( LENGTH_UNIT ( ) NAMED_UNIT ( * ) SI_UNIT ( .MILLI., .METRE. ) );
#26231 = DIRECTION ( 'NONE',  ( 0.000000000000000000, 1.000000000000000000, -0.000000000000000000 ) ) ;
#26232 = ORIENTED_EDGE ( 'NONE', *, *, #32935, .T. ) ;
#26233 = CARTESIAN_POINT ( 'NONE',  ( 12.21151522424549718, -3.711651800289232028, 33.01384336483936011 ) ) ;
#26234 = CARTESIAN_POINT ( 'NONE',  ( -14.30769230769199218, -2.255955759149395501, 30.00000000000324363 ) ) ;
#26235 = DIRECTION ( 'NONE',  ( -0.000000000000000000, -0.7660444431189791237, -0.6427876096865379196 ) ) ;
#26236 = VECTOR ( 'NONE', #27302, 1000.000000000000000 ) ;
#26237 = CARTESIAN_POINT ( 'NONE',  ( 7.146089767170317408, -12.38742843783360748, 31.66772728687926985 ) ) ;
#26238 = CARTESIAN_POINT ( 'NONE',  ( -5.076923076923075762, -9.819645486525091727, 36.12317359536749706 ) ) ;
#26239 = EDGE_LOOP ( 'NONE', ( #18307, #55051 ) ) ;
#26240 = CARTESIAN_POINT ( 'NONE',  ( -14.30769230769242739, -2.892918686052166066, 31.69288490824153470 ) ) ;
#26241 = ORIENTED_EDGE ( 'NONE', *, *, #75681, .T. ) ;
#26242 = CARTESIAN_POINT ( 'NONE',  ( -2.530619266599153150, -2.523278758544489353, 31.42238647778637528 ) ) ;
#26243 = CARTESIAN_POINT ( 'NONE',  ( -10.54931728203453822, -9.905515769479276145, 34.41647553114623292 ) ) ;
#26244 = EDGE_CURVE ( 'NONE', #88864, #25231, #73706, .T. ) ;
#26245 = B_SPLINE_CURVE_WITH_KNOTS ( 'NONE', 3,
 ( #32546, #19041, #88409, #66338, #46512, #67236, #68122, #73993, #73555, #24898 ),
 .UNSPECIFIED., .F., .F.,
 ( 4, 2, 2, 2, 4 ),
 ( 0.0007817246256747519429, 0.0009771112852218970073, 0.001172497944769042288, 0.001367884604316187353, 0.001563271263863332417 ),
 .UNSPECIFIED. ) ;
#26246 = CARTESIAN_POINT ( 'NONE',  ( 5.011652630962299959, -11.94971097300153140, 32.03036669348370680 ) ) ;
#26247 = EDGE_CURVE ( 'NONE', #61129, #78712, #80458, .T. ) ;
#26248 = DIRECTION ( 'NONE',  ( 0.000000000000000000, -1.000000000000000000, -8.673617379884033500E-16 ) ) ;
#26249 = DIRECTION ( 'NONE',  ( 0.000000000000000000, -6.938893903907222067E-15, 1.000000000000000000 ) ) ;
#26250 = ORIENTED_EDGE ( 'NONE', *, *, #7982, .T. ) ;
#26252 = EDGE_CURVE ( 'NONE', #81813, #35413, #67822, .T. ) ;
#26251 = ORIENTED_EDGE ( 'NONE', *, *, #9085, .F. ) ;
#26253 = ORIENTED_EDGE ( 'NONE', *, *, #1894, .T. ) ;
#26254 = EDGE_LOOP ( 'NONE', ( #69238, #79070, #57196, #59788 ) ) ;
#26255 = CARTESIAN_POINT ( 'NONE',  ( 2.307692307692187583, -5.219633306517616589, 34.19971097300220464 ) ) ;
#26256 = CARTESIAN_POINT ( 'NONE',  ( 4.376858997939548246, -10.01129605718032778, 34.36064277460058491 ) ) ;
#26257 = EDGE_CURVE ( 'NONE', #51846, #38427, #7432, .T. ) ;
#26258 = CARTESIAN_POINT ( 'NONE',  ( -15.45425417449318317, -10.81261337010820256, 33.49550067578627477 ) ) ;
#26259 = CARTESIAN_POINT ( 'NONE',  ( -8.069080805060693251, -3.395401636524185474, 33.02366814457250399 ) ) ;
#26260 = AXIS2_PLACEMENT_3D ( 'NONE', #46476, #12691, #73955 ) ;
#26261 = CARTESIAN_POINT ( 'NONE',  ( -10.03846153846153832, -3.499999999999999556, 29.75000000000000355 ) ) ;
#26262 = VECTOR ( 'NONE', #51809, 999.9999999999998863 ) ;
#26263 = DIRECTION ( 'NONE',  ( 0.000000000000000000, 0.9848077530122072432, -0.1736481776669354937 ) ) ;
#26264 = CARTESIAN_POINT ( 'NONE',  ( -2.176900499867520100, -3.530189275343204702, 32.79018710029569661 ) ) ;
#26265 = CARTESIAN_POINT ( 'NONE',  ( 17.14299142792552288, -2.538708090699994813, 30.37095296980875503 ) ) ;
#26266 = ORIENTED_EDGE ( 'NONE', *, *, #27598, .F. ) ;
#26267 = ORIENTED_EDGE ( 'NONE', *, *, #31657, .F. ) ;
#26268 = VECTOR ( 'NONE', #45277, 1000.000000000000000 ) ;
#26269 = EDGE_LOOP ( 'NONE', ( #47499, #44506, #4201, #51858 ) ) ;
#26271 = EDGE_LOOP ( 'NONE', ( #83870, #73871 ) ) ;
#26270 = CARTESIAN_POINT ( 'NONE',  ( 2.177545098254089151, -2.619462340734462380, 30.83744416345203021 ) ) ;
#26273 = DIRECTION ( 'NONE',  ( -0.000000000000000000, -0.8660254037844397068, -0.4999999999999978906 ) ) ;
#26272 = CARTESIAN_POINT ( 'NONE',  ( 16.40390046548446534, -11.79725096376909299, 32.30694842903960762 ) ) ;
#26274 = CARTESIAN_POINT ( 'NONE',  ( 15.93096747141751379, -7.630691491037286056, 34.74850469731152458 ) ) ;
#26275 = CARTESIAN_POINT ( 'NONE',  ( -9.822454901745910405, -6.852621066184266141, 34.70813303252209181 ) ) ;
#26276 = FACE_BOUND ( 'NONE', #27468, .T. ) ;
#26277 = ORIENTED_EDGE ( 'NONE', *, *, #54639, .T. ) ;
#26278 = ORIENTED_EDGE ( 'NONE', *, *, #22379, .T. ) ;
#26279 = CARTESIAN_POINT ( 'NONE',  ( 15.12820512820512953, -3.499999999999999556, 29.75000000000000355 ) ) ;
#26280 = EDGE_CURVE ( 'NONE', #69003, #10584, #86163, .T. ) ;
#26281 = ORIENTED_EDGE ( 'NONE', *, *, #50318, .T. ) ;
#26282 = FACE_BOUND ( 'NONE', #61078, .T. ) ;
#26283 = CARTESIAN_POINT ( 'NONE',  ( 9.692307692307695177, -5.471508081941601098, 34.59228464037088457 ) ) ;
#26284 = CARTESIAN_POINT ( 'NONE',  ( 18.22301135161285046, -4.887748414852792322, 34.01359900205217457 ) ) ;
#26285 = ORIENTED_EDGE ( 'NONE', *, *, #2061, .T. ) ;
#26286 = DIRECTION ( 'NONE',  ( 1.000000000000000000, 0.000000000000000000, 0.000000000000000000 ) ) ;
#26287 = CARTESIAN_POINT ( 'NONE',  ( 9.692307692307572609, -5.219633306517616589, 34.19971097300220464 ) ) ;
#26288 = CARTESIAN_POINT ( 'NONE',  ( 3.165499230212911019, -12.16647553114622049, 32.15551576947930812 ) ) ;
#26289 = VERTEX_POINT ( 'NONE', #25505 ) ;
#26290 = DIRECTION ( 'NONE',  ( -1.734723475976813750E-16, 1.000000000000000000, -0.000000000000000000 ) ) ;
#26291 = CYLINDRICAL_SURFACE ( 'NONE', #14087, 0.2500000000000012212 ) ;
#26292 = CARTESIAN_POINT ( 'NONE',  ( -3.480745961711585235, -2.779195860258149242, 31.39871582349837453 ) ) ;
#26293 = DIRECTION ( 'NONE',  ( 0.000000000000000000, 0.9848077530122072432, 0.1736481776669354937 ) ) ;
#26294 = ORIENTED_EDGE ( 'NONE', *, *, #7814, .F. ) ;
#26295 = ADVANCED_FACE ( 'NONE', ( #39476 ), #33596, .F. ) ;
#26296 = CARTESIAN_POINT ( 'NONE',  ( 27.00000000000000000, 0.7500000000000052180, 31.75000000000000000 ) ) ;
#26298 = CARTESIAN_POINT ( 'NONE',  ( 5.198717948717946236, -3.499999999999999556, 29.75000000000000355 ) ) ;
#26297 = VECTOR ( 'NONE', #15585, 1000.000000000000000 ) ;
#26300 = ORIENTED_EDGE ( 'NONE', *, *, #22463, .T. ) ;
#26299 = AXIS2_PLACEMENT_3D ( 'NONE', #35176, #15799, #43264 ) ;
#26301 = CARTESIAN_POINT ( 'NONE',  ( 0.4615384615383396616, -9.442884908241554243, 34.35708131394783038 ) ) ;
#26302 = CARTESIAN_POINT ( 'NONE',  ( -4.480769230769230838, -3.499999999999999556, 29.75000000000000355 ) ) ;
#26303 = CARTESIAN_POINT ( 'NONE',  ( 0.5276057948885365390, -10.67929555188718282, 33.92786785259544757 ) ) ;
#26304 = CARTESIAN_POINT ( 'NONE',  ( 12.46153846153846168, -12.34228464037088635, 31.77849191805839268 ) ) ;
#26305 = CARTESIAN_POINT ( 'NONE',  ( -16.08859058257012720, -4.481592998940251427, 33.73612834413965089 ) ) ;
#26306 = CARTESIAN_POINT ( 'NONE',  ( -39.05038313613820122, -2.499999999999999556, 29.75000000000000355 ) ) ;
#26308 = CARTESIAN_POINT ( 'NONE',  ( 8.638540166120458608, -2.845849958028613624, 32.17971566917920967 ) ) ;
#26307 = CARTESIAN_POINT ( 'NONE',  ( -1.514762594053604250, -5.195881422630166391, 34.18770438780619259 ) ) ;
#26309 = ADVANCED_FACE ( 'NONE', ( #46218 ), #74582, .T. ) ;
#26310 = EDGE_CURVE ( 'NONE', #48029, #12230, #12002, .T. ) ;
#26311 = DIRECTION ( 'NONE',  ( -1.000000000000000000, -0.000000000000000000, -0.000000000000000000 ) ) ;
#26312 = LINE ( 'NONE', #18677, #34872 ) ;
#26313 = CARTESIAN_POINT ( 'NONE',  ( 1.944543648263018731, -9.444543648262994751, 19.62500000000000000 ) ) ;
#26314 = VERTEX_POINT ( 'NONE', #33146 ) ;
#26315 = CARTESIAN_POINT ( 'NONE',  ( -4.153846153846152411, -5.471508081941601098, 34.59228464037088457 ) ) ;
#26316 = ORIENTED_EDGE ( 'NONE', *, *, #78163, .F. ) ;
#26317 = ORIENTED_EDGE ( 'NONE', *, *, #37284, .T. ) ;
#26318 = CARTESIAN_POINT ( 'NONE',  ( -16.82697766754503377, -4.176053281294517028, 33.81426240980091791 ) ) ;
#26319 = ORIENTED_EDGE ( 'NONE', *, *, #53367, .F. ) ;
#26320 = CARTESIAN_POINT ( 'NONE',  ( -5.326899820971665811, -11.47974371597207899, 33.17467449705390692 ) ) ;
#26321 = CARTESIAN_POINT ( 'NONE',  ( -2.749999999999998224, -7.500000000000015987, 17.59375000000000000 ) ) ;
#26322 = CARTESIAN_POINT ( 'NONE',  ( 4.153846153846154188, -2.721908614388771852, 31.22303859784724978 ) ) ;
#26323 = EDGE_CURVE ( 'NONE', #69118, #87423, #88123, .T. ) ;
#26324 = LINE ( 'NONE', #38509, #29478 ) ;
#26325 = CARTESIAN_POINT ( 'NONE',  ( 9.942253101685738059, -9.357781135181031829, 34.66075350412533851 ) ) ;
#26326 = CARTESIAN_POINT ( 'NONE',  ( 5.076923076923075762, -2.708943851104267164, 35.45975837776705220 ) ) ;
#26327 = DIRECTION ( 'NONE',  ( -0.000000000000000000, -0.8660254037844397068, -0.4999999999999978906 ) ) ;
#26328 = CARTESIAN_POINT ( 'NONE',  ( -11.76138775597768138, -4.887634598454295265, 34.01352882383564946 ) ) ;
#26329 = CARTESIAN_POINT ( 'NONE',  ( 2.651650429449569302, -10.15165042944953733, 22.12500000000000000 ) ) ;
#26330 = ADVANCED_FACE ( 'NONE', ( #61054 ), #66935, .F. ) ;
#26331 = EDGE_CURVE ( 'NONE', #66483, #22041, #88024, .T. ) ;
#26332 = CARTESIAN_POINT ( 'NONE',  ( 5.207713517890027788, -2.845873456487966635, 32.17976146951972538 ) ) ;
#26333 = DIRECTION ( 'NONE',  ( -0.000000000000000000, 1.000000000000000000, -0.000000000000000000 ) ) ;
#26334 = CARTESIAN_POINT ( 'NONE',  ( 5.749976775778544713, -3.520140089381497361, 33.17453946501458262 ) ) ;
#26335 = EDGE_CURVE ( 'NONE', #22078, #23906, #45289, .T. ) ;
#26336 = AXIS2_PLACEMENT_3D ( 'NONE', #9237, #22294, #48874 ) ;
#26337 = VERTEX_POINT ( 'NONE', #47980 ) ;
#26338 = ORIENTED_EDGE ( 'NONE', *, *, #31627, .T. ) ;
#26339 = CARTESIAN_POINT ( 'NONE',  ( 6.700150705560774966, -2.554751324335733820, 30.48935550225260727 ) ) ;
#26340 = CARTESIAN_POINT ( 'NONE',  ( 20.00000000000000000, -11.50000000000000000, 29.75000000000000355 ) ) ;
#26341 = CARTESIAN_POINT ( 'NONE',  ( 8.769230769230768274, -13.88283147151868846, 33.14645433367849847 ) ) ;
#26342 = CARTESIAN_POINT ( 'NONE',  ( -5.999999999999998224, -3.513871655860378418, 32.76840700105978499 ) ) ;
#26343 = CYLINDRICAL_SURFACE ( 'NONE', #80878, 0.2499999999999994726 ) ;
#26344 = AXIS2_PLACEMENT_3D ( 'NONE', #55476, #76187, #75315 ) ;
#26345 = CARTESIAN_POINT ( 'NONE',  ( -5.010855743573001675, -2.833524468853757750, 32.15551576947925838 ) ) ;
#26346 = DIRECTION ( 'NONE',  ( 0.000000000000000000, 0.8660254037844377084, -0.5000000000000015543 ) ) ;
#26347 = B_SPLINE_CURVE_WITH_KNOTS ( 'NONE', 3,
 ( #70684, #62252, #82554, #23367, #20831, #75771, #14076, #566, #50825, #16610 ),
 .UNSPECIFIED., .F., .F.,
 ( 4, 2, 2, 2, 4 ),
 ( 0.0007817359430256294638, 0.0009771253907249950223, 0.001172514838424360472, 0.001367904286123725922, 0.001563293733823091372 ),
 .UNSPECIFIED. ) ;
#26348 = VERTEX_POINT ( 'NONE', #40799 ) ;
#26349 = B_SPLINE_CURVE_WITH_KNOTS ( 'NONE', 3,
 ( #47042, #86739, #11502, #74530, #53363, #46614, #5625, #73657, #4288, #52472 ),
 .UNSPECIFIED., .F., .F.,
 ( 4, 2, 2, 2, 4 ),
 ( 0.000000000000000000, 0.0001954311564186864949, 0.0003908623128373729899, 0.0005862934692560594577, 0.0007817246256747459798 ),
 .UNSPECIFIED. ) ;
#26350 = CARTESIAN_POINT ( 'NONE',  ( 1.384615384615265343, -5.219633306517616589, 34.19971097300220464 ) ) ;
#26351 = VERTEX_POINT ( 'NONE', #6563 ) ;
#26352 = B_SPLINE_CURVE_WITH_KNOTS ( 'NONE', 3,
 ( #20868, #47898, #14117, #54203, #41151, #61400, #604, #33511, #13672, #27187 ),
 .UNSPECIFIED., .F., .F.,
 ( 4, 2, 2, 2, 4 ),
 ( 0.000000000000000000, 0.0001954311564186869015, 0.0003908623128373738030, 0.0005862934692560607588, 0.0007817246256747476061 ),
 .UNSPECIFIED. ) ;
#26354 = ADVANCED_FACE ( 'NONE', ( #88999 ), #39031, .F. ) ;
#26353 = EDGE_LOOP ( 'NONE', ( #58618, #36209, #22378, #28196 ) ) ;
#26355 = LINE ( 'NONE', #6087, #62257 ) ;
#26356 = DIRECTION ( 'NONE',  ( -1.000000000000000000, 0.000000000000000000, -0.000000000000000000 ) ) ;
#26357 = CARTESIAN_POINT ( 'NONE',  ( -7.173076923076919797, -7.566082377512563184, 35.00000000000000711 ) ) ;
#26358 = CARTESIAN_POINT ( 'NONE',  ( 6.249945409378045547, -8.476813868363244353, 34.90874843262270133 ) ) ;
#26359 = CYLINDRICAL_SURFACE ( 'NONE', #15074, 0.2500000000000009437 ) ;
#26360 = ORIENTED_EDGE ( 'NONE', *, *, #5391, .F. ) ;
#26361 = VECTOR ( 'NONE', #56172, 1000.000000000000114 ) ;
#26362 = EDGE_CURVE ( 'NONE', #40270, #33584, #87225, .T. ) ;
#26363 = VECTOR ( 'NONE', #37640, 1000.000000000000227 ) ;
#26364 = ORIENTED_EDGE ( 'NONE', *, *, #16220, .T. ) ;
#26365 = ORIENTED_EDGE ( 'NONE', *, *, #71227, .T. ) ;
#26366 = ORIENTED_EDGE ( 'NONE', *, *, #72413, .T. ) ;
#26367 = CARTESIAN_POINT ( 'NONE',  ( -17.07692307692307665, -10.51840700105979565, 33.73612834413961536 ) ) ;
#26368 = CYLINDRICAL_SURFACE ( 'NONE', #76161, 0.2499999999999994726 ) ;
#26369 = ADVANCED_FACE ( 'NONE', ( #63711 ), #69149, .F. ) ;
#26370 = CARTESIAN_POINT ( 'NONE',  ( 16.08859622207207707, -2.255955759149247619, 30.00000000000014211 ) ) ;
#26371 = CARTESIAN_POINT ( 'NONE',  ( 16.15384615384603251, -10.21337939537710326, 33.94971097300076224 ) ) ;
#26372 = CARTESIAN_POINT ( 'NONE',  ( -16.15384615384627409, -12.16647553114689728, 32.15551576947799362 ) ) ;
#26373 = DIRECTION ( 'NONE',  ( -0.000000000000000000, 0.7660444431189792347, -0.6427876096865379196 ) ) ;
#26374 = EDGE_LOOP ( 'NONE', ( #24223, #77328, #3925, #37829, #39560 ) ) ;
#26375 = VERTEX_POINT ( 'NONE', #7001 ) ;
#26376 = B_SPLINE_CURVE_WITH_KNOTS ( 'NONE', 3,
 ( #67588, #7215, #26596, #2643, #36455, #83322, #21159, #21603, #22056, #28358 ),
 .UNSPECIFIED., .F., .F.,
 ( 4, 2, 2, 2, 4 ),
 ( 0.0007817246256747503166, 0.0009771112852218946220, 0.001172497944769039036, 0.001367884604316183233, 0.001563271263863327647 ),
 .UNSPECIFIED. ) ;
#26377 = EDGE_CURVE ( 'NONE', #65002, #11510, #4468, .T. ) ;
#26379 = VERTEX_POINT ( 'NONE', #55622 ) ;
#26378 = CARTESIAN_POINT ( 'NONE',  ( 17.75000000000000000, -2.499999999999998668, 29.75000000000000355 ) ) ;
#26380 = DIRECTION ( 'NONE',  ( -0.000000000000000000, 1.000000000000000000, -0.000000000000000000 ) ) ;
#26381 = CARTESIAN_POINT ( 'NONE',  ( 11.53846153846153832, -3.886160181151819604, 36.00935417666054406 ) ) ;
#26382 = B_SPLINE_CURVE_WITH_KNOTS ( 'NONE', 3,
 ( #37100, #42111, #29479, #7872, #48847, #83986, #15515, #8318, #22268, #56052 ),
 .UNSPECIFIED., .F., .F.,
 ( 4, 2, 2, 2, 4 ),
 ( 0.000000000000000000, 0.0001954311564186867660, 0.0003908623128373735320, 0.0005862934692560603251, 0.0007817246256747470640 ),
 .UNSPECIFIED. ) ;
#26383 = CARTESIAN_POINT ( 'NONE',  ( 2.320192649118979489E-14, -11.25000000000000000, 22.28125000000000355 ) ) ;
#26384 = ORIENTED_EDGE ( 'NONE', *, *, #76189, .F. ) ;
#26385 = CARTESIAN_POINT ( 'NONE',  ( -3.007989689500821573, -12.44528174975671853, 30.48912976160716681 ) ) ;
#26386 = VERTEX_POINT ( 'NONE', #2017 ) ;
#26387 = DIRECTION ( 'NONE',  ( 0.000000000000000000, 0.7660444431189807890, 0.6427876096865361433 ) ) ;
#26388 = CARTESIAN_POINT ( 'NONE',  ( -9.692307692307691624, -9.780366693483667717, 34.19971097300155094 ) ) ;
#26389 = TOROIDAL_SURFACE ( 'NONE', #30685, 3.000000000000000888, 2.000000000000000000 ) ;
#26390 = LINE ( 'NONE', #5668, #62506 ) ;
#26391 = DIRECTION ( 'NONE',  ( 0.000000000000000000, 0.000000000000000000, -1.000000000000000000 ) ) ;
#26392 = VECTOR ( 'NONE', #82329, 1000.000000000000000 ) ;
#26393 = DIRECTION ( 'NONE',  ( -0.000000000000000000, 1.000000000000000000, -0.000000000000000000 ) ) ;
#26394 = ORIENTED_EDGE ( 'NONE', *, *, #74787, .F. ) ;
#26395 = EDGE_CURVE ( 'NONE', #54784, #31550, #44829, .T. ) ;
#26396 = CARTESIAN_POINT ( 'NONE',  ( -4.153846153846152411, -3.050289026998446396, 32.03036669348365706 ) ) ;
#26397 = CARTESIAN_POINT ( 'NONE',  ( -14.08468095607945969, -2.554770724473667265, 30.48948780036025852 ) ) ;
#26398 = EDGE_CURVE ( 'NONE', #12209, #4267, #7892, .T. ) ;
#26399 = CARTESIAN_POINT ( 'NONE',  ( 0.6845498131513099160, -12.39991518177334129, 30.74647679643404530 ) ) ;
#26400 = ORIENTED_EDGE ( 'NONE', *, *, #46509, .T. ) ;
#26401 = CARTESIAN_POINT ( 'NONE',  ( 14.30769230769218758, -6.879047030192662504, 34.71129190930017927 ) ) ;
#26402 = CARTESIAN_POINT ( 'NONE',  ( 1.515407192440173079, -8.147973898785416225, 34.70805048591653730 ) ) ;
#26403 = CARTESIAN_POINT ( 'NONE',  ( -23.50000000000000000, 8.999999999999996447, 23.75000000000000000 ) ) ;
#26404 = DIRECTION ( 'NONE',  ( -0.000000000000000000, -0.6427876096865404731, -0.7660444431189770143 ) ) ;
#26405 = CARTESIAN_POINT ( 'NONE',  ( -4.153846153846152411, -11.11383981884818262, 36.00935417666054406 ) ) ;
#26406 = FACE_BOUND ( 'NONE', #55453, .T. ) ;
#26408 = LINE ( 'NONE', #74597, #34500 ) ;
#26407 = CARTESIAN_POINT ( 'NONE',  ( -23.50000000000000000, -16.99999999999999289, 28.86437827766147279 ) ) ;
#26409 = ADVANCED_FACE ( 'NONE', ( #76342 ), #84010, .F. ) ;
#26410 = CARTESIAN_POINT ( 'NONE',  ( -9.561782254074053355, -12.15418822224088835, 32.17964115625579069 ) ) ;
#26412 = CARTESIAN_POINT ( 'NONE',  ( -9.561515884482908234, -10.54018710029568595, 33.71981072465678864 ) ) ;
#26411 = CARTESIAN_POINT ( 'NONE',  ( 2.980769230769232170, -7.566083408709834757, 34.74999999999999289 ) ) ;
#26413 = CARTESIAN_POINT ( 'NONE',  ( 13.25392478150508069, -2.494641256782728966, 31.33461815524612959 ) ) ;
#26414 = CARTESIAN_POINT ( 'NONE',  ( 1.077988221561464899, -4.724691934501233703, 15.23250670625848713 ) ) ;
#26415 = EDGE_LOOP ( 'NONE', ( #69775, #57289, #63872, #20384 ) ) ;
#26416 = CARTESIAN_POINT ( 'NONE',  ( 16.09615384615384670, -3.499999999999999556, 29.75000000000000355 ) ) ;
#26417 = ORIENTED_EDGE ( 'NONE', *, *, #11749, .F. ) ;
#26418 = B_SPLINE_CURVE_WITH_KNOTS ( 'NONE', 3,
 ( #46172, #73654, #42080, #20900, #6517, #76290, #22237, #69538, #49269, #69975 ),
 .UNSPECIFIED., .F., .F.,
 ( 4, 2, 2, 2, 4 ),
 ( 0.000000000000000000, 0.0001954311564186864949, 0.0003908623128373729899, 0.0005862934692560594577, 0.0007817246256747459798 ),
 .UNSPECIFIED. ) ;
#26419 = CARTESIAN_POINT ( 'NONE',  ( 18.25000000000141753, -7.500000000000154543, 35.00000000000007105 ) ) ;
#26420 = ORIENTED_EDGE ( 'NONE', *, *, #14209, .T. ) ;
#26421 = B_SPLINE_CURVE_WITH_KNOTS ( 'NONE', 3,
 ( #31112, #86078, #38327, #86533, #24807, #26149, #52719, #67139, #4542, #54497 ),
 .UNSPECIFIED., .F., .F.,
 ( 4, 2, 2, 2, 4 ),
 ( 0.000000000000000000, 0.0001954339857564080707, 0.0003908679715128161414, 0.0005863019572692241849, 0.0007817359430256322827 ),
 .UNSPECIFIED. ) ;
#26422 = CARTESIAN_POINT ( 'NONE',  ( -15.29609324357353550, -7.749976730030849303, 34.74374725381503737 ) ) ;
#26423 = FACE_OUTER_BOUND ( 'NONE', #43553, .T. ) ;
#26425 = ORIENTED_EDGE ( 'NONE', *, *, #37599, .T. ) ;
#26424 = CARTESIAN_POINT ( 'NONE',  ( -2.530618525208453651, -11.76352882383564769, 32.36236540154569497 ) ) ;
#26426 = CARTESIAN_POINT ( 'NONE',  ( -10.54931728203453822, -11.91647553114624358, 32.58852847137148245 ) ) ;
#26427 = DIRECTION ( 'NONE',  ( -0.000000000000000000, -0.9396926207859093161, -0.3420201433256663259 ) ) ;
#26428 = CARTESIAN_POINT ( 'NONE',  ( 3.775308065498768517, -8.992201783934554271, 26.79500670625849423 ) ) ;
#26429 = B_SPLINE_CURVE_WITH_KNOTS ( 'NONE', 3,
 ( #44322, #30827, #45680, #72705, #4251, #73161, #38039, #30388, #78570, #11015 ),
 .UNSPECIFIED., .F., .F.,
 ( 4, 2, 2, 2, 4 ),
 ( 0.0007817359430256316322, 0.0009771253907249980580, 0.001172514838424364592, 0.001367904286123731127, 0.001563293733823097661 ),
 .UNSPECIFIED. ) ;
#26430 = DIRECTION ( 'NONE',  ( -0.000000000000000000, -0.5000000000000009992, -0.8660254037844380415 ) ) ;
#26431 = CARTESIAN_POINT ( 'NONE',  ( 5.011652630962299959, -5.219633306516282545, 34.19971097300152252 ) ) ;
#26432 = VECTOR ( 'NONE', #21732, 1000.000000000000000 ) ;
#26433 = CARTESIAN_POINT ( 'NONE',  ( -0.08713905105068302237, -4.749995098204598420, 28.74997304012405763 ) ) ;
#26434 = DIRECTION ( 'NONE',  ( 1.000000000000000000, 0.000000000000000000, 0.000000000000000000 ) ) ;
#26435 = CARTESIAN_POINT ( 'NONE',  ( -12.33074802057151409, -8.191423895709840863, 34.95447573519442130 ) ) ;
#26436 = CARTESIAN_POINT ( 'NONE',  ( 13.19230769230769340, -3.499999999999999556, 29.75000000000000355 ) ) ;
#26437 = CARTESIAN_POINT ( 'NONE',  ( 1.492201783934598236, -11.27530806549875031, 17.45499329374151642 ) ) ;
#26438 = EDGE_CURVE ( 'NONE', #64311, #39901, #36257, .T. ) ;
#26439 = CARTESIAN_POINT ( 'NONE',  ( 5.326977496836530435, -2.544122305571457687, 31.48381861865059150 ) ) ;
#26440 = CARTESIAN_POINT ( 'NONE',  ( -1.161602540521989413, -11.98016756924215009, 32.48728574198911190 ) ) ;
#26441 = EDGE_LOOP ( 'NONE', ( #15049, #14852, #41765, #22656, #44775, #2545 ) ) ;
#26442 = CARTESIAN_POINT ( 'NONE',  ( 16.28437159207980045, -5.070358843744208421, 34.40418822224088302 ) ) ;
#26443 = CYLINDRICAL_SURFACE ( 'NONE', #70515, 0.2499999999999994726 ) ;
#26444 = CARTESIAN_POINT ( 'NONE',  ( 3.750000000000001776, -7.561099074964511502, 20.97061829374151642 ) ) ;
#26445 = CARTESIAN_POINT ( 'NONE',  ( -17.07692307692307665, -10.89733346790207413, 36.13435417666054406 ) ) ;
#26446 = CARTESIAN_POINT ( 'NONE',  ( -9.019207513279361876, -3.436278759898153901, 33.07459398097509506 ) ) ;
#26447 = ORIENTED_EDGE ( 'NONE', *, *, #67653, .T. ) ;
#26448 = LINE ( 'NONE', #89051, #31316 ) ;
#26449 = FACE_OUTER_BOUND ( 'NONE', #69433, .T. ) ;
#26451 = VERTEX_POINT ( 'NONE', #35815 ) ;
#26450 = CARTESIAN_POINT ( 'NONE',  ( 8.992243613324164997, -2.523321265292115534, 31.42251411153756990 ) ) ;
#26452 = LINE ( 'NONE', #40418, #12458 ) ;
#26453 = CARTESIAN_POINT ( 'NONE',  ( 5.326923076924495071, -7.500000000000154543, 35.00000000000007105 ) ) ;
#26454 = CARTESIAN_POINT ( 'NONE',  ( -11.76138849736838488, -2.523278758544489797, 31.42238647778637528 ) ) ;
#26455 = ORIENTED_EDGE ( 'NONE', *, *, #3415, .T. ) ;
#26456 = CARTESIAN_POINT ( 'NONE',  ( 3.164686851409095336, -2.486705287966279876, 31.30864560766542937 ) ) ;
#26457 = CARTESIAN_POINT ( 'NONE',  ( 9.692307692307695177, -6.343179335718451384, 34.87096338111211935 ) ) ;
#26458 = VECTOR ( 'NONE', #65006, 1000.000000000000227 ) ;
#26459 = LINE ( 'NONE', #20141, #19704 ) ;
#26460 = ORIENTED_EDGE ( 'NONE', *, *, #13978, .F. ) ;
#26461 = B_SPLINE_CURVE_WITH_KNOTS ( 'NONE', 3,
 ( #33762, #12610, #13926, #28326, #41858, #68428, #7176, #47717, #55796, #34649 ),
 .UNSPECIFIED., .F., .F.,
 ( 4, 2, 2, 2, 4 ),
 ( 0.0007817246256747494492, 0.0009771112852218935378, 0.001172497944769037518, 0.001367884604316181498, 0.001563271263863325695 ),
 .UNSPECIFIED. ) ;
#26462 = EDGE_LOOP ( 'NONE', ( #29924, #87658, #84421, #9814 ) ) ;
#26463 = ORIENTED_EDGE ( 'NONE', *, *, #7400, .F. ) ;
#26464 = B_SPLINE_CURVE_WITH_KNOTS ( 'NONE', 3,
 ( #2108, #29593, #16957, #76892, #83663, #1221, #57049, #7991, #23261, #50722 ),
 .UNSPECIFIED., .F., .F.,
 ( 4, 2, 2, 2, 4 ),
 ( 0.0007817246256747472808, 0.0009771112852218907189, 0.001172497944769034049, 0.001367884604316177595, 0.001563271263863320925 ),
 .UNSPECIFIED. ) ;
#26465 = AXIS2_PLACEMENT_3D ( 'NONE', #24893, #19911, #86625 ) ;
#26466 = ORIENTED_EDGE ( 'NONE', *, *, #86740, .F. ) ;
#26467 = VECTOR ( 'NONE', #21956, 999.9999999999998863 ) ;
#26468 = CARTESIAN_POINT ( 'NONE',  ( 12.46153846153833911, -10.33852847137269571, 34.16647553114546554 ) ) ;
#26469 = CARTESIAN_POINT ( 'NONE',  ( 14.24242186173153435, -4.481592998940162609, 33.73612834413957984 ) ) ;
#26470 = CARTESIAN_POINT ( 'NONE',  ( -13.38461538461550759, -12.16647553114689728, 32.15551576947799362 ) ) ;
#26471 = CARTESIAN_POINT ( 'NONE',  ( -7.976844449264153702, -10.70098750199973203, 33.91152734681376302 ) ) ;
#26472 = LINE ( 'NONE', #89075, #72221 ) ;
#26473 = ORIENTED_EDGE ( 'NONE', *, *, #64542, .F. ) ;
#26474 = EDGE_LOOP ( 'NONE', ( #7067, #17572, #14949, #9407 ) ) ;
#26475 = VERTEX_POINT ( 'NONE', #48870 ) ;
#26477 = ORIENTED_EDGE ( 'NONE', *, *, #2904, .F. ) ;
#26476 = CARTESIAN_POINT ( 'NONE',  ( -7.173053667125512511, -2.544273027872574922, 31.48422191005632342 ) ) ;
#26478 = CARTESIAN_POINT ( 'NONE',  ( -18.00000000000000000, -1.503186988994757778, 30.80739993210377747 ) ) ;
#26479 = CARTESIAN_POINT ( 'NONE',  ( 6.923076923076802558, -10.90142922262034020, 33.41473453929536674 ) ) ;
#26480 = CYLINDRICAL_SURFACE ( 'NONE', #34936, 0.2500000000000012212 ) ;
#26481 = DIRECTION ( 'NONE',  ( -0.000000000000000000, -0.000000000000000000, 1.000000000000000000 ) ) ;
#26482 = VERTEX_POINT ( 'NONE', #62374 ) ;
#26483 = ORIENTED_EDGE ( 'NONE', *, *, #21952, .T. ) ;
#26484 = VECTOR ( 'NONE', #56756, 1000.000000000000000 ) ;
#26485 = VERTEX_POINT ( 'NONE', #70029 ) ;
#26486 = CARTESIAN_POINT ( 'NONE',  ( -9.692307692307812417, -6.026961402154118019, 34.52809138561165270 ) ) ;
#26488 = VERTEX_POINT ( 'NONE', #50186 ) ;
#26487 = CYLINDRICAL_SURFACE ( 'NONE', #77587, 0.2500000000000008882 ) ;
#26489 = DIRECTION ( 'NONE',  ( 0.000000000000000000, 0.9396926207859126468, -0.3420201433256571111 ) ) ;
#26490 = CARTESIAN_POINT ( 'NONE',  ( 5.326923076924495071, -7.500000000000154543, 35.00000000000007105 ) ) ;
#26491 = ORIENTED_EDGE ( 'NONE', *, *, #43427, .F. ) ;
#26492 = LINE ( 'NONE', #67922, #57504 ) ;
#26493 = CARTESIAN_POINT ( 'NONE',  ( 9.942307692307695177, -2.249999999999998668, 29.75000000000000355 ) ) ;
#26494 = CARTESIAN_POINT ( 'NONE',  ( 18.25000000000143530, -7.500000000000155431, 34.75000000000007105 ) ) ;
#26495 = FACE_BOUND ( 'NONE', #11029, .T. ) ;
#26496 = CARTESIAN_POINT ( 'NONE',  ( -0.7115151924808155171, -9.943427161483782584, 34.11278801902876978 ) ) ;
#26497 = CARTESIAN_POINT ( 'NONE',  ( -1.254089682851818877, -11.93748526763465279, 32.05452791011430946 ) ) ;
#26498 = EDGE_CURVE ( 'NONE', #87793, #26079, #56073, .T. ) ;
#26499 = CARTESIAN_POINT ( 'NONE',  ( 11.76147289007438879, -12.39991518177334129, 30.74647679643404530 ) ) ;
#26501 = CARTESIAN_POINT ( 'NONE',  ( 14.43848274865926307, -2.845873456487966635, 32.17976146951972538 ) ) ;
#26500 = CARTESIAN_POINT ( 'NONE',  ( 0.2386115026316120158, -6.459968553980840689, 34.89616026154728701 ) ) ;
#26502 = DIRECTION ( 'NONE',  ( -0.000000000000000000, -4.336808689942017243E-16, -1.000000000000000000 ) ) ;
#26503 = DIRECTION ( 'NONE',  ( -0.000000000000000000, -0.6427876096865404731, -0.7660444431189771253 ) ) ;
#26504 = ORIENTED_EDGE ( 'NONE', *, *, #12023, .F. ) ;
#26505 = CARTESIAN_POINT ( 'NONE',  ( 14.30769230769231015, -12.37446782046654192, 30.86335684631486131 ) ) ;
#26506 = EDGE_CURVE ( 'NONE', #18801, #58277, #9889, .T. ) ;
#26507 = CARTESIAN_POINT ( 'NONE',  ( -17.07692307692319744, -6.835583212225970762, 34.95778746994575670 ) ) ;
#26508 = ORIENTED_EDGE ( 'NONE', *, *, #83353, .F. ) ;
#26509 = VERTEX_POINT ( 'NONE', #15096 ) ;
#26510 = CARTESIAN_POINT ( 'NONE',  ( 0.5267936010512993539, -8.656820664281605460, 34.87096338111211224 ) ) ;
#26511 = CARTESIAN_POINT ( 'NONE',  ( -15.29603967673000575, -2.625532179533444754, 30.86335684631481513 ) ) ;
#26512 = DIRECTION ( 'NONE',  ( -0.000000000000000000, 0.6427876096865404731, -0.7660444431189771253 ) ) ;
#26513 = EDGE_LOOP ( 'NONE', ( #81275, #67917 ) ) ;
#26514 = CARTESIAN_POINT ( 'NONE',  ( -16.02305434602136103, -11.18335022499818621, 33.13157742990016885 ) ) ;
#26515 = CARTESIAN_POINT ( 'NONE',  ( -7.053224132515143907, -10.19110544564092002, 33.96427741523702792 ) ) ;
#26516 = B_SPLINE_CURVE_WITH_KNOTS ( 'NONE', 3,
 ( #83199, #70563, #71002, #29146, #42654, #43088, #29581, #75986, #42217, #8866 ),
 .UNSPECIFIED., .F., .F.,
 ( 4, 2, 2, 2, 4 ),
 ( 0.000000000000000000, 0.0001954339857564075828, 0.0003908679715128151656, 0.0005863019572692227755, 0.0007817359430256303312 ),
 .UNSPECIFIED. ) ;
#26517 = VECTOR ( 'NONE', #54716, 1000.000000000000227 ) ;
#26518 = FACE_BOUND ( 'NONE', #37934, .T. ) ;
#26520 = CARTESIAN_POINT ( 'NONE',  ( -17.07692307692307665, -8.164416787775445883, 34.95778746994557906 ) ) ;
#26519 = CARTESIAN_POINT ( 'NONE',  ( -18.22348494372394967, -3.236172620538811717, 32.36188796281390267 ) ) ;
#26521 = CARTESIAN_POINT ( 'NONE',  ( 7.976945653978636308, -8.999086150933475636, 34.52020707165672775 ) ) ;
#26522 = EDGE_CURVE ( 'NONE', #37056, #53391, #42569, .T. ) ;
#26523 = B_SPLINE_CURVE_WITH_KNOTS ( 'NONE', 3,
 ( #3159, #45484, #50889, #44582, #86040, #17124, #51778, #71618, #37841, #24317 ),
 .UNSPECIFIED., .F., .F.,
 ( 4, 2, 2, 2, 4 ),
 ( 0.0007817246256747528103, 0.0009771112852218978746, 0.001172497944769042939, 0.001367884604316188003, 0.001563271263863333068 ),
 .UNSPECIFIED. ) ;
#26524 = CARTESIAN_POINT ( 'NONE',  ( 0.5923289025054098156, -4.684288915650983043, 34.18129842949671371 ) ) ;
#26526 = CARTESIAN_POINT ( 'NONE',  ( -14.55769230769230660, -7.566082377512564960, 35.00000000000000711 ) ) ;
#26525 = DIRECTION ( 'NONE',  ( 0.000000000000000000, 0.000000000000000000, 1.000000000000000000 ) ) ;
#26527 = CARTESIAN_POINT ( 'NONE',  ( 3.750000000000009770, -9.053300858899081760, 23.29687500000000000 ) ) ;
#26528 = ORIENTED_EDGE ( 'NONE', *, *, #47610, .F. ) ;
#26529 = VECTOR ( 'NONE', #35097, 1000.000000000000000 ) ;
#26530 = VERTEX_POINT ( 'NONE', #49754 ) ;
#26531 = AXIS2_PLACEMENT_3D ( 'NONE', #80156, #31057, #17108 ) ;
#26532 = DIRECTION ( 'NONE',  ( 0.000000000000000000, 0.000000000000000000, -1.000000000000000000 ) ) ;
#26533 = DIRECTION ( 'NONE',  ( -0.000000000000000000, 0.9396926207859093161, -0.3420201433256663259 ) ) ;
#26534 = DIRECTION ( 'NONE',  ( 0.000000000000000000, 0.4999999999999985567, 0.8660254037844395958 ) ) ;
#26535 = CARTESIAN_POINT ( 'NONE',  ( -0.3953693205758047058, -7.250054483168842268, 34.74374881642865631 ) ) ;
#26536 = DIRECTION ( 'NONE',  ( 0.000000000000000000, 0.9396926207859126468, -0.3420201433256571111 ) ) ;
#26537 = CARTESIAN_POINT ( 'NONE',  ( -3.750000000000008438, -5.946699141100917352, 25.17187500000000000 ) ) ;
#26538 = CARTESIAN_POINT ( 'NONE',  ( -1.634592128663975963, -4.075325502946085976, 33.72974371597207721 ) ) ;
#26539 = FACE_OUTER_BOUND ( 'NONE', #29597, .T. ) ;
#26540 = DIRECTION ( 'NONE',  ( -0.000000000000000000, 1.000000000000000000, -0.000000000000000000 ) ) ;
#26541 = CARTESIAN_POINT ( 'NONE',  ( 10.68063975489745232, -3.643525952247864463, 33.31231777344670064 ) ) ;
#26542 = CARTESIAN_POINT ( 'NONE',  ( -6.065270445960774026, -2.892918686051582089, 31.69288490824015270 ) ) ;
#26543 = DIRECTION ( 'NONE',  ( -0.000000000000000000, 0.8660254037844399289, -0.4999999999999980016 ) ) ;
#26544 = CARTESIAN_POINT ( 'NONE',  ( 5.776515056276052107, -12.24155766932282496, 31.33739205006857986 ) ) ;
#26545 = EDGE_CURVE ( 'NONE', #29700, #66822, #77229, .T. ) ;
#26546 = FACE_OUTER_BOUND ( 'NONE', #10536, .T. ) ;
#26547 = CARTESIAN_POINT ( 'NONE',  ( -7.715628144390283438, -12.45806712695776319, 30.39783852428763922 ) ) ;
#26548 = ADVANCED_FACE ( 'NONE', ( #48419 ), #43007, .F. ) ;
#26549 = VERTEX_POINT ( 'NONE', #59176 ) ;
#26550 = CARTESIAN_POINT ( 'NONE',  ( 1.161130440891439131, -2.599994579823203367, 30.74605699353653776 ) ) ;
#26551 = CARTESIAN_POINT ( 'NONE',  ( 18.06606733335007675, -4.661471528628508665, 34.16647553114624003 ) ) ;
#26552 = CARTESIAN_POINT ( 'NONE',  ( -1.987747218494638313, -9.401340078031370950, 15.18936829374151465 ) ) ;
#26553 = EDGE_CURVE ( 'NONE', #8324, #31532, #73225, .T. ) ;
#26554 = EDGE_CURVE ( 'NONE', #18617, #24402, #58281, .T. ) ;
#26555 = LINE ( 'NONE', #13913, #20211 ) ;
#26556 =( NAMED_UNIT ( * ) PLANE_ANGLE_UNIT ( ) SI_UNIT ( $, .RADIAN. ) );
#26557 = CARTESIAN_POINT ( 'NONE',  ( -0.4615384615384611200, -1.466349020453238561, 30.81389545987213907 ) ) ;
#26559 = VERTEX_POINT ( 'NONE', #44763 ) ;
#26558 = CARTESIAN_POINT ( 'NONE',  ( -18.12726022028586925, -2.249999999999999556, 29.52412087102020521 ) ) ;
#26560 = CARTESIAN_POINT ( 'NONE',  ( 1.944543648262996083, -5.555456351736983045, 23.06250000000000000 ) ) ;
#26561 = FACE_OUTER_BOUND ( 'NONE', #31819, .T. ) ;
#26562 = ORIENTED_EDGE ( 'NONE', *, *, #44846, .T. ) ;
#26563 = CARTESIAN_POINT ( 'NONE',  ( -16.08859058257013430, -10.21337939537593797, 33.94971097300152252 ) ) ;
#26564 = CARTESIAN_POINT ( 'NONE',  ( 0.2115152242454939047, -2.823816976329317718, 31.52131813110796443 ) ) ;
#26565 = VERTEX_POINT ( 'NONE', #24054 ) ;
#26566 = CARTESIAN_POINT ( 'NONE',  ( -5.076923076923075762, -11.69971097300155272, 32.46337939537588113 ) ) ;
#26567 = CARTESIAN_POINT ( 'NONE',  ( -14.98076923076916422, -7.434744860731433924, 35.00000000000000711 ) ) ;
#26568 = CARTESIAN_POINT ( 'NONE',  ( 2.084207383127977486, -12.69144148231606017, 30.53333754910549303 ) ) ;
#26569 = ORIENTED_EDGE ( 'NONE', *, *, #431, .T. ) ;
#26570 = ORIENTED_EDGE ( 'NONE', *, *, #24560, .F. ) ;
#26571 = ORIENTED_EDGE ( 'NONE', *, *, #17276, .F. ) ;
#26572 = DIRECTION ( 'NONE',  ( 0.000000000000000000, 0.4999999999999985567, 0.8660254037844395958 ) ) ;
#26573 = FACE_OUTER_BOUND ( 'NONE', #10734, .T. ) ;
#26574 = CARTESIAN_POINT ( 'NONE',  ( 18.22301284409339672, -10.01129605718032423, 34.36064277460058491 ) ) ;
#26575 = CARTESIAN_POINT ( 'NONE',  ( 9.626225312947559232, -9.058645607665454236, 34.76329471203372634 ) ) ;
#26576 = CARTESIAN_POINT ( 'NONE',  ( -10.61538461538473577, -12.16647553114689728, 32.15551576947799362 ) ) ;
#26577 = CARTESIAN_POINT ( 'NONE',  ( 9.757562831820530747, -10.33852847137154107, 34.16647553114620450 ) ) ;
#26578 = DIRECTION ( 'NONE',  ( 0.000000000000000000, 0.000000000000000000, 1.000000000000000000 ) ) ;
#26579 = CARTESIAN_POINT ( 'NONE',  ( -0.4615384615384611200, -12.34228464037088635, 31.77849191805839268 ) ) ;
#26580 = EDGE_CURVE ( 'NONE', #46286, #87539, #26014, .T. ) ;
#26581 = AXIS2_PLACEMENT_3D ( 'NONE', #59835, #60723, #81011 ) ;
#26582 = VERTEX_POINT ( 'NONE', #79005 ) ;
#26583 = VERTEX_POINT ( 'NONE', #2884 ) ;
#26585 = ORIENTED_EDGE ( 'NONE', *, *, #11533, .T. ) ;
#26584 = DIRECTION ( 'NONE',  ( 0.000000000000000000, 0.000000000000000000, -1.000000000000000000 ) ) ;
#26586 = CARTESIAN_POINT ( 'NONE',  ( 11.53846153846141576, -3.643525952248795718, 33.31231777344771672 ) ) ;
#26587 = CARTESIAN_POINT ( 'NONE',  ( 14.16025641025641235, -11.00000000000000000, 29.75000000000000355 ) ) ;
#26588 = ORIENTED_EDGE ( 'NONE', *, *, #65664, .T. ) ;
#26589 = B_SPLINE_CURVE_WITH_KNOTS ( 'NONE', 3,
 ( #43293, #49604, #55468, #82953, #70766, #21235, #15385, #9070, #28443, #76635 ),
 .UNSPECIFIED., .F., .F.,
 ( 4, 2, 2, 2, 4 ),
 ( 0.0007817246256747460882, 0.0009771112852218892010, 0.001172497944769032314, 0.001367884604316175427, 0.001563271263863318539 ),
 .UNSPECIFIED. ) ;
#26590 = CARTESIAN_POINT ( 'NONE',  ( -15.23076923076935252, -2.379036618888197729, 30.90682066428292885 ) ) ;
#26591 = EDGE_CURVE ( 'NONE', #19448, #2854, #68906, .T. ) ;
#26592 = ORIENTED_EDGE ( 'NONE', *, *, #39000, .T. ) ;
#26593 = CARTESIAN_POINT ( 'NONE',  ( 16.82689983963011926, -10.05641848906368097, 34.04755513067966177 ) ) ;
#26594 = ORIENTED_EDGE ( 'NONE', *, *, #39952, .T. ) ;
#26595 = LINE ( 'NONE', #31571, #40237 ) ;
#26596 = CARTESIAN_POINT ( 'NONE',  ( -6.792551484843278864, -5.070358843744210198, 34.40418822224088302 ) ) ;
#26597 = CARTESIAN_POINT ( 'NONE',  ( 12.33084785842815378, -2.295517848115769421, 30.44137282052137294 ) ) ;
#26598 = FACE_BOUND ( 'NONE', #58813, .T. ) ;
#26599 = CARTESIAN_POINT ( 'NONE',  ( 9.692307692307695177, -2.708943851104267164, 35.45975837776705220 ) ) ;
#26600 = CARTESIAN_POINT ( 'NONE',  ( 27.00000000000000000, 8.999999999999996447, 23.75000000000000000 ) ) ;
#26601 = ADVANCED_FACE ( 'NONE', ( #4235 ), #85328, .F. ) ;
#26602 = CARTESIAN_POINT ( 'NONE',  ( 13.60762822870878352, -4.762714258010881885, 34.23016756924214832 ) ) ;
#26603 = CARTESIAN_POINT ( 'NONE',  ( 10.48469401227430708, -9.929715669179220328, 34.40415004197138416 ) ) ;
#26604 = FACE_OUTER_BOUND ( 'NONE', #75656, .T. ) ;
#26605 = CARTESIAN_POINT ( 'NONE',  ( -7.912236225513983534, -9.058645607665454236, 34.76329471203372634 ) ) ;
#26606 = FACE_OUTER_BOUND ( 'NONE', #31729, .T. ) ;
#26607 = ADVANCED_FACE ( 'NONE', ( #51503 ), #2446, .F. ) ;
#26608 = ORIENTED_EDGE ( 'NONE', *, *, #79661, .F. ) ;
#26609 = ORIENTED_EDGE ( 'NONE', *, *, #17366, .F. ) ;
#26610 = AXIS2_PLACEMENT_3D ( 'NONE', #87473, #31620, #26639 ) ;
#26612 = DIRECTION ( 'NONE',  ( -0.000000000000000000, 0.8660254037844397068, -0.4999999999999978906 ) ) ;
#26611 = CARTESIAN_POINT ( 'NONE',  ( -14.30769230769242739, -12.27809138561165270, 31.22303859784587132 ) ) ;
#26613 = CARTESIAN_POINT ( 'NONE',  ( 16.40379156322419973, -11.56426240980093567, 33.07394671870546432 ) ) ;
#26614 = CARTESIAN_POINT ( 'NONE',  ( -0.4615384615385840772, -11.06231777344772027, 33.60647404775119895 ) ) ;
#26615 = LINE ( 'NONE', #53187, #42955 ) ;
#26616 = CARTESIAN_POINT ( 'NONE',  ( -12.39547011053602610, -4.098570777380720287, 33.41473453929635440 ) ) ;
#26617 = ORIENTED_EDGE ( 'NONE', *, *, #31700, .T. ) ;
#26618 = DIRECTION ( 'NONE',  ( 0.000000000000000000, 0.6427876096865373645, -0.7660444431189797898 ) ) ;
#26619 = B_SPLINE_CURVE_WITH_KNOTS ( 'NONE', 3,
 ( #79264, #84703, #22977, #50444, #64394, #78805, #86482, #57653, #71599, #58978 ),
 .UNSPECIFIED., .F., .F.,
 ( 4, 2, 2, 2, 4 ),
 ( 0.0007817359430256369448, 0.0009771253907250049969, 0.001172514838424373049, 0.001367904286123741101, 0.001563293733823109153 ),
 .UNSPECIFIED. ) ;
#26620 = CARTESIAN_POINT ( 'NONE',  ( 14.30769230769218758, -11.48612834414049644, 32.76840700105863391 ) ) ;
#26621 = CARTESIAN_POINT ( 'NONE',  ( 1.576923076923075762, -3.499999999999999556, 29.75000000000000355 ) ) ;
#26622 = ADVANCED_FACE ( 'NONE', ( #44307 ), #79460, .F. ) ;
#26623 = CARTESIAN_POINT ( 'NONE',  ( -3.480792454990687457, -12.68155406624981119, 30.59749803192733708 ) ) ;
#26624 = B_SPLINE_CURVE_WITH_KNOTS ( 'NONE', 3,
 ( #45131, #3257, #85687, #38384, #65839, #4140, #51415, #59089, #72605, #17218 ),
 .UNSPECIFIED., .F., .F.,
 ( 4, 2, 2, 2, 4 ),
 ( 0.0007817359430256322827, 0.0009771253907249989254, 0.001172514838424365676, 0.001367904286123732428, 0.001563293733823098962 ),
 .UNSPECIFIED. ) ;
#26625 = ORIENTED_EDGE ( 'NONE', *, *, #14287, .T. ) ;
#26626 = ORIENTED_EDGE ( 'NONE', *, *, #59236, .F. ) ;
#26628 = EDGE_CURVE ( 'NONE', #3856, #25471, #59242, .T. ) ;
#26627 = EDGE_LOOP ( 'NONE', ( #41454, #22928 ) ) ;
#26629 = FACE_OUTER_BOUND ( 'NONE', #65038, .T. ) ;
#26630 = ORIENTED_EDGE ( 'NONE', *, *, #57587, .F. ) ;
#26631 = ADVANCED_FACE ( 'NONE', ( #9233 ), #57397, .F. ) ;
#26632 = FACE_OUTER_BOUND ( 'NONE', #25258, .T. ) ;
#26633 = CARTESIAN_POINT ( 'NONE',  ( -5.300408020647022767, -2.847400154188068022, 31.58180166144859058 ) ) ;
#26634 = CARTESIAN_POINT ( 'NONE',  ( 3.296024370282069960, -5.941354392334606160, 34.76329471203374055 ) ) ;
#26635 = CARTESIAN_POINT ( 'NONE',  ( 1.634669804528839476, -6.523592122091591783, 34.90882529074906415 ) ) ;
#26636 = CARTESIAN_POINT ( 'NONE',  ( -19.50000000000000000, -3.499999999999999556, 29.75000000000000355 ) ) ;
#26637 = VERTEX_POINT ( 'NONE', #16419 ) ;
#26638 = CARTESIAN_POINT ( 'NONE',  ( -15.29685264172511161, -11.69971097300155272, 32.46337939537587403 ) ) ;
#26640 = EDGE_LOOP ( 'NONE', ( #6989, #72844 ) ) ;
#26639 = DIRECTION ( 'NONE',  ( 0.000000000000000000, 0.000000000000000000, 1.000000000000000000 ) ) ;
#26641 = FACE_OUTER_BOUND ( 'NONE', #69806, .T. ) ;
#26642 = CARTESIAN_POINT ( 'NONE',  ( -17.99999999999969447, -2.506253911140613244, 30.00000000000320455 ) ) ;
#26643 = DIRECTION ( 'NONE',  ( -0.000000000000000000, -0.9396926207859092051, -0.3420201433256662704 ) ) ;
#26644 = LINE ( 'NONE', #48677, #66829 ) ;
#26645 = CARTESIAN_POINT ( 'NONE',  ( -4.023055712879203050, -4.684288915650984819, 34.18129842949671371 ) ) ;
#26646 = EDGE_CURVE ( 'NONE', #4609, #68032, #43884, .T. ) ;
#26647 = CARTESIAN_POINT ( 'NONE',  ( 18.06525557127602610, -2.625532179533470512, 30.86335684631491105 ) ) ;
#26648 = CARTESIAN_POINT ( 'NONE',  ( -0.6850234052624097902, -12.44517049084099725, 30.48991314939691932 ) ) ;
#26649 = CARTESIAN_POINT ( 'NONE',  ( 0.06109907496451789238, -4.749999999999998224, 21.90811829374151642 ) ) ;
#26650 = ORIENTED_EDGE ( 'NONE', *, *, #79530, .T. ) ;
#26651 = CARTESIAN_POINT ( 'NONE',  ( -19.50000000000000000, -3.499999999999999556, 29.75000000000000355 ) ) ;
#26652 = CARTESIAN_POINT ( 'NONE',  ( -1.384615384615506484, -3.643525952248795718, 33.31231777344771672 ) ) ;
#26653 = EDGE_CURVE ( 'NONE', #74762, #85754, #69386, .T. ) ;
#26654 = EDGE_CURVE ( 'NONE', #13908, #49386, #5127, .T. ) ;
#26655 = EDGE_LOOP ( 'NONE', ( #40265, #82137 ) ) ;
#26656 = CARTESIAN_POINT ( 'NONE',  ( -6.000000000000119904, -2.625532179533778709, 30.86335684631627174 ) ) ;
#26657 = CARTESIAN_POINT ( 'NONE',  ( -2.980714919130916130, -5.728107161865378494, 34.42597550085002922 ) ) ;
#26658 = CARTESIAN_POINT ( 'NONE',  ( 24.00000000000000000, 5.000000000000023093, 29.24999999999999645 ) ) ;
#26659 = B_SPLINE_CURVE_WITH_KNOTS ( 'NONE', 3,
 ( #57741, #72582, #10889, #78446, #78894, #85661, #38360, #45106, #71688, #86109 ),
 .UNSPECIFIED., .F., .F.,
 ( 4, 2, 2, 2, 4 ),
 ( 0.0007817246256747445703, 0.0009771112852218872494, 0.001172497944769030145, 0.001367884604316172825, 0.001563271263863315504 ),
 .UNSPECIFIED. ) ;
#26660 = CARTESIAN_POINT ( 'NONE',  ( 7.173022441425066731, -5.852078868378311149, 34.47109172314383585 ) ) ;
#26661 = CARTESIAN_POINT ( 'NONE',  ( -14.37377468705243722, -2.833524468853757305, 32.15551576947924417 ) ) ;
#26662 = ORIENTED_EDGE ( 'NONE', *, *, #44820, .F. ) ;
#26663 = LINE ( 'NONE', #80286, #16073 ) ;
#26664 = FACE_OUTER_BOUND ( 'NONE', #4721, .T. ) ;
#26665 = CARTESIAN_POINT ( 'NONE',  ( 18.25005441991345734, -12.41089969410671223, 31.60739465890703670 ) ) ;
#26666 = ORIENTED_EDGE ( 'NONE', *, *, #25050, .T. ) ;
#26667 = DIRECTION ( 'NONE',  ( -0.000000000000000000, -0.3420201433256694901, -0.9396926207859082059 ) ) ;
#26668 = ORIENTED_EDGE ( 'NONE', *, *, #40228, .F. ) ;
#26669 = CYLINDRICAL_SURFACE ( 'NONE', #16959, 0.2499999999999973355 ) ;
#26670 = CARTESIAN_POINT ( 'NONE',  ( 11.76124120743959978, -6.717445702608402236, 34.94155399931962336 ) ) ;
#26671 = EDGE_CURVE ( 'NONE', #76071, #7867, #22804, .T. ) ;
#26672 = ORIENTED_EDGE ( 'NONE', *, *, #85279, .T. ) ;
#26673 = CARTESIAN_POINT ( 'NONE',  ( -39.05038313613820122, -2.499999999999999556, 29.75000000000000355 ) ) ;
#26674 = CARTESIAN_POINT ( 'NONE',  ( -6.249976744048591826, -2.318417181685854978, 30.59732222474233865 ) ) ;
#26675 = DIRECTION ( 'NONE',  ( -0.000000000000000000, 0.1736481776669307198, -0.9848077530122080203 ) ) ;
#26676 = VECTOR ( 'NONE', #54895, 1000.000000000000227 ) ;
#26677 = CARTESIAN_POINT ( 'NONE',  ( -2.307692307692305711, -1.629998284177014645, 34.34916445242399163 ) ) ;
#26678 = CARTESIAN_POINT ( 'NONE',  ( -2.241624974342230292, -10.67929555188718282, 33.92786785259544757 ) ) ;
#26679 = ADVANCED_FACE ( 'NONE', ( #4689 ), #12330, .F. ) ;
#26680 = B_SPLINE_CURVE_WITH_KNOTS ( 'NONE', 3,
 ( #1421, #22577, #64432, #28914, #57254, #30228, #50044, #77966, #73442, #58567 ),
 .UNSPECIFIED., .F., .F.,
 ( 4, 2, 2, 2, 4 ),
 ( 0.0007817246256747448956, 0.0009771112852218876831, 0.001172497944769030579, 0.001367884604316173475, 0.001563271263863316371 ),
 .UNSPECIFIED. ) ;
#26681 = ORIENTED_EDGE ( 'NONE', *, *, #7622, .F. ) ;
#26682 = DIRECTION ( 'NONE',  ( -0.000000000000000000, 0.9396926207859093161, -0.3420201433256663259 ) ) ;
#26683 = ORIENTED_EDGE ( 'NONE', *, *, #48219, .F. ) ;
#26684 = DIRECTION ( 'NONE',  ( -0.000000000000000000, 0.1736481776669307198, -0.9848077530122080203 ) ) ;
#26685 = ADVANCED_FACE ( 'NONE', ( #41919 ), #19525, .F. ) ;
#26686 = CARTESIAN_POINT ( 'NONE',  ( 18.03205128205128105, -7.500000000000000000, 33.75000000000000000 ) ) ;
#26687 = EDGE_CURVE ( 'NONE', #54790, #18166, #53752, .T. ) ;
#26688 = CARTESIAN_POINT ( 'NONE',  ( -18.13069060311030611, -10.70098750199973203, 33.91152734681374881 ) ) ;
#26689 = CARTESIAN_POINT ( 'NONE',  ( 3.230769230769108269, -11.67786785259630911, 32.92929555188603530 ) ) ;
#26690 = CARTESIAN_POINT ( 'NONE',  ( 17.07692307692307665, -2.538708090699994813, 30.37095296980875503 ) ) ;
#26691 = ORIENTED_EDGE ( 'NONE', *, *, #28535, .T. ) ;
#26692 = EDGE_CURVE ( 'NONE', #9304, #31091, #2387, .T. ) ;
#26693 = VERTEX_POINT ( 'NONE', #45664 ) ;
#26694 = ORIENTED_EDGE ( 'NONE', *, *, #45633, .T. ) ;
#26695 = VERTEX_POINT ( 'NONE', #66382 ) ;
#26696 = CARTESIAN_POINT ( 'NONE',  ( -4.219929564802032296, -5.557115091759785130, 34.35708131394839171 ) ) ;
#26697 = CARTESIAN_POINT ( 'NONE',  ( 16.40379156322419973, -10.92531984108285492, 33.72920026020278073 ) ) ;
#26698 = CARTESIAN_POINT ( 'NONE',  ( -9.822784400424156459, -7.276988635370452485, 34.74523720219453793 ) ) ;
#26699 = DIRECTION ( 'NONE',  ( -0.000000000000000000, 0.5000000000000011102, -0.8660254037844381525 ) ) ;
#26700 = CARTESIAN_POINT ( 'NONE',  ( 4.023285562104232937, -2.504760397472873823, 29.97295953869789997 ) ) ;
#26701 = CYLINDRICAL_SURFACE ( 'NONE', #23480, 8.000000000000000000 ) ;
#26702 = DIRECTION ( 'NONE',  ( -1.000000000000000000, -0.000000000000000000, -0.000000000000000000 ) ) ;
#26703 = CARTESIAN_POINT ( 'NONE',  ( -2.307692307692305711, -9.819645486525091727, 36.12317359536749706 ) ) ;
#26704 = ORIENTED_EDGE ( 'NONE', *, *, #1829, .F. ) ;
#26705 = B_SPLINE_CURVE_WITH_KNOTS ( 'NONE', 3,
 ( #85170, #50476, #77518, #15829, #77961, #3182, #22573, #23889, #50904, #16262 ),
 .UNSPECIFIED., .F., .F.,
 ( 4, 2, 2, 2, 4 ),
 ( 0.000000000000000000, 0.0001954311564186871184, 0.0003908623128373742367, 0.0005862934692560614093, 0.0007817246256747484735 ),
 .UNSPECIFIED. ) ;
#26706 = VECTOR ( 'NONE', #351, 1000.000000000000000 ) ;
#26707 = EDGE_CURVE ( 'NONE', #1158, #7863, #30136, .T. ) ;
#26708 = ORIENTED_EDGE ( 'NONE', *, *, #65444, .F. ) ;
#26709 = ORIENTED_EDGE ( 'NONE', *, *, #38362, .T. ) ;
#26711 = ORIENTED_EDGE ( 'NONE', *, *, #23816, .F. ) ;
#26710 = CARTESIAN_POINT ( 'NONE',  ( -1.384615384615383471, -3.513871655860378418, 32.76840700105978499 ) ) ;
#26712 = EDGE_CURVE ( 'NONE', #58521, #20099, #83931, .T. ) ;
#26714 = CARTESIAN_POINT ( 'NONE',  ( -5.934744428723973897, -3.835265460703683349, 33.15142922261929925 ) ) ;
#26713 = CYLINDRICAL_SURFACE ( 'NONE', #8659, 0.2499999999999994726 ) ;
#26715 = CARTESIAN_POINT ( 'NONE',  ( -0.2387587925603951444, -2.353885683473779356, 30.79025554430704759 ) ) ;
#26716 = FACE_OUTER_BOUND ( 'NONE', #46029, .T. ) ;
#26717 = FACE_BOUND ( 'NONE', #47741, .T. ) ;
#26718 = VERTEX_POINT ( 'NONE', #38924 ) ;
#26719 = CARTESIAN_POINT ( 'NONE',  ( 17.07692307692307665, -6.386643153685126251, 34.62446782046654192 ) ) ;
#26720 = FACE_OUTER_BOUND ( 'NONE', #484, .T. ) ;
#26721 = VERTEX_POINT ( 'NONE', #14435 ) ;
#26722 = CARTESIAN_POINT ( 'NONE',  ( 5.011653076366756387, -2.379036618887870436, 30.90682066428147934 ) ) ;
#26723 = EDGE_LOOP ( 'NONE', ( #81689, #5253 ) ) ;
#26724 = FACE_BOUND ( 'NONE', #22350, .T. ) ;
#26725 = LINE ( 'NONE', #80804, #20287 ) ;
#26726 = CARTESIAN_POINT ( 'NONE',  ( -13.63463862190834952, -10.76384336483936011, 33.53834819971076087 ) ) ;
#26727 = ORIENTED_EDGE ( 'NONE', *, *, #74732, .T. ) ;
#26728 = AXIS2_PLACEMENT_3D ( 'NONE', #16348, #54779, #54333 ) ;
#26729 = CARTESIAN_POINT ( 'NONE',  ( -5.869161581987236254, -7.277220443632450575, 34.74524770363009196 ) ) ;
#26730 = CARTESIAN_POINT ( 'NONE',  ( 17.07692307692307665, -11.91647553114624181, 32.58852847137148245 ) ) ;
#26731 = FACE_OUTER_BOUND ( 'NONE', #68018, .T. ) ;
#26732 = ORIENTED_EDGE ( 'NONE', *, *, #14044, .T. ) ;
#26733 = DIRECTION ( 'NONE',  ( 0.000000000000000000, 0.3420201433256610524, 0.9396926207859113145 ) ) ;
#26734 = CARTESIAN_POINT ( 'NONE',  ( 14.43821774592595553, -3.625058011473228703, 33.29252011169590020 ) ) ;
#26735 = CARTESIAN_POINT ( 'NONE',  ( 6.856993512121044354, -12.37446782046654192, 30.86335684631486487 ) ) ;
#26736 = CARTESIAN_POINT ( 'NONE',  ( -17.77722033102192967, -12.69155399931963046, 30.53255429739158444 ) ) ;
#26737 = ORIENTED_EDGE ( 'NONE', *, *, #35341, .T. ) ;
#26738 = AXIS2_PLACEMENT_3D ( 'NONE', #88066, #187, #54670 ) ;
#26739 = DIRECTION ( 'NONE',  ( 0.000000000000000000, 1.084202172485503448E-16, -1.000000000000000000 ) ) ;
#26740 = CARTESIAN_POINT ( 'NONE',  ( 2.307692307692309264, -3.322132147404559976, 32.92929555188717927 ) ) ;
#26741 = VERTEX_POINT ( 'NONE', #62611 ) ;
#26742 = LINE ( 'NONE', #74942, #14062 ) ;
#26743 = CARTESIAN_POINT ( 'NONE',  ( 9.442307692307695177, -7.433932668274256805, 35.00000000000000711 ) ) ;
#26744 = CARTESIAN_POINT ( 'NONE',  ( -8.069638770718178478, -12.47654668319379567, 31.42292124445336654 ) ) ;
#26745 = CARTESIAN_POINT ( 'NONE',  ( 6.673076923076925127, -7.500000000000001776, 34.75000000000000000 ) ) ;
#26746 = CARTESIAN_POINT ( 'NONE',  ( 7.596153846153846700, -7.500000000000001776, 35.00000000000000000 ) ) ;
#26747 = CARTESIAN_POINT ( 'NONE',  ( 15.23076923076910916, -5.941354392335915335, 34.76329471203413846 ) ) ;
#26749 = CARTESIAN_POINT ( 'NONE',  ( 6.923076923077238654, -2.255955759149395501, 30.00000000000324363 ) ) ;
#26748 = FACE_OUTER_BOUND ( 'NONE', #57997, .T. ) ;
#26750 = EDGE_CURVE ( 'NONE', #45168, #46953, #18654, .T. ) ;
#26751 = EDGE_CURVE ( 'NONE', #86970, #48041, #57822, .T. ) ;
#26752 = DIRECTION ( 'NONE',  ( 1.000000000000000000, 0.000000000000000000, 0.000000000000000000 ) ) ;
#26753 = B_SPLINE_CURVE_WITH_KNOTS ( 'NONE', 3,
 ( #61595, #20183, #75554, #40019, #47649, #60714, #21047, #47194, #48518, #75131 ),
 .UNSPECIFIED., .F., .F.,
 ( 4, 2, 2, 2, 4 ),
 ( 0.000000000000000000, 0.0001954311564186868202, 0.0003908623128373736404, 0.0005862934692560604335, 0.0007817246256747472808 ),
 .UNSPECIFIED. ) ;
#26754 = CARTESIAN_POINT ( 'NONE',  ( 1.139087296525997273, -4.749999999999992895, 19.23437500000000355 ) ) ;
#26755 = EDGE_LOOP ( 'NONE', ( #88368, #53437, #9419, #62148 ) ) ;
#26756 = DIRECTION ( 'NONE',  ( -1.000000000000000000, 0.000000000000000000, 0.000000000000000000 ) ) ;
#26757 = ORIENTED_EDGE ( 'NONE', *, *, #80077, .F. ) ;
#26758 = EDGE_CURVE ( 'NONE', #64904, #34679, #19465, .T. ) ;
#26759 = EDGE_LOOP ( 'NONE', ( #41238, #67805, #1560, #56385 ) ) ;
#26760 = DIRECTION ( 'NONE',  ( 0.000000000000000000, 0.000000000000000000, 1.000000000000000000 ) ) ;
#26761 = EDGE_CURVE ( 'NONE', #46856, #25490, #77902, .T. ) ;
#26762 = ORIENTED_EDGE ( 'NONE', *, *, #30884, .F. ) ;
#26763 = CARTESIAN_POINT ( 'NONE',  ( 10.61538461538461675, -5.557115091759785130, 34.35708131394839171 ) ) ;
#26764 = CARTESIAN_POINT ( 'NONE',  ( -1.944543648262992530, -9.444543648263016067, 21.18750000000000000 ) ) ;
#26765 = CARTESIAN_POINT ( 'NONE',  ( 12.52770506813010343, -7.250054591869670162, 34.99404684341514127 ) ) ;
#26766 = CARTESIAN_POINT ( 'NONE',  ( -11.31544869436814338, -10.01129605718032600, 34.36064277460058491 ) ) ;
#26767 = CYLINDRICAL_SURFACE ( 'NONE', #57635, 0.2499999999999986955 ) ;
#26768 = CARTESIAN_POINT ( 'NONE',  ( -11.66860874789975888, -11.47017969459904130, 32.78971311882034456 ) ) ;
#26769 = CARTESIAN_POINT ( 'NONE',  ( 9.757562831820532523, -12.51329471203373345, 31.30864560766537963 ) ) ;
#26770 = CYLINDRICAL_SURFACE ( 'NONE', #25256, 0.2499999999999998890 ) ;
#26771 = EDGE_CURVE ( 'NONE', #85779, #60579, #49986, .T. ) ;
#26772 = CARTESIAN_POINT ( 'NONE',  ( -4.219929564802033184, -3.513871655860377086, 32.76840700105978499 ) ) ;
#26773 = AXIS2_PLACEMENT_3D ( 'NONE', #84900, #15548, #42142 ) ;
#26774 = CARTESIAN_POINT ( 'NONE',  ( -6.923076923076922462, -4.661471528628507777, 34.16647553114623292 ) ) ;
#26775 = CARTESIAN_POINT ( 'NONE',  ( -13.25382357679059986, -6.413143153341454017, 34.63066358083362672 ) ) ;
#26776 = ADVANCED_FACE ( 'NONE', ( #63048 ), #1360, .F. ) ;
#26777 = CARTESIAN_POINT ( 'NONE',  ( 2.307692307692309264, -9.058645607665452459, 34.76329471203371924 ) ) ;
#26778 = EDGE_LOOP ( 'NONE', ( #58667, #30999 ) ) ;
#26779 = ORIENTED_EDGE ( 'NONE', *, *, #5308, .T. ) ;
#26780 = CARTESIAN_POINT ( 'NONE',  ( 6.673053685783957967, -2.587272538249754117, 30.68239716806877837 ) ) ;
#26781 = LINE ( 'NONE', #48817, #30212 ) ;
#26782 = DIRECTION ( 'NONE',  ( -0.000000000000000000, 1.000000000000000000, -0.000000000000000000 ) ) ;
#26783 = ADVANCED_FACE ( 'NONE', ( #15774 ), #63501, .F. ) ;
#26784 = CARTESIAN_POINT ( 'NONE',  ( 0.3313904918067653860, -10.31621877034669232, 34.18098118002069441 ) ) ;
#26785 = CARTESIAN_POINT ( 'NONE',  ( 15.23076923076910916, -12.51329471203414379, 31.30864560766407578 ) ) ;
#26786 = CARTESIAN_POINT ( 'NONE',  ( -13.51530598772569292, -10.70098750199973203, 33.91152734681376302 ) ) ;
#26787 = CARTESIAN_POINT ( 'NONE',  ( -3.230769230769229949, -2.499999999999998668, 29.75000000000001421 ) ) ;
#26788 = EDGE_CURVE ( 'NONE', #35812, #41427, #41963, .T. ) ;
#26789 = ORIENTED_EDGE ( 'NONE', *, *, #36183, .F. ) ;
#26790 = LINE ( 'NONE', #81744, #17029 ) ;
#26791 = ORIENTED_EDGE ( 'NONE', *, *, #48463, .F. ) ;
#26792 = B_SPLINE_CURVE_WITH_KNOTS ( 'NONE', 3,
 ( #40408, #20125, #39075, #80955, #87718, #18349, #25989, #45809, #66538, #4837 ),
 .UNSPECIFIED., .F., .F.,
 ( 4, 2, 2, 2, 4 ),
 ( 0.0007817359430256346680, 0.0009771253907250002264, 0.001172514838424365893, 0.001367904286123731560, 0.001563293733823104166 ),
 .UNSPECIFIED. ) ;
#26793 = ADVANCED_FACE ( 'NONE', ( #71143 ), #23395, .F. ) ;
#26794 = ORIENTED_EDGE ( 'NONE', *, *, #71323, .T. ) ;
#26795 = CARTESIAN_POINT ( 'NONE',  ( 18.00000000000000000, -3.050289026998446396, 32.03036669348365706 ) ) ;
#26796 = CARTESIAN_POINT ( 'NONE',  ( -1.576923076923076872, -3.499999999999999556, 29.75000000000000355 ) ) ;
#26797 = VECTOR ( 'NONE', #31076, 1000.000000000000114 ) ;
#26798 = CARTESIAN_POINT ( 'NONE',  ( -0.2115929431903193214, -6.696923467548660192, 34.68552623307873972 ) ) ;
#26799 = FACE_OUTER_BOUND ( 'NONE', #5898, .T. ) ;
#26800 = LINE ( 'NONE', #20043, #49400 ) ;
#26801 = VECTOR ( 'NONE', #20021, 1000.000000000000000 ) ;
#26802 = ORIENTED_EDGE ( 'NONE', *, *, #38387, .F. ) ;
#26803 = EDGE_CURVE ( 'NONE', #53825, #40554, #2672, .T. ) ;
#26804 = ORIENTED_EDGE ( 'NONE', *, *, #53761, .F. ) ;
#26805 = PRODUCT_DEFINITION_SHAPE ( 'NONE', 'NONE',  #41349 ) ;
#26806 = VERTEX_POINT ( 'NONE', #78339 ) ;
#26807 = EDGE_LOOP ( 'NONE', ( #21588, #58624 ) ) ;
#26808 = EDGE_CURVE ( 'NONE', #20400, #16925, #69348, .T. ) ;
#26809 = CARTESIAN_POINT ( 'NONE',  ( -14.30769230769230660, -13.04860791097971706, 34.73218667398347037 ) ) ;
#26810 = DIRECTION ( 'NONE',  ( -0.000000000000000000, -0.000000000000000000, -1.000000000000000000 ) ) ;
#26811 = APPLICATION_CONTEXT ( 'automotive_design' ) ;
#26812 = DIRECTION ( 'NONE',  ( -0.000000000000000000, 0.5000000000000011102, -0.8660254037844380415 ) ) ;
#26813 = CARTESIAN_POINT ( 'NONE',  ( -16.28399412357784826, -2.373036134822905208, 30.88089517874952250 ) ) ;
#26814 = SURFACE_STYLE_USAGE ( .BOTH. , #33125 ) ;
#26815 = CARTESIAN_POINT ( 'NONE',  ( -15.29685161012936767, -2.486705287966279432, 31.30864560766542937 ) ) ;
#26816 = ORIENTED_EDGE ( 'NONE', *, *, #26087, .F. ) ;
#26817 = EDGE_CURVE ( 'NONE', #87648, #8709, #70713, .T. ) ;
#26818 = ORIENTED_EDGE ( 'NONE', *, *, #21033, .T. ) ;
#26819 = ORIENTED_EDGE ( 'NONE', *, *, #27521, .F. ) ;
#26821 = ORIENTED_EDGE ( 'NONE', *, *, #24779, .F. ) ;
#26820 = CARTESIAN_POINT ( 'NONE',  ( -3.296039231325550212, -2.657715359629089225, 31.77849191805834295 ) ) ;
#26822 = EDGE_CURVE ( 'NONE', #37020, #55506, #15159, .T. ) ;
#26823 = B_SPLINE_CURVE_WITH_KNOTS ( 'NONE', 3,
 ( #38340, #23921, #36996, #18075, #11311, #3214, #3652, #50938, #10427, #58152 ),
 .UNSPECIFIED., .F., .F.,
 ( 4, 2, 2, 2, 4 ),
 ( 0.0007817359430256322827, 0.0009771253907249989254, 0.001172514838424365676, 0.001367904286123732428, 0.001563293733823099179 ),
 .UNSPECIFIED. ) ;
#26824 = CARTESIAN_POINT ( 'NONE',  ( 9.562159722575998444, -8.630895178749533159, 34.87696386517710323 ) ) ;
#26825 = DIRECTION ( 'NONE',  ( -0.000000000000000000, -0.000000000000000000, -1.000000000000000000 ) ) ;
#26826 = EDGE_CURVE ( 'NONE', #78424, #32882, #47374, .T. ) ;
#26827 = AXIS2_PLACEMENT_3D ( 'NONE', #69618, #47572, #83145 ) ;
#26828 = CARTESIAN_POINT ( 'NONE',  ( -3.750000000000007550, -5.946699141100917352, 20.17187500000000000 ) ) ;
#26829 = ORIENTED_EDGE ( 'NONE', *, *, #15624, .T. ) ;
#26830 = CARTESIAN_POINT ( 'NONE',  ( 7.846153846153723244, -4.320704448113951379, 33.92786785259630022 ) ) ;
#26831 = EDGE_LOOP ( 'NONE', ( #50317, #45161, #77044, #87356 ) ) ;
#26832 = CARTESIAN_POINT ( 'NONE',  ( 2.177000841024751665, -6.413092428213692742, 34.63065189839063152 ) ) ;
#26833 = FACE_BOUND ( 'NONE', #36596, .T. ) ;
#26834 = CARTESIAN_POINT ( 'NONE',  ( -10.61538461538461320, -9.780366693483667717, 34.19971097300155094 ) ) ;
#26835 = CARTESIAN_POINT ( 'NONE',  ( -0.4615384615384611200, -2.708943851104267164, 35.45975837776705220 ) ) ;
#26836 = VERTEX_POINT ( 'NONE', #38254 ) ;
#26837 = CARTESIAN_POINT ( 'NONE',  ( 19.50000000000000000, -4.000000000000000000, 29.75000000000000355 ) ) ;
#26838 = AXIS2_PLACEMENT_3D ( 'NONE', #84836, #20997, #27764 ) ;
#26839 = CARTESIAN_POINT ( 'NONE',  ( 8.834485908743602067, -8.656820664281605460, 34.87096338111211224 ) ) ;
#26840 = CARTESIAN_POINT ( 'NONE',  ( -17.07692307692319744, -12.70778746994576025, 30.41441678777401236 ) ) ;
#26841 = CARTESIAN_POINT ( 'NONE',  ( 14.30769230769218581, -9.528491918059723176, 34.59228464037033035 ) ) ;
#26842 = ORIENTED_EDGE ( 'NONE', *, *, #8488, .F. ) ;
#26843 = CYLINDRICAL_SURFACE ( 'NONE', #55917, 4.000000000000000000 ) ;
#26844 = CARTESIAN_POINT ( 'NONE',  ( -7.846153846153965716, -11.48612834414049644, 32.76840700105863391 ) ) ;
#26845 = CARTESIAN_POINT ( 'NONE',  ( -16.37671241690925683, -2.251424796025575770, 29.88072029997477586 ) ) ;
#26846 = CYLINDRICAL_SURFACE ( 'NONE', #65867, 0.2499999999999994726 ) ;
#26847 = CARTESIAN_POINT ( 'NONE',  ( 8.069165197766695385, -3.105924265160262543, 32.13625925475356127 ) ) ;
#26848 = FACE_BOUND ( 'NONE', #29126, .T. ) ;
#26850 = CARTESIAN_POINT ( 'NONE',  ( -17.07692307692319744, -11.06231777344772027, 33.60647404775119895 ) ) ;
#26849 = CARTESIAN_POINT ( 'NONE',  ( 13.38461538461538680, -11.91647553114624181, 32.58852847137148245 ) ) ;
#26851 = DIRECTION ( 'NONE',  ( 0.000000000000000000, 0.000000000000000000, 1.000000000000000000 ) ) ;
#26853 = CARTESIAN_POINT ( 'NONE',  ( -2.176901866725357682, -12.35292014791297710, 31.75344720912887198 ) ) ;
#26852 = CARTESIAN_POINT ( 'NONE',  ( -5.749945688361683516, -9.943054286541403997, 34.11300777759954883 ) ) ;
#26854 = CARTESIAN_POINT ( 'NONE',  ( -18.00000000000012079, -10.21337939537710504, 33.94971097300076224 ) ) ;
#26855 = CARTESIAN_POINT ( 'NONE',  ( 2.775308065498768517, -8.577988221561467341, 19.29500670625849068 ) ) ;
#26856 = ORIENTED_EDGE ( 'NONE', *, *, #62576, .F. ) ;
#26857 = CARTESIAN_POINT ( 'NONE',  ( -7.146561866800870355, -9.331801661448606566, 34.40259984581193464 ) ) ;
#26858 = ORIENTED_EDGE ( 'NONE', *, *, #77256, .F. ) ;
#26859 = CARTESIAN_POINT ( 'NONE',  ( 16.09615384615384670, -3.499999999999999556, 29.75000000000000355 ) ) ;
#26860 = VECTOR ( 'NONE', #43398, 999.9999999999998863 ) ;
#26861 = ORIENTED_EDGE ( 'NONE', *, *, #29886, .F. ) ;
#26862 = CARTESIAN_POINT ( 'NONE',  ( 7.846153846153846700, -4.102666532097928531, 36.13435417666054406 ) ) ;
#26863 = EDGE_CURVE ( 'NONE', #77695, #75748, #33347, .T. ) ;
#26864 = CYLINDRICAL_SURFACE ( 'NONE', #22919, 0.2499999999999994726 ) ;
#26866 = ORIENTED_EDGE ( 'NONE', *, *, #760, .T. ) ;
#26865 = CARTESIAN_POINT ( 'NONE',  ( -10.83886953994894498, -11.60425143139329940, 33.02411095842164457 ) ) ;
#26867 = CARTESIAN_POINT ( 'NONE',  ( 3.230769230769231726, -6.386643153685126251, 34.62446782046654192 ) ) ;
#26868 = CARTESIAN_POINT ( 'NONE',  ( 5.207713517890025123, -11.93129842949671726, 32.56571108434900452 ) ) ;
#26869 = CARTESIAN_POINT ( 'NONE',  ( 1.901340078031349856, -5.512252781505337929, 16.56063170625848713 ) ) ;
#26870 = CARTESIAN_POINT ( 'NONE',  ( 1.134615384615387246, -2.499999999999998668, 29.75000000000000355 ) ) ;
#26871 = LINE ( 'NONE', #20114, #50392 ) ;
#26872 = CARTESIAN_POINT ( 'NONE',  ( -5.076923076923075762, -11.91647553114624181, 32.58852847137148245 ) ) ;
#26873 = DIRECTION ( 'NONE',  ( 1.000000000000000000, 0.000000000000000000, 0.000000000000000000 ) ) ;
#26874 = DIRECTION ( 'NONE',  ( 0.000000000000000000, 1.000000000000000000, 0.000000000000000000 ) ) ;
#26875 = CARTESIAN_POINT ( 'NONE',  ( 11.66898724022510514, -3.816742781228458448, 33.13167719472716044 ) ) ;
#26876 = EDGE_CURVE ( 'NONE', #7644, #61382, #70828, .T. ) ;
#26877 = CARTESIAN_POINT ( 'NONE',  ( -1.614399933863613468, -11.22469193450124969, 25.11124329374151642 ) ) ;
#26878 = CARTESIAN_POINT ( 'NONE',  ( 9.561697332683166906, -7.722926236386453702, 34.74524107206102030 ) ) ;
#26879 = VECTOR ( 'NONE', #34059, 1000.000000000000000 ) ;
#26880 = ORIENTED_EDGE ( 'NONE', *, *, #34662, .F. ) ;
#26881 = ADVANCED_FACE ( 'NONE', ( #72924 ), #58069, .F. ) ;
#26882 = FACE_OUTER_BOUND ( 'NONE', #66447, .T. ) ;
#26883 = CARTESIAN_POINT ( 'NONE',  ( -2.608446859217920633, -4.805146000318815780, 24.25186829374150932 ) ) ;
#26884 = CARTESIAN_POINT ( 'NONE',  ( -16.02332071561251325, -12.50538340440932394, 31.33453814440721885 ) ) ;
#26885 = DIRECTION ( 'NONE',  ( 1.845450506358306311E-16, -1.000000000000000000, 5.102127870520020612E-17 ) ) ;
#26886 = VERTEX_POINT ( 'NONE', #17543 ) ;
#26887 = DIRECTION ( 'NONE',  ( -0.000000000000000000, 0.9848077530122085754, -0.1736481776669273613 ) ) ;
#26888 = CARTESIAN_POINT ( 'NONE',  ( 3.007284287045282056, -3.754499324213721234, 33.06261337010820256 ) ) ;
#26890 = ORIENTED_EDGE ( 'NONE', *, *, #25154, .F. ) ;
#26889 = CARTESIAN_POINT ( 'NONE',  ( 2.177545098254090927, -2.882441371585227508, 31.66841991370171527 ) ) ;
#26891 = CYLINDRICAL_SURFACE ( 'NONE', #61306, 0.2499999999999995559 ) ;
#26892 = CARTESIAN_POINT ( 'NONE',  ( 15.36129466900288065, -5.915461855592780260, 34.75538340440931506 ) ) ;
#26894 = EDGE_CURVE ( 'NONE', #64220, #34293, #39160, .T. ) ;
#26893 = CARTESIAN_POINT ( 'NONE',  ( -10.55012947587177941, -9.528491918058460186, 34.59228464037086326 ) ) ;
#26895 = ORIENTED_EDGE ( 'NONE', *, *, #67497, .F. ) ;
#26896 = CARTESIAN_POINT ( 'NONE',  ( 2.084765348785459160, -4.026226216239095379, 33.68668979543632958 ) ) ;
#26897 = CARTESIAN_POINT ( 'NONE',  ( 16.81410256410256565, -3.499999999999999556, 29.75000000000000355 ) ) ;
#26898 = AXIS2_PLACEMENT_3D ( 'NONE', #42402, #15365, #9481 ) ;
#26899 = CARTESIAN_POINT ( 'NONE',  ( 8.519207545009313876, -3.520140089381495585, 33.17453946501458262 ) ) ;
#26900 = ORIENTED_EDGE ( 'NONE', *, *, #4580, .T. ) ;
#26901 = EDGE_LOOP ( 'NONE', ( #9146, #75746, #75602, #61027 ) ) ;
#26902 = EDGE_LOOP ( 'NONE', ( #27303, #85412, #27273, #16569 ) ) ;
#26903 = EDGE_CURVE ( 'NONE', #58442, #50385, #44995, .T. ) ;
#26904 = VERTEX_POINT ( 'NONE', #86916 ) ;
#26905 = CARTESIAN_POINT ( 'NONE',  ( -9.915233909823840008, -2.758268499246657068, 31.33685645148948140 ) ) ;
#26906 = CARTESIAN_POINT ( 'NONE',  ( 0.3308469948709010233, -2.541943142973490666, 30.39792223712631980 ) ) ;
#26907 = EDGE_CURVE ( 'NONE', #46529, #292, #45444, .T. ) ;
#26908 = VECTOR ( 'NONE', #35085, 999.9999999999998863 ) ;
#26909 = CARTESIAN_POINT ( 'NONE',  ( -13.25382494364843389, -11.93129842949671726, 32.56571108434900452 ) ) ;
#26910 = DIRECTION ( 'NONE',  ( 0.000000000000000000, 0.000000000000000000, 1.000000000000000000 ) ) ;
#26911 = CARTESIAN_POINT ( 'NONE',  ( -17.75000000000000355, -7.500000000000000000, 35.00000000000000000 ) ) ;
#26912 = ORIENTED_EDGE ( 'NONE', *, *, #11129, .F. ) ;
#26913 = ORIENTED_EDGE ( 'NONE', *, *, #60481, .T. ) ;
#26914 = EDGE_CURVE ( 'NONE', #86693, #57379, #12128, .T. ) ;
#26915 = ORIENTED_EDGE ( 'NONE', *, *, #49145, .F. ) ;
#26917 = ORIENTED_EDGE ( 'NONE', *, *, #66680, .F. ) ;
#26916 = CARTESIAN_POINT ( 'NONE',  ( -6.989159302437059296, -8.164416787775445883, 34.95778746994557906 ) ) ;
#26918 = CARTESIAN_POINT ( 'NONE',  ( -1.384615384615383471, -2.833524468853757305, 32.15551576947925838 ) ) ;
#26919 = B_SPLINE_CURVE_WITH_KNOTS ( 'NONE', 3,
 ( #49378, #15153, #34968, #21461, #15594, #43061, #70535, #28210, #29555, #57010 ),
 .UNSPECIFIED., .F., .F.,
 ( 4, 2, 2, 2, 4 ),
 ( 0.0007817359430256283796, 0.0009771253907249943717, 0.001172514838424360255, 0.001367904286123726356, 0.001563293733823092240 ),
 .UNSPECIFIED. ) ;
#26920 = CARTESIAN_POINT ( 'NONE',  ( -10.86538461538461320, -7.500000000000001776, 34.75000000000000000 ) ) ;
#26921 = B_SPLINE_CURVE_WITH_KNOTS ( 'NONE', 3,
 ( #44462, #44916, #2162, #30087, #50339, #77820, #37274, #16563, #71067, #71951 ),
 .UNSPECIFIED., .F., .F.,
 ( 4, 2, 2, 2, 4 ),
 ( 0.000000000000000000, 0.0001954339857564086941, 0.0003908679715128173882, 0.0005863019572692261365, 0.0007817359430256347764 ),
 .UNSPECIFIED. ) ;
#26922 = AXIS2_PLACEMENT_3D ( 'NONE', #66488, #10211, #17410 ) ;
#26923 = LINE ( 'NONE', #68788, #88206 ) ;
#26924 = CARTESIAN_POINT ( 'NONE',  ( 18.00000000000000000, -10.67929555188718282, 33.92786785259544047 ) ) ;
#26925 = EDGE_LOOP ( 'NONE', ( #2338, #85152 ) ) ;
#26926 = EDGE_CURVE ( 'NONE', #34444, #74304, #46263, .T. ) ;
#26927 = ORIENTED_EDGE ( 'NONE', *, *, #23002, .F. ) ;
#26928 = ORIENTED_EDGE ( 'NONE', *, *, #58401, .F. ) ;
#26929 = CARTESIAN_POINT ( 'NONE',  ( -10.68146699474474914, -10.67929555188718460, 33.92786785259543336 ) ) ;
#26931 = ORIENTED_EDGE ( 'NONE', *, *, #13889, .T. ) ;
#26930 = CARTESIAN_POINT ( 'NONE',  ( -39.05038313613820122, -2.249999999999999556, 27.25000000000000000 ) ) ;
#26932 = CARTESIAN_POINT ( 'NONE',  ( 6.700150705560775855, -6.503392248772476236, 34.64988816332204635 ) ) ;
#26933 = ADVANCED_FACE ( 'NONE', ( #80132 ), #23827, .F. ) ;
#26934 = ADVANCED_FACE ( 'NONE', ( #38699 ), #58961, .F. ) ;
#26935 = CARTESIAN_POINT ( 'NONE',  ( -17.29985003582992320, -3.395401636524186362, 33.02366814457250399 ) ) ;
#26936 = ORIENTED_EDGE ( 'NONE', *, *, #80257, .T. ) ;
#26937 = CYLINDRICAL_SURFACE ( 'NONE', #53201, 0.2500000000000012212 ) ;
#26938 = CARTESIAN_POINT ( 'NONE',  ( -4.023054346021368133, -4.809403383903225304, 33.96459661697924304 ) ) ;
#26939 = CARTESIAN_POINT ( 'NONE',  ( -8.769230769230768274, -1.629998284177014645, 34.34916445242399163 ) ) ;
#26940 = ADVANCED_FACE ( 'NONE', ( #11229 ), #66160, .F. ) ;
#26941 = FACE_BOUND ( 'NONE', #41267, .T. ) ;
#26942 = EDGE_CURVE ( 'NONE', #48246, #85269, #37699, .T. ) ;
#26943 = B_SPLINE_CURVE_WITH_KNOTS ( 'NONE', 3,
 ( #6400, #19017, #74404, #12703, #61313, #88827, #66756, #46488, #27099, #54563 ),
 .UNSPECIFIED., .F., .F.,
 ( 4, 2, 2, 2, 4 ),
 ( 0.000000000000000000, 0.0001954311564186876063, 0.0003908623128373752125, 0.0005862934692560628188, 0.0007817246256747504250 ),
 .UNSPECIFIED. ) ;
#26944 = CARTESIAN_POINT ( 'NONE',  ( 6.000000000000001776, -2.708943851104267164, 35.45975837776705220 ) ) ;
#26945 = CARTESIAN_POINT ( 'NONE',  ( -0.4615384615384611200, -2.249999999999998668, 29.75000000000001776 ) ) ;
#26946 = DIRECTION ( 'NONE',  ( 0.000000000000000000, 0.000000000000000000, -1.000000000000000000 ) ) ;
#26948 = CARTESIAN_POINT ( 'NONE',  ( 18.24994551834813805, -4.336752205174650321, 33.62275283266504289 ) ) ;
#26947 = DIRECTION ( 'NONE',  ( 0.000000000000000000, 0.000000000000000000, -1.000000000000000000 ) ) ;
#26949 = LINE ( 'NONE', #88228, #59614 ) ;
#26950 = CARTESIAN_POINT ( 'NONE',  ( -15.84615384615384670, -7.500000000000000000, 33.75000000000000000 ) ) ;
#26951 = ORIENTED_EDGE ( 'NONE', *, *, #47102, .F. ) ;
#26952 = VECTOR ( 'NONE', #62970, 1000.000000000000000 ) ;
#26953 = FACE_OUTER_BOUND ( 'NONE', #6774, .T. ) ;
#26954 = VERTEX_POINT ( 'NONE', #7135 ) ;
#26955 = CARTESIAN_POINT ( 'NONE',  ( -14.30769230769242739, -5.219633306517616589, 34.19971097300220464 ) ) ;
#26956 = DIRECTION ( 'NONE',  ( -1.000000000000000000, -0.000000000000000000, -0.000000000000000000 ) ) ;
#26957 = ORIENTED_EDGE ( 'NONE', *, *, #42757, .T. ) ;
#26958 = VECTOR ( 'NONE', #57285, 1000.000000000000114 ) ;
#26959 = CARTESIAN_POINT ( 'NONE',  ( 11.28848479441294650, -10.06842814019191401, 34.32929386961144758 ) ) ;
#26960 = CARTESIAN_POINT ( 'NONE',  ( -15.00798956179116317, -12.69155399931963046, 30.53255429739157734 ) ) ;
#26961 = FACE_BOUND ( 'NONE', #13052, .T. ) ;
#26962 = B_SPLINE_CURVE_WITH_KNOTS ( 'NONE', 3,
 ( #75632, #46838, #41417, #5862, #33336, #47279, #74769, #8519, #70657, #8963 ),
 .UNSPECIFIED., .F., .F.,
 ( 4, 2, 2, 2, 4 ),
 ( 0.000000000000000000, 0.0001954311564186876063, 0.0003908623128373752125, 0.0005862934692560628188, 0.0007817246256747504250 ),
 .UNSPECIFIED. ) ;
#26964 = CARTESIAN_POINT ( 'NONE',  ( -17.01173008862841840, -2.255955759149234741, 29.99999999999988276 ) ) ;
#26963 = CARTESIAN_POINT ( 'NONE',  ( -18.06527044596078113, -3.300289026998416642, 32.46337939537583139 ) ) ;
#26965 = CARTESIAN_POINT ( 'NONE',  ( 10.61538461538461675, -8.120952969808772792, 34.71129190930000163 ) ) ;
#26966 = CARTESIAN_POINT ( 'NONE',  ( 15.23076923076923173, -2.517432740324522911, 35.29906147534542527 ) ) ;
#26968 = CARTESIAN_POINT ( 'NONE',  ( -18.00000000000000000, -11.10434399251292881, 35.99290692298802696 ) ) ;
#26967 = DIRECTION ( 'NONE',  ( 1.000000000000000000, 0.000000000000000000, 0.000000000000000000 ) ) ;
#26969 = B_SPLINE_CURVE_WITH_KNOTS ( 'NONE', 3,
 ( #57082, #62500, #49881, #84577, #83694, #43136, #50314, #71043, #42698, #23293 ),
 .UNSPECIFIED., .F., .F.,
 ( 4, 2, 2, 2, 4 ),
 ( 0.0007817359430256297891, 0.0009771253907249958896, 0.001172514838424361990, 0.001367904286123728091, 0.001563293733823094191 ),
 .UNSPECIFIED. ) ;
#26970 = AXIS2_PLACEMENT_3D ( 'NONE', #64399, #72054, #3593 ) ;
#26971 = CARTESIAN_POINT ( 'NONE',  ( 1.614399933863660985, -11.22469193450123193, 16.95125670625848713 ) ) ;
#26972 = ORIENTED_EDGE ( 'NONE', *, *, #59941, .F. ) ;
#26973 = ORIENTED_EDGE ( 'NONE', *, *, #26280, .F. ) ;
#26974 = FACE_OUTER_BOUND ( 'NONE', #51605, .T. ) ;
#26975 = AXIS2_PLACEMENT_3D ( 'NONE', #32088, #57779, #44239 ) ;
#26976 = CARTESIAN_POINT ( 'NONE',  ( -8.769230769230768274, -4.102666532097928531, 36.13435417666054406 ) ) ;
#26977 = CARTESIAN_POINT ( 'NONE',  ( -13.38461538461538325, -13.78497067705608181, 32.30358669280327177 ) ) ;
#26978 = CARTESIAN_POINT ( 'NONE',  ( 6.856993512121043466, -12.10708131394839349, 31.69288490824020244 ) ) ;
#26979 = FACE_OUTER_BOUND ( 'NONE', #79325, .T. ) ;
#26980 = CARTESIAN_POINT ( 'NONE',  ( -3.775308065498766297, -6.007798216065450170, 17.42000670625848713 ) ) ;
#26981 = LINE ( 'NONE', #54436, #35991 ) ;
#26982 = DIRECTION ( 'NONE',  ( 0.000000000000000000, 1.000000000000000000, 0.000000000000000000 ) ) ;
#26983 = FACE_OUTER_BOUND ( 'NONE', #80056, .T. ) ;
#26984 = CARTESIAN_POINT ( 'NONE',  ( -2.307692307692305711, -5.557115091759785130, 34.35708131394839171 ) ) ;
#26985 = CARTESIAN_POINT ( 'NONE',  ( -5.999999999999998224, -2.721908614388771852, 31.22303859784724978 ) ) ;
#26986 = DIRECTION ( 'NONE',  ( 0.000000000000000000, 0.4999999999999985567, 0.8660254037844395958 ) ) ;
#26987 = DIRECTION ( 'NONE',  ( -0.000000000000000000, -0.8660254037844397068, -0.4999999999999978906 ) ) ;
#26988 = CARTESIAN_POINT ( 'NONE',  ( 2.242369392200134204, -7.749976743299137993, 34.99404534957040624 ) ) ;
#26989 = CARTESIAN_POINT ( 'NONE',  ( -12.68440388374210315, -2.501496062324912284, 29.88072118266895671 ) ) ;
#26990 = ORIENTED_EDGE ( 'NONE', *, *, #10914, .F. ) ;
#26991 = CARTESIAN_POINT ( 'NONE',  ( 1.319344938654610333, -2.625532179533444754, 30.86335684631481513 ) ) ;
#26992 = DIRECTION ( 'NONE',  ( 1.000000000000000000, 0.000000000000000000, 0.000000000000000000 ) ) ;
#26993 = CARTESIAN_POINT ( 'NONE',  ( 1.987747218494642309, -5.598659921968629050, 14.56436829374151287 ) ) ;
#26994 = CARTESIAN_POINT ( 'NONE',  ( -9.942330916529149576, -10.92453946501458795, 33.72985991061850086 ) ) ;
#26995 = AXIS2_PLACEMENT_3D ( 'NONE', #76472, #54867, #6677 ) ;
#26996 = DIRECTION ( 'NONE',  ( -0.000000000000000000, -0.9848077530122085754, -0.1736481776669273613 ) ) ;
#26998 = EDGE_LOOP ( 'NONE', ( #6447, #43203, #3537, #77746 ) ) ;
#26997 = CARTESIAN_POINT ( 'NONE',  ( -1.253823576790597194, -4.118422570099827595, 33.43335022499816489 ) ) ;
#26999 = CARTESIAN_POINT ( 'NONE',  ( -1.409462824231155764E-14, -4.749999999999999112, 25.40625000000000000 ) ) ;
#27000 = CARTESIAN_POINT ( 'NONE',  ( -15.23076923076935074, -12.46129190930018460, 30.37095296980731973 ) ) ;
#27001 = EDGE_LOOP ( 'NONE', ( #25800, #22204 ) ) ;
#27002 = B_SPLINE_CURVE_WITH_KNOTS ( 'NONE', 3,
 ( #84128, #43128, #51174, #64708, #22406, #83684, #9344, #2562, #64262, #49440 ),
 .UNSPECIFIED., .F., .F.,
 ( 4, 2, 2, 2, 4 ),
 ( 0.0007817246256747453293, 0.0009771112852218889842, 0.001172497944769032747, 0.001367884604316176294, 0.001563271263863320057 ),
 .UNSPECIFIED. ) ;
#27003 = CARTESIAN_POINT ( 'NONE',  ( -15.90390063549801347, -10.05730279482229683, 34.04704008940765902 ) ) ;
#27004 = CARTESIAN_POINT ( 'NONE',  ( -6.923076923076922462, -11.35647404775217417, 33.31231777344666511 ) ) ;
#27005 = ORIENTED_EDGE ( 'NONE', *, *, #39872, .T. ) ;
#27006 = DIRECTION ( 'NONE',  ( -1.000000000000000000, -0.000000000000000000, -0.000000000000000000 ) ) ;
#27007 = DIRECTION ( 'NONE',  ( 0.000000000000000000, 0.000000000000000000, 1.000000000000000000 ) ) ;
#27008 = VECTOR ( 'NONE', #46712, 1000.000000000000000 ) ;
#27009 = CARTESIAN_POINT ( 'NONE',  ( -7.976301055592065481, -3.817052484675422797, 33.13202310037935661 ) ) ;
#27010 = ORIENTED_EDGE ( 'NONE', *, *, #29496, .F. ) ;
#27011 = ORIENTED_EDGE ( 'NONE', *, *, #55103, .T. ) ;
#27012 = CYLINDRICAL_SURFACE ( 'NONE', #16819, 0.2500000000000002220 ) ;
#27013 = EDGE_CURVE ( 'NONE', #80537, #37045, #39893, .T. ) ;
#27014 = VERTEX_POINT ( 'NONE', #55310 ) ;
#27015 = CARTESIAN_POINT ( 'NONE',  ( -7.846153846153967493, -2.379036618888197729, 30.90682066428292885 ) ) ;
#27016 = DIRECTION ( 'NONE',  ( -0.000000000000000000, 0.9396926207859093161, -0.3420201433256663259 ) ) ;
#27017 = CARTESIAN_POINT ( 'NONE',  ( -5.999999999999998224, -2.708943851104267164, 35.45975837776705220 ) ) ;
#27018 = CARTESIAN_POINT ( 'NONE',  ( 19.00000000000000000, 16.99999999999999289, 31.75000000000000000 ) ) ;
#27019 = CARTESIAN_POINT ( 'NONE',  ( 15.10007776410167324, -6.413092428213692742, 34.63065189839063152 ) ) ;
#27020 = CARTESIAN_POINT ( 'NONE',  ( 4.153846153846154188, -12.37446782046654192, 30.86335684631486131 ) ) ;
#27021 = CARTESIAN_POINT ( 'NONE',  ( -0.3954711281883850904, -12.34228464037088813, 31.77849191805839268 ) ) ;
#27022 = ORIENTED_EDGE ( 'NONE', *, *, #40973, .T. ) ;
#27023 = EDGE_CURVE ( 'NONE', #12236, #35073, #22648, .T. ) ;
#27024 = EDGE_LOOP ( 'NONE', ( #4577, #28228, #62241, #8690 ) ) ;
#27026 = ORIENTED_EDGE ( 'NONE', *, *, #81198, .F. ) ;
#27025 = CARTESIAN_POINT ( 'NONE',  ( -17.20707028636129721, -10.19110544564092002, 33.96427741523702792 ) ) ;
#27027 = VECTOR ( 'NONE', #53060, 1000.000000000000227 ) ;
#27028 = AXIS2_PLACEMENT_3D ( 'NONE', #55793, #54913, #69321 ) ;
#27029 = CARTESIAN_POINT ( 'NONE',  ( -8.703163435880695076, -10.67929555188718282, 33.92786785259544757 ) ) ;
#27030 = FACE_OUTER_BOUND ( 'NONE', #15836, .T. ) ;
#27031 = ORIENTED_EDGE ( 'NONE', *, *, #70670, .T. ) ;
#27032 = CARTESIAN_POINT ( 'NONE',  ( 14.30769230769218581, -12.16647553114689728, 32.15551576947799362 ) ) ;
#27033 = EDGE_LOOP ( 'NONE', ( #65760, #30814 ) ) ;
#27034 = CARTESIAN_POINT ( 'NONE',  ( 0.3962874713772188695, -2.506253911140460922, 30.00000000000013856 ) ) ;
#27035 = EDGE_LOOP ( 'NONE', ( #79294, #8308 ) ) ;
#27036 = B_SPLINE_CURVE_WITH_KNOTS ( 'NONE', 3,
 ( #8568, #479, #56744, #15325, #21183, #63497, #69382, #71137, #1356, #42804 ),
 .UNSPECIFIED., .F., .F.,
 ( 4, 2, 2, 2, 4 ),
 ( 0.000000000000000000, 0.0001954339857564072033, 0.0003908679715128144066, 0.0005863019572692215828, 0.0007817359430256288133 ),
 .UNSPECIFIED. ) ;
#27037 = CARTESIAN_POINT ( 'NONE',  ( -14.05763788777885281, -12.01375889529407281, 32.43194544308182969 ) ) ;
#27038 = EDGE_CURVE ( 'NONE', #58148, #38566, #17598, .T. ) ;
#27039 = EDGE_CURVE ( 'NONE', #64392, #15864, #4300, .T. ) ;
#27040 = ORIENTED_EDGE ( 'NONE', *, *, #87265, .F. ) ;
#27041 = CARTESIAN_POINT ( 'NONE',  ( -4.284536756956462966, -3.957541250942359756, 33.62499894934981626 ) ) ;
#27042 = CARTESIAN_POINT ( 'NONE',  ( 16.85343813319913053, -2.847400154188068910, 31.58180166144859768 ) ) ;
#27043 = FACE_BOUND ( 'NONE', #35567, .T. ) ;
#27044 = CARTESIAN_POINT ( 'NONE',  ( -14.53061926659915315, -9.172386477786396597, 34.72672124145550043 ) ) ;
#27045 = CARTESIAN_POINT ( 'NONE',  ( 1.318861956302054939, -7.249945578846654470, 34.99404164642496795 ) ) ;
#27046 = CARTESIAN_POINT ( 'NONE',  ( 13.38461538461526423, -5.094484230521993062, 34.41647553114689373 ) ) ;
#27047 = CARTESIAN_POINT ( 'NONE',  ( 1.161130460051053692, -12.47654668319379567, 31.42292124445336654 ) ) ;
#27048 = DIRECTION ( 'NONE',  ( -0.000000000000000000, -0.6427876096865404731, -0.7660444431189771253 ) ) ;
#27049 = CARTESIAN_POINT ( 'NONE',  ( 15.93091993633000136, -4.186968288167451036, 33.49512374952580274 ) ) ;
#27050 = FACE_OUTER_BOUND ( 'NONE', #82749, .T. ) ;
#27051 = EDGE_CURVE ( 'NONE', #49709, #8288, #81477, .T. ) ;
#27052 = ORIENTED_EDGE ( 'NONE', *, *, #59031, .T. ) ;
#27053 = ORIENTED_EDGE ( 'NONE', *, *, #72925, .T. ) ;
#27054 = VECTOR ( 'NONE', #55254, 1000.000000000000114 ) ;
#27056 = CARTESIAN_POINT ( 'NONE',  ( -18.25002322422145440, -10.18141759479407327, 34.26406193332782379 ) ) ;
#27055 = CARTESIAN_POINT ( 'NONE',  ( -5.326899820971665811, -12.01397095200673881, 32.43157075238190146 ) ) ;
#27057 = LINE ( 'NONE', #38801, #29854 ) ;
#27058 = CARTESIAN_POINT ( 'NONE',  ( 3.230769230769110045, -10.90142922262034020, 33.41473453929536674 ) ) ;
#27059 = DIRECTION ( 'NONE',  ( -0.000000000000000000, 1.000000000000000000, -0.000000000000000000 ) ) ;
#27060 = CARTESIAN_POINT ( 'NONE',  ( -12.46153846153858424, -5.094484230521993062, 34.41647553114689373 ) ) ;
#27061 = ORIENTED_EDGE ( 'NONE', *, *, #74142, .F. ) ;
#27062 = CARTESIAN_POINT ( 'NONE',  ( -11.60373198442231235, -12.27809138561121394, 31.22303859784730307 ) ) ;
#27063 = VECTOR ( 'NONE', #23882, 1000.000000000000000 ) ;
#27064 = CARTESIAN_POINT ( 'NONE',  ( 0.5276068125408998055, -9.780366693483669494, 34.19971097300155805 ) ) ;
#27065 = CARTESIAN_POINT ( 'NONE',  ( -3.360917200500926239, -11.66186481527757479, 32.95055677023626117 ) ) ;
#27066 = CARTESIAN_POINT ( 'NONE',  ( 7.846153846153725020, -10.90142922262034020, 33.41473453929536674 ) ) ;
#27067 = ORIENTED_EDGE ( 'NONE', *, *, #21776, .T. ) ;
#27068 = VERTEX_POINT ( 'NONE', #62070 ) ;
#27069 = EDGE_LOOP ( 'NONE', ( #32331, #25783, #73355, #81468 ) ) ;
#27070 = CARTESIAN_POINT ( 'NONE',  ( 0.4615384615384611200, -10.51840700105979565, 33.73612834413961536 ) ) ;
#27071 = ORIENTED_EDGE ( 'NONE', *, *, #62570, .F. ) ;
#27072 = DIRECTION ( 'NONE',  ( -0.000000000000000000, 1.000000000000000000, -0.000000000000000000 ) ) ;
#27073 = CARTESIAN_POINT ( 'NONE',  ( 15.00784301325308157, -9.086856451489515152, 34.49173150075333183 ) ) ;
#27074 = CARTESIAN_POINT ( 'NONE',  ( 3.453782074862625340, -10.01129605718032778, 34.36064277460058491 ) ) ;
#27075 = DIRECTION ( 'NONE',  ( -1.000000000000000000, -0.000000000000000000, -0.000000000000000000 ) ) ;
#27076 = CARTESIAN_POINT ( 'NONE',  ( 14.55774661933062575, -4.235687564193448829, 33.53795663066793509 ) ) ;
#27077 = ORIENTED_EDGE ( 'NONE', *, *, #59451, .T. ) ;
#27078 = CARTESIAN_POINT ( 'NONE',  ( 4.376625695114563008, -4.387253974876676565, 33.66317474335728832 ) ) ;
#27080 = EDGE_LOOP ( 'NONE', ( #63627, #32007, #87135, #13595 ) ) ;
#27079 = CARTESIAN_POINT ( 'NONE',  ( -13.25408968285182176, -4.459921816937791661, 33.71989282347011851 ) ) ;
#27081 = CARTESIAN_POINT ( 'NONE',  ( -5.207071046654771607, -2.373036134822904319, 30.88089517874952250 ) ) ;
#27082 = CARTESIAN_POINT ( 'NONE',  ( 8.834485908743607396, -12.51329471203373345, 31.30864560766537963 ) ) ;
#27083 = CARTESIAN_POINT ( 'NONE',  ( -11.53846153846153655, -7.500000000000001776, 35.04278698407183867 ) ) ;
#27084 = CARTESIAN_POINT ( 'NONE',  ( 8.769230769230645706, -12.16647553114689728, 32.15551576947799362 ) ) ;
#27085 = CARTESIAN_POINT ( 'NONE',  ( -12.46153846153846168, -2.721908614388771852, 31.22303859784724978 ) ) ;
#27086 = CARTESIAN_POINT ( 'NONE',  ( -5.300408001487409315, -10.97335522853832579, 33.68706563782419749 ) ) ;
#27087 = CARTESIAN_POINT ( 'NONE',  ( -0.5276218724943422256, -12.37446782046654192, 30.86335684631486487 ) ) ;
#27088 = CARTESIAN_POINT ( 'NONE',  ( -2.749999999999999112, -7.438900925035484057, 21.59561829374151287 ) ) ;
#27089 = ORIENTED_EDGE ( 'NONE', *, *, #88469, .F. ) ;
#27090 = AXIS2_PLACEMENT_3D ( 'NONE', #81343, #48313, #7344 ) ;
#27091 = DIRECTION ( 'NONE',  ( -0.000000000000000000, 0.9848077530122086864, -0.1736481776669273891 ) ) ;
#27092 = DIRECTION ( 'NONE',  ( 1.000000000000000000, -0.000000000000000000, -0.000000000000000000 ) ) ;
#27093 = B_SPLINE_CURVE_WITH_KNOTS ( 'NONE', 3,
 ( #23544, #2821, #37958, #30314, #65426, #58661, #57783, #45149, #72625, #10933 ),
 .UNSPECIFIED., .F., .F.,
 ( 4, 2, 2, 2, 4 ),
 ( 0.0007817359430256318490, 0.0009771253907249984917, 0.001172514838424365026, 0.001367904286123731560, 0.001563293733823098094 ),
 .UNSPECIFIED. ) ;
#27094 = CARTESIAN_POINT ( 'NONE',  ( 9.915087361285756629, -10.97394488606064122, 33.68653795673694873 ) ) ;
#27095 = ORIENTED_EDGE ( 'NONE', *, *, #25243, .T. ) ;
#27096 = CARTESIAN_POINT ( 'NONE',  ( 2.177217122616589950, -7.276987145209184327, 34.99546412871779211 ) ) ;
#27097 = CARTESIAN_POINT ( 'NONE',  ( -3.099977422944443006, -5.582136614379148654, 34.36778462344220486 ) ) ;
#27098 = ADVANCED_FACE ( 'NONE', ( #32833 ), #53536, .F. ) ;
#27099 = CARTESIAN_POINT ( 'NONE',  ( -10.68065461594093435, -2.379036618887870436, 30.90682066428147934 ) ) ;
#27100 = DIRECTION ( 'NONE',  ( -0.000000000000000000, 0.9848077530122086864, -0.1736481776669273891 ) ) ;
#27101 = CARTESIAN_POINT ( 'NONE',  ( 1.384615384615386802, -6.343179335718451384, 34.87096338111211935 ) ) ;
#27102 = ORIENTED_EDGE ( 'NONE', *, *, #65168, .T. ) ;
#27103 = CARTESIAN_POINT ( 'NONE',  ( 17.01083966596719321, -3.050289026998445951, 32.03036669348365706 ) ) ;
#27104 = DIRECTION ( 'NONE',  ( 0.000000000000000000, 0.000000000000000000, 1.000000000000000000 ) ) ;
#27105 = CARTESIAN_POINT ( 'NONE',  ( 7.596130608860880429, -10.05641848906368097, 34.04755513067966177 ) ) ;
#27106 = ORIENTED_EDGE ( 'NONE', *, *, #82211, .T. ) ;
#27107 = DIRECTION ( 'NONE',  ( 1.000000000000000000, 0.000000000000000000, 0.000000000000000000 ) ) ;
#27108 = B_SPLINE_CURVE_WITH_KNOTS ( 'NONE', 3,
 ( #50440, #44116, #36502, #70730, #63954, #58085, #37818, #71595, #1819, #23410 ),
 .UNSPECIFIED., .F., .F.,
 ( 4, 2, 2, 2, 4 ),
 ( 0.000000000000000000, 0.0001954339857564054144, 0.0003908679715128108288, 0.0005863019572692162703, 0.0007817359430256216575 ),
 .UNSPECIFIED. ) ;
#27109 = EDGE_CURVE ( 'NONE', #27279, #80982, #85969, .T. ) ;
#27110 = ORIENTED_EDGE ( 'NONE', *, *, #76555, .T. ) ;
#27111 = AXIS2_PLACEMENT_3D ( 'NONE', #38716, #58089, #66176 ) ;
#27112 = CARTESIAN_POINT ( 'NONE',  ( -16.40382288478850725, -5.728515186090277211, 34.42611988154120439 ) ) ;
#27113 = CARTESIAN_POINT ( 'NONE',  ( -5.933932666649922361, -11.91647553114624358, 32.58852847137148245 ) ) ;
#27114 = EDGE_LOOP ( 'NONE', ( #7747, #83113 ) ) ;
#27115 = EDGE_CURVE ( 'NONE', #42284, #22567, #54876, .T. ) ;
#27116 = CARTESIAN_POINT ( 'NONE',  ( 0.4615384615384611200, -11.11383981884818262, 36.00935417666054406 ) ) ;
#27117 = DIRECTION ( 'NONE',  ( -0.000000000000000000, 1.000000000000000000, 3.491481338843133355E-15 ) ) ;
#27118 = CARTESIAN_POINT ( 'NONE',  ( -6.673131513698879580, -12.45601412856602863, 31.48342859153981621 ) ) ;
#27119 = AXIS2_PLACEMENT_3D ( 'NONE', #80978, #32335, #12074 ) ;
#27120 = AXIS2_PLACEMENT_3D ( 'NONE', #16002, #14669, #43466 ) ;
#27121 = CARTESIAN_POINT ( 'NONE',  ( 15.23076923076911093, -3.835265460704628371, 33.15142922262033665 ) ) ;
#27122 = CARTESIAN_POINT ( 'NONE',  ( -2.176901866725355905, -10.70102852606553157, 33.91149625220312913 ) ) ;
#27123 = AXIS2_PLACEMENT_3D ( 'NONE', #81303, #39436, #67779 ) ;
#27124 = EDGE_LOOP ( 'NONE', ( #56987, #73619, #42729, #46409 ) ) ;
#27125 = B_SPLINE_CURVE_WITH_KNOTS ( 'NONE', 3,
 ( #11910, #39824, #11013, #59190, #12786, #86241, #67293, #4249, #25860, #18668 ),
 .UNSPECIFIED., .F., .F.,
 ( 4, 2, 2, 2, 4 ),
 ( 0.000000000000000000, 0.0001954311564186862781, 0.0003908623128373725562, 0.0005862934692560588072, 0.0007817246256747451124 ),
 .UNSPECIFIED. ) ;
#27126 = EDGE_CURVE ( 'NONE', #26386, #72566, #54877, .T. ) ;
#27127 = FACE_BOUND ( 'NONE', #66656, .T. ) ;
#27128 = EDGE_LOOP ( 'NONE', ( #83722, #60807, #51211, #21551 ) ) ;
#27129 = CARTESIAN_POINT ( 'NONE',  ( -17.78205128205128105, -7.500000000000000000, 33.75000000000000000 ) ) ;
#27130 = ADVANCED_FACE ( 'NONE', ( #77797 ), #76480, .F. ) ;
#27131 = CARTESIAN_POINT ( 'NONE',  ( 18.13052543823364360, -6.808710257144159783, 34.95449254468098843 ) ) ;
#27132 = CARTESIAN_POINT ( 'NONE',  ( 6.223012844093395834, -5.582272713120727481, 34.63742843783360570 ) ) ;
#27133 = CARTESIAN_POINT ( 'NONE',  ( -6.000000000000119904, -12.27809138561165270, 31.22303859784587132 ) ) ;
#27134 = VERTEX_POINT ( 'NONE', #78237 ) ;
#27135 = VERTEX_POINT ( 'NONE', #41815 ) ;
#27136 = ORIENTED_EDGE ( 'NONE', *, *, #29298, .T. ) ;
#27137 = VERTEX_POINT ( 'NONE', #70604 ) ;
#27138 = EDGE_CURVE ( 'NONE', #55802, #79573, #28741, .T. ) ;
#27139 = CARTESIAN_POINT ( 'NONE',  ( -4.854143535654666941, -5.114059244376869984, 34.14424750095245287 ) ) ;
#27140 = EDGE_CURVE ( 'NONE', #59157, #53967, #64271, .T. ) ;
#27141 = AXIS2_PLACEMENT_3D ( 'NONE', #8353, #35827, #22303 ) ;
#27142 = CARTESIAN_POINT ( 'NONE',  ( -15.23076923076935074, -10.90142922262034020, 33.41473453929536674 ) ) ;
#27143 = CARTESIAN_POINT ( 'NONE',  ( -1.384615384615505151, -10.90142922262034020, 33.41473453929536674 ) ) ;
#27144 = CARTESIAN_POINT ( 'NONE',  ( 17.93391658904412012, -9.780366693483667717, 34.19971097300155805 ) ) ;
#27145 = EDGE_CURVE ( 'NONE', #25133, #24082, #3334, .T. ) ;
#27146 = CARTESIAN_POINT ( 'NONE',  ( -0.6844646790546091708, -11.76352882383564769, 32.36236540154569497 ) ) ;
#27147 = EDGE_CURVE ( 'NONE', #22218, #5644, #36812, .T. ) ;
#27148 = DIRECTION ( 'NONE',  ( 0.000000000000000000, 0.6427876096865368094, 0.7660444431189802339 ) ) ;
#27149 = CARTESIAN_POINT ( 'NONE',  ( 11.40777007179398339, -9.804603061927743113, 34.18744698557895845 ) ) ;
#27150 = ORIENTED_EDGE ( 'NONE', *, *, #77421, .F. ) ;
#27151 = ORIENTED_EDGE ( 'NONE', *, *, #42999, .F. ) ;
#27152 = B_SPLINE_CURVE_WITH_KNOTS ( 'NONE', 3,
 ( #63928, #77893, #16196, #44534, #43661, #71132, #37340, #3113, #85543, #30587 ),
 .UNSPECIFIED., .F., .F.,
 ( 4, 2, 2, 2, 4 ),
 ( 0.0007817359430256400890, 0.0009771253907250091169, 0.001172514838424378253, 0.001367904286123747173, 0.001563293733823116309 ),
 .UNSPECIFIED. ) ;
#27153 = ORIENTED_EDGE ( 'NONE', *, *, #52963, .T. ) ;
#27154 = CARTESIAN_POINT ( 'NONE',  ( -13.51476335434708709, -12.50552854090298993, 31.33409797877408920 ) ) ;
#27156 = CARTESIAN_POINT ( 'NONE',  ( -9.757577692864012775, -4.320704448112771878, 33.92786785259540494 ) ) ;
#27155 = LINE ( 'NONE', #74911, #43243 ) ;
#27157 = PLANE ( 'NONE',  #39888 ) ;
#27158 = DIRECTION ( 'NONE',  ( 0.000000000000000000, -8.673617379884028076E-17, -1.000000000000000000 ) ) ;
#27159 = FACE_BOUND ( 'NONE', #28850, .T. ) ;
#27160 = ORIENTED_EDGE ( 'NONE', *, *, #81336, .T. ) ;
#27161 = DIRECTION ( 'NONE',  ( 1.000000000000000000, 0.000000000000000000, 0.000000000000000000 ) ) ;
#27162 = DIRECTION ( 'NONE',  ( 0.000000000000000000, 0.1736481776669275834, 0.9848077530122086864 ) ) ;
#27163 = CARTESIAN_POINT ( 'NONE',  ( 2.980745993476265898, -10.76384336483936011, 33.53834819971076087 ) ) ;
#27164 = VERTEX_POINT ( 'NONE', #28282 ) ;
#27165 = LINE ( 'NONE', #53300, #34186 ) ;
#27166 = ORIENTED_EDGE ( 'NONE', *, *, #57836, .T. ) ;
#27167 = FACE_BOUND ( 'NONE', #2100, .T. ) ;
#27168 = CARTESIAN_POINT ( 'NONE',  ( 9.442284455014730682, -5.851115903089112003, 34.47074536777953568 ) ) ;
#27169 = VECTOR ( 'NONE', #18722, 1000.000000000000000 ) ;
#27170 = ORIENTED_EDGE ( 'NONE', *, *, #52473, .F. ) ;
#27171 = LINE ( 'NONE', #27615, #325 ) ;
#27172 = DIRECTION ( 'NONE',  ( 1.000000000000000000, 0.000000000000000000, 0.000000000000000000 ) ) ;
#27173 = CARTESIAN_POINT ( 'NONE',  ( 1.318531973659506029, -3.050289026998445951, 32.03036669348365706 ) ) ;
#27174 = EDGE_LOOP ( 'NONE', ( #14735, #53305, #20432, #75422 ) ) ;
#27175 = CARTESIAN_POINT ( 'NONE',  ( -2.307692307692305711, -2.249999999999998668, 29.75000000000001776 ) ) ;
#27176 = CARTESIAN_POINT ( 'NONE',  ( -7.623374177175779032, -8.540255544307065350, 34.89611431652622286 ) ) ;
#27177 = CARTESIAN_POINT ( 'NONE',  ( 12.52679403281448600, -6.879047030191282275, 34.71129190930002295 ) ) ;
#27178 = CARTESIAN_POINT ( 'NONE',  ( 2.557637717070351702, -2.986452184633681117, 32.43230066228895225 ) ) ;
#27179 = ORIENTED_EDGE ( 'NONE', *, *, #2428, .T. ) ;
#27180 = VECTOR ( 'NONE', #5872, 1000.000000000000000 ) ;
#27181 = CARTESIAN_POINT ( 'NONE',  ( -5.076923076923075762, -4.661471528628507777, 34.16647553114623292 ) ) ;
#27182 = CARTESIAN_POINT ( 'NONE',  ( -15.29685264172511161, -4.098570777380719399, 33.41473453929634729 ) ) ;
#27183 = VECTOR ( 'NONE', #46358, 1000.000000000000114 ) ;
#27185 = ORIENTED_EDGE ( 'NONE', *, *, #61436, .T. ) ;
#27184 = CARTESIAN_POINT ( 'NONE',  ( -8.769230769230890843, -3.835265460704628371, 33.15142922262033665 ) ) ;
#27186 = CARTESIAN_POINT ( 'NONE',  ( 2.438217745925953750, -10.31582465632705237, 34.18122507451815295 ) ) ;
#27187 = CARTESIAN_POINT ( 'NONE',  ( 16.15384615384603251, -4.320704448113951379, 33.92786785259630022 ) ) ;
#27188 = CARTESIAN_POINT ( 'NONE',  ( -13.31854703361294590, -4.786620604624113540, 33.94971097300155805 ) ) ;
#27189 = CARTESIAN_POINT ( 'NONE',  ( -5.076923076923075762, -2.249999999999998668, 29.75000000000001776 ) ) ;
#27190 = CARTESIAN_POINT ( 'NONE',  ( 3.230769230769108269, -12.51329471203414379, 31.30864560766407578 ) ) ;
#27191 = EDGE_CURVE ( 'NONE', #80196, #66304, #26969, .T. ) ;
#27192 = CARTESIAN_POINT ( 'NONE',  ( 16.94677510719138169, -5.070767119584671079, 34.40440758774516183 ) ) ;
#27194 = CARTESIAN_POINT ( 'NONE',  ( 3.230769230769108269, -11.06231777344772027, 33.60647404775119895 ) ) ;
#27193 = CARTESIAN_POINT ( 'NONE',  ( 0.6843181305165255690, -11.60474049983370648, 33.02348890104160262 ) ) ;
#27195 = VECTOR ( 'NONE', #66944, 999.9999999999998863 ) ;
#27196 = CARTESIAN_POINT ( 'NONE',  ( -6.700065571464075553, -2.758310577978207778, 31.33698337089303010 ) ) ;
#27197 = CARTESIAN_POINT ( 'NONE',  ( -1.139087296526025916, -4.750000000000006217, 17.82812500000000000 ) ) ;
#27198 = ORIENTED_EDGE ( 'NONE', *, *, #80206, .F. ) ;
#27199 = LINE ( 'NONE', #7819, #27536 ) ;
#27200 = EDGE_LOOP ( 'NONE', ( #60517, #60498 ) ) ;
#27201 = B_SPLINE_CURVE_WITH_KNOTS ( 'NONE', 3,
 ( #71134, #64367, #57625, #16633, #50843, #86455, #31940, #85107, #17535, #23388 ),
 .UNSPECIFIED., .F., .F.,
 ( 4, 2, 2, 2, 4 ),
 ( 0.000000000000000000, 0.0001954339857564076912, 0.0003908679715128153824, 0.0005863019572692231007, 0.0007817359430256307648 ),
 .UNSPECIFIED. ) ;
#27202 = VERTEX_POINT ( 'NONE', #83239 ) ;
#27203 = CARTESIAN_POINT ( 'NONE',  ( -11.31544869436814338, -2.308499170217967134, 30.53291367094873721 ) ) ;
#27204 = ORIENTED_EDGE ( 'NONE', *, *, #9072, .T. ) ;
#27205 = CARTESIAN_POINT ( 'NONE',  ( 1.450682717965462665, -11.91647553114624358, 32.58852847137148245 ) ) ;
#27206 = CARTESIAN_POINT ( 'NONE',  ( -2.750000000000007105, -6.360912703474006946, 20.17187500000000000 ) ) ;
#27207 = CARTESIAN_POINT ( 'NONE',  ( 13.60762673622823371, -2.758310577978208666, 31.33698337089302299 ) ) ;
#27208 = CARTESIAN_POINT ( 'NONE',  ( -7.846153846153844924, -8.164416787775445883, 34.95778746994557906 ) ) ;
#27209 = CARTESIAN_POINT ( 'NONE',  ( 7.715593932540479649, -2.254533558242299396, 29.97296025877827930 ) ) ;
#27210 = EDGE_CURVE ( 'NONE', #30445, #83962, #31256, .T. ) ;
#27211 = DIRECTION ( 'NONE',  ( -0.000000000000000000, 0.6427876096865404731, -0.7660444431189770143 ) ) ;
#27212 = CARTESIAN_POINT ( 'NONE',  ( -4.153846153846152411, -1.790695186598648903, 34.54067556320373455 ) ) ;
#27213 = CARTESIAN_POINT ( 'NONE',  ( 2.242421861731533017, -10.21337939537584383, 33.94971097300158647 ) ) ;
#27214 = DIRECTION ( 'NONE',  ( -0.000000000000000000, 0.1736481776669307198, -0.9848077530122080203 ) ) ;
#27215 = CARTESIAN_POINT ( 'NONE',  ( -20.00000000000000000, -7.500000000000000000, 33.75000000000000000 ) ) ;
#27216 = CARTESIAN_POINT ( 'NONE',  ( -17.07692307692319744, -11.06231777344772027, 33.60647404775119895 ) ) ;
#27217 = CARTESIAN_POINT ( 'NONE',  ( 14.55769230769231015, -2.499999999999998668, 29.75000000000000355 ) ) ;
#27218 = VECTOR ( 'NONE', #40119, 1000.000000000000000 ) ;
#27220 = VERTEX_POINT ( 'NONE', #35490 ) ;
#27219 = EDGE_CURVE ( 'NONE', #47929, #33434, #21529, .T. ) ;
#27221 = VERTEX_POINT ( 'NONE', #56205 ) ;
#27222 = CARTESIAN_POINT ( 'NONE',  ( -14.98082371242109012, -8.433404298154334455, 34.66254593164985920 ) ) ;
#27223 = CYLINDRICAL_SURFACE ( 'NONE', #76222, 0.2499999999999994726 ) ;
#27224 = CARTESIAN_POINT ( 'NONE',  ( -6.857009589726848375, -11.91647553114624358, 32.58852847137148245 ) ) ;
#27225 = CARTESIAN_POINT ( 'NONE',  ( 9.692307692307570832, -12.16647553114689728, 32.15551576947799362 ) ) ;
#27226 = ADVANCED_FACE ( 'NONE', ( #21978 ), #49449, .F. ) ;
#27227 = DIRECTION ( 'NONE',  ( 0.000000000000000000, 0.8660254037844377084, 0.5000000000000015543 ) ) ;
#27228 = CARTESIAN_POINT ( 'NONE',  ( 11.66925197942849302, -3.957578996910242619, 33.62503395064540257 ) ) ;
#27229 = DIRECTION ( 'NONE',  ( -0.000000000000000000, 0.6427876096865404731, -0.7660444431189771253 ) ) ;
#27230 = ORIENTED_EDGE ( 'NONE', *, *, #23642, .F. ) ;
#27231 = ADVANCED_FACE ( 'NONE', ( #52977 ), #42028, .T. ) ;
#27232 = CARTESIAN_POINT ( 'NONE',  ( 16.08776274289027342, -2.721908614388770964, 31.22303859784723912 ) ) ;
#27233 = ORIENTED_EDGE ( 'NONE', *, *, #66581, .T. ) ;
#27234 = CARTESIAN_POINT ( 'NONE',  ( -14.55769230769230838, -7.433931650972299465, 34.75000000000000711 ) ) ;
#27235 = VECTOR ( 'NONE', #33078, 1000.000000000000000 ) ;
#27236 = DIRECTION ( 'NONE',  ( -0.000000000000000000, 0.9396926207859092051, -0.3420201433256662704 ) ) ;
#27237 = CARTESIAN_POINT ( 'NONE',  ( -4.284537620513710010, -4.118384482072085184, 33.43331474514187107 ) ) ;
#27238 = CARTESIAN_POINT ( 'NONE',  ( 3.007284306204900837, -8.539481045369598178, 34.89627647299170832 ) ) ;
#27239 = CARTESIAN_POINT ( 'NONE',  ( -7.846153846153844924, -6.681629849574314051, 35.83090037661290239 ) ) ;
#27240 = AXIS2_PLACEMENT_3D ( 'NONE', #47232, #74724, #19771 ) ;
#27241 = VECTOR ( 'NONE', #8540, 1000.000000000000000 ) ;
#27242 = ORIENTED_EDGE ( 'NONE', *, *, #10777, .T. ) ;
#27243 = AXIS2_PLACEMENT_3D ( 'NONE', #76728, #70418, #8721 ) ;
#27244 = ORIENTED_EDGE ( 'NONE', *, *, #86033, .F. ) ;
#27245 = VERTEX_POINT ( 'NONE', #25522 ) ;
#27246 = ORIENTED_EDGE ( 'NONE', *, *, #86706, .F. ) ;
#27247 = ADVANCED_FACE ( 'NONE', ( #51183 ), #16985, .F. ) ;
#27248 = CYLINDRICAL_SURFACE ( 'NONE', #74640, 0.2499999999999979738 ) ;
#27249 = CARTESIAN_POINT ( 'NONE',  ( -16.15384615384615330, -9.058645607665452459, 34.76329471203371924 ) ) ;
#27250 = CARTESIAN_POINT ( 'NONE',  ( -3.454254174493178731, -10.11188796281391511, 34.01382737946119050 ) ) ;
#27251 = EDGE_CURVE ( 'NONE', #2835, #4865, #65161, .T. ) ;
#27252 = CARTESIAN_POINT ( 'NONE',  ( -15.23076923076935074, -11.48612834414049644, 32.76840700105863391 ) ) ;
#27253 = CARTESIAN_POINT ( 'NONE',  ( -7.384615384615385025, -3.499999999999999556, 29.75000000000000355 ) ) ;
#27254 = ADVANCED_FACE ( 'NONE', ( #30497 ), #10677, .F. ) ;
#27255 = CARTESIAN_POINT ( 'NONE',  ( 2.307692307692309264, -1.129524287112498415, 32.06866353760679544 ) ) ;
#27256 = EDGE_LOOP ( 'NONE', ( #14733, #24698, #78190, #49207 ) ) ;
#27257 = VERTEX_POINT ( 'NONE', #58396 ) ;
#27258 = ORIENTED_EDGE ( 'NONE', *, *, #8581, .T. ) ;
#27260 = VERTEX_POINT ( 'NONE', #66509 ) ;
#27259 = CARTESIAN_POINT ( 'NONE',  ( 11.40831432902331954, -9.418419913701741919, 34.36755862841477693 ) ) ;
#27261 = CARTESIAN_POINT ( 'NONE',  ( 17.14217821643591932, -11.06231777344670952, 33.60647404775212266 ) ) ;
#27262 = CARTESIAN_POINT ( 'NONE',  ( -2.177166605928742005, -9.417988943895561960, 34.36773134775778260 ) ) ;
#27263 = CARTESIAN_POINT ( 'NONE',  ( -3.749999999999988454, -9.053300858899127945, 22.51562500000000000 ) ) ;
#27264 = EDGE_LOOP ( 'NONE', ( #64888, #8714, #34499, #78342 ) ) ;
#27265 = EDGE_CURVE ( 'NONE', #7759, #62397, #18348, .T. ) ;
#27266 = CARTESIAN_POINT ( 'NONE',  ( -1.318548051265308274, -2.486705287966280320, 31.30864560766543647 ) ) ;
#27267 = AXIS2_PLACEMENT_3D ( 'NONE', #62498, #35039, #38034 ) ;
#27268 = ORIENTED_EDGE ( 'NONE', *, *, #71332, .F. ) ;
#27269 = CARTESIAN_POINT ( 'NONE',  ( 7.912222197156284054, -12.10708131394839349, 31.69288490824020244 ) ) ;
#27270 = FACE_BOUND ( 'NONE', #60098, .T. ) ;
#27271 = CARTESIAN_POINT ( 'NONE',  ( -2.307692307692428724, -5.094484230521993062, 34.41647553114689373 ) ) ;
#27272 = CARTESIAN_POINT ( 'NONE',  ( -14.30769230769199929, -2.506253911140614576, 30.00000000000323297 ) ) ;
#27273 = ORIENTED_EDGE ( 'NONE', *, *, #16557, .T. ) ;
#27274 = EDGE_CURVE ( 'NONE', #43614, #87443, #17219, .T. ) ;
#27275 = CARTESIAN_POINT ( 'NONE',  ( 8.703148389870630552, -11.91647553114624181, 32.58852847137148245 ) ) ;
#27276 = CARTESIAN_POINT ( 'NONE',  ( 6.856994543716788293, -11.91647553114624181, 32.58852847137148245 ) ) ;
#27277 = CARTESIAN_POINT ( 'NONE',  ( 16.28437159207980045, -6.808710257144159783, 34.95449254468098843 ) ) ;
#27278 = CARTESIAN_POINT ( 'NONE',  ( 15.29602437028206907, -6.835583212224610072, 34.95778746994559327 ) ) ;
#27279 = VERTEX_POINT ( 'NONE', #24628 ) ;
#27280 = B_SPLINE_CURVE_WITH_KNOTS ( 'NONE', 3,
 ( #3267, #44687, #10485, #70861, #29871, #36627, #30739, #72170, #28997, #1513 ),
 .UNSPECIFIED., .F., .F.,
 ( 4, 2, 2, 2, 4 ),
 ( 0.0007817246256747517261, 0.0009771112852218961399, 0.001172497944769040771, 0.001367884604316185401, 0.001563271263863329815 ),
 .UNSPECIFIED. ) ;
#27281 = CARTESIAN_POINT ( 'NONE',  ( 15.93101946136715341, -7.369208160676171460, 34.74850200257122879 ) ) ;
#27282 = CARTESIAN_POINT ( 'NONE',  ( 1.134638640566794310, -4.075325502946085976, 33.72974371597207721 ) ) ;
#27283 = CARTESIAN_POINT ( 'NONE',  ( 11.53846153846141753, -6.026961402154118019, 34.52809138561165270 ) ) ;
#27284 = DIRECTION ( 'NONE',  ( -0.000000000000000000, 0.7660444431189791237, -0.6427876096865379196 ) ) ;
#27285 = DIRECTION ( 'NONE',  ( 0.000000000000000000, 0.9848077530122072432, -0.1736481776669354937 ) ) ;
#27286 = EDGE_CURVE ( 'NONE', #85898, #66653, #50556, .T. ) ;
#27287 = FACE_BOUND ( 'NONE', #59559, .T. ) ;
#27289 = CARTESIAN_POINT ( 'NONE',  ( 16.85399611801622299, -2.889293201056495786, 32.26117774369186009 ) ) ;
#27288 = CARTESIAN_POINT ( 'NONE',  ( 13.25392478150508246, -11.93127051446799847, 32.56575433478202797 ) ) ;
#27290 = B_SPLINE_CURVE_WITH_KNOTS ( 'NONE', 3,
 ( #15108, #70489, #8351, #57408, #83123, #35825, #21414, #14662, #29510, #56963 ),
 .UNSPECIFIED., .F., .F.,
 ( 4, 2, 2, 2, 4 ),
 ( 0.0007817359430256293554, 0.0009771253907249952391, 0.001172514838424361123, 0.001367904286123726790, 0.001563293733823092673 ),
 .UNSPECIFIED. ) ;
#27291 = AXIS2_PLACEMENT_3D ( 'NONE', #80254, #46011, #33830 ) ;
#27292 = CARTESIAN_POINT ( 'NONE',  ( 11.78851595837499211, -12.01375889529407281, 32.43194544308182969 ) ) ;
#27294 = CARTESIAN_POINT ( 'NONE',  ( 17.99999999999987566, -2.892918686052165622, 31.69288490824153470 ) ) ;
#27293 = DIRECTION ( 'NONE',  ( 0.000000000000000000, 0.000000000000000000, -1.000000000000000000 ) ) ;
#27295 = CARTESIAN_POINT ( 'NONE',  ( -8.069080805060693251, -4.026226216239094491, 33.68668979543634379 ) ) ;
#27296 = CARTESIAN_POINT ( 'NONE',  ( -2.775308065498764964, -6.422011778438537988, 18.67000670625849068 ) ) ;
#27298 = ADVANCED_FACE ( 'NONE', ( #64716 ), #11117, .T. ) ;
#27297 = ORIENTED_EDGE ( 'NONE', *, *, #41392, .F. ) ;
#27299 = CARTESIAN_POINT ( 'NONE',  ( -8.546267865669285868, -7.369474270740069777, 34.74850911626239736 ) ) ;
#27300 = EDGE_LOOP ( 'NONE', ( #67401, #30563 ) ) ;
#27301 = VECTOR ( 'NONE', #3898, 1000.000000000000000 ) ;
#27302 = DIRECTION ( 'NONE',  ( -0.000000000000000000, 1.000000000000000000, -0.000000000000000000 ) ) ;
#27303 = ORIENTED_EDGE ( 'NONE', *, *, #19636, .F. ) ;
#27304 = CARTESIAN_POINT ( 'NONE',  ( -11.47239420511146513, -6.343179335718452272, 34.87096338111212646 ) ) ;
#27305 = CARTESIAN_POINT ( 'NONE',  ( -16.02305571287920571, -11.93129842949672437, 32.56571108434900452 ) ) ;
#27307 = ORIENTED_EDGE ( 'NONE', *, *, #74425, .F. ) ;
#27306 = LINE ( 'NONE', #44230, #15105 ) ;
#27308 = CYLINDRICAL_SURFACE ( 'NONE', #41229, 0.2500000000000008882 ) ;
#27309 = CARTESIAN_POINT ( 'NONE',  ( 1.987747218494664292, -9.401340078031346081, 18.12313170625849068 ) ) ;
#27310 = AXIS2_PLACEMENT_3D ( 'NONE', #25100, #12920, #66985 ) ;
#27311 = CARTESIAN_POINT ( 'NONE',  ( -15.48074597481782178, -9.234221910056348293, 34.70572697212741531 ) ) ;
#27312 = LINE ( 'NONE', #46693, #10095 ) ;
#27313 = EDGE_CURVE ( 'NONE', #18683, #28039, #34451, .T. ) ;
#27314 = CARTESIAN_POINT ( 'NONE',  ( 17.07692307692307665, -12.37446782046654192, 30.86335684631486131 ) ) ;
#27315 = CARTESIAN_POINT ( 'NONE',  ( 4.023154687178596589, -11.71456829005830080, 32.44064028649416542 ) ) ;
#27316 = CARTESIAN_POINT ( 'NONE',  ( -0.3962828902624369598, -4.481592998940250538, 33.73612834413965089 ) ) ;
#27317 = CARTESIAN_POINT ( 'NONE',  ( 11.78840705680968171, -3.712312575010499494, 33.01462480002815170 ) ) ;
#27318 = STYLED_ITEM ( 'NONE', ( #72632 ), #37432 ) ;
#27319 = CARTESIAN_POINT ( 'NONE',  ( 3.750000000000001776, -7.561099074964511502, 22.22061829374151287 ) ) ;
#27320 = CARTESIAN_POINT ( 'NONE',  ( 13.13463864056679498, -6.524016743844655686, 34.90889640711025521 ) ) ;
#27321 = CARTESIAN_POINT ( 'NONE',  ( -4.153846153846152411, -2.833524468853757305, 32.15551576947925838 ) ) ;
#27322 = EDGE_CURVE ( 'NONE', #43247, #67219, #78471, .T. ) ;
#27323 = ORIENTED_EDGE ( 'NONE', *, *, #5689, .F. ) ;
#27324 = FACE_OUTER_BOUND ( 'NONE', #56314, .T. ) ;
#27325 = CARTESIAN_POINT ( 'NONE',  ( -1.553300858899125059, -3.750000000000009326, 14.07812500000000178 ) ) ;
#27326 = CARTESIAN_POINT ( 'NONE',  ( -14.98076923076922995, -2.249999999999998668, 29.75000000000000355 ) ) ;
#27327 = LINE ( 'NONE', #33643, #78589 ) ;
#27328 = ORIENTED_EDGE ( 'NONE', *, *, #82885, .F. ) ;
#27329 = CARTESIAN_POINT ( 'NONE',  ( 7.145856464345331283, -8.496831190052096971, 34.64984203495476578 ) ) ;
#27330 = CARTESIAN_POINT ( 'NONE',  ( 16.28463659481310799, -2.494656445102014342, 31.33466734024120015 ) ) ;
#27332 = ORIENTED_EDGE ( 'NONE', *, *, #29946, .T. ) ;
#27331 = FACE_OUTER_BOUND ( 'NONE', #53333, .T. ) ;
#27333 = CARTESIAN_POINT ( 'NONE',  ( -3.230769230769229949, -1.215029322943914858, 32.30358669280327177 ) ) ;
#27334 = EDGE_CURVE ( 'NONE', #19556, #37056, #82246, .T. ) ;
#27335 = CARTESIAN_POINT ( 'NONE',  ( 15.48082365068267841, -5.642605341092957971, 34.66089969410670335 ) ) ;
#27336 = CARTESIAN_POINT ( 'NONE',  ( 15.90382291655318880, -9.271318131107980420, 34.42618302367067429 ) ) ;
#27337 = EDGE_CURVE ( 'NONE', #45031, #79887, #73057, .T. ) ;
#27338 = CARTESIAN_POINT ( 'NONE',  ( 4.946775867484856093, -4.460286881179643004, 33.72017969459903242 ) ) ;
#27339 = B_SPLINE_CURVE_WITH_KNOTS ( 'NONE', 3,
 ( #5922, #32951, #27519, #87930, #68071, #73943, #27074, #33398, #74379, #41478 ),
 .UNSPECIFIED., .F., .F.,
 ( 4, 2, 2, 2, 4 ),
 ( 0.0007817246256747461966, 0.0009771112852218892010, 0.001172497944769032314, 0.001367884604316175427, 0.001563271263863318323 ),
 .UNSPECIFIED. ) ;
#27340 = CARTESIAN_POINT ( 'NONE',  ( 12.46153846153846168, -8.564572088678739092, 35.78748833219616898 ) ) ;
#27341 = VERTEX_POINT ( 'NONE', #41259 ) ;
#27342 = VERTEX_POINT ( 'NONE', #60182 ) ;
#27343 = ORIENTED_EDGE ( 'NONE', *, *, #21347, .F. ) ;
#27344 = AXIS2_PLACEMENT_3D ( 'NONE', #26636, #47341, #14003 ) ;
#27345 = EDGE_LOOP ( 'NONE', ( #46820, #25236 ) ) ;
#27346 = CARTESIAN_POINT ( 'NONE',  ( 0.4615384615384611200, -3.937682226553329556, 33.60647404775216529 ) ) ;
#27347 = CARTESIAN_POINT ( 'NONE',  ( 0.4615384615384611200, -2.538708090699994813, 30.37095296980875503 ) ) ;
#27348 = LINE ( 'NONE', #35427, #37867 ) ;
#27349 = DIRECTION ( 'NONE',  ( -0.000000000000000000, 0.8660254037844399289, -0.4999999999999980016 ) ) ;
#27350 = CARTESIAN_POINT ( 'NONE',  ( -16.85391172531022619, -4.887748414852789658, 34.01359900205216746 ) ) ;
#27351 = ORIENTED_EDGE ( 'NONE', *, *, #45934, .F. ) ;
#27352 = ORIENTED_EDGE ( 'NONE', *, *, #77302, .F. ) ;
#27353 = ORIENTED_EDGE ( 'NONE', *, *, #73458, .T. ) ;
#27355 = ORIENTED_EDGE ( 'NONE', *, *, #8452, .T. ) ;
#27354 = CARTESIAN_POINT ( 'NONE',  ( 5.999999999999878320, -11.67786785259630911, 32.92929555188603530 ) ) ;
#27356 = CARTESIAN_POINT ( 'NONE',  ( -1.449885385171703955, -3.083524468853724443, 32.58852847137143272 ) ) ;
#27357 = DIRECTION ( 'NONE',  ( 0.000000000000000000, 0.000000000000000000, 1.000000000000000000 ) ) ;
#27358 = EDGE_CURVE ( 'NONE', #42649, #13706, #80563, .T. ) ;
#27359 = B_SPLINE_CURVE_WITH_KNOTS ( 'NONE', 3,
 ( #55804, #34656, #81974, #55362, #68436, #81524, #21577, #7633, #6733, #62552 ),
 .UNSPECIFIED., .F., .F.,
 ( 4, 2, 2, 2, 4 ),
 ( 0.0007817246256747451124, 0.0009771112852218879000, 0.001172497944769030796, 0.001367884604316173692, 0.001563271263863316588 ),
 .UNSPECIFIED. ) ;
#27360 = VECTOR ( 'NONE', #14685, 1000.000000000000000 ) ;
#27361 = VECTOR ( 'NONE', #15972, 1000.000000000000114 ) ;
#27362 = CARTESIAN_POINT ( 'NONE',  ( 5.777073041093149897, -4.026226216239095379, 33.68668979543632958 ) ) ;
#27363 = CYLINDRICAL_SURFACE ( 'NONE', #6533, 0.2500000000000009437 ) ;
#27364 = ADVANCED_FACE ( 'NONE', ( #19212 ), #47109, .F. ) ;
#27365 = VERTEX_POINT ( 'NONE', #5688 ) ;
#27366 = AXIS2_PLACEMENT_3D ( 'NONE', #26651, #54552, #12249 ) ;
#27367 = ORIENTED_EDGE ( 'NONE', *, *, #3043, .F. ) ;
#27368 = AXIS2_PLACEMENT_3D ( 'NONE', #61046, #26825, #34898 ) ;
#27369 = VERTEX_POINT ( 'NONE', #54311 ) ;
#27370 = CARTESIAN_POINT ( 'NONE',  ( 0.4615384615384611200, -3.050289026998446396, 32.03036669348365706 ) ) ;
#27372 = VERTEX_POINT ( 'NONE', #27294 ) ;
#27371 = FACE_OUTER_BOUND ( 'NONE', #45525, .T. ) ;
#27373 = EDGE_CURVE ( 'NONE', #62668, #70987, #22474, .T. ) ;
#27374 = LINE ( 'NONE', #41329, #73337 ) ;
#27375 = B_SPLINE_CURVE_WITH_KNOTS ( 'NONE', 3,
 ( #74957, #51420, #58202, #78923, #16342, #10020, #37487, #49682, #56445, #84821 ),
 .UNSPECIFIED., .F., .F.,
 ( 4, 2, 2, 2, 4 ),
 ( 0.0007817359430256369448, 0.0009771253907250049969, 0.001172514838424373049, 0.001367904286123741101, 0.001563293733823109153 ),
 .UNSPECIFIED. ) ;
#27376 = CARTESIAN_POINT ( 'NONE',  ( -0.7115152055870529457, -6.524016743844655686, 34.90889640711025521 ) ) ;
#27377 = VERTEX_POINT ( 'NONE', #34049 ) ;
#27378 = CARTESIAN_POINT ( 'NONE',  ( -17.75005448165186195, -2.587454068350149239, 30.68340429815432557 ) ) ;
#27379 = EDGE_CURVE ( 'NONE', #14228, #58130, #21361, .T. ) ;
#27380 = CARTESIAN_POINT ( 'NONE',  ( 4.376857505459001096, -2.758310577978207778, 31.33698337089303010 ) ) ;
#27381 = EDGE_LOOP ( 'NONE', ( #41222, #55946, #3251, #12195 ) ) ;
#27382 = FACE_BOUND ( 'NONE', #10053, .T. ) ;
#27383 = CARTESIAN_POINT ( 'NONE',  ( 6.923076923076924238, -12.78798330534103123, 29.99999999999997868 ) ) ;
#27384 = CARTESIAN_POINT ( 'NONE',  ( 13.45068271796546178, -6.343179335718452272, 34.87096338111212646 ) ) ;
#27385 = CARTESIAN_POINT ( 'NONE',  ( 3.453548772037640546, -9.332535724633405749, 34.40230450496446224 ) ) ;
#27387 = CARTESIAN_POINT ( 'NONE',  ( 5.076923076922954969, -10.21337939537710326, 33.94971097300076224 ) ) ;
#27386 = CARTESIAN_POINT ( 'NONE',  ( 0.3313904918067649974, -6.809168938359898782, 34.95455904226513866 ) ) ;
#27388 = CARTESIAN_POINT ( 'NONE',  ( -3.230769230769352962, -3.643525952248796163, 33.31231777344771672 ) ) ;
#27389 = LINE ( 'NONE', #26950, #56286 ) ;
#27390 = EDGE_LOOP ( 'NONE', ( #12669, #29256 ) ) ;
#27391 = CARTESIAN_POINT ( 'NONE',  ( -18.13069146666756382, -10.54014554554151140, 33.71984207302941883 ) ) ;
#27392 = CARTESIAN_POINT ( 'NONE',  ( 0.2115152373170027800, -10.92453946501458439, 33.72985991061850086 ) ) ;
#27393 = EDGE_LOOP ( 'NONE', ( #54171, #4394, #326, #27061 ) ) ;
#27394 = DIRECTION ( 'NONE',  ( 0.000000000000000000, 0.000000000000000000, 1.000000000000000000 ) ) ;
#27395 = CYLINDRICAL_SURFACE ( 'NONE', #86468, 4.000000000000000000 ) ;
#27396 = ORIENTED_EDGE ( 'NONE', *, *, #44436, .T. ) ;
#27397 = CARTESIAN_POINT ( 'NONE',  ( -15.93106661257773915, -11.41317474335729543, 32.86274602512330034 ) ) ;
#27398 = CARTESIAN_POINT ( 'NONE',  ( -15.00775638667583678, -12.64618726649961289, 30.78989965857442712 ) ) ;
#27399 = FACE_BOUND ( 'NONE', #33307, .T. ) ;
#27401 = CARTESIAN_POINT ( 'NONE',  ( 4.087763774486016466, -12.34228464037088280, 31.77849191805838558 ) ) ;
#27400 = DIRECTION ( 'NONE',  ( -0.000000000000000000, -0.000000000000000000, -1.000000000000000000 ) ) ;
#27402 = DIRECTION ( 'NONE',  ( 0.000000000000000000, 0.000000000000000000, -1.000000000000000000 ) ) ;
#27403 = CARTESIAN_POINT ( 'NONE',  ( 1.515405825582336607, -12.62708834333097663, 30.88030960425257021 ) ) ;
#27405 = CARTESIAN_POINT ( 'NONE',  ( 2.177544337960610310, -11.04286588640298561, 33.62463336215343901 ) ) ;
#27404 = DIRECTION ( 'NONE',  ( 0.3831982898360153378, -0.9236661034522991587, 0.000000000000000000 ) ) ;
#27406 = AXIS2_PLACEMENT_3D ( 'NONE', #11131, #59764, #87258 ) ;
#27407 = CARTESIAN_POINT ( 'NONE',  ( 2.651650429449539104, -4.848349570550432475, 25.56250000000000355 ) ) ;
#27408 = VERTEX_POINT ( 'NONE', #14670 ) ;
#27409 = EDGE_CURVE ( 'NONE', #2192, #20400, #22744, .T. ) ;
#27410 = EDGE_LOOP ( 'NONE', ( #59618, #2889, #20848, #26662 ) ) ;
#27411 = CARTESIAN_POINT ( 'NONE',  ( -12.33074802057151409, -5.496552790871120031, 34.60292014791297532 ) ) ;
#27412 = CARTESIAN_POINT ( 'NONE',  ( -0.5922299282060184966, -2.729777683071817673, 31.24903638046269094 ) ) ;
#27413 = CARTESIAN_POINT ( 'NONE',  ( 1.384615384615386802, -9.058645607665452459, 34.76329471203371924 ) ) ;
#27414 = CARTESIAN_POINT ( 'NONE',  ( 10.68063975489745410, -3.083524468853784839, 32.58852847137153930 ) ) ;
#27415 = CARTESIAN_POINT ( 'NONE',  ( -3.453695448285377445, -5.667676309546437530, 34.40238873228292249 ) ) ;
#27416 = CARTESIAN_POINT ( 'NONE',  ( 2.694853999681214862, -10.10844685921789043, 15.62313170625848890 ) ) ;
#27417 = DIRECTION ( 'NONE',  ( 0.000000000000000000, 0.9396926207859126468, 0.3420201433256571111 ) ) ;
#27418 = DIRECTION ( 'NONE',  ( 0.000000000000000000, 0.9396926207859126468, 0.3420201433256571111 ) ) ;
#27419 = EDGE_CURVE ( 'NONE', #29899, #33691, #41785, .T. ) ;
#27420 = CARTESIAN_POINT ( 'NONE',  ( 9.692307692307570832, -11.06231777344772027, 33.60647404775119895 ) ) ;
#27421 = DIRECTION ( 'NONE',  ( 0.000000000000000000, 0.7660444431189822323, -0.6427876096865344779 ) ) ;
#27422 = CARTESIAN_POINT ( 'NONE',  ( 10.86533002476265963, -3.520799739797214389, 33.17531984108286025 ) ) ;
#27423 = CARTESIAN_POINT ( 'NONE',  ( -5.010855743573001675, -6.343179335718452272, 34.87096338111212646 ) ) ;
#27424 = CARTESIAN_POINT ( 'NONE',  ( -3.361459833879539172, -9.929715669179220328, 34.40415004197138416 ) ) ;
#27426 = EDGE_CURVE ( 'NONE', #6303, #622, #50379, .T. ) ;
#27425 = CARTESIAN_POINT ( 'NONE',  ( -6.857821783564084228, -3.643525952247864463, 33.31231777344670064 ) ) ;
#27427 = ADVANCED_FACE ( 'NONE', ( #49774 ), #41697, .F. ) ;
#27428 = AXIS2_PLACEMENT_3D ( 'NONE', #74263, #53080, #82354 ) ;
#27429 = CARTESIAN_POINT ( 'NONE',  ( 6.000000000000001776, -6.386643153685126251, 34.62446782046654192 ) ) ;
#27430 = ORIENTED_EDGE ( 'NONE', *, *, #50471, .T. ) ;
#27431 = CARTESIAN_POINT ( 'NONE',  ( -0.4615384615385826339, -3.835265460704628371, 33.15142922262033665 ) ) ;
#27432 = CARTESIAN_POINT ( 'NONE',  ( 10.61538461538461675, -5.471508081941601098, 34.59228464037088457 ) ) ;
#27433 = B_SPLINE_CURVE_WITH_KNOTS ( 'NONE', 3,
 ( #21430, #61965, #714, #55210, #35385, #56548, #82702, #70056, #14231, #76369 ),
 .UNSPECIFIED., .F., .F.,
 ( 4, 2, 2, 2, 4 ),
 ( 0.0007817246256747453293, 0.0009771112852218889842, 0.001172497944769032531, 0.001367884604316176294, 0.001563271263863319840 ),
 .UNSPECIFIED. ) ;
#27434 = CARTESIAN_POINT ( 'NONE',  ( 0.06109907496451789238, -4.749999999999998224, 21.90811829374151642 ) ) ;
#27435 = CIRCLE ( 'NONE', #77752, 4.000000000000000000 ) ;
#27436 = VECTOR ( 'NONE', #51728, 1000.000000000000000 ) ;
#27437 = CARTESIAN_POINT ( 'NONE',  ( 20.00000000000000000, -3.499999999999999556, 28.25000000000000000 ) ) ;
#27438 = CARTESIAN_POINT ( 'NONE',  ( 5.076923076923075762, -8.164416787775445883, 34.95778746994557906 ) ) ;
#27440 = VERTEX_POINT ( 'NONE', #20966 ) ;
#27439 = CARTESIAN_POINT ( 'NONE',  ( 7.846153846153846700, -2.538708090699994813, 30.37095296980875503 ) ) ;
#27441 = CARTESIAN_POINT ( 'NONE',  ( 2.750000000000001776, -7.499999999999984013, 25.71875000000000000 ) ) ;
#27442 = CARTESIAN_POINT ( 'NONE',  ( 12.52760579488853665, -5.471508081941601098, 34.59228464037088457 ) ) ;
#27443 = EDGE_CURVE ( 'NONE', #21602, #44682, #13853, .T. ) ;
#27444 = ORIENTED_EDGE ( 'NONE', *, *, #11854, .T. ) ;
#27445 = CARTESIAN_POINT ( 'NONE',  ( 11.53846153846141576, -9.528491918059723176, 34.59228464037033035 ) ) ;
#27446 = AXIS2_PLACEMENT_3D ( 'NONE', #73249, #39920, #25507 ) ;
#27447 = CARTESIAN_POINT ( 'NONE',  ( -15.23076923076922995, -1.044019251281081972, 31.83374038241031911 ) ) ;
#27448 = VERTEX_POINT ( 'NONE', #28631 ) ;
#27449 = CARTESIAN_POINT ( 'NONE',  ( 14.17700084102474811, -2.541943142973491554, 30.39792223712631980 ) ) ;
#27450 = ADVANCED_FACE ( 'NONE', ( #56095 ), #9253, .T. ) ;
#27451 = EDGE_CURVE ( 'NONE', #14199, #37091, #16103, .T. ) ;
#27452 = CARTESIAN_POINT ( 'NONE',  ( -16.28445651347068335, -7.722926236386454590, 34.74524107206102030 ) ) ;
#27453 = CARTESIAN_POINT ( 'NONE',  ( -15.23076923076935074, -12.46129190930018460, 30.37095296980731973 ) ) ;
#27454 = ORIENTED_EDGE ( 'NONE', *, *, #22317, .F. ) ;
#27455 = ORIENTED_EDGE ( 'NONE', *, *, #45330, .T. ) ;
#27456 = CARTESIAN_POINT ( 'NONE',  ( 15.29683656411930848, -4.661471528628508665, 34.16647553114624003 ) ) ;
#27457 = EDGE_CURVE ( 'NONE', #79057, #62627, #18174, .T. ) ;
#27458 = ORIENTED_EDGE ( 'NONE', *, *, #79281, .T. ) ;
#27459 = CARTESIAN_POINT ( 'NONE',  ( 7.715463243043540587, -9.084618155246140248, 34.75535874321725771 ) ) ;
#27460 = CARTESIAN_POINT ( 'NONE',  ( 5.299935921016468932, -4.762714258010880997, 34.23016756924214832 ) ) ;
#27461 = DIRECTION ( 'NONE',  ( -0.000000000000000000, -0.6427876096865404731, -0.7660444431189770143 ) ) ;
#27462 = CARTESIAN_POINT ( 'NONE',  ( -6.673131513698880468, -11.56426240980093745, 33.07394671870546432 ) ) ;
#27463 = CARTESIAN_POINT ( 'NONE',  ( 15.10062202133101295, -6.852621066184266141, 34.70813303252209181 ) ) ;
#27464 = CARTESIAN_POINT ( 'NONE',  ( -19.50000000000000000, -3.499999999999999556, 29.75000000000000355 ) ) ;
#27465 = CARTESIAN_POINT ( 'NONE',  ( 15.93036122928181975, -12.69144148231606017, 30.53333754910549303 ) ) ;
#27466 = AXIS2_PLACEMENT_3D ( 'NONE', #86399, #85935, #24218 ) ;
#27467 = VERTEX_POINT ( 'NONE', #31291 ) ;
#27468 = EDGE_LOOP ( 'NONE', ( #33786, #88447 ) ) ;
#27470 = ORIENTED_EDGE ( 'NONE', *, *, #50479, .T. ) ;
#27469 = CARTESIAN_POINT ( 'NONE',  ( -0.4615384615385826339, -12.27809138561165270, 31.22303859784587132 ) ) ;
#27471 = B_SPLINE_CURVE_WITH_KNOTS ( 'NONE', 3,
 ( #6572, #67829, #55631, #7464, #61065, #34919, #88569, #62382, #697, #28163 ),
 .UNSPECIFIED., .F., .F.,
 ( 4, 2, 2, 2, 4 ),
 ( 0.0007817246256747473893, 0.0009771112852218905021, 0.001172497944769033615, 0.001367884604316176944, 0.001563271263863320057 ),
 .UNSPECIFIED. ) ;
#27472 = B_SPLINE_CURVE_WITH_KNOTS ( 'NONE', 3,
 ( #67970, #18452, #80609, #87822, #53555, #19338, #88704, #59429, #46806, #74284 ),
 .UNSPECIFIED., .F., .F.,
 ( 4, 2, 2, 2, 4 ),
 ( 0.000000000000000000, 0.0001954339857564063089, 0.0003908679715128126177, 0.0005863019572692189808, 0.0007817359430256252354 ),
 .UNSPECIFIED. ) ;
#27473 = EDGE_CURVE ( 'NONE', #82350, #9234, #34286, .T. ) ;
#27474 = DIRECTION ( 'NONE',  ( -0.000000000000000000, 0.1736481776669307198, -0.9848077530122080203 ) ) ;
#27475 = CARTESIAN_POINT ( 'NONE',  ( -13.60744348225026634, -7.369209533119140509, 34.99857337881830688 ) ) ;
#27476 = CARTESIAN_POINT ( 'NONE',  ( 9.692307692307695177, -4.786620604624113540, 33.94971097300155094 ) ) ;
#27477 = VERTEX_POINT ( 'NONE', #16881 ) ;
#27478 = CARTESIAN_POINT ( 'NONE',  ( 1.384615384615265343, -3.835265460704628371, 33.15142922262033665 ) ) ;
#27479 = EDGE_LOOP ( 'NONE', ( #74453, #78960 ) ) ;
#27480 = CARTESIAN_POINT ( 'NONE',  ( 8.096208266067295156, -12.65882529074907126, 30.72640787790839312 ) ) ;
#27481 = EDGE_LOOP ( 'NONE', ( #44854, #8560, #2724, #12819 ) ) ;
#27482 = CARTESIAN_POINT ( 'NONE',  ( -14.24162497434223162, -11.91647553114624358, 32.58852847137148245 ) ) ;
#27483 = ORIENTED_EDGE ( 'NONE', *, *, #15532, .F. ) ;
#27484 = CARTESIAN_POINT ( 'NONE',  ( 1.515407192440173967, -6.413143153341454017, 34.63066358083362672 ) ) ;
#27485 = CARTESIAN_POINT ( 'NONE',  ( -8.769230769230890843, -2.892918686052166066, 31.69288490824153470 ) ) ;
#27486 = FACE_BOUND ( 'NONE', #16734, .T. ) ;
#27487 = CARTESIAN_POINT ( 'NONE',  ( -13.91025641025641058, -3.499999999999999556, 29.75000000000000355 ) ) ;
#27488 = CARTESIAN_POINT ( 'NONE',  ( 1.134615384615387246, -7.500000000000001776, 35.00000000000000000 ) ) ;
#27489 = CARTESIAN_POINT ( 'NONE',  ( 9.692307692307570832, -2.379036618888197729, 30.90682066428292885 ) ) ;
#27490 = CARTESIAN_POINT ( 'NONE',  ( 1.253924781505079800, -12.35290016733513951, 31.75349464988449455 ) ) ;
#27491 = DIRECTION ( 'NONE',  ( -1.000000000000000000, -0.000000000000000000, 0.000000000000000000 ) ) ;
#27492 = CARTESIAN_POINT ( 'NONE',  ( -5.749999999998562927, -7.500000000000155431, 34.75000000000007105 ) ) ;
#27493 = CARTESIAN_POINT ( 'NONE',  ( -13.38461538461538325, -6.189225973068211317, 35.74407628777942847 ) ) ;
#27494 = VERTEX_POINT ( 'NONE', #3811 ) ;
#27495 = ORIENTED_EDGE ( 'NONE', *, *, #30017, .F. ) ;
#27496 = AXIS2_PLACEMENT_3D ( 'NONE', #7581, #62940, #21077 ) ;
#27498 = CARTESIAN_POINT ( 'NONE',  ( 2.307692307692309264, -10.51840700105979565, 33.73612834413961536 ) ) ;
#27497 = CARTESIAN_POINT ( 'NONE',  ( 2.084765348785459604, -2.889293201056495786, 32.26117774369186009 ) ) ;
#27499 = ADVANCED_FACE ( 'NONE', ( #59200 ), #45238, .F. ) ;
#27500 = B_SPLINE_CURVE_WITH_KNOTS ( 'NONE', 3,
 ( #40207, #67669, #4181, #69878, #27118, #82524, #21688, #13166, #83854, #76186 ),
 .UNSPECIFIED., .F., .F.,
 ( 4, 2, 2, 2, 4 ),
 ( 0.0007817246256747519429, 0.0009771112852218970073, 0.001172497944769042288, 0.001367884604316187353, 0.001563271263863332417 ),
 .UNSPECIFIED. ) ;
#27501 = CARTESIAN_POINT ( 'NONE',  ( 7.053602624840485724, -6.852161475712352789, 34.70806712695775786 ) ) ;
#27502 = CARTESIAN_POINT ( 'NONE',  ( -4.023055712879202162, -9.084667340241226796, 34.75534355489798344 ) ) ;
#27503 = DIRECTION ( 'NONE',  ( -0.000000000000000000, 0.9396926207859092051, -0.3420201433256662704 ) ) ;
#27504 = DIRECTION ( 'NONE',  ( -0.000000000000000000, 0.6427876096865404731, -0.7660444431189771253 ) ) ;
#27506 = ORIENTED_EDGE ( 'NONE', *, *, #54803, .F. ) ;
#27505 = B_SPLINE_CURVE_WITH_KNOTS ( 'NONE', 3,
 ( #41245, #27278, #7460, #20953, #7899, #34033, #19634, #54744, #89005, #6125 ),
 .UNSPECIFIED., .F., .F.,
 ( 4, 2, 2, 2, 4 ),
 ( 0.0007817246256747473893, 0.0009771112852218909357, 0.001172497944769034482, 0.001367884604316178246, 0.001563271263863321792 ),
 .UNSPECIFIED. ) ;
#27507 = CARTESIAN_POINT ( 'NONE',  ( 2.177545098254087819, -9.418419913701741919, 34.36755862841477693 ) ) ;
#27508 = CARTESIAN_POINT ( 'NONE',  ( -6.250023237292964495, -6.695914987888143877, 34.68535235679833306 ) ) ;
#27509 = CARTESIAN_POINT ( 'NONE',  ( -6.923076923077044142, -11.48612834414049644, 32.76840700105863391 ) ) ;
#27510 = DIRECTION ( 'NONE',  ( -0.000000000000000000, 0.9396926207859093161, -0.3420201433256663259 ) ) ;
#27511 = ORIENTED_EDGE ( 'NONE', *, *, #59222, .F. ) ;
#27512 = EDGE_LOOP ( 'NONE', ( #8781, #37967 ) ) ;
#27513 = ORIENTED_EDGE ( 'NONE', *, *, #15921, .F. ) ;
#27514 = DIRECTION ( 'NONE',  ( 0.000000000000000000, 0.000000000000000000, 1.000000000000000000 ) ) ;
#27515 = EDGE_CURVE ( 'NONE', #85639, #36102, #59009, .T. ) ;
#27516 = ORIENTED_EDGE ( 'NONE', *, *, #88872, .T. ) ;
#27517 = CYLINDRICAL_SURFACE ( 'NONE', #52482, 0.2499999999999986955 ) ;
#27518 = CARTESIAN_POINT ( 'NONE',  ( 15.23076923076923173, -3.937682226553329556, 33.60647404775216529 ) ) ;
#27519 = CARTESIAN_POINT ( 'NONE',  ( 3.361294669002876656, -10.31582465632705237, 34.18122507451815295 ) ) ;
#27520 = CARTESIAN_POINT ( 'NONE',  ( -17.30040800148741198, -9.417330523894424488, 34.63758898049880486 ) ) ;
#27521 = EDGE_CURVE ( 'NONE', #21025, #54359, #72713, .T. ) ;
#27522 = CARTESIAN_POINT ( 'NONE',  ( 9.692307692307572609, -6.026961402154118019, 34.52809138561165270 ) ) ;
#27523 = EDGE_LOOP ( 'NONE', ( #47676, #84698, #43550, #75875, #19471, #30611 ) ) ;
#27524 = CARTESIAN_POINT ( 'NONE',  ( 11.40790094671961796, -2.504760397472875155, 29.97295953869789997 ) ) ;
#27526 = ORIENTED_EDGE ( 'NONE', *, *, #61368, .F. ) ;
#27525 = PLANE ( 'NONE',  #30970 ) ;
#27527 = DIRECTION ( 'NONE',  ( -1.000000000000000000, -0.000000000000000000, -0.000000000000000000 ) ) ;
#27528 = FACE_OUTER_BOUND ( 'NONE', #83086, .T. ) ;
#27529 = CARTESIAN_POINT ( 'NONE',  ( -11.60373153901786125, -11.06231777344662781, 33.60647404775220082 ) ) ;
#27530 = AXIS2_PLACEMENT_3D ( 'NONE', #75635, #68010, #62129 ) ;
#27531 = LINE ( 'NONE', #34282, #72544 ) ;
#27532 = FACE_OUTER_BOUND ( 'NONE', #34448, .T. ) ;
#27533 = EDGE_CURVE ( 'NONE', #78459, #79092, #83750, .T. ) ;
#27534 = CARTESIAN_POINT ( 'NONE',  ( 9.469381474791545017, -9.886141570436013382, 34.14413921362392301 ) ) ;
#27535 = CARTESIAN_POINT ( 'NONE',  ( -3.360916440207450506, -6.852621066184267029, 34.70813303252209181 ) ) ;
#27536 = VECTOR ( 'NONE', #6922, 999.9999999999998863 ) ;
#27537 = CARTESIAN_POINT ( 'NONE',  ( 1.901340078031373171, -9.487747218494639867, 22.37686829374150932 ) ) ;
#27538 = ORIENTED_EDGE ( 'NONE', *, *, #11943, .F. ) ;
#27539 = CARTESIAN_POINT ( 'NONE',  ( -7.053767526187229464, -10.70098750199973203, 33.91152734681376302 ) ) ;
#27540 = CARTESIAN_POINT ( 'NONE',  ( 12.71148387091650278, -4.932303261841489928, 34.32971442181322885 ) ) ;
#27541 = B_SPLINE_CURVE_WITH_KNOTS ( 'NONE', 3,
 ( #54683, #48816, #68650, #20469, #56019, #83510, #75852, #21793, #62328, #82178 ),
 .UNSPECIFIED., .F., .F.,
 ( 4, 2, 2, 2, 4 ),
 ( 0.000000000000000000, 0.0001954311564186873352, 0.0003908623128373746704, 0.0005862934692560620598, 0.0007817246256747493408 ),
 .UNSPECIFIED. ) ;
#27542 = LINE ( 'NONE', #14022, #74867 ) ;
#27543 =( NAMED_UNIT ( * ) SI_UNIT ( $, .STERADIAN. ) SOLID_ANGLE_UNIT ( ) );
#27544 = B_SPLINE_CURVE_WITH_KNOTS ( 'NONE', 3,
 ( #38141, #78235, #50751, #85446, #11115, #30060, #23726, #43565, #38590, #79131 ),
 .UNSPECIFIED., .F., .F.,
 ( 4, 2, 2, 2, 4 ),
 ( 0.0007817359430256215491, 0.0009771253907249856981, 0.001172514838424349847, 0.001367904286123713779, 0.001563293733823077928 ),
 .UNSPECIFIED. ) ;
#27545 = VERTEX_POINT ( 'NONE', #57866 ) ;
#27546 = CARTESIAN_POINT ( 'NONE',  ( -12.46153846153846168, -11.69971097300155272, 32.46337939537588113 ) ) ;
#27547 = CARTESIAN_POINT ( 'NONE',  ( -12.59222992820602371, -3.062553014421049546, 32.05460306192773601 ) ) ;
#27548 = B_SPLINE_CURVE_WITH_KNOTS ( 'NONE', 3,
 ( #54129, #47828, #74873, #41518, #33868, #6838, #12717, #68111, #61772, #88400 ),
 .UNSPECIFIED., .F., .F.,
 ( 4, 2, 2, 2, 4 ),
 ( 0.000000000000000000, 0.0001954311564186861426, 0.0003908623128373722852, 0.0005862934692560583735, 0.0007817246256747445703 ),
 .UNSPECIFIED. ) ;
#27549 = LINE ( 'NONE', #55022, #14317 ) ;
#27550 = CARTESIAN_POINT ( 'NONE',  ( 9.442307692307693401, -7.566082377512564960, 35.00000000000000711 ) ) ;
#27551 = FACE_OUTER_BOUND ( 'NONE', #50028, .T. ) ;
#27552 = VERTEX_POINT ( 'NONE', #85799 ) ;
#27553 = CARTESIAN_POINT ( 'NONE',  ( -15.45369544828537656, -2.758268499246657068, 31.33685645148948140 ) ) ;
#27554 = ADVANCED_FACE ( 'NONE', ( #17786 ), #44786, .F. ) ;
#27555 = CARTESIAN_POINT ( 'NONE',  ( 3.480714749117372886, -12.22109172314383052, 31.39792113162168263 ) ) ;
#27556 = CYLINDRICAL_SURFACE ( 'NONE', #57915, 0.2500000000000008882 ) ;
#27557 = ORIENTED_EDGE ( 'NONE', *, *, #53279, .F. ) ;
#27558 = CARTESIAN_POINT ( 'NONE',  ( 17.07692307692307665, -9.819645486525091727, 36.12317359536749706 ) ) ;
#27559 = VERTEX_POINT ( 'NONE', #78138 ) ;
#27560 = DIRECTION ( 'NONE',  ( 0.000000000000000000, 0.000000000000000000, -1.000000000000000000 ) ) ;
#27561 =( NAMED_UNIT ( * ) PLANE_ANGLE_UNIT ( ) SI_UNIT ( $, .RADIAN. ) );
#27562 = CARTESIAN_POINT ( 'NONE',  ( -19.50000000000000000, -4.000000000000000000, 29.75000000000000355 ) ) ;
#27563 = ORIENTED_EDGE ( 'NONE', *, *, #12424, .T. ) ;
#27564 = CARTESIAN_POINT ( 'NONE',  ( 9.692307692307695177, -13.53365097954675988, 30.81389545987213552 ) ) ;
#27565 = DIRECTION ( 'NONE',  ( -0.000000000000000000, -0.000000000000000000, -1.000000000000000000 ) ) ;
#27566 = CYLINDRICAL_SURFACE ( 'NONE', #60980, 0.2499999999999986955 ) ;
#27567 = VECTOR ( 'NONE', #25652, 1000.000000000000114 ) ;
#27568 = LINE ( 'NONE', #21241, #20601 ) ;
#27569 = CARTESIAN_POINT ( 'NONE',  ( -1.608100309179716358, -10.97335522853832579, 33.68706563782419749 ) ) ;
#27570 = VERTEX_POINT ( 'NONE', #85349 ) ;
#27571 = FACE_BOUND ( 'NONE', #51045, .T. ) ;
#27572 = ORIENTED_EDGE ( 'NONE', *, *, #53872, .T. ) ;
#27573 = CARTESIAN_POINT ( 'NONE',  ( 11.53846153846153832, -13.63283147151868846, 33.57946703557072254 ) ) ;
#27574 = CARTESIAN_POINT ( 'NONE',  ( 4.946775867484854317, -11.93770438780619259, 32.05411857736982029 ) ) ;
#27575 = CARTESIAN_POINT ( 'NONE',  ( 3.007842271862382955, -11.43668979543635089, 33.22377378376089752 ) ) ;
#27576 = CARTESIAN_POINT ( 'NONE',  ( 6.923076923076802558, -2.625532179533778709, 30.86335684631627174 ) ) ;
#27577 = EDGE_LOOP ( 'NONE', ( #59351, #38581, #67164, #11673 ) ) ;
#27578 = ORIENTED_EDGE ( 'NONE', *, *, #22161, .F. ) ;
#27579 = ORIENTED_EDGE ( 'NONE', *, *, #44820, .T. ) ;
#27580 = VECTOR ( 'NONE', #43440, 1000.000000000000114 ) ;
#27581 = CARTESIAN_POINT ( 'NONE',  ( 6.000000000000001776, -1.790695186598648903, 34.54067556320373455 ) ) ;
#27582 = VERTEX_POINT ( 'NONE', #64607 ) ;
#27583 = CARTESIAN_POINT ( 'NONE',  ( 15.00728430620490350, -3.562934362175799841, 33.22335522853832401 ) ) ;
#27584 = VECTOR ( 'NONE', #23872, 1000.000000000000227 ) ;
#27585 = CYLINDRICAL_SURFACE ( 'NONE', #69862, 0.2499999999999995559 ) ;
#27586 = CARTESIAN_POINT ( 'NONE',  ( 6.066068351002443571, -12.10708131394839882, 31.69288490824020954 ) ) ;
#27587 = CARTESIAN_POINT ( 'NONE',  ( 8.769230769230647482, -9.442884908241554243, 34.35708131394783038 ) ) ;
#27588 = CARTESIAN_POINT ( 'NONE',  ( -1.553300858899125059, -3.750000000000009326, 24.07812500000000355 ) ) ;
#27589 = CARTESIAN_POINT ( 'NONE',  ( -19.50000000000000000, -3.499999999999999556, 29.75000000000000355 ) ) ;
#27590 = DIRECTION ( 'NONE',  ( 0.000000000000000000, 2.546383084002652634E-16, 1.000000000000000000 ) ) ;
#27591 = CARTESIAN_POINT ( 'NONE',  ( -8.703163435880695076, -2.833524468853757305, 32.15551576947925838 ) ) ;
#27592 = ORIENTED_EDGE ( 'NONE', *, *, #10285, .F. ) ;
#27593 = ORIENTED_EDGE ( 'NONE', *, *, #38191, .F. ) ;
#27594 = ORIENTED_EDGE ( 'NONE', *, *, #82560, .T. ) ;
#27595 = CARTESIAN_POINT ( 'NONE',  ( 3.480769230770650147, -7.500000000000154543, 35.00000000000007105 ) ) ;
#27597 = CARTESIAN_POINT ( 'NONE',  ( -8.069080063669991532, -4.186968288167451036, 33.49512374952580274 ) ) ;
#27596 = CARTESIAN_POINT ( 'NONE',  ( 4.153846153846030731, -11.06231777344772027, 33.60647404775119895 ) ) ;
#27598 = EDGE_CURVE ( 'NONE', #2295, #26375, #77955, .T. ) ;
#27599 = DIRECTION ( 'NONE',  ( -1.000000000000000000, -0.000000000000000000, -0.000000000000000000 ) ) ;
#27600 = CARTESIAN_POINT ( 'NONE',  ( 7.846153846153846700, -8.564572088678739092, 35.78748833219616898 ) ) ;
#27601 = FACE_BOUND ( 'NONE', #28812, .T. ) ;
#27602 = CARTESIAN_POINT ( 'NONE',  ( -1.384615384615383471, -13.95598074871891292, 31.83374038241031911 ) ) ;
#27603 = EDGE_LOOP ( 'NONE', ( #71437, #29962, #69212, #48331 ) ) ;
#27604 = CARTESIAN_POINT ( 'NONE',  ( -15.23076923076892264, -2.506253911140614576, 30.00000000000323297 ) ) ;
#27605 = DIRECTION ( 'NONE',  ( -0.000000000000000000, 0.9848077530122086864, -0.1736481776669273891 ) ) ;
#27606 = DIRECTION ( 'NONE',  ( 0.000000000000000000, 0.8660254037844377084, -0.5000000000000015543 ) ) ;
#27607 = ORIENTED_EDGE ( 'NONE', *, *, #41002, .F. ) ;
#27608 = CARTESIAN_POINT ( 'NONE',  ( 6.000000000000001776, -10.67929555188718282, 33.92786785259544047 ) ) ;
#27609 = ORIENTED_EDGE ( 'NONE', *, *, #59658, .T. ) ;
#27610 = FACE_BOUND ( 'NONE', #40496, .T. ) ;
#27612 = VECTOR ( 'NONE', #22850, 1000.000000000000000 ) ;
#27611 = CARTESIAN_POINT ( 'NONE',  ( 14.30769230769218581, -12.51329471203414379, 31.30864560766407578 ) ) ;
#27613 = EDGE_CURVE ( 'NONE', #8179, #72902, #16440, .T. ) ;
#27614 = AXIS2_PLACEMENT_3D ( 'NONE', #76536, #43623, #27905 ) ;
#27615 = CARTESIAN_POINT ( 'NONE',  ( -11.00641025641025550, -7.500000000000000000, 33.75000000000000000 ) ) ;
#27616 = CYLINDRICAL_SURFACE ( 'NONE', #69157, 0.2499999999999994726 ) ;
#27617 = ORIENTED_EDGE ( 'NONE', *, *, #65855, .T. ) ;
#27618 = EDGE_CURVE ( 'NONE', #49301, #39942, #56482, .T. ) ;
#27619 = DIRECTION ( 'NONE',  ( 0.000000000000000000, 0.7660444431189807890, 0.6427876096865361433 ) ) ;
#27620 = DIRECTION ( 'NONE',  ( -1.000000000000000000, -0.000000000000000000, -0.000000000000000000 ) ) ;
#27621 = CARTESIAN_POINT ( 'NONE',  ( 18.06606733335007675, -10.67929555188718282, 33.92786785259544757 ) ) ;
#27622 = CARTESIAN_POINT ( 'NONE',  ( -4.946397638689432164, -5.915461855592777596, 34.75538340440931506 ) ) ;
#27623 = ORIENTED_EDGE ( 'NONE', *, *, #4814, .T. ) ;
#27624 = AXIS2_PLACEMENT_3D ( 'NONE', #65079, #3387, #38068 ) ;
#27625 = CARTESIAN_POINT ( 'NONE',  ( -12.46153846153858247, -3.300289026999228881, 32.46337939537708905 ) ) ;
#27626 = CARTESIAN_POINT ( 'NONE',  ( 4.088576153289833925, -10.33852847137145048, 34.16647553114627556 ) ) ;
#27628 = VERTEX_POINT ( 'NONE', #4259 ) ;
#27627 = LINE ( 'NONE', #602, #34067 ) ;
#27629 = LINE ( 'NONE', #6041, #84319 ) ;
#27630 = CARTESIAN_POINT ( 'NONE',  ( 0.6845513056318554002, -10.77377354290276301, 33.85451476688484718 ) ) ;
#27631 = DIRECTION ( 'NONE',  ( -0.000000000000000000, 1.000000000000000000, -0.000000000000000000 ) ) ;
#27632 = CARTESIAN_POINT ( 'NONE',  ( -13.25382357679060519, -3.530189275343204702, 32.79018710029569661 ) ) ;
#27633 = CARTESIAN_POINT ( 'NONE',  ( -2.544871794871793824, -11.50000000000000000, 29.75000000000000355 ) ) ;
#27635 = CARTESIAN_POINT ( 'NONE',  ( -2.557692307692319034, -2.499999999999999556, 29.81609845454692120 ) ) ;
#27634 = DIRECTION ( 'NONE',  ( 0.000000000000000000, 0.6427876096865368094, 0.7660444431189802339 ) ) ;
#27636 = ADVANCED_FACE ( 'NONE', ( #31742 ), #54211, .F. ) ;
#27637 = LINE ( 'NONE', #34833, #47854 ) ;
#27638 = CARTESIAN_POINT ( 'NONE',  ( -1.944543648262992530, -9.444543648263016067, 21.18750000000000000 ) ) ;
#27639 = ORIENTED_EDGE ( 'NONE', *, *, #2969, .F. ) ;
#27640 = CARTESIAN_POINT ( 'NONE',  ( -19.50000000000000000, -3.499999999999999556, 29.75000000000000355 ) ) ;
#27641 = EDGE_LOOP ( 'NONE', ( #13788, #41072, #16172, #23026 ) ) ;
#27642 = VERTEX_POINT ( 'NONE', #5152 ) ;
#27643 = CARTESIAN_POINT ( 'NONE',  ( -8.703163435880695076, -6.343179335718452272, 34.87096338111212646 ) ) ;
#27644 = EDGE_LOOP ( 'NONE', ( #42116, #31354 ) ) ;
#27645 = CARTESIAN_POINT ( 'NONE',  ( -5.207613680033385428, -11.37499894934982514, 33.29245874905763003 ) ) ;
#27646 = CARTESIAN_POINT ( 'NONE',  ( 2.749999999999995115, -6.360912703473971419, 19.39062500000000711 ) ) ;
#27647 = CARTESIAN_POINT ( 'NONE',  ( 14.43848411551709887, -11.18335022499818621, 33.13157742990016885 ) ) ;
#27648 = CARTESIAN_POINT ( 'NONE',  ( -30.00000000000000000, -15.00000000000000000, 0.000000000000000000 ) ) ;
#27649 = CARTESIAN_POINT ( 'NONE',  ( 3.007843013253083786, -8.239355502252617924, 34.69524867566427417 ) ) ;
#27650 = CARTESIAN_POINT ( 'NONE',  ( -8.769230769230892619, -12.70778746994576025, 30.41441678777401236 ) ) ;
#27651 = CARTESIAN_POINT ( 'NONE',  ( -15.23076923076935252, -5.094484230521993062, 34.41647553114689373 ) ) ;
#27652 = CARTESIAN_POINT ( 'NONE',  ( 4.153846153846154188, -3.513871655860378418, 32.76840700105978499 ) ) ;
#27653 = VECTOR ( 'NONE', #29940, 1000.000000000000000 ) ;
#27654 = CARTESIAN_POINT ( 'NONE',  ( -18.00000000000012079, -11.67786785259630733, 32.92929555188604240 ) ) ;
#27655 = CARTESIAN_POINT ( 'NONE',  ( 10.61538461538461675, -2.538708090699994813, 30.37095296980875503 ) ) ;
#27657 = EDGE_CURVE ( 'NONE', #56816, #66461, #26312, .T. ) ;
#27656 = CARTESIAN_POINT ( 'NONE',  ( -17.01085574357299990, -10.67929555188718282, 33.92786785259544757 ) ) ;
#27658 = ADVANCED_FACE ( 'NONE', ( #12357 ), #88481, .F. ) ;
#27659 = CARTESIAN_POINT ( 'NONE',  ( -12.46153846153858424, -11.06231777344772027, 33.60647404775119895 ) ) ;
#27660 = CARTESIAN_POINT ( 'NONE',  ( 11.60371710973756443, -5.219633306516380244, 34.19971097300157936 ) ) ;
#27661 = ORIENTED_EDGE ( 'NONE', *, *, #88469, .T. ) ;
#27663 = EDGE_CURVE ( 'NONE', #21233, #34931, #82641, .T. ) ;
#27662 = ORIENTED_EDGE ( 'NONE', *, *, #2936, .T. ) ;
#27664 = CARTESIAN_POINT ( 'NONE',  ( 12.68431813051652313, -2.612705202774698421, 31.66806509827799943 ) ) ;
#27665 = CARTESIAN_POINT ( 'NONE',  ( 0.5267936010512989098, -12.16647553114626490, 32.15551576947920864 ) ) ;
#27666 = CYLINDRICAL_SURFACE ( 'NONE', #74253, 0.2499999999999995559 ) ;
#27667 = CARTESIAN_POINT ( 'NONE',  ( 0.2115152373170036404, -10.18141759479407504, 34.26406193332783801 ) ) ;
#27668 = EDGE_CURVE ( 'NONE', #83905, #8169, #4713, .T. ) ;
#27669 = CARTESIAN_POINT ( 'NONE',  ( 12.21156173059610772, -9.148715823498378086, 34.47080413974185120 ) ) ;
#27670 = CARTESIAN_POINT ( 'NONE',  ( -9.757577692864012775, -6.835583212224499938, 34.95778746994557906 ) ) ;
#27671 = DIRECTION ( 'NONE',  ( 0.000000000000000000, 0.7660444431189822323, -0.6427876096865344779 ) ) ;
#27672 = ORIENTED_EDGE ( 'NONE', *, *, #6846, .T. ) ;
#27673 = CARTESIAN_POINT ( 'NONE',  ( 18.00000000000000000, -3.322132147404559976, 32.92929555188717927 ) ) ;
#27674 = VERTEX_POINT ( 'NONE', #88923 ) ;
#27675 = STYLED_ITEM ( 'NONE', ( #67197 ), #28008 ) ;
#27676 = CARTESIAN_POINT ( 'NONE',  ( 16.40390057375961064, -9.233818618650598609, 34.70587769442853698 ) ) ;
#27677 = VECTOR ( 'NONE', #57025, 1000.000000000000000 ) ;
#27678 = CARTESIAN_POINT ( 'NONE',  ( 8.834485908743603844, -9.528491918058460186, 34.59228464037086326 ) ) ;
#27679 = CARTESIAN_POINT ( 'NONE',  ( 11.78840705680968171, -10.76462480002816235, 33.53768742498949962 ) ) ;
#27680 = CARTESIAN_POINT ( 'NONE',  ( 3.903869409797562806, -6.524016743844655686, 34.90889640711025521 ) ) ;
#27681 = CARTESIAN_POINT ( 'NONE',  ( 5.750023269057650488, -2.779195860258147022, 31.39871582349836743 ) ) ;
#27682 = ORIENTED_EDGE ( 'NONE', *, *, #48574, .T. ) ;
#27683 = ORIENTED_EDGE ( 'NONE', *, *, #36117, .T. ) ;
#27684 = EDGE_CURVE ( 'NONE', #63003, #29891, #47456, .T. ) ;
#27685 = ORIENTED_EDGE ( 'NONE', *, *, #55578, .T. ) ;
#27686 = ORIENTED_EDGE ( 'NONE', *, *, #32996, .T. ) ;
#27687 = CARTESIAN_POINT ( 'NONE',  ( -10.74553258511631348, -12.50552854090298993, 31.33409797877408920 ) ) ;
#27688 = CARTESIAN_POINT ( 'NONE',  ( 22.00000000000000711, 9.999999999999991118, 0.000000000000000000 ) ) ;
#27689 = B_SPLINE_CURVE_WITH_KNOTS ( 'NONE', 3,
 ( #23457, #8637, #15834, #43301, #57255, #70773, #9079, #83409, #29788, #84746 ),
 .UNSPECIFIED., .F., .F.,
 ( 4, 2, 2, 2, 4 ),
 ( 0.0007817246256747473893, 0.0009771112852218905021, 0.001172497944769033615, 0.001367884604316176944, 0.001563271263863320057 ),
 .UNSPECIFIED. ) ;
#27690 = CARTESIAN_POINT ( 'NONE',  ( 14.30769230769231015, -2.486705287966279876, 31.30864560766543647 ) ) ;
#27691 = LINE ( 'NONE', #19607, #75824 ) ;
#27692 = CARTESIAN_POINT ( 'NONE',  ( 17.93472999944368240, -3.083524468853725775, 32.58852847137143272 ) ) ;
#27693 = FACE_OUTER_BOUND ( 'NONE', #66891, .T. ) ;
#27694 = ORIENTED_EDGE ( 'NONE', *, *, #24936, .F. ) ;
#27695 = B_SPLINE_CURVE_WITH_KNOTS ( 'NONE', 3,
 ( #38192, #65650, #74206, #26905, #11621, #19265, #73318, #60683, #33665, #61123 ),
 .UNSPECIFIED., .F., .F.,
 ( 4, 2, 2, 2, 4 ),
 ( 0.000000000000000000, 0.0001954339857564073388, 0.0003908679715128146777, 0.0005863019572692220165, 0.0007817359430256293554 ),
 .UNSPECIFIED. ) ;
#27696 = VERTEX_POINT ( 'NONE', #53328 ) ;
#27697 = ADVANCED_FACE ( 'NONE', ( #32184 ), #19991, .F. ) ;
#27698 = ORIENTED_EDGE ( 'NONE', *, *, #84389, .F. ) ;
#27700 = EDGE_LOOP ( 'NONE', ( #16193, #87472 ) ) ;
#27699 = CARTESIAN_POINT ( 'NONE',  ( 17.29993442853592711, -12.39991518177334129, 30.74647679643404530 ) ) ;
#27701 = FACE_OUTER_BOUND ( 'NONE', #15726, .T. ) ;
#27702 = FACE_OUTER_BOUND ( 'NONE', #10276, .T. ) ;
#27703 = AXIS2_PLACEMENT_3D ( 'NONE', #52101, #65606, #17441 ) ;
#27704 = CARTESIAN_POINT ( 'NONE',  ( -1.929879867024197893E-14, -3.750000000000000000, 19.15625000000000000 ) ) ;
#27705 = VERTEX_POINT ( 'NONE', #40281 ) ;
#27706 = ORIENTED_EDGE ( 'NONE', *, *, #43726, .T. ) ;
#27707 = FACE_OUTER_BOUND ( 'NONE', #59913, .T. ) ;
#27708 = FACE_BOUND ( 'NONE', #16886, .T. ) ;
#27709 = CARTESIAN_POINT ( 'NONE',  ( -2.177166869458661225, -5.070358843744209310, 34.40418822224088302 ) ) ;
#27710 = ADVANCED_FACE ( 'NONE', ( #59645 ), #61411, .F. ) ;
#27711 = CARTESIAN_POINT ( 'NONE',  ( -4.403869378067609475, -10.18141759479407327, 34.26406193332782379 ) ) ;
#27712 = ORIENTED_EDGE ( 'NONE', *, *, #22456, .T. ) ;
#27713 = CARTESIAN_POINT ( 'NONE',  ( -9.942330916529147800, -4.931416488878822335, 34.32920672191015399 ) ) ;
#27714 = FACE_OUTER_BOUND ( 'NONE', #20000, .T. ) ;
#27715 = EDGE_CURVE ( 'NONE', #37043, #5766, #70886, .T. ) ;
#27716 = CARTESIAN_POINT ( 'NONE',  ( -3.230769230769229949, -4.786620604624113540, 33.94971097300155094 ) ) ;
#27717 = DIRECTION ( 'NONE',  ( -0.000000000000000000, -0.9848077530122086864, -0.1736481776669273613 ) ) ;
#27718 = ORIENTED_EDGE ( 'NONE', *, *, #72945, .F. ) ;
#27719 = CARTESIAN_POINT ( 'NONE',  ( -0.3314910262880099157, -7.723484941389743952, 34.99544897038808955 ) ) ;
#27720 = CARTESIAN_POINT ( 'NONE',  ( -7.715362038329057981, -11.18335022499818621, 33.13157742990016885 ) ) ;
#27721 = CARTESIAN_POINT ( 'NONE',  ( -12.71151519248081740, -12.17611988154120972, 31.52148481390971213 ) ) ;
#27722 = CARTESIAN_POINT ( 'NONE',  ( -2.307692307692427391, -10.90142922262034020, 33.41473453929536674 ) ) ;
#27723 = CARTESIAN_POINT ( 'NONE',  ( -4.153846153846152411, -12.78798330534103123, 29.99999999999997868 ) ) ;
#27724 = FACE_BOUND ( 'NONE', #63684, .T. ) ;
#27726 = CARTESIAN_POINT ( 'NONE',  ( 11.31553532094539172, -12.39988816332205701, 30.74660775122750778 ) ) ;
#27725 = CARTESIAN_POINT ( 'NONE',  ( -8.834481759392012634, -2.506253911140460922, 30.00000000000013856 ) ) ;
#27727 = EDGE_CURVE ( 'NONE', #40013, #9491, #62201, .T. ) ;
#27728 = CARTESIAN_POINT ( 'NONE',  ( 5.299702745901139878, -9.418065098278011860, 34.63729479722530158 ) ) ;
#27730 = CARTESIAN_POINT ( 'NONE',  ( 17.86930853333243974, -11.18331474514187995, 33.13161551792790505 ) ) ;
#27729 = PLANE ( 'NONE',  #2662 ) ;
#27731 = B_SPLINE_CURVE_WITH_KNOTS ( 'NONE', 3,
 ( #56334, #14014, #22106, #76153, #20340, #48237, #47801, #55004, #75710, #508 ),
 .UNSPECIFIED., .F., .F.,
 ( 4, 2, 2, 2, 4 ),
 ( 0.000000000000000000, 0.0001954339881912783286, 0.0003908679763825566571, 0.0005863019645738349857, 0.0007817359527651133143 ),
 .UNSPECIFIED. ) ;
#27732 = CARTESIAN_POINT ( 'NONE',  ( -18.24997673094235395, -9.943427161483787913, 34.11278801902876978 ) ) ;
#27733 = CARTESIAN_POINT ( 'NONE',  ( 2.750000000000001332, -7.438900925035452083, 19.21688170625848358 ) ) ;
#27734 = B_SPLINE_CURVE_WITH_KNOTS ( 'NONE', 3,
 ( #36206, #37506, #71734, #56893, #15927, #72182, #37060, #49701, #3278, #44246 ),
 .UNSPECIFIED., .F., .F.,
 ( 4, 2, 2, 2, 4 ),
 ( 0.000000000000000000, 0.0001954339857564093175, 0.0003908679715128186350, 0.0005863019572692279796, 0.0007817359430256372700 ),
 .UNSPECIFIED. ) ;
#27735 = ORIENTED_EDGE ( 'NONE', *, *, #65232, .T. ) ;
#27736 = AXIS2_PLACEMENT_3D ( 'NONE', #78121, #62816, #1583 ) ;
#27737 = CARTESIAN_POINT ( 'NONE',  ( 19.00000000000000000, 9.000000000000001776, 2.999999999999999556 ) ) ;
#27738 = VERTEX_POINT ( 'NONE', #52882 ) ;
#27739 = EDGE_CURVE ( 'NONE', #20476, #29561, #85225, .T. ) ;
#27740 = CARTESIAN_POINT ( 'NONE',  ( 0.6849144022366444595, -2.501478030877322567, 29.88021232661720816 ) ) ;
#27741 = ORIENTED_EDGE ( 'NONE', *, *, #19062, .F. ) ;
#27742 = CARTESIAN_POINT ( 'NONE',  ( -11.40766973063675671, -2.729792928343269587, 31.24908615093345077 ) ) ;
#27744 = EDGE_CURVE ( 'NONE', #79573, #56516, #60535, .T. ) ;
#27743 = CARTESIAN_POINT ( 'NONE',  ( -14.30769230769230660, -3.886160181151819604, 36.00935417666054406 ) ) ;
#27746 = ORIENTED_EDGE ( 'NONE', *, *, #67821, .T. ) ;
#27745 = DIRECTION ( 'NONE',  ( 0.000000000000000000, 0.3420201433256641055, -0.9396926207859100932 ) ) ;
#27747 = FACE_OUTER_BOUND ( 'NONE', #25378, .T. ) ;
#27748 = CARTESIAN_POINT ( 'NONE',  ( -2.724691934501232371, -8.700186371490559623, 19.76375670625849423 ) ) ;
#27749 = CARTESIAN_POINT ( 'NONE',  ( -10.61538461538461320, -2.499999999999998668, 29.75000000000001421 ) ) ;
#27750 = CARTESIAN_POINT ( 'NONE',  ( -7.146003881983769013, -12.64616026154729411, 30.79003144601913533 ) ) ;
#27751 = CARTESIAN_POINT ( 'NONE',  ( 12.21151522424549540, -2.823816976329317274, 31.52131813110795733 ) ) ;
#27752 = CARTESIAN_POINT ( 'NONE',  ( 5.198717948717946236, -11.00000000000000000, 29.75000000000000355 ) ) ;
#27753 = CARTESIAN_POINT ( 'NONE',  ( 2.530471848960717640, -2.847695495035523550, 31.58253572463339154 ) ) ;
#27754 = LINE ( 'NONE', #41281, #55526 ) ;
#27755 = CARTESIAN_POINT ( 'NONE',  ( 1.492201783934598236, -11.27530806549875031, 22.45499329374151287 ) ) ;
#27756 = LINE ( 'NONE', #77273, #52016 ) ;
#27758 = EDGE_CURVE ( 'NONE', #45448, #66105, #5250, .T. ) ;
#27757 = CARTESIAN_POINT ( 'NONE',  ( 10.83839596699746544, -11.24521262558773493, 33.06293181088029343 ) ) ;
#27759 = ORIENTED_EDGE ( 'NONE', *, *, #75225, .T. ) ;
#27760 = CARTESIAN_POINT ( 'NONE',  ( 8.835299120233207404, -9.780366693483667717, 34.19971097300155805 ) ) ;
#27761 = CARTESIAN_POINT ( 'NONE',  ( 3.750000000000000888, -7.499999999999978684, 14.46875000000000000 ) ) ;
#27762 = B_SPLINE_CURVE_WITH_KNOTS ( 'NONE', 3,
 ( #4446, #86897, #12113, #25164, #52630, #60277, #12548, #60726, #87790, #88231 ),
 .UNSPECIFIED., .F., .F.,
 ( 4, 2, 2, 2, 4 ),
 ( 0.0007817359527651132059, 0.0009771254036996528287, 0.001172514854634192560, 0.001367904305568732291, 0.001563293756503272023 ),
 .UNSPECIFIED. ) ;
#27763 = LINE ( 'NONE', #13363, #13068 ) ;
#27764 = DIRECTION ( 'NONE',  ( 0.000000000000000000, 0.000000000000000000, 1.000000000000000000 ) ) ;
#27765 = ORIENTED_EDGE ( 'NONE', *, *, #20809, .F. ) ;
#27766 = CARTESIAN_POINT ( 'NONE',  ( 14.55774661933062397, -2.564540009722896752, 30.55348353981670684 ) ) ;
#27767 = CARTESIAN_POINT ( 'NONE',  ( 3.230769230769231726, -3.513871655860378418, 32.76840700105978499 ) ) ;
#27769 = ORIENTED_EDGE ( 'NONE', *, *, #70616, .F. ) ;
#27768 = LINE ( 'NONE', #13368, #21007 ) ;
#27770 = CARTESIAN_POINT ( 'NONE',  ( -5.076923076923075762, -5.557115091759785130, 34.35708131394839171 ) ) ;
#27771 = EDGE_CURVE ( 'NONE', #7100, #63601, #62300, .T. ) ;
#27772 = CARTESIAN_POINT ( 'NONE',  ( -1.515306851282940848, -10.54014554554150607, 33.71984207302941883 ) ) ;
#27773 = CARTESIAN_POINT ( 'NONE',  ( 6.923076923076800782, -12.16647553114689728, 32.15551576947799362 ) ) ;
#27774 = AXIS2_PLACEMENT_3D ( 'NONE', #14591, #49263, #69531 ) ;
#27775 = VECTOR ( 'NONE', #17611, 1000.000000000000114 ) ;
#27776 = CARTESIAN_POINT ( 'NONE',  ( -16.94639737515952049, -2.882268652242223617, 31.66798894389554064 ) ) ;
#27777 = CARTESIAN_POINT ( 'NONE',  ( 0.4615384615383382183, -2.379036618888197285, 30.90682066428292885 ) ) ;
#27778 = EDGE_LOOP ( 'NONE', ( #10424, #10876, #34468, #50913 ) ) ;
#27779 = EDGE_CURVE ( 'NONE', #31043, #84442, #27637, .T. ) ;
#27780 = ORIENTED_EDGE ( 'NONE', *, *, #31793, .T. ) ;
#27781 = EDGE_LOOP ( 'NONE', ( #60192, #71912 ) ) ;
#27782 = DIRECTION ( 'NONE',  ( -0.000000000000000000, 0.5000000000000011102, -0.8660254037844380415 ) ) ;
#27783 = CARTESIAN_POINT ( 'NONE',  ( 6.923076923076802558, -2.892918686052165622, 31.69288490824153470 ) ) ;
#27784 = EDGE_CURVE ( 'NONE', #75345, #16624, #8706, .T. ) ;
#27785 = FACE_OUTER_BOUND ( 'NONE', #74538, .T. ) ;
#27786 = DIRECTION ( 'NONE',  ( -0.000000000000000000, 0.8660254037844397068, -0.4999999999999978906 ) ) ;
#27787 = VERTEX_POINT ( 'NONE', #82601 ) ;
#27788 = CARTESIAN_POINT ( 'NONE',  ( -18.06575680251431137, -7.249945686854186278, 34.74374336980224598 ) ) ;
#27789 = ORIENTED_EDGE ( 'NONE', *, *, #70891, .F. ) ;
#27790 = EDGE_CURVE ( 'NONE', #37367, #53679, #69068, .T. ) ;
#27791 = VERTEX_POINT ( 'NONE', #28083 ) ;
#27792 = AXIS2_PLACEMENT_3D ( 'NONE', #63679, #1986, #29469 ) ;
#27793 = ORIENTED_EDGE ( 'NONE', *, *, #20185, .F. ) ;
#27795 = ORIENTED_EDGE ( 'NONE', *, *, #33304, .T. ) ;
#27794 = CARTESIAN_POINT ( 'NONE',  ( -7.173053667125516064, -8.347322224742351082, 34.93158281831414769 ) ) ;
#27796 = CARTESIAN_POINT ( 'NONE',  ( -19.50000000000000000, -3.499999999999999556, 29.75000000000000355 ) ) ;
#27797 = EDGE_CURVE ( 'NONE', #45094, #38831, #63318, .T. ) ;
#27798 = CARTESIAN_POINT ( 'NONE',  ( -5.999999999999998224, -6.189225973068211317, 35.74407628777942847 ) ) ;
#27799 = VECTOR ( 'NONE', #42305, 1000.000000000000000 ) ;
#27800 = ADVANCED_FACE ( 'NONE', ( #48790 ), #15018, .F. ) ;
#27801 = AXIS2_PLACEMENT_3D ( 'NONE', #19720, #6215, #22370 ) ;
#27802 = CARTESIAN_POINT ( 'NONE',  ( -12.33101275977489664, -12.27024696741798948, 31.24895572276497546 ) ) ;
#27803 = DIRECTION ( 'NONE',  ( 1.000000000000000000, 0.000000000000000000, 0.000000000000000000 ) ) ;
#27804 = ORIENTED_EDGE ( 'NONE', *, *, #65852, .T. ) ;
#27805 = ORIENTED_EDGE ( 'NONE', *, *, #37842, .F. ) ;
#27806 = EDGE_CURVE ( 'NONE', #13174, #76927, #56442, .T. ) ;
#27807 = ORIENTED_EDGE ( 'NONE', *, *, #1980, .T. ) ;
#27808 = LINE ( 'NONE', #55276, #14497 ) ;
#27810 = VERTEX_POINT ( 'NONE', #75821 ) ;
#27809 = CARTESIAN_POINT ( 'NONE',  ( -10.48459417441766206, -2.494656445102012565, 31.33466734024120015 ) ) ;
#27811 = B_SPLINE_CURVE_WITH_KNOTS ( 'NONE', 3,
 ( #2455, #10563, #83237, #37132, #84898, #71806, #23184, #78125, #85337, #24508 ),
 .UNSPECIFIED., .F., .F.,
 ( 4, 2, 2, 2, 4 ),
 ( 0.0007817246256747466303, 0.0009771112852218900684, 0.001172497944769033398, 0.001367884604316176728, 0.001563271263863320274 ),
 .UNSPECIFIED. ) ;
#27812 = LINE ( 'NONE', #48970, #47493 ) ;
#27813 = CYLINDRICAL_SURFACE ( 'NONE', #33569, 0.2499999999999995559 ) ;
#27814 = ORIENTED_EDGE ( 'NONE', *, *, #57939, .F. ) ;
#27815 = CARTESIAN_POINT ( 'NONE',  ( 9.822352748227467956, -2.254550872974306674, 29.97347326024527092 ) ) ;
#27816 = CARTESIAN_POINT ( 'NONE',  ( 12.46153846153846168, -9.058645607665452459, 34.76329471203371924 ) ) ;
#27817 = ORIENTED_EDGE ( 'NONE', *, *, #57477, .T. ) ;
#27818 = FACE_BOUND ( 'NONE', #62766, .T. ) ;
#27819 = CARTESIAN_POINT ( 'NONE',  ( -15.45369618967607828, -8.282780595021769443, 34.94152052738834158 ) ) ;
#27820 = CARTESIAN_POINT ( 'NONE',  ( 24.00000000000000000, 9.000000000000024869, 28.74999999999999645 ) ) ;
#27821 = CARTESIAN_POINT ( 'NONE',  ( 12.21151523731700550, -6.652501968072648708, 34.93155406624980941 ) ) ;
#27823 = DIRECTION ( 'NONE',  ( 0.000000000000000000, 0.000000000000000000, 1.000000000000000000 ) ) ;
#27822 = CARTESIAN_POINT ( 'NONE',  ( 7.911408985666684046, -11.06231777344671130, 33.60647404775212976 ) ) ;
#27824 = LINE ( 'NONE', #35022, #82652 ) ;
#27825 = CARTESIAN_POINT ( 'NONE',  ( -2.307692307692305711, -3.513871655860378418, 32.76840700105978499 ) ) ;
#27826 = ORIENTED_EDGE ( 'NONE', *, *, #5953, .T. ) ;
#27827 = CARTESIAN_POINT ( 'NONE',  ( -2.373774687052441212, -3.937682226553329556, 33.60647404775217240 ) ) ;
#27828 = FACE_OUTER_BOUND ( 'NONE', #50215, .T. ) ;
#27829 = EDGE_CURVE ( 'NONE', #28684, #26115, #3171, .T. ) ;
#27830 = B_SPLINE_CURVE_WITH_KNOTS ( 'NONE', 3,
 ( #70361, #76219, #8220, #36142, #14525, #1897, #83443, #77115, #29385, #56835 ),
 .UNSPECIFIED., .F., .F.,
 ( 4, 2, 2, 2, 4 ),
 ( 0.0007817359430256365111, 0.0009771253907250043464, 0.001172514838424372399, 0.001367904286123740234, 0.001563293733823108069 ),
 .UNSPECIFIED. ) ;
#27831 = ORIENTED_EDGE ( 'NONE', *, *, #67377, .T. ) ;
#27832 = B_SPLINE_CURVE_WITH_KNOTS ( 'NONE', 3,
 ( #5745, #54366, #75101, #33222, #46288, #60684, #47165, #13828, #41308, #68772 ),
 .UNSPECIFIED., .F., .F.,
 ( 4, 2, 2, 2, 4 ),
 ( 0.0007817359430256283796, 0.0009771253907249941549, 0.001172514838424359822, 0.001367904286123725489, 0.001563293733823091156 ),
 .UNSPECIFIED. ) ;
#27833 = AXIS2_PLACEMENT_3D ( 'NONE', #78833, #10386, #59462 ) ;
#27834 = AXIS2_PLACEMENT_3D ( 'NONE', #33009, #60474, #26249 ) ;
#27835 = DIRECTION ( 'NONE',  ( -0.000000000000000000, 1.000000000000000000, -0.000000000000000000 ) ) ;
#27836 = CARTESIAN_POINT ( 'NONE',  ( -7.596208436775802930, -2.341251567377310217, 30.72681386836322659 ) ) ;
#27837 = VERTEX_POINT ( 'NONE', #6919 ) ;
#27838 = CARTESIAN_POINT ( 'NONE',  ( 17.93391658904412012, -5.557115091759785130, 34.35708131394839171 ) ) ;
#27839 = CARTESIAN_POINT ( 'NONE',  ( 2.530705151785702878, -4.762714258010882773, 34.23016756924214832 ) ) ;
#27840 = FACE_BOUND ( 'NONE', #17638, .T. ) ;
#27842 = LINE ( 'NONE', #55307, #15731 ) ;
#27841 = CARTESIAN_POINT ( 'NONE',  ( -2.437839517130527156, -6.852621066184267029, 34.70813303252209181 ) ) ;
#27843 = CARTESIAN_POINT ( 'NONE',  ( 10.36540788444226102, -8.303909089506435137, 34.68538101551103381 ) ) ;
#27844 = CARTESIAN_POINT ( 'NONE',  ( -8.769230769230768274, -12.10708131394839349, 31.69288490824020244 ) ) ;
#27846 = CARTESIAN_POINT ( 'NONE',  ( 0.3954550505825806250, -5.557115091759785130, 34.35708131394839171 ) ) ;
#27845 = DIRECTION ( 'NONE',  ( 0.000000000000000000, 0.000000000000000000, 0.9999999999999997780 ) ) ;
#27847 = DIRECTION ( 'NONE',  ( -0.000000000000000000, 0.1736481776669307198, -0.9848077530122080203 ) ) ;
#27848 = CARTESIAN_POINT ( 'NONE',  ( 1.614399933863660985, -11.22469193450123193, 15.70125670625848890 ) ) ;
#27849 = ORIENTED_EDGE ( 'NONE', *, *, #24545, .F. ) ;
#27850 = VERTEX_POINT ( 'NONE', #35281 ) ;
#27851 = CARTESIAN_POINT ( 'NONE',  ( -4.230769230769229061, -4.000000000000000000, 29.75000000000000355 ) ) ;
#27852 = CARTESIAN_POINT ( 'NONE',  ( 14.53047197667037338, -12.69155399931963046, 30.53255429739157734 ) ) ;
#27853 = CARTESIAN_POINT ( 'NONE',  ( 6.673076923076925127, -7.500000000000001776, 35.00000000000000000 ) ) ;
#27854 = CARTESIAN_POINT ( 'NONE',  ( -0.7115152055870529457, -2.920706130388546651, 32.31842814019191223 ) ) ;
#27855 = CARTESIAN_POINT ( 'NONE',  ( -6.923076923076922462, -1.422936976036506707, 30.56769352161908415 ) ) ;
#27856 = CARTESIAN_POINT ( 'NONE',  ( 3.749999999999992006, -5.946699141100872943, 25.64062500000000000 ) ) ;
#27857 = CARTESIAN_POINT ( 'NONE',  ( 0.7114838709165043351, -4.176053281294515251, 33.81426240980091791 ) ) ;
#27858 = CARTESIAN_POINT ( 'NONE',  ( 2.307692307692623679, -2.255955759149395501, 30.00000000000324363 ) ) ;
#27859 = CARTESIAN_POINT ( 'NONE',  ( 2.307692307692309264, -13.20930481340135110, 34.54067556320372745 ) ) ;
#27860 = CARTESIAN_POINT ( 'NONE',  ( 10.61538461538461675, -6.343179335718451384, 34.87096338111211935 ) ) ;
#27861 = CARTESIAN_POINT ( 'NONE',  ( -15.00775787915638304, -11.24521262558773493, 33.06293181088029343 ) ) ;
#27862 = CARTESIAN_POINT ( 'NONE',  ( -4.853910232829680815, -6.460100341425561332, 34.89618726649961644 ) ) ;
#27863 = CARTESIAN_POINT ( 'NONE',  ( -0.4615384615385840772, -4.320704448113951379, 33.92786785259630022 ) ) ;
#27864 = VECTOR ( 'NONE', #41319, 1000.000000000000000 ) ;
#27865 = CARTESIAN_POINT ( 'NONE',  ( 14.43821800945587519, -11.93748526763465279, 32.05452791011430946 ) ) ;
#27866 = EDGE_CURVE ( 'NONE', #55482, #1586, #39205, .T. ) ;
#27867 = DIRECTION ( 'NONE',  ( -0.000000000000000000, 0.9396926207859092051, -0.3420201433256662704 ) ) ;
#27868 = EDGE_LOOP ( 'NONE', ( #41662, #88876, #5795, #52769 ) ) ;
#27869 = CARTESIAN_POINT ( 'NONE',  ( -0.2115929431903190994, -3.712312575010499938, 33.01462480002815170 ) ) ;
#27870 = CARTESIAN_POINT ( 'NONE',  ( 10.86543903529806698, -5.642605341092957971, 34.66089969410670335 ) ) ;
#27871 = CARTESIAN_POINT ( 'NONE',  ( -1.200186371490524317, -10.22469193450124791, 23.86124329374151998 ) ) ;
#27872 = B_SPLINE_CURVE_WITH_KNOTS ( 'NONE', 3,
 ( #33338, #26577, #45504, #66672, #54033, #25685, #31552, #59469, #81531, #26130 ),
 .UNSPECIFIED., .F., .F.,
 ( 4, 2, 2, 2, 4 ),
 ( 0.0007817246256747452209, 0.0009771112852218887673, 0.001172497944769032531, 0.001367884604316176294, 0.001563271263863319840 ),
 .UNSPECIFIED. ) ;
#27873 = VECTOR ( 'NONE', #43609, 1000.000000000000000 ) ;
#27874 = EDGE_CURVE ( 'NONE', #59207, #80088, #21767, .T. ) ;
#27875 = LINE ( 'NONE', #13475, #66296 ) ;
#27876 = CARTESIAN_POINT ( 'NONE',  ( -16.15384615384627409, -2.657715359629662988, 31.77849191805970364 ) ) ;
#27877 = ORIENTED_EDGE ( 'NONE', *, *, #53026, .T. ) ;
#27878 = CARTESIAN_POINT ( 'NONE',  ( -8.769230769230768274, -6.681629849574314051, 35.83090037661290239 ) ) ;
#27880 = ORIENTED_EDGE ( 'NONE', *, *, #33792, .F. ) ;
#27879 = CARTESIAN_POINT ( 'NONE',  ( -17.07692307692307665, -13.57706302396349152, 30.56769352161908060 ) ) ;
#27881 = CARTESIAN_POINT ( 'NONE',  ( -6.166666666666667851, -7.500000000000000000, 29.75000000000000355 ) ) ;
#27882 = CARTESIAN_POINT ( 'NONE',  ( 17.07692307692295586, -2.657715359629662544, 31.77849191805970364 ) ) ;
#27883 = EDGE_CURVE ( 'NONE', #60602, #1437, #77156, .T. ) ;
#27884 = B_SPLINE_CURVE_WITH_KNOTS ( 'NONE', 3,
 ( #67106, #33759, #11721, #5406, #18913, #26564, #12605, #61215, #47264, #74755 ),
 .UNSPECIFIED., .F., .F.,
 ( 4, 2, 2, 2, 4 ),
 ( 0.000000000000000000, 0.0001954339857564127327, 0.0003908679715128183640, 0.0005863019572692239681, 0.0007817359430256295722 ),
 .UNSPECIFIED. ) ;
#27885 = ORIENTED_EDGE ( 'NONE', *, *, #83287, .T. ) ;
#27886 = DIRECTION ( 'NONE',  ( -0.000000000000000000, 0.8660254037844399289, -0.4999999999999980016 ) ) ;
#27887 = CARTESIAN_POINT ( 'NONE',  ( -9.320512820512821150, -11.00000000000000000, 29.65000000000000213 ) ) ;
#27888 = EDGE_CURVE ( 'NONE', #18841, #9565, #50114, .T. ) ;
#27889 = ORIENTED_EDGE ( 'NONE', *, *, #23249, .T. ) ;
#27890 = CARTESIAN_POINT ( 'NONE',  ( 14.17754509825408960, -2.619462340734462380, 30.83744416345203021 ) ) ;
#27891 = CARTESIAN_POINT ( 'NONE',  ( -15.90384615384622613, -7.565270445406050648, 34.75000000000000000 ) ) ;
#27892 = DIRECTION ( 'NONE',  ( -0.000000000000000000, -0.9396926207859093161, -0.3420201433256663259 ) ) ;
#27893 = ORIENTED_EDGE ( 'NONE', *, *, #60568, .F. ) ;
#27894 = ORIENTED_EDGE ( 'NONE', *, *, #14083, .F. ) ;
#27895 = EDGE_CURVE ( 'NONE', #48157, #12391, #88087, .T. ) ;
#27896 = CARTESIAN_POINT ( 'NONE',  ( 3.100621261037533216, -3.069018819979302926, 32.56621877034667278 ) ) ;
#27897 = ORIENTED_EDGE ( 'NONE', *, *, #63299, .T. ) ;
#27898 = CARTESIAN_POINT ( 'NONE',  ( -15.23076923076922995, -3.937682226553329556, 33.60647404775216529 ) ) ;
#27899 = CARTESIAN_POINT ( 'NONE',  ( 5.299702745901139878, -4.989023458446560255, 34.36081565061822118 ) ) ;
#27900 = CARTESIAN_POINT ( 'NONE',  ( 9.469380733400845074, -9.172386477786396597, 34.72672124145550043 ) ) ;
#27901 = DIRECTION ( 'NONE',  ( -0.000000000000000000, -0.9396926207859092051, -0.3420201433256662704 ) ) ;
#27902 = CARTESIAN_POINT ( 'NONE',  ( 15.00728428704528561, -6.760086850603066466, 34.69517049084099369 ) ) ;
#27903 = CARTESIAN_POINT ( 'NONE',  ( 1.134638640566795420, -2.318417181685854533, 30.59732222474233865 ) ) ;
#27904 = CIRCLE ( 'NONE', #39433, 4.000000000000000000 ) ;
#27905 = DIRECTION ( 'NONE',  ( 0.000000000000000000, 0.3420201433256610524, 0.9396926207859113145 ) ) ;
#27906 = EDGE_LOOP ( 'NONE', ( #29025, #78291, #50157, #24306 ) ) ;
#27907 = ORIENTED_EDGE ( 'NONE', *, *, #27618, .F. ) ;
#27909 = EDGE_LOOP ( 'NONE', ( #38117, #20971 ) ) ;
#27908 = CARTESIAN_POINT ( 'NONE',  ( -1.607494067044030528, -7.630691491037286056, 34.74850469731152458 ) ) ;
#27910 = ADVANCED_FACE ( 'NONE', ( #23094 ), #70851, .F. ) ;
#27911 = CARTESIAN_POINT ( 'NONE',  ( -12.46153846153846168, -1.129524287112498415, 32.06866353760679544 ) ) ;
#27912 = VERTEX_POINT ( 'NONE', #78470 ) ;
#27913 = EDGE_CURVE ( 'NONE', #48093, #13650, #10473, .T. ) ;
#27914 = CARTESIAN_POINT ( 'NONE',  ( 11.78840694783958298, -3.520799739797214389, 33.17531984108286025 ) ) ;
#27915 = CARTESIAN_POINT ( 'NONE',  ( 5.142178648199100088, -3.835265460703683349, 33.15142922261929925 ) ) ;
#27916 = EDGE_LOOP ( 'NONE', ( #37990, #17072, #85934, #49521 ) ) ;
#27917 = CARTESIAN_POINT ( 'NONE',  ( -9.915173114511331320, -2.501496062324912284, 29.88072118266895671 ) ) ;
#27918 = EDGE_CURVE ( 'NONE', #6671, #50988, #64070, .T. ) ;
#27919 = ORIENTED_EDGE ( 'NONE', *, *, #41033, .F. ) ;
#27920 = CARTESIAN_POINT ( 'NONE',  ( -11.53846153846166089, -12.16647553114689728, 32.15551576947799362 ) ) ;
#27921 = ORIENTED_EDGE ( 'NONE', *, *, #44665, .T. ) ;
#27922 = CARTESIAN_POINT ( 'NONE',  ( -11.53846153846153655, -12.78798330534102945, 29.74999999999997868 ) ) ;
#27923 = ORIENTED_EDGE ( 'NONE', *, *, #369, .F. ) ;
#27924 = EDGE_CURVE ( 'NONE', #16798, #24594, #64952, .T. ) ;
#27925 = CARTESIAN_POINT ( 'NONE',  ( -8.992156986746914882, -4.887634598454295265, 34.01352882383564946 ) ) ;
#27926 = CARTESIAN_POINT ( 'NONE',  ( 12.21151523731700550, -2.341070481393819236, 30.72580821765574299 ) ) ;
#27927 = FACE_BOUND ( 'NONE', #61307, .T. ) ;
#27928 = VECTOR ( 'NONE', #48479, 1000.000000000000114 ) ;
#27929 = CARTESIAN_POINT ( 'NONE',  ( 5.776515075435670887, -2.353723527008295680, 30.78948104536958752 ) ) ;
#27930 = CARTESIAN_POINT ( 'NONE',  ( -17.86920819217521483, -12.11778462344220841, 31.66786338562085135 ) ) ;
#27931 = AXIS2_PLACEMENT_3D ( 'NONE', #62049, #82780, #70134 ) ;
#27932 = CARTESIAN_POINT ( 'NONE',  ( 9.468822767743363400, -2.353723527008296568, 30.78948104536958752 ) ) ;
#27933 = CARTESIAN_POINT ( 'NONE',  ( -12.46153846153846168, -13.49023893513002648, 31.06009739812518688 ) ) ;
#27934 = CARTESIAN_POINT ( 'NONE',  ( -3.100243529005665799, -3.285477652293413264, 32.44071101563363158 ) ) ;
#27935 = CARTESIAN_POINT ( 'NONE',  ( -4.153846153846273204, -11.48612834414049644, 32.76840700105863391 ) ) ;
#27936 = CARTESIAN_POINT ( 'NONE',  ( 8.769230769230768274, -3.050289026998446396, 32.03036669348365706 ) ) ;
#27937 = ORIENTED_EDGE ( 'NONE', *, *, #8228, .F. ) ;
#27938 = EDGE_CURVE ( 'NONE', #48865, #3633, #9048, .T. ) ;
#27939 = B_SPLINE_CURVE_WITH_KNOTS ( 'NONE', 3,
 ( #40708, #68170, #67729, #33053, #6034, #54637, #20426, #80814, #33502, #60961 ),
 .UNSPECIFIED., .F., .F.,
 ( 4, 2, 2, 2, 4 ),
 ( 0.000000000000000000, 0.0001954339857564073388, 0.0003908679715128146777, 0.0005863019572692220165, 0.0007817359430256293554 ),
 .UNSPECIFIED. ) ;
#27940 = ORIENTED_EDGE ( 'NONE', *, *, #84655, .T. ) ;
#27942 = CARTESIAN_POINT ( 'NONE',  ( 7.976679547917406410, -10.19071101563364756, 33.96452234770658407 ) ) ;
#27941 = CARTESIAN_POINT ( 'NONE',  ( 2.057715563643716994, -2.920706130388546651, 32.31842814019191223 ) ) ;
#27943 = CARTESIAN_POINT ( 'NONE',  ( -11.76194648218548622, -11.89387501736622710, 32.13663884655806413 ) ) ;
#27944 = CARTESIAN_POINT ( 'NONE',  ( -18.00000000000000000, -13.18701529485372070, 34.52197243641129631 ) ) ;
#27945 = EDGE_CURVE ( 'NONE', #32906, #3675, #14991, .T. ) ;
#27946 = CARTESIAN_POINT ( 'NONE',  ( 15.45378058238208041, -3.587049720035815348, 32.86302985866382897 ) ) ;
#27947 = DIRECTION ( 'NONE',  ( -0.000000000000000000, 1.000000000000000000, -0.000000000000000000 ) ) ;
#27948 = EDGE_CURVE ( 'NONE', #77695, #275, #79372, .T. ) ;
#27949 = VERTEX_POINT ( 'NONE', #71265 ) ;
#27950 = CARTESIAN_POINT ( 'NONE',  ( 8.769230769230768274, -13.04860791097971706, 34.73218667398347037 ) ) ;
#27951 = CARTESIAN_POINT ( 'NONE',  ( 3.296837581771669079, -11.16473453929635440, 33.15142922261926373 ) ) ;
#27952 = CARTESIAN_POINT ( 'NONE',  ( -14.24243716817946925, -12.51329471203373700, 31.30864560766537963 ) ) ;
#27953 = FACE_OUTER_BOUND ( 'NONE', #62719, .T. ) ;
#27954 = ORIENTED_EDGE ( 'NONE', *, *, #62377, .T. ) ;
#27955 = EDGE_CURVE ( 'NONE', #46303, #60075, #65379, .T. ) ;
#27956 = ORIENTED_EDGE ( 'NONE', *, *, #67448, .T. ) ;
#27957 = ORIENTED_EDGE ( 'NONE', *, *, #4128, .T. ) ;
#27958 = LINE ( 'NONE', #35154, #29073 ) ;
#27959 = VERTEX_POINT ( 'NONE', #37483 ) ;
#27960 = CARTESIAN_POINT ( 'NONE',  ( -9.626240358957616650, -9.905515769479276145, 34.41647553114623292 ) ) ;
#27961 = CARTESIAN_POINT ( 'NONE',  ( 22.75000000000000000, -7.500000000000000000, 29.75000000000000355 ) ) ;
#27962 = CARTESIAN_POINT ( 'NONE',  ( -5.999999999999998224, -12.78798330534102945, 29.74999999999997868 ) ) ;
#27963 = CARTESIAN_POINT ( 'NONE',  ( 20.00000000000000000, -7.500000000000000000, 29.75000000000000355 ) ) ;
#27964 = CARTESIAN_POINT ( 'NONE',  ( 14.30769230769218758, -4.481592998941358097, 33.73612834414048933 ) ) ;
#27966 = ORIENTED_EDGE ( 'NONE', *, *, #73095, .F. ) ;
#27965 = VECTOR ( 'NONE', #151, 1000.000000000000227 ) ;
#27967 = CARTESIAN_POINT ( 'NONE',  ( -1.105886215935217678E-14, 12.75000000000002487, 13.00000000000000178 ) ) ;
#27969 = EDGE_LOOP ( 'NONE', ( #32836, #41056 ) ) ;
#27968 = CARTESIAN_POINT ( 'NONE',  ( -7.846153846153844924, -1.044019251281081972, 31.83374038241031911 ) ) ;
#27970 = CARTESIAN_POINT ( 'NONE',  ( -9.442253380669374252, -4.235687564193447052, 33.53795663066793509 ) ) ;
#27971 = CARTESIAN_POINT ( 'NONE',  ( -8.899840424434849240, -7.722926974430166069, 34.99546784045485737 ) ) ;
#27972 = CARTESIAN_POINT ( 'NONE',  ( 13.38461538461526423, -11.67786785259630911, 32.92929555188603530 ) ) ;
#27973 = CARTESIAN_POINT ( 'NONE',  ( 11.78851595837499211, -10.06805714834173493, 34.32951233291982618 ) ) ;
#27974 = CARTESIAN_POINT ( 'NONE',  ( 2.530705151785704210, -2.523321265292116422, 31.42251411153756990 ) ) ;
#27975 = DIRECTION ( 'NONE',  ( 1.000000000000000000, 0.000000000000000000, 0.000000000000000000 ) ) ;
#27976 = CARTESIAN_POINT ( 'NONE',  ( -3.007806096502555704, -7.369474539155830506, 34.99858011523957657 ) ) ;
#27977 = CARTESIAN_POINT ( 'NONE',  ( -2.775308065498752086, -8.577988221561495763, 25.26749329374151642 ) ) ;
#27978 = ORIENTED_EDGE ( 'NONE', *, *, #55931, .F. ) ;
#27979 = CARTESIAN_POINT ( 'NONE',  ( -1.384615384615383471, -1.509761064869970415, 31.06009739812519044 ) ) ;
#27980 = LINE ( 'NONE', #68963, #60572 ) ;
#27981 = EDGE_CURVE ( 'NONE', #56983, #8169, #26624, .T. ) ;
#27982 = LINE ( 'NONE', #34739, #73449 ) ;
#27983 = ORIENTED_EDGE ( 'NONE', *, *, #44412, .F. ) ;
#27984 = CYLINDRICAL_SURFACE ( 'NONE', #31190, 0.2499999999999994726 ) ;
#27985 = CARTESIAN_POINT ( 'NONE',  ( 11.53846153846141576, -4.320704448113951379, 33.92786785259630022 ) ) ;
#27986 = CARTESIAN_POINT ( 'NONE',  ( 14.05769230769229061, -2.249999999999998668, 29.81609741502487410 ) ) ;
#27987 = CARTESIAN_POINT ( 'NONE',  ( -4.377331097570101193, -10.81261337010820256, 33.49550067578627477 ) ) ;
#27988 = EDGE_CURVE ( 'NONE', #50472, #4672, #35225, .T. ) ;
#27989 = B_SPLINE_CURVE_WITH_KNOTS ( 'NONE', 3,
 ( #20871, #21760, #6913, #607, #76253, #55544, #75381, #34386, #48340, #83027 ),
 .UNSPECIFIED., .F., .F.,
 ( 4, 2, 2, 2, 4 ),
 ( 0.000000000000000000, 0.0001954339857564073659, 0.0003908679715128147319, 0.0005863019572692221250, 0.0007817359430256294638 ),
 .UNSPECIFIED. ) ;
#27990 = EDGE_LOOP ( 'NONE', ( #39378, #53133 ) ) ;
#27991 = CARTESIAN_POINT ( 'NONE',  ( -12.39547011053602610, -8.973038597847271092, 34.52809138561121216 ) ) ;
#27992 = CIRCLE ( 'NONE', #32304, 0.2500000000000002220 ) ;
#27993 = DIRECTION ( 'NONE',  ( 1.000000000000000000, 0.000000000000000000, 0.000000000000000000 ) ) ;
#27994 = DIRECTION ( 'NONE',  ( -0.000000000000000000, -0.7660444431189791237, -0.6427876096865379196 ) ) ;
#27995 = ORIENTED_EDGE ( 'NONE', *, *, #69096, .F. ) ;
#27996 = ADVANCED_FACE ( 'NONE', ( #11808 ), #47352, .F. ) ;
#27997 = DIRECTION ( 'NONE',  ( -0.000000000000000000, 0.7660444431189791237, -0.6427876096865379196 ) ) ;
#27998 = VECTOR ( 'NONE', #25127, 1000.000000000000114 ) ;
#27999 = VECTOR ( 'NONE', #11915, 999.9999999999998863 ) ;
#28000 = ORIENTED_EDGE ( 'NONE', *, *, #72031, .T. ) ;
#28001 = CARTESIAN_POINT ( 'NONE',  ( -2.438383774359869083, -12.11776431015576172, 31.66791131148498906 ) ) ;
#28002 = DIRECTION ( 'NONE',  ( 0.000000000000000000, 0.000000000000000000, 1.000000000000000000 ) ) ;
#28003 = ORIENTED_EDGE ( 'NONE', *, *, #58076, .F. ) ;
#28004 = B_SPLINE_CURVE_WITH_KNOTS ( 'NONE', 3,
 ( #6415, #40644, #32539, #18147, #66330, #26233, #60014, #53700, #19909, #87515 ),
 .UNSPECIFIED., .F., .F.,
 ( 4, 2, 2, 2, 4 ),
 ( 0.000000000000000000, 0.0001954339857564093175, 0.0003908679715128186350, 0.0005863019572692279796, 0.0007817359430256372700 ),
 .UNSPECIFIED. ) ;
#28005 = CARTESIAN_POINT ( 'NONE',  ( 7.846153846153846700, -12.10708131394839349, 31.69288490824020244 ) ) ;
#28006 = CARTESIAN_POINT ( 'NONE',  ( 2.307692307692187583, -6.879047030192662504, 34.71129190930017927 ) ) ;
#28007 = CARTESIAN_POINT ( 'NONE',  ( 13.38461538461526601, -6.879047030192662504, 34.71129190930017927 ) ) ;
#28008 = MANIFOLD_SOLID_BREP ( 'Cut-Extrude2', #84621 ) ;
#28009 = EDGE_CURVE ( 'NONE', #46107, #47096, #46906, .T. ) ;
#28010 = CARTESIAN_POINT ( 'NONE',  ( 11.28843831424008215, -12.45566812827425451, 31.48439005359158926 ) ) ;
#28011 = PLANE ( 'NONE',  #58383 ) ;
#28012 = ORIENTED_EDGE ( 'NONE', *, *, #77522, .T. ) ;
#28013 = FACE_BOUND ( 'NONE', #32750, .T. ) ;
#28014 = ORIENTED_EDGE ( 'NONE', *, *, #63111, .F. ) ;
#28015 = CARTESIAN_POINT ( 'NONE',  ( -2.307692307692428724, -2.657715359629662544, 31.77849191805970364 ) ) ;
#28016 = ADVANCED_FACE ( 'NONE', ( #68085 ), #19004, .F. ) ;
#28017 = CARTESIAN_POINT ( 'NONE',  ( 4.403900465484466231, -11.79725096376909299, 32.30694842903960762 ) ) ;
#28018 = EDGE_CURVE ( 'NONE', #23009, #14315, #71753, .T. ) ;
#28019 = DIRECTION ( 'NONE',  ( -1.000000000000000000, -0.000000000000000000, -0.000000000000000000 ) ) ;
#28020 = CARTESIAN_POINT ( 'NONE',  ( 16.85343813319912698, -2.599994579823202923, 30.74605699353653776 ) ) ;
#28021 = ORIENTED_EDGE ( 'NONE', *, *, #60326, .T. ) ;
#28022 = AXIS2_PLACEMENT_3D ( 'NONE', #5047, #52335, #23971 ) ;
#28023 = ORIENTED_EDGE ( 'NONE', *, *, #54680, .F. ) ;
#28024 = ORIENTED_EDGE ( 'NONE', *, *, #88503, .T. ) ;
#28025 = CARTESIAN_POINT ( 'NONE',  ( -3.007756386675835003, -11.43677907613345113, 33.22367315496201456 ) ) ;
#28026 = ORIENTED_EDGE ( 'NONE', *, *, #59300, .T. ) ;
#28027 = EDGE_CURVE ( 'NONE', #42657, #9576, #56770, .T. ) ;
#28028 = CARTESIAN_POINT ( 'NONE',  ( 15.16468685140909400, -3.322132147404559532, 32.92929555188719348 ) ) ;
#28029 = CARTESIAN_POINT ( 'NONE',  ( -6.699701437304502960, -2.251407671071270489, 29.88021292934942252 ) ) ;
#28030 = CARTESIAN_POINT ( 'NONE',  ( -17.14219307747939425, -3.083524468853725775, 32.58852847137143272 ) ) ;
#28031 = CARTESIAN_POINT ( 'NONE',  ( -8.546451100252701494, -4.226511098958373402, 33.85474049983370293 ) ) ;
#28032 = B_SPLINE_CURVE_WITH_KNOTS ( 'NONE', 3,
 ( #9792, #30069, #3911, #43143, #30506, #16994, #23301, #36821, #85455, #57532 ),
 .UNSPECIFIED., .F., .F.,
 ( 4, 2, 2, 2, 4 ),
 ( 0.000000000000000000, 0.0001954311564186864949, 0.0003908623128373729899, 0.0005862934692560594577, 0.0007817246256747459798 ),
 .UNSPECIFIED. ) ;
#28033 = DIRECTION ( 'NONE',  ( 0.000000000000000000, 0.8660254037844377084, -0.5000000000000015543 ) ) ;
#28034 = LINE ( 'NONE', #83436, #6405 ) ;
#28035 = CARTESIAN_POINT ( 'NONE',  ( -5.207070286361297207, -3.817052484675422797, 33.13202310037935661 ) ) ;
#28036 = ORIENTED_EDGE ( 'NONE', *, *, #2425, .T. ) ;
#28037 = ORIENTED_EDGE ( 'NONE', *, *, #75699, .F. ) ;
#28038 = EDGE_CURVE ( 'NONE', #6878, #87412, #87041, .T. ) ;
#28039 = VERTEX_POINT ( 'NONE', #83823 ) ;
#28040 = DIRECTION ( 'NONE',  ( 0.000000000000000000, 0.6427876096865368094, 0.7660444431189802339 ) ) ;
#28042 = CARTESIAN_POINT ( 'NONE',  ( 10.68145296638705410, -6.386643153685127139, 34.62446782046654192 ) ) ;
#28041 = DIRECTION ( 'NONE',  ( -0.000000000000000000, 0.3420201433256694901, -0.9396926207859082059 ) ) ;
#28043 = CARTESIAN_POINT ( 'NONE',  ( -20.00000000000000355, -10.00000000000000533, 13.00000000000000178 ) ) ;
#28044 = CARTESIAN_POINT ( 'NONE',  ( 16.15384615384615330, -2.249999999999998668, 29.50000000000001421 ) ) ;
#28045 = ADVANCED_FACE ( 'NONE', ( #7716 ), #41491, .F. ) ;
#28046 = FACE_BOUND ( 'NONE', #77062, .T. ) ;
#28047 = CARTESIAN_POINT ( 'NONE',  ( 9.915319043920543862, -3.587049720035815348, 32.86302985866382897 ) ) ;
#28048 = EDGE_CURVE ( 'NONE', #12551, #5961, #82045, .T. ) ;
#28049 = EDGE_LOOP ( 'NONE', ( #14040, #76654 ) ) ;
#28050 = AXIS2_PLACEMENT_3D ( 'NONE', #8680, #63157, #29398 ) ;
#28051 = CARTESIAN_POINT ( 'NONE',  ( -7.846153846153844924, -1.129524287112498415, 32.06866353760679544 ) ) ;
#28052 = LINE ( 'NONE', #36585, #76160 ) ;
#28053 = DIRECTION ( 'NONE',  ( 0.000000000000000000, -1.000000000000000000, 0.000000000000000000 ) ) ;
#28054 = CARTESIAN_POINT ( 'NONE',  ( 3.453548899747295842, -11.60474049983370648, 33.02348890104160262 ) ) ;
#28055 = ORIENTED_EDGE ( 'NONE', *, *, #60734, .F. ) ;
#28056 = CARTESIAN_POINT ( 'NONE',  ( 5.076923076923075762, -12.62096338111211580, 30.90682066428153263 ) ) ;
#28057 = B_SPLINE_CURVE_WITH_KNOTS ( 'NONE', 3,
 ( #59217, #38064, #4731, #86725, #11040, #17803, #32207, #58773, #24541, #72728 ),
 .UNSPECIFIED., .F., .F.,
 ( 4, 2, 2, 2, 4 ),
 ( 0.000000000000000000, 0.0001954339857564078267, 0.0003908679715128156535, 0.0005863019572692235344, 0.0007817359430256313069 ),
 .UNSPECIFIED. ) ;
#28058 = ORIENTED_EDGE ( 'NONE', *, *, #29687, .T. ) ;
#28059 = FACE_BOUND ( 'NONE', #31783, .T. ) ;
#28060 = CARTESIAN_POINT ( 'NONE',  ( 9.627037246346917598, -6.026961402152685388, 34.52809138561120506 ) ) ;
#28061 = VECTOR ( 'NONE', #6345, 1000.000000000000000 ) ;
#28062 = CARTESIAN_POINT ( 'NONE',  ( -6.989159302437059296, -9.905515769479276145, 34.41647553114623292 ) ) ;
#28063 = DIRECTION ( 'NONE',  ( -0.000000000000000000, 0.3420201433256694901, -0.9396926207859082059 ) ) ;
#28064 = ORIENTED_EDGE ( 'NONE', *, *, #58669, .F. ) ;
#28065 = AXIS2_PLACEMENT_3D ( 'NONE', #66114, #58917, #11185 ) ;
#28066 = CARTESIAN_POINT ( 'NONE',  ( -14.37296275365308418, -12.46129190929999986, 30.37095296980880832 ) ) ;
#28067 = CARTESIAN_POINT ( 'NONE',  ( 15.23076923076923173, -2.292212530054420494, 30.41441678777542634 ) ) ;
#28068 = CARTESIAN_POINT ( 'NONE',  ( 12.71159277317677549, -6.567000820036036579, 34.66262288849541306 ) ) ;
#28069 = LINE ( 'NONE', #62284, #57636 ) ;
#28070 = ORIENTED_EDGE ( 'NONE', *, *, #7197, .F. ) ;
#28071 = CARTESIAN_POINT ( 'NONE',  ( 12.59158351745823445, -2.254550872974306674, 29.97347326024527092 ) ) ;
#28072 = VERTEX_POINT ( 'NONE', #41053 ) ;
#28074 = ORIENTED_EDGE ( 'NONE', *, *, #29772, .T. ) ;
#28073 = LINE ( 'NONE', #75376, #41277 ) ;
#28075 = FACE_OUTER_BOUND ( 'NONE', #67778, .T. ) ;
#28076 = CYLINDRICAL_SURFACE ( 'NONE', #59971, 0.2499999999999994726 ) ;
#28077 = CARTESIAN_POINT ( 'NONE',  ( 13.16113044089144068, -9.331801661448606566, 34.40259984581193464 ) ) ;
#28078 = CARTESIAN_POINT ( 'NONE',  ( -13.31935981333935359, -3.835265460703683349, 33.15142922261929925 ) ) ;
#28079 = CARTESIAN_POINT ( 'NONE',  ( 3.230769230769231726, -12.09954503811598769, 35.62045528018868623 ) ) ;
#28081 = CARTESIAN_POINT ( 'NONE',  ( -16.28399412357784826, -8.630895178749536711, 34.87696386517710323 ) ) ;
#28080 = CARTESIAN_POINT ( 'NONE',  ( 13.38461538461526601, -6.026961402154118019, 34.52809138561165270 ) ) ;
#28082 = B_SPLINE_CURVE_WITH_KNOTS ( 'NONE', 3,
 ( #4684, #16412, #17301, #44759, #9650, #10550, #37116, #64580, #2879, #30371 ),
 .UNSPECIFIED., .F., .F.,
 ( 4, 2, 2, 2, 4 ),
 ( 0.000000000000000000, 0.0001954311564186861968, 0.0003908623128373723936, 0.0005862934692560585904, 0.0007817246256747447872 ),
 .UNSPECIFIED. ) ;
#28083 = CARTESIAN_POINT ( 'NONE',  ( 6.923076923076800782, -3.083524468854526912, 32.58852847137268327 ) ) ;
#28084 = CARTESIAN_POINT ( 'NONE',  ( 1.944543648262996083, -5.555456351736983045, 20.56250000000000000 ) ) ;
#28085 = ORIENTED_EDGE ( 'NONE', *, *, #41772, .F. ) ;
#28086 = B_SPLINE_CURVE_WITH_KNOTS ( 'NONE', 3,
 ( #65960, #31750, #59208, #53338, #86714, #39842, #67309, #60542, #40288, #28090 ),
 .UNSPECIFIED., .F., .F.,
 ( 4, 2, 2, 2, 4 ),
 ( 0.0007817246256747471724, 0.0009771112852218905021, 0.001172497944769033615, 0.001367884604316176944, 0.001563271263863320274 ),
 .UNSPECIFIED. ) ;
#28087 = DIRECTION ( 'NONE',  ( 0.000000000000000000, 0.6427876096865373645, -0.7660444431189797898 ) ) ;
#28088 = ORIENTED_EDGE ( 'NONE', *, *, #312, .F. ) ;
#28089 = ORIENTED_EDGE ( 'NONE', *, *, #67908, .F. ) ;
#28090 = CARTESIAN_POINT ( 'NONE',  ( -3.230769230769229949, -9.058645607665452459, 34.76329471203371924 ) ) ;
#28091 = ORIENTED_EDGE ( 'NONE', *, *, #73017, .F. ) ;
#28092 = FACE_OUTER_BOUND ( 'NONE', #60221, .T. ) ;
#28093 = UNCERTAINTY_MEASURE_WITH_UNIT (LENGTH_MEASURE( 1.000000000000000082E-05 ), #47359, 'distance_accuracy_value', 'NONE');
#28094 = LINE ( 'NONE', #27648, #23733 ) ;
#28095 = CARTESIAN_POINT ( 'NONE',  ( 3.230769230769231726, -8.120952969808772792, 34.71129190930000163 ) ) ;
#28096 = VECTOR ( 'NONE', #70731, 1000.000000000000000 ) ;
#28097 = DIRECTION ( 'NONE',  ( -0.000000000000000000, 0.000000000000000000, 1.000000000000000000 ) ) ;
#28098 = CARTESIAN_POINT ( 'NONE',  ( 6.130525701763564150, -2.619367082507848554, 30.83698974864644171 ) ) ;
#28099 = DIRECTION ( 'NONE',  ( 0.000000000000000000, 0.6427876096865373645, -0.7660444431189797898 ) ) ;
#28100 = DIRECTION ( 'NONE',  ( -1.000000000000000000, -0.000000000000000000, -0.000000000000000000 ) ) ;
#28101 = CARTESIAN_POINT ( 'NONE',  ( -4.377331097570102969, -3.754499324213721234, 33.06261337010820256 ) ) ;
#28102 = CARTESIAN_POINT ( 'NONE',  ( 6.923076923076800782, -10.33852847137269571, 34.16647553114546554 ) ) ;
#28103 = DIRECTION ( 'NONE',  ( -0.000000000000000000, 0.7660444431189791237, -0.6427876096865379196 ) ) ;
#28104 = CARTESIAN_POINT ( 'NONE',  ( 11.53846153846141753, -5.219633306517616589, 34.19971097300220464 ) ) ;
#28105 = CARTESIAN_POINT ( 'NONE',  ( -9.692307692307814193, -11.67786785259630911, 32.92929555188603530 ) ) ;
#28106 = ORIENTED_EDGE ( 'NONE', *, *, #68461, .F. ) ;
#28107 = ORIENTED_EDGE ( 'NONE', *, *, #43185, .F. ) ;
#28108 = FACE_OUTER_BOUND ( 'NONE', #35266, .T. ) ;
#28109 = CARTESIAN_POINT ( 'NONE',  ( 1.634669804528839476, -3.435999193479609470, 33.07426656108011542 ) ) ;
#28110 = CARTESIAN_POINT ( 'NONE',  ( -6.700064078983527516, -11.98016756924215009, 32.48728574198911190 ) ) ;
#28111 = CARTESIAN_POINT ( 'NONE',  ( 9.915087361285756629, -12.11081565061823717, 32.26097654155341843 ) ) ;
#28112 = LINE ( 'NONE', #83963, #8977 ) ;
#28113 = CYLINDRICAL_SURFACE ( 'NONE', #55618, 0.2499999999999995559 ) ;
#28114 = CARTESIAN_POINT ( 'NONE',  ( 5.076923076923075762, -3.886160181151819604, 36.00935417666054406 ) ) ;
#28115 = EDGE_LOOP ( 'NONE', ( #83596, #14788, #8085, #39203 ) ) ;
#28116 = CARTESIAN_POINT ( 'NONE',  ( 6.000000000000001776, -7.500000000000001776, 35.04278698407183867 ) ) ;
#28117 = VERTEX_POINT ( 'NONE', #75282 ) ;
#28118 = DIRECTION ( 'NONE',  ( -1.000000000000000000, 0.000000000000000000, 0.000000000000000000 ) ) ;
#28119 = ADVANCED_FACE ( 'NONE', ( #8153 ), #1386, .F. ) ;
#28120 = CARTESIAN_POINT ( 'NONE',  ( 10.61538461538461675, -4.098570777380720287, 33.41473453929634729 ) ) ;
#28121 = CARTESIAN_POINT ( 'NONE',  ( -0.4615384615384611200, -6.386643153685126251, 34.62446782046654192 ) ) ;
#28122 = CARTESIAN_POINT ( 'NONE',  ( 4.153846153846030731, -6.835583212225970762, 34.95778746994575670 ) ) ;
#28123 = CARTESIAN_POINT ( 'NONE',  ( -3.453648747506816719, -7.630690623152302621, 34.99857592706774057 ) ) ;
#28124 = ORIENTED_EDGE ( 'NONE', *, *, #13715, .T. ) ;
#28125 = EDGE_LOOP ( 'NONE', ( #71322, #52707 ) ) ;
#28126 = EDGE_LOOP ( 'NONE', ( #29473, #62971, #51497, #17406 ) ) ;
#28127 = ORIENTED_EDGE ( 'NONE', *, *, #49098, .F. ) ;
#28128 = EDGE_CURVE ( 'NONE', #59563, #88887, #6811, .T. ) ;
#28129 = CARTESIAN_POINT ( 'NONE',  ( 13.13463865367303463, -3.137211980971221781, 32.19342716148376837 ) ) ;
#28130 = CARTESIAN_POINT ( 'NONE',  ( 7.596177115211490083, -3.627789207965226748, 32.91389620160131102 ) ) ;
#28131 = CARTESIAN_POINT ( 'NONE',  ( 1.384615384615386802, -12.48256725967547354, 35.29906147534542527 ) ) ;
#28132 = CARTESIAN_POINT ( 'NONE',  ( -15.23076923076922995, -11.16473453929635440, 33.15142922261926373 ) ) ;
#28133 = VECTOR ( 'NONE', #11348, 1000.000000000000000 ) ;
#28134 = CYLINDRICAL_SURFACE ( 'NONE', #19137, 4.000000000000000000 ) ;
#28135 = CARTESIAN_POINT ( 'NONE',  ( -2.307692307692427391, -3.300289026999228881, 32.46337939537708905 ) ) ;
#28136 = EDGE_LOOP ( 'NONE', ( #65212, #43244, #46892, #72328 ) ) ;
#28137 = EDGE_LOOP ( 'NONE', ( #489, #28598 ) ) ;
#28138 = AXIS2_PLACEMENT_3D ( 'NONE', #16020, #70521, #9272 ) ;
#28139 = ORIENTED_EDGE ( 'NONE', *, *, #52356, .F. ) ;
#28141 = ORIENTED_EDGE ( 'NONE', *, *, #4365, .F. ) ;
#28140 = CARTESIAN_POINT ( 'NONE',  ( 4.153846153846032507, -2.892918686052165622, 31.69288490824153470 ) ) ;
#28142 = FACE_OUTER_BOUND ( 'NONE', #76742, .T. ) ;
#28143 = CARTESIAN_POINT ( 'NONE',  ( -2.084912766423896002, -9.332535724633405749, 34.40230450496446224 ) ) ;
#28144 = EDGE_CURVE ( 'NONE', #52360, #81993, #6207, .T. ) ;
#28145 = CARTESIAN_POINT ( 'NONE',  ( 3.749999999999992006, -5.946699141100872943, 19.39062500000000355 ) ) ;
#28146 = EDGE_CURVE ( 'NONE', #10219, #13098, #63075, .T. ) ;
#28147 = ORIENTED_EDGE ( 'NONE', *, *, #14110, .T. ) ;
#28148 = EDGE_LOOP ( 'NONE', ( #26762, #54706 ) ) ;
#28149 = CARTESIAN_POINT ( 'NONE',  ( 4.087763774486017354, -3.937682226553329556, 33.60647404775217240 ) ) ;
#28150 = ORIENTED_EDGE ( 'NONE', *, *, #68677, .T. ) ;
#28151 = FACE_BOUND ( 'NONE', #42042, .T. ) ;
#28152 = CARTESIAN_POINT ( 'NONE',  ( 6.856993512121043466, -4.098570777380720287, 33.41473453929634729 ) ) ;
#28153 = EDGE_CURVE ( 'NONE', #77091, #15767, #27731, .T. ) ;
#28154 = CARTESIAN_POINT ( 'NONE',  ( -4.283994123577847368, -10.31621877034669588, 34.18098118002070152 ) ) ;
#28155 = ORIENTED_EDGE ( 'NONE', *, *, #32573, .F. ) ;
#28156 = CARTESIAN_POINT ( 'NONE',  ( 0.7115928814519137946, -8.346898887586323923, 34.93166121998716278 ) ) ;
#28157 = CARTESIAN_POINT ( 'NONE',  ( -15.93106648486808119, -12.69155399931963046, 30.53255429739158444 ) ) ;
#28158 = CARTESIAN_POINT ( 'NONE',  ( 9.019285189144222059, -8.346898887586323923, 34.93166121998716278 ) ) ;
#28159 = CARTESIAN_POINT ( 'NONE',  ( 0.5267940328144852247, -6.879047030191282275, 34.71129190930002295 ) ) ;
#28160 = CARTESIAN_POINT ( 'NONE',  ( -3.454254155333561283, -9.417330523894424488, 34.63758898049880486 ) ) ;
#28161 = EDGE_LOOP ( 'NONE', ( #29714, #51578 ) ) ;
#28162 = CARTESIAN_POINT ( 'NONE',  ( -12.33101302330481808, -2.372941743896879174, 30.88044141588253666 ) ) ;
#28163 = CARTESIAN_POINT ( 'NONE',  ( -5.999999999999998224, -3.937682226553329556, 33.60647404775216529 ) ) ;
#28164 = CARTESIAN_POINT ( 'NONE',  ( 0.2115152242454957365, -11.86270091957321071, 32.19358267280088626 ) ) ;
#28165 = DIRECTION ( 'NONE',  ( 1.000000000000000000, 0.000000000000000000, 0.000000000000000000 ) ) ;
#28166 = LINE ( 'NONE', #82690, #68874 ) ;
#28167 = VECTOR ( 'NONE', #53769, 1000.000000000000227 ) ;
#28168 = FACE_BOUND ( 'NONE', #29330, .T. ) ;
#28170 = DIRECTION ( 'NONE',  ( -0.000000000000000000, -0.3420201433256694346, -0.9396926207859080948 ) ) ;
#28169 = CARTESIAN_POINT ( 'NONE',  ( 4.853438133199128757, -11.41268669641500466, 32.86336882939237825 ) ) ;
#28171 = CARTESIAN_POINT ( 'NONE',  ( 5.142990410273152513, -9.058645607665452459, 34.76329471203371924 ) ) ;
#28173 = CARTESIAN_POINT ( 'NONE',  ( 15.45378058238208219, -9.886259254753566594, 34.14407573483972413 ) ) ;
#28172 = CARTESIAN_POINT ( 'NONE',  ( 3.930361229281823743, -5.827078755546623690, 34.72654668319379567 ) ) ;
#28174 = CARTESIAN_POINT ( 'NONE',  ( -15.23076923076922995, -3.886160181151819604, 36.00935417666054406 ) ) ;
#28175 = CARTESIAN_POINT ( 'NONE',  ( -2.724691934501232371, -8.700186371490559623, 19.76375670625849423 ) ) ;
#28176 = ORIENTED_EDGE ( 'NONE', *, *, #35171, .T. ) ;
#28177 = CARTESIAN_POINT ( 'NONE',  ( 12.52679403281448600, -2.625532179533470512, 30.86335684631491105 ) ) ;
#28178 = EDGE_LOOP ( 'NONE', ( #81194, #88098, #61005, #2742 ) ) ;
#28179 = DIRECTION ( 'NONE',  ( -0.000000000000000000, -0.1736481776669307198, -0.9848077530122080203 ) ) ;
#28180 = ORIENTED_EDGE ( 'NONE', *, *, #12587, .T. ) ;
#28181 = DIRECTION ( 'NONE',  ( 0.000000000000000000, 0.000000000000000000, 1.000000000000000000 ) ) ;
#28182 = CYLINDRICAL_SURFACE ( 'NONE', #34442, 0.2500000000000009437 ) ;
#28184 = ORIENTED_EDGE ( 'NONE', *, *, #42226, .F. ) ;
#28183 = VECTOR ( 'NONE', #54136, 1000.000000000000227 ) ;
#28185 = CARTESIAN_POINT ( 'NONE',  ( -15.23076923076935074, -5.219633306517616589, 34.19971097300220464 ) ) ;
#28186 = CARTESIAN_POINT ( 'NONE',  ( 2.775308065498768517, -8.577988221561467341, 16.79500670625849068 ) ) ;
#28187 = DIRECTION ( 'NONE',  ( 0.000000000000000000, 0.000000000000000000, -1.000000000000000000 ) ) ;
#28188 = CARTESIAN_POINT ( 'NONE',  ( -5.142193077479396912, -3.083524468853724443, 32.58852847137143272 ) ) ;
#28189 = CARTESIAN_POINT ( 'NONE',  ( 15.23076923076923173, -6.386643153685126251, 34.62446782046654192 ) ) ;
#28190 = CARTESIAN_POINT ( 'NONE',  ( 23.49999999999998934, 1.674711738930281374E-15, 13.00000000000000178 ) ) ;
#28191 = CARTESIAN_POINT ( 'NONE',  ( 6.989145274079363368, -4.098570777380720287, 33.41473453929635440 ) ) ;
#28192 = CARTESIAN_POINT ( 'NONE',  ( 11.76124107972994537, -3.755027918224367767, 33.06320215134714857 ) ) ;
#28193 = CARTESIAN_POINT ( 'NONE',  ( -1.492201783934593573, -3.724691934501250135, 20.57999329374151998 ) ) ;
#28194 = DIRECTION ( 'NONE',  ( -0.000000000000000000, 0.3420201433256694346, -0.9396926207859080948 ) ) ;
#28195 = DIRECTION ( 'NONE',  ( 0.000000000000000000, -6.938893903907222067E-15, 1.000000000000000000 ) ) ;
#28196 = ORIENTED_EDGE ( 'NONE', *, *, #48596, .F. ) ;
#28197 = DIRECTION ( 'NONE',  ( 0.000000000000000000, 0.000000000000000000, -1.000000000000000000 ) ) ;
#28198 = CARTESIAN_POINT ( 'NONE',  ( -1.492201783934593573, -3.724691934501250135, 21.82999329374151642 ) ) ;
#28199 = B_SPLINE_CURVE_WITH_KNOTS ( 'NONE', 3,
 ( #32759, #19252, #54351, #20135, #46718, #81404, #41299, #80516, #68319, #19687 ),
 .UNSPECIFIED., .F., .F.,
 ( 4, 2, 2, 2, 4 ),
 ( 0.000000000000000000, 0.0001954339857564082062, 0.0003908679715128164124, 0.0005863019572692246186, 0.0007817359430256328248 ),
 .UNSPECIFIED. ) ;
#28200 = CARTESIAN_POINT ( 'NONE',  ( -15.93083330975275658, -12.38742843783360748, 31.66772728687926985 ) ) ;
#28201 = CARTESIAN_POINT ( 'NONE',  ( -39.05038313613820122, -2.499999999999999556, 29.75000000000000355 ) ) ;
#28202 = ORIENTED_EDGE ( 'NONE', *, *, #67690, .T. ) ;
#28203 = B_SPLINE_CURVE_WITH_KNOTS ( 'NONE', 3,
 ( #53207, #40161, #11795, #87929, #75268, #46009, #26633, #73498, #67624, #60411 ),
 .UNSPECIFIED., .F., .F.,
 ( 4, 2, 2, 2, 4 ),
 ( 0.000000000000000000, 0.0001954339857564126514, 0.0003908679715128183098, 0.0005863019572692239681, 0.0007817359430256294638 ),
 .UNSPECIFIED. ) ;
#28204 = CIRCLE ( 'NONE', #49804, 4.000000000000000000 ) ;
#28205 = DIRECTION ( 'NONE',  ( -0.000000000000000000, 1.000000000000000000, 3.491481338843133355E-15 ) ) ;
#28206 = CARTESIAN_POINT ( 'NONE',  ( 16.15384615384615330, -8.564572088678739092, 35.78748833219616898 ) ) ;
#28208 = ORIENTED_EDGE ( 'NONE', *, *, #50505, .T. ) ;
#28207 = CARTESIAN_POINT ( 'NONE',  ( 4.088576153289833925, -9.528491918058357157, 34.59228464037090589 ) ) ;
#28209 = CARTESIAN_POINT ( 'NONE',  ( -7.976764205778374084, -7.722926236386456367, 34.74524107206103452 ) ) ;
#28210 = CARTESIAN_POINT ( 'NONE',  ( -3.099977422944444783, -4.809403383903226192, 33.96459661697924304 ) ) ;
#28211 = EDGE_CURVE ( 'NONE', #54822, #77202, #53586, .T. ) ;
#28212 = VECTOR ( 'NONE', #52127, 1000.000000000000000 ) ;
#28213 = DIRECTION ( 'NONE',  ( -0.000000000000000000, 0.8660254037844399289, -0.4999999999999980016 ) ) ;
#28214 = CARTESIAN_POINT ( 'NONE',  ( 4.826946345980720920, -4.236021600441998380, 33.53823185664189310 ) ) ;
#28215 = FACE_OUTER_BOUND ( 'NONE', #53865, .T. ) ;
#28216 = ORIENTED_EDGE ( 'NONE', *, *, #6301, .T. ) ;
#28217 = CARTESIAN_POINT ( 'NONE',  ( 6.989144256427000101, -11.35647404775217595, 33.31231777344667222 ) ) ;
#28218 = EDGE_LOOP ( 'NONE', ( #1188, #59127 ) ) ;
#28219 = VERTEX_POINT ( 'NONE', #42393 ) ;
#28220 = ADVANCED_FACE ( 'NONE', ( #69850 ), #14767, .F. ) ;
#28221 = CARTESIAN_POINT ( 'NONE',  ( -16.21911615440247090, -3.643525952247790300, 33.31231777344662959 ) ) ;
#28222 = CARTESIAN_POINT ( 'NONE',  ( -18.75000000000000000, -11.50000000000000000, 29.75000000000000355 ) ) ;
#28223 = EDGE_CURVE ( 'NONE', #22687, #70094, #80402, .T. ) ;
#28224 = LINE ( 'NONE', #55255, #42192 ) ;
#28225 = CARTESIAN_POINT ( 'NONE',  ( -17.14224599241525482, -7.749976743299138882, 34.99404534957040624 ) ) ;
#28226 = VERTEX_POINT ( 'NONE', #81461 ) ;
#28227 = CARTESIAN_POINT ( 'NONE',  ( -14.16025641025641058, -3.499999999999999556, 29.75000000000000355 ) ) ;
#28228 = ORIENTED_EDGE ( 'NONE', *, *, #35660, .T. ) ;
#28229 = VECTOR ( 'NONE', #83366, 999.9999999999998863 ) ;
#28230 = VERTEX_POINT ( 'NONE', #48987 ) ;
#28231 = B_SPLINE_CURVE_WITH_KNOTS ( 'NONE', 3,
 ( #70725, #9029, #36498, #84694, #44553, #72485, #18445, #30608, #10793, #24746 ),
 .UNSPECIFIED., .F., .F.,
 ( 4, 2, 2, 2, 4 ),
 ( 0.000000000000000000, 0.0001954311564186863323, 0.0003908623128373726646, 0.0005862934692560590241, 0.0007817246256747453293 ),
 .UNSPECIFIED. ) ;
#28233 = ORIENTED_EDGE ( 'NONE', *, *, #43823, .F. ) ;
#28232 = EDGE_CURVE ( 'NONE', #76954, #31022, #48092, .T. ) ;
#28235 = ORIENTED_EDGE ( 'NONE', *, *, #52746, .F. ) ;
#28234 = CARTESIAN_POINT ( 'NONE',  ( -9.692307692307691624, -6.343179335718451384, 34.87096338111211935 ) ) ;
#28236 = DIRECTION ( 'NONE',  ( -0.000000000000000000, 0.1736481776669307198, -0.9848077530122080203 ) ) ;
#28237 = CARTESIAN_POINT ( 'NONE',  ( 6.130525438233644486, -2.647132371071621471, 31.75357179365173010 ) ) ;
#28238 = EDGE_CURVE ( 'NONE', #41543, #79237, #68568, .T. ) ;
#28239 = CARTESIAN_POINT ( 'NONE',  ( -3.007989689500820241, -4.387253974876676565, 33.66317474335728832 ) ) ;
#28240 = CARTESIAN_POINT ( 'NONE',  ( 4.480769230769229061, -3.499999999999999556, 29.75000000000000355 ) ) ;
#28241 = EDGE_LOOP ( 'NONE', ( #86104, #22373, #46530, #25590 ) ) ;
#28242 = VERTEX_POINT ( 'NONE', #28268 ) ;
#28243 = ORIENTED_EDGE ( 'NONE', *, *, #15351, .T. ) ;
#28244 = CARTESIAN_POINT ( 'NONE',  ( -9.442253380669381357, -5.728107161865378494, 34.42597550085002922 ) ) ;
#28246 = EDGE_LOOP ( 'NONE', ( #25567, #58198 ) ) ;
#28245 = CARTESIAN_POINT ( 'NONE',  ( 1.253923917947828093, -8.147922237126337563, 34.70805685702651999 ) ) ;
#28247 = CARTESIAN_POINT ( 'NONE',  ( 2.307692307692186251, -2.657715359629662544, 31.77849191805970364 ) ) ;
#28248 = CARTESIAN_POINT ( 'NONE',  ( -0.4615384615384611200, -6.343179335718451384, 34.87096338111211935 ) ) ;
#28249 = ADVANCED_FACE ( 'NONE', ( #27828 ), #13429, .T. ) ;
#28250 = EDGE_LOOP ( 'NONE', ( #4622, #73314, #20974, #40113 ) ) ;
#28251 = EDGE_CURVE ( 'NONE', #9817, #88116, #40670, .T. ) ;
#28252 = CARTESIAN_POINT ( 'NONE',  ( -11.47239318745910275, -4.786620604624113540, 33.94971097300155805 ) ) ;
#28253 = CARTESIAN_POINT ( 'NONE',  ( -15.00798956179116317, -12.47679350104403007, 31.42216943046555855 ) ) ;
#28254 = ORIENTED_EDGE ( 'NONE', *, *, #34034, .F. ) ;
#28255 = FACE_BOUND ( 'NONE', #75545, .T. ) ;
#28256 = CARTESIAN_POINT ( 'NONE',  ( -10.86536135943320502, -4.818429247618089661, 34.26397095200675125 ) ) ;
#28257 = FACE_OUTER_BOUND ( 'NONE', #44203, .T. ) ;
#28258 = CARTESIAN_POINT ( 'NONE',  ( 13.19230769230769340, -3.499999999999999556, 29.75000000000000355 ) ) ;
#28260 = CARTESIAN_POINT ( 'NONE',  ( 4.853438133199126980, -10.11188796281391511, 34.01382737946119050 ) ) ;
#28259 = DIRECTION ( 'NONE',  ( -0.000000000000000000, 0.6427876096865404731, -0.7660444431189770143 ) ) ;
#28261 = ADVANCED_FACE ( 'NONE', ( #75567 ), #34141, .F. ) ;
#28262 = AXIS2_PLACEMENT_3D ( 'NONE', #18362, #46276, #73765 ) ;
#28263 = FACE_OUTER_BOUND ( 'NONE', #63255, .T. ) ;
#28264 = CARTESIAN_POINT ( 'NONE',  ( 17.99999999999987566, -2.892918686052165622, 31.69288490824153470 ) ) ;
#28265 = ORIENTED_EDGE ( 'NONE', *, *, #67894, .F. ) ;
#28266 = ADVANCED_FACE ( 'NONE', ( #55296 ), #82344, .F. ) ;
#28267 = CARTESIAN_POINT ( 'NONE',  ( 11.47319109250076430, -3.300289026998414865, 32.46337939537583139 ) ) ;
#28268 = CARTESIAN_POINT ( 'NONE',  ( 10.61538461538449596, -5.219633306517616589, 34.19971097300220464 ) ) ;
#28269 = ORIENTED_EDGE ( 'NONE', *, *, #59581, .F. ) ;
#28270 = B_SPLINE_CURVE_WITH_KNOTS ( 'NONE', 3,
 ( #8854, #9726, #23679, #16928, #42639, #70097, #1649, #29132, #84079, #22355 ),
 .UNSPECIFIED., .F., .F.,
 ( 4, 2, 2, 2, 4 ),
 ( 0.000000000000000000, 0.0001954311564186861968, 0.0003908623128373723936, 0.0005862934692560585904, 0.0007817246256747447872 ),
 .UNSPECIFIED. ) ;
#28271 = CARTESIAN_POINT ( 'NONE',  ( -7.846153846153844924, -12.09954503811598769, 35.62045528018868623 ) ) ;
#28272 = CARTESIAN_POINT ( 'NONE',  ( -7.780086512803768173, -2.292212530054420494, 30.41441678777542990 ) ) ;
#28273 = EDGE_LOOP ( 'NONE', ( #58154, #35775, #25557, #11799 ) ) ;
#28274 = CARTESIAN_POINT ( 'NONE',  ( 2.544871794871793824, -4.000000000000000000, 29.75000000000000355 ) ) ;
#28275 = CARTESIAN_POINT ( 'NONE',  ( 2.438482748659257737, -4.684288915650983043, 34.18129842949671371 ) ) ;
#28276 = FACE_BOUND ( 'NONE', #83640, .T. ) ;
#28278 = CARTESIAN_POINT ( 'NONE',  ( 15.23076923076911093, -12.27809138561165270, 31.22303859784587132 ) ) ;
#28277 = CARTESIAN_POINT ( 'NONE',  ( -1.634592128663975297, -6.524016743844655686, 34.90889640711025521 ) ) ;
#28279 = FACE_OUTER_BOUND ( 'NONE', #55300, .T. ) ;
#28280 = AXIS2_PLACEMENT_3D ( 'NONE', #84923, #64617, #37602 ) ;
#28281 = DIRECTION ( 'NONE',  ( 0.000000000000000000, 0.9848077530122072432, -0.1736481776669354937 ) ) ;
#28282 = CARTESIAN_POINT ( 'NONE',  ( 3.230769230769108269, -3.083524468854526912, 32.58852847137268327 ) ) ;
#28283 = DIRECTION ( 'NONE',  ( -0.000000000000000000, 0.7660444431189791237, -0.6427876096865379196 ) ) ;
#28284 = CARTESIAN_POINT ( 'NONE',  ( -3.775308065498766297, -6.007798216065450170, 17.42000670625848713 ) ) ;
#28285 = VERTEX_POINT ( 'NONE', #88232 ) ;
#28286 = VERTEX_POINT ( 'NONE', #21060 ) ;
#28287 = DIRECTION ( 'NONE',  ( -0.000000000000000000, 0.8660254037844397068, -0.4999999999999978906 ) ) ;
#28288 = CARTESIAN_POINT ( 'NONE',  ( 17.99999999999987566, -2.379036618888197729, 30.90682066428292885 ) ) ;
#28289 = CARTESIAN_POINT ( 'NONE',  ( 1.450682717965462443, -9.058645607665452459, 34.76329471203371924 ) ) ;
#28290 = CARTESIAN_POINT ( 'NONE',  ( -1.515306851282944400, -3.062553014421049546, 32.05460306192773601 ) ) ;
#28291 = CARTESIAN_POINT ( 'NONE',  ( -16.40386939113911779, -12.22074536777955345, 31.39888409691088356 ) ) ;
#28292 = CARTESIAN_POINT ( 'NONE',  ( -1.492201783934549164, -11.27530806549876807, 15.85750670625849068 ) ) ;
#28293 = MANIFOLD_SOLID_BREP ( 'Boss-Extrude6', #24219 ) ;
#28294 = CARTESIAN_POINT ( 'NONE',  ( 6.700149964170073247, -2.308479472611653094, 30.53278059502174457 ) ) ;
#28295 = CARTESIAN_POINT ( 'NONE',  ( 4.153846153846154188, -12.29105614889573062, 35.45975837776705220 ) ) ;
#28296 = CARTESIAN_POINT ( 'NONE',  ( 15.36129493253280032, -11.93748526763465279, 32.05452791011430946 ) ) ;
#28297 = LINE ( 'NONE', #61638, #40192 ) ;
#28298 = CARTESIAN_POINT ( 'NONE',  ( -1.134615384615446976, -7.565270000091922853, 34.99999999999999289 ) ) ;
#28299 = CARTESIAN_POINT ( 'NONE',  ( 16.28437185560972011, -5.195472089885680766, 34.18748526763464923 ) ) ;
#28300 = LINE ( 'NONE', #55771, #25157 ) ;
#28301 = EDGE_CURVE ( 'NONE', #84941, #72951, #11632, .T. ) ;
#28302 = VECTOR ( 'NONE', #37508, 1000.000000000000000 ) ;
#28303 = CARTESIAN_POINT ( 'NONE',  ( -14.05763799605399278, -3.136992222400443175, 32.19305428654138979 ) ) ;
#28304 = FACE_OUTER_BOUND ( 'NONE', #24425, .T. ) ;
#28305 = EDGE_LOOP ( 'NONE', ( #73456, #79417 ) ) ;
#28306 = EDGE_CURVE ( 'NONE', #86041, #69985, #3000, .T. ) ;
#28307 = CARTESIAN_POINT ( 'NONE',  ( 12.39626846098214230, -4.320704448112771878, 33.92786785259540494 ) ) ;
#28308 = DIRECTION ( 'NONE',  ( -0.000000000000000000, 1.000000000000000000, -0.000000000000000000 ) ) ;
#28309 = CARTESIAN_POINT ( 'NONE',  ( -1.077988221561493543, -4.724691934501247914, 23.07999329374151998 ) ) ;
#28310 = ADVANCED_FACE ( 'NONE', ( #83679, #21964 ), #22401, .F. ) ;
#28311 = FACE_BOUND ( 'NONE', #28932, .T. ) ;
#28312 = LINE ( 'NONE', #15254, #57017 ) ;
#28313 = EDGE_LOOP ( 'NONE', ( #16704, #31585 ) ) ;
#28314 = CYLINDRICAL_SURFACE ( 'NONE', #41333, 0.2500000000000009437 ) ;
#28316 = ORIENTED_EDGE ( 'NONE', *, *, #38878, .F. ) ;
#28315 = CARTESIAN_POINT ( 'NONE',  ( -1.319359813339359588, -4.481592998940251427, 33.73612834413965089 ) ) ;
#28317 = DIRECTION ( 'NONE',  ( -1.000000000000000000, -0.000000000000000000, -0.000000000000000000 ) ) ;
#28318 = DIRECTION ( 'NONE',  ( 0.000000000000000000, 0.1736481776669267785, -0.9848077530122087975 ) ) ;
#28319 = AXIS2_PLACEMENT_3D ( 'NONE', #40096, #68430, #67113 ) ;
#28320 = EDGE_LOOP ( 'NONE', ( #81306, #26818, #34203, #63173 ) ) ;
#28321 = CARTESIAN_POINT ( 'NONE',  ( -12.22435897435897267, -7.500000000000000000, 29.75000000000000355 ) ) ;
#28322 = EDGE_CURVE ( 'NONE', #16142, #52128, #76072, .T. ) ;
#28323 = CARTESIAN_POINT ( 'NONE',  ( 10.61538461538449418, -11.06231777344772027, 33.60647404775119895 ) ) ;
#28324 = ORIENTED_EDGE ( 'NONE', *, *, #21224, .F. ) ;
#28325 = CARTESIAN_POINT ( 'NONE',  ( 7.846153846153725020, -4.481592998941358097, 33.73612834414048933 ) ) ;
#28326 = CARTESIAN_POINT ( 'NONE',  ( 2.530471976670374712, -8.540255544307065350, 34.89611431652622286 ) ) ;
#28327 = CARTESIAN_POINT ( 'NONE',  ( 9.757562831820528970, -6.835583212224610072, 34.95778746994559327 ) ) ;
#28328 = ORIENTED_EDGE ( 'NONE', *, *, #46592, .T. ) ;
#28329 = EDGE_LOOP ( 'NONE', ( #35559, #61041, #56617, #60569 ) ) ;
#28330 = CARTESIAN_POINT ( 'NONE',  ( 15.23076923076923173, -10.51840700105979565, 33.73612834413961536 ) ) ;
#28331 = ORIENTED_EDGE ( 'NONE', *, *, #82842, .T. ) ;
#28332 = CARTESIAN_POINT ( 'NONE',  ( -7.976301815885541657, -2.373036134822904319, 30.88089517874952250 ) ) ;
#28333 = CARTESIAN_POINT ( 'NONE',  ( -6.923076923077045919, -2.657715359629662988, 31.77849191805970364 ) ) ;
#28334 = CARTESIAN_POINT ( 'NONE',  ( -5.933932666649923249, -5.471508081941601098, 34.59228464037088457 ) ) ;
#28335 = CARTESIAN_POINT ( 'NONE',  ( 23.00000000000000000, -10.75000000000000000, 27.25000000000000000 ) ) ;
#28337 = ADVANCED_FACE ( 'NONE', ( #63379 ), #2557, .F. ) ;
#28336 = CARTESIAN_POINT ( 'NONE',  ( 14.98074599347626368, -6.695914987888146541, 34.68535235679833306 ) ) ;
#28338 = CARTESIAN_POINT ( 'NONE',  ( 0.5923767920252209773, -7.277220318596960169, 34.99547417642776992 ) ) ;
#28339 = AXIS2_PLACEMENT_3D ( 'NONE', #18219, #51980, #52430 ) ;
#28340 = DIRECTION ( 'NONE',  ( -0.000000000000000000, 1.000000000000000000, -0.000000000000000000 ) ) ;
#28341 = EDGE_LOOP ( 'NONE', ( #9969, #5694, #80227, #60320 ) ) ;
#28342 = VERTEX_POINT ( 'NONE', #23713 ) ;
#28344 = ORIENTED_EDGE ( 'NONE', *, *, #72681, .T. ) ;
#28343 = DIRECTION ( 'NONE',  ( 0.000000000000000000, 0.8660254037844377084, 0.5000000000000015543 ) ) ;
#28345 = CARTESIAN_POINT ( 'NONE',  ( 7.715463243043541475, -2.494641256782728966, 31.33461815524612959 ) ) ;
#28346 = ORIENTED_EDGE ( 'NONE', *, *, #57599, .F. ) ;
#28347 = DIRECTION ( 'NONE',  ( -0.000000000000000000, -0.000000000000000000, -1.000000000000000000 ) ) ;
#28348 = CARTESIAN_POINT ( 'NONE',  ( 2.307692307692187583, -5.219633306517616589, 34.19971097300220464 ) ) ;
#28349 = EDGE_LOOP ( 'NONE', ( #76064, #45955 ) ) ;
#28350 = FACE_OUTER_BOUND ( 'NONE', #43399, .T. ) ;
#28351 = EDGE_LOOP ( 'NONE', ( #44396, #15811 ) ) ;
#28353 = VERTEX_POINT ( 'NONE', #44421 ) ;
#28352 = DIRECTION ( 'NONE',  ( -0.000000000000000000, 0.000000000000000000, 1.000000000000000000 ) ) ;
#28354 = CARTESIAN_POINT ( 'NONE',  ( -12.46153846153846168, -3.322132147404559976, 32.92929555188717927 ) ) ;
#28356 = ORIENTED_EDGE ( 'NONE', *, *, #33763, .F. ) ;
#28355 = ADVANCED_FACE ( 'NONE', ( #23280 ), #63826, .F. ) ;
#28357 = ADVANCED_FACE ( 'NONE', ( #70143 ), #36799, .F. ) ;
#28358 = CARTESIAN_POINT ( 'NONE',  ( -6.923076923076922462, -4.661471528628507777, 34.16647553114623292 ) ) ;
#28359 = CARTESIAN_POINT ( 'NONE',  ( -16.15384615384615330, -1.044019251281081972, 31.83374038241031911 ) ) ;
#28360 = B_SPLINE_CURVE_WITH_KNOTS ( 'NONE', 3,
 ( #78402, #51342, #67895, #16702, #33668, #39992, #6196, #88194, #44157, #17148 ),
 .UNSPECIFIED., .F., .F.,
 ( 4, 2, 2, 2, 4 ),
 ( 0.000000000000000000, 0.0001954311564186888531, 0.0003908623128373777062, 0.0005862934692560666135, 0.0007817246256747554124 ),
 .UNSPECIFIED. ) ;
#28361 = VECTOR ( 'NONE', #52388, 1000.000000000000000 ) ;
#28362 = FACE_BOUND ( 'NONE', #41161, .T. ) ;
#28363 = CARTESIAN_POINT ( 'NONE',  ( 7.846153846153846700, -9.819645486525091727, 36.12317359536749706 ) ) ;
#28365 = EDGE_CURVE ( 'NONE', #59530, #3191, #58824, .T. ) ;
#28364 = CARTESIAN_POINT ( 'NONE',  ( -5.076923076923075762, -13.53365097954675988, 30.81389545987213552 ) ) ;
#28366 = B_SPLINE_CURVE_WITH_KNOTS ( 'NONE', 3,
 ( #84158, #29212, #1724, #41834, #83262, #56665, #49021, #14806, #70179, #70624 ),
 .UNSPECIFIED., .F., .F.,
 ( 4, 2, 2, 2, 4 ),
 ( 0.0007817246256747505334, 0.0009771112852218954894, 0.001172497944769040554, 0.001367884604316185618, 0.001563271263863330682 ),
 .UNSPECIFIED. ) ;
#28367 = CARTESIAN_POINT ( 'NONE',  ( 9.627037691751372250, -2.379036618887870436, 30.90682066428147934 ) ) ;
#28368 = CARTESIAN_POINT ( 'NONE',  ( -17.07692307692319744, -12.51329471203414379, 31.30864560766407578 ) ) ;
#28369 = CARTESIAN_POINT ( 'NONE',  ( -4.946132635956124624, -3.957578996910242619, 33.62503395064540257 ) ) ;
#28370 = CARTESIAN_POINT ( 'NONE',  ( -16.15384615384615330, -2.486705287966279876, 31.30864560766543647 ) ) ;
#28371 = ORIENTED_EDGE ( 'NONE', *, *, #15405, .F. ) ;
#28372 = EDGE_CURVE ( 'NONE', #5766, #37043, #32114, .T. ) ;
#28373 = VECTOR ( 'NONE', #73851, 1000.000000000000000 ) ;
#28374 = CARTESIAN_POINT ( 'NONE',  ( -14.30769230769230660, -11.16473453929635440, 33.15142922261926373 ) ) ;
#28375 = VERTEX_POINT ( 'NONE', #79572 ) ;
#28376 = EDGE_LOOP ( 'NONE', ( #14295, #7157 ) ) ;
#28378 = CARTESIAN_POINT ( 'NONE',  ( 10.61538461538449418, -12.70778746994576025, 30.41441678777401236 ) ) ;
#28377 = CARTESIAN_POINT ( 'NONE',  ( 7.596177115211491859, -6.567427716900047230, 34.66269422305636283 ) ) ;
#28379 = CARTESIAN_POINT ( 'NONE',  ( 15.23076923076923173, -5.415277668671390821, 36.20867863119892149 ) ) ;
#28380 = CARTESIAN_POINT ( 'NONE',  ( 7.912221179503920787, -3.322132147404559976, 32.92929555188717927 ) ) ;
#28381 = CARTESIAN_POINT ( 'NONE',  ( -10.61538461538461320, -12.34228464037088635, 31.77849191805839268 ) ) ;
#28382 = LINE ( 'NONE', #35593, #44702 ) ;
#28383 = VERTEX_POINT ( 'NONE', #18310 ) ;
#28384 = CARTESIAN_POINT ( 'NONE',  ( 6.416666666666664298, -3.499999999999999556, 29.75000000000000355 ) ) ;
#28385 = CARTESIAN_POINT ( 'NONE',  ( -15.23076923076935074, -10.21337939537710326, 33.94971097300076224 ) ) ;
#28386 = CARTESIAN_POINT ( 'NONE',  ( 17.20771488474786892, -6.413143153341454017, 34.63066358083362672 ) ) ;
#28387 = DIRECTION ( 'NONE',  ( 0.000000000000000000, 0.7660444431189807890, 0.6427876096865361433 ) ) ;
#28388 = CARTESIAN_POINT ( 'NONE',  ( -15.36132982251114854, -2.504760397472875155, 29.97295953869789997 ) ) ;
#28389 = VERTEX_POINT ( 'NONE', #66939 ) ;
#28390 = EDGE_CURVE ( 'NONE', #55297, #61929, #23101, .T. ) ;
#28391 = ORIENTED_EDGE ( 'NONE', *, *, #14209, .F. ) ;
#28392 = B_SPLINE_CURVE_WITH_KNOTS ( 'NONE', 3,
 ( #42151, #35376, #15115, #15558, #42589, #22743, #50203, #70048, #8359, #36710 ),
 .UNSPECIFIED., .F., .F.,
 ( 4, 2, 2, 2, 4 ),
 ( 0.000000000000000000, 0.0001954311564186861697, 0.0003908623128373723394, 0.0005862934692560584820, 0.0007817246256747446788 ),
 .UNSPECIFIED. ) ;
#28393 = EDGE_LOOP ( 'NONE', ( #27005, #72760 ) ) ;
#28394 = AXIS2_PLACEMENT_3D ( 'NONE', #355, #34131, #7555 ) ;
#28395 = CARTESIAN_POINT ( 'NONE',  ( -7.146561866800870355, -8.496056993536548418, 34.65000542017679663 ) ) ;
#28396 = EDGE_CURVE ( 'NONE', #56689, #13581, #85823, .T. ) ;
#28397 = ORIENTED_EDGE ( 'NONE', *, *, #4874, .F. ) ;
#28398 = CARTESIAN_POINT ( 'NONE',  ( 12.46153846153833911, -4.481592998941358097, 33.73612834414048933 ) ) ;
#28399 = CARTESIAN_POINT ( 'NONE',  ( 15.29602437028207085, -4.320704448112861584, 33.92786785259548310 ) ) ;
#28400 = CARTESIAN_POINT ( 'NONE',  ( 19.00000000000000000, -1.249999999999999334, 30.25000000000000000 ) ) ;
#28401 = CARTESIAN_POINT ( 'NONE',  ( -16.85391172531022619, -12.15243808032446005, 31.58219941686247978 ) ) ;
#28402 = DIRECTION ( 'NONE',  ( 0.000000000000000000, 0.9396926207859126468, 0.3420201433256571111 ) ) ;
#28403 = VERTEX_POINT ( 'NONE', #58837 ) ;
#28404 = CARTESIAN_POINT ( 'NONE',  ( -14.30769230769230660, -8.564572088678739092, 35.78748833219616898 ) ) ;
#28406 = ORIENTED_EDGE ( 'NONE', *, *, #73070, .T. ) ;
#28405 = CARTESIAN_POINT ( 'NONE',  ( 15.23076923076923173, -9.819645486525091727, 36.12317359536749706 ) ) ;
#28407 = CARTESIAN_POINT ( 'NONE',  ( -5.198717948717948012, -7.500000000000000000, 29.75000000000000355 ) ) ;
#28408 = CARTESIAN_POINT ( 'NONE',  ( 18.00000000000000000, -9.780366693483667717, 34.19971097300155094 ) ) ;
#28410 = B_SPLINE_CURVE_WITH_KNOTS ( 'NONE', 3,
 ( #15576, #9267, #16898, #30849, #16456, #85813, #64180, #43924, #57432, #43043 ),
 .UNSPECIFIED., .F., .F.,
 ( 4, 2, 2, 2, 4 ),
 ( 0.0007817246256747528103, 0.0009771112852218980915, 0.001172497944769043156, 0.001367884604316188437, 0.001563271263863333718 ),
 .UNSPECIFIED. ) ;
#28409 = LINE ( 'NONE', #48232, #41516 ) ;
#28411 = CARTESIAN_POINT ( 'NONE',  ( -3.360916440207450950, -5.195881422630167279, 34.18770438780618548 ) ) ;
#28412 = EDGE_CURVE ( 'NONE', #59880, #45204, #17047, .T. ) ;
#28413 = CARTESIAN_POINT ( 'NONE',  ( -17.74994558008654622, -10.82426656108011720, 33.81400080652039009 ) ) ;
#28414 = AXIS2_PLACEMENT_3D ( 'NONE', #68418, #58655, #45143 ) ;
#28415 = DIRECTION ( 'NONE',  ( 0.000000000000000000, 0.7660444431189807890, 0.6427876096865361433 ) ) ;
#28416 = B_SPLINE_CURVE_WITH_KNOTS ( 'NONE', 3,
 ( #53170, #45973, #79775, #80218, #79326, #18958, #73464, #46423, #38785, #5001 ),
 .UNSPECIFIED., .F., .F.,
 ( 4, 2, 2, 2, 4 ),
 ( 0.0007817246256747486903, 0.0009771112852218918031, 0.001172497944769034699, 0.001367884604316177595, 0.001563271263863320708 ),
 .UNSPECIFIED. ) ;
#28417 = CYLINDRICAL_SURFACE ( 'NONE', #60818, 0.2500000000000009437 ) ;
#28418 = CARTESIAN_POINT ( 'NONE',  ( -3.749999999999997780, -7.438900925035489387, 15.34561829374151465 ) ) ;
#28419 = ORIENTED_EDGE ( 'NONE', *, *, #87760, .T. ) ;
#28420 = B_SPLINE_CURVE_WITH_KNOTS ( 'NONE', 3,
 ( #56166, #343, #21938, #63801, #76886, #49841, #7984, #14745, #35005, #14293 ),
 .UNSPECIFIED., .F., .F.,
 ( 4, 2, 2, 2, 4 ),
 ( 0.0007817246256747442451, 0.0009771112852218870326, 0.001172497944769029929, 0.001367884604316172825, 0.001563271263863315504 ),
 .UNSPECIFIED. ) ;
#28421 = ADVANCED_FACE ( 'NONE', ( #31830 ), #25945, .F. ) ;
#28422 = LINE ( 'NONE', #77058, #2852 ) ;
#28423 = CARTESIAN_POINT ( 'NONE',  ( 0.5267940328144856688, -3.300289026998475705, 32.46337939537591666 ) ) ;
#28424 = B_SPLINE_CURVE_WITH_KNOTS ( 'NONE', 3,
 ( #10911, #44672, #66741, #38381, #65836, #4138, #12242, #39728, #31625, #67192 ),
 .UNSPECIFIED., .F., .F.,
 ( 4, 2, 2, 2, 4 ),
 ( 0.0007817359430256320659, 0.0009771253907249987086, 0.001172514838424365460, 0.001367904286123732211, 0.001563293733823098962 ),
 .UNSPECIFIED. ) ;
#28425 = CARTESIAN_POINT ( 'NONE',  ( 8.096208157792158744, -2.564540009722895419, 30.55348353981670684 ) ) ;
#28426 = CARTESIAN_POINT ( 'NONE',  ( -2.980823821391186623, -10.92531984108285670, 33.72920026020278073 ) ) ;
#28427 = ORIENTED_EDGE ( 'NONE', *, *, #80603, .T. ) ;
#28428 = CARTESIAN_POINT ( 'NONE',  ( -2.749999999999998224, -7.500000000000015987, 15.09375000000000000 ) ) ;
#28429 = CARTESIAN_POINT ( 'NONE',  ( -3.453695448285375669, -10.61292498521070549, 33.66303323003028680 ) ) ;
#28430 = DIRECTION ( 'NONE',  ( -0.000000000000000000, 1.000000000000000000, -0.000000000000000000 ) ) ;
#28431 = EDGE_CURVE ( 'NONE', #38427, #57345, #82472, .T. ) ;
#28432 = CARTESIAN_POINT ( 'NONE',  ( 10.61538461538461675, -12.37446782046654192, 30.86335684631486131 ) ) ;
#28433 = VERTEX_POINT ( 'NONE', #25061 ) ;
#28434 = CARTESIAN_POINT ( 'NONE',  ( 17.01165263096229907, -3.300289026998414865, 32.46337939537583139 ) ) ;
#28435 = EDGE_CURVE ( 'NONE', #49386, #53248, #83590, .T. ) ;
#28436 = CARTESIAN_POINT ( 'NONE',  ( 7.912222197156284054, -5.557115091759786019, 34.35708131394839882 ) ) ;
#28437 = CARTESIAN_POINT ( 'NONE',  ( 7.716006636715624367, -10.19110544564092002, 33.96427741523702792 ) ) ;
#28438 = ORIENTED_EDGE ( 'NONE', *, *, #68324, .T. ) ;
#28439 = CARTESIAN_POINT ( 'NONE',  ( -2.372962308248626417, -12.16647553114622049, 32.15551576947930812 ) ) ;
#28440 = VECTOR ( 'NONE', #18851, 1000.000000000000000 ) ;
#28441 = ORIENTED_EDGE ( 'NONE', *, *, #78966, .F. ) ;
#28442 = CARTESIAN_POINT ( 'NONE',  ( -6.923076923076922462, -8.164416787775445883, 34.95778746994557906 ) ) ;
#28443 = CARTESIAN_POINT ( 'NONE',  ( 0.5276057948885364279, -9.905515769479277921, 34.41647553114623292 ) ) ;
#28444 = ORIENTED_EDGE ( 'NONE', *, *, #8622, .F. ) ;
#28445 = AXIS2_PLACEMENT_3D ( 'NONE', #77068, #8167, #961 ) ;
#28446 = FACE_OUTER_BOUND ( 'NONE', #82640, .T. ) ;
#28448 = EDGE_CURVE ( 'NONE', #47121, #8365, #8436, .T. ) ;
#28447 = CARTESIAN_POINT ( 'NONE',  ( -14.43784027742400689, -2.373036134822904319, 30.88089517874952250 ) ) ;
#28449 = CARTESIAN_POINT ( 'NONE',  ( -11.60373198442231413, -6.879047030191174805, 34.71129190930000163 ) ) ;
#28450 = MANIFOLD_SOLID_BREP ( 'Boss-Extrude3', #78941 ) ;
#28451 = B_SPLINE_CURVE_WITH_KNOTS ( 'NONE', 3,
 ( #58716, #86217, #24933, #52398, #60050, #87555, #19076, #51952, #79448, #45652 ),
 .UNSPECIFIED., .F., .F.,
 ( 4, 2, 2, 2, 4 ),
 ( 0.000000000000000000, 0.0001954339857564080165, 0.0003908679715128160329, 0.0005863019572692240765, 0.0007817359430256320659 ),
 .UNSPECIFIED. ) ;
#28452 = ADVANCED_FACE ( 'NONE', ( #27714 ), #44875, .F. ) ;
#28453 = B_SPLINE_CURVE_WITH_KNOTS ( 'NONE', 3,
 ( #85946, #72419, #3515, #51686, #79187, #11623, #18823, #72863, #66565, #73777 ),
 .UNSPECIFIED., .F., .F.,
 ( 4, 2, 2, 2, 4 ),
 ( 0.000000000000000000, 0.0001954339857564063360, 0.0003908679715128126719, 0.0005863019572692189808, 0.0007817359430256253438 ),
 .UNSPECIFIED. ) ;
#28454 = CARTESIAN_POINT ( 'NONE',  ( -11.47239420511146157, -5.471508081941601098, 34.59228464037088457 ) ) ;
#28455 = CARTESIAN_POINT ( 'NONE',  ( 20.00000000000000000, -11.00000000000000000, 28.25000000000000000 ) ) ;
#28456 = B_SPLINE_CURVE_WITH_KNOTS ( 'NONE', 3,
 ( #28132, #14179, #5650, #61471, #34454, #60590, #80888, #47069, #88105, #27252 ),
 .UNSPECIFIED., .F., .F.,
 ( 4, 2, 2, 2, 4 ),
 ( 0.000000000000000000, 0.0001954339857564063089, 0.0003908679715128126177, 0.0005863019572692189808, 0.0007817359430256252354 ),
 .UNSPECIFIED. ) ;
#28457 = B_SPLINE_CURVE_WITH_KNOTS ( 'NONE', 3,
 ( #46995, #27177, #47441, #33052, #74936, #28068, #83016, #6033, #33501, #6903 ),
 .UNSPECIFIED., .F., .F.,
 ( 4, 2, 2, 2, 4 ),
 ( 0.0007817359430256297891, 0.0009771253907249958896, 0.001172514838424361990, 0.001367904286123728091, 0.001563293733823094191 ),
 .UNSPECIFIED. ) ;
#28458 = EDGE_LOOP ( 'NONE', ( #15625, #32945, #50167, #27593 ) ) ;
#28459 = ORIENTED_EDGE ( 'NONE', *, *, #1948, .F. ) ;
#28460 = FACE_BOUND ( 'NONE', #77130, .T. ) ;
#28461 = ORIENTED_EDGE ( 'NONE', *, *, #65193, .T. ) ;
#28462 = DIRECTION ( 'NONE',  ( 0.000000000000000000, 1.000000000000000000, 0.000000000000000000 ) ) ;
#28463 = AXIS2_PLACEMENT_3D ( 'NONE', #32157, #79456, #58725 ) ;
#28464 = DIRECTION ( 'NONE',  ( 0.000000000000000000, 1.000000000000000000, 0.000000000000000000 ) ) ;
#28465 = CARTESIAN_POINT ( 'NONE',  ( -2.980769230767811084, -7.500000000000154543, 35.00000000000007105 ) ) ;
#28466 = CARTESIAN_POINT ( 'NONE',  ( -6.222926217516146608, -12.15238873228292071, 31.58232369045353849 ) ) ;
#28467 = EDGE_LOOP ( 'NONE', ( #12340, #36058, #35583, #65272 ) ) ;
#28468 = AXIS2_PLACEMENT_3D ( 'NONE', #9632, #24923, #58259 ) ;
#28469 = EDGE_LOOP ( 'NONE', ( #76073, #52887, #40256, #64534 ) ) ;
#28470 = VERTEX_POINT ( 'NONE', #68264 ) ;
#28471 = CYLINDRICAL_SURFACE ( 'NONE', #82210, 0.2499999999999995559 ) ;
#28472 = EDGE_LOOP ( 'NONE', ( #8759, #81697 ) ) ;
#28473 = AXIS2_PLACEMENT_3D ( 'NONE', #55907, #76181, #62657 ) ;
#28474 = FACE_OUTER_BOUND ( 'NONE', #63454, .T. ) ;
#28475 = FACE_OUTER_BOUND ( 'NONE', #74040, .T. ) ;
#28476 = CARTESIAN_POINT ( 'NONE',  ( -17.29985003582992320, -2.889293201056495786, 32.26117774369186009 ) ) ;
#28478 = EDGE_CURVE ( 'NONE', #42959, #87881, #88562, .T. ) ;
#28477 = CARTESIAN_POINT ( 'NONE',  ( 13.38461538461538680, -10.51840700105979565, 33.73612834413961536 ) ) ;
#28479 = CARTESIAN_POINT ( 'NONE',  ( -6.130147969731694069, -6.809168938359898782, 34.95455904226513866 ) ) ;
#28480 = CARTESIAN_POINT ( 'NONE',  ( 14.30769230769231015, -6.386643153685126251, 34.62446782046654192 ) ) ;
#28481 = CARTESIAN_POINT ( 'NONE',  ( -11.66915300512910214, -3.062553014421049546, 32.05460306192773601 ) ) ;
#28482 = ORIENTED_EDGE ( 'NONE', *, *, #5439, .F. ) ;
#28483 = EDGE_CURVE ( 'NONE', #26583, #81768, #67462, .T. ) ;
#28484 = ORIENTED_EDGE ( 'NONE', *, *, #32138, .T. ) ;
#28485 = ORIENTED_EDGE ( 'NONE', *, *, #393, .F. ) ;
#28486 = CARTESIAN_POINT ( 'NONE',  ( 4.153846153846030731, -3.083524468854526912, 32.58852847137268327 ) ) ;
#28487 = UNCERTAINTY_MEASURE_WITH_UNIT (LENGTH_MEASURE( 1.000000000000000082E-05 ), #73982, 'distance_accuracy_value', 'NONE');
#28489 = CARTESIAN_POINT ( 'NONE',  ( 1.634560793993429684, -11.56426240980093567, 33.07394671870546432 ) ) ;
#28488 = CARTESIAN_POINT ( 'NONE',  ( -3.164701897419154975, -9.905515769479277921, 34.41647553114623292 ) ) ;
#28490 = EDGE_CURVE ( 'NONE', #17200, #58944, #52464, .T. ) ;
#28491 = B_SPLINE_CURVE_WITH_KNOTS ( 'NONE', 3,
 ( #59329, #53005, #18799, #30959, #10264, #46268, #25104, #37725, #86837, #52566 ),
 .UNSPECIFIED., .F., .F.,
 ( 4, 2, 2, 2, 4 ),
 ( 0.0007817359430256303312, 0.0009771253907249965402, 0.001172514838424362641, 0.001367904286123728958, 0.001563293733823095059 ),
 .UNSPECIFIED. ) ;
#28492 = CARTESIAN_POINT ( 'NONE',  ( -6.923076923076922462, -5.180354513474913603, 36.12317359536750416 ) ) ;
#28493 = CARTESIAN_POINT ( 'NONE',  ( -2.057746898314264161, -2.589246495874657938, 31.60778113518102828 ) ) ;
#28494 = FACE_BOUND ( 'NONE', #20797, .T. ) ;
#28495 = CARTESIAN_POINT ( 'NONE',  ( 8.769230769230645706, -11.06231777344772027, 33.60647404775119895 ) ) ;
#28496 = ORIENTED_EDGE ( 'NONE', *, *, #58954, .T. ) ;
#28497 = DIRECTION ( 'NONE',  ( -1.000000000000000000, 0.000000000000000000, 0.000000000000000000 ) ) ;
#28498 = CARTESIAN_POINT ( 'NONE',  ( -9.692307692307691624, -6.189225973068211317, 35.74407628777942847 ) ) ;
#28499 = FACE_OUTER_BOUND ( 'NONE', #62569, .T. ) ;
#28500 = DIRECTION ( 'NONE',  ( -0.000000000000000000, 0.6427876096865404731, -0.7660444431189770143 ) ) ;
#28501 = ORIENTED_EDGE ( 'NONE', *, *, #19373, .F. ) ;
#28502 = EDGE_CURVE ( 'NONE', #36501, #31652, #19633, .T. ) ;
#28503 = CARTESIAN_POINT ( 'NONE',  ( 15.12820512820512953, -11.50000000000000000, 29.75000000000000355 ) ) ;
#28504 = VECTOR ( 'NONE', #32044, 1000.000000000000000 ) ;
#28505 = ORIENTED_EDGE ( 'NONE', *, *, #13114, .F. ) ;
#28506 = FACE_BOUND ( 'NONE', #65736, .T. ) ;
#28507 = CARTESIAN_POINT ( 'NONE',  ( 9.562160482869472844, -6.001485441113819874, 34.52039167877662607 ) ) ;
#28508 = ADVANCED_FACE ( 'NONE', ( #55626 ), #83116, .F. ) ;
#28509 = CARTESIAN_POINT ( 'NONE',  ( 4.403791563224195293, -2.589246495874657938, 31.60778113518102828 ) ) ;
#28510 = CARTESIAN_POINT ( 'NONE',  ( -3.165513659493205623, -8.613356846314928816, 34.62446782046653482 ) ) ;
#28511 = AXIS2_PLACEMENT_3D ( 'NONE', #66453, #31785, #32228 ) ;
#28512 = ORIENTED_EDGE ( 'NONE', *, *, #46620, .T. ) ;
#28513 = CARTESIAN_POINT ( 'NONE',  ( -14.55766903863466055, -12.41269422305637171, 30.68257228309993323 ) ) ;
#28514 = CARTESIAN_POINT ( 'NONE',  ( -5.999999999999998224, -9.058645607665452459, 34.76329471203371924 ) ) ;
#28515 = CARTESIAN_POINT ( 'NONE',  ( -9.942284423250045577, -3.137211980971221781, 32.19342716148376837 ) ) ;
#28516 = FACE_OUTER_BOUND ( 'NONE', #14171, .T. ) ;
#28517 = ORIENTED_EDGE ( 'NONE', *, *, #37652, .F. ) ;
#28518 = EDGE_CURVE ( 'NONE', #64799, #32448, #20255, .T. ) ;
#28519 = CARTESIAN_POINT ( 'NONE',  ( -12.21148414990014963, -3.136992222400443175, 32.19305428654138979 ) ) ;
#28520 = ORIENTED_EDGE ( 'NONE', *, *, #62123, .T. ) ;
#28522 = ORIENTED_EDGE ( 'NONE', *, *, #56450, .F. ) ;
#28521 = CARTESIAN_POINT ( 'NONE',  ( -9.019254006523736322, -3.711651800289232028, 33.01384336483936011 ) ) ;
#28523 = CARTESIAN_POINT ( 'NONE',  ( -9.019230769230768274, -7.500000000000001776, 34.75000000000000000 ) ) ;
#28524 = CARTESIAN_POINT ( 'NONE',  ( -10.74553182482283198, -12.45813303252208648, 30.39737893381572675 ) ) ;
#28525 = DIRECTION ( 'NONE',  ( -0.000000000000000000, -0.9396926207859093161, -0.3420201433256663259 ) ) ;
#28526 = DIRECTION ( 'NONE',  ( 0.000000000000000000, -0.000000000000000000, 1.000000000000000000 ) ) ;
#28527 = CARTESIAN_POINT ( 'NONE',  ( 16.94623247381277054, -4.684245665217972032, 34.18127051446801090 ) ) ;
#28529 = CARTESIAN_POINT ( 'NONE',  ( -16.82697755857493505, -8.433404298154332679, 34.66254593164985920 ) ) ;
#28528 = CARTESIAN_POINT ( 'NONE',  ( -3.100243792535585907, -4.299079248970732792, 33.91157788607253565 ) ) ;
#28530 = DIRECTION ( 'NONE',  ( -0.000000000000000000, 1.000000000000000000, -0.000000000000000000 ) ) ;
#28531 = B_SPLINE_CURVE_WITH_KNOTS ( 'NONE', 3,
 ( #31434, #17923, #58898, #86400, #24671, #52138, #46282, #52581, #72852, #66095 ),
 .UNSPECIFIED., .F., .F.,
 ( 4, 2, 2, 2, 4 ),
 ( 0.000000000000000000, 0.0001954311564186861697, 0.0003908623128373723394, 0.0005862934692560584820, 0.0007817246256747446788 ),
 .UNSPECIFIED. ) ;
#28532 = CARTESIAN_POINT ( 'NONE',  ( 2.750000000000001776, -7.499999999999984013, 25.71875000000000000 ) ) ;
#28533 =( REPRESENTATION_RELATIONSHIP ('NONE','NONE', #51743, #36256 ) REPRESENTATION_RELATIONSHIP_WITH_TRANSFORMATION ( #76589 )SHAPE_REPRESENTATION_RELATIONSHIP( ) );
#28534 = VERTEX_POINT ( 'NONE', #55185 ) ;
#28535 = EDGE_CURVE ( 'NONE', #33270, #38366, #82681, .T. ) ;
#28536 = CARTESIAN_POINT ( 'NONE',  ( -16.15384615384615330, -4.661471528628507777, 34.16647553114623292 ) ) ;
#28537 = VERTEX_POINT ( 'NONE', #22727 ) ;
#28538 = ORIENTED_EDGE ( 'NONE', *, *, #64257, .T. ) ;
#28539 = EDGE_CURVE ( 'NONE', #80310, #86521, #1135, .T. ) ;
#28540 = FACE_OUTER_BOUND ( 'NONE', #37305, .T. ) ;
#28541 = ORIENTED_EDGE ( 'NONE', *, *, #73003, .F. ) ;
#28542 = CARTESIAN_POINT ( 'NONE',  ( 17.01083966596719677, -4.786620604624113540, 33.94971097300155805 ) ) ;
#28543 = FACE_OUTER_BOUND ( 'NONE', #81867, .T. ) ;
#28544 = DIRECTION ( 'NONE',  ( 0.000000000000000000, 0.8660254037844377084, 0.5000000000000015543 ) ) ;
#28546 = CARTESIAN_POINT ( 'NONE',  ( 1.319345384059066539, -2.657715359629089225, 31.77849191805834295 ) ) ;
#28545 = VECTOR ( 'NONE', #86861, 1000.000000000000000 ) ;
#28547 = CARTESIAN_POINT ( 'NONE',  ( -4.826868765284762830, -3.627508038966690496, 32.91356715214248396 ) ) ;
#28548 = CARTESIAN_POINT ( 'NONE',  ( 8.769230769230768274, -11.16473453929635440, 33.15142922261926373 ) ) ;
#28549 = CARTESIAN_POINT ( 'NONE',  ( 15.93036121012220541, -11.89387501736623420, 32.13663884655804992 ) ) ;
#28550 = CARTESIAN_POINT ( 'NONE',  ( 6.250000000001421085, -7.500000000000154543, 35.00000000000007105 ) ) ;
#28551 = CARTESIAN_POINT ( 'NONE',  ( 10.39245839786846659, -2.554751324335735152, 30.48935550225260727 ) ) ;
#28552 = CARTESIAN_POINT ( 'NONE',  ( 15.23076923076923173, -9.058645607665452459, 34.76329471203371924 ) ) ;
#28553 = EDGE_CURVE ( 'NONE', #78547, #15822, #3296, .T. ) ;
#28554 = AXIS2_PLACEMENT_3D ( 'NONE', #48600, #69332, #76529 ) ;
#28555 = CARTESIAN_POINT ( 'NONE',  ( 5.076923076922954969, -2.892918686052165622, 31.69288490824153470 ) ) ;
#28556 = DIRECTION ( 'NONE',  ( -0.000000000000000000, -0.1736481776669307198, -0.9848077530122080203 ) ) ;
#28557 = B_SPLINE_CURVE_WITH_KNOTS ( 'NONE', 3,
 ( #26203, #27087, #60873, #88375, #60427, #87942, #26648, #47802, #39731, #68514 ),
 .UNSPECIFIED., .F., .F.,
 ( 4, 2, 2, 2, 4 ),
 ( 0.000000000000000000, 0.0001954339857564082604, 0.0003908679715128165208, 0.0005863019572692248355, 0.0007817359430256330417 ),
 .UNSPECIFIED. ) ;
#28558 = B_SPLINE_CURVE_WITH_KNOTS ( 'NONE', 3,
 ( #53204, #80707, #31610, #23945, #32056, #59964, #87024, #73495, #4582, #51396 ),
 .UNSPECIFIED., .F., .F.,
 ( 4, 2, 2, 2, 4 ),
 ( 0.0007817359430256282712, 0.0009771253907249945886, 0.001172514838424361123, 0.001367904286123727657, 0.001563293733823093975 ),
 .UNSPECIFIED. ) ;
#28559 = VERTEX_POINT ( 'NONE', #56523 ) ;
#28560 = VERTEX_POINT ( 'NONE', #69592 ) ;
#28561 = CARTESIAN_POINT ( 'NONE',  ( -15.16470087976679437, -8.120952969808772792, 34.71129190929999453 ) ) ;
#28562 = CARTESIAN_POINT ( 'NONE',  ( 1.384615384615386802, -2.517432740324522911, 35.29906147534542527 ) ) ;
#28563 = DIRECTION ( 'NONE',  ( -0.000000000000000000, 0.6427876096865404731, -0.7660444431189770143 ) ) ;
#28564 = ORIENTED_EDGE ( 'NONE', *, *, #1889, .T. ) ;
#28566 = EDGE_CURVE ( 'NONE', #45473, #86086, #35361, .T. ) ;
#28565 = CARTESIAN_POINT ( 'NONE',  ( 12.46153846153833911, -9.442884908241554243, 34.35708131394783038 ) ) ;
#28567 = DIRECTION ( 'NONE',  ( 0.000000000000000000, 0.4999999999999985567, 0.8660254037844395958 ) ) ;
#28568 = CARTESIAN_POINT ( 'NONE',  ( 9.019285080869083870, -4.235687564193448829, 33.53795663066793509 ) ) ;
#28569 = ADVANCED_FACE ( 'NONE', ( #16424 ), #43011, .F. ) ;
#28570 = EDGE_CURVE ( 'NONE', #16685, #21791, #63273, .T. ) ;
#28571 = VERTEX_POINT ( 'NONE', #9662 ) ;
#28572 = CARTESIAN_POINT ( 'NONE',  ( -14.43784027742400689, -12.70455904226513866, 30.44083106164009322 ) ) ;
#28573 = ORIENTED_EDGE ( 'NONE', *, *, #41553, .T. ) ;
#28574 = VECTOR ( 'NONE', #71469, 1000.000000000000114 ) ;
#28575 = EDGE_CURVE ( 'NONE', #41328, #32904, #2888, .T. ) ;
#28576 = CARTESIAN_POINT ( 'NONE',  ( 17.78205128205128105, -7.500000000000000000, 29.75000000000000355 ) ) ;
#28577 = CARTESIAN_POINT ( 'NONE',  ( 4.220012760437793276, -7.250054591869668386, 34.99404684341514127 ) ) ;
#28578 = CARTESIAN_POINT ( 'NONE',  ( -39.05038313613820122, -2.499999999999999556, 29.75000000000000355 ) ) ;
#28579 = LINE ( 'NONE', #217, #55153 ) ;
#28580 = CARTESIAN_POINT ( 'NONE',  ( -6.792551484843279752, -2.647132371071621471, 31.75357179365173010 ) ) ;
#28581 = ORIENTED_EDGE ( 'NONE', *, *, #5878, .T. ) ;
#28582 = ORIENTED_EDGE ( 'NONE', *, *, #27147, .F. ) ;
#28583 = VERTEX_POINT ( 'NONE', #2021 ) ;
#28584 = ORIENTED_EDGE ( 'NONE', *, *, #5089, .T. ) ;
#28585 = CARTESIAN_POINT ( 'NONE',  ( -3.453635493832329484, -2.251424796025575770, 29.88072029997477586 ) ) ;
#28586 = CARTESIAN_POINT ( 'NONE',  ( -2.531177232256636156, -10.23692288466677880, 34.23039457007281072 ) ) ;
#28587 = CARTESIAN_POINT ( 'NONE',  ( -12.21159305216042057, -12.45601412856602686, 31.48342859153981621 ) ) ;
#28588 = B_SPLINE_CURVE_WITH_KNOTS ( 'NONE', 3,
 ( #7933, #61095, #55226, #75070, #42175, #14244, #13356, #29869, #40837, #69188 ),
 .UNSPECIFIED., .F., .F.,
 ( 4, 2, 2, 2, 4 ),
 ( 0.0007817359430256215491, 0.0009771253907249856981, 0.001172514838424349847, 0.001367904286123713779, 0.001563293733823077928 ),
 .UNSPECIFIED. ) ;
#28589 = CARTESIAN_POINT ( 'NONE',  ( -2.307692307692428724, -11.67786785259630911, 32.92929555188603530 ) ) ;
#28590 = VECTOR ( 'NONE', #19125, 1000.000000000000000 ) ;
#28591 = CARTESIAN_POINT ( 'NONE',  ( -18.00000000000012079, -4.481592998941359873, 33.73612834414048933 ) ) ;
#28592 = CYLINDRICAL_SURFACE ( 'NONE', #12123, 0.2500000000000008882 ) ;
#28593 = VERTEX_POINT ( 'NONE', #8790 ) ;
#28594 = EDGE_LOOP ( 'NONE', ( #28733, #85647, #14269, #59577, #14940, #72112 ) ) ;
#28595 = VERTEX_POINT ( 'NONE', #57849 ) ;
#28596 = AXIS2_PLACEMENT_3D ( 'NONE', #61575, #40445, #82753 ) ;
#28598 = ORIENTED_EDGE ( 'NONE', *, *, #61260, .T. ) ;
#28597 = CARTESIAN_POINT ( 'NONE',  ( -10.61538461538461320, -2.499999999999998668, 29.75000000000001421 ) ) ;
#28600 = CARTESIAN_POINT ( 'NONE',  ( -5.299850035829924089, -12.64616026154729411, 30.79003144601913533 ) ) ;
#28599 = CARTESIAN_POINT ( 'NONE',  ( -16.82697755857493505, -9.272278438253401589, 34.42582936511637826 ) ) ;
#28601 = DIRECTION ( 'NONE',  ( -0.000000000000000000, -0.3420201433256694901, -0.9396926207859082059 ) ) ;
#28602 = CARTESIAN_POINT ( 'NONE',  ( 2.651650429449539104, -4.848349570550432475, 23.06250000000000000 ) ) ;
#28603 = VERTEX_POINT ( 'NONE', #84015 ) ;
#28604 = VECTOR ( 'NONE', #78677, 1000.000000000000114 ) ;
#28605 = ORIENTED_EDGE ( 'NONE', *, *, #6367, .F. ) ;
#28606 = CARTESIAN_POINT ( 'NONE',  ( 4.088576153289834814, -4.320704448112771878, 33.92786785259540494 ) ) ;
#28607 = ORIENTED_EDGE ( 'NONE', *, *, #26591, .F. ) ;
#28608 = FACE_BOUND ( 'NONE', #81426, .T. ) ;
#28609 = LINE ( 'NONE', #70028, #31667 ) ;
#28610 = CARTESIAN_POINT ( 'NONE',  ( -30.00000000000000000, -15.00000000000000000, 3.000000000000000000 ) ) ;
#28611 = ORIENTED_EDGE ( 'NONE', *, *, #7938, .F. ) ;
#28612 = CARTESIAN_POINT ( 'NONE',  ( 15.48076923076929567, -7.434744860731433924, 35.00000000000000711 ) ) ;
#28613 = CARTESIAN_POINT ( 'NONE',  ( -9.915234651214539952, -4.762599654559228846, 34.23009711892697737 ) ) ;
#28614 = DIRECTION ( 'NONE',  ( 0.000000000000000000, 0.000000000000000000, -1.000000000000000000 ) ) ;
#28615 = CARTESIAN_POINT ( 'NONE',  ( -12.94230769230769162, -7.500000000000000000, 29.75000000000000355 ) ) ;
#28616 = CARTESIAN_POINT ( 'NONE',  ( 0.5276068125408995835, -12.37446782046654192, 30.86335684631486842 ) ) ;
#28617 = ORIENTED_EDGE ( 'NONE', *, *, #36621, .T. ) ;
#28618 = B_SPLINE_CURVE_WITH_KNOTS ( 'NONE', 3,
 ( #26656, #68094, #68969, #13145, #12253, #20352, #81607, #6822, #75292, #33420 ),
 .UNSPECIFIED., .F., .F.,
 ( 4, 2, 2, 2, 4 ),
 ( 0.0007817359430256399806, 0.0009771253907250089001, 0.001172514838424378036, 0.001367904286123746956, 0.001563293733823115875 ),
 .UNSPECIFIED. ) ;
#28619 = B_SPLINE_CURVE_WITH_KNOTS ( 'NONE', 3,
 ( #41766, #21029, #76876, #21481, #34111, #331, #83196, #15176, #6208, #48502 ),
 .UNSPECIFIED., .F., .F.,
 ( 4, 2, 2, 2, 4 ),
 ( 0.0007817359430256282712, 0.0009771253907249939381, 0.001172514838424359822, 0.001367904286123725489, 0.001563293733823091156 ),
 .UNSPECIFIED. ) ;
#28620 = EDGE_CURVE ( 'NONE', #9998, #29143, #75260, .T. ) ;
#28621 = CARTESIAN_POINT ( 'NONE',  ( 6.066068351002440906, -8.120952969808772792, 34.71129190929999453 ) ) ;
#28622 = CARTESIAN_POINT ( 'NONE',  ( 2.241609928332172430, -11.91647553114624181, 32.58852847137148245 ) ) ;
#28623 = DIRECTION ( 'NONE',  ( -0.000000000000000000, 0.8660254037844397068, -0.4999999999999978906 ) ) ;
#28624 = FACE_OUTER_BOUND ( 'NONE', #57462, .T. ) ;
#28625 = CARTESIAN_POINT ( 'NONE',  ( -15.23076923076922995, -2.499999999999998668, 29.75000000000001421 ) ) ;
#28626 = FACE_BOUND ( 'NONE', #9496, .T. ) ;
#28628 = DIRECTION ( 'NONE',  ( -0.000000000000000000, -0.000000000000000000, -1.000000000000000000 ) ) ;
#28627 = CYLINDRICAL_SURFACE ( 'NONE', #49074, 0.2500000000000008882 ) ;
#28629 = CARTESIAN_POINT ( 'NONE',  ( -6.923076923077044142, -12.27809138561165270, 31.22303859784587132 ) ) ;
#28631 = CARTESIAN_POINT ( 'NONE',  ( 8.352564102564102200, -3.499999999999999556, 29.75000000000000355 ) ) ;
#28630 = CARTESIAN_POINT ( 'NONE',  ( -9.019230769230768274, -7.500000000000001776, 35.00000000000000000 ) ) ;
#28632 = CARTESIAN_POINT ( 'NONE',  ( -18.22348494372394967, -10.11188796281392221, 34.01382737946117629 ) ) ;
#28633 = VECTOR ( 'NONE', #62735, 1000.000000000000000 ) ;
#28634 = CARTESIAN_POINT ( 'NONE',  ( 1.987747218494664292, -9.401340078031346081, 24.37313170625848713 ) ) ;
#28635 = ORIENTED_EDGE ( 'NONE', *, *, #63136, .F. ) ;
#28636 = DIRECTION ( 'NONE',  ( -0.000000000000000000, -0.6427876096865404731, -0.7660444431189771253 ) ) ;
#28637 = ORIENTED_EDGE ( 'NONE', *, *, #75606, .F. ) ;
#28638 = CARTESIAN_POINT ( 'NONE',  ( -18.00000000000000000, -11.35647404775217240, 33.31231777344666511 ) ) ;
#28639 = VERTEX_POINT ( 'NONE', #43888 ) ;
#28640 = EDGE_CURVE ( 'NONE', #25404, #33571, #84711, .T. ) ;
#28641 = LINE ( 'NONE', #26862, #6684 ) ;
#28642 = CARTESIAN_POINT ( 'NONE',  ( -18.06527044596078113, -2.625532179533445198, 30.86335684631481513 ) ) ;
#28643 = ORIENTED_EDGE ( 'NONE', *, *, #1187, .T. ) ;
#28644 = CARTESIAN_POINT ( 'NONE',  ( -9.915186374736338237, -7.630691491037285168, 34.74850469731152458 ) ) ;
#28645 = CARTESIAN_POINT ( 'NONE',  ( -1.987747218494660295, -5.598659921968651254, 16.24813170625848713 ) ) ;
#28646 = CARTESIAN_POINT ( 'NONE',  ( -6.923076923076922462, -2.538708090699994813, 30.37095296980875503 ) ) ;
#28647 = FACE_OUTER_BOUND ( 'NONE', #487, .T. ) ;
#28648 = CARTESIAN_POINT ( 'NONE',  ( -5.207613680033387205, -2.845849958028613624, 32.17971566917920967 ) ) ;
#28649 = DIRECTION ( 'NONE',  ( 1.000000000000000000, 0.000000000000000000, 0.000000000000000000 ) ) ;
#28650 = CYLINDRICAL_SURFACE ( 'NONE', #41586, 0.2499999999999986955 ) ;
#28651 = CARTESIAN_POINT ( 'NONE',  ( -13.63463860883684120, -12.07920672191015221, 32.31858351112116168 ) ) ;
#28652 = CARTESIAN_POINT ( 'NONE',  ( -3.775308065498748977, -8.992201783934593351, 24.01749329374151287 ) ) ;
#28653 = CARTESIAN_POINT ( 'NONE',  ( -18.00000000000000000, -11.35647404775217240, 33.31231777344666511 ) ) ;
#28654 = DIRECTION ( 'NONE',  ( 0.000000000000000000, 0.000000000000000000, 1.000000000000000000 ) ) ;
#28655 = EDGE_CURVE ( 'NONE', #27642, #26164, #33543, .T. ) ;
#28656 = CARTESIAN_POINT ( 'NONE',  ( 20.00000000000000000, -4.000000000000000000, 29.75000000000000355 ) ) ;
#28657 = CARTESIAN_POINT ( 'NONE',  ( 2.608446859217924629, -10.19485399968118422, 23.62686829374151287 ) ) ;
#28658 = B_SPLINE_CURVE_WITH_KNOTS ( 'NONE', 3,
 ( #22775, #85378, #29550, #29989, #10605, #17814, #37625, #43501, #50685, #57005 ),
 .UNSPECIFIED., .F., .F.,
 ( 4, 2, 2, 2, 4 ),
 ( 0.0007817359430256288133, 0.0009771253907249948054, 0.001172514838424360689, 0.001367904286123726573, 0.001563293733823092457 ),
 .UNSPECIFIED. ) ;
#28659 = AXIS2_PLACEMENT_3D ( 'NONE', #34846, #27211, #47471 ) ;
#28661 = CARTESIAN_POINT ( 'NONE',  ( -14.05774678934416499, -10.76462480002816235, 33.53768742498949962 ) ) ;
#28660 = B_SPLINE_CURVE_WITH_KNOTS ( 'NONE', 3,
 ( #76815, #56089, #61953, #76358, #8355, #83584, #14219, #41253, #84026, #7908 ),
 .UNSPECIFIED., .F., .F.,
 ( 4, 2, 2, 2, 4 ),
 ( 0.0007817246256747517261, 0.0009771112852218961399, 0.001172497944769040771, 0.001367884604316185401, 0.001563271263863329815 ),
 .UNSPECIFIED. ) ;
#28662 = AXIS2_PLACEMENT_3D ( 'NONE', #44270, #25356, #38433 ) ;
#28663 = VERTEX_POINT ( 'NONE', #29504 ) ;
#28664 = CARTESIAN_POINT ( 'NONE',  ( 6.700198240648278514, -7.630691491037286056, 34.74850469731152458 ) ) ;
#28665 = CARTESIAN_POINT ( 'NONE',  ( 12.46153846153846168, -8.164416787775445883, 34.95778746994557906 ) ) ;
#28666 = CARTESIAN_POINT ( 'NONE',  ( 1.384615384615264011, -5.941354392335915335, 34.76329471203413846 ) ) ;
#28667 = CARTESIAN_POINT ( 'NONE',  ( -14.53117725141625627, -11.89387501736622710, 32.13663884655806413 ) ) ;
#28668 = B_SPLINE_CURVE_WITH_KNOTS ( 'NONE', 3,
 ( #25523, #73725, #31389, #12019, #24178, #40714, #68175, #6478, #33940, #85449 ),
 .UNSPECIFIED., .F., .F.,
 ( 4, 2, 2, 2, 4 ),
 ( 0.0007817246256747450040, 0.0009771112852218876831, 0.001172497944769030579, 0.001367884604316173258, 0.001563271263863315937 ),
 .UNSPECIFIED. ) ;
#28669 = CARTESIAN_POINT ( 'NONE',  ( -16.28453762051371712, -10.54014554554151140, 33.71984207302941883 ) ) ;
#28670 = CARTESIAN_POINT ( 'NONE',  ( 6.923076923076924238, -11.91647553114624181, 32.58852847137148245 ) ) ;
#28671 = CIRCLE ( 'NONE', #65999, 0.2500000000000002220 ) ;
#28672 = DIRECTION ( 'NONE',  ( 0.000000000000000000, 0.7660444431189807890, 0.6427876096865361433 ) ) ;
#28673 = CARTESIAN_POINT ( 'NONE',  ( 10.48523664565292002, -12.70455904226513866, 30.44083106164009322 ) ) ;
#28674 = ADVANCED_FACE ( 'NONE', ( #50190 ), #15100, .F. ) ;
#28675 = EDGE_CURVE ( 'NONE', #79746, #45649, #84453, .T. ) ;
#28676 = ORIENTED_EDGE ( 'NONE', *, *, #18711, .T. ) ;
#28677 = VERTEX_POINT ( 'NONE', #57401 ) ;
#28678 = ORIENTED_EDGE ( 'NONE', *, *, #750, .F. ) ;
#28679 = FACE_OUTER_BOUND ( 'NONE', #11391, .T. ) ;
#28680 = CARTESIAN_POINT ( 'NONE',  ( -6.673131404728781746, -4.336752205174647656, 33.62275283266504289 ) ) ;
#28681 = CARTESIAN_POINT ( 'NONE',  ( -15.48079245499068435, -10.92453946501458795, 33.72985991061850086 ) ) ;
#28682 = CARTESIAN_POINT ( 'NONE',  ( -13.25408968285181999, -12.27024696741798948, 31.24895572276497546 ) ) ;
#28683 = CARTESIAN_POINT ( 'NONE',  ( 17.99999999999987566, -9.528491918059723176, 34.59228464037033035 ) ) ;
#28684 = VERTEX_POINT ( 'NONE', #50642 ) ;
#28685 = CARTESIAN_POINT ( 'NONE',  ( 17.32686848630112308, -11.56426240980093567, 33.07394671870546432 ) ) ;
#28686 = ORIENTED_EDGE ( 'NONE', *, *, #80126, .T. ) ;
#28687 = ORIENTED_EDGE ( 'NONE', *, *, #73060, .T. ) ;
#28688 = B_SPLINE_CURVE_WITH_KNOTS ( 'NONE', 3,
 ( #63120, #43310, #44949, #10738, #82968, #62674 ),
 .UNSPECIFIED., .F., .F.,
 ( 4, 2, 4 ),
 ( 4.220987180333913997E-17, 0.0001954756301637150138, 0.0003909512603273878522 ),
 .UNSPECIFIED. ) ;
#28689 = ORIENTED_EDGE ( 'NONE', *, *, #77924, .F. ) ;
#28691 = EDGE_LOOP ( 'NONE', ( #40318, #46386, #8787, #62171, #75690 ) ) ;
#28690 = CARTESIAN_POINT ( 'NONE',  ( 11.53846153846153832, -3.322132147404559976, 32.92929555188717927 ) ) ;
#28692 = DIRECTION ( 'NONE',  ( -0.000000000000000000, 0.5000000000000011102, -0.8660254037844380415 ) ) ;
#28693 = AXIS2_PLACEMENT_3D ( 'NONE', #19977, #68610, #83472 ) ;
#28694 = CARTESIAN_POINT ( 'NONE',  ( 5.934729999443683290, -12.70778746994557551, 30.41441678777548319 ) ) ;
#28695 = CARTESIAN_POINT ( 'NONE',  ( -9.692307692307691624, -8.120952969808772792, 34.71129190930000163 ) ) ;
#28696 = CARTESIAN_POINT ( 'NONE',  ( 14.24193887937897607, -7.249945578846651806, 34.99404164642496795 ) ) ;
#28697 = VERTEX_POINT ( 'NONE', #15988 ) ;
#28698 = ORIENTED_EDGE ( 'NONE', *, *, #15165, .T. ) ;
#28699 = VERTEX_POINT ( 'NONE', #43452 ) ;
#28700 = DIRECTION ( 'NONE',  ( 1.000000000000000000, 0.000000000000000000, 0.000000000000000000 ) ) ;
#28702 = ORIENTED_EDGE ( 'NONE', *, *, #63735, .F. ) ;
#28701 = CARTESIAN_POINT ( 'NONE',  ( 4.153846153846154188, -11.16473453929635440, 33.15142922261926373 ) ) ;
#28703 = CARTESIAN_POINT ( 'NONE',  ( 3.230769230769108269, -3.643525952248796163, 33.31231777344771672 ) ) ;
#28704 = CARTESIAN_POINT ( 'NONE',  ( 9.692307692307695177, -11.69971097300155272, 32.46337939537588113 ) ) ;
#28705 = CARTESIAN_POINT ( 'NONE',  ( 10.61538461538461675, -10.05456864172156806, 36.03766855953608683 ) ) ;
#28706 = ORIENTED_EDGE ( 'NONE', *, *, #21500, .F. ) ;
#28707 = LINE ( 'NONE', #62471, #29297 ) ;
#28708 = DIRECTION ( 'NONE',  ( -0.000000000000000000, 0.9396926207859092051, -0.3420201433256662704 ) ) ;
#28709 = ORIENTED_EDGE ( 'NONE', *, *, #46650, .F. ) ;
#28710 = FACE_BOUND ( 'NONE', #65841, .T. ) ;
#28711 = CARTESIAN_POINT ( 'NONE',  ( 23.00000000000000000, -2.249999999999999556, 27.25000000000000000 ) ) ;
#28712 = CARTESIAN_POINT ( 'NONE',  ( 16.15384615384603251, -2.657715359629662544, 31.77849191805970364 ) ) ;
#28713 = CARTESIAN_POINT ( 'NONE',  ( 3.296837581771669079, -8.973038597847269315, 34.52809138561122637 ) ) ;
#28716 = CYLINDRICAL_SURFACE ( 'NONE', #8078, 4.000000000000000000 ) ;
#28715 = VECTOR ( 'NONE', #43340, 1000.000000000000227 ) ;
#28714 = CYLINDRICAL_SURFACE ( 'NONE', #76283, 0.2499999999999973355 ) ;
#28717 = VECTOR ( 'NONE', #39784, 1000.000000000000000 ) ;
#28718 = CARTESIAN_POINT ( 'NONE',  ( -4.826977558574934157, -10.76462480002816235, 33.53768742498949962 ) ) ;
#28719 = FACE_OUTER_BOUND ( 'NONE', #55116, .T. ) ;
#28720 = ORIENTED_EDGE ( 'NONE', *, *, #72957, .F. ) ;
#28721 = DIRECTION ( 'NONE',  ( 1.000000000000000000, 0.000000000000000000, 0.000000000000000000 ) ) ;
#28722 = CARTESIAN_POINT ( 'NONE',  ( -6.000000000000121680, -11.67786785259630911, 32.92929555188603530 ) ) ;
#28723 = AXIS2_PLACEMENT_3D ( 'NONE', #41374, #68837, #76931 ) ;
#28724 = ORIENTED_EDGE ( 'NONE', *, *, #77870, .T. ) ;
#28725 = EDGE_CURVE ( 'NONE', #75886, #40515, #768, .T. ) ;
#28726 = VECTOR ( 'NONE', #84434, 1000.000000000000114 ) ;
#28727 = EDGE_CURVE ( 'NONE', #83231, #949, #73607, .T. ) ;
#28728 = AXIS2_PLACEMENT_3D ( 'NONE', #33200, #79166, #17468 ) ;
#28729 = ADVANCED_FACE ( 'NONE', ( #86685 ), #38029, .F. ) ;
#28730 = CYLINDRICAL_SURFACE ( 'NONE', #37200, 4.000000000000000000 ) ;
#28731 = CARTESIAN_POINT ( 'NONE',  ( -15.93083480223330817, -10.61302985866384141, 33.66295027996417843 ) ) ;
#28732 = CARTESIAN_POINT ( 'NONE',  ( 9.627037246346919375, -2.892918686051582533, 31.69288490824015980 ) ) ;
#28733 = ORIENTED_EDGE ( 'NONE', *, *, #49892, .F. ) ;
#28734 = CARTESIAN_POINT ( 'NONE',  ( -10.36533019547115941, -2.920487667080175598, 32.31805714834170828 ) ) ;
#28735 = CARTESIAN_POINT ( 'NONE',  ( 4.219914504848593317, -9.780366693483667717, 34.19971097300155805 ) ) ;
#28736 = FACE_BOUND ( 'NONE', #72097, .T. ) ;
#28738 = CARTESIAN_POINT ( 'NONE',  ( -3.931066612577743147, -8.496831190052096971, 34.64984203495476578 ) ) ;
#28737 = CARTESIAN_POINT ( 'NONE',  ( 6.857806922520604864, -4.320704448112771878, 33.92786785259540494 ) ) ;
#28739 = CARTESIAN_POINT ( 'NONE',  ( 1.607628228708781970, -12.64618726649961289, 30.78989965857442712 ) ) ;
#28741 = LINE ( 'NONE', #16102, #27612 ) ;
#28740 = CARTESIAN_POINT ( 'NONE',  ( -3.007989689500819797, -11.89424750095246175, 32.13594075562311758 ) ) ;
#28742 = CARTESIAN_POINT ( 'NONE',  ( -19.00000000000000000, 1.250000000000004663, 23.75000000000000000 ) ) ;
#28743 = CARTESIAN_POINT ( 'NONE',  ( -1.553300858899081538, -11.25000000000000711, 26.10937500000001066 ) ) ;
#28744 = ORIENTED_EDGE ( 'NONE', *, *, #84632, .T. ) ;
#28745 = ORIENTED_EDGE ( 'NONE', *, *, #13550, .F. ) ;
#28746 = EDGE_CURVE ( 'NONE', #49489, #68389, #66834, .T. ) ;
#28747 = CARTESIAN_POINT ( 'NONE',  ( 1.326923076923076206, -4.000000000000000000, 29.75000000000000355 ) ) ;
#28748 = CARTESIAN_POINT ( 'NONE',  ( -12.33101302330481808, -6.808710257144161559, 34.95449254468098843 ) ) ;
#28749 = FACE_OUTER_BOUND ( 'NONE', #29095, .T. ) ;
#28750 = DIRECTION ( 'NONE',  ( -1.000000000000000000, 0.000000000000000000, -0.000000000000000000 ) ) ;
#28751 = EDGE_CURVE ( 'NONE', #6445, #46418, #29809, .T. ) ;
#28752 = DIRECTION ( 'NONE',  ( -0.000000000000000000, -0.9848077530122086864, -0.1736481776669273613 ) ) ;
#28753 = CARTESIAN_POINT ( 'NONE',  ( 2.651650429449569302, -10.15165042944953733, 25.87500000000000355 ) ) ;
#28754 = CARTESIAN_POINT ( 'NONE',  ( -12.59168643127016196, -4.299443229763728169, 33.91186481527756058 ) ) ;
#28755 = CARTESIAN_POINT ( 'NONE',  ( 4.023698184114460119, -12.15440758774515473, 32.17923288041532004 ) ) ;
#28756 = CARTESIAN_POINT ( 'NONE',  ( 9.562159722575998444, -11.04286588640298561, 33.62463336215343901 ) ) ;
#28757 = CARTESIAN_POINT ( 'NONE',  ( 8.352564102564102200, -7.500000000000000000, 29.75000000000000355 ) ) ;
#28758 = LINE ( 'NONE', #36397, #82746 ) ;
#28759 = FACE_OUTER_BOUND ( 'NONE', #56248, .T. ) ;
#28760 = B_SPLINE_CURVE_WITH_KNOTS ( 'NONE', 3,
 ( #47554, #41693, #54756, #69166, #61508, #89015, #48434, #7015, #42586, #26850 ),
 .UNSPECIFIED., .F., .F.,
 ( 4, 2, 2, 2, 4 ),
 ( 0.000000000000000000, 0.0001954311564186870371, 0.0003908623128373740741, 0.0005862934692560610840, 0.0007817246256747481482 ),
 .UNSPECIFIED. ) ;
#28761 = CARTESIAN_POINT ( 'NONE',  ( -5.869209559033047086, -11.37503395064541678, 33.29242100308974983 ) ) ;
#28762 = FACE_OUTER_BOUND ( 'NONE', #31559, .T. ) ;
#28763 = EDGE_CURVE ( 'NONE', #19281, #77760, #81339, .T. ) ;
#28764 = CARTESIAN_POINT ( 'NONE',  ( -3.512820512820513663, -7.500000000000000000, 29.75000000000000355 ) ) ;
#28765 = ORIENTED_EDGE ( 'NONE', *, *, #40740, .F. ) ;
#28766 = VECTOR ( 'NONE', #72488, 999.9999999999998863 ) ;
#28767 = CARTESIAN_POINT ( 'NONE',  ( 4.023154687178596589, -4.809359713505814149, 33.96456829005828837 ) ) ;
#28768 = CARTESIAN_POINT ( 'NONE',  ( 7.596130621932389637, -4.931416488878822335, 34.32920672191015399 ) ) ;
#28769 = CARTESIAN_POINT ( 'NONE',  ( 2.750000000000002665, -7.561099074964516831, 20.97061829374151642 ) ) ;
#28770 = CARTESIAN_POINT ( 'NONE',  ( 0.4615384615383382183, -3.643525952248795718, 33.31231777344771672 ) ) ;
#28771 = CARTESIAN_POINT ( 'NONE',  ( 16.82694633287449193, -11.47974371597207899, 33.17467449705390692 ) ) ;
#28772 = ORIENTED_EDGE ( 'NONE', *, *, #56596, .F. ) ;
#28773 = CARTESIAN_POINT ( 'NONE',  ( -9.915234651214538175, -5.582147617184174848, 34.63737895849758530 ) ) ;
#28775 = VERTEX_POINT ( 'NONE', #85332 ) ;
#28774 = LINE ( 'NONE', #21561, #56885 ) ;
#28776 = CARTESIAN_POINT ( 'NONE',  ( 8.096099364501988305, -3.712312575010499494, 33.01462480002815170 ) ) ;
#28777 = CARTESIAN_POINT ( 'NONE',  ( 0.4615384615384611200, -1.466349020453238561, 30.81389545987213907 ) ) ;
#28778 = EDGE_LOOP ( 'NONE', ( #24530, #3788 ) ) ;
#28779 = LINE ( 'NONE', #64309, #72171 ) ;
#28780 = CARTESIAN_POINT ( 'NONE',  ( 13.31934538405906743, -9.528491918058357157, 34.59228464037090589 ) ) ;
#28781 = VERTEX_POINT ( 'NONE', #23615 ) ;
#28782 = CARTESIAN_POINT ( 'NONE',  ( -4.230769230769230838, -7.500000000000000000, 29.75000000000000355 ) ) ;
#28783 = CARTESIAN_POINT ( 'NONE',  ( -16.02332045208259004, -3.285477652293413264, 32.44071101563363158 ) ) ;
#28784 = ADVANCED_FACE ( 'NONE', ( #51065 ), #24059, .F. ) ;
#28786 = CARTESIAN_POINT ( 'NONE',  ( -9.562262529472915773, -2.504778602574660340, 29.97347330155780654 ) ) ;
#28785 = VECTOR ( 'NONE', #59079, 1000.000000000000000 ) ;
#28787 = VERTEX_POINT ( 'NONE', #17310 ) ;
#28788 = ADVANCED_FACE ( 'NONE', ( #52863 ), #58734, .F. ) ;
#28789 = ORIENTED_EDGE ( 'NONE', *, *, #20410, .T. ) ;
#28790 = CARTESIAN_POINT ( 'NONE',  ( -10.48459417441766561, -2.295524264805589354, 30.44142389570982488 ) ) ;
#28791 = VERTEX_POINT ( 'NONE', #10105 ) ;
#28792 = AXIS2_PLACEMENT_3D ( 'NONE', #60179, #25957, #12447 ) ;
#28793 = EDGE_CURVE ( 'NONE', #17458, #48157, #44767, .T. ) ;
#28794 = CARTESIAN_POINT ( 'NONE',  ( 15.36155967173618286, -12.62708834333097663, 30.88030960425257021 ) ) ;
#28795 = CARTESIAN_POINT ( 'NONE',  ( -5.934744860487159102, -5.941354392334606160, 34.76329471203374055 ) ) ;
#28796 = ADVANCED_FACE ( 'NONE', ( #24502 ), #51969, .F. ) ;
#28797 = B_SPLINE_CURVE_WITH_KNOTS ( 'NONE', 3,
 ( #47316, #13101, #40581, #68049, #88780, #27056, #54517, #82009, #20305, #47766 ),
 .UNSPECIFIED., .F., .F.,
 ( 4, 2, 2, 2, 4 ),
 ( 0.000000000000000000, 0.0001954311564186870099, 0.0003908623128373740199, 0.0005862934692560609756, 0.0007817246256747480398 ),
 .UNSPECIFIED. ) ;
#28798 = CARTESIAN_POINT ( 'NONE',  ( 17.07692307692307665, -1.242168528481310874, 33.36296068462461051 ) ) ;
#28799 = B_SPLINE_CURVE_WITH_KNOTS ( 'NONE', 3,
 ( #80095, #80560, #72885, #11191, #53052, #4428, #39576, #59377, #5329, #19287 ),
 .UNSPECIFIED., .F., .F.,
 ( 4, 2, 2, 2, 4 ),
 ( 0.000000000000000000, 0.0001954311564186868473, 0.0003908623128373736946, 0.0005862934692560605419, 0.0007817246256747473893 ),
 .UNSPECIFIED. ) ;
#28800 = CARTESIAN_POINT ( 'NONE',  ( -7.596153846152408740, -7.500000000000155431, 34.75000000000007105 ) ) ;
#28801 = VECTOR ( 'NONE', #11813, 1000.000000000000114 ) ;
#28802 = DIRECTION ( 'NONE',  ( 0.000000000000000000, 0.1736481776669275834, 0.9848077530122086864 ) ) ;
#28803 = B_SPLINE_CURVE_WITH_KNOTS ( 'NONE', 3,
 ( #9479, #8161, #48688, #76164, #41950, #36521, #29323, #63969, #22114, #7723 ),
 .UNSPECIFIED., .F., .F.,
 ( 4, 2, 2, 2, 4 ),
 ( 0.000000000000000000, 0.0001954311564186868473, 0.0003908623128373736946, 0.0005862934692560605419, 0.0007817246256747473893 ),
 .UNSPECIFIED. ) ;
#28804 = ORIENTED_EDGE ( 'NONE', *, *, #73089, .F. ) ;
#28805 = ORIENTED_EDGE ( 'NONE', *, *, #13316, .T. ) ;
#28807 = ORIENTED_EDGE ( 'NONE', *, *, #85642, .T. ) ;
#28806 = CARTESIAN_POINT ( 'NONE',  ( 11.00641025641025550, -7.500000000000000000, 33.75000000000000000 ) ) ;
#28808 = CARTESIAN_POINT ( 'NONE',  ( -5.207071046654775159, -5.070767119584671079, 34.40440758774516183 ) ) ;
#28809 = ORIENTED_EDGE ( 'NONE', *, *, #15459, .F. ) ;
#28810 = LINE ( 'NONE', #8090, #56484 ) ;
#28811 = CARTESIAN_POINT ( 'NONE',  ( 6.857806922520603976, -9.528491918058357157, 34.59228464037090589 ) ) ;
#28812 = EDGE_LOOP ( 'NONE', ( #55714, #4754 ) ) ;
#28813 = LINE ( 'NONE', #83759, #45660 ) ;
#28814 = ORIENTED_EDGE ( 'NONE', *, *, #82560, .F. ) ;
#28816 = VERTEX_POINT ( 'NONE', #18206 ) ;
#28815 = CARTESIAN_POINT ( 'NONE',  ( -6.857821351800899023, -11.48612834413965977, 32.76840700105972815 ) ) ;
#28817 = CARTESIAN_POINT ( 'NONE',  ( -10.36538461538455103, -7.434744429011176159, 34.75000000000000711 ) ) ;
#28818 = EDGE_CURVE ( 'NONE', #14974, #84688, #2825, .T. ) ;
#28819 = ORIENTED_EDGE ( 'NONE', *, *, #19797, .F. ) ;
#28820 = CARTESIAN_POINT ( 'NONE',  ( 17.75002326905764960, -10.66389620160130036, 33.62221079203477103 ) ) ;
#28821 = B_SPLINE_CURVE_WITH_KNOTS ( 'NONE', 3,
 ( #64986, #37977, #53254, #3291, #19039, #25348, #80756, #66780, #30766, #58681 ),
 .UNSPECIFIED., .F., .F.,
 ( 4, 2, 2, 2, 4 ),
 ( 0.0007817246256747491240, 0.0009771112852218931041, 0.001172497944769036867, 0.001367884604316180631, 0.001563271263863324611 ),
 .UNSPECIFIED. ) ;
#28822 = VECTOR ( 'NONE', #72379, 1000.000000000000000 ) ;
#28823 = CARTESIAN_POINT ( 'NONE',  ( 17.99999999999987566, -12.51329471203414379, 31.30864560766407578 ) ) ;
#28824 = FACE_BOUND ( 'NONE', #41706, .T. ) ;
#28825 = B_SPLINE_CURVE_WITH_KNOTS ( 'NONE', 3,
 ( #40648, #16266, #85175, #57693, #36543, #70772, #15833, #83408, #35661, #41978 ),
 .UNSPECIFIED., .F., .F.,
 ( 4, 2, 2, 2, 4 ),
 ( 0.000000000000000000, 0.0001954311564186867931, 0.0003908623128373735862, 0.0005862934692560603251, 0.0007817246256747471724 ),
 .UNSPECIFIED. ) ;
#28826 = PLANE ( 'NONE',  #31217 ) ;
#28827 = DIRECTION ( 'NONE',  ( -1.000000000000000000, 0.000000000000000000, 0.000000000000000000 ) ) ;
#28828 = DIRECTION ( 'NONE',  ( -0.000000000000000000, 1.000000000000000000, 3.491481338843133355E-15 ) ) ;
#28829 = CARTESIAN_POINT ( 'NONE',  ( -0.4615384615384611200, -2.833524468853757305, 32.15551576947925838 ) ) ;
#28830 = CARTESIAN_POINT ( 'NONE',  ( 5.299934428535924447, -10.61302985866383963, 33.66295027996417843 ) ) ;
#28831 = CARTESIAN_POINT ( 'NONE',  ( -9.757557624081776737, -2.255955759149247619, 30.00000000000013856 ) ) ;
#28832 = ORIENTED_EDGE ( 'NONE', *, *, #23073, .F. ) ;
#28833 = CARTESIAN_POINT ( 'NONE',  ( 15.23076923076923173, -1.466349020453238561, 30.81389545987213907 ) ) ;
#28834 = ORIENTED_EDGE ( 'NONE', *, *, #29112, .T. ) ;
#28835 = ORIENTED_EDGE ( 'NONE', *, *, #9287, .T. ) ;
#28836 = EDGE_CURVE ( 'NONE', #83181, #19489, #71580, .T. ) ;
#28838 = CARTESIAN_POINT ( 'NONE',  ( 8.068933387422251968, -10.11255958852956027, 34.01340905677048454 ) ) ;
#28837 = DIRECTION ( 'NONE',  ( 0.000000000000000000, 0.4999999999999985567, 0.8660254037844395958 ) ) ;
#28839 = CYLINDRICAL_SURFACE ( 'NONE', #35571, 0.2499999999999995559 ) ;
#28840 = CARTESIAN_POINT ( 'NONE',  ( 17.07692307692307665, -5.415277668671390821, 36.20867863119892149 ) ) ;
#28841 = CYLINDRICAL_SURFACE ( 'NONE', #34390, 0.2500000000000002220 ) ;
#28842 = CARTESIAN_POINT ( 'NONE',  ( 9.915319043920543862, -2.554770724473668153, 30.48948780036025852 ) ) ;
#28843 = ORIENTED_EDGE ( 'NONE', *, *, #14594, .F. ) ;
#28844 = CARTESIAN_POINT ( 'NONE',  ( 1.384615384615264011, -5.094484230521993062, 34.41647553114689373 ) ) ;
#28845 = CARTESIAN_POINT ( 'NONE',  ( 16.40384615384615330, -2.499999999999998668, 29.75000000000000355 ) ) ;
#28846 = CARTESIAN_POINT ( 'NONE',  ( -12.52680846209478460, -11.67786785259540849, 32.92929555188721480 ) ) ;
#28847 = VECTOR ( 'NONE', #15753, 1000.000000000000114 ) ;
#28848 = CARTESIAN_POINT ( 'NONE',  ( -8.546217925137375104, -2.523321265292115534, 31.42251411153756990 ) ) ;
#28849 = CARTESIAN_POINT ( 'NONE',  ( 13.51540582558234149, -5.496552790871120031, 34.60292014791297532 ) ) ;
#28850 = EDGE_LOOP ( 'NONE', ( #17470, #59075 ) ) ;
#28851 = B_SPLINE_CURVE_WITH_KNOTS ( 'NONE', 3,
 ( #301, #1179, #69202, #41736, #742, #14704, #61546, #27330, #7946, #35411 ),
 .UNSPECIFIED., .F., .F.,
 ( 4, 2, 2, 2, 4 ),
 ( 0.0007817246256747469556, 0.0009771112852218889842, 0.001172497944769031013, 0.001367884604316173041, 0.001563271263863315070 ),
 .UNSPECIFIED. ) ;
#28852 = VERTEX_POINT ( 'NONE', #81245 ) ;
#28853 = VECTOR ( 'NONE', #24748, 1000.000000000000114 ) ;
#28854 = VECTOR ( 'NONE', #30263, 1000.000000000000227 ) ;
#28855 = ORIENTED_EDGE ( 'NONE', *, *, #64830, .T. ) ;
#28856 = ADVANCED_FACE ( 'NONE', ( #81688 ), #6029, .F. ) ;
#28857 = FACE_OUTER_BOUND ( 'NONE', #79984, .T. ) ;
#28858 = ORIENTED_EDGE ( 'NONE', *, *, #17944, .T. ) ;
#28859 = CARTESIAN_POINT ( 'NONE',  ( -1.254089682851820431, -8.586989748646450593, 34.63063291749215011 ) ) ;
#28860 = CARTESIAN_POINT ( 'NONE',  ( -12.21148414990014786, -6.567000820036036579, 34.66262288849541306 ) ) ;
#28861 = CARTESIAN_POINT ( 'NONE',  ( 14.05766908347085575, -10.18141759479407327, 34.26406193332782379 ) ) ;
#28862 = ADVANCED_FACE ( 'NONE', ( #69824 ), #19968, .F. ) ;
#28863 = CARTESIAN_POINT ( 'NONE',  ( -12.46153846153858424, -3.083524468854526912, 32.58852847137268327 ) ) ;
#28864 = CARTESIAN_POINT ( 'NONE',  ( -16.85414353565465717, -12.24180327182771855, 31.33663988360758168 ) ) ;
#28865 = VECTOR ( 'NONE', #65969, 1000.000000000000227 ) ;
#28866 = VECTOR ( 'NONE', #18309, 1000.000000000000227 ) ;
#28867 = DIRECTION ( 'NONE',  ( 0.000000000000000000, 0.7660444431189822323, -0.6427876096865344779 ) ) ;
#28868 = EDGE_LOOP ( 'NONE', ( #63705, #35235 ) ) ;
#28869 = CARTESIAN_POINT ( 'NONE',  ( 11.53846153846184563, -2.506253911140615021, 30.00000000000323297 ) ) ;
#28871 = ORIENTED_EDGE ( 'NONE', *, *, #32246, .F. ) ;
#28870 = CARTESIAN_POINT ( 'NONE',  ( -13.16183584334697265, -4.387253974876679230, 33.66317474335728832 ) ) ;
#28872 = CARTESIAN_POINT ( 'NONE',  ( -9.692307692307812417, -4.481592998941358097, 33.73612834414048933 ) ) ;
#28873 = LINE ( 'NONE', #50005, #71273 ) ;
#28874 = CARTESIAN_POINT ( 'NONE',  ( -0.5268084620947807162, -4.320704448112771878, 33.92786785259540494 ) ) ;
#28875 = CARTESIAN_POINT ( 'NONE',  ( -17.77722045873159473, -11.89424750095246175, 32.13594075562311758 ) ) ;
#28876 = CARTESIAN_POINT ( 'NONE',  ( -2.084912638714239375, -2.353885683473778023, 30.79025554430704759 ) ) ;
#28877 = CARTESIAN_POINT ( 'NONE',  ( -11.53846153846153655, -1.951392089020283160, 34.73218667398347748 ) ) ;
#28878 = EDGE_CURVE ( 'NONE', #50472, #42433, #19531, .T. ) ;
#28879 = CARTESIAN_POINT ( 'NONE',  ( -0.4615384615384611200, -12.78798330534102767, 29.49999999999997868 ) ) ;
#28880 = CARTESIAN_POINT ( 'NONE',  ( 1.987747218494642309, -5.598659921968629050, 24.56436829374151287 ) ) ;
#28881 = ORIENTED_EDGE ( 'NONE', *, *, #7546, .T. ) ;
#28882 = B_SPLINE_CURVE_WITH_KNOTS ( 'NONE', 3,
 ( #1962, #2826, #56463, #22232, #50579, #30317, #71290, #29445, #9596, #43392 ),
 .UNSPECIFIED., .F., .F.,
 ( 4, 2, 2, 2, 4 ),
 ( 0.0007817359430256294638, 0.0009771253907249974075, 0.001172514838424365243, 0.001367904286123733078, 0.001563293733823093758 ),
 .UNSPECIFIED. ) ;
#28883 = CARTESIAN_POINT ( 'NONE',  ( -15.45369618967607828, -6.459968553980841577, 34.89616026154728701 ) ) ;
#28884 = CARTESIAN_POINT ( 'NONE',  ( -1.384615384615383471, -12.10708131394839349, 31.69288490824020244 ) ) ;
#28885 = EDGE_CURVE ( 'NONE', #73515, #55297, #39164, .T. ) ;
#28886 = CARTESIAN_POINT ( 'NONE',  ( 8.992243613324164997, -10.77377354290276124, 33.85451476688484718 ) ) ;
#28887 = CARTESIAN_POINT ( 'NONE',  ( -3.230769230769229949, -10.67929555188718282, 33.92786785259544047 ) ) ;
#28888 = ORIENTED_EDGE ( 'NONE', *, *, #9067, .T. ) ;
#28889 = CARTESIAN_POINT ( 'NONE',  ( 0.3962684609821418569, -4.320704448112772766, 33.92786785259541915 ) ) ;
#28890 = CARTESIAN_POINT ( 'NONE',  ( -2.307692307692305711, -3.050289026998446396, 32.03036669348365706 ) ) ;
#28891 = EDGE_CURVE ( 'NONE', #13555, #35423, #52282, .T. ) ;
#28892 = ORIENTED_EDGE ( 'NONE', *, *, #76620, .T. ) ;
#28893 = CARTESIAN_POINT ( 'NONE',  ( 1.318531973659506251, -8.973038597847271092, 34.52809138561120506 ) ) ;
#28894 = CARTESIAN_POINT ( 'NONE',  ( -4.403869391139117795, -10.76384336483936011, 33.53834819971076087 ) ) ;
#28895 = VERTEX_POINT ( 'NONE', #74478 ) ;
#28896 = CARTESIAN_POINT ( 'NONE',  ( -15.48079246806219267, -2.823816976329319051, 31.52131813110795733 ) ) ;
#28897 = CARTESIAN_POINT ( 'NONE',  ( 3.903869422903798458, -3.627789207965226748, 32.91389620160131102 ) ) ;
#28898 = EDGE_CURVE ( 'NONE', #70465, #3756, #76587, .T. ) ;
#28899 = CARTESIAN_POINT ( 'NONE',  ( -0.6844654204453110014, -10.01117774369187252, 34.36070679894347535 ) ) ;
#28900 = CYLINDRICAL_SURFACE ( 'NONE', #39358, 0.2500000000000009437 ) ;
#28902 = ORIENTED_EDGE ( 'NONE', *, *, #46860, .T. ) ;
#28901 = VECTOR ( 'NONE', #57113, 1000.000000000000227 ) ;
#28903 = CARTESIAN_POINT ( 'NONE',  ( -3.007989561791163613, -2.353885683473778023, 30.79025554430704759 ) ) ;
#28904 = EDGE_CURVE ( 'NONE', #52308, #18841, #15773, .T. ) ;
#28906 = ORIENTED_EDGE ( 'NONE', *, *, #84053, .F. ) ;
#28905 = B_SPLINE_CURVE_WITH_KNOTS ( 'NONE', 3,
 ( #34245, #6772, #41013, #55845, #83332, #75671, #14418, #1787, #68472, #76569 ),
 .UNSPECIFIED., .F., .F.,
 ( 4, 2, 2, 2, 4 ),
 ( 0.0007817246256747473893, 0.0009771112852218909357, 0.001172497944769034482, 0.001367884604316178246, 0.001563271263863321792 ),
 .UNSPECIFIED. ) ;
#28907 = DIRECTION ( 'NONE',  ( -0.000000000000000000, 0.9848077530122086864, -0.1736481776669273891 ) ) ;
#28908 = DIRECTION ( 'NONE',  ( 0.000000000000000000, 0.9848077530122072432, 0.1736481776669354937 ) ) ;
#28909 = EDGE_LOOP ( 'NONE', ( #77024, #83685 ) ) ;
#28910 = ADVANCED_FACE ( 'NONE', ( #26731 ), #23610, .T. ) ;
#28911 = DIRECTION ( 'NONE',  ( 0.000000000000000000, 0.8660254037844377084, 0.5000000000000015543 ) ) ;
#28912 = CARTESIAN_POINT ( 'NONE',  ( -8.899377978668987055, -2.619462340734462380, 30.83744416345203021 ) ) ;
#28913 = CARTESIAN_POINT ( 'NONE',  ( 0.2115617305961063344, -4.236021600441995716, 33.53823185664188600 ) ) ;
#28914 = CARTESIAN_POINT ( 'NONE',  ( 13.60739505359345181, -12.11081565061823717, 32.26097654155341843 ) ) ;
#28915 = CARTESIAN_POINT ( 'NONE',  ( -8.096153846153844924, -7.500000000000001776, 34.75000000000000000 ) ) ;
#28916 = EDGE_LOOP ( 'NONE', ( #48130, #23144, #76515, #29524, #51054 ) ) ;
#28917 = ORIENTED_EDGE ( 'NONE', *, *, #7836, .T. ) ;
#28918 = VECTOR ( 'NONE', #71349, 1000.000000000000000 ) ;
#28919 = FACE_BOUND ( 'NONE', #27512, .T. ) ;
#28920 = ORIENTED_EDGE ( 'NONE', *, *, #17507, .F. ) ;
#28922 = EDGE_CURVE ( 'NONE', #11473, #47875, #20462, .T. ) ;
#28921 = CARTESIAN_POINT ( 'NONE',  ( -8.069080805060693251, -5.582147617184174848, 34.63737895849758530 ) ) ;
#28923 = CARTESIAN_POINT ( 'NONE',  ( 4.284371855609720114, -11.93748526763465279, 32.05452791011430946 ) ) ;
#28924 = EDGE_CURVE ( 'NONE', #66677, #63245, #61433, .T. ) ;
#28925 = CARTESIAN_POINT ( 'NONE',  ( -11.53846153846153655, -1.367168528481310208, 33.57946703557072254 ) ) ;
#28926 = CARTESIAN_POINT ( 'NONE',  ( -2.084679463598911653, -10.01129605718032778, 34.36064277460058491 ) ) ;
#28927 = VECTOR ( 'NONE', #24393, 1000.000000000000000 ) ;
#28928 = ORIENTED_EDGE ( 'NONE', *, *, #51658, .F. ) ;
#28929 = VERTEX_POINT ( 'NONE', #53796 ) ;
#28930 = VERTEX_POINT ( 'NONE', #27654 ) ;
#28931 = CARTESIAN_POINT ( 'NONE',  ( 13.31929137181107947, -7.749976730030849303, 34.74374725381503737 ) ) ;
#28932 = EDGE_LOOP ( 'NONE', ( #11091, #31645, #299, #18097 ) ) ;
#28933 = ADVANCED_FACE ( 'NONE', ( #74972 ), #41618, .F. ) ;
#28934 = DIRECTION ( 'NONE',  ( -0.000000000000000000, -0.9396926207859093161, -0.3420201433256663259 ) ) ;
#28935 = CARTESIAN_POINT ( 'NONE',  ( -2.557669051740897093, -12.41104346484419452, 31.60698883733904196 ) ) ;
#28936 = EDGE_CURVE ( 'NONE', #33889, #51136, #85634, .T. ) ;
#28937 = CARTESIAN_POINT ( 'NONE',  ( 13.60762822870878530, -11.43677907613344757, 33.22367315496202167 ) ) ;
#28938 = ORIENTED_EDGE ( 'NONE', *, *, #65778, .T. ) ;
#28939 = CARTESIAN_POINT ( 'NONE',  ( -8.703163435880695076, -3.937682226553329556, 33.60647404775216529 ) ) ;
#28940 = EDGE_CURVE ( 'NONE', #2419, #24282, #11468, .T. ) ;
#28941 = CYLINDRICAL_SURFACE ( 'NONE', #85041, 0.2499999999999995559 ) ;
#28942 = CARTESIAN_POINT ( 'NONE',  ( 6.000000000000001776, -13.88283147151868846, 33.14645433367849847 ) ) ;
#28943 = DIRECTION ( 'NONE',  ( 0.000000000000000000, 0.000000000000000000, -1.000000000000000000 ) ) ;
#28944 = EDGE_LOOP ( 'NONE', ( #31878, #65083 ) ) ;
#28945 = ORIENTED_EDGE ( 'NONE', *, *, #47745, .F. ) ;
#28946 = ORIENTED_EDGE ( 'NONE', *, *, #29295, .T. ) ;
#28948 = EDGE_CURVE ( 'NONE', #70346, #74779, #68410, .T. ) ;
#28947 = LINE ( 'NONE', #55067, #73283 ) ;
#28950 = CARTESIAN_POINT ( 'NONE',  ( 10.74617642320940369, -6.413143153341454017, 34.63066358083362672 ) ) ;
#28949 = DIRECTION ( 'NONE',  ( 0.000000000000000000, 0.000000000000000000, -1.000000000000000000 ) ) ;
#28951 = VECTOR ( 'NONE', #19472, 999.9999999999998863 ) ;
#28952 = CARTESIAN_POINT ( 'NONE',  ( -17.77698715590659972, -5.582272713120728369, 34.63742843783360570 ) ) ;
#28953 = CARTESIAN_POINT ( 'NONE',  ( -8.992715693795101828, -6.716662450894489211, 34.94144148231605840 ) ) ;
#28954 = FACE_BOUND ( 'NONE', #62597, .T. ) ;
#28955 = CARTESIAN_POINT ( 'NONE',  ( 8.703960768674447124, -11.06231777344662781, 33.60647404775220082 ) ) ;
#28956 = ORIENTED_EDGE ( 'NONE', *, *, #25762, .T. ) ;
#28957 = CARTESIAN_POINT ( 'NONE',  ( -8.069033362891428141, -7.630690623152299068, 34.99857592706772635 ) ) ;
#28958 = CARTESIAN_POINT ( 'NONE',  ( -14.16025641025641058, -3.499999999999999556, 29.75000000000000355 ) ) ;
#28959 = DIRECTION ( 'NONE',  ( 0.000000000000000000, 0.000000000000000000, -1.000000000000000000 ) ) ;
#28960 = CARTESIAN_POINT ( 'NONE',  ( -17.07692307692319744, -2.657715359629662988, 31.77849191805970364 ) ) ;
#28961 = ORIENTED_EDGE ( 'NONE', *, *, #40453, .F. ) ;
#28962 = CARTESIAN_POINT ( 'NONE',  ( 2.557746619330622639, -11.79725096376909654, 32.30694842903960762 ) ) ;
#28963 = ORIENTED_EDGE ( 'NONE', *, *, #5993, .F. ) ;
#28964 = FACE_BOUND ( 'NONE', #64107, .T. ) ;
#28965 = CARTESIAN_POINT ( 'NONE',  ( 20.00000000000000000, -7.500000000000000000, 29.75000000000000355 ) ) ;
#28966 = CARTESIAN_POINT ( 'NONE',  ( 16.94623161025552349, -11.71456829005830080, 32.44064028649416542 ) ) ;
#28967 = CARTESIAN_POINT ( 'NONE',  ( -11.47320596718551577, -11.94971097300157403, 32.03036669348361443 ) ) ;
#28968 = VERTEX_POINT ( 'NONE', #56459 ) ;
#28969 = CARTESIAN_POINT ( 'NONE',  ( -12.52680890749923570, -10.21337939537584383, 33.94971097300158647 ) ) ;
#28970 = CARTESIAN_POINT ( 'NONE',  ( -5.777220331021931443, -9.418065098278011860, 34.63729479722530158 ) ) ;
#28971 = CARTESIAN_POINT ( 'NONE',  ( -15.16551409125639260, -10.33852847137154107, 34.16647553114620450 ) ) ;
#28972 = EDGE_CURVE ( 'NONE', #8816, #15450, #87738, .T. ) ;
#28973 = FACE_OUTER_BOUND ( 'NONE', #10985, .T. ) ;
#28974 = ORIENTED_EDGE ( 'NONE', *, *, #32130, .F. ) ;
#28975 = B_SPLINE_CURVE_WITH_KNOTS ( 'NONE', 3,
 ( #13175, #40655, #68124, #33881, #61338, #57260, #69886, #2739, #71205, #70780 ),
 .UNSPECIFIED., .F., .F.,
 ( 4, 2, 2, 2, 4 ),
 ( 0.0007817359430256313069, 0.0009771253907249971907, 0.001172514838424363074, 0.001367904286123728958, 0.001563293733823094842 ),
 .UNSPECIFIED. ) ;
#28976 = CARTESIAN_POINT ( 'NONE',  ( 16.21910172512217585, -10.90142922261932057, 33.41473453929631887 ) ) ;
#28977 = ORIENTED_EDGE ( 'NONE', *, *, #30551, .T. ) ;
#28979 = ORIENTED_EDGE ( 'NONE', *, *, #11645, .F. ) ;
#28978 = CARTESIAN_POINT ( 'NONE',  ( 4.153846153846154188, -2.833524468853757305, 32.15551576947925838 ) ) ;
#28980 = CARTESIAN_POINT ( 'NONE',  ( -8.704084989898801084, -7.750023238201979581, 34.74374492549440419 ) ) ;
#28981 = CARTESIAN_POINT ( 'NONE',  ( -1.384615384615506484, -12.51329471203414379, 31.30864560766407578 ) ) ;
#28982 = CARTESIAN_POINT ( 'NONE',  ( -13.38461538461538325, -13.49023893513002648, 31.06009739812518688 ) ) ;
#28983 = CARTESIAN_POINT ( 'NONE',  ( -12.59222906464877134, -10.70098750199973203, 33.91152734681376302 ) ) ;
#28985 = CARTESIAN_POINT ( 'NONE',  ( 0.3309281019139320157, -7.722926236386453702, 34.74524107206102030 ) ) ;
#28984 = CARTESIAN_POINT ( 'NONE',  ( -5.750054590621955342, -6.653508905675592722, 34.93172785388651391 ) ) ;
#28986 = AXIS2_PLACEMENT_3D ( 'NONE', #65050, #16435, #10573 ) ;
#28987 = CARTESIAN_POINT ( 'NONE',  ( 0.4615384615384611200, -13.49023893513002648, 31.06009739812518688 ) ) ;
#28988 = CARTESIAN_POINT ( 'NONE',  ( -1.409462824231155764E-14, -4.749999999999999112, 22.90625000000000355 ) ) ;
#28989 = ORIENTED_EDGE ( 'NONE', *, *, #85460, .T. ) ;
#28990 = CARTESIAN_POINT ( 'NONE',  ( -8.769230769230892619, -10.33852847137269571, 34.16647553114546554 ) ) ;
#28991 = ORIENTED_EDGE ( 'NONE', *, *, #64087, .F. ) ;
#28992 = VECTOR ( 'NONE', #26503, 1000.000000000000227 ) ;
#28993 = ORIENTED_EDGE ( 'NONE', *, *, #69226, .T. ) ;
#28994 = CARTESIAN_POINT ( 'NONE',  ( 11.76124107972994537, -11.89424750095246175, 32.13594075562310337 ) ) ;
#28995 = EDGE_LOOP ( 'NONE', ( #70767, #88643 ) ) ;
#28996 = CARTESIAN_POINT ( 'NONE',  ( -10.74607608205217346, -11.18331474514187995, 33.13161551792790505 ) ) ;
#28997 = CARTESIAN_POINT ( 'NONE',  ( -5.010855743573001675, -12.62096338111211757, 30.90682066428152908 ) ) ;
#28998 = AXIS2_PLACEMENT_3D ( 'NONE', #7019, #54313, #13775 ) ;
#28999 = LINE ( 'NONE', #49692, #55722 ) ;
#29000 = CARTESIAN_POINT ( 'NONE',  ( -3.230769230769229949, -5.415277668671390821, 36.20867863119892149 ) ) ;
#29001 = DIRECTION ( 'NONE',  ( 0.000000000000000000, 0.000000000000000000, -1.000000000000000000 ) ) ;
#29002 = CARTESIAN_POINT ( 'NONE',  ( 15.90386942290380290, -11.79746400365624659, 32.30657167506340954 ) ) ;
#29003 = CARTESIAN_POINT ( 'NONE',  ( -15.10024379253558635, -8.630441415882550871, 34.87705825610312615 ) ) ;
#29004 = CARTESIAN_POINT ( 'NONE',  ( 10.54930120442873331, -2.538708090699994813, 30.37095296980875148 ) ) ;
#29005 = CARTESIAN_POINT ( 'NONE',  ( 11.47237812750565666, -10.51840700105979387, 33.73612834413961536 ) ) ;
#29006 = ADVANCED_FACE ( 'NONE', ( #10032 ), #77614, .F. ) ;
#29007 = CARTESIAN_POINT ( 'NONE',  ( -5.076923076923075762, -13.20930481340135110, 34.54067556320372745 ) ) ;
#29008 = CARTESIAN_POINT ( 'NONE',  ( 7.780883845597524662, -2.379036618887870436, 30.90682066428147579 ) ) ;
#29009 = EDGE_CURVE ( 'NONE', #61557, #48093, #12589, .T. ) ;
#29010 = ORIENTED_EDGE ( 'NONE', *, *, #77281, .F. ) ;
#29011 = VERTEX_POINT ( 'NONE', #42952 ) ;
#29012 = B_SPLINE_CURVE_WITH_KNOTS ( 'NONE', 3,
 ( #5502, #5945, #27539, #32966, #33848, #60431, #40620, #33415, #87947, #26206 ),
 .UNSPECIFIED., .F., .F.,
 ( 4, 2, 2, 2, 4 ),
 ( 0.000000000000000000, 0.0001954311564186865492, 0.0003908623128373730983, 0.0005862934692560596746, 0.0007817246256747461966 ),
 .UNSPECIFIED. ) ;
#29013 = DIRECTION ( 'NONE',  ( -0.000000000000000000, 0.8660254037844399289, -0.4999999999999980016 ) ) ;
#29014 = DIRECTION ( 'NONE',  ( 0.000000000000000000, -1.000000000000000000, 0.000000000000000000 ) ) ;
#29015 = CARTESIAN_POINT ( 'NONE',  ( 11.53846153846141753, -10.21337939537710326, 33.94971097300076224 ) ) ;
#29016 = DIRECTION ( 'NONE',  ( 0.000000000000000000, 0.8660254037844377084, -0.5000000000000015543 ) ) ;
#29017 = EDGE_LOOP ( 'NONE', ( #74252, #86234, #60031, #78735 ) ) ;
#29018 = ADVANCED_FACE ( 'NONE', ( #8725 ), #63650, .F. ) ;
#29019 = DIRECTION ( 'NONE',  ( -0.000000000000000000, 0.7660444431189791237, -0.6427876096865379196 ) ) ;
#29020 = CARTESIAN_POINT ( 'NONE',  ( -17.07692307692307665, -3.513871655860378418, 32.76840700105978499 ) ) ;
#29021 = ADVANCED_FACE ( 'NONE', ( #71284 ), #26389, .F. ) ;
#29022 = DIRECTION ( 'NONE',  ( 1.000000000000000000, 0.000000000000000000, 0.000000000000000000 ) ) ;
#29023 = ORIENTED_EDGE ( 'NONE', *, *, #69534, .T. ) ;
#29024 = CARTESIAN_POINT ( 'NONE',  ( -14.37296230824862775, -12.70778746994557551, 30.41441678777548319 ) ) ;
#29025 = ORIENTED_EDGE ( 'NONE', *, *, #87416, .T. ) ;
#29026 = AXIS2_PLACEMENT_3D ( 'NONE', #48365, #62756, #1073 ) ;
#29027 = ADVANCED_FACE ( 'NONE', ( #1956 ), #43386, .F. ) ;
#29028 = FACE_OUTER_BOUND ( 'NONE', #3752, .T. ) ;
#29029 = DIRECTION ( 'NONE',  ( 0.000000000000000000, 0.9396926207859126468, 0.3420201433256571111 ) ) ;
#29030 = CARTESIAN_POINT ( 'NONE',  ( 16.82692307692307665, -2.499999999999998668, 29.75000000000000355 ) ) ;
#29031 = DIRECTION ( 'NONE',  ( 1.000000000000000000, 0.000000000000000000, 0.000000000000000000 ) ) ;
#29032 = DIRECTION ( 'NONE',  ( 0.000000000000000000, 0.1736481776669267785, -0.9848077530122087975 ) ) ;
#29033 = ORIENTED_EDGE ( 'NONE', *, *, #33731, .F. ) ;
#29034 = ORIENTED_EDGE ( 'NONE', *, *, #82822, .F. ) ;
#29035 = ORIENTED_EDGE ( 'NONE', *, *, #60852, .F. ) ;
#29036 = B_SPLINE_CURVE_WITH_KNOTS ( 'NONE', 3,
 ( #7905, #56965, #22736, #42144, #84023, #35369, #84461, #2898, #43019, #29952 ),
 .UNSPECIFIED., .F., .F.,
 ( 4, 2, 2, 2, 4 ),
 ( 0.000000000000000000, 0.0001954339857564070678, 0.0003908679715128141356, 0.0005863019572692211492, 0.0007817359430256282712 ),
 .UNSPECIFIED. ) ;
#29037 = CARTESIAN_POINT ( 'NONE',  ( -10.61538461538473577, -12.51329471203414379, 31.30864560766407578 ) ) ;
#29038 = DIRECTION ( 'NONE',  ( 0.000000000000000000, 0.6427876096865373645, -0.7660444431189797898 ) ) ;
#29039 = ADVANCED_FACE ( 'NONE', ( #23110 ), #85263, .F. ) ;
#29040 = CARTESIAN_POINT ( 'NONE',  ( 0.7115928814519136836, -6.523592122091590895, 34.90882529074906415 ) ) ;
#29041 = VECTOR ( 'NONE', #49431, 1000.000000000000000 ) ;
#29042 = CARTESIAN_POINT ( 'NONE',  ( 0.2386115026316116827, -12.38737895849757820, 31.66785238281580206 ) ) ;
#29043 = VECTOR ( 'NONE', #18159, 1000.000000000000227 ) ;
#29044 = LINE ( 'NONE', #62790, #11946 ) ;
#29045 = CARTESIAN_POINT ( 'NONE',  ( 27.00000000000000000, 0.000000000000000000, 24.75000000000000000 ) ) ;
#29046 = ORIENTED_EDGE ( 'NONE', *, *, #48198, .F. ) ;
#29047 = ORIENTED_EDGE ( 'NONE', *, *, #36159, .T. ) ;
#29048 = AXIS2_PLACEMENT_3D ( 'NONE', #7499, #8830, #2060 ) ;
#29049 = VERTEX_POINT ( 'NONE', #56010 ) ;
#29052 = ORIENTED_EDGE ( 'NONE', *, *, #1961, .T. ) ;
#29051 = EDGE_CURVE ( 'NONE', #2574, #30732, #42508, .T. ) ;
#29050 = CARTESIAN_POINT ( 'NONE',  ( 16.15384615384615330, -4.661471528628507777, 34.16647553114623292 ) ) ;
#29054 = FACE_OUTER_BOUND ( 'NONE', #39940, .T. ) ;
#29053 = CARTESIAN_POINT ( 'NONE',  ( -13.38461538461538325, -10.89733346790207413, 36.13435417666054406 ) ) ;
#29055 = CARTESIAN_POINT ( 'NONE',  ( -2.307692307692305711, -8.973038597847269315, 34.52809138561121927 ) ) ;
#29056 = CARTESIAN_POINT ( 'NONE',  ( -2.651650429449535551, -10.15165042944956753, 23.68750000000000000 ) ) ;
#29057 = ORIENTED_EDGE ( 'NONE', *, *, #89162, .F. ) ;
#29058 = EDGE_CURVE ( 'NONE', #58205, #33472, #44240, .T. ) ;
#29059 = VERTEX_POINT ( 'NONE', #83499 ) ;
#29060 = CARTESIAN_POINT ( 'NONE',  ( 13.51540582558233794, -10.70102852606553157, 33.91149625220312913 ) ) ;
#29061 = ORIENTED_EDGE ( 'NONE', *, *, #77155, .F. ) ;
#29062 = FACE_BOUND ( 'NONE', #10007, .T. ) ;
#29063 = CARTESIAN_POINT ( 'NONE',  ( 6.673100192134569397, -4.236021600441998380, 33.53823185664189310 ) ) ;
#29064 = CARTESIAN_POINT ( 'NONE',  ( -4.403822897894744237, -10.06842814019191401, 34.32929386961144758 ) ) ;
#29065 = VERTEX_POINT ( 'NONE', #21785 ) ;
#29066 = CYLINDRICAL_SURFACE ( 'NONE', #11845, 4.000000000000000000 ) ;
#29067 = DIRECTION ( 'NONE',  ( 0.000000000000000000, 0.4999999999999985567, 0.8660254037844395958 ) ) ;
#29068 = DIRECTION ( 'NONE',  ( -0.000000000000000000, -0.3420201433256694346, -0.9396926207859080948 ) ) ;
#29069 = CARTESIAN_POINT ( 'NONE',  ( 4.088575707885378385, -11.48612834413959582, 32.76840700105983473 ) ) ;
#29070 = CARTESIAN_POINT ( 'NONE',  ( -17.01166750564705410, -2.625532179533469623, 30.86335684631491105 ) ) ;
#29072 = ORIENTED_EDGE ( 'NONE', *, *, #57744, .T. ) ;
#29071 = EDGE_CURVE ( 'NONE', #29311, #16242, #41621, .T. ) ;
#29073 = VECTOR ( 'NONE', #62180, 1000.000000000000000 ) ;
#29074 = CARTESIAN_POINT ( 'NONE',  ( 6.250054311638317373, -8.303483539816728154, 34.68545999027711702 ) ) ;
#29075 = LINE ( 'NONE', #70488, #59877 ) ;
#29076 = DIRECTION ( 'NONE',  ( -0.000000000000000000, 0.7660444431189791237, -0.6427876096865379196 ) ) ;
#29077 = CARTESIAN_POINT ( 'NONE',  ( -0.7115616857599184053, -4.931416488878823223, 34.32920672191015399 ) ) ;
#29078 = EDGE_CURVE ( 'NONE', #38958, #42531, #46041, .T. ) ;
#29080 = ADVANCED_FACE ( 'NONE', ( #86606 ), #24877, .F. ) ;
#29079 = CARTESIAN_POINT ( 'NONE',  ( -14.98082371242109012, -11.86320923018887541, 32.19269448109604781 ) ) ;
#29081 = CARTESIAN_POINT ( 'NONE',  ( 15.23076923076910916, -8.656820664282941280, 34.87096338111179961 ) ) ;
#29083 = FACE_OUTER_BOUND ( 'NONE', #58780, .T. ) ;
#29082 = CARTESIAN_POINT ( 'NONE',  ( 13.13459214732242408, -11.86270091957321249, 32.19358267280087915 ) ) ;
#29084 = CARTESIAN_POINT ( 'NONE',  ( -14.37296230824862775, -3.643525952247789412, 33.31231777344662959 ) ) ;
#29086 = CARTESIAN_POINT ( 'NONE',  ( 2.438217745925953750, -6.808710257144159783, 34.95449254468098843 ) ) ;
#29085 = FACE_OUTER_BOUND ( 'NONE', #45991, .T. ) ;
#29087 = AXIS2_PLACEMENT_3D ( 'NONE', #65872, #36318, #43508 ) ;
#29088 = CARTESIAN_POINT ( 'NONE',  ( -5.750054481651856619, -12.43552623307873972, 30.55307653245132826 ) ) ;
#29089 = CARTESIAN_POINT ( 'NONE',  ( -2.749999999999997780, -7.561099074964547917, 24.84188170625848713 ) ) ;
#29090 = ADVANCED_FACE ( 'NONE', ( #73072 ), #87057, .F. ) ;
#29091 = ORIENTED_EDGE ( 'NONE', *, *, #3084, .T. ) ;
#29092 = CARTESIAN_POINT ( 'NONE',  ( 12.71159277317677549, -2.564540009722896752, 30.55348353981670684 ) ) ;
#29093 = ORIENTED_EDGE ( 'NONE', *, *, #35371, .F. ) ;
#29094 = CARTESIAN_POINT ( 'NONE',  ( -13.31936024510254413, -9.528491918058460186, 34.59228464037086326 ) ) ;
#29095 = EDGE_LOOP ( 'NONE', ( #25253, #67430, #47826, #34014 ) ) ;
#29096 = CARTESIAN_POINT ( 'NONE',  ( 15.90386942290380290, -11.28823185664190376, 33.01397839955799896 ) ) ;
#29097 = DIRECTION ( 'NONE',  ( -0.000000000000000000, 1.000000000000000000, -0.000000000000000000 ) ) ;
#29098 = EDGE_LOOP ( 'NONE', ( #88655, #35244, #49215, #1654 ) ) ;
#29099 = CARTESIAN_POINT ( 'NONE',  ( -18.24997673094235751, -12.41269422305637171, 30.68257228309993323 ) ) ;
#29100 = CARTESIAN_POINT ( 'NONE',  ( 1.077988221561464899, -4.724691934501233703, 25.23250670625849068 ) ) ;
#29101 = CYLINDRICAL_SURFACE ( 'NONE', #9867, 0.2499999999999995559 ) ;
#29102 = CARTESIAN_POINT ( 'NONE',  ( -3.930470668073732909, -2.251407671071270489, 29.88021292934942252 ) ) ;
#29103 = CARTESIAN_POINT ( 'NONE',  ( 15.93091919493930320, -8.282780595021769443, 34.94152052738834868 ) ) ;
#29104 = CARTESIAN_POINT ( 'NONE',  ( 17.99999999999987566, -2.625532179533778709, 30.86335684631627174 ) ) ;
#29105 = CARTESIAN_POINT ( 'NONE',  ( 6.000000000000001776, -5.180354513474913603, 36.12317359536750416 ) ) ;
#29106 = LINE ( 'NONE', #30419, #32455 ) ;
#29107 = CARTESIAN_POINT ( 'NONE',  ( 2.320192649118979489E-14, -11.25000000000000000, 16.03125000000000000 ) ) ;
#29108 = CARTESIAN_POINT ( 'NONE',  ( -9.915792636031643070, -3.754499324213721234, 33.06261337010820256 ) ) ;
#29109 = CARTESIAN_POINT ( 'NONE',  ( 14.55763782604045176, -10.76462480002816235, 33.53768742498949962 ) ) ;
#29110 = CARTESIAN_POINT ( 'NONE',  ( -12.46153846153846168, -2.249999999999998668, 29.75000000000001776 ) ) ;
#29111 = CARTESIAN_POINT ( 'NONE',  ( -2.651650429449565305, -4.848349570550461785, 17.75000000000000355 ) ) ;
#29112 = EDGE_CURVE ( 'NONE', #87025, #32375, #44787, .T. ) ;
#29113 = AXIS2_PLACEMENT_3D ( 'NONE', #44101, #16641, #71581 ) ;
#29114 = CYLINDRICAL_SURFACE ( 'NONE', #17370, 0.2499999999999979738 ) ;
#29115 = EDGE_LOOP ( 'NONE', ( #71616, #83473, #18618, #58024 ) ) ;
#29116 = CARTESIAN_POINT ( 'NONE',  ( -3.230769230769229949, -6.435427911321262684, 35.78748833219616898 ) ) ;
#29117 = LINE ( 'NONE', #8390, #5714 ) ;
#29118 = CARTESIAN_POINT ( 'NONE',  ( 9.758376043310132530, -6.386643153685127139, 34.62446782046654192 ) ) ;
#29119 = CARTESIAN_POINT ( 'NONE',  ( -14.30769230769230660, -11.69971097300155272, 32.46337939537588113 ) ) ;
#29120 = EDGE_CURVE ( 'NONE', #25462, #8541, #25330, .T. ) ;
#29121 = CARTESIAN_POINT ( 'NONE',  ( -1.450698795571262689, -10.51840700105979387, 33.73612834413961536 ) ) ;
#29122 = AXIS2_PLACEMENT_3D ( 'NONE', #24214, #80059, #71963 ) ;
#29123 = CARTESIAN_POINT ( 'NONE',  ( -14.08491263871423449, -4.226511098958373402, 33.85474049983370293 ) ) ;
#29124 = EDGE_CURVE ( 'NONE', #36170, #15837, #59999, .T. ) ;
#29125 = FACE_OUTER_BOUND ( 'NONE', #62652, .T. ) ;
#29126 = EDGE_LOOP ( 'NONE', ( #14232, #86708 ) ) ;
#29127 = EDGE_LOOP ( 'NONE', ( #6668, #28391, #76636, #24239 ) ) ;
#29128 = EDGE_CURVE ( 'NONE', #558, #10433, #18581, .T. ) ;
#29129 = ORIENTED_EDGE ( 'NONE', *, *, #68330, .T. ) ;
#29130 = CARTESIAN_POINT ( 'NONE',  ( -13.60754160213153163, -3.586966769969701208, 32.86292498521069660 ) ) ;
#29131 = DIRECTION ( 'NONE',  ( 0.000000000000000000, 0.000000000000000000, -1.000000000000000000 ) ) ;
#29132 = CARTESIAN_POINT ( 'NONE',  ( 6.792928953345224841, -3.069018819979302926, 32.56621877034667278 ) ) ;
#29133 = CARTESIAN_POINT ( 'NONE',  ( 2.057715576749954867, -5.728515186090277211, 34.42611988154120439 ) ) ;
#29134 = CARTESIAN_POINT ( 'NONE',  ( 6.123233995736775897E-17, -2.085786437626902856, 29.75000000000000355 ) ) ;
#29135 = B_SPLINE_CURVE_WITH_KNOTS ( 'NONE', 3,
 ( #38108, #11086, #52058, #86770, #18738, #58363, #31810, #17850, #11984, #57931 ),
 .UNSPECIFIED., .F., .F.,
 ( 4, 2, 2, 2, 4 ),
 ( 0.0007817359430256328248, 0.0009771253907249995759, 0.001172514838424366327, 0.001367904286123733078, 0.001563293733823099829 ),
 .UNSPECIFIED. ) ;
#29137 = EDGE_CURVE ( 'NONE', #49988, #6788, #60909, .T. ) ;
#29136 = ORIENTED_EDGE ( 'NONE', *, *, #69105, .T. ) ;
#29138 = CARTESIAN_POINT ( 'NONE',  ( -18.25000000000000000, -7.500000000000001776, 34.75000000000000000 ) ) ;
#29139 = CIRCLE ( 'NONE', #9007, 4.000000000000000000 ) ;
#29140 = ORIENTED_EDGE ( 'NONE', *, *, #74782, .T. ) ;
#29141 = EDGE_LOOP ( 'NONE', ( #20351, #30640, #35888, #3502, #53926, #53197 ) ) ;
#29143 = VERTEX_POINT ( 'NONE', #24424 ) ;
#29142 = CARTESIAN_POINT ( 'NONE',  ( 4.284371592079798674, -12.50538340440932217, 31.33453814440721885 ) ) ;
#29144 = CARTESIAN_POINT ( 'NONE',  ( -19.50000000000000000, -3.499999999999999556, 29.75000000000000355 ) ) ;
#29145 = CARTESIAN_POINT ( 'NONE',  ( -10.68065506134539078, -5.219633306516282545, 34.19971097300152962 ) ) ;
#29146 = CARTESIAN_POINT ( 'NONE',  ( 3.930919936330006248, -4.186968288167446595, 33.49512374952580274 ) ) ;
#29147 = EDGE_CURVE ( 'NONE', #83740, #81428, #7156, .T. ) ;
#29148 = ORIENTED_EDGE ( 'NONE', *, *, #41033, .T. ) ;
#29149 = EDGE_CURVE ( 'NONE', #2479, #3057, #34997, .T. ) ;
#29150 = ORIENTED_EDGE ( 'NONE', *, *, #36816, .T. ) ;
#29151 = ORIENTED_EDGE ( 'NONE', *, *, #5423, .T. ) ;
#29152 = DIRECTION ( 'NONE',  ( -0.000000000000000000, 1.000000000000000000, 3.491481338843133355E-15 ) ) ;
#29154 = ORIENTED_EDGE ( 'NONE', *, *, #62276, .T. ) ;
#29153 = CYLINDRICAL_SURFACE ( 'NONE', #15738, 0.2499999999999973355 ) ;
#29155 = CARTESIAN_POINT ( 'NONE',  ( -17.78205128205128105, -11.00000000000000000, 29.75000000000000355 ) ) ;
#29156 = FACE_OUTER_BOUND ( 'NONE', #50837, .T. ) ;
#29157 = CARTESIAN_POINT ( 'NONE',  ( -3.007757879156380820, -9.886259254753566594, 34.14407573483972413 ) ) ;
#29158 = ORIENTED_EDGE ( 'NONE', *, *, #25703, .T. ) ;
#29159 = ADVANCED_FACE ( 'NONE', ( #58214 ), #18135, .F. ) ;
#29160 = EDGE_CURVE ( 'NONE', #37657, #12551, #62323, .T. ) ;
#29161 = CARTESIAN_POINT ( 'NONE',  ( -11.28840722682322273, -4.943051570960394159, 34.04725096376909477 ) ) ;
#29162 = FACE_OUTER_BOUND ( 'NONE', #9384, .T. ) ;
#29163 = B_SPLINE_CURVE_WITH_KNOTS ( 'NONE', 3,
 ( #23031, #42873, #84312, #50492, #1436, #36554, #83420, #16710, #77975, #64892 ),
 .UNSPECIFIED., .F., .F.,
 ( 4, 2, 2, 2, 4 ),
 ( 0.0007817246256747514008, 0.0009771112852218959231, 0.001172497944769040337, 0.001367884604316184968, 0.001563271263863329381 ),
 .UNSPECIFIED. ) ;
#29164 = ORIENTED_EDGE ( 'NONE', *, *, #20713, .F. ) ;
#29165 = FACE_BOUND ( 'NONE', #74880, .T. ) ;
#29166 = CARTESIAN_POINT ( 'NONE',  ( 11.53846153846141753, -5.219633306517616589, 34.19971097300220464 ) ) ;
#29167 = DIRECTION ( 'NONE',  ( -0.000000000000000000, -0.000000000000000000, -1.000000000000000000 ) ) ;
#29168 = B_SPLINE_CURVE_WITH_KNOTS ( 'NONE', 3,
 ( #25005, #52026, #38529, #86289, #78174, #30865, #43942, #3395, #10165, #72742 ),
 .UNSPECIFIED., .F., .F.,
 ( 4, 2, 2, 2, 4 ),
 ( 0.0007817246256747521597, 0.0009771112852218961399, 0.001172497944769040337, 0.001367884604316184534, 0.001563271263863328514 ),
 .UNSPECIFIED. ) ;
#29169 = AXIS2_PLACEMENT_3D ( 'NONE', #7117, #12990, #20625 ) ;
#29170 = CARTESIAN_POINT ( 'NONE',  ( 16.15384615384615330, -13.20930481340135110, 34.54067556320372745 ) ) ;
#29172 = CARTESIAN_POINT ( 'NONE',  ( 14.30769230769231015, -6.435427911321262684, 35.78748833219616898 ) ) ;
#29171 = CARTESIAN_POINT ( 'NONE',  ( -11.53846153846153655, -12.29105614889573062, 35.45975837776705220 ) ) ;
#29173 = VECTOR ( 'NONE', #11294, 1000.000000000000000 ) ;
#29174 = B_SPLINE_CURVE_WITH_KNOTS ( 'NONE', 3,
 ( #35049, #82367, #14338, #8030, #76035, #41822, #69287, #35499, #28289, #27413 ),
 .UNSPECIFIED., .F., .F.,
 ( 4, 2, 2, 2, 4 ),
 ( 0.0007817246256747471724, 0.0009771112852218905021, 0.001172497944769033832, 0.001367884604316177161, 0.001563271263863320491 ),
 .UNSPECIFIED. ) ;
#29175 = CARTESIAN_POINT ( 'NONE',  ( 17.06410256410256565, -4.000000000000000000, 29.75000000000000355 ) ) ;
#29176 = CARTESIAN_POINT ( 'NONE',  ( -4.376773112753000738, -10.77366814457252175, 33.85459836347579454 ) ) ;
#29177 = ORIENTED_EDGE ( 'NONE', *, *, #59019, .T. ) ;
#29178 = CARTESIAN_POINT ( 'NONE',  ( -11.47320596718551400, -4.481592998940250538, 33.73612834413965089 ) ) ;
#29179 = CARTESIAN_POINT ( 'NONE',  ( -8.769230769230768274, -13.87047571288749737, 32.06866353760679544 ) ) ;
#29180 = EDGE_LOOP ( 'NONE', ( #36777, #83038 ) ) ;
#29181 = FACE_OUTER_BOUND ( 'NONE', #41195, .T. ) ;
#29182 = CARTESIAN_POINT ( 'NONE',  ( -14.24162497434223162, -9.058645607665452459, 34.76329471203371924 ) ) ;
#29183 = CARTESIAN_POINT ( 'NONE',  ( 3.453732134330715908, -7.369474270740069777, 34.74850911626239736 ) ) ;
#29184 = CARTESIAN_POINT ( 'NONE',  ( -5.326946314216043810, -11.86270091957321249, 32.19358267280087915 ) ) ;
#29185 = CARTESIAN_POINT ( 'NONE',  ( -0.2114841499001468561, -12.41262288849542017, 30.68299917996395010 ) ) ;
#29186 = EDGE_CURVE ( 'NONE', #23103, #34892, #55024, .T. ) ;
#29187 = CARTESIAN_POINT ( 'NONE',  ( 2.372947447205147053, -5.094484230520773593, 34.41647553114626845 ) ) ;
#29188 = FACE_BOUND ( 'NONE', #64613, .T. ) ;
#29190 = CARTESIAN_POINT ( 'NONE',  ( 13.19230769230769340, -7.500000000000000000, 29.75000000000000355 ) ) ;
#29189 = FACE_OUTER_BOUND ( 'NONE', #33449, .T. ) ;
#29191 = FACE_OUTER_BOUND ( 'NONE', #42117, .T. ) ;
#29193 = CARTESIAN_POINT ( 'NONE',  ( 7.846153846154153122, -2.506253911140614576, 30.00000000000323297 ) ) ;
#29192 = CARTESIAN_POINT ( 'NONE',  ( -6.673022503163469565, -10.82426656108011720, 33.81400080652039009 ) ) ;
#29194 = CARTESIAN_POINT ( 'NONE',  ( -14.24243716817947281, -5.941354392334607049, 34.76329471203374055 ) ) ;
#29195 = CARTESIAN_POINT ( 'NONE',  ( -2.608446859217889546, -10.19485399968121264, 22.18563170625848713 ) ) ;
#29196 = EDGE_LOOP ( 'NONE', ( #74426, #28881 ) ) ;
#29197 = EDGE_LOOP ( 'NONE', ( #83889, #27204, #44861, #85324 ) ) ;
#29198 = CARTESIAN_POINT ( 'NONE',  ( -9.627052121031669074, -11.94971097300157403, 32.03036669348361443 ) ) ;
#29199 = CARTESIAN_POINT ( 'NONE',  ( -12.21148404162500967, -6.523592122091592671, 34.90882529074906415 ) ) ;
#29200 = CARTESIAN_POINT ( 'NONE',  ( 6.700248825442047362, -7.369209533119140509, 34.99857337881830688 ) ) ;
#29201 = CARTESIAN_POINT ( 'NONE',  ( 9.692307692307570832, -12.70778746994576025, 30.41441678777401236 ) ) ;
#29202 = LINE ( 'NONE', #69727, #18379 ) ;
#29203 = CARTESIAN_POINT ( 'NONE',  ( 0.06109907496455496689, -11.24999999999999822, 23.27938170625849068 ) ) ;
#29204 = DIRECTION ( 'NONE',  ( 0.000000000000000000, 0.1736481776669267785, -0.9848077530122087975 ) ) ;
#29205 = CARTESIAN_POINT ( 'NONE',  ( -7.846153846153844924, -2.249999999999998668, 29.75000000000001776 ) ) ;
#29206 = AXIS2_PLACEMENT_3D ( 'NONE', #51112, #51552, #10157 ) ;
#29207 = CARTESIAN_POINT ( 'NONE',  ( 15.48082354240754555, -11.79725096376909654, 32.30694842903959341 ) ) ;
#29208 = CARTESIAN_POINT ( 'NONE',  ( -3.230769230769229949, -11.91647553114624181, 32.58852847137148245 ) ) ;
#29209 = DIRECTION ( 'NONE',  ( -1.000000000000000000, 0.000000000000000000, -0.000000000000000000 ) ) ;
#29210 = CARTESIAN_POINT ( 'NONE',  ( -8.769230769230768274, -2.538708090699994813, 30.37095296980875503 ) ) ;
#29211 = AXIS2_PLACEMENT_3D ( 'NONE', #82046, #47353, #68959 ) ;
#29212 = CARTESIAN_POINT ( 'NONE',  ( 12.52679360105129724, -2.379036618887895305, 30.90682066428158592 ) ) ;
#29213 = B_SPLINE_CURVE_WITH_KNOTS ( 'NONE', 3,
 ( #25843, #88020, #88452, #46982, #81678, #88893 ),
 .UNSPECIFIED., .F., .F.,
 ( 4, 2, 4 ),
 ( 0.0003909569690057804843, 0.0005862646681846042955, 0.0007815723673634281067 ),
 .UNSPECIFIED. ) ;
#29214 = CARTESIAN_POINT ( 'NONE',  ( 7.911409417429874580, -6.879047030191282275, 34.71129190930002295 ) ) ;
#29215 = EDGE_LOOP ( 'NONE', ( #20579, #18594 ) ) ;
#29216 = CARTESIAN_POINT ( 'NONE',  ( 2.242422307135989445, -3.643525952247789412, 33.31231777344662959 ) ) ;
#29217 = FACE_OUTER_BOUND ( 'NONE', #61130, .T. ) ;
#29218 = CARTESIAN_POINT ( 'NONE',  ( -1.901340078031369618, -5.512252781505359245, 23.00186829374151287 ) ) ;
#29219 = CARTESIAN_POINT ( 'NONE',  ( 8.899275932065544126, -2.504778602574659896, 29.97347330155780654 ) ) ;
#29220 = CARTESIAN_POINT ( 'NONE',  ( 6.923076923076924238, -4.098570777380720287, 33.41473453929634729 ) ) ;
#29221 = EDGE_LOOP ( 'NONE', ( #761, #83737, #13128, #82931 ) ) ;
#29222 = LINE ( 'NONE', #27878, #77329 ) ;
#29224 = VERTEX_POINT ( 'NONE', #74406 ) ;
#29223 = CARTESIAN_POINT ( 'NONE',  ( 16.15384615384603251, -3.083524468854526912, 32.58852847137268327 ) ) ;
#29225 = CYLINDRICAL_SURFACE ( 'NONE', #16789, 0.2499999999999997502 ) ;
#29226 = CARTESIAN_POINT ( 'NONE',  ( -18.00000000000000000, -13.45340096658850904, 31.05360187035682884 ) ) ;
#29227 = VERTEX_POINT ( 'NONE', #40632 ) ;
#29228 = CARTESIAN_POINT ( 'NONE',  ( 5.999999999999880096, -2.625532179533778709, 30.86335684631627174 ) ) ;
#29229 = CARTESIAN_POINT ( 'NONE',  ( -6.988346923633242724, -11.67786785259541027, 32.92929555188721480 ) ) ;
#29230 = VERTEX_POINT ( 'NONE', #20786 ) ;
#29231 = CARTESIAN_POINT ( 'NONE',  ( 8.769230769230768274, -2.292212530054420494, 30.41441678777542634 ) ) ;
#29232 = CARTESIAN_POINT ( 'NONE',  ( -16.15384615384627409, -3.300289026999228437, 32.46337939537709616 ) ) ;
#29233 = CARTESIAN_POINT ( 'NONE',  ( 12.52679360105129724, -12.16647553114626490, 32.15551576947920864 ) ) ;
#29234 = VERTEX_POINT ( 'NONE', #48254 ) ;
#29235 = ORIENTED_EDGE ( 'NONE', *, *, #24713, .F. ) ;
#29236 = AXIS2_PLACEMENT_3D ( 'NONE', #16864, #44312, #71801 ) ;
#29237 = ORIENTED_EDGE ( 'NONE', *, *, #27981, .T. ) ;
#29238 = AXIS2_PLACEMENT_3D ( 'NONE', #17391, #52496, #44847 ) ;
#29239 = CARTESIAN_POINT ( 'NONE',  ( -6.923076923076922462, -2.292212530054420494, 30.41441678777542634 ) ) ;
#29240 = DIRECTION ( 'NONE',  ( -1.000000000000000000, 0.000000000000000000, -0.000000000000000000 ) ) ;
#29241 = CARTESIAN_POINT ( 'NONE',  ( -20.00000000000000355, 10.00000000000000711, 13.00000000000000178 ) ) ;
#29242 = B_SPLINE_CURVE_WITH_KNOTS ( 'NONE', 3,
 ( #76698, #35721, #8692, #34814, #55531, #9136, #77140, #22630, #50097, #83015 ),
 .UNSPECIFIED., .F., .F.,
 ( 4, 2, 2, 2, 4 ),
 ( 0.000000000000000000, 0.0001954339857564078267, 0.0003908679715128156535, 0.0005863019572692235344, 0.0007817359430256313069 ),
 .UNSPECIFIED. ) ;
#29243 = B_SPLINE_CURVE_WITH_KNOTS ( 'NONE', 3,
 ( #63248, #56498, #15514, #50616, #71326, #56929, #23587, #49295, #16833, #16393 ),
 .UNSPECIFIED., .F., .F.,
 ( 4, 2, 2, 2, 4 ),
 ( 0.0007817359430256314154, 0.0009771253907249980580, 0.001172514838424364592, 0.001367904286123731127, 0.001563293733823097661 ),
 .UNSPECIFIED. ) ;
#29244 = CARTESIAN_POINT ( 'NONE',  ( -17.32689980786543060, -6.567427716900048118, 34.66269422305636283 ) ) ;
#29245 = B_SPLINE_CURVE_WITH_KNOTS ( 'NONE', 3,
 ( #32765, #60232, #53474, #59792, #46283, #26899, #53022, #61118, #18814, #88627 ),
 .UNSPECIFIED., .F., .F.,
 ( 4, 2, 2, 2, 4 ),
 ( 0.000000000000000000, 0.0001954311564186858715, 0.0003908623128373717431, 0.0005862934692560576146, 0.0007817246256747434861 ),
 .UNSPECIFIED. ) ;
#29246 = B_SPLINE_CURVE_WITH_KNOTS ( 'NONE', 3,
 ( #65288, #63517, #50870, #9904, #71596, #57650, #3137, #30614, #58086, #3584 ),
 .UNSPECIFIED., .F., .F.,
 ( 4, 2, 2, 2, 4 ),
 ( 0.0007817359430256293554, 0.0009771253907249950223, 0.001172514838424360906, 0.001367904286123726790, 0.001563293733823092457 ),
 .UNSPECIFIED. ) ;
#29247 = ORIENTED_EDGE ( 'NONE', *, *, #89117, .F. ) ;
#29248 = VERTEX_POINT ( 'NONE', #46920 ) ;
#29250 = EDGE_LOOP ( 'NONE', ( #48286, #15440, #35602, #66498 ) ) ;
#29249 = CARTESIAN_POINT ( 'NONE',  ( -1.134615384613947953, -7.500000000000155431, 34.75000000000007105 ) ) ;
#29251 = CARTESIAN_POINT ( 'NONE',  ( 12.46153846153833911, -11.67786785259630911, 32.92929555188603530 ) ) ;
#29252 = ADVANCED_FACE ( 'NONE', ( #40193 ), #75298, .F. ) ;
#29253 = ORIENTED_EDGE ( 'NONE', *, *, #85045, .T. ) ;
#29254 = DIRECTION ( 'NONE',  ( -1.000000000000000000, 0.000000000000000000, 0.000000000000000000 ) ) ;
#29255 = CARTESIAN_POINT ( 'NONE',  ( -10.03846153846153832, -11.00000000000000000, 28.25000000000000000 ) ) ;
#29256 = ORIENTED_EDGE ( 'NONE', *, *, #48382, .F. ) ;
#29257 = CARTESIAN_POINT ( 'NONE',  ( -6.000000000000119904, -3.300289026999228881, 32.46337939537708905 ) ) ;
#29258 = ORIENTED_EDGE ( 'NONE', *, *, #47068, .F. ) ;
#29260 = ORIENTED_EDGE ( 'NONE', *, *, #14194, .T. ) ;
#29259 = CARTESIAN_POINT ( 'NONE',  ( -12.46153846153858247, -5.219633306517616589, 34.19971097300220464 ) ) ;
#29261 = VECTOR ( 'NONE', #653, 1000.000000000000000 ) ;
#29262 = CARTESIAN_POINT ( 'NONE',  ( -5.933931648997561759, -8.120952969808772792, 34.71129190929999453 ) ) ;
#29263 = CARTESIAN_POINT ( 'NONE',  ( -5.207614543590636913, -9.804603061927743113, 34.18744698557895845 ) ) ;
#29264 = VERTEX_POINT ( 'NONE', #75726 ) ;
#29265 = EDGE_CURVE ( 'NONE', #85537, #45384, #1964, .T. ) ;
#29266 = CARTESIAN_POINT ( 'NONE',  ( 15.23076923076923173, -3.050289026998446396, 32.03036669348365706 ) ) ;
#29267 = CARTESIAN_POINT ( 'NONE',  ( 5.326868595271218254, -11.37275283266503756, 32.91324779482534524 ) ) ;
#29268 = CARTESIAN_POINT ( 'NONE',  ( 6.673053698855467175, -5.765609946408404518, 34.70566812827425451 ) ) ;
#29269 = FACE_BOUND ( 'NONE', #48396, .T. ) ;
#29270 = CARTESIAN_POINT ( 'NONE',  ( 7.911408985666684046, -12.51329471203373700, 31.30864560766537963 ) ) ;
#29271 = CARTESIAN_POINT ( 'NONE',  ( -11.76138849736838488, -6.459968553980841577, 34.89616026154728701 ) ) ;
#29272 = CARTESIAN_POINT ( 'NONE',  ( 15.23076923076923173, -2.486705287966279876, 31.30864560766543647 ) ) ;
#29273 = CARTESIAN_POINT ( 'NONE',  ( 3.361559671736180199, -4.684288915650983043, 34.18129842949671371 ) ) ;
#29274 = CARTESIAN_POINT ( 'NONE',  ( -11.40793583669797506, -3.285477652293413264, 32.44071101563363158 ) ) ;
#29275 = CARTESIAN_POINT ( 'NONE',  ( -13.38461538461538325, -8.564572088678739092, 35.78748833219616898 ) ) ;
#29276 = ORIENTED_EDGE ( 'NONE', *, *, #77814, .F. ) ;
#29277 = LINE ( 'NONE', #42790, #61943 ) ;
#29278 = EDGE_LOOP ( 'NONE', ( #44204, #43527, #30099, #39550 ) ) ;
#29279 = ORIENTED_EDGE ( 'NONE', *, *, #60408, .F. ) ;
#29281 = CARTESIAN_POINT ( 'NONE',  ( 16.40379167219429490, -12.22109172314383052, 31.39792113162168263 ) ) ;
#29280 = CARTESIAN_POINT ( 'NONE',  ( 9.442307692307693401, -2.249999999999998668, 29.75000000000000355 ) ) ;
#29282 = CARTESIAN_POINT ( 'NONE',  ( -12.46153846153846168, -2.538708090699994813, 30.37095296980875503 ) ) ;
#29283 = CARTESIAN_POINT ( 'NONE',  ( 8.096099255531889582, -3.520799739797214389, 33.17531984108286025 ) ) ;
#29284 = LINE ( 'NONE', #56741, #1273 ) ;
#29285 = CARTESIAN_POINT ( 'NONE',  ( -0.3307466537136754536, -11.71459661697925903, 32.44059661609676937 ) ) ;
#29286 = ORIENTED_EDGE ( 'NONE', *, *, #9600, .T. ) ;
#29287 = EDGE_CURVE ( 'NONE', #29866, #52292, #13703, .T. ) ;
#29288 = CARTESIAN_POINT ( 'NONE',  ( -18.13069146666756382, -5.582088688514995845, 34.36776431015576350 ) ) ;
#29289 = CARTESIAN_POINT ( 'NONE',  ( 1.384615384615386802, -12.10708131394839349, 31.69288490824020244 ) ) ;
#29290 = LINE ( 'NONE', #57190, #80526 ) ;
#29291 = CARTESIAN_POINT ( 'NONE',  ( 15.48071464014727461, -12.45601412856602686, 31.48342859153981621 ) ) ;
#29292 = CARTESIAN_POINT ( 'NONE',  ( -15.29602022093047076, -2.506253911140460922, 30.00000000000013856 ) ) ;
#29293 = CARTESIAN_POINT ( 'NONE',  ( -1.553300858899081538, -11.25000000000000711, 18.60937500000000355 ) ) ;
#29294 = ORIENTED_EDGE ( 'NONE', *, *, #48482, .T. ) ;
#29295 = EDGE_CURVE ( 'NONE', #21236, #83780, #68974, .T. ) ;
#29296 = EDGE_LOOP ( 'NONE', ( #18154, #16450, #39448, #34230 ) ) ;
#29297 = VECTOR ( 'NONE', #48974, 1000.000000000000000 ) ;
#29298 = EDGE_CURVE ( 'NONE', #5455, #13666, #8283, .T. ) ;
#29299 = CARTESIAN_POINT ( 'NONE',  ( -7.846153846153967493, -12.16647553114689728, 32.15551576947799362 ) ) ;
#29300 = ORIENTED_EDGE ( 'NONE', *, *, #68789, .F. ) ;
#29301 = CARTESIAN_POINT ( 'NONE',  ( -9.942284423250047354, -12.41269422305637171, 30.68257228309993323 ) ) ;
#29302 = CARTESIAN_POINT ( 'NONE',  ( -1.161835715637317135, -10.23759521482555357, 34.22997729860117033 ) ) ;
#29303 = LINE ( 'NONE', #69833, #10665 ) ;
#29304 = CARTESIAN_POINT ( 'NONE',  ( 2.373759641042384239, -9.905515769479277921, 34.41647553114623292 ) ) ;
#29305 = CARTESIAN_POINT ( 'NONE',  ( -2.057637996053991003, -4.943051570960395047, 34.04725096376909477 ) ) ;
#29306 = B_SPLINE_CURVE_WITH_KNOTS ( 'NONE', 3,
 ( #49961, #16184, #51260, #79221, #43649, #16616, #17520, #38227, #78766, #44970 ),
 .UNSPECIFIED., .F., .F.,
 ( 4, 2, 2, 2, 4 ),
 ( 0.0007817359430256216575, 0.0009771253907249856981, 0.001172514838424349847, 0.001367904286123713779, 0.001563293733823077928 ),
 .UNSPECIFIED. ) ;
#29307 = CARTESIAN_POINT ( 'NONE',  ( 8.769230769230647482, -6.879047030192662504, 34.71129190930017927 ) ) ;
#29308 = ORIENTED_EDGE ( 'NONE', *, *, #75042, .F. ) ;
#29309 = LINE ( 'NONE', #44558, #71727 ) ;
#29311 = VERTEX_POINT ( 'NONE', #13150 ) ;
#29310 = CARTESIAN_POINT ( 'NONE',  ( -2.307692307692427391, -10.90142922262034020, 33.41473453929536674 ) ) ;
#29312 = CARTESIAN_POINT ( 'NONE',  ( 2.980792499826877329, -12.41269422305637171, 30.68257228309993323 ) ) ;
#29313 = DIRECTION ( 'NONE',  ( -1.000000000000000000, -0.000000000000000000, -0.000000000000000000 ) ) ;
#29314 = CARTESIAN_POINT ( 'NONE',  ( 6.130525438233648039, -9.503571793651733657, 34.60286762892837942 ) ) ;
#29315 = CARTESIAN_POINT ( 'NONE',  ( 6.699591998512594238, -3.562934362175799841, 33.22335522853832401 ) ) ;
#29316 = CYLINDRICAL_SURFACE ( 'NONE', #75232, 0.2499999999999995559 ) ;
#29317 = CARTESIAN_POINT ( 'NONE',  ( -2.724691934501246582, -6.299813628509474128, 24.17374329374151642 ) ) ;
#29318 = EDGE_LOOP ( 'NONE', ( #1366, #33558 ) ) ;
#29319 = CARTESIAN_POINT ( 'NONE',  ( -1.134669866267241423, -11.37275283266503756, 32.91324779482534524 ) ) ;
#29320 = CARTESIAN_POINT ( 'NONE',  ( -13.63463862190834952, -9.271318131107980420, 34.42618302367067429 ) ) ;
#29321 = CARTESIAN_POINT ( 'NONE',  ( -1.944543648263014957, -5.555456351737005249, 21.50000000000000000 ) ) ;
#29322 = CARTESIAN_POINT ( 'NONE',  ( 0.2386115026316118215, -5.582147617184174848, 34.63737895849758530 ) ) ;
#29323 = CARTESIAN_POINT ( 'NONE',  ( 9.468822767743363400, -6.716662450894489211, 34.94144148231605840 ) ) ;
#29324 = EDGE_LOOP ( 'NONE', ( #74663, #65027, #10413, #3435 ) ) ;
#29325 = CARTESIAN_POINT ( 'NONE',  ( 0.3313904918067645533, -4.299443229763728169, 33.91186481527756769 ) ) ;
#29326 = DIRECTION ( 'NONE',  ( -0.000000000000000000, -0.3420201433256694346, -0.9396926207859080948 ) ) ;
#29327 = VERTEX_POINT ( 'NONE', #27101 ) ;
#29328 = VECTOR ( 'NONE', #22610, 1000.000000000000000 ) ;
#29329 = CARTESIAN_POINT ( 'NONE',  ( 9.757452473027326434, -7.750023224968867197, 34.99404313364389907 ) ) ;
#29330 = EDGE_LOOP ( 'NONE', ( #36914, #4963 ) ) ;
#29331 = EDGE_CURVE ( 'NONE', #31770, #63430, #60907, .T. ) ;
#29332 = DIRECTION ( 'NONE',  ( 1.000000000000000000, 0.000000000000000000, 0.000000000000000000 ) ) ;
#29333 = CARTESIAN_POINT ( 'NONE',  ( -17.29985003582992320, -2.308479472611653094, 30.53278059502174457 ) ) ;
#29334 = CARTESIAN_POINT ( 'NONE',  ( -12.68446542044531178, -10.01117774369187252, 34.36070679894347535 ) ) ;
#29335 = DIRECTION ( 'NONE',  ( -0.000000000000000000, 0.6427876096865404731, -0.7660444431189770143 ) ) ;
#29336 = VERTEX_POINT ( 'NONE', #74861 ) ;
#29337 = CARTESIAN_POINT ( 'NONE',  ( -13.31936024510254413, -3.083524468853784839, 32.58852847137153930 ) ) ;
#29338 = B_SPLINE_CURVE_WITH_KNOTS ( 'NONE', 3,
 ( #56920, #77197, #84416, #64996, #78520, #2850, #63235, #1544, #70449, #71760 ),
 .UNSPECIFIED., .F., .F.,
 ( 4, 2, 2, 2, 4 ),
 ( 0.000000000000000000, 0.0001954311564186871184, 0.0003908623128373742367, 0.0005862934692560614093, 0.0007817246256747484735 ),
 .UNSPECIFIED. ) ;
#29339 = ORIENTED_EDGE ( 'NONE', *, *, #46342, .F. ) ;
#29340 = CARTESIAN_POINT ( 'NONE',  ( 5.999999999999878320, -5.094484230521993062, 34.41647553114689373 ) ) ;
#29341 = CARTESIAN_POINT ( 'NONE',  ( -10.61538461538473399, -2.892918686052166066, 31.69288490824153470 ) ) ;
#29342 = ORIENTED_EDGE ( 'NONE', *, *, #38128, .F. ) ;
#29343 = CARTESIAN_POINT ( 'NONE',  ( -6.249976744048590049, -10.82459398097509684, 33.81372124010185587 ) ) ;
#29344 = CARTESIAN_POINT ( 'NONE',  ( 10.83816415665302557, -3.236590943229499029, 32.36255958852954251 ) ) ;
#29345 = FACE_OUTER_BOUND ( 'NONE', #43881, .T. ) ;
#29346 = ADVANCED_FACE ( 'NONE', ( #27551 ), #4447, .F. ) ;
#29347 = DIRECTION ( 'NONE',  ( -0.000000000000000000, -0.000000000000000000, -1.000000000000000000 ) ) ;
#29348 = CARTESIAN_POINT ( 'NONE',  ( -18.00000000000000000, -4.098570777380720287, 33.41473453929634729 ) ) ;
#29349 = STYLED_ITEM ( 'NONE', ( #47702 ), #307 ) ;
#29350 = AXIS2_PLACEMENT_3D ( 'NONE', #11270, #38743, #66207 ) ;
#29351 = ORIENTED_EDGE ( 'NONE', *, *, #4814, .F. ) ;
#29352 = ORIENTED_EDGE ( 'NONE', *, *, #40433, .F. ) ;
#29353 = FACE_BOUND ( 'NONE', #52379, .T. ) ;
#29354 = ORIENTED_EDGE ( 'NONE', *, *, #74183, .F. ) ;
#29355 = CARTESIAN_POINT ( 'NONE',  ( 8.639083559792545941, -3.817052484675422797, 33.13202310037935661 ) ) ;
#29356 = VECTOR ( 'NONE', #3944, 1000.000000000000000 ) ;
#29357 = AXIS2_PLACEMENT_3D ( 'NONE', #12107, #5782, #87782 ) ;
#29358 = EDGE_CURVE ( 'NONE', #87090, #58189, #10766, .T. ) ;
#29359 = CYLINDRICAL_SURFACE ( 'NONE', #61683, 0.2499999999999995559 ) ;
#29360 = CARTESIAN_POINT ( 'NONE',  ( 13.63466969625370062, -10.66356715214248752, 33.62249196103329751 ) ) ;
#29361 = CARTESIAN_POINT ( 'NONE',  ( -2.176901866725357237, -9.929761469519744921, 34.40412654351204225 ) ) ;
#29362 = EDGE_CURVE ( 'NONE', #922, #55479, #79229, .T. ) ;
#29363 = EDGE_LOOP ( 'NONE', ( #74550, #37647 ) ) ;
#29364 = VERTEX_POINT ( 'NONE', #5789 ) ;
#29365 = ORIENTED_EDGE ( 'NONE', *, *, #58162, .T. ) ;
#29366 = DIRECTION ( 'NONE',  ( 0.000000000000000000, 0.9848077530122072432, 0.1736481776669354937 ) ) ;
#29367 = ORIENTED_EDGE ( 'NONE', *, *, #20410, .F. ) ;
#29368 = B_SPLINE_CURVE_WITH_KNOTS ( 'NONE', 3,
 ( #47001, #24960, #40271, #17773, #6040, #45227, #72703, #65940, #79913, #18217 ),
 .UNSPECIFIED., .F., .F.,
 ( 4, 2, 2, 2, 4 ),
 ( 0.0007817359430256301143, 0.0009771253907249963233, 0.001172514838424362641, 0.001367904286123728958, 0.001563293733823095276 ),
 .UNSPECIFIED. ) ;
#29369 = B_SPLINE_CURVE_WITH_KNOTS ( 'NONE', 3,
 ( #67386, #81354, #61946, #6573, #82237, #41249, #88570, #80918, #39928, #68271 ),
 .UNSPECIFIED., .F., .F.,
 ( 4, 2, 2, 2, 4 ),
 ( 0.0007817359430256365111, 0.0009771253907250045632, 0.001172514838424372399, 0.001367904286123740451, 0.001563293733823108503 ),
 .UNSPECIFIED. ) ;
#29370 = EDGE_CURVE ( 'NONE', #81013, #25396, #64090, .T. ) ;
#29371 = CYLINDRICAL_SURFACE ( 'NONE', #89109, 0.2499999999999998890 ) ;
#29372 = B_SPLINE_CURVE_WITH_KNOTS ( 'NONE', 3,
 ( #82451, #39693, #20732, #32920, #75670, #55401, #62159, #41451, #467, #27935 ),
 .UNSPECIFIED., .F., .F.,
 ( 4, 2, 2, 2, 4 ),
 ( 0.000000000000000000, 0.0001954339857564064444, 0.0003908679715128128888, 0.0005863019572692193060, 0.0007817359430256257775 ),
 .UNSPECIFIED. ) ;
#29373 = DIRECTION ( 'NONE',  ( -0.000000000000000000, -0.1736481776669307198, -0.9848077530122080203 ) ) ;
#29374 = CARTESIAN_POINT ( 'NONE',  ( 8.769230769230768274, -1.951392089020283160, 34.73218667398347748 ) ) ;
#29375 = ORIENTED_EDGE ( 'NONE', *, *, #43070, .F. ) ;
#29376 = CARTESIAN_POINT ( 'NONE',  ( 16.28437159207980045, -2.372941743896878286, 30.88044141588253311 ) ) ;
#29377 = EDGE_CURVE ( 'NONE', #8200, #54081, #80215, .T. ) ;
#29378 = LINE ( 'NONE', #71223, #4280 ) ;
#29379 = CARTESIAN_POINT ( 'NONE',  ( -17.77694319641476284, -12.75000000000000888, 29.61950345095122827 ) ) ;
#29380 = CARTESIAN_POINT ( 'NONE',  ( -1.254089946381742315, -3.068774925481847493, 32.56582465632704526 ) ) ;
#29381 = ORIENTED_EDGE ( 'NONE', *, *, #19799, .T. ) ;
#29382 = EDGE_CURVE ( 'NONE', #62209, #76336, #85985, .T. ) ;
#29383 = ORIENTED_EDGE ( 'NONE', *, *, #15560, .T. ) ;
#29384 = VERTEX_POINT ( 'NONE', #46329 ) ;
#29385 = CARTESIAN_POINT ( 'NONE',  ( -4.087777802843714170, -9.780366693483667717, 34.19971097300155805 ) ) ;
#29386 = CIRCLE ( 'NONE', #58159, 5.000000000000000888 ) ;
#29388 = CARTESIAN_POINT ( 'NONE',  ( 10.55011461482829738, -2.379036618887870436, 30.90682066428147934 ) ) ;
#29387 = DIRECTION ( 'NONE',  ( -0.000000000000000000, 1.000000000000000000, -0.000000000000000000 ) ) ;
#29389 = FACE_OUTER_BOUND ( 'NONE', #77221, .T. ) ;
#29390 = CARTESIAN_POINT ( 'NONE',  ( -3.361460697436787992, -11.18331474514187995, 33.13161551792790505 ) ) ;
#29391 = FACE_BOUND ( 'NONE', #5121, .T. ) ;
#29392 = CARTESIAN_POINT ( 'NONE',  ( -18.00000000000000000, -12.34228464037088635, 31.77849191805839268 ) ) ;
#29393 = ORIENTED_EDGE ( 'NONE', *, *, #13930, .F. ) ;
#29394 = ADVANCED_FACE ( 'NONE', ( #12114 ), #18417, .F. ) ;
#29395 = CARTESIAN_POINT ( 'NONE',  ( 17.20744877868664346, -10.88167719472716399, 33.43325721877153711 ) ) ;
#29396 = CARTESIAN_POINT ( 'NONE',  ( -14.30769230769242917, -12.70778746994576025, 30.41441678777401236 ) ) ;
#29397 = CARTESIAN_POINT ( 'NONE',  ( 4.403900465484469784, -9.148310452688871663, 34.47095581063188519 ) ) ;
#29398 = DIRECTION ( 'NONE',  ( 0.000000000000000000, 0.9848077530122072432, -0.1736481776669354937 ) ) ;
#29399 = ORIENTED_EDGE ( 'NONE', *, *, #68044, .F. ) ;
#29400 = CARTESIAN_POINT ( 'NONE',  ( 20.00000000000000355, 10.00000000000000533, 13.00000000000000178 ) ) ;
#29401 = EDGE_LOOP ( 'NONE', ( #51471, #75873, #77505, #76051 ) ) ;
#29402 = FACE_BOUND ( 'NONE', #42211, .T. ) ;
#29403 = CARTESIAN_POINT ( 'NONE',  ( 5.010839665967196765, -5.557115091759785130, 34.35708131394839171 ) ) ;
#29404 = ADVANCED_FACE ( 'NONE', ( #24262 ), #81016, .F. ) ;
#29405 = CARTESIAN_POINT ( 'NONE',  ( 10.61538461538449596, -6.026961402154118019, 34.52809138561165270 ) ) ;
#29407 = EDGE_CURVE ( 'NONE', #67015, #25023, #9224, .T. ) ;
#29406 = CARTESIAN_POINT ( 'NONE',  ( -2.980714919130914797, -8.303483539816728154, 34.68545999027711702 ) ) ;
#29408 = ORIENTED_EDGE ( 'NONE', *, *, #50007, .F. ) ;
#29409 = CARTESIAN_POINT ( 'NONE',  ( -14.37377571864818648, -12.37446782046654192, 30.86335684631486487 ) ) ;
#29410 = CARTESIAN_POINT ( 'NONE',  ( -17.77698715590660328, -4.026326845037963231, 33.68677907613344047 ) ) ;
#29411 = CARTESIAN_POINT ( 'NONE',  ( 8.519207545009312099, -2.341070481393819236, 30.72580821765574299 ) ) ;
#29412 = LINE ( 'NONE', #42036, #62010 ) ;
#29413 = ORIENTED_EDGE ( 'NONE', *, *, #41435, .F. ) ;
#29414 = CARTESIAN_POINT ( 'NONE',  ( 0.3589743589743582541, -7.500000000000000000, 29.75000000000000355 ) ) ;
#29415 = ORIENTED_EDGE ( 'NONE', *, *, #33312, .T. ) ;
#29417 = ORIENTED_EDGE ( 'NONE', *, *, #61333, .T. ) ;
#29416 = CARTESIAN_POINT ( 'NONE',  ( 16.82689983963011926, -10.76384336483936011, 33.53834819971076087 ) ) ;
#29418 = CARTESIAN_POINT ( 'NONE',  ( -14.98076923076779465, -7.500000000000155431, 34.75000000000007105 ) ) ;
#29419 = CARTESIAN_POINT ( 'NONE',  ( -1.449885385171703511, -12.51329471203370325, 31.30864560766548976 ) ) ;
#29420 = DIRECTION ( 'NONE',  ( -0.000000000000000000, 0.5000000000000011102, -0.8660254037844381525 ) ) ;
#29421 = B_SPLINE_CURVE_WITH_KNOTS ( 'NONE', 3,
 ( #50863, #31046, #37813, #24289, #9898, #18444, #78348, #16649, #44111, #71589 ),
 .UNSPECIFIED., .F., .F.,
 ( 4, 2, 2, 2, 4 ),
 ( 0.000000000000000000, 0.0001954339857564086941, 0.0003908679715128173882, 0.0005863019572692261365, 0.0007817359430256347764 ),
 .UNSPECIFIED. ) ;
#29422 = CARTESIAN_POINT ( 'NONE',  ( -12.46153846153846168, -2.721908614388771852, 31.22303859784724978 ) ) ;
#29425 = CARTESIAN_POINT ( 'NONE',  ( 8.769230769230645706, -4.320704448113951379, 33.92786785259630022 ) ) ;
#29424 = VECTOR ( 'NONE', #84430, 1000.000000000000000 ) ;
#29423 = FACE_OUTER_BOUND ( 'NONE', #85505, .T. ) ;
#29426 = CARTESIAN_POINT ( 'NONE',  ( 14.24242186173153435, -3.835265460703609186, 33.15142922261924241 ) ) ;
#29427 = CARTESIAN_POINT ( 'NONE',  ( -1.944543648262992530, -9.444543648263016067, 26.18750000000000355 ) ) ;
#29428 = ORIENTED_EDGE ( 'NONE', *, *, #82198, .T. ) ;
#29429 = CARTESIAN_POINT ( 'NONE',  ( 13.38461538461526423, -12.70778746994576025, 30.41441678777401236 ) ) ;
#29430 = CARTESIAN_POINT ( 'NONE',  ( -9.442253272394237840, -11.47946981652013498, 33.17500667209847620 ) ) ;
#29431 = ORIENTED_EDGE ( 'NONE', *, *, #80522, .F. ) ;
#29432 = VECTOR ( 'NONE', #55105, 1000.000000000000114 ) ;
#29433 = VERTEX_POINT ( 'NONE', #46776 ) ;
#29434 = ORIENTED_EDGE ( 'NONE', *, *, #69586, .T. ) ;
#29435 = CARTESIAN_POINT ( 'NONE',  ( -10.83831083290076158, -11.24512374952581872, 33.06303171183252942 ) ) ;
#29436 = CARTESIAN_POINT ( 'NONE',  ( -17.07692307692319744, -9.442884908241554243, 34.35708131394783038 ) ) ;
#29437 = CARTESIAN_POINT ( 'NONE',  ( -14.30769230769230660, -13.63283147151868846, 33.57946703557072254 ) ) ;
#29438 = CARTESIAN_POINT ( 'NONE',  ( -5.010854725920638408, -3.513871655860379306, 32.76840700105978499 ) ) ;
#29439 = CARTESIAN_POINT ( 'NONE',  ( -8.834500769787091201, -2.657715359629089225, 31.77849191805832874 ) ) ;
#29440 = CARTESIAN_POINT ( 'NONE',  ( 19.00000000000000000, -16.99999999999999289, 30.25000000000000000 ) ) ;
#29441 = CARTESIAN_POINT ( 'NONE',  ( 6.249999999999937828, -7.565270000091922853, 34.99999999999999289 ) ) ;
#29442 = EDGE_CURVE ( 'NONE', #23776, #30732, #62961, .T. ) ;
#29443 = LINE ( 'NONE', #9171, #21866 ) ;
#29444 = CARTESIAN_POINT ( 'NONE',  ( -24.00000000000000000, 9.000000000000024869, 28.74999999999999645 ) ) ;
#29445 = CARTESIAN_POINT ( 'NONE',  ( 7.976945653978630979, -2.729792928343270031, 31.24908615093345077 ) ) ;
#29446 = EDGE_CURVE ( 'NONE', #63242, #34093, #14641, .T. ) ;
#29447 = LINE ( 'NONE', #71736, #29789 ) ;
#29448 = EDGE_CURVE ( 'NONE', #9375, #76058, #45082, .T. ) ;
#29449 = EDGE_CURVE ( 'NONE', #76906, #1831, #26461, .T. ) ;
#29450 = VERTEX_POINT ( 'NONE', #40534 ) ;
#29451 = CARTESIAN_POINT ( 'NONE',  ( 8.769230769230768274, -2.833524468853757305, 32.15551576947925838 ) ) ;
#29452 = CARTESIAN_POINT ( 'NONE',  ( -16.15384615384583711, -2.255955759149395501, 30.00000000000324363 ) ) ;
#29453 = CARTESIAN_POINT ( 'NONE',  ( 10.03846153846153832, -11.00000000000000000, 29.25000000000000000 ) ) ;
#29454 = CYLINDRICAL_SURFACE ( 'NONE', #80085, 0.2500000000000008882 ) ;
#29455 = ORIENTED_EDGE ( 'NONE', *, *, #36064, .F. ) ;
#29456 = CARTESIAN_POINT ( 'NONE',  ( 10.03846153846153832, -7.500000000000000000, 29.75000000000000355 ) ) ;
#29457 = DIRECTION ( 'NONE',  ( 0.000000000000000000, 0.000000000000000000, 1.000000000000000000 ) ) ;
#29458 = EDGE_CURVE ( 'NONE', #47437, #45062, #859, .T. ) ;
#29459 = VECTOR ( 'NONE', #79252, 1000.000000000000000 ) ;
#29460 = CARTESIAN_POINT ( 'NONE',  ( -9.019207513279360100, -9.234221910056348293, 34.70572697212741531 ) ) ;
#29461 = B_SPLINE_CURVE_WITH_KNOTS ( 'NONE', 3,
 ( #65514, #58308, #29523, #44339, #71826, #64170, #37151, #10130, #37597, #24083 ),
 .UNSPECIFIED., .F., .F.,
 ( 4, 2, 2, 2, 4 ),
 ( 0.0007817359430256386795, 0.0009771253907250069485, 0.001172514838424375217, 0.001367904286123743486, 0.001563293733823111755 ),
 .UNSPECIFIED. ) ;
#29462 = ORIENTED_EDGE ( 'NONE', *, *, #22921, .F. ) ;
#29463 = CARTESIAN_POINT ( 'NONE',  ( 15.90382291655318880, -2.823816976329320827, 31.52131813110797154 ) ) ;
#29464 = VERTEX_POINT ( 'NONE', #69325 ) ;
#29465 = CARTESIAN_POINT ( 'NONE',  ( -7.846153846153967493, -2.379036618888197729, 30.90682066428292885 ) ) ;
#29466 = CARTESIAN_POINT ( 'NONE',  ( 9.019176178608812933, -9.357781135181031829, 34.66075350412533851 ) ) ;
#29467 = FACE_OUTER_BOUND ( 'NONE', #16868, .T. ) ;
#29468 = CARTESIAN_POINT ( 'NONE',  ( -10.61538461538461320, -2.499999999999998668, 29.50000000000001066 ) ) ;
#29469 = DIRECTION ( 'NONE',  ( 0.000000000000000000, 0.1736481776669275834, 0.9848077530122086864 ) ) ;
#29470 = EDGE_CURVE ( 'NONE', #10613, #2810, #82295, .T. ) ;
#29471 = EDGE_LOOP ( 'NONE', ( #4506, #30806, #10207, #74665, #52118, #76508 ) ) ;
#29472 = ORIENTED_EDGE ( 'NONE', *, *, #64014, .F. ) ;
#29473 = ORIENTED_EDGE ( 'NONE', *, *, #83264, .F. ) ;
#29474 = AXIS2_PLACEMENT_3D ( 'NONE', #14763, #42241, #34586 ) ;
#29475 = CARTESIAN_POINT ( 'NONE',  ( -3.230769230768915534, -2.255955759149395501, 30.00000000000324363 ) ) ;
#29476 = CARTESIAN_POINT ( 'NONE',  ( 13.51540719244017374, -9.804649428959608670, 34.18742332936588468 ) ) ;
#29477 = CARTESIAN_POINT ( 'NONE',  ( 0.5920638997721053842, -6.808710257144159783, 34.95449254468098843 ) ) ;
#29478 = VECTOR ( 'NONE', #60102, 1000.000000000000227 ) ;
#29479 = CARTESIAN_POINT ( 'NONE',  ( 16.94623247381276343, -9.929715669179216775, 34.40415004197138416 ) ) ;
#29480 = CARTESIAN_POINT ( 'NONE',  ( 7.596153846153846700, -7.500000000000001776, 35.00000000000000000 ) ) ;
#29481 = CARTESIAN_POINT ( 'NONE',  ( -7.846153846153844924, -6.386643153685126251, 34.62446782046654192 ) ) ;
#29482 = EDGE_LOOP ( 'NONE', ( #57634, #18540, #19053, #55611 ) ) ;
#29483 = ORIENTED_EDGE ( 'NONE', *, *, #16615, .F. ) ;
#29484 = EDGE_LOOP ( 'NONE', ( #44997, #86850, #66735, #76778 ) ) ;
#29486 = VERTEX_POINT ( 'NONE', #421 ) ;
#29485 = DIRECTION ( 'NONE',  ( -1.000000000000000000, -0.000000000000000000, -0.000000000000000000 ) ) ;
#29488 = CARTESIAN_POINT ( 'NONE',  ( 14.53070515178570332, -4.762714258010881885, 34.23016756924214832 ) ) ;
#29487 = CARTESIAN_POINT ( 'NONE',  ( -9.757578138268467427, -9.442884908240170461, 34.35708131394840592 ) ) ;
#29489 = CARTESIAN_POINT ( 'NONE',  ( -1.929879867024197893E-14, -3.750000000000000000, 25.40625000000000000 ) ) ;
#29490 = ORIENTED_EDGE ( 'NONE', *, *, #32205, .T. ) ;
#29491 = EDGE_CURVE ( 'NONE', #16480, #38892, #81965, .T. ) ;
#29492 = EDGE_CURVE ( 'NONE', #38006, #64208, #15599, .T. ) ;
#29493 = ORIENTED_EDGE ( 'NONE', *, *, #15095, .F. ) ;
#29494 = CYLINDRICAL_SURFACE ( 'NONE', #83111, 0.2500000000000004996 ) ;
#29496 = EDGE_CURVE ( 'NONE', #48420, #25149, #47269, .T. ) ;
#29495 = ORIENTED_EDGE ( 'NONE', *, *, #81425, .F. ) ;
#29497 = FACE_BOUND ( 'NONE', #59141, .T. ) ;
#29498 = CARTESIAN_POINT ( 'NONE',  ( -6.249976730942353953, -9.148715823498378086, 34.47080413974185120 ) ) ;
#29499 = CARTESIAN_POINT ( 'NONE',  ( 27.00000000000000000, -1.249999999999999112, 32.75000000000000000 ) ) ;
#29500 = ORIENTED_EDGE ( 'NONE', *, *, #5385, .T. ) ;
#29501 = CARTESIAN_POINT ( 'NONE',  ( -15.09997742294444478, -4.809403383903225304, 33.96459661697924304 ) ) ;
#29503 = EDGE_CURVE ( 'NONE', #5991, #328, #6727, .T. ) ;
#29502 = CARTESIAN_POINT ( 'NONE',  ( 16.37685750545900376, -4.187068189119696804, 33.49521262558774026 ) ) ;
#29504 = CARTESIAN_POINT ( 'NONE',  ( -8.769230769230890843, -6.026961402154118019, 34.52809138561165270 ) ) ;
#29505 = CARTESIAN_POINT ( 'NONE',  ( -11.66915300512910214, -5.582088688514999397, 34.36776431015576350 ) ) ;
#29506 = CARTESIAN_POINT ( 'NONE',  ( 4.153846153846154188, -3.050289026998446396, 32.03036669348365706 ) ) ;
#29507 = ADVANCED_FACE ( 'NONE', ( #82404 ), #75621, .F. ) ;
#29508 = CARTESIAN_POINT ( 'NONE',  ( 8.546303810323916395, -11.43668979543634734, 33.22377378376089752 ) ) ;
#29509 = CARTESIAN_POINT ( 'NONE',  ( -7.846153846153844924, -11.91647553114624181, 32.58852847137148245 ) ) ;
#29510 = CARTESIAN_POINT ( 'NONE',  ( 16.21991450484859598, -8.973038597847269315, 34.52809138561122637 ) ) ;
#29511 = CARTESIAN_POINT ( 'NONE',  ( 13.44987052412822059, -2.379036618887895305, 30.90682066428158592 ) ) ;
#29512 = CARTESIAN_POINT ( 'NONE',  ( 9.469380733400845074, -12.38737895849757820, 31.66785238281580206 ) ) ;
#29513 = CARTESIAN_POINT ( 'NONE',  ( 6.065255571276025215, -10.21337939537593620, 33.94971097300152252 ) ) ;
#29515 = CARTESIAN_POINT ( 'NONE',  ( 11.60462814505318008, -7.250054591869670162, 34.99404684341514127 ) ) ;
#29514 = DIRECTION ( 'NONE',  ( -0.000000000000000000, -0.7660444431189791237, -0.6427876096865379196 ) ) ;
#29516 = CARTESIAN_POINT ( 'NONE',  ( -14.30769230769230660, -8.164416787775445883, 34.95778746994557906 ) ) ;
#29518 = CARTESIAN_POINT ( 'NONE',  ( 5.933916589044121892, -10.51840700105979387, 33.73612834413961536 ) ) ;
#29517 = CARTESIAN_POINT ( 'NONE',  ( 4.023155550735844521, -5.496505350115500121, 34.60290016733514307 ) ) ;
#29519 = EDGE_CURVE ( 'NONE', #22275, #16729, #49406, .T. ) ;
#29520 = CARTESIAN_POINT ( 'NONE',  ( 2.307692307692309264, -13.78497067705608181, 32.30358669280327177 ) ) ;
#29521 = CARTESIAN_POINT ( 'NONE',  ( 1.077988221561464899, -4.724691934501233703, 23.98250670625849068 ) ) ;
#29522 = VERTEX_POINT ( 'NONE', #16579 ) ;
#29523 = CARTESIAN_POINT ( 'NONE',  ( 18.13052570176355971, -11.93748526763465279, 32.05452791011430946 ) ) ;
#29524 = ORIENTED_EDGE ( 'NONE', *, *, #60367, .T. ) ;
#29525 = DIRECTION ( 'NONE',  ( -1.000000000000000000, -0.000000000000000000, -0.000000000000000000 ) ) ;
#29526 = EDGE_CURVE ( 'NONE', #14701, #17652, #86611, .T. ) ;
#29527 = ORIENTED_EDGE ( 'NONE', *, *, #59358, .T. ) ;
#29528 = DIRECTION ( 'NONE',  ( -0.000000000000000000, 0.5000000000000011102, -0.8660254037844380415 ) ) ;
#29529 = CARTESIAN_POINT ( 'NONE',  ( -3.230769230769351186, -3.300289026999228881, 32.46337939537708905 ) ) ;
#29530 = EDGE_LOOP ( 'NONE', ( #39890, #10057 ) ) ;
#29531 = FACE_OUTER_BOUND ( 'NONE', #11926, .T. ) ;
#29532 = CARTESIAN_POINT ( 'NONE',  ( 2.724691934501235036, -6.299813628509441266, 24.13875670625849068 ) ) ;
#29533 = CARTESIAN_POINT ( 'NONE',  ( 7.596130621932389637, -8.475808217655753651, 34.90892951860618609 ) ) ;
#29534 = CARTESIAN_POINT ( 'NONE',  ( 12.22435897435897267, -7.500000000000000000, 29.75000000000000355 ) ) ;
#29535 = CARTESIAN_POINT ( 'NONE',  ( -5.299849294439222369, -4.887634598454295265, 34.01352882383564946 ) ) ;
#29536 = CARTESIAN_POINT ( 'NONE',  ( -20.00000000000000355, 10.00000000000000711, 13.00000000000000178 ) ) ;
#29537 = CARTESIAN_POINT ( 'NONE',  ( 11.53846153846141753, -2.892918686052165622, 31.69288490824153470 ) ) ;
#29538 = CARTESIAN_POINT ( 'NONE',  ( 6.923076923076924238, -8.120952969808772792, 34.71129190930000163 ) ) ;
#29539 = CARTESIAN_POINT ( 'NONE',  ( 3.750000000000009770, -9.053300858899081760, 14.54687500000000178 ) ) ;
#29541 = EDGE_CURVE ( 'NONE', #37415, #2917, #45743, .T. ) ;
#29540 = B_SPLINE_CURVE_WITH_KNOTS ( 'NONE', 3,
 ( #16837, #72667, #51041, #78534, #85752, #38001, #78983, #18180, #37101, #44743 ),
 .UNSPECIFIED., .F., .F.,
 ( 4, 2, 2, 2, 4 ),
 ( 0.0007817359430256379206, 0.0009771253907250060811, 0.001172514838424374133, 0.001367904286123742185, 0.001563293733823110238 ),
 .UNSPECIFIED. ) ;
#29542 = VECTOR ( 'NONE', #46886, 1000.000000000000000 ) ;
#29543 = LINE ( 'NONE', #48022, #39111 ) ;
#29544 = FACE_OUTER_BOUND ( 'NONE', #48897, .T. ) ;
#29545 = DIRECTION ( 'NONE',  ( -0.000000000000000000, 1.000000000000000000, -0.000000000000000000 ) ) ;
#29546 = CARTESIAN_POINT ( 'NONE',  ( 3.749999999999992006, -5.946699141100872943, 15.64062500000000178 ) ) ;
#29547 = EDGE_CURVE ( 'NONE', #48938, #5501, #9177, .T. ) ;
#29548 = DIRECTION ( 'NONE',  ( 0.000000000000000000, 0.000000000000000000, 1.000000000000000000 ) ) ;
#29549 = ORIENTED_EDGE ( 'NONE', *, *, #16349, .T. ) ;
#29550 = CARTESIAN_POINT ( 'NONE',  ( 14.43821800945587341, -5.195472089885680766, 34.18748526763464923 ) ) ;
#29551 = CARTESIAN_POINT ( 'NONE',  ( 11.60452988946397923, -5.557115091759786019, 34.35708131394839882 ) ) ;
#29552 = CARTESIAN_POINT ( 'NONE',  ( -8.834501215191544077, -11.48612834413959582, 32.76840700105983473 ) ) ;
#29553 = LINE ( 'NONE', #50240, #58538 ) ;
#29554 = VECTOR ( 'NONE', #24804, 1000.000000000000000 ) ;
#29555 = CARTESIAN_POINT ( 'NONE',  ( -3.164700879766792152, -4.786620604624113540, 33.94971097300155805 ) ) ;
#29556 = CARTESIAN_POINT ( 'NONE',  ( 19.00000000000000000, 16.99999999999999645, 23.75000000000000355 ) ) ;
#29557 = ADVANCED_FACE ( 'NONE', ( #63438 ), #70649, .F. ) ;
#29558 = DIRECTION ( 'NONE',  ( 0.000000000000000000, 0.000000000000000000, -1.000000000000000000 ) ) ;
#29559 = EDGE_CURVE ( 'NONE', #83441, #1531, #42743, .T. ) ;
#29560 = ORIENTED_EDGE ( 'NONE', *, *, #81328, .F. ) ;
#29561 = VERTEX_POINT ( 'NONE', #8951 ) ;
#29562 = ORIENTED_EDGE ( 'NONE', *, *, #18400, .F. ) ;
#29563 = CARTESIAN_POINT ( 'NONE',  ( -6.066082379360133281, -12.62096338111211580, 30.90682066428152197 ) ) ;
#29564 = CARTESIAN_POINT ( 'NONE',  ( 4.153846153846032507, -8.613356846316285953, 34.62446782046622218 ) ) ;
#29565 = LINE ( 'NONE', #44379, #64763 ) ;
#29566 = CARTESIAN_POINT ( 'NONE',  ( -6.223484943723947893, -3.236172620538810385, 32.36188796281390267 ) ) ;
#29567 = CARTESIAN_POINT ( 'NONE',  ( 9.692307692307695177, -3.050289026998446396, 32.03036669348365706 ) ) ;
#29568 = EDGE_CURVE ( 'NONE', #33767, #19270, #12408, .T. ) ;
#29569 = B_SPLINE_CURVE_WITH_KNOTS ( 'NONE', 3,
 ( #53243, #32987, #46497, #79844, #51441, #3725, #51899, #79398, #45154, #40199 ),
 .UNSPECIFIED., .F., .F.,
 ( 4, 2, 2, 2, 4 ),
 ( 0.0007817359430256297891, 0.0009771253907249958896, 0.001172514838424361990, 0.001367904286123728091, 0.001563293733823094191 ),
 .UNSPECIFIED. ) ;
#29570 = AXIS2_PLACEMENT_3D ( 'NONE', #50769, #21993, #8929 ) ;
#29571 = VERTEX_POINT ( 'NONE', #76522 ) ;
#29572 = EDGE_CURVE ( 'NONE', #43471, #70228, #14827, .T. ) ;
#29573 = CARTESIAN_POINT ( 'NONE',  ( -17.93383085903734298, -7.250054483168842268, 34.74374881642865631 ) ) ;
#29574 = ORIENTED_EDGE ( 'NONE', *, *, #20027, .F. ) ;
#29575 = B_SPLINE_CURVE_WITH_KNOTS ( 'NONE', 3,
 ( #1372, #82915, #56320, #48666, #49116, #28861, #77475, #76595, #14448, #15785 ),
 .UNSPECIFIED., .F., .F.,
 ( 4, 2, 2, 2, 4 ),
 ( 0.000000000000000000, 0.0001954311564186863052, 0.0003908623128373726104, 0.0005862934692560589156, 0.0007817246256747452209 ),
 .UNSPECIFIED. ) ;
#29576 = EDGE_LOOP ( 'NONE', ( #14374, #12486 ) ) ;
#29578 = ORIENTED_EDGE ( 'NONE', *, *, #59810, .T. ) ;
#29577 = CARTESIAN_POINT ( 'NONE',  ( -15.23076923076935074, -12.27809138561165270, 31.22303859784587132 ) ) ;
#29579 = CARTESIAN_POINT ( 'NONE',  ( 24.00000000000000000, 9.000000000000024869, 29.25000000000000000 ) ) ;
#29580 = DIRECTION ( 'NONE',  ( 1.000000000000000000, 0.000000000000000000, 0.000000000000000000 ) ) ;
#29581 = CARTESIAN_POINT ( 'NONE',  ( 3.930361210122205406, -4.386631170607603991, 33.66268669641500111 ) ) ;
#29582 = CARTESIAN_POINT ( 'NONE',  ( -16.02332071561251325, -5.915461855592777596, 34.75538340440931506 ) ) ;
#29583 = EDGE_LOOP ( 'NONE', ( #50383, #45715, #60543, #35150 ) ) ;
#29584 = ORIENTED_EDGE ( 'NONE', *, *, #77311, .T. ) ;
#29585 = CARTESIAN_POINT ( 'NONE',  ( -1.929879867024197893E-14, -3.750000000000000000, 20.40625000000000000 ) ) ;
#29586 = ORIENTED_EDGE ( 'NONE', *, *, #88513, .T. ) ;
#29587 = DIRECTION ( 'NONE',  ( 0.000000000000000000, 0.000000000000000000, -1.000000000000000000 ) ) ;
#29589 = ORIENTED_EDGE ( 'NONE', *, *, #76670, .F. ) ;
#29588 = CARTESIAN_POINT ( 'NONE',  ( 1.384615384615265343, -8.613356846316285953, 34.62446782046622218 ) ) ;
#29590 = DIRECTION ( 'NONE',  ( 0.000000000000000000, 0.9848077530122072432, -0.1736481776669354937 ) ) ;
#29591 = PLANE ( 'NONE',  #12967 ) ;
#29592 = AXIS2_PLACEMENT_3D ( 'NONE', #61073, #26851, #60180 ) ;
#29593 = CARTESIAN_POINT ( 'NONE',  ( -0.3962833220256229416, -9.528491918058460186, 34.59228464037085615 ) ) ;
#29594 = ORIENTED_EDGE ( 'NONE', *, *, #64006, .T. ) ;
#29595 = CARTESIAN_POINT ( 'NONE',  ( -11.28851602011339672, -5.057305518903948638, 34.11320923018887896 ) ) ;
#29596 = CARTESIAN_POINT ( 'NONE',  ( 15.23076923076910916, -2.657715359629662544, 31.77849191805970364 ) ) ;
#29597 = EDGE_LOOP ( 'NONE', ( #846, #1966, #27323, #81565 ) ) ;
#29598 = FACE_BOUND ( 'NONE', #86666, .T. ) ;
#29599 = CARTESIAN_POINT ( 'NONE',  ( -11.78848476268299628, -11.56360843649121684, 33.07473185843129926 ) ) ;
#29600 = CARTESIAN_POINT ( 'NONE',  ( 10.86543892702293412, -9.148310452688876993, 34.47095581063188519 ) ) ;
#29601 = DIRECTION ( 'NONE',  ( 0.000000000000000000, 0.000000000000000000, -1.000000000000000000 ) ) ;
#29603 = CARTESIAN_POINT ( 'NONE',  ( -10.61538461538461320, -5.471508081941601098, 34.59228464037088457 ) ) ;
#29602 = CARTESIAN_POINT ( 'NONE',  ( 7.976944287120795174, -10.70102852606553157, 33.91149625220312913 ) ) ;
#29604 = DIRECTION ( 'NONE',  ( -1.000000000000000000, 0.000000000000000000, 0.000000000000000000 ) ) ;
#29605 = CYLINDRICAL_SURFACE ( 'NONE', #60658, 0.2500000000000008882 ) ;
#29606 = EDGE_LOOP ( 'NONE', ( #13113, #56057 ) ) ;
#29607 = B_SPLINE_CURVE_WITH_KNOTS ( 'NONE', 3,
 ( #22841, #70594, #85438, #51173, #3006, #77788, #28731, #29616, #35931, #8900 ),
 .UNSPECIFIED., .F., .F.,
 ( 4, 2, 2, 2, 4 ),
 ( 0.0007817359430256221996, 0.0009771253907249863487, 0.001172514838424350498, 0.001367904286123714647, 0.001563293733823078796 ),
 .UNSPECIFIED. ) ;
#29609 = EDGE_CURVE ( 'NONE', #18998, #76633, #22895, .T. ) ;
#29608 = DIRECTION ( 'NONE',  ( -0.000000000000000000, -0.7660444431189791237, -0.6427876096865379196 ) ) ;
#29610 = VECTOR ( 'NONE', #84321, 1000.000000000000114 ) ;
#29611 = CARTESIAN_POINT ( 'NONE',  ( -16.94639763868943660, -6.808710257144159783, 34.95449254468098843 ) ) ;
#29612 = ORIENTED_EDGE ( 'NONE', *, *, #2045, .F. ) ;
#29613 = EDGE_CURVE ( 'NONE', #82495, #81637, #39329, .T. ) ;
#29614 = DIRECTION ( 'NONE',  ( 1.000000000000000000, 0.000000000000000000, 0.000000000000000000 ) ) ;
#29615 = CARTESIAN_POINT ( 'NONE',  ( -3.512820512820514995, -11.50000000000000000, 29.75000000000000355 ) ) ;
#29616 = CARTESIAN_POINT ( 'NONE',  ( -16.02305434602136813, -10.54018710029568595, 33.71981072465678864 ) ) ;
#29617 = CARTESIAN_POINT ( 'NONE',  ( 18.00000000000000000, -9.819645486525091727, 36.12317359536749706 ) ) ;
#29618 = CARTESIAN_POINT ( 'NONE',  ( 8.069166690247241647, -6.460100341425561332, 34.89618726649961644 ) ) ;
#29619 = FACE_OUTER_BOUND ( 'NONE', #51808, .T. ) ;
#29620 = FACE_BOUND ( 'NONE', #38030, .T. ) ;
#29622 = FACE_OUTER_BOUND ( 'NONE', #84432, .T. ) ;
#29621 = CARTESIAN_POINT ( 'NONE',  ( -1.384615384615506484, -6.835583212225970762, 34.95778746994575670 ) ) ;
#29623 = PLANE ( 'NONE',  #71306 ) ;
#29625 = CARTESIAN_POINT ( 'NONE',  ( 6.988332494352946789, -12.46129190930001052, 30.37095296980870174 ) ) ;
#29624 = LINE ( 'NONE', #57081, #40125 ) ;
#29626 = EDGE_CURVE ( 'NONE', #47623, #79680, #15266, .T. ) ;
#29627 = CARTESIAN_POINT ( 'NONE',  ( 1.319365452841301689, -2.255955759149247619, 30.00000000000013856 ) ) ;
#29628 = CARTESIAN_POINT ( 'NONE',  ( -1.614399933863656544, -3.775308065498769405, 22.57625670625848713 ) ) ;
#29629 = ORIENTED_EDGE ( 'NONE', *, *, #39221, .F. ) ;
#29630 = VERTEX_POINT ( 'NONE', #37291 ) ;
#29631 = DIRECTION ( 'NONE',  ( 1.000000000000000000, 0.000000000000000000, 0.000000000000000000 ) ) ;
#29632 = CARTESIAN_POINT ( 'NONE',  ( -14.30769230769242739, -6.879047030192662504, 34.71129190930017927 ) ) ;
#29633 = CARTESIAN_POINT ( 'NONE',  ( -0.5276208408985961773, -3.322132147404559976, 32.92929555188719348 ) ) ;
#29634 = CARTESIAN_POINT ( 'NONE',  ( 8.519230769230757616, -2.249999999999999556, 29.81609741502488120 ) ) ;
#29635 = CARTESIAN_POINT ( 'NONE',  ( -4.153846153846274980, -3.083524468854526912, 32.58852847137268327 ) ) ;
#29636 = CARTESIAN_POINT ( 'NONE',  ( -3.749999999999996447, -7.561099074964554134, 23.59188170625849068 ) ) ;
#29637 = MANIFOLD_SOLID_BREP ( 'Cavity2', #80432 ) ;
#29638 = CARTESIAN_POINT ( 'NONE',  ( -8.546219417617921366, -2.758310577978207778, 31.33698337089302299 ) ) ;
#29639 = CARTESIAN_POINT ( 'NONE',  ( 10.61538461538461675, -1.242168528481310874, 33.36296068462461051 ) ) ;
#29640 = EDGE_CURVE ( 'NONE', #32683, #10626, #79085, .T. ) ;
#29641 = CARTESIAN_POINT ( 'NONE',  ( 24.00000000000000000, 9.000000000000024869, 29.25000000000000000 ) ) ;
#29642 = DIRECTION ( 'NONE',  ( 0.000000000000000000, 0.4999999999999985567, 0.8660254037844395958 ) ) ;
#29643 = CARTESIAN_POINT ( 'NONE',  ( -3.360917200500926683, -4.299443229763728169, 33.91186481527756058 ) ) ;
#29644 = DIRECTION ( 'NONE',  ( 0.000000000000000000, 0.8660254037844377084, 0.5000000000000015543 ) ) ;
#29645 = CARTESIAN_POINT ( 'NONE',  ( -11.53846153846153655, -5.180354513474913603, 36.12317359536750416 ) ) ;
#29646 = CARTESIAN_POINT ( 'NONE',  ( 7.846153846153725020, -6.879047030192662504, 34.71129190930017927 ) ) ;
#29647 = EDGE_LOOP ( 'NONE', ( #57627, #67068 ) ) ;
#29648 = LINE ( 'NONE', #86383, #2421 ) ;
#29649 = CARTESIAN_POINT ( 'NONE',  ( -5.999999999999998224, -2.486705287966279876, 31.30864560766543647 ) ) ;
#29650 = CARTESIAN_POINT ( 'NONE',  ( 0.06109907496451789238, -4.749999999999998224, 24.40811829374151642 ) ) ;
#29651 = ADVANCED_FACE ( 'NONE', ( #11160 ), #80520, .F. ) ;
#29652 = CARTESIAN_POINT ( 'NONE',  ( -2.531177232256637932, -4.988325925672468131, 34.36044203135681130 ) ) ;
#29653 = FACE_OUTER_BOUND ( 'NONE', #32486, .T. ) ;
#29654 = ORIENTED_EDGE ( 'NONE', *, *, #74036, .F. ) ;
#29655 = CARTESIAN_POINT ( 'NONE',  ( -6.989159302437059296, -2.833524468853757305, 32.15551576947924417 ) ) ;
#29657 = EDGE_LOOP ( 'NONE', ( #33601, #67875 ) ) ;
#29656 = CARTESIAN_POINT ( 'NONE',  ( 6.923076923076924238, -1.367168528481310208, 33.57946703557072254 ) ) ;
#29658 = CARTESIAN_POINT ( 'NONE',  ( 8.068933387422253745, -3.755027918224369099, 33.06320215134714857 ) ) ;
#29659 = EDGE_CURVE ( 'NONE', #42538, #37962, #32832, .T. ) ;
#29660 = CARTESIAN_POINT ( 'NONE',  ( -13.13456107297706588, -9.943054286541403997, 34.11300777759954883 ) ) ;
#29661 = ORIENTED_EDGE ( 'NONE', *, *, #79507, .T. ) ;
#29662 = CARTESIAN_POINT ( 'NONE',  ( -5.299849294439222369, -11.24512374952581872, 33.06303171183252942 ) ) ;
#29663 = CARTESIAN_POINT ( 'NONE',  ( 8.835299120233207404, -4.786620604624113540, 33.94971097300155805 ) ) ;
#29664 = ORIENTED_EDGE ( 'NONE', *, *, #27426, .T. ) ;
#29665 = DIRECTION ( 'NONE',  ( 0.000000000000000000, 0.000000000000000000, -1.000000000000000000 ) ) ;
#29666 = SURFACE_SIDE_STYLE ('',( #78277 ) ) ;
#29667 = VECTOR ( 'NONE', #17212, 1000.000000000000000 ) ;
#29668 = EDGE_CURVE ( 'NONE', #55756, #74977, #79176, .T. ) ;
#29669 = CARTESIAN_POINT ( 'NONE',  ( -17.75000000000000355, -12.50000000000000000, 29.75000000000000355 ) ) ;
#29670 = EDGE_LOOP ( 'NONE', ( #47206, #2065, #39206, #61753 ) ) ;
#29671 = ORIENTED_EDGE ( 'NONE', *, *, #74816, .T. ) ;
#29672 = B_SPLINE_CURVE_WITH_KNOTS ( 'NONE', 3,
 ( #16447, #64172, #30841, #23640, #2042, #56982, #37155, #64614, #46477, #50213 ),
 .UNSPECIFIED., .F., .F.,
 ( 4, 2, 2, 2, 4 ),
 ( 0.000000000000000000, 0.0001954311564186861697, 0.0003908623128373723394, 0.0005862934692560584820, 0.0007817246256747446788 ),
 .UNSPECIFIED. ) ;
#29674 = ORIENTED_EDGE ( 'NONE', *, *, #8433, .T. ) ;
#29673 = B_SPLINE_CURVE_WITH_KNOTS ( 'NONE', 3,
 ( #73726, #19213, #80023, #67840, #6139, #39497, #25961, #46678, #74156, #39938 ),
 .UNSPECIFIED., .F., .F.,
 ( 4, 2, 2, 2, 4 ),
 ( 0.0007817246256747507503, 0.0009771112852218959231, 0.001172497944769040987, 0.001367884604316186052, 0.001563271263863331116 ),
 .UNSPECIFIED. ) ;
#29675 = CARTESIAN_POINT ( 'NONE',  ( 3.361294669002876212, -2.372941743896878286, 30.88044141588254377 ) ) ;
#29676 = CARTESIAN_POINT ( 'NONE',  ( 2.530705151785704210, -11.43677907613345113, 33.22367315496201456 ) ) ;
#29677 = CARTESIAN_POINT ( 'NONE',  ( -3.230769230769229949, -8.164416787775445883, 34.95778746994557906 ) ) ;
#29678 = EDGE_CURVE ( 'NONE', #35531, #61773, #17481, .T. ) ;
#29679 = CARTESIAN_POINT ( 'NONE',  ( 20.00000000000000000, -4.000000000000000000, 29.75000000000000355 ) ) ;
#29680 = EDGE_CURVE ( 'NONE', #2558, #24114, #28531, .T. ) ;
#29681 = EDGE_CURVE ( 'NONE', #44409, #59335, #4401, .T. ) ;
#29682 = VERTEX_POINT ( 'NONE', #73310 ) ;
#29683 = ORIENTED_EDGE ( 'NONE', *, *, #55445, .T. ) ;
#29685 = ORIENTED_EDGE ( 'NONE', *, *, #1808, .F. ) ;
#29684 = CARTESIAN_POINT ( 'NONE',  ( 4.376625822824220080, -8.540255544307065350, 34.89611431652622286 ) ) ;
#29686 = EDGE_CURVE ( 'NONE', #27365, #38356, #11613, .T. ) ;
#29687 = EDGE_CURVE ( 'NONE', #84823, #35118, #4859, .T. ) ;
#29688 = CARTESIAN_POINT ( 'NONE',  ( 12.68455130563185840, -11.43677907613344757, 33.22367315496202167 ) ) ;
#29689 = ORIENTED_EDGE ( 'NONE', *, *, #57052, .F. ) ;
#29690 = VECTOR ( 'NONE', #24666, 1000.000000000000227 ) ;
#29691 = CARTESIAN_POINT ( 'NONE',  ( -17.75005448165186195, -3.202959910592339199, 32.30730279482229150 ) ) ;
#29692 = CARTESIAN_POINT ( 'NONE',  ( 5.142991427925513115, -3.513871655860379306, 32.76840700105978499 ) ) ;
#29693 = ORIENTED_EDGE ( 'NONE', *, *, #23919, .F. ) ;
#29694 = AXIS2_PLACEMENT_3D ( 'NONE', #73983, #33436, #81185 ) ;
#29695 = EDGE_LOOP ( 'NONE', ( #55587, #76646 ) ) ;
#29697 = ORIENTED_EDGE ( 'NONE', *, *, #29668, .F. ) ;
#29696 = CYLINDRICAL_SURFACE ( 'NONE', #8537, 4.000000000000000000 ) ;
#29698 = CARTESIAN_POINT ( 'NONE',  ( -0.4615384615385826339, -10.90142922262034020, 33.41473453929536674 ) ) ;
#29699 = CARTESIAN_POINT ( 'NONE',  ( 14.24242230713598900, -5.941354392334499579, 34.76329471203369792 ) ) ;
#29700 = VERTEX_POINT ( 'NONE', #87287 ) ;
#29701 = AXIS2_PLACEMENT_3D ( 'NONE', #88256, #26533, #66627 ) ;
#29702 = CARTESIAN_POINT ( 'NONE',  ( 18.00000000000000000, -10.51840700105979565, 33.73612834413961536 ) ) ;
#29703 = B_SPLINE_CURVE_WITH_KNOTS ( 'NONE', 3,
 ( #957, #62212, #55455, #28429, #43276, #21223, #35186, #70750, #49588, #8612 ),
 .UNSPECIFIED., .F., .F.,
 ( 4, 2, 2, 2, 4 ),
 ( 0.000000000000000000, 0.0001954339857564054957, 0.0003908679715128109914, 0.0005863019572692164871, 0.0007817359430256219828 ),
 .UNSPECIFIED. ) ;
#29704 = CARTESIAN_POINT ( 'NONE',  ( 5.207714884747862705, -11.18335022499818621, 33.13157742990016885 ) ) ;
#29705 = CARTESIAN_POINT ( 'NONE',  ( 17.74997677577854205, -12.45566812827425096, 31.48439005359158926 ) ) ;
#29706 = FACE_BOUND ( 'NONE', #15965, .T. ) ;
#29707 = CARTESIAN_POINT ( 'NONE',  ( -11.76194648218548267, -2.599994579823203367, 30.74605699353653776 ) ) ;
#29708 = CARTESIAN_POINT ( 'NONE',  ( -18.00000000000012079, -12.27809138561165270, 31.22303859784587132 ) ) ;
#29709 = CARTESIAN_POINT ( 'NONE',  ( 14.30769230769218758, -12.27809138561165270, 31.22303859784587132 ) ) ;
#29711 = DIRECTION ( 'NONE',  ( -0.000000000000000000, 1.000000000000000000, -0.000000000000000000 ) ) ;
#29710 = CARTESIAN_POINT ( 'NONE',  ( 12.46153846153833911, -3.643525952248795718, 33.31231777344771672 ) ) ;
#29712 = DIRECTION ( 'NONE',  ( 0.000000000000000000, 0.000000000000000000, -1.000000000000000000 ) ) ;
#29713 = DIRECTION ( 'NONE',  ( -0.000000000000000000, 0.7660444431189791237, -0.6427876096865379196 ) ) ;
#29714 = ORIENTED_EDGE ( 'NONE', *, *, #80070, .F. ) ;
#29715 = CARTESIAN_POINT ( 'NONE',  ( 14.55769230769224620, -7.565270445406050648, 34.75000000000000000 ) ) ;
#29716 = ORIENTED_EDGE ( 'NONE', *, *, #21331, .F. ) ;
#29717 = ORIENTED_EDGE ( 'NONE', *, *, #62921, .F. ) ;
#29719 = CARTESIAN_POINT ( 'NONE',  ( -10.61538461538473577, -2.379036618888197729, 30.90682066428292885 ) ) ;
#29718 = CARTESIAN_POINT ( 'NONE',  ( -23.00000000000000000, -10.75000000000000000, 29.75000000000000355 ) ) ;
#29720 = CARTESIAN_POINT ( 'NONE',  ( 13.16168842570853670, -11.43668979543634734, 33.22377378376089752 ) ) ;
#29721 = FACE_OUTER_BOUND ( 'NONE', #30565, .T. ) ;
#29722 = CARTESIAN_POINT ( 'NONE',  ( 1.634669804528838588, -10.82426656108011720, 33.81400080652039009 ) ) ;
#29723 = CARTESIAN_POINT ( 'NONE',  ( 1.384615384615265343, -11.94971097300221174, 32.03036669348237098 ) ) ;
#29724 = ORIENTED_EDGE ( 'NONE', *, *, #73427, .T. ) ;
#29725 = AXIS2_PLACEMENT_3D ( 'NONE', #51426, #78928, #17228 ) ;
#29726 = CARTESIAN_POINT ( 'NONE',  ( -10.61538461538461320, -12.34228464037088635, 31.77849191805839268 ) ) ;
#29727 = CARTESIAN_POINT ( 'NONE',  ( 14.08420738312797837, -12.69144148231606017, 30.53333754910549303 ) ) ;
#29728 = CARTESIAN_POINT ( 'NONE',  ( -12.59168643127016196, -11.66186481527757302, 32.95055677023626117 ) ) ;
#29729 = CARTESIAN_POINT ( 'NONE',  ( -19.00000000000000000, -13.25000000000000533, 22.25000000000000000 ) ) ;
#29730 = CARTESIAN_POINT ( 'NONE',  ( -15.48076923076922995, -2.499999999999998668, 29.75000000000000355 ) ) ;
#29731 = CARTESIAN_POINT ( 'NONE',  ( -2.651650429449535551, -10.15165042944956753, 14.93750000000000000 ) ) ;
#29732 = ORIENTED_EDGE ( 'NONE', *, *, #4221, .T. ) ;
#29733 = ORIENTED_EDGE ( 'NONE', *, *, #76726, .F. ) ;
#29734 = CARTESIAN_POINT ( 'NONE',  ( -7.623141002060451754, -11.98016756924215009, 32.48728574198911190 ) ) ;
#29735 = ORIENTED_EDGE ( 'NONE', *, *, #49622, .T. ) ;
#29736 = CIRCLE ( 'NONE', #41241, 0.2500000000000002220 ) ;
#29737 = CARTESIAN_POINT ( 'NONE',  ( -17.93485422066803281, -7.750023238201980469, 34.74374492549440419 ) ) ;
#29738 = CARTESIAN_POINT ( 'NONE',  ( 17.86930939688969033, -11.37499894934982514, 33.29245874905763003 ) ) ;
#29739 = CARTESIAN_POINT ( 'NONE',  ( 3.230769230769231726, -6.343179335718451384, 34.87096338111211935 ) ) ;
#29740 = CARTESIAN_POINT ( 'NONE',  ( 2.307692307692186251, -10.33852847137269571, 34.16647553114546554 ) ) ;
#29741 = CARTESIAN_POINT ( 'NONE',  ( -3.750000000000008438, -5.946699141100917352, 18.92187500000000355 ) ) ;
#29743 = CARTESIAN_POINT ( 'NONE',  ( 0.5923289025054114809, -9.084667340241226796, 34.75534355489798344 ) ) ;
#29742 = B_SPLINE_CURVE_WITH_KNOTS ( 'NONE', 3,
 ( #66908, #87643, #53385, #5204, #11523, #67355, #33121, #5648, #60138, #39005 ),
 .UNSPECIFIED., .F., .F.,
 ( 4, 2, 2, 2, 4 ),
 ( 0.000000000000000000, 0.0001954311564186865763, 0.0003908623128373731525, 0.0005862934692560596746, 0.0007817246256747463051 ),
 .UNSPECIFIED. ) ;
#29744 = ORIENTED_EDGE ( 'NONE', *, *, #77988, .F. ) ;
#29745 = DIRECTION ( 'NONE',  ( 0.000000000000000000, 0.000000000000000000, -1.000000000000000000 ) ) ;
#29747 = EDGE_LOOP ( 'NONE', ( #64865, #83275 ) ) ;
#29746 = CARTESIAN_POINT ( 'NONE',  ( -2.307692307692305711, -10.51840700105979565, 33.73612834413961536 ) ) ;
#29748 = CARTESIAN_POINT ( 'NONE',  ( 3.100621261037533216, -12.50552854090298993, 31.33409797877408920 ) ) ;
#29749 = CARTESIAN_POINT ( 'NONE',  ( 17.14217864819910275, -11.48612834413965977, 32.76840700105972815 ) ) ;
#29750 = CARTESIAN_POINT ( 'NONE',  ( 11.31497659473759043, -4.386631170607603991, 33.66268669641500111 ) ) ;
#29751 = CARTESIAN_POINT ( 'NONE',  ( -2.176901866725357682, -2.295524264805589354, 30.44142389570982488 ) ) ;
#29752 = DIRECTION ( 'NONE',  ( -0.000000000000000000, 0.7660444431189791237, -0.6427876096865379196 ) ) ;
#29753 = CARTESIAN_POINT ( 'NONE',  ( -11.40793610022789828, -3.068774925481847493, 32.56582465632704526 ) ) ;
#29754 = CARTESIAN_POINT ( 'NONE',  ( -1.614399933863613468, -11.22469193450124969, 15.11124329374151287 ) ) ;
#29755 = ORIENTED_EDGE ( 'NONE', *, *, #49622, .F. ) ;
#29756 = CARTESIAN_POINT ( 'NONE',  ( -17.07692307692307665, -10.51840700105979565, 33.73612834413961536 ) ) ;
#29757 = CARTESIAN_POINT ( 'NONE',  ( -13.63459211555773720, -9.148715823498378086, 34.47080413974185120 ) ) ;
#29758 = CARTESIAN_POINT ( 'NONE',  ( -1.944543648263014957, -5.555456351737005249, 24.00000000000000000 ) ) ;
#29759 = EDGE_CURVE ( 'NONE', #12856, #20277, #83414, .T. ) ;
#29760 = CARTESIAN_POINT ( 'NONE',  ( 0.2115617305961059735, -3.627789207965226748, 32.91389620160131102 ) ) ;
#29762 = CARTESIAN_POINT ( 'NONE',  ( 2.372947447205147053, -12.16647553114626490, 32.15551576947920864 ) ) ;
#29761 = AXIS2_PLACEMENT_3D ( 'NONE', #52727, #81113, #51827 ) ;
#29763 = ORIENTED_EDGE ( 'NONE', *, *, #8168, .T. ) ;
#29764 = CARTESIAN_POINT ( 'NONE',  ( 7.912221179503920787, -11.91647553114624358, 32.58852847137148245 ) ) ;
#29765 = CARTESIAN_POINT ( 'NONE',  ( -16.15384615384627409, -12.27809138561165270, 31.22303859784587132 ) ) ;
#29766 = VERTEX_POINT ( 'NONE', #61117 ) ;
#29767 = AXIS2_PLACEMENT_3D ( 'NONE', #41486, #62629, #77049 ) ;
#29768 = CARTESIAN_POINT ( 'NONE',  ( -18.00000000000000000, -4.661471528628506000, 34.16647553114623292 ) ) ;
#29769 = VERTEX_POINT ( 'NONE', #26457 ) ;
#29770 = CARTESIAN_POINT ( 'NONE',  ( 17.86985279056177944, -6.852621066184266141, 34.70813303252209181 ) ) ;
#29771 = CARTESIAN_POINT ( 'NONE',  ( 16.85405765471943695, -2.501496062324911840, 29.88072118266895671 ) ) ;
#29772 = EDGE_CURVE ( 'NONE', #23619, #42406, #34537, .T. ) ;
#29773 = CIRCLE ( 'NONE', #70077, 0.2500000000000002220 ) ;
#29774 = DIRECTION ( 'NONE',  ( 0.000000000000000000, 0.000000000000000000, 1.000000000000000000 ) ) ;
#29775 = CARTESIAN_POINT ( 'NONE',  ( -13.38461538461550759, -12.70778746994576025, 30.41441678777401236 ) ) ;
#29776 = ORIENTED_EDGE ( 'NONE', *, *, #83633, .T. ) ;
#29777 = CARTESIAN_POINT ( 'NONE',  ( -19.00000000000000000, 0.7500000000000052180, 31.75000000000000000 ) ) ;
#29778 = ORIENTED_EDGE ( 'NONE', *, *, #34233, .T. ) ;
#29779 = CARTESIAN_POINT ( 'NONE',  ( -10.61538461538473577, -12.16647553114689728, 32.15551576947799362 ) ) ;
#29780 = CARTESIAN_POINT ( 'NONE',  ( 5.777121317571356052, -7.630691491037286056, 34.74850469731152458 ) ) ;
#29781 = ORIENTED_EDGE ( 'NONE', *, *, #73173, .F. ) ;
#29782 = B_SPLINE_CURVE_WITH_KNOTS ( 'NONE', 3,
 ( #7472, #62390, #83587, #14221, #40814, #1149, #34047, #54757, #82244, #28629 ),
 .UNSPECIFIED., .F., .F.,
 ( 4, 2, 2, 2, 4 ),
 ( 0.000000000000000000, 0.0001954339857564081520, 0.0003908679715128163040, 0.0005863019572692244018, 0.0007817359430256326080 ),
 .UNSPECIFIED. ) ;
#29783 = B_SPLINE_CURVE_WITH_KNOTS ( 'NONE', 3,
 ( #3622, #73433, #3180, #17139, #11732, #86514, #39209, #66669, #24333, #44150 ),
 .UNSPECIFIED., .F., .F.,
 ( 4, 2, 2, 2, 4 ),
 ( 0.0007817359430256334753, 0.0009771253907250058643, 0.001172514838424371098, 0.001367904286123736764, 0.001563293733823101998 ),
 .UNSPECIFIED. ) ;
#29784 = CARTESIAN_POINT ( 'NONE',  ( -6.000000000000121680, -11.06231777344772027, 33.60647404775119895 ) ) ;
#29785 = CARTESIAN_POINT ( 'NONE',  ( -14.37377571864818648, -10.51840700105979387, 33.73612834413961536 ) ) ;
#29786 = CARTESIAN_POINT ( 'NONE',  ( -11.66860874789975888, -2.882441371585227508, 31.66841991370172238 ) ) ;
#29787 = CARTESIAN_POINT ( 'NONE',  ( 2.307692307692309264, -1.466349020453238561, 30.81389545987213907 ) ) ;
#29788 = CARTESIAN_POINT ( 'NONE',  ( -4.087778820496078325, -3.937682226553329556, 33.60647404775216529 ) ) ;
#29789 = VECTOR ( 'NONE', #56894, 1000.000000000000000 ) ;
#29790 = EDGE_CURVE ( 'NONE', #38938, #30718, #614, .T. ) ;
#29791 = EDGE_CURVE ( 'NONE', #60435, #81436, #54360, .T. ) ;
#29792 = ORIENTED_EDGE ( 'NONE', *, *, #55076, .F. ) ;
#29793 = VERTEX_POINT ( 'NONE', #40857 ) ;
#29794 = FACE_BOUND ( 'NONE', #80644, .T. ) ;
#29795 = EDGE_LOOP ( 'NONE', ( #34394, #65907, #28993, #15598 ) ) ;
#29796 = CARTESIAN_POINT ( 'NONE',  ( 14.98079249982687777, -12.41269422305637171, 30.68257228309993323 ) ) ;
#29797 = AXIS2_PLACEMENT_3D ( 'NONE', #7417, #21810, #83528 ) ;
#29798 = EDGE_CURVE ( 'NONE', #16317, #28684, #13376, .T. ) ;
#29799 = CARTESIAN_POINT ( 'NONE',  ( -1.634615384615383027, -7.500000000000001776, 35.04278698407183867 ) ) ;
#29800 = AXIS2_PLACEMENT_3D ( 'NONE', #77405, #36855, #64316 ) ;
#29801 = LINE ( 'NONE', #28925, #6145 ) ;
#29802 = CARTESIAN_POINT ( 'NONE',  ( -2.242437168179467033, -10.33852847137154107, 34.16647553114620450 ) ) ;
#29803 = EDGE_LOOP ( 'NONE', ( #33002, #15175, #41606, #14751 ) ) ;
#29804 = EDGE_LOOP ( 'NONE', ( #76328, #75524 ) ) ;
#29805 = CARTESIAN_POINT ( 'NONE',  ( -1.634592115557738312, -11.79746400365624659, 32.30657167506340954 ) ) ;
#29806 = ORIENTED_EDGE ( 'NONE', *, *, #40551, .T. ) ;
#29807 = CARTESIAN_POINT ( 'NONE',  ( 16.08776274289027342, -9.780366693483667717, 34.19971097300155805 ) ) ;
#29808 = CARTESIAN_POINT ( 'NONE',  ( 3.164685819813350953, -2.721908614388772296, 31.22303859784724622 ) ) ;
#29809 = B_SPLINE_CURVE_WITH_KNOTS ( 'NONE', 3,
 ( #4239, #45218, #11899, #66386, #46119, #72695, #65034, #3791, #3345, #37571 ),
 .UNSPECIFIED., .F., .F.,
 ( 4, 2, 2, 2, 4 ),
 ( 0.000000000000000000, 0.0001954311564186869557, 0.0003908623128373739115, 0.0005862934692560608672, 0.0007817246256747478229 ),
 .UNSPECIFIED. ) ;
#29810 = CARTESIAN_POINT ( 'NONE',  ( 14.24242230713599078, -12.16647553114622049, 32.15551576947930812 ) ) ;
#29811 = FACE_BOUND ( 'NONE', #11207, .T. ) ;
#29812 = EDGE_LOOP ( 'NONE', ( #20705, #11890, #83210, #20176 ) ) ;
#29813 = CARTESIAN_POINT ( 'NONE',  ( -8.769230769230892619, -4.320704448113951379, 33.92786785259630022 ) ) ;
#29814 = CARTESIAN_POINT ( 'NONE',  ( 0.6845498131513104711, -11.76359900205217457, 32.36225158514719880 ) ) ;
#29815 = VECTOR ( 'NONE', #55727, 999.9999999999998863 ) ;
#29816 = CYLINDRICAL_SURFACE ( 'NONE', #9222, 0.2500000000000002220 ) ;
#29817 = DIRECTION ( 'NONE',  ( 0.000000000000000000, 0.000000000000000000, 1.000000000000000000 ) ) ;
#29818 = ORIENTED_EDGE ( 'NONE', *, *, #34363, .F. ) ;
#29819 = VERTEX_POINT ( 'NONE', #53920 ) ;
#29820 = ORIENTED_EDGE ( 'NONE', *, *, #36418, .T. ) ;
#29822 = CARTESIAN_POINT ( 'NONE',  ( 17.75000000000000000, -7.500000000000001776, 35.04278698407183867 ) ) ;
#29821 = CARTESIAN_POINT ( 'NONE',  ( 12.46153846153846168, -6.386643153685126251, 34.62446782046654192 ) ) ;
#29823 = CARTESIAN_POINT ( 'NONE',  ( -8.638440328263820689, -12.35292014791297710, 31.75344720912887198 ) ) ;
#29824 = CARTESIAN_POINT ( 'NONE',  ( 18.00000000000000000, -6.681629849574314051, 35.83090037661290239 ) ) ;
#29825 = DIRECTION ( 'NONE',  ( -1.000000000000000000, -0.000000000000000000, -0.000000000000000000 ) ) ;
#29826 = CARTESIAN_POINT ( 'NONE',  ( -15.48074597481782178, -3.436278759898153901, 33.07459398097509506 ) ) ;
#29827 = VERTEX_POINT ( 'NONE', #20138 ) ;
#29828 = CARTESIAN_POINT ( 'NONE',  ( -24.99999999999999645, 15.00000000000000355, 0.000000000000000000 ) ) ;
#29829 = CARTESIAN_POINT ( 'NONE',  ( -10.61538461538461320, -1.129524287112498415, 32.06866353760679544 ) ) ;
#29830 = CARTESIAN_POINT ( 'NONE',  ( 4.376625695114563008, -9.332535724633407526, 34.40230450496446224 ) ) ;
#29831 = CARTESIAN_POINT ( 'NONE',  ( 3.230769230769110045, -10.90142922262034020, 33.41473453929536674 ) ) ;
#29832 = ORIENTED_EDGE ( 'NONE', *, *, #34233, .F. ) ;
#29833 = CARTESIAN_POINT ( 'NONE',  ( 8.546303810323914618, -12.64616026154729411, 30.79003144601914244 ) ) ;
#29834 = ORIENTED_EDGE ( 'NONE', *, *, #33915, .F. ) ;
#29835 = FACE_BOUND ( 'NONE', #41529, .T. ) ;
#29836 = CARTESIAN_POINT ( 'NONE',  ( 5.011652630962299959, -6.026961402152685388, 34.52809138561120506 ) ) ;
#29837 = LINE ( 'NONE', #21296, #36265 ) ;
#29838 = CARTESIAN_POINT ( 'NONE',  ( 8.769230769230768274, -9.905515769479276145, 34.41647553114623292 ) ) ;
#29839 = ORIENTED_EDGE ( 'NONE', *, *, #5472, .T. ) ;
#29840 = CARTESIAN_POINT ( 'NONE',  ( 11.60371667797437567, -11.06231777344671130, 33.60647404775212976 ) ) ;
#29841 = CARTESIAN_POINT ( 'NONE',  ( -3.480745974817821775, -2.318417181685854533, 30.59732222474233865 ) ) ;
#29842 = CARTESIAN_POINT ( 'NONE',  ( 8.769230769230768274, -2.292212530054420494, 30.41441678777542634 ) ) ;
#29843 = CARTESIAN_POINT ( 'NONE',  ( 4.376858997939548246, -6.460100341425561332, 34.89618726649961644 ) ) ;
#29844 = ORIENTED_EDGE ( 'NONE', *, *, #54862, .T. ) ;
#29845 = ADVANCED_FACE ( 'NONE', ( #61555 ), #74199, .F. ) ;
#29846 = CYLINDRICAL_SURFACE ( 'NONE', #12864, 0.2500000000000012212 ) ;
#29847 = EDGE_LOOP ( 'NONE', ( #39405, #65015 ) ) ;
#29848 = B_SPLINE_CURVE_WITH_KNOTS ( 'NONE', 3,
 ( #38697, #58068, #59412, #17990, #44542, #4006, #10337, #23394, #65268, #85998 ),
 .UNSPECIFIED., .F., .F.,
 ( 4, 2, 2, 2, 4 ),
 ( 0.000000000000000000, 0.0001954311564186860884, 0.0003908623128373721767, 0.0005862934692560582651, 0.0007817246256747443535 ),
 .UNSPECIFIED. ) ;
#29850 = ORIENTED_EDGE ( 'NONE', *, *, #77727, .T. ) ;
#29849 = CARTESIAN_POINT ( 'NONE',  ( 13.38461538461538680, -12.10708131394839349, 31.69288490824020244 ) ) ;
#29851 = CARTESIAN_POINT ( 'NONE',  ( 9.561616225640133138, -3.530157926970578952, 32.79014554554150607 ) ) ;
#29852 = CARTESIAN_POINT ( 'NONE',  ( -6.673022611438609530, -11.79725096376909299, 32.30694842903960762 ) ) ;
#29853 = CARTESIAN_POINT ( 'NONE',  ( 7.596177102105253987, -10.06842814019191401, 34.32929386961144758 ) ) ;
#29854 = VECTOR ( 'NONE', #88343, 1000.000000000000227 ) ;
#29855 = CARTESIAN_POINT ( 'NONE',  ( -15.10072179551877802, -7.723484941389743952, 34.99544897038808955 ) ) ;
#29857 = DIRECTION ( 'NONE',  ( -0.000000000000000000, 0.5000000000000011102, -0.8660254037844381525 ) ) ;
#29856 = CARTESIAN_POINT ( 'NONE',  ( 0.4615384615383396616, -9.442884908241554243, 34.35708131394783038 ) ) ;
#29858 = CARTESIAN_POINT ( 'NONE',  ( -9.822455662039384805, -12.15440758774515473, 32.17923288041532004 ) ) ;
#29859 = CARTESIAN_POINT ( 'NONE',  ( 1.139087296526029469, -10.24999999999999467, 22.20312500000000000 ) ) ;
#29860 = ORIENTED_EDGE ( 'NONE', *, *, #73380, .F. ) ;
#29861 = AXIS2_PLACEMENT_3D ( 'NONE', #53171, #88769, #54508 ) ;
#29862 = DIRECTION ( 'NONE',  ( -0.000000000000000000, -0.8660254037844399289, -0.4999999999999980016 ) ) ;
#29863 = LINE ( 'NONE', #20547, #20818 ) ;
#29864 = VERTEX_POINT ( 'NONE', #12499 ) ;
#29865 = EDGE_CURVE ( 'NONE', #19590, #40270, #43741, .T. ) ;
#29866 = VERTEX_POINT ( 'NONE', #27777 ) ;
#29867 = ORIENTED_EDGE ( 'NONE', *, *, #59037, .T. ) ;
#29868 = CARTESIAN_POINT ( 'NONE',  ( 3.930919936330005360, -12.15238873228292071, 31.58232369045353849 ) ) ;
#29869 = CARTESIAN_POINT ( 'NONE',  ( -5.869208192175211281, -10.54018710029568595, 33.71981072465678864 ) ) ;
#29870 = EDGE_CURVE ( 'NONE', #79573, #65630, #68191, .T. ) ;
#29871 = CARTESIAN_POINT ( 'NONE',  ( -4.826977667545032880, -12.68172785388650681, 30.59649109432439573 ) ) ;
#29872 = FACE_OUTER_BOUND ( 'NONE', #76888, .T. ) ;
#29873 = CARTESIAN_POINT ( 'NONE',  ( 8.992010438208831502, -11.60474049983371003, 33.02348890104160262 ) ) ;
#29874 = CARTESIAN_POINT ( 'NONE',  ( -11.53846153846153655, -6.189225973068211317, 35.74407628777942847 ) ) ;
#29875 = CARTESIAN_POINT ( 'NONE',  ( 6.065144780719633921, -7.750023224968867197, 34.99404313364389907 ) ) ;
#29876 = ORIENTED_EDGE ( 'NONE', *, *, #49745, .T. ) ;
#29877 = B_SPLINE_CURVE_WITH_KNOTS ( 'NONE', 3,
 ( #13546, #73928, #80239, #19861, #61272, #39707, #12666, #67166, #5473, #52749 ),
 .UNSPECIFIED., .F., .F.,
 ( 4, 2, 2, 2, 4 ),
 ( 0.000000000000000000, 0.0001954311564186866034, 0.0003908623128373732067, 0.0005862934692560597830, 0.0007817246256747464135 ),
 .UNSPECIFIED. ) ;
#29878 = DIRECTION ( 'NONE',  ( 1.000000000000000000, 0.000000000000000000, 0.000000000000000000 ) ) ;
#29879 = CARTESIAN_POINT ( 'NONE',  ( -2.294871794871794712, -3.499999999999999556, 29.75000000000000355 ) ) ;
#29880 = B_SPLINE_CURVE_WITH_KNOTS ( 'NONE', 3,
 ( #107, #13179, #55047, #7754, #20814, #35214, #27132, #82087, #85183, #76652 ),
 .UNSPECIFIED., .F., .F.,
 ( 4, 2, 2, 2, 4 ),
 ( 0.0007817246256747459798, 0.0009771112852218896347, 0.001172497944769033181, 0.001367884604316176728, 0.001563271263863320491 ),
 .UNSPECIFIED. ) ;
#29881 = EDGE_CURVE ( 'NONE', #48748, #43361, #44609, .T. ) ;
#29882 = LINE ( 'NONE', #57343, #62767 ) ;
#29883 = DIRECTION ( 'NONE',  ( 0.000000000000000000, 0.9396926207859126468, -0.3420201433256571111 ) ) ;
#29884 = EDGE_LOOP ( 'NONE', ( #53317, #16408 ) ) ;
#29885 = LINE ( 'NONE', #57346, #6758 ) ;
#29886 = EDGE_CURVE ( 'NONE', #14701, #11434, #82736, .T. ) ;
#29887 = ORIENTED_EDGE ( 'NONE', *, *, #42090, .T. ) ;
#29888 = CARTESIAN_POINT ( 'NONE',  ( 8.769230769230645706, -3.083524468854526912, 32.58852847137268327 ) ) ;
#29889 = DIRECTION ( 'NONE',  ( 1.000000000000000000, 0.000000000000000000, 0.000000000000000000 ) ) ;
#29890 = FACE_OUTER_BOUND ( 'NONE', #79397, .T. ) ;
#29891 = VERTEX_POINT ( 'NONE', #41744 ) ;
#29892 = PLANE ( 'NONE',  #33422 ) ;
#29893 = DIRECTION ( 'NONE',  ( 0.000000000000000000, 0.6427876096865368094, 0.7660444431189802339 ) ) ;
#29894 = AXIS2_PLACEMENT_3D ( 'NONE', #37541, #65902, #78980 ) ;
#29895 = B_SPLINE_CURVE_WITH_KNOTS ( 'NONE', 3,
 ( #54199, #59187, #86690, #87578, #18665, #80818, #4700, #88470, #5140, #12782 ),
 .UNSPECIFIED., .F., .F.,
 ( 4, 2, 2, 2, 4 ),
 ( 0.000000000000000000, 0.0001954339857564071491, 0.0003908679715128142982, 0.0005863019572692214744, 0.0007817359430256285964 ),
 .UNSPECIFIED. ) ;
#29896 = CARTESIAN_POINT ( 'NONE',  ( -9.626240358957616650, -3.322132147404559976, 32.92929555188717927 ) ) ;
#29897 = ADVANCED_FACE ( 'NONE', ( #69210 ), #62871, .F. ) ;
#29898 = CIRCLE ( 'NONE', #28473, 4.000000000000000000 ) ;
#29899 = VERTEX_POINT ( 'NONE', #51452 ) ;
#29900 = DIRECTION ( 'NONE',  ( 1.799314243699348838E-16, 1.000000000000000000, -5.102127870520020612E-17 ) ) ;
#29901 = ADVANCED_FACE ( 'NONE', ( #16372 ), #85721, .F. ) ;
#29902 = ORIENTED_EDGE ( 'NONE', *, *, #12951, .F. ) ;
#29903 = CARTESIAN_POINT ( 'NONE',  ( 11.25641025641025550, -7.500000000000000000, 29.75000000000000355 ) ) ;
#29904 = CARTESIAN_POINT ( 'NONE',  ( -3.230769230769351186, -12.27809138561165270, 31.22303859784587132 ) ) ;
#29905 = ADVANCED_FACE ( 'NONE', ( #71746 ), #31206, .F. ) ;
#29906 = CARTESIAN_POINT ( 'NONE',  ( -7.846153846153967493, -2.657715359629662544, 31.77849191805970364 ) ) ;
#29907 = EDGE_CURVE ( 'NONE', #83302, #24853, #2837, .T. ) ;
#29908 = B_SPLINE_CURVE_WITH_KNOTS ( 'NONE', 3,
 ( #36144, #55510, #69472, #14980, #8222, #1899, #35698, #64029, #29388, #63147 ),
 .UNSPECIFIED., .F., .F.,
 ( 4, 2, 2, 2, 4 ),
 ( 0.000000000000000000, 0.0001954311564186876334, 0.0003908623128373752667, 0.0005862934692560629272, 0.0007817246256747505334 ),
 .UNSPECIFIED. ) ;
#29909 = CARTESIAN_POINT ( 'NONE',  ( -23.50000000000000000, 5.000000000000023093, 28.74999999999999645 ) ) ;
#29910 = DIRECTION ( 'NONE',  ( -0.000000000000000000, -0.3420201433256694901, -0.9396926207859082059 ) ) ;
#29911 = VERTEX_POINT ( 'NONE', #64983 ) ;
#29912 = B_SPLINE_CURVE_WITH_KNOTS ( 'NONE', 3,
 ( #27469, #14393, #54937, #81538, #20706, #61236, #69345, #7643, #440, #40553 ),
 .UNSPECIFIED., .F., .F.,
 ( 4, 2, 2, 2, 4 ),
 ( 0.0007817359430256232838, 0.0009771253907249930707, 0.001172514838424355702, 0.001367904286123718550, 0.001563293733823081181 ),
 .UNSPECIFIED. ) ;
#29913 = VECTOR ( 'NONE', #64591, 1000.000000000000000 ) ;
#29914 = EDGE_LOOP ( 'NONE', ( #23881, #55420, #11332, #56352 ) ) ;
#29915 = ORIENTED_EDGE ( 'NONE', *, *, #50058, .T. ) ;
#29916 = DIRECTION ( 'NONE',  ( -2.602085213965214586E-16, 1.000000000000000000, 0.000000000000000000 ) ) ;
#29917 = CARTESIAN_POINT ( 'NONE',  ( -17.07692307692307665, -3.513871655860378418, 32.76840700105978499 ) ) ;
#29918 = CARTESIAN_POINT ( 'NONE',  ( 0.6845513056318556222, -6.460100341425561332, 34.89618726649961644 ) ) ;
#29919 = CYLINDRICAL_SURFACE ( 'NONE', #67221, 0.2499999999999979738 ) ;
#29920 = CARTESIAN_POINT ( 'NONE',  ( -20.00000000000000000, -3.499999999999999556, 29.75000000000000355 ) ) ;
#29921 = CARTESIAN_POINT ( 'NONE',  ( 5.299934428535925335, -9.886259254753566594, 34.14407573483972413 ) ) ;
#29922 = VERTEX_POINT ( 'NONE', #78956 ) ;
#29923 = ORIENTED_EDGE ( 'NONE', *, *, #81831, .T. ) ;
#29924 = ORIENTED_EDGE ( 'NONE', *, *, #70651, .F. ) ;
#29926 = EDGE_LOOP ( 'NONE', ( #63970, #73359 ) ) ;
#29925 = FACE_OUTER_BOUND ( 'NONE', #17150, .T. ) ;
#29928 = CARTESIAN_POINT ( 'NONE',  ( -18.00000000000000000, -9.780366693483671270, 34.19971097300155094 ) ) ;
#29927 = CARTESIAN_POINT ( 'NONE',  ( -24.00000000000000000, -5.499999999999981348, 27.75000000000000000 ) ) ;
#29929 = EDGE_CURVE ( 'NONE', #18944, #34055, #76858, .T. ) ;
#29930 = DIRECTION ( 'NONE',  ( -0.000000000000000000, -0.5000000000000009992, -0.8660254037844380415 ) ) ;
#29931 = CARTESIAN_POINT ( 'NONE',  ( 1.553300858899129722, -11.24999999999999112, 23.45312500000000000 ) ) ;
#29932 = VERTEX_POINT ( 'NONE', #43837 ) ;
#29933 = EDGE_LOOP ( 'NONE', ( #84824, #40680, #36384, #68121 ) ) ;
#29934 = CARTESIAN_POINT ( 'NONE',  ( 5.326923076924495071, -7.500000000000154543, 35.00000000000007105 ) ) ;
#29935 = ORIENTED_EDGE ( 'NONE', *, *, #33229, .T. ) ;
#29936 = FACE_BOUND ( 'NONE', #22561, .T. ) ;
#29937 = DIRECTION ( 'NONE',  ( 0.000000000000000000, -1.000000000000000000, 0.000000000000000000 ) ) ;
#29938 = CARTESIAN_POINT ( 'NONE',  ( 16.15384615384603251, -6.879047030192662504, 34.71129190930017927 ) ) ;
#29939 = VERTEX_POINT ( 'NONE', #76407 ) ;
#29940 = DIRECTION ( 'NONE',  ( -1.000000000000000000, 0.000000000000000000, -0.000000000000000000 ) ) ;
#29941 = CARTESIAN_POINT ( 'NONE',  ( 3.480823542407545546, -3.136992222400443175, 32.19305428654138979 ) ) ;
#29942 = DIRECTION ( 'NONE',  ( -0.000000000000000000, -0.3420201433256694346, -0.9396926207859080948 ) ) ;
#29943 = CARTESIAN_POINT ( 'NONE',  ( -11.53846153846165912, -6.026961402154118019, 34.52809138561165270 ) ) ;
#29944 = CARTESIAN_POINT ( 'NONE',  ( 1.515405825582337718, -2.494656445102013453, 31.33466734024120015 ) ) ;
#29945 = EDGE_CURVE ( 'NONE', #38377, #61168, #17251, .T. ) ;
#29946 = EDGE_CURVE ( 'NONE', #25295, #55459, #58665, .T. ) ;
#29947 = AXIS2_PLACEMENT_3D ( 'NONE', #42314, #69767, #1305 ) ;
#29948 = CARTESIAN_POINT ( 'NONE',  ( -6.857821351800898135, -9.442884908240271713, 34.35708131394835618 ) ) ;
#29949 = DIRECTION ( 'NONE',  ( 0.000000000000000000, 0.7660444431189822323, -0.6427876096865344779 ) ) ;
#29950 = CARTESIAN_POINT ( 'NONE',  ( -7.715628144390283438, -6.852161475712352789, 34.70806712695775786 ) ) ;
#29951 = CARTESIAN_POINT ( 'NONE',  ( 7.384615384615385025, -3.499999999999999556, 29.75000000000000355 ) ) ;
#29952 = CARTESIAN_POINT ( 'NONE',  ( 5.999999999999880096, -5.219633306517616589, 34.19971097300220464 ) ) ;
#29953 = DIRECTION ( 'NONE',  ( -0.000000000000000000, -0.3420201433256694346, -0.9396926207859080948 ) ) ;
#29954 = CARTESIAN_POINT ( 'NONE',  ( 6.249945518348141604, -10.05730279482229683, 34.04704008940765902 ) ) ;
#29956 = CARTESIAN_POINT ( 'NONE',  ( 11.60371710973756620, -4.481592998940250538, 33.73612834413965089 ) ) ;
#29955 = CARTESIAN_POINT ( 'NONE',  ( -13.63463860883684120, -4.175268141568685643, 33.81360843649122216 ) ) ;
#29957 = CYLINDRICAL_SURFACE ( 'NONE', #18092, 0.2500000000000008882 ) ;
#29959 = CARTESIAN_POINT ( 'NONE',  ( 7.846153846153846700, -13.87047571288749737, 32.06866353760679544 ) ) ;
#29958 = DIRECTION ( 'NONE',  ( -0.000000000000000000, 0.6427876096865404731, -0.7660444431189770143 ) ) ;
#29960 = CYLINDRICAL_SURFACE ( 'NONE', #40504, 0.2500000000000009437 ) ;
#29961 = CARTESIAN_POINT ( 'NONE',  ( 1.077988221561464899, -4.724691934501233703, 20.23250670625849423 ) ) ;
#29962 = ORIENTED_EDGE ( 'NONE', *, *, #1070, .T. ) ;
#29963 = CARTESIAN_POINT ( 'NONE',  ( -3.931066484868086075, -5.827830569534415694, 34.72679350104403539 ) ) ;
#29964 = EDGE_LOOP ( 'NONE', ( #25754, #10407, #24036, #20606 ) ) ;
#29965 = CARTESIAN_POINT ( 'NONE',  ( -9.758391103263569732, -5.557115091759785130, 34.35708131394839171 ) ) ;
#29966 = EDGE_CURVE ( 'NONE', #66348, #77080, #38253, .T. ) ;
#29967 = ORIENTED_EDGE ( 'NONE', *, *, #50921, .T. ) ;
#29968 = CARTESIAN_POINT ( 'NONE',  ( 16.15384615384615330, -11.16473453929635440, 33.15142922261926373 ) ) ;
#29969 = ORIENTED_EDGE ( 'NONE', *, *, #80281, .T. ) ;
#29970 = CARTESIAN_POINT ( 'NONE',  ( -5.076923076923075762, -1.129524287112498415, 32.06866353760679544 ) ) ;
#29971 = CARTESIAN_POINT ( 'NONE',  ( 1.200186371490561621, -10.22469193450123193, 21.95125670625849068 ) ) ;
#29972 = CARTESIAN_POINT ( 'NONE',  ( -18.00000000000012079, -9.528491918059723176, 34.59228464037033035 ) ) ;
#29973 = EDGE_CURVE ( 'NONE', #61122, #29364, #70473, .T. ) ;
#29974 = CARTESIAN_POINT ( 'NONE',  ( 13.60739505359344825, -3.020022701398814569, 32.48759521482552515 ) ) ;
#29975 = FACE_OUTER_BOUND ( 'NONE', #25352, .T. ) ;
#29976 = CARTESIAN_POINT ( 'NONE',  ( -16.15384615384627409, -10.33852847137269571, 34.16647553114546554 ) ) ;
#29977 = DIRECTION ( 'NONE',  ( -0.000000000000000000, 0.9396926207859092051, -0.3420201433256662704 ) ) ;
#29978 = LINE ( 'NONE', #37168, #68401 ) ;
#29979 = CARTESIAN_POINT ( 'NONE',  ( -1.553300858899081538, -11.25000000000000711, 17.35937500000000000 ) ) ;
#29980 = CARTESIAN_POINT ( 'NONE',  ( 1.134638653673034181, -2.779195860258146134, 31.39871582349836032 ) ) ;
#29981 = CARTESIAN_POINT ( 'NONE',  ( 11.53846153846153832, -3.886160181151819604, 36.00935417666054406 ) ) ;
#29982 = B_SPLINE_CURVE_WITH_KNOTS ( 'NONE', 3,
 ( #24072, #51520, #72706, #4252, #11016, #57859, #10569, #85341, #30828, #78571 ),
 .UNSPECIFIED., .F., .F.,
 ( 4, 2, 2, 2, 4 ),
 ( 0.0007817359430256297891, 0.0009771253907249961065, 0.001172514838424362424, 0.001367904286123728741, 0.001563293733823095059 ),
 .UNSPECIFIED. ) ;
#29983 = ADVANCED_FACE ( 'NONE', ( #28215 ), #55683, .F. ) ;
#29984 = CARTESIAN_POINT ( 'NONE',  ( 14.37376065869474751, -3.050289026998446840, 32.03036669348366416 ) ) ;
#29985 = CIRCLE ( 'NONE', #52917, 0.5000000000000004441 ) ;
#29986 = CARTESIAN_POINT ( 'NONE',  ( -3.749999999999988454, -9.053300858899127945, 16.26562500000000000 ) ) ;
#29987 = CARTESIAN_POINT ( 'NONE',  ( -10.61538461538461320, -5.471508081941601098, 34.59228464037088457 ) ) ;
#29988 = ORIENTED_EDGE ( 'NONE', *, *, #18382, .T. ) ;
#29989 = CARTESIAN_POINT ( 'NONE',  ( 14.53047184896071542, -5.114059244376869984, 34.14424750095245287 ) ) ;
#29990 = LINE ( 'NONE', #43938, #79067 ) ;
#29991 = CARTESIAN_POINT ( 'NONE',  ( 1.134592147322421640, -12.43535235679832596, 30.55408501211184813 ) ) ;
#29992 = CARTESIAN_POINT ( 'NONE',  ( 18.25005431163831204, -10.66356715214248574, 33.62249196103329751 ) ) ;
#29993 = CARTESIAN_POINT ( 'NONE',  ( -24.00000000000000000, -9.499999999999982236, 27.74999999999999645 ) ) ;
#29994 = CARTESIAN_POINT ( 'NONE',  ( -8.899377978668987055, -8.587444163452046197, 34.63053765926554206 ) ) ;
#29995 = DIRECTION ( 'NONE',  ( -0.7071067811865510144, 0.7071067811865440200, 0.000000000000000000 ) ) ;
#29996 = EDGE_CURVE ( 'NONE', #30893, #88462, #83176, .T. ) ;
#29997 = ORIENTED_EDGE ( 'NONE', *, *, #9591, .T. ) ;
#29998 = CARTESIAN_POINT ( 'NONE',  ( 7.622668921589514035, -3.019605429927184836, 32.48692288466676814 ) ) ;
#29999 = ORIENTED_EDGE ( 'NONE', *, *, #3732, .F. ) ;
#30000 = ADVANCED_FACE ( 'NONE', ( #32995 ), #73988, .F. ) ;
#30001 = ORIENTED_EDGE ( 'NONE', *, *, #73558, .T. ) ;
#30002 = CARTESIAN_POINT ( 'NONE',  ( -11.40793610022789828, -11.66157788607254098, 32.95092075102925833 ) ) ;
#30003 = CARTESIAN_POINT ( 'NONE',  ( -8.899921372341079717, -2.295517848115769421, 30.44137282052137294 ) ) ;
#30004 = EDGE_CURVE ( 'NONE', #85209, #14132, #79692, .T. ) ;
#30005 = CARTESIAN_POINT ( 'NONE',  ( 1.607626736228236375, -11.76359900205217457, 32.36225158514719880 ) ) ;
#30006 = CARTESIAN_POINT ( 'NONE',  ( 14.30769230769231015, -12.78798330534102945, 29.74999999999997868 ) ) ;
#30007 = AXIS2_PLACEMENT_3D ( 'NONE', #66682, #39671, #4985 ) ;
#30008 = VERTEX_POINT ( 'NONE', #73090 ) ;
#30009 = DIRECTION ( 'NONE',  ( -0.000000000000000000, -0.9848077530122085754, -0.1736481776669273613 ) ) ;
#30010 = AXIS2_PLACEMENT_3D ( 'NONE', #24971, #38046, #11023 ) ;
#30011 = ORIENTED_EDGE ( 'NONE', *, *, #5431, .T. ) ;
#30012 = B_SPLINE_CURVE_WITH_KNOTS ( 'NONE', 3,
 ( #16033, #43503, #44365, #15150, #2500, #70976, #65086, #71404, #29118, #77724 ),
 .UNSPECIFIED., .F., .F.,
 ( 4, 2, 2, 2, 4 ),
 ( 0.0007817359430256297891, 0.0009771253907249958896, 0.001172514838424361990, 0.001367904286123728091, 0.001563293733823094191 ),
 .UNSPECIFIED. ) ;
#30013 = EDGE_LOOP ( 'NONE', ( #62305, #22854, #41000, #27089 ) ) ;
#30014 = VECTOR ( 'NONE', #19480, 1000.000000000000000 ) ;
#30015 = DIRECTION ( 'NONE',  ( -0.000000000000000000, -0.9848077530122085754, -0.1736481776669273613 ) ) ;
#30016 = DIRECTION ( 'NONE',  ( -1.000000000000000000, 0.000000000000000000, 0.000000000000000000 ) ) ;
#30017 = EDGE_CURVE ( 'NONE', #44792, #85917, #33441, .T. ) ;
#30018 = DIRECTION ( 'NONE',  ( -0.000000000000000000, -0.8660254037844397068, -0.4999999999999978906 ) ) ;
#30019 = EDGE_CURVE ( 'NONE', #85805, #7785, #18794, .T. ) ;
#30020 = CYLINDRICAL_SURFACE ( 'NONE', #80988, 0.2499999999999986955 ) ;
#30021 = CARTESIAN_POINT ( 'NONE',  ( 7.976679284387489410, -12.70449254468099198, 30.44128974285582956 ) ) ;
#30022 = ORIENTED_EDGE ( 'NONE', *, *, #39397, .T. ) ;
#30023 = ORIENTED_EDGE ( 'NONE', *, *, #59300, .F. ) ;
#30024 = CARTESIAN_POINT ( 'NONE',  ( -3.749999999999997335, -7.500000000000021316, 22.59375000000000355 ) ) ;
#30025 = ORIENTED_EDGE ( 'NONE', *, *, #19074, .F. ) ;
#30027 = VERTEX_POINT ( 'NONE', #88405 ) ;
#30026 = CARTESIAN_POINT ( 'NONE',  ( 4.284371855609715674, -11.46989282347013095, 32.79007818306219946 ) ) ;
#30028 = CARTESIAN_POINT ( 'NONE',  ( 13.38461538461526423, -9.528491918059723176, 34.59228464037033035 ) ) ;
#30029 = CARTESIAN_POINT ( 'NONE',  ( -8.102564102564102200, -7.500000000000000000, 29.75000000000000355 ) ) ;
#30030 = EDGE_CURVE ( 'NONE', #20476, #85537, #60459, .T. ) ;
#30031 = CYLINDRICAL_SURFACE ( 'NONE', #88237, 4.999999999999997335 ) ;
#30032 = ORIENTED_EDGE ( 'NONE', *, *, #42626, .T. ) ;
#30033 = CARTESIAN_POINT ( 'NONE',  ( -14.98071481085577972, -12.41089969410671223, 31.60739465890703670 ) ) ;
#30034 = VECTOR ( 'NONE', #9446, 1000.000000000000000 ) ;
#30035 = ORIENTED_EDGE ( 'NONE', *, *, #43878, .T. ) ;
#30036 = FACE_BOUND ( 'NONE', #30304, .T. ) ;
#30037 = EDGE_CURVE ( 'NONE', #37810, #10963, #53702, .T. ) ;
#30038 = CARTESIAN_POINT ( 'NONE',  ( 15.45354889974729495, -11.60474049983371003, 33.02348890104160262 ) ) ;
#30039 = CARTESIAN_POINT ( 'NONE',  ( 11.53846153846153832, -13.53365097954675988, 30.81389545987213552 ) ) ;
#30040 = CARTESIAN_POINT ( 'NONE',  ( 2.307692307692309264, -12.34228464037088635, 31.77849191805839268 ) ) ;
#30042 = CARTESIAN_POINT ( 'NONE',  ( 12.46153846153846168, -9.058645607665452459, 34.76329471203371924 ) ) ;
#30041 = CARTESIAN_POINT ( 'NONE',  ( -39.05038313613820122, -2.249999999999998668, 29.75000000000000355 ) ) ;
#30043 = ADVANCED_FACE ( 'NONE', ( #52364 ), #39319, .F. ) ;
#30044 = CARTESIAN_POINT ( 'NONE',  ( -0.4615384615384611200, -12.34228464037088635, 31.77849191805839268 ) ) ;
#30045 = CARTESIAN_POINT ( 'NONE',  ( -10.86536134632696893, -10.66389620160130036, 33.62221079203477103 ) ) ;
#30046 = ORIENTED_EDGE ( 'NONE', *, *, #83855, .T. ) ;
#30047 = CARTESIAN_POINT ( 'NONE',  ( -18.00000000000012079, -10.90142922262034020, 33.41473453929536674 ) ) ;
#30048 = ORIENTED_EDGE ( 'NONE', *, *, #47370, .T. ) ;
#30049 = EDGE_CURVE ( 'NONE', #30362, #61394, #81190, .T. ) ;
#30050 = CARTESIAN_POINT ( 'NONE',  ( -12.23852561744506495, -3.395485233115139057, 33.02377354290275946 ) ) ;
#30051 = CARTESIAN_POINT ( 'NONE',  ( 15.29683758177166908, -4.098570777380720287, 33.41473453929635440 ) ) ;
#30052 = CARTESIAN_POINT ( 'NONE',  ( -8.519230769230768274, -2.249999999999998668, 29.75000000000000355 ) ) ;
#30053 = LINE ( 'NONE', #78679, #66323 ) ;
#30054 = CARTESIAN_POINT ( 'NONE',  ( 7.846153846153723244, -6.835583212225970762, 34.95778746994575670 ) ) ;
#30055 = CARTESIAN_POINT ( 'NONE',  ( 7.622668902429897919, -8.496056993536548418, 34.65000542017679663 ) ) ;
#30056 = FACE_BOUND ( 'NONE', #68632, .T. ) ;
#30057 = EDGE_CURVE ( 'NONE', #47121, #85711, #87517, .T. ) ;
#30059 = CARTESIAN_POINT ( 'NONE',  ( 1.450683735617826153, -2.538708090699994813, 30.37095296980875503 ) ) ;
#30058 = CARTESIAN_POINT ( 'NONE',  ( 12.33084785842815378, -9.929715669179220328, 34.40415004197138416 ) ) ;
#30060 = CARTESIAN_POINT ( 'NONE',  ( -6.673022611438608642, -10.66356715214248396, 33.62249196103329751 ) ) ;
#30062 = CARTESIAN_POINT ( 'NONE',  ( 7.596153846153840483, -2.499999999999999556, 29.81609845454691765 ) ) ;
#30061 = CARTESIAN_POINT ( 'NONE',  ( -13.38461538461550582, -6.026961402154118019, 34.52809138561165270 ) ) ;
#30063 = CARTESIAN_POINT ( 'NONE',  ( -10.28846153846153832, -3.499999999999999556, 29.75000000000000355 ) ) ;
#30064 = CARTESIAN_POINT ( 'NONE',  ( 3.775308065498768517, -8.992201783934554271, 19.29500670625849068 ) ) ;
#30065 = VERTEX_POINT ( 'NONE', #80753 ) ;
#30066 = VECTOR ( 'NONE', #45397, 1000.000000000000000 ) ;
#30067 = CARTESIAN_POINT ( 'NONE',  ( -8.096177083446809419, -11.37209801155882971, 32.91403422569032955 ) ) ;
#30068 = LINE ( 'NONE', #57089, #32587 ) ;
#30069 = CARTESIAN_POINT ( 'NONE',  ( 5.933917620639865831, -5.471508081941601986, 34.59228464037088457 ) ) ;
#30070 = CARTESIAN_POINT ( 'NONE',  ( 0.4330127018922180770, -10.21569512280005299, 29.50000000000000355 ) ) ;
#30071 = CARTESIAN_POINT ( 'NONE',  ( 7.596130608860880429, -5.056417327199099532, 34.11270091957320716 ) ) ;
#30072 = CARTESIAN_POINT ( 'NONE',  ( -3.749999999999996447, -7.561099074964554134, 19.84188170625848713 ) ) ;
#30073 = EDGE_CURVE ( 'NONE', #10584, #7315, #46505, .T. ) ;
#30074 = CARTESIAN_POINT ( 'NONE',  ( -8.703975197954745724, -2.892918686051626498, 31.69288490824026638 ) ) ;
#30075 = DIRECTION ( 'NONE',  ( -0.000000000000000000, -0.3420201433256694901, -0.9396926207859082059 ) ) ;
#30076 = AXIS2_PLACEMENT_3D ( 'NONE', #10302, #72883, #73795 ) ;
#30077 = CARTESIAN_POINT ( 'NONE',  ( -8.069638770718178478, -3.019605429927184836, 32.48692288466676814 ) ) ;
#30078 = CARTESIAN_POINT ( 'NONE',  ( 10.36540787133602493, -6.524016743844655686, 34.90889640711025521 ) ) ;
#30079 = CARTESIAN_POINT ( 'NONE',  ( 5.326923076923079314, -2.499999999999999112, 29.81604066197450109 ) ) ;
#30080 = CARTESIAN_POINT ( 'NONE',  ( 12.46153846153833911, -12.70778746994576025, 30.41441678777401236 ) ) ;
#30081 = VECTOR ( 'NONE', #47130, 1000.000000000000114 ) ;
#30082 = CARTESIAN_POINT ( 'NONE',  ( -18.22348494372394967, -2.847400154188068022, 31.58180166144859768 ) ) ;
#30083 = AXIS2_PLACEMENT_3D ( 'NONE', #87582, #51978, #88040 ) ;
#30084 = DIRECTION ( 'NONE',  ( -0.000000000000000000, 1.000000000000000000, 3.491481338843133355E-15 ) ) ;
#30085 = EDGE_LOOP ( 'NONE', ( #20409, #57131, #10503, #26466 ) ) ;
#30086 = CARTESIAN_POINT ( 'NONE',  ( 25.00000000000000711, -9.999999999999957367, 13.00000000000000178 ) ) ;
#30087 = CARTESIAN_POINT ( 'NONE',  ( -17.29984929443922681, -2.758268499246657068, 31.33685645148948851 ) ) ;
#30088 = CARTESIAN_POINT ( 'NONE',  ( -3.775308065498748977, -8.992201783934593351, 15.26749329374151465 ) ) ;
#30089 = DIRECTION ( 'NONE',  ( 0.000000000000000000, 0.000000000000000000, 1.000000000000000000 ) ) ;
#30090 = CARTESIAN_POINT ( 'NONE',  ( 3.361294932532797208, -11.93748526763465279, 32.05452791011430946 ) ) ;
#30091 = EDGE_LOOP ( 'NONE', ( #740, #41856, #39679, #59517 ) ) ;
#30092 = CARTESIAN_POINT ( 'NONE',  ( -6.923076923076922462, -9.905515769479276145, 34.41647553114623292 ) ) ;
#30094 = EDGE_LOOP ( 'NONE', ( #40481, #69173 ) ) ;
#30093 = CARTESIAN_POINT ( 'NONE',  ( 7.780883400193072674, -2.625532179533445198, 30.86335684631481513 ) ) ;
#30095 = DIRECTION ( 'NONE',  ( 0.000000000000000000, 0.000000000000000000, -1.000000000000000000 ) ) ;
#30096 = DIRECTION ( 'NONE',  ( -0.000000000000000000, -0.1736481776669307198, -0.9848077530122080203 ) ) ;
#30097 = CARTESIAN_POINT ( 'NONE',  ( 16.15384615384603251, -10.21337939537710326, 33.94971097300076224 ) ) ;
#30098 = CARTESIAN_POINT ( 'NONE',  ( -24.99999999999999645, -19.99999999999999645, 3.000000000000000000 ) ) ;
#30099 = ORIENTED_EDGE ( 'NONE', *, *, #73024, .T. ) ;
#30100 = FACE_OUTER_BOUND ( 'NONE', #56735, .T. ) ;
#30101 = DIRECTION ( 'NONE',  ( 0.000000000000000000, 0.000000000000000000, -1.000000000000000000 ) ) ;
#30102 = CARTESIAN_POINT ( 'NONE',  ( -0.4615384615385826339, -6.026961402154118908, 34.52809138561165270 ) ) ;
#30103 = EDGE_LOOP ( 'NONE', ( #35495, #89175, #23793, #48405 ) ) ;
#30104 = VERTEX_POINT ( 'NONE', #74877 ) ;
#30105 = AXIS2_PLACEMENT_3D ( 'NONE', #32483, #87915, #5474 ) ;
#30106 = ADVANCED_FACE ( 'NONE', ( #12276 ), #38419, .F. ) ;
#30107 = ORIENTED_EDGE ( 'NONE', *, *, #9348, .T. ) ;
#30108 = FACE_OUTER_BOUND ( 'NONE', #3149, .T. ) ;
#30109 = CARTESIAN_POINT ( 'NONE',  ( -19.50000000000000000, -3.499999999999999556, 29.75000000000000355 ) ) ;
#30110 = EDGE_CURVE ( 'NONE', #18826, #60639, #31662, .T. ) ;
#30111 = B_SPLINE_CURVE_WITH_KNOTS ( 'NONE', 3,
 ( #29768, #37847, #36949, #23437, #9058, #44139, #78826, #31079, #86042, #63974 ),
 .UNSPECIFIED., .F., .F.,
 ( 4, 2, 2, 2, 4 ),
 ( 0.000000000000000000, 0.0001954311564186876334, 0.0003908623128373752667, 0.0005862934692560629272, 0.0007817246256747505334 ),
 .UNSPECIFIED. ) ;
#30112 = CARTESIAN_POINT ( 'NONE',  ( -4.023320715612507037, -12.70449254468099198, 30.44128974285582956 ) ) ;
#30113 = ADVANCED_FACE ( 'NONE', ( #39761 ), #67229, .F. ) ;
#30114 = CARTESIAN_POINT ( 'NONE',  ( -17.07692307692319744, -6.879047030192662504, 34.71129190930017927 ) ) ;
#30115 = ORIENTED_EDGE ( 'NONE', *, *, #43751, .F. ) ;
#30116 = ORIENTED_EDGE ( 'NONE', *, *, #33870, .T. ) ;
#30118 = VERTEX_POINT ( 'NONE', #46936 ) ;
#30117 = CYLINDRICAL_SURFACE ( 'NONE', #80367, 0.2499999999999994726 ) ;
#30119 = EDGE_CURVE ( 'NONE', #31805, #78822, #27500, .T. ) ;
#30120 = CARTESIAN_POINT ( 'NONE',  ( 16.40379156322419973, -8.476813868363244353, 34.90874843262270133 ) ) ;
#30121 = CIRCLE ( 'NONE', #8530, 0.2500000000000002220 ) ;
#30122 = DIRECTION ( 'NONE',  ( -0.000000000000000000, -0.9396926207859093161, -0.3420201433256663259 ) ) ;
#30123 = CARTESIAN_POINT ( 'NONE',  ( -8.703975629717932705, -12.70778746994558439, 30.41441678777536595 ) ) ;
#30124 = VERTEX_POINT ( 'NONE', #20803 ) ;
#30125 = AXIS2_PLACEMENT_3D ( 'NONE', #18780, #74609, #17889 ) ;
#30126 = VECTOR ( 'NONE', #11300, 999.9999999999998863 ) ;
#30127 = ORIENTED_EDGE ( 'NONE', *, *, #72331, .T. ) ;
#30129 = ORIENTED_EDGE ( 'NONE', *, *, #68190, .T. ) ;
#30128 = CARTESIAN_POINT ( 'NONE',  ( -8.519285250882628446, -8.433404298154334455, 34.66254593164985920 ) ) ;
#30130 = VECTOR ( 'NONE', #51666, 1000.000000000000227 ) ;
#30131 = DIRECTION ( 'NONE',  ( -0.000000000000000000, 0.9848077530122085754, -0.1736481776669273613 ) ) ;
#30132 = CARTESIAN_POINT ( 'NONE',  ( -5.076923076923075762, -9.780366693483667717, 34.19971097300155094 ) ) ;
#30133 = VERTEX_POINT ( 'NONE', #14489 ) ;
#30134 = B_SPLINE_CURVE_WITH_KNOTS ( 'NONE', 3,
 ( #84628, #28795, #57137, #21132, #22903, #50369, #77848, #869, #28334, #21579 ),
 .UNSPECIFIED., .F., .F.,
 ( 4, 2, 2, 2, 4 ),
 ( 0.0007817246256747459798, 0.0009771112852218896347, 0.001172497944769033181, 0.001367884604316176728, 0.001563271263863320491 ),
 .UNSPECIFIED. ) ;
#30135 = CARTESIAN_POINT ( 'NONE',  ( 15.36129493253279499, -3.285477652293413264, 32.44071101563363158 ) ) ;
#30136 = B_SPLINE_CURVE_WITH_KNOTS ( 'NONE', 3,
 ( #81241, #59622, #11441, #7688, #67278, #26726, #74927, #25399, #11895, #25847 ),
 .UNSPECIFIED., .F., .F.,
 ( 4, 2, 2, 2, 4 ),
 ( 0.000000000000000000, 0.0001954339857564054144, 0.0003908679715128108288, 0.0005863019572692162703, 0.0007817359430256216575 ),
 .UNSPECIFIED. ) ;
#30137 = CARTESIAN_POINT ( 'NONE',  ( 5.142991427925513115, -11.16473453929635440, 33.15142922261926373 ) ) ;
#30138 = CARTESIAN_POINT ( 'NONE',  ( -8.992715693795098275, -12.11044203135681840, 32.26167407432752299 ) ) ;
#30139 = FACE_BOUND ( 'NONE', #74338, .T. ) ;
#30140 = EDGE_CURVE ( 'NONE', #18183, #26741, #83339, .T. ) ;
#30141 = CARTESIAN_POINT ( 'NONE',  ( -9.442362282929650519, -4.176053281294518804, 33.81426240980091791 ) ) ;
#30142 = CARTESIAN_POINT ( 'NONE',  ( -6.700297254098854793, -9.418065098278011860, 34.63729479722530158 ) ) ;
#30143 = CARTESIAN_POINT ( 'NONE',  ( 8.545745825506822158, -2.599994579823202923, 30.74605699353653776 ) ) ;
#30145 = CYLINDRICAL_SURFACE ( 'NONE', #30320, 0.2499999999999994726 ) ;
#30144 = CARTESIAN_POINT ( 'NONE',  ( 3.361559671736182864, -3.338503747796865984, 32.95102852606552801 ) ) ;
#30146 = CARTESIAN_POINT ( 'NONE',  ( 6.416666666666664298, -7.500000000000000000, 29.75000000000000355 ) ) ;
#30147 = DIRECTION ( 'NONE',  ( -0.000000000000000000, 0.1736481776669307198, -0.9848077530122080203 ) ) ;
#30148 = ORIENTED_EDGE ( 'NONE', *, *, #30391, .T. ) ;
#30149 = CARTESIAN_POINT ( 'NONE',  ( 10.48469314871706182, -10.54014554554150607, 33.71984207302941883 ) ) ;
#30150 = VERTEX_POINT ( 'NONE', #56366 ) ;
#30151 = ORIENTED_EDGE ( 'NONE', *, *, #87128, .T. ) ;
#30153 = CARTESIAN_POINT ( 'NONE',  ( 15.00784227186237807, -2.889293201056495786, 32.26117774369186009 ) ) ;
#30152 = CARTESIAN_POINT ( 'NONE',  ( 9.442307692307679190, -2.249999999999998668, 29.81609741502487765 ) ) ;
#30154 = EDGE_CURVE ( 'NONE', #17995, #56514, #52217, .T. ) ;
#30155 = CARTESIAN_POINT ( 'NONE',  ( 11.40831356872984514, -8.630895178749533159, 34.87696386517710323 ) ) ;
#30156 = FACE_OUTER_BOUND ( 'NONE', #29197, .T. ) ;
#30157 = CARTESIAN_POINT ( 'NONE',  ( -19.99999999999996447, -15.00000000000000533, 13.00000000000000178 ) ) ;
#30158 = CARTESIAN_POINT ( 'NONE',  ( -2.307692307692305711, -11.35647404775217417, 33.31231777344666511 ) ) ;
#30159 = VERTEX_POINT ( 'NONE', #48270 ) ;
#30160 = CARTESIAN_POINT ( 'NONE',  ( 4.403900573759605308, -4.818054556918156095, 34.26375889529406749 ) ) ;
#30161 = EDGE_CURVE ( 'NONE', #41440, #10893, #55408, .T. ) ;
#30162 = EDGE_CURVE ( 'NONE', #80250, #53882, #49608, .T. ) ;
#30163 = CARTESIAN_POINT ( 'NONE',  ( 14.24160992833217243, -12.62096338111211580, 30.90682066428152908 ) ) ;
#30164 = FACE_OUTER_BOUND ( 'NONE', #7437, .T. ) ;
#30165 = CARTESIAN_POINT ( 'NONE',  ( -19.00000000000000000, -17.00000000000000000, 2.999999999999997780 ) ) ;
#30166 = DIRECTION ( 'NONE',  ( -0.000000000000000000, 1.000000000000000000, 3.491481338843133355E-15 ) ) ;
#30167 = AXIS2_PLACEMENT_3D ( 'NONE', #37930, #22201, #85676 ) ;
#30168 = CARTESIAN_POINT ( 'NONE',  ( 3.750000000000000888, -7.499999999999978684, 14.46875000000000000 ) ) ;
#30169 = EDGE_LOOP ( 'NONE', ( #17716, #61080, #56401, #37772 ) ) ;
#30170 = ORIENTED_EDGE ( 'NONE', *, *, #21548, .T. ) ;
#30171 = CARTESIAN_POINT ( 'NONE',  ( 14.08476534878545650, -12.38737895849757820, 31.66785238281580206 ) ) ;
#30172 = ORIENTED_EDGE ( 'NONE', *, *, #84530, .F. ) ;
#30173 = CARTESIAN_POINT ( 'NONE',  ( -6.923076923076922462, -2.538708090699994813, 30.37095296980875503 ) ) ;
#30174 = DIRECTION ( 'NONE',  ( -0.000000000000000000, -0.3420201433256694901, -0.9396926207859082059 ) ) ;
#30175 = CARTESIAN_POINT ( 'NONE',  ( 14.53047184896072075, -2.847695495035523550, 31.58253572463339154 ) ) ;
#30176 = DIRECTION ( 'NONE',  ( 0.000000000000000000, 0.6427876096865368094, 0.7660444431189802339 ) ) ;
#30177 = CARTESIAN_POINT ( 'NONE',  ( 1.553300858899129944, -11.24999999999998934, 19.70312500000000355 ) ) ;
#30178 = ADVANCED_FACE ( 'NONE', ( #6843 ), #27566, .F. ) ;
#30179 = DIRECTION ( 'NONE',  ( -0.000000000000000000, 0.000000000000000000, -1.000000000000000000 ) ) ;
#30180 = ORIENTED_EDGE ( 'NONE', *, *, #62429, .F. ) ;
#30181 = CARTESIAN_POINT ( 'NONE',  ( -1.384615384615383471, -9.584722331328613620, 36.20867863119891439 ) ) ;
#30183 = EDGE_LOOP ( 'NONE', ( #63973, #69983 ) ) ;
#30182 = CARTESIAN_POINT ( 'NONE',  ( -16.37677237136229991, -11.76352882383564769, 32.36236540154569497 ) ) ;
#30184 = DIRECTION ( 'NONE',  ( -0.000000000000000000, 1.000000000000000000, 3.491481338843133355E-15 ) ) ;
#30185 = CARTESIAN_POINT ( 'NONE',  ( 3.480823542407545990, -2.779044189368095719, 31.39831045268885745 ) ) ;
#30186 = B_SPLINE_CURVE_WITH_KNOTS ( 'NONE', 3,
 ( #59460, #31540, #86963, #59006, #86504, #80180, #73425, #11725, #13489, #61220 ),
 .UNSPECIFIED., .F., .F.,
 ( 4, 2, 2, 2, 4 ),
 ( 0.0007817359430256294638, 0.0009771253907249941549, 0.001172514838424358954, 0.001367904286123723754, 0.001563293733823095492 ),
 .UNSPECIFIED. ) ;
#30187 = B_SPLINE_CURVE_WITH_KNOTS ( 'NONE', 3,
 ( #44023, #71493, #35958, #50331, #16121, #9371 ),
 .UNSPECIFIED., .F., .F.,
 ( 4, 2, 4 ),
 ( 0.0003909512603273901832, 0.0005862562993132176088, 0.0007815613382990449802 ),
 .UNSPECIFIED. ) ;
#30188 = EDGE_CURVE ( 'NONE', #1645, #54361, #47922, .T. ) ;
#30189 = EDGE_CURVE ( 'NONE', #49069, #4865, #63909, .T. ) ;
#30190 = CARTESIAN_POINT ( 'NONE',  ( 11.47319109250076430, -4.481592998940162609, 33.73612834413957984 ) ) ;
#30191 = CARTESIAN_POINT ( 'NONE',  ( 9.692307692307695177, -11.33034616979429110, 35.88435417666054406 ) ) ;
#30192 = AXIS2_PLACEMENT_3D ( 'NONE', #82982, #72771, #4322 ) ;
#30193 = CARTESIAN_POINT ( 'NONE',  ( 4.153846153846154188, -6.435427911321262684, 35.78748833219616898 ) ) ;
#30194 = CARTESIAN_POINT ( 'NONE',  ( -7.911424292114620727, -12.46129190929999986, 30.37095296980880832 ) ) ;
#30195 = CARTESIAN_POINT ( 'NONE',  ( 3.750000000000001776, -7.561099074964511502, 19.72061829374151287 ) ) ;
#30196 = ORIENTED_EDGE ( 'NONE', *, *, #73424, .F. ) ;
#30197 = EDGE_CURVE ( 'NONE', #14162, #1369, #36542, .T. ) ;
#30198 = CARTESIAN_POINT ( 'NONE',  ( 2.307692307692309264, -2.249999999999998668, 29.75000000000001776 ) ) ;
#30199 = CARTESIAN_POINT ( 'NONE',  ( -13.60754160213153163, -9.086856451489515152, 34.49173150075333183 ) ) ;
#30200 = CARTESIAN_POINT ( 'NONE',  ( -1.944543648262992530, -9.444543648263016067, 23.68750000000000000 ) ) ;
#30201 = VECTOR ( 'NONE', #60532, 1000.000000000000000 ) ;
#30202 = CIRCLE ( 'NONE', #10061, 4.000000000000000000 ) ;
#30203 = CARTESIAN_POINT ( 'NONE',  ( -13.63463862190834952, -12.43535235679832596, 30.55408501211184813 ) ) ;
#30204 = CARTESIAN_POINT ( 'NONE',  ( -17.07692307692307665, -2.538708090699994813, 30.37095296980875503 ) ) ;
#30205 = ORIENTED_EDGE ( 'NONE', *, *, #88647, .F. ) ;
#30206 = CARTESIAN_POINT ( 'NONE',  ( 3.999999999999997335, 7.500000000000000888, 14.00000000000000178 ) ) ;
#30207 = CARTESIAN_POINT ( 'NONE',  ( 12.21153846153846168, -2.499999999999998668, 29.75000000000000355 ) ) ;
#30208 = VECTOR ( 'NONE', #46910, 1000.000000000000114 ) ;
#30209 = ORIENTED_EDGE ( 'NONE', *, *, #10027, .T. ) ;
#30210 = VECTOR ( 'NONE', #49308, 1000.000000000000000 ) ;
#30211 = CARTESIAN_POINT ( 'NONE',  ( -4.403822897894745125, -8.347322224742351082, 34.93158281831414769 ) ) ;
#30212 = VECTOR ( 'NONE', #60561, 1000.000000000000227 ) ;
#30213 = ORIENTED_EDGE ( 'NONE', *, *, #61282, .F. ) ;
#30214 = DIRECTION ( 'NONE',  ( -1.000000000000000000, -0.000000000000000000, -0.000000000000000000 ) ) ;
#30215 = CARTESIAN_POINT ( 'NONE',  ( 4.088575707885378385, -3.835265460703609186, 33.15142922261924241 ) ) ;
#30216 = CARTESIAN_POINT ( 'NONE',  ( -0.5922290646487698984, -9.929715669179220328, 34.40415004197138416 ) ) ;
#30217 = CARTESIAN_POINT ( 'NONE',  ( -12.39547112818838492, -10.67929555188718282, 33.92786785259544757 ) ) ;
#30218 = EDGE_LOOP ( 'NONE', ( #88824, #40444, #81645, #9788 ) ) ;
#30219 = CARTESIAN_POINT ( 'NONE',  ( -9.019230769230768274, -2.249999999999998668, 29.75000000000000355 ) ) ;
#30220 = EDGE_CURVE ( 'NONE', #47096, #998, #80153, .T. ) ;
#30221 = ORIENTED_EDGE ( 'NONE', *, *, #36171, .T. ) ;
#30222 = CARTESIAN_POINT ( 'NONE',  ( 2.437737470527086892, -2.504778602574659896, 29.97347330155780298 ) ) ;
#30223 = CYLINDRICAL_SURFACE ( 'NONE', #10984, 0.2500000000000008882 ) ;
#30224 = VERTEX_POINT ( 'NONE', #56801 ) ;
#30225 = CARTESIAN_POINT ( 'NONE',  ( -6.222926958906846551, -10.77366814457252175, 33.85459836347579454 ) ) ;
#30226 = DIRECTION ( 'NONE',  ( -0.000000000000000000, 0.1736481776669307198, -0.9848077530122080203 ) ) ;
#30227 = CARTESIAN_POINT ( 'NONE',  ( -11.60373153901786125, -3.083524468853724443, 32.58852847137143272 ) ) ;
#30228 = CARTESIAN_POINT ( 'NONE',  ( 13.63466980452883881, -12.01375889529407281, 32.43194544308182969 ) ) ;
#30229 = CYLINDRICAL_SURFACE ( 'NONE', #75634, 0.2500000000000009437 ) ;
#30230 = ORIENTED_EDGE ( 'NONE', *, *, #73537, .T. ) ;
#30231 = ORIENTED_EDGE ( 'NONE', *, *, #4853, .T. ) ;
#30232 = FACE_BOUND ( 'NONE', #21927, .T. ) ;
#30233 = VERTEX_POINT ( 'NONE', #3628 ) ;
#30234 = CARTESIAN_POINT ( 'NONE',  ( 15.16468581981334829, -12.37446782046654192, 30.86335684631486487 ) ) ;
#30235 = AXIS2_PLACEMENT_3D ( 'NONE', #54094, #68074, #28402 ) ;
#30236 = CYLINDRICAL_SURFACE ( 'NONE', #70888, 0.2499999999999998890 ) ;
#30237 = CARTESIAN_POINT ( 'NONE',  ( -2.307692307692305711, -9.905515769479276145, 34.41647553114623292 ) ) ;
#30238 = VERTEX_POINT ( 'NONE', #64431 ) ;
#30239 = B_SPLINE_CURVE_WITH_KNOTS ( 'NONE', 3,
 ( #45636, #86650, #38442, #37536, #31690, #78976, #57370, #65003, #3312, #85743 ),
 .UNSPECIFIED., .F., .F.,
 ( 4, 2, 2, 2, 4 ),
 ( 0.0007817359430256388964, 0.0009771253907250073822, 0.001172514838424375868, 0.001367904286123744571, 0.001563293733823113056 ),
 .UNSPECIFIED. ) ;
#30240 = VERTEX_POINT ( 'NONE', #72091 ) ;
#30241 = EDGE_CURVE ( 'NONE', #33427, #2097, #7077, .T. ) ;
#30242 = ORIENTED_EDGE ( 'NONE', *, *, #43074, .T. ) ;
#30243 = CARTESIAN_POINT ( 'NONE',  ( 3.453780582382079967, -4.887748414852789658, 34.01359900205216746 ) ) ;
#30244 = EDGE_LOOP ( 'NONE', ( #3552, #30713, #39357, #74415 ) ) ;
#30245 = CARTESIAN_POINT ( 'NONE',  ( 15.93091993633000136, -9.886141570436013382, 34.14413921362392301 ) ) ;
#30246 = VECTOR ( 'NONE', #19627, 1000.000000000000000 ) ;
#30247 = CARTESIAN_POINT ( 'NONE',  ( -5.999999999999998224, -9.584722331328613620, 36.20867863119891439 ) ) ;
#30248 = CARTESIAN_POINT ( 'NONE',  ( -11.53846153846153655, -12.62096338111211580, 30.90682066428153263 ) ) ;
#30249 = FACE_BOUND ( 'NONE', #3640, .T. ) ;
#30250 = ORIENTED_EDGE ( 'NONE', *, *, #15156, .F. ) ;
#30251 = CARTESIAN_POINT ( 'NONE',  ( 13.31853300525524908, -10.67929555188718460, 33.92786785259543336 ) ) ;
#30252 = AXIS2_PLACEMENT_3D ( 'NONE', #68583, #129, #69471 ) ;
#30253 = CARTESIAN_POINT ( 'NONE',  ( 10.61538461538461675, -2.499999999999998668, 29.75000000000001421 ) ) ;
#30254 = CARTESIAN_POINT ( 'NONE',  ( -14.43783951713053249, -9.418419913701741919, 34.36755862841477693 ) ) ;
#30255 = CARTESIAN_POINT ( 'NONE',  ( 11.53846153846141753, -8.613356846316285953, 34.62446782046622218 ) ) ;
#30256 = EDGE_LOOP ( 'NONE', ( #4509, #10182 ) ) ;
#30257 = EDGE_CURVE ( 'NONE', #23024, #30665, #59615, .T. ) ;
#30258 = PRODUCT_DEFINITION_CONTEXT ( 'detailed design', #8399, 'design' ) ;
#30259 = ORIENTED_EDGE ( 'NONE', *, *, #84287, .T. ) ;
#30260 = EDGE_CURVE ( 'NONE', #47846, #81242, #9075, .T. ) ;
#30261 = AXIS2_PLACEMENT_3D ( 'NONE', #68740, #7036, #34513 ) ;
#30262 = EDGE_LOOP ( 'NONE', ( #79648, #74371 ) ) ;
#30264 = CARTESIAN_POINT ( 'NONE',  ( 4.153846153846154188, -5.557115091759785130, 34.35708131394839171 ) ) ;
#30263 = DIRECTION ( 'NONE',  ( -0.000000000000000000, -0.6427876096865404731, -0.7660444431189771253 ) ) ;
#30265 = CARTESIAN_POINT ( 'NONE',  ( 15.90382291655318880, -5.851115903089112003, 34.47074536777953568 ) ) ;
#30266 = FACE_OUTER_BOUND ( 'NONE', #27641, .T. ) ;
#30267 = CARTESIAN_POINT ( 'NONE',  ( -18.25002322422145440, -5.765609946408404518, 34.70566812827425451 ) ) ;
#30268 = CARTESIAN_POINT ( 'NONE',  ( -15.23076923076922995, -12.29105614889573062, 35.45975837776705220 ) ) ;
#30269 = ORIENTED_EDGE ( 'NONE', *, *, #75639, .T. ) ;
#30270 = FACE_OUTER_BOUND ( 'NONE', #81143, .T. ) ;
#30271 = EDGE_CURVE ( 'NONE', #58140, #5565, #36105, .T. ) ;
#30272 = CARTESIAN_POINT ( 'NONE',  ( -27.00000000000000000, -1.250000000000001110, 22.25000000000000000 ) ) ;
#30273 = DIRECTION ( 'NONE',  ( -0.000000000000000000, 0.6427876096865404731, -0.7660444431189771253 ) ) ;
#30274 = CARTESIAN_POINT ( 'NONE',  ( 13.16168916709923664, -12.39988816332205701, 30.74660775122750778 ) ) ;
#30275 = ORIENTED_EDGE ( 'NONE', *, *, #8581, .F. ) ;
#30276 = EDGE_LOOP ( 'NONE', ( #88058, #6652 ) ) ;
#30277 = FACE_BOUND ( 'NONE', #83141, .T. ) ;
#30278 = CARTESIAN_POINT ( 'NONE',  ( 11.53846153846153832, -6.435427911321262684, 35.78748833219616898 ) ) ;
#30279 = CARTESIAN_POINT ( 'NONE',  ( 12.46153846153833911, -12.27809138561165270, 31.22303859784587132 ) ) ;
#30280 = ORIENTED_EDGE ( 'NONE', *, *, #77378, .F. ) ;
#30281 = CARTESIAN_POINT ( 'NONE',  ( -16.15384615384615330, -11.35647404775217417, 33.31231777344666511 ) ) ;
#30282 = CARTESIAN_POINT ( 'NONE',  ( 6.223012844093396723, -11.43677907613344757, 33.22367315496201456 ) ) ;
#30283 = CARTESIAN_POINT ( 'NONE',  ( -3.512820512820513663, -3.499999999999999556, 29.75000000000000355 ) ) ;
#30284 = CARTESIAN_POINT ( 'NONE',  ( 4.219101293358989757, -6.835583212224609184, 34.95778746994559327 ) ) ;
#30285 = ORIENTED_EDGE ( 'NONE', *, *, #11072, .F. ) ;
#30286 = FACE_OUTER_BOUND ( 'NONE', #21920, .T. ) ;
#30287 = ORIENTED_EDGE ( 'NONE', *, *, #3762, .F. ) ;
#30289 = EDGE_LOOP ( 'NONE', ( #72248, #30151, #2706, #67470 ) ) ;
#30288 = DIRECTION ( 'NONE',  ( -1.000000000000000000, -0.000000000000000000, -0.000000000000000000 ) ) ;
#30290 = CARTESIAN_POINT ( 'NONE',  ( -8.638705067467212118, -10.19071101563364756, 33.96452234770658407 ) ) ;
#30291 = CARTESIAN_POINT ( 'NONE',  ( 15.16549878480845770, -2.892918686051582533, 31.69288490824015980 ) ) ;
#30292 = CARTESIAN_POINT ( 'NONE',  ( -11.53846153846166089, -2.657715359629662544, 31.77849191805970364 ) ) ;
#30293 = ADVANCED_FACE ( 'NONE', ( #36966 ), #63558, .F. ) ;
#30294 = DIRECTION ( 'NONE',  ( -0.000000000000000000, 0.7660444431189791237, -0.6427876096865379196 ) ) ;
#30295 = PLANE ( 'NONE',  #33281 ) ;
#30296 = CARTESIAN_POINT ( 'NONE',  ( -9.757577692864012775, -12.16647553114622049, 32.15551576947930812 ) ) ;
#30297 = VECTOR ( 'NONE', #24312, 999.9999999999998863 ) ;
#30298 = CARTESIAN_POINT ( 'NONE',  ( 1.944543648263018731, -9.444543648262994751, 24.62500000000000000 ) ) ;
#30299 = ORIENTED_EDGE ( 'NONE', *, *, #14678, .F. ) ;
#30300 = CARTESIAN_POINT ( 'NONE',  ( -0.4615384615384611200, -5.557115091759785130, 34.35708131394839171 ) ) ;
#30301 = CARTESIAN_POINT ( 'NONE',  ( 13.16178728698051081, -7.369209533119137845, 34.99857337881830688 ) ) ;
#30302 = ORIENTED_EDGE ( 'NONE', *, *, #67457, .F. ) ;
#30303 = ORIENTED_EDGE ( 'NONE', *, *, #35419, .T. ) ;
#30304 = EDGE_LOOP ( 'NONE', ( #22633, #84850 ) ) ;
#30305 = CARTESIAN_POINT ( 'NONE',  ( 17.01165263096229907, -5.219633306516282545, 34.19971097300152252 ) ) ;
#30306 = CARTESIAN_POINT ( 'NONE',  ( 12.52679360105129724, -4.320704448112861584, 33.92786785259548310 ) ) ;
#30307 = CARTESIAN_POINT ( 'NONE',  ( 7.134615384615385025, -7.500000000000000000, 29.75000000000000355 ) ) ;
#30308 = CARTESIAN_POINT ( 'NONE',  ( 9.442284455014730682, -12.43535235679832596, 30.55408501211184813 ) ) ;
#30309 = LINE ( 'NONE', #57778, #71860 ) ;
#30310 = CYLINDRICAL_SURFACE ( 'NONE', #26975, 0.2500000000000008882 ) ;
#30311 = CARTESIAN_POINT ( 'NONE',  ( 5.750000000000002665, -7.500000000000001776, 35.00000000000000000 ) ) ;
#30312 = VERTEX_POINT ( 'NONE', #30657 ) ;
#30313 = CARTESIAN_POINT ( 'NONE',  ( 6.249945518348142492, -10.76462480002816235, 33.53768742498949962 ) ) ;
#30314 = CARTESIAN_POINT ( 'NONE',  ( -0.2387589202700521329, -8.496831190052095195, 34.64984203495477288 ) ) ;
#30315 = B_SPLINE_CURVE_WITH_KNOTS ( 'NONE', 3,
 ( #68397, #48118, #54887, #33732, #66630, #81042, #47234, #6695, #13015, #87816 ),
 .UNSPECIFIED., .F., .F.,
 ( 4, 2, 2, 2, 4 ),
 ( 0.0007817246256747444619, 0.0009771112852218868158, 0.001172497944769029061, 0.001367884604316171523, 0.001563271263863313769 ),
 .UNSPECIFIED. ) ;
#30316 = CARTESIAN_POINT ( 'NONE',  ( -6.000000000000119904, -6.026961402154118908, 34.52809138561165270 ) ) ;
#30317 = CARTESIAN_POINT ( 'NONE',  ( 8.096208157792164073, -2.779044189368097495, 31.39831045268886456 ) ) ;
#30318 = ORIENTED_EDGE ( 'NONE', *, *, #16746, .T. ) ;
#30319 = CARTESIAN_POINT ( 'NONE',  ( -7.846153846153965716, -8.613356846316285953, 34.62446782046622218 ) ) ;
#30320 = AXIS2_PLACEMENT_3D ( 'NONE', #64796, #78768, #65248 ) ;
#30321 = VECTOR ( 'NONE', #20309, 1000.000000000000000 ) ;
#30322 = VERTEX_POINT ( 'NONE', #37411 ) ;
#30323 = CARTESIAN_POINT ( 'NONE',  ( -17.07692307692319744, -2.657715359629662988, 31.77849191805970364 ) ) ;
#30324 = CARTESIAN_POINT ( 'NONE',  ( -3.230769230769351186, -2.892918686052166066, 31.69288490824153470 ) ) ;
#30325 = FACE_OUTER_BOUND ( 'NONE', #18837, .T. ) ;
#30326 = ORIENTED_EDGE ( 'NONE', *, *, #75306, .T. ) ;
#30327 = CARTESIAN_POINT ( 'NONE',  ( 5.750023269057647823, -9.943427161483782584, 34.11278801902876978 ) ) ;
#30328 = CARTESIAN_POINT ( 'NONE',  ( -10.48485891362104994, -10.88167719472716399, 33.43325721877153711 ) ) ;
#30329 = VECTOR ( 'NONE', #43351, 1000.000000000000114 ) ;
#30330 = CARTESIAN_POINT ( 'NONE',  ( -17.20748366866499879, -2.504760397472873823, 29.97295953869789997 ) ) ;
#30331 = EDGE_CURVE ( 'NONE', #55785, #25570, #42521, .T. ) ;
#30332 = CARTESIAN_POINT ( 'NONE',  ( -12.46153846153846168, -10.51840700105979565, 33.73612834413961536 ) ) ;
#30333 = ORIENTED_EDGE ( 'NONE', *, *, #2867, .F. ) ;
#30334 = CARTESIAN_POINT ( 'NONE',  ( 16.40390057375961064, -10.06805714834173138, 34.32951233291982618 ) ) ;
#30335 = ORIENTED_EDGE ( 'NONE', *, *, #30653, .T. ) ;
#30336 = DIRECTION ( 'NONE',  ( 0.000000000000000000, 0.9396926207859126468, 0.3420201433256571111 ) ) ;
#30337 = CARTESIAN_POINT ( 'NONE',  ( 9.019285189144222059, -9.233818618650603938, 34.70587769442853698 ) ) ;
#30338 = CARTESIAN_POINT ( 'NONE',  ( 7.846153846153723244, -2.657715359629662544, 31.77849191805970364 ) ) ;
#30339 = CARTESIAN_POINT ( 'NONE',  ( -5.076923076923075762, -8.120952969808772792, 34.71129190930000163 ) ) ;
#30340 = CARTESIAN_POINT ( 'NONE',  ( -7.596153846152425615, -7.500000000000154543, 35.00000000000007105 ) ) ;
#30341 = ORIENTED_EDGE ( 'NONE', *, *, #20694, .T. ) ;
#30342 = ORIENTED_EDGE ( 'NONE', *, *, #84991, .F. ) ;
#30343 = B_SPLINE_CURVE_WITH_KNOTS ( 'NONE', 3,
 ( #60588, #48401, #54267, #6544, #26370, #34005 ),
 .UNSPECIFIED., .F., .F.,
 ( 4, 2, 4 ),
 ( 5.307410501141271501E-17, 0.0001954756301637260456, 0.0003909512603273990194 ),
 .UNSPECIFIED. ) ;
#30345 = B_SPLINE_CURVE_WITH_KNOTS ( 'NONE', 3,
 ( #80742, #40635, #81616, #54123, #14479, #33861, #81, #68104, #55027, #12710 ),
 .UNSPECIFIED., .F., .F.,
 ( 4, 2, 2, 2, 4 ),
 ( 0.000000000000000000, 0.0001954339857564073388, 0.0003908679715128146777, 0.0005863019572692220165, 0.0007817359430256293554 ),
 .UNSPECIFIED. ) ;
#30344 = AXIS2_PLACEMENT_3D ( 'NONE', #54131, #47382, #13164 ) ;
#30346 = ORIENTED_EDGE ( 'NONE', *, *, #63023, .T. ) ;
#30347 = ORIENTED_EDGE ( 'NONE', *, *, #26788, .F. ) ;
#30348 = CARTESIAN_POINT ( 'NONE',  ( -10.36533030374629760, -8.303483539816728154, 34.68545999027711702 ) ) ;
#30349 = DIRECTION ( 'NONE',  ( -0.000000000000000000, -0.7660444431189791237, -0.6427876096865379196 ) ) ;
#30350 = VECTOR ( 'NONE', #2911, 1000.000000000000114 ) ;
#30351 = CARTESIAN_POINT ( 'NONE',  ( -15.16470087976679615, -8.973038597847271092, 34.52809138561121216 ) ) ;
#30352 = DIRECTION ( 'NONE',  ( -0.000000000000000000, -0.6427876096865404731, -0.7660444431189770143 ) ) ;
#30353 = CARTESIAN_POINT ( 'NONE',  ( -23.00000000000000000, -9.499999999999982236, 27.25000000000000000 ) ) ;
#30355 = ADVANCED_FACE ( 'NONE', ( #29345 ), #78400, .F. ) ;
#30354 = CARTESIAN_POINT ( 'NONE',  ( 8.519254038288416098, -9.148715823498378086, 34.47080413974185120 ) ) ;
#30356 = DIRECTION ( 'NONE',  ( 0.000000000000000000, 1.000000000000000000, 0.000000000000000000 ) ) ;
#30357 = CARTESIAN_POINT ( 'NONE',  ( 20.00000000000000000, -4.000000000000000000, 29.75000000000000355 ) ) ;
#30358 = VERTEX_POINT ( 'NONE', #43298 ) ;
#30359 = VERTEX_POINT ( 'NONE', #3184 ) ;
#30360 = ORIENTED_EDGE ( 'NONE', *, *, #37624, .F. ) ;
#30362 = VERTEX_POINT ( 'NONE', #58127 ) ;
#30361 = LINE ( 'NONE', #58713, #1401 ) ;
#30364 = CYLINDRICAL_SURFACE ( 'NONE', #70735, 0.2499999999999986955 ) ;
#30363 = CARTESIAN_POINT ( 'NONE',  ( 0.5267940328144846696, -8.613356846314930593, 34.62446782046653482 ) ) ;
#30365 = LINE ( 'NONE', #31250, #86414 ) ;
#30366 = CARTESIAN_POINT ( 'NONE',  ( 3.750000000000009770, -9.053300858899081760, 23.29687500000000000 ) ) ;
#30367 = VERTEX_POINT ( 'NONE', #85610 ) ;
#30368 = CIRCLE ( 'NONE', #37559, 0.2500000000000002220 ) ;
#30369 = EDGE_CURVE ( 'NONE', #42722, #12295, #17144, .T. ) ;
#30370 = VERTEX_POINT ( 'NONE', #78842 ) ;
#30371 = CARTESIAN_POINT ( 'NONE',  ( -11.53846153846166089, -12.16647553114689728, 32.15551576947799362 ) ) ;
#30372 = ORIENTED_EDGE ( 'NONE', *, *, #35682, .F. ) ;
#30373 = FACE_BOUND ( 'NONE', #7674, .T. ) ;
#30374 = FACE_OUTER_BOUND ( 'NONE', #38280, .T. ) ;
#30375 = AXIS2_PLACEMENT_3D ( 'NONE', #78458, #38373, #65826 ) ;
#30376 = CARTESIAN_POINT ( 'NONE',  ( 15.93036121012220541, -6.760086850603066466, 34.69517049084099369 ) ) ;
#30377 = EDGE_LOOP ( 'NONE', ( #28517, #9843, #58282, #17273 ) ) ;
#30378 = LINE ( 'NONE', #15098, #27653 ) ;
#30379 = DIRECTION ( 'NONE',  ( 0.000000000000000000, 0.000000000000000000, 1.000000000000000000 ) ) ;
#30380 = DIRECTION ( 'NONE',  ( -0.000000000000000000, 0.6427876096865404731, -0.7660444431189771253 ) ) ;
#30381 = ORIENTED_EDGE ( 'NONE', *, *, #19290, .F. ) ;
#30382 = CARTESIAN_POINT ( 'NONE',  ( 9.692307692307695177, -7.500000000000001776, 35.04278698407183867 ) ) ;
#30383 = CARTESIAN_POINT ( 'NONE',  ( -13.25408968285181821, -11.93748526763465279, 32.05452791011430946 ) ) ;
#30384 = ORIENTED_EDGE ( 'NONE', *, *, #59236, .T. ) ;
#30385 = CARTESIAN_POINT ( 'NONE',  ( 3.296837581771669523, -8.120952969808772792, 34.71129190929999453 ) ) ;
#30386 = CARTESIAN_POINT ( 'NONE',  ( 7.053867364043873600, -2.494656445102013453, 31.33466734024120015 ) ) ;
#30387 = CARTESIAN_POINT ( 'NONE',  ( -12.46153846153846168, -12.78798330534102945, 29.74999999999997868 ) ) ;
#30388 = CARTESIAN_POINT ( 'NONE',  ( -16.02305434602136103, -8.147973898785416225, 34.70805048591653730 ) ) ;
#30389 = CARTESIAN_POINT ( 'NONE',  ( -8.546451227962359454, -9.332535724633409302, 34.40230450496446934 ) ) ;
#30390 = CARTESIAN_POINT ( 'NONE',  ( -18.13014720943822056, -6.852621066184265253, 34.70813303252209181 ) ) ;
#30391 = EDGE_CURVE ( 'NONE', #221, #47746, #72641, .T. ) ;
#30392 = CARTESIAN_POINT ( 'NONE',  ( 8.096208266067296933, -2.920487667080175598, 32.31805714834170828 ) ) ;
#30394 = CARTESIAN_POINT ( 'NONE',  ( 7.173022441425065843, -3.202959910592335202, 32.30730279482227019 ) ) ;
#30393 = CARTESIAN_POINT ( 'NONE',  ( 19.00000000000000000, -8.999999999999998224, 22.25000000000000000 ) ) ;
#30395 = CARTESIAN_POINT ( 'NONE',  ( 23.49999999999998934, -5.499999999999981348, 27.75000000000000000 ) ) ;
#30397 = CARTESIAN_POINT ( 'NONE',  ( 12.46153846153833911, -5.094484230521993062, 34.41647553114689373 ) ) ;
#30396 = CARTESIAN_POINT ( 'NONE',  ( 12.59158589678891715, -7.723484941389743952, 34.99544897038808955 ) ) ;
#30398 = EDGE_CURVE ( 'NONE', #52292, #29866, #59717, .T. ) ;
#30399 = LINE ( 'NONE', #49775, #8857 ) ;
#30400 = CARTESIAN_POINT ( 'NONE',  ( 1.901340078031349856, -5.512252781505337929, 22.81063170625848713 ) ) ;
#30401 = ORIENTED_EDGE ( 'NONE', *, *, #2867, .T. ) ;
#30402 = EDGE_CURVE ( 'NONE', #19139, #81634, #4977, .T. ) ;
#30403 = CARTESIAN_POINT ( 'NONE',  ( 3.365693839367760010, -7.795565839780282502, 14.00000000000000178 ) ) ;
#30404 = EDGE_LOOP ( 'NONE', ( #8559, #12069, #54275, #68797 ) ) ;
#30405 = CARTESIAN_POINT ( 'NONE',  ( 9.561616225640134914, -6.413092428213692742, 34.63065189839063152 ) ) ;
#30406 = EDGE_CURVE ( 'NONE', #84690, #28560, #68339, .T. ) ;
#30407 = ORIENTED_EDGE ( 'NONE', *, *, #17151, .F. ) ;
#30408 = EDGE_CURVE ( 'NONE', #54790, #34521, #65768, .T. ) ;
#30409 = CARTESIAN_POINT ( 'NONE',  ( -13.38461538461550759, -2.379036618888197729, 30.90682066428292885 ) ) ;
#30410 = VERTEX_POINT ( 'NONE', #74323 ) ;
#30411 = CYLINDRICAL_SURFACE ( 'NONE', #21095, 4.000000000000000000 ) ;
#30412 = CARTESIAN_POINT ( 'NONE',  ( 1.901340078031349856, -5.512252781505337929, 21.56063170625849068 ) ) ;
#30413 = LINE ( 'NONE', #36725, #57328 ) ;
#30414 = CARTESIAN_POINT ( 'NONE',  ( 6.923076923076802558, -11.48612834414049644, 32.76840700105863391 ) ) ;
#30415 = CYLINDRICAL_SURFACE ( 'NONE', #70560, 1.999999999999998224 ) ;
#30416 = CARTESIAN_POINT ( 'NONE',  ( -14.55771553191376633, -10.92453946501458795, 33.72985991061850086 ) ) ;
#30417 = CARTESIAN_POINT ( 'NONE',  ( 7.846153846153846700, -7.500000000000001776, 35.04278698407183867 ) ) ;
#30418 = CARTESIAN_POINT ( 'NONE',  ( 15.10015887114470523, -7.722926236386453702, 34.74524107206102030 ) ) ;
#30419 = CARTESIAN_POINT ( 'NONE',  ( 20.00000000000000000, -4.000000000000000000, 29.75000000000000355 ) ) ;
#30420 = CARTESIAN_POINT ( 'NONE',  ( -3.750000000000008438, -5.946699141100917352, 17.67187500000000355 ) ) ;
#30421 = CARTESIAN_POINT ( 'NONE',  ( -10.61538461538461320, -2.721908614388771852, 31.22303859784724978 ) ) ;
#30422 = CARTESIAN_POINT ( 'NONE',  ( 14.30769230769231015, -10.51840700105979565, 33.73612834413961536 ) ) ;
#30423 = CIRCLE ( 'NONE', #43343, 4.000000000000000000 ) ;
#30424 = CARTESIAN_POINT ( 'NONE',  ( 13.38461538461526601, -4.481592998941358097, 33.73612834414048933 ) ) ;
#30425 = CARTESIAN_POINT ( 'NONE',  ( -2.651650429449565305, -4.848349570550461785, 15.25000000000000000 ) ) ;
#30426 = EDGE_LOOP ( 'NONE', ( #40212, #74806 ) ) ;
#30427 = CARTESIAN_POINT ( 'NONE',  ( -13.60754234352223335, -6.459968553980841577, 34.89616026154728701 ) ) ;
#30428 = PLANE ( 'NONE',  #1405 ) ;
#30429 = CARTESIAN_POINT ( 'NONE',  ( -39.05038313613820122, -2.249999999999998668, 29.75000000000000355 ) ) ;
#30430 = CARTESIAN_POINT ( 'NONE',  ( 18.24994551834813805, -10.76462480002816413, 33.53768742498949962 ) ) ;
#30431 = CARTESIAN_POINT ( 'NONE',  ( 15.45373213433071768, -7.369474270740069777, 34.74850911626239736 ) ) ;
#30432 = LINE ( 'NONE', #63328, #58650 ) ;
#30433 = EDGE_CURVE ( 'NONE', #61908, #10320, #73880, .T. ) ;
#30434 = ORIENTED_EDGE ( 'NONE', *, *, #83886, .F. ) ;
#30435 = LINE ( 'NONE', #16481, #32854 ) ;
#30436 = ORIENTED_EDGE ( 'NONE', *, *, #9324, .F. ) ;
#30437 = EDGE_LOOP ( 'NONE', ( #31973, #70197, #15759, #72993 ) ) ;
#30438 = AXIS2_PLACEMENT_3D ( 'NONE', #69588, #34910, #13755 ) ;
#30439 = CARTESIAN_POINT ( 'NONE',  ( 12.94230769230769340, -3.499999999999999556, 29.75000000000000355 ) ) ;
#30440 = LINE ( 'NONE', #36322, #61414 ) ;
#30441 = CARTESIAN_POINT ( 'NONE',  ( -15.23076923076935252, -11.06231777344772027, 33.60647404775119895 ) ) ;
#30442 = CARTESIAN_POINT ( 'NONE',  ( 1.515141086378952062, -11.93748526763465279, 32.05452791011430946 ) ) ;
#30443 = CARTESIAN_POINT ( 'NONE',  ( 6.000000000000001776, -8.318370150425687726, 35.83090037661290239 ) ) ;
#30444 = EDGE_CURVE ( 'NONE', #77110, #12785, #7818, .T. ) ;
#30445 = VERTEX_POINT ( 'NONE', #5422 ) ;
#30446 = CARTESIAN_POINT ( 'NONE',  ( 24.00000000000000000, -5.499999999999981348, 27.75000000000000000 ) ) ;
#30447 = ORIENTED_EDGE ( 'NONE', *, *, #43658, .F. ) ;
#30448 = EDGE_LOOP ( 'NONE', ( #69098, #87420 ) ) ;
#30449 = CARTESIAN_POINT ( 'NONE',  ( 13.16168842570853492, -4.762599654559228846, 34.23009711892697737 ) ) ;
#30450 = CARTESIAN_POINT ( 'NONE',  ( 8.545745825506823934, -2.847400154188068022, 31.58180166144859058 ) ) ;
#30451 = FACE_OUTER_BOUND ( 'NONE', #85516, .T. ) ;
#30452 = EDGE_CURVE ( 'NONE', #54595, #28559, #22072, .T. ) ;
#30453 = CARTESIAN_POINT ( 'NONE',  ( -11.53846153846166089, -8.656820664282941280, 34.87096338111179961 ) ) ;
#30454 = CARTESIAN_POINT ( 'NONE',  ( -16.15384615384627409, -5.941354392335915335, 34.76329471203413846 ) ) ;
#30455 = ORIENTED_EDGE ( 'NONE', *, *, #68324, .F. ) ;
#30456 = EDGE_CURVE ( 'NONE', #36253, #5298, #32889, .T. ) ;
#30457 = EDGE_LOOP ( 'NONE', ( #45895, #88124, #77143, #79630 ) ) ;
#30458 = CARTESIAN_POINT ( 'NONE',  ( -2.651650429449535551, -10.15165042944956753, 23.68750000000000000 ) ) ;
#30459 = EDGE_LOOP ( 'NONE', ( #37530, #72012, #15708, #70788 ) ) ;
#30461 = ORIENTED_EDGE ( 'NONE', *, *, #4038, .T. ) ;
#30460 = CARTESIAN_POINT ( 'NONE',  ( -13.60810030917971680, -5.827078755546623690, 34.72654668319379567 ) ) ;
#30462 = CARTESIAN_POINT ( 'NONE',  ( -7.173053654019277303, -12.41269422305637171, 30.68257228309993323 ) ) ;
#30463 = LINE ( 'NONE', #30900, #1459 ) ;
#30464 = VECTOR ( 'NONE', #20420, 1000.000000000000114 ) ;
#30465 = DIRECTION ( 'NONE',  ( -1.000000000000000000, 0.000000000000000000, 0.000000000000000000 ) ) ;
#30466 = ORIENTED_EDGE ( 'NONE', *, *, #54380, .T. ) ;
#30467 = EDGE_CURVE ( 'NONE', #8934, #42078, #33340, .T. ) ;
#30468 = VECTOR ( 'NONE', #31314, 1000.000000000000000 ) ;
#30469 = DIRECTION ( 'NONE',  ( -0.000000000000000000, 0.9848077530122086864, -0.1736481776669273891 ) ) ;
#30470 = ORIENTED_EDGE ( 'NONE', *, *, #16989, .T. ) ;
#30471 = CARTESIAN_POINT ( 'NONE',  ( 5.933917620639865831, -9.058645607665454236, 34.76329471203372634 ) ) ;
#30472 = LINE ( 'NONE', #3440, #70223 ) ;
#30473 = B_SPLINE_CURVE_WITH_KNOTS ( 'NONE', 3,
 ( #65523, #31304, #14805, #76046, #3377, #79042, #56222, #28761, #58769, #76499 ),
 .UNSPECIFIED., .F., .F.,
 ( 4, 2, 2, 2, 4 ),
 ( 0.0007817246256747474977, 0.0009771112852218909357, 0.001172497944769034482, 0.001367884604316178029, 0.001563271263863321575 ),
 .UNSPECIFIED. ) ;
#30474 = CARTESIAN_POINT ( 'NONE',  ( -2.307692307692305711, -13.87047571288749737, 32.06866353760679544 ) ) ;
#30476 = CARTESIAN_POINT ( 'NONE',  ( -6.857821351800899023, -2.625532179533470512, 30.86335684631491105 ) ) ;
#30475 = CARTESIAN_POINT ( 'NONE',  ( 5.776515075435669111, -12.47654668319379567, 31.42292124445336654 ) ) ;
#30477 = EDGE_CURVE ( 'NONE', #70917, #10589, #60799, .T. ) ;
#30478 = CARTESIAN_POINT ( 'NONE',  ( -0.5268084620947812713, -12.51329471203370325, 31.30864560766548976 ) ) ;
#30479 = CARTESIAN_POINT ( 'NONE',  ( -0.3310130233048159676, -12.70449254468099198, 30.44128974285582956 ) ) ;
#30480 = ORIENTED_EDGE ( 'NONE', *, *, #25178, .F. ) ;
#30481 = CARTESIAN_POINT ( 'NONE',  ( -10.83831083290076158, -9.886141570436013382, 34.14413921362392301 ) ) ;
#30482 = EDGE_CURVE ( 'NONE', #13813, #19489, #72533, .T. ) ;
#30483 = DIRECTION ( 'NONE',  ( -0.000000000000000000, 0.000000000000000000, -1.000000000000000000 ) ) ;
#30484 = ORIENTED_EDGE ( 'NONE', *, *, #40138, .T. ) ;
#30485 = CARTESIAN_POINT ( 'NONE',  ( 4.153846153846030731, -11.67786785259630911, 32.92929555188603530 ) ) ;
#30486 = CARTESIAN_POINT ( 'NONE',  ( 16.94677510719138169, -11.04286588640298916, 33.62463336215343901 ) ) ;
#30487 = DIRECTION ( 'NONE',  ( 0.000000000000000000, 0.000000000000000000, 1.000000000000000000 ) ) ;
#30488 = CARTESIAN_POINT ( 'NONE',  ( 10.61538461538461675, -12.78798330534102767, 29.49999999999997868 ) ) ;
#30489 = CYLINDRICAL_SURFACE ( 'NONE', #22674, 0.2500000000000009437 ) ;
#30490 = FACE_OUTER_BOUND ( 'NONE', #46973, .T. ) ;
#30491 = ADVANCED_FACE ( 'NONE', ( #34211 ), #21136, .F. ) ;
#30492 = FACE_BOUND ( 'NONE', #71073, .T. ) ;
#30494 = CARTESIAN_POINT ( 'NONE',  ( -6.923076923076922462, -10.05456864172156806, 36.03766855953608683 ) ) ;
#30493 = CARTESIAN_POINT ( 'NONE',  ( 12.46153846153833911, -3.300289026999228881, 32.46337939537708905 ) ) ;
#30495 = DIRECTION ( 'NONE',  ( 0.000000000000000000, 0.1736481776669275834, 0.9848077530122086864 ) ) ;
#30497 = FACE_OUTER_BOUND ( 'NONE', #47886, .T. ) ;
#30496 = CARTESIAN_POINT ( 'NONE',  ( -11.53846153846153655, -1.466349020453238561, 30.81389545987213907 ) ) ;
#30498 = CARTESIAN_POINT ( 'NONE',  ( 1.161749121552287711, -2.251424796025575770, 29.88072029997477586 ) ) ;
#30499 = CARTESIAN_POINT ( 'NONE',  ( 2.694853999681214862, -10.10844685921789043, 21.87313170625849068 ) ) ;
#30500 = AXIS2_PLACEMENT_3D ( 'NONE', #4924, #25630, #18874 ) ;
#30501 = VERTEX_POINT ( 'NONE', #68013 ) ;
#30502 = AXIS2_PLACEMENT_3D ( 'NONE', #67012, #54370, #82304 ) ;
#30503 = DIRECTION ( 'NONE',  ( -0.000000000000000000, -0.3420201433256694901, -0.9396926207859080948 ) ) ;
#30504 = EDGE_CURVE ( 'NONE', #69932, #26337, #2748, .T. ) ;
#30505 = CARTESIAN_POINT ( 'NONE',  ( -14.55766903863466055, -6.567427716900048118, 34.66269422305636283 ) ) ;
#30506 = CARTESIAN_POINT ( 'NONE',  ( 5.750023255951410839, -5.643011162660950042, 34.66104346484419096 ) ) ;
#30507 = CARTESIAN_POINT ( 'NONE',  ( -9.692307692307812417, -10.90142922262034020, 33.41473453929536674 ) ) ;
#30508 = CARTESIAN_POINT ( 'NONE',  ( -4.283994123577849145, -5.070767119584671079, 34.40440758774516183 ) ) ;
#30509 = CYLINDRICAL_SURFACE ( 'NONE', #9592, 0.2499999999999994726 ) ;
#30510 = CARTESIAN_POINT ( 'NONE',  ( -2.608446859217889546, -10.19485399968121264, 19.68563170625849068 ) ) ;
#30511 = AXIS2_PLACEMENT_3D ( 'NONE', #28321, #43170, #63876 ) ;
#30512 = CARTESIAN_POINT ( 'NONE',  ( -16.21992853320628569, -5.471508081941601986, 34.59228464037088457 ) ) ;
#30513 = DIRECTION ( 'NONE',  ( -0.000000000000000000, 1.000000000000000000, -0.000000000000000000 ) ) ;
#30514 = CARTESIAN_POINT ( 'NONE',  ( -17.01166750564705055, -6.026961402152789304, 34.52809138561124769 ) ) ;
#30515 = CARTESIAN_POINT ( 'NONE',  ( 17.75002325595141173, -8.347322224742351082, 34.93158281831414769 ) ) ;
#30516 = CARTESIAN_POINT ( 'NONE',  ( 4.153846153846032507, -12.46129190930018460, 30.37095296980731973 ) ) ;
#30517 = DIRECTION ( 'NONE',  ( -0.000000000000000000, -0.3420201433256694346, -0.9396926207859080948 ) ) ;
#30518 = CARTESIAN_POINT ( 'NONE',  ( -1.384615384615505151, -11.48612834414049644, 32.76840700105863391 ) ) ;
#30519 = CARTESIAN_POINT ( 'NONE',  ( -12.46153846153846168, -8.318370150425687726, 35.83090037661290239 ) ) ;
#30520 = ORIENTED_EDGE ( 'NONE', *, *, #48146, .T. ) ;
#30521 = CARTESIAN_POINT ( 'NONE',  ( 17.14299041027315695, -12.62096338111211757, 30.90682066428152908 ) ) ;
#30522 = CARTESIAN_POINT ( 'NONE',  ( 14.30769230769231015, -12.78798330534102945, 29.74999999999997868 ) ) ;
#30523 = CARTESIAN_POINT ( 'NONE',  ( -1.614399933863613468, -11.22469193450124969, 13.86124329374151820 ) ) ;
#30524 = CARTESIAN_POINT ( 'NONE',  ( 1.384615384615386802, -13.88283147151868846, 33.14645433367849847 ) ) ;
#30525 = DIRECTION ( 'NONE',  ( 1.000000000000000000, 0.000000000000000000, 0.000000000000000000 ) ) ;
#30526 = ORIENTED_EDGE ( 'NONE', *, *, #3481, .F. ) ;
#30527 = EDGE_CURVE ( 'NONE', #48794, #83351, #48607, .T. ) ;
#30528 = FACE_OUTER_BOUND ( 'NONE', #77530, .T. ) ;
#30529 = CARTESIAN_POINT ( 'NONE',  ( -10.61538461538473577, -9.528491918059723176, 34.59228464037033035 ) ) ;
#30531 = ORIENTED_EDGE ( 'NONE', *, *, #24612, .F. ) ;
#30530 = DIRECTION ( 'NONE',  ( 1.000000000000000000, 0.000000000000000000, 0.000000000000000000 ) ) ;
#30532 = CARTESIAN_POINT ( 'NONE',  ( 6.857806477116147548, -3.300289026998414865, 32.46337939537583139 ) ) ;
#30533 = CARTESIAN_POINT ( 'NONE',  ( -2.307692307692427391, -10.90142922262034020, 33.41473453929536674 ) ) ;
#30534 = CARTESIAN_POINT ( 'NONE',  ( -5.076923076923197442, -9.442884908241554243, 34.35708131394783038 ) ) ;
#30535 = DIRECTION ( 'NONE',  ( 0.000000000000000000, 0.8660254037844377084, -0.5000000000000015543 ) ) ;
#30536 = ORIENTED_EDGE ( 'NONE', *, *, #34763, .F. ) ;
#30537 = VECTOR ( 'NONE', #13996, 1000.000000000000000 ) ;
#30538 = LINE ( 'NONE', #77403, #30543 ) ;
#30539 = EDGE_CURVE ( 'NONE', #84142, #86621, #45209, .T. ) ;
#30540 = CARTESIAN_POINT ( 'NONE',  ( 1.576923076923075762, -7.500000000000000000, 29.75000000000000355 ) ) ;
#30541 = CARTESIAN_POINT ( 'NONE',  ( 4.023698944407931855, -10.19110544564092002, 33.96427741523702792 ) ) ;
#30542 = EDGE_LOOP ( 'NONE', ( #6689, #43314 ) ) ;
#30544 = ORIENTED_EDGE ( 'NONE', *, *, #4080, .F. ) ;
#30543 = VECTOR ( 'NONE', #58009, 1000.000000000000000 ) ;
#30545 = ADVANCED_FACE ( 'NONE', ( #434 ), #81532, .F. ) ;
#30546 = EDGE_LOOP ( 'NONE', ( #20254, #32489, #51534, #39278 ) ) ;
#30547 = EDGE_CURVE ( 'NONE', #44265, #18436, #71518, .T. ) ;
#30548 = CARTESIAN_POINT ( 'NONE',  ( -9.915233909823838232, -9.886141570436013382, 34.14413921362392301 ) ) ;
#30549 = CARTESIAN_POINT ( 'NONE',  ( 9.942362112221147186, -4.074993327901527351, 33.72946981652012255 ) ) ;
#30550 = FACE_OUTER_BOUND ( 'NONE', #38083, .T. ) ;
#30551 = EDGE_CURVE ( 'NONE', #3262, #12929, #61231, .T. ) ;
#30552 = DIRECTION ( 'NONE',  ( -0.000000000000000000, -0.000000000000000000, -1.000000000000000000 ) ) ;
#30553 = ORIENTED_EDGE ( 'NONE', *, *, #70435, .F. ) ;
#30554 = EDGE_LOOP ( 'NONE', ( #68961, #86534, #13185, #46654 ) ) ;
#30556 = EDGE_LOOP ( 'NONE', ( #61247, #34278 ) ) ;
#30555 = CARTESIAN_POINT ( 'NONE',  ( -1.318547033612945896, -4.786620604624113540, 33.94971097300155805 ) ) ;
#30557 = CARTESIAN_POINT ( 'NONE',  ( 16.40384615384615330, -2.499999999999998668, 29.75000000000000355 ) ) ;
#30558 = CARTESIAN_POINT ( 'NONE',  ( 1.634560902963528628, -10.76462480002816235, 33.53768742498949962 ) ) ;
#30559 = CARTESIAN_POINT ( 'NONE',  ( 15.93091919493930320, -11.43668979543635089, 33.22377378376089752 ) ) ;
#30560 = ORIENTED_EDGE ( 'NONE', *, *, #28144, .T. ) ;
#30561 = EDGE_CURVE ( 'NONE', #54522, #62121, #82860, .T. ) ;
#30562 = VECTOR ( 'NONE', #3940, 1000.000000000000114 ) ;
#30563 = ORIENTED_EDGE ( 'NONE', *, *, #4631, .T. ) ;
#30565 = EDGE_LOOP ( 'NONE', ( #55142, #6744, #20281, #38245 ) ) ;
#30564 = CARTESIAN_POINT ( 'NONE',  ( -9.692307692307691624, -12.62096338111211580, 30.90682066428153263 ) ) ;
#30566 = CARTESIAN_POINT ( 'NONE',  ( -5.869474298236436738, -8.586989748646452369, 34.63063291749215011 ) ) ;
#30567 = CARTESIAN_POINT ( 'NONE',  ( -10.74553258511630993, -9.504002272028875709, 34.60269587691767867 ) ) ;
#30568 = VERTEX_POINT ( 'NONE', #27020 ) ;
#30569 = DIRECTION ( 'NONE',  ( -0.000000000000000000, -1.000000000000000000, -0.000000000000000000 ) ) ;
#30570 = CARTESIAN_POINT ( 'NONE',  ( -14.30769230769230660, -12.62096338111211580, 30.90682066428153263 ) ) ;
#30571 = CARTESIAN_POINT ( 'NONE',  ( -8.992157728137616601, -11.98009711892699514, 32.48740034544076138 ) ) ;
#30572 = FACE_BOUND ( 'NONE', #158, .T. ) ;
#30573 = CARTESIAN_POINT ( 'NONE',  ( -11.78848477575450282, -2.587272538249755893, 30.68239716806877837 ) ) ;
#30574 = CARTESIAN_POINT ( 'NONE',  ( 2.307692307692187583, -8.613356846316285953, 34.62446782046622218 ) ) ;
#30575 = DIRECTION ( 'NONE',  ( -0.000000000000000000, -0.9848077530122086864, -0.1736481776669273613 ) ) ;
#30577 = CARTESIAN_POINT ( 'NONE',  ( 6.923076923076924238, -11.69971097300155272, 32.46337939537588113 ) ) ;
#30576 = CYLINDRICAL_SURFACE ( 'NONE', #73398, 0.2499999999999973355 ) ;
#30578 = CARTESIAN_POINT ( 'NONE',  ( -11.31545018684868964, -3.105924265160262543, 32.13625925475356127 ) ) ;
#30579 = CARTESIAN_POINT ( 'NONE',  ( 5.142991427925516668, -2.538708090699994813, 30.37095296980875503 ) ) ;
#30580 = ORIENTED_EDGE ( 'NONE', *, *, #32116, .F. ) ;
#30581 = CARTESIAN_POINT ( 'NONE',  ( -0.6089743589743589203, -4.000000000000000000, 29.75000000000000355 ) ) ;
#30582 = ORIENTED_EDGE ( 'NONE', *, *, #27779, .T. ) ;
#30583 = EDGE_LOOP ( 'NONE', ( #44959, #43642 ) ) ;
#30585 = CARTESIAN_POINT ( 'NONE',  ( 1.134592147322421418, -10.76384336483936011, 33.53834819971076087 ) ) ;
#30584 = CARTESIAN_POINT ( 'NONE',  ( -6.700065571464073777, -8.239487800360276282, 34.69522927552633718 ) ) ;
#30586 = VECTOR ( 'NONE', #29525, 1000.000000000000000 ) ;
#30587 = CARTESIAN_POINT ( 'NONE',  ( 2.307692307692309264, -2.538708090699994813, 30.37095296980875503 ) ) ;
#30588 = CARTESIAN_POINT ( 'NONE',  ( 14.53047197667037338, -4.226511098958373402, 33.85474049983370293 ) ) ;
#30589 = CYLINDRICAL_SURFACE ( 'NONE', #31491, 0.2499999999999973355 ) ;
#30590 = CARTESIAN_POINT ( 'NONE',  ( -4.153846153846274980, -3.643525952248796163, 33.31231777344771672 ) ) ;
#30591 = ORIENTED_EDGE ( 'NONE', *, *, #86924, .T. ) ;
#30592 = CARTESIAN_POINT ( 'NONE',  ( 18.00000000000000000, -2.486705287966279876, 31.30864560766543647 ) ) ;
#30593 = EDGE_CURVE ( 'NONE', #57207, #88166, #30808, .T. ) ;
#30594 = CARTESIAN_POINT ( 'NONE',  ( -15.16551365949320562, -10.21337939537593620, 33.94971097300152252 ) ) ;
#30595 = DIRECTION ( 'NONE',  ( 0.000000000000000000, 0.7660444431189822323, -0.6427876096865344779 ) ) ;
#30596 = LINE ( 'NONE', #4466, #32356 ) ;
#30597 = DIRECTION ( 'NONE',  ( -0.000000000000000000, -0.6427876096865404731, -0.7660444431189771253 ) ) ;
#30598 = CARTESIAN_POINT ( 'NONE',  ( -2.651650429449565305, -4.848349570550461785, 15.25000000000000000 ) ) ;
#30599 = ORIENTED_EDGE ( 'NONE', *, *, #2088, .F. ) ;
#30600 = EDGE_CURVE ( 'NONE', #61210, #66121, #88781, .T. ) ;
#30601 = EDGE_LOOP ( 'NONE', ( #71094, #52793 ) ) ;
#30602 = CARTESIAN_POINT ( 'NONE',  ( -10.61538461538461320, -1.951392089020283160, 34.73218667398347748 ) ) ;
#30604 = ORIENTED_EDGE ( 'NONE', *, *, #2404, .F. ) ;
#30603 = EDGE_CURVE ( 'NONE', #84061, #72551, #38184, .T. ) ;
#30605 = CARTESIAN_POINT ( 'NONE',  ( -5.076923076923075762, -1.129524287112498415, 32.06866353760679544 ) ) ;
#30606 = CARTESIAN_POINT ( 'NONE',  ( 18.00000000000000000, -11.35647404775217417, 33.31231777344666511 ) ) ;
#30607 = CARTESIAN_POINT ( 'NONE',  ( -14.05774678934416499, -6.696923467548660192, 34.68552623307873972 ) ) ;
#30608 = CARTESIAN_POINT ( 'NONE',  ( -0.5916864312701544115, -12.15440758774515473, 32.17923288041532004 ) ) ;
#30609 = CARTESIAN_POINT ( 'NONE',  ( 3.749999999999992006, -5.946699141100872943, 15.64062500000000178 ) ) ;
#30610 = DIRECTION ( 'NONE',  ( -0.000000000000000000, -0.5000000000000009992, -0.8660254037844380415 ) ) ;
#30611 = ORIENTED_EDGE ( 'NONE', *, *, #73094, .T. ) ;
#30612 = EDGE_CURVE ( 'NONE', #5024, #21466, #31711, .T. ) ;
#30613 = LINE ( 'NONE', #77917, #80370 ) ;
#30615 = EDGE_LOOP ( 'NONE', ( #55865, #72183, #37294, #39889 ) ) ;
#30614 = CARTESIAN_POINT ( 'NONE',  ( -1.253823576790596750, -8.999086150933472084, 34.52020707165672064 ) ) ;
#30616 = FACE_OUTER_BOUND ( 'NONE', #83104, .T. ) ;
#30617 = CARTESIAN_POINT ( 'NONE',  ( 3.453780582382079078, -2.758310577978208666, 31.33698337089302299 ) ) ;
#30618 = FACE_OUTER_BOUND ( 'NONE', #70130, .T. ) ;
#30619 = CARTESIAN_POINT ( 'NONE',  ( 0.7114839798866022802, -2.824170634883621744, 31.52227843825337317 ) ) ;
#30620 = LINE ( 'NONE', #58093, #82481 ) ;
#30621 = CARTESIAN_POINT ( 'NONE',  ( -2.980714919130917462, -11.28795663066794219, 33.01431243580653785 ) ) ;
#30622 = DIRECTION ( 'NONE',  ( -0.000000000000000000, 1.000000000000000000, 3.491481338843133355E-15 ) ) ;
#30623 = EDGE_CURVE ( 'NONE', #62427, #4695, #25102, .T. ) ;
#30624 = CARTESIAN_POINT ( 'NONE',  ( -3.775308065498748977, -8.992201783934593351, 19.01749329374151287 ) ) ;
#30625 = ORIENTED_EDGE ( 'NONE', *, *, #70658, .F. ) ;
#30626 = DIRECTION ( 'NONE',  ( 1.000000000000000000, 0.000000000000000000, 0.000000000000000000 ) ) ;
#30627 = CARTESIAN_POINT ( 'NONE',  ( -12.59214882116298995, -7.722926236386453702, 34.74524107206102030 ) ) ;
#30628 = LINE ( 'NONE', #70297, #56266 ) ;
#30629 = CARTESIAN_POINT ( 'NONE',  ( 2.749999999999995115, -6.360912703473971419, 24.39062500000000000 ) ) ;
#30630 = B_SPLINE_CURVE_WITH_KNOTS ( 'NONE', 3,
 ( #13241, #61406, #66850, #11461, #73165, #18224, #88046, #26307, #32181, #74060 ),
 .UNSPECIFIED., .F., .F.,
 ( 4, 2, 2, 2, 4 ),
 ( 0.000000000000000000, 0.0001954339857564071220, 0.0003908679715128142440, 0.0005863019572692213660, 0.0007817359430256284880 ),
 .UNSPECIFIED. ) ;
#30631 = CARTESIAN_POINT ( 'NONE',  ( -39.05038313613820122, -2.499999999999999556, 29.75000000000000355 ) ) ;
#30632 = CARTESIAN_POINT ( 'NONE',  ( 7.846153846153725020, -12.46129190930018460, 30.37095296980731973 ) ) ;
#30633 = EDGE_CURVE ( 'NONE', #49648, #60841, #3714, .T. ) ;
#30634 = ORIENTED_EDGE ( 'NONE', *, *, #1424, .T. ) ;
#30635 = CARTESIAN_POINT ( 'NONE',  ( -1.409462824231155764E-14, -4.749999999999999112, 20.40625000000000000 ) ) ;
#30636 = CARTESIAN_POINT ( 'NONE',  ( -15.36091720050092846, -4.299443229763728169, 33.91186481527756058 ) ) ;
#30637 = AXIS2_PLACEMENT_3D ( 'NONE', #2955, #71414, #85390 ) ;
#30638 = EDGE_LOOP ( 'NONE', ( #8192, #78825, #72272, #27328 ) ) ;
#30639 = CARTESIAN_POINT ( 'NONE',  ( -4.153846153846274980, -8.656820664282941280, 34.87096338111179961 ) ) ;
#30640 = ORIENTED_EDGE ( 'NONE', *, *, #82296, .F. ) ;
#30641 = CARTESIAN_POINT ( 'NONE',  ( 17.77707378248385339, -6.503392248772476236, 34.64988816332204635 ) ) ;
#30642 = B_SPLINE_CURVE_WITH_KNOTS ( 'NONE', 3,
 ( #25151, #80564, #31465, #11651, #32804, #59824 ),
 .UNSPECIFIED., .F., .F.,
 ( 4, 2, 4 ),
 ( 0.000000000000000000, 0.0001954784845028902421, 0.0003909569690057804843 ),
 .UNSPECIFIED. ) ;
#30643 = CARTESIAN_POINT ( 'NONE',  ( 17.01167208676183407, -2.506253911140460477, 30.00000000000013856 ) ) ;
#30644 = CARTESIAN_POINT ( 'NONE',  ( 2.294871794871793824, -11.50000000000000000, 29.75000000000000355 ) ) ;
#30645 = ORIENTED_EDGE ( 'NONE', *, *, #65322, .T. ) ;
#30646 = CARTESIAN_POINT ( 'NONE',  ( -12.23875879256039489, -10.97394488606064122, 33.68653795673694873 ) ) ;
#30647 = ORIENTED_EDGE ( 'NONE', *, *, #31910, .F. ) ;
#30648 = CARTESIAN_POINT ( 'NONE',  ( 13.25405547100202241, -2.254533558242299396, 29.97296025877827930 ) ) ;
#30649 = ADVANCED_FACE ( 'NONE', ( #70216 ), #63451, .F. ) ;
#30650 = ORIENTED_EDGE ( 'NONE', *, *, #87067, .F. ) ;
#30651 = CARTESIAN_POINT ( 'NONE',  ( -14.87820512820512953, -3.499999999999999556, 29.75000000000000355 ) ) ;
#30652 = FACE_OUTER_BOUND ( 'NONE', #34745, .T. ) ;
#30653 = EDGE_CURVE ( 'NONE', #5428, #85310, #56696, .T. ) ;
#30654 = ORIENTED_EDGE ( 'NONE', *, *, #38460, .F. ) ;
#30655 = CARTESIAN_POINT ( 'NONE',  ( 11.53846153846153832, -12.62096338111211580, 30.90682066428153263 ) ) ;
#30656 = CARTESIAN_POINT ( 'NONE',  ( 10.74591031714818179, -3.285477652293413264, 32.44071101563363158 ) ) ;
#30657 = CARTESIAN_POINT ( 'NONE',  ( -2.544871794871793824, -4.000000000000000000, 29.75000000000000355 ) ) ;
#30658 = EDGE_CURVE ( 'NONE', #39653, #67493, #72464, .T. ) ;
#30659 = AXIS2_PLACEMENT_3D ( 'NONE', #48259, #82948, #21230 ) ;
#30660 = CARTESIAN_POINT ( 'NONE',  ( -14.05774689831426372, -10.18230066228895758, 34.26354781536631577 ) ) ;
#30661 = DIRECTION ( 'NONE',  ( -0.000000000000000000, 1.000000000000000000, -0.000000000000000000 ) ) ;
#30662 = ORIENTED_EDGE ( 'NONE', *, *, #68172, .F. ) ;
#30664 = ADVANCED_FACE ( 'NONE', ( #30550 ), #51232, .F. ) ;
#30663 = EDGE_LOOP ( 'NONE', ( #77470, #36534, #76440, #84999 ) ) ;
#30665 = VERTEX_POINT ( 'NONE', #15277 ) ;
#30667 = VERTEX_POINT ( 'NONE', #23780 ) ;
#30666 = CARTESIAN_POINT ( 'NONE',  ( 15.23076923076911093, -2.625532179533778709, 30.86335684631627174 ) ) ;
#30668 = DIRECTION ( 'NONE',  ( -0.000000000000000000, 0.3420201433256694901, -0.9396926207859082059 ) ) ;
#30669 = CARTESIAN_POINT ( 'NONE',  ( 5.142991427925513115, -4.098570777380720287, 33.41473453929635440 ) ) ;
#30670 = VERTEX_POINT ( 'NONE', #85501 ) ;
#30671 = EDGE_CURVE ( 'NONE', #34205, #25462, #19325, .T. ) ;
#30672 = VERTEX_POINT ( 'NONE', #37300 ) ;
#30673 = B_SPLINE_CURVE_WITH_KNOTS ( 'NONE', 3,
 ( #70413, #83493, #1950, #8274, #35746, #8716, #63197, #84378, #15475, #78480 ),
 .UNSPECIFIED., .F., .F.,
 ( 4, 2, 2, 2, 4 ),
 ( 0.0007817246256747483650, 0.0009771112852218926705, 0.001172497944769037084, 0.001367884604316181498, 0.001563271263863325695 ),
 .UNSPECIFIED. ) ;
#30674 = EDGE_CURVE ( 'NONE', #26195, #75911, #42755, .T. ) ;
#30675 = ORIENTED_EDGE ( 'NONE', *, *, #24995, .T. ) ;
#30676 = CARTESIAN_POINT ( 'NONE',  ( 4.153846153846032507, -10.90142922262034020, 33.41473453929536674 ) ) ;
#30677 = ORIENTED_EDGE ( 'NONE', *, *, #50763, .F. ) ;
#30678 = CARTESIAN_POINT ( 'NONE',  ( 11.66925334628632882, -11.18335022499818621, 33.13157742990016885 ) ) ;
#30679 = ADVANCED_FACE ( 'NONE', ( #3069 ), #78739, .F. ) ;
#30680 = VECTOR ( 'NONE', #44951, 1000.000000000000000 ) ;
#30681 = CARTESIAN_POINT ( 'NONE',  ( -11.78848477575450282, -3.711651800289232028, 33.01384336483936011 ) ) ;
#30682 = FACE_OUTER_BOUND ( 'NONE', #31998, .T. ) ;
#30683 = FACE_BOUND ( 'NONE', #71076, .T. ) ;
#30684 = ORIENTED_EDGE ( 'NONE', *, *, #39559, .T. ) ;
#30685 = AXIS2_PLACEMENT_3D ( 'NONE', #15923, #84385, #22665 ) ;
#30686 = CARTESIAN_POINT ( 'NONE',  ( -1.450372187129693513, -7.249945686854186278, 34.74374336980224598 ) ) ;
#30687 = VECTOR ( 'NONE', #47858, 1000.000000000000000 ) ;
#30688 = CARTESIAN_POINT ( 'NONE',  ( -14.24162395668986747, -5.557115091759786019, 34.35708131394839882 ) ) ;
#30689 = CARTESIAN_POINT ( 'NONE',  ( 2.241609928332172874, -8.164416787775445883, 34.95778746994557906 ) ) ;
#30690 = CARTESIAN_POINT ( 'NONE',  ( 18.00000000000000000, -8.318370150425687726, 35.83090037661290239 ) ) ;
#30691 = ORIENTED_EDGE ( 'NONE', *, *, #45090, .T. ) ;
#30692 = DIRECTION ( 'NONE',  ( -0.000000000000000000, 0.6427876096865404731, -0.7660444431189770143 ) ) ;
#30693 = ORIENTED_EDGE ( 'NONE', *, *, #87714, .F. ) ;
#30694 = ORIENTED_EDGE ( 'NONE', *, *, #67351, .T. ) ;
#30696 = CARTESIAN_POINT ( 'NONE',  ( 8.769230769230768274, -6.681629849574314051, 35.83090037661290239 ) ) ;
#30695 = DIRECTION ( 'NONE',  ( 0.000000000000000000, 0.000000000000000000, 1.000000000000000000 ) ) ;
#30697 = CARTESIAN_POINT ( 'NONE',  ( 16.08857570788537572, -6.026961402152685388, 34.52809138561120506 ) ) ;
#30698 = CARTESIAN_POINT ( 'NONE',  ( -3.931066612577742259, -4.387253974876676565, 33.66317474335728832 ) ) ;
#30699 = CARTESIAN_POINT ( 'NONE',  ( -18.24997674404858827, -5.643011162660949154, 34.66104346484419096 ) ) ;
#30700 = CARTESIAN_POINT ( 'NONE',  ( -12.39628289026243380, -4.481592998940250538, 33.73612834413965089 ) ) ;
#30701 = ORIENTED_EDGE ( 'NONE', *, *, #25571, .T. ) ;
#30702 = CARTESIAN_POINT ( 'NONE',  ( 6.923076923076924238, -1.790695186598648903, 34.54067556320373455 ) ) ;
#30703 = CARTESIAN_POINT ( 'NONE',  ( 3.165499230212911908, -9.528491918058357157, 34.59228464037090589 ) ) ;
#30704 = CARTESIAN_POINT ( 'NONE',  ( 4.403791672194294016, -9.272278438253401589, 34.42582936511637826 ) ) ;
#30705 = CARTESIAN_POINT ( 'NONE',  ( 13.25392391794783187, -12.38065189839062263, 30.83690757178629482 ) ) ;
#30706 = VERTEX_POINT ( 'NONE', #84189 ) ;
#30707 = VERTEX_POINT ( 'NONE', #49932 ) ;
#30708 = FACE_BOUND ( 'NONE', #50983, .T. ) ;
#30709 = B_SPLINE_CURVE_WITH_KNOTS ( 'NONE', 3,
 ( #12383, #11499, #39864, #26339, #4745, #26780, #47486, #53804, #47039, #12822 ),
 .UNSPECIFIED., .F., .F.,
 ( 4, 2, 2, 2, 4 ),
 ( 0.000000000000000000, 0.0001954339857564099951, 0.0003908679715128199903, 0.0005863019572692300396, 0.0007817359430256399806 ),
 .UNSPECIFIED. ) ;
#30710 = VERTEX_POINT ( 'NONE', #11170 ) ;
#30711 = DIRECTION ( 'NONE',  ( -0.000000000000000000, -0.3420201433256694901, -0.9396926207859082059 ) ) ;
#30712 = CARTESIAN_POINT ( 'NONE',  ( -13.16183584334697265, -10.81320215134717344, 33.49497208177562868 ) ) ;
#30713 = ORIENTED_EDGE ( 'NONE', *, *, #61255, .T. ) ;
#30714 = CARTESIAN_POINT ( 'NONE',  ( 6.000000000000001776, -2.249999999999998668, 29.75000000000001776 ) ) ;
#30715 = CARTESIAN_POINT ( 'NONE',  ( 12.46153846153846168, -11.91647553114624181, 32.58852847137148245 ) ) ;
#30716 = CARTESIAN_POINT ( 'NONE',  ( -8.519176457592452678, -6.567000820036036579, 34.66262288849541306 ) ) ;
#30717 = CARTESIAN_POINT ( 'NONE',  ( 4.153846153846030731, -6.835583212225970762, 34.95778746994575670 ) ) ;
#30718 = VERTEX_POINT ( 'NONE', #24682 ) ;
#30719 = CARTESIAN_POINT ( 'NONE',  ( -4.153846153846273204, -6.879047030192662504, 34.71129190930017927 ) ) ;
#30720 = VERTEX_POINT ( 'NONE', #32773 ) ;
#30721 = ADVANCED_FACE ( 'NONE', ( #79635 ), #80076, .F. ) ;
#30723 = EDGE_LOOP ( 'NONE', ( #7500, #62423, #47423, #26802 ) ) ;
#30722 = CARTESIAN_POINT ( 'NONE',  ( 16.94623161025551639, -10.54014554554151140, 33.71984207302941883 ) ) ;
#30724 = DIRECTION ( 'NONE',  ( 0.000000000000000000, 1.000000000000000000, 0.000000000000000000 ) ) ;
#30725 = CARTESIAN_POINT ( 'NONE',  ( 14.98079248672063990, -4.818429247618089661, 34.26397095200675125 ) ) ;
#30726 = LINE ( 'NONE', #58192, #84663 ) ;
#30727 = CARTESIAN_POINT ( 'NONE',  ( -15.29609214626140634, -7.749976743299138882, 34.99404534957040624 ) ) ;
#30728 = CYLINDRICAL_SURFACE ( 'NONE', #75002, 0.2500000000000002220 ) ;
#30729 = CARTESIAN_POINT ( 'NONE',  ( 12.33139049180676494, -5.915902021225889484, 34.75552854090298638 ) ) ;
#30730 = EDGE_CURVE ( 'NONE', #219, #81991, #86862, .T. ) ;
#30731 = CARTESIAN_POINT ( 'NONE',  ( 0.06109907496451789238, -4.749999999999998224, 13.15811829374151642 ) ) ;
#30732 = VERTEX_POINT ( 'NONE', #52145 ) ;
#30733 = CARTESIAN_POINT ( 'NONE',  ( -10.61538461538473577, -3.643525952248795718, 33.31231777344771672 ) ) ;
#30734 = CARTESIAN_POINT ( 'NONE',  ( -0.4615384615384611200, -4.786620604624113540, 33.94971097300155094 ) ) ;
#30735 = ORIENTED_EDGE ( 'NONE', *, *, #53568, .F. ) ;
#30736 = ORIENTED_EDGE ( 'NONE', *, *, #65637, .T. ) ;
#30737 = CARTESIAN_POINT ( 'NONE',  ( 17.07692307692338218, -2.506253911140615021, 30.00000000000323297 ) ) ;
#30738 = CARTESIAN_POINT ( 'NONE',  ( -14.05763788777885281, -2.544122305571458575, 31.48381861865057729 ) ) ;
#30739 = CARTESIAN_POINT ( 'NONE',  ( -4.853910232829680815, -12.64618726649961289, 30.78989965857442712 ) ) ;
#30740 = CARTESIAN_POINT ( 'NONE',  ( 9.442330961365339448, -12.41269422305637171, 30.68257228309993323 ) ) ;
#30741 = CARTESIAN_POINT ( 'NONE',  ( 13.38461538461526423, -3.083524468854526912, 32.58852847137268327 ) ) ;
#30742 = EDGE_CURVE ( 'NONE', #44980, #49489, #57470, .T. ) ;
#30743 = LINE ( 'NONE', #52342, #22657 ) ;
#30744 = CARTESIAN_POINT ( 'NONE',  ( -15.00798956179115962, -8.540255544307065350, 34.89611431652622286 ) ) ;
#30745 = ORIENTED_EDGE ( 'NONE', *, *, #61928, .T. ) ;
#30746 = CARTESIAN_POINT ( 'NONE',  ( 6.000000000000001776, -12.34228464037088635, 31.77849191805839268 ) ) ;
#30747 = CARTESIAN_POINT ( 'NONE',  ( -17.07692307692319744, -12.27809138561165270, 31.22303859784587132 ) ) ;
#30748 = VECTOR ( 'NONE', #64669, 999.9999999999998863 ) ;
#30749 = CARTESIAN_POINT ( 'NONE',  ( 3.930966637108568307, -7.630690623152302621, 34.99857592706774057 ) ) ;
#30750 = PLANE ( 'NONE',  #9076 ) ;
#30751 = VERTEX_POINT ( 'NONE', #46733 ) ;
#30752 = CARTESIAN_POINT ( 'NONE',  ( 5.076923076923075762, -2.486705287966279876, 31.30864560766543647 ) ) ;
#30753 = ADVANCED_FACE ( 'NONE', ( #52592 ), #12508, .F. ) ;
#30754 = MECHANICAL_DESIGN_GEOMETRIC_PRESENTATION_REPRESENTATION (  '', ( #25030 ), #32241 ) ;
#30755 = VECTOR ( 'NONE', #67777, 1000.000000000000000 ) ;
#30756 = ORIENTED_EDGE ( 'NONE', *, *, #83416, .F. ) ;
#30757 = CARTESIAN_POINT ( 'NONE',  ( -17.93474486048716088, -8.656820664281605460, 34.87096338111211224 ) ) ;
#30758 = CARTESIAN_POINT ( 'NONE',  ( 16.28389120976593318, -2.254550872974305786, 29.97347326024527092 ) ) ;
#30759 = CARTESIAN_POINT ( 'NONE',  ( -2.084729404130821084, -7.369474270740069777, 34.74850911626239736 ) ) ;
#30760 = VERTEX_POINT ( 'NONE', #18378 ) ;
#30761 = EDGE_CURVE ( 'NONE', #75979, #62624, #28453, .T. ) ;
#30762 = CARTESIAN_POINT ( 'NONE',  ( -2.531177232256636156, -6.716662450894490100, 34.94144148231605840 ) ) ;
#30763 = CARTESIAN_POINT ( 'NONE',  ( -10.39237326377176451, -10.61302985866383963, 33.66295027996417843 ) ) ;
#30764 = CARTESIAN_POINT ( 'NONE',  ( -17.20707028636129721, -3.817052484675422797, 33.13202310037935661 ) ) ;
#30765 = LINE ( 'NONE', #73552, #19264 ) ;
#30766 = CARTESIAN_POINT ( 'NONE',  ( -5.010855743573001675, -8.164416787775445883, 34.95778746994558617 ) ) ;
#30767 = EDGE_CURVE ( 'NONE', #21486, #3366, #88624, .T. ) ;
#30768 = EDGE_LOOP ( 'NONE', ( #19259, #74836, #10173, #30180 ) ) ;
#30769 = CARTESIAN_POINT ( 'NONE',  ( 16.15384615384603251, -10.33852847137269571, 34.16647553114546554 ) ) ;
#30770 = ORIENTED_EDGE ( 'NONE', *, *, #87060, .F. ) ;
#30771 = CARTESIAN_POINT ( 'NONE',  ( -9.442253380669381357, -12.17597550085003633, 31.52189283813461884 ) ) ;
#30772 = CARTESIAN_POINT ( 'NONE',  ( -17.01085574357300345, -3.322132147404559532, 32.92929555188717927 ) ) ;
#30773 = CARTESIAN_POINT ( 'NONE',  ( 9.758375025657770152, -2.486705287966280320, 31.30864560766543647 ) ) ;
#30774 = DIRECTION ( 'NONE',  ( 0.000000000000000000, 0.000000000000000000, -1.000000000000000000 ) ) ;
#30775 = CARTESIAN_POINT ( 'NONE',  ( 12.46153846153846168, -3.513871655860378418, 32.76840700105978499 ) ) ;
#30776 = EDGE_CURVE ( 'NONE', #65772, #56866, #38645, .T. ) ;
#30777 = ORIENTED_EDGE ( 'NONE', *, *, #48550, .F. ) ;
#30778 = VECTOR ( 'NONE', #27158, 1000.000000000000000 ) ;
#30779 = ORIENTED_EDGE ( 'NONE', *, *, #10578, .T. ) ;
#30780 = EDGE_CURVE ( 'NONE', #23528, #86451, #13458, .T. ) ;
#30782 = ORIENTED_EDGE ( 'NONE', *, *, #1827, .F. ) ;
#30781 = EDGE_CURVE ( 'NONE', #12315, #72521, #67011, .T. ) ;
#30783 = ORIENTED_EDGE ( 'NONE', *, *, #82288, .F. ) ;
#30784 = FACE_OUTER_BOUND ( 'NONE', #43095, .T. ) ;
#30785 = CARTESIAN_POINT ( 'NONE',  ( -2.307692307692427391, -3.300289026999228881, 32.46337939537708905 ) ) ;
#30786 = CARTESIAN_POINT ( 'NONE',  ( -4.087778820496077437, -6.343179335718452272, 34.87096338111212646 ) ) ;
#30787 = ADVANCED_FACE ( 'NONE', ( #20583 ), #13387, .F. ) ;
#30788 = LINE ( 'NONE', #32135, #26458 ) ;
#30789 = CARTESIAN_POINT ( 'NONE',  ( 10.61538461538449596, -12.27809138561165270, 31.22303859784587132 ) ) ;
#30790 = CARTESIAN_POINT ( 'NONE',  ( -6.066082379360133281, -2.833524468853757305, 32.15551576947924417 ) ) ;
#30791 = DIRECTION ( 'NONE',  ( -0.000000000000000000, 0.8660254037844399289, -0.4999999999999980016 ) ) ;
#30792 = CARTESIAN_POINT ( 'NONE',  ( -7.623142494540998015, -3.105924265160262543, 32.13625925475356127 ) ) ;
#30793 = ORIENTED_EDGE ( 'NONE', *, *, #38397, .T. ) ;
#30794 = ORIENTED_EDGE ( 'NONE', *, *, #79960, .F. ) ;
#30795 = ORIENTED_EDGE ( 'NONE', *, *, #47807, .F. ) ;
#30797 = ORIENTED_EDGE ( 'NONE', *, *, #74137, .F. ) ;
#30796 = FACE_OUTER_BOUND ( 'NONE', #83411, .T. ) ;
#30799 = FACE_OUTER_BOUND ( 'NONE', #3161, .T. ) ;
#30798 = CARTESIAN_POINT ( 'NONE',  ( 16.40379167219429846, -11.86320923018887541, 32.19269448109604781 ) ) ;
#30800 = CARTESIAN_POINT ( 'NONE',  ( -1.607542343522233130, -4.762599654559228846, 34.23009711892697737 ) ) ;
#30801 = DIRECTION ( 'NONE',  ( 1.000000000000000000, 0.000000000000000000, 0.000000000000000000 ) ) ;
#30802 = VERTEX_POINT ( 'NONE', #62014 ) ;
#30803 = B_SPLINE_CURVE_WITH_KNOTS ( 'NONE', 3,
 ( #4420, #30995, #24236, #27362, #5319, #53941, #54383, #34564, #62027, #12962 ),
 .UNSPECIFIED., .F., .F.,
 ( 4, 2, 2, 2, 4 ),
 ( 0.000000000000000000, 0.0001954311564186868473, 0.0003908623128373736946, 0.0005862934692560605419, 0.0007817246256747473893 ),
 .UNSPECIFIED. ) ;
#30804 = VECTOR ( 'NONE', #75772, 1000.000000000000114 ) ;
#30805 = B_SPLINE_CURVE_WITH_KNOTS ( 'NONE', 3,
 ( #10026, #85697, #31179, #66308, #3265, #30738, #51884, #17684, #72617, #37047 ),
 .UNSPECIFIED., .F., .F.,
 ( 4, 2, 2, 2, 4 ),
 ( 0.0007817246256747446788, 0.0009771112852218874663, 0.001172497944769030145, 0.001367884604316172825, 0.001563271263863315720 ),
 .UNSPECIFIED. ) ;
#30806 = ORIENTED_EDGE ( 'NONE', *, *, #75404, .F. ) ;
#30807 = CARTESIAN_POINT ( 'NONE',  ( -2.531177251416254492, -12.44517049084099725, 30.48991314939691932 ) ) ;
#30808 = CIRCLE ( 'NONE', #75440, 4.000000000000000000 ) ;
#30809 = EDGE_LOOP ( 'NONE', ( #13390, #58294 ) ) ;
#30810 = FACE_BOUND ( 'NONE', #79905, .T. ) ;
#30811 = CARTESIAN_POINT ( 'NONE',  ( -5.999999999999998224, -8.973038597847269315, 34.52809138561121927 ) ) ;
#30812 = AXIS2_PLACEMENT_3D ( 'NONE', #23191, #70936, #17324 ) ;
#30813 = CARTESIAN_POINT ( 'NONE',  ( -4.153846153846273204, -11.94971097300221174, 32.03036669348237098 ) ) ;
#30814 = ORIENTED_EDGE ( 'NONE', *, *, #84715, .F. ) ;
#30815 = CARTESIAN_POINT ( 'NONE',  ( -15.09997742294444478, -12.11778462344220841, 31.66786338562085135 ) ) ;
#30816 = CARTESIAN_POINT ( 'NONE',  ( 16.37662569511456567, -4.387253974876675677, 33.66317474335728832 ) ) ;
#30817 = DIRECTION ( 'NONE',  ( -0.000000000000000000, 0.9848077530122085754, -0.1736481776669273613 ) ) ;
#30818 = ORIENTED_EDGE ( 'NONE', *, *, #19373, .T. ) ;
#30819 = DIRECTION ( 'NONE',  ( -0.000000000000000000, -0.3420201433256694346, -0.9396926207859080948 ) ) ;
#30820 = LINE ( 'NONE', #45671, #12162 ) ;
#30821 = VERTEX_POINT ( 'NONE', #88635 ) ;
#30822 = CARTESIAN_POINT ( 'NONE',  ( 6.250000000000063061, -7.434744860731433924, 35.00000000000000711 ) ) ;
#30823 = CARTESIAN_POINT ( 'NONE',  ( -9.561782254074051579, -9.503571793651731880, 34.60286762892837942 ) ) ;
#30824 = EDGE_LOOP ( 'NONE', ( #83619, #6030, #31791, #66471 ) ) ;
#30825 = DIRECTION ( 'NONE',  ( 0.000000000000000000, 0.000000000000000000, -1.000000000000000000 ) ) ;
#30826 = CARTESIAN_POINT ( 'NONE',  ( 13.13463865367303463, -2.564618984488975517, 30.55390908950641915 ) ) ;
#30827 = CARTESIAN_POINT ( 'NONE',  ( -16.08859058257012720, -8.613356846314930593, 34.62446782046653482 ) ) ;
#30828 = CARTESIAN_POINT ( 'NONE',  ( -10.54931626438217585, -5.557115091759786019, 34.35708131394839882 ) ) ;
#30829 = DIRECTION ( 'NONE',  ( 0.000000000000000000, 0.3420201433256610524, 0.9396926207859113145 ) ) ;
#30830 = CARTESIAN_POINT ( 'NONE',  ( 5.999999999999880096, -10.21337939537710326, 33.94971097300076224 ) ) ;
#30832 = CARTESIAN_POINT ( 'NONE',  ( 2.530471848960716752, -10.11255958852955850, 34.01340905677048454 ) ) ;
#30831 = CARTESIAN_POINT ( 'NONE',  ( -1.450698795571264688, -2.721908614388772296, 31.22303859784725688 ) ) ;
#30833 = DIRECTION ( 'NONE',  ( -0.000000000000000000, -0.000000000000000000, -1.000000000000000000 ) ) ;
#30835 = CARTESIAN_POINT ( 'NONE',  ( 12.33139049180676672, -5.070767119584671079, 34.40440758774516183 ) ) ;
#30834 = CARTESIAN_POINT ( 'NONE',  ( -15.48079246806219267, -11.86270091957321249, 32.19358267280087915 ) ) ;
#30836 = CARTESIAN_POINT ( 'NONE',  ( 13.44976016533501983, -7.750023224968867197, 34.99404313364389907 ) ) ;
#30837 = CARTESIAN_POINT ( 'NONE',  ( 2.724691934501235036, -6.299813628509441266, 25.38875670625849423 ) ) ;
#30838 = ORIENTED_EDGE ( 'NONE', *, *, #76110, .T. ) ;
#30839 = CARTESIAN_POINT ( 'NONE',  ( 1.337245517230120306, -4.028657149949338212, 14.00000000000000533 ) ) ;
#30840 = ORIENTED_EDGE ( 'NONE', *, *, #47824, .T. ) ;
#30841 = CARTESIAN_POINT ( 'NONE',  ( -2.438382910802615822, -2.845849958028613624, 32.17971566917920967 ) ) ;
#30842 = ORIENTED_EDGE ( 'NONE', *, *, #68437, .T. ) ;
#30843 = CARTESIAN_POINT ( 'NONE',  ( 17.93472955403922242, -12.27809138561121394, 31.22303859784730307 ) ) ;
#30844 = ORIENTED_EDGE ( 'NONE', *, *, #26903, .F. ) ;
#30845 = LINE ( 'NONE', #49356, #67086 ) ;
#30846 = CARTESIAN_POINT ( 'NONE',  ( -1.901340078031346525, -9.487747218494661183, 22.18563170625848713 ) ) ;
#30847 = FACE_OUTER_BOUND ( 'NONE', #63302, .T. ) ;
#30848 = CARTESIAN_POINT ( 'NONE',  ( 9.692307692307572609, -11.48612834414049644, 32.76840700105863391 ) ) ;
#30849 = CARTESIAN_POINT ( 'NONE',  ( -3.007989561791166278, -12.47679350104403007, 31.42216943046555855 ) ) ;
#30850 = CARTESIAN_POINT ( 'NONE',  ( -12.23852561744506495, -4.026326845037962343, 33.68677907613344047 ) ) ;
#30851 = DIRECTION ( 'NONE',  ( -0.000000000000000000, 0.9848077530122086864, -0.1736481776669273891 ) ) ;
#30852 = CYLINDRICAL_SURFACE ( 'NONE', #48780, 0.2499999999999973355 ) ;
#30853 = LINE ( 'NONE', #58324, #59786 ) ;
#30854 = CARTESIAN_POINT ( 'NONE',  ( -1.553300858899125059, -3.750000000000009326, 17.82812500000000000 ) ) ;
#30855 = CYLINDRICAL_SURFACE ( 'NONE', #268, 0.2500000000000008882 ) ;
#30856 = CARTESIAN_POINT ( 'NONE',  ( 13.38461538461538680, -3.322132147404559976, 32.92929555188717927 ) ) ;
#30857 = CARTESIAN_POINT ( 'NONE',  ( 13.45068373561782415, -4.098570777380720287, 33.41473453929635440 ) ) ;
#30858 = CARTESIAN_POINT ( 'NONE',  ( -3.749999999999997335, -7.500000000000021316, 16.34375000000000000 ) ) ;
#30859 = ADVANCED_FACE ( 'NONE', ( #5747 ), #81420, .T. ) ;
#30860 = VERTEX_POINT ( 'NONE', #34983 ) ;
#30861 = CARTESIAN_POINT ( 'NONE',  ( 17.29993442853592711, -12.15243808032446005, 31.58219941686247978 ) ) ;
#30862 = CARTESIAN_POINT ( 'NONE',  ( -14.30769230769230660, -8.120952969808772792, 34.71129190930000163 ) ) ;
#30863 = DIRECTION ( 'NONE',  ( -0.000000000000000000, -0.000000000000000000, -1.000000000000000000 ) ) ;
#30864 = DIRECTION ( 'NONE',  ( -0.000000000000000000, 1.000000000000000000, -0.000000000000000000 ) ) ;
#30865 = CARTESIAN_POINT ( 'NONE',  ( 17.32697749683652688, -12.41089969410671223, 31.60739465890703670 ) ) ;
#30866 = CARTESIAN_POINT ( 'NONE',  ( -3.007989561791163169, -5.827830569534416583, 34.72679350104403539 ) ) ;
#30867 = CIRCLE ( 'NONE', #42409, 4.000000000000000000 ) ;
#30868 = EDGE_CURVE ( 'NONE', #43223, #63578, #41311, .T. ) ;
#30869 = ORIENTED_EDGE ( 'NONE', *, *, #69442, .F. ) ;
#30870 = CARTESIAN_POINT ( 'NONE',  ( -1.161835843346975983, -10.11255958852956027, 34.01340905677048454 ) ) ;
#30871 = ORIENTED_EDGE ( 'NONE', *, *, #3770, .T. ) ;
#30872 = B_SPLINE_CURVE_WITH_KNOTS ( 'NONE', 3,
 ( #79565, #6888, #66029, #65583, #5230, #47876, #59279, #4793, #38575, #86785 ),
 .UNSPECIFIED., .F., .F.,
 ( 4, 2, 2, 2, 4 ),
 ( 0.0007817246256747507503, 0.0009771112852218959231, 0.001172497944769040987, 0.001367884604316186052, 0.001563271263863331116 ),
 .UNSPECIFIED. ) ;
#30873 = AXIS2_PLACEMENT_3D ( 'NONE', #14617, #29910, #57366 ) ;
#30874 = VERTEX_POINT ( 'NONE', #60686 ) ;
#30875 = CARTESIAN_POINT ( 'NONE',  ( 0.5920638997721079377, -12.50538340440932217, 31.33453814440721885 ) ) ;
#30876 = AXIS2_PLACEMENT_3D ( 'NONE', #25746, #53206, #80709 ) ;
#30877 = CARTESIAN_POINT ( 'NONE',  ( 3.453548772037639214, -5.913360116392399668, 34.49180327182771322 ) ) ;
#30878 = CARTESIAN_POINT ( 'NONE',  ( -0.3307001310517008186, -7.277220318596960169, 34.99547417642776992 ) ) ;
#30879 = DIRECTION ( 'NONE',  ( -0.000000000000000000, 0.1736481776669307198, -0.9848077530122080203 ) ) ;
#30880 = CARTESIAN_POINT ( 'NONE',  ( -2.241623956689867025, -11.69971097300155272, 32.46337939537588113 ) ) ;
#30881 = ORIENTED_EDGE ( 'NONE', *, *, #69139, .T. ) ;
#30882 = ORIENTED_EDGE ( 'NONE', *, *, #87144, .F. ) ;
#30883 = ADVANCED_FACE ( 'NONE', ( #55256 ), #75528, .F. ) ;
#30884 = EDGE_CURVE ( 'NONE', #58039, #22897, #69301, .T. ) ;
#30885 = ORIENTED_EDGE ( 'NONE', *, *, #18640, .F. ) ;
#30886 = CARTESIAN_POINT ( 'NONE',  ( 12.71153846153846168, -2.499999999999998668, 29.75000000000000355 ) ) ;
#30887 = CARTESIAN_POINT ( 'NONE',  ( 8.639083559792551270, -2.882441371585227508, 31.66841991370172238 ) ) ;
#30888 = CARTESIAN_POINT ( 'NONE',  ( 19.99999999999996803, 15.00000000000000711, 3.000000000000000000 ) ) ;
#30889 = CARTESIAN_POINT ( 'NONE',  ( -14.98082371242109012, -3.202959910592335646, 32.30730279482227019 ) ) ;
#30890 = CARTESIAN_POINT ( 'NONE',  ( -0.4615384615384611200, -10.89733346790207413, 36.13435417666054406 ) ) ;
#30891 = CARTESIAN_POINT ( 'NONE',  ( 5.999999999999880096, -9.442884908241554243, 34.35708131394783038 ) ) ;
#30892 = ORIENTED_EDGE ( 'NONE', *, *, #48750, .T. ) ;
#30893 = VERTEX_POINT ( 'NONE', #19706 ) ;
#30894 = CARTESIAN_POINT ( 'NONE',  ( 1.553300858899129944, -11.24999999999998934, 20.95312500000000000 ) ) ;
#30895 = AXIS2_PLACEMENT_3D ( 'NONE', #25640, #53096, #67075 ) ;
#30896 = VERTEX_POINT ( 'NONE', #758 ) ;
#30898 = EDGE_LOOP ( 'NONE', ( #30905, #88505 ) ) ;
#30897 = CARTESIAN_POINT ( 'NONE',  ( -14.30769230769230660, -11.11383981884818262, 36.00935417666054406 ) ) ;
#30899 = CARTESIAN_POINT ( 'NONE',  ( -9.822455662039388358, -10.31621877034669588, 34.18098118002070152 ) ) ;
#30900 = CARTESIAN_POINT ( 'NONE',  ( -2.307692307692305711, -13.04860791097971706, 34.73218667398347037 ) ) ;
#30901 = CARTESIAN_POINT ( 'NONE',  ( 14.30769230769218758, -3.835265460704628371, 33.15142922262033665 ) ) ;
#30902 = EDGE_LOOP ( 'NONE', ( #8980, #63344, #78099, #84071 ) ) ;
#30903 = B_SPLINE_CURVE_WITH_KNOTS ( 'NONE', 3,
 ( #86749, #79968, #18269, #74994, #27679, #61901, #81311, #6089, #48833, #67345 ),
 .UNSPECIFIED., .F., .F.,
 ( 4, 2, 2, 2, 4 ),
 ( 0.0007817359430256216575, 0.0009771253907249856981, 0.001172514838424349630, 0.001367904286123713779, 0.001563293733823077711 ),
 .UNSPECIFIED. ) ;
#30904 = DIRECTION ( 'NONE',  ( -0.000000000000000000, -0.9848077530122085754, -0.1736481776669273613 ) ) ;
#30905 = ORIENTED_EDGE ( 'NONE', *, *, #3068, .F. ) ;
#30906 = DIRECTION ( 'NONE',  ( 0.000000000000000000, -1.000000000000000000, 0.000000000000000000 ) ) ;
#30907 = DIRECTION ( 'NONE',  ( -0.000000000000000000, 0.8660254037844397068, -0.4999999999999978906 ) ) ;
#30908 = CARTESIAN_POINT ( 'NONE',  ( 2.084207383127976598, -12.47654668319379567, 31.42292124445336654 ) ) ;
#30910 = CARTESIAN_POINT ( 'NONE',  ( -6.923076923077044142, -2.625532179533778709, 30.86335684631627174 ) ) ;
#30909 = CARTESIAN_POINT ( 'NONE',  ( 5.934729999443682402, -12.51329471203370325, 31.30864560766548976 ) ) ;
#30911 = CARTESIAN_POINT ( 'NONE',  ( -1.161835715637317801, -8.540255544307065350, 34.89611431652622286 ) ) ;
#30912 = FACE_OUTER_BOUND ( 'NONE', #41150, .T. ) ;
#30913 = ORIENTED_EDGE ( 'NONE', *, *, #38015, .T. ) ;
#30914 = CARTESIAN_POINT ( 'NONE',  ( -10.86536134632696715, -9.943427161483782584, 34.11278801902876978 ) ) ;
#30915 = CARTESIAN_POINT ( 'NONE',  ( -8.992157728137618378, -4.026226216239094491, 33.68668979543634379 ) ) ;
#30916 = B_SPLINE_CURVE_WITH_KNOTS ( 'NONE', 3,
 ( #21439, #77268, #48909, #29535, #76380, #21884, #8822, #36294, #14686, #70959 ),
 .UNSPECIFIED., .F., .F.,
 ( 4, 2, 2, 2, 4 ),
 ( 0.000000000000000000, 0.0001954339857564070678, 0.0003908679715128141356, 0.0005863019572692211492, 0.0007817359430256282712 ),
 .UNSPECIFIED. ) ;
#30917 = ORIENTED_EDGE ( 'NONE', *, *, #15698, .T. ) ;
#30918 = CARTESIAN_POINT ( 'NONE',  ( -12.46153846153858424, -3.643525952248795718, 33.31231777344771672 ) ) ;
#30919 = CARTESIAN_POINT ( 'NONE',  ( 14.24242186173153435, -10.21337939537584383, 33.94971097300158647 ) ) ;
#30920 = CARTESIAN_POINT ( 'NONE',  ( -15.16470189741915320, -5.471508081941601098, 34.59228464037088457 ) ) ;
#30921 = CYLINDRICAL_SURFACE ( 'NONE', #18438, 0.2499999999999995559 ) ;
#30922 = DIRECTION ( 'NONE',  ( -0.000000000000000000, 0.8660254037844399289, -0.4999999999999980016 ) ) ;
#30923 = FACE_BOUND ( 'NONE', #48303, .T. ) ;
#30925 = CARTESIAN_POINT ( 'NONE',  ( 17.74997677577854560, -10.92453946501459328, 33.72985991061849376 ) ) ;
#30924 = CARTESIAN_POINT ( 'NONE',  ( 13.16168916709923664, -12.15238873228292071, 31.58232369045353849 ) ) ;
#30926 = CARTESIAN_POINT ( 'NONE',  ( 5.076923076923075762, -7.500000000000001776, 35.04278698407183867 ) ) ;
#30928 = CARTESIAN_POINT ( 'NONE',  ( 0.4615384615384611200, -12.29105614889573062, 35.45975837776705220 ) ) ;
#30927 = CARTESIAN_POINT ( 'NONE',  ( -11.78846153846153655, -7.566083408709835645, 34.74999999999999289 ) ) ;
#30929 = CARTESIAN_POINT ( 'NONE',  ( -15.23076923076935074, -2.892918686052166066, 31.69288490824153470 ) ) ;
#30930 = CARTESIAN_POINT ( 'NONE',  ( 8.900022577055551665, -10.54018710029568595, 33.71981072465678864 ) ) ;
#30931 = CARTESIAN_POINT ( 'NONE',  ( -1.492201783934549164, -11.27530806549876807, 19.60750670625849068 ) ) ;
#30932 = B_SPLINE_CURVE_WITH_KNOTS ( 'NONE', 3,
 ( #38241, #72017, #22948, #57621, #37338, #50408, #79233, #84671, #52185, #65696 ),
 .UNSPECIFIED., .F., .F.,
 ( 4, 2, 2, 2, 4 ),
 ( 0.0007817246256747448956, 0.0009771112852218876831, 0.001172497944769030579, 0.001367884604316173475, 0.001563271263863316371 ),
 .UNSPECIFIED. ) ;
#30933 = ORIENTED_EDGE ( 'NONE', *, *, #80659, .T. ) ;
#30934 = B_SPLINE_CURVE_WITH_KNOTS ( 'NONE', 3,
 ( #83224, #83678, #41348, #799, #49433, #7116, #8453, #55295, #62926, #61160 ),
 .UNSPECIFIED., .F., .F.,
 ( 4, 2, 2, 2, 4 ),
 ( 0.0007817359430256324996, 0.0009771253907249993591, 0.001172514838424366110, 0.001367904286123732861, 0.001563293733823099829 ),
 .UNSPECIFIED. ) ;
#30935 = CARTESIAN_POINT ( 'NONE',  ( -7.976301055592065481, -11.47017969459904130, 32.78971311882034456 ) ) ;
#30936 = CARTESIAN_POINT ( 'NONE',  ( -4.377331097570101193, -3.236172620538810385, 32.36188796281390267 ) ) ;
#30937 = DIRECTION ( 'NONE',  ( 0.000000000000000000, 0.8660254037844377084, -0.5000000000000015543 ) ) ;
#30939 = VECTOR ( 'NONE', #67024, 1000.000000000000114 ) ;
#30938 = DIRECTION ( 'NONE',  ( 1.000000000000000000, 0.000000000000000000, 0.000000000000000000 ) ) ;
#30940 = LINE ( 'NONE', #44900, #76104 ) ;
#30941 = CARTESIAN_POINT ( 'NONE',  ( -16.82686865700962642, -8.346898887586322147, 34.93166121998716278 ) ) ;
#30942 = CARTESIAN_POINT ( 'NONE',  ( -2.608446859217889546, -10.19485399968121264, 22.18563170625848713 ) ) ;
#30943 = EDGE_CURVE ( 'NONE', #58822, #59485, #22216, .T. ) ;
#30944 = CARTESIAN_POINT ( 'NONE',  ( -16.40382289789473802, -5.643011162660950042, 34.66104346484419096 ) ) ;
#30945 = CARTESIAN_POINT ( 'NONE',  ( -14.55771553191376633, -11.56360843649121684, 33.07473185843129926 ) ) ;
#30946 = CARTESIAN_POINT ( 'NONE',  ( -7.596099426240392027, -10.06805714834173493, 34.32951233291982618 ) ) ;
#30948 = B_SPLINE_CURVE_WITH_KNOTS ( 'NONE', 3,
 ( #70586, #8890, #65142, #2120, #3445, #58379, #85873, #51613, #10658, #38125 ),
 .UNSPECIFIED., .F., .F.,
 ( 4, 2, 2, 2, 4 ),
 ( 0.000000000000000000, 0.0001954339857564074473, 0.0003908679715128148945, 0.0005863019572692223418, 0.0007817359430256297891 ),
 .UNSPECIFIED. ) ;
#30947 = CARTESIAN_POINT ( 'NONE',  ( 5.207713517890025123, -12.62708834333097663, 30.88030960425257021 ) ) ;
#30949 = CARTESIAN_POINT ( 'NONE',  ( 0.4615384615383396616, -11.48612834414049644, 32.76840700105863391 ) ) ;
#30950 = CARTESIAN_POINT ( 'NONE',  ( 7.846153846153846700, -10.67929555188718282, 33.92786785259544047 ) ) ;
#30951 = B_SPLINE_CURVE_WITH_KNOTS ( 'NONE', 3,
 ( #50585, #49707, #1969, #64532, #63215, #1529, #56900, #64100, #2395, #7847 ),
 .UNSPECIFIED., .F., .F.,
 ( 4, 2, 2, 2, 4 ),
 ( 0.0007817246256747459798, 0.0009771112852218887673, 0.001172497944769031663, 0.001367884604316174559, 0.001563271263863317455 ),
 .UNSPECIFIED. ) ;
#30952 = FACE_OUTER_BOUND ( 'NONE', #84357, .T. ) ;
#30953 = CYLINDRICAL_SURFACE ( 'NONE', #83042, 0.2500000000000002220 ) ;
#30954 = VERTEX_POINT ( 'NONE', #47167 ) ;
#30955 = DIRECTION ( 'NONE',  ( -0.000000000000000000, 0.9848077530122085754, -0.1736481776669273613 ) ) ;
#30956 = LINE ( 'NONE', #51660, #24462 ) ;
#30957 = CARTESIAN_POINT ( 'NONE',  ( -2.608446859217920633, -4.805146000318815780, 13.00186829374151465 ) ) ;
#30958 = EDGE_CURVE ( 'NONE', #36124, #34697, #32762, .T. ) ;
#30959 = CARTESIAN_POINT ( 'NONE',  ( 6.222779541268410597, -4.387253974876676565, 33.66317474335728832 ) ) ;
#30960 = CARTESIAN_POINT ( 'NONE',  ( 2.307692307692309264, -8.973038597847269315, 34.52809138561121927 ) ) ;
#30961 = ORIENTED_EDGE ( 'NONE', *, *, #52688, .T. ) ;
#30962 = CARTESIAN_POINT ( 'NONE',  ( 1.634669696253701510, -4.235687564193446164, 33.53795663066793509 ) ) ;
#30963 = CARTESIAN_POINT ( 'NONE',  ( 2.438482748659258625, -10.70102852606553157, 33.91149625220312913 ) ) ;
#30965 = VERTEX_POINT ( 'NONE', #14274 ) ;
#30964 = CARTESIAN_POINT ( 'NONE',  ( 3.230769230769231726, -2.517432740324522911, 35.29906147534542527 ) ) ;
#30966 = CARTESIAN_POINT ( 'NONE',  ( -12.68446542044531000, -9.172386477786396597, 34.72672124145550043 ) ) ;
#30967 = CARTESIAN_POINT ( 'NONE',  ( -2.307692307692428724, -11.67786785259630911, 32.92929555188603530 ) ) ;
#30968 = EDGE_CURVE ( 'NONE', #59060, #45953, #40437, .T. ) ;
#30969 = CARTESIAN_POINT ( 'NONE',  ( -4.854143535654666941, -9.332535724633407526, 34.40230450496446224 ) ) ;
#30970 = AXIS2_PLACEMENT_3D ( 'NONE', #62191, #61291, #938 ) ;
#30971 = CARTESIAN_POINT ( 'NONE',  ( -14.05774678934416499, -11.37275283266504111, 32.91324779482534524 ) ) ;
#30972 = ORIENTED_EDGE ( 'NONE', *, *, #15935, .T. ) ;
#30973 = LINE ( 'NONE', #38185, #62176 ) ;
#30974 = CARTESIAN_POINT ( 'NONE',  ( 10.86543903529806698, -4.074993327901527351, 33.72946981652012255 ) ) ;
#30975 = CARTESIAN_POINT ( 'NONE',  ( -1.161835843346975539, -5.913360116392399668, 34.49180327182771322 ) ) ;
#30976 = ADVANCED_FACE ( 'NONE', ( #67896 ), #21473, .F. ) ;
#30977 = ORIENTED_EDGE ( 'NONE', *, *, #45958, .T. ) ;
#30978 = VERTEX_POINT ( 'NONE', #6197 ) ;
#30979 = ORIENTED_EDGE ( 'NONE', *, *, #20809, .T. ) ;
#30980 = ADVANCED_FACE ( 'NONE', ( #33669 ), #75104, .F. ) ;
#30981 = CARTESIAN_POINT ( 'NONE',  ( -9.692307692307691624, -9.780366693483667717, 34.19971097300155094 ) ) ;
#30982 = DIRECTION ( 'NONE',  ( -0.000000000000000000, -0.5000000000000009992, -0.8660254037844380415 ) ) ;
#30983 = CARTESIAN_POINT ( 'NONE',  ( -12.52762187249434156, -3.513871655860377086, 32.76840700105978499 ) ) ;
#30984 = CARTESIAN_POINT ( 'NONE',  ( 11.53846153846153832, -4.102666532097928531, 36.13435417666054406 ) ) ;
#30985 = AXIS2_PLACEMENT_3D ( 'NONE', #75230, #50713, #57926 ) ;
#30986 = EDGE_CURVE ( 'NONE', #22049, #23792, #45676, .T. ) ;
#30987 = ORIENTED_EDGE ( 'NONE', *, *, #32188, .T. ) ;
#30988 = VERTEX_POINT ( 'NONE', #29567 ) ;
#30991 = VERTEX_POINT ( 'NONE', #22357 ) ;
#30990 = EDGE_CURVE ( 'NONE', #40554, #24285, #83639, .T. ) ;
#30989 = CARTESIAN_POINT ( 'NONE',  ( 15.48082354240754555, -4.943051570960394159, 34.04725096376909477 ) ) ;
#30992 = CARTESIAN_POINT ( 'NONE',  ( 16.15384615384615330, -13.49023893513002648, 31.06009739812518688 ) ) ;
#30993 = EDGE_CURVE ( 'NONE', #75626, #26115, #8856, .T. ) ;
#30994 = EDGE_CURVE ( 'NONE', #21128, #50622, #87498, .T. ) ;
#30995 = CARTESIAN_POINT ( 'NONE',  ( 5.933917620639865831, -3.937682226553329556, 33.60647404775217240 ) ) ;
#30996 = CARTESIAN_POINT ( 'NONE',  ( -13.13456107297707121, -12.41262288849542017, 30.68299917996395010 ) ) ;
#30997 = B_SPLINE_CURVE_WITH_KNOTS ( 'NONE', 3,
 ( #54479, #47621, #49051, #35095, #21134, #33775, #61229, #75212, #62555, #54930 ),
 .UNSPECIFIED., .F., .F.,
 ( 4, 2, 2, 2, 4 ),
 ( 0.000000000000000000, 0.0001954339857564070949, 0.0003908679715128141898, 0.0005863019572692212576, 0.0007817359430256283796 ),
 .UNSPECIFIED. ) ;
#30998 = VECTOR ( 'NONE', #20289, 1000.000000000000114 ) ;
#30999 = ORIENTED_EDGE ( 'NONE', *, *, #8197, .T. ) ;
#31000 = ORIENTED_EDGE ( 'NONE', *, *, #66414, .F. ) ;
#31001 = B_SPLINE_CURVE_WITH_KNOTS ( 'NONE', 3,
 ( #68448, #6746, #34217, #60806, #61680, #2, #88313, #82864, #76086, #54486 ),
 .UNSPECIFIED., .F., .F.,
 ( 4, 2, 2, 2, 4 ),
 ( 0.0007817246256747517261, 0.0009771112852218961399, 0.001172497944769040771, 0.001367884604316185401, 0.001563271263863329815 ),
 .UNSPECIFIED. ) ;
#31002 = ORIENTED_EDGE ( 'NONE', *, *, #29331, .T. ) ;
#31004 = ORIENTED_EDGE ( 'NONE', *, *, #4011, .F. ) ;
#31003 = CARTESIAN_POINT ( 'NONE',  ( 8.992010310499177095, -2.600157965045224895, 30.74683119005207743 ) ) ;
#31005 = CARTESIAN_POINT ( 'NONE',  ( -0.5268089074992374776, -10.90142922261923886, 33.41473453929638993 ) ) ;
#31006 = CARTESIAN_POINT ( 'NONE',  ( -10.61538461538473577, -9.528491918059723176, 34.59228464037033035 ) ) ;
#31007 = ORIENTED_EDGE ( 'NONE', *, *, #86259, .F. ) ;
#31008 = CARTESIAN_POINT ( 'NONE',  ( 12.46153846153846168, -6.343179335718451384, 34.87096338111211935 ) ) ;
#31009 = CARTESIAN_POINT ( 'NONE',  ( -1.634638621908349077, -8.432397168068783699, 34.66272746175022945 ) ) ;
#31010 = CARTESIAN_POINT ( 'NONE',  ( 17.07692307692307665, -2.708943851104267164, 35.45975837776705220 ) ) ;
#31011 = FACE_BOUND ( 'NONE', #23381, .T. ) ;
#31012 = CARTESIAN_POINT ( 'NONE',  ( -5.999999999999998224, -2.499999999999998668, 29.75000000000001421 ) ) ;
#31013 = CARTESIAN_POINT ( 'NONE',  ( 2.438218009455871638, -8.586989748646452369, 34.63063291749215011 ) ) ;
#31014 = FACE_OUTER_BOUND ( 'NONE', #35745, .T. ) ;
#31016 = CARTESIAN_POINT ( 'NONE',  ( 9.942362003946010773, -3.136992222400443175, 32.19305428654138979 ) ) ;
#31015 = CARTESIAN_POINT ( 'NONE',  ( 16.82694633287449193, -9.234221910056350069, 34.70572697212741531 ) ) ;
#31017 = AXIS2_PLACEMENT_3D ( 'NONE', #3480, #37266, #29644 ) ;
#31018 = CARTESIAN_POINT ( 'NONE',  ( 17.93472999944368240, -6.835583212224500826, 34.95778746994557906 ) ) ;
#31019 = DIRECTION ( 'NONE',  ( 0.000000000000000000, 0.000000000000000000, 1.000000000000000000 ) ) ;
#31020 = EDGE_LOOP ( 'NONE', ( #7769, #42988 ) ) ;
#31021 = CARTESIAN_POINT ( 'NONE',  ( -2.307692307692305711, -2.833524468853757305, 32.15551576947925838 ) ) ;
#31022 = VERTEX_POINT ( 'NONE', #36756 ) ;
#31023 = EDGE_LOOP ( 'NONE', ( #59647, #50856, #60892, #49755 ) ) ;
#31024 = VECTOR ( 'NONE', #15685, 1000.000000000000000 ) ;
#31026 = CARTESIAN_POINT ( 'NONE',  ( 1.253923917947830313, -10.54014554554150607, 33.71984207302941883 ) ) ;
#31025 = CARTESIAN_POINT ( 'NONE',  ( -6.700297381808512753, -8.496831190052096971, 34.64984203495476578 ) ) ;
#31027 = CARTESIAN_POINT ( 'NONE',  ( -6.700065571464073777, -6.503523203565942268, 34.64991518177335195 ) ) ;
#31028 = CARTESIAN_POINT ( 'NONE',  ( -5.076923076923199218, -5.941354392335915335, 34.76329471203413846 ) ) ;
#31029 = CARTESIAN_POINT ( 'NONE',  ( -16.15384615384615330, -12.10708131394839349, 31.69288490824020244 ) ) ;
#31030 = ORIENTED_EDGE ( 'NONE', *, *, #56597, .T. ) ;
#31031 = EDGE_CURVE ( 'NONE', #67701, #47174, #25261, .T. ) ;
#31032 = CARTESIAN_POINT ( 'NONE',  ( 12.46153846153846168, -3.050289026998446396, 32.03036669348365706 ) ) ;
#31033 = CARTESIAN_POINT ( 'NONE',  ( 6.923076923076802558, -3.835265460704628371, 33.15142922262033665 ) ) ;
#31034 = CARTESIAN_POINT ( 'NONE',  ( -1.450697763975519194, -9.905515769479276145, 34.41647553114623292 ) ) ;
#31035 = DIRECTION ( 'NONE',  ( 0.000000000000000000, 1.000000000000000000, 0.000000000000000000 ) ) ;
#31036 = DIRECTION ( 'NONE',  ( 0.000000000000000000, 0.3420201433256610524, 0.9396926207859113145 ) ) ;
#31037 = B_SPLINE_CURVE_WITH_KNOTS ( 'NONE', 3,
 ( #49422, #71448, #49850, #28253, #2544, #30033, #84547, #83212, #35013, #56175 ),
 .UNSPECIFIED., .F., .F.,
 ( 4, 2, 2, 2, 4 ),
 ( 0.0007817246256747530271, 0.0009771112852218978746, 0.001172497944769042939, 0.001367884604316188003, 0.001563271263863332851 ),
 .UNSPECIFIED. ) ;
#31038 = CARTESIAN_POINT ( 'NONE',  ( -3.749999999999988454, -9.053300858899127945, 16.26562500000000000 ) ) ;
#31039 = EDGE_LOOP ( 'NONE', ( #57146, #87123, #62336, #17630 ) ) ;
#31041 = EDGE_CURVE ( 'NONE', #52632, #49352, #50701, .T. ) ;
#31040 = ORIENTED_EDGE ( 'NONE', *, *, #46962, .F. ) ;
#31042 = DIRECTION ( 'NONE',  ( 0.000000000000000000, 0.000000000000000000, 1.000000000000000000 ) ) ;
#31043 = VERTEX_POINT ( 'NONE', #14724 ) ;
#31044 = CARTESIAN_POINT ( 'NONE',  ( 17.14217821643591932, -4.320704448112858032, 33.92786785259548310 ) ) ;
#31045 = CARTESIAN_POINT ( 'NONE',  ( 7.846153846153723244, -12.51329471203414379, 31.30864560766407578 ) ) ;
#31046 = CARTESIAN_POINT ( 'NONE',  ( -16.21992956480203318, -2.721908614388770964, 31.22303859784723912 ) ) ;
#31047 = FACE_OUTER_BOUND ( 'NONE', #49423, .T. ) ;
#31048 = CARTESIAN_POINT ( 'NONE',  ( -1.929879867024197893E-14, -3.750000000000000000, 16.65625000000000000 ) ) ;
#31049 = EDGE_CURVE ( 'NONE', #70248, #87025, #2960, .T. ) ;
#31050 = CARTESIAN_POINT ( 'NONE',  ( 16.15384615384615330, -13.87047571288749737, 32.06866353760679544 ) ) ;
#31051 = ORIENTED_EDGE ( 'NONE', *, *, #8596, .T. ) ;
#31052 = CARTESIAN_POINT ( 'NONE',  ( -0.4615384615385840772, -3.083524468854526912, 32.58852847137268327 ) ) ;
#31054 = EDGE_LOOP ( 'NONE', ( #84100, #37720, #11315, #1549 ) ) ;
#31053 = CARTESIAN_POINT ( 'NONE',  ( -2.057746898314262385, -12.68172785388650681, 30.59649109432439218 ) ) ;
#31055 = CARTESIAN_POINT ( 'NONE',  ( -13.44988583057615905, -11.48612834413959582, 32.76840700105983473 ) ) ;
#31056 = CARTESIAN_POINT ( 'NONE',  ( -9.758391103263569732, -12.10708131394839349, 31.69288490824020244 ) ) ;
#31057 = DIRECTION ( 'NONE',  ( -0.000000000000000000, -0.8660254037844399289, -0.4999999999999980016 ) ) ;
#31059 = AXIS2_PLACEMENT_3D ( 'NONE', #30387, #57857, #69598 ) ;
#31058 = CARTESIAN_POINT ( 'NONE',  ( -1.576923076923076428, -11.50000000000000000, 29.75000000000000355 ) ) ;
#31060 = CARTESIAN_POINT ( 'NONE',  ( -5.869474561766355514, -5.070358843744210198, 34.40418822224088302 ) ) ;
#31061 = CARTESIAN_POINT ( 'NONE',  ( -4.403869391139118683, -9.271318131107980420, 34.42618302367067429 ) ) ;
#31062 = CARTESIAN_POINT ( 'NONE',  ( -6.989160334032801458, -4.786620604624113540, 33.94971097300155805 ) ) ;
#31063 = CARTESIAN_POINT ( 'NONE',  ( 2.694853999681185108, -4.891553140782077591, 19.56436829374151287 ) ) ;
#31064 = EDGE_LOOP ( 'NONE', ( #46758, #46812, #26316, #47000 ) ) ;
#31065 = CARTESIAN_POINT ( 'NONE',  ( -4.403822884788509029, -4.943428324936578910, 34.04746400365624481 ) ) ;
#31066 = DIRECTION ( 'NONE',  ( -5.997714145664496128E-17, -1.000000000000000000, 5.102127870520020612E-17 ) ) ;
#31067 = B_SPLINE_CURVE_WITH_KNOTS ( 'NONE', 3,
 ( #34860, #81295, #81736, #20020, #47487, #7404, #6951, #74979, #88954, #47040 ),
 .UNSPECIFIED., .F., .F.,
 ( 4, 2, 2, 2, 4 ),
 ( 0.0007817359430256294638, 0.0009771253907249952391, 0.001172514838424361123, 0.001367904286123726790, 0.001563293733823092673 ),
 .UNSPECIFIED. ) ;
#31068 = CARTESIAN_POINT ( 'NONE',  ( -4.219116154402471786, -5.941354392334500467, 34.76329471203369792 ) ) ;
#31069 = CARTESIAN_POINT ( 'NONE',  ( -2.750000000000007105, -6.360912703474006946, 23.92187500000000355 ) ) ;
#31070 = ADVANCED_FACE ( 'NONE', ( #77742 ), #2515, .F. ) ;
#31071 = CARTESIAN_POINT ( 'NONE',  ( -3.480792468062196221, -9.271318131107980420, 34.42618302367067429 ) ) ;
#31072 = CARTESIAN_POINT ( 'NONE',  ( 14.17700170458200404, -4.684245665217972032, 34.18127051446801090 ) ) ;
#31074 = VERTEX_POINT ( 'NONE', #23240 ) ;
#31073 = CARTESIAN_POINT ( 'NONE',  ( -13.25408994638174320, -6.808710257144161559, 34.95449254468098843 ) ) ;
#31075 = CARTESIAN_POINT ( 'NONE',  ( 1.944543648263018731, -9.444543648262994751, 17.12500000000000000 ) ) ;
#31076 = DIRECTION ( 'NONE',  ( -0.000000000000000000, 0.9396926207859092051, -0.3420201433256662704 ) ) ;
#31077 = EDGE_CURVE ( 'NONE', #14975, #6775, #42641, .T. ) ;
#31078 = ORIENTED_EDGE ( 'NONE', *, *, #22371, .F. ) ;
#31079 = CARTESIAN_POINT ( 'NONE',  ( -18.13014796973169851, -5.070767119584671079, 34.40440758774516183 ) ) ;
#31080 = VERTEX_POINT ( 'NONE', #16490 ) ;
#31081 = CARTESIAN_POINT ( 'NONE',  ( 14.37294787896833448, -12.27809138561124591, 31.22303859784720359 ) ) ;
#31082 = CARTESIAN_POINT ( 'NONE',  ( -1.450697763975519416, -11.91647553114624181, 32.58852847137148245 ) ) ;
#31083 = CARTESIAN_POINT ( 'NONE',  ( -0.3962833220256232192, -6.835583212224609184, 34.95778746994559327 ) ) ;
#31084 = ORIENTED_EDGE ( 'NONE', *, *, #53045, .T. ) ;
#31085 = CARTESIAN_POINT ( 'NONE',  ( -0.7115384615384606759, -2.249999999999998668, 29.75000000000000355 ) ) ;
#31086 = ORIENTED_EDGE ( 'NONE', *, *, #8407, .F. ) ;
#31087 = LINE ( 'NONE', #17134, #54261 ) ;
#31088 = EDGE_LOOP ( 'NONE', ( #20500, #52447 ) ) ;
#31089 = CARTESIAN_POINT ( 'NONE',  ( 2.241609928332172430, -9.058645607665454236, 34.76329471203372634 ) ) ;
#31090 = CARTESIAN_POINT ( 'NONE',  ( -6.923076923076922462, -13.87047571288749737, 32.06866353760679544 ) ) ;
#31091 = VERTEX_POINT ( 'NONE', #57022 ) ;
#31092 = CARTESIAN_POINT ( 'NONE',  ( 11.76124120743960333, -12.69155399931963046, 30.53255429739157734 ) ) ;
#31093 = CARTESIAN_POINT ( 'NONE',  ( -14.37296275365308418, -10.90142922261923886, 33.41473453929638993 ) ) ;
#31094 = CARTESIAN_POINT ( 'NONE',  ( -11.53846153846153655, -2.721908614388771852, 31.22303859784724978 ) ) ;
#31095 = VECTOR ( 'NONE', #19142, 1000.000000000000114 ) ;
#31096 = CARTESIAN_POINT ( 'NONE',  ( 5.010839665967195877, -8.973038597847269315, 34.52809138561120506 ) ) ;
#31097 = CARTESIAN_POINT ( 'NONE',  ( -11.28851612908349722, -3.520799739797214389, 33.17531984108286025 ) ) ;
#31098 = EDGE_CURVE ( 'NONE', #58205, #72630, #4855, .T. ) ;
#31099 = ORIENTED_EDGE ( 'NONE', *, *, #2425, .F. ) ;
#31100 = ORIENTED_EDGE ( 'NONE', *, *, #55361, .T. ) ;
#31101 = ORIENTED_EDGE ( 'NONE', *, *, #69682, .F. ) ;
#31103 = VERTEX_POINT ( 'NONE', #11517 ) ;
#31102 = CARTESIAN_POINT ( 'NONE',  ( 3.100621261037536769, -5.915902021225892149, 34.75552854090298638 ) ) ;
#31104 = EDGE_CURVE ( 'NONE', #80116, #14630, #20941, .T. ) ;
#31105 = EDGE_CURVE ( 'NONE', #67886, #76288, #73618, .T. ) ;
#31106 = DIRECTION ( 'NONE',  ( 0.000000000000000000, 0.6427876096865373645, -0.7660444431189797898 ) ) ;
#31107 = CARTESIAN_POINT ( 'NONE',  ( 6.130525438233648039, -10.31582465632705237, 34.18122507451815295 ) ) ;
#31108 = ORIENTED_EDGE ( 'NONE', *, *, #26331, .F. ) ;
#31109 = B_SPLINE_CURVE_WITH_KNOTS ( 'NONE', 3,
 ( #24716, #25159, #16617, #85977, #72008, #80108 ),
 .UNSPECIFIED., .F., .F.,
 ( 4, 2, 4 ),
 ( 0.0003909569690057772317, 0.0005862646681846011513, 0.0007815723673634250709 ),
 .UNSPECIFIED. ) ;
#31110 = ORIENTED_EDGE ( 'NONE', *, *, #4052, .T. ) ;
#31111 = EDGE_LOOP ( 'NONE', ( #5791, #44251, #67496, #50808, #70374 ) ) ;
#31112 = CARTESIAN_POINT ( 'NONE',  ( -10.61538461538461320, -3.050289026998446396, 32.03036669348365706 ) ) ;
#31113 = VERTEX_POINT ( 'NONE', #32664 ) ;
#31114 = B_SPLINE_CURVE_WITH_KNOTS ( 'NONE', 3,
 ( #69966, #86037, #48804, #83497, #77612, #45030, #35751, #14583, #7830, #1516 ),
 .UNSPECIFIED., .F., .F.,
 ( 4, 2, 2, 2, 4 ),
 ( 0.000000000000000000, 0.0001954339857564054144, 0.0003908679715128108288, 0.0005863019572692162703, 0.0007817359430256216575 ),
 .UNSPECIFIED. ) ;
#31115 = CARTESIAN_POINT ( 'NONE',  ( 11.78851585009985570, -11.28795663066794575, 33.01431243580653785 ) ) ;
#31116 = VECTOR ( 'NONE', #46152, 1000.000000000000000 ) ;
#31117 = CYLINDRICAL_SURFACE ( 'NONE', #73331, 0.2500000000000008882 ) ;
#31118 = EDGE_CURVE ( 'NONE', #36238, #18936, #540, .T. ) ;
#31119 = CARTESIAN_POINT ( 'NONE',  ( -19.99999999999998934, 12.00000000000000711, 10.00000000000000178 ) ) ;
#31120 = FACE_BOUND ( 'NONE', #34707, .T. ) ;
#31121 = ORIENTED_EDGE ( 'NONE', *, *, #20394, .T. ) ;
#31122 = CARTESIAN_POINT ( 'NONE',  ( -5.076923076923199218, -3.643525952248796163, 33.31231777344771672 ) ) ;
#31123 = LINE ( 'NONE', #80219, #78762 ) ;
#31124 = FACE_OUTER_BOUND ( 'NONE', #21119, .T. ) ;
#31125 = ADVANCED_FACE ( 'NONE', ( #16931 ), #4307, .F. ) ;
#31126 = LINE ( 'NONE', #16727, #79753 ) ;
#31127 = DIRECTION ( 'NONE',  ( -1.845450506358306311E-16, 1.000000000000000000, -5.102127870520021228E-17 ) ) ;
#31128 = VERTEX_POINT ( 'NONE', #59248 ) ;
#31129 = CARTESIAN_POINT ( 'NONE',  ( -7.146003140593069958, -6.503392248772476236, 34.64988816332204635 ) ) ;
#31130 = ORIENTED_EDGE ( 'NONE', *, *, #13994, .T. ) ;
#31131 = ORIENTED_EDGE ( 'NONE', *, *, #58604, .F. ) ;
#31133 = CARTESIAN_POINT ( 'NONE',  ( 1.384615384615386802, -3.937682226553329556, 33.60647404775216529 ) ) ;
#31132 = CARTESIAN_POINT ( 'NONE',  ( -0.5916856709766823430, -9.418419913701741919, 34.36755862841477693 ) ) ;
#31134 = CYLINDRICAL_SURFACE ( 'NONE', #68671, 0.2499999999999998890 ) ;
#31135 = CYLINDRICAL_SURFACE ( 'NONE', #83980, 4.000000000000000000 ) ;
#31136 = CARTESIAN_POINT ( 'NONE',  ( -14.30769230769230660, -11.91647553114624181, 32.58852847137148245 ) ) ;
#31137 = CARTESIAN_POINT ( 'NONE',  ( 14.30769230769231015, -2.833524468853757305, 32.15551576947925838 ) ) ;
#31138 = EDGE_LOOP ( 'NONE', ( #53784, #73211 ) ) ;
#31139 = EDGE_CURVE ( 'NONE', #45549, #57327, #62438, .T. ) ;
#31140 = CARTESIAN_POINT ( 'NONE',  ( -5.143005456283209931, -6.343179335718451384, 34.87096338111212646 ) ) ;
#31141 = CARTESIAN_POINT ( 'NONE',  ( 17.77651507543566822, -3.562934362175799841, 33.22335522853832401 ) ) ;
#31142 = CARTESIAN_POINT ( 'NONE',  ( -1.514762594053606692, -3.817052484675422797, 33.13202310037935661 ) ) ;
#31143 = CARTESIAN_POINT ( 'NONE',  ( -13.63463860883683942, -12.68155406624981119, 30.59749803192733708 ) ) ;
#31144 = ORIENTED_EDGE ( 'NONE', *, *, #67457, .T. ) ;
#31145 = ADVANCED_FACE ( 'NONE', ( #86751 ), #79078, .F. ) ;
#31146 = VERTEX_POINT ( 'NONE', #17830 ) ;
#31147 = FACE_BOUND ( 'NONE', #38198, .T. ) ;
#31148 = ORIENTED_EDGE ( 'NONE', *, *, #13473, .T. ) ;
#31149 = VECTOR ( 'NONE', #47099, 1000.000000000000000 ) ;
#31150 = DIRECTION ( 'NONE',  ( 0.000000000000000000, 0.9396926207859126468, -0.3420201433256571111 ) ) ;
#31151 = LINE ( 'NONE', #58623, #28927 ) ;
#31152 = ORIENTED_EDGE ( 'NONE', *, *, #13427, .T. ) ;
#31153 = CARTESIAN_POINT ( 'NONE',  ( -7.596099534515528440, -4.235687564193445276, 33.53795663066793509 ) ) ;
#31154 = CARTESIAN_POINT ( 'NONE',  ( -10.74607608205217346, -6.413092428213692742, 34.63065189839063152 ) ) ;
#31155 = CARTESIAN_POINT ( 'NONE',  ( 11.53846153846153832, -13.53365097954675988, 30.81389545987213552 ) ) ;
#31156 = DIRECTION ( 'NONE',  ( -0.000000000000000000, -0.8660254037844399289, -0.4999999999999980016 ) ) ;
#31157 = EDGE_LOOP ( 'NONE', ( #64251, #7757, #5524, #71593 ) ) ;
#31158 = EDGE_CURVE ( 'NONE', #41427, #35812, #37054, .T. ) ;
#31159 = CARTESIAN_POINT ( 'NONE',  ( -7.846153846153844924, -1.215029322943914858, 32.30358669280327177 ) ) ;
#31160 = ORIENTED_EDGE ( 'NONE', *, *, #65566, .T. ) ;
#31162 = ORIENTED_EDGE ( 'NONE', *, *, #30444, .T. ) ;
#31161 = CARTESIAN_POINT ( 'NONE',  ( 16.85399685940691938, -10.61292498521070549, 33.66303323003028680 ) ) ;
#31163 = CARTESIAN_POINT ( 'NONE',  ( 15.29683758177167086, -8.120952969808772792, 34.71129190929999453 ) ) ;
#31164 = CARTESIAN_POINT ( 'NONE',  ( 24.00000000000000000, -5.499999999999981348, 27.75000000000000000 ) ) ;
#31165 = CARTESIAN_POINT ( 'NONE',  ( -7.715628407920199550, -3.625058011473227815, 33.29252011169590020 ) ) ;
#31166 = CARTESIAN_POINT ( 'NONE',  ( 10.36540787133602670, -12.41104346484419452, 31.60698883733904196 ) ) ;
#31167 = DIRECTION ( 'NONE',  ( 0.000000000000000000, 0.9396926207859126468, 0.3420201433256571111 ) ) ;
#31168 = EDGE_CURVE ( 'NONE', #12391, #48157, #79974, .T. ) ;
#31169 = CIRCLE ( 'NONE', #34000, 0.2500000000000002220 ) ;
#31170 = CARTESIAN_POINT ( 'NONE',  ( -12.94230769230769162, -7.500000000000000000, 29.75000000000000355 ) ) ;
#31171 = CARTESIAN_POINT ( 'NONE',  ( 0.06109907496451789238, -4.749999999999998224, 14.40811829374151110 ) ) ;
#31172 = ORIENTED_EDGE ( 'NONE', *, *, #43182, .T. ) ;
#31173 = CARTESIAN_POINT ( 'NONE',  ( 14.24242230713598900, -2.379036618887870436, 30.90682066428147934 ) ) ;
#31174 = FACE_OUTER_BOUND ( 'NONE', #59794, .T. ) ;
#31175 = DIRECTION ( 'NONE',  ( 1.000000000000000000, -0.000000000000000000, -0.000000000000000000 ) ) ;
#31176 = ORIENTED_EDGE ( 'NONE', *, *, #19598, .T. ) ;
#31177 = EDGE_LOOP ( 'NONE', ( #83754, #65165, #89066, #23673 ) ) ;
#31178 = CARTESIAN_POINT ( 'NONE',  ( -4.153846153846152411, -12.78798330534102767, 29.49999999999997868 ) ) ;
#31179 = CARTESIAN_POINT ( 'NONE',  ( -14.17716686945866833, -2.647132371071621471, 31.75357179365171589 ) ) ;
#31180 = B_SPLINE_CURVE_WITH_KNOTS ( 'NONE', 3,
 ( #41857, #55795, #34648, #76521, #62115, #6726, #81962, #420, #8066, #40532 ),
 .UNSPECIFIED., .F., .F.,
 ( 4, 2, 2, 2, 4 ),
 ( 0.000000000000000000, 0.0001954339857564063089, 0.0003908679715128126177, 0.0005863019572692189808, 0.0007817359430256252354 ),
 .UNSPECIFIED. ) ;
#31181 = EDGE_CURVE ( 'NONE', #10084, #60048, #53379, .T. ) ;
#31182 = B_SPLINE_CURVE_WITH_KNOTS ( 'NONE', 3,
 ( #37768, #58466, #38659, #85960, #58924, #86430, #24241, #44958, #45856, #73340 ),
 .UNSPECIFIED., .F., .F.,
 ( 4, 2, 2, 2, 4 ),
 ( 0.000000000000000000, 0.0001954339857564097512, 0.0003908679715128195024, 0.0005863019572692292807, 0.0007817359430256390048 ),
 .UNSPECIFIED. ) ;
#31183 = CARTESIAN_POINT ( 'NONE',  ( 17.20771351789003489, -3.338503747796866872, 32.95102852606552801 ) ) ;
#31184 = CARTESIAN_POINT ( 'NONE',  ( 0.000000000000000000, 1.535740489026526408E-15, 28.00000000000000000 ) ) ;
#31185 = CARTESIAN_POINT ( 'NONE',  ( 16.02369818411445834, -10.31621877034669588, 34.18098118002070152 ) ) ;
#31186 = ADVANCED_FACE ( 'NONE', ( #19158 ), #26359, .F. ) ;
#31187 = CARTESIAN_POINT ( 'NONE',  ( 16.28463659481310799, -3.338503747796866872, 32.95102852606552801 ) ) ;
#31188 = CARTESIAN_POINT ( 'NONE',  ( -19.00000000000000000, -1.250000000000000222, 24.75000000000000000 ) ) ;
#31189 = ORIENTED_EDGE ( 'NONE', *, *, #21005, .F. ) ;
#31190 = AXIS2_PLACEMENT_3D ( 'NONE', #82503, #20781, #47361 ) ;
#31191 = CARTESIAN_POINT ( 'NONE',  ( 6.223011351612851350, -10.61302985866383963, 33.66295027996417843 ) ) ;
#31192 = DIRECTION ( 'NONE',  ( 0.000000000000000000, 0.000000000000000000, 1.000000000000000000 ) ) ;
#31193 = CARTESIAN_POINT ( 'NONE',  ( 7.173131342990376247, -6.523592122091591783, 34.90882529074906415 ) ) ;
#31194 = CARTESIAN_POINT ( 'NONE',  ( 9.469380733400841521, -2.523278758544489797, 31.42238647778637528 ) ) ;
#31195 = VERTEX_POINT ( 'NONE', #61458 ) ;
#31196 = CARTESIAN_POINT ( 'NONE',  ( -7.596099534515530216, -3.627508038966690496, 32.91356715214248396 ) ) ;
#31197 = AXIS2_PLACEMENT_3D ( 'NONE', #6308, #27016, #54477 ) ;
#31198 = ORIENTED_EDGE ( 'NONE', *, *, #47661, .T. ) ;
#31199 = CARTESIAN_POINT ( 'NONE',  ( -17.20761368003338987, -2.494641256782729855, 31.33461815524612959 ) ) ;
#31200 =( LENGTH_UNIT ( ) NAMED_UNIT ( * ) SI_UNIT ( .MILLI., .METRE. ) );
#31201 = CARTESIAN_POINT ( 'NONE',  ( 19.00000000000000000, -1.749999999999999334, 22.25000000000000000 ) ) ;
#31202 = CARTESIAN_POINT ( 'NONE',  ( 17.77707304109313924, -10.01117774369187252, 34.36070679894347535 ) ) ;
#31203 = ORIENTED_EDGE ( 'NONE', *, *, #32299, .F. ) ;
#31204 = VECTOR ( 'NONE', #41148, 1000.000000000000000 ) ;
#31205 = CARTESIAN_POINT ( 'NONE',  ( 12.59232890250541281, -10.70102852606553157, 33.91149625220312913 ) ) ;
#31206 = PLANE ( 'NONE',  #78197 ) ;
#31207 = DIRECTION ( 'NONE',  ( 0.000000000000000000, -1.000000000000000000, 0.000000000000000000 ) ) ;
#31208 = CARTESIAN_POINT ( 'NONE',  ( -4.946132635956127288, -10.70102852606553157, 33.91149625220312913 ) ) ;
#31209 = VERTEX_POINT ( 'NONE', #19597 ) ;
#31210 = FACE_OUTER_BOUND ( 'NONE', #46680, .T. ) ;
#31211 = VERTEX_POINT ( 'NONE', #61023 ) ;
#31212 = CARTESIAN_POINT ( 'NONE',  ( -10.61538461538461320, -12.37446782046654192, 30.86335684631486131 ) ) ;
#31213 = B_SPLINE_CURVE_WITH_KNOTS ( 'NONE', 3,
 ( #33895, #33461, #61353, #34781, #76663, #560 ),
 .UNSPECIFIED., .F., .F.,
 ( 4, 2, 4 ),
 ( 0.0003909569690057828153, 0.0005862646681846093912, 0.0007815723673634359129 ),
 .UNSPECIFIED. ) ;
#31214 = CARTESIAN_POINT ( 'NONE',  ( 6.000000000000001776, -1.117168528481311540, 33.14645433367849847 ) ) ;
#31215 = ADVANCED_FACE ( 'NONE', ( #47504 ), #34880, .F. ) ;
#31216 = CARTESIAN_POINT ( 'NONE',  ( -3.007342268907659655, -7.630147231320743018, 34.74852402298682819 ) ) ;
#31217 = AXIS2_PLACEMENT_3D ( 'NONE', #70241, #23805, #14869 ) ;
#31218 = CARTESIAN_POINT ( 'NONE',  ( 7.622668921589514035, -12.47654668319379567, 31.42292124445336654 ) ) ;
#31219 = EDGE_CURVE ( 'NONE', #70729, #30367, #39885, .T. ) ;
#31220 = CARTESIAN_POINT ( 'NONE',  ( -6.130691466667555822, -4.118384482072085184, 33.43331474514187107 ) ) ;
#31221 = CARTESIAN_POINT ( 'NONE',  ( 15.23076923076911093, -11.94971097300221174, 32.03036669348237098 ) ) ;
#31222 = B_SPLINE_CURVE_WITH_KNOTS ( 'NONE', 3,
 ( #56782, #62215, #62646, #69422, #22121, #55898, #22560, #7729, #83838, #14929 ),
 .UNSPECIFIED., .F., .F.,
 ( 4, 2, 2, 2, 4 ),
 ( 0.000000000000000000, 0.0001954339857564080707, 0.0003908679715128161414, 0.0005863019572692241849, 0.0007817359430256322827 ),
 .UNSPECIFIED. ) ;
#31223 = EDGE_LOOP ( 'NONE', ( #42373, #13486, #28208, #68875 ) ) ;
#31225 = EDGE_CURVE ( 'NONE', #23390, #4149, #26800, .T. ) ;
#31224 = ORIENTED_EDGE ( 'NONE', *, *, #81031, .F. ) ;
#31226 = VERTEX_POINT ( 'NONE', #41204 ) ;
#31227 = PRODUCT_DEFINITION_SHAPE ( 'NONE', 'NONE',  #89183 ) ;
#31228 = ORIENTED_EDGE ( 'NONE', *, *, #22729, .F. ) ;
#31229 = VERTEX_POINT ( 'NONE', #13729 ) ;
#31230 = AXIS2_PLACEMENT_3D ( 'NONE', #10811, #83937, #72058 ) ;
#31231 = DIRECTION ( 'NONE',  ( -0.000000000000000000, -0.7660444431189791237, -0.6427876096865379196 ) ) ;
#31232 = CARTESIAN_POINT ( 'NONE',  ( -1.318547033612945008, -12.37446782046654192, 30.86335684631486842 ) ) ;
#31233 = EDGE_CURVE ( 'NONE', #79258, #77986, #88969, .T. ) ;
#31234 = LINE ( 'NONE', #28240, #3624 ) ;
#31235 = LINE ( 'NONE', #37998, #20662 ) ;
#31236 = CARTESIAN_POINT ( 'NONE',  ( 7.715463243043538810, -12.62707690430377383, 30.88035979386743435 ) ) ;
#31237 = CARTESIAN_POINT ( 'NONE',  ( 6.923076923076924238, -3.669653830205710676, 35.88435417666054406 ) ) ;
#31238 = ADVANCED_FACE ( 'NONE', ( #20484 ), #67348, .F. ) ;
#31239 = DIRECTION ( 'NONE',  ( -0.000000000000000000, 0.9396926207859093161, -0.3420201433256663259 ) ) ;
#31240 = CARTESIAN_POINT ( 'NONE',  ( -5.207482990536439260, -2.254533558242299396, 29.97296025877828285 ) ) ;
#31241 = CARTESIAN_POINT ( 'NONE',  ( -4.283993363284373856, -10.19110544564092002, 33.96427741523702792 ) ) ;
#31242 = ORIENTED_EDGE ( 'NONE', *, *, #41490, .F. ) ;
#31243 = ORIENTED_EDGE ( 'NONE', *, *, #56904, .F. ) ;
#31244 = ORIENTED_EDGE ( 'NONE', *, *, #61308, .T. ) ;
#31245 = EDGE_CURVE ( 'NONE', #66835, #78733, #16630, .T. ) ;
#31247 = ORIENTED_EDGE ( 'NONE', *, *, #58663, .F. ) ;
#31246 = CARTESIAN_POINT ( 'NONE',  ( 6.065255139512837346, -12.51329471203373700, 31.30864560766537963 ) ) ;
#31249 = CARTESIAN_POINT ( 'NONE',  ( 18.00000000000031264, -2.255955759149395501, 30.00000000000324363 ) ) ;
#31248 = DIRECTION ( 'NONE',  ( -0.000000000000000000, -0.9848077530122086864, -0.1736481776669273613 ) ) ;
#31250 = CARTESIAN_POINT ( 'NONE',  ( 20.00000000000000000, -4.000000000000000000, 29.75000000000000355 ) ) ;
#31251 = AXIS2_PLACEMENT_3D ( 'NONE', #28043, #8672, #61822 ) ;
#31252 = FACE_OUTER_BOUND ( 'NONE', #80098, .T. ) ;
#31253 = ORIENTED_EDGE ( 'NONE', *, *, #43509, .F. ) ;
#31254 = B_SPLINE_CURVE_WITH_KNOTS ( 'NONE', 3,
 ( #22466, #8076, #48603, #55806, #77411, #36860, #15721, #14837, #43184, #83742 ),
 .UNSPECIFIED., .F., .F.,
 ( 4, 2, 2, 2, 4 ),
 ( 0.000000000000000000, 0.0001954339857564080707, 0.0003908679715128161414, 0.0005863019572692241849, 0.0007817359430256322827 ),
 .UNSPECIFIED. ) ;
#31255 = B_SPLINE_CURVE_WITH_KNOTS ( 'NONE', 3,
 ( #58276, #51498, #85767, #87117, #71346, #24942 ),
 .UNSPECIFIED., .F., .F.,
 ( 4, 2, 4 ),
 ( 0.0003909569690057874774, 0.0005862646681846157880, 0.0007815723673634440444 ),
 .UNSPECIFIED. ) ;
#31256 = B_SPLINE_CURVE_WITH_KNOTS ( 'NONE', 3,
 ( #55752, #63394, #42259, #1703, #77359, #15666, #49002, #63842, #69717, #2570 ),
 .UNSPECIFIED., .F., .F.,
 ( 4, 2, 2, 2, 4 ),
 ( 0.000000000000000000, 0.0001954339857564078267, 0.0003908679715128156535, 0.0005863019572692235344, 0.0007817359430256313069 ),
 .UNSPECIFIED. ) ;
#31257 = EDGE_LOOP ( 'NONE', ( #57905, #15103 ) ) ;
#31258 = CARTESIAN_POINT ( 'NONE',  ( -2.307692307692427391, -12.46129190930018460, 30.37095296980731973 ) ) ;
#31259 = AXIS2_PLACEMENT_3D ( 'NONE', #61357, #55058, #40227 ) ;
#31260 = B_SPLINE_CURVE_WITH_KNOTS ( 'NONE', 3,
 ( #33174, #87695, #32725, #88149, #26422, #52545, #11123, #38601, #52102, #18779 ),
 .UNSPECIFIED., .F., .F.,
 ( 4, 2, 2, 2, 4 ),
 ( 0.000000000000000000, 0.0001954339881912776238, 0.0003908679763825552477, 0.0005863019645738329257, 0.0007817359527651104954 ),
 .UNSPECIFIED. ) ;
#31261 = EDGE_CURVE ( 'NONE', #12327, #40886, #33114, .T. ) ;
#31262 = ORIENTED_EDGE ( 'NONE', *, *, #78491, .T. ) ;
#31263 = FACE_BOUND ( 'NONE', #35877, .T. ) ;
#31264 = CARTESIAN_POINT ( 'NONE',  ( 15.10062202133100939, -10.19110544564092002, 33.96427741523702792 ) ) ;
#31265 = DIRECTION ( 'NONE',  ( -0.000000000000000000, -0.5000000000000009992, -0.8660254037844380415 ) ) ;
#31266 = VERTEX_POINT ( 'NONE', #74548 ) ;
#31267 = CARTESIAN_POINT ( 'NONE',  ( 14.05766907039934033, -2.823816976329317274, 31.52131813110795733 ) ) ;
#31268 = ADVANCED_FACE ( 'NONE', ( #88096 ), #81314, .T. ) ;
#31269 = DIRECTION ( 'NONE',  ( -0.000000000000000000, -0.000000000000000000, -1.000000000000000000 ) ) ;
#31270 = AXIS2_PLACEMENT_3D ( 'NONE', #51431, #38398, #71726 ) ;
#31271 = CARTESIAN_POINT ( 'NONE',  ( -18.00000000000000000, -3.937682226553330445, 33.60647404775216529 ) ) ;
#31272 = ORIENTED_EDGE ( 'NONE', *, *, #52590, .T. ) ;
#31273 = DIRECTION ( 'NONE',  ( -0.000000000000000000, 0.3420201433256694901, -0.9396926207859082059 ) ) ;
#31274 = CARTESIAN_POINT ( 'NONE',  ( 3.164685819813350509, -12.10708131394839349, 31.69288490824020244 ) ) ;
#31275 = ORIENTED_EDGE ( 'NONE', *, *, #33261, .F. ) ;
#31276 = CARTESIAN_POINT ( 'NONE',  ( -6.792285115252135519, -8.999086150933472084, 34.52020707165672064 ) ) ;
#31277 = FACE_OUTER_BOUND ( 'NONE', #13096, .T. ) ;
#31278 = ORIENTED_EDGE ( 'NONE', *, *, #49061, .F. ) ;
#31279 = DIRECTION ( 'NONE',  ( 0.000000000000000000, 0.000000000000000000, 1.000000000000000000 ) ) ;
#31280 = DIRECTION ( 'NONE',  ( -0.000000000000000000, -0.7660444431189791237, -0.6427876096865379196 ) ) ;
#31281 = DIRECTION ( 'NONE',  ( 0.000000000000000000, 0.000000000000000000, -1.000000000000000000 ) ) ;
#31282 = CARTESIAN_POINT ( 'NONE',  ( 7.623327153674845036, -7.369208160676173236, 34.74850200257122879 ) ) ;
#31283 = CARTESIAN_POINT ( 'NONE',  ( 6.000000000000001776, -1.790695186598648903, 34.54067556320373455 ) ) ;
#31284 = CARTESIAN_POINT ( 'NONE',  ( 17.20744851515672025, -5.070358843744208421, 34.40418822224088302 ) ) ;
#31286 = CARTESIAN_POINT ( 'NONE',  ( 8.545745844666434721, -3.019605429927184392, 32.48692288466676814 ) ) ;
#31285 = CYLINDRICAL_SURFACE ( 'NONE', #57698, 0.2499999999999973355 ) ;
#31287 = ADVANCED_FACE ( 'NONE', ( #61903 ), #218, .F. ) ;
#31288 = EDGE_CURVE ( 'NONE', #24104, #81961, #64968, .T. ) ;
#31289 = CARTESIAN_POINT ( 'NONE',  ( 1.515141086378948954, -11.46989282347013095, 32.79007818306219946 ) ) ;
#31291 = CARTESIAN_POINT ( 'NONE',  ( -16.15384615384627409, -10.33852847137269571, 34.16647553114546554 ) ) ;
#31290 = CARTESIAN_POINT ( 'NONE',  ( 3.100209317155866007, -2.254533558242299396, 29.97296025877828285 ) ) ;
#31292 = CARTESIAN_POINT ( 'NONE',  ( -2.724691934501232371, -8.700186371490559623, 26.01375670625848713 ) ) ;
#31293 = VERTEX_POINT ( 'NONE', #22694 ) ;
#31294 = CARTESIAN_POINT ( 'NONE',  ( 3.014247786467086687, -7.171217661578389801, 14.00000000000001066 ) ) ;
#31295 = EDGE_LOOP ( 'NONE', ( #55098, #25914, #67599, #2712 ) ) ;
#31296 = AXIS2_PLACEMENT_3D ( 'NONE', #68037, #49079, #60824 ) ;
#31297 = VERTEX_POINT ( 'NONE', #42100 ) ;
#31298 = CARTESIAN_POINT ( 'NONE',  ( -7.846153846153967493, -2.657715359629662544, 31.77849191805970364 ) ) ;
#31299 = EDGE_LOOP ( 'NONE', ( #80342, #68475, #83680, #69673 ) ) ;
#31300 = DIRECTION ( 'NONE',  ( 1.000000000000000000, 0.000000000000000000, 0.000000000000000000 ) ) ;
#31301 = CARTESIAN_POINT ( 'NONE',  ( 1.139087296526029469, -10.24999999999999467, 15.95312500000000000 ) ) ;
#31302 = CARTESIAN_POINT ( 'NONE',  ( -17.75005448165186195, -5.852078868378308485, 34.47109172314382874 ) ) ;
#31303 = ADVANCED_FACE ( 'NONE', ( #1099 ), #16383, .F. ) ;
#31304 = CARTESIAN_POINT ( 'NONE',  ( -5.934744860487160878, -11.67786785259547777, 32.92929555188713664 ) ) ;
#31305 = CARTESIAN_POINT ( 'NONE',  ( -6.000000000000119904, -9.442884908241554243, 34.35708131394783038 ) ) ;
#31306 = DIRECTION ( 'NONE',  ( -0.000000000000000000, -0.8660254037844397068, -0.4999999999999978906 ) ) ;
#31307 = DIRECTION ( 'NONE',  ( -0.000000000000000000, -0.000000000000000000, -1.000000000000000000 ) ) ;
#31308 = LINE ( 'NONE', #51545, #42996 ) ;
#31309 = CARTESIAN_POINT ( 'NONE',  ( -7.780898274877817933, -12.27809138561124591, 31.22303859784720359 ) ) ;
#31310 = B_SPLINE_CURVE_WITH_KNOTS ( 'NONE', 3,
 ( #32433, #31083, #17130, #64864, #45492, #39200, #58553, #44590, #51785, #18035 ),
 .UNSPECIFIED., .F., .F.,
 ( 4, 2, 2, 2, 4 ),
 ( 0.0007817246256747470640, 0.0009771112852218905021, 0.001172497944769033832, 0.001367884604316177161, 0.001563271263863320491 ),
 .UNSPECIFIED. ) ;
#31311 = CARTESIAN_POINT ( 'NONE',  ( 3.750000000000000888, -7.499999999999978684, 20.71875000000000000 ) ) ;
#31312 = EDGE_CURVE ( 'NONE', #12423, #47330, #81106, .T. ) ;
#31313 = ADVANCED_FACE ( 'NONE', ( #63236 ), #83976, .F. ) ;
#31314 = DIRECTION ( 'NONE',  ( 0.000000000000000000, 1.000000000000000000, 8.673617379884034486E-16 ) ) ;
#31315 = CARTESIAN_POINT ( 'NONE',  ( 13.16113046005105680, -3.562934362175799841, 33.22335522853832401 ) ) ;
#31316 = VECTOR ( 'NONE', #54345, 1000.000000000000227 ) ;
#31317 = FACE_OUTER_BOUND ( 'NONE', #36320, .T. ) ;
#31318 = EDGE_CURVE ( 'NONE', #74870, #60596, #46510, .T. ) ;
#31319 = VERTEX_POINT ( 'NONE', #43851 ) ;
#31320 = VERTEX_POINT ( 'NONE', #78085 ) ;
#31321 = DIRECTION ( 'NONE',  ( -0.000000000000000000, -0.1736481776669307198, -0.9848077530122080203 ) ) ;
#31322 = DIRECTION ( 'NONE',  ( 0.000000000000000000, 0.000000000000000000, -1.000000000000000000 ) ) ;
#31323 = CARTESIAN_POINT ( 'NONE',  ( -3.230769230769229949, -12.37446782046654192, 30.86335684631486131 ) ) ;
#31324 = CARTESIAN_POINT ( 'NONE',  ( 5.076923076923075762, -2.721908614388771852, 31.22303859784724978 ) ) ;
#31325 = CARTESIAN_POINT ( 'NONE',  ( 8.546304551714618114, -11.76352882383564769, 32.36236540154569497 ) ) ;
#31326 = CARTESIAN_POINT ( 'NONE',  ( -0.6850234052624096792, -6.760086850603068243, 34.69517049084099369 ) ) ;
#31327 = AXIS2_PLACEMENT_3D ( 'NONE', #86122, #24397, #38371 ) ;
#31328 = ORIENTED_EDGE ( 'NONE', *, *, #29791, .F. ) ;
#31329 = CYLINDRICAL_SURFACE ( 'NONE', #12727, 0.2500000000000008882 ) ;
#31330 = VERTEX_POINT ( 'NONE', #42977 ) ;
#31331 = VECTOR ( 'NONE', #5338, 1000.000000000000000 ) ;
#31333 = ADVANCED_FACE ( 'NONE', ( #76309 ), #36225, .F. ) ;
#31332 = ORIENTED_EDGE ( 'NONE', *, *, #87497, .F. ) ;
#31334 = DIRECTION ( 'NONE',  ( -0.000000000000000000, 0.6427876096865404731, -0.7660444431189771253 ) ) ;
#31335 = CARTESIAN_POINT ( 'NONE',  ( 6.250000000001437961, -7.500000000000155431, 34.75000000000007105 ) ) ;
#31336 = CARTESIAN_POINT ( 'NONE',  ( 0.4615384615384611200, -13.78497067705608181, 32.30358669280327177 ) ) ;
#31337 = VECTOR ( 'NONE', #11506, 1000.000000000000000 ) ;
#31338 = DIRECTION ( 'NONE',  ( -0.000000000000000000, 0.1736481776669307198, -0.9848077530122080203 ) ) ;
#31339 = DIRECTION ( 'NONE',  ( -0.000000000000000000, 0.9848077530122086864, -0.1736481776669273891 ) ) ;
#31340 = VERTEX_POINT ( 'NONE', #84417 ) ;
#31341 = ORIENTED_EDGE ( 'NONE', *, *, #81092, .F. ) ;
#31342 = B_SPLINE_CURVE_WITH_KNOTS ( 'NONE', 3,
 ( #24170, #79579, #64710, #71917, #31381, #71036, #30055, #51623, #10229, #44883 ),
 .UNSPECIFIED., .F., .F.,
 ( 4, 2, 2, 2, 4 ),
 ( 0.000000000000000000, 0.0001954339857564079894, 0.0003908679715128159787, 0.0005863019572692239681, 0.0007817359430256319575 ),
 .UNSPECIFIED. ) ;
#31343 = EDGE_LOOP ( 'NONE', ( #37603, #52277, #83317, #24705 ) ) ;
#31344 = CARTESIAN_POINT ( 'NONE',  ( 1.253923917947829203, -11.18331474514187995, 33.13161551792790505 ) ) ;
#31345 = CARTESIAN_POINT ( 'NONE',  ( -16.08859101433330707, -9.528491918058456633, 34.59228464037085615 ) ) ;
#31346 = CARTESIAN_POINT ( 'NONE',  ( 4.284371592079798674, -3.625058011473227815, 33.29252011169590020 ) ) ;
#31347 = CARTESIAN_POINT ( 'NONE',  ( -15.16551365949320562, -3.300289026998473041, 32.46337939537591666 ) ) ;
#31348 = CIRCLE ( 'NONE', #81713, 5.000000000000000888 ) ;
#31349 = CARTESIAN_POINT ( 'NONE',  ( -4.153846153846273204, -8.613356846316285953, 34.62446782046622218 ) ) ;
#31350 = CARTESIAN_POINT ( 'NONE',  ( 17.93472955403921887, -8.613356846314824011, 34.62446782046655613 ) ) ;
#31351 = VERTEX_POINT ( 'NONE', #37087 ) ;
#31352 = ORIENTED_EDGE ( 'NONE', *, *, #63586, .F. ) ;
#31353 = CARTESIAN_POINT ( 'NONE',  ( 2.651650429449539104, -4.848349570550432475, 23.06250000000000000 ) ) ;
#31354 = ORIENTED_EDGE ( 'NONE', *, *, #45373, .T. ) ;
#31355 = ADVANCED_FACE ( 'NONE', ( #76764 ), #15950, .F. ) ;
#31357 = ORIENTED_EDGE ( 'NONE', *, *, #17336, .T. ) ;
#31356 = CARTESIAN_POINT ( 'NONE',  ( -12.52680890749923570, -11.48612834413959582, 32.76840700105983473 ) ) ;
#31358 = CARTESIAN_POINT ( 'NONE',  ( -10.55012947587177941, -4.320704448112861584, 33.92786785259548310 ) ) ;
#31359 = CARTESIAN_POINT ( 'NONE',  ( 11.00641025641025550, -7.500000000000000000, 29.75000000000000355 ) ) ;
#31360 = CARTESIAN_POINT ( 'NONE',  ( 3.750000000000000888, -7.499999999999978684, 15.71875000000000000 ) ) ;
#31361 = ORIENTED_EDGE ( 'NONE', *, *, #52920, .T. ) ;
#31362 = VECTOR ( 'NONE', #62762, 1000.000000000000000 ) ;
#31363 = CARTESIAN_POINT ( 'NONE',  ( -13.51530685128294529, -12.11776431015576172, 31.66791131148498906 ) ) ;
#31364 = ORIENTED_EDGE ( 'NONE', *, *, #82548, .T. ) ;
#31365 = FACE_OUTER_BOUND ( 'NONE', #987, .T. ) ;
#31366 = DIRECTION ( 'NONE',  ( 1.000000000000000000, 0.000000000000000000, 0.000000000000000000 ) ) ;
#31367 = CARTESIAN_POINT ( 'NONE',  ( 7.623226887246994821, -4.026226216239095379, 33.68668979543632958 ) ) ;
#31369 = LINE ( 'NONE', #25055, #7110 ) ;
#31368 = DIRECTION ( 'NONE',  ( -0.000000000000000000, 0.3420201433256694901, -0.9396926207859082059 ) ) ;
#31370 = DIRECTION ( 'NONE',  ( 0.000000000000000000, 0.6427876096865373645, -0.7660444431189797898 ) ) ;
#31371 = CARTESIAN_POINT ( 'NONE',  ( -10.74607608205217346, -10.54014554554150607, 33.71984207302941883 ) ) ;
#31372 = ORIENTED_EDGE ( 'NONE', *, *, #47455, .T. ) ;
#31373 = EDGE_CURVE ( 'NONE', #77667, #58446, #24125, .T. ) ;
#31374 = CARTESIAN_POINT ( 'NONE',  ( -25.00000000000000355, 9.999999999999971578, 13.00000000000000178 ) ) ;
#31375 = CARTESIAN_POINT ( 'NONE',  ( 15.00784301325308157, -4.186968288167450147, 33.49512374952580274 ) ) ;
#31376 = ORIENTED_EDGE ( 'NONE', *, *, #44057, .T. ) ;
#31377 = CARTESIAN_POINT ( 'NONE',  ( 6.700150705560774966, -9.886141570436013382, 34.14413921362392301 ) ) ;
#31378 = CARTESIAN_POINT ( 'NONE',  ( 17.07692307692295586, -11.06231777344772027, 33.60647404775119895 ) ) ;
#31379 = CARTESIAN_POINT ( 'NONE',  ( -2.307692307692427391, -11.94971097300221174, 32.03036669348237098 ) ) ;
#31380 = LINE ( 'NONE', #52529, #37120 ) ;
#31381 = CARTESIAN_POINT ( 'NONE',  ( 7.596177115211490971, -8.303909089506435137, 34.68538101551103381 ) ) ;
#31382 = FACE_BOUND ( 'NONE', #4427, .T. ) ;
#31384 = CARTESIAN_POINT ( 'NONE',  ( -10.68113804369794728, -7.249945578846652694, 34.99404164642496795 ) ) ;
#31383 = CARTESIAN_POINT ( 'NONE',  ( 12.39545505058258001, -3.050289026998445951, 32.03036669348365706 ) ) ;
#31385 = EDGE_CURVE ( 'NONE', #4203, #7957, #17609, .T. ) ;
#31386 = CARTESIAN_POINT ( 'NONE',  ( -2.307692307692305711, -13.20930481340135110, 34.54067556320372745 ) ) ;
#31388 = CARTESIAN_POINT ( 'NONE',  ( 0.5276057948885366500, -2.833524468853757750, 32.15551576947925838 ) ) ;
#31387 = FACE_OUTER_BOUND ( 'NONE', #3050, .T. ) ;
#31389 = CARTESIAN_POINT ( 'NONE',  ( 1.515140822849028401, -3.068774925481847493, 32.56582465632704526 ) ) ;
#31390 = CARTESIAN_POINT ( 'NONE',  ( 1.254055471002021971, -2.254533558242299396, 29.97296025877828285 ) ) ;
#31391 = B_SPLINE_CURVE_WITH_KNOTS ( 'NONE', 3,
 ( #40117, #68453, #81542, #19829, #5876, #47291, #74784, #6750, #6326, #54944 ),
 .UNSPECIFIED., .F., .F.,
 ( 4, 2, 2, 2, 4 ),
 ( 0.0007817359430256334753, 0.0009771253907250058643, 0.001172514838424371098, 0.001367904286123736764, 0.001563293733823101998 ),
 .UNSPECIFIED. ) ;
#31392 = CARTESIAN_POINT ( 'NONE',  ( 3.775308065498768517, -8.992201783934554271, 26.79500670625849423 ) ) ;
#31393 = ORIENTED_EDGE ( 'NONE', *, *, #4182, .F. ) ;
#31394 = CARTESIAN_POINT ( 'NONE',  ( -15.23076923076922995, -12.78798330534102945, 29.74999999999997868 ) ) ;
#31395 = B_SPLINE_CURVE_WITH_KNOTS ( 'NONE', 3,
 ( #596, #56859, #84354, #77583, #35263, #15891, #70834, #21300, #64056, #48772 ),
 .UNSPECIFIED., .F., .F.,
 ( 4, 2, 2, 2, 4 ),
 ( 0.0007817359527651090859, 0.0009771254036996478414, 0.001172514854634186489, 0.001367904305568725136, 0.001563293756503263783 ),
 .UNSPECIFIED. ) ;
#31396 = CARTESIAN_POINT ( 'NONE',  ( 8.096208266067295156, -10.06805714834173315, 34.32951233291982618 ) ) ;
#31397 = CARTESIAN_POINT ( 'NONE',  ( -0.7115152055870535008, -3.436278759898155233, 33.07459398097509506 ) ) ;
#31398 = LINE ( 'NONE', #16112, #25128 ) ;
#31399 = CARTESIAN_POINT ( 'NONE',  ( 1.653273178848927064E-15, -7.500000000000000000, 13.50000000000000178 ) ) ;
#31400 = FACE_OUTER_BOUND ( 'NONE', #71607, .T. ) ;
#31401 = CARTESIAN_POINT ( 'NONE',  ( 3.775308065498768517, -8.992201783934554271, 24.29500670625849423 ) ) ;
#31402 = CARTESIAN_POINT ( 'NONE',  ( -15.36145983387953606, -12.62707690430377383, 30.88035979386743435 ) ) ;
#31403 = CARTESIAN_POINT ( 'NONE',  ( 3.230769230769231726, -2.538708090699994813, 30.37095296980875503 ) ) ;
#31404 = CARTESIAN_POINT ( 'NONE',  ( 11.78846153846147793, -7.565270000091922853, 34.99999999999999289 ) ) ;
#31405 = CARTESIAN_POINT ( 'NONE',  ( -16.15384615384627409, -10.21337939537710326, 33.94971097300076224 ) ) ;
#31406 = CARTESIAN_POINT ( 'NONE',  ( 8.769230769230768274, -1.367168528481310208, 33.57946703557072254 ) ) ;
#31407 = CYLINDRICAL_SURFACE ( 'NONE', #44011, 0.2499999999999998890 ) ;
#31408 = EDGE_CURVE ( 'NONE', #61213, #16297, #13288, .T. ) ;
#31409 = EDGE_CURVE ( 'NONE', #72566, #46285, #23578, .T. ) ;
#31410 = CARTESIAN_POINT ( 'NONE',  ( -18.13069146666756382, -2.729777683071818117, 31.24903638046269450 ) ) ;
#31411 = DIRECTION ( 'NONE',  ( -0.000000000000000000, 1.000000000000000000, -0.000000000000000000 ) ) ;
#31412 = ORIENTED_EDGE ( 'NONE', *, *, #65264, .F. ) ;
#31414 = CARTESIAN_POINT ( 'NONE',  ( 14.98074600654777377, -11.56360843649121861, 33.07473185843129926 ) ) ;
#31413 = APPLICATION_CONTEXT ( 'automotive_design' ) ;
#31415 = CARTESIAN_POINT ( 'NONE',  ( 7.146088274689773812, -4.887748414852792322, 34.01359900205216746 ) ) ;
#31416 = CARTESIAN_POINT ( 'NONE',  ( 2.608446859217924629, -10.19485399968118422, 13.62686829374151642 ) ) ;
#31417 = B_SPLINE_CURVE_WITH_KNOTS ( 'NONE', 3,
 ( #83710, #70176, #15244, #36829, #44454, #76939, #2588, #42714, #8485, #29208 ),
 .UNSPECIFIED., .F., .F.,
 ( 4, 2, 2, 2, 4 ),
 ( 0.0007817246256747451124, 0.0009771112852218879000, 0.001172497944769030796, 0.001367884604316173692, 0.001563271263863316588 ),
 .UNSPECIFIED. ) ;
#31418 = CARTESIAN_POINT ( 'NONE',  ( -10.83831157429146330, -10.01117774369187252, 34.36070679894347535 ) ) ;
#31420 = CARTESIAN_POINT ( 'NONE',  ( 15.23076923076923173, -1.466349020453238561, 30.81389545987213907 ) ) ;
#31419 = AXIS2_PLACEMENT_3D ( 'NONE', #36704, #83579, #63723 ) ;
#31421 = ORIENTED_EDGE ( 'NONE', *, *, #23884, .T. ) ;
#31422 = CARTESIAN_POINT ( 'NONE',  ( 1.384615384615265343, -4.481592998941358097, 33.73612834414048933 ) ) ;
#31423 = CARTESIAN_POINT ( 'NONE',  ( 6.923076923076924238, -11.33034616979429110, 35.88435417666054406 ) ) ;
#31425 = VERTEX_POINT ( 'NONE', #24910 ) ;
#31424 = CARTESIAN_POINT ( 'NONE',  ( 7.976944287120804056, -2.494656445102014342, 31.33466734024120015 ) ) ;
#31426 = CARTESIAN_POINT ( 'NONE',  ( -12.59168643127015841, -9.504002272028875709, 34.60269587691767867 ) ) ;
#31427 = DIRECTION ( 'NONE',  ( -0.000000000000000000, -0.9848077530122086864, -0.1736481776669273613 ) ) ;
#31428 = LINE ( 'NONE', #25560, #69420 ) ;
#31429 = AXIS2_PLACEMENT_3D ( 'NONE', #41091, #82534, #62237 ) ;
#31430 = CARTESIAN_POINT ( 'NONE',  ( 17.99999999999987566, -11.67786785259630911, 32.92929555188603530 ) ) ;
#31431 = EDGE_LOOP ( 'NONE', ( #54821, #37039, #85287, #24498, #76875 ) ) ;
#31432 = AXIS2_PLACEMENT_3D ( 'NONE', #35618, #14005, #35165 ) ;
#31433 = LINE ( 'NONE', #87286, #332 ) ;
#31434 = CARTESIAN_POINT ( 'NONE',  ( -12.46153846153846168, -2.486705287966279876, 31.30864560766543647 ) ) ;
#31435 = AXIS2_PLACEMENT_3D ( 'NONE', #58790, #86293, #51563 ) ;
#31436 = CARTESIAN_POINT ( 'NONE',  ( 9.692307692307695177, -13.78497067705608181, 32.30358669280327177 ) ) ;
#31437 = VERTEX_POINT ( 'NONE', #25361 ) ;
#31438 = ORIENTED_EDGE ( 'NONE', *, *, #31219, .T. ) ;
#31439 = ORIENTED_EDGE ( 'NONE', *, *, #5157, .F. ) ;
#31440 = CARTESIAN_POINT ( 'NONE',  ( -9.758391103263571509, -9.780366693483667717, 34.19971097300155805 ) ) ;
#31441 = CARTESIAN_POINT ( 'NONE',  ( -5.076923076923075762, -3.669653830205710676, 35.88435417666054406 ) ) ;
#31442 = CARTESIAN_POINT ( 'NONE',  ( 2.438218009455871638, -6.001044277235011215, 34.52024696741798948 ) ) ;
#31443 = CYLINDRICAL_SURFACE ( 'NONE', #34809, 4.000000000000000000 ) ;
#31444 = ORIENTED_EDGE ( 'NONE', *, *, #48604, .T. ) ;
#31445 = ORIENTED_EDGE ( 'NONE', *, *, #11293, .T. ) ;
#31447 = ORIENTED_EDGE ( 'NONE', *, *, #58155, .T. ) ;
#31446 = CARTESIAN_POINT ( 'NONE',  ( 4.153846153846030731, -5.941354392335915335, 34.76329471203413846 ) ) ;
#31448 = CARTESIAN_POINT ( 'NONE',  ( -5.299850035829923200, -2.523278758544489797, 31.42238647778637528 ) ) ;
#31449 = CARTESIAN_POINT ( 'NONE',  ( -3.361459833879538284, -4.684245665217971144, 34.18127051446801090 ) ) ;
#31450 = CYLINDRICAL_SURFACE ( 'NONE', #62250, 0.2499999999999979738 ) ;
#31451 = CARTESIAN_POINT ( 'NONE',  ( -1.253824943648434109, -12.62708834333097663, 30.88030960425257021 ) ) ;
#31452 = ORIENTED_EDGE ( 'NONE', *, *, #20023, .F. ) ;
#31453 = VERTEX_POINT ( 'NONE', #30775 ) ;
#31454 = B_SPLINE_CURVE_WITH_KNOTS ( 'NONE', 3,
 ( #73609, #19534, #13227, #46994, #12777, #54635, #19971, #82134, #46121, #12337 ),
 .UNSPECIFIED., .F., .F.,
 ( 4, 2, 2, 2, 4 ),
 ( 0.000000000000000000, 0.0001954311564186865763, 0.0003908623128373731525, 0.0005862934692560596746, 0.0007817246256747463051 ),
 .UNSPECIFIED. ) ;
#31455 = B_SPLINE_CURVE_WITH_KNOTS ( 'NONE', 3,
 ( #70367, #82998, #76226, #36149, #63152, #35243, #1020, #1467, #28955, #28495 ),
 .UNSPECIFIED., .F., .F.,
 ( 4, 2, 2, 2, 4 ),
 ( 0.000000000000000000, 0.0001954311564186862781, 0.0003908623128373725562, 0.0005862934692560588072, 0.0007817246256747451124 ),
 .UNSPECIFIED. ) ;
#31456 = EDGE_LOOP ( 'NONE', ( #16604, #16780, #73417, #19540, #64000, #58724 ) ) ;
#31458 = ORIENTED_EDGE ( 'NONE', *, *, #19074, .T. ) ;
#31457 = PLANE ( 'NONE',  #86214 ) ;
#31459 = EDGE_CURVE ( 'NONE', #33835, #22118, #76623, .T. ) ;
#31460 = ADVANCED_FACE ( 'NONE', ( #85293 ), #51026, .F. ) ;
#31461 = CARTESIAN_POINT ( 'NONE',  ( 3.165498784808455479, -11.94971097300153140, 32.03036669348370680 ) ) ;
#31462 = CARTESIAN_POINT ( 'NONE',  ( 18.25005441991345378, -5.642605341092955307, 34.66089969410670335 ) ) ;
#31463 = ORIENTED_EDGE ( 'NONE', *, *, #3945, .T. ) ;
#31464 = CARTESIAN_POINT ( 'NONE',  ( -8.834501215191545853, -10.90142922261923886, 33.41473453929638993 ) ) ;
#31465 = CARTESIAN_POINT ( 'NONE',  ( -13.60748080681902294, -2.501496062324912284, 29.88072118266895671 ) ) ;
#31466 = CARTESIAN_POINT ( 'NONE',  ( -5.869209559033046197, -3.338503747796866872, 32.95102852606553512 ) ) ;
#31467 = FACE_BOUND ( 'NONE', #12057, .T. ) ;
#31468 = CARTESIAN_POINT ( 'NONE',  ( 15.23076923076911093, -6.026961402154118019, 34.52809138561165270 ) ) ;
#31469 = CARTESIAN_POINT ( 'NONE',  ( 9.442307692307693401, -7.433931650972300353, 34.75000000000000711 ) ) ;
#31470 = EDGE_CURVE ( 'NONE', #22047, #83223, #70234, .T. ) ;
#31471 = CARTESIAN_POINT ( 'NONE',  ( -7.976845312821408740, -12.11776431015576172, 31.66791131148498906 ) ) ;
#31473 = CARTESIAN_POINT ( 'NONE',  ( -8.703975629717930929, -12.16647553114626490, 32.15551576947920864 ) ) ;
#31472 = CARTESIAN_POINT ( 'NONE',  ( 16.94623247381277054, -9.084618155246140248, 34.75535874321725771 ) ) ;
#31474 = CARTESIAN_POINT ( 'NONE',  ( -11.53846153846153655, -3.050289026998446396, 32.03036669348365706 ) ) ;
#31475 = LINE ( 'NONE', #58940, #66322 ) ;
#31476 = ORIENTED_EDGE ( 'NONE', *, *, #59237, .T. ) ;
#31477 = CARTESIAN_POINT ( 'NONE',  ( -5.933931648997559982, -11.69971097300155272, 32.46337939537588113 ) ) ;
#31478 = EDGE_CURVE ( 'NONE', #34311, #53458, #26219, .T. ) ;
#31479 = CARTESIAN_POINT ( 'NONE',  ( -7.596099534515531104, -2.564540009722895419, 30.55348353981670684 ) ) ;
#31480 = ORIENTED_EDGE ( 'NONE', *, *, #51487, .F. ) ;
#31481 = VERTEX_POINT ( 'NONE', #45176 ) ;
#31482 = CIRCLE ( 'NONE', #54495, 2.000000000000001776 ) ;
#31484 = CARTESIAN_POINT ( 'NONE',  ( 14.98074600654777377, -2.985938066672154445, 32.43141759479405550 ) ) ;
#31483 = CARTESIAN_POINT ( 'NONE',  ( 5.869852790561781219, -6.852621066184267029, 34.70813303252209181 ) ) ;
#31485 = CARTESIAN_POINT ( 'NONE',  ( 15.23076923076923173, -5.180354513474913603, 36.12317359536750416 ) ) ;
#31486 = CYLINDRICAL_SURFACE ( 'NONE', #21396, 0.2500000000000008882 ) ;
#31487 = CARTESIAN_POINT ( 'NONE',  ( -15.16460008980657292, -7.250054483168843156, 34.74374881642865631 ) ) ;
#31488 = VERTEX_POINT ( 'NONE', #30340 ) ;
#31489 = CARTESIAN_POINT ( 'NONE',  ( 7.384615384615385025, -3.499999999999999556, 29.75000000000000355 ) ) ;
#31490 = CARTESIAN_POINT ( 'NONE',  ( 23.49999999999998934, 5.000000000000023093, 32.75000000000000000 ) ) ;
#31491 = AXIS2_PLACEMENT_3D ( 'NONE', #51731, #85545, #3115 ) ;
#31493 = DIRECTION ( 'NONE',  ( -0.000000000000000000, -0.7660444431189791237, -0.6427876096865379196 ) ) ;
#31492 = DIRECTION ( 'NONE',  ( -0.000000000000000000, 0.000000000000000000, 1.000000000000000000 ) ) ;
#31494 = CARTESIAN_POINT ( 'NONE',  ( 13.38461538461538680, -10.67929555188718282, 33.92786785259544047 ) ) ;
#31495 = ADVANCED_FACE ( 'NONE', ( #58692 ), #38886, .T. ) ;
#31496 = CARTESIAN_POINT ( 'NONE',  ( 10.86533013373275658, -4.336752205174649433, 33.62275283266504289 ) ) ;
#31497 = CARTESIAN_POINT ( 'NONE',  ( -6.923076923076922462, -2.708943851104267164, 35.45975837776705220 ) ) ;
#31498 = CARTESIAN_POINT ( 'NONE',  ( 2.651650429449569302, -10.15165042944953733, 20.87500000000000000 ) ) ;
#31499 = VERTEX_POINT ( 'NONE', #87087 ) ;
#31500 = ORIENTED_EDGE ( 'NONE', *, *, #80431, .T. ) ;
#31501 = CARTESIAN_POINT ( 'NONE',  ( -14.30769230769230660, -4.661471528628507777, 34.16647553114623292 ) ) ;
#31502 = DIRECTION ( 'NONE',  ( 1.000000000000000000, 0.000000000000000000, 0.000000000000000000 ) ) ;
#31503 = CARTESIAN_POINT ( 'NONE',  ( 10.61538461538449596, -2.625532179533778709, 30.86335684631627174 ) ) ;
#31504 = CARTESIAN_POINT ( 'NONE',  ( 3.903822929624695792, -10.92453946501458439, 33.72985991061850086 ) ) ;
#31505 = CARTESIAN_POINT ( 'NONE',  ( -18.00000000000000000, -12.27536236210233866, 35.44105525097462106 ) ) ;
#31506 = CARTESIAN_POINT ( 'NONE',  ( -3.750000000000008438, -5.946699141100917352, 17.67187500000000355 ) ) ;
#31507 = LINE ( 'NONE', #86477, #28853 ) ;
#31508 = CARTESIAN_POINT ( 'NONE',  ( -13.44988583057615905, -8.613356846314824011, 34.62446782046655613 ) ) ;
#31509 = CARTESIAN_POINT ( 'NONE',  ( 16.82689983963011215, -12.22074536777955345, 31.39888409691088356 ) ) ;
#31510 = CARTESIAN_POINT ( 'NONE',  ( 5.933917620639865831, -9.905515769479276145, 34.41647553114623292 ) ) ;
#31511 = CARTESIAN_POINT ( 'NONE',  ( -9.442307692306272315, -7.500000000000154543, 35.00000000000007105 ) ) ;
#31512 = CARTESIAN_POINT ( 'NONE',  ( 5.448717948717947124, -11.50000000000000000, 29.75000000000000355 ) ) ;
#31513 = B_SPLINE_CURVE_WITH_KNOTS ( 'NONE', 3,
 ( #51847, #23936, #78443, #37913, #37455, #65375, #4111, #79793, #3669, #51385 ),
 .UNSPECIFIED., .F., .F.,
 ( 4, 2, 2, 2, 4 ),
 ( 0.000000000000000000, 0.0001954311564186864407, 0.0003908623128373728815, 0.0005862934692560593493, 0.0007817246256747457630 ),
 .UNSPECIFIED. ) ;
#31514 = CARTESIAN_POINT ( 'NONE',  ( -3.480769230769229061, -7.433931650972300353, 34.75000000000000711 ) ) ;
#31515 = CARTESIAN_POINT ( 'NONE',  ( -3.165513659493203846, -11.94971097300157403, 32.03036669348361443 ) ) ;
#31516 = ADVANCED_FACE ( 'NONE', ( #57808 ), #82426, .F. ) ;
#31517 = CARTESIAN_POINT ( 'NONE',  ( -5.776987155906605942, -4.762714258010880997, 34.23016756924214832 ) ) ;
#31518 = CARTESIAN_POINT ( 'NONE',  ( 9.562159722575998444, -5.070767119584671079, 34.40440758774516183 ) ) ;
#31519 = CARTESIAN_POINT ( 'NONE',  ( -15.23076923076935074, -8.613356846316285953, 34.62446782046622218 ) ) ;
#31520 = EDGE_CURVE ( 'NONE', #88008, #78911, #48695, .T. ) ;
#31521 = ORIENTED_EDGE ( 'NONE', *, *, #73469, .F. ) ;
#31522 = AXIS2_PLACEMENT_3D ( 'NONE', #31283, #2028, #85342 ) ;
#31523 = CARTESIAN_POINT ( 'NONE',  ( -16.02305571287920571, -6.369690395747424461, 34.87708834333098196 ) ) ;
#31524 = CARTESIAN_POINT ( 'NONE',  ( -5.010756470331436674, -7.250054591869668386, 34.99404684341514127 ) ) ;
#31525 = DIRECTION ( 'NONE',  ( 2.891205793294679312E-16, -1.000000000000000000, 0.000000000000000000 ) ) ;
#31526 = CARTESIAN_POINT ( 'NONE',  ( 1.944543648263018731, -9.444543648262994751, 24.62500000000000000 ) ) ;
#31527 = EDGE_CURVE ( 'NONE', #80799, #47713, #14395, .T. ) ;
#31528 = CARTESIAN_POINT ( 'NONE',  ( 13.51540719244017374, -4.809403383903225304, 33.96459661697924304 ) ) ;
#31529 = CARTESIAN_POINT ( 'NONE',  ( -0.4615384615384611200, -2.499999999999998668, 29.75000000000001421 ) ) ;
#31530 = EDGE_CURVE ( 'NONE', #61423, #23488, #74003, .T. ) ;
#31532 = VERTEX_POINT ( 'NONE', #55379 ) ;
#31531 = DIRECTION ( 'NONE',  ( 1.000000000000000000, 0.000000000000000000, 0.000000000000000000 ) ) ;
#31533 = CARTESIAN_POINT ( 'NONE',  ( 1.944543648262996083, -5.555456351736983045, 20.56250000000000000 ) ) ;
#31534 = DIRECTION ( 'NONE',  ( 0.000000000000000000, 0.8660254037844377084, 0.5000000000000015543 ) ) ;
#31535 = ORIENTED_EDGE ( 'NONE', *, *, #54468, .F. ) ;
#31536 = CARTESIAN_POINT ( 'NONE',  ( 6.923076923076800782, -6.835583212225970762, 34.95778746994575670 ) ) ;
#31537 = ORIENTED_EDGE ( 'NONE', *, *, #3545, .F. ) ;
#31538 = CARTESIAN_POINT ( 'NONE',  ( -7.715628407920201326, -6.808710257144161559, 34.95449254468098843 ) ) ;
#31539 = CARTESIAN_POINT ( 'NONE',  ( -9.469528151039279251, -2.847695495035523550, 31.58253572463339154 ) ) ;
#31540 = CARTESIAN_POINT ( 'NONE',  ( 15.29602480204525428, -2.892918686051625166, 31.69288490824026638 ) ) ;
#31541 = ORIENTED_EDGE ( 'NONE', *, *, #55699, .T. ) ;
#31542 = CARTESIAN_POINT ( 'NONE',  ( 0.2115617174898691555, -4.818429247618089661, 34.26397095200675125 ) ) ;
#31543 = EDGE_LOOP ( 'NONE', ( #20318, #66573 ) ) ;
#31544 = CARTESIAN_POINT ( 'NONE',  ( 0.4615384615384611755, -10.05456864172156806, 36.03766855953608683 ) ) ;
#31545 = ORIENTED_EDGE ( 'NONE', *, *, #71436, .T. ) ;
#31546 = VECTOR ( 'NONE', #26073, 1000.000000000000000 ) ;
#31547 = VECTOR ( 'NONE', #36222, 1000.000000000000114 ) ;
#31548 = CARTESIAN_POINT ( 'NONE',  ( -16.08859101433330707, -2.379036618887895305, 30.90682066428158592 ) ) ;
#31549 = CARTESIAN_POINT ( 'NONE',  ( 0.5920641633020230499, -11.46989282347013095, 32.79007818306219946 ) ) ;
#31550 = VERTEX_POINT ( 'NONE', #76542 ) ;
#31551 = CARTESIAN_POINT ( 'NONE',  ( -6.000000000000121680, -10.33852847137269571, 34.16647553114546554 ) ) ;
#31552 = CARTESIAN_POINT ( 'NONE',  ( 9.915320536401090123, -10.01129605718032600, 34.36064277460058491 ) ) ;
#31553 = CARTESIAN_POINT ( 'NONE',  ( 0.3308478584281528412, -2.295517848115769421, 30.44137282052137294 ) ) ;
#31554 = AXIS2_PLACEMENT_3D ( 'NONE', #26930, #54389, #69241 ) ;
#31555 = AXIS2_PLACEMENT_3D ( 'NONE', #28206, #75959, #74635 ) ;
#31556 = DIRECTION ( 'NONE',  ( 0.000000000000000000, 1.000000000000000000, 0.000000000000000000 ) ) ;
#31557 = LINE ( 'NONE', #86520, #39302 ) ;
#31558 = EDGE_CURVE ( 'NONE', #6072, #52057, #34220, .T. ) ;
#31559 = EDGE_LOOP ( 'NONE', ( #77657, #8417, #40598, #84533 ) ) ;
#31560 = ORIENTED_EDGE ( 'NONE', *, *, #45090, .F. ) ;
#31561 = ORIENTED_EDGE ( 'NONE', *, *, #26104, .F. ) ;
#31563 = ORIENTED_EDGE ( 'NONE', *, *, #41216, .F. ) ;
#31562 = FACE_OUTER_BOUND ( 'NONE', #80790, .T. ) ;
#31564 = CARTESIAN_POINT ( 'NONE',  ( -18.00000000000000000, -2.249999999999989786, 29.74999999999998579 ) ) ;
#31565 = CARTESIAN_POINT ( 'NONE',  ( 9.627037691751372250, -5.941354392334499579, 34.76329471203369792 ) ) ;
#31566 = EDGE_LOOP ( 'NONE', ( #79815, #45791 ) ) ;
#31567 = EDGE_CURVE ( 'NONE', #46418, #81839, #55819, .T. ) ;
#31568 = ORIENTED_EDGE ( 'NONE', *, *, #70782, .T. ) ;
#31569 = LINE ( 'NONE', #84758, #45392 ) ;
#31570 = ORIENTED_EDGE ( 'NONE', *, *, #52049, .T. ) ;
#31571 = CARTESIAN_POINT ( 'NONE',  ( -12.46153846153846168, -3.669653830205710676, 35.88435417666054406 ) ) ;
#31572 = CARTESIAN_POINT ( 'NONE',  ( -11.66860874789976243, -3.817052484675422797, 33.13202310037935661 ) ) ;
#31573 = CARTESIAN_POINT ( 'NONE',  ( 0.3954550505825806250, -4.786620604624113540, 33.94971097300155805 ) ) ;
#31574 = FACE_BOUND ( 'NONE', #20082, .T. ) ;
#31575 = ORIENTED_EDGE ( 'NONE', *, *, #79717, .T. ) ;
#31576 = CARTESIAN_POINT ( 'NONE',  ( -11.25641025641025550, -11.50000000000000000, 29.75000000000000355 ) ) ;
#31577 = LINE ( 'NONE', #60825, #44228 ) ;
#31578 = EDGE_CURVE ( 'NONE', #15943, #38361, #54940, .T. ) ;
#31579 = CARTESIAN_POINT ( 'NONE',  ( 15.23076923076923173, -8.564572088678739092, 35.78748833219616898 ) ) ;
#31580 = CARTESIAN_POINT ( 'NONE',  ( -14.30769230769242739, -9.442884908241554243, 34.35708131394783038 ) ) ;
#31581 = CARTESIAN_POINT ( 'NONE',  ( -1.634592115557738534, -2.564618984488975961, 30.55390908950641915 ) ) ;
#31582 = ORIENTED_EDGE ( 'NONE', *, *, #78782, .T. ) ;
#31583 = FACE_OUTER_BOUND ( 'NONE', #80866, .T. ) ;
#31584 = EDGE_CURVE ( 'NONE', #84519, #80176, #65914, .T. ) ;
#31585 = ORIENTED_EDGE ( 'NONE', *, *, #32423, .F. ) ;
#31586 = VERTEX_POINT ( 'NONE', #56267 ) ;
#31588 = CARTESIAN_POINT ( 'NONE',  ( 5.777073782483851616, -3.105860786376062332, 32.13614157043599562 ) ) ;
#31587 = CARTESIAN_POINT ( 'NONE',  ( -6.989159302437059296, -3.937682226553329556, 33.60647404775217240 ) ) ;
#31589 = B_SPLINE_CURVE_WITH_KNOTS ( 'NONE', 3,
 ( #85699, #85257, #42945, #16350, #64512, #58209, #15917, #83940, #78482, #37951 ),
 .UNSPECIFIED., .F., .F.,
 ( 4, 2, 2, 2, 4 ),
 ( 0.0007817359430256257775, 0.0009771253907249911191, 0.001172514838424356352, 0.001367904286123721586, 0.001563293733823086819 ),
 .UNSPECIFIED. ) ;
#31590 = CARTESIAN_POINT ( 'NONE',  ( -11.53846153846153655, -1.629998284177014645, 34.34916445242399163 ) ) ;
#31591 = CARTESIAN_POINT ( 'NONE',  ( -15.23076923076935074, -12.27809138561165270, 31.22303859784587132 ) ) ;
#31592 = CARTESIAN_POINT ( 'NONE',  ( 1.450683735617825709, -9.780366693483669494, 34.19971097300155805 ) ) ;
#31593 = CARTESIAN_POINT ( 'NONE',  ( 1.384615384615264011, -4.320704448113951379, 33.92786785259630022 ) ) ;
#31594 = VERTEX_POINT ( 'NONE', #42324 ) ;
#31595 = LINE ( 'NONE', #85217, #74539 ) ;
#31596 = LINE ( 'NONE', #30272, #53139 ) ;
#31597 = CARTESIAN_POINT ( 'NONE',  ( -1.449885830576159940, -3.835265460703609186, 33.15142922261924241 ) ) ;
#31598 = EDGE_CURVE ( 'NONE', #26195, #11627, #36879, .T. ) ;
#31599 = CARTESIAN_POINT ( 'NONE',  ( 10.74617642320940369, -11.71459661697925903, 32.44059661609676937 ) ) ;
#31600 = ORIENTED_EDGE ( 'NONE', *, *, #44557, .F. ) ;
#31601 = ORIENTED_EDGE ( 'NONE', *, *, #17879, .T. ) ;
#31603 = FACE_BOUND ( 'NONE', #60494, .T. ) ;
#31602 = B_SPLINE_CURVE_WITH_KNOTS ( 'NONE', 3,
 ( #21656, #71162, #29314, #43261, #62631, #42390, #22104, #44121, #76606, #9038 ),
 .UNSPECIFIED., .F., .F.,
 ( 4, 2, 2, 2, 4 ),
 ( 0.0007817246256747472808, 0.0009771112852218907189, 0.001172497944769034265, 0.001367884604316177595, 0.001563271263863321141 ),
 .UNSPECIFIED. ) ;
#31604 = CIRCLE ( 'NONE', #28792, 4.000000000000000000 ) ;
#31606 = AXIS2_PLACEMENT_3D ( 'NONE', #20927, #81323, #41215 ) ;
#31605 = ITEM_DEFINED_TRANSFORMATION ( 'NONE', 'NONE', #7257,  #83448 ) ;
#31608 = ADVANCED_FACE ( 'NONE', ( #83306 ), #83751, .T. ) ;
#31607 = ORIENTED_EDGE ( 'NONE', *, *, #15690, .T. ) ;
#31609 = CARTESIAN_POINT ( 'NONE',  ( 7.846153846153846700, -2.721908614388771852, 31.22303859784724978 ) ) ;
#31610 = CARTESIAN_POINT ( 'NONE',  ( -7.715628144390283438, -5.195472089885680766, 34.18748526763464923 ) ) ;
#31611 = ORIENTED_EDGE ( 'NONE', *, *, #37792, .T. ) ;
#31612 = EDGE_CURVE ( 'NONE', #60674, #65236, #49060, .T. ) ;
#31613 = CARTESIAN_POINT ( 'NONE',  ( -7.715628144390280774, -4.459921816937788996, 33.71989282347011851 ) ) ;
#31614 = CYLINDRICAL_SURFACE ( 'NONE', #6883, 0.2500000000000008882 ) ;
#31615 = CARTESIAN_POINT ( 'NONE',  ( -17.07692307692307665, -13.20930481340135110, 34.54067556320372745 ) ) ;
#31616 = CARTESIAN_POINT ( 'NONE',  ( -1.254089946381739429, -4.299079248970732792, 33.91157788607253565 ) ) ;
#31617 = VECTOR ( 'NONE', #45967, 1000.000000000000000 ) ;
#31618 = DIRECTION ( 'NONE',  ( 0.000000000000000000, 0.000000000000000000, 1.000000000000000000 ) ) ;
#31619 = EDGE_LOOP ( 'NONE', ( #37763, #28512, #78390, #10379 ) ) ;
#31621 = EDGE_LOOP ( 'NONE', ( #6613, #35863 ) ) ;
#31620 = DIRECTION ( 'NONE',  ( -1.000000000000000000, -0.000000000000000000, -0.000000000000000000 ) ) ;
#31622 = CARTESIAN_POINT ( 'NONE',  ( 14.30769230769231015, -10.89733346790207413, 36.13435417666054406 ) ) ;
#31623 = CARTESIAN_POINT ( 'NONE',  ( 13.91025641025641235, -7.500000000000000000, 29.75000000000000355 ) ) ;
#31624 = CARTESIAN_POINT ( 'NONE',  ( 17.07692307692307665, -4.786620604624113540, 33.94971097300155094 ) ) ;
#31625 = CARTESIAN_POINT ( 'NONE',  ( 18.06606835100243913, -8.120952969808772792, 34.71129190929999453 ) ) ;
#31626 = CARTESIAN_POINT ( 'NONE',  ( -16.15384615384627409, -8.613356846316285953, 34.62446782046622218 ) ) ;
#31627 = EDGE_CURVE ( 'NONE', #84168, #66664, #32557, .T. ) ;
#31628 = DIRECTION ( 'NONE',  ( 1.000000000000000000, 0.000000000000000000, 0.000000000000000000 ) ) ;
#31629 = CARTESIAN_POINT ( 'NONE',  ( -1.077988221561493543, -4.724691934501247914, 16.82999329374151287 ) ) ;
#31630 = ORIENTED_EDGE ( 'NONE', *, *, #64324, .T. ) ;
#31631 = LINE ( 'NONE', #80271, #1457 ) ;
#31632 = CARTESIAN_POINT ( 'NONE',  ( 8.769230769231075584, -2.506253911140615021, 30.00000000000323297 ) ) ;
#31633 = CARTESIAN_POINT ( 'NONE',  ( 2.307692307692309264, -13.75783147151868846, 33.36296068462461051 ) ) ;
#31634 = EDGE_CURVE ( 'NONE', #63565, #63637, #71987, .T. ) ;
#31635 = ORIENTED_EDGE ( 'NONE', *, *, #78394, .F. ) ;
#31636 = EDGE_CURVE ( 'NONE', #88176, #47159, #84639, .T. ) ;
#31637 = ORIENTED_EDGE ( 'NONE', *, *, #715, .F. ) ;
#31638 = CARTESIAN_POINT ( 'NONE',  ( -9.019253993452226226, -5.765609946408404518, 34.70566812827425451 ) ) ;
#31639 = CARTESIAN_POINT ( 'NONE',  ( 12.22435897435897267, -7.500000000000000000, 29.75000000000000355 ) ) ;
#31640 = CARTESIAN_POINT ( 'NONE',  ( -0.3963444797551056165, -2.506253911140448487, 29.99999999999988987 ) ) ;
#31641 = B_SPLINE_CURVE_WITH_KNOTS ( 'NONE', 3,
 ( #50349, #77830, #25111, #2606, #64748, #52573, #58433, #24665, #71960, #37732 ),
 .UNSPECIFIED., .F., .F.,
 ( 4, 2, 2, 2, 4 ),
 ( 0.0007817246256747484735, 0.0009771112852218931041, 0.001172497944769037735, 0.001367884604316182365, 0.001563271263863326996 ),
 .UNSPECIFIED. ) ;
#31642 = CARTESIAN_POINT ( 'NONE',  ( 8.835298102580843249, -11.35647404775217595, 33.31231777344666511 ) ) ;
#31643 = CARTESIAN_POINT ( 'NONE',  ( 18.00000000000000000, -11.91647553114624181, 32.58852847137148245 ) ) ;
#31644 = CARTESIAN_POINT ( 'NONE',  ( -6.988347369037697376, -11.94971097300153140, 32.03036669348370680 ) ) ;
#31645 = ORIENTED_EDGE ( 'NONE', *, *, #11739, .T. ) ;
#31646 = CARTESIAN_POINT ( 'NONE',  ( 5.750023269057646047, -3.627789207965226748, 32.91389620160131102 ) ) ;
#31647 = CARTESIAN_POINT ( 'NONE',  ( -12.46153846153858247, -5.219633306517616589, 34.19971097300220464 ) ) ;
#31648 = CARTESIAN_POINT ( 'NONE',  ( -17.07692307692319744, -9.528491918059723176, 34.59228464037033035 ) ) ;
#31649 = EDGE_CURVE ( 'NONE', #48531, #77905, #72304, .T. ) ;
#31650 = CARTESIAN_POINT ( 'NONE',  ( -3.454254174493178287, -11.89387501736622710, 32.13663884655806413 ) ) ;
#31652 = VERTEX_POINT ( 'NONE', #2632 ) ;
#31651 = AXIS2_PLACEMENT_3D ( 'NONE', #74280, #41827, #7147 ) ;
#31653 = CARTESIAN_POINT ( 'NONE',  ( -12.46153846153846168, -12.37446782046654192, 30.86335684631486131 ) ) ;
#31654 = ORIENTED_EDGE ( 'NONE', *, *, #31997, .T. ) ;
#31655 = CARTESIAN_POINT ( 'NONE',  ( -0.3954701105360229896, -2.721908614388772740, 31.22303859784725333 ) ) ;
#31656 = CARTESIAN_POINT ( 'NONE',  ( -1.449885830576159940, -9.442884908240170461, 34.35708131394840592 ) ) ;
#31657 = EDGE_CURVE ( 'NONE', #88418, #77943, #80949, .T. ) ;
#31658 = CARTESIAN_POINT ( 'NONE',  ( 15.29602437028207085, -5.094484230520773593, 34.41647553114626845 ) ) ;
#31659 = EDGE_LOOP ( 'NONE', ( #49625, #77428 ) ) ;
#31660 = DIRECTION ( 'NONE',  ( -0.000000000000000000, -0.9848077530122085754, -0.1736481776669273613 ) ) ;
#31661 = FACE_OUTER_BOUND ( 'NONE', #33898, .T. ) ;
#31662 = LINE ( 'NONE', #18149, #40864 ) ;
#31663 = CARTESIAN_POINT ( 'NONE',  ( -6.249976744048591826, -5.643011162660950042, 34.66104346484419096 ) ) ;
#31664 = CARTESIAN_POINT ( 'NONE',  ( -9.692307692307691624, -13.87047571288749737, 32.06866353760679544 ) ) ;
#31665 = EDGE_CURVE ( 'NONE', #27545, #64872, #3522, .T. ) ;
#31666 = ORIENTED_EDGE ( 'NONE', *, *, #46138, .F. ) ;
#31667 = VECTOR ( 'NONE', #35814, 1000.000000000000227 ) ;
#31668 = DIRECTION ( 'NONE',  ( 0.000000000000000000, 0.4999999999999985567, 0.8660254037844395958 ) ) ;
#31669 = VERTEX_POINT ( 'NONE', #17048 ) ;
#31670 = CARTESIAN_POINT ( 'NONE',  ( 13.38461538461538680, -8.973038597847269315, 34.52809138561121927 ) ) ;
#31671 = EDGE_CURVE ( 'NONE', #86754, #22873, #38011, .T. ) ;
#31672 = CARTESIAN_POINT ( 'NONE',  ( -9.626239341305254271, -12.10708131394839882, 31.69288490824020954 ) ) ;
#31673 = B_SPLINE_CURVE_WITH_KNOTS ( 'NONE', 3,
 ( #70765, #71632, #36100, #22570, #63552, #72086, #10393, #9938, #77515, #9069 ),
 .UNSPECIFIED., .F., .F.,
 ( 4, 2, 2, 2, 4 ),
 ( 0.000000000000000000, 0.0001954311564186862239, 0.0003908623128373724478, 0.0005862934692560586988, 0.0007817246256747448956 ),
 .UNSPECIFIED. ) ;
#31674 = AXIS2_PLACEMENT_3D ( 'NONE', #27749, #6599, #83605 ) ;
#31675 = AXIS2_PLACEMENT_3D ( 'NONE', #61147, #80562, #81447 ) ;
#31676 = ADVANCED_FACE ( 'NONE', ( #23352 ), #70668, .F. ) ;
#31677 = CARTESIAN_POINT ( 'NONE',  ( -13.38461538461538325, -2.721908614388771852, 31.22303859784724978 ) ) ;
#31678 = FACE_OUTER_BOUND ( 'NONE', #69959, .T. ) ;
#31679 = CARTESIAN_POINT ( 'NONE',  ( 14.30769230769231015, -1.117168528481311540, 33.14645433367849847 ) ) ;
#31680 = DIRECTION ( 'NONE',  ( -1.000000000000000000, -0.000000000000000000, -0.000000000000000000 ) ) ;
#31681 = AXIS2_PLACEMENT_3D ( 'NONE', #25548, #32310, #46706 ) ;
#31682 = CIRCLE ( 'NONE', #57514, 4.000000000000000000 ) ;
#31683 = ORIENTED_EDGE ( 'NONE', *, *, #2831, .F. ) ;
#31684 = EDGE_CURVE ( 'NONE', #61379, #22275, #4677, .T. ) ;
#31685 = VERTEX_POINT ( 'NONE', #85510 ) ;
#31686 = STYLED_ITEM ( 'NONE', ( #53084 ), #923 ) ;
#31687 = ORIENTED_EDGE ( 'NONE', *, *, #3573, .T. ) ;
#31688 = ORIENTED_EDGE ( 'NONE', *, *, #35553, .T. ) ;
#31689 = ORIENTED_EDGE ( 'NONE', *, *, #39434, .F. ) ;
#31690 = CARTESIAN_POINT ( 'NONE',  ( 12.71148397988660328, -11.86320923018887719, 32.19269448109604070 ) ) ;
#31691 = CARTESIAN_POINT ( 'NONE',  ( -3.296851610129365451, -6.343179335718451384, 34.87096338111212646 ) ) ;
#31692 = CARTESIAN_POINT ( 'NONE',  ( -2.084265345830736305, -7.630147231320743018, 34.74852402298682819 ) ) ;
#31693 = CARTESIAN_POINT ( 'NONE',  ( -7.146003140593072622, -3.105860786376062332, 32.13614157043599562 ) ) ;
#31694 = CARTESIAN_POINT ( 'NONE',  ( -16.21911659980693443, -2.625532179533445198, 30.86335684631481513 ) ) ;
#31695 = DIRECTION ( 'NONE',  ( 0.000000000000000000, 0.1736481776669267785, -0.9848077530122087975 ) ) ;
#31696 = CYLINDRICAL_SURFACE ( 'NONE', #37836, 0.2500000000000012212 ) ;
#31697 = CARTESIAN_POINT ( 'NONE',  ( -7.596208327805703320, -3.202959910592335202, 32.30730279482227019 ) ) ;
#31698 = CARTESIAN_POINT ( 'NONE',  ( -4.403869391139119571, -10.05641848906368097, 34.04755513067966177 ) ) ;
#31699 = EDGE_LOOP ( 'NONE', ( #81968, #86507, #60359, #48851 ) ) ;
#31700 = EDGE_CURVE ( 'NONE', #29311, #33240, #58029, .T. ) ;
#31701 = ORIENTED_EDGE ( 'NONE', *, *, #21944, .T. ) ;
#31702 = ORIENTED_EDGE ( 'NONE', *, *, #57396, .F. ) ;
#31704 = ORIENTED_EDGE ( 'NONE', *, *, #73317, .F. ) ;
#31703 = CARTESIAN_POINT ( 'NONE',  ( 16.81410256410256565, -11.50000000000000000, 29.75000000000000355 ) ) ;
#31706 = DIRECTION ( 'NONE',  ( -0.000000000000000000, -0.9396926207859092051, -0.3420201433256662704 ) ) ;
#31705 = CARTESIAN_POINT ( 'NONE',  ( -12.46153846153846168, -1.215029322943914858, 32.30358669280327177 ) ) ;
#31707 = CARTESIAN_POINT ( 'NONE',  ( -11.53846153846153655, -8.164416787775445883, 34.95778746994557906 ) ) ;
#31708 = CARTESIAN_POINT ( 'NONE',  ( -14.55771554498526932, -10.05641848906368097, 34.04755513067966177 ) ) ;
#31709 = FACE_BOUND ( 'NONE', #656, .T. ) ;
#31710 = ORIENTED_EDGE ( 'NONE', *, *, #8228, .T. ) ;
#31711 = B_SPLINE_CURVE_WITH_KNOTS ( 'NONE', 3,
 ( #28800, #49504, #83744, #9401, #78289, #43186, #2624, #9835, #16586, #2187 ),
 .UNSPECIFIED., .F., .F.,
 ( 4, 2, 2, 2, 4 ),
 ( 0.0007817359527651106038, 0.0009771254036996469741, 0.001172514854634183236, 0.001367904305568724702, 0.001563293756503266168 ),
 .UNSPECIFIED. ) ;
#31712 = CIRCLE ( 'NONE', #67659, 0.2500000000000002220 ) ;
#31713 = VERTEX_POINT ( 'NONE', #1759 ) ;
#31714 = DIRECTION ( 'NONE',  ( 0.000000000000000000, 0.000000000000000000, 1.000000000000000000 ) ) ;
#31715 = ORIENTED_EDGE ( 'NONE', *, *, #79931, .T. ) ;
#31716 = FACE_BOUND ( 'NONE', #76365, .T. ) ;
#31717 = CARTESIAN_POINT ( 'NONE',  ( -9.626240358957616650, -2.292212530054420494, 30.41441678777542990 ) ) ;
#31718 = CARTESIAN_POINT ( 'NONE',  ( -14.53061926659915315, -6.459968553980841577, 34.89616026154728701 ) ) ;
#31719 = ORIENTED_EDGE ( 'NONE', *, *, #5740, .F. ) ;
#31720 = PLANE ( 'NONE',  #53483 ) ;
#31721 = CARTESIAN_POINT ( 'NONE',  ( 8.519230769230768274, -7.433932668274256805, 35.00000000000000711 ) ) ;
#31722 = CARTESIAN_POINT ( 'NONE',  ( -18.06527000055631405, -4.320704448112774543, 33.92786785259540494 ) ) ;
#31723 = ORIENTED_EDGE ( 'NONE', *, *, #78548, .F. ) ;
#31724 = CARTESIAN_POINT ( 'NONE',  ( -11.53846153846166089, -5.094484230521993062, 34.41647553114689373 ) ) ;
#31725 = CARTESIAN_POINT ( 'NONE',  ( -18.13014720943822056, -5.195881422630166391, 34.18770438780618548 ) ) ;
#31726 = EDGE_LOOP ( 'NONE', ( #80405, #27458 ) ) ;
#31727 = CYLINDRICAL_SURFACE ( 'NONE', #7158, 0.2499999999999979738 ) ;
#31728 = CARTESIAN_POINT ( 'NONE',  ( -9.469294848214296678, -9.172514111537584114, 34.72667873470787470 ) ) ;
#31729 = EDGE_LOOP ( 'NONE', ( #78067, #56599, #42702, #2865 ) ) ;
#31730 = CYLINDRICAL_SURFACE ( 'NONE', #30083, 0.2499999999999993616 ) ;
#31731 = CARTESIAN_POINT ( 'NONE',  ( -10.39237326377176451, -4.887748414852792322, 34.01359900205216746 ) ) ;
#31732 = CARTESIAN_POINT ( 'NONE',  ( 12.22435897435897267, -4.000000000000000000, 29.75000000000000355 ) ) ;
#31733 = CARTESIAN_POINT ( 'NONE',  ( 8.096153846153908873, -7.434744429011177935, 34.75000000000002132 ) ) ;
#31734 = DIRECTION ( 'NONE',  ( 0.000000000000000000, 0.000000000000000000, 1.000000000000000000 ) ) ;
#31735 = DIRECTION ( 'NONE',  ( -0.000000000000000000, -0.5000000000000009992, -0.8660254037844380415 ) ) ;
#31737 = CARTESIAN_POINT ( 'NONE',  ( -15.36146069743678844, -12.38065189839062263, 30.83690757178629482 ) ) ;
#31736 = CARTESIAN_POINT ( 'NONE',  ( -13.51530598772569469, -3.957541250942358424, 33.62499894934981626 ) ) ;
#31738 = EDGE_CURVE ( 'NONE', #52853, #71146, #35785, .T. ) ;
#31739 = CIRCLE ( 'NONE', #33212, 0.2500000000000002220 ) ;
#31740 = CARTESIAN_POINT ( 'NONE',  ( -15.93083480223330817, -11.76359900205217457, 32.36225158514719880 ) ) ;
#31742 = FACE_OUTER_BOUND ( 'NONE', #65908, .T. ) ;
#31741 = CARTESIAN_POINT ( 'NONE',  ( -15.48074596171158213, -11.79746400365624659, 32.30657167506340954 ) ) ;
#31743 = CARTESIAN_POINT ( 'NONE',  ( 1.944543648263018731, -9.444543648262994751, 15.87500000000000000 ) ) ;
#31744 = ORIENTED_EDGE ( 'NONE', *, *, #82783, .T. ) ;
#31745 = CARTESIAN_POINT ( 'NONE',  ( -3.903791733932699515, -5.642605341092957083, 34.66089969410670335 ) ) ;
#31746 = VERTEX_POINT ( 'NONE', #26479 ) ;
#31747 = ADVANCED_FACE ( 'NONE', ( #11635 ), #39113, .F. ) ;
#31748 = VECTOR ( 'NONE', #88341, 1000.000000000000227 ) ;
#31749 = VERTEX_POINT ( 'NONE', #87308 ) ;
#31750 = CARTESIAN_POINT ( 'NONE',  ( -3.165514091256391715, -9.528491918058460186, 34.59228464037085615 ) ) ;
#31751 = EDGE_CURVE ( 'NONE', #60833, #26904, #23957, .T. ) ;
#31752 = ORIENTED_EDGE ( 'NONE', *, *, #65204, .F. ) ;
#31753 = CARTESIAN_POINT ( 'NONE',  ( 17.93467598719568556, -7.749976730030849303, 34.74374725381503737 ) ) ;
#31754 = CARTESIAN_POINT ( 'NONE',  ( -1.944543648263014957, -5.555456351737005249, 16.50000000000000000 ) ) ;
#31755 = FACE_OUTER_BOUND ( 'NONE', #111, .T. ) ;
#31756 = CARTESIAN_POINT ( 'NONE',  ( -8.835314180186649935, -3.050289026998445951, 32.03036669348365706 ) ) ;
#31757 = FACE_OUTER_BOUND ( 'NONE', #19577, .T. ) ;
#31758 = CARTESIAN_POINT ( 'NONE',  ( -6.130690603110307002, -2.494641256782728966, 31.33461815524612959 ) ) ;
#31759 = VECTOR ( 'NONE', #57848, 1000.000000000000227 ) ;
#31760 = CYLINDRICAL_SURFACE ( 'NONE', #21452, 0.2499999999999995559 ) ;
#31761 = CARTESIAN_POINT ( 'NONE',  ( -9.692307692307814193, -5.941354392335915335, 34.76329471203413846 ) ) ;
#31762 = DIRECTION ( 'NONE',  ( -1.000000000000000000, -0.000000000000000000, 0.000000000000000000 ) ) ;
#31763 = ADVANCED_FACE ( 'NONE', ( #18832 ), #11181, .F. ) ;
#31764 = AXIS2_PLACEMENT_3D ( 'NONE', #48242, #27091, #66747 ) ;
#31765 = CARTESIAN_POINT ( 'NONE',  ( 1.553300858899087311, -3.749999999999992006, 20.48437500000000000 ) ) ;
#31766 = CARTESIAN_POINT ( 'NONE',  ( 1.634560902963529294, -3.202959910592336534, 32.30730279482227019 ) ) ;
#31767 = DIRECTION ( 'NONE',  ( -0.000000000000000000, -0.000000000000000000, -1.000000000000000000 ) ) ;
#31768 = EDGE_CURVE ( 'NONE', #26079, #81234, #38653, .T. ) ;
#31769 = CARTESIAN_POINT ( 'NONE',  ( 15.23076923076923173, -5.471508081941601098, 34.59228464037088457 ) ) ;
#31770 = VERTEX_POINT ( 'NONE', #52602 ) ;
#31771 = VERTEX_POINT ( 'NONE', #80084 ) ;
#31772 = CARTESIAN_POINT ( 'NONE',  ( 14.08476534878546005, -8.282780595021769443, 34.94152052738834868 ) ) ;
#31773 = CARTESIAN_POINT ( 'NONE',  ( -14.08491276642389423, -8.496831190052096971, 34.64984203495476578 ) ) ;
#31774 = CARTESIAN_POINT ( 'NONE',  ( 16.40390057375961064, -12.41089969410671223, 31.60739465890703670 ) ) ;
#31775 = DIRECTION ( 'NONE',  ( -1.000000000000000000, 0.000000000000000000, -0.000000000000000000 ) ) ;
#31776 = CARTESIAN_POINT ( 'NONE',  ( 8.703960323269992472, -11.94971097300153140, 32.03036669348370680 ) ) ;
#31777 = CARTESIAN_POINT ( 'NONE',  ( -5.076923076923199218, -3.083524468854526912, 32.58852847137268327 ) ) ;
#31778 = ORIENTED_EDGE ( 'NONE', *, *, #50109, .T. ) ;
#31779 = CARTESIAN_POINT ( 'NONE',  ( 7.780071466793709867, -2.833524468853757305, 32.15551576947924417 ) ) ;
#31780 = ORIENTED_EDGE ( 'NONE', *, *, #15508, .T. ) ;
#31781 = EDGE_CURVE ( 'NONE', #20358, #62888, #81053, .T. ) ;
#31782 = B_SPLINE_CURVE_WITH_KNOTS ( 'NONE', 3,
 ( #67859, #59321, #6161, #53899, #59768, #32737, #19669, #38612, #11589, #46257 ),
 .UNSPECIFIED., .F., .F.,
 ( 4, 2, 2, 2, 4 ),
 ( 0.000000000000000000, 0.0001954311564186858715, 0.0003908623128373717431, 0.0005862934692560576146, 0.0007817246256747434861 ),
 .UNSPECIFIED. ) ;
#31783 = EDGE_LOOP ( 'NONE', ( #67245, #12751 ) ) ;
#31784 = CARTESIAN_POINT ( 'NONE',  ( -9.692307692307691624, -2.833524468853757305, 32.15551576947925838 ) ) ;
#31785 = DIRECTION ( 'NONE',  ( 0.000000000000000000, 1.000000000000000000, 0.000000000000000000 ) ) ;
#31786 = CARTESIAN_POINT ( 'NONE',  ( 9.692307692307695177, -3.513871655860378418, 32.76840700105978499 ) ) ;
#31787 = CARTESIAN_POINT ( 'NONE',  ( -11.53846153846166089, -11.06231777344772027, 33.60647404775119895 ) ) ;
#31788 = CARTESIAN_POINT ( 'NONE',  ( 12.94230769230769340, -7.500000000000000000, 29.75000000000000355 ) ) ;
#31789 = ORIENTED_EDGE ( 'NONE', *, *, #4479, .T. ) ;
#31790 = ADVANCED_FACE ( 'NONE', ( #86869 ), #5317, .F. ) ;
#31791 = ORIENTED_EDGE ( 'NONE', *, *, #48060, .T. ) ;
#31792 = ORIENTED_EDGE ( 'NONE', *, *, #5472, .F. ) ;
#31793 = EDGE_CURVE ( 'NONE', #15793, #73783, #62729, .T. ) ;
#31794 = VECTOR ( 'NONE', #61297, 1000.000000000000227 ) ;
#31795 = CARTESIAN_POINT ( 'NONE',  ( 12.46153846153876898, -2.506253911140615021, 30.00000000000323297 ) ) ;
#31796 = CARTESIAN_POINT ( 'NONE',  ( 9.915320536401090123, -2.308499170217967134, 30.53291367094873721 ) ) ;
#31797 = CARTESIAN_POINT ( 'NONE',  ( 4.153846153846030731, -3.643525952248796163, 33.31231777344771672 ) ) ;
#31798 = AXIS2_PLACEMENT_3D ( 'NONE', #23049, #28943, #1892 ) ;
#31799 = VECTOR ( 'NONE', #18089, 999.9999999999998863 ) ;
#31800 = CARTESIAN_POINT ( 'NONE',  ( 2.241608896736428935, -11.16473453929635440, 33.15142922261925662 ) ) ;
#31801 = CARTESIAN_POINT ( 'NONE',  ( 11.53846153846141576, -11.06231777344772027, 33.60647404775119895 ) ) ;
#31802 = DIRECTION ( 'NONE',  ( -0.000000000000000000, 0.1736481776669307198, -0.9848077530122080203 ) ) ;
#31803 = ORIENTED_EDGE ( 'NONE', *, *, #82772, .T. ) ;
#31804 = EDGE_CURVE ( 'NONE', #39107, #47910, #25586, .T. ) ;
#31805 = VERTEX_POINT ( 'NONE', #32785 ) ;
#31806 = CARTESIAN_POINT ( 'NONE',  ( -3.750000000000008438, -5.946699141100917352, 25.17187500000000000 ) ) ;
#31807 = VECTOR ( 'NONE', #10557, 1000.000000000000000 ) ;
#31808 = B_SPLINE_CURVE_WITH_KNOTS ( 'NONE', 3,
 ( #85255, #62747, #76724, #42500, #59992, #87049, #71720, #37949, #87492, #51883 ),
 .UNSPECIFIED., .F., .F.,
 ( 4, 2, 2, 2, 4 ),
 ( 0.0007817246256747517261, 0.0009771112852218961399, 0.001172497944769040771, 0.001367884604316185401, 0.001563271263863329815 ),
 .UNSPECIFIED. ) ;
#31809 = ORIENTED_EDGE ( 'NONE', *, *, #52696, .F. ) ;
#31811 = EDGE_LOOP ( 'NONE', ( #57367, #86686, #61142, #35729 ) ) ;
#31810 = CARTESIAN_POINT ( 'NONE',  ( 2.530703659305157949, -12.39991518177334129, 30.74647679643404530 ) ) ;
#31812 = CARTESIAN_POINT ( 'NONE',  ( -19.00000000000000000, -3.499999999999999556, 29.75000000000000355 ) ) ;
#31813 = CARTESIAN_POINT ( 'NONE',  ( 20.00000000000000355, 10.00000000000000533, 13.00000000000000178 ) ) ;
#31814 = ADVANCED_FACE ( 'NONE', ( #80987 ), #58912, .F. ) ;
#31815 = EDGE_CURVE ( 'NONE', #27245, #52424, #60696, .T. ) ;
#31816 = CARTESIAN_POINT ( 'NONE',  ( 3.749999999999992006, -5.946699141100872943, 16.89062500000000000 ) ) ;
#31817 = EDGE_LOOP ( 'NONE', ( #55553, #35310 ) ) ;
#31818 = CARTESIAN_POINT ( 'NONE',  ( 12.22435897435897267, -3.499999999999999556, 29.75000000000000355 ) ) ;
#31819 = EDGE_LOOP ( 'NONE', ( #45488, #22065, #55050, #33395 ) ) ;
#31820 = ADVANCED_FACE ( 'NONE', ( #38204 ), #65663, .F. ) ;
#31821 = CARTESIAN_POINT ( 'NONE',  ( -13.63459212866397507, -11.47974371597208076, 33.17467449705390692 ) ) ;
#31822 = FACE_BOUND ( 'NONE', #66053, .T. ) ;
#31823 = FACE_BOUND ( 'NONE', #63807, .T. ) ;
#31825 = CARTESIAN_POINT ( 'NONE',  ( 7.846153846153846700, -11.91647553114624181, 32.58852847137148245 ) ) ;
#31824 = CARTESIAN_POINT ( 'NONE',  ( 10.39255792290561509, -7.369208160676172348, 34.74850200257122879 ) ) ;
#31826 = CARTESIAN_POINT ( 'NONE',  ( -1.384615384615506484, -3.643525952248795718, 33.31231777344771672 ) ) ;
#31827 = CARTESIAN_POINT ( 'NONE',  ( 18.06606835100243558, -2.721908614388772296, 31.22303859784725333 ) ) ;
#31828 = EDGE_LOOP ( 'NONE', ( #83763, #88914 ) ) ;
#31829 = CARTESIAN_POINT ( 'NONE',  ( 6.673053685783957967, -8.432397168068783699, 34.66272746175022945 ) ) ;
#31830 = FACE_OUTER_BOUND ( 'NONE', #9666, .T. ) ;
#31831 = ORIENTED_EDGE ( 'NONE', *, *, #73696, .F. ) ;
#31832 = CARTESIAN_POINT ( 'NONE',  ( 6.673053685783957967, -10.05641848906368097, 34.04755513067966177 ) ) ;
#31833 = VECTOR ( 'NONE', #10841, 1000.000000000000000 ) ;
#31834 = DIRECTION ( 'NONE',  ( 0.000000000000000000, 0.3420201433256610524, 0.9396926207859113145 ) ) ;
#31835 = CARTESIAN_POINT ( 'NONE',  ( -15.00775638667583500, -5.582272713120729257, 34.63742843783360570 ) ) ;
#31836 = CARTESIAN_POINT ( 'NONE',  ( 11.47237812750566022, -5.557115091759785130, 34.35708131394839171 ) ) ;
#31837 = FACE_OUTER_BOUND ( 'NONE', #37550, .T. ) ;
#31838 = FACE_BOUND ( 'NONE', #29926, .T. ) ;
#31840 = DIRECTION ( 'NONE',  ( -0.000000000000000000, -0.1736481776669307198, -0.9848077530122080203 ) ) ;
#31839 = CARTESIAN_POINT ( 'NONE',  ( 13.31934493865461455, -12.27809138561121394, 31.22303859784730307 ) ) ;
#31841 = CARTESIAN_POINT ( 'NONE',  ( -9.692307692307814193, -12.16647553114689728, 32.15551576947799362 ) ) ;
#31843 = CARTESIAN_POINT ( 'NONE',  ( 0.4615384615383382183, -3.083524468854526912, 32.58852847137268327 ) ) ;
#31842 = CARTESIAN_POINT ( 'NONE',  ( 1.161688425708537364, -12.64616026154729411, 30.79003144601913533 ) ) ;
#31844 = DIRECTION ( 'NONE',  ( 0.000000000000000000, 0.000000000000000000, -1.000000000000000000 ) ) ;
#31845 = CARTESIAN_POINT ( 'NONE',  ( -8.519285250882626670, -3.712312575010499049, 33.01462480002815170 ) ) ;
#31846 = CARTESIAN_POINT ( 'NONE',  ( -2.608446859217889546, -10.19485399968121264, 24.68563170625849068 ) ) ;
#31847 = ADVANCED_FACE ( 'NONE', ( #55708 ), #67907, .F. ) ;
#31848 = CARTESIAN_POINT ( 'NONE',  ( 16.15384615384603251, -5.094484230521993062, 34.41647553114689373 ) ) ;
#31849 = ORIENTED_EDGE ( 'NONE', *, *, #53727, .F. ) ;
#31850 = CARTESIAN_POINT ( 'NONE',  ( -6.923076923076922462, -13.53365097954675988, 30.81389545987213552 ) ) ;
#31851 = CARTESIAN_POINT ( 'NONE',  ( 2.241609928332172430, -2.292212530054419606, 30.41441678777542634 ) ) ;
#31852 = CARTESIAN_POINT ( 'NONE',  ( -1.384615384615383471, -2.721908614388771852, 31.22303859784724978 ) ) ;
#31853 = CARTESIAN_POINT ( 'NONE',  ( 20.99999999999999645, -10.75000000000000000, 27.25000000000000000 ) ) ;
#31854 = DIRECTION ( 'NONE',  ( 0.000000000000000000, 1.000000000000000000, 0.000000000000000000 ) ) ;
#31855 = CARTESIAN_POINT ( 'NONE',  ( 6.222779668978067669, -3.563462043263029955, 33.22394488606062879 ) ) ;
#31856 = CARTESIAN_POINT ( 'NONE',  ( -2.694853999681210865, -4.891553140782108677, 26.24813170625849068 ) ) ;
#31857 = CARTESIAN_POINT ( 'NONE',  ( -3.230769230769229949, -4.102666532097928531, 36.13435417666054406 ) ) ;
#31858 = DIRECTION ( 'NONE',  ( -0.000000000000000000, 1.000000000000000000, -0.000000000000000000 ) ) ;
#31859 = CARTESIAN_POINT ( 'NONE',  ( 0.3256479613346660584, -4.768304711466844203, 28.86076157308317391 ) ) ;
#31860 = CARTESIAN_POINT ( 'NONE',  ( -9.692307692307812417, -11.48612834414049644, 32.76840700105863391 ) ) ;
#31861 = DIRECTION ( 'NONE',  ( -0.000000000000000000, -0.8660254037844397068, -0.4999999999999978906 ) ) ;
#31862 = PLANE ( 'NONE',  #35337 ) ;
#31863 = ADVANCED_FACE ( 'NONE', ( #89087, #68787 ), #75538, .T. ) ;
#31864 = CARTESIAN_POINT ( 'NONE',  ( -6.130690603110307890, -11.93127051446800024, 32.56575433478200665 ) ) ;
#31865 = CYLINDRICAL_SURFACE ( 'NONE', #12572, 0.2499999999999994726 ) ;
#31866 = EDGE_LOOP ( 'NONE', ( #36690, #39311, #56505, #47413 ) ) ;
#31867 = EDGE_CURVE ( 'NONE', #85395, #1538, #77729, .T. ) ;
#31868 = FACE_OUTER_BOUND ( 'NONE', #64237, .T. ) ;
#31869 = CARTESIAN_POINT ( 'NONE',  ( 15.36129466900287532, -11.04252011169590020, 33.62494198852677130 ) ) ;
#31870 = CARTESIAN_POINT ( 'NONE',  ( -2.608446859217920633, -4.805146000318815780, 16.75186829374151287 ) ) ;
#31871 = AXIS2_PLACEMENT_3D ( 'NONE', #84890, #23176, #50638 ) ;
#31872 = CARTESIAN_POINT ( 'NONE',  ( 6.923076923076924238, -10.67929555188718282, 33.92786785259544047 ) ) ;
#31873 = DIRECTION ( 'NONE',  ( -0.000000000000000000, 0.9396926207859093161, -0.3420201433256663259 ) ) ;
#31874 = VERTEX_POINT ( 'NONE', #7086 ) ;
#31875 = CARTESIAN_POINT ( 'NONE',  ( -6.700064078983529292, -10.01129605718032778, 34.36064277460058491 ) ) ;
#31876 = CARTESIAN_POINT ( 'NONE',  ( -17.01166793741023042, -9.528491918058456633, 34.59228464037085615 ) ) ;
#31878 = ORIENTED_EDGE ( 'NONE', *, *, #77379, .T. ) ;
#31877 = CARTESIAN_POINT ( 'NONE',  ( 11.76183702423395872, -2.251407671071270489, 29.88021292934942963 ) ) ;
#31879 = CARTESIAN_POINT ( 'NONE',  ( -9.070512820512819374, -3.499999999999999556, 29.75000000000000355 ) ) ;
#31880 = CARTESIAN_POINT ( 'NONE',  ( -2.980823712421087901, -3.712312575010499938, 33.01462480002815170 ) ) ;
#31881 = DIRECTION ( 'NONE',  ( -0.000000000000000000, 0.1736481776669307198, -0.9848077530122080203 ) ) ;
#31883 = ADVANCED_FACE ( 'NONE', ( #34561 ), #62456, .F. ) ;
#31882 = CARTESIAN_POINT ( 'NONE',  ( 11.66898724022510514, -9.417988943895561960, 34.36773134775777550 ) ) ;
#31884 = EDGE_LOOP ( 'NONE', ( #30196, #76756 ) ) ;
#31885 = CYLINDRICAL_SURFACE ( 'NONE', #27466, 0.2499999999999995559 ) ;
#31886 = CARTESIAN_POINT ( 'NONE',  ( 10.74591005361826213, -4.299079248970732792, 33.91157788607253565 ) ) ;
#31887 = CARTESIAN_POINT ( 'NONE',  ( 13.38461538461538680, -13.87047571288749737, 32.06866353760679544 ) ) ;
#31888 = ORIENTED_EDGE ( 'NONE', *, *, #50155, .F. ) ;
#31889 = ORIENTED_EDGE ( 'NONE', *, *, #21944, .F. ) ;
#31890 = B_SPLINE_CURVE_WITH_KNOTS ( 'NONE', 3,
 ( #29775, #56790, #8175, #22566, #58117, #35647, #70311, #1852, #71187, #78386 ),
 .UNSPECIFIED., .F., .F.,
 ( 4, 2, 2, 2, 4 ),
 ( 0.0007817246256747507503, 0.0009771112852218957062, 0.001172497944769040771, 0.001367884604316185835, 0.001563271263863330682 ),
 .UNSPECIFIED. ) ;
#31891 = ORIENTED_EDGE ( 'NONE', *, *, #66233, .F. ) ;
#31892 = CARTESIAN_POINT ( 'NONE',  ( 5.207714884747862705, -12.11778462344220841, 31.66786338562085135 ) ) ;
#31893 = CARTESIAN_POINT ( 'NONE',  ( 9.822833130541340552, -4.299079248970732792, 33.91157788607253565 ) ) ;
#31894 = EDGE_CURVE ( 'NONE', #65345, #66107, #336, .T. ) ;
#31895 = CARTESIAN_POINT ( 'NONE',  ( -12.68446467905460473, -3.586966769969701208, 32.86292498521069660 ) ) ;
#31896 = DIRECTION ( 'NONE',  ( 0.000000000000000000, 0.9396926207859126468, 0.3420201433256571111 ) ) ;
#31897 = VECTOR ( 'NONE', #79889, 1000.000000000000000 ) ;
#31898 = ORIENTED_EDGE ( 'NONE', *, *, #12756, .F. ) ;
#31899 = EDGE_CURVE ( 'NONE', #27135, #55920, #23674, .T. ) ;
#31900 = VERTEX_POINT ( 'NONE', #54381 ) ;
#31901 = EDGE_CURVE ( 'NONE', #84958, #58400, #32581, .T. ) ;
#31903 = ORIENTED_EDGE ( 'NONE', *, *, #10581, .T. ) ;
#31902 = CARTESIAN_POINT ( 'NONE',  ( 4.284636594813102661, -5.496552790871117367, 34.60292014791297532 ) ) ;
#31904 = PLANE ( 'NONE',  #34366 ) ;
#31905 = CARTESIAN_POINT ( 'NONE',  ( 15.10007776410167324, -3.062553014421049546, 32.05460306192773601 ) ) ;
#31906 = B_SPLINE_CURVE_WITH_KNOTS ( 'NONE', 3,
 ( #80460, #46221, #19630, #73708, #25060, #31829, #59283, #86791, #74136, #12004 ),
 .UNSPECIFIED., .F., .F.,
 ( 4, 2, 2, 2, 4 ),
 ( 0.000000000000000000, 0.0001954339857564079894, 0.0003908679715128159787, 0.0005863019572692239681, 0.0007817359430256319575 ),
 .UNSPECIFIED. ) ;
#31907 = CARTESIAN_POINT ( 'NONE',  ( 2.530471848960718972, -3.755027918224367767, 33.06320215134714857 ) ) ;
#31908 = CYLINDRICAL_SURFACE ( 'NONE', #62573, 0.2499999999999979738 ) ;
#31909 = ORIENTED_EDGE ( 'NONE', *, *, #20273, .T. ) ;
#31910 = EDGE_CURVE ( 'NONE', #83780, #4543, #88645, .T. ) ;
#31911 = ORIENTED_EDGE ( 'NONE', *, *, #35341, .F. ) ;
#31912 = EDGE_LOOP ( 'NONE', ( #89116, #72585 ) ) ;
#31914 = ORIENTED_EDGE ( 'NONE', *, *, #50857, .F. ) ;
#31913 = CARTESIAN_POINT ( 'NONE',  ( 24.99999999999999645, -15.00000000000000000, 3.000000000000000000 ) ) ;
#31915 = CARTESIAN_POINT ( 'NONE',  ( -10.68063454715869831, -2.255955759149247619, 30.00000000000013856 ) ) ;
#31916 = EDGE_CURVE ( 'NONE', #17458, #73573, #64783, .T. ) ;
#31917 = EDGE_CURVE ( 'NONE', #25611, #33924, #47582, .T. ) ;
#31918 = CARTESIAN_POINT ( 'NONE',  ( 3.000000000000001776, -7.500000000000000000, 14.00000000000000178 ) ) ;
#31919 = EDGE_LOOP ( 'NONE', ( #42853, #61389, #2200, #35798 ) ) ;
#31920 = CYLINDRICAL_SURFACE ( 'NONE', #54679, 0.2499999999999998890 ) ;
#31921 = DIRECTION ( 'NONE',  ( -0.000000000000000000, 0.1736481776669307198, -0.9848077530122080203 ) ) ;
#31922 = CARTESIAN_POINT ( 'NONE',  ( 4.153846153846032507, -2.892918686052165622, 31.69288490824153470 ) ) ;
#31923 = FACE_BOUND ( 'NONE', #31912, .T. ) ;
#31924 = CARTESIAN_POINT ( 'NONE',  ( -0.5922299282060179415, -4.118384482072085184, 33.43331474514187107 ) ) ;
#31925 = CARTESIAN_POINT ( 'NONE',  ( -6.130147969731697621, -12.50552854090298993, 31.33409797877408920 ) ) ;
#31926 = FACE_OUTER_BOUND ( 'NONE', #43738, .T. ) ;
#31928 = CARTESIAN_POINT ( 'NONE',  ( 6.857806922520603088, -11.06231777344662781, 33.60647404775220082 ) ) ;
#31927 = CARTESIAN_POINT ( 'NONE',  ( 6.923076923076924238, -12.29105614889573062, 35.45975837776705220 ) ) ;
#31929 = AXIS2_PLACEMENT_3D ( 'NONE', #60023, #68126, #61341 ) ;
#31930 = CARTESIAN_POINT ( 'NONE',  ( -4.087679547254512435, -7.250054591869667497, 34.99404684341514127 ) ) ;
#31931 = CARTESIAN_POINT ( 'NONE',  ( 5.142178648199100977, -2.625532179533470512, 30.86335684631491105 ) ) ;
#31932 = ORIENTED_EDGE ( 'NONE', *, *, #26244, .T. ) ;
#31933 = CARTESIAN_POINT ( 'NONE',  ( -15.10024379253558635, -11.66157788607254098, 32.95092075102925833 ) ) ;
#31934 = CARTESIAN_POINT ( 'NONE',  ( 12.59206389977210705, -3.625058011473228703, 33.29252011169590020 ) ) ;
#31935 = EDGE_LOOP ( 'NONE', ( #42466, #13600 ) ) ;
#31936 = EDGE_LOOP ( 'NONE', ( #2720, #27179 ) ) ;
#31938 = DIRECTION ( 'NONE',  ( 0.000000000000000000, 0.1736481776669267785, -0.9848077530122087975 ) ) ;
#31937 = CARTESIAN_POINT ( 'NONE',  ( 6.000000000000001776, -6.386643153685126251, 34.62446782046654192 ) ) ;
#31939 = CARTESIAN_POINT ( 'NONE',  ( 16.15384615384603251, -4.481592998941358097, 33.73612834414048933 ) ) ;
#31940 = CARTESIAN_POINT ( 'NONE',  ( 1.161130440891438464, -6.760086850603068243, 34.69517049084099369 ) ) ;
#31941 = CARTESIAN_POINT ( 'NONE',  ( 12.46153846153833911, -11.06231777344772027, 33.60647404775119895 ) ) ;
#31942 = ORIENTED_EDGE ( 'NONE', *, *, #58628, .T. ) ;
#31943 = CARTESIAN_POINT ( 'NONE',  ( 8.545745844666436497, -12.69144148231606017, 30.53333754910549303 ) ) ;
#31944 = CARTESIAN_POINT ( 'NONE',  ( 17.99999999999987566, -4.320704448113951379, 33.92786785259630022 ) ) ;
#31946 = DIRECTION ( 'NONE',  ( 0.000000000000000000, 0.7660444431189822323, -0.6427876096865344779 ) ) ;
#31945 = CARTESIAN_POINT ( 'NONE',  ( 11.60371667797437212, -3.083524468853784839, 32.58852847137153930 ) ) ;
#31947 = CARTESIAN_POINT ( 'NONE',  ( -1.607542343522233796, -10.01117774369187252, 34.36070679894347535 ) ) ;
#31948 = FACE_OUTER_BOUND ( 'NONE', #8946, .T. ) ;
#31950 = CARTESIAN_POINT ( 'NONE',  ( -17.07692307692319744, -2.657715359629662988, 31.77849191805970364 ) ) ;
#31949 = SHAPE_REPRESENTATION_RELATIONSHIP ( 'NONE' , 'NONE' ,  #36256, #63293 ) ;
#31951 = CARTESIAN_POINT ( 'NONE',  ( -3.749999999999997335, -7.500000000000021316, 22.59375000000000355 ) ) ;
#31952 = ORIENTED_EDGE ( 'NONE', *, *, #53620, .T. ) ;
#31953 = EDGE_LOOP ( 'NONE', ( #50336, #72759, #82053, #62366 ) ) ;
#31954 = CARTESIAN_POINT ( 'NONE',  ( 24.00000000000000000, -5.499999999999981348, 27.25000000000000000 ) ) ;
#31955 = CARTESIAN_POINT ( 'NONE',  ( 12.68450136509994763, -7.369474270740069777, 34.74850911626239736 ) ) ;
#31956 = CARTESIAN_POINT ( 'NONE',  ( 10.74617642320940369, -2.541949514083464479, 30.39797389878540557 ) ) ;
#31957 = CARTESIAN_POINT ( 'NONE',  ( 14.30769230769218758, -2.892918686052165622, 31.69288490824153470 ) ) ;
#31958 = CARTESIAN_POINT ( 'NONE',  ( 2.438530725705071678, -7.277220443632450575, 34.74524770363009196 ) ) ;
#31959 = CARTESIAN_POINT ( 'NONE',  ( 2.651650429449569302, -10.15165042944953733, 24.62500000000000000 ) ) ;
#31960 = LINE ( 'NONE', #38266, #41 ) ;
#31961 = CARTESIAN_POINT ( 'NONE',  ( 1.515141086378949842, -5.195472089885680766, 34.18748526763464923 ) ) ;
#31962 = CARTESIAN_POINT ( 'NONE',  ( -8.834500769787091201, -12.70778746994557551, 30.41441678777548319 ) ) ;
#31963 = CARTESIAN_POINT ( 'NONE',  ( 3.230769230769231726, -1.129524287112498415, 32.06866353760679544 ) ) ;
#31964 = DIRECTION ( 'NONE',  ( 0.000000000000000000, 0.000000000000000000, 1.000000000000000000 ) ) ;
#31965 = CARTESIAN_POINT ( 'NONE',  ( 14.98074600654777377, -12.45566812827425451, 31.48439005359158926 ) ) ;
#31966 = VECTOR ( 'NONE', #57638, 1000.000000000000000 ) ;
#31967 = CARTESIAN_POINT ( 'NONE',  ( 19.50000000000000000, -11.00000000000000000, 29.75000000000000355 ) ) ;
#31968 = DIRECTION ( 'NONE',  ( -0.000000000000000000, -0.6427876096865404731, -0.7660444431189770143 ) ) ;
#31969 = CARTESIAN_POINT ( 'NONE',  ( -0.4615384615385826339, -11.48612834414049644, 32.76840700105863391 ) ) ;
#31970 = CARTESIAN_POINT ( 'NONE',  ( -2.980823712421087901, -11.37275283266503756, 32.91324779482534524 ) ) ;
#31971 = CARTESIAN_POINT ( 'NONE',  ( -3.360917200500928459, -12.50552854090298993, 31.33409797877408920 ) ) ;
#31972 = VECTOR ( 'NONE', #35873, 1000.000000000000000 ) ;
#31973 = ORIENTED_EDGE ( 'NONE', *, *, #21066, .T. ) ;
#31974 = DIRECTION ( 'NONE',  ( 0.000000000000000000, 0.000000000000000000, -1.000000000000000000 ) ) ;
#31975 = CARTESIAN_POINT ( 'NONE',  ( -12.71153846153846168, -7.566083408709835645, 34.74999999999999289 ) ) ;
#31976 = CARTESIAN_POINT ( 'NONE',  ( 13.13459216039393240, -6.652501968072648708, 34.93155406624980941 ) ) ;
#31977 = CARTESIAN_POINT ( 'NONE',  ( 0.06109907496451789238, -4.749999999999998224, 14.40811829374151110 ) ) ;
#31978 = CARTESIAN_POINT ( 'NONE',  ( 13.38461538461538680, -4.786620604624113540, 33.94971097300155094 ) ) ;
#31979 = DIRECTION ( 'NONE',  ( 0.000000000000000000, 0.3420201433256641055, -0.9396926207859100932 ) ) ;
#31981 = ORIENTED_EDGE ( 'NONE', *, *, #20508, .T. ) ;
#31980 = CARTESIAN_POINT ( 'NONE',  ( 10.74622294587137361, -7.277220318596961057, 34.99547417642776992 ) ) ;
#31982 = CARTESIAN_POINT ( 'NONE',  ( -2.749999999999998224, -7.500000000000015987, 20.09375000000000000 ) ) ;
#31983 = CARTESIAN_POINT ( 'NONE',  ( -1.634592115557737424, -9.943427161483782584, 34.11278801902876978 ) ) ;
#31984 = VERTEX_POINT ( 'NONE', #76877 ) ;
#31985 = B_SPLINE_CURVE_WITH_KNOTS ( 'NONE', 3,
 ( #58911, #66110, #11633, #81429, #4416, #80083, #19716, #5315, #87755, #46742 ),
 .UNSPECIFIED., .F., .F.,
 ( 4, 2, 2, 2, 4 ),
 ( 0.0007817246256747473893, 0.0009771112852218905021, 0.001172497944769033615, 0.001367884604316176944, 0.001563271263863320057 ),
 .UNSPECIFIED. ) ;
#31986 = CARTESIAN_POINT ( 'NONE',  ( -5.448717948717948012, -3.499999999999999556, 29.75000000000000355 ) ) ;
#31987 = EDGE_LOOP ( 'NONE', ( #19810, #44115 ) ) ;
#31988 = PRODUCT ( 'head base', 'head base', '', ( #5915 ) ) ;
#31989 = LINE ( 'NONE', #46387, #50463 ) ;
#31990 = CARTESIAN_POINT ( 'NONE',  ( -15.36145983387954139, -2.845849958028613624, 32.17971566917920967 ) ) ;
#31991 = DIRECTION ( 'NONE',  ( -0.000000000000000000, 0.8660254037844399289, -0.4999999999999980016 ) ) ;
#31992 = EDGE_LOOP ( 'NONE', ( #1215, #8440, #23449, #59023 ) ) ;
#31993 = CARTESIAN_POINT ( 'NONE',  ( -10.55012904410859065, -12.46129190930001052, 30.37095296980870174 ) ) ;
#31994 = EDGE_LOOP ( 'NONE', ( #82175, #76143, #26015, #57420, #67912 ) ) ;
#31995 = DIRECTION ( 'NONE',  ( -1.000000000000000000, -0.000000000000000000, -0.000000000000000000 ) ) ;
#31996 = VECTOR ( 'NONE', #5806, 1000.000000000000227 ) ;
#31997 = EDGE_CURVE ( 'NONE', #44682, #30667, #65112, .T. ) ;
#31998 = EDGE_LOOP ( 'NONE', ( #85844, #2095, #23032, #74760 ) ) ;
#32000 = CARTESIAN_POINT ( 'NONE',  ( -0.6844646790546096149, -3.105860786376062332, 32.13614157043599562 ) ) ;
#31999 = VECTOR ( 'NONE', #17610, 1000.000000000000000 ) ;
#32001 = CARTESIAN_POINT ( 'NONE',  ( 2.438218009455874302, -3.285477652293413264, 32.44071101563363158 ) ) ;
#32002 = DIRECTION ( 'NONE',  ( -0.000000000000000000, -0.000000000000000000, -1.000000000000000000 ) ) ;
#32003 = LINE ( 'NONE', #4066, #78086 ) ;
#32004 = CARTESIAN_POINT ( 'NONE',  ( 11.28843830116857383, -11.86270091957321249, 32.19358267280087915 ) ) ;
#32005 = LINE ( 'NONE', #59472, #86657 ) ;
#32006 = ORIENTED_EDGE ( 'NONE', *, *, #30547, .T. ) ;
#32007 = ORIENTED_EDGE ( 'NONE', *, *, #46738, .T. ) ;
#32008 = EDGE_CURVE ( 'NONE', #23542, #71435, #8421, .T. ) ;
#32009 = ORIENTED_EDGE ( 'NONE', *, *, #7040, .F. ) ;
#32011 = ORIENTED_EDGE ( 'NONE', *, *, #61443, .F. ) ;
#32010 = DIRECTION ( 'NONE',  ( -0.000000000000000000, 1.000000000000000000, 3.491481338843133355E-15 ) ) ;
#32012 = CYLINDRICAL_SURFACE ( 'NONE', #360, 0.2499999999999997502 ) ;
#32013 = DIRECTION ( 'NONE',  ( -0.000000000000000000, -0.1736481776669307198, -0.9848077530122080203 ) ) ;
#32014 = EDGE_LOOP ( 'NONE', ( #19864, #87114, #59261, #38641, #82578, #60285 ) ) ;
#32015 = CARTESIAN_POINT ( 'NONE',  ( -14.30769230769242739, -4.481592998941358097, 33.73612834414048933 ) ) ;
#32016 = ORIENTED_EDGE ( 'NONE', *, *, #28793, .T. ) ;
#32017 = CARTESIAN_POINT ( 'NONE',  ( 16.85343813319912698, -10.11188796281391511, 34.01382737946119050 ) ) ;
#32018 = ORIENTED_EDGE ( 'NONE', *, *, #25056, .F. ) ;
#32019 = VECTOR ( 'NONE', #44441, 1000.000000000000000 ) ;
#32020 = CARTESIAN_POINT ( 'NONE',  ( 9.758376043310132530, -8.120952969808772792, 34.71129190929999453 ) ) ;
#32021 = EDGE_CURVE ( 'NONE', #66205, #57379, #84123, .T. ) ;
#32022 = CARTESIAN_POINT ( 'NONE',  ( 4.153846153846154188, -12.62096338111211580, 30.90682066428153263 ) ) ;
#32023 = CARTESIAN_POINT ( 'NONE',  ( -11.40793610022789828, -12.15418822224088835, 32.17964115625579069 ) ) ;
#32024 = FACE_BOUND ( 'NONE', #50968, .T. ) ;
#32025 = ADVANCED_FACE ( 'NONE', ( #2970 ), #70559, .F. ) ;
#32026 = CARTESIAN_POINT ( 'NONE',  ( 2.531119269553878670, -7.630147231320743018, 34.74852402298682819 ) ) ;
#32027 = CARTESIAN_POINT ( 'NONE',  ( 12.46153846153846168, -5.557115091759785130, 34.35708131394839171 ) ) ;
#32028 = CYLINDRICAL_SURFACE ( 'NONE', #20854, 0.2500000000000004996 ) ;
#32029 = ADVANCED_FACE ( 'NONE', ( #43524 ), #9738, .T. ) ;
#32030 = CARTESIAN_POINT ( 'NONE',  ( 4.826899852701619587, -3.520140089381497361, 33.17453946501458262 ) ) ;
#32031 = CARTESIAN_POINT ( 'NONE',  ( -14.43838377435986686, -8.999036380462717588, 34.52022231692819076 ) ) ;
#32032 = DIRECTION ( 'NONE',  ( -0.000000000000000000, 0.1736481776669307198, -0.9848077530122080203 ) ) ;
#32033 = ORIENTED_EDGE ( 'NONE', *, *, #34301, .T. ) ;
#32034 = CYLINDRICAL_SURFACE ( 'NONE', #10069, 0.2500000000000008882 ) ;
#32035 = ORIENTED_EDGE ( 'NONE', *, *, #23175, .T. ) ;
#32036 = ORIENTED_EDGE ( 'NONE', *, *, #33206, .T. ) ;
#32038 = CARTESIAN_POINT ( 'NONE',  ( -9.692307692307691624, -8.164416787775445883, 34.95778746994557906 ) ) ;
#32037 = CARTESIAN_POINT ( 'NONE',  ( 10.86543892702293057, -12.41262288849542017, 30.68299917996395010 ) ) ;
#32039 = CARTESIAN_POINT ( 'NONE',  ( 3.007842271862381178, -3.395401636524185474, 33.02366814457250399 ) ) ;
#32040 = CARTESIAN_POINT ( 'NONE',  ( -13.38461538461538325, -2.833524468853757305, 32.15551576947925838 ) ) ;
#32041 = CARTESIAN_POINT ( 'NONE',  ( -19.50000000000000000, -3.499999999999999556, 28.25000000000000000 ) ) ;
#32042 = CARTESIAN_POINT ( 'NONE',  ( 1.384615384615386802, -3.937682226553329556, 33.60647404775216529 ) ) ;
#32043 = ORIENTED_EDGE ( 'NONE', *, *, #56622, .F. ) ;
#32044 = DIRECTION ( 'NONE',  ( -0.000000000000000000, -0.5000000000000009992, -0.8660254037844380415 ) ) ;
#32045 = B_SPLINE_CURVE_WITH_KNOTS ( 'NONE', 3,
 ( #24570, #32662, #3406, #30878, #79529, #4305, #17828, #60130, #58346, #66898 ),
 .UNSPECIFIED., .F., .F.,
 ( 4, 2, 2, 2, 4 ),
 ( 0.0007817246336856290608, 0.0009771112958940099402, 0.001172497958102391036, 0.001367884620310772133, 0.001563271282519153229 ),
 .UNSPECIFIED. ) ;
#32046 = CARTESIAN_POINT ( 'NONE',  ( -0.2115930521604181824, -3.520799739797214389, 33.17531984108286025 ) ) ;
#32047 = CARTESIAN_POINT ( 'NONE',  ( 2.438482748659258625, -12.62708834333097663, 30.88030960425257021 ) ) ;
#32048 = CARTESIAN_POINT ( 'NONE',  ( 5.011599064118766655, -7.749976730030849303, 34.74374725381503737 ) ) ;
#32049 = ORIENTED_EDGE ( 'NONE', *, *, #44420, .T. ) ;
#32050 = EDGE_LOOP ( 'NONE', ( #75001, #73586, #62641, #83350 ) ) ;
#32051 = AXIS2_PLACEMENT_3D ( 'NONE', #77599, #70404, #14566 ) ;
#32052 = SHAPE_DEFINITION_REPRESENTATION ( #57813, #85713 ) ;
#32053 = ORIENTED_EDGE ( 'NONE', *, *, #14252, .T. ) ;
#32054 = VECTOR ( 'NONE', #78298, 1000.000000000000000 ) ;
#32055 = CARTESIAN_POINT ( 'NONE',  ( 17.77717330752099301, -7.369208160676171460, 34.74850200257122879 ) ) ;
#32056 = CARTESIAN_POINT ( 'NONE',  ( -7.596208327805704208, -5.057305518903949526, 34.11320923018887896 ) ) ;
#32057 = VERTEX_POINT ( 'NONE', #36335 ) ;
#32058 = CARTESIAN_POINT ( 'NONE',  ( -3.480745961711584346, -12.41269422305637171, 30.68257228309993323 ) ) ;
#32059 = DIRECTION ( 'NONE',  ( -0.000000000000000000, 0.5000000000000011102, -0.8660254037844380415 ) ) ;
#32060 = CARTESIAN_POINT ( 'NONE',  ( -8.096130577096198877, -11.79746400365624659, 32.30657167506340954 ) ) ;
#32061 = CARTESIAN_POINT ( 'NONE',  ( 8.992010438208831502, -3.563462043263030399, 33.22394488606062879 ) ) ;
#32062 = DIRECTION ( 'NONE',  ( -0.000000000000000000, 0.9396926207859093161, -0.3420201433256663259 ) ) ;
#32063 = ORIENTED_EDGE ( 'NONE', *, *, #57350, .F. ) ;
#32065 = EDGE_LOOP ( 'NONE', ( #66477, #37278, #42463, #88528 ) ) ;
#32064 = CARTESIAN_POINT ( 'NONE',  ( -0.4615384615385840772, -12.16647553114689728, 32.15551576947799362 ) ) ;
#32066 = CARTESIAN_POINT ( 'NONE',  ( -7.846153846153844924, -8.973038597847269315, 34.52809138561121927 ) ) ;
#32067 = CARTESIAN_POINT ( 'NONE',  ( -2.530618525208453651, -9.086856451489515152, 34.49173150075333183 ) ) ;
#32068 = CARTESIAN_POINT ( 'NONE',  ( -9.692307692307691624, -1.367168528481310208, 33.57946703557072254 ) ) ;
#32069 = EDGE_CURVE ( 'NONE', #19996, #50277, #85405, .T. ) ;
#32070 = CARTESIAN_POINT ( 'NONE',  ( -10.61538461538461320, -3.322132147404559976, 32.92929555188717927 ) ) ;
#32071 = DIRECTION ( 'NONE',  ( -0.000000000000000000, 0.8660254037844399289, -0.4999999999999980016 ) ) ;
#32072 = CARTESIAN_POINT ( 'NONE',  ( -6.923076923076922462, -8.564572088678739092, 35.78748833219616898 ) ) ;
#32073 = CARTESIAN_POINT ( 'NONE',  ( -2.749999999999999112, -7.438900925035484057, 17.84561829374150932 ) ) ;
#32074 = EDGE_LOOP ( 'NONE', ( #52864, #47819 ) ) ;
#32075 = CARTESIAN_POINT ( 'NONE',  ( 17.29970274590113632, -3.020022701398814569, 32.48759521482552515 ) ) ;
#32076 = DIRECTION ( 'NONE',  ( -0.000000000000000000, 0.8660254037844399289, -0.4999999999999980016 ) ) ;
#32077 = DIRECTION ( 'NONE',  ( 1.000000000000000000, 0.000000000000000000, 0.000000000000000000 ) ) ;
#32078 = B_SPLINE_CURVE_WITH_KNOTS ( 'NONE', 3,
 ( #40034, #59838, #31933, #52180, #53968, #67494, #46327, #59394, #67939, #47208 ),
 .UNSPECIFIED., .F., .F.,
 ( 4, 2, 2, 2, 4 ),
 ( 0.0007817246256747463051, 0.0009771112852218896347, 0.001172497944769032747, 0.001367884604316176077, 0.001563271263863319407 ),
 .UNSPECIFIED. ) ;
#32079 = ORIENTED_EDGE ( 'NONE', *, *, #51343, .F. ) ;
#32080 = ORIENTED_EDGE ( 'NONE', *, *, #6581, .F. ) ;
#32081 = DIRECTION ( 'NONE',  ( -0.000000000000000000, 0.1736481776669307198, -0.9848077530122080203 ) ) ;
#32082 = CARTESIAN_POINT ( 'NONE',  ( 12.46153846153846168, -3.937682226553329556, 33.60647404775216529 ) ) ;
#32083 = LINE ( 'NONE', #66309, #86407 ) ;
#32084 = EDGE_CURVE ( 'NONE', #35421, #21173, #10090, .T. ) ;
#32085 = CARTESIAN_POINT ( 'NONE',  ( 10.54930120442873331, -4.098570777380720287, 33.41473453929634729 ) ) ;
#32086 = VECTOR ( 'NONE', #68308, 1000.000000000000000 ) ;
#32087 = B_SPLINE_CURVE_WITH_KNOTS ( 'NONE', 3,
 ( #55519, #23069, #1472, #36588, #14990, #77127, #586, #83004, #35250, #62710 ),
 .UNSPECIFIED., .F., .F.,
 ( 4, 2, 2, 2, 4 ),
 ( 0.0007817246256747472808, 0.0009771112852218907189, 0.001172497944769034265, 0.001367884604316177595, 0.001563271263863321141 ),
 .UNSPECIFIED. ) ;
#32088 = CARTESIAN_POINT ( 'NONE',  ( 6.000000000000001776, -13.87047571288749737, 32.06866353760679544 ) ) ;
#32089 = CARTESIAN_POINT ( 'NONE',  ( 5.999999999999880096, -8.613356846316285953, 34.62446782046622218 ) ) ;
#32090 = B_SPLINE_CURVE_WITH_KNOTS ( 'NONE', 3,
 ( #60220, #87278, #79167, #74189, #10711, #67433, #12056, #31424, #53010, #46273 ),
 .UNSPECIFIED., .F., .F.,
 ( 4, 2, 2, 2, 4 ),
 ( 0.0007817246256747448956, 0.0009771112852218879000, 0.001172497944769030796, 0.001367884604316173692, 0.001563271263863316805 ),
 .UNSPECIFIED. ) ;
#32091 = ORIENTED_EDGE ( 'NONE', *, *, #1628, .F. ) ;
#32092 = CARTESIAN_POINT ( 'NONE',  ( -3.099978789802280144, -12.62708834333097663, 30.88030960425257021 ) ) ;
#32093 = CARTESIAN_POINT ( 'NONE',  ( -2.307692307692305711, -9.780366693483667717, 34.19971097300155094 ) ) ;
#32094 = CARTESIAN_POINT ( 'NONE',  ( 16.94677586748485965, -9.418419913701741919, 34.36755862841477693 ) ) ;
#32095 = ORIENTED_EDGE ( 'NONE', *, *, #24522, .T. ) ;
#32096 = CARTESIAN_POINT ( 'NONE',  ( 10.39245765647776309, -9.172386477786396597, 34.72672124145550043 ) ) ;
#32097 = ADVANCED_FACE ( 'NONE', ( #49834 ), #70999, .F. ) ;
#32098 = ORIENTED_EDGE ( 'NONE', *, *, #85385, .T. ) ;
#32099 = CYLINDRICAL_SURFACE ( 'NONE', #64397, 0.2499999999999986955 ) ;
#32100 = CARTESIAN_POINT ( 'NONE',  ( -1.384615384615505151, -9.442884908241554243, 34.35708131394783038 ) ) ;
#32101 = CARTESIAN_POINT ( 'NONE',  ( 7.846153846153846700, -13.88283147151868846, 33.14645433367849847 ) ) ;
#32102 = ORIENTED_EDGE ( 'NONE', *, *, #79450, .F. ) ;
#32103 = EDGE_CURVE ( 'NONE', #25666, #43394, #57033, .T. ) ;
#32104 = CARTESIAN_POINT ( 'NONE',  ( -13.16160254052199008, -4.762714258010881885, 34.23016756924214832 ) ) ;
#32105 = CARTESIAN_POINT ( 'NONE',  ( -11.28851602011339672, -12.43552623307873972, 30.55307653245132826 ) ) ;
#32106 = CARTESIAN_POINT ( 'NONE',  ( -39.05038313613820122, -2.499999999999999556, 29.75000000000000355 ) ) ;
#32107 = CARTESIAN_POINT ( 'NONE',  ( -7.596099426240391139, -4.818054556918156983, 34.26375889529406749 ) ) ;
#32108 = CARTESIAN_POINT ( 'NONE',  ( 3.296024370282069516, -3.083524468853784839, 32.58852847137153930 ) ) ;
#32109 = ORIENTED_EDGE ( 'NONE', *, *, #13401, .F. ) ;
#32110 = ADVANCED_FACE ( 'NONE', ( #50263 ), #57924, .F. ) ;
#32111 = CARTESIAN_POINT ( 'NONE',  ( 14.30769230769231015, -13.78497067705608181, 32.30358669280327177 ) ) ;
#32112 = EDGE_LOOP ( 'NONE', ( #13234, #34905, #87638, #62446, #80997 ) ) ;
#32113 = PLANE ( 'NONE',  #37131 ) ;
#32114 = CIRCLE ( 'NONE', #20594, 4.000000000000000000 ) ;
#32115 = CYLINDRICAL_SURFACE ( 'NONE', #45034, 0.2499999999999986955 ) ;
#32116 = EDGE_CURVE ( 'NONE', #51881, #29248, #36767, .T. ) ;
#32117 = CYLINDRICAL_SURFACE ( 'NONE', #42780, 0.2500000000000004996 ) ;
#32118 = LINE ( 'NONE', #10517, #83309 ) ;
#32119 = ADVANCED_FACE ( 'NONE', ( #30451 ), #78641, .F. ) ;
#32120 = LINE ( 'NONE', #2517, #23354 ) ;
#32121 = CARTESIAN_POINT ( 'NONE',  ( 5.011672086761834066, -2.506253911140460477, 30.00000000000013856 ) ) ;
#32122 = CARTESIAN_POINT ( 'NONE',  ( 15.93091919493929964, -11.98009711892700224, 32.48740034544074007 ) ) ;
#32123 = CIRCLE ( 'NONE', #24718, 4.000000000000000000 ) ;
#32124 = EDGE_LOOP ( 'NONE', ( #53007, #62656, #86097, #53244 ) ) ;
#32125 = EDGE_LOOP ( 'NONE', ( #34610, #52250, #36962, #83648 ) ) ;
#32126 = ORIENTED_EDGE ( 'NONE', *, *, #5852, .T. ) ;
#32127 = B_SPLINE_CURVE_WITH_KNOTS ( 'NONE', 3,
 ( #61734, #21201, #55874, #48669, #41930, #69398, #14905, #21647, #7704, #35162 ),
 .UNSPECIFIED., .F., .F.,
 ( 4, 2, 2, 2, 4 ),
 ( 0.000000000000000000, 0.0001954339857564091007, 0.0003908679715128182013, 0.0005863019572692273291, 0.0007817359430256364027 ),
 .UNSPECIFIED. ) ;
#32128 = EDGE_LOOP ( 'NONE', ( #47973, #33638 ) ) ;
#32129 = ORIENTED_EDGE ( 'NONE', *, *, #31578, .T. ) ;
#32130 = EDGE_CURVE ( 'NONE', #66664, #12230, #12410, .T. ) ;
#32131 = DIRECTION ( 'NONE',  ( 1.000000000000000000, 0.000000000000000000, 0.000000000000000000 ) ) ;
#32132 = CARTESIAN_POINT ( 'NONE',  ( -3.360917200500926239, -6.809168938359898782, 34.95455904226513866 ) ) ;
#32133 = EDGE_CURVE ( 'NONE', #44386, #58630, #52494, .T. ) ;
#32134 = CARTESIAN_POINT ( 'NONE',  ( 15.00784301325308157, -4.887634598454295265, 34.01352882383564946 ) ) ;
#32135 = CARTESIAN_POINT ( 'NONE',  ( -12.46153846153846168, -13.88283147151868846, 33.14645433367849847 ) ) ;
#32136 = CARTESIAN_POINT ( 'NONE',  ( 3.230769230769231726, -1.242168528481310874, 33.36296068462461051 ) ) ;
#32137 = CARTESIAN_POINT ( 'NONE',  ( 4.153846153846032507, -12.27809138561165270, 31.22303859784587132 ) ) ;
#32138 = EDGE_CURVE ( 'NONE', #6007, #15407, #45324, .T. ) ;
#32139 = DIRECTION ( 'NONE',  ( -0.000000000000000000, 0.000000000000000000, 1.000000000000000000 ) ) ;
#32140 = EDGE_CURVE ( 'NONE', #14112, #52651, #87644, .T. ) ;
#32141 = CARTESIAN_POINT ( 'NONE',  ( -5.326923076923097966, -2.249999999999999112, 29.81609741502488120 ) ) ;
#32142 = LINE ( 'NONE', #5108, #67748 ) ;
#32143 = ORIENTED_EDGE ( 'NONE', *, *, #84375, .F. ) ;
#32144 = ORIENTED_EDGE ( 'NONE', *, *, #61203, .F. ) ;
#32145 = ORIENTED_EDGE ( 'NONE', *, *, #84510, .F. ) ;
#32147 = ORIENTED_EDGE ( 'NONE', *, *, #21835, .T. ) ;
#32146 = CARTESIAN_POINT ( 'NONE',  ( 0.2386115026316130983, -11.98009711892699691, 32.48740034544075428 ) ) ;
#32148 = AXIS2_PLACEMENT_3D ( 'NONE', #84124, #37685, #3452 ) ;
#32150 = LINE ( 'NONE', #4224, #82234 ) ;
#32149 = CARTESIAN_POINT ( 'NONE',  ( 12.46153846153833911, -3.643525952248795718, 33.31231777344771672 ) ) ;
#32151 = AXIS2_PLACEMENT_3D ( 'NONE', #33113, #74547, #45735 ) ;
#32152 = CARTESIAN_POINT ( 'NONE',  ( 5.076923076923075762, -1.129524287112498415, 32.06866353760679544 ) ) ;
#32153 = CARTESIAN_POINT ( 'NONE',  ( -14.43783951713053249, -10.19110544564092002, 33.96427741523702792 ) ) ;
#32154 = FACE_BOUND ( 'NONE', #36175, .T. ) ;
#32155 = VERTEX_POINT ( 'NONE', #65561 ) ;
#32156 = ORIENTED_EDGE ( 'NONE', *, *, #82230, .F. ) ;
#32157 = CARTESIAN_POINT ( 'NONE',  ( 11.53846153846153832, -5.180354513474913603, 36.12317359536750416 ) ) ;
#32158 = ORIENTED_EDGE ( 'NONE', *, *, #65335, .F. ) ;
#32159 = FACE_BOUND ( 'NONE', #68435, .T. ) ;
#32160 = CARTESIAN_POINT ( 'NONE',  ( -4.826923076921656452, -7.500000000000154543, 35.00000000000007105 ) ) ;
#32161 = DIRECTION ( 'NONE',  ( -1.000000000000000000, 0.000000000000000000, 0.000000000000000000 ) ) ;
#32162 = ORIENTED_EDGE ( 'NONE', *, *, #20140, .T. ) ;
#32163 = CARTESIAN_POINT ( 'NONE',  ( 17.93472955403922242, -2.892918686051582533, 31.69288490824015980 ) ) ;
#32164 = CARTESIAN_POINT ( 'NONE',  ( -1.384615384615506484, -8.656820664282941280, 34.87096338111179961 ) ) ;
#32165 = CARTESIAN_POINT ( 'NONE',  ( -5.207532732127157615, -7.722926974430166069, 34.99546784045485737 ) ) ;
#32166 = ORIENTED_EDGE ( 'NONE', *, *, #62979, .F. ) ;
#32167 = CARTESIAN_POINT ( 'NONE',  ( -3.230769230769229949, -12.29105614889573062, 35.45975837776705220 ) ) ;
#32168 = CARTESIAN_POINT ( 'NONE',  ( -16.15384615384615330, -1.242168528481310874, 33.36296068462461051 ) ) ;
#32169 = CARTESIAN_POINT ( 'NONE',  ( 8.102564102564102200, -7.500000000000000000, 29.75000000000000355 ) ) ;
#32170 = VERTEX_POINT ( 'NONE', #30888 ) ;
#32171 = DIRECTION ( 'NONE',  ( -0.000000000000000000, -0.9396926207859093161, -0.3420201433256663259 ) ) ;
#32172 = CARTESIAN_POINT ( 'NONE',  ( 7.173022441425065843, -10.76462480002816235, 33.53768742498949962 ) ) ;
#32173 = ORIENTED_EDGE ( 'NONE', *, *, #40039, .F. ) ;
#32174 = CARTESIAN_POINT ( 'NONE',  ( -17.29985003582992320, -12.64616026154729411, 30.79003144601914244 ) ) ;
#32175 = CARTESIAN_POINT ( 'NONE',  ( -10.55012904410859065, -5.219633306516380244, 34.19971097300157936 ) ) ;
#32176 = CARTESIAN_POINT ( 'NONE',  ( 15.93036122928182330, -3.019605429927187501, 32.48692288466676814 ) ) ;
#32177 = CARTESIAN_POINT ( 'NONE',  ( -8.638438961405979555, -8.999086150933475636, 34.52020707165672775 ) ) ;
#32178 = CARTESIAN_POINT ( 'NONE',  ( 0.4615384615384611755, -2.499999999999998668, 29.50000000000001066 ) ) ;
#32179 = ADVANCED_FACE ( 'NONE', ( #51585 ), #38551, .F. ) ;
#32180 = CARTESIAN_POINT ( 'NONE',  ( 6.923076923076802558, -9.442884908241554243, 34.35708131394783038 ) ) ;
#32182 = CARTESIAN_POINT ( 'NONE',  ( -20.00000000000000355, 10.00000000000000711, 3.000000000000000000 ) ) ;
#32181 = CARTESIAN_POINT ( 'NONE',  ( -1.449885830576159051, -5.219633306516282545, 34.19971097300152962 ) ) ;
#32183 = CARTESIAN_POINT ( 'NONE',  ( -15.90379184220784836, -11.79725096376909299, 32.30694842903960762 ) ) ;
#32184 = FACE_OUTER_BOUND ( 'NONE', #82331, .T. ) ;
#32185 = EDGE_CURVE ( 'NONE', #32252, #56816, #544, .T. ) ;
#32186 = CARTESIAN_POINT ( 'NONE',  ( 0.06109907496454976272, -10.25000000000000000, 25.77938170625848713 ) ) ;
#32188 = EDGE_CURVE ( 'NONE', #66117, #26375, #19169, .T. ) ;
#32187 = ORIENTED_EDGE ( 'NONE', *, *, #70394, .F. ) ;
#32189 = B_SPLINE_CURVE_WITH_KNOTS ( 'NONE', 3,
 ( #60900, #5074, #79851, #81189, #32105, #68114, #19473, #59569, #25793, #25345 ),
 .UNSPECIFIED., .F., .F.,
 ( 4, 2, 2, 2, 4 ),
 ( 0.0007817359430256326080, 0.0009771253907249993591, 0.001172514838424366327, 0.001367904286123733078, 0.001563293733823099829 ),
 .UNSPECIFIED. ) ;
#32190 = VECTOR ( 'NONE', #17973, 1000.000000000000114 ) ;
#32191 = DIRECTION ( 'NONE',  ( 0.000000000000000000, 0.000000000000000000, 1.000000000000000000 ) ) ;
#32192 = ORIENTED_EDGE ( 'NONE', *, *, #35179, .F. ) ;
#32193 = EDGE_CURVE ( 'NONE', #3057, #67027, #38099, .T. ) ;
#32194 = AXIS2_PLACEMENT_3D ( 'NONE', #32568, #32139, #4665 ) ;
#32195 = ORIENTED_EDGE ( 'NONE', *, *, #14646, .T. ) ;
#32196 = CARTESIAN_POINT ( 'NONE',  ( -2.084680956079457470, -12.39991518177334129, 30.74647679643404530 ) ) ;
#32197 = ORIENTED_EDGE ( 'NONE', *, *, #67821, .F. ) ;
#32198 = CARTESIAN_POINT ( 'NONE',  ( 17.86938964037546995, -7.722926236386454590, 34.74524107206102030 ) ) ;
#32199 = CARTESIAN_POINT ( 'NONE',  ( 2.775308065498768517, -8.577988221561467341, 26.79500670625849423 ) ) ;
#32200 = CARTESIAN_POINT ( 'NONE',  ( 12.71153846153988098, -7.500000000000154543, 35.00000000000007105 ) ) ;
#32201 = B_SPLINE_CURVE_WITH_KNOTS ( 'NONE', 3,
 ( #64646, #84067, #78175, #29123, #36317, #16037, #43507, #77288, #78615, #10166 ),
 .UNSPECIFIED., .F., .F.,
 ( 4, 2, 2, 2, 4 ),
 ( 0.0007817246256747465219, 0.0009771112852218900684, 0.001172497944769033615, 0.001367884604316177378, 0.001563271263863320925 ),
 .UNSPECIFIED. ) ;
#32202 = CARTESIAN_POINT ( 'NONE',  ( -15.29603923132554932, -12.51329471203370325, 31.30864560766548976 ) ) ;
#32203 = CARTESIAN_POINT ( 'NONE',  ( -3.230769230769351186, -9.442884908241554243, 34.35708131394783038 ) ) ;
#32204 = CARTESIAN_POINT ( 'NONE',  ( -14.43784027742400866, -11.04286588640298561, 33.62463336215343901 ) ) ;
#32205 = EDGE_CURVE ( 'NONE', #4047, #6648, #70073, .T. ) ;
#32206 = DIRECTION ( 'NONE',  ( -0.000000000000000000, 1.000000000000000000, 3.491481338843133355E-15 ) ) ;
#32207 = CARTESIAN_POINT ( 'NONE',  ( -10.83886955910856464, -4.386631170607603991, 33.66268669641500111 ) ) ;
#32208 = CARTESIAN_POINT ( 'NONE',  ( 0.7114838709165030028, -2.589246495874657938, 31.60778113518102828 ) ) ;
#32209 = CARTESIAN_POINT ( 'NONE',  ( -3.749999999999997335, -7.500000000000021316, 23.84375000000000000 ) ) ;
#32210 = CARTESIAN_POINT ( 'NONE',  ( 17.14299041027315695, -2.292212530054420050, 30.41441678777542990 ) ) ;
#32211 = CARTESIAN_POINT ( 'NONE',  ( -10.48533955946484220, -2.254550872974305342, 29.97347326024527092 ) ) ;
#32212 = CARTESIAN_POINT ( 'NONE',  ( 9.692307692307695177, -10.51840700105979565, 33.73612834413961536 ) ) ;
#32213 = VERTEX_POINT ( 'NONE', #52048 ) ;
#32214 = ORIENTED_EDGE ( 'NONE', *, *, #59548, .T. ) ;
#32215 = CARTESIAN_POINT ( 'NONE',  ( -9.019207500173124004, -12.41269422305637171, 30.68257228309993323 ) ) ;
#32216 = CARTESIAN_POINT ( 'NONE',  ( -17.20761454359063691, -8.147922237126337563, 34.70805685702651999 ) ) ;
#32217 = CARTESIAN_POINT ( 'NONE',  ( -2.373774687052442545, -2.292212530054419606, 30.41441678777542634 ) ) ;
#32218 = CARTESIAN_POINT ( 'NONE',  ( 8.769230769231082689, -2.255955759149395501, 30.00000000000324363 ) ) ;
#32219 = EDGE_CURVE ( 'NONE', #41186, #82649, #85850, .T. ) ;
#32220 = DIRECTION ( 'NONE',  ( -1.000000000000000000, -0.000000000000000000, -0.000000000000000000 ) ) ;
#32221 = CARTESIAN_POINT ( 'NONE',  ( -9.942284436356285227, -6.524016743844655686, 34.90889640711025521 ) ) ;
#32222 = AXIS2_PLACEMENT_3D ( 'NONE', #65022, #3331, #51052 ) ;
#32223 = EDGE_LOOP ( 'NONE', ( #43625, #40876 ) ) ;
#32224 = CARTESIAN_POINT ( 'NONE',  ( -15.23076923076922995, -4.786620604624113540, 33.94971097300155094 ) ) ;
#32225 = ORIENTED_EDGE ( 'NONE', *, *, #39857, .T. ) ;
#32226 = EDGE_LOOP ( 'NONE', ( #32656, #55357, #81209, #83403 ) ) ;
#32227 = CARTESIAN_POINT ( 'NONE',  ( -5.750054481651856619, -5.852078868378311149, 34.47109172314383585 ) ) ;
#32228 = DIRECTION ( 'NONE',  ( 0.000000000000000000, -0.000000000000000000, 1.000000000000000000 ) ) ;
#32229 = CARTESIAN_POINT ( 'NONE',  ( -4.153846153846274980, -12.70778746994576025, 30.41441678777401236 ) ) ;
#32230 = CARTESIAN_POINT ( 'NONE',  ( 6.066067333350077639, -8.164416787775445883, 34.95778746994558617 ) ) ;
#32231 = CARTESIAN_POINT ( 'NONE',  ( 13.31934538405906565, -8.656820664281498878, 34.87096338111211935 ) ) ;
#32232 = ORIENTED_EDGE ( 'NONE', *, *, #51303, .F. ) ;
#32233 = ORIENTED_EDGE ( 'NONE', *, *, #42090, .F. ) ;
#32234 = ORIENTED_EDGE ( 'NONE', *, *, #57936, .T. ) ;
#32235 = CIRCLE ( 'NONE', #33714, 0.2500000000000002220 ) ;
#32236 = ADVANCED_FACE ( 'NONE', ( #11077 ), #86760, .F. ) ;
#32237 = EDGE_CURVE ( 'NONE', #66936, #33331, #20607, .T. ) ;
#32238 = CARTESIAN_POINT ( 'NONE',  ( 13.16113046005105680, -4.988325925672468131, 34.36044203135681130 ) ) ;
#32239 = CARTESIAN_POINT ( 'NONE',  ( -0.2115930521604179604, -10.18230066228895758, 34.26354781536631577 ) ) ;
#32240 = CARTESIAN_POINT ( 'NONE',  ( 8.900021210197719412, -5.496552790871120031, 34.60292014791297532 ) ) ;
#32241 =( GEOMETRIC_REPRESENTATION_CONTEXT ( 3 ) GLOBAL_UNCERTAINTY_ASSIGNED_CONTEXT ( ( #14577 ) ) GLOBAL_UNIT_ASSIGNED_CONTEXT ( ( #80064, #37741, #3504 ) ) REPRESENTATION_CONTEXT ( 'NONE', 'WORKASPACE' ) );
#32242 = EDGE_CURVE ( 'NONE', #88972, #56388, #62353, .T. ) ;
#32243 = VECTOR ( 'NONE', #77630, 1000.000000000000000 ) ;
#32244 = CYLINDRICAL_SURFACE ( 'NONE', #34158, 0.2499999999999994726 ) ;
#32245 = CARTESIAN_POINT ( 'NONE',  ( -14.98082382139119062, -9.357781135181031829, 34.66075350412533851 ) ) ;
#32246 = EDGE_CURVE ( 'NONE', #32412, #5555, #80773, .T. ) ;
#32247 = CARTESIAN_POINT ( 'NONE',  ( -15.90379184220783593, -2.779044189368096607, 31.39831045268885035 ) ) ;
#32248 = ORIENTED_EDGE ( 'NONE', *, *, #12267, .F. ) ;
#32249 = ORIENTED_EDGE ( 'NONE', *, *, #69763, .T. ) ;
#32250 = CARTESIAN_POINT ( 'NONE',  ( 11.66850670129631595, -2.504778602574659896, 29.97347330155780654 ) ) ;
#32252 = VERTEX_POINT ( 'NONE', #48846 ) ;
#32251 = CARTESIAN_POINT ( 'NONE',  ( -1.384615384615383471, -12.78798330534102767, 29.49999999999997868 ) ) ;
#32253 = ADVANCED_FACE ( 'NONE', ( #82656 ), #20492, .F. ) ;
#32254 = B_SPLINE_CURVE_WITH_KNOTS ( 'NONE', 3,
 ( #38790, #79329, #32031, #50511, #77991, #17634, #16295, #30254, #4097, #31580 ),
 .UNSPECIFIED., .F., .F.,
 ( 4, 2, 2, 2, 4 ),
 ( 0.000000000000000000, 0.0001954339857564073659, 0.0003908679715128147319, 0.0005863019572692221250, 0.0007817359430256294638 ),
 .UNSPECIFIED. ) ;
#32255 = DIRECTION ( 'NONE',  ( 1.000000000000000000, 0.000000000000000000, 0.000000000000000000 ) ) ;
#32256 = DIRECTION ( 'NONE',  ( -1.000000000000000000, 0.000000000000000000, 0.000000000000000000 ) ) ;
#32257 = CARTESIAN_POINT ( 'NONE',  ( -3.750000000000007550, -5.946699141100917352, 17.67187500000000355 ) ) ;
#32258 = ORIENTED_EDGE ( 'NONE', *, *, #67609, .F. ) ;
#32259 = EDGE_CURVE ( 'NONE', #9873, #58140, #5649, .T. ) ;
#32260 = CARTESIAN_POINT ( 'NONE',  ( -14.55766905174089665, -12.41104346484419452, 31.60698883733904196 ) ) ;
#32261 = ORIENTED_EDGE ( 'NONE', *, *, #32138, .F. ) ;
#32262 = CARTESIAN_POINT ( 'NONE',  ( 5.999999999999878320, -9.528491918059723176, 34.59228464037033035 ) ) ;
#32263 = CARTESIAN_POINT ( 'NONE',  ( -8.096153846153844924, -2.249999999999998668, 29.75000000000000355 ) ) ;
#32264 = FACE_BOUND ( 'NONE', #63670, .T. ) ;
#32266 = DIRECTION ( 'NONE',  ( 0.000000000000000000, -1.084202172485503448E-16, 1.000000000000000000 ) ) ;
#32265 = CARTESIAN_POINT ( 'NONE',  ( -6.673131404728780858, -12.43552623307873972, 30.55307653245132826 ) ) ;
#32267 = CARTESIAN_POINT ( 'NONE',  ( -14.24249832590895082, -2.506253911140448487, 29.99999999999988631 ) ) ;
#32268 = ORIENTED_EDGE ( 'NONE', *, *, #77500, .F. ) ;
#32269 = EDGE_CURVE ( 'NONE', #7422, #76471, #42109, .T. ) ;
#32270 = CARTESIAN_POINT ( 'NONE',  ( 11.31497661389721010, -11.60425143139329940, 33.02411095842164457 ) ) ;
#32271 = CYLINDRICAL_SURFACE ( 'NONE', #63888, 0.2499999999999986955 ) ;
#32272 = ORIENTED_EDGE ( 'NONE', *, *, #68538, .F. ) ;
#32273 = DIRECTION ( 'NONE',  ( -1.000000000000000000, -0.000000000000000000, -0.000000000000000000 ) ) ;
#32274 = CARTESIAN_POINT ( 'NONE',  ( -6.223484943723948781, -10.81261337010820256, 33.49550067578627477 ) ) ;
#32275 = CARTESIAN_POINT ( 'NONE',  ( -13.16160254052198830, -11.43677907613344757, 33.22367315496202167 ) ) ;
#32276 = CARTESIAN_POINT ( 'NONE',  ( -0.7115384615384605649, -7.566083408709834757, 34.74999999999999289 ) ) ;
#32277 = EDGE_CURVE ( 'NONE', #16715, #80414, #74383, .T. ) ;
#32278 = FACE_BOUND ( 'NONE', #4655, .T. ) ;
#32280 = CARTESIAN_POINT ( 'NONE',  ( 10.28846153846153832, -7.500000000000000000, 33.75000000000000000 ) ) ;
#32279 = DIRECTION ( 'NONE',  ( -0.000000000000000000, -1.000000000000000000, -0.000000000000000000 ) ) ;
#32281 = CARTESIAN_POINT ( 'NONE',  ( -10.61538461538461320, -4.786620604624113540, 33.94971097300155094 ) ) ;
#32283 = DIRECTION ( 'NONE',  ( 1.000000000000000000, 0.000000000000000000, 0.000000000000000000 ) ) ;
#32282 = CARTESIAN_POINT ( 'NONE',  ( 3.230769230769231726, -4.098570777380720287, 33.41473453929634729 ) ) ;
#32284 = DIRECTION ( 'NONE',  ( 1.000000000000000000, 0.000000000000000000, 0.000000000000000000 ) ) ;
#32285 = DIRECTION ( 'NONE',  ( 0.000000000000000000, 0.9396926207859126468, 0.3420201433256571111 ) ) ;
#32286 = CARTESIAN_POINT ( 'NONE',  ( 1.614399933863660985, -11.22469193450123193, 26.95125670625849068 ) ) ;
#32287 = ADVANCED_FACE ( 'NONE', ( #83090, #20928, #19606 ), #75005, .T. ) ;
#32288 = CARTESIAN_POINT ( 'NONE',  ( -6.923076923076922462, -8.973038597847269315, 34.52809138561121927 ) ) ;
#32289 = EDGE_LOOP ( 'NONE', ( #12739, #60863 ) ) ;
#32290 = CARTESIAN_POINT ( 'NONE',  ( -5.999999999999998224, -3.937682226553329556, 33.60647404775216529 ) ) ;
#32291 = CARTESIAN_POINT ( 'NONE',  ( -6.923076923077045919, -12.70778746994576025, 30.41441678777401236 ) ) ;
#32292 = CARTESIAN_POINT ( 'NONE',  ( -1.161604033002534564, -10.61302985866383963, 33.66295027996417843 ) ) ;
#32293 = PLANE ( 'NONE',  #15052 ) ;
#32294 = CARTESIAN_POINT ( 'NONE',  ( -17.01085574357300345, -2.292212530054420494, 30.41441678777542990 ) ) ;
#32295 = CARTESIAN_POINT ( 'NONE',  ( -12.71151520558705528, -6.524016743844655686, 34.90889640711025521 ) ) ;
#32296 = CARTESIAN_POINT ( 'NONE',  ( 1.200186371490561621, -10.22469193450123193, 15.70125670625848890 ) ) ;
#32297 = CYLINDRICAL_SURFACE ( 'NONE', #50365, 0.2500000000000008882 ) ;
#32298 = CARTESIAN_POINT ( 'NONE',  ( 11.00641025641025550, -4.000000000000000000, 29.75000000000000355 ) ) ;
#32299 = EDGE_CURVE ( 'NONE', #88887, #51951, #30343, .T. ) ;
#32300 = LINE ( 'NONE', #32734, #18758 ) ;
#32301 = CARTESIAN_POINT ( 'NONE',  ( 9.562159722575998444, -4.299443229763728169, 33.91186481527756058 ) ) ;
#32302 = CARTESIAN_POINT ( 'NONE',  ( 8.769230769230647482, -10.21337939537710326, 33.94971097300076224 ) ) ;
#32303 = FACE_OUTER_BOUND ( 'NONE', #50823, .T. ) ;
#32304 = AXIS2_PLACEMENT_3D ( 'NONE', #3103, #2653, #16187 ) ;
#32305 = CARTESIAN_POINT ( 'NONE',  ( 14.30769230769231015, -1.466349020453238561, 30.81389545987213907 ) ) ;
#32306 = ADVANCED_FACE ( 'NONE', ( #67799 ), #14178, .T. ) ;
#32307 = CARTESIAN_POINT ( 'NONE',  ( 16.15384615384603251, -2.657715359629662544, 31.77849191805970364 ) ) ;
#32308 = ORIENTED_EDGE ( 'NONE', *, *, #53165, .T. ) ;
#32309 = DIRECTION ( 'NONE',  ( 0.000000000000000000, 0.3420201433256610524, 0.9396926207859113145 ) ) ;
#32310 = DIRECTION ( 'NONE',  ( -0.000000000000000000, -0.8660254037844399289, -0.4999999999999980016 ) ) ;
#32311 = CARTESIAN_POINT ( 'NONE',  ( -0.06109907496450878162, -11.25000000000000000, 18.78311829374151287 ) ) ;
#32312 = VECTOR ( 'NONE', #62882, 1000.000000000000000 ) ;
#32313 = VECTOR ( 'NONE', #35278, 1000.000000000000000 ) ;
#32314 = LINE ( 'NONE', #66988, #24565 ) ;
#32315 = CARTESIAN_POINT ( 'NONE',  ( -8.835313148590904220, -3.322132147404559532, 32.92929555188719348 ) ) ;
#32316 = EDGE_LOOP ( 'NONE', ( #14534, #28520, #39162, #64895 ) ) ;
#32317 = CARTESIAN_POINT ( 'NONE',  ( 1.576923076923075762, -7.500000000000000000, 29.75000000000000355 ) ) ;
#32318 = CARTESIAN_POINT ( 'NONE',  ( -12.21148404162501144, -12.65882529074907126, 30.72640787790839312 ) ) ;
#32320 = ORIENTED_EDGE ( 'NONE', *, *, #45740, .T. ) ;
#32319 = CARTESIAN_POINT ( 'NONE',  ( 4.946232473812767871, -12.35290016733513951, 31.75349464988449455 ) ) ;
#32321 = CARTESIAN_POINT ( 'NONE',  ( -13.38461538461550759, -10.33852847137269571, 34.16647553114546554 ) ) ;
#32322 = CARTESIAN_POINT ( 'NONE',  ( -2.438301962896387565, -7.722926974430166069, 34.99546784045485737 ) ) ;
#32323 = EDGE_CURVE ( 'NONE', #2266, #19388, #8826, .T. ) ;
#32324 = CARTESIAN_POINT ( 'NONE',  ( -8.546219417617921366, -2.554770724473667265, 30.48948780036025852 ) ) ;
#32325 = CARTESIAN_POINT ( 'NONE',  ( -12.46153846153846168, -4.661471528628507777, 34.16647553114623292 ) ) ;
#32326 = EDGE_CURVE ( 'NONE', #72856, #62783, #83985, .T. ) ;
#32327 = ORIENTED_EDGE ( 'NONE', *, *, #1517, .F. ) ;
#32328 = CARTESIAN_POINT ( 'NONE',  ( -14.30769230769230660, -9.584722331328613620, 36.20867863119891439 ) ) ;
#32329 = CARTESIAN_POINT ( 'NONE',  ( -5.076923076923075762, -12.78798330534103123, 29.99999999999997868 ) ) ;
#32330 = CARTESIAN_POINT ( 'NONE',  ( 0.000000000000000000, -11.00000000000000000, 29.75000000000000355 ) ) ;
#32331 = ORIENTED_EDGE ( 'NONE', *, *, #29678, .F. ) ;
#32332 = ORIENTED_EDGE ( 'NONE', *, *, #23348, .F. ) ;
#32333 = ORIENTED_EDGE ( 'NONE', *, *, #69647, .T. ) ;
#32334 = CARTESIAN_POINT ( 'NONE',  ( 18.75000000000000000, -11.00000000000000000, 29.75000000000000355 ) ) ;
#32335 = DIRECTION ( 'NONE',  ( -0.000000000000000000, 0.1736481776669307198, -0.9848077530122080203 ) ) ;
#32336 = CARTESIAN_POINT ( 'NONE',  ( 2.557746619330622639, -5.728107161865378494, 34.42597550085002922 ) ) ;
#32337 = FACE_OUTER_BOUND ( 'NONE', #19310, .T. ) ;
#32338 = VERTEX_POINT ( 'NONE', #2860 ) ;
#32339 = ORIENTED_EDGE ( 'NONE', *, *, #53299, .T. ) ;
#32340 = ORIENTED_EDGE ( 'NONE', *, *, #20337, .T. ) ;
#32342 = ORIENTED_EDGE ( 'NONE', *, *, #29945, .T. ) ;
#32341 = CARTESIAN_POINT ( 'NONE',  ( 15.45354877203763522, -5.114059244376869984, 34.14424750095245287 ) ) ;
#32343 = CARTESIAN_POINT ( 'NONE',  ( -5.300408001487411092, -2.612411019501189813, 31.66733052389439962 ) ) ;
#32344 = CARTESIAN_POINT ( 'NONE',  ( -3.360917200500926683, -5.070767119584671967, 34.40440758774516183 ) ) ;
#32345 = CARTESIAN_POINT ( 'NONE',  ( -13.38461538461538325, -8.973038597847269315, 34.52809138561121927 ) ) ;
#32346 = CARTESIAN_POINT ( 'NONE',  ( -13.13466986626724164, -12.43552623307873972, 30.55307653245132826 ) ) ;
#32347 = ADVANCED_FACE ( 'NONE', ( #22266 ), #15073, .F. ) ;
#32348 = VERTEX_POINT ( 'NONE', #85305 ) ;
#32349 = ORIENTED_EDGE ( 'NONE', *, *, #44481, .F. ) ;
#32350 = ORIENTED_EDGE ( 'NONE', *, *, #64657, .F. ) ;
#32351 = CARTESIAN_POINT ( 'NONE',  ( -5.326923076923076650, -7.566083408709834757, 34.74999999999999289 ) ) ;
#32353 = EDGE_LOOP ( 'NONE', ( #7274, #85556, #1881, #78275 ) ) ;
#32352 = CARTESIAN_POINT ( 'NONE',  ( 5.299702618191483694, -5.114059244376869984, 34.14424750095245287 ) ) ;
#32354 = EDGE_CURVE ( 'NONE', #3876, #70755, #78092, .T. ) ;
#32355 = FACE_OUTER_BOUND ( 'NONE', #4628, .T. ) ;
#32356 = VECTOR ( 'NONE', #57631, 1000.000000000000227 ) ;
#32357 = CARTESIAN_POINT ( 'NONE',  ( -13.45069879557126136, -6.386643153685125363, 34.62446782046654903 ) ) ;
#32358 = DIRECTION ( 'NONE',  ( -0.000000000000000000, 0.1736481776669307198, -0.9848077530122080203 ) ) ;
#32359 = DIRECTION ( 'NONE',  ( -0.000000000000000000, 0.3420201433256694901, -0.9396926207859082059 ) ) ;
#32360 = ADVANCED_FACE ( 'NONE', ( #36233 ), #84426, .F. ) ;
#32361 = CARTESIAN_POINT ( 'NONE',  ( 10.74617642320940369, -3.530189275343204702, 32.79018710029569661 ) ) ;
#32362 = FACE_BOUND ( 'NONE', #48501, .T. ) ;
#32363 = B_SPLINE_CURVE_WITH_KNOTS ( 'NONE', 3,
 ( #73645, #65527, #38969, #3382, #16901, #10597, #11937, #71841, #78598, #52898 ),
 .UNSPECIFIED., .F., .F.,
 ( 4, 2, 2, 2, 4 ),
 ( 0.0007817359430256293554, 0.0009771253907249971907, 0.001172514838424365026, 0.001367904286123733078, 0.001563293733823093758 ),
 .UNSPECIFIED. ) ;
#32364 = CARTESIAN_POINT ( 'NONE',  ( -5.076923076923075762, -9.905515769479276145, 34.41647553114623292 ) ) ;
#32365 = DIRECTION ( 'NONE',  ( -0.000000000000000000, -0.6427876096865404731, -0.7660444431189770143 ) ) ;
#32366 = CYLINDRICAL_SURFACE ( 'NONE', #29357, 0.2499999999999986955 ) ;
#32368 = CARTESIAN_POINT ( 'NONE',  ( 6.673053698855467175, -10.92453946501458439, 33.72985991061850086 ) ) ;
#32367 = CARTESIAN_POINT ( 'NONE',  ( 9.442284455014730682, -3.202444869320336451, 32.30641848906366675 ) ) ;
#32369 = CARTESIAN_POINT ( 'NONE',  ( 0.2380535178145107567, -12.24155766932282496, 31.33739205006857986 ) ) ;
#32370 = CARTESIAN_POINT ( 'NONE',  ( 1.384615384615264011, -2.379036618888197285, 30.90682066428292885 ) ) ;
#32371 = ORIENTED_EDGE ( 'NONE', *, *, #84873, .F. ) ;
#32372 = DIRECTION ( 'NONE',  ( 0.000000000000000000, 0.7660444431189822323, -0.6427876096865344779 ) ) ;
#32373 = AXIS2_PLACEMENT_3D ( 'NONE', #38208, #52604, #3081 ) ;
#32374 = CARTESIAN_POINT ( 'NONE',  ( -5.999999999999998224, -3.886160181151819604, 36.00935417666054406 ) ) ;
#32375 = VERTEX_POINT ( 'NONE', #22702 ) ;
#32376 = ORIENTED_EDGE ( 'NONE', *, *, #58103, .F. ) ;
#32377 = CARTESIAN_POINT ( 'NONE',  ( -17.32689980786543060, -11.28823185664190376, 33.01397839955799896 ) ) ;
#32378 = EDGE_CURVE ( 'NONE', #83375, #34892, #29243, .T. ) ;
#32379 = CARTESIAN_POINT ( 'NONE',  ( -13.63461538461537970, -7.566083408709835645, 34.74999999999999289 ) ) ;
#32380 = DIRECTION ( 'NONE',  ( -0.000000000000000000, 1.000000000000000000, -0.000000000000000000 ) ) ;
#32381 = CARTESIAN_POINT ( 'NONE',  ( 12.23805353697412990, -10.97335522853832579, 33.68706563782419749 ) ) ;
#32382 = EDGE_LOOP ( 'NONE', ( #70081, #88971, #21221, #2988, #39999, #4308 ) ) ;
#32383 = FACE_OUTER_BOUND ( 'NONE', #58617, .T. ) ;
#32384 = CARTESIAN_POINT ( 'NONE',  ( -4.283994123577847368, -9.504002272028875709, 34.60269587691767867 ) ) ;
#32386 = CARTESIAN_POINT ( 'NONE',  ( 6.000000000000001776, -9.780366693483667717, 34.19971097300155094 ) ) ;
#32385 = CARTESIAN_POINT ( 'NONE',  ( 18.00000000000000000, -3.513871655860378418, 32.76840700105978499 ) ) ;
#32387 = CARTESIAN_POINT ( 'NONE',  ( -12.52762187249433978, -4.786620604624113540, 33.94971097300155805 ) ) ;
#32388 = DIRECTION ( 'NONE',  ( 0.000000000000000000, 0.000000000000000000, 1.000000000000000000 ) ) ;
#32389 = CARTESIAN_POINT ( 'NONE',  ( -8.769230769230768274, -6.435427911321262684, 35.78748833219616898 ) ) ;
#32390 = CARTESIAN_POINT ( 'NONE',  ( -3.749999999999997335, -7.500000000000021316, 21.34375000000000000 ) ) ;
#32391 = VERTEX_POINT ( 'NONE', #21823 ) ;
#32392 = EDGE_CURVE ( 'NONE', #40861, #73086, #86195, .T. ) ;
#32393 = ORIENTED_EDGE ( 'NONE', *, *, #73999, .T. ) ;
#32394 = CARTESIAN_POINT ( 'NONE',  ( 4.853996118016225658, -10.77366814457252175, 33.85459836347579454 ) ) ;
#32395 = EDGE_CURVE ( 'NONE', #3633, #17957, #83540, .T. ) ;
#32396 = CARTESIAN_POINT ( 'NONE',  ( 6.923076923076802558, -12.27809138561165270, 31.22303859784587132 ) ) ;
#32397 = CARTESIAN_POINT ( 'NONE',  ( 16.15384615384603251, -3.083524468854526912, 32.58852847137268327 ) ) ;
#32398 = CARTESIAN_POINT ( 'NONE',  ( 17.32692307692307665, -2.249999999999998668, 29.75000000000000355 ) ) ;
#32399 = DIRECTION ( 'NONE',  ( 0.000000000000000000, 0.6427876096865368094, 0.7660444431189802339 ) ) ;
#32400 = CARTESIAN_POINT ( 'NONE',  ( -1.553300858899081538, -11.25000000000000711, 24.85937500000001421 ) ) ;
#32401 = CARTESIAN_POINT ( 'NONE',  ( -9.692307692307691624, -1.117168528481311540, 33.14645433367849847 ) ) ;
#32402 = CARTESIAN_POINT ( 'NONE',  ( 2.307692307692309264, -1.422936976036506707, 30.56769352161908415 ) ) ;
#32403 = CARTESIAN_POINT ( 'NONE',  ( -13.13461538461531752, -7.434744429011176159, 34.75000000000000711 ) ) ;
#32404 = CARTESIAN_POINT ( 'NONE',  ( 5.869309396889692110, -9.929715669179216775, 34.40415004197138416 ) ) ;
#32405 = FACE_OUTER_BOUND ( 'NONE', #67655, .T. ) ;
#32406 = DIRECTION ( 'NONE',  ( -0.000000000000000000, 0.3420201433256694901, -0.9396926207859082059 ) ) ;
#32407 = CARTESIAN_POINT ( 'NONE',  ( -3.361245938885694784, -7.276988635370450709, 34.74523720219453793 ) ) ;
#32408 = CYLINDRICAL_SURFACE ( 'NONE', #17079, 0.2499999999999979738 ) ;
#32410 = EDGE_CURVE ( 'NONE', #13761, #6434, #26044, .T. ) ;
#32409 = CARTESIAN_POINT ( 'NONE',  ( 10.83816415665302557, -2.847695495035523550, 31.58253572463339154 ) ) ;
#32411 = DIRECTION ( 'NONE',  ( 0.000000000000000000, 0.000000000000000000, 1.000000000000000000 ) ) ;
#32412 = VERTEX_POINT ( 'NONE', #2424 ) ;
#32413 = LINE ( 'NONE', #59882, #9627 ) ;
#32414 = CARTESIAN_POINT ( 'NONE',  ( -8.769230769230768274, -3.322132147404559976, 32.92929555188717927 ) ) ;
#32415 = CARTESIAN_POINT ( 'NONE',  ( -0.2115384615370421995, -7.500000000000154543, 35.00000000000007105 ) ) ;
#32416 = CARTESIAN_POINT ( 'NONE',  ( -2.775308065498752086, -8.577988221561495763, 16.51749329374151642 ) ) ;
#32417 = CARTESIAN_POINT ( 'NONE',  ( 13.38461538461526601, -10.90142922262034020, 33.41473453929536674 ) ) ;
#32418 = DIRECTION ( 'NONE',  ( 0.000000000000000000, 0.1736481776669275834, 0.9848077530122086864 ) ) ;
#32420 = ORIENTED_EDGE ( 'NONE', *, *, #44057, .F. ) ;
#32419 = DIRECTION ( 'NONE',  ( 0.000000000000000000, 0.000000000000000000, 1.000000000000000000 ) ) ;
#32421 = CARTESIAN_POINT ( 'NONE',  ( -1.139087296526025250, -4.750000000000006217, 16.57812500000000000 ) ) ;
#32422 = DIRECTION ( 'NONE',  ( 0.000000000000000000, 0.000000000000000000, 1.000000000000000000 ) ) ;
#32423 = EDGE_CURVE ( 'NONE', #558, #18982, #43280, .T. ) ;
#32424 = ORIENTED_EDGE ( 'NONE', *, *, #80208, .F. ) ;
#32425 = CARTESIAN_POINT ( 'NONE',  ( -2.084680956079457026, -2.554770724473667709, 30.48948780036025852 ) ) ;
#32426 = EDGE_LOOP ( 'NONE', ( #27053, #63144 ) ) ;
#32427 = B_SPLINE_CURVE_WITH_KNOTS ( 'NONE', 3,
 ( #48563, #13020, #89145, #88703, #54441, #75174, #62089, #20659, #28298, #76497 ),
 .UNSPECIFIED., .F., .F.,
 ( 4, 2, 2, 2, 4 ),
 ( 0.000000000000000000, 0.0001954311584214073465, 0.0003908623168428146930, 0.0005862934752642220667, 0.0007817246336856293861 ),
 .UNSPECIFIED. ) ;
#32428 = CARTESIAN_POINT ( 'NONE',  ( -7.623141002060451754, -6.460100341425560444, 34.89618726649961644 ) ) ;
#32429 = ADVANCED_FACE ( 'NONE', ( #10976 ), #71770, .F. ) ;
#32430 = EDGE_CURVE ( 'NONE', #68029, #12728, #30788, .T. ) ;
#32431 = CARTESIAN_POINT ( 'NONE',  ( 13.25446817517716980, -10.19110544564092002, 33.96427741523702792 ) ) ;
#32432 = VECTOR ( 'NONE', #30833, 1000.000000000000000 ) ;
#32433 = CARTESIAN_POINT ( 'NONE',  ( -0.4615384615385840772, -6.835583212225970762, 34.95778746994575670 ) ) ;
#32434 = ORIENTED_EDGE ( 'NONE', *, *, #81956, .T. ) ;
#32435 = CARTESIAN_POINT ( 'NONE',  ( -11.53846153846153655, -11.35647404775217417, 33.31231777344666511 ) ) ;
#32436 = ORIENTED_EDGE ( 'NONE', *, *, #65168, .F. ) ;
#32437 = EDGE_CURVE ( 'NONE', #65096, #62997, #72216, .T. ) ;
#32438 = EDGE_LOOP ( 'NONE', ( #28709, #83039, #84405, #69284 ) ) ;
#32439 = CARTESIAN_POINT ( 'NONE',  ( 13.51540719244017374, -11.71459661697925903, 32.44059661609676937 ) ) ;
#32440 = CARTESIAN_POINT ( 'NONE',  ( 6.000000000000001776, -1.466349020453238561, 30.81389545987213907 ) ) ;
#32441 = CARTESIAN_POINT ( 'NONE',  ( -10.61538461538461320, -6.386643153685126251, 34.62446782046654192 ) ) ;
#32442 = DIRECTION ( 'NONE',  ( -0.000000000000000000, -0.8660254037844399289, -0.4999999999999980016 ) ) ;
#32443 = DIRECTION ( 'NONE',  ( 0.000000000000000000, 0.7660444431189807890, 0.6427876096865361433 ) ) ;
#32444 = CARTESIAN_POINT ( 'NONE',  ( 11.31497659473759043, -11.89387501736622710, 32.13663884655806413 ) ) ;
#32445 = DIRECTION ( 'NONE',  ( 0.000000000000000000, 0.000000000000000000, 1.000000000000000000 ) ) ;
#32446 = ORIENTED_EDGE ( 'NONE', *, *, #50110, .F. ) ;
#32447 = ORIENTED_EDGE ( 'NONE', *, *, #77565, .F. ) ;
#32448 = VERTEX_POINT ( 'NONE', #73116 ) ;
#32450 = ORIENTED_EDGE ( 'NONE', *, *, #16401, .T. ) ;
#32449 = CARTESIAN_POINT ( 'NONE',  ( -4.153846153846274980, -8.656820664282941280, 34.87096338111179961 ) ) ;
#32451 = CARTESIAN_POINT ( 'NONE',  ( -9.019254006523732770, -10.05641848906368097, 34.04755513067966177 ) ) ;
#32452 = CARTESIAN_POINT ( 'NONE',  ( 1.634669696253701510, -2.779044189368096607, 31.39831045268885035 ) ) ;
#32453 = EDGE_LOOP ( 'NONE', ( #18900, #14732 ) ) ;
#32454 = CYLINDRICAL_SURFACE ( 'NONE', #77544, 0.2500000000000002220 ) ;
#32455 = VECTOR ( 'NONE', #49363, 1000.000000000000000 ) ;
#32456 = VERTEX_POINT ( 'NONE', #79875 ) ;
#32457 = CARTESIAN_POINT ( 'NONE',  ( 0.2115384615384550415, -2.499999999999999556, 29.81609845454691765 ) ) ;
#32458 = VERTEX_POINT ( 'NONE', #17280 ) ;
#32459 = CARTESIAN_POINT ( 'NONE',  ( 5.076923076923075762, -2.249999999999998668, 29.75000000000001776 ) ) ;
#32460 = CYLINDRICAL_SURFACE ( 'NONE', #37383, 0.2499999999999998890 ) ;
#32461 = CARTESIAN_POINT ( 'NONE',  ( -16.08777882049607655, -10.67929555188718282, 33.92786785259544757 ) ) ;
#32462 = FACE_BOUND ( 'NONE', #48383, .T. ) ;
#32463 = DIRECTION ( 'NONE',  ( 1.000000000000000000, 0.000000000000000000, 0.000000000000000000 ) ) ;
#32464 = FACE_OUTER_BOUND ( 'NONE', #56947, .T. ) ;
#32465 = DIRECTION ( 'NONE',  ( 0.000000000000000000, 0.000000000000000000, 1.000000000000000000 ) ) ;
#32466 = CARTESIAN_POINT ( 'NONE',  ( 4.826946332874483936, -3.436278759898155677, 33.07459398097509506 ) ) ;
#32467 = CARTESIAN_POINT ( 'NONE',  ( 10.74543222164029821, -7.723484964179501588, 34.74522123443823318 ) ) ;
#32468 = DIRECTION ( 'NONE',  ( 1.000000000000000000, 0.000000000000000000, 0.000000000000000000 ) ) ;
#32469 = ORIENTED_EDGE ( 'NONE', *, *, #6318, .T. ) ;
#32470 = DIRECTION ( 'NONE',  ( -0.000000000000000000, 0.6427876096865404731, -0.7660444431189771253 ) ) ;
#32471 = ORIENTED_EDGE ( 'NONE', *, *, #1781, .F. ) ;
#32472 = ORIENTED_EDGE ( 'NONE', *, *, #20346, .F. ) ;
#32474 = FACE_OUTER_BOUND ( 'NONE', #905, .T. ) ;
#32473 = CARTESIAN_POINT ( 'NONE',  ( 10.61538461538449596, -12.46129190930018460, 30.37095296980731973 ) ) ;
#32475 = CARTESIAN_POINT ( 'NONE',  ( 16.28463659481310799, -11.37503395064541678, 33.29242100308974983 ) ) ;
#32476 = CARTESIAN_POINT ( 'NONE',  ( -14.53061926659915315, -11.98009711892699514, 32.48740034544076138 ) ) ;
#32477 = LINE ( 'NONE', #59950, #37142 ) ;
#32478 = CARTESIAN_POINT ( 'NONE',  ( -2.177166605928743781, -2.882268652242222284, 31.66798894389554064 ) ) ;
#32479 = VERTEX_POINT ( 'NONE', #24028 ) ;
#32480 = VECTOR ( 'NONE', #39228, 1000.000000000000000 ) ;
#32481 = CARTESIAN_POINT ( 'NONE',  ( 8.352564102564102200, -3.499999999999999556, 29.75000000000000355 ) ) ;
#32482 = CARTESIAN_POINT ( 'NONE',  ( 0.5267940328144847806, -10.21337939537593797, 33.94971097300152252 ) ) ;
#32483 = CARTESIAN_POINT ( 'NONE',  ( -4.480769230769230838, -7.500000000000000000, 29.75000000000000355 ) ) ;
#32484 = DIRECTION ( 'NONE',  ( 0.000000000000000000, 0.3420201433256610524, 0.9396926207859113145 ) ) ;
#32485 = ORIENTED_EDGE ( 'NONE', *, *, #47633, .T. ) ;
#32486 = EDGE_LOOP ( 'NONE', ( #84970, #25037, #13381, #47161 ) ) ;
#32487 = EDGE_CURVE ( 'NONE', #61793, #64477, #31235, .T. ) ;
#32488 = SHAPE_DEFINITION_REPRESENTATION ( #64260, #51743 ) ;
#32489 = ORIENTED_EDGE ( 'NONE', *, *, #6324, .F. ) ;
#32490 = CARTESIAN_POINT ( 'NONE',  ( 15.36129493253279676, -6.852161475712352789, 34.70806712695775786 ) ) ;
#32491 = CARTESIAN_POINT ( 'NONE',  ( 11.53846153846141576, -3.643525952248795718, 33.31231777344771672 ) ) ;
#32492 = ORIENTED_EDGE ( 'NONE', *, *, #79422, .F. ) ;
#32493 = VECTOR ( 'NONE', #43546, 999.9999999999998863 ) ;
#32494 = CARTESIAN_POINT ( 'NONE',  ( 3.100621261037534993, -12.70455904226513866, 30.44083106164009322 ) ) ;
#32495 = DIRECTION ( 'NONE',  ( -0.000000000000000000, 0.5000000000000011102, -0.8660254037844381525 ) ) ;
#32496 = CARTESIAN_POINT ( 'NONE',  ( 0.6843180028068707177, -12.24180327182771855, 31.33663988360758168 ) ) ;
#32497 = CARTESIAN_POINT ( 'NONE',  ( 8.900021210197719412, -3.338503747796866872, 32.95102852606553512 ) ) ;
#32498 = FACE_OUTER_BOUND ( 'NONE', #48842, .T. ) ;
#32499 = ORIENTED_EDGE ( 'NONE', *, *, #14947, .T. ) ;
#32501 = ORIENTED_EDGE ( 'NONE', *, *, #52677, .F. ) ;
#32500 = CARTESIAN_POINT ( 'NONE',  ( 0.3954550505825797924, -9.780366693483667717, 34.19971097300155805 ) ) ;
#32502 = LINE ( 'NONE', #18999, #19570 ) ;
#32503 = CARTESIAN_POINT ( 'NONE',  ( 15.93098073164252249, -2.501496062324911840, 29.88072118266895671 ) ) ;
#32504 = CARTESIAN_POINT ( 'NONE',  ( -7.846153846153844924, -6.343179335718451384, 34.87096338111211935 ) ) ;
#32505 = CARTESIAN_POINT ( 'NONE',  ( 15.23076923076911093, -12.46129190930018460, 30.37095296980731973 ) ) ;
#32506 = DIRECTION ( 'NONE',  ( 0.000000000000000000, 0.000000000000000000, 1.000000000000000000 ) ) ;
#32507 = EDGE_CURVE ( 'NONE', #33215, #63487, #68185, .T. ) ;
#32508 = DIRECTION ( 'NONE',  ( -0.000000000000000000, -0.9396926207859092051, -0.3420201433256662704 ) ) ;
#32509 = CARTESIAN_POINT ( 'NONE',  ( -1.077988221561493543, -4.724691934501247914, 15.57999329374151110 ) ) ;
#32510 = VERTEX_POINT ( 'NONE', #72664 ) ;
#32511 = CARTESIAN_POINT ( 'NONE',  ( 11.78840705680968348, -2.824170634883621744, 31.52227843825338738 ) ) ;
#32512 = CARTESIAN_POINT ( 'NONE',  ( 8.069580245068634028, -7.630147987733840509, 34.99859428049666121 ) ) ;
#32513 = CARTESIAN_POINT ( 'NONE',  ( -13.38461538461538325, -4.661471528628507777, 34.16647553114623292 ) ) ;
#32515 = VERTEX_POINT ( 'NONE', #58258 ) ;
#32514 = AXIS2_PLACEMENT_3D ( 'NONE', #61640, #56221, #62518 ) ;
#32516 = ORIENTED_EDGE ( 'NONE', *, *, #76405, .F. ) ;
#32517 = CARTESIAN_POINT ( 'NONE',  ( -11.53846153846165912, -10.90142922262034020, 33.41473453929536674 ) ) ;
#32518 = CARTESIAN_POINT ( 'NONE',  ( 8.769230769230647482, -8.613356846316285953, 34.62446782046622218 ) ) ;
#32519 = CARTESIAN_POINT ( 'NONE',  ( -0.2381625208402778360, -2.501478030877323011, 29.88021232661721172 ) ) ;
#32520 = VECTOR ( 'NONE', #6717, 999.9999999999998863 ) ;
#32521 = LINE ( 'NONE', #81610, #12842 ) ;
#32522 = CARTESIAN_POINT ( 'NONE',  ( -17.78205128205128105, -3.499999999999999556, 29.75000000000000355 ) ) ;
#32523 = CARTESIAN_POINT ( 'NONE',  ( -7.173100160369890510, -11.86270091957321249, 32.19358267280087915 ) ) ;
#32524 = ORIENTED_EDGE ( 'NONE', *, *, #25312, .T. ) ;
#32526 = EDGE_CURVE ( 'NONE', #60729, #46284, #51479, .T. ) ;
#32525 = CARTESIAN_POINT ( 'NONE',  ( 9.627037246346917598, -10.90142922261923886, 33.41473453929638993 ) ) ;
#32527 = EDGE_CURVE ( 'NONE', #33691, #29899, #78675, .T. ) ;
#32528 = CARTESIAN_POINT ( 'NONE',  ( -2.241623956689867470, -9.780366693483667717, 34.19971097300155805 ) ) ;
#32529 = CARTESIAN_POINT ( 'NONE',  ( -5.076923076923075762, -9.058645607665452459, 34.76329471203371924 ) ) ;
#32530 = ORIENTED_EDGE ( 'NONE', *, *, #36992, .T. ) ;
#32531 = CARTESIAN_POINT ( 'NONE',  ( 12.46153846153846168, -2.486705287966279876, 31.30864560766543647 ) ) ;
#32532 = ORIENTED_EDGE ( 'NONE', *, *, #30154, .T. ) ;
#32533 = EDGE_CURVE ( 'NONE', #60409, #47762, #49643, .T. ) ;
#32534 = CARTESIAN_POINT ( 'NONE',  ( 13.60739492588379740, -3.755027918224367767, 33.06320215134714857 ) ) ;
#32535 =( NAMED_UNIT ( * ) SI_UNIT ( $, .STERADIAN. ) SOLID_ANGLE_UNIT ( ) );
#32536 = DIRECTION ( 'NONE',  ( -1.799314243699348838E-16, -1.000000000000000000, 5.102127870520021228E-17 ) ) ;
#32537 = CARTESIAN_POINT ( 'NONE',  ( 15.23076923076923173, -4.661471528628507777, 34.16647553114623292 ) ) ;
#32538 = ORIENTED_EDGE ( 'NONE', *, *, #64913, .T. ) ;
#32539 = CARTESIAN_POINT ( 'NONE',  ( 12.33084699487089964, -3.530157926970578952, 32.79014554554150607 ) ) ;
#32540 = DIRECTION ( 'NONE',  ( -0.000000000000000000, 0.3420201433256694346, -0.9396926207859080948 ) ) ;
#32541 = CARTESIAN_POINT ( 'NONE',  ( -16.15384615384615330, -1.951392089020283160, 34.73218667398347748 ) ) ;
#32542 = CARTESIAN_POINT ( 'NONE',  ( 23.49999999999998934, 1.674711738930281374E-15, 28.74999999999999645 ) ) ;
#32543 = CARTESIAN_POINT ( 'NONE',  ( -5.076923076923199218, -11.06231777344772027, 33.60647404775119895 ) ) ;
#32544 = ORIENTED_EDGE ( 'NONE', *, *, #30049, .F. ) ;
#32545 = B_SPLINE_CURVE_WITH_KNOTS ( 'NONE', 3,
 ( #77679, #38037, #44320, #85786, #65501, #22733, #3800, #30386, #56961, #58746 ),
 .UNSPECIFIED., .F., .F.,
 ( 4, 2, 2, 2, 4 ),
 ( 0.0007817246256747457630, 0.0009771112852218887673, 0.001172497944769031880, 0.001367884604316174993, 0.001563271263863318106 ),
 .UNSPECIFIED. ) ;
#32546 = CARTESIAN_POINT ( 'NONE',  ( -4.153846153846274980, -12.51329471203414379, 31.30864560766407578 ) ) ;
#32547 = ORIENTED_EDGE ( 'NONE', *, *, #34356, .F. ) ;
#32548 = CARTESIAN_POINT ( 'NONE',  ( -5.076923076923075762, -9.584722331328613620, 36.20867863119891439 ) ) ;
#32549 = B_SPLINE_CURVE_WITH_KNOTS ( 'NONE', 3,
 ( #43219, #14874, #8110, #35582, #63028, #44525, #86895, #16620, #9869, #45423 ),
 .UNSPECIFIED., .F., .F.,
 ( 4, 2, 2, 2, 4 ),
 ( 0.000000000000000000, 0.0001954339857564079080, 0.0003908679715128158161, 0.0005863019572692237513, 0.0007817359430256316322 ),
 .UNSPECIFIED. ) ;
#32550 = B_SPLINE_CURVE_WITH_KNOTS ( 'NONE', 3,
 ( #53558, #6703, #74286, #46808, #75178, #20661, #12584, #5386, #34176, #81938 ),
 .UNSPECIFIED., .F., .F.,
 ( 4, 2, 2, 2, 4 ),
 ( 0.0007817246256747444619, 0.0009771112852218868158, 0.001172497944769029061, 0.001367884604316171523, 0.001563271263863313769 ),
 .UNSPECIFIED. ) ;
#32551 = DIRECTION ( 'NONE',  ( 0.000000000000000000, 0.9396926207859126468, 0.3420201433256571111 ) ) ;
#32552 = CARTESIAN_POINT ( 'NONE',  ( -3.453647913197877894, -7.630691491037286056, 34.74850469731152458 ) ) ;
#32553 = CARTESIAN_POINT ( 'NONE',  ( 11.00641025641025550, -7.500000000000000000, 29.75000000000000355 ) ) ;
#32554 = VECTOR ( 'NONE', #18919, 1000.000000000000000 ) ;
#32555 = DIRECTION ( 'NONE',  ( -0.000000000000000000, -0.000000000000000000, -1.000000000000000000 ) ) ;
#32556 = PLANE ( 'NONE',  #82509 ) ;
#32557 = LINE ( 'NONE', #60029, #62318 ) ;
#32558 = ORIENTED_EDGE ( 'NONE', *, *, #47438, .F. ) ;
#32559 = ORIENTED_EDGE ( 'NONE', *, *, #76740, .T. ) ;
#32560 = ORIENTED_EDGE ( 'NONE', *, *, #68039, .F. ) ;
#32561 = ORIENTED_EDGE ( 'NONE', *, *, #27126, .F. ) ;
#32562 = CARTESIAN_POINT ( 'NONE',  ( -10.61538461538473399, -11.48612834414049644, 32.76840700105863391 ) ) ;
#32563 = DIRECTION ( 'NONE',  ( -0.000000000000000000, 0.3420201433256694901, -0.9396926207859082059 ) ) ;
#32564 = CARTESIAN_POINT ( 'NONE',  ( 8.769230769230768274, -2.249999999999998668, 29.75000000000001776 ) ) ;
#32565 = CARTESIAN_POINT ( 'NONE',  ( 3.903822916553187028, -3.202444869320336451, 32.30641848906366675 ) ) ;
#32566 = CARTESIAN_POINT ( 'NONE',  ( 17.93472955403921887, -10.21337939537584383, 33.94971097300158647 ) ) ;
#32567 = VECTOR ( 'NONE', #71961, 1000.000000000000227 ) ;
#32568 = CARTESIAN_POINT ( 'NONE',  ( 6.416666666666664298, -3.499999999999999556, 29.75000000000000355 ) ) ;
#32569 = CARTESIAN_POINT ( 'NONE',  ( 13.38461538461538680, -2.708943851104267164, 35.45975837776705220 ) ) ;
#32570 = CARTESIAN_POINT ( 'NONE',  ( 0.2115617305961072503, -3.137211980971221781, 32.19342716148376837 ) ) ;
#32571 = VERTEX_POINT ( 'NONE', #87096 ) ;
#32572 = VERTEX_POINT ( 'NONE', #25370 ) ;
#32573 = EDGE_CURVE ( 'NONE', #77030, #88830, #80332, .T. ) ;
#32574 = B_SPLINE_CURVE_WITH_KNOTS ( 'NONE', 3,
 ( #2079, #64212, #22789, #84954, #85392, #43952, #43073, #50253, #71867, #63338 ),
 .UNSPECIFIED., .F., .F.,
 ( 4, 2, 2, 2, 4 ),
 ( 0.0007817359430256346680, 0.0009771253907250002264, 0.001172514838424365893, 0.001367904286123731560, 0.001563293733823104166 ),
 .UNSPECIFIED. ) ;
#32575 = AXIS2_PLACEMENT_3D ( 'NONE', #534, #13162, #80749 ) ;
#32576 = ORIENTED_EDGE ( 'NONE', *, *, #18921, .T. ) ;
#32578 = VERTEX_POINT ( 'NONE', #37540 ) ;
#32577 = CARTESIAN_POINT ( 'NONE',  ( -1.634638621908349077, -11.37209801155882971, 32.91403422569032955 ) ) ;
#32580 = DIRECTION ( 'NONE',  ( -0.000000000000000000, -0.7660444431189791237, -0.6427876096865379196 ) ) ;
#32579 = CARTESIAN_POINT ( 'NONE',  ( -7.134615384615385025, -7.500000000000000000, 33.75000000000000000 ) ) ;
#32581 = B_SPLINE_CURVE_WITH_KNOTS ( 'NONE', 3,
 ( #48503, #33679, #55267, #82757, #76433, #6643, #74671, #14285, #28694, #41767 ),
 .UNSPECIFIED., .F., .F.,
 ( 4, 2, 2, 2, 4 ),
 ( 0.000000000000000000, 0.0001954311564186879315, 0.0003908623128373758630, 0.0005862934692560637946, 0.0007817246256747517261 ),
 .UNSPECIFIED. ) ;
#32582 = B_SPLINE_CURVE_WITH_KNOTS ( 'NONE', 3,
 ( #10494, #72626, #4167, #67217, #52349, #31193, #72181, #65427, #38855, #3722 ),
 .UNSPECIFIED., .F., .F.,
 ( 4, 2, 2, 2, 4 ),
 ( 0.0007817246256747484735, 0.0009771112852218920199, 0.001172497944769035783, 0.001367884604316179330, 0.001563271263863322876 ),
 .UNSPECIFIED. ) ;
#32583 = CARTESIAN_POINT ( 'NONE',  ( -0.3954711281883849794, -2.292212530054420494, 30.41441678777542990 ) ) ;
#32584 = CARTESIAN_POINT ( 'NONE',  ( 4.153846153846154188, -2.538708090699994813, 30.37095296980875503 ) ) ;
#32585 = FACE_BOUND ( 'NONE', #76375, .T. ) ;
#32586 = ORIENTED_EDGE ( 'NONE', *, *, #76801, .F. ) ;
#32587 = VECTOR ( 'NONE', #36386, 1000.000000000000000 ) ;
#32588 = ORIENTED_EDGE ( 'NONE', *, *, #61694, .F. ) ;
#32589 = CYLINDRICAL_SURFACE ( 'NONE', #41395, 0.2500000000000002220 ) ;
#32590 = EDGE_LOOP ( 'NONE', ( #71345, #21382, #57697, #47037 ) ) ;
#32591 = FACE_BOUND ( 'NONE', #73127, .T. ) ;
#32592 = CARTESIAN_POINT ( 'NONE',  ( 7.780070435197965040, -11.69971097300155272, 32.46337939537587403 ) ) ;
#32593 = EDGE_CURVE ( 'NONE', #59060, #83471, #46091, .T. ) ;
#32594 = CARTESIAN_POINT ( 'NONE',  ( 8.096153846153860911, -2.249999999999999112, 29.81603969181031033 ) ) ;
#32595 = VERTEX_POINT ( 'NONE', #70757 ) ;
#32596 = DIRECTION ( 'NONE',  ( -0.000000000000000000, -0.9848077530122085754, -0.1736481776669273613 ) ) ;
#32597 = DIRECTION ( 'NONE',  ( 1.000000000000000000, 0.000000000000000000, 0.000000000000000000 ) ) ;
#32598 = DIRECTION ( 'NONE',  ( 0.000000000000000000, 0.7660444431189822323, -0.6427876096865344779 ) ) ;
#32599 = EDGE_LOOP ( 'NONE', ( #33509, #57423 ) ) ;
#32600 = ADVANCED_FACE ( 'NONE', ( #84286 ), #49594, .F. ) ;
#32601 = CARTESIAN_POINT ( 'NONE',  ( 14.55763771707035303, -3.520799739797214389, 33.17531984108286025 ) ) ;
#32602 = CARTESIAN_POINT ( 'NONE',  ( 7.173131342990376247, -5.642605341092957083, 34.66089969410670335 ) ) ;
#32603 = CARTESIAN_POINT ( 'NONE',  ( -13.38461538461538325, -6.343179335718451384, 34.87096338111211935 ) ) ;
#32604 = ORIENTED_EDGE ( 'NONE', *, *, #61591, .F. ) ;
#32605 = PLANE ( 'NONE',  #25802 ) ;
#32606 = CARTESIAN_POINT ( 'NONE',  ( -9.442253272394237840, -9.233818618650603938, 34.70587769442853698 ) ) ;
#32607 = EDGE_LOOP ( 'NONE', ( #19834, #24447 ) ) ;
#32608 = CARTESIAN_POINT ( 'NONE',  ( 3.361559671736181087, -6.369690395747422684, 34.87708834333098196 ) ) ;
#32609 = DIRECTION ( 'NONE',  ( 0.000000000000000000, 0.6427876096865373645, -0.7660444431189797898 ) ) ;
#32610 = CARTESIAN_POINT ( 'NONE',  ( -7.911423846710164298, -12.51329471203370325, 31.30864560766548976 ) ) ;
#32611 = CARTESIAN_POINT ( 'NONE',  ( -11.78848477575450282, -8.432397168068783699, 34.66272746175022945 ) ) ;
#32612 = DIRECTION ( 'NONE',  ( -1.000000000000000000, 0.000000000000000000, 0.000000000000000000 ) ) ;
#32613 = VECTOR ( 'NONE', #69842, 1000.000000000000000 ) ;
#32614 = CARTESIAN_POINT ( 'NONE',  ( 2.307692307692309264, -3.886160181151819604, 36.00935417666054406 ) ) ;
#32616 = CARTESIAN_POINT ( 'NONE',  ( -20.99999999999999645, -10.75000000000000000, 27.25000000000000000 ) ) ;
#32615 = CARTESIAN_POINT ( 'NONE',  ( 6.000000000000001776, -11.69971097300155272, 32.46337939537588113 ) ) ;
#32617 = EDGE_CURVE ( 'NONE', #70140, #40157, #65752, .T. ) ;
#32618 = CARTESIAN_POINT ( 'NONE',  ( 10.86543903529806876, -9.233818618650603938, 34.70587769442853698 ) ) ;
#32619 = CARTESIAN_POINT ( 'NONE',  ( -12.23852710992561299, -11.24521262558773493, 33.06293181088029343 ) ) ;
#32620 = CARTESIAN_POINT ( 'NONE',  ( 2.775308065498768517, -8.577988221561467341, 25.54500670625849779 ) ) ;
#32621 = ORIENTED_EDGE ( 'NONE', *, *, #11352, .F. ) ;
#32622 = CIRCLE ( 'NONE', #82966, 4.000000000000000000 ) ;
#32623 = PLANE ( 'NONE',  #44736 ) ;
#32624 = VERTEX_POINT ( 'NONE', #42846 ) ;
#32625 = EDGE_CURVE ( 'NONE', #78937, #37879, #21729, .T. ) ;
#32626 = VERTEX_POINT ( 'NONE', #9061 ) ;
#32627 = CARTESIAN_POINT ( 'NONE',  ( -7.596099426240389363, -2.544122305571458575, 31.48381861865057729 ) ) ;
#32628 = VERTEX_POINT ( 'NONE', #83843 ) ;
#32629 = CARTESIAN_POINT ( 'NONE',  ( 3.453780582382081743, -9.886259254753566594, 34.14407573483972413 ) ) ;
#32630 = CARTESIAN_POINT ( 'NONE',  ( -1.944543648263014957, -5.555456351737005249, 14.00000000000000000 ) ) ;
#32631 = CARTESIAN_POINT ( 'NONE',  ( 12.71153846153852385, -7.434744860731433924, 35.00000000000000711 ) ) ;
#32632 = DIRECTION ( 'NONE',  ( 0.000000000000000000, 0.7660444431189822323, -0.6427876096865344779 ) ) ;
#32633 = CARTESIAN_POINT ( 'NONE',  ( -7.780085495151407571, -5.557115091759786019, 34.35708131394839882 ) ) ;
#32634 = CARTESIAN_POINT ( 'NONE',  ( 9.915320536401091900, -2.889357225399416418, 32.26129605718031002 ) ) ;
#32635 = CARTESIAN_POINT ( 'NONE',  ( -10.36543920600657209, -3.520799739797214389, 33.17531984108286025 ) ) ;
#32636 = CARTESIAN_POINT ( 'NONE',  ( 0.7114838709165038910, -5.766571408460172243, 34.70601412856602508 ) ) ;
#32637 = DIRECTION ( 'NONE',  ( -0.000000000000000000, -0.000000000000000000, -1.000000000000000000 ) ) ;
#32638 = CARTESIAN_POINT ( 'NONE',  ( 1.553300858899129944, -11.24999999999998934, 22.20312500000000000 ) ) ;
#32639 = CARTESIAN_POINT ( 'NONE',  ( 5.326868486301119532, -2.986452184633680673, 32.43230066228895225 ) ) ;
#32641 = EDGE_CURVE ( 'NONE', #60920, #83778, #77559, .T. ) ;
#32640 = CARTESIAN_POINT ( 'NONE',  ( -13.13466986626724164, -6.696923467548660192, 34.68552623307873972 ) ) ;
#32642 = ADVANCED_FACE ( 'NONE', ( #44588 ), #77072, .F. ) ;
#32643 = DIRECTION ( 'NONE',  ( -1.000000000000000000, -0.000000000000000000, 0.000000000000000000 ) ) ;
#32644 = ORIENTED_EDGE ( 'NONE', *, *, #36042, .F. ) ;
#32646 = EDGE_CURVE ( 'NONE', #29234, #33682, #6740, .T. ) ;
#32645 = ORIENTED_EDGE ( 'NONE', *, *, #60924, .F. ) ;
#32647 = AXIS2_PLACEMENT_3D ( 'NONE', #78953, #10502, #29016 ) ;
#32648 = CARTESIAN_POINT ( 'NONE',  ( -11.40766973063675316, -5.582136614379148654, 34.36778462344220486 ) ) ;
#32649 = DIRECTION ( 'NONE',  ( -0.000000000000000000, -0.3420201433256694346, -0.9396926207859080948 ) ) ;
#32650 = CARTESIAN_POINT ( 'NONE',  ( -2.749999999999998224, -7.500000000000000000, 29.50000000000000355 ) ) ;
#32651 = CARTESIAN_POINT ( 'NONE',  ( -16.08859058257013430, -12.46129190930001052, 30.37095296980869819 ) ) ;
#32652 = EDGE_CURVE ( 'NONE', #10983, #83460, #57139, .T. ) ;
#32653 = DIRECTION ( 'NONE',  ( -0.000000000000000000, 0.8660254037844397068, -0.4999999999999978906 ) ) ;
#32654 = CARTESIAN_POINT ( 'NONE',  ( -5.011667937410239304, -3.083524468853784839, 32.58852847137153930 ) ) ;
#32655 = VECTOR ( 'NONE', #81715, 1000.000000000000000 ) ;
#32656 = ORIENTED_EDGE ( 'NONE', *, *, #30994, .T. ) ;
#32657 = CARTESIAN_POINT ( 'NONE',  ( 15.93091993633000847, -2.758268499246657068, 31.33685645148948851 ) ) ;
#32658 = ORIENTED_EDGE ( 'NONE', *, *, #27334, .F. ) ;
#32659 = EDGE_LOOP ( 'NONE', ( #57781, #75431 ) ) ;
#32660 = CARTESIAN_POINT ( 'NONE',  ( 17.99999999999987566, -3.300289026999228437, 32.46337939537709616 ) ) ;
#32661 = CARTESIAN_POINT ( 'NONE',  ( -2.437840277424001556, -9.504002272028875709, 34.60269587691767867 ) ) ;
#32662 = CARTESIAN_POINT ( 'NONE',  ( -0.2115384615383984479, -7.434744860731433036, 35.00000000000000000 ) ) ;
#32663 = CARTESIAN_POINT ( 'NONE',  ( 4.153846153846154188, -6.343179335718451384, 34.87096338111211935 ) ) ;
#32664 = CARTESIAN_POINT ( 'NONE',  ( 9.692307692307695177, -6.386643153685126251, 34.62446782046654192 ) ) ;
#32665 = ORIENTED_EDGE ( 'NONE', *, *, #11464, .F. ) ;
#32666 = ORIENTED_EDGE ( 'NONE', *, *, #66581, .F. ) ;
#32667 = ADVANCED_FACE ( 'NONE', ( #71624 ), #9929, .F. ) ;
#32668 = AXIS2_PLACEMENT_3D ( 'NONE', #11152, #64305, #66086 ) ;
#32669 = ORIENTED_EDGE ( 'NONE', *, *, #29519, .T. ) ;
#32670 = DIRECTION ( 'NONE',  ( -0.000000000000000000, -0.8660254037844399289, -0.4999999999999980016 ) ) ;
#32671 = PLANE ( 'NONE',  #1393 ) ;
#32672 = AXIS2_PLACEMENT_3D ( 'NONE', #14857, #68895, #70230 ) ;
#32673 = DIRECTION ( 'NONE',  ( 0.000000000000000000, 0.000000000000000000, -1.000000000000000000 ) ) ;
#32674 = CARTESIAN_POINT ( 'NONE',  ( -11.53846153846165912, -12.27809138561165270, 31.22303859784587132 ) ) ;
#32675 = CARTESIAN_POINT ( 'NONE',  ( -18.00000000000000000, -8.317224813626184599, 35.82440484884453724 ) ) ;
#32676 = CARTESIAN_POINT ( 'NONE',  ( -2.307692307692427391, -6.026961402154118908, 34.52809138561165270 ) ) ;
#32677 = ORIENTED_EDGE ( 'NONE', *, *, #4309, .T. ) ;
#32678 = EDGE_CURVE ( 'NONE', #2810, #30821, #51327, .T. ) ;
#32679 = ORIENTED_EDGE ( 'NONE', *, *, #58514, .T. ) ;
#32680 = CARTESIAN_POINT ( 'NONE',  ( 3.750000000000009770, -9.053300858899081760, 25.79687500000000355 ) ) ;
#32681 = EDGE_CURVE ( 'NONE', #76616, #7349, #16303, .T. ) ;
#32683 = VERTEX_POINT ( 'NONE', #60339 ) ;
#32682 = CARTESIAN_POINT ( 'NONE',  ( 11.40777007179398161, -8.999036380462717588, 34.52022231692819076 ) ) ;
#32684 = CARTESIAN_POINT ( 'NONE',  ( 1.161689167099237974, -9.886141570436013382, 34.14413921362392301 ) ) ;
#32685 = CARTESIAN_POINT ( 'NONE',  ( -9.822999158975250111, -11.71456829005830080, 32.44064028649416542 ) ) ;
#32686 = ORIENTED_EDGE ( 'NONE', *, *, #61432, .T. ) ;
#32687 = CARTESIAN_POINT ( 'NONE',  ( -1.254089946381740983, -11.66157788607254275, 32.95092075102925833 ) ) ;
#32688 = EDGE_LOOP ( 'NONE', ( #47891, #12366 ) ) ;
#32689 = CARTESIAN_POINT ( 'NONE',  ( -5.076923076923199218, -8.656820664282941280, 34.87096338111179961 ) ) ;
#32690 = CYLINDRICAL_SURFACE ( 'NONE', #81746, 0.2500000000000002220 ) ;
#32691 = CARTESIAN_POINT ( 'NONE',  ( 12.46153846153833911, -10.21337939537710326, 33.94971097300076224 ) ) ;
#32692 = CARTESIAN_POINT ( 'NONE',  ( 16.15384615384615330, -2.708943851104267164, 35.45975837776705220 ) ) ;
#32693 = EDGE_CURVE ( 'NONE', #36501, #85855, #68948, .T. ) ;
#32694 = CIRCLE ( 'NONE', #26922, 4.000000000000000000 ) ;
#32695 = CARTESIAN_POINT ( 'NONE',  ( 4.153846153846154188, -1.215029322943914858, 32.30358669280327177 ) ) ;
#32696 = VERTEX_POINT ( 'NONE', #65755 ) ;
#32697 = CARTESIAN_POINT ( 'NONE',  ( -0.4615384615384611200, -2.292212530054420494, 30.41441678777542634 ) ) ;
#32698 = CARTESIAN_POINT ( 'NONE',  ( 15.23076923076911093, -4.481592998941358097, 33.73612834414048933 ) ) ;
#32699 = EDGE_CURVE ( 'NONE', #1879, #11337, #33377, .T. ) ;
#32700 = CARTESIAN_POINT ( 'NONE',  ( -14.05774678934416677, -2.824170634883621744, 31.52227843825338738 ) ) ;
#32701 = ORIENTED_EDGE ( 'NONE', *, *, #65048, .T. ) ;
#32702 = CARTESIAN_POINT ( 'NONE',  ( 6.416666666666664298, -7.500000000000000000, 29.75000000000000355 ) ) ;
#32704 = CARTESIAN_POINT ( 'NONE',  ( 10.61538461538449418, -8.656820664282941280, 34.87096338111179961 ) ) ;
#32703 = PRODUCT_DEFINITION_SHAPE ( 'NONE', 'NONE',  #89191 ) ;
#32705 = CARTESIAN_POINT ( 'NONE',  ( -4.023055712879203938, -2.295524264805589354, 30.44142389570982488 ) ) ;
#32706 = CARTESIAN_POINT ( 'NONE',  ( 11.40831432902331954, -6.001485441113819874, 34.52039167877662607 ) ) ;
#32707 = CARTESIAN_POINT ( 'NONE',  ( 8.096208157792158744, -3.136992222400443175, 32.19305428654138979 ) ) ;
#32708 = FACE_BOUND ( 'NONE', #5995, .T. ) ;
#32710 = CARTESIAN_POINT ( 'NONE',  ( 4.219913487196229163, -12.62096338111211757, 30.90682066428152908 ) ) ;
#32709 = LINE ( 'NONE', #26407, #7302 ) ;
#32711 = VECTOR ( 'NONE', #78720, 1000.000000000000000 ) ;
#32712 = B_SPLINE_CURVE_WITH_KNOTS ( 'NONE', 3,
 ( #57008, #57452, #70534, #24108, #51558, #50688 ),
 .UNSPECIFIED., .F., .F.,
 ( 4, 2, 4 ),
 ( 0.0003909569690057850379, 0.0005862646681846119933, 0.0007815723673634389487 ),
 .UNSPECIFIED. ) ;
#32713 = EDGE_CURVE ( 'NONE', #7735, #79114, #4513, .T. ) ;
#32714 = DIRECTION ( 'NONE',  ( -0.000000000000000000, -0.9848077530122086864, -0.1736481776669273613 ) ) ;
#32716 = DIRECTION ( 'NONE',  ( 0.000000000000000000, 0.1736481776669267785, -0.9848077530122087975 ) ) ;
#32715 = CARTESIAN_POINT ( 'NONE',  ( -11.78846153846153832, -7.500000000000001776, 34.75000000000000000 ) ) ;
#32717 = CYLINDRICAL_SURFACE ( 'NONE', #36197, 0.2499999999999986955 ) ;
#32718 = B_SPLINE_CURVE_WITH_KNOTS ( 'NONE', 3,
 ( #34787, #53732, #46967, #20833, #6874, #40233, #61812, #42007, #27591, #569 ),
 .UNSPECIFIED., .F., .F.,
 ( 4, 2, 2, 2, 4 ),
 ( 0.0007817246256747442451, 0.0009771112852218865989, 0.001172497944769029061, 0.001367884604316171523, 0.001563271263863313986 ),
 .UNSPECIFIED. ) ;
#32719 = CARTESIAN_POINT ( 'NONE',  ( 2.694853999681214862, -10.10844685921789043, 23.12313170625848713 ) ) ;
#32720 = ORIENTED_EDGE ( 'NONE', *, *, #25744, .F. ) ;
#32721 = CARTESIAN_POINT ( 'NONE',  ( -9.692307692307691624, -13.78497067705608181, 32.30358669280327177 ) ) ;
#32722 = ORIENTED_EDGE ( 'NONE', *, *, #45451, .T. ) ;
#32723 = CARTESIAN_POINT ( 'NONE',  ( 0.2115152242454954312, -6.695914987888143877, 34.68535235679833306 ) ) ;
#32724 = EDGE_LOOP ( 'NONE', ( #17466, #14961, #60280, #48141 ) ) ;
#32725 = CARTESIAN_POINT ( 'NONE',  ( -15.45364791319787834, -7.630691491037285168, 34.74850469731152458 ) ) ;
#32726 = CARTESIAN_POINT ( 'NONE',  ( -13.44986531638946836, -2.255955759149247175, 30.00000000000013856 ) ) ;
#32728 = ORIENTED_EDGE ( 'NONE', *, *, #28566, .T. ) ;
#32727 = CARTESIAN_POINT ( 'NONE',  ( -4.854143407945009869, -9.418065098278011860, 34.63729479722530158 ) ) ;
#32729 = CARTESIAN_POINT ( 'NONE',  ( -16.28453762051371712, -2.541943142973489334, 30.39792223712631980 ) ) ;
#32730 = CARTESIAN_POINT ( 'NONE',  ( -3.230769230769352962, -6.835583212225970762, 34.95778746994575670 ) ) ;
#32731 = CARTESIAN_POINT ( 'NONE',  ( 1.614399933863660985, -11.22469193450123193, 25.70125670625848713 ) ) ;
#32732 = DIRECTION ( 'NONE',  ( -0.000000000000000000, -0.8660254037844399289, -0.4999999999999980016 ) ) ;
#32733 = DIRECTION ( 'NONE',  ( 0.000000000000000000, 0.000000000000000000, -1.000000000000000000 ) ) ;
#32734 = CARTESIAN_POINT ( 'NONE',  ( -2.294871794871794712, -7.500000000000000000, 33.75000000000000000 ) ) ;
#32735 = CYLINDRICAL_SURFACE ( 'NONE', #84744, 0.2500000000000002220 ) ;
#32736 = CARTESIAN_POINT ( 'NONE',  ( 15.23076923076923173, -4.945431358278436385, 36.03766855953609394 ) ) ;
#32737 = CARTESIAN_POINT ( 'NONE',  ( 9.442284468086239002, -3.520140089381495585, 33.17453946501458262 ) ) ;
#32738 = CARTESIAN_POINT ( 'NONE',  ( 2.694853999681185108, -4.891553140782077591, 15.81436829374151465 ) ) ;
#32739 = AXIS2_PLACEMENT_3D ( 'NONE', #13981, #42797, #20306 ) ;
#32741 = EDGE_CURVE ( 'NONE', #36624, #13172, #76444, .T. ) ;
#32740 = LINE ( 'NONE', #60209, #85173 ) ;
#32742 = CARTESIAN_POINT ( 'NONE',  ( 19.00000000000000000, 0.7500000000000061062, 23.75000000000000000 ) ) ;
#32743 = VERTEX_POINT ( 'NONE', #51784 ) ;
#32744 = CARTESIAN_POINT ( 'NONE',  ( 7.173076923076861178, -7.565270000091922853, 34.99999999999999289 ) ) ;
#32745 = CARTESIAN_POINT ( 'NONE',  ( 8.992010310499175318, -11.41317474335729543, 32.86274602512330034 ) ) ;
#32746 = CARTESIAN_POINT ( 'NONE',  ( -3.749999999999997780, -7.438900925035489387, 17.84561829374150932 ) ) ;
#32747 = EDGE_CURVE ( 'NONE', #21625, #1947, #39925, .T. ) ;
#32748 = CARTESIAN_POINT ( 'NONE',  ( 6.989144256427000990, -10.67929555188718282, 33.92786785259544757 ) ) ;
#32749 = CARTESIAN_POINT ( 'NONE',  ( 17.20744877868664346, -11.93748526763465279, 32.05452791011430946 ) ) ;
#32750 = EDGE_LOOP ( 'NONE', ( #7682, #78897 ) ) ;
#32751 = DIRECTION ( 'NONE',  ( -0.000000000000000000, 1.000000000000000000, -0.000000000000000000 ) ) ;
#32752 = CARTESIAN_POINT ( 'NONE',  ( 6.000000000000001776, -3.322132147404559976, 32.92929555188717927 ) ) ;
#32754 = VERTEX_POINT ( 'NONE', #81077 ) ;
#32753 = CARTESIAN_POINT ( 'NONE',  ( 4.853438152358743096, -12.47654668319379567, 31.42292124445336654 ) ) ;
#32755 = CARTESIAN_POINT ( 'NONE',  ( 16.15384615384615330, -12.09954503811598769, 35.62045528018868623 ) ) ;
#32756 = CARTESIAN_POINT ( 'NONE',  ( -2.557692307692306155, -7.566082377512563184, 35.00000000000000711 ) ) ;
#32757 = ADVANCED_FACE ( 'NONE', ( #17591 ), #86503, .T. ) ;
#32758 = AXIS2_PLACEMENT_3D ( 'NONE', #60566, #12390, #24559 ) ;
#32759 = CARTESIAN_POINT ( 'NONE',  ( 2.307692307692309264, -12.37446782046654192, 30.86335684631486131 ) ) ;
#32760 = CARTESIAN_POINT ( 'NONE',  ( 11.60371710973756443, -9.442884908240273489, 34.35708131394835618 ) ) ;
#32761 = EDGE_LOOP ( 'NONE', ( #4228, #26594, #18704, #83008 ) ) ;
#32762 = B_SPLINE_CURVE_WITH_KNOTS ( 'NONE', 3,
 ( #74660, #7075, #321, #6633, #28225, #55694, #54816, #12947, #75974, #83186 ),
 .UNSPECIFIED., .F., .F.,
 ( 4, 2, 2, 2, 4 ),
 ( 0.000000000000000000, 0.0001954311584214072923, 0.0003908623168428145846, 0.0005862934752642218498, 0.0007817246336856291692 ),
 .UNSPECIFIED. ) ;
#32763 = CYLINDRICAL_SURFACE ( 'NONE', #47779, 0.2499999999999986955 ) ;
#32764 = B_SPLINE_CURVE_WITH_KNOTS ( 'NONE', 3,
 ( #36168, #28971, #83468, #78022, #49227, #49665, #35264, #77141, #83915, #71252 ),
 .UNSPECIFIED., .F., .F.,
 ( 4, 2, 2, 2, 4 ),
 ( 0.0007817246256747453293, 0.0009771112852218889842, 0.001172497944769032531, 0.001367884604316176294, 0.001563271263863319840 ),
 .UNSPECIFIED. ) ;
#32765 = CARTESIAN_POINT ( 'NONE',  ( 8.769230769230768274, -3.322132147404559976, 32.92929555188717927 ) ) ;
#32766 = ORIENTED_EDGE ( 'NONE', *, *, #52737, .F. ) ;
#32767 = ORIENTED_EDGE ( 'NONE', *, *, #73558, .F. ) ;
#32768 = ADVANCED_FACE ( 'NONE', ( #18734 ), #72327, .F. ) ;
#32769 = ORIENTED_EDGE ( 'NONE', *, *, #80843, .F. ) ;
#32770 = CARTESIAN_POINT ( 'NONE',  ( -16.15384615384615330, -3.322132147404559976, 32.92929555188717927 ) ) ;
#32771 = CARTESIAN_POINT ( 'NONE',  ( 14.30769230769218758, -4.481592998941358097, 33.73612834414048933 ) ) ;
#32772 = EDGE_CURVE ( 'NONE', #80449, #33353, #25035, .T. ) ;
#32773 = CARTESIAN_POINT ( 'NONE',  ( -18.00000000000000000, -6.343179335718452272, 34.87096338111211935 ) ) ;
#32774 = AXIS2_PLACEMENT_3D ( 'NONE', #40061, #74276, #12576 ) ;
#32775 = CARTESIAN_POINT ( 'NONE',  ( 15.93036121012220541, -5.113361153441931428, 34.14387501736621999 ) ) ;
#32776 = ORIENTED_EDGE ( 'NONE', *, *, #49260, .F. ) ;
#32777 = ADVANCED_FACE ( 'NONE', ( #17844 ), #45295, .F. ) ;
#32778 = ORIENTED_EDGE ( 'NONE', *, *, #18388, .T. ) ;
#32779 = VECTOR ( 'NONE', #7845, 1000.000000000000000 ) ;
#32780 = ORIENTED_EDGE ( 'NONE', *, *, #39256, .T. ) ;
#32782 = VERTEX_POINT ( 'NONE', #11979 ) ;
#32781 = CARTESIAN_POINT ( 'NONE',  ( -2.980769230769226841, -2.499999999999999556, 29.81604066197450109 ) ) ;
#32783 = LINE ( 'NONE', #12516, #20035 ) ;
#32784 = EDGE_CURVE ( 'NONE', #6435, #12084, #52937, .T. ) ;
#32785 = CARTESIAN_POINT ( 'NONE',  ( -6.923076923077045919, -12.51329471203414379, 31.30864560766407578 ) ) ;
#32786 = B_SPLINE_CURVE_WITH_KNOTS ( 'NONE', 3,
 ( #17245, #85715, #46053, #25787, #18590, #59564, #67664, #5069, #31655, #38861 ),
 .UNSPECIFIED., .F., .F.,
 ( 4, 2, 2, 2, 4 ),
 ( 0.0007817359430256293554, 0.0009771253907249974075, 0.001172514838424365460, 0.001367904286123733512, 0.001563293733823094625 ),
 .UNSPECIFIED. ) ;
#32787 = EDGE_CURVE ( 'NONE', #19289, #23594, #23781, .T. ) ;
#32788 = B_SPLINE_CURVE_WITH_KNOTS ( 'NONE', 3,
 ( #18762, #80012, #3454, #59739, #24620, #3893, #51621, #66945, #72800, #32704 ),
 .UNSPECIFIED., .F., .F.,
 ( 4, 2, 2, 2, 4 ),
 ( 0.000000000000000000, 0.0001954311564186870913, 0.0003908623128373741825, 0.0005862934692560613009, 0.0007817246256747483650 ),
 .UNSPECIFIED. ) ;
#32789 = CARTESIAN_POINT ( 'NONE',  ( 7.053867364043873600, -4.684288915650984819, 34.18129842949671371 ) ) ;
#32790 = LINE ( 'NONE', #88648, #78396 ) ;
#32791 = VERTEX_POINT ( 'NONE', #32676 ) ;
#32792 = B_SPLINE_CURVE_WITH_KNOTS ( 'NONE', 3,
 ( #83477, #64065, #605, #1048, #42044, #29852, #49674, #77150, #43363, #70845 ),
 .UNSPECIFIED., .F., .F.,
 ( 4, 2, 2, 2, 4 ),
 ( 0.0007817359430256390048, 0.0009771253907250075990, 0.001172514838424376085, 0.001367904286123744571, 0.001563293733823113056 ),
 .UNSPECIFIED. ) ;
#32793 = ORIENTED_EDGE ( 'NONE', *, *, #70440, .F. ) ;
#32794 = EDGE_CURVE ( 'NONE', #63168, #42657, #65116, .T. ) ;
#32795 = ORIENTED_EDGE ( 'NONE', *, *, #59685, .T. ) ;
#32796 = CARTESIAN_POINT ( 'NONE',  ( 14.55774672760575861, -10.82426656108012075, 33.81400080652039009 ) ) ;
#32798 = VERTEX_POINT ( 'NONE', #79546 ) ;
#32797 = CARTESIAN_POINT ( 'NONE',  ( -13.13461538461538325, -2.249999999999998668, 29.75000000000000355 ) ) ;
#32799 = CARTESIAN_POINT ( 'NONE',  ( 18.13079044096694759, -11.93129842949672437, 32.56571108434900452 ) ) ;
#32800 = B_SPLINE_CURVE_WITH_KNOTS ( 'NONE', 3,
 ( #69611, #6588, #27299, #34934, #54763, #76824, #7917, #41263, #62396, #41701 ),
 .UNSPECIFIED., .F., .F.,
 ( 4, 2, 2, 2, 4 ),
 ( 0.0007817359527651104954, 0.0009771254036996493593, 0.001172514854634188223, 0.001367904305568727087, 0.001563293756503265951 ),
 .UNSPECIFIED. ) ;
#32801 = CIRCLE ( 'NONE', #83154, 4.000000000000000000 ) ;
#32802 = CARTESIAN_POINT ( 'NONE',  ( 12.21151522424549718, -11.37209801155882793, 32.91403422569033665 ) ) ;
#32803 = DIRECTION ( 'NONE',  ( 0.000000000000000000, 0.3420201433256641055, -0.9396926207859100932 ) ) ;
#32804 = CARTESIAN_POINT ( 'NONE',  ( -13.44986637477662761, -2.506253911140460922, 30.00000000000013856 ) ) ;
#32805 = CARTESIAN_POINT ( 'NONE',  ( 8.834486340506792601, -6.026961402152789304, 34.52809138561124769 ) ) ;
#32806 = VECTOR ( 'NONE', #36584, 1000.000000000000114 ) ;
#32807 = FACE_BOUND ( 'NONE', #19947, .T. ) ;
#32808 = CARTESIAN_POINT ( 'NONE',  ( -8.546217925137375104, -2.308499170217967134, 30.53291367094873721 ) ) ;
#32809 = DIRECTION ( 'NONE',  ( 0.000000000000000000, 0.000000000000000000, 1.000000000000000000 ) ) ;
#32810 = DIRECTION ( 'NONE',  ( -0.000000000000000000, -0.6427876096865404731, -0.7660444431189770143 ) ) ;
#32812 = CARTESIAN_POINT ( 'NONE',  ( -5.076923076923075762, -3.050289026998446396, 32.03036669348365706 ) ) ;
#32811 = FACE_OUTER_BOUND ( 'NONE', #51345, .T. ) ;
#32813 = CARTESIAN_POINT ( 'NONE',  ( -5.076923076923197442, -10.90142922262034020, 33.41473453929536674 ) ) ;
#32814 = CARTESIAN_POINT ( 'NONE',  ( -4.088591014333314178, -11.67786785259547777, 32.92929555188713664 ) ) ;
#32815 = ORIENTED_EDGE ( 'NONE', *, *, #23600, .F. ) ;
#32816 = AXIS2_PLACEMENT_3D ( 'NONE', #22902, #86409, #16584 ) ;
#32817 = CARTESIAN_POINT ( 'NONE',  ( -6.923076923076922462, -13.37000171582298513, 34.34916445242398453 ) ) ;
#32818 = CARTESIAN_POINT ( 'NONE',  ( -13.51476335434707821, -9.504002272028875709, 34.60269587691767867 ) ) ;
#32819 = ORIENTED_EDGE ( 'NONE', *, *, #60581, .F. ) ;
#32820 = EDGE_CURVE ( 'NONE', #67660, #28595, #56026, .T. ) ;
#32821 = VERTEX_POINT ( 'NONE', #85853 ) ;
#32822 = FACE_OUTER_BOUND ( 'NONE', #19552, .T. ) ;
#32823 = CARTESIAN_POINT ( 'NONE',  ( 16.15384615384615330, -2.292212530054420494, 30.41441678777542634 ) ) ;
#32824 = DIRECTION ( 'NONE',  ( -1.000000000000000000, -0.000000000000000000, -0.000000000000000000 ) ) ;
#32825 = VERTEX_POINT ( 'NONE', #30891 ) ;
#32826 = CARTESIAN_POINT ( 'NONE',  ( -19.50000000000000000, -3.499999999999999556, 29.75000000000000355 ) ) ;
#32827 = CARTESIAN_POINT ( 'NONE',  ( -6.989160334032804123, -9.780366693483667717, 34.19971097300155805 ) ) ;
#32829 = DIRECTION ( 'NONE',  ( -0.000000000000000000, -0.000000000000000000, -1.000000000000000000 ) ) ;
#32828 = CARTESIAN_POINT ( 'NONE',  ( -15.48074596171158213, -5.728515186090277211, 34.42611988154120439 ) ) ;
#32830 = CARTESIAN_POINT ( 'NONE',  ( -13.60810030917971858, -2.353723527008296568, 30.78948104536958752 ) ) ;
#32831 = CARTESIAN_POINT ( 'NONE',  ( -5.326946314216043810, -9.271318131107980420, 34.42618302367067429 ) ) ;
#32833 = FACE_OUTER_BOUND ( 'NONE', #8639, .T. ) ;
#32832 = B_SPLINE_CURVE_WITH_KNOTS ( 'NONE', 3,
 ( #71970, #18368, #31886, #65205, #86852, #30974, #78731, #58439, #18812, #79623 ),
 .UNSPECIFIED., .F., .F.,
 ( 4, 2, 2, 2, 4 ),
 ( 0.0007817246256747464135, 0.0009771112852218900684, 0.001172497944769033615, 0.001367884604316177161, 0.001563271263863320925 ),
 .UNSPECIFIED. ) ;
#32834 = CARTESIAN_POINT ( 'NONE',  ( -2.651650429449535551, -10.15165042944956753, 19.93750000000000000 ) ) ;
#32835 = ORIENTED_EDGE ( 'NONE', *, *, #32880, .T. ) ;
#32836 = ORIENTED_EDGE ( 'NONE', *, *, #18608, .T. ) ;
#32837 =( BOUNDED_CURVE ( )  B_SPLINE_CURVE ( 2, ( #71178, #77498, #36946, #83833, #70749, #1842, #21222, #63086, #36524, #56779, #956, #7725, #35185, #49140, #28428, #21672, #69860, #22116, #15812, #63971, #35638, #64409, #63535, #84279, #42837, #70302, #22556, #2267, #57229, #84722, #58107, #50888, #25220, #32421, #80172, #51777, #4956, #85589, #66198, #52682, #31075, #79280, #10377, #18471, #45925, #59447, #86039, #71617, #37387, #44580, #37840, #23865, #73414, #72066, #78376, #58996, #4504, #72962, #16680, #11718, #39193, #38292, #4043, #65747, #3158, #17582, #44136, #66654, #3606, #11263, #51320, #64856, #38736, #85150, #9923, #78823, #23433, #45032, #31982, #58542, #24316, #86952, #30635, #17123, #31533, #65308, #72510, #10821, #86497, #24771, #52236, #79726, #18026, #45483, #20244, #33318, #46382, #54014, #60330, #87843, #60776, #47706, #40525, #68862, #12600, #81953, #6291, #12159, #80628, #7169, #26109, #18910, #73863, #5842, #19353, #39641, #26560, #81508, #13480, #88285, #59889, #67991, #67543, #75192, #61211, #46821, #40088, #33754, #87385, #68421, #74299, #19796, #47259, #74751, #61655, #53123, #67101, #25667, #40956, #5402, #89161, #32868, #53574, #13040, #88721, #81069, #26999, #54457, #6719, #34191, #27441, #54909, #82392, #20678, #48142, #75612, #13918, #41400, #35975, #43601, #7614 ),
 .UNSPECIFIED., .F., .F. ) 
 B_SPLINE_CURVE_WITH_KNOTS ( ( 3, 2, 2, 2, 2, 2, 2, 2, 2, 2, 2, 2, 2, 2, 2, 2, 2, 2, 2, 2, 2, 2, 2, 2, 2, 2, 2, 2, 2, 2, 2, 2, 2, 2, 2, 2, 2, 2, 2, 2, 2, 2, 2, 2, 2, 2, 2, 2, 2, 2, 2, 2, 2, 2, 2, 2, 2, 2, 2, 2, 2, 2, 2, 2, 2, 2, 2, 2, 2, 2, 2, 2, 2, 2, 2, 2, 2, 2, 2, 2, 3 ),
 ( 0.000000000000000000, 0.01250000000000000069, 0.02500000000000000139, 0.03749999999999999861, 0.05000000000000000278, 0.06250000000000000000, 0.07499999999999999722, 0.08749999999999999445, 0.1000000000000000056, 0.1125000000000000028, 0.1250000000000000000, 0.1375000000000000111, 0.1499999999999999944, 0.1625000000000000056, 0.1749999999999999889, 0.1875000000000000000, 0.2000000000000000111, 0.2124999999999999944, 0.2250000000000000056, 0.2374999999999999889, 0.2500000000000000000, 0.2625000000000000111, 0.2750000000000000222, 0.2874999999999999778, 0.2999999999999999889, 0.3125000000000000000, 0.3250000000000000111, 0.3375000000000000222, 0.3499999999999999778, 0.3624999999999999889, 0.3750000000000000000, 0.3875000000000000111, 0.4000000000000000222, 0.4124999999999999778, 0.4249999999999999889, 0.4375000000000000000, 0.4500000000000000111, 0.4625000000000000222, 0.4749999999999999778, 0.4874999999999999889, 0.5000000000000000000, 0.5124999999999999556, 0.5250000000000000222, 0.5374999999999999778, 0.5500000000000000444, 0.5625000000000000000, 0.5749999999999999556, 0.5875000000000000222, 0.5999999999999999778, 0.6125000000000000444, 0.6250000000000000000, 0.6374999999999999556, 0.6500000000000000222, 0.6624999999999999778, 0.6750000000000000444, 0.6875000000000000000, 0.6999999999999999556, 0.7125000000000000222, 0.7249999999999999778, 0.7375000000000000444, 0.7500000000000000000, 0.7624999999999999556, 0.7750000000000000222, 0.7874999999999999778, 0.8000000000000000444, 0.8125000000000000000, 0.8249999999999999556, 0.8375000000000000222, 0.8499999999999999778, 0.8625000000000000444, 0.8750000000000000000, 0.8874999999999999556, 0.9000000000000000222, 0.9124999999999999778, 0.9250000000000000444, 0.9375000000000000000, 0.9499999999999999556, 0.9625000000000000222, 0.9749999999999999778, 0.9875000000000000444, 1.000000000000000000 ),
 .UNSPECIFIED. ) 
 CURVE ( )  GEOMETRIC_REPRESENTATION_ITEM ( )  RATIONAL_B_SPLINE_CURVE ( ( 1.000000000000000000, 0.9238795325112867385, 1.000000000000000000, 0.9238795325112867385, 1.000000000000000000, 0.9238795325112867385, 1.000000000000000000, 0.9238795325112867385, 1.000000000000000000, 0.9238795325112867385, 1.000000000000000000, 0.9238795325112867385, 1.000000000000000000, 0.9238795325112867385, 1.000000000000000000, 0.9238795325112867385, 1.000000000000000000, 0.9238795325112867385, 1.000000000000000000, 0.9238795325112867385, 1.000000000000000000, 0.9238795325112867385, 1.000000000000000000, 0.9238795325112867385, 1.000000000000000000, 0.9238795325112867385, 1.000000000000000000, 0.9238795325112867385, 1.000000000000000000, 0.9238795325112867385, 1.000000000000000000, 0.9238795325112867385, 1.000000000000000000, 0.9238795325112867385, 1.000000000000000000, 0.9238795325112867385, 1.000000000000000000, 0.9238795325112867385, 1.000000000000000000, 0.9238795325112867385, 1.000000000000000000, 0.9238795325112867385, 1.000000000000000000, 0.9238795325112867385, 1.000000000000000000, 0.9238795325112867385, 1.000000000000000000, 0.9238795325112867385, 1.000000000000000000, 0.9238795325112867385, 1.000000000000000000, 0.9238795325112867385, 1.000000000000000000, 0.9238795325112867385, 1.000000000000000000, 0.9238795325112867385, 1.000000000000000000, 0.9238795325112867385, 1.000000000000000000, 0.9238795325112867385, 1.000000000000000000, 0.9238795325112867385, 1.000000000000000000, 0.9238795325112867385, 1.000000000000000000, 0.9238795325112867385, 1.000000000000000000, 0.9238795325112867385, 1.000000000000000000, 0.9238795325112867385, 1.000000000000000000, 0.9238795325112867385, 1.000000000000000000, 0.9238795325112867385, 1.000000000000000000, 0.9238795325112867385, 1.000000000000000000, 0.9238795325112867385, 1.000000000000000000, 0.9238795325112867385, 1.000000000000000000, 0.9238795325112867385, 1.000000000000000000, 0.9238795325112867385, 1.000000000000000000, 0.9238795325112867385, 1.000000000000000000, 0.9238795325112867385, 1.000000000000000000, 0.9238795325112867385, 1.000000000000000000, 0.9238795325112867385, 1.000000000000000000, 0.9238795325112867385, 1.000000000000000000, 0.9238795325112867385, 1.000000000000000000, 0.9238795325112867385, 1.000000000000000000, 0.9238795325112867385, 1.000000000000000000, 0.9238795325112867385, 1.000000000000000000, 0.9238795325112867385, 1.000000000000000000, 0.9238795325112867385, 1.000000000000000000, 0.9238795325112867385, 1.000000000000000000, 0.9238795325112867385, 1.000000000000000000, 0.9238795325112867385, 1.000000000000000000, 0.9238795325112867385, 1.000000000000000000, 0.9238795325112867385, 1.000000000000000000, 0.9238795325112867385, 1.000000000000000000, 0.9238795325112867385, 1.000000000000000000, 0.9238795325112867385, 1.000000000000000000, 0.9238795325112867385, 1.000000000000000000, 0.9238795325112867385, 1.000000000000000000, 0.9238795325112867385, 1.000000000000000000, 0.9238795325112867385, 1.000000000000000000, 0.9238795325112867385, 1.000000000000000000, 0.9238795325112867385, 1.000000000000000000, 0.9238795325112867385, 1.000000000000000000, 0.9238795325112867385, 1.000000000000000000, 0.9238795325112867385, 1.000000000000000000, 0.9238795325112867385, 1.000000000000000000, 0.9238795325112867385, 1.000000000000000000, 0.9238795325112867385, 1.000000000000000000, 0.9238795325112867385, 1.000000000000000000, 0.9238795325112867385, 1.000000000000000000, 0.9238795325112867385, 1.000000000000000000, 0.9238795325112867385, 1.000000000000000000, 0.9238795325112867385, 1.000000000000000000, 0.9238795325112867385, 1.000000000000000000, 0.9238795325112867385, 1.000000000000000000 ) ) 
 REPRESENTATION_ITEM ( '' )  );
#32838 = VECTOR ( 'NONE', #53869, 1000.000000000000114 ) ;
#32839 = LINE ( 'NONE', #47679, #44930 ) ;
#32840 = CARTESIAN_POINT ( 'NONE',  ( 6.000000000000001776, -13.53365097954675988, 30.81389545987213552 ) ) ;
#32841 = DIRECTION ( 'NONE',  ( 0.000000000000000000, 0.000000000000000000, -1.000000000000000000 ) ) ;
#32842 = CARTESIAN_POINT ( 'NONE',  ( 6.792385456409363087, -12.11776431015576172, 31.66791131148498906 ) ) ;
#32843 = CARTESIAN_POINT ( 'NONE',  ( -3.230769230769351186, -6.026961402154118908, 34.52809138561165270 ) ) ;
#32844 = CARTESIAN_POINT ( 'NONE',  ( 3.750000000000009770, -9.053300858899081760, 23.29687500000000000 ) ) ;
#32845 = CARTESIAN_POINT ( 'NONE',  ( -7.596208327805704208, -8.433404298154334455, 34.66254593164985920 ) ) ;
#32846 = CARTESIAN_POINT ( 'NONE',  ( -13.45069879557126136, -8.120952969808774569, 34.71129190930000163 ) ) ;
#32847 = CARTESIAN_POINT ( 'NONE',  ( -13.16165248105389907, -7.369474270740069777, 34.74850911626239736 ) ) ;
#32848 = CARTESIAN_POINT ( 'NONE',  ( 12.39545608217832218, -11.35647404775217595, 33.31231777344666511 ) ) ;
#32849 = DIRECTION ( 'NONE',  ( -1.000000000000000000, -0.000000000000000000, -0.000000000000000000 ) ) ;
#32850 = DIRECTION ( 'NONE',  ( 0.000000000000000000, 0.3420201433256610524, 0.9396926207859113145 ) ) ;
#32851 = LINE ( 'NONE', #61643, #61036 ) ;
#32852 = CARTESIAN_POINT ( 'NONE',  ( 4.153846153846032507, -12.46129190930018460, 30.37095296980731973 ) ) ;
#32853 = CARTESIAN_POINT ( 'NONE',  ( 12.46153846153846168, -1.790695186598648903, 34.54067556320373455 ) ) ;
#32854 = VECTOR ( 'NONE', #57903, 1000.000000000000000 ) ;
#32855 = CARTESIAN_POINT ( 'NONE',  ( -15.45425417449318317, -10.11188796281391511, 34.01382737946119050 ) ) ;
#32856 = VERTEX_POINT ( 'NONE', #58812 ) ;
#32857 = DIRECTION ( 'NONE',  ( -0.000000000000000000, -0.7660444431189791237, -0.6427876096865379196 ) ) ;
#32858 = CARTESIAN_POINT ( 'NONE',  ( -17.07692307692319744, -6.835583212225970762, 34.95778746994575670 ) ) ;
#32859 = DIRECTION ( 'NONE',  ( -0.000000000000000000, -0.9396926207859092051, -0.3420201433256662704 ) ) ;
#32860 = CARTESIAN_POINT ( 'NONE',  ( 1.901340078031373171, -9.487747218494639867, 14.87686829374151465 ) ) ;
#32861 = ADVANCED_FACE ( 'NONE', ( #58358 ), #24137, .F. ) ;
#32862 = B_SPLINE_CURVE_WITH_KNOTS ( 'NONE', 3,
 ( #77580, #49660, #78018, #8689, #23078, #64480, #15888, #16320, #2783, #30279 ),
 .UNSPECIFIED., .F., .F.,
 ( 4, 2, 2, 2, 4 ),
 ( 0.000000000000000000, 0.0001954339857564083688, 0.0003908679715128167377, 0.0005863019572692250523, 0.0007817359430256334753 ),
 .UNSPECIFIED. ) ;
#32863 = CARTESIAN_POINT ( 'NONE',  ( 5.326977496836529546, -10.06805714834173848, 34.32951233291982618 ) ) ;
#32864 = DIRECTION ( 'NONE',  ( -1.000000000000000000, 0.000000000000000000, 0.000000000000000000 ) ) ;
#32865 = FACE_OUTER_BOUND ( 'NONE', #42195, .T. ) ;
#32867 = VERTEX_POINT ( 'NONE', #24588 ) ;
#32866 = CARTESIAN_POINT ( 'NONE',  ( 6.000000000000001776, -3.886160181151819604, 36.00935417666054406 ) ) ;
#32868 = CARTESIAN_POINT ( 'NONE',  ( -2.749999999999991562, -8.639087296526026805, 25.01562500000000000 ) ) ;
#32869 = CARTESIAN_POINT ( 'NONE',  ( -14.43784027742400333, -5.915902021225889484, 34.75552854090298638 ) ) ;
#32870 = EDGE_CURVE ( 'NONE', #33781, #87066, #43096, .T. ) ;
#32871 = VERTEX_POINT ( 'NONE', #59707 ) ;
#32872 = CARTESIAN_POINT ( 'NONE',  ( -17.74994568836168085, -3.627508038966687831, 32.91356715214246265 ) ) ;
#32873 = ADVANCED_FACE ( 'NONE', ( #87204 ), #46199, .F. ) ;
#32874 = EDGE_LOOP ( 'NONE', ( #58531, #556 ) ) ;
#32875 = DIRECTION ( 'NONE',  ( -0.000000000000000000, -0.1736481776669307198, -0.9848077530122080203 ) ) ;
#32876 = CARTESIAN_POINT ( 'NONE',  ( -9.442253380669376028, -2.779044189368095275, 31.39831045268885745 ) ) ;
#32877 = FACE_OUTER_BOUND ( 'NONE', #70144, .T. ) ;
#32878 = ORIENTED_EDGE ( 'NONE', *, *, #50008, .T. ) ;
#32879 = ORIENTED_EDGE ( 'NONE', *, *, #47564, .T. ) ;
#32880 = EDGE_CURVE ( 'NONE', #75011, #16582, #3384, .T. ) ;
#32881 = AXIS2_PLACEMENT_3D ( 'NONE', #10670, #72802, #57962 ) ;
#32882 = VERTEX_POINT ( 'NONE', #75010 ) ;
#32883 = CARTESIAN_POINT ( 'NONE',  ( 0.4615384615384611200, -1.629998284177014645, 34.34916445242399163 ) ) ;
#32884 = CARTESIAN_POINT ( 'NONE',  ( 12.33084699487090319, -12.38065189839062263, 30.83690757178629482 ) ) ;
#32885 = CARTESIAN_POINT ( 'NONE',  ( 18.24994540937804643, -10.18230066228895758, 34.26354781536631577 ) ) ;
#32886 = CARTESIAN_POINT ( 'NONE',  ( -1.449885385171704177, -11.67786785259541027, 32.92929555188721480 ) ) ;
#32887 = FACE_OUTER_BOUND ( 'NONE', #48949, .T. ) ;
#32888 = CARTESIAN_POINT ( 'NONE',  ( 1.384615384615265343, -10.90142922262034020, 33.41473453929536674 ) ) ;
#32889 = LINE ( 'NONE', #60353, #43806 ) ;
#32890 = CARTESIAN_POINT ( 'NONE',  ( 10.48523740594639087, -12.27039167877662251, 31.24851455888617835 ) ) ;
#32891 = ORIENTED_EDGE ( 'NONE', *, *, #72180, .T. ) ;
#32892 = ORIENTED_EDGE ( 'NONE', *, *, #47586, .T. ) ;
#32893 = VERTEX_POINT ( 'NONE', #6547 ) ;
#32895 = EDGE_LOOP ( 'NONE', ( #48509, #42771, #31172, #23570 ) ) ;
#32894 = CARTESIAN_POINT ( 'NONE',  ( -4.153846153846152411, -8.164416787775445883, 34.95778746994557906 ) ) ;
#32896 = ADVANCED_FACE ( 'NONE', ( #27693 ), #7436, .F. ) ;
#32897 = AXIS2_PLACEMENT_3D ( 'NONE', #50873, #71161, #9468 ) ;
#32898 = DIRECTION ( 'NONE',  ( -0.000000000000000000, 0.9848077530122085754, -0.1736481776669273613 ) ) ;
#32899 = CARTESIAN_POINT ( 'NONE',  ( 12.71148397988660150, -3.202959910592335646, 32.30730279482227019 ) ) ;
#32900 = ORIENTED_EDGE ( 'NONE', *, *, #54747, .F. ) ;
#32901 = CARTESIAN_POINT ( 'NONE',  ( 17.07692307692307665, -13.04860791097971706, 34.73218667398347037 ) ) ;
#32902 = VECTOR ( 'NONE', #7531, 1000.000000000000227 ) ;
#32903 = EDGE_CURVE ( 'NONE', #51992, #5606, #38799, .T. ) ;
#32904 = VERTEX_POINT ( 'NONE', #67359 ) ;
#32905 = DIRECTION ( 'NONE',  ( -0.000000000000000000, 0.7660444431189791237, -0.6427876096865379196 ) ) ;
#32906 = VERTEX_POINT ( 'NONE', #47961 ) ;
#32907 = VECTOR ( 'NONE', #64834, 1000.000000000000000 ) ;
#32908 = CARTESIAN_POINT ( 'NONE',  ( -16.81410256410256565, -7.500000000000000000, 33.75000000000000000 ) ) ;
#32909 = ADVANCED_FACE ( 'NONE', ( #60144 ), #12852, .F. ) ;
#32910 = VECTOR ( 'NONE', #82235, 1000.000000000000000 ) ;
#32911 = EDGE_CURVE ( 'NONE', #6496, #28389, #14182, .T. ) ;
#32912 = CARTESIAN_POINT ( 'NONE',  ( -16.21992956480203318, -6.386643153685125363, 34.62446782046654903 ) ) ;
#32913 = CARTESIAN_POINT ( 'NONE',  ( -11.31568186948347154, -12.11081565061824250, 32.26097654155340422 ) ) ;
#32914 = FACE_BOUND ( 'NONE', #46144, .T. ) ;
#32915 = DIRECTION ( 'NONE',  ( -0.000000000000000000, 0.3420201433256694901, -0.9396926207859082059 ) ) ;
#32916 = DIRECTION ( 'NONE',  ( -0.000000000000000000, 0.1736481776669307198, -0.9848077530122080203 ) ) ;
#32917 = CARTESIAN_POINT ( 'NONE',  ( 13.45068271796546178, -4.661471528628508665, 34.16647553114624003 ) ) ;
#32918 = CARTESIAN_POINT ( 'NONE',  ( 3.296024370282069516, -5.094484230520773593, 34.41647553114626845 ) ) ;
#32919 = LINE ( 'NONE', #88772, #3534 ) ;
#32920 = CARTESIAN_POINT ( 'NONE',  ( -4.376772371362299019, -11.24512374952581872, 33.06303171183252942 ) ) ;
#32921 = ORIENTED_EDGE ( 'NONE', *, *, #2006, .T. ) ;
#32922 = CARTESIAN_POINT ( 'NONE',  ( -6.988347369037697376, -6.879047030191174805, 34.71129190930000163 ) ) ;
#32923 = ORIENTED_EDGE ( 'NONE', *, *, #11082, .F. ) ;
#32924 = EDGE_CURVE ( 'NONE', #22118, #67341, #74117, .T. ) ;
#32925 = ORIENTED_EDGE ( 'NONE', *, *, #34052, .T. ) ;
#32926 = B_SPLINE_CURVE_WITH_KNOTS ( 'NONE', 3,
 ( #26918, #54379, #47630, #75113, #13395, #40880, #61577, #89084, #27356, #82312 ),
 .UNSPECIFIED., .F., .F.,
 ( 4, 2, 2, 2, 4 ),
 ( 0.000000000000000000, 0.0001954311564186862510, 0.0003908623128373725020, 0.0005862934692560588072, 0.0007817246256747450040 ),
 .UNSPECIFIED. ) ;
#32928 = CARTESIAN_POINT ( 'NONE',  ( 23.49999999999998579, 8.999999999999996447, 30.36437827766148345 ) ) ;
#32927 = LINE ( 'NONE', #13979, #80622 ) ;
#32929 = CARTESIAN_POINT ( 'NONE',  ( -6.923076923077045919, -11.67786785259630911, 32.92929555188603530 ) ) ;
#32931 = B_SPLINE_CURVE_WITH_KNOTS ( 'NONE', 3,
 ( #87188, #25466, #80420, #19155, #18721, #46623, #12396, #39880, #19592, #47054 ),
 .UNSPECIFIED., .F., .F.,
 ( 4, 2, 2, 2, 4 ),
 ( 0.0007817246256747474977, 0.0009771112852218911526, 0.001172497944769034699, 0.001367884604316178462, 0.001563271263863322009 ),
 .UNSPECIFIED. ) ;
#32930 = CARTESIAN_POINT ( 'NONE',  ( -14.30769230769230660, -2.292212530054420494, 30.41441678777542634 ) ) ;
#32932 = EDGE_CURVE ( 'NONE', #40761, #69679, #72123, .T. ) ;
#32933 = CARTESIAN_POINT ( 'NONE',  ( 1.384615384615264011, -11.06231777344772027, 33.60647404775119895 ) ) ;
#32934 = CARTESIAN_POINT ( 'NONE',  ( -13.16160403300253812, -2.758310577978207778, 31.33698337089302299 ) ) ;
#32935 = EDGE_CURVE ( 'NONE', #61593, #44583, #78508, .T. ) ;
#32936 = ORIENTED_EDGE ( 'NONE', *, *, #7468, .F. ) ;
#32937 = CARTESIAN_POINT ( 'NONE',  ( -5.999999999999998224, -8.164416787775445883, 34.95778746994557906 ) ) ;
#32938 = FACE_OUTER_BOUND ( 'NONE', #77732, .T. ) ;
#32939 = CARTESIAN_POINT ( 'NONE',  ( 10.36540788444226102, -3.137211980971221781, 32.19342716148376837 ) ) ;
#32940 = CARTESIAN_POINT ( 'NONE',  ( -14.30769230769230660, -1.422936976036506707, 30.56769352161908415 ) ) ;
#32941 = VERTEX_POINT ( 'NONE', #81326 ) ;
#32942 = ADVANCED_FACE ( 'NONE', ( #21381 ), #28592, .F. ) ;
#32943 = ORIENTED_EDGE ( 'NONE', *, *, #44423, .F. ) ;
#32944 = CONTEXT_DEPENDENT_SHAPE_REPRESENTATION ( #17617, #52083 ) ;
#32945 = ORIENTED_EDGE ( 'NONE', *, *, #66768, .T. ) ;
#32946 = CARTESIAN_POINT ( 'NONE',  ( 0.5276068125408981402, -10.51840700105979565, 33.73612834413962247 ) ) ;
#32947 = LINE ( 'NONE', #41816, #34699 ) ;
#32948 = ORIENTED_EDGE ( 'NONE', *, *, #53979, .F. ) ;
#32949 = FACE_OUTER_BOUND ( 'NONE', #76465, .T. ) ;
#32950 = CARTESIAN_POINT ( 'NONE',  ( 6.923076923076924238, -2.249999999999998668, 29.75000000000001776 ) ) ;
#32951 = CARTESIAN_POINT ( 'NONE',  ( 3.296024370282069516, -10.33852847137154107, 34.16647553114620450 ) ) ;
#32952 = CARTESIAN_POINT ( 'NONE',  ( -2.557715544985270650, -8.432397168068783699, 34.66272746175022945 ) ) ;
#32953 = LINE ( 'NONE', #52766, #1430 ) ;
#32954 = ORIENTED_EDGE ( 'NONE', *, *, #43390, .F. ) ;
#32956 = ORIENTED_EDGE ( 'NONE', *, *, #39798, .F. ) ;
#32955 = FACE_OUTER_BOUND ( 'NONE', #51123, .T. ) ;
#32957 = FACE_OUTER_BOUND ( 'NONE', #18052, .T. ) ;
#32958 = CARTESIAN_POINT ( 'NONE',  ( 11.78846153846154010, -7.500000000000001776, 35.04278698407183867 ) ) ;
#32959 = DIRECTION ( 'NONE',  ( -1.000000000000000000, 0.000000000000000000, 0.000000000000000000 ) ) ;
#32960 = CARTESIAN_POINT ( 'NONE',  ( -3.903791842207838148, -12.41262288849542017, 30.68299917996395010 ) ) ;
#32961 = CARTESIAN_POINT ( 'NONE',  ( -3.903791733932700847, -4.818054556918156095, 34.26375889529406749 ) ) ;
#32962 = CARTESIAN_POINT ( 'NONE',  ( -8.638705330997126453, -9.503571793651731880, 34.60286762892837942 ) ) ;
#32963 = DIRECTION ( 'NONE',  ( -0.000000000000000000, -0.7660444431189791237, -0.6427876096865379196 ) ) ;
#32964 = CARTESIAN_POINT ( 'NONE',  ( -0.06109907496451398579, -10.25000000000000178, 21.28311829374151287 ) ) ;
#32965 = VERTEX_POINT ( 'NONE', #28135 ) ;
#32966 = CARTESIAN_POINT ( 'NONE',  ( -7.146003881983769013, -10.77366814457252175, 33.85459836347579454 ) ) ;
#32967 = DIRECTION ( 'NONE',  ( 0.000000000000000000, 0.000000000000000000, 1.000000000000000000 ) ) ;
#32968 = ADVANCED_FACE ( 'NONE', ( #70008 ), #42114, .F. ) ;
#32969 = B_SPLINE_CURVE_WITH_KNOTS ( 'NONE', 3,
 ( #1967, #64530, #31199, #9181, #58671, #16366, #58227, #56898, #79402, #30323 ),
 .UNSPECIFIED., .F., .F.,
 ( 4, 2, 2, 2, 4 ),
 ( 0.000000000000000000, 0.0001954311564186867389, 0.0003908623128373734778, 0.0005862934692560602167, 0.0007817246256747469556 ),
 .UNSPECIFIED. ) ;
#32970 = B_SPLINE_CURVE_WITH_KNOTS ( 'NONE', 3,
 ( #26849, #82241, #27288, #54755, #54306, #60178, #53420, #53874, #80922, #46232 ),
 .UNSPECIFIED., .F., .F.,
 ( 4, 2, 2, 2, 4 ),
 ( 0.000000000000000000, 0.0001954311564186862239, 0.0003908623128373724478, 0.0005862934692560586988, 0.0007817246256747448956 ),
 .UNSPECIFIED. ) ;
#32971 = VECTOR ( 'NONE', #75752, 1000.000000000000227 ) ;
#32972 = VERTEX_POINT ( 'NONE', #1113 ) ;
#32973 = B_SPLINE_CURVE_WITH_KNOTS ( 'NONE', 3,
 ( #65509, #85347, #31289, #23632, #78577, #58756, #70496, #8803, #16879, #63730 ),
 .UNSPECIFIED., .F., .F.,
 ( 4, 2, 2, 2, 4 ),
 ( 0.0007817359430256258859, 0.0009771253907249909023, 0.001172514838424355919, 0.001367904286123720935, 0.001563293733823085951 ),
 .UNSPECIFIED. ) ;
#32974 = ORIENTED_EDGE ( 'NONE', *, *, #17901, .T. ) ;
#32975 = CARTESIAN_POINT ( 'NONE',  ( 2.241938879378976068, -7.249945578846654470, 34.99404164642496795 ) ) ;
#32976 = CARTESIAN_POINT ( 'NONE',  ( -12.46153846153858247, -3.300289026999228881, 32.46337939537708905 ) ) ;
#32977 = CARTESIAN_POINT ( 'NONE',  ( -9.019253993452228002, -10.92453946501458795, 33.72985991061850086 ) ) ;
#32978 = CARTESIAN_POINT ( 'NONE',  ( 6.988332494352946789, -6.026961402152789304, 34.52809138561124769 ) ) ;
#32979 = EDGE_CURVE ( 'NONE', #2085, #47848, #15518, .T. ) ;
#32980 = DIRECTION ( 'NONE',  ( -0.000000000000000000, -0.6427876096865404731, -0.7660444431189771253 ) ) ;
#32981 = VERTEX_POINT ( 'NONE', #14629 ) ;
#32982 = B_SPLINE_CURVE_WITH_KNOTS ( 'NONE', 3,
 ( #35635, #55016, #75289, #27094, #82051, #20349, #47809, #68519, #6818, #70 ),
 .UNSPECIFIED., .F., .F.,
 ( 4, 2, 2, 2, 4 ),
 ( 0.0007817246256747451124, 0.0009771112852218885505, 0.001172497944769032097, 0.001367884604316175427, 0.001563271263863318973 ),
 .UNSPECIFIED. ) ;
#32983 = CARTESIAN_POINT ( 'NONE',  ( -3.230769230769229949, -12.62096338111211580, 30.90682066428153263 ) ) ;
#32984 = CARTESIAN_POINT ( 'NONE',  ( 15.23076923076923173, -3.886160181151819604, 36.00935417666054406 ) ) ;
#32985 = CARTESIAN_POINT ( 'NONE',  ( 9.626225312947559232, -2.486705287966279432, 31.30864560766542937 ) ) ;
#32986 = EDGE_LOOP ( 'NONE', ( #88926, #67700, #18965, #40185 ) ) ;
#32987 = CARTESIAN_POINT ( 'NONE',  ( 13.44987095589141468, -6.879047030191282275, 34.71129190930002295 ) ) ;
#32988 = ORIENTED_EDGE ( 'NONE', *, *, #46940, .F. ) ;
#32989 = CARTESIAN_POINT ( 'NONE',  ( -5.076923076923199218, -3.083524468854526912, 32.58852847137268327 ) ) ;
#32990 = SURFACE_STYLE_USAGE ( .BOTH. , #20368 ) ;
#32991 = LINE ( 'NONE', #27562, #11056 ) ;
#32992 = ORIENTED_EDGE ( 'NONE', *, *, #83040, .F. ) ;
#32993 = CARTESIAN_POINT ( 'NONE',  ( -13.13456096470193302, -4.818054556918156983, 34.26375889529406749 ) ) ;
#32994 = FACE_OUTER_BOUND ( 'NONE', #50248, .T. ) ;
#32995 = FACE_OUTER_BOUND ( 'NONE', #44746, .T. ) ;
#32996 = EDGE_CURVE ( 'NONE', #28226, #43633, #88290, .T. ) ;
#32997 = DIRECTION ( 'NONE',  ( -0.000000000000000000, -0.7660444431189791237, -0.6427876096865379196 ) ) ;
#32998 = CARTESIAN_POINT ( 'NONE',  ( 10.03846153846153832, -3.499999999999999556, 29.75000000000000355 ) ) ;
#32999 = B_SPLINE_CURVE_WITH_KNOTS ( 'NONE', 3,
 ( #46521, #12733, #88414, #74000, #12289, #67242, #33006, #46946, #74434, #40216 ),
 .UNSPECIFIED., .F., .F.,
 ( 4, 2, 2, 2, 4 ),
 ( 0.0007817359430256294638, 0.0009771253907249952391, 0.001172514838424361123, 0.001367904286123726790, 0.001563293733823092673 ),
 .UNSPECIFIED. ) ;
#33000 = EDGE_LOOP ( 'NONE', ( #31144, #78043, #8875, #36868 ) ) ;
#33001 = CARTESIAN_POINT ( 'NONE',  ( -1.384615384615383471, -12.10708131394839349, 31.69288490824020244 ) ) ;
#33002 = ORIENTED_EDGE ( 'NONE', *, *, #31530, .F. ) ;
#33003 = CARTESIAN_POINT ( 'NONE',  ( 5.142178216435913107, -11.67786785259547777, 32.92929555188713664 ) ) ;
#33004 = VECTOR ( 'NONE', #81030, 1000.000000000000227 ) ;
#33005 = LINE ( 'NONE', #87082, #9110 ) ;
#33006 = CARTESIAN_POINT ( 'NONE',  ( 6.223011351612851350, -9.086983370893049639, 34.49168942202179267 ) ) ;
#33007 = EDGE_CURVE ( 'NONE', #6141, #60344, #56054, .T. ) ;
#33008 = CARTESIAN_POINT ( 'NONE',  ( -14.08491276642389245, -12.24180327182772388, 31.33663988360758168 ) ) ;
#33009 = CARTESIAN_POINT ( 'NONE',  ( 12.46153846153846168, -12.78798330534102945, 29.74999999999997868 ) ) ;
#33010 = ADVANCED_FACE ( 'NONE', ( #42549 ), #21827, .T. ) ;
#33011 = VERTEX_POINT ( 'NONE', #22272 ) ;
#33012 = ORIENTED_EDGE ( 'NONE', *, *, #57218, .F. ) ;
#33013 = VERTEX_POINT ( 'NONE', #35796 ) ;
#33014 = VERTEX_POINT ( 'NONE', #70463 ) ;
#33015 = EDGE_CURVE ( 'NONE', #51776, #11880, #50166, .T. ) ;
#33016 = CARTESIAN_POINT ( 'NONE',  ( -5.207071046654771607, -4.299443229763728169, 33.91186481527756058 ) ) ;
#33017 = CARTESIAN_POINT ( 'NONE',  ( -6.065270445960774914, -12.46129190929999986, 30.37095296980880832 ) ) ;
#33018 = CARTESIAN_POINT ( 'NONE',  ( -4.023320452082588261, -9.417988943895561960, 34.36773134775778260 ) ) ;
#33019 = DIRECTION ( 'NONE',  ( 0.000000000000000000, 0.3420201433256610524, 0.9396926207859113145 ) ) ;
#33020 = CARTESIAN_POINT ( 'NONE',  ( 3.903846153846143530, -2.499999999999999556, 29.81609845454692120 ) ) ;
#33021 = VECTOR ( 'NONE', #76230, 1000.000000000000000 ) ;
#33022 = VECTOR ( 'NONE', #50615, 1000.000000000000000 ) ;
#33023 = DIRECTION ( 'NONE',  ( 0.000000000000000000, 1.000000000000000000, 0.000000000000000000 ) ) ;
#33024 = CARTESIAN_POINT ( 'NONE',  ( -2.307692307692305711, -3.513871655860378418, 32.76840700105978499 ) ) ;
#33025 = CARTESIAN_POINT ( 'NONE',  ( 20.00000000000000000, -4.000000000000000000, 28.25000000000000000 ) ) ;
#33026 = ORIENTED_EDGE ( 'NONE', *, *, #32185, .F. ) ;
#33027 = ORIENTED_EDGE ( 'NONE', *, *, #40606, .T. ) ;
#33028 = AXIS2_PLACEMENT_3D ( 'NONE', #53993, #46797, #88257 ) ;
#33029 = EDGE_LOOP ( 'NONE', ( #68092, #77826, #48275, #65016 ) ) ;
#33030 = VECTOR ( 'NONE', #61367, 1000.000000000000000 ) ;
#33032 = ORIENTED_EDGE ( 'NONE', *, *, #32392, .F. ) ;
#33031 = CARTESIAN_POINT ( 'NONE',  ( 2.057669070399344324, -2.587272538249755449, 30.68239716806877837 ) ) ;
#33034 = CARTESIAN_POINT ( 'NONE',  ( -7.596208436775802930, -9.357781135181033605, 34.66075350412533851 ) ) ;
#33033 = CARTESIAN_POINT ( 'NONE',  ( 6.673100179028334189, -11.47974371597207899, 33.17467449705390692 ) ) ;
#33035 = DIRECTION ( 'NONE',  ( -0.000000000000000000, -0.3420201433256694346, -0.9396926207859080948 ) ) ;
#33036 = DIRECTION ( 'NONE',  ( 0.000000000000000000, 0.7660444431189807890, 0.6427876096865361433 ) ) ;
#33037 = EDGE_CURVE ( 'NONE', #9922, #73822, #1557, .T. ) ;
#33038 = FACE_BOUND ( 'NONE', #33130, .T. ) ;
#33039 = ORIENTED_EDGE ( 'NONE', *, *, #87169, .T. ) ;
#33040 = ORIENTED_EDGE ( 'NONE', *, *, #1572, .F. ) ;
#33041 = CARTESIAN_POINT ( 'NONE',  ( 2.307692307692309264, -9.819645486525091727, 36.12317359536749706 ) ) ;
#33042 = ORIENTED_EDGE ( 'NONE', *, *, #48830, .F. ) ;
#33043 = FACE_BOUND ( 'NONE', #36675, .T. ) ;
#33044 = DIRECTION ( 'NONE',  ( -0.000000000000000000, -0.1736481776669307198, -0.9848077530122080203 ) ) ;
#33045 = CARTESIAN_POINT ( 'NONE',  ( 8.096153846153846700, -2.249999999999998668, 29.75000000000000355 ) ) ;
#33046 = ORIENTED_EDGE ( 'NONE', *, *, #87847, .F. ) ;
#33047 = CARTESIAN_POINT ( 'NONE',  ( -8.096153846153844924, -2.249999999999998668, 29.75000000000000355 ) ) ;
#33048 = CARTESIAN_POINT ( 'NONE',  ( -3.262820512820514107, -3.499999999999999556, 29.75000000000000355 ) ) ;
#33049 = CARTESIAN_POINT ( 'NONE',  ( 3.100621261037538545, -12.15440758774515473, 32.17923288041532004 ) ) ;
#33050 = ORIENTED_EDGE ( 'NONE', *, *, #68209, .T. ) ;
#33051 = CARTESIAN_POINT ( 'NONE',  ( 6.000000000000001776, -1.466349020453238561, 30.81389545987213907 ) ) ;
#33052 = CARTESIAN_POINT ( 'NONE',  ( 12.68431800280686694, -6.760870238392817200, 34.69528174975672385 ) ) ;
#33053 = CARTESIAN_POINT ( 'NONE',  ( -8.069080063669991532, -2.758268499246657068, 31.33685645148948140 ) ) ;
#33054 = ORIENTED_EDGE ( 'NONE', *, *, #30161, .F. ) ;
#33055 = DIRECTION ( 'NONE',  ( 0.000000000000000000, 0.7660444431189822323, -0.6427876096865344779 ) ) ;
#33056 = CARTESIAN_POINT ( 'NONE',  ( 4.023155550735844521, -9.929715669179216775, 34.40415004197138416 ) ) ;
#33057 = ORIENTED_EDGE ( 'NONE', *, *, #2186, .F. ) ;
#33058 = CARTESIAN_POINT ( 'NONE',  ( 3.453782074862625340, -6.460100341425561332, 34.89618726649961644 ) ) ;
#33059 = DIRECTION ( 'NONE',  ( -1.000000000000000000, 0.000000000000000000, 0.000000000000000000 ) ) ;
#33060 = CARTESIAN_POINT ( 'NONE',  ( -7.846153846153844924, -12.34228464037088635, 31.77849191805839268 ) ) ;
#33061 = CARTESIAN_POINT ( 'NONE',  ( -5.076923076923075762, -8.120952969808772792, 34.71129190930000163 ) ) ;
#33062 = CARTESIAN_POINT ( 'NONE',  ( -6.988830351390253881, -7.249945578846651806, 34.99404164642496795 ) ) ;
#33063 = CARTESIAN_POINT ( 'NONE',  ( 17.32686848630112308, -4.932303261841487263, 34.32971442181322885 ) ) ;
#33064 = B_SPLINE_CURVE_WITH_KNOTS ( 'NONE', 3,
 ( #21703, #15402, #50491, #23030, #50922, #42872, #78409, #77536, #84753, #14958 ),
 .UNSPECIFIED., .F., .F.,
 ( 4, 2, 2, 2, 4 ),
 ( 0.000000000000000000, 0.0001954311564186868473, 0.0003908623128373736946, 0.0005862934692560605419, 0.0007817246256747473893 ),
 .UNSPECIFIED. ) ;
#33066 = CARTESIAN_POINT ( 'NONE',  ( 5.076923076923075762, -4.098570777380720287, 33.41473453929634729 ) ) ;
#33065 = CARTESIAN_POINT ( 'NONE',  ( 6.223011351612851350, -11.76359900205217457, 32.36225158514719880 ) ) ;
#33067 = CARTESIAN_POINT ( 'NONE',  ( 11.25641025641025550, -11.50000000000000000, 29.75000000000000355 ) ) ;
#33068 = CARTESIAN_POINT ( 'NONE',  ( 5.448717948717947124, -7.500000000000000000, 29.75000000000000355 ) ) ;
#33069 = CARTESIAN_POINT ( 'NONE',  ( -1.139087296525992166, -10.25000000000000533, 17.35937500000000000 ) ) ;
#33070 = VERTEX_POINT ( 'NONE', #36237 ) ;
#33071 = CARTESIAN_POINT ( 'NONE',  ( -12.52680890749923570, -8.613356846314824011, 34.62446782046655613 ) ) ;
#33072 = VERTEX_POINT ( 'NONE', #63692 ) ;
#33073 = EDGE_LOOP ( 'NONE', ( #54427, #30048, #29046, #84611 ) ) ;
#33074 = CARTESIAN_POINT ( 'NONE',  ( -17.07692307692319744, -4.320704448113951379, 33.92786785259630022 ) ) ;
#33075 = ORIENTED_EDGE ( 'NONE', *, *, #2520, .T. ) ;
#33076 = LINE ( 'NONE', #60544, #8125 ) ;
#33077 = CARTESIAN_POINT ( 'NONE',  ( -2.724691934501232371, -8.700186371490559623, 27.26375670625849423 ) ) ;
#33078 = DIRECTION ( 'NONE',  ( -0.000000000000000000, 1.000000000000000000, -0.000000000000000000 ) ) ;
#33079 = CARTESIAN_POINT ( 'NONE',  ( -8.769230769230768274, -3.050289026998446396, 32.03036669348365706 ) ) ;
#33080 = CARTESIAN_POINT ( 'NONE',  ( -3.164700879766792152, -8.973038597847269315, 34.52809138561122637 ) ) ;
#33081 = CARTESIAN_POINT ( 'NONE',  ( -5.326899820971668476, -3.436278759898155677, 33.07459398097509506 ) ) ;
#33082 = DIRECTION ( 'NONE',  ( -0.000000000000000000, -0.9396926207859093161, -0.3420201433256663259 ) ) ;
#33083 = CARTESIAN_POINT ( 'NONE',  ( 2.373760658694747061, -11.16473453929635440, 33.15142922261926373 ) ) ;
#33084 = B_SPLINE_CURVE_WITH_KNOTS ( 'NONE', 3,
 ( #27522, #88363, #41480, #54992, #75700, #20759, #6800, #934, #81587, #7255 ),
 .UNSPECIFIED., .F., .F.,
 ( 4, 2, 2, 2, 4 ),
 ( 0.0007817359430256297891, 0.0009771253907249958896, 0.001172514838424362207, 0.001367904286123728524, 0.001563293733823094625 ),
 .UNSPECIFIED. ) ;
#33085 = CARTESIAN_POINT ( 'NONE',  ( -1.929879867024197893E-14, -3.750000000000000000, 19.15625000000000000 ) ) ;
#33086 = CARTESIAN_POINT ( 'NONE',  ( 17.29970274590113632, -2.353885683473779800, 30.79025554430704759 ) ) ;
#33087 = CARTESIAN_POINT ( 'NONE',  ( -10.61538461538429878, -2.255955759149395501, 30.00000000000324363 ) ) ;
#33088 = CIRCLE ( 'NONE', #30375, 0.2500000000000002220 ) ;
#33089 = DIRECTION ( 'NONE',  ( -1.000000000000000000, -0.000000000000000000, 0.000000000000000000 ) ) ;
#33090 = VECTOR ( 'NONE', #4810, 1000.000000000000227 ) ;
#33091 = VECTOR ( 'NONE', #51049, 1000.000000000000227 ) ;
#33092 = ORIENTED_EDGE ( 'NONE', *, *, #82743, .T. ) ;
#33093 = ORIENTED_EDGE ( 'NONE', *, *, #58173, .T. ) ;
#33094 = LINE ( 'NONE', #4285, #57269 ) ;
#33095 = CARTESIAN_POINT ( 'NONE',  ( 15.48082365068268373, -12.01375889529407281, 32.43194544308182969 ) ) ;
#33096 = CARTESIAN_POINT ( 'NONE',  ( -6.673131513698880468, -12.07971442181322352, 32.31769673815850297 ) ) ;
#33097 = CARTESIAN_POINT ( 'NONE',  ( 6.065192988294654697, -2.255955759149235629, 29.99999999999988631 ) ) ;
#33098 = B_SPLINE_CURVE_WITH_KNOTS ( 'NONE', 3,
 ( #86432, #66589, #25146, #67034, #31915, #72439 ),
 .UNSPECIFIED., .F., .F.,
 ( 4, 2, 4 ),
 ( 3.165870343657672947E-17, 0.0001954756301637032231, 0.0003909512603273747875 ),
 .UNSPECIFIED. ) ;
#33099 = VECTOR ( 'NONE', #22875, 1000.000000000000000 ) ;
#33100 = LINE ( 'NONE', #47044, #63623 ) ;
#33101 = VECTOR ( 'NONE', #32470, 1000.000000000000227 ) ;
#33102 = CARTESIAN_POINT ( 'NONE',  ( -0.7115616988314269475, -6.695914987888143877, 34.68535235679833306 ) ) ;
#33103 = B_SPLINE_CURVE_WITH_KNOTS ( 'NONE', 3,
 ( #71538, #35103, #49939, #29684, #22910, #50377, #77858, #35558, #83748, #878 ),
 .UNSPECIFIED., .F., .F.,
 ( 4, 2, 2, 2, 4 ),
 ( 0.0007817246256747491240, 0.0009771112852218931041, 0.001172497944769036867, 0.001367884604316180631, 0.001563271263863324611 ),
 .UNSPECIFIED. ) ;
#33104 = VERTEX_POINT ( 'NONE', #1999 ) ;
#33105 = CARTESIAN_POINT ( 'NONE',  ( 3.230769230769108269, -6.835583212225970762, 34.95778746994575670 ) ) ;
#33106 = ORIENTED_EDGE ( 'NONE', *, *, #53239, .F. ) ;
#33107 = VERTEX_POINT ( 'NONE', #29481 ) ;
#33108 = CYLINDRICAL_SURFACE ( 'NONE', #86596, 0.2499999999999973355 ) ;
#33109 = EDGE_CURVE ( 'NONE', #74160, #16329, #15964, .T. ) ;
#33110 = CARTESIAN_POINT ( 'NONE',  ( -2.438382910802615378, -9.084618155246140248, 34.75535874321725771 ) ) ;
#33111 = CARTESIAN_POINT ( 'NONE',  ( 14.30769230769231015, -4.786620604624113540, 33.94971097300155094 ) ) ;
#33112 = EDGE_CURVE ( 'NONE', #41653, #28230, #61265, .T. ) ;
#33113 = CARTESIAN_POINT ( 'NONE',  ( 1.384615384615386802, -2.249999999999998668, 29.75000000000001776 ) ) ;
#33114 = LINE ( 'NONE', #34440, #13463 ) ;
#33115 = EDGE_LOOP ( 'NONE', ( #385, #21814 ) ) ;
#33116 = ORIENTED_EDGE ( 'NONE', *, *, #60734, .T. ) ;
#33117 = VERTEX_POINT ( 'NONE', #78097 ) ;
#33118 = ORIENTED_EDGE ( 'NONE', *, *, #35016, .F. ) ;
#33119 = EDGE_CURVE ( 'NONE', #35898, #60361, #16397, .T. ) ;
#33120 = CARTESIAN_POINT ( 'NONE',  ( 5.776515056276055660, -2.599994579823202923, 30.74605699353653776 ) ) ;
#33121 = CARTESIAN_POINT ( 'NONE',  ( 10.39189969082028675, -11.60425143139329940, 33.02411095842164457 ) ) ;
#33122 = AXIS2_PLACEMENT_3D ( 'NONE', #66424, #78596, #38511 ) ;
#33123 = CARTESIAN_POINT ( 'NONE',  ( 4.153846153846154188, -11.91647553114624181, 32.58852847137148245 ) ) ;
#33124 = CARTESIAN_POINT ( 'NONE',  ( 5.076923076922953193, -8.656820664282941280, 34.87096338111179961 ) ) ;
#33125 = SURFACE_SIDE_STYLE ('',( #61472 ) ) ;
#33126 = CARTESIAN_POINT ( 'NONE',  ( -15.36091720050093734, -2.647304123082328875, 31.75400227202885972 ) ) ;
#33127 = ORIENTED_EDGE ( 'NONE', *, *, #2083, .F. ) ;
#33128 = ORIENTED_EDGE ( 'NONE', *, *, #64727, .T. ) ;
#33130 = EDGE_LOOP ( 'NONE', ( #81572, #87749 ) ) ;
#33129 = FACE_OUTER_BOUND ( 'NONE', #7647, .T. ) ;
#33131 = CARTESIAN_POINT ( 'NONE',  ( 17.32697749683652688, -10.82426656108011720, 33.81400080652039009 ) ) ;
#33132 = CARTESIAN_POINT ( 'NONE',  ( 7.053915341089685320, -7.277220443632450575, 34.74524770363009196 ) ) ;
#33133 = CARTESIAN_POINT ( 'NONE',  ( 3.750000000000009770, -9.053300858899081760, 18.29687500000000000 ) ) ;
#33134 = EDGE_CURVE ( 'NONE', #61316, #35118, #15189, .T. ) ;
#33135 = VERTEX_POINT ( 'NONE', #4666 ) ;
#33136 = EDGE_CURVE ( 'NONE', #48109, #1161, #7707, .T. ) ;
#33137 = CARTESIAN_POINT ( 'NONE',  ( 3.480769230769230838, -2.249999999999998668, 29.75000000000000355 ) ) ;
#33138 = ORIENTED_EDGE ( 'NONE', *, *, #16147, .T. ) ;
#33139 = DIRECTION ( 'NONE',  ( -0.000000000000000000, 0.6427876096865404731, -0.7660444431189770143 ) ) ;
#33140 = DIRECTION ( 'NONE',  ( 0.000000000000000000, -6.938893903907222067E-15, 1.000000000000000000 ) ) ;
#33141 = EDGE_CURVE ( 'NONE', #66010, #32904, #60334, .T. ) ;
#33142 = CARTESIAN_POINT ( 'NONE',  ( -12.21159294319032185, -12.43552623307873972, 30.55307653245132826 ) ) ;
#33144 = CIRCLE ( 'NONE', #5834, 4.000000000000000000 ) ;
#33143 = CARTESIAN_POINT ( 'NONE',  ( -6.700065571464072889, -12.39991518177334129, 30.74647679643404530 ) ) ;
#33145 = EDGE_CURVE ( 'NONE', #52583, #65133, #83967, .T. ) ;
#33146 = CARTESIAN_POINT ( 'NONE',  ( -1.134615384615383915, -2.249999999999998668, 29.75000000000000355 ) ) ;
#33147 = ORIENTED_EDGE ( 'NONE', *, *, #11680, .F. ) ;
#33148 = CARTESIAN_POINT ( 'NONE',  ( -11.31568186948346977, -8.540255544307065350, 34.89611431652622286 ) ) ;
#33149 = CARTESIAN_POINT ( 'NONE',  ( -14.24243673641627694, -2.625532179533470512, 30.86335684631491105 ) ) ;
#33150 = CARTESIAN_POINT ( 'NONE',  ( 6.923076923076924238, -11.35647404775217417, 33.31231777344666511 ) ) ;
#33151 = VERTEX_POINT ( 'NONE', #17286 ) ;
#33152 = AXIS2_PLACEMENT_3D ( 'NONE', #22066, #25, #76116 ) ;
#33153 = AXIS2_PLACEMENT_3D ( 'NONE', #7134, #61623, #19761 ) ;
#33154 = FACE_OUTER_BOUND ( 'NONE', #56648, .T. ) ;
#33155 = CARTESIAN_POINT ( 'NONE',  ( -7.780085495151407571, -11.16473453929635440, 33.15142922261926373 ) ) ;
#33156 = CARTESIAN_POINT ( 'NONE',  ( 4.219913487196230939, -11.35647404775217595, 33.31231777344667222 ) ) ;
#33157 = DIRECTION ( 'NONE',  ( 0.000000000000000000, 0.7660444431189822323, -0.6427876096865344779 ) ) ;
#33158 = CARTESIAN_POINT ( 'NONE',  ( 10.36536137809165403, -11.86270091957321249, 32.19358267280087915 ) ) ;
#33159 = FACE_BOUND ( 'NONE', #26778, .T. ) ;
#33161 = CARTESIAN_POINT ( 'NONE',  ( 4.403791563224197070, -12.68172785388650681, 30.59649109432439573 ) ) ;
#33160 = CARTESIAN_POINT ( 'NONE',  ( 5.999999999999878320, -5.094484230521993062, 34.41647553114689373 ) ) ;
#33162 = B_SPLINE_CURVE_WITH_KNOTS ( 'NONE', 3,
 ( #51981, #52876, #18671, #17776, #79916, #58298, #18220, #45681, #38942, #37584 ),
 .UNSPECIFIED., .F., .F.,
 ( 4, 2, 2, 2, 4 ),
 ( 0.000000000000000000, 0.0001954311564186876876, 0.0003908623128373753751, 0.0005862934692560630356, 0.0007817246256747507503 ),
 .UNSPECIFIED. ) ;
#33163 = LINE ( 'NONE', #66046, #49713 ) ;
#33165 = CARTESIAN_POINT ( 'NONE',  ( -11.53846153846153655, -10.67929555188718282, 33.92786785259544047 ) ) ;
#33164 = CARTESIAN_POINT ( 'NONE',  ( -6.000000000000119904, -10.21337939537710326, 33.94971097300076224 ) ) ;
#33166 = CARTESIAN_POINT ( 'NONE',  ( 13.38461538461538680, -2.486705287966279876, 31.30864560766543647 ) ) ;
#33167 = CARTESIAN_POINT ( 'NONE',  ( 1.614399933863660985, -11.22469193450123193, 25.70125670625848713 ) ) ;
#33168 = B_SPLINE_CURVE_WITH_KNOTS ( 'NONE', 3,
 ( #43933, #65533, #2062, #36304, #85374, #2494, #65080, #3835, #29984, #57888 ),
 .UNSPECIFIED., .F., .F.,
 ( 4, 2, 2, 2, 4 ),
 ( 0.0007817359430256322827, 0.0009771253907249989254, 0.001172514838424365676, 0.001367904286123732428, 0.001563293733823099179 ),
 .UNSPECIFIED. ) ;
#33169 = ORIENTED_EDGE ( 'NONE', *, *, #35893, .T. ) ;
#33170 = CARTESIAN_POINT ( 'NONE',  ( -12.68436655917334654, -7.369209533119140509, 34.99857337881830688 ) ) ;
#33171 = ORIENTED_EDGE ( 'NONE', *, *, #82173, .T. ) ;
#33172 = CARTESIAN_POINT ( 'NONE',  ( -5.198717948717948012, -7.500000000000000000, 29.75000000000000355 ) ) ;
#33173 = ORIENTED_EDGE ( 'NONE', *, *, #76329, .T. ) ;
#33174 = CARTESIAN_POINT ( 'NONE',  ( -15.48076923076922995, -7.500000000000001776, 34.75000000000000000 ) ) ;
#33175 = CARTESIAN_POINT ( 'NONE',  ( -13.38461538461506883, -2.255955759149395501, 30.00000000000324363 ) ) ;
#33177 = VERTEX_POINT ( 'NONE', #17738 ) ;
#33176 = FACE_OUTER_BOUND ( 'NONE', #21114, .T. ) ;
#33178 = CARTESIAN_POINT ( 'NONE',  ( -10.61538461538461320, -11.91647553114624181, 32.58852847137148245 ) ) ;
#33179 = CARTESIAN_POINT ( 'NONE',  ( -12.71156168575991785, -6.652501968072648708, 34.93155406624980941 ) ) ;
#33180 = CARTESIAN_POINT ( 'NONE',  ( 1.492201783934554493, -3.724691934501233703, 26.48250670625848713 ) ) ;
#33181 = CARTESIAN_POINT ( 'NONE',  ( 30.00000000000000000, -15.00000000000000000, 3.000000000000000000 ) ) ;
#33182 = CARTESIAN_POINT ( 'NONE',  ( 0.4615384615384611200, -5.180354513474913603, 36.12317359536750416 ) ) ;
#33183 = CARTESIAN_POINT ( 'NONE',  ( -12.23875879256039489, -9.418065098278013636, 34.63729479722530158 ) ) ;
#33184 = DIRECTION ( 'NONE',  ( -1.000000000000000000, -0.000000000000000000, -0.000000000000000000 ) ) ;
#33185 = CYLINDRICAL_SURFACE ( 'NONE', #61190, 0.2499999999999973355 ) ;
#33186 = FACE_OUTER_BOUND ( 'NONE', #59803, .T. ) ;
#33187 = CARTESIAN_POINT ( 'NONE',  ( -1.492201783934593573, -3.724691934501250135, 15.57999329374151110 ) ) ;
#33188 = EDGE_CURVE ( 'NONE', #2843, #67618, #73121, .T. ) ;
#33189 = CARTESIAN_POINT ( 'NONE',  ( -4.376773112753001627, -2.889293201056495786, 32.26117774369186009 ) ) ;
#33190 = CARTESIAN_POINT ( 'NONE',  ( 13.38461538461526601, -2.625532179533778709, 30.86335684631627174 ) ) ;
#33191 = ORIENTED_EDGE ( 'NONE', *, *, #49384, .T. ) ;
#33192 = FACE_OUTER_BOUND ( 'NONE', #24315, .T. ) ;
#33193 = CARTESIAN_POINT ( 'NONE',  ( 15.23076923076910916, -11.06231777344772027, 33.60647404775119895 ) ) ;
#33194 = CARTESIAN_POINT ( 'NONE',  ( 2.694853999681185108, -4.891553140782077591, 18.31436829374150932 ) ) ;
#33195 = B_SPLINE_CURVE_WITH_KNOTS ( 'NONE', 3,
 ( #87213, #4782, #32685, #87655, #86323, #44857, #17404, #24146, #18290, #11537 ),
 .UNSPECIFIED., .F., .F.,
 ( 4, 2, 2, 2, 4 ),
 ( 0.000000000000000000, 0.0001954339857564097241, 0.0003908679715128194482, 0.0005863019572692291723, 0.0007817359430256388964 ),
 .UNSPECIFIED. ) ;
#33196 = CARTESIAN_POINT ( 'NONE',  ( -18.00000000000012079, -12.46129190930018460, 30.37095296980731973 ) ) ;
#33197 = CARTESIAN_POINT ( 'NONE',  ( 17.14299142792552288, -11.69971097300155272, 32.46337939537588113 ) ) ;
#33198 = ORIENTED_EDGE ( 'NONE', *, *, #70661, .F. ) ;
#33199 = DIRECTION ( 'NONE',  ( -0.000000000000000000, 0.9396926207859092051, -0.3420201433256662704 ) ) ;
#33200 = CARTESIAN_POINT ( 'NONE',  ( -0.4615384615384611200, -1.129524287112498415, 32.06866353760679544 ) ) ;
#33202 = EDGE_LOOP ( 'NONE', ( #63518, #22597, #86263, #9857 ) ) ;
#33201 = CARTESIAN_POINT ( 'NONE',  ( -7.715363405186896451, -12.35292014791297710, 31.75344720912887198 ) ) ;
#33203 = DIRECTION ( 'NONE',  ( -1.000000000000000000, -0.000000000000000000, -0.000000000000000000 ) ) ;
#33204 = B_SPLINE_CURVE_WITH_KNOTS ( 'NONE', 3,
 ( #14075, #18737, #41110, #25927, #11983, #73232, #52940, #39461, #82100, #41548 ),
 .UNSPECIFIED., .F., .F.,
 ( 4, 2, 2, 2, 4 ),
 ( 0.000000000000000000, 0.0001954311564186865221, 0.0003908623128373730441, 0.0005862934692560595662, 0.0007817246256747460882 ),
 .UNSPECIFIED. ) ;
#33205 = LINE ( 'NONE', #33650, #43506 ) ;
#33206 = EDGE_CURVE ( 'NONE', #79365, #14132, #4213, .T. ) ;
#33207 = CARTESIAN_POINT ( 'NONE',  ( -11.60454391782167249, -2.486705287966279432, 31.30864560766542937 ) ) ;
#33208 = B_SPLINE_CURVE_WITH_KNOTS ( 'NONE', 3,
 ( #38810, #80241, #66270, #4574, #32048, #87017, #23500, #50956, #25291, #73489 ),
 .UNSPECIFIED., .F., .F.,
 ( 4, 2, 2, 2, 4 ),
 ( 0.000000000000000000, 0.0001954339881912772715, 0.0003908679763825545429, 0.0005863019645738318415, 0.0007817359527651090859 ),
 .UNSPECIFIED. ) ;
#33209 = ORIENTED_EDGE ( 'NONE', *, *, #75218, .F. ) ;
#33210 = DIRECTION ( 'NONE',  ( -0.000000000000000000, -0.6427876096865404731, -0.7660444431189770143 ) ) ;
#33211 = DIRECTION ( 'NONE',  ( 0.000000000000000000, 0.000000000000000000, -1.000000000000000000 ) ) ;
#33213 = CARTESIAN_POINT ( 'NONE',  ( 1.161688425708536920, -2.889293201056495786, 32.26117774369186009 ) ) ;
#33212 = AXIS2_PLACEMENT_3D ( 'NONE', #74714, #20636, #18869 ) ;
#33214 = EDGE_LOOP ( 'NONE', ( #23703, #48792, #59917, #81341 ) ) ;
#33215 = VERTEX_POINT ( 'NONE', #51042 ) ;
#33216 = ORIENTED_EDGE ( 'NONE', *, *, #44242, .F. ) ;
#33217 = ORIENTED_EDGE ( 'NONE', *, *, #55076, .T. ) ;
#33218 = AXIS2_PLACEMENT_3D ( 'NONE', #54667, #1066, #28544 ) ;
#33219 = VECTOR ( 'NONE', #20741, 1000.000000000000114 ) ;
#33220 = EDGE_CURVE ( 'NONE', #53, #59603, #79440, .T. ) ;
#33221 = DIRECTION ( 'NONE',  ( 0.000000000000000000, 0.9848077530122072432, -0.1736481776669354937 ) ) ;
#33222 = CARTESIAN_POINT ( 'NONE',  ( -2.084912766423897779, -5.913360116392399668, 34.49180327182771322 ) ) ;
#33223 = EDGE_CURVE ( 'NONE', #64477, #17545, #22683, .T. ) ;
#33224 = CARTESIAN_POINT ( 'NONE',  ( -11.53846153846153655, -3.322132147404559976, 32.92929555188717927 ) ) ;
#33225 = DIRECTION ( 'NONE',  ( 0.000000000000000000, 0.9396926207859126468, -0.3420201433256571111 ) ) ;
#33226 = CARTESIAN_POINT ( 'NONE',  ( -5.076923076923075762, -5.557115091759785130, 34.35708131394839171 ) ) ;
#33227 = ORIENTED_EDGE ( 'NONE', *, *, #63586, .T. ) ;
#33228 = ORIENTED_EDGE ( 'NONE', *, *, #75798, .F. ) ;
#33230 = EDGE_LOOP ( 'NONE', ( #86422, #11406, #58311, #27526 ) ) ;
#33229 = EDGE_CURVE ( 'NONE', #83978, #68708, #2249, .T. ) ;
#33232 = EDGE_LOOP ( 'NONE', ( #85834, #80338 ) ) ;
#33231 = CYLINDRICAL_SURFACE ( 'NONE', #28596, 0.2499999999999994726 ) ;
#33233 = CARTESIAN_POINT ( 'NONE',  ( -16.40382289789473802, -12.41104346484419452, 31.60698883733904196 ) ) ;
#33234 = CARTESIAN_POINT ( 'NONE',  ( 6.923076923076924238, -13.75783147151868846, 33.36296068462461051 ) ) ;
#33235 = ADVANCED_FACE ( 'NONE', ( #68139 ), #6004, .F. ) ;
#33236 = DIRECTION ( 'NONE',  ( -0.000000000000000000, 1.000000000000000000, -0.000000000000000000 ) ) ;
#33237 = CARTESIAN_POINT ( 'NONE',  ( -5.750054481651857508, -4.336752205174647656, 33.62275283266504289 ) ) ;
#33238 = ADVANCED_FACE ( 'NONE', ( #123 ), #88874, .F. ) ;
#33239 = ORIENTED_EDGE ( 'NONE', *, *, #19058, .F. ) ;
#33240 = VERTEX_POINT ( 'NONE', #74016 ) ;
#33241 = ORIENTED_EDGE ( 'NONE', *, *, #67812, .T. ) ;
#33242 = CARTESIAN_POINT ( 'NONE',  ( -9.442307692306256328, -7.500000000000155431, 34.75000000000007105 ) ) ;
#33244 = ORIENTED_EDGE ( 'NONE', *, *, #67861, .F. ) ;
#33243 = CYLINDRICAL_SURFACE ( 'NONE', #17145, 0.2500000000000002220 ) ;
#33245 = B_SPLINE_CURVE_WITH_KNOTS ( 'NONE', 3,
 ( #9988, #77569, #58170, #3232, #83901, #70372, #1471, #8679, #70820, #22617 ),
 .UNSPECIFIED., .F., .F.,
 ( 4, 2, 2, 2, 4 ),
 ( 0.0007817359527651101701, 0.0009771254036996489256, 0.001172514854634187790, 0.001367904305568726653, 0.001563293756503265517 ),
 .UNSPECIFIED. ) ;
#33246 = CARTESIAN_POINT ( 'NONE',  ( 3.164685819813349177, -11.69971097300155272, 32.46337939537587403 ) ) ;
#33247 = VECTOR ( 'NONE', #32002, 1000.000000000000000 ) ;
#33248 = CARTESIAN_POINT ( 'NONE',  ( -17.14219307747939425, -3.643525952247790300, 33.31231777344662959 ) ) ;
#33249 = ADVANCED_FACE ( 'NONE', ( #40232 ), #39789, .F. ) ;
#33250 = ORIENTED_EDGE ( 'NONE', *, *, #56551, .T. ) ;
#33251 = CARTESIAN_POINT ( 'NONE',  ( -11.47320639894870276, -4.320704448112861584, 33.92786785259548310 ) ) ;
#33252 = AXIS2_PLACEMENT_3D ( 'NONE', #6492, #83037, #28087 ) ;
#33253 = CARTESIAN_POINT ( 'NONE',  ( 8.992242120843620512, -12.39991518177334129, 30.74647679643404530 ) ) ;
#33254 = CYLINDRICAL_SURFACE ( 'NONE', #68441, 0.2499999999999994726 ) ;
#33255 = FACE_BOUND ( 'NONE', #9000, .T. ) ;
#33256 = CARTESIAN_POINT ( 'NONE',  ( 18.00000000000000000, -5.557115091759785130, 34.35708131394839171 ) ) ;
#33257 = CARTESIAN_POINT ( 'NONE',  ( -18.00000000000000000, -2.249999999999988898, 29.99999999999998579 ) ) ;
#33258 = CARTESIAN_POINT ( 'NONE',  ( -9.019254006523732770, -4.335965774309648246, 33.62209801155881905 ) ) ;
#33260 = CARTESIAN_POINT ( 'NONE',  ( 15.48071464014727283, -10.18230066228895758, 34.26354781536631577 ) ) ;
#33259 = CARTESIAN_POINT ( 'NONE',  ( 9.442330961365341224, -3.137211980971221781, 32.19342716148376837 ) ) ;
#33261 = EDGE_CURVE ( 'NONE', #55459, #22454, #73582, .T. ) ;
#33262 = CARTESIAN_POINT ( 'NONE',  ( 0.4615384615384611200, -12.10708131394839349, 31.69288490824020244 ) ) ;
#33263 = CARTESIAN_POINT ( 'NONE',  ( -0.6844646790546099480, -3.586966769969700763, 32.86292498521069660 ) ) ;
#33264 = ORIENTED_EDGE ( 'NONE', *, *, #79636, .T. ) ;
#33265 = EDGE_CURVE ( 'NONE', #79311, #26451, #54914, .T. ) ;
#33266 = LINE ( 'NONE', #32817, #40365 ) ;
#33267 = CARTESIAN_POINT ( 'NONE',  ( 0.2115617174898699049, -10.82459398097509684, 33.81372124010185587 ) ) ;
#33268 = VERTEX_POINT ( 'NONE', #20832 ) ;
#33269 = B_SPLINE_CURVE_WITH_KNOTS ( 'NONE', 3,
 ( #45528, #4997, #60819, #53163, #59036, #86992, #88322, #53619, #67585, #47300 ),
 .UNSPECIFIED., .F., .F.,
 ( 4, 2, 2, 2, 4 ),
 ( 0.000000000000000000, 0.0001954311564186870371, 0.0003908623128373740741, 0.0005862934692560610840, 0.0007817246256747481482 ),
 .UNSPECIFIED. ) ;
#33270 = VERTEX_POINT ( 'NONE', #19941 ) ;
#33271 = CARTESIAN_POINT ( 'NONE',  ( 6.416666666666664298, -7.500000000000000000, 29.75000000000000355 ) ) ;
#33272 = CARTESIAN_POINT ( 'NONE',  ( 16.02315555073584363, -2.295517848115769421, 30.44137282052136939 ) ) ;
#33273 = DIRECTION ( 'NONE',  ( -0.000000000000000000, 0.3420201433256694901, -0.9396926207859082059 ) ) ;
#33274 = ORIENTED_EDGE ( 'NONE', *, *, #2520, .F. ) ;
#33275 = CARTESIAN_POINT ( 'NONE',  ( 11.53846153846141576, -10.33852847137269571, 34.16647553114546554 ) ) ;
#33276 = CARTESIAN_POINT ( 'NONE',  ( 2.557692307693744560, -7.500000000000155431, 34.75000000000007105 ) ) ;
#33277 = FACE_BOUND ( 'NONE', #35440, .T. ) ;
#33279 = CARTESIAN_POINT ( 'NONE',  ( -9.822454901745910405, -4.460286881179643004, 33.72017969459903242 ) ) ;
#33278 = DIRECTION ( 'NONE',  ( 0.000000000000000000, 1.000000000000000000, 0.000000000000000000 ) ) ;
#33280 = CARTESIAN_POINT ( 'NONE',  ( 8.068933387422255521, -9.332535724633405749, 34.40230450496446934 ) ) ;
#33281 = AXIS2_PLACEMENT_3D ( 'NONE', #23525, #16337, #78468 ) ;
#33282 = CARTESIAN_POINT ( 'NONE',  ( 2.557746619330623528, -4.943051570960395047, 34.04725096376909477 ) ) ;
#33284 = CARTESIAN_POINT ( 'NONE',  ( 0.2380535178145126718, -5.912607949931405926, 34.49155766932282319 ) ) ;
#33283 = CARTESIAN_POINT ( 'NONE',  ( 0.000000000000000000, 0.000000000000000000, 0.000000000000000000 ) ) ;
#33285 = CARTESIAN_POINT ( 'NONE',  ( -1.553300858899081538, -11.25000000000000711, 22.35937500000000711 ) ) ;
#33286 = ORIENTED_EDGE ( 'NONE', *, *, #74646, .F. ) ;
#33287 = AXIS2_PLACEMENT_3D ( 'NONE', #61158, #67047, #46325 ) ;
#33288 = ORIENTED_EDGE ( 'NONE', *, *, #62600, .F. ) ;
#33289 = CARTESIAN_POINT ( 'NONE',  ( 9.692307692307695177, -13.75783147151868846, 33.36296068462461051 ) ) ;
#33290 = ADVANCED_FACE ( 'NONE', ( #19502 ), #54606, .F. ) ;
#33291 = LINE ( 'NONE', #26976, #74329 ) ;
#33292 = CARTESIAN_POINT ( 'NONE',  ( -10.61538461538461320, -6.386643153685126251, 34.62446782046654192 ) ) ;
#33293 = CARTESIAN_POINT ( 'NONE',  ( 6.923076923076802558, -12.27809138561165270, 31.22303859784587132 ) ) ;
#33294 = CARTESIAN_POINT ( 'NONE',  ( -7.596153846153844924, -2.249999999999998668, 29.75000000000000355 ) ) ;
#33295 = CARTESIAN_POINT ( 'NONE',  ( 2.651650429449539104, -4.848349570550432475, 21.81250000000000000 ) ) ;
#33296 = AXIS2_PLACEMENT_3D ( 'NONE', #77377, #42718, #63414 ) ;
#33297 = CARTESIAN_POINT ( 'NONE',  ( -1.450697763975518306, -3.937682226553329556, 33.60647404775217240 ) ) ;
#33298 = CARTESIAN_POINT ( 'NONE',  ( -6.249976744048591826, -8.347322224742351082, 34.93158281831414769 ) ) ;
#33299 = CARTESIAN_POINT ( 'NONE',  ( 16.82694634598072270, -12.17611988154120795, 31.52148481390971213 ) ) ;
#33300 = CARTESIAN_POINT ( 'NONE',  ( 13.13463864056679498, -10.06842814019191401, 34.32929386961144758 ) ) ;
#33301 = DIRECTION ( 'NONE',  ( 0.000000000000000000, 0.9396926207859126468, -0.3420201433256571111 ) ) ;
#33302 = CARTESIAN_POINT ( 'NONE',  ( 13.16113044089144068, -4.386631170607603991, 33.66268669641500111 ) ) ;
#33303 = CYLINDRICAL_SURFACE ( 'NONE', #68310, 0.2500000000000002220 ) ;
#33304 = EDGE_CURVE ( 'NONE', #9576, #42657, #50592, .T. ) ;
#33305 = FACE_OUTER_BOUND ( 'NONE', #40700, .T. ) ;
#33306 = CARTESIAN_POINT ( 'NONE',  ( -3.296851610129366339, -12.34228464037088280, 31.77849191805838558 ) ) ;
#33307 = EDGE_LOOP ( 'NONE', ( #64882, #55209 ) ) ;
#33308 = CARTESIAN_POINT ( 'NONE',  ( 1.253923917947826538, -2.541943142973489778, 30.39792223712631980 ) ) ;
#33309 = EDGE_CURVE ( 'NONE', #79691, #54317, #5464, .T. ) ;
#33310 = CARTESIAN_POINT ( 'NONE',  ( -16.15384615384615330, -4.786620604624113540, 33.94971097300155094 ) ) ;
#33311 = CARTESIAN_POINT ( 'NONE',  ( 1.901340078031373171, -9.487747218494639867, 17.37686829374151287 ) ) ;
#33312 = EDGE_CURVE ( 'NONE', #81634, #19254, #46537, .T. ) ;
#33313 = DIRECTION ( 'NONE',  ( 0.000000000000000000, 0.000000000000000000, -1.000000000000000000 ) ) ;
#33314 = FACE_OUTER_BOUND ( 'NONE', #67156, .T. ) ;
#33315 = CARTESIAN_POINT ( 'NONE',  ( 10.36540788444226102, -5.728515186090277211, 34.42611988154120439 ) ) ;
#33317 = EDGE_LOOP ( 'NONE', ( #64914, #14541, #19521, #61366 ) ) ;
#33316 = CARTESIAN_POINT ( 'NONE',  ( -18.22629316816001932, -2.249999999999999556, 29.62232573653512446 ) ) ;
#33318 = CARTESIAN_POINT ( 'NONE',  ( -2.750000000000006217, -6.360912703474006946, 21.42187500000000000 ) ) ;
#33319 = CARTESIAN_POINT ( 'NONE',  ( 17.74997676270703550, -3.711651800289232916, 33.01384336483936011 ) ) ;
#33320 = VERTEX_POINT ( 'NONE', #81660 ) ;
#33321 = CARTESIAN_POINT ( 'NONE',  ( -16.15384615384627409, -10.21337939537710326, 33.94971097300076224 ) ) ;
#33322 = EDGE_CURVE ( 'NONE', #4010, #4115, #25886, .T. ) ;
#33323 = CARTESIAN_POINT ( 'NONE',  ( -2.176900499867520988, -2.541949514083463590, 30.39797389878540557 ) ) ;
#33324 = ORIENTED_EDGE ( 'NONE', *, *, #69763, .F. ) ;
#33325 = AXIS2_PLACEMENT_3D ( 'NONE', #69375, #7676, #910 ) ;
#33326 = DIRECTION ( 'NONE',  ( -0.000000000000000000, -0.7660444431189791237, -0.6427876096865379196 ) ) ;
#33327 = CARTESIAN_POINT ( 'NONE',  ( -1.326923076923076872, -7.500000000000000000, 33.75000000000000000 ) ) ;
#33328 = CARTESIAN_POINT ( 'NONE',  ( 6.000000000000001776, -13.20930481340135110, 34.54067556320372745 ) ) ;
#33329 = ORIENTED_EDGE ( 'NONE', *, *, #13634, .F. ) ;
#33331 = VERTEX_POINT ( 'NONE', #77550 ) ;
#33330 = CIRCLE ( 'NONE', #44811, 4.000000000000000000 ) ;
#33332 = VERTEX_POINT ( 'NONE', #69464 ) ;
#33333 = CARTESIAN_POINT ( 'NONE',  ( -17.93474486048716088, -5.094484230520770929, 34.41647553114626845 ) ) ;
#33334 = CARTESIAN_POINT ( 'NONE',  ( 6.988332062589762472, -11.67786785259547777, 32.92929555188713664 ) ) ;
#33335 = CARTESIAN_POINT ( 'NONE',  ( -9.626239341305252495, -9.780366693483667717, 34.19971097300155805 ) ) ;
#33336 = CARTESIAN_POINT ( 'NONE',  ( -15.48074597481782178, -2.318417181685855422, 30.59732222474233865 ) ) ;
#33337 = CARTESIAN_POINT ( 'NONE',  ( 13.38461538461526423, -6.835583212225970762, 34.95778746994575670 ) ) ;
#33339 = EDGE_CURVE ( 'NONE', #4576, #58726, #62689, .T. ) ;
#33338 = CARTESIAN_POINT ( 'NONE',  ( 9.692307692307570832, -10.33852847137269571, 34.16647553114546554 ) ) ;
#33340 = LINE ( 'NONE', #51800, #49531 ) ;
#33341 = EDGE_CURVE ( 'NONE', #40963, #13065, #32235, .T. ) ;
#33342 = LINE ( 'NONE', #14507, #37701 ) ;
#33343 = ORIENTED_EDGE ( 'NONE', *, *, #55970, .T. ) ;
#33344 = VERTEX_POINT ( 'NONE', #14519 ) ;
#33346 = VERTEX_POINT ( 'NONE', #55944 ) ;
#33345 = CARTESIAN_POINT ( 'NONE',  ( -17.30040802064702987, -10.11188796281391511, 34.01382737946119050 ) ) ;
#33347 = B_SPLINE_CURVE_WITH_KNOTS ( 'NONE', 3,
 ( #11682, #4467, #52200, #18433, #72028, #79689, #51282, #17992, #59856, #17090 ),
 .UNSPECIFIED., .F., .F.,
 ( 4, 2, 2, 2, 4 ),
 ( 0.0007817246256747453293, 0.0009771112852218889842, 0.001172497944769032531, 0.001367884604316176294, 0.001563271263863319840 ),
 .UNSPECIFIED. ) ;
#33348 = AXIS2_PLACEMENT_3D ( 'NONE', #84993, #72350, #79569 ) ;
#33349 = CARTESIAN_POINT ( 'NONE',  ( 10.36538461538460076, -2.249999999999998668, 29.81609741502487765 ) ) ;
#33350 = DIRECTION ( 'NONE',  ( -0.000000000000000000, 0.000000000000000000, 1.000000000000000000 ) ) ;
#33351 = ORIENTED_EDGE ( 'NONE', *, *, #42574, .T. ) ;
#33352 = PLANE ( 'NONE',  #78963 ) ;
#33353 = VERTEX_POINT ( 'NONE', #15861 ) ;
#33354 = CARTESIAN_POINT ( 'NONE',  ( 15.90384615384615330, -7.500000000000001776, 34.75000000000000000 ) ) ;
#33355 = EDGE_LOOP ( 'NONE', ( #9185, #11313, #22366, #57846 ) ) ;
#33356 = DIRECTION ( 'NONE',  ( -0.000000000000000000, 1.000000000000000000, -0.000000000000000000 ) ) ;
#33357 = EDGE_CURVE ( 'NONE', #19254, #4576, #21719, .T. ) ;
#33358 = EDGE_CURVE ( 'NONE', #46099, #42810, #68778, .T. ) ;
#33359 = CARTESIAN_POINT ( 'NONE',  ( 1.450683735617825043, -6.386643153685127139, 34.62446782046654192 ) ) ;
#33360 = DIRECTION ( 'NONE',  ( 1.000000000000000000, 0.000000000000000000, 0.000000000000000000 ) ) ;
#33361 = FACE_BOUND ( 'NONE', #26925, .T. ) ;
#33362 = CARTESIAN_POINT ( 'NONE',  ( 14.30769230769231015, -13.49023893513002648, 31.06009739812518688 ) ) ;
#33364 = EDGE_CURVE ( 'NONE', #82738, #77091, #28034, .T. ) ;
#33363 = CARTESIAN_POINT ( 'NONE',  ( 15.93091919493929964, -3.395401636524186362, 33.02366814457250399 ) ) ;
#33365 = CARTESIAN_POINT ( 'NONE',  ( -18.00000000000000000, -12.08385125132259574, 35.60175215339625510 ) ) ;
#33366 = CARTESIAN_POINT ( 'NONE',  ( -6.923076923076922462, -11.69971097300155272, 32.46337939537588113 ) ) ;
#33367 = CARTESIAN_POINT ( 'NONE',  ( 10.86538461538455280, -7.565270445406050648, 34.75000000000000000 ) ) ;
#33368 = CARTESIAN_POINT ( 'NONE',  ( -8.069638770718176701, -9.417330523894424488, 34.63758898049880486 ) ) ;
#33369 = ADVANCED_FACE ( 'NONE', ( #69904 ), #29816, .F. ) ;
#33370 = CARTESIAN_POINT ( 'NONE',  ( 1.384615384615701439, -2.255955759149395501, 30.00000000000324363 ) ) ;
#33371 = ORIENTED_EDGE ( 'NONE', *, *, #4938, .F. ) ;
#33372 = B_SPLINE_CURVE_WITH_KNOTS ( 'NONE', 3,
 ( #30717, #30284, #85232, #65391, #86124, #36600, #29843, #52318, #24847, #10002 ),
 .UNSPECIFIED., .F., .F.,
 ( 4, 2, 2, 2, 4 ),
 ( 0.0007817246256747484735, 0.0009771112852218920199, 0.001172497944769035783, 0.001367884604316179330, 0.001563271263863322876 ),
 .UNSPECIFIED. ) ;
#33373 = ORIENTED_EDGE ( 'NONE', *, *, #10350, .T. ) ;
#33375 = CARTESIAN_POINT ( 'NONE',  ( -14.24243673641628050, -12.46129190930001052, 30.37095296980870174 ) ) ;
#33374 = CARTESIAN_POINT ( 'NONE',  ( -7.846153846153844924, -12.10708131394839349, 31.69288490824020244 ) ) ;
#33376 = EDGE_CURVE ( 'NONE', #78512, #43106, #8661, .T. ) ;
#33377 = B_SPLINE_CURVE_WITH_KNOTS ( 'NONE', 3,
 ( #38300, #24322, #4965, #52691, #72519, #80179, #39199, #32431, #10383, #59897 ),
 .UNSPECIFIED., .F., .F.,
 ( 4, 2, 2, 2, 4 ),
 ( 0.000000000000000000, 0.0001954339857564091007, 0.0003908679715128182013, 0.0005863019572692273291, 0.0007817359430256364027 ),
 .UNSPECIFIED. ) ;
#33378 = AXIS2_PLACEMENT_3D ( 'NONE', #67175, #27514, #73937 ) ;
#33379 = CARTESIAN_POINT ( 'NONE',  ( 16.28437159207980045, -11.66157788607254275, 32.95092075102925833 ) ) ;
#33380 = CARTESIAN_POINT ( 'NONE',  ( -14.55771553191376100, -12.07920672191015221, 32.31858351112116168 ) ) ;
#33381 = CARTESIAN_POINT ( 'NONE',  ( 19.00000000000000000, 0.000000000000000000, 23.75000000000000000 ) ) ;
#33382 = CARTESIAN_POINT ( 'NONE',  ( -2.057746789344165439, -2.824170634883621744, 31.52227843825338738 ) ) ;
#33383 = ORIENTED_EDGE ( 'NONE', *, *, #65796, .T. ) ;
#33384 = CARTESIAN_POINT ( 'NONE',  ( -5.326899820971668476, -5.643011162660950042, 34.66104346484419096 ) ) ;
#33385 = DIRECTION ( 'NONE',  ( -1.734723475976812518E-16, 1.000000000000000000, 0.000000000000000000 ) ) ;
#33386 = CARTESIAN_POINT ( 'NONE',  ( -14.30769230769242739, -8.613356846316285953, 34.62446782046622218 ) ) ;
#33387 = LINE ( 'NONE', #40590, #29542 ) ;
#33388 = VECTOR ( 'NONE', #64088, 1000.000000000000000 ) ;
#33389 = ORIENTED_EDGE ( 'NONE', *, *, #33322, .F. ) ;
#33390 = EDGE_CURVE ( 'NONE', #41890, #60580, #8214, .T. ) ;
#33391 = ORIENTED_EDGE ( 'NONE', *, *, #11968, .F. ) ;
#33392 = ORIENTED_EDGE ( 'NONE', *, *, #50268, .F. ) ;
#33393 = LINE ( 'NONE', #19868, #30537 ) ;
#33394 = EDGE_CURVE ( 'NONE', #33011, #81813, #25706, .T. ) ;
#33395 = ORIENTED_EDGE ( 'NONE', *, *, #17783, .T. ) ;
#33396 = CARTESIAN_POINT ( 'NONE',  ( 3.100078627658923835, -12.62707690430377383, 30.88035979386743435 ) ) ;
#33397 = CARTESIAN_POINT ( 'NONE',  ( -8.769230769230768274, -3.669653830205710676, 35.88435417666054406 ) ) ;
#33398 = CARTESIAN_POINT ( 'NONE',  ( 3.361559671736181087, -9.929761469519744921, 34.40412654351204225 ) ) ;
#33399 = LINE ( 'NONE', #60859, #47478 ) ;
#33400 = FACE_OUTER_BOUND ( 'NONE', #24047, .T. ) ;
#33401 = ORIENTED_EDGE ( 'NONE', *, *, #28435, .F. ) ;
#33402 = CARTESIAN_POINT ( 'NONE',  ( -15.36146069743679021, -11.71456829005830080, 32.44064028649416542 ) ) ;
#33404 = ORIENTED_EDGE ( 'NONE', *, *, #42491, .T. ) ;
#33403 = CARTESIAN_POINT ( 'NONE',  ( -15.45369618967607828, -11.98009711892699514, 32.48740034544076138 ) ) ;
#33405 = DIRECTION ( 'NONE',  ( 0.000000000000000000, 0.4999999999999960032, -0.8660254037844410391 ) ) ;
#33406 = CARTESIAN_POINT ( 'NONE',  ( -9.019230769230766498, -7.566082377512564960, 35.00000000000000711 ) ) ;
#33407 = CARTESIAN_POINT ( 'NONE',  ( -13.51530685128294351, -4.809359713505814149, 33.96456829005828837 ) ) ;
#33408 = CARTESIAN_POINT ( 'NONE',  ( -15.90384615384473399, -7.500000000000154543, 35.00000000000007105 ) ) ;
#33409 = CARTESIAN_POINT ( 'NONE',  ( -8.769230769230892619, -8.656820664282941280, 34.87096338111179961 ) ) ;
#33410 = CARTESIAN_POINT ( 'NONE',  ( -8.519176349317316266, -9.233818618650603938, 34.70587769442853698 ) ) ;
#33411 = CARTESIAN_POINT ( 'NONE',  ( 12.68454981315131036, -11.24521262558773493, 33.06293181088029343 ) ) ;
#33412 = CARTESIAN_POINT ( 'NONE',  ( -1.077988221561493543, -4.724691934501247914, 20.57999329374151998 ) ) ;
#33413 = EDGE_LOOP ( 'NONE', ( #1761, #11002, #42037, #25059 ) ) ;
#33414 = EDGE_CURVE ( 'NONE', #40774, #6072, #76277, .T. ) ;
#33415 = CARTESIAN_POINT ( 'NONE',  ( -7.053224892808620083, -11.04286588640298561, 33.62463336215343901 ) ) ;
#33416 = CARTESIAN_POINT ( 'NONE',  ( 1.161688425708536698, -9.172386477786396597, 34.72672124145550043 ) ) ;
#33417 = VECTOR ( 'NONE', #11571, 1000.000000000000227 ) ;
#33418 = ORIENTED_EDGE ( 'NONE', *, *, #34261, .T. ) ;
#33419 = ORIENTED_EDGE ( 'NONE', *, *, #49895, .F. ) ;
#33420 = CARTESIAN_POINT ( 'NONE',  ( -5.999999999999998224, -2.538708090699994813, 30.37095296980875503 ) ) ;
#33421 = CARTESIAN_POINT ( 'NONE',  ( 3.165518240607989142, -2.506253911140460922, 30.00000000000013856 ) ) ;
#33422 = AXIS2_PLACEMENT_3D ( 'NONE', #43836, #78503, #58676 ) ;
#33423 = CARTESIAN_POINT ( 'NONE',  ( -8.992715693795101828, -10.97335522853832579, 33.68706563782419749 ) ) ;
#33424 = ADVANCED_FACE ( 'NONE', ( #567 ), #64022, .F. ) ;
#33425 = CYLINDRICAL_SURFACE ( 'NONE', #68682, 0.2499999999999997502 ) ;
#33426 = CARTESIAN_POINT ( 'NONE',  ( 0.4615384615383382183, -2.379036618888197285, 30.90682066428292885 ) ) ;
#33427 = VERTEX_POINT ( 'NONE', #78429 ) ;
#33428 = DIRECTION ( 'NONE',  ( -0.000000000000000000, -0.5000000000000009992, -0.8660254037844380415 ) ) ;
#33429 = EDGE_CURVE ( 'NONE', #84305, #50475, #4554, .T. ) ;
#33430 = CARTESIAN_POINT ( 'NONE',  ( 17.07692307692295586, -6.026961402154118908, 34.52809138561165270 ) ) ;
#33431 = CARTESIAN_POINT ( 'NONE',  ( 7.715462379486288214, -9.804603061927743113, 34.18744698557895845 ) ) ;
#33432 = EDGE_LOOP ( 'NONE', ( #36139, #79642, #25132, #44009 ) ) ;
#33433 = CARTESIAN_POINT ( 'NONE',  ( -17.01085574357299990, -11.91647553114624358, 32.58852847137148245 ) ) ;
#33434 = VERTEX_POINT ( 'NONE', #64458 ) ;
#33435 = CARTESIAN_POINT ( 'NONE',  ( 14.30769230769231015, -12.29105614889573062, 35.45975837776705220 ) ) ;
#33436 = DIRECTION ( 'NONE',  ( -1.000000000000000000, 0.000000000000000000, 0.000000000000000000 ) ) ;
#33437 = ORIENTED_EDGE ( 'NONE', *, *, #69998, .T. ) ;
#33438 = LINE ( 'NONE', #81188, #28951 ) ;
#33440 = ADVANCED_FACE ( 'NONE', ( #17175 ), #45536, .F. ) ;
#33439 = CARTESIAN_POINT ( 'NONE',  ( 13.60762822870878352, -9.172514111537584114, 34.72667873470787470 ) ) ;
#33441 = LINE ( 'NONE', #54133, #2013 ) ;
#33442 = ADVANCED_FACE ( 'NONE', ( #37896 ), #59497, .F. ) ;
#33443 = VECTOR ( 'NONE', #40385, 1000.000000000000000 ) ;
#33444 = DIRECTION ( 'NONE',  ( -0.000000000000000000, -0.000000000000000000, -1.000000000000000000 ) ) ;
#33445 = CARTESIAN_POINT ( 'NONE',  ( -1.384615384615506484, -11.06231777344772027, 33.60647404775119895 ) ) ;
#33446 = EDGE_CURVE ( 'NONE', #1831, #76906, #11844, .T. ) ;
#33447 = VERTEX_POINT ( 'NONE', #43760 ) ;
#33448 = FACE_BOUND ( 'NONE', #63606, .T. ) ;
#33449 = EDGE_LOOP ( 'NONE', ( #70540, #87626, #27563, #60541 ) ) ;
#33450 = CARTESIAN_POINT ( 'NONE',  ( -8.899921372341076165, -12.35290016733513951, 31.75349464988449455 ) ) ;
#33451 = CARTESIAN_POINT ( 'NONE',  ( 9.019230769232203571, -7.500000000000155431, 34.75000000000007105 ) ) ;
#33452 = CARTESIAN_POINT ( 'NONE',  ( 18.24994551834813805, -12.22109172314383052, 31.39792113162168263 ) ) ;
#33453 = CARTESIAN_POINT ( 'NONE',  ( 3.230769230769231726, -13.49023893513002648, 31.06009739812518688 ) ) ;
#33454 = CARTESIAN_POINT ( 'NONE',  ( -6.249976730942353065, -12.17611988154120972, 31.52148481390971213 ) ) ;
#33455 = EDGE_LOOP ( 'NONE', ( #33957, #71564, #17394, #68153 ) ) ;
#33456 = ORIENTED_EDGE ( 'NONE', *, *, #88259, .T. ) ;
#33457 = ORIENTED_EDGE ( 'NONE', *, *, #33429, .T. ) ;
#33458 = ORIENTED_EDGE ( 'NONE', *, *, #87789, .F. ) ;
#33459 = FACE_OUTER_BOUND ( 'NONE', #15614, .T. ) ;
#33460 = CARTESIAN_POINT ( 'NONE',  ( -6.000000000000119904, -12.46129190930018460, 30.37095296980731973 ) ) ;
#33461 = CARTESIAN_POINT ( 'NONE',  ( -17.01172909513971732, -2.506253911140448043, 29.99999999999988631 ) ) ;
#33462 = CARTESIAN_POINT ( 'NONE',  ( 13.38461538461538680, -11.11383981884818262, 36.00935417666054406 ) ) ;
#33463 = B_SPLINE_CURVE_WITH_KNOTS ( 'NONE', 3,
 ( #82634, #83066, #42525, #49274, #35311, #69980, #77186, #41192, #643, #35771 ),
 .UNSPECIFIED., .F., .F.,
 ( 4, 2, 2, 2, 4 ),
 ( 0.0007817246256747477145, 0.0009771112852218907189, 0.001172497944769033615, 0.001367884604316176511, 0.001563271263863319407 ),
 .UNSPECIFIED. ) ;
#33464 = AXIS2_PLACEMENT_3D ( 'NONE', #47905, #13679, #88049 ) ;
#33465 = CARTESIAN_POINT ( 'NONE',  ( 17.77651505627605033, -10.11188796281391511, 34.01382737946119050 ) ) ;
#33466 = VECTOR ( 'NONE', #32555, 1000.000000000000000 ) ;
#33467 = DIRECTION ( 'NONE',  ( -0.000000000000000000, 0.7660444431189791237, -0.6427876096865379196 ) ) ;
#33468 = CARTESIAN_POINT ( 'NONE',  ( -4.946131269098287930, -4.118422570099827595, 33.43335022499816489 ) ) ;
#33469 = DIRECTION ( 'NONE',  ( -0.000000000000000000, 0.3420201433256694346, -0.9396926207859080948 ) ) ;
#33470 = ORIENTED_EDGE ( 'NONE', *, *, #5698, .F. ) ;
#33471 = B_SPLINE_CURVE_WITH_KNOTS ( 'NONE', 3,
 ( #34179, #20664, #56227, #41387, #55332, #14350, #47695, #21998, #49472, #34627 ),
 .UNSPECIFIED., .F., .F.,
 ( 4, 2, 2, 2, 4 ),
 ( 0.000000000000000000, 0.0001954339857564100222, 0.0003908679715128200445, 0.0005863019572692300396, 0.0007817359430256400890 ),
 .UNSPECIFIED. ) ;
#33472 = VERTEX_POINT ( 'NONE', #72115 ) ;
#33473 = AXIS2_PLACEMENT_3D ( 'NONE', #871, #83298, #47729 ) ;
#33474 = EDGE_LOOP ( 'NONE', ( #79742, #73197 ) ) ;
#33476 = ORIENTED_EDGE ( 'NONE', *, *, #25044, .F. ) ;
#33475 = LINE ( 'NONE', #33907, #87706 ) ;
#33478 = CARTESIAN_POINT ( 'NONE',  ( -5.869208192175211281, -3.530189275343204702, 32.79018710029569661 ) ) ;
#33477 = CARTESIAN_POINT ( 'NONE',  ( -2.980714810855778385, -10.06805714834173848, 34.32951233291982618 ) ) ;
#33479 = EDGE_CURVE ( 'NONE', #71762, #51826, #26823, .T. ) ;
#33480 = LINE ( 'NONE', #60052, #55743 ) ;
#33481 = DIRECTION ( 'NONE',  ( 0.000000000000000000, 0.9848077530122072432, 0.1736481776669354937 ) ) ;
#33482 = FACE_BOUND ( 'NONE', #30809, .T. ) ;
#33483 = VERTEX_POINT ( 'NONE', #65362 ) ;
#33484 = DIRECTION ( 'NONE',  ( 1.000000000000000000, 2.602085213965214586E-16, 0.000000000000000000 ) ) ;
#33485 = CARTESIAN_POINT ( 'NONE',  ( -3.007757879156380820, -6.503523203565942268, 34.64991518177335195 ) ) ;
#33486 = VERTEX_POINT ( 'NONE', #78875 ) ;
#33487 = EDGE_CURVE ( 'NONE', #19576, #46099, #31126, .T. ) ;
#33488 = CARTESIAN_POINT ( 'NONE',  ( -4.854143535654666941, -6.760870238392817200, 34.69528174975672385 ) ) ;
#33489 = B_SPLINE_CURVE_WITH_KNOTS ( 'NONE', 3,
 ( #87606, #44805, #73187, #18694, #32636, #60107, #79046, #72284, #45256, #79942 ),
 .UNSPECIFIED., .F., .F.,
 ( 4, 2, 2, 2, 4 ),
 ( 0.0007817246256747460882, 0.0009771112852218892010, 0.001172497944769032314, 0.001367884604316175643, 0.001563271263863318756 ),
 .UNSPECIFIED. ) ;
#33490 = ORIENTED_EDGE ( 'NONE', *, *, #55475, .T. ) ;
#33491 = FACE_BOUND ( 'NONE', #26239, .T. ) ;
#33492 = CARTESIAN_POINT ( 'NONE',  ( -9.561782254074051579, -2.372941743896879174, 30.88044141588253666 ) ) ;
#33493 = CARTESIAN_POINT ( 'NONE',  ( 18.24994551834813805, -5.057305518903949526, 34.11320923018887896 ) ) ;
#33494 = EDGE_LOOP ( 'NONE', ( #33545, #26180, #62057, #75197 ) ) ;
#33495 = CARTESIAN_POINT ( 'NONE',  ( -23.50000000000000000, 1.250000000000003775, 28.00000000000000000 ) ) ;
#33496 = CARTESIAN_POINT ( 'NONE',  ( -12.68446542044531000, -11.98009711892699514, 32.48740034544076138 ) ) ;
#33497 = DIRECTION ( 'NONE',  ( -0.000000000000000000, 0.6427876096865404731, -0.7660444431189771253 ) ) ;
#33498 = ORIENTED_EDGE ( 'NONE', *, *, #88741, .T. ) ;
#33499 = FACE_OUTER_BOUND ( 'NONE', #20301, .T. ) ;
#33500 = CARTESIAN_POINT ( 'NONE',  ( 11.25641025641025550, -7.500000000000000000, 33.75000000000000000 ) ) ;
#33501 = CARTESIAN_POINT ( 'NONE',  ( 12.52760681254089903, -6.386643153685127139, 34.62446782046654192 ) ) ;
#33502 = CARTESIAN_POINT ( 'NONE',  ( -7.911424292114620727, -2.892918686051583421, 31.69288490824015980 ) ) ;
#33503 = EDGE_LOOP ( 'NONE', ( #63527, #60904 ) ) ;
#33504 = EDGE_CURVE ( 'NONE', #87552, #60114, #24366, .T. ) ;
#33505 = DIRECTION ( 'NONE',  ( -0.000000000000000000, -0.000000000000000000, -1.000000000000000000 ) ) ;
#33507 = CARTESIAN_POINT ( 'NONE',  ( -16.02332071561251325, -10.31582465632704704, 34.18122507451815295 ) ) ;
#33506 = AXIS2_PLACEMENT_3D ( 'NONE', #23660, #71398, #16909 ) ;
#33509 = ORIENTED_EDGE ( 'NONE', *, *, #60770, .F. ) ;
#33508 = AXIS2_PLACEMENT_3D ( 'NONE', #16069, #85417, #29590 ) ;
#33510 = CARTESIAN_POINT ( 'NONE',  ( 16.15384615384615330, -1.367168528481310208, 33.57946703557072254 ) ) ;
#33511 = CARTESIAN_POINT ( 'NONE',  ( 16.02369818411445834, -4.299443229763728169, 33.91186481527756058 ) ) ;
#33512 = CARTESIAN_POINT ( 'NONE',  ( -14.37296230824862953, -2.657715359629089225, 31.77849191805832874 ) ) ;
#33513 = CARTESIAN_POINT ( 'NONE',  ( 16.37685899793954292, -11.98016756924215187, 32.48728574198911190 ) ) ;
#33514 = CARTESIAN_POINT ( 'NONE',  ( 0.2115152373170014477, -2.588893531581426988, 31.60682220781848528 ) ) ;
#33515 = CARTESIAN_POINT ( 'NONE',  ( 14.98079248672064345, -5.643011162660950042, 34.66104346484419096 ) ) ;
#33517 = CARTESIAN_POINT ( 'NONE',  ( 5.076923076923075762, -13.04860791097971706, 34.73218667398347037 ) ) ;
#33516 = CARTESIAN_POINT ( 'NONE',  ( 6.130791807824786943, -11.71459661697925903, 32.44059661609676937 ) ) ;
#33518 = B_SPLINE_CURVE_WITH_KNOTS ( 'NONE', 3,
 ( #81929, #19773, #75169, #27415, #53097, #67964, #67076, #6266, #5374, #32843 ),
 .UNSPECIFIED., .F., .F.,
 ( 4, 2, 2, 2, 4 ),
 ( 0.000000000000000000, 0.0001954339857564070949, 0.0003908679715128141898, 0.0005863019572692212576, 0.0007817359430256283796 ),
 .UNSPECIFIED. ) ;
#33519 = DIRECTION ( 'NONE',  ( 0.000000000000000000, -2.546383084002652634E-16, -1.000000000000000000 ) ) ;
#33520 = B_SPLINE_CURVE_WITH_KNOTS ( 'NONE', 3,
 ( #28264, #1235, #1685, #48984, #76464, #11549, #79113, #57506, #31827, #59281 ),
 .UNSPECIFIED., .F., .F.,
 ( 4, 2, 2, 2, 4 ),
 ( 0.0007817359430256346680, 0.0009771253907250002264, 0.001172514838424365893, 0.001367904286123731560, 0.001563293733823104166 ),
 .UNSPECIFIED. ) ;
#33521 = CARTESIAN_POINT ( 'NONE',  ( 1.944543648262996083, -5.555456351736983045, 18.06250000000000355 ) ) ;
#33522 = ORIENTED_EDGE ( 'NONE', *, *, #20039, .T. ) ;
#33523 = EDGE_CURVE ( 'NONE', #21721, #68660, #32254, .T. ) ;
#33524 = FACE_OUTER_BOUND ( 'NONE', #88973, .T. ) ;
#33525 = ORIENTED_EDGE ( 'NONE', *, *, #54802, .T. ) ;
#33526 = ORIENTED_EDGE ( 'NONE', *, *, #83797, .T. ) ;
#33527 = ADVANCED_FACE ( 'NONE', ( #71224 ), #57721, .F. ) ;
#33528 = CARTESIAN_POINT ( 'NONE',  ( -11.47320639894870276, -2.379036618887895305, 30.90682066428158592 ) ) ;
#33529 = VERTEX_POINT ( 'NONE', #9972 ) ;
#33530 = CARTESIAN_POINT ( 'NONE',  ( 14.05766907039934210, -8.432397168068783699, 34.66272746175022945 ) ) ;
#33531 = CARTESIAN_POINT ( 'NONE',  ( 1.799775606325937360E-14, -10.25000000000000000, 19.78125000000000000 ) ) ;
#33532 = CARTESIAN_POINT ( 'NONE',  ( 14.30769230769231015, -11.16473453929635440, 33.15142922261926373 ) ) ;
#33533 = CARTESIAN_POINT ( 'NONE',  ( 5.750023269057647823, -11.28823185664190376, 33.01397839955799896 ) ) ;
#33534 = CARTESIAN_POINT ( 'NONE',  ( -0.2115929431903192381, -5.852078868378310261, 34.47109172314383585 ) ) ;
#33535 = CARTESIAN_POINT ( 'NONE',  ( -8.546451227962359454, -5.114059244376869984, 34.14424750095245287 ) ) ;
#33536 = CARTESIAN_POINT ( 'NONE',  ( -0.4615384615384611200, -11.91647553114624181, 32.58852847137148245 ) ) ;
#33537 = FACE_OUTER_BOUND ( 'NONE', #79768, .T. ) ;
#33538 = CARTESIAN_POINT ( 'NONE',  ( 6.923076923076800782, -12.51329471203414379, 31.30864560766407578 ) ) ;
#33539 = CARTESIAN_POINT ( 'NONE',  ( 10.61538461538461675, -9.780366693483667717, 34.19971097300155094 ) ) ;
#33540 = CARTESIAN_POINT ( 'NONE',  ( -17.07692307692319744, -4.320704448113951379, 33.92786785259630022 ) ) ;
#33541 = ADVANCED_FACE ( 'NONE', ( #37439 ), #81118, .F. ) ;
#33542 = CARTESIAN_POINT ( 'NONE',  ( 5.934729999443682402, -3.643525952247789412, 33.31231777344662959 ) ) ;
#33543 = CIRCLE ( 'NONE', #76666, 4.000000000000000000 ) ;
#33544 = VECTOR ( 'NONE', #54831, 1000.000000000000000 ) ;
#33545 = ORIENTED_EDGE ( 'NONE', *, *, #31598, .T. ) ;
#33546 = ORIENTED_EDGE ( 'NONE', *, *, #37887, .T. ) ;
#33547 = CARTESIAN_POINT ( 'NONE',  ( 14.17700170458200581, -8.191372820521381826, 34.95448215188423546 ) ) ;
#33548 = DIRECTION ( 'NONE',  ( 0.000000000000000000, -6.938893903907222067E-15, 1.000000000000000000 ) ) ;
#33549 = DIRECTION ( 'NONE',  ( -1.000000000000000000, -0.000000000000000000, -0.000000000000000000 ) ) ;
#33550 = CARTESIAN_POINT ( 'NONE',  ( 12.46153846153833911, -6.026961402154118019, 34.52809138561165270 ) ) ;
#33552 = EDGE_CURVE ( 'NONE', #47571, #66205, #39243, .T. ) ;
#33551 = CARTESIAN_POINT ( 'NONE',  ( -12.46153846153846168, -2.833524468853757305, 32.15551576947925838 ) ) ;
#33553 = VECTOR ( 'NONE', #50876, 1000.000000000000000 ) ;
#33554 = CARTESIAN_POINT ( 'NONE',  ( -13.45069776397551742, -10.67929555188718460, 33.92786785259543336 ) ) ;
#33555 = CARTESIAN_POINT ( 'NONE',  ( 13.38461538461526601, -6.026961402154118019, 34.52809138561165270 ) ) ;
#33556 = EDGE_CURVE ( 'NONE', #12929, #58001, #18521, .T. ) ;
#33557 = ADVANCED_FACE ( 'NONE', ( #80223 ), #5895, .T. ) ;
#33558 = ORIENTED_EDGE ( 'NONE', *, *, #60998, .T. ) ;
#33559 = CARTESIAN_POINT ( 'NONE',  ( -7.846153846153844924, -9.780366693483667717, 34.19971097300155094 ) ) ;
#33560 = VERTEX_POINT ( 'NONE', #81559 ) ;
#33561 = EDGE_CURVE ( 'NONE', #34382, #77626, #35432, .T. ) ;
#33562 = ORIENTED_EDGE ( 'NONE', *, *, #4202, .T. ) ;
#33563 = CARTESIAN_POINT ( 'NONE',  ( 5.207448778686639024, -8.586989748646452369, 34.63063291749215011 ) ) ;
#33564 = CARTESIAN_POINT ( 'NONE',  ( -7.846153846153844924, -2.721908614388771852, 31.22303859784724978 ) ) ;
#33565 = CARTESIAN_POINT ( 'NONE',  ( 14.30769230769218758, -5.219633306517616589, 34.19971097300220464 ) ) ;
#33566 = CARTESIAN_POINT ( 'NONE',  ( 4.023155550735846298, -6.369640206132550553, 34.87707690430378449 ) ) ;
#33567 = DIRECTION ( 'NONE',  ( 0.000000000000000000, 0.4999999999999985567, 0.8660254037844395958 ) ) ;
#33568 = ORIENTED_EDGE ( 'NONE', *, *, #79894, .T. ) ;
#33569 = AXIS2_PLACEMENT_3D ( 'NONE', #7548, #48514, #75127 ) ;
#33570 = AXIS2_PLACEMENT_3D ( 'NONE', #73564, #65888, #17266 ) ;
#33571 = VERTEX_POINT ( 'NONE', #33802 ) ;
#33572 = ORIENTED_EDGE ( 'NONE', *, *, #31233, .F. ) ;
#33573 = ORIENTED_EDGE ( 'NONE', *, *, #79189, .T. ) ;
#33574 = CARTESIAN_POINT ( 'NONE',  ( -6.065270000556319374, -5.094484230520674117, 34.41647553114621161 ) ) ;
#33575 = DIRECTION ( 'NONE',  ( -1.000000000000000000, 0.000000000000000000, 0.000000000000000000 ) ) ;
#33576 = CARTESIAN_POINT ( 'NONE',  ( 4.219101293358988869, -12.16647553114626490, 32.15551576947920864 ) ) ;
#33577 = CYLINDRICAL_SURFACE ( 'NONE', #51350, 0.2499999999999997502 ) ;
#33578 = CARTESIAN_POINT ( 'NONE',  ( -15.16470189741915675, -9.058645607665452459, 34.76329471203371924 ) ) ;
#33579 = CARTESIAN_POINT ( 'NONE',  ( 12.46153846153833911, -3.083524468854526912, 32.58852847137268327 ) ) ;
#33580 = ORIENTED_EDGE ( 'NONE', *, *, #21248, .T. ) ;
#33581 = VERTEX_POINT ( 'NONE', #87437 ) ;
#33582 = ORIENTED_EDGE ( 'NONE', *, *, #23491, .F. ) ;
#33584 = VERTEX_POINT ( 'NONE', #40136 ) ;
#33583 = CARTESIAN_POINT ( 'NONE',  ( -10.61538461538461320, -11.69971097300155272, 32.46337939537588113 ) ) ;
#33585 = CARTESIAN_POINT ( 'NONE',  ( 17.32686848630112308, -10.92531984108285492, 33.72920026020278073 ) ) ;
#33586 = CARTESIAN_POINT ( 'NONE',  ( -4.826977558574935045, -11.37275283266503756, 32.91324779482534524 ) ) ;
#33587 = CARTESIAN_POINT ( 'NONE',  ( -1.553300858899125059, -3.750000000000009326, 22.82812500000000355 ) ) ;
#33588 = EDGE_LOOP ( 'NONE', ( #36471, #70973, #15883, #12294 ) ) ;
#33589 = CARTESIAN_POINT ( 'NONE',  ( -1.319360245102545459, -11.67786785259547777, 32.92929555188713664 ) ) ;
#33590 = ORIENTED_EDGE ( 'NONE', *, *, #27913, .T. ) ;
#33591 = CARTESIAN_POINT ( 'NONE',  ( -14.30769230769230660, -12.78798330534102767, 29.49999999999997868 ) ) ;
#33592 = AXIS2_PLACEMENT_3D ( 'NONE', #38236, #87337, #67050 ) ;
#33593 = FACE_BOUND ( 'NONE', #73238, .T. ) ;
#33594 = LINE ( 'NONE', #73245, #30246 ) ;
#33595 = VECTOR ( 'NONE', #70577, 1000.000000000000000 ) ;
#33596 = CYLINDRICAL_SURFACE ( 'NONE', #10314, 0.2499999999999994726 ) ;
#33597 = ORIENTED_EDGE ( 'NONE', *, *, #37589, .F. ) ;
#33598 = FACE_OUTER_BOUND ( 'NONE', #18968, .T. ) ;
#33599 = CARTESIAN_POINT ( 'NONE',  ( -14.17716660592874334, -2.619367082507849442, 30.83698974864643461 ) ) ;
#33600 = CARTESIAN_POINT ( 'NONE',  ( 14.17700170458200404, -9.084618155246140248, 34.75535874321725771 ) ) ;
#33601 = ORIENTED_EDGE ( 'NONE', *, *, #43239, .T. ) ;
#33602 = CYLINDRICAL_SURFACE ( 'NONE', #86158, 0.2500000000000008882 ) ;
#33603 = CARTESIAN_POINT ( 'NONE',  ( -3.903900744468109529, -10.18230066228895758, 34.26354781536631577 ) ) ;
#33604 = CARTESIAN_POINT ( 'NONE',  ( -12.68502340526241312, -12.24155766932282496, 31.33739205006857986 ) ) ;
#33605 = CARTESIAN_POINT ( 'NONE',  ( 10.61538461538461675, -6.189225973068211317, 35.74407628777942847 ) ) ;
#33606 = CARTESIAN_POINT ( 'NONE',  ( 8.068933387422253745, -3.236590943229497697, 32.36255958852954251 ) ) ;
#33607 = FACE_BOUND ( 'NONE', #3527, .T. ) ;
#33609 = DIRECTION ( 'NONE',  ( -1.000000000000000000, 0.000000000000000000, 0.000000000000000000 ) ) ;
#33608 = CARTESIAN_POINT ( 'NONE',  ( 1.634615384615323297, -7.565270000091922853, 34.99999999999999289 ) ) ;
#33610 = CARTESIAN_POINT ( 'NONE',  ( -7.846153846153844924, -1.367168528481310208, 33.57946703557072254 ) ) ;
#33612 = CARTESIAN_POINT ( 'NONE',  ( -2.057637887778852814, -12.41089969410671223, 31.60739465890703670 ) ) ;
#33611 = CARTESIAN_POINT ( 'NONE',  ( -8.546219417617917813, -11.76359900205217457, 32.36225158514719880 ) ) ;
#33613 = CARTESIAN_POINT ( 'NONE',  ( -8.769230769230890843, -3.835265460704628371, 33.15142922262033665 ) ) ;
#33614 = CARTESIAN_POINT ( 'NONE',  ( 2.750000000000001332, -7.438900925035452083, 17.96688170625848713 ) ) ;
#33615 = ORIENTED_EDGE ( 'NONE', *, *, #77302, .T. ) ;
#33616 = CARTESIAN_POINT ( 'NONE',  ( -7.053768389744481837, -8.999036380462719364, 34.52022231692819076 ) ) ;
#33617 = ORIENTED_EDGE ( 'NONE', *, *, #59328, .T. ) ;
#33618 = EDGE_CURVE ( 'NONE', #4333, #60674, #11764, .T. ) ;
#33619 = CARTESIAN_POINT ( 'NONE',  ( 0.3954550505825804030, -6.386643153685125363, 34.62446782046654903 ) ) ;
#33620 = EDGE_LOOP ( 'NONE', ( #67711, #43812 ) ) ;
#33621 = LINE ( 'NONE', #73274, #65678 ) ;
#33622 = CARTESIAN_POINT ( 'NONE',  ( 14.05769230769230838, -7.500000000000001776, 35.00000000000000000 ) ) ;
#33624 = EDGE_LOOP ( 'NONE', ( #11329, #48924, #1346, #85322 ) ) ;
#33623 = CARTESIAN_POINT ( 'NONE',  ( 14.98076923076922995, -2.499999999999999556, 29.81609845454691765 ) ) ;
#33625 = LINE ( 'NONE', #66523, #67316 ) ;
#33626 = CARTESIAN_POINT ( 'NONE',  ( 5.933917620639864943, -10.67929555188718460, 33.92786785259543336 ) ) ;
#33627 = CARTESIAN_POINT ( 'NONE',  ( -2.724691934501232371, -8.700186371490559623, 17.26375670625849068 ) ) ;
#33628 = CARTESIAN_POINT ( 'NONE',  ( 14.24242186173153435, -10.90142922261923886, 33.41473453929638993 ) ) ;
#33629 = CARTESIAN_POINT ( 'NONE',  ( -7.053767526187231240, -12.62707690430377383, 30.88035979386743435 ) ) ;
#33630 = DIRECTION ( 'NONE',  ( -0.000000000000000000, 0.3420201433256694901, -0.9396926207859082059 ) ) ;
#33631 = CARTESIAN_POINT ( 'NONE',  ( 12.71153846153846168, -2.249999999999998668, 29.75000000000000355 ) ) ;
#33632 = CARTESIAN_POINT ( 'NONE',  ( 2.307692307692309264, -1.466349020453238561, 30.81389545987213907 ) ) ;
#33633 = LINE ( 'NONE', #61532, #16695 ) ;
#33634 = CARTESIAN_POINT ( 'NONE',  ( 3.724691934501251023, -9.114399933863618131, 23.54874329374151642 ) ) ;
#33635 = CARTESIAN_POINT ( 'NONE',  ( 9.757453471639660592, -7.750023238201979581, 34.74374492549440419 ) ) ;
#33636 = ADVANCED_FACE ( 'NONE', ( #88334 ), #25272, .T. ) ;
#33637 = CARTESIAN_POINT ( 'NONE',  ( -9.019207513279361876, -2.920706130388546651, 32.31842814019191223 ) ) ;
#33638 = ORIENTED_EDGE ( 'NONE', *, *, #19777, .F. ) ;
#33639 = CARTESIAN_POINT ( 'NONE',  ( -5.198717948717948012, -11.50000000000000000, 29.75000000000000355 ) ) ;
#33640 = CARTESIAN_POINT ( 'NONE',  ( -1.492201783934593573, -3.724691934501250135, 19.32999329374151642 ) ) ;
#33641 = B_SPLINE_CURVE_WITH_KNOTS ( 'NONE', 3,
 ( #86277, #50229, #37171, #44809, #17354, #57439, #64188, #71396, #11044, #16024 ),
 .UNSPECIFIED., .F., .F.,
 ( 4, 2, 2, 2, 4 ),
 ( 0.0007817246256747451124, 0.0009771112852218879000, 0.001172497944769030796, 0.001367884604316173692, 0.001563271263863316588 ),
 .UNSPECIFIED. ) ;
#33642 = LINE ( 'NONE', #6611, #64867 ) ;
#33643 = CARTESIAN_POINT ( 'NONE',  ( 0.4615384615384611200, -1.044019251281081972, 31.83374038241031911 ) ) ;
#33644 = ORIENTED_EDGE ( 'NONE', *, *, #6854, .F. ) ;
#33645 = CARTESIAN_POINT ( 'NONE',  ( 7.053602624840485724, -8.586989748646452369, 34.63063291749215011 ) ) ;
#33646 = DIRECTION ( 'NONE',  ( -1.000000000000000000, 0.000000000000000000, -0.000000000000000000 ) ) ;
#33648 = ORIENTED_EDGE ( 'NONE', *, *, #37573, .F. ) ;
#33647 = CARTESIAN_POINT ( 'NONE',  ( 1.318533005255250634, -5.471508081941601986, 34.59228464037088457 ) ) ;
#33649 = CARTESIAN_POINT ( 'NONE',  ( 12.68454981315131391, -12.39991518177334129, 30.74647679643404530 ) ) ;
#33650 = CARTESIAN_POINT ( 'NONE',  ( 9.692307692307695177, -8.318370150425687726, 35.83090037661290239 ) ) ;
#33651 = CARTESIAN_POINT ( 'NONE',  ( -12.52680846209478460, -5.094484230520674117, 34.41647553114621161 ) ) ;
#33652 = ORIENTED_EDGE ( 'NONE', *, *, #32772, .F. ) ;
#33653 = CARTESIAN_POINT ( 'NONE',  ( 2.084207383127977042, -4.225889041578354544, 33.85425143139329407 ) ) ;
#33654 = CARTESIAN_POINT ( 'NONE',  ( -18.00000000000012079, -12.27809138561165270, 31.22303859784587132 ) ) ;
#33655 = ADVANCED_FACE ( 'NONE', ( #26604 ), #20297, .F. ) ;
#33656 = ADVANCED_FACE ( 'NONE', ( #19846 ), #75242, .F. ) ;
#33657 = CARTESIAN_POINT ( 'NONE',  ( 19.99999999999996803, 15.00000000000000711, 13.00000000000000178 ) ) ;
#33658 = ORIENTED_EDGE ( 'NONE', *, *, #26712, .F. ) ;
#33659 = ORIENTED_EDGE ( 'NONE', *, *, #25470, .F. ) ;
#33660 = VERTEX_POINT ( 'NONE', #13093 ) ;
#33662 = AXIS2_PLACEMENT_3D ( 'NONE', #38870, #26675, #66778 ) ;
#33661 = B_SPLINE_CURVE_WITH_KNOTS ( 'NONE', 3,
 ( #76479, #76921, #70156, #84137, #15665, #43135, #52976, #66954, #5248, #24176 ),
 .UNSPECIFIED., .F., .F.,
 ( 4, 2, 2, 2, 4 ),
 ( 0.0007817359430256358606, 0.0009771253907250034790, 0.001172514838424371098, 0.001367904286123738716, 0.001563293733823106334 ),
 .UNSPECIFIED. ) ;
#33663 = VERTEX_POINT ( 'NONE', #13531 ) ;
#33664 = CIRCLE ( 'NONE', #60983, 4.000000000000000000 ) ;
#33665 = CARTESIAN_POINT ( 'NONE',  ( -9.757578138268467427, -2.892918686051582977, 31.69288490824015980 ) ) ;
#33666 = DIRECTION ( 'NONE',  ( -0.000000000000000000, -0.000000000000000000, -1.000000000000000000 ) ) ;
#33667 = EDGE_CURVE ( 'NONE', #14549, #54915, #73912, .T. ) ;
#33668 = CARTESIAN_POINT ( 'NONE',  ( -16.40382289789474157, -2.920706130388546651, 32.31842814019191223 ) ) ;
#33669 = FACE_OUTER_BOUND ( 'NONE', #56253, .T. ) ;
#33670 = CARTESIAN_POINT ( 'NONE',  ( -17.93129618099654010, -7.250074905162718686, 34.99404781541490195 ) ) ;
#33671 = EDGE_LOOP ( 'NONE', ( #1411, #47013, #3247, #53215 ) ) ;
#33672 = ORIENTED_EDGE ( 'NONE', *, *, #23452, .T. ) ;
#33673 = B_SPLINE_CURVE_WITH_KNOTS ( 'NONE', 3,
 ( #47987, #34482, #28162, #55630, #76352, #75466, #15106, #42578, #14211, #44776 ),
 .UNSPECIFIED., .F., .F.,
 ( 4, 2, 2, 2, 4 ),
 ( 0.0007817246256747504250, 0.0009771112852218954894, 0.001172497944769040554, 0.001367884604316185401, 0.001563271263863330466 ),
 .UNSPECIFIED. ) ;
#33674 = B_SPLINE_CURVE_WITH_KNOTS ( 'NONE', 3,
 ( #75039, #20957, #40369, #48429, #75915, #74591, #12879, #32705, #87677, #53416 ),
 .UNSPECIFIED., .F., .F.,
 ( 4, 2, 2, 2, 4 ),
 ( 0.0007817246256747516176, 0.0009771112852218965736, 0.001172497944769041421, 0.001367884604316186269, 0.001563271263863331333 ),
 .UNSPECIFIED. ) ;
#33675 = ORIENTED_EDGE ( 'NONE', *, *, #14522, .T. ) ;
#33677 = ORIENTED_EDGE ( 'NONE', *, *, #23485, .F. ) ;
#33676 = CARTESIAN_POINT ( 'NONE',  ( -7.053224892808621860, -2.647304123082328875, 31.75400227202885262 ) ) ;
#33678 = DIRECTION ( 'NONE',  ( -0.000000000000000000, 0.9848077530122085754, -0.1736481776669273613 ) ) ;
#33679 = CARTESIAN_POINT ( 'NONE',  ( 5.933917620639864943, -12.62096338111211580, 30.90682066428152197 ) ) ;
#33680 = PLANE ( 'NONE',  #75263 ) ;
#33681 = CARTESIAN_POINT ( 'NONE',  ( -5.933931648997561759, -4.098570777380720287, 33.41473453929635440 ) ) ;
#33682 = VERTEX_POINT ( 'NONE', #53630 ) ;
#33683 = ORIENTED_EDGE ( 'NONE', *, *, #69657, .F. ) ;
#33684 = VECTOR ( 'NONE', #8346, 1000.000000000000000 ) ;
#33685 = EDGE_LOOP ( 'NONE', ( #46171, #45262, #33573, #24264 ) ) ;
#33686 = DIRECTION ( 'NONE',  ( -0.000000000000000000, -0.9396926207859092051, -0.3420201433256662704 ) ) ;
#33688 = ORIENTED_EDGE ( 'NONE', *, *, #76926, .T. ) ;
#33687 = DIRECTION ( 'NONE',  ( -0.000000000000000000, 0.5000000000000011102, -0.8660254037844380415 ) ) ;
#33689 = CARTESIAN_POINT ( 'NONE',  ( -2.057746789344164995, -8.433404298154334455, 34.66254593164985920 ) ) ;
#33690 = LINE ( 'NONE', #22820, #26361 ) ;
#33691 = VERTEX_POINT ( 'NONE', #52731 ) ;
#33692 = CARTESIAN_POINT ( 'NONE',  ( 6.000000000000001776, -1.951392089020283160, 34.73218667398347748 ) ) ;
#33693 = CARTESIAN_POINT ( 'NONE',  ( 9.757500680602349874, -2.255955759149235629, 29.99999999999988987 ) ) ;
#33694 = CARTESIAN_POINT ( 'NONE',  ( 12.46153846153833911, -9.528491918059723176, 34.59228464037033035 ) ) ;
#33695 = FACE_BOUND ( 'NONE', #72880, .T. ) ;
#33696 = CARTESIAN_POINT ( 'NONE',  ( 10.61538461538449596, -10.21337939537710326, 33.94971097300076224 ) ) ;
#33697 = CARTESIAN_POINT ( 'NONE',  ( 9.320512820512821150, -11.00000000000000000, 28.25000000000000000 ) ) ;
#33698 = DIRECTION ( 'NONE',  ( -0.000000000000000000, 1.000000000000000000, 3.491481338843133355E-15 ) ) ;
#33700 = CARTESIAN_POINT ( 'NONE',  ( 5.076923076923075762, -9.780366693483667717, 34.19971097300155094 ) ) ;
#33699 = CARTESIAN_POINT ( 'NONE',  ( 9.692307692307695177, -3.050289026998446396, 32.03036669348365706 ) ) ;
#33701 = DIRECTION ( 'NONE',  ( -0.000000000000000000, -0.1736481776669307198, -0.9848077530122080203 ) ) ;
#33702 = CARTESIAN_POINT ( 'NONE',  ( -0.5922299282060231596, -3.530157926970578508, 32.79014554554150607 ) ) ;
#33703 = ORIENTED_EDGE ( 'NONE', *, *, #76983, .T. ) ;
#33704 = CARTESIAN_POINT ( 'NONE',  ( 2.438218009455872526, -6.852161475712352789, 34.70806712695775786 ) ) ;
#33705 = ORIENTED_EDGE ( 'NONE', *, *, #1889, .F. ) ;
#33706 = EDGE_CURVE ( 'NONE', #16142, #23267, #32919, .T. ) ;
#33707 = B_SPLINE_CURVE_WITH_KNOTS ( 'NONE', 3,
 ( #18040, #86050, #79738, #72977, #45496, #11276, #38749, #66212, #60503, #52848 ),
 .UNSPECIFIED., .F., .F.,
 ( 4, 2, 2, 2, 4 ),
 ( 0.000000000000000000, 0.0001954339857564093175, 0.0003908679715128186350, 0.0005863019572692279796, 0.0007817359430256372700 ),
 .UNSPECIFIED. ) ;
#33708 = CARTESIAN_POINT ( 'NONE',  ( -6.857008572074484221, -4.786620604624113540, 33.94971097300155805 ) ) ;
#33709 = CARTESIAN_POINT ( 'NONE',  ( -14.53117725141625627, -5.113361153441934093, 34.14387501736622710 ) ) ;
#33710 = CARTESIAN_POINT ( 'NONE',  ( -7.715363405186898227, -2.295524264805589354, 30.44142389570982488 ) ) ;
#33711 = ORIENTED_EDGE ( 'NONE', *, *, #39736, .F. ) ;
#33712 = DIRECTION ( 'NONE',  ( 0.000000000000000000, 0.7660444431189807890, 0.6427876096865361433 ) ) ;
#33713 = CARTESIAN_POINT ( 'NONE',  ( -15.10024379253558635, -12.70449254468099198, 30.44128974285582956 ) ) ;
#33714 = AXIS2_PLACEMENT_3D ( 'NONE', #1009, #35230, #56397 ) ;
#33715 = FACE_BOUND ( 'NONE', #79491, .T. ) ;
#33717 = FACE_OUTER_BOUND ( 'NONE', #40683, .T. ) ;
#33716 = CARTESIAN_POINT ( 'NONE',  ( -14.30769230769230660, -3.937682226553329556, 33.60647404775216529 ) ) ;
#33718 = CARTESIAN_POINT ( 'NONE',  ( -6.923076923076922462, -2.499999999999998668, 29.75000000000001421 ) ) ;
#33719 = CARTESIAN_POINT ( 'NONE',  ( 0.5276057948885366500, -4.661471528628508665, 34.16647553114624003 ) ) ;
#33721 = CARTESIAN_POINT ( 'NONE',  ( -14.37301522318448299, -7.749976743299138882, 34.99404534957040624 ) ) ;
#33720 =( NAMED_UNIT ( * ) PLANE_ANGLE_UNIT ( ) SI_UNIT ( $, .RADIAN. ) );
#33722 = CARTESIAN_POINT ( 'NONE',  ( 3.724691934501232815, -5.885600066136343678, 16.63875670625849068 ) ) ;
#33723 = VERTEX_POINT ( 'NONE', #82003 ) ;
#33724 = VECTOR ( 'NONE', #42202, 1000.000000000000114 ) ;
#33725 = ORIENTED_EDGE ( 'NONE', *, *, #1970, .T. ) ;
#33726 = EDGE_CURVE ( 'NONE', #22286, #86499, #22510, .T. ) ;
#33727 = CARTESIAN_POINT ( 'NONE',  ( 23.49999999999998934, 9.000000000000024869, 28.74999999999999645 ) ) ;
#33728 = CARTESIAN_POINT ( 'NONE',  ( -17.77698715590660328, -3.395485233115134172, 33.02377354290275946 ) ) ;
#33729 = CARTESIAN_POINT ( 'NONE',  ( -5.999999999999998224, -13.75783147151868846, 33.36296068462461051 ) ) ;
#33730 = CARTESIAN_POINT ( 'NONE',  ( 6.673100192134571174, -12.17611988154120972, 31.52148481390971213 ) ) ;
#33731 = EDGE_CURVE ( 'NONE', #64564, #41090, #80607, .T. ) ;
#33732 = CARTESIAN_POINT ( 'NONE',  ( 5.299702745901141654, -3.563462043263029955, 33.22394488606062879 ) ) ;
#33733 = CARTESIAN_POINT ( 'NONE',  ( 2.320192649118979489E-14, -11.25000000000000000, 22.28125000000000355 ) ) ;
#33734 = CARTESIAN_POINT ( 'NONE',  ( 1.384615384615386802, -11.11383981884818262, 36.00935417666054406 ) ) ;
#33735 = FACE_OUTER_BOUND ( 'NONE', #49686, .T. ) ;
#33736 = CARTESIAN_POINT ( 'NONE',  ( 7.596177102105255763, -5.643011162660950042, 34.66104346484419096 ) ) ;
#33737 = CARTESIAN_POINT ( 'NONE',  ( -12.46153846153846168, -1.629998284177014645, 34.34916445242399163 ) ) ;
#33738 = CARTESIAN_POINT ( 'NONE',  ( 16.15384615384615330, -1.129524287112498415, 32.06866353760679544 ) ) ;
#33739 = CARTESIAN_POINT ( 'NONE',  ( -17.07692307692307665, -2.499999999999998668, 29.75000000000001421 ) ) ;
#33740 = CARTESIAN_POINT ( 'NONE',  ( 6.856993512121044354, -11.16473453929635440, 33.15142922261925662 ) ) ;
#33741 = CARTESIAN_POINT ( 'NONE',  ( -8.769230769230892619, -11.67786785259630911, 32.92929555188603530 ) ) ;
#33742 = EDGE_CURVE ( 'NONE', #81743, #5990, #61705, .T. ) ;
#33743 = CARTESIAN_POINT ( 'NONE',  ( 17.07692307692295586, -12.70778746994576025, 30.41441678777401236 ) ) ;
#33744 = VERTEX_POINT ( 'NONE', #7225 ) ;
#33745 = CARTESIAN_POINT ( 'NONE',  ( 1.254468175177166689, -2.619462340734462380, 30.83744416345203021 ) ) ;
#33746 = CARTESIAN_POINT ( 'NONE',  ( -6.923076923077044142, -12.46129190930018460, 30.37095296980731973 ) ) ;
#33747 = CARTESIAN_POINT ( 'NONE',  ( 1.077988221561497539, -10.27530806549875386, 17.45499329374151642 ) ) ;
#33748 = EDGE_CURVE ( 'NONE', #18312, #2392, #54962, .T. ) ;
#33749 = CARTESIAN_POINT ( 'NONE',  ( 5.142990410273152513, -9.905515769479277921, 34.41647553114623292 ) ) ;
#33750 = LINE ( 'NONE', #4953, #65657 ) ;
#33751 = CARTESIAN_POINT ( 'NONE',  ( -8.769230769230768274, -11.91647553114624181, 32.58852847137148245 ) ) ;
#33753 = VERTEX_POINT ( 'NONE', #83329 ) ;
#33752 = CARTESIAN_POINT ( 'NONE',  ( -1.161604033002534342, -4.187068189119697692, 33.49521262558774026 ) ) ;
#33754 = CARTESIAN_POINT ( 'NONE',  ( -2.750000000000006217, -6.360912703474006946, 23.92187500000000355 ) ) ;
#33755 = DIRECTION ( 'NONE',  ( -0.000000000000000000, 0.3420201433256694346, -0.9396926207859080948 ) ) ;
#33756 = ORIENTED_EDGE ( 'NONE', *, *, #47288, .T. ) ;
#33757 = CARTESIAN_POINT ( 'NONE',  ( 10.61538461538461675, -2.499999999999998668, 29.50000000000001066 ) ) ;
#33758 = VECTOR ( 'NONE', #61523, 1000.000000000000000 ) ;
#33759 = CARTESIAN_POINT ( 'NONE',  ( 0.3954550505825801809, -2.721908614388771408, 31.22303859784724267 ) ) ;
#33760 = ORIENTED_EDGE ( 'NONE', *, *, #3526, .T. ) ;
#33761 = CARTESIAN_POINT ( 'NONE',  ( 3.230769230769231726, -4.786620604624113540, 33.94971097300155094 ) ) ;
#33762 = CARTESIAN_POINT ( 'NONE',  ( 2.307692307692186251, -8.656820664282941280, 34.87096338111179961 ) ) ;
#33763 = EDGE_CURVE ( 'NONE', #52641, #87211, #75669, .T. ) ;
#33764 = FACE_OUTER_BOUND ( 'NONE', #80954, .T. ) ;
#33765 = EDGE_LOOP ( 'NONE', ( #71648, #23787 ) ) ;
#33766 = EDGE_CURVE ( 'NONE', #22482, #58674, #78329, .T. ) ;
#33767 = VERTEX_POINT ( 'NONE', #13971 ) ;
#33768 = ORIENTED_EDGE ( 'NONE', *, *, #74852, .T. ) ;
#33769 = CARTESIAN_POINT ( 'NONE',  ( -17.86947456176635640, -5.070358843744208421, 34.40418822224088302 ) ) ;
#33770 = CARTESIAN_POINT ( 'NONE',  ( -5.076923076923075762, -6.435427911321262684, 35.78748833219616898 ) ) ;
#33771 = EDGE_CURVE ( 'NONE', #39, #7626, #41450, .T. ) ;
#33772 = DIRECTION ( 'NONE',  ( -0.000000000000000000, -0.9396926207859092051, -0.3420201433256662704 ) ) ;
#33773 = CARTESIAN_POINT ( 'NONE',  ( -1.384615384615383471, -11.35647404775217417, 33.31231777344666511 ) ) ;
#33774 = EDGE_CURVE ( 'NONE', #56271, #33346, #64448, .T. ) ;
#33775 = CARTESIAN_POINT ( 'NONE',  ( -2.557715544985271094, -5.851115903089112003, 34.47074536777953568 ) ) ;
#33776 = CARTESIAN_POINT ( 'NONE',  ( -4.403869391139119571, -6.695914987888143877, 34.68535235679833306 ) ) ;
#33777 = CARTESIAN_POINT ( 'NONE',  ( 13.63466969625370062, -3.136992222400443175, 32.19305428654138979 ) ) ;
#33778 = CARTESIAN_POINT ( 'NONE',  ( 16.08857615328983925, -12.70778746994557551, 30.41441678777548319 ) ) ;
#33779 = AXIS2_PLACEMENT_3D ( 'NONE', #37228, #84992, #31370 ) ;
#33780 = VERTEX_POINT ( 'NONE', #83776 ) ;
#33781 = VERTEX_POINT ( 'NONE', #8109 ) ;
#33783 = ORIENTED_EDGE ( 'NONE', *, *, #23229, .F. ) ;
#33782 = CARTESIAN_POINT ( 'NONE',  ( -17.14300648787895653, -9.780366693483667717, 34.19971097300155805 ) ) ;
#33784 = DIRECTION ( 'NONE',  ( -0.000000000000000000, -0.7660444431189791237, -0.6427876096865379196 ) ) ;
#33785 = CYLINDRICAL_SURFACE ( 'NONE', #25165, 0.2500000000000012212 ) ;
#33786 = ORIENTED_EDGE ( 'NONE', *, *, #66473, .F. ) ;
#33787 = CARTESIAN_POINT ( 'NONE',  ( 14.30769230769231015, -11.91647553114624181, 32.58852847137148245 ) ) ;
#33788 = ORIENTED_EDGE ( 'NONE', *, *, #20145, .F. ) ;
#33789 = CARTESIAN_POINT ( 'NONE',  ( 17.29970274590113632, -9.418065098278011860, 34.63729479722530158 ) ) ;
#33790 = ORIENTED_EDGE ( 'NONE', *, *, #78457, .T. ) ;
#33791 = CARTESIAN_POINT ( 'NONE',  ( -10.83821130786361664, -7.369208160676171460, 34.74850200257122879 ) ) ;
#33792 = EDGE_CURVE ( 'NONE', #17306, #61727, #35581, .T. ) ;
#33793 = ORIENTED_EDGE ( 'NONE', *, *, #20448, .T. ) ;
#33794 = LINE ( 'NONE', #18953, #4339 ) ;
#33795 = CARTESIAN_POINT ( 'NONE',  ( -8.899377978668987055, -2.882441371585227508, 31.66841991370172238 ) ) ;
#33796 = FACE_BOUND ( 'NONE', #75733, .T. ) ;
#33797 = CARTESIAN_POINT ( 'NONE',  ( 5.750023255951410839, -2.318417181685854978, 30.59732222474233865 ) ) ;
#33798 = CARTESIAN_POINT ( 'NONE',  ( 15.90386940979756503, -3.436278759898155677, 33.07459398097509506 ) ) ;
#33799 = EDGE_CURVE ( 'NONE', #22240, #19556, #22063, .T. ) ;
#33800 = CARTESIAN_POINT ( 'NONE',  ( 13.19230769230769340, -3.499999999999999556, 29.75000000000000355 ) ) ;
#33801 = CARTESIAN_POINT ( 'NONE',  ( 10.61538461538449418, -10.33852847137269571, 34.16647553114546554 ) ) ;
#33802 = CARTESIAN_POINT ( 'NONE',  ( 10.61538461538449596, -2.892918686052165622, 31.69288490824153470 ) ) ;
#33803 = CARTESIAN_POINT ( 'NONE',  ( -7.976844449264155479, -9.084618155246140248, 34.75535874321725771 ) ) ;
#33804 = DIRECTION ( 'NONE',  ( -0.000000000000000000, -0.9396926207859093161, -0.3420201433256663259 ) ) ;
#33805 = ORIENTED_EDGE ( 'NONE', *, *, #10063, .F. ) ;
#33806 = ORIENTED_EDGE ( 'NONE', *, *, #23416, .T. ) ;
#33807 = EDGE_CURVE ( 'NONE', #77497, #68692, #56960, .T. ) ;
#33808 = AXIS2_PLACEMENT_3D ( 'NONE', #72045, #85132, #58520 ) ;
#33810 = CARTESIAN_POINT ( 'NONE',  ( 2.530471848960718972, -10.81320215134717344, 33.49497208177562868 ) ) ;
#33809 = FACE_OUTER_BOUND ( 'NONE', #1570, .T. ) ;
#33811 = CARTESIAN_POINT ( 'NONE',  ( -3.903846153844733102, -7.500000000000154543, 35.00000000000007105 ) ) ;
#33812 = CARTESIAN_POINT ( 'NONE',  ( -3.930833309752757909, -9.172514111537584114, 34.72667873470787470 ) ) ;
#33813 = DIRECTION ( 'NONE',  ( 0.000000000000000000, 0.000000000000000000, -1.000000000000000000 ) ) ;
#33814 = CARTESIAN_POINT ( 'NONE',  ( 13.60762673622823726, -11.24521262558773493, 33.06293181088029343 ) ) ;
#33815 = ORIENTED_EDGE ( 'NONE', *, *, #60482, .F. ) ;
#33816 = CARTESIAN_POINT ( 'NONE',  ( -11.76138775597768138, -12.15238873228292071, 31.58232369045353849 ) ) ;
#33817 = CARTESIAN_POINT ( 'NONE',  ( 9.692307692307570832, -3.643525952248795718, 33.31231777344771672 ) ) ;
#33818 = CARTESIAN_POINT ( 'NONE',  ( -3.480792454990689233, -11.56360843649121861, 33.07473185843129926 ) ) ;
#33819 = CARTESIAN_POINT ( 'NONE',  ( -3.361459833879538728, -12.62707690430377383, 30.88035979386743435 ) ) ;
#33820 = EDGE_LOOP ( 'NONE', ( #19027, #18663, #41221, #8311 ) ) ;
#33821 = VERTEX_POINT ( 'NONE', #50401 ) ;
#33822 = VERTEX_POINT ( 'NONE', #58939 ) ;
#33823 = EDGE_CURVE ( 'NONE', #11728, #39, #55303, .T. ) ;
#33824 = CARTESIAN_POINT ( 'NONE',  ( 10.48469401227430708, -3.957541250942358424, 33.62499894934981626 ) ) ;
#33825 = ORIENTED_EDGE ( 'NONE', *, *, #71210, .T. ) ;
#33826 = CARTESIAN_POINT ( 'NONE',  ( 3.930361229281821966, -11.60425143139329940, 33.02411095842164457 ) ) ;
#33827 = CARTESIAN_POINT ( 'NONE',  ( 15.10062202133100939, -9.418419913701741919, 34.36755862841477693 ) ) ;
#33828 = CARTESIAN_POINT ( 'NONE',  ( -5.143006487878958310, -4.098570777380720287, 33.41473453929634729 ) ) ;
#33829 = EDGE_CURVE ( 'NONE', #79174, #60125, #83785, .T. ) ;
#33830 = DIRECTION ( 'NONE',  ( 0.000000000000000000, 0.000000000000000000, 1.000000000000000000 ) ) ;
#33831 = CARTESIAN_POINT ( 'NONE',  ( 14.53047184896071542, -4.387253974876679230, 33.66317474335728832 ) ) ;
#33832 = EDGE_LOOP ( 'NONE', ( #16945, #14899 ) ) ;
#33833 = CARTESIAN_POINT ( 'NONE',  ( 4.153846153846468603, -2.255955759149395501, 30.00000000000324363 ) ) ;
#33835 = VERTEX_POINT ( 'NONE', #24719 ) ;
#33834 = CARTESIAN_POINT ( 'NONE',  ( -13.31854703361294767, -4.098570777380720287, 33.41473453929635440 ) ) ;
#33836 = CARTESIAN_POINT ( 'NONE',  ( -5.076923076923075762, -2.292212530054420494, 30.41441678777542634 ) ) ;
#33837 = CARTESIAN_POINT ( 'NONE',  ( -2.557715544985271094, -9.271318131107980420, 34.42618302367067429 ) ) ;
#33839 = B_SPLINE_CURVE_WITH_KNOTS ( 'NONE', 3,
 ( #24192, #30074, #64728, #84591, #63853, #23306, #29638, #3027, #72821, #78249 ),
 .UNSPECIFIED., .F., .F.,
 ( 4, 2, 2, 2, 4 ),
 ( 0.0007817359430256293554, 0.0009771253907249941549, 0.001172514838424358954, 0.001367904286123723537, 0.001563293733823095276 ),
 .UNSPECIFIED. ) ;
#33838 = CYLINDRICAL_SURFACE ( 'NONE', #14180, 0.2500000000000002220 ) ;
#33840 = CARTESIAN_POINT ( 'NONE',  ( 9.915087233576100445, -10.81320215134717344, 33.49497208177562868 ) ) ;
#33842 = AXIS2_PLACEMENT_3D ( 'NONE', #83238, #20639, #83692 ) ;
#33841 = DIRECTION ( 'NONE',  ( 0.000000000000000000, 0.9396926207859126468, -0.3420201433256571111 ) ) ;
#33843 = CARTESIAN_POINT ( 'NONE',  ( -8.546217925137375104, -9.172514111537584114, 34.72667873470787470 ) ) ;
#33844 = CARTESIAN_POINT ( 'NONE',  ( -3.361460697436787104, -6.413092428213692742, 34.63065189839063152 ) ) ;
#33845 = CARTESIAN_POINT ( 'NONE',  ( -1.200186371490524317, -10.22469193450124791, 22.61124329374151287 ) ) ;
#33846 = ORIENTED_EDGE ( 'NONE', *, *, #34494, .F. ) ;
#33847 = B_SPLINE_CURVE_WITH_KNOTS ( 'NONE', 3,
 ( #28523, #22205, #84812, #84363, #16333, #28980, #43362, #36176, #2799, #8256 ),
 .UNSPECIFIED., .F., .F.,
 ( 4, 2, 2, 2, 4 ),
 ( 0.000000000000000000, 0.0001954339881912776238, 0.0003908679763825552477, 0.0005863019645738329257, 0.0007817359527651104954 ),
 .UNSPECIFIED. ) ;
#33848 = CARTESIAN_POINT ( 'NONE',  ( -7.173053667125515176, -10.82459398097509684, 33.81372124010185587 ) ) ;
#33849 = CARTESIAN_POINT ( 'NONE',  ( 12.46153846153846168, -4.661471528628507777, 34.16647553114623292 ) ) ;
#33850 = VERTEX_POINT ( 'NONE', #44973 ) ;
#33851 = EDGE_LOOP ( 'NONE', ( #45380, #52767, #72850, #22942, #7002, #42246 ) ) ;
#33852 = CARTESIAN_POINT ( 'NONE',  ( 2.057692307692309708, -7.500000000000001776, 35.00000000000000000 ) ) ;
#33853 = CARTESIAN_POINT ( 'NONE',  ( -5.207614543590634248, -6.413092428213692742, 34.63065189839063152 ) ) ;
#33854 = VECTOR ( 'NONE', #51699, 1000.000000000000114 ) ;
#33855 = CARTESIAN_POINT ( 'NONE',  ( 1.384615384615386802, -3.513871655860378418, 32.76840700105978499 ) ) ;
#33856 = CARTESIAN_POINT ( 'NONE',  ( 7.146088274689773812, -5.667800583137508674, 34.40243808032445827 ) ) ;
#33857 = CARTESIAN_POINT ( 'NONE',  ( -14.43784027742400866, -3.069018819979302926, 32.56621877034667278 ) ) ;
#33858 = ORIENTED_EDGE ( 'NONE', *, *, #3092, .T. ) ;
#33859 = CARTESIAN_POINT ( 'NONE',  ( 12.39628852976437656, -2.255955759149247619, 30.00000000000013856 ) ) ;
#33860 = EDGE_CURVE ( 'NONE', #45495, #67170, #27992, .T. ) ;
#33861 = CARTESIAN_POINT ( 'NONE',  ( -14.55771554498527287, -2.823816976329319051, 31.52131813110795733 ) ) ;
#33862 = DIRECTION ( 'NONE',  ( -0.000000000000000000, 0.9396926207859093161, -0.3420201433256663259 ) ) ;
#33863 = ORIENTED_EDGE ( 'NONE', *, *, #86036, .T. ) ;
#33864 = CARTESIAN_POINT ( 'NONE',  ( -9.019230769230768274, -7.433932668274256805, 35.00000000000000711 ) ) ;
#33865 = EDGE_CURVE ( 'NONE', #69118, #18312, #61098, .T. ) ;
#33866 = ORIENTED_EDGE ( 'NONE', *, *, #22430, .T. ) ;
#33867 = FACE_OUTER_BOUND ( 'NONE', #25872, .T. ) ;
#33868 = CARTESIAN_POINT ( 'NONE',  ( 11.28848479441295005, -2.544273027872575366, 31.48422191005632342 ) ) ;
#33869 = ORIENTED_EDGE ( 'NONE', *, *, #69907, .F. ) ;
#33870 = EDGE_CURVE ( 'NONE', #68708, #83978, #48362, .T. ) ;
#33871 = CARTESIAN_POINT ( 'NONE',  ( 0.6843180028068700516, -4.387253974876678342, 33.66317474335728832 ) ) ;
#33872 = CARTESIAN_POINT ( 'NONE',  ( 16.15384615384615330, -12.78798330534102945, 29.74999999999997868 ) ) ;
#33873 = CARTESIAN_POINT ( 'NONE',  ( 1.134592147322421418, -4.335965774309649134, 33.62209801155881905 ) ) ;
#33874 = VECTOR ( 'NONE', #51546, 1000.000000000000000 ) ;
#33875 = CARTESIAN_POINT ( 'NONE',  ( 11.31553457955468645, -12.38737895849757820, 31.66785238281580206 ) ) ;
#33876 = DIRECTION ( 'NONE',  ( 0.000000000000000000, 0.9396926207859126468, 0.3420201433256571111 ) ) ;
#33877 = B_SPLINE_CURVE_WITH_KNOTS ( 'NONE', 3,
 ( #80437, #86312, #16942, #85851, #3861, #79980, #66007, #24586, #87645, #73682 ),
 .UNSPECIFIED., .F., .F.,
 ( 4, 2, 2, 2, 4 ),
 ( 0.000000000000000000, 0.0001954311564186871184, 0.0003908623128373742367, 0.0005862934692560614093, 0.0007817246256747484735 ),
 .UNSPECIFIED. ) ;
#33878 = ORIENTED_EDGE ( 'NONE', *, *, #52924, .F. ) ;
#33879 = FACE_BOUND ( 'NONE', #48413, .T. ) ;
#33880 = VERTEX_POINT ( 'NONE', #52177 ) ;
#33882 = EDGE_CURVE ( 'NONE', #47735, #64358, #7525, .T. ) ;
#33881 = CARTESIAN_POINT ( 'NONE',  ( -8.546451227962359454, -4.387253974876679230, 33.66317474335728832 ) ) ;
#33883 = CARTESIAN_POINT ( 'NONE',  ( -10.61538461538473577, -10.33852847137269571, 34.16647553114546554 ) ) ;
#33884 = CARTESIAN_POINT ( 'NONE',  ( 18.25005441991345734, -6.523592122091590895, 34.90882529074906415 ) ) ;
#33885 = EDGE_CURVE ( 'NONE', #82401, #38474, #44524, .T. ) ;
#33886 = FACE_OUTER_BOUND ( 'NONE', #31223, .T. ) ;
#33887 = CARTESIAN_POINT ( 'NONE',  ( -11.53846153846165912, -2.625532179533778709, 30.86335684631627174 ) ) ;
#33888 = ORIENTED_EDGE ( 'NONE', *, *, #82321, .F. ) ;
#33889 = VERTEX_POINT ( 'NONE', #65688 ) ;
#33890 = ORIENTED_EDGE ( 'NONE', *, *, #72273, .F. ) ;
#33891 = ORIENTED_EDGE ( 'NONE', *, *, #50711, .T. ) ;
#33892 = EDGE_CURVE ( 'NONE', #80428, #25943, #23623, .T. ) ;
#33893 = CIRCLE ( 'NONE', #2256, 4.000000000000000000 ) ;
#33894 = CARTESIAN_POINT ( 'NONE',  ( -17.07692307692319744, -10.33852847137269571, 34.16647553114546554 ) ) ;
#33895 = CARTESIAN_POINT ( 'NONE',  ( -17.07692307692277112, -2.506253911140615021, 30.00000000000323297 ) ) ;
#33896 = ADVANCED_FACE ( 'NONE', ( #79225, #17524 ), #18855, .T. ) ;
#33897 = CARTESIAN_POINT ( 'NONE',  ( 6.000000000000001776, -12.10708131394839349, 31.69288490824020244 ) ) ;
#33898 = EDGE_LOOP ( 'NONE', ( #13009, #87733, #1786, #1853 ) ) ;
#33899 = CARTESIAN_POINT ( 'NONE',  ( 11.47319109250076430, -2.625532179533445198, 30.86335684631481513 ) ) ;
#33900 = CARTESIAN_POINT ( 'NONE',  ( -2.557669038634660996, -4.943428324936578910, 34.04746400365624481 ) ) ;
#33901 = CARTESIAN_POINT ( 'NONE',  ( -2.177166605928740672, -3.816742781228458448, 33.13167719472716044 ) ) ;
#33902 = CARTESIAN_POINT ( 'NONE',  ( -17.76215049426127024, 12.75000000000001421, 13.00000000000000178 ) ) ;
#33903 = VERTEX_POINT ( 'NONE', #19300 ) ;
#33904 = AXIS2_PLACEMENT_3D ( 'NONE', #54157, #13193, #20826 ) ;
#33905 = EDGE_LOOP ( 'NONE', ( #51346, #81857 ) ) ;
#33906 = ORIENTED_EDGE ( 'NONE', *, *, #34392, .T. ) ;
#33908 = ADVANCED_FACE ( 'NONE', ( #53065 ), #66139, .F. ) ;
#33907 = CARTESIAN_POINT ( 'NONE',  ( -9.320512820512821150, -1.926643599941765039, 28.25000000000000000 ) ) ;
#33910 = LINE ( 'NONE', #48306, #5992 ) ;
#33909 = CARTESIAN_POINT ( 'NONE',  ( 1.607626736228236819, -5.667800583137508674, 34.40243808032445827 ) ) ;
#33911 = CARTESIAN_POINT ( 'NONE',  ( -1.384615384615383471, -1.215029322943914858, 32.30358669280327177 ) ) ;
#33912 = CARTESIAN_POINT ( 'NONE',  ( -10.83886955910856464, -3.754499324213721234, 33.06261337010820256 ) ) ;
#33913 = FACE_BOUND ( 'NONE', #18728, .T. ) ;
#33914 = EDGE_LOOP ( 'NONE', ( #11221, #33825, #30287, #41925 ) ) ;
#33915 = EDGE_CURVE ( 'NONE', #57709, #19174, #45870, .T. ) ;
#33916 = DIRECTION ( 'NONE',  ( 0.000000000000000000, 0.9848077530122072432, 0.1736481776669354937 ) ) ;
#33917 = CARTESIAN_POINT ( 'NONE',  ( -5.076923076923075762, -12.29105614889573062, 35.45975837776705220 ) ) ;
#33918 = CARTESIAN_POINT ( 'NONE',  ( 3.007843013253084674, -10.61292498521070549, 33.66303323003028680 ) ) ;
#33919 = ORIENTED_EDGE ( 'NONE', *, *, #68976, .F. ) ;
#33920 = CARTESIAN_POINT ( 'NONE',  ( 17.20744851515672025, -5.915461855592777596, 34.75538340440931506 ) ) ;
#33921 = EDGE_LOOP ( 'NONE', ( #84544, #13507, #80895, #70250 ) ) ;
#33922 = FACE_BOUND ( 'NONE', #28351, .T. ) ;
#33923 = LINE ( 'NONE', #82580, #74953 ) ;
#33924 = VERTEX_POINT ( 'NONE', #80110 ) ;
#33925 = AXIS2_PLACEMENT_3D ( 'NONE', #8040, #42716, #34623 ) ;
#33926 = CARTESIAN_POINT ( 'NONE',  ( -6.923076923076922462, -9.905515769479276145, 34.41647553114623292 ) ) ;
#33927 = DIRECTION ( 'NONE',  ( 0.000000000000000000, 0.000000000000000000, -1.000000000000000000 ) ) ;
#33928 = DIRECTION ( 'NONE',  ( 0.000000000000000000, 0.3420201433256610524, 0.9396926207859113145 ) ) ;
#33929 = EDGE_LOOP ( 'NONE', ( #38656, #14999, #46881, #34655, #7168 ) ) ;
#33930 = CARTESIAN_POINT ( 'NONE',  ( -8.769230769230768274, -3.322132147404559976, 32.92929555188717927 ) ) ;
#33931 = CARTESIAN_POINT ( 'NONE',  ( -4.153846153846152411, -1.129524287112498415, 32.06866353760679544 ) ) ;
#33932 = CARTESIAN_POINT ( 'NONE',  ( -16.37733109757010652, -12.44517049084099725, 30.48991314939691932 ) ) ;
#33933 = EDGE_CURVE ( 'NONE', #39364, #64018, #52627, .T. ) ;
#33934 = CARTESIAN_POINT ( 'NONE',  ( -9.561515884482906458, -2.541949514083464479, 30.39797389878540557 ) ) ;
#33935 = ORIENTED_EDGE ( 'NONE', *, *, #34268, .T. ) ;
#33936 = VECTOR ( 'NONE', #23225, 1000.000000000000000 ) ;
#33937 = EDGE_CURVE ( 'NONE', #28389, #83231, #30867, .T. ) ;
#33938 = CARTESIAN_POINT ( 'NONE',  ( -4.946397638689432164, -5.070358843744210198, 34.40418822224088302 ) ) ;
#33939 = CARTESIAN_POINT ( 'NONE',  ( -15.93083330975275658, -10.01129605718032423, 34.36064277460058491 ) ) ;
#33941 = ORIENTED_EDGE ( 'NONE', *, *, #77262, .T. ) ;
#33940 = CARTESIAN_POINT ( 'NONE',  ( 1.450682717965462221, -2.833524468853757750, 32.15551576947925838 ) ) ;
#33942 = CARTESIAN_POINT ( 'NONE',  ( 2.372947447205146609, -10.33852847137154107, 34.16647553114620450 ) ) ;
#33943 = DIRECTION ( 'NONE',  ( -0.000000000000000000, 1.000000000000000000, -0.000000000000000000 ) ) ;
#33944 = CARTESIAN_POINT ( 'NONE',  ( -13.25382357679059986, -4.809403383903225304, 33.96459661697924304 ) ) ;
#33945 = CARTESIAN_POINT ( 'NONE',  ( 13.60762673622823904, -12.39991518177334129, 30.74647679643404530 ) ) ;
#33946 = CARTESIAN_POINT ( 'NONE',  ( -13.13466986626724164, -3.712312575010499049, 33.01462480002815170 ) ) ;
#33947 = DIRECTION ( 'NONE',  ( 1.000000000000000000, 0.000000000000000000, 0.000000000000000000 ) ) ;
#33949 = CARTESIAN_POINT ( 'NONE',  ( -23.50000000000000000, -13.25000000000000533, 27.31828373317831549 ) ) ;
#33948 = CARTESIAN_POINT ( 'NONE',  ( 8.769230769231082689, -2.255955759149395501, 30.00000000000324363 ) ) ;
#33950 = CARTESIAN_POINT ( 'NONE',  ( -12.23875892027005108, -11.41317474335729543, 32.86274602512330034 ) ) ;
#33951 = CARTESIAN_POINT ( 'NONE',  ( 2.750000000000008438, -8.639087296525996607, 19.54687499999999645 ) ) ;
#33952 = ORIENTED_EDGE ( 'NONE', *, *, #78671, .F. ) ;
#33953 = CARTESIAN_POINT ( 'NONE',  ( -3.262820512820514107, -11.00000000000000000, 29.75000000000000355 ) ) ;
#33954 = ORIENTED_EDGE ( 'NONE', *, *, #8448, .T. ) ;
#33955 = VERTEX_POINT ( 'NONE', #6237 ) ;
#33956 = FACE_OUTER_BOUND ( 'NONE', #25593, .T. ) ;
#33957 = ORIENTED_EDGE ( 'NONE', *, *, #65614, .F. ) ;
#33958 = CARTESIAN_POINT ( 'NONE',  ( 14.17700084102474989, -8.147922237126337563, 34.70805685702651999 ) ) ;
#33959 = CARTESIAN_POINT ( 'NONE',  ( 1.139087296526029469, -10.24999999999999467, 22.20312500000000000 ) ) ;
#33960 = LINE ( 'NONE', #20003, #2725 ) ;
#33961 = CARTESIAN_POINT ( 'NONE',  ( -11.28851612908349544, -10.18230066228895758, 34.26354781536631577 ) ) ;
#33962 = DIRECTION ( 'NONE',  ( -0.000000000000000000, 0.3420201433256694346, -0.9396926207859080948 ) ) ;
#33963 = CARTESIAN_POINT ( 'NONE',  ( 1.384615384615264011, -2.657715359629662544, 31.77849191805970364 ) ) ;
#33964 = LINE ( 'NONE', #60551, #41651 ) ;
#33965 = CYLINDRICAL_SURFACE ( 'NONE', #26738, 4.000000000000000000 ) ;
#33966 = CARTESIAN_POINT ( 'NONE',  ( 3.750000000000009770, -9.053300858899081760, 25.79687500000000355 ) ) ;
#33967 = VECTOR ( 'NONE', #61847, 1000.000000000000227 ) ;
#33968 = DIRECTION ( 'NONE',  ( -0.000000000000000000, 1.000000000000000000, 3.491481338843133355E-15 ) ) ;
#33969 = CARTESIAN_POINT ( 'NONE',  ( -13.31854703361294590, -6.386643153685127139, 34.62446782046654192 ) ) ;
#33970 = FACE_OUTER_BOUND ( 'NONE', #9180, .T. ) ;
#33971 = B_SPLINE_CURVE_WITH_KNOTS ( 'NONE', 3,
 ( #42030, #23077, #50535, #23505, #4122, #39269, #10454, #66726, #58177, #3240 ),
 .UNSPECIFIED., .F., .F.,
 ( 4, 2, 2, 2, 4 ),
 ( 0.0007817246256747519429, 0.0009771112852218959231, 0.001172497944769039686, 0.001367884604316183667, 0.001563271263863327647 ),
 .UNSPECIFIED. ) ;
#33972 = EDGE_CURVE ( 'NONE', #80082, #45222, #48099, .T. ) ;
#33973 = B_SPLINE_CURVE_WITH_KNOTS ( 'NONE', 3,
 ( #74601, #53425, #59301, #87245, #25077, #72811, #40380, #5690, #12020, #52540 ),
 .UNSPECIFIED., .F., .F.,
 ( 4, 2, 2, 2, 4 ),
 ( 0.0007817246256747503166, 0.0009771112852218946220, 0.001172497944769039036, 0.001367884604316183233, 0.001563271263863327647 ),
 .UNSPECIFIED. ) ;
#33974 = ORIENTED_EDGE ( 'NONE', *, *, #53015, .T. ) ;
#33975 = ORIENTED_EDGE ( 'NONE', *, *, #37289, .F. ) ;
#33976 = CARTESIAN_POINT ( 'NONE',  ( -6.923076923076607159, -2.255955759149395501, 30.00000000000324363 ) ) ;
#33977 = CARTESIAN_POINT ( 'NONE',  ( 0.6845513056318550671, -11.98016756924214832, 32.48728574198911190 ) ) ;
#33978 = CARTESIAN_POINT ( 'NONE',  ( 6.923076923076924238, -8.973038597847269315, 34.52809138561121927 ) ) ;
#33979 = LINE ( 'NONE', #41631, #19655 ) ;
#33980 = EDGE_CURVE ( 'NONE', #31080, #19898, #18215, .T. ) ;
#33981 = AXIS2_PLACEMENT_3D ( 'NONE', #72782, #30469, #64686 ) ;
#33982 = CARTESIAN_POINT ( 'NONE',  ( 14.17754433796061875, -3.625366637846545892, 33.29286588640298561 ) ) ;
#33983 = CARTESIAN_POINT ( 'NONE',  ( 11.53846153846153832, -3.937682226553329556, 33.60647404775216529 ) ) ;
#33984 = EDGE_CURVE ( 'NONE', #16191, #70346, #60274, .T. ) ;
#33985 = CARTESIAN_POINT ( 'NONE',  ( -6.923076923076922462, -3.050289026998446396, 32.03036669348365706 ) ) ;
#33986 = ORIENTED_EDGE ( 'NONE', *, *, #11285, .T. ) ;
#33987 = CARTESIAN_POINT ( 'NONE',  ( -6.673022611438605978, -9.943054286541403997, 34.11300777759954883 ) ) ;
#33988 = EDGE_LOOP ( 'NONE', ( #75900, #72702, #36560, #65311 ) ) ;
#33989 = ADVANCED_FACE ( 'NONE', ( #40031 ), #5785, .F. ) ;
#33990 = DIRECTION ( 'NONE',  ( -0.000000000000000000, 0.9848077530122085754, -0.1736481776669273613 ) ) ;
#33991 = CARTESIAN_POINT ( 'NONE',  ( 3.903846153846154632, -7.500000000000001776, 35.00000000000000000 ) ) ;
#33992 = VECTOR ( 'NONE', #47813, 1000.000000000000000 ) ;
#33993 = CARTESIAN_POINT ( 'NONE',  ( 14.17700084102474989, -4.809359713505814149, 33.96456829005828837 ) ) ;
#33994 = PLANE ( 'NONE',  #88238 ) ;
#33995 = DIRECTION ( 'NONE',  ( -1.000000000000000000, 0.000000000000000000, 0.000000000000000000 ) ) ;
#33996 = ORIENTED_EDGE ( 'NONE', *, *, #29547, .T. ) ;
#33997 = ORIENTED_EDGE ( 'NONE', *, *, #7623, .T. ) ;
#33998 = EDGE_LOOP ( 'NONE', ( #19390, #70091, #79522, #72635 ) ) ;
#33999 = VERTEX_POINT ( 'NONE', #38676 ) ;
#34000 = AXIS2_PLACEMENT_3D ( 'NONE', #79250, #45000, #24743 ) ;
#34001 = CARTESIAN_POINT ( 'NONE',  ( -6.000000000000121680, -5.094484230521993062, 34.41647553114689373 ) ) ;
#34002 = B_SPLINE_CURVE_WITH_KNOTS ( 'NONE', 3,
 ( #12702, #87954, #68524, #39297, #74402, #75293, #13583, #26213, #66753, #46486 ),
 .UNSPECIFIED., .F., .F.,
 ( 4, 2, 2, 2, 4 ),
 ( 0.000000000000000000, 0.0001954311564186876876, 0.0003908623128373753751, 0.0005862934692560630356, 0.0007817246256747507503 ),
 .UNSPECIFIED. ) ;
#34003 = CARTESIAN_POINT ( 'NONE',  ( 4.853438133199127869, -10.81261337010820256, 33.49550067578627477 ) ) ;
#34004 = EDGE_CURVE ( 'NONE', #24055, #84960, #26949, .T. ) ;
#34005 = CARTESIAN_POINT ( 'NONE',  ( 16.15384615384646949, -2.255955759149395501, 30.00000000000324363 ) ) ;
#34006 = DIRECTION ( 'NONE',  ( -1.000000000000000000, -0.000000000000000000, -0.000000000000000000 ) ) ;
#34007 = CARTESIAN_POINT ( 'NONE',  ( -15.00798956179116317, -9.418065098278013636, 34.63729479722530158 ) ) ;
#34008 = CARTESIAN_POINT ( 'NONE',  ( -15.36145983387953962, -2.494641256782728966, 31.33461815524612959 ) ) ;
#34009 = ORIENTED_EDGE ( 'NONE', *, *, #23915, .F. ) ;
#34010 = VERTEX_POINT ( 'NONE', #12545 ) ;
#34011 = EDGE_LOOP ( 'NONE', ( #14260, #22698, #22165, #81745, #86065, #16843 ) ) ;
#34014 = ORIENTED_EDGE ( 'NONE', *, *, #32103, .F. ) ;
#34013 = EDGE_CURVE ( 'NONE', #61361, #61570, #82667, .T. ) ;
#34012 = CARTESIAN_POINT ( 'NONE',  ( -10.36543909703646982, -11.86320923018887541, 32.19269448109604781 ) ) ;
#34015 = DIRECTION ( 'NONE',  ( 1.000000000000000000, 0.000000000000000000, 0.000000000000000000 ) ) ;
#34016 = CARTESIAN_POINT ( 'NONE',  ( -12.21148404162500967, -12.01375889529407281, 32.43194544308182969 ) ) ;
#34017 = VECTOR ( 'NONE', #58652, 1000.000000000000000 ) ;
#34018 = CARTESIAN_POINT ( 'NONE',  ( -2.651650429449535551, -10.15165042944956753, 22.43750000000000000 ) ) ;
#34019 = ORIENTED_EDGE ( 'NONE', *, *, #31158, .F. ) ;
#34020 = EDGE_CURVE ( 'NONE', #54784, #63016, #12180, .T. ) ;
#34021 = EDGE_CURVE ( 'NONE', #17811, #42433, #4156, .T. ) ;
#34022 = LINE ( 'NONE', #5223, #39716 ) ;
#34023 = ORIENTED_EDGE ( 'NONE', *, *, #57744, .F. ) ;
#34024 = CARTESIAN_POINT ( 'NONE',  ( 7.976945653978634532, -12.11778462344221197, 31.66786338562085135 ) ) ;
#34025 = FACE_BOUND ( 'NONE', #85185, .T. ) ;
#34026 = CARTESIAN_POINT ( 'NONE',  ( 7.846153846153846700, -12.78798330534102945, 29.74999999999997868 ) ) ;
#34027 = CARTESIAN_POINT ( 'NONE',  ( -14.08431636699412337, -2.501478030877323455, 29.88021232661721172 ) ) ;
#34028 = ORIENTED_EDGE ( 'NONE', *, *, #20139, .T. ) ;
#34029 = CARTESIAN_POINT ( 'NONE',  ( -2.294871794871794712, -3.499999999999999556, 29.75000000000000355 ) ) ;
#34030 = AXIS2_PLACEMENT_3D ( 'NONE', #24430, #86610, #46494 ) ;
#34031 = CARTESIAN_POINT ( 'NONE',  ( 8.835298102580845025, -8.164416787775445883, 34.95778746994558617 ) ) ;
#34032 = CARTESIAN_POINT ( 'NONE',  ( 16.15384615384615330, -2.538708090699994813, 30.37095296980875503 ) ) ;
#34033 = CARTESIAN_POINT ( 'NONE',  ( 15.48082365068268373, -6.523592122091592671, 34.90882529074906415 ) ) ;
#34035 = ORIENTED_EDGE ( 'NONE', *, *, #13651, .F. ) ;
#34034 = EDGE_CURVE ( 'NONE', #83533, #15199, #24577, .T. ) ;
#34036 = B_SPLINE_CURVE_WITH_KNOTS ( 'NONE', 3,
 ( #66866, #45248, #17796, #18237, #11033, #60099, #79039, #10590, #5607, #73638 ),
 .UNSPECIFIED., .F., .F.,
 ( 4, 2, 2, 2, 4 ),
 ( 0.0007817246256747460882, 0.0009771112852218892010, 0.001172497944769032314, 0.001367884604316175210, 0.001563271263863318323 ),
 .UNSPECIFIED. ) ;
#34037 = CARTESIAN_POINT ( 'NONE',  ( 16.40384615384759215, -7.500000000000155431, 34.75000000000007105 ) ) ;
#34038 = CARTESIAN_POINT ( 'NONE',  ( -7.715628144390285215, -11.46989282347013095, 32.79007818306219946 ) ) ;
#34039 = CARTESIAN_POINT ( 'NONE',  ( 4.219101293358989757, -11.67786785259547777, 32.92929555188713664 ) ) ;
#34040 = CARTESIAN_POINT ( 'NONE',  ( -2.177166869458661225, -9.503571793651733657, 34.60286762892837942 ) ) ;
#34041 = EDGE_CURVE ( 'NONE', #83971, #56983, #27824, .T. ) ;
#34043 = ADVANCED_FACE ( 'NONE', ( #22395 ), #42678, .F. ) ;
#34042 = CARTESIAN_POINT ( 'NONE',  ( -13.91025641025641058, -7.500000000000000000, 29.75000000000000355 ) ) ;
#34044 = FACE_BOUND ( 'NONE', #16762, .T. ) ;
#34046 = CARTESIAN_POINT ( 'NONE',  ( 11.53846153846141753, -12.46129190930018460, 30.37095296980731973 ) ) ;
#34045 = CARTESIAN_POINT ( 'NONE',  ( -4.500000000000003553, 7.499999999999996447, 13.50000000000000178 ) ) ;
#34047 = CARTESIAN_POINT ( 'NONE',  ( -7.146561866800873020, -12.24155766932282496, 31.33739205006857986 ) ) ;
#34049 = CARTESIAN_POINT ( 'NONE',  ( 6.923076923076800782, -2.657715359629662988, 31.77849191805970364 ) ) ;
#34048 = CARTESIAN_POINT ( 'NONE',  ( -8.769230769230768274, -11.69971097300155272, 32.46337939537588113 ) ) ;
#34050 = DIRECTION ( 'NONE',  ( -0.000000000000000000, 0.9848077530122085754, -0.1736481776669273613 ) ) ;
#34051 = CARTESIAN_POINT ( 'NONE',  ( 1.901340078031349856, -5.512252781505337929, 15.31063170625849068 ) ) ;
#34052 = EDGE_CURVE ( 'NONE', #54472, #26695, #62922, .T. ) ;
#34053 = VERTEX_POINT ( 'NONE', #1234 ) ;
#34054 = CARTESIAN_POINT ( 'NONE',  ( 1.384615384615386802, -12.10708131394839349, 31.69288490824020244 ) ) ;
#34055 = VERTEX_POINT ( 'NONE', #29175 ) ;
#34056 = CARTESIAN_POINT ( 'NONE',  ( -15.00798968950081758, -4.387253974876679230, 33.66317474335728832 ) ) ;
#34057 = VECTOR ( 'NONE', #76746, 999.9999999999998863 ) ;
#34058 = ORIENTED_EDGE ( 'NONE', *, *, #84303, .T. ) ;
#34059 = DIRECTION ( 'NONE',  ( 1.000000000000000000, 0.000000000000000000, 0.000000000000000000 ) ) ;
#34060 = DIRECTION ( 'NONE',  ( 0.000000000000000000, 0.8660254037844377084, -0.5000000000000015543 ) ) ;
#34062 = ORIENTED_EDGE ( 'NONE', *, *, #83178, .T. ) ;
#34061 = CARTESIAN_POINT ( 'NONE',  ( -4.826977667545033768, -9.357781135181031829, 34.66075350412533851 ) ) ;
#34063 = CARTESIAN_POINT ( 'NONE',  ( -12.94230769230769162, -3.499999999999999556, 29.75000000000000355 ) ) ;
#34064 = CARTESIAN_POINT ( 'NONE',  ( 2.750000000000001332, -7.438900925035452083, 19.21688170625848358 ) ) ;
#34065 = CARTESIAN_POINT ( 'NONE',  ( -15.23076923076922995, -9.058645607665452459, 34.76329471203371924 ) ) ;
#34066 = CARTESIAN_POINT ( 'NONE',  ( -7.173100147298380413, -12.68155406624981119, 30.59749803192733708 ) ) ;
#34067 = VECTOR ( 'NONE', #8698, 1000.000000000000000 ) ;
#34068 = CARTESIAN_POINT ( 'NONE',  ( 17.07692307692295586, -12.46129190930018460, 30.37095296980731973 ) ) ;
#34069 = CARTESIAN_POINT ( 'NONE',  ( 1.134592160393929072, -4.931416488878823223, 34.32920672191015399 ) ) ;
#34070 = CARTESIAN_POINT ( 'NONE',  ( -1.318548051265308274, -6.343179335718451384, 34.87096338111212646 ) ) ;
#34071 = CARTESIAN_POINT ( 'NONE',  ( -24.00000000000000000, -5.499999999999981348, 27.25000000000000000 ) ) ;
#34072 = CARTESIAN_POINT ( 'NONE',  ( -3.724691934501248802, -5.885600066136383646, 24.17374329374151642 ) ) ;
#34073 = CARTESIAN_POINT ( 'NONE',  ( 9.469429009879048564, -7.630691491037285168, 34.74850469731152458 ) ) ;
#34074 = AXIS2_PLACEMENT_3D ( 'NONE', #4369, #86365, #24637 ) ;
#34075 = ORIENTED_EDGE ( 'NONE', *, *, #45316, .T. ) ;
#34076 = LINE ( 'NONE', #21893, #19103 ) ;
#34077 = CARTESIAN_POINT ( 'NONE',  ( -3.724691934501248802, -5.885600066136383646, 25.42374329374151998 ) ) ;
#34078 = ADVANCED_FACE ( 'NONE', ( #28263 ), #13424, .F. ) ;
#34079 = DIRECTION ( 'NONE',  ( -1.000000000000000000, -0.000000000000000000, -0.000000000000000000 ) ) ;
#34080 = DIRECTION ( 'NONE',  ( -0.000000000000000000, -0.000000000000000000, -1.000000000000000000 ) ) ;
#34081 = VERTEX_POINT ( 'NONE', #1684 ) ;
#34082 = CARTESIAN_POINT ( 'NONE',  ( 6.923076923076802558, -8.613356846316285953, 34.62446782046622218 ) ) ;
#34083 = CARTESIAN_POINT ( 'NONE',  ( -0.2115929431903202929, -10.05730279482229683, 34.04704008940765902 ) ) ;
#34085 = ORIENTED_EDGE ( 'NONE', *, *, #61984, .F. ) ;
#34084 = CARTESIAN_POINT ( 'NONE',  ( -16.82692307692300915, -7.434744429011174383, 34.75000000000000711 ) ) ;
#34086 = DIRECTION ( 'NONE',  ( -0.000000000000000000, -0.9396926207859093161, -0.3420201433256663259 ) ) ;
#34087 = CARTESIAN_POINT ( 'NONE',  ( -14.98071481085577972, -12.01375889529407281, 32.43194544308182969 ) ) ;
#34088 = CARTESIAN_POINT ( 'NONE',  ( 16.08857570788537572, -9.442884908240170461, 34.35708131394840592 ) ) ;
#34089 = CARTESIAN_POINT ( 'NONE',  ( -9.442253272394236063, -2.544122305571458575, 31.48381861865057729 ) ) ;
#34090 = CARTESIAN_POINT ( 'NONE',  ( -18.06608341095587278, -12.10708131394839349, 31.69288490824020244 ) ) ;
#34091 = VECTOR ( 'NONE', #28317, 1000.000000000000000 ) ;
#34092 = LINE ( 'NONE', #33657, #16805 ) ;
#34093 = VERTEX_POINT ( 'NONE', #76904 ) ;
#34094 = EDGE_LOOP ( 'NONE', ( #23042, #31780 ) ) ;
#34095 = ORIENTED_EDGE ( 'NONE', *, *, #65557, .T. ) ;
#34096 = AXIS2_PLACEMENT_3D ( 'NONE', #56142, #68771, #7520 ) ;
#34097 = ORIENTED_EDGE ( 'NONE', *, *, #19160, .F. ) ;
#34098 = CARTESIAN_POINT ( 'NONE',  ( -9.469296340694842939, -3.105924265160262543, 32.13625925475356127 ) ) ;
#34099 = DIRECTION ( 'NONE',  ( 0.000000000000000000, 0.4999999999999985567, 0.8660254037844395958 ) ) ;
#34100 = VECTOR ( 'NONE', #37742, 1000.000000000000114 ) ;
#34101 = CARTESIAN_POINT ( 'NONE',  ( 9.757563263583717728, -5.219633306516380244, 34.19971097300157936 ) ) ;
#34102 = CARTESIAN_POINT ( 'NONE',  ( -8.769230769230768274, -13.63283147151868846, 33.57946703557072254 ) ) ;
#34103 = EDGE_CURVE ( 'NONE', #76906, #7653, #56628, .T. ) ;
#34104 = CARTESIAN_POINT ( 'NONE',  ( 16.08776274289027342, -4.786620604624113540, 33.94971097300155805 ) ) ;
#34105 = ORIENTED_EDGE ( 'NONE', *, *, #32678, .F. ) ;
#34106 = ORIENTED_EDGE ( 'NONE', *, *, #6293, .F. ) ;
#34107 = B_SPLINE_CURVE_WITH_KNOTS ( 'NONE', 3,
 ( #45250, #25880, #38963, #86718, #66868, #5163, #51540, #59212, #4270, #18689 ),
 .UNSPECIFIED., .F., .F.,
 ( 4, 2, 2, 2, 4 ),
 ( 0.0007817246256747451124, 0.0009771112852218881168, 0.001172497944769031230, 0.001367884604316174126, 0.001563271263863317238 ),
 .UNSPECIFIED. ) ;
#34108 = ORIENTED_EDGE ( 'NONE', *, *, #3163, .T. ) ;
#34110 = ORIENTED_EDGE ( 'NONE', *, *, #7982, .F. ) ;
#34109 = FACE_OUTER_BOUND ( 'NONE', #52381, .T. ) ;
#34111 = CARTESIAN_POINT ( 'NONE',  ( 4.403791672194295792, -5.852078868378311149, 34.47109172314383585 ) ) ;
#34112 = CARTESIAN_POINT ( 'NONE',  ( -3.230769230769229949, -11.91647553114624181, 32.58852847137148245 ) ) ;
#34113 = AXIS2_PLACEMENT_3D ( 'NONE', #63370, #70132, #71451 ) ;
#34114 = CARTESIAN_POINT ( 'NONE',  ( 7.146089767170317408, -4.762714258010880997, 34.23016756924214832 ) ) ;
#34115 = EDGE_CURVE ( 'NONE', #5202, #36170, #14860, .T. ) ;
#34116 = DIRECTION ( 'NONE',  ( 0.000000000000000000, 0.1736481776669275834, 0.9848077530122086864 ) ) ;
#34117 = EDGE_LOOP ( 'NONE', ( #22605, #39074, #31575, #46407 ) ) ;
#34118 = EDGE_LOOP ( 'NONE', ( #84445, #7992 ) ) ;
#34119 = ORIENTED_EDGE ( 'NONE', *, *, #59357, .F. ) ;
#34120 = CARTESIAN_POINT ( 'NONE',  ( -4.946875470667394303, -7.723484964179500700, 34.74522123443823318 ) ) ;
#34122 = ORIENTED_EDGE ( 'NONE', *, *, #58212, .T. ) ;
#34121 = LINE ( 'NONE', #82324, #70391 ) ;
#34123 = CARTESIAN_POINT ( 'NONE',  ( 13.16174996241175066, -2.501496062324912284, 29.88072118266895671 ) ) ;
#34124 = DIRECTION ( 'NONE',  ( -0.000000000000000000, 0.9396926207859094271, -0.3420201433256663259 ) ) ;
#34125 = VERTEX_POINT ( 'NONE', #13864 ) ;
#34126 = ADVANCED_FACE ( 'NONE', ( #68812 ), #7113, .F. ) ;
#34127 = AXIS2_PLACEMENT_3D ( 'NONE', #71608, #11254, #59437 ) ;
#34128 = FACE_OUTER_BOUND ( 'NONE', #31111, .T. ) ;
#34129 = CARTESIAN_POINT ( 'NONE',  ( 2.307692307692309264, -9.905515769479276145, 34.41647553114623292 ) ) ;
#34130 = FACE_BOUND ( 'NONE', #46845, .T. ) ;
#34131 = DIRECTION ( 'NONE',  ( 8.673617379884044347E-16, -1.000000000000000000, 5.102127870520021228E-17 ) ) ;
#34132 = CARTESIAN_POINT ( 'NONE',  ( 16.15384615384615330, -2.486705287966279876, 31.30864560766543647 ) ) ;
#34133 = DIRECTION ( 'NONE',  ( -0.000000000000000000, 0.1736481776669307198, -0.9848077530122080203 ) ) ;
#34134 = B_SPLINE_CURVE_WITH_KNOTS ( 'NONE', 3,
 ( #35585, #61707, #82452, #36032, #84228, #1345 ),
 .UNSPECIFIED., .F., .F.,
 ( 4, 2, 4 ),
 ( 0.000000000000000000, 0.0001954784845028921395, 0.0003909569690057842790 ),
 .UNSPECIFIED. ) ;
#34136 = CARTESIAN_POINT ( 'NONE',  ( 5.010839665967194989, -9.780366693483667717, 34.19971097300155805 ) ) ;
#34135 = DIRECTION ( 'NONE',  ( -0.000000000000000000, 1.000000000000000000, 3.491481338843133355E-15 ) ) ;
#34137 = CARTESIAN_POINT ( 'NONE',  ( 3.512820512820510555, -3.499999999999999556, 29.75000000000000355 ) ) ;
#34138 = CARTESIAN_POINT ( 'NONE',  ( 12.52679360105129724, -3.083524468853784839, 32.58852847137153930 ) ) ;
#34139 = EDGE_LOOP ( 'NONE', ( #11063, #51618 ) ) ;
#34140 = FACE_OUTER_BOUND ( 'NONE', #30902, .T. ) ;
#34141 = CYLINDRICAL_SURFACE ( 'NONE', #75206, 0.2499999999999997502 ) ;
#34142 = VERTEX_POINT ( 'NONE', #69696 ) ;
#34143 = B_SPLINE_CURVE_WITH_KNOTS ( 'NONE', 3,
 ( #53534, #59855, #67065, #18873, #40921, #12127, #45891, #26524, #33719, #67953 ),
 .UNSPECIFIED., .F., .F.,
 ( 4, 2, 2, 2, 4 ),
 ( 0.0007817246256747502082, 0.0009771112852218944052, 0.001172497944769038819, 0.001367884604316183233, 0.001563271263863327430 ),
 .UNSPECIFIED. ) ;
#34144 = CARTESIAN_POINT ( 'NONE',  ( 14.24160889673642849, -9.780366693483667717, 34.19971097300155805 ) ) ;
#34145 = FACE_OUTER_BOUND ( 'NONE', #63032, .T. ) ;
#34146 = ORIENTED_EDGE ( 'NONE', *, *, #18377, .F. ) ;
#34147 = AXIS2_PLACEMENT_3D ( 'NONE', #32152, #59610, #21278 ) ;
#34148 = CARTESIAN_POINT ( 'NONE',  ( 11.40777093535123043, -9.929715669179220328, 34.40415004197138416 ) ) ;
#34149 = ADVANCED_FACE ( 'NONE', ( #361 ), #55292, .F. ) ;
#34150 = CARTESIAN_POINT ( 'NONE',  ( -18.03205128205128105, -7.500000000000000000, 29.75000000000000355 ) ) ;
#34151 = FACE_BOUND ( 'NONE', #50387, .T. ) ;
#34153 = CARTESIAN_POINT ( 'NONE',  ( -17.01166750564705055, -12.46129190930001052, 30.37095296980869819 ) ) ;
#34152 = CARTESIAN_POINT ( 'NONE',  ( -18.24997673094235040, -3.137211980971222225, 32.19342716148376837 ) ) ;
#34154 = CARTESIAN_POINT ( 'NONE',  ( 10.39245839786846837, -8.239355502252617924, 34.69524867566427417 ) ) ;
#34155 = DIRECTION ( 'NONE',  ( -0.000000000000000000, 0.6427876096865404731, -0.7660444431189770143 ) ) ;
#34157 = CARTESIAN_POINT ( 'NONE',  ( -8.769230769230768274, -13.37000171582298513, 34.34916445242398453 ) ) ;
#34156 = SURFACE_STYLE_USAGE ( .BOTH. , #41364 ) ;
#34158 = AXIS2_PLACEMENT_3D ( 'NONE', #11526, #39009, #4773 ) ;
#34159 = CARTESIAN_POINT ( 'NONE',  ( -3.749999999999997335, -7.500000000000021316, 25.09374999999999645 ) ) ;
#34160 = VERTEX_POINT ( 'NONE', #48526 ) ;
#34161 = EDGE_LOOP ( 'NONE', ( #6329, #34722 ) ) ;
#34162 = CARTESIAN_POINT ( 'NONE',  ( -25.00000000000000000, -10.00000000000000533, 13.00000000000000178 ) ) ;
#34163 = AXIS2_PLACEMENT_3D ( 'NONE', #12258, #39746, #67210 ) ;
#34164 = CARTESIAN_POINT ( 'NONE',  ( -10.39237177129122003, -8.282913670948747864, 34.94150082978203642 ) ) ;
#34165 = DIRECTION ( 'NONE',  ( 0.000000000000000000, 0.7660444431189822323, -0.6427876096865344779 ) ) ;
#34166 = CARTESIAN_POINT ( 'NONE',  ( 10.86543903529806698, -2.920487667080175598, 32.31805714834170828 ) ) ;
#34167 = CARTESIAN_POINT ( 'NONE',  ( 10.61538461538461675, -2.900454961884010974, 35.62045528018868623 ) ) ;
#34168 = CARTESIAN_POINT ( 'NONE',  ( 1.614399933863660985, -11.22469193450123193, 18.20125670625849068 ) ) ;
#34169 = CARTESIAN_POINT ( 'NONE',  ( -7.846153846153965716, -8.613356846316285953, 34.62446782046622218 ) ) ;
#34170 = CARTESIAN_POINT ( 'NONE',  ( 1.319345384059066539, -10.33852847137145048, 34.16647553114627556 ) ) ;
#34171 = CARTESIAN_POINT ( 'NONE',  ( 17.77651507543566822, -4.225889041578354544, 33.85425143139329407 ) ) ;
#34172 = DIRECTION ( 'NONE',  ( 0.000000000000000000, 0.000000000000000000, -1.000000000000000000 ) ) ;
#34173 = LINE ( 'NONE', #89146, #58345 ) ;
#34174 = CARTESIAN_POINT ( 'NONE',  ( 6.223012844093396723, -6.460100341425561332, 34.89618726649961644 ) ) ;
#34175 = B_SPLINE_CURVE_WITH_KNOTS ( 'NONE', 3,
 ( #19417, #75255, #87015, #5909, #68057, #6363, #12222, #25288, #80697, #26620 ),
 .UNSPECIFIED., .F., .F.,
 ( 4, 2, 2, 2, 4 ),
 ( 0.000000000000000000, 0.0001954339857564063360, 0.0003908679715128126719, 0.0005863019572692189808, 0.0007817359430256253438 ),
 .UNSPECIFIED. ) ;
#34176 = CARTESIAN_POINT ( 'NONE',  ( 6.989144256426998325, -3.322132147404559976, 32.92929555188717927 ) ) ;
#34177 = B_SPLINE_CURVE_WITH_KNOTS ( 'NONE', 3,
 ( #26586, #34677, #19386, #88752, #27914, #76092, #61684, #445, #74783, #34223 ),
 .UNSPECIFIED., .F., .F.,
 ( 4, 2, 2, 2, 4 ),
 ( 0.0007817246256747434861, 0.0009771112852218861652, 0.001172497944769028844, 0.001367884604316171740, 0.001563271263863314419 ),
 .UNSPECIFIED. ) ;
#34178 = CARTESIAN_POINT ( 'NONE',  ( 2.372837088411941409, -7.750023224968865421, 34.99404313364389907 ) ) ;
#34179 = CARTESIAN_POINT ( 'NONE',  ( 3.230769230769231726, -2.538708090699994813, 30.37095296980875503 ) ) ;
#34180 = ORIENTED_EDGE ( 'NONE', *, *, #57948, .F. ) ;
#34181 = CARTESIAN_POINT ( 'NONE',  ( -4.153846153846273204, -5.219633306517616589, 34.19971097300220464 ) ) ;
#34182 = CARTESIAN_POINT ( 'NONE',  ( -8.769230769230768274, -5.180354513474913603, 36.12317359536750416 ) ) ;
#34183 = CARTESIAN_POINT ( 'NONE',  ( -0.06109907496451398579, -10.25000000000000178, 23.78311829374151998 ) ) ;
#34184 = AXIS2_PLACEMENT_3D ( 'NONE', #81504, #40084, #32418 ) ;
#34185 = DIRECTION ( 'NONE',  ( -0.000000000000000000, -0.000000000000000000, -1.000000000000000000 ) ) ;
#34187 = DIRECTION ( 'NONE',  ( -0.000000000000000000, 0.5000000000000011102, -0.8660254037844381525 ) ) ;
#34186 = VECTOR ( 'NONE', #12326, 1000.000000000000000 ) ;
#34188 = DIRECTION ( 'NONE',  ( 0.000000000000000000, 8.673617379884035472E-17, 1.000000000000000000 ) ) ;
#34190 = VERTEX_POINT ( 'NONE', #8003 ) ;
#34189 = CARTESIAN_POINT ( 'NONE',  ( -1.318547033612945452, -4.098570777380720287, 33.41473453929635440 ) ) ;
#34191 = CARTESIAN_POINT ( 'NONE',  ( 2.749999999999995115, -6.360912703473971419, 25.64062500000000000 ) ) ;
#34192 = CARTESIAN_POINT ( 'NONE',  ( -19.50000000000000000, -3.499999999999999556, 29.75000000000000355 ) ) ;
#34193 = ORIENTED_EDGE ( 'NONE', *, *, #22907, .F. ) ;
#34194 = CARTESIAN_POINT ( 'NONE',  ( -11.47326855016688185, -2.255955759149236073, 29.99999999999988987 ) ) ;
#34195 = AXIS2_PLACEMENT_3D ( 'NONE', #40502, #4934, #32399 ) ;
#34196 = CARTESIAN_POINT ( 'NONE',  ( 10.61538461538461675, -10.67929555188718282, 33.92786785259544047 ) ) ;
#34197 = B_SPLINE_CURVE_WITH_KNOTS ( 'NONE', 3,
 ( #55749, #29948, #44773, #64152, #14779, #57854, #44318, #31276, #69714, #86238 ),
 .UNSPECIFIED., .F., .F.,
 ( 4, 2, 2, 2, 4 ),
 ( 0.0007817359430256294638, 0.0009771253907249952391, 0.001172514838424361123, 0.001367904286123726790, 0.001563293733823092673 ),
 .UNSPECIFIED. ) ;
#34198 = ORIENTED_EDGE ( 'NONE', *, *, #42513, .F. ) ;
#34199 = LINE ( 'NONE', #7175, #39183 ) ;
#34200 = CARTESIAN_POINT ( 'NONE',  ( 8.769230769230768274, -12.09954503811598769, 35.62045528018868623 ) ) ;
#34201 = CARTESIAN_POINT ( 'NONE',  ( 0.000000000000000000, -11.00000000000000000, 29.75000000000000355 ) ) ;
#34202 = ORIENTED_EDGE ( 'NONE', *, *, #7865, .T. ) ;
#34203 = ORIENTED_EDGE ( 'NONE', *, *, #86586, .F. ) ;
#34204 = CARTESIAN_POINT ( 'NONE',  ( 6.250054419913455561, -12.01375889529407281, 32.43194544308182969 ) ) ;
#34205 = VERTEX_POINT ( 'NONE', #35469 ) ;
#34206 = CARTESIAN_POINT ( 'NONE',  ( 7.622668921589514923, -9.417330523894422711, 34.63758898049880486 ) ) ;
#34207 = CARTESIAN_POINT ( 'NONE',  ( -9.561515884482904681, -9.804649428959608670, 34.18742332936588468 ) ) ;
#34208 = CARTESIAN_POINT ( 'NONE',  ( -1.514763354347081092, -11.66186481527757479, 32.95055677023626117 ) ) ;
#34209 = DIRECTION ( 'NONE',  ( -0.000000000000000000, 0.1736481776669307198, -0.9848077530122080203 ) ) ;
#34210 = DIRECTION ( 'NONE',  ( 0.000000000000000000, 0.000000000000000000, -1.000000000000000000 ) ) ;
#34211 = FACE_OUTER_BOUND ( 'NONE', #41317, .T. ) ;
#34212 = CARTESIAN_POINT ( 'NONE',  ( -12.59168567097668401, -6.852621066184266141, 34.70813303252209181 ) ) ;
#34213 = EDGE_CURVE ( 'NONE', #85801, #72479, #17078, .T. ) ;
#34214 = VECTOR ( 'NONE', #81691, 1000.000000000000227 ) ;
#34215 = EDGE_LOOP ( 'NONE', ( #10651, #22592, #28089, #22797 ) ) ;
#34216 = VERTEX_POINT ( 'NONE', #63822 ) ;
#34218 = EDGE_LOOP ( 'NONE', ( #1389, #24741, #31888, #81626 ) ) ;
#34217 = CARTESIAN_POINT ( 'NONE',  ( 7.053602361310570501, -12.70449254468099198, 30.44128974285582956 ) ) ;
#34219 = AXIS2_PLACEMENT_3D ( 'NONE', #57275, #1007, #62249 ) ;
#34220 = LINE ( 'NONE', #62568, #40791 ) ;
#34221 = ADVANCED_FACE ( 'NONE', ( #36795 ), #50292, .F. ) ;
#34222 = CIRCLE ( 'NONE', #75963, 4.000000000000000000 ) ;
#34223 = CARTESIAN_POINT ( 'NONE',  ( 11.53846153846153832, -3.322132147404559976, 32.92929555188717927 ) ) ;
#34224 = CARTESIAN_POINT ( 'NONE',  ( -4.153846153846152411, -13.75783147151868846, 33.36296068462461051 ) ) ;
#34226 = EDGE_LOOP ( 'NONE', ( #67584, #26779, #48349, #63707 ) ) ;
#34225 = EDGE_CURVE ( 'NONE', #17236, #28791, #40713, .T. ) ;
#34227 = CARTESIAN_POINT ( 'NONE',  ( -16.15384615384615330, -1.129524287112498415, 32.06866353760679544 ) ) ;
#34228 = ORIENTED_EDGE ( 'NONE', *, *, #79525, .F. ) ;
#34229 = FACE_OUTER_BOUND ( 'NONE', #12093, .T. ) ;
#34230 = ORIENTED_EDGE ( 'NONE', *, *, #54286, .F. ) ;
#34231 = CARTESIAN_POINT ( 'NONE',  ( -14.17716686945866833, -12.15418822224088835, 32.17964115625579069 ) ) ;
#34232 = VERTEX_POINT ( 'NONE', #85428 ) ;
#34233 = EDGE_CURVE ( 'NONE', #23252, #87267, #15971, .T. ) ;
#34234 = CARTESIAN_POINT ( 'NONE',  ( -4.219116154402471786, -4.320704448112771878, 33.92786785259540494 ) ) ;
#34235 = CARTESIAN_POINT ( 'NONE',  ( 12.23861150263161335, -2.308479472611653094, 30.53278059502174457 ) ) ;
#34236 = FACE_BOUND ( 'NONE', #12569, .T. ) ;
#34237 = B_SPLINE_CURVE_WITH_KNOTS ( 'NONE', 3,
 ( #41084, #82960, #48717, #33875, #53703, #28010, #34318, #81191, #68548, #6844 ),
 .UNSPECIFIED., .F., .F.,
 ( 4, 2, 2, 2, 4 ),
 ( 0.000000000000000000, 0.0001954311564186881213, 0.0003908623128373762425, 0.0005862934692560643367, 0.0007817246256747524850 ),
 .UNSPECIFIED. ) ;
#34238 = CARTESIAN_POINT ( 'NONE',  ( -17.75000000000000000, -2.499999999999999556, 29.75000000000000355 ) ) ;
#34239 = CARTESIAN_POINT ( 'NONE',  ( 1.515453715102147658, -7.277220318596959281, 34.99547417642776992 ) ) ;
#34240 = CARTESIAN_POINT ( 'NONE',  ( -19.99999999999996447, -15.00000000000000533, 13.00000000000000178 ) ) ;
#34241 = B_SPLINE_CURVE_WITH_KNOTS ( 'NONE', 3,
 ( #50630, #57386, #52400, #30800, #38461, #11431, #23601, #65481, #17750, #86220 ),
 .UNSPECIFIED., .F., .F.,
 ( 4, 2, 2, 2, 4 ),
 ( 0.000000000000000000, 0.0001954311564186875792, 0.0003908623128373751583, 0.0005862934692560627103, 0.0007817246256747503166 ),
 .UNSPECIFIED. ) ;
#34242 = LINE ( 'NONE', #5894, #66106 ) ;
#34243 = CARTESIAN_POINT ( 'NONE',  ( -4.854143407945009869, -4.226511098958374291, 33.85474049983370293 ) ) ;
#34244 = CARTESIAN_POINT ( 'NONE',  ( -10.86538461538461320, -7.500000000000001776, 34.75000000000000000 ) ) ;
#34245 = CARTESIAN_POINT ( 'NONE',  ( 14.30769230769218581, -6.835583212225970762, 34.95778746994575670 ) ) ;
#34246 = B_SPLINE_CURVE_WITH_KNOTS ( 'NONE', 3,
 ( #28323, #49491, #41854, #8507, #63435, #13923, #6724, #49039, #76517, #34196 ),
 .UNSPECIFIED., .F., .F.,
 ( 4, 2, 2, 2, 4 ),
 ( 0.0007817246256747451124, 0.0009771112852218885505, 0.001172497944769032097, 0.001367884604316175427, 0.001563271263863318973 ),
 .UNSPECIFIED. ) ;
#34247 = ORIENTED_EDGE ( 'NONE', *, *, #55425, .F. ) ;
#34248 = ORIENTED_EDGE ( 'NONE', *, *, #3721, .T. ) ;
#34250 = FACE_OUTER_BOUND ( 'NONE', #6201, .T. ) ;
#34249 = CARTESIAN_POINT ( 'NONE',  ( 2.084207363968360038, -10.81261337010820256, 33.49550067578627477 ) ) ;
#34251 = CARTESIAN_POINT ( 'NONE',  ( 7.173022441425065843, -6.696923467548660192, 34.68552623307873972 ) ) ;
#34252 = CARTESIAN_POINT ( 'NONE',  ( 15.23076923076923173, -13.88283147151868846, 33.14645433367849847 ) ) ;
#34253 = CARTESIAN_POINT ( 'NONE',  ( 6.923076923076924238, -8.564572088678739092, 35.78748833219616898 ) ) ;
#34254 = DIRECTION ( 'NONE',  ( 0.000000000000000000, 0.000000000000000000, 1.000000000000000000 ) ) ;
#34255 = VERTEX_POINT ( 'NONE', #10217 ) ;
#34256 = EDGE_CURVE ( 'NONE', #71506, #64660, #48182, .T. ) ;
#34257 = DIRECTION ( 'NONE',  ( 0.000000000000000000, 0.8660254037844377084, -0.5000000000000015543 ) ) ;
#34258 = AXIS2_PLACEMENT_3D ( 'NONE', #65537, #31321, #58782 ) ;
#34259 = CARTESIAN_POINT ( 'NONE',  ( -5.076923076923199218, -4.320704448113951379, 33.92786785259630022 ) ) ;
#34260 = CARTESIAN_POINT ( 'NONE',  ( 10.61538461538461675, -13.87047571288749737, 32.06866353760679544 ) ) ;
#34261 = EDGE_CURVE ( 'NONE', #60372, #22195, #45272, .T. ) ;
#34262 = CARTESIAN_POINT ( 'NONE',  ( -7.173100147298380413, -6.652501968072646932, 34.93155406624980941 ) ) ;
#34263 = EDGE_LOOP ( 'NONE', ( #52629, #31710 ) ) ;
#34264 = EDGE_LOOP ( 'NONE', ( #49040, #43510, #22461, #37871 ) ) ;
#34265 = VERTEX_POINT ( 'NONE', #3885 ) ;
#34266 = EDGE_CURVE ( 'NONE', #2983, #17599, #30948, .T. ) ;
#34267 = CARTESIAN_POINT ( 'NONE',  ( 10.36540787133602670, -4.075325502946081535, 33.72974371597206300 ) ) ;
#34268 = EDGE_CURVE ( 'NONE', #36170, #5202, #21390, .T. ) ;
#34269 = ORIENTED_EDGE ( 'NONE', *, *, #19419, .T. ) ;
#34270 = FACE_OUTER_BOUND ( 'NONE', #59024, .T. ) ;
#34271 = CARTESIAN_POINT ( 'NONE',  ( 17.07692307692295586, -6.879047030192662504, 34.71129190930017927 ) ) ;
#34272 = CARTESIAN_POINT ( 'NONE',  ( 4.826946345980721809, -6.567427716900047230, 34.66269422305636283 ) ) ;
#34273 = CARTESIAN_POINT ( 'NONE',  ( -17.07692307692319744, -9.528491918059723176, 34.59228464037033035 ) ) ;
#34274 = CARTESIAN_POINT ( 'NONE',  ( 14.43848411551709887, -4.118422570099828484, 33.43335022499816489 ) ) ;
#34275 = EDGE_LOOP ( 'NONE', ( #26709, #68673, #28091, #2270 ) ) ;
#34276 = DIRECTION ( 'NONE',  ( 0.000000000000000000, 0.9848077530122072432, 0.1736481776669354937 ) ) ;
#34278 = ORIENTED_EDGE ( 'NONE', *, *, #50162, .F. ) ;
#34277 = LINE ( 'NONE', #61737, #66919 ) ;
#34279 = CARTESIAN_POINT ( 'NONE',  ( 0.4615384615384611200, -9.819645486525091727, 36.12317359536749706 ) ) ;
#34280 = CARTESIAN_POINT ( 'NONE',  ( -8.545804370315979170, -7.630147987733840509, 34.99859428049665411 ) ) ;
#34281 = FACE_OUTER_BOUND ( 'NONE', #1491, .T. ) ;
#34282 = CARTESIAN_POINT ( 'NONE',  ( -39.05038313613820122, -2.249999999999998668, 29.75000000000000355 ) ) ;
#34283 = DIRECTION ( 'NONE',  ( -0.000000000000000000, -0.8660254037844399289, -0.4999999999999980016 ) ) ;
#34284 = CARTESIAN_POINT ( 'NONE',  ( -3.480745974817820887, -10.82459398097509684, 33.81372124010185587 ) ) ;
#34285 = CARTESIAN_POINT ( 'NONE',  ( 11.53846153846153832, -12.34228464037088635, 31.77849191805839268 ) ) ;
#34286 = B_SPLINE_CURVE_WITH_KNOTS ( 'NONE', 3,
 ( #72268, #37592, #78579, #79485, #10577, #38951, #10126, #51989, #65511, #9678 ),
 .UNSPECIFIED., .F., .F.,
 ( 4, 2, 2, 2, 4 ),
 ( 0.000000000000000000, 0.0001954339857564078809, 0.0003908679715128157619, 0.0005863019572692236428, 0.0007817359430256315238 ),
 .UNSPECIFIED. ) ;
#34287 = CARTESIAN_POINT ( 'NONE',  ( -2.724691934501246582, -6.299813628509474128, 22.92374329374151998 ) ) ;
#34288 = ORIENTED_EDGE ( 'NONE', *, *, #28898, .F. ) ;
#34289 = VECTOR ( 'NONE', #79105, 1000.000000000000000 ) ;
#34290 = CARTESIAN_POINT ( 'NONE',  ( 11.66925334628632349, -2.729792928343269587, 31.24908615093345077 ) ) ;
#34291 = CARTESIAN_POINT ( 'NONE',  ( -14.30769230769230660, -10.51840700105979565, 33.73612834413961536 ) ) ;
#34292 = CARTESIAN_POINT ( 'NONE',  ( 9.942362112221145409, -2.920487667080175598, 32.31805714834170828 ) ) ;
#34293 = VERTEX_POINT ( 'NONE', #41567 ) ;
#34294 = ORIENTED_EDGE ( 'NONE', *, *, #39320, .F. ) ;
#34295 = FACE_OUTER_BOUND ( 'NONE', #12071, .T. ) ;
#34296 = CARTESIAN_POINT ( 'NONE',  ( -12.46153846153846168, -3.050289026998446396, 32.03036669348365706 ) ) ;
#34297 = CARTESIAN_POINT ( 'NONE',  ( -8.834500769787089425, -11.06231777344662781, 33.60647404775220082 ) ) ;
#34298 = CARTESIAN_POINT ( 'NONE',  ( 9.942307692307633005, -7.565270000091922853, 34.99999999999999289 ) ) ;
#34299 = CARTESIAN_POINT ( 'NONE',  ( 17.77707304109314279, -2.523278758544490241, 31.42238647778636818 ) ) ;
#34300 = ORIENTED_EDGE ( 'NONE', *, *, #35968, .T. ) ;
#34301 = EDGE_CURVE ( 'NONE', #22580, #14205, #76916, .T. ) ;
#34302 = CARTESIAN_POINT ( 'NONE',  ( 12.33097854792509551, -2.254533558242299396, 29.97296025877828285 ) ) ;
#34303 = DIRECTION ( 'NONE',  ( 1.681660752236433198E-16, 1.000000000000000000, -5.102127870520021228E-17 ) ) ;
#34304 = CARTESIAN_POINT ( 'NONE',  ( 7.623227628637697428, -9.886141570436013382, 34.14413921362392301 ) ) ;
#34305 = ORIENTED_EDGE ( 'NONE', *, *, #2973, .F. ) ;
#34306 = CARTESIAN_POINT ( 'NONE',  ( -8.546267634964095805, -7.369474539155828730, 34.99858011523957657 ) ) ;
#34307 = ORIENTED_EDGE ( 'NONE', *, *, #84672, .T. ) ;
#34308 = CARTESIAN_POINT ( 'NONE',  ( 1.134615384615387246, -7.500000000000001776, 34.75000000000000000 ) ) ;
#34309 = DIRECTION ( 'NONE',  ( 0.000000000000000000, 0.000000000000000000, 1.000000000000000000 ) ) ;
#34310 = CARTESIAN_POINT ( 'NONE',  ( 5.076923076923075762, -4.786620604624113540, 33.94971097300155094 ) ) ;
#34311 = VERTEX_POINT ( 'NONE', #88891 ) ;
#34312 = CARTESIAN_POINT ( 'NONE',  ( 7.715462379486285549, -12.11776431015576172, 31.66791131148498906 ) ) ;
#34313 = CARTESIAN_POINT ( 'NONE',  ( -14.98076923076922995, -2.499999999999998668, 29.75000000000000355 ) ) ;
#34314 = CARTESIAN_POINT ( 'NONE',  ( 13.13459214732242408, -6.695914987888146541, 34.68535235679833306 ) ) ;
#34315 = B_SPLINE_CURVE_WITH_KNOTS ( 'NONE', 3,
 ( #20324, #81586, #39276, #66732, #59969, #32952, #87470, #12679, #40163, #67626 ),
 .UNSPECIFIED., .F., .F.,
 ( 4, 2, 2, 2, 4 ),
 ( 0.000000000000000000, 0.0001954339857564079352, 0.0003908679715128158703, 0.0005863019572692237513, 0.0007817359430256317406 ),
 .UNSPECIFIED. ) ;
#34316 = EDGE_CURVE ( 'NONE', #37130, #86943, #24608, .T. ) ;
#34317 = AXIS2_PLACEMENT_3D ( 'NONE', #76981, #4414, #59807 ) ;
#34318 = CARTESIAN_POINT ( 'NONE',  ( 11.31497661389720477, -12.47654668319379567, 31.42292124445336654 ) ) ;
#34319 = CARTESIAN_POINT ( 'NONE',  ( -2.084679463598911653, -10.77377354290276301, 33.85451476688484718 ) ) ;
#34320 = ORIENTED_EDGE ( 'NONE', *, *, #72442, .T. ) ;
#34321 = FACE_BOUND ( 'NONE', #53949, .T. ) ;
#34322 = ORIENTED_EDGE ( 'NONE', *, *, #42653, .F. ) ;
#34323 = DIRECTION ( 'NONE',  ( 0.000000000000000000, 0.000000000000000000, 1.000000000000000000 ) ) ;
#34324 = ADVANCED_FACE ( 'NONE', ( #26720 ), #82575, .F. ) ;
#34325 = CARTESIAN_POINT ( 'NONE',  ( 18.22277966897806678, -6.717445702608400460, 34.94155399931962336 ) ) ;
#34326 = DIRECTION ( 'NONE',  ( 0.000000000000000000, 0.4999999999999960032, -0.8660254037844410391 ) ) ;
#34327 = CARTESIAN_POINT ( 'NONE',  ( 17.01165263096229907, -2.625532179533444754, 30.86335684631481513 ) ) ;
#34328 = ADVANCED_FACE ( 'NONE', ( #66030 ), #61378, .F. ) ;
#34329 = ORIENTED_EDGE ( 'NONE', *, *, #58595, .T. ) ;
#34330 = EDGE_LOOP ( 'NONE', ( #554, #54297 ) ) ;
#34331 = ORIENTED_EDGE ( 'NONE', *, *, #4221, .F. ) ;
#34332 = DIRECTION ( 'NONE',  ( -0.000000000000000000, 0.6427876096865404731, -0.7660444431189771253 ) ) ;
#34333 = VERTEX_POINT ( 'NONE', #79568 ) ;
#34334 = ADVANCED_FACE ( 'NONE', ( #67713 ), #17864, .F. ) ;
#34335 = CARTESIAN_POINT ( 'NONE',  ( -6.223484943723947005, -12.44517049084099725, 30.48991314939691932 ) ) ;
#34336 = CARTESIAN_POINT ( 'NONE',  ( 7.846153846153723244, -10.33852847137269571, 34.16647553114546554 ) ) ;
#34337 = FACE_OUTER_BOUND ( 'NONE', #47930, .T. ) ;
#34338 = CARTESIAN_POINT ( 'NONE',  ( 3.453782074862625784, -9.172514111537584114, 34.72667873470787470 ) ) ;
#34339 = EDGE_CURVE ( 'NONE', #58442, #17248, #64287, .T. ) ;
#34340 = CARTESIAN_POINT ( 'NONE',  ( 3.749999999999992006, -5.946699141100872943, 25.64062500000000000 ) ) ;
#34341 = CARTESIAN_POINT ( 'NONE',  ( 5.076923076922954969, -11.48612834414049644, 32.76840700105863391 ) ) ;
#34342 = CARTESIAN_POINT ( 'NONE',  ( 17.86985279056177944, -2.619462340734461048, 30.83744416345203021 ) ) ;
#34343 = CARTESIAN_POINT ( 'NONE',  ( 7.912221179503920787, -4.661471528628508665, 34.16647553114624003 ) ) ;
#34344 = ORIENTED_EDGE ( 'NONE', *, *, #54830, .T. ) ;
#34345 = EDGE_CURVE ( 'NONE', #25224, #45114, #72604, .T. ) ;
#34346 = ORIENTED_EDGE ( 'NONE', *, *, #88259, .F. ) ;
#34347 = ORIENTED_EDGE ( 'NONE', *, *, #85194, .F. ) ;
#34348 = DIRECTION ( 'NONE',  ( -0.000000000000000000, 0.5000000000000011102, -0.8660254037844381525 ) ) ;
#34350 = CARTESIAN_POINT ( 'NONE',  ( -7.846153846153967493, -9.528491918059723176, 34.59228464037033035 ) ) ;
#34349 = CARTESIAN_POINT ( 'NONE',  ( 11.53846153846153832, -2.499999999999998668, 29.75000000000001421 ) ) ;
#34351 = CARTESIAN_POINT ( 'NONE',  ( 1.449870524128224591, -12.51329471203373700, 31.30864560766537963 ) ) ;
#34352 = CARTESIAN_POINT ( 'NONE',  ( -10.74553182482283198, -3.817052484675422797, 33.13202310037935661 ) ) ;
#34353 = FACE_BOUND ( 'NONE', #23701, .T. ) ;
#34354 = CARTESIAN_POINT ( 'NONE',  ( -7.146561847641252463, -3.562934362175799841, 33.22335522853832401 ) ) ;
#34355 = ORIENTED_EDGE ( 'NONE', *, *, #30767, .F. ) ;
#34356 = EDGE_CURVE ( 'NONE', #50903, #42078, #68612, .T. ) ;
#34357 = FACE_OUTER_BOUND ( 'NONE', #45428, .T. ) ;
#34358 = CARTESIAN_POINT ( 'NONE',  ( -1.318547033612945452, -2.721908614388772740, 31.22303859784725333 ) ) ;
#34359 = DIRECTION ( 'NONE',  ( 0.000000000000000000, 0.8660254037844377084, 0.5000000000000015543 ) ) ;
#34360 = ORIENTED_EDGE ( 'NONE', *, *, #858, .F. ) ;
#34361 = CARTESIAN_POINT ( 'NONE',  ( -5.011667505647053211, -6.879047030191282275, 34.71129190930002295 ) ) ;
#34363 = EDGE_CURVE ( 'NONE', #22155, #46498, #65421, .T. ) ;
#34362 = ORIENTED_EDGE ( 'NONE', *, *, #18880, .T. ) ;
#34364 = FACE_BOUND ( 'NONE', #28393, .T. ) ;
#34365 = LINE ( 'NONE', #7353, #10184 ) ;
#34366 = AXIS2_PLACEMENT_3D ( 'NONE', #52600, #25585, #47175 ) ;
#34367 = LINE ( 'NONE', #12333, #30464 ) ;
#34369 = EDGE_CURVE ( 'NONE', #37924, #37932, #35707, .T. ) ;
#34368 = CARTESIAN_POINT ( 'NONE',  ( 16.94677510719138169, -12.15440758774515473, 32.17923288041532004 ) ) ;
#34370 = ORIENTED_EDGE ( 'NONE', *, *, #18267, .T. ) ;
#34371 = FACE_OUTER_BOUND ( 'NONE', #9951, .T. ) ;
#34372 = DIRECTION ( 'NONE',  ( -0.000000000000000000, 0.1736481776669307198, -0.9848077530122080203 ) ) ;
#34373 = CARTESIAN_POINT ( 'NONE',  ( 6.792929713638703682, -12.45813303252208648, 30.39737893381572675 ) ) ;
#34374 = CARTESIAN_POINT ( 'NONE',  ( 0.000000000000000000, -11.00000000000000000, 29.25000000000000000 ) ) ;
#34375 = ORIENTED_EDGE ( 'NONE', *, *, #81799, .F. ) ;
#34376 = VECTOR ( 'NONE', #62034, 1000.000000000000227 ) ;
#34377 = B_SPLINE_CURVE_WITH_KNOTS ( 'NONE', 3,
 ( #2300, #1871, #58133, #15841, #56377, #49169, #64440, #29355, #83863, #14952 ),
 .UNSPECIFIED., .F., .F.,
 ( 4, 2, 2, 2, 4 ),
 ( 0.000000000000000000, 0.0001954339857564093175, 0.0003908679715128186350, 0.0005863019572692279796, 0.0007817359430256372700 ),
 .UNSPECIFIED. ) ;
#34378 = CARTESIAN_POINT ( 'NONE',  ( -22.00000000000000355, -15.00000000000000000, 0.000000000000000000 ) ) ;
#34379 = CARTESIAN_POINT ( 'NONE',  ( -15.23076923076922995, -8.120952969808772792, 34.71129190930000163 ) ) ;
#34380 = VECTOR ( 'NONE', #16554, 999.9999999999998863 ) ;
#34382 = VERTEX_POINT ( 'NONE', #9124 ) ;
#34381 = CARTESIAN_POINT ( 'NONE',  ( 4.376858997939550910, -2.889357225399416862, 32.26129605718031002 ) ) ;
#34383 = CARTESIAN_POINT ( 'NONE',  ( -4.377331097570100304, -2.599994579823202923, 30.74605699353653776 ) ) ;
#34384 = CARTESIAN_POINT ( 'NONE',  ( 0.6843181305165253470, -10.97394488606064122, 33.68653795673694873 ) ) ;
#34385 = CARTESIAN_POINT ( 'NONE',  ( -11.53846153846165912, -8.613356846316285953, 34.62446782046622218 ) ) ;
#34386 = CARTESIAN_POINT ( 'NONE',  ( 14.17754509825408960, -9.418419913701741919, 34.36755862841477693 ) ) ;
#34387 = CARTESIAN_POINT ( 'NONE',  ( -13.31854805126531005, -3.322132147404559976, 32.92929555188717927 ) ) ;
#34389 = DIRECTION ( 'NONE',  ( 0.000000000000000000, 0.9396926207859126468, -0.3420201433256571111 ) ) ;
#34388 = CARTESIAN_POINT ( 'NONE',  ( -3.230769230769229949, -3.937682226553329556, 33.60647404775216529 ) ) ;
#34390 = AXIS2_PLACEMENT_3D ( 'NONE', #1796, #9010, #13983 ) ;
#34391 = DIRECTION ( 'NONE',  ( -0.000000000000000000, -0.5000000000000009992, -0.8660254037844380415 ) ) ;
#34392 = EDGE_CURVE ( 'NONE', #14741, #23084, #89059, .T. ) ;
#34393 = CARTESIAN_POINT ( 'NONE',  ( -1.139087296526025916, -4.750000000000006217, 19.07812500000000000 ) ) ;
#34394 = ORIENTED_EDGE ( 'NONE', *, *, #42310, .F. ) ;
#34395 = DIRECTION ( 'NONE',  ( -0.000000000000000000, -0.8660254037844399289, -0.4999999999999980016 ) ) ;
#34396 = ORIENTED_EDGE ( 'NONE', *, *, #1631, .F. ) ;
#34397 = ADVANCED_FACE ( 'NONE', ( #15437 ), #50086, .F. ) ;
#34398 = ORIENTED_EDGE ( 'NONE', *, *, #82408, .F. ) ;
#34399 = DIRECTION ( 'NONE',  ( -0.000000000000000000, -0.000000000000000000, -1.000000000000000000 ) ) ;
#34400 = ORIENTED_EDGE ( 'NONE', *, *, #37353, .T. ) ;
#34401 = CARTESIAN_POINT ( 'NONE',  ( -4.153846153846152411, -2.486705287966279876, 31.30864560766543647 ) ) ;
#34402 = CARTESIAN_POINT ( 'NONE',  ( -2.749999999999998224, -7.500000000000015987, 18.84375000000000000 ) ) ;
#34403 = CARTESIAN_POINT ( 'NONE',  ( 13.45068373561782593, -2.721908614388771852, 31.22303859784725333 ) ) ;
#34404 = PLANE ( 'NONE',  #71190 ) ;
#34405 = CARTESIAN_POINT ( 'NONE',  ( 7.846153846154160227, -2.255955759149395501, 30.00000000000324363 ) ) ;
#34406 = CARTESIAN_POINT ( 'NONE',  ( -23.50000000000000000, -5.499999999999981348, 27.75000000000000000 ) ) ;
#34407 = CARTESIAN_POINT ( 'NONE',  ( -13.51530685128294884, -2.541943142973491554, 30.39792223712631980 ) ) ;
#34408 = CARTESIAN_POINT ( 'NONE',  ( -11.53846153846153655, -4.786620604624113540, 33.94971097300155094 ) ) ;
#34409 = CARTESIAN_POINT ( 'NONE',  ( -1.929879867024197893E-14, -3.750000000000000000, 24.15625000000000000 ) ) ;
#34410 = EDGE_CURVE ( 'NONE', #24943, #87423, #36666, .T. ) ;
#34411 = CARTESIAN_POINT ( 'NONE',  ( 6.792928953345229282, -10.31621877034669588, 34.18098118002070152 ) ) ;
#34412 = CARTESIAN_POINT ( 'NONE',  ( -16.82697766754503377, -10.92531984108285670, 33.72920026020278073 ) ) ;
#34413 = CARTESIAN_POINT ( 'NONE',  ( 10.61538461538461675, -13.04860791097971706, 34.73218667398347037 ) ) ;
#34414 = B_SPLINE_CURVE_WITH_KNOTS ( 'NONE', 3,
 ( #24359, #31573, #67144, #86994, #79772, #65355, #18513, #18069, #73005, #52283 ),
 .UNSPECIFIED., .F., .F.,
 ( 4, 2, 2, 2, 4 ),
 ( 0.000000000000000000, 0.0001954339857564071491, 0.0003908679715128142982, 0.0005863019572692214744, 0.0007817359430256285964 ),
 .UNSPECIFIED. ) ;
#34415 = AXIS2_PLACEMENT_3D ( 'NONE', #16433, #58750, #84904 ) ;
#34416 = CARTESIAN_POINT ( 'NONE',  ( -9.915792616872021625, -3.562934362175800285, 33.22335522853832401 ) ) ;
#34417 = EDGE_CURVE ( 'NONE', #77757, #22218, #22187, .T. ) ;
#34418 = B_SPLINE_CURVE_WITH_KNOTS ( 'NONE', 3,
 ( #86517, #60798, #88308, #87406, #66218, #24791, #74322, #45946, #87863, #39212 ),
 .UNSPECIFIED., .F., .F.,
 ( 4, 2, 2, 2, 4 ),
 ( 0.0007817246256747491240, 0.0009771112852218931041, 0.001172497944769036867, 0.001367884604316180631, 0.001563271263863324611 ),
 .UNSPECIFIED. ) ;
#34419 = EDGE_CURVE ( 'NONE', #2875, #28403, #32087, .T. ) ;
#34420 = EDGE_LOOP ( 'NONE', ( #2700, #55701, #21806, #86991 ) ) ;
#34421 = ORIENTED_EDGE ( 'NONE', *, *, #67116, .T. ) ;
#34422 = B_SPLINE_CURVE_WITH_KNOTS ( 'NONE', 3,
 ( #65301, #31975, #58100, #30627, #9475, #44129, #58533, #86030, #24309, #85144 ),
 .UNSPECIFIED., .F., .F.,
 ( 4, 2, 2, 2, 4 ),
 ( 0.000000000000000000, 0.0001954339881912776238, 0.0003908679763825552477, 0.0005863019645738329257, 0.0007817359527651104954 ),
 .UNSPECIFIED. ) ;
#34423 = CARTESIAN_POINT ( 'NONE',  ( -15.23076923076922995, -13.75783147151868846, 33.36296068462461051 ) ) ;
#34424 = LINE ( 'NONE', #26340, #38829 ) ;
#34425 = FACE_OUTER_BOUND ( 'NONE', #65209, .T. ) ;
#34426 = CARTESIAN_POINT ( 'NONE',  ( 5.999999999999880096, -6.026961402154118908, 34.52809138561165270 ) ) ;
#34427 = CARTESIAN_POINT ( 'NONE',  ( 9.822833130541336999, -11.66157788607254098, 32.95092075102925833 ) ) ;
#34428 = CARTESIAN_POINT ( 'NONE',  ( -9.442362282929646966, -10.92531984108285670, 33.72920026020278073 ) ) ;
#34429 = ADVANCED_FACE ( 'NONE', ( #21739 ), #77570, .T. ) ;
#34430 = DIRECTION ( 'NONE',  ( 0.000000000000000000, -1.000000000000000000, 0.000000000000000000 ) ) ;
#34431 = EDGE_LOOP ( 'NONE', ( #38325, #30736, #3430, #10291 ) ) ;
#34432 = CARTESIAN_POINT ( 'NONE',  ( 18.24994540937804643, -3.520799739797213501, 33.17531984108286025 ) ) ;
#34433 = ORIENTED_EDGE ( 'NONE', *, *, #1520, .T. ) ;
#34434 = CARTESIAN_POINT ( 'NONE',  ( -8.546451100252703270, -4.989023458446560255, 34.36081565061822118 ) ) ;
#34435 = VECTOR ( 'NONE', #62497, 1000.000000000000227 ) ;
#34436 = AXIS2_PLACEMENT_3D ( 'NONE', #1444, #7762, #56389 ) ;
#34437 = CARTESIAN_POINT ( 'NONE',  ( 0.4615384615383396616, -4.481592998941358097, 33.73612834414048933 ) ) ;
#34438 = CARTESIAN_POINT ( 'NONE',  ( 10.28846153846153832, -7.500000000000000000, 29.75000000000000355 ) ) ;
#34439 = LINE ( 'NONE', #62779, #6245 ) ;
#34440 = CARTESIAN_POINT ( 'NONE',  ( 6.000000000000001776, -11.33034616979429110, 35.88435417666054406 ) ) ;
#34441 = ADVANCED_FACE ( 'NONE', ( #69924 ), #8234, .F. ) ;
#34442 = AXIS2_PLACEMENT_3D ( 'NONE', #81817, #76374, #75485 ) ;
#34443 = AXIS2_PLACEMENT_3D ( 'NONE', #27922, #81994, #892 ) ;
#34444 = VERTEX_POINT ( 'NONE', #28960 ) ;
#34445 = VECTOR ( 'NONE', #43817, 1000.000000000000114 ) ;
#34446 = EDGE_LOOP ( 'NONE', ( #31108, #23243, #75356, #59589, #51384, #26626 ) ) ;
#34447 = VERTEX_POINT ( 'NONE', #42908 ) ;
#34448 = EDGE_LOOP ( 'NONE', ( #240, #87374, #44760, #49949 ) ) ;
#34449 = CARTESIAN_POINT ( 'NONE',  ( 6.000000000000001776, -2.538708090699994813, 30.37095296980875503 ) ) ;
#34450 = CARTESIAN_POINT ( 'NONE',  ( -12.68446542044531000, -12.64616026154729411, 30.79003144601914244 ) ) ;
#34451 = B_SPLINE_CURVE_WITH_KNOTS ( 'NONE', 3,
 ( #71924, #52538, #80021, #59748, #87243, #10237, #40816, #61075, #267, #33165 ),
 .UNSPECIFIED., .F., .F.,
 ( 4, 2, 2, 2, 4 ),
 ( 0.0007817246256747453293, 0.0009771112852218889842, 0.001172497944769032531, 0.001367884604316176294, 0.001563271263863319840 ),
 .UNSPECIFIED. ) ;
#34452 = B_SPLINE_CURVE_WITH_KNOTS ( 'NONE', 3,
 ( #30409, #71831, #23643, #64175, #50217, #58313, #1608, #15570, #43036, #85806 ),
 .UNSPECIFIED., .F., .F.,
 ( 4, 2, 2, 2, 4 ),
 ( 0.0007817246256747504250, 0.0009771112852218954894, 0.001172497944769040554, 0.001367884604316185401, 0.001563271263863330466 ),
 .UNSPECIFIED. ) ;
#34453 = CARTESIAN_POINT ( 'NONE',  ( -3.360916440207451839, -10.19110544564092002, 33.96427741523702792 ) ) ;
#34454 = CARTESIAN_POINT ( 'NONE',  ( -15.48074596171158390, -11.28823185664190376, 33.01397839955799896 ) ) ;
#34455 = CARTESIAN_POINT ( 'NONE',  ( 5.076923076923075762, -1.367168528481310208, 33.57946703557072254 ) ) ;
#34456 = CARTESIAN_POINT ( 'NONE',  ( -10.61538461538461320, -12.10708131394839349, 31.69288490824020244 ) ) ;
#34457 = EDGE_LOOP ( 'NONE', ( #37874, #13482, #2109, #33250 ) ) ;
#34458 = ORIENTED_EDGE ( 'NONE', *, *, #36642, .T. ) ;
#34459 = ORIENTED_EDGE ( 'NONE', *, *, #38932, .F. ) ;
#34461 = VERTEX_POINT ( 'NONE', #56414 ) ;
#34460 = CARTESIAN_POINT ( 'NONE',  ( 17.07692307692295586, -12.46129190930018460, 30.37095296980731973 ) ) ;
#34462 = CARTESIAN_POINT ( 'NONE',  ( 17.07692307692307665, -10.67929555188718282, 33.92786785259544047 ) ) ;
#34463 = CARTESIAN_POINT ( 'NONE',  ( 4.153846153846154188, -12.62096338111211580, 30.90682066428153263 ) ) ;
#34464 = CARTESIAN_POINT ( 'NONE',  ( 1.553300858899086867, -3.749999999999992006, 21.73437500000000000 ) ) ;
#34465 = VERTEX_POINT ( 'NONE', #83902 ) ;
#34466 = EDGE_CURVE ( 'NONE', #13098, #23856, #979, .T. ) ;
#34467 = VECTOR ( 'NONE', #33505, 1000.000000000000000 ) ;
#34468 = ORIENTED_EDGE ( 'NONE', *, *, #27784, .T. ) ;
#34469 = CARTESIAN_POINT ( 'NONE',  ( 2.294871794871793380, -3.499999999999999556, 29.75000000000000355 ) ) ;
#34470 = ADVANCED_FACE ( 'NONE', ( #57293 ), #50526, .F. ) ;
#34471 = FACE_BOUND ( 'NONE', #48262, .T. ) ;
#34472 = DIRECTION ( 'NONE',  ( -1.000000000000000000, -0.000000000000000000, -0.000000000000000000 ) ) ;
#34473 = CARTESIAN_POINT ( 'NONE',  ( 8.068933515131911705, -5.827830569534417471, 34.72679350104403539 ) ) ;
#34474 = ORIENTED_EDGE ( 'NONE', *, *, #67381, .F. ) ;
#34476 = EDGE_CURVE ( 'NONE', #5555, #32412, #26659, .T. ) ;
#34475 = CARTESIAN_POINT ( 'NONE',  ( -6.000000000000121680, -5.941354392335915335, 34.76329471203413846 ) ) ;
#34477 = CARTESIAN_POINT ( 'NONE',  ( 6.792928953345230170, -12.15440758774515473, 32.17923288041532004 ) ) ;
#34478 = CARTESIAN_POINT ( 'NONE',  ( -17.01085574357299990, -12.62096338111211757, 30.90682066428152908 ) ) ;
#34479 = CARTESIAN_POINT ( 'NONE',  ( 14.30769230769231015, -9.058645607665452459, 34.76329471203371924 ) ) ;
#34480 = VERTEX_POINT ( 'NONE', #16747 ) ;
#34481 = EDGE_CURVE ( 'NONE', #83601, #64427, #76099, .T. ) ;
#34482 = CARTESIAN_POINT ( 'NONE',  ( -12.39628332202562433, -2.379036618887895305, 30.90682066428158592 ) ) ;
#34483 = CARTESIAN_POINT ( 'NONE',  ( -6.923076923076922462, -11.16473453929635440, 33.15142922261926373 ) ) ;
#34484 = CARTESIAN_POINT ( 'NONE',  ( -16.15384615384583711, -2.255955759149395501, 30.00000000000324363 ) ) ;
#34485 = CARTESIAN_POINT ( 'NONE',  ( -2.372962753653082402, -10.90142922261923886, 33.41473453929638993 ) ) ;
#34486 = CYLINDRICAL_SURFACE ( 'NONE', #41496, 0.2500000000000002220 ) ;
#34487 = FACE_BOUND ( 'NONE', #77238, .T. ) ;
#34489 = CARTESIAN_POINT ( 'NONE',  ( -6.223484924564328225, -10.23692288466677880, 34.23039457007281072 ) ) ;
#34488 = CARTESIAN_POINT ( 'NONE',  ( 5.076923076923075762, -11.16473453929635440, 33.15142922261926373 ) ) ;
#34490 = AXIS2_PLACEMENT_3D ( 'NONE', #16758, #51402, #18109 ) ;
#34491 = CARTESIAN_POINT ( 'NONE',  ( -6.923076923076922462, -9.819645486525091727, 36.12317359536749706 ) ) ;
#34493 = CARTESIAN_POINT ( 'NONE',  ( 17.77651505627604678, -11.41268669641499756, 32.86336882939238535 ) ) ;
#34492 = CARTESIAN_POINT ( 'NONE',  ( -5.934744428723974785, -10.21337939537593620, 33.94971097300152252 ) ) ;
#34494 = EDGE_CURVE ( 'NONE', #1913, #16308, #59997, .T. ) ;
#34495 = CARTESIAN_POINT ( 'NONE',  ( -18.06608341095587633, -9.780366693483671270, 34.19971097300155805 ) ) ;
#34496 = CARTESIAN_POINT ( 'NONE',  ( -2.724691934501232371, -8.700186371490559623, 18.51375670625849068 ) ) ;
#34497 = ORIENTED_EDGE ( 'NONE', *, *, #51470, .T. ) ;
#34498 = CARTESIAN_POINT ( 'NONE',  ( -5.750054590621957118, -10.92531984108285670, 33.72920026020278073 ) ) ;
#34499 = ORIENTED_EDGE ( 'NONE', *, *, #83793, .F. ) ;
#34500 = VECTOR ( 'NONE', #59295, 1000.000000000000000 ) ;
#34501 = AXIS2_PLACEMENT_3D ( 'NONE', #3093, #4432, #72890 ) ;
#34502 = CARTESIAN_POINT ( 'NONE',  ( 12.46153846153846168, -8.120952969808772792, 34.71129190930000163 ) ) ;
#34503 = EDGE_LOOP ( 'NONE', ( #71201, #83304, #85200, #79783 ) ) ;
#34504 = CARTESIAN_POINT ( 'NONE',  ( -19.50000000000000000, -11.50000000000000000, 29.75000000000000355 ) ) ;
#34505 = CARTESIAN_POINT ( 'NONE',  ( 7.846153846153846700, -5.180354513474913603, 36.12317359536750416 ) ) ;
#34507 = EDGE_LOOP ( 'NONE', ( #59436, #54378 ) ) ;
#34506 = CARTESIAN_POINT ( 'NONE',  ( 5.750023255951410839, -8.347322224742351082, 34.93158281831414769 ) ) ;
#34508 = CARTESIAN_POINT ( 'NONE',  ( 18.06616660659164353, -7.250054591869668386, 34.99404684341514127 ) ) ;
#34509 = CARTESIAN_POINT ( 'NONE',  ( -1.987747218494660295, -5.598659921968651254, 17.49813170625848713 ) ) ;
#34510 = AXIS2_PLACEMENT_3D ( 'NONE', #12049, #40409, #67866 ) ;
#34511 = CARTESIAN_POINT ( 'NONE',  ( -15.36091720050092846, -9.504002272028875709, 34.60269587691767867 ) ) ;
#34512 = PLANE ( 'NONE',  #7285 ) ;
#34513 = DIRECTION ( 'NONE',  ( 0.000000000000000000, 0.000000000000000000, -1.000000000000000000 ) ) ;
#34514 = LINE ( 'NONE', #61093, #74643 ) ;
#34515 = DIRECTION ( 'NONE',  ( -0.000000000000000000, 0.6427876096865404731, -0.7660444431189770143 ) ) ;
#34516 = CYLINDRICAL_SURFACE ( 'NONE', #23886, 0.2500000000000004996 ) ;
#34517 =( GEOMETRIC_REPRESENTATION_CONTEXT ( 3 ) GLOBAL_UNCERTAINTY_ASSIGNED_CONTEXT ( ( #57234 ) ) GLOBAL_UNIT_ASSIGNED_CONTEXT ( ( #25788, #25340, #87511 ) ) REPRESENTATION_CONTEXT ( 'NONE', 'WORKASPACE' ) );
#34518 = CARTESIAN_POINT ( 'NONE',  ( 2.608446859217924629, -10.19485399968118422, 21.12686829374151287 ) ) ;
#34519 = DIRECTION ( 'NONE',  ( -0.000000000000000000, -0.9848077530122086864, -0.1736481776669273613 ) ) ;
#34520 = CARTESIAN_POINT ( 'NONE',  ( 10.74591031714818001, -11.46989282347013095, 32.79007818306219946 ) ) ;
#34521 = VERTEX_POINT ( 'NONE', #3233 ) ;
#34522 = CARTESIAN_POINT ( 'NONE',  ( 9.019285080869083870, -9.943054286541403997, 34.11300777759954883 ) ) ;
#34523 = CARTESIAN_POINT ( 'NONE',  ( 3.749999999999992006, -5.946699141100872943, 14.39062500000000178 ) ) ;
#34524 = EDGE_CURVE ( 'NONE', #798, #13779, #19162, .T. ) ;
#34525 = CYLINDRICAL_SURFACE ( 'NONE', #80725, 0.2500000000000009437 ) ;
#34526 = DIRECTION ( 'NONE',  ( -0.000000000000000000, 0.8660254037844399289, -0.4999999999999980016 ) ) ;
#34527 = EDGE_LOOP ( 'NONE', ( #86155, #45092 ) ) ;
#34528 = DIRECTION ( 'NONE',  ( 0.000000000000000000, 0.9848077530122072432, -0.1736481776669354937 ) ) ;
#34529 = CYLINDRICAL_SURFACE ( 'NONE', #31555, 0.2499999999999995559 ) ;
#34531 = EDGE_LOOP ( 'NONE', ( #15653, #79342, #14280, #36160 ) ) ;
#34530 = CARTESIAN_POINT ( 'NONE',  ( 2.084766090176162212, -2.758268499246657068, 31.33685645148949561 ) ) ;
#34532 = LINE ( 'NONE', #745, #41201 ) ;
#34533 = CARTESIAN_POINT ( 'NONE',  ( -5.999999999999998224, -4.102666532097928531, 36.13435417666054406 ) ) ;
#34534 = CARTESIAN_POINT ( 'NONE',  ( 16.08776274289027342, -8.973038597847269315, 34.52809138561120506 ) ) ;
#34535 = EDGE_CURVE ( 'NONE', #24282, #2419, #57916, .T. ) ;
#34536 = DIRECTION ( 'NONE',  ( -0.000000000000000000, -0.7660444431189791237, -0.6427876096865379196 ) ) ;
#34537 = LINE ( 'NONE', #26897, #82607 ) ;
#34538 = EDGE_CURVE ( 'NONE', #57919, #80616, #33208, .T. ) ;
#34539 = EDGE_LOOP ( 'NONE', ( #10114, #14335, #36857, #70225 ) ) ;
#34540 = ORIENTED_EDGE ( 'NONE', *, *, #81297, .T. ) ;
#34541 = VECTOR ( 'NONE', #2153, 1000.000000000000227 ) ;
#34542 = VERTEX_POINT ( 'NONE', #11782 ) ;
#34543 = CARTESIAN_POINT ( 'NONE',  ( -9.561515884482908234, -3.062576670634119758, 32.05464942895959979 ) ) ;
#34544 = DIRECTION ( 'NONE',  ( -0.000000000000000000, 0.9848077530122085754, -0.1736481776669273613 ) ) ;
#34545 = CARTESIAN_POINT ( 'NONE',  ( -13.16160403300253634, -12.15243808032446005, 31.58219941686247978 ) ) ;
#34546 = DIRECTION ( 'NONE',  ( -1.000000000000000000, -0.000000000000000000, -0.000000000000000000 ) ) ;
#34547 = EDGE_CURVE ( 'NONE', #52607, #66583, #48213, .T. ) ;
#34548 = B_SPLINE_CURVE_WITH_KNOTS ( 'NONE', 3,
 ( #1550, #83983, #15071, #7868, #28129, #77204, #82654, #70458, #55157, #1106 ),
 .UNSPECIFIED., .F., .F.,
 ( 4, 2, 2, 2, 4 ),
 ( 0.000000000000000000, 0.0001954339857564080707, 0.0003908679715128161414, 0.0005863019572692241849, 0.0007817359430256322827 ),
 .UNSPECIFIED. ) ;
#34549 = ORIENTED_EDGE ( 'NONE', *, *, #88056, .F. ) ;
#34550 = LINE ( 'NONE', #76870, #27677 ) ;
#34551 = ORIENTED_EDGE ( 'NONE', *, *, #7796, .F. ) ;
#34552 = ADVANCED_FACE ( 'NONE', ( #6365 ), #53194, .F. ) ;
#34553 = EDGE_CURVE ( 'NONE', #21434, #34265, #33387, .T. ) ;
#34554 = EDGE_LOOP ( 'NONE', ( #26165, #71719 ) ) ;
#34555 = VECTOR ( 'NONE', #34135, 1000.000000000000000 ) ;
#34556 = ORIENTED_EDGE ( 'NONE', *, *, #2680, .F. ) ;
#34558 = ORIENTED_EDGE ( 'NONE', *, *, #17249, .F. ) ;
#34557 = FACE_OUTER_BOUND ( 'NONE', #53692, .T. ) ;
#34559 = CARTESIAN_POINT ( 'NONE',  ( -5.010855743572999899, -12.34228464037088813, 31.77849191805839268 ) ) ;
#34560 = EDGE_CURVE ( 'NONE', #75253, #76436, #22348, .T. ) ;
#34561 = FACE_OUTER_BOUND ( 'NONE', #67013, .T. ) ;
#34562 = VECTOR ( 'NONE', #81706, 999.9999999999998863 ) ;
#34563 = CIRCLE ( 'NONE', #83507, 8.000000000000000000 ) ;
#34564 = CARTESIAN_POINT ( 'NONE',  ( 5.869852030268304155, -4.299443229763728169, 33.91186481527756058 ) ) ;
#34565 = CARTESIAN_POINT ( 'NONE',  ( -5.777220458731587627, -4.387253974876676565, 33.66317474335728832 ) ) ;
#34566 = ORIENTED_EDGE ( 'NONE', *, *, #28575, .F. ) ;
#34567 = VECTOR ( 'NONE', #43045, 1000.000000000000000 ) ;
#34568 = EDGE_LOOP ( 'NONE', ( #9684, #65939, #48183, #88854 ) ) ;
#34569 = ORIENTED_EDGE ( 'NONE', *, *, #47763, .F. ) ;
#34570 = CARTESIAN_POINT ( 'NONE',  ( -6.923076923076922462, -2.833524468853757305, 32.15551576947925838 ) ) ;
#34572 = VERTEX_POINT ( 'NONE', #27066 ) ;
#34571 = CARTESIAN_POINT ( 'NONE',  ( -2.307692307692305711, -12.62096338111211580, 30.90682066428153263 ) ) ;
#34573 = CARTESIAN_POINT ( 'NONE',  ( -2.307692307692427391, -8.613356846316285953, 34.62446782046622218 ) ) ;
#34574 = CARTESIAN_POINT ( 'NONE',  ( -17.32689982097166848, -3.436278759898155677, 33.07459398097509506 ) ) ;
#34575 = EDGE_LOOP ( 'NONE', ( #16696, #4101, #19117, #87411 ) ) ;
#34576 = DIRECTION ( 'NONE',  ( 1.000000000000000000, 0.000000000000000000, 0.000000000000000000 ) ) ;
#34577 = CARTESIAN_POINT ( 'NONE',  ( 12.59232890250541281, -9.084667340241226796, 34.75534355489798344 ) ) ;
#34578 = VERTEX_POINT ( 'NONE', #5475 ) ;
#34579 = FACE_BOUND ( 'NONE', #63964, .T. ) ;
#34580 = FACE_OUTER_BOUND ( 'NONE', #40204, .T. ) ;
#34581 = CARTESIAN_POINT ( 'NONE',  ( 13.38461538461538680, -6.343179335718451384, 34.87096338111211935 ) ) ;
#34582 = EDGE_CURVE ( 'NONE', #66717, #58944, #41028, .T. ) ;
#34583 = CARTESIAN_POINT ( 'NONE',  ( 12.39545608217832395, -6.343179335718451384, 34.87096338111212646 ) ) ;
#34585 = DIRECTION ( 'NONE',  ( 0.000000000000000000, -0.000000000000000000, -1.000000000000000000 ) ) ;
#34584 = CARTESIAN_POINT ( 'NONE',  ( -14.30769230769230660, -5.557115091759785130, 34.35708131394839171 ) ) ;
#34586 = DIRECTION ( 'NONE',  ( 0.000000000000000000, -6.938893903907222067E-15, 1.000000000000000000 ) ) ;
#34587 = CARTESIAN_POINT ( 'NONE',  ( -0.7115151924808165163, -3.627789207965226748, 32.91389620160131102 ) ) ;
#34588 = EDGE_LOOP ( 'NONE', ( #70763, #11404 ) ) ;
#34589 = CARTESIAN_POINT ( 'NONE',  ( -2.530619266599155370, -4.026226216239095379, 33.68668979543632958 ) ) ;
#34590 = CARTESIAN_POINT ( 'NONE',  ( 13.45078452557804738, -7.250054483168843156, 34.74374881642865631 ) ) ;
#34591 = VERTEX_POINT ( 'NONE', #19863 ) ;
#34592 = EDGE_CURVE ( 'NONE', #88588, #74576, #42458, .T. ) ;
#34593 = CYLINDRICAL_SURFACE ( 'NONE', #71732, 0.2500000000000004996 ) ;
#34594 = DIRECTION ( 'NONE',  ( -0.000000000000000000, 0.9396926207859092051, -0.3420201433256662704 ) ) ;
#34595 = EDGE_LOOP ( 'NONE', ( #38960, #78988 ) ) ;
#34596 = DIRECTION ( 'NONE',  ( 0.000000000000000000, 0.8660254037844377084, -0.5000000000000015543 ) ) ;
#34597 = DIRECTION ( 'NONE',  ( 0.000000000000000000, 0.6427876096865373645, -0.7660444431189797898 ) ) ;
#34598 = FACE_BOUND ( 'NONE', #2274, .T. ) ;
#34600 = CARTESIAN_POINT ( 'NONE',  ( -4.088590582570128973, -8.613356846314928816, 34.62446782046653482 ) ) ;
#34599 = CARTESIAN_POINT ( 'NONE',  ( -15.23076923076935074, -6.026961402154118019, 34.52809138561165270 ) ) ;
#34601 = CARTESIAN_POINT ( 'NONE',  ( -8.899377978668990608, -6.852621066184266141, 34.70813303252209181 ) ) ;
#34602 = CARTESIAN_POINT ( 'NONE',  ( 12.21151523731700372, -12.45566812827425451, 31.48439005359158926 ) ) ;
#34604 = CARTESIAN_POINT ( 'NONE',  ( 0.3313912521002405631, -6.001485441113819874, 34.52039167877662607 ) ) ;
#34603 = CARTESIAN_POINT ( 'NONE',  ( -3.686287386450715076E-15, 15.00000000000000000, 1.499999999999996225 ) ) ;
#34605 = AXIS2_PLACEMENT_3D ( 'NONE', #1394, #62208, #69415 ) ;
#34606 = EDGE_CURVE ( 'NONE', #86693, #47571, #3031, .T. ) ;
#34607 = CARTESIAN_POINT ( 'NONE',  ( -9.692307692307691624, -4.661471528628507777, 34.16647553114623292 ) ) ;
#34608 = CARTESIAN_POINT ( 'NONE',  ( -3.775308065498766297, -6.007798216065450170, 16.17000670625848713 ) ) ;
#34609 = ORIENTED_EDGE ( 'NONE', *, *, #38387, .T. ) ;
#34610 = ORIENTED_EDGE ( 'NONE', *, *, #76776, .F. ) ;
#34611 = CARTESIAN_POINT ( 'NONE',  ( -9.942330916529147800, -2.341070481393819236, 30.72580821765574299 ) ) ;
#34612 = CARTESIAN_POINT ( 'NONE',  ( -15.29603923132555110, -5.941354392334499579, 34.76329471203369792 ) ) ;
#34613 = LINE ( 'NONE', #69725, #81980 ) ;
#34614 = CARTESIAN_POINT ( 'NONE',  ( -8.899921372341079717, -8.191372820521381826, 34.95448215188424967 ) ) ;
#34615 = CARTESIAN_POINT ( 'NONE',  ( -8.769230769230890843, -3.300289026999228881, 32.46337939537708905 ) ) ;
#34616 = CARTESIAN_POINT ( 'NONE',  ( 2.694853999681214862, -10.10844685921789043, 18.12313170625849068 ) ) ;
#34617 = CARTESIAN_POINT ( 'NONE',  ( 3.903846153846154632, -7.500000000000001776, 34.75000000000000000 ) ) ;
#34618 = CARTESIAN_POINT ( 'NONE',  ( 2.177132394078943545, -2.254533558242299396, 29.97296025877828285 ) ) ;
#34619 = EDGE_CURVE ( 'NONE', #17855, #69894, #59957, .T. ) ;
#34620 = CARTESIAN_POINT ( 'NONE',  ( 9.468822767743363400, -10.97335522853832579, 33.68706563782419749 ) ) ;
#34621 = CYLINDRICAL_SURFACE ( 'NONE', #89060, 0.2499999999999979738 ) ;
#34622 = PLANE ( 'NONE',  #41016 ) ;
#34623 = DIRECTION ( 'NONE',  ( 0.000000000000000000, 0.000000000000000000, 1.000000000000000000 ) ) ;
#34624 = CARTESIAN_POINT ( 'NONE',  ( -3.296039231325551100, -10.33852847137145048, 34.16647553114627556 ) ) ;
#34625 = CARTESIAN_POINT ( 'NONE',  ( -8.769230769230768274, -11.35647404775217417, 33.31231777344666511 ) ) ;
#34626 = VECTOR ( 'NONE', #25179, 999.9999999999998863 ) ;
#34627 = CARTESIAN_POINT ( 'NONE',  ( 3.230769230769110045, -2.625532179533779154, 30.86335684631627174 ) ) ;
#34628 = ORIENTED_EDGE ( 'NONE', *, *, #5914, .F. ) ;
#34629 = CARTESIAN_POINT ( 'NONE',  ( 4.087762742890273415, -4.786620604624113540, 33.94971097300155805 ) ) ;
#34630 = CARTESIAN_POINT ( 'NONE',  ( 0.7115927731767751618, -2.564540009722895419, 30.55348353981670684 ) ) ;
#34631 = CARTESIAN_POINT ( 'NONE',  ( 2.775308065498755195, -6.422011778438505125, 19.64249329374151642 ) ) ;
#34632 = EDGE_CURVE ( 'NONE', #88595, #74089, #20283, .T. ) ;
#34633 = AXIS2_PLACEMENT_3D ( 'NONE', #29617, #23719, #18210 ) ;
#34634 = CARTESIAN_POINT ( 'NONE',  ( -9.019230769230768274, -7.500000000000001776, 35.04278698407183867 ) ) ;
#34635 = CARTESIAN_POINT ( 'NONE',  ( 17.01165307636675905, -11.67786785259541027, 32.92929555188721480 ) ) ;
#34636 = ORIENTED_EDGE ( 'NONE', *, *, #5138, .F. ) ;
#34637 = CARTESIAN_POINT ( 'NONE',  ( -7.146561847641256016, -3.019605429927184836, 32.48692288466676814 ) ) ;
#34639 = ORIENTED_EDGE ( 'NONE', *, *, #13149, .F. ) ;
#34638 = CARTESIAN_POINT ( 'NONE',  ( -14.53061852520844965, -12.15238873228292071, 31.58232369045353849 ) ) ;
#34640 = CARTESIAN_POINT ( 'NONE',  ( 9.822833130541338775, -12.70449254468099198, 30.44128974285582956 ) ) ;
#34641 = ADVANCED_FACE ( 'NONE', ( #40153 ), #12224, .F. ) ;
#34642 = CARTESIAN_POINT ( 'NONE',  ( -5.076923076923075762, -9.780366693483667717, 34.19971097300155094 ) ) ;
#34643 = EDGE_LOOP ( 'NONE', ( #71014, #84825, #61770, #59331 ) ) ;
#34644 = CARTESIAN_POINT ( 'NONE',  ( 8.519207531937803779, -8.432397168068783699, 34.66272746175022945 ) ) ;
#34645 = VECTOR ( 'NONE', #1134, 1000.000000000000000 ) ;
#34646 = DIRECTION ( 'NONE',  ( 0.000000000000000000, 0.000000000000000000, -1.000000000000000000 ) ) ;
#34647 = EDGE_LOOP ( 'NONE', ( #25813, #46181, #1063, #49843 ) ) ;
#34648 = CARTESIAN_POINT ( 'NONE',  ( 16.94623161025552704, -11.18331474514187995, 33.13161551792790505 ) ) ;
#34649 = CARTESIAN_POINT ( 'NONE',  ( 2.307692307692309264, -8.164416787775445883, 34.95778746994557906 ) ) ;
#34650 = ADVANCED_FACE ( 'NONE', ( #47326 ), #68488, .T. ) ;
#34651 = CARTESIAN_POINT ( 'NONE',  ( 2.307692307692309264, -12.62096338111211580, 30.90682066428153263 ) ) ;
#34652 = ORIENTED_EDGE ( 'NONE', *, *, #53688, .F. ) ;
#34653 = ORIENTED_EDGE ( 'NONE', *, *, #13293, .T. ) ;
#34654 = CARTESIAN_POINT ( 'NONE',  ( -10.48485917715097138, -2.372941743896879174, 30.88044141588253666 ) ) ;
#34655 = ORIENTED_EDGE ( 'NONE', *, *, #68461, .T. ) ;
#34656 = CARTESIAN_POINT ( 'NONE',  ( 3.296024370282068627, -12.16647553114626490, 32.15551576947920864 ) ) ;
#34657 = CARTESIAN_POINT ( 'NONE',  ( -1.254089682851821541, -2.619367082507848998, 30.83698974864644171 ) ) ;
#34658 = CARTESIAN_POINT ( 'NONE',  ( -1.634638608836842089, -11.56360843649122216, 33.07473185843129926 ) ) ;
#34659 = DIRECTION ( 'NONE',  ( -0.000000000000000000, 2.413528314402514090E-16, -1.000000000000000000 ) ) ;
#34660 = CARTESIAN_POINT ( 'NONE',  ( -0.4615384615384611200, -5.471508081941601098, 34.59228464037088457 ) ) ;
#34661 = CARTESIAN_POINT ( 'NONE',  ( 1.318533005255250190, -2.292212530054419606, 30.41441678777542634 ) ) ;
#34662 = EDGE_CURVE ( 'NONE', #3616, #7165, #72910, .T. ) ;
#34663 = B_SPLINE_CURVE_WITH_KNOTS ( 'NONE', 3,
 ( #22511, #3997, #85990, #50841, #10328, #84674, #31027, #58492, #36902, #24269 ),
 .UNSPECIFIED., .F., .F.,
 ( 4, 2, 2, 2, 4 ),
 ( 0.0007817359430256308733, 0.0009771253907249971907, 0.001172514838424363725, 0.001367904286123730259, 0.001563293733823096577 ),
 .UNSPECIFIED. ) ;
#34664 = B_SPLINE_CURVE_WITH_KNOTS ( 'NONE', 3,
 ( #54067, #81566, #19852, #47315, #27055, #82008, #44088, #63490, #22070, #70253 ),
 .UNSPECIFIED., .F., .F.,
 ( 4, 2, 2, 2, 4 ),
 ( 0.000000000000000000, 0.0001954311564186861697, 0.0003908623128373723394, 0.0005862934692560584820, 0.0007817246256747446788 ),
 .UNSPECIFIED. ) ;
#34665 = CARTESIAN_POINT ( 'NONE',  ( 10.48469314871705649, -12.11776431015576172, 31.66791131148498906 ) ) ;
#34667 = B_SPLINE_CURVE_WITH_KNOTS ( 'NONE', 3,
 ( #33430, #81178, #19463, #60890, #82947, #60444, #74865, #87963, #55461, #21229 ),
 .UNSPECIFIED., .F., .F.,
 ( 4, 2, 2, 2, 4 ),
 ( 0.0007817359430256296806, 0.0009771253907249958896, 0.001172514838424361990, 0.001367904286123728091, 0.001563293733823094408 ),
 .UNSPECIFIED. ) ;
#34666 = VECTOR ( 'NONE', #37740, 1000.000000000000114 ) ;
#34668 = ADVANCED_FACE ( 'NONE', ( #2234 ), #14434, .F. ) ;
#34669 = ADVANCED_FACE ( 'NONE', ( #22958 ), #1803, .F. ) ;
#34670 = ORIENTED_EDGE ( 'NONE', *, *, #8332, .F. ) ;
#34671 = VERTEX_POINT ( 'NONE', #49553 ) ;
#34673 = VERTEX_POINT ( 'NONE', #69385 ) ;
#34672 = CARTESIAN_POINT ( 'NONE',  ( -1.634615384615382805, -7.566083408709834757, 34.74999999999999289 ) ) ;
#34674 = AXIS2_PLACEMENT_3D ( 'NONE', #26416, #5254, #18327 ) ;
#34675 = CARTESIAN_POINT ( 'NONE',  ( 17.01084069756293715, -2.292212530054419606, 30.41441678777542634 ) ) ;
#34676 = VERTEX_POINT ( 'NONE', #8129 ) ;
#34677 = CARTESIAN_POINT ( 'NONE',  ( 11.60371667797437567, -3.643525952247864463, 33.31231777344670064 ) ) ;
#34678 = DIRECTION ( 'NONE',  ( 0.000000000000000000, 0.4999999999999985567, 0.8660254037844395958 ) ) ;
#34679 = VERTEX_POINT ( 'NONE', #49985 ) ;
#34680 = CARTESIAN_POINT ( 'NONE',  ( 8.096208157792162297, -8.303483539816731707, 34.68545999027711702 ) ) ;
#34681 = ORIENTED_EDGE ( 'NONE', *, *, #70552, .F. ) ;
#34682 = CARTESIAN_POINT ( 'NONE',  ( -12.33149329870368405, -2.504778602574660340, 29.97347330155780654 ) ) ;
#34683 = VERTEX_POINT ( 'NONE', #15772 ) ;
#34684 = FACE_OUTER_BOUND ( 'NONE', #65285, .T. ) ;
#34685 = ORIENTED_EDGE ( 'NONE', *, *, #36274, .T. ) ;
#34686 = CARTESIAN_POINT ( 'NONE',  ( -12.46153846153846168, -9.905515769479276145, 34.41647553114623292 ) ) ;
#34687 = CARTESIAN_POINT ( 'NONE',  ( -16.15384615384615330, -5.557115091759785130, 34.35708131394839171 ) ) ;
#34688 = FACE_BOUND ( 'NONE', #76656, .T. ) ;
#34689 = CARTESIAN_POINT ( 'NONE',  ( -14.30769230769242917, -9.528491918059723176, 34.59228464037033035 ) ) ;
#34690 = CARTESIAN_POINT ( 'NONE',  ( -6.857821351800899023, -12.27809138561124591, 31.22303859784720359 ) ) ;
#34691 = B_SPLINE_CURVE_WITH_KNOTS ( 'NONE', 3,
 ( #82898, #41461, #15765, #63494, #69813, #21179, #2228, #70704, #69379, #28381 ),
 .UNSPECIFIED., .F., .F.,
 ( 4, 2, 2, 2, 4 ),
 ( 0.0007817246256747530271, 0.0009771112852218978746, 0.001172497944769042939, 0.001367884604316188003, 0.001563271263863332851 ),
 .UNSPECIFIED. ) ;
#34692 = CARTESIAN_POINT ( 'NONE',  ( 11.53846153846153832, -2.833524468853757305, 32.15551576947925838 ) ) ;
#34693 = CARTESIAN_POINT ( 'NONE',  ( 4.376857505459002873, -8.239487800360276282, 34.69522927552633718 ) ) ;
#34694 = CARTESIAN_POINT ( 'NONE',  ( -5.076923076923075762, -3.937682226553329556, 33.60647404775216529 ) ) ;
#34695 = CARTESIAN_POINT ( 'NONE',  ( 16.15384615384603251, -4.481592998941358097, 33.73612834414048933 ) ) ;
#34696 = DIRECTION ( 'NONE',  ( 0.000000000000000000, 0.6427876096865368094, 0.7660444431189802339 ) ) ;
#34697 = VERTEX_POINT ( 'NONE', #63500 ) ;
#34698 = EDGE_LOOP ( 'NONE', ( #76551, #22097, #76061, #70341 ) ) ;
#34699 = VECTOR ( 'NONE', #67176, 1000.000000000000000 ) ;
#34701 = DIRECTION ( 'NONE',  ( 0.000000000000000000, 0.000000000000000000, -1.000000000000000000 ) ) ;
#34700 = CARTESIAN_POINT ( 'NONE',  ( 2.241609928332171986, -2.833524468853757305, 32.15551576947924417 ) ) ;
#34702 = B_SPLINE_CURVE_WITH_KNOTS ( 'NONE', 3,
 ( #42019, #55958, #28957, #42459, #69478, #83454, #15432, #21736, #43339, #76685 ),
 .UNSPECIFIED., .F., .F.,
 ( 4, 2, 2, 2, 4 ),
 ( 0.000000000000000000, 0.0001954311584214086476, 0.0003908623168428172951, 0.0005862934752642233677, 0.0007817246336856293861 ),
 .UNSPECIFIED. ) ;
#34703 = CARTESIAN_POINT ( 'NONE',  ( -12.71151519248081740, -2.564618984488975073, 30.55390908950641915 ) ) ;
#34704 = DIRECTION ( 'NONE',  ( -0.000000000000000000, -0.9848077530122086864, -0.1736481776669273613 ) ) ;
#34705 = FACE_OUTER_BOUND ( 'NONE', #89180, .T. ) ;
#34706 = CARTESIAN_POINT ( 'NONE',  ( 9.692307692307695177, -2.538708090699994813, 30.37095296980875503 ) ) ;
#34707 = EDGE_LOOP ( 'NONE', ( #30544, #52367 ) ) ;
#34708 = DIRECTION ( 'NONE',  ( 0.000000000000000000, 0.9396926207859126468, 0.3420201433256571111 ) ) ;
#34709 = CARTESIAN_POINT ( 'NONE',  ( 1.634669696253701066, -12.17597550085003455, 31.52189283813461884 ) ) ;
#34710 = CARTESIAN_POINT ( 'NONE',  ( -14.17716686945866300, -12.50538340440932394, 31.33453814440721885 ) ) ;
#34711 = CARTESIAN_POINT ( 'NONE',  ( 3.230769230769110045, -3.300289026999228881, 32.46337939537708905 ) ) ;
#34712 = ORIENTED_EDGE ( 'NONE', *, *, #68195, .T. ) ;
#34713 = ORIENTED_EDGE ( 'NONE', *, *, #84971, .T. ) ;
#34714 = ORIENTED_EDGE ( 'NONE', *, *, #84510, .T. ) ;
#34715 = DIRECTION ( 'NONE',  ( -0.000000000000000000, 0.9396926207859092051, -0.3420201433256662704 ) ) ;
#34716 = ORIENTED_EDGE ( 'NONE', *, *, #52412, .F. ) ;
#34717 = CARTESIAN_POINT ( 'NONE',  ( -9.561782254074048026, -10.31582465632705237, 34.18122507451815295 ) ) ;
#34718 = CARTESIAN_POINT ( 'NONE',  ( -12.23852710992561299, -6.503523203565941380, 34.64991518177335195 ) ) ;
#34719 = CARTESIAN_POINT ( 'NONE',  ( -0.3589743589743593088, -3.499999999999999556, 29.75000000000000355 ) ) ;
#34720 = CARTESIAN_POINT ( 'NONE',  ( -8.769230769230892619, -5.094484230521993062, 34.41647553114689373 ) ) ;
#34721 = CYLINDRICAL_SURFACE ( 'NONE', #30235, 0.2499999999999986955 ) ;
#34722 = ORIENTED_EDGE ( 'NONE', *, *, #86116, .F. ) ;
#34723 = CARTESIAN_POINT ( 'NONE',  ( 4.403846153846153300, -2.249999999999998668, 29.75000000000000355 ) ) ;
#34725 = ORIENTED_EDGE ( 'NONE', *, *, #48556, .T. ) ;
#34724 = LINE ( 'NONE', #27968, #51072 ) ;
#34726 = CARTESIAN_POINT ( 'NONE',  ( -17.07692307692307665, -8.164416787775445883, 34.95778746994557906 ) ) ;
#34727 = CARTESIAN_POINT ( 'NONE',  ( -10.55012904410858710, -3.835265460703683349, 33.15142922261929925 ) ) ;
#34728 = LINE ( 'NONE', #9037, #18501 ) ;
#34729 = AXIS2_PLACEMENT_3D ( 'NONE', #52260, #18491, #73437 ) ;
#34730 = CARTESIAN_POINT ( 'NONE',  ( 9.019285189144222059, -12.01375889529407281, 32.43194544308182969 ) ) ;
#34731 = DIRECTION ( 'NONE',  ( -0.000000000000000000, -0.3420201433256694901, -0.9396926207859082059 ) ) ;
#34732 = CARTESIAN_POINT ( 'NONE',  ( 9.442284455014730682, -10.05641848906368097, 34.04755513067966177 ) ) ;
#34733 = CARTESIAN_POINT ( 'NONE',  ( -2.980769230769166445, -7.434744860731434812, 35.00000000000000711 ) ) ;
#34734 = CARTESIAN_POINT ( 'NONE',  ( -2.749999999999999112, -7.438900925035484057, 19.09561829374150932 ) ) ;
#34735 = ORIENTED_EDGE ( 'NONE', *, *, #85194, .T. ) ;
#34736 = CARTESIAN_POINT ( 'NONE',  ( -3.230769230769229949, -6.343179335718451384, 34.87096338111211935 ) ) ;
#34737 = CARTESIAN_POINT ( 'NONE',  ( 0.7114839798866033904, -3.202959910592335202, 32.30730279482227019 ) ) ;
#34738 = EDGE_CURVE ( 'NONE', #58816, #75080, #50419, .T. ) ;
#34739 = CARTESIAN_POINT ( 'NONE',  ( -7.173076923076921574, -7.500000000000001776, 35.04278698407183867 ) ) ;
#34740 = VERTEX_POINT ( 'NONE', #21187 ) ;
#34741 = PLANE ( 'NONE',  #75744 ) ;
#34742 = CARTESIAN_POINT ( 'NONE',  ( 11.40831356872984514, -4.299443229763728169, 33.91186481527756058 ) ) ;
#34743 = CARTESIAN_POINT ( 'NONE',  ( -3.480769230769229061, -2.249999999999998668, 29.75000000000000355 ) ) ;
#34744 = DIRECTION ( 'NONE',  ( -0.000000000000000000, -0.000000000000000000, -1.000000000000000000 ) ) ;
#34745 = EDGE_LOOP ( 'NONE', ( #54996, #81304, #50600, #66032 ) ) ;
#34746 = CARTESIAN_POINT ( 'NONE',  ( 3.230769230769231726, -11.91647553114624181, 32.58852847137148245 ) ) ;
#34747 = EDGE_CURVE ( 'NONE', #27559, #66547, #62175, .T. ) ;
#34748 = CARTESIAN_POINT ( 'NONE',  ( 3.296837581771669967, -12.10708131394839704, 31.69288490824020954 ) ) ;
#34749 = CARTESIAN_POINT ( 'NONE',  ( 7.780883400193070898, -10.21337939537584383, 33.94971097300158647 ) ) ;
#34750 = ORIENTED_EDGE ( 'NONE', *, *, #59703, .F. ) ;
#34751 = PLANE ( 'NONE',  #88761 ) ;
#34752 = VECTOR ( 'NONE', #8786, 1000.000000000000114 ) ;
#34753 = EDGE_LOOP ( 'NONE', ( #59282, #87316, #2418, #38953 ) ) ;
#34754 = CARTESIAN_POINT ( 'NONE',  ( -17.07692307692307665, -13.53365097954675988, 30.81389545987213552 ) ) ;
#34755 = DIRECTION ( 'NONE',  ( 1.000000000000000000, 0.000000000000000000, 0.000000000000000000 ) ) ;
#34756 = ORIENTED_EDGE ( 'NONE', *, *, #60146, .T. ) ;
#34757 = FACE_OUTER_BOUND ( 'NONE', #26068, .T. ) ;
#34758 = CARTESIAN_POINT ( 'NONE',  ( -14.53061926659915315, -2.308479472611653094, 30.53278059502174457 ) ) ;
#34759 = CARTESIAN_POINT ( 'NONE',  ( -11.53846153846153655, -6.386643153685126251, 34.62446782046654192 ) ) ;
#34760 = VECTOR ( 'NONE', #23314, 999.9999999999998863 ) ;
#34761 = CARTESIAN_POINT ( 'NONE',  ( -1.384615384615383471, -1.242168528481310874, 33.36296068462461051 ) ) ;
#34762 = CARTESIAN_POINT ( 'NONE',  ( 3.296837581771669967, -12.37446782046654192, 30.86335684631486842 ) ) ;
#34763 = EDGE_CURVE ( 'NONE', #23390, #31550, #56843, .T. ) ;
#34764 = ORIENTED_EDGE ( 'NONE', *, *, #65649, .T. ) ;
#34765 = FACE_BOUND ( 'NONE', #74785, .T. ) ;
#34766 = ORIENTED_EDGE ( 'NONE', *, *, #62074, .T. ) ;
#34767 = CARTESIAN_POINT ( 'NONE',  ( 7.846153846153846700, -12.29105614889573062, 35.45975837776705220 ) ) ;
#34768 = ADVANCED_FACE ( 'NONE', ( #27953 ), #13989, .F. ) ;
#34769 = CARTESIAN_POINT ( 'NONE',  ( 5.076923076922954969, -11.94971097300221174, 32.03036669348237098 ) ) ;
#34770 = CARTESIAN_POINT ( 'NONE',  ( -2.307692307692305711, -2.499999999999998668, 29.75000000000001421 ) ) ;
#34771 = CARTESIAN_POINT ( 'NONE',  ( 6.989145274079363368, -9.780366693483667717, 34.19971097300155805 ) ) ;
#34772 = VERTEX_POINT ( 'NONE', #1359 ) ;
#34773 = ORIENTED_EDGE ( 'NONE', *, *, #866, .F. ) ;
#34774 = ORIENTED_EDGE ( 'NONE', *, *, #49220, .T. ) ;
#34775 = B_SPLINE_CURVE_WITH_KNOTS ( 'NONE', 3,
 ( #9162, #1951, #23536, #50993, #2375, #77165, #71279, #84380, #9584, #29436 ),
 .UNSPECIFIED., .F., .F.,
 ( 4, 2, 2, 2, 4 ),
 ( 0.000000000000000000, 0.0001954339857564073388, 0.0003908679715128146777, 0.0005863019572692220165, 0.0007817359430256293554 ),
 .UNSPECIFIED. ) ;
#34776 = VECTOR ( 'NONE', #86554, 1000.000000000000114 ) ;
#34777 = CARTESIAN_POINT ( 'NONE',  ( -10.74553258511630993, -8.630895178749533159, 34.87696386517710323 ) ) ;
#34778 = ORIENTED_EDGE ( 'NONE', *, *, #79259, .F. ) ;
#34779 = DIRECTION ( 'NONE',  ( -0.000000000000000000, 0.8660254037844399289, -0.4999999999999980016 ) ) ;
#34780 = AXIS2_PLACEMENT_3D ( 'NONE', #7396, #35756, #82624 ) ;
#34781 = CARTESIAN_POINT ( 'NONE',  ( -16.85354713622489342, -2.501478030877323011, 29.88021232661721172 ) ) ;
#34782 = FACE_OUTER_BOUND ( 'NONE', #41648, .T. ) ;
#34783 = CARTESIAN_POINT ( 'NONE',  ( 16.28463659481310799, -2.295524264805589354, 30.44142389570982488 ) ) ;
#34784 = CARTESIAN_POINT ( 'NONE',  ( 2.651650429449539104, -4.848349570550432475, 25.56250000000000355 ) ) ;
#34785 = CARTESIAN_POINT ( 'NONE',  ( -14.08491263871423982, -12.69155399931963046, 30.53255429739157734 ) ) ;
#34786 = CARTESIAN_POINT ( 'NONE',  ( -18.22559223176555321, -7.628091957228972930, 34.99866226681163539 ) ) ;
#34787 = CARTESIAN_POINT ( 'NONE',  ( -8.769230769230892619, -3.083524468854526912, 32.58852847137268327 ) ) ;
#34788 = ORIENTED_EDGE ( 'NONE', *, *, #22741, .F. ) ;
#34789 = ORIENTED_EDGE ( 'NONE', *, *, #69448, .T. ) ;
#34790 = VERTEX_POINT ( 'NONE', #76584 ) ;
#34791 = CARTESIAN_POINT ( 'NONE',  ( -9.692307692307691624, -13.20930481340135110, 34.54067556320372745 ) ) ;
#34793 = CARTESIAN_POINT ( 'NONE',  ( 10.74591031714818179, -6.852161475712352789, 34.70806712695775786 ) ) ;
#34792 = FACE_OUTER_BOUND ( 'NONE', #38298, .T. ) ;
#34794 = CARTESIAN_POINT ( 'NONE',  ( 1.607395053593450474, -12.47679350104403007, 31.42216943046557276 ) ) ;
#34795 = LINE ( 'NONE', #29824, #29328 ) ;
#34796 = FACE_OUTER_BOUND ( 'NONE', #84249, .T. ) ;
#34797 = CARTESIAN_POINT ( 'NONE',  ( 9.692307692307572609, -3.835265460704628371, 33.15142922262033665 ) ) ;
#34798 = ORIENTED_EDGE ( 'NONE', *, *, #6606, .T. ) ;
#34799 = FACE_OUTER_BOUND ( 'NONE', #70916, .T. ) ;
#34801 = VECTOR ( 'NONE', #22992, 1000.000000000000000 ) ;
#34800 = CARTESIAN_POINT ( 'NONE',  ( -8.769230769230768274, -3.050289026998446396, 32.03036669348365706 ) ) ;
#34802 = CARTESIAN_POINT ( 'NONE',  ( -14.30769230769230660, -13.53365097954675988, 30.81389545987213552 ) ) ;
#34803 = CARTESIAN_POINT ( 'NONE',  ( -5.999999999999998224, -1.951392089020283160, 34.73218667398347748 ) ) ;
#34804 = EDGE_LOOP ( 'NONE', ( #46887, #51496 ) ) ;
#34805 = CARTESIAN_POINT ( 'NONE',  ( 18.24994551834813805, -12.43552623307873972, 30.55307653245132826 ) ) ;
#34806 = VERTEX_POINT ( 'NONE', #69821 ) ;
#34807 = FACE_BOUND ( 'NONE', #4000, .T. ) ;
#34808 = CARTESIAN_POINT ( 'NONE',  ( 9.561616225640133138, -5.582088688514999397, 34.36776431015576350 ) ) ;
#34809 = AXIS2_PLACEMENT_3D ( 'NONE', #23346, #11172, #57581 ) ;
#34810 = CARTESIAN_POINT ( 'NONE',  ( -12.23852710992561299, -8.239487800360276282, 34.69522927552633718 ) ) ;
#34811 = FACE_OUTER_BOUND ( 'NONE', #3556, .T. ) ;
#34812 = ORIENTED_EDGE ( 'NONE', *, *, #11464, .T. ) ;
#34813 = CARTESIAN_POINT ( 'NONE',  ( -18.23784950573857344, 12.75000000000000711, 30.81664701255125394 ) ) ;
#34814 = CARTESIAN_POINT ( 'NONE',  ( -14.53061852520844965, -4.186968288167449259, 33.49512374952580274 ) ) ;
#34815 = CARTESIAN_POINT ( 'NONE',  ( 6.699591979352976345, -12.44517049084099725, 30.48991314939691932 ) ) ;
#34816 = CARTESIAN_POINT ( 'NONE',  ( -7.173100160369890510, -10.76384336483936011, 33.53834819971076087 ) ) ;
#34817 = ORIENTED_EDGE ( 'NONE', *, *, #22136, .F. ) ;
#34818 = EDGE_CURVE ( 'NONE', #29700, #84739, #38457, .T. ) ;
#34819 = B_SPLINE_CURVE_WITH_KNOTS ( 'NONE', 3,
 ( #41965, #41073, #34306, #81619, #68107, #74869, #20793, #61768, #33864, #19904 ),
 .UNSPECIFIED., .F., .F.,
 ( 4, 2, 2, 2, 4 ),
 ( 0.0007817246336856291692, 0.0009771112958940105907, 0.001172497958102391904, 0.001367884620310773434, 0.001563271282519154747 ),
 .UNSPECIFIED. ) ;
#34820 = B_SPLINE_CURVE_WITH_KNOTS ( 'NONE', 3,
 ( #4223, #38912, #45199, #59607, #79888, #86669, #18189, #39359, #66370, #5115 ),
 .UNSPECIFIED., .F., .F.,
 ( 4, 2, 2, 2, 4 ),
 ( 0.0007817359430256301143, 0.0009771253907249963233, 0.001172514838424362641, 0.001367904286123728958, 0.001563293733823095059 ),
 .UNSPECIFIED. ) ;
#34821 = CARTESIAN_POINT ( 'NONE',  ( 16.15384615384615330, -10.51840700105979565, 33.73612834413961536 ) ) ;
#34822 = CARTESIAN_POINT ( 'NONE',  ( 11.53846153846153832, -12.48256725967547354, 35.29906147534542527 ) ) ;
#34824 = VERTEX_POINT ( 'NONE', #22082 ) ;
#34823 = CARTESIAN_POINT ( 'NONE',  ( -8.834501215191544077, -3.835265460703609186, 33.15142922261924241 ) ) ;
#34825 = CARTESIAN_POINT ( 'NONE',  ( -5.076923076923075762, -12.48256725967547354, 35.29906147534542527 ) ) ;
#34826 = CARTESIAN_POINT ( 'NONE',  ( 4.153846153846154188, -13.75783147151868846, 33.36296068462461051 ) ) ;
#34827 = CARTESIAN_POINT ( 'NONE',  ( 13.25392391794783009, -8.999036380462717588, 34.52022231692819076 ) ) ;
#34828 = B_SPLINE_CURVE_WITH_KNOTS ( 'NONE', 3,
 ( #58478, #45417, #50397, #16183, #3544, #17518, #38671, #71558, #66134, #4439 ),
 .UNSPECIFIED., .F., .F.,
 ( 4, 2, 2, 2, 4 ),
 ( 0.000000000000000000, 0.0001954339857564079623, 0.0003908679715128159245, 0.0005863019572692238597, 0.0007817359430256318490 ),
 .UNSPECIFIED. ) ;
#34829 = CARTESIAN_POINT ( 'NONE',  ( -10.39260507411620260, -2.600157965045224451, 30.74683119005207743 ) ) ;
#34830 = CARTESIAN_POINT ( 'NONE',  ( 17.07692307692295586, -5.094484230521993062, 34.41647553114689373 ) ) ;
#34832 = DIRECTION ( 'NONE',  ( 0.000000000000000000, 0.000000000000000000, -1.000000000000000000 ) ) ;
#34831 = CYLINDRICAL_SURFACE ( 'NONE', #63473, 0.2499999999999997502 ) ;
#34833 = CARTESIAN_POINT ( 'NONE',  ( 14.87820512820512953, -3.499999999999999556, 29.75000000000000355 ) ) ;
#34834 = CARTESIAN_POINT ( 'NONE',  ( -2.750000000000007105, -6.360912703474006946, 17.67187500000000355 ) ) ;
#34835 = EDGE_LOOP ( 'NONE', ( #81888, #42596, #54051, #70352 ) ) ;
#34836 = CARTESIAN_POINT ( 'NONE',  ( 2.307692307692309264, -12.78798330534102767, 29.49999999999997868 ) ) ;
#34837 = EDGE_LOOP ( 'NONE', ( #75108, #37454, #60725, #23684 ) ) ;
#34838 = EDGE_CURVE ( 'NONE', #55677, #45298, #1928, .T. ) ;
#34839 = EDGE_LOOP ( 'NONE', ( #13685, #1559, #15568, #69777 ) ) ;
#34840 = CYLINDRICAL_SURFACE ( 'NONE', #84422, 0.2500000000000009437 ) ;
#34841 = ORIENTED_EDGE ( 'NONE', *, *, #38878, .T. ) ;
#34842 = FACE_OUTER_BOUND ( 'NONE', #42565, .T. ) ;
#34843 = EDGE_CURVE ( 'NONE', #68924, #89067, #24737, .T. ) ;
#34844 = DIRECTION ( 'NONE',  ( -0.000000000000000000, -1.000000000000000000, -0.000000000000000000 ) ) ;
#34845 = CARTESIAN_POINT ( 'NONE',  ( -15.93106661257773560, -5.913360116392398780, 34.49180327182771322 ) ) ;
#34846 = CARTESIAN_POINT ( 'NONE',  ( 8.769230769230768274, -12.29105614889573062, 35.45975837776705220 ) ) ;
#34847 = CARTESIAN_POINT ( 'NONE',  ( -7.846153846153844924, -1.129524287112498415, 32.06866353760679544 ) ) ;
#34848 = CARTESIAN_POINT ( 'NONE',  ( -4.480769230769230838, -7.500000000000000000, 29.75000000000000355 ) ) ;
#34849 = CARTESIAN_POINT ( 'NONE',  ( -4.403822884788509029, -3.627789207965226748, 32.91389620160131102 ) ) ;
#34850 = CARTESIAN_POINT ( 'NONE',  ( -0.7115616988314262814, -2.587272538249754117, 30.68239716806877837 ) ) ;
#34851 = CARTESIAN_POINT ( 'NONE',  ( -2.057746898314263273, -2.986452184633681117, 32.43230066228895225 ) ) ;
#34852 = ADVANCED_FACE ( 'NONE', ( #37803 ), #37348, .F. ) ;
#34853 = CIRCLE ( 'NONE', #85196, 2.750000000000000000 ) ;
#34854 = DIRECTION ( 'NONE',  ( -0.000000000000000000, -0.9848077530122086864, -0.1736481776669273613 ) ) ;
#34855 = CARTESIAN_POINT ( 'NONE',  ( -7.911424292114620727, -8.613356846314824011, 34.62446782046655613 ) ) ;
#34856 = EDGE_CURVE ( 'NONE', #75329, #73584, #16532, .T. ) ;
#34857 = VERTEX_POINT ( 'NONE', #52198 ) ;
#34858 = VERTEX_POINT ( 'NONE', #72474 ) ;
#34859 = CARTESIAN_POINT ( 'NONE',  ( -15.00775787915638304, -8.239487800360276282, 34.69522927552633718 ) ) ;
#34860 = CARTESIAN_POINT ( 'NONE',  ( 5.076923076922954969, -9.442884908241554243, 34.35708131394783038 ) ) ;
#34861 = CARTESIAN_POINT ( 'NONE',  ( -6.857821783564084228, -12.16647553114626490, 32.15551576947920864 ) ) ;
#34862 = CARTESIAN_POINT ( 'NONE',  ( 0.3962684609821410242, -10.33852847137145226, 34.16647553114627556 ) ) ;
#34863 = B_SPLINE_CURVE_WITH_KNOTS ( 'NONE', 3,
 ( #66738, #45572, #30290, #10467, #11802, #71706, #11347, #24854, #37935, #65398 ),
 .UNSPECIFIED., .F., .F.,
 ( 4, 2, 2, 2, 4 ),
 ( 0.0007817359430256360774, 0.0009771253907250041296, 0.001172514838424371965, 0.001367904286123740017, 0.001563293733823108069 ),
 .UNSPECIFIED. ) ;
#34864 = CARTESIAN_POINT ( 'NONE',  ( 9.758375025657770152, -11.35647404775217595, 33.31231777344666511 ) ) ;
#34865 = CARTESIAN_POINT ( 'NONE',  ( -6.249976730942353953, -8.303909089506435137, 34.68538101551103381 ) ) ;
#34866 = DIRECTION ( 'NONE',  ( 0.000000000000000000, -0.000000000000000000, -1.000000000000000000 ) ) ;
#34867 = EDGE_CURVE ( 'NONE', #43627, #8235, #29848, .T. ) ;
#34868 = ORIENTED_EDGE ( 'NONE', *, *, #18715, .T. ) ;
#34869 = CARTESIAN_POINT ( 'NONE',  ( -13.51476259405360203, -10.19110544564092002, 33.96427741523702792 ) ) ;
#34870 = EDGE_CURVE ( 'NONE', #18944, #44728, #64816, .T. ) ;
#34871 = ORIENTED_EDGE ( 'NONE', *, *, #70006, .T. ) ;
#34872 = VECTOR ( 'NONE', #66855, 1000.000000000000000 ) ;
#34873 = CARTESIAN_POINT ( 'NONE',  ( 13.13459216039392885, -12.45566812827425451, 31.48439005359158926 ) ) ;
#34874 = AXIS2_PLACEMENT_3D ( 'NONE', #67681, #88416, #69000 ) ;
#34875 = CARTESIAN_POINT ( 'NONE',  ( -19.50000000000000000, -3.499999999999999556, 29.75000000000000355 ) ) ;
#34876 = EDGE_CURVE ( 'NONE', #49681, #57294, #52531, .T. ) ;
#34877 = DIRECTION ( 'NONE',  ( 0.000000000000000000, 0.000000000000000000, 1.000000000000000000 ) ) ;
#34878 = EDGE_CURVE ( 'NONE', #54784, #11728, #10782, .T. ) ;
#34879 = CARTESIAN_POINT ( 'NONE',  ( -15.23076923076935074, -3.300289026999228881, 32.46337939537708905 ) ) ;
#34880 = CYLINDRICAL_SURFACE ( 'NONE', #34990, 0.2500000000000002220 ) ;
#34881 = CIRCLE ( 'NONE', #7568, 0.4999999999999994449 ) ;
#34882 = VERTEX_POINT ( 'NONE', #3121 ) ;
#34883 = VERTEX_POINT ( 'NONE', #71142 ) ;
#34884 = VERTEX_POINT ( 'NONE', #9449 ) ;
#34885 = VERTEX_POINT ( 'NONE', #17089 ) ;
#34886 = CARTESIAN_POINT ( 'NONE',  ( -16.15384615384615330, -13.49023893513002648, 31.06009739812518688 ) ) ;
#34887 = CARTESIAN_POINT ( 'NONE',  ( -12.59222906464876779, -12.62707690430377383, 30.88035979386743435 ) ) ;
#34888 = CARTESIAN_POINT ( 'NONE',  ( 14.05766908347084865, -2.588893531581426988, 31.60682220781847818 ) ) ;
#34889 = CARTESIAN_POINT ( 'NONE',  ( 14.08481279095472694, -7.630690623152299956, 34.99857592706774057 ) ) ;
#34890 = CARTESIAN_POINT ( 'NONE',  ( 7.912320452745487565, -7.250054591869670162, 34.99404684341514127 ) ) ;
#34891 = CARTESIAN_POINT ( 'NONE',  ( 14.30769230769231015, -10.05456864172156806, 36.03766855953608683 ) ) ;
#34892 = VERTEX_POINT ( 'NONE', #36911 ) ;
#34893 = ORIENTED_EDGE ( 'NONE', *, *, #61999, .F. ) ;
#34894 = ORIENTED_EDGE ( 'NONE', *, *, #75843, .F. ) ;
#34896 = ORIENTED_EDGE ( 'NONE', *, *, #61453, .F. ) ;
#34895 = DIRECTION ( 'NONE',  ( -0.000000000000000000, -0.6427876096865404731, -0.7660444431189771253 ) ) ;
#34897 = CARTESIAN_POINT ( 'NONE',  ( 10.48469314871706004, -12.38065189839062263, 30.83690757178629482 ) ) ;
#34898 = DIRECTION ( 'NONE',  ( -1.000000000000000000, 0.000000000000000000, 0.000000000000000000 ) ) ;
#34899 = EDGE_CURVE ( 'NONE', #69130, #68662, #44994, .T. ) ;
#34900 = CARTESIAN_POINT ( 'NONE',  ( 2.651650429449569302, -10.15165042944953733, 22.12500000000000000 ) ) ;
#34901 = ORIENTED_EDGE ( 'NONE', *, *, #72524, .F. ) ;
#34902 = EDGE_CURVE ( 'NONE', #57842, #22025, #30596, .T. ) ;
#34903 = ORIENTED_EDGE ( 'NONE', *, *, #54738, .F. ) ;
#34904 = CARTESIAN_POINT ( 'NONE',  ( 4.153846153846154188, -3.937682226553329556, 33.60647404775216529 ) ) ;
#34905 = ORIENTED_EDGE ( 'NONE', *, *, #24131, .F. ) ;
#34906 = FACE_BOUND ( 'NONE', #16344, .T. ) ;
#34907 = B_SPLINE_CURVE_WITH_KNOTS ( 'NONE', 3,
 ( #68280, #55642, #89020, #27295, #54760, #75926, #82248, #55204, #14224, #20535 ),
 .UNSPECIFIED., .F., .F.,
 ( 4, 2, 2, 2, 4 ),
 ( 0.000000000000000000, 0.0001954311564186866305, 0.0003908623128373732609, 0.0005862934692560598914, 0.0007817246256747465219 ),
 .UNSPECIFIED. ) ;
#34908 = CARTESIAN_POINT ( 'NONE',  ( -2.307692307692305711, -4.661471528628507777, 34.16647553114623292 ) ) ;
#34909 = EDGE_CURVE ( 'NONE', #24019, #16297, #65709, .T. ) ;
#34910 = DIRECTION ( 'NONE',  ( -1.000000000000000000, 0.000000000000000000, 0.000000000000000000 ) ) ;
#34911 = ORIENTED_EDGE ( 'NONE', *, *, #64050, .F. ) ;
#34912 = CARTESIAN_POINT ( 'NONE',  ( -16.15384615384627409, -12.70778746994576025, 30.41441678777401236 ) ) ;
#34913 = CARTESIAN_POINT ( 'NONE',  ( -14.30769230769230660, -2.538708090699994813, 30.37095296980875503 ) ) ;
#34914 = CARTESIAN_POINT ( 'NONE',  ( 0.000000000000000000, -11.00000000000000000, 29.75000000000000355 ) ) ;
#34915 = CARTESIAN_POINT ( 'NONE',  ( 7.846153846153846700, -12.78798330534103123, 29.99999999999997868 ) ) ;
#34916 = EDGE_LOOP ( 'NONE', ( #18392, #47052 ) ) ;
#34917 = EDGE_CURVE ( 'NONE', #38437, #22109, #78338, .T. ) ;
#34918 = CARTESIAN_POINT ( 'NONE',  ( 16.40384615384621725, -7.434744429011175271, 34.75000000000000711 ) ) ;
#34919 = CARTESIAN_POINT ( 'NONE',  ( -5.749945580086545327, -4.074993327901525575, 33.72946981652012255 ) ) ;
#34920 = CYLINDRICAL_SURFACE ( 'NONE', #55649, 0.2499999999999997502 ) ;
#34921 = CYLINDRICAL_SURFACE ( 'NONE', #51502, 0.2499999999999998890 ) ;
#34922 = CARTESIAN_POINT ( 'NONE',  ( -13.38461538461550582, -11.48612834414049644, 32.76840700105863391 ) ) ;
#34923 = FACE_BOUND ( 'NONE', #24669, .T. ) ;
#34925 = FACE_OUTER_BOUND ( 'NONE', #26112, .T. ) ;
#34924 = LINE ( 'NONE', #55197, #1642 ) ;
#34926 = CARTESIAN_POINT ( 'NONE',  ( -17.07692307692307665, -6.386643153685126251, 34.62446782046654192 ) ) ;
#34928 = CARTESIAN_POINT ( 'NONE',  ( 8.899756470994327984, -2.882268652242222284, 31.66798894389554064 ) ) ;
#34927 = PLANE ( 'NONE',  #83260 ) ;
#34929 = CARTESIAN_POINT ( 'NONE',  ( -10.61538461538473577, -6.835583212225970762, 34.95778746994575670 ) ) ;
#34930 = CARTESIAN_POINT ( 'NONE',  ( -0.06109907496454585613, -4.750000000000000000, 17.65438170625849068 ) ) ;
#34931 = VERTEX_POINT ( 'NONE', #51737 ) ;
#34933 = AXIS2_PLACEMENT_3D ( 'NONE', #77234, #7896, #56957 ) ;
#34932 = B_SPLINE_CURVE_WITH_KNOTS ( 'NONE', 3,
 ( #33409, #81158, #47350, #18561, #87480, #79823, #66293, #40175, #39285, #19003 ),
 .UNSPECIFIED., .F., .F.,
 ( 4, 2, 2, 2, 4 ),
 ( 0.0007817246256747484735, 0.0009771112852218928873, 0.001172497944769037084, 0.001367884604316181498, 0.001563271263863325912 ),
 .UNSPECIFIED. ) ;
#34934 = CARTESIAN_POINT ( 'NONE',  ( -8.638392351218003640, -7.277220443632450575, 34.74524770363009196 ) ) ;
#34935 = ORIENTED_EDGE ( 'NONE', *, *, #87946, .F. ) ;
#34936 = AXIS2_PLACEMENT_3D ( 'NONE', #55269, #41321, #73788 ) ;
#34937 = CARTESIAN_POINT ( 'NONE',  ( -13.25382494364843389, -9.084667340241226796, 34.75534355489798344 ) ) ;
#34938 = EDGE_LOOP ( 'NONE', ( #73519, #29383, #11093, #47626 ) ) ;
#34939 = PLANE ( 'NONE',  #68533 ) ;
#34940 = CARTESIAN_POINT ( 'NONE',  ( -7.846153846153965716, -10.21337939537710326, 33.94971097300076224 ) ) ;
#34941 = ORIENTED_EDGE ( 'NONE', *, *, #38871, .F. ) ;
#34942 = CARTESIAN_POINT ( 'NONE',  ( -9.627161912975726210, -7.750023238201979581, 34.74374492549440419 ) ) ;
#34943 = CARTESIAN_POINT ( 'NONE',  ( -1.077988221561460236, -10.27530806549876452, 18.35750670625849068 ) ) ;
#34944 = EDGE_CURVE ( 'NONE', #53967, #40946, #44100, .T. ) ;
#34945 = VECTOR ( 'NONE', #45163, 1000.000000000000114 ) ;
#34946 = CARTESIAN_POINT ( 'NONE',  ( 4.023698944407932743, -9.418419913701741919, 34.36755862841477693 ) ) ;
#34947 = CARTESIAN_POINT ( 'NONE',  ( -5.143005456283213483, -2.833524468853757305, 32.15551576947924417 ) ) ;
#34948 = CYLINDRICAL_SURFACE ( 'NONE', #5635, 0.2499999999999973355 ) ;
#34949 = CARTESIAN_POINT ( 'NONE',  ( -1.384615384615383471, -8.318370150425687726, 35.83090037661290239 ) ) ;
#34950 = CARTESIAN_POINT ( 'NONE',  ( -0.2385271099256122129, -4.187068189119697692, 33.49521262558774026 ) ) ;
#34951 = LINE ( 'NONE', #34071, #59834 ) ;
#34952 = B_SPLINE_CURVE_WITH_KNOTS ( 'NONE', 3,
 ( #1615, #55656, #83147, #29102, #56557, #84046 ),
 .UNSPECIFIED., .F., .F.,
 ( 4, 2, 4 ),
 ( 0.0003909512603273918637, 0.0005862562993132197772, 0.0007815613382990476907 ),
 .UNSPECIFIED. ) ;
#34953 = CARTESIAN_POINT ( 'NONE',  ( -1.492201783934593573, -3.724691934501250135, 21.82999329374151642 ) ) ;
#34954 = CARTESIAN_POINT ( 'NONE',  ( -9.942284423250045577, -3.627789207965226748, 32.91389620160131102 ) ) ;
#34955 = CARTESIAN_POINT ( 'NONE',  ( -5.999999999999998224, -3.050289026998446396, 32.03036669348365706 ) ) ;
#34956 = ORIENTED_EDGE ( 'NONE', *, *, #75531, .T. ) ;
#34957 = CARTESIAN_POINT ( 'NONE',  ( -3.230769230769351186, -3.300289026999228881, 32.46337939537708905 ) ) ;
#34958 = B_SPLINE_CURVE_WITH_KNOTS ( 'NONE', 3,
 ( #56867, #2357, #29851, #15455, #48783, #22638, #49235, #15010, #76250, #57315 ),
 .UNSPECIFIED., .F., .F.,
 ( 4, 2, 2, 2, 4 ),
 ( 0.000000000000000000, 0.0001954339857564093175, 0.0003908679715128186350, 0.0005863019572692279796, 0.0007817359430256372700 ),
 .UNSPECIFIED. ) ;
#34959 = CARTESIAN_POINT ( 'NONE',  ( -2.694853999681181556, -10.10844685921792241, 21.43936829374151642 ) ) ;
#34960 = CARTESIAN_POINT ( 'NONE',  ( 2.084765348785459604, -4.762599654559228846, 34.23009711892697737 ) ) ;
#34961 = CARTESIAN_POINT ( 'NONE',  ( -8.899921372341079717, -11.37499894934982692, 33.29245874905763003 ) ) ;
#34962 = ORIENTED_EDGE ( 'NONE', *, *, #61553, .T. ) ;
#34963 = CARTESIAN_POINT ( 'NONE',  ( 14.37294787896833625, -2.625532179533470512, 30.86335684631491105 ) ) ;
#34964 = CARTESIAN_POINT ( 'NONE',  ( -14.30769230769242739, -11.48612834414049644, 32.76840700105863391 ) ) ;
#34966 = ORIENTED_EDGE ( 'NONE', *, *, #55926, .F. ) ;
#34965 = CARTESIAN_POINT ( 'NONE',  ( -17.20739978503954148, -7.276988635370451597, 34.74523720219453793 ) ) ;
#34967 = CARTESIAN_POINT ( 'NONE',  ( 8.519207545009310323, -5.765609946408404518, 34.70566812827425451 ) ) ;
#34968 = CARTESIAN_POINT ( 'NONE',  ( -3.100243529005666687, -5.195472089885680766, 34.18748526763464923 ) ) ;
#34969 = CARTESIAN_POINT ( 'NONE',  ( 4.153846153846154188, -12.48256725967547354, 35.29906147534542527 ) ) ;
#34970 = VECTOR ( 'NONE', #1523, 1000.000000000000000 ) ;
#34971 = CARTESIAN_POINT ( 'NONE',  ( -9.692307692307691624, -2.486705287966279876, 31.30864560766543647 ) ) ;
#34972 = CARTESIAN_POINT ( 'NONE',  ( -18.24997673094235395, -12.17611988154120795, 31.52148481390971213 ) ) ;
#34973 = EDGE_CURVE ( 'NONE', #71827, #4784, #70676, .T. ) ;
#34974 = ADVANCED_FACE ( 'NONE', ( #31948 ), #40490, .T. ) ;
#34975 = ORIENTED_EDGE ( 'NONE', *, *, #68061, .F. ) ;
#34976 = VERTEX_POINT ( 'NONE', #80589 ) ;
#34977 = EDGE_CURVE ( 'NONE', #56750, #27705, #34143, .T. ) ;
#34978 = ORIENTED_EDGE ( 'NONE', *, *, #56606, .T. ) ;
#34979 = CARTESIAN_POINT ( 'NONE',  ( -13.45069879557126491, -3.513871655860377086, 32.76840700105978499 ) ) ;
#34980 = LINE ( 'NONE', #48940, #27054 ) ;
#34981 = ADVANCED_FACE ( 'NONE', ( #46343 ), #74717, .F. ) ;
#34982 = DIRECTION ( 'NONE',  ( -0.000000000000000000, 0.5000000000000011102, -0.8660254037844381525 ) ) ;
#34983 = CARTESIAN_POINT ( 'NONE',  ( -3.230769230769229949, -2.249999999999998668, 29.50000000000001421 ) ) ;
#34984 = B_SPLINE_CURVE_WITH_KNOTS ( 'NONE', 3,
 ( #70859, #2373, #9161, #29868, #57331, #78044, #35289, #43813, #7825, #71277 ),
 .UNSPECIFIED., .F., .F.,
 ( 4, 2, 2, 2, 4 ),
 ( 0.000000000000000000, 0.0001954339857564081520, 0.0003908679715128163040, 0.0005863019572692244018, 0.0007817359430256326080 ),
 .UNSPECIFIED. ) ;
#34985 = VERTEX_POINT ( 'NONE', #88248 ) ;
#34986 = CARTESIAN_POINT ( 'NONE',  ( -19.99999999999996447, -12.00000000000000355, 10.00000000000000178 ) ) ;
#34987 = ORIENTED_EDGE ( 'NONE', *, *, #35682, .T. ) ;
#34988 = B_SPLINE_CURVE_WITH_KNOTS ( 'NONE', 3,
 ( #8564, #15320, #56301, #1795, #29283, #56740, #63929, #42357, #28380, #77458 ),
 .UNSPECIFIED., .F., .F.,
 ( 4, 2, 2, 2, 4 ),
 ( 0.0007817246256747435946, 0.0009771112852218863821, 0.001172497944769029061, 0.001367884604316171957, 0.001563271263863314636 ),
 .UNSPECIFIED. ) ;
#34989 = ORIENTED_EDGE ( 'NONE', *, *, #70344, .F. ) ;
#34990 = AXIS2_PLACEMENT_3D ( 'NONE', #74108, #82647, #33995 ) ;
#34991 = ORIENTED_EDGE ( 'NONE', *, *, #63089, .T. ) ;
#34993 = ORIENTED_EDGE ( 'NONE', *, *, #36655, .T. ) ;
#34992 = CARTESIAN_POINT ( 'NONE',  ( 8.769230769230645706, -12.51329471203414379, 31.30864560766407578 ) ) ;
#34994 = CARTESIAN_POINT ( 'NONE',  ( -4.946397638689431275, -12.50538340440932217, 31.33453814440721885 ) ) ;
#34995 = EDGE_CURVE ( 'NONE', #28389, #72492, #25628, .T. ) ;
#34996 = CARTESIAN_POINT ( 'NONE',  ( 5.999999999999878320, -2.657715359629662988, 31.77849191805970364 ) ) ;
#34997 = CIRCLE ( 'NONE', #66648, 8.000000000000000000 ) ;
#34998 = CIRCLE ( 'NONE', #85356, 0.2500000000000002220 ) ;
#34999 = EDGE_CURVE ( 'NONE', #54833, #86900, #78176, .T. ) ;
#35000 = DIRECTION ( 'NONE',  ( -0.000000000000000000, 0.7660444431189791237, -0.6427876096865379196 ) ) ;
#35001 = CARTESIAN_POINT ( 'NONE',  ( 6.923076923076924238, -12.48256725967547354, 35.29906147534542527 ) ) ;
#35002 = ORIENTED_EDGE ( 'NONE', *, *, #21795, .T. ) ;
#35003 = ORIENTED_EDGE ( 'NONE', *, *, #32784, .F. ) ;
#35004 = EDGE_LOOP ( 'NONE', ( #22993, #55596, #58422, #81136 ) ) ;
#35005 = CARTESIAN_POINT ( 'NONE',  ( -2.241624974342231180, -3.322132147404559976, 32.92929555188717927 ) ) ;
#35007 = VERTEX_POINT ( 'NONE', #87804 ) ;
#35006 = LINE ( 'NONE', #40891, #68896 ) ;
#35008 = CARTESIAN_POINT ( 'NONE',  ( 9.561616225640136690, -11.71456829005830080, 32.44064028649416542 ) ) ;
#35009 = ADVANCED_FACE ( 'NONE', ( #81032 ), #88688, .F. ) ;
#35010 = CARTESIAN_POINT ( 'NONE',  ( 24.00000000000000000, -5.499999999999981348, 27.25000000000000000 ) ) ;
#35011 = VERTEX_POINT ( 'NONE', #87351 ) ;
#35012 = CARTESIAN_POINT ( 'NONE',  ( 14.98074599347626368, -10.76384336483936011, 33.53834819971076087 ) ) ;
#35013 = CARTESIAN_POINT ( 'NONE',  ( -15.16470189741915320, -12.34228464037088813, 31.77849191805839268 ) ) ;
#35014 = VERTEX_POINT ( 'NONE', #11681 ) ;
#35015 = FACE_BOUND ( 'NONE', #34554, .T. ) ;
#35016 = EDGE_CURVE ( 'NONE', #53989, #56689, #46789, .T. ) ;
#35017 = CARTESIAN_POINT ( 'NONE',  ( -17.75005448165186195, -8.433404298154332679, 34.66254593164985920 ) ) ;
#35018 = DIRECTION ( 'NONE',  ( 0.000000000000000000, 0.000000000000000000, 1.000000000000000000 ) ) ;
#35019 = CARTESIAN_POINT ( 'NONE',  ( 12.23805353697412812, -6.716662450894489211, 34.94144148231605840 ) ) ;
#35021 = CARTESIAN_POINT ( 'NONE',  ( 18.06606835100243913, -4.098570777380720287, 33.41473453929635440 ) ) ;
#35020 = CYLINDRICAL_SURFACE ( 'NONE', #77688, 4.000000000000000000 ) ;
#35022 = CARTESIAN_POINT ( 'NONE',  ( 5.076923076923075762, -13.57706302396349152, 30.56769352161908060 ) ) ;
#35023 = DIRECTION ( 'NONE',  ( 1.000000000000000000, 0.000000000000000000, 0.000000000000000000 ) ) ;
#35024 = ORIENTED_EDGE ( 'NONE', *, *, #9454, .T. ) ;
#35025 = CARTESIAN_POINT ( 'NONE',  ( -7.846153846153967493, -6.835583212225970762, 34.95778746994575670 ) ) ;
#35026 = CARTESIAN_POINT ( 'NONE',  ( 13.51545380262814788, -7.277220443632450575, 34.74524770363009196 ) ) ;
#35027 = EDGE_LOOP ( 'NONE', ( #4424, #64381, #54348, #74932 ) ) ;
#35028 = ADVANCED_FACE ( 'NONE', ( #74266 ), #12563, .F. ) ;
#35029 = LINE ( 'NONE', #28271, #81854 ) ;
#35030 = DIRECTION ( 'NONE',  ( -0.000000000000000000, -0.000000000000000000, -1.000000000000000000 ) ) ;
#35031 = B_SPLINE_CURVE_WITH_KNOTS ( 'NONE', 3,
 ( #7051, #7503, #48027, #34960, #89048, #47593, #75507, #5722, #53908, #13806 ),
 .UNSPECIFIED., .F., .F.,
 ( 4, 2, 2, 2, 4 ),
 ( 0.000000000000000000, 0.0001954311564186874978, 0.0003908623128373749957, 0.0005862934692560624935, 0.0007817246256747499913 ),
 .UNSPECIFIED. ) ;
#35032 = ORIENTED_EDGE ( 'NONE', *, *, #64848, .T. ) ;
#35033 = CARTESIAN_POINT ( 'NONE',  ( -9.942330916529149576, -9.356822207818506598, 34.66110646841856635 ) ) ;
#35034 = CARTESIAN_POINT ( 'NONE',  ( -18.00000000000000000, -12.75000000000000888, 29.74999999999997868 ) ) ;
#35035 = FACE_BOUND ( 'NONE', #34507, .T. ) ;
#35036 = EDGE_CURVE ( 'NONE', #7995, #34447, #13442, .T. ) ;
#35038 = CARTESIAN_POINT ( 'NONE',  ( 18.00000000000000000, -13.63283147151868846, 33.57946703557072254 ) ) ;
#35037 = FACE_OUTER_BOUND ( 'NONE', #19185, .T. ) ;
#35039 = DIRECTION ( 'NONE',  ( -0.000000000000000000, 0.7660444431189791237, -0.6427876096865379196 ) ) ;
#35040 = CARTESIAN_POINT ( 'NONE',  ( -15.45425417449318317, -9.331801661448606566, 34.40259984581193464 ) ) ;
#35042 = CARTESIAN_POINT ( 'NONE',  ( -1.576923076923076872, -3.499999999999999556, 29.75000000000000355 ) ) ;
#35041 = DIRECTION ( 'NONE',  ( 1.000000000000000000, 0.000000000000000000, 0.000000000000000000 ) ) ;
#35043 = CARTESIAN_POINT ( 'NONE',  ( -14.08491263871423982, -5.827830569534417471, 34.72679350104403539 ) ) ;
#35044 = CARTESIAN_POINT ( 'NONE',  ( -2.608446859217889546, -10.19485399968121264, 15.93563170625849068 ) ) ;
#35045 = VERTEX_POINT ( 'NONE', #75158 ) ;
#35046 = ORIENTED_EDGE ( 'NONE', *, *, #3721, .F. ) ;
#35047 = DIRECTION ( 'NONE',  ( 0.000000000000000000, 0.000000000000000000, -1.000000000000000000 ) ) ;
#35048 = CARTESIAN_POINT ( 'NONE',  ( -15.36091720050093024, -5.915902021225889484, 34.75552854090298638 ) ) ;
#35049 = CARTESIAN_POINT ( 'NONE',  ( 1.384615384615264011, -9.528491918059723176, 34.59228464037033035 ) ) ;
#35050 = CARTESIAN_POINT ( 'NONE',  ( -17.01085472592063752, -11.16473453929635440, 33.15142922261926373 ) ) ;
#35051 = CARTESIAN_POINT ( 'NONE',  ( 3.007284287045284277, -11.41268669641500466, 32.86336882939237825 ) ) ;
#35052 = CARTESIAN_POINT ( 'NONE',  ( 3.724691934501232815, -5.885600066136343678, 15.38875670625848890 ) ) ;
#35053 = EDGE_CURVE ( 'NONE', #19610, #53313, #41650, .T. ) ;
#35054 = CARTESIAN_POINT ( 'NONE',  ( 0.6845513056318560663, -4.026326845037962343, 33.68677907613344047 ) ) ;
#35055 = CARTESIAN_POINT ( 'NONE',  ( 5.869852030268303267, -3.069018819979302926, 32.56621877034667278 ) ) ;
#35056 = EDGE_CURVE ( 'NONE', #77538, #44792, #85678, .T. ) ;
#35057 = CARTESIAN_POINT ( 'NONE',  ( 9.626225312947561008, -10.67929555188718460, 33.92786785259543336 ) ) ;
#35058 = CARTESIAN_POINT ( 'NONE',  ( 17.86930939688968678, -3.957541250942358424, 33.62499894934981626 ) ) ;
#35059 = CARTESIAN_POINT ( 'NONE',  ( 16.15384615384615330, -9.058645607665452459, 34.76329471203371924 ) ) ;
#35060 = CARTESIAN_POINT ( 'NONE',  ( 7.846153846153846700, -9.584722331328613620, 36.20867863119891439 ) ) ;
#35061 = DIRECTION ( 'NONE',  ( -0.000000000000000000, -0.1736481776669307198, -0.9848077530122080203 ) ) ;
#35062 = AXIS2_PLACEMENT_3D ( 'NONE', #35792, #8317, #1554 ) ;
#35063 = CARTESIAN_POINT ( 'NONE',  ( -11.53846153846153655, -4.945431358278436385, 36.03766855953609394 ) ) ;
#35064 = DIRECTION ( 'NONE',  ( -0.000000000000000000, 0.000000000000000000, 1.000000000000000000 ) ) ;
#35065 = VERTEX_POINT ( 'NONE', #76025 ) ;
#35066 = CARTESIAN_POINT ( 'NONE',  ( 12.33084785842815378, -3.957541250942358424, 33.62499894934981626 ) ) ;
#35067 = CARTESIAN_POINT ( 'NONE',  ( 0.4615384615383396616, -2.625532179533779154, 30.86335684631627174 ) ) ;
#35068 = CARTESIAN_POINT ( 'NONE',  ( 1.901340078031373171, -9.487747218494639867, 22.37686829374150932 ) ) ;
#35069 = AXIS2_PLACEMENT_3D ( 'NONE', #27340, #68766, #67884 ) ;
#35070 = CIRCLE ( 'NONE', #73979, 3.000000000000000000 ) ;
#35071 = CARTESIAN_POINT ( 'NONE',  ( -5.777220331021931443, -12.47679350104403007, 31.42216943046555855 ) ) ;
#35072 = CARTESIAN_POINT ( 'NONE',  ( -17.93393164899756087, -10.51840700105979387, 33.73612834413962247 ) ) ;
#35073 = VERTEX_POINT ( 'NONE', #27844 ) ;
#35074 = CARTESIAN_POINT ( 'NONE',  ( -16.21909714400740299, -2.506253911140460477, 30.00000000000013856 ) ) ;
#35076 = ORIENTED_EDGE ( 'NONE', *, *, #74588, .F. ) ;
#35075 = CARTESIAN_POINT ( 'NONE',  ( -6.065322915492173728, -7.749976743299137993, 34.99404534957040624 ) ) ;
#35077 = CARTESIAN_POINT ( 'NONE',  ( 8.096208157792158744, -3.627508038966690496, 32.91356715214248396 ) ) ;
#35078 = CYLINDRICAL_SURFACE ( 'NONE', #64194, 0.2500000000000008882 ) ;
#35079 = ORIENTED_EDGE ( 'NONE', *, *, #6944, .T. ) ;
#35080 = CARTESIAN_POINT ( 'NONE',  ( -5.207614543590636913, -12.11776431015576172, 31.66791131148498906 ) ) ;
#35081 = CARTESIAN_POINT ( 'NONE',  ( 13.13463864056679675, -9.234221910056348293, 34.70572697212741531 ) ) ;
#35082 = ORIENTED_EDGE ( 'NONE', *, *, #34944, .T. ) ;
#35083 = CARTESIAN_POINT ( 'NONE',  ( -10.61538461538473577, -4.320704448113951379, 33.92786785259630022 ) ) ;
#35084 = DIRECTION ( 'NONE',  ( -1.000000000000000000, -0.000000000000000000, -0.000000000000000000 ) ) ;
#35085 = DIRECTION ( 'NONE',  ( -0.000000000000000000, -0.9848077530122086864, -0.1736481776669273613 ) ) ;
#35086 = ORIENTED_EDGE ( 'NONE', *, *, #24867, .F. ) ;
#35087 = ORIENTED_EDGE ( 'NONE', *, *, #81092, .T. ) ;
#35088 = CARTESIAN_POINT ( 'NONE',  ( 6.065255571276025215, -6.879047030191282275, 34.71129190930002295 ) ) ;
#35089 = ADVANCED_FACE ( 'NONE', ( #63840 ), #68828, .F. ) ;
#35090 = ORIENTED_EDGE ( 'NONE', *, *, #69317, .F. ) ;
#35091 = CARTESIAN_POINT ( 'NONE',  ( 7.846153846153723244, -9.528491918059723176, 34.59228464037033035 ) ) ;
#35092 = CARTESIAN_POINT ( 'NONE',  ( 12.68431800280687050, -9.332535724633409302, 34.40230450496446934 ) ) ;
#35093 = CARTESIAN_POINT ( 'NONE',  ( 2.438217745925951085, -11.66157788607254275, 32.95092075102925833 ) ) ;
#35094 = EDGE_CURVE ( 'NONE', #29011, #83562, #12624, .T. ) ;
#35095 = CARTESIAN_POINT ( 'NONE',  ( -2.530618525208453207, -5.667676309546437530, 34.40238873228292249 ) ) ;
#35096 = CARTESIAN_POINT ( 'NONE',  ( -4.219929564802032296, -6.386643153685125363, 34.62446782046654903 ) ) ;
#35097 = DIRECTION ( 'NONE',  ( -1.000000000000000000, -0.000000000000000000, -0.000000000000000000 ) ) ;
#35098 = AXIS2_PLACEMENT_3D ( 'NONE', #86557, #86101, #65371 ) ;
#35099 = ADVANCED_FACE ( 'NONE', ( #43134 ), #8466, .F. ) ;
#35100 = LINE ( 'NONE', #83745, #43499 ) ;
#35101 = VERTEX_POINT ( 'NONE', #56643 ) ;
#35102 = ORIENTED_EDGE ( 'NONE', *, *, #55268, .T. ) ;
#35104 = EDGE_LOOP ( 'NONE', ( #36523, #79038 ) ) ;
#35103 = CARTESIAN_POINT ( 'NONE',  ( 4.219101293358989757, -8.656820664281605460, 34.87096338111211224 ) ) ;
#35105 = EDGE_CURVE ( 'NONE', #456, #31984, #1249, .T. ) ;
#35106 = CARTESIAN_POINT ( 'NONE',  ( 17.01165307636676260, -2.379036618887870436, 30.90682066428148644 ) ) ;
#35107 = ORIENTED_EDGE ( 'NONE', *, *, #38640, .T. ) ;
#35108 = CARTESIAN_POINT ( 'NONE',  ( -17.77722045873158763, -3.236590943229503914, 32.36255958852954251 ) ) ;
#35109 = CARTESIAN_POINT ( 'NONE',  ( -8.096130590202436750, -10.06842814019191401, 34.32929386961144758 ) ) ;
#35110 = VERTEX_POINT ( 'NONE', #82801 ) ;
#35111 = CARTESIAN_POINT ( 'NONE',  ( 7.912222197156284054, -8.120952969808772792, 34.71129190929999453 ) ) ;
#35112 = ADVANCED_FACE ( 'NONE', ( #70602 ), #69276, .F. ) ;
#35113 = ORIENTED_EDGE ( 'NONE', *, *, #70021, .F. ) ;
#35115 = ORIENTED_EDGE ( 'NONE', *, *, #27790, .F. ) ;
#35114 = FACE_OUTER_BOUND ( 'NONE', #85603, .T. ) ;
#35116 = CARTESIAN_POINT ( 'NONE',  ( -10.68114141789892102, -7.249945686854186278, 34.74374336980224598 ) ) ;
#35117 = AXIS2_PLACEMENT_3D ( 'NONE', #40781, #26373, #47516 ) ;
#35118 = VERTEX_POINT ( 'NONE', #13882 ) ;
#35119 = CARTESIAN_POINT ( 'NONE',  ( 15.23076923076911093, -3.300289026999228881, 32.46337939537708905 ) ) ;
#35120 = B_SPLINE_CURVE_WITH_KNOTS ( 'NONE', 3,
 ( #57964, #3458, #30058, #9779, #45332, #10673, #51178, #16534, #71919, #11566 ),
 .UNSPECIFIED., .F., .F.,
 ( 4, 2, 2, 2, 4 ),
 ( 0.000000000000000000, 0.0001954311564186863052, 0.0003908623128373726104, 0.0005862934692560589156, 0.0007817246256747452209 ),
 .UNSPECIFIED. ) ;
#35121 = CARTESIAN_POINT ( 'NONE',  ( 16.82689983963011215, -2.823816976329320827, 31.52131813110797154 ) ) ;
#35122 = FACE_BOUND ( 'NONE', #48068, .T. ) ;
#35123 = EDGE_CURVE ( 'NONE', #23593, #48855, #87694, .T. ) ;
#35124 = AXIS2_PLACEMENT_3D ( 'NONE', #7523, #54368, #69219 ) ;
#35125 = CARTESIAN_POINT ( 'NONE',  ( -14.53117723225663482, -9.417330523894424488, 34.63758898049880486 ) ) ;
#35126 = CARTESIAN_POINT ( 'NONE',  ( -6.792551221313357424, -12.27024696741798770, 31.24895572276497546 ) ) ;
#35127 = VECTOR ( 'NONE', #72193, 1000.000000000000000 ) ;
#35128 = CARTESIAN_POINT ( 'NONE',  ( 15.29683656411930848, -2.486705287966280320, 31.30864560766543647 ) ) ;
#35129 = CARTESIAN_POINT ( 'NONE',  ( 12.23805353697412990, -3.562934362175799841, 33.22335522853832401 ) ) ;
#35130 = CARTESIAN_POINT ( 'NONE',  ( 5.207448778686640800, -10.88167719472716399, 33.43325721877153711 ) ) ;
#35131 = CARTESIAN_POINT ( 'NONE',  ( 10.61538461538449418, -11.06231777344772027, 33.60647404775119895 ) ) ;
#35132 = ORIENTED_EDGE ( 'NONE', *, *, #58021, .T. ) ;
#35133 = EDGE_CURVE ( 'NONE', #82999, #54572, #61998, .T. ) ;
#35134 = CARTESIAN_POINT ( 'NONE',  ( -14.24162395668986747, -3.513871655860379306, 32.76840700105978499 ) ) ;
#35135 = ORIENTED_EDGE ( 'NONE', *, *, #74705, .F. ) ;
#35136 = ORIENTED_EDGE ( 'NONE', *, *, #75633, .T. ) ;
#35138 = CARTESIAN_POINT ( 'NONE',  ( -0.4615384615384611200, -12.37446782046654192, 30.86335684631486131 ) ) ;
#35137 = CARTESIAN_POINT ( 'NONE',  ( -1.134560964701931018, -4.818054556918156983, 34.26375889529406749 ) ) ;
#35139 = CARTESIAN_POINT ( 'NONE',  ( -12.59168567097668223, -2.619462340734462380, 30.83744416345203021 ) ) ;
#35140 = CARTESIAN_POINT ( 'NONE',  ( -16.82686865700962286, -10.06805714834173138, 34.32951233291982618 ) ) ;
#35141 = CARTESIAN_POINT ( 'NONE',  ( 15.29602480204525783, -3.835265460703683349, 33.15142922261929925 ) ) ;
#35142 = CARTESIAN_POINT ( 'NONE',  ( 18.00000000000000000, -13.20930481340135110, 34.54067556320372745 ) ) ;
#35143 = ORIENTED_EDGE ( 'NONE', *, *, #35094, .T. ) ;
#35144 = CARTESIAN_POINT ( 'NONE',  ( 11.31553457955469000, -3.395401636524185474, 33.02366814457250399 ) ) ;
#35145 = ADVANCED_FACE ( 'NONE', ( #29191 ), #3900, .F. ) ;
#35146 = DIRECTION ( 'NONE',  ( -0.000000000000000000, 0.7660444431189791237, -0.6427876096865379196 ) ) ;
#35147 = CARTESIAN_POINT ( 'NONE',  ( -4.153846153846152411, -2.249999999999998668, 29.75000000000001776 ) ) ;
#35148 = CARTESIAN_POINT ( 'NONE',  ( 3.100077764101671463, -3.062553014421049991, 32.05460306192774311 ) ) ;
#35149 = CARTESIAN_POINT ( 'NONE',  ( -5.076923076923075762, -11.33034616979429110, 35.88435417666054406 ) ) ;
#35150 = ORIENTED_EDGE ( 'NONE', *, *, #39912, .T. ) ;
#35151 = ORIENTED_EDGE ( 'NONE', *, *, #49248, .F. ) ;
#35152 = CONTEXT_DEPENDENT_SHAPE_REPRESENTATION ( #60744, #85883 ) ;
#35153 = EDGE_LOOP ( 'NONE', ( #84229, #61585, #36319, #8638 ) ) ;
#35154 = CARTESIAN_POINT ( 'NONE',  ( 2.750000000000001776, -7.500000000000000000, 29.50000000000000355 ) ) ;
#35155 = ORIENTED_EDGE ( 'NONE', *, *, #20039, .F. ) ;
#35156 = CARTESIAN_POINT ( 'NONE',  ( -9.442253272394237840, -10.06805714834173493, 34.32951233291982618 ) ) ;
#35157 = CARTESIAN_POINT ( 'NONE',  ( 2.544871794871792936, -7.500000000000000000, 29.75000000000000355 ) ) ;
#35158 = LINE ( 'NONE', #22093, #79785 ) ;
#35159 = CARTESIAN_POINT ( 'NONE',  ( -2.242436736416282717, -5.219633306516380244, 34.19971097300157936 ) ) ;
#35160 = EDGE_CURVE ( 'NONE', #73867, #33320, #37252, .T. ) ;
#35161 = B_SPLINE_CURVE_WITH_KNOTS ( 'NONE', 3,
 ( #58868, #60199, #87700, #18783, #46250, #53892, #45349, #87255, #39508, #59313 ),
 .UNSPECIFIED., .F., .F.,
 ( 4, 2, 2, 2, 4 ),
 ( 0.000000000000000000, 0.0001954311564186866305, 0.0003908623128373732609, 0.0005862934692560598914, 0.0007817246256747465219 ),
 .UNSPECIFIED. ) ;
#35162 = CARTESIAN_POINT ( 'NONE',  ( 12.46153846153833911, -10.21337939537710326, 33.94971097300076224 ) ) ;
#35164 = EDGE_LOOP ( 'NONE', ( #16233, #42427 ) ) ;
#35163 = AXIS2_PLACEMENT_3D ( 'NONE', #14000, #7251, #47338 ) ;
#35165 = DIRECTION ( 'NONE',  ( 0.000000000000000000, 0.000000000000000000, -1.000000000000000000 ) ) ;
#35167 = ORIENTED_EDGE ( 'NONE', *, *, #32437, .T. ) ;
#35166 = DIRECTION ( 'NONE',  ( -0.000000000000000000, 0.6427876096865404731, -0.7660444431189771253 ) ) ;
#35168 = CARTESIAN_POINT ( 'NONE',  ( 13.19230769230769340, -3.499999999999999556, 29.75000000000000355 ) ) ;
#35169 = CYLINDRICAL_SURFACE ( 'NONE', #29767, 0.2500000000000009437 ) ;
#35170 = CARTESIAN_POINT ( 'NONE',  ( 17.07692307692307665, -3.513871655860378418, 32.76840700105978499 ) ) ;
#35171 = EDGE_CURVE ( 'NONE', #19139, #1878, #10675, .T. ) ;
#35172 = EDGE_CURVE ( 'NONE', #29433, #30896, #27544, .T. ) ;
#35173 = CARTESIAN_POINT ( 'NONE',  ( 9.942362003946010773, -10.66356715214248752, 33.62249196103329751 ) ) ;
#35174 = CARTESIAN_POINT ( 'NONE',  ( -17.77722033102192967, -10.97394488606064122, 33.68653795673696294 ) ) ;
#35175 = CARTESIAN_POINT ( 'NONE',  ( -3.361459833879537840, -10.70098750199973203, 33.91152734681376302 ) ) ;
#35176 = CARTESIAN_POINT ( 'NONE',  ( 18.75000000000000000, -7.500000000000000000, 29.75000000000000355 ) ) ;
#35177 = CARTESIAN_POINT ( 'NONE',  ( 2.724691934501250135, -8.700186371490531201, 23.54874329374151642 ) ) ;
#35178 = EDGE_LOOP ( 'NONE', ( #26473, #69228, #84774, #19094, #85669 ) ) ;
#35179 = EDGE_CURVE ( 'NONE', #34683, #48673, #64051, .T. ) ;
#35180 = CARTESIAN_POINT ( 'NONE',  ( -4.853959942656404181, -7.369474539155828730, 34.99858011523957657 ) ) ;
#35181 = CARTESIAN_POINT ( 'NONE',  ( 1.134592160393928850, -9.356822207818506598, 34.66110646841856635 ) ) ;
#35182 = CARTESIAN_POINT ( 'NONE',  ( -6.923076923076922462, -1.790695186598648903, 34.54067556320373455 ) ) ;
#35183 = LINE ( 'NONE', #50021, #102 ) ;
#35184 = EDGE_LOOP ( 'NONE', ( #76849, #16577 ) ) ;
#35185 = CARTESIAN_POINT ( 'NONE',  ( -1.944543648262992530, -9.444543648263016067, 14.93750000000000000 ) ) ;
#35186 = CARTESIAN_POINT ( 'NONE',  ( -3.454254174493178731, -10.81261337010820256, 33.49550067578627477 ) ) ;
#35187 = CARTESIAN_POINT ( 'NONE',  ( 14.08482604462921195, -2.251424796025574881, 29.88072029997477586 ) ) ;
#35188 = CARTESIAN_POINT ( 'NONE',  ( -4.284537620513709122, -10.54014554554150607, 33.71984207302941883 ) ) ;
#35189 = ORIENTED_EDGE ( 'NONE', *, *, #48054, .T. ) ;
#35190 = CARTESIAN_POINT ( 'NONE',  ( 6.130525701763564150, -6.001044277235011215, 34.52024696741798948 ) ) ;
#35191 = VECTOR ( 'NONE', #49964, 1000.000000000000000 ) ;
#35192 = CARTESIAN_POINT ( 'NONE',  ( 7.976945653978634532, -5.582136614379148654, 34.36778462344220486 ) ) ;
#35193 = CARTESIAN_POINT ( 'NONE',  ( -14.17685397720554441, -7.277220318596961057, 34.99547417642776992 ) ) ;
#35194 = B_SPLINE_CURVE_WITH_KNOTS ( 'NONE', 3,
 ( #83795, #76128, #41465, #7685, #15770, #14430, #35596, #70264, #63045, #76581 ),
 .UNSPECIFIED., .F., .F.,
 ( 4, 2, 2, 2, 4 ),
 ( 0.000000000000000000, 0.0001954311564186863323, 0.0003908623128373726646, 0.0005862934692560590241, 0.0007817246256747453293 ),
 .UNSPECIFIED. ) ;
#35195 = ORIENTED_EDGE ( 'NONE', *, *, #24750, .T. ) ;
#35196 = DIRECTION ( 'NONE',  ( 0.000000000000000000, 0.6427876096865373645, -0.7660444431189797898 ) ) ;
#35197 = AXIS2_PLACEMENT_3D ( 'NONE', #4196, #31680, #66347 ) ;
#35198 = AXIS2_PLACEMENT_3D ( 'NONE', #42488, #63631, #77596 ) ;
#35199 = ORIENTED_EDGE ( 'NONE', *, *, #86142, .F. ) ;
#35200 = CARTESIAN_POINT ( 'NONE',  ( -2.372962753653081514, -12.27809138561121394, 31.22303859784730307 ) ) ;
#35201 = CARTESIAN_POINT ( 'NONE',  ( 6.130047606255684123, -7.723484964179500700, 34.74522123443823318 ) ) ;
#35202 = ORIENTED_EDGE ( 'NONE', *, *, #61308, .F. ) ;
#35203 = CARTESIAN_POINT ( 'NONE',  ( -17.86947456176635640, -10.31582465632705770, 34.18122507451815295 ) ) ;
#35204 = CARTESIAN_POINT ( 'NONE',  ( 5.076923076923075762, -7.500000000000001776, 35.04278698407183867 ) ) ;
#35205 = CARTESIAN_POINT ( 'NONE',  ( -10.68146802634049486, -5.557115091759785130, 34.35708131394839171 ) ) ;
#35206 = CARTESIAN_POINT ( 'NONE',  ( -11.40793610022789650, -5.915461855592780260, 34.75538340440931506 ) ) ;
#35207 = CYLINDRICAL_SURFACE ( 'NONE', #74225, 0.2500000000000002220 ) ;
#35208 = ORIENTED_EDGE ( 'NONE', *, *, #5988, .T. ) ;
#35209 = ORIENTED_EDGE ( 'NONE', *, *, #47419, .T. ) ;
#35210 = FACE_BOUND ( 'NONE', #38773, .T. ) ;
#35211 = VERTEX_POINT ( 'NONE', #17432 ) ;
#35212 = CARTESIAN_POINT ( 'NONE',  ( -8.834500769787091201, -12.51329471203370325, 31.30864560766548976 ) ) ;
#35213 = LINE ( 'NONE', #76651, #30066 ) ;
#35214 = CARTESIAN_POINT ( 'NONE',  ( 6.250054419913455561, -5.642605341092957083, 34.66089969410670335 ) ) ;
#35215 = CARTESIAN_POINT ( 'NONE',  ( 14.43821774592595553, -8.630441415882550871, 34.87705825610312615 ) ) ;
#35216 = ORIENTED_EDGE ( 'NONE', *, *, #6924, .F. ) ;
#35217 = VECTOR ( 'NONE', #36619, 1000.000000000000000 ) ;
#35218 = ADVANCED_FACE ( 'NONE', ( #44887 ), #37242, .F. ) ;
#35219 = ORIENTED_EDGE ( 'NONE', *, *, #45638, .T. ) ;
#35220 = ORIENTED_EDGE ( 'NONE', *, *, #55422, .T. ) ;
#35221 = CARTESIAN_POINT ( 'NONE',  ( -3.165514091256390827, -11.67786785259547777, 32.92929555188713664 ) ) ;
#35222 = ORIENTED_EDGE ( 'NONE', *, *, #86616, .F. ) ;
#35223 = B_SPLINE_CURVE_WITH_KNOTS ( 'NONE', 3,
 ( #39847, #67313, #20885, #47024, #46596, #54224, #27207, #75833, #34403, #68635 ),
 .UNSPECIFIED., .F., .F.,
 ( 4, 2, 2, 2, 4 ),
 ( 0.0007817359430256294638, 0.0009771253907249941549, 0.001172514838424358954, 0.001367904286123723754, 0.001563293733823095492 ),
 .UNSPECIFIED. ) ;
#35224 = CARTESIAN_POINT ( 'NONE',  ( -4.853911725310226188, -4.887748414852792322, 34.01359900205216746 ) ) ;
#35225 = B_SPLINE_CURVE_WITH_KNOTS ( 'NONE', 3,
 ( #12245, #60426, #25760, #66743, #67639, #87941, #27086, #59984, #40176, #53672 ),
 .UNSPECIFIED., .F., .F.,
 ( 4, 2, 2, 2, 4 ),
 ( 0.000000000000000000, 0.0001954311564186865492, 0.0003908623128373730983, 0.0005862934692560596746, 0.0007817246256747461966 ),
 .UNSPECIFIED. ) ;
#35226 = CARTESIAN_POINT ( 'NONE',  ( -11.60373153901785948, -5.941354392334499579, 34.76329471203369792 ) ) ;
#35227 = CARTESIAN_POINT ( 'NONE',  ( -17.20761368003338987, -2.845849958028613624, 32.17971566917920967 ) ) ;
#35228 = CARTESIAN_POINT ( 'NONE',  ( -12.46153846153846168, -1.242168528481310874, 33.36296068462461051 ) ) ;
#35229 = FACE_OUTER_BOUND ( 'NONE', #23469, .T. ) ;
#35230 = DIRECTION ( 'NONE',  ( -0.000000000000000000, 1.000000000000000000, -0.000000000000000000 ) ) ;
#35231 = CARTESIAN_POINT ( 'NONE',  ( 11.31553532094539172, -9.886141570436013382, 34.14413921362392301 ) ) ;
#35232 = ORIENTED_EDGE ( 'NONE', *, *, #32533, .T. ) ;
#35233 = ADVANCED_FACE ( 'NONE', ( #64269 ), #29623, .F. ) ;
#35234 = B_SPLINE_CURVE_WITH_KNOTS ( 'NONE', 3,
 ( #76837, #84047, #77710, #22760, #43925, #15577, #70069, #49793, #7929, #64181 ),
 .UNSPECIFIED., .F., .F.,
 ( 4, 2, 2, 2, 4 ),
 ( 0.0007817359430256294638, 0.0009771253907249952391, 0.001172514838424361123, 0.001367904286123726790, 0.001563293733823092673 ),
 .UNSPECIFIED. ) ;
#35235 = ORIENTED_EDGE ( 'NONE', *, *, #33479, .T. ) ;
#35236 = ORIENTED_EDGE ( 'NONE', *, *, #40107, .T. ) ;
#35237 = CYLINDRICAL_SURFACE ( 'NONE', #44507, 0.2499999999999995559 ) ;
#35239 = CARTESIAN_POINT ( 'NONE',  ( 1.607628228708781970, -11.43677907613345113, 33.22367315496201456 ) ) ;
#35238 = CARTESIAN_POINT ( 'NONE',  ( 12.46153846153846168, -2.486705287966279876, 31.30864560766543647 ) ) ;
#35240 = CARTESIAN_POINT ( 'NONE',  ( 11.31497661389720832, -2.353723527008296568, 30.78948104536958752 ) ) ;
#35241 = LINE ( 'NONE', #83450, #26432 ) ;
#35242 = FACE_BOUND ( 'NONE', #67808, .T. ) ;
#35243 = CARTESIAN_POINT ( 'NONE',  ( 8.519207545009310323, -10.92453946501458795, 33.72985991061850086 ) ) ;
#35244 = ORIENTED_EDGE ( 'NONE', *, *, #62968, .F. ) ;
#35245 = AXIS2_PLACEMENT_3D ( 'NONE', #55860, #41918, #82904 ) ;
#35246 = CARTESIAN_POINT ( 'NONE',  ( 17.14299041027315695, -11.91647553114624358, 32.58852847137148245 ) ) ;
#35247 = ADVANCED_FACE ( 'NONE', ( #16100 ), #51627, .T. ) ;
#35248 = CARTESIAN_POINT ( 'NONE',  ( -1.384615384615383471, -11.16473453929635440, 33.15142922261926373 ) ) ;
#35249 = CARTESIAN_POINT ( 'NONE',  ( -1.134561072977068319, -2.779044189368096607, 31.39831045268885035 ) ) ;
#35250 = CARTESIAN_POINT ( 'NONE',  ( 6.989144256427000101, -9.058645607665452459, 34.76329471203371924 ) ) ;
#35251 = ORIENTED_EDGE ( 'NONE', *, *, #66269, .F. ) ;
#35252 = CARTESIAN_POINT ( 'NONE',  ( 6.249945409378046435, -10.92531984108285670, 33.72920026020278073 ) ) ;
#35253 = ORIENTED_EDGE ( 'NONE', *, *, #11981, .T. ) ;
#35254 = FACE_BOUND ( 'NONE', #20690, .T. ) ;
#35255 = CARTESIAN_POINT ( 'NONE',  ( -17.14300545628320904, -3.937682226553330445, 33.60647404775217240 ) ) ;
#35256 = AXIS2_PLACEMENT_3D ( 'NONE', #30714, #52315, #58180 ) ;
#35257 = B_SPLINE_CURVE_WITH_KNOTS ( 'NONE', 3,
 ( #70141, #27827, #21963, #34589, #76466, #75144, #56187, #13428, #62055, #1237 ),
 .UNSPECIFIED., .F., .F.,
 ( 4, 2, 2, 2, 4 ),
 ( 0.000000000000000000, 0.0001954311564186868202, 0.0003908623128373736404, 0.0005862934692560604335, 0.0007817246256747472808 ),
 .UNSPECIFIED. ) ;
#35258 = CARTESIAN_POINT ( 'NONE',  ( -7.173100147298381302, -10.18141759479407327, 34.26406193332782379 ) ) ;
#35259 = CARTESIAN_POINT ( 'NONE',  ( 1.384615384615386802, -2.499999999999998668, 29.75000000000001421 ) ) ;
#35260 = ORIENTED_EDGE ( 'NONE', *, *, #83946, .F. ) ;
#35261 = AXIS2_PLACEMENT_3D ( 'NONE', #81099, #33350, #68892 ) ;
#35262 = CARTESIAN_POINT ( 'NONE',  ( -12.71156169883143150, -10.05641848906368097, 34.04755513067966177 ) ) ;
#35263 = CARTESIAN_POINT ( 'NONE',  ( 5.143092217885731898, -7.250054483168843156, 34.74374881642865631 ) ) ;
#35264 = CARTESIAN_POINT ( 'NONE',  ( -15.00775638667583678, -10.01129605718032600, 34.36064277460058491 ) ) ;
#35265 = CARTESIAN_POINT ( 'NONE',  ( -6.988347369037697376, -10.90142922261923886, 33.41473453929638993 ) ) ;
#35266 = EDGE_LOOP ( 'NONE', ( #49304, #12381, #17660, #51325 ) ) ;
#35267 = CARTESIAN_POINT ( 'NONE',  ( 13.16168916709923664, -5.667676309546437530, 34.40238873228292249 ) ) ;
#35268 = VERTEX_POINT ( 'NONE', #16537 ) ;
#35270 = ORIENTED_EDGE ( 'NONE', *, *, #47955, .T. ) ;
#35269 = CARTESIAN_POINT ( 'NONE',  ( 15.93101805621127731, -7.369209533119136069, 34.99857337881830688 ) ) ;
#35271 = CYLINDRICAL_SURFACE ( 'NONE', #2309, 0.2499999999999986955 ) ;
#35272 = CARTESIAN_POINT ( 'NONE',  ( -10.68146802634049308, -12.37446782046654192, 30.86335684631486487 ) ) ;
#35273 = B_SPLINE_CURVE_WITH_KNOTS ( 'NONE', 3,
 ( #29015, #71297, #43397, #36641, #84844, #36211, #56021, #76745, #77624, #9604 ),
 .UNSPECIFIED., .F., .F.,
 ( 4, 2, 2, 2, 4 ),
 ( 0.0007817359430256364027, 0.0009771253907250043464, 0.001172514838424372399, 0.001367904286123740234, 0.001563293733823108286 ),
 .UNSPECIFIED. ) ;
#35274 = CARTESIAN_POINT ( 'NONE',  ( 5.010840697562940704, -2.486705287966279432, 31.30864560766542937 ) ) ;
#35275 = CARTESIAN_POINT ( 'NONE',  ( -39.05038313613820122, -2.499999999999999556, 29.75000000000000355 ) ) ;
#35276 = ADVANCED_FACE ( 'NONE', ( #17880 ), #23291, .F. ) ;
#35277 = ADVANCED_FACE ( 'NONE', ( #44432 ), #3460, .F. ) ;
#35278 = DIRECTION ( 'NONE',  ( -0.000000000000000000, 1.000000000000000000, 3.491481338843133355E-15 ) ) ;
#35280 = CARTESIAN_POINT ( 'NONE',  ( 16.37662569511456567, -5.913360116392396115, 34.49180327182771322 ) ) ;
#35279 = FACE_OUTER_BOUND ( 'NONE', #31953, .T. ) ;
#35281 = CARTESIAN_POINT ( 'NONE',  ( -4.153846153846273204, -12.27809138561165270, 31.22303859784587132 ) ) ;
#35282 = CARTESIAN_POINT ( 'NONE',  ( 1.139087296525997273, -4.749999999999992895, 25.48437500000000000 ) ) ;
#35283 = VERTEX_POINT ( 'NONE', #25520 ) ;
#35284 = CARTESIAN_POINT ( 'NONE',  ( -17.75005448165186195, -9.272278438253398036, 34.42582936511637826 ) ) ;
#35285 = VERTEX_POINT ( 'NONE', #19645 ) ;
#35286 = EDGE_LOOP ( 'NONE', ( #54708, #32992 ) ) ;
#35287 = CARTESIAN_POINT ( 'NONE',  ( 3.230769230769110045, -5.219633306517616589, 34.19971097300220464 ) ) ;
#35288 = ORIENTED_EDGE ( 'NONE', *, *, #4881, .T. ) ;
#35289 = CARTESIAN_POINT ( 'NONE',  ( 3.930361210122202742, -12.24155766932282496, 31.33739205006857986 ) ) ;
#35290 = UNCERTAINTY_MEASURE_WITH_UNIT (LENGTH_MEASURE( 1.000000000000000082E-05 ), #39286, 'distance_accuracy_value', 'NONE');
#35291 = CARTESIAN_POINT ( 'NONE',  ( -7.911423846710166075, -8.656820664281498878, 34.87096338111211935 ) ) ;
#35292 = CARTESIAN_POINT ( 'NONE',  ( 3.164685819813350065, -8.120952969808774569, 34.71129190930000163 ) ) ;
#35293 = VECTOR ( 'NONE', #10354, 1000.000000000000114 ) ;
#35294 = CARTESIAN_POINT ( 'NONE',  ( 14.87820512820512953, -11.50000000000000000, 29.75000000000000355 ) ) ;
#35295 = CARTESIAN_POINT ( 'NONE',  ( 10.86533002476265786, -6.653508905675592722, 34.93172785388651391 ) ) ;
#35296 = CARTESIAN_POINT ( 'NONE',  ( -13.13456096470193302, -6.523592122091592671, 34.90882529074906415 ) ) ;
#35297 = CARTESIAN_POINT ( 'NONE',  ( 17.07692307692295586, -11.48612834414049644, 32.76840700105863391 ) ) ;
#35298 = CARTESIAN_POINT ( 'NONE',  ( -1.553300858899081538, -11.25000000000000711, 26.10937500000001066 ) ) ;
#35299 = B_SPLINE_CURVE_WITH_KNOTS ( 'NONE', 3,
 ( #75684, #49100, #69819, #1800, #48653, #27508, #1357, #77026, #8127, #8569 ),
 .UNSPECIFIED., .F., .F.,
 ( 4, 2, 2, 2, 4 ),
 ( 0.000000000000000000, 0.0001954339857564077183, 0.0003908679715128154366, 0.0005863019572692231007, 0.0007817359430256308733 ),
 .UNSPECIFIED. ) ;
#35300 = CARTESIAN_POINT ( 'NONE',  ( -0.4615384615385826339, -2.625532179533779598, 30.86335684631627174 ) ) ;
#35301 = CARTESIAN_POINT ( 'NONE',  ( 14.98074600654777377, -9.356822207818506598, 34.66110646841856635 ) ) ;
#35302 = CARTESIAN_POINT ( 'NONE',  ( 5.142990410273152513, -10.67929555188718282, 33.92786785259544757 ) ) ;
#35303 = CARTESIAN_POINT ( 'NONE',  ( -9.942330916529147800, -11.56360843649121684, 33.07473185843129926 ) ) ;
#35304 = ORIENTED_EDGE ( 'NONE', *, *, #48830, .T. ) ;
#35305 = EDGE_LOOP ( 'NONE', ( #52041, #71631 ) ) ;
#35306 = CARTESIAN_POINT ( 'NONE',  ( -17.75000000000000355, -12.50000000000000000, 29.75000000000000355 ) ) ;
#35307 = DIRECTION ( 'NONE',  ( 1.000000000000000000, 0.000000000000000000, 0.000000000000000000 ) ) ;
#35308 = CARTESIAN_POINT ( 'NONE',  ( -2.980714919130916130, -2.779044189368095719, 31.39831045268885745 ) ) ;
#35309 = CARTESIAN_POINT ( 'NONE',  ( 6.000000000000001776, -5.557115091759785130, 34.35708131394839171 ) ) ;
#35310 = ORIENTED_EDGE ( 'NONE', *, *, #83898, .F. ) ;
#35311 = CARTESIAN_POINT ( 'NONE',  ( -15.90390074446811042, -8.476813868363244353, 34.90874843262270133 ) ) ;
#35312 = CARTESIAN_POINT ( 'NONE',  ( 11.78851595837499566, -4.074993327901527351, 33.72946981652012255 ) ) ;
#35313 = B_SPLINE_CURVE_WITH_KNOTS ( 'NONE', 3,
 ( #27625, #13232, #48333, #6476, #74939, #28519, #55536, #7363, #82589, #75808 ),
 .UNSPECIFIED., .F., .F.,
 ( 4, 2, 2, 2, 4 ),
 ( 0.0007817359430256322827, 0.0009771253907249989254, 0.001172514838424365676, 0.001367904286123732428, 0.001563293733823098962 ),
 .UNSPECIFIED. ) ;
#35314 = DIRECTION ( 'NONE',  ( 0.000000000000000000, 1.000000000000000000, 0.000000000000000000 ) ) ;
#35315 = VECTOR ( 'NONE', #24970, 1000.000000000000000 ) ;
#35316 = EDGE_LOOP ( 'NONE', ( #1214, #79570, #3969, #78357, #60765, #74111, #14808, #14601, #38051, #32669, #37044, #54337, #23682, #25121, #24022, #71955, #59209, #46294, #27470, #43764, #18776, #40016, #65397, #25145, #72736, #41588, #57598, #69841, #54159, #47529, #12283, #12211, #15881, #19040, #43869, #88007, #42878, #13733, #42164, #78303, #15840, #25830, #22637, #88892, #11194, #66796, #38537, #29902, #61302, #78862, #22825, #69346, #15090, #52225, #42424, #1059, #5621, #29594, #62450, #15315, #72991, #8810, #35883, #87867, #19618, #6191, #74251, #58945, #78111, #14543, #7980, #1101, #61044, #28021, #73933, #33227, #59003, #21965, #62803, #74330, #67459, #45757, #88933, #69919, #60662, #85333, #46381, #17379, #23785, #54598, #19075, #88398, #67284, #2830, #88339, #88387, #23501, #50959, #77069, #1806, #21568, #16300, #20819, #74680, #49946, #81292, #81082, #2819, #21671, #71784, #85739, #50635, #71209, #18572, #76765, #77566, #42040, #68931, #7357, #61281, #54492, #82900, #22998, #2417 ) ) ;
#35317 = CARTESIAN_POINT ( 'NONE',  ( 18.13052543823364360, -3.625058011473227815, 33.29252011169590020 ) ) ;
#35318 = EDGE_LOOP ( 'NONE', ( #10452, #39086, #19709, #44667 ) ) ;
#35319 = DIRECTION ( 'NONE',  ( -0.000000000000000000, -0.7660444431189792347, -0.6427876096865379196 ) ) ;
#35320 = CARTESIAN_POINT ( 'NONE',  ( 4.376809288112829321, -7.369474539155828730, 34.99858011523957657 ) ) ;
#35321 = CARTESIAN_POINT ( 'NONE',  ( -1.514763354347078872, -9.504002272028875709, 34.60269587691767867 ) ) ;
#35322 = AXIS2_PLACEMENT_3D ( 'NONE', #12979, #60266, #14301 ) ;
#35323 = CARTESIAN_POINT ( 'NONE',  ( -15.48074596171158213, -3.137211980971221781, 32.19342716148376837 ) ) ;
#35324 = CARTESIAN_POINT ( 'NONE',  ( -6.923076923077045919, -2.657715359629662988, 31.77849191805970364 ) ) ;
#35325 = EDGE_CURVE ( 'NONE', #22188, #61316, #20092, .T. ) ;
#35326 = ORIENTED_EDGE ( 'NONE', *, *, #74713, .T. ) ;
#35327 = B_SPLINE_CURVE_WITH_KNOTS ( 'NONE', 3,
 ( #74218, #26916, #26028, #12954, #27794, #13393, #7082, #40877, #82310, #6640 ),
 .UNSPECIFIED., .F., .F.,
 ( 4, 2, 2, 2, 4 ),
 ( 0.000000000000000000, 0.0001954311564186872810, 0.0003908623128373745620, 0.0005862934692560618430, 0.0007817246256747491240 ),
 .UNSPECIFIED. ) ;
#35328 = ORIENTED_EDGE ( 'NONE', *, *, #67934, .T. ) ;
#35329 = EDGE_CURVE ( 'NONE', #12315, #85264, #80190, .T. ) ;
#35330 = ORIENTED_EDGE ( 'NONE', *, *, #80549, .F. ) ;
#35331 = ORIENTED_EDGE ( 'NONE', *, *, #9138, .F. ) ;
#35332 = CYLINDRICAL_SURFACE ( 'NONE', #74703, 0.2500000000000012212 ) ;
#35333 = CARTESIAN_POINT ( 'NONE',  ( -12.68502338610279523, -12.69144148231606017, 30.53333754910549303 ) ) ;
#35334 = CARTESIAN_POINT ( 'NONE',  ( 0.5276057948885360949, -6.343179335718451384, 34.87096338111212646 ) ) ;
#35336 = EDGE_CURVE ( 'NONE', #3335, #13990, #14614, .T. ) ;
#35335 = DIRECTION ( 'NONE',  ( -0.000000000000000000, 0.5000000000000011102, -0.8660254037844380415 ) ) ;
#35337 = AXIS2_PLACEMENT_3D ( 'NONE', #45805, #60649, #60206 ) ;
#35338 = CARTESIAN_POINT ( 'NONE',  ( -7.846153846153967493, -4.320704448113951379, 33.92786785259630022 ) ) ;
#35339 = CARTESIAN_POINT ( 'NONE',  ( 14.53047184896071542, -10.11255958852956027, 34.01340905677048454 ) ) ;
#35340 = ORIENTED_EDGE ( 'NONE', *, *, #3514, .F. ) ;
#35341 = EDGE_CURVE ( 'NONE', #3675, #32906, #76987, .T. ) ;
#35342 = ORIENTED_EDGE ( 'NONE', *, *, #21597, .T. ) ;
#35343 = ORIENTED_EDGE ( 'NONE', *, *, #20611, .F. ) ;
#35345 = ORIENTED_EDGE ( 'NONE', *, *, #44662, .F. ) ;
#35344 = CARTESIAN_POINT ( 'NONE',  ( 4.087762742890272527, -2.721908614388772740, 31.22303859784724622 ) ) ;
#35347 = CARTESIAN_POINT ( 'NONE',  ( 13.38461538461526423, -4.320704448113951379, 33.92786785259630022 ) ) ;
#35346 = CARTESIAN_POINT ( 'NONE',  ( 16.15384615384615330, -8.120952969808772792, 34.71129190930000163 ) ) ;
#35348 = CARTESIAN_POINT ( 'NONE',  ( 9.692307692307572609, -2.625532179533778709, 30.86335684631627174 ) ) ;
#35349 = CARTESIAN_POINT ( 'NONE',  ( 13.60739492588379562, -8.496831190052093419, 34.64984203495476578 ) ) ;
#35350 = ORIENTED_EDGE ( 'NONE', *, *, #81640, .F. ) ;
#35351 = EDGE_CURVE ( 'NONE', #47861, #2266, #33163, .T. ) ;
#35352 = EDGE_LOOP ( 'NONE', ( #35990, #21256 ) ) ;
#35353 = CARTESIAN_POINT ( 'NONE',  ( 4.023698184114455678, -4.299443229763728169, 33.91186481527756058 ) ) ;
#35354 = VERTEX_POINT ( 'NONE', #88580 ) ;
#35355 = FACE_BOUND ( 'NONE', #17834, .T. ) ;
#35356 = CARTESIAN_POINT ( 'NONE',  ( 6.792929713638703682, -4.460286881179643004, 33.72017969459903242 ) ) ;
#35357 = DIRECTION ( 'NONE',  ( -0.000000000000000000, -0.1736481776669307198, -0.9848077530122080203 ) ) ;
#35358 = ORIENTED_EDGE ( 'NONE', *, *, #32678, .T. ) ;
#35359 = CARTESIAN_POINT ( 'NONE',  ( -14.05763788777885637, -8.346898887586323923, 34.93166121998716278 ) ) ;
#35360 = PLANE ( 'NONE',  #2928 ) ;
#35361 = LINE ( 'NONE', #56078, #53650 ) ;
#35362 = B_SPLINE_CURVE_WITH_KNOTS ( 'NONE', 3,
 ( #3844, #47045, #4751, #39871, #19147, #86742, #53366, #10610, #73206, #80412 ),
 .UNSPECIFIED., .F., .F.,
 ( 4, 2, 2, 2, 4 ),
 ( 0.000000000000000000, 0.0001954339857564073388, 0.0003908679715128146777, 0.0005863019572692220165, 0.0007817359430256293554 ),
 .UNSPECIFIED. ) ;
#35363 = CARTESIAN_POINT ( 'NONE',  ( 0.6843180028068696075, -6.760870238392817200, 34.69528174975672385 ) ) ;
#35364 = CARTESIAN_POINT ( 'NONE',  ( 0.5920641633020236050, -12.45806712695776319, 30.39783852428763922 ) ) ;
#35365 = EDGE_LOOP ( 'NONE', ( #30172, #73302, #48406, #20677 ) ) ;
#35366 = LINE ( 'NONE', #61944, #32910 ) ;
#35367 = DIRECTION ( 'NONE',  ( -0.000000000000000000, -0.9396926207859092051, -0.3420201433256662704 ) ) ;
#35368 = LINE ( 'NONE', #83578, #18252 ) ;
#35369 = CARTESIAN_POINT ( 'NONE',  ( 5.749976762707037281, -5.056417327199099532, 34.11270091957320716 ) ) ;
#35370 = DIRECTION ( 'NONE',  ( 0.000000000000000000, -0.000000000000000000, -1.000000000000000000 ) ) ;
#35371 = EDGE_CURVE ( 'NONE', #20780, #5299, #11420, .T. ) ;
#35372 = FACE_BOUND ( 'NONE', #35479, .T. ) ;
#35374 = DIRECTION ( 'NONE',  ( -0.000000000000000000, 0.8660254037844397068, -0.4999999999999978906 ) ) ;
#35373 = CARTESIAN_POINT ( 'NONE',  ( -9.019230769230773603, -2.499999999999999556, 29.81609845454691765 ) ) ;
#35375 = LINE ( 'NONE', #76817, #43930 ) ;
#35377 = DIRECTION ( 'NONE',  ( -1.000000000000000000, 0.000000000000000000, -0.000000000000000000 ) ) ;
#35376 = CARTESIAN_POINT ( 'NONE',  ( -3.296851610129365451, -2.833524468853757305, 32.15551576947924417 ) ) ;
#35378 = EDGE_CURVE ( 'NONE', #27260, #19610, #39493, .T. ) ;
#35379 = CARTESIAN_POINT ( 'NONE',  ( -10.68146699474474914, -6.343179335718451384, 34.87096338111212646 ) ) ;
#35380 = CARTESIAN_POINT ( 'NONE',  ( -0.06109907496454585613, -4.750000000000000000, 16.40438170625849068 ) ) ;
#35381 = ORIENTED_EDGE ( 'NONE', *, *, #78843, .T. ) ;
#35382 = B_SPLINE_CURVE_WITH_KNOTS ( 'NONE', 3,
 ( #29452, #70431, #84396, #8736, #2394, #1081 ),
 .UNSPECIFIED., .F., .F.,
 ( 4, 2, 4 ),
 ( 0.0003909512603273650297, 0.0005862562993131907206, 0.0007815613382990164656 ),
 .UNSPECIFIED. ) ;
#35383 = CARTESIAN_POINT ( 'NONE',  ( -1.399447498061196837, -4.021041001012671146, 14.00000000000000711 ) ) ;
#35384 = ORIENTED_EDGE ( 'NONE', *, *, #79544, .T. ) ;
#35385 = CARTESIAN_POINT ( 'NONE',  ( -13.13466997523734037, -10.92531984108285670, 33.72920026020278073 ) ) ;
#35386 = EDGE_CURVE ( 'NONE', #52135, #34125, #4358, .T. ) ;
#35387 = ORIENTED_EDGE ( 'NONE', *, *, #49265, .F. ) ;
#35388 = EDGE_CURVE ( 'NONE', #4412, #83978, #66507, .T. ) ;
#35389 = CARTESIAN_POINT ( 'NONE',  ( 4.500000000000003553, -7.499999999999998224, 13.00000000000000178 ) ) ;
#35390 = CARTESIAN_POINT ( 'NONE',  ( -8.069080063669991532, -9.886141570436013382, 34.14413921362392301 ) ) ;
#35391 = EDGE_LOOP ( 'NONE', ( #68886, #72436, #16177, #56937 ) ) ;
#35392 = CARTESIAN_POINT ( 'NONE',  ( -9.757631705111998954, -7.749976730030849303, 34.74374725381503737 ) ) ;
#35393 = CARTESIAN_POINT ( 'NONE',  ( 0.06109907496454976272, -10.25000000000000000, 19.52938170625848713 ) ) ;
#35394 = DIRECTION ( 'NONE',  ( -0.000000000000000000, -0.7660444431189791237, -0.6427876096865379196 ) ) ;
#35395 = CARTESIAN_POINT ( 'NONE',  ( 4.153846153846154188, -7.500000000000001776, 35.04278698407183867 ) ) ;
#35396 = CARTESIAN_POINT ( 'NONE',  ( -5.207070286361294542, -12.45813303252208648, 30.39737893381572675 ) ) ;
#35397 = CARTESIAN_POINT ( 'NONE',  ( 14.87820512820512953, -11.00000000000000000, 29.75000000000000355 ) ) ;
#35398 = CARTESIAN_POINT ( 'NONE',  ( 5.010839665967194989, -8.120952969808774569, 34.71129190930000163 ) ) ;
#35399 = DIRECTION ( 'NONE',  ( -0.000000000000000000, 1.000000000000000000, -0.000000000000000000 ) ) ;
#35400 = CARTESIAN_POINT ( 'NONE',  ( 1.492201783934598236, -11.27530806549875031, 23.70499329374151642 ) ) ;
#35401 = CYLINDRICAL_SURFACE ( 'NONE', #77928, 0.2499999999999986955 ) ;
#35402 = CARTESIAN_POINT ( 'NONE',  ( 14.37294787896832915, -10.90142922261932057, 33.41473453929631887 ) ) ;
#35403 = B_SPLINE_CURVE_WITH_KNOTS ( 'NONE', 3,
 ( #82145, #55101, #61849, #88043, #81258, #14119, #33513, #19544, #40274, #47004 ),
 .UNSPECIFIED., .F., .F.,
 ( 4, 2, 2, 2, 4 ),
 ( 0.0007817246256747469556, 0.0009771112852218896347, 0.001172497944769032531, 0.001367884604316175427, 0.001563271263863318106 ),
 .UNSPECIFIED. ) ;
#35404 = CARTESIAN_POINT ( 'NONE',  ( -0.6089743589743593644, -7.500000000000000000, 29.75000000000000355 ) ) ;
#35405 = CARTESIAN_POINT ( 'NONE',  ( -3.775308065498748977, -8.992201783934593351, 21.51749329374151998 ) ) ;
#35406 = CARTESIAN_POINT ( 'NONE',  ( -14.17716660592874334, -10.88167719472716399, 33.43325721877153711 ) ) ;
#35407 = CARTESIAN_POINT ( 'NONE',  ( -9.692307692307812417, -11.48612834414049644, 32.76840700105863391 ) ) ;
#35408 = ORIENTED_EDGE ( 'NONE', *, *, #86332, .F. ) ;
#35409 = AXIS2_PLACEMENT_3D ( 'NONE', #38715, #4488, #46360 ) ;
#35410 = CARTESIAN_POINT ( 'NONE',  ( 6.673076923076925127, -7.500000000000001776, 34.75000000000000000 ) ) ;
#35411 = CARTESIAN_POINT ( 'NONE',  ( 16.15384615384615330, -2.486705287966279876, 31.30864560766543647 ) ) ;
#35413 = VERTEX_POINT ( 'NONE', #4811 ) ;
#35412 = DIRECTION ( 'NONE',  ( -0.000000000000000000, 0.000000000000000000, 1.000000000000000000 ) ) ;
#35414 = CARTESIAN_POINT ( 'NONE',  ( -14.55766903863466055, -11.79746400365624659, 32.30657167506340954 ) ) ;
#35415 = CARTESIAN_POINT ( 'NONE',  ( -1.514762594053603584, -10.88202310037936194, 33.43294751532457099 ) ) ;
#35416 = AXIS2_PLACEMENT_3D ( 'NONE', #81842, #75512, #20132 ) ;
#35417 = CARTESIAN_POINT ( 'NONE',  ( 7.146089767170319185, -11.98016756924215009, 32.48728574198911190 ) ) ;
#35418 = DIRECTION ( 'NONE',  ( 1.000000000000000000, 0.000000000000000000, 0.000000000000000000 ) ) ;
#35419 = EDGE_CURVE ( 'NONE', #10751, #3063, #72731, .T. ) ;
#35420 = CARTESIAN_POINT ( 'NONE',  ( -10.54931626438217585, -10.51840700105979565, 33.73612834413962247 ) ) ;
#35421 = VERTEX_POINT ( 'NONE', #32281 ) ;
#35422 = CYLINDRICAL_SURFACE ( 'NONE', #44062, 0.2499999999999995559 ) ;
#35423 = VERTEX_POINT ( 'NONE', #59746 ) ;
#35424 = VERTEX_POINT ( 'NONE', #25958 ) ;
#35425 = CARTESIAN_POINT ( 'NONE',  ( 5.076923076922954969, -11.94971097300221174, 32.03036669348237098 ) ) ;
#35426 = CARTESIAN_POINT ( 'NONE',  ( -17.07692307692307665, -4.945431358278436385, 36.03766855953609394 ) ) ;
#35427 = CARTESIAN_POINT ( 'NONE',  ( -23.50000000000000000, -1.749999999999991118, 32.75000000000000000 ) ) ;
#35428 = CARTESIAN_POINT ( 'NONE',  ( 13.25392478150507891, -8.191372820521381826, 34.95448215188423546 ) ) ;
#35429 = B_SPLINE_CURVE_WITH_KNOTS ( 'NONE', 3,
 ( #5451, #32918, #60381, #87895, #53629, #14414, #36028, #29273, #48634, #1340 ),
 .UNSPECIFIED., .F., .F.,
 ( 4, 2, 2, 2, 4 ),
 ( 0.0007817246256747499913, 0.0009771112852218944052, 0.001172497944769038819, 0.001367884604316183016, 0.001563271263863327430 ),
 .UNSPECIFIED. ) ;
#35430 = ADVANCED_FACE ( 'NONE', ( #54309 ), #80925, .F. ) ;
#35431 = ORIENTED_EDGE ( 'NONE', *, *, #41527, .T. ) ;
#35432 = B_SPLINE_CURVE_WITH_KNOTS ( 'NONE', 3,
 ( #67151, #73472, #25719, #45978, #54062, #46870, #32467, #74353, #33367, #60829 ),
 .UNSPECIFIED., .F., .F.,
 ( 4, 2, 2, 2, 4 ),
 ( 0.000000000000000000, 0.0001954339881912775425, 0.0003908679763825550850, 0.0005863019645738326005, 0.0007817359527651101701 ),
 .UNSPECIFIED. ) ;
#35433 = CARTESIAN_POINT ( 'NONE',  ( 13.38461538461538680, -2.721908614388771852, 31.22303859784724978 ) ) ;
#35434 = VERTEX_POINT ( 'NONE', #34926 ) ;
#35435 = B_SPLINE_CURVE_WITH_KNOTS ( 'NONE', 3,
 ( #69524, #42506, #42949, #70419, #63647, #17580, #76276, #1954, #29439, #630 ),
 .UNSPECIFIED., .F., .F.,
 ( 4, 2, 2, 2, 4 ),
 ( 0.000000000000000000, 0.0001954311564186861697, 0.0003908623128373723394, 0.0005862934692560584820, 0.0007817246256747446788 ),
 .UNSPECIFIED. ) ;
#35436 = AXIS2_PLACEMENT_3D ( 'NONE', #62193, #21653, #65174 ) ;
#35437 = ORIENTED_EDGE ( 'NONE', *, *, #1768, .T. ) ;
#35438 = ORIENTED_EDGE ( 'NONE', *, *, #63015, .T. ) ;
#35440 = EDGE_LOOP ( 'NONE', ( #86755, #23604 ) ) ;
#35439 = CARTESIAN_POINT ( 'NONE',  ( 13.38461538461538680, -4.661471528628507777, 34.16647553114623292 ) ) ;
#35441 = CARTESIAN_POINT ( 'NONE',  ( -4.826868657009623753, -12.41089969410671223, 31.60739465890703670 ) ) ;
#35442 = DIRECTION ( 'NONE',  ( 1.000000000000000000, 0.000000000000000000, -0.000000000000000000 ) ) ;
#35443 = EDGE_CURVE ( 'NONE', #33344, #59859, #29782, .T. ) ;
#35444 = CARTESIAN_POINT ( 'NONE',  ( -3.230769230769229949, -4.098570777380720287, 33.41473453929634729 ) ) ;
#35445 = CARTESIAN_POINT ( 'NONE',  ( -3.903900744468109973, -6.653508905675592722, 34.93172785388651391 ) ) ;
#35446 = AXIS2_PLACEMENT_3D ( 'NONE', #79163, #31873, #17465 ) ;
#35448 = ORIENTED_EDGE ( 'NONE', *, *, #38128, .T. ) ;
#35447 = CIRCLE ( 'NONE', #57602, 3.000000000000000000 ) ;
#35449 = EDGE_CURVE ( 'NONE', #20712, #86240, #35375, .T. ) ;
#35450 = EDGE_LOOP ( 'NONE', ( #18285, #31242, #11471, #12749 ) ) ;
#35451 = ORIENTED_EDGE ( 'NONE', *, *, #60056, .F. ) ;
#35452 = CARTESIAN_POINT ( 'NONE',  ( -3.262820512820514107, -7.500000000000000000, 29.75000000000000355 ) ) ;
#35454 = ORIENTED_EDGE ( 'NONE', *, *, #64434, .T. ) ;
#35453 = LINE ( 'NONE', #8428, #48777 ) ;
#35455 = CARTESIAN_POINT ( 'NONE',  ( 11.31497659473759043, -6.760086850603066466, 34.69517049084099369 ) ) ;
#35456 = CARTESIAN_POINT ( 'NONE',  ( 6.857806477116147548, -6.879047030191174805, 34.71129190930000163 ) ) ;
#35457 = CARTESIAN_POINT ( 'NONE',  ( 2.557746727605761272, -9.233818618650603938, 34.70587769442853698 ) ) ;
#35458 = ORIENTED_EDGE ( 'NONE', *, *, #30241, .T. ) ;
#35459 = EDGE_CURVE ( 'NONE', #39506, #27738, #9361, .T. ) ;
#35460 = CARTESIAN_POINT ( 'NONE',  ( 15.00728428704528561, -10.81261337010820256, 33.49550067578627477 ) ) ;
#35461 = CARTESIAN_POINT ( 'NONE',  ( 3.230769230769231726, -13.95598074871891292, 31.83374038241031911 ) ) ;
#35462 = ORIENTED_EDGE ( 'NONE', *, *, #68716, .F. ) ;
#35463 = FACE_BOUND ( 'NONE', #39327, .T. ) ;
#35464 = LINE ( 'NONE', #28711, #8289 ) ;
#35465 = CARTESIAN_POINT ( 'NONE',  ( -12.94230769230769162, -7.500000000000000000, 29.75000000000000355 ) ) ;
#35466 = CARTESIAN_POINT ( 'NONE',  ( -11.00641025641025550, -7.500000000000000000, 29.75000000000000355 ) ) ;
#35468 = CARTESIAN_POINT ( 'NONE',  ( 24.00000000000000000, -5.499999999999981348, 27.75000000000000000 ) ) ;
#35467 = CARTESIAN_POINT ( 'NONE',  ( -8.769230769230768274, -12.78798330534103123, 29.99999999999997868 ) ) ;
#35469 = CARTESIAN_POINT ( 'NONE',  ( 10.28846153846153832, -7.500000000000000000, 33.75000000000000000 ) ) ;
#35470 = CARTESIAN_POINT ( 'NONE',  ( 14.55763771707035303, -2.341251567377310217, 30.72681386836322659 ) ) ;
#35471 = ORIENTED_EDGE ( 'NONE', *, *, #26761, .T. ) ;
#35472 = CARTESIAN_POINT ( 'NONE',  ( -18.00000000000000000, -10.51840700105979387, 33.73612834413961536 ) ) ;
#35473 = EDGE_CURVE ( 'NONE', #37880, #48065, #78098, .T. ) ;
#35474 = CARTESIAN_POINT ( 'NONE',  ( -6.223484924564330889, -11.60425143139329940, 33.02411095842164457 ) ) ;
#35475 = ORIENTED_EDGE ( 'NONE', *, *, #13042, .T. ) ;
#35476 = B_SPLINE_CURVE_WITH_KNOTS ( 'NONE', 3,
 ( #32015, #80207, #26146, #45963, #60813, #18505, #46414, #53611, #59923, #68025 ),
 .UNSPECIFIED., .F., .F.,
 ( 4, 2, 2, 2, 4 ),
 ( 0.0007817359430256313069, 0.0009771253907249971907, 0.001172514838424363074, 0.001367904286123728958, 0.001563293733823094842 ),
 .UNSPECIFIED. ) ;
#35477 = CARTESIAN_POINT ( 'NONE',  ( -4.153846153846152411, -13.49023893513002648, 31.06009739812518688 ) ) ;
#35478 = DIRECTION ( 'NONE',  ( -0.000000000000000000, -0.9396926207859093161, -0.3420201433256663259 ) ) ;
#35479 = EDGE_LOOP ( 'NONE', ( #76862, #1644 ) ) ;
#35480 = LINE ( 'NONE', #70597, #19845 ) ;
#35481 = CARTESIAN_POINT ( 'NONE',  ( 4.153846153846032507, -10.21337939537710326, 33.94971097300076224 ) ) ;
#35482 = EDGE_CURVE ( 'NONE', #32338, #71873, #8358, .T. ) ;
#35483 = FACE_BOUND ( 'NONE', #9109, .T. ) ;
#35485 = CARTESIAN_POINT ( 'NONE',  ( -16.82697755857493149, -12.43552623307873972, 30.55307653245132826 ) ) ;
#35484 = CARTESIAN_POINT ( 'NONE',  ( -6.249999999999997335, -7.500000000000001776, 35.00000000000000000 ) ) ;
#35486 = CARTESIAN_POINT ( 'NONE',  ( 3.361294932532794100, -8.586989748646452369, 34.63063291749215011 ) ) ;
#35487 = VECTOR ( 'NONE', #45897, 1000.000000000000000 ) ;
#35488 = CARTESIAN_POINT ( 'NONE',  ( 12.23861150263161157, -12.38737895849757820, 31.66785238281580206 ) ) ;
#35490 = CARTESIAN_POINT ( 'NONE',  ( 5.999999999999880096, -3.835265460704628371, 33.15142922262033665 ) ) ;
#35489 = CARTESIAN_POINT ( 'NONE',  ( -7.623141002060451754, -12.64618726649961289, 30.78989965857442712 ) ) ;
#35491 = FACE_OUTER_BOUND ( 'NONE', #85727, .T. ) ;
#35492 = CARTESIAN_POINT ( 'NONE',  ( -2.651650429449565305, -4.848349570550461785, 26.50000000000000355 ) ) ;
#35493 = VERTEX_POINT ( 'NONE', #68277 ) ;
#35494 = EDGE_CURVE ( 'NONE', #11273, #57, #83382, .T. ) ;
#35495 = ORIENTED_EDGE ( 'NONE', *, *, #47177, .T. ) ;
#35496 = CARTESIAN_POINT ( 'NONE',  ( 5.999999999999880096, -3.300289026999228881, 32.46337939537708905 ) ) ;
#35497 = EDGE_CURVE ( 'NONE', #69942, #62711, #52258, .T. ) ;
#35498 = CARTESIAN_POINT ( 'NONE',  ( -10.61538461538461320, -8.164416787775445883, 34.95778746994557906 ) ) ;
#35499 = CARTESIAN_POINT ( 'NONE',  ( 1.515405825582337052, -9.084667340241226796, 34.75534355489798344 ) ) ;
#35500 = B_SPLINE_CURVE_WITH_KNOTS ( 'NONE', 3,
 ( #62002, #13375, #27776, #55244, #40856, #89061, #83174, #82735, #48478, #14265 ),
 .UNSPECIFIED., .F., .F.,
 ( 4, 2, 2, 2, 4 ),
 ( 0.0007817359430256347764, 0.0009771253907250036959, 0.001172514838424372832, 0.001367904286123741969, 0.001563293733823103949 ),
 .UNSPECIFIED. ) ;
#35501 = CARTESIAN_POINT ( 'NONE',  ( -9.019253993452222673, -8.475808217655753651, 34.90892951860618609 ) ) ;
#35502 = CARTESIAN_POINT ( 'NONE',  ( -13.13466997523734392, -2.589246495874658383, 31.60778113518102828 ) ) ;
#35503 = CARTESIAN_POINT ( 'NONE',  ( 3.749999999999999556, -7.438900925035446754, 15.46688170625848713 ) ) ;
#35504 = B_SPLINE_CURVE_WITH_KNOTS ( 'NONE', 3,
 ( #74121, #40785, #32682, #66920, #88986, #55168, #68250, #27259, #54721, #47521 ),
 .UNSPECIFIED., .F., .F.,
 ( 4, 2, 2, 2, 4 ),
 ( 0.000000000000000000, 0.0001954339857564073659, 0.0003908679715128147319, 0.0005863019572692221250, 0.0007817359430256294638 ),
 .UNSPECIFIED. ) ;
#35505 = CARTESIAN_POINT ( 'NONE',  ( 0.5920638997721056063, -4.299079248970732792, 33.91157788607253565 ) ) ;
#35506 = CARTESIAN_POINT ( 'NONE',  ( -9.692307692307691624, -1.215029322943914858, 32.30358669280327177 ) ) ;
#35507 = DIRECTION ( 'NONE',  ( -0.000000000000000000, -0.1736481776669307198, -0.9848077530122080203 ) ) ;
#35508 = CARTESIAN_POINT ( 'NONE',  ( 7.596130621932389637, -5.765609946408403630, 34.70566812827425451 ) ) ;
#35509 = DIRECTION ( 'NONE',  ( 0.000000000000000000, -4.336808689942017243E-16, 1.000000000000000000 ) ) ;
#35510 = CARTESIAN_POINT ( 'NONE',  ( 16.40390046548447245, -4.943051570960395047, 34.04725096376909477 ) ) ;
#35511 = CYLINDRICAL_SURFACE ( 'NONE', #736, 0.2499999999999979738 ) ;
#35512 = VECTOR ( 'NONE', #31995, 1000.000000000000000 ) ;
#35513 = CARTESIAN_POINT ( 'NONE',  ( 10.48477496018053223, -7.722926974430166069, 34.99546784045485737 ) ) ;
#35514 = CARTESIAN_POINT ( 'NONE',  ( -0.4615384615384611200, -9.058645607665452459, 34.76329471203371924 ) ) ;
#35515 = ADVANCED_FACE ( 'NONE', ( #7016 ), #77248, .F. ) ;
#35516 = VERTEX_POINT ( 'NONE', #29516 ) ;
#35517 = CARTESIAN_POINT ( 'NONE',  ( -14.55766903863466055, -3.627789207965226748, 32.91389620160131102 ) ) ;
#35518 = CARTESIAN_POINT ( 'NONE',  ( 7.780071466793709867, -4.661471528628507777, 34.16647553114621871 ) ) ;
#35519 = AXIS2_PLACEMENT_3D ( 'NONE', #84848, #1974, #29457 ) ;
#35520 = CARTESIAN_POINT ( 'NONE',  ( 2.724691934501250135, -8.700186371490531201, 19.79874329374151287 ) ) ;
#35521 = CARTESIAN_POINT ( 'NONE',  ( 6.857806922520602200, -5.094484230520674117, 34.41647553114621161 ) ) ;
#35522 = LINE ( 'NONE', #2165, #59671 ) ;
#35523 = VERTEX_POINT ( 'NONE', #70940 ) ;
#35524 = ADVANCED_FACE ( 'NONE', ( #77689 ), #29957, .F. ) ;
#35525 = CYLINDRICAL_SURFACE ( 'NONE', #54308, 4.500000000000001776 ) ;
#35527 = ORIENTED_EDGE ( 'NONE', *, *, #67587, .F. ) ;
#35526 = LINE ( 'NONE', #27879, #45374 ) ;
#35528 = CARTESIAN_POINT ( 'NONE',  ( -25.00000000000000355, 9.999999999999971578, 13.00000000000000178 ) ) ;
#35529 = CARTESIAN_POINT ( 'NONE',  ( -2.530619266599154038, -10.77366814457252175, 33.85459836347579454 ) ) ;
#35530 = AXIS2_PLACEMENT_3D ( 'NONE', #83735, #16146, #15267 ) ;
#35531 = VERTEX_POINT ( 'NONE', #36709 ) ;
#35532 = CARTESIAN_POINT ( 'NONE',  ( -5.076923076923197442, -12.27809138561165270, 31.22303859784587132 ) ) ;
#35533 = CARTESIAN_POINT ( 'NONE',  ( 13.25392478150507891, -9.084618155246140248, 34.75535874321725771 ) ) ;
#35534 = EDGE_LOOP ( 'NONE', ( #58695, #57771 ) ) ;
#35535 = CYLINDRICAL_SURFACE ( 'NONE', #38986, 0.2500000000000008882 ) ;
#35536 = EDGE_CURVE ( 'NONE', #15565, #29065, #82429, .T. ) ;
#35537 = CARTESIAN_POINT ( 'NONE',  ( 5.326923076923089084, -2.249999999999999112, 29.81603969181031033 ) ) ;
#35538 = DIRECTION ( 'NONE',  ( -0.000000000000000000, 1.000000000000000000, -0.000000000000000000 ) ) ;
#35539 = ORIENTED_EDGE ( 'NONE', *, *, #5117, .F. ) ;
#35540 = ORIENTED_EDGE ( 'NONE', *, *, #5486, .F. ) ;
#35541 = CARTESIAN_POINT ( 'NONE',  ( 6.130791807824788719, -6.413143153341454017, 34.63066358083362672 ) ) ;
#35542 = EDGE_CURVE ( 'NONE', #28852, #30322, #57688, .T. ) ;
#35543 = ORIENTED_EDGE ( 'NONE', *, *, #58662, .F. ) ;
#35544 = EDGE_CURVE ( 'NONE', #60075, #74684, #57415, .T. ) ;
#35545 = FACE_OUTER_BOUND ( 'NONE', #59944, .T. ) ;
#35546 = VECTOR ( 'NONE', #77241, 1000.000000000000227 ) ;
#35547 = CARTESIAN_POINT ( 'NONE',  ( -1.161835843346975095, -2.600157965045225783, 30.74683119005207743 ) ) ;
#35548 = CARTESIAN_POINT ( 'NONE',  ( 2.373759641042385127, -11.35647404775217595, 33.31231777344667222 ) ) ;
#35549 = B_SPLINE_CURVE_WITH_KNOTS ( 'NONE', 3,
 ( #60885, #46919, #13148, #6401, #54564, #19896 ),
 .UNSPECIFIED., .F., .F.,
 ( 4, 2, 4 ),
 ( 0.0003909569690057842790, 0.0005862646681846108007, 0.0007815723673634373224 ),
 .UNSPECIFIED. ) ;
#35550 = DIRECTION ( 'NONE',  ( -0.000000000000000000, 0.9848077530122085754, -0.1736481776669273613 ) ) ;
#35551 = CARTESIAN_POINT ( 'NONE',  ( 1.161688425708537808, -2.308479472611653094, 30.53278059502174457 ) ) ;
#35552 = VECTOR ( 'NONE', #18670, 1000.000000000000000 ) ;
#35553 = EDGE_CURVE ( 'NONE', #4801, #44215, #50202, .T. ) ;
#35554 = CARTESIAN_POINT ( 'NONE',  ( 15.23076923076953904, -2.506253911140615021, 30.00000000000323297 ) ) ;
#35555 = ORIENTED_EDGE ( 'NONE', *, *, #19475, .F. ) ;
#35556 = AXIS2_PLACEMENT_3D ( 'NONE', #69632, #8384, #82720 ) ;
#35557 = ORIENTED_EDGE ( 'NONE', *, *, #6817, .F. ) ;
#35559 = ORIENTED_EDGE ( 'NONE', *, *, #88636, .T. ) ;
#35558 = CARTESIAN_POINT ( 'NONE',  ( 4.284636594813103549, -8.191423895709842640, 34.95447573519442130 ) ) ;
#35560 = CARTESIAN_POINT ( 'NONE',  ( 16.82694633287449193, -2.318417181685854978, 30.59732222474233865 ) ) ;
#35561 = EDGE_LOOP ( 'NONE', ( #83242, #11186 ) ) ;
#35562 = LINE ( 'NONE', #77424, #17657 ) ;
#35563 = CARTESIAN_POINT ( 'NONE',  ( -10.61538461538473577, -12.70778746994576025, 30.41441678777401236 ) ) ;
#35564 = ORIENTED_EDGE ( 'NONE', *, *, #59345, .T. ) ;
#35565 = ADVANCED_FACE ( 'NONE', ( #44784 ), #50655, .F. ) ;
#35566 = CARTESIAN_POINT ( 'NONE',  ( -12.21159294319032185, -5.852078868378309373, 34.47109172314383585 ) ) ;
#35567 = EDGE_LOOP ( 'NONE', ( #17502, #44241 ) ) ;
#35569 = EDGE_LOOP ( 'NONE', ( #39669, #7517, #57495, #13552 ) ) ;
#35568 = CARTESIAN_POINT ( 'NONE',  ( -8.519176457592454454, -8.303483539816728154, 34.68545999027711702 ) ) ;
#35570 = CARTESIAN_POINT ( 'NONE',  ( -14.08491263871423982, -12.11081565061824250, 32.26097654155340422 ) ) ;
#35571 = AXIS2_PLACEMENT_3D ( 'NONE', #56300, #2226, #23386 ) ;
#35572 = EDGE_LOOP ( 'NONE', ( #37511, #2961 ) ) ;
#35573 = DIRECTION ( 'NONE',  ( 0.000000000000000000, 0.000000000000000000, 1.000000000000000000 ) ) ;
#35574 = CARTESIAN_POINT ( 'NONE',  ( -16.15384615384615330, -13.87047571288749737, 32.06866353760679544 ) ) ;
#35575 = VECTOR ( 'NONE', #11078, 1000.000000000000000 ) ;
#35576 = FACE_BOUND ( 'NONE', #40784, .T. ) ;
#35577 = CARTESIAN_POINT ( 'NONE',  ( -11.66915300512910036, -2.541943142973491554, 30.39792223712631980 ) ) ;
#35578 = CYLINDRICAL_SURFACE ( 'NONE', #65842, 0.2500000000000009437 ) ;
#35579 = CARTESIAN_POINT ( 'NONE',  ( 9.468822767743363400, -11.60425143139329940, 33.02411095842164457 ) ) ;
#35580 = CARTESIAN_POINT ( 'NONE',  ( -0.4615384615385840772, -3.083524468854526912, 32.58852847137268327 ) ) ;
#35581 = LINE ( 'NONE', #42786, #62494 ) ;
#35582 = CARTESIAN_POINT ( 'NONE',  ( -16.37677237136229991, -8.239355502252617924, 34.69524867566427417 ) ) ;
#35583 = ORIENTED_EDGE ( 'NONE', *, *, #17694, .T. ) ;
#35584 = VECTOR ( 'NONE', #58421, 1000.000000000000000 ) ;
#35585 = CARTESIAN_POINT ( 'NONE',  ( -6.249999999999997335, -2.499999999999998668, 29.75000000000000355 ) ) ;
#35586 = ORIENTED_EDGE ( 'NONE', *, *, #55113, .F. ) ;
#35587 = ORIENTED_EDGE ( 'NONE', *, *, #40950, .F. ) ;
#35589 = CARTESIAN_POINT ( 'NONE',  ( 15.16549878480845948, -12.27809138561121394, 31.22303859784730307 ) ) ;
#35588 = CARTESIAN_POINT ( 'NONE',  ( -1.134669975237340811, -4.932303261841489039, 34.32971442181322885 ) ) ;
#35590 = FACE_OUTER_BOUND ( 'NONE', #14007, .T. ) ;
#35591 = CYLINDRICAL_SURFACE ( 'NONE', #52320, 0.2500000000000008882 ) ;
#35592 = CARTESIAN_POINT ( 'NONE',  ( -12.46153846153858424, -2.657715359629662544, 31.77849191805970364 ) ) ;
#35593 = CARTESIAN_POINT ( 'NONE',  ( -8.102564102564102200, -3.499999999999999556, 29.75000000000000355 ) ) ;
#35594 = ORIENTED_EDGE ( 'NONE', *, *, #77412, .T. ) ;
#35595 = CARTESIAN_POINT ( 'NONE',  ( -5.142193077479396024, -5.941354392334500467, 34.76329471203369792 ) ) ;
#35596 = CARTESIAN_POINT ( 'NONE',  ( -14.53117723225663660, -10.23692288466677880, 34.23039457007281072 ) ) ;
#35597 = DIRECTION ( 'NONE',  ( -0.000000000000000000, -5.102127870520021228E-17, -1.000000000000000000 ) ) ;
#35598 = CARTESIAN_POINT ( 'NONE',  ( -8.769230769230892619, -2.657715359629662544, 31.77849191805970364 ) ) ;
#35599 = CARTESIAN_POINT ( 'NONE',  ( 2.530471976670374712, -5.827830569534416583, 34.72679350104403539 ) ) ;
#35600 = ORIENTED_EDGE ( 'NONE', *, *, #60319, .F. ) ;
#35601 = CARTESIAN_POINT ( 'NONE',  ( -0.7115152055870527237, -2.318417181685854533, 30.59732222474233865 ) ) ;
#35602 = ORIENTED_EDGE ( 'NONE', *, *, #5734, .T. ) ;
#35603 = EDGE_CURVE ( 'NONE', #59616, #82973, #16438, .T. ) ;
#35604 = ORIENTED_EDGE ( 'NONE', *, *, #9767, .F. ) ;
#35605 = AXIS2_PLACEMENT_3D ( 'NONE', #80567, #18850, #86440 ) ;
#35606 = CYLINDRICAL_SURFACE ( 'NONE', #52063, 0.2500000000000009437 ) ;
#35608 = ORIENTED_EDGE ( 'NONE', *, *, #36509, .T. ) ;
#35607 = EDGE_CURVE ( 'NONE', #72717, #12426, #16839, .T. ) ;
#35609 = CARTESIAN_POINT ( 'NONE',  ( -1.134669866267242311, -8.433404298154336232, 34.66254593164985920 ) ) ;
#35610 = CARTESIAN_POINT ( 'NONE',  ( -17.14300648787895653, -3.050289026998445951, 32.03036669348365706 ) ) ;
#35611 = DIRECTION ( 'NONE',  ( -0.000000000000000000, 0.7660444431189791237, -0.6427876096865379196 ) ) ;
#35612 = CARTESIAN_POINT ( 'NONE',  ( -4.854143407945007205, -3.563462043263029955, 33.22394488606062879 ) ) ;
#35613 = FACE_OUTER_BOUND ( 'NONE', #45630, .T. ) ;
#35614 = B_SPLINE_CURVE_WITH_KNOTS ( 'NONE', 3,
 ( #3227, #30700, #85654, #17186, #72128, #65373, #54072, #12219, #26616, #66716 ),
 .UNSPECIFIED., .F., .F.,
 ( 4, 2, 2, 2, 4 ),
 ( 0.0007817359430256313069, 0.0009771253907249971907, 0.001172514838424363074, 0.001367904286123728958, 0.001563293733823094842 ),
 .UNSPECIFIED. ) ;
#35615 = CARTESIAN_POINT ( 'NONE',  ( 0.4615384615383382183, -9.528491918059723176, 34.59228464037033035 ) ) ;
#35616 = VERTEX_POINT ( 'NONE', #30395 ) ;
#35617 = EDGE_CURVE ( 'NONE', #47387, #81622, #32973, .T. ) ;
#35618 = CARTESIAN_POINT ( 'NONE',  ( 8.352564102564102200, -7.500000000000000000, 29.75000000000000355 ) ) ;
#35620 = EDGE_LOOP ( 'NONE', ( #64171, #11012, #77655, #19587 ) ) ;
#35619 = CARTESIAN_POINT ( 'NONE',  ( -12.23875892027004753, -11.89424750095246175, 32.13594075562311758 ) ) ;
#35621 = CARTESIAN_POINT ( 'NONE',  ( -5.326923076923075762, -2.499999999999998668, 29.75000000000000355 ) ) ;
#35622 = CARTESIAN_POINT ( 'NONE',  ( 6.000000000000001776, -8.564572088678739092, 35.78748833219616898 ) ) ;
#35623 = CARTESIAN_POINT ( 'NONE',  ( -17.07692307692319744, -12.16647553114689728, 32.15551576947799362 ) ) ;
#35624 = B_SPLINE_CURVE_WITH_KNOTS ( 'NONE', 3,
 ( #62985, #1297, #28786, #8954, #56251, #15713 ),
 .UNSPECIFIED., .F., .F.,
 ( 4, 2, 4 ),
 ( 0.0003909569690057804843, 0.0005862646681846042955, 0.0007815723673634281067 ),
 .UNSPECIFIED. ) ;
#35625 = B_SPLINE_CURVE_WITH_KNOTS ( 'NONE', 3,
 ( #15792, #43257, #49570, #8591, #84700, #9034 ),
 .UNSPECIFIED., .F., .F.,
 ( 4, 2, 4 ),
 ( 5.648016952424533599E-17, 0.0001954756301637301926, 0.0003909512603274038984 ),
 .UNSPECIFIED. ) ;
#35626 = CARTESIAN_POINT ( 'NONE',  ( -2.372962308248625529, -12.70778746994557551, 30.41441678777548319 ) ) ;
#35627 = DIRECTION ( 'NONE',  ( 0.000000000000000000, 0.4999999999999960032, -0.8660254037844410391 ) ) ;
#35628 = CARTESIAN_POINT ( 'NONE',  ( -3.296851610129365451, -10.67929555188718460, 33.92786785259543336 ) ) ;
#35629 = LINE ( 'NONE', #28879, #17690 ) ;
#35630 = EDGE_CURVE ( 'NONE', #64075, #45937, #65169, .T. ) ;
#35631 = CARTESIAN_POINT ( 'NONE',  ( -2.749999999999999112, -7.438900925035484057, 25.34561829374151642 ) ) ;
#35632 = EDGE_LOOP ( 'NONE', ( #13028, #20246, #84640, #53260, #28745, #26491 ) ) ;
#35633 = CARTESIAN_POINT ( 'NONE',  ( -16.85414353565466072, -10.81320215134717166, 33.49497208177562868 ) ) ;
#35634 = CARTESIAN_POINT ( 'NONE',  ( -1.515306851282938849, -12.11776431015575994, 31.66791131148498906 ) ) ;
#35635 = CARTESIAN_POINT ( 'NONE',  ( 9.692307692307570832, -11.06231777344772027, 33.60647404775119895 ) ) ;
#35636 = CARTESIAN_POINT ( 'NONE',  ( 13.91025641025641235, -3.499999999999999556, 29.75000000000000355 ) ) ;
#35637 = ORIENTED_EDGE ( 'NONE', *, *, #58929, .T. ) ;
#35638 = CARTESIAN_POINT ( 'NONE',  ( 1.944543648262996083, -5.555456351736983045, 15.56250000000000000 ) ) ;
#35639 = CARTESIAN_POINT ( 'NONE',  ( -2.557669038634660108, -3.137211980971222669, 32.19342716148376837 ) ) ;
#35640 = CARTESIAN_POINT ( 'NONE',  ( 14.17713239407894044, -2.254533558242299396, 29.97296025877828285 ) ) ;
#35641 = LINE ( 'NONE', #63090, #55758 ) ;
#35642 = ORIENTED_EDGE ( 'NONE', *, *, #87224, .T. ) ;
#35643 = VECTOR ( 'NONE', #85334, 1000.000000000000000 ) ;
#35644 = CARTESIAN_POINT ( 'NONE',  ( -12.39628289026243557, -9.442884908240273489, 34.35708131394835618 ) ) ;
#35645 = CARTESIAN_POINT ( 'NONE',  ( 11.53846153846153832, -7.500000000000001776, 35.04278698407183867 ) ) ;
#35646 = DIRECTION ( 'NONE',  ( 0.000000000000000000, 0.1736481776669267785, -0.9848077530122087975 ) ) ;
#35647 = CARTESIAN_POINT ( 'NONE',  ( -13.13456096470193302, -12.65882529074907126, 30.72640787790839312 ) ) ;
#35648 = ORIENTED_EDGE ( 'NONE', *, *, #78782, .F. ) ;
#35649 = CARTESIAN_POINT ( 'NONE',  ( -6.673131513698878692, -6.653508905675592722, 34.93172785388651391 ) ) ;
#35650 = AXIS2_PLACEMENT_3D ( 'NONE', #12647, #67148, #87890 ) ;
#35651 = EDGE_CURVE ( 'NONE', #54682, #82221, #19114, .T. ) ;
#35652 = ORIENTED_EDGE ( 'NONE', *, *, #36731, .T. ) ;
#35653 = CARTESIAN_POINT ( 'NONE',  ( 12.68455130563185662, -12.38742843783360748, 31.66772728687926985 ) ) ;
#35654 = CARTESIAN_POINT ( 'NONE',  ( -10.83886955910855932, -2.847400154188067578, 31.58180166144859058 ) ) ;
#35655 = EDGE_LOOP ( 'NONE', ( #22010, #61610 ) ) ;
#35656 = AXIS2_PLACEMENT_3D ( 'NONE', #42191, #8395, #69643 ) ;
#35657 = LINE ( 'NONE', #55036, #17423 ) ;
#35658 = CARTESIAN_POINT ( 'NONE',  ( -14.55766905174089665, -2.318417181685855422, 30.59732222474233865 ) ) ;
#35659 = CARTESIAN_POINT ( 'NONE',  ( 13.16113044089144068, -6.760086850603066466, 34.69517049084099369 ) ) ;
#35660 = EDGE_CURVE ( 'NONE', #78029, #19388, #11919, .T. ) ;
#35661 = CARTESIAN_POINT ( 'NONE',  ( 1.319345384059066983, -6.835583212224499938, 34.95778746994557906 ) ) ;
#35662 = FACE_OUTER_BOUND ( 'NONE', #55984, .T. ) ;
#35663 = EDGE_CURVE ( 'NONE', #10540, #59654, #8245, .T. ) ;
#35664 = VERTEX_POINT ( 'NONE', #87145 ) ;
#35666 = ORIENTED_EDGE ( 'NONE', *, *, #21421, .T. ) ;
#35665 = EDGE_CURVE ( 'NONE', #15081, #50717, #25868, .T. ) ;
#35667 = FACE_BOUND ( 'NONE', #17494, .T. ) ;
#35668 = ORIENTED_EDGE ( 'NONE', *, *, #20344, .F. ) ;
#35669 = LINE ( 'NONE', #70334, #76041 ) ;
#35670 = AXIS2_PLACEMENT_3D ( 'NONE', #39470, #88555, #66930 ) ;
#35671 = LINE ( 'NONE', #85953, #55969 ) ;
#35672 = DIRECTION ( 'NONE',  ( -0.000000000000000000, -0.8660254037844399289, -0.4999999999999980016 ) ) ;
#35673 = DIRECTION ( 'NONE',  ( -0.000000000000000000, 0.000000000000000000, 1.000000000000000000 ) ) ;
#35674 = B_SPLINE_CURVE_WITH_KNOTS ( 'NONE', 3,
 ( #17588, #60337, #31538, #86502, #52690, #4964, #32428, #87393, #55352, #48150 ),
 .UNSPECIFIED., .F., .F.,
 ( 4, 2, 2, 2, 4 ),
 ( 0.0007817246256747474977, 0.0009771112852218911526, 0.001172497944769034916, 0.001367884604316178679, 0.001563271263863322443 ),
 .UNSPECIFIED. ) ;
#35675 = EDGE_CURVE ( 'NONE', #40586, #14645, #20040, .T. ) ;
#35676 = ORIENTED_EDGE ( 'NONE', *, *, #82110, .F. ) ;
#35677 = AXIS2_PLACEMENT_3D ( 'NONE', #19938, #67252, #33019 ) ;
#35678 = ORIENTED_EDGE ( 'NONE', *, *, #67022, .F. ) ;
#35679 = ORIENTED_EDGE ( 'NONE', *, *, #87460, .T. ) ;
#35680 = CARTESIAN_POINT ( 'NONE',  ( -3.100243792535588128, -11.66157788607254275, 32.95092075102925833 ) ) ;
#35681 = EDGE_CURVE ( 'NONE', #81564, #79445, #75867, .T. ) ;
#35683 = ORIENTED_EDGE ( 'NONE', *, *, #35603, .F. ) ;
#35682 = EDGE_CURVE ( 'NONE', #9934, #79961, #39395, .T. ) ;
#35684 = AXIS2_PLACEMENT_3D ( 'NONE', #34423, #29013, #41627 ) ;
#35685 = CARTESIAN_POINT ( 'NONE',  ( 3.165498784808456367, -2.892918686051582533, 31.69288490824015270 ) ) ;
#35686 = CARTESIAN_POINT ( 'NONE',  ( 12.21151522424549896, -2.587272538249754117, 30.68239716806877837 ) ) ;
#35687 = EDGE_CURVE ( 'NONE', #34255, #21400, #38494, .T. ) ;
#35688 = CARTESIAN_POINT ( 'NONE',  ( -18.22292621751613950, -11.24512374952582050, 33.06303171183252942 ) ) ;
#35689 = LINE ( 'NONE', #77987, #60059 ) ;
#35690 = CARTESIAN_POINT ( 'NONE',  ( -6.066082379360132393, -6.343179335718451384, 34.87096338111212646 ) ) ;
#35691 = CARTESIAN_POINT ( 'NONE',  ( 20.00000000000000000, -4.000000000000000000, 29.75000000000000355 ) ) ;
#35692 = CARTESIAN_POINT ( 'NONE',  ( 8.992010438208831502, -6.717445702608402236, 34.94155399931962336 ) ) ;
#35693 = ORIENTED_EDGE ( 'NONE', *, *, #42620, .T. ) ;
#35694 = ORIENTED_EDGE ( 'NONE', *, *, #80430, .T. ) ;
#35695 = ORIENTED_EDGE ( 'NONE', *, *, #3064, .T. ) ;
#35696 = CARTESIAN_POINT ( 'NONE',  ( 3.295914011488863871, -7.750023224968865421, 34.99404313364389907 ) ) ;
#35698 = CARTESIAN_POINT ( 'NONE',  ( 10.39189969082028497, -2.353723527008296568, 30.78948104536958752 ) ) ;
#35697 = DIRECTION ( 'NONE',  ( 1.000000000000000000, -1.799314243699348838E-16, 1.560656329602356967E-32 ) ) ;
#35699 = CARTESIAN_POINT ( 'NONE',  ( 1.634669804528839476, -12.41089969410671223, 31.60739465890703670 ) ) ;
#35700 = CARTESIAN_POINT ( 'NONE',  ( 12.59206389977210705, -12.70449254468099198, 30.44128974285582956 ) ) ;
#35701 = FACE_BOUND ( 'NONE', #81175, .T. ) ;
#35702 = CARTESIAN_POINT ( 'NONE',  ( 16.28437185560972011, -3.285477652293413264, 32.44071101563363158 ) ) ;
#35703 = ORIENTED_EDGE ( 'NONE', *, *, #6817, .T. ) ;
#35704 = CARTESIAN_POINT ( 'NONE',  ( 17.07692307692307665, -10.51840700105979565, 33.73612834413961536 ) ) ;
#35705 = LINE ( 'NONE', #56845, #35860 ) ;
#35706 = DIRECTION ( 'NONE',  ( 1.000000000000000000, 0.000000000000000000, 0.000000000000000000 ) ) ;
#35707 = LINE ( 'NONE', #43779, #25147 ) ;
#35708 = EDGE_LOOP ( 'NONE', ( #37117, #29490, #78, #30885 ) ) ;
#35709 = CARTESIAN_POINT ( 'NONE',  ( -18.06608341095587633, -8.120952969808774569, 34.71129190930000163 ) ) ;
#35710 = AXIS2_PLACEMENT_3D ( 'NONE', #18536, #50953, #23497 ) ;
#35711 = ORIENTED_EDGE ( 'NONE', *, *, #16155, .T. ) ;
#35712 = FACE_BOUND ( 'NONE', #9293, .T. ) ;
#35714 = EDGE_CURVE ( 'NONE', #34892, #83375, #2784, .T. ) ;
#35713 = B_SPLINE_CURVE_WITH_KNOTS ( 'NONE', 3,
 ( #84388, #43389, #84835, #64972, #50577, #16358, #44244, #72179, #50133, #9594 ),
 .UNSPECIFIED., .F., .F.,
 ( 4, 2, 2, 2, 4 ),
 ( 0.000000000000000000, 0.0001954339857564076912, 0.0003908679715128153824, 0.0005863019572692231007, 0.0007817359430256307648 ),
 .UNSPECIFIED. ) ;
#35715 = CARTESIAN_POINT ( 'NONE',  ( -17.32694630114453105, -4.175268141568689195, 33.81360843649122216 ) ) ;
#35716 = CARTESIAN_POINT ( 'NONE',  ( -7.146003881983773454, -10.01117774369187252, 34.36070679894347535 ) ) ;
#35717 = CARTESIAN_POINT ( 'NONE',  ( -8.769230769230768274, -13.49023893513002648, 31.06009739812518688 ) ) ;
#35718 = VECTOR ( 'NONE', #69216, 1000.000000000000000 ) ;
#35719 = VERTEX_POINT ( 'NONE', #51359 ) ;
#35720 = CARTESIAN_POINT ( 'NONE',  ( -12.52762187249434156, -9.780366693483667717, 34.19971097300155805 ) ) ;
#35721 = CARTESIAN_POINT ( 'NONE',  ( -14.37377571864818648, -4.098570777380719399, 33.41473453929634729 ) ) ;
#35722 = FACE_OUTER_BOUND ( 'NONE', #87232, .T. ) ;
#35723 = CYLINDRICAL_SURFACE ( 'NONE', #15798, 0.2499999999999995559 ) ;
#35724 = ORIENTED_EDGE ( 'NONE', *, *, #47807, .T. ) ;
#35725 = CARTESIAN_POINT ( 'NONE',  ( 13.13463865367303463, -5.728515186090277211, 34.42611988154120439 ) ) ;
#35726 = ORIENTED_EDGE ( 'NONE', *, *, #4419, .F. ) ;
#35727 = EDGE_CURVE ( 'NONE', #33332, #57312, #64898, .T. ) ;
#35729 = ORIENTED_EDGE ( 'NONE', *, *, #27023, .F. ) ;
#35728 = DIRECTION ( 'NONE',  ( -0.000000000000000000, 0.8660254037844399289, -0.4999999999999980016 ) ) ;
#35730 = DIRECTION ( 'NONE',  ( -0.000000000000000000, -0.9396926207859092051, -0.3420201433256662704 ) ) ;
#35731 = CARTESIAN_POINT ( 'NONE',  ( -1.515305987725690695, -12.35290016733513951, 31.75349464988449455 ) ) ;
#35732 = FACE_OUTER_BOUND ( 'NONE', #79758, .T. ) ;
#35733 = CARTESIAN_POINT ( 'NONE',  ( -12.23875892027005108, -2.847695495035523550, 31.58253572463339154 ) ) ;
#35735 = CARTESIAN_POINT ( 'NONE',  ( 0.2386597791098133969, -7.630691491037286056, 34.74850469731152458 ) ) ;
#35734 = CARTESIAN_POINT ( 'NONE',  ( 8.899275825150539276, -2.254550872974305342, 29.97347326024527092 ) ) ;
#35736 = DIRECTION ( 'NONE',  ( 0.000000000000000000, 0.000000000000000000, -1.000000000000000000 ) ) ;
#35737 = EDGE_CURVE ( 'NONE', #80445, #1486, #24354, .T. ) ;
#35738 = CARTESIAN_POINT ( 'NONE',  ( 2.749999999999995115, -6.360912703473971419, 24.39062500000000000 ) ) ;
#35739 = VERTEX_POINT ( 'NONE', #85189 ) ;
#35740 = CARTESIAN_POINT ( 'NONE',  ( -16.37733107841048863, -4.988325925672468131, 34.36044203135681130 ) ) ;
#35741 = ORIENTED_EDGE ( 'NONE', *, *, #17231, .T. ) ;
#35742 =( BOUNDED_SURFACE ( )  B_SPLINE_SURFACE ( 3, 2, ( 
 ( #933, #41929, #20758, #493, #69397, #63513, #7252, #82916, #1815, #49, #48224, #14002, #68943, #62186, #55430, #21199, #7701, #15787, #72486, #16219, #9461, #30609, #22533, #79254, #43252, #10794, #17100, #63950, #85565, #78798, #9030, #50865, #2245, #65283, #31048, #58082, #2686, #23839, #58516, #3579, #50435, #51293, #44554, #72040, #10349, #17554, #4019, #31506, #77914, #43685, #16651, #37815, #45004, #3133, #86010, #57644, #38265, #24291, #51751, #65723, #58972, #49997, #77477, #29741, #70726, #71154, #36499, #23407, #84695, #57205, #36924, #22970, #64387, #30177, #85127, #78351, #44113, #71591, #9900, #37362, #64829, #53550, #74277, #24747, #18001, #40503, #74727, #87363, #19333, #38710, #52658, #6267, #40062, #87817, #81488, #25642, #67965, #18446, #45456, #52211, #33295, #46354, #86930, #81043, #11693, #73841, #33733, #66631, #25194, #39171, #53098, #26086, #46800, #19774, #12577, #80145, #67521, #5818, #18887, #32844, #86475, #4482, #4935, #45901, #79700, #60753, #12139, #47235, #13016, #72937, #39618, #80601, #88261, #67077, #11239, #66170, #31959, #59423, #73387, #32400, #59865, #5375, #60308, #26537, #53996, #62950, #8033, #54435, #75170, #27856, #61634, #20654, #28753, #42271, #89139, #61187, #76038, #69290, #41825, #88699, #13896 ),
 ( #13452, #14795, #69728, #7591, #41377, #35052, #35503, #1262, #27416, #62512, #828, #28292, #49013, #56215, #42709, #70172, #54888, #82370, #55323, #55763, #83705, #83252, #21539, #7145, #76934, #21988, #49461, #76491, #15237, #8479, #68398, #26980, #81930, #40935, #48119, #14341, #20220, #68840, #6696, #47684, #34616, #34168, #75590, #62082, #392, #82814, #21086, #48558, #71938, #57978, #44902, #63406, #15679, #84589, #10249, #43579, #8924, #22860, #37708, #37258, #30510, #78702, #30072, #22426, #51194, #16998, #85459, #71488, #72377, #9796, #58410, #36824, #43146, #1714, #64726, #84150, #49891, #24191, #9366, #70615, #85905, #23742, #57535, #85023, #44448, #65175, #16550, #77807, #23304, #77370, #3474, #50762, #30942, #71052, #3026, #78248, #64281, #36390, #16114, #2582, #51643, #50326, #44017, #79146, #17447, #35951, #29203, #63852, #2151, #56656, #29636, #57093, #3915, #60642, #4374, #86820, #18784, #10690, #67411, #31401, #88155, #5265, #52107, #73740, #66971, #86370, #39065, #79596, #53440, #19227, #46251, #80036, #12033, #46691, #80942, #38606, #39509, #32731, #60200, #87701, #5707, #81380, #19663, #66062, #31856, #4826, #25975, #33180, #80488, #74169, #45798, #26428, #12466, #11583, #39951, #25537, #58869, #53893, #24642, #52990, #47124 ),
 ( #38156, #59314, #65613, #17893, #25087, #45350, #72820, #11128, #52551, #32296, #18335, #73280, #66525, #59761, #87256, #6154, #28645, #62844, #75489, #7489, #26869, #40829, #83603, #28186, #75938, #69619, #13790, #56109, #6598, #33627, #40395, #21436, #34509, #75064, #69182, #89033, #61972, #21881, #54772, #13349, #27309, #41273, #14237, #34943, #7927, #62406, #68294, #55655, #41712, #7033, #20981, #74614, #81821, #82263, #34064, #12904, #722, #281, #35393, #1163, #67853, #27748, #68737, #48905, #55219, #61089, #88598, #54327, #20110, #47573, #61526, #20550, #48012, #82709, #83146, #48452, #76377, #14684, #42166, #63304, #16014, #49789, #8818, #16895, #30412, #77265, #49357, #64178, #57430, #29971, #76834, #2049, #30846, #15574, #58316, #23646, #50220, #84926, #51097, #70513, #2481, #23207, #36290, #50668, #65069, #35846, #78151, #36724, #85809, #2922, #43040, #15131, #63747, #77706, #84044, #56555, #56989, #29532, #3375, #16452, #43921, #44347, #71834, #42605, #71385, #43482, #85362, #9691, #70065, #8373, #1612, #29100, #22324, #84481, #22757, #70955, #9265, #37160, #64620, #78592, #10141, #57877, #37605, #79936, #24534, #72722, #80841, #5162, #52001, #24090, #38962, #32199, #4725, #51539, #65963, #5608, #79495, #33077, #87601, #24983, #59656 ),
 ( #32630, #60100, #17797, #87156, #25434, #52891, #11931, #19124, #60545, #79040, #45249, #11034, #18238, #80391, #46595, #18688, #46153, #59211, #39846, #66867, #25879, #53341, #73639, #74074, #39409, #31301, #12368, #67312, #38057, #38507, #66420, #17341, #31754, #58767, #44798, #86717, #72278, #86265, #10591, #65521, #3822, #4269, #52449, #45699, #73181, #11478, #26321, #67754, #47466, #63530, #6498, #60989, #74964, #1834, #179, #82615, #41611, #82161, #74509, #14134, #70298, #20884, #34402, #36518, #61864, #22551, #88935, #6057, #53788, #27646, #47023, #12805, #77494, #61425, #33531, #50019, #48355, #55118, #84273, #27206, #70745, #20002, #19560, #81277, #36079, #47914, #88491, #75832, #13252, #75396, #9047, #68199, #26764, #40733, #54663, #8605, #29321, #15806, #56775, #54223, #43271, #88060, #20453, #40291, #81718, #33959, #13690, #41168, #68634, #6931, #78818, #58989, #86492, #72956, #51313, #3153, #10814, #17119, #45477, #63967, #11257, #84718, #57225, #18020, #30200, #2263, #37381, #31069, #29758, #65740, #38286, #22989, #77934, #30629, #64404, #23426, #31526, #45026, #2703, #50454, #44573, #72061, #10373, #16237, #16672, #43702, #57664, #71172, #4037, #64852, #37833, #24766, #85146, #65303, #3600, #50884, #58535, #79721, #9477, #86032, #24311 ),
 ( #58102, #36941, #85585, #51771, #79275, #78371, #44131, #71612, #17576, #72504, #9919, #23860, #52229, #39635, #11711, #20236, #66647, #40518, #31977, #25661, #26993, #60769, #73405, #59440, #32860, #59885, #53116, #5833, #26552, #66189, #86947, #81947, #54451, #67094, #88276, #80165, #4951, #47699, #81502, #47253, #46815, #18904, #74293, #74745, #19788, #32416, #12593, #40082, #67536, #54009, #6282, #75185, #38729, #87378, #80620, #60323, #33311, #33747, #19348, #13031, #73857, #4499, #67983, #61202, #88714, #25215, #52676, #18465, #45919, #39188, #46374, #12154, #5395, #53567, #87834, #26103, #81060, #76505, #48573, #42725, #48135, #56231, #13471, #40949, #75605, #34631, #49476, #35520, #22441, #68414, #82385, #62099, #76948, #21102, #13911, #407, #15252, #14811, #8050, #83719, #7607, #89155, #28769, #22003, #62967, #49027, #49906, #42287, #35966, #14354, #20669, #6711, #69743, #61649, #27434, #1729, #76054, #41391, #63422, #1279, #35068, #62527, #70185, #8494, #83269, #55338, #843, #54903, #29218, #28309, #56670, #41840, #84163, #55777, #69308, #68856, #82829, #21555, #34183, #27871, #7162, #65189, #65626, #58883, #43160, #22876, #29650, #85921, #3042, #57111, #70630, #38169, #71068, #64297, #85473, #77384, #44917, #8937, #3929, #71952, #84604 ),
 ( #30957, #58425, #24203, #78716, #51661, #57994, #50340, #79160, #31416, #2163, #16128, #30523, #86385, #85039, #77821, #51208, #23319, #17461, #43594, #72391, #15694, #36408, #9378, #36837, #10703, #10263, #24655, #63866, #2598, #30088, #57550, #50776, #78262, #16564, #44030, #17012, #37723, #71503, #9809, #37275, #3487, #64740, #23755, #44463, #88610, #87720, #74629, #53004, #31870, #17906, #25991, #11143, #66078, #40410, #25550, #86836, #12921, #74182, #46266, #12050, #12483, #67425, #32746, #4839, #39524, #38619, #5721, #66987, #33194, #87270, #19242, #5280, #80504, #59327, #32311, #18798, #67867, #11598, #73756, #39966, #6168, #33640, #45362, #25101, #4387, #60657, #60214, #52564, #72836, #61103, #45811, #39077, #53454, #52121, #19677, #80049, #79609, #46707, #18352, #80957, #88169, #73295, #26444, #66540, #53906, #81395, #47141, #59774, #34959, #35405, #7940, #54787, #62420, #28198, #55669, #14696, #83615, #8386, #35858, #82277, #20562, #20994, #83161, #21894, #7502, #48920, #61988, #42617, #55232, #68309, #69633, #62859, #735, #7050, #21451, #1174, #28657, #48026, #76394, #42180, #56125, #49368, #76847, #63320, #26883, #75504, #13805, #48467, #15144, #70079, #54340, #81834, #294, #20126, #47590, #75075, #13362, #40843, #6610, #34077, #61541 ),
 ( #89046, #27325, #75954, #41290, #68752, #34523, #27761, #82721, #14251, #41731, #69195, #43496, #9704, #77278, #2063, #3389, #30425, #16468, #16910, #70970, #65081, #29546, #84058, #56568, #85375, #2495, #36305, #71399, #22770, #29986, #30858, #50231, #63759, #77719, #9277, #43934, #37174, #44360, #64635, #57001, #57889, #2939, #64190, #50679, #1630, #70527, #16027, #84494, #29111, #23661, #78165, #37622, #22337, #49801, #51113, #84939, #10158, #78605, #15587, #43052, #8834, #57443, #23219, #36738, #71848, #22812, #23694, #86318, #79549, #63799, #43529, #50270, #17396, #51146, #77759, #2098, #58815, #2531, #84973, #16948, #8871, #65568, #29585, #24591, #3427, #16065, #71887, #65120, #84535, #30894, #43970, #52056, #51592, #79093, #44851, #10197, #72330, #78649, #71006, #10641, #17847, #9315, #36774, #44398, #45299, #16503, #64230, #37658, #71438, #38105, #30024, #3867, #36340, #57041, #57484, #23254, #31353, #58361, #50716, #78203, #9744, #37211, #64676, #2978, #30458, #57929, #85413, #85856, #24140, #27588, #66918, #59264, #121, #55060, #6871, #20395, #21267, #47857, #7326, #73688, #52501, #38558, #75341, #31806, #86768, #62251, #46202, #18286, #34784, #34340, #5214, #32680, #61808, #82553, #54604, #25488, #60148, #25038, #20830, #87650, #48296 ) ),
 .UNSPECIFIED., .T., .F., .F. ) 
 B_SPLINE_SURFACE_WITH_KNOTS ( ( 4, 3, 4 ),
 ( 3, 2, 2, 2, 2, 2, 2, 2, 2, 2, 2, 2, 2, 2, 2, 2, 2, 2, 2, 2, 2, 2, 2, 2, 2, 2, 2, 2, 2, 2, 2, 2, 2, 2, 2, 2, 2, 2, 2, 2, 2, 2, 2, 2, 2, 2, 2, 2, 2, 2, 2, 2, 2, 2, 2, 2, 2, 2, 2, 2, 2, 2, 2, 2, 2, 2, 2, 2, 2, 2, 2, 2, 2, 2, 2, 2, 2, 2, 2, 2, 3 ),
 ( 0.000000000000000000, 0.5000000000000000000, 1.000000000000000000 ),
 ( 0.000000000000000000, 0.01250000000000000069, 0.02500000000000000139, 0.03749999999999999861, 0.05000000000000000278, 0.06250000000000000000, 0.07499999999999999722, 0.08749999999999999445, 0.1000000000000000056, 0.1125000000000000028, 0.1250000000000000000, 0.1375000000000000111, 0.1499999999999999944, 0.1625000000000000056, 0.1749999999999999889, 0.1875000000000000000, 0.2000000000000000111, 0.2124999999999999944, 0.2250000000000000056, 0.2374999999999999889, 0.2500000000000000000, 0.2625000000000000111, 0.2750000000000000222, 0.2874999999999999778, 0.2999999999999999889, 0.3125000000000000000, 0.3250000000000000111, 0.3375000000000000222, 0.3499999999999999778, 0.3624999999999999889, 0.3750000000000000000, 0.3875000000000000111, 0.4000000000000000222, 0.4124999999999999778, 0.4249999999999999889, 0.4375000000000000000, 0.4500000000000000111, 0.4625000000000000222, 0.4749999999999999778, 0.4874999999999999889, 0.5000000000000000000, 0.5124999999999999556, 0.5250000000000000222, 0.5374999999999999778, 0.5500000000000000444, 0.5625000000000000000, 0.5749999999999999556, 0.5875000000000000222, 0.5999999999999999778, 0.6125000000000000444, 0.6250000000000000000, 0.6374999999999999556, 0.6500000000000000222, 0.6624999999999999778, 0.6750000000000000444, 0.6875000000000000000, 0.6999999999999999556, 0.7125000000000000222, 0.7249999999999999778, 0.7375000000000000444, 0.7500000000000000000, 0.7624999999999999556, 0.7750000000000000222, 0.7874999999999999778, 0.8000000000000000444, 0.8125000000000000000, 0.8249999999999999556, 0.8375000000000000222, 0.8499999999999999778, 0.8625000000000000444, 0.8750000000000000000, 0.8874999999999999556, 0.9000000000000000222, 0.9124999999999999778, 0.9250000000000000444, 0.9375000000000000000, 0.9499999999999999556, 0.9625000000000000222, 0.9749999999999999778, 0.9875000000000000444, 1.000000000000000000 ),
 .UNSPECIFIED. ) 
 GEOMETRIC_REPRESENTATION_ITEM ( )  RATIONAL_B_SPLINE_SURFACE ( (
 ( 1.000000000000000000, 0.9238795325112867385, 1.000000000000000000, 0.9238795325112867385, 1.000000000000000000, 0.9238795325112867385, 1.000000000000000000, 0.9238795325112867385, 1.000000000000000000, 0.9238795325112867385, 1.000000000000000000, 0.9238795325112867385, 1.000000000000000000, 0.9238795325112867385, 1.000000000000000000, 0.9238795325112867385, 1.000000000000000000, 0.9238795325112867385, 1.000000000000000000, 0.9238795325112867385, 1.000000000000000000, 0.9238795325112867385, 1.000000000000000000, 0.9238795325112867385, 1.000000000000000000, 0.9238795325112867385, 1.000000000000000000, 0.9238795325112867385, 1.000000000000000000, 0.9238795325112867385, 1.000000000000000000, 0.9238795325112867385, 1.000000000000000000, 0.9238795325112867385, 1.000000000000000000, 0.9238795325112867385, 1.000000000000000000, 0.9238795325112867385, 1.000000000000000000, 0.9238795325112867385, 1.000000000000000000, 0.9238795325112867385, 1.000000000000000000, 0.9238795325112867385, 1.000000000000000000, 0.9238795325112867385, 1.000000000000000000, 0.9238795325112867385, 1.000000000000000000, 0.9238795325112867385, 1.000000000000000000, 0.9238795325112867385, 1.000000000000000000, 0.9238795325112867385, 1.000000000000000000, 0.9238795325112867385, 1.000000000000000000, 0.9238795325112867385, 1.000000000000000000, 0.9238795325112867385, 1.000000000000000000, 0.9238795325112867385, 1.000000000000000000, 0.9238795325112867385, 1.000000000000000000, 0.9238795325112867385, 1.000000000000000000, 0.9238795325112867385, 1.000000000000000000, 0.9238795325112867385, 1.000000000000000000, 0.9238795325112867385, 1.000000000000000000, 0.9238795325112867385, 1.000000000000000000, 0.9238795325112867385, 1.000000000000000000, 0.9238795325112867385, 1.000000000000000000, 0.9238795325112867385, 1.000000000000000000, 0.9238795325112867385, 1.000000000000000000, 0.9238795325112867385, 1.000000000000000000, 0.9238795325112867385, 1.000000000000000000, 0.9238795325112867385, 1.000000000000000000, 0.9238795325112867385, 1.000000000000000000, 0.9238795325112867385, 1.000000000000000000, 0.9238795325112867385, 1.000000000000000000, 0.9238795325112867385, 1.000000000000000000, 0.9238795325112867385, 1.000000000000000000, 0.9238795325112867385, 1.000000000000000000, 0.9238795325112867385, 1.000000000000000000, 0.9238795325112867385, 1.000000000000000000, 0.9238795325112867385, 1.000000000000000000, 0.9238795325112867385, 1.000000000000000000, 0.9238795325112867385, 1.000000000000000000, 0.9238795325112867385, 1.000000000000000000, 0.9238795325112867385, 1.000000000000000000, 0.9238795325112867385, 1.000000000000000000, 0.9238795325112867385, 1.000000000000000000, 0.9238795325112867385, 1.000000000000000000, 0.9238795325112867385, 1.000000000000000000, 0.9238795325112867385, 1.000000000000000000, 0.9238795325112867385, 1.000000000000000000, 0.9238795325112867385, 1.000000000000000000, 0.9238795325112867385, 1.000000000000000000, 0.9238795325112867385, 1.000000000000000000, 0.9238795325112867385, 1.000000000000000000, 0.9238795325112867385, 1.000000000000000000, 0.9238795325112867385, 1.000000000000000000, 0.9238795325112867385, 1.000000000000000000, 0.9238795325112867385, 1.000000000000000000, 0.9238795325112867385, 1.000000000000000000, 0.9238795325112867385, 1.000000000000000000, 0.9238795325112867385, 1.000000000000000000, 0.9238795325112867385, 1.000000000000000000, 0.9238795325112867385, 1.000000000000000000, 0.9238795325112867385, 1.000000000000000000, 0.9238795325112867385, 1.000000000000000000, 0.9238795325112867385, 1.000000000000000000, 0.9238795325112867385, 1.000000000000000000),
 ( 0.3333333333333333703, 0.3079598441704289313, 0.3333333333333333703, 0.3079598441704289313, 0.3333333333333333703, 0.3079598441704289313, 0.3333333333333333703, 0.3079598441704289313, 0.3333333333333333703, 0.3079598441704289313, 0.3333333333333333703, 0.3079598441704289313, 0.3333333333333333703, 0.3079598441704289313, 0.3333333333333333703, 0.3079598441704289313, 0.3333333333333333703, 0.3079598441704289313, 0.3333333333333333703, 0.3079598441704289313, 0.3333333333333333703, 0.3079598441704289313, 0.3333333333333333703, 0.3079598441704289313, 0.3333333333333333703, 0.3079598441704289313, 0.3333333333333333703, 0.3079598441704289313, 0.3333333333333333703, 0.3079598441704289313, 0.3333333333333333703, 0.3079598441704289313, 0.3333333333333333703, 0.3079598441704289313, 0.3333333333333333703, 0.3079598441704289313, 0.3333333333333333703, 0.3079598441704289313, 0.3333333333333333703, 0.3079598441704289313, 0.3333333333333333703, 0.3079598441704289313, 0.3333333333333333703, 0.3079598441704289313, 0.3333333333333333703, 0.3079598441704289313, 0.3333333333333333703, 0.3079598441704289313, 0.3333333333333333703, 0.3079598441704289313, 0.3333333333333333703, 0.3079598441704289313, 0.3333333333333333703, 0.3079598441704289313, 0.3333333333333333703, 0.3079598441704289313, 0.3333333333333333703, 0.3079598441704289313, 0.3333333333333333703, 0.3079598441704289313, 0.3333333333333333703, 0.3079598441704289313, 0.3333333333333333703, 0.3079598441704289313, 0.3333333333333333703, 0.3079598441704289313, 0.3333333333333333703, 0.3079598441704289313, 0.3333333333333333703, 0.3079598441704289313, 0.3333333333333333703, 0.3079598441704289313, 0.3333333333333333703, 0.3079598441704289313, 0.3333333333333333703, 0.3079598441704289313, 0.3333333333333333703, 0.3079598441704289313, 0.3333333333333333703, 0.3079598441704289313, 0.3333333333333333703, 0.3079598441704289313, 0.3333333333333333703, 0.3079598441704289313, 0.3333333333333333703, 0.3079598441704289313, 0.3333333333333333703, 0.3079598441704289313, 0.3333333333333333703, 0.3079598441704289313, 0.3333333333333333703, 0.3079598441704289313, 0.3333333333333333703, 0.3079598441704289313, 0.3333333333333333703, 0.3079598441704289313, 0.3333333333333333703, 0.3079598441704289313, 0.3333333333333333703, 0.3079598441704289313, 0.3333333333333333703, 0.3079598441704289313, 0.3333333333333333703, 0.3079598441704289313, 0.3333333333333333703, 0.3079598441704289313, 0.3333333333333333703, 0.3079598441704289313, 0.3333333333333333703, 0.3079598441704289313, 0.3333333333333333703, 0.3079598441704289313, 0.3333333333333333703, 0.3079598441704289313, 0.3333333333333333703, 0.3079598441704289313, 0.3333333333333333703, 0.3079598441704289313, 0.3333333333333333703, 0.3079598441704289313, 0.3333333333333333703, 0.3079598441704289313, 0.3333333333333333703, 0.3079598441704289313, 0.3333333333333333703, 0.3079598441704289313, 0.3333333333333333703, 0.3079598441704289313, 0.3333333333333333703, 0.3079598441704289313, 0.3333333333333333703, 0.3079598441704289313, 0.3333333333333333703, 0.3079598441704289313, 0.3333333333333333703, 0.3079598441704289313, 0.3333333333333333703, 0.3079598441704289313, 0.3333333333333333703, 0.3079598441704289313, 0.3333333333333333703, 0.3079598441704289313, 0.3333333333333333703, 0.3079598441704289313, 0.3333333333333333703, 0.3079598441704289313, 0.3333333333333333703, 0.3079598441704289313, 0.3333333333333333703, 0.3079598441704289313, 0.3333333333333333703, 0.3079598441704289313, 0.3333333333333333703, 0.3079598441704289313, 0.3333333333333333703, 0.3079598441704289313, 0.3333333333333333703, 0.3079598441704289313, 0.3333333333333333703, 0.3079598441704289313, 0.3333333333333333703),
 ( 0.3333333333333333703, 0.3079598441704289313, 0.3333333333333333703, 0.3079598441704289313, 0.3333333333333333703, 0.3079598441704289313, 0.3333333333333333703, 0.3079598441704289313, 0.3333333333333333703, 0.3079598441704289313, 0.3333333333333333703, 0.3079598441704289313, 0.3333333333333333703, 0.3079598441704289313, 0.3333333333333333703, 0.3079598441704289313, 0.3333333333333333703, 0.3079598441704289313, 0.3333333333333333703, 0.3079598441704289313, 0.3333333333333333703, 0.3079598441704289313, 0.3333333333333333703, 0.3079598441704289313, 0.3333333333333333703, 0.3079598441704289313, 0.3333333333333333703, 0.3079598441704289313, 0.3333333333333333703, 0.3079598441704289313, 0.3333333333333333703, 0.3079598441704289313, 0.3333333333333333703, 0.3079598441704289313, 0.3333333333333333703, 0.3079598441704289313, 0.3333333333333333703, 0.3079598441704289313, 0.3333333333333333703, 0.3079598441704289313, 0.3333333333333333703, 0.3079598441704289313, 0.3333333333333333703, 0.3079598441704289313, 0.3333333333333333703, 0.3079598441704289313, 0.3333333333333333703, 0.3079598441704289313, 0.3333333333333333703, 0.3079598441704289313, 0.3333333333333333703, 0.3079598441704289313, 0.3333333333333333703, 0.3079598441704289313, 0.3333333333333333703, 0.3079598441704289313, 0.3333333333333333703, 0.3079598441704289313, 0.3333333333333333703, 0.3079598441704289313, 0.3333333333333333703, 0.3079598441704289313, 0.3333333333333333703, 0.3079598441704289313, 0.3333333333333333703, 0.3079598441704289313, 0.3333333333333333703, 0.3079598441704289313, 0.3333333333333333703, 0.3079598441704289313, 0.3333333333333333703, 0.3079598441704289313, 0.3333333333333333703, 0.3079598441704289313, 0.3333333333333333703, 0.3079598441704289313, 0.3333333333333333703, 0.3079598441704289313, 0.3333333333333333703, 0.3079598441704289313, 0.3333333333333333703, 0.3079598441704289313, 0.3333333333333333703, 0.3079598441704289313, 0.3333333333333333703, 0.3079598441704289313, 0.3333333333333333703, 0.3079598441704289313, 0.3333333333333333703, 0.3079598441704289313, 0.3333333333333333703, 0.3079598441704289313, 0.3333333333333333703, 0.3079598441704289313, 0.3333333333333333703, 0.3079598441704289313, 0.3333333333333333703, 0.3079598441704289313, 0.3333333333333333703, 0.3079598441704289313, 0.3333333333333333703, 0.3079598441704289313, 0.3333333333333333703, 0.3079598441704289313, 0.3333333333333333703, 0.3079598441704289313, 0.3333333333333333703, 0.3079598441704289313, 0.3333333333333333703, 0.3079598441704289313, 0.3333333333333333703, 0.3079598441704289313, 0.3333333333333333703, 0.3079598441704289313, 0.3333333333333333703, 0.3079598441704289313, 0.3333333333333333703, 0.3079598441704289313, 0.3333333333333333703, 0.3079598441704289313, 0.3333333333333333703, 0.3079598441704289313, 0.3333333333333333703, 0.3079598441704289313, 0.3333333333333333703, 0.3079598441704289313, 0.3333333333333333703, 0.3079598441704289313, 0.3333333333333333703, 0.3079598441704289313, 0.3333333333333333703, 0.3079598441704289313, 0.3333333333333333703, 0.3079598441704289313, 0.3333333333333333703, 0.3079598441704289313, 0.3333333333333333703, 0.3079598441704289313, 0.3333333333333333703, 0.3079598441704289313, 0.3333333333333333703, 0.3079598441704289313, 0.3333333333333333703, 0.3079598441704289313, 0.3333333333333333703, 0.3079598441704289313, 0.3333333333333333703, 0.3079598441704289313, 0.3333333333333333703, 0.3079598441704289313, 0.3333333333333333703, 0.3079598441704289313, 0.3333333333333333703, 0.3079598441704289313, 0.3333333333333333703, 0.3079598441704289313, 0.3333333333333333703, 0.3079598441704289313, 0.3333333333333333703, 0.3079598441704289313, 0.3333333333333333703),
 ( 1.000000000000000000, 0.9238795325112867385, 1.000000000000000000, 0.9238795325112867385, 1.000000000000000000, 0.9238795325112867385, 1.000000000000000000, 0.9238795325112867385, 1.000000000000000000, 0.9238795325112867385, 1.000000000000000000, 0.9238795325112867385, 1.000000000000000000, 0.9238795325112867385, 1.000000000000000000, 0.9238795325112867385, 1.000000000000000000, 0.9238795325112867385, 1.000000000000000000, 0.9238795325112867385, 1.000000000000000000, 0.9238795325112867385, 1.000000000000000000, 0.9238795325112867385, 1.000000000000000000, 0.9238795325112867385, 1.000000000000000000, 0.9238795325112867385, 1.000000000000000000, 0.9238795325112867385, 1.000000000000000000, 0.9238795325112867385, 1.000000000000000000, 0.9238795325112867385, 1.000000000000000000, 0.9238795325112867385, 1.000000000000000000, 0.9238795325112867385, 1.000000000000000000, 0.9238795325112867385, 1.000000000000000000, 0.9238795325112867385, 1.000000000000000000, 0.9238795325112867385, 1.000000000000000000, 0.9238795325112867385, 1.000000000000000000, 0.9238795325112867385, 1.000000000000000000, 0.9238795325112867385, 1.000000000000000000, 0.9238795325112867385, 1.000000000000000000, 0.9238795325112867385, 1.000000000000000000, 0.9238795325112867385, 1.000000000000000000, 0.9238795325112867385, 1.000000000000000000, 0.9238795325112867385, 1.000000000000000000, 0.9238795325112867385, 1.000000000000000000, 0.9238795325112867385, 1.000000000000000000, 0.9238795325112867385, 1.000000000000000000, 0.9238795325112867385, 1.000000000000000000, 0.9238795325112867385, 1.000000000000000000, 0.9238795325112867385, 1.000000000000000000, 0.9238795325112867385, 1.000000000000000000, 0.9238795325112867385, 1.000000000000000000, 0.9238795325112867385, 1.000000000000000000, 0.9238795325112867385, 1.000000000000000000, 0.9238795325112867385, 1.000000000000000000, 0.9238795325112867385, 1.000000000000000000, 0.9238795325112867385, 1.000000000000000000, 0.9238795325112867385, 1.000000000000000000, 0.9238795325112867385, 1.000000000000000000, 0.9238795325112867385, 1.000000000000000000, 0.9238795325112867385, 1.000000000000000000, 0.9238795325112867385, 1.000000000000000000, 0.9238795325112867385, 1.000000000000000000, 0.9238795325112867385, 1.000000000000000000, 0.9238795325112867385, 1.000000000000000000, 0.9238795325112867385, 1.000000000000000000, 0.9238795325112867385, 1.000000000000000000, 0.9238795325112867385, 1.000000000000000000, 0.9238795325112867385, 1.000000000000000000, 0.9238795325112867385, 1.000000000000000000, 0.9238795325112867385, 1.000000000000000000, 0.9238795325112867385, 1.000000000000000000, 0.9238795325112867385, 1.000000000000000000, 0.9238795325112867385, 1.000000000000000000, 0.9238795325112867385, 1.000000000000000000, 0.9238795325112867385, 1.000000000000000000, 0.9238795325112867385, 1.000000000000000000, 0.9238795325112867385, 1.000000000000000000, 0.9238795325112867385, 1.000000000000000000, 0.9238795325112867385, 1.000000000000000000, 0.9238795325112867385, 1.000000000000000000, 0.9238795325112867385, 1.000000000000000000, 0.9238795325112867385, 1.000000000000000000, 0.9238795325112867385, 1.000000000000000000, 0.9238795325112867385, 1.000000000000000000, 0.9238795325112867385, 1.000000000000000000, 0.9238795325112867385, 1.000000000000000000, 0.9238795325112867385, 1.000000000000000000, 0.9238795325112867385, 1.000000000000000000, 0.9238795325112867385, 1.000000000000000000, 0.9238795325112867385, 1.000000000000000000, 0.9238795325112867385, 1.000000000000000000, 0.9238795325112867385, 1.000000000000000000, 0.9238795325112867385, 1.000000000000000000),
 ( 0.3333333333333333703, 0.3079598441704289313, 0.3333333333333333703, 0.3079598441704289313, 0.3333333333333333703, 0.3079598441704289313, 0.3333333333333333703, 0.3079598441704289313, 0.3333333333333333703, 0.3079598441704289313, 0.3333333333333333703, 0.3079598441704289313, 0.3333333333333333703, 0.3079598441704289313, 0.3333333333333333703, 0.3079598441704289313, 0.3333333333333333703, 0.3079598441704289313, 0.3333333333333333703, 0.3079598441704289313, 0.3333333333333333703, 0.3079598441704289313, 0.3333333333333333703, 0.3079598441704289313, 0.3333333333333333703, 0.3079598441704289313, 0.3333333333333333703, 0.3079598441704289313, 0.3333333333333333703, 0.3079598441704289313, 0.3333333333333333703, 0.3079598441704289313, 0.3333333333333333703, 0.3079598441704289313, 0.3333333333333333703, 0.3079598441704289313, 0.3333333333333333703, 0.3079598441704289313, 0.3333333333333333703, 0.3079598441704289313, 0.3333333333333333703, 0.3079598441704289313, 0.3333333333333333703, 0.3079598441704289313, 0.3333333333333333703, 0.3079598441704289313, 0.3333333333333333703, 0.3079598441704289313, 0.3333333333333333703, 0.3079598441704289313, 0.3333333333333333703, 0.3079598441704289313, 0.3333333333333333703, 0.3079598441704289313, 0.3333333333333333703, 0.3079598441704289313, 0.3333333333333333703, 0.3079598441704289313, 0.3333333333333333703, 0.3079598441704289313, 0.3333333333333333703, 0.3079598441704289313, 0.3333333333333333703, 0.3079598441704289313, 0.3333333333333333703, 0.3079598441704289313, 0.3333333333333333703, 0.3079598441704289313, 0.3333333333333333703, 0.3079598441704289313, 0.3333333333333333703, 0.3079598441704289313, 0.3333333333333333703, 0.3079598441704289313, 0.3333333333333333703, 0.3079598441704289313, 0.3333333333333333703, 0.3079598441704289313, 0.3333333333333333703, 0.3079598441704289313, 0.3333333333333333703, 0.3079598441704289313, 0.3333333333333333703, 0.3079598441704289313, 0.3333333333333333703, 0.3079598441704289313, 0.3333333333333333703, 0.3079598441704289313, 0.3333333333333333703, 0.3079598441704289313, 0.3333333333333333703, 0.3079598441704289313, 0.3333333333333333703, 0.3079598441704289313, 0.3333333333333333703, 0.3079598441704289313, 0.3333333333333333703, 0.3079598441704289313, 0.3333333333333333703, 0.3079598441704289313, 0.3333333333333333703, 0.3079598441704289313, 0.3333333333333333703, 0.3079598441704289313, 0.3333333333333333703, 0.3079598441704289313, 0.3333333333333333703, 0.3079598441704289313, 0.3333333333333333703, 0.3079598441704289313, 0.3333333333333333703, 0.3079598441704289313, 0.3333333333333333703, 0.3079598441704289313, 0.3333333333333333703, 0.3079598441704289313, 0.3333333333333333703, 0.3079598441704289313, 0.3333333333333333703, 0.3079598441704289313, 0.3333333333333333703, 0.3079598441704289313, 0.3333333333333333703, 0.3079598441704289313, 0.3333333333333333703, 0.3079598441704289313, 0.3333333333333333703, 0.3079598441704289313, 0.3333333333333333703, 0.3079598441704289313, 0.3333333333333333703, 0.3079598441704289313, 0.3333333333333333703, 0.3079598441704289313, 0.3333333333333333703, 0.3079598441704289313, 0.3333333333333333703, 0.3079598441704289313, 0.3333333333333333703, 0.3079598441704289313, 0.3333333333333333703, 0.3079598441704289313, 0.3333333333333333703, 0.3079598441704289313, 0.3333333333333333703, 0.3079598441704289313, 0.3333333333333333703, 0.3079598441704289313, 0.3333333333333333703, 0.3079598441704289313, 0.3333333333333333703, 0.3079598441704289313, 0.3333333333333333703, 0.3079598441704289313, 0.3333333333333333703, 0.3079598441704289313, 0.3333333333333333703, 0.3079598441704289313, 0.3333333333333333703, 0.3079598441704289313, 0.3333333333333333703),
 ( 0.3333333333333333703, 0.3079598441704289313, 0.3333333333333333703, 0.3079598441704289313, 0.3333333333333333703, 0.3079598441704289313, 0.3333333333333333703, 0.3079598441704289313, 0.3333333333333333703, 0.3079598441704289313, 0.3333333333333333703, 0.3079598441704289313, 0.3333333333333333703, 0.3079598441704289313, 0.3333333333333333703, 0.3079598441704289313, 0.3333333333333333703, 0.3079598441704289313, 0.3333333333333333703, 0.3079598441704289313, 0.3333333333333333703, 0.3079598441704289313, 0.3333333333333333703, 0.3079598441704289313, 0.3333333333333333703, 0.3079598441704289313, 0.3333333333333333703, 0.3079598441704289313, 0.3333333333333333703, 0.3079598441704289313, 0.3333333333333333703, 0.3079598441704289313, 0.3333333333333333703, 0.3079598441704289313, 0.3333333333333333703, 0.3079598441704289313, 0.3333333333333333703, 0.3079598441704289313, 0.3333333333333333703, 0.3079598441704289313, 0.3333333333333333703, 0.3079598441704289313, 0.3333333333333333703, 0.3079598441704289313, 0.3333333333333333703, 0.3079598441704289313, 0.3333333333333333703, 0.3079598441704289313, 0.3333333333333333703, 0.3079598441704289313, 0.3333333333333333703, 0.3079598441704289313, 0.3333333333333333703, 0.3079598441704289313, 0.3333333333333333703, 0.3079598441704289313, 0.3333333333333333703, 0.3079598441704289313, 0.3333333333333333703, 0.3079598441704289313, 0.3333333333333333703, 0.3079598441704289313, 0.3333333333333333703, 0.3079598441704289313, 0.3333333333333333703, 0.3079598441704289313, 0.3333333333333333703, 0.3079598441704289313, 0.3333333333333333703, 0.3079598441704289313, 0.3333333333333333703, 0.3079598441704289313, 0.3333333333333333703, 0.3079598441704289313, 0.3333333333333333703, 0.3079598441704289313, 0.3333333333333333703, 0.3079598441704289313, 0.3333333333333333703, 0.3079598441704289313, 0.3333333333333333703, 0.3079598441704289313, 0.3333333333333333703, 0.3079598441704289313, 0.3333333333333333703, 0.3079598441704289313, 0.3333333333333333703, 0.3079598441704289313, 0.3333333333333333703, 0.3079598441704289313, 0.3333333333333333703, 0.3079598441704289313, 0.3333333333333333703, 0.3079598441704289313, 0.3333333333333333703, 0.3079598441704289313, 0.3333333333333333703, 0.3079598441704289313, 0.3333333333333333703, 0.3079598441704289313, 0.3333333333333333703, 0.3079598441704289313, 0.3333333333333333703, 0.3079598441704289313, 0.3333333333333333703, 0.3079598441704289313, 0.3333333333333333703, 0.3079598441704289313, 0.3333333333333333703, 0.3079598441704289313, 0.3333333333333333703, 0.3079598441704289313, 0.3333333333333333703, 0.3079598441704289313, 0.3333333333333333703, 0.3079598441704289313, 0.3333333333333333703, 0.3079598441704289313, 0.3333333333333333703, 0.3079598441704289313, 0.3333333333333333703, 0.3079598441704289313, 0.3333333333333333703, 0.3079598441704289313, 0.3333333333333333703, 0.3079598441704289313, 0.3333333333333333703, 0.3079598441704289313, 0.3333333333333333703, 0.3079598441704289313, 0.3333333333333333703, 0.3079598441704289313, 0.3333333333333333703, 0.3079598441704289313, 0.3333333333333333703, 0.3079598441704289313, 0.3333333333333333703, 0.3079598441704289313, 0.3333333333333333703, 0.3079598441704289313, 0.3333333333333333703, 0.3079598441704289313, 0.3333333333333333703, 0.3079598441704289313, 0.3333333333333333703, 0.3079598441704289313, 0.3333333333333333703, 0.3079598441704289313, 0.3333333333333333703, 0.3079598441704289313, 0.3333333333333333703, 0.3079598441704289313, 0.3333333333333333703, 0.3079598441704289313, 0.3333333333333333703, 0.3079598441704289313, 0.3333333333333333703, 0.3079598441704289313, 0.3333333333333333703, 0.3079598441704289313, 0.3333333333333333703),
 ( 1.000000000000000000, 0.9238795325112867385, 1.000000000000000000, 0.9238795325112867385, 1.000000000000000000, 0.9238795325112867385, 1.000000000000000000, 0.9238795325112867385, 1.000000000000000000, 0.9238795325112867385, 1.000000000000000000, 0.9238795325112867385, 1.000000000000000000, 0.9238795325112867385, 1.000000000000000000, 0.9238795325112867385, 1.000000000000000000, 0.9238795325112867385, 1.000000000000000000, 0.9238795325112867385, 1.000000000000000000, 0.9238795325112867385, 1.000000000000000000, 0.9238795325112867385, 1.000000000000000000, 0.9238795325112867385, 1.000000000000000000, 0.9238795325112867385, 1.000000000000000000, 0.9238795325112867385, 1.000000000000000000, 0.9238795325112867385, 1.000000000000000000, 0.9238795325112867385, 1.000000000000000000, 0.9238795325112867385, 1.000000000000000000, 0.9238795325112867385, 1.000000000000000000, 0.9238795325112867385, 1.000000000000000000, 0.9238795325112867385, 1.000000000000000000, 0.9238795325112867385, 1.000000000000000000, 0.9238795325112867385, 1.000000000000000000, 0.9238795325112867385, 1.000000000000000000, 0.9238795325112867385, 1.000000000000000000, 0.9238795325112867385, 1.000000000000000000, 0.9238795325112867385, 1.000000000000000000, 0.9238795325112867385, 1.000000000000000000, 0.9238795325112867385, 1.000000000000000000, 0.9238795325112867385, 1.000000000000000000, 0.9238795325112867385, 1.000000000000000000, 0.9238795325112867385, 1.000000000000000000, 0.9238795325112867385, 1.000000000000000000, 0.9238795325112867385, 1.000000000000000000, 0.9238795325112867385, 1.000000000000000000, 0.9238795325112867385, 1.000000000000000000, 0.9238795325112867385, 1.000000000000000000, 0.9238795325112867385, 1.000000000000000000, 0.9238795325112867385, 1.000000000000000000, 0.9238795325112867385, 1.000000000000000000, 0.9238795325112867385, 1.000000000000000000, 0.9238795325112867385, 1.000000000000000000, 0.9238795325112867385, 1.000000000000000000, 0.9238795325112867385, 1.000000000000000000, 0.9238795325112867385, 1.000000000000000000, 0.9238795325112867385, 1.000000000000000000, 0.9238795325112867385, 1.000000000000000000, 0.9238795325112867385, 1.000000000000000000, 0.9238795325112867385, 1.000000000000000000, 0.9238795325112867385, 1.000000000000000000, 0.9238795325112867385, 1.000000000000000000, 0.9238795325112867385, 1.000000000000000000, 0.9238795325112867385, 1.000000000000000000, 0.9238795325112867385, 1.000000000000000000, 0.9238795325112867385, 1.000000000000000000, 0.9238795325112867385, 1.000000000000000000, 0.9238795325112867385, 1.000000000000000000, 0.9238795325112867385, 1.000000000000000000, 0.9238795325112867385, 1.000000000000000000, 0.9238795325112867385, 1.000000000000000000, 0.9238795325112867385, 1.000000000000000000, 0.9238795325112867385, 1.000000000000000000, 0.9238795325112867385, 1.000000000000000000, 0.9238795325112867385, 1.000000000000000000, 0.9238795325112867385, 1.000000000000000000, 0.9238795325112867385, 1.000000000000000000, 0.9238795325112867385, 1.000000000000000000, 0.9238795325112867385, 1.000000000000000000, 0.9238795325112867385, 1.000000000000000000, 0.9238795325112867385, 1.000000000000000000, 0.9238795325112867385, 1.000000000000000000, 0.9238795325112867385, 1.000000000000000000, 0.9238795325112867385, 1.000000000000000000, 0.9238795325112867385, 1.000000000000000000, 0.9238795325112867385, 1.000000000000000000, 0.9238795325112867385, 1.000000000000000000, 0.9238795325112867385, 1.000000000000000000, 0.9238795325112867385, 1.000000000000000000, 0.9238795325112867385, 1.000000000000000000, 0.9238795325112867385, 1.000000000000000000) ) ) 
 REPRESENTATION_ITEM ( '' )  SURFACE ( )  );
#35743 = ORIENTED_EDGE ( 'NONE', *, *, #25275, .F. ) ;
#35744 = CARTESIAN_POINT ( 'NONE',  ( 11.60371710973756443, -11.94971097300157403, 32.03036669348361443 ) ) ;
#35745 = EDGE_LOOP ( 'NONE', ( #73886, #2949, #65144, #74066 ) ) ;
#35746 = CARTESIAN_POINT ( 'NONE',  ( 10.86533002476265963, -8.476813868363244353, 34.90874843262270133 ) ) ;
#35747 = CARTESIAN_POINT ( 'NONE',  ( 7.596153846153829825, -2.249999999999999112, 29.81609741502488120 ) ) ;
#35749 = CARTESIAN_POINT ( 'NONE',  ( -2.307692307692305711, -1.790695186598648903, 34.54067556320373455 ) ) ;
#35748 = AXIS2_PLACEMENT_3D ( 'NONE', #30109, #76079, #29240 ) ;
#35750 = CARTESIAN_POINT ( 'NONE',  ( 6.250054311638314708, -2.564540009722896752, 30.55348353981670684 ) ) ;
#35752 = EDGE_CURVE ( 'NONE', #15407, #2983, #18062, .T. ) ;
#35751 = CARTESIAN_POINT ( 'NONE',  ( 12.23805351781451201, -10.81261337010820256, 33.49550067578627477 ) ) ;
#35753 = CARTESIAN_POINT ( 'NONE',  ( 7.053868730901711182, -11.18335022499818621, 33.13157742990016885 ) ) ;
#35754 = CIRCLE ( 'NONE', #9876, 4.000000000000000000 ) ;
#35755 = CARTESIAN_POINT ( 'NONE',  ( -11.53846153846153655, -8.564572088678739092, 35.78748833219616898 ) ) ;
#35756 = DIRECTION ( 'NONE',  ( -0.000000000000000000, -0.1736481776669307198, -0.9848077530122080203 ) ) ;
#35757 = CARTESIAN_POINT ( 'NONE',  ( -2.084912638714241151, -3.020022701398814124, 32.48759521482552515 ) ) ;
#35758 = CIRCLE ( 'NONE', #21344, 0.2500000000000002220 ) ;
#35759 = CARTESIAN_POINT ( 'NONE',  ( 5.207448515156719360, -11.04252011169590020, 33.62494198852677130 ) ) ;
#35760 = B_SPLINE_CURVE_WITH_KNOTS ( 'NONE', 3,
 ( #18522, #23922, #18964, #58153, #53176, #45979, #73473, #3653, #10428, #11765 ),
 .UNSPECIFIED., .F., .F.,
 ( 4, 2, 2, 2, 4 ),
 ( 0.0007817359430256293554, 0.0009771253907249952391, 0.001172514838424361123, 0.001367904286123726790, 0.001563293733823092673 ),
 .UNSPECIFIED. ) ;
#35761 = CARTESIAN_POINT ( 'NONE',  ( -17.20748299053643748, -2.254533558242299396, 29.97296025877828640 ) ) ;
#35762 = ORIENTED_EDGE ( 'NONE', *, *, #50921, .F. ) ;
#35763 = VERTEX_POINT ( 'NONE', #30676 ) ;
#35764 = CARTESIAN_POINT ( 'NONE',  ( -14.98071491913091791, -8.303483539816728154, 34.68545999027711702 ) ) ;
#35765 = FILL_AREA_STYLE ('',( #70876 ) ) ;
#35766 = CARTESIAN_POINT ( 'NONE',  ( -3.100243529005668019, -2.882268652242222284, 31.66798894389554064 ) ) ;
#35767 = DIRECTION ( 'NONE',  ( 0.000000000000000000, 0.000000000000000000, 1.000000000000000000 ) ) ;
#35768 = ORIENTED_EDGE ( 'NONE', *, *, #4166, .F. ) ;
#35769 = EDGE_CURVE ( 'NONE', #36896, #13945, #44578, .T. ) ;
#35770 = EDGE_CURVE ( 'NONE', #38055, #7411, #46839, .T. ) ;
#35771 = CARTESIAN_POINT ( 'NONE',  ( -16.15384615384615330, -8.164416787775445883, 34.95778746994557906 ) ) ;
#35772 = FACE_OUTER_BOUND ( 'NONE', #40552, .T. ) ;
#35773 = CARTESIAN_POINT ( 'NONE',  ( 8.899756470994335089, -4.459921816937791661, 33.71989282347011851 ) ) ;
#35774 = EDGE_CURVE ( 'NONE', #45628, #23088, #31569, .T. ) ;
#35775 = ORIENTED_EDGE ( 'NONE', *, *, #25624, .T. ) ;
#35776 = CARTESIAN_POINT ( 'NONE',  ( 0.6843180028068694964, -5.913360116392399668, 34.49180327182771322 ) ) ;
#35777 = VERTEX_POINT ( 'NONE', #50497 ) ;
#35778 = TOROIDAL_SURFACE ( 'NONE', #32881, 3.250000000000001332, 2.000000000000000000 ) ;
#35779 = CARTESIAN_POINT ( 'NONE',  ( 25.00000000000000355, 9.999999999999971578, 13.00000000000000178 ) ) ;
#35780 = CARTESIAN_POINT ( 'NONE',  ( 18.00000000000000000, -3.322132147404559976, 32.92929555188717927 ) ) ;
#35781 = CARTESIAN_POINT ( 'NONE',  ( -6.065270445960774914, -2.625532179533445198, 30.86335684631481513 ) ) ;
#35782 = CARTESIAN_POINT ( 'NONE',  ( -9.692307692307814193, -6.835583212225970762, 34.95778746994575670 ) ) ;
#35783 = CARTESIAN_POINT ( 'NONE',  ( 18.13079044096695469, -8.191423895709842640, 34.95447573519442130 ) ) ;
#35784 = VERTEX_POINT ( 'NONE', #64447 ) ;
#35785 = B_SPLINE_CURVE_WITH_KNOTS ( 'NONE', 3,
 ( #29251, #78745, #8971, #44500, #36440, #63894, #29688, #60251, #40004, #3964 ),
 .UNSPECIFIED., .F., .F.,
 ( 4, 2, 2, 2, 4 ),
 ( 0.0007817246256747463051, 0.0009771112852218896347, 0.001172497944769033181, 0.001367884604316176728, 0.001563271263863320057 ),
 .UNSPECIFIED. ) ;
#35786 = ORIENTED_EDGE ( 'NONE', *, *, #69, .T. ) ;
#35787 = EDGE_CURVE ( 'NONE', #12459, #12780, #38206, .T. ) ;
#35788 = EDGE_LOOP ( 'NONE', ( #71125, #59406, #21708, #25187 ) ) ;
#35789 = EDGE_LOOP ( 'NONE', ( #44278, #78539, #52826, #32588 ) ) ;
#35790 = CARTESIAN_POINT ( 'NONE',  ( -17.20761454359064047, -10.54014554554151140, 33.71984207302941883 ) ) ;
#35791 = DIRECTION ( 'NONE',  ( -1.000000000000000000, -0.000000000000000000, -0.000000000000000000 ) ) ;
#35792 = CARTESIAN_POINT ( 'NONE',  ( -17.07692307692307665, -11.11383981884818262, 36.00935417666054406 ) ) ;
#35793 = LINE ( 'NONE', #15962, #83035 ) ;
#35794 = VECTOR ( 'NONE', #67190, 1000.000000000000000 ) ;
#35795 = CARTESIAN_POINT ( 'NONE',  ( -7.596099426240392027, -4.074993327901524687, 33.72946981652012255 ) ) ;
#35796 = CARTESIAN_POINT ( 'NONE',  ( 18.00000000000000000, -3.050289026998446396, 32.03036669348365706 ) ) ;
#35797 = ORIENTED_EDGE ( 'NONE', *, *, #74300, .F. ) ;
#35798 = ORIENTED_EDGE ( 'NONE', *, *, #54468, .T. ) ;
#35799 = VERTEX_POINT ( 'NONE', #65350 ) ;
#35800 = AXIS2_PLACEMENT_3D ( 'NONE', #25476, #54264, #13734 ) ;
#35802 = ORIENTED_EDGE ( 'NONE', *, *, #25797, .T. ) ;
#35801 = CARTESIAN_POINT ( 'NONE',  ( -3.007989689500820241, -10.81320215134717344, 33.49497208177562868 ) ) ;
#35804 = CARTESIAN_POINT ( 'NONE',  ( -5.076923076923075762, -12.62096338111211580, 30.90682066428153263 ) ) ;
#35803 = DIRECTION ( 'NONE',  ( -0.000000000000000000, 0.8660254037844399289, -0.4999999999999980016 ) ) ;
#35805 = CARTESIAN_POINT ( 'NONE',  ( -17.14300648787895298, -12.37446782046654192, 30.86335684631486487 ) ) ;
#35806 = VECTOR ( 'NONE', #45706, 1000.000000000000000 ) ;
#35807 = CARTESIAN_POINT ( 'NONE',  ( -3.750000000000007550, -5.946699141100917352, 26.42187500000000000 ) ) ;
#35808 = ORIENTED_EDGE ( 'NONE', *, *, #45508, .T. ) ;
#35809 = CIRCLE ( 'NONE', #70328, 4.000000000000000000 ) ;
#35810 = ORIENTED_EDGE ( 'NONE', *, *, #49892, .T. ) ;
#35811 = CARTESIAN_POINT ( 'NONE',  ( 3.903822929624696680, -4.175268141568689195, 33.81360843649122216 ) ) ;
#35812 = VERTEX_POINT ( 'NONE', #59034 ) ;
#35813 = FACE_BOUND ( 'NONE', #20747, .T. ) ;
#35814 = DIRECTION ( 'NONE',  ( -0.000000000000000000, 0.7660444431189791237, -0.6427876096865379196 ) ) ;
#35815 = CARTESIAN_POINT ( 'NONE',  ( -2.307692307692305711, -3.513871655860378418, 32.76840700105978499 ) ) ;
#35816 = ORIENTED_EDGE ( 'NONE', *, *, #4980, .T. ) ;
#35817 = CARTESIAN_POINT ( 'NONE',  ( -14.05774689831426372, -8.476813868363244353, 34.90874843262270133 ) ) ;
#35818 = LINE ( 'NONE', #50189, #47546 ) ;
#35819 = CARTESIAN_POINT ( 'NONE',  ( -13.38461538461538325, -5.415277668671390821, 36.20867863119892149 ) ) ;
#35820 = CARTESIAN_POINT ( 'NONE',  ( -15.29603967673000575, -6.879047030191174805, 34.71129190930000163 ) ) ;
#35821 = CARTESIAN_POINT ( 'NONE',  ( 18.00000000000000000, -10.89733346790207413, 36.13435417666054406 ) ) ;
#35822 = ORIENTED_EDGE ( 'NONE', *, *, #88877, .T. ) ;
#35823 = CARTESIAN_POINT ( 'NONE',  ( 11.76124107972994537, -3.236590943229499029, 32.36255958852954251 ) ) ;
#35824 = CARTESIAN_POINT ( 'NONE',  ( -9.692307692307691624, -2.900454961884010974, 35.62045528018868623 ) ) ;
#35825 = CARTESIAN_POINT ( 'NONE',  ( 16.40390046548447245, -9.148310452688871663, 34.47095581063188519 ) ) ;
#35826 = CARTESIAN_POINT ( 'NONE',  ( 15.23076923076923173, -11.33034616979429110, 35.88435417666054406 ) ) ;
#35827 = DIRECTION ( 'NONE',  ( -0.000000000000000000, -0.9396926207859093161, -0.3420201433256663259 ) ) ;
#35828 = CARTESIAN_POINT ( 'NONE',  ( 8.769230769230768274, -3.937682226553329556, 33.60647404775216529 ) ) ;
#35830 = CARTESIAN_POINT ( 'NONE',  ( 6.923076923076802558, -3.300289026999228881, 32.46337939537708905 ) ) ;
#35829 = DIRECTION ( 'NONE',  ( -0.000000000000000000, -0.3420201433256694901, -0.9396926207859082059 ) ) ;
#35831 = CARTESIAN_POINT ( 'NONE',  ( -14.37377468705243722, -3.322132147404559532, 32.92929555188719348 ) ) ;
#35833 = CARTESIAN_POINT ( 'NONE',  ( -18.06527000055631760, -3.083524468853727551, 32.58852847137143272 ) ) ;
#35832 = CARTESIAN_POINT ( 'NONE',  ( 5.076923076923075762, -13.37000171582298513, 34.34916445242398453 ) ) ;
#35834 = CARTESIAN_POINT ( 'NONE',  ( -10.83886953994894675, -6.716662450894489211, 34.94144148231605840 ) ) ;
#35835 = VECTOR ( 'NONE', #2772, 1000.000000000000227 ) ;
#35836 = CARTESIAN_POINT ( 'NONE',  ( -1.901340078031346525, -9.487747218494661183, 24.68563170625849068 ) ) ;
#35837 = ORIENTED_EDGE ( 'NONE', *, *, #7897, .T. ) ;
#35838 = CARTESIAN_POINT ( 'NONE',  ( -2.333004543783647744, -4.556662903998644154, 13.99999999999999289 ) ) ;
#35839 = ORIENTED_EDGE ( 'NONE', *, *, #75793, .F. ) ;
#35840 = DIRECTION ( 'NONE',  ( -0.000000000000000000, -0.000000000000000000, -1.000000000000000000 ) ) ;
#35841 = ORIENTED_EDGE ( 'NONE', *, *, #2376, .F. ) ;
#35842 = DIRECTION ( 'NONE',  ( -1.000000000000000000, -0.000000000000000000, -0.000000000000000000 ) ) ;
#35843 = CYLINDRICAL_SURFACE ( 'NONE', #38825, 0.2499999999999986955 ) ;
#35844 = VERTEX_POINT ( 'NONE', #3641 ) ;
#35845 = CARTESIAN_POINT ( 'NONE',  ( -18.22292621751613950, -12.39988816332205701, 30.74660775122750778 ) ) ;
#35846 = CARTESIAN_POINT ( 'NONE',  ( 1.200186371490561621, -10.22469193450123193, 23.20125670625849068 ) ) ;
#35847 = CARTESIAN_POINT ( 'NONE',  ( 1.384615384615386802, -1.117168528481311540, 33.14645433367849847 ) ) ;
#35848 = B_SPLINE_CURVE_WITH_KNOTS ( 'NONE', 3,
 ( #46061, #19038, #46506, #12278, #44711, #38420, #3290, #24005, #65442, #3734 ),
 .UNSPECIFIED., .F., .F.,
 ( 4, 2, 2, 2, 4 ),
 ( 0.000000000000000000, 0.0001954339881912775425, 0.0003908679763825550850, 0.0005863019645738326005, 0.0007817359527651101701 ),
 .UNSPECIFIED. ) ;
#35849 = CARTESIAN_POINT ( 'NONE',  ( 15.23076923076910916, -12.16647553114689728, 32.15551576947799362 ) ) ;
#35850 = DIRECTION ( 'NONE',  ( -1.000000000000000000, 0.000000000000000000, 0.000000000000000000 ) ) ;
#35851 = LINE ( 'NONE', #63310, #56162 ) ;
#35852 = CARTESIAN_POINT ( 'NONE',  ( 11.28848480751918615, -2.779195860258146578, 31.39871582349836032 ) ) ;
#35853 = DIRECTION ( 'NONE',  ( 1.000000000000000000, 0.000000000000000000, 0.000000000000000000 ) ) ;
#35854 = CARTESIAN_POINT ( 'NONE',  ( -3.749999999999988454, -9.053300858899127945, 17.51562500000000000 ) ) ;
#35855 = CARTESIAN_POINT ( 'NONE',  ( -18.06527000055631405, -11.67786785259541205, 32.92929555188721480 ) ) ;
#35856 = LINE ( 'NONE', #732, #80816 ) ;
#35857 = CARTESIAN_POINT ( 'NONE',  ( 1.653273178848927064E-15, -7.500000000000000000, 13.50000000000000178 ) ) ;
#35858 = CARTESIAN_POINT ( 'NONE',  ( 3.750000000000001776, -7.561099074964511502, 22.22061829374151287 ) ) ;
#35859 = EDGE_CURVE ( 'NONE', #74923, #1726, #26421, .T. ) ;
#35860 = VECTOR ( 'NONE', #1024, 1000.000000000000000 ) ;
#35861 = CARTESIAN_POINT ( 'NONE',  ( 17.07692307692295586, -2.379036618888197729, 30.90682066428292885 ) ) ;
#35862 = VECTOR ( 'NONE', #65994, 1000.000000000000000 ) ;
#35863 = ORIENTED_EDGE ( 'NONE', *, *, #45382, .T. ) ;
#35864 = CARTESIAN_POINT ( 'NONE',  ( 1.634669804528839698, -8.346898887586323923, 34.93166121998716278 ) ) ;
#35865 = CARTESIAN_POINT ( 'NONE',  ( -11.53846153846153655, -8.120952969808772792, 34.71129190930000163 ) ) ;
#35866 = LINE ( 'NONE', #36313, #88675 ) ;
#35867 = CARTESIAN_POINT ( 'NONE',  ( 8.769230769230768274, -5.471508081941601098, 34.59228464037088457 ) ) ;
#35868 = PRODUCT_DEFINITION ( 'UNKNOWN', '', #11625, #50941 ) ;
#35869 = DIRECTION ( 'NONE',  ( -1.000000000000000000, 0.000000000000000000, -0.000000000000000000 ) ) ;
#35870 = VECTOR ( 'NONE', #24024, 1000.000000000000227 ) ;
#35871 = CARTESIAN_POINT ( 'NONE',  ( 2.241608896736428491, -12.10708131394839349, 31.69288490824020244 ) ) ;
#35872 = VECTOR ( 'NONE', #2378, 1000.000000000000000 ) ;
#35873 = DIRECTION ( 'NONE',  ( -0.000000000000000000, 1.000000000000000000, -0.000000000000000000 ) ) ;
#35874 = EDGE_CURVE ( 'NONE', #80757, #69974, #53615, .T. ) ;
#35875 = ORIENTED_EDGE ( 'NONE', *, *, #44877, .T. ) ;
#35876 = ORIENTED_EDGE ( 'NONE', *, *, #57448, .T. ) ;
#35877 = EDGE_LOOP ( 'NONE', ( #41873, #81709 ) ) ;
#35878 = CYLINDRICAL_SURFACE ( 'NONE', #16992, 0.2499999999999979738 ) ;
#35879 = CARTESIAN_POINT ( 'NONE',  ( 11.53846153846153832, -13.49023893513002648, 31.06009739812518688 ) ) ;
#35880 = CARTESIAN_POINT ( 'NONE',  ( -8.769230769230892619, -2.379036618888197729, 30.90682066428292885 ) ) ;
#35881 = CARTESIAN_POINT ( 'NONE',  ( -13.31854703361294945, -12.10708131394839882, 31.69288490824020954 ) ) ;
#35882 = CARTESIAN_POINT ( 'NONE',  ( 13.16113046005105680, -8.539481045369596401, 34.89627647299170832 ) ) ;
#35883 = ORIENTED_EDGE ( 'NONE', *, *, #29945, .F. ) ;
#35884 = CARTESIAN_POINT ( 'NONE',  ( -11.53846153846153655, -1.242168528481310874, 33.36296068462461051 ) ) ;
#35885 = ORIENTED_EDGE ( 'NONE', *, *, #26395, .T. ) ;
#35886 = ADVANCED_FACE ( 'NONE', ( #46857 ), #80210, .F. ) ;
#35887 = VERTEX_POINT ( 'NONE', #38775 ) ;
#35888 = ORIENTED_EDGE ( 'NONE', *, *, #26025, .F. ) ;
#35890 = ORIENTED_EDGE ( 'NONE', *, *, #55480, .T. ) ;
#35889 = CARTESIAN_POINT ( 'NONE',  ( -12.46153846153846168, -2.900454961884010974, 35.62045528018868623 ) ) ;
#35891 = CARTESIAN_POINT ( 'NONE',  ( 8.769230769230647482, -2.892918686052165622, 31.69288490824153470 ) ) ;
#35892 = VECTOR ( 'NONE', #87133, 1000.000000000000114 ) ;
#35893 = EDGE_CURVE ( 'NONE', #61168, #71998, #60699, .T. ) ;
#35894 = CARTESIAN_POINT ( 'NONE',  ( -19.50000000000000000, -11.50000000000000000, 29.75000000000000355 ) ) ;
#35895 = B_SPLINE_CURVE_WITH_KNOTS ( 'NONE', 3,
 ( #62829, #49773, #69606, #70497, #36276, #1150, #7912, #9252, #84467, #78137 ),
 .UNSPECIFIED., .F., .F.,
 ( 4, 2, 2, 2, 4 ),
 ( 0.0007817359430256252354, 0.0009771253907249898181, 0.001172514838424354401, 0.001367904286123718983, 0.001563293733823083566 ),
 .UNSPECIFIED. ) ;
#35896 = ADVANCED_FACE ( 'NONE', ( #12194 ), #87882, .F. ) ;
#35897 = CARTESIAN_POINT ( 'NONE',  ( 2.084826885488670456, -2.501496062324912284, 29.88072118266895671 ) ) ;
#35898 = VERTEX_POINT ( 'NONE', #74339 ) ;
#35899 = EDGE_LOOP ( 'NONE', ( #61519, #47355, #21303, #54938 ) ) ;
#35900 = ORIENTED_EDGE ( 'NONE', *, *, #62653, .T. ) ;
#35901 = CARTESIAN_POINT ( 'NONE',  ( -14.24254652836034118, -7.750023238201979581, 34.74374492549440419 ) ) ;
#35903 = VERTEX_POINT ( 'NONE', #33354 ) ;
#35902 = LINE ( 'NONE', #2534, #22863 ) ;
#35904 = CARTESIAN_POINT ( 'NONE',  ( 11.53846153846141753, -6.879047030192662504, 34.71129190930017927 ) ) ;
#35905 = FACE_OUTER_BOUND ( 'NONE', #87150, .T. ) ;
#35906 = B_SPLINE_CURVE_WITH_KNOTS ( 'NONE', 3,
 ( #34065, #82264, #68738, #75940, #27311, #54774, #61973, #34511, #8375, #1165 ),
 .UNSPECIFIED., .F., .F.,
 ( 4, 2, 2, 2, 4 ),
 ( 0.000000000000000000, 0.0001954311564186865221, 0.0003908623128373730441, 0.0005862934692560595662, 0.0007817246256747460882 ),
 .UNSPECIFIED. ) ;
#35907 = B_SPLINE_CURVE_WITH_KNOTS ( 'NONE', 3,
 ( #205, #63222, #76751, #1537, #42967, #2839, #85283, #15053, #63669, #30332 ),
 .UNSPECIFIED., .F., .F.,
 ( 4, 2, 2, 2, 4 ),
 ( 0.0007817359430256216575, 0.0009771253907249856981, 0.001172514838424349847, 0.001367904286123713779, 0.001563293733823077928 ),
 .UNSPECIFIED. ) ;
#35908 = DIRECTION ( 'NONE',  ( -0.000000000000000000, -0.3420201433256694346, -0.9396926207859080948 ) ) ;
#35909 = VERTEX_POINT ( 'NONE', #12638 ) ;
#35910 = B_SPLINE_CURVE_WITH_KNOTS ( 'NONE', 3,
 ( #55358, #8514, #83738, #49046, #76074, #76971, #13932, #68873, #7628, #28330 ),
 .UNSPECIFIED., .F., .F.,
 ( 4, 2, 2, 2, 4 ),
 ( 0.0007817359430256216575, 0.0009771253907249856981, 0.001172514838424349630, 0.001367904286123713779, 0.001563293733823077711 ),
 .UNSPECIFIED. ) ;
#35911 = CARTESIAN_POINT ( 'NONE',  ( -11.53846153846165912, -5.219633306517616589, 34.19971097300220464 ) ) ;
#35912 = DIRECTION ( 'NONE',  ( -0.000000000000000000, -0.6427876096865404731, -0.7660444431189770143 ) ) ;
#35913 = ORIENTED_EDGE ( 'NONE', *, *, #19152, .T. ) ;
#35914 = FACE_BOUND ( 'NONE', #1040, .T. ) ;
#35915 = CARTESIAN_POINT ( 'NONE',  ( 11.31497659473759043, -5.113361153441934093, 34.14387501736622710 ) ) ;
#35916 = CARTESIAN_POINT ( 'NONE',  ( -18.00000000000012079, -12.51329471203414379, 31.30864560766407578 ) ) ;
#35917 = DIRECTION ( 'NONE',  ( -1.000000000000000000, 0.000000000000000000, 0.000000000000000000 ) ) ;
#35920 = DIRECTION ( 'NONE',  ( 1.000000000000000000, 0.000000000000000000, 0.000000000000000000 ) ) ;
#35919 = AXIS2_PLACEMENT_3D ( 'NONE', #72363, #57078, #50750 ) ;
#35918 = FACE_OUTER_BOUND ( 'NONE', #10538, .T. ) ;
#35921 = CARTESIAN_POINT ( 'NONE',  ( -5.076923076923075762, -10.51840700105979565, 33.73612834413961536 ) ) ;
#35922 = CARTESIAN_POINT ( 'NONE',  ( -16.08777780284371772, -8.973038597847269315, 34.52809138561122637 ) ) ;
#35923 = ORIENTED_EDGE ( 'NONE', *, *, #50180, .F. ) ;
#35924 = FACE_OUTER_BOUND ( 'NONE', #9456, .T. ) ;
#35925 = CARTESIAN_POINT ( 'NONE',  ( 5.010840697562940704, -3.937682226553329556, 33.60647404775217240 ) ) ;
#35926 = VECTOR ( 'NONE', #52986, 1000.000000000000000 ) ;
#35927 = ORIENTED_EDGE ( 'NONE', *, *, #64141, .T. ) ;
#35928 = CIRCLE ( 'NONE', #22920, 0.2500000000000002220 ) ;
#35929 = CARTESIAN_POINT ( 'NONE',  ( -16.21992853320628925, -12.62096338111211580, 30.90682066428152908 ) ) ;
#35930 = CARTESIAN_POINT ( 'NONE',  ( -14.08491263871423982, -9.418065098278013636, 34.63729479722530158 ) ) ;
#35931 = CARTESIAN_POINT ( 'NONE',  ( -16.08777780284372128, -10.51840700105979565, 33.73612834413962247 ) ) ;
#35932 = DIRECTION ( 'NONE',  ( -0.000000000000000000, 1.000000000000000000, 3.491481338843133355E-15 ) ) ;
#35933 = EDGE_CURVE ( 'NONE', #58351, #10580, #47785, .T. ) ;
#35934 = CARTESIAN_POINT ( 'NONE',  ( 15.23076923076923173, -2.292212530054420494, 30.41441678777542634 ) ) ;
#35935 = CARTESIAN_POINT ( 'NONE',  ( 18.00000000000000000, -5.180354513474913603, 36.12317359536750416 ) ) ;
#35936 = FACE_BOUND ( 'NONE', #64129, .T. ) ;
#35938 = CARTESIAN_POINT ( 'NONE',  ( 15.36156103859402045, -12.11778462344221019, 31.66786338562085135 ) ) ;
#35937 = CARTESIAN_POINT ( 'NONE',  ( -2.373775718648186928, -6.386643153685125363, 34.62446782046654903 ) ) ;
#35939 = CARTESIAN_POINT ( 'NONE',  ( -15.29603967673000575, -9.442884908240170461, 34.35708131394840592 ) ) ;
#35941 = DIRECTION ( 'NONE',  ( -0.000000000000000000, -0.6427876096865404731, -0.7660444431189770143 ) ) ;
#35940 = CYLINDRICAL_SURFACE ( 'NONE', #14191, 0.2500000000000008882 ) ;
#35942 = CARTESIAN_POINT ( 'NONE',  ( -7.846153846153967493, -3.643525952248795718, 33.31231777344771672 ) ) ;
#35943 = CARTESIAN_POINT ( 'NONE',  ( 1.492201783934554493, -3.724691934501233703, 18.98250670625849068 ) ) ;
#35944 = ORIENTED_EDGE ( 'NONE', *, *, #82182, .F. ) ;
#35945 = ORIENTED_EDGE ( 'NONE', *, *, #27883, .F. ) ;
#35946 = FACE_OUTER_BOUND ( 'NONE', #20510, .T. ) ;
#35947 = FACE_OUTER_BOUND ( 'NONE', #60936, .T. ) ;
#35948 = FACE_OUTER_BOUND ( 'NONE', #29482, .T. ) ;
#35949 = DIRECTION ( 'NONE',  ( -0.000000000000000000, 0.5000000000000011102, -0.8660254037844380415 ) ) ;
#35950 = LINE ( 'NONE', #62949, #73021 ) ;
#35951 = CARTESIAN_POINT ( 'NONE',  ( 1.614399933863660985, -11.22469193450123193, 23.20125670625849068 ) ) ;
#35952 = EDGE_CURVE ( 'NONE', #31103, #32628, #85431, .T. ) ;
#35953 = CARTESIAN_POINT ( 'NONE',  ( 4.284684571858915270, -7.277220443632450575, 34.74524770363009196 ) ) ;
#35955 = DIRECTION ( 'NONE',  ( -0.000000000000000000, -0.9396926207859092051, -0.3420201433256662704 ) ) ;
#35954 = B_SPLINE_CURVE_WITH_KNOTS ( 'NONE', 3,
 ( #12754, #61369, #75350, #88881, #42012, #40240, #82991, #69028, #55951, #74457 ),
 .UNSPECIFIED., .F., .F.,
 ( 4, 2, 2, 2, 4 ),
 ( 0.000000000000000000, 0.0001954311564186863865, 0.0003908623128373727731, 0.0005862934692560591325, 0.0007817246256747455461 ),
 .UNSPECIFIED. ) ;
#35956 = DIRECTION ( 'NONE',  ( 0.000000000000000000, 0.000000000000000000, 1.000000000000000000 ) ) ;
#35957 = LINE ( 'NONE', #23746, #22868 ) ;
#35958 = CARTESIAN_POINT ( 'NONE',  ( 2.437737363612081598, -2.254550872974306674, 29.97347326024527447 ) ) ;
#35959 = CARTESIAN_POINT ( 'NONE',  ( -4.826977667545033768, -6.653508905675592722, 34.93172785388651391 ) ) ;
#35960 = DIRECTION ( 'NONE',  ( -0.000000000000000000, -0.3420201433256694901, -0.9396926207859082059 ) ) ;
#35961 = CARTESIAN_POINT ( 'NONE',  ( -5.999999999999998224, -3.669653830205710676, 35.88435417666054406 ) ) ;
#35962 = EDGE_LOOP ( 'NONE', ( #22444, #20181, #5122, #3815 ) ) ;
#35963 = AXIS2_PLACEMENT_3D ( 'NONE', #40506, #88701, #27418 ) ;
#35964 = CARTESIAN_POINT ( 'NONE',  ( 2.307692307692309264, -3.322132147404559976, 32.92929555188717927 ) ) ;
#35965 = CARTESIAN_POINT ( 'NONE',  ( 10.74591005361826390, -5.915461855592780260, 34.75538340440931506 ) ) ;
#35966 = CARTESIAN_POINT ( 'NONE',  ( -1.987747218494638313, -9.401340078031370950, 21.43936829374151642 ) ) ;
#35967 = PRODUCT_DEFINITION ( 'UNKNOWN', '', #72043, #57280 ) ;
#35968 = EDGE_CURVE ( 'NONE', #76747, #67048, #74789, .T. ) ;
#35969 = CARTESIAN_POINT ( 'NONE',  ( 6.792386319966615460, -4.684245665217972032, 34.18127051446801090 ) ) ;
#35970 = DIRECTION ( 'NONE',  ( 1.000000000000000000, 0.000000000000000000, 0.000000000000000000 ) ) ;
#35971 = ORIENTED_EDGE ( 'NONE', *, *, #50109, .F. ) ;
#35972 = FACE_OUTER_BOUND ( 'NONE', #44383, .T. ) ;
#35974 = ORIENTED_EDGE ( 'NONE', *, *, #25983, .T. ) ;
#35973 = LINE ( 'NONE', #24210, #56938 ) ;
#35975 = CARTESIAN_POINT ( 'NONE',  ( -2.749999999999998224, -7.500000000000015987, 26.34375000000000000 ) ) ;
#35976 = CARTESIAN_POINT ( 'NONE',  ( -4.946397375159515164, -10.19071101563364756, 33.96452234770658407 ) ) ;
#35977 = EDGE_CURVE ( 'NONE', #10638, #78414, #54320, .T. ) ;
#35978 = EDGE_LOOP ( 'NONE', ( #75331, #85694 ) ) ;
#35979 = DIRECTION ( 'NONE',  ( -0.000000000000000000, -0.7660444431189791237, -0.6427876096865379196 ) ) ;
#35980 = CARTESIAN_POINT ( 'NONE',  ( 7.596153846153846700, -7.500000000000001776, 34.75000000000000000 ) ) ;
#35981 = ORIENTED_EDGE ( 'NONE', *, *, #77434, .F. ) ;
#35982 = DIRECTION ( 'NONE',  ( -0.000000000000000000, 0.6427876096865404731, -0.7660444431189770143 ) ) ;
#35983 = CARTESIAN_POINT ( 'NONE',  ( -15.93083480223330461, -3.105924265160262099, 32.13625925475356127 ) ) ;
#35985 = CARTESIAN_POINT ( 'NONE',  ( 18.00000000000000000, -8.564572088678739092, 35.78748833219616898 ) ) ;
#35984 = AXIS2_PLACEMENT_3D ( 'NONE', #58151, #72114, #59496 ) ;
#35986 = EDGE_CURVE ( 'NONE', #3292, #345, #11751, .T. ) ;
#35987 = ORIENTED_EDGE ( 'NONE', *, *, #88960, .F. ) ;
#35988 = EDGE_LOOP ( 'NONE', ( #10040, #58621, #18091, #35923 ) ) ;
#35989 = CARTESIAN_POINT ( 'NONE',  ( -6.792551484843277976, -8.630441415882550871, 34.87705825610312615 ) ) ;
#35990 = ORIENTED_EDGE ( 'NONE', *, *, #25569, .T. ) ;
#35991 = VECTOR ( 'NONE', #68399, 1000.000000000000000 ) ;
#35992 = ADVANCED_FACE ( 'NONE', ( #34229 ), #71003, .F. ) ;
#35993 = DIRECTION ( 'NONE',  ( -0.000000000000000000, 0.7660444431189791237, -0.6427876096865379196 ) ) ;
#35994 = CARTESIAN_POINT ( 'NONE',  ( 17.07692307692307665, -12.37446782046654192, 30.86335684631486131 ) ) ;
#35995 = B_SPLINE_CURVE_WITH_KNOTS ( 'NONE', 3,
 ( #82687, #75467, #76353, #20085, #258, #13764, #47098, #26402, #14661, #6129 ),
 .UNSPECIFIED., .F., .F.,
 ( 4, 2, 2, 2, 4 ),
 ( 0.0007817359430256318490, 0.0009771253907249984917, 0.001172514838424365026, 0.001367904286123731560, 0.001563293733823098311 ),
 .UNSPECIFIED. ) ;
#35996 = ADVANCED_FACE ( 'NONE', ( #16062 ), #75655, .T. ) ;
#35997 = DIRECTION ( 'NONE',  ( -0.000000000000000000, -0.000000000000000000, -1.000000000000000000 ) ) ;
#35998 = AXIS2_PLACEMENT_3D ( 'NONE', #88216, #58926, #3972 ) ;
#35999 = CARTESIAN_POINT ( 'NONE',  ( 3.164686851409094892, -9.905515769479276145, 34.41647553114623292 ) ) ;
#36000 = B_SPLINE_CURVE_WITH_KNOTS ( 'NONE', 3,
 ( #29429, #9577, #22653, #44679, #3260, #37041, #44229, #85251, #72163, #2808 ),
 .UNSPECIFIED., .F., .F.,
 ( 4, 2, 2, 2, 4 ),
 ( 0.0007817246256747507503, 0.0009771112852218959231, 0.001172497944769040987, 0.001367884604316186052, 0.001563271263863331116 ),
 .UNSPECIFIED. ) ;
#36001 = EDGE_CURVE ( 'NONE', #27696, #15288, #54950, .T. ) ;
#36002 = VERTEX_POINT ( 'NONE', #64227 ) ;
#36003 = ORIENTED_EDGE ( 'NONE', *, *, #79002, .F. ) ;
#36005 = ORIENTED_EDGE ( 'NONE', *, *, #21248, .F. ) ;
#36004 = CARTESIAN_POINT ( 'NONE',  ( -2.176853977205544854, -7.277220318596959281, 34.99547417642776992 ) ) ;
#36006 = CARTESIAN_POINT ( 'NONE',  ( 17.07692307692307665, -4.786620604624113540, 33.94971097300155094 ) ) ;
#36007 = ORIENTED_EDGE ( 'NONE', *, *, #47431, .F. ) ;
#36008 = EDGE_CURVE ( 'NONE', #74006, #23956, #16678, .T. ) ;
#36009 = ADVANCED_FACE ( 'NONE', ( #49837 ), #68458, .F. ) ;
#36010 = CARTESIAN_POINT ( 'NONE',  ( -3.230769230769229949, -12.78798330534102767, 29.49999999999997868 ) ) ;
#36011 = CARTESIAN_POINT ( 'NONE',  ( 6.000000000000001776, -2.499999999999998668, 29.75000000000001421 ) ) ;
#36012 = EDGE_LOOP ( 'NONE', ( #58611, #45101, #79731, #71872 ) ) ;
#36013 = CARTESIAN_POINT ( 'NONE',  ( 7.976679547917409963, -8.586989748646452369, 34.63063291749215011 ) ) ;
#36014 = VERTEX_POINT ( 'NONE', #27920 ) ;
#36016 = VERTEX_POINT ( 'NONE', #36769 ) ;
#36015 = DIRECTION ( 'NONE',  ( -0.000000000000000000, 0.5000000000000011102, -0.8660254037844381525 ) ) ;
#36017 = DIRECTION ( 'NONE',  ( 0.000000000000000000, 0.9396926207859126468, -0.3420201433256571111 ) ) ;
#36018 = CARTESIAN_POINT ( 'NONE',  ( -16.08859058257013075, -3.835265460703683349, 33.15142922261929925 ) ) ;
#36019 = ORIENTED_EDGE ( 'NONE', *, *, #66122, .T. ) ;
#36020 = CARTESIAN_POINT ( 'NONE',  ( 15.90386942290380290, -12.41269422305637171, 30.68257228309993323 ) ) ;
#36021 = AXIS2_PLACEMENT_3D ( 'NONE', #2927, #4273, #72282 ) ;
#36022 = CARTESIAN_POINT ( 'NONE',  ( 6.792386319966616348, -5.496505350115500121, 34.60290016733514307 ) ) ;
#36023 =( REPRESENTATION_RELATIONSHIP ('NONE','NONE', #51743, #60984 ) REPRESENTATION_RELATIONSHIP_WITH_TRANSFORMATION ( #18985 )SHAPE_REPRESENTATION_RELATIONSHIP( ) );
#36024 = FACE_BOUND ( 'NONE', #86966, .T. ) ;
#36025 = CARTESIAN_POINT ( 'NONE',  ( -1.634615384615383027, -2.249999999999998668, 29.75000000000000355 ) ) ;
#36026 = CYLINDRICAL_SURFACE ( 'NONE', #62941, 4.000000000000000000 ) ;
#36027 = CARTESIAN_POINT ( 'NONE',  ( 6.000000000000309086, -2.506253911140614576, 30.00000000000323297 ) ) ;
#36028 = CARTESIAN_POINT ( 'NONE',  ( 3.453782074862624896, -4.762714258010882773, 34.23016756924214832 ) ) ;
#36029 = DIRECTION ( 'NONE',  ( -0.000000000000000000, 1.000000000000000000, -0.000000000000000000 ) ) ;
#36030 = CARTESIAN_POINT ( 'NONE',  ( -16.21992853320628925, -2.486705287966280320, 31.30864560766543647 ) ) ;
#36031 = ORIENTED_EDGE ( 'NONE', *, *, #52518, .F. ) ;
#36032 = CARTESIAN_POINT ( 'NONE',  ( -6.130560591741918586, -2.504760397472873823, 29.97295953869789997 ) ) ;
#36033 = VERTEX_POINT ( 'NONE', #2975 ) ;
#36034 = ORIENTED_EDGE ( 'NONE', *, *, #40073, .F. ) ;
#36036 = CARTESIAN_POINT ( 'NONE',  ( 16.15384615384615330, -12.10708131394839349, 31.69288490824020244 ) ) ;
#36035 = CARTESIAN_POINT ( 'NONE',  ( -1.253824943648434553, -4.684288915650983043, 34.18129842949671371 ) ) ;
#36037 = CARTESIAN_POINT ( 'NONE',  ( 6.923076923076924238, -6.386643153685126251, 34.62446782046654192 ) ) ;
#36038 = DIRECTION ( 'NONE',  ( -0.000000000000000000, -0.000000000000000000, -1.000000000000000000 ) ) ;
#36039 = DIRECTION ( 'NONE',  ( 0.000000000000000000, 0.6427876096865373645, -0.7660444431189797898 ) ) ;
#36040 = CARTESIAN_POINT ( 'NONE',  ( 14.53047197667037516, -11.60474049983371003, 33.02348890104160262 ) ) ;
#36041 = ORIENTED_EDGE ( 'NONE', *, *, #78791, .T. ) ;
#36042 = EDGE_CURVE ( 'NONE', #34976, #46832, #23783, .T. ) ;
#36043 = CARTESIAN_POINT ( 'NONE',  ( -18.00000000000000000, -5.557115091759784242, 34.35708131394839171 ) ) ;
#36044 = CARTESIAN_POINT ( 'NONE',  ( 1.634560902963529072, -12.22109172314383052, 31.39792113162168263 ) ) ;
#36045 = CARTESIAN_POINT ( 'NONE',  ( -12.59222906464877134, -11.37499894934982692, 33.29245874905763003 ) ) ;
#36046 = CARTESIAN_POINT ( 'NONE',  ( 2.980745993476265010, -3.202444869320336451, 32.30641848906366675 ) ) ;
#36047 = CARTESIAN_POINT ( 'NONE',  ( 13.38461538461538680, -5.471508081941601098, 34.59228464037088457 ) ) ;
#36048 = EDGE_CURVE ( 'NONE', #79283, #15980, #13498, .T. ) ;
#36049 = EDGE_CURVE ( 'NONE', #23814, #12523, #9198, .T. ) ;
#36050 = B_SPLINE_CURVE_WITH_KNOTS ( 'NONE', 3,
 ( #1257, #69723, #76929, #15231, #48114, #42703, #50757, #22855, #10682, #16991 ),
 .UNSPECIFIED., .F., .F.,
 ( 4, 2, 2, 2, 4 ),
 ( 0.000000000000000000, 0.0001954311564186871184, 0.0003908623128373742367, 0.0005862934692560614093, 0.0007817246256747484735 ),
 .UNSPECIFIED. ) ;
#36051 = CARTESIAN_POINT ( 'NONE',  ( -1.553300858899125059, -3.750000000000009326, 16.57812500000000000 ) ) ;
#36052 = EDGE_LOOP ( 'NONE', ( #54882, #48042 ) ) ;
#36053 = AXIS2_PLACEMENT_3D ( 'NONE', #47575, #32732, #20113 ) ;
#36054 = VECTOR ( 'NONE', #13644, 1000.000000000000227 ) ;
#36056 = ADVANCED_FACE ( 'NONE', ( #63796 ), #8867, .F. ) ;
#36055 = EDGE_LOOP ( 'NONE', ( #35387, #3887, #7126, #47074 ) ) ;
#36057 = DIRECTION ( 'NONE',  ( 0.000000000000000000, 0.000000000000000000, -1.000000000000000000 ) ) ;
#36058 = ORIENTED_EDGE ( 'NONE', *, *, #26128, .T. ) ;
#36059 = DIRECTION ( 'NONE',  ( 0.000000000000000000, -6.938893903907222067E-15, 1.000000000000000000 ) ) ;
#36060 = CARTESIAN_POINT ( 'NONE',  ( -12.21159294319032185, -6.696923467548660192, 34.68552623307873972 ) ) ;
#36061 = CARTESIAN_POINT ( 'NONE',  ( -14.08491276642389423, -6.760870238392817200, 34.69528174975672385 ) ) ;
#36062 = DIRECTION ( 'NONE',  ( 0.000000000000000000, 0.000000000000000000, -1.000000000000000000 ) ) ;
#36063 = AXIS2_PLACEMENT_3D ( 'NONE', #44295, #3778, #10092 ) ;
#36064 = EDGE_CURVE ( 'NONE', #42886, #88546, #23251, .T. ) ;
#36065 = CARTESIAN_POINT ( 'NONE',  ( -8.769230769230768274, -8.564572088678739092, 35.78748833219616898 ) ) ;
#36066 = ORIENTED_EDGE ( 'NONE', *, *, #53227, .T. ) ;
#36067 = DIRECTION ( 'NONE',  ( 0.000000000000000000, 0.3420201433256641055, -0.9396926207859100932 ) ) ;
#36069 = EDGE_LOOP ( 'NONE', ( #37377, #77993, #70441, #27343 ) ) ;
#36068 = CARTESIAN_POINT ( 'NONE',  ( -16.15384615384627409, -11.94971097300221174, 32.03036669348237098 ) ) ;
#36070 = DIRECTION ( 'NONE',  ( 1.000000000000000000, 0.000000000000000000, 0.000000000000000000 ) ) ;
#36071 = CARTESIAN_POINT ( 'NONE',  ( 7.846153846153846700, -12.78798330534102945, 29.74999999999997868 ) ) ;
#36072 = CARTESIAN_POINT ( 'NONE',  ( 11.40777007179398339, -4.118384482072086072, 33.43331474514187107 ) ) ;
#36073 = DIRECTION ( 'NONE',  ( 0.000000000000000000, 0.000000000000000000, 1.000000000000000000 ) ) ;
#36074 = CYLINDRICAL_SURFACE ( 'NONE', #73818, 0.2499999999999997502 ) ;
#36075 = CARTESIAN_POINT ( 'NONE',  ( -2.608446859217920633, -4.805146000318815780, 14.25186829374151465 ) ) ;
#36076 = VERTEX_POINT ( 'NONE', #43967 ) ;
#36077 = CARTESIAN_POINT ( 'NONE',  ( -15.23076923076935252, -6.835583212225970762, 34.95778746994575670 ) ) ;
#36078 = CARTESIAN_POINT ( 'NONE',  ( -17.07692307692319744, -5.094484230521993062, 34.41647553114689373 ) ) ;
#36079 = CARTESIAN_POINT ( 'NONE',  ( 1.944543648262996083, -5.555456351736983045, 20.56250000000000000 ) ) ;
#36080 = DIRECTION ( 'NONE',  ( 1.000000000000000000, 0.000000000000000000, 0.000000000000000000 ) ) ;
#36081 = CARTESIAN_POINT ( 'NONE',  ( -3.099978789802280144, -10.70102852606553157, 33.91149625220312913 ) ) ;
#36082 = ORIENTED_EDGE ( 'NONE', *, *, #21722, .F. ) ;
#36083 = CARTESIAN_POINT ( 'NONE',  ( 0.4615384615384611200, -3.937682226553329556, 33.60647404775216529 ) ) ;
#36084 = CARTESIAN_POINT ( 'NONE',  ( -2.531177251416254936, -3.236172620538810385, 32.36188796281390267 ) ) ;
#36085 = EDGE_CURVE ( 'NONE', #7957, #9491, #71432, .T. ) ;
#36086 = ORIENTED_EDGE ( 'NONE', *, *, #61798, .T. ) ;
#36087 = CARTESIAN_POINT ( 'NONE',  ( -1.253823576790596750, -6.413143153341454017, 34.63066358083362672 ) ) ;
#36088 = EDGE_CURVE ( 'NONE', #52651, #87412, #42528, .T. ) ;
#36089 = CARTESIAN_POINT ( 'NONE',  ( 9.626984776815520561, -7.749976743299138882, 34.99404534957040624 ) ) ;
#36090 = ORIENTED_EDGE ( 'NONE', *, *, #41283, .T. ) ;
#36091 = B_SPLINE_CURVE_WITH_KNOTS ( 'NONE', 3,
 ( #17782, #4711, #65947, #47904, #28529, #7375, #61407, #68186, #21315, #40280 ),
 .UNSPECIFIED., .F., .F.,
 ( 4, 2, 2, 2, 4 ),
 ( 0.0007817359430256316322, 0.0009771253907249980580, 0.001172514838424364592, 0.001367904286123731127, 0.001563293733823097661 ),
 .UNSPECIFIED. ) ;
#36092 = CARTESIAN_POINT ( 'NONE',  ( 0.4615384615384611200, -8.564572088678739092, 35.78748833219616898 ) ) ;
#36093 = CARTESIAN_POINT ( 'NONE',  ( -5.749999999999995559, -2.499999999999999112, 29.81604066197450109 ) ) ;
#36094 = LINE ( 'NONE', #63545, #9531 ) ;
#36095 = CARTESIAN_POINT ( 'NONE',  ( -12.33074802057151409, -10.70102852606553157, 33.91149625220312913 ) ) ;
#36097 = EDGE_LOOP ( 'NONE', ( #28611, #15406, #57927, #5692, #81519, #73338 ) ) ;
#36096 = VECTOR ( 'NONE', #70080, 1000.000000000000000 ) ;
#36098 = LINE ( 'NONE', #8178, #75816 ) ;
#36099 = ORIENTED_EDGE ( 'NONE', *, *, #35787, .F. ) ;
#36100 = CARTESIAN_POINT ( 'NONE',  ( 12.33084785842815911, -11.93127051446799847, 32.56575433478202797 ) ) ;
#36101 = CARTESIAN_POINT ( 'NONE',  ( 5.934675987195693558, -7.749976730030849303, 34.74374725381503737 ) ) ;
#36102 = VERTEX_POINT ( 'NONE', #30052 ) ;
#36103 = DIRECTION ( 'NONE',  ( 1.000000000000000000, 0.000000000000000000, 0.000000000000000000 ) ) ;
#36104 = CARTESIAN_POINT ( 'NONE',  ( -14.53117723225664015, -2.353723527008296568, 30.78948104536958752 ) ) ;
#36105 = LINE ( 'NONE', #77964, #56671 ) ;
#36106 = CYLINDRICAL_SURFACE ( 'NONE', #76675, 0.2499999999999973355 ) ;
#36107 = LINE ( 'NONE', #28455, #16682 ) ;
#36108 = EDGE_CURVE ( 'NONE', #19870, #9301, #78228, .T. ) ;
#36110 = ORIENTED_EDGE ( 'NONE', *, *, #33799, .F. ) ;
#36109 = ADVANCED_FACE ( 'NONE', ( #36803 ), #9343, .F. ) ;
#36111 = ORIENTED_EDGE ( 'NONE', *, *, #51099, .T. ) ;
#36112 = FACE_BOUND ( 'NONE', #44591, .T. ) ;
#36113 = ORIENTED_EDGE ( 'NONE', *, *, #56562, .F. ) ;
#36114 = CARTESIAN_POINT ( 'NONE',  ( 15.45378058238208041, -2.554770724473668153, 30.48948780036025852 ) ) ;
#36115 = EDGE_CURVE ( 'NONE', #72492, #949, #33893, .T. ) ;
#36116 = CARTESIAN_POINT ( 'NONE',  ( -18.00000000000012079, -11.06231777344772027, 33.60647404775119895 ) ) ;
#36117 = EDGE_CURVE ( 'NONE', #70063, #33903, #79062, .T. ) ;
#36118 = CARTESIAN_POINT ( 'NONE',  ( 13.51514108637895184, -10.88167719472716399, 33.43325721877153711 ) ) ;
#36119 = FACE_OUTER_BOUND ( 'NONE', #61582, .T. ) ;
#36120 = AXIS2_PLACEMENT_3D ( 'NONE', #78238, #23730, #58855 ) ;
#36121 = ORIENTED_EDGE ( 'NONE', *, *, #16677, .F. ) ;
#36123 = EDGE_CURVE ( 'NONE', #72614, #70706, #29607, .T. ) ;
#36122 = EDGE_LOOP ( 'NONE', ( #84668, #42539, #65750, #14483 ) ) ;
#36124 = VERTEX_POINT ( 'NONE', #56194 ) ;
#36125 = FACE_OUTER_BOUND ( 'NONE', #2629, .T. ) ;
#36126 = B_SPLINE_CURVE_WITH_KNOTS ( 'NONE', 3,
 ( #22254, #84411, #71757, #37526, #2848, #84856, #37983, #56485, #30772, #36656 ),
 .UNSPECIFIED., .F., .F.,
 ( 4, 2, 2, 2, 4 ),
 ( 0.0007817246256747452209, 0.0009771112852218879000, 0.001172497944769030362, 0.001367884604316172825, 0.001563271263863315504 ),
 .UNSPECIFIED. ) ;
#36127 = EDGE_LOOP ( 'NONE', ( #8556, #76202 ) ) ;
#36128 = B_SPLINE_CURVE_WITH_KNOTS ( 'NONE', 3,
 ( #6779, #67161, #46438, #32476, #5014, #33380, #73482, #74362, #19411, #46878 ),
 .UNSPECIFIED., .F., .F.,
 ( 4, 2, 2, 2, 4 ),
 ( 0.000000000000000000, 0.0001954311564186861968, 0.0003908623128373723936, 0.0005862934692560585904, 0.0007817246256747447872 ),
 .UNSPECIFIED. ) ;
#36129 = CARTESIAN_POINT ( 'NONE',  ( 16.15384615384615330, -5.557115091759785130, 34.35708131394839171 ) ) ;
#36130 = EDGE_CURVE ( 'NONE', #77977, #25611, #22405, .T. ) ;
#36131 = CARTESIAN_POINT ( 'NONE',  ( 17.01084069756294781, -3.322132147404559976, 32.92929555188719348 ) ) ;
#36132 = CARTESIAN_POINT ( 'NONE',  ( -18.22348492456433178, -6.716662450894492764, 34.94144148231605840 ) ) ;
#36133 = ORIENTED_EDGE ( 'NONE', *, *, #55478, .T. ) ;
#36134 = CARTESIAN_POINT ( 'NONE',  ( -8.519285359852728945, -4.176053281294518804, 33.81426240980091791 ) ) ;
#36135 = DIRECTION ( 'NONE',  ( 0.000000000000000000, 0.000000000000000000, -1.000000000000000000 ) ) ;
#36136 = EDGE_CURVE ( 'NONE', #31320, #15649, #13768, .T. ) ;
#36137 = CARTESIAN_POINT ( 'NONE',  ( 4.153846153846030731, -2.657715359629662988, 31.77849191805970364 ) ) ;
#36138 = CARTESIAN_POINT ( 'NONE',  ( 11.78851585009985214, -8.303483539816731707, 34.68545999027711702 ) ) ;
#36139 = ORIENTED_EDGE ( 'NONE', *, *, #40617, .T. ) ;
#36140 = ORIENTED_EDGE ( 'NONE', *, *, #44557, .T. ) ;
#36141 = ORIENTED_EDGE ( 'NONE', *, *, #51398, .T. ) ;
#36142 = CARTESIAN_POINT ( 'NONE',  ( -3.931066612577744923, -10.11255958852956027, 34.01340905677048454 ) ) ;
#36144 = CARTESIAN_POINT ( 'NONE',  ( 10.61538461538461675, -2.292212530054420494, 30.41441678777542634 ) ) ;
#36143 = CARTESIAN_POINT ( 'NONE',  ( -5.076923076923075762, -2.708943851104267164, 35.45975837776705220 ) ) ;
#36145 = VECTOR ( 'NONE', #76080, 1000.000000000000114 ) ;
#36146 = LINE ( 'NONE', #75781, #84506 ) ;
#36147 = CARTESIAN_POINT ( 'NONE',  ( -12.46153846153858247, -6.879047030192662504, 34.71129190930017927 ) ) ;
#36148 = FACE_BOUND ( 'NONE', #22773, .T. ) ;
#36149 = CARTESIAN_POINT ( 'NONE',  ( 8.546303810323916395, -10.77366814457252175, 33.85459836347579454 ) ) ;
#36150 = ORIENTED_EDGE ( 'NONE', *, *, #81964, .T. ) ;
#36151 = EDGE_CURVE ( 'NONE', #34125, #14249, #45721, .T. ) ;
#36152 = CARTESIAN_POINT ( 'NONE',  ( -3.164700879766790820, -2.538708090699994813, 30.37095296980875503 ) ) ;
#36153 = CARTESIAN_POINT ( 'NONE',  ( 2.307692307692309264, -1.044019251281081972, 31.83374038241031911 ) ) ;
#36154 = LINE ( 'NONE', #42907, #50207 ) ;
#36155 = CARTESIAN_POINT ( 'NONE',  ( -11.53846153846165912, -3.835265460704628371, 33.15142922262033665 ) ) ;
#36156 = VECTOR ( 'NONE', #52228, 1000.000000000000000 ) ;
#36157 = ORIENTED_EDGE ( 'NONE', *, *, #6580, .F. ) ;
#36158 = CARTESIAN_POINT ( 'NONE',  ( -18.00000000000012079, -8.613356846316285953, 34.62446782046622218 ) ) ;
#36159 = EDGE_CURVE ( 'NONE', #16890, #43377, #69335, .T. ) ;
#36160 = ORIENTED_EDGE ( 'NONE', *, *, #1614, .T. ) ;
#36161 = FACE_BOUND ( 'NONE', #18565, .T. ) ;
#36162 = CARTESIAN_POINT ( 'NONE',  ( -16.94639737515951339, -4.459921816937789885, 33.71989282347011851 ) ) ;
#36163 = CYLINDRICAL_SURFACE ( 'NONE', #50646, 0.2500000000000008882 ) ;
#36164 = CARTESIAN_POINT ( 'NONE',  ( -6.673076923075486278, -7.500000000000155431, 34.75000000000007105 ) ) ;
#36165 = ORIENTED_EDGE ( 'NONE', *, *, #57238, .T. ) ;
#36166 = CARTESIAN_POINT ( 'NONE',  ( 0.4615384615384611200, -10.51840700105979565, 33.73612834413961536 ) ) ;
#36167 = CARTESIAN_POINT ( 'NONE',  ( 15.29683656411930848, -2.292212530054420494, 30.41441678777542990 ) ) ;
#36168 = CARTESIAN_POINT ( 'NONE',  ( -15.23076923076935252, -10.33852847137269571, 34.16647553114546554 ) ) ;
#36169 = DIRECTION ( 'NONE',  ( 0.000000000000000000, 0.7660444431189822323, -0.6427876096865344779 ) ) ;
#36170 = VERTEX_POINT ( 'NONE', #23284 ) ;
#36171 = EDGE_CURVE ( 'NONE', #74862, #60729, #568, .T. ) ;
#36172 = FACE_OUTER_BOUND ( 'NONE', #33073, .T. ) ;
#36173 = ORIENTED_EDGE ( 'NONE', *, *, #87151, .F. ) ;
#36175 = EDGE_LOOP ( 'NONE', ( #73124, #38148 ) ) ;
#36174 = CARTESIAN_POINT ( 'NONE',  ( 13.45068271796546178, -8.164416787775445883, 34.95778746994558617 ) ) ;
#36176 = CARTESIAN_POINT ( 'NONE',  ( -8.545803807369198424, -7.630147231320743018, 34.74852402298682819 ) ) ;
#36177 = CARTESIAN_POINT ( 'NONE',  ( -10.83886955910856464, -12.44517049084099725, 30.48991314939691932 ) ) ;
#36178 = CARTESIAN_POINT ( 'NONE',  ( 4.826946332874485712, -2.544273027872574922, 31.48422191005632342 ) ) ;
#36179 = B_SPLINE_CURVE_WITH_KNOTS ( 'NONE', 3,
 ( #28770, #78264, #36839, #70187, #63867, #84605, #56235, #2164, #83720, #49480 ),
 .UNSPECIFIED., .F., .F.,
 ( 4, 2, 2, 2, 4 ),
 ( 0.0007817246256747443535, 0.0009771112852218868158, 0.001172497944769029278, 0.001367884604316171523, 0.001563271263863313986 ),
 .UNSPECIFIED. ) ;
#36180 = CARTESIAN_POINT ( 'NONE',  ( -3.903900635498011251, -12.43552623307873972, 30.55307653245132826 ) ) ;
#36182 = CARTESIAN_POINT ( 'NONE',  ( 8.703148389870632329, -3.937682226553330445, 33.60647404775217240 ) ) ;
#36181 = DIRECTION ( 'NONE',  ( -1.000000000000000000, -0.000000000000000000, -0.000000000000000000 ) ) ;
#36183 = EDGE_CURVE ( 'NONE', #82502, #68350, #39927, .T. ) ;
#36184 = AXIS2_PLACEMENT_3D ( 'NONE', #58641, #9151, #37481 ) ;
#36185 = CARTESIAN_POINT ( 'NONE',  ( 12.21153846153846168, -7.566083408709835645, 34.74999999999999289 ) ) ;
#36186 = CARTESIAN_POINT ( 'NONE',  ( -1.944543648262992530, -9.444543648263016067, 24.93750000000000000 ) ) ;
#36187 = ORIENTED_EDGE ( 'NONE', *, *, #84194, .F. ) ;
#36188 = LINE ( 'NONE', #50117, #74989 ) ;
#36189 = CARTESIAN_POINT ( 'NONE',  ( -9.469528023329623068, -11.60474049983371003, 33.02348890104160262 ) ) ;
#36190 = ORIENTED_EDGE ( 'NONE', *, *, #48127, .T. ) ;
#36191 = AXIS2_PLACEMENT_3D ( 'NONE', #50834, #78321, #31019 ) ;
#36192 = ORIENTED_EDGE ( 'NONE', *, *, #81766, .F. ) ;
#36193 = ORIENTED_EDGE ( 'NONE', *, *, #46475, .F. ) ;
#36194 = CARTESIAN_POINT ( 'NONE',  ( 16.85343813319912698, -5.113361153441931428, 34.14387501736621999 ) ) ;
#36195 = ADVANCED_FACE ( 'NONE', ( #65593 ), #52969, .F. ) ;
#36196 = CARTESIAN_POINT ( 'NONE',  ( 3.007284287045282944, -10.11188796281391511, 34.01382737946119050 ) ) ;
#36197 = AXIS2_PLACEMENT_3D ( 'NONE', #80928, #52096, #32285 ) ;
#36198 = CARTESIAN_POINT ( 'NONE',  ( 0.6849648604532480034, -7.630147987733843173, 34.99859428049665411 ) ) ;
#36199 = CARTESIAN_POINT ( 'NONE',  ( 10.61538461538492406, -2.506253911140615021, 30.00000000000323297 ) ) ;
#36200 = CARTESIAN_POINT ( 'NONE',  ( -16.15384615384627409, -3.300289026999228437, 32.46337939537709616 ) ) ;
#36201 = EDGE_CURVE ( 'NONE', #69909, #58148, #73714, .T. ) ;
#36202 = FACE_OUTER_BOUND ( 'NONE', #82256, .T. ) ;
#36203 = CARTESIAN_POINT ( 'NONE',  ( 0.2115384615384438560, -2.249999999999999112, 29.81609741502488120 ) ) ;
#36204 = CARTESIAN_POINT ( 'NONE',  ( 2.980792499826877773, -6.567427716900047230, 34.66269422305636283 ) ) ;
#36205 = CARTESIAN_POINT ( 'NONE',  ( 11.53846153846153832, -10.51840700105979565, 33.73612834413961536 ) ) ;
#36206 = CARTESIAN_POINT ( 'NONE',  ( 2.307692307692309264, -3.513871655860378418, 32.76840700105978499 ) ) ;
#36207 = CARTESIAN_POINT ( 'NONE',  ( -17.07692307692319744, -11.67786785259630911, 32.92929555188603530 ) ) ;
#36208 = B_SPLINE_CURVE_WITH_KNOTS ( 'NONE', 3,
 ( #75996, #55720, #67919, #26935, #34574, #88657, #54392, #61592, #33248, #61145 ),
 .UNSPECIFIED., .F., .F.,
 ( 4, 2, 2, 2, 4 ),
 ( 0.000000000000000000, 0.0001954311564186863052, 0.0003908623128373726104, 0.0005862934692560589156, 0.0007817246256747452209 ),
 .UNSPECIFIED. ) ;
#36209 = ORIENTED_EDGE ( 'NONE', *, *, #81640, .T. ) ;
#36210 = CARTESIAN_POINT ( 'NONE',  ( 15.10007776410167324, -11.18331474514187995, 33.13161551792790505 ) ) ;
#36211 = CARTESIAN_POINT ( 'NONE',  ( 11.78851585009985570, -9.943054286541403997, 34.11300777759954883 ) ) ;
#36212 = CARTESIAN_POINT ( 'NONE',  ( -2.557692307692305267, -7.433931650972300353, 34.75000000000000711 ) ) ;
#36213 = ORIENTED_EDGE ( 'NONE', *, *, #83434, .F. ) ;
#36214 = LINE ( 'NONE', #56905, #50690 ) ;
#36215 = CARTESIAN_POINT ( 'NONE',  ( -10.74553258511630993, -12.70455904226513866, 30.44083106164009322 ) ) ;
#36216 = CARTESIAN_POINT ( 'NONE',  ( -3.164700879766793040, -12.10708131394839704, 31.69288490824020954 ) ) ;
#36217 = ORIENTED_EDGE ( 'NONE', *, *, #52722, .F. ) ;
#36218 = CARTESIAN_POINT ( 'NONE',  ( 18.22301284409340028, -3.395485233115139501, 33.02377354290276656 ) ) ;
#36219 = ORIENTED_EDGE ( 'NONE', *, *, #33414, .T. ) ;
#36220 = CARTESIAN_POINT ( 'NONE',  ( 9.915087233576100445, -11.89424750095246175, 32.13594075562310337 ) ) ;
#36221 = CARTESIAN_POINT ( 'NONE',  ( 7.146089767170321849, -2.889357225399416862, 32.26129605718031002 ) ) ;
#36222 = DIRECTION ( 'NONE',  ( -0.000000000000000000, -0.9396926207859092051, -0.3420201433256662704 ) ) ;
#36223 = EDGE_CURVE ( 'NONE', #87922, #52641, #85884, .T. ) ;
#36224 = CARTESIAN_POINT ( 'NONE',  ( -9.692307692307691624, -1.951392089020283160, 34.73218667398347748 ) ) ;
#36225 = CYLINDRICAL_SURFACE ( 'NONE', #27792, 0.2500000000000009437 ) ;
#36226 = ORIENTED_EDGE ( 'NONE', *, *, #45459, .F. ) ;
#36227 = ADVANCED_FACE ( 'NONE', ( #45327 ), #38135, .F. ) ;
#36228 = VERTEX_POINT ( 'NONE', #39487 ) ;
#36229 = EDGE_LOOP ( 'NONE', ( #75377, #73065, #75994, #70663 ) ) ;
#36230 = CARTESIAN_POINT ( 'NONE',  ( -3.361329144382594336, -2.254533558242299396, 29.97296025877828285 ) ) ;
#36231 = CARTESIAN_POINT ( 'NONE',  ( 13.45068373561782593, -9.780366693483667717, 34.19971097300155805 ) ) ;
#36232 = EDGE_CURVE ( 'NONE', #82664, #8847, #32788, .T. ) ;
#36233 = FACE_OUTER_BOUND ( 'NONE', #54835, .T. ) ;
#36234 = CARTESIAN_POINT ( 'NONE',  ( 0.3313904918067623884, -12.50552854090298993, 31.33409797877408920 ) ) ;
#36235 = AXIS2_PLACEMENT_3D ( 'NONE', #64544, #78964, #86185 ) ;
#36236 = CARTESIAN_POINT ( 'NONE',  ( 15.48076923076923173, -2.249999999999998668, 29.75000000000000355 ) ) ;
#36237 = CARTESIAN_POINT ( 'NONE',  ( -10.61538461538461320, -9.905515769479276145, 34.41647553114623292 ) ) ;
#36238 = VERTEX_POINT ( 'NONE', #31379 ) ;
#36239 = ORIENTED_EDGE ( 'NONE', *, *, #78957, .F. ) ;
#36240 = VERTEX_POINT ( 'NONE', #4805 ) ;
#36241 = EDGE_CURVE ( 'NONE', #70755, #59129, #46228, .T. ) ;
#36243 = VERTEX_POINT ( 'NONE', #60172 ) ;
#36242 = CARTESIAN_POINT ( 'NONE',  ( 12.59233026936324684, -8.147973898785416225, 34.70805048591653730 ) ) ;
#36245 = CARTESIAN_POINT ( 'NONE',  ( 13.45068271796546178, -3.937682226553329556, 33.60647404775216529 ) ) ;
#36244 = DIRECTION ( 'NONE',  ( -0.000000000000000000, 0.8660254037844397068, -0.4999999999999978906 ) ) ;
#36246 = B_SPLINE_CURVE_WITH_KNOTS ( 'NONE', 3,
 ( #69273, #27401, #68383, #1248, #48540, #21975, #54872, #76022, #14326, #42694 ),
 .UNSPECIFIED., .F., .F.,
 ( 4, 2, 2, 2, 4 ),
 ( 0.000000000000000000, 0.0001954311564186879586, 0.0003908623128373759172, 0.0005862934692560639030, 0.0007817246256747518345 ),
 .UNSPECIFIED. ) ;
#36247 = CARTESIAN_POINT ( 'NONE',  ( 2.320192649118979489E-14, -11.25000000000000000, 23.53125000000000000 ) ) ;
#36248 = ORIENTED_EDGE ( 'NONE', *, *, #37888, .F. ) ;
#36249 = B_SPLINE_CURVE_WITH_KNOTS ( 'NONE', 3,
 ( #68452, #40991, #13950, #75649, #60810, #81098, #53608, #60364, #27029, #20275 ),
 .UNSPECIFIED., .F., .F.,
 ( 4, 2, 2, 2, 4 ),
 ( 0.0007817246256747453293, 0.0009771112852218889842, 0.001172497944769032531, 0.001367884604316176294, 0.001563271263863319840 ),
 .UNSPECIFIED. ) ;
#36250 = EDGE_LOOP ( 'NONE', ( #67201, #73935, #64540, #39998 ) ) ;
#36251 = CARTESIAN_POINT ( 'NONE',  ( 4.826923076923077538, -7.566082377512563184, 35.00000000000000711 ) ) ;
#36252 = EDGE_CURVE ( 'NONE', #24676, #53273, #64995, .T. ) ;
#36253 = VERTEX_POINT ( 'NONE', #72358 ) ;
#36254 = FACE_BOUND ( 'NONE', #58215, .T. ) ;
#36255 = CARTESIAN_POINT ( 'NONE',  ( -5.776987155906601501, -2.889357225399416862, 32.26129605718031002 ) ) ;
#36256 = SHAPE_REPRESENTATION ( 'Ultra-Thin Hypoallergenic Micro-Foil Screen', ( #83448 ), #14453 ) ;
#36257 = LINE ( 'NONE', #22723, #6024 ) ;
#36258 = ORIENTED_EDGE ( 'NONE', *, *, #51487, .T. ) ;
#36259 = CARTESIAN_POINT ( 'NONE',  ( -4.219097144007394107, -2.506253911140460477, 30.00000000000013856 ) ) ;
#36260 = EDGE_CURVE ( 'NONE', #28816, #54248, #76829, .T. ) ;
#36261 = LINE ( 'NONE', #3344, #31759 ) ;
#36262 = CARTESIAN_POINT ( 'NONE',  ( 10.39245839786846837, -2.758268499246657068, 31.33685645148948140 ) ) ;
#36263 = CARTESIAN_POINT ( 'NONE',  ( -15.23076923076935074, -6.879047030192662504, 34.71129190930017927 ) ) ;
#36264 = CARTESIAN_POINT ( 'NONE',  ( -13.31935981333935892, -11.94971097300157403, 32.03036669348361443 ) ) ;
#36265 = VECTOR ( 'NONE', #57301, 1000.000000000000000 ) ;
#36266 = CARTESIAN_POINT ( 'NONE',  ( -6.923076923077044142, -11.48612834414049644, 32.76840700105863391 ) ) ;
#36267 = CARTESIAN_POINT ( 'NONE',  ( -8.069080805060693251, -11.98009711892699514, 32.48740034544076138 ) ) ;
#36268 = FACE_OUTER_BOUND ( 'NONE', #35450, .T. ) ;
#36269 = CARTESIAN_POINT ( 'NONE',  ( 13.63466980452883526, -2.318338780012835443, 30.59689888758630261 ) ) ;
#36270 = CARTESIAN_POINT ( 'NONE',  ( 9.692307692307570832, -12.51329471203414379, 31.30864560766407578 ) ) ;
#36271 = CARTESIAN_POINT ( 'NONE',  ( -13.16160254052199008, -12.38742843783360748, 31.66772728687926985 ) ) ;
#36273 = CARTESIAN_POINT ( 'NONE',  ( 3.230769230769231726, -11.35647404775217417, 33.31231777344666511 ) ) ;
#36272 = CARTESIAN_POINT ( 'NONE',  ( 4.946775867484857869, -11.47017969459903952, 32.78971311882034456 ) ) ;
#36274 = EDGE_CURVE ( 'NONE', #15372, #34740, #3748, .T. ) ;
#36275 = CARTESIAN_POINT ( 'NONE',  ( 8.638670177488846136, -2.504760397472875155, 29.97295953869789997 ) ) ;
#36277 = CARTESIAN_POINT ( 'NONE',  ( 2.373759641042384239, -6.343179335718452272, 34.87096338111212646 ) ) ;
#36276 = CARTESIAN_POINT ( 'NONE',  ( -11.28851602011339672, -11.37275283266504111, 32.91324779482534524 ) ) ;
#36278 = CIRCLE ( 'NONE', #70796, 0.4999999999999994449 ) ;
#36279 = CARTESIAN_POINT ( 'NONE',  ( 13.13461538461538680, -7.500000000000001776, 35.00000000000000000 ) ) ;
#36280 = CARTESIAN_POINT ( 'NONE',  ( -1.077988221561460236, -10.27530806549876452, 23.35750670625849423 ) ) ;
#36281 = ORIENTED_EDGE ( 'NONE', *, *, #73317, .T. ) ;
#36282 = CARTESIAN_POINT ( 'NONE',  ( 3.318022706343656925, -6.194818042847236583, 14.00000000000015099 ) ) ;
#36283 = ORIENTED_EDGE ( 'NONE', *, *, #49314, .T. ) ;
#36284 = CARTESIAN_POINT ( 'NONE',  ( 9.692307692307695177, -6.386643153685126251, 34.62446782046654192 ) ) ;
#36285 = EDGE_LOOP ( 'NONE', ( #29744, #36714, #48683, #26184 ) ) ;
#36286 = DIRECTION ( 'NONE',  ( -0.000000000000000000, -0.5000000000000009992, -0.8660254037844380415 ) ) ;
#36287 = CARTESIAN_POINT ( 'NONE',  ( 17.14217821643592288, -3.083524468853783951, 32.58852847137153930 ) ) ;
#36288 = VERTEX_POINT ( 'NONE', #34483 ) ;
#36289 = CARTESIAN_POINT ( 'NONE',  ( 5.934729999443681514, -11.06231777344662781, 33.60647404775220082 ) ) ;
#36290 = CARTESIAN_POINT ( 'NONE',  ( 2.750000000000001332, -7.438900925035452083, 22.96688170625849068 ) ) ;
#36291 = CARTESIAN_POINT ( 'NONE',  ( 7.846153846153846700, -8.164416787775445883, 34.95778746994557906 ) ) ;
#36292 = EDGE_CURVE ( 'NONE', #15704, #46513, #19869, .T. ) ;
#36293 = CARTESIAN_POINT ( 'NONE',  ( -5.934744428723972121, -9.442884908240271713, 34.35708131394835618 ) ) ;
#36294 = CARTESIAN_POINT ( 'NONE',  ( -5.207070286361298095, -5.195881422630167279, 34.18770438780618548 ) ) ;
#36295 = CARTESIAN_POINT ( 'NONE',  ( 14.98074600654777733, -8.475808217655753651, 34.90892951860618609 ) ) ;
#36296 = DIRECTION ( 'NONE',  ( 0.000000000000000000, -1.000000000000000000, -8.673617379884033500E-16 ) ) ;
#36297 = CARTESIAN_POINT ( 'NONE',  ( 0.4615384615384611200, -1.422936976036506707, 30.56769352161908415 ) ) ;
#36298 = CARTESIAN_POINT ( 'NONE',  ( -1.929879867024197893E-14, -3.750000000000000000, 14.15625000000000000 ) ) ;
#36299 = EDGE_CURVE ( 'NONE', #75150, #65922, #35995, .T. ) ;
#36300 = EDGE_CURVE ( 'NONE', #58446, #67262, #74590, .T. ) ;
#36301 = CARTESIAN_POINT ( 'NONE',  ( 11.31553457955468645, -5.582147617184174848, 34.63737895849758530 ) ) ;
#36302 = CARTESIAN_POINT ( 'NONE',  ( 14.55774661933062575, -10.66356715214248752, 33.62249196103329751 ) ) ;
#36303 = ADVANCED_FACE ( 'NONE', ( #81795 ), #47548, .F. ) ;
#36304 = CARTESIAN_POINT ( 'NONE',  ( 14.53047184896071542, -3.236590943229499029, 32.36255958852954251 ) ) ;
#36305 = CARTESIAN_POINT ( 'NONE',  ( 2.320192649118979489E-14, -11.25000000000000000, 16.03125000000000000 ) ) ;
#36306 = EDGE_CURVE ( 'NONE', #58277, #18801, #66051, .T. ) ;
#36307 = AXIS2_PLACEMENT_3D ( 'NONE', #5249, #67395, #32716 ) ;
#36308 = DIRECTION ( 'NONE',  ( -1.000000000000000000, 5.637851296924618008E-14, 0.000000000000000000 ) ) ;
#36309 = VECTOR ( 'NONE', #30552, 1000.000000000000000 ) ;
#36310 = EDGE_LOOP ( 'NONE', ( #56055, #55239, #63625, #15312, #49628 ) ) ;
#36311 = CARTESIAN_POINT ( 'NONE',  ( 14.53070365930516061, -2.554770724473668153, 30.48948780036025852 ) ) ;
#36312 = CARTESIAN_POINT ( 'NONE',  ( 11.78851585009985214, -5.728107161865378494, 34.42597550085002922 ) ) ;
#36313 = CARTESIAN_POINT ( 'NONE',  ( 17.07692307692307665, -13.49023893513002648, 31.06009739812518688 ) ) ;
#36314 = CARTESIAN_POINT ( 'NONE',  ( 18.13079180782478872, -10.54018710029568595, 33.71981072465678864 ) ) ;
#36315 = CARTESIAN_POINT ( 'NONE',  ( -16.28399336328437386, -10.88202310037936194, 33.43294751532457099 ) ) ;
#36316 = AXIS2_PLACEMENT_3D ( 'NONE', #75086, #75517, #13371 ) ;
#36317 = CARTESIAN_POINT ( 'NONE',  ( -14.05774689831426372, -4.176053281294518804, 33.81426240980091791 ) ) ;
#36318 = DIRECTION ( 'NONE',  ( -0.000000000000000000, 0.7660444431189791237, -0.6427876096865379196 ) ) ;
#36319 = ORIENTED_EDGE ( 'NONE', *, *, #58703, .T. ) ;
#36320 = EDGE_LOOP ( 'NONE', ( #24467, #22954, #37746, #66278 ) ) ;
#36321 = ORIENTED_EDGE ( 'NONE', *, *, #62117, .F. ) ;
#36322 = CARTESIAN_POINT ( 'NONE',  ( -1.384615384615383471, -1.117168528481311540, 33.14645433367849847 ) ) ;
#36323 = CARTESIAN_POINT ( 'NONE',  ( 6.416666666666664298, -11.00000000000000000, 29.75000000000000355 ) ) ;
#36324 = CARTESIAN_POINT ( 'NONE',  ( 4.153846153846030731, -2.657715359629662988, 31.77849191805970364 ) ) ;
#36325 = B_SPLINE_CURVE_WITH_KNOTS ( 'NONE', 3,
 ( #82854, #77410, #43183, #21131, #48602, #76078, #58449, #85944, #85499, #71528 ),
 .UNSPECIFIED., .F., .F.,
 ( 4, 2, 2, 2, 4 ),
 ( 0.000000000000000000, 0.0001954311564186868202, 0.0003908623128373736404, 0.0005862934692560604335, 0.0007817246256747472808 ),
 .UNSPECIFIED. ) ;
#36326 = CARTESIAN_POINT ( 'NONE',  ( 4.153846153846154188, -3.513871655860378418, 32.76840700105978499 ) ) ;
#36327 = CARTESIAN_POINT ( 'NONE',  ( 18.00000000000000000, -8.973038597847269315, 34.52809138561121927 ) ) ;
#36328 = VERTEX_POINT ( 'NONE', #41687 ) ;
#36329 = LINE ( 'NONE', #63785, #75140 ) ;
#36330 = EDGE_LOOP ( 'NONE', ( #32900, #17621, #23086, #2655 ) ) ;
#36331 = ORIENTED_EDGE ( 'NONE', *, *, #52559, .T. ) ;
#36333 = VERTEX_POINT ( 'NONE', #53867 ) ;
#36332 = CARTESIAN_POINT ( 'NONE',  ( 8.639082799499071541, -12.50552854090298638, 31.33409797877408920 ) ) ;
#36334 = LINE ( 'NONE', #70109, #47406 ) ;
#36335 = CARTESIAN_POINT ( 'NONE',  ( 1.384615384615265343, -10.21337939537710326, 33.94971097300076224 ) ) ;
#36336 = CARTESIAN_POINT ( 'NONE',  ( -18.00000000000000000, -10.51840700105979387, 33.73612834413961536 ) ) ;
#36337 = DIRECTION ( 'NONE',  ( -0.000000000000000000, -0.7660444431189791237, -0.6427876096865379196 ) ) ;
#36338 = EDGE_LOOP ( 'NONE', ( #9841, #57388 ) ) ;
#36339 = ORIENTED_EDGE ( 'NONE', *, *, #8932, .T. ) ;
#36340 = CARTESIAN_POINT ( 'NONE',  ( -2.651650429449565305, -4.848349570550461785, 22.75000000000000000 ) ) ;
#36341 = ORIENTED_EDGE ( 'NONE', *, *, #46319, .T. ) ;
#36342 = LINE ( 'NONE', #83204, #104 ) ;
#36344 = EDGE_LOOP ( 'NONE', ( #64786, #6082 ) ) ;
#36343 = CARTESIAN_POINT ( 'NONE',  ( 1.254468175177165357, -8.587444163452046197, 34.63053765926554206 ) ) ;
#36345 = CARTESIAN_POINT ( 'NONE',  ( -19.50000000000000000, -11.50000000000000000, 29.75000000000000355 ) ) ;
#36346 = CARTESIAN_POINT ( 'NONE',  ( 5.011652630962299959, -3.835265460703609186, 33.15142922261924241 ) ) ;
#36347 = LINE ( 'NONE', #64236, #76703 ) ;
#36348 = ORIENTED_EDGE ( 'NONE', *, *, #14299, .T. ) ;
#36349 = CYLINDRICAL_SURFACE ( 'NONE', #88279, 0.2499999999999997502 ) ;
#36350 = CARTESIAN_POINT ( 'NONE',  ( 4.826923076923055334, -2.249999999999999112, 29.81609741502488120 ) ) ;
#36351 = ORIENTED_EDGE ( 'NONE', *, *, #65458, .T. ) ;
#36352 = FACE_BOUND ( 'NONE', #72583, .T. ) ;
#36353 = B_SPLINE_CURVE_WITH_KNOTS ( 'NONE', 3,
 ( #51897, #79396, #86162, #87063, #17698, #66319, #11376, #32094, #10935, #12263 ),
 .UNSPECIFIED., .F., .F.,
 ( 4, 2, 2, 2, 4 ),
 ( 0.000000000000000000, 0.0001954339857564073388, 0.0003908679715128146777, 0.0005863019572692220165, 0.0007817359430256293554 ),
 .UNSPECIFIED. ) ;
#36354 = CARTESIAN_POINT ( 'NONE',  ( -11.66915214157184444, -11.37499894934982692, 33.29245874905763003 ) ) ;
#36355 = CARTESIAN_POINT ( 'NONE',  ( -6.988347369037698265, -2.892918686051582089, 31.69288490824015270 ) ) ;
#36356 = VECTOR ( 'NONE', #50657, 1000.000000000000000 ) ;
#36357 = EDGE_CURVE ( 'NONE', #84497, #17395, #27471, .T. ) ;
#36358 = DIRECTION ( 'NONE',  ( 1.000000000000000000, 0.000000000000000000, 0.000000000000000000 ) ) ;
#36360 = CARTESIAN_POINT ( 'NONE',  ( 15.23076923076954614, -2.255955759149395501, 30.00000000000324363 ) ) ;
#36359 = DIRECTION ( 'NONE',  ( -0.000000000000000000, 0.7660444431189791237, -0.6427876096865379196 ) ) ;
#36361 = CARTESIAN_POINT ( 'NONE',  ( 4.826946345980720032, -2.564618984488975961, 30.55390908950641915 ) ) ;
#36362 = CARTESIAN_POINT ( 'NONE',  ( 14.43848274865925774, -2.295524264805589354, 30.44142389570982488 ) ) ;
#36363 = ORIENTED_EDGE ( 'NONE', *, *, #13533, .F. ) ;
#36364 = DIRECTION ( 'NONE',  ( 0.000000000000000000, 0.3420201433256610524, 0.9396926207859113145 ) ) ;
#36365 = DIRECTION ( 'NONE',  ( -0.000000000000000000, -0.8660254037844399289, -0.4999999999999980016 ) ) ;
#36366 = ORIENTED_EDGE ( 'NONE', *, *, #210, .T. ) ;
#36367 = VECTOR ( 'NONE', #13165, 1000.000000000000114 ) ;
#36368 = CARTESIAN_POINT ( 'NONE',  ( 11.31497661389721010, -12.11044203135681840, 32.26167407432752299 ) ) ;
#36369 = CARTESIAN_POINT ( 'NONE',  ( -4.946397375159516052, -6.001044277235011215, 34.52024696741798948 ) ) ;
#36370 = CARTESIAN_POINT ( 'NONE',  ( -4.153846153846273204, -2.625532179533778709, 30.86335684631627174 ) ) ;
#36371 = CARTESIAN_POINT ( 'NONE',  ( 2.084765348785459604, -5.582147617184174848, 34.63737895849758530 ) ) ;
#36372 = CARTESIAN_POINT ( 'NONE',  ( 16.15384615384615330, -1.790695186598648903, 34.54067556320373455 ) ) ;
#36373 = CARTESIAN_POINT ( 'NONE',  ( 11.00641025641025550, -3.499999999999999556, 29.75000000000000355 ) ) ;
#36374 = FACE_BOUND ( 'NONE', #1468, .T. ) ;
#36376 = CARTESIAN_POINT ( 'NONE',  ( 13.38461538461538680, -2.708943851104267164, 35.45975837776705220 ) ) ;
#36375 = CARTESIAN_POINT ( 'NONE',  ( 6.673100179028332413, -4.075325502946086864, 33.72974371597207721 ) ) ;
#36377 = ADVANCED_FACE ( 'NONE', ( #83122 ), #21413, .T. ) ;
#36378 = CARTESIAN_POINT ( 'NONE',  ( 12.39626846098214408, -12.51329471203370325, 31.30864560766548976 ) ) ;
#36380 = CARTESIAN_POINT ( 'NONE',  ( 7.053868730901709405, -12.38066358083363738, 30.83685684665853444 ) ) ;
#36379 = CARTESIAN_POINT ( 'NONE',  ( -2.980714919130917462, -11.79725096376909654, 32.30694842903960762 ) ) ;
#36381 = FACE_OUTER_BOUND ( 'NONE', #24116, .T. ) ;
#36382 = CARTESIAN_POINT ( 'NONE',  ( 1.492201783934554493, -3.724691934501233703, 21.48250670625849068 ) ) ;
#36383 = ORIENTED_EDGE ( 'NONE', *, *, #83803, .F. ) ;
#36384 = ORIENTED_EDGE ( 'NONE', *, *, #87121, .T. ) ;
#36385 = LINE ( 'NONE', #69285, #85262 ) ;
#36386 = DIRECTION ( 'NONE',  ( -1.000000000000000000, -0.000000000000000000, -0.000000000000000000 ) ) ;
#36387 = CARTESIAN_POINT ( 'NONE',  ( -7.780086512803769949, -11.35647404775217595, 33.31231777344667222 ) ) ;
#36388 = CARTESIAN_POINT ( 'NONE',  ( -0.5276208408985973985, -2.833524468853757305, 32.15551576947924417 ) ) ;
#36389 = CARTESIAN_POINT ( 'NONE',  ( -7.846153846153967493, -12.70778746994576025, 30.41441678777401236 ) ) ;
#36390 = CARTESIAN_POINT ( 'NONE',  ( -1.614399933863656544, -3.775308065498769405, 22.57625670625848713 ) ) ;
#36391 = B_SPLINE_CURVE_WITH_KNOTS ( 'NONE', 3,
 ( #33699, #48084, #4903, #40902, #33259, #32367, #5340, #47201, #61155, #59831 ),
 .UNSPECIFIED., .F., .F.,
 ( 4, 2, 2, 2, 4 ),
 ( 0.000000000000000000, 0.0001954339857564080707, 0.0003908679715128161414, 0.0005863019572692241849, 0.0007817359430256322827 ),
 .UNSPECIFIED. ) ;
#36392 = FACE_OUTER_BOUND ( 'NONE', #43196, .T. ) ;
#36393 = LINE ( 'NONE', #43581, #46108 ) ;
#36394 = VECTOR ( 'NONE', #42956, 1000.000000000000227 ) ;
#36395 = CARTESIAN_POINT ( 'NONE',  ( -17.32694631421604115, -5.056417327199097755, 34.11270091957320716 ) ) ;
#36396 = FACE_OUTER_BOUND ( 'NONE', #29964, .T. ) ;
#36397 = CARTESIAN_POINT ( 'NONE',  ( 15.23076923076923173, -13.04860791097971706, 34.73218667398347037 ) ) ;
#36398 = FACE_OUTER_BOUND ( 'NONE', #41710, .T. ) ;
#36399 = VECTOR ( 'NONE', #32963, 1000.000000000000227 ) ;
#36400 = B_SPLINE_CURVE_WITH_KNOTS ( 'NONE', 3,
 ( #67874, #33647, #2944, #85380, #57895, #84944, #16915, #37627, #50239, #28666 ),
 .UNSPECIFIED., .F., .F.,
 ( 4, 2, 2, 2, 4 ),
 ( 0.000000000000000000, 0.0001954311564186866305, 0.0003908623128373732609, 0.0005862934692560598914, 0.0007817246256747465219 ),
 .UNSPECIFIED. ) ;
#36401 = EDGE_CURVE ( 'NONE', #5654, #76326, #5944, .T. ) ;
#36402 = EDGE_CURVE ( 'NONE', #2497, #82763, #29075, .T. ) ;
#36403 = LINE ( 'NONE', #35063, #63488 ) ;
#36404 = CARTESIAN_POINT ( 'NONE',  ( -2.307692307692427391, -8.613356846316285953, 34.62446782046622218 ) ) ;
#36405 = EDGE_LOOP ( 'NONE', ( #10681, #29235 ) ) ;
#36406 = CARTESIAN_POINT ( 'NONE',  ( 4.023698944407932743, -5.195881422630167279, 34.18770438780618548 ) ) ;
#36407 = CARTESIAN_POINT ( 'NONE',  ( -6.923076923076922462, -13.87047571288749737, 32.06866353760679544 ) ) ;
#36408 = CARTESIAN_POINT ( 'NONE',  ( 3.775308065498752086, -6.007798216065404873, 14.64249329374151110 ) ) ;
#36409 = EDGE_CURVE ( 'NONE', #28375, #67914, #7049, .T. ) ;
#36410 = CARTESIAN_POINT ( 'NONE',  ( 6.699591998512592461, -4.988325925672468131, 34.36044203135681130 ) ) ;
#36411 = DIRECTION ( 'NONE',  ( -0.000000000000000000, 0.8660254037844397068, -0.4999999999999978906 ) ) ;
#36412 = VERTEX_POINT ( 'NONE', #42579 ) ;
#36413 = CARTESIAN_POINT ( 'NONE',  ( -16.40384615384615330, -2.499999999999998668, 29.75000000000000355 ) ) ;
#36415 = ORIENTED_EDGE ( 'NONE', *, *, #54687, .T. ) ;
#36414 = CARTESIAN_POINT ( 'NONE',  ( 7.716006636715625255, -2.619462340734462380, 30.83744416345203021 ) ) ;
#36416 = LINE ( 'NONE', #16136, #19693 ) ;
#36417 = CARTESIAN_POINT ( 'NONE',  ( -13.25382357679059986, -9.804649428959608670, 34.18742332936588468 ) ) ;
#36418 = EDGE_CURVE ( 'NONE', #77986, #33107, #23149, .T. ) ;
#36419 = ORIENTED_EDGE ( 'NONE', *, *, #20299, .T. ) ;
#36420 = CARTESIAN_POINT ( 'NONE',  ( -5.076923076923075762, -12.10708131394839349, 31.69288490824020244 ) ) ;
#36421 = CARTESIAN_POINT ( 'NONE',  ( 8.834486340506792601, -5.219633306516380244, 34.19971097300157936 ) ) ;
#36422 = ORIENTED_EDGE ( 'NONE', *, *, #6543, .F. ) ;
#36423 = CARTESIAN_POINT ( 'NONE',  ( -12.68502338610279523, -2.353723527008296568, 30.78948104536958752 ) ) ;
#36424 = CARTESIAN_POINT ( 'NONE',  ( -16.15384615384615330, -3.050289026998446396, 32.03036669348365706 ) ) ;
#36425 = FACE_OUTER_BOUND ( 'NONE', #74205, .T. ) ;
#36426 = ORIENTED_EDGE ( 'NONE', *, *, #27219, .T. ) ;
#36427 = VERTEX_POINT ( 'NONE', #70039 ) ;
#36428 = VECTOR ( 'NONE', #33497, 1000.000000000000227 ) ;
#36429 = ORIENTED_EDGE ( 'NONE', *, *, #80149, .T. ) ;
#36430 = VECTOR ( 'NONE', #15180, 1000.000000000000227 ) ;
#36431 = CARTESIAN_POINT ( 'NONE',  ( 5.207448515156719360, -5.070358843744210198, 34.40418822224088302 ) ) ;
#36432 = CARTESIAN_POINT ( 'NONE',  ( 13.60762822870878530, -3.395485233115139057, 33.02377354290275946 ) ) ;
#36433 = DIRECTION ( 'NONE',  ( 1.000000000000000000, 0.000000000000000000, 0.000000000000000000 ) ) ;
#36434 = AXIS2_PLACEMENT_3D ( 'NONE', #46944, #66786, #5087 ) ;
#36435 = CARTESIAN_POINT ( 'NONE',  ( 19.00000000000000000, -16.99999999999999645, 22.25000000000000355 ) ) ;
#36436 = EDGE_LOOP ( 'NONE', ( #20588, #14486, #71830, #41819 ) ) ;
#36437 = ORIENTED_EDGE ( 'NONE', *, *, #32242, .F. ) ;
#36439 = VERTEX_POINT ( 'NONE', #2025 ) ;
#36438 = FACE_OUTER_BOUND ( 'NONE', #27410, .T. ) ;
#36440 = CARTESIAN_POINT ( 'NONE',  ( 12.71148387091650278, -11.56426240980093745, 33.07394671870546432 ) ) ;
#36441 = ORIENTED_EDGE ( 'NONE', *, *, #61024, .F. ) ;
#36442 = CARTESIAN_POINT ( 'NONE',  ( 15.48076923076923173, -2.249999999999998668, 29.75000000000000355 ) ) ;
#36443 = CARTESIAN_POINT ( 'NONE',  ( -24.99999999999999645, 20.00000000000000355, 3.000000000000000000 ) ) ;
#36444 = EDGE_LOOP ( 'NONE', ( #2473, #65289 ) ) ;
#36445 = EDGE_CURVE ( 'NONE', #35739, #69118, #77101, .T. ) ;
#36446 = B_SPLINE_CURVE_WITH_KNOTS ( 'NONE', 3,
 ( #18376, #73319, #85945, #44939, #24226, #72417, #11169, #71529, #3067, #45836 ),
 .UNSPECIFIED., .F., .F.,
 ( 4, 2, 2, 2, 4 ),
 ( 0.0007817246256747446788, 0.0009771112852218872494, 0.001172497944769029929, 0.001367884604316172391, 0.001563271263863315070 ),
 .UNSPECIFIED. ) ;
#36447 = CIRCLE ( 'NONE', #9142, 4.000000000000000000 ) ;
#36448 = ORIENTED_EDGE ( 'NONE', *, *, #59694, .F. ) ;
#36450 = VERTEX_POINT ( 'NONE', #1141 ) ;
#36449 = CARTESIAN_POINT ( 'NONE',  ( -12.23852710992561299, -4.887748414852792322, 34.01359900205216746 ) ) ;
#36451 = VECTOR ( 'NONE', #87532, 1000.000000000000114 ) ;
#36452 = CARTESIAN_POINT ( 'NONE',  ( 4.376625695114563008, -5.114059244376869984, 34.14424750095245287 ) ) ;
#36453 = CARTESIAN_POINT ( 'NONE',  ( -5.326899807865430603, -9.943427161483782584, 34.11278801902876978 ) ) ;
#36454 = ORIENTED_EDGE ( 'NONE', *, *, #57396, .T. ) ;
#36455 = CARTESIAN_POINT ( 'NONE',  ( -6.673131513698878692, -4.932303261841489039, 34.32971442181322885 ) ) ;
#36456 = DIRECTION ( 'NONE',  ( -1.000000000000000000, -0.000000000000000000, 0.000000000000000000 ) ) ;
#36457 = CARTESIAN_POINT ( 'NONE',  ( 16.15384615384603251, -12.27809138561165270, 31.22303859784587132 ) ) ;
#36458 = FACE_BOUND ( 'NONE', #46954, .T. ) ;
#36459 = CARTESIAN_POINT ( 'NONE',  ( 1.515407192440172413, -12.38066358083363738, 30.83685684665853444 ) ) ;
#36460 = CARTESIAN_POINT ( 'NONE',  ( -11.53846153846153655, -6.343179335718451384, 34.87096338111211935 ) ) ;
#36461 = EDGE_CURVE ( 'NONE', #3816, #41163, #43477, .T. ) ;
#36462 = DIRECTION ( 'NONE',  ( -0.000000000000000000, -0.000000000000000000, -1.000000000000000000 ) ) ;
#36464 = LINE ( 'NONE', #9429, #8733 ) ;
#36463 = FACE_OUTER_BOUND ( 'NONE', #22471, .T. ) ;
#36465 = CARTESIAN_POINT ( 'NONE',  ( 11.31497659473759043, -11.41268669641499756, 32.86336882939238535 ) ) ;
#36466 = CARTESIAN_POINT ( 'NONE',  ( 10.55011461482829560, -11.06231777344662781, 33.60647404775220082 ) ) ;
#36467 = ORIENTED_EDGE ( 'NONE', *, *, #85408, .F. ) ;
#36468 = CARTESIAN_POINT ( 'NONE',  ( 14.17708194806778010, -7.722926236386453702, 34.74524107206102030 ) ) ;
#36469 = ADVANCED_FACE ( 'NONE', ( #71361 ), #2896, .F. ) ;
#36470 = ORIENTED_EDGE ( 'NONE', *, *, #42893, .F. ) ;
#36471 = ORIENTED_EDGE ( 'NONE', *, *, #41224, .T. ) ;
#36473 = CARTESIAN_POINT ( 'NONE',  ( 16.28463796167094557, -12.11778462344220841, 31.66786338562085135 ) ) ;
#36472 = CARTESIAN_POINT ( 'NONE',  ( -1.318548051265308052, -4.661471528628508665, 34.16647553114624003 ) ) ;
#36474 = CARTESIAN_POINT ( 'NONE',  ( -6.000000000000119904, -6.879047030192662504, 34.71129190930017927 ) ) ;
#36475 = DIRECTION ( 'NONE',  ( 0.000000000000000000, 0.3420201433256610524, 0.9396926207859113145 ) ) ;
#36476 = CARTESIAN_POINT ( 'NONE',  ( 15.23076923076923173, -1.790695186598648903, 34.54067556320373455 ) ) ;
#36477 = CARTESIAN_POINT ( 'NONE',  ( -2.557715531913763662, -11.56360843649121861, 33.07473185843129926 ) ) ;
#36478 = EDGE_LOOP ( 'NONE', ( #27639, #24524 ) ) ;
#36479 = DIRECTION ( 'NONE',  ( -0.000000000000000000, 0.3420201433256694346, -0.9396926207859080948 ) ) ;
#36480 = VECTOR ( 'NONE', #76772, 1000.000000000000000 ) ;
#36481 = CARTESIAN_POINT ( 'NONE',  ( -15.09997742294444478, -9.804649428959608670, 34.18742332936588468 ) ) ;
#36482 = DIRECTION ( 'NONE',  ( 1.000000000000000000, 0.000000000000000000, 0.000000000000000000 ) ) ;
#36483 = EDGE_CURVE ( 'NONE', #57772, #55252, #7903, .T. ) ;
#36484 = CARTESIAN_POINT ( 'NONE',  ( 15.36155967173618286, -12.35292014791297710, 31.75344720912887198 ) ) ;
#36485 = DIRECTION ( 'NONE',  ( 0.000000000000000000, 0.3420201433256641055, -0.9396926207859100932 ) ) ;
#36486 = B_SPLINE_CURVE_WITH_KNOTS ( 'NONE', 3,
 ( #3437, #44407, #58825, #45309, #32260, #78658, #59722, #24151, #52511, #87217 ),
 .UNSPECIFIED., .F., .F.,
 ( 4, 2, 2, 2, 4 ),
 ( 0.000000000000000000, 0.0001954311564186882568, 0.0003908623128373765136, 0.0005862934692560647703, 0.0007817246256747530271 ),
 .UNSPECIFIED. ) ;
#36487 = CARTESIAN_POINT ( 'NONE',  ( -3.750000000000008438, -5.946699141100917352, 17.67187500000000355 ) ) ;
#36488 = ORIENTED_EDGE ( 'NONE', *, *, #41010, .F. ) ;
#36489 = AXIS2_PLACEMENT_3D ( 'NONE', #35755, #69968, #57338 ) ;
#36491 = EDGE_CURVE ( 'NONE', #79975, #55599, #49332, .T. ) ;
#36490 = ORIENTED_EDGE ( 'NONE', *, *, #59124, .F. ) ;
#36492 = B_SPLINE_CURVE_WITH_KNOTS ( 'NONE', 3,
 ( #79608, #64739, #3041, #9377, #36836, #84603, #31415, #58882, #58424, #57549 ),
 .UNSPECIFIED., .F., .F.,
 ( 4, 2, 2, 2, 4 ),
 ( 0.0007817359430256282712, 0.0009771253907249945886, 0.001172514838424360689, 0.001367904286123726790, 0.001563293733823093107 ),
 .UNSPECIFIED. ) ;
#36493 = CARTESIAN_POINT ( 'NONE',  ( -7.596208436775802930, -12.07971442181322352, 32.31769673815850297 ) ) ;
#36494 = ORIENTED_EDGE ( 'NONE', *, *, #30551, .F. ) ;
#36495 = LINE ( 'NONE', #43680, #965 ) ;
#36496 = CARTESIAN_POINT ( 'NONE',  ( -12.23852710992561299, -9.886259254753566594, 34.14407573483972413 ) ) ;
#36497 = CARTESIAN_POINT ( 'NONE',  ( -13.19230769230769162, -3.499999999999999556, 29.75000000000000355 ) ) ;
#36498 = CARTESIAN_POINT ( 'NONE',  ( -0.5922290646487684551, -11.93127051446800024, 32.56575433478200665 ) ) ;
#36499 = CARTESIAN_POINT ( 'NONE',  ( -1.929879867024197893E-14, -3.750000000000000000, 19.15625000000000000 ) ) ;
#36500 = CARTESIAN_POINT ( 'NONE',  ( 8.545745825506822158, -6.760086850603066466, 34.69517049084099369 ) ) ;
#36501 = VERTEX_POINT ( 'NONE', #72257 ) ;
#36502 = CARTESIAN_POINT ( 'NONE',  ( -12.59222992820602194, -10.54014554554150607, 33.71984207302941883 ) ) ;
#36504 = VERTEX_POINT ( 'NONE', #11456 ) ;
#36503 = CARTESIAN_POINT ( 'NONE',  ( -2.084680956079457470, -10.61302985866383963, 33.66295027996417843 ) ) ;
#36505 = CARTESIAN_POINT ( 'NONE',  ( -12.46153846153814726, -2.255955759149395501, 30.00000000000324363 ) ) ;
#36506 = CARTESIAN_POINT ( 'NONE',  ( -17.07692307692307665, -11.91647553114624181, 32.58852847137148245 ) ) ;
#36507 = CARTESIAN_POINT ( 'NONE',  ( -17.77698864838715309, -11.76359900205217635, 32.36225158514719169 ) ) ;
#36508 = DIRECTION ( 'NONE',  ( -0.000000000000000000, 1.000000000000000000, -0.000000000000000000 ) ) ;
#36509 = EDGE_CURVE ( 'NONE', #87198, #2477, #62858, .T. ) ;
#36510 = DIRECTION ( 'NONE',  ( -0.000000000000000000, 0.3420201433256694346, -0.9396926207859080948 ) ) ;
#36511 = CARTESIAN_POINT ( 'NONE',  ( -11.31544869436814338, -2.889357225399414197, 32.26129605718031002 ) ) ;
#36512 = EDGE_CURVE ( 'NONE', #40093, #26721, #67098, .T. ) ;
#36513 = CARTESIAN_POINT ( 'NONE',  ( 1.077988221561497539, -10.27530806549875386, 24.95499329374151287 ) ) ;
#36514 = ORIENTED_EDGE ( 'NONE', *, *, #52049, .F. ) ;
#36515 = CARTESIAN_POINT ( 'NONE',  ( 13.63461538461682210, -7.500000000000155431, 34.75000000000007105 ) ) ;
#36516 = B_SPLINE_CURVE_WITH_KNOTS ( 'NONE', 3,
 ( #22119, #69863, #21674, #71957, #82941, #21225, #69421, #48693, #49142, #49590 ),
 .UNSPECIFIED., .F., .F.,
 ( 4, 2, 2, 2, 4 ),
 ( 0.000000000000000000, 0.0001954311564186878502, 0.0003908623128373757004, 0.0005862934692560635777, 0.0007817246256747514008 ),
 .UNSPECIFIED. ) ;
#36517 = CARTESIAN_POINT ( 'NONE',  ( -1.450698795571264021, -12.10708131394839349, 31.69288490824020244 ) ) ;
#36518 = CARTESIAN_POINT ( 'NONE',  ( -2.750000000000007105, -6.360912703474006946, 18.92187500000000355 ) ) ;
#36519 = EDGE_CURVE ( 'NONE', #21173, #35421, #6955, .T. ) ;
#36520 = CARTESIAN_POINT ( 'NONE',  ( -13.38461538461550582, -12.46129190930018460, 30.37095296980731973 ) ) ;
#36521 = CARTESIAN_POINT ( 'NONE',  ( 9.442284468086239002, -6.652501968072648708, 34.93155406624980941 ) ) ;
#36522 = EDGE_CURVE ( 'NONE', #84175, #43394, #10137, .T. ) ;
#36523 = ORIENTED_EDGE ( 'NONE', *, *, #59287, .T. ) ;
#36524 = CARTESIAN_POINT ( 'NONE',  ( 1.944543648263018731, -9.444543648262994751, 14.62500000000000000 ) ) ;
#36525 = CARTESIAN_POINT ( 'NONE',  ( 11.40777093535123043, -3.957541250942358424, 33.62499894934981626 ) ) ;
#36526 = ORIENTED_EDGE ( 'NONE', *, *, #12586, .T. ) ;
#36527 = CARTESIAN_POINT ( 'NONE',  ( -17.07692307692307665, -8.564572088678739092, 35.78748833219616898 ) ) ;
#36528 = UNCERTAINTY_MEASURE_WITH_UNIT (LENGTH_MEASURE( 1.000000000000000082E-05 ), #4174, 'distance_accuracy_value', 'NONE');
#36529 = ORIENTED_EDGE ( 'NONE', *, *, #37861, .T. ) ;
#36530 = CARTESIAN_POINT ( 'NONE',  ( 6.923076923076800782, -4.320704448113951379, 33.92786785259630022 ) ) ;
#36531 = CARTESIAN_POINT ( 'NONE',  ( -17.32689982097166492, -2.318417181685854978, 30.59732222474233865 ) ) ;
#36532 = CARTESIAN_POINT ( 'NONE',  ( 8.069165197766697162, -5.667800583137507786, 34.40243808032445827 ) ) ;
#36533 = CARTESIAN_POINT ( 'NONE',  ( -12.21159305216042057, -10.92531984108285670, 33.72920026020278073 ) ) ;
#36534 = ORIENTED_EDGE ( 'NONE', *, *, #40988, .F. ) ;
#36535 = CARTESIAN_POINT ( 'NONE',  ( -17.76215049426127024, 12.75000000000001599, 32.75000000000000000 ) ) ;
#36536 = VERTEX_POINT ( 'NONE', #58747 ) ;
#36537 = CARTESIAN_POINT ( 'NONE',  ( 2.372886289475665489, -2.506253911140448043, 29.99999999999988631 ) ) ;
#36538 = CARTESIAN_POINT ( 'NONE',  ( 4.853996118016226546, -5.582147617184174848, 34.63737895849758530 ) ) ;
#36539 = EDGE_LOOP ( 'NONE', ( #88034, #69213, #41738, #73687 ) ) ;
#36540 = CARTESIAN_POINT ( 'NONE',  ( 11.78840694783958476, -12.68172785388650681, 30.59649109432439218 ) ) ;
#36541 = CARTESIAN_POINT ( 'NONE',  ( -14.30769230769242739, -10.90142922262034020, 33.41473453929536674 ) ) ;
#36542 = LINE ( 'NONE', #77520, #6341 ) ;
#36543 = CARTESIAN_POINT ( 'NONE',  ( 1.134638640566794976, -6.524016743844655686, 34.90889640711025521 ) ) ;
#36544 = CARTESIAN_POINT ( 'NONE',  ( -18.00000000000012079, -4.481592998941359873, 33.73612834414048933 ) ) ;
#36545 = ADVANCED_FACE ( 'NONE', ( #24961 ), #87583, .F. ) ;
#36546 = AXIS2_PLACEMENT_3D ( 'NONE', #17393, #11529, #86314 ) ;
#36547 = ORIENTED_EDGE ( 'NONE', *, *, #69144, .F. ) ;
#36548 = ORIENTED_EDGE ( 'NONE', *, *, #25178, .T. ) ;
#36549 = FACE_BOUND ( 'NONE', #79951, .T. ) ;
#36550 = VERTEX_POINT ( 'NONE', #58296 ) ;
#36551 = LINE ( 'NONE', #64001, #38684 ) ;
#36552 = FACE_OUTER_BOUND ( 'NONE', #11786, .T. ) ;
#36553 = CARTESIAN_POINT ( 'NONE',  ( 9.442330961365341224, -12.17611988154120972, 31.52148481390971213 ) ) ;
#36554 = CARTESIAN_POINT ( 'NONE',  ( 0.7115928814519131285, -12.65882529074907126, 30.72640787790839312 ) ) ;
#36555 = EDGE_CURVE ( 'NONE', #74216, #41990, #5144, .T. ) ;
#36556 = ORIENTED_EDGE ( 'NONE', *, *, #34268, .F. ) ;
#36557 = ADVANCED_FACE ( 'NONE', ( #73621 ), #86242, .F. ) ;
#36558 = VERTEX_POINT ( 'NONE', #60077 ) ;
#36559 = CARTESIAN_POINT ( 'NONE',  ( -14.30769230769230660, -3.669653830205710676, 35.88435417666054406 ) ) ;
#36560 = ORIENTED_EDGE ( 'NONE', *, *, #62043, .T. ) ;
#36561 = CARTESIAN_POINT ( 'NONE',  ( 16.15384615384615330, -9.780366693483667717, 34.19971097300155094 ) ) ;
#36562 = CARTESIAN_POINT ( 'NONE',  ( 13.16168916709924019, -2.758268499246657068, 31.33685645148948140 ) ) ;
#36563 = CARTESIAN_POINT ( 'NONE',  ( 16.85343815235874487, -3.562934362175799841, 33.22335522853832401 ) ) ;
#36564 = CARTESIAN_POINT ( 'NONE',  ( 13.63456079399342791, -11.56426240980093745, 33.07394671870546432 ) ) ;
#36565 = ORIENTED_EDGE ( 'NONE', *, *, #15907, .F. ) ;
#36566 = CARTESIAN_POINT ( 'NONE',  ( -5.142193522883852452, -10.90142922261923886, 33.41473453929638993 ) ) ;
#36567 = EDGE_CURVE ( 'NONE', #59816, #85420, #53319, .T. ) ;
#36568 = CYLINDRICAL_SURFACE ( 'NONE', #10054, 0.2500000000000004996 ) ;
#36569 = CARTESIAN_POINT ( 'NONE',  ( -18.06870381900347766, -7.749925094837281314, 34.99404781541490905 ) ) ;
#36570 = DIRECTION ( 'NONE',  ( -0.000000000000000000, -0.5000000000000009992, -0.8660254037844380415 ) ) ;
#36571 = ORIENTED_EDGE ( 'NONE', *, *, #49753, .F. ) ;
#36572 = UNCERTAINTY_MEASURE_WITH_UNIT (LENGTH_MEASURE( 1.000000000000000082E-05 ), #18432, 'distance_accuracy_value', 'NONE');
#36573 = ADVANCED_FACE ( 'NONE', ( #45679 ), #85787, .F. ) ;
#36574 = ORIENTED_EDGE ( 'NONE', *, *, #61964, .F. ) ;
#36575 = EDGE_LOOP ( 'NONE', ( #37441, #17211, #88433, #38053 ) ) ;
#36576 = VECTOR ( 'NONE', #69155, 1000.000000000000000 ) ;
#36578 = LINE ( 'NONE', #69914, #66429 ) ;
#36577 = CARTESIAN_POINT ( 'NONE',  ( 3.230769230769231726, -8.120952969808772792, 34.71129190930000163 ) ) ;
#36579 = CARTESIAN_POINT ( 'NONE',  ( -1.384615384615383471, -1.790695186598648903, 34.54067556320373455 ) ) ;
#36580 = CARTESIAN_POINT ( 'NONE',  ( -3.480792468062195333, -11.37209801155882971, 32.91403422569032955 ) ) ;
#36581 = FACE_BOUND ( 'NONE', #2710, .T. ) ;
#36582 = CARTESIAN_POINT ( 'NONE',  ( -2.307692307692427391, -10.21337939537710326, 33.94971097300076224 ) ) ;
#36583 = ORIENTED_EDGE ( 'NONE', *, *, #4798, .F. ) ;
#36584 = DIRECTION ( 'NONE',  ( -0.000000000000000000, 0.9396926207859092051, -0.3420201433256662704 ) ) ;
#36585 = CARTESIAN_POINT ( 'NONE',  ( -14.30769230769230660, -1.951392089020283160, 34.73218667398347748 ) ) ;
#36586 = DIRECTION ( 'NONE',  ( 0.000000000000000000, 0.9396926207859126468, 0.3420201433256571111 ) ) ;
#36587 = EDGE_CURVE ( 'NONE', #47272, #71093, #81256, .T. ) ;
#36588 = CARTESIAN_POINT ( 'NONE',  ( 7.145856592054988354, -9.418065098278011860, 34.63729479722530158 ) ) ;
#36589 = ORIENTED_EDGE ( 'NONE', *, *, #53568, .T. ) ;
#36590 = CARTESIAN_POINT ( 'NONE',  ( 2.438484115517095319, -11.71459661697925903, 32.44059661609676937 ) ) ;
#36591 = ORIENTED_EDGE ( 'NONE', *, *, #72421, .F. ) ;
#36592 = FACE_BOUND ( 'NONE', #76103, .T. ) ;
#36593 = CARTESIAN_POINT ( 'NONE',  ( -19.50000000000000000, -11.50000000000000000, 29.75000000000000355 ) ) ;
#36594 = CARTESIAN_POINT ( 'NONE',  ( -6.988346923633242724, -10.33852847137145048, 34.16647553114627556 ) ) ;
#36595 = CARTESIAN_POINT ( 'NONE',  ( 14.17754509825409137, -11.93770438780619259, 32.05411857736982029 ) ) ;
#36596 = EDGE_LOOP ( 'NONE', ( #10939, #35328 ) ) ;
#36597 = CARTESIAN_POINT ( 'NONE',  ( 5.142178648199100088, -3.300289026998475705, 32.46337939537591666 ) ) ;
#36598 = CARTESIAN_POINT ( 'NONE',  ( -17.93474486048716088, -4.320704448112861584, 33.92786785259548310 ) ) ;
#36599 = CARTESIAN_POINT ( 'NONE',  ( -9.692307692307812417, -3.300289026999228881, 32.46337939537708905 ) ) ;
#36600 = CARTESIAN_POINT ( 'NONE',  ( 4.403900573759605308, -6.523592122091591783, 34.90882529074906415 ) ) ;
#36601 = ORIENTED_EDGE ( 'NONE', *, *, #48347, .F. ) ;
#36602 = DIRECTION ( 'NONE',  ( 0.000000000000000000, -1.000000000000000000, -4.336808689942017736E-16 ) ) ;
#36603 = ORIENTED_EDGE ( 'NONE', *, *, #5308, .F. ) ;
#36605 = ORIENTED_EDGE ( 'NONE', *, *, #28027, .T. ) ;
#36604 = DIRECTION ( 'NONE',  ( 0.000000000000000000, 0.000000000000000000, -1.000000000000000000 ) ) ;
#36606 = CARTESIAN_POINT ( 'NONE',  ( 3.453780582382079967, -2.554770724473667709, 30.48948780036025852 ) ) ;
#36607 = CARTESIAN_POINT ( 'NONE',  ( -1.384615384615383471, -12.34228464037088635, 31.77849191805839268 ) ) ;
#36608 = CARTESIAN_POINT ( 'NONE',  ( -5.999999999999998224, -8.120952969808772792, 34.71129190930000163 ) ) ;
#36609 = CARTESIAN_POINT ( 'NONE',  ( -12.46153846153858247, -2.892918686052166066, 31.69288490824153470 ) ) ;
#36612 = DIRECTION ( 'NONE',  ( 0.000000000000000000, 0.000000000000000000, -1.000000000000000000 ) ) ;
#36611 = AXIS2_PLACEMENT_3D ( 'NONE', #67596, #5005, #19402 ) ;
#36610 = CARTESIAN_POINT ( 'NONE',  ( -7.912237257109724808, -8.973038597847271092, 34.52809138561120506 ) ) ;
#36613 = EDGE_CURVE ( 'NONE', #49704, #71861, #19542, .T. ) ;
#36614 = DIRECTION ( 'NONE',  ( -0.000000000000000000, -0.000000000000000000, -1.000000000000000000 ) ) ;
#36615 = CARTESIAN_POINT ( 'NONE',  ( -2.749999999999991562, -8.639087296526025028, 22.51562500000000000 ) ) ;
#36616 = ORIENTED_EDGE ( 'NONE', *, *, #7447, .T. ) ;
#36617 = VECTOR ( 'NONE', #80193, 1000.000000000000000 ) ;
#36618 = CARTESIAN_POINT ( 'NONE',  ( -16.15384615384615330, -3.886160181151819604, 36.00935417666054406 ) ) ;
#36619 = DIRECTION ( 'NONE',  ( -0.000000000000000000, 1.000000000000000000, -0.000000000000000000 ) ) ;
#36620 = ORIENTED_EDGE ( 'NONE', *, *, #55821, .F. ) ;
#36621 = EDGE_CURVE ( 'NONE', #14768, #60046, #26352, .T. ) ;
#36622 = ORIENTED_EDGE ( 'NONE', *, *, #40936, .F. ) ;
#36623 = ADVANCED_FACE ( 'NONE', ( #28075 ), #74055, .F. ) ;
#36624 = VERTEX_POINT ( 'NONE', #75378 ) ;
#36625 = CARTESIAN_POINT ( 'NONE',  ( -15.23076923076922995, -10.05456864172156806, 36.03766855953608683 ) ) ;
#36626 = B_SPLINE_CURVE_WITH_KNOTS ( 'NONE', 3,
 ( #62432, #7065, #749, #75519, #28214, #61554, #47604, #27338, #5733, #74644 ),
 .UNSPECIFIED., .F., .F.,
 ( 4, 2, 2, 2, 4 ),
 ( 0.000000000000000000, 0.0001954339857564075828, 0.0003908679715128151656, 0.0005863019572692227755, 0.0007817359430256303312 ),
 .UNSPECIFIED. ) ;
#36627 = CARTESIAN_POINT ( 'NONE',  ( -4.826868657009622865, -12.65882529074907126, 30.72640787790839312 ) ) ;
#36628 = CARTESIAN_POINT ( 'NONE',  ( 0.2386589448008749614, -7.630690623152302621, 34.99857592706774057 ) ) ;
#36629 = CARTESIAN_POINT ( 'NONE',  ( 1.384615384615386802, -1.422936976036506707, 30.56769352161908415 ) ) ;
#36630 = DIRECTION ( 'NONE',  ( -1.000000000000000000, 0.000000000000000000, -0.000000000000000000 ) ) ;
#36631 = FACE_OUTER_BOUND ( 'NONE', #87195, .T. ) ;
#36632 = CARTESIAN_POINT ( 'NONE',  ( -22.75000000000000000, -7.500000000000000000, 29.75000000000000355 ) ) ;
#36633 = ORIENTED_EDGE ( 'NONE', *, *, #75691, .F. ) ;
#36634 = LINE ( 'NONE', #43388, #33388 ) ;
#36635 = DIRECTION ( 'NONE',  ( 1.000000000000000000, 0.000000000000000000, 0.000000000000000000 ) ) ;
#36636 = EDGE_CURVE ( 'NONE', #86110, #53273, #19107, .T. ) ;
#36637 = FACE_OUTER_BOUND ( 'NONE', #16501, .T. ) ;
#36638 = CARTESIAN_POINT ( 'NONE',  ( 12.46153846153833911, -12.70778746994576025, 30.41441678777401236 ) ) ;
#36639 = ORIENTED_EDGE ( 'NONE', *, *, #45640, .T. ) ;
#36640 = DIRECTION ( 'NONE',  ( -0.000000000000000000, 0.8660254037844397068, -0.4999999999999978906 ) ) ;
#36641 = CARTESIAN_POINT ( 'NONE',  ( 11.76124107972994537, -10.11255958852956027, 34.01340905677048454 ) ) ;
#36642 = EDGE_CURVE ( 'NONE', #30027, #18184, #82593, .T. ) ;
#36643 = CARTESIAN_POINT ( 'NONE',  ( 6.222779668978067669, -12.69155399931963046, 30.53255429739158444 ) ) ;
#36644 = EDGE_LOOP ( 'NONE', ( #67864, #1302 ) ) ;
#36645 = CARTESIAN_POINT ( 'NONE',  ( 12.52679360105129902, -11.06231777344671130, 33.60647404775212976 ) ) ;
#36646 = CARTESIAN_POINT ( 'NONE',  ( -10.86536135943320502, -12.65889640711025521, 30.72598325615533454 ) ) ;
#36647 = VECTOR ( 'NONE', #5816, 1000.000000000000000 ) ;
#36648 = FACE_OUTER_BOUND ( 'NONE', #35178, .T. ) ;
#36649 = EDGE_CURVE ( 'NONE', #14249, #34125, #2722, .T. ) ;
#36650 = EDGE_LOOP ( 'NONE', ( #34110, #53023, #53154, #12360 ) ) ;
#36651 = DIRECTION ( 'NONE',  ( -0.000000000000000000, 0.3420201433256694901, -0.9396926207859082059 ) ) ;
#36652 = ORIENTED_EDGE ( 'NONE', *, *, #16201, .F. ) ;
#36653 = EDGE_CURVE ( 'NONE', #84875, #83291, #67294, .T. ) ;
#36654 = CARTESIAN_POINT ( 'NONE',  ( 10.68064018666064108, -8.613356846314928816, 34.62446782046653482 ) ) ;
#36655 = EDGE_CURVE ( 'NONE', #71705, #67458, #27629, .T. ) ;
#36656 = CARTESIAN_POINT ( 'NONE',  ( -17.07692307692307665, -3.322132147404559976, 32.92929555188717927 ) ) ;
#36657 = B_SPLINE_CURVE_WITH_KNOTS ( 'NONE', 3,
 ( #56212, #47681, #49010, #75167, #68394, #40931, #7588, #29200, #82811, #27853 ),
 .UNSPECIFIED., .F., .F.,
 ( 4, 2, 2, 2, 4 ),
 ( 0.0007817246336856291692, 0.0009771112958940103739, 0.001172497958102391470, 0.001367884620310772566, 0.001563271282519153879 ),
 .UNSPECIFIED. ) ;
#36658 = DIRECTION ( 'NONE',  ( 0.000000000000000000, 1.000000000000000000, 0.000000000000000000 ) ) ;
#36659 = CARTESIAN_POINT ( 'NONE',  ( -9.469528023329623068, -6.717445702608402236, 34.94155399931962336 ) ) ;
#36660 = CARTESIAN_POINT ( 'NONE',  ( -3.165624450049597360, -7.750023224968865421, 34.99404313364389907 ) ) ;
#36661 = B_SPLINE_CURVE_WITH_KNOTS ( 'NONE', 3,
 ( #38484, #44774, #45675, #71807, #32172, #11011, #87579, #86691, #11453, #38035 ),
 .UNSPECIFIED., .F., .F.,
 ( 4, 2, 2, 2, 4 ),
 ( 0.0007817359430256215491, 0.0009771253907249856981, 0.001172514838424349847, 0.001367904286123713779, 0.001563293733823077928 ),
 .UNSPECIFIED. ) ;
#36662 = ORIENTED_EDGE ( 'NONE', *, *, #30260, .T. ) ;
#36663 = EDGE_CURVE ( 'NONE', #4672, #17811, #48337, .T. ) ;
#36664 = EDGE_LOOP ( 'NONE', ( #66201, #81711 ) ) ;
#36665 = ORIENTED_EDGE ( 'NONE', *, *, #54042, .F. ) ;
#36666 = CIRCLE ( 'NONE', #72659, 4.000000000000000000 ) ;
#36667 = EDGE_CURVE ( 'NONE', #49416, #38795, #55378, .T. ) ;
#36668 = CARTESIAN_POINT ( 'NONE',  ( -1.134669866267241201, -3.202959910592336534, 32.30730279482227019 ) ) ;
#36669 = CARTESIAN_POINT ( 'NONE',  ( -16.94613126909828793, -3.530189275343204702, 32.79018710029569661 ) ) ;
#36670 = CARTESIAN_POINT ( 'NONE',  ( 0.5923289025054111478, -6.369690395747424461, 34.87708834333098196 ) ) ;
#36671 = VECTOR ( 'NONE', #88937, 1000.000000000000114 ) ;
#36672 = CARTESIAN_POINT ( 'NONE',  ( 0.4615384615383382183, -12.51329471203414379, 31.30864560766407578 ) ) ;
#36673 = DIRECTION ( 'NONE',  ( 0.000000000000000000, -6.938893903907222067E-15, 1.000000000000000000 ) ) ;
#36674 = CARTESIAN_POINT ( 'NONE',  ( 5.299702618191482806, -10.11255958852956027, 34.01340905677048454 ) ) ;
#36675 = EDGE_LOOP ( 'NONE', ( #56165, #29047 ) ) ;
#36676 = VECTOR ( 'NONE', #15845, 1000.000000000000227 ) ;
#36677 = EDGE_CURVE ( 'NONE', #53825, #52479, #40717, .T. ) ;
#36678 = VERTEX_POINT ( 'NONE', #55099 ) ;
#36679 = ORIENTED_EDGE ( 'NONE', *, *, #1281, .T. ) ;
#36681 = ORIENTED_EDGE ( 'NONE', *, *, #80063, .T. ) ;
#36680 = CARTESIAN_POINT ( 'NONE',  ( 4.219913487196228274, -3.937682226553329556, 33.60647404775216529 ) ) ;
#36683 = CARTESIAN_POINT ( 'NONE',  ( -5.326946301144536378, -12.68155406624981119, 30.59749803192733708 ) ) ;
#36682 = CARTESIAN_POINT ( 'NONE',  ( 6.923076923076924238, -13.63283147151868846, 33.57946703557072254 ) ) ;
#36684 = CARTESIAN_POINT ( 'NONE',  ( 13.63466969625370062, -8.303483539816731707, 34.68545999027711702 ) ) ;
#36685 = VERTEX_POINT ( 'NONE', #75812 ) ;
#36686 = B_SPLINE_CURVE_WITH_KNOTS ( 'NONE', 3,
 ( #60160, #87663, #19186, #74129, #1571, #42564, #50182, #29060, #84886, #14200 ),
 .UNSPECIFIED., .F., .F.,
 ( 4, 2, 2, 2, 4 ),
 ( 0.0007817246256747451124, 0.0009771112852218885505, 0.001172497944769032097, 0.001367884604316175427, 0.001563271263863318973 ),
 .UNSPECIFIED. ) ;
#36687 = B_SPLINE_CURVE_WITH_KNOTS ( 'NONE', 3,
 ( #76905, #797, #83676, #29176, #22833, #77780, #55293, #43116, #8450, #82785 ),
 .UNSPECIFIED., .F., .F.,
 ( 4, 2, 2, 2, 4 ),
 ( 0.000000000000000000, 0.0001954311564186865492, 0.0003908623128373730983, 0.0005862934692560596746, 0.0007817246256747461966 ),
 .UNSPECIFIED. ) ;
#36688 = ORIENTED_EDGE ( 'NONE', *, *, #36445, .F. ) ;
#36689 = CARTESIAN_POINT ( 'NONE',  ( 3.930361229281822855, -4.225889041578354544, 33.85425143139329407 ) ) ;
#36690 = ORIENTED_EDGE ( 'NONE', *, *, #74210, .T. ) ;
#36691 = FACE_BOUND ( 'NONE', #78206, .T. ) ;
#36692 = CARTESIAN_POINT ( 'NONE',  ( -12.46153846153858247, -9.442884908241554243, 34.35708131394783038 ) ) ;
#36693 = CARTESIAN_POINT ( 'NONE',  ( -14.30769230769242917, -6.835583212225970762, 34.95778746994575670 ) ) ;
#36694 = ORIENTED_EDGE ( 'NONE', *, *, #64173, .T. ) ;
#36695 = CARTESIAN_POINT ( 'NONE',  ( -17.07692307692319744, -10.21337939537710326, 33.94971097300076224 ) ) ;
#36696 = CYLINDRICAL_SURFACE ( 'NONE', #70567, 0.2499999999999994726 ) ;
#36697 = CARTESIAN_POINT ( 'NONE',  ( 1.384615384615386802, -3.322132147404559976, 32.92929555188717927 ) ) ;
#36698 = CARTESIAN_POINT ( 'NONE',  ( -15.29685264172511161, -6.386643153685125363, 34.62446782046654903 ) ) ;
#36699 = CARTESIAN_POINT ( 'NONE',  ( 1.634669804528840586, -2.544122305571458575, 31.48381861865057729 ) ) ;
#36700 = CIRCLE ( 'NONE', #39621, 0.2500000000000002220 ) ;
#36701 = CARTESIAN_POINT ( 'NONE',  ( 8.545745844666438273, -11.60425143139329940, 33.02411095842164457 ) ) ;
#36702 = DIRECTION ( 'NONE',  ( 1.000000000000000000, 0.000000000000000000, 0.000000000000000000 ) ) ;
#36703 = DIRECTION ( 'NONE',  ( -1.000000000000000000, 0.000000000000000000, -0.000000000000000000 ) ) ;
#36704 = CARTESIAN_POINT ( 'NONE',  ( 5.448717948717947124, -7.500000000000000000, 29.75000000000000355 ) ) ;
#36705 = CARTESIAN_POINT ( 'NONE',  ( 9.468822767743359847, -12.47654668319379567, 31.42292124445336654 ) ) ;
#36706 = CARTESIAN_POINT ( 'NONE',  ( 9.019176178608809380, -4.176053281294518804, 33.81426240980091791 ) ) ;
#36708 = CARTESIAN_POINT ( 'NONE',  ( 11.78846153846295763, -7.500000000000154543, 35.00000000000007105 ) ) ;
#36707 = CARTESIAN_POINT ( 'NONE',  ( 4.946775867484856093, -12.45813303252208648, 30.39737893381572675 ) ) ;
#36709 = CARTESIAN_POINT ( 'NONE',  ( -17.78205128205128105, -4.000000000000000000, 29.75000000000000355 ) ) ;
#36711 = CARTESIAN_POINT ( 'NONE',  ( -6.066083410955878108, -4.786620604624113540, 33.94971097300155805 ) ) ;
#36710 = CARTESIAN_POINT ( 'NONE',  ( -3.230769230769352962, -3.083524468854526912, 32.58852847137268327 ) ) ;
#36712 = CARTESIAN_POINT ( 'NONE',  ( -5.869208192175213945, -12.38066358083363738, 30.83685684665853444 ) ) ;
#36713 = CARTESIAN_POINT ( 'NONE',  ( -1.901340078031346525, -9.487747218494661183, 20.93563170625849068 ) ) ;
#36714 = ORIENTED_EDGE ( 'NONE', *, *, #21331, .T. ) ;
#36715 = CARTESIAN_POINT ( 'NONE',  ( 3.116851723387825235, -7.815776116252264316, 14.00000000000001066 ) ) ;
#36716 = ORIENTED_EDGE ( 'NONE', *, *, #70562, .F. ) ;
#36717 = EDGE_CURVE ( 'NONE', #20364, #60609, #78030, .T. ) ;
#36718 = DIRECTION ( 'NONE',  ( -0.000000000000000000, -0.1736481776669307198, -0.9848077530122080203 ) ) ;
#36719 = ORIENTED_EDGE ( 'NONE', *, *, #43407, .F. ) ;
#36720 = DIRECTION ( 'NONE',  ( 0.000000000000000000, 1.000000000000000000, 0.000000000000000000 ) ) ;
#36721 = EDGE_CURVE ( 'NONE', #20451, #34572, #13416, .T. ) ;
#36722 = EDGE_LOOP ( 'NONE', ( #80442, #3371, #83344, #45599 ) ) ;
#36723 = CARTESIAN_POINT ( 'NONE',  ( -8.069638789877792817, -5.912607949931405926, 34.49155766932282319 ) ) ;
#36724 = CARTESIAN_POINT ( 'NONE',  ( -1.077988221561460236, -10.27530806549876452, 23.35750670625849423 ) ) ;
#36725 = CARTESIAN_POINT ( 'NONE',  ( 2.307692307692309264, -1.367168528481310208, 33.57946703557072254 ) ) ;
#36726 = CARTESIAN_POINT ( 'NONE',  ( -5.776988648387149539, -9.086983370893049639, 34.49168942202179267 ) ) ;
#36727 = CARTESIAN_POINT ( 'NONE',  ( 17.77651507543566822, -2.353723527008297012, 30.78948104536958752 ) ) ;
#36728 = CARTESIAN_POINT ( 'NONE',  ( 15.16549923021291058, -8.656820664281498878, 34.87096338111211935 ) ) ;
#36729 = CARTESIAN_POINT ( 'NONE',  ( 15.00789054834058511, -7.630691491037285168, 34.74850469731152458 ) ) ;
#36730 = CARTESIAN_POINT ( 'NONE',  ( -13.51476335434707821, -12.15440758774515473, 32.17923288041532004 ) ) ;
#36731 = EDGE_CURVE ( 'NONE', #19674, #18184, #33847, .T. ) ;
#36732 = CARTESIAN_POINT ( 'NONE',  ( 3.750000000000009770, -9.053300858899081760, 17.04687500000000000 ) ) ;
#36733 = VECTOR ( 'NONE', #49653, 1000.000000000000000 ) ;
#36734 = LINE ( 'NONE', #44357, #80855 ) ;
#36735 = CYLINDRICAL_SURFACE ( 'NONE', #50623, 0.2500000000000009437 ) ;
#36736 = ADVANCED_FACE ( 'NONE', ( #83924 ), #35271, .F. ) ;
#36737 = CARTESIAN_POINT ( 'NONE',  ( 13.51540719244018263, -4.118422570099828484, 33.43335022499816489 ) ) ;
#36738 = CARTESIAN_POINT ( 'NONE',  ( -3.750000000000008438, -5.946699141100917352, 18.92187500000000355 ) ) ;
#36739 = CARTESIAN_POINT ( 'NONE',  ( -39.05038313613820122, -2.499999999999999556, 29.75000000000000355 ) ) ;
#36740 = ORIENTED_EDGE ( 'NONE', *, *, #83793, .T. ) ;
#36741 = CARTESIAN_POINT ( 'NONE',  ( -13.38461538461550759, -6.835583212225970762, 34.95778746994575670 ) ) ;
#36742 = CARTESIAN_POINT ( 'NONE',  ( 15.93036121012220185, -12.24155766932282496, 31.33739205006857986 ) ) ;
#36743 = LINE ( 'NONE', #22777, #33936 ) ;
#36744 = CARTESIAN_POINT ( 'NONE',  ( 15.16544631527705533, -7.749976743299138882, 34.99404534957040624 ) ) ;
#36745 = FACE_OUTER_BOUND ( 'NONE', #14481, .T. ) ;
#36746 = CARTESIAN_POINT ( 'NONE',  ( 2.307692307692187583, -12.27809138561165270, 31.22303859784587132 ) ) ;
#36747 = CARTESIAN_POINT ( 'NONE',  ( 8.519207531937803779, -10.76384336483936011, 33.53834819971076087 ) ) ;
#36748 = ORIENTED_EDGE ( 'NONE', *, *, #21033, .F. ) ;
#36749 = ORIENTED_EDGE ( 'NONE', *, *, #34256, .F. ) ;
#36750 = EDGE_CURVE ( 'NONE', #5178, #10414, #86509, .T. ) ;
#36751 = VERTEX_POINT ( 'NONE', #29418 ) ;
#36752 = B_SPLINE_CURVE_WITH_KNOTS ( 'NONE', 3,
 ( #32823, #40479, #33272, #74707, #86905, #25618, #47663, #60283, #60731, #53525 ),
 .UNSPECIFIED., .F., .F.,
 ( 4, 2, 2, 2, 4 ),
 ( 0.000000000000000000, 0.0001954311564186882568, 0.0003908623128373765136, 0.0005862934692560647703, 0.0007817246256747530271 ),
 .UNSPECIFIED. ) ;
#36753 = CARTESIAN_POINT ( 'NONE',  ( 6.923076923076802558, -10.21337939537710326, 33.94971097300076224 ) ) ;
#36754 = CARTESIAN_POINT ( 'NONE',  ( -8.769230769230768274, -2.292212530054420494, 30.41441678777542634 ) ) ;
#36755 = CARTESIAN_POINT ( 'NONE',  ( -13.25408968285182354, -9.417988943895561960, 34.36773134775777550 ) ) ;
#36756 = CARTESIAN_POINT ( 'NONE',  ( -19.99999999999996803, 15.00000000000000711, 3.000000000000000000 ) ) ;
#36757 = ORIENTED_EDGE ( 'NONE', *, *, #82065, .T. ) ;
#36758 = EDGE_CURVE ( 'NONE', #78695, #1002, #34958, .T. ) ;
#36759 = DIRECTION ( 'NONE',  ( -1.000000000000000000, -0.000000000000000000, -0.000000000000000000 ) ) ;
#36760 = VERTEX_POINT ( 'NONE', #62732 ) ;
#36761 = B_SPLINE_CURVE_WITH_KNOTS ( 'NONE', 3,
 ( #70150, #63388, #57075, #84570, #13876, #7128, #57520, #77791, #64264, #85886 ),
 .UNSPECIFIED., .F., .F.,
 ( 4, 2, 2, 2, 4 ),
 ( 0.000000000000000000, 0.0001954339857564074473, 0.0003908679715128148945, 0.0005863019572692223418, 0.0007817359430256297891 ),
 .UNSPECIFIED. ) ;
#36762 = ORIENTED_EDGE ( 'NONE', *, *, #84515, .F. ) ;
#36763 = EDGE_CURVE ( 'NONE', #63786, #4010, #42464, .T. ) ;
#36764 = EDGE_CURVE ( 'NONE', #5458, #19800, #83305, .T. ) ;
#36765 = LINE ( 'NONE', #43521, #32902 ) ;
#36766 = DIRECTION ( 'NONE',  ( -0.000000000000000000, 0.1736481776669307198, -0.9848077530122080203 ) ) ;
#36767 = LINE ( 'NONE', #2523, #52348 ) ;
#36768 = DIRECTION ( 'NONE',  ( -1.000000000000000000, -0.000000000000000000, -0.000000000000000000 ) ) ;
#36769 = CARTESIAN_POINT ( 'NONE',  ( 12.46153846153846168, -12.62096338111211580, 30.90682066428153263 ) ) ;
#36770 = ORIENTED_EDGE ( 'NONE', *, *, #69093, .T. ) ;
#36771 = ADVANCED_FACE ( 'NONE', ( #38378 ), #44220, .F. ) ;
#36772 = VERTEX_POINT ( 'NONE', #39281 ) ;
#36773 = B_SPLINE_CURVE_WITH_KNOTS ( 'NONE', 3,
 ( #65463, #79432, #17731, #10970, #43856, #30348, #9628, #2857, #57817, #78526 ),
 .UNSPECIFIED., .F., .F.,
 ( 4, 2, 2, 2, 4 ),
 ( 0.0007817359430256315238, 0.0009771253907249980580, 0.001172514838424364592, 0.001367904286123730910, 0.001563293733823097444 ),
 .UNSPECIFIED. ) ;
#36774 = CARTESIAN_POINT ( 'NONE',  ( 3.750000000000000888, -7.499999999999978684, 21.96875000000000355 ) ) ;
#36775 = ORIENTED_EDGE ( 'NONE', *, *, #57199, .T. ) ;
#36777 = ORIENTED_EDGE ( 'NONE', *, *, #80319, .T. ) ;
#36776 = CARTESIAN_POINT ( 'NONE',  ( -2.557669038634661440, -2.779195860258149242, 31.39871582349837453 ) ) ;
#36778 = CARTESIAN_POINT ( 'NONE',  ( -10.61538461538461320, -5.557115091759785130, 34.35708131394839171 ) ) ;
#36779 = CARTESIAN_POINT ( 'NONE',  ( 8.519230769230768274, -7.500000000000001776, 35.00000000000000000 ) ) ;
#36780 = ADVANCED_FACE ( 'NONE', ( #23521 ), #44668, .F. ) ;
#36781 = EDGE_CURVE ( 'NONE', #59185, #45658, #56968, .T. ) ;
#36782 = VECTOR ( 'NONE', #64672, 1000.000000000000114 ) ;
#36783 = CARTESIAN_POINT ( 'NONE',  ( 7.053602624840490165, -11.93748526763465279, 32.05452791011430946 ) ) ;
#36784 = ORIENTED_EDGE ( 'NONE', *, *, #27715, .F. ) ;
#36785 = DIRECTION ( 'NONE',  ( -0.000000000000000000, -0.1736481776669307198, -0.9848077530122080203 ) ) ;
#36786 = CARTESIAN_POINT ( 'NONE',  ( 5.011673145148991537, -2.255955759149247619, 30.00000000000013856 ) ) ;
#36787 = EDGE_LOOP ( 'NONE', ( #87018, #10510, #69222, #4083 ) ) ;
#36788 = FACE_BOUND ( 'NONE', #82701, .T. ) ;
#36789 = EDGE_CURVE ( 'NONE', #28895, #53468, #43569, .T. ) ;
#36790 = CARTESIAN_POINT ( 'NONE',  ( 15.23076923076910916, -11.67786785259630911, 32.92929555188603530 ) ) ;
#36791 = CARTESIAN_POINT ( 'NONE',  ( 10.83816415665302380, -9.332535724633409302, 34.40230450496446934 ) ) ;
#36792 = CARTESIAN_POINT ( 'NONE',  ( -15.16551409125639260, -3.083524468853784839, 32.58852847137153930 ) ) ;
#36794 = CARTESIAN_POINT ( 'NONE',  ( -19.99999999999996447, -12.00000000000000355, 13.00000000000000178 ) ) ;
#36793 = DIRECTION ( 'NONE',  ( -0.000000000000000000, 0.7660444431189791237, -0.6427876096865379196 ) ) ;
#36795 = FACE_OUTER_BOUND ( 'NONE', #4449, .T. ) ;
#36796 = CARTESIAN_POINT ( 'NONE',  ( 14.53047197667037338, -2.353885683473779800, 30.79025554430704403 ) ) ;
#36797 = EDGE_LOOP ( 'NONE', ( #83272, #56018, #84323, #50074 ) ) ;
#36798 = CARTESIAN_POINT ( 'NONE',  ( -11.31545018684868964, -4.187068189119696804, 33.49521262558774026 ) ) ;
#36799 = CYLINDRICAL_SURFACE ( 'NONE', #6211, 0.2500000000000008882 ) ;
#36800 = ORIENTED_EDGE ( 'NONE', *, *, #46518, .T. ) ;
#36801 = CARTESIAN_POINT ( 'NONE',  ( 5.448717948717947124, -11.50000000000000000, 29.75000000000000355 ) ) ;
#36802 = CARTESIAN_POINT ( 'NONE',  ( 10.36536137809165403, -6.695914987888146541, 34.68535235679833306 ) ) ;
#36803 = FACE_OUTER_BOUND ( 'NONE', #65980, .T. ) ;
#36804 = CARTESIAN_POINT ( 'NONE',  ( -6.000000000000121680, -6.835583212225970762, 34.95778746994575670 ) ) ;
#36805 = CARTESIAN_POINT ( 'NONE',  ( -10.48485917715097138, -3.068774925481847493, 32.56582465632704526 ) ) ;
#36806 = CARTESIAN_POINT ( 'NONE',  ( -20.00000000000000355, -10.00000000000000533, 0.000000000000000000 ) ) ;
#36807 = FACE_BOUND ( 'NONE', #24918, .T. ) ;
#36809 = CARTESIAN_POINT ( 'NONE',  ( 18.00000000000000000, -6.435427911321262684, 35.78748833219616898 ) ) ;
#36808 = CARTESIAN_POINT ( 'NONE',  ( -1.634638608836841200, -6.652501968072646932, 34.93155406624980941 ) ) ;
#36810 = DIRECTION ( 'NONE',  ( 0.000000000000000000, 0.1736481776669275834, 0.9848077530122086864 ) ) ;
#36812 = LINE ( 'NONE', #35042, #88090 ) ;
#36811 = CARTESIAN_POINT ( 'NONE',  ( -6.857821783564083340, -11.06231777344671130, 33.60647404775212976 ) ) ;
#36813 = CARTESIAN_POINT ( 'NONE',  ( -5.999999999999998224, -12.78798330534103123, 29.99999999999997868 ) ) ;
#36814 = CARTESIAN_POINT ( 'NONE',  ( 1.614399933863660985, -11.22469193450123193, 19.45125670625849068 ) ) ;
#36816 = EDGE_CURVE ( 'NONE', #85269, #5298, #16765, .T. ) ;
#36815 = B_SPLINE_CURVE_WITH_KNOTS ( 'NONE', 3,
 ( #20571, #48035, #47152, #26003, #46277, #34087, #5730, #47602, #88179, #74639 ),
 .UNSPECIFIED., .F., .F.,
 ( 4, 2, 2, 2, 4 ),
 ( 0.0007817246256747447872, 0.0009771112852218876831, 0.001172497944769030579, 0.001367884604316173475, 0.001563271263863316371 ),
 .UNSPECIFIED. ) ;
#36817 = ORIENTED_EDGE ( 'NONE', *, *, #36241, .T. ) ;
#36818 = CARTESIAN_POINT ( 'NONE',  ( -8.069080063669991532, -11.24512374952581872, 33.06303171183252942 ) ) ;
#36819 = AXIS2_PLACEMENT_3D ( 'NONE', #66532, #52114, #79603 ) ;
#36820 = CARTESIAN_POINT ( 'NONE',  ( -2.939152317953646711E-15, 7.500000000000000000, 14.00000000000000178 ) ) ;
#36821 = CARTESIAN_POINT ( 'NONE',  ( 5.869852030268306819, -5.915902021225892149, 34.75552854090298638 ) ) ;
#36822 = CARTESIAN_POINT ( 'NONE',  ( 0.1741240272142571821, -10.24553155050938358, 28.77324492963869673 ) ) ;
#36823 = DIRECTION ( 'NONE',  ( -1.000000000000000000, -0.000000000000000000, 0.000000000000000000 ) ) ;
#36824 = CARTESIAN_POINT ( 'NONE',  ( 3.775308065498768517, -8.992201783934554271, 20.54500670625849068 ) ) ;
#36825 = CARTESIAN_POINT ( 'NONE',  ( -2.557715531913761886, -3.520140089381496473, 33.17453946501458262 ) ) ;
#36826 = CARTESIAN_POINT ( 'NONE',  ( -2.307692307692305711, -11.16473453929635440, 33.15142922261926373 ) ) ;
#36827 = AXIS2_PLACEMENT_3D ( 'NONE', #51118, #9283, #77284 ) ;
#36828 = CARTESIAN_POINT ( 'NONE',  ( -7.912236225513983534, -2.833524468853757305, 32.15551576947924417 ) ) ;
#36829 = CARTESIAN_POINT ( 'NONE',  ( -3.007989561791164945, -12.11081565061823717, 32.26097654155341843 ) ) ;
#36830 = CARTESIAN_POINT ( 'NONE',  ( 5.300299017621258990, -2.501478030877322567, 29.88021232661720816 ) ) ;
#36831 = CARTESIAN_POINT ( 'NONE',  ( 4.153846153846032507, -10.90142922262034020, 33.41473453929536674 ) ) ;
#36832 = CARTESIAN_POINT ( 'NONE',  ( 14.30769230769231015, -13.04860791097971706, 34.73218667398347037 ) ) ;
#36833 = CARTESIAN_POINT ( 'NONE',  ( 8.096099364501988305, -6.696923467548660192, 34.68552623307873972 ) ) ;
#36834 = ORIENTED_EDGE ( 'NONE', *, *, #84193, .F. ) ;
#36835 = CARTESIAN_POINT ( 'NONE',  ( 3.361559671736180643, -12.35292014791297710, 31.75344720912887198 ) ) ;
#36836 = CARTESIAN_POINT ( 'NONE',  ( 7.173022441425065843, -5.057305518903949526, 34.11320923018887896 ) ) ;
#36837 = CARTESIAN_POINT ( 'NONE',  ( 3.724691934501251023, -9.114399933863618131, 14.79874329374151642 ) ) ;
#36838 = B_SPLINE_CURVE_WITH_KNOTS ( 'NONE', 3,
 ( #33833, #68947, #7258, #937, #42383, #34723 ),
 .UNSPECIFIED., .F., .F.,
 ( 4, 2, 4 ),
 ( 0.0003909512603273906169, 0.0005862562993132179340, 0.0007815613382990451970 ),
 .UNSPECIFIED. ) ;
#36839 = CARTESIAN_POINT ( 'NONE',  ( 0.5920638997721061614, -3.625058011473228259, 33.29252011169590020 ) ) ;
#36840 = DIRECTION ( 'NONE',  ( -0.000000000000000000, -0.1736481776669307198, -0.9848077530122080203 ) ) ;
#36841 = EDGE_LOOP ( 'NONE', ( #71136, #4009 ) ) ;
#36842 = CARTESIAN_POINT ( 'NONE',  ( 23.49999999999998579, 0.000000000000000000, 30.36437827766148345 ) ) ;
#36844 = EDGE_LOOP ( 'NONE', ( #73894, #55507, #82071, #78087 ) ) ;
#36843 = FACE_OUTER_BOUND ( 'NONE', #29471, .T. ) ;
#36845 = CARTESIAN_POINT ( 'NONE',  ( -11.28846153846153477, -2.499999999999999556, 29.81604066197449754 ) ) ;
#36846 = CARTESIAN_POINT ( 'NONE',  ( 9.692307692307695177, -13.37000171582298513, 34.34916445242398453 ) ) ;
#36847 = CARTESIAN_POINT ( 'NONE',  ( -5.300408020647024543, -11.41268669641500466, 32.86336882939237825 ) ) ;
#36849 = EDGE_CURVE ( 'NONE', #20099, #87653, #85681, .T. ) ;
#36848 = CARTESIAN_POINT ( 'NONE',  ( -15.23076923076935252, -5.094484230521993062, 34.41647553114689373 ) ) ;
#36850 = ORIENTED_EDGE ( 'NONE', *, *, #44864, .F. ) ;
#36851 = CARTESIAN_POINT ( 'NONE',  ( -12.59168643127016196, -2.373036134822904319, 30.88089517874952250 ) ) ;
#36852 = CARTESIAN_POINT ( 'NONE',  ( -15.93106661257774270, -3.236590943229499473, 32.36255958852954251 ) ) ;
#36853 = AXIS2_PLACEMENT_3D ( 'NONE', #5036, #60421, #20766 ) ;
#36854 = B_SPLINE_CURVE_WITH_KNOTS ( 'NONE', 3,
 ( #7665, #40132, #67591, #27044, #61700, #54507, #35125, #5889, #76108, #34689 ),
 .UNSPECIFIED., .F., .F.,
 ( 4, 2, 2, 2, 4 ),
 ( 0.000000000000000000, 0.0001954311564186865221, 0.0003908623128373730441, 0.0005862934692560595662, 0.0007817246256747460882 ),
 .UNSPECIFIED. ) ;
#36855 = DIRECTION ( 'NONE',  ( 0.000000000000000000, 0.000000000000000000, -1.000000000000000000 ) ) ;
#36856 = ORIENTED_EDGE ( 'NONE', *, *, #9836, .F. ) ;
#36857 = ORIENTED_EDGE ( 'NONE', *, *, #59364, .F. ) ;
#36858 = ORIENTED_EDGE ( 'NONE', *, *, #22123, .F. ) ;
#36859 = CARTESIAN_POINT ( 'NONE',  ( -9.822999158975250111, -9.804603061927743113, 34.18744698557895845 ) ) ;
#36860 = CARTESIAN_POINT ( 'NONE',  ( -14.55771554498526932, -3.202444869320336451, 32.30641848906366675 ) ) ;
#36861 = EDGE_CURVE ( 'NONE', #54248, #43633, #72152, .T. ) ;
#36862 = AXIS2_PLACEMENT_3D ( 'NONE', #1409, #29774, #8623 ) ;
#36863 = EDGE_CURVE ( 'NONE', #4267, #35011, #34863, .T. ) ;
#36864 = CARTESIAN_POINT ( 'NONE',  ( -3.099978789802281032, -8.191423895709840863, 34.95447573519442130 ) ) ;
#36865 = CARTESIAN_POINT ( 'NONE',  ( -2.307692307692305711, -13.53365097954675988, 30.81389545987213552 ) ) ;
#36866 = ORIENTED_EDGE ( 'NONE', *, *, #48820, .F. ) ;
#36867 = ADVANCED_FACE ( 'NONE', ( #79366 ), #85241, .F. ) ;
#36868 = ORIENTED_EDGE ( 'NONE', *, *, #45591, .F. ) ;
#36870 = EDGE_LOOP ( 'NONE', ( #46124, #60455 ) ) ;
#36869 = DIRECTION ( 'NONE',  ( -1.000000000000000000, -0.000000000000000000, -0.000000000000000000 ) ) ;
#36871 = CARTESIAN_POINT ( 'NONE',  ( 16.37685899793955357, -8.282913670948747864, 34.94150082978203642 ) ) ;
#36872 = CARTESIAN_POINT ( 'NONE',  ( 7.846153846153846700, -11.91647553114624181, 32.58852847137148245 ) ) ;
#36873 = DIRECTION ( 'NONE',  ( -0.000000000000000000, -0.9396926207859092051, -0.3420201433256662704 ) ) ;
#36874 = EDGE_LOOP ( 'NONE', ( #81911, #24507, #85299, #2667 ) ) ;
#36875 = AXIS2_PLACEMENT_3D ( 'NONE', #58397, #32284, #31844 ) ;
#36876 = ORIENTED_EDGE ( 'NONE', *, *, #41973, .T. ) ;
#36878 = EDGE_LOOP ( 'NONE', ( #15120, #59688 ) ) ;
#36877 = DIRECTION ( 'NONE',  ( 0.000000000000000000, 0.4999999999999985567, 0.8660254037844395958 ) ) ;
#36879 = B_SPLINE_CURVE_WITH_KNOTS ( 'NONE', 3,
 ( #68887, #34675, #7646, #62138, #35560, #21145, #63002, #41879, #35106, #69347 ),
 .UNSPECIFIED., .F., .F.,
 ( 4, 2, 2, 2, 4 ),
 ( 0.000000000000000000, 0.0001954311564186882568, 0.0003908623128373765136, 0.0005862934692560647703, 0.0007817246256747530271 ),
 .UNSPECIFIED. ) ;
#36880 = CARTESIAN_POINT ( 'NONE',  ( 4.284371855609715674, -5.195472089885680766, 34.18748526763464923 ) ) ;
#36881 = EDGE_CURVE ( 'NONE', #31211, #69454, #14444, .T. ) ;
#36882 = CARTESIAN_POINT ( 'NONE',  ( -10.68146699474474914, -9.058645607665454236, 34.76329471203372634 ) ) ;
#36883 = ORIENTED_EDGE ( 'NONE', *, *, #88427, .T. ) ;
#36884 = VECTOR ( 'NONE', #15127, 1000.000000000000114 ) ;
#36885 = CARTESIAN_POINT ( 'NONE',  ( 16.02315468717859659, -12.38065189839062263, 30.83690757178629482 ) ) ;
#36886 = DIRECTION ( 'NONE',  ( -0.000000000000000000, -0.9848077530122086864, -0.1736481776669273613 ) ) ;
#36887 = CARTESIAN_POINT ( 'NONE',  ( 12.46153846153833911, -2.892918686052165622, 31.69288490824153470 ) ) ;
#36888 = FACE_BOUND ( 'NONE', #83144, .T. ) ;
#36889 = CARTESIAN_POINT ( 'NONE',  ( 1.384615384615386802, -12.37446782046654192, 30.86335684631486131 ) ) ;
#36890 = CARTESIAN_POINT ( 'NONE',  ( -4.219116599806928214, -12.27809138561121394, 31.22303859784730307 ) ) ;
#36891 = CYLINDRICAL_SURFACE ( 'NONE', #82610, 0.2499999999999979738 ) ;
#36893 = CARTESIAN_POINT ( 'NONE',  ( 4.153846153846154188, -2.292212530054420494, 30.41441678777542634 ) ) ;
#36892 = DIRECTION ( 'NONE',  ( 0.000000000000000000, 0.000000000000000000, -1.000000000000000000 ) ) ;
#36894 = CARTESIAN_POINT ( 'NONE',  ( 17.75002325595141173, -6.524016743844656574, 34.90889640711025521 ) ) ;
#36895 = CARTESIAN_POINT ( 'NONE',  ( -7.846153846153967493, -12.51329471203414379, 31.30864560766407578 ) ) ;
#36896 = VERTEX_POINT ( 'NONE', #79816 ) ;
#36897 = CARTESIAN_POINT ( 'NONE',  ( -5.934744428723973897, -11.94971097300157403, 32.03036669348361443 ) ) ;
#36898 = VERTEX_POINT ( 'NONE', #18115 ) ;
#36899 = ORIENTED_EDGE ( 'NONE', *, *, #50264, .F. ) ;
#36901 = CARTESIAN_POINT ( 'NONE',  ( -5.749945688361684404, -12.17597550085003633, 31.52189283813461884 ) ) ;
#36900 = DIRECTION ( 'NONE',  ( 0.000000000000000000, 0.8660254037844377084, -0.5000000000000015543 ) ) ;
#36902 = CARTESIAN_POINT ( 'NONE',  ( -6.857008572074484221, -6.386643153685127139, 34.62446782046654192 ) ) ;
#36903 = CARTESIAN_POINT ( 'NONE',  ( 14.30769230769218581, -4.320704448113951379, 33.92786785259630022 ) ) ;
#36904 = CARTESIAN_POINT ( 'NONE',  ( 2.373759641042385571, -2.292212530054420494, 30.41441678777542990 ) ) ;
#36905 = CARTESIAN_POINT ( 'NONE',  ( 1.134638653673031961, -11.79746400365624659, 32.30657167506340954 ) ) ;
#36906 = ORIENTED_EDGE ( 'NONE', *, *, #71332, .T. ) ;
#36907 = VECTOR ( 'NONE', #75720, 1000.000000000000227 ) ;
#36908 = CARTESIAN_POINT ( 'NONE',  ( 4.153846153846154188, -4.661471528628507777, 34.16647553114623292 ) ) ;
#36909 = CARTESIAN_POINT ( 'NONE',  ( 6.700150705560775855, -3.586966769969700763, 32.86292498521069660 ) ) ;
#36910 = LINE ( 'NONE', #55859, #43085 ) ;
#36911 = CARTESIAN_POINT ( 'NONE',  ( 17.07692307692307665, -4.098570777380720287, 33.41473453929634729 ) ) ;
#36912 = DIRECTION ( 'NONE',  ( -0.000000000000000000, -0.6427876096865404731, -0.7660444431189770143 ) ) ;
#36913 = CARTESIAN_POINT ( 'NONE',  ( 2.651650429449539104, -4.848349570550432475, 18.06250000000000355 ) ) ;
#36914 = ORIENTED_EDGE ( 'NONE', *, *, #48845, .T. ) ;
#36915 = B_SPLINE_CURVE_WITH_KNOTS ( 'NONE', 3,
 ( #86102, #24376, #51844, #79340, #17644, #65807, #45099, #4108, #31592, #59058 ),
 .UNSPECIFIED., .F., .F.,
 ( 4, 2, 2, 2, 4 ),
 ( 0.0007817359430256366195, 0.0009771253907250045632, 0.001172514838424372615, 0.001367904286123740668, 0.001563293733823108503 ),
 .UNSPECIFIED. ) ;
#36916 = ORIENTED_EDGE ( 'NONE', *, *, #36117, .F. ) ;
#36917 = CYLINDRICAL_SURFACE ( 'NONE', #42070, 5.000000000000000888 ) ;
#36918 = ORIENTED_EDGE ( 'NONE', *, *, #83864, .T. ) ;
#36919 = AXIS2_PLACEMENT_3D ( 'NONE', #528, #27993, #23442 ) ;
#36920 = CARTESIAN_POINT ( 'NONE',  ( -9.692307692307814193, -6.835583212225970762, 34.95778746994575670 ) ) ;
#36921 = CARTESIAN_POINT ( 'NONE',  ( 0.000000000000000000, -4.000000000000000000, 29.25000000000000000 ) ) ;
#36922 = CARTESIAN_POINT ( 'NONE',  ( 3.230769230769110045, -6.879047030192662504, 34.71129190930017927 ) ) ;
#36923 = CARTESIAN_POINT ( 'NONE',  ( 16.82692307692307665, -7.500000000000001776, 35.00000000000000000 ) ) ;
#36924 = CARTESIAN_POINT ( 'NONE',  ( 3.750000000000000888, -7.499999999999978684, 19.46875000000000000 ) ) ;
#36925 = LINE ( 'NONE', #77915, #87740 ) ;
#36926 = ORIENTED_EDGE ( 'NONE', *, *, #3311, .T. ) ;
#36927 = CARTESIAN_POINT ( 'NONE',  ( 4.403846153846090239, -7.565270445406050648, 34.75000000000000000 ) ) ;
#36929 = EDGE_LOOP ( 'NONE', ( #26708, #8203 ) ) ;
#36928 = DIRECTION ( 'NONE',  ( -0.000000000000000000, 0.3420201433256694901, -0.9396926207859082059 ) ) ;
#36930 = CARTESIAN_POINT ( 'NONE',  ( 3.230769230769231726, -12.34228464037088635, 31.77849191805839268 ) ) ;
#36931 = LINE ( 'NONE', #78359, #74631 ) ;
#36932 = B_SPLINE_CURVE_WITH_KNOTS ( 'NONE', 3,
 ( #2334, #77124, #42905, #43776, #49650, #14986, #8677, #64037, #36152, #71237 ),
 .UNSPECIFIED., .F., .F.,
 ( 4, 2, 2, 2, 4 ),
 ( 0.0007817359430256400890, 0.0009771253907250091169, 0.001172514838424378253, 0.001367904286123747173, 0.001563293733823116309 ),
 .UNSPECIFIED. ) ;
#36933 = CARTESIAN_POINT ( 'NONE',  ( 5.076923076923075762, -12.10708131394839349, 31.69288490824020244 ) ) ;
#36934 = CARTESIAN_POINT ( 'NONE',  ( 11.76147438255493149, -8.282913670948747864, 34.94150082978203642 ) ) ;
#36935 = CARTESIAN_POINT ( 'NONE',  ( -12.68446467905460828, -12.39988816332205701, 30.74660775122750778 ) ) ;
#36936 = DIRECTION ( 'NONE',  ( 1.000000000000000000, 0.000000000000000000, 0.000000000000000000 ) ) ;
#36937 = CARTESIAN_POINT ( 'NONE',  ( -2.749999999999999112, -7.438900925035484057, 24.09561829374151287 ) ) ;
#36938 = VERTEX_POINT ( 'NONE', #59531 ) ;
#36939 = CARTESIAN_POINT ( 'NONE',  ( 1.161130440891438687, -5.912607949931405038, 34.49155766932282319 ) ) ;
#36940 = CARTESIAN_POINT ( 'NONE',  ( -1.634592115557737646, -12.17611988154120972, 31.52148481390971213 ) ) ;
#36941 = CARTESIAN_POINT ( 'NONE',  ( -1.077988221561493543, -4.724691934501247914, 13.07999329374151642 ) ) ;
#36942 = CARTESIAN_POINT ( 'NONE',  ( -16.02332071561251325, -11.66157788607254275, 32.95092075102925833 ) ) ;
#36944 = CARTESIAN_POINT ( 'NONE',  ( -7.596208436775802930, -2.986452184633680229, 32.43230066228895225 ) ) ;
#36943 = VECTOR ( 'NONE', #5241, 1000.000000000000227 ) ;
#36945 = ORIENTED_EDGE ( 'NONE', *, *, #21888, .F. ) ;
#36946 = CARTESIAN_POINT ( 'NONE',  ( -1.409462824231155764E-14, -4.749999999999999112, 14.15625000000000000 ) ) ;
#36947 = CARTESIAN_POINT ( 'NONE',  ( 3.165498784808455923, -9.442884908240170461, 34.35708131394840592 ) ) ;
#36948 = ORIENTED_EDGE ( 'NONE', *, *, #59810, .F. ) ;
#36949 = CARTESIAN_POINT ( 'NONE',  ( -18.13069060311030967, -4.684245665217971144, 34.18127051446801090 ) ) ;
#36950 = ORIENTED_EDGE ( 'NONE', *, *, #42763, .T. ) ;
#36951 = CARTESIAN_POINT ( 'NONE',  ( 7.173022332454967120, -4.176053281294514363, 33.81426240980091791 ) ) ;
#36952 = CARTESIAN_POINT ( 'NONE',  ( 3.230769230769231726, -3.937682226553329556, 33.60647404775216529 ) ) ;
#36953 = AXIS2_PLACEMENT_3D ( 'NONE', #66984, #5719, #81833 ) ;
#36954 = CARTESIAN_POINT ( 'NONE',  ( -1.515306851282940181, -4.118384482072085184, 33.43331474514187107 ) ) ;
#36955 = LINE ( 'NONE', #2278, #40769 ) ;
#36956 = ORIENTED_EDGE ( 'NONE', *, *, #70331, .F. ) ;
#36957 = CARTESIAN_POINT ( 'NONE',  ( -8.992097032293871806, -2.251424796025575326, 29.88072029997477941 ) ) ;
#36958 = EDGE_CURVE ( 'NONE', #52415, #1493, #80260, .T. ) ;
#36959 = VERTEX_POINT ( 'NONE', #46468 ) ;
#36960 = CARTESIAN_POINT ( 'NONE',  ( -17.77722033102192967, -12.11081565061824250, 32.26097654155340422 ) ) ;
#36961 = CARTESIAN_POINT ( 'NONE',  ( -3.903846153846087574, -7.434744429011176159, 34.75000000000000711 ) ) ;
#36962 = ORIENTED_EDGE ( 'NONE', *, *, #25122, .T. ) ;
#36963 = EDGE_CURVE ( 'NONE', #57712, #51469, #57646, .T. ) ;
#36964 = CARTESIAN_POINT ( 'NONE',  ( 11.53846153846141576, -12.70778746994576025, 30.41441678777401236 ) ) ;
#36965 = CARTESIAN_POINT ( 'NONE',  ( 10.68145296638705410, -3.050289026998446840, 32.03036669348366416 ) ) ;
#36966 = FACE_OUTER_BOUND ( 'NONE', #86096, .T. ) ;
#36967 = LINE ( 'NONE', #84300, #46323 ) ;
#36968 = CARTESIAN_POINT ( 'NONE',  ( -18.24997673094235395, -4.236021600441996604, 33.53823185664189310 ) ) ;
#36969 = ORIENTED_EDGE ( 'NONE', *, *, #48723, .F. ) ;
#36970 = EDGE_LOOP ( 'NONE', ( #30745, #17298, #45853, #39697 ) ) ;
#36971 = ADVANCED_FACE ( 'NONE', ( #81154 ), #48230, .T. ) ;
#36972 = FACE_BOUND ( 'NONE', #28349, .T. ) ;
#36973 = ORIENTED_EDGE ( 'NONE', *, *, #54235, .T. ) ;
#36974 = CARTESIAN_POINT ( 'NONE',  ( -8.096130590202436750, -5.643011162660950042, 34.66104346484419096 ) ) ;
#36975 = B_SPLINE_CURVE_WITH_KNOTS ( 'NONE', 3,
 ( #74393, #510, #33844, #12692, #12246, #40177, #64, #27535, #20772, #75711 ),
 .UNSPECIFIED., .F., .F.,
 ( 4, 2, 2, 2, 4 ),
 ( 0.000000000000000000, 0.0001954339857564076641, 0.0003908679715128153282, 0.0005863019572692229923, 0.0007817359430256306564 ),
 .UNSPECIFIED. ) ;
#36976 = VECTOR ( 'NONE', #9617, 1000.000000000000000 ) ;
#36977 = CARTESIAN_POINT ( 'NONE',  ( 6.000000000000001776, -10.67929555188718282, 33.92786785259544047 ) ) ;
#36978 = CARTESIAN_POINT ( 'NONE',  ( -14.17690049986751433, -8.999086150933475636, 34.52020707165672775 ) ) ;
#36979 = VERTEX_POINT ( 'NONE', #61293 ) ;
#36980 = ORIENTED_EDGE ( 'NONE', *, *, #34632, .F. ) ;
#36981 = CARTESIAN_POINT ( 'NONE',  ( 16.82694634598072270, -4.236021600441997492, 33.53823185664189310 ) ) ;
#36982 = ORIENTED_EDGE ( 'NONE', *, *, #13527, .T. ) ;
#36983 = FACE_OUTER_BOUND ( 'NONE', #2595, .T. ) ;
#36984 = EDGE_CURVE ( 'NONE', #80414, #84227, #53667, .T. ) ;
#36985 = DIRECTION ( 'NONE',  ( 0.000000000000000000, 0.3420201433256641055, -0.9396926207859100932 ) ) ;
#36986 = EDGE_CURVE ( 'NONE', #23542, #1333, #80718, .T. ) ;
#36987 = CARTESIAN_POINT ( 'NONE',  ( -12.46153846153814726, -2.255955759149395501, 30.00000000000324363 ) ) ;
#36988 = FACE_BOUND ( 'NONE', #8868, .T. ) ;
#36989 = ORIENTED_EDGE ( 'NONE', *, *, #24444, .T. ) ;
#36990 = B_SPLINE_CURVE_WITH_KNOTS ( 'NONE', 3,
 ( #39831, #11916, #81261, #47453, #60974, #19112, #33065, #33516, #88479, #32615 ),
 .UNSPECIFIED., .F., .F.,
 ( 4, 2, 2, 2, 4 ),
 ( 0.0007817359430256390048, 0.0009771253907250075990, 0.001172514838424376085, 0.001367904286123744571, 0.001563293733823113056 ),
 .UNSPECIFIED. ) ;
#36991 = CARTESIAN_POINT ( 'NONE',  ( -9.692307692307691624, -11.33034616979429110, 35.88435417666054406 ) ) ;
#36992 = EDGE_CURVE ( 'NONE', #21128, #67701, #87936, .T. ) ;
#36993 = CARTESIAN_POINT ( 'NONE',  ( -6.250023224221455287, -6.652501968072646932, 34.93155406624980941 ) ) ;
#36994 = AXIS2_PLACEMENT_3D ( 'NONE', #85090, #57607, #15306 ) ;
#36995 = ADVANCED_FACE ( 'NONE', ( #32957 ), #20331, .F. ) ;
#36996 = CARTESIAN_POINT ( 'NONE',  ( 8.899756470994335089, -3.285477652293413264, 32.44071101563363158 ) ) ;
#36997 = CARTESIAN_POINT ( 'NONE',  ( -1.319360245102545681, -3.083524468853784839, 32.58852847137153930 ) ) ;
#36998 = ORIENTED_EDGE ( 'NONE', *, *, #7321, .F. ) ;
#36999 = EDGE_LOOP ( 'NONE', ( #26182, #15364 ) ) ;
#37000 = VERTEX_POINT ( 'NONE', #67188 ) ;
#37002 = CARTESIAN_POINT ( 'NONE',  ( 5.934729554039225974, -3.300289026998414865, 32.46337939537583139 ) ) ;
#37001 = DIRECTION ( 'NONE',  ( 0.000000000000000000, 0.000000000000000000, 1.000000000000000000 ) ) ;
#37003 = FACE_OUTER_BOUND ( 'NONE', #43316, .T. ) ;
#37004 = CARTESIAN_POINT ( 'NONE',  ( -3.903900635498011251, -4.336752205174647656, 33.62275283266504289 ) ) ;
#37005 = CARTESIAN_POINT ( 'NONE',  ( 7.780883400193070898, -12.46129190929999986, 30.37095296980880832 ) ) ;
#37006 = CARTESIAN_POINT ( 'NONE',  ( -15.36145983387954139, -3.338472653186243644, 32.95098750199972670 ) ) ;
#37007 = ORIENTED_EDGE ( 'NONE', *, *, #46527, .T. ) ;
#37008 = LINE ( 'NONE', #64471, #21290 ) ;
#37009 = CARTESIAN_POINT ( 'NONE',  ( -0.2114840416250089172, -3.435999193479610803, 33.07426656108012963 ) ) ;
#37011 = DIRECTION ( 'NONE',  ( -1.000000000000000000, -0.000000000000000000, -0.000000000000000000 ) ) ;
#37010 = B_SPLINE_CURVE_WITH_KNOTS ( 'NONE', 3,
 ( #50350, #77831, #16137, #9386, #80966, #74638, #80058, #53013, #87729, #26001 ),
 .UNSPECIFIED., .F., .F.,
 ( 4, 2, 2, 2, 4 ),
 ( 0.000000000000000000, 0.0001954339857564079894, 0.0003908679715128159787, 0.0005863019572692239681, 0.0007817359430256319575 ),
 .UNSPECIFIED. ) ;
#37012 = CARTESIAN_POINT ( 'NONE',  ( 6.166666666666664298, -7.500000000000000000, 29.75000000000000355 ) ) ;
#37013 = EDGE_LOOP ( 'NONE', ( #54281, #24200 ) ) ;
#37014 = B_SPLINE_CURVE_WITH_KNOTS ( 'NONE', 3,
 ( #25377, #11875, #65906, #52840, #32570, #39352, #39790, #46096, #25826, #73122 ),
 .UNSPECIFIED., .F., .F.,
 ( 4, 2, 2, 2, 4 ),
 ( 0.000000000000000000, 0.0001954339857564081791, 0.0003908679715128163582, 0.0005863019572692245102, 0.0007817359430256327164 ),
 .UNSPECIFIED. ) ;
#37015 = EDGE_LOOP ( 'NONE', ( #16298, #85581, #231, #18051 ) ) ;
#37017 = FACE_BOUND ( 'NONE', #47498, .T. ) ;
#37016 = B_SPLINE_CURVE_WITH_KNOTS ( 'NONE', 3,
 ( #88813, #6387, #82925, #12688, #54546, #27973, #20338, #26201, #82042, #61 ),
 .UNSPECIFIED., .F., .F.,
 ( 4, 2, 2, 2, 4 ),
 ( 0.0007817246256747452209, 0.0009771112852218887673, 0.001172497944769032531, 0.001367884604316176294, 0.001563271263863319840 ),
 .UNSPECIFIED. ) ;
#37018 = DIRECTION ( 'NONE',  ( 0.000000000000000000, 0.4999999999999960032, -0.8660254037844410391 ) ) ;
#37019 = CARTESIAN_POINT ( 'NONE',  ( 14.30769230769218758, -11.94971097300221174, 32.03036669348237098 ) ) ;
#37020 = VERTEX_POINT ( 'NONE', #88369 ) ;
#37021 = CARTESIAN_POINT ( 'NONE',  ( 4.087763774486018242, -11.35647404775217595, 33.31231777344666511 ) ) ;
#37022 = CARTESIAN_POINT ( 'NONE',  ( 6.923076923076924238, -10.51840700105979565, 33.73612834413961536 ) ) ;
#37023 = CARTESIAN_POINT ( 'NONE',  ( 8.638540166120462160, -8.191372820521381826, 34.95448215188423546 ) ) ;
#37024 = CARTESIAN_POINT ( 'NONE',  ( -4.153846153846152411, -4.102666532097928531, 36.13435417666054406 ) ) ;
#37025 = ORIENTED_EDGE ( 'NONE', *, *, #39848, .T. ) ;
#37026 = DIRECTION ( 'NONE',  ( 0.000000000000000000, 0.3420201433256641055, -0.9396926207859100932 ) ) ;
#37027 = EDGE_LOOP ( 'NONE', ( #64138, #14568, #69514, #33046 ) ) ;
#37029 = ORIENTED_EDGE ( 'NONE', *, *, #61153, .F. ) ;
#37028 = CARTESIAN_POINT ( 'NONE',  ( 13.51540719244017730, -12.11778462344221019, 31.66786338562085135 ) ) ;
#37030 = CARTESIAN_POINT ( 'NONE',  ( -18.22305672590244896, -12.75000000000001066, 29.61950333530916168 ) ) ;
#37031 = CARTESIAN_POINT ( 'NONE',  ( 14.98074599347626545, -2.823816976329317274, 31.52131813110795733 ) ) ;
#37032 = DIRECTION ( 'NONE',  ( 0.000000000000000000, 0.000000000000000000, 1.000000000000000000 ) ) ;
#37033 = EDGE_CURVE ( 'NONE', #17504, #20844, #32502, .T. ) ;
#37034 = AXIS2_PLACEMENT_3D ( 'NONE', #21731, #62262, #48753 ) ;
#37035 = CARTESIAN_POINT ( 'NONE',  ( -12.33074665371367828, -2.729792928343269587, 31.24908615093345077 ) ) ;
#37036 = CARTESIAN_POINT ( 'NONE',  ( 6.923076923076924238, -12.78798330534102945, 29.74999999999997868 ) ) ;
#37037 = CARTESIAN_POINT ( 'NONE',  ( 12.39626846098214052, -5.941354392334499579, 34.76329471203369792 ) ) ;
#37038 = CARTESIAN_POINT ( 'NONE',  ( 1.139087296526029469, -10.24999999999999467, 24.70312500000000000 ) ) ;
#37039 = ORIENTED_EDGE ( 'NONE', *, *, #34870, .F. ) ;
#37040 = AXIS2_PLACEMENT_3D ( 'NONE', #59829, #32365, #88665 ) ;
#37041 = CARTESIAN_POINT ( 'NONE',  ( 13.63466980452883526, -12.65882529074907126, 30.72640787790839312 ) ) ;
#37042 = LINE ( 'NONE', #23099, #35217 ) ;
#37043 = VERTEX_POINT ( 'NONE', #60867 ) ;
#37044 = ORIENTED_EDGE ( 'NONE', *, *, #47610, .T. ) ;
#37045 = VERTEX_POINT ( 'NONE', #13566 ) ;
#37046 = CARTESIAN_POINT ( 'NONE',  ( -19.50000000000000000, -3.499999999999999556, 29.75000000000000355 ) ) ;
#37047 = CARTESIAN_POINT ( 'NONE',  ( -14.30769230769230660, -2.486705287966279876, 31.30864560766543647 ) ) ;
#37048 = CARTESIAN_POINT ( 'NONE',  ( 2.980792499826877773, -9.943427161483782584, 34.11278801902876978 ) ) ;
#37049 = ADVANCED_FACE ( 'NONE', ( #82039 ), #59976, .F. ) ;
#37050 = B_SPLINE_CURVE_WITH_KNOTS ( 'NONE', 3,
 ( #21262, #41997, #60485, #40224, #67692, #48736, #34335, #5997, #33017, #33460 ),
 .UNSPECIFIED., .F., .F.,
 ( 4, 2, 2, 2, 4 ),
 ( 0.000000000000000000, 0.0001954339857564080707, 0.0003908679715128161414, 0.0005863019572692241849, 0.0007817359430256322827 ),
 .UNSPECIFIED. ) ;
#37051 = CARTESIAN_POINT ( 'NONE',  ( 9.626224281351811740, -12.37446782046654192, 30.86335684631486487 ) ) ;
#37052 = CARTESIAN_POINT ( 'NONE',  ( -4.826977558574935045, -3.712312575010499494, 33.01462480002815170 ) ) ;
#37053 = CARTESIAN_POINT ( 'NONE',  ( -9.019254006523732770, -11.86270091957321249, 32.19358267280087915 ) ) ;
#37054 = B_SPLINE_CURVE_WITH_KNOTS ( 'NONE', 3,
 ( #79970, #45282, #18272, #10179, #73217, #37641, #85842, #66456, #4762, #52926 ),
 .UNSPECIFIED., .F., .F.,
 ( 4, 2, 2, 2, 4 ),
 ( 0.000000000000000000, 0.0001954311564186862510, 0.0003908623128373725020, 0.0005862934692560588072, 0.0007817246256747450040 ),
 .UNSPECIFIED. ) ;
#37055 = CARTESIAN_POINT ( 'NONE',  ( 6.130047435250454591, -7.723484941389743952, 34.99544897038808955 ) ) ;
#37056 = VERTEX_POINT ( 'NONE', #41047 ) ;
#37057 = CARTESIAN_POINT ( 'NONE',  ( -1.576923076923076872, -7.500000000000000000, 29.75000000000000355 ) ) ;
#37058 = CYLINDRICAL_SURFACE ( 'NONE', #52039, 0.2500000000000008882 ) ;
#37059 = CARTESIAN_POINT ( 'NONE',  ( -8.769230769230768274, -11.35647404775217417, 33.31231777344666511 ) ) ;
#37060 = CARTESIAN_POINT ( 'NONE',  ( 2.084207363968359150, -3.754499324213721234, 33.06261337010820256 ) ) ;
#37061 = VERTEX_POINT ( 'NONE', #58 ) ;
#37062 = DIRECTION ( 'NONE',  ( -0.000000000000000000, 0.7660444431189791237, -0.6427876096865379196 ) ) ;
#37063 = ADVANCED_FACE ( 'NONE', ( #26641 ), #47796, .F. ) ;
#37064 = VERTEX_POINT ( 'NONE', #68079 ) ;
#37065 = AXIS2_PLACEMENT_3D ( 'NONE', #70024, #1126, #49316 ) ;
#37066 = CARTESIAN_POINT ( 'NONE',  ( 14.98074599347626545, -11.37209801155882793, 32.91403422569033665 ) ) ;
#37067 = CARTESIAN_POINT ( 'NONE',  ( -3.165513659493206067, -2.892918686051626498, 31.69288490824026638 ) ) ;
#37068 = CARTESIAN_POINT ( 'NONE',  ( -2.438169015808770546, -7.276988635370450709, 34.74523720219453793 ) ) ;
#37069 = ORIENTED_EDGE ( 'NONE', *, *, #34867, .F. ) ;
#37070 = ADVANCED_FACE ( 'NONE', ( #54099 ), #6805, .F. ) ;
#37071 = CARTESIAN_POINT ( 'NONE',  ( -23.50000000000000000, 5.000000000000023093, 32.75000000000000000 ) ) ;
#37072 = DIRECTION ( 'NONE',  ( 1.000000000000000000, 0.000000000000000000, 0.000000000000000000 ) ) ;
#37073 = CARTESIAN_POINT ( 'NONE',  ( -4.230769230769230838, -3.499999999999999556, 29.75000000000000355 ) ) ;
#37074 = CYLINDRICAL_SURFACE ( 'NONE', #6344, 0.2500000000000012212 ) ;
#37075 = AXIS2_PLACEMENT_3D ( 'NONE', #37406, #58121, #37859 ) ;
#37076 = ORIENTED_EDGE ( 'NONE', *, *, #72866, .F. ) ;
#37077 = ADVANCED_FACE ( 'NONE', ( #87475 ), #41485, .F. ) ;
#37078 = CARTESIAN_POINT ( 'NONE',  ( -0.7115616988314267255, -8.432397168068783699, 34.66272746175022945 ) ) ;
#37079 = VERTEX_POINT ( 'NONE', #53216 ) ;
#37080 = CARTESIAN_POINT ( 'NONE',  ( -9.692307692307812417, -12.27809138561165270, 31.22303859784587132 ) ) ;
#37081 = EDGE_CURVE ( 'NONE', #21191, #3730, #83818, .T. ) ;
#37082 = CARTESIAN_POINT ( 'NONE',  ( -16.28453762051371356, -11.18331474514187995, 33.13161551792790505 ) ) ;
#37083 = CARTESIAN_POINT ( 'NONE',  ( -6.250023237292963607, -2.587272538249754117, 30.68239716806877837 ) ) ;
#37084 = EDGE_CURVE ( 'NONE', #53391, #59157, #9795, .T. ) ;
#37085 = LINE ( 'NONE', #36224, #63771 ) ;
#37086 = B_SPLINE_CURVE_WITH_KNOTS ( 'NONE', 3,
 ( #68508, #74841, #32503, #53668, #59977, #60868 ),
 .UNSPECIFIED., .F., .F.,
 ( 4, 2, 4 ),
 ( 0.000000000000000000, 0.0001954784845028913534, 0.0003909569690057827069 ),
 .UNSPECIFIED. ) ;
#37087 = CARTESIAN_POINT ( 'NONE',  ( -13.63461538461538325, -7.500000000000001776, 35.00000000000000000 ) ) ;
#37088 = EDGE_LOOP ( 'NONE', ( #69224, #50056 ) ) ;
#37089 = B_SPLINE_CURVE_WITH_KNOTS ( 'NONE', 3,
 ( #13778, #28177, #76366, #1604, #48002, #29092, #82700, #49348, #56545, #1155 ),
 .UNSPECIFIED., .F., .F.,
 ( 4, 2, 2, 2, 4 ),
 ( 0.0007817359430256390048, 0.0009771253907250078159, 0.001172514838424376735, 0.001367904286123745655, 0.001563293733823114574 ),
 .UNSPECIFIED. ) ;
#37090 = AXIS2_PLACEMENT_3D ( 'NONE', #32950, #60857, #46458 ) ;
#37091 = VERTEX_POINT ( 'NONE', #69403 ) ;
#37092 = ORIENTED_EDGE ( 'NONE', *, *, #34902, .T. ) ;
#37093 = EDGE_CURVE ( 'NONE', #29234, #87291, #64725, .T. ) ;
#37094 = CARTESIAN_POINT ( 'NONE',  ( 1.384615384615386802, -9.058645607665452459, 34.76329471203371924 ) ) ;
#37095 = CARTESIAN_POINT ( 'NONE',  ( 11.53846153846153832, -9.058645607665452459, 34.76329471203371924 ) ) ;
#37096 = AXIS2_PLACEMENT_3D ( 'NONE', #22955, #44989, #66154 ) ;
#37097 = CARTESIAN_POINT ( 'NONE',  ( -15.00775787915638126, -9.086983370893049639, 34.49168942202179267 ) ) ;
#37098 = DIRECTION ( 'NONE',  ( -0.000000000000000000, -0.9396926207859092051, -0.3420201433256662704 ) ) ;
#37099 = CARTESIAN_POINT ( 'NONE',  ( 7.716005876422150855, -12.70455904226513866, 30.44083106164009322 ) ) ;
#37100 = CARTESIAN_POINT ( 'NONE',  ( 17.07692307692307665, -9.905515769479276145, 34.41647553114623292 ) ) ;
#37101 = CARTESIAN_POINT ( 'NONE',  ( -17.93393164899755732, -9.780366693483671270, 34.19971097300155805 ) ) ;
#37102 = ADVANCED_FACE ( 'NONE', ( #49572 ), #940, .T. ) ;
#37103 = CARTESIAN_POINT ( 'NONE',  ( 9.692307692307570832, -10.33852847137269571, 34.16647553114546554 ) ) ;
#37104 = ORIENTED_EDGE ( 'NONE', *, *, #74459, .F. ) ;
#37105 = ORIENTED_EDGE ( 'NONE', *, *, #24529, .F. ) ;
#37106 = EDGE_LOOP ( 'NONE', ( #62460, #44615 ) ) ;
#37108 = ORIENTED_EDGE ( 'NONE', *, *, #33742, .T. ) ;
#37107 = CARTESIAN_POINT ( 'NONE',  ( 11.60452887181161508, -2.486705287966280320, 31.30864560766543647 ) ) ;
#37110 = CARTESIAN_POINT ( 'NONE',  ( -10.48485917715097138, -6.808710257144161559, 34.95449254468098843 ) ) ;
#37109 = DIRECTION ( 'NONE',  ( -1.000000000000000000, -0.000000000000000000, 0.000000000000000000 ) ) ;
#37111 = CYLINDRICAL_SURFACE ( 'NONE', #60475, 0.2499999999999973355 ) ;
#37112 = CARTESIAN_POINT ( 'NONE',  ( -10.74607608205217346, -11.71456829005830080, 32.44064028649416542 ) ) ;
#37113 = ORIENTED_EDGE ( 'NONE', *, *, #41639, .T. ) ;
#37114 = ADVANCED_FACE ( 'NONE', ( #55879 ), #58409, .F. ) ;
#37115 = ORIENTED_EDGE ( 'NONE', *, *, #69892, .T. ) ;
#37116 = CARTESIAN_POINT ( 'NONE',  ( -11.76194646302586477, -12.11044203135681840, 32.26167407432752299 ) ) ;
#37117 = ORIENTED_EDGE ( 'NONE', *, *, #65655, .F. ) ;
#37118 = FACE_BOUND ( 'NONE', #60812, .T. ) ;
#37119 = CYLINDRICAL_SURFACE ( 'NONE', #40425, 0.2499999999999995559 ) ;
#37120 = VECTOR ( 'NONE', #80013, 1000.000000000000000 ) ;
#37121 = CARTESIAN_POINT ( 'NONE',  ( -4.153846153846152411, -11.69971097300155272, 32.46337939537588113 ) ) ;
#37122 = ORIENTED_EDGE ( 'NONE', *, *, #57477, .F. ) ;
#37123 = EDGE_CURVE ( 'NONE', #82411, #18197, #25439, .T. ) ;
#37124 = CARTESIAN_POINT ( 'NONE',  ( -14.17690186672535901, -8.191423895709840863, 34.95447573519442130 ) ) ;
#37125 = CARTESIAN_POINT ( 'NONE',  ( 3.361294932532796764, -3.285477652293413264, 32.44071101563363158 ) ) ;
#37126 = DIRECTION ( 'NONE',  ( -0.000000000000000000, -0.3420201433256694346, -0.9396926207859080948 ) ) ;
#37127 = ORIENTED_EDGE ( 'NONE', *, *, #11838, .F. ) ;
#37128 = CARTESIAN_POINT ( 'NONE',  ( 17.86939034479591726, -7.722926974430166069, 34.99546784045485737 ) ) ;
#37129 = CYLINDRICAL_SURFACE ( 'NONE', #20760, 0.2500000000000008882 ) ;
#37130 = VERTEX_POINT ( 'NONE', #8148 ) ;
#37131 = AXIS2_PLACEMENT_3D ( 'NONE', #52370, #72199, #72647 ) ;
#37132 = CARTESIAN_POINT ( 'NONE',  ( 8.068933515131909928, -11.60474049983371003, 33.02348890104160262 ) ) ;
#37133 = CARTESIAN_POINT ( 'NONE',  ( -14.30769230769230660, -6.343179335718451384, 34.87096338111211935 ) ) ;
#37134 = CARTESIAN_POINT ( 'NONE',  ( 3.361294932532796320, -4.459921816937789885, 33.71989282347011851 ) ) ;
#37135 = FACE_OUTER_BOUND ( 'NONE', #5490, .T. ) ;
#37136 = CARTESIAN_POINT ( 'NONE',  ( 13.38461538461538680, -2.292212530054420494, 30.41441678777542634 ) ) ;
#37137 = CYLINDRICAL_SURFACE ( 'NONE', #43029, 0.2500000000000002220 ) ;
#37138 = EDGE_CURVE ( 'NONE', #14427, #49108, #3025, .T. ) ;
#37139 = CARTESIAN_POINT ( 'NONE',  ( -13.38461538461550759, -12.51329471203414379, 31.30864560766407578 ) ) ;
#37141 = CYLINDRICAL_SURFACE ( 'NONE', #61805, 0.2499999999999979738 ) ;
#37140 = CARTESIAN_POINT ( 'NONE',  ( -11.53846153846153655, -6.681629849574314051, 35.83090037661290239 ) ) ;
#37142 = VECTOR ( 'NONE', #27503, 1000.000000000000114 ) ;
#37143 = CARTESIAN_POINT ( 'NONE',  ( -0.3954711281883858676, -8.164416787775445883, 34.95778746994558617 ) ) ;
#37145 = DIRECTION ( 'NONE',  ( -0.000000000000000000, 0.3420201433256694346, -0.9396926207859080948 ) ) ;
#37144 = CYLINDRICAL_SURFACE ( 'NONE', #30010, 0.2500000000000009437 ) ;
#37146 = DIRECTION ( 'NONE',  ( 1.000000000000000000, 0.000000000000000000, 0.000000000000000000 ) ) ;
#37147 = CARTESIAN_POINT ( 'NONE',  ( -1.987747218494660295, -5.598659921968651254, 21.24813170625848713 ) ) ;
#37149 = EDGE_CURVE ( 'NONE', #20800, #84823, #1816, .T. ) ;
#37148 = EDGE_LOOP ( 'NONE', ( #26477, #63893, #76861, #3294 ) ) ;
#37150 = B_SPLINE_CURVE_WITH_KNOTS ( 'NONE', 3,
 ( #41265, #29094, #13781, #63297, #75482, #56103, #83597, #34937, #48005, #1606 ),
 .UNSPECIFIED., .F., .F.,
 ( 4, 2, 2, 2, 4 ),
 ( 0.0007817246256747460882, 0.0009771112852218900684, 0.001172497944769033832, 0.001367884604316177595, 0.001563271263863321575 ),
 .UNSPECIFIED. ) ;
#37151 = CARTESIAN_POINT ( 'NONE',  ( 18.22301135161285046, -11.76359900205217457, 32.36225158514719880 ) ) ;
#37152 = ORIENTED_EDGE ( 'NONE', *, *, #7791, .F. ) ;
#37153 = B_SPLINE_CURVE_WITH_KNOTS ( 'NONE', 3,
 ( #45559, #10895, #66727, #52758, #5026, #64935, #80248, #72141, #59073, #87465 ),
 .UNSPECIFIED., .F., .F.,
 ( 4, 2, 2, 2, 4 ),
 ( 0.000000000000000000, 0.0001954311564186861968, 0.0003908623128373723936, 0.0005862934692560585904, 0.0007817246256747447872 ),
 .UNSPECIFIED. ) ;
#37154 = EDGE_CURVE ( 'NONE', #55599, #20857, #39483, .T. ) ;
#37155 = CARTESIAN_POINT ( 'NONE',  ( -2.531177232256639709, -3.019605429927184836, 32.48692288466676814 ) ) ;
#37156 = EDGE_LOOP ( 'NONE', ( #76397, #31253 ) ) ;
#37157 = CARTESIAN_POINT ( 'NONE',  ( -3.931066612577743147, -11.41317474335729187, 32.86274602512330034 ) ) ;
#37158 = ORIENTED_EDGE ( 'NONE', *, *, #25992, .T. ) ;
#37159 = DIRECTION ( 'NONE',  ( -0.000000000000000000, -0.000000000000000000, -1.000000000000000000 ) ) ;
#37160 = CARTESIAN_POINT ( 'NONE',  ( 1.200186371490561621, -10.22469193450123193, 25.70125670625848713 ) ) ;
#37161 = CARTESIAN_POINT ( 'NONE',  ( 17.29970261819148902, -8.496831190052089866, 34.64984203495476578 ) ) ;
#37162 = CARTESIAN_POINT ( 'NONE',  ( -4.153846153846152411, -6.189225973068211317, 35.74407628777942847 ) ) ;
#37163 = FACE_OUTER_BOUND ( 'NONE', #17093, .T. ) ;
#37164 = CARTESIAN_POINT ( 'NONE',  ( 17.99999999999987566, -2.379036618888197729, 30.90682066428292885 ) ) ;
#37165 = EDGE_CURVE ( 'NONE', #28537, #49979, #82922, .T. ) ;
#37166 = DIRECTION ( 'NONE',  ( -1.000000000000000000, 0.000000000000000000, 0.000000000000000000 ) ) ;
#37167 = CARTESIAN_POINT ( 'NONE',  ( -13.51476335434707821, -8.630895178749533159, 34.87696386517710323 ) ) ;
#37168 = CARTESIAN_POINT ( 'NONE',  ( -10.61538461538461320, -1.367168528481310208, 33.57946703557072254 ) ) ;
#37169 = CARTESIAN_POINT ( 'NONE',  ( 1.553300858899129944, -11.24999999999998934, 15.95312500000000000 ) ) ;
#37170 = CARTESIAN_POINT ( 'NONE',  ( -11.53846153846166089, -2.657715359629662544, 31.77849191805970364 ) ) ;
#37171 = CARTESIAN_POINT ( 'NONE',  ( -2.177166869458663889, -12.15418822224088657, 32.17964115625579069 ) ) ;
#37172 = CARTESIAN_POINT ( 'NONE',  ( 10.36540787133602670, -5.643011162660950042, 34.66104346484419096 ) ) ;
#37173 = VECTOR ( 'NONE', #12881, 1000.000000000000227 ) ;
#37174 = CARTESIAN_POINT ( 'NONE',  ( 2.651650429449539104, -4.848349570550432475, 16.81250000000000000 ) ) ;
#37175 = EDGE_LOOP ( 'NONE', ( #73732, #70837, #43917, #59240 ) ) ;
#37176 = CARTESIAN_POINT ( 'NONE',  ( 17.32686859527121470, -12.22109172314383052, 31.39792113162168263 ) ) ;
#37177 = CARTESIAN_POINT ( 'NONE',  ( 12.39545608217832218, -8.164416787775445883, 34.95778746994557906 ) ) ;
#37178 = CARTESIAN_POINT ( 'NONE',  ( -8.992156986746914882, -11.24512374952581872, 33.06303171183252942 ) ) ;
#37179 = CARTESIAN_POINT ( 'NONE',  ( 5.299934428535923558, -2.758310577978207778, 31.33698337089303010 ) ) ;
#37180 = ADVANCED_FACE ( 'NONE', ( #41935 ), #30509, .F. ) ;
#37181 = DIRECTION ( 'NONE',  ( -0.000000000000000000, -0.1736481776669307198, -0.9848077530122080203 ) ) ;
#37182 = CARTESIAN_POINT ( 'NONE',  ( -18.00000000000012079, -2.379036618888197285, 30.90682066428292885 ) ) ;
#37183 = B_SPLINE_CURVE_WITH_KNOTS ( 'NONE', 3,
 ( #20597, #338, #27802, #40884, #75117, #20166, #87761, #40006, #46301, #68347 ),
 .UNSPECIFIED., .F., .F.,
 ( 4, 2, 2, 2, 4 ),
 ( 0.0007817359430256333669, 0.0009771253907250056474, 0.001172514838424370881, 0.001367904286123736331, 0.001563293733823101564 ),
 .UNSPECIFIED. ) ;
#37184 = ORIENTED_EDGE ( 'NONE', *, *, #59065, .T. ) ;
#37185 = DIRECTION ( 'NONE',  ( -1.000000000000000000, -0.000000000000000000, -0.000000000000000000 ) ) ;
#37186 = ORIENTED_EDGE ( 'NONE', *, *, #43900, .T. ) ;
#37187 = B_SPLINE_CURVE_WITH_KNOTS ( 'NONE', 3,
 ( #53446, #73747, #87710, #47132, #12911, #58876, #25982, #24648, #66069, #52996 ),
 .UNSPECIFIED., .F., .F.,
 ( 4, 2, 2, 2, 4 ),
 ( 0.0007817359430256360774, 0.0009771253907250041296, 0.001172514838424371965, 0.001367904286123740017, 0.001563293733823108069 ),
 .UNSPECIFIED. ) ;
#37188 = EDGE_LOOP ( 'NONE', ( #63640, #68292, #2194, #11074 ) ) ;
#37189 = CARTESIAN_POINT ( 'NONE',  ( -5.749945688361685292, -5.728107161865375829, 34.42597550085002922 ) ) ;
#37190 = CIRCLE ( 'NONE', #51568, 2.000000000000001776 ) ;
#37191 = CARTESIAN_POINT ( 'NONE',  ( 3.230769230769231726, -5.557115091759785130, 34.35708131394839171 ) ) ;
#37192 = CARTESIAN_POINT ( 'NONE',  ( -15.29685161012936767, -10.67929555188718460, 33.92786785259543336 ) ) ;
#37193 = CARTESIAN_POINT ( 'NONE',  ( 4.219914504848592429, -3.513871655860379306, 32.76840700105978499 ) ) ;
#37194 = CARTESIAN_POINT ( 'NONE',  ( 17.86930853333243618, -8.999036380462719364, 34.52022231692819076 ) ) ;
#37195 = ORIENTED_EDGE ( 'NONE', *, *, #48700, .F. ) ;
#37196 = CARTESIAN_POINT ( 'NONE',  ( 6.923076923076924238, -1.466349020453238561, 30.81389545987213907 ) ) ;
#37197 = VECTOR ( 'NONE', #70284, 1000.000000000000227 ) ;
#37198 = ORIENTED_EDGE ( 'NONE', *, *, #28435, .T. ) ;
#37199 = EDGE_LOOP ( 'NONE', ( #16625, #88319, #31932, #47705 ) ) ;
#37200 = AXIS2_PLACEMENT_3D ( 'NONE', #62059, #56193, #27394 ) ;
#37201 = EDGE_CURVE ( 'NONE', #58674, #22482, #19054, .T. ) ;
#37202 = CARTESIAN_POINT ( 'NONE',  ( 18.06525513951284267, -2.379036618887895305, 30.90682066428158592 ) ) ;
#37203 = CARTESIAN_POINT ( 'NONE',  ( 17.07692307692307665, -1.466349020453238561, 30.81389545987213907 ) ) ;
#37204 = CARTESIAN_POINT ( 'NONE',  ( -16.37677237136229991, -4.186968288167451036, 33.49512374952580274 ) ) ;
#37205 = EDGE_CURVE ( 'NONE', #85285, #88692, #75990, .T. ) ;
#37206 = CARTESIAN_POINT ( 'NONE',  ( 11.31497661389720655, -10.97335522853832579, 33.68706563782419749 ) ) ;
#37207 = EDGE_CURVE ( 'NONE', #74314, #68579, #87848, .T. ) ;
#37208 = CARTESIAN_POINT ( 'NONE',  ( -6.923076923076922462, -1.044019251281081972, 31.83374038241031911 ) ) ;
#37209 = ORIENTED_EDGE ( 'NONE', *, *, #5978, .T. ) ;
#37210 = VERTEX_POINT ( 'NONE', #32730 ) ;
#37211 = CARTESIAN_POINT ( 'NONE',  ( 1.553300858899129944, -11.24999999999998934, 23.45312500000000000 ) ) ;
#37212 = ORIENTED_EDGE ( 'NONE', *, *, #15160, .F. ) ;
#37214 = ORIENTED_EDGE ( 'NONE', *, *, #73661, .F. ) ;
#37213 = CARTESIAN_POINT ( 'NONE',  ( -2.530618525208453651, -2.758268499246657068, 31.33685645148949561 ) ) ;
#37215 = ADVANCED_FACE ( 'NONE', ( #31400 ), #66061, .F. ) ;
#37216 = CARTESIAN_POINT ( 'NONE',  ( -6.989160334032801458, -12.37446782046654192, 30.86335684631486487 ) ) ;
#37217 = LINE ( 'NONE', #64681, #63309 ) ;
#37218 = CARTESIAN_POINT ( 'NONE',  ( 9.692307692307695177, -9.819645486525091727, 36.12317359536749706 ) ) ;
#37219 = EDGE_LOOP ( 'NONE', ( #45677, #54017, #18605, #75552, #40994, #87303, #36800, #28324 ) ) ;
#37220 = ADVANCED_FACE ( 'NONE', ( #17892 ), #65612, .T. ) ;
#37221 = CARTESIAN_POINT ( 'NONE',  ( -11.28846153846153655, -7.500000000000001776, 35.04278698407183867 ) ) ;
#37222 = ORIENTED_EDGE ( 'NONE', *, *, #759, .F. ) ;
#37223 = CARTESIAN_POINT ( 'NONE',  ( -10.68065461594093435, -5.094484230520674117, 34.41647553114621161 ) ) ;
#37224 = CARTESIAN_POINT ( 'NONE',  ( 17.99999999999987566, -12.70778746994576025, 30.41441678777401236 ) ) ;
#37225 = PLANE ( 'NONE',  #84076 ) ;
#37227 = CARTESIAN_POINT ( 'NONE',  ( 4.946231610255517275, -3.062553014421049546, 32.05460306192773601 ) ) ;
#37226 = CARTESIAN_POINT ( 'NONE',  ( -18.00000000000000000, -13.49681301100524244, 30.80739993210377392 ) ) ;
#37228 = CARTESIAN_POINT ( 'NONE',  ( -8.769230769230768274, -1.790695186598648903, 34.54067556320373455 ) ) ;
#37229 = FACE_OUTER_BOUND ( 'NONE', #64649, .T. ) ;
#37230 = VERTEX_POINT ( 'NONE', #73279 ) ;
#37231 = CARTESIAN_POINT ( 'NONE',  ( 5.076923076922953193, -4.320704448113951379, 33.92786785259630022 ) ) ;
#37232 = ORIENTED_EDGE ( 'NONE', *, *, #80169, .F. ) ;
#37233 = CARTESIAN_POINT ( 'NONE',  ( 11.40831356872984870, -12.15440758774515473, 32.17923288041532004 ) ) ;
#37234 = DIRECTION ( 'NONE',  ( 0.000000000000000000, 0.000000000000000000, -1.000000000000000000 ) ) ;
#37235 = DIRECTION ( 'NONE',  ( -0.000000000000000000, 1.000000000000000000, 3.491481338843133355E-15 ) ) ;
#37236 = CARTESIAN_POINT ( 'NONE',  ( 2.242422307135989890, -5.941354392334500467, 34.76329471203369792 ) ) ;
#37237 = CARTESIAN_POINT ( 'NONE',  ( -0.3962828902624366822, -12.46129190930001052, 30.37095296980870174 ) ) ;
#37238 = LINE ( 'NONE', #52087, #42971 ) ;
#37239 = FACE_BOUND ( 'NONE', #85860, .T. ) ;
#37241 = CARTESIAN_POINT ( 'NONE',  ( 1.449870955891410906, -2.625532179533470067, 30.86335684631491105 ) ) ;
#37240 = CARTESIAN_POINT ( 'NONE',  ( -11.53846153846153655, -13.57706302396349152, 30.56769352161908060 ) ) ;
#37242 = CYLINDRICAL_SURFACE ( 'NONE', #5099, 0.2500000000000009437 ) ;
#37244 = CARTESIAN_POINT ( 'NONE',  ( 9.942362003946010773, -4.235687564193448829, 33.53795663066793509 ) ) ;
#37243 = CARTESIAN_POINT ( 'NONE',  ( -3.007757879156381264, -11.76359900205217457, 32.36225158514719880 ) ) ;
#37245 = CARTESIAN_POINT ( 'NONE',  ( 2.307692307692309264, -4.786620604624113540, 33.94971097300155094 ) ) ;
#37246 = CARTESIAN_POINT ( 'NONE',  ( -3.775308065498766297, -6.007798216065450170, 21.17000670625848713 ) ) ;
#37247 = EDGE_CURVE ( 'NONE', #48006, #14278, #35161, .T. ) ;
#37248 = ORIENTED_EDGE ( 'NONE', *, *, #73615, .T. ) ;
#37249 = AXIS2_PLACEMENT_3D ( 'NONE', #3747, #37527, #45624 ) ;
#37250 = CARTESIAN_POINT ( 'NONE',  ( -7.912237257109724808, -11.16473453929635440, 33.15142922261925662 ) ) ;
#37251 = EDGE_CURVE ( 'NONE', #78822, #33344, #86369, .T. ) ;
#37252 = B_SPLINE_CURVE_WITH_KNOTS ( 'NONE', 3,
 ( #58850, #86356, #71474, #10235, #2568, #78689, #9781, #72807, #22848, #37693 ),
 .UNSPECIFIED., .F., .F.,
 ( 4, 2, 2, 2, 4 ),
 ( 0.000000000000000000, 0.0001954339857564079352, 0.0003908679715128158703, 0.0005863019572692237513, 0.0007817359430256317406 ),
 .UNSPECIFIED. ) ;
#37253 = CARTESIAN_POINT ( 'NONE',  ( 8.769230769230768274, -6.343179335718451384, 34.87096338111211935 ) ) ;
#37254 = CARTESIAN_POINT ( 'NONE',  ( -9.442253380669374252, -9.148310452688876993, 34.47095581063188519 ) ) ;
#37255 = CARTESIAN_POINT ( 'NONE',  ( -9.915233909823836456, -10.61292498521070549, 33.66303323003028680 ) ) ;
#37256 = CARTESIAN_POINT ( 'NONE',  ( 3.361294932532794988, -6.852161475712352789, 34.70806712695775786 ) ) ;
#37257 = CARTESIAN_POINT ( 'NONE',  ( -9.692307692307691624, -4.098570777380720287, 33.41473453929634729 ) ) ;
#37258 = CARTESIAN_POINT ( 'NONE',  ( -1.492201783934549164, -11.27530806549876807, 19.60750670625849068 ) ) ;
#37259 = CARTESIAN_POINT ( 'NONE',  ( -11.28846153846160050, -7.565270000091922853, 34.99999999999999289 ) ) ;
#37260 = DIRECTION ( 'NONE',  ( -0.000000000000000000, 1.000000000000000000, -0.000000000000000000 ) ) ;
#37261 = VECTOR ( 'NONE', #10075, 1000.000000000000227 ) ;
#37262 = EDGE_CURVE ( 'NONE', #66893, #72317, #71677, .T. ) ;
#37263 = DIRECTION ( 'NONE',  ( -0.000000000000000000, -0.000000000000000000, -1.000000000000000000 ) ) ;
#37264 = CARTESIAN_POINT ( 'NONE',  ( 10.54930223602447903, -6.343179335718451384, 34.87096338111212646 ) ) ;
#37265 = DIRECTION ( 'NONE',  ( 1.000000000000000000, 0.000000000000000000, 0.000000000000000000 ) ) ;
#37266 = DIRECTION ( 'NONE',  ( -0.000000000000000000, 0.5000000000000011102, -0.8660254037844381525 ) ) ;
#37267 = VECTOR ( 'NONE', #65075, 1000.000000000000000 ) ;
#37268 = B_SPLINE_CURVE_WITH_KNOTS ( 'NONE', 3,
 ( #49029, #40519, #19790, #42288, #69744, #67986, #6286, #1730, #15695, #43161 ),
 .UNSPECIFIED., .F., .F.,
 ( 4, 2, 2, 2, 4 ),
 ( 0.000000000000000000, 0.0001954311564186875792, 0.0003908623128373751583, 0.0005862934692560627103, 0.0007817246256747503166 ),
 .UNSPECIFIED. ) ;
#37269 = CARTESIAN_POINT ( 'NONE',  ( -6.223484924564329113, -12.11044203135681840, 32.26167407432752299 ) ) ;
#37270 = EDGE_CURVE ( 'NONE', #55151, #81591, #39064, .T. ) ;
#37271 = DIRECTION ( 'NONE',  ( -1.000000000000000000, 0.000000000000000000, -0.000000000000000000 ) ) ;
#37272 = EDGE_LOOP ( 'NONE', ( #76980, #53072, #55615, #36226 ) ) ;
#37273 = DIRECTION ( 'NONE',  ( -0.000000000000000000, 0.5000000000000011102, -0.8660254037844381525 ) ) ;
#37274 = CARTESIAN_POINT ( 'NONE',  ( -17.30040802064702632, -2.847400154188068910, 31.58180166144859768 ) ) ;
#37275 = CARTESIAN_POINT ( 'NONE',  ( 3.724691934501251023, -9.114399933863618131, 16.04874329374151287 ) ) ;
#37276 = CARTESIAN_POINT ( 'NONE',  ( 6.923076923076800782, -5.094484230521993062, 34.41647553114689373 ) ) ;
#37277 = CARTESIAN_POINT ( 'NONE',  ( -5.326899807865432379, -2.564618984488975961, 30.55390908950641915 ) ) ;
#37278 = ORIENTED_EDGE ( 'NONE', *, *, #56870, .T. ) ;
#37279 = CARTESIAN_POINT ( 'NONE',  ( -6.792286482109972212, -9.929761469519744921, 34.40412654351204225 ) ) ;
#37281 = EDGE_LOOP ( 'NONE', ( #26364, #78753, #37558, #12161 ) ) ;
#37280 = CARTESIAN_POINT ( 'NONE',  ( 4.088575707885377497, -6.026961402152685388, 34.52809138561120506 ) ) ;
#37282 = CARTESIAN_POINT ( 'NONE',  ( -12.52762084089859407, -9.058645607665454236, 34.76329471203372634 ) ) ;
#37283 = DIRECTION ( 'NONE',  ( -0.000000000000000000, 0.8660254037844399289, -0.4999999999999980016 ) ) ;
#37284 = EDGE_CURVE ( 'NONE', #78742, #72334, #55581, .T. ) ;
#37285 = CARTESIAN_POINT ( 'NONE',  ( -8.638705067467203236, -2.619367082507849442, 30.83698974864643461 ) ) ;
#37286 = DIRECTION ( 'NONE',  ( -0.000000000000000000, 0.9848077530122086864, -0.1736481776669273891 ) ) ;
#37287 = VERTEX_POINT ( 'NONE', #40828 ) ;
#37288 = LINE ( 'NONE', #56686, #131 ) ;
#37289 = EDGE_CURVE ( 'NONE', #20449, #20445, #42165, .T. ) ;
#37290 = ADVANCED_FACE ( 'NONE', ( #27747 ), #54326, .F. ) ;
#37291 = CARTESIAN_POINT ( 'NONE',  ( -15.84615384615384670, -11.00000000000000000, 29.75000000000000355 ) ) ;
#37292 = B_SPLINE_CURVE_WITH_KNOTS ( 'NONE', 3,
 ( #68556, #68127, #19927, #81202, #33452, #6427, #7309, #54591, #61790, #14057 ),
 .UNSPECIFIED., .F., .F.,
 ( 4, 2, 2, 2, 4 ),
 ( 0.0007817359430256339090, 0.0009771253907250065148, 0.001172514838424371965, 0.001367904286123737632, 0.001563293733823103299 ),
 .UNSPECIFIED. ) ;
#37293 = CARTESIAN_POINT ( 'NONE',  ( -1.318547033612945896, -5.557115091759786019, 34.35708131394839882 ) ) ;
#37294 = ORIENTED_EDGE ( 'NONE', *, *, #9784, .F. ) ;
#37295 = EDGE_LOOP ( 'NONE', ( #31078, #30381 ) ) ;
#37296 = EDGE_CURVE ( 'NONE', #60879, #24900, #66257, .T. ) ;
#37297 = ORIENTED_EDGE ( 'NONE', *, *, #28018, .F. ) ;
#37298 = CARTESIAN_POINT ( 'NONE',  ( 3.453548899747296730, -2.353885683473778023, 30.79025554430704759 ) ) ;
#37299 = CARTESIAN_POINT ( 'NONE',  ( -8.769230769230890843, -3.300289026999228881, 32.46337939537708905 ) ) ;
#37300 = CARTESIAN_POINT ( 'NONE',  ( 3.230769230769231726, -12.62096338111211580, 30.90682066428153263 ) ) ;
#37301 = FACE_OUTER_BOUND ( 'NONE', #12171, .T. ) ;
#37302 = ORIENTED_EDGE ( 'NONE', *, *, #48133, .F. ) ;
#37303 = VERTEX_POINT ( 'NONE', #88597 ) ;
#37305 = EDGE_LOOP ( 'NONE', ( #30662, #81778, #62134, #72119 ) ) ;
#37304 = CARTESIAN_POINT ( 'NONE',  ( 11.76147438255493327, -11.43677907613344757, 33.22367315496202167 ) ) ;
#37306 = CARTESIAN_POINT ( 'NONE',  ( 9.757563263583717728, -12.46129190930001052, 30.37095296980870174 ) ) ;
#37307 = AXIS2_PLACEMENT_3D ( 'NONE', #26176, #13110, #5019 ) ;
#37308 = VECTOR ( 'NONE', #8420, 1000.000000000000227 ) ;
#37309 = CARTESIAN_POINT ( 'NONE',  ( 10.36536137809165403, -11.37209801155882793, 32.91403422569033665 ) ) ;
#37310 = CARTESIAN_POINT ( 'NONE',  ( 16.15384615384615330, -11.35647404775217417, 33.31231777344666511 ) ) ;
#37311 = VERTEX_POINT ( 'NONE', #81820 ) ;
#37312 = VECTOR ( 'NONE', #10917, 1000.000000000000000 ) ;
#37313 = VERTEX_POINT ( 'NONE', #82708 ) ;
#37315 = ORIENTED_EDGE ( 'NONE', *, *, #86831, .T. ) ;
#37314 = DIRECTION ( 'NONE',  ( -0.000000000000000000, 0.8660254037844399289, -0.4999999999999980016 ) ) ;
#37316 = ADVANCED_FACE ( 'NONE', ( #76376 ), #27308, .F. ) ;
#37317 = VECTOR ( 'NONE', #15370, 1000.000000000000000 ) ;
#37318 = CARTESIAN_POINT ( 'NONE',  ( -14.16025641025641058, -11.00000000000000000, 29.75000000000000355 ) ) ;
#37319 = CARTESIAN_POINT ( 'NONE',  ( -16.08777780284371417, -3.513871655860379306, 32.76840700105978499 ) ) ;
#37320 = ORIENTED_EDGE ( 'NONE', *, *, #89058, .F. ) ;
#37321 = DIRECTION ( 'NONE',  ( -0.000000000000000000, 0.9848077530122086864, -0.1736481776669273891 ) ) ;
#37322 = CARTESIAN_POINT ( 'NONE',  ( -14.30769230769242917, -12.70778746994576025, 30.41441678777401236 ) ) ;
#37323 = ADVANCED_FACE ( 'NONE', ( #40394 ), #56108, .F. ) ;
#37324 = CARTESIAN_POINT ( 'NONE',  ( -8.835313148590907772, -11.91647553114624181, 32.58852847137148245 ) ) ;
#37325 = FACE_BOUND ( 'NONE', #637, .T. ) ;
#37326 = CARTESIAN_POINT ( 'NONE',  ( 8.096208266067295156, -12.41089969410671223, 31.60739465890703670 ) ) ;
#37327 = CARTESIAN_POINT ( 'NONE',  ( 4.087763774486016466, -2.292212530054419606, 30.41441678777542634 ) ) ;
#37328 = CARTESIAN_POINT ( 'NONE',  ( 13.38461538461538680, -10.51840700105979565, 33.73612834413961536 ) ) ;
#37330 = CARTESIAN_POINT ( 'NONE',  ( 6.857806477116148436, -11.94971097300153140, 32.03036669348370680 ) ) ;
#37329 = CARTESIAN_POINT ( 'NONE',  ( 16.28463659481311154, -3.957578996910245284, 33.62503395064540257 ) ) ;
#37331 = DIRECTION ( 'NONE',  ( 0.000000000000000000, -1.000000000000000000, 5.421010862427522170E-17 ) ) ;
#37332 = FACE_OUTER_BOUND ( 'NONE', #27124, .T. ) ;
#37333 = VERTEX_POINT ( 'NONE', #48011 ) ;
#37334 = FACE_OUTER_BOUND ( 'NONE', #66091, .T. ) ;
#37335 = ORIENTED_EDGE ( 'NONE', *, *, #30482, .F. ) ;
#37336 = ORIENTED_EDGE ( 'NONE', *, *, #82986, .T. ) ;
#37338 = CARTESIAN_POINT ( 'NONE',  ( 10.86533002476265786, -12.07971442181322352, 32.31769673815850297 ) ) ;
#37337 = CARTESIAN_POINT ( 'NONE',  ( 8.769230769230768274, -8.164416787775445883, 34.95778746994557906 ) ) ;
#37339 = EDGE_CURVE ( 'NONE', #44873, #88199, #14743, .T. ) ;
#37340 = CARTESIAN_POINT ( 'NONE',  ( 2.530703659305157949, -2.554770724473667709, 30.48948780036025852 ) ) ;
#37341 = CARTESIAN_POINT ( 'NONE',  ( -5.076923076923075762, -12.62096338111211580, 30.90682066428153263 ) ) ;
#37342 = CARTESIAN_POINT ( 'NONE',  ( -9.692307692307691624, -11.11383981884818262, 36.00935417666054406 ) ) ;
#37343 = CARTESIAN_POINT ( 'NONE',  ( 1.253923917947830091, -11.71456829005830080, 32.44064028649416542 ) ) ;
#37344 = ORIENTED_EDGE ( 'NONE', *, *, #62613, .F. ) ;
#37345 = CARTESIAN_POINT ( 'NONE',  ( 4.219913487196229163, -4.661471528628508665, 34.16647553114624003 ) ) ;
#37346 = CARTESIAN_POINT ( 'NONE',  ( 14.08476534878545650, -12.64616026154729411, 30.79003144601914244 ) ) ;
#37347 = CARTESIAN_POINT ( 'NONE',  ( 0.000000000000000000, -11.00000000000000000, 29.75000000000000355 ) ) ;
#37348 = CYLINDRICAL_SURFACE ( 'NONE', #13717, 0.2499999999999973355 ) ;
#37349 = DIRECTION ( 'NONE',  ( -0.000000000000000000, 0.9396926207859092051, -0.3420201433256662704 ) ) ;
#37350 = AXIS2_PLACEMENT_3D ( 'NONE', #84255, #30179, #57647 ) ;
#37351 = CARTESIAN_POINT ( 'NONE',  ( 1.553300858899087311, -3.749999999999992006, 16.73437500000000000 ) ) ;
#37352 = ORIENTED_EDGE ( 'NONE', *, *, #5682, .F. ) ;
#37353 = EDGE_CURVE ( 'NONE', #71459, #48865, #55654, .T. ) ;
#37354 = EDGE_LOOP ( 'NONE', ( #4640, #56393 ) ) ;
#37355 = CARTESIAN_POINT ( 'NONE',  ( 14.24242230713598900, -12.51329471203370325, 31.30864560766548976 ) ) ;
#37356 = EDGE_CURVE ( 'NONE', #17504, #48285, #72797, .T. ) ;
#37357 = ORIENTED_EDGE ( 'NONE', *, *, #50321, .T. ) ;
#37358 = CARTESIAN_POINT ( 'NONE',  ( -6.923076923077044142, -2.625532179533778709, 30.86335684631627174 ) ) ;
#37359 = CARTESIAN_POINT ( 'NONE',  ( -1.384615384615383471, -9.905515769479276145, 34.41647553114623292 ) ) ;
#37360 = FACE_OUTER_BOUND ( 'NONE', #7343, .T. ) ;
#37361 = DIRECTION ( 'NONE',  ( -0.000000000000000000, 0.7660444431189791237, -0.6427876096865379196 ) ) ;
#37362 = CARTESIAN_POINT ( 'NONE',  ( -3.750000000000008438, -5.946699141100917352, 20.17187500000000000 ) ) ;
#37363 = LINE ( 'NONE', #77043, #7217 ) ;
#37364 = VERTEX_POINT ( 'NONE', #14236 ) ;
#37365 = CARTESIAN_POINT ( 'NONE',  ( 4.153846153846030731, -12.51329471203414379, 31.30864560766407578 ) ) ;
#37367 = VERTEX_POINT ( 'NONE', #6153 ) ;
#37366 = CARTESIAN_POINT ( 'NONE',  ( -2.057637887778853703, -12.65882529074907126, 30.72640787790839312 ) ) ;
#37368 = DIRECTION ( 'NONE',  ( -0.000000000000000000, 0.7660444431189791237, -0.6427876096865379196 ) ) ;
#37369 = DIRECTION ( 'NONE',  ( 0.000000000000000000, -6.938893903907222067E-15, 1.000000000000000000 ) ) ;
#37370 = CARTESIAN_POINT ( 'NONE',  ( -3.230769230769229949, -9.905515769479276145, 34.41647553114623292 ) ) ;
#37371 = CARTESIAN_POINT ( 'NONE',  ( 6.923076923076800782, -3.643525952248796163, 33.31231777344771672 ) ) ;
#37373 = EDGE_CURVE ( 'NONE', #58562, #44876, #79191, .T. ) ;
#37372 = CARTESIAN_POINT ( 'NONE',  ( -6.250023237292966272, -10.05641848906368097, 34.04755513067966177 ) ) ;
#37374 = CARTESIAN_POINT ( 'NONE',  ( -4.377331097570100304, -9.331801661448606566, 34.40259984581193464 ) ) ;
#37375 = CARTESIAN_POINT ( 'NONE',  ( -8.069638789877792817, -12.44517049084099725, 30.48991314939691932 ) ) ;
#37376 = CARTESIAN_POINT ( 'NONE',  ( -3.775308065498748977, -8.992201783934593351, 20.26749329374151998 ) ) ;
#37377 = ORIENTED_EDGE ( 'NONE', *, *, #18067, .T. ) ;
#37378 = CARTESIAN_POINT ( 'NONE',  ( -4.284537620513710010, -4.809359713505814149, 33.96456829005828837 ) ) ;
#37379 = LINE ( 'NONE', #51311, #67627 ) ;
#37380 = CARTESIAN_POINT ( 'NONE',  ( -1.161602540521987859, -3.395485233115138168, 33.02377354290276656 ) ) ;
#37381 = CARTESIAN_POINT ( 'NONE',  ( -2.749999999999998224, -7.500000000000015987, 23.84375000000000000 ) ) ;
#37382 = VECTOR ( 'NONE', #80471, 1000.000000000000000 ) ;
#37383 = AXIS2_PLACEMENT_3D ( 'NONE', #38779, #85633, #18068 ) ;
#37384 = DIRECTION ( 'NONE',  ( -0.000000000000000000, -0.5000000000000009992, -0.8660254037844380415 ) ) ;
#37385 = CARTESIAN_POINT ( 'NONE',  ( 8.519254025182176449, -10.06842814019191401, 34.32929386961144758 ) ) ;
#37386 = VERTEX_POINT ( 'NONE', #57876 ) ;
#37387 = CARTESIAN_POINT ( 'NONE',  ( -1.944543648263014957, -5.555456351737005249, 17.75000000000000355 ) ) ;
#37388 = CARTESIAN_POINT ( 'NONE',  ( -15.36145983387954139, -3.957541250942358424, 33.62499894934981626 ) ) ;
#37389 = VECTOR ( 'NONE', #28308, 1000.000000000000000 ) ;
#37390 = EDGE_CURVE ( 'NONE', #8057, #17639, #68501, .T. ) ;
#37391 = EDGE_LOOP ( 'NONE', ( #62018, #33050, #19406, #45651 ) ) ;
#37392 = AXIS2_PLACEMENT_3D ( 'NONE', #67155, #33804, #5457 ) ;
#37393 = CARTESIAN_POINT ( 'NONE',  ( -4.284536756956459413, -8.191372820521381826, 34.95448215188423546 ) ) ;
#37394 = VECTOR ( 'NONE', #14152, 1000.000000000000227 ) ;
#37395 = EDGE_LOOP ( 'NONE', ( #1735, #80715, #32349, #13544, #2681, #3082 ) ) ;
#37396 = CARTESIAN_POINT ( 'NONE',  ( -13.38461538461538325, -2.517432740324522911, 35.29906147534542527 ) ) ;
#37397 = EDGE_CURVE ( 'NONE', #44468, #54188, #30845, .T. ) ;
#37398 = ADVANCED_FACE ( 'NONE', ( #43039 ), #16894, .F. ) ;
#37399 = CARTESIAN_POINT ( 'NONE',  ( -0.4615384615384611200, -6.435427911321262684, 35.78748833219616898 ) ) ;
#37400 = CYLINDRICAL_SURFACE ( 'NONE', #2451, 0.2499999999999993616 ) ;
#37401 = VERTEX_POINT ( 'NONE', #43920 ) ;
#37402 = DIRECTION ( 'NONE',  ( 0.000000000000000000, 0.1736481776669275834, 0.9848077530122086864 ) ) ;
#37403 = ORIENTED_EDGE ( 'NONE', *, *, #72075, .T. ) ;
#37404 = DIRECTION ( 'NONE',  ( -0.000000000000000000, 0.3420201433256694901, -0.9396926207859082059 ) ) ;
#37405 = ORIENTED_EDGE ( 'NONE', *, *, #45747, .F. ) ;
#37406 = CARTESIAN_POINT ( 'NONE',  ( 18.00000000000000000, -9.819645486525091727, 36.12317359536749706 ) ) ;
#37407 = CARTESIAN_POINT ( 'NONE',  ( 2.373760658694747061, -3.050289026998446840, 32.03036669348366416 ) ) ;
#37408 = VERTEX_POINT ( 'NONE', #71384 ) ;
#37409 = CARTESIAN_POINT ( 'NONE',  ( -5.999999999999998224, -10.67929555188718282, 33.92786785259544047 ) ) ;
#37410 = DIRECTION ( 'NONE',  ( -0.000000000000000000, 0.1736481776669307198, -0.9848077530122080203 ) ) ;
#37411 = CARTESIAN_POINT ( 'NONE',  ( -1.384615384615383471, -9.058645607665452459, 34.76329471203371924 ) ) ;
#37412 = CYLINDRICAL_SURFACE ( 'NONE', #67933, 0.2499999999999979738 ) ;
#37413 = DIRECTION ( 'NONE',  ( 0.000000000000000000, 0.000000000000000000, 1.000000000000000000 ) ) ;
#37414 = ORIENTED_EDGE ( 'NONE', *, *, #4863, .T. ) ;
#37415 = VERTEX_POINT ( 'NONE', #57429 ) ;
#37416 = FACE_BOUND ( 'NONE', #3620, .T. ) ;
#37417 = EDGE_LOOP ( 'NONE', ( #32621, #36571 ) ) ;
#37419 = ORIENTED_EDGE ( 'NONE', *, *, #37284, .F. ) ;
#37418 = CARTESIAN_POINT ( 'NONE',  ( 15.10062202133100939, -12.45813303252208648, 30.39737893381572675 ) ) ;
#37420 = AXIS2_PLACEMENT_3D ( 'NONE', #27437, #54904, #88716 ) ;
#37421 = B_SPLINE_CURVE_WITH_KNOTS ( 'NONE', 3,
 ( #79420, #24903, #51463, #65883, #43847, #58244, #3744, #11396, #38879, #17260 ),
 .UNSPECIFIED., .F., .F.,
 ( 4, 2, 2, 2, 4 ),
 ( 0.000000000000000000, 0.0001954339857564081520, 0.0003908679715128163040, 0.0005863019572692244018, 0.0007817359430256326080 ),
 .UNSPECIFIED. ) ;
#37422 = CARTESIAN_POINT ( 'NONE',  ( 6.065255139512839122, -3.083524468853784839, 32.58852847137153930 ) ) ;
#37423 = CARTESIAN_POINT ( 'NONE',  ( 5.142178648199100088, -4.481592998940251427, 33.73612834413965089 ) ) ;
#37424 = ORIENTED_EDGE ( 'NONE', *, *, #19517, .T. ) ;
#37425 = ORIENTED_EDGE ( 'NONE', *, *, #62093, .F. ) ;
#37426 = ORIENTED_EDGE ( 'NONE', *, *, #38683, .F. ) ;
#37427 = CARTESIAN_POINT ( 'NONE',  ( 17.01083966596719321, -4.098570777380720287, 33.41473453929634729 ) ) ;
#37428 = ORIENTED_EDGE ( 'NONE', *, *, #23564, .T. ) ;
#37429 = CARTESIAN_POINT ( 'NONE',  ( 11.53846153846141753, -11.48612834414049644, 32.76840700105863391 ) ) ;
#37430 = CARTESIAN_POINT ( 'NONE',  ( -11.53846153846153655, -3.513871655860378418, 32.76840700105978499 ) ) ;
#37431 = DIRECTION ( 'NONE',  ( 0.000000000000000000, 0.000000000000000000, 1.000000000000000000 ) ) ;
#37432 = ADVANCED_BREP_SHAPE_REPRESENTATION ( '', ( #9, #83448 ), #34517 ) ;
#37433 = FACE_BOUND ( 'NONE', #17421, .T. ) ;
#37434 = ORIENTED_EDGE ( 'NONE', *, *, #13168, .F. ) ;
#37435 = CARTESIAN_POINT ( 'NONE',  ( 13.51540719244018263, -8.999086150933475636, 34.52020707165672775 ) ) ;
#37436 = CIRCLE ( 'NONE', #43180, 4.000000000000000000 ) ;
#37437 = AXIS2_PLACEMENT_3D ( 'NONE', #17531, #24726, #72461 ) ;
#37438 = CARTESIAN_POINT ( 'NONE',  ( 5.010840697562940704, -3.322132147404559976, 32.92929555188719348 ) ) ;
#37439 = FACE_OUTER_BOUND ( 'NONE', #39876, .T. ) ;
#37440 = DIRECTION ( 'NONE',  ( -0.000000000000000000, -0.6427876096865404731, -0.7660444431189771253 ) ) ;
#37441 = ORIENTED_EDGE ( 'NONE', *, *, #86303, .F. ) ;
#37442 = CARTESIAN_POINT ( 'NONE',  ( -6.923076923076922462, -6.386643153685126251, 34.62446782046654192 ) ) ;
#37443 = ORIENTED_EDGE ( 'NONE', *, *, #1182, .T. ) ;
#37444 = AXIS2_PLACEMENT_3D ( 'NONE', #63410, #83709, #35956 ) ;
#37445 = ORIENTED_EDGE ( 'NONE', *, *, #48241, .T. ) ;
#37446 = AXIS2_PLACEMENT_3D ( 'NONE', #44084, #84667, #15758 ) ;
#37448 = CARTESIAN_POINT ( 'NONE',  ( -9.469294848214296678, -8.282913670948747864, 34.94150082978203642 ) ) ;
#37447 = CARTESIAN_POINT ( 'NONE',  ( -18.25000000000000711, -2.249999999999999556, 29.81919447696817471 ) ) ;
#37449 = MECHANICAL_DESIGN_GEOMETRIC_PRESENTATION_REPRESENTATION (  '', ( #31686 ), #50373 ) ;
#37450 = CARTESIAN_POINT ( 'NONE',  ( -8.769230769230892619, -12.51329471203414379, 31.30864560766407578 ) ) ;
#37451 = DIRECTION ( 'NONE',  ( -0.000000000000000000, -0.3420201433256694346, -0.9396926207859080948 ) ) ;
#37452 = DIRECTION ( 'NONE',  ( -0.000000000000000000, 0.000000000000000000, 1.000000000000000000 ) ) ;
#37453 = CARTESIAN_POINT ( 'NONE',  ( 14.24160992833217065, -2.833524468853757305, 32.15551576947924417 ) ) ;
#37454 = ORIENTED_EDGE ( 'NONE', *, *, #5138, .T. ) ;
#37455 = CARTESIAN_POINT ( 'NONE',  ( 6.673100179028335077, -2.544273027872574922, 31.48422191005632342 ) ) ;
#37456 = CARTESIAN_POINT ( 'NONE',  ( -0.4615384615385840772, -3.643525952248795718, 33.31231777344771672 ) ) ;
#37457 = CARTESIAN_POINT ( 'NONE',  ( 4.219101725122178514, -9.442884908240271713, 34.35708131394835618 ) ) ;
#37458 = CARTESIAN_POINT ( 'NONE',  ( 10.68064018666063930, -11.94971097300157403, 32.03036669348361443 ) ) ;
#37459 = EDGE_LOOP ( 'NONE', ( #46898, #75628 ) ) ;
#37460 = B_SPLINE_CURVE_WITH_KNOTS ( 'NONE', 3,
 ( #62758, #41623, #76735, #54676, #54234, #15040, #13264, #83503, #6512, #55568 ),
 .UNSPECIFIED., .F., .F.,
 ( 4, 2, 2, 2, 4 ),
 ( 0.000000000000000000, 0.0001954311564186868744, 0.0003908623128373737488, 0.0005862934692560606504, 0.0007817246256747474977 ),
 .UNSPECIFIED. ) ;
#37461 = EDGE_LOOP ( 'NONE', ( #62439, #419, #69940, #61278 ) ) ;
#37462 = FACE_BOUND ( 'NONE', #12801, .T. ) ;
#37463 = EDGE_CURVE ( 'NONE', #25475, #37415, #71833, .T. ) ;
#37464 = ORIENTED_EDGE ( 'NONE', *, *, #26069, .T. ) ;
#37465 = CARTESIAN_POINT ( 'NONE',  ( 18.22296290356148418, -7.369474270740072441, 34.74850911626239736 ) ) ;
#37466 = CARTESIAN_POINT ( 'NONE',  ( -13.25382357679060519, -10.54018710029568595, 33.71981072465678864 ) ) ;
#37467 = VERTEX_POINT ( 'NONE', #44346 ) ;
#37468 = FACE_OUTER_BOUND ( 'NONE', #81884, .T. ) ;
#37469 = CARTESIAN_POINT ( 'NONE',  ( -10.86540785267757947, -6.695914987888146541, 34.68535235679833306 ) ) ;
#37470 = DIRECTION ( 'NONE',  ( -1.000000000000000000, 0.000000000000000000, -0.000000000000000000 ) ) ;
#37471 = FACE_OUTER_BOUND ( 'NONE', #31054, .T. ) ;
#37472 = ORIENTED_EDGE ( 'NONE', *, *, #79490, .F. ) ;
#37473 = CARTESIAN_POINT ( 'NONE',  ( -7.846153846153844924, -8.120952969808772792, 34.71129190930000163 ) ) ;
#37474 = ORIENTED_EDGE ( 'NONE', *, *, #3834, .T. ) ;
#37476 = ORIENTED_EDGE ( 'NONE', *, *, #59107, .F. ) ;
#37475 = CARTESIAN_POINT ( 'NONE',  ( -20.74999999999999645, -10.50000000000000000, 29.75000000000000355 ) ) ;
#37477 = DIRECTION ( 'NONE',  ( -0.000000000000000000, -0.3420201433256694901, -0.9396926207859082059 ) ) ;
#37478 = CARTESIAN_POINT ( 'NONE',  ( 3.930919936330005360, -6.503392248772476236, 34.64988816332204635 ) ) ;
#37479 = CARTESIAN_POINT ( 'NONE',  ( 11.53846153846153832, -13.37000171582298513, 34.34916445242398453 ) ) ;
#37480 = CARTESIAN_POINT ( 'NONE',  ( -12.33101275977490019, -2.882268652242222284, 31.66798894389554064 ) ) ;
#37481 = DIRECTION ( 'NONE',  ( 0.000000000000000000, 0.000000000000000000, 1.000000000000000000 ) ) ;
#37482 = ADVANCED_FACE ( 'NONE', ( #29531 ), #43481, .F. ) ;
#37483 = CARTESIAN_POINT ( 'NONE',  ( 0.4615384615383396616, -6.879047030192662504, 34.71129190930017927 ) ) ;
#37484 = VECTOR ( 'NONE', #34185, 1000.000000000000000 ) ;
#37485 = CARTESIAN_POINT ( 'NONE',  ( -1.901340078031369618, -5.512252781505359245, 15.50186829374151287 ) ) ;
#37486 = VERTEX_POINT ( 'NONE', #23206 ) ;
#37487 = CARTESIAN_POINT ( 'NONE',  ( -15.00775787915638304, -3.587049720035815348, 32.86302985866382897 ) ) ;
#37488 = CARTESIAN_POINT ( 'NONE',  ( 13.13461538461538680, -7.433932668274256805, 35.00000000000000711 ) ) ;
#37489 = EDGE_LOOP ( 'NONE', ( #52799, #59010 ) ) ;
#37490 = ORIENTED_EDGE ( 'NONE', *, *, #67558, .T. ) ;
#37491 = CARTESIAN_POINT ( 'NONE',  ( -11.66915300512909504, -10.54014554554150607, 33.71984207302941883 ) ) ;
#37492 = LINE ( 'NONE', #45588, #3764 ) ;
#37493 = LINE ( 'NONE', #64962, #84966 ) ;
#37494 = B_SPLINE_CURVE_WITH_KNOTS ( 'NONE', 3,
 ( #7223, #61703, #26603, #68041, #22, #46869, #40574, #6346, #74352, #33801 ),
 .UNSPECIFIED., .F., .F.,
 ( 4, 2, 2, 2, 4 ),
 ( 0.000000000000000000, 0.0001954311564186863052, 0.0003908623128373726104, 0.0005862934692560589156, 0.0007817246256747452209 ),
 .UNSPECIFIED. ) ;
#37495 = CARTESIAN_POINT ( 'NONE',  ( 9.561616225640136690, -12.38065189839062263, 30.83690757178629482 ) ) ;
#37496 = LINE ( 'NONE', #58211, #56044 ) ;
#37497 = LINE ( 'NONE', #65856, #77299 ) ;
#37498 = CARTESIAN_POINT ( 'NONE',  ( 0.4615384615387756462, -2.255955759149395501, 30.00000000000324363 ) ) ;
#37499 = ORIENTED_EDGE ( 'NONE', *, *, #3194, .T. ) ;
#37501 = EDGE_CURVE ( 'NONE', #87990, #51727, #21116, .T. ) ;
#37500 = DIRECTION ( 'NONE',  ( -0.000000000000000000, -0.9396926207859092051, -0.3420201433256662704 ) ) ;
#37503 = ADVANCED_FACE ( 'NONE', ( #50667 ), #30411, .T. ) ;
#37502 = DIRECTION ( 'NONE',  ( -0.000000000000000000, 1.000000000000000000, -0.000000000000000000 ) ) ;
#37504 = AXIS2_PLACEMENT_3D ( 'NONE', #63710, #29937, #24496 ) ;
#37505 = CARTESIAN_POINT ( 'NONE',  ( 3.903846153846154632, -7.500000000000001776, 35.00000000000000000 ) ) ;
#37506 = CARTESIAN_POINT ( 'NONE',  ( 2.241608896736428047, -3.513871655860377086, 32.76840700105978499 ) ) ;
#37507 = ORIENTED_EDGE ( 'NONE', *, *, #26506, .F. ) ;
#37508 = DIRECTION ( 'NONE',  ( 1.000000000000000000, 0.000000000000000000, 0.000000000000000000 ) ) ;
#37509 = VECTOR ( 'NONE', #58709, 1000.000000000000000 ) ;
#37510 = VECTOR ( 'NONE', #77350, 1000.000000000000000 ) ;
#37512 = EDGE_CURVE ( 'NONE', #38908, #6875, #22245, .T. ) ;
#37511 = ORIENTED_EDGE ( 'NONE', *, *, #61056, .F. ) ;
#37513 = CARTESIAN_POINT ( 'NONE',  ( 0.6843180028068702736, -9.332535724633405749, 34.40230450496446224 ) ) ;
#37514 = CARTESIAN_POINT ( 'NONE',  ( -1.384615384615383471, -8.973038597847269315, 34.52809138561121927 ) ) ;
#37515 = CARTESIAN_POINT ( 'NONE',  ( -3.230769230769229949, -8.564572088678739092, 35.78748833219616898 ) ) ;
#37516 = ORIENTED_EDGE ( 'NONE', *, *, #87452, .T. ) ;
#37517 = CARTESIAN_POINT ( 'NONE',  ( -2.298097038856290464, -5.201902961143733961, 14.00000000000000000 ) ) ;
#37518 = CARTESIAN_POINT ( 'NONE',  ( 10.39189967166066531, -3.754499324213721234, 33.06261337010820256 ) ) ;
#37519 = AXIS2_PLACEMENT_3D ( 'NONE', #87125, #32597, #80809 ) ;
#37520 = CARTESIAN_POINT ( 'NONE',  ( 14.30769230769231015, -11.91647553114624181, 32.58852847137148245 ) ) ;
#37521 = CARTESIAN_POINT ( 'NONE',  ( 8.900022577055558770, -4.118422570099828484, 33.43335022499816489 ) ) ;
#37522 = ORIENTED_EDGE ( 'NONE', *, *, #35769, .F. ) ;
#37523 = CARTESIAN_POINT ( 'NONE',  ( 18.00000000000000000, -11.16473453929635440, 33.15142922261926373 ) ) ;
#37524 = ORIENTED_EDGE ( 'NONE', *, *, #73588, .T. ) ;
#37525 = DIRECTION ( 'NONE',  ( 0.000000000000000000, 1.000000000000000000, -0.000000000000000000 ) ) ;
#37526 = CARTESIAN_POINT ( 'NONE',  ( -16.85414340794500276, -3.563462043263029955, 33.22394488606062879 ) ) ;
#37527 = DIRECTION ( 'NONE',  ( -0.000000000000000000, 0.7660444431189791237, -0.6427876096865379196 ) ) ;
#37528 = CARTESIAN_POINT ( 'NONE',  ( -14.17690049986752321, -9.804649428959608670, 34.18742332936588468 ) ) ;
#37529 = CARTESIAN_POINT ( 'NONE',  ( 14.98079249982687777, -11.79746400365624659, 32.30657167506340954 ) ) ;
#37530 = ORIENTED_EDGE ( 'NONE', *, *, #55584, .F. ) ;
#37531 = ORIENTED_EDGE ( 'NONE', *, *, #87442, .T. ) ;
#37532 = B_SPLINE_CURVE_WITH_KNOTS ( 'NONE', 3,
 ( #4113, #86107, #24833, #39708, #66268, #4572, #52305, #32047, #45105, #79796 ),
 .UNSPECIFIED., .F., .F.,
 ( 4, 2, 2, 2, 4 ),
 ( 0.0007817246256747511840, 0.0009771112852218952725, 0.001172497944769039470, 0.001367884604316183667, 0.001563271263863327864 ),
 .UNSPECIFIED. ) ;
#37533 = AXIS2_PLACEMENT_3D ( 'NONE', #27116, #75739, #28911 ) ;
#37534 = VERTEX_POINT ( 'NONE', #72721 ) ;
#37535 = VERTEX_POINT ( 'NONE', #86264 ) ;
#37536 = CARTESIAN_POINT ( 'NONE',  ( 12.68431800280686694, -11.89424750095246175, 32.13594075562310337 ) ) ;
#37537 = CARTESIAN_POINT ( 'NONE',  ( 15.93036122928182330, -5.827078755546626354, 34.72654668319379567 ) ) ;
#37538 = VECTOR ( 'NONE', #83003, 1000.000000000000000 ) ;
#37539 = CARTESIAN_POINT ( 'NONE',  ( -4.153846153846274980, -6.835583212225970762, 34.95778746994575670 ) ) ;
#37540 = CARTESIAN_POINT ( 'NONE',  ( -4.153846153846152411, -2.833524468853757305, 32.15551576947925838 ) ) ;
#37541 = CARTESIAN_POINT ( 'NONE',  ( -15.23076923076922995, -12.78798330534102945, 29.74999999999997868 ) ) ;
#37542 = CARTESIAN_POINT ( 'NONE',  ( 8.519207531937803779, -9.271318131107980420, 34.42618302367067429 ) ) ;
#37543 = CARTESIAN_POINT ( 'NONE',  ( -3.230769230769229949, -13.75783147151868846, 33.36296068462461051 ) ) ;
#37544 = CARTESIAN_POINT ( 'NONE',  ( -17.75005448165186195, -6.696923467548661968, 34.68552623307873972 ) ) ;
#37545 = ORIENTED_EDGE ( 'NONE', *, *, #25744, .T. ) ;
#37546 = B_SPLINE_CURVE_WITH_KNOTS ( 'NONE', 3,
 ( #35347, #7882, #56510, #42995, #8774, #1121, #62798, #83995, #36245, #84437 ),
 .UNSPECIFIED., .F., .F.,
 ( 4, 2, 2, 2, 4 ),
 ( 0.0007817246256747464135, 0.0009771112852218900684, 0.001172497944769033615, 0.001367884604316177161, 0.001563271263863320925 ),
 .UNSPECIFIED. ) ;
#37547 = ORIENTED_EDGE ( 'NONE', *, *, #67265, .F. ) ;
#37548 = B_SPLINE_CURVE_WITH_KNOTS ( 'NONE', 3,
 ( #12196, #46859, #19835, #74791, #13079, #40566, #73002, #38777, #32020, #59486 ),
 .UNSPECIFIED., .F., .F.,
 ( 4, 2, 2, 2, 4 ),
 ( 0.0007817359430256318490, 0.0009771253907249984917, 0.001172514838424365026, 0.001367904286123731560, 0.001563293733823098311 ),
 .UNSPECIFIED. ) ;
#37549 = EDGE_CURVE ( 'NONE', #56816, #83848, #59655, .T. ) ;
#37550 = EDGE_LOOP ( 'NONE', ( #5156, #3595, #84522, #72761 ) ) ;
#37552 = ORIENTED_EDGE ( 'NONE', *, *, #11397, .T. ) ;
#37551 = CARTESIAN_POINT ( 'NONE',  ( 11.76124120743959978, -2.612705202774698421, 31.66806509827799943 ) ) ;
#37553 = B_SPLINE_CURVE_WITH_KNOTS ( 'NONE', 3,
 ( #38644, #66102, #31893, #66563, #44488, #30549, #59353, #50801, #37748, #65216 ),
 .UNSPECIFIED., .F., .F.,
 ( 4, 2, 2, 2, 4 ),
 ( 0.0007817246256747464135, 0.0009771112852218900684, 0.001172497944769033615, 0.001367884604316177161, 0.001563271263863320925 ),
 .UNSPECIFIED. ) ;
#37555 = DIRECTION ( 'NONE',  ( 0.000000000000000000, 0.8660254037844377084, -0.5000000000000015543 ) ) ;
#37554 = CARTESIAN_POINT ( 'NONE',  ( 16.21910172512217585, -11.94971097300157403, 32.03036669348361443 ) ) ;
#37556 = CARTESIAN_POINT ( 'NONE',  ( 9.019230769232203571, -7.500000000000155431, 34.75000000000007105 ) ) ;
#37557 = CARTESIAN_POINT ( 'NONE',  ( -14.30769230769230660, -9.780366693483667717, 34.19971097300155094 ) ) ;
#37558 = ORIENTED_EDGE ( 'NONE', *, *, #88848, .F. ) ;
#37559 = AXIS2_PLACEMENT_3D ( 'NONE', #46474, #13135, #32506 ) ;
#37560 = ORIENTED_EDGE ( 'NONE', *, *, #46847, .T. ) ;
#37561 = CYLINDRICAL_SURFACE ( 'NONE', #28463, 0.2499999999999986955 ) ;
#37562 = EDGE_LOOP ( 'NONE', ( #29258, #44529 ) ) ;
#37563 = FACE_BOUND ( 'NONE', #3274, .T. ) ;
#37565 = VECTOR ( 'NONE', #61706, 1000.000000000000114 ) ;
#37564 = CARTESIAN_POINT ( 'NONE',  ( 13.38461538461526423, -12.51329471203414379, 31.30864560766407578 ) ) ;
#37566 = EDGE_CURVE ( 'NONE', #83933, #74576, #65520, .T. ) ;
#37567 = CARTESIAN_POINT ( 'NONE',  ( 16.02369894440793630, -6.852621066184266141, 34.70813303252209181 ) ) ;
#37568 = ORIENTED_EDGE ( 'NONE', *, *, #27883, .T. ) ;
#37569 = CARTESIAN_POINT ( 'NONE',  ( -15.16551365949320562, -12.27809138561124591, 31.22303859784720359 ) ) ;
#37570 = CARTESIAN_POINT ( 'NONE',  ( 3.453548772037641434, -3.236590943229497253, 32.36255958852954251 ) ) ;
#37571 = CARTESIAN_POINT ( 'NONE',  ( 2.307692307692186251, -11.67786785259630911, 32.92929555188603530 ) ) ;
#37572 = EDGE_LOOP ( 'NONE', ( #71749, #86713, #34714, #84624 ) ) ;
#37573 = EDGE_CURVE ( 'NONE', #2295, #52380, #58766, .T. ) ;
#37574 = DIRECTION ( 'NONE',  ( 0.000000000000000000, 0.1736481776669267785, -0.9848077530122087975 ) ) ;
#37575 = DIRECTION ( 'NONE',  ( -0.000000000000000000, 0.5000000000000011102, -0.8660254037844381525 ) ) ;
#37576 = EDGE_LOOP ( 'NONE', ( #23923, #15638, #53734, #57793 ) ) ;
#37577 = VECTOR ( 'NONE', #12451, 1000.000000000000114 ) ;
#37578 = DIRECTION ( 'NONE',  ( -0.000000000000000000, 0.9848077530122086864, -0.1736481776669273891 ) ) ;
#37579 = CARTESIAN_POINT ( 'NONE',  ( -9.626240358957616650, -9.058645607665452459, 34.76329471203371924 ) ) ;
#37580 = EDGE_LOOP ( 'NONE', ( #28928, #2635, #68212, #88300 ) ) ;
#37581 = CARTESIAN_POINT ( 'NONE',  ( -13.38461538461538325, -12.78798330534102945, 29.74999999999997868 ) ) ;
#37582 = CARTESIAN_POINT ( 'NONE',  ( 10.61538461538461675, -2.708943851104267164, 35.45975837776705220 ) ) ;
#37583 = DIRECTION ( 'NONE',  ( 1.000000000000000000, 0.000000000000000000, 0.000000000000000000 ) ) ;
#37584 = CARTESIAN_POINT ( 'NONE',  ( 15.23076923076910916, -12.70778746994576025, 30.41441678777401236 ) ) ;
#37585 = CARTESIAN_POINT ( 'NONE',  ( 9.561617089197389063, -12.35290016733513951, 31.75349464988449455 ) ) ;
#37586 = FACE_BOUND ( 'NONE', #53475, .T. ) ;
#37588 = LINE ( 'NONE', #51082, #60402 ) ;
#37587 = CARTESIAN_POINT ( 'NONE',  ( 4.403900465484466231, -12.17597550085003633, 31.52189283813461884 ) ) ;
#37589 = EDGE_CURVE ( 'NONE', #14975, #60707, #34036, .T. ) ;
#37590 = CARTESIAN_POINT ( 'NONE',  ( -1.134560964701931018, -9.233818618650603938, 34.70587769442853698 ) ) ;
#37592 = CARTESIAN_POINT ( 'NONE',  ( -10.68146802634049308, -8.120952969808774569, 34.71129190930000163 ) ) ;
#37591 = CARTESIAN_POINT ( 'NONE',  ( 12.71153846153840128, -7.565270000091922853, 34.99999999999999289 ) ) ;
#37593 = LINE ( 'NONE', #70499, #5972 ) ;
#37594 = CARTESIAN_POINT ( 'NONE',  ( 1.944543648262996083, -5.555456351736983045, 14.31250000000000000 ) ) ;
#37595 = VERTEX_POINT ( 'NONE', #24089 ) ;
#37596 = B_SPLINE_CURVE_WITH_KNOTS ( 'NONE', 3,
 ( #47941, #6530, #82191, #34434, #19154, #20480, #67783, #80872, #41199, #46622 ),
 .UNSPECIFIED., .F., .F.,
 ( 4, 2, 2, 2, 4 ),
 ( 0.0007817246256747484735, 0.0009771112852218922368, 0.001172497944769036217, 0.001367884604316180197, 0.001563271263863323960 ),
 .UNSPECIFIED. ) ;
#37597 = CARTESIAN_POINT ( 'NONE',  ( 18.06606835100244268, -11.69971097300155272, 32.46337939537588113 ) ) ;
#37598 = ORIENTED_EDGE ( 'NONE', *, *, #48048, .T. ) ;
#37599 = EDGE_CURVE ( 'NONE', #11498, #34673, #38506, .T. ) ;
#37600 = CARTESIAN_POINT ( 'NONE',  ( 4.153846153846154188, -1.044019251281081972, 31.83374038241031911 ) ) ;
#37601 = ORIENTED_EDGE ( 'NONE', *, *, #70774, .T. ) ;
#37602 = DIRECTION ( 'NONE',  ( 0.000000000000000000, 0.8660254037844377084, -0.5000000000000015543 ) ) ;
#37603 = ORIENTED_EDGE ( 'NONE', *, *, #47212, .T. ) ;
#37604 = CARTESIAN_POINT ( 'NONE',  ( -7.912237257109728361, -5.557115091759785130, 34.35708131394839171 ) ) ;
#37605 = CARTESIAN_POINT ( 'NONE',  ( -2.749999999999997780, -7.561099074964547917, 26.09188170625848358 ) ) ;
#37606 = CARTESIAN_POINT ( 'NONE',  ( 3.100078627658923391, -2.295517848115769421, 30.44137282052137294 ) ) ;
#37607 = B_SPLINE_CURVE_WITH_KNOTS ( 'NONE', 3,
 ( #19673, #8279, #2379, #49695, #50129, #22228, #67863, #35753, #12917, #63202 ),
 .UNSPECIFIED., .F., .F.,
 ( 4, 2, 2, 2, 4 ),
 ( 0.0007817359430256257775, 0.0009771253907249911191, 0.001172514838424356352, 0.001367904286123721586, 0.001563293733823086819 ),
 .UNSPECIFIED. ) ;
#37608 = CARTESIAN_POINT ( 'NONE',  ( -9.758390071667825794, -12.62096338111211580, 30.90682066428152908 ) ) ;
#37609 = CARTESIAN_POINT ( 'NONE',  ( -5.869208192175211281, -8.999086150933472084, 34.52020707165672064 ) ) ;
#37610 = CARTESIAN_POINT ( 'NONE',  ( -12.39547112818838670, -3.937682226553329556, 33.60647404775216529 ) ) ;
#37611 = CARTESIAN_POINT ( 'NONE',  ( -23.00000000000000000, -5.499999999999981348, 27.75000000000000000 ) ) ;
#37612 = CARTESIAN_POINT ( 'NONE',  ( -39.05038313613820122, -2.499999999999999556, 29.75000000000000355 ) ) ;
#37613 = CARTESIAN_POINT ( 'NONE',  ( 5.869852790561781219, -4.460286881179643004, 33.72017969459903242 ) ) ;
#37614 = AXIS2_PLACEMENT_3D ( 'NONE', #49973, #69810, #8117 ) ;
#37615 = CARTESIAN_POINT ( 'NONE',  ( 3.750000000000009770, -9.053300858899081760, 15.79687500000000178 ) ) ;
#37616 = CARTESIAN_POINT ( 'NONE',  ( 1.134592147322419420, -2.823816976329317718, 31.52131813110795733 ) ) ;
#37618 = EDGE_CURVE ( 'NONE', #87573, #20844, #13619, .T. ) ;
#37617 = FACE_OUTER_BOUND ( 'NONE', #22724, .T. ) ;
#37619 = EDGE_CURVE ( 'NONE', #23459, #46284, #82397, .T. ) ;
#37620 = CIRCLE ( 'NONE', #66356, 0.2500000000000002220 ) ;
#37621 = CARTESIAN_POINT ( 'NONE',  ( 13.63466969625370240, -4.235687564193448829, 33.53795663066793509 ) ) ;
#37622 = CARTESIAN_POINT ( 'NONE',  ( 1.553300858899087311, -3.749999999999992006, 17.98437500000000000 ) ) ;
#37623 = VERTEX_POINT ( 'NONE', #4724 ) ;
#37624 = EDGE_CURVE ( 'NONE', #32743, #73490, #9316, .T. ) ;
#37625 = CARTESIAN_POINT ( 'NONE',  ( 14.53070365930516061, -4.887748414852792322, 34.01359900205216746 ) ) ;
#37626 = CARTESIAN_POINT ( 'NONE',  ( 4.153846153846154188, -9.819645486525091727, 36.12317359536749706 ) ) ;
#37627 = CARTESIAN_POINT ( 'NONE',  ( 1.254467414883692289, -5.915902021225892149, 34.75552854090298638 ) ) ;
#37628 = CARTESIAN_POINT ( 'NONE',  ( 5.076923076922954969, -2.892918686052165622, 31.69288490824153470 ) ) ;
#37629 = EDGE_CURVE ( 'NONE', #60953, #23257, #53340, .T. ) ;
#37630 = CARTESIAN_POINT ( 'NONE',  ( 8.519207531937803779, -11.86270091957321249, 32.19358267280087915 ) ) ;
#37631 = CARTESIAN_POINT ( 'NONE',  ( -3.100243792535585463, -5.915461855592777596, 34.75538340440931506 ) ) ;
#37632 = VERTEX_POINT ( 'NONE', #74073 ) ;
#37633 = CARTESIAN_POINT ( 'NONE',  ( 7.716005876422148191, -3.069018819979302926, 32.56621877034667278 ) ) ;
#37634 = EDGE_LOOP ( 'NONE', ( #88544, #51579, #57718, #13834 ) ) ;
#37635 = EDGE_LOOP ( 'NONE', ( #71973, #29237 ) ) ;
#37636 = AXIS2_PLACEMENT_3D ( 'NONE', #75904, #14204, #71796 ) ;
#37637 = CARTESIAN_POINT ( 'NONE',  ( -9.469294848214296678, -2.889357225399414197, 32.26129605718031002 ) ) ;
#37638 = CARTESIAN_POINT ( 'NONE',  ( -6.223484924564330889, -12.69144148231606017, 30.53333754910549303 ) ) ;
#37639 = CARTESIAN_POINT ( 'NONE',  ( -9.019253993452226226, -2.341070481393819236, 30.72580821765574299 ) ) ;
#37640 = DIRECTION ( 'NONE',  ( -0.000000000000000000, 0.7660444431189791237, -0.6427876096865379196 ) ) ;
#37641 = CARTESIAN_POINT ( 'NONE',  ( 13.13459216039392885, -5.765609946408404518, 34.70566812827425451 ) ) ;
#37642 = AXIS2_PLACEMENT_3D ( 'NONE', #29981, #9702, #4279 ) ;
#37643 = ORIENTED_EDGE ( 'NONE', *, *, #33119, .F. ) ;
#37644 = CARTESIAN_POINT ( 'NONE',  ( 8.992010310499178871, -3.755027918224367767, 33.06320215134714857 ) ) ;
#37645 = ORIENTED_EDGE ( 'NONE', *, *, #8544, .T. ) ;
#37646 = EDGE_CURVE ( 'NONE', #72317, #66893, #11559, .T. ) ;
#37647 = ORIENTED_EDGE ( 'NONE', *, *, #88787, .F. ) ;
#37648 = CARTESIAN_POINT ( 'NONE',  ( 13.31934538405906565, -5.094484230520674117, 34.41647553114621161 ) ) ;
#37649 = FACE_OUTER_BOUND ( 'NONE', #46749, .T. ) ;
#37650 = ADVANCED_FACE ( 'NONE', ( #34842 ), #19559, .F. ) ;
#37651 = CARTESIAN_POINT ( 'NONE',  ( -19.50000000000000000, -11.50000000000000000, 29.75000000000000355 ) ) ;
#37652 = EDGE_CURVE ( 'NONE', #58112, #54935, #47913, .T. ) ;
#37653 = CARTESIAN_POINT ( 'NONE',  ( -8.638440328263820689, -9.929761469519743144, 34.40412654351204225 ) ) ;
#37654 = CARTESIAN_POINT ( 'NONE',  ( -4.284537620513711786, -8.147922237126337563, 34.70805685702651999 ) ) ;
#37655 = CARTESIAN_POINT ( 'NONE',  ( -16.08777780284371772, -2.721908614388772740, 31.22303859784725333 ) ) ;
#37656 = ORIENTED_EDGE ( 'NONE', *, *, #2297, .F. ) ;
#37657 = VERTEX_POINT ( 'NONE', #40290 ) ;
#37658 = CARTESIAN_POINT ( 'NONE',  ( -1.553300858899081538, -11.25000000000000711, 22.35937500000000711 ) ) ;
#37659 = B_SPLINE_CURVE_WITH_KNOTS ( 'NONE', 3,
 ( #23285, #42689, #8460, #11449, #84567, #29184, #38933, #16529, #77789, #43559 ),
 .UNSPECIFIED., .F., .F.,
 ( 4, 2, 2, 2, 4 ),
 ( 0.000000000000000000, 0.0001954339857564097512, 0.0003908679715128195024, 0.0005863019572692292807, 0.0007817359430256390048 ),
 .UNSPECIFIED. ) ;
#37660 = EDGE_CURVE ( 'NONE', #14030, #72338, #58581, .T. ) ;
#37661 = EDGE_LOOP ( 'NONE', ( #39248, #82719, #24835, #69557 ) ) ;
#37663 = VERTEX_POINT ( 'NONE', #625 ) ;
#37662 = DIRECTION ( 'NONE',  ( -0.000000000000000000, 1.000000000000000000, -0.000000000000000000 ) ) ;
#37664 = CARTESIAN_POINT ( 'NONE',  ( 7.846153846153846700, -12.37446782046654192, 30.86335684631486131 ) ) ;
#37665 = DIRECTION ( 'NONE',  ( 1.000000000000000000, 0.000000000000000000, 0.000000000000000000 ) ) ;
#37667 = B_SPLINE_CURVE_WITH_KNOTS ( 'NONE', 3,
 ( #3483, #77817, #43590, #85469, #16560, #2594, #44026, #23315, #64735, #71498 ),
 .UNSPECIFIED., .F., .F.,
 ( 4, 2, 2, 2, 4 ),
 ( 0.0007817246256747469556, 0.0009771112852218889842, 0.001172497944769031013, 0.001367884604316173041, 0.001563271263863315070 ),
 .UNSPECIFIED. ) ;
#37666 = VECTOR ( 'NONE', #88900, 1000.000000000000114 ) ;
#37668 = CARTESIAN_POINT ( 'NONE',  ( -1.553300858899125059, -3.750000000000009326, 15.32812500000000178 ) ) ;
#37669 = EDGE_LOOP ( 'NONE', ( #44140, #71236, #7256, #1354 ) ) ;
#37670 = VECTOR ( 'NONE', #60110, 1000.000000000000000 ) ;
#37671 = FACE_OUTER_BOUND ( 'NONE', #61107, .T. ) ;
#37672 = VERTEX_POINT ( 'NONE', #26763 ) ;
#37673 = CARTESIAN_POINT ( 'NONE',  ( -9.019253993452222673, -4.931416488878822335, 34.32920672191015399 ) ) ;
#37674 = CARTESIAN_POINT ( 'NONE',  ( 17.93391762063986050, -12.62096338111211580, 30.90682066428152908 ) ) ;
#37675 = DIRECTION ( 'NONE',  ( 0.000000000000000000, 0.1736481776669267785, -0.9848077530122087975 ) ) ;
#37677 = CARTESIAN_POINT ( 'NONE',  ( -39.05038313613820122, -2.499999999999999556, 29.75000000000000355 ) ) ;
#37676 = DIRECTION ( 'NONE',  ( -0.000000000000000000, 0.9848077530122086864, -0.1736481776669273891 ) ) ;
#37678 = CARTESIAN_POINT ( 'NONE',  ( -1.134669975237340811, -8.476813868363244353, 34.90874843262270133 ) ) ;
#37679 = CARTESIAN_POINT ( 'NONE',  ( -19.50000000000000000, -3.499999999999999556, 29.75000000000000355 ) ) ;
#37680 = VERTEX_POINT ( 'NONE', #6056 ) ;
#37681 = DIRECTION ( 'NONE',  ( 1.000000000000000000, 0.000000000000000000, 0.000000000000000000 ) ) ;
#37682 = CARTESIAN_POINT ( 'NONE',  ( 11.28846153846152411, -2.249999999999998668, 29.81609741502487765 ) ) ;
#37683 = EDGE_CURVE ( 'NONE', #27696, #22240, #2382, .T. ) ;
#37684 = ORIENTED_EDGE ( 'NONE', *, *, #24274, .F. ) ;
#37685 = DIRECTION ( 'NONE',  ( -0.000000000000000000, -0.8660254037844399289, -0.4999999999999980016 ) ) ;
#37686 = CARTESIAN_POINT ( 'NONE',  ( 16.85343815235874487, -10.97335522853832934, 33.68706563782419749 ) ) ;
#37687 = DIRECTION ( 'NONE',  ( -0.000000000000000000, 0.6427876096865404731, -0.7660444431189771253 ) ) ;
#37688 = CARTESIAN_POINT ( 'NONE',  ( -16.21911615440247090, -12.16647553114622049, 32.15551576947930812 ) ) ;
#37689 = CARTESIAN_POINT ( 'NONE',  ( 12.21151522424549896, -4.335965774309649134, 33.62209801155881905 ) ) ;
#37690 = FACE_BOUND ( 'NONE', #11967, .T. ) ;
#37692 = CARTESIAN_POINT ( 'NONE',  ( -10.86538461538461320, -7.433932668274256805, 35.00000000000000711 ) ) ;
#37691 = CARTESIAN_POINT ( 'NONE',  ( 13.31853197365950692, -12.10708131394839349, 31.69288490824020244 ) ) ;
#37693 = CARTESIAN_POINT ( 'NONE',  ( 16.15384615384603251, -3.300289026999228437, 32.46337939537709616 ) ) ;
#37695 = DIRECTION ( 'NONE',  ( 0.000000000000000000, 0.000000000000000000, -1.000000000000000000 ) ) ;
#37694 = CARTESIAN_POINT ( 'NONE',  ( -1.134561072977069873, -12.17597550085003455, 31.52189283813461884 ) ) ;
#37696 = FACE_OUTER_BOUND ( 'NONE', #73248, .T. ) ;
#37697 = CARTESIAN_POINT ( 'NONE',  ( 9.019176287578909879, -10.76462480002816235, 33.53768742498949962 ) ) ;
#37698 = CARTESIAN_POINT ( 'NONE',  ( -3.724691934501229262, -9.114399933863657211, 21.01375670625849068 ) ) ;
#37699 = CIRCLE ( 'NONE', #30500, 4.000000000000000000 ) ;
#37700 = ORIENTED_EDGE ( 'NONE', *, *, #86722, .F. ) ;
#37701 = VECTOR ( 'NONE', #75638, 1000.000000000000114 ) ;
#37702 = CARTESIAN_POINT ( 'NONE',  ( -15.23076923076935074, -11.48612834414049644, 32.76840700105863391 ) ) ;
#37703 = CARTESIAN_POINT ( 'NONE',  ( 5.076923076922953193, -3.083524468854526912, 32.58852847137268327 ) ) ;
#37704 = CARTESIAN_POINT ( 'NONE',  ( 0.000000000000000000, -4.000000000000000000, 29.25000000000000000 ) ) ;
#37705 = LINE ( 'NONE', #16547, #66873 ) ;
#37706 = CARTESIAN_POINT ( 'NONE',  ( 7.622668902429897919, -5.113361153441932316, 34.14387501736621999 ) ) ;
#37707 = CARTESIAN_POINT ( 'NONE',  ( 3.230769230769231726, -11.11383981884818262, 36.00935417666054406 ) ) ;
#37708 = CARTESIAN_POINT ( 'NONE',  ( 0.06109907496455496689, -11.24999999999999822, 19.52938170625848713 ) ) ;
#37709 = AXIS2_PLACEMENT_3D ( 'NONE', #2070, #70086, #35869 ) ;
#37710 = CARTESIAN_POINT ( 'NONE',  ( -11.60378445395371472, -7.749976743299138882, 34.99404534957040624 ) ) ;
#37711 = CARTESIAN_POINT ( 'NONE',  ( 0.7115927731767749398, -3.627508038966689163, 32.91356715214248396 ) ) ;
#37712 = CARTESIAN_POINT ( 'NONE',  ( -7.596208436775802930, -10.18230066228895758, 34.26354781536631577 ) ) ;
#37713 = CARTESIAN_POINT ( 'NONE',  ( 9.468822767743363400, -4.225889041578353655, 33.85425143139329407 ) ) ;
#37714 = CARTESIAN_POINT ( 'NONE',  ( 14.30769230769231015, -5.557115091759785130, 34.35708131394839171 ) ) ;
#37715 = DIRECTION ( 'NONE',  ( 0.000000000000000000, 0.6427876096865368094, 0.7660444431189802339 ) ) ;
#37717 = EDGE_CURVE ( 'NONE', #26721, #40093, #20007, .T. ) ;
#37716 = CARTESIAN_POINT ( 'NONE',  ( -16.81410256410256565, -3.499999999999999556, 29.75000000000000355 ) ) ;
#37718 = EDGE_CURVE ( 'NONE', #49073, #43765, #43604, .T. ) ;
#37719 = CARTESIAN_POINT ( 'NONE',  ( 8.096208157792160520, -6.567000820036036579, 34.66262288849541306 ) ) ;
#37720 = ORIENTED_EDGE ( 'NONE', *, *, #73500, .T. ) ;
#37721 = CARTESIAN_POINT ( 'NONE',  ( 15.10062126103753322, -11.66186481527757302, 32.95055677023626117 ) ) ;
#37722 = CARTESIAN_POINT ( 'NONE',  ( 1.384615384615386802, -6.189225973068211317, 35.74407628777942847 ) ) ;
#37723 = CARTESIAN_POINT ( 'NONE',  ( 2.694853999681185108, -4.891553140782077591, 15.81436829374151465 ) ) ;
#37724 = ADVANCED_FACE ( 'NONE', ( #48354 ), #14133, .F. ) ;
#37725 = CARTESIAN_POINT ( 'NONE',  ( 6.130791807824788719, -4.118422570099827595, 33.43335022499816489 ) ) ;
#37726 = CARTESIAN_POINT ( 'NONE',  ( 3.230769230769110045, -11.94971097300221174, 32.03036669348237098 ) ) ;
#37727 = ORIENTED_EDGE ( 'NONE', *, *, #59902, .T. ) ;
#37728 = CARTESIAN_POINT ( 'NONE',  ( -6.700297254098854793, -10.23759521482555357, 34.22997729860117033 ) ) ;
#37729 = CARTESIAN_POINT ( 'NONE',  ( 2.373759641042385127, -10.67929555188718282, 33.92786785259544757 ) ) ;
#37731 = ORIENTED_EDGE ( 'NONE', *, *, #36008, .F. ) ;
#37730 = CARTESIAN_POINT ( 'NONE',  ( 12.23805351781451201, -5.912607949931405926, 34.49155766932282319 ) ) ;
#37732 = CARTESIAN_POINT ( 'NONE',  ( 11.53846153846153832, -4.661471528628507777, 34.16647553114623292 ) ) ;
#37733 = CARTESIAN_POINT ( 'NONE',  ( -16.15384615384615330, -9.819645486525091727, 36.12317359536749706 ) ) ;
#37734 = ADVANCED_FACE ( 'NONE', ( #28092 ), #83044, .F. ) ;
#37735 = B_SPLINE_CURVE_WITH_KNOTS ( 'NONE', 3,
 ( #8760, #75877, #28585, #36230, #41656, #29475 ),
 .UNSPECIFIED., .F., .F.,
 ( 4, 2, 4 ),
 ( 4.220987180333914613E-17, 0.0001954756301637168027, 0.0003909512603273914300 ),
 .UNSPECIFIED. ) ;
#37736 = LINE ( 'NONE', #17023, #1767 ) ;
#37737 = CARTESIAN_POINT ( 'NONE',  ( -15.48076923076923528, -2.249999999999999556, 29.81609741502490607 ) ) ;
#37738 = ORIENTED_EDGE ( 'NONE', *, *, #5852, .F. ) ;
#37739 = VECTOR ( 'NONE', #54765, 1000.000000000000000 ) ;
#37740 = DIRECTION ( 'NONE',  ( -0.000000000000000000, 0.9848077530122085754, -0.1736481776669273613 ) ) ;
#37741 =( NAMED_UNIT ( * ) PLANE_ANGLE_UNIT ( ) SI_UNIT ( $, .RADIAN. ) );
#37742 = DIRECTION ( 'NONE',  ( -0.000000000000000000, 0.9396926207859092051, -0.3420201433256662704 ) ) ;
#37743 = ORIENTED_EDGE ( 'NONE', *, *, #26142, .F. ) ;
#37744 = ORIENTED_EDGE ( 'NONE', *, *, #13391, .F. ) ;
#37745 = EDGE_CURVE ( 'NONE', #22022, #55623, #33076, .T. ) ;
#37746 = ORIENTED_EDGE ( 'NONE', *, *, #986, .T. ) ;
#37747 = CARTESIAN_POINT ( 'NONE',  ( -18.25002323729296805, -3.711651800289232028, 33.01384336483935300 ) ) ;
#37748 = CARTESIAN_POINT ( 'NONE',  ( 9.758375025657770152, -3.937682226553329556, 33.60647404775216529 ) ) ;
#37749 = EDGE_CURVE ( 'NONE', #8847, #82664, #30673, .T. ) ;
#37750 = CARTESIAN_POINT ( 'NONE',  ( -3.931066484868085187, -12.69155399931963046, 30.53255429739158444 ) ) ;
#37751 = DIRECTION ( 'NONE',  ( 1.000000000000000000, 2.602085213965214586E-16, 0.000000000000000000 ) ) ;
#37752 = EDGE_CURVE ( 'NONE', #77905, #48531, #80146, .T. ) ;
#37753 = ORIENTED_EDGE ( 'NONE', *, *, #23163, .F. ) ;
#37754 = EDGE_LOOP ( 'NONE', ( #28235, #77423, #5656, #36494 ) ) ;
#37756 = EDGE_LOOP ( 'NONE', ( #66016, #49371 ) ) ;
#37755 = CARTESIAN_POINT ( 'NONE',  ( 10.86538461538461675, -2.249999999999998668, 29.75000000000000355 ) ) ;
#37757 = EDGE_CURVE ( 'NONE', #26530, #81582, #49688, .T. ) ;
#37758 = CARTESIAN_POINT ( 'NONE',  ( 9.942253210655836781, -12.43552623307873972, 30.55307653245132826 ) ) ;
#37759 = VECTOR ( 'NONE', #60087, 1000.000000000000114 ) ;
#37760 = B_SPLINE_CURVE_WITH_KNOTS ( 'NONE', 3,
 ( #12461, #80032, #47119, #72816, #32726, #33175 ),
 .UNSPECIFIED., .F., .F.,
 ( 4, 2, 4 ),
 ( 2.453269466693398621E-17, 0.0001954756301636960945, 0.0003909512603273676860 ),
 .UNSPECIFIED. ) ;
#37761 = CARTESIAN_POINT ( 'NONE',  ( -8.638438961405983108, -12.38066358083363738, 30.83685684665853444 ) ) ;
#37762 = CARTESIAN_POINT ( 'NONE',  ( 13.44987052412822237, -10.33852847137154107, 34.16647553114620450 ) ) ;
#37763 = ORIENTED_EDGE ( 'NONE', *, *, #14946, .F. ) ;
#37764 = B_SPLINE_CURVE_WITH_KNOTS ( 'NONE', 3,
 ( #12149, #33306, #25654, #38722, #47249, #66183, #67977, #31971, #59435, #58984 ),
 .UNSPECIFIED., .F., .F.,
 ( 4, 2, 2, 2, 4 ),
 ( 0.000000000000000000, 0.0001954311564186882026, 0.0003908623128373764051, 0.0005862934692560646619, 0.0007817246256747528103 ),
 .UNSPECIFIED. ) ;
#37765 = ORIENTED_EDGE ( 'NONE', *, *, #57673, .T. ) ;
#37766 = EDGE_CURVE ( 'NONE', #82473, #48855, #84826, .T. ) ;
#37767 = VERTEX_POINT ( 'NONE', #69960 ) ;
#37769 = ORIENTED_EDGE ( 'NONE', *, *, #2281, .T. ) ;
#37768 = CARTESIAN_POINT ( 'NONE',  ( 15.23076923076923173, -2.538708090699994813, 30.37095296980875503 ) ) ;
#37770 = CARTESIAN_POINT ( 'NONE',  ( -0.4615384615384611200, -10.51840700105979565, 33.73612834413961536 ) ) ;
#37771 = CARTESIAN_POINT ( 'NONE',  ( -5.142193522883852452, -10.21337939537584383, 33.94971097300158647 ) ) ;
#37772 = ORIENTED_EDGE ( 'NONE', *, *, #23238, .F. ) ;
#37773 = EDGE_CURVE ( 'NONE', #4310, #61816, #75837, .T. ) ;
#37774 = DIRECTION ( 'NONE',  ( 0.000000000000000000, 0.6427876096865373645, -0.7660444431189797898 ) ) ;
#37775 = CARTESIAN_POINT ( 'NONE',  ( 10.61538461538461675, -5.471508081941601098, 34.59228464037088457 ) ) ;
#37776 = DIRECTION ( 'NONE',  ( -0.000000000000000000, 0.9848077530122085754, -0.1736481776669273613 ) ) ;
#37777 = FACE_BOUND ( 'NONE', #11740, .T. ) ;
#37778 = CARTESIAN_POINT ( 'NONE',  ( -0.7115616988314267255, -4.335965774309649134, 33.62209801155881905 ) ) ;
#37779 = CARTESIAN_POINT ( 'NONE',  ( 9.758476833270350426, -7.250054483168843156, 34.74374881642865631 ) ) ;
#37780 = DIRECTION ( 'NONE',  ( -0.000000000000000000, -0.1736481776669307198, -0.9848077530122080203 ) ) ;
#37782 = CARTESIAN_POINT ( 'NONE',  ( 6.923076923076802558, -11.94971097300221174, 32.03036669348237098 ) ) ;
#37781 = CARTESIAN_POINT ( 'NONE',  ( 6.250000000000000888, -2.499999999999998668, 29.75000000000000355 ) ) ;
#37783 = CARTESIAN_POINT ( 'NONE',  ( 17.86930939688969033, -6.369640206132551441, 34.87707690430378449 ) ) ;
#37784 = CYLINDRICAL_SURFACE ( 'NONE', #64890, 8.000000000000000000 ) ;
#37785 = EDGE_LOOP ( 'NONE', ( #35151, #8471, #86766, #5728 ) ) ;
#37786 = CARTESIAN_POINT ( 'NONE',  ( -5.999999999999998224, -11.69971097300155272, 32.46337939537588113 ) ) ;
#37787 = ORIENTED_EDGE ( 'NONE', *, *, #33304, .F. ) ;
#37788 = ADVANCED_FACE ( 'NONE', ( #42944 ), #50123, .F. ) ;
#37789 = ORIENTED_EDGE ( 'NONE', *, *, #56043, .T. ) ;
#37791 = CARTESIAN_POINT ( 'NONE',  ( 15.23076923076910916, -3.083524468854526912, 32.58852847137268327 ) ) ;
#37790 = CYLINDRICAL_SURFACE ( 'NONE', #37437, 0.2500000000000002220 ) ;
#37792 = EDGE_CURVE ( 'NONE', #33486, #5632, #34984, .T. ) ;
#37793 = VECTOR ( 'NONE', #79508, 1000.000000000000114 ) ;
#37794 = AXIS2_PLACEMENT_3D ( 'NONE', #320, #34982, #75103 ) ;
#37795 = CARTESIAN_POINT ( 'NONE',  ( 13.13459216039392707, -11.56360843649121861, 33.07473185843129926 ) ) ;
#37796 = CARTESIAN_POINT ( 'NONE',  ( 7.846153846153846700, -9.905515769479276145, 34.41647553114623292 ) ) ;
#37797 = CARTESIAN_POINT ( 'NONE',  ( -4.153846153846152411, -3.322132147404559976, 32.92929555188717927 ) ) ;
#37798 = ORIENTED_EDGE ( 'NONE', *, *, #282, .F. ) ;
#37799 = LINE ( 'NONE', #85110, #58779 ) ;
#37800 = CARTESIAN_POINT ( 'NONE',  ( 14.17754433796061875, -12.70455904226513866, 30.44083106164009322 ) ) ;
#37802 = CARTESIAN_POINT ( 'NONE',  ( -12.59222992820602194, -4.809359713505814149, 33.96456829005828837 ) ) ;
#37801 = B_SPLINE_CURVE_WITH_KNOTS ( 'NONE', 3,
 ( #53748, #63160, #1911, #84345, #35252, #14542, #1028, #42465, #49214, #27608 ),
 .UNSPECIFIED., .F., .F.,
 ( 4, 2, 2, 2, 4 ),
 ( 0.0007817246256747461966, 0.0009771112852218892010, 0.001172497944769032314, 0.001367884604316175427, 0.001563271263863318323 ),
 .UNSPECIFIED. ) ;
#37803 = FACE_OUTER_BOUND ( 'NONE', #52611, .T. ) ;
#37804 = DIRECTION ( 'NONE',  ( 1.000000000000000000, 0.000000000000000000, 0.000000000000000000 ) ) ;
#37805 = CARTESIAN_POINT ( 'NONE',  ( 2.651650429449539104, -4.848349570550432475, 19.31250000000000000 ) ) ;
#37806 = ORIENTED_EDGE ( 'NONE', *, *, #53561, .F. ) ;
#37807 = B_SPLINE_CURVE_WITH_KNOTS ( 'NONE', 3,
 ( #74377, #54534, #82030, #68496, #46893, #87928, #47787, #46008, #18549, #67623 ),
 .UNSPECIFIED., .F., .F.,
 ( 4, 2, 2, 2, 4 ),
 ( 0.0007817359430256285964, 0.0009771253907249945886, 0.001172514838424360472, 0.001367904286123726356, 0.001563293733823092457 ),
 .UNSPECIFIED. ) ;
#37808 = EDGE_LOOP ( 'NONE', ( #27592, #42811 ) ) ;
#37809 = CARTESIAN_POINT ( 'NONE',  ( -14.43784027742400689, -5.070767119584671079, 34.40440758774516183 ) ) ;
#37810 = VERTEX_POINT ( 'NONE', #9582 ) ;
#37811 = CARTESIAN_POINT ( 'NONE',  ( -27.00000000000000000, -8.999999999999996447, 22.25000000000000000 ) ) ;
#37812 = CARTESIAN_POINT ( 'NONE',  ( 17.93391762063986050, -11.35647404775217595, 33.31231777344666511 ) ) ;
#37813 = CARTESIAN_POINT ( 'NONE',  ( -16.28453762051371356, -2.729777683071817229, 31.24903638046269450 ) ) ;
#37814 = DIRECTION ( 'NONE',  ( -0.000000000000000000, 0.6427876096865404731, -0.7660444431189770143 ) ) ;
#37815 = CARTESIAN_POINT ( 'NONE',  ( 1.553300858899087311, -3.749999999999992006, 17.98437500000000000 ) ) ;
#37816 = CARTESIAN_POINT ( 'NONE',  ( 1.384615384615386802, -9.905515769479276145, 34.41647553114623292 ) ) ;
#37817 = ORIENTED_EDGE ( 'NONE', *, *, #47841, .T. ) ;
#37818 = CARTESIAN_POINT ( 'NONE',  ( -12.68502340526241312, -10.81261337010820256, 33.49550067578627477 ) ) ;
#37820 = EDGE_LOOP ( 'NONE', ( #32501, #68132, #66, #78926, #61814 ) ) ;
#37819 = CARTESIAN_POINT ( 'NONE',  ( -16.40382288478850725, -11.79746400365624659, 32.30657167506340954 ) ) ;
#37821 = CARTESIAN_POINT ( 'NONE',  ( -9.562260257057236146, -7.723484941389743952, 34.99544897038808955 ) ) ;
#37822 = FACE_OUTER_BOUND ( 'NONE', #19504, .T. ) ;
#37823 = CARTESIAN_POINT ( 'NONE',  ( -8.769230769230768274, -6.343179335718451384, 34.87096338111211935 ) ) ;
#37824 = DIRECTION ( 'NONE',  ( -0.000000000000000000, 0.5000000000000011102, -0.8660254037844380415 ) ) ;
#37825 = DIRECTION ( 'NONE',  ( -0.000000000000000000, -0.3420201433256694901, -0.9396926207859082059 ) ) ;
#37826 = CARTESIAN_POINT ( 'NONE',  ( 9.442330948259101575, -4.818429247618089661, 34.26397095200675125 ) ) ;
#37827 = PLANE ( 'NONE',  #48487 ) ;
#37828 = CARTESIAN_POINT ( 'NONE',  ( -2.608446859217920633, -4.805146000318815780, 19.25186829374151287 ) ) ;
#37829 = ORIENTED_EDGE ( 'NONE', *, *, #67680, .T. ) ;
#37830 = CARTESIAN_POINT ( 'NONE',  ( -13.91025641025641058, -7.500000000000000000, 29.75000000000000355 ) ) ;
#37831 = CARTESIAN_POINT ( 'NONE',  ( -13.38461538461538325, -9.905515769479276145, 34.41647553114623292 ) ) ;
#37832 = CARTESIAN_POINT ( 'NONE',  ( -12.46153846153858247, -11.94971097300221174, 32.03036669348237098 ) ) ;
#37833 = CARTESIAN_POINT ( 'NONE',  ( 2.750000000000001776, -7.499999999999984013, 25.71875000000000000 ) ) ;
#37834 = VECTOR ( 'NONE', #10558, 1000.000000000000000 ) ;
#37835 = EDGE_CURVE ( 'NONE', #48938, #31226, #49252, .T. ) ;
#37836 = AXIS2_PLACEMENT_3D ( 'NONE', #2427, #65011, #59154 ) ;
#37837 = CARTESIAN_POINT ( 'NONE',  ( 0.3962680155776850399, -3.835265460703609186, 33.15142922261924241 ) ) ;
#37838 = CARTESIAN_POINT ( 'NONE',  ( 8.545745844666440050, -10.23692288466677880, 34.23039457007281072 ) ) ;
#37839 = ORIENTED_EDGE ( 'NONE', *, *, #24956, .T. ) ;
#37840 = CARTESIAN_POINT ( 'NONE',  ( -1.409462824231155764E-14, -4.749999999999999112, 17.90625000000000000 ) ) ;
#37841 = CARTESIAN_POINT ( 'NONE',  ( -1.318548051265307386, -12.34228464037088813, 31.77849191805839268 ) ) ;
#37842 = EDGE_CURVE ( 'NONE', #78742, #31319, #15027, .T. ) ;
#37843 = VECTOR ( 'NONE', #42095, 1000.000000000000000 ) ;
#37844 = ORIENTED_EDGE ( 'NONE', *, *, #18373, .T. ) ;
#37845 = B_SPLINE_CURVE_WITH_KNOTS ( 'NONE', 3,
 ( #49759, #36698, #49327, #15544, #43013, #76805, #70485, #15101, #35820, #36263 ),
 .UNSPECIFIED., .F., .F.,
 ( 4, 2, 2, 2, 4 ),
 ( 0.000000000000000000, 0.0001954339857564074473, 0.0003908679715128148945, 0.0005863019572692223418, 0.0007817359430256297891 ),
 .UNSPECIFIED. ) ;
#37846 = B_SPLINE_CURVE_WITH_KNOTS ( 'NONE', 3,
 ( #11219, #44987, #18424, #12119, #53975, #67502, #5794, #38244, #58950, #66614 ),
 .UNSPECIFIED., .F., .F.,
 ( 4, 2, 2, 2, 4 ),
 ( 0.000000000000000000, 0.0001954311564186863323, 0.0003908623128373726646, 0.0005862934692560590241, 0.0007817246256747453293 ),
 .UNSPECIFIED. ) ;
#37847 = CARTESIAN_POINT ( 'NONE',  ( -18.06608237936013595, -4.661471528628505112, 34.16647553114621871 ) ) ;
#37848 = EDGE_CURVE ( 'NONE', #80960, #24436, #31808, .T. ) ;
#37849 = ORIENTED_EDGE ( 'NONE', *, *, #50533, .F. ) ;
#37850 = LINE ( 'NONE', #15375, #79418 ) ;
#37851 = CARTESIAN_POINT ( 'NONE',  ( -7.715362038329056205, -11.71459661697926080, 32.44059661609675516 ) ) ;
#37852 = CARTESIAN_POINT ( 'NONE',  ( 9.692307692307570832, -8.656820664282941280, 34.87096338111179961 ) ) ;
#37853 = VERTEX_POINT ( 'NONE', #72168 ) ;
#37854 = DIRECTION ( 'NONE',  ( -0.000000000000000000, 1.000000000000000000, -0.000000000000000000 ) ) ;
#37855 = ORIENTED_EDGE ( 'NONE', *, *, #55764, .T. ) ;
#37856 = EDGE_CURVE ( 'NONE', #36253, #72492, #73521, .T. ) ;
#37857 = CARTESIAN_POINT ( 'NONE',  ( -5.934744860487159102, -2.379036618887895305, 30.90682066428159303 ) ) ;
#37858 = ORIENTED_EDGE ( 'NONE', *, *, #24115, .F. ) ;
#37859 = DIRECTION ( 'NONE',  ( 0.000000000000000000, 0.9396926207859126468, 0.3420201433256571111 ) ) ;
#37860 = CARTESIAN_POINT ( 'NONE',  ( 0.6843180028068690524, -11.41317474335729187, 32.86274602512330034 ) ) ;
#37861 = EDGE_CURVE ( 'NONE', #38356, #35065, #8201, .T. ) ;
#37862 = ORIENTED_EDGE ( 'NONE', *, *, #39053, .F. ) ;
#37863 = DIRECTION ( 'NONE',  ( -0.000000000000000000, 0.000000000000000000, 1.000000000000000000 ) ) ;
#37864 = FACE_OUTER_BOUND ( 'NONE', #44061, .T. ) ;
#37865 = CARTESIAN_POINT ( 'NONE',  ( -11.78848476268299628, -2.985938066672154445, 32.43141759479405550 ) ) ;
#37866 = EDGE_CURVE ( 'NONE', #18168, #45741, #86599, .T. ) ;
#37867 = VECTOR ( 'NONE', #21017, 1000.000000000000000 ) ;
#37868 = DIRECTION ( 'NONE',  ( 0.000000000000000000, 1.000000000000000000, 0.000000000000000000 ) ) ;
#37869 = CARTESIAN_POINT ( 'NONE',  ( -7.912236225513979981, -12.62096338111211580, 30.90682066428152908 ) ) ;
#37870 = ORIENTED_EDGE ( 'NONE', *, *, #75008, .F. ) ;
#37871 = ORIENTED_EDGE ( 'NONE', *, *, #59448, .T. ) ;
#37872 = ORIENTED_EDGE ( 'NONE', *, *, #4017, .T. ) ;
#37874 = ORIENTED_EDGE ( 'NONE', *, *, #17262, .F. ) ;
#37873 = CARTESIAN_POINT ( 'NONE',  ( -4.023055712879202162, -8.191423895709842640, 34.95447573519442130 ) ) ;
#37875 = EDGE_CURVE ( 'NONE', #22236, #18827, #84457, .T. ) ;
#37876 = EDGE_CURVE ( 'NONE', #41430, #60227, #2744, .T. ) ;
#37877 = CARTESIAN_POINT ( 'NONE',  ( -14.30769230769230660, -10.67929555188718282, 33.92786785259544047 ) ) ;
#37878 = CARTESIAN_POINT ( 'NONE',  ( 6.065255139512838234, -10.33852847137154107, 34.16647553114620450 ) ) ;
#37879 = VERTEX_POINT ( 'NONE', #30737 ) ;
#37880 = VERTEX_POINT ( 'NONE', #25769 ) ;
#37881 = ORIENTED_EDGE ( 'NONE', *, *, #73070, .F. ) ;
#37882 = CARTESIAN_POINT ( 'NONE',  ( 16.85399685940691938, -4.186968288167451036, 33.49512374952580274 ) ) ;
#37883 = EDGE_LOOP ( 'NONE', ( #26912, #82090 ) ) ;
#37884 = B_SPLINE_CURVE_WITH_KNOTS ( 'NONE', 3,
 ( #74711, #82352, #12998, #53980, #60287, #87799, #74261, #40483, #67948, #6251 ),
 .UNSPECIFIED., .F., .F.,
 ( 4, 2, 2, 2, 4 ),
 ( 0.000000000000000000, 0.0001954311564186872810, 0.0003908623128373745620, 0.0005862934692560618430, 0.0007817246256747491240 ),
 .UNSPECIFIED. ) ;
#37885 = LINE ( 'NONE', #64012, #51974 ) ;
#37886 = VECTOR ( 'NONE', #49515, 1000.000000000000227 ) ;
#37887 = EDGE_CURVE ( 'NONE', #72513, #4656, #19013, .T. ) ;
#37888 = EDGE_CURVE ( 'NONE', #39612, #80371, #3868, .T. ) ;
#37889 = CARTESIAN_POINT ( 'NONE',  ( -11.66915300512910214, -3.530157926970578952, 32.79014554554150607 ) ) ;
#37890 = CARTESIAN_POINT ( 'NONE',  ( -15.93083330975275658, -10.77377354290276301, 33.85451476688484718 ) ) ;
#37891 = FACE_BOUND ( 'NONE', #18393, .T. ) ;
#37892 = ORIENTED_EDGE ( 'NONE', *, *, #60697, .F. ) ;
#37893 = DIRECTION ( 'NONE',  ( 0.000000000000000000, 0.000000000000000000, 1.000000000000000000 ) ) ;
#37894 = CARTESIAN_POINT ( 'NONE',  ( 13.51514108637895006, -9.417988943895561960, 34.36773134775777550 ) ) ;
#37895 = CARTESIAN_POINT ( 'NONE',  ( -4.153846153846273204, -2.892918686052165622, 31.69288490824153470 ) ) ;
#37896 = FACE_OUTER_BOUND ( 'NONE', #40619, .T. ) ;
#37897 = CARTESIAN_POINT ( 'NONE',  ( 13.38461538461538680, -1.242168528481310874, 33.36296068462461051 ) ) ;
#37898 = ORIENTED_EDGE ( 'NONE', *, *, #82981, .F. ) ;
#37899 = DIRECTION ( 'NONE',  ( -0.000000000000000000, -0.000000000000000000, -1.000000000000000000 ) ) ;
#37900 = B_SPLINE_CURVE_WITH_KNOTS ( 'NONE', 3,
 ( #71611, #84272, #78817, #9918, #58101, #8604, #50018, #23859, #63082, #36078 ),
 .UNSPECIFIED., .F., .F.,
 ( 4, 2, 2, 2, 4 ),
 ( 0.000000000000000000, 0.0001954311564186878502, 0.0003908623128373757004, 0.0005862934692560635777, 0.0007817246256747514008 ),
 .UNSPECIFIED. ) ;
#37901 = EDGE_LOOP ( 'NONE', ( #81983, #42092, #33419, #42914 ) ) ;
#37902 = ADVANCED_FACE ( 'NONE', ( #39296 ), #85696, .F. ) ;
#37903 = ORIENTED_EDGE ( 'NONE', *, *, #61255, .F. ) ;
#37905 = CARTESIAN_POINT ( 'NONE',  ( -1.608100309179714360, -5.827078755546626354, 34.72654668319379567 ) ) ;
#37904 = DIRECTION ( 'NONE',  ( -0.000000000000000000, -0.9396926207859092051, -0.3420201433256662704 ) ) ;
#37906 = CARTESIAN_POINT ( 'NONE',  ( -10.86540785267757947, -12.22074536777954989, 31.39888409691088356 ) ) ;
#37907 = CARTESIAN_POINT ( 'NONE',  ( -13.63459212866397685, -2.920706130388546651, 32.31842814019191223 ) ) ;
#37908 = ADVANCED_FACE ( 'NONE', ( #64960 ), #23974, .F. ) ;
#37909 = DIRECTION ( 'NONE',  ( 1.000000000000000000, 0.000000000000000000, 0.000000000000000000 ) ) ;
#37910 = CARTESIAN_POINT ( 'NONE',  ( 14.08420738312797482, -3.019605429927184392, 32.48692288466676814 ) ) ;
#37911 = EDGE_CURVE ( 'NONE', #46479, #11121, #82054, .T. ) ;
#37912 = ORIENTED_EDGE ( 'NONE', *, *, #69690, .T. ) ;
#37913 = CARTESIAN_POINT ( 'NONE',  ( 6.700149964170075023, -2.523278758544489797, 31.42238647778637528 ) ) ;
#37914 = DIRECTION ( 'NONE',  ( -0.000000000000000000, 1.000000000000000000, -0.000000000000000000 ) ) ;
#37915 = CARTESIAN_POINT ( 'NONE',  ( 10.55011416942384095, -3.300289026998414865, 32.46337939537583139 ) ) ;
#37916 = CARTESIAN_POINT ( 'NONE',  ( -13.44988538517170440, -12.70778746994557551, 30.41441678777548319 ) ) ;
#37917 = ORIENTED_EDGE ( 'NONE', *, *, #23479, .T. ) ;
#37918 = EDGE_CURVE ( 'NONE', #49110, #12728, #65121, .T. ) ;
#37919 = ORIENTED_EDGE ( 'NONE', *, *, #85776, .F. ) ;
#37920 = FACE_BOUND ( 'NONE', #1893, .T. ) ;
#37921 = VERTEX_POINT ( 'NONE', #41061 ) ;
#37922 = CARTESIAN_POINT ( 'NONE',  ( 11.53846153846141576, -12.51329471203414379, 31.30864560766407578 ) ) ;
#37923 = CARTESIAN_POINT ( 'NONE',  ( -8.769230769230768274, -5.415277668671390821, 36.20867863119892149 ) ) ;
#37924 = VERTEX_POINT ( 'NONE', #520 ) ;
#37925 = CARTESIAN_POINT ( 'NONE',  ( -3.230769230769229949, -12.37446782046654192, 30.86335684631486131 ) ) ;
#37926 = CARTESIAN_POINT ( 'NONE',  ( -2.307692307692305711, -4.098570777380720287, 33.41473453929634729 ) ) ;
#37927 = CARTESIAN_POINT ( 'NONE',  ( 0.5276068125408989173, -12.10708131394839704, 31.69288490824020954 ) ) ;
#37928 = CARTESIAN_POINT ( 'NONE',  ( -1.318548051265309162, -3.937682226553329556, 33.60647404775216529 ) ) ;
#37929 = EDGE_LOOP ( 'NONE', ( #35900, #21003, #22834, #13108 ) ) ;
#37930 = CARTESIAN_POINT ( 'NONE',  ( -17.07692307692307665, -6.435427911321262684, 35.78748833219616898 ) ) ;
#37932 = VERTEX_POINT ( 'NONE', #12701 ) ;
#37931 = CIRCLE ( 'NONE', #55222, 4.000000000000000000 ) ;
#37934 = EDGE_LOOP ( 'NONE', ( #72147, #60571 ) ) ;
#37933 = FACE_OUTER_BOUND ( 'NONE', #19175, .T. ) ;
#37935 = CARTESIAN_POINT ( 'NONE',  ( -8.703162418228330921, -9.780366693483667717, 34.19971097300155805 ) ) ;
#37936 = CARTESIAN_POINT ( 'NONE',  ( -12.68446542044531178, -2.889293201056495786, 32.26117774369186009 ) ) ;
#37937 = FACE_OUTER_BOUND ( 'NONE', #39266, .T. ) ;
#37938 = DIRECTION ( 'NONE',  ( -0.000000000000000000, 0.3420201433256694901, -0.9396926207859082059 ) ) ;
#37939 = CARTESIAN_POINT ( 'NONE',  ( -14.53117723225663838, -8.539481045369596401, 34.89627647299170832 ) ) ;
#37940 = DIRECTION ( 'NONE',  ( -0.000000000000000000, 0.3420201433256694901, -0.9396926207859082059 ) ) ;
#37941 = CARTESIAN_POINT ( 'NONE',  ( 2.750000000000002665, -7.561099074964516831, 13.47061829374151465 ) ) ;
#37942 = VERTEX_POINT ( 'NONE', #61310 ) ;
#37943 = B_SPLINE_CURVE_WITH_KNOTS ( 'NONE', 3,
 ( #80422, #59696, #25468, #52925, #53823, #39884, #80876, #52037, #17829, #18723 ),
 .UNSPECIFIED., .F., .F.,
 ( 4, 2, 2, 2, 4 ),
 ( 0.000000000000000000, 0.0001954311564186869286, 0.0003908623128373738573, 0.0005862934692560607588, 0.0007817246256747477145 ),
 .UNSPECIFIED. ) ;
#37944 = CARTESIAN_POINT ( 'NONE',  ( 4.946775107191381693, -12.15440758774515473, 32.17923288041532004 ) ) ;
#37945 = LINE ( 'NONE', #65408, #62041 ) ;
#37946 = DIRECTION ( 'NONE',  ( 0.000000000000000000, 0.000000000000000000, 1.000000000000000000 ) ) ;
#37947 = VERTEX_POINT ( 'NONE', #46914 ) ;
#37948 = ORIENTED_EDGE ( 'NONE', *, *, #9223, .T. ) ;
#37949 = CARTESIAN_POINT ( 'NONE',  ( -5.869209559033047974, -12.62708834333097663, 30.88030960425257021 ) ) ;
#37950 = CARTESIAN_POINT ( 'NONE',  ( 7.715463243043539698, -6.369640206132550553, 34.87707690430378449 ) ) ;
#37951 = CARTESIAN_POINT ( 'NONE',  ( 6.000000000000001776, -11.16473453929635440, 33.15142922261926373 ) ) ;
#37952 = PLANE ( 'NONE',  #61509 ) ;
#37953 = CARTESIAN_POINT ( 'NONE',  ( 2.307692307692309264, -5.415277668671390821, 36.20867863119892149 ) ) ;
#37954 = CARTESIAN_POINT ( 'NONE',  ( -17.01166793741023753, -11.67786785259547777, 32.92929555188713664 ) ) ;
#37955 = CARTESIAN_POINT ( 'NONE',  ( 5.869308533332442401, -8.147922237126337563, 34.70805685702651999 ) ) ;
#37956 = ORIENTED_EDGE ( 'NONE', *, *, #22708, .F. ) ;
#37957 = CARTESIAN_POINT ( 'NONE',  ( -4.023320452082591814, -6.001044277235011215, 34.52024696741798948 ) ) ;
#37958 = CARTESIAN_POINT ( 'NONE',  ( -0.3310127597748976358, -8.586989748646448817, 34.63063291749215011 ) ) ;
#37959 = AXIS2_PLACEMENT_3D ( 'NONE', #2092, #29580, #44391 ) ;
#37960 = CARTESIAN_POINT ( 'NONE',  ( -5.776573038138430150, -7.630147231320743018, 34.74852402298682819 ) ) ;
#37961 = CARTESIAN_POINT ( 'NONE',  ( 12.33139125210024289, -11.93770438780619259, 32.05411857736982029 ) ) ;
#37962 = VERTEX_POINT ( 'NONE', #19453 ) ;
#37963 = CARTESIAN_POINT ( 'NONE',  ( 10.48523664565292179, -9.504002272028875709, 34.60269587691767867 ) ) ;
#37965 = AXIS2_PLACEMENT_3D ( 'NONE', #48934, #58233, #21909 ) ;
#37964 = B_SPLINE_CURVE_WITH_KNOTS ( 'NONE', 3,
 ( #23292, #56204, #50752, #21527, #15225, #78236, #21977, #16538, #63393, #69716 ),
 .UNSPECIFIED., .F., .F.,
 ( 4, 2, 2, 2, 4 ),
 ( 0.0007817246256747460882, 0.0009771112852218892010, 0.001172497944769032314, 0.001367884604316175210, 0.001563271263863318323 ),
 .UNSPECIFIED. ) ;
#37966 = VECTOR ( 'NONE', #33698, 1000.000000000000000 ) ;
#37967 = ORIENTED_EDGE ( 'NONE', *, *, #82316, .F. ) ;
#37968 = CARTESIAN_POINT ( 'NONE',  ( 14.98079249982687777, -11.28823185664190376, 33.01397839955799896 ) ) ;
#37969 = SURFACE_STYLE_USAGE ( .BOTH. , #53246 ) ;
#37970 = CARTESIAN_POINT ( 'NONE',  ( 10.36540787133602493, -3.436278759898153901, 33.07459398097509506 ) ) ;
#37971 = CARTESIAN_POINT ( 'NONE',  ( 15.48082365068268373, -4.818054556918156983, 34.26375889529406749 ) ) ;
#37972 = ORIENTED_EDGE ( 'NONE', *, *, #81264, .F. ) ;
#37973 = CARTESIAN_POINT ( 'NONE',  ( 12.46153846153833911, -11.06231777344772027, 33.60647404775119895 ) ) ;
#37974 = DIRECTION ( 'NONE',  ( 0.000000000000000000, 0.000000000000000000, -1.000000000000000000 ) ) ;
#37975 = EDGE_CURVE ( 'NONE', #73916, #47875, #28618, .T. ) ;
#37976 = CARTESIAN_POINT ( 'NONE',  ( -6.222926958906846551, -5.582147617184174848, 34.63737895849758530 ) ) ;
#37977 = CARTESIAN_POINT ( 'NONE',  ( -5.011667937410237528, -8.656820664281605460, 34.87096338111211224 ) ) ;
#37978 = ORIENTED_EDGE ( 'NONE', *, *, #84164, .T. ) ;
#37979 = DIRECTION ( 'NONE',  ( -0.000000000000000000, 0.8660254037844399289, -0.4999999999999980016 ) ) ;
#37980 = ORIENTED_EDGE ( 'NONE', *, *, #23773, .T. ) ;
#37981 = CARTESIAN_POINT ( 'NONE',  ( -27.00000000000000000, 0.000000000000000000, 0.000000000000000000 ) ) ;
#37982 = CYLINDRICAL_SURFACE ( 'NONE', #36235, 0.2499999999999995559 ) ;
#37983 = CARTESIAN_POINT ( 'NONE',  ( -16.85391023282967637, -3.395485233115139501, 33.02377354290276656 ) ) ;
#37984 = LINE ( 'NONE', #11399, #24331 ) ;
#37985 = ADVANCED_FACE ( 'NONE', ( #34295 ), #34741, .T. ) ;
#37986 = CARTESIAN_POINT ( 'NONE',  ( 6.923076923076802558, -10.21337939537710326, 33.94971097300076224 ) ) ;
#37987 = CARTESIAN_POINT ( 'NONE',  ( 9.442330961365339448, -8.303909089506435137, 34.68538101551103381 ) ) ;
#37988 = ORIENTED_EDGE ( 'NONE', *, *, #38274, .T. ) ;
#37989 = VECTOR ( 'NONE', #57752, 1000.000000000000000 ) ;
#37990 = ORIENTED_EDGE ( 'NONE', *, *, #55597, .F. ) ;
#37991 = ORIENTED_EDGE ( 'NONE', *, *, #39848, .F. ) ;
#37992 = ORIENTED_EDGE ( 'NONE', *, *, #66318, .T. ) ;
#37993 = VERTEX_POINT ( 'NONE', #73 ) ;
#37994 = ADVANCED_FACE ( 'NONE', ( #55019 ), #27984, .F. ) ;
#37995 = CARTESIAN_POINT ( 'NONE',  ( -12.46153846153814726, -2.255955759149395501, 30.00000000000324363 ) ) ;
#37996 = CARTESIAN_POINT ( 'NONE',  ( 11.47319153790521717, -9.528491918058357157, 34.59228464037090589 ) ) ;
#37997 = CARTESIAN_POINT ( 'NONE',  ( -3.930833309752757021, -6.460100341425561332, 34.89618726649961644 ) ) ;
#37998 = CARTESIAN_POINT ( 'NONE',  ( -18.00000000000000000, -6.682775186373817178, 35.82440484884453724 ) ) ;
#37999 = CARTESIAN_POINT ( 'NONE',  ( -13.60754234352223335, -3.395401636524185474, 33.02366814457250399 ) ) ;
#38000 = CARTESIAN_POINT ( 'NONE',  ( 0.5276068125408989173, -4.786620604624113540, 33.94971097300155805 ) ) ;
#38001 = CARTESIAN_POINT ( 'NONE',  ( -17.74994568836168440, -9.943054286541400444, 34.11300777759954883 ) ) ;
#38002 = CARTESIAN_POINT ( 'NONE',  ( -17.93474442872397034, -6.879047030191283163, 34.71129190930002295 ) ) ;
#38003 = CARTESIAN_POINT ( 'NONE',  ( -4.377331097570101193, -10.11188796281391511, 34.01382737946119050 ) ) ;
#38004 = ORIENTED_EDGE ( 'NONE', *, *, #5208, .T. ) ;
#38005 = ORIENTED_EDGE ( 'NONE', *, *, #79497, .T. ) ;
#38006 = VERTEX_POINT ( 'NONE', #88825 ) ;
#38008 = ORIENTED_EDGE ( 'NONE', *, *, #58741, .T. ) ;
#38007 = CYLINDRICAL_SURFACE ( 'NONE', #18635, 0.2500000000000004996 ) ;
#38010 = CARTESIAN_POINT ( 'NONE',  ( 1.384615384615386802, -2.538708090699994813, 30.37095296980875503 ) ) ;
#38009 = CARTESIAN_POINT ( 'NONE',  ( -15.23076923076922995, -13.87047571288749737, 32.06866353760679544 ) ) ;
#38011 = B_SPLINE_CURVE_WITH_KNOTS ( 'NONE', 3,
 ( #24234, #49942, #43195, #50380, #30120, #77861, #36871, #16164, #51696, #79202 ),
 .UNSPECIFIED., .F., .F.,
 ( 4, 2, 2, 2, 4 ),
 ( 0.0007817246256747476061, 0.0009771112852218902852, 0.001172497944769033181, 0.001367884604316175860, 0.001563271263863318539 ),
 .UNSPECIFIED. ) ;
#38012 = CARTESIAN_POINT ( 'NONE',  ( 4.230769230769229061, -3.499999999999999556, 29.75000000000000355 ) ) ;
#38013 = EDGE_CURVE ( 'NONE', #6050, #8255, #48247, .T. ) ;
#38014 = CARTESIAN_POINT ( 'NONE',  ( -10.68065506134539078, -11.94971097300153140, 32.03036669348370680 ) ) ;
#38015 = EDGE_CURVE ( 'NONE', #45914, #68800, #71513, .T. ) ;
#38016 = ORIENTED_EDGE ( 'NONE', *, *, #23568, .T. ) ;
#38017 = VECTOR ( 'NONE', #8767, 1000.000000000000000 ) ;
#38018 = ORIENTED_EDGE ( 'NONE', *, *, #57121, .T. ) ;
#38019 = CARTESIAN_POINT ( 'NONE',  ( -17.14219307747939780, -11.67786785259541027, 32.92929555188721480 ) ) ;
#38020 = AXIS2_PLACEMENT_3D ( 'NONE', #52703, #59018, #24792 ) ;
#38021 = EDGE_LOOP ( 'NONE', ( #33677, #89068 ) ) ;
#38022 = FACE_BOUND ( 'NONE', #29606, .T. ) ;
#38023 = CARTESIAN_POINT ( 'NONE',  ( 17.07692307692295586, -8.656820664282941280, 34.87096338111179961 ) ) ;
#38024 = CIRCLE ( 'NONE', #88397, 0.2500000000000002220 ) ;
#38025 = CARTESIAN_POINT ( 'NONE',  ( -3.903900635498009919, -11.86320923018887719, 32.19269448109604781 ) ) ;
#38026 = VERTEX_POINT ( 'NONE', #74401 ) ;
#38027 = CARTESIAN_POINT ( 'NONE',  ( -15.00775787915638126, -12.15243808032446005, 31.58219941686247978 ) ) ;
#38028 = CARTESIAN_POINT ( 'NONE',  ( -6.857821783564084228, -2.379036618887895305, 30.90682066428159303 ) ) ;
#38029 = CYLINDRICAL_SURFACE ( 'NONE', #72343, 0.2499999999999979738 ) ;
#38030 = EDGE_LOOP ( 'NONE', ( #76429, #24652 ) ) ;
#38031 = CARTESIAN_POINT ( 'NONE',  ( 17.93467708450782183, -7.749976743299138882, 34.99404534957040624 ) ) ;
#38032 = CARTESIAN_POINT ( 'NONE',  ( 6.000000000000001776, -12.78798330534102945, 29.74999999999997868 ) ) ;
#38033 = ORIENTED_EDGE ( 'NONE', *, *, #1341, .F. ) ;
#38034 = DIRECTION ( 'NONE',  ( 0.000000000000000000, 0.6427876096865368094, 0.7660444431189802339 ) ) ;
#38035 = CARTESIAN_POINT ( 'NONE',  ( 6.923076923076924238, -10.51840700105979565, 33.73612834413961536 ) ) ;
#38036 = ORIENTED_EDGE ( 'NONE', *, *, #21023, .T. ) ;
#38037 = CARTESIAN_POINT ( 'NONE',  ( 6.988332062589762472, -2.657715359629131857, 31.77849191805844242 ) ) ;
#38038 = CARTESIAN_POINT ( 'NONE',  ( -12.23875892027004753, -2.600157965045224451, 30.74683119005207743 ) ) ;
#38039 = CARTESIAN_POINT ( 'NONE',  ( -15.93083480223330817, -8.239487800360276282, 34.69522927552633718 ) ) ;
#38040 = CARTESIAN_POINT ( 'NONE',  ( 7.780397043639536214, -7.249945686854188942, 34.74374336980223887 ) ) ;
#38041 = CARTESIAN_POINT ( 'NONE',  ( 9.562159722575998444, -12.50552854090298638, 31.33409797877408920 ) ) ;
#38042 = CYLINDRICAL_SURFACE ( 'NONE', #56726, 0.2499999999999994726 ) ;
#38044 = CARTESIAN_POINT ( 'NONE',  ( -15.23076923076935074, -12.46129190930018460, 30.37095296980731973 ) ) ;
#38043 = LINE ( 'NONE', #37140, #83630 ) ;
#38045 = CARTESIAN_POINT ( 'NONE',  ( -0.3962833220256229416, -8.656820664281605460, 34.87096338111211224 ) ) ;
#38047 = CARTESIAN_POINT ( 'NONE',  ( -8.545855283458346108, -2.251407671071268712, 29.88021292934943673 ) ) ;
#38046 = DIRECTION ( 'NONE',  ( -0.000000000000000000, 0.9848077530122086864, -0.1736481776669273891 ) ) ;
#38048 = CARTESIAN_POINT ( 'NONE',  ( -2.749999999999998224, -7.500000000000015987, 15.09375000000000000 ) ) ;
#38049 = ORIENTED_EDGE ( 'NONE', *, *, #13427, .F. ) ;
#38050 = CARTESIAN_POINT ( 'NONE',  ( 3.056863809964074807, -7.383657973411067665, 13.99999999999999467 ) ) ;
#38051 = ORIENTED_EDGE ( 'NONE', *, *, #60428, .F. ) ;
#38052 = B_SPLINE_CURVE_WITH_KNOTS ( 'NONE', 3,
 ( #76755, #69984, #42969, #35776, #56479, #48384, #1978, #70442, #83970, #22250 ),
 .UNSPECIFIED., .F., .F.,
 ( 4, 2, 2, 2, 4 ),
 ( 0.0007817359430256289217, 0.0009771253907249950223, 0.001172514838424361123, 0.001367904286123727007, 0.001563293733823093107 ),
 .UNSPECIFIED. ) ;
#38053 = ORIENTED_EDGE ( 'NONE', *, *, #40624, .F. ) ;
#38054 = CARTESIAN_POINT ( 'NONE',  ( -17.01166793741023042, -4.320704448112858032, 33.92786785259548310 ) ) ;
#38055 = VERTEX_POINT ( 'NONE', #5950 ) ;
#38056 = CARTESIAN_POINT ( 'NONE',  ( 3.296024802045255164, -10.21337939537593797, 33.94971097300152252 ) ) ;
#38057 = CARTESIAN_POINT ( 'NONE',  ( -1.944543648262992530, -9.444543648263016067, 16.18750000000000000 ) ) ;
#38058 = DIRECTION ( 'NONE',  ( -0.000000000000000000, 0.8660254037844399289, -0.4999999999999980016 ) ) ;
#38059 = CARTESIAN_POINT ( 'NONE',  ( 17.07692307692307665, -2.721908614388771852, 31.22303859784724978 ) ) ;
#38060 = CARTESIAN_POINT ( 'NONE',  ( -0.3962828902624371263, -6.026961402152789304, 34.52809138561124769 ) ) ;
#38061 = CYLINDRICAL_SURFACE ( 'NONE', #33122, 0.2500000000000009437 ) ;
#38062 = AXIS2_PLACEMENT_3D ( 'NONE', #71717, #78040, #27745 ) ;
#38063 = CARTESIAN_POINT ( 'NONE',  ( -8.769230769230890843, -5.219633306517616589, 34.19971097300220464 ) ) ;
#38064 = CARTESIAN_POINT ( 'NONE',  ( -10.68146802634049308, -4.098570777380719399, 33.41473453929634729 ) ) ;
#38065 = CARTESIAN_POINT ( 'NONE',  ( 0.5923289025054128132, -2.494656445102013453, 31.33466734024120015 ) ) ;
#38066 = CARTESIAN_POINT ( 'NONE',  ( 2.651650429449569302, -10.15165042944953733, 19.62500000000000000 ) ) ;
#38067 = CARTESIAN_POINT ( 'NONE',  ( -11.31568186948347154, -2.612705202774698421, 31.66806509827799943 ) ) ;
#38068 = DIRECTION ( 'NONE',  ( 0.000000000000000000, 1.000000000000000000, -2.546383084002652634E-16 ) ) ;
#38069 = LINE ( 'NONE', #10602, #26297 ) ;
#38070 = ORIENTED_EDGE ( 'NONE', *, *, #2176, .F. ) ;
#38071 = ORIENTED_EDGE ( 'NONE', *, *, #20197, .F. ) ;
#38072 = CARTESIAN_POINT ( 'NONE',  ( 17.14299142792551933, -12.10708131394839882, 31.69288490824020954 ) ) ;
#38073 = CARTESIAN_POINT ( 'NONE',  ( 18.00000000000000000, -1.422936976036506707, 30.56769352161908415 ) ) ;
#38074 = FACE_OUTER_BOUND ( 'NONE', #77513, .T. ) ;
#38075 = CARTESIAN_POINT ( 'NONE',  ( 16.21899093456577745, -7.750023224968865421, 34.99404313364389907 ) ) ;
#38076 = LINE ( 'NONE', #23228, #88097 ) ;
#38077 = CYLINDRICAL_SURFACE ( 'NONE', #71565, 0.2500000000000008882 ) ;
#38078 = EDGE_CURVE ( 'NONE', #46711, #21870, #51070, .T. ) ;
#38079 = ADVANCED_FACE ( 'NONE', ( #8611 ), #22994, .F. ) ;
#38080 = VECTOR ( 'NONE', #59391, 1000.000000000000114 ) ;
#38081 = ORIENTED_EDGE ( 'NONE', *, *, #58854, .T. ) ;
#38082 = CARTESIAN_POINT ( 'NONE',  ( -10.39195821646982587, -7.630147987733840509, 34.99859428049665411 ) ) ;
#38083 = EDGE_LOOP ( 'NONE', ( #81523, #19055, #23507, #63828 ) ) ;
#38084 = ORIENTED_EDGE ( 'NONE', *, *, #19312, .T. ) ;
#38085 = CARTESIAN_POINT ( 'NONE',  ( -5.933931648997561759, -5.557115091759786019, 34.35708131394839882 ) ) ;
#38086 = CIRCLE ( 'NONE', #35256, 0.2500000000000002220 ) ;
#38087 = EDGE_CURVE ( 'NONE', #4529, #2835, #67230, .T. ) ;
#38088 = CARTESIAN_POINT ( 'NONE',  ( -23.00000000000000000, -12.50000000000000000, 27.25000000000000000 ) ) ;
#38089 = CARTESIAN_POINT ( 'NONE',  ( 9.757563263583723057, -12.27809138561124591, 31.22303859784720359 ) ) ;
#38090 = EDGE_CURVE ( 'NONE', #24436, #33117, #14925, .T. ) ;
#38091 = CARTESIAN_POINT ( 'NONE',  ( -6.249976730942353953, -3.137211980971221781, 32.19342716148376837 ) ) ;
#38092 = DIRECTION ( 'NONE',  ( 0.000000000000000000, 0.000000000000000000, -1.000000000000000000 ) ) ;
#38093 = VERTEX_POINT ( 'NONE', #69418 ) ;
#38094 = ORIENTED_EDGE ( 'NONE', *, *, #6529, .F. ) ;
#38095 = EDGE_LOOP ( 'NONE', ( #27789, #73298 ) ) ;
#38096 = EDGE_CURVE ( 'NONE', #31128, #43735, #41952, .T. ) ;
#38097 = CARTESIAN_POINT ( 'NONE',  ( -1.384615384615505151, -3.300289026999228881, 32.46337939537708905 ) ) ;
#38098 = DIRECTION ( 'NONE',  ( 0.000000000000000000, 0.8660254037844377084, -0.5000000000000015543 ) ) ;
#38099 = LINE ( 'NONE', #66909, #46577 ) ;
#38100 = CARTESIAN_POINT ( 'NONE',  ( -15.23076923076922995, -3.050289026998446396, 32.03036669348365706 ) ) ;
#38101 = CARTESIAN_POINT ( 'NONE',  ( 1.384615384615386802, -12.10708131394839349, 31.69288490824020244 ) ) ;
#38102 = CARTESIAN_POINT ( 'NONE',  ( 17.93391658904412012, -8.120952969808774569, 34.71129190930000163 ) ) ;
#38103 = ORIENTED_EDGE ( 'NONE', *, *, #56372, .T. ) ;
#38104 = ORIENTED_EDGE ( 'NONE', *, *, #73434, .T. ) ;
#38105 = CARTESIAN_POINT ( 'NONE',  ( -3.749999999999988454, -9.053300858899127945, 22.51562500000000000 ) ) ;
#38106 = VECTOR ( 'NONE', #46359, 1000.000000000000227 ) ;
#38107 = ORIENTED_EDGE ( 'NONE', *, *, #61330, .T. ) ;
#38109 = EDGE_LOOP ( 'NONE', ( #5345, #75449, #9991, #27578 ) ) ;
#38108 = CARTESIAN_POINT ( 'NONE',  ( 2.307692307692187583, -12.46129190930018460, 30.37095296980731973 ) ) ;
#38110 = CARTESIAN_POINT ( 'NONE',  ( 1.161130440891437132, -10.11188796281391333, 34.01382737946119050 ) ) ;
#38111 = CARTESIAN_POINT ( 'NONE',  ( 12.68455130563185662, -8.282913670948747864, 34.94150082978203642 ) ) ;
#38112 = CARTESIAN_POINT ( 'NONE',  ( -1.929879867024197893E-14, -3.750000000000000000, 17.90625000000000000 ) ) ;
#38113 = ADVANCED_FACE ( 'NONE', ( #43707 ), #16243, .F. ) ;
#38114 = VERTEX_POINT ( 'NONE', #30206 ) ;
#38115 = EDGE_CURVE ( 'NONE', #1316, #83223, #56347, .T. ) ;
#38116 = CARTESIAN_POINT ( 'NONE',  ( -1.319360245102546347, -2.657715359629131857, 31.77849191805844242 ) ) ;
#38117 = ORIENTED_EDGE ( 'NONE', *, *, #22169, .F. ) ;
#38118 = CARTESIAN_POINT ( 'NONE',  ( -8.769230769230892619, -5.094484230521993062, 34.41647553114689373 ) ) ;
#38119 = CARTESIAN_POINT ( 'NONE',  ( -7.173053654019277303, -2.779195860258147022, 31.39871582349836743 ) ) ;
#38120 = B_SPLINE_CURVE_WITH_KNOTS ( 'NONE', 3,
 ( #85793, #4255, #31736, #59196, #52434, #29955, #43463, #57412, #23192, #50653 ),
 .UNSPECIFIED., .F., .F.,
 ( 4, 2, 2, 2, 4 ),
 ( 0.000000000000000000, 0.0001954311564186866305, 0.0003908623128373732609, 0.0005862934692560598914, 0.0007817246256747465219 ),
 .UNSPECIFIED. ) ;
#38121 = FACE_BOUND ( 'NONE', #79973, .T. ) ;
#38123 = CARTESIAN_POINT ( 'NONE',  ( 9.692307692307695177, -3.669653830205710676, 35.88435417666054406 ) ) ;
#38122 = CARTESIAN_POINT ( 'NONE',  ( 10.54962781287031071, -7.249945686854186278, 34.74374336980224598 ) ) ;
#38124 = EDGE_CURVE ( 'NONE', #76825, #28286, #32837, .T. ) ;
#38125 = CARTESIAN_POINT ( 'NONE',  ( 8.769230769230647482, -6.026961402154118019, 34.52809138561165270 ) ) ;
#38126 = CARTESIAN_POINT ( 'NONE',  ( -3.480792454990687457, -8.475808217655753651, 34.90892951860618609 ) ) ;
#38127 = ORIENTED_EDGE ( 'NONE', *, *, #750, .T. ) ;
#38128 = EDGE_CURVE ( 'NONE', #3529, #84875, #42717, .T. ) ;
#38129 = CARTESIAN_POINT ( 'NONE',  ( 13.38461538461538680, -13.04860791097971706, 34.73218667398347037 ) ) ;
#38130 = SURFACE_STYLE_FILL_AREA ( #10663 ) ;
#38131 = ORIENTED_EDGE ( 'NONE', *, *, #45902, .F. ) ;
#38132 = CARTESIAN_POINT ( 'NONE',  ( -7.384615384615385025, -11.50000000000000000, 29.75000000000000355 ) ) ;
#38133 = B_SPLINE_CURVE_WITH_KNOTS ( 'NONE', 3,
 ( #44905, #30512, #78703, #16551, #30944, #44018, #11130, #9797, #85906, #22861 ),
 .UNSPECIFIED., .F., .F.,
 ( 4, 2, 2, 2, 4 ),
 ( 0.000000000000000000, 0.0001954311564186867660, 0.0003908623128373735320, 0.0005862934692560603251, 0.0007817246256747470640 ),
 .UNSPECIFIED. ) ;
#38134 = CARTESIAN_POINT ( 'NONE',  ( 14.17754509825408960, -10.19110544564092002, 33.96427741523702792 ) ) ;
#38135 = CYLINDRICAL_SURFACE ( 'NONE', #49768, 0.2499999999999986955 ) ;
#38136 = CARTESIAN_POINT ( 'NONE',  ( 11.28843830116857383, -5.851115903089112003, 34.47074536777953568 ) ) ;
#38137 = LINE ( 'NONE', #43999, #28574 ) ;
#38138 = FACE_BOUND ( 'NONE', #86955, .T. ) ;
#38140 = LINE ( 'NONE', #22411, #71903 ) ;
#38139 = DIRECTION ( 'NONE',  ( -0.000000000000000000, 0.9848077530122085754, -0.1736481776669273613 ) ) ;
#38141 = CARTESIAN_POINT ( 'NONE',  ( -6.923076923077044142, -10.90142922262034020, 33.41473453929536674 ) ) ;
#38143 = CARTESIAN_POINT ( 'NONE',  ( 9.758376043310132530, -4.098570777380720287, 33.41473453929635440 ) ) ;
#38142 = DIRECTION ( 'NONE',  ( 0.000000000000000000, 0.3420201433256610524, 0.9396926207859113145 ) ) ;
#38144 = CARTESIAN_POINT ( 'NONE',  ( 15.90386942290380290, -10.66389620160130036, 33.62221079203477103 ) ) ;
#38145 = DIRECTION ( 'NONE',  ( -0.000000000000000000, 0.5000000000000011102, -0.8660254037844381525 ) ) ;
#38146 = CARTESIAN_POINT ( 'NONE',  ( 3.749999999999999556, -7.438900925035446754, 22.96688170625849068 ) ) ;
#38147 = B_SPLINE_CURVE_WITH_KNOTS ( 'NONE', 3,
 ( #73510, #80722, #18118, #87037, #5497, #45128, #17216, #11805, #3694, #23963 ),
 .UNSPECIFIED., .F., .F.,
 ( 4, 2, 2, 2, 4 ),
 ( 0.0007817359430256324996, 0.0009771253907249993591, 0.001172514838424366110, 0.001367904286123732861, 0.001563293733823099829 ),
 .UNSPECIFIED. ) ;
#38148 = ORIENTED_EDGE ( 'NONE', *, *, #52222, .F. ) ;
#38149 = CARTESIAN_POINT ( 'NONE',  ( -18.00000000000000000, -5.184797716151534175, 36.11096599634342397 ) ) ;
#38150 = CARTESIAN_POINT ( 'NONE',  ( 8.068933515131909928, -10.23759521482555357, 34.22997729860117033 ) ) ;
#38151 = CARTESIAN_POINT ( 'NONE',  ( -7.780898706641008467, -11.67786785259547777, 32.92929555188713664 ) ) ;
#38153 = AXIS2_PLACEMENT_3D ( 'NONE', #36011, #78299, #71101 ) ;
#38152 = CARTESIAN_POINT ( 'NONE',  ( -0.4765651934480722995, -10.20875367119844590, 29.07531184057631890 ) ) ;
#38154 = CARTESIAN_POINT ( 'NONE',  ( 6.923076923076924238, -12.62096338111211580, 30.90682066428153263 ) ) ;
#38155 = CARTESIAN_POINT ( 'NONE',  ( -12.68502338610279523, -6.716662450894489211, 34.94144148231605840 ) ) ;
#38156 = CARTESIAN_POINT ( 'NONE',  ( -1.987747218494660295, -5.598659921968651254, 14.99813170625848713 ) ) ;
#38157 = CARTESIAN_POINT ( 'NONE',  ( -1.450368812928716000, -7.249945578846654470, 34.99404164642496795 ) ) ;
#38158 = FACE_OUTER_BOUND ( 'NONE', #30289, .T. ) ;
#38159 = CARTESIAN_POINT ( 'NONE',  ( -7.623141002060450866, -10.01129605718032600, 34.36064277460058491 ) ) ;
#38160 = CARTESIAN_POINT ( 'NONE',  ( 5.142178216435913107, -12.70778746994558439, 30.41441678777537305 ) ) ;
#38161 = CARTESIAN_POINT ( 'NONE',  ( 12.46153846153833911, -12.46129190930018460, 30.37095296980731973 ) ) ;
#38162 = CYLINDRICAL_SURFACE ( 'NONE', #41136, 0.2499999999999997502 ) ;
#38163 = EDGE_CURVE ( 'NONE', #47709, #83085, #5973, .T. ) ;
#38164 = CARTESIAN_POINT ( 'NONE',  ( -14.30769230769230660, -3.050289026998446396, 32.03036669348365706 ) ) ;
#38165 = CARTESIAN_POINT ( 'NONE',  ( 8.069166690247241647, -9.172514111537584114, 34.72667873470787470 ) ) ;
#38166 = ORIENTED_EDGE ( 'NONE', *, *, #49998, .T. ) ;
#38167 = CARTESIAN_POINT ( 'NONE',  ( 3.361294669002873992, -12.50538340440932217, 31.33453814440721885 ) ) ;
#38168 = CARTESIAN_POINT ( 'NONE',  ( 8.834486340506794377, -11.48612834413965977, 32.76840700105972815 ) ) ;
#38169 = CARTESIAN_POINT ( 'NONE',  ( 2.724691934501250135, -8.700186371490531201, 24.79874329374151998 ) ) ;
#38170 = CARTESIAN_POINT ( 'NONE',  ( -10.61538461538461320, -2.486705287966279876, 31.30864560766543647 ) ) ;
#38171 = CARTESIAN_POINT ( 'NONE',  ( -12.46153846153858424, -12.51329471203414379, 31.30864560766407578 ) ) ;
#38172 = ORIENTED_EDGE ( 'NONE', *, *, #45342, .F. ) ;
#38173 = CARTESIAN_POINT ( 'NONE',  ( -6.673131513698878692, -10.18230066228895758, 34.26354781536631577 ) ) ;
#38174 = LINE ( 'NONE', #31423, #38762 ) ;
#38176 = EDGE_LOOP ( 'NONE', ( #22352, #12955, #75738, #42758 ) ) ;
#38175 = CARTESIAN_POINT ( 'NONE',  ( 8.835298102580843249, -2.486705287966280320, 31.30864560766543647 ) ) ;
#38177 = CARTESIAN_POINT ( 'NONE',  ( -13.51530598772569469, -9.929715669179220328, 34.40415004197138416 ) ) ;
#38178 = LINE ( 'NONE', #43602, #46963 ) ;
#38179 = CARTESIAN_POINT ( 'NONE',  ( 11.97435897435897267, -7.500000000000000000, 29.75000000000000355 ) ) ;
#38180 = ADVANCED_FACE ( 'NONE', ( #21563 ), #29225, .F. ) ;
#38181 = CIRCLE ( 'NONE', #75594, 0.2500000000000002220 ) ;
#38182 = CARTESIAN_POINT ( 'NONE',  ( -14.05763799605399633, -11.28795663066794575, 33.01431243580653785 ) ) ;
#38183 = ORIENTED_EDGE ( 'NONE', *, *, #30402, .F. ) ;
#38184 = B_SPLINE_CURVE_WITH_KNOTS ( 'NONE', 3,
 ( #69338, #62557, #873, #28338, #55810, #14840, #21582, #76535, #42317, #10286 ),
 .UNSPECIFIED., .F., .F.,
 ( 4, 2, 2, 2, 4 ),
 ( 0.0007817246336856290608, 0.0009771112958940101571, 0.001172497958102391036, 0.001367884620310772133, 0.001563271282519153446 ),
 .UNSPECIFIED. ) ;
#38185 = CARTESIAN_POINT ( 'NONE',  ( -16.15384615384615330, -13.37000171582298513, 34.34916445242398453 ) ) ;
#38186 = CARTESIAN_POINT ( 'NONE',  ( -11.76132780152463830, -2.251424796025575326, 29.88072029997477941 ) ) ;
#38187 = CARTESIAN_POINT ( 'NONE',  ( 3.930919936330004472, -9.886141570436013382, 34.14413921362392301 ) ) ;
#38188 = VERTEX_POINT ( 'NONE', #49486 ) ;
#38189 = ORIENTED_EDGE ( 'NONE', *, *, #70528, .F. ) ;
#38190 = ORIENTED_EDGE ( 'NONE', *, *, #59658, .F. ) ;
#38191 = EDGE_CURVE ( 'NONE', #26565, #44547, #22069, .T. ) ;
#38192 = CARTESIAN_POINT ( 'NONE',  ( -9.692307692307691624, -2.721908614388771852, 31.22303859784724978 ) ) ;
#38193 = LINE ( 'NONE', #65651, #86076 ) ;
#38194 = EDGE_CURVE ( 'NONE', #68109, #83936, #74729, .T. ) ;
#38195 = CARTESIAN_POINT ( 'NONE',  ( 2.307692307692309264, -5.557115091759785130, 34.35708131394839171 ) ) ;
#38196 = DIRECTION ( 'NONE',  ( -0.000000000000000000, -0.5000000000000009992, -0.8660254037844380415 ) ) ;
#38197 = AXIS2_PLACEMENT_3D ( 'NONE', #84969, #36337, #2094 ) ;
#38198 = EDGE_LOOP ( 'NONE', ( #23170, #75073 ) ) ;
#38200 = VERTEX_POINT ( 'NONE', #14361 ) ;
#38199 = EDGE_CURVE ( 'NONE', #75748, #62404, #36416, .T. ) ;
#38202 = ORIENTED_EDGE ( 'NONE', *, *, #88861, .T. ) ;
#38201 = CARTESIAN_POINT ( 'NONE',  ( 15.36156103859402222, -4.809403383903225304, 33.96459661697924304 ) ) ;
#38203 = CARTESIAN_POINT ( 'NONE',  ( -18.22348492456433178, -10.97335522853832934, 33.68706563782419749 ) ) ;
#38204 = FACE_OUTER_BOUND ( 'NONE', #13274, .T. ) ;
#38205 = EDGE_CURVE ( 'NONE', #66225, #56583, #41849, .T. ) ;
#38206 = B_SPLINE_CURVE_WITH_KNOTS ( 'NONE', 3,
 ( #77978, #23907, #2746, #16282, #45073, #9516, #72550, #44618, #10417, #10861 ),
 .UNSPECIFIED., .F., .F.,
 ( 4, 2, 2, 2, 4 ),
 ( 0.000000000000000000, 0.0001954311564186873894, 0.0003908623128373747788, 0.0005862934692560621682, 0.0007817246256747495577 ),
 .UNSPECIFIED. ) ;
#38207 = CARTESIAN_POINT ( 'NONE',  ( 1.515141086378950952, -10.88167719472716399, 33.43325721877153711 ) ) ;
#38208 = CARTESIAN_POINT ( 'NONE',  ( 20.75000000000001066, -7.500000000000000000, 29.75000000000000355 ) ) ;
#38209 = EDGE_CURVE ( 'NONE', #72149, #47713, #83726, .T. ) ;
#38210 = EDGE_LOOP ( 'NONE', ( #53202, #10195, #85080, #30447 ) ) ;
#38211 = ORIENTED_EDGE ( 'NONE', *, *, #36653, .T. ) ;
#38212 = ORIENTED_EDGE ( 'NONE', *, *, #35651, .F. ) ;
#38214 = EDGE_LOOP ( 'NONE', ( #58264, #83438, #57309, #16804 ) ) ;
#38213 = CARTESIAN_POINT ( 'NONE',  ( 5.142178648199100977, -5.219633306516380244, 34.19971097300157936 ) ) ;
#38215 = CARTESIAN_POINT ( 'NONE',  ( 18.06525513951284267, -12.16647553114626490, 32.15551576947920864 ) ) ;
#38216 = B_SPLINE_CURVE_WITH_KNOTS ( 'NONE', 3,
 ( #76687, #55518, #6889, #21286, #40691, #35249, #68154, #6457, #34358, #48760 ),
 .UNSPECIFIED., .F., .F.,
 ( 4, 2, 2, 2, 4 ),
 ( 0.0007817359430256293554, 0.0009771253907249974075, 0.001172514838424365460, 0.001367904286123733512, 0.001563293733823094625 ),
 .UNSPECIFIED. ) ;
#38217 = CARTESIAN_POINT ( 'NONE',  ( 12.46153846153846168, -11.16473453929635440, 33.15142922261926373 ) ) ;
#38219 = VERTEX_POINT ( 'NONE', #70640 ) ;
#38218 = EDGE_CURVE ( 'NONE', #60596, #12315, #56527, .T. ) ;
#38220 = DIRECTION ( 'NONE',  ( -0.000000000000000000, -0.7660444431189791237, -0.6427876096865379196 ) ) ;
#38221 = CARTESIAN_POINT ( 'NONE',  ( -1.515306851282942624, -8.147922237126337563, 34.70805685702651999 ) ) ;
#38222 = CARTESIAN_POINT ( 'NONE',  ( 8.769230769230647482, -6.026961402154118019, 34.52809138561165270 ) ) ;
#38223 = FACE_BOUND ( 'NONE', #23829, .T. ) ;
#38224 = CARTESIAN_POINT ( 'NONE',  ( -5.076923076923199218, -10.33852847137269571, 34.16647553114546554 ) ) ;
#38226 = EDGE_CURVE ( 'NONE', #40782, #441, #77392, .T. ) ;
#38225 = CARTESIAN_POINT ( 'NONE',  ( -6.923076923076922462, -9.058645607665452459, 34.76329471203371924 ) ) ;
#38227 = CARTESIAN_POINT ( 'NONE',  ( -15.09997742294444834, -10.54018710029568595, 33.71981072465678864 ) ) ;
#38229 = CARTESIAN_POINT ( 'NONE',  ( -6.000000000000119904, -2.892918686052165622, 31.69288490824153470 ) ) ;
#38228 = CARTESIAN_POINT ( 'NONE',  ( 17.01084069756293715, -9.058645607665454236, 34.76329471203372634 ) ) ;
#38230 = AXIS2_PLACEMENT_3D ( 'NONE', #18341, #4833, #46697 ) ;
#38231 = CARTESIAN_POINT ( 'NONE',  ( 17.74997677577853850, -6.652501968072647820, 34.93155406624980941 ) ) ;
#38232 = CARTESIAN_POINT ( 'NONE',  ( 16.15384615384615330, -2.249999999999998668, 29.75000000000001776 ) ) ;
#38233 = EDGE_LOOP ( 'NONE', ( #63800, #3181 ) ) ;
#38234 = EDGE_CURVE ( 'NONE', #6887, #63695, #31641, .T. ) ;
#38235 = CARTESIAN_POINT ( 'NONE',  ( -18.00000000000012079, -6.026961402154117131, 34.52809138561165270 ) ) ;
#38236 = CARTESIAN_POINT ( 'NONE',  ( 11.53846153846153832, -11.11383981884818262, 36.00935417666054406 ) ) ;
#38237 = ORIENTED_EDGE ( 'NONE', *, *, #2474, .F. ) ;
#38238 = ORIENTED_EDGE ( 'NONE', *, *, #14828, .T. ) ;
#38239 = AXIS2_PLACEMENT_3D ( 'NONE', #33632, #727, #56996 ) ;
#38241 = CARTESIAN_POINT ( 'NONE',  ( 10.61538461538449418, -12.16647553114689728, 32.15551576947799362 ) ) ;
#38240 = LINE ( 'NONE', #58490, #27436 ) ;
#38242 = CARTESIAN_POINT ( 'NONE',  ( -6.923076923076922462, -9.058645607665452459, 34.76329471203371924 ) ) ;
#38243 = FACE_OUTER_BOUND ( 'NONE', #8749, .T. ) ;
#38244 = CARTESIAN_POINT ( 'NONE',  ( -11.66860950819323328, -10.31621877034669588, 34.18098118002070152 ) ) ;
#38245 = ORIENTED_EDGE ( 'NONE', *, *, #15929, .F. ) ;
#38246 = DIRECTION ( 'NONE',  ( -0.000000000000000000, 1.000000000000000000, -0.000000000000000000 ) ) ;
#38247 = CARTESIAN_POINT ( 'NONE',  ( -22.00000000000000711, 9.999999999999971578, 13.00000000000000178 ) ) ;
#38249 = CARTESIAN_POINT ( 'NONE',  ( -9.822999158975250111, -4.118384482072085184, 33.43331474514187107 ) ) ;
#38248 = DIRECTION ( 'NONE',  ( 1.000000000000000000, 0.000000000000000000, 0.000000000000000000 ) ) ;
#38250 = DIRECTION ( 'NONE',  ( -0.000000000000000000, -0.6427876096865404731, -0.7660444431189770143 ) ) ;
#38251 = CARTESIAN_POINT ( 'NONE',  ( 10.83816415665302380, -4.387253974876679230, 33.66317474335728832 ) ) ;
#38254 = CARTESIAN_POINT ( 'NONE',  ( 5.076923076922953193, -11.67786785259630911, 32.92929555188603530 ) ) ;
#38253 = B_SPLINE_CURVE_WITH_KNOTS ( 'NONE', 3,
 ( #79409, #17711, #30328, #7954, #56136, #21465, #30763, #51013, #35420, #78504 ),
 .UNSPECIFIED., .F., .F.,
 ( 4, 2, 2, 2, 4 ),
 ( 0.0007817359430256216575, 0.0009771253907249856981, 0.001172514838424349847, 0.001367904286123713779, 0.001563293733823077928 ),
 .UNSPECIFIED. ) ;
#38252 =( NAMED_UNIT ( * ) PLANE_ANGLE_UNIT ( ) SI_UNIT ( $, .RADIAN. ) );
#38255 = ADVANCED_FACE ( 'NONE', ( #65198 ), #52129, .F. ) ;
#38256 = CARTESIAN_POINT ( 'NONE',  ( -3.749999999999988454, -9.053300858899127945, 22.51562500000000000 ) ) ;
#38257 = VERTEX_POINT ( 'NONE', #58002 ) ;
#38258 = ORIENTED_EDGE ( 'NONE', *, *, #80880, .F. ) ;
#38259 = CARTESIAN_POINT ( 'NONE',  ( 14.24160992833216888, -12.34228464037088280, 31.77849191805838558 ) ) ;
#38260 = EDGE_CURVE ( 'NONE', #53380, #54393, #80057, .T. ) ;
#38261 = CARTESIAN_POINT ( 'NONE',  ( -17.75000000000006750, -7.565270445406050648, 34.75000000000000000 ) ) ;
#38262 = DIRECTION ( 'NONE',  ( 0.000000000000000000, 0.000000000000000000, 1.000000000000000000 ) ) ;
#38263 = CARTESIAN_POINT ( 'NONE',  ( -16.21911659980693443, -5.219633306516282545, 34.19971097300152252 ) ) ;
#38264 = FACE_OUTER_BOUND ( 'NONE', #30768, .T. ) ;
#38265 = CARTESIAN_POINT ( 'NONE',  ( 2.651650429449569302, -10.15165042944953733, 18.37500000000000355 ) ) ;
#38266 = CARTESIAN_POINT ( 'NONE',  ( 7.173076923076923350, -7.500000000000001776, 35.04278698407183867 ) ) ;
#38267 = CARTESIAN_POINT ( 'NONE',  ( 8.769230769230647482, -10.90142922262034020, 33.41473453929536674 ) ) ;
#38268 = VERTEX_POINT ( 'NONE', #31879 ) ;
#38269 = FACE_BOUND ( 'NONE', #25324, .T. ) ;
#38270 = CARTESIAN_POINT ( 'NONE',  ( -18.25000000000000355, -12.50000000000000000, 29.75000000000000355 ) ) ;
#38271 = CARTESIAN_POINT ( 'NONE',  ( -9.822917347511772590, -7.722926974430166069, 34.99546784045485737 ) ) ;
#38272 = LINE ( 'NONE', #3587, #48707 ) ;
#38273 = CARTESIAN_POINT ( 'NONE',  ( -3.164600089806574257, -7.250054483168843156, 34.74374881642865631 ) ) ;
#38274 = EDGE_CURVE ( 'NONE', #70465, #81224, #71496, .T. ) ;
#38276 = VECTOR ( 'NONE', #63279, 1000.000000000000227 ) ;
#38275 = CARTESIAN_POINT ( 'NONE',  ( 4.023154687178596589, -12.38065189839062263, 30.83690757178629482 ) ) ;
#38277 = CARTESIAN_POINT ( 'NONE',  ( -5.750054590621955342, -4.932303261841489039, 34.32971442181322885 ) ) ;
#38278 = CARTESIAN_POINT ( 'NONE',  ( -3.164700879766792152, -11.16473453929635440, 33.15142922261926373 ) ) ;
#38279 = CARTESIAN_POINT ( 'NONE',  ( -11.40767109749459074, -2.845873456487965747, 32.17976146951972538 ) ) ;
#38280 = EDGE_LOOP ( 'NONE', ( #51242, #12670, #66306, #80171 ) ) ;
#38281 = CARTESIAN_POINT ( 'NONE',  ( -16.08777882049607655, -6.343179335718451384, 34.87096338111212646 ) ) ;
#38282 = EDGE_CURVE ( 'NONE', #73496, #10700, #25474, .T. ) ;
#38283 = CARTESIAN_POINT ( 'NONE',  ( -9.692307692307691624, -2.486705287966279876, 31.30864560766543647 ) ) ;
#38285 = CARTESIAN_POINT ( 'NONE',  ( 13.31934538405906565, -6.835583212224499938, 34.95778746994557906 ) ) ;
#38284 = B_SPLINE_CURVE_WITH_KNOTS ( 'NONE', 3,
 ( #29299, #43245, #70720, #9023, #36493, #2239, #29734, #84689, #22964, #50428 ),
 .UNSPECIFIED., .F., .F.,
 ( 4, 2, 2, 2, 4 ),
 ( 0.0007817246256747447872, 0.0009771112852218879000, 0.001172497944769031013, 0.001367884604316173909, 0.001563271263863317022 ),
 .UNSPECIFIED. ) ;
#38286 = CARTESIAN_POINT ( 'NONE',  ( -1.409462824231155764E-14, -4.749999999999999112, 24.15625000000000000 ) ) ;
#38287 = EDGE_CURVE ( 'NONE', #79996, #3529, #58496, .T. ) ;
#38288 = CARTESIAN_POINT ( 'NONE',  ( -19.50000000000000000, -11.50000000000000000, 29.75000000000000355 ) ) ;
#38289 = FILL_AREA_STYLE ('',( #45029 ) ) ;
#38291 = EDGE_LOOP ( 'NONE', ( #14682, #40998 ) ) ;
#38290 = CARTESIAN_POINT ( 'NONE',  ( 8.546304551714619890, -11.24512374952581872, 33.06303171183252942 ) ) ;
#38292 = CARTESIAN_POINT ( 'NONE',  ( -2.749999999999991562, -8.639087296526026805, 18.76562500000000000 ) ) ;
#38293 = CARTESIAN_POINT ( 'NONE',  ( 2.980745993476265898, -9.271318131107980420, 34.42618302367067429 ) ) ;
#38294 = VECTOR ( 'NONE', #50045, 1000.000000000000000 ) ;
#38295 = ORIENTED_EDGE ( 'NONE', *, *, #48036, .F. ) ;
#38296 = EDGE_CURVE ( 'NONE', #69130, #34806, #40266, .T. ) ;
#38297 = CARTESIAN_POINT ( 'NONE',  ( -4.088591014333314178, -2.657715359629131857, 31.77849191805844242 ) ) ;
#38298 = EDGE_LOOP ( 'NONE', ( #78522, #35136, #21042, #44297 ) ) ;
#38299 = FACE_OUTER_BOUND ( 'NONE', #19554, .T. ) ;
#38300 = CARTESIAN_POINT ( 'NONE',  ( 13.38461538461538680, -9.780366693483667717, 34.19971097300155094 ) ) ;
#38301 = DIRECTION ( 'NONE',  ( -0.000000000000000000, 0.9396926207859092051, -0.3420201433256662704 ) ) ;
#38302 = ORIENTED_EDGE ( 'NONE', *, *, #67661, .T. ) ;
#38303 = CARTESIAN_POINT ( 'NONE',  ( 20.00000000000000000, -4.000000000000000000, 29.75000000000000355 ) ) ;
#38304 = VERTEX_POINT ( 'NONE', #79169 ) ;
#38305 = CARTESIAN_POINT ( 'NONE',  ( -12.46153846153846168, -13.20930481340135110, 34.54067556320372745 ) ) ;
#38306 = VERTEX_POINT ( 'NONE', #45370 ) ;
#38307 = CARTESIAN_POINT ( 'NONE',  ( -15.90379173393269596, -2.318338780012836775, 30.59689888758630616 ) ) ;
#38308 = DIRECTION ( 'NONE',  ( -0.000000000000000000, -0.3420201433256694901, -0.9396926207859082059 ) ) ;
#38309 = AXIS2_PLACEMENT_3D ( 'NONE', #6292, #33755, #25668 ) ;
#38310 = EDGE_LOOP ( 'NONE', ( #82771, #1347 ) ) ;
#38311 = CARTESIAN_POINT ( 'NONE',  ( 9.442330961365341224, -9.148715823498378086, 34.47080413974185120 ) ) ;
#38313 = EDGE_CURVE ( 'NONE', #66445, #88887, #67142, .T. ) ;
#38312 = CARTESIAN_POINT ( 'NONE',  ( 7.846153846153846700, -2.499999999999998668, 29.50000000000001066 ) ) ;
#38314 = CARTESIAN_POINT ( 'NONE',  ( -1.254089946381741427, -11.04252011169590020, 33.62494198852677130 ) ) ;
#38315 = AXIS2_PLACEMENT_3D ( 'NONE', #6616, #35412, #41737 ) ;
#38316 = CARTESIAN_POINT ( 'NONE',  ( 5.076923076923075762, -8.973038597847269315, 34.52809138561121927 ) ) ;
#38317 = CARTESIAN_POINT ( 'NONE',  ( -13.38461538461538325, -11.91647553114624181, 32.58852847137148245 ) ) ;
#38318 = ORIENTED_EDGE ( 'NONE', *, *, #61298, .T. ) ;
#38319 = ORIENTED_EDGE ( 'NONE', *, *, #64830, .F. ) ;
#38320 = ORIENTED_EDGE ( 'NONE', *, *, #76437, .T. ) ;
#38322 = ORIENTED_EDGE ( 'NONE', *, *, #6606, .F. ) ;
#38321 = CARTESIAN_POINT ( 'NONE',  ( 3.230769230769108269, -5.941354392335915335, 34.76329471203413846 ) ) ;
#38323 = CARTESIAN_POINT ( 'NONE',  ( -8.899377978668987055, -10.19110544564092002, 33.96427741523702792 ) ) ;
#38324 = CARTESIAN_POINT ( 'NONE',  ( 1.450683735617825709, -2.721908614388772740, 31.22303859784725333 ) ) ;
#38325 = ORIENTED_EDGE ( 'NONE', *, *, #69296, .F. ) ;
#38326 = ORIENTED_EDGE ( 'NONE', *, *, #56224, .T. ) ;
#38327 = CARTESIAN_POINT ( 'NONE',  ( -10.74607608205217346, -3.062553014421049546, 32.05460306192773601 ) ) ;
#38328 = VERTEX_POINT ( 'NONE', #50784 ) ;
#38329 = CARTESIAN_POINT ( 'NONE',  ( -10.39237326377176451, -9.086983370893049639, 34.49168942202179267 ) ) ;
#38330 = VECTOR ( 'NONE', #57773, 1000.000000000000227 ) ;
#38331 = EDGE_CURVE ( 'NONE', #34679, #18725, #3709, .T. ) ;
#38332 = DIRECTION ( 'NONE',  ( 0.000000000000000000, 0.000000000000000000, -1.000000000000000000 ) ) ;
#38333 = CARTESIAN_POINT ( 'NONE',  ( 12.23805351781451201, -2.599994579823202923, 30.74605699353653776 ) ) ;
#38334 = FACE_BOUND ( 'NONE', #9091, .T. ) ;
#38335 = ORIENTED_EDGE ( 'NONE', *, *, #54353, .T. ) ;
#38336 = CARTESIAN_POINT ( 'NONE',  ( 2.057692307692309708, -7.566083408709834757, 34.74999999999999289 ) ) ;
#38338 = EDGE_CURVE ( 'NONE', #55087, #2893, #82212, .T. ) ;
#38337 = DIRECTION ( 'NONE',  ( -0.000000000000000000, -0.1736481776669307198, -0.9848077530122080203 ) ) ;
#38339 = CARTESIAN_POINT ( 'NONE',  ( -14.24243673641628050, -6.026961402152789304, 34.52809138561124769 ) ) ;
#38340 = CARTESIAN_POINT ( 'NONE',  ( 8.769230769230647482, -3.300289026999228881, 32.46337939537708905 ) ) ;
#38341 = LINE ( 'NONE', #45088, #4472 ) ;
#38342 = EDGE_LOOP ( 'NONE', ( #18081, #81543, #79183, #57026 ) ) ;
#38343 = EDGE_CURVE ( 'NONE', #33560, #7422, #56367, .T. ) ;
#38344 = B_SPLINE_CURVE_WITH_KNOTS ( 'NONE', 3,
 ( #84450, #85330, #50188, #63271, #15986, #2886, #22292, #70925, #9235, #2449 ),
 .UNSPECIFIED., .F., .F.,
 ( 4, 2, 2, 2, 4 ),
 ( 0.0007817359430256252354, 0.0009771253907249902518, 0.001172514838424355051, 0.001367904286123720068, 0.001563293733823085084 ),
 .UNSPECIFIED. ) ;
#38345 = VECTOR ( 'NONE', #23987, 1000.000000000000227 ) ;
#38346 = CARTESIAN_POINT ( 'NONE',  ( -7.173053654019277303, -6.567427716900047230, 34.66269422305636283 ) ) ;
#38347 = ORIENTED_EDGE ( 'NONE', *, *, #7455, .T. ) ;
#38348 = ORIENTED_EDGE ( 'NONE', *, *, #82525, .F. ) ;
#38350 = CARTESIAN_POINT ( 'NONE',  ( -7.846153846153844924, -5.415277668671390821, 36.20867863119892149 ) ) ;
#38349 = CARTESIAN_POINT ( 'NONE',  ( -7.173100147298380413, -4.175268141568689195, 33.81360843649122216 ) ) ;
#38351 = EDGE_CURVE ( 'NONE', #64930, #79014, #11213, .T. ) ;
#38352 = DIRECTION ( 'NONE',  ( 0.000000000000000000, 0.6427876096865373645, -0.7660444431189797898 ) ) ;
#38353 = CARTESIAN_POINT ( 'NONE',  ( -2.241623956689868802, -12.10708131394839704, 31.69288490824020954 ) ) ;
#38354 = CARTESIAN_POINT ( 'NONE',  ( 17.32692307692451195, -7.500000000000155431, 34.75000000000007105 ) ) ;
#38355 = CARTESIAN_POINT ( 'NONE',  ( -3.230769230769352962, -11.06231777344772027, 33.60647404775119895 ) ) ;
#38356 = VERTEX_POINT ( 'NONE', #69532 ) ;
#38357 = CARTESIAN_POINT ( 'NONE',  ( 17.01083966596719321, -5.557115091759785130, 34.35708131394839171 ) ) ;
#38358 = CARTESIAN_POINT ( 'NONE',  ( 17.75002325595140817, -3.436278759898155677, 33.07459398097509506 ) ) ;
#38359 = DIRECTION ( 'NONE',  ( 0.000000000000000000, 0.000000000000000000, 1.000000000000000000 ) ) ;
#38360 = CARTESIAN_POINT ( 'NONE',  ( 14.53070515178570865, -2.523321265292115534, 31.42251411153756990 ) ) ;
#38361 = VERTEX_POINT ( 'NONE', #55129 ) ;
#38362 = EDGE_CURVE ( 'NONE', #1867, #57235, #44530, .T. ) ;
#38363 = ORIENTED_EDGE ( 'NONE', *, *, #44201, .T. ) ;
#38364 = FACE_BOUND ( 'NONE', #74441, .T. ) ;
#38365 = CONTEXT_DEPENDENT_SHAPE_REPRESENTATION ( #36023, #72969 ) ;
#38366 = VERTEX_POINT ( 'NONE', #26000 ) ;
#38367 = CARTESIAN_POINT ( 'NONE',  ( 11.78840694783958298, -12.45601412856602686, 31.48342859153981621 ) ) ;
#38368 = CARTESIAN_POINT ( 'NONE',  ( -7.173076923076921574, -7.500000000000001776, 34.75000000000000000 ) ) ;
#38369 = ORIENTED_EDGE ( 'NONE', *, *, #11590, .T. ) ;
#38370 = CARTESIAN_POINT ( 'NONE',  ( -7.846153846153965716, -4.481592998941358097, 33.73612834414048933 ) ) ;
#38371 = DIRECTION ( 'NONE',  ( 0.000000000000000000, 0.3420201433256641055, -0.9396926207859100932 ) ) ;
#38372 = CARTESIAN_POINT ( 'NONE',  ( -7.976301055592065481, -11.93770438780619259, 32.05411857736982029 ) ) ;
#38373 = DIRECTION ( 'NONE',  ( -0.000000000000000000, 1.000000000000000000, -0.000000000000000000 ) ) ;
#38374 = LINE ( 'NONE', #19435, #20069 ) ;
#38375 = ORIENTED_EDGE ( 'NONE', *, *, #10285, .T. ) ;
#38377 = VERTEX_POINT ( 'NONE', #76286 ) ;
#38376 = CARTESIAN_POINT ( 'NONE',  ( -15.00775638667583678, -2.308499170217967134, 30.53291367094873721 ) ) ;
#38378 = FACE_OUTER_BOUND ( 'NONE', #9480, .T. ) ;
#38379 = DIRECTION ( 'NONE',  ( 0.000000000000000000, 0.7660444431189822323, -0.6427876096865344779 ) ) ;
#38380 = CARTESIAN_POINT ( 'NONE',  ( -12.46153846153846168, -13.53365097954675988, 30.81389545987213552 ) ) ;
#38381 = CARTESIAN_POINT ( 'NONE',  ( 18.22277954126840172, -8.496831190052089866, 34.64984203495476578 ) ) ;
#38382 = CARTESIAN_POINT ( 'NONE',  ( 7.846153846153723244, -11.67786785259630911, 32.92929555188603530 ) ) ;
#38383 = AXIS2_PLACEMENT_3D ( 'NONE', #48007, #48448, #75484 ) ;
#38384 = CARTESIAN_POINT ( 'NONE',  ( 5.299702618191483694, -12.44528174975671853, 30.48912976160716681 ) ) ;
#38385 = CARTESIAN_POINT ( 'NONE',  ( 1.200186371490529202, -4.775308065498752974, 13.23624329374151465 ) ) ;
#38386 = ORIENTED_EDGE ( 'NONE', *, *, #18440, .T. ) ;
#38387 = EDGE_CURVE ( 'NONE', #6352, #20065, #5288, .T. ) ;
#38388 = CARTESIAN_POINT ( 'NONE',  ( -3.480745961711583458, -3.137211980971222669, 32.19342716148376837 ) ) ;
#38389 = CARTESIAN_POINT ( 'NONE',  ( -9.692307692307691624, -8.120952969808772792, 34.71129190930000163 ) ) ;
#38390 = CARTESIAN_POINT ( 'NONE',  ( 6.250000000000004441, -2.499999999999999112, 29.81604066197450109 ) ) ;
#38391 = ORIENTED_EDGE ( 'NONE', *, *, #20807, .F. ) ;
#38392 = ORIENTED_EDGE ( 'NONE', *, *, #66195, .F. ) ;
#38393 = CARTESIAN_POINT ( 'NONE',  ( -9.019207513279360100, -5.643011162660950042, 34.66104346484419096 ) ) ;
#38394 = CARTESIAN_POINT ( 'NONE',  ( 11.28848479441294650, -4.818429247618089661, 34.26397095200675125 ) ) ;
#38395 = CARTESIAN_POINT ( 'NONE',  ( 17.07692307692295586, -3.643525952248796163, 33.31231777344771672 ) ) ;
#38396 = CARTESIAN_POINT ( 'NONE',  ( 8.900021210197717636, -11.37503395064541678, 33.29242100308974273 ) ) ;
#38397 = EDGE_CURVE ( 'NONE', #2182, #49089, #635, .T. ) ;
#38398 = DIRECTION ( 'NONE',  ( -0.000000000000000000, -0.1736481776669307198, -0.9848077530122080203 ) ) ;
#38399 = CARTESIAN_POINT ( 'NONE',  ( 5.776515056276054771, -8.496056993536548418, 34.65000542017679663 ) ) ;
#38400 = ORIENTED_EDGE ( 'NONE', *, *, #18150, .T. ) ;
#38401 = AXIS2_PLACEMENT_3D ( 'NONE', #15485, #50135, #2389 ) ;
#38402 = CARTESIAN_POINT ( 'NONE',  ( 10.61538461538461675, -13.53365097954675988, 30.81389545987213552 ) ) ;
#38403 = CARTESIAN_POINT ( 'NONE',  ( 8.769230769230768274, -8.120952969808772792, 34.71129190930000163 ) ) ;
#38404 = EDGE_CURVE ( 'NONE', #86388, #23968, #69292, .T. ) ;
#38405 = CARTESIAN_POINT ( 'NONE',  ( 4.218990934565787221, -7.750023224968867197, 34.99404313364389907 ) ) ;
#38406 = CARTESIAN_POINT ( 'NONE',  ( -3.453695448285377445, -11.76352882383564769, 32.36236540154569497 ) ) ;
#38407 = ORIENTED_EDGE ( 'NONE', *, *, #31181, .T. ) ;
#38408 = CARTESIAN_POINT ( 'NONE',  ( -7.780085495151406683, -3.513871655860379306, 32.76840700105978499 ) ) ;
#38409 = VECTOR ( 'NONE', #41752, 1000.000000000000114 ) ;
#38410 = ORIENTED_EDGE ( 'NONE', *, *, #81522, .T. ) ;
#38411 = DIRECTION ( 'NONE',  ( 0.000000000000000000, 0.9396926207859126468, -0.3420201433256571111 ) ) ;
#38412 = CARTESIAN_POINT ( 'NONE',  ( 16.09615384615384670, -7.500000000000000000, 29.75000000000000355 ) ) ;
#38413 = CYLINDRICAL_SURFACE ( 'NONE', #74374, 0.2500000000000002220 ) ;
#38414 = EDGE_LOOP ( 'NONE', ( #77162, #14394, #33404, #9108 ) ) ;
#38415 = CIRCLE ( 'NONE', #78646, 0.2500000000000002220 ) ;
#38416 = FACE_OUTER_BOUND ( 'NONE', #24088, .T. ) ;
#38418 = EDGE_CURVE ( 'NONE', #7925, #79557, #77890, .T. ) ;
#38417 = LINE ( 'NONE', #3286, #34945 ) ;
#38419 = CYLINDRICAL_SURFACE ( 'NONE', #86921, 0.2500000000000004996 ) ;
#38420 = CARTESIAN_POINT ( 'NONE',  ( 8.834376548562733689, -7.750023238201979581, 34.74374492549440419 ) ) ;
#38421 = LINE ( 'NONE', #72194, #20978 ) ;
#38422 = EDGE_CURVE ( 'NONE', #9533, #67226, #60671, .T. ) ;
#38423 = EDGE_CURVE ( 'NONE', #39262, #32155, #50581, .T. ) ;
#38424 = B_SPLINE_CURVE_WITH_KNOTS ( 'NONE', 3,
 ( #36291, #61642, #78152, #57878, #16453, #29533, #70956, #64621, #2923, #9266 ),
 .UNSPECIFIED., .F., .F.,
 ( 4, 2, 2, 2, 4 ),
 ( 0.000000000000000000, 0.0001954311564186870642, 0.0003908623128373741283, 0.0005862934692560611925, 0.0007817246256747482566 ),
 .UNSPECIFIED. ) ;
#38425 = ORIENTED_EDGE ( 'NONE', *, *, #61409, .T. ) ;
#38426 = CYLINDRICAL_SURFACE ( 'NONE', #70262, 0.2500000000000009437 ) ;
#38427 = VERTEX_POINT ( 'NONE', #63210 ) ;
#38428 = CARTESIAN_POINT ( 'NONE',  ( 5.299702745901138101, -11.60474049983371003, 33.02348890104160262 ) ) ;
#38429 = EDGE_CURVE ( 'NONE', #34985, #16890, #29885, .T. ) ;
#38430 = DIRECTION ( 'NONE',  ( -0.000000000000000000, -0.9848077530122085754, -0.1736481776669273613 ) ) ;
#38431 = CARTESIAN_POINT ( 'NONE',  ( -7.846153846153844924, -1.242168528481310874, 33.36296068462461051 ) ) ;
#38432 = VECTOR ( 'NONE', #10312, 1000.000000000000000 ) ;
#38433 = DIRECTION ( 'NONE',  ( 0.000000000000000000, 0.6427876096865368094, 0.7660444431189802339 ) ) ;
#38434 = DIRECTION ( 'NONE',  ( -1.000000000000000000, -0.000000000000000000, -0.000000000000000000 ) ) ;
#38435 = DIRECTION ( 'NONE',  ( -0.000000000000000000, -0.8660254037844399289, -0.4999999999999980016 ) ) ;
#38436 = ORIENTED_EDGE ( 'NONE', *, *, #44581, .F. ) ;
#38437 = VERTEX_POINT ( 'NONE', #57787 ) ;
#38438 = VERTEX_POINT ( 'NONE', #15928 ) ;
#38439 = ORIENTED_EDGE ( 'NONE', *, *, #88427, .F. ) ;
#38440 = ORIENTED_EDGE ( 'NONE', *, *, #3674, .F. ) ;
#38441 = CIRCLE ( 'NONE', #68591, 4.500000000000001776 ) ;
#38442 = CARTESIAN_POINT ( 'NONE',  ( 12.59206416330202671, -11.93748526763465279, 32.05452791011430946 ) ) ;
#38443 = CARTESIAN_POINT ( 'NONE',  ( -3.480745974817821331, -6.524016743844655686, 34.90889640711025521 ) ) ;
#38444 = CARTESIAN_POINT ( 'NONE',  ( -10.55012947587177941, -5.094484230520773593, 34.41647553114626845 ) ) ;
#38445 = CARTESIAN_POINT ( 'NONE',  ( -15.23076923076922995, -4.945431358278436385, 36.03766855953609394 ) ) ;
#38446 = CARTESIAN_POINT ( 'NONE',  ( 13.38461538461538680, -8.120952969808772792, 34.71129190930000163 ) ) ;
#38447 = EDGE_CURVE ( 'NONE', #88550, #70465, #22670, .T. ) ;
#38448 = CARTESIAN_POINT ( 'NONE',  ( 8.769230769230768274, -8.973038597847269315, 34.52809138561121927 ) ) ;
#38449 = CYLINDRICAL_SURFACE ( 'NONE', #40797, 0.2500000000000009437 ) ;
#38450 = CARTESIAN_POINT ( 'NONE',  ( -3.903791842207838148, -10.66356715214248396, 33.62249196103329751 ) ) ;
#38451 = LINE ( 'NONE', #80337, #37509 ) ;
#38452 = VERTEX_POINT ( 'NONE', #49264 ) ;
#38453 = ORIENTED_EDGE ( 'NONE', *, *, #68513, .T. ) ;
#38454 = EDGE_LOOP ( 'NONE', ( #9474, #33590, #41664, #54214 ) ) ;
#38456 = ORIENTED_EDGE ( 'NONE', *, *, #84122, .T. ) ;
#38455 = CARTESIAN_POINT ( 'NONE',  ( 6.130790440966951138, -12.35292014791297710, 31.75344720912887198 ) ) ;
#38457 = B_SPLINE_CURVE_WITH_KNOTS ( 'NONE', 3,
 ( #35598, #63047, #41468, #70712, #14891, #42364, #28848, #84684, #56309, #83798 ),
 .UNSPECIFIED., .F., .F.,
 ( 4, 2, 2, 2, 4 ),
 ( 0.0007817246256747446788, 0.0009771112852218874663, 0.001172497944769030145, 0.001367884604316172825, 0.001563271263863315720 ),
 .UNSPECIFIED. ) ;
#38459 = CARTESIAN_POINT ( 'NONE',  ( 10.55011416942384095, -9.442884908240170461, 34.35708131394840592 ) ) ;
#38458 = LINE ( 'NONE', #31705, #77700 ) ;
#38460 = EDGE_CURVE ( 'NONE', #61394, #27134, #77219, .T. ) ;
#38461 = CARTESIAN_POINT ( 'NONE',  ( -1.634592128663975741, -4.818429247618089661, 34.26397095200675125 ) ) ;
#38462 = VECTOR ( 'NONE', #51842, 1000.000000000000227 ) ;
#38463 = CARTESIAN_POINT ( 'NONE',  ( -16.81410256410256565, -3.499999999999999556, 29.75000000000000355 ) ) ;
#38464 = FACE_BOUND ( 'NONE', #39738, .T. ) ;
#38465 = VERTEX_POINT ( 'NONE', #64094 ) ;
#38466 = ORIENTED_EDGE ( 'NONE', *, *, #23312, .F. ) ;
#38467 = EDGE_CURVE ( 'NONE', #67881, #36002, #70873, .T. ) ;
#38468 = CARTESIAN_POINT ( 'NONE',  ( -17.20761368003338632, -11.37499894934982514, 33.29245874905763003 ) ) ;
#38469 = VECTOR ( 'NONE', #78642, 1000.000000000000000 ) ;
#38470 = EDGE_LOOP ( 'NONE', ( #60247, #47611, #88212, #71333 ) ) ;
#38471 = FACE_BOUND ( 'NONE', #58360, .T. ) ;
#38472 = CARTESIAN_POINT ( 'NONE',  ( 13.38461538461538680, -8.810774026931790459, 35.74407628777942847 ) ) ;
#38473 = DIRECTION ( 'NONE',  ( 0.000000000000000000, 0.6427876096865368094, 0.7660444431189802339 ) ) ;
#38474 = VERTEX_POINT ( 'NONE', #43393 ) ;
#38475 = CARTESIAN_POINT ( 'NONE',  ( -15.23076923076935074, -12.27809138561165270, 31.22303859784587132 ) ) ;
#38476 = DIRECTION ( 'NONE',  ( -1.000000000000000000, 0.000000000000000000, -0.000000000000000000 ) ) ;
#38477 = CARTESIAN_POINT ( 'NONE',  ( -18.13014796973170206, -4.299443229763728169, 33.91186481527756058 ) ) ;
#38478 = ORIENTED_EDGE ( 'NONE', *, *, #13308, .T. ) ;
#38479 = FACE_OUTER_BOUND ( 'NONE', #32590, .T. ) ;
#38480 = CARTESIAN_POINT ( 'NONE',  ( 3.230769230769108269, -5.094484230521993062, 34.41647553114689373 ) ) ;
#38481 = VERTEX_POINT ( 'NONE', #36638 ) ;
#38482 = ADVANCED_FACE ( 'NONE', ( #63658 ), #43827, .F. ) ;
#38483 = DIRECTION ( 'NONE',  ( 0.000000000000000000, 0.3420201433256641055, -0.9396926207859100932 ) ) ;
#38484 = CARTESIAN_POINT ( 'NONE',  ( 6.923076923076802558, -10.90142922262034020, 33.41473453929536674 ) ) ;
#38485 = ORIENTED_EDGE ( 'NONE', *, *, #16956, .T. ) ;
#38486 = CARTESIAN_POINT ( 'NONE',  ( 0.2115152242454953480, -9.271318131107980420, 34.42618302367067429 ) ) ;
#38487 = CARTESIAN_POINT ( 'NONE',  ( 14.55763782604044998, -8.433404298154334455, 34.66254593164985920 ) ) ;
#38488 = CARTESIAN_POINT ( 'NONE',  ( 16.02369818411445834, -3.069018819979304702, 32.56621877034667278 ) ) ;
#38489 = LINE ( 'NONE', #66846, #44306 ) ;
#38490 = CARTESIAN_POINT ( 'NONE',  ( 18.00000000000000000, -7.500000000000001776, 35.04278698407183867 ) ) ;
#38491 = CARTESIAN_POINT ( 'NONE',  ( 6.673053685783957967, -9.271318131107980420, 34.42618302367067429 ) ) ;
#38493 = CARTESIAN_POINT ( 'NONE',  ( 8.769230769230645706, -3.083524468854526912, 32.58852847137268327 ) ) ;
#38492 = CARTESIAN_POINT ( 'NONE',  ( 11.53846153846153832, -12.29105614889573062, 35.45975837776705220 ) ) ;
#38494 = LINE ( 'NONE', #33067, #51109 ) ;
#38496 = CARTESIAN_POINT ( 'NONE',  ( -14.30769230769230660, -2.499999999999998668, 29.75000000000001421 ) ) ;
#38495 = CARTESIAN_POINT ( 'NONE',  ( -15.23076923076922995, -11.69971097300155272, 32.46337939537588113 ) ) ;
#38497 = CARTESIAN_POINT ( 'NONE',  ( -1.901340078031346525, -9.487747218494661183, 25.93563170625849423 ) ) ;
#38498 = ORIENTED_EDGE ( 'NONE', *, *, #67609, .T. ) ;
#38499 = CARTESIAN_POINT ( 'NONE',  ( 16.15384615384615330, -2.721908614388771852, 31.22303859784724978 ) ) ;
#38500 = VERTEX_POINT ( 'NONE', #30752 ) ;
#38501 = CIRCLE ( 'NONE', #86003, 3.000000000000000444 ) ;
#38502 = ORIENTED_EDGE ( 'NONE', *, *, #78629, .T. ) ;
#38503 = EDGE_CURVE ( 'NONE', #57712, #7553, #69972, .T. ) ;
#38504 = CARTESIAN_POINT ( 'NONE',  ( -2.177166605928743337, -12.45806712695776319, 30.39783852428763922 ) ) ;
#38505 = ORIENTED_EDGE ( 'NONE', *, *, #53106, .T. ) ;
#38506 = LINE ( 'NONE', #38961, #88707 ) ;
#38507 = CARTESIAN_POINT ( 'NONE',  ( -2.749999999999991562, -8.639087296526025028, 16.26562500000000000 ) ) ;
#38508 = DIRECTION ( 'NONE',  ( -0.000000000000000000, 1.000000000000000000, 3.491481338843133355E-15 ) ) ;
#38509 = CARTESIAN_POINT ( 'NONE',  ( -6.923076923076922462, -13.88283147151868846, 33.14645433367849847 ) ) ;
#38510 = CARTESIAN_POINT ( 'NONE',  ( -7.715362038329057981, -5.582136614379148654, 34.36778462344220486 ) ) ;
#38511 = DIRECTION ( 'NONE',  ( 0.000000000000000000, 0.4999999999999985567, 0.8660254037844395958 ) ) ;
#38512 = CARTESIAN_POINT ( 'NONE',  ( -5.299850035829926753, -3.395401636524186362, 33.02366814457250399 ) ) ;
#38513 = FACE_OUTER_BOUND ( 'NONE', #43673, .T. ) ;
#38514 = CARTESIAN_POINT ( 'NONE',  ( 6.000000000000309086, -2.506253911140614576, 30.00000000000323297 ) ) ;
#38515 = CARTESIAN_POINT ( 'NONE',  ( 2.651650429449569302, -10.15165042944953733, 20.87500000000000000 ) ) ;
#38516 = CARTESIAN_POINT ( 'NONE',  ( -11.28851612908349722, -2.589246495874658383, 31.60778113518102828 ) ) ;
#38517 = CARTESIAN_POINT ( 'NONE',  ( 14.53070365930516061, -10.61302985866384141, 33.66295027996417843 ) ) ;
#38518 = EDGE_CURVE ( 'NONE', #24368, #25168, #53159, .T. ) ;
#38519 = VECTOR ( 'NONE', #10486, 999.9999999999998863 ) ;
#38520 = EDGE_CURVE ( 'NONE', #12295, #27221, #4851, .T. ) ;
#38521 = CARTESIAN_POINT ( 'NONE',  ( -2.437839517130526712, -4.460286881179643004, 33.72017969459903242 ) ) ;
#38522 = ORIENTED_EDGE ( 'NONE', *, *, #51990, .T. ) ;
#38523 = ORIENTED_EDGE ( 'NONE', *, *, #40562, .F. ) ;
#38524 = DIRECTION ( 'NONE',  ( -1.000000000000000000, -0.000000000000000000, 0.000000000000000000 ) ) ;
#38525 = CARTESIAN_POINT ( 'NONE',  ( -14.24243673641628050, -8.613356846314928816, 34.62446782046653482 ) ) ;
#38526 = CARTESIAN_POINT ( 'NONE',  ( -11.53846153846153655, -3.669653830205710676, 35.88435417666054406 ) ) ;
#38527 = CARTESIAN_POINT ( 'NONE',  ( 14.30769230769231015, -4.945431358278436385, 36.03766855953609394 ) ) ;
#38528 = B_SPLINE_CURVE_WITH_KNOTS ( 'NONE', 3,
 ( #43874, #22713, #37110, #48857, #21392, #83101, #63701, #9642, #70015, #64571 ),
 .UNSPECIFIED., .F., .F.,
 ( 4, 2, 2, 2, 4 ),
 ( 0.0007817246256747474977, 0.0009771112852218911526, 0.001172497944769034699, 0.001367884604316178462, 0.001563271263863322009 ),
 .UNSPECIFIED. ) ;
#38529 = CARTESIAN_POINT ( 'NONE',  ( 17.20744851515672025, -12.50538340440932394, 31.33453814440721885 ) ) ;
#38530 = CARTESIAN_POINT ( 'NONE',  ( -3.230769230769229949, -5.471508081941601098, 34.59228464037088457 ) ) ;
#38531 = B_SPLINE_CURVE_WITH_KNOTS ( 'NONE', 3,
 ( #25583, #85507, #72868, #66108, #24690, #79198, #71985, #11176, #30555, #18384 ),
 .UNSPECIFIED., .F., .F.,
 ( 4, 2, 2, 2, 4 ),
 ( 0.0007817359430256284880, 0.0009771253907249941549, 0.001172514838424359822, 0.001367904286123725489, 0.001563293733823091156 ),
 .UNSPECIFIED. ) ;
#38532 = B_SPLINE_CURVE_WITH_KNOTS ( 'NONE', 3,
 ( #2265, #29762, #57227, #16241, #43705, #11260, #4040, #86035, #85148, #65305 ),
 .UNSPECIFIED., .F., .F.,
 ( 4, 2, 2, 2, 4 ),
 ( 0.0007817246256747451124, 0.0009771112852218879000, 0.001172497944769030796, 0.001367884604316173692, 0.001563271263863316588 ),
 .UNSPECIFIED. ) ;
#38533 = AXIS2_PLACEMENT_3D ( 'NONE', #31485, #58948, #62817 ) ;
#38534 = ADVANCED_FACE ( 'NONE', ( #85712 ), #8285, .F. ) ;
#38535 = ORIENTED_EDGE ( 'NONE', *, *, #68499, .T. ) ;
#38536 = CARTESIAN_POINT ( 'NONE',  ( 17.86985279056177944, -12.45813303252208648, 30.39737893381572675 ) ) ;
#38537 = ORIENTED_EDGE ( 'NONE', *, *, #34876, .T. ) ;
#38538 = VECTOR ( 'NONE', #77335, 1000.000000000000000 ) ;
#38539 = EDGE_LOOP ( 'NONE', ( #75876, #16844, #57259, #11164 ) ) ;
#38540 = CARTESIAN_POINT ( 'NONE',  ( 7.846153846153723244, -11.06231777344772027, 33.60647404775119895 ) ) ;
#38541 = CARTESIAN_POINT ( 'NONE',  ( -2.307692307692305711, -9.058645607665452459, 34.76329471203371924 ) ) ;
#38542 = CARTESIAN_POINT ( 'NONE',  ( -9.692307692307812417, -6.879047030192662504, 34.71129190930017927 ) ) ;
#38543 = CARTESIAN_POINT ( 'NONE',  ( -10.61538461538461320, -10.05456864172156806, 36.03766855953608683 ) ) ;
#38544 = CARTESIAN_POINT ( 'NONE',  ( -2.177166605928741117, -11.93748526763465279, 32.05452791011430946 ) ) ;
#38545 = ORIENTED_EDGE ( 'NONE', *, *, #4365, .T. ) ;
#38546 = ORIENTED_EDGE ( 'NONE', *, *, #3661, .F. ) ;
#38547 = EDGE_LOOP ( 'NONE', ( #41425, #47250, #79870, #76334 ) ) ;
#38548 = CARTESIAN_POINT ( 'NONE',  ( 1.576923076923075762, -3.499999999999999556, 29.75000000000000355 ) ) ;
#38549 = CARTESIAN_POINT ( 'NONE',  ( 9.942362112221147186, -2.318338780012835443, 30.59689888758630261 ) ) ;
#38550 = B_SPLINE_CURVE_WITH_KNOTS ( 'NONE', 3,
 ( #2989, #79558, #65132, #65577, #38568, #66484, #79995, #45763, #11541, #51156 ),
 .UNSPECIFIED., .F., .F.,
 ( 4, 2, 2, 2, 4 ),
 ( 0.0007817246256747505334, 0.0009771112852218954894, 0.001172497944769040554, 0.001367884604316185618, 0.001563271263863330682 ),
 .UNSPECIFIED. ) ;
#38551 = CYLINDRICAL_SURFACE ( 'NONE', #25024, 0.2499999999999979738 ) ;
#38552 = CARTESIAN_POINT ( 'NONE',  ( -8.546217925137375104, -10.01129605718032600, 34.36064277460058491 ) ) ;
#38553 = B_SPLINE_CURVE_WITH_KNOTS ( 'NONE', 3,
 ( #64285, #36828, #17896, #57983, #17451, #2154, #30077, #77810, #43583, #9800 ),
 .UNSPECIFIED., .F., .F.,
 ( 4, 2, 2, 2, 4 ),
 ( 0.000000000000000000, 0.0001954311564186860613, 0.0003908623128373721225, 0.0005862934692560581567, 0.0007817246256747442451 ),
 .UNSPECIFIED. ) ;
#38554 = DIRECTION ( 'NONE',  ( -0.000000000000000000, 0.8660254037844397068, -0.4999999999999978906 ) ) ;
#38555 = CARTESIAN_POINT ( 'NONE',  ( 5.933916589044120116, -12.37446782046654192, 30.86335684631486487 ) ) ;
#38556 = ORIENTED_EDGE ( 'NONE', *, *, #8794, .T. ) ;
#38557 = ORIENTED_EDGE ( 'NONE', *, *, #89130, .F. ) ;
#38558 = CARTESIAN_POINT ( 'NONE',  ( -3.749999999999988454, -9.053300858899127945, 25.01562500000000000 ) ) ;
#38559 = VERTEX_POINT ( 'NONE', #42957 ) ;
#38560 = AXIS2_PLACEMENT_3D ( 'NONE', #5983, #28462, #34323 ) ;
#38562 = ORIENTED_EDGE ( 'NONE', *, *, #31910, .T. ) ;
#38561 = CARTESIAN_POINT ( 'NONE',  ( -5.750054481651857508, -3.202959910592335202, 32.30730279482227019 ) ) ;
#38563 = CARTESIAN_POINT ( 'NONE',  ( -7.134615384615385025, -3.499999999999999556, 29.75000000000000355 ) ) ;
#38564 = CARTESIAN_POINT ( 'NONE',  ( -7.173076923076942002, -2.249999999999999112, 29.81609741502488120 ) ) ;
#38565 = CARTESIAN_POINT ( 'NONE',  ( -2.307692307691991296, -2.255955759149395501, 30.00000000000324363 ) ) ;
#38566 = VERTEX_POINT ( 'NONE', #70427 ) ;
#38567 = AXIS2_PLACEMENT_3D ( 'NONE', #48372, #83958, #55572 ) ;
#38568 = CARTESIAN_POINT ( 'NONE',  ( 10.86533002476265963, -2.341251567377310217, 30.72681386836322659 ) ) ;
#38569 = VERTEX_POINT ( 'NONE', #44249 ) ;
#38570 = ADVANCED_BREP_SHAPE_REPRESENTATION ( '', ( #29637, #83448 ), #80635 ) ;
#38571 = CARTESIAN_POINT ( 'NONE',  ( -8.769230769230768274, -4.661471528628507777, 34.16647553114623292 ) ) ;
#38572 = CARTESIAN_POINT ( 'NONE',  ( 0.4615384615383382183, -11.67786785259630911, 32.92929555188603530 ) ) ;
#38573 = FACE_BOUND ( 'NONE', #29576, .T. ) ;
#38575 = CARTESIAN_POINT ( 'NONE',  ( 7.912221179503920787, -2.292212530054420494, 30.41441678777542990 ) ) ;
#38574 = CARTESIAN_POINT ( 'NONE',  ( -0.2114840416250085564, -11.47946981652013498, 33.17500667209846910 ) ) ;
#38576 = CARTESIAN_POINT ( 'NONE',  ( -1.608100309179714360, -3.562934362175799841, 33.22335522853832401 ) ) ;
#38577 = CARTESIAN_POINT ( 'NONE',  ( -3.296039231325549324, -8.656820664281497102, 34.87096338111211935 ) ) ;
#38578 = ORIENTED_EDGE ( 'NONE', *, *, #74004, .T. ) ;
#38579 = CARTESIAN_POINT ( 'NONE',  ( 11.40777093535123399, -11.37499894934982692, 33.29245874905763003 ) ) ;
#38580 = CARTESIAN_POINT ( 'NONE',  ( 8.992242120843620512, -6.503523203565941380, 34.64991518177335195 ) ) ;
#38581 = ORIENTED_EDGE ( 'NONE', *, *, #78565, .T. ) ;
#38582 = CARTESIAN_POINT ( 'NONE',  ( -8.703975629717930929, -3.643525952247864463, 33.31231777344670064 ) ) ;
#38583 = CARTESIAN_POINT ( 'NONE',  ( 16.15384615384615330, -11.16473453929635440, 33.15142922261926373 ) ) ;
#38584 = CARTESIAN_POINT ( 'NONE',  ( -6.065270445960775803, -10.90142922261923886, 33.41473453929638993 ) ) ;
#38585 = CARTESIAN_POINT ( 'NONE',  ( -19.50000000000000000, -3.499999999999999556, 29.75000000000000355 ) ) ;
#38586 = DIRECTION ( 'NONE',  ( -1.000000000000000000, -0.000000000000000000, -0.000000000000000000 ) ) ;
#38587 = FACE_BOUND ( 'NONE', #68004, .T. ) ;
#38589 = FACE_OUTER_BOUND ( 'NONE', #29324, .T. ) ;
#38588 = CARTESIAN_POINT ( 'NONE',  ( 5.326868486301119532, -5.766571408460171355, 34.70601412856602508 ) ) ;
#38590 = CARTESIAN_POINT ( 'NONE',  ( -6.857008572074485109, -10.51840700105979565, 33.73612834413962247 ) ) ;
#38592 = CARTESIAN_POINT ( 'NONE',  ( -11.53846153846153655, -5.180354513474913603, 36.12317359536750416 ) ) ;
#38591 = CYLINDRICAL_SURFACE ( 'NONE', #64517, 0.2500000000000008882 ) ;
#38593 = CARTESIAN_POINT ( 'NONE',  ( -3.931066484868087851, -10.97394488606064122, 33.68653795673694873 ) ) ;
#38594 = CARTESIAN_POINT ( 'NONE',  ( 13.19230769230769340, -11.00000000000000000, 29.75000000000000355 ) ) ;
#38595 = VECTOR ( 'NONE', #22079, 999.9999999999998863 ) ;
#38596 = CARTESIAN_POINT ( 'NONE',  ( 0.06109907496455496689, -11.24999999999999822, 24.52938170625849423 ) ) ;
#38597 = B_SPLINE_CURVE_WITH_KNOTS ( 'NONE', 3,
 ( #52119, #64738, #79607, #17904, #23317, #50774, #78260, #9807, #30521, #54338 ),
 .UNSPECIFIED., .F., .F.,
 ( 4, 2, 2, 2, 4 ),
 ( 0.0007817246256747519429, 0.0009771112852218959231, 0.001172497944769039686, 0.001367884604316183667, 0.001563271263863327647 ),
 .UNSPECIFIED. ) ;
#38598 = VERTEX_POINT ( 'NONE', #36207 ) ;
#38599 = EDGE_CURVE ( 'NONE', #18170, #77088, #29447, .T. ) ;
#38600 = CARTESIAN_POINT ( 'NONE',  ( 9.320512820512821150, -1.926643599941765039, 28.25000000000000000 ) ) ;
#38601 = CARTESIAN_POINT ( 'NONE',  ( -15.00734226890766188, -7.630147231320743018, 34.74852402298682819 ) ) ;
#38602 = CARTESIAN_POINT ( 'NONE',  ( -1.319359813339359366, -10.90142922261932057, 33.41473453929631887 ) ) ;
#38603 = CARTESIAN_POINT ( 'NONE',  ( -10.83831157429145975, -11.43668979543635089, 33.22377378376089752 ) ) ;
#38604 = CARTESIAN_POINT ( 'NONE',  ( -4.153846153846152411, -4.661471528628507777, 34.16647553114623292 ) ) ;
#38605 = CARTESIAN_POINT ( 'NONE',  ( 6.223012844093396723, -3.395485233115139057, 33.02377354290275946 ) ) ;
#38606 = CARTESIAN_POINT ( 'NONE',  ( 3.775308065498768517, -8.992201783934554271, 25.54500670625849779 ) ) ;
#38607 = CARTESIAN_POINT ( 'NONE',  ( 14.08420736396836226, -10.81261337010820256, 33.49550067578627477 ) ) ;
#38608 = CARTESIAN_POINT ( 'NONE',  ( -14.43784027742400333, -11.66186481527757302, 32.95055677023626117 ) ) ;
#38609 = CARTESIAN_POINT ( 'NONE',  ( 8.096099364501986528, -11.86320923018887719, 32.19269448109604070 ) ) ;
#38610 = CARTESIAN_POINT ( 'NONE',  ( 5.299935921016470708, -12.64618726649961289, 30.78989965857442712 ) ) ;
#38611 = CARTESIAN_POINT ( 'NONE',  ( 8.639083559792549494, -10.19110544564092002, 33.96427741523702792 ) ) ;
#38612 = CARTESIAN_POINT ( 'NONE',  ( 9.562159722576001997, -3.625366637846545892, 33.29286588640298561 ) ) ;
#38613 = CARTESIAN_POINT ( 'NONE',  ( -3.230769230769229949, -5.471508081941601098, 34.59228464037088457 ) ) ;
#38614 = EDGE_CURVE ( 'NONE', #5068, #30150, #84391, .T. ) ;
#38615 = DIRECTION ( 'NONE',  ( 0.000000000000000000, 0.8660254037844377084, -0.5000000000000015543 ) ) ;
#38616 = ORIENTED_EDGE ( 'NONE', *, *, #22796, .F. ) ;
#38617 = CARTESIAN_POINT ( 'NONE',  ( -5.076923076923075762, -11.11383981884818262, 36.00935417666054406 ) ) ;
#38618 = LINE ( 'NONE', #86835, #84860 ) ;
#38619 = CARTESIAN_POINT ( 'NONE',  ( -1.492201783934593573, -3.724691934501250135, 18.07999329374151287 ) ) ;
#38620 = CARTESIAN_POINT ( 'NONE',  ( -10.74607521849492464, -9.929715669179220328, 34.40415004197138416 ) ) ;
#38621 = CARTESIAN_POINT ( 'NONE',  ( -5.326946314216041145, -2.587272538249754117, 30.68239716806877837 ) ) ;
#38622 = ORIENTED_EDGE ( 'NONE', *, *, #24501, .T. ) ;
#38623 = CARTESIAN_POINT ( 'NONE',  ( 7.134615384615385025, -7.500000000000000000, 29.75000000000000355 ) ) ;
#38624 = DIRECTION ( 'NONE',  ( 1.000000000000000000, 0.000000000000000000, -0.000000000000000000 ) ) ;
#38626 = ORIENTED_EDGE ( 'NONE', *, *, #33007, .T. ) ;
#38625 = CARTESIAN_POINT ( 'NONE',  ( -7.596099426240392027, -12.41089969410671223, 31.60739465890703670 ) ) ;
#38627 = CARTESIAN_POINT ( 'NONE',  ( -2.939152317953646711E-15, 7.500000000000000000, 10.00000000000000178 ) ) ;
#38628 = CARTESIAN_POINT ( 'NONE',  ( 12.52679403281448600, -12.46129190930001052, 30.37095296980870174 ) ) ;
#38629 = FACE_OUTER_BOUND ( 'NONE', #36970, .T. ) ;
#38630 = VECTOR ( 'NONE', #36869, 1000.000000000000000 ) ;
#38631 = CARTESIAN_POINT ( 'NONE',  ( -16.21959958215948916, -7.249945578846654470, 34.99404164642496795 ) ) ;
#38632 = VERTEX_POINT ( 'NONE', #64976 ) ;
#38633 = CARTESIAN_POINT ( 'NONE',  ( 10.61538461538461675, -13.20930481340135110, 34.54067556320372745 ) ) ;
#38634 = CARTESIAN_POINT ( 'NONE',  ( -11.60371147023562344, -2.255955759149247619, 30.00000000000013856 ) ) ;
#38635 = EDGE_CURVE ( 'NONE', #64411, #28677, #57467, .T. ) ;
#38636 = CIRCLE ( 'NONE', #63044, 0.2500000000000002220 ) ;
#38637 = CARTESIAN_POINT ( 'NONE',  ( 4.153846153846032507, -10.21337939537710326, 33.94971097300076224 ) ) ;
#38638 = EDGE_LOOP ( 'NONE', ( #13115, #11407, #77735, #526 ) ) ;
#38639 = EDGE_LOOP ( 'NONE', ( #77939, #31535, #73452, #33116 ) ) ;
#38640 = EDGE_CURVE ( 'NONE', #81137, #5354, #72460, .T. ) ;
#38641 = ORIENTED_EDGE ( 'NONE', *, *, #30781, .T. ) ;
#38642 = EDGE_CURVE ( 'NONE', #73914, #84701, #72184, .T. ) ;
#38643 = CARTESIAN_POINT ( 'NONE',  ( 0.3954550505825804030, -8.120952969808774569, 34.71129190930000163 ) ) ;
#38644 = CARTESIAN_POINT ( 'NONE',  ( 9.692307692307570832, -4.320704448113951379, 33.92786785259630022 ) ) ;
#38645 = LINE ( 'NONE', #87747, #55314 ) ;
#38646 = CARTESIAN_POINT ( 'NONE',  ( -10.39260507411620438, -3.236590943229499029, 32.36255958852954251 ) ) ;
#38647 = VERTEX_POINT ( 'NONE', #31653 ) ;
#38648 = VERTEX_POINT ( 'NONE', #12265 ) ;
#38650 = ORIENTED_EDGE ( 'NONE', *, *, #76556, .T. ) ;
#38649 = CARTESIAN_POINT ( 'NONE',  ( 4.376625822824220080, -5.827830569534416583, 34.72679350104403539 ) ) ;
#38651 = CARTESIAN_POINT ( 'NONE',  ( -16.21992853320628925, -12.34228464037088280, 31.77849191805838558 ) ) ;
#38652 = AXIS2_PLACEMENT_3D ( 'NONE', #28625, #7012, #56087 ) ;
#38653 = LINE ( 'NONE', #52152, #30680 ) ;
#38654 = CARTESIAN_POINT ( 'NONE',  ( -8.546451227962359454, -12.44528174975671853, 30.48912976160716681 ) ) ;
#38655 = LINE ( 'NONE', #51241, #33854 ) ;
#38656 = ORIENTED_EDGE ( 'NONE', *, *, #39042, .T. ) ;
#38657 = ORIENTED_EDGE ( 'NONE', *, *, #23379, .T. ) ;
#38658 = ORIENTED_EDGE ( 'NONE', *, *, #9679, .F. ) ;
#38660 = EDGE_LOOP ( 'NONE', ( #43826, #65894, #65700, #49539, #78800 ) ) ;
#38659 = CARTESIAN_POINT ( 'NONE',  ( 15.10007776410167502, -2.541943142973491554, 30.39792223712631980 ) ) ;
#38661 = B_SPLINE_CURVE_WITH_KNOTS ( 'NONE', 3,
 ( #79687, #17541, #24277, #51736, #44993, #58958, #24736, #17989, #45442, #4464 ),
 .UNSPECIFIED., .F., .F.,
 ( 4, 2, 2, 2, 4 ),
 ( 0.000000000000000000, 0.0001954339857564070678, 0.0003908679715128141356, 0.0005863019572692211492, 0.0007817359430256282712 ),
 .UNSPECIFIED. ) ;
#38662 = CARTESIAN_POINT ( 'NONE',  ( 2.307692307692309264, -13.04860791097971706, 34.73218667398347037 ) ) ;
#38663 = EDGE_CURVE ( 'NONE', #59654, #10540, #71334, .T. ) ;
#38664 = CARTESIAN_POINT ( 'NONE',  ( -13.60810032833933469, -6.760086850603066466, 34.69517049084099369 ) ) ;
#38665 = ORIENTED_EDGE ( 'NONE', *, *, #8635, .T. ) ;
#38666 = CARTESIAN_POINT ( 'NONE',  ( -9.320512820512821150, -3.499999999999999556, 29.75000000000000355 ) ) ;
#38667 = CARTESIAN_POINT ( 'NONE',  ( 16.15384615384615330, -12.34228464037088635, 31.77849191805839268 ) ) ;
#38668 = CARTESIAN_POINT ( 'NONE',  ( 4.219101725122175850, -2.892918686051625166, 31.69288490824025928 ) ) ;
#38669 = FACE_BOUND ( 'NONE', #28909, .T. ) ;
#38670 = CARTESIAN_POINT ( 'NONE',  ( -5.999999999999998224, -10.05456864172156806, 36.03766855953608683 ) ) ;
#38671 = CARTESIAN_POINT ( 'NONE',  ( 11.31497659473759043, -8.496056993536548418, 34.65000542017679663 ) ) ;
#38672 = CARTESIAN_POINT ( 'NONE',  ( -8.769230769230768274, -4.098570777380720287, 33.41473453929634729 ) ) ;
#38674 = CARTESIAN_POINT ( 'NONE',  ( 14.30769230769231015, -2.833524468853757305, 32.15551576947925838 ) ) ;
#38673 = CARTESIAN_POINT ( 'NONE',  ( 17.07692307692307665, -9.058645607665452459, 34.76329471203371924 ) ) ;
#38675 = CIRCLE ( 'NONE', #51636, 0.2500000000000002220 ) ;
#38676 = CARTESIAN_POINT ( 'NONE',  ( 6.000000000000317080, -2.255955759149395501, 30.00000000000324363 ) ) ;
#38677 = CARTESIAN_POINT ( 'NONE',  ( 8.769230769230647482, -3.835265460704628371, 33.15142922262033665 ) ) ;
#38678 = ORIENTED_EDGE ( 'NONE', *, *, #83520, .F. ) ;
#38679 = CARTESIAN_POINT ( 'NONE',  ( -17.07692307692319744, -5.941354392335915335, 34.76329471203413846 ) ) ;
#38680 = CARTESIAN_POINT ( 'NONE',  ( -13.38461538461538325, -9.058645607665452459, 34.76329471203371924 ) ) ;
#38681 = ORIENTED_EDGE ( 'NONE', *, *, #20068, .F. ) ;
#38682 = ORIENTED_EDGE ( 'NONE', *, *, #16212, .T. ) ;
#38683 = EDGE_CURVE ( 'NONE', #59958, #1686, #15523, .T. ) ;
#38684 = VECTOR ( 'NONE', #16274, 1000.000000000000000 ) ;
#38686 = CARTESIAN_POINT ( 'NONE',  ( 10.86543903529806876, -12.65882529074907126, 30.72640787790839312 ) ) ;
#38685 = FACE_OUTER_BOUND ( 'NONE', #7585, .T. ) ;
#38687 = CARTESIAN_POINT ( 'NONE',  ( 16.40379167219429846, -2.587454068350149239, 30.68340429815432557 ) ) ;
#38688 = FACE_OUTER_BOUND ( 'NONE', #83410, .T. ) ;
#38689 = CARTESIAN_POINT ( 'NONE',  ( -10.61538461538473399, -11.94971097300221174, 32.03036669348237098 ) ) ;
#38690 = ORIENTED_EDGE ( 'NONE', *, *, #13519, .F. ) ;
#38691 = FACE_OUTER_BOUND ( 'NONE', #37148, .T. ) ;
#38692 = CARTESIAN_POINT ( 'NONE',  ( 18.13052543823364360, -4.299079248970731015, 33.91157788607253565 ) ) ;
#38693 = AXIS2_PLACEMENT_3D ( 'NONE', #78568, #71360, #9668 ) ;
#38695 = DIRECTION ( 'NONE',  ( -0.7071067811865510144, 0.7071067811865440200, 0.000000000000000000 ) ) ;
#38694 = CARTESIAN_POINT ( 'NONE',  ( 4.826899839630109490, -5.851115903089112003, 34.47074536777953568 ) ) ;
#38696 = CARTESIAN_POINT ( 'NONE',  ( -12.46153846153846168, -4.786620604624113540, 33.94971097300155094 ) ) ;
#38697 = CARTESIAN_POINT ( 'NONE',  ( 0.4615384615384611200, -3.322132147404559976, 32.92929555188717927 ) ) ;
#38699 = FACE_OUTER_BOUND ( 'NONE', #29278, .T. ) ;
#38698 =( NAMED_UNIT ( * ) SI_UNIT ( $, .STERADIAN. ) SOLID_ANGLE_UNIT ( ) );
#38700 = CARTESIAN_POINT ( 'NONE',  ( -1.553300858899081538, -11.25000000000000711, 23.60937500000000711 ) ) ;
#38701 = ORIENTED_EDGE ( 'NONE', *, *, #48382, .T. ) ;
#38702 = ORIENTED_EDGE ( 'NONE', *, *, #18150, .F. ) ;
#38703 = EDGE_CURVE ( 'NONE', #46051, #31453, #539, .T. ) ;
#38704 = LINE ( 'NONE', #30602, #82305 ) ;
#38705 = CARTESIAN_POINT ( 'NONE',  ( -4.403869391139118683, -12.43535235679832596, 30.55408501211184813 ) ) ;
#38706 = CARTESIAN_POINT ( 'NONE',  ( 10.86543892702293057, -2.564540009722896752, 30.55348353981670684 ) ) ;
#38707 = CARTESIAN_POINT ( 'NONE',  ( 4.087763774486018242, -10.67929555188718460, 33.92786785259543336 ) ) ;
#38708 = EDGE_CURVE ( 'NONE', #10893, #41440, #29569, .T. ) ;
#38709 = CARTESIAN_POINT ( 'NONE',  ( 17.32692307692314415, -7.434744860731433924, 35.00000000000000711 ) ) ;
#38710 = CARTESIAN_POINT ( 'NONE',  ( 1.553300858899129944, -11.24999999999998934, 20.95312500000000000 ) ) ;
#38711 = LINE ( 'NONE', #8263, #60470 ) ;
#38712 = DIRECTION ( 'NONE',  ( -0.000000000000000000, 0.9396926207859092051, -0.3420201433256662704 ) ) ;
#38713 = CARTESIAN_POINT ( 'NONE',  ( -8.992715693795103604, -12.69144148231606017, 30.53333754910549303 ) ) ;
#38714 = LINE ( 'NONE', #66174, #88495 ) ;
#38715 = CARTESIAN_POINT ( 'NONE',  ( 7.384615384615385025, -7.500000000000000000, 29.75000000000000355 ) ) ;
#38716 = CARTESIAN_POINT ( 'NONE',  ( 16.15384615384615330, -1.242168528481310874, 33.36296068462461051 ) ) ;
#38717 = CARTESIAN_POINT ( 'NONE',  ( 2.177545098254088263, -3.285722584762969856, 32.44110544564090759 ) ) ;
#38718 = CARTESIAN_POINT ( 'NONE',  ( 8.068933515131911705, -8.540255544307065350, 34.89611431652622286 ) ) ;
#38719 = CARTESIAN_POINT ( 'NONE',  ( -6.223484943723947893, -10.11188796281391511, 34.01382737946119050 ) ) ;
#38720 = EDGE_CURVE ( 'NONE', #59530, #64959, #60893, .T. ) ;
#38721 = CARTESIAN_POINT ( 'NONE',  ( -4.153846153846152411, -8.973038597847269315, 34.52809138561121927 ) ) ;
#38722 = CARTESIAN_POINT ( 'NONE',  ( -3.453696189676078276, -12.38737895849757820, 31.66785238281580206 ) ) ;
#38723 = ORIENTED_EDGE ( 'NONE', *, *, #44384, .F. ) ;
#38724 = B_SPLINE_CURVE_WITH_KNOTS ( 'NONE', 3,
 ( #80782, #19061, #67251, #59150, #60486, #87999, #26258, #10974, #65900, #27142 ),
 .UNSPECIFIED., .F., .F.,
 ( 4, 2, 2, 2, 4 ),
 ( 0.000000000000000000, 0.0001954339857564054144, 0.0003908679715128108288, 0.0005863019572692162703, 0.0007817359430256216575 ),
 .UNSPECIFIED. ) ;
#38725 = VECTOR ( 'NONE', #16745, 1000.000000000000000 ) ;
#38726 = CARTESIAN_POINT ( 'NONE',  ( 11.53846153846141753, -11.94971097300221174, 32.03036669348237098 ) ) ;
#38727 = DIRECTION ( 'NONE',  ( 0.000000000000000000, 0.000000000000000000, 1.000000000000000000 ) ) ;
#38728 = CARTESIAN_POINT ( 'NONE',  ( 13.31853300525525086, -6.343179335718451384, 34.87096338111212646 ) ) ;
#38729 = CARTESIAN_POINT ( 'NONE',  ( 1.987747218494642309, -5.598659921968629050, 17.06436829374151287 ) ) ;
#38730 = ADVANCED_FACE ( 'NONE', ( #82950 ), #82070, .F. ) ;
#38731 = B_SPLINE_CURVE_WITH_KNOTS ( 'NONE', 3,
 ( #33193, #74628, #31869, #25990, #11597, #80048, #53453, #74181, #46265, #12482 ),
 .UNSPECIFIED., .F., .F.,
 ( 4, 2, 2, 2, 4 ),
 ( 0.0007817246256747451124, 0.0009771112852218885505, 0.001172497944769032097, 0.001367884604316175427, 0.001563271263863318973 ),
 .UNSPECIFIED. ) ;
#38732 = CARTESIAN_POINT ( 'NONE',  ( -18.22286542220362904, -2.501496062324911396, 29.88072118266894250 ) ) ;
#38733 = CARTESIAN_POINT ( 'NONE',  ( 14.17754433796061875, -5.070767119584671079, 34.40440758774516183 ) ) ;
#38735 = ORIENTED_EDGE ( 'NONE', *, *, #52820, .T. ) ;
#38734 = CARTESIAN_POINT ( 'NONE',  ( 5.142178216435913107, -4.320704448112861584, 33.92786785259548310 ) ) ;
#38736 = CARTESIAN_POINT ( 'NONE',  ( 1.944543648263018731, -9.444543648262994751, 19.62500000000000000 ) ) ;
#38737 = CARTESIAN_POINT ( 'NONE',  ( 2.980792499826877773, -9.148715823498378086, 34.47080413974185120 ) ) ;
#38738 = ADVANCED_FACE ( 'NONE', ( #40638 ), #55030, .F. ) ;
#38739 = ORIENTED_EDGE ( 'NONE', *, *, #16825, .F. ) ;
#38740 = DIRECTION ( 'NONE',  ( 0.000000000000000000, 0.6427876096865373645, -0.7660444431189797898 ) ) ;
#38741 = EDGE_LOOP ( 'NONE', ( #6894, #17915 ) ) ;
#38742 = CARTESIAN_POINT ( 'NONE',  ( 15.23076923076923173, -2.486705287966279876, 31.30864560766543647 ) ) ;
#38743 = DIRECTION ( 'NONE',  ( 0.000000000000000000, 8.673617379884033500E-16, -1.000000000000000000 ) ) ;
#38744 = EDGE_CURVE ( 'NONE', #11362, #61129, #55242, .T. ) ;
#38745 = CARTESIAN_POINT ( 'NONE',  ( 16.15384615384615330, -8.120952969808772792, 34.71129190930000163 ) ) ;
#38746 = EDGE_LOOP ( 'NONE', ( #18265, #76134, #7518, #16646 ) ) ;
#38747 = FACE_OUTER_BOUND ( 'NONE', #8061, .T. ) ;
#38748 = VERTEX_POINT ( 'NONE', #85 ) ;
#38749 = CARTESIAN_POINT ( 'NONE',  ( 11.31497659473758866, -3.754499324213721234, 33.06261337010820256 ) ) ;
#38750 = B_SPLINE_CURVE_WITH_KNOTS ( 'NONE', 3,
 ( #60219, #17913, #87277, #80510, #18803, #66993, #46713, #60664, #88174, #45367 ),
 .UNSPECIFIED., .F., .F.,
 ( 4, 2, 2, 2, 4 ),
 ( 0.000000000000000000, 0.0001954311564186876876, 0.0003908623128373753751, 0.0005862934692560630356, 0.0007817246256747507503 ),
 .UNSPECIFIED. ) ;
#38751 = ORIENTED_EDGE ( 'NONE', *, *, #32533, .F. ) ;
#38752 = CARTESIAN_POINT ( 'NONE',  ( 2.307692307692186251, -9.528491918059723176, 34.59228464037033035 ) ) ;
#38753 = CARTESIAN_POINT ( 'NONE',  ( 0.4615384615383396616, -11.48612834414049644, 32.76840700105863391 ) ) ;
#38754 = ADVANCED_FACE ( 'NONE', ( #69429 ), #41514, .F. ) ;
#38755 = EDGE_LOOP ( 'NONE', ( #83654, #54533, #52599, #12712 ) ) ;
#38756 = EDGE_CURVE ( 'NONE', #30027, #86745, #34819, .T. ) ;
#38757 = CARTESIAN_POINT ( 'NONE',  ( -5.326923076923075762, -7.500000000000001776, 35.00000000000000000 ) ) ;
#38758 = CARTESIAN_POINT ( 'NONE',  ( -11.00641025641025550, -11.50000000000000000, 29.75000000000000355 ) ) ;
#38759 = CARTESIAN_POINT ( 'NONE',  ( 12.59206416330202671, -5.195472089885680766, 34.18748526763464923 ) ) ;
#38760 = AXIS2_PLACEMENT_3D ( 'NONE', #33729, #46351, #26534 ) ;
#38761 = AXIS2_PLACEMENT_3D ( 'NONE', #71324, #29916, #4204 ) ;
#38762 = VECTOR ( 'NONE', #58889, 1000.000000000000114 ) ;
#38763 = PLANE ( 'NONE',  #24786 ) ;
#38764 = EDGE_LOOP ( 'NONE', ( #54925, #56317 ) ) ;
#38765 = EDGE_LOOP ( 'NONE', ( #29999, #63953, #70358, #88142 ) ) ;
#38766 = B_SPLINE_CURVE_WITH_KNOTS ( 'NONE', 3,
 ( #16585, #51229, #3954, #58904, #86410, #64765, #79186, #24680, #58020, #80074 ),
 .UNSPECIFIED., .F., .F.,
 ( 4, 2, 2, 2, 4 ),
 ( 0.0007817246256747516176, 0.0009771112852218965736, 0.001172497944769041421, 0.001367884604316186269, 0.001563271263863331333 ),
 .UNSPECIFIED. ) ;
#38767 = VERTEX_POINT ( 'NONE', #61321 ) ;
#38769 = ORIENTED_EDGE ( 'NONE', *, *, #609, .F. ) ;
#38768 = CARTESIAN_POINT ( 'NONE',  ( 3.296024370282069071, -12.70778746994558439, 30.41441678777536595 ) ) ;
#38770 = B_SPLINE_CURVE_WITH_KNOTS ( 'NONE', 3,
 ( #50758, #57531, #3469, #51189, #30505, #58404, #85900, #50322, #8919, #29632 ),
 .UNSPECIFIED., .F., .F.,
 ( 4, 2, 2, 2, 4 ),
 ( 0.000000000000000000, 0.0001954339857564074473, 0.0003908679715128148945, 0.0005863019572692223418, 0.0007817359430256297891 ),
 .UNSPECIFIED. ) ;
#38771 = CARTESIAN_POINT ( 'NONE',  ( -14.30769230769242917, -11.06231777344772027, 33.60647404775119895 ) ) ;
#38772 = CARTESIAN_POINT ( 'NONE',  ( -10.28846153846153832, -11.00000000000000000, 29.75000000000000355 ) ) ;
#38773 = EDGE_LOOP ( 'NONE', ( #30797, #39779 ) ) ;
#38774 = EDGE_LOOP ( 'NONE', ( #83646, #78004, #86855, #3157 ) ) ;
#38775 = CARTESIAN_POINT ( 'NONE',  ( -7.846153846153967493, -11.67786785259630911, 32.92929555188603530 ) ) ;
#38776 = VERTEX_POINT ( 'NONE', #76179 ) ;
#38777 = CARTESIAN_POINT ( 'NONE',  ( 9.823099500132480344, -8.147973898785416225, 34.70805048591653730 ) ) ;
#38778 = EDGE_CURVE ( 'NONE', #88550, #35014, #68981, .T. ) ;
#38779 = CARTESIAN_POINT ( 'NONE',  ( -4.153846153846152411, -1.790695186598648903, 34.54067556320373455 ) ) ;
#38780 = EDGE_CURVE ( 'NONE', #30410, #5644, #7287, .T. ) ;
#38781 = AXIS2_PLACEMENT_3D ( 'NONE', #3797, #57405, #85783 ) ;
#38782 = CARTESIAN_POINT ( 'NONE',  ( -11.47239420511146513, -11.91647553114624358, 32.58852847137148245 ) ) ;
#38783 = ADVANCED_FACE ( 'NONE', ( #19467 ), #34751, .T. ) ;
#38784 = FACE_BOUND ( 'NONE', #15847, .T. ) ;
#38785 = CARTESIAN_POINT ( 'NONE',  ( 17.14299041027315695, -6.343179335718452272, 34.87096338111212646 ) ) ;
#38786 = CARTESIAN_POINT ( 'NONE',  ( -1.318446243652726890, -7.250054483168843156, 34.74374881642865631 ) ) ;
#38787 = ADVANCED_FACE ( 'NONE', ( #48261 ), #47825, .F. ) ;
#38788 = PLANE ( 'NONE',  #42414 ) ;
#38789 = DIRECTION ( 'NONE',  ( -0.000000000000000000, 0.1736481776669307198, -0.9848077530122080203 ) ) ;
#38790 = CARTESIAN_POINT ( 'NONE',  ( -14.30769230769230660, -8.973038597847269315, 34.52809138561121927 ) ) ;
#38791 = CARTESIAN_POINT ( 'NONE',  ( 12.46153846153846168, -3.322132147404559976, 32.92929555188717927 ) ) ;
#38792 = ORIENTED_EDGE ( 'NONE', *, *, #86903, .T. ) ;
#38793 = CARTESIAN_POINT ( 'NONE',  ( -11.60373153901785948, -3.643525952247789412, 33.31231777344662959 ) ) ;
#38794 = VERTEX_POINT ( 'NONE', #531 ) ;
#38795 = VERTEX_POINT ( 'NONE', #75304 ) ;
#38796 = ADVANCED_FACE ( 'NONE', ( #21232 ), #48704, .F. ) ;
#38798 = CARTESIAN_POINT ( 'NONE',  ( -1.634638608836841200, -5.765609946408405406, 34.70566812827424741 ) ) ;
#38797 = CARTESIAN_POINT ( 'NONE',  ( 12.46153846153846168, -10.67929555188718282, 33.92786785259544047 ) ) ;
#38799 = B_SPLINE_CURVE_WITH_KNOTS ( 'NONE', 3,
 ( #6105, #75444, #55163, #88107, #41220, #81767, #47072, #82661, #20932, #48404 ),
 .UNSPECIFIED., .F., .F.,
 ( 4, 2, 2, 2, 4 ),
 ( 0.000000000000000000, 0.0001954339857564081249, 0.0003908679715128162498, 0.0005863019572692244018, 0.0007817359430256324996 ),
 .UNSPECIFIED. ) ;
#38800 = B_SPLINE_CURVE_WITH_KNOTS ( 'NONE', 3,
 ( #79152, #87262, #66977, #80042, #25981, #53445, #17453, #44909, #28191, #7038 ),
 .UNSPECIFIED., .F., .F.,
 ( 4, 2, 2, 2, 4 ),
 ( 0.0007817359430256303312, 0.0009771253907249965402, 0.001172514838424362641, 0.001367904286123728958, 0.001563293733823095059 ),
 .UNSPECIFIED. ) ;
#38801 = CARTESIAN_POINT ( 'NONE',  ( 6.000000000000001776, -13.63283147151868846, 33.57946703557072254 ) ) ;
#38802 = DIRECTION ( 'NONE',  ( 0.000000000000000000, 0.4999999999999985567, 0.8660254037844395958 ) ) ;
#38803 = LINE ( 'NONE', #32041, #77463 ) ;
#38804 = CARTESIAN_POINT ( 'NONE',  ( -13.25408968285182532, -2.882268652242222284, 31.66798894389554064 ) ) ;
#38805 = VERTEX_POINT ( 'NONE', #63548 ) ;
#38806 = CARTESIAN_POINT ( 'NONE',  ( 16.85399685940691938, -5.667676309546437530, 34.40238873228292249 ) ) ;
#38807 = CARTESIAN_POINT ( 'NONE',  ( -0.4615384615384611200, -3.322132147404559976, 32.92929555188717927 ) ) ;
#38808 = CARTESIAN_POINT ( 'NONE',  ( -1.384615384615505151, -3.835265460704628371, 33.15142922262033665 ) ) ;
#38809 = AXIS2_PLACEMENT_3D ( 'NONE', #31579, #38789, #3651 ) ;
#38810 = CARTESIAN_POINT ( 'NONE',  ( 4.826923076923076650, -7.500000000000001776, 34.75000000000000000 ) ) ;
#38811 = ORIENTED_EDGE ( 'NONE', *, *, #63531, .T. ) ;
#38812 = ORIENTED_EDGE ( 'NONE', *, *, #55059, .T. ) ;
#38813 = AXIS2_PLACEMENT_3D ( 'NONE', #16982, #44431, #58849 ) ;
#38815 = AXIS2_PLACEMENT_3D ( 'NONE', #2968, #56600, #30016 ) ;
#38814 = APPLICATION_PROTOCOL_DEFINITION ( 'draft international standard', 'automotive_design', 1998, #26811 ) ;
#38816 = VERTEX_POINT ( 'NONE', #76631 ) ;
#38817 = CARTESIAN_POINT ( 'NONE',  ( 18.06616914096265702, -7.250054483168842268, 34.74374881642865631 ) ) ;
#38818 = LINE ( 'NONE', #86118, #20303 ) ;
#38819 = ORIENTED_EDGE ( 'NONE', *, *, #5963, .T. ) ;
#38820 = CARTESIAN_POINT ( 'NONE',  ( -2.307692307692428724, -12.51329471203414379, 31.30864560766407578 ) ) ;
#38821 = CARTESIAN_POINT ( 'NONE',  ( 6.699591979352975457, -10.81261337010820256, 33.49550067578627477 ) ) ;
#38822 = CARTESIAN_POINT ( 'NONE',  ( 0.5920641633020261585, -12.27024696741798770, 31.24895572276497546 ) ) ;
#38823 = EDGE_CURVE ( 'NONE', #30118, #76426, #70415, .T. ) ;
#38824 = CARTESIAN_POINT ( 'NONE',  ( 5.076923076923075762, -6.343179335718451384, 34.87096338111211935 ) ) ;
#38825 = AXIS2_PLACEMENT_3D ( 'NONE', #85690, #4143, #11356 ) ;
#38826 = AXIS2_PLACEMENT_3D ( 'NONE', #87553, #34348, #13203 ) ;
#38827 = CARTESIAN_POINT ( 'NONE',  ( -0.4615384615385826339, -11.48612834414049644, 32.76840700105863391 ) ) ;
#38828 = ORIENTED_EDGE ( 'NONE', *, *, #27379, .T. ) ;
#38829 = VECTOR ( 'NONE', #48373, 1000.000000000000000 ) ;
#38831 = VERTEX_POINT ( 'NONE', #50470 ) ;
#38830 = CARTESIAN_POINT ( 'NONE',  ( -15.29603923132555110, -12.16647553114622049, 32.15551576947930812 ) ) ;
#38832 = CARTESIAN_POINT ( 'NONE',  ( 15.23076923076923173, -8.120952969808772792, 34.71129190930000163 ) ) ;
#38833 = CARTESIAN_POINT ( 'NONE',  ( 14.98074600654777733, -4.931416488878822335, 34.32920672191015399 ) ) ;
#38834 = DIRECTION ( 'NONE',  ( -0.000000000000000000, 0.1736481776669307198, -0.9848077530122080203 ) ) ;
#38835 = CARTESIAN_POINT ( 'NONE',  ( -2.294871794871794712, -11.50000000000000000, 29.75000000000000355 ) ) ;
#38836 = CARTESIAN_POINT ( 'NONE',  ( 6.923076923076924238, -8.164416787775445883, 34.95778746994557906 ) ) ;
#38837 = CARTESIAN_POINT ( 'NONE',  ( 18.13079180782478872, -2.541949514083464479, 30.39797389878540557 ) ) ;
#38838 = CARTESIAN_POINT ( 'NONE',  ( -1.987747218494638313, -9.401340078031370950, 17.68936829374151287 ) ) ;
#38839 = EDGE_LOOP ( 'NONE', ( #77621, #22817, #79468, #50361 ) ) ;
#38840 = CARTESIAN_POINT ( 'NONE',  ( 17.07692307692295586, -3.083524468854526912, 32.58852847137268327 ) ) ;
#38841 = CARTESIAN_POINT ( 'NONE',  ( 2.372947447205147942, -4.320704448112861584, 33.92786785259548310 ) ) ;
#38842 = DIRECTION ( 'NONE',  ( 2.891205793294678326E-16, -1.000000000000000000, 0.000000000000000000 ) ) ;
#38843 = EDGE_LOOP ( 'NONE', ( #49315, #27579 ) ) ;
#38844 = EDGE_LOOP ( 'NONE', ( #15633, #34903 ) ) ;
#38845 = CARTESIAN_POINT ( 'NONE',  ( -11.76194648218548622, -10.81261337010820256, 33.49550067578627477 ) ) ;
#38846 = CARTESIAN_POINT ( 'NONE',  ( 1.653273178848927064E-15, -7.500000000000000000, 14.00000000000000178 ) ) ;
#38847 = CARTESIAN_POINT ( 'NONE',  ( -10.61538461538461320, -13.75783147151868846, 33.36296068462461051 ) ) ;
#38848 = DIRECTION ( 'NONE',  ( -0.000000000000000000, 0.3420201433256694901, -0.9396926207859082059 ) ) ;
#38849 = CARTESIAN_POINT ( 'NONE',  ( 17.99999999999987566, -12.16647553114689728, 32.15551576947799362 ) ) ;
#38850 = CARTESIAN_POINT ( 'NONE',  ( 12.46153846153846168, -11.11383981884818262, 36.00935417666054406 ) ) ;
#38851 = ORIENTED_EDGE ( 'NONE', *, *, #42333, .F. ) ;
#38852 = CARTESIAN_POINT ( 'NONE',  ( 5.869852790561777667, -3.817052484675422797, 33.13202310037935661 ) ) ;
#38853 = EDGE_CURVE ( 'NONE', #519, #64802, #36098, .T. ) ;
#38854 = EDGE_CURVE ( 'NONE', #28470, #85639, #9163, .T. ) ;
#38855 = CARTESIAN_POINT ( 'NONE',  ( 6.989144256426998325, -6.343179335718452272, 34.87096338111212646 ) ) ;
#38856 = CARTESIAN_POINT ( 'NONE',  ( -12.46153846153846168, -2.499999999999998668, 29.75000000000001421 ) ) ;
#38857 = ORIENTED_EDGE ( 'NONE', *, *, #38423, .F. ) ;
#38858 = CARTESIAN_POINT ( 'NONE',  ( -7.623374304885432551, -3.755027918224367767, 33.06320215134714857 ) ) ;
#38859 = EDGE_CURVE ( 'NONE', #69859, #68982, #57310, .T. ) ;
#38860 = ORIENTED_EDGE ( 'NONE', *, *, #63206, .T. ) ;
#38861 = CARTESIAN_POINT ( 'NONE',  ( -0.4615384615384611200, -2.721908614388771852, 31.22303859784724978 ) ) ;
#38862 =( NAMED_UNIT ( * ) PLANE_ANGLE_UNIT ( ) SI_UNIT ( $, .RADIAN. ) );
#38863 = CARTESIAN_POINT ( 'NONE',  ( -1.634638621908349077, -9.271318131107980420, 34.42618302367067429 ) ) ;
#38864 = CARTESIAN_POINT ( 'NONE',  ( 3.230769230769231726, -2.833524468853757305, 32.15551576947925838 ) ) ;
#38865 = EDGE_LOOP ( 'NONE', ( #22908, #15563 ) ) ;
#38866 = ADVANCED_FACE ( 'NONE', ( #62654 ), #84291, .F. ) ;
#38867 = B_SPLINE_CURVE_WITH_KNOTS ( 'NONE', 3,
 ( #80177, #86044, #59457, #24321, #73868, #86959, #39198, #12165, #59004, #25226 ),
 .UNSPECIFIED., .F., .F.,
 ( 4, 2, 2, 2, 4 ),
 ( 0.000000000000000000, 0.0001954339857564067696, 0.0003908679715128135393, 0.0005863019572692202818, 0.0007817359430256270785 ),
 .UNSPECIFIED. ) ;
#38868 = CARTESIAN_POINT ( 'NONE',  ( -13.38461538461550759, -5.094484230521993062, 34.41647553114689373 ) ) ;
#38869 = CARTESIAN_POINT ( 'NONE',  ( -14.55769230769230660, -7.500000000000001776, 34.75000000000000000 ) ) ;
#38870 = CARTESIAN_POINT ( 'NONE',  ( -1.384615384615383471, -8.564572088678739092, 35.78748833219616898 ) ) ;
#38871 = EDGE_CURVE ( 'NONE', #76436, #75253, #20783, .T. ) ;
#38872 = CARTESIAN_POINT ( 'NONE',  ( 11.53846153846153832, -1.242168528481310874, 33.36296068462461051 ) ) ;
#38873 = CARTESIAN_POINT ( 'NONE',  ( -2.057746898314262385, -10.92531984108285670, 33.72920026020278073 ) ) ;
#38874 = EDGE_LOOP ( 'NONE', ( #32248, #79279, #50738, #45072, #12753, #16043 ) ) ;
#38875 = FACE_BOUND ( 'NONE', #23561, .T. ) ;
#38876 = ORIENTED_EDGE ( 'NONE', *, *, #68157, .F. ) ;
#38878 = EDGE_CURVE ( 'NONE', #26509, #53886, #83172, .T. ) ;
#38877 = CARTESIAN_POINT ( 'NONE',  ( 5.326868486301118644, -11.56426240980093745, 33.07394671870546432 ) ) ;
#38879 = CARTESIAN_POINT ( 'NONE',  ( 5.011652630962300847, -12.27809138561121394, 31.22303859784730307 ) ) ;
#38880 = AXIS2_PLACEMENT_3D ( 'NONE', #6916, #54210, #34832 ) ;
#38881 = AXIS2_PLACEMENT_3D ( 'NONE', #38009, #53289, #19511 ) ;
#38882 = FACE_OUTER_BOUND ( 'NONE', #74400, .T. ) ;
#38883 = CARTESIAN_POINT ( 'NONE',  ( 9.942253101685734507, -2.589246495874658383, 31.60778113518102828 ) ) ;
#38884 = EDGE_CURVE ( 'NONE', #21923, #25224, #8626, .T. ) ;
#38885 = CARTESIAN_POINT ( 'NONE',  ( -8.102564102564102200, -7.500000000000000000, 33.75000000000000000 ) ) ;
#38886 = CYLINDRICAL_SURFACE ( 'NONE', #35197, 4.000000000000000000 ) ;
#38887 = CIRCLE ( 'NONE', #73416, 5.000000000000000888 ) ;
#38888 = CIRCLE ( 'NONE', #35998, 4.000000000000000000 ) ;
#38889 = ORIENTED_EDGE ( 'NONE', *, *, #25235, .T. ) ;
#38890 = EDGE_LOOP ( 'NONE', ( #20173, #34817 ) ) ;
#38891 = MECHANICAL_DESIGN_GEOMETRIC_PRESENTATION_REPRESENTATION (  '', ( #48969 ), #10152 ) ;
#38892 = VERTEX_POINT ( 'NONE', #29777 ) ;
#38893 = VERTEX_POINT ( 'NONE', #57244 ) ;
#38895 = ORIENTED_EDGE ( 'NONE', *, *, #60141, .T. ) ;
#38894 = EDGE_CURVE ( 'NONE', #63694, #8816, #51863, .T. ) ;
#38896 = PLANE ( 'NONE',  #1327 ) ;
#38897 = CARTESIAN_POINT ( 'NONE',  ( -11.78848477575450282, -9.271318131107980420, 34.42618302367067429 ) ) ;
#38898 = DIRECTION ( 'NONE',  ( 0.000000000000000000, 0.000000000000000000, 1.000000000000000000 ) ) ;
#38899 = EDGE_CURVE ( 'NONE', #37767, #11473, #73440, .T. ) ;
#38900 = CARTESIAN_POINT ( 'NONE',  ( -7.053224132515142131, -3.285722584762969856, 32.44110544564090759 ) ) ;
#38901 = CARTESIAN_POINT ( 'NONE',  ( 13.13459214732242408, -8.432397168068783699, 34.66272746175022945 ) ) ;
#38902 = CARTESIAN_POINT ( 'NONE',  ( -12.68502338610279523, -12.47654668319379567, 31.42292124445336654 ) ) ;
#38903 = CARTESIAN_POINT ( 'NONE',  ( -0.7115616988314266145, -11.86270091957321071, 32.19358267280088626 ) ) ;
#38904 = CARTESIAN_POINT ( 'NONE',  ( -7.780085495151406683, -3.050289026998446840, 32.03036669348366416 ) ) ;
#38905 = CARTESIAN_POINT ( 'NONE',  ( 12.46153846153833911, -11.94971097300221174, 32.03036669348237098 ) ) ;
#38906 = ORIENTED_EDGE ( 'NONE', *, *, #6975, .T. ) ;
#38907 = EDGE_LOOP ( 'NONE', ( #75259, #60702, #1742, #60329 ) ) ;
#38908 = VERTEX_POINT ( 'NONE', #52697 ) ;
#38911 = ORIENTED_EDGE ( 'NONE', *, *, #45490, .T. ) ;
#38910 = EDGE_CURVE ( 'NONE', #38361, #64945, #24327, .T. ) ;
#38909 = CARTESIAN_POINT ( 'NONE',  ( 0.3313904918067679950, -12.15440758774515473, 32.17923288041532004 ) ) ;
#38913 = CARTESIAN_POINT ( 'NONE',  ( 6.000000000000001776, -6.435427911321262684, 35.78748833219616898 ) ) ;
#38912 = CARTESIAN_POINT ( 'NONE',  ( -16.08859058257012720, -6.879047030191284051, 34.71129190930002295 ) ) ;
#38914 = DIRECTION ( 'NONE',  ( 0.000000000000000000, 0.7660444431189807890, 0.6427876096865361433 ) ) ;
#38915 = CARTESIAN_POINT ( 'NONE',  ( 4.403791672194295792, -2.587454068350147462, 30.68340429815432202 ) ) ;
#38916 = FACE_BOUND ( 'NONE', #25877, .T. ) ;
#38917 = ORIENTED_EDGE ( 'NONE', *, *, #20179, .F. ) ;
#38918 = EDGE_CURVE ( 'NONE', #4960, #59157, #66665, .T. ) ;
#38919 = EDGE_LOOP ( 'NONE', ( #87562, #49940 ) ) ;
#38920 = DIRECTION ( 'NONE',  ( -0.000000000000000000, -0.000000000000000000, -1.000000000000000000 ) ) ;
#38921 = EDGE_LOOP ( 'NONE', ( #85523, #44608 ) ) ;
#38922 = FACE_BOUND ( 'NONE', #26005, .T. ) ;
#38923 = CARTESIAN_POINT ( 'NONE',  ( 7.716006636715625255, -11.93770438780619259, 32.05411857736982029 ) ) ;
#38924 = CARTESIAN_POINT ( 'NONE',  ( -2.307692307692427391, -11.48612834414049644, 32.76840700105863391 ) ) ;
#38925 = ORIENTED_EDGE ( 'NONE', *, *, #10410, .T. ) ;
#38926 = CARTESIAN_POINT ( 'NONE',  ( 17.93391658904412012, -2.721908614388770964, 31.22303859784723912 ) ) ;
#38927 = CARTESIAN_POINT ( 'NONE',  ( -1.634638608836840978, -8.475808217655753651, 34.90892951860618609 ) ) ;
#38928 = DIRECTION ( 'NONE',  ( -0.000000000000000000, 0.9848077530122086864, -0.1736481776669273891 ) ) ;
#38929 = ORIENTED_EDGE ( 'NONE', *, *, #40551, .F. ) ;
#38930 = CARTESIAN_POINT ( 'NONE',  ( 9.692307692307695177, -11.91647553114624181, 32.58852847137148245 ) ) ;
#38931 = CARTESIAN_POINT ( 'NONE',  ( -18.06527044596078113, -5.219633306516281657, 34.19971097300152252 ) ) ;
#38932 = EDGE_CURVE ( 'NONE', #22144, #85987, #51789, .T. ) ;
#38933 = CARTESIAN_POINT ( 'NONE',  ( -5.300408020647025431, -11.89387501736622710, 32.13663884655806413 ) ) ;
#38934 = ORIENTED_EDGE ( 'NONE', *, *, #22721, .T. ) ;
#38935 = ADVANCED_FACE ( 'NONE', ( #59464 ), #52251, .F. ) ;
#38936 = CARTESIAN_POINT ( 'NONE',  ( 8.769230769230768274, -10.89733346790207413, 36.13435417666054406 ) ) ;
#38937 = CARTESIAN_POINT ( 'NONE',  ( -17.01166750564705055, -11.94971097300157403, 32.03036669348361443 ) ) ;
#38938 = VERTEX_POINT ( 'NONE', #65321 ) ;
#38939 = CARTESIAN_POINT ( 'NONE',  ( -17.20761368003338632, -12.62707690430377383, 30.88035979386743435 ) ) ;
#38940 = CARTESIAN_POINT ( 'NONE',  ( 14.37376065869474751, -8.120952969808772792, 34.71129190929999453 ) ) ;
#38941 = CARTESIAN_POINT ( 'NONE',  ( -2.307692307692305711, -2.538708090699994813, 30.37095296980875503 ) ) ;
#38942 = CARTESIAN_POINT ( 'NONE',  ( 15.16549923021291058, -12.70778746994557551, 30.41441678777548319 ) ) ;
#38943 = DIRECTION ( 'NONE',  ( -0.000000000000000000, 0.1736481776669307198, -0.9848077530122080203 ) ) ;
#38944 = CYLINDRICAL_SURFACE ( 'NONE', #63916, 4.000000000000000000 ) ;
#38946 = CARTESIAN_POINT ( 'NONE',  ( -15.23076923076922995, -12.37446782046654192, 30.86335684631486131 ) ) ;
#38945 = CARTESIAN_POINT ( 'NONE',  ( 0.4615384615383382183, -11.67786785259630911, 32.92929555188603530 ) ) ;
#38947 = B_SPLINE_CURVE_WITH_KNOTS ( 'NONE', 3,
 ( #40571, #55836, #6342, #62154, #33797, #462, #27929, #83325, #61253, #44076 ),
 .UNSPECIFIED., .F., .F.,
 ( 4, 2, 2, 2, 4 ),
 ( 0.000000000000000000, 0.0001954311564186879044, 0.0003908623128373758088, 0.0005862934692560636861, 0.0007817246256747516176 ),
 .UNSPECIFIED. ) ;
#38948 = VECTOR ( 'NONE', #5801, 1000.000000000000114 ) ;
#38949 = CARTESIAN_POINT ( 'NONE',  ( 10.68145194873469173, -9.058645607665452459, 34.76329471203371924 ) ) ;
#38951 = CARTESIAN_POINT ( 'NONE',  ( -10.86540785267757947, -8.432397168068783699, 34.66272746175022945 ) ) ;
#38950 = CARTESIAN_POINT ( 'NONE',  ( -14.98082382139119062, -2.589246495874658383, 31.60778113518102828 ) ) ;
#38952 = CARTESIAN_POINT ( 'NONE',  ( -1.987747218494660295, -5.598659921968651254, 27.49813170625849068 ) ) ;
#38953 = ORIENTED_EDGE ( 'NONE', *, *, #30260, .F. ) ;
#38954 = FACE_OUTER_BOUND ( 'NONE', #58814, .T. ) ;
#38955 = ORIENTED_EDGE ( 'NONE', *, *, #11943, .T. ) ;
#38956 = VECTOR ( 'NONE', #45589, 1000.000000000000000 ) ;
#38957 = AXIS2_PLACEMENT_3D ( 'NONE', #4450, #44981, #85541 ) ;
#38958 = VERTEX_POINT ( 'NONE', #65761 ) ;
#38959 = DIRECTION ( 'NONE',  ( -0.000000000000000000, 0.9848077530122085754, -0.1736481776669273613 ) ) ;
#38960 = ORIENTED_EDGE ( 'NONE', *, *, #8008, .T. ) ;
#38961 = CARTESIAN_POINT ( 'NONE',  ( 20.00000000000000000, -4.000000000000000000, 29.75000000000000355 ) ) ;
#38962 = CARTESIAN_POINT ( 'NONE',  ( 2.750000000000001332, -7.438900925035452083, 26.71688170625849068 ) ) ;
#38963 = CARTESIAN_POINT ( 'NONE',  ( -13.25408994638174143, -5.915461855592780260, 34.75538340440931506 ) ) ;
#38964 = CARTESIAN_POINT ( 'NONE',  ( 5.933916589044121892, -11.16473453929635440, 33.15142922261925662 ) ) ;
#38965 = CYLINDRICAL_SURFACE ( 'NONE', #80675, 0.2500000000000004996 ) ;
#38966 = CARTESIAN_POINT ( 'NONE',  ( -14.30769230769242917, -11.06231777344772027, 33.60647404775119895 ) ) ;
#38967 = VECTOR ( 'NONE', #66142, 1000.000000000000000 ) ;
#38968 = DIRECTION ( 'NONE',  ( 1.000000000000000000, 0.000000000000000000, 0.000000000000000000 ) ) ;
#38969 = CARTESIAN_POINT ( 'NONE',  ( -7.715628144390285215, -2.882268652242222728, 31.66798894389554064 ) ) ;
#38970 = CARTESIAN_POINT ( 'NONE',  ( -14.17690186672535901, -4.684288915650983043, 34.18129842949671371 ) ) ;
#38971 = CARTESIAN_POINT ( 'NONE',  ( 1.384615384615386802, -1.367168528481310208, 33.57946703557072254 ) ) ;
#38972 = CARTESIAN_POINT ( 'NONE',  ( 1.553300858899129944, -11.24999999999998934, 23.45312500000000000 ) ) ;
#38973 = CARTESIAN_POINT ( 'NONE',  ( 10.74591005361826213, -12.50538340440932394, 31.33453814440721885 ) ) ;
#38974 = CARTESIAN_POINT ( 'NONE',  ( -17.74994558008654622, -2.318338780012836331, 30.59689888758630616 ) ) ;
#38975 = CARTESIAN_POINT ( 'NONE',  ( -2.531177251416254936, -4.386631170607603991, 33.66268669641500111 ) ) ;
#38976 = ORIENTED_EDGE ( 'NONE', *, *, #60093, .T. ) ;
#38977 = VERTEX_POINT ( 'NONE', #78835 ) ;
#38978 = CARTESIAN_POINT ( 'NONE',  ( -9.561781990544126586, -3.816742781228458004, 33.13167719472716044 ) ) ;
#38979 = DIRECTION ( 'NONE',  ( -0.000000000000000000, -0.9848077530122086864, -0.1736481776669273613 ) ) ;
#38980 = CARTESIAN_POINT ( 'NONE',  ( -2.307692307692305711, -12.34228464037088635, 31.77849191805839268 ) ) ;
#38981 = DIRECTION ( 'NONE',  ( 0.000000000000000000, 0.000000000000000000, -1.000000000000000000 ) ) ;
#38982 = EDGE_CURVE ( 'NONE', #75052, #27477, #31087, .T. ) ;
#38983 = CARTESIAN_POINT ( 'NONE',  ( 4.153846153846030731, -3.643525952248796163, 33.31231777344771672 ) ) ;
#38984 = CARTESIAN_POINT ( 'NONE',  ( -0.4615384615385826339, -6.879047030192662504, 34.71129190930017927 ) ) ;
#38985 = ADVANCED_FACE ( 'NONE', ( #25234 ), #59011, .T. ) ;
#38986 = AXIS2_PLACEMENT_3D ( 'NONE', #84180, #15709, #8950 ) ;
#38987 = B_SPLINE_CURVE_WITH_KNOTS ( 'NONE', 3,
 ( #4894, #32357, #3975, #73343, #11193, #51710, #38664, #46757, #40015, #86434 ),
 .UNSPECIFIED., .F., .F.,
 ( 4, 2, 2, 2, 4 ),
 ( 0.000000000000000000, 0.0001954339857564074473, 0.0003908679715128148945, 0.0005863019572692223418, 0.0007817359430256297891 ),
 .UNSPECIFIED. ) ;
#38988 = ORIENTED_EDGE ( 'NONE', *, *, #45057, .T. ) ;
#38989 = CARTESIAN_POINT ( 'NONE',  ( 3.165499230212911908, -6.835583212224499938, 34.95778746994557906 ) ) ;
#38990 = EDGE_LOOP ( 'NONE', ( #18716, #18876 ) ) ;
#38991 = VECTOR ( 'NONE', #55233, 1000.000000000000114 ) ;
#38992 = ADVANCED_FACE ( 'NONE', ( #86508 ), #24784, .F. ) ;
#38993 = ORIENTED_EDGE ( 'NONE', *, *, #33141, .F. ) ;
#38994 = CARTESIAN_POINT ( 'NONE',  ( 10.03846153846153832, -7.500000000000000000, 29.75000000000000355 ) ) ;
#38995 = CARTESIAN_POINT ( 'NONE',  ( 5.777173307520998335, -7.369208160676172348, 34.74850200257122879 ) ) ;
#38996 = CARTESIAN_POINT ( 'NONE',  ( 9.915087233576102221, -12.24180327182771855, 31.33663988360758879 ) ) ;
#38997 = CARTESIAN_POINT ( 'NONE',  ( 6.223012844093396723, -8.282913670948747864, 34.94150082978203642 ) ) ;
#38998 = DIRECTION ( 'NONE',  ( 0.000000000000000000, 0.1736481776669275834, 0.9848077530122086864 ) ) ;
#39000 = EDGE_CURVE ( 'NONE', #83351, #89000, #33707, .T. ) ;
#38999 = ORIENTED_EDGE ( 'NONE', *, *, #85698, .T. ) ;
#39001 = ORIENTED_EDGE ( 'NONE', *, *, #67861, .T. ) ;
#39002 = ORIENTED_EDGE ( 'NONE', *, *, #67974, .F. ) ;
#39003 = VECTOR ( 'NONE', #36508, 1000.000000000000000 ) ;
#39004 = CARTESIAN_POINT ( 'NONE',  ( 1.134592147322421196, -11.37209801155882971, 32.91403422569032955 ) ) ;
#39005 = CARTESIAN_POINT ( 'NONE',  ( 10.61538461538449418, -11.67786785259630911, 32.92929555188603530 ) ) ;
#39006 = ADVANCED_FACE ( 'NONE', ( #60940 ), #74026, .F. ) ;
#39007 = CARTESIAN_POINT ( 'NONE',  ( 9.019176178608811156, -5.766571408460171355, 34.70601412856602508 ) ) ;
#39008 = VECTOR ( 'NONE', #76470, 999.9999999999998863 ) ;
#39009 = DIRECTION ( 'NONE',  ( -0.000000000000000000, -0.5000000000000009992, -0.8660254037844380415 ) ) ;
#39010 = CARTESIAN_POINT ( 'NONE',  ( -3.930419191984583005, -7.630147231320743018, 34.74852402298682819 ) ) ;
#39011 = ADVANCED_FACE ( 'NONE', ( #87111 ), #73592, .F. ) ;
#39012 = CARTESIAN_POINT ( 'NONE',  ( 5.934729554039225974, -12.46129190929999986, 30.37095296980880832 ) ) ;
#39013 = ORIENTED_EDGE ( 'NONE', *, *, #36984, .F. ) ;
#39014 = ORIENTED_EDGE ( 'NONE', *, *, #78657, .F. ) ;
#39015 = CYLINDRICAL_SURFACE ( 'NONE', #30192, 0.2499999999999986955 ) ;
#39016 = VECTOR ( 'NONE', #27847, 1000.000000000000000 ) ;
#39018 = ORIENTED_EDGE ( 'NONE', *, *, #30539, .F. ) ;
#39017 = CARTESIAN_POINT ( 'NONE',  ( -12.68502340526241134, -11.41268669641500466, 32.86336882939237825 ) ) ;
#39019 = CYLINDRICAL_SURFACE ( 'NONE', #16265, 0.2499999999999994726 ) ;
#39020 = CARTESIAN_POINT ( 'NONE',  ( -2.241624974342231180, -3.937682226553329556, 33.60647404775216529 ) ) ;
#39021 = CARTESIAN_POINT ( 'NONE',  ( -1.553300858899125059, -3.750000000000009326, 16.57812500000000000 ) ) ;
#39022 = ORIENTED_EDGE ( 'NONE', *, *, #68440, .F. ) ;
#39023 = EDGE_CURVE ( 'NONE', #35903, #81809, #62725, .T. ) ;
#39024 = CARTESIAN_POINT ( 'NONE',  ( -13.63463862190834952, -12.22074536777954989, 31.39888409691088356 ) ) ;
#39025 = ORIENTED_EDGE ( 'NONE', *, *, #16353, .T. ) ;
#39026 = CARTESIAN_POINT ( 'NONE',  ( 5.934729999443682402, -9.528491918058357157, 34.59228464037090589 ) ) ;
#39027 = FACE_OUTER_BOUND ( 'NONE', #56791, .T. ) ;
#39028 = CARTESIAN_POINT ( 'NONE',  ( -12.33074665371367651, -12.38066358083363738, 30.83685684665853444 ) ) ;
#39030 = CARTESIAN_POINT ( 'NONE',  ( -15.10072406793445765, -2.504778602574660340, 29.97347330155780654 ) ) ;
#39029 = CARTESIAN_POINT ( 'NONE',  ( -6.988347369037697376, -3.835265460703609186, 33.15142922261924241 ) ) ;
#39031 = CYLINDRICAL_SURFACE ( 'NONE', #26141, 0.2499999999999994726 ) ;
#39032 = EDGE_LOOP ( 'NONE', ( #52235, #45775, #55075, #77280 ) ) ;
#39033 = CARTESIAN_POINT ( 'NONE',  ( 11.53846153846141576, -11.67786785259630911, 32.92929555188603530 ) ) ;
#39034 = DIRECTION ( 'NONE',  ( 0.000000000000000000, 0.000000000000000000, 1.000000000000000000 ) ) ;
#39035 = DIRECTION ( 'NONE',  ( -0.000000000000000000, 0.5000000000000011102, -0.8660254037844380415 ) ) ;
#39037 = VERTEX_POINT ( 'NONE', #53742 ) ;
#39036 = EDGE_CURVE ( 'NONE', #72151, #65829, #33480, .T. ) ;
#39038 = CIRCLE ( 'NONE', #204, 0.2500000000000002220 ) ;
#39039 = CARTESIAN_POINT ( 'NONE',  ( -18.22348492456433178, -12.69144148231606017, 30.53333754910549303 ) ) ;
#39040 = CARTESIAN_POINT ( 'NONE',  ( -12.46153846153846168, -9.819645486525091727, 36.12317359536749706 ) ) ;
#39041 = DIRECTION ( 'NONE',  ( 0.000000000000000000, 0.000000000000000000, 1.000000000000000000 ) ) ;
#39042 = EDGE_CURVE ( 'NONE', #38776, #15438, #77291, .T. ) ;
#39044 = ADVANCED_FACE ( 'NONE', ( #80795 ), #27157, .F. ) ;
#39043 = LINE ( 'NONE', #68273, #4116 ) ;
#39045 = FACE_BOUND ( 'NONE', #12336, .T. ) ;
#39047 = CARTESIAN_POINT ( 'NONE',  ( 4.284371592079800450, -12.70449254468099198, 30.44128974285582956 ) ) ;
#39046 = CARTESIAN_POINT ( 'NONE',  ( 12.46153846153846168, -3.050289026998446396, 32.03036669348365706 ) ) ;
#39048 = CARTESIAN_POINT ( 'NONE',  ( 2.307692307692186251, -10.33852847137269571, 34.16647553114546554 ) ) ;
#39050 = DIRECTION ( 'NONE',  ( 0.000000000000000000, 0.7660444431189807890, 0.6427876096865361433 ) ) ;
#39049 = CARTESIAN_POINT ( 'NONE',  ( 1.384615384615386802, -12.62096338111211580, 30.90682066428153263 ) ) ;
#39051 = CARTESIAN_POINT ( 'NONE',  ( 16.02369894440793630, -10.88202310037936194, 33.43294751532457099 ) ) ;
#39052 = VECTOR ( 'NONE', #82497, 999.9999999999998863 ) ;
#39053 = EDGE_CURVE ( 'NONE', #34461, #16936, #47870, .T. ) ;
#39054 = CARTESIAN_POINT ( 'NONE',  ( 13.25446741488368296, -2.647304123082328875, 31.75400227202885972 ) ) ;
#39055 = CARTESIAN_POINT ( 'NONE',  ( -0.06109907496455085213, -3.750000000000000888, 23.90438170625849068 ) ) ;
#39056 = EDGE_CURVE ( 'NONE', #75394, #76215, #13206, .T. ) ;
#39057 = CARTESIAN_POINT ( 'NONE',  ( -8.703162418228330921, -5.557115091759786019, 34.35708131394839882 ) ) ;
#39058 = ORIENTED_EDGE ( 'NONE', *, *, #65264, .T. ) ;
#39059 = DIRECTION ( 'NONE',  ( 0.000000000000000000, 0.4999999999999985567, 0.8660254037844395958 ) ) ;
#39060 = CARTESIAN_POINT ( 'NONE',  ( 16.15384615384603251, -12.70778746994576025, 30.41441678777401236 ) ) ;
#39061 = PLANE ( 'NONE',  #11424 ) ;
#39062 = FACE_OUTER_BOUND ( 'NONE', #43274, .T. ) ;
#39063 = CARTESIAN_POINT ( 'NONE',  ( -8.769230769230768274, -5.557115091759785130, 34.35708131394839171 ) ) ;
#39064 = LINE ( 'NONE', #39950, #22516 ) ;
#39065 = CARTESIAN_POINT ( 'NONE',  ( -3.749999999999996447, -7.561099074964554134, 24.84188170625848713 ) ) ;
#39066 = CARTESIAN_POINT ( 'NONE',  ( 2.177545098254086930, -11.93770438780619259, 32.05411857736982029 ) ) ;
#39067 = DIRECTION ( 'NONE',  ( -0.000000000000000000, 0.1736481776669307198, -0.9848077530122080203 ) ) ;
#39068 = LINE ( 'NONE', #66529, #84928 ) ;
#39069 = CARTESIAN_POINT ( 'NONE',  ( 5.326868486301119532, -12.68172785388650681, 30.59649109432439573 ) ) ;
#39070 = DIRECTION ( 'NONE',  ( 0.000000000000000000, 1.000000000000000000, -0.000000000000000000 ) ) ;
#39071 = LINE ( 'NONE', #74175, #12397 ) ;
#39072 = CARTESIAN_POINT ( 'NONE',  ( 14.24242186173153435, -6.026961402152685388, 34.52809138561120506 ) ) ;
#39073 = CARTESIAN_POINT ( 'NONE',  ( 7.846153846153723244, -9.528491918059723176, 34.59228464037033035 ) ) ;
#39074 = ORIENTED_EDGE ( 'NONE', *, *, #61282, .T. ) ;
#39075 = CARTESIAN_POINT ( 'NONE',  ( 17.20744877868662925, -2.882268652242222728, 31.66798894389554064 ) ) ;
#39076 = CARTESIAN_POINT ( 'NONE',  ( 9.019176287578911655, -11.37275283266504111, 32.91324779482534524 ) ) ;
#39077 = CARTESIAN_POINT ( 'NONE',  ( -1.614399933863613468, -11.22469193450124969, 20.11124329374151642 ) ) ;
#39078 = B_SPLINE_CURVE_WITH_KNOTS ( 'NONE', 3,
 ( #52460, #80401, #54233, #47033, #61001, #40743 ),
 .UNSPECIFIED., .F., .F.,
 ( 4, 2, 4 ),
 ( 0.000000000000000000, 0.0001954784845028902421, 0.0003909569690057804843 ),
 .UNSPECIFIED. ) ;
#39079 = VECTOR ( 'NONE', #40255, 1000.000000000000000 ) ;
#39080 = CARTESIAN_POINT ( 'NONE',  ( -15.23076923076891553, -2.255955759149395501, 30.00000000000324363 ) ) ;
#39081 = CARTESIAN_POINT ( 'NONE',  ( 17.07692307692295586, -11.94971097300221174, 32.03036669348237098 ) ) ;
#39082 = EDGE_LOOP ( 'NONE', ( #69131, #54319 ) ) ;
#39083 = CARTESIAN_POINT ( 'NONE',  ( 7.173131234715238946, -8.303483539816728154, 34.68545999027711702 ) ) ;
#39084 = CARTESIAN_POINT ( 'NONE',  ( 7.134615384615385025, -3.499999999999999556, 29.75000000000000355 ) ) ;
#39086 = ORIENTED_EDGE ( 'NONE', *, *, #59387, .T. ) ;
#39085 = CARTESIAN_POINT ( 'NONE',  ( 5.011653076366756387, -12.51329471203370325, 31.30864560766548976 ) ) ;
#39087 = CARTESIAN_POINT ( 'NONE',  ( -13.25382357679059986, -11.18335022499818621, 33.13157742990016885 ) ) ;
#39088 = DIRECTION ( 'NONE',  ( 0.000000000000000000, 0.9848077530122072432, -0.1736481776669354937 ) ) ;
#39089 = CARTESIAN_POINT ( 'NONE',  ( -12.46153846153858424, -8.656820664282941280, 34.87096338111179961 ) ) ;
#39090 = VECTOR ( 'NONE', #21867, 1000.000000000000000 ) ;
#39091 = CARTESIAN_POINT ( 'NONE',  ( -16.08767954725451332, -7.250054591869668386, 34.99404684341514127 ) ) ;
#39092 = EDGE_LOOP ( 'NONE', ( #6261, #78009, #5964, #55847, #14091 ) ) ;
#39093 = CARTESIAN_POINT ( 'NONE',  ( 2.373760658694747061, -12.10708131394839704, 31.69288490824020954 ) ) ;
#39094 = CARTESIAN_POINT ( 'NONE',  ( -39.05038313613820122, -2.499999999999999556, 29.75000000000000355 ) ) ;
#39095 = CARTESIAN_POINT ( 'NONE',  ( 3.903822916553186584, -10.05641848906368097, 34.04755513067966177 ) ) ;
#39096 = VERTEX_POINT ( 'NONE', #40243 ) ;
#39097 = ORIENTED_EDGE ( 'NONE', *, *, #48367, .T. ) ;
#39098 = B_SPLINE_CURVE_WITH_KNOTS ( 'NONE', 3,
 ( #72050, #16660, #84707, #16229, #9470, #24301, #36934, #79266, #10361, #64396 ),
 .UNSPECIFIED., .F., .F.,
 ( 4, 2, 2, 2, 4 ),
 ( 0.0007817246256747483650, 0.0009771112852218926705, 0.001172497944769037084, 0.001367884604316181498, 0.001563271263863325695 ),
 .UNSPECIFIED. ) ;
#39099 = EDGE_LOOP ( 'NONE', ( #5790, #18615, #9590, #56128, #23796, #21395 ) ) ;
#39100 = DIRECTION ( 'NONE',  ( 0.000000000000000000, 0.000000000000000000, 1.000000000000000000 ) ) ;
#39101 = CARTESIAN_POINT ( 'NONE',  ( -8.703162418228330921, -3.050289026998446840, 32.03036669348366416 ) ) ;
#39102 = CARTESIAN_POINT ( 'NONE',  ( -12.71151519248081740, -3.627789207965226748, 32.91389620160131102 ) ) ;
#39103 = CARTESIAN_POINT ( 'NONE',  ( 15.00728428704528383, -3.754499324213721234, 33.06261337010820256 ) ) ;
#39104 = ORIENTED_EDGE ( 'NONE', *, *, #37792, .F. ) ;
#39105 = B_SPLINE_CURVE_WITH_KNOTS ( 'NONE', 3,
 ( #4635, #11846, #64985, #24445, #59571, #32107, #60017, #17712, #87520, #59125 ),
 .UNSPECIFIED., .F., .F.,
 ( 4, 2, 2, 2, 4 ),
 ( 0.0007817246256747484735, 0.0009771112852218928873, 0.001172497944769037518, 0.001367884604316181932, 0.001563271263863326346 ),
 .UNSPECIFIED. ) ;
#39106 = ORIENTED_EDGE ( 'NONE', *, *, #201, .T. ) ;
#39107 = VERTEX_POINT ( 'NONE', #46547 ) ;
#39109 = VERTEX_POINT ( 'NONE', #6013 ) ;
#39108 = CARTESIAN_POINT ( 'NONE',  ( 4.376858997939548246, -5.582272713120727481, 34.63742843783360570 ) ) ;
#39110 = CARTESIAN_POINT ( 'NONE',  ( 9.442307692307693401, -7.500000000000001776, 34.75000000000000000 ) ) ;
#39111 = VECTOR ( 'NONE', #34519, 999.9999999999998863 ) ;
#39112 = B_SPLINE_CURVE_WITH_KNOTS ( 'NONE', 3,
 ( #58481, #44080, #23375, #43651, #22939, #15754, #71561, #24256, #63919, #36893 ),
 .UNSPECIFIED., .F., .F.,
 ( 4, 2, 2, 2, 4 ),
 ( 0.0007817246256747516176, 0.0009771112852218965736, 0.001172497944769041421, 0.001367884604316186269, 0.001563271263863331333 ),
 .UNSPECIFIED. ) ;
#39113 = CYLINDRICAL_SURFACE ( 'NONE', #14888, 0.2499999999999994726 ) ;
#39114 = EDGE_CURVE ( 'NONE', #37680, #16668, #6452, .T. ) ;
#39115 = CARTESIAN_POINT ( 'NONE',  ( 10.36540788444226102, -11.28823185664190376, 33.01397839955799896 ) ) ;
#39116 = CARTESIAN_POINT ( 'NONE',  ( 16.08776377448601735, -11.35647404775217595, 33.31231777344666511 ) ) ;
#39117 = ORIENTED_EDGE ( 'NONE', *, *, #31318, .F. ) ;
#39118 = ORIENTED_EDGE ( 'NONE', *, *, #70213, .F. ) ;
#39119 = ORIENTED_EDGE ( 'NONE', *, *, #56126, .T. ) ;
#39120 = DIRECTION ( 'NONE',  ( -0.000000000000000000, 0.7660444431189791237, -0.6427876096865379196 ) ) ;
#39122 = EDGE_LOOP ( 'NONE', ( #38876, #33906, #31458, #21816 ) ) ;
#39121 = CARTESIAN_POINT ( 'NONE',  ( 5.207448778686639024, -5.195472089885680766, 34.18748526763464923 ) ) ;
#39123 = CARTESIAN_POINT ( 'NONE',  ( 2.980745993476266342, -11.86270091957321249, 32.19358267280087915 ) ) ;
#39124 = CARTESIAN_POINT ( 'NONE',  ( -19.50000000000000000, -3.499999999999999556, 29.75000000000000355 ) ) ;
#39125 = EDGE_CURVE ( 'NONE', #18841, #52308, #26216, .T. ) ;
#39126 = CARTESIAN_POINT ( 'NONE',  ( 12.52679360105129724, -6.835583212224610072, 34.95778746994559327 ) ) ;
#39127 = LINE ( 'NONE', #72891, #19191 ) ;
#39128 = CARTESIAN_POINT ( 'NONE',  ( -17.07692307692307665, -12.10708131394839349, 31.69288490824020244 ) ) ;
#39129 = FACE_BOUND ( 'NONE', #71254, .T. ) ;
#39130 = CARTESIAN_POINT ( 'NONE',  ( -5.326946301144532825, -10.18141759479407327, 34.26406193332782379 ) ) ;
#39131 = CARTESIAN_POINT ( 'NONE',  ( -6.065270000556318486, -12.51329471203370325, 31.30864560766548976 ) ) ;
#39132 = AXIS2_PLACEMENT_3D ( 'NONE', #31497, #87352, #65270 ) ;
#39133 = CARTESIAN_POINT ( 'NONE',  ( -8.834501215191544077, -4.481592998940162609, 33.73612834413957984 ) ) ;
#39135 = CARTESIAN_POINT ( 'NONE',  ( 14.43821774592595375, -3.068774925481848825, 32.56582465632704526 ) ) ;
#39134 = DIRECTION ( 'NONE',  ( -0.000000000000000000, -0.9848077530122085754, -0.1736481776669273613 ) ) ;
#39136 = VECTOR ( 'NONE', #86976, 1000.000000000000000 ) ;
#39137 = CARTESIAN_POINT ( 'NONE',  ( 0.3308469948709059638, -12.11776431015575994, 31.66791131148498906 ) ) ;
#39138 = CYLINDRICAL_SURFACE ( 'NONE', #36191, 4.000000000000000000 ) ;
#39139 = ORIENTED_EDGE ( 'NONE', *, *, #64949, .F. ) ;
#39140 = CARTESIAN_POINT ( 'NONE',  ( 11.31497659473759043, -3.236172620538810385, 32.36188796281390267 ) ) ;
#39141 = CARTESIAN_POINT ( 'NONE',  ( 12.71159288145191013, -3.435999193479609914, 33.07426656108010832 ) ) ;
#39142 = VERTEX_POINT ( 'NONE', #67266 ) ;
#39143 = EDGE_LOOP ( 'NONE', ( #49166, #40537, #46116, #64102, #26694, #31162 ) ) ;
#39144 = AXIS2_PLACEMENT_3D ( 'NONE', #81072, #27886, #88288 ) ;
#39145 = B_SPLINE_CURVE_WITH_KNOTS ( 'NONE', 3,
 ( #54394, #42557, #59823, #87324, #39578, #12533, #62797, #5332, #19291, #35346 ),
 .UNSPECIFIED., .F., .F.,
 ( 4, 2, 2, 2, 4 ),
 ( 0.0007817359430256320659, 0.0009771253907249987086, 0.001172514838424365460, 0.001367904286123732211, 0.001563293733823098962 ),
 .UNSPECIFIED. ) ;
#39147 = CARTESIAN_POINT ( 'NONE',  ( 24.00000000000000000, -5.499999999999981348, 27.75000000000000000 ) ) ;
#39146 = CARTESIAN_POINT ( 'NONE',  ( -11.60373153901785948, -12.70778746994557551, 30.41441678777548319 ) ) ;
#39148 = DIRECTION ( 'NONE',  ( 0.000000000000000000, 0.8660254037844377084, -0.5000000000000015543 ) ) ;
#39149 = CARTESIAN_POINT ( 'NONE',  ( -13.38461538461550759, -5.094484230521993062, 34.41647553114689373 ) ) ;
#39150 = LINE ( 'NONE', #59846, #80676 ) ;
#39151 = ORIENTED_EDGE ( 'NONE', *, *, #49875, .T. ) ;
#39153 = EDGE_CURVE ( 'NONE', #55647, #54542, #54174, .T. ) ;
#39152 = CARTESIAN_POINT ( 'NONE',  ( 14.37376065869474751, -8.973038597847271092, 34.52809138561121216 ) ) ;
#39154 = ADVANCED_FACE ( 'NONE', ( #41121 ), #4678, .F. ) ;
#39155 = CARTESIAN_POINT ( 'NONE',  ( -0.4615384615384611200, -13.53365097954675988, 30.81389545987213552 ) ) ;
#39157 = CARTESIAN_POINT ( 'NONE',  ( -25.00000000000000000, -10.00000000000000533, 3.000000000000000000 ) ) ;
#39156 = FACE_OUTER_BOUND ( 'NONE', #50170, .T. ) ;
#39158 = CARTESIAN_POINT ( 'NONE',  ( -39.05038313613820122, -2.249999999999998668, 29.75000000000000355 ) ) ;
#39159 = DIRECTION ( 'NONE',  ( 0.000000000000000000, 0.9396926207859126468, -0.3420201433256571111 ) ) ;
#39160 = LINE ( 'NONE', #73832, #54941 ) ;
#39161 = CARTESIAN_POINT ( 'NONE',  ( -3.749999999999988454, -9.053300858899127945, 23.76562499999999645 ) ) ;
#39162 = ORIENTED_EDGE ( 'NONE', *, *, #51673, .F. ) ;
#39163 = EDGE_LOOP ( 'NONE', ( #16444, #62453, #25907, #49783 ) ) ;
#39164 =( BOUNDED_CURVE ( )  B_SPLINE_CURVE ( 3, ( #87572, #19093, #53308, #88904 ),
 .UNSPECIFIED., .F., .F. ) 
 B_SPLINE_CURVE_WITH_KNOTS ( ( 4, 4 ),
 ( 1.570796326794895892, 1.579613961134529010 ),
 .UNSPECIFIED. ) 
 CURVE ( )  GEOMETRIC_REPRESENTATION_ITEM ( )  RATIONAL_B_SPLINE_CURVE ( ( 1.000000000000000000, 0.9999935207875494392, 0.9999935207875494392, 1.000000000000000000 ) ) 
 REPRESENTATION_ITEM ( '' )  );
#39165 = ADVANCED_FACE ( 'NONE', ( #82566 ), #83449, .F. ) ;
#39166 = CARTESIAN_POINT ( 'NONE',  ( 5.076923076923075762, -10.67929555188718282, 33.92786785259544047 ) ) ;
#39167 = CARTESIAN_POINT ( 'NONE',  ( -17.93474486048716088, -3.643525952247861355, 33.31231777344670064 ) ) ;
#39168 = CYLINDRICAL_SURFACE ( 'NONE', #38760, 0.2500000000000009437 ) ;
#39169 = CARTESIAN_POINT ( 'NONE',  ( -0.3307000435256987059, -7.277220443632451463, 34.74524770363009196 ) ) ;
#39170 = FACE_OUTER_BOUND ( 'NONE', #40728, .T. ) ;
#39171 = CARTESIAN_POINT ( 'NONE',  ( -3.749999999999988454, -9.053300858899127945, 22.51562500000000000 ) ) ;
#39172 = CARTESIAN_POINT ( 'NONE',  ( -12.59222906464877134, -3.957541250942358424, 33.62499894934981626 ) ) ;
#39173 = CARTESIAN_POINT ( 'NONE',  ( 1.634560902963528184, -5.057305518903949526, 34.11320923018887896 ) ) ;
#39174 = CARTESIAN_POINT ( 'NONE',  ( 16.94677586748485609, -12.27039167877662251, 31.24851455888617835 ) ) ;
#39175 = CARTESIAN_POINT ( 'NONE',  ( -5.999999999999683808, -2.255955759149395501, 30.00000000000324363 ) ) ;
#39176 = CARTESIAN_POINT ( 'NONE',  ( -10.61538461538461320, -4.945431358278436385, 36.03766855953609394 ) ) ;
#39177 = CARTESIAN_POINT ( 'NONE',  ( 15.00728430620489995, -12.47654668319379567, 31.42292124445336654 ) ) ;
#39178 = AXIS2_PLACEMENT_3D ( 'NONE', #23944, #30711, #31150 ) ;
#39179 = CARTESIAN_POINT ( 'NONE',  ( -2.980769230767794653, -7.500000000000155431, 34.75000000000007105 ) ) ;
#39180 = CARTESIAN_POINT ( 'NONE',  ( -4.153846153846152411, -2.708943851104267164, 35.45975837776705220 ) ) ;
#39181 = CYLINDRICAL_SURFACE ( 'NONE', #68073, 0.2499999999999986955 ) ;
#39182 = LINE ( 'NONE', #88272, #18283 ) ;
#39183 = VECTOR ( 'NONE', #54021, 1000.000000000000227 ) ;
#39184 = ORIENTED_EDGE ( 'NONE', *, *, #26252, .F. ) ;
#39185 = CARTESIAN_POINT ( 'NONE',  ( 8.835298102580845025, -4.661471528628508665, 34.16647553114624003 ) ) ;
#39186 = CARTESIAN_POINT ( 'NONE',  ( 18.24994540937804643, -4.932303261841487263, 34.32971442181322885 ) ) ;
#39187 = CARTESIAN_POINT ( 'NONE',  ( 13.25392478150507891, -6.369640206132551441, 34.87707690430378449 ) ) ;
#39188 = CARTESIAN_POINT ( 'NONE',  ( 2.775308065498755195, -6.422011778438505125, 18.39249329374151642 ) ) ;
#39189 = CARTESIAN_POINT ( 'NONE',  ( 13.51514108637895006, -5.195472089885680766, 34.18748526763464923 ) ) ;
#39190 = CARTESIAN_POINT ( 'NONE',  ( 14.05766908347085042, -4.931416488878822335, 34.32920672191015399 ) ) ;
#39192 = ORIENTED_EDGE ( 'NONE', *, *, #39667, .T. ) ;
#39191 = CARTESIAN_POINT ( 'NONE',  ( -0.3310127597748989681, -2.619367082507848998, 30.83698974864644171 ) ) ;
#39193 = CARTESIAN_POINT ( 'NONE',  ( -1.944543648262992530, -9.444543648263016067, 18.68750000000000000 ) ) ;
#39194 = CARTESIAN_POINT ( 'NONE',  ( 18.00000000000000000, -3.513871655860378418, 32.76840700105978499 ) ) ;
#39195 = ORIENTED_EDGE ( 'NONE', *, *, #52394, .T. ) ;
#39196 = CYLINDRICAL_SURFACE ( 'NONE', #65848, 0.2499999999999998890 ) ;
#39197 = ORIENTED_EDGE ( 'NONE', *, *, #23278, .F. ) ;
#39198 = CARTESIAN_POINT ( 'NONE',  ( -18.22348494372394967, -11.89387501736623243, 32.13663884655804992 ) ) ;
#39199 = CARTESIAN_POINT ( 'NONE',  ( 13.16113044089144068, -10.11188796281391511, 34.01382737946119050 ) ) ;
#39200 = CARTESIAN_POINT ( 'NONE',  ( -0.2114840416250086119, -6.523592122091592671, 34.90882529074906415 ) ) ;
#39201 = ORIENTED_EDGE ( 'NONE', *, *, #21835, .F. ) ;
#39202 = LINE ( 'NONE', #38303, #1926 ) ;
#39203 = ORIENTED_EDGE ( 'NONE', *, *, #20291, .F. ) ;
#39204 = DIRECTION ( 'NONE',  ( 1.000000000000000000, -1.799314243699348838E-16, 0.000000000000000000 ) ) ;
#39205 = CIRCLE ( 'NONE', #72292, 0.2500000000000002220 ) ;
#39206 = ORIENTED_EDGE ( 'NONE', *, *, #85141, .T. ) ;
#39208 = LINE ( 'NONE', #25237, #73096 ) ;
#39207 = VECTOR ( 'NONE', #48174, 1000.000000000000227 ) ;
#39209 = CARTESIAN_POINT ( 'NONE',  ( 12.68454981315131214, -12.15243808032445827, 31.58219941686247978 ) ) ;
#39210 = CARTESIAN_POINT ( 'NONE',  ( -10.48459280755982803, -6.413143153341454017, 34.63066358083362672 ) ) ;
#39211 = CARTESIAN_POINT ( 'NONE',  ( 2.307692307692309264, -13.57706302396349152, 30.56769352161908060 ) ) ;
#39212 = CARTESIAN_POINT ( 'NONE',  ( 6.923076923076924238, -8.164416787775445883, 34.95778746994557906 ) ) ;
#39213 = CARTESIAN_POINT ( 'NONE',  ( 11.40831432902331954, -11.93770438780619259, 32.05411857736982029 ) ) ;
#39214 = EDGE_CURVE ( 'NONE', #60261, #58859, #54115, .T. ) ;
#39215 = CARTESIAN_POINT ( 'NONE',  ( -16.15384615384627409, -6.835583212225970762, 34.95778746994575670 ) ) ;
#39216 = ORIENTED_EDGE ( 'NONE', *, *, #7224, .T. ) ;
#39217 = EDGE_LOOP ( 'NONE', ( #66352, #50141 ) ) ;
#39218 = ORIENTED_EDGE ( 'NONE', *, *, #86541, .T. ) ;
#39220 = VERTEX_POINT ( 'NONE', #14530 ) ;
#39219 = CARTESIAN_POINT ( 'NONE',  ( 3.480823542407545546, -3.627508038966689163, 32.91356715214248396 ) ) ;
#39221 = EDGE_CURVE ( 'NONE', #68176, #32696, #70364, .T. ) ;
#39222 = LINE ( 'NONE', #17618, #42096 ) ;
#39223 = CARTESIAN_POINT ( 'NONE',  ( 9.561617089197383734, -5.496505350115501010, 34.60290016733514307 ) ) ;
#39225 = VERTEX_POINT ( 'NONE', #84335 ) ;
#39224 = EDGE_CURVE ( 'NONE', #17051, #81438, #72988, .T. ) ;
#39226 = CARTESIAN_POINT ( 'NONE',  ( -12.39628332202562433, -11.67786785259547777, 32.92929555188713664 ) ) ;
#39227 = ORIENTED_EDGE ( 'NONE', *, *, #51825, .F. ) ;
#39228 = DIRECTION ( 'NONE',  ( 0.000000000000000000, 0.000000000000000000, -1.000000000000000000 ) ) ;
#39229 = EDGE_LOOP ( 'NONE', ( #18293, #52337, #29693, #70304 ) ) ;
#39230 = VECTOR ( 'NONE', #13342, 999.9999999999998863 ) ;
#39231 = CARTESIAN_POINT ( 'NONE',  ( -7.846153846153844924, -9.584722331328613620, 36.20867863119891439 ) ) ;
#39232 = ADVANCED_FACE ( 'NONE', ( #7339 ), #41559, .F. ) ;
#39233 = CARTESIAN_POINT ( 'NONE',  ( -11.53846153846165912, -10.90142922262034020, 33.41473453929536674 ) ) ;
#39234 = CARTESIAN_POINT ( 'NONE',  ( -6.000000000000121680, -2.657715359629662988, 31.77849191805970364 ) ) ;
#39235 = B_SPLINE_CURVE_WITH_KNOTS ( 'NONE', 3,
 ( #21874, #48899, #82255, #34056, #83140, #14677, #70507, #41705, #69176, #42160 ),
 .UNSPECIFIED., .F., .F.,
 ( 4, 2, 2, 2, 4 ),
 ( 0.0007817359430256313069, 0.0009771253907249971907, 0.001172514838424363291, 0.001367904286123729392, 0.001563293733823095276 ),
 .UNSPECIFIED. ) ;
#39236 = FACE_BOUND ( 'NONE', #68248, .T. ) ;
#39237 = CARTESIAN_POINT ( 'NONE',  ( -16.15384615384615330, -9.905515769479276145, 34.41647553114623292 ) ) ;
#39238 = FACE_OUTER_BOUND ( 'NONE', #77178, .T. ) ;
#39239 = B_SPLINE_CURVE_WITH_KNOTS ( 'NONE', 3,
 ( #43910, #23197, #57867, #10127, #29088, #2468, #22311, #36712, #44336, #3364 ),
 .UNSPECIFIED., .F., .F.,
 ( 4, 2, 2, 2, 4 ),
 ( 0.0007817359430256322827, 0.0009771253907249989254, 0.001172514838424365676, 0.001367904286123732428, 0.001563293733823098962 ),
 .UNSPECIFIED. ) ;
#39240 = EDGE_CURVE ( 'NONE', #48079, #79735, #8978, .T. ) ;
#39241 = FACE_OUTER_BOUND ( 'NONE', #25163, .T. ) ;
#39242 = CARTESIAN_POINT ( 'NONE',  ( 5.076923076923075762, -3.322132147404559976, 32.92929555188717927 ) ) ;
#39243 = LINE ( 'NONE', #87896, #63904 ) ;
#39244 = CARTESIAN_POINT ( 'NONE',  ( -5.076923076923075762, -2.721908614388771852, 31.22303859784724978 ) ) ;
#39245 = ORIENTED_EDGE ( 'NONE', *, *, #65346, .T. ) ;
#39246 = DIRECTION ( 'NONE',  ( -0.000000000000000000, -0.8660254037844399289, -0.4999999999999980016 ) ) ;
#39247 = EDGE_LOOP ( 'NONE', ( #77417, #69117, #66823, #28147 ) ) ;
#39248 = ORIENTED_EDGE ( 'NONE', *, *, #78781, .F. ) ;
#39250 = CARTESIAN_POINT ( 'NONE',  ( 2.557746619330623528, -10.66356715214248396, 33.62249196103329751 ) ) ;
#39249 = CARTESIAN_POINT ( 'NONE',  ( -0.7115616988314267255, -9.271318131107980420, 34.42618302367067429 ) ) ;
#39251 = CARTESIAN_POINT ( 'NONE',  ( 3.230769230769108269, -3.643525952248796163, 33.31231777344771672 ) ) ;
#39252 = CARTESIAN_POINT ( 'NONE',  ( 4.153846153846154188, -2.292212530054420494, 30.41441678777542634 ) ) ;
#39253 = DIRECTION ( 'NONE',  ( 1.000000000000000000, 0.000000000000000000, 0.000000000000000000 ) ) ;
#39254 = CARTESIAN_POINT ( 'NONE',  ( -13.16183584334697443, -2.847695495035523550, 31.58253572463339154 ) ) ;
#39255 = ORIENTED_EDGE ( 'NONE', *, *, #47770, .F. ) ;
#39256 = EDGE_CURVE ( 'NONE', #6548, #27134, #36146, .T. ) ;
#39257 = DIRECTION ( 'NONE',  ( 0.000000000000000000, 0.9848077530122072432, 0.1736481776669354937 ) ) ;
#39258 = CARTESIAN_POINT ( 'NONE',  ( -5.076923076923197442, -2.625532179533778709, 30.86335684631627174 ) ) ;
#39259 = CARTESIAN_POINT ( 'NONE',  ( 10.48523740594639619, -3.285722584762969856, 32.44110544564090759 ) ) ;
#39260 = ADVANCED_FACE ( 'NONE', ( #15427 ), #63597, .F. ) ;
#39261 = CARTESIAN_POINT ( 'NONE',  ( -3.453696189676078276, -12.64616026154729411, 30.79003144601913533 ) ) ;
#39262 = VERTEX_POINT ( 'NONE', #83893 ) ;
#39263 = ORIENTED_EDGE ( 'NONE', *, *, #59844, .T. ) ;
#39264 = AXIS2_PLACEMENT_3D ( 'NONE', #40361, #41682, #60611 ) ;
#39265 = APPLICATION_PROTOCOL_DEFINITION ( 'draft international standard', 'automotive_design', 1998, #56140 ) ;
#39266 = EDGE_LOOP ( 'NONE', ( #58910, #67888, #32195, #21999 ) ) ;
#39267 = CIRCLE ( 'NONE', #43547, 0.2500000000000002220 ) ;
#39268 = ADVANCED_FACE ( 'NONE', ( #29389 ), #22609, .F. ) ;
#39269 = CARTESIAN_POINT ( 'NONE',  ( 18.25005441991345734, -12.65882529074907126, 30.72640787790838601 ) ) ;
#39271 = EDGE_CURVE ( 'NONE', #24035, #44409, #82056, .T. ) ;
#39270 = CARTESIAN_POINT ( 'NONE',  ( -6.130475185075718869, -7.276987145209185215, 34.99546412871779211 ) ) ;
#39272 = EDGE_LOOP ( 'NONE', ( #57474, #22172 ) ) ;
#39273 = CARTESIAN_POINT ( 'NONE',  ( -15.23076923076922995, -12.62096338111211580, 30.90682066428153263 ) ) ;
#39274 = DIRECTION ( 'NONE',  ( 0.000000000000000000, 1.000000000000000000, 0.000000000000000000 ) ) ;
#39275 = CARTESIAN_POINT ( 'NONE',  ( -8.769230769230890843, -6.879047030192662504, 34.71129190930017927 ) ) ;
#39276 = CARTESIAN_POINT ( 'NONE',  ( -2.438383774359864198, -8.147922237126337563, 34.70805685702651999 ) ) ;
#39277 = CARTESIAN_POINT ( 'NONE',  ( 6.000000000000001776, -2.499999999999998668, 29.75000000000001421 ) ) ;
#39278 = ORIENTED_EDGE ( 'NONE', *, *, #1517, .T. ) ;
#39280 = ORIENTED_EDGE ( 'NONE', *, *, #26133, .T. ) ;
#39279 = CARTESIAN_POINT ( 'NONE',  ( -15.00798956179116317, -2.353885683473779800, 30.79025554430704403 ) ) ;
#39281 = CARTESIAN_POINT ( 'NONE',  ( -24.00000000000000000, -9.499999999999982236, 27.74999999999999645 ) ) ;
#39282 = CARTESIAN_POINT ( 'NONE',  ( 0.000000000000000000, -2.085786437626902856, 29.25000000000000000 ) ) ;
#39283 = CARTESIAN_POINT ( 'NONE',  ( -13.60810032833933469, -5.113361153441934093, 34.14387501736622710 ) ) ;
#39284 = CARTESIAN_POINT ( 'NONE',  ( 10.48469401227431419, -12.35290016733513951, 31.75349464988449455 ) ) ;
#39285 = CARTESIAN_POINT ( 'NONE',  ( -8.703163435880695076, -8.164416787775445883, 34.95778746994558617 ) ) ;
#39286 =( LENGTH_UNIT ( ) NAMED_UNIT ( * ) SI_UNIT ( .MILLI., .METRE. ) );
#39287 = B_SPLINE_CURVE_WITH_KNOTS ( 'NONE', 3,
 ( #26342, #25900, #19143, #67335, #18708, #11053, #59233, #60119, #53807, #88078 ),
 .UNSPECIFIED., .F., .F.,
 ( 4, 2, 2, 2, 4 ),
 ( 0.000000000000000000, 0.0001954339857564093175, 0.0003908679715128186350, 0.0005863019572692279796, 0.0007817359430256372700 ),
 .UNSPECIFIED. ) ;
#39288 = DIRECTION ( 'NONE',  ( -0.000000000000000000, -0.5000000000000009992, -0.8660254037844380415 ) ) ;
#39289 = CARTESIAN_POINT ( 'NONE',  ( 1.901340078031373171, -9.487747218494639867, 14.87686829374151465 ) ) ;
#39290 = ORIENTED_EDGE ( 'NONE', *, *, #70057, .F. ) ;
#39291 = CARTESIAN_POINT ( 'NONE',  ( -8.769230769230768274, -5.471508081941601098, 34.59228464037088457 ) ) ;
#39292 = CARTESIAN_POINT ( 'NONE',  ( -9.626239341305252495, -8.120952969808772792, 34.71129190929999453 ) ) ;
#39293 = CARTESIAN_POINT ( 'NONE',  ( 23.49999999999998934, 1.250000000000002220, 32.75000000000000000 ) ) ;
#39294 = ORIENTED_EDGE ( 'NONE', *, *, #71828, .T. ) ;
#39295 = ORIENTED_EDGE ( 'NONE', *, *, #46698, .F. ) ;
#39296 = FACE_OUTER_BOUND ( 'NONE', #33000, .T. ) ;
#39297 = CARTESIAN_POINT ( 'NONE',  ( 11.31553457955468645, -12.64616026154729411, 30.79003144601914244 ) ) ;
#39298 = CARTESIAN_POINT ( 'NONE',  ( -0.6844654204453112234, -9.172386477786396597, 34.72672124145550043 ) ) ;
#39299 = CARTESIAN_POINT ( 'NONE',  ( -7.146561866800870355, -5.912607949931405038, 34.49155766932282319 ) ) ;
#39300 = AXIS2_PLACEMENT_3D ( 'NONE', #72627, #59558, #18586 ) ;
#39301 = CARTESIAN_POINT ( 'NONE',  ( 20.00000000000000000, -4.000000000000000000, 29.75000000000000355 ) ) ;
#39302 = VECTOR ( 'NONE', #24795, 1000.000000000000000 ) ;
#39303 = CARTESIAN_POINT ( 'NONE',  ( -6.989160334032803235, -11.69971097300155272, 32.46337939537587403 ) ) ;
#39304 = ORIENTED_EDGE ( 'NONE', *, *, #29519, .F. ) ;
#39305 = EDGE_CURVE ( 'NONE', #64026, #47786, #63149, .T. ) ;
#39306 = CARTESIAN_POINT ( 'NONE',  ( -3.007756386675835447, -12.64618726649961289, 30.78989965857442712 ) ) ;
#39307 = DIRECTION ( 'NONE',  ( -0.000000000000000000, 0.9848077530122086864, -0.1736481776669273891 ) ) ;
#39308 = CARTESIAN_POINT ( 'NONE',  ( 4.088576153289833925, -8.656820664281497102, 34.87096338111211935 ) ) ;
#39309 = ORIENTED_EDGE ( 'NONE', *, *, #83753, .F. ) ;
#39310 = CARTESIAN_POINT ( 'NONE',  ( 12.71148397988660328, -3.712312575010499494, 33.01462480002815170 ) ) ;
#39311 = ORIENTED_EDGE ( 'NONE', *, *, #77988, .T. ) ;
#39312 = CARTESIAN_POINT ( 'NONE',  ( 13.44987095589141468, -3.835265460703683349, 33.15142922261929925 ) ) ;
#39313 = CYLINDRICAL_SURFACE ( 'NONE', #2352, 0.2499999999999993616 ) ;
#39314 = CARTESIAN_POINT ( 'NONE',  ( 15.48071464014727283, -4.932303261841489928, 34.32971442181322885 ) ) ;
#39315 = ORIENTED_EDGE ( 'NONE', *, *, #33339, .T. ) ;
#39316 = CARTESIAN_POINT ( 'NONE',  ( -13.16183571563731647, -4.989023458446560255, 34.36081565061822118 ) ) ;
#39318 = ADVANCED_FACE ( 'NONE', ( #9537 ), #31134, .F. ) ;
#39317 = CYLINDRICAL_SURFACE ( 'NONE', #53601, 0.2500000000000002220 ) ;
#39319 = CYLINDRICAL_SURFACE ( 'NONE', #33662, 0.2499999999999995559 ) ;
#39320 = EDGE_CURVE ( 'NONE', #43306, #36328, #15368, .T. ) ;
#39321 = B_SPLINE_CURVE_WITH_KNOTS ( 'NONE', 3,
 ( #35119, #22491, #30135, #42778, #57161, #1776, #2208, #63908, #49076, #29266 ),
 .UNSPECIFIED., .F., .F.,
 ( 4, 2, 2, 2, 4 ),
 ( 0.0007817359430256322827, 0.0009771253907249989254, 0.001172514838424365676, 0.001367904286123732428, 0.001563293733823099179 ),
 .UNSPECIFIED. ) ;
#39322 = CARTESIAN_POINT ( 'NONE',  ( -6.066082379360133281, -5.471508081941601986, 34.59228464037088457 ) ) ;
#39323 = CARTESIAN_POINT ( 'NONE',  ( -4.853910232829682592, -10.77377354290276301, 33.85451476688484718 ) ) ;
#39324 = VECTOR ( 'NONE', #44272, 1000.000000000000000 ) ;
#39325 = ORIENTED_EDGE ( 'NONE', *, *, #89058, .T. ) ;
#39326 = CARTESIAN_POINT ( 'NONE',  ( -4.153846153846274980, -5.941354392335915335, 34.76329471203413846 ) ) ;
#39327 = EDGE_LOOP ( 'NONE', ( #41921, #85826 ) ) ;
#39328 = CARTESIAN_POINT ( 'NONE',  ( -15.16551409125639260, -6.835583212224610072, 34.95778746994559327 ) ) ;
#39329 = CIRCLE ( 'NONE', #78142, 4.000000000000000000 ) ;
#39330 = CYLINDRICAL_SURFACE ( 'NONE', #31929, 0.2499999999999986955 ) ;
#39331 = VECTOR ( 'NONE', #38554, 1000.000000000000227 ) ;
#39333 = ADVANCED_FACE ( 'NONE', ( #23059 ), #52298, .F. ) ;
#39332 = DIRECTION ( 'NONE',  ( -0.000000000000000000, 0.8660254037844399289, -0.4999999999999980016 ) ) ;
#39334 = CARTESIAN_POINT ( 'NONE',  ( 5.076923076923075762, -11.69971097300155272, 32.46337939537588113 ) ) ;
#39335 = CARTESIAN_POINT ( 'NONE',  ( -14.05763799605399278, -12.17597550085003633, 31.52189283813461884 ) ) ;
#39336 = CARTESIAN_POINT ( 'NONE',  ( 4.946362485181154511, -2.504760397472873823, 29.97295953869789997 ) ) ;
#39337 = CARTESIAN_POINT ( 'NONE',  ( 9.627037246346917598, -8.613356846314824011, 34.62446782046655613 ) ) ;
#39338 = EDGE_CURVE ( 'NONE', #51322, #23856, #58607, .T. ) ;
#39339 = EDGE_LOOP ( 'NONE', ( #73608, #77571, #61309, #68236 ) ) ;
#39340 = ORIENTED_EDGE ( 'NONE', *, *, #48036, .T. ) ;
#39341 = ORIENTED_EDGE ( 'NONE', *, *, #58025, .T. ) ;
#39342 = ORIENTED_EDGE ( 'NONE', *, *, #69703, .F. ) ;
#39343 = EDGE_LOOP ( 'NONE', ( #39373, #78433 ) ) ;
#39344 = DIRECTION ( 'NONE',  ( 0.000000000000000000, 0.000000000000000000, 1.000000000000000000 ) ) ;
#39345 = EDGE_CURVE ( 'NONE', #75643, #24805, #23931, .T. ) ;
#39346 = CARTESIAN_POINT ( 'NONE',  ( -11.53846153846165912, -9.442884908241554243, 34.35708131394783038 ) ) ;
#39347 = CARTESIAN_POINT ( 'NONE',  ( 15.23076923076923173, -4.786620604624113540, 33.94971097300155094 ) ) ;
#39348 = CARTESIAN_POINT ( 'NONE',  ( 4.153846153846154188, -3.050289026998446396, 32.03036669348365706 ) ) ;
#39349 = CARTESIAN_POINT ( 'NONE',  ( 0.5267940328144847806, -5.219633306516380244, 34.19971097300157936 ) ) ;
#39350 = DIRECTION ( 'NONE',  ( 0.000000000000000000, 0.6427876096865368094, 0.7660444431189802339 ) ) ;
#39351 = CARTESIAN_POINT ( 'NONE',  ( 17.93472955403921887, -2.625532179533444754, 30.86335684631481513 ) ) ;
#39352 = CARTESIAN_POINT ( 'NONE',  ( 0.2115152242454947096, -3.202444869320336451, 32.30641848906366675 ) ) ;
#39353 = ORIENTED_EDGE ( 'NONE', *, *, #33414, .F. ) ;
#39354 = ORIENTED_EDGE ( 'NONE', *, *, #39881, .F. ) ;
#39355 = ORIENTED_EDGE ( 'NONE', *, *, #72651, .F. ) ;
#39357 = ORIENTED_EDGE ( 'NONE', *, *, #40772, .T. ) ;
#39356 = CARTESIAN_POINT ( 'NONE',  ( 24.00000000000000000, -9.499999999999982236, 27.25000000000000000 ) ) ;
#39358 = AXIS2_PLACEMENT_3D ( 'NONE', #44145, #57678, #37402 ) ;
#39360 = CARTESIAN_POINT ( 'NONE',  ( 10.48469314871706182, -8.999036380462717588, 34.52022231692819076 ) ) ;
#39359 = CARTESIAN_POINT ( 'NONE',  ( -16.02305434602136103, -6.413143153341451352, 34.63066358083362672 ) ) ;
#39361 = CARTESIAN_POINT ( 'NONE',  ( -0.3310130233048166892, -2.372941743896879618, 30.88044141588254377 ) ) ;
#39362 = CARTESIAN_POINT ( 'NONE',  ( 3.230769230769231726, -5.557115091759785130, 34.35708131394839171 ) ) ;
#39363 = FACE_BOUND ( 'NONE', #36878, .T. ) ;
#39364 = VERTEX_POINT ( 'NONE', #85651 ) ;
#39365 = ADVANCED_FACE ( 'NONE', ( #37003 ), #78438, .F. ) ;
#39366 = ORIENTED_EDGE ( 'NONE', *, *, #20674, .F. ) ;
#39367 = LINE ( 'NONE', #80800, #21249 ) ;
#39369 = EDGE_CURVE ( 'NONE', #59454, #64208, #24826, .T. ) ;
#39368 = ORIENTED_EDGE ( 'NONE', *, *, #65771, .F. ) ;
#39370 = FACE_BOUND ( 'NONE', #17870, .T. ) ;
#39371 = CARTESIAN_POINT ( 'NONE',  ( -9.442253272394237840, -2.318338780012835443, 30.59689888758630261 ) ) ;
#39372 = CARTESIAN_POINT ( 'NONE',  ( 18.13052570176355971, -5.195472089885680766, 34.18748526763464923 ) ) ;
#39373 = ORIENTED_EDGE ( 'NONE', *, *, #75939, .F. ) ;
#39374 = CARTESIAN_POINT ( 'NONE',  ( 2.057669070399343880, -8.432397168068783699, 34.66272746175022945 ) ) ;
#39376 = ADVANCED_FACE ( 'NONE', ( #9981 ), #79788, .F. ) ;
#39375 = CARTESIAN_POINT ( 'NONE',  ( -1.450697763975519194, -8.164416787775445883, 34.95778746994557906 ) ) ;
#39377 = CARTESIAN_POINT ( 'NONE',  ( -18.06608237936013239, -3.937682226553330445, 33.60647404775217240 ) ) ;
#39378 = ORIENTED_EDGE ( 'NONE', *, *, #29759, .F. ) ;
#39379 = CARTESIAN_POINT ( 'NONE',  ( -7.715628407920200438, -8.630441415882550871, 34.87705825610312615 ) ) ;
#39380 = CARTESIAN_POINT ( 'NONE',  ( 7.053602361310569613, -5.915461855592777596, 34.75538340440931506 ) ) ;
#39381 = DIRECTION ( 'NONE',  ( -0.000000000000000000, 0.5000000000000011102, -0.8660254037844381525 ) ) ;
#39382 = ORIENTED_EDGE ( 'NONE', *, *, #60698, .T. ) ;
#39383 = CARTESIAN_POINT ( 'NONE',  ( 2.372947447205147942, -12.51329471203373700, 31.30864560766537963 ) ) ;
#39384 = CARTESIAN_POINT ( 'NONE',  ( -17.07692307692307665, -11.69971097300155272, 32.46337939537588113 ) ) ;
#39385 = VERTEX_POINT ( 'NONE', #86100 ) ;
#39386 = CARTESIAN_POINT ( 'NONE',  ( 3.480714640147274164, -6.653508905675590945, 34.93172785388651391 ) ) ;
#39387 = CARTESIAN_POINT ( 'NONE',  ( 14.37294787896833270, -8.613356846314928816, 34.62446782046653482 ) ) ;
#39388 = CARTESIAN_POINT ( 'NONE',  ( -14.55766905174089665, -2.544273027872575366, 31.48422191005632342 ) ) ;
#39389 = CARTESIAN_POINT ( 'NONE',  ( -4.153846153846152411, -11.33034616979429110, 35.88435417666054406 ) ) ;
#39390 = DIRECTION ( 'NONE',  ( 0.000000000000000000, 0.9848077530122072432, -0.1736481776669354937 ) ) ;
#39391 = CARTESIAN_POINT ( 'NONE',  ( 17.07692307692307665, -4.661471528628507777, 34.16647553114623292 ) ) ;
#39393 = CARTESIAN_POINT ( 'NONE',  ( 20.99999999999999645, -2.249999999999999556, 27.25000000000000000 ) ) ;
#39392 = CARTESIAN_POINT ( 'NONE',  ( -8.769230769230768274, -4.098570777380720287, 33.41473453929634729 ) ) ;
#39394 = B_SPLINE_CURVE_WITH_KNOTS ( 'NONE', 3,
 ( #42212, #75984, #76432, #48952, #6642, #14283, #69231, #7533, #55706, #14736 ),
 .UNSPECIFIED., .F., .F.,
 ( 4, 2, 2, 2, 4 ),
 ( 0.000000000000000000, 0.0001954339857564071762, 0.0003908679715128143524, 0.0005863019572692215828, 0.0007817359430256287049 ),
 .UNSPECIFIED. ) ;
#39395 = LINE ( 'NONE', #66854, #7990 ) ;
#39396 = DIRECTION ( 'NONE',  ( 0.000000000000000000, 0.4999999999999985567, 0.8660254037844395958 ) ) ;
#39397 = EDGE_CURVE ( 'NONE', #80197, #16713, #1487, .T. ) ;
#39398 = CARTESIAN_POINT ( 'NONE',  ( -1.139087296526025916, -4.750000000000006217, 16.57812500000000000 ) ) ;
#39399 = B_SPLINE_CURVE_WITH_KNOTS ( 'NONE', 3,
 ( #15974, #8331, #7884, #35349, #84881, #36684, #64134, #62801, #1123, #70018 ),
 .UNSPECIFIED., .F., .F.,
 ( 4, 2, 2, 2, 4 ),
 ( 0.0007817359430256318490, 0.0009771253907249984917, 0.001172514838424365026, 0.001367904286123731560, 0.001563293733823098311 ),
 .UNSPECIFIED. ) ;
#39400 = EDGE_LOOP ( 'NONE', ( #6900, #81018 ) ) ;
#39401 = VECTOR ( 'NONE', #66556, 1000.000000000000000 ) ;
#39402 = CARTESIAN_POINT ( 'NONE',  ( 5.011653076366756387, -6.835583212224499938, 34.95778746994557906 ) ) ;
#39403 = ORIENTED_EDGE ( 'NONE', *, *, #13149, .T. ) ;
#39404 = EDGE_CURVE ( 'NONE', #69679, #40761, #17608, .T. ) ;
#39405 = ORIENTED_EDGE ( 'NONE', *, *, #9784, .T. ) ;
#39406 = DIRECTION ( 'NONE',  ( -0.000000000000000000, -0.5000000000000009992, -0.8660254037844380415 ) ) ;
#39407 = ORIENTED_EDGE ( 'NONE', *, *, #16155, .F. ) ;
#39408 = CARTESIAN_POINT ( 'NONE',  ( 18.25000000000143530, -7.500000000000155431, 34.75000000000007105 ) ) ;
#39409 = CARTESIAN_POINT ( 'NONE',  ( 1.944543648263018731, -9.444543648262994751, 15.87500000000000000 ) ) ;
#39410 = CARTESIAN_POINT ( 'NONE',  ( -17.74994568836168440, -5.728107161865374941, 34.42597550085002922 ) ) ;
#39411 = CARTESIAN_POINT ( 'NONE',  ( 5.869852790561783884, -11.47017969459903952, 32.78971311882034456 ) ) ;
#39412 = CARTESIAN_POINT ( 'NONE',  ( -0.3310127597748990791, -6.001044277235011215, 34.52024696741798948 ) ) ;
#39413 = FACE_OUTER_BOUND ( 'NONE', #38210, .T. ) ;
#39414 = CARTESIAN_POINT ( 'NONE',  ( -4.946397638689434828, -2.647132371071621471, 31.75357179365173010 ) ) ;
#39415 = CARTESIAN_POINT ( 'NONE',  ( -7.846153846153844924, -5.557115091759785130, 34.35708131394839171 ) ) ;
#39416 = CARTESIAN_POINT ( 'NONE',  ( -7.715628144390278997, -12.27024696741798770, 31.24895572276497546 ) ) ;
#39417 = CARTESIAN_POINT ( 'NONE',  ( -2.651650429449565305, -4.848349570550461785, 20.25000000000000000 ) ) ;
#39418 = EDGE_CURVE ( 'NONE', #80757, #19260, #41205, .T. ) ;
#39419 = CARTESIAN_POINT ( 'NONE',  ( 1.576923076923076428, -4.000000000000000000, 29.75000000000000355 ) ) ;
#39420 = CARTESIAN_POINT ( 'NONE',  ( -4.283994123577847368, -12.15440758774515473, 32.17923288041532004 ) ) ;
#39421 = CARTESIAN_POINT ( 'NONE',  ( 6.000000000000001776, -8.810774026931790459, 35.74407628777942847 ) ) ;
#39422 = EDGE_CURVE ( 'NONE', #27582, #62474, #27057, .T. ) ;
#39423 = EDGE_CURVE ( 'NONE', #14877, #37595, #60836, .T. ) ;
#39424 = ORIENTED_EDGE ( 'NONE', *, *, #53715, .T. ) ;
#39425 = ORIENTED_EDGE ( 'NONE', *, *, #40882, .T. ) ;
#39426 = CARTESIAN_POINT ( 'NONE',  ( -9.561515884482908234, -3.530189275343204702, 32.79018710029569661 ) ) ;
#39427 = CARTESIAN_POINT ( 'NONE',  ( 7.780883400193070898, -11.48612834413959582, 32.76840700105983473 ) ) ;
#39428 = LINE ( 'NONE', #65539, #49811 ) ;
#39429 = CARTESIAN_POINT ( 'NONE',  ( 15.48076923076917133, -7.565270000091922853, 34.99999999999999289 ) ) ;
#39430 = CARTESIAN_POINT ( 'NONE',  ( -10.61538461538461320, -11.11383981884818262, 36.00935417666054406 ) ) ;
#39431 = CARTESIAN_POINT ( 'NONE',  ( -9.692307692307691624, -6.343179335718451384, 34.87096338111211935 ) ) ;
#39432 = EDGE_CURVE ( 'NONE', #19898, #31080, #16476, .T. ) ;
#39433 = AXIS2_PLACEMENT_3D ( 'NONE', #24827, #52299, #73026 ) ;
#39434 = EDGE_CURVE ( 'NONE', #40036, #18264, #85235, .T. ) ;
#39435 = ORIENTED_EDGE ( 'NONE', *, *, #22314, .T. ) ;
#39436 = DIRECTION ( 'NONE',  ( 1.000000000000000000, 0.000000000000000000, 0.000000000000000000 ) ) ;
#39437 = ORIENTED_EDGE ( 'NONE', *, *, #38663, .F. ) ;
#39438 = ORIENTED_EDGE ( 'NONE', *, *, #30037, .F. ) ;
#39439 = CARTESIAN_POINT ( 'NONE',  ( 5.142178648199100088, -8.613356846314928816, 34.62446782046653482 ) ) ;
#39440 = CARTESIAN_POINT ( 'NONE',  ( -0.4615384615385840772, -5.094484230521993062, 34.41647553114689373 ) ) ;
#39441 = CARTESIAN_POINT ( 'NONE',  ( 9.758376043310134307, -12.10708131394839704, 31.69288490824020954 ) ) ;
#39442 = CARTESIAN_POINT ( 'NONE',  ( 11.78851595837499211, -2.318338780012835443, 30.59689888758630261 ) ) ;
#39443 = CARTESIAN_POINT ( 'NONE',  ( -13.25382357679060519, -3.062576670634119758, 32.05464942895959979 ) ) ;
#39444 = EDGE_CURVE ( 'NONE', #68800, #9134, #39700, .T. ) ;
#39445 = ORIENTED_EDGE ( 'NONE', *, *, #27771, .F. ) ;
#39446 = ORIENTED_EDGE ( 'NONE', *, *, #48726, .F. ) ;
#39448 = ORIENTED_EDGE ( 'NONE', *, *, #29149, .F. ) ;
#39447 = B_SPLINE_CURVE_WITH_KNOTS ( 'NONE', 3,
 ( #16934, #44385, #71871, #37644, #65106, #4648, #60027, #87531, #48283, #82539 ),
 .UNSPECIFIED., .F., .F.,
 ( 4, 2, 2, 2, 4 ),
 ( 0.0007817359430256372700, 0.0009771253907250054306, 0.001172514838424373483, 0.001367904286123741535, 0.001563293733823109804 ),
 .UNSPECIFIED. ) ;
#39449 = VECTOR ( 'NONE', #12651, 1000.000000000000000 ) ;
#39450 = CARTESIAN_POINT ( 'NONE',  ( 17.20771351789002424, -9.929761469519743144, 34.40412654351204225 ) ) ;
#39451 = CARTESIAN_POINT ( 'NONE',  ( 9.692307692307695177, -2.292212530054420494, 30.41441678777542634 ) ) ;
#39452 = APPLICATION_CONTEXT ( 'automotive_design' ) ;
#39453 = CARTESIAN_POINT ( 'NONE',  ( 8.835298102580843249, -5.471508081941601098, 34.59228464037088457 ) ) ;
#39454 = VECTOR ( 'NONE', #77404, 1000.000000000000227 ) ;
#39455 = VECTOR ( 'NONE', #6080, 1000.000000000000000 ) ;
#39456 = CARTESIAN_POINT ( 'NONE',  ( -8.769230769230892619, -10.33852847137269571, 34.16647553114546554 ) ) ;
#39457 = CARTESIAN_POINT ( 'NONE',  ( 17.93391658904412012, -4.786620604624113540, 33.94971097300155805 ) ) ;
#39458 = CARTESIAN_POINT ( 'NONE',  ( -16.08859058257013430, -2.892918686051626054, 31.69288490824025928 ) ) ;
#39459 = ORIENTED_EDGE ( 'NONE', *, *, #59045, .T. ) ;
#39460 = ORIENTED_EDGE ( 'NONE', *, *, #461, .T. ) ;
#39461 = CARTESIAN_POINT ( 'NONE',  ( 4.946775107191381693, -10.31621877034669588, 34.18098118002070152 ) ) ;
#39463 = ORIENTED_EDGE ( 'NONE', *, *, #10938, .T. ) ;
#39462 = CARTESIAN_POINT ( 'NONE',  ( -4.826923076923076650, -2.249999999999998668, 29.75000000000000355 ) ) ;
#39464 = CARTESIAN_POINT ( 'NONE',  ( 8.096208157792160520, -12.41262288849542017, 30.68299917996395010 ) ) ;
#39465 = DIRECTION ( 'NONE',  ( 0.000000000000000000, 0.000000000000000000, 1.000000000000000000 ) ) ;
#39466 = CARTESIAN_POINT ( 'NONE',  ( -3.750000000000007550, -5.946699141100917352, 16.42187500000000000 ) ) ;
#39467 = VERTEX_POINT ( 'NONE', #32929 ) ;
#39468 = CARTESIAN_POINT ( 'NONE',  ( 7.912221179503920787, -3.937682226553329556, 33.60647404775216529 ) ) ;
#39469 = EDGE_LOOP ( 'NONE', ( #42940, #81270 ) ) ;
#39470 = CARTESIAN_POINT ( 'NONE',  ( 7.846153846153846700, -6.435427911321262684, 35.78748833219616898 ) ) ;
#39471 = CARTESIAN_POINT ( 'NONE',  ( 14.55763771707035126, -12.45601412856602686, 31.48342859153981621 ) ) ;
#39472 = ADVANCED_FACE ( 'NONE', ( #60390 ), #59505, .F. ) ;
#39473 = CARTESIAN_POINT ( 'NONE',  ( -12.46153846153858247, -12.46129190930018460, 30.37095296980731973 ) ) ;
#39475 = CARTESIAN_POINT ( 'NONE',  ( -9.692307692307691624, -8.564572088678739092, 35.78748833219616898 ) ) ;
#39474 = CYLINDRICAL_SURFACE ( 'NONE', #40347, 0.2500000000000002220 ) ;
#39476 = FACE_OUTER_BOUND ( 'NONE', #70319, .T. ) ;
#39477 = ORIENTED_EDGE ( 'NONE', *, *, #7844, .F. ) ;
#39479 = ADVANCED_FACE ( 'NONE', ( #5466 ), #26169, .F. ) ;
#39478 = CARTESIAN_POINT ( 'NONE',  ( 16.15384615384615330, -13.04860791097971706, 34.73218667398347037 ) ) ;
#39480 = DIRECTION ( 'NONE',  ( 1.000000000000000000, 0.000000000000000000, 0.000000000000000000 ) ) ;
#39481 = CYLINDRICAL_SURFACE ( 'NONE', #10611, 2.000000000000001776 ) ;
#39482 = VERTEX_POINT ( 'NONE', #45987 ) ;
#39483 = B_SPLINE_CURVE_WITH_KNOTS ( 'NONE', 3,
 ( #28872, #51642, #500, #77048, #1381, #27970, #62628, #16549, #44016, #37257 ),
 .UNSPECIFIED., .F., .F.,
 ( 4, 2, 2, 2, 4 ),
 ( 0.0007817359430256313069, 0.0009771253907249971907, 0.001172514838424363074, 0.001367904286123728958, 0.001563293733823094842 ),
 .UNSPECIFIED. ) ;
#39484 = VECTOR ( 'NONE', #62722, 1000.000000000000000 ) ;
#39485 = ADVANCED_FACE ( 'NONE', ( #5903 ), #73481, .F. ) ;
#39486 = CARTESIAN_POINT ( 'NONE',  ( -9.692307692307814193, -5.094484230521993062, 34.41647553114689373 ) ) ;
#39487 = CARTESIAN_POINT ( 'NONE',  ( -0.4615384615384611200, -5.471508081941601098, 34.59228464037088457 ) ) ;
#39488 = CARTESIAN_POINT ( 'NONE',  ( 11.31553532094538994, -5.667676309546437530, 34.40238873228292249 ) ) ;
#39489 = CARTESIAN_POINT ( 'NONE',  ( 8.992243613324164997, -10.01129605718032600, 34.36064277460058491 ) ) ;
#39490 = FACE_BOUND ( 'NONE', #56060, .T. ) ;
#39492 = CARTESIAN_POINT ( 'NONE',  ( -3.230769230769229949, -13.53365097954675988, 30.81389545987213552 ) ) ;
#39491 = DIRECTION ( 'NONE',  ( -0.000000000000000000, 0.000000000000000000, 1.000000000000000000 ) ) ;
#39493 = LINE ( 'NONE', #67836, #10885 ) ;
#39495 = CARTESIAN_POINT ( 'NONE',  ( -9.561781990544128362, -10.88167719472716399, 33.43325721877153711 ) ) ;
#39494 = CARTESIAN_POINT ( 'NONE',  ( 1.384615384615264011, -12.70778746994576025, 30.41441678777401236 ) ) ;
#39496 = EDGE_CURVE ( 'NONE', #61245, #19826, #44368, .T. ) ;
#39497 = CARTESIAN_POINT ( 'NONE',  ( 9.019285189144222059, -12.65882529074907126, 30.72640787790839312 ) ) ;
#39498 = CARTESIAN_POINT ( 'NONE',  ( -2.694853999681210865, -4.891553140782108677, 24.99813170625849423 ) ) ;
#39499 = EDGE_LOOP ( 'NONE', ( #73520, #31121, #31244, #58880 ) ) ;
#39500 = PLANE ( 'NONE',  #85013 ) ;
#39501 = ORIENTED_EDGE ( 'NONE', *, *, #6543, .T. ) ;
#39502 = CARTESIAN_POINT ( 'NONE',  ( 1.384615384615693667, -2.506253911140615021, 30.00000000000323297 ) ) ;
#39503 = CARTESIAN_POINT ( 'NONE',  ( -3.931066612577741370, -12.24180327182771855, 31.33663988360758168 ) ) ;
#39504 = DIRECTION ( 'NONE',  ( 1.000000000000000000, 0.000000000000000000, 0.000000000000000000 ) ) ;
#39506 = VERTEX_POINT ( 'NONE', #15319 ) ;
#39505 = CARTESIAN_POINT ( 'NONE',  ( -2.438383774359863754, -11.71456829005830080, 32.44064028649416542 ) ) ;
#39507 = CARTESIAN_POINT ( 'NONE',  ( -9.942307692307691624, -7.500000000000001776, 35.00000000000000000 ) ) ;
#39508 = CARTESIAN_POINT ( 'NONE',  ( -11.60373153901785770, -4.320704448112771878, 33.92786785259540494 ) ) ;
#39509 = CARTESIAN_POINT ( 'NONE',  ( 2.694853999681214862, -10.10844685921789043, 25.62313170625849068 ) ) ;
#39510 = CARTESIAN_POINT ( 'NONE',  ( 15.10062126103754210, -12.15440758774515473, 32.17923288041532004 ) ) ;
#39511 = CARTESIAN_POINT ( 'NONE',  ( 8.545745844666436497, -2.612411019501189369, 31.66733052389439962 ) ) ;
#39512 = CARTESIAN_POINT ( 'NONE',  ( -0.5001402707344744236, -4.795862479435460735, 29.33712102935293231 ) ) ;
#39513 = CARTESIAN_POINT ( 'NONE',  ( 5.299702745901141654, -12.69155399931963046, 30.53255429739158444 ) ) ;
#39514 = CARTESIAN_POINT ( 'NONE',  ( -7.146561866800870355, -4.386631170607603991, 33.66268669641500111 ) ) ;
#39515 = CARTESIAN_POINT ( 'NONE',  ( 1.384615384615386802, -9.905515769479276145, 34.41647553114623292 ) ) ;
#39516 = CARTESIAN_POINT ( 'NONE',  ( 3.750000000000001776, -7.561099074964511502, 15.97061829374151287 ) ) ;
#39517 = VECTOR ( 'NONE', #78769, 1000.000000000000114 ) ;
#39518 = CARTESIAN_POINT ( 'NONE',  ( -4.377331078410485077, -3.019605429927184836, 32.48692288466676814 ) ) ;
#39519 = FACE_OUTER_BOUND ( 'NONE', #82629, .T. ) ;
#39520 = ORIENTED_EDGE ( 'NONE', *, *, #87422, .T. ) ;
#39521 = B_SPLINE_CURVE_WITH_KNOTS ( 'NONE', 3,
 ( #53400, #33589, #32687, #19184, #80902, #54283, #60158, #88553, #81340, #11992 ),
 .UNSPECIFIED., .F., .F.,
 ( 4, 2, 2, 2, 4 ),
 ( 0.0007817246256747477145, 0.0009771112852218909357, 0.001172497944769034265, 0.001367884604316177595, 0.001563271263863320708 ),
 .UNSPECIFIED. ) ;
#39522 = DIRECTION ( 'NONE',  ( -0.000000000000000000, 0.5000000000000011102, -0.8660254037844381525 ) ) ;
#39523 = CARTESIAN_POINT ( 'NONE',  ( 8.835299120233205628, -11.16473453929635440, 33.15142922261926373 ) ) ;
#39524 = CARTESIAN_POINT ( 'NONE',  ( -2.608446859217920633, -4.805146000318815780, 18.00186829374151287 ) ) ;
#39525 = EDGE_CURVE ( 'NONE', #43394, #84175, #60495, .T. ) ;
#39526 = VECTOR ( 'NONE', #27786, 1000.000000000000227 ) ;
#39527 = AXIS2_PLACEMENT_3D ( 'NONE', #52433, #4254, #18223 ) ;
#39529 = CARTESIAN_POINT ( 'NONE',  ( -10.83831157429146508, -2.523278758544489797, 31.42238647778637528 ) ) ;
#39528 = B_SPLINE_CURVE_WITH_KNOTS ( 'NONE', 3,
 ( #65488, #22720, #70922, #3786, #71795, #57395, #50637, #31264, #86228, #78116 ),
 .UNSPECIFIED., .F., .F.,
 ( 4, 2, 2, 2, 4 ),
 ( 0.000000000000000000, 0.0001954339857564091007, 0.0003908679715128182013, 0.0005863019572692273291, 0.0007817359430256364027 ),
 .UNSPECIFIED. ) ;
#39530 = CARTESIAN_POINT ( 'NONE',  ( -16.15384615384615330, -10.67929555188718282, 33.92786785259544047 ) ) ;
#39531 = ORIENTED_EDGE ( 'NONE', *, *, #53932, .T. ) ;
#39532 = CARTESIAN_POINT ( 'NONE',  ( 6.989145274079363368, -8.120952969808772792, 34.71129190929999453 ) ) ;
#39533 = CARTESIAN_POINT ( 'NONE',  ( 15.12820512820512953, -3.499999999999999556, 29.75000000000000355 ) ) ;
#39535 = VERTEX_POINT ( 'NONE', #82458 ) ;
#39534 = CARTESIAN_POINT ( 'NONE',  ( 11.28843831424008393, -2.985938066672154445, 32.43141759479405550 ) ) ;
#39536 = CARTESIAN_POINT ( 'NONE',  ( -13.31935981333936070, -11.48612834413965977, 32.76840700105972815 ) ) ;
#39537 = CARTESIAN_POINT ( 'NONE',  ( 4.480769230769229061, -7.500000000000000000, 29.75000000000000355 ) ) ;
#39538 = B_SPLINE_CURVE_WITH_KNOTS ( 'NONE', 3,
 ( #39431, #18258, #45723, #81300, #32221, #59682, #66889, #14157, #27670, #56025 ),
 .UNSPECIFIED., .F., .F.,
 ( 4, 2, 2, 2, 4 ),
 ( 0.000000000000000000, 0.0001954311564186868744, 0.0003908623128373737488, 0.0005862934692560606504, 0.0007817246256747474977 ),
 .UNSPECIFIED. ) ;
#39539 = CARTESIAN_POINT ( 'NONE',  ( 15.36155967173618286, -5.496552790871120031, 34.60292014791297532 ) ) ;
#39540 = CARTESIAN_POINT ( 'NONE',  ( -14.24162395668986747, -11.16473453929635440, 33.15142922261926373 ) ) ;
#39541 = EDGE_CURVE ( 'NONE', #88546, #54362, #56190, .T. ) ;
#39542 = VERTEX_POINT ( 'NONE', #8563 ) ;
#39543 = CARTESIAN_POINT ( 'NONE',  ( 7.053121978996697017, -2.254550872974306674, 29.97347326024527447 ) ) ;
#39544 = CARTESIAN_POINT ( 'NONE',  ( -15.45369618967607828, -11.43668979543635089, 33.22377378376089752 ) ) ;
#39545 = EDGE_CURVE ( 'NONE', #3, #39385, #88435, .T. ) ;
#39546 = EDGE_CURVE ( 'NONE', #44275, #2005, #63492, .T. ) ;
#39547 = LINE ( 'NONE', #61556, #58510 ) ;
#39548 = ORIENTED_EDGE ( 'NONE', *, *, #9409, .T. ) ;
#39549 = ORIENTED_EDGE ( 'NONE', *, *, #5266, .F. ) ;
#39550 = ORIENTED_EDGE ( 'NONE', *, *, #85621, .F. ) ;
#39551 = CARTESIAN_POINT ( 'NONE',  ( -7.846153846153967493, -3.083524468854526912, 32.58852847137268327 ) ) ;
#39552 = DIRECTION ( 'NONE',  ( -1.000000000000000000, -0.000000000000000000, -0.000000000000000000 ) ) ;
#39553 = CARTESIAN_POINT ( 'NONE',  ( -12.46153846153858247, -3.835265460704628371, 33.15142922262033665 ) ) ;
#39554 = EDGE_CURVE ( 'NONE', #46850, #83826, #62558, .T. ) ;
#39555 = AXIS2_PLACEMENT_3D ( 'NONE', #31853, #79143, #30938 ) ;
#39556 = CARTESIAN_POINT ( 'NONE',  ( 5.142178648199100977, -6.026961402152789304, 34.52809138561124769 ) ) ;
#39557 = VERTEX_POINT ( 'NONE', #69377 ) ;
#39558 = ADVANCED_FACE ( 'NONE', ( #30 ), #21621, .F. ) ;
#39559 = EDGE_CURVE ( 'NONE', #46752, #31330, #911, .T. ) ;
#39560 = ORIENTED_EDGE ( 'NONE', *, *, #24136, .T. ) ;
#39561 = EDGE_LOOP ( 'NONE', ( #63989, #66324 ) ) ;
#39563 = ORIENTED_EDGE ( 'NONE', *, *, #31245, .T. ) ;
#39562 = CYLINDRICAL_SURFACE ( 'NONE', #88985, 4.000000000000000000 ) ;
#39564 = CARTESIAN_POINT ( 'NONE',  ( -16.28453675695646652, -12.35290016733513951, 31.75349464988449455 ) ) ;
#39565 = ADVANCED_FACE ( 'NONE', ( #14881 ), #63038, .F. ) ;
#39566 = DIRECTION ( 'NONE',  ( 0.000000000000000000, 0.000000000000000000, -1.000000000000000000 ) ) ;
#39567 = CARTESIAN_POINT ( 'NONE',  ( 7.173022332454967120, -4.932303261841489039, 34.32971442181322885 ) ) ;
#39568 = CARTESIAN_POINT ( 'NONE',  ( 16.08857615328983570, -11.67786785259541027, 32.92929555188721480 ) ) ;
#39569 = EDGE_LOOP ( 'NONE', ( #14053, #38018, #10856, #54643 ) ) ;
#39570 = B_SPLINE_CURVE_WITH_KNOTS ( 'NONE', 3,
 ( #84930, #34947, #28648, #50671, #78156, #83606, #70517, #62408, #28188, #55657 ),
 .UNSPECIFIED., .F., .F.,
 ( 4, 2, 2, 2, 4 ),
 ( 0.000000000000000000, 0.0001954311564186861968, 0.0003908623128373723936, 0.0005862934692560585904, 0.0007817246256747447872 ),
 .UNSPECIFIED. ) ;
#39571 = ORIENTED_EDGE ( 'NONE', *, *, #45524, .T. ) ;
#39572 = EDGE_LOOP ( 'NONE', ( #77953, #75000 ) ) ;
#39573 = CARTESIAN_POINT ( 'NONE',  ( 14.43821774592595197, -11.04252011169590020, 33.62494198852677130 ) ) ;
#39575 = ORIENTED_EDGE ( 'NONE', *, *, #88791, .F. ) ;
#39574 = CARTESIAN_POINT ( 'NONE',  ( -8.769230769230768274, -12.37446782046654192, 30.86335684631486131 ) ) ;
#39576 = CARTESIAN_POINT ( 'NONE',  ( 16.85343815235874132, -5.827078755546626354, 34.72654668319379567 ) ) ;
#39577 = CARTESIAN_POINT ( 'NONE',  ( 3.230769230769231726, -12.34228464037088635, 31.77849191805839268 ) ) ;
#39578 = CARTESIAN_POINT ( 'NONE',  ( 16.40379167219429490, -8.433404298154332679, 34.66254593164985920 ) ) ;
#39579 = LINE ( 'NONE', #45861, #42216 ) ;
#39580 = CARTESIAN_POINT ( 'NONE',  ( -2.057746789344163663, -11.37275283266503756, 32.91324779482534524 ) ) ;
#39581 = FACE_BOUND ( 'NONE', #5258, .T. ) ;
#39582 = CARTESIAN_POINT ( 'NONE',  ( -5.300408001487407539, -10.23692288466677880, 34.23039457007281072 ) ) ;
#39583 = CARTESIAN_POINT ( 'NONE',  ( -18.06608237936013595, -12.34228464037088280, 31.77849191805838558 ) ) ;
#39584 = ADVANCED_FACE ( 'NONE', ( #35590 ), #28839, .F. ) ;
#39585 = VECTOR ( 'NONE', #27072, 1000.000000000000000 ) ;
#39586 = CARTESIAN_POINT ( 'NONE',  ( 11.66898724022510514, -12.45806712695776319, 30.39783852428763922 ) ) ;
#39588 = CARTESIAN_POINT ( 'NONE',  ( -18.00000000000012079, -10.90142922262034020, 33.41473453929536674 ) ) ;
#39587 = DIRECTION ( 'NONE',  ( 0.000000000000000000, 0.1736481776669267785, -0.9848077530122087975 ) ) ;
#39589 = CARTESIAN_POINT ( 'NONE',  ( 0.3313912521002370104, -12.27039167877662251, 31.24851455888617835 ) ) ;
#39590 = CARTESIAN_POINT ( 'NONE',  ( -0.5276218724943423366, -3.513871655860377086, 32.76840700105978499 ) ) ;
#39591 = ORIENTED_EDGE ( 'NONE', *, *, #29298, .F. ) ;
#39592 = CARTESIAN_POINT ( 'NONE',  ( 2.557746619330622639, -6.567000820036038355, 34.66262288849541306 ) ) ;
#39593 = CARTESIAN_POINT ( 'NONE',  ( -13.13456096470193124, -4.074993327901527351, 33.72946981652012255 ) ) ;
#39594 = ORIENTED_EDGE ( 'NONE', *, *, #54569, .F. ) ;
#39595 = ORIENTED_EDGE ( 'NONE', *, *, #81406, .T. ) ;
#39596 = DIRECTION ( 'NONE',  ( 0.000000000000000000, 0.000000000000000000, -1.000000000000000000 ) ) ;
#39597 = EDGE_CURVE ( 'NONE', #25676, #43597, #34663, .T. ) ;
#39598 = B_SPLINE_CURVE_WITH_KNOTS ( 'NONE', 3,
 ( #65633, #5286, #25556, #87726, #25109, #39534, #18804, #88175, #80511, #80963 ),
 .UNSPECIFIED., .F., .F.,
 ( 4, 2, 2, 2, 4 ),
 ( 0.000000000000000000, 0.0001954311564186860071, 0.0003908623128373720141, 0.0005862934692560580483, 0.0007817246256747440282 ),
 .UNSPECIFIED. ) ;
#39599 = CARTESIAN_POINT ( 'NONE',  ( 15.93036121012220541, -3.754499324213721234, 33.06261337010820256 ) ) ;
#39600 = CARTESIAN_POINT ( 'NONE',  ( 12.33084785842815378, -10.70098750199973203, 33.91152734681376302 ) ) ;
#39601 = ORIENTED_EDGE ( 'NONE', *, *, #29331, .F. ) ;
#39602 = LINE ( 'NONE', #31489, #81641 ) ;
#39603 = CARTESIAN_POINT ( 'NONE',  ( -6.988347369037697376, -10.21337939537584383, 33.94971097300158647 ) ) ;
#39605 = DIRECTION ( 'NONE',  ( -1.000000000000000000, -0.000000000000000000, -0.000000000000000000 ) ) ;
#39604 = CARTESIAN_POINT ( 'NONE',  ( -15.48079246806219267, -5.851115903089112003, 34.47074536777953568 ) ) ;
#39606 = CARTESIAN_POINT ( 'NONE',  ( -3.230769230769229949, -6.343179335718451384, 34.87096338111211935 ) ) ;
#39607 = CARTESIAN_POINT ( 'NONE',  ( -18.75000000000000000, -3.499999999999999556, 29.75000000000000355 ) ) ;
#39609 = CARTESIAN_POINT ( 'NONE',  ( -16.15384615384615330, -2.900454961884010974, 35.62045528018868623 ) ) ;
#39608 =( LENGTH_UNIT ( ) NAMED_UNIT ( * ) SI_UNIT ( .MILLI., .METRE. ) );
#39610 = CARTESIAN_POINT ( 'NONE',  ( 3.749999999999992006, -5.946699141100872943, 19.39062500000000711 ) ) ;
#39611 = ORIENTED_EDGE ( 'NONE', *, *, #46588, .T. ) ;
#39612 = VERTEX_POINT ( 'NONE', #64806 ) ;
#39613 = DIRECTION ( 'NONE',  ( 0.000000000000000000, 0.4999999999999985567, 0.8660254037844395958 ) ) ;
#39614 = CARTESIAN_POINT ( 'NONE',  ( -17.75005459062195712, -3.520799739797213501, 33.17531984108286025 ) ) ;
#39615 = CARTESIAN_POINT ( 'NONE',  ( 4.219040135629509081, -2.506253911140448487, 29.99999999999988631 ) ) ;
#39616 = DIRECTION ( 'NONE',  ( -0.000000000000000000, 0.6427876096865404731, -0.7660444431189770143 ) ) ;
#39617 = DIRECTION ( 'NONE',  ( -0.000000000000000000, -0.6427876096865404731, -0.7660444431189771253 ) ) ;
#39618 = CARTESIAN_POINT ( 'NONE',  ( -1.929879867024197893E-14, -3.750000000000000000, 24.15625000000000000 ) ) ;
#39619 = LINE ( 'NONE', #11695, #73407 ) ;
#39620 = CARTESIAN_POINT ( 'NONE',  ( 14.17754433796061875, -6.809168938359901446, 34.95455904226513866 ) ) ;
#39621 = AXIS2_PLACEMENT_3D ( 'NONE', #82485, #55877, #48672 ) ;
#39622 = EDGE_CURVE ( 'NONE', #8848, #78089, #47574, .T. ) ;
#39623 = CARTESIAN_POINT ( 'NONE',  ( -13.63461538461538680, -7.433931650972299465, 34.75000000000000711 ) ) ;
#39624 = CARTESIAN_POINT ( 'NONE',  ( 5.934729999443682402, -10.33852847137145048, 34.16647553114627556 ) ) ;
#39625 = CARTESIAN_POINT ( 'NONE',  ( 18.13052570176356326, -10.19071101563364401, 33.96452234770658407 ) ) ;
#39626 = CARTESIAN_POINT ( 'NONE',  ( 8.519207531937805555, -12.22074536777954989, 31.39888409691088356 ) ) ;
#39627 = CARTESIAN_POINT ( 'NONE',  ( -19.50000000000000000, -3.499999999999999556, 29.75000000000000355 ) ) ;
#39628 = LINE ( 'NONE', #65732, #63037 ) ;
#39629 = LINE ( 'NONE', #67087, #13167 ) ;
#39630 = DIRECTION ( 'NONE',  ( -0.000000000000000000, 1.000000000000000000, -0.000000000000000000 ) ) ;
#39631 = ORIENTED_EDGE ( 'NONE', *, *, #48921, .F. ) ;
#39632 = CARTESIAN_POINT ( 'NONE',  ( 1.384615384615386802, -2.538708090699994813, 30.37095296980875503 ) ) ;
#39633 = DIRECTION ( 'NONE',  ( -1.000000000000000000, 0.000000000000000000, 0.000000000000000000 ) ) ;
#39634 = CARTESIAN_POINT ( 'NONE',  ( 13.16113046005105680, -6.716662450894489211, 34.94144148231605840 ) ) ;
#39635 = CARTESIAN_POINT ( 'NONE',  ( -2.775308065498752086, -8.577988221561495763, 14.01749329374151642 ) ) ;
#39636 = DIRECTION ( 'NONE',  ( -0.000000000000000000, -0.7660444431189791237, -0.6427876096865379196 ) ) ;
#39637 = CARTESIAN_POINT ( 'NONE',  ( 20.00000000000000355, 10.00000000000000533, 3.000000000000000000 ) ) ;
#39638 = DIRECTION ( 'NONE',  ( -0.000000000000000000, -0.9848077530122085754, -0.1736481776669273613 ) ) ;
#39640 = ORIENTED_EDGE ( 'NONE', *, *, #44247, .T. ) ;
#39639 = CARTESIAN_POINT ( 'NONE',  ( -18.06973409430282729, -2.249999999999999556, 29.49970722874968843 ) ) ;
#39641 = CARTESIAN_POINT ( 'NONE',  ( 1.139087296525997051, -4.749999999999992895, 22.98437500000000000 ) ) ;
#39642 = EDGE_CURVE ( 'NONE', #2951, #66107, #70067, .T. ) ;
#39643 = CARTESIAN_POINT ( 'NONE',  ( 3.230769230769231726, -8.164416787775445883, 34.95778746994557906 ) ) ;
#39644 = EDGE_CURVE ( 'NONE', #14452, #61423, #11055, .T. ) ;
#39645 = ORIENTED_EDGE ( 'NONE', *, *, #75056, .T. ) ;
#39646 = CARTESIAN_POINT ( 'NONE',  ( -2.084912766423896446, -2.600157965045225783, 30.74683119005207743 ) ) ;
#39647 = VERTEX_POINT ( 'NONE', #38242 ) ;
#39648 = CARTESIAN_POINT ( 'NONE',  ( 0.4615384615383382183, -6.835583212225970762, 34.95778746994575670 ) ) ;
#39649 = CARTESIAN_POINT ( 'NONE',  ( -9.627052121031669074, -2.892918686051626498, 31.69288490824026638 ) ) ;
#39650 = VECTOR ( 'NONE', #5247, 1000.000000000000227 ) ;
#39651 = EDGE_CURVE ( 'NONE', #42406, #82638, #5425, .T. ) ;
#39652 = CARTESIAN_POINT ( 'NONE',  ( 2.307692307692186251, -12.70778746994576025, 30.41441678777401236 ) ) ;
#39653 = VERTEX_POINT ( 'NONE', #58059 ) ;
#39654 = ORIENTED_EDGE ( 'NONE', *, *, #69804, .T. ) ;
#39655 = ORIENTED_EDGE ( 'NONE', *, *, #12544, .F. ) ;
#39656 = CARTESIAN_POINT ( 'NONE',  ( -15.93083330975275658, -2.308499170217968466, 30.53291367094874076 ) ) ;
#39657 = CARTESIAN_POINT ( 'NONE',  ( 7.173022332454966232, -11.56426240980093745, 33.07394671870546432 ) ) ;
#39658 = CARTESIAN_POINT ( 'NONE',  ( 27.00000000000000000, -13.24999999999999822, 29.02772085586297734 ) ) ;
#39659 = CARTESIAN_POINT ( 'NONE',  ( -10.68146802634049486, -2.538708090699994813, 30.37095296980875148 ) ) ;
#39660 = B_SPLINE_CURVE_WITH_KNOTS ( 'NONE', 3,
 ( #10396, #72531, #65327, #24335, #3625, #63556, #44152, #9497, #9941, #43295 ),
 .UNSPECIFIED., .F., .F.,
 ( 4, 2, 2, 2, 4 ),
 ( 0.0007817359430256257775, 0.0009771253907249911191, 0.001172514838424356352, 0.001367904286123721586, 0.001563293733823086819 ),
 .UNSPECIFIED. ) ;
#39661 = VECTOR ( 'NONE', #72003, 1000.000000000000000 ) ;
#39662 = DIRECTION ( 'NONE',  ( -0.000000000000000000, 0.6427876096865404731, -0.7660444431189770143 ) ) ;
#39663 = CARTESIAN_POINT ( 'NONE',  ( -3.164701897419154530, -4.661471528628508665, 34.16647553114624003 ) ) ;
#39664 = CARTESIAN_POINT ( 'NONE',  ( 0.2386115026316118215, -2.308479472611653094, 30.53278059502174457 ) ) ;
#39665 = B_SPLINE_CURVE_WITH_KNOTS ( 'NONE', 3,
 ( #77749, #1657, #69229, #21928, #49402, #76874, #70555, #36332, #15174, #34992 ),
 .UNSPECIFIED., .F., .F.,
 ( 4, 2, 2, 2, 4 ),
 ( 0.000000000000000000, 0.0001954311564186881213, 0.0003908623128373762425, 0.0005862934692560643367, 0.0007817246256747524850 ),
 .UNSPECIFIED. ) ;
#39666 = LINE ( 'NONE', #81091, #73669 ) ;
#39667 = EDGE_CURVE ( 'NONE', #60483, #57327, #17081, .T. ) ;
#39668 = ORIENTED_EDGE ( 'NONE', *, *, #60401, .F. ) ;
#39669 = ORIENTED_EDGE ( 'NONE', *, *, #31665, .F. ) ;
#39670 = ORIENTED_EDGE ( 'NONE', *, *, #74043, .T. ) ;
#39672 = EDGE_LOOP ( 'NONE', ( #28744, #7207, #54834, #24808, #39919 ) ) ;
#39671 = DIRECTION ( 'NONE',  ( -0.000000000000000000, -0.000000000000000000, -1.000000000000000000 ) ) ;
#39673 = AXIS2_PLACEMENT_3D ( 'NONE', #25414, #51077, #51519 ) ;
#39674 = FACE_OUTER_BOUND ( 'NONE', #17651, .T. ) ;
#39675 = CARTESIAN_POINT ( 'NONE',  ( -8.769230769230768274, -9.905515769479276145, 34.41647553114623292 ) ) ;
#39676 = EDGE_LOOP ( 'NONE', ( #65641, #10282, #2795, #47986 ) ) ;
#39677 = CARTESIAN_POINT ( 'NONE',  ( 14.30769230769218581, -8.656820664282941280, 34.87096338111179961 ) ) ;
#39678 = CIRCLE ( 'NONE', #51133, 4.000000000000000000 ) ;
#39679 = ORIENTED_EDGE ( 'NONE', *, *, #9098, .F. ) ;
#39680 = CARTESIAN_POINT ( 'NONE',  ( 0.3309778697965401473, -2.504760397472875155, 29.97295953869789997 ) ) ;
#39681 = ORIENTED_EDGE ( 'NONE', *, *, #47092, .T. ) ;
#39682 = CARTESIAN_POINT ( 'NONE',  ( -5.448717948717948012, -11.00000000000000000, 29.75000000000000355 ) ) ;
#39683 = CARTESIAN_POINT ( 'NONE',  ( -8.992715712954719720, -5.113361153441934093, 34.14387501736622710 ) ) ;
#39684 = B_SPLINE_CURVE_WITH_KNOTS ( 'NONE', 3,
 ( #38222, #32805, #11197, #78761, #53057, #80565, #11652, #44517, #5334, #44965 ),
 .UNSPECIFIED., .F., .F.,
 ( 4, 2, 2, 2, 4 ),
 ( 0.0007817359430256297891, 0.0009771253907249958896, 0.001172514838424362207, 0.001367904286123728524, 0.001563293733823094625 ),
 .UNSPECIFIED. ) ;
#39685 = CARTESIAN_POINT ( 'NONE',  ( 1.384615384615386802, -6.435427911321262684, 35.78748833219616898 ) ) ;
#39686 = FACE_BOUND ( 'NONE', #83725, .T. ) ;
#39687 = B_SPLINE_CURVE_WITH_KNOTS ( 'NONE', 3,
 ( #50905, #29785, #22574, #10397, #71196, #23890, #64430, #16698, #31093, #36541 ),
 .UNSPECIFIED., .F., .F.,
 ( 4, 2, 2, 2, 4 ),
 ( 0.000000000000000000, 0.0001954339857564054144, 0.0003908679715128108288, 0.0005863019572692162703, 0.0007817359430256216575 ),
 .UNSPECIFIED. ) ;
#39688 = DIRECTION ( 'NONE',  ( -1.000000000000000000, 0.000000000000000000, 0.000000000000000000 ) ) ;
#39689 = LINE ( 'NONE', #59935, #6893 ) ;
#39690 = CARTESIAN_POINT ( 'NONE',  ( -1.450697763975520083, -2.292212530054419606, 30.41441678777542634 ) ) ;
#39691 = CARTESIAN_POINT ( 'NONE',  ( 4.403791672194294904, -8.433404298154334455, 34.66254593164985920 ) ) ;
#39692 = DIRECTION ( 'NONE',  ( 0.000000000000000000, -1.000000000000000000, -8.673617379884033500E-16 ) ) ;
#39693 = CARTESIAN_POINT ( 'NONE',  ( -4.219929564802032296, -11.16473453929635440, 33.15142922261925662 ) ) ;
#39694 = EDGE_LOOP ( 'NONE', ( #4264, #70237, #29260, #28501 ) ) ;
#39695 = LINE ( 'NONE', #5008, #33101 ) ;
#39696 = ORIENTED_EDGE ( 'NONE', *, *, #69196, .T. ) ;
#39697 = ORIENTED_EDGE ( 'NONE', *, *, #2312, .F. ) ;
#39699 = CARTESIAN_POINT ( 'NONE',  ( -3.230769230769229949, -3.513871655860378418, 32.76840700105978499 ) ) ;
#39698 = CARTESIAN_POINT ( 'NONE',  ( -19.00000000000000000, 8.999999999999996447, 23.75000000000000000 ) ) ;
#39700 = LINE ( 'NONE', #67160, #58569 ) ;
#39701 = CARTESIAN_POINT ( 'NONE',  ( -23.50000000000000000, -5.499999999999981348, 27.24999999999999645 ) ) ;
#39702 = CARTESIAN_POINT ( 'NONE',  ( 0.000000000000000000, -11.00000000000000000, 29.75000000000000355 ) ) ;
#39703 = CARTESIAN_POINT ( 'NONE',  ( 12.46153846153833911, -10.33852847137269571, 34.16647553114546554 ) ) ;
#39704 = ORIENTED_EDGE ( 'NONE', *, *, #20541, .F. ) ;
#39705 = VECTOR ( 'NONE', #44321, 1000.000000000000114 ) ;
#39706 = CARTESIAN_POINT ( 'NONE',  ( 17.32697738856139580, -3.136992222400443175, 32.19305428654138979 ) ) ;
#39707 = CARTESIAN_POINT ( 'NONE',  ( 14.98074600654777377, -4.175268141568685643, 33.81360843649122216 ) ) ;
#39708 = CARTESIAN_POINT ( 'NONE',  ( 2.530471976670372936, -12.69155399931963046, 30.53255429739157734 ) ) ;
#39709 = CARTESIAN_POINT ( 'NONE',  ( -24.00000000000000000, -5.499999999999981348, 27.25000000000000000 ) ) ;
#39710 = EDGE_LOOP ( 'NONE', ( #81024, #17707, #59081, #49778 ) ) ;
#39711 = EDGE_LOOP ( 'NONE', ( #68516, #88434, #31101, #48353 ) ) ;
#39712 = ORIENTED_EDGE ( 'NONE', *, *, #16714, .F. ) ;
#39713 = CARTESIAN_POINT ( 'NONE',  ( 4.153846153846030731, -12.16647553114689728, 32.15551576947799362 ) ) ;
#39714 = CARTESIAN_POINT ( 'NONE',  ( -14.05763788777885281, -5.642605341092957971, 34.66089969410670335 ) ) ;
#39715 = VERTEX_POINT ( 'NONE', #84234 ) ;
#39716 = VECTOR ( 'NONE', #87660, 1000.000000000000000 ) ;
#39717 = CARTESIAN_POINT ( 'NONE',  ( 3.230769230769231726, -12.62096338111211580, 30.90682066428153263 ) ) ;
#39718 = CARTESIAN_POINT ( 'NONE',  ( 15.23076923076911093, -9.442884908241554243, 34.35708131394783038 ) ) ;
#39719 = FACE_OUTER_BOUND ( 'NONE', #73815, .T. ) ;
#39720 = CARTESIAN_POINT ( 'NONE',  ( 14.53065521125379611, -7.369474270740069777, 34.74850911626239736 ) ) ;
#39721 = DIRECTION ( 'NONE',  ( -0.000000000000000000, -0.9396926207859093161, -0.3420201433256663259 ) ) ;
#39722 = ORIENTED_EDGE ( 'NONE', *, *, #36049, .F. ) ;
#39724 = ORIENTED_EDGE ( 'NONE', *, *, #31636, .T. ) ;
#39723 = CARTESIAN_POINT ( 'NONE',  ( -7.596208327805704208, -10.05730279482229683, 34.04704008940765902 ) ) ;
#39725 = CARTESIAN_POINT ( 'NONE',  ( 2.307692307692309264, -13.20930481340135110, 34.54067556320372745 ) ) ;
#39726 = DIRECTION ( 'NONE',  ( 0.000000000000000000, -1.000000000000000000, 0.000000000000000000 ) ) ;
#39727 = LINE ( 'NONE', #47798, #35794 ) ;
#39728 = CARTESIAN_POINT ( 'NONE',  ( 18.13079180782478872, -8.147973898785416225, 34.70805048591653730 ) ) ;
#39729 = CARTESIAN_POINT ( 'NONE',  ( 2.438217745925951530, -2.647132371071621471, 31.75357179365173010 ) ) ;
#39730 = CARTESIAN_POINT ( 'NONE',  ( -8.703975629717932705, -9.528491918058460186, 34.59228464037086326 ) ) ;
#39731 = CARTESIAN_POINT ( 'NONE',  ( -0.5268089074992375886, -12.46129190929999986, 30.37095296980880832 ) ) ;
#39732 = CARTESIAN_POINT ( 'NONE',  ( 2.775308065498755195, -6.422011778438505125, 20.89249329374151642 ) ) ;
#39733 = ORIENTED_EDGE ( 'NONE', *, *, #50588, .T. ) ;
#39734 = DIRECTION ( 'NONE',  ( 0.000000000000000000, 0.000000000000000000, -1.000000000000000000 ) ) ;
#39735 = CARTESIAN_POINT ( 'NONE',  ( 1.384615384615386802, -3.669653830205710676, 35.88435417666054406 ) ) ;
#39736 = EDGE_CURVE ( 'NONE', #15629, #5929, #27152, .T. ) ;
#39738 = EDGE_LOOP ( 'NONE', ( #42205, #60187 ) ) ;
#39737 = VECTOR ( 'NONE', #55329, 1000.000000000000000 ) ;
#39739 = ORIENTED_EDGE ( 'NONE', *, *, #73799, .T. ) ;
#39740 = CARTESIAN_POINT ( 'NONE',  ( -18.75000000000000000, -7.500000000000000000, 29.75000000000000355 ) ) ;
#39741 = FACE_OUTER_BOUND ( 'NONE', #63507, .T. ) ;
#39742 = ADVANCED_FACE ( 'NONE', ( #23819 ), #72019, .F. ) ;
#39743 = CARTESIAN_POINT ( 'NONE',  ( 13.16113044089143713, -3.754499324213721234, 33.06261337010820256 ) ) ;
#39744 = AXIS2_PLACEMENT_3D ( 'NONE', #79615, #17914, #45368 ) ;
#39745 = CARTESIAN_POINT ( 'NONE',  ( -0.4615384615385826339, -2.892918686052166066, 31.69288490824153470 ) ) ;
#39746 = DIRECTION ( 'NONE',  ( 0.000000000000000000, 0.000000000000000000, -1.000000000000000000 ) ) ;
#39747 = DIRECTION ( 'NONE',  ( -0.000000000000000000, 0.9396926207859092051, -0.3420201433256662704 ) ) ;
#39748 = ORIENTED_EDGE ( 'NONE', *, *, #59833, .T. ) ;
#39749 = DIRECTION ( 'NONE',  ( 1.000000000000000000, 0.000000000000000000, 0.000000000000000000 ) ) ;
#39750 = EDGE_CURVE ( 'NONE', #84034, #42820, #82988, .T. ) ;
#39751 = CARTESIAN_POINT ( 'NONE',  ( 11.53846153846153832, -13.88283147151868846, 33.14645433367849847 ) ) ;
#39752 = CARTESIAN_POINT ( 'NONE',  ( -3.360916440207452283, -11.93770438780619259, 32.05411857736982029 ) ) ;
#39753 = ORIENTED_EDGE ( 'NONE', *, *, #64153, .F. ) ;
#39754 = CARTESIAN_POINT ( 'NONE',  ( 15.93091919493930320, -12.38737895849757820, 31.66785238281580206 ) ) ;
#39755 = ORIENTED_EDGE ( 'NONE', *, *, #53833, .F. ) ;
#39756 = CARTESIAN_POINT ( 'NONE',  ( 13.38461538461526601, -3.300289026999228881, 32.46337939537708905 ) ) ;
#39757 = CARTESIAN_POINT ( 'NONE',  ( 6.000000000000001776, -11.16473453929635440, 33.15142922261926373 ) ) ;
#39758 = EDGE_LOOP ( 'NONE', ( #47335, #13562, #60957, #65694 ) ) ;
#39759 = DIRECTION ( 'NONE',  ( 0.000000000000000000, 0.3420201433256641055, -0.9396926207859100932 ) ) ;
#39760 = CARTESIAN_POINT ( 'NONE',  ( 13.51540582558233794, -9.084667340241226796, 34.75534355489798344 ) ) ;
#39761 = FACE_OUTER_BOUND ( 'NONE', #12938, .T. ) ;
#39762 = CARTESIAN_POINT ( 'NONE',  ( 13.19230769230769340, -11.50000000000000000, 29.75000000000000355 ) ) ;
#39763 = CARTESIAN_POINT ( 'NONE',  ( -0.7115616857599196265, -11.56360843649122216, 33.07473185843129926 ) ) ;
#39764 = VECTOR ( 'NONE', #52448, 1000.000000000000000 ) ;
#39765 = EDGE_CURVE ( 'NONE', #84875, #65515, #13759, .T. ) ;
#39766 = EDGE_LOOP ( 'NONE', ( #43699, #6117 ) ) ;
#39767 = DIRECTION ( 'NONE',  ( -0.000000000000000000, 0.9396926207859092051, -0.3420201433256662704 ) ) ;
#39768 = EDGE_CURVE ( 'NONE', #38893, #46048, #2415, .T. ) ;
#39769 = ORIENTED_EDGE ( 'NONE', *, *, #75948, .F. ) ;
#39770 = CARTESIAN_POINT ( 'NONE',  ( 8.769230769230647482, -12.46129190930018460, 30.37095296980731973 ) ) ;
#39771 = EDGE_CURVE ( 'NONE', #1868, #83195, #68944, .T. ) ;
#39772 = CARTESIAN_POINT ( 'NONE',  ( -12.33074802057151409, -2.845873456487965747, 32.17976146951972538 ) ) ;
#39773 = CARTESIAN_POINT ( 'NONE',  ( 4.480769230769229061, -7.500000000000000000, 29.75000000000000355 ) ) ;
#39774 = EDGE_CURVE ( 'NONE', #72479, #85801, #59372, .T. ) ;
#39775 = CYLINDRICAL_SURFACE ( 'NONE', #71774, 0.2499999999999979738 ) ;
#39776 = VECTOR ( 'NONE', #82280, 1000.000000000000227 ) ;
#39777 = CARTESIAN_POINT ( 'NONE',  ( -6.923076923077044142, -6.026961402154118908, 34.52809138561165270 ) ) ;
#39778 = CARTESIAN_POINT ( 'NONE',  ( 20.00000000000000711, -9.999999999999994671, 13.00000000000000178 ) ) ;
#39779 = ORIENTED_EDGE ( 'NONE', *, *, #2412, .F. ) ;
#39780 = ORIENTED_EDGE ( 'NONE', *, *, #63381, .T. ) ;
#39781 = EDGE_LOOP ( 'NONE', ( #76438, #17179, #79001, #242 ) ) ;
#39782 = EDGE_LOOP ( 'NONE', ( #62226, #47117, #88618, #81545 ) ) ;
#39783 = CARTESIAN_POINT ( 'NONE',  ( -16.40382288478850725, -3.627789207965226304, 32.91389620160131102 ) ) ;
#39784 = DIRECTION ( 'NONE',  ( -0.000000000000000000, -0.000000000000000000, -1.000000000000000000 ) ) ;
#39785 = DIRECTION ( 'NONE',  ( 0.000000000000000000, 0.000000000000000000, -1.000000000000000000 ) ) ;
#39786 = CARTESIAN_POINT ( 'NONE',  ( 3.930361210122205406, -3.236172620538810385, 32.36188796281390267 ) ) ;
#39787 = CARTESIAN_POINT ( 'NONE',  ( -5.076923076923075762, -10.51840700105979565, 33.73612834413961536 ) ) ;
#39788 = CARTESIAN_POINT ( 'NONE',  ( -5.143006487878958310, -8.120952969808774569, 34.71129190930000163 ) ) ;
#39789 = PLANE ( 'NONE',  #19315 ) ;
#39790 = CARTESIAN_POINT ( 'NONE',  ( 0.2380535178145122277, -3.236172620538810829, 32.36188796281390267 ) ) ;
#39791 = ORIENTED_EDGE ( 'NONE', *, *, #35607, .T. ) ;
#39792 = VERTEX_POINT ( 'NONE', #31939 ) ;
#39793 = ORIENTED_EDGE ( 'NONE', *, *, #79530, .F. ) ;
#39795 = ORIENTED_EDGE ( 'NONE', *, *, #15711, .F. ) ;
#39794 = CARTESIAN_POINT ( 'NONE',  ( 2.307692307692309264, -2.538708090699994813, 30.37095296980875503 ) ) ;
#39797 = CARTESIAN_POINT ( 'NONE',  ( -7.911424292114620727, -4.481592998940162609, 33.73612834413957984 ) ) ;
#39796 = CARTESIAN_POINT ( 'NONE',  ( 1.653273178848927064E-15, -7.500000000000000000, 14.00000000000000178 ) ) ;
#39798 = EDGE_CURVE ( 'NONE', #33903, #70063, #50740, .T. ) ;
#39799 = CARTESIAN_POINT ( 'NONE',  ( -0.2385256174450677280, -2.308499170217967134, 30.53291367094873721 ) ) ;
#39800 = CARTESIAN_POINT ( 'NONE',  ( -15.45369618967607828, -10.01117774369187252, 34.36070679894347535 ) ) ;
#39801 = FACE_BOUND ( 'NONE', #74525, .T. ) ;
#39802 = ORIENTED_EDGE ( 'NONE', *, *, #50777, .F. ) ;
#39803 = AXIS2_PLACEMENT_3D ( 'NONE', #50861, #85561, #84691 ) ;
#39804 = EDGE_LOOP ( 'NONE', ( #88693, #60135 ) ) ;
#39805 = CARTESIAN_POINT ( 'NONE',  ( -4.826977558574935045, -6.696923467548660192, 34.68552623307873972 ) ) ;
#39806 = VERTEX_POINT ( 'NONE', #80119 ) ;
#39807 = FACE_BOUND ( 'NONE', #42684, .T. ) ;
#39808 = CARTESIAN_POINT ( 'NONE',  ( 9.692307692307570832, -5.941354392335915335, 34.76329471203413846 ) ) ;
#39809 = CARTESIAN_POINT ( 'NONE',  ( 7.846153846154160227, -2.255955759149395501, 30.00000000000324363 ) ) ;
#39810 = ORIENTED_EDGE ( 'NONE', *, *, #20494, .T. ) ;
#39811 = LINE ( 'NONE', #46989, #47767 ) ;
#39812 = LINE ( 'NONE', #33048, #31807 ) ;
#39813 = CARTESIAN_POINT ( 'NONE',  ( -4.826923076923140599, -7.565270000091922853, 34.99999999999999289 ) ) ;
#39814 = ORIENTED_EDGE ( 'NONE', *, *, #33261, .T. ) ;
#39815 = B_SPLINE_CURVE_WITH_KNOTS ( 'NONE', 3,
 ( #49920, #44042, #23769, #57565, #85490, #64312, #51221, #57126, #70648, #43608 ),
 .UNSPECIFIED., .F., .F.,
 ( 4, 2, 2, 2, 4 ),
 ( 0.000000000000000000, 0.0001954339857564078267, 0.0003908679715128156535, 0.0005863019572692235344, 0.0007817359430256313069 ),
 .UNSPECIFIED. ) ;
#39816 = CARTESIAN_POINT ( 'NONE',  ( -8.769230769230890843, -4.481592998941358097, 33.73612834414048933 ) ) ;
#39817 = CARTESIAN_POINT ( 'NONE',  ( -3.453695448285377889, -2.758268499246657068, 31.33685645148949561 ) ) ;
#39818 = CARTESIAN_POINT ( 'NONE',  ( 2.438482748659261734, -2.845873456487966635, 32.17976146951972538 ) ) ;
#39819 = ORIENTED_EDGE ( 'NONE', *, *, #83296, .F. ) ;
#39820 = ADVANCED_FACE ( 'NONE', ( #68705 ), #75909, .F. ) ;
#39821 = CARTESIAN_POINT ( 'NONE',  ( -2.437839517130524492, -11.47017969459903952, 32.78971311882034456 ) ) ;
#39822 = CARTESIAN_POINT ( 'NONE',  ( 2.557637717070352146, -3.520799739797214389, 33.17531984108286025 ) ) ;
#39823 = ORIENTED_EDGE ( 'NONE', *, *, #18566, .T. ) ;
#39824 = CARTESIAN_POINT ( 'NONE',  ( -12.52762084089859407, -5.471508081941602875, 34.59228464037088457 ) ) ;
#39825 = CARTESIAN_POINT ( 'NONE',  ( -4.153846153846273204, -2.625532179533778709, 30.86335684631627174 ) ) ;
#39826 = CARTESIAN_POINT ( 'NONE',  ( -14.43784027742400866, -2.647304123082328875, 31.75400227202885972 ) ) ;
#39827 = CARTESIAN_POINT ( 'NONE',  ( -11.66915300512910214, -8.147922237126337563, 34.70805685702651999 ) ) ;
#39828 = CARTESIAN_POINT ( 'NONE',  ( 0.3962684609821413018, -2.657715359629089669, 31.77849191805833584 ) ) ;
#39829 = VECTOR ( 'NONE', #9176, 1000.000000000000000 ) ;
#39830 = CARTESIAN_POINT ( 'NONE',  ( -0.3963454732438077555, -2.255955759149235185, 29.99999999999988987 ) ) ;
#39832 = DIRECTION ( 'NONE',  ( 0.000000000000000000, 0.7660444431189822323, -0.6427876096865344779 ) ) ;
#39831 = CARTESIAN_POINT ( 'NONE',  ( 5.999999999999880096, -11.94971097300221174, 32.03036669348237098 ) ) ;
#39833 = CARTESIAN_POINT ( 'NONE',  ( 8.835299120233209180, -12.10708131394839704, 31.69288490824020954 ) ) ;
#39834 = CARTESIAN_POINT ( 'NONE',  ( -12.39547011053602610, -11.16473453929635440, 33.15142922261926373 ) ) ;
#39835 = CARTESIAN_POINT ( 'NONE',  ( -1.944543648263014957, -5.555456351737005249, 19.00000000000000000 ) ) ;
#39836 = VERTEX_POINT ( 'NONE', #27716 ) ;
#39837 = VECTOR ( 'NONE', #33772, 1000.000000000000114 ) ;
#39838 = CARTESIAN_POINT ( 'NONE',  ( 4.826946332874483936, -6.524016743844655686, 34.90889640711025521 ) ) ;
#39839 = ORIENTED_EDGE ( 'NONE', *, *, #22253, .T. ) ;
#39840 = ADVANCED_FACE ( 'NONE', ( #55186 ), #82682, .F. ) ;
#39841 = EDGE_LOOP ( 'NONE', ( #27230, #34023, #7481, #19218 ) ) ;
#39842 = CARTESIAN_POINT ( 'NONE',  ( -2.980714810855777497, -9.233818618650603938, 34.70587769442853698 ) ) ;
#39844 = ORIENTED_EDGE ( 'NONE', *, *, #26069, .F. ) ;
#39843 = AXIS2_PLACEMENT_3D ( 'NONE', #35985, #43176, #2180 ) ;
#39845 = CARTESIAN_POINT ( 'NONE',  ( 1.449870524128224814, -12.16647553114626490, 32.15551576947920864 ) ) ;
#39846 = CARTESIAN_POINT ( 'NONE',  ( -1.409462824231155764E-14, -4.749999999999999112, 15.40625000000000000 ) ) ;
#39847 = CARTESIAN_POINT ( 'NONE',  ( 13.38461538461526601, -2.892918686052165622, 31.69288490824153470 ) ) ;
#39848 = EDGE_CURVE ( 'NONE', #53945, #79249, #55627, .T. ) ;
#39849 = CARTESIAN_POINT ( 'NONE',  ( -18.22348492456433178, -12.11044203135682018, 32.26167407432752299 ) ) ;
#39850 = CARTESIAN_POINT ( 'NONE',  ( -7.596099534515530216, -5.728107161865378494, 34.42597550085002922 ) ) ;
#39851 = CARTESIAN_POINT ( 'NONE',  ( -8.546219417617919589, -4.887748414852792322, 34.01359900205216746 ) ) ;
#39852 = DIRECTION ( 'NONE',  ( -0.000000000000000000, 1.000000000000000000, -0.000000000000000000 ) ) ;
#39853 = CARTESIAN_POINT ( 'NONE',  ( -10.61538461538461320, -12.78798330534103123, 29.99999999999997868 ) ) ;
#39854 = CARTESIAN_POINT ( 'NONE',  ( 2.651650429449539104, -4.848349570550432475, 23.06250000000000000 ) ) ;
#39855 = CARTESIAN_POINT ( 'NONE',  ( -7.053767526187232129, -4.684245665217972032, 34.18127051446801090 ) ) ;
#39856 = CARTESIAN_POINT ( 'NONE',  ( -4.403869378067612139, -12.07920672191015221, 32.31858351112116168 ) ) ;
#39857 = EDGE_CURVE ( 'NONE', #18166, #30238, #15989, .T. ) ;
#39858 = CARTESIAN_POINT ( 'NONE',  ( -16.15384615384615330, -1.215029322943914858, 32.30358669280327177 ) ) ;
#39859 = EDGE_CURVE ( 'NONE', #49704, #72244, #48609, .T. ) ;
#39860 = ORIENTED_EDGE ( 'NONE', *, *, #66275, .T. ) ;
#39861 = ORIENTED_EDGE ( 'NONE', *, *, #87230, .T. ) ;
#39862 = B_SPLINE_CURVE_WITH_KNOTS ( 'NONE', 3,
 ( #72609, #56985, #3700, #25319, #56552, #63301, #59540, #37944, #45582, #18567 ),
 .UNSPECIFIED., .F., .F.,
 ( 4, 2, 2, 2, 4 ),
 ( 0.000000000000000000, 0.0001954311564186861697, 0.0003908623128373723394, 0.0005862934692560584820, 0.0007817246256747446788 ),
 .UNSPECIFIED. ) ;
#39863 = AXIS2_PLACEMENT_3D ( 'NONE', #1142, #1590, #49333 ) ;
#39864 = CARTESIAN_POINT ( 'NONE',  ( 6.792385456409365752, -2.541943142973490666, 30.39792223712631980 ) ) ;
#39865 = CARTESIAN_POINT ( 'NONE',  ( 13.38461538461526423, -3.643525952248795718, 33.31231777344771672 ) ) ;
#39866 = CARTESIAN_POINT ( 'NONE',  ( 16.37662582282421653, -12.47679350104403007, 31.42216943046555855 ) ) ;
#39867 = DIRECTION ( 'NONE',  ( -0.000000000000000000, -0.9848077530122085754, -0.1736481776669273613 ) ) ;
#39868 = ADVANCED_FACE ( 'NONE', ( #42138 ), #691, .F. ) ;
#39869 = LINE ( 'NONE', #46615, #79444 ) ;
#39870 = CIRCLE ( 'NONE', #22559, 5.250000000000000888 ) ;
#39871 = CARTESIAN_POINT ( 'NONE',  ( -16.37677237136229991, -9.086856451489516928, 34.49173150075333183 ) ) ;
#39872 = EDGE_CURVE ( 'NONE', #53910, #44756, #77555, .T. ) ;
#39873 = AXIS2_PLACEMENT_3D ( 'NONE', #51659, #71500, #77819 ) ;
#39874 = VERTEX_POINT ( 'NONE', #77236 ) ;
#39875 = CARTESIAN_POINT ( 'NONE',  ( -6.857008572074483332, -9.780366693483667717, 34.19971097300155805 ) ) ;
#39876 = EDGE_LOOP ( 'NONE', ( #54098, #16283, #65546, #65647 ) ) ;
#39877 = B_SPLINE_CURVE_WITH_KNOTS ( 'NONE', 3,
 ( #80847, #25884, #34407, #60995, #13257, #54228, #68204, #81725, #75402, #12374 ),
 .UNSPECIFIED., .F., .F.,
 ( 4, 2, 2, 2, 4 ),
 ( 0.000000000000000000, 0.0001954339857564098054, 0.0003908679715128196108, 0.0005863019572692293891, 0.0007817359430256392216 ),
 .UNSPECIFIED. ) ;
#39878 = VERTEX_POINT ( 'NONE', #43890 ) ;
#39879 = CARTESIAN_POINT ( 'NONE',  ( -14.17685388967953664, -7.277220443632450575, 34.74524770363009196 ) ) ;
#39880 = CARTESIAN_POINT ( 'NONE',  ( -14.17690186672535901, -6.369690395747422684, 34.87708834333098196 ) ) ;
#39881 = EDGE_CURVE ( 'NONE', #27959, #58891, #46462, .T. ) ;
#39882 = DIRECTION ( 'NONE',  ( 0.000000000000000000, 0.000000000000000000, 1.000000000000000000 ) ) ;
#39883 = EDGE_CURVE ( 'NONE', #3633, #86305, #78828, .T. ) ;
#39884 = CARTESIAN_POINT ( 'NONE',  ( 1.134592160393928406, -11.56360843649122216, 33.07473185843129926 ) ) ;
#39885 = LINE ( 'NONE', #81752, #76734 ) ;
#39886 = VERTEX_POINT ( 'NONE', #21851 ) ;
#39887 = ORIENTED_EDGE ( 'NONE', *, *, #76776, .T. ) ;
#39888 = AXIS2_PLACEMENT_3D ( 'NONE', #46976, #13641, #66819 ) ;
#39889 = ORIENTED_EDGE ( 'NONE', *, *, #1768, .F. ) ;
#39890 = ORIENTED_EDGE ( 'NONE', *, *, #87918, .F. ) ;
#39891 = CARTESIAN_POINT ( 'NONE',  ( 5.749976762707036393, -2.587272538249754117, 30.68239716806877837 ) ) ;
#39892 = CARTESIAN_POINT ( 'NONE',  ( 9.823098133274644539, -2.295524264805589354, 30.44142389570982488 ) ) ;
#39893 = B_SPLINE_CURVE_WITH_KNOTS ( 'NONE', 3,
 ( #12565, #27846, #53987, #382, #54424, #14330, #33284, #34604, #81034, #40052 ),
 .UNSPECIFIED., .F., .F.,
 ( 4, 2, 2, 2, 4 ),
 ( 0.000000000000000000, 0.0001954339857564072304, 0.0003908679715128144608, 0.0005863019572692216913, 0.0007817359430256289217 ),
 .UNSPECIFIED. ) ;
#39894 = AXIS2_PLACEMENT_3D ( 'NONE', #48402, #39896, #41218 ) ;
#39895 = CARTESIAN_POINT ( 'NONE',  ( -15.23076923076922995, -2.708943851104267164, 35.45975837776705220 ) ) ;
#39896 = DIRECTION ( 'NONE',  ( 1.000000000000000000, 0.000000000000000000, 0.000000000000000000 ) ) ;
#39897 = EDGE_CURVE ( 'NONE', #66304, #80196, #37845, .T. ) ;
#39898 = PRESENTATION_STYLE_ASSIGNMENT (( #26814 ) ) ;
#39899 = CARTESIAN_POINT ( 'NONE',  ( -10.39260507411620083, -12.24180327182772388, 31.33663988360758168 ) ) ;
#39900 = VECTOR ( 'NONE', #76501, 1000.000000000000227 ) ;
#39901 = VERTEX_POINT ( 'NONE', #84454 ) ;
#39902 = EDGE_LOOP ( 'NONE', ( #12972, #62784, #20302, #84087 ) ) ;
#39904 = ORIENTED_EDGE ( 'NONE', *, *, #57231, .T. ) ;
#39903 = CARTESIAN_POINT ( 'NONE',  ( 17.32686859527121825, -12.43552623307873972, 30.55307653245132826 ) ) ;
#39905 = CARTESIAN_POINT ( 'NONE',  ( 10.61538461538461675, -11.11383981884818262, 36.00935417666054406 ) ) ;
#39906 = CARTESIAN_POINT ( 'NONE',  ( 7.976199008988623440, -2.504778602574660340, 29.97347330155780654 ) ) ;
#39907 = EDGE_CURVE ( 'NONE', #4994, #45619, #73253, .T. ) ;
#39908 = CARTESIAN_POINT ( 'NONE',  ( 2.651650429449539104, -4.848349570550432475, 18.06250000000000355 ) ) ;
#39909 = EDGE_LOOP ( 'NONE', ( #48172, #34685 ) ) ;
#39910 = CARTESIAN_POINT ( 'NONE',  ( -11.97435897435897623, -4.000000000000000000, 29.75000000000000355 ) ) ;
#39911 = ORIENTED_EDGE ( 'NONE', *, *, #27744, .T. ) ;
#39912 = EDGE_CURVE ( 'NONE', #37056, #4960, #23181, .T. ) ;
#39913 = DIRECTION ( 'NONE',  ( -0.000000000000000000, -0.5000000000000009992, -0.8660254037844380415 ) ) ;
#39914 = CARTESIAN_POINT ( 'NONE',  ( 14.43848274865925774, -12.35292014791297710, 31.75344720912887198 ) ) ;
#39915 = DIRECTION ( 'NONE',  ( 1.000000000000000000, 0.000000000000000000, 0.000000000000000000 ) ) ;
#39916 = CARTESIAN_POINT ( 'NONE',  ( -7.053768389744485390, -3.530157926970578508, 32.79014554554150607 ) ) ;
#39917 = ADVANCED_FACE ( 'NONE', ( #38479 ), #10107, .F. ) ;
#39918 = CARTESIAN_POINT ( 'NONE',  ( -17.07692307692307665, -13.63283147151868846, 33.57946703557072254 ) ) ;
#39919 = ORIENTED_EDGE ( 'NONE', *, *, #82254, .T. ) ;
#39920 = DIRECTION ( 'NONE',  ( -1.000000000000000000, -0.000000000000000000, -0.000000000000000000 ) ) ;
#39921 = DIRECTION ( 'NONE',  ( 0.000000000000000000, -1.000000000000000000, 0.000000000000000000 ) ) ;
#39922 = CYLINDRICAL_SURFACE ( 'NONE', #40888, 0.2500000000000009437 ) ;
#39923 = ORIENTED_EDGE ( 'NONE', *, *, #78427, .F. ) ;
#39924 = EDGE_CURVE ( 'NONE', #48285, #17504, #42168, .T. ) ;
#39925 = B_SPLINE_CURVE_WITH_KNOTS ( 'NONE', 3,
 ( #12166, #39649, #45491, #31539, #5409, #32876, #72971, #79288, #87853, #26118 ),
 .UNSPECIFIED., .F., .F.,
 ( 4, 2, 2, 2, 4 ),
 ( 0.0007817359430256293554, 0.0009771253907249941549, 0.001172514838424358954, 0.001367904286123723537, 0.001563293733823095276 ),
 .UNSPECIFIED. ) ;
#39926 = DIRECTION ( 'NONE',  ( -1.000000000000000000, -0.000000000000000000, -0.000000000000000000 ) ) ;
#39927 = LINE ( 'NONE', #58388, #5172 ) ;
#39928 = CARTESIAN_POINT ( 'NONE',  ( 17.14299142792552288, -9.780366693483667717, 34.19971097300155805 ) ) ;
#39929 = CARTESIAN_POINT ( 'NONE',  ( -2.373775718648185595, -10.51840700105979387, 33.73612834413961536 ) ) ;
#39930 = CARTESIAN_POINT ( 'NONE',  ( 0.4615384615384611200, -13.63283147151868846, 33.57946703557072254 ) ) ;
#39931 = FACE_BOUND ( 'NONE', #24387, .T. ) ;
#39933 = LINE ( 'NONE', #59745, #56101 ) ;
#39932 = CARTESIAN_POINT ( 'NONE',  ( -7.146003881983771677, -12.38737895849757820, 31.66785238281580206 ) ) ;
#39934 = VECTOR ( 'NONE', #84381, 1000.000000000000227 ) ;
#39935 = CARTESIAN_POINT ( 'NONE',  ( -9.469528023329626620, -12.11081565061824250, 32.26097654155340422 ) ) ;
#39937 = CARTESIAN_POINT ( 'NONE',  ( 17.77707378248385339, -11.24512374952581872, 33.06303171183252942 ) ) ;
#39936 = CARTESIAN_POINT ( 'NONE',  ( -8.703162418228330921, -11.69971097300155272, 32.46337939537588113 ) ) ;
#39938 = CARTESIAN_POINT ( 'NONE',  ( 8.769230769230768274, -12.62096338111211580, 30.90682066428153263 ) ) ;
#39939 = CARTESIAN_POINT ( 'NONE',  ( -0.06109907496455085213, -3.750000000000000888, 25.15438170625849068 ) ) ;
#39940 = EDGE_LOOP ( 'NONE', ( #87152, #8266, #5314, #10003 ) ) ;
#39941 = CARTESIAN_POINT ( 'NONE',  ( 10.48469401227431419, -11.93127051446799847, 32.56575433478202797 ) ) ;
#39942 = VERTEX_POINT ( 'NONE', #79012 ) ;
#39943 = CARTESIAN_POINT ( 'NONE',  ( 16.09615384615384670, -4.000000000000000000, 29.75000000000000355 ) ) ;
#39944 = VERTEX_POINT ( 'NONE', #38930 ) ;
#39945 = CARTESIAN_POINT ( 'NONE',  ( 7.716006636715625255, -9.418419913701741919, 34.36755862841477693 ) ) ;
#39946 = CARTESIAN_POINT ( 'NONE',  ( -7.846153846153844924, -11.35647404775217417, 33.31231777344666511 ) ) ;
#39948 = ORIENTED_EDGE ( 'NONE', *, *, #69732, .F. ) ;
#39947 = CARTESIAN_POINT ( 'NONE',  ( 6.000000000000001776, -9.058645607665452459, 34.76329471203371924 ) ) ;
#39949 = CARTESIAN_POINT ( 'NONE',  ( -17.07692307692307665, -2.292212530054420494, 30.41441678777542634 ) ) ;
#39950 = CARTESIAN_POINT ( 'NONE',  ( -7.846153846153844924, -13.78497067705608181, 32.30358669280327177 ) ) ;
#39951 = CARTESIAN_POINT ( 'NONE',  ( 0.06109907496455496689, -11.24999999999999822, 27.02938170625848358 ) ) ;
#39952 = EDGE_CURVE ( 'NONE', #71524, #24900, #3793, .T. ) ;
#39953 = CARTESIAN_POINT ( 'NONE',  ( 2.177000841024752109, -11.71456829005830080, 32.44064028649416542 ) ) ;
#39954 = DIRECTION ( 'NONE',  ( -0.000000000000000000, 0.3420201433256694346, -0.9396926207859080948 ) ) ;
#39955 = DIRECTION ( 'NONE',  ( 1.000000000000000000, 0.000000000000000000, 0.000000000000000000 ) ) ;
#39956 = CARTESIAN_POINT ( 'NONE',  ( -11.53846153846153655, -11.33034616979429110, 35.88435417666054406 ) ) ;
#39957 = CARTESIAN_POINT ( 'NONE',  ( -1.384615384615506484, -6.835583212225970762, 34.95778746994575670 ) ) ;
#39958 = FACE_OUTER_BOUND ( 'NONE', #78999, .T. ) ;
#39959 = CARTESIAN_POINT ( 'NONE',  ( -1.492201783934593573, -3.724691934501250135, 16.82999329374151287 ) ) ;
#39960 = CARTESIAN_POINT ( 'NONE',  ( 9.915734654169265028, -7.630147231320743018, 34.74852402298682819 ) ) ;
#39961 = DIRECTION ( 'NONE',  ( -0.000000000000000000, 0.5000000000000011102, -0.8660254037844381525 ) ) ;
#39962 = ORIENTED_EDGE ( 'NONE', *, *, #63219, .F. ) ;
#39963 = CARTESIAN_POINT ( 'NONE',  ( 4.480769230769229061, -11.50000000000000000, 29.75000000000000355 ) ) ;
#39964 = CARTESIAN_POINT ( 'NONE',  ( 19.00000000000000000, -16.99999999999999289, 30.25000000000000000 ) ) ;
#39965 = AXIS2_PLACEMENT_3D ( 'NONE', #5449, #32916, #61701 ) ;
#39966 = CARTESIAN_POINT ( 'NONE',  ( -3.724691934501248802, -5.885600066136383646, 19.17374329374151642 ) ) ;
#39967 = CARTESIAN_POINT ( 'NONE',  ( -0.6089743589743593644, -7.500000000000000000, 29.75000000000000355 ) ) ;
#39968 = CARTESIAN_POINT ( 'NONE',  ( -8.992157728137618378, -3.395401636524185474, 33.02366814457250399 ) ) ;
#39969 = ORIENTED_EDGE ( 'NONE', *, *, #44983, .T. ) ;
#39970 = CARTESIAN_POINT ( 'NONE',  ( 3.230769230769231726, -12.10708131394839349, 31.69288490824020244 ) ) ;
#39971 = DIRECTION ( 'NONE',  ( -1.000000000000000000, 0.000000000000000000, -0.000000000000000000 ) ) ;
#39973 = ORIENTED_EDGE ( 'NONE', *, *, #20438, .T. ) ;
#39972 = CARTESIAN_POINT ( 'NONE',  ( 5.010840697562939816, -12.34228464037088280, 31.77849191805838558 ) ) ;
#39974 = CARTESIAN_POINT ( 'NONE',  ( 12.59206416330202671, -12.45806712695776319, 30.39783852428763922 ) ) ;
#39975 = VECTOR ( 'NONE', #26114, 1000.000000000000000 ) ;
#39976 = CARTESIAN_POINT ( 'NONE',  ( -17.32692307692307665, -7.433932668274255917, 35.00000000000000711 ) ) ;
#39977 = DIRECTION ( 'NONE',  ( 1.000000000000000000, 0.000000000000000000, 0.000000000000000000 ) ) ;
#39978 = VERTEX_POINT ( 'NONE', #86687 ) ;
#39979 = CYLINDRICAL_SURFACE ( 'NONE', #56390, 0.2499999999999979738 ) ;
#39980 = DIRECTION ( 'NONE',  ( 0.000000000000000000, 0.000000000000000000, 1.000000000000000000 ) ) ;
#39981 = ADVANCED_FACE ( 'NONE', ( #23617 ), #51067, .F. ) ;
#39982 = EDGE_CURVE ( 'NONE', #73792, #77192, #18208, .T. ) ;
#39983 = CARTESIAN_POINT ( 'NONE',  ( -13.13466997523734037, -8.476813868363244353, 34.90874843262270133 ) ) ;
#39984 = ORIENTED_EDGE ( 'NONE', *, *, #67974, .T. ) ;
#39985 = EDGE_LOOP ( 'NONE', ( #8913, #84872, #8419, #42634 ) ) ;
#39986 = EDGE_CURVE ( 'NONE', #84435, #67271, #45670, .T. ) ;
#39987 = ORIENTED_EDGE ( 'NONE', *, *, #23262, .T. ) ;
#39988 = AXIS2_PLACEMENT_3D ( 'NONE', #32826, #72917, #11223 ) ;
#39989 = CARTESIAN_POINT ( 'NONE',  ( 0.2115617305961063066, -8.303909089506435137, 34.68538101551103381 ) ) ;
#39990 = FACE_OUTER_BOUND ( 'NONE', #767, .T. ) ;
#39991 = EDGE_CURVE ( 'NONE', #28559, #54595, #5627, .T. ) ;
#39992 = CARTESIAN_POINT ( 'NONE',  ( -16.40386937806761125, -2.985938066672154445, 32.43141759479405550 ) ) ;
#39993 = DIRECTION ( 'NONE',  ( 0.000000000000000000, 0.000000000000000000, -1.000000000000000000 ) ) ;
#39994 = B_SPLINE_CURVE_WITH_KNOTS ( 'NONE', 3,
 ( #80778, #59593, #5100, #53724, #19495, #81211, #18620, #33016, #12740, #11868 ),
 .UNSPECIFIED., .F., .F.,
 ( 4, 2, 2, 2, 4 ),
 ( 0.000000000000000000, 0.0001954311564186868473, 0.0003908623128373736946, 0.0005862934692560605419, 0.0007817246256747473893 ),
 .UNSPECIFIED. ) ;
#39995 = EDGE_CURVE ( 'NONE', #67434, #67903, #84121, .T. ) ;
#39996 = CARTESIAN_POINT ( 'NONE',  ( -16.94639737515951339, -5.195472089885680766, 34.18748526763464923 ) ) ;
#39997 = EDGE_LOOP ( 'NONE', ( #9562, #43762 ) ) ;
#39998 = ORIENTED_EDGE ( 'NONE', *, *, #49325, .F. ) ;
#39999 = ORIENTED_EDGE ( 'NONE', *, *, #84173, .F. ) ;
#40001 = ORIENTED_EDGE ( 'NONE', *, *, #44604, .F. ) ;
#40000 = CARTESIAN_POINT ( 'NONE',  ( -8.069638789877792817, -5.113361153441934093, 34.14387501736622710 ) ) ;
#40002 = CARTESIAN_POINT ( 'NONE',  ( -25.00000000000000000, -10.00000000000000533, 13.00000000000000178 ) ) ;
#40003 = ADVANCED_FACE ( 'NONE', ( #10560 ), #79466, .F. ) ;
#40004 = CARTESIAN_POINT ( 'NONE',  ( 12.52760579488853665, -11.35647404775217595, 33.31231777344666511 ) ) ;
#40005 = ADVANCED_FACE ( 'NONE', ( #4696 ), #45220, .F. ) ;
#40006 = CARTESIAN_POINT ( 'NONE',  ( -12.33074665371367651, -12.11778462344220841, 31.66786338562085135 ) ) ;
#40007 = CARTESIAN_POINT ( 'NONE',  ( -5.448717948717948012, -7.500000000000000000, 33.75000000000000000 ) ) ;
#40008 = ORIENTED_EDGE ( 'NONE', *, *, #51307, .F. ) ;
#40009 = EDGE_LOOP ( 'NONE', ( #43258, #59975 ) ) ;
#40010 = ORIENTED_EDGE ( 'NONE', *, *, #51268, .F. ) ;
#40011 = CARTESIAN_POINT ( 'NONE',  ( -10.61538461538461320, -10.67929555188718282, 33.92786785259544047 ) ) ;
#40013 = VERTEX_POINT ( 'NONE', #52865 ) ;
#40012 = CARTESIAN_POINT ( 'NONE',  ( -1.384615384615383471, -3.669653830205710676, 35.88435417666054406 ) ) ;
#40014 = CARTESIAN_POINT ( 'NONE',  ( 2.242422307135989001, -2.657715359629089225, 31.77849191805834295 ) ) ;
#40015 = CARTESIAN_POINT ( 'NONE',  ( -13.44988583057615905, -6.879047030191174805, 34.71129190930000163 ) ) ;
#40016 = ORIENTED_EDGE ( 'NONE', *, *, #17407, .T. ) ;
#40017 = DIRECTION ( 'NONE',  ( -0.000000000000000000, -0.5000000000000009992, -0.8660254037844380415 ) ) ;
#40018 = CARTESIAN_POINT ( 'NONE',  ( 8.992010310499175318, -12.44528174975671853, 30.48912976160716681 ) ) ;
#40019 = CARTESIAN_POINT ( 'NONE',  ( 0.2386115026316108223, -9.172386477786396597, 34.72672124145550043 ) ) ;
#40020 = B_SPLINE_CURVE_WITH_KNOTS ( 'NONE', 3,
 ( #14855, #30123, #42767, #22917, #57590, #2198, #2634, #43199, #85077, #49945 ),
 .UNSPECIFIED., .F., .F.,
 ( 4, 2, 2, 2, 4 ),
 ( 0.0007817246256747507503, 0.0009771112852218957062, 0.001172497944769040771, 0.001367884604316185835, 0.001563271263863330682 ),
 .UNSPECIFIED. ) ;
#40021 = AXIS2_PLACEMENT_3D ( 'NONE', #30702, #65811, #59511 ) ;
#40022 = FACE_BOUND ( 'NONE', #39400, .T. ) ;
#40023 = ADVANCED_FACE ( 'NONE', ( #47440 ), #87574, .F. ) ;
#40024 = CARTESIAN_POINT ( 'NONE',  ( -0.5922299282060213832, -9.804603061927743113, 34.18744698557895845 ) ) ;
#40025 = LINE ( 'NONE', #33257, #31331 ) ;
#40026 = CARTESIAN_POINT ( 'NONE',  ( -10.61538461538461320, -10.67929555188718282, 33.92786785259544047 ) ) ;
#40028 = CARTESIAN_POINT ( 'NONE',  ( -5.999999999999998224, -2.721908614388771852, 31.22303859784724978 ) ) ;
#40027 = CARTESIAN_POINT ( 'NONE',  ( -7.145955605505568187, -7.630691491037286056, 34.74850469731152458 ) ) ;
#40029 = EDGE_CURVE ( 'NONE', #30874, #11346, #6902, .T. ) ;
#40030 = B_SPLINE_CURVE_WITH_KNOTS ( 'NONE', 3,
 ( #56319, #77038, #1812, #29302, #56755, #84251, #22530, #49994, #77474, #37359 ),
 .UNSPECIFIED., .F., .F.,
 ( 4, 2, 2, 2, 4 ),
 ( 0.0007817246256747457630, 0.0009771112852218887673, 0.001172497944769031663, 0.001367884604316174559, 0.001563271263863317672 ),
 .UNSPECIFIED. ) ;
#40031 = FACE_OUTER_BOUND ( 'NONE', #20070, .T. ) ;
#40032 = CARTESIAN_POINT ( 'NONE',  ( 12.46153846153846168, -2.833524468853757305, 32.15551576947925838 ) ) ;
#40033 = ORIENTED_EDGE ( 'NONE', *, *, #60948, .T. ) ;
#40034 = CARTESIAN_POINT ( 'NONE',  ( -15.23076923076935252, -11.67786785259630911, 32.92929555188603530 ) ) ;
#40035 = CARTESIAN_POINT ( 'NONE',  ( -13.16183571563731469, -4.226511098958373402, 33.85474049983370293 ) ) ;
#40036 = VERTEX_POINT ( 'NONE', #40262 ) ;
#40037 = ORIENTED_EDGE ( 'NONE', *, *, #16464, .T. ) ;
#40038 = FACE_OUTER_BOUND ( 'NONE', #37669, .T. ) ;
#40039 = EDGE_CURVE ( 'NONE', #47287, #51433, #68015, .T. ) ;
#40040 = CARTESIAN_POINT ( 'NONE',  ( -15.23076923076935074, -2.625532179533778709, 30.86335684631627174 ) ) ;
#40041 = CARTESIAN_POINT ( 'NONE',  ( 1.326923076923076206, -3.499999999999999556, 29.75000000000000355 ) ) ;
#40042 = ORIENTED_EDGE ( 'NONE', *, *, #70797, .T. ) ;
#40043 = LINE ( 'NONE', #9550, #24134 ) ;
#40044 = CARTESIAN_POINT ( 'NONE',  ( -6.923076923077045919, -9.528491918059723176, 34.59228464037033035 ) ) ;
#40045 = FACE_BOUND ( 'NONE', #8472, .T. ) ;
#40046 = ADVANCED_FACE ( 'NONE', ( #61391 ), #26291, .F. ) ;
#40048 = CARTESIAN_POINT ( 'NONE',  ( 5.776515075435670887, -6.716662450894490100, 34.94144148231605840 ) ) ;
#40047 = CARTESIAN_POINT ( 'NONE',  ( -9.070512820512819374, -3.499999999999999556, 29.75000000000000355 ) ) ;
#40049 = CARTESIAN_POINT ( 'NONE',  ( 14.30769230769231015, -3.050289026998446396, 32.03036669348365706 ) ) ;
#40050 = DIRECTION ( 'NONE',  ( 0.000000000000000000, 0.7660444431189807890, 0.6427876096865361433 ) ) ;
#40052 = CARTESIAN_POINT ( 'NONE',  ( 0.4615384615383396616, -6.026961402154118908, 34.52809138561165270 ) ) ;
#40051 = CARTESIAN_POINT ( 'NONE',  ( 6.927495775892239749, 10.37398717377011614, 1.734723475976807094E-15 ) ) ;
#40053 = CARTESIAN_POINT ( 'NONE',  ( 1.553300858899129944, -11.24999999999998934, 20.95312500000000000 ) ) ;
#40054 = EDGE_LOOP ( 'NONE', ( #32350, #41412 ) ) ;
#40055 = ORIENTED_EDGE ( 'NONE', *, *, #62373, .T. ) ;
#40056 = VECTOR ( 'NONE', #84365, 1000.000000000000114 ) ;
#40057 = DIRECTION ( 'NONE',  ( 1.000000000000000000, 0.000000000000000000, 0.000000000000000000 ) ) ;
#40058 = CARTESIAN_POINT ( 'NONE',  ( 16.15384615384615330, -6.386643153685126251, 34.62446782046654192 ) ) ;
#40059 = DIRECTION ( 'NONE',  ( -1.000000000000000000, 0.000000000000000000, -0.000000000000000000 ) ) ;
#40060 = CARTESIAN_POINT ( 'NONE',  ( 17.32692307692309797, -2.249999999999997780, 29.81603969181029612 ) ) ;
#40061 = CARTESIAN_POINT ( 'NONE',  ( -15.23076923076922995, -1.129524287112498415, 32.06866353760679544 ) ) ;
#40062 = CARTESIAN_POINT ( 'NONE',  ( -2.651650429449535551, -10.15165042944956753, 21.18750000000000000 ) ) ;
#40063 = EDGE_CURVE ( 'NONE', #88099, #7820, #31454, .T. ) ;
#40064 = CARTESIAN_POINT ( 'NONE',  ( -15.23076923076922995, -8.973038597847269315, 34.52809138561121927 ) ) ;
#40065 = CARTESIAN_POINT ( 'NONE',  ( -6.065270000556318486, -8.656820664281497102, 34.87096338111211935 ) ) ;
#40066 = VECTOR ( 'NONE', #14722, 1000.000000000000227 ) ;
#40067 = EDGE_CURVE ( 'NONE', #15438, #48507, #5134, .T. ) ;
#40068 = CARTESIAN_POINT ( 'NONE',  ( 17.01165263096230262, -12.27809138561121394, 31.22303859784730307 ) ) ;
#40069 = CARTESIAN_POINT ( 'NONE',  ( 12.33084785842815378, -11.37499894934982692, 33.29245874905763003 ) ) ;
#40070 = DIRECTION ( 'NONE',  ( -0.000000000000000000, -0.9396926207859093161, -0.3420201433256663259 ) ) ;
#40071 = VECTOR ( 'NONE', #56973, 1000.000000000000227 ) ;
#40072 = CARTESIAN_POINT ( 'NONE',  ( 8.703960323269996024, -12.27809138561121394, 31.22303859784730307 ) ) ;
#40073 = EDGE_CURVE ( 'NONE', #19302, #6432, #60959, .T. ) ;
#40074 = CARTESIAN_POINT ( 'NONE',  ( -0.3310130233048168558, -4.299079248970732792, 33.91157788607253565 ) ) ;
#40075 = CARTESIAN_POINT ( 'NONE',  ( 14.98076923076923173, -2.249999999999998668, 29.75000000000000355 ) ) ;
#40076 = VECTOR ( 'NONE', #66783, 1000.000000000000000 ) ;
#40077 = B_SPLINE_CURVE_WITH_KNOTS ( 'NONE', 3,
 ( #62820, #7008, #1140, #55190, #83121, #29074, #41247, #21412, #28621, #69597 ),
 .UNSPECIFIED., .F., .F.,
 ( 4, 2, 2, 2, 4 ),
 ( 0.0007817359430256319575, 0.0009771253907249984917, 0.001172514838424365026, 0.001367904286123731343, 0.001563293733823097878 ),
 .UNSPECIFIED. ) ;
#40078 = CARTESIAN_POINT ( 'NONE',  ( -17.07692307692307665, -2.833524468853757305, 32.15551576947925838 ) ) ;
#40079 = EDGE_LOOP ( 'NONE', ( #83383, #69572, #15258, #43973 ) ) ;
#40080 = CYLINDRICAL_SURFACE ( 'NONE', #80099, 0.2499999999999995559 ) ;
#40081 = CARTESIAN_POINT ( 'NONE',  ( -17.32689982097166492, -6.524016743844656574, 34.90889640711025521 ) ) ;
#40082 = CARTESIAN_POINT ( 'NONE',  ( -2.724691934501246582, -6.299813628509474128, 16.67374329374151998 ) ) ;
#40083 = DIRECTION ( 'NONE',  ( 0.000000000000000000, 0.6427876096865373645, -0.7660444431189797898 ) ) ;
#40084 = DIRECTION ( 'NONE',  ( -0.000000000000000000, 0.9848077530122086864, -0.1736481776669273891 ) ) ;
#40085 = FACE_OUTER_BOUND ( 'NONE', #84864, .T. ) ;
#40087 = ORIENTED_EDGE ( 'NONE', *, *, #77870, .F. ) ;
#40086 = CARTESIAN_POINT ( 'NONE',  ( 5.326977496836527770, -4.074993327901525575, 33.72946981652012255 ) ) ;
#40088 = CARTESIAN_POINT ( 'NONE',  ( -2.749999999999998224, -7.500000000000015987, 23.84375000000000000 ) ) ;
#40089 = CARTESIAN_POINT ( 'NONE',  ( -3.230769230769229949, -6.681629849574314051, 35.83090037661290239 ) ) ;
#40090 = ORIENTED_EDGE ( 'NONE', *, *, #80630, .T. ) ;
#40091 = CARTESIAN_POINT ( 'NONE',  ( 8.703960323269994248, -8.613356846314824011, 34.62446782046655613 ) ) ;
#40092 = CARTESIAN_POINT ( 'NONE',  ( -17.86947429823644029, -3.816742781228455783, 33.13167719472716044 ) ) ;
#40093 = VERTEX_POINT ( 'NONE', #82585 ) ;
#40094 = CARTESIAN_POINT ( 'NONE',  ( 4.153846153846154188, -12.78798330534102945, 29.74999999999997868 ) ) ;
#40095 = CARTESIAN_POINT ( 'NONE',  ( -16.37672483627479636, -7.630691491037286056, 34.74850469731152458 ) ) ;
#40096 = CARTESIAN_POINT ( 'NONE',  ( 20.74999999999999645, -7.500000000000000000, 29.75000000000000355 ) ) ;
#40097 = ORIENTED_EDGE ( 'NONE', *, *, #21815, .F. ) ;
#40098 = ORIENTED_EDGE ( 'NONE', *, *, #12961, .T. ) ;
#40099 = ORIENTED_EDGE ( 'NONE', *, *, #78363, .T. ) ;
#40100 = LINE ( 'NONE', #24787, #9755 ) ;
#40101 = DIRECTION ( 'NONE',  ( -0.000000000000000000, -0.9848077530122085754, -0.1736481776669273613 ) ) ;
#40102 = CARTESIAN_POINT ( 'NONE',  ( 18.22277966897806678, -10.23759521482555357, 34.22997729860117033 ) ) ;
#40103 = CARTESIAN_POINT ( 'NONE',  ( 20.00000000000000355, 10.00000000000000533, 3.000000000000000000 ) ) ;
#40104 = DIRECTION ( 'NONE',  ( -0.000000000000000000, 0.8660254037844397068, -0.4999999999999978906 ) ) ;
#40105 = CYLINDRICAL_SURFACE ( 'NONE', #43554, 0.2499999999999973355 ) ;
#40106 = DIRECTION ( 'NONE',  ( -1.000000000000000000, -0.000000000000000000, -0.000000000000000000 ) ) ;
#40107 = EDGE_CURVE ( 'NONE', #63332, #68729, #80812, .T. ) ;
#40108 = CARTESIAN_POINT ( 'NONE',  ( -12.52680890749923570, -6.879047030191174805, 34.71129190930000163 ) ) ;
#40109 = ORIENTED_EDGE ( 'NONE', *, *, #51871, .T. ) ;
#40110 = ORIENTED_EDGE ( 'NONE', *, *, #67265, .T. ) ;
#40111 = ORIENTED_EDGE ( 'NONE', *, *, #5495, .F. ) ;
#40113 = ORIENTED_EDGE ( 'NONE', *, *, #25126, .F. ) ;
#40112 = CARTESIAN_POINT ( 'NONE',  ( 1.384615384615386802, -12.78798330534102945, 29.74999999999997868 ) ) ;
#40114 = EDGE_CURVE ( 'NONE', #34882, #65891, #86191, .T. ) ;
#40115 = AXIS2_PLACEMENT_3D ( 'NONE', #3823, #24091, #80392 ) ;
#40116 = CARTESIAN_POINT ( 'NONE',  ( -13.13461538461532108, -7.434744860731433924, 35.00000000000000711 ) ) ;
#40117 = CARTESIAN_POINT ( 'NONE',  ( 11.53846153846141753, -12.27809138561165270, 31.22303859784587132 ) ) ;
#40118 = VERTEX_POINT ( 'NONE', #39816 ) ;
#40119 = DIRECTION ( 'NONE',  ( -0.000000000000000000, 0.1736481776669307198, -0.9848077530122080203 ) ) ;
#40120 = VECTOR ( 'NONE', #17941, 1000.000000000000000 ) ;
#40121 = EDGE_CURVE ( 'NONE', #33177, #37079, #75370, .T. ) ;
#40122 = VERTEX_POINT ( 'NONE', #68605 ) ;
#40123 = CARTESIAN_POINT ( 'NONE',  ( 11.78840705680968171, -2.587454068350148351, 30.68340429815432202 ) ) ;
#40124 = VERTEX_POINT ( 'NONE', #55089 ) ;
#40125 = VECTOR ( 'NONE', #71042, 1000.000000000000000 ) ;
#40126 = CARTESIAN_POINT ( 'NONE',  ( -12.33149102628801153, -7.723484941389743952, 34.99544897038808955 ) ) ;
#40127 = AXIS2_PLACEMENT_3D ( 'NONE', #67828, #81794, #59289 ) ;
#40128 = CARTESIAN_POINT ( 'NONE',  ( 1.384615384615386802, -6.386643153685126251, 34.62446782046654192 ) ) ;
#40129 = CARTESIAN_POINT ( 'NONE',  ( -4.153846153846152411, -6.343179335718451384, 34.87096338111211935 ) ) ;
#40130 = FACE_BOUND ( 'NONE', #32074, .T. ) ;
#40131 = ADVANCED_FACE ( 'NONE', ( #67286 ), #5579, .F. ) ;
#40132 = CARTESIAN_POINT ( 'NONE',  ( -14.37377468705243722, -9.058645607665454236, 34.76329471203372634 ) ) ;
#40133 = CYLINDRICAL_SURFACE ( 'NONE', #54339, 0.2499999999999994726 ) ;
#40134 = CARTESIAN_POINT ( 'NONE',  ( 13.44987052412822059, -5.094484230520773593, 34.41647553114626845 ) ) ;
#40135 = CARTESIAN_POINT ( 'NONE',  ( -19.50000000000000000, -3.499999999999999556, 29.75000000000000355 ) ) ;
#40136 = CARTESIAN_POINT ( 'NONE',  ( -30.00000000000000000, -15.00000000000000000, 3.000000000000000000 ) ) ;
#40137 = DIRECTION ( 'NONE',  ( 0.000000000000000000, 0.3420201433256641055, -0.9396926207859100932 ) ) ;
#40138 = EDGE_CURVE ( 'NONE', #82649, #52040, #29242, .T. ) ;
#40139 = CARTESIAN_POINT ( 'NONE',  ( -13.25457022178060562, -2.504778602574660340, 29.97347330155780654 ) ) ;
#40140 = ORIENTED_EDGE ( 'NONE', *, *, #6791, .F. ) ;
#40141 = ORIENTED_EDGE ( 'NONE', *, *, #29120, .T. ) ;
#40143 = CARTESIAN_POINT ( 'NONE',  ( 2.438218009455872970, -10.88167719472716399, 33.43325721877153711 ) ) ;
#40142 = CARTESIAN_POINT ( 'NONE',  ( 2.177544337960609866, -3.069018819979302926, 32.56621877034667278 ) ) ;
#40144 = CARTESIAN_POINT ( 'NONE',  ( 15.36155967173618286, -8.191423895709840863, 34.95447573519442130 ) ) ;
#40145 = DIRECTION ( 'NONE',  ( -0.000000000000000000, 0.9848077530122085754, -0.1736481776669273613 ) ) ;
#40146 = CARTESIAN_POINT ( 'NONE',  ( -17.07692307692307665, -12.34228464037088635, 31.77849191805839268 ) ) ;
#40147 = CARTESIAN_POINT ( 'NONE',  ( 8.096153846153846700, -2.499999999999998668, 29.75000000000000355 ) ) ;
#40148 = ORIENTED_EDGE ( 'NONE', *, *, #34419, .T. ) ;
#40149 = CARTESIAN_POINT ( 'NONE',  ( -11.76194648218548444, -12.24155766932282496, 31.33739205006857986 ) ) ;
#40150 = EDGE_CURVE ( 'NONE', #53886, #26509, #81879, .T. ) ;
#40151 = DIRECTION ( 'NONE',  ( 1.000000000000000000, 1.734723475976812518E-16, -0.000000000000000000 ) ) ;
#40152 = CARTESIAN_POINT ( 'NONE',  ( -8.899922235898330314, -12.11776431015576172, 31.66791131148498906 ) ) ;
#40153 = FACE_OUTER_BOUND ( 'NONE', #41293, .T. ) ;
#40154 = ORIENTED_EDGE ( 'NONE', *, *, #28448, .T. ) ;
#40155 = ORIENTED_EDGE ( 'NONE', *, *, #68224, .T. ) ;
#40156 = PRODUCT_CONTEXT ( 'NONE', #80885, 'mechanical' ) ;
#40157 = VERTEX_POINT ( 'NONE', #42477 ) ;
#40158 = CARTESIAN_POINT ( 'NONE',  ( 0.5920641633020254924, -10.88167719472716399, 33.43325721877153711 ) ) ;
#40159 = ORIENTED_EDGE ( 'NONE', *, *, #60778, .F. ) ;
#40160 = CARTESIAN_POINT ( 'NONE',  ( 4.088576153289833037, -11.67786785259541027, 32.92929555188721480 ) ) ;
#40161 = CARTESIAN_POINT ( 'NONE',  ( -5.143006487878958310, -2.721908614388772740, 31.22303859784724622 ) ) ;
#40162 = CYLINDRICAL_SURFACE ( 'NONE', #81207, 0.2499999999999986955 ) ;
#40163 = CARTESIAN_POINT ( 'NONE',  ( -2.372962753653082402, -8.613356846314824011, 34.62446782046655613 ) ) ;
#40164 = EDGE_CURVE ( 'NONE', #79737, #21202, #16299, .T. ) ;
#40165 = DIRECTION ( 'NONE',  ( 1.000000000000000000, 0.000000000000000000, 0.000000000000000000 ) ) ;
#40166 = ORIENTED_EDGE ( 'NONE', *, *, #87128, .F. ) ;
#40168 = ORIENTED_EDGE ( 'NONE', *, *, #23874, .F. ) ;
#40167 = CARTESIAN_POINT ( 'NONE',  ( -0.3962833220256234967, -12.16647553114626490, 32.15551576947920864 ) ) ;
#40169 = DIRECTION ( 'NONE',  ( 0.000000000000000000, 0.6427876096865368094, 0.7660444431189802339 ) ) ;
#40170 = CARTESIAN_POINT ( 'NONE',  ( 8.769230769230645706, -12.51329471203414379, 31.30864560766407578 ) ) ;
#40171 = CARTESIAN_POINT ( 'NONE',  ( 9.692307692307695177, -12.37446782046654192, 30.86335684631486131 ) ) ;
#40172 = EDGE_CURVE ( 'NONE', #86079, #77001, #57249, .T. ) ;
#40173 = EDGE_CURVE ( 'NONE', #77760, #19281, #43197, .T. ) ;
#40174 = CARTESIAN_POINT ( 'NONE',  ( -16.40384615384615330, -7.566082377512564960, 35.00000000000000711 ) ) ;
#40175 = CARTESIAN_POINT ( 'NONE',  ( -8.638440328263820689, -8.191423895709840863, 34.95447573519442130 ) ) ;
#40176 = CARTESIAN_POINT ( 'NONE',  ( -5.142193077479396912, -11.06231777344662781, 33.60647404775220082 ) ) ;
#40177 = CARTESIAN_POINT ( 'NONE',  ( -3.480792468062196221, -6.695914987888143877, 34.68535235679833306 ) ) ;
#40178 = CARTESIAN_POINT ( 'NONE',  ( 1.901340078031373171, -9.487747218494639867, 18.62686829374151642 ) ) ;
#40179 = VERTEX_POINT ( 'NONE', #1921 ) ;
#40180 = EDGE_CURVE ( 'NONE', #80616, #57919, #31395, .T. ) ;
#40181 = LINE ( 'NONE', #6393, #57512 ) ;
#40182 = CARTESIAN_POINT ( 'NONE',  ( 1.384615384615386802, -4.945431358278436385, 36.03766855953609394 ) ) ;
#40183 = VECTOR ( 'NONE', #21450, 1000.000000000000227 ) ;
#40184 = AXIS2_PLACEMENT_3D ( 'NONE', #66789, #71758, #10064 ) ;
#40185 = ORIENTED_EDGE ( 'NONE', *, *, #22837, .F. ) ;
#40186 = ORIENTED_EDGE ( 'NONE', *, *, #45992, .F. ) ;
#40187 = CARTESIAN_POINT ( 'NONE',  ( 7.911408985666682270, -12.16647553114626490, 32.15551576947920864 ) ) ;
#40188 = DIRECTION ( 'NONE',  ( -0.000000000000000000, 1.000000000000000000, 3.491481338843133355E-15 ) ) ;
#40189 = AXIS2_PLACEMENT_3D ( 'NONE', #44064, #36015, #64340 ) ;
#40190 = CARTESIAN_POINT ( 'NONE',  ( 6.923076923076924238, -8.564572088678739092, 35.78748833219616898 ) ) ;
#40191 = DIRECTION ( 'NONE',  ( 0.000000000000000000, 0.4999999999999985567, 0.8660254037844395958 ) ) ;
#40192 = VECTOR ( 'NONE', #55768, 999.9999999999998863 ) ;
#40193 = FACE_OUTER_BOUND ( 'NONE', #48747, .T. ) ;
#40194 = VERTEX_POINT ( 'NONE', #76242 ) ;
#40195 = CARTESIAN_POINT ( 'NONE',  ( 6.000000000000001776, -3.513871655860378418, 32.76840700105978499 ) ) ;
#40196 = DIRECTION ( 'NONE',  ( 0.000000000000000000, 0.6427876096865373645, -0.7660444431189797898 ) ) ;
#40197 = CARTESIAN_POINT ( 'NONE',  ( 18.00000000000000000, -12.34228464037088635, 31.77849191805839268 ) ) ;
#40198 = VERTEX_POINT ( 'NONE', #30715 ) ;
#40199 = CARTESIAN_POINT ( 'NONE',  ( 13.38461538461538680, -6.386643153685126251, 34.62446782046654192 ) ) ;
#40200 = B_SPLINE_CURVE_WITH_KNOTS ( 'NONE', 3,
 ( #20013, #5174, #53799, #74974, #32640, #6511, #80854, #26775, #33969, #68208 ),
 .UNSPECIFIED., .F., .F.,
 ( 4, 2, 2, 2, 4 ),
 ( 0.0007817359430256297891, 0.0009771253907249958896, 0.001172514838424361990, 0.001367904286123728091, 0.001563293733823094191 ),
 .UNSPECIFIED. ) ;
#40201 = ORIENTED_EDGE ( 'NONE', *, *, #57195, .T. ) ;
#40202 = FACE_OUTER_BOUND ( 'NONE', #86, .T. ) ;
#40203 = CARTESIAN_POINT ( 'NONE',  ( 11.66898697669518548, -6.808710257144161559, 34.95449254468098843 ) ) ;
#40204 = EDGE_LOOP ( 'NONE', ( #29351, #45286, #68695, #61350, #40527, #61016 ) ) ;
#40205 = CARTESIAN_POINT ( 'NONE',  ( 0.4615384615383396616, -4.481592998941358097, 33.73612834414048933 ) ) ;
#40206 = CARTESIAN_POINT ( 'NONE',  ( -6.066082379360135945, -2.292212530054419606, 30.41441678777542634 ) ) ;
#40207 = CARTESIAN_POINT ( 'NONE',  ( -6.923076923077045919, -12.51329471203414379, 31.30864560766407578 ) ) ;
#40208 = DIRECTION ( 'NONE',  ( -0.000000000000000000, -0.8660254037844399289, -0.4999999999999980016 ) ) ;
#40209 = DIRECTION ( 'NONE',  ( -0.000000000000000000, 0.3420201433256694346, -0.9396926207859080948 ) ) ;
#40210 = ORIENTED_EDGE ( 'NONE', *, *, #58232, .F. ) ;
#40211 = FACE_BOUND ( 'NONE', #13216, .T. ) ;
#40212 = ORIENTED_EDGE ( 'NONE', *, *, #23919, .T. ) ;
#40213 = CARTESIAN_POINT ( 'NONE',  ( 17.07692307692307665, -3.513871655860378418, 32.76840700105978499 ) ) ;
#40214 = VECTOR ( 'NONE', #9015, 1000.000000000000000 ) ;
#40215 = CARTESIAN_POINT ( 'NONE',  ( -12.33101302330481808, -3.068774925481847493, 32.56582465632704526 ) ) ;
#40216 = CARTESIAN_POINT ( 'NONE',  ( 6.000000000000001776, -8.973038597847269315, 34.52809138561121927 ) ) ;
#40217 = CARTESIAN_POINT ( 'NONE',  ( 8.769230769230768274, -1.117168528481311540, 33.14645433367849847 ) ) ;
#40218 = DIRECTION ( 'NONE',  ( 0.000000000000000000, 0.7660444431189822323, -0.6427876096865344779 ) ) ;
#40219 = VERTEX_POINT ( 'NONE', #65389 ) ;
#40220 = EDGE_LOOP ( 'NONE', ( #81422, #88755 ) ) ;
#40221 = ORIENTED_EDGE ( 'NONE', *, *, #9040, .F. ) ;
#40222 = ORIENTED_EDGE ( 'NONE', *, *, #61599, .F. ) ;
#40223 = DIRECTION ( 'NONE',  ( 1.000000000000000000, 0.000000000000000000, 0.000000000000000000 ) ) ;
#40224 = CARTESIAN_POINT ( 'NONE',  ( -6.222926217516146608, -12.39988816332205701, 30.74660775122750778 ) ) ;
#40225 = CARTESIAN_POINT ( 'NONE',  ( -7.846153846153965716, -10.21337939537710326, 33.94971097300076224 ) ) ;
#40226 = CARTESIAN_POINT ( 'NONE',  ( -7.846153846153844924, -3.322132147404559976, 32.92929555188717927 ) ) ;
#40228 = EDGE_CURVE ( 'NONE', #8255, #15080, #75427, .T. ) ;
#40227 = DIRECTION ( 'NONE',  ( 0.000000000000000000, 0.9848077530122072432, -0.1736481776669354937 ) ) ;
#40229 = VECTOR ( 'NONE', #2669, 1000.000000000000000 ) ;
#40230 = VECTOR ( 'NONE', #79086, 1000.000000000000000 ) ;
#40231 = CARTESIAN_POINT ( 'NONE',  ( -5.300408020647025431, -8.496056993536548418, 34.65000542017679663 ) ) ;
#40232 = FACE_OUTER_BOUND ( 'NONE', #66826, .T. ) ;
#40233 = CARTESIAN_POINT ( 'NONE',  ( -8.519176349317316266, -2.920487667080175598, 32.31805714834170828 ) ) ;
#40234 = ORIENTED_EDGE ( 'NONE', *, *, #45402, .F. ) ;
#40235 = VERTEX_POINT ( 'NONE', #59077 ) ;
#40236 = ORIENTED_EDGE ( 'NONE', *, *, #27051, .F. ) ;
#40237 = VECTOR ( 'NONE', #87426, 1000.000000000000000 ) ;
#40239 = ORIENTED_EDGE ( 'NONE', *, *, #53430, .T. ) ;
#40238 = CARTESIAN_POINT ( 'NONE',  ( -11.53846153846153655, -12.37446782046654192, 30.86335684631486131 ) ) ;
#40241 = CARTESIAN_POINT ( 'NONE',  ( -9.915234651214539952, -4.026226216239094491, 33.68668979543634379 ) ) ;
#40240 = CARTESIAN_POINT ( 'NONE',  ( -1.634638608836843421, -2.588893531581426544, 31.60682220781847818 ) ) ;
#40242 = AXIS2_PLACEMENT_3D ( 'NONE', #23664, #56573, #84063 ) ;
#40243 = CARTESIAN_POINT ( 'NONE',  ( -11.53846153846153655, -4.786620604624113540, 33.94971097300155094 ) ) ;
#40244 = CARTESIAN_POINT ( 'NONE',  ( -15.36091720050092846, -10.31621877034669588, 34.18098118002070152 ) ) ;
#40245 = FACE_BOUND ( 'NONE', #60524, .T. ) ;
#40246 = EDGE_LOOP ( 'NONE', ( #17928, #65871, #44148, #76882 ) ) ;
#40247 = EDGE_CURVE ( 'NONE', #48730, #11070, #85168, .T. ) ;
#40248 = FACE_OUTER_BOUND ( 'NONE', #28469, .T. ) ;
#40249 = DIRECTION ( 'NONE',  ( -0.000000000000000000, -0.7660444431189791237, -0.6427876096865379196 ) ) ;
#40250 = EDGE_LOOP ( 'NONE', ( #8968, #23993 ) ) ;
#40251 = DIRECTION ( 'NONE',  ( -0.000000000000000000, 0.8660254037844397068, -0.4999999999999978906 ) ) ;
#40252 = ORIENTED_EDGE ( 'NONE', *, *, #79741, .F. ) ;
#40253 = FACE_BOUND ( 'NONE', #33232, .T. ) ;
#40254 = CARTESIAN_POINT ( 'NONE',  ( -10.83831157429146330, -2.889293201056495786, 32.26117774369186009 ) ) ;
#40255 = DIRECTION ( 'NONE',  ( 0.000000000000000000, 0.000000000000000000, 1.000000000000000000 ) ) ;
#40256 = ORIENTED_EDGE ( 'NONE', *, *, #24576, .T. ) ;
#40257 = DIRECTION ( 'NONE',  ( -1.000000000000000000, -0.000000000000000000, -0.000000000000000000 ) ) ;
#40258 = DIRECTION ( 'NONE',  ( -0.000000000000000000, 0.5000000000000011102, -0.8660254037844381525 ) ) ;
#40259 = CARTESIAN_POINT ( 'NONE',  ( -0.5916864312701585193, -2.373036134822905208, 30.88089517874951540 ) ) ;
#40260 = ORIENTED_EDGE ( 'NONE', *, *, #62348, .T. ) ;
#40261 = DIRECTION ( 'NONE',  ( -1.000000000000000000, 0.000000000000000000, 0.000000000000000000 ) ) ;
#40262 = CARTESIAN_POINT ( 'NONE',  ( 3.230769230769231726, -3.322132147404559976, 32.92929555188717927 ) ) ;
#40263 = CARTESIAN_POINT ( 'NONE',  ( 18.24994540937804643, -10.92531984108285492, 33.72920026020278073 ) ) ;
#40264 = CYLINDRICAL_SURFACE ( 'NONE', #11686, 0.2499999999999979738 ) ;
#40265 = ORIENTED_EDGE ( 'NONE', *, *, #47490, .F. ) ;
#40266 = B_SPLINE_CURVE_WITH_KNOTS ( 'NONE', 3,
 ( #59336, #37282, #72845, #30966, #17916, #17021, #9818, #31426, #86393, #51669 ),
 .UNSPECIFIED., .F., .F.,
 ( 4, 2, 2, 2, 4 ),
 ( 0.000000000000000000, 0.0001954311564186865221, 0.0003908623128373730441, 0.0005862934692560595662, 0.0007817246256747460882 ),
 .UNSPECIFIED. ) ;
#40267 = B_SPLINE_CURVE_WITH_KNOTS ( 'NONE', 3,
 ( #58269, #30363, #2435, #23160, #57833, #78543, #78105, #77658, #50627, #83994 ),
 .UNSPECIFIED., .F., .F.,
 ( 4, 2, 2, 2, 4 ),
 ( 0.0007817359430256320659, 0.0009771253907249987086, 0.001172514838424365243, 0.001367904286123731994, 0.001563293733823098528 ),
 .UNSPECIFIED. ) ;
#40268 = CARTESIAN_POINT ( 'NONE',  ( -2.307692307692305711, -13.37000171582298513, 34.34916445242398453 ) ) ;
#40269 = CARTESIAN_POINT ( 'NONE',  ( 2.530471976670375600, -3.563462043263030399, 33.22394488606062879 ) ) ;
#40270 = VERTEX_POINT ( 'NONE', #17662 ) ;
#40271 = CARTESIAN_POINT ( 'NONE',  ( 18.13052570176355971, -6.852161475712351013, 34.70806712695775786 ) ) ;
#40272 = DIRECTION ( 'NONE',  ( -0.000000000000000000, 1.000000000000000000, -0.000000000000000000 ) ) ;
#40273 = CARTESIAN_POINT ( 'NONE',  ( -14.55771553191376633, -2.588893531581426988, 31.60682220781847818 ) ) ;
#40274 = CARTESIAN_POINT ( 'NONE',  ( 16.21991348719623360, -11.91647553114624358, 32.58852847137148245 ) ) ;
#40275 = CARTESIAN_POINT ( 'NONE',  ( 0.2386115026316125431, -2.523278758544489797, 31.42238647778637528 ) ) ;
#40276 = EDGE_CURVE ( 'NONE', #47301, #72614, #50965, .T. ) ;
#40277 = EDGE_CURVE ( 'NONE', #36504, #1046, #65824, .T. ) ;
#40278 = DIRECTION ( 'NONE',  ( 1.000000000000000000, 0.000000000000000000, 0.000000000000000000 ) ) ;
#40280 = CARTESIAN_POINT ( 'NONE',  ( -17.07692307692307665, -8.120952969808772792, 34.71129190930000163 ) ) ;
#40279 = CARTESIAN_POINT ( 'NONE',  ( -24.00000000000000000, 9.000000000000024869, 29.25000000000000000 ) ) ;
#40281 = CARTESIAN_POINT ( 'NONE',  ( 0.4615384615384611200, -4.661471528628507777, 34.16647553114623292 ) ) ;
#40282 = VECTOR ( 'NONE', #83708, 1000.000000000000000 ) ;
#40283 = CARTESIAN_POINT ( 'NONE',  ( -1.944543648262992530, -9.444543648263016067, 19.93750000000000000 ) ) ;
#40284 = ORIENTED_EDGE ( 'NONE', *, *, #34899, .T. ) ;
#40285 = DIRECTION ( 'NONE',  ( -0.000000000000000000, 1.000000000000000000, -0.000000000000000000 ) ) ;
#40286 = ORIENTED_EDGE ( 'NONE', *, *, #11829, .T. ) ;
#40287 = ORIENTED_EDGE ( 'NONE', *, *, #1802, .F. ) ;
#40288 = CARTESIAN_POINT ( 'NONE',  ( -3.164701897419154530, -9.058645607665452459, 34.76329471203371924 ) ) ;
#40289 = VERTEX_POINT ( 'NONE', #23948 ) ;
#40290 = CARTESIAN_POINT ( 'NONE',  ( -0.3589743589743593088, -7.500000000000000000, 33.75000000000000000 ) ) ;
#40291 = CARTESIAN_POINT ( 'NONE',  ( 2.750000000000008438, -8.639087296525996607, 22.04687500000000000 ) ) ;
#40292 = CARTESIAN_POINT ( 'NONE',  ( -14.05774689831426372, -2.986452184633680229, 32.43230066228895225 ) ) ;
#40293 = CARTESIAN_POINT ( 'NONE',  ( -15.23076923076935252, -12.51329471203414379, 31.30864560766407578 ) ) ;
#40294 = CYLINDRICAL_SURFACE ( 'NONE', #50425, 0.2500000000000004996 ) ;
#40295 = CARTESIAN_POINT ( 'NONE',  ( -5.010855743573001675, -2.486705287966279876, 31.30864560766543647 ) ) ;
#40296 = CARTESIAN_POINT ( 'NONE',  ( -15.29685161012936589, -4.661471528628507777, 34.16647553114621871 ) ) ;
#40297 = CYLINDRICAL_SURFACE ( 'NONE', #16627, 0.2499999999999995559 ) ;
#40298 = CARTESIAN_POINT ( 'NONE',  ( 6.673053698855467175, -12.45566812827425096, 31.48439005359158926 ) ) ;
#40299 = DIRECTION ( 'NONE',  ( -0.000000000000000000, -0.5000000000000009992, -0.8660254037844380415 ) ) ;
#40300 = CARTESIAN_POINT ( 'NONE',  ( -4.153846153846274980, -12.16647553114689728, 32.15551576947799362 ) ) ;
#40301 = CARTESIAN_POINT ( 'NONE',  ( 6.000000000000001776, -3.322132147404559976, 32.92929555188717927 ) ) ;
#40302 = B_SPLINE_CURVE_WITH_KNOTS ( 'NONE', 3,
 ( #72527, #31548, #19366, #17601, #12172, #38307, #39656, #67118, #5416, #87858 ),
 .UNSPECIFIED., .F., .F.,
 ( 4, 2, 2, 2, 4 ),
 ( 0.0007817246256747528103, 0.0009771112852218970073, 0.001172497944769041421, 0.001367884604316185835, 0.001563271263863330032 ),
 .UNSPECIFIED. ) ;
#40303 = AXIS2_PLACEMENT_3D ( 'NONE', #32182, #46137, #73628 ) ;
#40304 = VECTOR ( 'NONE', #31248, 999.9999999999998863 ) ;
#40305 = EDGE_LOOP ( 'NONE', ( #908, #72 ) ) ;
#40306 = VERTEX_POINT ( 'NONE', #10458 ) ;
#40307 = CARTESIAN_POINT ( 'NONE',  ( -8.769230769230768274, -12.37446782046654192, 30.86335684631486131 ) ) ;
#40308 = CARTESIAN_POINT ( 'NONE',  ( 15.36129466900287532, -12.15418822224088657, 32.17964115625579069 ) ) ;
#40309 = LINE ( 'NONE', #641, #2291 ) ;
#40310 = CARTESIAN_POINT ( 'NONE',  ( 6.223375485772421278, -2.251407671071270489, 29.88021292934942252 ) ) ;
#40311 = AXIS2_PLACEMENT_3D ( 'NONE', #88275, #19347, #25658 ) ;
#40312 = CARTESIAN_POINT ( 'NONE',  ( 6.065255571276025215, -5.219633306516380244, 34.19971097300157936 ) ) ;
#40313 = CARTESIAN_POINT ( 'NONE',  ( -6.065270445960775803, -8.613356846314824011, 34.62446782046655613 ) ) ;
#40314 = DIRECTION ( 'NONE',  ( -0.000000000000000000, -0.3420201433256694346, -0.9396926207859080948 ) ) ;
#40315 = ORIENTED_EDGE ( 'NONE', *, *, #13935, .T. ) ;
#40316 = CARTESIAN_POINT ( 'NONE',  ( 1.318531973659506251, -4.786620604624113540, 33.94971097300155805 ) ) ;
#40317 = EDGE_LOOP ( 'NONE', ( #10448, #67140 ) ) ;
#40318 = ORIENTED_EDGE ( 'NONE', *, *, #25018, .F. ) ;
#40319 = CARTESIAN_POINT ( 'NONE',  ( -14.53051900017131359, -7.369208160676171460, 34.74850200257122879 ) ) ;
#40320 = CARTESIAN_POINT ( 'NONE',  ( 0.4615384615384611200, -12.09954503811598769, 35.62045528018868623 ) ) ;
#40321 = CARTESIAN_POINT ( 'NONE',  ( -17.07692307692319744, -10.90142922262034020, 33.41473453929536674 ) ) ;
#40322 = CARTESIAN_POINT ( 'NONE',  ( 6.250054419913455561, -8.346898887586323923, 34.93166121998716278 ) ) ;
#40323 = CARTESIAN_POINT ( 'NONE',  ( -17.93474486048716088, -12.51329471203373700, 31.30864560766537963 ) ) ;
#40324 = EDGE_CURVE ( 'NONE', #72998, #31746, #64624, .T. ) ;
#40325 = EDGE_LOOP ( 'NONE', ( #12416, #2605 ) ) ;
#40326 = ORIENTED_EDGE ( 'NONE', *, *, #41996, .T. ) ;
#40327 = ORIENTED_EDGE ( 'NONE', *, *, #15778, .F. ) ;
#40328 = ORIENTED_EDGE ( 'NONE', *, *, #81286, .T. ) ;
#40329 = FACE_OUTER_BOUND ( 'NONE', #85479, .T. ) ;
#40330 = CARTESIAN_POINT ( 'NONE',  ( 17.99999999999987566, -11.48612834414049644, 32.76840700105863391 ) ) ;
#40331 = AXIS2_PLACEMENT_3D ( 'NONE', #73282, #11585, #3917 ) ;
#40332 = CARTESIAN_POINT ( 'NONE',  ( 4.219913487196229163, -11.91647553114624358, 32.58852847137148245 ) ) ;
#40334 = EDGE_CURVE ( 'NONE', #40827, #40441, #80769, .T. ) ;
#40333 = CARTESIAN_POINT ( 'NONE',  ( -16.15384615384615330, -2.292212530054420494, 30.41441678777542634 ) ) ;
#40335 = CARTESIAN_POINT ( 'NONE',  ( 9.320512820512821150, -1.926643599941765039, 29.65000000000000213 ) ) ;
#40336 = CARTESIAN_POINT ( 'NONE',  ( -10.36533030374630293, -12.17597550085003633, 31.52189283813461884 ) ) ;
#40337 = ORIENTED_EDGE ( 'NONE', *, *, #55873, .F. ) ;
#40338 = ADVANCED_FACE ( 'NONE', ( #58626 ), #45116, .F. ) ;
#40339 = ORIENTED_EDGE ( 'NONE', *, *, #60659, .F. ) ;
#40340 = ORIENTED_EDGE ( 'NONE', *, *, #5689, .T. ) ;
#40342 = EDGE_LOOP ( 'NONE', ( #410, #16748 ) ) ;
#40341 = DIRECTION ( 'NONE',  ( -0.000000000000000000, 0.3420201433256694346, -0.9396926207859080948 ) ) ;
#40343 = CYLINDRICAL_SURFACE ( 'NONE', #21801, 0.2499999999999994726 ) ;
#40344 = CARTESIAN_POINT ( 'NONE',  ( -12.21159305216042057, -12.07971442181322175, 32.31769673815850297 ) ) ;
#40345 = CARTESIAN_POINT ( 'NONE',  ( -2.651650429449535551, -10.15165042944956753, 19.93750000000000000 ) ) ;
#40346 = ORIENTED_EDGE ( 'NONE', *, *, #41092, .F. ) ;
#40347 = AXIS2_PLACEMENT_3D ( 'NONE', #34026, #87222, #61491 ) ;
#40348 = ADVANCED_FACE ( 'NONE', ( #4126 ), #31614, .F. ) ;
#40349 = CARTESIAN_POINT ( 'NONE',  ( -12.46153846153858247, -11.48612834414049644, 32.76840700105863391 ) ) ;
#40350 = ORIENTED_EDGE ( 'NONE', *, *, #10864, .T. ) ;
#40351 = CYLINDRICAL_SURFACE ( 'NONE', #1079, 0.2499999999999994726 ) ;
#40352 = FACE_BOUND ( 'NONE', #46942, .T. ) ;
#40353 = B_SPLINE_CURVE_WITH_KNOTS ( 'NONE', 3,
 ( #14785, #29194, #53655, #35043, #82804, #39714, #62071, #8023, #69718, #81142 ),
 .UNSPECIFIED., .F., .F.,
 ( 4, 2, 2, 2, 4 ),
 ( 0.0007817246256747451124, 0.0009771112852218881168, 0.001172497944769031230, 0.001367884604316174126, 0.001563271263863317238 ),
 .UNSPECIFIED. ) ;
#40355 = AXIS2_PLACEMENT_3D ( 'NONE', #15680, #62084, #69730 ) ;
#40354 = FACE_OUTER_BOUND ( 'NONE', #55905, .T. ) ;
#40356 = AXIS2_PLACEMENT_3D ( 'NONE', #49206, #7779, #48756 ) ;
#40357 = ADVANCED_FACE ( 'NONE', ( #73043 ), #11339, .F. ) ;
#40358 = DIRECTION ( 'NONE',  ( 0.000000000000000000, 1.000000000000000000, 0.000000000000000000 ) ) ;
#40359 = ORIENTED_EDGE ( 'NONE', *, *, #70151, .F. ) ;
#40360 = DIRECTION ( 'NONE',  ( -1.000000000000000000, 0.000000000000000000, 0.000000000000000000 ) ) ;
#40361 = CARTESIAN_POINT ( 'NONE',  ( -11.00641025641025550, -3.499999999999999556, 29.75000000000000355 ) ) ;
#40362 = AXIS2_PLACEMENT_3D ( 'NONE', #79451, #4225, #59164 ) ;
#40363 = CARTESIAN_POINT ( 'NONE',  ( -3.230769230769229949, -9.058645607665452459, 34.76329471203371924 ) ) ;
#40364 = ORIENTED_EDGE ( 'NONE', *, *, #12940, .T. ) ;
#40365 = VECTOR ( 'NONE', #53069, 1000.000000000000227 ) ;
#40366 =( GEOMETRIC_REPRESENTATION_CONTEXT ( 3 ) GLOBAL_UNCERTAINTY_ASSIGNED_CONTEXT ( ( #64461 ) ) GLOBAL_UNIT_ASSIGNED_CONTEXT ( ( #82359, #33720, #53986 ) ) REPRESENTATION_CONTEXT ( 'NONE', 'WORKASPACE' ) );
#40367 = CYLINDRICAL_SURFACE ( 'NONE', #40127, 0.2500000000000012212 ) ;
#40368 = CARTESIAN_POINT ( 'NONE',  ( -3.903791733932700847, -10.06805714834173848, 34.32951233291982618 ) ) ;
#40369 = CARTESIAN_POINT ( 'NONE',  ( -4.023320715612507925, -2.372941743896878286, 30.88044141588254377 ) ) ;
#40370 = CARTESIAN_POINT ( 'NONE',  ( -2.437839517130526268, -10.88202310037936194, 33.43294751532457099 ) ) ;
#40371 = CARTESIAN_POINT ( 'NONE',  ( 8.900021210197715860, -9.929761469519743144, 34.40412654351204225 ) ) ;
#40372 = EDGE_CURVE ( 'NONE', #78354, #33346, #88802, .T. ) ;
#40373 = FACE_BOUND ( 'NONE', #43746, .T. ) ;
#40375 = CARTESIAN_POINT ( 'NONE',  ( 4.153846153846030731, -12.70778746994576025, 30.41441678777401236 ) ) ;
#40374 = CARTESIAN_POINT ( 'NONE',  ( 5.776515075435670887, -4.988325925672468131, 34.36044203135681130 ) ) ;
#40376 = CARTESIAN_POINT ( 'NONE',  ( 2.057715563643717438, -10.06842814019191401, 34.32929386961144758 ) ) ;
#40378 = DIRECTION ( 'NONE',  ( -1.000000000000000000, -0.000000000000000000, 0.000000000000000000 ) ) ;
#40377 = CARTESIAN_POINT ( 'NONE',  ( 7.846153846153846700, -6.435427911321262684, 35.78748833219616898 ) ) ;
#40379 = EDGE_CURVE ( 'NONE', #9486, #34081, #75947, .T. ) ;
#40380 = CARTESIAN_POINT ( 'NONE',  ( 6.223012844093394946, -4.762714258010880997, 34.23016756924214832 ) ) ;
#40381 = CARTESIAN_POINT ( 'NONE',  ( 1.200186371490561621, -10.22469193450123193, 15.70125670625848890 ) ) ;
#40382 = ORIENTED_EDGE ( 'NONE', *, *, #74200, .T. ) ;
#40383 = CARTESIAN_POINT ( 'NONE',  ( -5.076923076923075762, -12.34228464037088635, 31.77849191805839268 ) ) ;
#40384 = EDGE_LOOP ( 'NONE', ( #66902, #32258 ) ) ;
#40385 = DIRECTION ( 'NONE',  ( -0.000000000000000000, 1.000000000000000000, -0.000000000000000000 ) ) ;
#40386 = EDGE_CURVE ( 'NONE', #45661, #35777, #3468, .T. ) ;
#40387 = EDGE_LOOP ( 'NONE', ( #69143, #49513, #86435, #22538, #83871 ) ) ;
#40388 = EDGE_CURVE ( 'NONE', #21202, #79737, #19593, .T. ) ;
#40389 = CARTESIAN_POINT ( 'NONE',  ( 16.40390057375961064, -12.65882529074907126, 30.72640787790838601 ) ) ;
#40390 = DIRECTION ( 'NONE',  ( 1.000000000000000000, 0.000000000000000000, 0.000000000000000000 ) ) ;
#40392 = ORIENTED_EDGE ( 'NONE', *, *, #43621, .F. ) ;
#40391 = CARTESIAN_POINT ( 'NONE',  ( -5.076923076923075762, -9.058645607665452459, 34.76329471203371924 ) ) ;
#40393 = DIRECTION ( 'NONE',  ( -0.000000000000000000, 1.000000000000000000, -0.000000000000000000 ) ) ;
#40394 = FACE_OUTER_BOUND ( 'NONE', #37391, .T. ) ;
#40395 = CARTESIAN_POINT ( 'NONE',  ( -2.749999999999997780, -7.561099074964547917, 17.34188170625849068 ) ) ;
#40396 = LINE ( 'NONE', #33181, #76287 ) ;
#40397 = CARTESIAN_POINT ( 'NONE',  ( 2.307692307692187583, -9.442884908241554243, 34.35708131394783038 ) ) ;
#40398 = CARTESIAN_POINT ( 'NONE',  ( 0.3891064303782384992, -4.777307027835201225, 28.92407589458995432 ) ) ;
#40399 = CARTESIAN_POINT ( 'NONE',  ( 4.088575707885377497, -11.94971097300153140, 32.03036669348370680 ) ) ;
#40400 = CARTESIAN_POINT ( 'NONE',  ( -12.46153846153846168, -8.164416787775445883, 34.95778746994557906 ) ) ;
#40401 = CARTESIAN_POINT ( 'NONE',  ( 1.449870524128224591, -10.33852847137154107, 34.16647553114620450 ) ) ;
#40402 = B_SPLINE_CURVE_WITH_KNOTS ( 'NONE', 3,
 ( #36708, #79025, #85346, #22740, #29515, #71818, #1595, #84027, #23631, #43906 ),
 .UNSPECIFIED., .F., .F.,
 ( 4, 2, 2, 2, 4 ),
 ( 0.0007817246336856289524, 0.0009771112958940101571, 0.001172497958102391253, 0.001367884620310772350, 0.001563271282519153446 ),
 .UNSPECIFIED. ) ;
#40403 = CARTESIAN_POINT ( 'NONE',  ( 1.614399933863618797, -3.775308065498751198, 21.98624329374151642 ) ) ;
#40404 = CARTESIAN_POINT ( 'NONE',  ( -24.00000000000000000, -9.499999999999982236, 27.25000000000000000 ) ) ;
#40405 = CYLINDRICAL_SURFACE ( 'NONE', #47073, 0.2499999999999994726 ) ;
#40406 = VERTEX_POINT ( 'NONE', #25747 ) ;
#40407 = VECTOR ( 'NONE', #84940, 1000.000000000000114 ) ;
#40408 = CARTESIAN_POINT ( 'NONE',  ( 17.07692307692295586, -2.892918686052165622, 31.69288490824153470 ) ) ;
#40409 = DIRECTION ( 'NONE',  ( 0.000000000000000000, 0.000000000000000000, -1.000000000000000000 ) ) ;
#40410 = CARTESIAN_POINT ( 'NONE',  ( 3.775308065498752086, -6.007798216065404873, 17.14249329374151287 ) ) ;
#40411 = CARTESIAN_POINT ( 'NONE',  ( -17.77722045873158763, -12.44528174975671853, 30.48912976160715615 ) ) ;
#40412 = CYLINDRICAL_SURFACE ( 'NONE', #51231, 0.2499999999999994726 ) ;
#40413 = EDGE_LOOP ( 'NONE', ( #39860, #24216 ) ) ;
#40414 = CYLINDRICAL_SURFACE ( 'NONE', #45711, 0.2499999999999995559 ) ;
#40415 = CARTESIAN_POINT ( 'NONE',  ( -14.53117725141625094, -11.41268669641500466, 32.86336882939237825 ) ) ;
#40417 = ORIENTED_EDGE ( 'NONE', *, *, #34034, .T. ) ;
#40416 = CARTESIAN_POINT ( 'NONE',  ( -16.15384615384615330, -12.34228464037088635, 31.77849191805839268 ) ) ;
#40418 = CARTESIAN_POINT ( 'NONE',  ( -6.923076923076922462, -4.102666532097928531, 36.13435417666054406 ) ) ;
#40419 = CARTESIAN_POINT ( 'NONE',  ( 5.143089683514715738, -7.250054591869668386, 34.99404684341514127 ) ) ;
#40420 = CARTESIAN_POINT ( 'NONE',  ( -12.59222906464877134, -4.684245665217972032, 34.18127051446801090 ) ) ;
#40421 = EDGE_LOOP ( 'NONE', ( #68197, #78652 ) ) ;
#40422 = CARTESIAN_POINT ( 'NONE',  ( 2.241609928332173762, -3.937682226553329556, 33.60647404775217240 ) ) ;
#40423 = EDGE_CURVE ( 'NONE', #75445, #28787, #68070, .T. ) ;
#40424 = CARTESIAN_POINT ( 'NONE',  ( 6.792385456409367528, -4.809359713505814149, 33.96456829005828837 ) ) ;
#40426 = CARTESIAN_POINT ( 'NONE',  ( -13.31936024510254768, -8.656820664281605460, 34.87096338111211224 ) ) ;
#40425 = AXIS2_PLACEMENT_3D ( 'NONE', #25398, #33044, #46556 ) ;
#40427 = EDGE_LOOP ( 'NONE', ( #75654, #42220, #47719, #35683 ) ) ;
#40428 = ORIENTED_EDGE ( 'NONE', *, *, #12529, .F. ) ;
#40429 = EDGE_LOOP ( 'NONE', ( #6203, #39424, #37912, #15782 ) ) ;
#40430 = EDGE_LOOP ( 'NONE', ( #66209, #55844, #70530, #16754 ) ) ;
#40431 = VECTOR ( 'NONE', #23976, 1000.000000000000227 ) ;
#40432 = VECTOR ( 'NONE', #22953, 1000.000000000000000 ) ;
#40433 = EDGE_CURVE ( 'NONE', #25506, #85233, #28203, .T. ) ;
#40434 = CARTESIAN_POINT ( 'NONE',  ( 5.076923076923075762, -12.34228464037088635, 31.77849191805839268 ) ) ;
#40435 = CYLINDRICAL_SURFACE ( 'NONE', #87518, 2.000000000000001776 ) ;
#40436 = CARTESIAN_POINT ( 'NONE',  ( 1.653273178848927064E-15, -7.500000000000000000, 14.00000000000000178 ) ) ;
#40437 = LINE ( 'NONE', #41757, #86982 ) ;
#40438 = CIRCLE ( 'NONE', #27496, 3.000000000000000444 ) ;
#40439 = EDGE_CURVE ( 'NONE', #74505, #66117, #9775, .T. ) ;
#40440 = CARTESIAN_POINT ( 'NONE',  ( 5.299934428535925335, -5.667800583137508674, 34.40243808032445827 ) ) ;
#40441 = VERTEX_POINT ( 'NONE', #74830 ) ;
#40442 = B_SPLINE_CURVE_WITH_KNOTS ( 'NONE', 3,
 ( #50842, #78331, #5236, #87673, #32700, #64807, #5675, #23387, #71133, #25946 ),
 .UNSPECIFIED., .F., .F.,
 ( 4, 2, 2, 2, 4 ),
 ( 0.0007817359430256293554, 0.0009771253907249941549, 0.001172514838424358954, 0.001367904286123723537, 0.001563293733823095276 ),
 .UNSPECIFIED. ) ;
#40443 = ORIENTED_EDGE ( 'NONE', *, *, #14812, .F. ) ;
#40444 = ORIENTED_EDGE ( 'NONE', *, *, #44490, .T. ) ;
#40446 = EDGE_LOOP ( 'NONE', ( #2998, #62054, #10047, #41783 ) ) ;
#40445 = DIRECTION ( 'NONE',  ( -0.000000000000000000, -0.5000000000000009992, -0.8660254037844380415 ) ) ;
#40447 = CYLINDRICAL_SURFACE ( 'NONE', #43055, 0.2500000000000008882 ) ;
#40448 = CARTESIAN_POINT ( 'NONE',  ( -3.361459833879538284, -11.93127051446800024, 32.56575433478200665 ) ) ;
#40449 = EDGE_CURVE ( 'NONE', #13183, #42562, #59523, .T. ) ;
#40450 = FACE_OUTER_BOUND ( 'NONE', #50405, .T. ) ;
#40451 = CARTESIAN_POINT ( 'NONE',  ( 15.90382292962469535, -11.56360843649121861, 33.07473185843129926 ) ) ;
#40452 = ORIENTED_EDGE ( 'NONE', *, *, #4573, .T. ) ;
#40453 = EDGE_CURVE ( 'NONE', #45514, #23762, #7792, .T. ) ;
#40454 = VERTEX_POINT ( 'NONE', #13557 ) ;
#40455 = VERTEX_POINT ( 'NONE', #6374 ) ;
#40456 = CARTESIAN_POINT ( 'NONE',  ( -10.74553258511631348, -11.04286588640298561, 33.62463336215343901 ) ) ;
#40458 = EDGE_LOOP ( 'NONE', ( #26417, #26737, #50187, #66287 ) ) ;
#40457 = LINE ( 'NONE', #40012, #18576 ) ;
#40459 = CARTESIAN_POINT ( 'NONE',  ( 9.442284455014730682, -11.86270091957321249, 32.19358267280087915 ) ) ;
#40460 = DIRECTION ( 'NONE',  ( 1.000000000000000000, 0.000000000000000000, 0.000000000000000000 ) ) ;
#40461 = ORIENTED_EDGE ( 'NONE', *, *, #23163, .T. ) ;
#40462 = CARTESIAN_POINT ( 'NONE',  ( -17.07692307692307665, -8.973038597847269315, 34.52809138561121927 ) ) ;
#40463 = VECTOR ( 'NONE', #11027, 1000.000000000000000 ) ;
#40464 = CARTESIAN_POINT ( 'NONE',  ( -17.77698864838715309, -2.554770724473667709, 30.48948780036025852 ) ) ;
#40465 = CARTESIAN_POINT ( 'NONE',  ( 4.403900465484468896, -2.779044189368096163, 31.39831045268886456 ) ) ;
#40466 = FACE_BOUND ( 'NONE', #84618, .T. ) ;
#40467 = CARTESIAN_POINT ( 'NONE',  ( 17.07692307692295586, -2.892918686052165622, 31.69288490824153470 ) ) ;
#40468 = CARTESIAN_POINT ( 'NONE',  ( -6.222926958906846551, -12.38737895849757820, 31.66785238281580206 ) ) ;
#40469 = CARTESIAN_POINT ( 'NONE',  ( -10.48485917715097138, -11.04252011169590020, 33.62494198852677130 ) ) ;
#40471 = CARTESIAN_POINT ( 'NONE',  ( 17.07692307692307665, -8.973038597847269315, 34.52809138561121927 ) ) ;
#40470 = LINE ( 'NONE', #12541, #34555 ) ;
#40472 = DIRECTION ( 'NONE',  ( -0.000000000000000000, 0.9848077530122086864, -0.1736481776669273891 ) ) ;
#40473 = CARTESIAN_POINT ( 'NONE',  ( 6.923076923077231548, -2.506253911140614576, 30.00000000000323297 ) ) ;
#40474 = VERTEX_POINT ( 'NONE', #20322 ) ;
#40475 = LINE ( 'NONE', #46774, #38967 ) ;
#40476 = CARTESIAN_POINT ( 'NONE',  ( 0.2380535369741281215, -10.97335522853832579, 33.68706563782419749 ) ) ;
#40477 = ORIENTED_EDGE ( 'NONE', *, *, #75668, .T. ) ;
#40478 = CARTESIAN_POINT ( 'NONE',  ( -6.700065571464073777, -4.887748414852792322, 34.01359900205216746 ) ) ;
#40479 = CARTESIAN_POINT ( 'NONE',  ( 16.08776377448601735, -2.292212530054419606, 30.41441678777542634 ) ) ;
#40480 = CARTESIAN_POINT ( 'NONE',  ( -7.780898706641008467, -2.379036618887895305, 30.90682066428158592 ) ) ;
#40481 = ORIENTED_EDGE ( 'NONE', *, *, #47455, .F. ) ;
#40482 = CARTESIAN_POINT ( 'NONE',  ( -16.08777780284371772, -11.16473453929635440, 33.15142922261926373 ) ) ;
#40483 = CARTESIAN_POINT ( 'NONE',  ( 6.792928953345229282, -8.630895178749536711, 34.87696386517710323 ) ) ;
#40484 = EDGE_CURVE ( 'NONE', #13555, #24183, #87027, .T. ) ;
#40485 = FACE_BOUND ( 'NONE', #45195, .T. ) ;
#40487 = CARTESIAN_POINT ( 'NONE',  ( -17.07692307692276046, -2.255955759149395501, 30.00000000000324363 ) ) ;
#40486 = CARTESIAN_POINT ( 'NONE',  ( -18.22292621751613240, -3.105860786376063221, 32.13614157043599562 ) ) ;
#40488 = CARTESIAN_POINT ( 'NONE',  ( 8.096099364501986528, -9.272278438253398036, 34.42582936511637115 ) ) ;
#40489 = CIRCLE ( 'NONE', #28986, 4.000000000000000000 ) ;
#40490 = CYLINDRICAL_SURFACE ( 'NONE', #85597, 4.000000000000000000 ) ;
#40491 = CARTESIAN_POINT ( 'NONE',  ( -14.53057182442989337, -7.630690623152299956, 34.99857592706774057 ) ) ;
#40492 = CARTESIAN_POINT ( 'NONE',  ( 2.608446859217893099, -4.805146000318787358, 15.31063170625849068 ) ) ;
#40493 = ORIENTED_EDGE ( 'NONE', *, *, #74804, .T. ) ;
#40494 = EDGE_CURVE ( 'NONE', #73366, #61830, #32801, .T. ) ;
#40495 = AXIS2_PLACEMENT_3D ( 'NONE', #87787, #81458, #81902 ) ;
#40496 = EDGE_LOOP ( 'NONE', ( #30917, #78220 ) ) ;
#40497 = CARTESIAN_POINT ( 'NONE',  ( 5.010840697562940704, -10.67929555188718460, 33.92786785259543336 ) ) ;
#40498 = EDGE_CURVE ( 'NONE', #79559, #53989, #23885, .T. ) ;
#40499 = CARTESIAN_POINT ( 'NONE',  ( -17.77722033102192967, -3.563462043263028178, 33.22394488606062879 ) ) ;
#40500 = CARTESIAN_POINT ( 'NONE',  ( 16.28437159207979334, -3.068774925481847937, 32.56582465632704526 ) ) ;
#40501 = CARTESIAN_POINT ( 'NONE',  ( 10.86533002476265786, -2.986452184633680673, 32.43230066228895225 ) ) ;
#40502 = CARTESIAN_POINT ( 'NONE',  ( -15.23076923076922995, -13.20930481340135110, 34.54067556320372745 ) ) ;
#40503 = CARTESIAN_POINT ( 'NONE',  ( 3.749999999999992006, -5.946699141100872943, 20.64062500000000000 ) ) ;
#40504 = AXIS2_PLACEMENT_3D ( 'NONE', #23635, #57418, #16882 ) ;
#40505 = CARTESIAN_POINT ( 'NONE',  ( 5.076923076923075762, -1.629998284177014645, 34.34916445242399163 ) ) ;
#40506 = CARTESIAN_POINT ( 'NONE',  ( 8.769230769230768274, -9.819645486525091727, 36.12317359536749706 ) ) ;
#40507 = DIRECTION ( 'NONE',  ( -1.000000000000000000, 0.000000000000000000, -0.000000000000000000 ) ) ;
#40508 = CARTESIAN_POINT ( 'NONE',  ( -18.00000000000012079, -11.94971097300221352, 32.03036669348236387 ) ) ;
#40509 = CARTESIAN_POINT ( 'NONE',  ( -17.07692307692307665, -1.044019251281081972, 31.83374038241031911 ) ) ;
#40510 = CARTESIAN_POINT ( 'NONE',  ( -2.307692307692305711, -13.75783147151868846, 33.36296068462461051 ) ) ;
#40511 = CARTESIAN_POINT ( 'NONE',  ( -17.78205128205128105, -11.50000000000000000, 29.75000000000000355 ) ) ;
#40512 = CARTESIAN_POINT ( 'NONE',  ( -8.703163435880695076, -11.35647404775217595, 33.31231777344666511 ) ) ;
#40513 = CARTESIAN_POINT ( 'NONE',  ( -16.82686865700962642, -2.920487667080175154, 32.31805714834170828 ) ) ;
#40514 = EDGE_CURVE ( 'NONE', #62375, #48447, #44276, .T. ) ;
#40515 = VERTEX_POINT ( 'NONE', #82914 ) ;
#40516 = CARTESIAN_POINT ( 'NONE',  ( -4.946397375159510723, -11.93748526763465279, 32.05452791011430946 ) ) ;
#40517 = PLANE ( 'NONE',  #87765 ) ;
#40518 = CARTESIAN_POINT ( 'NONE',  ( -1.077988221561493543, -4.724691934501247914, 14.32999329374151465 ) ) ;
#40519 = CARTESIAN_POINT ( 'NONE',  ( 4.087763774486018242, -4.661471528628507777, 34.16647553114621871 ) ) ;
#40520 = CYLINDRICAL_SURFACE ( 'NONE', #47591, 0.2499999999999994726 ) ;
#40521 = EDGE_CURVE ( 'NONE', #40709, #77395, #55812, .T. ) ;
#40522 = CARTESIAN_POINT ( 'NONE',  ( -2.307692307692428724, -8.656820664282941280, 34.87096338111179961 ) ) ;
#40524 = ORIENTED_EDGE ( 'NONE', *, *, #77846, .T. ) ;
#40523 = CARTESIAN_POINT ( 'NONE',  ( -5.750000000000062172, -7.565270000091922853, 34.99999999999999289 ) ) ;
#40525 = CARTESIAN_POINT ( 'NONE',  ( 2.750000000000001776, -7.499999999999984013, 21.96875000000000355 ) ) ;
#40526 = CARTESIAN_POINT ( 'NONE',  ( 17.75002326905764960, -3.627789207965226304, 32.91389620160131102 ) ) ;
#40527 = ORIENTED_EDGE ( 'NONE', *, *, #11285, .F. ) ;
#40528 = CARTESIAN_POINT ( 'NONE',  ( 11.78840694783958476, -9.357781135181031829, 34.66075350412533851 ) ) ;
#40529 = DIRECTION ( 'NONE',  ( -0.000000000000000000, -0.8660254037844397068, -0.4999999999999978906 ) ) ;
#40530 = ORIENTED_EDGE ( 'NONE', *, *, #61583, .F. ) ;
#40531 = AXIS2_PLACEMENT_3D ( 'NONE', #47211, #83114, #31938 ) ;
#40532 = CARTESIAN_POINT ( 'NONE',  ( 17.07692307692295586, -11.48612834414049644, 32.76840700105863391 ) ) ;
#40533 = EDGE_CURVE ( 'NONE', #66377, #10085, #76545, .T. ) ;
#40534 = CARTESIAN_POINT ( 'NONE',  ( 0.4615384615384611200, -2.721908614388771852, 31.22303859784724978 ) ) ;
#40535 = DIRECTION ( 'NONE',  ( 0.000000000000000000, 0.6427876096865368094, 0.7660444431189802339 ) ) ;
#40536 = ORIENTED_EDGE ( 'NONE', *, *, #77379, .F. ) ;
#40537 = ORIENTED_EDGE ( 'NONE', *, *, #81186, .F. ) ;
#40538 = EDGE_CURVE ( 'NONE', #84649, #14645, #42815, .T. ) ;
#40540 = ORIENTED_EDGE ( 'NONE', *, *, #50599, .T. ) ;
#40539 = B_SPLINE_CURVE_WITH_KNOTS ( 'NONE', 3,
 ( #23279, #85877, #44874, #30481, #30914, #16087, #64700, #51616, #43551, #72352 ),
 .UNSPECIFIED., .F., .F.,
 ( 4, 2, 2, 2, 4 ),
 ( 0.000000000000000000, 0.0001954339857564090194, 0.0003908679715128180387, 0.0005863019572692270039, 0.0007817359430256360774 ),
 .UNSPECIFIED. ) ;
#40541 = CARTESIAN_POINT ( 'NONE',  ( -15.09997878980228059, -3.957578996910242619, 33.62503395064540257 ) ) ;
#40542 = DIRECTION ( 'NONE',  ( 1.000000000000000000, 0.000000000000000000, 0.000000000000000000 ) ) ;
#40543 = CARTESIAN_POINT ( 'NONE',  ( 9.627037691751372250, -3.083524468853724443, 32.58852847137143272 ) ) ;
#40544 = CARTESIAN_POINT ( 'NONE',  ( -17.14300648787895653, -5.557115091759785130, 34.35708131394839171 ) ) ;
#40545 = CARTESIAN_POINT ( 'NONE',  ( -6.700297254098857458, -11.60474049983371003, 33.02348890104160262 ) ) ;
#40546 = CARTESIAN_POINT ( 'NONE',  ( 15.23076923076923173, -13.95598074871891292, 31.83374038241031911 ) ) ;
#40547 = CARTESIAN_POINT ( 'NONE',  ( 13.45068373561782593, -3.050289026998446840, 32.03036669348366416 ) ) ;
#40548 = EDGE_CURVE ( 'NONE', #1790, #34883, #65835, .T. ) ;
#40549 = CARTESIAN_POINT ( 'NONE',  ( 16.08776377448601735, -12.62096338111211580, 30.90682066428152908 ) ) ;
#40551 = EDGE_CURVE ( 'NONE', #6432, #3401, #87250, .T. ) ;
#40550 = VERTEX_POINT ( 'NONE', #34271 ) ;
#40552 = EDGE_LOOP ( 'NONE', ( #44838, #14366, #24952, #57264 ) ) ;
#40554 = VERTEX_POINT ( 'NONE', #63059 ) ;
#40553 = CARTESIAN_POINT ( 'NONE',  ( -0.4615384615384611200, -12.10708131394839349, 31.69288490824020244 ) ) ;
#40555 = VECTOR ( 'NONE', #88849, 1000.000000000000227 ) ;
#40556 = CARTESIAN_POINT ( 'NONE',  ( -13.16165225034871078, -7.369474539155828730, 34.99858011523957657 ) ) ;
#40557 = CARTESIAN_POINT ( 'NONE',  ( 6.130790440966950250, -9.929761469519744921, 34.40412654351204225 ) ) ;
#40558 = ORIENTED_EDGE ( 'NONE', *, *, #15608, .F. ) ;
#40559 = ADVANCED_FACE ( 'NONE', ( #69832 ), #491, .F. ) ;
#40560 = LINE ( 'NONE', #4539, #27218 ) ;
#40561 = AXIS2_PLACEMENT_3D ( 'NONE', #42614, #56123, #62416 ) ;
#40562 = EDGE_CURVE ( 'NONE', #41231, #47411, #40030, .T. ) ;
#40563 = ORIENTED_EDGE ( 'NONE', *, *, #16777, .T. ) ;
#40564 = CARTESIAN_POINT ( 'NONE',  ( 1.384615384615386802, -12.09954503811598769, 35.62045528018868623 ) ) ;
#40565 = ORIENTED_EDGE ( 'NONE', *, *, #67576, .F. ) ;
#40566 = CARTESIAN_POINT ( 'NONE',  ( 9.942362003946010773, -8.303483539816731707, 34.68545999027711702 ) ) ;
#40567 = ORIENTED_EDGE ( 'NONE', *, *, #47979, .F. ) ;
#40568 = CARTESIAN_POINT ( 'NONE',  ( -16.15384615384615330, -6.386643153685126251, 34.62446782046654192 ) ) ;
#40569 = CARTESIAN_POINT ( 'NONE',  ( 10.86533013373275658, -5.057305518903948638, 34.11320923018887896 ) ) ;
#40570 = FACE_BOUND ( 'NONE', #79884, .T. ) ;
#40571 = CARTESIAN_POINT ( 'NONE',  ( 6.000000000000001776, -2.292212530054420494, 30.41441678777542634 ) ) ;
#40572 = DIRECTION ( 'NONE',  ( 1.000000000000000000, 0.000000000000000000, 0.000000000000000000 ) ) ;
#40573 = CARTESIAN_POINT ( 'NONE',  ( -1.384615384615383471, -2.249999999999998668, 29.50000000000001421 ) ) ;
#40574 = CARTESIAN_POINT ( 'NONE',  ( 10.39189969082028675, -10.23692288466677880, 34.23039457007281072 ) ) ;
#40575 = CARTESIAN_POINT ( 'NONE',  ( -8.769230769230768274, -12.09954503811598769, 35.62045528018868623 ) ) ;
#40576 = CARTESIAN_POINT ( 'NONE',  ( -19.50000000000000000, -3.499999999999999556, 29.75000000000000355 ) ) ;
#40577 = CARTESIAN_POINT ( 'NONE',  ( -10.61538461538473399, -4.481592998941358097, 33.73612834414048933 ) ) ;
#40578 = VERTEX_POINT ( 'NONE', #71151 ) ;
#40579 = ORIENTED_EDGE ( 'NONE', *, *, #67426, .T. ) ;
#40581 = CARTESIAN_POINT ( 'NONE',  ( -18.13069060311030611, -9.929715669179222104, 34.40415004197138416 ) ) ;
#40580 = CARTESIAN_POINT ( 'NONE',  ( 2.307692307692309264, -10.51840700105979565, 33.73612834413961536 ) ) ;
#40582 = CARTESIAN_POINT ( 'NONE',  ( -4.403846153846151523, -7.500000000000001776, 35.00000000000000000 ) ) ;
#40583 = DIRECTION ( 'NONE',  ( 0.000000000000000000, 0.000000000000000000, 1.000000000000000000 ) ) ;
#40584 = DIRECTION ( 'NONE',  ( -0.000000000000000000, 1.000000000000000000, -0.000000000000000000 ) ) ;
#40585 = CARTESIAN_POINT ( 'NONE',  ( -13.38461538461538325, -13.95598074871891292, 31.83374038241031911 ) ) ;
#40586 = VERTEX_POINT ( 'NONE', #10791 ) ;
#40587 = DIRECTION ( 'NONE',  ( -0.000000000000000000, -0.7660444431189791237, -0.6427876096865379196 ) ) ;
#40588 = CARTESIAN_POINT ( 'NONE',  ( 11.60360731779350374, -7.750023238201979581, 34.74374492549440419 ) ) ;
#40589 = CARTESIAN_POINT ( 'NONE',  ( -14.17690186672535901, -12.35292014791297710, 31.75344720912887198 ) ) ;
#40590 = CARTESIAN_POINT ( 'NONE',  ( -19.50000000000000000, -11.50000000000000000, 29.75000000000000355 ) ) ;
#40591 = VECTOR ( 'NONE', #71184, 1000.000000000000114 ) ;
#40592 = ORIENTED_EDGE ( 'NONE', *, *, #77504, .T. ) ;
#40593 = EDGE_LOOP ( 'NONE', ( #44195, #22021 ) ) ;
#40594 = EDGE_CURVE ( 'NONE', #18500, #86292, #63613, .T. ) ;
#40595 = VERTEX_POINT ( 'NONE', #50432 ) ;
#40596 = CARTESIAN_POINT ( 'NONE',  ( 10.39245765647776309, -4.026226216239094491, 33.68668979543634379 ) ) ;
#40598 = ORIENTED_EDGE ( 'NONE', *, *, #54037, .T. ) ;
#40597 = EDGE_CURVE ( 'NONE', #85310, #75827, #55015, .T. ) ;
#40599 = CYLINDRICAL_SURFACE ( 'NONE', #30876, 0.2499999999999979738 ) ;
#40600 = CARTESIAN_POINT ( 'NONE',  ( 15.23076923076923173, -8.973038597847269315, 34.52809138561121927 ) ) ;
#40601 = CARTESIAN_POINT ( 'NONE',  ( 3.296836564119306701, -5.471508081941601098, 34.59228464037088457 ) ) ;
#40602 = CARTESIAN_POINT ( 'NONE',  ( 8.835298102580843249, -3.322132147404559976, 32.92929555188717927 ) ) ;
#40603 = B_SPLINE_CURVE_WITH_KNOTS ( 'NONE', 3,
 ( #26045, #33246, #10749, #4893, #65675, #39123, #59821, #60708, #31461, #18842 ),
 .UNSPECIFIED., .F., .F.,
 ( 4, 2, 2, 2, 4 ),
 ( 0.000000000000000000, 0.0001954339857564098054, 0.0003908679715128196108, 0.0005863019572692293891, 0.0007817359430256392216 ),
 .UNSPECIFIED. ) ;
#40604 = PLANE ( 'NONE',  #27344 ) ;
#40605 = ORIENTED_EDGE ( 'NONE', *, *, #2360, .T. ) ;
#40606 = EDGE_CURVE ( 'NONE', #69003, #59070, #63947, .T. ) ;
#40607 = CARTESIAN_POINT ( 'NONE',  ( -11.76128963609641964, -7.369209533119140509, 34.99857337881830688 ) ) ;
#40609 = ORIENTED_EDGE ( 'NONE', *, *, #54738, .T. ) ;
#40608 = CARTESIAN_POINT ( 'NONE',  ( -0.5268084620947810492, -5.941354392334500467, 34.76329471203369792 ) ) ;
#40610 = CARTESIAN_POINT ( 'NONE',  ( -5.142193077479395136, -2.379036618887870436, 30.90682066428147934 ) ) ;
#40611 = CARTESIAN_POINT ( 'NONE',  ( -2.437839517130527156, -9.418419913701741919, 34.36755862841477693 ) ) ;
#40612 = CARTESIAN_POINT ( 'NONE',  ( -3.230769230769352962, -10.33852847137269571, 34.16647553114546554 ) ) ;
#40613 = CARTESIAN_POINT ( 'NONE',  ( 9.942253210655835005, -10.76462480002816235, 33.53768742498949962 ) ) ;
#40614 = CARTESIAN_POINT ( 'NONE',  ( 13.31934538405906565, -4.320704448112771878, 33.92786785259540494 ) ) ;
#40615 = CARTESIAN_POINT ( 'NONE',  ( 18.22301135161285046, -2.554770724473668597, 30.48948780036025852 ) ) ;
#40616 = CARTESIAN_POINT ( 'NONE',  ( -0.5276208408985966214, -2.486705287966279876, 31.30864560766542937 ) ) ;
#40617 = EDGE_CURVE ( 'NONE', #11323, #3349, #72222, .T. ) ;
#40618 = CARTESIAN_POINT ( 'NONE',  ( 2.724691934501250135, -8.700186371490531201, 22.29874329374151642 ) ) ;
#40619 = EDGE_LOOP ( 'NONE', ( #74407, #40239, #45486, #3638, #40847 ) ) ;
#40620 = CARTESIAN_POINT ( 'NONE',  ( -7.146561847641256016, -10.97335522853832579, 33.68706563782419749 ) ) ;
#40621 = CARTESIAN_POINT ( 'NONE',  ( 1.384615384615386802, -9.058645607665452459, 34.76329471203371924 ) ) ;
#40622 = VECTOR ( 'NONE', #69822, 1000.000000000000000 ) ;
#40623 = AXIS2_PLACEMENT_3D ( 'NONE', #56260, #42318, #22906 ) ;
#40624 = EDGE_CURVE ( 'NONE', #77202, #54822, #18489, .T. ) ;
#40625 = CARTESIAN_POINT ( 'NONE',  ( 5.076923076923075762, -2.292212530054420494, 30.41441678777542634 ) ) ;
#40626 = VERTEX_POINT ( 'NONE', #65280 ) ;
#40627 = CARTESIAN_POINT ( 'NONE',  ( -12.59222992820601839, -11.71456829005830080, 32.44064028649416542 ) ) ;
#40628 = CARTESIAN_POINT ( 'NONE',  ( -12.68502340526241312, -3.236172620538810385, 32.36188796281390267 ) ) ;
#40629 = AXIS2_PLACEMENT_3D ( 'NONE', #78727, #11609, #4850 ) ;
#40630 = CARTESIAN_POINT ( 'NONE',  ( 10.61538461538461675, -4.661471528628507777, 34.16647553114623292 ) ) ;
#40631 = CARTESIAN_POINT ( 'NONE',  ( -7.846153846153844924, -2.900454961884010974, 35.62045528018868623 ) ) ;
#40632 = CARTESIAN_POINT ( 'NONE',  ( -0.4615384615384611200, -2.499999999999998668, 29.50000000000001066 ) ) ;
#40633 = ORIENTED_EDGE ( 'NONE', *, *, #78644, .F. ) ;
#40634 = CYLINDRICAL_SURFACE ( 'NONE', #66433, 0.2499999999999995559 ) ;
#40635 = CARTESIAN_POINT ( 'NONE',  ( -14.37377571864818648, -2.721908614388770964, 31.22303859784723912 ) ) ;
#40636 = CARTESIAN_POINT ( 'NONE',  ( -14.24152570110066307, -7.250054591869670162, 34.99404684341514127 ) ) ;
#40637 = VERTEX_POINT ( 'NONE', #31045 ) ;
#40638 = FACE_OUTER_BOUND ( 'NONE', #20521, .T. ) ;
#40639 = ADVANCED_FACE ( 'NONE', ( #2683 ), #17551, .F. ) ;
#40640 = EDGE_LOOP ( 'NONE', ( #32340, #10547 ) ) ;
#40641 = CARTESIAN_POINT ( 'NONE',  ( 12.59232890250541281, -12.35292014791297710, 31.75344720912887198 ) ) ;
#40642 = CARTESIAN_POINT ( 'NONE',  ( 11.60452887181161330, -6.343179335718452272, 34.87096338111212646 ) ) ;
#40643 = ORIENTED_EDGE ( 'NONE', *, *, #82132, .T. ) ;
#40644 = CARTESIAN_POINT ( 'NONE',  ( 12.39545505058257824, -3.513871655860377086, 32.76840700105978499 ) ) ;
#40645 = CARTESIAN_POINT ( 'NONE',  ( -14.55769230769230660, -2.249999999999998668, 29.75000000000000355 ) ) ;
#40646 = CARTESIAN_POINT ( 'NONE',  ( 13.38461538461538680, -6.386643153685126251, 34.62446782046654192 ) ) ;
#40647 = AXIS2_PLACEMENT_3D ( 'NONE', #14790, #29631, #42266 ) ;
#40648 = CARTESIAN_POINT ( 'NONE',  ( 1.384615384615386802, -6.343179335718451384, 34.87096338111211935 ) ) ;
#40649 = FACE_OUTER_BOUND ( 'NONE', #84256, .T. ) ;
#40650 = EDGE_CURVE ( 'NONE', #40554, #15501, #47412, .T. ) ;
#40651 = ORIENTED_EDGE ( 'NONE', *, *, #23986, .F. ) ;
#40652 = EDGE_CURVE ( 'NONE', #9053, #70948, #65720, .T. ) ;
#40653 = DIRECTION ( 'NONE',  ( -0.000000000000000000, 1.000000000000000000, -0.000000000000000000 ) ) ;
#40654 = ORIENTED_EDGE ( 'NONE', *, *, #27945, .T. ) ;
#40655 = CARTESIAN_POINT ( 'NONE',  ( -8.703975197954740395, -4.481592998940250538, 33.73612834413965089 ) ) ;
#40656 = CARTESIAN_POINT ( 'NONE',  ( -12.39628332202562433, -3.083524468853784839, 32.58852847137153930 ) ) ;
#40657 = DIRECTION ( 'NONE',  ( -1.000000000000000000, -0.000000000000000000, -0.000000000000000000 ) ) ;
#40658 = CYLINDRICAL_SURFACE ( 'NONE', #46393, 0.2499999999999986955 ) ;
#40659 = CARTESIAN_POINT ( 'NONE',  ( 5.999999999999880096, -5.219633306517616589, 34.19971097300220464 ) ) ;
#40660 = EDGE_CURVE ( 'NONE', #83423, #53882, #51795, .T. ) ;
#40661 = VERTEX_POINT ( 'NONE', #81927 ) ;
#40662 = ORIENTED_EDGE ( 'NONE', *, *, #52045, .T. ) ;
#40663 = ORIENTED_EDGE ( 'NONE', *, *, #66937, .F. ) ;
#40664 = PRODUCT_DEFINITION_SHAPE ( 'NONE', 'NONE',  #89184 ) ;
#40665 = EDGE_CURVE ( 'NONE', #21924, #7139, #80489, .T. ) ;
#40667 = ORIENTED_EDGE ( 'NONE', *, *, #13462, .T. ) ;
#40666 = EDGE_CURVE ( 'NONE', #87523, #74505, #79745, .T. ) ;
#40668 = CARTESIAN_POINT ( 'NONE',  ( 11.28846153846153832, -2.249999999999998668, 29.75000000000000355 ) ) ;
#40669 = CARTESIAN_POINT ( 'NONE',  ( -17.30040800148741198, -10.23692288466677880, 34.23039457007281072 ) ) ;
#40670 = B_SPLINE_CURVE_WITH_KNOTS ( 'NONE', 3,
 ( #62056, #55737, #21510, #6670, #54860, #6241 ),
 .UNSPECIFIED., .F., .F.,
 ( 4, 2, 4 ),
 ( 0.000000000000000000, 0.0001954784845028895374, 0.0003909569690057790748 ),
 .UNSPECIFIED. ) ;
#40671 = CARTESIAN_POINT ( 'NONE',  ( 1.515141086378952506, -3.816742781228458448, 33.13167719472716044 ) ) ;
#40672 = ADVANCED_FACE ( 'NONE', ( #60750 ), #52655, .F. ) ;
#40673 = CARTESIAN_POINT ( 'NONE',  ( -7.846153846153967493, -3.643525952248795718, 33.31231777344771672 ) ) ;
#40674 = VECTOR ( 'NONE', #27975, 1000.000000000000000 ) ;
#40675 = CARTESIAN_POINT ( 'NONE',  ( -5.207614543590632472, -10.54014554554150607, 33.71984207302941883 ) ) ;
#40676 = VECTOR ( 'NONE', #63897, 1000.000000000000000 ) ;
#40677 = CARTESIAN_POINT ( 'NONE',  ( -2.373775718648186484, -4.786620604624113540, 33.94971097300155805 ) ) ;
#40678 = CARTESIAN_POINT ( 'NONE',  ( -17.86950326799833633, -12.75000000000001066, 29.52694330344912643 ) ) ;
#40679 = CARTESIAN_POINT ( 'NONE',  ( -5.143006487878956534, -3.513871655860377086, 32.76840700105978499 ) ) ;
#40680 = ORIENTED_EDGE ( 'NONE', *, *, #85300, .T. ) ;
#40681 = EDGE_LOOP ( 'NONE', ( #50059, #37297 ) ) ;
#40682 = VECTOR ( 'NONE', #37410, 1000.000000000000000 ) ;
#40683 = EDGE_LOOP ( 'NONE', ( #13078, #84924, #23461, #57267 ) ) ;
#40684 = CARTESIAN_POINT ( 'NONE',  ( -8.769230769230768274, -1.044019251281081972, 31.83374038241031911 ) ) ;
#40686 = CARTESIAN_POINT ( 'NONE',  ( -9.692307692307814193, -4.320704448113951379, 33.92786785259630022 ) ) ;
#40685 = DIRECTION ( 'NONE',  ( 1.000000000000000000, 0.000000000000000000, 0.000000000000000000 ) ) ;
#40687 = DIRECTION ( 'NONE',  ( -0.000000000000000000, 0.5000000000000011102, -0.8660254037844380415 ) ) ;
#40688 = CARTESIAN_POINT ( 'NONE',  ( -15.23076923076935252, -10.33852847137269571, 34.16647553114546554 ) ) ;
#40689 = FACE_BOUND ( 'NONE', #42230, .T. ) ;
#40690 = EDGE_LOOP ( 'NONE', ( #47016, #18251 ) ) ;
#40691 = CARTESIAN_POINT ( 'NONE',  ( -1.134669866267242311, -2.824170634883621744, 31.52227843825337317 ) ) ;
#40692 = CARTESIAN_POINT ( 'NONE',  ( 3.164685819813352285, -10.51840700105979387, 33.73612834413961536 ) ) ;
#40693 = ORIENTED_EDGE ( 'NONE', *, *, #21182, .F. ) ;
#40694 = FACE_OUTER_BOUND ( 'NONE', #47949, .T. ) ;
#40695 = ORIENTED_EDGE ( 'NONE', *, *, #67606, .T. ) ;
#40696 = FACE_BOUND ( 'NONE', #49291, .T. ) ;
#40697 = ADVANCED_FACE ( 'NONE', ( #19330 ), #80598, .F. ) ;
#40698 = CARTESIAN_POINT ( 'NONE',  ( -5.076923076922769340, -2.506253911140614576, 30.00000000000323297 ) ) ;
#40699 = B_SPLINE_CURVE_WITH_KNOTS ( 'NONE', 3,
 ( #81120, #87440, #60831, #6350, #25722, #53632, #18525, #74356, #38793, #11314 ),
 .UNSPECIFIED., .F., .F.,
 ( 4, 2, 2, 2, 4 ),
 ( 0.000000000000000000, 0.0001954311564186858715, 0.0003908623128373717431, 0.0005862934692560576146, 0.0007817246256747434861 ),
 .UNSPECIFIED. ) ;
#40700 = EDGE_LOOP ( 'NONE', ( #587, #14476, #28906, #58056 ) ) ;
#40701 = CARTESIAN_POINT ( 'NONE',  ( -12.33074665371367651, -8.147973898785416225, 34.70805048591653730 ) ) ;
#40702 = DIRECTION ( 'NONE',  ( -1.000000000000000000, -0.000000000000000000, 0.000000000000000000 ) ) ;
#40703 = CARTESIAN_POINT ( 'NONE',  ( -4.946875641672624724, -7.723484941389743952, 34.99544897038808955 ) ) ;
#40704 = ORIENTED_EDGE ( 'NONE', *, *, #64805, .T. ) ;
#40705 = CARTESIAN_POINT ( 'NONE',  ( 6.792385456409363975, -5.582088688514999397, 34.36776431015576350 ) ) ;
#40706 = CARTESIAN_POINT ( 'NONE',  ( -7.596099426240392027, -8.346898887586323923, 34.93166121998716278 ) ) ;
#40707 = CARTESIAN_POINT ( 'NONE',  ( 6.923076923076924238, -12.37446782046654192, 30.86335684631486131 ) ) ;
#40708 = CARTESIAN_POINT ( 'NONE',  ( -7.846153846153844924, -2.721908614388771852, 31.22303859784724978 ) ) ;
#40709 = VERTEX_POINT ( 'NONE', #72934 ) ;
#40710 = B_SPLINE_CURVE_WITH_KNOTS ( 'NONE', 3,
 ( #84112, #27822, #49857, #77337, #15644, #48981, #2118, #29602, #358, #55290 ),
 .UNSPECIFIED., .F., .F.,
 ( 4, 2, 2, 2, 4 ),
 ( 0.0007817246256747453293, 0.0009771112852218889842, 0.001172497944769032531, 0.001367884604316176294, 0.001563271263863319840 ),
 .UNSPECIFIED. ) ;
#40711 = CARTESIAN_POINT ( 'NONE',  ( -5.076923076923199218, -5.094484230521993062, 34.41647553114689373 ) ) ;
#40712 = CARTESIAN_POINT ( 'NONE',  ( -15.23076923076922995, -4.098570777380720287, 33.41473453929634729 ) ) ;
#40713 = B_SPLINE_CURVE_WITH_KNOTS ( 'NONE', 3,
 ( #58833, #78666, #16084, #16520, #36361, #44416, #9335, #23275, #17415, #64249 ),
 .UNSPECIFIED., .F., .F.,
 ( 4, 2, 2, 2, 4 ),
 ( 0.000000000000000000, 0.0001954339857564099951, 0.0003908679715128199903, 0.0005863019572692300396, 0.0007817359430256399806 ),
 .UNSPECIFIED. ) ;
#40715 = ORIENTED_EDGE ( 'NONE', *, *, #59340, .T. ) ;
#40714 = CARTESIAN_POINT ( 'NONE',  ( 1.634669804528839476, -2.920487667080174710, 32.31805714834170828 ) ) ;
#40716 = LINE ( 'NONE', #68177, #8348 ) ;
#40717 = LINE ( 'NONE', #6481, #6637 ) ;
#40718 = CARTESIAN_POINT ( 'NONE',  ( -14.43838291080261271, -2.494641256782728966, 31.33461815524612959 ) ) ;
#40719 = CARTESIAN_POINT ( 'NONE',  ( -4.854143535654666941, -8.496831190052096971, 34.64984203495476578 ) ) ;
#40720 = CARTESIAN_POINT ( 'NONE',  ( 19.99999999999999289, -11.99999999999999467, 13.00000000000000178 ) ) ;
#40721 = CARTESIAN_POINT ( 'NONE',  ( 17.07692307692307665, -4.661471528628507777, 34.16647553114623292 ) ) ;
#40723 = CARTESIAN_POINT ( 'NONE',  ( -2.557692307692305267, -2.499999999999998668, 29.75000000000000355 ) ) ;
#40722 = DIRECTION ( 'NONE',  ( 1.000000000000000000, 0.000000000000000000, 0.000000000000000000 ) ) ;
#40724 = CARTESIAN_POINT ( 'NONE',  ( -6.923076923076922462, -2.721908614388771852, 31.22303859784724978 ) ) ;
#40725 = CARTESIAN_POINT ( 'NONE',  ( -2.750000000000007105, -6.360912703474006946, 18.92187500000000355 ) ) ;
#40726 = EDGE_LOOP ( 'NONE', ( #6084, #41388, #42603, #322 ) ) ;
#40727 = FACE_OUTER_BOUND ( 'NONE', #53783, .T. ) ;
#40728 = EDGE_LOOP ( 'NONE', ( #36856, #74190, #67016, #59674 ) ) ;
#40729 = ORIENTED_EDGE ( 'NONE', *, *, #12961, .F. ) ;
#40730 = DIRECTION ( 'NONE',  ( 0.000000000000000000, 0.1736481776669275834, 0.9848077530122086864 ) ) ;
#40731 = VERTEX_POINT ( 'NONE', #87360 ) ;
#40732 = CARTESIAN_POINT ( 'NONE',  ( -5.076923076923075762, -11.35647404775217417, 33.31231777344666511 ) ) ;
#40733 = CARTESIAN_POINT ( 'NONE',  ( -2.749999999999991562, -8.639087296526025028, 21.26562500000000000 ) ) ;
#40734 = CARTESIAN_POINT ( 'NONE',  ( 17.77651507543566112, -4.988325925672468131, 34.36044203135681130 ) ) ;
#40735 = LINE ( 'NONE', #42063, #36671 ) ;
#40736 = CARTESIAN_POINT ( 'NONE',  ( 11.53846153846153832, -8.973038597847269315, 34.52809138561121927 ) ) ;
#40737 = DIRECTION ( 'NONE',  ( 0.000000000000000000, 0.4999999999999960032, -0.8660254037844410391 ) ) ;
#40738 = FACE_OUTER_BOUND ( 'NONE', #31295, .T. ) ;
#40740 = EDGE_CURVE ( 'NONE', #83471, #48416, #18883, .T. ) ;
#40739 = CARTESIAN_POINT ( 'NONE',  ( 2.177000841024749889, -9.804603061927743113, 34.18744698557895845 ) ) ;
#40741 = CARTESIAN_POINT ( 'NONE',  ( 1.553300858899087311, -3.749999999999992006, 25.48437500000000000 ) ) ;
#40742 = CARTESIAN_POINT ( 'NONE',  ( 17.07692307692307665, -2.292212530054420494, 30.41441678777542634 ) ) ;
#40743 = CARTESIAN_POINT ( 'NONE',  ( -14.30769230769199929, -2.506253911140614576, 30.00000000000323297 ) ) ;
#40744 = CARTESIAN_POINT ( 'NONE',  ( 5.299935921016469820, -10.77377354290276301, 33.85451476688484718 ) ) ;
#40745 = AXIS2_PLACEMENT_3D ( 'NONE', #79464, #38928, #24951 ) ;
#40746 = VECTOR ( 'NONE', #58810, 1000.000000000000114 ) ;
#40747 = ORIENTED_EDGE ( 'NONE', *, *, #71798, .T. ) ;
#40748 = ORIENTED_EDGE ( 'NONE', *, *, #54458, .F. ) ;
#40749 = DIRECTION ( 'NONE',  ( -0.000000000000000000, 0.8660254037844399289, -0.4999999999999980016 ) ) ;
#40750 = CARTESIAN_POINT ( 'NONE',  ( 15.45378207486262667, -11.98016756924215009, 32.48728574198911190 ) ) ;
#40751 = CARTESIAN_POINT ( 'NONE',  ( -19.50000000000000000, -11.50000000000000000, 29.75000000000000355 ) ) ;
#40752 = CARTESIAN_POINT ( 'NONE',  ( 0.2115617174898691277, -10.06842814019191401, 34.32929386961144758 ) ) ;
#40753 = ADVANCED_FACE ( 'NONE', ( #53095 ), #39168, .F. ) ;
#40754 = CYLINDRICAL_SURFACE ( 'NONE', #367, 0.2500000000000009437 ) ;
#40755 = CIRCLE ( 'NONE', #47738, 0.2500000000000002220 ) ;
#40756 = CARTESIAN_POINT ( 'NONE',  ( -9.692307692307691624, -10.67929555188718282, 33.92786785259544047 ) ) ;
#40757 = DIRECTION ( 'NONE',  ( -0.000000000000000000, -0.3420201433256694901, -0.9396926207859082059 ) ) ;
#40758 = ADVANCED_FACE ( 'NONE', ( #12136 ), #26083, .F. ) ;
#40759 = ORIENTED_EDGE ( 'NONE', *, *, #77562, .F. ) ;
#40760 = CYLINDRICAL_SURFACE ( 'NONE', #15615, 0.2499999999999994726 ) ;
#40761 = VERTEX_POINT ( 'NONE', #81484 ) ;
#40762 = CARTESIAN_POINT ( 'NONE',  ( -14.05769230769087130, -7.500000000000155431, 34.75000000000007105 ) ) ;
#40763 = CARTESIAN_POINT ( 'NONE',  ( 15.45378207486262667, -3.395485233115139057, 33.02377354290275946 ) ) ;
#40764 = DIRECTION ( 'NONE',  ( -1.000000000000000000, -0.000000000000000000, -0.000000000000000000 ) ) ;
#40765 = B_SPLINE_CURVE_WITH_KNOTS ( 'NONE', 3,
 ( #37409, #1860, #84297, #30225, #29343, #17142, #64876, #85608, #17604, #29784 ),
 .UNSPECIFIED., .F., .F.,
 ( 4, 2, 2, 2, 4 ),
 ( 0.000000000000000000, 0.0001954311564186865492, 0.0003908623128373730983, 0.0005862934692560596746, 0.0007817246256747461966 ),
 .UNSPECIFIED. ) ;
#40766 = CARTESIAN_POINT ( 'NONE',  ( 14.30769230769231015, -1.129524287112498415, 32.06866353760679544 ) ) ;
#40767 = CARTESIAN_POINT ( 'NONE',  ( 5.999999999999880096, -2.892918686052165622, 31.69288490824153470 ) ) ;
#40768 = ORIENTED_EDGE ( 'NONE', *, *, #76895, .T. ) ;
#40769 = VECTOR ( 'NONE', #9064, 1000.000000000000114 ) ;
#40770 = VECTOR ( 'NONE', #57911, 1000.000000000000000 ) ;
#40771 = ORIENTED_EDGE ( 'NONE', *, *, #36461, .T. ) ;
#40772 = EDGE_CURVE ( 'NONE', #4390, #9985, #73838, .T. ) ;
#40773 = EDGE_CURVE ( 'NONE', #68727, #4543, #11236, .T. ) ;
#40774 = VERTEX_POINT ( 'NONE', #12574 ) ;
#40775 = EDGE_LOOP ( 'NONE', ( #81773, #74203, #82559, #51332 ) ) ;
#40776 = DIRECTION ( 'NONE',  ( -0.000000000000000000, -0.6427876096865404731, -0.7660444431189770143 ) ) ;
#40777 = CARTESIAN_POINT ( 'NONE',  ( -2.307692307692428724, -10.33852847137269571, 34.16647553114546554 ) ) ;
#40778 = CARTESIAN_POINT ( 'NONE',  ( 4.376625822824220080, -12.11081565061823717, 32.26097654155341843 ) ) ;
#40779 = CARTESIAN_POINT ( 'NONE',  ( -16.15384615384627409, -2.379036618888197285, 30.90682066428292885 ) ) ;
#40780 =( NAMED_UNIT ( * ) SI_UNIT ( $, .STERADIAN. ) SOLID_ANGLE_UNIT ( ) );
#40781 = CARTESIAN_POINT ( 'NONE',  ( -18.00000000000000000, -13.18701529485372070, 34.52197243641129631 ) ) ;
#40782 = VERTEX_POINT ( 'NONE', #67518 ) ;
#40783 = VERTEX_POINT ( 'NONE', #5815 ) ;
#40784 = EDGE_LOOP ( 'NONE', ( #83728, #12181 ) ) ;
#40786 = ORIENTED_EDGE ( 'NONE', *, *, #58741, .F. ) ;
#40785 = CARTESIAN_POINT ( 'NONE',  ( 11.47237812750566022, -8.973038597847271092, 34.52809138561120506 ) ) ;
#40787 = CARTESIAN_POINT ( 'NONE',  ( 10.61538461538461675, -12.37446782046654192, 30.86335684631486131 ) ) ;
#40788 = CARTESIAN_POINT ( 'NONE',  ( -12.23875879256039667, -12.11081565061824250, 32.26097654155340422 ) ) ;
#40789 = CARTESIAN_POINT ( 'NONE',  ( 3.750000000000000888, -7.499999999999978684, 20.71875000000000000 ) ) ;
#40790 = ORIENTED_EDGE ( 'NONE', *, *, #41534, .F. ) ;
#40791 = VECTOR ( 'NONE', #46524, 1000.000000000000000 ) ;
#40792 = FACE_OUTER_BOUND ( 'NONE', #63538, .T. ) ;
#40793 = ORIENTED_EDGE ( 'NONE', *, *, #60356, .F. ) ;
#40794 = DIRECTION ( 'NONE',  ( 1.000000000000000000, 0.000000000000000000, 0.000000000000000000 ) ) ;
#40795 = FACE_BOUND ( 'NONE', #73753, .T. ) ;
#40796 = CARTESIAN_POINT ( 'NONE',  ( -18.00000000000000000, -9.058645607665452459, 34.76329471203371924 ) ) ;
#40797 = AXIS2_PLACEMENT_3D ( 'NONE', #37543, #30791, #79439 ) ;
#40798 = B_SPLINE_CURVE_WITH_KNOTS ( 'NONE', 3,
 ( #9045, #2261, #8157, #35633, #63081, #83827, #50017, #515, #76158, #29756 ),
 .UNSPECIFIED., .F., .F.,
 ( 4, 2, 2, 2, 4 ),
 ( 0.0007817359430256221996, 0.0009771253907249863487, 0.001172514838424350498, 0.001367904286123714647, 0.001563293733823078796 ),
 .UNSPECIFIED. ) ;
#40799 = CARTESIAN_POINT ( 'NONE',  ( 3.230769230769231726, -9.058645607665452459, 34.76329471203371924 ) ) ;
#40800 = ORIENTED_EDGE ( 'NONE', *, *, #12535, .T. ) ;
#40801 = CARTESIAN_POINT ( 'NONE',  ( -9.692307692307691624, -4.661471528628507777, 34.16647553114623292 ) ) ;
#40802 = DIRECTION ( 'NONE',  ( -0.000000000000000000, 1.000000000000000000, -0.000000000000000000 ) ) ;
#40803 = CARTESIAN_POINT ( 'NONE',  ( -13.16118842275381340, -7.630147231320743018, 34.74852402298682819 ) ) ;
#40804 = CARTESIAN_POINT ( 'NONE',  ( 14.05771556364371833, -9.234221910056348293, 34.70572697212741531 ) ) ;
#40805 = ORIENTED_EDGE ( 'NONE', *, *, #55195, .T. ) ;
#40806 = CARTESIAN_POINT ( 'NONE',  ( -1.384615384615383471, -4.786620604624113540, 33.94971097300155094 ) ) ;
#40807 = CARTESIAN_POINT ( 'NONE',  ( -7.596099534515530216, -11.28795663066794575, 33.01431243580653785 ) ) ;
#40808 = CARTESIAN_POINT ( 'NONE',  ( 4.153846153846154188, -11.35647404775217417, 33.31231777344666511 ) ) ;
#40809 = CARTESIAN_POINT ( 'NONE',  ( -2.438383774359862866, -10.54014554554150607, 33.71984207302941883 ) ) ;
#40810 = LINE ( 'NONE', #87679, #22824 ) ;
#40811 = FACE_BOUND ( 'NONE', #11212, .T. ) ;
#40813 = CARTESIAN_POINT ( 'NONE',  ( 6.673076923076925127, -2.249999999999998668, 29.75000000000000355 ) ) ;
#40812 = CARTESIAN_POINT ( 'NONE',  ( -7.173100147298380413, -12.45566812827425096, 31.48439005359158926 ) ) ;
#40814 = CARTESIAN_POINT ( 'NONE',  ( -7.173053654019276415, -12.17611988154120972, 31.52148481390971213 ) ) ;
#40816 = CARTESIAN_POINT ( 'NONE',  ( -11.31544869436814338, -10.77377354290276124, 33.85451476688484718 ) ) ;
#40815 = CARTESIAN_POINT ( 'NONE',  ( -18.13014796973169851, -2.373036134822904319, 30.88089517874953316 ) ) ;
#40817 = CARTESIAN_POINT ( 'NONE',  ( -5.300408001487409315, -12.47654668319379567, 31.42292124445336654 ) ) ;
#40818 = CARTESIAN_POINT ( 'NONE',  ( 2.750000000000001332, -7.438900925035452083, 15.46688170625848713 ) ) ;
#40819 = ORIENTED_EDGE ( 'NONE', *, *, #37646, .T. ) ;
#40820 = CYLINDRICAL_SURFACE ( 'NONE', #46182, 0.2499999999999998890 ) ;
#40821 = ORIENTED_EDGE ( 'NONE', *, *, #60369, .F. ) ;
#40822 = CARTESIAN_POINT ( 'NONE',  ( 20.00000000000000000, -4.000000000000000000, 29.75000000000000355 ) ) ;
#40823 = ORIENTED_EDGE ( 'NONE', *, *, #10778, .F. ) ;
#40824 = DIRECTION ( 'NONE',  ( -0.000000000000000000, 0.9848077530122086864, -0.1736481776669273891 ) ) ;
#40825 = DIRECTION ( 'NONE',  ( 0.000000000000000000, 0.9396926207859126468, -0.3420201433256571111 ) ) ;
#40827 = VERTEX_POINT ( 'NONE', #33292 ) ;
#40826 = CARTESIAN_POINT ( 'NONE',  ( 5.076923076923075762, -1.242168528481310874, 33.36296068462461051 ) ) ;
#40828 = CARTESIAN_POINT ( 'NONE',  ( -18.00000000000012079, -2.625532179533778709, 30.86335684631627174 ) ) ;
#40829 = CARTESIAN_POINT ( 'NONE',  ( 2.724691934501235036, -6.299813628509441266, 16.63875670625849068 ) ) ;
#40830 = LINE ( 'NONE', #20983, #27360 ) ;
#40831 = CYLINDRICAL_SURFACE ( 'NONE', #83, 0.2499999999999986955 ) ;
#40832 = AXIS2_PLACEMENT_3D ( 'NONE', #27600, #60504, #33481 ) ;
#40833 = CARTESIAN_POINT ( 'NONE',  ( 16.85399685940693004, -12.39988816332205701, 30.74660775122750778 ) ) ;
#40834 = CARTESIAN_POINT ( 'NONE',  ( 10.54930223602447903, -2.486705287966279432, 31.30864560766542937 ) ) ;
#40835 = DIRECTION ( 'NONE',  ( 0.000000000000000000, 0.000000000000000000, 1.000000000000000000 ) ) ;
#40836 = ADVANCED_FACE ( 'NONE', ( #73383 ), #11690, .F. ) ;
#40837 = CARTESIAN_POINT ( 'NONE',  ( -5.933931648997560870, -10.51840700105979565, 33.73612834413962247 ) ) ;
#40838 = EDGE_CURVE ( 'NONE', #70678, #19537, #69047, .T. ) ;
#40839 = CARTESIAN_POINT ( 'NONE',  ( -3.775308065498748977, -8.992201783934593351, 21.51749329374151998 ) ) ;
#40840 = CARTESIAN_POINT ( 'NONE',  ( 14.30769230769218758, -6.026961402154118019, 34.52809138561165270 ) ) ;
#40841 = ORIENTED_EDGE ( 'NONE', *, *, #74086, .T. ) ;
#40842 = DIRECTION ( 'NONE',  ( -0.000000000000000000, 1.000000000000000000, 0.000000000000000000 ) ) ;
#40843 = CARTESIAN_POINT ( 'NONE',  ( -3.775308065498748977, -8.992201783934593351, 25.26749329374151642 ) ) ;
#40844 = ADVANCED_FACE ( 'NONE', ( #35948 ), #84147, .F. ) ;
#40845 = CARTESIAN_POINT ( 'NONE',  ( -16.02305571287920571, -12.35292014791297710, 31.75344720912887198 ) ) ;
#40846 = CARTESIAN_POINT ( 'NONE',  ( 17.14217864819909920, -11.94971097300157403, 32.03036669348361443 ) ) ;
#40847 = ORIENTED_EDGE ( 'NONE', *, *, #2502, .T. ) ;
#40848 = CARTESIAN_POINT ( 'NONE',  ( -18.00000000000012079, -2.892918686052166066, 31.69288490824153470 ) ) ;
#40849 = CARTESIAN_POINT ( 'NONE',  ( 3.165498784808455479, -3.835265460703609186, 33.15142922261924241 ) ) ;
#40851 = VERTEX_POINT ( 'NONE', #21083 ) ;
#40850 = LINE ( 'NONE', #14259, #69938 ) ;
#40852 = CARTESIAN_POINT ( 'NONE',  ( 8.703148389870632329, -5.471508081941602875, 34.59228464037088457 ) ) ;
#40853 = EDGE_CURVE ( 'NONE', #61249, #20169, #36657, .T. ) ;
#40854 = CARTESIAN_POINT ( 'NONE',  ( -2.102533092329708531, -5.360057338231124291, 13.56786352175840626 ) ) ;
#40855 = CARTESIAN_POINT ( 'NONE',  ( 6.988332062589762472, -12.16647553114626490, 32.15551576947920864 ) ) ;
#40856 = CARTESIAN_POINT ( 'NONE',  ( -16.82697755857492794, -2.824170634883621744, 31.52227843825337317 ) ) ;
#40857 = CARTESIAN_POINT ( 'NONE',  ( -18.00000000000000711, -12.74702886152665471, 29.99985851721553587 ) ) ;
#40858 = AXIS2_PLACEMENT_3D ( 'NONE', #48954, #6210, #27357 ) ;
#40859 = CARTESIAN_POINT ( 'NONE',  ( -8.769230769230768274, -2.249999999999998668, 29.75000000000001776 ) ) ;
#40860 = ADVANCED_FACE ( 'NONE', ( #28749 ), #21536, .F. ) ;
#40861 = VERTEX_POINT ( 'NONE', #61631 ) ;
#40862 = ORIENTED_EDGE ( 'NONE', *, *, #3500, .F. ) ;
#40863 = EDGE_LOOP ( 'NONE', ( #59144, #59033, #59858, #60962 ) ) ;
#40864 = VECTOR ( 'NONE', #19474, 1000.000000000000000 ) ;
#40865 = ORIENTED_EDGE ( 'NONE', *, *, #18031, .F. ) ;
#40866 = AXIS2_PLACEMENT_3D ( 'NONE', #7558, #26946, #14759 ) ;
#40867 = DIRECTION ( 'NONE',  ( 0.000000000000000000, 0.7660444431189822323, -0.6427876096865344779 ) ) ;
#40868 = DIRECTION ( 'NONE',  ( -1.000000000000000000, 0.000000000000000000, 0.000000000000000000 ) ) ;
#40869 = CARTESIAN_POINT ( 'NONE',  ( 9.823099500132483897, -4.809403383903225304, 33.96459661697924304 ) ) ;
#40870 = CARTESIAN_POINT ( 'NONE',  ( -7.846153846153967493, -11.06231777344772027, 33.60647404775119895 ) ) ;
#40871 = LINE ( 'NONE', #67455, #21896 ) ;
#40872 = B_SPLINE_CURVE_WITH_KNOTS ( 'NONE', 3,
 ( #40712, #27182, #54641, #20430, #80819, #47894, #19104, #46568, #75375, #13669 ),
 .UNSPECIFIED., .F., .F.,
 ( 4, 2, 2, 2, 4 ),
 ( 0.000000000000000000, 0.0001954339857564078267, 0.0003908679715128156535, 0.0005863019572692235344, 0.0007817359430256313069 ),
 .UNSPECIFIED. ) ;
#40873 = ORIENTED_EDGE ( 'NONE', *, *, #37918, .T. ) ;
#40874 = ADVANCED_FACE ( 'NONE', ( #56653 ), #89136, .F. ) ;
#40875 = ORIENTED_EDGE ( 'NONE', *, *, #59031, .F. ) ;
#40876 = ORIENTED_EDGE ( 'NONE', *, *, #69768, .T. ) ;
#40879 = ORIENTED_EDGE ( 'NONE', *, *, #19484, .T. ) ;
#40878 = EDGE_CURVE ( 'NONE', #57134, #49278, #29174, .T. ) ;
#40877 = CARTESIAN_POINT ( 'NONE',  ( -7.053224892808618307, -8.630895178749536711, 34.87696386517710323 ) ) ;
#40880 = CARTESIAN_POINT ( 'NONE',  ( -1.634638608836841200, -2.985938066672154445, 32.43141759479405550 ) ) ;
#40881 = DIRECTION ( 'NONE',  ( -0.000000000000000000, 0.6427876096865404731, -0.7660444431189770143 ) ) ;
#40882 = EDGE_CURVE ( 'NONE', #35898, #79443, #9848, .T. ) ;
#40883 = EDGE_CURVE ( 'NONE', #35887, #15372, #34613, .T. ) ;
#40884 = CARTESIAN_POINT ( 'NONE',  ( -12.23875892027004930, -12.24180327182772388, 31.33663988360758168 ) ) ;
#40885 = FACE_OUTER_BOUND ( 'NONE', #13636, .T. ) ;
#40886 = VERTEX_POINT ( 'NONE', #1259 ) ;
#40887 = ORIENTED_EDGE ( 'NONE', *, *, #31158, .T. ) ;
#40888 = AXIS2_PLACEMENT_3D ( 'NONE', #18311, #3114, #46664 ) ;
#40889 = ORIENTED_EDGE ( 'NONE', *, *, #45579, .T. ) ;
#40890 = CARTESIAN_POINT ( 'NONE',  ( -5.299801759351723263, -7.630691491037286056, 34.74850469731152458 ) ) ;
#40892 = ORIENTED_EDGE ( 'NONE', *, *, #38899, .F. ) ;
#40891 = CARTESIAN_POINT ( 'NONE',  ( -39.05038313613820122, -2.499999999999999556, 29.75000000000000355 ) ) ;
#40893 = CARTESIAN_POINT ( 'NONE',  ( -12.46153846153858247, -2.892918686052166066, 31.69288490824153470 ) ) ;
#40894 = DIRECTION ( 'NONE',  ( 0.000000000000000000, 0.3420201433256671586, 0.9396926207859089830 ) ) ;
#40895 = EDGE_LOOP ( 'NONE', ( #75970, #40382, #86427, #27694 ) ) ;
#40896 = CARTESIAN_POINT ( 'NONE',  ( -4.087777802843713282, -4.786620604624113540, 33.94971097300155805 ) ) ;
#40897 = CARTESIAN_POINT ( 'NONE',  ( 12.52679360105129724, -9.528491918058460186, 34.59228464037086326 ) ) ;
#40898 = FACE_BOUND ( 'NONE', #52055, .T. ) ;
#40899 = DIRECTION ( 'NONE',  ( -1.000000000000000000, -0.000000000000000000, -0.000000000000000000 ) ) ;
#40900 = DIRECTION ( 'NONE',  ( -0.000000000000000000, -0.8660254037844397068, -0.4999999999999978906 ) ) ;
#40901 = CARTESIAN_POINT ( 'NONE',  ( -23.50000000000000000, 9.000000000000024869, 32.75000000000000000 ) ) ;
#40903 = CARTESIAN_POINT ( 'NONE',  ( 4.946775867484853428, -10.19110544564092002, 33.96427741523702792 ) ) ;
#40902 = CARTESIAN_POINT ( 'NONE',  ( 9.469381474791543241, -3.105860786376062332, 32.13614157043599562 ) ) ;
#40904 = CARTESIAN_POINT ( 'NONE',  ( -3.903791842207838148, -2.779044189368096163, 31.39831045268886456 ) ) ;
#40905 = CARTESIAN_POINT ( 'NONE',  ( 12.71148387091650278, -2.986452184633680673, 32.43230066228895225 ) ) ;
#40906 = ORIENTED_EDGE ( 'NONE', *, *, #70455, .T. ) ;
#40907 = CYLINDRICAL_SURFACE ( 'NONE', #25948, 0.2499999999999973355 ) ;
#40908 = DIRECTION ( 'NONE',  ( 0.000000000000000000, -0.000000000000000000, -1.000000000000000000 ) ) ;
#40909 = ORIENTED_EDGE ( 'NONE', *, *, #58788, .F. ) ;
#40910 = CARTESIAN_POINT ( 'NONE',  ( 15.90386942290380290, -3.627789207965226304, 32.91389620160131102 ) ) ;
#40911 = CYLINDRICAL_SURFACE ( 'NONE', #13090, 0.2500000000000012212 ) ;
#40912 = ORIENTED_EDGE ( 'NONE', *, *, #68039, .T. ) ;
#40913 = ADVANCED_FACE ( 'NONE', ( #83702 ), #21985, .F. ) ;
#40914 = FACE_OUTER_BOUND ( 'NONE', #62451, .T. ) ;
#40915 = CARTESIAN_POINT ( 'NONE',  ( -15.23076923076922995, -12.62096338111211580, 30.90682066428153263 ) ) ;
#40916 = VECTOR ( 'NONE', #51832, 1000.000000000000114 ) ;
#40917 = FACE_BOUND ( 'NONE', #83432, .T. ) ;
#40919 = CARTESIAN_POINT ( 'NONE',  ( 1.326923076923075762, -3.499999999999999556, 29.75000000000000355 ) ) ;
#40918 = LINE ( 'NONE', #89124, #60533 ) ;
#40920 = CARTESIAN_POINT ( 'NONE',  ( 5.076923076923075762, -12.48256725967547354, 35.29906147534542527 ) ) ;
#40921 = CARTESIAN_POINT ( 'NONE',  ( 0.7114838709165038910, -4.932303261841488151, 34.32971442181322885 ) ) ;
#40923 = CARTESIAN_POINT ( 'NONE',  ( -10.61538461538461320, -11.35647404775217417, 33.31231777344666511 ) ) ;
#40922 = DIRECTION ( 'NONE',  ( 1.000000000000000000, 0.000000000000000000, 0.000000000000000000 ) ) ;
#40924 = CARTESIAN_POINT ( 'NONE',  ( 1.553300858899129944, -11.24999999999998934, 24.70312500000000000 ) ) ;
#40925 = ORIENTED_EDGE ( 'NONE', *, *, #54155, .T. ) ;
#40926 = VECTOR ( 'NONE', #76423, 1000.000000000000000 ) ;
#40927 = ORIENTED_EDGE ( 'NONE', *, *, #89074, .T. ) ;
#40928 = VECTOR ( 'NONE', #40278, 1000.000000000000000 ) ;
#40929 = CARTESIAN_POINT ( 'NONE',  ( -9.692307692307814193, -2.657715359629662544, 31.77849191805970364 ) ) ;
#40930 = CYLINDRICAL_SURFACE ( 'NONE', #55600, 0.2500000000000002220 ) ;
#40931 = CARTESIAN_POINT ( 'NONE',  ( 6.857323494763590155, -7.249945578846651806, 34.99404164642496795 ) ) ;
#40932 = B_SPLINE_CURVE_WITH_KNOTS ( 'NONE', 3,
 ( #22666, #72177, #37957, #77616, #15924, #16357, #43821, #71286, #10034, #9593 ),
 .UNSPECIFIED., .F., .F.,
 ( 4, 2, 2, 2, 4 ),
 ( 0.0007817359430256282712, 0.0009771253907249941549, 0.001172514838424359822, 0.001367904286123725706, 0.001563293733823091589 ),
 .UNSPECIFIED. ) ;
#40933 = CARTESIAN_POINT ( 'NONE',  ( -1.384615384615383471, -13.75783147151868846, 33.36296068462461051 ) ) ;
#40934 = CARTESIAN_POINT ( 'NONE',  ( 7.846153846153723244, -12.16647553114689728, 32.15551576947799362 ) ) ;
#40935 = CARTESIAN_POINT ( 'NONE',  ( -1.614399933863656544, -3.775308065498769405, 17.57625670625849068 ) ) ;
#40936 = EDGE_CURVE ( 'NONE', #58918, #37595, #46396, .T. ) ;
#40937 = CARTESIAN_POINT ( 'NONE',  ( -12.71151520558705172, -4.075325502946081535, 33.72974371597206300 ) ) ;
#40938 = CARTESIAN_POINT ( 'NONE',  ( 1.161688425708536032, -10.01117774369187252, 34.36070679894347535 ) ) ;
#40939 = CARTESIAN_POINT ( 'NONE',  ( -19.50000000000000000, -3.499999999999999556, 29.75000000000000355 ) ) ;
#40940 = CARTESIAN_POINT ( 'NONE',  ( 10.86543903529806521, -3.435999193479609914, 33.07426656108010832 ) ) ;
#40941 = CARTESIAN_POINT ( 'NONE',  ( -4.946132635956126400, -6.369690395747422684, 34.87708834333098196 ) ) ;
#40942 = CARTESIAN_POINT ( 'NONE',  ( 13.16168916709923664, -4.186968288167450147, 33.49512374952580274 ) ) ;
#40943 = CARTESIAN_POINT ( 'NONE',  ( -3.360917200500924906, -10.31621877034669588, 34.18098118002070152 ) ) ;
#40944 = CARTESIAN_POINT ( 'NONE',  ( -3.480745961711584346, -8.303909089506435137, 34.68538101551103381 ) ) ;
#40945 = DIRECTION ( 'NONE',  ( 0.000000000000000000, 0.000000000000000000, -1.000000000000000000 ) ) ;
#40946 = VERTEX_POINT ( 'NONE', #2579 ) ;
#40947 = CARTESIAN_POINT ( 'NONE',  ( 1.161689167099237752, -2.554751324335734264, 30.48935550225260727 ) ) ;
#40948 = CARTESIAN_POINT ( 'NONE',  ( -3.296039676730006640, -3.835265460703609186, 33.15142922261924241 ) ) ;
#40949 = CARTESIAN_POINT ( 'NONE',  ( 1.200186371490529202, -4.775308065498752974, 19.48624329374152353 ) ) ;
#40950 = EDGE_CURVE ( 'NONE', #79461, #72151, #28032, .T. ) ;
#40951 = CARTESIAN_POINT ( 'NONE',  ( -9.915792616872023402, -10.97335522853832579, 33.68706563782419749 ) ) ;
#40952 = CARTESIAN_POINT ( 'NONE',  ( 5.076923076923075762, -11.16473453929635440, 33.15142922261926373 ) ) ;
#40953 = CARTESIAN_POINT ( 'NONE',  ( 10.55011416942384095, -6.026961402152685388, 34.52809138561120506 ) ) ;
#40955 = ORIENTED_EDGE ( 'NONE', *, *, #32130, .T. ) ;
#40954 = DIRECTION ( 'NONE',  ( -0.000000000000000000, 0.8660254037844397068, -0.4999999999999978906 ) ) ;
#40956 = CARTESIAN_POINT ( 'NONE',  ( 1.799775606325937360E-14, -10.25000000000000000, 24.78125000000000000 ) ) ;
#40957 = CARTESIAN_POINT ( 'NONE',  ( 17.99999999999987566, -3.835265460704628815, 33.15142922262033665 ) ) ;
#40958 = EDGE_CURVE ( 'NONE', #42418, #42284, #3300, .T. ) ;
#40959 = ORIENTED_EDGE ( 'NONE', *, *, #21630, .F. ) ;
#40960 = CARTESIAN_POINT ( 'NONE',  ( -11.40841648254176732, -2.254550872974305342, 29.97347326024527092 ) ) ;
#40961 = AXIS2_PLACEMENT_3D ( 'NONE', #86927, #52656, #80143 ) ;
#40962 = CARTESIAN_POINT ( 'NONE',  ( -11.53846153846153655, -6.343179335718451384, 34.87096338111211935 ) ) ;
#40963 = VERTEX_POINT ( 'NONE', #49888 ) ;
#40964 = CARTESIAN_POINT ( 'NONE',  ( 7.716006636715624367, -4.460286881179643004, 33.72017969459903242 ) ) ;
#40965 = CARTESIAN_POINT ( 'NONE',  ( 12.46153846153846168, -13.88283147151868846, 33.14645433367849847 ) ) ;
#40966 = CARTESIAN_POINT ( 'NONE',  ( 23.49999999999999645, -1.749999999999996447, 28.00000000000000000 ) ) ;
#40967 = ADVANCED_FACE ( 'NONE', ( #85901 ), #71049, .F. ) ;
#40968 = ORIENTED_EDGE ( 'NONE', *, *, #72138, .T. ) ;
#40969 = ORIENTED_EDGE ( 'NONE', *, *, #5655, .T. ) ;
#40970 = CARTESIAN_POINT ( 'NONE',  ( 17.86930939688968678, -9.929715669179216775, 34.40415004197138416 ) ) ;
#40971 = B_SPLINE_CURVE_WITH_KNOTS ( 'NONE', 3,
 ( #62430, #56577, #14262, #55241, #84066, #43505, #49809, #747, #42627, #83624 ),
 .UNSPECIFIED., .F., .F.,
 ( 4, 2, 2, 2, 4 ),
 ( 0.0007817359430256390048, 0.0009771253907250078159, 0.001172514838424376735, 0.001367904286123745655, 0.001563293733823114574 ),
 .UNSPECIFIED. ) ;
#40972 = VERTEX_POINT ( 'NONE', #3022 ) ;
#40973 = EDGE_CURVE ( 'NONE', #14205, #31293, #78244, .T. ) ;
#40974 = CARTESIAN_POINT ( 'NONE',  ( 6.000000000000001776, -12.09954503811598769, 35.62045528018868623 ) ) ;
#40975 = DIRECTION ( 'NONE',  ( 0.000000000000000000, 0.8660254037844377084, 0.5000000000000015543 ) ) ;
#40976 = CARTESIAN_POINT ( 'NONE',  ( -10.61538461538473399, -2.625532179533778709, 30.86335684631627174 ) ) ;
#40977 = ADVANCED_FACE ( 'NONE', ( #2146 ), #57974, .F. ) ;
#40978 = CARTESIAN_POINT ( 'NONE',  ( -6.792551484843279752, -11.66157788607254275, 32.95092075102925833 ) ) ;
#40979 = LINE ( 'NONE', #13940, #47864 ) ;
#40980 = CARTESIAN_POINT ( 'NONE',  ( -13.38461538461538325, -2.249999999999998668, 29.75000000000001776 ) ) ;
#40981 = CARTESIAN_POINT ( 'NONE',  ( 16.15384615384615330, -12.62096338111211580, 30.90682066428153263 ) ) ;
#40982 = AXIS2_PLACEMENT_3D ( 'NONE', #41128, #20413, #46980 ) ;
#40983 = ADVANCED_FACE ( 'NONE', ( #51190 ), #71934, .F. ) ;
#40984 = ORIENTED_EDGE ( 'NONE', *, *, #8813, .T. ) ;
#40985 = ORIENTED_EDGE ( 'NONE', *, *, #39125, .T. ) ;
#40987 = ORIENTED_EDGE ( 'NONE', *, *, #7212, .T. ) ;
#40986 = DIRECTION ( 'NONE',  ( -0.000000000000000000, 0.6427876096865404731, -0.7660444431189771253 ) ) ;
#40988 = EDGE_CURVE ( 'NONE', #15501, #40554, #63237, .T. ) ;
#40989 = CARTESIAN_POINT ( 'NONE',  ( -5.326899820971668476, -4.818429247618089661, 34.26397095200675125 ) ) ;
#40990 = EDGE_CURVE ( 'NONE', #88116, #9579, #45264, .T. ) ;
#40991 = CARTESIAN_POINT ( 'NONE',  ( -8.703975629717929152, -11.06231777344671130, 33.60647404775212976 ) ) ;
#40992 = DIRECTION ( 'NONE',  ( -0.000000000000000000, -0.3420201433256694346, -0.9396926207859080948 ) ) ;
#40993 = CIRCLE ( 'NONE', #32373, 5.000000000000000888 ) ;
#40994 = ORIENTED_EDGE ( 'NONE', *, *, #30477, .T. ) ;
#40995 = CARTESIAN_POINT ( 'NONE',  ( 9.692307692307695177, -12.34228464037088635, 31.77849191805839268 ) ) ;
#40996 = EDGE_LOOP ( 'NONE', ( #34962, #42836, #6972, #34105 ) ) ;
#40997 = CARTESIAN_POINT ( 'NONE',  ( 7.911408985666682270, -12.70778746994558439, 30.41441678777536595 ) ) ;
#40998 = ORIENTED_EDGE ( 'NONE', *, *, #50958, .F. ) ;
#40999 = CARTESIAN_POINT ( 'NONE',  ( -10.54921547442195795, -7.250054483168843156, 34.74374881642865631 ) ) ;
#41000 = ORIENTED_EDGE ( 'NONE', *, *, #40324, .F. ) ;
#41001 = CARTESIAN_POINT ( 'NONE',  ( -16.37733109757010652, -6.760086850603066466, 34.69517049084099369 ) ) ;
#41002 = EDGE_CURVE ( 'NONE', #35887, #73980, #15125, .T. ) ;
#41003 = CARTESIAN_POINT ( 'NONE',  ( 10.61538461538461675, -4.786620604624113540, 33.94971097300155094 ) ) ;
#41004 = FACE_BOUND ( 'NONE', #88086, .T. ) ;
#41005 = B_SPLINE_CURVE_WITH_KNOTS ( 'NONE', 3,
 ( #24286, #2682, #45452, #72482, #44109, #29737, #10790, #58967, #38261, #52207 ),
 .UNSPECIFIED., .F., .F.,
 ( 4, 2, 2, 2, 4 ),
 ( 0.000000000000000000, 0.0001954339881912783015, 0.0003908679763825566029, 0.0005863019645738348773, 0.0007817359527651132059 ),
 .UNSPECIFIED. ) ;
#41006 = DIRECTION ( 'NONE',  ( -0.000000000000000000, 1.000000000000000000, -0.000000000000000000 ) ) ;
#41007 = CARTESIAN_POINT ( 'NONE',  ( 17.07692307692295586, -2.625532179533778709, 30.86335684631627174 ) ) ;
#41008 = FACE_OUTER_BOUND ( 'NONE', #64076, .T. ) ;
#41009 = DIRECTION ( 'NONE',  ( -1.000000000000000000, -0.000000000000000000, -0.000000000000000000 ) ) ;
#41010 = EDGE_CURVE ( 'NONE', #71780, #65753, #8613, .T. ) ;
#41011 = CARTESIAN_POINT ( 'NONE',  ( -5.011667937410237528, -4.320704448112861584, 33.92786785259548310 ) ) ;
#41012 = LINE ( 'NONE', #47760, #63479 ) ;
#41013 = CARTESIAN_POINT ( 'NONE',  ( 14.43821774592595197, -6.808710257144161559, 34.95449254468098843 ) ) ;
#41014 = EDGE_LOOP ( 'NONE', ( #36429, #31952 ) ) ;
#41015 = VERTEX_POINT ( 'NONE', #24638 ) ;
#41016 = AXIS2_PLACEMENT_3D ( 'NONE', #47240, #834, #69299 ) ;
#41018 = CARTESIAN_POINT ( 'NONE',  ( -7.846153846153844924, -13.63283147151868846, 33.57946703557072254 ) ) ;
#41017 = CARTESIAN_POINT ( 'NONE',  ( 2.177545098254088707, -10.88202310037936194, 33.43294751532457099 ) ) ;
#41019 = CARTESIAN_POINT ( 'NONE',  ( 7.053868730901711182, -6.413143153341454017, 34.63066358083362672 ) ) ;
#41020 = DIRECTION ( 'NONE',  ( -0.000000000000000000, 0.8660254037844397068, -0.4999999999999978906 ) ) ;
#41021 = CARTESIAN_POINT ( 'NONE',  ( 12.22435897435897267, -3.499999999999999556, 29.75000000000000355 ) ) ;
#41022 = DIRECTION ( 'NONE',  ( -0.000000000000000000, 0.9848077530122085754, -0.1736481776669273613 ) ) ;
#41023 = ORIENTED_EDGE ( 'NONE', *, *, #9679, .T. ) ;
#41024 = EDGE_CURVE ( 'NONE', #20214, #48033, #73736, .T. ) ;
#41025 = CARTESIAN_POINT ( 'NONE',  ( 17.32686859527121470, -3.202959910592336090, 32.30730279482227019 ) ) ;
#41026 = CARTESIAN_POINT ( 'NONE',  ( -4.946397375159516052, -2.619367082507848554, 30.83698974864644171 ) ) ;
#41027 = CYLINDRICAL_SURFACE ( 'NONE', #74670, 0.2499999999999973355 ) ;
#41028 = LINE ( 'NONE', #32940, #48236 ) ;
#41029 = ORIENTED_EDGE ( 'NONE', *, *, #79066, .T. ) ;
#41030 = EDGE_CURVE ( 'NONE', #62505, #24326, #45794, .T. ) ;
#41031 = VERTEX_POINT ( 'NONE', #19658 ) ;
#41033 = EDGE_CURVE ( 'NONE', #70251, #76766, #53435, .T. ) ;
#41032 = ORIENTED_EDGE ( 'NONE', *, *, #29496, .T. ) ;
#41034 = CARTESIAN_POINT ( 'NONE',  ( 15.48082354240754555, -6.567000820036036579, 34.66262288849541306 ) ) ;
#41035 = VERTEX_POINT ( 'NONE', #33622 ) ;
#41036 = FACE_OUTER_BOUND ( 'NONE', #60276, .T. ) ;
#41037 = DIRECTION ( 'NONE',  ( -0.000000000000000000, -0.7660444431189791237, -0.6427876096865379196 ) ) ;
#41038 = CARTESIAN_POINT ( 'NONE',  ( 10.03846153846153832, -4.000000000000000000, 29.75000000000000355 ) ) ;
#41039 = CARTESIAN_POINT ( 'NONE',  ( -2.307692307692305711, -4.786620604624113540, 33.94971097300155094 ) ) ;
#41040 = B_SPLINE_CURVE_WITH_KNOTS ( 'NONE', 3,
 ( #50950, #4109, #78003, #56841, #16307, #17645, #64469, #50080, #77564, #9540 ),
 .UNSPECIFIED., .F., .F.,
 ( 4, 2, 2, 2, 4 ),
 ( 0.000000000000000000, 0.0001954311564186876063, 0.0003908623128373752125, 0.0005862934692560628188, 0.0007817246256747504250 ),
 .UNSPECIFIED. ) ;
#41041 = EDGE_CURVE ( 'NONE', #81906, #29384, #45345, .T. ) ;
#41042 = CARTESIAN_POINT ( 'NONE',  ( 14.30769230769231015, -4.098570777380720287, 33.41473453929634729 ) ) ;
#41043 = ORIENTED_EDGE ( 'NONE', *, *, #9325, .F. ) ;
#41044 = CARTESIAN_POINT ( 'NONE',  ( 1.576923076923075762, -3.499999999999999556, 29.75000000000000355 ) ) ;
#41046 = ORIENTED_EDGE ( 'NONE', *, *, #66343, .T. ) ;
#41045 = CARTESIAN_POINT ( 'NONE',  ( -12.21148414990014963, -11.79725096376909299, 32.30694842903960762 ) ) ;
#41047 = CARTESIAN_POINT ( 'NONE',  ( 13.91025641025641235, -11.00000000000000000, 29.75000000000000355 ) ) ;
#41048 = CARTESIAN_POINT ( 'NONE',  ( 18.00000000000000000, -2.721908614388771852, 31.22303859784724978 ) ) ;
#41049 = DIRECTION ( 'NONE',  ( 0.000000000000000000, 0.9396926207859126468, -0.3420201433256571111 ) ) ;
#41050 = DIRECTION ( 'NONE',  ( -0.000000000000000000, -0.9396926207859092051, -0.3420201433256662704 ) ) ;
#41052 = VECTOR ( 'NONE', #16983, 1000.000000000000000 ) ;
#41051 = FACE_OUTER_BOUND ( 'NONE', #73219, .T. ) ;
#41053 = CARTESIAN_POINT ( 'NONE',  ( -0.4615384615384611200, -12.10708131394839349, 31.69288490824020244 ) ) ;
#41054 = CARTESIAN_POINT ( 'NONE',  ( -2.307692307692428724, -5.094484230521993062, 34.41647553114689373 ) ) ;
#41055 = CARTESIAN_POINT ( 'NONE',  ( 1.987747218494642309, -5.598659921968629050, 18.31436829374150932 ) ) ;
#41056 = ORIENTED_EDGE ( 'NONE', *, *, #49941, .T. ) ;
#41057 = CARTESIAN_POINT ( 'NONE',  ( 15.00728428704528561, -8.496056993536548418, 34.65000542017679663 ) ) ;
#41058 = CARTESIAN_POINT ( 'NONE',  ( -9.692307692307814193, -9.528491918059723176, 34.59228464037033035 ) ) ;
#41059 = DIRECTION ( 'NONE',  ( -0.000000000000000000, -0.000000000000000000, -1.000000000000000000 ) ) ;
#41060 = ORIENTED_EDGE ( 'NONE', *, *, #82508, .F. ) ;
#41061 = CARTESIAN_POINT ( 'NONE',  ( -4.153846153846152411, -6.343179335718451384, 34.87096338111211935 ) ) ;
#41062 = DIRECTION ( 'NONE',  ( -1.000000000000000000, -0.000000000000000000, 0.000000000000000000 ) ) ;
#41063 = VECTOR ( 'NONE', #24921, 1000.000000000000000 ) ;
#41064 = EDGE_CURVE ( 'NONE', #77857, #998, #87252, .T. ) ;
#41065 = CARTESIAN_POINT ( 'NONE',  ( 10.86543903529806876, -4.818054556918156983, 34.26375889529406749 ) ) ;
#41066 = LINE ( 'NONE', #39301, #49967 ) ;
#41067 = CARTESIAN_POINT ( 'NONE',  ( -14.55766905174090020, -2.920706130388546651, 32.31842814019191223 ) ) ;
#41068 = ORIENTED_EDGE ( 'NONE', *, *, #37084, .T. ) ;
#41069 = LINE ( 'NONE', #42407, #59225 ) ;
#41070 = CARTESIAN_POINT ( 'NONE',  ( -5.076923076923075762, -9.780366693483667717, 34.19971097300155094 ) ) ;
#41071 = CARTESIAN_POINT ( 'NONE',  ( -14.55769230769230838, -7.433932668274256805, 35.00000000000000711 ) ) ;
#41072 = ORIENTED_EDGE ( 'NONE', *, *, #60991, .F. ) ;
#41073 = CARTESIAN_POINT ( 'NONE',  ( -8.519230769230702549, -7.434744860731433924, 35.00000000000000711 ) ) ;
#41074 = B_SPLINE_CURVE_WITH_KNOTS ( 'NONE', 3,
 ( #39486, #5239, #11107, #66499, #12877, #5677, #19637, #88568, #73255, #81352 ),
 .UNSPECIFIED., .F., .F.,
 ( 4, 2, 2, 2, 4 ),
 ( 0.0007817246256747484735, 0.0009771112852218922368, 0.001172497944769036217, 0.001367884604316180197, 0.001563271263863323960 ),
 .UNSPECIFIED. ) ;
#41075 = ORIENTED_EDGE ( 'NONE', *, *, #23642, .T. ) ;
#41076 = CARTESIAN_POINT ( 'NONE',  ( -16.21992956480203318, -5.557115091759785130, 34.35708131394839171 ) ) ;
#41077 = CARTESIAN_POINT ( 'NONE',  ( 0.000000000000000000, 0.000000000000000000, 0.000000000000000000 ) ) ;
#41078 = DIRECTION ( 'NONE',  ( -0.000000000000000000, 0.000000000000000000, 1.000000000000000000 ) ) ;
#41079 = ORIENTED_EDGE ( 'NONE', *, *, #78657, .T. ) ;
#41080 = CYLINDRICAL_SURFACE ( 'NONE', #44731, 0.2500000000000004996 ) ;
#41081 = CARTESIAN_POINT ( 'NONE',  ( -8.899922235898330314, -2.541943142973491554, 30.39792223712631980 ) ) ;
#41082 = CARTESIAN_POINT ( 'NONE',  ( -10.61538461538473399, -6.026961402154118019, 34.52809138561165270 ) ) ;
#41083 = VECTOR ( 'NONE', #35853, 1000.000000000000000 ) ;
#41084 = CARTESIAN_POINT ( 'NONE',  ( 11.53846153846153832, -12.34228464037088635, 31.77849191805839268 ) ) ;
#41085 = CARTESIAN_POINT ( 'NONE',  ( -1.449885385171704399, -11.06231777344662781, 33.60647404775220082 ) ) ;
#41086 = B_SPLINE_CURVE_WITH_KNOTS ( 'NONE', 3,
 ( #35481, #21068, #22408, #48994, #62933, #1245, #15219, #8903, #28735, #75574 ),
 .UNSPECIFIED., .F., .F.,
 ( 4, 2, 2, 2, 4 ),
 ( 0.0007817359430256367279, 0.0009771253907250045632, 0.001172514838424372615, 0.001367904286123740668, 0.001563293733823108503 ),
 .UNSPECIFIED. ) ;
#41088 = ORIENTED_EDGE ( 'NONE', *, *, #55492, .F. ) ;
#41087 = ADVANCED_FACE ( 'NONE', ( #11579 ), #39061, .F. ) ;
#41089 = FACE_BOUND ( 'NONE', #4911, .T. ) ;
#41090 = VERTEX_POINT ( 'NONE', #52546 ) ;
#41091 = CARTESIAN_POINT ( 'NONE',  ( 17.78205128205128105, -7.500000000000000000, 29.75000000000000355 ) ) ;
#41092 = EDGE_CURVE ( 'NONE', #59157, #60898, #80484, .T. ) ;
#41093 = FACE_OUTER_BOUND ( 'NONE', #54824, .T. ) ;
#41094 = EDGE_CURVE ( 'NONE', #24532, #29384, #18633, .T. ) ;
#41095 = DIRECTION ( 'NONE',  ( -0.000000000000000000, -0.9396926207859092051, -0.3420201433256662704 ) ) ;
#41096 = CARTESIAN_POINT ( 'NONE',  ( 17.01083966596718611, -2.538708090699995257, 30.37095296980875148 ) ) ;
#41097 = B_SPLINE_CURVE_WITH_KNOTS ( 'NONE', 3,
 ( #12353, #39830, #65945, #79480, #45233, #3806 ),
 .UNSPECIFIED., .F., .F.,
 ( 4, 2, 4 ),
 ( 0.0003909512603273928937, 0.0005862562993132217288, 0.0007815613382990504012 ),
 .UNSPECIFIED. ) ;
#41098 = ORIENTED_EDGE ( 'NONE', *, *, #15801, .T. ) ;
#41100 = EDGE_CURVE ( 'NONE', #81906, #30233, #25083, .T. ) ;
#41099 = ORIENTED_EDGE ( 'NONE', *, *, #7551, .F. ) ;
#41101 = EDGE_LOOP ( 'NONE', ( #84449, #61082 ) ) ;
#41102 = CARTESIAN_POINT ( 'NONE',  ( -3.099978789802278367, -11.37503395064541678, 33.29242100308974983 ) ) ;
#41103 = ORIENTED_EDGE ( 'NONE', *, *, #9819, .T. ) ;
#41104 = AXIS2_PLACEMENT_3D ( 'NONE', #19210, #21863, #6582 ) ;
#41105 = CARTESIAN_POINT ( 'NONE',  ( 4.376625822824220080, -10.23759521482555357, 34.22997729860117033 ) ) ;
#41106 = EDGE_CURVE ( 'NONE', #8808, #67806, #46686, .T. ) ;
#41107 = CARTESIAN_POINT ( 'NONE',  ( -11.53846153846166089, -5.941354392335915335, 34.76329471203413846 ) ) ;
#41108 = CARTESIAN_POINT ( 'NONE',  ( 4.023698944407932743, -3.285722584762969856, 32.44110544564090759 ) ) ;
#41109 = CARTESIAN_POINT ( 'NONE',  ( 4.088595163684911604, -2.506253911140460477, 30.00000000000013856 ) ) ;
#41110 = CARTESIAN_POINT ( 'NONE',  ( 4.946232473812766095, -9.929715669179216775, 34.40415004197138416 ) ) ;
#41111 = CARTESIAN_POINT ( 'NONE',  ( -4.219096085620237524, -2.255955759149247619, 30.00000000000013856 ) ) ;
#41112 = CARTESIAN_POINT ( 'NONE',  ( -2.084680956079456582, -3.587049720035815348, 32.86302985866382897 ) ) ;
#41113 = CARTESIAN_POINT ( 'NONE',  ( 11.53846153846141753, -10.21337939537710326, 33.94971097300076224 ) ) ;
#41114 = ORIENTED_EDGE ( 'NONE', *, *, #50596, .F. ) ;
#41115 = AXIS2_PLACEMENT_3D ( 'NONE', #22595, #50064, #37431 ) ;
#41116 = ORIENTED_EDGE ( 'NONE', *, *, #1423, .T. ) ;
#41117 = ORIENTED_EDGE ( 'NONE', *, *, #73017, .T. ) ;
#41118 = CARTESIAN_POINT ( 'NONE',  ( -1.515306851282941292, -11.18331474514187995, 33.13161551792790505 ) ) ;
#41120 = CARTESIAN_POINT ( 'NONE',  ( 13.63461538461538680, -2.249999999999998668, 29.75000000000000355 ) ) ;
#41119 = CARTESIAN_POINT ( 'NONE',  ( 1.515141086378948954, -6.001044277235011215, 34.52024696741798948 ) ) ;
#41121 = FACE_OUTER_BOUND ( 'NONE', #57390, .T. ) ;
#41122 = CARTESIAN_POINT ( 'NONE',  ( 10.61538461538461675, -12.29105614889573062, 35.45975837776705220 ) ) ;
#41123 = FACE_BOUND ( 'NONE', #59841, .T. ) ;
#41124 = CARTESIAN_POINT ( 'NONE',  ( -7.146003881983771677, -3.395401636524186362, 33.02366814457250399 ) ) ;
#41125 = EDGE_LOOP ( 'NONE', ( #36193, #66185 ) ) ;
#41126 = DIRECTION ( 'NONE',  ( 0.000000000000000000, 0.000000000000000000, -1.000000000000000000 ) ) ;
#41127 = CYLINDRICAL_SURFACE ( 'NONE', #47588, 0.2499999999999993616 ) ;
#41128 = CARTESIAN_POINT ( 'NONE',  ( -20.00000000000000355, -10.00000000000000533, 3.000000000000000000 ) ) ;
#41129 = EDGE_LOOP ( 'NONE', ( #19379, #14521, #6525, #4518 ) ) ;
#41130 = CARTESIAN_POINT ( 'NONE',  ( 4.826899852701618698, -2.341070481393820124, 30.72580821765574299 ) ) ;
#41131 = EDGE_CURVE ( 'NONE', #85190, #19800, #11124, .T. ) ;
#41132 = VERTEX_POINT ( 'NONE', #31852 ) ;
#41133 = FACE_BOUND ( 'NONE', #23833, .T. ) ;
#41134 = B_SPLINE_CURVE_WITH_KNOTS ( 'NONE', 3,
 ( #60669, #61551, #26892, #61113, #89056, #27335, #80967, #39539, #12060, #18808 ),
 .UNSPECIFIED., .F., .F.,
 ( 4, 2, 2, 2, 4 ),
 ( 0.0007817246256747450040, 0.0009771112852218881168, 0.001172497944769031230, 0.001367884604316174342, 0.001563271263863317455 ),
 .UNSPECIFIED. ) ;
#41135 = DIRECTION ( 'NONE',  ( -0.000000000000000000, -0.7660444431189792347, -0.6427876096865379196 ) ) ;
#41136 = AXIS2_PLACEMENT_3D ( 'NONE', #43152, #70622, #37715 ) ;
#41137 = CARTESIAN_POINT ( 'NONE',  ( 20.00000000000000000, -7.500000000000000000, 33.75000000000000000 ) ) ;
#41138 = LINE ( 'NONE', #35717, #30329 ) ;
#41139 = EDGE_LOOP ( 'NONE', ( #41306, #5211, #38819, #4118 ) ) ;
#41140 = CYLINDRICAL_SURFACE ( 'NONE', #66674, 5.000000000000000888 ) ;
#41141 = DIRECTION ( 'NONE',  ( 0.000000000000000000, 0.3420201433256641055, -0.9396926207859100932 ) ) ;
#41142 = LINE ( 'NONE', #60519, #27965 ) ;
#41143 = DIRECTION ( 'NONE',  ( 1.000000000000000000, 0.000000000000000000, 0.000000000000000000 ) ) ;
#41144 = ORIENTED_EDGE ( 'NONE', *, *, #27322, .T. ) ;
#41145 = VECTOR ( 'NONE', #12824, 1000.000000000000000 ) ;
#41146 = ADVANCED_FACE ( 'NONE', ( #26423 ), #74164, .F. ) ;
#41147 = CARTESIAN_POINT ( 'NONE',  ( -6.923076923076922462, -11.11383981884818262, 36.00935417666054406 ) ) ;
#41148 = DIRECTION ( 'NONE',  ( -0.000000000000000000, 1.000000000000000000, -0.000000000000000000 ) ) ;
#41150 = EDGE_LOOP ( 'NONE', ( #31809, #55381, #2076, #17095 ) ) ;
#41149 = CARTESIAN_POINT ( 'NONE',  ( 14.30769230769218581, -12.70778746994576025, 30.41441678777401236 ) ) ;
#41151 = CARTESIAN_POINT ( 'NONE',  ( 15.90386940979756503, -4.075325502946085976, 33.72974371597207721 ) ) ;
#41152 = CARTESIAN_POINT ( 'NONE',  ( 5.933916589044120116, -8.973038597847269315, 34.52809138561120506 ) ) ;
#41153 = CARTESIAN_POINT ( 'NONE',  ( -11.76194648218548622, -8.496056993536548418, 34.65000542017679663 ) ) ;
#41154 = CARTESIAN_POINT ( 'NONE',  ( -4.153846153846152411, -6.681629849574314051, 35.83090037661290239 ) ) ;
#41155 = CARTESIAN_POINT ( 'NONE',  ( -13.16160254052198830, -3.395485233115139057, 33.02377354290275946 ) ) ;
#41157 = PLANE ( 'NONE',  #38880 ) ;
#41156 = CARTESIAN_POINT ( 'NONE',  ( 12.46153846153846168, -2.517432740324522911, 35.29906147534542527 ) ) ;
#41158 = EDGE_CURVE ( 'NONE', #86621, #63322, #37760, .T. ) ;
#41159 = CARTESIAN_POINT ( 'NONE',  ( 5.076923076923075762, -13.49023893513002648, 31.06009739812518688 ) ) ;
#41160 = CARTESIAN_POINT ( 'NONE',  ( 1.799775606325937360E-14, -10.25000000000000000, 18.53125000000000000 ) ) ;
#41161 = EDGE_LOOP ( 'NONE', ( #10352, #9314 ) ) ;
#41162 = DIRECTION ( 'NONE',  ( -0.000000000000000000, 1.000000000000000000, 3.491481338843133355E-15 ) ) ;
#41163 = VERTEX_POINT ( 'NONE', #60637 ) ;
#41164 = ORIENTED_EDGE ( 'NONE', *, *, #85063, .F. ) ;
#41165 = DIRECTION ( 'NONE',  ( 1.799314243699348838E-16, 1.000000000000000000, -5.102127870520020612E-17 ) ) ;
#41166 = EDGE_LOOP ( 'NONE', ( #26672, #26794, #19685, #3968 ) ) ;
#41167 = CARTESIAN_POINT ( 'NONE',  ( 14.08476609017615644, -8.239355502252617924, 34.69524867566427417 ) ) ;
#41168 = CARTESIAN_POINT ( 'NONE',  ( -1.139087296525992166, -10.25000000000000533, 22.35937500000000711 ) ) ;
#41169 = CARTESIAN_POINT ( 'NONE',  ( -14.17716686945866655, -3.068774925481847493, 32.56582465632704526 ) ) ;
#41170 = EDGE_CURVE ( 'NONE', #47265, #65473, #20542, .T. ) ;
#41171 = FACE_OUTER_BOUND ( 'NONE', #39092, .T. ) ;
#41172 = CARTESIAN_POINT ( 'NONE',  ( 6.223011351612850461, -3.105924265160262543, 32.13625925475356127 ) ) ;
#41173 = CARTESIAN_POINT ( 'NONE',  ( -11.76138775597768138, -11.24512374952581872, 33.06303171183252942 ) ) ;
#41174 = CARTESIAN_POINT ( 'NONE',  ( -15.36145983387954139, -4.684245665217972032, 34.18127051446801090 ) ) ;
#41175 = CARTESIAN_POINT ( 'NONE',  ( -10.61538461538461320, -12.78798330534102945, 29.74999999999997868 ) ) ;
#41176 = CARTESIAN_POINT ( 'NONE',  ( -3.749999999999997335, -7.500000000000021316, 26.34375000000000000 ) ) ;
#41177 = ADVANCED_FACE ( 'NONE', ( #62841 ), #26864, .F. ) ;
#41178 = EDGE_CURVE ( 'NONE', #6173, #37287, #62481, .T. ) ;
#41179 = FACE_OUTER_BOUND ( 'NONE', #78659, .T. ) ;
#41180 = CARTESIAN_POINT ( 'NONE',  ( 23.49999999999998579, 12.75000000000000711, 29.19862367942584314 ) ) ;
#41181 = B_SPLINE_CURVE_WITH_KNOTS ( 'NONE', 3,
 ( #79474, #53768, #81255, #53318, #39386, #5587, #33058, #32608, #80821, #24511 ),
 .UNSPECIFIED., .F., .F.,
 ( 4, 2, 2, 2, 4 ),
 ( 0.0007817246256747469556, 0.0009771112852218902852, 0.001172497944769033615, 0.001367884604316176728, 0.001563271263863320057 ),
 .UNSPECIFIED. ) ;
#41182 = CYLINDRICAL_SURFACE ( 'NONE', #23454, 0.2499999999999986955 ) ;
#41183 = CARTESIAN_POINT ( 'NONE',  ( -13.25408968285182532, -11.46989282347013095, 32.79007818306219946 ) ) ;
#41184 = EDGE_CURVE ( 'NONE', #6648, #70140, #7029, .T. ) ;
#41185 = B_SPLINE_CURVE_WITH_KNOTS ( 'NONE', 3,
 ( #5610, #45701, #11036, #65966, #12370, #60547, #39849, #18690, #52893, #47025 ),
 .UNSPECIFIED., .F., .F.,
 ( 4, 2, 2, 2, 4 ),
 ( 0.000000000000000000, 0.0001954311564186856818, 0.0003908623128373713636, 0.0005862934692560570725, 0.0007817246256747427272 ),
 .UNSPECIFIED. ) ;
#41186 = VERTEX_POINT ( 'NONE', #61522 ) ;
#41187 = ORIENTED_EDGE ( 'NONE', *, *, #26758, .F. ) ;
#41188 = FACE_OUTER_BOUND ( 'NONE', #78656, .T. ) ;
#41189 = CARTESIAN_POINT ( 'NONE',  ( 1.384615384615264011, -3.643525952248795718, 33.31231777344771672 ) ) ;
#41190 = CARTESIAN_POINT ( 'NONE',  ( -6.923076923076922462, -11.91647553114624181, 32.58852847137148245 ) ) ;
#41191 = CARTESIAN_POINT ( 'NONE',  ( -11.47229239749887952, -7.250054483168843156, 34.74374881642865631 ) ) ;
#41192 = CARTESIAN_POINT ( 'NONE',  ( -16.02305571287920216, -8.191423895709842640, 34.95447573519442130 ) ) ;
#41193 = CARTESIAN_POINT ( 'NONE',  ( 11.76147438255493327, -4.026326845037962343, 33.68677907613344047 ) ) ;
#41194 = DIRECTION ( 'NONE',  ( 0.000000000000000000, -1.000000000000000000, 0.000000000000000000 ) ) ;
#41195 = EDGE_LOOP ( 'NONE', ( #17682, #51595, #1199, #15735 ) ) ;
#41196 = LINE ( 'NONE', #14608, #6996 ) ;
#41197 = ORIENTED_EDGE ( 'NONE', *, *, #25687, .T. ) ;
#41198 = ADVANCED_FACE ( 'NONE', ( #54322 ), #28182, .F. ) ;
#41199 = CARTESIAN_POINT ( 'NONE',  ( -8.703163435880695076, -4.661471528628508665, 34.16647553114624003 ) ) ;
#41200 = CARTESIAN_POINT ( 'NONE',  ( 3.931018056211275535, -7.369209533119140509, 34.99857337881830688 ) ) ;
#41201 = VECTOR ( 'NONE', #41739, 1000.000000000000000 ) ;
#41202 = CARTESIAN_POINT ( 'NONE',  ( 14.24160889673642849, -4.786620604624113540, 33.94971097300155805 ) ) ;
#41203 = CARTESIAN_POINT ( 'NONE',  ( -15.45369544828538011, -3.105860786376062332, 32.13614157043599562 ) ) ;
#41204 = CARTESIAN_POINT ( 'NONE',  ( 2.294871794871793824, -3.499999999999999556, 29.75000000000000355 ) ) ;
#41205 = B_SPLINE_CURVE_WITH_KNOTS ( 'NONE', 3,
 ( #45097, #73921, #33379, #4564, #26613, #6356, #11319, #32475, #13102, #88782 ),
 .UNSPECIFIED., .F., .F.,
 ( 4, 2, 2, 2, 4 ),
 ( 0.0007817246256747489071, 0.0009771112852218922368, 0.001172497944769035350, 0.001367884604316178679, 0.001563271263863322009 ),
 .UNSPECIFIED. ) ;
#41206 = VECTOR ( 'NONE', #15491, 1000.000000000000000 ) ;
#41207 = ORIENTED_EDGE ( 'NONE', *, *, #58722, .F. ) ;
#41208 = ADVANCED_FACE ( 'NONE', ( #68733 ), #21878, .F. ) ;
#41209 = VERTEX_POINT ( 'NONE', #89029 ) ;
#41210 = PRODUCT_DEFINITION_SHAPE ( 'NONE', 'NONE',  #47945 ) ;
#41211 = ORIENTED_EDGE ( 'NONE', *, *, #84948, .T. ) ;
#41212 = EDGE_LOOP ( 'NONE', ( #57153, #33343, #13076, #29455 ) ) ;
#41213 = VECTOR ( 'NONE', #36286, 1000.000000000000000 ) ;
#41214 = CARTESIAN_POINT ( 'NONE',  ( -6.249976744048591826, -4.818429247618089661, 34.26397095200675125 ) ) ;
#41215 = DIRECTION ( 'NONE',  ( 0.000000000000000000, 0.1736481776669267785, -0.9848077530122087975 ) ) ;
#41216 = EDGE_CURVE ( 'NONE', #59376, #37064, #67768, .T. ) ;
#41217 = CARTESIAN_POINT ( 'NONE',  ( 4.480769230769229061, -7.500000000000000000, 29.75000000000000355 ) ) ;
#41218 = DIRECTION ( 'NONE',  ( 0.000000000000000000, 0.000000000000000000, -1.000000000000000000 ) ) ;
#41219 = CARTESIAN_POINT ( 'NONE',  ( -15.16551409125639260, -9.528491918058460186, 34.59228464037086326 ) ) ;
#41220 = CARTESIAN_POINT ( 'NONE',  ( 14.05771557674995442, -12.41269422305637171, 30.68257228309993323 ) ) ;
#41221 = ORIENTED_EDGE ( 'NONE', *, *, #10470, .T. ) ;
#41222 = ORIENTED_EDGE ( 'NONE', *, *, #14727, .F. ) ;
#41223 = ORIENTED_EDGE ( 'NONE', *, *, #75090, .F. ) ;
#41224 = EDGE_CURVE ( 'NONE', #25798, #57772, #55941, .T. ) ;
#41226 = ORIENTED_EDGE ( 'NONE', *, *, #4682, .T. ) ;
#41225 = CARTESIAN_POINT ( 'NONE',  ( -10.48459280755982803, -11.71459661697925903, 32.44059661609676937 ) ) ;
#41227 = DIRECTION ( 'NONE',  ( 0.000000000000000000, 0.1736481776669275834, 0.9848077530122086864 ) ) ;
#41228 = CARTESIAN_POINT ( 'NONE',  ( -12.46153846153846168, -11.91647553114624181, 32.58852847137148245 ) ) ;
#41229 = AXIS2_PLACEMENT_3D ( 'NONE', #20109, #41711, #7488 ) ;
#41230 = CARTESIAN_POINT ( 'NONE',  ( -2.651650429449565305, -4.848349570550461785, 21.50000000000000000 ) ) ;
#41231 = VERTEX_POINT ( 'NONE', #41269 ) ;
#41232 = ORIENTED_EDGE ( 'NONE', *, *, #5566, .F. ) ;
#41233 = CARTESIAN_POINT ( 'NONE',  ( 7.846153846153725020, -12.27809138561165270, 31.22303859784587132 ) ) ;
#41234 = EDGE_CURVE ( 'NONE', #44863, #20097, #78608, .T. ) ;
#41235 = FACE_BOUND ( 'NONE', #38921, .T. ) ;
#41236 = CARTESIAN_POINT ( 'NONE',  ( 6.792385456409367528, -4.118384482072085184, 33.43331474514187107 ) ) ;
#41237 = CARTESIAN_POINT ( 'NONE',  ( -4.153846153846152411, -9.905515769479276145, 34.41647553114623292 ) ) ;
#41238 = ORIENTED_EDGE ( 'NONE', *, *, #22159, .T. ) ;
#41239 = EDGE_CURVE ( 'NONE', #77888, #46688, #719, .T. ) ;
#41240 = CARTESIAN_POINT ( 'NONE',  ( -9.915792616872025178, -4.988325925672468131, 34.36044203135681130 ) ) ;
#41241 = AXIS2_PLACEMENT_3D ( 'NONE', #63095, #49147, #9063 ) ;
#41242 = AXIS2_PLACEMENT_3D ( 'NONE', #48138, #60325, #12596 ) ;
#41243 = CARTESIAN_POINT ( 'NONE',  ( 9.019176178608812933, -8.476813868363244353, 34.90874843262270133 ) ) ;
#41244 = CARTESIAN_POINT ( 'NONE',  ( 16.28463659481310444, -6.369690395747422684, 34.87708834333098196 ) ) ;
#41245 = CARTESIAN_POINT ( 'NONE',  ( 15.23076923076910916, -6.835583212225970762, 34.95778746994575670 ) ) ;
#41246 = ORIENTED_EDGE ( 'NONE', *, *, #61436, .F. ) ;
#41247 = CARTESIAN_POINT ( 'NONE',  ( 6.223011351612851350, -8.239487800360276282, 34.69522927552633718 ) ) ;
#41248 = CARTESIAN_POINT ( 'NONE',  ( 15.23076923076923173, -11.11383981884818262, 36.00935417666054406 ) ) ;
#41249 = CARTESIAN_POINT ( 'NONE',  ( 17.32697738856138869, -9.943054286541403997, 34.11300777759954883 ) ) ;
#41250 = CARTESIAN_POINT ( 'NONE',  ( -2.057637887778853703, -9.233818618650603938, 34.70587769442853698 ) ) ;
#41251 = CARTESIAN_POINT ( 'NONE',  ( -15.10024352900566846, -11.93748526763465279, 32.05452791011430946 ) ) ;
#41252 = FACE_BOUND ( 'NONE', #43091, .T. ) ;
#41254 = CARTESIAN_POINT ( 'NONE',  ( -6.250023224221455287, -10.18141759479407327, 34.26406193332782379 ) ) ;
#41253 = CARTESIAN_POINT ( 'NONE',  ( -6.792286482109971324, -12.62708834333097663, 30.88030960425257021 ) ) ;
#41255 = EDGE_CURVE ( 'NONE', #81196, #9998, #51878, .T. ) ;
#41256 = EDGE_CURVE ( 'NONE', #41090, #64564, #76370, .T. ) ;
#41257 = CARTESIAN_POINT ( 'NONE',  ( 11.60371667797437567, -12.16647553114626490, 32.15551576947920864 ) ) ;
#41259 = CARTESIAN_POINT ( 'NONE',  ( 10.03846153846153832, -3.499999999999999556, 29.75000000000000355 ) ) ;
#41258 = CARTESIAN_POINT ( 'NONE',  ( 3.454196192630801576, -7.630147231320743018, 34.74852402298682819 ) ) ;
#41260 = CARTESIAN_POINT ( 'NONE',  ( -5.207613680033384540, -12.35290016733513951, 31.75349464988449455 ) ) ;
#41261 = CARTESIAN_POINT ( 'NONE',  ( 1.200186371490561621, -10.22469193450123193, 18.20125670625849068 ) ) ;
#41262 = ORIENTED_EDGE ( 'NONE', *, *, #26894, .T. ) ;
#41263 = CARTESIAN_POINT ( 'NONE',  ( -8.992057461709771715, -7.369208160676171460, 34.74850200257122879 ) ) ;
#41264 = ORIENTED_EDGE ( 'NONE', *, *, #77054, .F. ) ;
#41265 = CARTESIAN_POINT ( 'NONE',  ( -13.38461538461550759, -9.528491918059723176, 34.59228464037033035 ) ) ;
#41266 = VECTOR ( 'NONE', #66886, 1000.000000000000114 ) ;
#41267 = EDGE_LOOP ( 'NONE', ( #28023, #48779 ) ) ;
#41268 = LINE ( 'NONE', #70061, #36884 ) ;
#41269 = CARTESIAN_POINT ( 'NONE',  ( -1.384615384615506484, -10.33852847137269571, 34.16647553114546554 ) ) ;
#41271 = EDGE_LOOP ( 'NONE', ( #39733, #79639, #47509, #17059 ) ) ;
#41270 = CARTESIAN_POINT ( 'NONE',  ( -9.692307692307814193, -11.67786785259630911, 32.92929555188603530 ) ) ;
#41272 = CARTESIAN_POINT ( 'NONE',  ( 5.142990410273151625, -11.91647553114624358, 32.58852847137148245 ) ) ;
#41273 = CARTESIAN_POINT ( 'NONE',  ( 1.200186371490561621, -10.22469193450123193, 18.20125670625849068 ) ) ;
#41274 = EDGE_CURVE ( 'NONE', #72334, #78742, #39862, .T. ) ;
#41275 = CARTESIAN_POINT ( 'NONE',  ( -10.39260494640654819, -12.69155399931963046, 30.53255429739157734 ) ) ;
#41276 = CARTESIAN_POINT ( 'NONE',  ( -7.146561847641255127, -12.69144148231606017, 30.53333754910549303 ) ) ;
#41277 = VECTOR ( 'NONE', #76248, 1000.000000000000000 ) ;
#41278 = PLANE ( 'NONE',  #30261 ) ;
#41279 = LINE ( 'NONE', #68741, #1270 ) ;
#41280 = CARTESIAN_POINT ( 'NONE',  ( 2.530703659305157061, -2.758310577978208666, 31.33698337089302299 ) ) ;
#41281 = CARTESIAN_POINT ( 'NONE',  ( -18.00000000000000000, -13.54022505542197408, 30.56119799385072255 ) ) ;
#41282 = CARTESIAN_POINT ( 'NONE',  ( 2.694853999681185108, -4.891553140782077591, 22.06436829374151287 ) ) ;
#41283 = EDGE_CURVE ( 'NONE', #19865, #59616, #87703, .T. ) ;
#41284 = EDGE_CURVE ( 'NONE', #57930, #11539, #49785, .T. ) ;
#41285 = CARTESIAN_POINT ( 'NONE',  ( 11.40831356872984514, -5.915902021225889484, 34.75552854090298638 ) ) ;
#41286 = CARTESIAN_POINT ( 'NONE',  ( 10.83816415665302202, -11.41317474335729543, 32.86274602512330034 ) ) ;
#41287 = AXIS2_PLACEMENT_3D ( 'NONE', #74071, #66864, #52888 ) ;
#41288 = ORIENTED_EDGE ( 'NONE', *, *, #87197, .T. ) ;
#41289 = CARTESIAN_POINT ( 'NONE',  ( 24.00000000000000000, -9.499999999999982236, 27.74999999999999645 ) ) ;
#41290 = CARTESIAN_POINT ( 'NONE',  ( 1.553300858899087311, -3.749999999999992006, 14.23437500000000355 ) ) ;
#41291 = DIRECTION ( 'NONE',  ( 0.000000000000000000, 1.000000000000000000, 0.000000000000000000 ) ) ;
#41292 = CARTESIAN_POINT ( 'NONE',  ( 4.023236498642070558, -7.722926974430166069, 34.99546784045485737 ) ) ;
#41293 = EDGE_LOOP ( 'NONE', ( #36770, #43968, #3169, #26842 ) ) ;
#41294 = FACE_OUTER_BOUND ( 'NONE', #4323, .T. ) ;
#41295 = CARTESIAN_POINT ( 'NONE',  ( -14.37377571864818293, -11.16473453929635440, 33.15142922261925662 ) ) ;
#41297 = ORIENTED_EDGE ( 'NONE', *, *, #72421, .T. ) ;
#41296 = LINE ( 'NONE', #7057, #46917 ) ;
#41298 = CARTESIAN_POINT ( 'NONE',  ( -5.299849294439224145, -5.667676309546437530, 34.40238873228292249 ) ) ;
#41299 = CARTESIAN_POINT ( 'NONE',  ( 2.084207363968360482, -12.44517049084099725, 30.48991314939691932 ) ) ;
#41300 = FACE_OUTER_BOUND ( 'NONE', #33921, .T. ) ;
#41301 = LINE ( 'NONE', #68765, #85001 ) ;
#41302 = CARTESIAN_POINT ( 'NONE',  ( 6.673053685783958855, -5.056417327199099532, 34.11270091957320716 ) ) ;
#41303 = ORIENTED_EDGE ( 'NONE', *, *, #69442, .T. ) ;
#41304 = ORIENTED_EDGE ( 'NONE', *, *, #12075, .F. ) ;
#41306 = ORIENTED_EDGE ( 'NONE', *, *, #15723, .F. ) ;
#41305 = B_SPLINE_CURVE_WITH_KNOTS ( 'NONE', 3,
 ( #37429, #10863, #84317, #58144, #64900, #31115, #3205, #30678, #4085, #85631 ),
 .UNSPECIFIED., .F., .F.,
 ( 4, 2, 2, 2, 4 ),
 ( 0.0007817359430256253438, 0.0009771253907249898181, 0.001172514838424354401, 0.001367904286123718983, 0.001563293733823083566 ),
 .UNSPECIFIED. ) ;
#41307 = DIRECTION ( 'NONE',  ( 0.000000000000000000, 0.000000000000000000, 1.000000000000000000 ) ) ;
#41308 = CARTESIAN_POINT ( 'NONE',  ( -2.241623956689868358, -5.557115091759786019, 34.35708131394839882 ) ) ;
#41309 = VECTOR ( 'NONE', #58115, 1000.000000000000000 ) ;
#41310 = CARTESIAN_POINT ( 'NONE',  ( -15.12820512820512953, -3.499999999999999556, 29.75000000000000355 ) ) ;
#41311 = LINE ( 'NONE', #34102, #39526 ) ;
#41312 = CARTESIAN_POINT ( 'NONE',  ( -17.07692307692319744, -4.481592998941358097, 33.73612834414048933 ) ) ;
#41313 = ORIENTED_EDGE ( 'NONE', *, *, #58628, .F. ) ;
#41314 = ORIENTED_EDGE ( 'NONE', *, *, #29568, .F. ) ;
#41315 = ORIENTED_EDGE ( 'NONE', *, *, #48700, .T. ) ;
#41317 = EDGE_LOOP ( 'NONE', ( #64936, #86505, #64860, #88353 ) ) ;
#41316 = CARTESIAN_POINT ( 'NONE',  ( -13.91025641025641058, -7.500000000000000000, 29.75000000000000355 ) ) ;
#41318 = CARTESIAN_POINT ( 'NONE',  ( -5.011667937410238416, -12.51329471203373700, 31.30864560766537963 ) ) ;
#41319 = DIRECTION ( 'NONE',  ( -1.000000000000000000, -0.000000000000000000, -0.000000000000000000 ) ) ;
#41320 = AXIS2_PLACEMENT_3D ( 'NONE', #5666, #33139, #26387 ) ;
#41321 = DIRECTION ( 'NONE',  ( -0.000000000000000000, -0.9396926207859093161, -0.3420201433256663259 ) ) ;
#41322 = CARTESIAN_POINT ( 'NONE',  ( -18.00000000000000000, -1.077559353945483744, 31.82153278338624602 ) ) ;
#41323 = ORIENTED_EDGE ( 'NONE', *, *, #66680, .T. ) ;
#41324 = EDGE_LOOP ( 'NONE', ( #28441, #47186 ) ) ;
#41325 = ORIENTED_EDGE ( 'NONE', *, *, #44800, .F. ) ;
#41326 = LINE ( 'NONE', #68795, #23119 ) ;
#41328 = VERTEX_POINT ( 'NONE', #79827 ) ;
#41327 = CARTESIAN_POINT ( 'NONE',  ( -10.48485917715097138, -2.647132371071621471, 31.75357179365171589 ) ) ;
#41329 = CARTESIAN_POINT ( 'NONE',  ( -4.153846153846152411, -1.422936976036506707, 30.56769352161908415 ) ) ;
#41330 = B_SPLINE_CURVE_WITH_KNOTS ( 'NONE', 3,
 ( #74236, #33693, #27815, #81890, #87777, #26493 ),
 .UNSPECIFIED., .F., .F.,
 ( 4, 2, 4 ),
 ( 0.0003909512603273880690, 0.0005862562993132132720, 0.0007815613382990384750 ),
 .UNSPECIFIED. ) ;
#41331 = LINE ( 'NONE', #74683, #55152 ) ;
#41332 = ORIENTED_EDGE ( 'NONE', *, *, #63620, .F. ) ;
#41333 = AXIS2_PLACEMENT_3D ( 'NONE', #42291, #21107, #76059 ) ;
#41334 = CARTESIAN_POINT ( 'NONE',  ( 9.019285080869085647, -12.41262288849542017, 30.68299917996395010 ) ) ;
#41335 = CARTESIAN_POINT ( 'NONE',  ( -5.326923076923075762, -2.499999999999998668, 29.75000000000000355 ) ) ;
#41336 = B_SPLINE_CURVE_WITH_KNOTS ( 'NONE', 3,
 ( #11204, #86893, #39135, #45420, #72899, #80109, #52625, #26501, #60272, #38674 ),
 .UNSPECIFIED., .F., .F.,
 ( 4, 2, 2, 2, 4 ),
 ( 0.0007817246256747440282, 0.0009771112852218863821, 0.001172497944769028844, 0.001367884604316171307, 0.001563271263863313769 ),
 .UNSPECIFIED. ) ;
#41337 = ORIENTED_EDGE ( 'NONE', *, *, #31671, .F. ) ;
#41338 = FACE_BOUND ( 'NONE', #84213, .T. ) ;
#41339 = CARTESIAN_POINT ( 'NONE',  ( 1.653273178848927064E-15, -7.500000000000000000, 29.50000000000000355 ) ) ;
#41340 = CARTESIAN_POINT ( 'NONE',  ( 15.93091919493929609, -2.523278758544490241, 31.42238647778636818 ) ) ;
#41341 = EDGE_CURVE ( 'NONE', #20954, #11784, #72062, .T. ) ;
#41342 = CARTESIAN_POINT ( 'NONE',  ( 3.361561038594018225, -8.999086150933472084, 34.52020707165672064 ) ) ;
#41344 = LINE ( 'NONE', #69258, #49786 ) ;
#41343 = CARTESIAN_POINT ( 'NONE',  ( 1.384615384615386802, -2.249999999999998668, 29.50000000000001421 ) ) ;
#41345 = CARTESIAN_POINT ( 'NONE',  ( -4.023320452082589149, -2.882268652242224505, 31.66798894389554064 ) ) ;
#41346 = CARTESIAN_POINT ( 'NONE',  ( -4.153846153846152411, -11.35647404775217417, 33.31231777344666511 ) ) ;
#41347 = VERTEX_POINT ( 'NONE', #44678 ) ;
#41348 = CARTESIAN_POINT ( 'NONE',  ( 14.43821800945587341, -12.45806712695776319, 30.39783852428763922 ) ) ;
#41349 = PRODUCT_DEFINITION ( 'UNKNOWN', '', #15939, #9532 ) ;
#41350 = SURFACE_SIDE_STYLE ('',( #47209 ) ) ;
#41351 = EDGE_LOOP ( 'NONE', ( #70219, #37403, #73001, #4187 ) ) ;
#41352 = DIRECTION ( 'NONE',  ( -0.000000000000000000, -0.8660254037844399289, -0.4999999999999980016 ) ) ;
#41353 = CYLINDRICAL_SURFACE ( 'NONE', #2972, 4.000000000000000000 ) ;
#41354 = ORIENTED_EDGE ( 'NONE', *, *, #62673, .T. ) ;
#41355 = AXIS2_PLACEMENT_3D ( 'NONE', #52741, #19410, #18531 ) ;
#41356 = DIRECTION ( 'NONE',  ( -0.000000000000000000, -0.7660444431189791237, -0.6427876096865379196 ) ) ;
#41357 = CARTESIAN_POINT ( 'NONE',  ( -4.153846153846152411, -2.292212530054420494, 30.41441678777542634 ) ) ;
#41358 = FACE_BOUND ( 'NONE', #43291, .T. ) ;
#41360 = LINE ( 'NONE', #20637, #4211 ) ;
#41359 = CARTESIAN_POINT ( 'NONE',  ( 8.769230769230768274, -3.322132147404559976, 32.92929555188717927 ) ) ;
#41361 = CARTESIAN_POINT ( 'NONE',  ( 10.36536137809165403, -8.432397168068783699, 34.66272746175022945 ) ) ;
#41362 = ADVANCED_FACE ( 'NONE', ( #84041 ), #35843, .F. ) ;
#41363 = CARTESIAN_POINT ( 'NONE',  ( 12.46153846153846168, -12.34228464037088635, 31.77849191805839268 ) ) ;
#41365 = CARTESIAN_POINT ( 'NONE',  ( -8.519176457592454454, -12.17597550085003633, 31.52189283813461884 ) ) ;
#41364 = SURFACE_SIDE_STYLE ('',( #13883 ) ) ;
#41366 = CARTESIAN_POINT ( 'NONE',  ( 24.00000000000000000, -5.499999999999981348, 27.75000000000000000 ) ) ;
#41367 = AXIS2_PLACEMENT_3D ( 'NONE', #35465, #75558, #15641 ) ;
#41368 = CARTESIAN_POINT ( 'NONE',  ( 3.775308065498768517, -8.992201783934554271, 15.54500670625849246 ) ) ;
#41369 = ORIENTED_EDGE ( 'NONE', *, *, #82435, .T. ) ;
#41370 = EDGE_LOOP ( 'NONE', ( #51488, #55814 ) ) ;
#41371 = CARTESIAN_POINT ( 'NONE',  ( -14.30769230769242739, -2.625532179533778709, 30.86335684631627174 ) ) ;
#41372 = VECTOR ( 'NONE', #70180, 1000.000000000000000 ) ;
#41373 = CARTESIAN_POINT ( 'NONE',  ( -10.36543920600657209, -8.476813868363244353, 34.90874843262270133 ) ) ;
#41374 = CARTESIAN_POINT ( 'NONE',  ( -5.999999999999998224, -13.87047571288749737, 32.06866353760679544 ) ) ;
#41375 = CARTESIAN_POINT ( 'NONE',  ( -0.6850233861027947846, -3.019605429927184836, 32.48692288466676814 ) ) ;
#41376 = CARTESIAN_POINT ( 'NONE',  ( 3.007843013253084230, -11.24512374952581872, 33.06303171183252942 ) ) ;
#41377 = CARTESIAN_POINT ( 'NONE',  ( 2.608446859217893099, -4.805146000318787358, 15.31063170625849068 ) ) ;
#41378 = CARTESIAN_POINT ( 'NONE',  ( -12.52680846209478460, -4.320704448112771878, 33.92786785259540494 ) ) ;
#41379 = DIRECTION ( 'NONE',  ( 0.000000000000000000, 0.6427876096865368094, 0.7660444431189802339 ) ) ;
#41380 = CARTESIAN_POINT ( 'NONE',  ( 15.36156103859402222, -11.71459661697925903, 32.44059661609676937 ) ) ;
#41381 = DIRECTION ( 'NONE',  ( -0.000000000000000000, 0.000000000000000000, 1.000000000000000000 ) ) ;
#41382 = LINE ( 'NONE', #7597, #45300 ) ;
#41383 = CARTESIAN_POINT ( 'NONE',  ( 5.299702745901139878, -8.540255544307065350, 34.89611431652622286 ) ) ;
#41384 = CARTESIAN_POINT ( 'NONE',  ( -16.15384615384615330, -12.78798330534102945, 29.74999999999997868 ) ) ;
#41385 = EDGE_CURVE ( 'NONE', #77968, #33107, #31631, .T. ) ;
#41386 = CARTESIAN_POINT ( 'NONE',  ( -6.857009589726848375, -3.322132147404559976, 32.92929555188717927 ) ) ;
#41387 = CARTESIAN_POINT ( 'NONE',  ( 3.007843013253082010, -2.554751324335734264, 30.48935550225260727 ) ) ;
#41388 = ORIENTED_EDGE ( 'NONE', *, *, #37289, .T. ) ;
#41389 = FACE_OUTER_BOUND ( 'NONE', #30615, .T. ) ;
#41390 = CARTESIAN_POINT ( 'NONE',  ( -19.50000000000000000, -3.499999999999999556, 29.75000000000000355 ) ) ;
#41391 = CARTESIAN_POINT ( 'NONE',  ( 2.775308065498755195, -6.422011778438505125, 22.14249329374151998 ) ) ;
#41392 = EDGE_CURVE ( 'NONE', #65630, #14162, #58646, .T. ) ;
#41393 = EDGE_CURVE ( 'NONE', #26228, #80339, #73198, .T. ) ;
#41394 = LINE ( 'NONE', #34634, #37484 ) ;
#41396 = CARTESIAN_POINT ( 'NONE',  ( -4.153846153846152411, -1.129524287112498415, 32.06866353760679544 ) ) ;
#41395 = AXIS2_PLACEMENT_3D ( 'NONE', #74033, #60508, #142 ) ;
#41397 = CARTESIAN_POINT ( 'NONE',  ( -9.757577692864012775, -5.941354392334499579, 34.76329471203369792 ) ) ;
#41399 = ORIENTED_EDGE ( 'NONE', *, *, #53826, .T. ) ;
#41398 = CARTESIAN_POINT ( 'NONE',  ( 7.715462379486288214, -2.541943142973490666, 30.39792223712631980 ) ) ;
#41400 = CARTESIAN_POINT ( 'NONE',  ( -2.749999999999991562, -8.639087296526026805, 26.26562500000000000 ) ) ;
#41401 = CARTESIAN_POINT ( 'NONE',  ( -9.561517251340742263, -5.496552790871120031, 34.60292014791297532 ) ) ;
#41402 = ORIENTED_EDGE ( 'NONE', *, *, #72354, .T. ) ;
#41403 = CARTESIAN_POINT ( 'NONE',  ( -4.153846153846152411, -2.517432740324522911, 35.29906147534542527 ) ) ;
#41404 = AXIS2_PLACEMENT_3D ( 'NONE', #81487, #53549, #87362 ) ;
#41405 = CARTESIAN_POINT ( 'NONE',  ( 7.596153846153846700, -7.566083408709834757, 34.74999999999999289 ) ) ;
#41406 = ORIENTED_EDGE ( 'NONE', *, *, #63050, .F. ) ;
#41407 = CARTESIAN_POINT ( 'NONE',  ( 7.596177115211490971, -4.236021600441998380, 33.53823185664189310 ) ) ;
#41408 = CARTESIAN_POINT ( 'NONE',  ( 8.703148389870632329, -6.343179335718451384, 34.87096338111212646 ) ) ;
#41409 = VECTOR ( 'NONE', #51793, 1000.000000000000227 ) ;
#41410 = DIRECTION ( 'NONE',  ( 0.000000000000000000, 0.000000000000000000, 1.000000000000000000 ) ) ;
#41411 = ORIENTED_EDGE ( 'NONE', *, *, #39872, .F. ) ;
#41412 = ORIENTED_EDGE ( 'NONE', *, *, #41968, .F. ) ;
#41413 = CARTESIAN_POINT ( 'NONE',  ( -6.792286482109971324, -8.191423895709842640, 34.95447573519442130 ) ) ;
#41414 = EDGE_LOOP ( 'NONE', ( #41315, #82275, #2775, #66882 ) ) ;
#41415 = LINE ( 'NONE', #40974, #60112 ) ;
#41416 = CARTESIAN_POINT ( 'NONE',  ( 5.142178216435913107, -5.094484230520773593, 34.41647553114626845 ) ) ;
#41417 = CARTESIAN_POINT ( 'NONE',  ( -15.36145983387954139, -2.295517848115769421, 30.44137282052137294 ) ) ;
#41418 = DIRECTION ( 'NONE',  ( 0.000000000000000000, 0.9848077530122072432, -0.1736481776669354937 ) ) ;
#41419 = DIRECTION ( 'NONE',  ( 0.000000000000000000, 0.4999999999999960032, -0.8660254037844410391 ) ) ;
#41420 = DIRECTION ( 'NONE',  ( 1.000000000000000000, 0.000000000000000000, 0.000000000000000000 ) ) ;
#41421 = CARTESIAN_POINT ( 'NONE',  ( -5.076923076923199218, -12.16647553114689728, 32.15551576947799362 ) ) ;
#41422 = B_SPLINE_CURVE_WITH_KNOTS ( 'NONE', 3,
 ( #33196, #12923, #48468, #40411, #54788, #61990, #20563, #81836, #67868, #81396 ),
 .UNSPECIFIED., .F., .F.,
 ( 4, 2, 2, 2, 4 ),
 ( 0.0007817359430256326080, 0.0009771253907249993591, 0.001172514838424366110, 0.001367904286123732861, 0.001563293733823099612 ),
 .UNSPECIFIED. ) ;
#41423 = VECTOR ( 'NONE', #32059, 1000.000000000000114 ) ;
#41424 = ORIENTED_EDGE ( 'NONE', *, *, #25623, .F. ) ;
#41425 = ORIENTED_EDGE ( 'NONE', *, *, #64913, .F. ) ;
#41427 = VERTEX_POINT ( 'NONE', #20347 ) ;
#41426 = CARTESIAN_POINT ( 'NONE',  ( -10.61538461538461320, -2.833524468853757305, 32.15551576947925838 ) ) ;
#41428 = VECTOR ( 'NONE', #76127, 1000.000000000000000 ) ;
#41429 = CARTESIAN_POINT ( 'NONE',  ( 7.623226887246997485, -2.523278758544489797, 31.42238647778637528 ) ) ;
#41430 = VERTEX_POINT ( 'NONE', #39291 ) ;
#41431 = CARTESIAN_POINT ( 'NONE',  ( -4.153846153846152411, -1.629998284177014645, 34.34916445242399163 ) ) ;
#41432 = DIRECTION ( 'NONE',  ( 0.000000000000000000, 0.3420201433256641055, -0.9396926207859100932 ) ) ;
#41433 = ORIENTED_EDGE ( 'NONE', *, *, #7447, .F. ) ;
#41434 = CARTESIAN_POINT ( 'NONE',  ( 2.307692307692186251, -10.33852847137269571, 34.16647553114546554 ) ) ;
#41435 = EDGE_CURVE ( 'NONE', #53468, #28895, #74317, .T. ) ;
#41436 = ORIENTED_EDGE ( 'NONE', *, *, #48568, .T. ) ;
#41437 = CARTESIAN_POINT ( 'NONE',  ( 7.912221179503920787, -12.62096338111211757, 30.90682066428152908 ) ) ;
#41438 = VERTEX_POINT ( 'NONE', #61303 ) ;
#41439 = CARTESIAN_POINT ( 'NONE',  ( -14.30769230769242917, -2.379036618888197729, 30.90682066428292885 ) ) ;
#41440 = VERTEX_POINT ( 'NONE', #19449 ) ;
#41441 = CARTESIAN_POINT ( 'NONE',  ( -16.40386939113911779, -6.695914987888146541, 34.68535235679833306 ) ) ;
#41442 = CARTESIAN_POINT ( 'NONE',  ( -4.153846153846274980, -6.835583212225970762, 34.95778746994575670 ) ) ;
#41443 = FACE_BOUND ( 'NONE', #5097, .T. ) ;
#41444 = FACE_OUTER_BOUND ( 'NONE', #24822, .T. ) ;
#41445 = CARTESIAN_POINT ( 'NONE',  ( -6.673022611438610419, -12.17597550085003633, 31.52189283813461884 ) ) ;
#41446 = ADVANCED_FACE ( 'NONE', ( #82496 ), #80728, .F. ) ;
#41447 = CARTESIAN_POINT ( 'NONE',  ( 4.403791672194296680, -12.43552623307873972, 30.55307653245132826 ) ) ;
#41448 = CARTESIAN_POINT ( 'NONE',  ( -3.480745961711584346, -4.236021600441998380, 33.53823185664189310 ) ) ;
#41449 = AXIS2_PLACEMENT_3D ( 'NONE', #75469, #54303, #62384 ) ;
#41450 = LINE ( 'NONE', #42347, #4981 ) ;
#41451 = CARTESIAN_POINT ( 'NONE',  ( -4.283993363284372080, -11.47017969459903952, 32.78971311882034456 ) ) ;
#41452 = CARTESIAN_POINT ( 'NONE',  ( -17.07692307692307665, -12.37446782046654192, 30.86335684631486131 ) ) ;
#41453 = EDGE_CURVE ( 'NONE', #45729, #40586, #68517, .T. ) ;
#41454 = ORIENTED_EDGE ( 'NONE', *, *, #53478, .T. ) ;
#41455 = VERTEX_POINT ( 'NONE', #55011 ) ;
#41456 = VECTOR ( 'NONE', #990, 1000.000000000000227 ) ;
#41458 = CARTESIAN_POINT ( 'NONE',  ( -3.230769230769352962, -5.941354392335915335, 34.76329471203413846 ) ) ;
#41457 = CARTESIAN_POINT ( 'NONE',  ( 2.307692307692187583, -10.90142922262034020, 33.41473453929536674 ) ) ;
#41459 = CARTESIAN_POINT ( 'NONE',  ( -11.66860874789975888, -11.93770438780619259, 32.05411857736982029 ) ) ;
#41460 = CARTESIAN_POINT ( 'NONE',  ( -7.846153846153844924, -13.95598074871891292, 31.83374038241031911 ) ) ;
#41461 = CARTESIAN_POINT ( 'NONE',  ( -10.55012947587177408, -12.51329471203373700, 31.30864560766537963 ) ) ;
#41462 = CARTESIAN_POINT ( 'NONE',  ( 7.846153846153725020, -6.026961402154118019, 34.52809138561165270 ) ) ;
#41463 = ORIENTED_EDGE ( 'NONE', *, *, #49395, .T. ) ;
#41464 = CARTESIAN_POINT ( 'NONE',  ( 17.14299142792551578, -3.050289026998446840, 32.03036669348366416 ) ) ;
#41465 = CARTESIAN_POINT ( 'NONE',  ( -14.43838291080261627, -9.929715669179220328, 34.40415004197138416 ) ) ;
#41466 = CARTESIAN_POINT ( 'NONE',  ( -14.37296275365308418, -8.613356846314824011, 34.62446782046655613 ) ) ;
#41467 = ADVANCED_FACE ( 'NONE', ( #19008 ), #67644, .F. ) ;
#41468 = CARTESIAN_POINT ( 'NONE',  ( -8.638705330997128229, -2.647132371071621471, 31.75357179365171589 ) ) ;
#41469 = EDGE_LOOP ( 'NONE', ( #50756, #66097 ) ) ;
#41470 = ORIENTED_EDGE ( 'NONE', *, *, #3068, .T. ) ;
#41471 = B_SPLINE_CURVE_WITH_KNOTS ( 'NONE', 3,
 ( #77360, #70606, #30498, #31390, #29627, #71926 ),
 .UNSPECIFIED., .F., .F.,
 ( 4, 2, 4 ),
 ( 4.224605973302673136E-17, 0.0001954756301637161251, 0.0003909512603273899664 ),
 .UNSPECIFIED. ) ;
#41473 = EDGE_CURVE ( 'NONE', #38026, #38006, #40181, .T. ) ;
#41472 = ORIENTED_EDGE ( 'NONE', *, *, #84530, .T. ) ;
#41474 = CARTESIAN_POINT ( 'NONE',  ( 0.5923768795512234231, -7.277220443632451463, 34.74524770363009196 ) ) ;
#41475 = ORIENTED_EDGE ( 'NONE', *, *, #15289, .T. ) ;
#41476 = CARTESIAN_POINT ( 'NONE',  ( -9.692307692307814193, -10.33852847137269571, 34.16647553114546554 ) ) ;
#41477 = CARTESIAN_POINT ( 'NONE',  ( 15.23076923076910916, -4.320704448113951379, 33.92786785259630022 ) ) ;
#41478 = CARTESIAN_POINT ( 'NONE',  ( 3.230769230769231726, -9.905515769479276145, 34.41647553114623292 ) ) ;
#41479 = DIRECTION ( 'NONE',  ( -1.000000000000000000, -0.000000000000000000, -0.000000000000000000 ) ) ;
#41480 = CARTESIAN_POINT ( 'NONE',  ( 9.822833394071261992, -6.001044277235009439, 34.52024696741798948 ) ) ;
#41481 = ORIENTED_EDGE ( 'NONE', *, *, #42491, .F. ) ;
#41482 = CARTESIAN_POINT ( 'NONE',  ( -11.60421496677487063, -7.249945578846652694, 34.99404164642496795 ) ) ;
#41484 = VERTEX_POINT ( 'NONE', #74396 ) ;
#41483 = CARTESIAN_POINT ( 'NONE',  ( -12.33074665371367651, -11.71459661697925903, 32.44059661609676937 ) ) ;
#41485 = PLANE ( 'NONE',  #46882 ) ;
#41486 = CARTESIAN_POINT ( 'NONE',  ( 16.15384615384615330, -13.53365097954675988, 30.81389545987213552 ) ) ;
#41487 = CARTESIAN_POINT ( 'NONE',  ( -19.00000000000000000, -7.500000000000000000, 29.75000000000000355 ) ) ;
#41488 = CARTESIAN_POINT ( 'NONE',  ( 8.992010438208831502, -12.11081565061823717, 32.26097654155341843 ) ) ;
#41489 = DIRECTION ( 'NONE',  ( 1.000000000000000000, 0.000000000000000000, 0.000000000000000000 ) ) ;
#41490 = EDGE_CURVE ( 'NONE', #85035, #75229, #47805, .T. ) ;
#41491 = CYLINDRICAL_SURFACE ( 'NONE', #6142, 0.2499999999999973355 ) ;
#41492 = CARTESIAN_POINT ( 'NONE',  ( -0.7115616857599206257, -2.588893531581426988, 31.60682220781847818 ) ) ;
#41493 = EDGE_CURVE ( 'NONE', #72231, #5606, #81164, .T. ) ;
#41494 = CARTESIAN_POINT ( 'NONE',  ( -1.077988221561493543, -4.724691934501247914, 19.32999329374151642 ) ) ;
#41495 = ORIENTED_EDGE ( 'NONE', *, *, #30623, .T. ) ;
#41496 = AXIS2_PLACEMENT_3D ( 'NONE', #20959, #83581, #21858 ) ;
#41497 = DIRECTION ( 'NONE',  ( 1.000000000000000000, 0.000000000000000000, 0.000000000000000000 ) ) ;
#41498 = CARTESIAN_POINT ( 'NONE',  ( 1.384615384615264011, -9.528491918059723176, 34.59228464037033035 ) ) ;
#41499 = ADVANCED_FACE ( 'NONE', ( #54108 ), #6815, .F. ) ;
#41500 = CARTESIAN_POINT ( 'NONE',  ( -15.23076923076922995, -8.318370150425687726, 35.83090037661290239 ) ) ;
#41501 = CARTESIAN_POINT ( 'NONE',  ( -13.25382357679060519, -8.147973898785416225, 34.70805048591653730 ) ) ;
#41502 = EDGE_CURVE ( 'NONE', #76098, #22173, #18304, .T. ) ;
#41503 = ORIENTED_EDGE ( 'NONE', *, *, #61789, .F. ) ;
#41504 = CARTESIAN_POINT ( 'NONE',  ( -12.68446467905461006, -11.76352882383564769, 32.36236540154569497 ) ) ;
#41505 = CARTESIAN_POINT ( 'NONE',  ( -15.93106661257773915, -12.24180327182771855, 31.33663988360758168 ) ) ;
#41506 = CARTESIAN_POINT ( 'NONE',  ( 1.384615384615265343, -9.442884908241554243, 34.35708131394783038 ) ) ;
#41507 = DIRECTION ( 'NONE',  ( -0.000000000000000000, -0.9848077530122085754, -0.1736481776669273613 ) ) ;
#41508 = CARTESIAN_POINT ( 'NONE',  ( -11.97435897435897267, -3.499999999999999556, 29.75000000000000355 ) ) ;
#41509 = ORIENTED_EDGE ( 'NONE', *, *, #38520, .T. ) ;
#41510 = CARTESIAN_POINT ( 'NONE',  ( -15.29603967673000575, -2.892918686051582977, 31.69288490824015980 ) ) ;
#41511 = CARTESIAN_POINT ( 'NONE',  ( 3.480823542407545101, -12.17597550085003455, 31.52189283813461884 ) ) ;
#41512 = CARTESIAN_POINT ( 'NONE',  ( 5.207448515156721136, -12.50538340440932217, 31.33453814440721885 ) ) ;
#41513 = VERTEX_POINT ( 'NONE', #61749 ) ;
#41514 = CYLINDRICAL_SURFACE ( 'NONE', #11071, 0.2499999999999998890 ) ;
#41515 = ORIENTED_EDGE ( 'NONE', *, *, #88412, .T. ) ;
#41516 = VECTOR ( 'NONE', #43260, 999.9999999999998863 ) ;
#41517 = CARTESIAN_POINT ( 'NONE',  ( -7.846153846153844924, -5.471508081941601098, 34.59228464037088457 ) ) ;
#41518 = CARTESIAN_POINT ( 'NONE',  ( 11.31553457955468467, -2.523278758544489797, 31.42238647778637528 ) ) ;
#41519 = ORIENTED_EDGE ( 'NONE', *, *, #83803, .T. ) ;
#41520 = CARTESIAN_POINT ( 'NONE',  ( 7.780883400193071786, -12.27809138561121394, 31.22303859784730307 ) ) ;
#41521 = DIRECTION ( 'NONE',  ( -0.000000000000000000, 0.9396926207859092051, -0.3420201433256662704 ) ) ;
#41522 = DIRECTION ( 'NONE',  ( -0.000000000000000000, 0.3420201433256694346, -0.9396926207859080948 ) ) ;
#41523 = VECTOR ( 'NONE', #48843, 1000.000000000000227 ) ;
#41524 = VECTOR ( 'NONE', #16223, 1000.000000000000227 ) ;
#41525 = CARTESIAN_POINT ( 'NONE',  ( -7.846153846153967493, -5.094484230521993062, 34.41647553114689373 ) ) ;
#41526 = CARTESIAN_POINT ( 'NONE',  ( 3.480823542407545546, -12.41262288849542017, 30.68299917996395010 ) ) ;
#41527 = EDGE_CURVE ( 'NONE', #5856, #88899, #29012, .T. ) ;
#41528 = VECTOR ( 'NONE', #4914, 1000.000000000000114 ) ;
#41529 = EDGE_LOOP ( 'NONE', ( #75791, #35637 ) ) ;
#41530 = FACE_BOUND ( 'NONE', #60156, .T. ) ;
#41531 = ORIENTED_EDGE ( 'NONE', *, *, #15305, .T. ) ;
#41532 = LINE ( 'NONE', #83415, #65875 ) ;
#41533 = EDGE_CURVE ( 'NONE', #1706, #17127, #69828, .T. ) ;
#41534 = EDGE_CURVE ( 'NONE', #26475, #38566, #28422, .T. ) ;
#41535 = CYLINDRICAL_SURFACE ( 'NONE', #66055, 0.2500000000000012212 ) ;
#41536 = CARTESIAN_POINT ( 'NONE',  ( 11.53846153846141753, -2.625532179533778709, 30.86335684631627174 ) ) ;
#41537 = CARTESIAN_POINT ( 'NONE',  ( -11.47320596718551045, -2.625532179533470512, 30.86335684631491105 ) ) ;
#41538 = ORIENTED_EDGE ( 'NONE', *, *, #85486, .T. ) ;
#41539 = EDGE_CURVE ( 'NONE', #51846, #58941, #14919, .T. ) ;
#41540 = ORIENTED_EDGE ( 'NONE', *, *, #45959, .F. ) ;
#41541 = EDGE_LOOP ( 'NONE', ( #76925, #60691, #35543, #66213 ) ) ;
#41542 = CARTESIAN_POINT ( 'NONE',  ( -10.61538461538461320, -8.164416787775445883, 34.95778746994557906 ) ) ;
#41543 = VERTEX_POINT ( 'NONE', #36515 ) ;
#41544 = CYLINDRICAL_SURFACE ( 'NONE', #15808, 0.2500000000000009437 ) ;
#41545 = CARTESIAN_POINT ( 'NONE',  ( -9.915134384786696842, -7.369208160676171460, 34.74850200257122879 ) ) ;
#41546 = FACE_OUTER_BOUND ( 'NONE', #1942, .T. ) ;
#41547 = CARTESIAN_POINT ( 'NONE',  ( 11.28848480751918437, -2.564618984488975517, 30.55390908950641915 ) ) ;
#41548 = CARTESIAN_POINT ( 'NONE',  ( 5.076923076922953193, -10.33852847137269571, 34.16647553114546554 ) ) ;
#41549 = CARTESIAN_POINT ( 'NONE',  ( 0.000000000000000000, -11.00000000000000000, 29.75000000000000355 ) ) ;
#41550 = CARTESIAN_POINT ( 'NONE',  ( 14.43848411551709709, -6.413143153341454017, 34.63066358083362672 ) ) ;
#41551 = CARTESIAN_POINT ( 'NONE',  ( 17.32697738856138869, -2.564540009722896752, 30.55348353981672105 ) ) ;
#41552 = ORIENTED_EDGE ( 'NONE', *, *, #57121, .F. ) ;
#41553 = EDGE_CURVE ( 'NONE', #54188, #22025, #11762, .T. ) ;
#41554 = ORIENTED_EDGE ( 'NONE', *, *, #85118, .T. ) ;
#41555 = ORIENTED_EDGE ( 'NONE', *, *, #21148, .F. ) ;
#41556 = CARTESIAN_POINT ( 'NONE',  ( 3.165446315277056222, -7.749976743299137993, 34.99404534957040624 ) ) ;
#41558 = CARTESIAN_POINT ( 'NONE',  ( 10.61538461538449596, -6.879047030192662504, 34.71129190930017927 ) ) ;
#41557 = DIRECTION ( 'NONE',  ( 0.000000000000000000, -1.000000000000000000, 0.000000000000000000 ) ) ;
#41559 = CYLINDRICAL_SURFACE ( 'NONE', #57158, 0.2500000000000009437 ) ;
#41560 = CARTESIAN_POINT ( 'NONE',  ( -10.61538461538473399, -3.835265460704628371, 33.15142922262033665 ) ) ;
#41561 = FACE_BOUND ( 'NONE', #55466, .T. ) ;
#41562 = CARTESIAN_POINT ( 'NONE',  ( 9.915087233576105774, -3.755027918224367767, 33.06320215134714857 ) ) ;
#41563 = VERTEX_POINT ( 'NONE', #42832 ) ;
#41564 = CARTESIAN_POINT ( 'NONE',  ( 0.3962684609821406911, -11.67786785259540672, 32.92929555188720059 ) ) ;
#41565 = DIRECTION ( 'NONE',  ( -0.000000000000000000, 0.7660444431189791237, -0.6427876096865379196 ) ) ;
#41566 = CARTESIAN_POINT ( 'NONE',  ( 16.85399685940693004, -6.503392248772476236, 34.64988816332204635 ) ) ;
#41567 = CARTESIAN_POINT ( 'NONE',  ( 9.070512820512819374, -3.499999999999999556, 29.75000000000000355 ) ) ;
#41568 = ORIENTED_EDGE ( 'NONE', *, *, #73588, .F. ) ;
#41569 = CARTESIAN_POINT ( 'NONE',  ( 17.99999999999987566, -12.46129190930018460, 30.37095296980731973 ) ) ;
#41570 = ORIENTED_EDGE ( 'NONE', *, *, #80, .T. ) ;
#41571 = FACE_BOUND ( 'NONE', #74938, .T. ) ;
#41572 = CARTESIAN_POINT ( 'NONE',  ( -17.20707104665477161, -4.299443229763728169, 33.91186481527756058 ) ) ;
#41573 = B_SPLINE_CURVE_WITH_KNOTS ( 'NONE', 3,
 ( #25940, #53858, #39916, #11546, #5229, #81345, #67376, #25501, #39029, #88558 ),
 .UNSPECIFIED., .F., .F.,
 ( 4, 2, 2, 2, 4 ),
 ( 0.000000000000000000, 0.0001954339857564093175, 0.0003908679715128186350, 0.0005863019572692279796, 0.0007817359430256372700 ),
 .UNSPECIFIED. ) ;
#41574 = AXIS2_PLACEMENT_3D ( 'NONE', #14613, #77196, #36658 ) ;
#41575 = CARTESIAN_POINT ( 'NONE',  ( -8.069020109216943126, -2.251424796025575770, 29.88072029997477230 ) ) ;
#41576 = CARTESIAN_POINT ( 'NONE',  ( -12.68502338610278990, -12.11044203135681840, 32.26167407432752299 ) ) ;
#41577 = ORIENTED_EDGE ( 'NONE', *, *, #64417, .T. ) ;
#41579 = CARTESIAN_POINT ( 'NONE',  ( 0.3954550505825812912, -10.51840700105979387, 33.73612834413961536 ) ) ;
#41578 = B_SPLINE_CURVE_WITH_KNOTS ( 'NONE', 3,
 ( #3903, #18771, #85895, #38593, #59299, #25076, #45786, #59749, #4813, #46238 ),
 .UNSPECIFIED., .F., .F.,
 ( 4, 2, 2, 2, 4 ),
 ( 0.0007817246256747461966, 0.0009771112852218892010, 0.001172497944769032314, 0.001367884604316175427, 0.001563271263863318323 ),
 .UNSPECIFIED. ) ;
#41580 = CARTESIAN_POINT ( 'NONE',  ( -3.230769230769352962, -2.379036618888197285, 30.90682066428292885 ) ) ;
#41581 = CARTESIAN_POINT ( 'NONE',  ( -3.230769230769229949, -2.721908614388771852, 31.22303859784724978 ) ) ;
#41582 = DIRECTION ( 'NONE',  ( 0.000000000000000000, 0.9848077530122072432, -0.1736481776669354937 ) ) ;
#41583 = EDGE_LOOP ( 'NONE', ( #10429, #78790, #74270, #73429 ) ) ;
#41584 = CARTESIAN_POINT ( 'NONE',  ( 16.37662569511456567, -10.81320215134717166, 33.49497208177562868 ) ) ;
#41585 = CARTESIAN_POINT ( 'NONE',  ( 3.903869409797563250, -10.06842814019191401, 34.32929386961144758 ) ) ;
#41586 = AXIS2_PLACEMENT_3D ( 'NONE', #29105, #49795, #70520 ) ;
#41588 = ORIENTED_EDGE ( 'NONE', *, *, #81159, .T. ) ;
#41587 = CARTESIAN_POINT ( 'NONE',  ( 14.30769230769231015, -11.16473453929635440, 33.15142922261926373 ) ) ;
#41589 = CARTESIAN_POINT ( 'NONE',  ( -4.153846153846152411, -2.538708090699994813, 30.37095296980875503 ) ) ;
#41590 = DIRECTION ( 'NONE',  ( -0.000000000000000000, 0.8660254037844399289, -0.4999999999999980016 ) ) ;
#41591 = CARTESIAN_POINT ( 'NONE',  ( 13.51540719244017730, -12.38066358083363738, 30.83685684665853444 ) ) ;
#41593 = CARTESIAN_POINT ( 'NONE',  ( -13.38461538461538325, -3.513871655860378418, 32.76840700105978499 ) ) ;
#41592 = B_SPLINE_CURVE_WITH_KNOTS ( 'NONE', 3,
 ( #5836, #79722, #38732, #52232, #12594, #5396 ),
 .UNSPECIFIED., .F., .F.,
 ( 4, 2, 4 ),
 ( 0.000000000000000000, 0.0001954784845028772859, 0.0003909569690057545718 ),
 .UNSPECIFIED. ) ;
#41594 = CARTESIAN_POINT ( 'NONE',  ( 9.758376043310132530, -8.973038597847271092, 34.52809138561121216 ) ) ;
#41596 = CYLINDRICAL_SURFACE ( 'NONE', #61879, 4.000000000000000000 ) ;
#41595 = CARTESIAN_POINT ( 'NONE',  ( -9.692307692307691624, -2.538708090699994813, 30.37095296980875503 ) ) ;
#41597 = ADVANCED_FACE ( 'NONE', ( #70296 ), #21216, .F. ) ;
#41598 = AXIS2_PLACEMENT_3D ( 'NONE', #48989, #21967, #48094 ) ;
#41599 = EDGE_CURVE ( 'NONE', #78839, #34884, #40798, .T. ) ;
#41600 = CARTESIAN_POINT ( 'NONE',  ( 12.39621444873415257, -7.749976730030849303, 34.74374725381503737 ) ) ;
#41601 = CARTESIAN_POINT ( 'NONE',  ( 1.944543648262996083, -5.555456351736983045, 16.81250000000000000 ) ) ;
#41602 = VERTEX_POINT ( 'NONE', #22110 ) ;
#41603 = CARTESIAN_POINT ( 'NONE',  ( 2.307692307692309264, -11.16473453929635440, 33.15142922261926373 ) ) ;
#41604 = ORIENTED_EDGE ( 'NONE', *, *, #38429, .F. ) ;
#41605 = EDGE_CURVE ( 'NONE', #37210, #8934, #50509, .T. ) ;
#41606 = ORIENTED_EDGE ( 'NONE', *, *, #56180, .T. ) ;
#41607 = CARTESIAN_POINT ( 'NONE',  ( -8.638440328263818913, -6.369690395747422684, 34.87708834333098196 ) ) ;
#41608 = EDGE_CURVE ( 'NONE', #36439, #80539, #62204, .T. ) ;
#41609 = EDGE_LOOP ( 'NONE', ( #58495, #7737, #25305, #69830 ) ) ;
#41610 = CARTESIAN_POINT ( 'NONE',  ( -15.23076923076922995, -6.435427911321262684, 35.78748833219616898 ) ) ;
#41611 = CARTESIAN_POINT ( 'NONE',  ( 1.944543648263018731, -9.444543648262994751, 18.37500000000000355 ) ) ;
#41612 = CARTESIAN_POINT ( 'NONE',  ( 0.4615384615384611755, -8.810774026931790459, 35.74407628777942847 ) ) ;
#41613 = CARTESIAN_POINT ( 'NONE',  ( -15.93083480223330817, -5.667800583137506898, 34.40243808032445827 ) ) ;
#41614 = CARTESIAN_POINT ( 'NONE',  ( -5.999999999999998224, -2.499999999999998668, 29.75000000000001421 ) ) ;
#41615 = DIRECTION ( 'NONE',  ( -0.000000000000000000, -0.000000000000000000, -1.000000000000000000 ) ) ;
#41616 = CARTESIAN_POINT ( 'NONE',  ( 2.084766090176159992, -9.886141570436013382, 34.14413921362392301 ) ) ;
#41617 = EDGE_CURVE ( 'NONE', #39653, #10726, #14467, .T. ) ;
#41618 = CYLINDRICAL_SURFACE ( 'NONE', #43674, 0.2499999999999995559 ) ;
#41619 = FACE_OUTER_BOUND ( 'NONE', #83631, .T. ) ;
#41620 = CARTESIAN_POINT ( 'NONE',  ( -5.076923076923197442, -8.613356846316285953, 34.62446782046622218 ) ) ;
#41621 = B_SPLINE_CURVE_WITH_KNOTS ( 'NONE', 3,
 ( #63203, #1519, #29003, #30744, #51432, #85705, #11371, #80283, #45146, #4616 ),
 .UNSPECIFIED., .F., .F.,
 ( 4, 2, 2, 2, 4 ),
 ( 0.0007817246256747484735, 0.0009771112852218928873, 0.001172497944769037084, 0.001367884604316181498, 0.001563271263863325912 ),
 .UNSPECIFIED. ) ;
#41622 = EDGE_CURVE ( 'NONE', #84688, #14974, #84841, .T. ) ;
#41623 = CARTESIAN_POINT ( 'NONE',  ( 5.933917620639864943, -11.35647404775217595, 33.31231777344666511 ) ) ;
#41624 = CARTESIAN_POINT ( 'NONE',  ( -9.692307692307691624, -3.322132147404559976, 32.92929555188717927 ) ) ;
#41625 = ORIENTED_EDGE ( 'NONE', *, *, #14594, .T. ) ;
#41626 = ORIENTED_EDGE ( 'NONE', *, *, #74615, .F. ) ;
#41627 = DIRECTION ( 'NONE',  ( 0.000000000000000000, 0.4999999999999985567, 0.8660254037844395958 ) ) ;
#41628 = CARTESIAN_POINT ( 'NONE',  ( 15.45354889974729495, -12.11081565061823717, 32.26097654155341843 ) ) ;
#41629 = PLANE ( 'NONE',  #61244 ) ;
#41630 = EDGE_CURVE ( 'NONE', #7422, #33560, #66649, .T. ) ;
#41631 = CARTESIAN_POINT ( 'NONE',  ( -11.53846153846153655, -12.48256725967547354, 35.29906147534542527 ) ) ;
#41632 = CARTESIAN_POINT ( 'NONE',  ( 12.39626801557768587, -9.442884908240170461, 34.35708131394840592 ) ) ;
#41633 = CARTESIAN_POINT ( 'NONE',  ( -13.38461538461538325, -10.67929555188718282, 33.92786785259544047 ) ) ;
#41634 = CARTESIAN_POINT ( 'NONE',  ( -2.307692307692428724, -8.656820664282941280, 34.87096338111179961 ) ) ;
#41635 = ADVANCED_FACE ( 'NONE', ( #64402 ), #50452, .F. ) ;
#41636 = ORIENTED_EDGE ( 'NONE', *, *, #26247, .T. ) ;
#41637 = CARTESIAN_POINT ( 'NONE',  ( 16.02369894440793985, -2.882441371585227508, 31.66841991370172238 ) ) ;
#41638 = ORIENTED_EDGE ( 'NONE', *, *, #67908, .T. ) ;
#41639 = EDGE_CURVE ( 'NONE', #52419, #41861, #34422, .T. ) ;
#41640 = CARTESIAN_POINT ( 'NONE',  ( 9.758376043310132530, -11.69971097300155272, 32.46337939537588113 ) ) ;
#41641 = AXIS2_PLACEMENT_3D ( 'NONE', #29829, #9121, #14537 ) ;
#41642 = AXIS2_PLACEMENT_3D ( 'NONE', #50063, #28934, #36985 ) ;
#41643 = LINE ( 'NONE', #49283, #60007 ) ;
#41644 = CARTESIAN_POINT ( 'NONE',  ( -4.153846153846152411, -4.098570777380720287, 33.41473453929634729 ) ) ;
#41645 = CYLINDRICAL_SURFACE ( 'NONE', #62346, 0.2500000000000012212 ) ;
#41646 = DIRECTION ( 'NONE',  ( -0.000000000000000000, -0.000000000000000000, -1.000000000000000000 ) ) ;
#41647 = VECTOR ( 'NONE', #46419, 1000.000000000000000 ) ;
#41648 = EDGE_LOOP ( 'NONE', ( #49637, #53990, #86049, #65927 ) ) ;
#41649 = EDGE_CURVE ( 'NONE', #87319, #41602, #46217, .T. ) ;
#41650 = B_SPLINE_CURVE_WITH_KNOTS ( 'NONE', 3,
 ( #89127, #6685, #67510, #80131, #68385, #33282, #52647, #60741, #53985, #81475 ),
 .UNSPECIFIED., .F., .F.,
 ( 4, 2, 2, 2, 4 ),
 ( 0.0007817359430256283796, 0.0009771253907249943717, 0.001172514838424360255, 0.001367904286123726356, 0.001563293733823092240 ),
 .UNSPECIFIED. ) ;
#41651 = VECTOR ( 'NONE', #26327, 1000.000000000000227 ) ;
#41652 = ORIENTED_EDGE ( 'NONE', *, *, #88791, .T. ) ;
#41653 = VERTEX_POINT ( 'NONE', #71170 ) ;
#41654 = ORIENTED_EDGE ( 'NONE', *, *, #60401, .T. ) ;
#41655 = EDGE_CURVE ( 'NONE', #13933, #17114, #37379, .T. ) ;
#41656 = CARTESIAN_POINT ( 'NONE',  ( -3.296019162543315062, -2.255955759149247619, 30.00000000000013856 ) ) ;
#41657 = CARTESIAN_POINT ( 'NONE',  ( -2.307692307692305711, -9.905515769479276145, 34.41647553114623292 ) ) ;
#41658 = CARTESIAN_POINT ( 'NONE',  ( -3.361460697436789768, -9.804603061927743113, 34.18744698557895845 ) ) ;
#41659 = FACE_OUTER_BOUND ( 'NONE', #7301, .T. ) ;
#41660 = CARTESIAN_POINT ( 'NONE',  ( 7.596153846153847589, -7.433932668274256805, 35.00000000000000711 ) ) ;
#41661 = CARTESIAN_POINT ( 'NONE',  ( -15.48079245499068612, -2.588893531581426988, 31.60682220781847818 ) ) ;
#41662 = ORIENTED_EDGE ( 'NONE', *, *, #76005, .T. ) ;
#41663 = EDGE_CURVE ( 'NONE', #68176, #40963, #63306, .T. ) ;
#41664 = ORIENTED_EDGE ( 'NONE', *, *, #71709, .F. ) ;
#41665 = EDGE_LOOP ( 'NONE', ( #67937, #55423 ) ) ;
#41667 = EDGE_LOOP ( 'NONE', ( #5724, #43281 ) ) ;
#41666 = CARTESIAN_POINT ( 'NONE',  ( 8.769230769230768274, -2.517432740324522911, 35.29906147534542527 ) ) ;
#41668 = EDGE_CURVE ( 'NONE', #34542, #65424, #48281, .T. ) ;
#41669 = CARTESIAN_POINT ( 'NONE',  ( 17.07692307692295586, -11.06231777344772027, 33.60647404775119895 ) ) ;
#41670 = CYLINDRICAL_SURFACE ( 'NONE', #54690, 0.2499999999999994726 ) ;
#41671 = CARTESIAN_POINT ( 'NONE',  ( -3.749999999999997335, -7.500000000000021316, 21.34375000000000000 ) ) ;
#41672 = ORIENTED_EDGE ( 'NONE', *, *, #15284, .T. ) ;
#41673 = VECTOR ( 'NONE', #85996, 1000.000000000000000 ) ;
#41674 = ORIENTED_EDGE ( 'NONE', *, *, #49188, .T. ) ;
#41675 = CARTESIAN_POINT ( 'NONE',  ( -17.74994558008654622, -2.920487667080175154, 32.31805714834172960 ) ) ;
#41676 = VERTEX_POINT ( 'NONE', #38283 ) ;
#41677 = FACE_BOUND ( 'NONE', #73556, .T. ) ;
#41678 = LINE ( 'NONE', #77227, #82020 ) ;
#41679 = CARTESIAN_POINT ( 'NONE',  ( -4.219116154402471786, -10.33852847137145048, 34.16647553114627556 ) ) ;
#41680 = EDGE_LOOP ( 'NONE', ( #69610, #72715, #9212, #76031 ) ) ;
#41681 = LINE ( 'NONE', #54292, #48964 ) ;
#41682 = DIRECTION ( 'NONE',  ( -0.000000000000000000, 0.000000000000000000, 1.000000000000000000 ) ) ;
#41683 = DIRECTION ( 'NONE',  ( 1.000000000000000000, 0.000000000000000000, 0.000000000000000000 ) ) ;
#41684 = LINE ( 'NONE', #34915, #9269 ) ;
#41685 = ORIENTED_EDGE ( 'NONE', *, *, #60141, .F. ) ;
#41686 = CARTESIAN_POINT ( 'NONE',  ( 11.66898724022510159, -3.285477652293413264, 32.44071101563363158 ) ) ;
#41687 = CARTESIAN_POINT ( 'NONE',  ( -8.769230769230768274, -12.34228464037088635, 31.77849191805839268 ) ) ;
#41688 = CARTESIAN_POINT ( 'NONE',  ( -12.46153846153858247, -12.27809138561165270, 31.22303859784587132 ) ) ;
#41689 = DIRECTION ( 'NONE',  ( -0.000000000000000000, -0.8660254037844399289, -0.4999999999999980016 ) ) ;
#41690 = FACE_OUTER_BOUND ( 'NONE', #57593, .T. ) ;
#41691 = FACE_BOUND ( 'NONE', #11922, .T. ) ;
#41693 = CARTESIAN_POINT ( 'NONE',  ( -17.14300545628321260, -10.67929555188718460, 33.92786785259543336 ) ) ;
#41692 = DIRECTION ( 'NONE',  ( -0.000000000000000000, -0.9848077530122085754, -0.1736481776669273613 ) ) ;
#41694 = CIRCLE ( 'NONE', #57493, 0.2500000000000002220 ) ;
#41695 = CARTESIAN_POINT ( 'NONE',  ( 11.78840694783958298, -12.07971442181322352, 32.31769673815850297 ) ) ;
#41697 = PLANE ( 'NONE',  #75136 ) ;
#41696 = CARTESIAN_POINT ( 'NONE',  ( 2.307692307692309264, -13.87047571288749737, 32.06866353760679544 ) ) ;
#41698 = CARTESIAN_POINT ( 'NONE',  ( -10.83831157429146330, -6.459968553980841577, 34.89616026154728701 ) ) ;
#41699 = CARTESIAN_POINT ( 'NONE',  ( 2.775308065498768517, -8.577988221561467341, 16.79500670625849068 ) ) ;
#41700 = ORIENTED_EDGE ( 'NONE', *, *, #69326, .T. ) ;
#41701 = CARTESIAN_POINT ( 'NONE',  ( -9.019230769230768274, -7.500000000000001776, 34.75000000000000000 ) ) ;
#41702 = VERTEX_POINT ( 'NONE', #58987 ) ;
#41703 = AXIS2_PLACEMENT_3D ( 'NONE', #55637, #28628, #7909 ) ;
#41704 = VECTOR ( 'NONE', #71999, 1000.000000000000000 ) ;
#41705 = CARTESIAN_POINT ( 'NONE',  ( -15.09997742294443945, -4.118422570099827595, 33.43335022499816489 ) ) ;
#41706 = EDGE_LOOP ( 'NONE', ( #55995, #62660 ) ) ;
#41707 = CARTESIAN_POINT ( 'NONE',  ( 17.93391658904412012, -12.10708131394839349, 31.69288490824020244 ) ) ;
#41708 = EDGE_CURVE ( 'NONE', #82006, #23503, #49407, .T. ) ;
#41709 = CARTESIAN_POINT ( 'NONE',  ( -7.976301055592065481, -10.19110544564092002, 33.96427741523702792 ) ) ;
#41710 = EDGE_LOOP ( 'NONE', ( #45808, #52488, #57349, #10769 ) ) ;
#41711 = DIRECTION ( 'NONE',  ( -0.000000000000000000, -0.9848077530122085754, -0.1736481776669273613 ) ) ;
#41712 = CARTESIAN_POINT ( 'NONE',  ( -1.987747218494660295, -5.598659921968651254, 18.74813170625849068 ) ) ;
#41713 = B_SPLINE_CURVE_WITH_KNOTS ( 'NONE', 3,
 ( #86881, #73797, #45858, #60262, #53501, #46753, #74232, #12530, #40014, #28247 ),
 .UNSPECIFIED., .F., .F.,
 ( 4, 2, 2, 2, 4 ),
 ( 0.000000000000000000, 0.0001954311564186863865, 0.0003908623128373727731, 0.0005862934692560591325, 0.0007817246256747455461 ),
 .UNSPECIFIED. ) ;
#41714 = AXIS2_PLACEMENT_3D ( 'NONE', #34182, #4949, #53114 ) ;
#41715 = FACE_OUTER_BOUND ( 'NONE', #78913, .T. ) ;
#41716 = CARTESIAN_POINT ( 'NONE',  ( 4.826946345980720032, -4.943428324936578910, 34.04746400365624481 ) ) ;
#41717 = AXIS2_PLACEMENT_3D ( 'NONE', #81886, #13849, #42228 ) ;
#41718 = B_SPLINE_CURVE_WITH_KNOTS ( 'NONE', 3,
 ( #31446, #79641, #44496, #38649, #64773, #11630, #39108, #31902, #52149, #86866 ),
 .UNSPECIFIED., .F., .F.,
 ( 4, 2, 2, 2, 4 ),
 ( 0.0007817246256747459798, 0.0009771112852218896347, 0.001172497944769033181, 0.001367884604316176728, 0.001563271263863320491 ),
 .UNSPECIFIED. ) ;
#41719 = CARTESIAN_POINT ( 'NONE',  ( -2.980769230769215739, -2.249999999999999112, 29.81603969181031033 ) ) ;
#41720 = LINE ( 'NONE', #28190, #51653 ) ;
#41721 = CARTESIAN_POINT ( 'NONE',  ( -1.384615384615383471, -3.937682226553329556, 33.60647404775216529 ) ) ;
#41722 = CARTESIAN_POINT ( 'NONE',  ( 5.076923076923075762, -8.810774026931790459, 35.74407628777942847 ) ) ;
#41723 = EDGE_CURVE ( 'NONE', #17051, #22580, #6281, .T. ) ;
#41724 = MECHANICAL_DESIGN_GEOMETRIC_PRESENTATION_REPRESENTATION (  '', ( #80559 ), #23003 ) ;
#41725 = CARTESIAN_POINT ( 'NONE',  ( -2.694853999681181556, -10.10844685921792241, 25.18936829374151642 ) ) ;
#41726 = CARTESIAN_POINT ( 'NONE',  ( -17.06410256410256565, -11.50000000000000000, 29.75000000000000355 ) ) ;
#41727 = CARTESIAN_POINT ( 'NONE',  ( -6.130147969731693181, -3.625366637846544560, 33.29286588640298561 ) ) ;
#41728 = VERTEX_POINT ( 'NONE', #33310 ) ;
#41729 = ADVANCED_FACE ( 'NONE', ( #52674 ), #12152, .F. ) ;
#41730 = DIRECTION ( 'NONE',  ( -0.000000000000000000, -0.8660254037844397068, -0.4999999999999978906 ) ) ;
#41731 = CARTESIAN_POINT ( 'NONE',  ( 1.553300858899129944, -11.24999999999998934, 14.70312500000000355 ) ) ;
#41732 = CARTESIAN_POINT ( 'NONE',  ( -15.90379173393269951, -12.41089969410671223, 31.60739465890703670 ) ) ;
#41733 = CYLINDRICAL_SURFACE ( 'NONE', #18235, 0.2500000000000009437 ) ;
#41734 = VERTEX_POINT ( 'NONE', #18902 ) ;
#41735 = CARTESIAN_POINT ( 'NONE',  ( -18.00000000000000000, -2.721908614388771852, 31.22303859784724978 ) ) ;
#41736 = CARTESIAN_POINT ( 'NONE',  ( 16.37662582282421653, -2.612705202774696200, 31.66806509827799943 ) ) ;
#41738 = ORIENTED_EDGE ( 'NONE', *, *, #15634, .F. ) ;
#41737 = DIRECTION ( 'NONE',  ( 1.000000000000000000, 0.000000000000000000, 0.000000000000000000 ) ) ;
#41739 = DIRECTION ( 'NONE',  ( 1.000000000000000000, 0.000000000000000000, 0.000000000000000000 ) ) ;
#41740 = CARTESIAN_POINT ( 'NONE',  ( -1.384615384615505151, -4.481592998941358097, 33.73612834414048933 ) ) ;
#41742 = ADVANCED_FACE ( 'NONE', ( #67535 ), #25213, .T. ) ;
#41741 = CARTESIAN_POINT ( 'NONE',  ( 7.173131342990377135, -12.01375889529407281, 32.43194544308182969 ) ) ;
#41743 = CARTESIAN_POINT ( 'NONE',  ( 3.007842271862382066, -2.523278758544489353, 31.42238647778637528 ) ) ;
#41744 = CARTESIAN_POINT ( 'NONE',  ( -9.692307692307812417, -6.879047030192662504, 34.71129190930017927 ) ) ;
#41745 = ORIENTED_EDGE ( 'NONE', *, *, #55433, .T. ) ;
#41746 = EDGE_LOOP ( 'NONE', ( #3813, #15183, #43069, #47981 ) ) ;
#41747 = VECTOR ( 'NONE', #25750, 1000.000000000000227 ) ;
#41749 = EDGE_CURVE ( 'NONE', #72951, #84941, #41923, .T. ) ;
#41748 = B_SPLINE_CURVE_WITH_KNOTS ( 'NONE', 3,
 ( #84410, #2407, #14166, #36220, #63674, #83972, #62339, #14610, #41640, #1981 ),
 .UNSPECIFIED., .F., .F.,
 ( 4, 2, 2, 2, 4 ),
 ( 0.0007817359430256388964, 0.0009771253907250073822, 0.001172514838424375868, 0.001367904286123744571, 0.001563293733823113056 ),
 .UNSPECIFIED. ) ;
#41750 = EDGE_LOOP ( 'NONE', ( #75143, #10293, #77976, #2678 ) ) ;
#41751 = B_SPLINE_CURVE_WITH_KNOTS ( 'NONE', 3,
 ( #52111, #79600, #87260, #87707, #25540, #40398, #31859, #80040, #75067, #26433, #4377, #67856, #66066, #73744, #5710, #39512, #46254, #19666 ),
 .UNSPECIFIED., .F., .F.,
 ( 4, 2, 2, 2, 2, 2, 2, 2, 4 ),
 ( 0.000000000000000000, 0.0002610006692907291767, 0.0005220013385814583533, 0.0007830020078721875842, 0.001044002677162916707, 0.001305003346453645829, 0.001566004015744375168, 0.001827004685035104291, 0.002088005354325833413 ),
 .UNSPECIFIED. ) ;
#41752 = DIRECTION ( 'NONE',  ( -0.000000000000000000, -0.3420201433256694346, -0.9396926207859080948 ) ) ;
#41753 = CARTESIAN_POINT ( 'NONE',  ( -6.700065571464073777, -4.187068189119697692, 33.49521262558774026 ) ) ;
#41754 = ADVANCED_FACE ( 'NONE', ( #13030 ), #60322, .F. ) ;
#41755 = B_SPLINE_CURVE_WITH_KNOTS ( 'NONE', 3,
 ( #54691, #76298, #88959, #68656, #34428, #75857, #61892, #74983, #62769, #40756 ),
 .UNSPECIFIED., .F., .F.,
 ( 4, 2, 2, 2, 4 ),
 ( 0.0007817246256747453293, 0.0009771112852218889842, 0.001172497944769032531, 0.001367884604316176294, 0.001563271263863319840 ),
 .UNSPECIFIED. ) ;
#41756 = CYLINDRICAL_SURFACE ( 'NONE', #81021, 0.2499999999999995559 ) ;
#41757 = CARTESIAN_POINT ( 'NONE',  ( -19.50000000000000000, -11.50000000000000000, 29.75000000000000355 ) ) ;
#41758 = VERTEX_POINT ( 'NONE', #33746 ) ;
#41759 = CARTESIAN_POINT ( 'NONE',  ( 17.32697749683652688, -11.47946981652013498, 33.17500667209846910 ) ) ;
#41760 = EDGE_LOOP ( 'NONE', ( #2037, #3574 ) ) ;
#41761 = EDGE_LOOP ( 'NONE', ( #56429, #74607 ) ) ;
#41762 = EDGE_CURVE ( 'NONE', #83278, #82873, #61201, .T. ) ;
#41763 = ORIENTED_EDGE ( 'NONE', *, *, #819, .F. ) ;
#41765 = ORIENTED_EDGE ( 'NONE', *, *, #69096, .T. ) ;
#41764 = CARTESIAN_POINT ( 'NONE',  ( -7.911424292114620727, -5.219633306516282545, 34.19971097300152962 ) ) ;
#41766 = CARTESIAN_POINT ( 'NONE',  ( 4.153846153846032507, -6.026961402154118908, 34.52809138561165270 ) ) ;
#41767 = CARTESIAN_POINT ( 'NONE',  ( 5.999999999999878320, -12.70778746994576025, 30.41441678777401236 ) ) ;
#41768 = VECTOR ( 'NONE', #51542, 1000.000000000000000 ) ;
#41769 = CARTESIAN_POINT ( 'NONE',  ( 2.307692307692615685, -2.506253911140615021, 30.00000000000323297 ) ) ;
#41770 = DIRECTION ( 'NONE',  ( -0.000000000000000000, 0.1736481776669307198, -0.9848077530122080203 ) ) ;
#41771 = ORIENTED_EDGE ( 'NONE', *, *, #44662, .T. ) ;
#41772 = EDGE_CURVE ( 'NONE', #15837, #83400, #63447, .T. ) ;
#41773 = EDGE_LOOP ( 'NONE', ( #29154, #73599 ) ) ;
#41774 = ORIENTED_EDGE ( 'NONE', *, *, #53015, .F. ) ;
#41775 = LINE ( 'NONE', #21040, #83565 ) ;
#41777 = ORIENTED_EDGE ( 'NONE', *, *, #48048, .F. ) ;
#41776 = CARTESIAN_POINT ( 'NONE',  ( -10.61538461538461320, -11.11383981884818262, 36.00935417666054406 ) ) ;
#41778 =( GEOMETRIC_REPRESENTATION_CONTEXT ( 3 ) GLOBAL_UNCERTAINTY_ASSIGNED_CONTEXT ( ( #14978 ) ) GLOBAL_UNIT_ASSIGNED_CONTEXT ( ( #26230, #60453, #87970 ) ) REPRESENTATION_CONTEXT ( 'NONE', 'WORKASPACE' ) );
#41779 = CARTESIAN_POINT ( 'NONE',  ( -11.47239420511146513, -12.62096338111211757, 30.90682066428152908 ) ) ;
#41780 = ADVANCED_FACE ( 'NONE', ( #88712 ), #40517, .T. ) ;
#41781 = EDGE_CURVE ( 'NONE', #32578, #52323, #81946, .T. ) ;
#41782 = CARTESIAN_POINT ( 'NONE',  ( -14.53061852520844965, -2.554751324335734708, 30.48935550225260727 ) ) ;
#41783 = ORIENTED_EDGE ( 'NONE', *, *, #970, .F. ) ;
#41784 = B_SPLINE_CURVE_WITH_KNOTS ( 'NONE', 3,
 ( #19984, #20870, #39827, #13674, #47450, #32611, #41153, #5590, #74945, #34385 ),
 .UNSPECIFIED., .F., .F.,
 ( 4, 2, 2, 2, 4 ),
 ( 0.000000000000000000, 0.0001954339857564078538, 0.0003908679715128157077, 0.0005863019572692235344, 0.0007817359430256314154 ),
 .UNSPECIFIED. ) ;
#41785 = B_SPLINE_CURVE_WITH_KNOTS ( 'NONE', 3,
 ( #49342, #36711, #43467, #707, #21424, #83132, #76362, #22310, #83589, #42152 ),
 .UNSPECIFIED., .F., .F.,
 ( 4, 2, 2, 2, 4 ),
 ( 0.000000000000000000, 0.0001954339857564070678, 0.0003908679715128141356, 0.0005863019572692211492, 0.0007817359430256282712 ),
 .UNSPECIFIED. ) ;
#41786 = CARTESIAN_POINT ( 'NONE',  ( -17.77722045873159473, -2.600157965045223563, 30.74683119005207033 ) ) ;
#41787 = LINE ( 'NONE', #74237, #78453 ) ;
#41788 = ORIENTED_EDGE ( 'NONE', *, *, #81451, .T. ) ;
#41789 = FACE_BOUND ( 'NONE', #18038, .T. ) ;
#41790 = ADVANCED_FACE ( 'NONE', ( #20235 ), #47698, .F. ) ;
#41791 = B_SPLINE_CURVE_WITH_KNOTS ( 'NONE', 3,
 ( #40301, #6070, #79949, #18249, #19134, #26334, #67326, #4738, #33542, #52465 ),
 .UNSPECIFIED., .F., .F.,
 ( 4, 2, 2, 2, 4 ),
 ( 0.000000000000000000, 0.0001954311564186861155, 0.0003908623128373722310, 0.0005862934692560583735, 0.0007817246256747444619 ),
 .UNSPECIFIED. ) ;
#41792 = CARTESIAN_POINT ( 'NONE',  ( 10.86533013373275658, -10.05730279482229683, 34.04704008940765902 ) ) ;
#41793 = LINE ( 'NONE', #69253, #2509 ) ;
#41794 = CARTESIAN_POINT ( 'NONE',  ( 3.453780582382082631, -9.086983370893047862, 34.49168942202179267 ) ) ;
#41796 = FACE_OUTER_BOUND ( 'NONE', #7423, .T. ) ;
#41795 = CARTESIAN_POINT ( 'NONE',  ( 13.38461538461538680, -11.91647553114624181, 32.58852847137148245 ) ) ;
#41797 = CARTESIAN_POINT ( 'NONE',  ( -4.088590582570128973, -2.892918686051625166, 31.69288490824025928 ) ) ;
#41798 = CARTESIAN_POINT ( 'NONE',  ( -16.15384615384615330, -8.973038597847269315, 34.52809138561121927 ) ) ;
#41799 = EDGE_LOOP ( 'NONE', ( #78403, #25448, #29674, #64590 ) ) ;
#41800 = CARTESIAN_POINT ( 'NONE',  ( -18.25000000000000000, -7.500000000000001776, 34.75000000000000000 ) ) ;
#41801 = CARTESIAN_POINT ( 'NONE',  ( 13.31885858210107898, -7.249945686854186278, 34.74374336980224598 ) ) ;
#41802 = B_SPLINE_CURVE_WITH_KNOTS ( 'NONE', 3,
 ( #84152, #22428, #43148, #50328, #44019, #77372, #21541, #77809, #76494, #70618 ),
 .UNSPECIFIED., .F., .F.,
 ( 4, 2, 2, 2, 4 ),
 ( 0.0007817359430256317406, 0.0009771253907249982749, 0.001172514838424365026, 0.001367904286123731560, 0.001563293733823098094 ),
 .UNSPECIFIED. ) ;
#41803 = EDGE_LOOP ( 'NONE', ( #6849, #49355, #23465, #3992 ) ) ;
#41804 = CYLINDRICAL_SURFACE ( 'NONE', #19990, 8.000000000000000000 ) ;
#41805 = CARTESIAN_POINT ( 'NONE',  ( -7.134615384615385025, -7.500000000000000000, 29.75000000000000355 ) ) ;
#41806 = VERTEX_POINT ( 'NONE', #32414 ) ;
#41807 = CARTESIAN_POINT ( 'NONE',  ( 17.77707378248384629, -5.667676309546437530, 34.40238873228292249 ) ) ;
#41808 = FACE_OUTER_BOUND ( 'NONE', #60805, .T. ) ;
#41809 = FACE_BOUND ( 'NONE', #80558, .T. ) ;
#41811 = CARTESIAN_POINT ( 'NONE',  ( 23.49999999999998579, -8.999999999999996447, 22.25000000000000000 ) ) ;
#41810 = CARTESIAN_POINT ( 'NONE',  ( 2.294871794871793380, -7.500000000000000000, 29.75000000000000355 ) ) ;
#41812 = CARTESIAN_POINT ( 'NONE',  ( 5.750000000000002665, -7.500000000000001776, 35.00000000000000000 ) ) ;
#41813 = CARTESIAN_POINT ( 'NONE',  ( 12.39545608217832395, -12.34228464037088280, 31.77849191805838558 ) ) ;
#41815 = CARTESIAN_POINT ( 'NONE',  ( 15.48076923076923173, -2.499999999999998668, 29.75000000000000355 ) ) ;
#41814 = CARTESIAN_POINT ( 'NONE',  ( 0.000000000000000000, 0.000000000000000000, 0.000000000000000000 ) ) ;
#41816 = CARTESIAN_POINT ( 'NONE',  ( 20.00000000000000000, -4.000000000000000000, 29.75000000000000355 ) ) ;
#41817 = CARTESIAN_POINT ( 'NONE',  ( -2.651650429449535551, -10.15165042944956753, 24.93750000000000000 ) ) ;
#41818 = ORIENTED_EDGE ( 'NONE', *, *, #7090, .T. ) ;
#41819 = ORIENTED_EDGE ( 'NONE', *, *, #67104, .F. ) ;
#41820 = CARTESIAN_POINT ( 'NONE',  ( -10.61538461538461320, -1.466349020453238561, 30.81389545987213907 ) ) ;
#41821 = CARTESIAN_POINT ( 'NONE',  ( 13.38461538461538680, -12.78798330534102945, 29.74999999999997868 ) ) ;
#41822 = CARTESIAN_POINT ( 'NONE',  ( 1.634669804528839254, -9.233818618650603938, 34.70587769442853698 ) ) ;
#41823 = CARTESIAN_POINT ( 'NONE',  ( -16.85391172531022619, -11.24521262558773493, 33.06293181088029343 ) ) ;
#41824 = CARTESIAN_POINT ( 'NONE',  ( -4.088591014333315066, -3.083524468853784839, 32.58852847137153930 ) ) ;
#41825 = CARTESIAN_POINT ( 'NONE',  ( -3.749999999999997335, -7.500000000000021316, 26.34375000000000000 ) ) ;
#41826 = DIRECTION ( 'NONE',  ( -0.000000000000000000, -0.9848077530122085754, -0.1736481776669273613 ) ) ;
#41827 = DIRECTION ( 'NONE',  ( 0.000000000000000000, 1.000000000000000000, 0.000000000000000000 ) ) ;
#41828 = CARTESIAN_POINT ( 'NONE',  ( -17.32689980786543060, -4.943428324936578910, 34.04746400365624481 ) ) ;
#41829 = CARTESIAN_POINT ( 'NONE',  ( 7.846153846153846700, -5.471508081941601098, 34.59228464037088457 ) ) ;
#41830 = CARTESIAN_POINT ( 'NONE',  ( 9.692307692307695177, -12.78798330534102767, 29.49999999999997868 ) ) ;
#41831 = CYLINDRICAL_SURFACE ( 'NONE', #32514, 4.000000000000000000 ) ;
#41832 = B_SPLINE_CURVE_WITH_KNOTS ( 'NONE', 3,
 ( #47704, #62104, #48580, #34638, #69314, #14817, #55344, #1286, #68419, #67989 ),
 .UNSPECIFIED., .F., .F.,
 ( 4, 2, 2, 2, 4 ),
 ( 0.000000000000000000, 0.0001954339857564083417, 0.0003908679715128166835, 0.0005863019572692250523, 0.0007817359430256333669 ),
 .UNSPECIFIED. ) ;
#41833 = CARTESIAN_POINT ( 'NONE',  ( 9.942253210655838558, -11.37275283266504111, 32.91324779482534524 ) ) ;
#41834 = CARTESIAN_POINT ( 'NONE',  ( 12.68431813051652668, -2.353885683473779800, 30.79025554430704403 ) ) ;
#41835 = AXIS2_PLACEMENT_3D ( 'NONE', #57844, #65029, #3340 ) ;
#41836 = CARTESIAN_POINT ( 'NONE',  ( 12.52679403281448423, -2.892918686051625166, 31.69288490824026638 ) ) ;
#41837 = ORIENTED_EDGE ( 'NONE', *, *, #10389, .F. ) ;
#41838 = CARTESIAN_POINT ( 'NONE',  ( -14.55771554498527642, -3.711651800289232028, 33.01384336483936011 ) ) ;
#41839 = CARTESIAN_POINT ( 'NONE',  ( 10.86533002476265786, -5.766571408460171355, 34.70601412856602508 ) ) ;
#41840 = CARTESIAN_POINT ( 'NONE',  ( 1.200186371490529202, -4.775308065498752974, 23.23624329374151642 ) ) ;
#41841 = AXIS2_PLACEMENT_3D ( 'NONE', #38847, #25772, #79385 ) ;
#41842 = CIRCLE ( 'NONE', #79246, 0.2500000000000002220 ) ;
#41843 = CARTESIAN_POINT ( 'NONE',  ( -0.4615384615384611200, -10.67929555188718282, 33.92786785259544047 ) ) ;
#41844 = CARTESIAN_POINT ( 'NONE',  ( 16.94623247381277054, -11.37499894934982514, 33.29245874905763003 ) ) ;
#41845 = ORIENTED_EDGE ( 'NONE', *, *, #83582, .T. ) ;
#41846 = CYLINDRICAL_SURFACE ( 'NONE', #48516, 0.2500000000000002220 ) ;
#41848 = ORIENTED_EDGE ( 'NONE', *, *, #84638, .F. ) ;
#41847 = CARTESIAN_POINT ( 'NONE',  ( 22.00000000000000711, 9.999999999999991118, 13.00000000000000178 ) ) ;
#41849 = LINE ( 'NONE', #35528, #84439 ) ;
#41850 = FACE_OUTER_BOUND ( 'NONE', #24482, .T. ) ;
#41851 = VERTEX_POINT ( 'NONE', #62966 ) ;
#41852 = DIRECTION ( 'NONE',  ( -0.000000000000000000, 0.7660444431189791237, -0.6427876096865379196 ) ) ;
#41853 = CIRCLE ( 'NONE', #184, 0.2500000000000002220 ) ;
#41854 = CARTESIAN_POINT ( 'NONE',  ( 10.74591005361826035, -11.04252011169590020, 33.62494198852677130 ) ) ;
#41855 = DIRECTION ( 'NONE',  ( -1.000000000000000000, 0.000000000000000000, 0.000000000000000000 ) ) ;
#41856 = ORIENTED_EDGE ( 'NONE', *, *, #59911, .T. ) ;
#41857 = CARTESIAN_POINT ( 'NONE',  ( 17.07692307692307665, -11.16473453929635440, 33.15142922261926373 ) ) ;
#41858 = CARTESIAN_POINT ( 'NONE',  ( 2.557637717070351258, -8.476813868363244353, 34.90874843262270133 ) ) ;
#41859 = CARTESIAN_POINT ( 'NONE',  ( -15.23076923076922995, -12.37446782046654192, 30.86335684631486131 ) ) ;
#41860 = ORIENTED_EDGE ( 'NONE', *, *, #21133, .T. ) ;
#41861 = VERTEX_POINT ( 'NONE', #69742 ) ;
#41862 = CARTESIAN_POINT ( 'NONE',  ( 6.249945518348142492, -6.696923467548660192, 34.68552623307873972 ) ) ;
#41863 = EDGE_LOOP ( 'NONE', ( #35330, #80892 ) ) ;
#41864 = CARTESIAN_POINT ( 'NONE',  ( -15.00798956179115962, -4.226511098958373402, 33.85474049983370293 ) ) ;
#41865 = CARTESIAN_POINT ( 'NONE',  ( 15.48071464014727283, -12.68172785388650681, 30.59649109432439218 ) ) ;
#41866 = CARTESIAN_POINT ( 'NONE',  ( 13.38461538461526423, -3.643525952248795718, 33.31231777344771672 ) ) ;
#41867 = CYLINDRICAL_SURFACE ( 'NONE', #27530, 0.2499999999999986955 ) ;
#41868 = DIRECTION ( 'NONE',  ( -0.000000000000000000, 0.6427876096865404731, -0.7660444431189770143 ) ) ;
#41869 = CARTESIAN_POINT ( 'NONE',  ( -2.557692307692330136, -2.249999999999999112, 29.81609741502488120 ) ) ;
#41870 = CYLINDRICAL_SURFACE ( 'NONE', #55014, 0.2500000000000009437 ) ;
#41871 = B_SPLINE_CURVE_WITH_KNOTS ( 'NONE', 3,
 ( #38696, #32387, #37802, #59853, #25627, #87350, #80588, #3565, #12126, #3120 ),
 .UNSPECIFIED., .F., .F.,
 ( 4, 2, 2, 2, 4 ),
 ( 0.000000000000000000, 0.0001954339857564071762, 0.0003908679715128143524, 0.0005863019572692215828, 0.0007817359430256287049 ),
 .UNSPECIFIED. ) ;
#41872 = VECTOR ( 'NONE', #73087, 1000.000000000000000 ) ;
#41873 = ORIENTED_EDGE ( 'NONE', *, *, #14731, .T. ) ;
#41874 = EDGE_CURVE ( 'NONE', #64241, #78478, #42286, .T. ) ;
#41875 = ORIENTED_EDGE ( 'NONE', *, *, #31558, .T. ) ;
#41877 = ORIENTED_EDGE ( 'NONE', *, *, #29377, .F. ) ;
#41876 = CARTESIAN_POINT ( 'NONE',  ( -17.32689980786543060, -9.943427161483782584, 34.11278801902876978 ) ) ;
#41878 = AXIS2_PLACEMENT_3D ( 'NONE', #27737, #20970, #48442 ) ;
#41879 = CARTESIAN_POINT ( 'NONE',  ( 16.94677510719138169, -2.373036134822905208, 30.88089517874952250 ) ) ;
#41880 = VERTEX_POINT ( 'NONE', #20668 ) ;
#41881 = DIRECTION ( 'NONE',  ( -0.000000000000000000, 0.8660254037844399289, -0.4999999999999980016 ) ) ;
#41882 = CARTESIAN_POINT ( 'NONE',  ( 6.223012844093395834, -10.01129605718032778, 34.36064277460058491 ) ) ;
#41883 = VERTEX_POINT ( 'NONE', #56230 ) ;
#41884 = CARTESIAN_POINT ( 'NONE',  ( 0.000000000000000000, -4.750000000000000000, 29.25000000000000000 ) ) ;
#41885 = ORIENTED_EDGE ( 'NONE', *, *, #83385, .T. ) ;
#41886 = ORIENTED_EDGE ( 'NONE', *, *, #43754, .T. ) ;
#41887 = CARTESIAN_POINT ( 'NONE',  ( -12.68446542044531178, -3.395401636524185474, 33.02366814457250399 ) ) ;
#41888 = EDGE_CURVE ( 'NONE', #23097, #65576, #54829, .T. ) ;
#41889 = EDGE_CURVE ( 'NONE', #6007, #17599, #83718, .T. ) ;
#41890 = VERTEX_POINT ( 'NONE', #14810 ) ;
#41891 = AXIS2_PLACEMENT_3D ( 'NONE', #87940, #45576, #67194 ) ;
#41892 = CARTESIAN_POINT ( 'NONE',  ( -7.846153846153844924, -13.04860791097971706, 34.73218667398347037 ) ) ;
#41893 = DIRECTION ( 'NONE',  ( 0.000000000000000000, 0.000000000000000000, -1.000000000000000000 ) ) ;
#41894 = FACE_BOUND ( 'NONE', #22363, .T. ) ;
#41895 = CYLINDRICAL_SURFACE ( 'NONE', #62896, 0.2499999999999986955 ) ;
#41896 = CARTESIAN_POINT ( 'NONE',  ( -6.673131404728779970, -12.22109172314383052, 31.39792113162168263 ) ) ;
#41897 = AXIS2_PLACEMENT_3D ( 'NONE', #10762, #59392, #58483 ) ;
#41898 = AXIS2_PLACEMENT_3D ( 'NONE', #57720, #14518, #55942 ) ;
#41899 = LINE ( 'NONE', #69366, #78389 ) ;
#41900 = CARTESIAN_POINT ( 'NONE',  ( -13.38461538461538325, -12.37446782046654192, 30.86335684631486131 ) ) ;
#41901 = CARTESIAN_POINT ( 'NONE',  ( -19.50000000000000000, -11.50000000000000000, 29.75000000000000355 ) ) ;
#41902 = CARTESIAN_POINT ( 'NONE',  ( -12.46153846153846168, -2.292212530054420494, 30.41441678777542634 ) ) ;
#41903 = ORIENTED_EDGE ( 'NONE', *, *, #76194, .F. ) ;
#41904 = CARTESIAN_POINT ( 'NONE',  ( 10.61538461538449596, -10.21337939537710326, 33.94971097300076224 ) ) ;
#41905 = VERTEX_POINT ( 'NONE', #22001 ) ;
#41906 = EDGE_LOOP ( 'NONE', ( #69580, #85616, #2086, #80820 ) ) ;
#41907 = CIRCLE ( 'NONE', #56297, 4.000000000000000000 ) ;
#41909 = CARTESIAN_POINT ( 'NONE',  ( 15.10062202133100939, -12.27039167877662251, 31.24851455888617835 ) ) ;
#41908 = CARTESIAN_POINT ( 'NONE',  ( -5.999999999999998224, -11.11383981884818262, 36.00935417666054406 ) ) ;
#41910 = CARTESIAN_POINT ( 'NONE',  ( -11.60373198442231590, -11.94971097300153140, 32.03036669348370680 ) ) ;
#41911 = CARTESIAN_POINT ( 'NONE',  ( -17.01166793741023042, -10.33852847137154107, 34.16647553114620450 ) ) ;
#41912 = CARTESIAN_POINT ( 'NONE',  ( 15.36156103859402045, -3.530189275343204702, 32.79018710029569661 ) ) ;
#41913 = CARTESIAN_POINT ( 'NONE',  ( -12.33074802057151409, -4.684288915650983043, 34.18129842949671371 ) ) ;
#41914 = VERTEX_POINT ( 'NONE', #8936 ) ;
#41915 = CARTESIAN_POINT ( 'NONE',  ( -18.22348494372394967, -5.912607949931402374, 34.49155766932282319 ) ) ;
#41916 = CARTESIAN_POINT ( 'NONE',  ( 1.515407192440173745, -12.11778462344221019, 31.66786338562085135 ) ) ;
#41917 = DIRECTION ( 'NONE',  ( -0.000000000000000000, 0.9396926207859093161, -0.3420201433256663259 ) ) ;
#41918 = DIRECTION ( 'NONE',  ( -0.000000000000000000, -0.6427876096865404731, -0.7660444431189770143 ) ) ;
#41919 = FACE_OUTER_BOUND ( 'NONE', #23940, .T. ) ;
#41920 = VERTEX_POINT ( 'NONE', #62098 ) ;
#41921 = ORIENTED_EDGE ( 'NONE', *, *, #72745, .F. ) ;
#41922 = ORIENTED_EDGE ( 'NONE', *, *, #52615, .F. ) ;
#41923 = B_SPLINE_CURVE_WITH_KNOTS ( 'NONE', 3,
 ( #46372, #67092, #54450, #60767, #40081, #87376, #6710, #75184, #5393, #32858 ),
 .UNSPECIFIED., .F., .F.,
 ( 4, 2, 2, 2, 4 ),
 ( 0.000000000000000000, 0.0001954311564186870371, 0.0003908623128373740741, 0.0005862934692560610840, 0.0007817246256747481482 ),
 .UNSPECIFIED. ) ;
#41924 = CARTESIAN_POINT ( 'NONE',  ( -7.053768389744481837, -8.147922237126337563, 34.70805685702651999 ) ) ;
#41925 = ORIENTED_EDGE ( 'NONE', *, *, #315, .F. ) ;
#41926 = CARTESIAN_POINT ( 'NONE',  ( -9.469294848214296678, -10.01129605718032600, 34.36064277460058491 ) ) ;
#41927 = DIRECTION ( 'NONE',  ( -1.000000000000000000, -0.000000000000000000, -0.000000000000000000 ) ) ;
#41928 = CARTESIAN_POINT ( 'NONE',  ( -5.999999999999998224, -8.810774026931790459, 35.74407628777942847 ) ) ;
#41929 = CARTESIAN_POINT ( 'NONE',  ( -1.553300858899125059, -3.750000000000009326, 14.07812500000000178 ) ) ;
#41930 = CARTESIAN_POINT ( 'NONE',  ( 12.21156173059610772, -9.943427161483782584, 34.11278801902876978 ) ) ;
#41931 = ORIENTED_EDGE ( 'NONE', *, *, #9653, .F. ) ;
#41932 = CARTESIAN_POINT ( 'NONE',  ( -11.78846153846153832, -7.500000000000001776, 35.00000000000000000 ) ) ;
#41934 = ORIENTED_EDGE ( 'NONE', *, *, #79069, .F. ) ;
#41933 = CARTESIAN_POINT ( 'NONE',  ( -12.39547011053602432, -11.69971097300155272, 32.46337939537588113 ) ) ;
#41935 = FACE_OUTER_BOUND ( 'NONE', #72314, .T. ) ;
#41936 = CARTESIAN_POINT ( 'NONE',  ( -10.61538461538461320, -3.513871655860378418, 32.76840700105978499 ) ) ;
#41937 = CARTESIAN_POINT ( 'NONE',  ( -10.61538461538461320, -9.058645607665452459, 34.76329471203371924 ) ) ;
#41938 = AXIS2_PLACEMENT_3D ( 'NONE', #50517, #84776, #8670 ) ;
#41939 = CARTESIAN_POINT ( 'NONE',  ( -15.93041975493136597, -7.630147987733843173, 34.99859428049665411 ) ) ;
#41940 = CARTESIAN_POINT ( 'NONE',  ( 2.373759641042383794, -2.486705287966280320, 31.30864560766543647 ) ) ;
#41941 = CARTESIAN_POINT ( 'NONE',  ( -39.05038313613820122, -2.249999999999998668, 29.75000000000000355 ) ) ;
#41942 = CARTESIAN_POINT ( 'NONE',  ( -12.59222992820602371, -12.38065189839062263, 30.83690757178629482 ) ) ;
#41943 = VECTOR ( 'NONE', #32859, 1000.000000000000114 ) ;
#41944 = CARTESIAN_POINT ( 'NONE',  ( 1.614399933863618797, -3.775308065498751198, 14.48624329374151465 ) ) ;
#41945 = ORIENTED_EDGE ( 'NONE', *, *, #84756, .F. ) ;
#41946 = CARTESIAN_POINT ( 'NONE',  ( -4.153846153846152411, -13.57706302396349152, 30.56769352161908060 ) ) ;
#41947 = B_SPLINE_CURVE_WITH_KNOTS ( 'NONE', 3,
 ( #82058, #20354, #47815, #75294, #13584, #68526, #42840, #30963, #37729, #3494 ),
 .UNSPECIFIED., .F., .F.,
 ( 4, 2, 2, 2, 4 ),
 ( 0.0007817246256747459798, 0.0009771112852218887673, 0.001172497944769031663, 0.001367884604316174559, 0.001563271263863317455 ),
 .UNSPECIFIED. ) ;
#41948 = CARTESIAN_POINT ( 'NONE',  ( 1.318533005255250856, -9.058645607665454236, 34.76329471203372634 ) ) ;
#41949 = DIRECTION ( 'NONE',  ( 0.000000000000000000, 0.9848077530122072432, 0.1736481776669354937 ) ) ;
#41950 = CARTESIAN_POINT ( 'NONE',  ( 9.442330948259101575, -6.524016743844655686, 34.90889640711025521 ) ) ;
#41951 = ORIENTED_EDGE ( 'NONE', *, *, #63439, .F. ) ;
#41952 = LINE ( 'NONE', #9054, #78632 ) ;
#41953 = CARTESIAN_POINT ( 'NONE',  ( -2.438383774359866418, -3.062553014421049991, 32.05460306192774311 ) ) ;
#41954 = ADVANCED_FACE ( 'NONE', ( #29217 ), #49475, .F. ) ;
#41955 = CARTESIAN_POINT ( 'NONE',  ( -1.384615384615505151, -6.879047030192662504, 34.71129190930017927 ) ) ;
#41956 = CARTESIAN_POINT ( 'NONE',  ( 8.769230769230768274, -5.557115091759785130, 34.35708131394839171 ) ) ;
#41957 = ADVANCED_FACE ( 'NONE', ( #76053 ), #15251, .F. ) ;
#41958 = VERTEX_POINT ( 'NONE', #69307 ) ;
#41959 = CARTESIAN_POINT ( 'NONE',  ( 6.065255571276025215, -6.026961402152789304, 34.52809138561124769 ) ) ;
#41960 = B_SPLINE_CURVE_WITH_KNOTS ( 'NONE', 3,
 ( #41866, #76975, #71089, #49050, #43620, #56257, #36432, #7635, #64322, #70215 ),
 .UNSPECIFIED., .F., .F.,
 ( 4, 2, 2, 2, 4 ),
 ( 0.0007817246256747434861, 0.0009771112852218861652, 0.001172497944769028844, 0.001367884604316171740, 0.001563271263863314419 ),
 .UNSPECIFIED. ) ;
#41961 = CARTESIAN_POINT ( 'NONE',  ( -11.53846153846165912, -2.892918686052166066, 31.69288490824153470 ) ) ;
#41962 = DIRECTION ( 'NONE',  ( -0.000000000000000000, 1.000000000000000000, -0.000000000000000000 ) ) ;
#41963 = B_SPLINE_CURVE_WITH_KNOTS ( 'NONE', 3,
 ( #43671, #1804, #14892, #57632, #85115, #70267, #9017, #28849, #43238, #36047 ),
 .UNSPECIFIED., .F., .F.,
 ( 4, 2, 2, 2, 4 ),
 ( 0.0007817246256747450040, 0.0009771112852218881168, 0.001172497944769031230, 0.001367884604316174342, 0.001563271263863317455 ),
 .UNSPECIFIED. ) ;
#41964 = EDGE_LOOP ( 'NONE', ( #19382, #10965 ) ) ;
#41965 = CARTESIAN_POINT ( 'NONE',  ( -8.519230769229348965, -7.500000000000154543, 35.00000000000007105 ) ) ;
#41966 = B_SPLINE_CURVE_WITH_KNOTS ( 'NONE', 3,
 ( #14680, #56105, #61967, #62840, #83599, #276, #8368, #27742, #1159, #61083 ),
 .UNSPECIFIED., .F., .F.,
 ( 4, 2, 2, 2, 4 ),
 ( 0.0007817359430256293554, 0.0009771253907249941549, 0.001172514838424358954, 0.001367904286123723537, 0.001563293733823095276 ),
 .UNSPECIFIED. ) ;
#41967 = VECTOR ( 'NONE', #42679, 1000.000000000000000 ) ;
#41968 = EDGE_CURVE ( 'NONE', #52756, #60044, #59135, .T. ) ;
#41969 = ORIENTED_EDGE ( 'NONE', *, *, #23529, .T. ) ;
#41970 = CARTESIAN_POINT ( 'NONE',  ( 10.28846153846153832, -3.499999999999999556, 29.75000000000000355 ) ) ;
#41971 = CARTESIAN_POINT ( 'NONE',  ( 4.946232473812766983, -5.496505350115500121, 34.60290016733514307 ) ) ;
#41972 = ORIENTED_EDGE ( 'NONE', *, *, #65114, .F. ) ;
#41973 = EDGE_CURVE ( 'NONE', #45581, #38569, #65516, .T. ) ;
#41974 = DIRECTION ( 'NONE',  ( -0.000000000000000000, 0.9848077530122086864, -0.1736481776669273891 ) ) ;
#41975 = FACE_OUTER_BOUND ( 'NONE', #37634, .T. ) ;
#41976 = CARTESIAN_POINT ( 'NONE',  ( 1.253923917947830757, -4.118384482072085184, 33.43331474514187107 ) ) ;
#41977 = VECTOR ( 'NONE', #51001, 1000.000000000000000 ) ;
#41978 = CARTESIAN_POINT ( 'NONE',  ( 1.384615384615264011, -6.835583212225970762, 34.95778746994575670 ) ) ;
#41979 = DIRECTION ( 'NONE',  ( -0.000000000000000000, 0.9848077530122086864, -0.1736481776669273891 ) ) ;
#41980 = VERTEX_POINT ( 'NONE', #82828 ) ;
#41981 = ORIENTED_EDGE ( 'NONE', *, *, #79701, .T. ) ;
#41982 = ADVANCED_FACE ( 'NONE', ( #48134 ), #75604, .F. ) ;
#41983 = FACE_BOUND ( 'NONE', #23864, .T. ) ;
#41984 = ORIENTED_EDGE ( 'NONE', *, *, #82463, .T. ) ;
#41985 = CARTESIAN_POINT ( 'NONE',  ( 3.230769230769231726, -1.509761064869970415, 31.06009739812519044 ) ) ;
#41986 = DIRECTION ( 'NONE',  ( 0.000000000000000000, 0.000000000000000000, -1.000000000000000000 ) ) ;
#41987 = CARTESIAN_POINT ( 'NONE',  ( 3.230769230769231726, -1.044019251281081972, 31.83374038241031911 ) ) ;
#41988 = CARTESIAN_POINT ( 'NONE',  ( 7.146088274689774700, -9.886259254753566594, 34.14407573483972413 ) ) ;
#41989 = B_SPLINE_CURVE_WITH_KNOTS ( 'NONE', 3,
 ( #63621, #1923, #27622, #48330, #1039, #55533, #21302, #56861, #15449, #14553 ),
 .UNSPECIFIED., .F., .F.,
 ( 4, 2, 2, 2, 4 ),
 ( 0.0007817246256747459798, 0.0009771112852218896347, 0.001172497944769033181, 0.001367884604316176728, 0.001563271263863320491 ),
 .UNSPECIFIED. ) ;
#41990 = VERTEX_POINT ( 'NONE', #21100 ) ;
#41991 = ORIENTED_EDGE ( 'NONE', *, *, #17818, .T. ) ;
#41992 = ORIENTED_EDGE ( 'NONE', *, *, #47035, .F. ) ;
#41993 = AXIS2_PLACEMENT_3D ( 'NONE', #75799, #82581, #13222 ) ;
#41994 = CYLINDRICAL_SURFACE ( 'NONE', #64894, 3.000000000000000444 ) ;
#41995 = ORIENTED_EDGE ( 'NONE', *, *, #86924, .F. ) ;
#41996 = EDGE_CURVE ( 'NONE', #84941, #57639, #14353, .T. ) ;
#41997 = CARTESIAN_POINT ( 'NONE',  ( -6.066083410955879884, -12.37446782046654192, 30.86335684631486487 ) ) ;
#41998 = EDGE_CURVE ( 'NONE', #29327, #54013, #11141, .T. ) ;
#41999 = CARTESIAN_POINT ( 'NONE',  ( -11.76194646302587010, -5.827078755546623690, 34.72654668319379567 ) ) ;
#42000 = CARTESIAN_POINT ( 'NONE',  ( -18.13014720943822056, -11.47017969459903597, 32.78971311882035167 ) ) ;
#42001 = ORIENTED_EDGE ( 'NONE', *, *, #33892, .T. ) ;
#42002 = CARTESIAN_POINT ( 'NONE',  ( 8.992010310499175318, -9.332535724633409302, 34.40230450496446934 ) ) ;
#42003 = EDGE_CURVE ( 'NONE', #2192, #82502, #30956, .T. ) ;
#42004 = DIRECTION ( 'NONE',  ( -0.000000000000000000, 0.7660444431189791237, -0.6427876096865379196 ) ) ;
#42005 = ADVANCED_FACE ( 'NONE', ( #24654 ), #85472, .F. ) ;
#42006 = CARTESIAN_POINT ( 'NONE',  ( 14.55774661933062397, -6.567000820036036579, 34.66262288849541306 ) ) ;
#42007 = CARTESIAN_POINT ( 'NONE',  ( -8.638440328263820689, -2.845873456487965747, 32.17976146951972538 ) ) ;
#42008 = EDGE_LOOP ( 'NONE', ( #55421, #65918 ) ) ;
#42009 = ORIENTED_EDGE ( 'NONE', *, *, #78124, .T. ) ;
#42010 = ORIENTED_EDGE ( 'NONE', *, *, #18714, .T. ) ;
#42011 = CARTESIAN_POINT ( 'NONE',  ( 3.007889714031644957, -7.630690623152302621, 34.99857592706774057 ) ) ;
#42013 = CARTESIAN_POINT ( 'NONE',  ( -16.15384615384615330, -6.386643153685126251, 34.62446782046654192 ) ) ;
#42012 = CARTESIAN_POINT ( 'NONE',  ( -1.634592128663973076, -2.544273027872574922, 31.48422191005632342 ) ) ;
#42014 = CARTESIAN_POINT ( 'NONE',  ( -17.86920955903304886, -5.496552790871120031, 34.60292014791297532 ) ) ;
#42015 = CARTESIAN_POINT ( 'NONE',  ( -6.673131404728781746, -3.712312575010499494, 33.01462480002815170 ) ) ;
#42016 = FACE_BOUND ( 'NONE', #19969, .T. ) ;
#42017 = CARTESIAN_POINT ( 'NONE',  ( 16.21991450484859243, -3.050289026998446840, 32.03036669348366416 ) ) ;
#42018 = VERTEX_POINT ( 'NONE', #44029 ) ;
#42019 = CARTESIAN_POINT ( 'NONE',  ( -8.096153846153844924, -7.500000000000001776, 35.00000000000000000 ) ) ;
#42020 = DIRECTION ( 'NONE',  ( -0.000000000000000000, -0.1736481776669307198, -0.9848077530122080203 ) ) ;
#42021 = CARTESIAN_POINT ( 'NONE',  ( 10.03846153846153832, -1.926643599941765039, 28.25000000000000000 ) ) ;
#42022 = CARTESIAN_POINT ( 'NONE',  ( 3.361294669002873992, -11.66157788607254275, 32.95092075102925833 ) ) ;
#42023 = EDGE_LOOP ( 'NONE', ( #23263, #17529, #48776, #6369, #30480 ) ) ;
#42024 = CARTESIAN_POINT ( 'NONE',  ( 10.61538461538461675, -8.973038597847269315, 34.52809138561121927 ) ) ;
#42025 = EDGE_LOOP ( 'NONE', ( #64810, #87013, #6789, #31000 ) ) ;
#42026 = FACE_BOUND ( 'NONE', #7519, .T. ) ;
#42028 = TOROIDAL_SURFACE ( 'NONE', #60718, 3.250000000000001332, 2.000000000000000000 ) ;
#42027 = DIRECTION ( 'NONE',  ( -1.000000000000000000, -0.000000000000000000, -0.000000000000000000 ) ) ;
#42029 = VECTOR ( 'NONE', #1653, 1000.000000000000227 ) ;
#42030 = CARTESIAN_POINT ( 'NONE',  ( 17.99999999999987566, -12.70778746994576025, 30.41441678777401236 ) ) ;
#42031 = DIRECTION ( 'NONE',  ( -1.000000000000000000, -0.000000000000000000, 0.000000000000000000 ) ) ;
#42032 = ORIENTED_EDGE ( 'NONE', *, *, #33823, .F. ) ;
#42033 = CARTESIAN_POINT ( 'NONE',  ( 5.076923076923075762, -3.050289026998446396, 32.03036669348365706 ) ) ;
#42034 = CARTESIAN_POINT ( 'NONE',  ( 15.48082365068268018, -2.318338780012835443, 30.59689888758630261 ) ) ;
#42035 = DIRECTION ( 'NONE',  ( -0.000000000000000000, -0.6427876096865404731, -0.7660444431189771253 ) ) ;
#42036 = CARTESIAN_POINT ( 'NONE',  ( 5.076923076923075762, -3.669653830205710676, 35.88435417666054406 ) ) ;
#42037 = ORIENTED_EDGE ( 'NONE', *, *, #41655, .T. ) ;
#42038 = AXIS2_PLACEMENT_3D ( 'NONE', #4397, #31881, #86847 ) ;
#42039 = CARTESIAN_POINT ( 'NONE',  ( -5.010855743573000787, -4.661471528628508665, 34.16647553114624003 ) ) ;
#42040 = ORIENTED_EDGE ( 'NONE', *, *, #18171, .F. ) ;
#42042 = EDGE_LOOP ( 'NONE', ( #1634, #30972 ) ) ;
#42041 = CARTESIAN_POINT ( 'NONE',  ( -8.899922235898330314, -3.530157926970578952, 32.79014554554150607 ) ) ;
#42043 = CARTESIAN_POINT ( 'NONE',  ( -18.24999999999999289, -12.75000000000000711, 29.68455015305019273 ) ) ;
#42045 = B_SPLINE_CURVE_WITH_KNOTS ( 'NONE', 3,
 ( #80376, #46574, #49238, #34829, #75815, #6484, #88919, #61850, #13675, #13239 ),
 .UNSPECIFIED., .F., .F.,
 ( 4, 2, 2, 2, 4 ),
 ( 0.0007817359430256392216, 0.0009771253907250080327, 0.001172514838424376952, 0.001367904286123745872, 0.001563293733823114791 ),
 .UNSPECIFIED. ) ;
#42044 = CARTESIAN_POINT ( 'NONE',  ( -6.673131404728780858, -11.86320923018887541, 32.19269448109604781 ) ) ;
#42046 = CYLINDRICAL_SURFACE ( 'NONE', #54364, 0.2499999999999994726 ) ;
#42047 = DIRECTION ( 'NONE',  ( 1.000000000000000000, 0.000000000000000000, 0.000000000000000000 ) ) ;
#42048 = EDGE_CURVE ( 'NONE', #75687, #65093, #8579, .T. ) ;
#42049 = CARTESIAN_POINT ( 'NONE',  ( -39.05038313613820122, -2.249999999999998668, 29.75000000000000355 ) ) ;
#42051 = CARTESIAN_POINT ( 'NONE',  ( 15.23076923076923173, -13.75783147151868846, 33.36296068462461051 ) ) ;
#42050 = DIRECTION ( 'NONE',  ( 0.000000000000000000, 0.000000000000000000, 1.000000000000000000 ) ) ;
#42052 = CARTESIAN_POINT ( 'NONE',  ( 7.911409417429874580, -4.481592998940250538, 33.73612834413965089 ) ) ;
#42053 = CARTESIAN_POINT ( 'NONE',  ( -1.409462824231155764E-14, -4.749999999999999112, 24.15625000000000000 ) ) ;
#42054 = ORIENTED_EDGE ( 'NONE', *, *, #65965, .F. ) ;
#42055 = DIRECTION ( 'NONE',  ( 1.000000000000000000, 0.000000000000000000, 0.000000000000000000 ) ) ;
#42056 = ORIENTED_EDGE ( 'NONE', *, *, #34944, .F. ) ;
#42057 =( BOUNDED_CURVE ( )  B_SPLINE_CURVE ( 2, ( #45306, #11990, #52946, #17854, #66019, #59270, #25932, #11538, #86775, #60155, #53398, #80899, #25045, #11090, #18742, #52509, #19180, #37668, #86326, #87215, #65129, #3433, #31360, #72778, #25493, #65575, #58368, #66482, #52064, #85863, #4783, #39466, #4328, #39021, #24147, #3875, #51600, #31816, #80448, #58821, #79992, #79556, #79099, #72337, #17405, #46208, #18291, #32257, #73694, #10647, #38112, #83103, #39908, #61485, #62365, #33133, #20506, #6994, #13748, #54726, #239, #47525, #61047, #54280, #81337, #82670, #27704, #12861, #88549, #28145, #82218, #5661, #48412, #55172, #69137, #19617, #40345, #46651, #75020, #26828, #81777, #20064, #75894, #67811, #61925, #47969, #40789, #75452, #20942, #88990, #7445, #74572, #74125, #13307, #41671, #68254, #41230, #68691, #12422, #34464, #88115, #14192, #6114, #60599, #34900, #67368, #26383, #6556, #34018, #27263, #678, #53849, #47082, #33587, #55614, #43441, #28602, #15530, #63702, #30366, #70915, #29931, #36247, #2874, #29056, #14638, #49746, #56512, #56064, #21394, #48860, #70471, #63261, #83555, #23164, #21839, #83997, #69577, #22281, #77220, #16407, #42998, #50631, #2438, #8775, #2009, #29489, #64575, #22714, #56944, #43876, #71343, #57837, #84440, #50177, #57387, #77661, #76333, #42124, #35807, #9220 ),
 .UNSPECIFIED., .F., .F. ) 
 B_SPLINE_CURVE_WITH_KNOTS ( ( 3, 2, 2, 2, 2, 2, 2, 2, 2, 2, 2, 2, 2, 2, 2, 2, 2, 2, 2, 2, 2, 2, 2, 2, 2, 2, 2, 2, 2, 2, 2, 2, 2, 2, 2, 2, 2, 2, 2, 2, 2, 2, 2, 2, 2, 2, 2, 2, 2, 2, 2, 2, 2, 2, 2, 2, 2, 2, 2, 2, 2, 2, 2, 2, 2, 2, 2, 2, 2, 2, 2, 2, 2, 2, 2, 2, 2, 2, 2, 2, 3 ),
 ( 0.000000000000000000, 0.01250000000000000069, 0.02500000000000000139, 0.03749999999999999861, 0.05000000000000000278, 0.06250000000000000000, 0.07499999999999999722, 0.08749999999999999445, 0.1000000000000000056, 0.1125000000000000028, 0.1250000000000000000, 0.1375000000000000111, 0.1499999999999999944, 0.1625000000000000056, 0.1749999999999999889, 0.1875000000000000000, 0.2000000000000000111, 0.2124999999999999944, 0.2250000000000000056, 0.2374999999999999889, 0.2500000000000000000, 0.2625000000000000111, 0.2750000000000000222, 0.2874999999999999778, 0.2999999999999999889, 0.3125000000000000000, 0.3250000000000000111, 0.3375000000000000222, 0.3499999999999999778, 0.3624999999999999889, 0.3750000000000000000, 0.3875000000000000111, 0.4000000000000000222, 0.4124999999999999778, 0.4249999999999999889, 0.4375000000000000000, 0.4500000000000000111, 0.4625000000000000222, 0.4749999999999999778, 0.4874999999999999889, 0.5000000000000000000, 0.5124999999999999556, 0.5250000000000000222, 0.5374999999999999778, 0.5500000000000000444, 0.5625000000000000000, 0.5749999999999999556, 0.5875000000000000222, 0.5999999999999999778, 0.6125000000000000444, 0.6250000000000000000, 0.6374999999999999556, 0.6500000000000000222, 0.6624999999999999778, 0.6750000000000000444, 0.6875000000000000000, 0.6999999999999999556, 0.7125000000000000222, 0.7249999999999999778, 0.7375000000000000444, 0.7500000000000000000, 0.7624999999999999556, 0.7750000000000000222, 0.7874999999999999778, 0.8000000000000000444, 0.8125000000000000000, 0.8249999999999999556, 0.8375000000000000222, 0.8499999999999999778, 0.8625000000000000444, 0.8750000000000000000, 0.8874999999999999556, 0.9000000000000000222, 0.9124999999999999778, 0.9250000000000000444, 0.9375000000000000000, 0.9499999999999999556, 0.9625000000000000222, 0.9749999999999999778, 0.9875000000000000444, 1.000000000000000000 ),
 .UNSPECIFIED. ) 
 CURVE ( )  GEOMETRIC_REPRESENTATION_ITEM ( )  RATIONAL_B_SPLINE_CURVE ( ( 1.000000000000000000, 0.9238795325112867385, 1.000000000000000000, 0.9238795325112867385, 1.000000000000000000, 0.9238795325112867385, 1.000000000000000000, 0.9238795325112867385, 1.000000000000000000, 0.9238795325112867385, 1.000000000000000000, 0.9238795325112867385, 1.000000000000000000, 0.9238795325112867385, 1.000000000000000000, 0.9238795325112867385, 1.000000000000000000, 0.9238795325112867385, 1.000000000000000000, 0.9238795325112867385, 1.000000000000000000, 0.9238795325112867385, 1.000000000000000000, 0.9238795325112867385, 1.000000000000000000, 0.9238795325112867385, 1.000000000000000000, 0.9238795325112867385, 1.000000000000000000, 0.9238795325112867385, 1.000000000000000000, 0.9238795325112867385, 1.000000000000000000, 0.9238795325112867385, 1.000000000000000000, 0.9238795325112867385, 1.000000000000000000, 0.9238795325112867385, 1.000000000000000000, 0.9238795325112867385, 1.000000000000000000, 0.9238795325112867385, 1.000000000000000000, 0.9238795325112867385, 1.000000000000000000, 0.9238795325112867385, 1.000000000000000000, 0.9238795325112867385, 1.000000000000000000, 0.9238795325112867385, 1.000000000000000000, 0.9238795325112867385, 1.000000000000000000, 0.9238795325112867385, 1.000000000000000000, 0.9238795325112867385, 1.000000000000000000, 0.9238795325112867385, 1.000000000000000000, 0.9238795325112867385, 1.000000000000000000, 0.9238795325112867385, 1.000000000000000000, 0.9238795325112867385, 1.000000000000000000, 0.9238795325112867385, 1.000000000000000000, 0.9238795325112867385, 1.000000000000000000, 0.9238795325112867385, 1.000000000000000000, 0.9238795325112867385, 1.000000000000000000, 0.9238795325112867385, 1.000000000000000000, 0.9238795325112867385, 1.000000000000000000, 0.9238795325112867385, 1.000000000000000000, 0.9238795325112867385, 1.000000000000000000, 0.9238795325112867385, 1.000000000000000000, 0.9238795325112867385, 1.000000000000000000, 0.9238795325112867385, 1.000000000000000000, 0.9238795325112867385, 1.000000000000000000, 0.9238795325112867385, 1.000000000000000000, 0.9238795325112867385, 1.000000000000000000, 0.9238795325112867385, 1.000000000000000000, 0.9238795325112867385, 1.000000000000000000, 0.9238795325112867385, 1.000000000000000000, 0.9238795325112867385, 1.000000000000000000, 0.9238795325112867385, 1.000000000000000000, 0.9238795325112867385, 1.000000000000000000, 0.9238795325112867385, 1.000000000000000000, 0.9238795325112867385, 1.000000000000000000, 0.9238795325112867385, 1.000000000000000000, 0.9238795325112867385, 1.000000000000000000, 0.9238795325112867385, 1.000000000000000000, 0.9238795325112867385, 1.000000000000000000, 0.9238795325112867385, 1.000000000000000000, 0.9238795325112867385, 1.000000000000000000, 0.9238795325112867385, 1.000000000000000000, 0.9238795325112867385, 1.000000000000000000, 0.9238795325112867385, 1.000000000000000000, 0.9238795325112867385, 1.000000000000000000, 0.9238795325112867385, 1.000000000000000000, 0.9238795325112867385, 1.000000000000000000, 0.9238795325112867385, 1.000000000000000000, 0.9238795325112867385, 1.000000000000000000, 0.9238795325112867385, 1.000000000000000000, 0.9238795325112867385, 1.000000000000000000, 0.9238795325112867385, 1.000000000000000000, 0.9238795325112867385, 1.000000000000000000, 0.9238795325112867385, 1.000000000000000000, 0.9238795325112867385, 1.000000000000000000, 0.9238795325112867385, 1.000000000000000000, 0.9238795325112867385, 1.000000000000000000, 0.9238795325112867385, 1.000000000000000000, 0.9238795325112867385, 1.000000000000000000, 0.9238795325112867385, 1.000000000000000000, 0.9238795325112867385, 1.000000000000000000 ) ) 
 REPRESENTATION_ITEM ( '' )  );
#42058 = VERTEX_POINT ( 'NONE', #65625 ) ;
#42059 = CARTESIAN_POINT ( 'NONE',  ( -8.546217925137376881, -6.460100341425560444, 34.89618726649961644 ) ) ;
#42060 = VERTEX_POINT ( 'NONE', #86384 ) ;
#42061 = DIRECTION ( 'NONE',  ( -0.000000000000000000, -0.9848077530122085754, -0.1736481776669273613 ) ) ;
#42062 = EDGE_CURVE ( 'NONE', #20364, #40851, #56897, .T. ) ;
#42063 = CARTESIAN_POINT ( 'NONE',  ( 11.53846153846153832, -13.57706302396349152, 30.56769352161908060 ) ) ;
#42064 = CARTESIAN_POINT ( 'NONE',  ( -16.08777780284371772, -5.557115091759786019, 34.35708131394839882 ) ) ;
#42065 = ADVANCED_FACE ( 'NONE', ( #72390 ), #17011, .F. ) ;
#42066 = CARTESIAN_POINT ( 'NONE',  ( -11.66915300512910214, -11.18331474514187995, 33.13161551792790505 ) ) ;
#42067 = CARTESIAN_POINT ( 'NONE',  ( 10.61538461538449418, -6.835583212225970762, 34.95778746994575670 ) ) ;
#42068 = CARTESIAN_POINT ( 'NONE',  ( -13.13466997523734214, -6.653508905675592722, 34.93172785388651391 ) ) ;
#42069 = DIRECTION ( 'NONE',  ( -0.000000000000000000, -0.1736481776669307198, -0.9848077530122080203 ) ) ;
#42070 = AXIS2_PLACEMENT_3D ( 'NONE', #47229, #81482, #67071 ) ;
#42071 = CARTESIAN_POINT ( 'NONE',  ( -3.749999999999988454, -9.053300858899127945, 25.01562500000000000 ) ) ;
#42072 = CARTESIAN_POINT ( 'NONE',  ( -0.5916856709766814548, -2.619462340734461048, 30.83744416345203021 ) ) ;
#42073 = CARTESIAN_POINT ( 'NONE',  ( -16.82686865700962286, -10.82426656108011720, 33.81400080652039009 ) ) ;
#42074 = AXIS2_PLACEMENT_3D ( 'NONE', #19360, #81076, #87852 ) ;
#42075 = CARTESIAN_POINT ( 'NONE',  ( 14.43773747052708778, -2.504778602574659896, 29.97347330155780654 ) ) ;
#42076 = CARTESIAN_POINT ( 'NONE',  ( -13.38461538461538325, -6.681629849574314051, 35.83090037661290239 ) ) ;
#42078 = VERTEX_POINT ( 'NONE', #10262 ) ;
#42077 = EDGE_CURVE ( 'NONE', #56304, #45063, #26921, .T. ) ;
#42079 = ORIENTED_EDGE ( 'NONE', *, *, #57836, .F. ) ;
#42080 = CARTESIAN_POINT ( 'NONE',  ( 3.100078627658924280, -10.70098750199973203, 33.91152734681376302 ) ) ;
#42081 =( NAMED_UNIT ( * ) PLANE_ANGLE_UNIT ( ) SI_UNIT ( $, .RADIAN. ) );
#42082 = PLANE ( 'NONE',  #59910 ) ;
#42083 = CARTESIAN_POINT ( 'NONE',  ( -11.76128823094054354, -7.369208160676171460, 34.74850200257122879 ) ) ;
#42084 = ORIENTED_EDGE ( 'NONE', *, *, #20611, .T. ) ;
#42085 = EDGE_CURVE ( 'NONE', #81436, #60435, #36492, .T. ) ;
#42086 = DIRECTION ( 'NONE',  ( -0.000000000000000000, 0.9848077530122085754, -0.1736481776669273613 ) ) ;
#42087 = CARTESIAN_POINT ( 'NONE',  ( -13.19230769230769162, -11.00000000000000000, 29.75000000000000355 ) ) ;
#42088 = LINE ( 'NONE', #74534, #22150 ) ;
#42089 = ORIENTED_EDGE ( 'NONE', *, *, #72745, .T. ) ;
#42090 = EDGE_CURVE ( 'NONE', #6115, #60613, #85919, .T. ) ;
#42091 = CARTESIAN_POINT ( 'NONE',  ( 17.99999999999987566, -3.643525952248796163, 33.31231777344771672 ) ) ;
#42092 = ORIENTED_EDGE ( 'NONE', *, *, #25530, .T. ) ;
#42093 = B_SPLINE_CURVE_WITH_KNOTS ( 'NONE', 3,
 ( #61658, #34194, #40960, #19356, #60780, #68424 ),
 .UNSPECIFIED., .F., .F.,
 ( 4, 2, 4 ),
 ( 0.0003909512603273759801, 0.0005862562993132019963, 0.0007815613382990279582 ),
 .UNSPECIFIED. ) ;
#42094 = VECTOR ( 'NONE', #28530, 1000.000000000000000 ) ;
#42095 = DIRECTION ( 'NONE',  ( -1.000000000000000000, -0.000000000000000000, -0.000000000000000000 ) ) ;
#42096 = VECTOR ( 'NONE', #30668, 999.9999999999998863 ) ;
#42097 = CARTESIAN_POINT ( 'NONE',  ( 15.36155967173618286, -3.338503747796866872, 32.95102852606553512 ) ) ;
#42098 = CARTESIAN_POINT ( 'NONE',  ( -1.607542343522233352, -9.172386477786396597, 34.72672124145550043 ) ) ;
#42099 = CARTESIAN_POINT ( 'NONE',  ( 17.78205128205128105, -4.000000000000000000, 29.75000000000000355 ) ) ;
#42100 = CARTESIAN_POINT ( 'NONE',  ( 11.53846153846153832, -4.098570777380720287, 33.41473453929634729 ) ) ;
#42101 = AXIS2_PLACEMENT_3D ( 'NONE', #65200, #3499, #85932 ) ;
#42102 = VERTEX_POINT ( 'NONE', #10702 ) ;
#42103 = ORIENTED_EDGE ( 'NONE', *, *, #50335, .F. ) ;
#42104 = EDGE_LOOP ( 'NONE', ( #31421, #26250, #53521, #75307 ) ) ;
#42105 = EDGE_LOOP ( 'NONE', ( #47271, #88951, #67449, #16920 ) ) ;
#42106 = EDGE_CURVE ( 'NONE', #53666, #14815, #16060, .T. ) ;
#42107 = CARTESIAN_POINT ( 'NONE',  ( -17.32694631421604115, -10.76384336483936011, 33.53834819971076087 ) ) ;
#42108 = CARTESIAN_POINT ( 'NONE',  ( 7.716006636715624367, -3.817052484675424129, 33.13202310037935661 ) ) ;
#42109 = LINE ( 'NONE', #76319, #24968 ) ;
#42110 = EDGE_CURVE ( 'NONE', #76174, #57828, #87269, .T. ) ;
#42111 = CARTESIAN_POINT ( 'NONE',  ( 17.01084069756293715, -9.905515769479276145, 34.41647553114623292 ) ) ;
#42112 = CARTESIAN_POINT ( 'NONE',  ( -17.77722045873158763, -4.387253974876677454, 33.66317474335728832 ) ) ;
#42113 = ADVANCED_FACE ( 'NONE', ( #60656 ), #26443, .F. ) ;
#42114 = CYLINDRICAL_SURFACE ( 'NONE', #73972, 0.2499999999999986955 ) ;
#42115 = ORIENTED_EDGE ( 'NONE', *, *, #9346, .F. ) ;
#42116 = ORIENTED_EDGE ( 'NONE', *, *, #28153, .T. ) ;
#42117 = EDGE_LOOP ( 'NONE', ( #64491, #37948, #66254, #24493 ) ) ;
#42119 = VERTEX_POINT ( 'NONE', #73755 ) ;
#42118 = CARTESIAN_POINT ( 'NONE',  ( -0.4615384615384611200, -13.20930481340135110, 34.54067556320372745 ) ) ;
#42121 = CARTESIAN_POINT ( 'NONE',  ( 14.55763771707034948, -4.932303261841489928, 34.32971442181322885 ) ) ;
#42120 = CARTESIAN_POINT ( 'NONE',  ( -11.53846153846166089, -4.320704448113951379, 33.92786785259630022 ) ) ;
#42122 = CARTESIAN_POINT ( 'NONE',  ( 3.230769230769231726, -2.499999999999998668, 29.75000000000001421 ) ) ;
#42123 = VECTOR ( 'NONE', #89026, 1000.000000000000000 ) ;
#42124 = CARTESIAN_POINT ( 'NONE',  ( -3.749999999999997335, -7.500000000000021316, 26.34375000000000000 ) ) ;
#42125 = EDGE_LOOP ( 'NONE', ( #16375, #87593 ) ) ;
#42126 = ADVANCED_FACE ( 'NONE', ( #60213 ), #66539, .F. ) ;
#42127 = VERTEX_POINT ( 'NONE', #80956 ) ;
#42128 = CARTESIAN_POINT ( 'NONE',  ( -17.77698715590659972, -2.889357225399417306, 32.26129605718031712 ) ) ;
#42129 = ORIENTED_EDGE ( 'NONE', *, *, #39444, .F. ) ;
#42130 = FACE_BOUND ( 'NONE', #36841, .T. ) ;
#42131 = CARTESIAN_POINT ( 'NONE',  ( 4.853438152358743984, -4.988325925672468131, 34.36044203135681130 ) ) ;
#42132 = CARTESIAN_POINT ( 'NONE',  ( 7.846153846153846700, -5.471508081941601098, 34.59228464037088457 ) ) ;
#42133 = ORIENTED_EDGE ( 'NONE', *, *, #2408, .F. ) ;
#42134 = ADVANCED_FACE ( 'NONE', ( #53905 ), #53003, .F. ) ;
#42135 = DIRECTION ( 'NONE',  ( 0.000000000000000000, 0.6427876096865368094, 0.7660444431189802339 ) ) ;
#42136 = CARTESIAN_POINT ( 'NONE',  ( -16.08777882049607655, -12.62096338111211757, 30.90682066428152908 ) ) ;
#42137 = CARTESIAN_POINT ( 'NONE',  ( 10.36536137809164870, -2.823816976329317274, 31.52131813110795733 ) ) ;
#42138 = FACE_OUTER_BOUND ( 'NONE', #75084, .T. ) ;
#42139 = CARTESIAN_POINT ( 'NONE',  ( 14.24242230713598900, -9.528491918058357157, 34.59228464037090589 ) ) ;
#42140 = ORIENTED_EDGE ( 'NONE', *, *, #13397, .F. ) ;
#42141 = CARTESIAN_POINT ( 'NONE',  ( -11.40793610022789473, -12.50538340440932394, 31.33453814440721885 ) ) ;
#42142 = DIRECTION ( 'NONE',  ( 0.000000000000000000, 0.000000000000000000, -1.000000000000000000 ) ) ;
#42143 = CARTESIAN_POINT ( 'NONE',  ( 0.4615384615383396616, -11.94971097300221174, 32.03036669348237098 ) ) ;
#42144 = CARTESIAN_POINT ( 'NONE',  ( 5.777073782483852504, -4.887634598454295265, 34.01352882383564946 ) ) ;
#42145 = DIRECTION ( 'NONE',  ( -0.000000000000000000, -0.1736481776669307198, -0.9848077530122080203 ) ) ;
#42146 = EDGE_CURVE ( 'NONE', #57707, #59177, #18350, .T. ) ;
#42147 = FACE_BOUND ( 'NONE', #1203, .T. ) ;
#42149 = FACE_OUTER_BOUND ( 'NONE', #42978, .T. ) ;
#42148 = CARTESIAN_POINT ( 'NONE',  ( -4.153846153846152411, -5.180354513474913603, 36.12317359536750416 ) ) ;
#42150 = CARTESIAN_POINT ( 'NONE',  ( 5.207713517890025123, -2.295524264805589354, 30.44142389570982488 ) ) ;
#42152 = CARTESIAN_POINT ( 'NONE',  ( -6.000000000000119904, -5.219633306517616589, 34.19971097300220464 ) ) ;
#42151 = CARTESIAN_POINT ( 'NONE',  ( -3.230769230769229949, -2.833524468853757305, 32.15551576947925838 ) ) ;
#42153 = CARTESIAN_POINT ( 'NONE',  ( -10.28846153846153832, -3.499999999999999556, 29.75000000000000355 ) ) ;
#42154 = CARTESIAN_POINT ( 'NONE',  ( -1.200186371490556958, -4.775308065498765409, 20.07625670625849068 ) ) ;
#42156 = EDGE_CURVE ( 'NONE', #45741, #74119, #15865, .T. ) ;
#42155 = ORIENTED_EDGE ( 'NONE', *, *, #8922, .T. ) ;
#42157 = CARTESIAN_POINT ( 'NONE',  ( 1.253923917947832312, -12.11776431015575994, 31.66791131148498906 ) ) ;
#42158 = ORIENTED_EDGE ( 'NONE', *, *, #72862, .F. ) ;
#42159 = EDGE_CURVE ( 'NONE', #87108, #1750, #5279, .T. ) ;
#42160 = CARTESIAN_POINT ( 'NONE',  ( -15.23076923076922995, -4.098570777380720287, 33.41473453929634729 ) ) ;
#42161 = ORIENTED_EDGE ( 'NONE', *, *, #46928, .F. ) ;
#42162 = CARTESIAN_POINT ( 'NONE',  ( -3.930834802233301950, -12.15243808032446005, 31.58219941686247978 ) ) ;
#42163 = CARTESIAN_POINT ( 'NONE',  ( -18.13069146666756382, -2.541943142973489778, 30.39792223712632335 ) ) ;
#42164 = ORIENTED_EDGE ( 'NONE', *, *, #14947, .F. ) ;
#42165 = LINE ( 'NONE', #20549, #85791 ) ;
#42166 = CARTESIAN_POINT ( 'NONE',  ( -2.749999999999997780, -7.561099074964547917, 21.09188170625849068 ) ) ;
#42167 = AXIS2_PLACEMENT_3D ( 'NONE', #7742, #14047, #49607 ) ;
#42168 = B_SPLINE_CURVE_WITH_KNOTS ( 'NONE', 3,
 ( #72697, #2891, #79906, #37128, #38031, #80363, #44314, #52422, #44769, #65495 ),
 .UNSPECIFIED., .F., .F.,
 ( 4, 2, 2, 2, 4 ),
 ( 0.000000000000000000, 0.0001954311584214072381, 0.0003908623168428144762, 0.0005862934752642217414, 0.0007817246336856289524 ),
 .UNSPECIFIED. ) ;
#42169 = DIRECTION ( 'NONE',  ( 0.000000000000000000, 0.6427876096865373645, -0.7660444431189797898 ) ) ;
#42170 = CARTESIAN_POINT ( 'NONE',  ( 17.77707304109314634, -2.308479472611653094, 30.53278059502174457 ) ) ;
#42171 = EDGE_CURVE ( 'NONE', #63925, #72548, #38731, .T. ) ;
#42172 = CARTESIAN_POINT ( 'NONE',  ( 12.46153846153833911, -2.892918686052165622, 31.69288490824153470 ) ) ;
#42173 = CARTESIAN_POINT ( 'NONE',  ( 15.36081683702491674, -7.723484964179501588, 34.74522123443823318 ) ) ;
#42174 = DIRECTION ( 'NONE',  ( -0.000000000000000000, -0.1736481776669307198, -0.9848077530122080203 ) ) ;
#42175 = CARTESIAN_POINT ( 'NONE',  ( -5.750054481651856619, -10.76462480002816235, 33.53768742498949962 ) ) ;
#42176 = CARTESIAN_POINT ( 'NONE',  ( -3.724691934501248802, -5.885600066136383646, 25.42374329374151998 ) ) ;
#42177 = DIRECTION ( 'NONE',  ( 1.000000000000000000, 0.000000000000000000, 0.000000000000000000 ) ) ;
#42178 = CARTESIAN_POINT ( 'NONE',  ( 14.30769230769218758, -10.90142922262034020, 33.41473453929536674 ) ) ;
#42179 = DIRECTION ( 'NONE',  ( -0.000000000000000000, -0.5000000000000009992, -0.8660254037844380415 ) ) ;
#42180 = CARTESIAN_POINT ( 'NONE',  ( -1.614399933863613468, -11.22469193450124969, 23.86124329374151998 ) ) ;
#42181 = DIRECTION ( 'NONE',  ( -0.000000000000000000, -0.6427876096865404731, -0.7660444431189770143 ) ) ;
#42182 = CARTESIAN_POINT ( 'NONE',  ( 10.03846153846153832, -7.500000000000000000, 33.75000000000000000 ) ) ;
#42183 = VERTEX_POINT ( 'NONE', #19676 ) ;
#42184 = CARTESIAN_POINT ( 'NONE',  ( 1.515405825582336607, -8.191423895709840863, 34.95447573519442130 ) ) ;
#42185 = CARTESIAN_POINT ( 'NONE',  ( -0.3307466537136748985, -9.804649428959606894, 34.18742332936587047 ) ) ;
#42187 = ORIENTED_EDGE ( 'NONE', *, *, #22696, .F. ) ;
#42186 = DIRECTION ( 'NONE',  ( -0.000000000000000000, -0.9396926207859092051, -0.3420201433256662704 ) ) ;
#42188 = CARTESIAN_POINT ( 'NONE',  ( -14.37377571864818648, -11.69971097300155272, 32.46337939537587403 ) ) ;
#42189 = ADVANCED_FACE ( 'NONE', ( #4838 ), #59326, .F. ) ;
#42190 = LINE ( 'NONE', #72301, #49230 ) ;
#42191 = CARTESIAN_POINT ( 'NONE',  ( -9.692307692307691624, -12.78798330534102945, 29.74999999999997868 ) ) ;
#42192 = VECTOR ( 'NONE', #13829, 1000.000000000000000 ) ;
#42193 = DIRECTION ( 'NONE',  ( 0.000000000000000000, 0.1736481776669267785, -0.9848077530122087975 ) ) ;
#42194 = CARTESIAN_POINT ( 'NONE',  ( 10.48469401227430886, -12.62707690430377383, 30.88035979386743435 ) ) ;
#42195 = EDGE_LOOP ( 'NONE', ( #15129, #40985, #41845, #42773 ) ) ;
#42196 = CYLINDRICAL_SURFACE ( 'NONE', #45507, 0.2500000000000008882 ) ;
#42197 = ORIENTED_EDGE ( 'NONE', *, *, #72273, .T. ) ;
#42198 = ORIENTED_EDGE ( 'NONE', *, *, #20337, .F. ) ;
#42199 = CARTESIAN_POINT ( 'NONE',  ( -9.442362173959550020, -3.202959910592335646, 32.30730279482227019 ) ) ;
#42200 = CARTESIAN_POINT ( 'NONE',  ( 6.673053685783957079, -2.823816976329319495, 31.52131813110795733 ) ) ;
#42201 = CARTESIAN_POINT ( 'NONE',  ( -12.46153846153858247, -10.21337939537710326, 33.94971097300076224 ) ) ;
#42202 = DIRECTION ( 'NONE',  ( -0.000000000000000000, 0.5000000000000011102, -0.8660254037844380415 ) ) ;
#42203 = EDGE_LOOP ( 'NONE', ( #11361, #24601, #86617, #23935 ) ) ;
#42204 = DIRECTION ( 'NONE',  ( -0.000000000000000000, -0.6427876096865404731, -0.7660444431189770143 ) ) ;
#42205 = ORIENTED_EDGE ( 'NONE', *, *, #38362, .F. ) ;
#42206 = B_SPLINE_CURVE_WITH_KNOTS ( 'NONE', 3,
 ( #79562, #44866, #10653, #57498, #38119, #84987, #8886, #23269, #36355, #63817 ),
 .UNSPECIFIED., .F., .F.,
 ( 4, 2, 2, 2, 4 ),
 ( 0.000000000000000000, 0.0001954339857564126514, 0.0003908679715128183098, 0.0005863019572692239681, 0.0007817359430256294638 ),
 .UNSPECIFIED. ) ;
#42207 = ORIENTED_EDGE ( 'NONE', *, *, #73130, .F. ) ;
#42208 = AXIS2_PLACEMENT_3D ( 'NONE', #17499, #59365, #39566 ) ;
#42209 = ORIENTED_EDGE ( 'NONE', *, *, #63400, .F. ) ;
#42211 = EDGE_LOOP ( 'NONE', ( #42368, #46326 ) ) ;
#42210 = LINE ( 'NONE', #69665, #83255 ) ;
#42212 = CARTESIAN_POINT ( 'NONE',  ( -0.4615384615384611200, -4.786620604624113540, 33.94971097300155094 ) ) ;
#42213 = DIRECTION ( 'NONE',  ( 0.000000000000000000, 0.6427876096865368094, 0.7660444431189802339 ) ) ;
#42214 = VECTOR ( 'NONE', #631, 1000.000000000000227 ) ;
#42215 = EDGE_CURVE ( 'NONE', #35812, #60430, #38618, .T. ) ;
#42216 = VECTOR ( 'NONE', #66594, 1000.000000000000227 ) ;
#42217 = CARTESIAN_POINT ( 'NONE',  ( 4.088575707885377497, -4.481592998940161721, 33.73612834413957984 ) ) ;
#42218 = CARTESIAN_POINT ( 'NONE',  ( -5.010753935960420513, -7.250054483168843156, 34.74374881642865631 ) ) ;
#42219 = ADVANCED_FACE ( 'NONE', ( #72234 ), #37111, .F. ) ;
#42220 = ORIENTED_EDGE ( 'NONE', *, *, #2087, .T. ) ;
#42221 = ORIENTED_EDGE ( 'NONE', *, *, #46861, .T. ) ;
#42222 = ORIENTED_EDGE ( 'NONE', *, *, #82740, .F. ) ;
#42223 = CARTESIAN_POINT ( 'NONE',  ( -6.857821783564085116, -3.083524468853784839, 32.58852847137153930 ) ) ;
#42225 = VERTEX_POINT ( 'NONE', #45201 ) ;
#42224 = CARTESIAN_POINT ( 'NONE',  ( 4.153846153846032507, -11.48612834414049644, 32.76840700105863391 ) ) ;
#42226 = EDGE_CURVE ( 'NONE', #86676, #79746, #34241, .T. ) ;
#42227 = DIRECTION ( 'NONE',  ( -1.000000000000000000, 0.000000000000000000, 0.000000000000000000 ) ) ;
#42228 = DIRECTION ( 'NONE',  ( 0.000000000000000000, 0.9848077530122072432, -0.1736481776669354937 ) ) ;
#42229 = LINE ( 'NONE', #13850, #85384 ) ;
#42230 = EDGE_LOOP ( 'NONE', ( #47426, #25615 ) ) ;
#42231 = CARTESIAN_POINT ( 'NONE',  ( 15.16549878480845770, -10.90142922261923886, 33.41473453929638993 ) ) ;
#42232 = EDGE_CURVE ( 'NONE', #7100, #37311, #80529, .T. ) ;
#42233 = LINE ( 'NONE', #35461, #800 ) ;
#42234 = ORIENTED_EDGE ( 'NONE', *, *, #66514, .T. ) ;
#42235 = FACE_BOUND ( 'NONE', #69510, .T. ) ;
#42236 = FACE_OUTER_BOUND ( 'NONE', #32065, .T. ) ;
#42237 = CARTESIAN_POINT ( 'NONE',  ( 1.384615384615386802, -1.509761064869970415, 31.06009739812519044 ) ) ;
#42238 = CARTESIAN_POINT ( 'NONE',  ( 12.33139049180676672, -6.809168938359901446, 34.95455904226513866 ) ) ;
#42240 = CARTESIAN_POINT ( 'NONE',  ( 18.25005431163831204, -4.235687564193445276, 33.53795663066793509 ) ) ;
#42239 = CARTESIAN_POINT ( 'NONE',  ( 7.846153846153846700, -13.37000171582298513, 34.34916445242398453 ) ) ;
#42241 = DIRECTION ( 'NONE',  ( -0.000000000000000000, 1.000000000000000000, 3.491481338843133355E-15 ) ) ;
#42242 = CARTESIAN_POINT ( 'NONE',  ( -15.93083480223330817, -9.086983370893049639, 34.49168942202179267 ) ) ;
#42243 = ORIENTED_EDGE ( 'NONE', *, *, #66158, .F. ) ;
#42244 = DIRECTION ( 'NONE',  ( -0.000000000000000000, 0.6427876096865404731, -0.7660444431189770143 ) ) ;
#42245 = DIRECTION ( 'NONE',  ( -0.000000000000000000, 0.7660444431189791237, -0.6427876096865379196 ) ) ;
#42246 = ORIENTED_EDGE ( 'NONE', *, *, #20014, .F. ) ;
#42247 = VECTOR ( 'NONE', #64683, 999.9999999999998863 ) ;
#42248 = CARTESIAN_POINT ( 'NONE',  ( 8.519207531937803779, -3.202444869320336451, 32.30641848906366675 ) ) ;
#42249 = CARTESIAN_POINT ( 'NONE',  ( -4.403822897894744237, -3.436278759898155677, 33.07459398097509506 ) ) ;
#42250 = EDGE_LOOP ( 'NONE', ( #25739, #63797, #67270, #52307 ) ) ;
#42251 = DIRECTION ( 'NONE',  ( -0.000000000000000000, -0.8660254037844397068, -0.4999999999999978906 ) ) ;
#42252 = CARTESIAN_POINT ( 'NONE',  ( 2.530471976670374712, -4.989023458446561143, 34.36081565061822118 ) ) ;
#42253 = FACE_BOUND ( 'NONE', #35104, .T. ) ;
#42255 = CARTESIAN_POINT ( 'NONE',  ( 15.29602480204525961, -12.27809138561124591, 31.22303859784720359 ) ) ;
#42254 = CARTESIAN_POINT ( 'NONE',  ( 1.326923076923075762, -7.500000000000000000, 33.75000000000000000 ) ) ;
#42256 = FACE_OUTER_BOUND ( 'NONE', #80891, .T. ) ;
#42257 = CARTESIAN_POINT ( 'NONE',  ( 1.384615384615386802, -12.62096338111211580, 30.90682066428153263 ) ) ;
#42259 = CARTESIAN_POINT ( 'NONE',  ( -12.59222992820602371, -4.118384482072085184, 33.43331474514187107 ) ) ;
#42258 = CARTESIAN_POINT ( 'NONE',  ( -7.780898706641008467, -12.70778746994558439, 30.41441678777536595 ) ) ;
#42260 = DIRECTION ( 'NONE',  ( 1.000000000000000000, -5.421010862427522170E-17, 0.000000000000000000 ) ) ;
#42261 = CARTESIAN_POINT ( 'NONE',  ( -3.749999999999997335, -7.500000000000021316, 26.34375000000000000 ) ) ;
#42262 = ORIENTED_EDGE ( 'NONE', *, *, #61521, .F. ) ;
#42263 = EDGE_CURVE ( 'NONE', #16936, #71861, #24536, .T. ) ;
#42264 = B_SPLINE_CURVE_WITH_KNOTS ( 'NONE', 3,
 ( #14248, #61983, #34520, #41286, #7937, #62854, #27757, #14693, #63757, #13801 ),
 .UNSPECIFIED., .F., .F.,
 ( 4, 2, 2, 2, 4 ),
 ( 0.0007817359430256253438, 0.0009771253907249898181, 0.001172514838424354401, 0.001367904286123718983, 0.001563293733823083566 ),
 .UNSPECIFIED. ) ;
#42265 = ORIENTED_EDGE ( 'NONE', *, *, #72554, .T. ) ;
#42266 = DIRECTION ( 'NONE',  ( 0.000000000000000000, 0.000000000000000000, -1.000000000000000000 ) ) ;
#42267 = CARTESIAN_POINT ( 'NONE',  ( 14.55763771707035303, -12.68172785388650681, 30.59649109432439218 ) ) ;
#42268 = DIRECTION ( 'NONE',  ( -0.000000000000000000, 0.1736481776669307198, -0.9848077530122080203 ) ) ;
#42269 = CARTESIAN_POINT ( 'NONE',  ( -0.5922290646487710086, -2.845849958028613624, 32.17971566917920967 ) ) ;
#42270 = CARTESIAN_POINT ( 'NONE',  ( -3.903791733932699515, -2.920487667080175154, 32.31805714834170828 ) ) ;
#42271 = CARTESIAN_POINT ( 'NONE',  ( 1.553300858899129944, -11.24999999999998934, 25.95312500000000000 ) ) ;
#42272 = CARTESIAN_POINT ( 'NONE',  ( 3.903846153846154632, -7.433931650972300353, 34.75000000000000711 ) ) ;
#42273 = DIRECTION ( 'NONE',  ( -0.000000000000000000, -0.8660254037844399289, -0.4999999999999980016 ) ) ;
#42274 = EDGE_CURVE ( 'NONE', #57045, #32941, #12715, .T. ) ;
#42275 = CARTESIAN_POINT ( 'NONE',  ( -17.07692307692307665, -4.786620604624113540, 33.94971097300155094 ) ) ;
#42276 = CARTESIAN_POINT ( 'NONE',  ( -4.826977667545033768, -2.341251567377310217, 30.72681386836322659 ) ) ;
#42277 = LINE ( 'NONE', #33737, #87075 ) ;
#42278 = DIRECTION ( 'NONE',  ( -0.000000000000000000, 1.000000000000000000, -0.000000000000000000 ) ) ;
#42279 = CARTESIAN_POINT ( 'NONE',  ( -4.946131269098293259, -2.729792928343270919, 31.24908615093345077 ) ) ;
#42281 = EDGE_CURVE ( 'NONE', #65093, #26314, #66468, .T. ) ;
#42280 = CARTESIAN_POINT ( 'NONE',  ( 10.74543205063506868, -7.723484941389743952, 34.99544897038808955 ) ) ;
#42282 = ADVANCED_FACE ( 'NONE', ( #66373 ), #58272, .F. ) ;
#42283 = LINE ( 'NONE', #83265, #72995 ) ;
#42284 = VERTEX_POINT ( 'NONE', #16850 ) ;
#42285 = CARTESIAN_POINT ( 'NONE',  ( -14.30769230769242739, -3.835265460704628371, 33.15142922262033665 ) ) ;
#42286 = LINE ( 'NONE', #49026, #37389 ) ;
#42287 = CARTESIAN_POINT ( 'NONE',  ( -1.200186371490524317, -10.22469193450124791, 21.36124329374151642 ) ) ;
#42288 = CARTESIAN_POINT ( 'NONE',  ( 3.930919194939304084, -4.762599654559228846, 34.23009711892697737 ) ) ;
#42289 = LINE ( 'NONE', #8939, #81520 ) ;
#42290 = ORIENTED_EDGE ( 'NONE', *, *, #30776, .T. ) ;
#42291 = CARTESIAN_POINT ( 'NONE',  ( -4.153846153846152411, -13.53365097954675988, 30.81389545987213552 ) ) ;
#42293 = ORIENTED_EDGE ( 'NONE', *, *, #31867, .T. ) ;
#42292 = CARTESIAN_POINT ( 'NONE',  ( -9.561781990544128362, -5.195472089885680766, 34.18748526763464923 ) ) ;
#42294 = CARTESIAN_POINT ( 'NONE',  ( 9.915087361285756629, -12.69155399931963046, 30.53255429739157734 ) ) ;
#42295 = CARTESIAN_POINT ( 'NONE',  ( -4.854143535654668717, -10.11255958852956027, 34.01340905677048454 ) ) ;
#42296 = EDGE_CURVE ( 'NONE', #52150, #73790, #45654, .T. ) ;
#42297 = ORIENTED_EDGE ( 'NONE', *, *, #4011, .T. ) ;
#42298 = CARTESIAN_POINT ( 'NONE',  ( 10.03846153846153832, -11.00000000000000000, 29.75000000000000355 ) ) ;
#42299 = CARTESIAN_POINT ( 'NONE',  ( -2.307692307692305711, -6.343179335718451384, 34.87096338111211935 ) ) ;
#42300 = VERTEX_POINT ( 'NONE', #31707 ) ;
#42301 = B_SPLINE_CURVE_WITH_KNOTS ( 'NONE', 3,
 ( #52340, #53232, #72618, #87494, #80735, #19015, #39743, #46487, #73965, #12255 ),
 .UNSPECIFIED., .F., .F.,
 ( 4, 2, 2, 2, 4 ),
 ( 0.000000000000000000, 0.0001954339857564093175, 0.0003908679715128186350, 0.0005863019572692279796, 0.0007817359430256372700 ),
 .UNSPECIFIED. ) ;
#42302 = CARTESIAN_POINT ( 'NONE',  ( -10.86540783960607115, -4.175268141568685643, 33.81360843649122216 ) ) ;
#42303 = EDGE_CURVE ( 'NONE', #15714, #53825, #30365, .T. ) ;
#42304 = ADVANCED_FACE ( 'NONE', ( #85763 ), #58718, .F. ) ;
#42305 = DIRECTION ( 'NONE',  ( -0.000000000000000000, 1.000000000000000000, 3.491481338843133355E-15 ) ) ;
#42306 = CARTESIAN_POINT ( 'NONE',  ( -10.61538461538461320, -2.249999999999998668, 29.75000000000001776 ) ) ;
#42307 = ORIENTED_EDGE ( 'NONE', *, *, #30017, .T. ) ;
#42308 = ORIENTED_EDGE ( 'NONE', *, *, #42296, .T. ) ;
#42309 = CARTESIAN_POINT ( 'NONE',  ( -10.61538461538473577, -2.379036618888197729, 30.90682066428292885 ) ) ;
#42310 = EDGE_CURVE ( 'NONE', #87005, #58712, #42713, .T. ) ;
#42311 = ORIENTED_EDGE ( 'NONE', *, *, #68582, .T. ) ;
#42312 = CARTESIAN_POINT ( 'NONE',  ( -17.77698715590660328, -4.762714258010878332, 34.23016756924214832 ) ) ;
#42313 = CARTESIAN_POINT ( 'NONE',  ( -1.319359813339359588, -2.625532179533470067, 30.86335684631491105 ) ) ;
#42314 = CARTESIAN_POINT ( 'NONE',  ( 23.49999999999998579, 8.999999999999996447, 23.75000000000000000 ) ) ;
#42315 = FACE_OUTER_BOUND ( 'NONE', #2172, .T. ) ;
#42316 = CARTESIAN_POINT ( 'NONE',  ( 27.00000000000000000, -9.000000000000001776, 2.999999999999999556 ) ) ;
#42317 = CARTESIAN_POINT ( 'NONE',  ( 0.2115384615384615363, -7.433932668274254141, 35.00000000000001421 ) ) ;
#42318 = DIRECTION ( 'NONE',  ( -0.000000000000000000, -0.3420201433256694901, -0.9396926207859082059 ) ) ;
#42319 = ORIENTED_EDGE ( 'NONE', *, *, #39256, .F. ) ;
#42320 = ORIENTED_EDGE ( 'NONE', *, *, #62462, .T. ) ;
#42322 = VERTEX_POINT ( 'NONE', #43149 ) ;
#42321 = CARTESIAN_POINT ( 'NONE',  ( 9.692307692307695177, -4.098570777380720287, 33.41473453929634729 ) ) ;
#42323 = EDGE_CURVE ( 'NONE', #57930, #40306, #65342, .T. ) ;
#42324 = CARTESIAN_POINT ( 'NONE',  ( -16.15384615384615330, -11.16473453929635440, 33.15142922261926373 ) ) ;
#42325 = ORIENTED_EDGE ( 'NONE', *, *, #87428, .F. ) ;
#42326 = CARTESIAN_POINT ( 'NONE',  ( -18.00000000000012079, -3.300289026999231545, 32.46337939537709616 ) ) ;
#42327 = CARTESIAN_POINT ( 'NONE',  ( 3.903846153846154632, -2.249999999999998668, 29.75000000000000355 ) ) ;
#42328 = VERTEX_POINT ( 'NONE', #397 ) ;
#42329 = DIRECTION ( 'NONE',  ( -0.000000000000000000, -0.1736481776669307198, -0.9848077530122080203 ) ) ;
#42330 = ORIENTED_EDGE ( 'NONE', *, *, #57128, .F. ) ;
#42332 = EDGE_LOOP ( 'NONE', ( #15701, #63574 ) ) ;
#42331 = CARTESIAN_POINT ( 'NONE',  ( -8.638705067467206788, -8.586989748646452369, 34.63063291749215011 ) ) ;
#42333 = EDGE_CURVE ( 'NONE', #60048, #48024, #75099, .T. ) ;
#42334 = CARTESIAN_POINT ( 'NONE',  ( -12.71151520558705528, -3.436278759898153901, 33.07459398097509506 ) ) ;
#42335 = B_SPLINE_CURVE_WITH_KNOTS ( 'NONE', 3,
 ( #60751, #75168, #81485, #20652, #40060, #32398 ),
 .UNSPECIFIED., .F., .F.,
 ( 4, 2, 4 ),
 ( 0.0003909512603273935984, 0.0005862562993132163077, 0.0007815613382990390171 ),
 .UNSPECIFIED. ) ;
#42336 = VECTOR ( 'NONE', #62356, 999.9999999999998863 ) ;
#42337 = ORIENTED_EDGE ( 'NONE', *, *, #70263, .F. ) ;
#42338 = CARTESIAN_POINT ( 'NONE',  ( 16.08776274289027342, -12.37446782046654192, 30.86335684631486487 ) ) ;
#42339 = CARTESIAN_POINT ( 'NONE',  ( -14.30769230769230660, -11.33034616979429110, 35.88435417666054406 ) ) ;
#42340 = APPLICATION_CONTEXT ( 'automotive_design' ) ;
#42341 = FACE_BOUND ( 'NONE', #33503, .T. ) ;
#42342 = AXIS2_PLACEMENT_3D ( 'NONE', #71869, #31339, #38998 ) ;
#42343 = CARTESIAN_POINT ( 'NONE',  ( 1.634669696253701288, -12.41262288849542017, 30.68299917996395010 ) ) ;
#42344 = CARTESIAN_POINT ( 'NONE',  ( -6.700297381808510089, -12.24180327182771855, 31.33663988360758168 ) ) ;
#42345 = LINE ( 'NONE', #76564, #49601 ) ;
#42346 = CARTESIAN_POINT ( 'NONE',  ( 20.00000000000000000, -4.000000000000000000, 29.75000000000000355 ) ) ;
#42347 = CARTESIAN_POINT ( 'NONE',  ( -27.00000000000000000, 17.00000000000000000, 2.999999999999999112 ) ) ;
#42348 = LINE ( 'NONE', #69802, #7382 ) ;
#42349 = ORIENTED_EDGE ( 'NONE', *, *, #74545, .T. ) ;
#42350 = LINE ( 'NONE', #55402, #43253 ) ;
#42351 = ORIENTED_EDGE ( 'NONE', *, *, #85294, .T. ) ;
#42352 = VERTEX_POINT ( 'NONE', #7595 ) ;
#42354 = CARTESIAN_POINT ( 'NONE',  ( -16.15384615384627409, -11.48612834414049644, 32.76840700105863391 ) ) ;
#42353 = CARTESIAN_POINT ( 'NONE',  ( -5.076923076923075762, -3.050289026998446396, 32.03036669348365706 ) ) ;
#42355 = EDGE_CURVE ( 'NONE', #42183, #78937, #50, .T. ) ;
#42356 = CARTESIAN_POINT ( 'NONE',  ( 6.000000000000001776, -1.242168528481310874, 33.36296068462461051 ) ) ;
#42357 = CARTESIAN_POINT ( 'NONE',  ( 7.976944287120798727, -3.338503747796866872, 32.95102852606553512 ) ) ;
#42358 = FACE_OUTER_BOUND ( 'NONE', #29250, .T. ) ;
#42359 = DIRECTION ( 'NONE',  ( -0.000000000000000000, 0.7660444431189791237, -0.6427876096865379196 ) ) ;
#42360 = ORIENTED_EDGE ( 'NONE', *, *, #73024, .F. ) ;
#42361 = LINE ( 'NONE', #49099, #38595 ) ;
#42362 = DIRECTION ( 'NONE',  ( -1.000000000000000000, 0.000000000000000000, -0.000000000000000000 ) ) ;
#42363 = CARTESIAN_POINT ( 'NONE',  ( -19.50000000000000000, -11.50000000000000000, 29.75000000000000355 ) ) ;
#42364 = CARTESIAN_POINT ( 'NONE',  ( -8.519176349317316266, -2.544122305571458575, 31.48381861865057729 ) ) ;
#42365 = DIRECTION ( 'NONE',  ( 0.000000000000000000, 0.7660444431189822323, -0.6427876096865344779 ) ) ;
#42366 = VERTEX_POINT ( 'NONE', #21991 ) ;
#42367 = CARTESIAN_POINT ( 'NONE',  ( 5.076923076923075762, -13.87047571288749737, 32.06866353760679544 ) ) ;
#42368 = ORIENTED_EDGE ( 'NONE', *, *, #27013, .T. ) ;
#42369 = B_SPLINE_CURVE_WITH_KNOTS ( 'NONE', 3,
 ( #85387, #19588, #61015, #45728, #11957, #33987, #25906, #47049, #39875, #46180 ),
 .UNSPECIFIED., .F., .F.,
 ( 4, 2, 2, 2, 4 ),
 ( 0.0007817359430256365111, 0.0009771253907250043464, 0.001172514838424372399, 0.001367904286123740234, 0.001563293733823108069 ),
 .UNSPECIFIED. ) ;
#42370 = ORIENTED_EDGE ( 'NONE', *, *, #81290, .F. ) ;
#42371 = CARTESIAN_POINT ( 'NONE',  ( 7.846153846153846700, -13.78497067705608181, 32.30358669280327177 ) ) ;
#42372 = EDGE_CURVE ( 'NONE', #519, #22135, #78263, .T. ) ;
#42373 = ORIENTED_EDGE ( 'NONE', *, *, #75433, .F. ) ;
#42374 = DIRECTION ( 'NONE',  ( -1.000000000000000000, -8.673617379884044347E-16, 0.000000000000000000 ) ) ;
#42375 = CARTESIAN_POINT ( 'NONE',  ( -17.14219352288385778, -3.300289026998414865, 32.46337939537583850 ) ) ;
#42376 = CYLINDRICAL_SURFACE ( 'NONE', #49506, 0.2500000000000002220 ) ;
#42377 = CARTESIAN_POINT ( 'NONE',  ( -4.946132635956123735, -3.338503747796866872, 32.95102852606553512 ) ) ;
#42378 = CYLINDRICAL_SURFACE ( 'NONE', #2841, 0.2500000000000002220 ) ;
#42379 = ADVANCED_FACE ( 'NONE', ( #49465 ), #8037, .F. ) ;
#42380 = CARTESIAN_POINT ( 'NONE',  ( 8.638539302563209787, -6.413092428213692742, 34.63065189839063152 ) ) ;
#42382 = VERTEX_POINT ( 'NONE', #76042 ) ;
#42381 = VECTOR ( 'NONE', #35611, 1000.000000000000227 ) ;
#42383 = CARTESIAN_POINT ( 'NONE',  ( 4.403846153846169287, -2.249999999999999112, 29.81603969181031033 ) ) ;
#42385 = ORIENTED_EDGE ( 'NONE', *, *, #28251, .F. ) ;
#42384 = CARTESIAN_POINT ( 'NONE',  ( -12.46153846153846168, -9.058645607665452459, 34.76329471203371924 ) ) ;
#42386 = CARTESIAN_POINT ( 'NONE',  ( -3.230769230768923084, -2.506253911140615021, 30.00000000000323297 ) ) ;
#42387 = DIRECTION ( 'NONE',  ( -0.000000000000000000, -0.3420201433256694346, -0.9396926207859080948 ) ) ;
#42388 = CARTESIAN_POINT ( 'NONE',  ( -0.5922290646487706756, -3.957541250942359756, 33.62499894934981626 ) ) ;
#42389 = B_SPLINE_CURVE_WITH_KNOTS ( 'NONE', 3,
 ( #85802, #79033, #3814, #22748, #86257, #57422, #17334, #24525, #44791, #51994 ),
 .UNSPECIFIED., .F., .F.,
 ( 4, 2, 2, 2, 4 ),
 ( 0.000000000000000000, 0.0001954339857564081791, 0.0003908679715128163582, 0.0005863019572692245102, 0.0007817359430256327164 ),
 .UNSPECIFIED. ) ;
#42390 = CARTESIAN_POINT ( 'NONE',  ( 6.250054419913455561, -9.233818618650603938, 34.70587769442853698 ) ) ;
#42391 = LINE ( 'NONE', #88814, #4465 ) ;
#42392 = EDGE_CURVE ( 'NONE', #82786, #2951, #62515, .T. ) ;
#42393 = CARTESIAN_POINT ( 'NONE',  ( 11.53846153846153832, -8.120952969808772792, 34.71129190930000163 ) ) ;
#42394 = DIRECTION ( 'NONE',  ( -0.000000000000000000, -0.9848077530122085754, -0.1736481776669273613 ) ) ;
#42395 = CARTESIAN_POINT ( 'NONE',  ( -2.608446859217920633, -4.805146000318815780, 13.00186829374151465 ) ) ;
#42396 = ORIENTED_EDGE ( 'NONE', *, *, #28390, .F. ) ;
#42397 = CARTESIAN_POINT ( 'NONE',  ( -1.319359813339359588, -11.48612834413965977, 32.76840700105972815 ) ) ;
#42398 = CARTESIAN_POINT ( 'NONE',  ( 12.46153846153833911, -5.094484230521993062, 34.41647553114689373 ) ) ;
#42399 = CARTESIAN_POINT ( 'NONE',  ( 7.846153846153725020, -2.625532179533779154, 30.86335684631627174 ) ) ;
#42400 = DIRECTION ( 'NONE',  ( 0.000000000000000000, 0.9848077530122072432, 0.1736481776669354937 ) ) ;
#42401 = ORIENTED_EDGE ( 'NONE', *, *, #35977, .F. ) ;
#42402 = CARTESIAN_POINT ( 'NONE',  ( 10.61538461538461675, -1.790695186598648903, 34.54067556320373455 ) ) ;
#42403 = CARTESIAN_POINT ( 'NONE',  ( -2.372962753653082402, -3.300289026998414865, 32.46337939537583139 ) ) ;
#42404 = CARTESIAN_POINT ( 'NONE',  ( -1.254089682851820209, -6.852161475712352789, 34.70806712695775786 ) ) ;
#42405 = CARTESIAN_POINT ( 'NONE',  ( -4.219929564802032296, -10.51840700105979387, 33.73612834413961536 ) ) ;
#42406 = VERTEX_POINT ( 'NONE', #832 ) ;
#42407 = CARTESIAN_POINT ( 'NONE',  ( -16.15384615384615330, -12.78798330534103123, 29.99999999999997868 ) ) ;
#42408 = EDGE_CURVE ( 'NONE', #53458, #34311, #21324, .T. ) ;
#42409 = AXIS2_PLACEMENT_3D ( 'NONE', #53965, #73809, #11205 ) ;
#42410 = FACE_OUTER_BOUND ( 'NONE', #16159, .T. ) ;
#42411 = CYLINDRICAL_SURFACE ( 'NONE', #17746, 0.2499999999999973355 ) ;
#42412 = ORIENTED_EDGE ( 'NONE', *, *, #4052, .F. ) ;
#42413 = CARTESIAN_POINT ( 'NONE',  ( -8.769230769230455635, -2.255955759149395501, 30.00000000000324363 ) ) ;
#42414 = AXIS2_PLACEMENT_3D ( 'NONE', #33800, #12648, #52729 ) ;
#42415 = ORIENTED_EDGE ( 'NONE', *, *, #41094, .F. ) ;
#42416 = PLANE ( 'NONE',  #19860 ) ;
#42417 = DIRECTION ( 'NONE',  ( 0.000000000000000000, 0.8660254037844377084, -0.5000000000000015543 ) ) ;
#42418 = VERTEX_POINT ( 'NONE', #84154 ) ;
#42419 = CARTESIAN_POINT ( 'NONE',  ( 10.68145194873469350, -11.35647404775217595, 33.31231777344666511 ) ) ;
#42420 = CARTESIAN_POINT ( 'NONE',  ( -9.019207500173124004, -2.564618984488975073, 30.55390908950641915 ) ) ;
#42421 = CARTESIAN_POINT ( 'NONE',  ( -10.83886955910856464, -5.912607949931405926, 34.49155766932282319 ) ) ;
#42422 = CARTESIAN_POINT ( 'NONE',  ( -11.40767109749458541, -5.496552790871120031, 34.60292014791297532 ) ) ;
#42423 = DIRECTION ( 'NONE',  ( 0.000000000000000000, 0.1736481776669275834, 0.9848077530122086864 ) ) ;
#42424 = ORIENTED_EDGE ( 'NONE', *, *, #4545, .T. ) ;
#42425 = ORIENTED_EDGE ( 'NONE', *, *, #5838, .T. ) ;
#42426 = FACE_BOUND ( 'NONE', #9111, .T. ) ;
#42427 = ORIENTED_EDGE ( 'NONE', *, *, #41599, .T. ) ;
#42428 = CARTESIAN_POINT ( 'NONE',  ( 15.23076923076923173, -12.37446782046654192, 30.86335684631486131 ) ) ;
#42429 = B_SPLINE_CURVE_WITH_KNOTS ( 'NONE', 3,
 ( #17403, #24145, #24595, #59268, #86773, #16953, #79990, #30899, #46206, #73691 ),
 .UNSPECIFIED., .F., .F.,
 ( 4, 2, 2, 2, 4 ),
 ( 0.000000000000000000, 0.0001954311564186863323, 0.0003908623128373726646, 0.0005862934692560590241, 0.0007817246256747453293 ),
 .UNSPECIFIED. ) ;
#42430 = CARTESIAN_POINT ( 'NONE',  ( -14.24243716817946925, -11.67786785259547777, 32.92929555188713664 ) ) ;
#42431 = CARTESIAN_POINT ( 'NONE',  ( 9.562160482869471068, -12.27039167877662251, 31.24851455888617835 ) ) ;
#42432 = CARTESIAN_POINT ( 'NONE',  ( -10.61538461538461320, -12.09954503811598769, 35.62045528018868623 ) ) ;
#42433 = VERTEX_POINT ( 'NONE', #75595 ) ;
#42434 = AXIS2_PLACEMENT_3D ( 'NONE', #73737, #11580, #46687 ) ;
#42435 = EDGE_LOOP ( 'NONE', ( #28184, #35350 ) ) ;
#42436 = VERTEX_POINT ( 'NONE', #68845 ) ;
#42437 = CARTESIAN_POINT ( 'NONE',  ( 13.13461538461538858, -7.566083408709835645, 34.74999999999999289 ) ) ;
#42438 = EDGE_LOOP ( 'NONE', ( #56850, #76625 ) ) ;
#42439 = FACE_OUTER_BOUND ( 'NONE', #29115, .T. ) ;
#42440 = CARTESIAN_POINT ( 'NONE',  ( -6.673076923076909139, -2.249999999999999112, 29.81603969181031033 ) ) ;
#42441 = LINE ( 'NONE', #29374, #11171 ) ;
#42442 = CARTESIAN_POINT ( 'NONE',  ( 9.019176287578908102, -9.272278438253398036, 34.42582936511637115 ) ) ;
#42443 = CARTESIAN_POINT ( 'NONE',  ( 6.000000000000001776, -8.564572088678739092, 35.78748833219616898 ) ) ;
#42444 = CARTESIAN_POINT ( 'NONE',  ( 14.37294787896833448, -6.879047030191282275, 34.71129190930002295 ) ) ;
#42445 = CARTESIAN_POINT ( 'NONE',  ( -1.134669975237340811, -2.986452184633681117, 32.43230066228895225 ) ) ;
#42446 = ORIENTED_EDGE ( 'NONE', *, *, #13527, .F. ) ;
#42447 = ORIENTED_EDGE ( 'NONE', *, *, #37390, .F. ) ;
#42448 = ORIENTED_EDGE ( 'NONE', *, *, #64002, .T. ) ;
#42449 = CARTESIAN_POINT ( 'NONE',  ( 2.980769230769232170, -7.500000000000001776, 35.00000000000000000 ) ) ;
#42451 = CARTESIAN_POINT ( 'NONE',  ( -13.51530685128294529, -5.582088688514999397, 34.36776431015576350 ) ) ;
#42450 = CARTESIAN_POINT ( 'NONE',  ( -6.000000000000119904, -9.442884908241554243, 34.35708131394783038 ) ) ;
#42452 = B_SPLINE_CURVE_WITH_KNOTS ( 'NONE', 3,
 ( #10594, #38060, #39412, #59660, #33534, #72725, #60103, #4728, #53344, #60548 ),
 .UNSPECIFIED., .F., .F.,
 ( 4, 2, 2, 2, 4 ),
 ( 0.0007817359430256288133, 0.0009771253907249945886, 0.001172514838424360472, 0.001367904286123726356, 0.001563293733823092240 ),
 .UNSPECIFIED. ) ;
#42453 = CARTESIAN_POINT ( 'NONE',  ( 1.384615384615386802, -12.34228464037088635, 31.77849191805839268 ) ) ;
#42454 = CARTESIAN_POINT ( 'NONE',  ( 12.68431813051652668, -12.69155399931963046, 30.53255429739157734 ) ) ;
#42455 = FACE_BOUND ( 'NONE', #25582, .T. ) ;
#42456 = CARTESIAN_POINT ( 'NONE',  ( 8.068933387422250192, -11.41317474335729543, 32.86274602512330034 ) ) ;
#42457 = ORIENTED_EDGE ( 'NONE', *, *, #76324, .F. ) ;
#42458 = CIRCLE ( 'NONE', #46756, 0.2500000000000002220 ) ;
#42459 = CARTESIAN_POINT ( 'NONE',  ( -7.976763501357926778, -7.722926974430166069, 34.99546784045486447 ) ) ;
#42460 = CARTESIAN_POINT ( 'NONE',  ( 9.627037691751372250, -12.16647553114622049, 32.15551576947930812 ) ) ;
#42461 = CARTESIAN_POINT ( 'NONE',  ( 15.12820512820512953, -7.500000000000000000, 29.75000000000000355 ) ) ;
#42462 = DIRECTION ( 'NONE',  ( 0.000000000000000000, 0.000000000000000000, 1.000000000000000000 ) ) ;
#42463 = ORIENTED_EDGE ( 'NONE', *, *, #4243, .F. ) ;
#42464 = B_SPLINE_CURVE_WITH_KNOTS ( 'NONE', 3,
 ( #9568, #42043, #37030, #69501, #42485, #69943 ),
 .UNSPECIFIED., .F., .F.,
 ( 4, 2, 4 ),
 ( 0.000000000000000000, 0.1250000000000000000, 0.2500000000000000000 ),
 .UNSPECIFIED. ) ;
#42465 = CARTESIAN_POINT ( 'NONE',  ( 6.130790440966950250, -10.70102852606553157, 33.91149625220312913 ) ) ;
#42466 = ORIENTED_EDGE ( 'NONE', *, *, #2613, .T. ) ;
#42468 = FACE_BOUND ( 'NONE', #47345, .T. ) ;
#42467 = B_SPLINE_CURVE_WITH_KNOTS ( 'NONE', 3,
 ( #1269, #48125, #28299, #21545, #49019, #35510, #70178, #76941, #13902, #7151 ),
 .UNSPECIFIED., .F., .F.,
 ( 4, 2, 2, 2, 4 ),
 ( 0.0007817359430256285964, 0.0009771253907249948054, 0.001172514838424360906, 0.001367904286123727223, 0.001563293733823093324 ),
 .UNSPECIFIED. ) ;
#42469 = LINE ( 'NONE', #8240, #44695 ) ;
#42470 = EDGE_CURVE ( 'NONE', #83460, #10983, #60094, .T. ) ;
#42471 = CARTESIAN_POINT ( 'NONE',  ( 17.07692307692295586, -11.94971097300221174, 32.03036669348237098 ) ) ;
#42472 = CARTESIAN_POINT ( 'NONE',  ( 12.46153846153833911, -11.67786785259630911, 32.92929555188603530 ) ) ;
#42473 = ORIENTED_EDGE ( 'NONE', *, *, #39771, .F. ) ;
#42474 = VECTOR ( 'NONE', #10528, 1000.000000000000114 ) ;
#42475 = EDGE_CURVE ( 'NONE', #9551, #4412, #38553, .T. ) ;
#42476 = CARTESIAN_POINT ( 'NONE',  ( 19.00000000000000000, 1.250000000000002665, 31.75000000000000000 ) ) ;
#42477 = CARTESIAN_POINT ( 'NONE',  ( 4.153846153846032507, -3.835265460704628371, 33.15142922262033665 ) ) ;
#42478 = LINE ( 'NONE', #50098, #39484 ) ;
#42479 = DIRECTION ( 'NONE',  ( -0.000000000000000000, 0.6427876096865404731, -0.7660444431189771253 ) ) ;
#42480 = ORIENTED_EDGE ( 'NONE', *, *, #69845, .F. ) ;
#42481 = CARTESIAN_POINT ( 'NONE',  ( 13.31853197365950692, -5.557115091759785130, 34.35708131394839171 ) ) ;
#42482 = ORIENTED_EDGE ( 'NONE', *, *, #30884, .T. ) ;
#42484 = ORIENTED_EDGE ( 'NONE', *, *, #3173, .F. ) ;
#42483 = CARTESIAN_POINT ( 'NONE',  ( 4.376625822824218304, -3.020022701398814124, 32.48759521482552515 ) ) ;
#42485 = CARTESIAN_POINT ( 'NONE',  ( -18.06544984694978595, -12.75000000000000888, 29.49999999999998224 ) ) ;
#42486 = LINE ( 'NONE', #56436, #51323 ) ;
#42487 = CARTESIAN_POINT ( 'NONE',  ( 4.853996118016228323, -2.523278758544489797, 31.42238647778637528 ) ) ;
#42488 = CARTESIAN_POINT ( 'NONE',  ( -8.769230769230768274, -5.180354513474913603, 36.12317359536750416 ) ) ;
#42490 = CYLINDRICAL_SURFACE ( 'NONE', #74886, 0.2499999999999994726 ) ;
#42489 = CARTESIAN_POINT ( 'NONE',  ( -7.134615384615385025, -3.499999999999999556, 29.75000000000000355 ) ) ;
#42491 = EDGE_CURVE ( 'NONE', #26806, #32798, #45353, .T. ) ;
#42492 = DIRECTION ( 'NONE',  ( -0.000000000000000000, 0.000000000000000000, 1.000000000000000000 ) ) ;
#42493 = CARTESIAN_POINT ( 'NONE',  ( -2.749999999999998224, -7.500000000000015987, 26.34375000000000000 ) ) ;
#42494 = ORIENTED_EDGE ( 'NONE', *, *, #45740, .F. ) ;
#42495 = CARTESIAN_POINT ( 'NONE',  ( -16.40382289789474513, -4.818429247618091438, 34.26397095200675125 ) ) ;
#42496 = ORIENTED_EDGE ( 'NONE', *, *, #28751, .F. ) ;
#42497 = ORIENTED_EDGE ( 'NONE', *, *, #65048, .F. ) ;
#42498 = CARTESIAN_POINT ( 'NONE',  ( 15.23076923076910916, -11.06231777344772027, 33.60647404775119895 ) ) ;
#42499 = ORIENTED_EDGE ( 'NONE', *, *, #21898, .F. ) ;
#42500 = CARTESIAN_POINT ( 'NONE',  ( -5.777220331021931443, -12.69155399931963046, 30.53255429739158444 ) ) ;
#42501 = FACE_OUTER_BOUND ( 'NONE', #74068, .T. ) ;
#42502 = B_SPLINE_CURVE_WITH_KNOTS ( 'NONE', 3,
 ( #43318, #23039, #15411, #36562, #70795, #63580, #63129, #49629, #1882, #23473 ),
 .UNSPECIFIED., .F., .F.,
 ( 4, 2, 2, 2, 4 ),
 ( 0.000000000000000000, 0.0001954339857564073659, 0.0003908679715128147319, 0.0005863019572692221250, 0.0007817359430256294638 ),
 .UNSPECIFIED. ) ;
#42503 = VECTOR ( 'NONE', #36928, 999.9999999999998863 ) ;
#42504 = LINE ( 'NONE', #74969, #67489 ) ;
#42505 = CYLINDRICAL_SURFACE ( 'NONE', #12912, 0.2500000000000009437 ) ;
#42506 = CARTESIAN_POINT ( 'NONE',  ( -8.835313148590902443, -2.486705287966279432, 31.30864560766542937 ) ) ;
#42507 = DIRECTION ( 'NONE',  ( -1.000000000000000000, 0.000000000000000000, -0.000000000000000000 ) ) ;
#42508 = LINE ( 'NONE', #78487, #69533 ) ;
#42509 = B_SPLINE_CURVE_WITH_KNOTS ( 'NONE', 3,
 ( #38448, #18178, #80334, #73580, #30354, #37542, #65009, #3318, #75768, #27587 ),
 .UNSPECIFIED., .F., .F.,
 ( 4, 2, 2, 2, 4 ),
 ( 0.000000000000000000, 0.0001954339857564073659, 0.0003908679715128147319, 0.0005863019572692221250, 0.0007817359430256294638 ),
 .UNSPECIFIED. ) ;
#42510 = CARTESIAN_POINT ( 'NONE',  ( 6.699591998512593349, -10.23692288466677880, 34.23039457007281072 ) ) ;
#42512 = EDGE_CURVE ( 'NONE', #58364, #2406, #79401, .T. ) ;
#42511 = CARTESIAN_POINT ( 'NONE',  ( -2.307692307692428724, -3.083524468854526912, 32.58852847137268327 ) ) ;
#42513 = EDGE_CURVE ( 'NONE', #39107, #89080, #23556, .T. ) ;
#42514 = LINE ( 'NONE', #75847, #17688 ) ;
#42515 = DIRECTION ( 'NONE',  ( -0.000000000000000000, -0.000000000000000000, -1.000000000000000000 ) ) ;
#42516 = ADVANCED_FACE ( 'NONE', ( #78251 ), #72381, .F. ) ;
#42517 = ORIENTED_EDGE ( 'NONE', *, *, #55493, .T. ) ;
#42519 = EDGE_CURVE ( 'NONE', #80969, #57045, #23745, .T. ) ;
#42518 = ORIENTED_EDGE ( 'NONE', *, *, #28891, .F. ) ;
#42520 = CARTESIAN_POINT ( 'NONE',  ( 12.71159288145191901, -2.544122305571458575, 31.48381861865057729 ) ) ;
#42521 = LINE ( 'NONE', #64531, #63313 ) ;
#42522 = CARTESIAN_POINT ( 'NONE',  ( 10.61538461538461675, -13.95598074871891292, 31.83374038241031911 ) ) ;
#42523 = CARTESIAN_POINT ( 'NONE',  ( 19.00000000000000000, 16.99999999999999289, 31.75000000000000000 ) ) ;
#42524 = ORIENTED_EDGE ( 'NONE', *, *, #39768, .F. ) ;
#42525 = CARTESIAN_POINT ( 'NONE',  ( -16.02332071561251325, -8.630441415882549094, 34.87705825610312615 ) ) ;
#42526 = CARTESIAN_POINT ( 'NONE',  ( -13.44988538517170795, -11.06231777344662781, 33.60647404775220082 ) ) ;
#42527 = DIRECTION ( 'NONE',  ( 0.000000000000000000, 0.000000000000000000, -1.000000000000000000 ) ) ;
#42528 = CIRCLE ( 'NONE', #61219, 0.2500000000000002220 ) ;
#42529 = ORIENTED_EDGE ( 'NONE', *, *, #72866, .T. ) ;
#42530 = CARTESIAN_POINT ( 'NONE',  ( -13.45069879557126669, -9.780366693483667717, 34.19971097300155805 ) ) ;
#42531 = VERTEX_POINT ( 'NONE', #3029 ) ;
#42532 = CARTESIAN_POINT ( 'NONE',  ( 4.153846153846032507, -9.442884908241554243, 34.35708131394783038 ) ) ;
#42533 = PLANE ( 'NONE',  #21162 ) ;
#42534 = CARTESIAN_POINT ( 'NONE',  ( -8.069080805060693251, -2.523278758544489797, 31.42238647778637528 ) ) ;
#42535 = VECTOR ( 'NONE', #4547, 1000.000000000000000 ) ;
#42536 = CARTESIAN_POINT ( 'NONE',  ( -14.05763799605399456, -11.79725096376909299, 32.30694842903960762 ) ) ;
#42537 = DIRECTION ( 'NONE',  ( -0.000000000000000000, 0.9396926207859093161, -0.3420201433256663259 ) ) ;
#42538 = VERTEX_POINT ( 'NONE', #78705 ) ;
#42539 = ORIENTED_EDGE ( 'NONE', *, *, #12553, .T. ) ;
#42540 = EDGE_CURVE ( 'NONE', #9337, #67157, #81481, .T. ) ;
#42541 = ORIENTED_EDGE ( 'NONE', *, *, #31049, .F. ) ;
#42542 = ORIENTED_EDGE ( 'NONE', *, *, #18455, .F. ) ;
#42543 = CARTESIAN_POINT ( 'NONE',  ( -10.86536135943320502, -12.41104346484419452, 31.60698883733904196 ) ) ;
#42544 = CARTESIAN_POINT ( 'NONE',  ( -16.85414353565466783, -3.755027918224367767, 33.06320215134714857 ) ) ;
#42545 = CARTESIAN_POINT ( 'NONE',  ( 0.4615384615383382183, -6.835583212225970762, 34.95778746994575670 ) ) ;
#42546 = CARTESIAN_POINT ( 'NONE',  ( 1.576923076923075762, -7.500000000000000000, 33.75000000000000000 ) ) ;
#42547 = AXIS2_PLACEMENT_3D ( 'NONE', #38846, #78481, #17229 ) ;
#42548 = CARTESIAN_POINT ( 'NONE',  ( -7.623374177175779032, -4.226511098958374291, 33.85474049983370293 ) ) ;
#42549 = FACE_OUTER_BOUND ( 'NONE', #73172, .T. ) ;
#42550 = ORIENTED_EDGE ( 'NONE', *, *, #81703, .F. ) ;
#42551 = ORIENTED_EDGE ( 'NONE', *, *, #32924, .F. ) ;
#42552 = EDGE_CURVE ( 'NONE', #88650, #16692, #41751, .T. ) ;
#42553 = VECTOR ( 'NONE', #10255, 999.9999999999998863 ) ;
#42554 = VERTEX_POINT ( 'NONE', #6157 ) ;
#42556 = EDGE_LOOP ( 'NONE', ( #26463, #16644, #55534, #38212 ) ) ;
#42555 = CARTESIAN_POINT ( 'NONE',  ( -3.100243529005665799, -10.88167719472716399, 33.43325721877153711 ) ) ;
#42558 = CARTESIAN_POINT ( 'NONE',  ( -8.769230769230890843, -11.48612834414049644, 32.76840700105863391 ) ) ;
#42557 = CARTESIAN_POINT ( 'NONE',  ( 16.21910172512217585, -8.613356846314930593, 34.62446782046653482 ) ) ;
#42559 = DIRECTION ( 'NONE',  ( 0.000000000000000000, 0.7660444431189807890, 0.6427876096865361433 ) ) ;
#42560 = CARTESIAN_POINT ( 'NONE',  ( -10.74553182482283198, -11.93770438780619259, 32.05411857736982029 ) ) ;
#42561 = ORIENTED_EDGE ( 'NONE', *, *, #54042, .T. ) ;
#42562 = VERTEX_POINT ( 'NONE', #18787 ) ;
#42563 = B_SPLINE_CURVE_WITH_KNOTS ( 'NONE', 3,
 ( #25388, #78995, #11432, #86672, #79452, #24938, #59611, #65916, #46105, #17297 ),
 .UNSPECIFIED., .F., .F.,
 ( 4, 2, 2, 2, 4 ),
 ( 0.0007817359430256399806, 0.0009771253907250089001, 0.001172514838424378036, 0.001367904286123746956, 0.001563293733823115875 ),
 .UNSPECIFIED. ) ;
#42564 = CARTESIAN_POINT ( 'NONE',  ( 13.63466980452883526, -10.82426656108012075, 33.81400080652039009 ) ) ;
#42565 = EDGE_LOOP ( 'NONE', ( #1116, #30127, #83677, #15337 ) ) ;
#42566 = FACE_BOUND ( 'NONE', #72964, .T. ) ;
#42567 = CARTESIAN_POINT ( 'NONE',  ( -1.254570221780606287, -2.504778602574659896, 29.97347330155780298 ) ) ;
#42568 = EDGE_CURVE ( 'NONE', #56977, #7644, #32300, .T. ) ;
#42569 = LINE ( 'NONE', #22289, #3099 ) ;
#42570 = ORIENTED_EDGE ( 'NONE', *, *, #83868, .T. ) ;
#42571 = CARTESIAN_POINT ( 'NONE',  ( 15.16501580245589764, -7.249945578846651806, 34.99404164642496795 ) ) ;
#42572 = CARTESIAN_POINT ( 'NONE',  ( 11.28843831424008926, -6.652501968072648708, 34.93155406624980941 ) ) ;
#42573 = CARTESIAN_POINT ( 'NONE',  ( 10.61538461538449596, -2.892918686052165622, 31.69288490824153470 ) ) ;
#42574 = EDGE_CURVE ( 'NONE', #58249, #55087, #12037, .T. ) ;
#42575 = DIRECTION ( 'NONE',  ( -1.000000000000000000, -0.000000000000000000, 0.000000000000000000 ) ) ;
#42576 = CARTESIAN_POINT ( 'NONE',  ( 1.634560793993428796, -2.589246495874657938, 31.60778113518102828 ) ) ;
#42577 = EDGE_LOOP ( 'NONE', ( #33042, #39355 ) ) ;
#42578 = CARTESIAN_POINT ( 'NONE',  ( -12.33074802057151409, -2.295524264805589354, 30.44142389570982488 ) ) ;
#42579 = CARTESIAN_POINT ( 'NONE',  ( 17.07692307692295586, -12.46129190930018460, 30.37095296980731973 ) ) ;
#42580 = DIRECTION ( 'NONE',  ( -0.000000000000000000, -0.8660254037844397068, -0.4999999999999978906 ) ) ;
#42581 = CARTESIAN_POINT ( 'NONE',  ( 13.38461538461526423, -2.379036618888197729, 30.90682066428292885 ) ) ;
#42582 = FACE_OUTER_BOUND ( 'NONE', #81782, .T. ) ;
#42583 = AXIS2_PLACEMENT_3D ( 'NONE', #37582, #52429, #46131 ) ;
#42584 = FACE_BOUND ( 'NONE', #59806, .T. ) ;
#42586 = CARTESIAN_POINT ( 'NONE',  ( -17.14219307747939069, -11.06231777344663136, 33.60647404775220082 ) ) ;
#42585 = CARTESIAN_POINT ( 'NONE',  ( 17.32686859527121825, -3.712312575010499494, 33.01462480002815170 ) ) ;
#42587 = EDGE_CURVE ( 'NONE', #16922, #74826, #5844, .T. ) ;
#42588 = CARTESIAN_POINT ( 'NONE',  ( 11.76147438255493327, -11.98016756924215009, 32.48728574198911190 ) ) ;
#42590 = CARTESIAN_POINT ( 'NONE',  ( -18.00000000000000000, -2.833524468853757305, 32.15551576947926549 ) ) ;
#42589 = CARTESIAN_POINT ( 'NONE',  ( -3.480745974817821775, -2.920706130388546651, 32.31842814019191223 ) ) ;
#42591 = CYLINDRICAL_SURFACE ( 'NONE', #21780, 0.2499999999999994726 ) ;
#42592 = CARTESIAN_POINT ( 'NONE',  ( 0.06109907496454976272, -10.25000000000000000, 22.02938170625849068 ) ) ;
#42593 = ORIENTED_EDGE ( 'NONE', *, *, #24274, .T. ) ;
#42594 = B_SPLINE_CURVE_WITH_KNOTS ( 'NONE', 3,
 ( #31609, #59072, #65820, #59519, #44654, #44207, #71694, #72140, #86571, #50961 ),
 .UNSPECIFIED., .F., .F.,
 ( 4, 2, 2, 2, 4 ),
 ( 0.000000000000000000, 0.0001954339857564126514, 0.0003908679715128183098, 0.0005863019572692239681, 0.0007817359430256294638 ),
 .UNSPECIFIED. ) ;
#42595 = CARTESIAN_POINT ( 'NONE',  ( -5.777220331021934108, -10.97394488606064122, 33.68653795673694873 ) ) ;
#42596 = ORIENTED_EDGE ( 'NONE', *, *, #83767, .T. ) ;
#42597 = EDGE_CURVE ( 'NONE', #34806, #69130, #55779, .T. ) ;
#42598 = CARTESIAN_POINT ( 'NONE',  ( 14.30769230769231015, -12.78798330534103123, 29.99999999999997868 ) ) ;
#42599 = ORIENTED_EDGE ( 'NONE', *, *, #11324, .T. ) ;
#42600 = CARTESIAN_POINT ( 'NONE',  ( -11.47320639894870276, -6.835583212224610072, 34.95778746994559327 ) ) ;
#42602 = EDGE_CURVE ( 'NONE', #37879, #65133, #39068, .T. ) ;
#42601 = CARTESIAN_POINT ( 'NONE',  ( -18.24997673094235395, -2.564618984488975961, 30.55390908950641915 ) ) ;
#42603 = ORIENTED_EDGE ( 'NONE', *, *, #74545, .F. ) ;
#42604 = CARTESIAN_POINT ( 'NONE',  ( -18.06608341095587633, -12.37446782046654192, 30.86335684631486487 ) ) ;
#42605 = CARTESIAN_POINT ( 'NONE',  ( -1.077988221561460236, -10.27530806549876452, 24.60750670625849779 ) ) ;
#42606 = CARTESIAN_POINT ( 'NONE',  ( 6.222779668978068557, -6.717445702608402236, 34.94155399931962336 ) ) ;
#42607 = CARTESIAN_POINT ( 'NONE',  ( -10.39237177129122003, -12.64618726649961289, 30.78989965857442712 ) ) ;
#42608 = DIRECTION ( 'NONE',  ( -1.000000000000000000, -0.000000000000000000, -0.000000000000000000 ) ) ;
#42609 = CARTESIAN_POINT ( 'NONE',  ( -5.326899807865431491, -12.41269422305637171, 30.68257228309993323 ) ) ;
#42610 = CARTESIAN_POINT ( 'NONE',  ( 0.4615384615383382183, -12.16647553114689728, 32.15551576947799362 ) ) ;
#42611 = CARTESIAN_POINT ( 'NONE',  ( -14.08467946359891165, -4.762714258010881885, 34.23016756924214832 ) ) ;
#42612 = CARTESIAN_POINT ( 'NONE',  ( 3.749999999999992006, -5.946699141100872943, 18.14062500000000711 ) ) ;
#42613 = CARTESIAN_POINT ( 'NONE',  ( -18.24997674404858827, -11.47974371597207899, 33.17467449705390692 ) ) ;
#42615 = EDGE_CURVE ( 'NONE', #39647, #56424, #74619, .T. ) ;
#42614 = CARTESIAN_POINT ( 'NONE',  ( 2.307692307692309264, -2.708943851104267164, 35.45975837776705220 ) ) ;
#42616 = CARTESIAN_POINT ( 'NONE',  ( 8.769230769230647482, -10.21337939537710326, 33.94971097300076224 ) ) ;
#42617 = CARTESIAN_POINT ( 'NONE',  ( -3.724691934501248802, -5.885600066136383646, 22.92374329374151998 ) ) ;
#42618 = CARTESIAN_POINT ( 'NONE',  ( -15.23076923076922995, -13.49023893513002648, 31.06009739812518688 ) ) ;
#42619 = EDGE_LOOP ( 'NONE', ( #51564, #6814, #16961, #75392 ) ) ;
#42620 = EDGE_CURVE ( 'NONE', #57617, #79299, #70783, .T. ) ;
#42621 = AXIS2_PLACEMENT_3D ( 'NONE', #17917, #37283, #45371 ) ;
#42622 = CARTESIAN_POINT ( 'NONE',  ( -17.93474442872397745, -2.892918686051626498, 31.69288490824025928 ) ) ;
#42623 = CARTESIAN_POINT ( 'NONE',  ( 15.93091993633000136, -12.15238873228291716, 31.58232369045353849 ) ) ;
#42624 = DIRECTION ( 'NONE',  ( -0.000000000000000000, -0.6427876096865404731, -0.7660444431189770143 ) ) ;
#42625 = CARTESIAN_POINT ( 'NONE',  ( -8.096153846153844924, -7.500000000000001776, 34.75000000000000000 ) ) ;
#42626 = EDGE_CURVE ( 'NONE', #34010, #8684, #12470, .T. ) ;
#42627 = CARTESIAN_POINT ( 'NONE',  ( 13.45068373561782593, -2.538708090699994813, 30.37095296980875503 ) ) ;
#42628 = VECTOR ( 'NONE', #66440, 1000.000000000000000 ) ;
#42629 = DIRECTION ( 'NONE',  ( 0.000000000000000000, 0.8660254037844377084, -0.5000000000000015543 ) ) ;
#42630 = CARTESIAN_POINT ( 'NONE',  ( -2.298097038856290464, -5.201902961143733961, 14.00000000000000000 ) ) ;
#42631 = B_SPLINE_CURVE_WITH_KNOTS ( 'NONE', 3,
 ( #3422, #59259, #37654, #65115, #10636, #24587, #3862, #4774, #23690, #31349 ),
 .UNSPECIFIED., .F., .F.,
 ( 4, 2, 2, 2, 4 ),
 ( 0.000000000000000000, 0.0001954339857564079894, 0.0003908679715128159787, 0.0005863019572692239681, 0.0007817359430256319575 ),
 .UNSPECIFIED. ) ;
#42632 = ORIENTED_EDGE ( 'NONE', *, *, #76266, .T. ) ;
#42633 = B_SPLINE_CURVE_WITH_KNOTS ( 'NONE', 3,
 ( #15813, #7276, #36525, #70303, #521, #22117, #15366, #34742, #76618, #27985 ),
 .UNSPECIFIED., .F., .F.,
 ( 4, 2, 2, 2, 4 ),
 ( 0.000000000000000000, 0.0001954311564186866034, 0.0003908623128373732067, 0.0005862934692560597830, 0.0007817246256747464135 ),
 .UNSPECIFIED. ) ;
#42634 = ORIENTED_EDGE ( 'NONE', *, *, #51685, .F. ) ;
#42635 = ORIENTED_EDGE ( 'NONE', *, *, #3661, .T. ) ;
#42636 = CARTESIAN_POINT ( 'NONE',  ( -9.442253380669379581, -3.136992222400443175, 32.19305428654138979 ) ) ;
#42637 = DIRECTION ( 'NONE',  ( -0.000000000000000000, 0.9396926207859093161, -0.3420201433256663259 ) ) ;
#42638 = EDGE_CURVE ( 'NONE', #19405, #49519, #901, .T. ) ;
#42639 = CARTESIAN_POINT ( 'NONE',  ( 6.673100179028331524, -2.920706130388546651, 32.31842814019191223 ) ) ;
#42640 = FACE_OUTER_BOUND ( 'NONE', #67369, .T. ) ;
#42641 = LINE ( 'NONE', #21919, #33724 ) ;
#42642 = EDGE_LOOP ( 'NONE', ( #51017, #82424 ) ) ;
#42643 = DIRECTION ( 'NONE',  ( 1.000000000000000000, 2.602085213965214586E-16, -0.000000000000000000 ) ) ;
#42644 = VERTEX_POINT ( 'NONE', #68297 ) ;
#42645 = ADVANCED_FACE ( 'NONE', ( #69625 ), #34948, .F. ) ;
#42646 = ORIENTED_EDGE ( 'NONE', *, *, #5978, .F. ) ;
#42647 = ORIENTED_EDGE ( 'NONE', *, *, #81328, .T. ) ;
#42649 = VERTEX_POINT ( 'NONE', #6601 ) ;
#42648 = PLANE ( 'NONE',  #21386 ) ;
#42650 = CARTESIAN_POINT ( 'NONE',  ( 16.21910172512217585, -12.46129190930001052, 30.37095296980869819 ) ) ;
#42651 = EDGE_CURVE ( 'NONE', #42644, #52424, #53542, .T. ) ;
#42652 = DIRECTION ( 'NONE',  ( 0.000000000000000000, -6.938893903907222067E-15, 1.000000000000000000 ) ) ;
#42653 = EDGE_CURVE ( 'NONE', #47496, #36412, #46052, .T. ) ;
#42654 = CARTESIAN_POINT ( 'NONE',  ( 3.903869422903799347, -4.236021600441998380, 33.53823185664189310 ) ) ;
#42655 = CARTESIAN_POINT ( 'NONE',  ( -5.326923076923075762, -7.500000000000001776, 34.75000000000000000 ) ) ;
#42656 = AXIS2_PLACEMENT_3D ( 'NONE', #61318, #88834, #54570 ) ;
#42657 = VERTEX_POINT ( 'NONE', #29104 ) ;
#42658 = ORIENTED_EDGE ( 'NONE', *, *, #26181, .F. ) ;
#42659 = ADVANCED_FACE ( 'NONE', ( #62410 ), #61529, .T. ) ;
#42660 = ORIENTED_EDGE ( 'NONE', *, *, #5670, .F. ) ;
#42661 = DIRECTION ( 'NONE',  ( -0.000000000000000000, 0.1736481776669307198, -0.9848077530122080203 ) ) ;
#42663 = ORIENTED_EDGE ( 'NONE', *, *, #31567, .T. ) ;
#42662 = DIRECTION ( 'NONE',  ( 0.000000000000000000, 0.7660444431189807890, 0.6427876096865361433 ) ) ;
#42664 = CARTESIAN_POINT ( 'NONE',  ( 1.384615384615265343, -9.442884908241554243, 34.35708131394783038 ) ) ;
#42665 = DIRECTION ( 'NONE',  ( 0.000000000000000000, 0.9396926207859126468, 0.3420201433256571111 ) ) ;
#42666 = CARTESIAN_POINT ( 'NONE',  ( -3.007989689500821573, -10.11255958852955850, 34.01340905677048454 ) ) ;
#42667 = VERTEX_POINT ( 'NONE', #7930 ) ;
#42668 = DIRECTION ( 'NONE',  ( -0.000000000000000000, -0.6427876096865404731, -0.7660444431189770143 ) ) ;
#42669 = CARTESIAN_POINT ( 'NONE',  ( -16.15384615384627409, -12.70778746994576025, 30.41441678777401236 ) ) ;
#42670 = ORIENTED_EDGE ( 'NONE', *, *, #41041, .T. ) ;
#42671 = FACE_BOUND ( 'NONE', #75286, .T. ) ;
#42672 = CARTESIAN_POINT ( 'NONE',  ( 11.53846153846153832, -4.786620604624113540, 33.94971097300155094 ) ) ;
#42673 = CARTESIAN_POINT ( 'NONE',  ( -18.22292695890684655, -12.38737895849757820, 31.66785238281580206 ) ) ;
#42674 = CARTESIAN_POINT ( 'NONE',  ( -11.53846153846153655, -4.098570777380720287, 33.41473453929634729 ) ) ;
#42676 = DIRECTION ( 'NONE',  ( -1.000000000000000000, -0.000000000000000000, -0.000000000000000000 ) ) ;
#42675 = CARTESIAN_POINT ( 'NONE',  ( 19.99999999999997158, -14.99999999999999467, 13.00000000000000178 ) ) ;
#42677 = VECTOR ( 'NONE', #47549, 1000.000000000000227 ) ;
#42678 = CYLINDRICAL_SURFACE ( 'NONE', #63979, 0.2500000000000008882 ) ;
#42679 = DIRECTION ( 'NONE',  ( -1.000000000000000000, -0.000000000000000000, -0.000000000000000000 ) ) ;
#42680 = VERTEX_POINT ( 'NONE', #28189 ) ;
#42681 = CARTESIAN_POINT ( 'NONE',  ( -8.069080805060693251, -6.459968553980841577, 34.89616026154728701 ) ) ;
#42682 = DIRECTION ( 'NONE',  ( 0.000000000000000000, 0.9848077530122072432, -0.1736481776669354937 ) ) ;
#42683 = EDGE_CURVE ( 'NONE', #8176, #70654, #69185, .T. ) ;
#42684 = EDGE_LOOP ( 'NONE', ( #21306, #9932 ) ) ;
#42685 = VECTOR ( 'NONE', #2833, 1000.000000000000114 ) ;
#42686 = ADVANCED_FACE ( 'NONE', ( #20985 ), #41278, .F. ) ;
#42687 = CARTESIAN_POINT ( 'NONE',  ( 8.545745825506822158, -3.236172620538810385, 32.36188796281390267 ) ) ;
#42688 = CARTESIAN_POINT ( 'NONE',  ( -4.023054346021367245, -2.541949514083464479, 30.39797389878540557 ) ) ;
#42689 = CARTESIAN_POINT ( 'NONE',  ( -5.143006487878958310, -11.69971097300155272, 32.46337939537587403 ) ) ;
#42690 = CARTESIAN_POINT ( 'NONE',  ( 6.923076923076924238, -13.57706302396349152, 30.56769352161908060 ) ) ;
#42691 = DIRECTION ( 'NONE',  ( -0.000000000000000000, 1.000000000000000000, -0.000000000000000000 ) ) ;
#42692 = FACE_BOUND ( 'NONE', #70697, .T. ) ;
#42694 = CARTESIAN_POINT ( 'NONE',  ( 4.153846153846030731, -12.51329471203414379, 31.30864560766407578 ) ) ;
#42693 = DIRECTION ( 'NONE',  ( -1.000000000000000000, -0.000000000000000000, -0.000000000000000000 ) ) ;
#42695 = AXIS2_PLACEMENT_3D ( 'NONE', #32840, #12573, #61630 ) ;
#42696 = CARTESIAN_POINT ( 'NONE',  ( 1.607395053593452694, -12.69155399931963046, 30.53255429739158444 ) ) ;
#42698 = CARTESIAN_POINT ( 'NONE',  ( -15.16470087976679437, -6.386643153685127139, 34.62446782046654192 ) ) ;
#42697 = CARTESIAN_POINT ( 'NONE',  ( -6.923076923076922462, -10.67929555188718282, 33.92786785259544047 ) ) ;
#42699 = DIRECTION ( 'NONE',  ( 1.000000000000000000, 0.000000000000000000, 0.000000000000000000 ) ) ;
#42700 = CARTESIAN_POINT ( 'NONE',  ( 3.749999999999999556, -7.438900925035446754, 21.71688170625848713 ) ) ;
#42701 = EDGE_LOOP ( 'NONE', ( #38557, #16590, #34609, #83989 ) ) ;
#42702 = ORIENTED_EDGE ( 'NONE', *, *, #67426, .F. ) ;
#42703 = CARTESIAN_POINT ( 'NONE',  ( 15.90382292962469535, -9.356822207818511927, 34.66110646841856635 ) ) ;
#42704 = CARTESIAN_POINT ( 'NONE',  ( -0.5276218724943421146, -2.721908614388772296, 31.22303859784725688 ) ) ;
#42705 = CARTESIAN_POINT ( 'NONE',  ( -9.561781990544128362, -9.417988943895561960, 34.36773134775777550 ) ) ;
#42707 = B_SPLINE_CURVE_WITH_KNOTS ( 'NONE', 3,
 ( #84402, #50143, #77629, #78070, #23128, #15938, #16373, #60794, #40543, #47726 ),
 .UNSPECIFIED., .F., .F.,
 ( 4, 2, 2, 2, 4 ),
 ( 0.000000000000000000, 0.0001954311564186860071, 0.0003908623128373720141, 0.0005862934692560580483, 0.0007817246256747440282 ),
 .UNSPECIFIED. ) ;
#42706 = CARTESIAN_POINT ( 'NONE',  ( -16.94639737515951694, -11.46989282347013095, 32.79007818306219946 ) ) ;
#42708 = CARTESIAN_POINT ( 'NONE',  ( -16.82697755857493505, -6.696923467548659303, 34.68552623307873972 ) ) ;
#42709 = CARTESIAN_POINT ( 'NONE',  ( -3.749999999999996447, -7.561099074964554134, 16.09188170625848713 ) ) ;
#42710 = B_SPLINE_CURVE_WITH_KNOTS ( 'NONE', 3,
 ( #4973, #60793, #76412, #69650, #60348, #87403, #14717, #46395, #88302, #61225 ),
 .UNSPECIFIED., .F., .F.,
 ( 4, 2, 2, 2, 4 ),
 ( 0.0007817359430256218744, 0.0009771253907249859150, 0.001172514838424350064, 0.001367904286123714213, 0.001563293733823078145 ),
 .UNSPECIFIED. ) ;
#42711 = CARTESIAN_POINT ( 'NONE',  ( -11.78846153846153832, -7.500000000000001776, 35.00000000000000000 ) ) ;
#42712 = DIRECTION ( 'NONE',  ( -0.000000000000000000, -0.000000000000000000, -1.000000000000000000 ) ) ;
#42713 = LINE ( 'NONE', #83256, #2924 ) ;
#42714 = CARTESIAN_POINT ( 'NONE',  ( -3.099978789802282364, -11.93129842949671726, 32.56571108434900452 ) ) ;
#42715 = CARTESIAN_POINT ( 'NONE',  ( -3.453696189676080053, -4.026226216239095379, 33.68668979543632958 ) ) ;
#42716 = DIRECTION ( 'NONE',  ( -0.000000000000000000, 1.000000000000000000, -0.000000000000000000 ) ) ;
#42717 = CIRCLE ( 'NONE', #45595, 4.000000000000000000 ) ;
#42719 = EDGE_CURVE ( 'NONE', #13624, #20560, #85772, .T. ) ;
#42718 = DIRECTION ( 'NONE',  ( -0.000000000000000000, -0.8660254037844399289, -0.4999999999999980016 ) ) ;
#42720 = EDGE_CURVE ( 'NONE', #64611, #10442, #67594, .T. ) ;
#42721 = CYLINDRICAL_SURFACE ( 'NONE', #44165, 0.2500000000000009437 ) ;
#42722 = VERTEX_POINT ( 'NONE', #48911 ) ;
#42723 = CARTESIAN_POINT ( 'NONE',  ( -14.53061852520844965, -3.586966769969701208, 32.86292498521069660 ) ) ;
#42724 = DIRECTION ( 'NONE',  ( -0.000000000000000000, -0.5000000000000009992, -0.8660254037844380415 ) ) ;
#42725 = CARTESIAN_POINT ( 'NONE',  ( -2.724691934501246582, -6.299813628509474128, 19.17374329374151642 ) ) ;
#42726 = EDGE_CURVE ( 'NONE', #48943, #55647, #35851, .T. ) ;
#42727 = LINE ( 'NONE', #30524, #28901 ) ;
#42728 = DIRECTION ( 'NONE',  ( -0.000000000000000000, -0.6427876096865404731, -0.7660444431189771253 ) ) ;
#42729 = ORIENTED_EDGE ( 'NONE', *, *, #75681, .F. ) ;
#42730 = DIRECTION ( 'NONE',  ( -0.000000000000000000, 0.5000000000000011102, -0.8660254037844380415 ) ) ;
#42732 = ORIENTED_EDGE ( 'NONE', *, *, #28372, .T. ) ;
#42731 = DIRECTION ( 'NONE',  ( -0.000000000000000000, -0.6427876096865404731, -0.7660444431189771253 ) ) ;
#42733 = CARTESIAN_POINT ( 'NONE',  ( 9.757562831820528970, -12.70778746994558439, 30.41441678777536595 ) ) ;
#42734 = DIRECTION ( 'NONE',  ( 1.000000000000000000, -0.000000000000000000, -0.000000000000000000 ) ) ;
#42735 = EDGE_CURVE ( 'NONE', #85269, #72492, #71390, .T. ) ;
#42736 = VECTOR ( 'NONE', #54200, 1000.000000000000000 ) ;
#42737 = ORIENTED_EDGE ( 'NONE', *, *, #15179, .T. ) ;
#42738 = CARTESIAN_POINT ( 'NONE',  ( -13.16183584334697265, -2.600157965045224451, 30.74683119005207743 ) ) ;
#42739 = CARTESIAN_POINT ( 'NONE',  ( -19.50000000000000000, -3.499999999999999556, 29.75000000000000355 ) ) ;
#42740 = EDGE_CURVE ( 'NONE', #31080, #66517, #77711, .T. ) ;
#42741 = EDGE_LOOP ( 'NONE', ( #915, #30818 ) ) ;
#42742 = CYLINDRICAL_SURFACE ( 'NONE', #75114, 0.2499999999999973355 ) ;
#42743 = LINE ( 'NONE', #56687, #55178 ) ;
#42744 = CYLINDRICAL_SURFACE ( 'NONE', #39843, 0.2499999999999995559 ) ;
#42745 = ORIENTED_EDGE ( 'NONE', *, *, #72681, .F. ) ;
#42746 = EDGE_LOOP ( 'NONE', ( #8326, #10491, #69452, #40955 ) ) ;
#42747 = ADVANCED_FACE ( 'NONE', ( #50672 ), #9696, .F. ) ;
#42748 = CARTESIAN_POINT ( 'NONE',  ( 6.130525701763564150, -6.852161475712352789, 34.70806712695775786 ) ) ;
#42749 = ORIENTED_EDGE ( 'NONE', *, *, #78970, .T. ) ;
#42750 = VECTOR ( 'NONE', #75134, 999.9999999999998863 ) ;
#42751 = CARTESIAN_POINT ( 'NONE',  ( 15.45354889974729318, -12.69155399931963046, 30.53255429739157734 ) ) ;
#42752 = CYLINDRICAL_SURFACE ( 'NONE', #6935, 0.2499999999999995559 ) ;
#42753 = EDGE_CURVE ( 'NONE', #36102, #6730, #78157, .T. ) ;
#42754 = B_SPLINE_CURVE_WITH_KNOTS ( 'NONE', 3,
 ( #63751, #56992, #84485, #42170, #50223, #9268, #36727, #65073, #3827, #37164 ),
 .UNSPECIFIED., .F., .F.,
 ( 4, 2, 2, 2, 4 ),
 ( 0.000000000000000000, 0.0001954311564186882568, 0.0003908623128373765136, 0.0005862934692560647703, 0.0007817246256747530271 ),
 .UNSPECIFIED. ) ;
#42755 = LINE ( 'NONE', #64767, #13597 ) ;
#42756 = CARTESIAN_POINT ( 'NONE',  ( -2.307692307692305711, -5.471508081941601098, 34.59228464037088457 ) ) ;
#42757 = EDGE_CURVE ( 'NONE', #75394, #27467, #58965, .T. ) ;
#42758 = ORIENTED_EDGE ( 'NONE', *, *, #79634, .F. ) ;
#42759 = AXIS2_PLACEMENT_3D ( 'NONE', #11927, #39406, #81273 ) ;
#42760 = ORIENTED_EDGE ( 'NONE', *, *, #55353, .T. ) ;
#42762 = ORIENTED_EDGE ( 'NONE', *, *, #35172, .T. ) ;
#42761 = DIRECTION ( 'NONE',  ( 1.000000000000000000, 0.000000000000000000, 0.000000000000000000 ) ) ;
#42763 = EDGE_CURVE ( 'NONE', #19730, #42722, #66303, .T. ) ;
#42764 = CARTESIAN_POINT ( 'NONE',  ( 16.15384615384645883, -2.506253911140615021, 30.00000000000323297 ) ) ;
#42765 = ORIENTED_EDGE ( 'NONE', *, *, #50429, .F. ) ;
#42766 = CARTESIAN_POINT ( 'NONE',  ( -17.74994568836168440, -3.136992222400446728, 32.19305428654138268 ) ) ;
#42767 = CARTESIAN_POINT ( 'NONE',  ( -8.638705330997126453, -12.70449254468099198, 30.44128974285582956 ) ) ;
#42768 = ORIENTED_EDGE ( 'NONE', *, *, #49289, .F. ) ;
#42769 = CARTESIAN_POINT ( 'NONE',  ( -16.15384615384627409, -9.442884908241554243, 34.35708131394783038 ) ) ;
#42770 = EDGE_CURVE ( 'NONE', #19826, #61245, #82427, .T. ) ;
#42771 = ORIENTED_EDGE ( 'NONE', *, *, #20911, .T. ) ;
#42773 = ORIENTED_EDGE ( 'NONE', *, *, #70405, .F. ) ;
#42772 = CARTESIAN_POINT ( 'NONE',  ( 14.30769230769231015, -13.75783147151868846, 33.36296068462461051 ) ) ;
#42774 = CYLINDRICAL_SURFACE ( 'NONE', #61758, 5.000000000000000888 ) ;
#42775 = CARTESIAN_POINT ( 'NONE',  ( -12.46153846153846168, -8.973038597847269315, 34.52809138561121927 ) ) ;
#42776 = EDGE_LOOP ( 'NONE', ( #38522, #70477, #32558, #23004 ) ) ;
#42777 = ADVANCED_FACE ( 'NONE', ( #79045 ), #57434, .F. ) ;
#42778 = CARTESIAN_POINT ( 'NONE',  ( 15.45354877203763522, -3.236590943229499029, 32.36255958852954251 ) ) ;
#42779 = LINE ( 'NONE', #3095, #82789 ) ;
#42780 = AXIS2_PLACEMENT_3D ( 'NONE', #38431, #18160, #45623 ) ;
#42781 = FACE_BOUND ( 'NONE', #43473, .T. ) ;
#42782 = CARTESIAN_POINT ( 'NONE',  ( 7.846153846153723244, -12.51329471203414379, 31.30864560766407578 ) ) ;
#42783 = CARTESIAN_POINT ( 'NONE',  ( -6.792551484843277976, -9.503571793651733657, 34.60286762892837942 ) ) ;
#42784 = CARTESIAN_POINT ( 'NONE',  ( -16.08777882049607655, -4.661471528628508665, 34.16647553114624003 ) ) ;
#42785 = CARTESIAN_POINT ( 'NONE',  ( -16.94613263595612906, -12.35292014791297710, 31.75344720912887198 ) ) ;
#42786 = CARTESIAN_POINT ( 'NONE',  ( -3.230769230769229949, -10.05456864172156806, 36.03766855953608683 ) ) ;
#42787 = CARTESIAN_POINT ( 'NONE',  ( -16.40382289789474157, -2.544273027872574922, 31.48422191005632342 ) ) ;
#42788 = VERTEX_POINT ( 'NONE', #10149 ) ;
#42789 = VECTOR ( 'NONE', #47816, 1000.000000000000000 ) ;
#42790 = CARTESIAN_POINT ( 'NONE',  ( -5.076923076923075762, -1.215029322943914858, 32.30358669280327177 ) ) ;
#42791 = ORIENTED_EDGE ( 'NONE', *, *, #76632, .T. ) ;
#42792 = EDGE_CURVE ( 'NONE', #38465, #53590, #38887, .T. ) ;
#42793 = VERTEX_POINT ( 'NONE', #15578 ) ;
#42795 = CARTESIAN_POINT ( 'NONE',  ( -3.296851610129365007, -5.471508081941601986, 34.59228464037088457 ) ) ;
#42794 = CARTESIAN_POINT ( 'NONE',  ( 14.30769230769231015, -3.513871655860378418, 32.76840700105978499 ) ) ;
#42796 = EDGE_CURVE ( 'NONE', #2346, #60982, #71840, .T. ) ;
#42797 = DIRECTION ( 'NONE',  ( -0.000000000000000000, 1.000000000000000000, 3.491481338843133355E-15 ) ) ;
#42798 = B_SPLINE_CURVE_WITH_KNOTS ( 'NONE', 3,
 ( #15878, #22616, #70819, #21285, #64038, #69479, #55959, #1470, #42460, #2335 ),
 .UNSPECIFIED., .F., .F.,
 ( 4, 2, 2, 2, 4 ),
 ( 0.000000000000000000, 0.0001954311564186862239, 0.0003908623128373724478, 0.0005862934692560586988, 0.0007817246256747448956 ),
 .UNSPECIFIED. ) ;
#42799 = DIRECTION ( 'NONE',  ( 0.000000000000000000, 0.3420201433256610524, 0.9396926207859113145 ) ) ;
#42800 = CARTESIAN_POINT ( 'NONE',  ( -12.39547112818838670, -2.486705287966280320, 31.30864560766543647 ) ) ;
#42801 = CARTESIAN_POINT ( 'NONE',  ( 13.60739492588379385, -11.41317474335729543, 32.86274602512330034 ) ) ;
#42802 = ADVANCED_FACE ( 'NONE', ( #77269 ), #65526, .F. ) ;
#42803 = ORIENTED_EDGE ( 'NONE', *, *, #88896, .F. ) ;
#42804 = CARTESIAN_POINT ( 'NONE',  ( 13.38461538461526601, -5.219633306517616589, 34.19971097300220464 ) ) ;
#42805 = FACE_OUTER_BOUND ( 'NONE', #59374, .T. ) ;
#42806 = DIRECTION ( 'NONE',  ( -1.000000000000000000, -0.000000000000000000, 0.000000000000000000 ) ) ;
#42807 = CARTESIAN_POINT ( 'NONE',  ( 15.36129466900287888, -12.50538340440932394, 31.33453814440721885 ) ) ;
#42808 = DIRECTION ( 'NONE',  ( 0.000000000000000000, 0.000000000000000000, -1.000000000000000000 ) ) ;
#42809 = CARTESIAN_POINT ( 'NONE',  ( -5.076923076923075762, -12.09954503811598769, 35.62045528018868623 ) ) ;
#42810 = VERTEX_POINT ( 'NONE', #51544 ) ;
#42811 = ORIENTED_EDGE ( 'NONE', *, *, #32277, .F. ) ;
#42812 = CARTESIAN_POINT ( 'NONE',  ( -9.469296340694842939, -12.39991518177334129, 30.74647679643404530 ) ) ;
#42813 = ORIENTED_EDGE ( 'NONE', *, *, #13208, .F. ) ;
#42814 = CARTESIAN_POINT ( 'NONE',  ( -5.076923076923075762, -13.87047571288749737, 32.06866353760679544 ) ) ;
#42815 = LINE ( 'NONE', #63509, #54335 ) ;
#42816 = CARTESIAN_POINT ( 'NONE',  ( -14.17716660592874689, -6.852161475712352789, 34.70806712695775786 ) ) ;
#42817 = CARTESIAN_POINT ( 'NONE',  ( 1.384615384615264011, -4.320704448113951379, 33.92786785259630022 ) ) ;
#42818 = FACE_OUTER_BOUND ( 'NONE', #69495, .T. ) ;
#42819 = PLANE ( 'NONE',  #37350 ) ;
#42820 = VERTEX_POINT ( 'NONE', #2487 ) ;
#42821 = CARTESIAN_POINT ( 'NONE',  ( 4.403846153847589484, -7.500000000000155431, 34.75000000000007105 ) ) ;
#42823 = EDGE_LOOP ( 'NONE', ( #10826, #49966, #15848, #74814 ) ) ;
#42822 = CARTESIAN_POINT ( 'NONE',  ( -10.61538461538461320, -2.517432740324522911, 35.29906147534542527 ) ) ;
#42825 = B_SPLINE_CURVE_WITH_KNOTS ( 'NONE', 3,
 ( #53663, #10903, #81149, #45567, #12235, #46897, #53211, #65828, #5487, #38827 ),
 .UNSPECIFIED., .F., .F.,
 ( 4, 2, 2, 2, 4 ),
 ( 0.000000000000000000, 0.0001954339857564064444, 0.0003908679715128128888, 0.0005863019572692193060, 0.0007817359430256257775 ),
 .UNSPECIFIED. ) ;
#42824 = FACE_OUTER_BOUND ( 'NONE', #61615, .T. ) ;
#42826 = CARTESIAN_POINT ( 'NONE',  ( -17.32694630114453105, -12.07920672191015221, 32.31858351112116168 ) ) ;
#42827 = CARTESIAN_POINT ( 'NONE',  ( -17.86920819217521483, -11.71459661697926258, 32.44059661609676937 ) ) ;
#42828 = DIRECTION ( 'NONE',  ( -0.000000000000000000, 0.8660254037844399289, -0.4999999999999980016 ) ) ;
#42829 = CARTESIAN_POINT ( 'NONE',  ( -12.52680890749923570, -12.46129190929999986, 30.37095296980880832 ) ) ;
#42830 = CARTESIAN_POINT ( 'NONE',  ( -0.06109907496450878162, -11.25000000000000000, 13.78311829374151287 ) ) ;
#42831 = ORIENTED_EDGE ( 'NONE', *, *, #27274, .F. ) ;
#42832 = CARTESIAN_POINT ( 'NONE',  ( -15.23076923076935074, -10.21337939537710326, 33.94971097300076224 ) ) ;
#42833 = CARTESIAN_POINT ( 'NONE',  ( -5.076923076923075762, -2.708943851104267164, 35.45975837776705220 ) ) ;
#42834 = DIRECTION ( 'NONE',  ( -0.000000000000000000, -0.3420201433256694346, -0.9396926207859080948 ) ) ;
#42835 = CARTESIAN_POINT ( 'NONE',  ( 14.87820512820512953, -7.500000000000000000, 29.75000000000000355 ) ) ;
#42836 = ORIENTED_EDGE ( 'NONE', *, *, #54231, .T. ) ;
#42837 = CARTESIAN_POINT ( 'NONE',  ( 1.944543648263018731, -9.444543648262994751, 15.87500000000000000 ) ) ;
#42838 = CARTESIAN_POINT ( 'NONE',  ( -16.02305434602136813, -12.11778462344220841, 31.66786338562085135 ) ) ;
#42839 = ORIENTED_EDGE ( 'NONE', *, *, #60581, .T. ) ;
#42840 = CARTESIAN_POINT ( 'NONE',  ( 2.530705151785703322, -10.77377354290276301, 33.85451476688484718 ) ) ;
#42841 = DIRECTION ( 'NONE',  ( 0.000000000000000000, 0.1736481776669267785, -0.9848077530122087975 ) ) ;
#42842 = EDGE_CURVE ( 'NONE', #72489, #42562, #11599, .T. ) ;
#42843 = EDGE_LOOP ( 'NONE', ( #2611, #37765, #54407, #62146 ) ) ;
#42844 = AXIS2_PLACEMENT_3D ( 'NONE', #27961, #41927, #21197 ) ;
#42845 = DIRECTION ( 'NONE',  ( -1.000000000000000000, -0.000000000000000000, -0.000000000000000000 ) ) ;
#42846 = CARTESIAN_POINT ( 'NONE',  ( -3.230769230769351186, -8.613356846316285953, 34.62446782046622218 ) ) ;
#42847 = CARTESIAN_POINT ( 'NONE',  ( -15.23076923076922995, -1.466349020453238561, 30.81389545987213907 ) ) ;
#42848 = LINE ( 'NONE', #77952, #4829 ) ;
#42849 = ORIENTED_EDGE ( 'NONE', *, *, #82926, .T. ) ;
#42850 = EDGE_CURVE ( 'NONE', #12394, #70222, #78095, .T. ) ;
#42851 = CARTESIAN_POINT ( 'NONE',  ( -3.165514091256391271, -2.379036618887895305, 30.90682066428159303 ) ) ;
#42852 = AXIS2_PLACEMENT_3D ( 'NONE', #59043, #65794, #4094 ) ;
#42853 = ORIENTED_EDGE ( 'NONE', *, *, #32507, .T. ) ;
#42854 = CARTESIAN_POINT ( 'NONE',  ( -17.75005459062195712, -12.07971442181322352, 32.31769673815850297 ) ) ;
#42855 = CARTESIAN_POINT ( 'NONE',  ( 6.249999999999937828, -7.565270445406050648, 34.75000000000000000 ) ) ;
#42856 = VERTEX_POINT ( 'NONE', #5612 ) ;
#42857 = AXIS2_PLACEMENT_3D ( 'NONE', #50461, #78380, #16684 ) ;
#42858 = CYLINDRICAL_SURFACE ( 'NONE', #37533, 0.2499999999999994726 ) ;
#42859 = CARTESIAN_POINT ( 'NONE',  ( -14.30769230769230660, -2.292212530054420494, 30.41441678777542634 ) ) ;
#42860 = CARTESIAN_POINT ( 'NONE',  ( -3.903846153846149303, -2.499999999999999112, 29.81604066197450109 ) ) ;
#42861 = EDGE_CURVE ( 'NONE', #73366, #31226, #59663, .T. ) ;
#42862 = FACE_OUTER_BOUND ( 'NONE', #37580, .T. ) ;
#42863 = CARTESIAN_POINT ( 'NONE',  ( 8.352564102564102200, -11.50000000000000000, 29.75000000000000355 ) ) ;
#42864 = ORIENTED_EDGE ( 'NONE', *, *, #7080, .F. ) ;
#42865 = ORIENTED_EDGE ( 'NONE', *, *, #47833, .T. ) ;
#42866 = FACE_BOUND ( 'NONE', #36405, .T. ) ;
#42867 = EDGE_LOOP ( 'NONE', ( #72882, #72542 ) ) ;
#42868 = CARTESIAN_POINT ( 'NONE',  ( 15.48071474911737333, -2.587454068350148351, 30.68340429815432202 ) ) ;
#42869 = EDGE_CURVE ( 'NONE', #30240, #84116, #66425, .T. ) ;
#42870 = LINE ( 'NONE', #8196, #44440 ) ;
#42871 = EDGE_CURVE ( 'NONE', #50717, #72564, #60550, .T. ) ;
#42872 = CARTESIAN_POINT ( 'NONE',  ( 17.74997677577853850, -5.765609946408405406, 34.70566812827424741 ) ) ;
#42873 = CARTESIAN_POINT ( 'NONE',  ( 0.5267936010512993539, -12.70778746994558439, 30.41441678777537305 ) ) ;
#42874 = B_SPLINE_CURVE_WITH_KNOTS ( 'NONE', 3,
 ( #51219, #72405, #44477, #3501, #30971, #38182, #58436, #65640, #39540, #80968 ),
 .UNSPECIFIED., .F., .F.,
 ( 4, 2, 2, 2, 4 ),
 ( 0.0007817359430256252354, 0.0009771253907249898181, 0.001172514838424354401, 0.001367904286123718983, 0.001563293733823083566 ),
 .UNSPECIFIED. ) ;
#42875 = ORIENTED_EDGE ( 'NONE', *, *, #35630, .F. ) ;
#42876 = AXIS2_PLACEMENT_3D ( 'NONE', #18624, #19063, #74013 ) ;
#42877 = ORIENTED_EDGE ( 'NONE', *, *, #61807, .F. ) ;
#42878 = ORIENTED_EDGE ( 'NONE', *, *, #57128, .T. ) ;
#42879 = CARTESIAN_POINT ( 'NONE',  ( -10.86536135943320502, -8.347322224742351082, 34.93158281831414058 ) ) ;
#42880 = EDGE_LOOP ( 'NONE', ( #15817, #61128, #87535, #37127 ) ) ;
#42881 = EDGE_CURVE ( 'NONE', #77088, #61773, #24989, .T. ) ;
#42882 = AXIS2_PLACEMENT_3D ( 'NONE', #59230, #40749, #66883 ) ;
#42883 = CARTESIAN_POINT ( 'NONE',  ( -17.07692307692307665, -13.37000171582298513, 34.34916445242398453 ) ) ;
#42884 = CARTESIAN_POINT ( 'NONE',  ( 16.94623247381276698, -3.338472653186243200, 32.95098750199972670 ) ) ;
#42885 = CARTESIAN_POINT ( 'NONE',  ( 13.44987052412822059, -11.67786785259547777, 32.92929555188713664 ) ) ;
#42886 = VERTEX_POINT ( 'NONE', #81283 ) ;
#42887 = CARTESIAN_POINT ( 'NONE',  ( 12.46153846153833911, -9.528491918059723176, 34.59228464037033035 ) ) ;
#42888 = FACE_OUTER_BOUND ( 'NONE', #6985, .T. ) ;
#42889 = CARTESIAN_POINT ( 'NONE',  ( 3.903822929624694904, -2.588893531581426544, 31.60682220781847818 ) ) ;
#42890 = CARTESIAN_POINT ( 'NONE',  ( -1.384615384615506484, -3.083524468854526912, 32.58852847137268327 ) ) ;
#42891 = ORIENTED_EDGE ( 'NONE', *, *, #69579, .T. ) ;
#42892 = ORIENTED_EDGE ( 'NONE', *, *, #58544, .T. ) ;
#42893 = EDGE_CURVE ( 'NONE', #19715, #78412, #87161, .T. ) ;
#42894 = ORIENTED_EDGE ( 'NONE', *, *, #50794, .T. ) ;
#42895 = DIRECTION ( 'NONE',  ( 0.000000000000000000, 0.000000000000000000, 1.000000000000000000 ) ) ;
#42897 = CARTESIAN_POINT ( 'NONE',  ( -19.50000000000000000, -3.499999999999999556, 29.75000000000000355 ) ) ;
#42896 = CARTESIAN_POINT ( 'NONE',  ( 12.33084699487090319, -6.413092428213692742, 34.63065189839063152 ) ) ;
#42898 = CARTESIAN_POINT ( 'NONE',  ( -18.00000000000012079, -5.941354392335914447, 34.76329471203413846 ) ) ;
#42899 = CARTESIAN_POINT ( 'NONE',  ( -2.084679463598911209, -2.523321265292116422, 31.42251411153756990 ) ) ;
#42900 = EDGE_CURVE ( 'NONE', #41883, #75445, #87874, .T. ) ;
#42901 = FACE_BOUND ( 'NONE', #25222, .T. ) ;
#42902 = CARTESIAN_POINT ( 'NONE',  ( 9.758376043310132530, -3.513871655860379306, 32.76840700105978499 ) ) ;
#42903 = EDGE_CURVE ( 'NONE', #27494, #47764, #7290, .T. ) ;
#42904 = ORIENTED_EDGE ( 'NONE', *, *, #36849, .F. ) ;
#42905 = CARTESIAN_POINT ( 'NONE',  ( -3.100243529005667575, -2.619367082507848998, 30.83698974864644171 ) ) ;
#42906 = CARTESIAN_POINT ( 'NONE',  ( 18.00000000000000000, -13.20930481340135110, 34.54067556320372745 ) ) ;
#42907 = CARTESIAN_POINT ( 'NONE',  ( -12.46153846153846168, -12.78798330534102767, 29.49999999999997868 ) ) ;
#42908 = CARTESIAN_POINT ( 'NONE',  ( 10.03846153846153832, -11.00000000000000000, 29.65000000000000213 ) ) ;
#42909 = VERTEX_POINT ( 'NONE', #80846 ) ;
#42910 = ADVANCED_FACE ( 'NONE', ( #12373 ), #74514, .F. ) ;
#42911 = CARTESIAN_POINT ( 'NONE',  ( 5.076923076922953193, -12.70778746994576025, 30.41441678777401236 ) ) ;
#42912 = ADVANCED_FACE ( 'NONE', ( #60994 ), #31760, .F. ) ;
#42913 = B_SPLINE_CURVE_WITH_KNOTS ( 'NONE', 3,
 ( #12591, #80617, #40516, #67534, #19786, #47697, #5392, #54007, #13468, #87831 ),
 .UNSPECIFIED., .F., .F.,
 ( 4, 2, 2, 2, 4 ),
 ( 0.0007817359430256390048, 0.0009771253907250075990, 0.001172514838424376085, 0.001367904286123744571, 0.001563293733823113056 ),
 .UNSPECIFIED. ) ;
#42914 = ORIENTED_EDGE ( 'NONE', *, *, #87978, .F. ) ;
#42915 = FACE_BOUND ( 'NONE', #41761, .T. ) ;
#42916 = CARTESIAN_POINT ( 'NONE',  ( 18.13079180782478872, -3.530189275343204702, 32.79018710029569661 ) ) ;
#42917 = CARTESIAN_POINT ( 'NONE',  ( 4.403900573759607973, -2.544122305571457687, 31.48381861865059150 ) ) ;
#42918 = CARTESIAN_POINT ( 'NONE',  ( -3.230769230769229949, -8.120952969808772792, 34.71129190930000163 ) ) ;
#42919 = ORIENTED_EDGE ( 'NONE', *, *, #38013, .F. ) ;
#42920 = CARTESIAN_POINT ( 'NONE',  ( 5.142991427925514891, -3.050289026998446840, 32.03036669348366416 ) ) ;
#42921 = CARTESIAN_POINT ( 'NONE',  ( -3.454254155333561283, -2.353723527008296568, 30.78948104536958752 ) ) ;
#42922 = CARTESIAN_POINT ( 'NONE',  ( 8.769230769230645706, -8.656820664282941280, 34.87096338111179961 ) ) ;
#42923 = CARTESIAN_POINT ( 'NONE',  ( 3.230769230769231726, -1.790695186598648903, 34.54067556320373455 ) ) ;
#42924 = ORIENTED_EDGE ( 'NONE', *, *, #53086, .T. ) ;
#42925 = CARTESIAN_POINT ( 'NONE',  ( -4.153846153846152411, -6.386643153685126251, 34.62446782046654192 ) ) ;
#42926 = ORIENTED_EDGE ( 'NONE', *, *, #37835, .F. ) ;
#42928 = EDGE_LOOP ( 'NONE', ( #81413, #19249, #68980, #28720 ) ) ;
#42927 = DIRECTION ( 'NONE',  ( -0.000000000000000000, 0.3420201433256694901, -0.9396926207859082059 ) ) ;
#42929 = CARTESIAN_POINT ( 'NONE',  ( 11.53846153846141753, -6.879047030192662504, 34.71129190930017927 ) ) ;
#42930 = CARTESIAN_POINT ( 'NONE',  ( -10.74607608205217346, -12.38065189839062263, 30.83690757178629482 ) ) ;
#42931 = CARTESIAN_POINT ( 'NONE',  ( 7.846153846153723244, -10.33852847137269571, 34.16647553114546554 ) ) ;
#42932 = CARTESIAN_POINT ( 'NONE',  ( -15.48076923076922995, -7.500000000000001776, 35.00000000000000000 ) ) ;
#42934 = CARTESIAN_POINT ( 'NONE',  ( 8.519207545009310323, -4.175268141568685643, 33.81360843649122216 ) ) ;
#42933 = CARTESIAN_POINT ( 'NONE',  ( -2.980823821391186623, -4.176053281294514363, 33.81426240980091791 ) ) ;
#42935 = CARTESIAN_POINT ( 'NONE',  ( -17.07692307692307665, -13.95598074871891292, 31.83374038241031911 ) ) ;
#42936 = CARTESIAN_POINT ( 'NONE',  ( 1.139087296525997273, -4.749999999999992895, 24.23437500000000355 ) ) ;
#42937 = ORIENTED_EDGE ( 'NONE', *, *, #12816, .T. ) ;
#42938 = DIRECTION ( 'NONE',  ( 0.000000000000000000, 0.4999999999999960032, -0.8660254037844410391 ) ) ;
#42939 = PLANE ( 'NONE',  #76884 ) ;
#42940 = ORIENTED_EDGE ( 'NONE', *, *, #36401, .F. ) ;
#42941 = AXIS2_PLACEMENT_3D ( 'NONE', #25513, #66946, #39041 ) ;
#42942 = ORIENTED_EDGE ( 'NONE', *, *, #51046, .T. ) ;
#42943 = VERTEX_POINT ( 'NONE', #27650 ) ;
#42944 = FACE_OUTER_BOUND ( 'NONE', #85967, .T. ) ;
#42945 = CARTESIAN_POINT ( 'NONE',  ( 6.130525701763564150, -11.46989282347013095, 32.79007818306219946 ) ) ;
#42947 = CARTESIAN_POINT ( 'NONE',  ( 0.2115384615384615641, -7.500000000000001776, 35.00000000000000000 ) ) ;
#42946 = AXIS2_PLACEMENT_3D ( 'NONE', #37981, #11394, #80311 ) ;
#42948 = CARTESIAN_POINT ( 'NONE',  ( 10.74617505635156611, -6.369690395747422684, 34.87708834333098196 ) ) ;
#42949 = CARTESIAN_POINT ( 'NONE',  ( -8.899921372341076165, -2.494641256782728966, 31.33461815524612959 ) ) ;
#42950 = CARTESIAN_POINT ( 'NONE',  ( -12.46153846153846168, -2.486705287966279876, 31.30864560766543647 ) ) ;
#42951 = VECTOR ( 'NONE', #21203, 1000.000000000000114 ) ;
#42952 = CARTESIAN_POINT ( 'NONE',  ( 1.384615384615264011, -12.70778746994576025, 30.41441678777401236 ) ) ;
#42953 = LINE ( 'NONE', #49698, #3147 ) ;
#42954 = CARTESIAN_POINT ( 'NONE',  ( 11.53846153846141753, -10.90142922262034020, 33.41473453929536674 ) ) ;
#42955 = VECTOR ( 'NONE', #27059, 1000.000000000000000 ) ;
#42956 = DIRECTION ( 'NONE',  ( -0.000000000000000000, 0.8660254037844397068, -0.4999999999999978906 ) ) ;
#42957 = CARTESIAN_POINT ( 'NONE',  ( 7.846153846153723244, -9.528491918059723176, 34.59228464037033035 ) ) ;
#42958 = ORIENTED_EDGE ( 'NONE', *, *, #82498, .F. ) ;
#42959 = VERTEX_POINT ( 'NONE', #35294 ) ;
#42960 = CARTESIAN_POINT ( 'NONE',  ( 8.992010438208827949, -3.020022701398814569, 32.48759521482552515 ) ) ;
#42961 = SURFACE_STYLE_USAGE ( .BOTH. , #63214 ) ;
#42962 = CARTESIAN_POINT ( 'NONE',  ( 19.00000000000000000, -7.500000000000000000, 29.75000000000000355 ) ) ;
#42963 = CARTESIAN_POINT ( 'NONE',  ( -2.057692307690870415, -7.500000000000155431, 34.75000000000007105 ) ) ;
#42964 = VERTEX_POINT ( 'NONE', #20458 ) ;
#42965 = CARTESIAN_POINT ( 'NONE',  ( 27.00000000000000000, -1.250000000000000000, 22.25000000000000000 ) ) ;
#42966 = CARTESIAN_POINT ( 'NONE',  ( -10.68146699474474914, -12.62096338111211580, 30.90682066428152908 ) ) ;
#42967 = CARTESIAN_POINT ( 'NONE',  ( -12.21159294319032185, -10.76462480002816235, 33.53768742498949962 ) ) ;
#42968 = ORIENTED_EDGE ( 'NONE', *, *, #63050, .T. ) ;
#42969 = CARTESIAN_POINT ( 'NONE',  ( 0.5920641633020238270, -6.001044277235011215, 34.52024696741798948 ) ) ;
#42970 = EDGE_LOOP ( 'NONE', ( #70390, #66366, #46741, #28809 ) ) ;
#42971 = VECTOR ( 'NONE', #38586, 1000.000000000000000 ) ;
#42972 = CARTESIAN_POINT ( 'NONE',  ( 10.83839596699746544, -8.239487800360276282, 34.69522927552633718 ) ) ;
#42973 = EDGE_CURVE ( 'NONE', #84284, #88629, #61989, .T. ) ;
#42974 = CARTESIAN_POINT ( 'NONE',  ( 8.835298102580845025, -9.058645607665452459, 34.76329471203371924 ) ) ;
#42975 = LINE ( 'NONE', #70448, #31547 ) ;
#42976 = CARTESIAN_POINT ( 'NONE',  ( -9.561782254074051579, -6.808710257144161559, 34.95449254468098843 ) ) ;
#42977 = CARTESIAN_POINT ( 'NONE',  ( 15.23076923076911093, -6.026961402154118019, 34.52809138561165270 ) ) ;
#42978 = EDGE_LOOP ( 'NONE', ( #27307, #63158, #65239, #5051 ) ) ;
#42979 = ORIENTED_EDGE ( 'NONE', *, *, #55361, .F. ) ;
#42980 = ORIENTED_EDGE ( 'NONE', *, *, #9040, .T. ) ;
#42981 = EDGE_CURVE ( 'NONE', #39647, #7402, #22269, .T. ) ;
#42982 = CARTESIAN_POINT ( 'NONE',  ( -6.223484943723947005, -11.41268669641500466, 32.86336882939237825 ) ) ;
#42983 = DIRECTION ( 'NONE',  ( 0.000000000000000000, 0.000000000000000000, 1.000000000000000000 ) ) ;
#42984 = CARTESIAN_POINT ( 'NONE',  ( -4.219928533206290133, -12.34228464037088280, 31.77849191805838558 ) ) ;
#42985 = CARTESIAN_POINT ( 'NONE',  ( -2.176901866725354573, -11.37503395064541678, 33.29242100308974983 ) ) ;
#42986 = CARTESIAN_POINT ( 'NONE',  ( -7.623141002060451754, -4.026326845037962343, 33.68677907613344047 ) ) ;
#42987 = CARTESIAN_POINT ( 'NONE',  ( 14.55763782604044998, -10.05730279482229683, 34.04704008940765902 ) ) ;
#42988 = ORIENTED_EDGE ( 'NONE', *, *, #88145, .F. ) ;
#42989 = EDGE_LOOP ( 'NONE', ( #7642, #11717, #82648, #64922 ) ) ;
#42990 = ORIENTED_EDGE ( 'NONE', *, *, #29265, .F. ) ;
#42991 = VECTOR ( 'NONE', #1994, 999.9999999999998863 ) ;
#42993 = ORIENTED_EDGE ( 'NONE', *, *, #18407, .F. ) ;
#42992 = CARTESIAN_POINT ( 'NONE',  ( 4.219101293358989757, -4.320704448112861584, 33.92786785259548310 ) ) ;
#42995 = CARTESIAN_POINT ( 'NONE',  ( 13.60739505359345536, -4.226511098958373402, 33.85474049983370293 ) ) ;
#42994 = CARTESIAN_POINT ( 'NONE',  ( 8.992242120843616959, -8.239487800360276282, 34.69522927552633718 ) ) ;
#42996 = VECTOR ( 'NONE', #10150, 1000.000000000000227 ) ;
#42997 = EDGE_CURVE ( 'NONE', #68861, #40709, #82620, .T. ) ;
#42998 = CARTESIAN_POINT ( 'NONE',  ( -3.749999999999988454, -9.053300858899127945, 25.01562500000000000 ) ) ;
#42999 = EDGE_CURVE ( 'NONE', #14363, #69353, #14450, .T. ) ;
#43000 = VERTEX_POINT ( 'NONE', #21781 ) ;
#43001 = VECTOR ( 'NONE', #79576, 999.9999999999998863 ) ;
#43002 = VERTEX_POINT ( 'NONE', #55559 ) ;
#43003 = CARTESIAN_POINT ( 'NONE',  ( 4.153846153846030731, -4.320704448113951379, 33.92786785259630022 ) ) ;
#43004 = VERTEX_POINT ( 'NONE', #34406 ) ;
#43005 = FACE_BOUND ( 'NONE', #75583, .T. ) ;
#43006 = CARTESIAN_POINT ( 'NONE',  ( -2.084912638714239819, -4.989023458446561143, 34.36081565061822118 ) ) ;
#43007 = CYLINDRICAL_SURFACE ( 'NONE', #37636, 0.2500000000000002220 ) ;
#43008 = ORIENTED_EDGE ( 'NONE', *, *, #66434, .T. ) ;
#43009 = CARTESIAN_POINT ( 'NONE',  ( 14.98076923076923350, -7.433932668274256805, 35.00000000000000711 ) ) ;
#43010 = DIRECTION ( 'NONE',  ( -1.000000000000000000, 1.897353801849632760E-16, -8.673617379884035472E-16 ) ) ;
#43011 = PLANE ( 'NONE',  #27736 ) ;
#43012 = ADVANCED_FACE ( 'NONE', ( #76727 ), #7392, .F. ) ;
#43013 = CARTESIAN_POINT ( 'NONE',  ( -15.48074596171158390, -6.567427716900048118, 34.66269422305636283 ) ) ;
#43014 = CARTESIAN_POINT ( 'NONE',  ( -16.82686876528476105, -2.564540009722896752, 30.55348353981672105 ) ) ;
#43015 = EDGE_LOOP ( 'NONE', ( #88321, #64847, #17378, #81153 ) ) ;
#43016 = DIRECTION ( 'NONE',  ( 1.000000000000000000, 0.000000000000000000, 0.000000000000000000 ) ) ;
#43017 = CARTESIAN_POINT ( 'NONE',  ( 3.453780582382080411, -4.187068189119697692, 33.49521262558774026 ) ) ;
#43018 = CARTESIAN_POINT ( 'NONE',  ( -6.673076923076923350, -2.249999999999998668, 29.75000000000000355 ) ) ;
#43019 = CARTESIAN_POINT ( 'NONE',  ( 5.934729554039226862, -5.219633306516282545, 34.19971097300152252 ) ) ;
#43020 = DIRECTION ( 'NONE',  ( -0.000000000000000000, 0.7660444431189791237, -0.6427876096865379196 ) ) ;
#43021 = CARTESIAN_POINT ( 'NONE',  ( 6.000000000000001776, -9.780366693483667717, 34.19971097300155094 ) ) ;
#43023 = CARTESIAN_POINT ( 'NONE',  ( 11.76147289007438701, -4.187068189119697692, 33.49521262558774026 ) ) ;
#43022 = CARTESIAN_POINT ( 'NONE',  ( -1.384615384615506484, -6.835583212225970762, 34.95778746994575670 ) ) ;
#43024 = CARTESIAN_POINT ( 'NONE',  ( 16.15384615384615330, -8.564572088678739092, 35.78748833219616898 ) ) ;
#43026 = CARTESIAN_POINT ( 'NONE',  ( 15.36156103859402222, -9.804649428959608670, 34.18742332936588468 ) ) ;
#43025 = CARTESIAN_POINT ( 'NONE',  ( 3.480769230770666578, -7.500000000000155431, 34.75000000000007105 ) ) ;
#43027 = CARTESIAN_POINT ( 'NONE',  ( -2.557715531913763662, -5.765609946408404518, 34.70566812827425451 ) ) ;
#43028 = B_SPLINE_CURVE_WITH_KNOTS ( 'NONE', 3,
 ( #22162, #36131, #42884, #64453, #49630, #9522, #36563, #63131, #2753, #77103 ),
 .UNSPECIFIED., .F., .F.,
 ( 4, 2, 2, 2, 4 ),
 ( 0.000000000000000000, 0.0001954311564186862510, 0.0003908623128373725020, 0.0005862934692560588072, 0.0007817246256747450040 ),
 .UNSPECIFIED. ) ;
#43029 = AXIS2_PLACEMENT_3D ( 'NONE', #51521, #64601, #2899 ) ;
#43030 = CARTESIAN_POINT ( 'NONE',  ( -1.987747218494660295, -5.598659921968651254, 22.49813170625848713 ) ) ;
#43031 = ORIENTED_EDGE ( 'NONE', *, *, #42323, .F. ) ;
#43032 = CARTESIAN_POINT ( 'NONE',  ( -4.088591014333315066, -5.941354392334606160, 34.76329471203374055 ) ) ;
#43033 = ORIENTED_EDGE ( 'NONE', *, *, #14588, .T. ) ;
#43034 = LINE ( 'NONE', #71829, #30586 ) ;
#43035 = ORIENTED_EDGE ( 'NONE', *, *, #24163, .T. ) ;
#43036 = CARTESIAN_POINT ( 'NONE',  ( -13.31854805126531005, -2.292212530054420494, 30.41441678777542990 ) ) ;
#43037 = CARTESIAN_POINT ( 'NONE',  ( 17.20771351789003489, -2.845873456487966635, 32.17976146951972538 ) ) ;
#43038 = ORIENTED_EDGE ( 'NONE', *, *, #55374, .F. ) ;
#43039 = FACE_OUTER_BOUND ( 'NONE', #59521, .T. ) ;
#43040 = CARTESIAN_POINT ( 'NONE',  ( -2.749999999999997780, -7.561099074964547917, 23.59188170625849068 ) ) ;
#43041 = CARTESIAN_POINT ( 'NONE',  ( 6.249945409378045547, -6.653508905675592722, 34.93172785388651391 ) ) ;
#43042 = B_SPLINE_CURVE_WITH_KNOTS ( 'NONE', 3,
 ( #10825, #38297, #24319, #44585, #9926, #72070, #43712, #3610, #2711, #23870 ),
 .UNSPECIFIED., .F., .F.,
 ( 4, 2, 2, 2, 4 ),
 ( 0.0007817246256747457630, 0.0009771112852218887673, 0.001172497944769031880, 0.001367884604316174993, 0.001563271263863318106 ),
 .UNSPECIFIED. ) ;
#43043 = CARTESIAN_POINT ( 'NONE',  ( -3.230769230769229949, -12.34228464037088635, 31.77849191805839268 ) ) ;
#43044 = DIRECTION ( 'NONE',  ( 0.000000000000000000, 0.8660254037844377084, 0.5000000000000015543 ) ) ;
#43045 = DIRECTION ( 'NONE',  ( 1.000000000000000000, 0.000000000000000000, 0.000000000000000000 ) ) ;
#43046 = CARTESIAN_POINT ( 'NONE',  ( 15.29591501010119892, -7.750023238201979581, 34.74374492549440419 ) ) ;
#43047 = LINE ( 'NONE', #1619, #41083 ) ;
#43048 = CARTESIAN_POINT ( 'NONE',  ( -1.553300858899125059, -3.750000000000009326, 14.07812500000000178 ) ) ;
#43049 = DIRECTION ( 'NONE',  ( 0.000000000000000000, 0.000000000000000000, -1.000000000000000000 ) ) ;
#43050 = FACE_OUTER_BOUND ( 'NONE', #81163, .T. ) ;
#43051 = CARTESIAN_POINT ( 'NONE',  ( 13.38461538461538680, -4.098570777380720287, 33.41473453929634729 ) ) ;
#43052 = CARTESIAN_POINT ( 'NONE',  ( -1.553300858899081538, -11.25000000000000711, 18.60937500000000355 ) ) ;
#43053 = AXIS2_PLACEMENT_3D ( 'NONE', #47220, #74715, #13001 ) ;
#43054 = CARTESIAN_POINT ( 'NONE',  ( 16.15384615384615330, -6.189225973068211317, 35.74407628777942847 ) ) ;
#43055 = AXIS2_PLACEMENT_3D ( 'NONE', #26478, #4880, #73786 ) ;
#43056 = ORIENTED_EDGE ( 'NONE', *, *, #22904, .T. ) ;
#43057 = DIRECTION ( 'NONE',  ( 1.000000000000000000, 0.000000000000000000, 0.000000000000000000 ) ) ;
#43058 = CARTESIAN_POINT ( 'NONE',  ( 16.02315468717859304, -12.11776431015576172, 31.66791131148498906 ) ) ;
#43059 = CARTESIAN_POINT ( 'NONE',  ( 1.253923917947828537, -12.38065189839062263, 30.83690757178629482 ) ) ;
#43060 = CARTESIAN_POINT ( 'NONE',  ( -0.3589743589743593088, -3.499999999999999556, 29.75000000000000355 ) ) ;
#43061 = CARTESIAN_POINT ( 'NONE',  ( -2.980714919130914353, -4.943051570960395047, 34.04725096376909477 ) ) ;
#43062 = ADVANCED_FACE ( 'NONE', ( #628 ), #15031, .F. ) ;
#43063 = CARTESIAN_POINT ( 'NONE',  ( -8.834501215191545853, -8.613356846314824011, 34.62446782046655613 ) ) ;
#43064 = AXIS2_PLACEMENT_3D ( 'NONE', #62312, #81284, #19566 ) ;
#43065 = DIRECTION ( 'NONE',  ( 1.000000000000000000, 0.000000000000000000, 0.000000000000000000 ) ) ;
#43066 = B_SPLINE_CURVE_WITH_KNOTS ( 'NONE', 3,
 ( #83295, #63886, #35093, #2185, #62554, #22028, #29676, #49503, #35548, #82855 ),
 .UNSPECIFIED., .F., .F.,
 ( 4, 2, 2, 2, 4 ),
 ( 0.0007817246256747478229, 0.0009771112852218913694, 0.001172497944769034916, 0.001367884604316178679, 0.001563271263863322226 ),
 .UNSPECIFIED. ) ;
#43067 = EDGE_LOOP ( 'NONE', ( #10461, #56763, #41636, #28459 ) ) ;
#43068 = EDGE_LOOP ( 'NONE', ( #76192, #40892 ) ) ;
#43069 = ORIENTED_EDGE ( 'NONE', *, *, #34266, .F. ) ;
#43070 = EDGE_CURVE ( 'NONE', #4983, #58791, #42504, .T. ) ;
#43071 = CARTESIAN_POINT ( 'NONE',  ( 3.230769230769110045, -6.026961402154118908, 34.52809138561165270 ) ) ;
#43072 = CARTESIAN_POINT ( 'NONE',  ( 6.700150705560778519, -2.758268499246657957, 31.33685645148948140 ) ) ;
#43073 = CARTESIAN_POINT ( 'NONE',  ( 16.37685750545900731, -2.758310577978207778, 31.33698337089302299 ) ) ;
#43074 = EDGE_CURVE ( 'NONE', #79653, #88101, #10479, .T. ) ;
#43075 = CARTESIAN_POINT ( 'NONE',  ( 4.403791672194295792, -3.712312575010499494, 33.01462480002815170 ) ) ;
#43076 = CARTESIAN_POINT ( 'NONE',  ( 17.99999999999987566, -9.442884908241554243, 34.35708131394783038 ) ) ;
#43077 = ORIENTED_EDGE ( 'NONE', *, *, #19375, .F. ) ;
#43078 = CARTESIAN_POINT ( 'NONE',  ( -8.769230769230768274, -2.900454961884010974, 35.62045528018868623 ) ) ;
#43079 = ORIENTED_EDGE ( 'NONE', *, *, #60289, .T. ) ;
#43080 = ORIENTED_EDGE ( 'NONE', *, *, #88585, .F. ) ;
#43081 = ADVANCED_FACE ( 'NONE', ( #75401 ), #14581, .F. ) ;
#43083 = ORIENTED_EDGE ( 'NONE', *, *, #39924, .T. ) ;
#43082 = CARTESIAN_POINT ( 'NONE',  ( -15.23076923076935074, -9.442884908241554243, 34.35708131394783038 ) ) ;
#43084 = FACE_OUTER_BOUND ( 'NONE', #62461, .T. ) ;
#43085 = VECTOR ( 'NONE', #63936, 1000.000000000000000 ) ;
#43086 = CARTESIAN_POINT ( 'NONE',  ( -10.36538461538317790, -7.500000000000155431, 34.75000000000007105 ) ) ;
#43087 = EDGE_CURVE ( 'NONE', #148, #84960, #47106, .T. ) ;
#43088 = CARTESIAN_POINT ( 'NONE',  ( 3.903822916553187472, -4.335965774309649134, 33.62209801155881905 ) ) ;
#43089 = CARTESIAN_POINT ( 'NONE',  ( -16.02305571287920216, -5.496552790871120031, 34.60292014791297532 ) ) ;
#43090 = ORIENTED_EDGE ( 'NONE', *, *, #45271, .F. ) ;
#43091 = EDGE_LOOP ( 'NONE', ( #23484, #45273 ) ) ;
#43092 = ORIENTED_EDGE ( 'NONE', *, *, #40652, .T. ) ;
#43093 = DIRECTION ( 'NONE',  ( -0.000000000000000000, 0.1736481776669307198, -0.9848077530122080203 ) ) ;
#43095 = EDGE_LOOP ( 'NONE', ( #53924, #15728, #52939, #18063 ) ) ;
#43094 = CARTESIAN_POINT ( 'NONE',  ( 4.219914504848592429, -11.16473453929635440, 33.15142922261926373 ) ) ;
#43096 = B_SPLINE_CURVE_WITH_KNOTS ( 'NONE', 3,
 ( #52053, #38555, #66009, #86765, #52497, #79983, #18282, #45750, #39012, #4775 ),
 .UNSPECIFIED., .F., .F.,
 ( 4, 2, 2, 2, 4 ),
 ( 0.000000000000000000, 0.0001954339857564080707, 0.0003908679715128161414, 0.0005863019572692241849, 0.0007817359430256322827 ),
 .UNSPECIFIED. ) ;
#43097 = CARTESIAN_POINT ( 'NONE',  ( 1.634669696253702176, -9.148310452688873440, 34.47095581063188519 ) ) ;
#43098 = CARTESIAN_POINT ( 'NONE',  ( 4.946231610255514610, -3.530157926970578508, 32.79014554554150607 ) ) ;
#43099 = B_SPLINE_CURVE_WITH_KNOTS ( 'NONE', 3,
 ( #58416, #17898, #45804, #58875, #46256, #59320, #52556, #45355, #11588, #37714 ),
 .UNSPECIFIED., .F., .F.,
 ( 4, 2, 2, 2, 4 ),
 ( 0.0007817359430256297891, 0.0009771253907249958896, 0.001172514838424362207, 0.001367904286123728524, 0.001563293733823094625 ),
 .UNSPECIFIED. ) ;
#43100 = DIRECTION ( 'NONE',  ( 0.000000000000000000, 0.9396926207859126468, 0.3420201433256571111 ) ) ;
#43101 = ADVANCED_FACE ( 'NONE', ( #29872 ), #15477, .F. ) ;
#43102 = VERTEX_POINT ( 'NONE', #50126 ) ;
#43103 = ADVANCED_FACE ( 'NONE', ( #9164 ), #84829, .T. ) ;
#43104 = DIRECTION ( 'NONE',  ( -0.000000000000000000, -0.9848077530122086864, -0.1736481776669273613 ) ) ;
#43105 = CYLINDRICAL_SURFACE ( 'NONE', #10898, 0.2499999999999998890 ) ;
#43106 = VERTEX_POINT ( 'NONE', #85258 ) ;
#43107 = FACE_BOUND ( 'NONE', #79784, .T. ) ;
#43108 = CARTESIAN_POINT ( 'NONE',  ( 11.47319109250076430, -5.219633306516282545, 34.19971097300152962 ) ) ;
#43109 = FACE_OUTER_BOUND ( 'NONE', #71499, .T. ) ;
#43110 = CARTESIAN_POINT ( 'NONE',  ( 2.177544337960610754, -12.50552854090298993, 31.33409797877408920 ) ) ;
#43113 = CARTESIAN_POINT ( 'NONE',  ( -10.61538461538473577, -5.941354392335915335, 34.76329471203413846 ) ) ;
#43112 = VECTOR ( 'NONE', #24077, 1000.000000000000114 ) ;
#43111 = DIRECTION ( 'NONE',  ( -1.000000000000000000, -0.000000000000000000, -0.000000000000000000 ) ) ;
#43114 = EDGE_CURVE ( 'NONE', #48549, #58504, #28999, .T. ) ;
#43115 = CARTESIAN_POINT ( 'NONE',  ( -1.319360245102545015, -8.656820664281605460, 34.87096338111211224 ) ) ;
#43116 = CARTESIAN_POINT ( 'NONE',  ( -4.283994123577851809, -11.04286588640298561, 33.62463336215343901 ) ) ;
#43117 = ORIENTED_EDGE ( 'NONE', *, *, #80323, .F. ) ;
#43118 = EDGE_CURVE ( 'NONE', #42531, #15081, #43816, .T. ) ;
#43119 = CARTESIAN_POINT ( 'NONE',  ( -18.13014720943822056, -10.88202310037936194, 33.43294751532457099 ) ) ;
#43120 = CARTESIAN_POINT ( 'NONE',  ( -17.01166793741023042, -6.835583212224605631, 34.95778746994559327 ) ) ;
#43121 = AXIS2_PLACEMENT_3D ( 'NONE', #36921, #72483, #38262 ) ;
#43122 = VERTEX_POINT ( 'NONE', #10029 ) ;
#43123 = AXIS2_PLACEMENT_3D ( 'NONE', #32459, #54052, #80667 ) ;
#43124 = VECTOR ( 'NONE', #87616, 1000.000000000000000 ) ;
#43125 = CARTESIAN_POINT ( 'NONE',  ( -12.21148404162501144, -3.435999193479609914, 33.07426656108010832 ) ) ;
#43126 = CARTESIAN_POINT ( 'NONE',  ( -12.22435897435897267, -3.499999999999999556, 29.75000000000000355 ) ) ;
#43127 = CARTESIAN_POINT ( 'NONE',  ( 15.90382292962469535, -6.652501968072647820, 34.93155406624980941 ) ) ;
#43128 = CARTESIAN_POINT ( 'NONE',  ( -7.780898706641008467, -11.06231777344671130, 33.60647404775212976 ) ) ;
#43129 = DIRECTION ( 'NONE',  ( -0.000000000000000000, 0.8660254037844399289, -0.4999999999999980016 ) ) ;
#43130 = CARTESIAN_POINT ( 'NONE',  ( -4.153846153846274980, -2.379036618888197729, 30.90682066428292885 ) ) ;
#43131 = FACE_BOUND ( 'NONE', #73292, .T. ) ;
#43133 = CARTESIAN_POINT ( 'NONE',  ( 1.607394925883794068, -2.600157965045225783, 30.74683119005207743 ) ) ;
#43132 = CARTESIAN_POINT ( 'NONE',  ( -2.557669038634660108, -6.567427716900047230, 34.66269422305636283 ) ) ;
#43134 = FACE_OUTER_BOUND ( 'NONE', #54921, .T. ) ;
#43136 = CARTESIAN_POINT ( 'NONE',  ( -14.98071491913091791, -6.567000820036036579, 34.66262288849541306 ) ) ;
#43135 = CARTESIAN_POINT ( 'NONE',  ( -17.74994568836168440, -11.28795663066794575, 33.01431243580655206 ) ) ;
#43137 = CARTESIAN_POINT ( 'NONE',  ( -19.99999999999996803, 15.00000000000000711, 13.00000000000000178 ) ) ;
#43138 = CARTESIAN_POINT ( 'NONE',  ( 2.608446859217893099, -4.805146000318787358, 21.56063170625849068 ) ) ;
#43139 = ORIENTED_EDGE ( 'NONE', *, *, #51201, .F. ) ;
#43140 = ORIENTED_EDGE ( 'NONE', *, *, #81102, .T. ) ;
#43141 = CARTESIAN_POINT ( 'NONE',  ( 5.299934428535925335, -6.503523203565942268, 34.64991518177335195 ) ) ;
#43142 = CARTESIAN_POINT ( 'NONE',  ( -4.826977558574935045, -3.202959910592335202, 32.30730279482227019 ) ) ;
#43143 = CARTESIAN_POINT ( 'NONE',  ( 5.777073041093152561, -5.582147617184174848, 34.63737895849758530 ) ) ;
#43144 = CARTESIAN_POINT ( 'NONE',  ( 8.769230769231082689, -2.255955759149395501, 30.00000000000324363 ) ) ;
#43145 = CARTESIAN_POINT ( 'NONE',  ( -4.153846153846152411, -2.833524468853757305, 32.15551576947925838 ) ) ;
#43146 = CARTESIAN_POINT ( 'NONE',  ( 2.694853999681214862, -10.10844685921789043, 20.62313170625849068 ) ) ;
#43147 = CARTESIAN_POINT ( 'NONE',  ( 6.699591998512592461, -2.353723527008295680, 30.78948104536958752 ) ) ;
#43148 = CARTESIAN_POINT ( 'NONE',  ( 18.13052570176355971, -3.285477652293413264, 32.44071101563363158 ) ) ;
#43149 = CARTESIAN_POINT ( 'NONE',  ( -17.07692307692319744, -10.33852847137269571, 34.16647553114546554 ) ) ;
#43150 = CARTESIAN_POINT ( 'NONE',  ( -1.608100328339332030, -12.44517049084099725, 30.48991314939691932 ) ) ;
#43151 = FACE_OUTER_BOUND ( 'NONE', #82766, .T. ) ;
#43152 = CARTESIAN_POINT ( 'NONE',  ( 6.000000000000001776, -13.20930481340135110, 34.54067556320372745 ) ) ;
#43153 = EDGE_CURVE ( 'NONE', #25462, #21400, #78047, .T. ) ;
#43154 = CARTESIAN_POINT ( 'NONE',  ( 14.55763782604045176, -11.86320923018887719, 32.19269448109604070 ) ) ;
#43155 = CARTESIAN_POINT ( 'NONE',  ( 14.08420736396836226, -6.760086850603066466, 34.69517049084099369 ) ) ;
#43156 = EDGE_LOOP ( 'NONE', ( #50684, #63100 ) ) ;
#43157 = AXIS2_PLACEMENT_3D ( 'NONE', #82816, #21089, #48560 ) ;
#43158 = DIRECTION ( 'NONE',  ( -0.000000000000000000, 0.9396926207859092051, -0.3420201433256662704 ) ) ;
#43159 = DIRECTION ( 'NONE',  ( 0.000000000000000000, 0.8660254037844377084, -0.5000000000000015543 ) ) ;
#43160 = CARTESIAN_POINT ( 'NONE',  ( -1.901340078031369618, -5.512252781505359245, 24.25186829374150932 ) ) ;
#43161 = CARTESIAN_POINT ( 'NONE',  ( 4.153846153846030731, -5.094484230521993062, 34.41647553114689373 ) ) ;
#43162 = CARTESIAN_POINT ( 'NONE',  ( -16.15384615384615330, -2.486705287966279876, 31.30864560766543647 ) ) ;
#43163 = ORIENTED_EDGE ( 'NONE', *, *, #63073, .T. ) ;
#43164 = CARTESIAN_POINT ( 'NONE',  ( -7.053767526187232129, -2.845849958028613624, 32.17971566917920967 ) ) ;
#43166 = ORIENTED_EDGE ( 'NONE', *, *, #5177, .F. ) ;
#43165 = CARTESIAN_POINT ( 'NONE',  ( 12.33084699487089964, -5.582088688514999397, 34.36776431015576350 ) ) ;
#43167 = CARTESIAN_POINT ( 'NONE',  ( 7.976945653978629203, -3.530189275343204702, 32.79018710029569661 ) ) ;
#43168 = CARTESIAN_POINT ( 'NONE',  ( 16.85399611801622299, -2.523278758544490241, 31.42238647778636818 ) ) ;
#43169 = ORIENTED_EDGE ( 'NONE', *, *, #15846, .T. ) ;
#43170 = DIRECTION ( 'NONE',  ( 1.000000000000000000, 0.000000000000000000, 0.000000000000000000 ) ) ;
#43171 = ADVANCED_FACE ( 'NONE', ( #16351 ), #37952, .T. ) ;
#43172 = DIRECTION ( 'NONE',  ( -1.000000000000000000, -0.000000000000000000, 0.000000000000000000 ) ) ;
#43173 = ORIENTED_EDGE ( 'NONE', *, *, #75205, .F. ) ;
#43174 = CARTESIAN_POINT ( 'NONE',  ( 8.835298102580845025, -2.292212530054420494, 30.41441678777542990 ) ) ;
#43175 = CARTESIAN_POINT ( 'NONE',  ( -11.60373153901785948, -12.51329471203370325, 31.30864560766548976 ) ) ;
#43176 = DIRECTION ( 'NONE',  ( -0.000000000000000000, 0.1736481776669307198, -0.9848077530122080203 ) ) ;
#43177 = VERTEX_POINT ( 'NONE', #50994 ) ;
#43178 = ORIENTED_EDGE ( 'NONE', *, *, #85734, .T. ) ;
#43179 = ORIENTED_EDGE ( 'NONE', *, *, #84303, .F. ) ;
#43180 = AXIS2_PLACEMENT_3D ( 'NONE', #63307, #723, #28187 ) ;
#43181 = VECTOR ( 'NONE', #83552, 1000.000000000000227 ) ;
#43182 = EDGE_CURVE ( 'NONE', #11993, #37408, #56454, .T. ) ;
#43183 = CARTESIAN_POINT ( 'NONE',  ( -5.207613680033384540, -9.084618155246140248, 34.75535874321725771 ) ) ;
#43184 = CARTESIAN_POINT ( 'NONE',  ( -14.37296275365308418, -3.300289026998414865, 32.46337939537583139 ) ) ;
#43185 = EDGE_CURVE ( 'NONE', #56880, #23776, #2377, .T. ) ;
#43186 = CARTESIAN_POINT ( 'NONE',  ( -7.911910648668153634, -7.249945686854186278, 34.74374336980223887 ) ) ;
#43187 = AXIS2_PLACEMENT_3D ( 'NONE', #45917, #18463, #12592 ) ;
#43188 = AXIS2_PLACEMENT_3D ( 'NONE', #14637, #83102, #20062 ) ;
#43189 = CARTESIAN_POINT ( 'NONE',  ( -5.076923076923075762, -2.292212530054420494, 30.41441678777542634 ) ) ;
#43190 = EDGE_LOOP ( 'NONE', ( #34106, #75321 ) ) ;
#43192 = VERTEX_POINT ( 'NONE', #1514 ) ;
#43191 = EDGE_CURVE ( 'NONE', #72551, #84061, #25464, .T. ) ;
#43194 = ORIENTED_EDGE ( 'NONE', *, *, #9819, .F. ) ;
#43193 = CARTESIAN_POINT ( 'NONE',  ( -1.515225744239911521, -7.722926236386453702, 34.74524107206102030 ) ) ;
#43195 = CARTESIAN_POINT ( 'NONE',  ( 16.28437159207980045, -8.630441415882549094, 34.87705825610312615 ) ) ;
#43196 = EDGE_LOOP ( 'NONE', ( #69666, #78734, #12738, #9083 ) ) ;
#43197 = B_SPLINE_CURVE_WITH_KNOTS ( 'NONE', 3,
 ( #8248, #36598, #7359, #48328, #43354, #21749, #29410, #75803, #69492, #63618 ),
 .UNSPECIFIED., .F., .F.,
 ( 4, 2, 2, 2, 4 ),
 ( 0.0007817246256747505334, 0.0009771112852218941883, 0.001172497944769037952, 0.001367884604316181498, 0.001563271263863325261 ),
 .UNSPECIFIED. ) ;
#43198 = CARTESIAN_POINT ( 'NONE',  ( 19.99999999999997158, -14.99999999999999467, 13.00000000000000178 ) ) ;
#43199 = CARTESIAN_POINT ( 'NONE',  ( -8.638440328263820689, -12.62708834333097663, 30.88030960425257021 ) ) ;
#43200 = ORIENTED_EDGE ( 'NONE', *, *, #13570, .T. ) ;
#43201 = ORIENTED_EDGE ( 'NONE', *, *, #22136, .T. ) ;
#43203 = ORIENTED_EDGE ( 'NONE', *, *, #26029, .T. ) ;
#43202 = CARTESIAN_POINT ( 'NONE',  ( -8.769230769230768274, -8.120952969808772792, 34.71129190930000163 ) ) ;
#43204 = CARTESIAN_POINT ( 'NONE',  ( -3.230769230769351186, -6.879047030192662504, 34.71129190930017927 ) ) ;
#43205 = CARTESIAN_POINT ( 'NONE',  ( -0.4615384615385840772, -5.094484230521993062, 34.41647553114689373 ) ) ;
#43207 = ORIENTED_EDGE ( 'NONE', *, *, #80149, .F. ) ;
#43206 = EDGE_CURVE ( 'NONE', #45365, #65338, #1952, .T. ) ;
#43208 = LINE ( 'NONE', #41892, #80547 ) ;
#43209 = CARTESIAN_POINT ( 'NONE',  ( -14.05774689831426372, -12.68172785388650681, 30.59649109432439218 ) ) ;
#43210 = CARTESIAN_POINT ( 'NONE',  ( 18.00000000000000000, -12.34228464037088635, 31.77849191805839268 ) ) ;
#43211 = FACE_BOUND ( 'NONE', #38095, .T. ) ;
#43212 = CARTESIAN_POINT ( 'NONE',  ( 1.449870955891411350, -12.46129190930001052, 30.37095296980870174 ) ) ;
#43214 = ADVANCED_FACE ( 'NONE', ( #64965 ), #15918, .F. ) ;
#43213 = FACE_OUTER_BOUND ( 'NONE', #56753, .T. ) ;
#43215 = CYLINDRICAL_SURFACE ( 'NONE', #46589, 0.2500000000000002220 ) ;
#43217 = CARTESIAN_POINT ( 'NONE',  ( 9.757563263583719504, -3.300289026998473041, 32.46337939537591666 ) ) ;
#43216 = CARTESIAN_POINT ( 'NONE',  ( 0.4615384615387756462, -2.255955759149395501, 30.00000000000324363 ) ) ;
#43218 = CARTESIAN_POINT ( 'NONE',  ( -3.007989689500818464, -3.236590943229497253, 32.36255958852954251 ) ) ;
#43219 = CARTESIAN_POINT ( 'NONE',  ( -16.15384615384615330, -8.120952969808772792, 34.71129190930000163 ) ) ;
#43220 = VERTEX_POINT ( 'NONE', #16784 ) ;
#43221 = EDGE_CURVE ( 'NONE', #77943, #88418, #59919, .T. ) ;
#43222 = CARTESIAN_POINT ( 'NONE',  ( 10.61538461538461675, -10.51840700105979565, 33.73612834413961536 ) ) ;
#43223 = VERTEX_POINT ( 'NONE', #33751 ) ;
#43224 = VERTEX_POINT ( 'NONE', #27438 ) ;
#43226 = CARTESIAN_POINT ( 'NONE',  ( 7.846153846153846700, -9.780366693483667717, 34.19971097300155094 ) ) ;
#43225 = CARTESIAN_POINT ( 'NONE',  ( -7.134615384615385025, -4.000000000000000000, 29.75000000000000355 ) ) ;
#43227 = CARTESIAN_POINT ( 'NONE',  ( 11.53846153846153832, -8.164416787775445883, 34.95778746994557906 ) ) ;
#43228 = CARTESIAN_POINT ( 'NONE',  ( 0.2115384615384615641, -7.500000000000001776, 35.04278698407183867 ) ) ;
#43229 = CARTESIAN_POINT ( 'NONE',  ( -12.46153846153846168, -2.486705287966279876, 31.30864560766543647 ) ) ;
#43230 = CARTESIAN_POINT ( 'NONE',  ( 1.384615384615386802, -1.215029322943914858, 32.30358669280327177 ) ) ;
#43231 = ORIENTED_EDGE ( 'NONE', *, *, #52356, .T. ) ;
#43232 = CARTESIAN_POINT ( 'NONE',  ( -9.692307692307691624, -9.819645486525091727, 36.12317359536749706 ) ) ;
#43233 = CARTESIAN_POINT ( 'NONE',  ( 3.230769230769110045, -11.48612834414049644, 32.76840700105863391 ) ) ;
#43235 = DIRECTION ( 'NONE',  ( 0.000000000000000000, 0.9396926207859126468, -0.3420201433256571111 ) ) ;
#43234 = B_SPLINE_CURVE_WITH_KNOTS ( 'NONE', 3,
 ( #36790, #64243, #2547, #30038, #57497, #83216, #49425, #16514, #43981, #21498 ),
 .UNSPECIFIED., .F., .F.,
 ( 4, 2, 2, 2, 4 ),
 ( 0.0007817246256747463051, 0.0009771112852218896347, 0.001172497944769033181, 0.001367884604316176728, 0.001563271263863320057 ),
 .UNSPECIFIED. ) ;
#43236 = CIRCLE ( 'NONE', #21694, 4.000000000000000000 ) ;
#43237 = DIRECTION ( 'NONE',  ( -0.000000000000000000, 0.9396926207859092051, -0.3420201433256662704 ) ) ;
#43238 = CARTESIAN_POINT ( 'NONE',  ( 13.45068271796546178, -5.471508081941601098, 34.59228464037088457 ) ) ;
#43239 = EDGE_CURVE ( 'NONE', #37672, #16542, #13656, .T. ) ;
#43240 = CARTESIAN_POINT ( 'NONE',  ( 2.651650429449539104, -4.848349570550432475, 16.81250000000000000 ) ) ;
#43241 = ORIENTED_EDGE ( 'NONE', *, *, #43555, .F. ) ;
#43242 = VECTOR ( 'NONE', #47641, 1000.000000000000000 ) ;
#43243 = VECTOR ( 'NONE', #40685, 1000.000000000000000 ) ;
#43244 = ORIENTED_EDGE ( 'NONE', *, *, #86968, .F. ) ;
#43245 = CARTESIAN_POINT ( 'NONE',  ( -7.780898706641008467, -12.16647553114626490, 32.15551576947920864 ) ) ;
#43246 = ADVANCED_FACE ( 'NONE', ( #13915 ), #81505, .F. ) ;
#43247 = VERTEX_POINT ( 'NONE', #40522 ) ;
#43248 = CARTESIAN_POINT ( 'NONE',  ( -9.692307692307812417, -12.46129190930018460, 30.37095296980731973 ) ) ;
#43249 = CARTESIAN_POINT ( 'NONE',  ( 15.45354889974729673, -4.226511098958373402, 33.85474049983370293 ) ) ;
#43250 = LINE ( 'NONE', #41928, #22176 ) ;
#43251 = DIRECTION ( 'NONE',  ( 1.000000000000000000, 0.000000000000000000, 0.000000000000000000 ) ) ;
#43252 = CARTESIAN_POINT ( 'NONE',  ( 2.651650429449569302, -10.15165042944953733, 15.87500000000000000 ) ) ;
#43253 = VECTOR ( 'NONE', #47761, 1000.000000000000114 ) ;
#43254 = FACE_OUTER_BOUND ( 'NONE', #82320, .T. ) ;
#43255 = VERTEX_POINT ( 'NONE', #17686 ) ;
#43256 = CARTESIAN_POINT ( 'NONE',  ( 4.283893760101836534, -7.723484964179500700, 34.74522123443823318 ) ) ;
#43258 = ORIENTED_EDGE ( 'NONE', *, *, #78343, .T. ) ;
#43257 = CARTESIAN_POINT ( 'NONE',  ( 17.74999999999998224, -2.249999999999998668, 29.81609741502487054 ) ) ;
#43259 = CARTESIAN_POINT ( 'NONE',  ( -10.54931626438217585, -3.513871655860379306, 32.76840700105978499 ) ) ;
#43260 = DIRECTION ( 'NONE',  ( -0.000000000000000000, 0.3420201433256694901, -0.9396926207859082059 ) ) ;
#43261 = CARTESIAN_POINT ( 'NONE',  ( 6.222779668978068557, -9.418065098278011860, 34.63729479722530158 ) ) ;
#43262 = ADVANCED_FACE ( 'NONE', ( #20675 ), #54906, .F. ) ;
#43263 = CARTESIAN_POINT ( 'NONE',  ( -2.084679463598912097, -2.308499170217967134, 30.53291367094873721 ) ) ;
#43264 = DIRECTION ( 'NONE',  ( 0.000000000000000000, 0.000000000000000000, -1.000000000000000000 ) ) ;
#43265 = CARTESIAN_POINT ( 'NONE',  ( -0.4615384615384611200, -12.78798330534103123, 29.99999999999997868 ) ) ;
#43266 = CARTESIAN_POINT ( 'NONE',  ( -1.492201783934593573, -3.724691934501250135, 14.32999329374151465 ) ) ;
#43267 = ORIENTED_EDGE ( 'NONE', *, *, #12775, .T. ) ;
#43268 = ADVANCED_FACE ( 'NONE', ( #40085 ), #74296, .F. ) ;
#43269 = CARTESIAN_POINT ( 'NONE',  ( -3.165514091256391271, -6.835583212224609184, 34.95778746994559327 ) ) ;
#43270 = CARTESIAN_POINT ( 'NONE',  ( -1.384615384615505151, -12.27809138561165270, 31.22303859784587132 ) ) ;
#43271 = CARTESIAN_POINT ( 'NONE',  ( 1.944543648262996083, -5.555456351736983045, 21.81250000000000000 ) ) ;
#43272 = CARTESIAN_POINT ( 'NONE',  ( 14.30769230769231015, -5.415277668671390821, 36.20867863119892149 ) ) ;
#43273 = CARTESIAN_POINT ( 'NONE',  ( -2.980714810855778829, -10.82426656108011720, 33.81400080652039009 ) ) ;
#43274 = EDGE_LOOP ( 'NONE', ( #83645, #68285, #59049, #6494 ) ) ;
#43275 = CARTESIAN_POINT ( 'NONE',  ( 0.4615384615383382183, -4.320704448113951379, 33.92786785259630022 ) ) ;
#43276 = CARTESIAN_POINT ( 'NONE',  ( -3.480745961711583902, -10.66389620160130036, 33.62221079203477103 ) ) ;
#43277 = ORIENTED_EDGE ( 'NONE', *, *, #11939, .T. ) ;
#43278 = EDGE_CURVE ( 'NONE', #7349, #7411, #60773, .T. ) ;
#43279 = DIRECTION ( 'NONE',  ( -0.000000000000000000, 1.000000000000000000, 3.491481338843133355E-15 ) ) ;
#43280 = B_SPLINE_CURVE_WITH_KNOTS ( 'NONE', 3,
 ( #57372, #84867, #43859, #62788, #28587, #9631, #23150, #56051, #70004, #3315 ),
 .UNSPECIFIED., .F., .F.,
 ( 4, 2, 2, 2, 4 ),
 ( 0.0007817246256747530271, 0.0009771112852218978746, 0.001172497944769042939, 0.001367884604316188003, 0.001563271263863332851 ),
 .UNSPECIFIED. ) ;
#43281 = ORIENTED_EDGE ( 'NONE', *, *, #50072, .T. ) ;
#43282 = B_SPLINE_CURVE_WITH_KNOTS ( 'NONE', 3,
 ( #39081, #40846, #32749, #68312, #54789, #18800, #6172, #45815, #33197, #89049 ),
 .UNSPECIFIED., .F., .F.,
 ( 4, 2, 2, 2, 4 ),
 ( 0.0007817359430256386795, 0.0009771253907250069485, 0.001172514838424375217, 0.001367904286123743486, 0.001563293733823111755 ),
 .UNSPECIFIED. ) ;
#43283 = CARTESIAN_POINT ( 'NONE',  ( 7.053867364043876265, -3.957578996910242619, 33.62503395064540257 ) ) ;
#43284 = CARTESIAN_POINT ( 'NONE',  ( 16.94636248518114741, -2.504760397472873823, 29.97295953869789997 ) ) ;
#43285 = ADVANCED_FACE ( 'NONE', ( #47703 ), #53571, .F. ) ;
#43286 = CARTESIAN_POINT ( 'NONE',  ( -8.769230769230768274, -5.471508081941601098, 34.59228464037088457 ) ) ;
#43287 = DIRECTION ( 'NONE',  ( 0.000000000000000000, 0.7660444431189807890, 0.6427876096865361433 ) ) ;
#43289 = ORIENTED_EDGE ( 'NONE', *, *, #10065, .F. ) ;
#43288 = CIRCLE ( 'NONE', #79214, 2.750000000000000000 ) ;
#43290 = CARTESIAN_POINT ( 'NONE',  ( -3.100243792535585907, -2.372941743896878286, 30.88044141588254377 ) ) ;
#43291 = EDGE_LOOP ( 'NONE', ( #50898, #43008 ) ) ;
#43292 = CARTESIAN_POINT ( 'NONE',  ( -3.512820512820513663, -3.499999999999999556, 29.75000000000000355 ) ) ;
#43293 = CARTESIAN_POINT ( 'NONE',  ( 0.4615384615383382183, -10.33852847137269571, 34.16647553114546554 ) ) ;
#43294 = ORIENTED_EDGE ( 'NONE', *, *, #84200, .F. ) ;
#43295 = CARTESIAN_POINT ( 'NONE',  ( -5.999999999999998224, -11.16473453929635440, 33.15142922261926373 ) ) ;
#43297 = ADVANCED_FACE ( 'NONE', ( #32865 ), #6288, .F. ) ;
#43296 = DIRECTION ( 'NONE',  ( 0.000000000000000000, 0.000000000000000000, -1.000000000000000000 ) ) ;
#43298 = CARTESIAN_POINT ( 'NONE',  ( 8.769230769230768274, -2.249999999999998668, 29.50000000000001421 ) ) ;
#43299 = ADVANCED_FACE ( 'NONE', ( #81950 ), #88718, .F. ) ;
#43300 = DIRECTION ( 'NONE',  ( 0.000000000000000000, 1.000000000000000000, -8.673617379884028076E-17 ) ) ;
#43301 = CARTESIAN_POINT ( 'NONE',  ( -3.931066484868084299, -4.226511098958374291, 33.85474049983370293 ) ) ;
#43302 = ORIENTED_EDGE ( 'NONE', *, *, #30162, .F. ) ;
#43303 = ORIENTED_EDGE ( 'NONE', *, *, #22167, .T. ) ;
#43304 = AXIS2_PLACEMENT_3D ( 'NONE', #82491, #34731, #33841 ) ;
#43305 = FACE_BOUND ( 'NONE', #64337, .T. ) ;
#43306 = VERTEX_POINT ( 'NONE', #86151 ) ;
#43307 = CARTESIAN_POINT ( 'NONE',  ( 15.23076923076911093, -12.46129190930018460, 30.37095296980731973 ) ) ;
#43308 = VECTOR ( 'NONE', #904, 1000.000000000000114 ) ;
#43309 = VECTOR ( 'NONE', #60520, 1000.000000000000227 ) ;
#43310 = CARTESIAN_POINT ( 'NONE',  ( 6.673076923076905587, -2.249999999999999112, 29.81609741502488120 ) ) ;
#43311 = FACE_OUTER_BOUND ( 'NONE', #46219, .T. ) ;
#43312 = CARTESIAN_POINT ( 'NONE',  ( -2.057746898314262385, -10.18230066228895758, 34.26354781536631577 ) ) ;
#43313 = AXIS2_PLACEMENT_3D ( 'NONE', #82129, #48325, #68164 ) ;
#43314 = ORIENTED_EDGE ( 'NONE', *, *, #20534, .T. ) ;
#43315 = ORIENTED_EDGE ( 'NONE', *, *, #59387, .F. ) ;
#43316 = EDGE_LOOP ( 'NONE', ( #60005, #74828, #71908, #24590, #7540, #32187 ) ) ;
#43317 = CARTESIAN_POINT ( 'NONE',  ( 6.923076923076924238, -13.87047571288749737, 32.06866353760679544 ) ) ;
#43318 = CARTESIAN_POINT ( 'NONE',  ( 13.38461538461538680, -2.721908614388771852, 31.22303859784724978 ) ) ;
#43319 = CARTESIAN_POINT ( 'NONE',  ( 14.05766908347085042, -12.07920672191015221, 32.31858351112116168 ) ) ;
#43320 = CARTESIAN_POINT ( 'NONE',  ( -18.00000000000012079, -6.835583212225971650, 34.95778746994575670 ) ) ;
#43321 = EDGE_LOOP ( 'NONE', ( #3528, #45498, #43747, #63007 ) ) ;
#43323 = EDGE_CURVE ( 'NONE', #67903, #67434, #63101, .T. ) ;
#43322 = CARTESIAN_POINT ( 'NONE',  ( 16.37662582282421653, -2.353885683473779800, 30.79025554430704759 ) ) ;
#43324 = CARTESIAN_POINT ( 'NONE',  ( 10.61538461538449596, -2.625532179533778709, 30.86335684631627174 ) ) ;
#43325 = CARTESIAN_POINT ( 'NONE',  ( 4.153846153846154188, -2.486705287966279876, 31.30864560766543647 ) ) ;
#43326 = DIRECTION ( 'NONE',  ( 1.000000000000000000, 0.000000000000000000, -0.000000000000000000 ) ) ;
#43327 = ORIENTED_EDGE ( 'NONE', *, *, #26522, .T. ) ;
#43328 = ADVANCED_FACE ( 'NONE', ( #61652 ), #89158, .F. ) ;
#43329 = ORIENTED_EDGE ( 'NONE', *, *, #69050, .F. ) ;
#43330 = ORIENTED_EDGE ( 'NONE', *, *, #58099, .T. ) ;
#43332 = CARTESIAN_POINT ( 'NONE',  ( 1.634669804528839476, -11.47946981652013498, 33.17500667209846910 ) ) ;
#43331 = CARTESIAN_POINT ( 'NONE',  ( 12.33139125210024112, -6.852621066184266141, 34.70813303252209181 ) ) ;
#43333 = EDGE_CURVE ( 'NONE', #19690, #88317, #4075, .T. ) ;
#43334 = CARTESIAN_POINT ( 'NONE',  ( 16.02315468717859304, -5.582088688514999397, 34.36776431015576350 ) ) ;
#43335 = CARTESIAN_POINT ( 'NONE',  ( 1.576923076923075762, -11.50000000000000000, 29.75000000000000355 ) ) ;
#43336 = CARTESIAN_POINT ( 'NONE',  ( 15.23076923076923173, -12.34228464037088635, 31.77849191805839268 ) ) ;
#43337 = CARTESIAN_POINT ( 'NONE',  ( -2.530618525208453651, -9.886141570436013382, 34.14413921362392301 ) ) ;
#43338 = ORIENTED_EDGE ( 'NONE', *, *, #56315, .T. ) ;
#43339 = CARTESIAN_POINT ( 'NONE',  ( -7.596153846153909761, -7.565270000091922853, 34.99999999999999289 ) ) ;
#43340 = DIRECTION ( 'NONE',  ( -0.000000000000000000, -0.8660254037844397068, -0.4999999999999978906 ) ) ;
#43341 = LINE ( 'NONE', #78445, #12818 ) ;
#43342 = CARTESIAN_POINT ( 'NONE',  ( -11.40766973063675493, -3.530189275343204702, 32.79018710029569661 ) ) ;
#43343 = AXIS2_PLACEMENT_3D ( 'NONE', #3701, #23970, #10477 ) ;
#43344 = ORIENTED_EDGE ( 'NONE', *, *, #51805, .T. ) ;
#43345 = ADVANCED_FACE ( 'NONE', ( #55343 ), #35525, .T. ) ;
#43346 = CARTESIAN_POINT ( 'NONE',  ( -18.25002323729296450, -8.432397168068783699, 34.66272746175022945 ) ) ;
#43347 = ORIENTED_EDGE ( 'NONE', *, *, #76416, .F. ) ;
#43348 = FACE_BOUND ( 'NONE', #10071, .T. ) ;
#43349 = CARTESIAN_POINT ( 'NONE',  ( -16.85391172531022619, -4.187068189119696804, 33.49521262558774026 ) ) ;
#43350 = LINE ( 'NONE', #14546, #13259 ) ;
#43351 = DIRECTION ( 'NONE',  ( -0.000000000000000000, 0.9848077530122085754, -0.1736481776669273613 ) ) ;
#43352 = ORIENTED_EDGE ( 'NONE', *, *, #64115, .T. ) ;
#43353 = DIRECTION ( 'NONE',  ( 1.000000000000000000, 0.000000000000000000, 0.000000000000000000 ) ) ;
#43354 = CARTESIAN_POINT ( 'NONE',  ( -17.75005459062195712, -4.176053281294518804, 33.81426240980091791 ) ) ;
#43355 = CARTESIAN_POINT ( 'NONE',  ( 8.639082799499073317, -8.630895178749533159, 34.87696386517710323 ) ) ;
#43356 = CARTESIAN_POINT ( 'NONE',  ( -7.173053654019277303, -10.66389620160130036, 33.62221079203477103 ) ) ;
#43357 = ORIENTED_EDGE ( 'NONE', *, *, #6285, .F. ) ;
#43358 = CARTESIAN_POINT ( 'NONE',  ( -9.822998295418001291, -2.845849958028613624, 32.17971566917920967 ) ) ;
#43359 = ORIENTED_EDGE ( 'NONE', *, *, #65055, .T. ) ;
#43361 = VERTEX_POINT ( 'NONE', #62103 ) ;
#43360 = PLANE ( 'NONE',  #10797 ) ;
#43362 = CARTESIAN_POINT ( 'NONE',  ( -8.639183162975086816, -7.723484964179501588, 34.74522123443823318 ) ) ;
#43363 = CARTESIAN_POINT ( 'NONE',  ( -6.857008572074483332, -11.69971097300155272, 32.46337939537588113 ) ) ;
#43364 = CARTESIAN_POINT ( 'NONE',  ( 4.946775107191377252, -2.647304123082328875, 31.75400227202885262 ) ) ;
#43365 = CARTESIAN_POINT ( 'NONE',  ( 12.71159277317677549, -4.235687564193448829, 33.53795663066793509 ) ) ;
#43367 = CARTESIAN_POINT ( 'NONE',  ( -15.23076923076935074, -6.026961402154118019, 34.52809138561165270 ) ) ;
#43366 = CARTESIAN_POINT ( 'NONE',  ( -14.30769230769230660, -8.164416787775445883, 34.95778746994557906 ) ) ;
#43368 = CARTESIAN_POINT ( 'NONE',  ( 5.999999999999880096, -2.892918686052165622, 31.69288490824153470 ) ) ;
#43369 = CARTESIAN_POINT ( 'NONE',  ( 1.944543648262996083, -5.555456351736983045, 21.81250000000000000 ) ) ;
#43370 = ORIENTED_EDGE ( 'NONE', *, *, #1090, .T. ) ;
#43371 = EDGE_CURVE ( 'NONE', #50664, #23467, #56728, .T. ) ;
#43372 = CARTESIAN_POINT ( 'NONE',  ( 11.53846153846141576, -4.320704448113951379, 33.92786785259630022 ) ) ;
#43373 = LINE ( 'NONE', #23531, #87006 ) ;
#43374 = EDGE_LOOP ( 'NONE', ( #26278, #38036, #84408, #52406 ) ) ;
#43375 = B_SPLINE_CURVE_WITH_KNOTS ( 'NONE', 3,
 ( #47135, #46701, #13359, #80952, #19237, #26439, #67862, #19671, #81830, #89043 ),
 .UNSPECIFIED., .F., .F.,
 ( 4, 2, 2, 2, 4 ),
 ( 0.0007817246256747457630, 0.0009771112852218887673, 0.001172497944769031880, 0.001367884604316174993, 0.001563271263863318106 ),
 .UNSPECIFIED. ) ;
#43376 = ORIENTED_EDGE ( 'NONE', *, *, #2088, .T. ) ;
#43377 = VERTEX_POINT ( 'NONE', #83273 ) ;
#43378 = DIRECTION ( 'NONE',  ( -0.000000000000000000, 0.8660254037844397068, -0.4999999999999978906 ) ) ;
#43379 = LINE ( 'NONE', #78046, #44701 ) ;
#43380 = AXIS2_PLACEMENT_3D ( 'NONE', #43317, #78864, #79321 ) ;
#43381 = DIRECTION ( 'NONE',  ( -0.000000000000000000, -0.000000000000000000, -1.000000000000000000 ) ) ;
#43382 = CARTESIAN_POINT ( 'NONE',  ( 8.899756207464411872, -11.66157788607254098, 32.95092075102925833 ) ) ;
#43383 = FACE_OUTER_BOUND ( 'NONE', #18582, .T. ) ;
#43384 = ADVANCED_FACE ( 'NONE', ( #68859 ), #28314, .F. ) ;
#43385 = DIRECTION ( 'NONE',  ( 0.000000000000000000, 0.000000000000000000, -1.000000000000000000 ) ) ;
#43386 = CYLINDRICAL_SURFACE ( 'NONE', #53712, 0.2499999999999995559 ) ;
#43387 = EDGE_LOOP ( 'NONE', ( #81080, #57068, #9280, #83190 ) ) ;
#43388 = CARTESIAN_POINT ( 'NONE',  ( 11.25641025641025550, -3.499999999999999556, 29.75000000000000355 ) ) ;
#43389 = CARTESIAN_POINT ( 'NONE',  ( -1.450698795571264021, -6.386643153685125363, 34.62446782046654903 ) ) ;
#43390 = EDGE_CURVE ( 'NONE', #47437, #20712, #64329, .T. ) ;
#43391 = EDGE_CURVE ( 'NONE', #56650, #36450, #49483, .T. ) ;
#43392 = CARTESIAN_POINT ( 'NONE',  ( 7.846153846153846700, -2.721908614388771852, 31.22303859784724978 ) ) ;
#43393 = CARTESIAN_POINT ( 'NONE',  ( 17.99999999999987566, -12.27809138561165270, 31.22303859784587132 ) ) ;
#43394 = VERTEX_POINT ( 'NONE', #55783 ) ;
#43395 = CARTESIAN_POINT ( 'NONE',  ( 12.33139049180676672, -9.504002272028875709, 34.60269587691767867 ) ) ;
#43396 =( LENGTH_UNIT ( ) NAMED_UNIT ( * ) SI_UNIT ( .MILLI., .METRE. ) );
#43397 = CARTESIAN_POINT ( 'NONE',  ( 11.66898724022509981, -10.19071101563364756, 33.96452234770658407 ) ) ;
#43398 = DIRECTION ( 'NONE',  ( -0.000000000000000000, -0.9848077530122086864, -0.1736481776669273613 ) ) ;
#43399 = EDGE_LOOP ( 'NONE', ( #41197, #84765, #39002, #24868 ) ) ;
#43401 = EDGE_CURVE ( 'NONE', #85626, #87991, #72837, .T. ) ;
#43400 = CARTESIAN_POINT ( 'NONE',  ( -2.373774687052440768, -6.343179335718451384, 34.87096338111212646 ) ) ;
#43402 = CARTESIAN_POINT ( 'NONE',  ( -12.59201516965492473, -7.276988635370452485, 34.74523720219453793 ) ) ;
#43403 = B_SPLINE_CURVE_WITH_KNOTS ( 'NONE', 3,
 ( #67208, #80279, #5509, #39298, #4152, #18132, #3708, #66754, #18575, #87053 ),
 .UNSPECIFIED., .F., .F.,
 ( 4, 2, 2, 2, 4 ),
 ( 0.000000000000000000, 0.0001954311564186868202, 0.0003908623128373736404, 0.0005862934692560604335, 0.0007817246256747472808 ),
 .UNSPECIFIED. ) ;
#43404 = VECTOR ( 'NONE', #22178, 1000.000000000000000 ) ;
#43405 = CARTESIAN_POINT ( 'NONE',  ( -8.769230769230892619, -9.528491918059723176, 34.59228464037033035 ) ) ;
#43406 = ADVANCED_FACE ( 'NONE', ( #35972 ), #41846, .F. ) ;
#43407 = EDGE_CURVE ( 'NONE', #5574, #82155, #29222, .T. ) ;
#43408 = EDGE_LOOP ( 'NONE', ( #31278, #66746, #30871, #89025 ) ) ;
#43409 = B_SPLINE_CURVE_WITH_KNOTS ( 'NONE', 3,
 ( #72634, #79405, #47723, #52804, #17706, #34204, #45160, #80297, #81969, #46055 ),
 .UNSPECIFIED., .F., .F.,
 ( 4, 2, 2, 2, 4 ),
 ( 0.0007817246256747446788, 0.0009771112852218879000, 0.001172497944769031013, 0.001367884604316174126, 0.001563271263863317238 ),
 .UNSPECIFIED. ) ;
#43410 = CARTESIAN_POINT ( 'NONE',  ( -10.74594520712653534, -2.504760397472875155, 29.97295953869789997 ) ) ;
#43411 = VERTEX_POINT ( 'NONE', #76952 ) ;
#43412 = AXIS2_PLACEMENT_3D ( 'NONE', #45596, #73074, #39749 ) ;
#43413 = B_SPLINE_CURVE_WITH_KNOTS ( 'NONE', 3,
 ( #26486, #53947, #89093, #15627, #62033, #28244, #56609, #49414, #69677, #63359 ),
 .UNSPECIFIED., .F., .F.,
 ( 4, 2, 2, 2, 4 ),
 ( 0.0007817359430256297891, 0.0009771253907249961065, 0.001172514838424362424, 0.001367904286123728741, 0.001563293733823095059 ),
 .UNSPECIFIED. ) ;
#43414 = ADVANCED_FACE ( 'NONE', ( #82834 ), #77389, .F. ) ;
#43415 = B_SPLINE_CURVE_WITH_KNOTS ( 'NONE', 3,
 ( #59431, #52666, #18009, #59875, #79265, #45464, #72049, #38717, #3142, #58090 ),
 .UNSPECIFIED., .F., .F.,
 ( 4, 2, 2, 2, 4 ),
 ( 0.000000000000000000, 0.0001954339857564081791, 0.0003908679715128163582, 0.0005863019572692245102, 0.0007817359430256327164 ),
 .UNSPECIFIED. ) ;
#43416 = DIRECTION ( 'NONE',  ( -0.000000000000000000, -0.000000000000000000, -1.000000000000000000 ) ) ;
#43417 = CARTESIAN_POINT ( 'NONE',  ( 7.173131342990374471, -2.920487667080175154, 32.31805714834170828 ) ) ;
#43418 = CARTESIAN_POINT ( 'NONE',  ( -8.096177070375304652, -2.588893531581426988, 31.60682220781847818 ) ) ;
#43419 = CARTESIAN_POINT ( 'NONE',  ( 1.384615384615264011, -8.656820664282941280, 34.87096338111179961 ) ) ;
#43420 = CARTESIAN_POINT ( 'NONE',  ( -3.480769230769229061, -7.500000000000001776, 35.00000000000000000 ) ) ;
#43421 = ORIENTED_EDGE ( 'NONE', *, *, #1312, .F. ) ;
#43422 = ORIENTED_EDGE ( 'NONE', *, *, #34535, .F. ) ;
#43423 = EDGE_LOOP ( 'NONE', ( #87285, #22786 ) ) ;
#43424 = CYLINDRICAL_SURFACE ( 'NONE', #73218, 0.2499999999999979738 ) ;
#43425 = CARTESIAN_POINT ( 'NONE',  ( 15.93091919493930320, -5.582147617184174848, 34.63737895849758530 ) ) ;
#43426 = CARTESIAN_POINT ( 'NONE',  ( -12.94230769230769162, -7.500000000000000000, 33.75000000000000000 ) ) ;
#43427 = EDGE_CURVE ( 'NONE', #54250, #54586, #52413, .T. ) ;
#43428 = VECTOR ( 'NONE', #49554, 1000.000000000000000 ) ;
#43429 = CARTESIAN_POINT ( 'NONE',  ( -2.177166869458664333, -11.66157788607254275, 32.95092075102925833 ) ) ;
#43430 = VECTOR ( 'NONE', #6425, 1000.000000000000000 ) ;
#43431 = CARTESIAN_POINT ( 'NONE',  ( 4.284371855609715674, -6.852161475712352789, 34.70806712695775786 ) ) ;
#43432 = CARTESIAN_POINT ( 'NONE',  ( 5.207448778686637247, -10.19071101563364756, 33.96452234770658407 ) ) ;
#43433 = ORIENTED_EDGE ( 'NONE', *, *, #47154, .T. ) ;
#43434 = ORIENTED_EDGE ( 'NONE', *, *, #26554, .T. ) ;
#43435 = B_SPLINE_CURVE_WITH_KNOTS ( 'NONE', 3,
 ( #65912, #59162, #80343, #72232, #33033, #3775, #88011, #66817, #24483, #11883 ),
 .UNSPECIFIED., .F., .F.,
 ( 4, 2, 2, 2, 4 ),
 ( 0.000000000000000000, 0.0001954311564186868744, 0.0003908623128373737488, 0.0005862934692560606504, 0.0007817246256747474977 ),
 .UNSPECIFIED. ) ;
#43436 = ORIENTED_EDGE ( 'NONE', *, *, #40666, .F. ) ;
#43438 = ORIENTED_EDGE ( 'NONE', *, *, #53817, .T. ) ;
#43437 = CARTESIAN_POINT ( 'NONE',  ( 12.52679403281448600, -8.613356846314928816, 34.62446782046653482 ) ) ;
#43440 = DIRECTION ( 'NONE',  ( -0.000000000000000000, -0.3420201433256694346, -0.9396926207859080948 ) ) ;
#43439 = CARTESIAN_POINT ( 'NONE',  ( 8.900022577055551665, -8.147973898785416225, 34.70805048591653730 ) ) ;
#43441 = CARTESIAN_POINT ( 'NONE',  ( 1.553300858899086867, -3.749999999999992006, 22.98437500000000000 ) ) ;
#43442 = VERTEX_POINT ( 'NONE', #51665 ) ;
#43443 = EDGE_LOOP ( 'NONE', ( #35555, #10615, #74761, #35768 ) ) ;
#43444 = CARTESIAN_POINT ( 'NONE',  ( 13.38461538461569411, -2.506253911140615021, 30.00000000000323297 ) ) ;
#43445 = VERTEX_POINT ( 'NONE', #16133 ) ;
#43446 = FACE_BOUND ( 'NONE', #57178, .T. ) ;
#43447 = CARTESIAN_POINT ( 'NONE',  ( 13.60762822870878352, -12.38742843783360748, 31.66772728687926985 ) ) ;
#43448 = CARTESIAN_POINT ( 'NONE',  ( -14.37296230824862775, -6.835583212224499938, 34.95778746994557906 ) ) ;
#43449 = ORIENTED_EDGE ( 'NONE', *, *, #6928, .T. ) ;
#43450 = CARTESIAN_POINT ( 'NONE',  ( -14.24243716817947281, -8.656820664281605460, 34.87096338111211224 ) ) ;
#43451 = CARTESIAN_POINT ( 'NONE',  ( 16.21910172512217585, -4.481592998940251427, 33.73612834413965089 ) ) ;
#43452 = CARTESIAN_POINT ( 'NONE',  ( -10.28846153846153832, -11.50000000000000000, 29.75000000000000355 ) ) ;
#43453 = CARTESIAN_POINT ( 'NONE',  ( -11.78848477575450460, -5.851115903089112003, 34.47074536777953568 ) ) ;
#43454 = FACE_OUTER_BOUND ( 'NONE', #68194, .T. ) ;
#43455 = EDGE_CURVE ( 'NONE', #56514, #17995, #84659, .T. ) ;
#43456 = CIRCLE ( 'NONE', #4634, 0.2500000000000002220 ) ;
#43457 = CYLINDRICAL_SURFACE ( 'NONE', #89063, 4.000000000000000000 ) ;
#43458 = CARTESIAN_POINT ( 'NONE',  ( -7.596099534515530216, -6.567000820036036579, 34.66262288849541306 ) ) ;
#43459 = CARTESIAN_POINT ( 'NONE',  ( 0.3954550505825793483, -11.69971097300155272, 32.46337939537587403 ) ) ;
#43460 = CARTESIAN_POINT ( 'NONE',  ( 13.45068271796546178, -2.292212530054420494, 30.41441678777542990 ) ) ;
#43461 = CYLINDRICAL_SURFACE ( 'NONE', #47329, 0.2500000000000008882 ) ;
#43462 = FACE_BOUND ( 'NONE', #71545, .T. ) ;
#43464 = CARTESIAN_POINT ( 'NONE',  ( 2.307692307692309264, -9.780366693483667717, 34.19971097300155094 ) ) ;
#43463 = CARTESIAN_POINT ( 'NONE',  ( -13.60810030917971858, -4.225889041578353655, 33.85425143139329407 ) ) ;
#43465 = CARTESIAN_POINT ( 'NONE',  ( -0.2115930521604184600, -8.476813868363244353, 34.90874843262270133 ) ) ;
#43467 = CARTESIAN_POINT ( 'NONE',  ( -6.130691466667557599, -4.809359713505814149, 33.96456829005828837 ) ) ;
#43466 = DIRECTION ( 'NONE',  ( 0.000000000000000000, 0.1736481776669267785, -0.9848077530122087975 ) ) ;
#43468 = VECTOR ( 'NONE', #2072, 1000.000000000000227 ) ;
#43469 = CARTESIAN_POINT ( 'NONE',  ( -2.531177232256636156, -5.827078755546623690, 34.72654668319379567 ) ) ;
#43470 = CARTESIAN_POINT ( 'NONE',  ( -2.749999999999997780, -7.561099074964547917, 22.34188170625849068 ) ) ;
#43471 = VERTEX_POINT ( 'NONE', #24208 ) ;
#43472 = CARTESIAN_POINT ( 'NONE',  ( -4.153846153846274980, -5.941354392335915335, 34.76329471203413846 ) ) ;
#43473 = EDGE_LOOP ( 'NONE', ( #79764, #28963 ) ) ;
#43474 = B_SPLINE_CURVE_WITH_KNOTS ( 'NONE', 3,
 ( #57247, #78391, #16693, #36960, #42854, #44149, #8628, #15826, #51335, #3179 ),
 .UNSPECIFIED., .F., .F.,
 ( 4, 2, 2, 2, 4 ),
 ( 0.0007817246256747427272, 0.0009771112852218844305, 0.001172497944769026242, 0.001367884604316168054, 0.001563271263863309649 ),
 .UNSPECIFIED. ) ;
#43475 = DIRECTION ( 'NONE',  ( 0.000000000000000000, 0.8660254037844377084, 0.5000000000000015543 ) ) ;
#43476 = EDGE_LOOP ( 'NONE', ( #12193, #73686 ) ) ;
#43477 = B_SPLINE_CURVE_WITH_KNOTS ( 'NONE', 3,
 ( #23186, #28622, #50648, #22300, #78127, #77240, #16430, #43897, #9669, #64598 ),
 .UNSPECIFIED., .F., .F.,
 ( 4, 2, 2, 2, 4 ),
 ( 0.000000000000000000, 0.0001954311564186862781, 0.0003908623128373725562, 0.0005862934692560588072, 0.0007817246256747451124 ),
 .UNSPECIFIED. ) ;
#43478 = EDGE_CURVE ( 'NONE', #61793, #30720, #48113, .T. ) ;
#43479 = DIRECTION ( 'NONE',  ( 0.000000000000000000, 0.000000000000000000, 1.000000000000000000 ) ) ;
#43480 = EDGE_LOOP ( 'NONE', ( #77665, #9035 ) ) ;
#43481 = CYLINDRICAL_SURFACE ( 'NONE', #54137, 0.2499999999999993616 ) ;
#43482 = CARTESIAN_POINT ( 'NONE',  ( -2.724691934501232371, -8.700186371490559623, 24.76375670625848713 ) ) ;
#43483 = CARTESIAN_POINT ( 'NONE',  ( 17.14299142792551578, -8.120952969808772792, 34.71129190929999453 ) ) ;
#43484 = EDGE_CURVE ( 'NONE', #47571, #86693, #6170, .T. ) ;
#43485 = CARTESIAN_POINT ( 'NONE',  ( 13.38461538461538680, -2.833524468853757305, 32.15551576947925838 ) ) ;
#43486 = CARTESIAN_POINT ( 'NONE',  ( 16.08776377448601735, -8.164416787775445883, 34.95778746994557906 ) ) ;
#43487 = CARTESIAN_POINT ( 'NONE',  ( -16.37733107841048508, -10.23692288466677880, 34.23039457007281072 ) ) ;
#43488 = CARTESIAN_POINT ( 'NONE',  ( -13.60754234352223158, -8.282780595021769443, 34.94152052738834158 ) ) ;
#43489 = CARTESIAN_POINT ( 'NONE',  ( 4.826899839630110378, -8.432397168068783699, 34.66272746175022945 ) ) ;
#43490 = CARTESIAN_POINT ( 'NONE',  ( 2.651650429449539104, -4.848349570550432475, 14.31250000000000000 ) ) ;
#43491 = B_SPLINE_CURVE_WITH_KNOTS ( 'NONE', 3,
 ( #30300, #83934, #77159, #23098, #22217, #64955, #57767, #63638, #50561, #2368 ),
 .UNSPECIFIED., .F., .F.,
 ( 4, 2, 2, 2, 4 ),
 ( 0.000000000000000000, 0.0001954339857564072033, 0.0003908679715128144066, 0.0005863019572692215828, 0.0007817359430256288133 ),
 .UNSPECIFIED. ) ;
#43492 = FACE_OUTER_BOUND ( 'NONE', #55978, .T. ) ;
#43493 = CARTESIAN_POINT ( 'NONE',  ( 15.84615384615384670, -3.499999999999999556, 29.75000000000000355 ) ) ;
#43494 = EDGE_CURVE ( 'NONE', #28603, #15849, #45366, .T. ) ;
#43495 = CARTESIAN_POINT ( 'NONE',  ( 6.923076923076924238, -2.486705287966279876, 31.30864560766543647 ) ) ;
#43496 = CARTESIAN_POINT ( 'NONE',  ( -1.553300858899081538, -11.25000000000000711, 14.85937500000000355 ) ) ;
#43497 = VECTOR ( 'NONE', #36614, 1000.000000000000000 ) ;
#43498 = CARTESIAN_POINT ( 'NONE',  ( -14.30769230769230660, -10.51840700105979565, 33.73612834413961536 ) ) ;
#43499 = VECTOR ( 'NONE', #28340, 1000.000000000000000 ) ;
#43500 = ORIENTED_EDGE ( 'NONE', *, *, #86178, .T. ) ;
#43501 = CARTESIAN_POINT ( 'NONE',  ( 14.43848411551709709, -4.809403383903225304, 33.96459661697924304 ) ) ;
#43502 = CARTESIAN_POINT ( 'NONE',  ( -11.28840722682322628, -8.303483539816728154, 34.68545999027711702 ) ) ;
#43503 = CARTESIAN_POINT ( 'NONE',  ( 9.757563263583719504, -6.879047030191282275, 34.71129190930002295 ) ) ;
#43504 = CARTESIAN_POINT ( 'NONE',  ( 15.00788971403164496, -7.630690623152299956, 34.99857592706774057 ) ) ;
#43505 = CARTESIAN_POINT ( 'NONE',  ( 13.63466969625370062, -2.564540009722896752, 30.55348353981670684 ) ) ;
#43506 = VECTOR ( 'NONE', #53916, 1000.000000000000000 ) ;
#43507 = CARTESIAN_POINT ( 'NONE',  ( -14.08467946359890988, -4.026326845037962343, 33.68677907613344047 ) ) ;
#43508 = DIRECTION ( 'NONE',  ( 0.000000000000000000, 0.6427876096865368094, 0.7660444431189802339 ) ) ;
#43509 = EDGE_CURVE ( 'NONE', #33104, #56650, #19088, .T. ) ;
#43510 = ORIENTED_EDGE ( 'NONE', *, *, #65273, .F. ) ;
#43511 = EDGE_LOOP ( 'NONE', ( #11425, #15283, #37787, #8600 ) ) ;
#43512 = EDGE_LOOP ( 'NONE', ( #52927, #37560 ) ) ;
#43513 = CARTESIAN_POINT ( 'NONE',  ( 6.222962903561486847, -7.369474270740069777, 34.74850911626239736 ) ) ;
#43514 = CYLINDRICAL_SURFACE ( 'NONE', #60471, 0.2499999999999997502 ) ;
#43515 = CARTESIAN_POINT ( 'NONE',  ( 1.384615384615265343, -12.46129190930018460, 30.37095296980731973 ) ) ;
#43516 = CARTESIAN_POINT ( 'NONE',  ( 10.74617505635156789, -9.929761469519743144, 34.40412654351204225 ) ) ;
#43517 = VERTEX_POINT ( 'NONE', #3933 ) ;
#43518 = LINE ( 'NONE', #80316, #68005 ) ;
#43519 = EDGE_LOOP ( 'NONE', ( #11422, #29997 ) ) ;
#43520 = VERTEX_POINT ( 'NONE', #57555 ) ;
#43521 = CARTESIAN_POINT ( 'NONE',  ( 0.4615384615384611755, -1.367168528481310208, 33.57946703557072254 ) ) ;
#43522 = LINE ( 'NONE', #66464, #63231 ) ;
#43523 = B_SPLINE_CURVE_WITH_KNOTS ( 'NONE', 3,
 ( #36284, #25316, #30405, #63741, #44341, #57872, #46027, #11809, #2916, #87482 ),
 .UNSPECIFIED., .F., .F.,
 ( 4, 2, 2, 2, 4 ),
 ( 0.000000000000000000, 0.0001954339857564074473, 0.0003908679715128148945, 0.0005863019572692223418, 0.0007817359430256297891 ),
 .UNSPECIFIED. ) ;
#43524 = FACE_OUTER_BOUND ( 'NONE', #48613, .T. ) ;
#43525 = DIRECTION ( 'NONE',  ( 0.000000000000000000, 0.6427876096865368094, 0.7660444431189802339 ) ) ;
#43526 = CARTESIAN_POINT ( 'NONE',  ( -12.46153846153815437, -2.506253911140614576, 30.00000000000323297 ) ) ;
#43527 = ORIENTED_EDGE ( 'NONE', *, *, #48854, .T. ) ;
#43528 = ORIENTED_EDGE ( 'NONE', *, *, #84415, .T. ) ;
#43529 = CARTESIAN_POINT ( 'NONE',  ( 3.750000000000000888, -7.499999999999978684, 19.46875000000000000 ) ) ;
#43530 = EDGE_LOOP ( 'NONE', ( #71010, #57815, #5348, #73885 ) ) ;
#43532 = ORIENTED_EDGE ( 'NONE', *, *, #50296, .T. ) ;
#43531 = CARTESIAN_POINT ( 'NONE',  ( 1.319344938654610999, -8.613356846314824011, 34.62446782046655613 ) ) ;
#43533 = LINE ( 'NONE', #31812, #52188 ) ;
#43534 = CARTESIAN_POINT ( 'NONE',  ( 4.853996859406925601, -3.586966769969700763, 32.86292498521069660 ) ) ;
#43535 = CARTESIAN_POINT ( 'NONE',  ( 2.307692307692309264, -9.058645607665452459, 34.76329471203371924 ) ) ;
#43536 = EDGE_LOOP ( 'NONE', ( #25429, #42307, #72915, #52916 ) ) ;
#43537 = CARTESIAN_POINT ( 'NONE',  ( -16.15384615384615330, -6.681629849574314051, 35.83090037661290239 ) ) ;
#43538 = CARTESIAN_POINT ( 'NONE',  ( 4.946363163309711375, -2.254533558242299396, 29.97296025877828285 ) ) ;
#43539 = ORIENTED_EDGE ( 'NONE', *, *, #25814, .F. ) ;
#43540 = FACE_BOUND ( 'NONE', #657, .T. ) ;
#43541 = CARTESIAN_POINT ( 'NONE',  ( 11.28843830116857383, -5.056417327199099532, 34.11270091957321426 ) ) ;
#43542 = CARTESIAN_POINT ( 'NONE',  ( -19.50000000000000000, -11.50000000000000000, 29.75000000000000355 ) ) ;
#43543 = VECTOR ( 'NONE', #33519, 1000.000000000000000 ) ;
#43544 = CARTESIAN_POINT ( 'NONE',  ( -17.77722033102192967, -2.612705202774696200, 31.66806509827799943 ) ) ;
#43546 = DIRECTION ( 'NONE',  ( -0.000000000000000000, 0.3420201433256694901, -0.9396926207859082059 ) ) ;
#43545 = FACE_OUTER_BOUND ( 'NONE', #58307, .T. ) ;
#43547 = AXIS2_PLACEMENT_3D ( 'NONE', #34770, #61791, #74435 ) ;
#43548 = CARTESIAN_POINT ( 'NONE',  ( -1.318548051265307830, -8.164416787775445883, 34.95778746994558617 ) ) ;
#43549 = CARTESIAN_POINT ( 'NONE',  ( -39.05038313613820122, -2.499999999999999556, 29.75000000000000355 ) ) ;
#43550 = ORIENTED_EDGE ( 'NONE', *, *, #20204, .F. ) ;
#43551 = CARTESIAN_POINT ( 'NONE',  ( -10.68065506134539078, -10.21337939537584383, 33.94971097300158647 ) ) ;
#43552 = CARTESIAN_POINT ( 'NONE',  ( 5.076923076922953193, -4.320704448113951379, 33.92786785259630022 ) ) ;
#43553 = EDGE_LOOP ( 'NONE', ( #71379, #85278, #68672, #26294 ) ) ;
#43554 = AXIS2_PLACEMENT_3D ( 'NONE', #19371, #79748, #32443 ) ;
#43555 = EDGE_CURVE ( 'NONE', #67271, #40972, #43629, .T. ) ;
#43556 = LINE ( 'NONE', #36801, #12036 ) ;
#43557 = CARTESIAN_POINT ( 'NONE',  ( 10.48469314871705826, -6.413092428213692742, 34.63065189839063152 ) ) ;
#43558 = CARTESIAN_POINT ( 'NONE',  ( 18.00000000000000000, -12.09954503811598769, 35.62045528018868623 ) ) ;
#43559 = CARTESIAN_POINT ( 'NONE',  ( -5.076923076923197442, -11.94971097300221174, 32.03036669348237098 ) ) ;
#43560 = CARTESIAN_POINT ( 'NONE',  ( -10.55012947587177941, -3.083524468853784839, 32.58852847137153930 ) ) ;
#43561 = CARTESIAN_POINT ( 'NONE',  ( -8.068981943788728017, -7.369209533119140509, 34.99857337881830688 ) ) ;
#43562 = FACE_BOUND ( 'NONE', #57850, .T. ) ;
#43564 = CARTESIAN_POINT ( 'NONE',  ( 17.07692307692307665, -6.435427911321262684, 35.78748833219616898 ) ) ;
#43563 = CARTESIAN_POINT ( 'NONE',  ( 14.30769230769231015, -8.564572088678739092, 35.78748833219616898 ) ) ;
#43565 = CARTESIAN_POINT ( 'NONE',  ( -6.792285115252136407, -10.54018710029568595, 33.71981072465678864 ) ) ;
#43567 = CARTESIAN_POINT ( 'NONE',  ( 6.923076923076924238, -12.37446782046654192, 30.86335684631486131 ) ) ;
#43566 = CARTESIAN_POINT ( 'NONE',  ( -11.00641025641025550, -4.000000000000000000, 29.75000000000000355 ) ) ;
#43568 = DIRECTION ( 'NONE',  ( -0.000000000000000000, -0.000000000000000000, -1.000000000000000000 ) ) ;
#43569 = B_SPLINE_CURVE_WITH_KNOTS ( 'NONE', 3,
 ( #45124, #72599, #23960, #58636, #18557, #78464, #57759, #52770, #31163, #38832 ),
 .UNSPECIFIED., .F., .F.,
 ( 4, 2, 2, 2, 4 ),
 ( 0.0007817359430256318490, 0.0009771253907249984917, 0.001172514838424365026, 0.001367904286123731560, 0.001563293733823098311 ),
 .UNSPECIFIED. ) ;
#43570 = CARTESIAN_POINT ( 'NONE',  ( -2.608446859217889546, -10.19485399968121264, 18.43563170625848713 ) ) ;
#43571 = EDGE_LOOP ( 'NONE', ( #77833, #35143, #66958, #80974 ) ) ;
#43572 = ADVANCED_FACE ( 'NONE', ( #23323 ), #50781, .F. ) ;
#43573 = CARTESIAN_POINT ( 'NONE',  ( -4.403822884788507253, -11.79746400365624659, 32.30657167506340954 ) ) ;
#43574 = LINE ( 'NONE', #9791, #51252 ) ;
#43575 = CARTESIAN_POINT ( 'NONE',  ( -7.623374177175780808, -11.60474049983371003, 33.02348890104160262 ) ) ;
#43576 = CARTESIAN_POINT ( 'NONE',  ( 10.86538461538461675, -2.499999999999998668, 29.75000000000000355 ) ) ;
#43577 = ADVANCED_FACE ( 'NONE', ( #30528 ), #6174, .F. ) ;
#43578 = LINE ( 'NONE', #17445, #5461 ) ;
#43579 = CARTESIAN_POINT ( 'NONE',  ( 3.775308065498768517, -8.992201783934554271, 19.29500670625849068 ) ) ;
#43580 = CARTESIAN_POINT ( 'NONE',  ( -11.66907119366561396, -7.722926974430166069, 34.99546784045485737 ) ) ;
#43581 = CARTESIAN_POINT ( 'NONE',  ( -19.50000000000000000, -3.499999999999999556, 29.75000000000000355 ) ) ;
#43582 = AXIS2_PLACEMENT_3D ( 'NONE', #51438, #10495, #22669 ) ;
#43583 = CARTESIAN_POINT ( 'NONE',  ( -7.911423846710166075, -3.083524468853724443, 32.58852847137143272 ) ) ;
#43584 = DIRECTION ( 'NONE',  ( -0.000000000000000000, -0.6427876096865404731, -0.7660444431189771253 ) ) ;
#43585 = DIRECTION ( 'NONE',  ( 0.000000000000000000, 0.000000000000000000, -1.000000000000000000 ) ) ;
#43586 = CARTESIAN_POINT ( 'NONE',  ( 3.930919936330007136, -10.61292498521070549, 33.66303323003028680 ) ) ;
#43587 = VECTOR ( 'NONE', #23698, 1000.000000000000000 ) ;
#43588 = CARTESIAN_POINT ( 'NONE',  ( 10.83881101429940408, -7.630147987733840509, 34.99859428049665411 ) ) ;
#43589 = EDGE_CURVE ( 'NONE', #78986, #69985, #62918, .T. ) ;
#43590 = CARTESIAN_POINT ( 'NONE',  ( 17.20744851515672025, -2.647132371071621471, 31.75357179365173010 ) ) ;
#43591 = ORIENTED_EDGE ( 'NONE', *, *, #21788, .F. ) ;
#43592 = CARTESIAN_POINT ( 'NONE',  ( 3.480823650682684622, -12.41089969410671223, 31.60739465890703670 ) ) ;
#43593 = CARTESIAN_POINT ( 'NONE',  ( -5.776987155906605054, -2.523321265292115090, 31.42251411153756280 ) ) ;
#43594 = CARTESIAN_POINT ( 'NONE',  ( 0.06109907496451268821, -3.749999999999999556, 14.40811829374151110 ) ) ;
#43595 = CARTESIAN_POINT ( 'NONE',  ( 6.673053698855467175, -4.931416488878822335, 34.32920672191015399 ) ) ;
#43596 = CARTESIAN_POINT ( 'NONE',  ( -16.94639763868943660, -5.915461855592777596, 34.75538340440931506 ) ) ;
#43597 = VERTEX_POINT ( 'NONE', #61545 ) ;
#43598 = CARTESIAN_POINT ( 'NONE',  ( -17.86947456176635640, -6.808710257144159783, 34.95449254468098843 ) ) ;
#43600 = ORIENTED_EDGE ( 'NONE', *, *, #31225, .F. ) ;
#43599 = CARTESIAN_POINT ( 'NONE',  ( 3.903869422903799347, -5.728515186090277211, 34.42611988154120439 ) ) ;
#43601 = CARTESIAN_POINT ( 'NONE',  ( -2.750000000000006217, -6.360912703474006946, 26.42187500000000000 ) ) ;
#43602 = CARTESIAN_POINT ( 'NONE',  ( -12.46153846153846168, -1.367168528481310208, 33.57946703557072254 ) ) ;
#43603 = CARTESIAN_POINT ( 'NONE',  ( -5.076923076923197442, -11.48612834414049644, 32.76840700105863391 ) ) ;
#43604 = B_SPLINE_CURVE_WITH_KNOTS ( 'NONE', 3,
 ( #34401, #61863, #55117, #82614, #60988, #12804, #20883, #76271, #88490, #54222 ),
 .UNSPECIFIED., .F., .F.,
 ( 4, 2, 2, 2, 4 ),
 ( 0.000000000000000000, 0.0001954311564186864407, 0.0003908623128373728815, 0.0005862934692560593493, 0.0007817246256747457630 ),
 .UNSPECIFIED. ) ;
#43605 = B_SPLINE_CURVE_WITH_KNOTS ( 'NONE', 3,
 ( #76661, #29808, #57271, #85195, #64015, #2751, #84761, #69898, #35685, #57715 ),
 .UNSPECIFIED., .F., .F.,
 ( 4, 2, 2, 2, 4 ),
 ( 0.000000000000000000, 0.0001954339857564126514, 0.0003908679715128183098, 0.0005863019572692239681, 0.0007817359430256294638 ),
 .UNSPECIFIED. ) ;
#43606 = CARTESIAN_POINT ( 'NONE',  ( 12.46153846153833911, -8.613356846316285953, 34.62446782046622218 ) ) ;
#43607 = ORIENTED_EDGE ( 'NONE', *, *, #33206, .F. ) ;
#43608 = CARTESIAN_POINT ( 'NONE',  ( -11.53846153846165912, -4.481592998941358097, 33.73612834414048933 ) ) ;
#43609 = DIRECTION ( 'NONE',  ( -0.000000000000000000, -0.1736481776669307198, -0.9848077530122080203 ) ) ;
#43610 = EDGE_CURVE ( 'NONE', #58985, #41090, #18357, .T. ) ;
#43611 = CARTESIAN_POINT ( 'NONE',  ( 9.915320536401090123, -6.460100341425560444, 34.89618726649961644 ) ) ;
#43612 = ORIENTED_EDGE ( 'NONE', *, *, #40067, .T. ) ;
#43613 = ADVANCED_FACE ( 'NONE', ( #73299 ), #53459, .F. ) ;
#43614 = VERTEX_POINT ( 'NONE', #11603 ) ;
#43615 = AXIS2_PLACEMENT_3D ( 'NONE', #86792, #3450, #39034 ) ;
#43616 = VERTEX_POINT ( 'NONE', #39970 ) ;
#43617 = PRESENTATION_LAYER_ASSIGNMENT (  '', '', ( #79567 ) ) ;
#43618 = ADVANCED_FACE ( 'NONE', ( #12054 ), #61108, .T. ) ;
#43619 = CARTESIAN_POINT ( 'NONE',  ( 7.846153846153846700, -1.242168528481310874, 33.36296068462461051 ) ) ;
#43620 = CARTESIAN_POINT ( 'NONE',  ( 13.63456079399343146, -3.520799739797214389, 33.17531984108286025 ) ) ;
#43621 = EDGE_CURVE ( 'NONE', #20169, #77592, #20130, .T. ) ;
#43622 = CARTESIAN_POINT ( 'NONE',  ( 10.28846153846153832, -7.500000000000000000, 29.75000000000000355 ) ) ;
#43623 = DIRECTION ( 'NONE',  ( -0.000000000000000000, 0.9396926207859093161, -0.3420201433256663259 ) ) ;
#43624 = VERTEX_POINT ( 'NONE', #67431 ) ;
#43625 = ORIENTED_EDGE ( 'NONE', *, *, #84515, .T. ) ;
#43627 = VERTEX_POINT ( 'NONE', #88615 ) ;
#43626 = CARTESIAN_POINT ( 'NONE',  ( -1.449939397419692355, -7.749976730030849303, 34.74374725381503737 ) ) ;
#43628 = CARTESIAN_POINT ( 'NONE',  ( 9.822833394071260216, -12.45806712695776319, 30.39783852428763922 ) ) ;
#43629 = B_SPLINE_CURVE_WITH_KNOTS ( 'NONE', 3,
 ( #72841, #85480, #11148, #10709, #85046, #17017, #65194, #3493, #24661, #79613 ),
 .UNSPECIFIED., .F., .F.,
 ( 4, 2, 2, 2, 4 ),
 ( 0.000000000000000000, 0.0001954339857564072304, 0.0003908679715128144608, 0.0005863019572692216913, 0.0007817359430256289217 ),
 .UNSPECIFIED. ) ;
#43630 = B_SPLINE_CURVE_WITH_KNOTS ( 'NONE', 3,
 ( #76021, #57077, #55306, #8905, #36375, #14325, #15662, #83235, #28737, #21071 ),
 .UNSPECIFIED., .F., .F.,
 ( 4, 2, 2, 2, 4 ),
 ( 0.000000000000000000, 0.0001954311564186868473, 0.0003908623128373736946, 0.0005862934692560605419, 0.0007817246256747473893 ),
 .UNSPECIFIED. ) ;
#43631 = CARTESIAN_POINT ( 'NONE',  ( -17.93393164899755732, -3.050289026998447728, 32.03036669348366416 ) ) ;
#43632 = DIRECTION ( 'NONE',  ( 1.000000000000000000, 0.000000000000000000, 0.000000000000000000 ) ) ;
#43633 = VERTEX_POINT ( 'NONE', #53911 ) ;
#43634 = B_SPLINE_CURVE_WITH_KNOTS ( 'NONE', 3,
 ( #74056, #6042, #12347, #34384, #160, #19543, #27630, #19108, #26303, #67295 ),
 .UNSPECIFIED., .F., .F.,
 ( 4, 2, 2, 2, 4 ),
 ( 0.0007817246256747461966, 0.0009771112852218889842, 0.001172497944769031880, 0.001367884604316174776, 0.001563271263863317672 ),
 .UNSPECIFIED. ) ;
#43635 = ORIENTED_EDGE ( 'NONE', *, *, #50449, .T. ) ;
#43637 = ORIENTED_EDGE ( 'NONE', *, *, #21445, .T. ) ;
#43636 = CARTESIAN_POINT ( 'NONE',  ( -39.05038313613820122, -12.75000000000000178, 27.25000000000000000 ) ) ;
#43638 = VECTOR ( 'NONE', #46523, 1000.000000000000000 ) ;
#43639 = CARTESIAN_POINT ( 'NONE',  ( -6.000000000000119904, -8.613356846316285953, 34.62446782046622218 ) ) ;
#43640 = EDGE_CURVE ( 'NONE', #83562, #34160, #60663, .T. ) ;
#43641 = DIRECTION ( 'NONE',  ( 0.000000000000000000, 0.000000000000000000, -1.000000000000000000 ) ) ;
#43642 = ORIENTED_EDGE ( 'NONE', *, *, #63704, .F. ) ;
#43643 = CARTESIAN_POINT ( 'NONE',  ( 17.93391658904412012, -10.51840700105979565, 33.73612834413961536 ) ) ;
#43644 = CARTESIAN_POINT ( 'NONE',  ( -19.50000000000000000, -3.499999999999999556, 29.75000000000000355 ) ) ;
#43645 = CARTESIAN_POINT ( 'NONE',  ( 10.68064018666064285, -3.835265460703683349, 33.15142922261929925 ) ) ;
#43646 = FACE_BOUND ( 'NONE', #78077, .T. ) ;
#43647 = LINE ( 'NONE', #58044, #70058 ) ;
#43648 = CARTESIAN_POINT ( 'NONE',  ( -4.376772371362299019, -12.15238873228292071, 31.58232369045353849 ) ) ;
#43649 = CARTESIAN_POINT ( 'NONE',  ( -14.98082371242109012, -10.76462480002816235, 33.53768742498949962 ) ) ;
#43651 = CARTESIAN_POINT ( 'NONE',  ( 4.376625822824220080, -2.353885683473779800, 30.79025554430704759 ) ) ;
#43650 = CARTESIAN_POINT ( 'NONE',  ( -0.2114840416250086119, -2.920487667080175154, 32.31805714834172250 ) ) ;
#43652 = CARTESIAN_POINT ( 'NONE',  ( 8.769230769230768274, -9.058645607665452459, 34.76329471203371924 ) ) ;
#43653 = CARTESIAN_POINT ( 'NONE',  ( 10.39189969082028675, -10.97335522853832579, 33.68706563782419749 ) ) ;
#43654 = ORIENTED_EDGE ( 'NONE', *, *, #73434, .F. ) ;
#43655 = CARTESIAN_POINT ( 'NONE',  ( -15.93083330975275658, -3.395485233115139501, 33.02377354290276656 ) ) ;
#43656 = VERTEX_POINT ( 'NONE', #60218 ) ;
#43657 = VERTEX_POINT ( 'NONE', #53008 ) ;
#43658 = EDGE_CURVE ( 'NONE', #51433, #9533, #66992, .T. ) ;
#43660 = LINE ( 'NONE', #71131, #72124 ) ;
#43659 = CARTESIAN_POINT ( 'NONE',  ( 7.780883400193072674, -6.879047030191174805, 34.71129190930000163 ) ) ;
#43661 = CARTESIAN_POINT ( 'NONE',  ( 2.557637826040451312, -2.587454068350147907, 30.68340429815432202 ) ) ;
#43662 = DIRECTION ( 'NONE',  ( -0.000000000000000000, 0.6427876096865404731, -0.7660444431189770143 ) ) ;
#43663 = CARTESIAN_POINT ( 'NONE',  ( -15.23076923076922995, -3.937682226553329556, 33.60647404775216529 ) ) ;
#43664 = CARTESIAN_POINT ( 'NONE',  ( -0.2115929431903184610, -11.86320923018887719, 32.19269448109604781 ) ) ;
#43665 = ORIENTED_EDGE ( 'NONE', *, *, #10745, .T. ) ;
#43666 = CARTESIAN_POINT ( 'NONE',  ( -18.00000000000012079, -6.026961402154117131, 34.52809138561165270 ) ) ;
#43667 = VECTOR ( 'NONE', #10078, 1000.000000000000000 ) ;
#43668 = CARTESIAN_POINT ( 'NONE',  ( 14.98079248672064345, -10.82459398097509329, 33.81372124010185587 ) ) ;
#43669 = CARTESIAN_POINT ( 'NONE',  ( 7.846153846153846700, -13.49023893513002648, 31.06009739812518688 ) ) ;
#43670 = DIRECTION ( 'NONE',  ( -0.000000000000000000, -0.5000000000000009992, -0.8660254037844380415 ) ) ;
#43671 = CARTESIAN_POINT ( 'NONE',  ( 13.38461538461526423, -5.941354392335915335, 34.76329471203413846 ) ) ;
#43672 = CARTESIAN_POINT ( 'NONE',  ( -2.651650429449565305, -4.848349570550461785, 17.75000000000000355 ) ) ;
#43673 = EDGE_LOOP ( 'NONE', ( #36883, #65062, #88201, #60985 ) ) ;
#43674 = AXIS2_PLACEMENT_3D ( 'NONE', #13260, #27214, #81287 ) ;
#43675 = ORIENTED_EDGE ( 'NONE', *, *, #29470, .T. ) ;
#43676 = AXIS2_PLACEMENT_3D ( 'NONE', #83666, #42668, #27671 ) ;
#43677 = EDGE_CURVE ( 'NONE', #46850, #13379, #80509, .T. ) ;
#43678 = CARTESIAN_POINT ( 'NONE',  ( -9.561781990544128362, -12.45806712695776319, 30.39783852428763922 ) ) ;
#43679 = EDGE_LOOP ( 'NONE', ( #79512, #11286 ) ) ;
#43680 = CARTESIAN_POINT ( 'NONE',  ( -1.326923076923076872, -3.499999999999999556, 29.75000000000000355 ) ) ;
#43681 = CARTESIAN_POINT ( 'NONE',  ( 9.915319043920545639, -9.886259254753566594, 34.14407573483972413 ) ) ;
#43682 = LINE ( 'NONE', #70724, #6379 ) ;
#43683 = EDGE_CURVE ( 'NONE', #70465, #23070, #87724, .T. ) ;
#43684 = CARTESIAN_POINT ( 'NONE',  ( -8.546219417617919589, -10.61302985866383963, 33.66295027996417843 ) ) ;
#43685 = CARTESIAN_POINT ( 'NONE',  ( -1.553300858899125059, -3.750000000000009326, 17.82812500000000000 ) ) ;
#43686 = LINE ( 'NONE', #84697, #80592 ) ;
#43687 = VERTEX_POINT ( 'NONE', #19682 ) ;
#43688 = CARTESIAN_POINT ( 'NONE',  ( 1.384615384615386802, -13.95598074871891292, 31.83374038241031911 ) ) ;
#43690 = ORIENTED_EDGE ( 'NONE', *, *, #23750, .T. ) ;
#43689 = CARTESIAN_POINT ( 'NONE',  ( -2.084679463598910765, -12.64618726649961289, 30.78989965857442712 ) ) ;
#43691 = CYLINDRICAL_SURFACE ( 'NONE', #2285, 0.2500000000000009437 ) ;
#43692 = CYLINDRICAL_SURFACE ( 'NONE', #32897, 0.2499999999999997502 ) ;
#43693 = CARTESIAN_POINT ( 'NONE',  ( 3.230769230769231726, -13.20930481340135110, 34.54067556320372745 ) ) ;
#43694 = CARTESIAN_POINT ( 'NONE',  ( 0.6845498131513093609, -2.758310577978207334, 31.33698337089302299 ) ) ;
#43695 = EDGE_CURVE ( 'NONE', #65515, #50542, #74634, .T. ) ;
#43696 = CARTESIAN_POINT ( 'NONE',  ( -12.71151519248081740, -12.41269422305637171, 30.68257228309993323 ) ) ;
#43697 = CARTESIAN_POINT ( 'NONE',  ( -11.47320639894870276, -3.083524468853784839, 32.58852847137153930 ) ) ;
#43698 = CARTESIAN_POINT ( 'NONE',  ( -1.901340078031369618, -5.512252781505359245, 24.25186829374150932 ) ) ;
#43699 = ORIENTED_EDGE ( 'NONE', *, *, #18930, .F. ) ;
#43700 = CARTESIAN_POINT ( 'NONE',  ( 1.134638653673032849, -5.728515186090277211, 34.42611988154120439 ) ) ;
#43701 = CARTESIAN_POINT ( 'NONE',  ( 4.376858997939548246, -10.77377354290276301, 33.85451476688484718 ) ) ;
#43702 = CARTESIAN_POINT ( 'NONE',  ( -1.139087296526025916, -4.750000000000006217, 25.32812500000000711 ) ) ;
#43703 = ADVANCED_FACE ( 'NONE', ( #12926 ), #40414, .F. ) ;
#43704 = CARTESIAN_POINT ( 'NONE',  ( -15.23076923076922995, -8.120952969808772792, 34.71129190930000163 ) ) ;
#43705 = CARTESIAN_POINT ( 'NONE',  ( 2.557637717070351258, -12.07971442181321997, 32.31769673815850297 ) ) ;
#43706 = EDGE_LOOP ( 'NONE', ( #79247, #77259 ) ) ;
#43707 = FACE_OUTER_BOUND ( 'NONE', #14023, .T. ) ;
#43708 = CARTESIAN_POINT ( 'NONE',  ( -17.07692307692307665, -2.499999999999998668, 29.50000000000001066 ) ) ;
#43709 = EDGE_CURVE ( 'NONE', #40731, #24676, #26448, .T. ) ;
#43710 = VERTEX_POINT ( 'NONE', #13366 ) ;
#43711 = VECTOR ( 'NONE', #50948, 1000.000000000000000 ) ;
#43712 = CARTESIAN_POINT ( 'NONE',  ( -3.930833309752757909, -2.523321265292115090, 31.42251411153756280 ) ) ;
#43713 = UNCERTAINTY_MEASURE_WITH_UNIT (LENGTH_MEASURE( 1.000000000000000082E-05 ), #56899, 'distance_accuracy_value', 'NONE');
#43714 = EDGE_LOOP ( 'NONE', ( #39591, #40633 ) ) ;
#43715 = CARTESIAN_POINT ( 'NONE',  ( 6.923076923076924238, -10.89733346790207413, 36.13435417666054406 ) ) ;
#43716 = CARTESIAN_POINT ( 'NONE',  ( 2.980746006547775107, -4.175268141568689195, 33.81360843649122216 ) ) ;
#43717 = EDGE_CURVE ( 'NONE', #40179, #24050, #2778, .T. ) ;
#43718 = CARTESIAN_POINT ( 'NONE',  ( -1.384615384615383471, -4.098570777380720287, 33.41473453929634729 ) ) ;
#43719 = CARTESIAN_POINT ( 'NONE',  ( -4.219928533206288357, -11.35647404775217595, 33.31231777344666511 ) ) ;
#43720 = ORIENTED_EDGE ( 'NONE', *, *, #81722, .F. ) ;
#43721 = CARTESIAN_POINT ( 'NONE',  ( -3.230769230769352962, -2.379036618888197285, 30.90682066428292885 ) ) ;
#43722 = VERTEX_POINT ( 'NONE', #62424 ) ;
#43723 = CARTESIAN_POINT ( 'NONE',  ( -39.05038313613820122, -12.50000000000000000, 29.75000000000000355 ) ) ;
#43724 = CARTESIAN_POINT ( 'NONE',  ( 9.692307692307695177, -3.886160181151819604, 36.00935417666054406 ) ) ;
#43725 = ORIENTED_EDGE ( 'NONE', *, *, #823, .T. ) ;
#43726 = EDGE_CURVE ( 'NONE', #5488, #11611, #44741, .T. ) ;
#43727 = LINE ( 'NONE', #12176, #18843 ) ;
#43728 = CARTESIAN_POINT ( 'NONE',  ( 5.076923076922954969, -10.90142922262034020, 33.41473453929536674 ) ) ;
#43729 = CARTESIAN_POINT ( 'NONE',  ( -39.05038313613820122, -2.249999999999998668, 29.75000000000000355 ) ) ;
#43730 = CARTESIAN_POINT ( 'NONE',  ( -19.99999999999998934, 12.00000000000000711, 13.00000000000000178 ) ) ;
#43731 = CARTESIAN_POINT ( 'NONE',  ( -14.30769230769230660, -12.78798330534102945, 29.74999999999997868 ) ) ;
#43732 = B_SPLINE_CURVE_WITH_KNOTS ( 'NONE', 3,
 ( #85995, #10780, #38249, #58957, #86461, #24735, #5802, #33279, #46340, #59410 ),
 .UNSPECIFIED., .F., .F.,
 ( 4, 2, 2, 2, 4 ),
 ( 0.000000000000000000, 0.0001954339857564078267, 0.0003908679715128156535, 0.0005863019572692235344, 0.0007817359430256313069 ),
 .UNSPECIFIED. ) ;
#43733 = B_SPLINE_CURVE_WITH_KNOTS ( 'NONE', 3,
 ( #5, #40116, #40556, #7203, #13071, #68022, #47739, #27475, #6749, #54489 ),
 .UNSPECIFIED., .F., .F.,
 ( 4, 2, 2, 2, 4 ),
 ( 0.0007817246336856291692, 0.0009771112958940105907, 0.001172497958102391904, 0.001367884620310773434, 0.001563271282519154747 ),
 .UNSPECIFIED. ) ;
#43734 = ORIENTED_EDGE ( 'NONE', *, *, #3194, .F. ) ;
#43735 = VERTEX_POINT ( 'NONE', #20566 ) ;
#43736 = FACE_BOUND ( 'NONE', #76586, .T. ) ;
#43737 = B_SPLINE_CURVE_WITH_KNOTS ( 'NONE', 3,
 ( #78686, #24173, #72362, #64712, #38588, #86354, #25071, #51625, #65157, #3011 ),
 .UNSPECIFIED., .F., .F.,
 ( 4, 2, 2, 2, 4 ),
 ( 0.0007817246256747459798, 0.0009771112852218896347, 0.001172497944769033181, 0.001367884604316176728, 0.001563271263863320491 ),
 .UNSPECIFIED. ) ;
#43738 = EDGE_LOOP ( 'NONE', ( #26625, #6327, #53576, #66751 ) ) ;
#43740 = EDGE_CURVE ( 'NONE', #42183, #53607, #63763, .T. ) ;
#43739 = DIRECTION ( 'NONE',  ( -0.000000000000000000, 1.000000000000000000, -0.000000000000000000 ) ) ;
#43741 = CIRCLE ( 'NONE', #4928, 5.000000000000000888 ) ;
#43742 = VECTOR ( 'NONE', #59830, 1000.000000000000000 ) ;
#43743 = EDGE_CURVE ( 'NONE', #26475, #21434, #84545, .T. ) ;
#43744 = CARTESIAN_POINT ( 'NONE',  ( 9.626224281351813516, -12.10708131394839349, 31.69288490824020244 ) ) ;
#43745 = CARTESIAN_POINT ( 'NONE',  ( -14.30769230769242739, -9.442884908241554243, 34.35708131394783038 ) ) ;
#43746 = EDGE_LOOP ( 'NONE', ( #76767, #44957 ) ) ;
#43747 = ORIENTED_EDGE ( 'NONE', *, *, #44950, .T. ) ;
#43748 = CARTESIAN_POINT ( 'NONE',  ( 16.82689983963011926, -4.335965774309648246, 33.62209801155881905 ) ) ;
#43749 = VERTEX_POINT ( 'NONE', #13810 ) ;
#43750 = CARTESIAN_POINT ( 'NONE',  ( 2.057692307692309708, -7.566082377512563184, 35.00000000000000711 ) ) ;
#43751 = EDGE_CURVE ( 'NONE', #77592, #1771, #8241, .T. ) ;
#43752 = CARTESIAN_POINT ( 'NONE',  ( -5.076923076923199218, -5.094484230521993062, 34.41647553114689373 ) ) ;
#43753 = CARTESIAN_POINT ( 'NONE',  ( 14.05771556364372188, -12.01397095200674059, 32.43157075238190146 ) ) ;
#43754 = EDGE_CURVE ( 'NONE', #21774, #44514, #68364, .T. ) ;
#43755 = FACE_BOUND ( 'NONE', #63932, .T. ) ;
#43756 = VERTEX_POINT ( 'NONE', #49372 ) ;
#43757 = CARTESIAN_POINT ( 'NONE',  ( 12.68454981315131391, -5.667800583137506010, 34.40243808032445827 ) ) ;
#43758 = ADVANCED_FACE ( 'NONE', ( #41294 ), #56572, .F. ) ;
#43759 = DIRECTION ( 'NONE',  ( -1.000000000000000000, -0.000000000000000000, -0.000000000000000000 ) ) ;
#43760 = CARTESIAN_POINT ( 'NONE',  ( 10.61538461538449418, -5.094484230521993062, 34.41647553114689373 ) ) ;
#43761 = CARTESIAN_POINT ( 'NONE',  ( -1.318548051265308052, -2.833524468853757750, 32.15551576947925838 ) ) ;
#43762 = ORIENTED_EDGE ( 'NONE', *, *, #47770, .T. ) ;
#43763 = UNCERTAINTY_MEASURE_WITH_UNIT (LENGTH_MEASURE( 1.000000000000000082E-05 ), #43396, 'distance_accuracy_value', 'NONE');
#43764 = ORIENTED_EDGE ( 'NONE', *, *, #43087, .T. ) ;
#43765 = VERTEX_POINT ( 'NONE', #7055 ) ;
#43766 = EDGE_CURVE ( 'NONE', #25678, #58364, #15148, .T. ) ;
#43767 = B_SPLINE_CURVE_WITH_KNOTS ( 'NONE', 3,
 ( #12085, #18386, #3962, #31448, #86423, #45846, #32343, #59809, #24692, #52151 ),
 .UNSPECIFIED., .F., .F.,
 ( 4, 2, 2, 2, 4 ),
 ( 0.000000000000000000, 0.0001954311564186864407, 0.0003908623128373728815, 0.0005862934692560593493, 0.0007817246256747457630 ),
 .UNSPECIFIED. ) ;
#43768 = VECTOR ( 'NONE', #14109, 1000.000000000000114 ) ;
#43770 = CARTESIAN_POINT ( 'NONE',  ( -18.00000000000000000, -4.112162358433185005, 36.11790692298802696 ) ) ;
#43769 = CARTESIAN_POINT ( 'NONE',  ( -6.923076923077044142, -10.21337939537710326, 33.94971097300076224 ) ) ;
#43771 = CARTESIAN_POINT ( 'NONE',  ( -10.86536134632696715, -12.17611988154120972, 31.52148481390971213 ) ) ;
#43772 = CARTESIAN_POINT ( 'NONE',  ( -6.857821351800897247, -3.835265460703683349, 33.15142922261929925 ) ) ;
#43773 = FACE_OUTER_BOUND ( 'NONE', #77255, .T. ) ;
#43774 = CARTESIAN_POINT ( 'NONE',  ( -15.48079245499068435, -3.520140089381495585, 33.17453946501458262 ) ) ;
#43775 = ORIENTED_EDGE ( 'NONE', *, *, #46014, .F. ) ;
#43776 = CARTESIAN_POINT ( 'NONE',  ( -3.007989689500820241, -2.600157965045225783, 30.74683119005207743 ) ) ;
#43777 = CARTESIAN_POINT ( 'NONE',  ( 3.230769230769231726, -9.058645607665452459, 34.76329471203371924 ) ) ;
#43778 = CARTESIAN_POINT ( 'NONE',  ( -17.14219352288385778, -11.94971097300153140, 32.03036669348370680 ) ) ;
#43779 = CARTESIAN_POINT ( 'NONE',  ( -4.153846153846152411, -3.669653830205710676, 35.88435417666054406 ) ) ;
#43780 = ORIENTED_EDGE ( 'NONE', *, *, #20179, .T. ) ;
#43781 = DIRECTION ( 'NONE',  ( 0.000000000000000000, 0.9848077530122072432, 0.1736481776669354937 ) ) ;
#43782 = ORIENTED_EDGE ( 'NONE', *, *, #6205, .F. ) ;
#43783 = FACE_BOUND ( 'NONE', #16225, .T. ) ;
#43784 = CARTESIAN_POINT ( 'NONE',  ( 4.153846153846154188, -2.486705287966279876, 31.30864560766543647 ) ) ;
#43785 = CARTESIAN_POINT ( 'NONE',  ( -17.92071683142037486, 12.74206001580630954, 30.82086045927834661 ) ) ;
#43786 = ORIENTED_EDGE ( 'NONE', *, *, #61024, .T. ) ;
#43787 = CARTESIAN_POINT ( 'NONE',  ( -7.623142494540996239, -4.187068189119696804, 33.49521262558774026 ) ) ;
#43788 = CARTESIAN_POINT ( 'NONE',  ( -2.176900499867519212, -4.118422570099827595, 33.43335022499816489 ) ) ;
#43789 = CARTESIAN_POINT ( 'NONE',  ( 5.076923076923075762, -2.900454961884010974, 35.62045528018868623 ) ) ;
#43790 = ADVANCED_FACE ( 'NONE', ( #1635 ), #8389, .F. ) ;
#43791 = CYLINDRICAL_SURFACE ( 'NONE', #76206, 0.2500000000000004996 ) ;
#43792 = EDGE_LOOP ( 'NONE', ( #83158, #78850, #10890, #20587 ) ) ;
#43793 = CYLINDRICAL_SURFACE ( 'NONE', #30167, 0.2499999999999995559 ) ;
#43794 = ORIENTED_EDGE ( 'NONE', *, *, #60360, .T. ) ;
#43796 = VERTEX_POINT ( 'NONE', #49805 ) ;
#43795 = DIRECTION ( 'NONE',  ( -0.000000000000000000, 0.8660254037844397068, -0.4999999999999978906 ) ) ;
#43797 = CARTESIAN_POINT ( 'NONE',  ( 3.230769230769110045, -2.625532179533779154, 30.86335684631627174 ) ) ;
#43798 = CARTESIAN_POINT ( 'NONE',  ( 15.00784301325307979, -2.758268499246657068, 31.33685645148948140 ) ) ;
#43799 = CARTESIAN_POINT ( 'NONE',  ( -7.715363405186892898, -3.338503747796866872, 32.95102852606553512 ) ) ;
#43800 = CARTESIAN_POINT ( 'NONE',  ( -12.59168643127016374, -11.04286588640298561, 33.62463336215343901 ) ) ;
#43802 = AXIS2_PLACEMENT_3D ( 'NONE', #14096, #54180, #34359 ) ;
#43801 = DIRECTION ( 'NONE',  ( -0.000000000000000000, -0.6427876096865404731, -0.7660444431189771253 ) ) ;
#43803 = DIRECTION ( 'NONE',  ( -0.000000000000000000, 0.000000000000000000, 1.000000000000000000 ) ) ;
#43804 = CARTESIAN_POINT ( 'NONE',  ( -1.139087296526025916, -4.750000000000006217, 22.82812500000000355 ) ) ;
#43805 = ORIENTED_EDGE ( 'NONE', *, *, #49102, .F. ) ;
#43806 = VECTOR ( 'NONE', #40106, 1000.000000000000000 ) ;
#43807 = CARTESIAN_POINT ( 'NONE',  ( 6.923076923076924238, -1.129524287112498415, 32.06866353760679544 ) ) ;
#43808 = LINE ( 'NONE', #71270, #75465 ) ;
#43809 = ORIENTED_EDGE ( 'NONE', *, *, #12844, .T. ) ;
#43810 = VECTOR ( 'NONE', #52878, 1000.000000000000227 ) ;
#43811 = ORIENTED_EDGE ( 'NONE', *, *, #84070, .F. ) ;
#43812 = ORIENTED_EDGE ( 'NONE', *, *, #47227, .T. ) ;
#43813 = CARTESIAN_POINT ( 'NONE',  ( 4.023698944407930078, -12.27039167877662251, 31.24851455888617835 ) ) ;
#43814 = CARTESIAN_POINT ( 'NONE',  ( 3.230769230769231726, -1.951392089020283160, 34.73218667398347748 ) ) ;
#43815 = DIRECTION ( 'NONE',  ( -0.000000000000000000, 1.000000000000000000, -0.000000000000000000 ) ) ;
#43816 = LINE ( 'NONE', #71724, #8298 ) ;
#43817 = DIRECTION ( 'NONE',  ( -0.000000000000000000, -0.3420201433256694346, -0.9396926207859080948 ) ) ;
#43818 = CARTESIAN_POINT ( 'NONE',  ( -17.01085574357300345, -11.35647404775217595, 33.31231777344667222 ) ) ;
#43819 = CARTESIAN_POINT ( 'NONE',  ( 6.223426398914789992, -7.630147987733840509, 34.99859428049665411 ) ) ;
#43820 = ORIENTED_EDGE ( 'NONE', *, *, #85776, .T. ) ;
#43821 = CARTESIAN_POINT ( 'NONE',  ( -3.930834802233303282, -5.667800583137508674, 34.40243808032445827 ) ) ;
#43822 = CARTESIAN_POINT ( 'NONE',  ( -17.14219352288385423, -12.27809138561121394, 31.22303859784730307 ) ) ;
#43823 = EDGE_CURVE ( 'NONE', #47862, #66121, #9707, .T. ) ;
#43824 = CARTESIAN_POINT ( 'NONE',  ( -8.834500769787091201, -11.67786785259540849, 32.92929555188721480 ) ) ;
#43825 = CARTESIAN_POINT ( 'NONE',  ( 12.46153846153846168, -11.69971097300155272, 32.46337939537588113 ) ) ;
#43826 = ORIENTED_EDGE ( 'NONE', *, *, #70345, .F. ) ;
#43827 = CYLINDRICAL_SURFACE ( 'NONE', #38401, 0.2499999999999979738 ) ;
#43828 = EDGE_CURVE ( 'NONE', #72161, #46109, #71541, .T. ) ;
#43829 = ORIENTED_EDGE ( 'NONE', *, *, #29929, .F. ) ;
#43830 = CARTESIAN_POINT ( 'NONE',  ( 8.899756207464410096, -3.068774925481848825, 32.56582465632704526 ) ) ;
#43831 = CARTESIAN_POINT ( 'NONE',  ( -7.846153846153844924, -13.75783147151868846, 33.36296068462461051 ) ) ;
#43832 = DIRECTION ( 'NONE',  ( -1.000000000000000000, -0.000000000000000000, -0.000000000000000000 ) ) ;
#43833 = CARTESIAN_POINT ( 'NONE',  ( 12.52760681254089903, -10.51840700105979565, 33.73612834413962247 ) ) ;
#43834 = ORIENTED_EDGE ( 'NONE', *, *, #8168, .F. ) ;
#43835 = EDGE_CURVE ( 'NONE', #74179, #37853, #23663, .T. ) ;
#43836 = CARTESIAN_POINT ( 'NONE',  ( 19.00000000000000000, -3.499999999999999556, 29.75000000000000355 ) ) ;
#43837 = CARTESIAN_POINT ( 'NONE',  ( 9.692307692307695177, -5.557115091759785130, 34.35708131394839171 ) ) ;
#43838 = CARTESIAN_POINT ( 'NONE',  ( -12.21153846153702638, -7.500000000000155431, 34.75000000000007105 ) ) ;
#43839 = VECTOR ( 'NONE', #50562, 999.9999999999998863 ) ;
#43840 = EDGE_CURVE ( 'NONE', #62614, #27628, #64639, .T. ) ;
#43841 = CARTESIAN_POINT ( 'NONE',  ( -8.992715693795100051, -9.417330523894424488, 34.63758898049880486 ) ) ;
#43842 = B_SPLINE_CURVE_WITH_KNOTS ( 'NONE', 3,
 ( #29972, #2050, #56990, #57431, #23208, #77707, #49790, #84482, #83604, #50669 ),
 .UNSPECIFIED., .F., .F.,
 ( 4, 2, 2, 2, 4 ),
 ( 0.0007817246256747481482, 0.0009771112852218911526, 0.001172497944769034049, 0.001367884604316176944, 0.001563271263863319840 ),
 .UNSPECIFIED. ) ;
#43843 = ORIENTED_EDGE ( 'NONE', *, *, #70057, .T. ) ;
#43844 = CARTESIAN_POINT ( 'NONE',  ( 16.40379156322419973, -10.18230066228895758, 34.26354781536631577 ) ) ;
#43845 = ORIENTED_EDGE ( 'NONE', *, *, #43978, .F. ) ;
#43846 = ADVANCED_FACE ( 'NONE', ( #58331 ), #16913, .F. ) ;
#43847 = CARTESIAN_POINT ( 'NONE',  ( 4.826946345980721809, -12.17611988154120972, 31.52148481390971213 ) ) ;
#43848 = CARTESIAN_POINT ( 'NONE',  ( 7.053602361310566948, -3.068774925481847937, 32.56582465632704526 ) ) ;
#43849 = CARTESIAN_POINT ( 'NONE',  ( -6.066083410955879884, -2.538708090699994813, 30.37095296980875148 ) ) ;
#43850 = CARTESIAN_POINT ( 'NONE',  ( 1.253924781505079356, -8.191372820521381826, 34.95448215188423546 ) ) ;
#43851 = CARTESIAN_POINT ( 'NONE',  ( 5.076923076922954969, -11.94971097300221174, 32.03036669348237098 ) ) ;
#43852 = ORIENTED_EDGE ( 'NONE', *, *, #29382, .T. ) ;
#43853 = ORIENTED_EDGE ( 'NONE', *, *, #45342, .T. ) ;
#43854 = ORIENTED_EDGE ( 'NONE', *, *, #20083, .F. ) ;
#43855 = AXIS2_PLACEMENT_3D ( 'NONE', #49212, #76688, #42462 ) ;
#43856 = CARTESIAN_POINT ( 'NONE',  ( -10.36543909703647337, -8.433404298154334455, 34.66254593164985920 ) ) ;
#43857 = DIRECTION ( 'NONE',  ( -0.000000000000000000, 1.000000000000000000, -0.000000000000000000 ) ) ;
#43858 = EDGE_CURVE ( 'NONE', #11982, #8529, #28658, .T. ) ;
#43859 = CARTESIAN_POINT ( 'NONE',  ( -12.33101302330481985, -12.50538340440932394, 31.33453814440721885 ) ) ;
#43860 = CARTESIAN_POINT ( 'NONE',  ( -13.31935981333936070, -6.026961402152789304, 34.52809138561124769 ) ) ;
#43861 = AXIS2_PLACEMENT_3D ( 'NONE', #75267, #11794, #66729 ) ;
#43862 = FACE_OUTER_BOUND ( 'NONE', #84318, .T. ) ;
#43863 = EDGE_CURVE ( 'NONE', #82908, #2182, #81308, .T. ) ;
#43864 = CARTESIAN_POINT ( 'NONE',  ( 10.61538461538461675, -9.058645607665452459, 34.76329471203371924 ) ) ;
#43865 = DIRECTION ( 'NONE',  ( 0.000000000000000000, 0.9396926207859126468, -0.3420201433256571111 ) ) ;
#43866 = ORIENTED_EDGE ( 'NONE', *, *, #72651, .T. ) ;
#43867 = AXIS2_PLACEMENT_3D ( 'NONE', #8199, #35673, #64005 ) ;
#43868 = ORIENTED_EDGE ( 'NONE', *, *, #71932, .T. ) ;
#43869 = ORIENTED_EDGE ( 'NONE', *, *, #2376, .T. ) ;
#43872 = ORIENTED_EDGE ( 'NONE', *, *, #37149, .T. ) ;
#43871 = ADVANCED_FACE ( 'NONE', ( #79058 ), #43937, .T. ) ;
#43870 = CARTESIAN_POINT ( 'NONE',  ( 11.76147438255493327, -2.523321265292115534, 31.42251411153756990 ) ) ;
#43874 = CARTESIAN_POINT ( 'NONE',  ( -10.61538461538473577, -6.835583212225970762, 34.95778746994575670 ) ) ;
#43873 = CARTESIAN_POINT ( 'NONE',  ( -9.942284423250045577, -9.148715823498378086, 34.47080413974185120 ) ) ;
#43875 = CARTESIAN_POINT ( 'NONE',  ( 8.835399910193425299, -7.250054483168843156, 34.74374881642865631 ) ) ;
#43876 = CARTESIAN_POINT ( 'NONE',  ( 3.750000000000000888, -7.499999999999978684, 25.71875000000000000 ) ) ;
#43877 = VERTEX_POINT ( 'NONE', #78170 ) ;
#43878 = EDGE_CURVE ( 'NONE', #41031, #65326, #44816, .T. ) ;
#43879 = ORIENTED_EDGE ( 'NONE', *, *, #20145, .T. ) ;
#43880 = LINE ( 'NONE', #59617, #64379 ) ;
#43881 = EDGE_LOOP ( 'NONE', ( #51758, #5460, #72615, #51360 ) ) ;
#43882 = FACE_BOUND ( 'NONE', #40305, .T. ) ;
#43883 = CARTESIAN_POINT ( 'NONE',  ( 13.60739505359344825, -12.47679350104403007, 31.42216943046555855 ) ) ;
#43884 = LINE ( 'NONE', #47432, #70689 ) ;
#43885 = ORIENTED_EDGE ( 'NONE', *, *, #1424, .F. ) ;
#43886 = CARTESIAN_POINT ( 'NONE',  ( -4.403846153846151523, -2.499999999999998668, 29.75000000000000355 ) ) ;
#43887 = CARTESIAN_POINT ( 'NONE',  ( 3.361561038594016004, -3.062576670634119758, 32.05464942895959979 ) ) ;
#43888 = CARTESIAN_POINT ( 'NONE',  ( 18.00000000000030553, -2.506253911140615021, 30.00000000000323297 ) ) ;
#43889 = ORIENTED_EDGE ( 'NONE', *, *, #33726, .T. ) ;
#43890 = CARTESIAN_POINT ( 'NONE',  ( 1.634615384615386580, -2.249999999999998668, 29.75000000000000355 ) ) ;
#43891 = CARTESIAN_POINT ( 'NONE',  ( -13.16183584334697443, -11.89424750095246175, 32.13594075562311758 ) ) ;
#43892 = ADVANCED_FACE ( 'NONE', ( #64195 ), #9281, .F. ) ;
#43893 = VERTEX_POINT ( 'NONE', #86284 ) ;
#43894 = VECTOR ( 'NONE', #24296, 1000.000000000000227 ) ;
#43895 = CARTESIAN_POINT ( 'NONE',  ( 3.230769230769231726, -8.120952969808772792, 34.71129190930000163 ) ) ;
#43896 = PLANE ( 'NONE',  #38693 ) ;
#43897 = CARTESIAN_POINT ( 'NONE',  ( 2.177544337960616527, -12.15440758774515473, 32.17923288041532004 ) ) ;
#43898 = CARTESIAN_POINT ( 'NONE',  ( 15.93091919493929964, -2.889293201056495786, 32.26117774369186009 ) ) ;
#43899 = CARTESIAN_POINT ( 'NONE',  ( -0.4615384615384611200, -4.661471528628507777, 34.16647553114623292 ) ) ;
#43900 = EDGE_CURVE ( 'NONE', #26375, #19635, #24150, .T. ) ;
#43902 = EDGE_CURVE ( 'NONE', #45619, #4994, #88821, .T. ) ;
#43901 = CARTESIAN_POINT ( 'NONE',  ( 9.320512820512821150, -11.00000000000000000, 29.65000000000000213 ) ) ;
#43903 = CARTESIAN_POINT ( 'NONE',  ( 7.911408985666682270, -3.083524468853784839, 32.58852847137153930 ) ) ;
#43904 = B_SPLINE_CURVE_WITH_KNOTS ( 'NONE', 3,
 ( #38316, #31096, #85611, #80195, #51341, #64880, #78844, #86060, #18495, #11738 ),
 .UNSPECIFIED., .F., .F.,
 ( 4, 2, 2, 2, 4 ),
 ( 0.000000000000000000, 0.0001954339857564073659, 0.0003908679715128147319, 0.0005863019572692221250, 0.0007817359430256294638 ),
 .UNSPECIFIED. ) ;
#43906 = CARTESIAN_POINT ( 'NONE',  ( 11.28846153846153832, -7.500000000000001776, 35.00000000000000000 ) ) ;
#43905 = CARTESIAN_POINT ( 'NONE',  ( 4.153846153846154188, -12.10708131394839349, 31.69288490824020244 ) ) ;
#43907 = CARTESIAN_POINT ( 'NONE',  ( -3.999999999999998224, -7.500000000000000000, 14.00000000000000178 ) ) ;
#43909 = CARTESIAN_POINT ( 'NONE',  ( -8.639185713310999049, -2.254550872974305342, 29.97347326024527092 ) ) ;
#43908 = CARTESIAN_POINT ( 'NONE',  ( 4.153846153846030731, -5.941354392335915335, 34.76329471203413846 ) ) ;
#43910 = CARTESIAN_POINT ( 'NONE',  ( -6.000000000000119904, -12.46129190930018460, 30.37095296980731973 ) ) ;
#43911 = CARTESIAN_POINT ( 'NONE',  ( 0.06109907496454976272, -10.25000000000000000, 20.77938170625848713 ) ) ;
#43912 = ADVANCED_FACE ( 'NONE', ( #20019 ), #19578, .F. ) ;
#43913 = ORIENTED_EDGE ( 'NONE', *, *, #72828, .F. ) ;
#43914 = CARTESIAN_POINT ( 'NONE',  ( 3.205095948332795430, -8.038739123764113259, 14.00000000000000355 ) ) ;
#43915 = EDGE_LOOP ( 'NONE', ( #36437, #35808, #34300, #14893 ) ) ;
#43916 = CARTESIAN_POINT ( 'NONE',  ( -9.822999158975251888, -5.582088688514999397, 34.36776431015576350 ) ) ;
#43917 = ORIENTED_EDGE ( 'NONE', *, *, #85740, .F. ) ;
#43918 = CARTESIAN_POINT ( 'NONE',  ( 16.08857570788537927, -11.48612834413959582, 32.76840700105983473 ) ) ;
#43919 = ORIENTED_EDGE ( 'NONE', *, *, #62582, .T. ) ;
#43920 = CARTESIAN_POINT ( 'NONE',  ( 17.06410256410256565, -11.50000000000000000, 29.75000000000000355 ) ) ;
#43921 = CARTESIAN_POINT ( 'NONE',  ( 1.987747218494664292, -9.401340078031346081, 24.37313170625848713 ) ) ;
#43922 = CARTESIAN_POINT ( 'NONE',  ( 24.99999999999999645, 20.00000000000000355, 3.000000000000000000 ) ) ;
#43923 = CARTESIAN_POINT ( 'NONE',  ( 6.673053685783957967, -11.37209801155882971, 32.91403422569032955 ) ) ;
#43924 = CARTESIAN_POINT ( 'NONE',  ( -3.099978789802281920, -12.35292014791297710, 31.75344720912887198 ) ) ;
#43925 = CARTESIAN_POINT ( 'NONE',  ( 7.173022441425063178, -9.272278438253401589, 34.42582936511637826 ) ) ;
#43926 = CARTESIAN_POINT ( 'NONE',  ( 15.10062126103753855, -8.630895178749533159, 34.87696386517710323 ) ) ;
#43927 = DIRECTION ( 'NONE',  ( -1.000000000000000000, 0.000000000000000000, -0.000000000000000000 ) ) ;
#43928 = CARTESIAN_POINT ( 'NONE',  ( 6.000000000000001776, -6.189225973068211317, 35.74407628777942847 ) ) ;
#43929 = CARTESIAN_POINT ( 'NONE',  ( 1.553300858899087311, -3.749999999999992006, 17.98437500000000000 ) ) ;
#43930 = VECTOR ( 'NONE', #48435, 1000.000000000000000 ) ;
#43931 = CARTESIAN_POINT ( 'NONE',  ( 1.319344938654611443, -2.892918686051582977, 31.69288490824016691 ) ) ;
#43932 = CARTESIAN_POINT ( 'NONE',  ( 11.53846153846141576, -12.70778746994576025, 30.41441678777401236 ) ) ;
#43933 = CARTESIAN_POINT ( 'NONE',  ( 14.30769230769218758, -3.300289026999228881, 32.46337939537708905 ) ) ;
#43934 = CARTESIAN_POINT ( 'NONE',  ( 1.553300858899087311, -3.749999999999992006, 16.73437500000000000 ) ) ;
#43935 = EDGE_CURVE ( 'NONE', #25274, #38093, #58620, .T. ) ;
#43936 = ORIENTED_EDGE ( 'NONE', *, *, #36201, .F. ) ;
#43937 = CYLINDRICAL_SURFACE ( 'NONE', #15556, 4.500000000000001776 ) ;
#43938 = CARTESIAN_POINT ( 'NONE',  ( -11.53846153846153655, -12.78798330534102767, 29.49999999999997868 ) ) ;
#43939 = CARTESIAN_POINT ( 'NONE',  ( -8.769230769230768274, -11.16473453929635440, 33.15142922261926373 ) ) ;
#43940 = CARTESIAN_POINT ( 'NONE',  ( 15.90384615384615330, -7.566082377512564960, 35.00000000000000711 ) ) ;
#43941 = VECTOR ( 'NONE', #70129, 1000.000000000000000 ) ;
#43942 = CARTESIAN_POINT ( 'NONE',  ( 17.29993592101647337, -12.38742843783360748, 31.66772728687926985 ) ) ;
#43943 = DIRECTION ( 'NONE',  ( -0.000000000000000000, -0.1736481776669307198, -0.9848077530122080203 ) ) ;
#43944 = ADVANCED_FACE ( 'NONE', ( #87615 ), #5622, .F. ) ;
#43945 = ORIENTED_EDGE ( 'NONE', *, *, #57618, .T. ) ;
#43946 = CARTESIAN_POINT ( 'NONE',  ( -1.384615384615505151, -10.21337939537710326, 33.94971097300076224 ) ) ;
#43947 = ORIENTED_EDGE ( 'NONE', *, *, #16268, .F. ) ;
#43948 = EDGE_CURVE ( 'NONE', #65065, #8429, #24329, .T. ) ;
#43949 = EDGE_LOOP ( 'NONE', ( #21742, #60030, #49970, #41540 ) ) ;
#43950 = DIRECTION ( 'NONE',  ( -0.000000000000000000, -0.9396926207859092051, -0.3420201433256662704 ) ) ;
#43951 = DIRECTION ( 'NONE',  ( 0.000000000000000000, 1.000000000000000000, -0.000000000000000000 ) ) ;
#43952 = CARTESIAN_POINT ( 'NONE',  ( 16.40390046548446534, -2.779044189368097051, 31.39831045268885745 ) ) ;
#43953 = CARTESIAN_POINT ( 'NONE',  ( 4.376857505459002873, -3.587049720035815792, 32.86302985866382897 ) ) ;
#43954 = CARTESIAN_POINT ( 'NONE',  ( 17.77651507543566822, -9.417330523894424488, 34.63758898049880486 ) ) ;
#43956 = EDGE_CURVE ( 'NONE', #20735, #87881, #33094, .T. ) ;
#43955 = ORIENTED_EDGE ( 'NONE', *, *, #72534, .F. ) ;
#43957 = DIRECTION ( 'NONE',  ( -0.000000000000000000, -0.3420201433256694901, -0.9396926207859082059 ) ) ;
#43958 = VERTEX_POINT ( 'NONE', #74090 ) ;
#43959 = ORIENTED_EDGE ( 'NONE', *, *, #85508, .F. ) ;
#43960 = CARTESIAN_POINT ( 'NONE',  ( 12.52673244332181568, -2.506253911140448043, 29.99999999999988631 ) ) ;
#43961 = CARTESIAN_POINT ( 'NONE',  ( 23.49999999999998579, -13.24999999999999822, 27.31828373317832970 ) ) ;
#43963 = EDGE_CURVE ( 'NONE', #42436, #19174, #30709, .T. ) ;
#43962 = B_SPLINE_CURVE_WITH_KNOTS ( 'NONE', 3,
 ( #58794, #11064, #52033, #25015, #32227, #37189, #3850, #64654, #38085, #66451 ),
 .UNSPECIFIED., .F., .F.,
 ( 4, 2, 2, 2, 4 ),
 ( 0.0007817359430256282712, 0.0009771253907249941549, 0.001172514838424359822, 0.001367904286123725489, 0.001563293733823091372 ),
 .UNSPECIFIED. ) ;
#43964 = CARTESIAN_POINT ( 'NONE',  ( -10.48533700912893174, -7.723484964179501588, 34.74522123443823318 ) ) ;
#43965 = LINE ( 'NONE', #30890, #40746 ) ;
#43966 = EDGE_CURVE ( 'NONE', #49557, #72270, #84495, .T. ) ;
#43967 = CARTESIAN_POINT ( 'NONE',  ( -7.846153846153965716, -12.27809138561165270, 31.22303859784587132 ) ) ;
#43968 = ORIENTED_EDGE ( 'NONE', *, *, #35737, .T. ) ;
#43969 = ORIENTED_EDGE ( 'NONE', *, *, #68408, .T. ) ;
#43970 = CARTESIAN_POINT ( 'NONE',  ( 2.320192649118979489E-14, -11.25000000000000000, 21.03125000000000000 ) ) ;
#43971 = EDGE_LOOP ( 'NONE', ( #74231, #88312 ) ) ;
#43973 = ORIENTED_EDGE ( 'NONE', *, *, #4658, .F. ) ;
#43972 = CARTESIAN_POINT ( 'NONE',  ( -14.08467946359890988, -2.308499170217967134, 30.53291367094873721 ) ) ;
#43974 = CYLINDRICAL_SURFACE ( 'NONE', #33508, 0.2499999999999995559 ) ;
#43975 = CARTESIAN_POINT ( 'NONE',  ( 6.222779541268409709, -12.44528174975671853, 30.48912976160716681 ) ) ;
#43976 = CARTESIAN_POINT ( 'NONE',  ( 2.372947447205147942, -9.528491918058460186, 34.59228464037085615 ) ) ;
#43977 = ORIENTED_EDGE ( 'NONE', *, *, #72789, .T. ) ;
#43978 = EDGE_CURVE ( 'NONE', #25915, #23361, #26418, .T. ) ;
#43979 = CARTESIAN_POINT ( 'NONE',  ( 14.98079248672064345, -2.544273027872575366, 31.48422191005632342 ) ) ;
#43980 = ORIENTED_EDGE ( 'NONE', *, *, #46074, .F. ) ;
#43981 = CARTESIAN_POINT ( 'NONE',  ( 15.29683656411930848, -11.35647404775217595, 33.31231777344666511 ) ) ;
#43982 = FACE_OUTER_BOUND ( 'NONE', #63029, .T. ) ;
#43983 = CARTESIAN_POINT ( 'NONE',  ( -18.00000000000000000, -2.486705287966279876, 31.30864560766543647 ) ) ;
#43985 = CARTESIAN_POINT ( 'NONE',  ( -10.86540783960607293, -5.765609946408404518, 34.70566812827425451 ) ) ;
#43984 = CARTESIAN_POINT ( 'NONE',  ( -0.2385256174450662847, -11.43677907613345113, 33.22367315496201456 ) ) ;
#43986 = CARTESIAN_POINT ( 'NONE',  ( 16.08857570788537572, -2.625532179533444754, 30.86335684631481513 ) ) ;
#43987 = CARTESIAN_POINT ( 'NONE',  ( -0.3962833220256231082, -12.70778746994558439, 30.41441678777537305 ) ) ;
#43988 = ORIENTED_EDGE ( 'NONE', *, *, #63726, .F. ) ;
#43989 = CARTESIAN_POINT ( 'NONE',  ( -11.47320596718551400, -12.27809138561124591, 31.22303859784720359 ) ) ;
#43990 = CARTESIAN_POINT ( 'NONE',  ( -6.249976744048589161, -11.47974371597207899, 33.17467449705390692 ) ) ;
#43992 = ORIENTED_EDGE ( 'NONE', *, *, #31997, .F. ) ;
#43991 = ADVANCED_FACE ( 'NONE', ( #28108 ), #56468, .F. ) ;
#43993 = CARTESIAN_POINT ( 'NONE',  ( -1.384615384615383471, -10.51840700105979565, 33.73612834413961536 ) ) ;
#43994 = CARTESIAN_POINT ( 'NONE',  ( -4.854143535654667829, -5.913360116392398780, 34.49180327182771322 ) ) ;
#43995 = CARTESIAN_POINT ( 'NONE',  ( 3.296938371731887862, -7.250054483168843156, 34.74374881642865631 ) ) ;
#43996 = CARTESIAN_POINT ( 'NONE',  ( 2.057669083470851756, -5.765609946408404518, 34.70566812827425451 ) ) ;
#43997 = CARTESIAN_POINT ( 'NONE',  ( 17.93472955403921887, -6.026961402152685388, 34.52809138561120506 ) ) ;
#43998 = EDGE_CURVE ( 'NONE', #19270, #82252, #14597, .T. ) ;
#44000 = ADVANCED_FACE ( 'NONE', ( #41188 ), #69099, .F. ) ;
#43999 = CARTESIAN_POINT ( 'NONE',  ( 13.38461538461538680, -13.95598074871891292, 31.83374038241031911 ) ) ;
#44001 = FACE_BOUND ( 'NONE', #24123, .T. ) ;
#44003 = FACE_OUTER_BOUND ( 'NONE', #19811, .T. ) ;
#44002 = DIRECTION ( 'NONE',  ( -0.000000000000000000, 0.9396926207859092051, -0.3420201433256662704 ) ) ;
#44004 = DIRECTION ( 'NONE',  ( -0.000000000000000000, 0.7660444431189791237, -0.6427876096865379196 ) ) ;
#44006 = CARTESIAN_POINT ( 'NONE',  ( 9.823099500132483897, -4.118422570099828484, 33.43335022499816489 ) ) ;
#44005 = CARTESIAN_POINT ( 'NONE',  ( -6.792286482109972212, -10.70102852606553157, 33.91149625220312913 ) ) ;
#44007 = DIRECTION ( 'NONE',  ( -0.000000000000000000, 0.3420201433256694346, -0.9396926207859080948 ) ) ;
#44008 = CARTESIAN_POINT ( 'NONE',  ( -3.749999999999996447, -7.561099074964554134, 19.84188170625848713 ) ) ;
#44009 = ORIENTED_EDGE ( 'NONE', *, *, #78246, .F. ) ;
#44010 = CARTESIAN_POINT ( 'NONE',  ( 18.00000000000000000, -3.669653830205710676, 35.88435417666054406 ) ) ;
#44011 = AXIS2_PLACEMENT_3D ( 'NONE', #85029, #84157, #2157 ) ;
#44012 = CARTESIAN_POINT ( 'NONE',  ( -12.33074802057151409, -6.369690395747422684, 34.87708834333098196 ) ) ;
#44013 = CARTESIAN_POINT ( 'NONE',  ( -0.7115616857599182943, -3.520140089381497361, 33.17453946501458262 ) ) ;
#44014 = CARTESIAN_POINT ( 'NONE',  ( -10.86536135943320502, -11.47974371597208076, 33.17467449705390692 ) ) ;
#44015 = CARTESIAN_POINT ( 'NONE',  ( 6.700149964170075023, -12.64616026154729411, 30.79003144601913533 ) ) ;
#44016 = CARTESIAN_POINT ( 'NONE',  ( -9.626239341305254271, -4.098570777380720287, 33.41473453929635440 ) ) ;
#44017 = CARTESIAN_POINT ( 'NONE',  ( 3.749999999999999556, -7.438900925035446754, 22.96688170625849068 ) ) ;
#44018 = CARTESIAN_POINT ( 'NONE',  ( -16.40386937806761125, -5.765609946408405406, 34.70566812827424741 ) ) ;
#44019 = CARTESIAN_POINT ( 'NONE',  ( 18.24994551834813805, -3.202959910592336090, 32.30730279482227019 ) ) ;
#44020 = VECTOR ( 'NONE', #48032, 1000.000000000000227 ) ;
#44021 = DIRECTION ( 'NONE',  ( 0.000000000000000000, 0.1736481776669267785, -0.9848077530122087975 ) ) ;
#44022 = CARTESIAN_POINT ( 'NONE',  ( 10.48469401227430708, -6.369640206132551441, 34.87707690430378449 ) ) ;
#44023 = CARTESIAN_POINT ( 'NONE',  ( 2.307692307692623679, -2.255955759149395501, 30.00000000000324363 ) ) ;
#44024 = CARTESIAN_POINT ( 'NONE',  ( 6.000000000000001776, -13.87047571288749737, 32.06866353760679544 ) ) ;
#44025 = FACE_OUTER_BOUND ( 'NONE', #24222, .T. ) ;
#44026 = CARTESIAN_POINT ( 'NONE',  ( 17.29993592101647693, -2.523321265292116866, 31.42251411153756990 ) ) ;
#44027 = EDGE_LOOP ( 'NONE', ( #41984, #84002, #71096, #19932 ) ) ;
#44028 = CARTESIAN_POINT ( 'NONE',  ( -15.90384615384471800, -7.500000000000155431, 34.75000000000007105 ) ) ;
#44029 = CARTESIAN_POINT ( 'NONE',  ( -4.230769230769230838, -7.500000000000000000, 33.75000000000000000 ) ) ;
#44030 = CARTESIAN_POINT ( 'NONE',  ( 0.06109907496451268821, -3.749999999999999556, 15.65811829374151287 ) ) ;
#44031 = CARTESIAN_POINT ( 'NONE',  ( 7.145856592054987466, -10.97394488606064122, 33.68653795673694873 ) ) ;
#44032 = CARTESIAN_POINT ( 'NONE',  ( -8.769230769230892619, -8.656820664282941280, 34.87096338111179961 ) ) ;
#44033 = ORIENTED_EDGE ( 'NONE', *, *, #48219, .T. ) ;
#44034 = CARTESIAN_POINT ( 'NONE',  ( -16.21992853320628925, -3.937682226553330445, 33.60647404775217240 ) ) ;
#44036 = ORIENTED_EDGE ( 'NONE', *, *, #52575, .F. ) ;
#44035 = CARTESIAN_POINT ( 'NONE',  ( 12.23861224402230619, -5.667676309546437530, 34.40238873228292249 ) ) ;
#44037 = CARTESIAN_POINT ( 'NONE',  ( 6.699591979352975457, -3.236172620538810385, 32.36188796281390267 ) ) ;
#44038 = CARTESIAN_POINT ( 'NONE',  ( -13.16160403300253279, -9.886259254753566594, 34.14407573483972413 ) ) ;
#44039 = LINE ( 'NONE', #23765, #44836 ) ;
#44040 = DIRECTION ( 'NONE',  ( -0.000000000000000000, 0.9396926207859093161, -0.3420201433256663259 ) ) ;
#44041 = ORIENTED_EDGE ( 'NONE', *, *, #874, .T. ) ;
#44042 = CARTESIAN_POINT ( 'NONE',  ( -11.60454494941741999, -4.098570777380719399, 33.41473453929634729 ) ) ;
#44043 = SURFACE_STYLE_USAGE ( .BOTH. , #29666 ) ;
#44044 = CARTESIAN_POINT ( 'NONE',  ( -1.384615384615505151, -6.026961402154118908, 34.52809138561165270 ) ) ;
#44045 = ORIENTED_EDGE ( 'NONE', *, *, #23416, .F. ) ;
#44046 = VERTEX_POINT ( 'NONE', #33976 ) ;
#44047 = VERTEX_POINT ( 'NONE', #49706 ) ;
#44048 = CARTESIAN_POINT ( 'NONE',  ( -8.769230769230890843, -10.21337939537710326, 33.94971097300076224 ) ) ;
#44049 = CARTESIAN_POINT ( 'NONE',  ( -8.638438961405983108, -3.062576670634119758, 32.05464942895959979 ) ) ;
#44050 = CARTESIAN_POINT ( 'NONE',  ( -3.930833309752757021, -12.64618726649961289, 30.78989965857442712 ) ) ;
#44051 = CARTESIAN_POINT ( 'NONE',  ( -10.39237326377176451, -3.105924265160262543, 32.13625925475356127 ) ) ;
#44052 = VERTEX_POINT ( 'NONE', #197 ) ;
#44053 = ORIENTED_EDGE ( 'NONE', *, *, #7105, .F. ) ;
#44055 = ORIENTED_EDGE ( 'NONE', *, *, #24394, .F. ) ;
#44054 = CARTESIAN_POINT ( 'NONE',  ( -2.057692307690886846, -7.500000000000154543, 35.00000000000007105 ) ) ;
#44056 = CARTESIAN_POINT ( 'NONE',  ( 9.692307692307695177, -12.37446782046654192, 30.86335684631486131 ) ) ;
#44057 = EDGE_CURVE ( 'NONE', #1586, #8757, #83378, .T. ) ;
#44058 = AXIS2_PLACEMENT_3D ( 'NONE', #54015, #81509, #32422 ) ;
#44059 = CARTESIAN_POINT ( 'NONE',  ( 2.307692307692309264, -3.513871655860378418, 32.76840700105978499 ) ) ;
#44060 = DIRECTION ( 'NONE',  ( -0.000000000000000000, -0.6427876096865404731, -0.7660444431189770143 ) ) ;
#44061 = EDGE_LOOP ( 'NONE', ( #21709, #13201, #20030, #32767 ) ) ;
#44062 = AXIS2_PLACEMENT_3D ( 'NONE', #33770, #25682, #48936 ) ;
#44063 = ORIENTED_EDGE ( 'NONE', *, *, #41030, .T. ) ;
#44065 = ORIENTED_EDGE ( 'NONE', *, *, #10210, .T. ) ;
#44064 = CARTESIAN_POINT ( 'NONE',  ( -16.15384615384615330, -11.11383981884818262, 36.00935417666054406 ) ) ;
#44066 = B_SPLINE_CURVE_WITH_KNOTS ( 'NONE', 3,
 ( #87880, #61242, #59482, #81101, #73453, #88318, #13513, #67137, #6328, #81990 ),
 .UNSPECIFIED., .F., .F.,
 ( 4, 2, 2, 2, 4 ),
 ( 0.0007817246256747459798, 0.0009771112852218896347, 0.001172497944769033398, 0.001367884604316177161, 0.001563271263863320708 ),
 .UNSPECIFIED. ) ;
#44067 = CARTESIAN_POINT ( 'NONE',  ( -2.294871794871794712, -7.500000000000000000, 29.75000000000000355 ) ) ;
#44068 = CARTESIAN_POINT ( 'NONE',  ( -16.02332045208259004, -3.816742781228458448, 33.13167719472716044 ) ) ;
#44069 = ORIENTED_EDGE ( 'NONE', *, *, #69534, .F. ) ;
#44070 = EDGE_CURVE ( 'NONE', #17127, #80196, #77181, .T. ) ;
#44071 = AXIS2_PLACEMENT_3D ( 'NONE', #55651, #6592, #7027 ) ;
#44072 = CARTESIAN_POINT ( 'NONE',  ( 12.52760579488853665, -6.343179335718452272, 34.87096338111212646 ) ) ;
#44073 = LINE ( 'NONE', #13630, #45085 ) ;
#44074 = LINE ( 'NONE', #42339, #87103 ) ;
#44075 = FACE_BOUND ( 'NONE', #25411, .T. ) ;
#44076 = CARTESIAN_POINT ( 'NONE',  ( 5.999999999999878320, -2.379036618888197729, 30.90682066428292885 ) ) ;
#44077 = CARTESIAN_POINT ( 'NONE',  ( 2.307692307692309264, -8.120952969808772792, 34.71129190930000163 ) ) ;
#44078 = CARTESIAN_POINT ( 'NONE',  ( 8.769230769230768274, -2.708943851104267164, 35.45975837776705220 ) ) ;
#44080 = CARTESIAN_POINT ( 'NONE',  ( 4.219101293358989757, -2.379036618887895305, 30.90682066428159303 ) ) ;
#44079 = CARTESIAN_POINT ( 'NONE',  ( 3.361294669002876656, -3.625058011473228259, 33.29252011169590020 ) ) ;
#44081 = CARTESIAN_POINT ( 'NONE',  ( -7.976845312821408740, -3.062553014421049546, 32.05460306192773601 ) ) ;
#44082 = DIRECTION ( 'NONE',  ( 0.000000000000000000, 0.000000000000000000, -1.000000000000000000 ) ) ;
#44083 = EDGE_LOOP ( 'NONE', ( #45832, #63739, #83321, #73064 ) ) ;
#44084 = CARTESIAN_POINT ( 'NONE',  ( -5.076923076923075762, -3.886160181151819604, 36.00935417666054406 ) ) ;
#44085 = B_SPLINE_CURVE_WITH_KNOTS ( 'NONE', 3,
 ( #40205, #87072, #11841, #33871, #52806, #18595, #59568, #67667, #67227, #60457 ),
 .UNSPECIFIED., .F., .F.,
 ( 4, 2, 2, 2, 4 ),
 ( 0.0007817359430256304396, 0.0009771253907249963233, 0.001172514838424362424, 0.001367904286123728308, 0.001563293733823094191 ),
 .UNSPECIFIED. ) ;
#44086 = ORIENTED_EDGE ( 'NONE', *, *, #59201, .F. ) ;
#44087 = ORIENTED_EDGE ( 'NONE', *, *, #85675, .F. ) ;
#44089 = CARTESIAN_POINT ( 'NONE',  ( 10.74591005361826035, -12.70449254468099198, 30.44128974285582956 ) ) ;
#44088 = CARTESIAN_POINT ( 'NONE',  ( -5.300408001487405762, -12.11044203135681840, 32.26167407432752299 ) ) ;
#44090 = CARTESIAN_POINT ( 'NONE',  ( -5.749945688361685292, -6.567000820036038355, 34.66262288849541306 ) ) ;
#44091 = CARTESIAN_POINT ( 'NONE',  ( 14.37375964104238335, -3.937682226553329556, 33.60647404775216529 ) ) ;
#44092 = CARTESIAN_POINT ( 'NONE',  ( -16.15384615384615330, -2.499999999999998668, 29.50000000000001066 ) ) ;
#44093 = CARTESIAN_POINT ( 'NONE',  ( -24.00000000000000000, -5.499999999999981348, 27.75000000000000000 ) ) ;
#44094 = EDGE_LOOP ( 'NONE', ( #4889, #12567, #86237, #62724, #53890 ) ) ;
#44095 = EDGE_CURVE ( 'NONE', #33240, #10922, #16836, .T. ) ;
#44096 = EDGE_CURVE ( 'NONE', #84840, #79197, #27541, .T. ) ;
#44097 = CARTESIAN_POINT ( 'NONE',  ( 18.00000000000000000, -3.937682226553329556, 33.60647404775216529 ) ) ;
#44098 = CARTESIAN_POINT ( 'NONE',  ( 6.792385456409363087, -3.530157926970578508, 32.79014554554150607 ) ) ;
#44099 = CARTESIAN_POINT ( 'NONE',  ( 17.32697738856138869, -6.567000820036036579, 34.66262288849541306 ) ) ;
#44100 = LINE ( 'NONE', #71579, #65462 ) ;
#44101 = CARTESIAN_POINT ( 'NONE',  ( -20.00000000000000355, 10.00000000000000711, 10.00000000000000178 ) ) ;
#44102 = CARTESIAN_POINT ( 'NONE',  ( -1.553300858899125059, -3.750000000000009326, 15.32812500000000355 ) ) ;
#44103 = ORIENTED_EDGE ( 'NONE', *, *, #3332, .T. ) ;
#44104 = ORIENTED_EDGE ( 'NONE', *, *, #75165, .F. ) ;
#44105 = EDGE_CURVE ( 'NONE', #5354, #81137, #23220, .T. ) ;
#44106 = CARTESIAN_POINT ( 'NONE',  ( -7.846153846153844924, -11.35647404775217417, 33.31231777344666511 ) ) ;
#44107 = ORIENTED_EDGE ( 'NONE', *, *, #67088, .T. ) ;
#44108 = AXIS2_PLACEMENT_3D ( 'NONE', #40859, #60677, #6624 ) ;
#44109 = CARTESIAN_POINT ( 'NONE',  ( -18.06532401280430733, -7.749976730030849303, 34.74374725381503737 ) ) ;
#44110 = CARTESIAN_POINT ( 'NONE',  ( 9.692307692307695177, -9.780366693483667717, 34.19971097300155094 ) ) ;
#44111 = CARTESIAN_POINT ( 'NONE',  ( -16.21911659980692733, -2.892918686051582089, 31.69288490824015980 ) ) ;
#44112 = CARTESIAN_POINT ( 'NONE',  ( 5.777133736936903574, -2.251424796025575770, 29.88072029997477586 ) ) ;
#44113 = CARTESIAN_POINT ( 'NONE',  ( -2.651650429449535551, -10.15165042944956753, 19.93750000000000000 ) ) ;
#44114 = DIRECTION ( 'NONE',  ( -1.000000000000000000, -0.000000000000000000, -0.000000000000000000 ) ) ;
#44115 = ORIENTED_EDGE ( 'NONE', *, *, #77511, .T. ) ;
#44116 = CARTESIAN_POINT ( 'NONE',  ( -12.52762187249433978, -10.51840700105979387, 33.73612834413961536 ) ) ;
#44118 = ORIENTED_EDGE ( 'NONE', *, *, #60369, .T. ) ;
#44117 = CARTESIAN_POINT ( 'NONE',  ( -16.40386939113912135, -11.86270091957321071, 32.19358267280088626 ) ) ;
#44119 = LINE ( 'NONE', #2692, #13809 ) ;
#44120 = DIRECTION ( 'NONE',  ( 0.000000000000000000, 0.9848077530122072432, 0.1736481776669354937 ) ) ;
#44121 = CARTESIAN_POINT ( 'NONE',  ( 6.130790440966952026, -9.084667340241226796, 34.75534355489798344 ) ) ;
#44122 = CARTESIAN_POINT ( 'NONE',  ( -2.307692307692305711, -2.292212530054420494, 30.41441678777542634 ) ) ;
#44123 = CARTESIAN_POINT ( 'NONE',  ( -6.000000000000119904, -10.21337939537710326, 33.94971097300076224 ) ) ;
#44124 = CARTESIAN_POINT ( 'NONE',  ( 11.28848480751918437, -6.567427716900048118, 34.66269422305636283 ) ) ;
#44125 = CARTESIAN_POINT ( 'NONE',  ( -7.053768389744481837, -4.809359713505814149, 33.96456829005828837 ) ) ;
#44126 = CARTESIAN_POINT ( 'NONE',  ( -1.614399933863613468, -11.22469193450124969, 17.61124329374151642 ) ) ;
#44127 = ORIENTED_EDGE ( 'NONE', *, *, #4741, .T. ) ;
#44128 = DIRECTION ( 'NONE',  ( 1.000000000000000000, 0.000000000000000000, 0.000000000000000000 ) ) ;
#44129 = CARTESIAN_POINT ( 'NONE',  ( -12.39639268220649271, -7.750023238201979581, 34.74374492549440419 ) ) ;
#44130 = DIRECTION ( 'NONE',  ( -0.000000000000000000, 0.3420201433256694901, -0.9396926207859082059 ) ) ;
#44131 = CARTESIAN_POINT ( 'NONE',  ( 2.750000000000002665, -7.561099074964516831, 13.47061829374151465 ) ) ;
#44132 = CARTESIAN_POINT ( 'NONE',  ( 0.4615384615384611200, -3.513871655860378418, 32.76840700105978499 ) ) ;
#44134 = CARTESIAN_POINT ( 'NONE',  ( -17.32689980786543060, -2.564618984488975517, 30.55390908950641915 ) ) ;
#44133 = VECTOR ( 'NONE', #86171, 1000.000000000000227 ) ;
#44135 = ORIENTED_EDGE ( 'NONE', *, *, #17173, .T. ) ;
#44136 = CARTESIAN_POINT ( 'NONE',  ( -1.409462824231155764E-14, -4.749999999999999112, 19.15625000000000000 ) ) ;
#44137 = LINE ( 'NONE', #18027, #48389 ) ;
#44138 = EDGE_LOOP ( 'NONE', ( #28346, #50040 ) ) ;
#44139 = CARTESIAN_POINT ( 'NONE',  ( -18.25002322422145085, -4.931416488878823223, 34.32920672191015399 ) ) ;
#44140 = ORIENTED_EDGE ( 'NONE', *, *, #8742, .T. ) ;
#44141 = CARTESIAN_POINT ( 'NONE',  ( 17.75002326905764605, -6.567427716900048118, 34.66269422305636283 ) ) ;
#44142 = CARTESIAN_POINT ( 'NONE',  ( 3.230769230769108269, -4.320704448113951379, 33.92786785259630022 ) ) ;
#44143 = AXIS2_PLACEMENT_3D ( 'NONE', #10261, #37273, #58881 ) ;
#44144 = CARTESIAN_POINT ( 'NONE',  ( -0.7115616857599186273, -10.18141759479407327, 34.26406193332782379 ) ) ;
#44145 = CARTESIAN_POINT ( 'NONE',  ( -12.46153846153846168, -13.53365097954675988, 30.81389545987213552 ) ) ;
#44146 = EDGE_LOOP ( 'NONE', ( #79100, #29778, #69516, #9229 ) ) ;
#44147 = CARTESIAN_POINT ( 'NONE',  ( -13.38461538461538325, -2.833524468853757305, 32.15551576947925838 ) ) ;
#44148 = ORIENTED_EDGE ( 'NONE', *, *, #33561, .F. ) ;
#44149 = CARTESIAN_POINT ( 'NONE',  ( -17.74994558008654622, -12.01375889529407992, 32.43194544308182969 ) ) ;
#44150 = CARTESIAN_POINT ( 'NONE',  ( 12.46153846153846168, -12.10708131394839349, 31.69288490824020244 ) ) ;
#44151 = ORIENTED_EDGE ( 'NONE', *, *, #78893, .T. ) ;
#44152 = CARTESIAN_POINT ( 'NONE',  ( -5.776988648387149539, -11.24521262558773671, 33.06293181088029343 ) ) ;
#44153 = CARTESIAN_POINT ( 'NONE',  ( 10.83839596699746544, -3.105924265160262543, 32.13625925475356127 ) ) ;
#44154 = CARTESIAN_POINT ( 'NONE',  ( -4.023800991011373895, -2.504778602574660340, 29.97347330155780298 ) ) ;
#44155 = EDGE_CURVE ( 'NONE', #84107, #43411, #6950, .T. ) ;
#44156 = CARTESIAN_POINT ( 'NONE',  ( -14.17716686945866300, -10.31582465632705237, 34.18122507451815295 ) ) ;
#44157 = CARTESIAN_POINT ( 'NONE',  ( -16.21911615440247090, -3.083524468853725775, 32.58852847137143272 ) ) ;
#44158 = VECTOR ( 'NONE', #8163, 1000.000000000000114 ) ;
#44159 = EDGE_LOOP ( 'NONE', ( #19149, #36341, #73445, #46063 ) ) ;
#44160 = ORIENTED_EDGE ( 'NONE', *, *, #81193, .T. ) ;
#44161 = FACE_BOUND ( 'NONE', #72205, .T. ) ;
#44162 = EDGE_LOOP ( 'NONE', ( #11640, #81351 ) ) ;
#44163 = DIRECTION ( 'NONE',  ( -1.000000000000000000, -0.000000000000000000, 0.000000000000000000 ) ) ;
#44164 = EDGE_CURVE ( 'NONE', #87031, #79680, #69487, .T. ) ;
#44165 = AXIS2_PLACEMENT_3D ( 'NONE', #61645, #49023, #54899 ) ;
#44166 = CARTESIAN_POINT ( 'NONE',  ( 13.44987095589141290, -10.90142922261932057, 33.41473453929631887 ) ) ;
#44167 = DIRECTION ( 'NONE',  ( -1.000000000000000000, -0.000000000000000000, -0.000000000000000000 ) ) ;
#44169 = ORIENTED_EDGE ( 'NONE', *, *, #24687, .F. ) ;
#44168 = EDGE_CURVE ( 'NONE', #21769, #5830, #79054, .T. ) ;
#44170 = ORIENTED_EDGE ( 'NONE', *, *, #61909, .T. ) ;
#44171 = ORIENTED_EDGE ( 'NONE', *, *, #19585, .T. ) ;
#44172 = CARTESIAN_POINT ( 'NONE',  ( -1.515306851282940626, -11.71456829005830080, 32.44064028649416542 ) ) ;
#44173 = ORIENTED_EDGE ( 'NONE', *, *, #41874, .F. ) ;
#44174 = CARTESIAN_POINT ( 'NONE',  ( 2.438218009455873858, -4.459921816937789885, 33.71989282347011851 ) ) ;
#44175 = EDGE_CURVE ( 'NONE', #74304, #34444, #32969, .T. ) ;
#44176 = CARTESIAN_POINT ( 'NONE',  ( -7.912237257109728361, -2.538708090699994813, 30.37095296980875148 ) ) ;
#44177 = CARTESIAN_POINT ( 'NONE',  ( -5.076923076923075762, -13.20930481340135110, 34.54067556320372745 ) ) ;
#44178 = FACE_BOUND ( 'NONE', #49120, .T. ) ;
#44179 = ORIENTED_EDGE ( 'NONE', *, *, #1970, .F. ) ;
#44180 = CARTESIAN_POINT ( 'NONE',  ( 5.076923076923075762, -3.513871655860378418, 32.76840700105978499 ) ) ;
#44181 = EDGE_CURVE ( 'NONE', #2618, #10136, #23044, .T. ) ;
#44182 = CYLINDRICAL_SURFACE ( 'NONE', #38809, 0.2499999999999995559 ) ;
#44183 = DIRECTION ( 'NONE',  ( -1.000000000000000000, 0.000000000000000000, -0.000000000000000000 ) ) ;
#44184 = CARTESIAN_POINT ( 'NONE',  ( -11.60454494941741999, -3.050289026998445951, 32.03036669348365706 ) ) ;
#44185 = EDGE_LOOP ( 'NONE', ( #17274, #53122, #16214, #69097 ) ) ;
#44186 = CARTESIAN_POINT ( 'NONE',  ( -2.557692307692305267, -7.500000000000001776, 35.00000000000000000 ) ) ;
#44187 = ORIENTED_EDGE ( 'NONE', *, *, #26174, .T. ) ;
#44188 = ORIENTED_EDGE ( 'NONE', *, *, #86637, .F. ) ;
#44190 = DIRECTION ( 'NONE',  ( -0.000000000000000000, -0.5000000000000011102, -0.8660254037844380415 ) ) ;
#44189 = CARTESIAN_POINT ( 'NONE',  ( -3.148799926473854489E-16, -1.749999999999995781, 28.00000000000000000 ) ) ;
#44191 = CARTESIAN_POINT ( 'NONE',  ( -8.546217925137375104, -12.38742843783360748, 31.66772728687926985 ) ) ;
#44192 = CARTESIAN_POINT ( 'NONE',  ( -4.087777802843714170, -4.098570777380720287, 33.41473453929635440 ) ) ;
#44193 = CARTESIAN_POINT ( 'NONE',  ( 17.20776149493583773, -7.277220443632451463, 34.74524770363009196 ) ) ;
#44194 = CARTESIAN_POINT ( 'NONE',  ( -2.373775718648187372, -9.780366693483667717, 34.19971097300155805 ) ) ;
#44195 = ORIENTED_EDGE ( 'NONE', *, *, #45992, .T. ) ;
#44196 = EDGE_CURVE ( 'NONE', #85987, #22316, #20972, .T. ) ;
#44197 = CARTESIAN_POINT ( 'NONE',  ( -5.207613680033384540, -6.369640206132550553, 34.87707690430378449 ) ) ;
#44198 = AXIS2_PLACEMENT_3D ( 'NONE', #32317, #73760, #59779 ) ;
#44199 = CARTESIAN_POINT ( 'NONE',  ( -11.60454494941741999, -9.780366693483667717, 34.19971097300155805 ) ) ;
#44200 = LINE ( 'NONE', #78007, #8515 ) ;
#44201 = EDGE_CURVE ( 'NONE', #48673, #34683, #68211, .T. ) ;
#44202 = CARTESIAN_POINT ( 'NONE',  ( -13.63459212866397685, -12.65889640711025521, 30.72598325615533454 ) ) ;
#44203 = EDGE_LOOP ( 'NONE', ( #65042, #88215, #45107, #14185 ) ) ;
#44204 = ORIENTED_EDGE ( 'NONE', *, *, #69170, .F. ) ;
#44205 = FACE_BOUND ( 'NONE', #36644, .T. ) ;
#44206 = EDGE_CURVE ( 'NONE', #88485, #64018, #32786, .T. ) ;
#44207 = CARTESIAN_POINT ( 'NONE',  ( 7.596130608860879541, -2.823816976329319495, 31.52131813110795733 ) ) ;
#44209 = EDGE_CURVE ( 'NONE', #66098, #33822, #60009, .T. ) ;
#44208 = CARTESIAN_POINT ( 'NONE',  ( -6.792238505064159604, -7.277220443632450575, 34.74524770363009196 ) ) ;
#44210 = EDGE_LOOP ( 'NONE', ( #6279, #54238 ) ) ;
#44211 = CARTESIAN_POINT ( 'NONE',  ( 3.903869409797563250, -11.47974371597208076, 33.17467449705390692 ) ) ;
#44212 = CARTESIAN_POINT ( 'NONE',  ( 6.222779668978065004, -11.60474049983371003, 33.02348890104160262 ) ) ;
#44213 = CARTESIAN_POINT ( 'NONE',  ( 0.7115927731767749398, -12.17597550085003455, 31.52189283813461884 ) ) ;
#44214 = FACE_OUTER_BOUND ( 'NONE', #17131, .T. ) ;
#44215 = VERTEX_POINT ( 'NONE', #25339 ) ;
#44216 = CYLINDRICAL_SURFACE ( 'NONE', #47391, 0.2499999999999998890 ) ;
#44217 = EDGE_LOOP ( 'NONE', ( #50515, #23533, #780, #30170, #55794, #13705, #5559, #26927, #16261, #52962, #46280, #72749, #61289, #18394, #46003, #56492, #26856, #25925, #23946, #17656, #64761, #66765, #38319, #55463, #39118, #66391, #7026, #16484, #25999, #7690, #72770, #77230, #66773, #79487, #87290, #14292, #26704, #56605, #59238, #28974, #54908, #8768, #14063, #86579, #24691, #48486, #86198, #31439, #44934, #68133, #81459, #12637, #80552, #2125, #64389, #62491, #63042, #12675, #48548, #3128, #68001, #32272, #51668, #59393, #17622, #65260, #27849, #76267, #12080, #8299, #37991, #28037, #28356, #87551, #51407, #10475, #56268, #32658, #44231, #13575, #55166, #83214, #77309, #17493, #73992, #42446, #66961, #54655, #14302, #88299, #31438, #67339, #85774, #17595, #85016 ) ) ;
#44219 = EDGE_LOOP ( 'NONE', ( #55082, #55702 ) ) ;
#44218 = CARTESIAN_POINT ( 'NONE',  ( 24.99999999999999645, 15.00000000000000355, 3.000000000000000000 ) ) ;
#44220 = CYLINDRICAL_SURFACE ( 'NONE', #52668, 0.2500000000000009437 ) ;
#44221 = CARTESIAN_POINT ( 'NONE',  ( 15.23076923076911093, -2.892918686052165622, 31.69288490824153470 ) ) ;
#44222 = DIRECTION ( 'NONE',  ( 0.000000000000000000, 0.000000000000000000, -1.000000000000000000 ) ) ;
#44223 = DIRECTION ( 'NONE',  ( 0.000000000000000000, 0.000000000000000000, 1.000000000000000000 ) ) ;
#44224 = CARTESIAN_POINT ( 'NONE',  ( -14.43784027742400689, -8.630895178749533159, 34.87696386517710323 ) ) ;
#44225 = CARTESIAN_POINT ( 'NONE',  ( 12.39545608217832395, -5.471508081941602875, 34.59228464037088457 ) ) ;
#44226 = CARTESIAN_POINT ( 'NONE',  ( -2.749999999999999112, -7.438900925035484057, 16.59561829374151287 ) ) ;
#44227 = ORIENTED_EDGE ( 'NONE', *, *, #6984, .T. ) ;
#44228 = VECTOR ( 'NONE', #68467, 1000.000000000000114 ) ;
#44229 = CARTESIAN_POINT ( 'NONE',  ( 13.60762822870878352, -12.64618726649961289, 30.78989965857442712 ) ) ;
#44230 = CARTESIAN_POINT ( 'NONE',  ( -24.00000000000000000, -5.499999999999981348, 27.25000000000000000 ) ) ;
#44231 = ORIENTED_EDGE ( 'NONE', *, *, #88396, .F. ) ;
#44233 = ORIENTED_EDGE ( 'NONE', *, *, #30406, .T. ) ;
#44232 = VECTOR ( 'NONE', #67548, 1000.000000000000114 ) ;
#44234 = CARTESIAN_POINT ( 'NONE',  ( -10.83886955910856109, -11.41268669641500466, 32.86336882939237825 ) ) ;
#44235 = CARTESIAN_POINT ( 'NONE',  ( -7.596208436775802930, -5.766571408460171355, 34.70601412856602508 ) ) ;
#44236 = CYLINDRICAL_SURFACE ( 'NONE', #69147, 0.2499999999999973355 ) ;
#44237 = CARTESIAN_POINT ( 'NONE',  ( 24.00000000000000000, 5.000000000000023093, 29.24999999999999645 ) ) ;
#44238 = CARTESIAN_POINT ( 'NONE',  ( 13.38461538461538680, -2.833524468853757305, 32.15551576947925838 ) ) ;
#44239 = DIRECTION ( 'NONE',  ( 0.000000000000000000, 0.3420201433256610524, 0.9396926207859113145 ) ) ;
#44240 = LINE ( 'NONE', #8280, #14896 ) ;
#44241 = ORIENTED_EDGE ( 'NONE', *, *, #62026, .F. ) ;
#44242 = EDGE_CURVE ( 'NONE', #24932, #87868, #87969, .T. ) ;
#44243 = CARTESIAN_POINT ( 'NONE',  ( 6.250054311638314708, -10.66356715214248396, 33.62249196103329751 ) ) ;
#44244 = CARTESIAN_POINT ( 'NONE',  ( -1.608100328339332252, -6.760086850603068243, 34.69517049084099369 ) ) ;
#44245 = FACE_OUTER_BOUND ( 'NONE', #42619, .T. ) ;
#44246 = CARTESIAN_POINT ( 'NONE',  ( 2.307692307692187583, -3.835265460704628371, 33.15142922262033665 ) ) ;
#44247 = EDGE_CURVE ( 'NONE', #42119, #35523, #64992, .T. ) ;
#44248 = ORIENTED_EDGE ( 'NONE', *, *, #67285, .F. ) ;
#44249 = CARTESIAN_POINT ( 'NONE',  ( 0.4615384615384611200, -2.538708090699994813, 30.37095296980875503 ) ) ;
#44250 = ADVANCED_FACE ( 'NONE', ( #53245 ), #46499, .F. ) ;
#44251 = ORIENTED_EDGE ( 'NONE', *, *, #37683, .T. ) ;
#44252 = AXIS2_PLACEMENT_3D ( 'NONE', #62492, #13436, #55301 ) ;
#44253 = CARTESIAN_POINT ( 'NONE',  ( -17.77722033102192967, -8.540255544307065350, 34.89611431652622286 ) ) ;
#44254 =( NAMED_UNIT ( * ) PLANE_ANGLE_UNIT ( ) SI_UNIT ( $, .RADIAN. ) );
#44255 = DIRECTION ( 'NONE',  ( -1.000000000000000000, 1.897353801849632760E-16, -3.469446951953614189E-15 ) ) ;
#44256 = DIRECTION ( 'NONE',  ( -0.000000000000000000, 0.1736481776669307198, -0.9848077530122080203 ) ) ;
#44257 = ORIENTED_EDGE ( 'NONE', *, *, #34524, .F. ) ;
#44258 = CARTESIAN_POINT ( 'NONE',  ( 5.749976762707036393, -10.05641848906368097, 34.04755513067966177 ) ) ;
#44259 = B_SPLINE_CURVE_WITH_KNOTS ( 'NONE', 3,
 ( #16495, #51583, #31344, #24129, #65110, #39004, #64665, #72320, #3416, #45287 ),
 .UNSPECIFIED., .F., .F.,
 ( 4, 2, 2, 2, 4 ),
 ( 0.000000000000000000, 0.0001954339857564064715, 0.0003908679715128129430, 0.0005863019572692194144, 0.0007817359430256258859 ),
 .UNSPECIFIED. ) ;
#44260 = CARTESIAN_POINT ( 'NONE',  ( 10.39189969082028497, -12.69144148231606017, 30.53333754910549303 ) ) ;
#44261 = CARTESIAN_POINT ( 'NONE',  ( -10.86540783960607293, -12.68155406624981119, 30.59749803192733708 ) ) ;
#44262 = ADVANCED_FACE ( 'NONE', ( #79846 ), #26669, .F. ) ;
#44263 = AXIS2_PLACEMENT_3D ( 'NONE', #31505, #37814, #10348 ) ;
#44264 = PLANE ( 'NONE',  #85407 ) ;
#44265 = VERTEX_POINT ( 'NONE', #39756 ) ;
#44266 = CARTESIAN_POINT ( 'NONE',  ( 7.596130621932387861, -11.56360843649121861, 33.07473185843129926 ) ) ;
#44267 = ORIENTED_EDGE ( 'NONE', *, *, #18597, .T. ) ;
#44268 = LINE ( 'NONE', #73559, #60860 ) ;
#44269 = CARTESIAN_POINT ( 'NONE',  ( 8.992010438208831502, -9.418065098278013636, 34.63729479722530158 ) ) ;
#44270 = CARTESIAN_POINT ( 'NONE',  ( -0.4615384615384611200, -13.20930481340135110, 34.54067556320372745 ) ) ;
#44271 = CARTESIAN_POINT ( 'NONE',  ( -14.24162395668986747, -9.780366693483667717, 34.19971097300155805 ) ) ;
#44272 = DIRECTION ( 'NONE',  ( -0.000000000000000000, -0.000000000000000000, -1.000000000000000000 ) ) ;
#44273 = ADVANCED_FACE ( 'NONE', ( #52802 ), #67223, .F. ) ;
#44274 = EDGE_LOOP ( 'NONE', ( #18480, #72699, #850, #54363 ) ) ;
#44275 = VERTEX_POINT ( 'NONE', #32989 ) ;
#44276 = CIRCLE ( 'NONE', #81670, 4.000000000000000000 ) ;
#44277 = EDGE_LOOP ( 'NONE', ( #17743, #72210, #56834, #63455 ) ) ;
#44278 = ORIENTED_EDGE ( 'NONE', *, *, #37718, .T. ) ;
#44279 = CARTESIAN_POINT ( 'NONE',  ( -1.384615384615383471, -3.050289026998446396, 32.03036669348365706 ) ) ;
#44280 = CARTESIAN_POINT ( 'NONE',  ( 13.51514108637894829, -10.19071101563364756, 33.96452234770658407 ) ) ;
#44281 = CARTESIAN_POINT ( 'NONE',  ( -7.053637514818842824, -2.504760397472873823, 29.97295953869789997 ) ) ;
#44282 = CARTESIAN_POINT ( 'NONE',  ( -5.933931648997560870, -4.786620604624113540, 33.94971097300155805 ) ) ;
#44283 = FACE_OUTER_BOUND ( 'NONE', #62808, .T. ) ;
#44284 = CARTESIAN_POINT ( 'NONE',  ( -6.065270000556318486, -3.083524468853724443, 32.58852847137143272 ) ) ;
#44285 = CARTESIAN_POINT ( 'NONE',  ( 12.46153846153846168, -4.102666532097928531, 36.13435417666054406 ) ) ;
#44286 = CARTESIAN_POINT ( 'NONE',  ( -17.93393164899756087, -6.386643153685127139, 34.62446782046654192 ) ) ;
#44287 = AXIS2_PLACEMENT_3D ( 'NONE', #43619, #78736, #63885 ) ;
#44288 = ORIENTED_EDGE ( 'NONE', *, *, #13280, .F. ) ;
#44289 = ORIENTED_EDGE ( 'NONE', *, *, #52601, .F. ) ;
#44290 = ORIENTED_EDGE ( 'NONE', *, *, #839, .F. ) ;
#44292 = ORIENTED_EDGE ( 'NONE', *, *, #53582, .F. ) ;
#44291 = CARTESIAN_POINT ( 'NONE',  ( 0.6089743589743582541, -3.499999999999999556, 29.75000000000000355 ) ) ;
#44294 = CARTESIAN_POINT ( 'NONE',  ( 10.36536137809165403, -9.271318131107980420, 34.42618302367067429 ) ) ;
#44293 = CARTESIAN_POINT ( 'NONE',  ( -16.15384615384615330, -4.661471528628507777, 34.16647553114623292 ) ) ;
#44295 = CARTESIAN_POINT ( 'NONE',  ( -10.28846153846153832, -7.500000000000000000, 29.75000000000000355 ) ) ;
#44296 = DIRECTION ( 'NONE',  ( -0.000000000000000000, 1.000000000000000000, -0.000000000000000000 ) ) ;
#44297 = ORIENTED_EDGE ( 'NONE', *, *, #17285, .F. ) ;
#44298 = ADVANCED_FACE ( 'NONE', ( #60452 ), #12716, .F. ) ;
#44299 = ADVANCED_FACE ( 'NONE', ( #40202 ), #45158, .F. ) ;
#44300 = ORIENTED_EDGE ( 'NONE', *, *, #68476, .F. ) ;
#44301 = FACE_OUTER_BOUND ( 'NONE', #10073, .T. ) ;
#44303 = ADVANCED_FACE ( 'NONE', ( #72631 ), #32099, .F. ) ;
#44302 = ORIENTED_EDGE ( 'NONE', *, *, #56829, .T. ) ;
#44304 = FACE_BOUND ( 'NONE', #4172, .T. ) ;
#44305 = LINE ( 'NONE', #15982, #50359 ) ;
#44306 = VECTOR ( 'NONE', #24964, 1000.000000000000114 ) ;
#44307 = FACE_OUTER_BOUND ( 'NONE', #36787, .T. ) ;
#44308 = ORIENTED_EDGE ( 'NONE', *, *, #34662, .T. ) ;
#44309 = CYLINDRICAL_SURFACE ( 'NONE', #3141, 0.2500000000000008882 ) ;
#44311 = EDGE_CURVE ( 'NONE', #64217, #25231, #82253, .T. ) ;
#44310 = CARTESIAN_POINT ( 'NONE',  ( 16.40390046548447245, -4.235687564193445276, 33.53795663066793509 ) ) ;
#44312 = DIRECTION ( 'NONE',  ( -0.000000000000000000, 1.000000000000000000, 3.491481338843133355E-15 ) ) ;
#44313 = VERTEX_POINT ( 'NONE', #41517 ) ;
#44314 = CARTESIAN_POINT ( 'NONE',  ( 18.13004743525045370, -7.723484941389743952, 34.99544897038808955 ) ) ;
#44315 = DIRECTION ( 'NONE',  ( 0.000000000000000000, 0.1736481776669267785, -0.9848077530122087975 ) ) ;
#44316 = ORIENTED_EDGE ( 'NONE', *, *, #81418, .F. ) ;
#44317 = AXIS2_PLACEMENT_3D ( 'NONE', #22788, #48491, #21915 ) ;
#44318 = CARTESIAN_POINT ( 'NONE',  ( -6.700065571464073777, -9.086983370893049639, 34.49168942202179267 ) ) ;
#44319 = DIRECTION ( 'NONE',  ( 1.000000000000000000, 0.000000000000000000, 0.000000000000000000 ) ) ;
#44320 = CARTESIAN_POINT ( 'NONE',  ( 7.053602361310566948, -2.647132371071621471, 31.75357179365173010 ) ) ;
#44321 = DIRECTION ( 'NONE',  ( -0.000000000000000000, 0.9848077530122085754, -0.1736481776669273613 ) ) ;
#44322 = CARTESIAN_POINT ( 'NONE',  ( -16.15384615384627409, -8.613356846316285953, 34.62446782046622218 ) ) ;
#44323 = CARTESIAN_POINT ( 'NONE',  ( 7.596153846153846700, -7.500000000000001776, 34.75000000000000000 ) ) ;
#44324 = LINE ( 'NONE', #71813, #45915 ) ;
#44325 = CLOSED_SHELL ( 'NONE', ( #19678, #71875, #39006, #63524 ) ) ;
#44326 = CARTESIAN_POINT ( 'NONE',  ( -6.923076923076922462, -13.57706302396349152, 30.56769352161908060 ) ) ;
#44328 = CARTESIAN_POINT ( 'NONE',  ( 2.557637826040449980, -10.05730279482229683, 34.04704008940765902 ) ) ;
#44327 = CARTESIAN_POINT ( 'NONE',  ( 4.376625695114563008, -12.24180327182771855, 31.33663988360758168 ) ) ;
#44329 = AXIS2_PLACEMENT_3D ( 'NONE', #83451, #22181, #78002 ) ;
#44330 = B_SPLINE_CURVE_WITH_KNOTS ( 'NONE', 3,
 ( #2685, #38709, #66169, #65722, #51750, #52210, #79699, #17553, #58971, #36923 ),
 .UNSPECIFIED., .F., .F.,
 ( 4, 2, 2, 2, 4 ),
 ( 0.0007817246336856289524, 0.0009771112958940099402, 0.001172497958102391036, 0.001367884620310772133, 0.001563271282519153229 ),
 .UNSPECIFIED. ) ;
#44331 = B_SPLINE_CURVE_WITH_KNOTS ( 'NONE', 3,
 ( #85423, #30471, #11543, #24602, #65134, #59274, #79561, #11094, #39026, #32262 ),
 .UNSPECIFIED., .F., .F.,
 ( 4, 2, 2, 2, 4 ),
 ( 0.000000000000000000, 0.0001954311564186868202, 0.0003908623128373736404, 0.0005862934692560604335, 0.0007817246256747472808 ),
 .UNSPECIFIED. ) ;
#44332 = DIRECTION ( 'NONE',  ( 0.000000000000000000, 0.3420201433256610524, 0.9396926207859113145 ) ) ;
#44334 = CARTESIAN_POINT ( 'NONE',  ( 12.46153846153846168, -4.661471528628507777, 34.16647553114623292 ) ) ;
#44333 = FACE_OUTER_BOUND ( 'NONE', #66251, .T. ) ;
#44335 = ADVANCED_FACE ( 'NONE', ( #33867 ), #42416, .F. ) ;
#44336 = CARTESIAN_POINT ( 'NONE',  ( -5.933931648997560870, -12.37446782046654192, 30.86335684631486842 ) ) ;
#44337 = CARTESIAN_POINT ( 'NONE',  ( -2.775308065498764964, -6.422011778438537988, 23.67000670625849779 ) ) ;
#44338 = ORIENTED_EDGE ( 'NONE', *, *, #72002, .F. ) ;
#44339 = CARTESIAN_POINT ( 'NONE',  ( 18.22277954126840172, -11.89424750095246175, 32.13594075562311758 ) ) ;
#44340 = ORIENTED_EDGE ( 'NONE', *, *, #16842, .T. ) ;
#44341 = CARTESIAN_POINT ( 'NONE',  ( 9.442330961365339448, -6.567427716900048118, 34.66269422305636283 ) ) ;
#44342 = EDGE_CURVE ( 'NONE', #20467, #50087, #564, .T. ) ;
#44343 = ORIENTED_EDGE ( 'NONE', *, *, #1290, .F. ) ;
#44344 = CARTESIAN_POINT ( 'NONE',  ( 16.15384615384615330, -12.62096338111211580, 30.90682066428153263 ) ) ;
#44345 = ORIENTED_EDGE ( 'NONE', *, *, #25056, .T. ) ;
#44346 = CARTESIAN_POINT ( 'NONE',  ( -2.307692307692305711, -2.292212530054420494, 30.41441678777542634 ) ) ;
#44347 = CARTESIAN_POINT ( 'NONE',  ( 1.200186371490561621, -10.22469193450123193, 24.45125670625849423 ) ) ;
#44348 = CARTESIAN_POINT ( 'NONE',  ( 6.130525438233648039, -6.808710257144159783, 34.95449254468098843 ) ) ;
#44349 = CARTESIAN_POINT ( 'NONE',  ( 9.823099500132483897, -11.18335022499818621, 33.13157742990016885 ) ) ;
#44350 = CARTESIAN_POINT ( 'NONE',  ( 4.153846153846154188, -6.386643153685126251, 34.62446782046654192 ) ) ;
#44351 = DIRECTION ( 'NONE',  ( -0.000000000000000000, 0.1736481776669307198, -0.9848077530122080203 ) ) ;
#44352 = CARTESIAN_POINT ( 'NONE',  ( -17.93026593459031659, -2.250000000000000000, 29.50029277152256668 ) ) ;
#44353 = CARTESIAN_POINT ( 'NONE',  ( -17.07692307692307665, -12.29105614889573062, 35.45975837776705220 ) ) ;
#44354 = CARTESIAN_POINT ( 'NONE',  ( 0.5276057948885359838, -2.486705287966280320, 31.30864560766543647 ) ) ;
#44355 = CARTESIAN_POINT ( 'NONE',  ( 2.651650429449569302, -10.15165042944953733, 14.62500000000000000 ) ) ;
#44356 = EDGE_CURVE ( 'NONE', #25459, #82973, #29898, .T. ) ;
#44357 = CARTESIAN_POINT ( 'NONE',  ( -39.05038313613820122, -2.499999999999999556, 29.75000000000000355 ) ) ;
#44358 = CARTESIAN_POINT ( 'NONE',  ( -2.307692307692305711, -6.189225973068211317, 35.74407628777942847 ) ) ;
#44359 = DIRECTION ( 'NONE',  ( 0.000000000000000000, 0.3420201433256641055, -0.9396926207859100932 ) ) ;
#44360 = CARTESIAN_POINT ( 'NONE',  ( 3.749999999999992006, -5.946699141100872943, 16.89062500000000000 ) ) ;
#44361 = EDGE_CURVE ( 'NONE', #32571, #22055, #62224, .T. ) ;
#44362 = EDGE_LOOP ( 'NONE', ( #73138, #53237 ) ) ;
#44363 = CARTESIAN_POINT ( 'NONE',  ( 17.29970261819148902, -12.24180327182771855, 31.33663988360758168 ) ) ;
#44364 = DIRECTION ( 'NONE',  ( 0.000000000000000000, 0.000000000000000000, -1.000000000000000000 ) ) ;
#44365 = CARTESIAN_POINT ( 'NONE',  ( 9.822833394071258439, -6.852161475712352789, 34.70806712695775786 ) ) ;
#44366 = CARTESIAN_POINT ( 'NONE',  ( 5.207714884747860040, -2.729792928343270919, 31.24908615093345077 ) ) ;
#44367 = DIRECTION ( 'NONE',  ( -1.000000000000000000, -0.000000000000000000, -0.000000000000000000 ) ) ;
#44368 = B_SPLINE_CURVE_WITH_KNOTS ( 'NONE', 3,
 ( #59948, #87447, #53638, #81126, #74361, #12659, #25727, #40144, #67604, #70256 ),
 .UNSPECIFIED., .F., .F.,
 ( 4, 2, 2, 2, 4 ),
 ( 0.0007817246256747483650, 0.0009771112852218926705, 0.001172497944769037084, 0.001367884604316181498, 0.001563271263863325695 ),
 .UNSPECIFIED. ) ;
#44369 = CARTESIAN_POINT ( 'NONE',  ( 2.307692307692309264, -12.10708131394839349, 31.69288490824020244 ) ) ;
#44370 = ADVANCED_FACE ( 'NONE', ( #48708 ), #14484, .F. ) ;
#44371 = EDGE_CURVE ( 'NONE', #66098, #27341, #88840, .T. ) ;
#44372 = ORIENTED_EDGE ( 'NONE', *, *, #32641, .F. ) ;
#44373 = CARTESIAN_POINT ( 'NONE',  ( 17.93391658904412012, -12.37446782046654192, 30.86335684631486487 ) ) ;
#44374 = ORIENTED_EDGE ( 'NONE', *, *, #68976, .T. ) ;
#44375 = EDGE_LOOP ( 'NONE', ( #21696, #58274 ) ) ;
#44376 = CARTESIAN_POINT ( 'NONE',  ( 7.596130621932386973, -10.92453946501458795, 33.72985991061850086 ) ) ;
#44377 = VECTOR ( 'NONE', #78593, 1000.000000000000000 ) ;
#44378 = CARTESIAN_POINT ( 'NONE',  ( -6.222926958906846551, -12.64616026154729411, 30.79003144601913533 ) ) ;
#44379 = CARTESIAN_POINT ( 'NONE',  ( -16.15384615384615330, -9.584722331328613620, 36.20867863119891439 ) ) ;
#44380 = CARTESIAN_POINT ( 'NONE',  ( -5.999999999999998224, -3.050289026998446396, 32.03036669348365706 ) ) ;
#44381 = DIRECTION ( 'NONE',  ( 0.000000000000000000, 0.000000000000000000, 1.000000000000000000 ) ) ;
#44382 = ADVANCED_FACE ( 'NONE', ( #14041 ), #82072, .F. ) ;
#44383 = EDGE_LOOP ( 'NONE', ( #78181, #38453, #2868, #12456, #78852, #64899 ) ) ;
#44384 = EDGE_CURVE ( 'NONE', #76146, #32981, #53198, .T. ) ;
#44385 = CARTESIAN_POINT ( 'NONE',  ( 8.834486340506796154, -3.835265460703683349, 33.15142922261929925 ) ) ;
#44386 = VERTEX_POINT ( 'NONE', #28442 ) ;
#44387 = EDGE_LOOP ( 'NONE', ( #34305, #5470, #48988, #78563, #77916, #4515 ) ) ;
#44388 = VECTOR ( 'NONE', #32273, 1000.000000000000000 ) ;
#44389 = CARTESIAN_POINT ( 'NONE',  ( 18.24994540937804643, -2.341251567377310217, 30.72681386836322659 ) ) ;
#44390 = CARTESIAN_POINT ( 'NONE',  ( 16.40390046548447245, -12.41262288849542017, 30.68299917996395010 ) ) ;
#44391 = DIRECTION ( 'NONE',  ( 0.000000000000000000, 0.000000000000000000, -1.000000000000000000 ) ) ;
#44392 = B_SPLINE_CURVE_WITH_KNOTS ( 'NONE', 3,
 ( #87625, #40316, #46618, #67340, #47497, #52915, #60570, #88085, #54696, #26350 ),
 .UNSPECIFIED., .F., .F.,
 ( 4, 2, 2, 2, 4 ),
 ( 0.000000000000000000, 0.0001954339857564071220, 0.0003908679715128142440, 0.0005863019572692213660, 0.0007817359430256284880 ),
 .UNSPECIFIED. ) ;
#44393 = CARTESIAN_POINT ( 'NONE',  ( 1.384615384615265343, -3.835265460704628371, 33.15142922262033665 ) ) ;
#44394 = CARTESIAN_POINT ( 'NONE',  ( -4.023798547590470065, -7.723484964179500700, 34.74522123443823318 ) ) ;
#44395 = CARTESIAN_POINT ( 'NONE',  ( -15.93083480223330284, -2.758310577978207334, 31.33698337089302299 ) ) ;
#44396 = ORIENTED_EDGE ( 'NONE', *, *, #70101, .T. ) ;
#44397 = ORIENTED_EDGE ( 'NONE', *, *, #58792, .T. ) ;
#44398 = CARTESIAN_POINT ( 'NONE',  ( 3.750000000000009770, -9.053300858899081760, 22.04687500000000000 ) ) ;
#44399 = ORIENTED_EDGE ( 'NONE', *, *, #72386, .F. ) ;
#44401 = ORIENTED_EDGE ( 'NONE', *, *, #48735, .T. ) ;
#44400 = CARTESIAN_POINT ( 'NONE',  ( 15.45378058238208219, -5.667800583137506010, 34.40243808032445827 ) ) ;
#44402 = CARTESIAN_POINT ( 'NONE',  ( -10.39237177129121825, -4.026326845037962343, 33.68677907613344047 ) ) ;
#44403 = CYLINDRICAL_SURFACE ( 'NONE', #59000, 0.2499999999999986955 ) ;
#44404 = B_SPLINE_CURVE_WITH_KNOTS ( 'NONE', 3,
 ( #60604, #19623, #4335, #83000, #39471, #87664, #14092, #39914, #45312, #87220 ),
 .UNSPECIFIED., .F., .F.,
 ( 4, 2, 2, 2, 4 ),
 ( 0.0007817246256747524850, 0.0009771112852218972241, 0.001172497944769042072, 0.001367884604316186702, 0.001563271263863331550 ),
 .UNSPECIFIED. ) ;
#44405 = CARTESIAN_POINT ( 'NONE',  ( -3.165513659493206067, -10.21337939537593797, 33.94971097300152252 ) ) ;
#44406 = ORIENTED_EDGE ( 'NONE', *, *, #89162, .T. ) ;
#44407 = CARTESIAN_POINT ( 'NONE',  ( -14.37377468705244077, -12.34228464037088280, 31.77849191805838558 ) ) ;
#44408 = VECTOR ( 'NONE', #50085, 1000.000000000000227 ) ;
#44409 = VERTEX_POINT ( 'NONE', #63103 ) ;
#44410 = CARTESIAN_POINT ( 'NONE',  ( 2.307692307692309264, -8.973038597847269315, 34.52809138561121927 ) ) ;
#44411 = CARTESIAN_POINT ( 'NONE',  ( 17.75002325595141173, -12.65889640711025521, 30.72598325615533454 ) ) ;
#44412 = EDGE_CURVE ( 'NONE', #44792, #77538, #16673, .T. ) ;
#44413 = CARTESIAN_POINT ( 'NONE',  ( -17.93393266664992680, -2.486705287966280320, 31.30864560766543647 ) ) ;
#44415 = CARTESIAN_POINT ( 'NONE',  ( -6.700065571464074665, -2.554770724473668153, 30.48948780036025852 ) ) ;
#44414 = CYLINDRICAL_SURFACE ( 'NONE', #86401, 0.2500000000000009437 ) ;
#44416 = CARTESIAN_POINT ( 'NONE',  ( 4.826899839630110378, -2.587272538249754117, 30.68239716806877837 ) ) ;
#44417 = DIRECTION ( 'NONE',  ( 0.000000000000000000, 0.3420201433256610524, 0.9396926207859113145 ) ) ;
#44418 = ORIENTED_EDGE ( 'NONE', *, *, #85975, .F. ) ;
#44420 = EDGE_CURVE ( 'NONE', #5961, #7880, #20798, .T. ) ;
#44419 = CARTESIAN_POINT ( 'NONE',  ( -9.692307692307812417, -6.026961402154118019, 34.52809138561165270 ) ) ;
#44421 = CARTESIAN_POINT ( 'NONE',  ( 2.307692307692309264, -2.833524468853757305, 32.15551576947925838 ) ) ;
#44422 = ORIENTED_EDGE ( 'NONE', *, *, #6810, .T. ) ;
#44423 = EDGE_CURVE ( 'NONE', #58471, #29571, #82519, .T. ) ;
#44424 = CARTESIAN_POINT ( 'NONE',  ( 11.47319153790522073, -12.16647553114622049, 32.15551576947930812 ) ) ;
#44425 = CARTESIAN_POINT ( 'NONE',  ( 15.29602480204525605, -4.481592998940250538, 33.73612834413965089 ) ) ;
#44426 = CARTESIAN_POINT ( 'NONE',  ( -3.931066612577743147, -2.600157965045225339, 30.74683119005207743 ) ) ;
#44427 = CARTESIAN_POINT ( 'NONE',  ( -5.999999999999998224, -5.557115091759785130, 34.35708131394839171 ) ) ;
#44428 = CARTESIAN_POINT ( 'NONE',  ( -7.976629031229566458, -7.276987145209185215, 34.99546412871779211 ) ) ;
#44429 = FACE_BOUND ( 'NONE', #15147, .T. ) ;
#44431 = DIRECTION ( 'NONE',  ( -0.000000000000000000, -0.3420201433256694901, -0.9396926207859082059 ) ) ;
#44430 = CARTESIAN_POINT ( 'NONE',  ( 13.38461538461526423, -2.379036618888197729, 30.90682066428292885 ) ) ;
#44432 = FACE_OUTER_BOUND ( 'NONE', #84713, .T. ) ;
#44434 = CARTESIAN_POINT ( 'NONE',  ( 14.17754433796061342, -11.04286588640298561, 33.62463336215343901 ) ) ;
#44433 = CARTESIAN_POINT ( 'NONE',  ( -1.384615384615383471, -12.10708131394839349, 31.69288490824020244 ) ) ;
#44435 = DIRECTION ( 'NONE',  ( -0.000000000000000000, 0.1736481776669307198, -0.9848077530122080203 ) ) ;
#44436 = EDGE_CURVE ( 'NONE', #17506, #12547, #84737, .T. ) ;
#44437 = CARTESIAN_POINT ( 'NONE',  ( 9.019285080869085647, -10.66356715214248752, 33.62249196103329751 ) ) ;
#44438 = CARTESIAN_POINT ( 'NONE',  ( 3.724691934501232815, -5.885600066136343678, 19.13875670625849068 ) ) ;
#44439 = VERTEX_POINT ( 'NONE', #29779 ) ;
#44440 = VECTOR ( 'NONE', #24233, 1000.000000000000000 ) ;
#44441 = DIRECTION ( 'NONE',  ( -0.000000000000000000, -0.1736481776669307198, -0.9848077530122080203 ) ) ;
#44442 = EDGE_CURVE ( 'NONE', #16132, #83475, #22112, .T. ) ;
#44443 = FACE_OUTER_BOUND ( 'NONE', #60089, .T. ) ;
#44444 = CARTESIAN_POINT ( 'NONE',  ( -19.99999999999996447, -15.00000000000000533, 3.000000000000000000 ) ) ;
#44445 = CARTESIAN_POINT ( 'NONE',  ( -9.758391103263571509, -10.51840700105979387, 33.73612834413961536 ) ) ;
#44446 = CARTESIAN_POINT ( 'NONE',  ( 10.68064018666064641, -12.27809138561124591, 31.22303859784720359 ) ) ;
#44447 = DIRECTION ( 'NONE',  ( 0.000000000000000000, 0.8660254037844377084, 0.5000000000000015543 ) ) ;
#44448 = CARTESIAN_POINT ( 'NONE',  ( 2.608446859217893099, -4.805146000318787358, 21.56063170625849068 ) ) ;
#44449 = CARTESIAN_POINT ( 'NONE',  ( -15.23076923076922995, -12.62096338111211580, 30.90682066428153263 ) ) ;
#44450 = CARTESIAN_POINT ( 'NONE',  ( -2.177166869458661669, -6.808710257144159783, 34.95449254468098843 ) ) ;
#44451 = AXIS2_PLACEMENT_3D ( 'NONE', #64554, #72661, #58255 ) ;
#44452 = ADVANCED_FACE ( 'NONE', ( #56361 ), #57685, .F. ) ;
#44453 = CARTESIAN_POINT ( 'NONE',  ( -16.94639737515951339, -6.001044277235011215, 34.52024696741798948 ) ) ;
#44454 = CARTESIAN_POINT ( 'NONE',  ( -2.980823821391187955, -12.07971442181321997, 32.31769673815850297 ) ) ;
#44455 = LINE ( 'NONE', #85028, #20935 ) ;
#44456 = CARTESIAN_POINT ( 'NONE',  ( 12.33084785842815734, -12.62707690430377383, 30.88035979386743435 ) ) ;
#44457 = AXIS2_PLACEMENT_3D ( 'NONE', #12580, #67524, #51756 ) ;
#44458 = CARTESIAN_POINT ( 'NONE',  ( -18.00000000000000000, -2.721908614388771852, 31.22303859784724978 ) ) ;
#44459 = CARTESIAN_POINT ( 'NONE',  ( 14.17700084102474989, -6.413092428213692742, 34.63065189839063152 ) ) ;
#44460 = ORIENTED_EDGE ( 'NONE', *, *, #58038, .T. ) ;
#44461 = LINE ( 'NONE', #17459, #78688 ) ;
#44462 = CARTESIAN_POINT ( 'NONE',  ( -17.07692307692307665, -2.721908614388771852, 31.22303859784724978 ) ) ;
#44463 = CARTESIAN_POINT ( 'NONE',  ( -1.614399933863613468, -11.22469193450124969, 16.36124329374151642 ) ) ;
#44464 = ADVANCED_FACE ( 'NONE', ( #65324 ), #85165, .F. ) ;
#44465 = B_SPLINE_CURVE_WITH_KNOTS ( 'NONE', 3,
 ( #15561, #8806, #50206, #51087, #71822, #43027, #43469, #78580, #64167, #1600 ),
 .UNSPECIFIED., .F., .F.,
 ( 4, 2, 2, 2, 4 ),
 ( 0.000000000000000000, 0.0001954311564186864678, 0.0003908623128373729357, 0.0005862934692560594577, 0.0007817246256747458714 ),
 .UNSPECIFIED. ) ;
#44466 = CARTESIAN_POINT ( 'NONE',  ( 6.792928953345226617, -5.070767119584671079, 34.40440758774516183 ) ) ;
#44467 = CARTESIAN_POINT ( 'NONE',  ( -5.300408020647024543, -2.599994579823202923, 30.74605699353653776 ) ) ;
#44468 = VERTEX_POINT ( 'NONE', #9494 ) ;
#44469 = CARTESIAN_POINT ( 'NONE',  ( 1.450683735617825043, -4.098570777380720287, 33.41473453929635440 ) ) ;
#44470 = DIRECTION ( 'NONE',  ( 0.000000000000000000, 1.000000000000000000, 0.000000000000000000 ) ) ;
#44472 = ORIENTED_EDGE ( 'NONE', *, *, #4103, .T. ) ;
#44471 = CARTESIAN_POINT ( 'NONE',  ( -12.21153846153704237, -7.500000000000154543, 35.00000000000007105 ) ) ;
#44473 = DIRECTION ( 'NONE',  ( 0.000000000000000000, 0.000000000000000000, 1.000000000000000000 ) ) ;
#44474 = EDGE_CURVE ( 'NONE', #11720, #57615, #1856, .T. ) ;
#44475 = CYLINDRICAL_SURFACE ( 'NONE', #71401, 0.2499999999999986955 ) ;
#44476 = CYLINDRICAL_SURFACE ( 'NONE', #29122, 0.2500000000000002220 ) ;
#44477 = CARTESIAN_POINT ( 'NONE',  ( -14.17716660592875044, -11.46989282347013095, 32.79007818306219946 ) ) ;
#44478 = VERTEX_POINT ( 'NONE', #29340 ) ;
#44479 = CARTESIAN_POINT ( 'NONE',  ( 24.00000000000000000, -9.499999999999982236, 27.74999999999999645 ) ) ;
#44480 = CARTESIAN_POINT ( 'NONE',  ( -11.53846153846122391, -2.255955759149395501, 30.00000000000324363 ) ) ;
#44481 = EDGE_CURVE ( 'NONE', #64117, #73491, #74763, .T. ) ;
#44482 = CARTESIAN_POINT ( 'NONE',  ( 16.15384615384603251, -12.51329471203414379, 31.30864560766407578 ) ) ;
#44483 = EDGE_LOOP ( 'NONE', ( #68431, #86127 ) ) ;
#44484 = VERTEX_POINT ( 'NONE', #70317 ) ;
#44485 = AXIS2_PLACEMENT_3D ( 'NONE', #9667, #37578, #65039 ) ;
#44486 = ORIENTED_EDGE ( 'NONE', *, *, #26751, .T. ) ;
#44487 = CARTESIAN_POINT ( 'NONE',  ( 3.296024370282069071, -2.379036618887895305, 30.90682066428159303 ) ) ;
#44488 = CARTESIAN_POINT ( 'NONE',  ( 9.942253101685736283, -4.176053281294518804, 33.81426240980091791 ) ) ;
#44489 = DIRECTION ( 'NONE',  ( -1.000000000000000000, 0.000000000000000000, 0.000000000000000000 ) ) ;
#44490 = EDGE_CURVE ( 'NONE', #61936, #35844, #43474, .T. ) ;
#44491 = LINE ( 'NONE', #30984, #10392 ) ;
#44492 = EDGE_CURVE ( 'NONE', #35283, #35014, #64425, .T. ) ;
#44493 = ADVANCED_FACE ( 'NONE', ( #2726 ), #78837, .F. ) ;
#44494 = ORIENTED_EDGE ( 'NONE', *, *, #61757, .F. ) ;
#44495 = ORIENTED_EDGE ( 'NONE', *, *, #53365, .T. ) ;
#44497 = EDGE_LOOP ( 'NONE', ( #47162, #44151 ) ) ;
#44496 = CARTESIAN_POINT ( 'NONE',  ( 4.284371592079798674, -5.915461855592777596, 34.75538340440931506 ) ) ;
#44498 = EDGE_CURVE ( 'NONE', #40198, #48420, #31673, .T. ) ;
#44499 = B_SPLINE_CURVE_WITH_KNOTS ( 'NONE', 3,
 ( #87939, #14011, #506, #33840, #40613, #35173, #88372, #74389, #62196, #55002 ),
 .UNSPECIFIED., .F., .F.,
 ( 4, 2, 2, 2, 4 ),
 ( 0.0007817359430256216575, 0.0009771253907249856981, 0.001172514838424349630, 0.001367904286123713779, 0.001563293733823077711 ),
 .UNSPECIFIED. ) ;
#44500 = CARTESIAN_POINT ( 'NONE',  ( 12.68431813051652846, -11.60474049983371003, 33.02348890104160262 ) ) ;
#44501 = VECTOR ( 'NONE', #73370, 1000.000000000000000 ) ;
#44502 = AXIS2_PLACEMENT_3D ( 'NONE', #15513, #10076, #57371 ) ;
#44503 = CARTESIAN_POINT ( 'NONE',  ( 2.438218009455874746, -3.816742781228458448, 33.13167719472716044 ) ) ;
#44504 = CARTESIAN_POINT ( 'NONE',  ( -17.99999999841483955, -2.249999999999995115, 29.50000000010503953 ) ) ;
#44505 = VERTEX_POINT ( 'NONE', #30651 ) ;
#44506 = ORIENTED_EDGE ( 'NONE', *, *, #45523, .T. ) ;
#44507 = AXIS2_PLACEMENT_3D ( 'NONE', #62696, #1014, #55950 ) ;
#44508 = ORIENTED_EDGE ( 'NONE', *, *, #60924, .T. ) ;
#44510 = ORIENTED_EDGE ( 'NONE', *, *, #6347, .T. ) ;
#44509 = DIRECTION ( 'NONE',  ( 1.000000000000000000, 0.000000000000000000, 0.000000000000000000 ) ) ;
#44511 = AXIS2_PLACEMENT_3D ( 'NONE', #37626, #22776, #77723 ) ;
#44512 = DIRECTION ( 'NONE',  ( 0.000000000000000000, 0.4999999999999960032, -0.8660254037844410391 ) ) ;
#44513 = FACE_OUTER_BOUND ( 'NONE', #50624, .T. ) ;
#44514 = VERTEX_POINT ( 'NONE', #85604 ) ;
#44515 = CARTESIAN_POINT ( 'NONE',  ( -8.769230769230768274, -10.51840700105979565, 33.73612834413961536 ) ) ;
#44516 = DIRECTION ( 'NONE',  ( -0.000000000000000000, -0.9396926207859093161, -0.3420201433256663259 ) ) ;
#44517 = CARTESIAN_POINT ( 'NONE',  ( 8.900022577055556994, -5.582136614379148654, 34.36778462344220486 ) ) ;
#44518 = FACE_BOUND ( 'NONE', #77930, .T. ) ;
#44519 = CARTESIAN_POINT ( 'NONE',  ( 15.10062202133100939, -6.001485441113819874, 34.52039167877662607 ) ) ;
#44520 = CARTESIAN_POINT ( 'NONE',  ( -6.700064078983528404, -9.172514111537584114, 34.72667873470787470 ) ) ;
#44521 = CARTESIAN_POINT ( 'NONE',  ( 13.31934538405906565, -12.70778746994557551, 30.41441678777548319 ) ) ;
#44523 = CARTESIAN_POINT ( 'NONE',  ( 9.692307692307572609, -3.300289026999228881, 32.46337939537708905 ) ) ;
#44522 = CARTESIAN_POINT ( 'NONE',  ( 5.076923076922953193, -12.70778746994576025, 30.41441678777401236 ) ) ;
#44524 = LINE ( 'NONE', #10318, #39517 ) ;
#44525 = CARTESIAN_POINT ( 'NONE',  ( -16.40386939113911779, -8.432397168068783699, 34.66272746175022945 ) ) ;
#44526 = VERTEX_POINT ( 'NONE', #80645 ) ;
#44527 = CARTESIAN_POINT ( 'NONE',  ( -16.02332071561251325, -3.625058011473227815, 33.29252011169590020 ) ) ;
#44528 = ORIENTED_EDGE ( 'NONE', *, *, #42796, .F. ) ;
#44529 = ORIENTED_EDGE ( 'NONE', *, *, #64284, .F. ) ;
#44530 = B_SPLINE_CURVE_WITH_KNOTS ( 'NONE', 3,
 ( #21346, #59783, #53012, #82627, #80513, #35303, #12058, #48811, #68646, #28105 ),
 .UNSPECIFIED., .F., .F.,
 ( 4, 2, 2, 2, 4 ),
 ( 0.000000000000000000, 0.0001954311564186865763, 0.0003908623128373731525, 0.0005862934692560596746, 0.0007817246256747463051 ),
 .UNSPECIFIED. ) ;
#44531 = B_SPLINE_CURVE_WITH_KNOTS ( 'NONE', 3,
 ( #29821, #77557, #42896, #22607, #15868, #21727, #70362, #43331, #9535, #49201 ),
 .UNSPECIFIED., .F., .F.,
 ( 4, 2, 2, 2, 4 ),
 ( 0.000000000000000000, 0.0001954339857564074473, 0.0003908679715128148945, 0.0005863019572692223418, 0.0007817359430256297891 ),
 .UNSPECIFIED. ) ;
#44533 = CARTESIAN_POINT ( 'NONE',  ( -5.776988648387147762, -12.15243808032446005, 31.58219941686247978 ) ) ;
#44532 = LINE ( 'NONE', #65255, #10133 ) ;
#44534 = CARTESIAN_POINT ( 'NONE',  ( 2.530471848960717640, -2.600157965045225783, 30.74683119005207743 ) ) ;
#44535 = B_SPLINE_CURVE_WITH_KNOTS ( 'NONE', 3,
 ( #76774, #64560, #63690, #49296, #16395, #49734, #76320, #83541, #2862, #21825 ),
 .UNSPECIFIED., .F., .F.,
 ( 4, 2, 2, 2, 4 ),
 ( 0.000000000000000000, 0.0001954339857564083688, 0.0003908679715128167377, 0.0005863019572692250523, 0.0007817359430256334753 ),
 .UNSPECIFIED. ) ;
#44536 = FACE_OUTER_BOUND ( 'NONE', #63399, .T. ) ;
#44537 = CARTESIAN_POINT ( 'NONE',  ( -0.4615384615384611200, -11.69971097300155272, 32.46337939537588113 ) ) ;
#44538 = VERTEX_POINT ( 'NONE', #46835 ) ;
#44539 = CARTESIAN_POINT ( 'NONE',  ( 18.25005441991345378, -2.544122305571458575, 31.48381861865057729 ) ) ;
#44540 = CARTESIAN_POINT ( 'NONE',  ( 15.16549923021291058, -11.06231777344662781, 33.60647404775220082 ) ) ;
#44541 = CARTESIAN_POINT ( 'NONE',  ( -1.449885385171703955, -10.33852847137145048, 34.16647553114627556 ) ) ;
#44542 = CARTESIAN_POINT ( 'NONE',  ( 0.2115617174898687114, -3.436278759898155233, 33.07459398097509506 ) ) ;
#44543 = CARTESIAN_POINT ( 'NONE',  ( -19.50000000000000000, -3.499999999999999556, 29.75000000000000355 ) ) ;
#44544 = VECTOR ( 'NONE', #35955, 1000.000000000000114 ) ;
#44545 = CARTESIAN_POINT ( 'NONE',  ( -2.651650429449565305, -4.848349570550461785, 16.50000000000000000 ) ) ;
#44546 = VERTEX_POINT ( 'NONE', #4972 ) ;
#44547 = VERTEX_POINT ( 'NONE', #46394 ) ;
#44548 = CARTESIAN_POINT ( 'NONE',  ( -14.43838291080261627, -4.684245665217972032, 34.18127051446801090 ) ) ;
#44549 = ORIENTED_EDGE ( 'NONE', *, *, #43484, .F. ) ;
#44550 = CARTESIAN_POINT ( 'NONE',  ( -13.38461538461538325, -11.11383981884818262, 36.00935417666054406 ) ) ;
#44551 = CARTESIAN_POINT ( 'NONE',  ( -12.33074665371367651, -9.804649428959608670, 34.18742332936588468 ) ) ;
#44552 = CARTESIAN_POINT ( 'NONE',  ( 14.37376065869474751, -2.721908614388771852, 31.22303859784725333 ) ) ;
#44553 = CARTESIAN_POINT ( 'NONE',  ( -0.7115152055870517245, -12.01397095200673881, 32.43157075238190146 ) ) ;
#44554 = CARTESIAN_POINT ( 'NONE',  ( 2.320192649118979489E-14, -11.25000000000000000, 17.28125000000000000 ) ) ;
#44555 = CARTESIAN_POINT ( 'NONE',  ( 1.449870955891410684, -5.219633306516380244, 34.19971097300157936 ) ) ;
#44556 = ORIENTED_EDGE ( 'NONE', *, *, #29071, .F. ) ;
#44557 = EDGE_CURVE ( 'NONE', #43627, #11372, #59466, .T. ) ;
#44558 = CARTESIAN_POINT ( 'NONE',  ( -12.46153846153846168, -12.48256725967547354, 35.29906147534542527 ) ) ;
#44560 = ORIENTED_EDGE ( 'NONE', *, *, #70839, .T. ) ;
#44559 = CYLINDRICAL_SURFACE ( 'NONE', #33808, 0.2500000000000008882 ) ;
#44561 = CARTESIAN_POINT ( 'NONE',  ( -9.627162911588058591, -7.750023224968867197, 34.99404313364389907 ) ) ;
#44562 = CARTESIAN_POINT ( 'NONE',  ( 14.24242186173153613, -12.27809138561121394, 31.22303859784730307 ) ) ;
#44563 = CARTESIAN_POINT ( 'NONE',  ( 17.07692307692307665, -10.89733346790207413, 36.13435417666054406 ) ) ;
#44564 = CARTESIAN_POINT ( 'NONE',  ( -2.241624974342229848, -2.292212530054420494, 30.41441678777542990 ) ) ;
#44565 = CARTESIAN_POINT ( 'NONE',  ( -0.2115929431903188496, -11.37275283266503756, 32.91324779482534524 ) ) ;
#44566 = CARTESIAN_POINT ( 'NONE',  ( -3.007989689500822017, -11.41317474335729187, 32.86274602512330034 ) ) ;
#44567 = CARTESIAN_POINT ( 'NONE',  ( 15.29683758177167086, -11.16473453929635440, 33.15142922261926373 ) ) ;
#44568 = CARTESIAN_POINT ( 'NONE',  ( -2.694853999681181556, -10.10844685921792241, 17.68936829374151287 ) ) ;
#44569 = ORIENTED_EDGE ( 'NONE', *, *, #25797, .F. ) ;
#44570 = CARTESIAN_POINT ( 'NONE',  ( -12.46153846153846168, -10.67929555188718282, 33.92786785259544047 ) ) ;
#44571 = CARTESIAN_POINT ( 'NONE',  ( -5.326923076923075762, -7.433932668274256805, 35.00000000000000711 ) ) ;
#44572 = LINE ( 'NONE', #72060, #17498 ) ;
#44573 = CARTESIAN_POINT ( 'NONE',  ( -1.944543648262992530, -9.444543648263016067, 24.93750000000000000 ) ) ;
#44574 = VECTOR ( 'NONE', #23193, 1000.000000000000000 ) ;
#44575 = VECTOR ( 'NONE', #60499, 1000.000000000000000 ) ;
#44576 = CARTESIAN_POINT ( 'NONE',  ( -13.60810032833933469, -12.44517049084099725, 30.48991314939691932 ) ) ;
#44577 = CARTESIAN_POINT ( 'NONE',  ( 8.638540166120458608, -9.929715669179220328, 34.40415004197138416 ) ) ;
#44578 = B_SPLINE_CURVE_WITH_KNOTS ( 'NONE', 3,
 ( #57711, #50927, #78861, #79767, #79319, #78415, #30243, #58142, #52276, #71213 ),
 .UNSPECIFIED., .F., .F.,
 ( 4, 2, 2, 2, 4 ),
 ( 0.0007817359430256283796, 0.0009771253907249943717, 0.001172514838424360255, 0.001367904286123726356, 0.001563293733823092240 ),
 .UNSPECIFIED. ) ;
#44579 = ORIENTED_EDGE ( 'NONE', *, *, #76754, .T. ) ;
#44580 = CARTESIAN_POINT ( 'NONE',  ( -1.139087296526025250, -4.750000000000006217, 17.82812500000000000 ) ) ;
#44581 = EDGE_CURVE ( 'NONE', #530, #13588, #40100, .T. ) ;
#44582 = CARTESIAN_POINT ( 'NONE',  ( -1.161835715637319577, -12.47679350104403007, 31.42216943046557276 ) ) ;
#44583 = VERTEX_POINT ( 'NONE', #72979 ) ;
#44584 = AXIS2_PLACEMENT_3D ( 'NONE', #87003, #39246, #66708 ) ;
#44585 = CARTESIAN_POINT ( 'NONE',  ( -3.931066484868086963, -2.612705202774697533, 31.66806509827799943 ) ) ;
#44586 = ORIENTED_EDGE ( 'NONE', *, *, #75699, .T. ) ;
#44587 = CARTESIAN_POINT ( 'NONE',  ( -9.692307692307691624, -10.51840700105979565, 33.73612834413961536 ) ) ;
#44588 = FACE_OUTER_BOUND ( 'NONE', #32050, .T. ) ;
#44589 = EDGE_CURVE ( 'NONE', #57339, #43411, #19866, .T. ) ;
#44590 = CARTESIAN_POINT ( 'NONE',  ( -0.3307480205715113697, -6.369690395747422684, 34.87708834333098196 ) ) ;
#44591 = EDGE_LOOP ( 'NONE', ( #44748, #83188 ) ) ;
#44592 = CARTESIAN_POINT ( 'NONE',  ( 1.576923076923075762, -3.499999999999999556, 29.75000000000000355 ) ) ;
#44593 = ORIENTED_EDGE ( 'NONE', *, *, #42869, .T. ) ;
#44594 = DIRECTION ( 'NONE',  ( -0.000000000000000000, 0.9848077530122086864, -0.1736481776669273891 ) ) ;
#44595 = ORIENTED_EDGE ( 'NONE', *, *, #68647, .T. ) ;
#44596 = CARTESIAN_POINT ( 'NONE',  ( 2.307692307692615685, -2.506253911140615021, 30.00000000000323297 ) ) ;
#44597 = DIRECTION ( 'NONE',  ( -0.000000000000000000, 0.8660254037844399289, -0.4999999999999980016 ) ) ;
#44598 = ORIENTED_EDGE ( 'NONE', *, *, #84572, .F. ) ;
#44599 = LINE ( 'NONE', #64429, #31833 ) ;
#44600 = CYLINDRICAL_SURFACE ( 'NONE', #3306, 0.2499999999999994726 ) ;
#44601 = CARTESIAN_POINT ( 'NONE',  ( -11.60454494941741999, -2.721908614388770964, 31.22303859784723912 ) ) ;
#44602 = CARTESIAN_POINT ( 'NONE',  ( 7.846153846153846700, -1.951392089020283160, 34.73218667398347748 ) ) ;
#44603 = CARTESIAN_POINT ( 'NONE',  ( -13.13466997523734392, -12.07971442181322175, 32.31769673815850297 ) ) ;
#44604 = EDGE_CURVE ( 'NONE', #33104, #81317, #39208, .T. ) ;
#44605 = EDGE_CURVE ( 'NONE', #64975, #25175, #1681, .T. ) ;
#44606 = VERTEX_POINT ( 'NONE', #4521 ) ;
#44607 = ORIENTED_EDGE ( 'NONE', *, *, #18303, .F. ) ;
#44608 = ORIENTED_EDGE ( 'NONE', *, *, #13721, .T. ) ;
#44609 = B_SPLINE_CURVE_WITH_KNOTS ( 'NONE', 3,
 ( #6187, #60676, #68322, #74645, #55247, #47605, #75091, #7066, #62004, #310 ),
 .UNSPECIFIED., .F., .F.,
 ( 4, 2, 2, 2, 4 ),
 ( 0.000000000000000000, 0.0001954339857564097241, 0.0003908679715128194482, 0.0005863019572692291723, 0.0007817359430256388964 ),
 .UNSPECIFIED. ) ;
#44611 = EDGE_LOOP ( 'NONE', ( #2222, #87959 ) ) ;
#44610 = CARTESIAN_POINT ( 'NONE',  ( 3.100078627658922503, -5.496505350115500121, 34.60290016733514307 ) ) ;
#44612 = VECTOR ( 'NONE', #44351, 1000.000000000000000 ) ;
#44613 = CARTESIAN_POINT ( 'NONE',  ( -14.24243716817946570, -11.06231777344671130, 33.60647404775212976 ) ) ;
#44614 = CARTESIAN_POINT ( 'NONE',  ( 5.076923076923075762, -4.098570777380720287, 33.41473453929634729 ) ) ;
#44615 = ORIENTED_EDGE ( 'NONE', *, *, #32378, .T. ) ;
#44616 = EDGE_LOOP ( 'NONE', ( #84196, #28706, #26136, #85044 ) ) ;
#44617 = ORIENTED_EDGE ( 'NONE', *, *, #22803, .F. ) ;
#44618 = CARTESIAN_POINT ( 'NONE',  ( 0.3313904918067661076, -8.630895178749536711, 34.87696386517710323 ) ) ;
#44619 = ORIENTED_EDGE ( 'NONE', *, *, #67033, .T. ) ;
#44620 = CARTESIAN_POINT ( 'NONE',  ( 2.438484115517095763, -4.118422570099827595, 33.43335022499816489 ) ) ;
#44621 = CARTESIAN_POINT ( 'NONE',  ( 16.94677510719138169, -12.50552854090298638, 31.33409797877408920 ) ) ;
#44622 = LINE ( 'NONE', #83876, #29610 ) ;
#44623 = B_SPLINE_CURVE_WITH_KNOTS ( 'NONE', 3,
 ( #1709, #29198, #57088, #56210, #83246, #15673, #84145, #49456, #76033, #82809 ),
 .UNSPECIFIED., .F., .F.,
 ( 4, 2, 2, 2, 4 ),
 ( 0.0007817359430256388964, 0.0009771253907250075990, 0.001172514838424376085, 0.001367904286123744571, 0.001563293733823113273 ),
 .UNSPECIFIED. ) ;
#44624 = FACE_BOUND ( 'NONE', #8697, .T. ) ;
#44625 = ORIENTED_EDGE ( 'NONE', *, *, #64417, .F. ) ;
#44626 = CARTESIAN_POINT ( 'NONE',  ( 12.71148397988660328, -5.852078868378309373, 34.47109172314383585 ) ) ;
#44627 = B_SPLINE_CURVE_WITH_KNOTS ( 'NONE', 3,
 ( #10455, #18988, #11336, #30712, #66277, #46006, #46454, #37466, #17659, #58178 ),
 .UNSPECIFIED., .F., .F.,
 ( 4, 2, 2, 2, 4 ),
 ( 0.0007817359430256216575, 0.0009771253907249856981, 0.001172514838424349847, 0.001367904286123713779, 0.001563293733823077928 ),
 .UNSPECIFIED. ) ;
#44628 = AXIS2_PLACEMENT_3D ( 'NONE', #76256, #75385, #34389 ) ;
#44629 = CARTESIAN_POINT ( 'NONE',  ( -24.99999999999999645, 20.00000000000000355, 3.000000000000000000 ) ) ;
#44630 = DIRECTION ( 'NONE',  ( -0.000000000000000000, -0.3420201433256694901, -0.9396926207859082059 ) ) ;
#44631 = CARTESIAN_POINT ( 'NONE',  ( 7.911409417429871027, -10.90142922261932057, 33.41473453929631887 ) ) ;
#44632 = VERTEX_POINT ( 'NONE', #25681 ) ;
#44633 = DIRECTION ( 'NONE',  ( -1.000000000000000000, -0.000000000000000000, -0.000000000000000000 ) ) ;
#44634 = EDGE_LOOP ( 'NONE', ( #34558, #41945 ) ) ;
#44635 = AXIS2_PLACEMENT_3D ( 'NONE', #30417, #86271, #37166 ) ;
#44636 = ORIENTED_EDGE ( 'NONE', *, *, #17908, .F. ) ;
#44637 = VECTOR ( 'NONE', #14313, 1000.000000000000114 ) ;
#44639 = CARTESIAN_POINT ( 'NONE',  ( -1.515305987725692027, -5.496505350115500121, 34.60290016733514307 ) ) ;
#44638 = CARTESIAN_POINT ( 'NONE',  ( -0.5276218724943415594, -8.973038597847271092, 34.52809138561120506 ) ) ;
#44640 = COLOUR_RGB ( '', 0.72549020, 0.75294118, 0.79215686) ;
#44641 = CARTESIAN_POINT ( 'NONE',  ( -10.68146802634049486, -12.10708131394839349, 31.69288490824020244 ) ) ;
#44642 = CARTESIAN_POINT ( 'NONE',  ( -2.057746789344164107, -12.22109172314383052, 31.39792113162168263 ) ) ;
#44643 = CARTESIAN_POINT ( 'NONE',  ( -18.06527000055631760, -5.941354392334500467, 34.76329471203369792 ) ) ;
#44644 = CARTESIAN_POINT ( 'NONE',  ( -6.923076923077045919, -3.643525952248796163, 33.31231777344771672 ) ) ;
#44645 = EDGE_LOOP ( 'NONE', ( #38172, #54138 ) ) ;
#44646 = LINE ( 'NONE', #24831, #28504 ) ;
#44647 = CARTESIAN_POINT ( 'NONE',  ( 17.86930939688968678, -3.338472653186243200, 32.95098750199972670 ) ) ;
#44648 = CARTESIAN_POINT ( 'NONE',  ( 10.55011461482829560, -3.083524468853724443, 32.58852847137143272 ) ) ;
#44649 = CARTESIAN_POINT ( 'NONE',  ( 13.38461538461526601, -12.46129190930018460, 30.37095296980731973 ) ) ;
#44650 = ORIENTED_EDGE ( 'NONE', *, *, #7715, .F. ) ;
#44651 = ORIENTED_EDGE ( 'NONE', *, *, #72418, .T. ) ;
#44652 = FACE_BOUND ( 'NONE', #9831, .T. ) ;
#44653 = ORIENTED_EDGE ( 'NONE', *, *, #8844, .T. ) ;
#44654 = CARTESIAN_POINT ( 'NONE',  ( 7.596177115211495412, -2.779195860258147022, 31.39871582349836743 ) ) ;
#44655 = LINE ( 'NONE', #37923, #76350 ) ;
#44656 = ORIENTED_EDGE ( 'NONE', *, *, #31312, .F. ) ;
#44657 = CARTESIAN_POINT ( 'NONE',  ( -3.360916440207450506, -12.45813303252208648, 30.39737893381572675 ) ) ;
#44658 = CARTESIAN_POINT ( 'NONE',  ( -2.084912766423896446, -4.387253974876676565, 33.66317474335728832 ) ) ;
#44659 = DIRECTION ( 'NONE',  ( 0.000000000000000000, 0.1736481776669275834, 0.9848077530122086864 ) ) ;
#44660 = PLANE ( 'NONE',  #34490 ) ;
#44661 = ORIENTED_EDGE ( 'NONE', *, *, #80924, .T. ) ;
#44662 = EDGE_CURVE ( 'NONE', #21693, #81733, #57500, .T. ) ;
#44663 = CARTESIAN_POINT ( 'NONE',  ( -6.923076923076922462, -2.721908614388771852, 31.22303859784724978 ) ) ;
#44664 = ORIENTED_EDGE ( 'NONE', *, *, #55803, .F. ) ;
#44665 = EDGE_CURVE ( 'NONE', #65223, #86258, #40302, .T. ) ;
#44667 = ORIENTED_EDGE ( 'NONE', *, *, #19997, .F. ) ;
#44666 = CARTESIAN_POINT ( 'NONE',  ( -2.307692307692428724, -12.16647553114689728, 32.15551576947799362 ) ) ;
#44668 = CYLINDRICAL_SURFACE ( 'NONE', #87214, 0.2499999999999994726 ) ;
#44669 = ADVANCED_FACE ( 'NONE', ( #74315 ), #59013, .F. ) ;
#44670 = CARTESIAN_POINT ( 'NONE',  ( 15.10007862765892206, -4.684245665217972032, 34.18127051446801090 ) ) ;
#44671 = CARTESIAN_POINT ( 'NONE',  ( 2.307692307692309264, -1.790695186598648903, 34.54067556320373455 ) ) ;
#44672 = CARTESIAN_POINT ( 'NONE',  ( 18.06525557127601900, -8.613356846314930593, 34.62446782046653482 ) ) ;
#44673 = FACE_OUTER_BOUND ( 'NONE', #87649, .T. ) ;
#44674 = CARTESIAN_POINT ( 'NONE',  ( 12.33084785842815378, -5.496505350115501010, 34.60290016733514307 ) ) ;
#44675 = B_SPLINE_CURVE_WITH_KNOTS ( 'NONE', 3,
 ( #55347, #49915, #8945, #62536, #89163, #62107, #69318, #21111, #27442, #62976 ),
 .UNSPECIFIED., .F., .F.,
 ( 4, 2, 2, 2, 4 ),
 ( 0.0007817246256747450040, 0.0009771112852218881168, 0.001172497944769031230, 0.001367884604316174342, 0.001563271263863317455 ),
 .UNSPECIFIED. ) ;
#44676 = CARTESIAN_POINT ( 'NONE',  ( 2.750000000000002665, -7.561099074964516831, 15.97061829374151287 ) ) ;
#44677 = ORIENTED_EDGE ( 'NONE', *, *, #85121, .F. ) ;
#44678 = CARTESIAN_POINT ( 'NONE',  ( -16.15384615384615330, -12.37446782046654192, 30.86335684631486131 ) ) ;
#44679 = CARTESIAN_POINT ( 'NONE',  ( 13.60739505359345181, -12.69155399931963046, 30.53255429739157734 ) ) ;
#44680 = DIRECTION ( 'NONE',  ( -1.000000000000000000, -0.000000000000000000, 0.000000000000000000 ) ) ;
#44681 = ADVANCED_FACE ( 'NONE', ( #12617 ), #10837, .F. ) ;
#44682 = VERTEX_POINT ( 'NONE', #89179 ) ;
#44683 = ORIENTED_EDGE ( 'NONE', *, *, #69170, .T. ) ;
#44684 = CARTESIAN_POINT ( 'NONE',  ( -11.76138775597768316, -10.61292498521070549, 33.66303323003028680 ) ) ;
#44685 = CARTESIAN_POINT ( 'NONE',  ( 7.596130621932389637, -6.652501968072646932, 34.93155406624980941 ) ) ;
#44686 = EDGE_CURVE ( 'NONE', #21246, #38559, #3745, .T. ) ;
#44687 = CARTESIAN_POINT ( 'NONE',  ( -5.011667937410237528, -12.70778746994558439, 30.41441678777537305 ) ) ;
#44688 = DIRECTION ( 'NONE',  ( -0.000000000000000000, -0.9848077530122086864, -0.1736481776669273613 ) ) ;
#44689 = CARTESIAN_POINT ( 'NONE',  ( 10.36540788444226102, -4.236021600441997492, 33.53823185664189310 ) ) ;
#44690 = CARTESIAN_POINT ( 'NONE',  ( -16.94613263595612551, -11.37503395064541678, 33.29242100308974983 ) ) ;
#44691 = DIRECTION ( 'NONE',  ( -1.000000000000000000, -0.000000000000000000, -0.000000000000000000 ) ) ;
#44692 = ORIENTED_EDGE ( 'NONE', *, *, #24694, .F. ) ;
#44693 = CARTESIAN_POINT ( 'NONE',  ( -14.30769230769230660, -6.681629849574314051, 35.83090037661290239 ) ) ;
#44694 = CARTESIAN_POINT ( 'NONE',  ( -4.230769230769230838, -3.499999999999999556, 29.75000000000000355 ) ) ;
#44695 = VECTOR ( 'NONE', #63164, 1000.000000000000000 ) ;
#44696 = EDGE_CURVE ( 'NONE', #2574, #56880, #45714, .T. ) ;
#44697 = FACE_OUTER_BOUND ( 'NONE', #17911, .T. ) ;
#44698 = DIRECTION ( 'NONE',  ( -1.000000000000000000, 0.000000000000000000, 0.000000000000000000 ) ) ;
#44699 = ORIENTED_EDGE ( 'NONE', *, *, #72434, .F. ) ;
#44700 = CARTESIAN_POINT ( 'NONE',  ( 12.23805353697412635, -2.612411019501189369, 31.66733052389439962 ) ) ;
#44701 = VECTOR ( 'NONE', #71722, 1000.000000000000114 ) ;
#44702 = VECTOR ( 'NONE', #27947, 1000.000000000000000 ) ;
#44703 = EDGE_LOOP ( 'NONE', ( #75110, #11190, #47587, #85706 ) ) ;
#44704 = CARTESIAN_POINT ( 'NONE',  ( 13.38461538461538680, -13.63283147151868846, 33.57946703557072254 ) ) ;
#44705 = CARTESIAN_POINT ( 'NONE',  ( 10.39245765647776309, -3.395401636524185474, 33.02366814457250399 ) ) ;
#44706 = DIRECTION ( 'NONE',  ( -0.000000000000000000, -0.9848077530122085754, -0.1736481776669273613 ) ) ;
#44707 = VERTEX_POINT ( 'NONE', #76077 ) ;
#44708 = LINE ( 'NONE', #57355, #62213 ) ;
#44709 = CARTESIAN_POINT ( 'NONE',  ( 10.61538461538449596, -3.835265460704628371, 33.15142922262033665 ) ) ;
#44710 = AXIS2_PLACEMENT_3D ( 'NONE', #59625, #11004, #38476 ) ;
#44711 = CARTESIAN_POINT ( 'NONE',  ( 8.703906756426460944, -7.749976730030849303, 34.74374725381503737 ) ) ;
#44712 = DIRECTION ( 'NONE',  ( -0.000000000000000000, 0.9396926207859093161, -0.3420201433256663259 ) ) ;
#44713 = B_SPLINE_CURVE_WITH_KNOTS ( 'NONE', 3,
 ( #38541, #67785, #33110, #87631, #60575, #11962, #88093, #32661, #5637, #4759 ),
 .UNSPECIFIED., .F., .F.,
 ( 4, 2, 2, 2, 4 ),
 ( 0.000000000000000000, 0.0001954311564186867931, 0.0003908623128373735862, 0.0005862934692560603251, 0.0007817246256747471724 ),
 .UNSPECIFIED. ) ;
#44714 = B_SPLINE_CURVE_WITH_KNOTS ( 'NONE', 3,
 ( #34479, #68706, #33600, #13760, #40804, #81350, #68266, #76348, #42139, #26841 ),
 .UNSPECIFIED., .F., .F.,
 ( 4, 2, 2, 2, 4 ),
 ( 0.000000000000000000, 0.0001954311564186864949, 0.0003908623128373729899, 0.0005862934692560594577, 0.0007817246256747459798 ),
 .UNSPECIFIED. ) ;
#44715 = EDGE_CURVE ( 'NONE', #58562, #6303, #41415, .T. ) ;
#44716 = ORIENTED_EDGE ( 'NONE', *, *, #52633, .T. ) ;
#44717 = CARTESIAN_POINT ( 'NONE',  ( -1.134561072977069651, -3.627508038966689163, 32.91356715214248396 ) ) ;
#44718 = EDGE_CURVE ( 'NONE', #17646, #78512, #84325, .T. ) ;
#44719 = ORIENTED_EDGE ( 'NONE', *, *, #43153, .T. ) ;
#44720 = CYLINDRICAL_SURFACE ( 'NONE', #18449, 0.2500000000000008882 ) ;
#44721 = DIRECTION ( 'NONE',  ( -0.000000000000000000, 0.9396926207859093161, -0.3420201433256663259 ) ) ;
#44722 = CARTESIAN_POINT ( 'NONE',  ( -16.28399336328438096, -11.47017969459903952, 32.78971311882035167 ) ) ;
#44723 = EDGE_CURVE ( 'NONE', #35423, #13555, #27359, .T. ) ;
#44724 = CARTESIAN_POINT ( 'NONE',  ( 11.53846153846141576, -5.941354392335915335, 34.76329471203413846 ) ) ;
#44725 = EDGE_CURVE ( 'NONE', #16932, #45628, #77935, .T. ) ;
#44726 = FACE_OUTER_BOUND ( 'NONE', #7740, .T. ) ;
#44727 = CARTESIAN_POINT ( 'NONE',  ( 15.90386940979756503, -12.01397095200673881, 32.43157075238190146 ) ) ;
#44728 = VERTEX_POINT ( 'NONE', #82853 ) ;
#44729 = ORIENTED_EDGE ( 'NONE', *, *, #36223, .T. ) ;
#44730 = ORIENTED_EDGE ( 'NONE', *, *, #76368, .F. ) ;
#44731 = AXIS2_PLACEMENT_3D ( 'NONE', #68545, #7741, #536 ) ;
#44732 = ORIENTED_EDGE ( 'NONE', *, *, #80015, .F. ) ;
#44733 = VERTEX_POINT ( 'NONE', #867 ) ;
#44734 = CARTESIAN_POINT ( 'NONE',  ( -12.59209837515182784, -2.254533558242299396, 29.97296025877828285 ) ) ;
#44735 = CARTESIAN_POINT ( 'NONE',  ( -2.241623956689868358, -3.050289026998446840, 32.03036669348366416 ) ) ;
#44736 = AXIS2_PLACEMENT_3D ( 'NONE', #80385, #60091, #65956 ) ;
#44737 = CARTESIAN_POINT ( 'NONE',  ( -7.145942345280561270, -2.501496062324911840, 29.88072118266895671 ) ) ;
#44738 = CARTESIAN_POINT ( 'NONE',  ( -6.989160334032800570, -3.050289026998445951, 32.03036669348365706 ) ) ;
#44739 = CARTESIAN_POINT ( 'NONE',  ( -13.38461538461550582, -6.026961402154118019, 34.52809138561165270 ) ) ;
#44740 = CARTESIAN_POINT ( 'NONE',  ( -1.576923076923076428, -4.000000000000000000, 29.75000000000000355 ) ) ;
#44741 = B_SPLINE_CURVE_WITH_KNOTS ( 'NONE', 3,
 ( #75958, #34963, #84062, #1178, #14703, #27766, #36311, #15590, #14257, #741 ),
 .UNSPECIFIED., .F., .F.,
 ( 4, 2, 2, 2, 4 ),
 ( 0.0007817359430256390048, 0.0009771253907250078159, 0.001172514838424376735, 0.001367904286123745655, 0.001563293733823114574 ),
 .UNSPECIFIED. ) ;
#44742 = B_SPLINE_CURVE_WITH_KNOTS ( 'NONE', 3,
 ( #7014, #35373, #14666, #77245, #27725, #55636 ),
 .UNSPECIFIED., .F., .F.,
 ( 4, 2, 4 ),
 ( 0.000000000000000000, 0.0001954784845028902421, 0.0003909569690057804843 ),
 .UNSPECIFIED. ) ;
#44743 = CARTESIAN_POINT ( 'NONE',  ( -18.00000000000000000, -9.780366693483671270, 34.19971097300155094 ) ) ;
#44744 = DIRECTION ( 'NONE',  ( 1.000000000000000000, 0.000000000000000000, 0.000000000000000000 ) ) ;
#44745 = CARTESIAN_POINT ( 'NONE',  ( -4.284537620513712675, -9.804603061927743113, 34.18744698557895845 ) ) ;
#44746 = EDGE_LOOP ( 'NONE', ( #76592, #73336, #29472, #71779, #32766 ) ) ;
#44747 = EDGE_LOOP ( 'NONE', ( #47881, #15188, #19378, #29431 ) ) ;
#44748 = ORIENTED_EDGE ( 'NONE', *, *, #53472, .F. ) ;
#44750 = EDGE_LOOP ( 'NONE', ( #47144, #57661 ) ) ;
#44749 = CARTESIAN_POINT ( 'NONE',  ( 0.4615384615384611200, -2.833524468853757305, 32.15551576947925838 ) ) ;
#44752 = CARTESIAN_POINT ( 'NONE',  ( 10.54930120442873687, -8.973038597847271092, 34.52809138561120506 ) ) ;
#44751 = CYLINDRICAL_SURFACE ( 'NONE', #51772, 0.2500000000000012212 ) ;
#44753 = ADVANCED_FACE ( 'NONE', ( #21130 ), #49048, .F. ) ;
#44754 = DIRECTION ( 'NONE',  ( -0.000000000000000000, -0.3420201433256694346, -0.9396926207859080948 ) ) ;
#44755 = CYLINDRICAL_SURFACE ( 'NONE', #32222, 0.2499999999999997502 ) ;
#44756 = VERTEX_POINT ( 'NONE', #64650 ) ;
#44757 = AXIS2_PLACEMENT_3D ( 'NONE', #30393, #72262, #15999 ) ;
#44758 = ORIENTED_EDGE ( 'NONE', *, *, #65218, .F. ) ;
#44759 = CARTESIAN_POINT ( 'NONE',  ( -11.76138849736838132, -11.98009711892699514, 32.48740034544076138 ) ) ;
#44760 = ORIENTED_EDGE ( 'NONE', *, *, #5641, .F. ) ;
#44761 = FACE_BOUND ( 'NONE', #40009, .T. ) ;
#44762 = LINE ( 'NONE', #10999, #51894 ) ;
#44763 = CARTESIAN_POINT ( 'NONE',  ( 11.53846153846141753, -3.300289026999228881, 32.46337939537708905 ) ) ;
#44764 = EDGE_LOOP ( 'NONE', ( #58907, #37898 ) ) ;
#44765 = CARTESIAN_POINT ( 'NONE',  ( 14.08476609017615822, -2.758268499246657068, 31.33685645148948140 ) ) ;
#44766 = CARTESIAN_POINT ( 'NONE',  ( 8.835397375822410027, -7.250054591869670162, 34.99404684341514127 ) ) ;
#44767 = LINE ( 'NONE', #45668, #17718 ) ;
#44768 = ORIENTED_EDGE ( 'NONE', *, *, #36008, .T. ) ;
#44769 = CARTESIAN_POINT ( 'NONE',  ( 18.24999999999993250, -7.565270000091922853, 34.99999999999999289 ) ) ;
#44770 = DIRECTION ( 'NONE',  ( 0.000000000000000000, 0.8660254037844377084, 0.5000000000000015543 ) ) ;
#44771 = ORIENTED_EDGE ( 'NONE', *, *, #75162, .T. ) ;
#44772 = ADVANCED_FACE ( 'NONE', ( #24113 ), #23672, .F. ) ;
#44773 = CARTESIAN_POINT ( 'NONE',  ( -6.792551221313359200, -9.417988943895561960, 34.36773134775778260 ) ) ;
#44774 = CARTESIAN_POINT ( 'NONE',  ( 6.988332494352947677, -10.90142922261932057, 33.41473453929631887 ) ) ;
#44775 = ORIENTED_EDGE ( 'NONE', *, *, #67001, .F. ) ;
#44776 = CARTESIAN_POINT ( 'NONE',  ( -12.46153846153846168, -2.292212530054420494, 30.41441678777542634 ) ) ;
#44777 = CARTESIAN_POINT ( 'NONE',  ( 14.43821800945587341, -8.586989748646452369, 34.63063291749215011 ) ) ;
#44778 = FACE_OUTER_BOUND ( 'NONE', #997, .T. ) ;
#44779 = LINE ( 'NONE', #3356, #14129 ) ;
#44780 = CARTESIAN_POINT ( 'NONE',  ( 24.99999999999999645, -15.00000000000000000, 0.000000000000000000 ) ) ;
#44781 = CARTESIAN_POINT ( 'NONE',  ( 8.992243613324164997, -4.026326845037962343, 33.68677907613344047 ) ) ;
#44783 = CARTESIAN_POINT ( 'NONE',  ( 6.923076923076924238, -3.050289026998446396, 32.03036669348365706 ) ) ;
#44782 = CARTESIAN_POINT ( 'NONE',  ( -1.449885830576159496, -2.892918686051582977, 31.69288490824016691 ) ) ;
#44784 = FACE_OUTER_BOUND ( 'NONE', #26122, .T. ) ;
#44786 = CYLINDRICAL_SURFACE ( 'NONE', #295, 0.2499999999999986955 ) ;
#44785 = CARTESIAN_POINT ( 'NONE',  ( 3.360814393604009354, -2.504778602574659896, 29.97347330155780298 ) ) ;
#44787 = B_SPLINE_CURVE_WITH_KNOTS ( 'NONE', 3,
 ( #73968, #79838, #37955, #59105, #52343, #45593, #38399, #51890, #52792, #32089 ),
 .UNSPECIFIED., .F., .F.,
 ( 4, 2, 2, 2, 4 ),
 ( 0.000000000000000000, 0.0001954339857564079894, 0.0003908679715128159787, 0.0005863019572692239681, 0.0007817359430256319575 ),
 .UNSPECIFIED. ) ;
#44788 = CARTESIAN_POINT ( 'NONE',  ( -1.944543648263014957, -5.555456351737005249, 15.25000000000000000 ) ) ;
#44789 = B_SPLINE_CURVE_WITH_KNOTS ( 'NONE', 3,
 ( #49225, #29409, #63169, #2347, #28513, #14107, #76697, #55974, #28066, #20859 ),
 .UNSPECIFIED., .F., .F.,
 ( 4, 2, 2, 2, 4 ),
 ( 0.000000000000000000, 0.0001954339857564081520, 0.0003908679715128163040, 0.0005863019572692244018, 0.0007817359430256326080 ),
 .UNSPECIFIED. ) ;
#44790 = EDGE_LOOP ( 'NONE', ( #1769, #40452 ) ) ;
#44791 = CARTESIAN_POINT ( 'NONE',  ( 0.3962680155776847624, -12.46129190929999986, 30.37095296980880832 ) ) ;
#44792 = VERTEX_POINT ( 'NONE', #24563 ) ;
#44793 = ADVANCED_FACE ( 'NONE', ( #35545 ), #2950, .F. ) ;
#44794 = ORIENTED_EDGE ( 'NONE', *, *, #29124, .F. ) ;
#44795 = FACE_OUTER_BOUND ( 'NONE', #36330, .T. ) ;
#44796 = EDGE_LOOP ( 'NONE', ( #19510, #39595, #1476, #16171 ) ) ;
#44797 = CARTESIAN_POINT ( 'NONE',  ( 3.230769230769110045, -10.21337939537710326, 33.94971097300076224 ) ) ;
#44798 = CARTESIAN_POINT ( 'NONE',  ( -1.409462824231155764E-14, -4.749999999999999112, 16.65625000000000000 ) ) ;
#44799 = CARTESIAN_POINT ( 'NONE',  ( 3.007284306204901281, -2.353723527008296568, 30.78948104536958752 ) ) ;
#44800 = EDGE_CURVE ( 'NONE', #77977, #59461, #6947, .T. ) ;
#44801 = CARTESIAN_POINT ( 'NONE',  ( -5.076923076923075762, -2.721908614388771852, 31.22303859784724978 ) ) ;
#44802 = DIRECTION ( 'NONE',  ( -0.000000000000000000, -0.000000000000000000, -1.000000000000000000 ) ) ;
#44803 = CARTESIAN_POINT ( 'NONE',  ( -12.23875879256039312, -4.226511098958373402, 33.85474049983370293 ) ) ;
#44804 = CARTESIAN_POINT ( 'NONE',  ( -16.37677311275300340, -10.01117774369187252, 34.36070679894347535 ) ) ;
#44805 = CARTESIAN_POINT ( 'NONE',  ( 0.5267936010512993539, -5.941354392334606160, 34.76329471203374055 ) ) ;
#44806 = CARTESIAN_POINT ( 'NONE',  ( -14.24162497434223162, -4.661471528628508665, 34.16647553114624003 ) ) ;
#44807 = CARTESIAN_POINT ( 'NONE',  ( 3.750000000000009770, -9.053300858899081760, 19.54687499999999645 ) ) ;
#44808 = CARTESIAN_POINT ( 'NONE',  ( 18.22301284409340028, -11.43677907613345113, 33.22367315496201456 ) ) ;
#44809 = CARTESIAN_POINT ( 'NONE',  ( -2.084912638714241151, -12.11081565061823717, 32.26097654155341843 ) ) ;
#44810 = EDGE_CURVE ( 'NONE', #85360, #33072, #4883, .T. ) ;
#44811 = AXIS2_PLACEMENT_3D ( 'NONE', #81176, #87503, #87960 ) ;
#44812 = DIRECTION ( 'NONE',  ( 0.000000000000000000, 0.000000000000000000, -1.000000000000000000 ) ) ;
#44813 = EDGE_CURVE ( 'NONE', #41031, #3673, #13494, .T. ) ;
#44814 = ORIENTED_EDGE ( 'NONE', *, *, #78394, .T. ) ;
#44815 = ORIENTED_EDGE ( 'NONE', *, *, #66787, .T. ) ;
#44816 = LINE ( 'NONE', #72296, #48593 ) ;
#44817 = CARTESIAN_POINT ( 'NONE',  ( -14.17690049986752143, -8.147973898785416225, 34.70805048591653730 ) ) ;
#44818 = LINE ( 'NONE', #32650, #6620 ) ;
#44819 = CARTESIAN_POINT ( 'NONE',  ( 15.23076923076923173, -1.044019251281081972, 31.83374038241031911 ) ) ;
#44820 = EDGE_CURVE ( 'NONE', #30159, #2090, #46659, .T. ) ;
#44821 = FACE_OUTER_BOUND ( 'NONE', #33914, .T. ) ;
#44822 = CARTESIAN_POINT ( 'NONE',  ( -3.099978789802280144, -5.496552790871119143, 34.60292014791297532 ) ) ;
#44823 = ADVANCED_FACE ( 'NONE', ( #86744 ), #31329, .F. ) ;
#44824 = ORIENTED_EDGE ( 'NONE', *, *, #27419, .T. ) ;
#44825 = CARTESIAN_POINT ( 'NONE',  ( 18.00000000000000000, -12.37446782046654192, 30.86335684631486131 ) ) ;
#44826 = EDGE_LOOP ( 'NONE', ( #25704, #43665, #19766, #35676 ) ) ;
#44827 = EDGE_CURVE ( 'NONE', #14132, #87104, #30435, .T. ) ;
#44828 = EDGE_LOOP ( 'NONE', ( #73034, #40109, #80046, #10644 ) ) ;
#44829 = CIRCLE ( 'NONE', #30438, 8.000000000000000000 ) ;
#44830 = CARTESIAN_POINT ( 'NONE',  ( 0.7115928814519140166, -12.41089969410671223, 31.60739465890703670 ) ) ;
#44831 = CARTESIAN_POINT ( 'NONE',  ( -11.47320639894870276, -11.67786785259547777, 32.92929555188713664 ) ) ;
#44832 = CARTESIAN_POINT ( 'NONE',  ( -14.30769230769230660, -2.833524468853757305, 32.15551576947925838 ) ) ;
#44833 = EDGE_CURVE ( 'NONE', #34232, #11498, #71410, .T. ) ;
#44834 = CARTESIAN_POINT ( 'NONE',  ( 9.692307692307572609, -3.300289026999228881, 32.46337939537708905 ) ) ;
#44835 = CARTESIAN_POINT ( 'NONE',  ( -2.307692307692427391, -11.94971097300221174, 32.03036669348237098 ) ) ;
#44836 = VECTOR ( 'NONE', #45824, 1000.000000000000000 ) ;
#44837 = ORIENTED_EDGE ( 'NONE', *, *, #32354, .T. ) ;
#44838 = ORIENTED_EDGE ( 'NONE', *, *, #67670, .F. ) ;
#44839 = B_SPLINE_CURVE_WITH_KNOTS ( 'NONE', 3,
 ( #70046, #20530, #55198, #27726, #14667, #6579, #7471, #75045, #47994, #34046 ),
 .UNSPECIFIED., .F., .F.,
 ( 4, 2, 2, 2, 4 ),
 ( 0.000000000000000000, 0.0001954339857564081249, 0.0003908679715128162498, 0.0005863019572692244018, 0.0007817359430256324996 ),
 .UNSPECIFIED. ) ;
#44840 = ORIENTED_EDGE ( 'NONE', *, *, #47063, .F. ) ;
#44841 = CARTESIAN_POINT ( 'NONE',  ( 13.25446741488368829, -5.070767119584671079, 34.40440758774516183 ) ) ;
#44842 = CARTESIAN_POINT ( 'NONE',  ( 9.692307692307570832, -2.379036618888197729, 30.90682066428292885 ) ) ;
#44843 = EDGE_CURVE ( 'NONE', #81317, #36450, #42369, .T. ) ;
#44844 = CARTESIAN_POINT ( 'NONE',  ( 4.153846153846154188, -12.78798330534102767, 29.49999999999997868 ) ) ;
#44845 = CARTESIAN_POINT ( 'NONE',  ( -15.00775787915638304, -3.105924265160262543, 32.13625925475356127 ) ) ;
#44846 = EDGE_CURVE ( 'NONE', #67618, #67129, #5631, .T. ) ;
#44847 = DIRECTION ( 'NONE',  ( 0.000000000000000000, 0.8660254037844377084, -0.5000000000000015543 ) ) ;
#44848 = CARTESIAN_POINT ( 'NONE',  ( 4.153846153846154188, -12.09954503811598769, 35.62045528018868623 ) ) ;
#44849 = ORIENTED_EDGE ( 'NONE', *, *, #53331, .T. ) ;
#44850 = ORIENTED_EDGE ( 'NONE', *, *, #3712, .F. ) ;
#44851 = CARTESIAN_POINT ( 'NONE',  ( -3.749999999999997335, -7.500000000000021316, 21.34375000000000000 ) ) ;
#44852 = EDGE_LOOP ( 'NONE', ( #36784, #64801 ) ) ;
#44854 = ORIENTED_EDGE ( 'NONE', *, *, #42303, .F. ) ;
#44853 = CARTESIAN_POINT ( 'NONE',  ( 15.48082354240754555, -5.728107161865378494, 34.42597550085002922 ) ) ;
#44855 = CARTESIAN_POINT ( 'NONE',  ( 6.416666666666664298, -11.50000000000000000, 29.75000000000000355 ) ) ;
#44856 = B_SPLINE_CURVE_WITH_KNOTS ( 'NONE', 3,
 ( #81932, #54891, #5820, #81490, #14343, #20223, #19776, #35055, #13018, #89141 ),
 .UNSPECIFIED., .F., .F.,
 ( 4, 2, 2, 2, 4 ),
 ( 0.000000000000000000, 0.0001954311564186861968, 0.0003908623128373723936, 0.0005862934692560585904, 0.0007817246256747447872 ),
 .UNSPECIFIED. ) ;
#44857 = CARTESIAN_POINT ( 'NONE',  ( -9.942330929600657896, -11.86270091957321249, 32.19358267280087915 ) ) ;
#44858 = VECTOR ( 'NONE', #52860, 1000.000000000000000 ) ;
#44859 = EDGE_CURVE ( 'NONE', #67881, #9159, #9020, .T. ) ;
#44860 = CARTESIAN_POINT ( 'NONE',  ( 10.28846153846153832, -3.499999999999999556, 29.75000000000000355 ) ) ;
#44861 = ORIENTED_EDGE ( 'NONE', *, *, #79878, .F. ) ;
#44862 = CARTESIAN_POINT ( 'NONE',  ( -39.05038313613820122, -2.249999999999998668, 29.75000000000000355 ) ) ;
#44863 = VERTEX_POINT ( 'NONE', #33559 ) ;
#44864 = EDGE_CURVE ( 'NONE', #3680, #37287, #4755, .T. ) ;
#44865 = DIRECTION ( 'NONE',  ( -0.000000000000000000, -0.8660254037844397068, -0.4999999999999978906 ) ) ;
#44866 = CARTESIAN_POINT ( 'NONE',  ( -6.989160334032804123, -2.721908614388772740, 31.22303859784724622 ) ) ;
#44867 = CARTESIAN_POINT ( 'NONE',  ( -12.46153846153846168, -12.37446782046654192, 30.86335684631486131 ) ) ;
#44869 = CARTESIAN_POINT ( 'NONE',  ( 4.153846153846154188, -3.669653830205710676, 35.88435417666054406 ) ) ;
#44868 = CARTESIAN_POINT ( 'NONE',  ( -15.23076923076922995, -13.37000171582298513, 34.34916445242398453 ) ) ;
#44870 = EDGE_CURVE ( 'NONE', #20057, #63601, #44392, .T. ) ;
#44871 = CARTESIAN_POINT ( 'NONE',  ( -0.5276208408985981757, -12.34228464037088280, 31.77849191805838558 ) ) ;
#44872 = CARTESIAN_POINT ( 'NONE',  ( -3.453696189676077832, -8.282780595021769443, 34.94152052738834868 ) ) ;
#44873 = VERTEX_POINT ( 'NONE', #32224 ) ;
#44874 = CARTESIAN_POINT ( 'NONE',  ( -10.74607608205217346, -9.804603061927743113, 34.18744698557895845 ) ) ;
#44875 = PLANE ( 'NONE',  #39264 ) ;
#44876 = VERTEX_POINT ( 'NONE', #74099 ) ;
#44877 = EDGE_CURVE ( 'NONE', #52424, #42644, #4719, .T. ) ;
#44878 = CARTESIAN_POINT ( 'NONE',  ( 19.00000000000000000, 0.000000000000000000, 22.25000000000000000 ) ) ;
#44879 = CARTESIAN_POINT ( 'NONE',  ( 14.30769230769218758, -10.21337939537710326, 33.94971097300076224 ) ) ;
#44881 = DIRECTION ( 'NONE',  ( 0.000000000000000000, 0.9396926207859126468, 0.3420201433256571111 ) ) ;
#44880 = PRODUCT_DEFINITION_SHAPE ( 'NONE', 'NONE',  #89189 ) ;
#44882 = DIRECTION ( 'NONE',  ( 0.000000000000000000, 0.000000000000000000, -1.000000000000000000 ) ) ;
#44883 = CARTESIAN_POINT ( 'NONE',  ( 7.846153846153725020, -8.613356846316285953, 34.62446782046622218 ) ) ;
#44884 = FACE_BOUND ( 'NONE', #41760, .T. ) ;
#44886 = DIRECTION ( 'NONE',  ( -0.000000000000000000, -0.1736481776669307198, -0.9848077530122080203 ) ) ;
#44885 = CARTESIAN_POINT ( 'NONE',  ( 13.13463865367303463, -12.17611988154120972, 31.52148481390971213 ) ) ;
#44887 = FACE_OUTER_BOUND ( 'NONE', #36436, .T. ) ;
#44889 = DIRECTION ( 'NONE',  ( 1.000000000000000000, 0.000000000000000000, 0.000000000000000000 ) ) ;
#44888 = CARTESIAN_POINT ( 'NONE',  ( 3.100622021331010725, -4.460286881179643004, 33.72017969459903242 ) ) ;
#44890 = DIRECTION ( 'NONE',  ( -0.000000000000000000, 0.9396926207859092051, -0.3420201433256662704 ) ) ;
#44891 = CARTESIAN_POINT ( 'NONE',  ( 11.53846153846153832, -12.78798330534102767, 29.49999999999997868 ) ) ;
#44892 = CARTESIAN_POINT ( 'NONE',  ( -2.608446859217889546, -10.19485399968121264, 25.93563170625849423 ) ) ;
#44893 = AXIS2_PLACEMENT_3D ( 'NONE', #30928, #73264, #39050 ) ;
#44894 = ORIENTED_EDGE ( 'NONE', *, *, #81635, .T. ) ;
#44895 = VECTOR ( 'NONE', #76425, 1000.000000000000000 ) ;
#44896 = DIRECTION ( 'NONE',  ( -0.000000000000000000, 0.8660254037844397068, -0.4999999999999978906 ) ) ;
#44897 = CARTESIAN_POINT ( 'NONE',  ( 7.911408985666682270, -10.33852847137154107, 34.16647553114620450 ) ) ;
#44898 = DIRECTION ( 'NONE',  ( 0.000000000000000000, 0.000000000000000000, 1.000000000000000000 ) ) ;
#44899 = CARTESIAN_POINT ( 'NONE',  ( 17.01084069756293715, -8.164416787775445883, 34.95778746994557906 ) ) ;
#44900 = CARTESIAN_POINT ( 'NONE',  ( 0.000000000000000000, -11.00000000000000000, 29.75000000000000355 ) ) ;
#44901 = CARTESIAN_POINT ( 'NONE',  ( 5.142178216435913107, -12.16647553114626490, 32.15551576947920864 ) ) ;
#44902 = CARTESIAN_POINT ( 'NONE',  ( -0.06109907496455085213, -3.750000000000000888, 18.90438170625848713 ) ) ;
#44903 = EDGE_CURVE ( 'NONE', #48041, #61963, #2616, .T. ) ;
#44904 = AXIS2_PLACEMENT_3D ( 'NONE', #78955, #86174, #71301 ) ;
#44905 = CARTESIAN_POINT ( 'NONE',  ( -16.15384615384615330, -5.471508081941601098, 34.59228464037088457 ) ) ;
#44906 = CARTESIAN_POINT ( 'NONE',  ( 0.5267940328144861128, -3.835265460703683349, 33.15142922261929925 ) ) ;
#44907 = CARTESIAN_POINT ( 'NONE',  ( 11.31558202172395511, -7.630690623152299956, 34.99857592706774057 ) ) ;
#44908 = CARTESIAN_POINT ( 'NONE',  ( -0.4615384615384611200, -8.164416787775445883, 34.95778746994557906 ) ) ;
#44909 = CARTESIAN_POINT ( 'NONE',  ( 7.053868730901711182, -4.118422570099827595, 33.43335022499816489 ) ) ;
#44910 = FACE_OUTER_BOUND ( 'NONE', #54858, .T. ) ;
#44911 = CARTESIAN_POINT ( 'NONE',  ( 4.153846153846032507, -4.481592998941358097, 33.73612834414048933 ) ) ;
#44912 = CARTESIAN_POINT ( 'NONE',  ( 17.20744851515672025, -8.630441415882549094, 34.87705825610312615 ) ) ;
#44913 = ORIENTED_EDGE ( 'NONE', *, *, #45952, .F. ) ;
#44914 = B_SPLINE_CURVE_WITH_KNOTS ( 'NONE', 3,
 ( #67371, #61487, #88993, #26385, #6116, #51915, #11390, #73553, #66335, #86628 ),
 .UNSPECIFIED., .F., .F.,
 ( 4, 2, 2, 2, 4 ),
 ( 0.0007817359430256328248, 0.0009771253907249995759, 0.001172514838424366327, 0.001367904286123733078, 0.001563293733823099829 ),
 .UNSPECIFIED. ) ;
#44915 = CARTESIAN_POINT ( 'NONE',  ( 1.634615384616822320, -7.500000000000155431, 34.75000000000007105 ) ) ;
#44916 = CARTESIAN_POINT ( 'NONE',  ( -17.14300648787895298, -2.721908614388770964, 31.22303859784723912 ) ) ;
#44917 = CARTESIAN_POINT ( 'NONE',  ( -1.987747218494638313, -9.401340078031370950, 25.18936829374151642 ) ) ;
#44918 = CARTESIAN_POINT ( 'NONE',  ( -10.86540783960607293, -10.18141759479407327, 34.26406193332782379 ) ) ;
#44919 = CARTESIAN_POINT ( 'NONE',  ( 1.384615384615265343, -9.442884908241554243, 34.35708131394783038 ) ) ;
#44920 = ORIENTED_EDGE ( 'NONE', *, *, #31804, .F. ) ;
#44921 = CARTESIAN_POINT ( 'NONE',  ( -17.77722033102192967, -6.717445702608402236, 34.94155399931962336 ) ) ;
#44922 = CARTESIAN_POINT ( 'NONE',  ( 1.384615384615264011, -2.657715359629662544, 31.77849191805970364 ) ) ;
#44924 = VERTEX_POINT ( 'NONE', #6083 ) ;
#44923 = CARTESIAN_POINT ( 'NONE',  ( -7.596208436775802930, -12.45601412856602686, 31.48342859153981621 ) ) ;
#44925 = CARTESIAN_POINT ( 'NONE',  ( -11.28846153846153655, -2.499999999999998668, 29.75000000000000355 ) ) ;
#44926 = CARTESIAN_POINT ( 'NONE',  ( 16.85404356018549521, -7.630690623152299956, 34.99857592706774057 ) ) ;
#44927 = CARTESIAN_POINT ( 'NONE',  ( -7.846153846153844924, -12.34228464037088635, 31.77849191805839268 ) ) ;
#44928 = CARTESIAN_POINT ( 'NONE',  ( 6.000000000000001776, -3.886160181151819604, 36.00935417666054406 ) ) ;
#44929 = ORIENTED_EDGE ( 'NONE', *, *, #1205, .F. ) ;
#44930 = VECTOR ( 'NONE', #59860, 1000.000000000000000 ) ;
#44931 = FACE_OUTER_BOUND ( 'NONE', #88381, .T. ) ;
#44932 = EDGE_CURVE ( 'NONE', #50951, #26741, #26790, .T. ) ;
#44933 = DIRECTION ( 'NONE',  ( -1.000000000000000000, 0.000000000000000000, 0.000000000000000000 ) ) ;
#44934 = ORIENTED_EDGE ( 'NONE', *, *, #16294, .F. ) ;
#44935 = ORIENTED_EDGE ( 'NONE', *, *, #68089, .T. ) ;
#44936 = ADVANCED_FACE ( 'NONE', ( #13275 ), #40760, .F. ) ;
#44937 = EDGE_LOOP ( 'NONE', ( #14440, #21853 ) ) ;
#44938 = CARTESIAN_POINT ( 'NONE',  ( -10.61538461538461320, -11.16473453929635440, 33.15142922261926373 ) ) ;
#44939 = CARTESIAN_POINT ( 'NONE',  ( -3.007989561791165389, -3.020022701398814124, 32.48759521482552515 ) ) ;
#44940 = EDGE_CURVE ( 'NONE', #12084, #82763, #86406, .T. ) ;
#44941 = CARTESIAN_POINT ( 'NONE',  ( -9.561517251340744039, -12.62708834333097663, 30.88030960425257021 ) ) ;
#44942 = EDGE_CURVE ( 'NONE', #16715, #53257, #77191, .T. ) ;
#44943 = CARTESIAN_POINT ( 'NONE',  ( -10.61538461538461320, -3.050289026998446396, 32.03036669348365706 ) ) ;
#44944 = VERTEX_POINT ( 'NONE', #61897 ) ;
#44945 = B_SPLINE_CURVE_WITH_KNOTS ( 'NONE', 3,
 ( #55543, #8702, #83926, #2359, #29853, #21311, #22207, #8258, #57317, #42931 ),
 .UNSPECIFIED., .F., .F.,
 ( 4, 2, 2, 2, 4 ),
 ( 0.000000000000000000, 0.0001954311564186863052, 0.0003908623128373726104, 0.0005862934692560589156, 0.0007817246256747452209 ),
 .UNSPECIFIED. ) ;
#44946 = ORIENTED_EDGE ( 'NONE', *, *, #22796, .T. ) ;
#44948 = ORIENTED_EDGE ( 'NONE', *, *, #33134, .T. ) ;
#44947 = CARTESIAN_POINT ( 'NONE',  ( 11.76124120743959978, -11.60474049983371003, 33.02348890104160262 ) ) ;
#44949 = CARTESIAN_POINT ( 'NONE',  ( 6.700210660013824260, -2.251424796025575770, 29.88072029997477586 ) ) ;
#44950 = EDGE_CURVE ( 'NONE', #6564, #71441, #83075, .T. ) ;
#44951 = DIRECTION ( 'NONE',  ( -1.000000000000000000, -0.000000000000000000, -0.000000000000000000 ) ) ;
#44952 = VECTOR ( 'NONE', #37940, 999.9999999999998863 ) ;
#44953 = DIRECTION ( 'NONE',  ( 0.000000000000000000, 0.7660444431189822323, -0.6427876096865344779 ) ) ;
#44954 = CARTESIAN_POINT ( 'NONE',  ( -1.254089946381738319, -12.70449254468099198, 30.44128974285582956 ) ) ;
#44955 = ORIENTED_EDGE ( 'NONE', *, *, #54830, .F. ) ;
#44956 = VERTEX_POINT ( 'NONE', #83524 ) ;
#44957 = ORIENTED_EDGE ( 'NONE', *, *, #88896, .T. ) ;
#44959 = ORIENTED_EDGE ( 'NONE', *, *, #84784, .F. ) ;
#44958 = CARTESIAN_POINT ( 'NONE',  ( 15.10062202133101295, -2.619462340734462380, 30.83744416345203021 ) ) ;
#44960 = CARTESIAN_POINT ( 'NONE',  ( -10.61538461538473577, -5.941354392335915335, 34.76329471203413846 ) ) ;
#44961 = CARTESIAN_POINT ( 'NONE',  ( 18.13052543823364360, -5.915461855592777596, 34.75538340440931506 ) ) ;
#44962 = ORIENTED_EDGE ( 'NONE', *, *, #20076, .T. ) ;
#44963 = CARTESIAN_POINT ( 'NONE',  ( -13.44988583057615905, -4.481592998940162609, 33.73612834413957984 ) ) ;
#44964 = FACE_OUTER_BOUND ( 'NONE', #34457, .T. ) ;
#44965 = CARTESIAN_POINT ( 'NONE',  ( 8.769230769230768274, -5.557115091759785130, 34.35708131394839171 ) ) ;
#44966 = FACE_BOUND ( 'NONE', #53564, .T. ) ;
#44967 = ADVANCED_FACE ( 'NONE', ( #209 ), #1539, .F. ) ;
#44968 = CARTESIAN_POINT ( 'NONE',  ( -5.142193077479396024, -10.33852847137145048, 34.16647553114627556 ) ) ;
#44969 = CARTESIAN_POINT ( 'NONE',  ( -4.377331097570102969, -12.24155766932282496, 31.33739205006857986 ) ) ;
#44970 = CARTESIAN_POINT ( 'NONE',  ( -15.23076923076922995, -10.51840700105979565, 33.73612834413961536 ) ) ;
#44972 = LINE ( 'NONE', #16618, #26016 ) ;
#44971 = CARTESIAN_POINT ( 'NONE',  ( 16.28437159207980045, -4.299079248970731015, 33.91157788607253565 ) ) ;
#44973 = CARTESIAN_POINT ( 'NONE',  ( 5.076923076922954969, -12.27809138561165270, 31.22303859784587132 ) ) ;
#44974 = CARTESIAN_POINT ( 'NONE',  ( 1.634560793993430128, -2.341251567377310217, 30.72681386836322659 ) ) ;
#44975 = ORIENTED_EDGE ( 'NONE', *, *, #44164, .F. ) ;
#44976 = CARTESIAN_POINT ( 'NONE',  ( -9.692307692307691624, -1.129524287112498415, 32.06866353760679544 ) ) ;
#44977 = CARTESIAN_POINT ( 'NONE',  ( -7.715628144390286103, -2.619367082507848554, 30.83698974864644171 ) ) ;
#44978 = ORIENTED_EDGE ( 'NONE', *, *, #20140, .F. ) ;
#44979 = B_SPLINE_CURVE_WITH_KNOTS ( 'NONE', 3,
 ( #66475, #4778, #59710, #87208, #56828, #57276, #29814, #76669, #84326, #50068 ),
 .UNSPECIFIED., .F., .F.,
 ( 4, 2, 2, 2, 4 ),
 ( 0.0007817359430256394385, 0.0009771253907250078159, 0.001172514838424376085, 0.001367904286123744571, 0.001563293733823112840 ),
 .UNSPECIFIED. ) ;
#44980 = VERTEX_POINT ( 'NONE', #21805 ) ;
#44982 = CARTESIAN_POINT ( 'NONE',  ( 10.86533002476265963, -12.68172785388650681, 30.59649109432439218 ) ) ;
#44981 = DIRECTION ( 'NONE',  ( -0.000000000000000000, -0.6427876096865404731, -0.7660444431189770143 ) ) ;
#44983 = EDGE_CURVE ( 'NONE', #86342, #76471, #58447, .T. ) ;
#44984 = AXIS2_PLACEMENT_3D ( 'NONE', #55693, #70099, #21918 ) ;
#44985 = CARTESIAN_POINT ( 'NONE',  ( -5.750054481651856619, -6.696923467548660192, 34.68552623307873972 ) ) ;
#44986 = CARTESIAN_POINT ( 'NONE',  ( -10.61538461538473577, -5.094484230521993062, 34.41647553114689373 ) ) ;
#44987 = CARTESIAN_POINT ( 'NONE',  ( -11.60454391782167427, -9.905515769479276145, 34.41647553114623292 ) ) ;
#44988 = EDGE_LOOP ( 'NONE', ( #27907, #2658, #38008, #81237, #594, #18914 ) ) ;
#44989 = DIRECTION ( 'NONE',  ( -0.000000000000000000, -0.7660444431189791237, -0.6427876096865379196 ) ) ;
#44990 = EDGE_CURVE ( 'NONE', #56583, #33821, #41196, .T. ) ;
#44992 = CARTESIAN_POINT ( 'NONE',  ( -3.230769230769229949, -1.790695186598648903, 34.54067556320373455 ) ) ;
#44991 = DIRECTION ( 'NONE',  ( 1.000000000000000000, 0.000000000000000000, 0.000000000000000000 ) ) ;
#44993 = CARTESIAN_POINT ( 'NONE',  ( 7.596177115211492747, -5.728515186090277211, 34.42611988154120439 ) ) ;
#44994 = LINE ( 'NONE', #64373, #12244 ) ;
#44995 = LINE ( 'NONE', #72475, #85162 ) ;
#44996 = CARTESIAN_POINT ( 'NONE',  ( -1.929879867024197893E-14, -3.750000000000000000, 16.65625000000000000 ) ) ;
#44997 = ORIENTED_EDGE ( 'NONE', *, *, #10164, .T. ) ;
#44998 = ORIENTED_EDGE ( 'NONE', *, *, #86161, .T. ) ;
#44999 = CARTESIAN_POINT ( 'NONE',  ( -7.596153846153844924, -2.249999999999998668, 29.75000000000000355 ) ) ;
#45000 = DIRECTION ( 'NONE',  ( -0.000000000000000000, 1.000000000000000000, -0.000000000000000000 ) ) ;
#45001 = DIRECTION ( 'NONE',  ( 0.000000000000000000, 0.9396926207859126468, -0.3420201433256571111 ) ) ;
#45002 = FACE_OUTER_BOUND ( 'NONE', #43536, .T. ) ;
#45003 = CARTESIAN_POINT ( 'NONE',  ( 0.4615384615384611200, -13.87047571288749737, 32.06866353760679544 ) ) ;
#45004 = CARTESIAN_POINT ( 'NONE',  ( 2.651650429449539104, -4.848349570550432475, 18.06250000000000355 ) ) ;
#45005 = EDGE_CURVE ( 'NONE', #40289, #4801, #57348, .T. ) ;
#45006 = CARTESIAN_POINT ( 'NONE',  ( 3.262820512820511443, -4.000000000000000000, 29.75000000000000355 ) ) ;
#45007 = CARTESIAN_POINT ( 'NONE',  ( -13.38461538461538325, -13.53365097954675988, 30.81389545987213552 ) ) ;
#45008 = ORIENTED_EDGE ( 'NONE', *, *, #60326, .F. ) ;
#45009 = DIRECTION ( 'NONE',  ( -0.000000000000000000, 1.000000000000000000, 3.491481338843133355E-15 ) ) ;
#45011 = ORIENTED_EDGE ( 'NONE', *, *, #55538, .F. ) ;
#45010 = CARTESIAN_POINT ( 'NONE',  ( -6.249999999999997335, -2.249999999999998668, 29.75000000000000355 ) ) ;
#45012 = CARTESIAN_POINT ( 'NONE',  ( -9.942307692307691624, -7.500000000000001776, 35.00000000000000000 ) ) ;
#45013 = FACE_OUTER_BOUND ( 'NONE', #69388, .T. ) ;
#45014 = EDGE_CURVE ( 'NONE', #66369, #22022, #85273, .T. ) ;
#45015 = EDGE_CURVE ( 'NONE', #37045, #80537, #38052, .T. ) ;
#45016 = CARTESIAN_POINT ( 'NONE',  ( -3.296526033283539991, -7.249945686854185389, 34.74374336980224598 ) ) ;
#45017 = CARTESIAN_POINT ( 'NONE',  ( 7.053602361310569613, -2.372941743896878286, 30.88044141588254377 ) ) ;
#45018 = LINE ( 'NONE', #72497, #33553 ) ;
#45019 = CARTESIAN_POINT ( 'NONE',  ( 9.469380733400843297, -4.762599654559228846, 34.23009711892697737 ) ) ;
#45020 = LINE ( 'NONE', #43265, #62875 ) ;
#45021 = ORIENTED_EDGE ( 'NONE', *, *, #54483, .T. ) ;
#45022 = EDGE_CURVE ( 'NONE', #43002, #57014, #48724, .T. ) ;
#45023 = CARTESIAN_POINT ( 'NONE',  ( 11.60452988946397923, -11.69971097300155272, 32.46337939537588113 ) ) ;
#45024 = CARTESIAN_POINT ( 'NONE',  ( -13.31936024510254590, -10.33852847137154107, 34.16647553114620450 ) ) ;
#45025 = CARTESIAN_POINT ( 'NONE',  ( -18.00000000000000000, -1.163064389776900187, 32.05645593858272235 ) ) ;
#45026 = CARTESIAN_POINT ( 'NONE',  ( 1.139087296526029469, -10.24999999999999467, 24.70312500000000000 ) ) ;
#45027 = CIRCLE ( 'NONE', #68065, 4.000000000000000000 ) ;
#45028 = DIRECTION ( 'NONE',  ( 0.000000000000000000, -1.000000000000000000, 0.000000000000000000 ) ) ;
#45029 = FILL_AREA_STYLE_COLOUR ( '', #68183 ) ;
#45031 = VERTEX_POINT ( 'NONE', #37523 ) ;
#45030 = CARTESIAN_POINT ( 'NONE',  ( 12.21151522424549896, -10.76384336483936011, 33.53834819971076087 ) ) ;
#45032 = CARTESIAN_POINT ( 'NONE',  ( -2.749999999999991562, -8.639087296526026805, 20.01562500000000355 ) ) ;
#45033 = CARTESIAN_POINT ( 'NONE',  ( -15.45369618967607828, -4.026226216239094491, 33.68668979543634379 ) ) ;
#45034 = AXIS2_PLACEMENT_3D ( 'NONE', #74432, #59579, #32551 ) ;
#45035 = ORIENTED_EDGE ( 'NONE', *, *, #25126, .T. ) ;
#45036 = DIRECTION ( 'NONE',  ( 0.000000000000000000, 0.000000000000000000, -1.000000000000000000 ) ) ;
#45037 = ORIENTED_EDGE ( 'NONE', *, *, #13168, .T. ) ;
#45038 = DIRECTION ( 'NONE',  ( 0.000000000000000000, 0.1736481776669275834, 0.9848077530122086864 ) ) ;
#45039 = CARTESIAN_POINT ( 'NONE',  ( -15.45369618967607828, -2.889293201056495786, 32.26117774369186009 ) ) ;
#45040 = CARTESIAN_POINT ( 'NONE',  ( 16.85343815235874132, -6.716662450894490988, 34.94144148231605840 ) ) ;
#45041 = ORIENTED_EDGE ( 'NONE', *, *, #28322, .T. ) ;
#45042 = DIRECTION ( 'NONE',  ( 1.000000000000000000, 0.000000000000000000, 0.000000000000000000 ) ) ;
#45043 = ORIENTED_EDGE ( 'NONE', *, *, #4714, .F. ) ;
#45044 = CARTESIAN_POINT ( 'NONE',  ( -5.869474561766354626, -2.372941743896878286, 30.88044141588254377 ) ) ;
#45045 = ADVANCED_FACE ( 'NONE', ( #72196 ), #38426, .F. ) ;
#45046 = ORIENTED_EDGE ( 'NONE', *, *, #79140, .F. ) ;
#45047 = CARTESIAN_POINT ( 'NONE',  ( 13.60739492588379385, -11.89424750095246175, 32.13594075562310337 ) ) ;
#45048 = FACE_OUTER_BOUND ( 'NONE', #4617, .T. ) ;
#45049 = VERTEX_POINT ( 'NONE', #51018 ) ;
#45050 = B_SPLINE_CURVE_WITH_KNOTS ( 'NONE', 3,
 ( #35804, #69574, #9219, #28600, #71340, #36683, #83553, #64133, #2436, #49307 ),
 .UNSPECIFIED., .F., .F.,
 ( 4, 2, 2, 2, 4 ),
 ( 0.000000000000000000, 0.0001954311564186879315, 0.0003908623128373758630, 0.0005862934692560637946, 0.0007817246256747517261 ),
 .UNSPECIFIED. ) ;
#45051 = DIRECTION ( 'NONE',  ( 1.000000000000000000, 0.000000000000000000, 0.000000000000000000 ) ) ;
#45052 = LINE ( 'NONE', #78398, #40682 ) ;
#45053 = B_SPLINE_CURVE_WITH_KNOTS ( 'NONE', 3,
 ( #25382, #31246, #71337, #58267, #85759, #24037, #10986, #38455, #51490, #64568 ),
 .UNSPECIFIED., .F., .F.,
 ( 4, 2, 2, 2, 4 ),
 ( 0.0007817246256747519429, 0.0009771112852218970073, 0.001172497944769042288, 0.001367884604316187353, 0.001563271263863332417 ),
 .UNSPECIFIED. ) ;
#45054 = DIRECTION ( 'NONE',  ( 0.000000000000000000, 0.000000000000000000, 1.000000000000000000 ) ) ;
#45055 = B_SPLINE_CURVE_WITH_KNOTS ( 'NONE', 3,
 ( #42428, #30234, #76650, #77531, #29796, #22584, #63566, #37418, #63119, #43307 ),
 .UNSPECIFIED., .F., .F.,
 ( 4, 2, 2, 2, 4 ),
 ( 0.000000000000000000, 0.0001954339857564081249, 0.0003908679715128162498, 0.0005863019572692244018, 0.0007817359430256324996 ),
 .UNSPECIFIED. ) ;
#45056 = AXIS2_PLACEMENT_3D ( 'NONE', #37218, #78209, #43100 ) ;
#45057 = EDGE_CURVE ( 'NONE', #17031, #27837, #86180, .T. ) ;
#45058 = VECTOR ( 'NONE', #51927, 1000.000000000000227 ) ;
#45059 = FACE_OUTER_BOUND ( 'NONE', #69910, .T. ) ;
#45060 = CARTESIAN_POINT ( 'NONE',  ( -11.47239420511146157, -3.322132147404559976, 32.92929555188717927 ) ) ;
#45061 = VERTEX_POINT ( 'NONE', #10953 ) ;
#45062 = VERTEX_POINT ( 'NONE', #64541 ) ;
#45063 = VERTEX_POINT ( 'NONE', #10055 ) ;
#45065 = ORIENTED_EDGE ( 'NONE', *, *, #20037, .T. ) ;
#45064 = CARTESIAN_POINT ( 'NONE',  ( 15.36156103859401867, -2.541949514083464479, 30.39797389878540557 ) ) ;
#45066 = EDGE_CURVE ( 'NONE', #4986, #85950, #83198, .T. ) ;
#45067 = LINE ( 'NONE', #13510, #86733 ) ;
#45068 = CARTESIAN_POINT ( 'NONE',  ( -10.83831083290076158, -9.086856451489515152, 34.49173150075333183 ) ) ;
#45069 = ORIENTED_EDGE ( 'NONE', *, *, #32069, .F. ) ;
#45070 = ORIENTED_EDGE ( 'NONE', *, *, #76162, .T. ) ;
#45071 = ADVANCED_FACE ( 'NONE', ( #31210 ), #3740, .F. ) ;
#45072 = ORIENTED_EDGE ( 'NONE', *, *, #55704, .T. ) ;
#45073 = CARTESIAN_POINT ( 'NONE',  ( 0.2115617174898693220, -8.347322224742351082, 34.93158281831414769 ) ) ;
#45074 = ORIENTED_EDGE ( 'NONE', *, *, #69093, .F. ) ;
#45075 = CARTESIAN_POINT ( 'NONE',  ( 16.02315468717859304, -9.804603061927743113, 34.18744698557895845 ) ) ;
#45076 = AXIS2_PLACEMENT_3D ( 'NONE', #49726, #70450, #29032 ) ;
#45077 = CARTESIAN_POINT ( 'NONE',  ( -8.096130577096198877, -2.564618984488975073, 30.55390908950641915 ) ) ;
#45078 = B_SPLINE_CURVE_WITH_KNOTS ( 'NONE', 3,
 ( #83769, #37324, #49077, #30571, #71113, #76559, #30138, #14867, #77004, #77874 ),
 .UNSPECIFIED., .F., .F.,
 ( 4, 2, 2, 2, 4 ),
 ( 0.000000000000000000, 0.0001954311564186861968, 0.0003908623128373723936, 0.0005862934692560585904, 0.0007817246256747447872 ),
 .UNSPECIFIED. ) ;
#45079 = CARTESIAN_POINT ( 'NONE',  ( -18.03205128205128105, -3.499999999999999556, 29.75000000000000355 ) ) ;
#45080 = FACE_BOUND ( 'NONE', #6190, .T. ) ;
#45081 = ORIENTED_EDGE ( 'NONE', *, *, #82770, .T. ) ;
#45082 = CIRCLE ( 'NONE', #13472, 2.750000000000000000 ) ;
#45083 = CARTESIAN_POINT ( 'NONE',  ( 3.230769230769231726, -7.500000000000001776, 35.04278698407183867 ) ) ;
#45084 = CARTESIAN_POINT ( 'NONE',  ( 13.16168842570853670, -10.77366814457252175, 33.85459836347579454 ) ) ;
#45085 = VECTOR ( 'NONE', #36886, 999.9999999999998863 ) ;
#45086 = CARTESIAN_POINT ( 'NONE',  ( 14.30769230769231015, -6.435427911321262684, 35.78748833219616898 ) ) ;
#45087 = CARTESIAN_POINT ( 'NONE',  ( 2.084765348785460048, -8.282780595021769443, 34.94152052738834868 ) ) ;
#45088 = CARTESIAN_POINT ( 'NONE',  ( -14.30769230769230660, -2.900454961884010974, 35.62045528018868623 ) ) ;
#45089 = ORIENTED_EDGE ( 'NONE', *, *, #50557, .F. ) ;
#45090 = EDGE_CURVE ( 'NONE', #27014, #63342, #54143, .T. ) ;
#45091 = CARTESIAN_POINT ( 'NONE',  ( -2.084680956079455250, -9.086983370893047862, 34.49168942202179267 ) ) ;
#45092 = ORIENTED_EDGE ( 'NONE', *, *, #40882, .F. ) ;
#45093 = EDGE_CURVE ( 'NONE', #67353, #50385, #65958, .T. ) ;
#45094 = VERTEX_POINT ( 'NONE', #22688 ) ;
#45096 = DIRECTION ( 'NONE',  ( -0.000000000000000000, -0.3420201433256694901, -0.9396926207859082059 ) ) ;
#45095 = CARTESIAN_POINT ( 'NONE',  ( 1.384615384615386802, -2.721908614388771852, 31.22303859784724978 ) ) ;
#45097 = CARTESIAN_POINT ( 'NONE',  ( 16.15384615384603251, -11.67786785259630911, 32.92929555188603530 ) ) ;
#45098 = CARTESIAN_POINT ( 'NONE',  ( 18.00000000000000000, -2.517432740324522911, 35.29906147534542527 ) ) ;
#45099 = CARTESIAN_POINT ( 'NONE',  ( 1.607626736228236375, -9.886259254753564818, 34.14407573483972413 ) ) ;
#45100 = LINE ( 'NONE', #23934, #56158 ) ;
#45101 = ORIENTED_EDGE ( 'NONE', *, *, #27115, .T. ) ;
#45102 = CARTESIAN_POINT ( 'NONE',  ( -5.076923076923075762, -6.343179335718451384, 34.87096338111211935 ) ) ;
#45103 = EDGE_CURVE ( 'NONE', #52344, #50406, #67095, .T. ) ;
#45104 = CARTESIAN_POINT ( 'NONE',  ( 3.007842271862380290, -9.172386477786396597, 34.72672124145550043 ) ) ;
#45105 = CARTESIAN_POINT ( 'NONE',  ( 2.373759641042385127, -12.62096338111211757, 30.90682066428152908 ) ) ;
#45106 = CARTESIAN_POINT ( 'NONE',  ( 14.43848274865926129, -2.494656445102012565, 31.33466734024120015 ) ) ;
#45107 = ORIENTED_EDGE ( 'NONE', *, *, #85566, .T. ) ;
#45108 = B_SPLINE_CURVE_WITH_KNOTS ( 'NONE', 3,
 ( #4392, #31876, #59333, #86841, #75082, #21001, #53912, #48472, #6175, #62425 ),
 .UNSPECIFIED., .F., .F.,
 ( 4, 2, 2, 2, 4 ),
 ( 0.0007817246256747481482, 0.0009771112852218911526, 0.001172497944769034049, 0.001367884604316176944, 0.001563271263863319840 ),
 .UNSPECIFIED. ) ;
#45109 = EDGE_LOOP ( 'NONE', ( #77214, #49632 ) ) ;
#45110 = FACE_BOUND ( 'NONE', #20028, .T. ) ;
#45111 = ORIENTED_EDGE ( 'NONE', *, *, #21764, .F. ) ;
#45112 = DIRECTION ( 'NONE',  ( -0.000000000000000000, -0.5000000000000009992, -0.8660254037844380415 ) ) ;
#45113 = CARTESIAN_POINT ( 'NONE',  ( -5.749999999999936051, -7.434744860731433924, 35.00000000000000711 ) ) ;
#45114 = VERTEX_POINT ( 'NONE', #59575 ) ;
#45115 = DIRECTION ( 'NONE',  ( 0.000000000000000000, 1.000000000000000000, 0.000000000000000000 ) ) ;
#45116 = CYLINDRICAL_SURFACE ( 'NONE', #31327, 0.2500000000000012212 ) ;
#45117 = CARTESIAN_POINT ( 'NONE',  ( -8.069638789877792817, -11.89387501736622710, 32.13663884655806413 ) ) ;
#45118 = DIRECTION ( 'NONE',  ( -0.000000000000000000, 1.000000000000000000, -0.000000000000000000 ) ) ;
#45119 = DIRECTION ( 'NONE',  ( 1.000000000000000000, 0.000000000000000000, 0.000000000000000000 ) ) ;
#45121 = ORIENTED_EDGE ( 'NONE', *, *, #68936, .T. ) ;
#45120 = VECTOR ( 'NONE', #85652, 1000.000000000000000 ) ;
#45123 = ORIENTED_EDGE ( 'NONE', *, *, #11046, .T. ) ;
#45122 = CARTESIAN_POINT ( 'NONE',  ( 17.07692307692307665, -10.51840700105979565, 33.73612834413961536 ) ) ;
#45124 = CARTESIAN_POINT ( 'NONE',  ( 15.23076923076911093, -8.613356846316285953, 34.62446782046622218 ) ) ;
#45125 = CARTESIAN_POINT ( 'NONE',  ( -12.68502338610279523, -3.019605429927184836, 32.48692288466676814 ) ) ;
#45126 = DIRECTION ( 'NONE',  ( -0.000000000000000000, 0.3420201433256694901, -0.9396926207859082059 ) ) ;
#45127 = EDGE_CURVE ( 'NONE', #34142, #683, #12282, .T. ) ;
#45128 = CARTESIAN_POINT ( 'NONE',  ( 15.48082354240754555, -12.41262288849542017, 30.68299917996395010 ) ) ;
#45129 = CARTESIAN_POINT ( 'NONE',  ( -7.976845312821404299, -8.999036380462717588, 34.52022231692819076 ) ) ;
#45130 = B_SPLINE_CURVE_WITH_KNOTS ( 'NONE', 3,
 ( #67831, #81797, #34040, #13766, #14214, #41250, #81355, #47100, #69162, #12442 ),
 .UNSPECIFIED., .F., .F.,
 ( 4, 2, 2, 2, 4 ),
 ( 0.0007817246256747471724, 0.0009771112852218905021, 0.001172497944769033615, 0.001367884604316176944, 0.001563271263863320274 ),
 .UNSPECIFIED. ) ;
#45131 = CARTESIAN_POINT ( 'NONE',  ( 5.076923076922954969, -12.46129190930018460, 30.37095296980731973 ) ) ;
#45132 = CARTESIAN_POINT ( 'NONE',  ( -1.077988221561493543, -4.724691934501247914, 14.32999329374151465 ) ) ;
#45133 = ORIENTED_EDGE ( 'NONE', *, *, #81970, .F. ) ;
#45134 = B_SPLINE_CURVE_WITH_KNOTS ( 'NONE', 3,
 ( #56229, #8048, #49474, #42723, #35517, #41838, #14809, #75603, #70183, #42285 ),
 .UNSPECIFIED., .F., .F.,
 ( 4, 2, 2, 2, 4 ),
 ( 0.000000000000000000, 0.0001954339857564092362, 0.0003908679715128184724, 0.0005863019572692276544, 0.0007817359430256369448 ),
 .UNSPECIFIED. ) ;
#45135 = CARTESIAN_POINT ( 'NONE',  ( -3.296039676730006196, -3.300289026998414865, 32.46337939537583139 ) ) ;
#45136 = CYLINDRICAL_SURFACE ( 'NONE', #4517, 4.000000000000000000 ) ;
#45137 = CARTESIAN_POINT ( 'NONE',  ( 6.130045162834781181, -2.504778602574660340, 29.97347330155780298 ) ) ;
#45138 = ORIENTED_EDGE ( 'NONE', *, *, #38642, .T. ) ;
#45139 = VERTEX_POINT ( 'NONE', #39326 ) ;
#45140 = CARTESIAN_POINT ( 'NONE',  ( -19.00000000000000000, -3.499999999999999556, 29.75000000000000355 ) ) ;
#45141 = CARTESIAN_POINT ( 'NONE',  ( -7.596099426240391139, -5.642605341092958859, 34.66089969410670335 ) ) ;
#45142 = CARTESIAN_POINT ( 'NONE',  ( -0.2115384615384616196, -2.499999999999998668, 29.75000000000000355 ) ) ;
#45143 = DIRECTION ( 'NONE',  ( 0.000000000000000000, 0.3420201433256641055, -0.9396926207859100932 ) ) ;
#45144 = CARTESIAN_POINT ( 'NONE',  ( 10.61538461538461675, -4.098570777380720287, 33.41473453929634729 ) ) ;
#45145 = CARTESIAN_POINT ( 'NONE',  ( -8.899377978668988831, -11.93770438780619259, 32.05411857736982029 ) ) ;
#45146 = CARTESIAN_POINT ( 'NONE',  ( -15.16470189741915675, -8.164416787775445883, 34.95778746994558617 ) ) ;
#45147 = ORIENTED_EDGE ( 'NONE', *, *, #80851, .F. ) ;
#45148 = CYLINDRICAL_SURFACE ( 'NONE', #72198, 0.2499999999999979738 ) ;
#45149 = CARTESIAN_POINT ( 'NONE',  ( -0.3307466537136752871, -8.147973898785416225, 34.70805048591653730 ) ) ;
#45150 = AXIS2_PLACEMENT_3D ( 'NONE', #66005, #11976, #32673 ) ;
#45151 = CARTESIAN_POINT ( 'NONE',  ( -6.249999999999997335, -7.500000000000001776, 34.75000000000000000 ) ) ;
#45152 = CARTESIAN_POINT ( 'NONE',  ( 9.692307692307570832, -2.657715359629662544, 31.77849191805970364 ) ) ;
#45153 = EDGE_LOOP ( 'NONE', ( #40667, #37336 ) ) ;
#45154 = CARTESIAN_POINT ( 'NONE',  ( 13.45068373561782593, -6.386643153685127139, 34.62446782046654192 ) ) ;
#45155 = VECTOR ( 'NONE', #85281, 1000.000000000000000 ) ;
#45156 = VECTOR ( 'NONE', #8887, 1000.000000000000000 ) ;
#45157 = ORIENTED_EDGE ( 'NONE', *, *, #10334, .T. ) ;
#45158 = CYLINDRICAL_SURFACE ( 'NONE', #52903, 0.2500000000000004996 ) ;
#45159 = CARTESIAN_POINT ( 'NONE',  ( -1.515306851282941958, -8.999036380462717588, 34.52022231692819076 ) ) ;
#45160 = CARTESIAN_POINT ( 'NONE',  ( 6.223012844093396723, -11.98016756924215009, 32.48728574198911190 ) ) ;
#45161 = ORIENTED_EDGE ( 'NONE', *, *, #85298, .T. ) ;
#45162 = CARTESIAN_POINT ( 'NONE',  ( 3.230769230769108269, -12.70778746994576025, 30.41441678777401236 ) ) ;
#45163 = DIRECTION ( 'NONE',  ( -0.000000000000000000, -0.3420201433256694346, -0.9396926207859080948 ) ) ;
#45164 = CARTESIAN_POINT ( 'NONE',  ( 10.61538461538461675, -3.513871655860378418, 32.76840700105978499 ) ) ;
#45165 = DIRECTION ( 'NONE',  ( -0.000000000000000000, -0.6427876096865404731, -0.7660444431189771253 ) ) ;
#45166 = LINE ( 'NONE', #65443, #10959 ) ;
#45167 = B_SPLINE_CURVE_WITH_KNOTS ( 'NONE', 3,
 ( #72285, #10598, #73188, #18695, #32208, #24542, #78599, #38065, #44354, #46162 ),
 .UNSPECIFIED., .F., .F.,
 ( 4, 2, 2, 2, 4 ),
 ( 0.0007817246256747452209, 0.0009771112852218879000, 0.001172497944769030579, 0.001367884604316173258, 0.001563271263863315937 ),
 .UNSPECIFIED. ) ;
#45168 = VERTEX_POINT ( 'NONE', #45618 ) ;
#45169 = CARTESIAN_POINT ( 'NONE',  ( -0.6850234052624101233, -8.496056993536548418, 34.65000542017679663 ) ) ;
#45170 = EDGE_LOOP ( 'NONE', ( #53720, #24378, #48216, #77919 ) ) ;
#45171 = DIRECTION ( 'NONE',  ( 1.000000000000000000, -0.000000000000000000, -0.000000000000000000 ) ) ;
#45172 = CYLINDRICAL_SURFACE ( 'NONE', #17523, 0.2500000000000008882 ) ;
#45173 = CARTESIAN_POINT ( 'NONE',  ( -13.60810032833933114, -2.847400154188067578, 31.58180166144859058 ) ) ;
#45174 = CARTESIAN_POINT ( 'NONE',  ( 9.823098133274648092, -2.494656445102012565, 31.33466734024120015 ) ) ;
#45175 = CARTESIAN_POINT ( 'NONE',  ( 6.988332494352946789, -10.21337939537593620, 33.94971097300152252 ) ) ;
#45176 = CARTESIAN_POINT ( 'NONE',  ( 19.00000000000000000, 12.75000000000000711, 30.81664701255128236 ) ) ;
#45177 = VERTEX_POINT ( 'NONE', #87079 ) ;
#45178 = AXIS2_PLACEMENT_3D ( 'NONE', #38032, #65496, #3794 ) ;
#45179 = ORIENTED_EDGE ( 'NONE', *, *, #48045, .F. ) ;
#45180 = EDGE_LOOP ( 'NONE', ( #4910, #17180, #22658, #52059, #50037, #72396 ) ) ;
#45181 = ORIENTED_EDGE ( 'NONE', *, *, #66937, .T. ) ;
#45182 = EDGE_LOOP ( 'NONE', ( #72769, #52693, #57228, #58902 ) ) ;
#45183 = LINE ( 'NONE', #2422, #37261 ) ;
#45184 = FACE_OUTER_BOUND ( 'NONE', #18940, .T. ) ;
#45185 = CARTESIAN_POINT ( 'NONE',  ( 15.23076923076910916, -6.835583212225970762, 34.95778746994575670 ) ) ;
#45186 = CARTESIAN_POINT ( 'NONE',  ( -5.999999999999998224, -4.786620604624113540, 33.94971097300155094 ) ) ;
#45187 = CARTESIAN_POINT ( 'NONE',  ( -13.38461538461550759, -3.643525952248795718, 33.31231777344771672 ) ) ;
#45189 = ADVANCED_FACE ( 'NONE', ( #25351 ), #18604, .F. ) ;
#45188 = CARTESIAN_POINT ( 'NONE',  ( 1.576923076923075762, -3.499999999999999556, 29.75000000000000355 ) ) ;
#45190 = CARTESIAN_POINT ( 'NONE',  ( -0.5276218724943428917, -11.69971097300155272, 32.46337939537587403 ) ) ;
#45191 = CARTESIAN_POINT ( 'NONE',  ( -17.77698864838715309, -6.503523203565942268, 34.64991518177335195 ) ) ;
#45192 = CARTESIAN_POINT ( 'NONE',  ( -4.153846153846273204, -10.21337939537710326, 33.94971097300076224 ) ) ;
#45193 = EDGE_LOOP ( 'NONE', ( #81251, #71374, #18755, #80935, #67503, #41972 ) ) ;
#45194 = PRODUCT_DEFINITION ( 'UNKNOWN', '', #56247, #2324 ) ;
#45195 = EDGE_LOOP ( 'NONE', ( #24064, #76323 ) ) ;
#45196 = VERTEX_POINT ( 'NONE', #26240 ) ;
#45198 = ORIENTED_EDGE ( 'NONE', *, *, #54616, .F. ) ;
#45197 = CARTESIAN_POINT ( 'NONE',  ( 0.3954560821783248414, -11.91647553114624181, 32.58852847137148245 ) ) ;
#45200 = CYLINDRICAL_SURFACE ( 'NONE', #23260, 0.2499999999999995559 ) ;
#45199 = CARTESIAN_POINT ( 'NONE',  ( -16.02332045208259359, -6.852161475712351013, 34.70806712695775786 ) ) ;
#45201 = CARTESIAN_POINT ( 'NONE',  ( -13.38461538461550759, -3.643525952248795718, 33.31231777344771672 ) ) ;
#45202 = LINE ( 'NONE', #52401, #48015 ) ;
#45203 = FACE_BOUND ( 'NONE', #49938, .T. ) ;
#45204 = VERTEX_POINT ( 'NONE', #59128 ) ;
#45205 = VECTOR ( 'NONE', #66249, 1000.000000000000227 ) ;
#45206 = ADVANCED_FACE ( 'NONE', ( #52813 ), #4639, .F. ) ;
#45207 = EDGE_LOOP ( 'NONE', ( #88964, #16387 ) ) ;
#45208 = DIRECTION ( 'NONE',  ( -0.000000000000000000, -0.7660444431189791237, -0.6427876096865379196 ) ) ;
#45209 = CIRCLE ( 'NONE', #58135, 0.2500000000000002220 ) ;
#45210 = ORIENTED_EDGE ( 'NONE', *, *, #65297, .T. ) ;
#45211 = FACE_BOUND ( 'NONE', #75310, .T. ) ;
#45212 = CARTESIAN_POINT ( 'NONE',  ( -6.065270445960775803, -9.442884908240170461, 34.35708131394840592 ) ) ;
#45213 = VECTOR ( 'NONE', #26987, 1000.000000000000227 ) ;
#45214 = CARTESIAN_POINT ( 'NONE',  ( -4.023320452082587373, -11.93748526763465279, 32.05452791011430946 ) ) ;
#45215 = VERTEX_POINT ( 'NONE', #53259 ) ;
#45216 = FACE_OUTER_BOUND ( 'NONE', #74365, .T. ) ;
#45217 = FACE_OUTER_BOUND ( 'NONE', #37188, .T. ) ;
#45218 = CARTESIAN_POINT ( 'NONE',  ( 2.241609928332172874, -11.35647404775217595, 33.31231777344666511 ) ) ;
#45219 = ORIENTED_EDGE ( 'NONE', *, *, #68647, .F. ) ;
#45220 = CYLINDRICAL_SURFACE ( 'NONE', #1102, 0.2499999999999973355 ) ;
#45221 = CARTESIAN_POINT ( 'NONE',  ( 6.988332062589762472, -5.941354392334606160, 34.76329471203374055 ) ) ;
#45222 = VERTEX_POINT ( 'NONE', #80758 ) ;
#45223 = B_SPLINE_CURVE_WITH_KNOTS ( 'NONE', 3,
 ( #82214, #75016, #75448, #13744, #67364, #25928, #53394, #60150, #26820, #81772 ),
 .UNSPECIFIED., .F., .F.,
 ( 4, 2, 2, 2, 4 ),
 ( 0.000000000000000000, 0.0001954311564186863865, 0.0003908623128373727731, 0.0005862934692560591325, 0.0007817246256747455461 ),
 .UNSPECIFIED. ) ;
#45224 = CARTESIAN_POINT ( 'NONE',  ( 2.307692307692186251, -12.51329471203414379, 31.30864560766407578 ) ) ;
#45225 = CARTESIAN_POINT ( 'NONE',  ( -19.50000000000000000, -3.499999999999999556, 29.75000000000000355 ) ) ;
#45226 = ORIENTED_EDGE ( 'NONE', *, *, #27274, .T. ) ;
#45227 = CARTESIAN_POINT ( 'NONE',  ( 18.25005431163831204, -6.567000820036036579, 34.66262288849541306 ) ) ;
#45228 = CARTESIAN_POINT ( 'NONE',  ( -10.61538461538461320, -4.786620604624113540, 33.94971097300155094 ) ) ;
#45229 = CARTESIAN_POINT ( 'NONE',  ( -2.557669038634660552, -2.564618984488975961, 30.55390908950641915 ) ) ;
#45230 = LINE ( 'NONE', #65943, #70245 ) ;
#45231 = FACE_OUTER_BOUND ( 'NONE', #74526, .T. ) ;
#45232 = EDGE_CURVE ( 'NONE', #50514, #79802, #5082, .T. ) ;
#45233 = CARTESIAN_POINT ( 'NONE',  ( -0.2115384615384473255, -2.249999999999998668, 29.81603969181031033 ) ) ;
#45235 = CARTESIAN_POINT ( 'NONE',  ( -15.45425417449318317, -12.44517049084099725, 30.48991314939691932 ) ) ;
#45234 = CARTESIAN_POINT ( 'NONE',  ( 5.010839665967194989, -12.37446782046654192, 30.86335684631486487 ) ) ;
#45236 = CARTESIAN_POINT ( 'NONE',  ( -3.230769230769229949, -11.33034616979429110, 35.88435417666054406 ) ) ;
#45238 = CYLINDRICAL_SURFACE ( 'NONE', #20479, 0.2500000000000008882 ) ;
#45237 = CARTESIAN_POINT ( 'NONE',  ( 3.295963212552587507, -2.506253911140448043, 29.99999999999988631 ) ) ;
#45239 = CARTESIAN_POINT ( 'NONE',  ( -1.944543648262992530, -9.444543648263016067, 14.93750000000000000 ) ) ;
#45240 = ORIENTED_EDGE ( 'NONE', *, *, #48592, .T. ) ;
#45241 = EDGE_CURVE ( 'NONE', #21562, #22635, #18155, .T. ) ;
#45242 = CARTESIAN_POINT ( 'NONE',  ( -12.71156169883143150, -8.432397168068783699, 34.66272746175022945 ) ) ;
#45243 = ORIENTED_EDGE ( 'NONE', *, *, #65789, .T. ) ;
#45244 = ADVANCED_FACE ( 'NONE', ( #6422 ), #80309, .F. ) ;
#45245 = VERTEX_POINT ( 'NONE', #33001 ) ;
#45246 = CARTESIAN_POINT ( 'NONE',  ( -16.85391023282967637, -4.026326845037968560, 33.68677907613345468 ) ) ;
#45247 = ORIENTED_EDGE ( 'NONE', *, *, #27210, .T. ) ;
#45248 = CARTESIAN_POINT ( 'NONE',  ( -5.934744860487159102, -10.33852847137154107, 34.16647553114620450 ) ) ;
#45249 = CARTESIAN_POINT ( 'NONE',  ( 1.799775606325937360E-14, -10.25000000000000000, 14.78125000000000178 ) ) ;
#45250 = CARTESIAN_POINT ( 'NONE',  ( -13.38461538461550759, -5.941354392335915335, 34.76329471203413846 ) ) ;
#45251 = LINE ( 'NONE', #73641, #46767 ) ;
#45252 = CARTESIAN_POINT ( 'NONE',  ( 1.634615384615386580, -7.500000000000001776, 35.04278698407183867 ) ) ;
#45253 = CARTESIAN_POINT ( 'NONE',  ( -6.223484924564333554, -2.612411019501189813, 31.66733052389439962 ) ) ;
#45254 = VECTOR ( 'NONE', #73839, 1000.000000000000227 ) ;
#45255 = CARTESIAN_POINT ( 'NONE',  ( -10.39237177129121825, -3.395485233115139057, 33.02377354290275946 ) ) ;
#45256 = CARTESIAN_POINT ( 'NONE',  ( 0.5276057948885363169, -5.471508081941601098, 34.59228464037088457 ) ) ;
#45257 = CARTESIAN_POINT ( 'NONE',  ( 5.777073782483853392, -4.186968288167446595, 33.49512374952580274 ) ) ;
#45258 = CARTESIAN_POINT ( 'NONE',  ( -2.651650429449535551, -10.15165042944956753, 23.68750000000000000 ) ) ;
#45259 = CARTESIAN_POINT ( 'NONE',  ( 1.607626736228235265, -3.105924265160262099, 32.13625925475356127 ) ) ;
#45260 = CARTESIAN_POINT ( 'NONE',  ( -14.98082371242109012, -2.587454068350147018, 30.68340429815432202 ) ) ;
#45261 = LINE ( 'NONE', #67765, #37793 ) ;
#45262 = ORIENTED_EDGE ( 'NONE', *, *, #23874, .T. ) ;
#45263 = ORIENTED_EDGE ( 'NONE', *, *, #42156, .T. ) ;
#45264 = B_SPLINE_CURVE_WITH_KNOTS ( 'NONE', 3,
 ( #65171, #57090, #58405, #79142, #77804, #72373 ),
 .UNSPECIFIED., .F., .F.,
 ( 4, 2, 4 ),
 ( 0.0003909569690057790748, 0.0005862646681846021271, 0.0007815723673634251793 ),
 .UNSPECIFIED. ) ;
#45265 = CARTESIAN_POINT ( 'NONE',  ( -11.53846153846165912, -6.026961402154118019, 34.52809138561165270 ) ) ;
#45266 = DIRECTION ( 'NONE',  ( -1.000000000000000000, 0.000000000000000000, -0.000000000000000000 ) ) ;
#45267 = CARTESIAN_POINT ( 'NONE',  ( 16.15384615384603251, -12.51329471203414379, 31.30864560766407578 ) ) ;
#45268 = CARTESIAN_POINT ( 'NONE',  ( 6.250000000000000888, -2.249999999999998668, 29.75000000000000355 ) ) ;
#45269 = CARTESIAN_POINT ( 'NONE',  ( -15.23076923076892264, -2.506253911140614576, 30.00000000000323297 ) ) ;
#45270 = CYLINDRICAL_SURFACE ( 'NONE', #71635, 0.2499999999999986955 ) ;
#45271 = EDGE_CURVE ( 'NONE', #73086, #40861, #26245, .T. ) ;
#45272 = CIRCLE ( 'NONE', #69709, 1.999999999999998224 ) ;
#45273 = ORIENTED_EDGE ( 'NONE', *, *, #16168, .T. ) ;
#45274 = CARTESIAN_POINT ( 'NONE',  ( 17.07692307692307665, -13.87047571288749737, 32.06866353760679544 ) ) ;
#45275 = EDGE_LOOP ( 'NONE', ( #15825, #3519, #32049, #50705 ) ) ;
#45276 = ORIENTED_EDGE ( 'NONE', *, *, #74804, .F. ) ;
#45277 = DIRECTION ( 'NONE',  ( -1.000000000000000000, 0.000000000000000000, 0.000000000000000000 ) ) ;
#45278 = VECTOR ( 'NONE', #88801, 1000.000000000000000 ) ;
#45279 = DIRECTION ( 'NONE',  ( 0.000000000000000000, 0.000000000000000000, -1.000000000000000000 ) ) ;
#45280 = CARTESIAN_POINT ( 'NONE',  ( -14.17690186672535901, -2.845873456487965747, 32.17976146951972538 ) ) ;
#45281 = CARTESIAN_POINT ( 'NONE',  ( 11.60371667797437567, -2.379036618887895305, 30.90682066428158592 ) ) ;
#45282 = CARTESIAN_POINT ( 'NONE',  ( 13.31853300525525086, -5.471508081941602875, 34.59228464037088457 ) ) ;
#45283 = EDGE_CURVE ( 'NONE', #38452, #63694, #38636, .T. ) ;
#45284 = ORIENTED_EDGE ( 'NONE', *, *, #79116, .F. ) ;
#45285 = ORIENTED_EDGE ( 'NONE', *, *, #42871, .T. ) ;
#45286 = ORIENTED_EDGE ( 'NONE', *, *, #16815, .T. ) ;
#45287 = CARTESIAN_POINT ( 'NONE',  ( 1.384615384615265343, -11.48612834414049644, 32.76840700105863391 ) ) ;
#45288 = DIRECTION ( 'NONE',  ( -1.000000000000000000, -0.000000000000000000, 0.000000000000000000 ) ) ;
#45289 = B_SPLINE_CURVE_WITH_KNOTS ( 'NONE', 3,
 ( #12431, #61493, #53859, #75459, #5671, #68261, #81346, #19628, #54290, #13317 ),
 .UNSPECIFIED., .F., .F.,
 ( 4, 2, 2, 2, 4 ),
 ( 0.000000000000000000, 0.0001954339857564072033, 0.0003908679715128144066, 0.0005863019572692215828, 0.0007817359430256288133 ),
 .UNSPECIFIED. ) ;
#45290 = B_SPLINE_CURVE_WITH_KNOTS ( 'NONE', 3,
 ( #55319, #42704, #27412, #76034, #76930, #69286, #75166, #13891, #15233, #1710 ),
 .UNSPECIFIED., .F., .F.,
 ( 4, 2, 2, 2, 4 ),
 ( 0.000000000000000000, 0.0001954339857564125972, 0.0003908679715128181471, 0.0005863019572692237513, 0.0007817359430256293554 ),
 .UNSPECIFIED. ) ;
#45291 = CARTESIAN_POINT ( 'NONE',  ( -15.23076923076922995, -12.78798330534102767, 29.49999999999997868 ) ) ;
#45293 = ADVANCED_FACE ( 'NONE', ( #60466, #40211, #46065, #87983, #81195, #38875, #60020, #74427, #11851, #87524, #86631, #25799, #12729, #67674, #47388, #5981, #33448, #74882, #7749, #33879, #27571, #82963, #54585, #68552, #55043, #14950, #34321, #28013, #21695, #55481, #35210, #83861, #22146, #41530, #21245, #61336, #55921, #61785, #49167, #88853, #47837, #68994, #62235, #48720, #49616, #82532, #14052, #63117, #7304, #83412, #99, #42426, #20810, #76648, #82082, #62670, #6848, #1427, #69884, #42866, #76191, #20377, #27127, #69445, #8191, #48276, #988, #28460, #14494, #75747, #35667, #34765, #28919, #56375, #546, #41983, #77090, #15395, #70332, #75320, #13612, #41089, #57699, #15839, #43736, #71203, #16272, #36549, #36972, #43305, #50915, #9505, #63999, #2298, #50048, #23025, #78405, #57258, #36112, #85180, #29794, #84750, #44161, #64438, #50487, #16706, #9952, #2737, #77529, #37416, #30232, #64885, #77970, #23460, #71645, #8640, #63564, #1869, #29353, #56807, #84307, #22582, #70778, #9082, #30683, #17629, #38784, #72111, #23041, #58147, #64903, #10423, #29811, #86085, #17168, #84764, #38334, #43755, #66241, #57273, #2754, #37433, #9968, #30249, #51365, #31574, #85638, #50506, #72557, #3210, #23475, #71219, #65791, #24360, #77985, #85199, #44624, #9523, #23916, #78869, #50933, #16288, #65357, #36988, #64454, #57717, #78423, #31120, #16722, #37891, #44178, #71665, #3646, #58591, #51823, #11305, #79324, #18070, #45080, #10867, #4091, #59040, #86540, #24813, #52284, #79773, #45531, #73006, #87888, #73905, #75237, #26598, #81998, #53624, #26155, #46422, #53169, #13524, #12201, #5888, #33361, #46864, #86995, #5446, #39686, #74347, #4548, #60823, #81111, #59489, #13085, #18514, #41004, #32024, #66697, #25266, #52726, #12645, #67146, #27043, #40130, #80217, #47305, #19840, #45972, #73463, #47754, #60377, #80672, #11756, #19397, #39236, #5000, #67590, #74796, #87431, #88327, #54056, #81554, #32914, #40570, #25714, #68036, #32462, #6339, #61252, #33796, #88767, #20290, #59932, #18957, #54506, #28824, #48630, #29269, #1336, #35122, #36024, #84218, #62585, #34236, #896, #56282, #76107, #56722, #83771, #28362, #63476, #22495, #42341, #7219, #49957, #49078, #69795, #15749, #76560, #83324, #70240, #1778, #6762, #35576, #68465, #63020, #55835, #61699, #77005, #82445, #77438, #18, #41443, #27486, #54956, #21606, #21163, #20723, #14868, #68908, #75663, #48190, #8104, #14410, #22058, #34688, #49530, #62153, #15304, #13966, #42781, #460, #69363, #8548, #27927, #55395, #82882, #7663, #41894, #85528, #43211, #10310, #30572, #8992, #85089, #37777, #36888, #72446, #44518, #50827, #23369, #16181, #64790, #44966, #24250, #43646, #3541, #2211, #72004, #77875, #44075, #31011, #52171, #23804, #63912, #36458, #78763, #51715, #64350, #17063, #65243, #51256, #78312, #58476, #2647, #10755, #85972, #16612, #71556, #71114, #3096, #38223, #9861, #29706, #37325, #79217, #58043, #3981, #17516, #65682, #31467, #9424, #58933, #86439, #24710, #79660, #70686, #57166, #84654, #22934, #50395, #30139, #57606, #87779, #25603, #19294, #46763, #66596, #6230, #5779, #11653, #53058, #32807, #87327, #80103, #33695, #18849, #61150, #18404, #59826, #54398, #4898, #80566, #12104, #46315, #40466, #60267, #45863, #33255, #45415, #31923, #88663, #73803, #32362, #26941, #67040, #38669, #72893, #53507, #88222, #39129, #81004, #74238, #26052, #39581, #5335, #12537, #40022, #17962, #67484, #74688, #60715, #26495, #11199, #66132, #52620, #53959, #81450, #19735, #67925, #47196, #12980, #4436, #59384, #86888, #25153, #73347, #63369, #76898, #62475, #27818, #21049, #76002, #70131, #13857, #62046, #21951, #55286, #42235, #82332, #62914, #20615, #69688, #40898, #6658, #35914, #48520, #68806, #1676, #41789, #13417, #47650, #28255, #1228, #75556, #55726, #83215, #789, #34579, #76456, #7996, #7104, #48080, #28710, #82776, #29165, #41338, #353, #81893, #14303, #69251, #7554, #89102, #35015, #21497, #48977, #20184, #35463, #14755, #56177, #83669, #49424, #15200, #8441, #34130, #75132, #42671, #68360, #61598, #27382, #54848, #29598, #16077, #84108, #59612, #45656, #59166, #38464, #9329, #52402, #50283, #87113, #86673, #64242, #25389, #65917, #79892, #73594, #66821, #2113, #51956, #18194, #36788, #18644, #73133, #24487, #52851, #11888, #31709, #84549, #39363, #4227, #24939, #5120, #11433, #43540, #46106, #38916, #77772, #2546, #72684, #30036, #66375, #4680, #32154, #57496, #80347, #71018, #56621, #22389, #84985, #79453, #57056, #17752, #49852, #77333, #22826, #45203, #15639, #10992, #43107, #70580, #8884, #36352, #63815, #6454, #60505, #75783, #13209, #33913, #69033, #40689, #47422, #34353, #33482, #67710, #74915, #32585, #14089, #40245, #61373, #88886, #81230, #20842, #20407, #26276, #6015, #68152, #12760, #5564, #48310, #60942, #41561, #33038, #60054, #88016, #25839, #53294, #27159, #74463, #55073, #54619, #46549, #82569, #26717, #61824, #53744, #88446, #67269, #19515, #68587, #74028, #87560, #82114, #134, #46978, #80797, #27601, #47873, #75354, #54176, #81672, #19080, #12323, #39801, #13643, #19954, #41123, #6885, #76225, #55513, #579, #8674, #14532, #1466, #84780, #28494, #76682, #36581, #69917, #56840, #7778, #77563, #35242, #84337, #82997, #36148, #42016, #8226, #22611, #16306, #49646, #28046, #35701, #42901, #15874, #1019, #70366, #63599, #77121, #49205, #1902, #55955, #64032, #29391, #14983, #42455, #69475, #28954, #9117, #63151, #62264, #50079, #56408 ), #21281, .T. ) ;
#45292 = CARTESIAN_POINT ( 'NONE',  ( -15.00798968950081758, -3.236590943229499029, 32.36255958852954251 ) ) ;
#45294 = FACE_OUTER_BOUND ( 'NONE', #87186, .T. ) ;
#45295 = CYLINDRICAL_SURFACE ( 'NONE', #50910, 0.2499999999999995559 ) ;
#45296 = ORIENTED_EDGE ( 'NONE', *, *, #29626, .F. ) ;
#45297 = ADVANCED_FACE ( 'NONE', ( #43773 ), #48755, .F. ) ;
#45298 = VERTEX_POINT ( 'NONE', #43336 ) ;
#45299 = CARTESIAN_POINT ( 'NONE',  ( 2.651650429449569302, -10.15165042944953733, 22.12500000000000000 ) ) ;
#45300 = VECTOR ( 'NONE', #74734, 1000.000000000000227 ) ;
#45301 = ORIENTED_EDGE ( 'NONE', *, *, #1988, .F. ) ;
#45303 = ORIENTED_EDGE ( 'NONE', *, *, #40439, .F. ) ;
#45302 = CARTESIAN_POINT ( 'NONE',  ( -13.45069776397551564, -5.471508081941602875, 34.59228464037088457 ) ) ;
#45304 = DIRECTION ( 'NONE',  ( 0.000000000000000000, 0.6427876096865368094, 0.7660444431189802339 ) ) ;
#45305 = CARTESIAN_POINT ( 'NONE',  ( 12.68431813051652846, -8.540255544307065350, 34.89611431652622286 ) ) ;
#45306 = CARTESIAN_POINT ( 'NONE',  ( -2.651650429449565305, -4.848349570550461785, 14.00000000000000178 ) ) ;
#45307 = ORIENTED_EDGE ( 'NONE', *, *, #16938, .F. ) ;
#45308 = EDGE_CURVE ( 'NONE', #60674, #21879, #2331, .T. ) ;
#45309 = CARTESIAN_POINT ( 'NONE',  ( -14.53061926659915315, -12.38737895849757820, 31.66785238281580206 ) ) ;
#45310 = EDGE_LOOP ( 'NONE', ( #16742, #10449 ) ) ;
#45311 = CARTESIAN_POINT ( 'NONE',  ( -13.63463860883684120, -11.56360843649121684, 33.07473185843129926 ) ) ;
#45312 = CARTESIAN_POINT ( 'NONE',  ( 14.37375964104238513, -12.34228464037088813, 31.77849191805839268 ) ) ;
#45313 = FACE_BOUND ( 'NONE', #78950, .T. ) ;
#45315 = CARTESIAN_POINT ( 'NONE',  ( -15.16557524898587594, -2.506253911140448487, 29.99999999999988631 ) ) ;
#45314 = DIRECTION ( 'NONE',  ( -0.000000000000000000, 0.5000000000000011102, -0.8660254037844380415 ) ) ;
#45316 = EDGE_CURVE ( 'NONE', #14607, #28677, #7341, .T. ) ;
#45317 = CARTESIAN_POINT ( 'NONE',  ( -1.450697763975518306, -3.322132147404559976, 32.92929555188719348 ) ) ;
#45318 = CYLINDRICAL_SURFACE ( 'NONE', #47737, 0.2500000000000002220 ) ;
#45319 = ORIENTED_EDGE ( 'NONE', *, *, #32259, .F. ) ;
#45320 = CARTESIAN_POINT ( 'NONE',  ( -11.53846153846153655, -8.164416787775445883, 34.95778746994557906 ) ) ;
#45321 = ADVANCED_FACE ( 'NONE', ( #34796 ), #23062, .F. ) ;
#45322 = CARTESIAN_POINT ( 'NONE',  ( 2.139942661768877041, -5.397466907670289693, 13.88036352175840626 ) ) ;
#45323 = VERTEX_POINT ( 'NONE', #10882 ) ;
#45324 = B_SPLINE_CURVE_WITH_KNOTS ( 'NONE', 3,
 ( #72322, #58354, #79087, #24132, #39007, #18732, #72765, #32240, #39453, #46196 ),
 .UNSPECIFIED., .F., .F.,
 ( 4, 2, 2, 2, 4 ),
 ( 0.0007817246256747450040, 0.0009771112852218881168, 0.001172497944769031230, 0.001367884604316174342, 0.001563271263863317455 ),
 .UNSPECIFIED. ) ;
#45325 = CARTESIAN_POINT ( 'NONE',  ( 6.700150705560774966, -5.667676309546437530, 34.40238873228292249 ) ) ;
#45326 = CARTESIAN_POINT ( 'NONE',  ( -11.53846153846153655, -10.05456864172156806, 36.03766855953608683 ) ) ;
#45327 = FACE_OUTER_BOUND ( 'NONE', #18949, .T. ) ;
#45328 = CARTESIAN_POINT ( 'NONE',  ( 13.38461538461526423, -4.320704448113951379, 33.92786785259630022 ) ) ;
#45329 = DIRECTION ( 'NONE',  ( -1.000000000000000000, -0.000000000000000000, -0.000000000000000000 ) ) ;
#45330 = EDGE_CURVE ( 'NONE', #19105, #273, #56232, .T. ) ;
#45331 = FACE_BOUND ( 'NONE', #77829, .T. ) ;
#45333 = CARTESIAN_POINT ( 'NONE',  ( 4.376858997939548246, -12.64618726649961289, 30.78989965857442712 ) ) ;
#45332 = CARTESIAN_POINT ( 'NONE',  ( 12.21156171748986985, -10.06842814019191401, 34.32929386961144758 ) ) ;
#45334 = DIRECTION ( 'NONE',  ( -0.000000000000000000, 0.9848077530122086864, -0.1736481776669273891 ) ) ;
#45336 = CARTESIAN_POINT ( 'NONE',  ( 14.30769230769218581, -11.06231777344772027, 33.60647404775119895 ) ) ;
#45335 = CARTESIAN_POINT ( 'NONE',  ( -11.60378555126584388, -7.749976730030849303, 34.74374725381503737 ) ) ;
#45337 = CARTESIAN_POINT ( 'NONE',  ( 16.15384615384615330, -10.51840700105979565, 33.73612834413961536 ) ) ;
#45338 = CARTESIAN_POINT ( 'NONE',  ( -8.546219417617921366, -3.587049720035815348, 32.86302985866382897 ) ) ;
#45339 = CARTESIAN_POINT ( 'NONE',  ( -1.614399933863656544, -3.775308065498769405, 26.32625670625849068 ) ) ;
#45340 = ORIENTED_EDGE ( 'NONE', *, *, #58006, .T. ) ;
#45341 = DIRECTION ( 'NONE',  ( -0.000000000000000000, 1.000000000000000000, 3.491481338843133355E-15 ) ) ;
#45342 = EDGE_CURVE ( 'NONE', #58859, #60261, #73466, .T. ) ;
#45343 = EDGE_CURVE ( 'NONE', #40578, #2477, #23494, .T. ) ;
#45344 = CARTESIAN_POINT ( 'NONE',  ( 16.15384615384615330, -9.905515769479276145, 34.41647553114623292 ) ) ;
#45345 = LINE ( 'NONE', #81374, #58920 ) ;
#45347 = VECTOR ( 'NONE', #40992, 1000.000000000000114 ) ;
#45346 = CARTESIAN_POINT ( 'NONE',  ( -0.3891064303782384992, -10.22269297216479877, 28.92407589458995432 ) ) ;
#45348 = CARTESIAN_POINT ( 'NONE',  ( 3.296024802045255164, -6.879047030191282275, 34.71129190930002295 ) ) ;
#45349 = CARTESIAN_POINT ( 'NONE',  ( -11.76194646302587010, -4.225889041578353655, 33.85425143139329407 ) ) ;
#45350 = CARTESIAN_POINT ( 'NONE',  ( 2.724691934501235036, -6.299813628509441266, 15.38875670625848890 ) ) ;
#45351 = CARTESIAN_POINT ( 'NONE',  ( -15.23076923076935252, -12.70778746994576025, 30.41441678777401236 ) ) ;
#45352 = CARTESIAN_POINT ( 'NONE',  ( -2.084679463598912097, -6.460100341425561332, 34.89618726649961644 ) ) ;
#45353 = LINE ( 'NONE', #29641, #87845 ) ;
#45354 = CARTESIAN_POINT ( 'NONE',  ( -6.923076923076922462, -12.62096338111211580, 30.90682066428153263 ) ) ;
#45355 = CARTESIAN_POINT ( 'NONE',  ( 14.43848411551709709, -5.582136614379148654, 34.36778462344220486 ) ) ;
#45356 = CARTESIAN_POINT ( 'NONE',  ( 0.3589743589743582541, -7.500000000000000000, 33.75000000000000000 ) ) ;
#45357 = CARTESIAN_POINT ( 'NONE',  ( -18.00000000000000000, -10.05012543904494748, 36.02546096051201374 ) ) ;
#45358 = CARTESIAN_POINT ( 'NONE',  ( 7.976944287120795174, -9.084667340241226796, 34.75534355489798344 ) ) ;
#45359 = EDGE_LOOP ( 'NONE', ( #56138, #39460, #74986, #49599 ) ) ;
#45360 = CARTESIAN_POINT ( 'NONE',  ( 15.16549923021291058, -11.67786785259540849, 32.92929555188721480 ) ) ;
#45361 = CARTESIAN_POINT ( 'NONE',  ( -1.607481647678483005, -2.251424796025575770, 29.88072029997477586 ) ) ;
#45362 = CARTESIAN_POINT ( 'NONE',  ( 0.06109907496451268821, -3.749999999999999556, 19.40811829374151287 ) ) ;
#45363 = CARTESIAN_POINT ( 'NONE',  ( -10.68146699474474914, -2.486705287966279432, 31.30864560766542937 ) ) ;
#45364 = CARTESIAN_POINT ( 'NONE',  ( -5.207614543590636913, -2.541943142973490666, 30.39792223712631980 ) ) ;
#45365 = VERTEX_POINT ( 'NONE', #31136 ) ;
#45366 = LINE ( 'NONE', #36842, #32711 ) ;
#45367 = CARTESIAN_POINT ( 'NONE',  ( 9.692307692307570832, -12.70778746994576025, 30.41441678777401236 ) ) ;
#45369 = ORIENTED_EDGE ( 'NONE', *, *, #11817, .T. ) ;
#45368 = DIRECTION ( 'NONE',  ( 0.000000000000000000, 0.000000000000000000, -1.000000000000000000 ) ) ;
#45370 = CARTESIAN_POINT ( 'NONE',  ( -9.692307692307691624, -11.16473453929635440, 33.15142922261926373 ) ) ;
#45371 = DIRECTION ( 'NONE',  ( 0.000000000000000000, 0.4999999999999985567, 0.8660254037844395958 ) ) ;
#45372 = CARTESIAN_POINT ( 'NONE',  ( -8.703162418228330921, -2.538708090699994813, 30.37095296980875503 ) ) ;
#45373 = EDGE_CURVE ( 'NONE', #15767, #77091, #70271, .T. ) ;
#45374 = VECTOR ( 'NONE', #49484, 1000.000000000000114 ) ;
#45375 = DIRECTION ( 'NONE',  ( -0.000000000000000000, 1.000000000000000000, -0.000000000000000000 ) ) ;
#45376 = ORIENTED_EDGE ( 'NONE', *, *, #3907, .T. ) ;
#45377 = CARTESIAN_POINT ( 'NONE',  ( 2.557637826040450868, -12.22109172314383052, 31.39792113162168263 ) ) ;
#45378 = ADVANCED_FACE ( 'NONE', ( #4566 ), #66262, .F. ) ;
#45379 = FACE_OUTER_BOUND ( 'NONE', #57279, .T. ) ;
#45380 = ORIENTED_EDGE ( 'NONE', *, *, #9087, .F. ) ;
#45381 = ORIENTED_EDGE ( 'NONE', *, *, #51021, .F. ) ;
#45382 = EDGE_CURVE ( 'NONE', #32057, #73835, #36915, .T. ) ;
#45383 = ADVANCED_FACE ( 'NONE', ( #86558 ), #24828, .F. ) ;
#45384 = VERTEX_POINT ( 'NONE', #73027 ) ;
#45385 = EDGE_CURVE ( 'NONE', #51674, #30978, #38803, .T. ) ;
#45386 = CARTESIAN_POINT ( 'NONE',  ( -18.22292621751613950, -3.586966769969697211, 32.86292498521068950 ) ) ;
#45387 = CARTESIAN_POINT ( 'NONE',  ( -4.153846153846152411, -1.242168528481310874, 33.36296068462461051 ) ) ;
#45388 = CARTESIAN_POINT ( 'NONE',  ( -9.442253272394237840, -12.65882529074907126, 30.72640787790839312 ) ) ;
#45389 = B_SPLINE_CURVE_WITH_KNOTS ( 'NONE', 3,
 ( #46320, #46768, #39586, #67930, #86891, #5339, #26499, #52174, #53061, #53962 ),
 .UNSPECIFIED., .F., .F.,
 ( 4, 2, 2, 2, 4 ),
 ( 0.0007817359430256324996, 0.0009771253907249993591, 0.001172514838424366110, 0.001367904286123732861, 0.001563293733823099829 ),
 .UNSPECIFIED. ) ;
#45390 = EDGE_CURVE ( 'NONE', #42964, #19767, #16498, .T. ) ;
#45391 = LINE ( 'NONE', #65654, #60722 ) ;
#45392 = VECTOR ( 'NONE', #23034, 1000.000000000000227 ) ;
#45393 = ORIENTED_EDGE ( 'NONE', *, *, #71929, .F. ) ;
#45394 = ORIENTED_EDGE ( 'NONE', *, *, #42869, .F. ) ;
#45396 = ORIENTED_EDGE ( 'NONE', *, *, #42719, .F. ) ;
#45395 = CARTESIAN_POINT ( 'NONE',  ( 11.53846153846141576, -11.67786785259630911, 32.92929555188603530 ) ) ;
#45397 = DIRECTION ( 'NONE',  ( -0.000000000000000000, -0.000000000000000000, 1.000000000000000000 ) ) ;
#45398 = CARTESIAN_POINT ( 'NONE',  ( 15.16549878480845770, -3.300289026998414865, 32.46337939537583139 ) ) ;
#45399 = CARTESIAN_POINT ( 'NONE',  ( -8.703975197954745724, -12.46129190930001052, 30.37095296980870174 ) ) ;
#45400 = CARTESIAN_POINT ( 'NONE',  ( -1.384615384615506484, -12.70778746994576025, 30.41441678777401236 ) ) ;
#45401 = EDGE_LOOP ( 'NONE', ( #877, #58801 ) ) ;
#45402 = EDGE_CURVE ( 'NONE', #87727, #60602, #78872, .T. ) ;
#45403 = ORIENTED_EDGE ( 'NONE', *, *, #51180, .F. ) ;
#45404 = ADVANCED_FACE ( 'NONE', ( #46439 ), #73483, .F. ) ;
#45405 = VERTEX_POINT ( 'NONE', #61268 ) ;
#45407 = ORIENTED_EDGE ( 'NONE', *, *, #30658, .T. ) ;
#45406 = DIRECTION ( 'NONE',  ( 0.000000000000000000, 0.000000000000000000, -1.000000000000000000 ) ) ;
#45408 = CARTESIAN_POINT ( 'NONE',  ( 17.99999999999987566, -12.16647553114689728, 32.15551576947799362 ) ) ;
#45409 = CARTESIAN_POINT ( 'NONE',  ( -7.134615384615385025, -7.500000000000000000, 29.75000000000000355 ) ) ;
#45410 = VERTEX_POINT ( 'NONE', #53640 ) ;
#45411 = CYLINDRICAL_SURFACE ( 'NONE', #70506, 0.2500000000000009437 ) ;
#45412 = CARTESIAN_POINT ( 'NONE',  ( -6.923076923076922462, -7.500000000000001776, 35.04278698407183867 ) ) ;
#45413 = CARTESIAN_POINT ( 'NONE',  ( 0.4615384615384611755, -13.95598074871891292, 31.83374038241031911 ) ) ;
#45414 = B_SPLINE_CURVE_WITH_KNOTS ( 'NONE', 3,
 ( #53717, #86641, #10960, #39336, #32121, #10518 ),
 .UNSPECIFIED., .F., .F.,
 ( 4, 2, 4 ),
 ( 0.000000000000000000, 0.0001954784845028921395, 0.0003909569690057842790 ),
 .UNSPECIFIED. ) ;
#45415 = FACE_BOUND ( 'NONE', #88252, .T. ) ;
#45416 = DIRECTION ( 'NONE',  ( -1.000000000000000000, 0.000000000000000000, -0.000000000000000000 ) ) ;
#45417 = CARTESIAN_POINT ( 'NONE',  ( 11.47237812750566022, -8.120952969808774569, 34.71129190930000163 ) ) ;
#45418 = CARTESIAN_POINT ( 'NONE',  ( -8.096130577096198877, -12.17611988154120972, 31.52148481390971213 ) ) ;
#45420 = CARTESIAN_POINT ( 'NONE',  ( 14.53047197667037160, -3.020022701398814569, 32.48759521482552515 ) ) ;
#45419 = CARTESIAN_POINT ( 'NONE',  ( 3.480714640147274608, -3.520799739797214389, 33.17531984108286025 ) ) ;
#45421 = AXIS2_PLACEMENT_3D ( 'NONE', #57100, #71058, #85911 ) ;
#45422 = CARTESIAN_POINT ( 'NONE',  ( 8.638540166120458608, -9.084618155246140248, 34.75535874321725771 ) ) ;
#45423 = CARTESIAN_POINT ( 'NONE',  ( -16.15384615384627409, -8.613356846316285953, 34.62446782046622218 ) ) ;
#45424 = ORIENTED_EDGE ( 'NONE', *, *, #83655, .T. ) ;
#45425 = DIRECTION ( 'NONE',  ( 1.000000000000000000, 0.000000000000000000, 0.000000000000000000 ) ) ;
#45426 = CARTESIAN_POINT ( 'NONE',  ( 12.68431813051652846, -3.563462043263030399, 33.22394488606062879 ) ) ;
#45427 = ORIENTED_EDGE ( 'NONE', *, *, #18474, .T. ) ;
#45428 = EDGE_LOOP ( 'NONE', ( #20233, #32018, #21144, #51147, #30654 ) ) ;
#45429 = AXIS2_PLACEMENT_3D ( 'NONE', #61886, #20471, #13709 ) ;
#45431 = CARTESIAN_POINT ( 'NONE',  ( 1.515140822849032176, -5.915461855592777596, 34.75538340440931506 ) ) ;
#45430 = CARTESIAN_POINT ( 'NONE',  ( -11.53846153846153655, -12.62096338111211580, 30.90682066428153263 ) ) ;
#45432 = CARTESIAN_POINT ( 'NONE',  ( -16.82697766754503377, -12.68172785388650681, 30.59649109432439573 ) ) ;
#45433 = CARTESIAN_POINT ( 'NONE',  ( 2.438217745925953750, -2.372941743896878286, 30.88044141588254377 ) ) ;
#45434 = DIRECTION ( 'NONE',  ( -0.000000000000000000, 0.1736481776669307198, -0.9848077530122080203 ) ) ;
#45435 = ORIENTED_EDGE ( 'NONE', *, *, #43717, .F. ) ;
#45436 = CARTESIAN_POINT ( 'NONE',  ( 8.639082799499073317, -12.70455904226513866, 30.44083106164009322 ) ) ;
#45437 = DIRECTION ( 'NONE',  ( -0.000000000000000000, -0.000000000000000000, -1.000000000000000000 ) ) ;
#45438 = ADVANCED_FACE ( 'NONE', ( #61715 ), #5905, .T. ) ;
#45439 = EDGE_CURVE ( 'NONE', #67446, #427, #5015, .T. ) ;
#45441 = CARTESIAN_POINT ( 'NONE',  ( 0.3954560821783247304, -12.62096338111211580, 30.90682066428152197 ) ) ;
#45440 = CARTESIAN_POINT ( 'NONE',  ( 9.692307692307695177, -1.509761064869970415, 31.06009739812519044 ) ) ;
#45442 = CARTESIAN_POINT ( 'NONE',  ( 7.780883400193070898, -6.026961402152685388, 34.52809138561120506 ) ) ;
#45443 = CARTESIAN_POINT ( 'NONE',  ( 10.68145296638705410, -4.098570777380720287, 33.41473453929635440 ) ) ;
#45444 = LINE ( 'NONE', #53085, #76543 ) ;
#45445 = CARTESIAN_POINT ( 'NONE',  ( 2.651650429449569302, -10.15165042944953733, 22.12500000000000000 ) ) ;
#45446 = ORIENTED_EDGE ( 'NONE', *, *, #54589, .T. ) ;
#45447 = EDGE_CURVE ( 'NONE', #40122, #46874, #74574, .T. ) ;
#45448 = VERTEX_POINT ( 'NONE', #88345 ) ;
#45449 = SHAPE_REPRESENTATION ( 'Outer Protective Cap', ( #83448 ), #80635 ) ;
#45450 = CARTESIAN_POINT ( 'NONE',  ( 14.17754433796061342, -12.50552854090298638, 31.33409797877408920 ) ) ;
#45451 = EDGE_CURVE ( 'NONE', #78478, #34673, #26615, .T. ) ;
#45452 = CARTESIAN_POINT ( 'NONE',  ( -18.22287868242863951, -7.630691491037286056, 34.74850469731152458 ) ) ;
#45453 = CARTESIAN_POINT ( 'NONE',  ( -14.30769230769230660, -12.78798330534103123, 29.99999999999997868 ) ) ;
#45454 = CARTESIAN_POINT ( 'NONE',  ( 14.30769230769231015, -2.721908614388771852, 31.22303859784724978 ) ) ;
#45455 = CYLINDRICAL_SURFACE ( 'NONE', #80229, 0.2499999999999995559 ) ;
#45456 = CARTESIAN_POINT ( 'NONE',  ( -1.929879867024197893E-14, -3.750000000000000000, 21.65625000000000355 ) ) ;
#45457 = FACE_OUTER_BOUND ( 'NONE', #72981, .T. ) ;
#45458 = CARTESIAN_POINT ( 'NONE',  ( -13.60810032833933469, -8.496056993536548418, 34.65000542017679663 ) ) ;
#45459 = EDGE_CURVE ( 'NONE', #74166, #19286, #32477, .T. ) ;
#45460 = CARTESIAN_POINT ( 'NONE',  ( -8.992157728137618378, -12.64616026154729411, 30.79003144601914244 ) ) ;
#45461 = CARTESIAN_POINT ( 'NONE',  ( 12.23805353697412990, -11.60425143139329940, 33.02411095842164457 ) ) ;
#45462 = CARTESIAN_POINT ( 'NONE',  ( -39.05038313613820122, -2.499999999999999556, 29.75000000000000355 ) ) ;
#45463 = CYLINDRICAL_SURFACE ( 'NONE', #27111, 0.2500000000000004996 ) ;
#45464 = CARTESIAN_POINT ( 'NONE',  ( 2.057669070399342992, -3.202444869320336451, 32.30641848906366675 ) ) ;
#45466 = VECTOR ( 'NONE', #159, 1000.000000000000000 ) ;
#45465 = DIRECTION ( 'NONE',  ( -0.000000000000000000, 0.9396926207859093161, -0.3420201433256663259 ) ) ;
#45467 = DIRECTION ( 'NONE',  ( 0.000000000000000000, 0.000000000000000000, 1.000000000000000000 ) ) ;
#45468 = B_SPLINE_CURVE_WITH_KNOTS ( 'NONE', 3,
 ( #68269, #7463, #63278, #84020, #257, #48879, #27719, #13324, #89008, #54749 ),
 .UNSPECIFIED., .F., .F.,
 ( 4, 2, 2, 2, 4 ),
 ( 0.000000000000000000, 0.0001954311584214072652, 0.0003908623168428145304, 0.0005862934752642217414, 0.0007817246336856290608 ),
 .UNSPECIFIED. ) ;
#45469 = B_SPLINE_CURVE_WITH_KNOTS ( 'NONE', 3,
 ( #8993, #56724, #70687, #63914, #22935, #2648, #32808, #52172, #60268, #58477 ),
 .UNSPECIFIED., .F., .F.,
 ( 4, 2, 2, 2, 4 ),
 ( 0.0007817246256747504250, 0.0009771112852218954894, 0.001172497944769040554, 0.001367884604316185401, 0.001563271263863330466 ),
 .UNSPECIFIED. ) ;
#45470 = CARTESIAN_POINT ( 'NONE',  ( -3.100243529005668019, -11.46989282347013095, 32.79007818306219946 ) ) ;
#45471 = CARTESIAN_POINT ( 'NONE',  ( -17.01166793741023042, -3.083524468853783951, 32.58852847137153930 ) ) ;
#45472 = EDGE_CURVE ( 'NONE', #51215, #80969, #88486, .T. ) ;
#45473 = VERTEX_POINT ( 'NONE', #82461 ) ;
#45474 = CARTESIAN_POINT ( 'NONE',  ( -7.384615384615385025, -7.500000000000000000, 29.75000000000000355 ) ) ;
#45475 = CARTESIAN_POINT ( 'NONE',  ( 8.992010310499177095, -11.89424750095246175, 32.13594075562310337 ) ) ;
#45476 = CARTESIAN_POINT ( 'NONE',  ( -4.403869378067610363, -5.765609946408404518, 34.70566812827425451 ) ) ;
#45477 = CARTESIAN_POINT ( 'NONE',  ( 2.750000000000001776, -7.499999999999984013, 23.21875000000000000 ) ) ;
#45478 = CARTESIAN_POINT ( 'NONE',  ( -17.07692307692307665, -5.471508081941601098, 34.59228464037088457 ) ) ;
#45479 = CARTESIAN_POINT ( 'NONE',  ( 8.546303810323914618, -10.01117774369187252, 34.36070679894347535 ) ) ;
#45480 = EDGE_CURVE ( 'NONE', #19270, #43177, #35758, .T. ) ;
#45482 = ORIENTED_EDGE ( 'NONE', *, *, #64115, .F. ) ;
#45481 = CARTESIAN_POINT ( 'NONE',  ( -0.2115929431903192937, -2.587454068350147907, 30.68340429815432202 ) ) ;
#45483 = CARTESIAN_POINT ( 'NONE',  ( -2.749999999999991562, -8.639087296526026805, 21.26562500000000000 ) ) ;
#45484 = CARTESIAN_POINT ( 'NONE',  ( -1.319360245102545681, -12.51329471203373700, 31.30864560766537963 ) ) ;
#45485 = VECTOR ( 'NONE', #8447, 1000.000000000000000 ) ;
#45486 = ORIENTED_EDGE ( 'NONE', *, *, #67606, .F. ) ;
#45487 = CARTESIAN_POINT ( 'NONE',  ( 6.792386319966616348, -6.369640206132550553, 34.87707690430378449 ) ) ;
#45488 = ORIENTED_EDGE ( 'NONE', *, *, #58420, .F. ) ;
#45489 = CYLINDRICAL_SURFACE ( 'NONE', #69387, 0.2500000000000002220 ) ;
#45490 = EDGE_CURVE ( 'NONE', #72293, #21038, #45989, .T. ) ;
#45491 = CARTESIAN_POINT ( 'NONE',  ( -9.561781990544133691, -2.882268652242222284, 31.66798894389554064 ) ) ;
#45492 = CARTESIAN_POINT ( 'NONE',  ( -0.2115930521604184322, -6.653508905675590945, 34.93172785388651391 ) ) ;
#45493 = ORIENTED_EDGE ( 'NONE', *, *, #50969, .F. ) ;
#45494 = CYLINDRICAL_SURFACE ( 'NONE', #27833, 0.2499999999999998890 ) ;
#45495 = VERTEX_POINT ( 'NONE', #25729 ) ;
#45496 = CARTESIAN_POINT ( 'NONE',  ( 11.28848480751918437, -3.627789207965226748, 32.91389620160131102 ) ) ;
#45497 = EDGE_CURVE ( 'NONE', #34333, #17369, #73923, .T. ) ;
#45498 = ORIENTED_EDGE ( 'NONE', *, *, #67301, .T. ) ;
#45499 = CARTESIAN_POINT ( 'NONE',  ( 2.084207383127978375, -9.417330523894424488, 34.63758898049880486 ) ) ;
#45500 = CARTESIAN_POINT ( 'NONE',  ( -7.846153846153844924, -5.180354513474913603, 36.12317359536750416 ) ) ;
#45501 = AXIS2_PLACEMENT_3D ( 'NONE', #62428, #61549, #1181 ) ;
#45502 = ORIENTED_EDGE ( 'NONE', *, *, #68228, .F. ) ;
#45503 = DIRECTION ( 'NONE',  ( 0.000000000000000000, 0.4999999999999960032, -0.8660254037844410391 ) ) ;
#45504 = CARTESIAN_POINT ( 'NONE',  ( 9.822833130541340552, -10.31582465632705237, 34.18122507451815295 ) ) ;
#45505 = CARTESIAN_POINT ( 'NONE',  ( 12.68431800280687050, -5.114059244376869984, 34.14424750095245287 ) ) ;
#45506 = B_SPLINE_CURVE_WITH_KNOTS ( 'NONE', 3,
 ( #79232, #3557, #24266, #31025, #11668, #58946, #30584, #17076, #79674, #86452 ),
 .UNSPECIFIED., .F., .F.,
 ( 4, 2, 2, 2, 4 ),
 ( 0.0007817359430256319575, 0.0009771253907249984917, 0.001172514838424365026, 0.001367904286123731343, 0.001563293733823097878 ),
 .UNSPECIFIED. ) ;
#45507 = AXIS2_PLACEMENT_3D ( 'NONE', #32440, #40101, #59905 ) ;
#45508 = EDGE_CURVE ( 'NONE', #88972, #76747, #66911, .T. ) ;
#45509 = CARTESIAN_POINT ( 'NONE',  ( -4.153846153846152411, -13.78497067705608181, 32.30358669280327177 ) ) ;
#45510 = CARTESIAN_POINT ( 'NONE',  ( -7.846153846153844924, -12.62096338111211580, 30.90682066428153263 ) ) ;
#45511 = B_SPLINE_CURVE_WITH_KNOTS ( 'NONE', 3,
 ( #6870, #33020, #75340, #26700, #41109, #20829 ),
 .UNSPECIFIED., .F., .F.,
 ( 4, 2, 4 ),
 ( 0.000000000000000000, 0.0001954784845028921395, 0.0003909569690057842790 ),
 .UNSPECIFIED. ) ;
#45512 = B_SPLINE_CURVE_WITH_KNOTS ( 'NONE', 3,
 ( #52987, #46248, #39505, #26424, #25971, #54323, #18332, #45795, #53436, #73276 ),
 .UNSPECIFIED., .F., .F.,
 ( 4, 2, 2, 2, 4 ),
 ( 0.000000000000000000, 0.0001954339857564098054, 0.0003908679715128196108, 0.0005863019572692293891, 0.0007817359430256392216 ),
 .UNSPECIFIED. ) ;
#45513 = ORIENTED_EDGE ( 'NONE', *, *, #20816, .F. ) ;
#45515 = ADVANCED_FACE ( 'NONE', ( #42358 ), #28841, .F. ) ;
#45514 = VERTEX_POINT ( 'NONE', #55852 ) ;
#45516 = AXIS2_PLACEMENT_3D ( 'NONE', #10685, #64277, #79141 ) ;
#45517 = ORIENTED_EDGE ( 'NONE', *, *, #38447, .T. ) ;
#45519 = EDGE_LOOP ( 'NONE', ( #38081, #65773, #73503, #82976 ) ) ;
#45518 = CARTESIAN_POINT ( 'NONE',  ( -7.846153846153844924, -11.11383981884818262, 36.00935417666054406 ) ) ;
#45520 = DIRECTION ( 'NONE',  ( -0.000000000000000000, 0.7660444431189791237, -0.6427876096865379196 ) ) ;
#45521 = FACE_OUTER_BOUND ( 'NONE', #45359, .T. ) ;
#45522 = ORIENTED_EDGE ( 'NONE', *, *, #70965, .T. ) ;
#45523 = EDGE_CURVE ( 'NONE', #31425, #7198, #34691, .T. ) ;
#45524 = EDGE_CURVE ( 'NONE', #57246, #23981, #20646, .T. ) ;
#45525 = EDGE_LOOP ( 'NONE', ( #58362, #35876, #79755, #80416 ) ) ;
#45526 = CARTESIAN_POINT ( 'NONE',  ( 16.94677586748485965, -10.19110544564092002, 33.96427741523702792 ) ) ;
#45527 = ORIENTED_EDGE ( 'NONE', *, *, #52412, .T. ) ;
#45528 = CARTESIAN_POINT ( 'NONE',  ( -18.00000000000000000, -9.058645607665452459, 34.76329471203371924 ) ) ;
#45529 = CARTESIAN_POINT ( 'NONE',  ( -13.38461538461550759, -5.941354392335915335, 34.76329471203413846 ) ) ;
#45530 = CARTESIAN_POINT ( 'NONE',  ( -16.15384615384627409, -11.06231777344772027, 33.60647404775119895 ) ) ;
#45531 = FACE_BOUND ( 'NONE', #8456, .T. ) ;
#45532 = CARTESIAN_POINT ( 'NONE',  ( -0.4615384615384611200, -7.500000000000001776, 35.04278698407183867 ) ) ;
#45533 = CARTESIAN_POINT ( 'NONE',  ( 12.46153846153846168, -8.973038597847269315, 34.52809138561121927 ) ) ;
#45534 = DIRECTION ( 'NONE',  ( 0.000000000000000000, 0.9396926207859126468, -0.3420201433256571111 ) ) ;
#45535 = DIRECTION ( 'NONE',  ( -0.000000000000000000, -0.3420201433256694901, -0.9396926207859082059 ) ) ;
#45536 = CYLINDRICAL_SURFACE ( 'NONE', #56716, 0.2499999999999986955 ) ;
#45537 = CARTESIAN_POINT ( 'NONE',  ( -16.15384615384627409, -3.083524468854526912, 32.58852847137268327 ) ) ;
#45538 = VERTEX_POINT ( 'NONE', #68922 ) ;
#45539 = CARTESIAN_POINT ( 'NONE',  ( -2.057637996053991447, -9.148310452688873440, 34.47095581063188519 ) ) ;
#45540 = ORIENTED_EDGE ( 'NONE', *, *, #26335, .T. ) ;
#45541 = ORIENTED_EDGE ( 'NONE', *, *, #29681, .F. ) ;
#45543 = CARTESIAN_POINT ( 'NONE',  ( 10.83839596699746721, -5.667800583137506010, 34.40243808032445827 ) ) ;
#45542 = CARTESIAN_POINT ( 'NONE',  ( 10.68064018666064108, -12.46129190930001052, 30.37095296980870174 ) ) ;
#45544 = B_SPLINE_CURVE_WITH_KNOTS ( 'NONE', 3,
 ( #65844, #38841, #26207, #12250, #67203, #51879, #79376, #59094, #5503, #86593 ),
 .UNSPECIFIED., .F., .F.,
 ( 4, 2, 2, 2, 4 ),
 ( 0.0007817246256747472808, 0.0009771112852218905021, 0.001172497944769033832, 0.001367884604316177161, 0.001563271263863320274 ),
 .UNSPECIFIED. ) ;
#45545 = CARTESIAN_POINT ( 'NONE',  ( 2.980792486720639456, -3.436278759898155233, 33.07459398097509506 ) ) ;
#45546 = CARTESIAN_POINT ( 'NONE',  ( -11.00641025641025550, -7.500000000000000000, 29.75000000000000355 ) ) ;
#45547 = DIRECTION ( 'NONE',  ( -1.000000000000000000, 0.000000000000000000, -0.000000000000000000 ) ) ;
#45548 = CARTESIAN_POINT ( 'NONE',  ( 1.515405825582337718, -3.957578996910242619, 33.62503395064540257 ) ) ;
#45549 = VERTEX_POINT ( 'NONE', #913 ) ;
#45550 = DIRECTION ( 'NONE',  ( -0.000000000000000000, 0.1736481776669307198, -0.9848077530122080203 ) ) ;
#45551 = CARTESIAN_POINT ( 'NONE',  ( -5.749999999999999112, -2.249999999999998668, 29.75000000000000355 ) ) ;
#45552 = CARTESIAN_POINT ( 'NONE',  ( -1.634638621908348632, -3.711651800289232028, 33.01384336483936011 ) ) ;
#45553 = CARTESIAN_POINT ( 'NONE',  ( -4.088590582570129861, -3.835265460703683349, 33.15142922261929925 ) ) ;
#45554 = ORIENTED_EDGE ( 'NONE', *, *, #26591, .T. ) ;
#45555 = VERTEX_POINT ( 'NONE', #476 ) ;
#45556 = EDGE_LOOP ( 'NONE', ( #42001, #50282, #56718, #62192 ) ) ;
#45557 = VECTOR ( 'NONE', #64198, 1000.000000000000000 ) ;
#45558 = CARTESIAN_POINT ( 'NONE',  ( -17.75000000000000711, -2.249999999999999112, 29.81889780837710902 ) ) ;
#45559 = CARTESIAN_POINT ( 'NONE',  ( 5.076923076923075762, -2.833524468853757305, 32.15551576947925838 ) ) ;
#45561 = ORIENTED_EDGE ( 'NONE', *, *, #15690, .F. ) ;
#45560 = ADVANCED_FACE ( 'NONE', ( #49095 ), #48649, .F. ) ;
#45562 = CARTESIAN_POINT ( 'NONE',  ( -3.230769230769229949, -1.790695186598648903, 34.54067556320373455 ) ) ;
#45563 = CARTESIAN_POINT ( 'NONE',  ( 6.130525438233644486, -11.66157788607254275, 32.95092075102925833 ) ) ;
#45564 = CARTESIAN_POINT ( 'NONE',  ( -8.703975197954740395, -6.879047030191282275, 34.71129190930002295 ) ) ;
#45565 = CARTESIAN_POINT ( 'NONE',  ( -1.384615384615506484, -4.320704448113951379, 33.92786785259630022 ) ) ;
#45566 = CIRCLE ( 'NONE', #85880, 4.000000000000000000 ) ;
#45567 = CARTESIAN_POINT ( 'NONE',  ( -0.6844646790546086157, -11.24512374952581872, 33.06303171183252942 ) ) ;
#45568 = ORIENTED_EDGE ( 'NONE', *, *, #54665, .T. ) ;
#45569 = ADVANCED_FACE ( 'NONE', ( #34705 ), #7680, .F. ) ;
#45571 = ORIENTED_EDGE ( 'NONE', *, *, #23441, .F. ) ;
#45570 = CARTESIAN_POINT ( 'NONE',  ( 0.2115617305961068062, -9.943427161483782584, 34.11278801902876978 ) ) ;
#45572 = CARTESIAN_POINT ( 'NONE',  ( -8.703975197954747500, -10.21337939537593620, 33.94971097300152252 ) ) ;
#45573 = CARTESIAN_POINT ( 'NONE',  ( 4.023154687178596589, -6.413092428213692742, 34.63065189839063152 ) ) ;
#45574 = CYLINDRICAL_SURFACE ( 'NONE', #45814, 0.2499999999999997502 ) ;
#45575 = CARTESIAN_POINT ( 'NONE',  ( -10.74553258511630993, -3.625366637846544116, 33.29286588640298561 ) ) ;
#45576 = DIRECTION ( 'NONE',  ( -0.000000000000000000, 0.9848077530122086864, -0.1736481776669273891 ) ) ;
#45577 = AXIS2_PLACEMENT_3D ( 'NONE', #77382, #15692, #8935 ) ;
#45578 =( NAMED_UNIT ( * ) PLANE_ANGLE_UNIT ( ) SI_UNIT ( $, .RADIAN. ) );
#45579 = EDGE_CURVE ( 'NONE', #24114, #2558, #72323, .T. ) ;
#45580 = CARTESIAN_POINT ( 'NONE',  ( 1.077988221561497539, -10.27530806549875386, 17.45499329374151642 ) ) ;
#45581 = VERTEX_POINT ( 'NONE', #70258 ) ;
#45582 = CARTESIAN_POINT ( 'NONE',  ( 5.011653076366755499, -12.16647553114622049, 32.15551576947930812 ) ) ;
#45583 = CARTESIAN_POINT ( 'NONE',  ( -9.469296340694842939, -8.239487800360276282, 34.69522927552633718 ) ) ;
#45584 = CARTESIAN_POINT ( 'NONE',  ( -0.3307466537136757867, -4.809403383903225304, 33.96459661697924304 ) ) ;
#45585 = VERTEX_POINT ( 'NONE', #8565 ) ;
#45586 = ORIENTED_EDGE ( 'NONE', *, *, #12433, .T. ) ;
#45587 = CARTESIAN_POINT ( 'NONE',  ( 9.692307692307695177, -3.322132147404559976, 32.92929555188717927 ) ) ;
#45588 = CARTESIAN_POINT ( 'NONE',  ( 25.00000000000000355, 9.999999999999971578, 3.000000000000000000 ) ) ;
#45589 = DIRECTION ( 'NONE',  ( -1.000000000000000000, -0.000000000000000000, -0.000000000000000000 ) ) ;
#45590 = DIRECTION ( 'NONE',  ( 0.000000000000000000, 0.000000000000000000, -1.000000000000000000 ) ) ;
#45591 = EDGE_CURVE ( 'NONE', #81768, #85253, #29284, .T. ) ;
#45592 = CARTESIAN_POINT ( 'NONE',  ( 17.77651507543566822, -12.11044203135681840, 32.26167407432752299 ) ) ;
#45593 = CARTESIAN_POINT ( 'NONE',  ( 5.749976762707035505, -8.432397168068783699, 34.66272746175022945 ) ) ;
#45594 = EDGE_LOOP ( 'NONE', ( #85240, #39722 ) ) ;
#45595 = AXIS2_PLACEMENT_3D ( 'NONE', #27881, #8502, #15702 ) ;
#45596 = CARTESIAN_POINT ( 'NONE',  ( 20.00000000000000711, -9.999999999999994671, 10.00000000000000178 ) ) ;
#45597 = CARTESIAN_POINT ( 'NONE',  ( -2.084912766423897779, -10.11255958852955850, 34.01340905677048454 ) ) ;
#45598 = CARTESIAN_POINT ( 'NONE',  ( 9.468822767743361624, -2.612411019501189369, 31.66733052389439962 ) ) ;
#45599 = ORIENTED_EDGE ( 'NONE', *, *, #52245, .F. ) ;
#45600 = CARTESIAN_POINT ( 'NONE',  ( -7.715362038329059757, -3.530189275343204702, 32.79018710029569661 ) ) ;
#45601 = VECTOR ( 'NONE', #15076, 1000.000000000000000 ) ;
#45602 = ADVANCED_FACE ( 'NONE', ( #49977 ), #30589, .F. ) ;
#45603 = ORIENTED_EDGE ( 'NONE', *, *, #30030, .F. ) ;
#45604 = DIRECTION ( 'NONE',  ( -0.000000000000000000, -0.3420201433256694901, -0.9396926207859082059 ) ) ;
#45605 = SURFACE_SIDE_STYLE ('',( #18591 ) ) ;
#45606 = CARTESIAN_POINT ( 'NONE',  ( -5.076923076923075762, -13.37000171582298513, 34.34916445242398453 ) ) ;
#45607 = DIRECTION ( 'NONE',  ( 0.000000000000000000, 0.3420201433256641055, -0.9396926207859100932 ) ) ;
#45608 = ORIENTED_EDGE ( 'NONE', *, *, #33376, .F. ) ;
#45609 = ADVANCED_FACE ( 'NONE', ( #72913 ), #78332, .F. ) ;
#45610 = VECTOR ( 'NONE', #10113, 1000.000000000000227 ) ;
#45611 = CARTESIAN_POINT ( 'NONE',  ( -17.32692307692307665, -7.500000000000001776, 35.04278698407183867 ) ) ;
#45612 = CARTESIAN_POINT ( 'NONE',  ( 13.63456079399343146, -9.357781135181031829, 34.66075350412533851 ) ) ;
#45613 = CARTESIAN_POINT ( 'NONE',  ( -1.384615384615383471, -13.20930481340135110, 34.54067556320372745 ) ) ;
#45614 = CARTESIAN_POINT ( 'NONE',  ( -6.223484924564328225, -5.827078755546623690, 34.72654668319379567 ) ) ;
#45615 = CARTESIAN_POINT ( 'NONE',  ( -2.177166869458664333, -11.04252011169590020, 33.62494198852677130 ) ) ;
#45616 = EDGE_CURVE ( 'NONE', #62505, #78112, #84676, .T. ) ;
#45617 = VERTEX_POINT ( 'NONE', #17082 ) ;
#45618 = CARTESIAN_POINT ( 'NONE',  ( 3.512820512820511443, -11.50000000000000000, 29.75000000000000355 ) ) ;
#45619 = VERTEX_POINT ( 'NONE', #58061 ) ;
#45620 = CARTESIAN_POINT ( 'NONE',  ( 8.639083559792549494, -12.45813303252208648, 30.39737893381572675 ) ) ;
#45621 = B_SPLINE_CURVE_WITH_KNOTS ( 'NONE', 3,
 ( #57862, #30831, #24517, #24076, #51985, #79481, #9674, #51523, #44782, #3807 ),
 .UNSPECIFIED., .F., .F.,
 ( 4, 2, 2, 2, 4 ),
 ( 0.000000000000000000, 0.0001954339857564125972, 0.0003908679715128181471, 0.0005863019572692237513, 0.0007817359430256293554 ),
 .UNSPECIFIED. ) ;
#45622 = FACE_OUTER_BOUND ( 'NONE', #75659, .T. ) ;
#45623 = DIRECTION ( 'NONE',  ( 0.000000000000000000, 0.4999999999999960032, -0.8660254037844410391 ) ) ;
#45624 = DIRECTION ( 'NONE',  ( 0.000000000000000000, 0.6427876096865368094, 0.7660444431189802339 ) ) ;
#45625 = CARTESIAN_POINT ( 'NONE',  ( -9.692307692307691624, -6.343179335718451384, 34.87096338111211935 ) ) ;
#45626 = CARTESIAN_POINT ( 'NONE',  ( 9.469381474791545017, -8.239355502252617924, 34.69524867566427417 ) ) ;
#45627 = ADVANCED_FACE ( 'NONE', ( #44536 ), #3560, .F. ) ;
#45628 = VERTEX_POINT ( 'NONE', #43663 ) ;
#45629 = ORIENTED_EDGE ( 'NONE', *, *, #46126, .F. ) ;
#45630 = EDGE_LOOP ( 'NONE', ( #55689, #64999, #7247, #24843, #32043, #64819 ) ) ;
#45631 = B_SPLINE_CURVE_WITH_KNOTS ( 'NONE', 3,
 ( #31305, #36293, #2051, #2484, #77709, #65524, #36726, #37609, #58770, #86269 ),
 .UNSPECIFIED., .F., .F.,
 ( 4, 2, 2, 2, 4 ),
 ( 0.0007817359430256294638, 0.0009771253907249952391, 0.001172514838424361123, 0.001367904286123726790, 0.001563293733823092673 ),
 .UNSPECIFIED. ) ;
#45632 = ADVANCED_FACE ( 'NONE', ( #38688 ), #85991, .T. ) ;
#45634 = ORIENTED_EDGE ( 'NONE', *, *, #42408, .T. ) ;
#45633 = EDGE_CURVE ( 'NONE', #3517, #77110, #81923, .T. ) ;
#45635 = VERTEX_POINT ( 'NONE', #24729 ) ;
#45636 = CARTESIAN_POINT ( 'NONE',  ( 12.46153846153833911, -11.94971097300221174, 32.03036669348237098 ) ) ;
#45637 = DIRECTION ( 'NONE',  ( -0.000000000000000000, -0.1736481776669307198, -0.9848077530122080203 ) ) ;
#45638 = EDGE_CURVE ( 'NONE', #75555, #74750, #58279, .T. ) ;
#45639 = CARTESIAN_POINT ( 'NONE',  ( -10.36533019547116119, -4.818054556918156983, 34.26375889529406749 ) ) ;
#45640 = EDGE_CURVE ( 'NONE', #54013, #82892, #27201, .T. ) ;
#45641 = CARTESIAN_POINT ( 'NONE',  ( -7.173053654019276415, -3.137211980971221781, 32.19342716148376837 ) ) ;
#45642 = CARTESIAN_POINT ( 'NONE',  ( 13.16168916709923664, -8.239355502252617924, 34.69524867566427417 ) ) ;
#45643 = CARTESIAN_POINT ( 'NONE',  ( -6.000000000000121680, -3.083524468854526912, 32.58852847137268327 ) ) ;
#45644 = CARTESIAN_POINT ( 'NONE',  ( -0.4615384615385826339, -11.94971097300221174, 32.03036669348237098 ) ) ;
#45645 = CARTESIAN_POINT ( 'NONE',  ( 16.82692307692307665, -2.249999999999998668, 29.75000000000000355 ) ) ;
#45646 = LINE ( 'NONE', #18182, #64820 ) ;
#45647 = EDGE_LOOP ( 'NONE', ( #12770, #57941 ) ) ;
#45648 = VERTEX_POINT ( 'NONE', #52190 ) ;
#45649 = VERTEX_POINT ( 'NONE', #72466 ) ;
#45651 = ORIENTED_EDGE ( 'NONE', *, *, #36861, .F. ) ;
#45650 = CARTESIAN_POINT ( 'NONE',  ( 11.60371667797437212, -2.657715359629132301, 31.77849191805844242 ) ) ;
#45653 = CARTESIAN_POINT ( 'NONE',  ( 18.13004505591977278, -2.254550872974305342, 29.97347326024528158 ) ) ;
#45652 = CARTESIAN_POINT ( 'NONE',  ( 7.846153846153725020, -3.300289026999228881, 32.46337939537708905 ) ) ;
#45654 = LINE ( 'NONE', #38012, #51837 ) ;
#45655 = CARTESIAN_POINT ( 'NONE',  ( 4.376625695114562120, -2.600157965045225339, 30.74683119005207743 ) ) ;
#45656 = FACE_BOUND ( 'NONE', #25210, .T. ) ;
#45657 = EDGE_LOOP ( 'NONE', ( #81753, #62782, #65367, #51904 ) ) ;
#45658 = VERTEX_POINT ( 'NONE', #44092 ) ;
#45659 = CARTESIAN_POINT ( 'NONE',  ( -17.32694630114453105, -11.56360843649121861, 33.07473185843129926 ) ) ;
#45660 = VECTOR ( 'NONE', #83313, 1000.000000000000114 ) ;
#45661 = VERTEX_POINT ( 'NONE', #10329 ) ;
#45662 = FACE_BOUND ( 'NONE', #82199, .T. ) ;
#45663 = CYLINDRICAL_SURFACE ( 'NONE', #72026, 0.2499999999999998890 ) ;
#45664 = CARTESIAN_POINT ( 'NONE',  ( -16.15384615384615330, -2.486705287966279876, 31.30864560766543647 ) ) ;
#45665 = VERTEX_POINT ( 'NONE', #37796 ) ;
#45666 = CARTESIAN_POINT ( 'NONE',  ( -1.318548051265308274, -5.471508081941601098, 34.59228464037088457 ) ) ;
#45667 = LINE ( 'NONE', #46560, #54746 ) ;
#45668 = CARTESIAN_POINT ( 'NONE',  ( 6.000000000000001776, -1.215029322943914858, 32.30358669280327177 ) ) ;
#45669 = EDGE_LOOP ( 'NONE', ( #68975, #6071 ) ) ;
#45670 = LINE ( 'NONE', #16866, #85965 ) ;
#45671 = CARTESIAN_POINT ( 'NONE',  ( 10.03846153846153832, -4.000000000000000000, 29.25000000000000000 ) ) ;
#45672 = DIRECTION ( 'NONE',  ( 0.000000000000000000, 0.000000000000000000, 1.000000000000000000 ) ) ;
#45673 = VERTEX_POINT ( 'NONE', #44986 ) ;
#45674 = CARTESIAN_POINT ( 'NONE',  ( -2.373775718648186039, -11.16473453929635440, 33.15142922261925662 ) ) ;
#45675 = CARTESIAN_POINT ( 'NONE',  ( 7.053602624840488389, -10.88167719472716399, 33.43325721877153711 ) ) ;
#45676 = B_SPLINE_CURVE_WITH_KNOTS ( 'NONE', 3,
 ( #22791, #57912, #16047, #84956, #23681, #63340, #51132, #43516, #85394, #71418 ),
 .UNSPECIFIED., .F., .F.,
 ( 4, 2, 2, 2, 4 ),
 ( 0.0007817246256747452209, 0.0009771112852218887673, 0.001172497944769032531, 0.001367884604316176294, 0.001563271263863319840 ),
 .UNSPECIFIED. ) ;
#45677 = ORIENTED_EDGE ( 'NONE', *, *, #81732, .F. ) ;
#45678 = CARTESIAN_POINT ( 'NONE',  ( 2.307692307692186251, -11.67786785259630911, 32.92929555188603530 ) ) ;
#45679 = FACE_OUTER_BOUND ( 'NONE', #40996, .T. ) ;
#45680 = CARTESIAN_POINT ( 'NONE',  ( -16.02332045208259359, -8.586989748646450593, 34.63063291749215011 ) ) ;
#45681 = CARTESIAN_POINT ( 'NONE',  ( 15.10062126103753855, -12.70455904226513866, 30.44083106164009322 ) ) ;
#45682 = CARTESIAN_POINT ( 'NONE',  ( 5.076923076923075762, -12.37446782046654192, 30.86335684631486131 ) ) ;
#45683 = B_SPLINE_CURVE_WITH_KNOTS ( 'NONE', 3,
 ( #67287, #81692, #597, #55532, #40263, #67728, #68606, #75804, #27621, #54196 ),
 .UNSPECIFIED., .F., .F.,
 ( 4, 2, 2, 2, 4 ),
 ( 0.0007817246256747485819, 0.0009771112852218918031, 0.001172497944769034916, 0.001367884604316178029, 0.001563271263863321358 ),
 .UNSPECIFIED. ) ;
#45684 = CARTESIAN_POINT ( 'NONE',  ( 15.12820512820512953, -7.500000000000000000, 29.75000000000000355 ) ) ;
#45686 = CARTESIAN_POINT ( 'NONE',  ( -1.384615384615506484, -8.656820664282941280, 34.87096338111179961 ) ) ;
#45685 = CARTESIAN_POINT ( 'NONE',  ( 2.307692307692309264, -12.29105614889573062, 35.45975837776705220 ) ) ;
#45687 = CARTESIAN_POINT ( 'NONE',  ( -3.480792468062195333, -2.587272538249755449, 30.68239716806877837 ) ) ;
#45689 = CARTESIAN_POINT ( 'NONE',  ( -8.519230769230768274, -2.249999999999998668, 29.75000000000000355 ) ) ;
#45688 = CARTESIAN_POINT ( 'NONE',  ( -15.16551409125639083, -2.657715359629131857, 31.77849191805844242 ) ) ;
#45690 = CARTESIAN_POINT ( 'NONE',  ( -2.724691934501232371, -8.700186371490559623, 27.26375670625849423 ) ) ;
#45691 = ORIENTED_EDGE ( 'NONE', *, *, #50911, .T. ) ;
#45692 = CARTESIAN_POINT ( 'NONE',  ( 17.77651505627605033, -4.386631170607603991, 33.66268669641500111 ) ) ;
#45693 = VERTEX_POINT ( 'NONE', #31028 ) ;
#45694 = VECTOR ( 'NONE', #82122, 1000.000000000000000 ) ;
#45695 = ORIENTED_EDGE ( 'NONE', *, *, #52253, .T. ) ;
#45696 = CARTESIAN_POINT ( 'NONE',  ( -12.71153846153846168, -2.499999999999998668, 29.75000000000000355 ) ) ;
#45697 = VERTEX_POINT ( 'NONE', #10773 ) ;
#45698 = CARTESIAN_POINT ( 'NONE',  ( -15.09997742294444478, -5.582136614379148654, 34.36778462344220486 ) ) ;
#45699 = CARTESIAN_POINT ( 'NONE',  ( -1.139087296525992166, -10.25000000000000533, 17.35937500000000000 ) ) ;
#45700 = LINE ( 'NONE', #11479, #28590 ) ;
#45701 = CARTESIAN_POINT ( 'NONE',  ( -18.06608237936013239, -11.91647553114624358, 32.58852847137148245 ) ) ;
#45702 = DIRECTION ( 'NONE',  ( -0.000000000000000000, -0.8660254037844399289, -0.4999999999999980016 ) ) ;
#45703 = CARTESIAN_POINT ( 'NONE',  ( 7.846153846153723244, -11.06231777344772027, 33.60647404775119895 ) ) ;
#45705 = CARTESIAN_POINT ( 'NONE',  ( -8.519285250882628446, -5.057305518903948638, 34.11320923018887896 ) ) ;
#45704 = VECTOR ( 'NONE', #52105, 1000.000000000000000 ) ;
#45706 = DIRECTION ( 'NONE',  ( -1.000000000000000000, -0.000000000000000000, -0.000000000000000000 ) ) ;
#45707 = CARTESIAN_POINT ( 'NONE',  ( -24.00000000000000000, -5.499999999999981348, 27.75000000000000000 ) ) ;
#45708 = CARTESIAN_POINT ( 'NONE',  ( 3.750000000000000888, -7.499999999999978684, 23.21875000000000000 ) ) ;
#45709 = CARTESIAN_POINT ( 'NONE',  ( 5.326977496836527770, -2.920487667080175154, 32.31805714834170828 ) ) ;
#45710 = CARTESIAN_POINT ( 'NONE',  ( -16.15384615384615330, -2.538708090699994813, 30.37095296980875503 ) ) ;
#45711 = AXIS2_PLACEMENT_3D ( 'NONE', #5284, #5725, #88173 ) ;
#45712 = CARTESIAN_POINT ( 'NONE',  ( 6.923076923076924238, -11.91647553114624181, 32.58852847137148245 ) ) ;
#45713 = ADVANCED_FACE ( 'NONE', ( #38243 ), #31486, .F. ) ;
#45714 = B_SPLINE_CURVE_WITH_KNOTS ( 'NONE', 3,
 ( #48158, #14835, #54926, #20259, #60792, #68006, #20695, #28332, #13934, #27015 ),
 .UNSPECIFIED., .F., .F.,
 ( 4, 2, 2, 2, 4 ),
 ( 0.000000000000000000, 0.0001954311564186876063, 0.0003908623128373752125, 0.0005862934692560628188, 0.0007817246256747504250 ),
 .UNSPECIFIED. ) ;
#45715 = ORIENTED_EDGE ( 'NONE', *, *, #63569, .F. ) ;
#45716 = ORIENTED_EDGE ( 'NONE', *, *, #48862, .F. ) ;
#45717 = CARTESIAN_POINT ( 'NONE',  ( -8.835314180186648159, -12.37446782046654192, 30.86335684631486487 ) ) ;
#45718 = CYLINDRICAL_SURFACE ( 'NONE', #4295, 0.2500000000000004996 ) ;
#45719 = CARTESIAN_POINT ( 'NONE',  ( -2.557669051740897537, -2.318417181685854533, 30.59732222474233865 ) ) ;
#45720 = FACE_OUTER_BOUND ( 'NONE', #2626, .T. ) ;
#45721 = B_SPLINE_CURVE_WITH_KNOTS ( 'NONE', 3,
 ( #36370, #76911, #57959, #44426, #8459, #15216, #57072, #42688, #49870, #78678 ),
 .UNSPECIFIED., .F., .F.,
 ( 4, 2, 2, 2, 4 ),
 ( 0.0007817359430256399806, 0.0009771253907250089001, 0.001172514838424378036, 0.001367904286123746956, 0.001563293733823115875 ),
 .UNSPECIFIED. ) ;
#45722 = DIRECTION ( 'NONE',  ( 0.000000000000000000, 0.9848077530122072432, -0.1736481776669354937 ) ) ;
#45723 = CARTESIAN_POINT ( 'NONE',  ( -9.822998295418001291, -6.369640206132551441, 34.87707690430378449 ) ) ;
#45724 = B_SPLINE_CURVE_WITH_KNOTS ( 'NONE', 3,
 ( #76848, #57002, #84496, #22772, #69634, #64192, #83618, #2496, #21895, #29987 ),
 .UNSPECIFIED., .F., .F.,
 ( 4, 2, 2, 2, 4 ),
 ( 0.0007817246256747451124, 0.0009771112852218881168, 0.001172497944769031230, 0.001367884604316174126, 0.001563271263863317238 ),
 .UNSPECIFIED. ) ;
#45725 = VECTOR ( 'NONE', #30819, 1000.000000000000114 ) ;
#45726 = EDGE_CURVE ( 'NONE', #72078, #78012, #61470, .T. ) ;
#45727 = EDGE_LOOP ( 'NONE', ( #10943, #64229, #85187, #68648, #62124, #11777 ) ) ;
#45728 = CARTESIAN_POINT ( 'NONE',  ( -6.700297381808513641, -10.11255958852956027, 34.01340905677048454 ) ) ;
#45729 = VERTEX_POINT ( 'NONE', #19751 ) ;
#45730 = AXIS2_PLACEMENT_3D ( 'NONE', #76563, #76109, #28827 ) ;
#45731 = ORIENTED_EDGE ( 'NONE', *, *, #5592, .F. ) ;
#45732 = CARTESIAN_POINT ( 'NONE',  ( 0.5267936010512997980, -12.51329471203373700, 31.30864560766537963 ) ) ;
#45733 = CARTESIAN_POINT ( 'NONE',  ( -23.50000000000000000, -5.499999999999981348, 32.75000000000000000 ) ) ;
#45734 = CARTESIAN_POINT ( 'NONE',  ( 9.915319043920545639, -12.15243808032445827, 31.58219941686247978 ) ) ;
#45735 = DIRECTION ( 'NONE',  ( 0.000000000000000000, 0.000000000000000000, 1.000000000000000000 ) ) ;
#45736 = CARTESIAN_POINT ( 'NONE',  ( 20.00000000000000711, -9.999999999999994671, 3.000000000000000000 ) ) ;
#45737 = ORIENTED_EDGE ( 'NONE', *, *, #67363, .T. ) ;
#45738 = VERTEX_POINT ( 'NONE', #73364 ) ;
#45739 = EDGE_CURVE ( 'NONE', #65392, #42328, #36752, .T. ) ;
#45740 = EDGE_CURVE ( 'NONE', #78212, #78525, #8850, .T. ) ;
#45741 = VERTEX_POINT ( 'NONE', #26066 ) ;
#45742 = CARTESIAN_POINT ( 'NONE',  ( -7.173100147298381302, -12.07920672191015221, 32.31858351112116168 ) ) ;
#45743 = B_SPLINE_CURVE_WITH_KNOTS ( 'NONE', 3,
 ( #29232, #49495, #28783, #36852, #64754, #16145, #35983, #85491, #84181, #36424 ),
 .UNSPECIFIED., .F., .F.,
 ( 4, 2, 2, 2, 4 ),
 ( 0.0007817359430256315238, 0.0009771253907249980580, 0.001172514838424364592, 0.001367904286123731127, 0.001563293733823097661 ),
 .UNSPECIFIED. ) ;
#45744 = DIRECTION ( 'NONE',  ( -1.000000000000000000, -0.000000000000000000, -0.000000000000000000 ) ) ;
#45745 = CARTESIAN_POINT ( 'NONE',  ( 4.219913487196228274, -3.322132147404559976, 32.92929555188717927 ) ) ;
#45746 = DIRECTION ( 'NONE',  ( -1.000000000000000000, -0.000000000000000000, -0.000000000000000000 ) ) ;
#45747 = EDGE_CURVE ( 'NONE', #68539, #9053, #86227, .T. ) ;
#45748 = VECTOR ( 'NONE', #17321, 1000.000000000000114 ) ;
#45749 = CARTESIAN_POINT ( 'NONE',  ( -4.219170166650461518, -7.749976730030849303, 34.74374725381503737 ) ) ;
#45750 = CARTESIAN_POINT ( 'NONE',  ( 5.869852790561782108, -12.45813303252208648, 30.39737893381572675 ) ) ;
#45751 = EDGE_LOOP ( 'NONE', ( #62022, #56141 ) ) ;
#45752 = EDGE_CURVE ( 'NONE', #57312, #70118, #22878, .T. ) ;
#45753 = EDGE_LOOP ( 'NONE', ( #1896, #60335, #3611, #70117 ) ) ;
#45754 = CARTESIAN_POINT ( 'NONE',  ( 11.78846153846154010, -2.499999999999998668, 29.75000000000000355 ) ) ;
#45755 = AXIS2_PLACEMENT_3D ( 'NONE', #19703, #73776, #88193 ) ;
#45757 = ORIENTED_EDGE ( 'NONE', *, *, #75798, .T. ) ;
#45756 = CARTESIAN_POINT ( 'NONE',  ( 15.23076923076923173, -5.557115091759785130, 34.35708131394839171 ) ) ;
#45758 = LINE ( 'NONE', #4781, #23455 ) ;
#45759 = CARTESIAN_POINT ( 'NONE',  ( -2.307692307692428724, -4.320704448113951379, 33.92786785259630022 ) ) ;
#45760 = CARTESIAN_POINT ( 'NONE',  ( -3.230769230769229949, -9.780366693483667717, 34.19971097300155094 ) ) ;
#45761 = ORIENTED_EDGE ( 'NONE', *, *, #59037, .F. ) ;
#45762 = AXIS2_PLACEMENT_3D ( 'NONE', #48925, #83620, #76850 ) ;
#45763 = CARTESIAN_POINT ( 'NONE',  ( 10.74617505635156789, -2.295524264805589354, 30.44142389570982488 ) ) ;
#45764 = VERTEX_POINT ( 'NONE', #66613 ) ;
#45765 = LINE ( 'NONE', #52513, #85943 ) ;
#45766 = CARTESIAN_POINT ( 'NONE',  ( -19.50000000000000000, -3.499999999999999556, 29.75000000000000355 ) ) ;
#45767 = CARTESIAN_POINT ( 'NONE',  ( 7.622668921589514923, -4.225889041578354544, 33.85425143139329407 ) ) ;
#45769 = CYLINDRICAL_SURFACE ( 'NONE', #22783, 0.2499999999999995559 ) ;
#45768 = CARTESIAN_POINT ( 'NONE',  ( -6.857008572074484221, -12.37446782046654192, 30.86335684631486842 ) ) ;
#45770 = DIRECTION ( 'NONE',  ( 1.000000000000000000, -1.799314243699348838E-16, 1.560656329602356967E-32 ) ) ;
#45771 = ORIENTED_EDGE ( 'NONE', *, *, #64704, .T. ) ;
#45772 = CARTESIAN_POINT ( 'NONE',  ( 0.4615384615384611200, -2.292212530054420494, 30.41441678777542634 ) ) ;
#45773 = CARTESIAN_POINT ( 'NONE',  ( 11.31559527539844190, -2.251424796025574881, 29.88072029997477230 ) ) ;
#45774 = CYLINDRICAL_SURFACE ( 'NONE', #645, 0.2500000000000002220 ) ;
#45775 = ORIENTED_EDGE ( 'NONE', *, *, #86211, .T. ) ;
#45776 = CARTESIAN_POINT ( 'NONE',  ( -9.320512820512821150, -3.499999999999999556, 29.75000000000000355 ) ) ;
#45777 = CARTESIAN_POINT ( 'NONE',  ( -6.066083410955878108, -10.51840700105979387, 33.73612834413961536 ) ) ;
#45778 = DIRECTION ( 'NONE',  ( -1.000000000000000000, 0.000000000000000000, -0.000000000000000000 ) ) ;
#45779 = CARTESIAN_POINT ( 'NONE',  ( 10.55011416942383917, -11.94971097300153140, 32.03036669348370680 ) ) ;
#45780 = FACE_BOUND ( 'NONE', #40220, .T. ) ;
#45782 = CARTESIAN_POINT ( 'NONE',  ( -1.384615384615383471, -8.120952969808772792, 34.71129190930000163 ) ) ;
#45781 = CARTESIAN_POINT ( 'NONE',  ( 12.33139125210024112, -3.285722584762969856, 32.44110544564090759 ) ) ;
#45783 = CARTESIAN_POINT ( 'NONE',  ( -9.626240358957616650, -11.91647553114624358, 32.58852847137148245 ) ) ;
#45785 = CARTESIAN_POINT ( 'NONE',  ( 14.05771556364371833, -10.82459398097509329, 33.81372124010185587 ) ) ;
#45784 = CARTESIAN_POINT ( 'NONE',  ( -1.134669866267241423, -12.22109172314383052, 31.39792113162168263 ) ) ;
#45786 = CARTESIAN_POINT ( 'NONE',  ( -3.930833309752758797, -10.77377354290276301, 33.85451476688484718 ) ) ;
#45787 = CARTESIAN_POINT ( 'NONE',  ( 13.13459216039392707, -2.588893531581426988, 31.60682220781847818 ) ) ;
#45788 = AXIS2_PLACEMENT_3D ( 'NONE', #56844, #84340, #84783 ) ;
#45789 = CARTESIAN_POINT ( 'NONE',  ( 2.608446859217893099, -4.805146000318787358, 22.81063170625848713 ) ) ;
#45790 = CARTESIAN_POINT ( 'NONE',  ( -8.638705067467205012, -6.001044277235009439, 34.52024696741798948 ) ) ;
#45791 = ORIENTED_EDGE ( 'NONE', *, *, #81635, .F. ) ;
#45792 = CARTESIAN_POINT ( 'NONE',  ( 0.2380535178145125608, -6.760086850603068243, 34.69517049084099369 ) ) ;
#45793 = DIRECTION ( 'NONE',  ( -0.000000000000000000, 1.000000000000000000, -0.000000000000000000 ) ) ;
#45794 = LINE ( 'NONE', #25970, #35926 ) ;
#45795 = CARTESIAN_POINT ( 'NONE',  ( -2.437839517130528044, -11.93770438780619259, 32.05411857736982029 ) ) ;
#45796 = CARTESIAN_POINT ( 'NONE',  ( -17.01166793741023042, -2.379036618887895305, 30.90682066428158592 ) ) ;
#45797 = CARTESIAN_POINT ( 'NONE',  ( 6.130525438233648039, -3.625058011473227815, 33.29252011169590020 ) ) ;
#45798 = CARTESIAN_POINT ( 'NONE',  ( 3.749999999999999556, -7.438900925035446754, 26.71688170625849068 ) ) ;
#45799 = EDGE_CURVE ( 'NONE', #60707, #58077, #6673, .T. ) ;
#45800 = CARTESIAN_POINT ( 'NONE',  ( -9.692307692307814193, -3.643525952248795718, 33.31231777344771672 ) ) ;
#45801 = CYLINDRICAL_SURFACE ( 'NONE', #40331, 0.2499999999999997502 ) ;
#45802 = CARTESIAN_POINT ( 'NONE',  ( -12.46153846153846168, -9.058645607665452459, 34.76329471203371924 ) ) ;
#45803 = CARTESIAN_POINT ( 'NONE',  ( 5.076923076923075762, -9.058645607665452459, 34.76329471203371924 ) ) ;
#45804 = CARTESIAN_POINT ( 'NONE',  ( 14.43821800945587519, -6.001044277235009439, 34.52024696741798948 ) ) ;
#45805 = CARTESIAN_POINT ( 'NONE',  ( -19.99999999999996447, -12.00000000000000355, 13.00000000000000178 ) ) ;
#45806 = CARTESIAN_POINT ( 'NONE',  ( -2.057692307692291500, -2.249999999999999112, 29.81603969181031033 ) ) ;
#45807 = CARTESIAN_POINT ( 'NONE',  ( -11.40766973063675493, -10.54018710029568595, 33.71981072465678864 ) ) ;
#45808 = ORIENTED_EDGE ( 'NONE', *, *, #26817, .F. ) ;
#45809 = CARTESIAN_POINT ( 'NONE',  ( 17.20771488474786182, -2.729792928343269587, 31.24908615093345077 ) ) ;
#45810 = CARTESIAN_POINT ( 'NONE',  ( 8.769230769230768274, -11.16473453929635440, 33.15142922261926373 ) ) ;
#45811 = CARTESIAN_POINT ( 'NONE',  ( -0.06109907496450878162, -11.25000000000000000, 20.03311829374151287 ) ) ;
#45812 = EDGE_CURVE ( 'NONE', #20712, #77757, #54412, .T. ) ;
#45813 = CARTESIAN_POINT ( 'NONE',  ( 0.4615384615384611200, -3.513871655860378418, 32.76840700105978499 ) ) ;
#45815 = CARTESIAN_POINT ( 'NONE',  ( 17.20771488474786537, -11.71459661697925903, 32.44059661609676937 ) ) ;
#45814 = AXIS2_PLACEMENT_3D ( 'NONE', #10910, #3254, #11349 ) ;
#45816 = ORIENTED_EDGE ( 'NONE', *, *, #16777, .F. ) ;
#45817 = CARTESIAN_POINT ( 'NONE',  ( -3.230769230769229949, -1.117168528481311540, 33.14645433367849847 ) ) ;
#45818 = LINE ( 'NONE', #73300, #87711 ) ;
#45820 = ORIENTED_EDGE ( 'NONE', *, *, #79541, .F. ) ;
#45819 = CARTESIAN_POINT ( 'NONE',  ( -1.384615384615506484, -3.083524468854526912, 32.58852847137268327 ) ) ;
#45821 = CARTESIAN_POINT ( 'NONE',  ( -11.53846153846123102, -2.506253911140614576, 30.00000000000323297 ) ) ;
#45822 = CARTESIAN_POINT ( 'NONE',  ( 12.59233026936325039, -12.38066358083363738, 30.83685684665853444 ) ) ;
#45823 = ADVANCED_FACE ( 'NONE', ( #87342 ), #46334, .F. ) ;
#45824 = DIRECTION ( 'NONE',  ( -0.000000000000000000, -0.1736481776669307198, -0.9848077530122080203 ) ) ;
#45825 = DIRECTION ( 'NONE',  ( -0.000000000000000000, -0.6427876096865404731, -0.7660444431189771253 ) ) ;
#45826 = EDGE_LOOP ( 'NONE', ( #88189, #15525 ) ) ;
#45827 = CARTESIAN_POINT ( 'NONE',  ( 2.372947878968333590, -12.27809138561124591, 31.22303859784720359 ) ) ;
#45828 = DIRECTION ( 'NONE',  ( -0.000000000000000000, 0.9396926207859092051, -0.3420201433256662704 ) ) ;
#45829 = LINE ( 'NONE', #31436, #34100 ) ;
#45830 = ADVANCED_FACE ( 'NONE', ( #75569 ), #41804, .T. ) ;
#45831 = ORIENTED_EDGE ( 'NONE', *, *, #64306, .T. ) ;
#45832 = ORIENTED_EDGE ( 'NONE', *, *, #71929, .T. ) ;
#45833 = VERTEX_POINT ( 'NONE', #49869 ) ;
#45834 = ADVANCED_FACE ( 'NONE', ( #13872 ), #803, .F. ) ;
#45835 = CARTESIAN_POINT ( 'NONE',  ( -9.692307692307691624, -6.435427911321262684, 35.78748833219616898 ) ) ;
#45836 = CARTESIAN_POINT ( 'NONE',  ( -3.230769230769229949, -2.833524468853757305, 32.15551576947925838 ) ) ;
#45837 = CARTESIAN_POINT ( 'NONE',  ( -12.46153846153846168, -3.513871655860378418, 32.76840700105978499 ) ) ;
#45838 = B_SPLINE_CURVE_WITH_KNOTS ( 'NONE', 3,
 ( #2858, #22265, #56049, #43425, #85303, #83984, #37537, #49731, #23585, #63687 ),
 .UNSPECIFIED., .F., .F.,
 ( 4, 2, 2, 2, 4 ),
 ( 0.000000000000000000, 0.0001954311564186868473, 0.0003908623128373736946, 0.0005862934692560605419, 0.0007817246256747473893 ),
 .UNSPECIFIED. ) ;
#45839 = CARTESIAN_POINT ( 'NONE',  ( 20.00000000000000000, -4.000000000000000000, 29.75000000000000355 ) ) ;
#45840 = EDGE_CURVE ( 'NONE', #64311, #53642, #15655, .T. ) ;
#45841 = ORIENTED_EDGE ( 'NONE', *, *, #28390, .T. ) ;
#45842 = ORIENTED_EDGE ( 'NONE', *, *, #59827, .F. ) ;
#45845 = VERTEX_POINT ( 'NONE', #14318 ) ;
#45844 = EDGE_CURVE ( 'NONE', #51826, #71762, #14270, .T. ) ;
#45843 = CARTESIAN_POINT ( 'NONE',  ( 11.60371667797437567, -11.67786785259547777, 32.92929555188713664 ) ) ;
#45846 = CARTESIAN_POINT ( 'NONE',  ( -5.326946301144536378, -2.588893531581426544, 31.60682220781847818 ) ) ;
#45847 = AXIS2_PLACEMENT_3D ( 'NONE', #3118, #65261, #3563 ) ;
#45848 = CARTESIAN_POINT ( 'NONE',  ( -3.480745974817821775, -4.818429247618089661, 34.26397095200675125 ) ) ;
#45849 = ADVANCED_FACE ( 'NONE', ( #69704 ), #34593, .F. ) ;
#45850 = EDGE_CURVE ( 'NONE', #67493, #28342, #7123, .T. ) ;
#45851 = FACE_OUTER_BOUND ( 'NONE', #12186, .T. ) ;
#45852 = CARTESIAN_POINT ( 'NONE',  ( 13.45068271796546178, -9.905515769479276145, 34.41647553114623292 ) ) ;
#45853 = ORIENTED_EDGE ( 'NONE', *, *, #12099, .F. ) ;
#45854 = ORIENTED_EDGE ( 'NONE', *, *, #58953, .F. ) ;
#45855 = EDGE_LOOP ( 'NONE', ( #39984, #11788 ) ) ;
#45857 = EDGE_LOOP ( 'NONE', ( #83413, #13921, #48465, #74883 ) ) ;
#45856 = CARTESIAN_POINT ( 'NONE',  ( 15.16549878480846125, -2.625532179533445198, 30.86335684631481513 ) ) ;
#45858 = CARTESIAN_POINT ( 'NONE',  ( 2.177001704582003594, -2.494641256782728966, 31.33461815524612959 ) ) ;
#45859 = CARTESIAN_POINT ( 'NONE',  ( -0.2387587925603958106, -4.989023458446561143, 34.36081565061822118 ) ) ;
#45860 = CARTESIAN_POINT ( 'NONE',  ( -9.019254006523732770, -10.76384336483936011, 33.53834819971076087 ) ) ;
#45861 = CARTESIAN_POINT ( 'NONE',  ( 10.61538461538461675, -12.09954503811598769, 35.62045528018868623 ) ) ;
#45862 = CARTESIAN_POINT ( 'NONE',  ( -2.057637996053991891, -11.28795663066794219, 33.01431243580653785 ) ) ;
#45863 = FACE_BOUND ( 'NONE', #59007, .T. ) ;
#45864 = CARTESIAN_POINT ( 'NONE',  ( 15.23076923076923173, -5.557115091759785130, 34.35708131394839171 ) ) ;
#45865 = CARTESIAN_POINT ( 'NONE',  ( 17.07692307692307665, -12.09954503811598769, 35.62045528018868623 ) ) ;
#45866 = CARTESIAN_POINT ( 'NONE',  ( -7.976301055592070810, -12.27039167877662251, 31.24851455888617835 ) ) ;
#45868 = CARTESIAN_POINT ( 'NONE',  ( -5.207614543590636913, -3.062553014421049546, 32.05460306192773601 ) ) ;
#45867 = CARTESIAN_POINT ( 'NONE',  ( 16.21991348719623005, -3.937682226553329556, 33.60647404775216529 ) ) ;
#45869 = AXIS2_PLACEMENT_3D ( 'NONE', #55147, #82645, #34877 ) ;
#45870 = LINE ( 'NONE', #88669, #23670 ) ;
#45871 = CARTESIAN_POINT ( 'NONE',  ( -19.00000000000000000, -8.999999999999994671, 30.24999999999999645 ) ) ;
#45872 = ORIENTED_EDGE ( 'NONE', *, *, #819, .T. ) ;
#45873 = CARTESIAN_POINT ( 'NONE',  ( 11.28848480751918437, -3.137211980971221781, 32.19342716148376837 ) ) ;
#45874 = CARTESIAN_POINT ( 'NONE',  ( -7.846153846153844924, -6.435427911321262684, 35.78748833219616898 ) ) ;
#45875 = ORIENTED_EDGE ( 'NONE', *, *, #7511, .T. ) ;
#45876 = ORIENTED_EDGE ( 'NONE', *, *, #6509, .T. ) ;
#45877 = VECTOR ( 'NONE', #37662, 1000.000000000000000 ) ;
#45879 = CYLINDRICAL_SURFACE ( 'NONE', #40531, 0.2500000000000008882 ) ;
#45878 = CARTESIAN_POINT ( 'NONE',  ( 5.999999999999880096, -6.879047030192662504, 34.71129190930017927 ) ) ;
#45880 = VECTOR ( 'NONE', #82818, 1000.000000000000114 ) ;
#45881 = CARTESIAN_POINT ( 'NONE',  ( 16.28463796167094202, -2.541949514083464479, 30.39797389878540557 ) ) ;
#45882 = CARTESIAN_POINT ( 'NONE',  ( -13.38461538461538325, -4.661471528628507777, 34.16647553114623292 ) ) ;
#45883 = CARTESIAN_POINT ( 'NONE',  ( 12.39545608217832218, -10.67929555188718460, 33.92786785259543336 ) ) ;
#45884 = ORIENTED_EDGE ( 'NONE', *, *, #5857, .T. ) ;
#45885 = ADVANCED_FACE ( 'NONE', ( #62929 ), #28730, .T. ) ;
#45886 = DIRECTION ( 'NONE',  ( -1.000000000000000000, 0.000000000000000000, -0.000000000000000000 ) ) ;
#45887 = CARTESIAN_POINT ( 'NONE',  ( 18.13079044096695469, -2.494656445102014342, 31.33466734024120015 ) ) ;
#45889 = CARTESIAN_POINT ( 'NONE',  ( 15.23076923076911093, -12.27809138561165270, 31.22303859784587132 ) ) ;
#45888 = FACE_OUTER_BOUND ( 'NONE', #9995, .T. ) ;
#45890 = CARTESIAN_POINT ( 'NONE',  ( 17.07692307692307665, -6.386643153685126251, 34.62446782046654192 ) ) ;
#45891 = CARTESIAN_POINT ( 'NONE',  ( 0.6845513056318550671, -4.762714258010882773, 34.23016756924214832 ) ) ;
#45892 = CARTESIAN_POINT ( 'NONE',  ( 2.438482748659258625, -5.496552790871119143, 34.60292014791297532 ) ) ;
#45893 = CARTESIAN_POINT ( 'NONE',  ( 2.651650429449539104, -4.848349570550432475, 23.06250000000000000 ) ) ;
#45894 = ORIENTED_EDGE ( 'NONE', *, *, #77281, .T. ) ;
#45895 = ORIENTED_EDGE ( 'NONE', *, *, #23274, .T. ) ;
#45896 = CARTESIAN_POINT ( 'NONE',  ( 5.142178648199100977, -6.879047030191282275, 34.71129190930002295 ) ) ;
#45897 = DIRECTION ( 'NONE',  ( -0.000000000000000000, -0.1736481776669307198, -0.9848077530122080203 ) ) ;
#45898 = DIRECTION ( 'NONE',  ( -0.000000000000000000, 1.000000000000000000, -0.000000000000000000 ) ) ;
#45899 = CARTESIAN_POINT ( 'NONE',  ( -14.08468095607945969, -6.503523203565941380, 34.64991518177335195 ) ) ;
#45900 = CARTESIAN_POINT ( 'NONE',  ( 1.384615384615386802, -13.20930481340135110, 34.54067556320372745 ) ) ;
#45901 = CARTESIAN_POINT ( 'NONE',  ( -1.553300858899081538, -11.25000000000000711, 23.60937500000000711 ) ) ;
#45902 = EDGE_CURVE ( 'NONE', #43445, #85648, #63709, .T. ) ;
#45903 = EDGE_CURVE ( 'NONE', #82221, #31128, #77348, .T. ) ;
#45904 = DIRECTION ( 'NONE',  ( -0.000000000000000000, 0.5000000000000011102, -0.8660254037844381525 ) ) ;
#45905 = CARTESIAN_POINT ( 'NONE',  ( 1.450683735617824599, -4.786620604624113540, 33.94971097300155805 ) ) ;
#45906 = CARTESIAN_POINT ( 'NONE',  ( -8.769230769230892619, -12.70778746994576025, 30.41441678777401236 ) ) ;
#45907 = CARTESIAN_POINT ( 'NONE',  ( 12.46153846153833911, -11.67786785259630911, 32.92929555188603530 ) ) ;
#45908 = LINE ( 'NONE', #39176, #10920 ) ;
#45909 = CARTESIAN_POINT ( 'NONE',  ( 13.44987052412822059, -2.657715359629132301, 31.77849191805844242 ) ) ;
#45910 = CYLINDRICAL_SURFACE ( 'NONE', #19327, 0.2499999999999986955 ) ;
#45911 = CARTESIAN_POINT ( 'NONE',  ( 6.989144256427000990, -2.292212530054420494, 30.41441678777542990 ) ) ;
#45912 = CARTESIAN_POINT ( 'NONE',  ( -6.249976730942353065, -9.943427161483782584, 34.11278801902876978 ) ) ;
#45913 = CARTESIAN_POINT ( 'NONE',  ( 23.00000000000000000, -5.499999999999981348, 27.25000000000000000 ) ) ;
#45914 = VERTEX_POINT ( 'NONE', #55298 ) ;
#45915 = VECTOR ( 'NONE', #17777, 1000.000000000000114 ) ;
#45916 = CARTESIAN_POINT ( 'NONE',  ( 8.992010438208831502, -4.989023458446560255, 34.36081565061822118 ) ) ;
#45917 = CARTESIAN_POINT ( 'NONE',  ( 20.99999999999999645, -10.75000000000000000, 29.75000000000000355 ) ) ;
#45918 = CARTESIAN_POINT ( 'NONE',  ( -4.153846153846274980, -5.941354392335915335, 34.76329471203413846 ) ) ;
#45919 = CARTESIAN_POINT ( 'NONE',  ( 1.987747218494642309, -5.598659921968629050, 18.31436829374150932 ) ) ;
#45920 = EDGE_CURVE ( 'NONE', #58039, #73779, #35029, .T. ) ;
#45921 = DIRECTION ( 'NONE',  ( 1.000000000000000000, 0.000000000000000000, 0.000000000000000000 ) ) ;
#45922 = CARTESIAN_POINT ( 'NONE',  ( 14.30769230769218581, -5.094484230521993062, 34.41647553114689373 ) ) ;
#45924 = EDGE_LOOP ( 'NONE', ( #50423, #69756, #32492, #19057, #71145 ) ) ;
#45923 = CARTESIAN_POINT ( 'NONE',  ( -0.2385271099256127125, -2.554770724473667709, 30.48948780036025852 ) ) ;
#45925 = CARTESIAN_POINT ( 'NONE',  ( -1.944543648262992530, -9.444543648263016067, 17.43750000000000000 ) ) ;
#45926 = CARTESIAN_POINT ( 'NONE',  ( 3.361294669002875324, -8.630441415882550871, 34.87705825610312615 ) ) ;
#45927 = EDGE_CURVE ( 'NONE', #43633, #28226, #15399, .T. ) ;
#45928 = ORIENTED_EDGE ( 'NONE', *, *, #89077, .F. ) ;
#45929 = CARTESIAN_POINT ( 'NONE',  ( -7.146003881983769901, -11.43668979543635089, 33.22377378376089752 ) ) ;
#45930 = ORIENTED_EDGE ( 'NONE', *, *, #23986, .T. ) ;
#45931 = CARTESIAN_POINT ( 'NONE',  ( 3.230769230769108269, -5.094484230521993062, 34.41647553114689373 ) ) ;
#45932 = CARTESIAN_POINT ( 'NONE',  ( -1.384615384615383471, -11.91647553114624181, 32.58852847137148245 ) ) ;
#45933 = CARTESIAN_POINT ( 'NONE',  ( -1.634592115557738312, -4.236021600441998380, 33.53823185664189310 ) ) ;
#45934 = EDGE_CURVE ( 'NONE', #63430, #27372, #85882, .T. ) ;
#45935 = ORIENTED_EDGE ( 'NONE', *, *, #81970, .T. ) ;
#45936 = CARTESIAN_POINT ( 'NONE',  ( 6.923076923076924238, -13.53365097954675988, 30.81389545987213552 ) ) ;
#45937 = VERTEX_POINT ( 'NONE', #65151 ) ;
#45938 = CARTESIAN_POINT ( 'NONE',  ( -5.777220331021931443, -2.353885683473779800, 30.79025554430704759 ) ) ;
#45939 = ORIENTED_EDGE ( 'NONE', *, *, #15646, .T. ) ;
#45940 = CIRCLE ( 'NONE', #68964, 8.000000000000000000 ) ;
#45941 = VECTOR ( 'NONE', #1003, 999.9999999999998863 ) ;
#45942 = CARTESIAN_POINT ( 'NONE',  ( 2.084765348785458272, -9.172386477786396597, 34.72672124145550043 ) ) ;
#45943 = CARTESIAN_POINT ( 'NONE',  ( 0.5276068125408986953, -11.16473453929635440, 33.15142922261926373 ) ) ;
#45944 = CARTESIAN_POINT ( 'NONE',  ( -10.36533030374629938, -6.567000820036036579, 34.66262288849541306 ) ) ;
#45945 = CARTESIAN_POINT ( 'NONE',  ( -39.05038313613820122, -2.499999999999999556, 29.75000000000000355 ) ) ;
#45946 = CARTESIAN_POINT ( 'NONE',  ( 7.053867364043876265, -8.191423895709842640, 34.95447573519442130 ) ) ;
#45947 = CARTESIAN_POINT ( 'NONE',  ( -7.134615384615385025, -3.499999999999999556, 29.75000000000000355 ) ) ;
#45948 = VECTOR ( 'NONE', #63145, 1000.000000000000000 ) ;
#45949 = CIRCLE ( 'NONE', #2796, 4.000000000000000000 ) ;
#45950 = LINE ( 'NONE', #24340, #39136 ) ;
#45951 = B_SPLINE_CURVE_WITH_KNOTS ( 'NONE', 3,
 ( #87617, #18255, #58333, #85829, #25002, #18707, #25899, #52471, #79955, #24107 ),
 .UNSPECIFIED., .F., .F.,
 ( 4, 2, 2, 2, 4 ),
 ( 0.000000000000000000, 0.0001954311564186865492, 0.0003908623128373730983, 0.0005862934692560596746, 0.0007817246256747461966 ),
 .UNSPECIFIED. ) ;
#45952 = EDGE_CURVE ( 'NONE', #73958, #44944, #84165, .T. ) ;
#45953 = VERTEX_POINT ( 'NONE', #29615 ) ;
#45954 = ORIENTED_EDGE ( 'NONE', *, *, #66564, .F. ) ;
#45955 = ORIENTED_EDGE ( 'NONE', *, *, #57448, .F. ) ;
#45957 = ORIENTED_EDGE ( 'NONE', *, *, #83055, .F. ) ;
#45956 = CYLINDRICAL_SURFACE ( 'NONE', #30007, 4.000000000000000000 ) ;
#45958 = EDGE_CURVE ( 'NONE', #37534, #68628, #57958, .T. ) ;
#45959 = EDGE_CURVE ( 'NONE', #70825, #58033, #62588, .T. ) ;
#45960 = CARTESIAN_POINT ( 'NONE',  ( 10.48469314871705826, -4.809359713505814149, 33.96456829005828837 ) ) ;
#45961 = CARTESIAN_POINT ( 'NONE',  ( 1.515407192440170636, -2.729792928343270031, 31.24908615093345432 ) ) ;
#45962 = ORIENTED_EDGE ( 'NONE', *, *, #57618, .F. ) ;
#45963 = CARTESIAN_POINT ( 'NONE',  ( -14.08491276642389423, -4.387253974876679230, 33.66317474335728832 ) ) ;
#45964 = ORIENTED_EDGE ( 'NONE', *, *, #85260, .T. ) ;
#45965 = CARTESIAN_POINT ( 'NONE',  ( 0.4615384615387678746, -2.506253911140615021, 30.00000000000323297 ) ) ;
#45966 = ORIENTED_EDGE ( 'NONE', *, *, #51582, .F. ) ;
#45967 = DIRECTION ( 'NONE',  ( -0.000000000000000000, 0.1736481776669307198, -0.9848077530122080203 ) ) ;
#45968 = CARTESIAN_POINT ( 'NONE',  ( -7.976845312821407852, -2.541943142973491554, 30.39792223712631980 ) ) ;
#45969 = EDGE_CURVE ( 'NONE', #40626, #51674, #85437, .T. ) ;
#45970 = CIRCLE ( 'NONE', #14284, 8.000000000000000000 ) ;
#45971 = CARTESIAN_POINT ( 'NONE',  ( -14.30769230769242739, -11.94971097300221174, 32.03036669348237098 ) ) ;
#45972 = FACE_BOUND ( 'NONE', #76779, .T. ) ;
#45973 = CARTESIAN_POINT ( 'NONE',  ( 17.14217821643591932, -6.835583212224605631, 34.95778746994559327 ) ) ;
#45974 = FACE_OUTER_BOUND ( 'NONE', #22795, .T. ) ;
#45975 = DIRECTION ( 'NONE',  ( -0.000000000000000000, -0.3420201433256694901, -0.9396926207859082059 ) ) ;
#45976 = CYLINDRICAL_SURFACE ( 'NONE', #14371, 0.2499999999999986955 ) ;
#45977 = EDGE_CURVE ( 'NONE', #13581, #56689, #6765, .T. ) ;
#45978 = CARTESIAN_POINT ( 'NONE',  ( 10.48477425576008848, -7.722926236386453702, 34.74524107206102030 ) ) ;
#45979 = CARTESIAN_POINT ( 'NONE',  ( 17.32697738856138869, -9.148310452688871663, 34.47095581063188519 ) ) ;
#45980 = ORIENTED_EDGE ( 'NONE', *, *, #1553, .T. ) ;
#45981 = CYLINDRICAL_SURFACE ( 'NONE', #37392, 0.2500000000000012212 ) ;
#45982 = ORIENTED_EDGE ( 'NONE', *, *, #8433, .F. ) ;
#45983 = ORIENTED_EDGE ( 'NONE', *, *, #61951, .F. ) ;
#45985 = DIRECTION ( 'NONE',  ( 0.000000000000000000, 0.8660254037844377084, -0.5000000000000015543 ) ) ;
#45984 = CARTESIAN_POINT ( 'NONE',  ( 5.934729999443680626, -12.16647553114622049, 32.15551576947930812 ) ) ;
#45986 = B_SPLINE_CURVE_WITH_KNOTS ( 'NONE', 3,
 ( #26965, #81474, #75157, #34154, #27843, #41361, #68827, #55308, #7577, #16428 ),
 .UNSPECIFIED., .F., .F.,
 ( 4, 2, 2, 2, 4 ),
 ( 0.000000000000000000, 0.0001954339857564079623, 0.0003908679715128159245, 0.0005863019572692238597, 0.0007817359430256318490 ),
 .UNSPECIFIED. ) ;
#45987 = CARTESIAN_POINT ( 'NONE',  ( -17.07692307692319744, -3.643525952248796163, 33.31231777344771672 ) ) ;
#45988 = CARTESIAN_POINT ( 'NONE',  ( -3.903791842207837259, -4.235687564193446164, 33.53795663066793509 ) ) ;
#45989 = LINE ( 'NONE', #41021, #86082 ) ;
#45990 = CARTESIAN_POINT ( 'NONE',  ( -2.241623956689868358, -2.721908614388771852, 31.22303859784725333 ) ) ;
#45991 = EDGE_LOOP ( 'NONE', ( #33562, #62833, #41406, #85993 ) ) ;
#45992 = EDGE_CURVE ( 'NONE', #43517, #59172, #24945, .T. ) ;
#45993 = CARTESIAN_POINT ( 'NONE',  ( 13.38461538461538680, -9.819645486525091727, 36.12317359536749706 ) ) ;
#45994 = CARTESIAN_POINT ( 'NONE',  ( -4.853911725310227077, -2.554770724473668153, 30.48948780036025852 ) ) ;
#45995 = CARTESIAN_POINT ( 'NONE',  ( -14.43838377435986864, -8.147922237126337563, 34.70805685702651999 ) ) ;
#45996 = AXIS2_PLACEMENT_3D ( 'NONE', #68573, #69017, #28033 ) ;
#45997 = CARTESIAN_POINT ( 'NONE',  ( 13.13459214732242408, -12.43535235679832596, 30.55408501211184813 ) ) ;
#45998 = ORIENTED_EDGE ( 'NONE', *, *, #15028, .T. ) ;
#45999 = EDGE_CURVE ( 'NONE', #56065, #44047, #17462, .T. ) ;
#46000 = ORIENTED_EDGE ( 'NONE', *, *, #70440, .T. ) ;
#46001 = CIRCLE ( 'NONE', #87758, 4.000000000000000000 ) ;
#46002 = PRODUCT_CONTEXT ( 'NONE', #13007, 'mechanical' ) ;
#46004 = EDGE_CURVE ( 'NONE', #765, #79986, #77605, .T. ) ;
#46003 = ORIENTED_EDGE ( 'NONE', *, *, #82932, .F. ) ;
#46005 = CARTESIAN_POINT ( 'NONE',  ( -11.25641025641025550, -11.00000000000000000, 29.75000000000000355 ) ) ;
#46006 = CARTESIAN_POINT ( 'NONE',  ( -13.13456107297706588, -10.66356715214248396, 33.62249196103329751 ) ) ;
#46007 = VERTEX_POINT ( 'NONE', #38583 ) ;
#46008 = CARTESIAN_POINT ( 'NONE',  ( -16.02305434602136103, -4.809403383903226192, 33.96459661697924304 ) ) ;
#46009 = CARTESIAN_POINT ( 'NONE',  ( -5.326946314216042921, -2.823816976329319495, 31.52131813110795733 ) ) ;
#46010 = CARTESIAN_POINT ( 'NONE',  ( -7.846153846153844924, -11.69971097300155272, 32.46337939537588113 ) ) ;
#46011 = DIRECTION ( 'NONE',  ( -1.000000000000000000, -0.000000000000000000, -0.000000000000000000 ) ) ;
#46012 = VECTOR ( 'NONE', #87486, 1000.000000000000000 ) ;
#46013 = AXIS2_PLACEMENT_3D ( 'NONE', #17637, #30692, #42559 ) ;
#46014 = EDGE_CURVE ( 'NONE', #40406, #53195, #41074, .T. ) ;
#46015 = DIRECTION ( 'NONE',  ( 0.000000000000000000, 1.000000000000000000, 0.000000000000000000 ) ) ;
#46016 = ORIENTED_EDGE ( 'NONE', *, *, #45726, .F. ) ;
#46017 = AXIS2_PLACEMENT_3D ( 'NONE', #58783, #86285, #25001 ) ;
#46019 = ORIENTED_EDGE ( 'NONE', *, *, #29865, .F. ) ;
#46018 = CYLINDRICAL_SURFACE ( 'NONE', #26610, 4.000000000000000000 ) ;
#46020 = CARTESIAN_POINT ( 'NONE',  ( -19.50000000000000000, -3.499999999999999556, 29.75000000000000355 ) ) ;
#46021 = LINE ( 'NONE', #32958, #24017 ) ;
#46022 = B_SPLINE_CURVE_WITH_KNOTS ( 'NONE', 3,
 ( #21220, #954, #63533, #70300, #36944, #84277, #84720, #63084, #69858, #49585 ),
 .UNSPECIFIED., .F., .F.,
 ( 4, 2, 2, 2, 4 ),
 ( 0.0007817246256747442451, 0.0009771112852218868158, 0.001172497944769029278, 0.001367884604316171740, 0.001563271263863314203 ),
 .UNSPECIFIED. ) ;
#46023 = CARTESIAN_POINT ( 'NONE',  ( -13.63463862190834952, -5.056417327199099532, 34.11270091957321426 ) ) ;
#46024 = CYLINDRICAL_SURFACE ( 'NONE', #58136, 4.000000000000000000 ) ;
#46025 = CARTESIAN_POINT ( 'NONE',  ( 13.13459216039392707, -4.175268141568685643, 33.81360843649122216 ) ) ;
#46026 = EDGE_CURVE ( 'NONE', #30760, #15316, #4804, .T. ) ;
#46027 = CARTESIAN_POINT ( 'NONE',  ( 9.468822748583747284, -6.760086850603066466, 34.69517049084099369 ) ) ;
#46028 = CARTESIAN_POINT ( 'NONE',  ( 1.987747218494642309, -5.598659921968629050, 14.56436829374151287 ) ) ;
#46029 = EDGE_LOOP ( 'NONE', ( #27683, #17244, #85942, #17793 ) ) ;
#46030 = CARTESIAN_POINT ( 'NONE',  ( -3.480792468062196221, -3.202444869320336451, 32.30641848906366675 ) ) ;
#46031 = CARTESIAN_POINT ( 'NONE',  ( 5.076923076923075762, -1.790695186598648903, 34.54067556320373455 ) ) ;
#46032 = LINE ( 'NONE', #17680, #695 ) ;
#46033 = EDGE_LOOP ( 'NONE', ( #12313, #62524, #75968, #53497 ) ) ;
#46034 = EDGE_LOOP ( 'NONE', ( #63335, #27242, #84282, #44169 ) ) ;
#46035 = CARTESIAN_POINT ( 'NONE',  ( -11.53846153846153655, -10.51840700105979565, 33.73612834413961536 ) ) ;
#46036 = CARTESIAN_POINT ( 'NONE',  ( 12.71148387091650278, -4.176053281294518804, 33.81426240980091791 ) ) ;
#46037 = EDGE_CURVE ( 'NONE', #60033, #80094, #19200, .T. ) ;
#46038 = CARTESIAN_POINT ( 'NONE',  ( -4.153846153846273204, -8.613356846316285953, 34.62446782046622218 ) ) ;
#46039 = CARTESIAN_POINT ( 'NONE',  ( -19.00000000000000000, 0.7500000000000059952, 24.75000000000000000 ) ) ;
#46040 = DIRECTION ( 'NONE',  ( 0.000000000000000000, 0.6427876096865368094, 0.7660444431189802339 ) ) ;
#46041 = LINE ( 'NONE', #17691, #10582 ) ;
#46042 = VERTEX_POINT ( 'NONE', #45776 ) ;
#46043 = CARTESIAN_POINT ( 'NONE',  ( -16.37677311275299985, -6.459968553980840689, 34.89616026154728701 ) ) ;
#46044 = CARTESIAN_POINT ( 'NONE',  ( -2.177166605928744669, -10.19071101563364401, 33.96452234770658407 ) ) ;
#46045 = CARTESIAN_POINT ( 'NONE',  ( 3.903869409797562806, -8.347322224742351082, 34.93158281831414769 ) ) ;
#46046 = B_SPLINE_CURVE_WITH_KNOTS ( 'NONE', 3,
 ( #72339, #38116, #3877, #54729, #5664, #13310, #82220, #81781, #27266, #61049 ),
 .UNSPECIFIED., .F., .F.,
 ( 4, 2, 2, 2, 4 ),
 ( 0.0007817246256747455461, 0.0009771112852218885505, 0.001172497944769031446, 0.001367884604316174559, 0.001563271263863317455 ),
 .UNSPECIFIED. ) ;
#46048 = VERTEX_POINT ( 'NONE', #53414 ) ;
#46047 = AXIS2_PLACEMENT_3D ( 'NONE', #29639, #42273, #14797 ) ;
#46049 = CARTESIAN_POINT ( 'NONE',  ( 12.46153846153833911, -3.835265460704628371, 33.15142922262033665 ) ) ;
#46050 = B_SPLINE_CURVE_WITH_KNOTS ( 'NONE', 3,
 ( #9910, #85577, #79267, #18457, #45912, #37372, #38719, #73396, #66180, #44123 ),
 .UNSPECIFIED., .F., .F.,
 ( 4, 2, 2, 2, 4 ),
 ( 0.000000000000000000, 0.0001954339857564091278, 0.0003908679715128182556, 0.0005863019572692274375, 0.0007817359430256365111 ),
 .UNSPECIFIED. ) ;
#46051 = VERTEX_POINT ( 'NONE', #25511 ) ;
#46052 = B_SPLINE_CURVE_WITH_KNOTS ( 'NONE', 3,
 ( #27314, #48016, #1617, #40833, #56115, #75493, #76381, #55223, #54776, #34068 ),
 .UNSPECIFIED., .F., .F.,
 ( 4, 2, 2, 2, 4 ),
 ( 0.000000000000000000, 0.0001954339857564080978, 0.0003908679715128161956, 0.0005863019572692242934, 0.0007817359430256323911 ),
 .UNSPECIFIED. ) ;
#46053 = CARTESIAN_POINT ( 'NONE',  ( -0.3310127597748995232, -2.882268652242222728, 31.66798894389554064 ) ) ;
#46054 = CARTESIAN_POINT ( 'NONE',  ( 16.15384615384646949, -2.255955759149395501, 30.00000000000324363 ) ) ;
#46055 = CARTESIAN_POINT ( 'NONE',  ( 6.000000000000001776, -11.91647553114624181, 32.58852847137148245 ) ) ;
#46056 = ORIENTED_EDGE ( 'NONE', *, *, #55918, .T. ) ;
#46057 = B_SPLINE_CURVE_WITH_KNOTS ( 'NONE', 3,
 ( #24215, #36421, #50354, #58895, #77837, #63877, #2175, #51672, #29663, #16141 ),
 .UNSPECIFIED., .F., .F.,
 ( 4, 2, 2, 2, 4 ),
 ( 0.0007817359430256288133, 0.0009771253907249948054, 0.001172514838424360689, 0.001367904286123726573, 0.001563293733823092457 ),
 .UNSPECIFIED. ) ;
#46058 = CARTESIAN_POINT ( 'NONE',  ( -8.769230769230768274, -10.67929555188718282, 33.92786785259544047 ) ) ;
#46059 = CARTESIAN_POINT ( 'NONE',  ( 13.38461538461538680, -9.058645607665452459, 34.76329471203371924 ) ) ;
#46060 = CARTESIAN_POINT ( 'NONE',  ( -9.757578138268465651, -2.625532179533444754, 30.86335684631481513 ) ) ;
#46061 = CARTESIAN_POINT ( 'NONE',  ( 8.519230769230768274, -7.500000000000001776, 34.75000000000000000 ) ) ;
#46062 = CARTESIAN_POINT ( 'NONE',  ( -5.011667937410237528, -11.06231777344671130, 33.60647404775212976 ) ) ;
#46063 = ORIENTED_EDGE ( 'NONE', *, *, #48215, .F. ) ;
#46064 = VECTOR ( 'NONE', #36359, 1000.000000000000227 ) ;
#46065 = FACE_BOUND ( 'NONE', #50547, .T. ) ;
#46066 = ORIENTED_EDGE ( 'NONE', *, *, #48301, .T. ) ;
#46067 = CARTESIAN_POINT ( 'NONE',  ( -14.98071481085577972, -6.523592122091592671, 34.90882529074906415 ) ) ;
#46068 = B_SPLINE_CURVE_WITH_KNOTS ( 'NONE', 3,
 ( #6518, #27665, #14598, #13708, #640, #68215, #33977, #54241, #54684, #61441 ),
 .UNSPECIFIED., .F., .F.,
 ( 4, 2, 2, 2, 4 ),
 ( 0.0007817246256747454377, 0.0009771112852218883336, 0.001172497944769031446, 0.001367884604316174342, 0.001563271263863317238 ),
 .UNSPECIFIED. ) ;
#46069 = CARTESIAN_POINT ( 'NONE',  ( -12.23875879256039489, -3.020022701398813236, 32.48759521482552515 ) ) ;
#46070 = EDGE_CURVE ( 'NONE', #27377, #5535, #80916, .T. ) ;
#46071 = VECTOR ( 'NONE', #24372, 1000.000000000000114 ) ;
#46072 = FACE_OUTER_BOUND ( 'NONE', #75291, .T. ) ;
#46073 = CARTESIAN_POINT ( 'NONE',  ( 12.46153846153833911, -5.094484230521993062, 34.41647553114689373 ) ) ;
#46074 = EDGE_CURVE ( 'NONE', #26040, #6052, #66038, .T. ) ;
#46075 = DIRECTION ( 'NONE',  ( 0.000000000000000000, 0.1736481776669267785, -0.9848077530122087975 ) ) ;
#46076 = LINE ( 'NONE', #38885, #43638 ) ;
#46077 = CARTESIAN_POINT ( 'NONE',  ( 12.46153846153846168, -9.780366693483667717, 34.19971097300155094 ) ) ;
#46078 = VECTOR ( 'NONE', #31307, 1000.000000000000000 ) ;
#46079 = AXIS2_PLACEMENT_3D ( 'NONE', #22504, #16190, #85983 ) ;
#46080 = ORIENTED_EDGE ( 'NONE', *, *, #49818, .F. ) ;
#46082 = ADVANCED_FACE ( 'NONE', ( #33154 ), #26843, .T. ) ;
#46081 = EDGE_LOOP ( 'NONE', ( #12737, #62543, #28397, #55598, #57569, #5367 ) ) ;
#46083 = AXIS2_PLACEMENT_3D ( 'NONE', #40051, #27845, #27404 ) ;
#46084 = ORIENTED_EDGE ( 'NONE', *, *, #46164, .T. ) ;
#46085 = ORIENTED_EDGE ( 'NONE', *, *, #81406, .F. ) ;
#46086 = ORIENTED_EDGE ( 'NONE', *, *, #79201, .T. ) ;
#46087 = CARTESIAN_POINT ( 'NONE',  ( 2.057669070399344768, -5.056417327199099532, 34.11270091957320716 ) ) ;
#46088 = CARTESIAN_POINT ( 'NONE',  ( -11.66915300512909859, -8.999036380462717588, 34.52022231692819076 ) ) ;
#46089 = EDGE_CURVE ( 'NONE', #73852, #9873, #25950, .T. ) ;
#46090 = CARTESIAN_POINT ( 'NONE',  ( -4.230769230769230838, -7.500000000000000000, 29.75000000000000355 ) ) ;
#46091 = LINE ( 'NONE', #85156, #19257 ) ;
#46092 = CARTESIAN_POINT ( 'NONE',  ( 13.38461538461526601, -8.613356846316285953, 34.62446782046622218 ) ) ;
#46093 = CARTESIAN_POINT ( 'NONE',  ( -6.130690603110308778, -2.845849958028613624, 32.17971566917920967 ) ) ;
#46094 = CARTESIAN_POINT ( 'NONE',  ( 20.00000000000000000, -7.500000000000000000, 33.75000000000000000 ) ) ;
#46095 = CARTESIAN_POINT ( 'NONE',  ( -3.903900635498011251, -10.76462480002816235, 33.53768742498949962 ) ) ;
#46096 = CARTESIAN_POINT ( 'NONE',  ( 0.3313912521002406741, -3.285722584762970744, 32.44110544564090759 ) ) ;
#46097 = ORIENTED_EDGE ( 'NONE', *, *, #80430, .F. ) ;
#46098 = ORIENTED_EDGE ( 'NONE', *, *, #68543, .T. ) ;
#46099 = VERTEX_POINT ( 'NONE', #26401 ) ;
#46101 = ORIENTED_EDGE ( 'NONE', *, *, #57479, .F. ) ;
#46100 = CARTESIAN_POINT ( 'NONE',  ( -11.66860874789975888, -12.45813303252208648, 30.39737893381572675 ) ) ;
#46103 = CARTESIAN_POINT ( 'NONE',  ( 18.25000000000000000, -2.249999999999998668, 29.75000000000000355 ) ) ;
#46102 = DIRECTION ( 'NONE',  ( -0.000000000000000000, -0.9396926207859092051, -0.3420201433256662704 ) ) ;
#46104 = CARTESIAN_POINT ( 'NONE',  ( 16.40384615384759215, -7.500000000000155431, 34.75000000000007105 ) ) ;
#46105 = CARTESIAN_POINT ( 'NONE',  ( 6.989145274079363368, -2.538708090699994813, 30.37095296980875503 ) ) ;
#46106 = FACE_BOUND ( 'NONE', #62998, .T. ) ;
#46107 = VERTEX_POINT ( 'NONE', #74589 ) ;
#46108 = VECTOR ( 'NONE', #71054, 1000.000000000000000 ) ;
#46109 = VERTEX_POINT ( 'NONE', #59738 ) ;
#46110 = DIRECTION ( 'NONE',  ( 0.000000000000000000, 0.9396926207859126468, 0.3420201433256571111 ) ) ;
#46111 = ADVANCED_FACE ( 'NONE', ( #67384 ), #33602, .F. ) ;
#46112 = ORIENTED_EDGE ( 'NONE', *, *, #80734, .T. ) ;
#46113 = FACE_BOUND ( 'NONE', #20602, .T. ) ;
#46114 = CARTESIAN_POINT ( 'NONE',  ( 18.75000000000000000, -3.499999999999999556, 29.75000000000000355 ) ) ;
#46115 = CARTESIAN_POINT ( 'NONE',  ( -13.38461538461538325, -1.129524287112498415, 32.06866353760679544 ) ) ;
#46116 = ORIENTED_EDGE ( 'NONE', *, *, #64839, .F. ) ;
#46117 = CARTESIAN_POINT ( 'NONE',  ( -1.254089946381738763, -5.915461855592777596, 34.75538340440931506 ) ) ;
#46118 = CARTESIAN_POINT ( 'NONE',  ( -6.792551484843277976, -2.372941743896878286, 30.88044141588254377 ) ) ;
#46119 = CARTESIAN_POINT ( 'NONE',  ( 2.057715563643718326, -11.47974371597207899, 33.17467449705390692 ) ) ;
#46120 = EDGE_LOOP ( 'NONE', ( #35762, #53011, #88354, #34569 ) ) ;
#46121 = CARTESIAN_POINT ( 'NONE',  ( 14.24242230713598900, -11.67786785259540849, 32.92929555188721480 ) ) ;
#46122 = CARTESIAN_POINT ( 'NONE',  ( 3.100622021331007172, -12.27039167877662251, 31.24851455888617835 ) ) ;
#46123 = CARTESIAN_POINT ( 'NONE',  ( -9.469528151039279251, -2.600157965045224451, 30.74683119005207743 ) ) ;
#46124 = ORIENTED_EDGE ( 'NONE', *, *, #15039, .F. ) ;
#46125 = B_SPLINE_CURVE_WITH_KNOTS ( 'NONE', 3,
 ( #58596, #85641, #86090, #82002, #39691, #6768, #34693, #81117, #13092, #12649 ),
 .UNSPECIFIED., .F., .F.,
 ( 4, 2, 2, 2, 4 ),
 ( 0.0007817359430256319575, 0.0009771253907249984917, 0.001172514838424365026, 0.001367904286123731343, 0.001563293733823097878 ),
 .UNSPECIFIED. ) ;
#46126 = EDGE_CURVE ( 'NONE', #65351, #40455, #80011, .T. ) ;
#46127 = FACE_OUTER_BOUND ( 'NONE', #69121, .T. ) ;
#46128 = CARTESIAN_POINT ( 'NONE',  ( -16.94613126909828793, -11.71459661697925903, 32.44059661609676937 ) ) ;
#46129 = EDGE_LOOP ( 'NONE', ( #61029, #68749 ) ) ;
#46130 = LINE ( 'NONE', #33510, #50179 ) ;
#46131 = DIRECTION ( 'NONE',  ( 0.000000000000000000, 0.7660444431189822323, -0.6427876096865344779 ) ) ;
#46132 = CARTESIAN_POINT ( 'NONE',  ( -14.37377468705243899, -2.486705287966279432, 31.30864560766542937 ) ) ;
#46133 = CARTESIAN_POINT ( 'NONE',  ( 16.08857615328984281, -11.06231777344662959, 33.60647404775220082 ) ) ;
#46134 = DIRECTION ( 'NONE',  ( 1.000000000000000000, 0.000000000000000000, 0.000000000000000000 ) ) ;
#46135 = DIRECTION ( 'NONE',  ( -0.000000000000000000, 0.6427876096865404731, -0.7660444431189771253 ) ) ;
#46137 = DIRECTION ( 'NONE',  ( 0.000000000000000000, 0.000000000000000000, 1.000000000000000000 ) ) ;
#46136 = CARTESIAN_POINT ( 'NONE',  ( -12.22435897435897267, -3.499999999999999556, 29.75000000000000355 ) ) ;
#46138 = EDGE_CURVE ( 'NONE', #43687, #46293, #6128, .T. ) ;
#46139 = ADVANCED_FACE ( 'NONE', ( #54299 ), #40367, .F. ) ;
#46140 = AXIS2_PLACEMENT_3D ( 'NONE', #41810, #22846, #83690 ) ;
#46141 = CARTESIAN_POINT ( 'NONE',  ( -3.453695448285378333, -2.554751324335734264, 30.48935550225260727 ) ) ;
#46142 = DIRECTION ( 'NONE',  ( -0.000000000000000000, -0.7660444431189791237, -0.6427876096865379196 ) ) ;
#46143 = CARTESIAN_POINT ( 'NONE',  ( -2.749999999999998224, -7.500000000000015987, 16.34375000000000000 ) ) ;
#46144 = EDGE_LOOP ( 'NONE', ( #44730, #22290 ) ) ;
#46145 = FACE_OUTER_BOUND ( 'NONE', #55392, .T. ) ;
#46146 = ORIENTED_EDGE ( 'NONE', *, *, #33556, .T. ) ;
#46147 = AXIS2_PLACEMENT_3D ( 'NONE', #15476, #8719, #16783 ) ;
#46148 = AXIS2_PLACEMENT_3D ( 'NONE', #11903, #39381, #46565 ) ;
#46149 = ORIENTED_EDGE ( 'NONE', *, *, #61937, .T. ) ;
#46150 = CYLINDRICAL_SURFACE ( 'NONE', #42759, 0.2499999999999994726 ) ;
#46151 = ORIENTED_EDGE ( 'NONE', *, *, #74618, .T. ) ;
#46152 = DIRECTION ( 'NONE',  ( 1.000000000000000000, 0.000000000000000000, 0.000000000000000000 ) ) ;
#46153 = CARTESIAN_POINT ( 'NONE',  ( -1.944543648263014957, -5.555456351737005249, 15.25000000000000000 ) ) ;
#46154 = CARTESIAN_POINT ( 'NONE',  ( -17.86947429823643674, -6.001044277235007662, 34.52024696741798948 ) ) ;
#46155 = ADVANCED_FACE ( 'NONE', ( #86795 ), #25066, .F. ) ;
#46156 = CARTESIAN_POINT ( 'NONE',  ( 5.749976762707035505, -11.37209801155882971, 32.91403422569032955 ) ) ;
#46157 = CARTESIAN_POINT ( 'NONE',  ( -7.846153846153965716, -6.026961402154118019, 34.52809138561165270 ) ) ;
#46158 = CARTESIAN_POINT ( 'NONE',  ( 8.769230769230768274, -10.67929555188718282, 33.92786785259544047 ) ) ;
#46159 = VECTOR ( 'NONE', #22851, 999.9999999999998863 ) ;
#46160 = CARTESIAN_POINT ( 'NONE',  ( -8.769230769230768274, -12.48256725967547354, 35.29906147534542527 ) ) ;
#46161 = CARTESIAN_POINT ( 'NONE',  ( 2.307692307692309264, -13.63283147151868846, 33.57946703557072254 ) ) ;
#46162 = CARTESIAN_POINT ( 'NONE',  ( 0.4615384615384611200, -2.486705287966279876, 31.30864560766543647 ) ) ;
#46163 = CARTESIAN_POINT ( 'NONE',  ( -2.651650429449565305, -4.848349570550461785, 21.50000000000000000 ) ) ;
#46164 = EDGE_CURVE ( 'NONE', #3413, #55616, #35366, .T. ) ;
#46165 = EDGE_CURVE ( 'NONE', #17652, #14701, #52950, .T. ) ;
#46166 = CARTESIAN_POINT ( 'NONE',  ( -6.989159302437059296, -4.661471528628507777, 34.16647553114621871 ) ) ;
#46167 = CARTESIAN_POINT ( 'NONE',  ( -16.15384615384584777, -2.506253911140615021, 30.00000000000323297 ) ) ;
#46168 = DIRECTION ( 'NONE',  ( -0.000000000000000000, 0.9848077530122086864, -0.1736481776669273891 ) ) ;
#46169 = EDGE_CURVE ( 'NONE', #32375, #87025, #40077, .T. ) ;
#46170 = ORIENTED_EDGE ( 'NONE', *, *, #50214, .F. ) ;
#46171 = ORIENTED_EDGE ( 'NONE', *, *, #46860, .F. ) ;
#46172 = CARTESIAN_POINT ( 'NONE',  ( 3.230769230769231726, -10.67929555188718282, 33.92786785259544047 ) ) ;
#46173 = CARTESIAN_POINT ( 'NONE',  ( 10.61538461538461675, -4.786620604624113540, 33.94971097300155094 ) ) ;
#46174 = CARTESIAN_POINT ( 'NONE',  ( -2.372962308248625085, -2.379036618887870880, 30.90682066428147934 ) ) ;
#46175 = CARTESIAN_POINT ( 'NONE',  ( 15.48076923077065103, -7.500000000000154543, 35.00000000000007105 ) ) ;
#46176 = CARTESIAN_POINT ( 'NONE',  ( 14.05771556364371655, -3.436278759898153901, 33.07459398097509506 ) ) ;
#46177 = CYLINDRICAL_SURFACE ( 'NONE', #74346, 0.2499999999999986955 ) ;
#46178 = AXIS2_PLACEMENT_3D ( 'NONE', #62982, #85055, #8509 ) ;
#46179 = VERTEX_POINT ( 'NONE', #69159 ) ;
#46180 = CARTESIAN_POINT ( 'NONE',  ( -6.923076923076922462, -9.780366693483667717, 34.19971097300155094 ) ) ;
#46181 = ORIENTED_EDGE ( 'NONE', *, *, #53042, .T. ) ;
#46182 = AXIS2_PLACEMENT_3D ( 'NONE', #66516, #4818, #74159 ) ;
#46184 = EDGE_CURVE ( 'NONE', #26559, #64833, #57270, .T. ) ;
#46183 = ORIENTED_EDGE ( 'NONE', *, *, #11494, .F. ) ;
#46185 = LINE ( 'NONE', #53374, #435 ) ;
#46186 = CARTESIAN_POINT ( 'NONE',  ( -5.076923076923199218, -11.06231777344772027, 33.60647404775119895 ) ) ;
#46187 = CARTESIAN_POINT ( 'NONE',  ( 9.942253210655836781, -12.22109172314383052, 31.39792113162168263 ) ) ;
#46188 = CARTESIAN_POINT ( 'NONE',  ( -0.4615384615385840772, -2.379036618888197285, 30.90682066428292885 ) ) ;
#46189 = CARTESIAN_POINT ( 'NONE',  ( 5.777073782483853392, -2.758268499246657957, 31.33685645148948140 ) ) ;
#46190 = ORIENTED_EDGE ( 'NONE', *, *, #58219, .T. ) ;
#46191 = B_SPLINE_CURVE_WITH_KNOTS ( 'NONE', 3,
 ( #13384, #6195, #67893, #68332, #6630, #60239, #12505, #61124, #26469, #32771 ),
 .UNSPECIFIED., .F., .F.,
 ( 4, 2, 2, 2, 4 ),
 ( 0.000000000000000000, 0.0001954339857564078809, 0.0003908679715128157619, 0.0005863019572692236428, 0.0007817359430256315238 ),
 .UNSPECIFIED. ) ;
#46192 = ORIENTED_EDGE ( 'NONE', *, *, #12099, .T. ) ;
#46193 = EDGE_LOOP ( 'NONE', ( #2356, #55619, #52929, #20018 ) ) ;
#46194 = CARTESIAN_POINT ( 'NONE',  ( 17.32697749683652688, -10.06805714834173138, 34.32951233291982618 ) ) ;
#46195 = LINE ( 'NONE', #17837, #53140 ) ;
#46196 = CARTESIAN_POINT ( 'NONE',  ( 8.769230769230768274, -5.471508081941601098, 34.59228464037088457 ) ) ;
#46197 = VECTOR ( 'NONE', #49085, 1000.000000000000227 ) ;
#46198 = CARTESIAN_POINT ( 'NONE',  ( 1.253923917947825206, -3.530157926970578508, 32.79014554554150607 ) ) ;
#46199 = CYLINDRICAL_SURFACE ( 'NONE', #49525, 0.2500000000000012212 ) ;
#46200 = ORIENTED_EDGE ( 'NONE', *, *, #9062, .T. ) ;
#46201 = ORIENTED_EDGE ( 'NONE', *, *, #42651, .T. ) ;
#46202 = CARTESIAN_POINT ( 'NONE',  ( -1.929879867024197893E-14, -3.750000000000000000, 25.40625000000000000 ) ) ;
#46203 = EDGE_CURVE ( 'NONE', #8388, #12765, #45468, .T. ) ;
#46205 = ORIENTED_EDGE ( 'NONE', *, *, #19278, .F. ) ;
#46204 = CARTESIAN_POINT ( 'NONE',  ( -5.933931648997560870, -3.050289026998446840, 32.03036669348366416 ) ) ;
#46206 = CARTESIAN_POINT ( 'NONE',  ( -9.757577692864012775, -10.33852847137145048, 34.16647553114627556 ) ) ;
#46207 = CARTESIAN_POINT ( 'NONE',  ( -11.53846153846153655, -3.322132147404559976, 32.92929555188717927 ) ) ;
#46208 = CARTESIAN_POINT ( 'NONE',  ( -3.749999999999988454, -9.053300858899127945, 17.51562500000000000 ) ) ;
#46209 = ORIENTED_EDGE ( 'NONE', *, *, #925, .T. ) ;
#46210 = DIRECTION ( 'NONE',  ( -0.000000000000000000, -0.000000000000000000, -1.000000000000000000 ) ) ;
#46211 = VERTEX_POINT ( 'NONE', #40806 ) ;
#46212 = CARTESIAN_POINT ( 'NONE',  ( -8.835313148590904220, -4.661471528628507777, 34.16647553114621871 ) ) ;
#46213 = DIRECTION ( 'NONE',  ( -0.000000000000000000, -0.5000000000000009992, -0.8660254037844380415 ) ) ;
#46214 = CARTESIAN_POINT ( 'NONE',  ( 7.846153846153723244, -4.320704448113951379, 33.92786785259630022 ) ) ;
#46216 = DIRECTION ( 'NONE',  ( 1.000000000000000000, 0.000000000000000000, 0.000000000000000000 ) ) ;
#46215 = CARTESIAN_POINT ( 'NONE',  ( -6.792285115252136407, -12.38066358083363738, 30.83685684665853444 ) ) ;
#46217 = B_SPLINE_CURVE_WITH_KNOTS ( 'NONE', 3,
 ( #23424, #4497, #51769, #65738, #43700, #78369, #36939, #2701, #23858, #9917 ),
 .UNSPECIFIED., .F., .F.,
 ( 4, 2, 2, 2, 4 ),
 ( 0.000000000000000000, 0.0001954339857564071491, 0.0003908679715128142982, 0.0005863019572692214744, 0.0007817359430256285964 ),
 .UNSPECIFIED. ) ;
#46218 = FACE_OUTER_BOUND ( 'NONE', #78585, .T. ) ;
#46219 = EDGE_LOOP ( 'NONE', ( #43992, #3570, #74823, #85078 ) ) ;
#46220 = EDGE_CURVE ( 'NONE', #81809, #35903, #51818, .T. ) ;
#46221 = CARTESIAN_POINT ( 'NONE',  ( 6.856993512121043466, -8.120952969808774569, 34.71129190930000163 ) ) ;
#46222 = CARTESIAN_POINT ( 'NONE',  ( -9.019207513279360100, -4.075325502946081535, 33.72974371597206300 ) ) ;
#46223 = EDGE_CURVE ( 'NONE', #76945, #25666, #33673, .T. ) ;
#46224 = DIRECTION ( 'NONE',  ( 1.000000000000000000, 0.000000000000000000, 0.000000000000000000 ) ) ;
#46225 = ORIENTED_EDGE ( 'NONE', *, *, #76943, .F. ) ;
#46226 = VECTOR ( 'NONE', #5863, 1000.000000000000000 ) ;
#46227 = DIRECTION ( 'NONE',  ( 1.000000000000000000, 0.000000000000000000, 0.000000000000000000 ) ) ;
#46228 = LINE ( 'NONE', #18314, #81423 ) ;
#46229 = CARTESIAN_POINT ( 'NONE',  ( -19.50000000000000000, -11.50000000000000000, 29.75000000000000355 ) ) ;
#46230 = CARTESIAN_POINT ( 'NONE',  ( 8.834485908743602067, -10.33852847137154107, 34.16647553114620450 ) ) ;
#46231 = FACE_BOUND ( 'NONE', #57591, .T. ) ;
#46233 = CARTESIAN_POINT ( 'NONE',  ( 16.15384615384615330, -8.164416787775445883, 34.95778746994557906 ) ) ;
#46232 = CARTESIAN_POINT ( 'NONE',  ( 13.38461538461526423, -12.16647553114689728, 32.15551576947799362 ) ) ;
#46234 = ADVANCED_FACE ( 'NONE', ( #2456 ), #71809, .F. ) ;
#46235 = CARTESIAN_POINT ( 'NONE',  ( -9.442253272394237840, -12.01375889529407281, 32.43194544308182969 ) ) ;
#46237 = CARTESIAN_POINT ( 'NONE',  ( 18.00000000000000000, -11.16473453929635440, 33.15142922261926373 ) ) ;
#46236 = CARTESIAN_POINT ( 'NONE',  ( 18.13052570176356326, -11.46989282347013095, 32.79007818306219946 ) ) ;
#46238 = CARTESIAN_POINT ( 'NONE',  ( -4.153846153846152411, -10.67929555188718282, 33.92786785259544047 ) ) ;
#46239 = VECTOR ( 'NONE', #86031, 1000.000000000000227 ) ;
#46240 = CARTESIAN_POINT ( 'NONE',  ( -8.769230769230768274, -3.513871655860378418, 32.76840700105978499 ) ) ;
#46241 = CARTESIAN_POINT ( 'NONE',  ( -3.775308065498766297, -6.007798216065450170, 27.42000670625849068 ) ) ;
#46242 = ORIENTED_EDGE ( 'NONE', *, *, #4871, .T. ) ;
#46243 = CARTESIAN_POINT ( 'NONE',  ( -8.546219417617917813, -5.667800583137506010, 34.40243808032445827 ) ) ;
#46244 = ORIENTED_EDGE ( 'NONE', *, *, #18792, .T. ) ;
#46245 = CARTESIAN_POINT ( 'NONE',  ( 1.161749962411747772, -2.501496062324912284, 29.88072118266895671 ) ) ;
#46246 = CARTESIAN_POINT ( 'NONE',  ( 16.15384615384615330, -12.62096338111211580, 30.90682066428153263 ) ) ;
#46247 = DIRECTION ( 'NONE',  ( 0.000000000000000000, 0.8660254037844377084, -0.5000000000000015543 ) ) ;
#46248 = CARTESIAN_POINT ( 'NONE',  ( -2.373775718648187816, -11.69971097300155272, 32.46337939537587403 ) ) ;
#46249 = CARTESIAN_POINT ( 'NONE',  ( 3.480714749117373774, -6.696923467548660192, 34.68552623307873972 ) ) ;
#46250 = CARTESIAN_POINT ( 'NONE',  ( -11.78843828251013015, -4.075325502946081535, 33.72974371597206300 ) ) ;
#46251 = CARTESIAN_POINT ( 'NONE',  ( -0.06109907496455085213, -3.750000000000000888, 25.15438170625849068 ) ) ;
#46252 = CARTESIAN_POINT ( 'NONE',  ( 15.00784227186238162, -11.98009711892699514, 32.48740034544076138 ) ) ;
#46253 = CARTESIAN_POINT ( 'NONE',  ( 6.923076923076924238, -8.810774026931790459, 35.74407628777942847 ) ) ;
#46254 = CARTESIAN_POINT ( 'NONE',  ( -0.4769952865663709130, -4.791317821203144867, 29.42381992869616880 ) ) ;
#46255 = CARTESIAN_POINT ( 'NONE',  ( 5.142990410273152513, -12.62096338111211757, 30.90682066428152908 ) ) ;
#46256 = CARTESIAN_POINT ( 'NONE',  ( 14.55763782604045176, -5.852078868378309373, 34.47109172314383585 ) ) ;
#46257 = CARTESIAN_POINT ( 'NONE',  ( 9.692307692307570832, -3.643525952248795718, 33.31231777344771672 ) ) ;
#46258 = CARTESIAN_POINT ( 'NONE',  ( -3.724691934501248802, -5.885600066136383646, 17.92374329374151287 ) ) ;
#46259 = EDGE_CURVE ( 'NONE', #29065, #43002, #57406, .T. ) ;
#46260 = CARTESIAN_POINT ( 'NONE',  ( 3.296935837360872146, -7.250054591869667497, 34.99404684341514127 ) ) ;
#46261 = CARTESIAN_POINT ( 'NONE',  ( 7.976679284387489410, -9.503571793651731880, 34.60286762892837942 ) ) ;
#46262 = VERTEX_POINT ( 'NONE', #24069 ) ;
#46263 = B_SPLINE_CURVE_WITH_KNOTS ( 'NONE', 3,
 ( #31950, #4007, #46345, #25184, #10783, #85999, #66622, #85553, #78787, #52649 ),
 .UNSPECIFIED., .F., .F.,
 ( 4, 2, 2, 2, 4 ),
 ( 0.0007817246256747469556, 0.0009771112852218892010, 0.001172497944769031230, 0.001367884604316173258, 0.001563271263863315504 ),
 .UNSPECIFIED. ) ;
#46264 = CARTESIAN_POINT ( 'NONE',  ( 16.40379156322419973, -4.932303261841487263, 34.32971442181322885 ) ) ;
#46265 = CARTESIAN_POINT ( 'NONE',  ( 15.29683656411930848, -10.67929555188718282, 33.92786785259544757 ) ) ;
#46266 = CARTESIAN_POINT ( 'NONE',  ( -0.06109907496450878162, -11.25000000000000000, 17.53311829374151287 ) ) ;
#46267 = B_SPLINE_CURVE_WITH_KNOTS ( 'NONE', 3,
 ( #69724, #49457, #28748, #8475, #63402, #29199, #56652, #44012, #22422, #23300 ),
 .UNSPECIFIED., .F., .F.,
 ( 4, 2, 2, 2, 4 ),
 ( 0.0007817246256747474977, 0.0009771112852218911526, 0.001172497944769034699, 0.001367884604316178462, 0.001563271263863322009 ),
 .UNSPECIFIED. ) ;
#46268 = CARTESIAN_POINT ( 'NONE',  ( 6.250054311638314708, -4.235687564193446164, 33.53795663066793509 ) ) ;
#46269 = CARTESIAN_POINT ( 'NONE',  ( -8.899921372341079717, -3.338472653186243644, 32.95098750199972670 ) ) ;
#46270 = ORIENTED_EDGE ( 'NONE', *, *, #31041, .T. ) ;
#46271 = DIRECTION ( 'NONE',  ( -0.000000000000000000, 1.000000000000000000, 3.491481338843133355E-15 ) ) ;
#46272 = DIRECTION ( 'NONE',  ( -1.000000000000000000, -0.000000000000000000, -0.000000000000000000 ) ) ;
#46274 = ORIENTED_EDGE ( 'NONE', *, *, #15660, .F. ) ;
#46273 = CARTESIAN_POINT ( 'NONE',  ( 7.846153846153846700, -2.486705287966279876, 31.30864560766543647 ) ) ;
#46275 = CARTESIAN_POINT ( 'NONE',  ( -13.63463860883683942, -10.18141759479407327, 34.26406193332782379 ) ) ;
#46276 = DIRECTION ( 'NONE',  ( -0.000000000000000000, 0.5000000000000011102, -0.8660254037844381525 ) ) ;
#46277 = CARTESIAN_POINT ( 'NONE',  ( -14.98082382139119062, -12.07971442181322175, 32.31769673815850297 ) ) ;
#46278 = AXIS2_PLACEMENT_3D ( 'NONE', #32853, #74739, #61197 ) ;
#46279 = CARTESIAN_POINT ( 'NONE',  ( -15.90384615384608757, -7.434744860731433924, 35.00000000000000711 ) ) ;
#46280 = ORIENTED_EDGE ( 'NONE', *, *, #3332, .F. ) ;
#46281 = CARTESIAN_POINT ( 'NONE',  ( -4.153846153846152411, -3.322132147404559976, 32.92929555188717927 ) ) ;
#46282 = CARTESIAN_POINT ( 'NONE',  ( -12.68502338610279523, -2.612411019501189369, 31.66733052389439962 ) ) ;
#46283 = CARTESIAN_POINT ( 'NONE',  ( 8.519254025182176449, -3.436278759898153901, 33.07459398097509506 ) ) ;
#46284 = VERTEX_POINT ( 'NONE', #64154 ) ;
#46285 = VERTEX_POINT ( 'NONE', #23185 ) ;
#46286 = VERTEX_POINT ( 'NONE', #37133 ) ;
#46287 = CARTESIAN_POINT ( 'NONE',  ( 0.2380535178145121722, -8.496056993536548418, 34.65000542017679663 ) ) ;
#46288 = CARTESIAN_POINT ( 'NONE',  ( -2.057746789344163663, -5.852078868378310261, 34.47109172314383585 ) ) ;
#46289 = CARTESIAN_POINT ( 'NONE',  ( 2.438484115517096651, -5.582136614379148654, 34.36778462344220486 ) ) ;
#46290 = CARTESIAN_POINT ( 'NONE',  ( -10.61538461538473577, -6.835583212225970762, 34.95778746994575670 ) ) ;
#46292 = B_SPLINE_CURVE_WITH_KNOTS ( 'NONE', 3,
 ( #8046, #88709, #26989, #6706, #54447, #69304 ),
 .UNSPECIFIED., .F., .F.,
 ( 4, 2, 4 ),
 ( 0.000000000000000000, 0.0001954784845028902421, 0.0003909569690057804843 ),
 .UNSPECIFIED. ) ;
#46291 = VECTOR ( 'NONE', #130, 1000.000000000000000 ) ;
#46293 = VERTEX_POINT ( 'NONE', #63719 ) ;
#46294 = ORIENTED_EDGE ( 'NONE', *, *, #81193, .F. ) ;
#46295 = ORIENTED_EDGE ( 'NONE', *, *, #52203, .F. ) ;
#46297 = ORIENTED_EDGE ( 'NONE', *, *, #75421, .T. ) ;
#46296 = CARTESIAN_POINT ( 'NONE',  ( -0.6089743589743593644, -7.500000000000000000, 33.75000000000000000 ) ) ;
#46298 = FACE_OUTER_BOUND ( 'NONE', #24915, .T. ) ;
#46299 = VECTOR ( 'NONE', #66878, 1000.000000000000000 ) ;
#46300 = CARTESIAN_POINT ( 'NONE',  ( 11.28846153846153832, -7.500000000000001776, 35.04278698407183867 ) ) ;
#46301 = CARTESIAN_POINT ( 'NONE',  ( -12.39547011053602610, -12.10708131394839882, 31.69288490824020954 ) ) ;
#46302 = CARTESIAN_POINT ( 'NONE',  ( -15.23076923076935074, -9.442884908241554243, 34.35708131394783038 ) ) ;
#46303 = VERTEX_POINT ( 'NONE', #50647 ) ;
#46304 = EDGE_LOOP ( 'NONE', ( #36850, #45568, #61729, #41685 ) ) ;
#46305 = ORIENTED_EDGE ( 'NONE', *, *, #77736, .F. ) ;
#46306 = CARTESIAN_POINT ( 'NONE',  ( -10.74607521849492464, -10.70098750199973203, 33.91152734681376302 ) ) ;
#46308 = ORIENTED_EDGE ( 'NONE', *, *, #2186, .T. ) ;
#46307 = FACE_OUTER_BOUND ( 'NONE', #25689, .T. ) ;
#46309 = CARTESIAN_POINT ( 'NONE',  ( 9.070512820512819374, -11.00000000000000000, 29.75000000000000355 ) ) ;
#46310 = CARTESIAN_POINT ( 'NONE',  ( -0.3310130233048168558, -5.070358843744209310, 34.40418822224088302 ) ) ;
#46311 = CARTESIAN_POINT ( 'NONE',  ( -11.40793610022789650, -4.299079248970732792, 33.91157788607253565 ) ) ;
#46312 = AXIS2_PLACEMENT_3D ( 'NONE', #42835, #1395, #82937 ) ;
#46313 = CARTESIAN_POINT ( 'NONE',  ( -1.450698795571263799, -8.120952969808774569, 34.71129190930000163 ) ) ;
#46314 = DIRECTION ( 'NONE',  ( -0.000000000000000000, -0.6427876096865404731, -0.7660444431189770143 ) ) ;
#46315 = FACE_BOUND ( 'NONE', #28161, .T. ) ;
#46316 = CARTESIAN_POINT ( 'NONE',  ( -5.207071046654770718, -10.31621877034669588, 34.18098118002070152 ) ) ;
#46317 = CARTESIAN_POINT ( 'NONE',  ( -12.68502340526241312, -9.331801661448606566, 34.40259984581193464 ) ) ;
#46318 = AXIS2_PLACEMENT_3D ( 'NONE', #3567, #86464, #31036 ) ;
#46319 = EDGE_CURVE ( 'NONE', #4757, #3, #70487, .T. ) ;
#46320 = CARTESIAN_POINT ( 'NONE',  ( 11.53846153846141753, -12.46129190930018460, 30.37095296980731973 ) ) ;
#46322 = CYLINDRICAL_SURFACE ( 'NONE', #13089, 0.2500000000000004996 ) ;
#46321 = CARTESIAN_POINT ( 'NONE',  ( -7.173076923076921574, -7.500000000000001776, 34.75000000000000000 ) ) ;
#46323 = VECTOR ( 'NONE', #63113, 1000.000000000000000 ) ;
#46324 = CARTESIAN_POINT ( 'NONE',  ( -3.930883019579477278, -7.369474539155830506, 34.99858011523957657 ) ) ;
#46325 = DIRECTION ( 'NONE',  ( 0.000000000000000000, 0.1736481776669267785, -0.9848077530122087975 ) ) ;
#46326 = ORIENTED_EDGE ( 'NONE', *, *, #45015, .T. ) ;
#46327 = CARTESIAN_POINT ( 'NONE',  ( -15.00775638667583500, -11.43677907613344757, 33.22367315496202167 ) ) ;
#46328 = ADVANCED_FACE ( 'NONE', ( #10566 ), #10115, .F. ) ;
#46329 = CARTESIAN_POINT ( 'NONE',  ( 12.94230769230769340, -11.50000000000000000, 29.75000000000000355 ) ) ;
#46330 = ORIENTED_EDGE ( 'NONE', *, *, #34606, .T. ) ;
#46331 = EDGE_LOOP ( 'NONE', ( #23231, #41211, #84247, #51069 ) ) ;
#46332 = AXIS2_PLACEMENT_3D ( 'NONE', #69320, #41852, #8947 ) ;
#46333 = DIRECTION ( 'NONE',  ( 0.000000000000000000, 0.000000000000000000, -1.000000000000000000 ) ) ;
#46334 = PLANE ( 'NONE',  #17086 ) ;
#46335 = LINE ( 'NONE', #66151, #51902 ) ;
#46336 = VERTEX_POINT ( 'NONE', #58295 ) ;
#46337 = CYLINDRICAL_SURFACE ( 'NONE', #18374, 0.2499999999999995559 ) ;
#46338 = CARTESIAN_POINT ( 'NONE',  ( -7.173053654019277303, -9.943427161483782584, 34.11278801902876978 ) ) ;
#46340 = CARTESIAN_POINT ( 'NONE',  ( -9.757578138268465651, -4.481592998940162609, 33.73612834413957984 ) ) ;
#46339 = DIRECTION ( 'NONE',  ( 0.000000000000000000, 0.000000000000000000, 1.000000000000000000 ) ) ;
#46341 = CARTESIAN_POINT ( 'NONE',  ( 18.00000000000000000, -11.11383981884818262, 36.00935417666054406 ) ) ;
#46342 = EDGE_CURVE ( 'NONE', #38566, #83848, #35809, .T. ) ;
#46343 = FACE_OUTER_BOUND ( 'NONE', #20934, .T. ) ;
#46345 = CARTESIAN_POINT ( 'NONE',  ( -16.94639763868943660, -2.647132371071621471, 31.75357179365173010 ) ) ;
#46344 = SHAPE_REPRESENTATION_RELATIONSHIP ( 'NONE' , 'NONE' ,  #60984, #923 ) ;
#46346 = CARTESIAN_POINT ( 'NONE',  ( -3.750000000000008438, -5.946699141100917352, 23.92187500000000355 ) ) ;
#46347 = EDGE_LOOP ( 'NONE', ( #12112, #47322, #72411, #50696, #32333 ) ) ;
#46348 = EDGE_LOOP ( 'NONE', ( #62884, #54169, #24724, #3039 ) ) ;
#46349 = CARTESIAN_POINT ( 'NONE',  ( -15.23076923076935252, -6.835583212225970762, 34.95778746994575670 ) ) ;
#46350 = CARTESIAN_POINT ( 'NONE',  ( 7.053602624840490165, -12.27024696741798770, 31.24895572276497546 ) ) ;
#46351 = DIRECTION ( 'NONE',  ( -0.000000000000000000, 0.8660254037844399289, -0.4999999999999980016 ) ) ;
#46352 = DIRECTION ( 'NONE',  ( -0.000000000000000000, -0.6427876096865404731, -0.7660444431189771253 ) ) ;
#46353 = DIRECTION ( 'NONE',  ( -0.000000000000000000, -0.9848077530122085754, -0.1736481776669273613 ) ) ;
#46354 = CARTESIAN_POINT ( 'NONE',  ( 3.749999999999992006, -5.946699141100872943, 21.89062500000000355 ) ) ;
#46355 = B_SPLINE_CURVE_WITH_KNOTS ( 'NONE', 3,
 ( #88424, #26696, #49070, #87093, #54154, #55829, #25367, #81651, #19934, #47400 ),
 .UNSPECIFIED., .F., .F.,
 ( 4, 2, 2, 2, 4 ),
 ( 0.000000000000000000, 0.0001954339857564070678, 0.0003908679715128141356, 0.0005863019572692211492, 0.0007817359430256282712 ),
 .UNSPECIFIED. ) ;
#46356 = CARTESIAN_POINT ( 'NONE',  ( -7.780085495151406683, -8.120952969808772792, 34.71129190929999453 ) ) ;
#46357 = DIRECTION ( 'NONE',  ( 0.000000000000000000, 0.1736481776669275834, 0.9848077530122086864 ) ) ;
#46358 = DIRECTION ( 'NONE',  ( -0.000000000000000000, 0.9848077530122085754, -0.1736481776669273613 ) ) ;
#46359 = DIRECTION ( 'NONE',  ( -0.000000000000000000, -0.7660444431189791237, -0.6427876096865379196 ) ) ;
#46360 = DIRECTION ( 'NONE',  ( 0.000000000000000000, 0.000000000000000000, -1.000000000000000000 ) ) ;
#46361 = CARTESIAN_POINT ( 'NONE',  ( 2.544871794871792936, -7.500000000000000000, 29.75000000000000355 ) ) ;
#46362 = VECTOR ( 'NONE', #19528, 1000.000000000000000 ) ;
#46363 = CARTESIAN_POINT ( 'NONE',  ( -12.68502338610279523, -8.539481045369596401, 34.89627647299170832 ) ) ;
#46364 = CARTESIAN_POINT ( 'NONE',  ( 6.923076923076800782, -2.379036618888197729, 30.90682066428292885 ) ) ;
#46365 = ADVANCED_FACE ( 'NONE', ( #79018 ), #43457, .T. ) ;
#46366 = CARTESIAN_POINT ( 'NONE',  ( -3.230769230769229949, -8.120952969808772792, 34.71129190930000163 ) ) ;
#46367 = LINE ( 'NONE', #24761, #28373 ) ;
#46368 = ADVANCED_FACE ( 'NONE', ( #16429 ), #43896, .F. ) ;
#46369 = AXIS2_PLACEMENT_3D ( 'NONE', #11269, #33326, #73422 ) ;
#46370 = ORIENTED_EDGE ( 'NONE', *, *, #87530, .T. ) ;
#46371 = LINE ( 'NONE', #67980, #74391 ) ;
#46372 = CARTESIAN_POINT ( 'NONE',  ( -17.07692307692307665, -6.343179335718451384, 34.87096338111211935 ) ) ;
#46373 = LINE ( 'NONE', #73856, #41943 ) ;
#46374 = CARTESIAN_POINT ( 'NONE',  ( 2.750000000000002665, -7.561099074964516831, 18.47061829374151287 ) ) ;
#46375 = EDGE_CURVE ( 'NONE', #27377, #64638, #32545, .T. ) ;
#46376 = EDGE_CURVE ( 'NONE', #36288, #8676, #22799, .T. ) ;
#46377 = FACE_OUTER_BOUND ( 'NONE', #14064, .T. ) ;
#46378 = SURFACE_STYLE_USAGE ( .BOTH. , #20673 ) ;
#46379 = EDGE_CURVE ( 'NONE', #68002, #16148, #25047, .T. ) ;
#46381 = ORIENTED_EDGE ( 'NONE', *, *, #14522, .F. ) ;
#46380 = CARTESIAN_POINT ( 'NONE',  ( 5.299702745901139878, -4.226511098958374291, 33.85474049983370293 ) ) ;
#46382 = CARTESIAN_POINT ( 'NONE',  ( -1.944543648263014957, -5.555456351737005249, 21.50000000000000000 ) ) ;
#46383 = CARTESIAN_POINT ( 'NONE',  ( -4.403846153846151523, -2.249999999999998668, 29.75000000000000355 ) ) ;
#46384 = ORIENTED_EDGE ( 'NONE', *, *, #54889, .F. ) ;
#46385 = CARTESIAN_POINT ( 'NONE',  ( 18.24994551834813805, -9.272278438253401589, 34.42582936511637826 ) ) ;
#46386 = ORIENTED_EDGE ( 'NONE', *, *, #30271, .F. ) ;
#46387 = CARTESIAN_POINT ( 'NONE',  ( 17.07692307692307665, -6.681629849574314051, 35.83090037661290239 ) ) ;
#46388 = CARTESIAN_POINT ( 'NONE',  ( -1.607542343522231576, -11.98009711892699691, 32.48740034544075428 ) ) ;
#46389 = CYLINDRICAL_SURFACE ( 'NONE', #25484, 0.2500000000000012212 ) ;
#46390 = ORIENTED_EDGE ( 'NONE', *, *, #68663, .T. ) ;
#46391 = VERTEX_POINT ( 'NONE', #25412 ) ;
#46392 = ORIENTED_EDGE ( 'NONE', *, *, #2631, .T. ) ;
#46394 = CARTESIAN_POINT ( 'NONE',  ( 7.846153846153846700, -3.513871655860378418, 32.76840700105978499 ) ) ;
#46393 = AXIS2_PLACEMENT_3D ( 'NONE', #75755, #14059, #76198 ) ;
#46395 = CARTESIAN_POINT ( 'NONE',  ( -0.3307466537136757312, -10.54018710029568595, 33.71981072465678864 ) ) ;
#46396 = B_SPLINE_CURVE_WITH_KNOTS ( 'NONE', 3,
 ( #49458, #15234, #42705, #62079, #1711, #37254, #16111, #64278, #9363, #78698 ),
 .UNSPECIFIED., .F., .F.,
 ( 4, 2, 2, 2, 4 ),
 ( 0.0007817359430256294638, 0.0009771253907249948054, 0.001172514838424360255, 0.001367904286123725489, 0.001563293733823090939 ),
 .UNSPECIFIED. ) ;
#46397 = CYLINDRICAL_SURFACE ( 'NONE', #72926, 0.2499999999999998890 ) ;
#46398 = FACE_OUTER_BOUND ( 'NONE', #4780, .T. ) ;
#46399 = LINE ( 'NONE', #59468, #74984 ) ;
#46400 = CARTESIAN_POINT ( 'NONE',  ( -3.007756386675836779, -4.762714258010882773, 34.23016756924214832 ) ) ;
#46401 = CARTESIAN_POINT ( 'NONE',  ( -1.134560964701931463, -10.82426656108011720, 33.81400080652039009 ) ) ;
#46402 = VECTOR ( 'NONE', #77726, 1000.000000000000227 ) ;
#46403 = CARTESIAN_POINT ( 'NONE',  ( -12.52762187249433978, -6.386643153685125363, 34.62446782046654903 ) ) ;
#46404 = EDGE_CURVE ( 'NONE', #70678, #33320, #46130, .T. ) ;
#46405 = ORIENTED_EDGE ( 'NONE', *, *, #56978, .F. ) ;
#46406 = ORIENTED_EDGE ( 'NONE', *, *, #83055, .T. ) ;
#46407 = ORIENTED_EDGE ( 'NONE', *, *, #31649, .F. ) ;
#46409 = ORIENTED_EDGE ( 'NONE', *, *, #66910, .F. ) ;
#46408 = CARTESIAN_POINT ( 'NONE',  ( -3.931066484868086075, -8.540255544307065350, 34.89611431652622286 ) ) ;
#46410 = B_SPLINE_CURVE_WITH_KNOTS ( 'NONE', 3,
 ( #59319, #11133, #86826, #80041, #18339, #4831, #37713, #32301, #17452, #73745 ),
 .UNSPECIFIED., .F., .F.,
 ( 4, 2, 2, 2, 4 ),
 ( 0.000000000000000000, 0.0001954311564186866034, 0.0003908623128373732067, 0.0005862934692560597830, 0.0007817246256747464135 ),
 .UNSPECIFIED. ) ;
#46411 = CARTESIAN_POINT ( 'NONE',  ( -11.53846153846153655, -1.790695186598648903, 34.54067556320373455 ) ) ;
#46412 = CARTESIAN_POINT ( 'NONE',  ( -4.153846153846273204, -11.94971097300221174, 32.03036669348237098 ) ) ;
#46413 = ORIENTED_EDGE ( 'NONE', *, *, #86511, .F. ) ;
#46414 = CARTESIAN_POINT ( 'NONE',  ( -14.08468095607945614, -4.187068189119699468, 33.49521262558774026 ) ) ;
#46415 = EDGE_CURVE ( 'NONE', #22316, #85987, #86328, .T. ) ;
#46416 = ORIENTED_EDGE ( 'NONE', *, *, #47419, .F. ) ;
#46417 = CARTESIAN_POINT ( 'NONE',  ( 11.66925334628632349, -2.541949514083464479, 30.39797389878540557 ) ) ;
#46418 = VERTEX_POINT ( 'NONE', #45678 ) ;
#46419 = DIRECTION ( 'NONE',  ( -0.000000000000000000, -1.000000000000000000, -8.673617379884033500E-16 ) ) ;
#46420 = CARTESIAN_POINT ( 'NONE',  ( -9.019207500173124004, -4.943428324936578910, 34.04746400365624481 ) ) ;
#46421 = CARTESIAN_POINT ( 'NONE',  ( -9.758061120621023932, -7.249945578846652694, 34.99404164642496795 ) ) ;
#46422 = FACE_BOUND ( 'NONE', #58252, .T. ) ;
#46423 = CARTESIAN_POINT ( 'NONE',  ( 17.20771351789002424, -6.369690395747422684, 34.87708834333098196 ) ) ;
#46424 = CYLINDRICAL_SURFACE ( 'NONE', #39965, 0.2499999999999995559 ) ;
#46425 = ADVANCED_FACE ( 'NONE', ( #4704 ), #31730, .F. ) ;
#46426 = DIRECTION ( 'NONE',  ( 0.000000000000000000, 0.000000000000000000, -1.000000000000000000 ) ) ;
#46427 = CARTESIAN_POINT ( 'NONE',  ( -3.296039676730006640, -4.481592998940161721, 33.73612834413957984 ) ) ;
#46428 = DIRECTION ( 'NONE',  ( -0.000000000000000000, -0.6427876096865404731, -0.7660444431189771253 ) ) ;
#46429 = LINE ( 'NONE', #73913, #37565 ) ;
#46430 = EDGE_LOOP ( 'NONE', ( #41771, #46725 ) ) ;
#46431 = CARTESIAN_POINT ( 'NONE',  ( -10.39237326377176451, -4.187068189119699468, 33.49521262558774026 ) ) ;
#46432 = EDGE_CURVE ( 'NONE', #72869, #36033, #27125, .T. ) ;
#46433 = ORIENTED_EDGE ( 'NONE', *, *, #25591, .T. ) ;
#46434 = ORIENTED_EDGE ( 'NONE', *, *, #31478, .T. ) ;
#46436 = FACE_OUTER_BOUND ( 'NONE', #87723, .T. ) ;
#46435 = CARTESIAN_POINT ( 'NONE',  ( -7.146003881983773454, -4.026226216239095379, 33.68668979543632958 ) ) ;
#46437 = CARTESIAN_POINT ( 'NONE',  ( 3.164686851409096224, -3.322132147404559976, 32.92929555188719348 ) ) ;
#46438 = CARTESIAN_POINT ( 'NONE',  ( -14.43838291080261449, -11.93127051446799847, 32.56575433478202797 ) ) ;
#46439 = FACE_OUTER_BOUND ( 'NONE', #49133, .T. ) ;
#46440 = CARTESIAN_POINT ( 'NONE',  ( -13.25382357679060341, -2.729792928343269587, 31.24908615093345077 ) ) ;
#46441 = ORIENTED_EDGE ( 'NONE', *, *, #77311, .F. ) ;
#46442 = CARTESIAN_POINT ( 'NONE',  ( -8.769230769230768274, -3.886160181151819604, 36.00935417666054406 ) ) ;
#46443 = CARTESIAN_POINT ( 'NONE',  ( 0.6843180028068690524, -10.11255958852955672, 34.01340905677048454 ) ) ;
#46444 = DIRECTION ( 'NONE',  ( 0.000000000000000000, 0.000000000000000000, -1.000000000000000000 ) ) ;
#46445 = EDGE_CURVE ( 'NONE', #9159, #67881, #41181, .T. ) ;
#46446 = CARTESIAN_POINT ( 'NONE',  ( -3.480745974817820887, -12.65889640711025521, 30.72598325615533454 ) ) ;
#46447 = ORIENTED_EDGE ( 'NONE', *, *, #84629, .F. ) ;
#46448 = ORIENTED_EDGE ( 'NONE', *, *, #48643, .F. ) ;
#46449 = VECTOR ( 'NONE', #8343, 1000.000000000000000 ) ;
#46451 = ADVANCED_FACE ( 'NONE', ( #52428 ), #19106, .F. ) ;
#46450 = EDGE_LOOP ( 'NONE', ( #86597, #26683, #40821, #58762 ) ) ;
#46452 = CIRCLE ( 'NONE', #85289, 2.750000000000000000 ) ;
#46453 = CARTESIAN_POINT ( 'NONE',  ( 10.48523664565292002, -4.299443229763728169, 33.91186481527756058 ) ) ;
#46454 = CARTESIAN_POINT ( 'NONE',  ( -13.16160403300253634, -10.61302985866383963, 33.66295027996417843 ) ) ;
#46455 = ORIENTED_EDGE ( 'NONE', *, *, #20111, .F. ) ;
#46456 = EDGE_CURVE ( 'NONE', #34857, #33744, #29368, .T. ) ;
#46457 = DIRECTION ( 'NONE',  ( 0.000000000000000000, 0.6427876096865373645, -0.7660444431189797898 ) ) ;
#46458 = DIRECTION ( 'NONE',  ( 0.000000000000000000, 0.000000000000000000, 1.000000000000000000 ) ) ;
#46459 = CARTESIAN_POINT ( 'NONE',  ( 3.453548899747296730, -5.827830569534416583, 34.72679350104403539 ) ) ;
#46460 = CARTESIAN_POINT ( 'NONE',  ( -16.94639737515950983, -12.27024696741798770, 31.24895572276497546 ) ) ;
#46461 = AXIS2_PLACEMENT_3D ( 'NONE', #11736, #18932, #81088 ) ;
#46462 = B_SPLINE_CURVE_WITH_KNOTS ( 'NONE', 3,
 ( #48875, #28159, #7459, #35363, #76347, #14655, #8345, #56079, #7898, #56524 ),
 .UNSPECIFIED., .F., .F.,
 ( 4, 2, 2, 2, 4 ),
 ( 0.0007817359430256304396, 0.0009771253907249967570, 0.001172514838424363291, 0.001367904286123729609, 0.001563293733823095926 ),
 .UNSPECIFIED. ) ;
#46463 = B_SPLINE_CURVE_WITH_KNOTS ( 'NONE', 3,
 ( #17536, #1797, #57626, #64809, #43664, #51732, #2229, #29285, #56742, #44537 ),
 .UNSPECIFIED., .F., .F.,
 ( 4, 2, 2, 2, 4 ),
 ( 0.0007817359430256393300, 0.0009771253907250075990, 0.001172514838424376085, 0.001367904286123744571, 0.001563293733823112840 ),
 .UNSPECIFIED. ) ;
#46464 = DIRECTION ( 'NONE',  ( 1.000000000000000000, 0.000000000000000000, 0.000000000000000000 ) ) ;
#46465 = ORIENTED_EDGE ( 'NONE', *, *, #8671, .F. ) ;
#46467 = EDGE_LOOP ( 'NONE', ( #70190, #11972, #59205, #68649 ) ) ;
#46466 = CARTESIAN_POINT ( 'NONE',  ( 0.3308469948709013009, -9.804603061927743113, 34.18744698557895845 ) ) ;
#46468 = CARTESIAN_POINT ( 'NONE',  ( -5.999999999999998224, -3.513871655860378418, 32.76840700105978499 ) ) ;
#46469 = FACE_OUTER_BOUND ( 'NONE', #26998, .T. ) ;
#46470 = CARTESIAN_POINT ( 'NONE',  ( -7.846153846153965716, -6.879047030192662504, 34.71129190930017927 ) ) ;
#46471 = B_SPLINE_CURVE_WITH_KNOTS ( 'NONE', 3,
 ( #63980, #76628, #50032, #70310, #50896, #22127, #21678, #14933, #50466, #43286 ),
 .UNSPECIFIED., .F., .F.,
 ( 4, 2, 2, 2, 4 ),
 ( 0.0007817246256747451124, 0.0009771112852218881168, 0.001172497944769031230, 0.001367884604316174126, 0.001563271263863317238 ),
 .UNSPECIFIED. ) ;
#46472 = B_SPLINE_CURVE_WITH_KNOTS ( 'NONE', 3,
 ( #38217, #80999, #12100, #66127, #18399, #32802, #72886, #60263, #11648, #80097 ),
 .UNSPECIFIED., .F., .F.,
 ( 4, 2, 2, 2, 4 ),
 ( 0.000000000000000000, 0.0001954339857564063360, 0.0003908679715128126719, 0.0005863019572692189808, 0.0007817359430256253438 ),
 .UNSPECIFIED. ) ;
#46473 = DIRECTION ( 'NONE',  ( -1.000000000000000000, -0.000000000000000000, -0.000000000000000000 ) ) ;
#46474 = CARTESIAN_POINT ( 'NONE',  ( 18.00000000000000000, -2.499999999999998668, 29.75000000000001421 ) ) ;
#46475 = EDGE_CURVE ( 'NONE', #42820, #84034, #73397, .T. ) ;
#46476 = CARTESIAN_POINT ( 'NONE',  ( 11.53846153846153832, -9.819645486525091727, 36.12317359536749706 ) ) ;
#46477 = CARTESIAN_POINT ( 'NONE',  ( -2.372962308248625529, -3.083524468853724443, 32.58852847137143272 ) ) ;
#46478 = CARTESIAN_POINT ( 'NONE',  ( -1.901340078031369618, -5.512252781505359245, 20.50186829374151287 ) ) ;
#46479 = VERTEX_POINT ( 'NONE', #54202 ) ;
#46480 = CARTESIAN_POINT ( 'NONE',  ( 15.10007776410167324, -8.147922237126337563, 34.70805685702651999 ) ) ;
#46481 = CARTESIAN_POINT ( 'NONE',  ( -9.561781990544128362, -8.586989748646452369, 34.63063291749215011 ) ) ;
#46482 = CARTESIAN_POINT ( 'NONE',  ( -13.38461538461538325, -8.120952969808772792, 34.71129190930000163 ) ) ;
#46483 = EDGE_CURVE ( 'NONE', #78412, #54915, #70205, .T. ) ;
#46484 = VERTEX_POINT ( 'NONE', #49996 ) ;
#46485 = CARTESIAN_POINT ( 'NONE',  ( 8.068933515131909928, -12.11081565061823717, 32.26097654155341843 ) ) ;
#46486 = CARTESIAN_POINT ( 'NONE',  ( 11.53846153846141576, -12.70778746994576025, 30.41441678777401236 ) ) ;
#46487 = CARTESIAN_POINT ( 'NONE',  ( 13.25446817517716447, -3.817052484675422797, 33.13202310037935661 ) ) ;
#46488 = CARTESIAN_POINT ( 'NONE',  ( -10.74553258511630993, -2.373036134822904319, 30.88089517874952250 ) ) ;
#46489 = FACE_OUTER_BOUND ( 'NONE', #34568, .T. ) ;
#46490 = CIRCLE ( 'NONE', #11970, 4.000000000000000000 ) ;
#46491 = DIRECTION ( 'NONE',  ( 1.000000000000000000, 0.000000000000000000, 0.000000000000000000 ) ) ;
#46492 = ORIENTED_EDGE ( 'NONE', *, *, #55778, .T. ) ;
#46493 = DIRECTION ( 'NONE',  ( -0.000000000000000000, 0.9848077530122086864, -0.1736481776669273891 ) ) ;
#46494 = DIRECTION ( 'NONE',  ( 0.000000000000000000, 0.9396926207859126468, -0.3420201433256571111 ) ) ;
#46495 = CARTESIAN_POINT ( 'NONE',  ( -2.177166869458661225, -5.915461855592777596, 34.75538340440931506 ) ) ;
#46496 = ORIENTED_EDGE ( 'NONE', *, *, #50471, .F. ) ;
#46497 = CARTESIAN_POINT ( 'NONE',  ( 13.51514108637895006, -6.852161475712352789, 34.70806712695775786 ) ) ;
#46498 = VERTEX_POINT ( 'NONE', #69834 ) ;
#46499 = CYLINDRICAL_SURFACE ( 'NONE', #62984, 0.2499999999999986955 ) ;
#46500 = DIRECTION ( 'NONE',  ( 0.000000000000000000, 0.6427876096865373645, -0.7660444431189797898 ) ) ;
#46501 = EDGE_CURVE ( 'NONE', #40626, #15955, #13235, .T. ) ;
#46502 = ORIENTED_EDGE ( 'NONE', *, *, #18680, .F. ) ;
#46503 = LINE ( 'NONE', #26673, #10225 ) ;
#46504 = CARTESIAN_POINT ( 'NONE',  ( -14.37294223946638994, -2.255955759149247619, 30.00000000000013856 ) ) ;
#46505 = LINE ( 'NONE', #32106, #76794 ) ;
#46506 = CARTESIAN_POINT ( 'NONE',  ( 8.546352086802123438, -7.630691491037285168, 34.74850469731152458 ) ) ;
#46507 = CYLINDRICAL_SURFACE ( 'NONE', #85735, 0.2499999999999986955 ) ;
#46508 = B_SPLINE_CURVE_WITH_KNOTS ( 'NONE', 3,
 ( #71452, #37674, #57943, #71900, #44411, #86334, #85424, #70582, #71020, #37224 ),
 .UNSPECIFIED., .F., .F.,
 ( 4, 2, 2, 2, 4 ),
 ( 0.000000000000000000, 0.0001954311564186879857, 0.0003908623128373759715, 0.0005862934692560640114, 0.0007817246256747519429 ),
 .UNSPECIFIED. ) ;
#46509 = EDGE_CURVE ( 'NONE', #48052, #50514, #4022, .T. ) ;
#46510 = CIRCLE ( 'NONE', #74034, 0.2500000000000002220 ) ;
#46511 = ORIENTED_EDGE ( 'NONE', *, *, #33885, .T. ) ;
#46512 = CARTESIAN_POINT ( 'NONE',  ( -3.903900744468109973, -12.45601412856602863, 31.48342859153981621 ) ) ;
#46513 = VERTEX_POINT ( 'NONE', #42817 ) ;
#46514 = CARTESIAN_POINT ( 'NONE',  ( -15.16470189741915675, -6.343179335718452272, 34.87096338111212646 ) ) ;
#46515 = EDGE_CURVE ( 'NONE', #75445, #41883, #82017, .T. ) ;
#46516 = AXIS2_PLACEMENT_3D ( 'NONE', #10490, #72175, #65857 ) ;
#46517 = CYLINDRICAL_SURFACE ( 'NONE', #24911, 0.2499999999999998890 ) ;
#46518 = EDGE_CURVE ( 'NONE', #27949, #15069, #8586, .T. ) ;
#46519 = AXIS2_PLACEMENT_3D ( 'NONE', #43644, #57162, #64347 ) ;
#46520 = CARTESIAN_POINT ( 'NONE',  ( -16.15384615384627409, -11.48612834414049644, 32.76840700105863391 ) ) ;
#46521 = CARTESIAN_POINT ( 'NONE',  ( 5.999999999999880096, -9.442884908241554243, 34.35708131394783038 ) ) ;
#46522 = CYLINDRICAL_SURFACE ( 'NONE', #78081, 0.2499999999999986955 ) ;
#46523 = DIRECTION ( 'NONE',  ( -1.000000000000000000, -0.000000000000000000, -0.000000000000000000 ) ) ;
#46524 = DIRECTION ( 'NONE',  ( -0.000000000000000000, -0.000000000000000000, -1.000000000000000000 ) ) ;
#46525 = B_SPLINE_CURVE_WITH_KNOTS ( 'NONE', 3,
 ( #37139, #84025, #22305, #64160, #9673, #16434, #36271, #78131, #2462, #49769 ),
 .UNSPECIFIED., .F., .F.,
 ( 4, 2, 2, 2, 4 ),
 ( 0.0007817246256747530271, 0.0009771112852218978746, 0.001172497944769042939, 0.001367884604316188003, 0.001563271263863332851 ),
 .UNSPECIFIED. ) ;
#46526 = ORIENTED_EDGE ( 'NONE', *, *, #64727, .F. ) ;
#46527 = EDGE_CURVE ( 'NONE', #43756, #37230, #26742, .T. ) ;
#46528 = ORIENTED_EDGE ( 'NONE', *, *, #76194, .T. ) ;
#46529 = VERTEX_POINT ( 'NONE', #63061 ) ;
#46530 = ORIENTED_EDGE ( 'NONE', *, *, #81563, .T. ) ;
#46531 = CARTESIAN_POINT ( 'NONE',  ( 2.177000841024750333, -4.809359713505814149, 33.96456829005828837 ) ) ;
#46532 = CARTESIAN_POINT ( 'NONE',  ( 11.28843831424008393, -9.356822207818506598, 34.66110646841856635 ) ) ;
#46533 = CARTESIAN_POINT ( 'NONE',  ( 15.16468581981335184, -4.786620604624113540, 33.94971097300155805 ) ) ;
#46534 = CARTESIAN_POINT ( 'NONE',  ( 4.087762742890272527, -3.050289026998445951, 32.03036669348365706 ) ) ;
#46535 = CARTESIAN_POINT ( 'NONE',  ( 20.74999999999999645, -2.499999999999999556, 29.75000000000000355 ) ) ;
#46536 = FACE_OUTER_BOUND ( 'NONE', #14392, .T. ) ;
#46537 = LINE ( 'NONE', #67697, #86910 ) ;
#46538 = LINE ( 'NONE', #33025, #8851 ) ;
#46539 = ORIENTED_EDGE ( 'NONE', *, *, #2904, .T. ) ;
#46540 = EDGE_CURVE ( 'NONE', #17613, #54993, #40716, .T. ) ;
#46541 = ORIENTED_EDGE ( 'NONE', *, *, #28575, .T. ) ;
#46542 = EDGE_LOOP ( 'NONE', ( #66272, #69825, #27160, #74587 ) ) ;
#46544 = VERTEX_POINT ( 'NONE', #28863 ) ;
#46543 = CARTESIAN_POINT ( 'NONE',  ( -11.76138775597768138, -12.39988816332205701, 30.74660775122750778 ) ) ;
#46546 = FACE_OUTER_BOUND ( 'NONE', #88420, .T. ) ;
#46545 = DIRECTION ( 'NONE',  ( 0.000000000000000000, 0.000000000000000000, 1.000000000000000000 ) ) ;
#46547 = CARTESIAN_POINT ( 'NONE',  ( 11.28846153846153832, -7.500000000000001776, 35.00000000000000000 ) ) ;
#46548 = CARTESIAN_POINT ( 'NONE',  ( -10.86536134632696715, -3.627789207965226748, 32.91389620160131102 ) ) ;
#46549 = FACE_BOUND ( 'NONE', #43714, .T. ) ;
#46550 = ORIENTED_EDGE ( 'NONE', *, *, #73424, .T. ) ;
#46551 = ORIENTED_EDGE ( 'NONE', *, *, #43740, .F. ) ;
#46552 = CARTESIAN_POINT ( 'NONE',  ( 9.320512820512821150, -11.50000000000000000, 29.75000000000000355 ) ) ;
#46553 = VERTEX_POINT ( 'NONE', #77476 ) ;
#46554 = FACE_BOUND ( 'NONE', #62615, .T. ) ;
#46555 = B_SPLINE_CURVE_WITH_KNOTS ( 'NONE', 3,
 ( #76389, #83156, #56565, #49366, #83612, #84055, #22335, #41727, #55229, #82718 ),
 .UNSPECIFIED., .F., .F.,
 ( 4, 2, 2, 2, 4 ),
 ( 0.000000000000000000, 0.0001954311564186861155, 0.0003908623128373722310, 0.0005862934692560583735, 0.0007817246256747444619 ),
 .UNSPECIFIED. ) ;
#46556 = DIRECTION ( 'NONE',  ( 0.000000000000000000, 0.9848077530122072432, -0.1736481776669354937 ) ) ;
#46557 = CARTESIAN_POINT ( 'NONE',  ( 14.98074600654777733, -6.652501968072648708, 34.93155406624980941 ) ) ;
#46558 = ORIENTED_EDGE ( 'NONE', *, *, #14850, .F. ) ;
#46559 = DIRECTION ( 'NONE',  ( -0.000000000000000000, 0.1736481776669307198, -0.9848077530122080203 ) ) ;
#46560 = CARTESIAN_POINT ( 'NONE',  ( -3.480769230769229061, -7.500000000000001776, 35.04278698407183867 ) ) ;
#46561 = DIRECTION ( 'NONE',  ( 1.000000000000000000, 0.000000000000000000, 0.000000000000000000 ) ) ;
#46562 = VERTEX_POINT ( 'NONE', #61399 ) ;
#46563 = CARTESIAN_POINT ( 'NONE',  ( 14.37375964104238335, -3.322132147404559976, 32.92929555188717927 ) ) ;
#46564 = CARTESIAN_POINT ( 'NONE',  ( -18.06608341095587633, -4.786620604624111763, 33.94971097300155805 ) ) ;
#46565 = DIRECTION ( 'NONE',  ( 0.000000000000000000, 0.8660254037844377084, 0.5000000000000015543 ) ) ;
#46566 = ORIENTED_EDGE ( 'NONE', *, *, #12586, .F. ) ;
#46567 = CARTESIAN_POINT ( 'NONE',  ( 2.530471976670372491, -12.47679350104403007, 31.42216943046555855 ) ) ;
#46568 = CARTESIAN_POINT ( 'NONE',  ( -15.36091644020745051, -4.460286881179644780, 33.72017969459903242 ) ) ;
#46569 = EDGE_LOOP ( 'NONE', ( #25995, #82944, #79296, #53656 ) ) ;
#46570 = DIRECTION ( 'NONE',  ( -0.000000000000000000, 0.9396926207859093161, -0.3420201433256663259 ) ) ;
#46571 = CARTESIAN_POINT ( 'NONE',  ( -4.403822884788509029, -2.564618984488975961, 30.55390908950641915 ) ) ;
#46572 = CARTESIAN_POINT ( 'NONE',  ( -0.2115384615384615641, -7.500000000000001776, 35.04278698407183867 ) ) ;
#46573 = CARTESIAN_POINT ( 'NONE',  ( 13.38461538461526601, -12.46129190930018460, 30.37095296980731973 ) ) ;
#46574 = CARTESIAN_POINT ( 'NONE',  ( -10.55012904410858532, -2.625532179533470512, 30.86335684631491105 ) ) ;
#46575 = CARTESIAN_POINT ( 'NONE',  ( 6.673100192134570285, -9.148715823498378086, 34.47080413974185120 ) ) ;
#46578 = CARTESIAN_POINT ( 'NONE',  ( 9.758375025657770152, -4.661471528628508665, 34.16647553114624003 ) ) ;
#46577 = VECTOR ( 'NONE', #3860, 1000.000000000000000 ) ;
#46576 = CARTESIAN_POINT ( 'NONE',  ( 0.7115928814519140166, -11.47946981652013498, 33.17500667209846910 ) ) ;
#46579 = EDGE_CURVE ( 'NONE', #5299, #20780, #4638, .T. ) ;
#46580 = CARTESIAN_POINT ( 'NONE',  ( 10.74591005361826035, -9.503571793651731880, 34.60286762892837942 ) ) ;
#46581 = CARTESIAN_POINT ( 'NONE',  ( -12.21159294319032185, -11.37275283266504111, 32.91324779482534524 ) ) ;
#46582 = CARTESIAN_POINT ( 'NONE',  ( -2.775308065498764964, -6.422011778438537988, 27.42000670625849068 ) ) ;
#46583 = ORIENTED_EDGE ( 'NONE', *, *, #34004, .T. ) ;
#46585 = VECTOR ( 'NONE', #45828, 1000.000000000000114 ) ;
#46584 = B_SPLINE_CURVE_WITH_KNOTS ( 'NONE', 3,
 ( #46364, #52220, #45017, #79712, #86938, #86484, #52667, #66639, #45911, #10805 ),
 .UNSPECIFIED., .F., .F.,
 ( 4, 2, 2, 2, 4 ),
 ( 0.0007817246256747516176, 0.0009771112852218965736, 0.001172497944769041421, 0.001367884604316186269, 0.001563271263863331333 ),
 .UNSPECIFIED. ) ;
#46586 = DIRECTION ( 'NONE',  ( -0.000000000000000000, -0.000000000000000000, -1.000000000000000000 ) ) ;
#46587 = EDGE_LOOP ( 'NONE', ( #48599, #49592, #2675, #46205 ) ) ;
#46588 = EDGE_CURVE ( 'NONE', #39037, #71584, #15786, .T. ) ;
#46589 = AXIS2_PLACEMENT_3D ( 'NONE', #24254, #36462, #85532 ) ;
#46590 = ORIENTED_EDGE ( 'NONE', *, *, #16152, .T. ) ;
#46591 = CARTESIAN_POINT ( 'NONE',  ( -2.307692307692427391, -12.46129190930018460, 30.37095296980731973 ) ) ;
#46592 = EDGE_CURVE ( 'NONE', #88144, #62981, #28231, .T. ) ;
#46593 = ORIENTED_EDGE ( 'NONE', *, *, #36677, .F. ) ;
#46594 = DIRECTION ( 'NONE',  ( -0.000000000000000000, 0.7660444431189791237, -0.6427876096865379196 ) ) ;
#46595 = CARTESIAN_POINT ( 'NONE',  ( -2.749999999999998224, -7.500000000000015987, 15.09375000000000000 ) ) ;
#46596 = CARTESIAN_POINT ( 'NONE',  ( 13.63456090296353018, -2.824170634883621744, 31.52227843825338738 ) ) ;
#46597 = CARTESIAN_POINT ( 'NONE',  ( 10.61538461538449418, -2.657715359629662544, 31.77849191805970364 ) ) ;
#46598 = CARTESIAN_POINT ( 'NONE',  ( 3.230769230769231726, -11.69971097300155272, 32.46337939537588113 ) ) ;
#46599 = CARTESIAN_POINT ( 'NONE',  ( -10.39260494640654642, -3.563462043263030399, 33.22394488606062879 ) ) ;
#46600 = CARTESIAN_POINT ( 'NONE',  ( -15.36091720050093024, -5.070767119584671079, 34.40440758774516183 ) ) ;
#46601 = CARTESIAN_POINT ( 'NONE',  ( 2.307692307692309264, -11.16473453929635440, 33.15142922261926373 ) ) ;
#46602 = ADVANCED_FACE ( 'NONE', ( #73386 ), #4018, .F. ) ;
#46603 = B_SPLINE_CURVE_WITH_KNOTS ( 'NONE', 3,
 ( #77609, #56883, #49690, #64079, #37048, #17230, #36196, #10028, #57775, #23106 ),
 .UNSPECIFIED., .F., .F.,
 ( 4, 2, 2, 2, 4 ),
 ( 0.000000000000000000, 0.0001954339857564090465, 0.0003908679715128180929, 0.0005863019572692271123, 0.0007817359430256361858 ),
 .UNSPECIFIED. ) ;
#46604 = CARTESIAN_POINT ( 'NONE',  ( 2.651650429449539104, -4.848349570550432475, 21.81250000000000000 ) ) ;
#46605 = LINE ( 'NONE', #74083, #46299 ) ;
#46606 = CARTESIAN_POINT ( 'NONE',  ( -4.153846153846152411, -11.91647553114624181, 32.58852847137148245 ) ) ;
#46607 = ADVANCED_FACE ( 'NONE', ( #38264 ), #72039, .F. ) ;
#46608 = LINE ( 'NONE', #73194, #50766 ) ;
#46609 = EDGE_LOOP ( 'NONE', ( #19012, #10094, #12949, #6396, #37029 ) ) ;
#46610 = ORIENTED_EDGE ( 'NONE', *, *, #68582, .F. ) ;
#46611 = CARTESIAN_POINT ( 'NONE',  ( -11.28840722682322273, -5.728107161865378494, 34.42597550085002922 ) ) ;
#46612 = CARTESIAN_POINT ( 'NONE',  ( -17.14300648787895298, -8.120952969808774569, 34.71129190930000163 ) ) ;
#46613 = DIRECTION ( 'NONE',  ( 0.000000000000000000, 0.3420201433256610524, 0.9396926207859113145 ) ) ;
#46614 = CARTESIAN_POINT ( 'NONE',  ( -7.173100147298380413, -5.765609946408404518, 34.70566812827425451 ) ) ;
#46615 = CARTESIAN_POINT ( 'NONE',  ( -7.596153846153844924, -7.500000000000001776, 35.04278698407183867 ) ) ;
#46616 = CARTESIAN_POINT ( 'NONE',  ( -4.826977667545031991, -2.986452184633680673, 32.43230066228895225 ) ) ;
#46617 = ORIENTED_EDGE ( 'NONE', *, *, #12940, .F. ) ;
#46618 = CARTESIAN_POINT ( 'NONE',  ( 1.253923917947828315, -4.809359713505814149, 33.96456829005828837 ) ) ;
#46619 = ORIENTED_EDGE ( 'NONE', *, *, #73665, .T. ) ;
#46620 = EDGE_CURVE ( 'NONE', #36760, #82738, #44330, .T. ) ;
#46621 = ORIENTED_EDGE ( 'NONE', *, *, #63148, .F. ) ;
#46622 = CARTESIAN_POINT ( 'NONE',  ( -8.769230769230768274, -4.661471528628507777, 34.16647553114623292 ) ) ;
#46623 = CARTESIAN_POINT ( 'NONE',  ( -14.05763788777885281, -6.523592122091592671, 34.90882529074906415 ) ) ;
#46624 = ADVANCED_FACE ( 'NONE', ( #86474 ), #85564, .F. ) ;
#46625 = CARTESIAN_POINT ( 'NONE',  ( -9.561781990544126586, -6.852161475712352789, 34.70806712695775786 ) ) ;
#46626 = CARTESIAN_POINT ( 'NONE',  ( -4.153846153846152411, -9.905515769479276145, 34.41647553114623292 ) ) ;
#46627 = CARTESIAN_POINT ( 'NONE',  ( -13.38461538461538325, -2.486705287966279876, 31.30864560766543647 ) ) ;
#46628 = B_SPLINE_CURVE_WITH_KNOTS ( 'NONE', 3,
 ( #46974, #67704, #6011, #1015, #13204, #33477, #20403, #14084, #28488, #48751 ),
 .UNSPECIFIED., .F., .F.,
 ( 4, 2, 2, 2, 4 ),
 ( 0.0007817246256747461966, 0.0009771112852218892010, 0.001172497944769032314, 0.001367884604316175427, 0.001563271263863318323 ),
 .UNSPECIFIED. ) ;
#46629 = ORIENTED_EDGE ( 'NONE', *, *, #41341, .T. ) ;
#46630 = ADVANCED_FACE ( 'NONE', ( #58515 ), #45455, .F. ) ;
#46631 = ORIENTED_EDGE ( 'NONE', *, *, #76135, .F. ) ;
#46632 = B_SPLINE_CURVE_WITH_KNOTS ( 'NONE', 3,
 ( #10757, #78765, #17065, #72006, #37779, #10313, #65684, #3983, #31469, #86441 ),
 .UNSPECIFIED., .F., .F.,
 ( 4, 2, 2, 2, 4 ),
 ( 0.0007817359527651101701, 0.0009771254036996489256, 0.001172514854634187790, 0.001367904305568726653, 0.001563293756503265517 ),
 .UNSPECIFIED. ) ;
#46633 = ORIENTED_EDGE ( 'NONE', *, *, #73529, .F. ) ;
#46634 = EDGE_CURVE ( 'NONE', #7438, #9134, #3505, .T. ) ;
#46635 = CARTESIAN_POINT ( 'NONE',  ( -16.15384615384615330, -2.708943851104267164, 35.45975837776705220 ) ) ;
#46636 = CARTESIAN_POINT ( 'NONE',  ( -0.3310130233048168558, -10.31582465632705237, 34.18122507451815295 ) ) ;
#46637 = CARTESIAN_POINT ( 'NONE',  ( 16.37685899793955357, -5.582272713120730145, 34.63742843783360570 ) ) ;
#46638 = AXIS2_PLACEMENT_3D ( 'NONE', #27464, #49053, #83299 ) ;
#46639 = CARTESIAN_POINT ( 'NONE',  ( -16.28453675695646652, -2.295517848115768089, 30.44137282052136939 ) ) ;
#46640 = CARTESIAN_POINT ( 'NONE',  ( 4.153846153846154188, -1.509761064869970415, 31.06009739812519044 ) ) ;
#46641 = DIRECTION ( 'NONE',  ( 0.000000000000000000, 0.3420201433256641055, -0.9396926207859100932 ) ) ;
#46642 = ORIENTED_EDGE ( 'NONE', *, *, #43743, .F. ) ;
#46643 = ADVANCED_FACE ( 'NONE', ( #31047 ), #80144, .F. ) ;
#46644 = ORIENTED_EDGE ( 'NONE', *, *, #24872, .T. ) ;
#46646 = ORIENTED_EDGE ( 'NONE', *, *, #68789, .T. ) ;
#46645 = CARTESIAN_POINT ( 'NONE',  ( -10.54931626438217585, -11.69971097300155272, 32.46337939537588113 ) ) ;
#46647 = EDGE_CURVE ( 'NONE', #82252, #33999, #67976, .T. ) ;
#46648 = DIRECTION ( 'NONE',  ( -0.000000000000000000, 0.3420201433256694346, -0.9396926207859080948 ) ) ;
#46649 = CARTESIAN_POINT ( 'NONE',  ( -2.084912638714238486, -4.226511098958374291, 33.85474049983370293 ) ) ;
#46650 = EDGE_CURVE ( 'NONE', #73234, #41543, #3132, .T. ) ;
#46651 = CARTESIAN_POINT ( 'NONE',  ( -3.749999999999988454, -9.053300858899127945, 20.01562500000000355 ) ) ;
#46652 = EDGE_LOOP ( 'NONE', ( #20108, #46981, #85506, #89099 ) ) ;
#46653 = CARTESIAN_POINT ( 'NONE',  ( 8.069166690247241647, -4.026326845037962343, 33.68677907613344047 ) ) ;
#46654 = ORIENTED_EDGE ( 'NONE', *, *, #45799, .F. ) ;
#46655 = EDGE_CURVE ( 'NONE', #71986, #37663, #47527, .T. ) ;
#46656 = CARTESIAN_POINT ( 'NONE',  ( 2.242421861731533017, -6.879047030191174805, 34.71129190930000163 ) ) ;
#46657 = CARTESIAN_POINT ( 'NONE',  ( 0.3313904918067637762, -11.66186481527757124, 32.95055677023625407 ) ) ;
#46658 = CARTESIAN_POINT ( 'NONE',  ( -12.39547011053602432, -12.37446782046654192, 30.86335684631486842 ) ) ;
#46659 = B_SPLINE_CURVE_WITH_KNOTS ( 'NONE', 3,
 ( #43946, #57460, #17823, #30870, #65545, #58340, #85835, #59239, #78180, #3847 ),
 .UNSPECIFIED., .F., .F.,
 ( 4, 2, 2, 2, 4 ),
 ( 0.0007817359430256366195, 0.0009771253907250045632, 0.001172514838424372615, 0.001367904286123740668, 0.001563293733823108503 ),
 .UNSPECIFIED. ) ;
#46660 = CARTESIAN_POINT ( 'NONE',  ( -5.010854725920638408, -12.10708131394839882, 31.69288490824020954 ) ) ;
#46661 = CARTESIAN_POINT ( 'NONE',  ( -3.262820512820514107, -3.499999999999999556, 29.75000000000000355 ) ) ;
#46662 = ORIENTED_EDGE ( 'NONE', *, *, #64306, .F. ) ;
#46663 = CARTESIAN_POINT ( 'NONE',  ( -11.28840711854808632, -8.346898887586323923, 34.93166121998716278 ) ) ;
#46664 = DIRECTION ( 'NONE',  ( 0.000000000000000000, 0.1736481776669275834, 0.9848077530122086864 ) ) ;
#46665 = ORIENTED_EDGE ( 'NONE', *, *, #80762, .T. ) ;
#46666 = AXIS2_PLACEMENT_3D ( 'NONE', #9441, #53411, #66497 ) ;
#46667 = CARTESIAN_POINT ( 'NONE',  ( -18.00000000000012079, -12.70778746994576025, 30.41441678777401236 ) ) ;
#46668 = CARTESIAN_POINT ( 'NONE',  ( 14.43848274865925774, -9.929761469519743144, 34.40412654351204225 ) ) ;
#46669 = CARTESIAN_POINT ( 'NONE',  ( -10.61538461538461320, -2.292212530054420494, 30.41441678777542634 ) ) ;
#46670 = CARTESIAN_POINT ( 'NONE',  ( 0.4615384615384611200, -2.708943851104267164, 35.45975837776705220 ) ) ;
#46671 = DIRECTION ( 'NONE',  ( -0.000000000000000000, 0.1736481776669307198, -0.9848077530122080203 ) ) ;
#46672 = FACE_BOUND ( 'NONE', #16321, .T. ) ;
#46674 = CARTESIAN_POINT ( 'NONE',  ( 16.15384615384615330, -6.681629849574314051, 35.83090037661290239 ) ) ;
#46673 = DIRECTION ( 'NONE',  ( -0.000000000000000000, 0.8660254037844397068, -0.4999999999999978906 ) ) ;
#46675 = CARTESIAN_POINT ( 'NONE',  ( 9.822352855142472805, -2.504778602574659896, 29.97347330155780654 ) ) ;
#46677 = CARTESIAN_POINT ( 'NONE',  ( -2.307692307692428724, -12.51329471203414379, 31.30864560766407578 ) ) ;
#46676 = CARTESIAN_POINT ( 'NONE',  ( -18.22292695890684655, -2.308479472611653094, 30.53278059502174457 ) ) ;
#46678 = CARTESIAN_POINT ( 'NONE',  ( 8.900021210197715860, -12.62708834333097663, 30.88030960425257021 ) ) ;
#46679 = CARTESIAN_POINT ( 'NONE',  ( -1.614399933863656544, -3.775308065498769405, 23.82625670625849068 ) ) ;
#46680 = EDGE_LOOP ( 'NONE', ( #44267, #44187, #9914, #60159, #36331 ) ) ;
#46681 = CARTESIAN_POINT ( 'NONE',  ( 10.61538461538461675, -11.91647553114624181, 32.58852847137148245 ) ) ;
#46682 = ORIENTED_EDGE ( 'NONE', *, *, #33774, .F. ) ;
#46683 = CARTESIAN_POINT ( 'NONE',  ( -18.06608237936013239, -3.322132147404557312, 32.92929555188717217 ) ) ;
#46684 = EDGE_LOOP ( 'NONE', ( #46416, #54272, #24998, #31084 ) ) ;
#46685 = CARTESIAN_POINT ( 'NONE',  ( 7.596177115211490971, -9.148715823498378086, 34.47080413974185120 ) ) ;
#46686 = LINE ( 'NONE', #6149, #84805 ) ;
#46688 = VERTEX_POINT ( 'NONE', #88698 ) ;
#46687 = DIRECTION ( 'NONE',  ( 0.000000000000000000, 0.000000000000000000, 1.000000000000000000 ) ) ;
#46689 = CARTESIAN_POINT ( 'NONE',  ( 3.453548772037639214, -6.760870238392817200, 34.69528174975672385 ) ) ;
#46690 = DIRECTION ( 'NONE',  ( -1.000000000000000000, 0.000000000000000000, 0.000000000000000000 ) ) ;
#46691 = CARTESIAN_POINT ( 'NONE',  ( 3.724691934501232815, -5.885600066136343678, 25.38875670625849423 ) ) ;
#46692 = CARTESIAN_POINT ( 'NONE',  ( -12.21153846153846168, -2.499999999999998668, 29.75000000000000355 ) ) ;
#46693 = CARTESIAN_POINT ( 'NONE',  ( 0.000000000000000000, -11.00000000000000000, 29.75000000000000355 ) ) ;
#46694 = DIRECTION ( 'NONE',  ( -1.000000000000000000, -0.000000000000000000, -0.000000000000000000 ) ) ;
#46695 = DIRECTION ( 'NONE',  ( -1.000000000000000000, -0.000000000000000000, -0.000000000000000000 ) ) ;
#46696 = CARTESIAN_POINT ( 'NONE',  ( -7.146003140593069070, -4.186968288167446595, 33.49512374952580274 ) ) ;
#46697 = DIRECTION ( 'NONE',  ( 0.000000000000000000, 0.9396926207859126468, 0.3420201433256571111 ) ) ;
#46698 = EDGE_CURVE ( 'NONE', #36558, #16973, #63654, .T. ) ;
#46699 = CARTESIAN_POINT ( 'NONE',  ( -1.614399933863613468, -11.22469193450124969, 16.36124329374151642 ) ) ;
#46700 = AXIS2_PLACEMENT_3D ( 'NONE', #4443, #40472, #47656 ) ;
#46701 = CARTESIAN_POINT ( 'NONE',  ( 5.142178216435913107, -2.657715359629131857, 31.77849191805844242 ) ) ;
#46702 = CARTESIAN_POINT ( 'NONE',  ( -11.53846153846153655, -10.51840700105979565, 33.73612834413961536 ) ) ;
#46703 = ORIENTED_EDGE ( 'NONE', *, *, #2310, .T. ) ;
#46704 = ADVANCED_FACE ( 'NONE', ( #26979 ), #20219, .F. ) ;
#46705 = CARTESIAN_POINT ( 'NONE',  ( 16.15384615384603251, -5.094484230521993062, 34.41647553114689373 ) ) ;
#46706 = DIRECTION ( 'NONE',  ( 0.000000000000000000, 0.4999999999999960032, -0.8660254037844410391 ) ) ;
#46707 = CARTESIAN_POINT ( 'NONE',  ( -1.492201783934593573, -3.724691934501250135, 20.57999329374151998 ) ) ;
#46708 = VECTOR ( 'NONE', #22477, 1000.000000000000000 ) ;
#46709 = CARTESIAN_POINT ( 'NONE',  ( -10.74553258511631704, -2.647304123082328875, 31.75400227202885972 ) ) ;
#46710 = LINE ( 'NONE', #6612, #16730 ) ;
#46711 = VERTEX_POINT ( 'NONE', #40934 ) ;
#46712 = DIRECTION ( 'NONE',  ( -1.000000000000000000, -0.000000000000000000, -0.000000000000000000 ) ) ;
#46713 = CARTESIAN_POINT ( 'NONE',  ( 9.468822767743363400, -12.69144148231606017, 30.53333754910549303 ) ) ;
#46715 = ORIENTED_EDGE ( 'NONE', *, *, #59685, .F. ) ;
#46714 = CARTESIAN_POINT ( 'NONE',  ( 5.076923076922953193, -12.51329471203414379, 31.30864560766407578 ) ) ;
#46716 = CARTESIAN_POINT ( 'NONE',  ( -8.096130577096200653, -8.303909089506435137, 34.68538101551103381 ) ) ;
#46717 = CARTESIAN_POINT ( 'NONE',  ( -3.164700879766791708, -3.513871655860379306, 32.76840700105978499 ) ) ;
#46718 = CARTESIAN_POINT ( 'NONE',  ( 2.057715576749954423, -12.41269422305637171, 30.68257228309993323 ) ) ;
#46720 = ADVANCED_FACE ( 'NONE', ( #39170 ), #74726, .F. ) ;
#46719 = CARTESIAN_POINT ( 'NONE',  ( 11.76147289007438701, -9.086983370893049639, 34.49168942202179267 ) ) ;
#46721 = ORIENTED_EDGE ( 'NONE', *, *, #65950, .F. ) ;
#46722 = CARTESIAN_POINT ( 'NONE',  ( 2.307692307692186251, -6.835583212225970762, 34.95778746994575670 ) ) ;
#46723 = CARTESIAN_POINT ( 'NONE',  ( -15.48079245499068612, -11.56360843649121684, 33.07473185843129926 ) ) ;
#46724 = CARTESIAN_POINT ( 'NONE',  ( -13.25408994638174143, -8.630441415882550871, 34.87705825610312615 ) ) ;
#46725 = ORIENTED_EDGE ( 'NONE', *, *, #53694, .T. ) ;
#46726 = ORIENTED_EDGE ( 'NONE', *, *, #70965, .F. ) ;
#46727 = EDGE_CURVE ( 'NONE', #26582, #41513, #30315, .T. ) ;
#46729 = ORIENTED_EDGE ( 'NONE', *, *, #66799, .T. ) ;
#46728 = B_SPLINE_CURVE_WITH_KNOTS ( 'NONE', 3,
 ( #69738, #55331, #83714, #35513, #21997, #50333, #42280, #43588, #49471, #69303 ),
 .UNSPECIFIED., .F., .F.,
 ( 4, 2, 2, 2, 4 ),
 ( 0.000000000000000000, 0.0001954311584214072381, 0.0003908623168428144762, 0.0005862934752642217414, 0.0007817246336856289524 ),
 .UNSPECIFIED. ) ;
#46730 = CARTESIAN_POINT ( 'NONE',  ( 24.00000000000000000, -5.499999999999981348, 27.75000000000000000 ) ) ;
#46731 = CARTESIAN_POINT ( 'NONE',  ( -6.857821351800898135, -4.481592998940251427, 33.73612834413965089 ) ) ;
#46732 = ADVANCED_FACE ( 'NONE', ( #54434 ), #11692, .F. ) ;
#46733 = CARTESIAN_POINT ( 'NONE',  ( 13.91025641025641235, -3.499999999999999556, 29.75000000000000355 ) ) ;
#46734 = AXIS2_PLACEMENT_3D ( 'NONE', #78924, #79829, #18125 ) ;
#46735 = CARTESIAN_POINT ( 'NONE',  ( -18.25000000000001066, -7.431102191622666275, 35.00000000000000711 ) ) ;
#46736 = ORIENTED_EDGE ( 'NONE', *, *, #57441, .F. ) ;
#46737 = ORIENTED_EDGE ( 'NONE', *, *, #50912, .T. ) ;
#46738 = EDGE_CURVE ( 'NONE', #42538, #71827, #59864, .T. ) ;
#46739 = ORIENTED_EDGE ( 'NONE', *, *, #71759, .T. ) ;
#46741 = ORIENTED_EDGE ( 'NONE', *, *, #22430, .F. ) ;
#46740 = CARTESIAN_POINT ( 'NONE',  ( -6.989159302437059296, -2.486705287966279432, 31.30864560766542937 ) ) ;
#46742 = CARTESIAN_POINT ( 'NONE',  ( -6.923076923076922462, -3.937682226553329556, 33.60647404775216529 ) ) ;
#46743 = CARTESIAN_POINT ( 'NONE',  ( -3.296851610129365451, -4.661471528628506888, 34.16647553114621871 ) ) ;
#46744 = CYLINDRICAL_SURFACE ( 'NONE', #52231, 0.2500000000000012212 ) ;
#46745 = CARTESIAN_POINT ( 'NONE',  ( 16.15384615384615330, -5.180354513474913603, 36.12317359536750416 ) ) ;
#46746 = ORIENTED_EDGE ( 'NONE', *, *, #50911, .F. ) ;
#46747 = ADVANCED_FACE ( 'NONE', ( #46799 ), #47683, .F. ) ;
#46748 = ORIENTED_EDGE ( 'NONE', *, *, #436, .T. ) ;
#46749 = EDGE_LOOP ( 'NONE', ( #86331, #85618, #22147, #55278 ) ) ;
#46750 = CARTESIAN_POINT ( 'NONE',  ( 10.61538461538461675, -10.51840700105979565, 33.73612834413961536 ) ) ;
#46752 = VERTEX_POINT ( 'NONE', #25641 ) ;
#46751 = CARTESIAN_POINT ( 'NONE',  ( -10.61538461538461320, -2.486705287966279876, 31.30864560766543647 ) ) ;
#46753 = CARTESIAN_POINT ( 'NONE',  ( 2.057669083470849980, -2.588893531581426544, 31.60682220781847818 ) ) ;
#46754 = EDGE_CURVE ( 'NONE', #66607, #42352, #33518, .T. ) ;
#46755 = ADVANCED_FACE ( 'NONE', ( #61186 ), #26085, .F. ) ;
#46756 = AXIS2_PLACEMENT_3D ( 'NONE', #5911, #47778, #12668 ) ;
#46757 = CARTESIAN_POINT ( 'NONE',  ( -13.51476259405360381, -6.852621066184266141, 34.70813303252209181 ) ) ;
#46758 = ORIENTED_EDGE ( 'NONE', *, *, #16946, .T. ) ;
#46759 = FACE_OUTER_BOUND ( 'NONE', #87463, .T. ) ;
#46760 = B_SPLINE_CURVE_WITH_KNOTS ( 'NONE', 3,
 ( #35867, #40852, #7510, #15151, #63326, #34967, #68318, #82287, #14707, #1638 ),
 .UNSPECIFIED., .F., .F.,
 ( 4, 2, 2, 2, 4 ),
 ( 0.000000000000000000, 0.0001954311564186862510, 0.0003908623128373725020, 0.0005862934692560588072, 0.0007817246256747450040 ),
 .UNSPECIFIED. ) ;
#46761 = CARTESIAN_POINT ( 'NONE',  ( -3.903900635498011251, -5.057305518903949526, 34.11320923018887896 ) ) ;
#46762 = LINE ( 'NONE', #89101, #72741 ) ;
#46763 = FACE_BOUND ( 'NONE', #83575, .T. ) ;
#46764 = CARTESIAN_POINT ( 'NONE',  ( -18.00000000000000000, -8.120952969808772792, 34.71129190930000163 ) ) ;
#46765 = DIRECTION ( 'NONE',  ( -0.000000000000000000, 0.3420201433256694901, -0.9396926207859082059 ) ) ;
#46766 = B_SPLINE_CURVE_WITH_KNOTS ( 'NONE', 3,
 ( #65620, #58417, #64733, #43586, #51651, #22434, #49899, #9372, #50770, #36831 ),
 .UNSPECIFIED., .F., .F.,
 ( 4, 2, 2, 2, 4 ),
 ( 0.000000000000000000, 0.0001954339857564053873, 0.0003908679715128107746, 0.0005863019572692161618, 0.0007817359430256215491 ),
 .UNSPECIFIED. ) ;
#46767 = VECTOR ( 'NONE', #6933, 999.9999999999998863 ) ;
#46768 = CARTESIAN_POINT ( 'NONE',  ( 11.60371710973756443, -12.46129190930001052, 30.37095296980870174 ) ) ;
#46770 = FACE_OUTER_BOUND ( 'NONE', #49501, .T. ) ;
#46769 = CARTESIAN_POINT ( 'NONE',  ( 11.53846153846153832, -6.681629849574314051, 35.83090037661290239 ) ) ;
#46771 = DIRECTION ( 'NONE',  ( -0.000000000000000000, -0.9848077530122086864, -0.1736481776669273613 ) ) ;
#46772 = CARTESIAN_POINT ( 'NONE',  ( -0.4615384615384611200, -3.513871655860378418, 32.76840700105978499 ) ) ;
#46773 = ORIENTED_EDGE ( 'NONE', *, *, #59019, .F. ) ;
#46774 = CARTESIAN_POINT ( 'NONE',  ( -11.97435897435897267, -3.499999999999999556, 29.75000000000000355 ) ) ;
#46775 = AXIS2_PLACEMENT_3D ( 'NONE', #59369, #23790, #24237 ) ;
#46776 = CARTESIAN_POINT ( 'NONE',  ( -6.923076923077044142, -10.90142922262034020, 33.41473453929536674 ) ) ;
#46777 = ORIENTED_EDGE ( 'NONE', *, *, #24673, .T. ) ;
#46778 = ORIENTED_EDGE ( 'NONE', *, *, #28620, .T. ) ;
#46779 = CARTESIAN_POINT ( 'NONE',  ( -6.857821351800898135, -5.219633306516380244, 34.19971097300157936 ) ) ;
#46780 = CARTESIAN_POINT ( 'NONE',  ( -13.44988538517170440, -5.094484230520674117, 34.41647553114621161 ) ) ;
#46781 = CARTESIAN_POINT ( 'NONE',  ( -15.48076923076923173, -7.433931650972299465, 34.75000000000000711 ) ) ;
#46782 = ORIENTED_EDGE ( 'NONE', *, *, #58788, .T. ) ;
#46783 = CARTESIAN_POINT ( 'NONE',  ( 14.43821800945587341, -9.417988943895561960, 34.36773134775777550 ) ) ;
#46784 = CARTESIAN_POINT ( 'NONE',  ( -20.00000000000000355, -10.00000000000000533, 13.00000000000000178 ) ) ;
#46785 = FACE_BOUND ( 'NONE', #17205, .T. ) ;
#46787 = CARTESIAN_POINT ( 'NONE',  ( -24.99999999999999645, 20.00000000000000355, 0.000000000000000000 ) ) ;
#46786 = CARTESIAN_POINT ( 'NONE',  ( -15.45425417449318317, -5.912607949931405926, 34.49155766932282319 ) ) ;
#46788 = LINE ( 'NONE', #40920, #33004 ) ;
#46789 = LINE ( 'NONE', #26966, #55372 ) ;
#46791 = CARTESIAN_POINT ( 'NONE',  ( 2.057669083470850424, -10.92453946501458439, 33.72985991061850086 ) ) ;
#46790 = DIRECTION ( 'NONE',  ( 1.000000000000000000, 0.000000000000000000, 0.000000000000000000 ) ) ;
#46792 = CARTESIAN_POINT ( 'NONE',  ( -3.750000000000008438, -5.946699141100917352, 20.17187500000000000 ) ) ;
#46793 = ORIENTED_EDGE ( 'NONE', *, *, #64593, .F. ) ;
#46794 = ORIENTED_EDGE ( 'NONE', *, *, #11265, .T. ) ;
#46795 = CARTESIAN_POINT ( 'NONE',  ( 2.307692307692187583, -12.27809138561165270, 31.22303859784587132 ) ) ;
#46796 = CARTESIAN_POINT ( 'NONE',  ( -17.74994558008654622, -3.435999193479609470, 33.07426656108012253 ) ) ;
#46797 = DIRECTION ( 'NONE',  ( -0.000000000000000000, -0.9396926207859093161, -0.3420201433256663259 ) ) ;
#46798 = LINE ( 'NONE', #47682, #36647 ) ;
#46799 = FACE_OUTER_BOUND ( 'NONE', #38539, .T. ) ;
#46800 = CARTESIAN_POINT ( 'NONE',  ( -2.651650429449565305, -4.848349570550461785, 22.75000000000000000 ) ) ;
#46801 = CARTESIAN_POINT ( 'NONE',  ( -1.384615384615383471, -3.937682226553329556, 33.60647404775216529 ) ) ;
#46802 = FACE_OUTER_BOUND ( 'NONE', #44796, .T. ) ;
#46803 = AXIS2_PLACEMENT_3D ( 'NONE', #31963, #79706, #12581 ) ;
#46804 = DIRECTION ( 'NONE',  ( -0.000000000000000000, -0.9396926207859092051, -0.3420201433256662704 ) ) ;
#46805 = CARTESIAN_POINT ( 'NONE',  ( 13.38461538461538680, -9.905515769479276145, 34.41647553114623292 ) ) ;
#46806 = CARTESIAN_POINT ( 'NONE',  ( -9.757578138268467427, -11.48612834413959582, 32.76840700105983473 ) ) ;
#46807 = CARTESIAN_POINT ( 'NONE',  ( 13.38461538461538680, -2.486705287966279876, 31.30864560766543647 ) ) ;
#46808 = CARTESIAN_POINT ( 'NONE',  ( 7.145856592054990131, -3.563462043263029955, 33.22394488606062879 ) ) ;
#46809 = CARTESIAN_POINT ( 'NONE',  ( -13.38461538461538325, -9.780366693483667717, 34.19971097300155094 ) ) ;
#46810 = CARTESIAN_POINT ( 'NONE',  ( 2.531118706607095703, -7.630147987733843173, 34.99859428049665411 ) ) ;
#46811 = CARTESIAN_POINT ( 'NONE',  ( 7.846153846153846700, -2.249999999999998668, 29.75000000000001776 ) ) ;
#46812 = ORIENTED_EDGE ( 'NONE', *, *, #75606, .T. ) ;
#46813 = DIRECTION ( 'NONE',  ( 0.000000000000000000, 0.000000000000000000, 1.000000000000000000 ) ) ;
#46814 = CARTESIAN_POINT ( 'NONE',  ( -3.480792468062194889, -3.711651800289232916, 33.01384336483936011 ) ) ;
#46815 = CARTESIAN_POINT ( 'NONE',  ( 1.901340078031373171, -9.487747218494639867, 16.12686829374151287 ) ) ;
#46816 = CYLINDRICAL_SURFACE ( 'NONE', #53297, 0.2499999999999998890 ) ;
#46817 = CYLINDRICAL_SURFACE ( 'NONE', #85271, 0.2499999999999986955 ) ;
#46818 = CARTESIAN_POINT ( 'NONE',  ( 7.846153846153846700, -1.466349020453238561, 30.81389545987213907 ) ) ;
#46820 = ORIENTED_EDGE ( 'NONE', *, *, #8742, .F. ) ;
#46819 = CARTESIAN_POINT ( 'NONE',  ( 0.2115384615384616196, -2.249999999999998668, 29.75000000000000355 ) ) ;
#46821 = CARTESIAN_POINT ( 'NONE',  ( -2.749999999999991562, -8.639087296526026805, 23.76562500000000000 ) ) ;
#46822 = CARTESIAN_POINT ( 'NONE',  ( 3.480823650682684178, -8.346898887586323923, 34.93166121998716278 ) ) ;
#46823 = ORIENTED_EDGE ( 'NONE', *, *, #43743, .T. ) ;
#46824 = CARTESIAN_POINT ( 'NONE',  ( 8.519254038288414321, -8.303909089506435137, 34.68538101551103381 ) ) ;
#46825 = CARTESIAN_POINT ( 'NONE',  ( -17.93393164899755732, -3.513871655860376642, 32.76840700105978499 ) ) ;
#46826 = ORIENTED_EDGE ( 'NONE', *, *, #21437, .F. ) ;
#46827 = CARTESIAN_POINT ( 'NONE',  ( 3.164686851409094892, -4.661471528628506888, 34.16647553114621871 ) ) ;
#46828 = CARTESIAN_POINT ( 'NONE',  ( -15.23076923076935252, -3.083524468854526912, 32.58852847137268327 ) ) ;
#46829 = AXIS2_PLACEMENT_3D ( 'NONE', #61690, #48181, #16500 ) ;
#46830 = DIRECTION ( 'NONE',  ( -0.000000000000000000, -0.3420201433256694901, -0.9396926207859082059 ) ) ;
#46831 = ORIENTED_EDGE ( 'NONE', *, *, #40853, .F. ) ;
#46832 = VERTEX_POINT ( 'NONE', #67520 ) ;
#46833 = EDGE_CURVE ( 'NONE', #46874, #6628, #35950, .T. ) ;
#46834 = ORIENTED_EDGE ( 'NONE', *, *, #69, .F. ) ;
#46835 = CARTESIAN_POINT ( 'NONE',  ( 7.134615384615385025, -7.500000000000000000, 33.75000000000000000 ) ) ;
#46836 = DIRECTION ( 'NONE',  ( 1.000000000000000000, 0.000000000000000000, 0.000000000000000000 ) ) ;
#46837 = CARTESIAN_POINT ( 'NONE',  ( -7.846153846153844924, -11.11383981884818262, 36.00935417666054406 ) ) ;
#46838 = CARTESIAN_POINT ( 'NONE',  ( -15.29685161012936589, -2.292212530054419606, 30.41441678777542634 ) ) ;
#46839 = B_SPLINE_CURVE_WITH_KNOTS ( 'NONE', 3,
 ( #72106, #16716, #44172, #17160, #29805, #17623, #71657, #9961, #85629, #57266 ),
 .UNSPECIFIED., .F., .F.,
 ( 4, 2, 2, 2, 4 ),
 ( 0.000000000000000000, 0.0001954339857564097783, 0.0003908679715128195566, 0.0005863019572692293891, 0.0007817359430256391132 ),
 .UNSPECIFIED. ) ;
#46840 = CYLINDRICAL_SURFACE ( 'NONE', #63453, 0.2499999999999998890 ) ;
#46841 = CARTESIAN_POINT ( 'NONE',  ( -3.230769230769352962, -5.094484230521993062, 34.41647553114689373 ) ) ;
#46842 = CARTESIAN_POINT ( 'NONE',  ( 11.40777007179398339, -11.71456829005830080, 32.44064028649416542 ) ) ;
#46843 = CARTESIAN_POINT ( 'NONE',  ( -12.71151519248081740, -6.567427716900048118, 34.66269422305636283 ) ) ;
#46844 = B_SPLINE_CURVE_WITH_KNOTS ( 'NONE', 3,
 ( #23320, #50778, #16567, #44031, #71504, #9811, #64742, #73296, #32748, #31872 ),
 .UNSPECIFIED., .F., .F.,
 ( 4, 2, 2, 2, 4 ),
 ( 0.0007817246256747461966, 0.0009771112852218892010, 0.001172497944769032314, 0.001367884604316175427, 0.001563271263863318323 ),
 .UNSPECIFIED. ) ;
#46845 = EDGE_LOOP ( 'NONE', ( #32815, #36603 ) ) ;
#46846 = EDGE_LOOP ( 'NONE', ( #66795, #3109 ) ) ;
#46847 = EDGE_CURVE ( 'NONE', #57639, #35434, #61410, .T. ) ;
#46848 = ORIENTED_EDGE ( 'NONE', *, *, #8916, .T. ) ;
#46850 = VERTEX_POINT ( 'NONE', #69289 ) ;
#46849 = CARTESIAN_POINT ( 'NONE',  ( 18.22301284409339672, -9.172514111537580561, 34.72667873470787470 ) ) ;
#46851 = LINE ( 'NONE', #41431, #39207 ) ;
#46852 = CARTESIAN_POINT ( 'NONE',  ( 9.469381474791545017, -4.887634598454295265, 34.01352882383564946 ) ) ;
#46853 = ORIENTED_EDGE ( 'NONE', *, *, #60668, .T. ) ;
#46854 = CARTESIAN_POINT ( 'NONE',  ( 22.00000000000000711, 9.999999999999971578, 13.00000000000000178 ) ) ;
#46855 = VECTOR ( 'NONE', #52113, 1000.000000000000227 ) ;
#46856 = VERTEX_POINT ( 'NONE', #36389 ) ;
#46857 = FACE_OUTER_BOUND ( 'NONE', #6423, .T. ) ;
#46858 = ORIENTED_EDGE ( 'NONE', *, *, #37745, .T. ) ;
#46859 = CARTESIAN_POINT ( 'NONE',  ( 9.757563263583717728, -8.613356846314928816, 34.62446782046653482 ) ) ;
#46860 = EDGE_CURVE ( 'NONE', #67070, #314, #29202, .T. ) ;
#46861 = EDGE_CURVE ( 'NONE', #67515, #48597, #4460, .T. ) ;
#46862 = CARTESIAN_POINT ( 'NONE',  ( 1.607394925883795400, -6.760870238392817200, 34.69528174975672385 ) ) ;
#46863 = CARTESIAN_POINT ( 'NONE',  ( -4.403822897894745125, -6.524016743844655686, 34.90889640711025521 ) ) ;
#46864 = FACE_BOUND ( 'NONE', #5033, .T. ) ;
#46865 = FACE_OUTER_BOUND ( 'NONE', #25427, .T. ) ;
#46866 = CARTESIAN_POINT ( 'NONE',  ( 16.08857615328984281, -3.643525952247789856, 33.31231777344662959 ) ) ;
#46867 = CARTESIAN_POINT ( 'NONE',  ( -1.634592128663975075, -2.318417181685854533, 30.59732222474233865 ) ) ;
#46868 = EDGE_CURVE ( 'NONE', #78733, #66835, #19462, .T. ) ;
#46869 = CARTESIAN_POINT ( 'NONE',  ( 10.36536139116316058, -10.18141759479407327, 34.26406193332782379 ) ) ;
#46870 = CARTESIAN_POINT ( 'NONE',  ( 10.68053039471658394, -7.750023238201979581, 34.74374492549440419 ) ) ;
#46871 = CARTESIAN_POINT ( 'NONE',  ( 10.54930223602447903, -10.67929555188718460, 33.92786785259543336 ) ) ;
#46872 = CARTESIAN_POINT ( 'NONE',  ( -8.102564102564102200, -11.50000000000000000, 29.75000000000000355 ) ) ;
#46873 = EDGE_LOOP ( 'NONE', ( #23140, #9769 ) ) ;
#46874 = VERTEX_POINT ( 'NONE', #83704 ) ;
#46876 = CARTESIAN_POINT ( 'NONE',  ( 2.373760658694746173, -10.51840700105979565, 33.73612834413962247 ) ) ;
#46875 = CARTESIAN_POINT ( 'NONE',  ( 2.057669070399343880, -10.76384336483936011, 33.53834819971076087 ) ) ;
#46877 = DIRECTION ( 'NONE',  ( -0.000000000000000000, -0.000000000000000000, -1.000000000000000000 ) ) ;
#46878 = CARTESIAN_POINT ( 'NONE',  ( -14.30769230769242917, -12.16647553114689728, 32.15551576947799362 ) ) ;
#46879 = CARTESIAN_POINT ( 'NONE',  ( 17.01165263096229907, -8.613356846314824011, 34.62446782046655613 ) ) ;
#46880 = CARTESIAN_POINT ( 'NONE',  ( 1.515140822849031732, -4.299079248970732792, 33.91157788607253565 ) ) ;
#46881 = ORIENTED_EDGE ( 'NONE', *, *, #18414, .T. ) ;
#46882 = AXIS2_PLACEMENT_3D ( 'NONE', #13129, #61739, #25755 ) ;
#46883 = DIRECTION ( 'NONE',  ( -0.000000000000000000, -0.7660444431189791237, -0.6427876096865379196 ) ) ;
#46884 = CARTESIAN_POINT ( 'NONE',  ( 0.4615384615383396616, -10.21337939537710326, 33.94971097300076224 ) ) ;
#46885 = CARTESIAN_POINT ( 'NONE',  ( 17.01084069756293715, -3.937682226553330445, 33.60647404775217240 ) ) ;
#46886 = DIRECTION ( 'NONE',  ( 1.000000000000000000, 0.000000000000000000, 0.000000000000000000 ) ) ;
#46887 = ORIENTED_EDGE ( 'NONE', *, *, #1439, .T. ) ;
#46888 = ORIENTED_EDGE ( 'NONE', *, *, #40624, .T. ) ;
#46889 = PRODUCT_CONTEXT ( 'NONE', #82604, 'mechanical' ) ;
#46890 = EDGE_LOOP ( 'NONE', ( #79331, #74385 ) ) ;
#46891 = CARTESIAN_POINT ( 'NONE',  ( 10.55011461482829738, -4.320704448112771878, 33.92786785259540494 ) ) ;
#46892 = ORIENTED_EDGE ( 'NONE', *, *, #9810, .T. ) ;
#46893 = CARTESIAN_POINT ( 'NONE',  ( -15.90390063549801347, -5.057305518903949526, 34.11320923018887896 ) ) ;
#46894 = CARTESIAN_POINT ( 'NONE',  ( -6.222926958906846551, -9.172386477786396597, 34.72672124145550043 ) ) ;
#46895 = CARTESIAN_POINT ( 'NONE',  ( -6.249999999999997335, -7.500000000000001776, 34.75000000000000000 ) ) ;
#46896 = CARTESIAN_POINT ( 'NONE',  ( -18.75000000000000000, -7.500000000000000000, 33.75000000000000000 ) ) ;
#46897 = CARTESIAN_POINT ( 'NONE',  ( -0.7115616988314271696, -11.37209801155882971, 32.91403422569032955 ) ) ;
#46898 = ORIENTED_EDGE ( 'NONE', *, *, #85376, .T. ) ;
#46900 = ORIENTED_EDGE ( 'NONE', *, *, #79931, .F. ) ;
#46899 = CARTESIAN_POINT ( 'NONE',  ( -0.2114840416250080568, -12.01375889529407637, 32.43194544308182969 ) ) ;
#46901 = CARTESIAN_POINT ( 'NONE',  ( -5.300408001487407539, -2.353723527008295680, 30.78948104536958752 ) ) ;
#46902 = CARTESIAN_POINT ( 'NONE',  ( -2.980823821391188844, -2.589246495874657938, 31.60778113518102828 ) ) ;
#46903 = CARTESIAN_POINT ( 'NONE',  ( -11.78848476268299628, -10.92453946501458795, 33.72985991061850086 ) ) ;
#46904 = CARTESIAN_POINT ( 'NONE',  ( 8.769230769230768274, -11.91647553114624181, 32.58852847137148245 ) ) ;
#46905 = CARTESIAN_POINT ( 'NONE',  ( 13.31853300525525086, -3.937682226553330445, 33.60647404775217240 ) ) ;
#46906 = LINE ( 'NONE', #74392, #50680 ) ;
#46907 = CARTESIAN_POINT ( 'NONE',  ( -0.5268084620947811603, -2.657715359629089225, 31.77849191805834295 ) ) ;
#46908 = CARTESIAN_POINT ( 'NONE',  ( 2.775308065498755195, -6.422011778438505125, 19.64249329374151642 ) ) ;
#46909 = ORIENTED_EDGE ( 'NONE', *, *, #12352, .T. ) ;
#46910 = DIRECTION ( 'NONE',  ( -0.000000000000000000, 0.9396926207859092051, -0.3420201433256662704 ) ) ;
#46911 = CARTESIAN_POINT ( 'NONE',  ( -9.469528151039281028, -8.496831190052096971, 34.64984203495476578 ) ) ;
#46912 = ORIENTED_EDGE ( 'NONE', *, *, #70339, .T. ) ;
#46913 = ORIENTED_EDGE ( 'NONE', *, *, #51303, .T. ) ;
#46914 = CARTESIAN_POINT ( 'NONE',  ( -12.46153846153846168, -11.35647404775217417, 33.31231777344666511 ) ) ;
#46915 = CARTESIAN_POINT ( 'NONE',  ( 3.007903808565593362, -2.501496062324912284, 29.88072118266895671 ) ) ;
#46916 = EDGE_CURVE ( 'NONE', #79454, #78447, #21085, .T. ) ;
#46917 = VECTOR ( 'NONE', #42186, 1000.000000000000114 ) ;
#46918 = CARTESIAN_POINT ( 'NONE',  ( -6.923076923077044142, -6.026961402154118908, 34.52809138561165270 ) ) ;
#46919 = CARTESIAN_POINT ( 'NONE',  ( -5.011729095139719092, -2.506253911140448487, 29.99999999999988631 ) ) ;
#46920 = CARTESIAN_POINT ( 'NONE',  ( -2.307692307692305711, -3.050289026998446396, 32.03036669348365706 ) ) ;
#46921 = ORIENTED_EDGE ( 'NONE', *, *, #32870, .T. ) ;
#46922 = CARTESIAN_POINT ( 'NONE',  ( 5.776515056276052995, -3.754499324213721234, 33.06261337010820256 ) ) ;
#46923 = B_SPLINE_CURVE_WITH_KNOTS ( 'NONE', 3,
 ( #29765, #69419, #68970, #41505, #50024, #8164, #48691, #42838, #1398, #83834 ),
 .UNSPECIFIED., .F., .F.,
 ( 4, 2, 2, 2, 4 ),
 ( 0.0007817359430256338006, 0.0009771253907250062980, 0.001172514838424371531, 0.001367904286123736981, 0.001563293733823102431 ),
 .UNSPECIFIED. ) ;
#46924 = DIRECTION ( 'NONE',  ( -1.000000000000000000, -0.000000000000000000, -0.000000000000000000 ) ) ;
#46925 = CARTESIAN_POINT ( 'NONE',  ( -2.176901866725356793, -5.496552790871119143, 34.60292014791297532 ) ) ;
#46926 = ORIENTED_EDGE ( 'NONE', *, *, #81052, .F. ) ;
#46927 = DIRECTION ( 'NONE',  ( -0.000000000000000000, 0.6427876096865404731, -0.7660444431189770143 ) ) ;
#46928 = EDGE_CURVE ( 'NONE', #82406, #75693, #70020, .T. ) ;
#46929 = VERTEX_POINT ( 'NONE', #34615 ) ;
#46930 = CARTESIAN_POINT ( 'NONE',  ( 13.45068373561782593, -3.513871655860379306, 32.76840700105978499 ) ) ;
#46931 = CARTESIAN_POINT ( 'NONE',  ( -6.000000000000121680, -12.16647553114689728, 32.15551576947799362 ) ) ;
#46932 = EDGE_LOOP ( 'NONE', ( #70385, #72035 ) ) ;
#46933 = EDGE_CURVE ( 'NONE', #28537, #32578, #74343, .T. ) ;
#46934 = DIRECTION ( 'NONE',  ( 1.000000000000000000, 0.000000000000000000, 0.000000000000000000 ) ) ;
#46935 = CARTESIAN_POINT ( 'NONE',  ( 13.38461538461526423, -9.528491918059723176, 34.59228464037033035 ) ) ;
#46936 = CARTESIAN_POINT ( 'NONE',  ( -13.38461538461550759, -3.083524468854526912, 32.58852847137268327 ) ) ;
#46937 = CARTESIAN_POINT ( 'NONE',  ( -8.069080805060693251, -4.762599654559228846, 34.23009711892697737 ) ) ;
#46938 = CARTESIAN_POINT ( 'NONE',  ( -2.307692307692305711, -10.67929555188718282, 33.92786785259544047 ) ) ;
#46939 = ORIENTED_EDGE ( 'NONE', *, *, #35665, .F. ) ;
#46940 = EDGE_CURVE ( 'NONE', #72513, #73958, #51454, .T. ) ;
#46941 = DIRECTION ( 'NONE',  ( -0.000000000000000000, -0.7660444431189791237, -0.6427876096865379196 ) ) ;
#46942 = EDGE_LOOP ( 'NONE', ( #26173, #68426 ) ) ;
#46943 = DIRECTION ( 'NONE',  ( -0.000000000000000000, 0.3420201433256694901, -0.9396926207859082059 ) ) ;
#46944 = CARTESIAN_POINT ( 'NONE',  ( 0.6089743589743582541, -7.500000000000000000, 29.75000000000000355 ) ) ;
#46945 = EDGE_CURVE ( 'NONE', #47170, #46688, #60290, .T. ) ;
#46946 = CARTESIAN_POINT ( 'NONE',  ( 6.130791807824788719, -8.999086150933472084, 34.52020707165672064 ) ) ;
#46947 = AXIS2_PLACEMENT_3D ( 'NONE', #32984, #20362, #69426 ) ;
#46948 = CARTESIAN_POINT ( 'NONE',  ( 2.980792486720641232, -11.47974371597207899, 33.17467449705390692 ) ) ;
#46949 = CARTESIAN_POINT ( 'NONE',  ( 14.30769230769218581, -8.656820664282941280, 34.87096338111179961 ) ) ;
#46950 = ORIENTED_EDGE ( 'NONE', *, *, #53054, .F. ) ;
#46951 = B_SPLINE_CURVE_WITH_KNOTS ( 'NONE', 3,
 ( #79873, #52833, #46088, #11410, #10971, #38897, #17278, #11869, #66355, #39346 ),
 .UNSPECIFIED., .F., .F.,
 ( 4, 2, 2, 2, 4 ),
 ( 0.000000000000000000, 0.0001954339857564073659, 0.0003908679715128147319, 0.0005863019572692221250, 0.0007817359430256294638 ),
 .UNSPECIFIED. ) ;
#46952 = EDGE_LOOP ( 'NONE', ( #59613, #13125 ) ) ;
#46953 = VERTEX_POINT ( 'NONE', #10688 ) ;
#46954 = EDGE_LOOP ( 'NONE', ( #36749, #76190 ) ) ;
#46955 = EDGE_CURVE ( 'NONE', #37924, #67105, #77528, .T. ) ;
#46956 = CARTESIAN_POINT ( 'NONE',  ( 2.177545098254087819, -5.195881422630167279, 34.18770438780618548 ) ) ;
#46957 = CARTESIAN_POINT ( 'NONE',  ( 4.153846153846030731, -10.33852847137269571, 34.16647553114546554 ) ) ;
#46958 = EDGE_CURVE ( 'NONE', #82973, #25459, #71594, .T. ) ;
#46959 = CARTESIAN_POINT ( 'NONE',  ( -2.057692307692370104, -7.565270445406050648, 34.75000000000000000 ) ) ;
#46960 = CARTESIAN_POINT ( 'NONE',  ( 6.130525701763567703, -12.27024696741798770, 31.24895572276497546 ) ) ;
#46961 = CARTESIAN_POINT ( 'NONE',  ( 17.86985279056177944, -10.19110544564092002, 33.96427741523702792 ) ) ;
#46962 = EDGE_CURVE ( 'NONE', #57615, #59590, #43578, .T. ) ;
#46963 = VECTOR ( 'NONE', #16574, 1000.000000000000227 ) ;
#46964 = CARTESIAN_POINT ( 'NONE',  ( -5.326899807865431491, -8.303909089506435137, 34.68538101551103381 ) ) ;
#46965 = EDGE_CURVE ( 'NONE', #60579, #17730, #30940, .T. ) ;
#46966 = CARTESIAN_POINT ( 'NONE',  ( -2.084912766423895558, -3.755027918224367767, 33.06320215134714857 ) ) ;
#46967 = CARTESIAN_POINT ( 'NONE',  ( -8.638705330997126453, -3.068774925481847493, 32.56582465632704526 ) ) ;
#46968 = ORIENTED_EDGE ( 'NONE', *, *, #68716, .T. ) ;
#46969 = ORIENTED_EDGE ( 'NONE', *, *, #16815, .F. ) ;
#46970 = AXIS2_PLACEMENT_3D ( 'NONE', #62225, #41078, #34755 ) ;
#46971 = ORIENTED_EDGE ( 'NONE', *, *, #83157, .T. ) ;
#46973 = EDGE_LOOP ( 'NONE', ( #87293, #62061, #44248, #54539 ) ) ;
#46972 = CARTESIAN_POINT ( 'NONE',  ( -13.44988538517170440, -12.51329471203370325, 31.30864560766548976 ) ) ;
#46975 = CARTESIAN_POINT ( 'NONE',  ( -9.758390071667825794, -3.937682226553330445, 33.60647404775217240 ) ) ;
#46974 = CARTESIAN_POINT ( 'NONE',  ( -3.230769230769352962, -10.33852847137269571, 34.16647553114546554 ) ) ;
#46976 = CARTESIAN_POINT ( 'NONE',  ( -13.19230769230769162, -7.500000000000000000, 29.75000000000000355 ) ) ;
#46977 = FACE_OUTER_BOUND ( 'NONE', #83660, .T. ) ;
#46978 = FACE_BOUND ( 'NONE', #42125, .T. ) ;
#46979 = ORIENTED_EDGE ( 'NONE', *, *, #57670, .T. ) ;
#46980 = DIRECTION ( 'NONE',  ( -1.000000000000000000, 0.000000000000000000, 0.000000000000000000 ) ) ;
#46981 = ORIENTED_EDGE ( 'NONE', *, *, #44723, .T. ) ;
#46982 = CARTESIAN_POINT ( 'NONE',  ( -8.545854828532586822, -2.501478030877323455, 29.88021232661721172 ) ) ;
#46983 = ORIENTED_EDGE ( 'NONE', *, *, #5301, .T. ) ;
#46984 = FACE_BOUND ( 'NONE', #6973, .T. ) ;
#46985 = DIRECTION ( 'NONE',  ( -0.000000000000000000, -0.000000000000000000, -1.000000000000000000 ) ) ;
#46986 = B_SPLINE_CURVE_WITH_KNOTS ( 'NONE', 3,
 ( #69585, #48418, #14648, #15537, #7000, #62810, #42131, #88998, #22288, #246 ),
 .UNSPECIFIED., .F., .F.,
 ( 4, 2, 2, 2, 4 ),
 ( 0.000000000000000000, 0.0001954311564186875792, 0.0003908623128373751583, 0.0005862934692560627103, 0.0007817246256747503166 ),
 .UNSPECIFIED. ) ;
#46987 = CARTESIAN_POINT ( 'NONE',  ( 17.99999999999987566, -5.219633306517616589, 34.19971097300220464 ) ) ;
#46988 = ORIENTED_EDGE ( 'NONE', *, *, #32507, .F. ) ;
#46989 = CARTESIAN_POINT ( 'NONE',  ( 3.230769230769231726, -1.422936976036506707, 30.56769352161908415 ) ) ;
#46990 = CARTESIAN_POINT ( 'NONE',  ( 12.46153846153846168, -11.11383981884818262, 36.00935417666054406 ) ) ;
#46991 = CARTESIAN_POINT ( 'NONE',  ( 3.230769230769231726, -11.91647553114624181, 32.58852847137148245 ) ) ;
#46992 = ORIENTED_EDGE ( 'NONE', *, *, #70292, .T. ) ;
#46993 = CARTESIAN_POINT ( 'NONE',  ( 6.699591979352975457, -10.11188796281391511, 34.01382737946119050 ) ) ;
#46994 = CARTESIAN_POINT ( 'NONE',  ( 14.08476534878546360, -11.43668979543634734, 33.22377378376089752 ) ) ;
#46995 = CARTESIAN_POINT ( 'NONE',  ( 12.46153846153833911, -6.879047030192662504, 34.71129190930017927 ) ) ;
#46996 = CARTESIAN_POINT ( 'NONE',  ( 5.076923076923075762, -6.386643153685126251, 34.62446782046654192 ) ) ;
#46997 = EDGE_LOOP ( 'NONE', ( #11684, #63380, #55868, #86315 ) ) ;
#46998 = CARTESIAN_POINT ( 'NONE',  ( 2.307692307692309264, -12.34228464037088635, 31.77849191805839268 ) ) ;
#46999 = CARTESIAN_POINT ( 'NONE',  ( -16.15384615384627409, -10.33852847137269571, 34.16647553114546554 ) ) ;
#47000 = ORIENTED_EDGE ( 'NONE', *, *, #45127, .F. ) ;
#47001 = CARTESIAN_POINT ( 'NONE',  ( 17.99999999999987566, -6.879047030192662504, 34.71129190930017927 ) ) ;
#47002 = CARTESIAN_POINT ( 'NONE',  ( 9.942307692307759126, -7.434744860731433924, 35.00000000000000711 ) ) ;
#47003 = DIRECTION ( 'NONE',  ( -0.000000000000000000, -0.000000000000000000, -1.000000000000000000 ) ) ;
#47004 = CARTESIAN_POINT ( 'NONE',  ( 16.15384615384615330, -11.91647553114624181, 32.58852847137148245 ) ) ;
#47005 = CARTESIAN_POINT ( 'NONE',  ( 0.4615384615384611200, -2.486705287966279876, 31.30864560766543647 ) ) ;
#47006 = ADVANCED_FACE ( 'NONE', ( #50325 ), #64280, .F. ) ;
#47007 = VECTOR ( 'NONE', #37404, 999.9999999999998863 ) ;
#47008 = DIRECTION ( 'NONE',  ( 0.000000000000000000, 0.9848077530122072432, -0.1736481776669354937 ) ) ;
#47010 = CARTESIAN_POINT ( 'NONE',  ( 15.12820512820512953, -3.499999999999999556, 29.75000000000000355 ) ) ;
#47009 = CARTESIAN_POINT ( 'NONE',  ( 0.5923289025054125911, -11.37503395064541678, 33.29242100308974983 ) ) ;
#47011 = CARTESIAN_POINT ( 'NONE',  ( -6.792551221313360088, -2.882268652242224505, 31.66798894389554064 ) ) ;
#47012 = CARTESIAN_POINT ( 'NONE',  ( -1.409462824231155764E-14, -4.749999999999999112, 17.90625000000000000 ) ) ;
#47013 = ORIENTED_EDGE ( 'NONE', *, *, #84625, .T. ) ;
#47014 = VECTOR ( 'NONE', #75418, 1000.000000000000000 ) ;
#47015 = CARTESIAN_POINT ( 'NONE',  ( 17.75002326905764960, -4.236021600441997492, 33.53823185664189310 ) ) ;
#47016 = ORIENTED_EDGE ( 'NONE', *, *, #34524, .T. ) ;
#47017 = EDGE_CURVE ( 'NONE', #43624, #46336, #57104, .T. ) ;
#47018 = EDGE_LOOP ( 'NONE', ( #34652, #8111, #21469, #65819 ) ) ;
#47019 = CARTESIAN_POINT ( 'NONE',  ( -3.230769230769229949, -13.57706302396349152, 30.56769352161908060 ) ) ;
#47021 = VERTEX_POINT ( 'NONE', #78247 ) ;
#47020 = VECTOR ( 'NONE', #3946, 1000.000000000000227 ) ;
#47022 = CARTESIAN_POINT ( 'NONE',  ( 1.607628228708781304, -11.98016756924215009, 32.48728574198911190 ) ) ;
#47023 = CARTESIAN_POINT ( 'NONE',  ( 2.750000000000001776, -7.499999999999984013, 19.46875000000000000 ) ) ;
#47024 = CARTESIAN_POINT ( 'NONE',  ( 13.60739492588379917, -2.847695495035523550, 31.58253572463339154 ) ) ;
#47025 = CARTESIAN_POINT ( 'NONE',  ( -18.00000000000012079, -12.16647553114689906, 32.15551576947799362 ) ) ;
#47026 = DIRECTION ( 'NONE',  ( 0.000000000000000000, -1.000000000000000000, 5.421010862427522170E-17 ) ) ;
#47027 = EDGE_CURVE ( 'NONE', #59987, #74290, #73222, .T. ) ;
#47028 = CARTESIAN_POINT ( 'NONE',  ( -5.076923076923075762, -3.322132147404559976, 32.92929555188717927 ) ) ;
#47029 = CARTESIAN_POINT ( 'NONE',  ( -15.48079245499068612, -4.931416488878822335, 34.32920672191015399 ) ) ;
#47030 = CYLINDRICAL_SURFACE ( 'NONE', #78483, 0.2500000000000002220 ) ;
#47031 = CARTESIAN_POINT ( 'NONE',  ( 3.750000000000009770, -9.053300858899081760, 24.54687500000000000 ) ) ;
#47032 = FACE_OUTER_BOUND ( 'NONE', #67622, .T. ) ;
#47033 = CARTESIAN_POINT ( 'NONE',  ( -14.43825289943422696, -2.504760397472875155, 29.97295953869789997 ) ) ;
#47034 = LINE ( 'NONE', #39421, #65105 ) ;
#47036 = EDGE_LOOP ( 'NONE', ( #2201, #35195, #71358, #12272 ) ) ;
#47035 = EDGE_CURVE ( 'NONE', #31499, #85628, #9794, .T. ) ;
#47037 = ORIENTED_EDGE ( 'NONE', *, *, #64573, .F. ) ;
#47038 = CIRCLE ( 'NONE', #85872, 0.2500000000000002220 ) ;
#47039 = CARTESIAN_POINT ( 'NONE',  ( 6.857806477116147548, -2.625532179533445198, 30.86335684631481513 ) ) ;
#47040 = CARTESIAN_POINT ( 'NONE',  ( 5.076923076923075762, -8.973038597847269315, 34.52809138561121927 ) ) ;
#47041 = FACE_OUTER_BOUND ( 'NONE', #75646, .T. ) ;
#47042 = CARTESIAN_POINT ( 'NONE',  ( -6.923076923076922462, -5.471508081941601098, 34.59228464037088457 ) ) ;
#47043 = EDGE_CURVE ( 'NONE', #67813, #36002, #166, .T. ) ;
#47044 = CARTESIAN_POINT ( 'NONE',  ( 0.000000000000000000, -11.00000000000000000, 29.75000000000000355 ) ) ;
#47045 = CARTESIAN_POINT ( 'NONE',  ( -16.21992956480203318, -8.973038597847269315, 34.52809138561120506 ) ) ;
#47046 = CARTESIAN_POINT ( 'NONE',  ( 17.07692307692295586, -3.643525952248796163, 33.31231777344771672 ) ) ;
#47047 = AXIS2_PLACEMENT_3D ( 'NONE', #29110, #7501, #48466 ) ;
#47048 = ORIENTED_EDGE ( 'NONE', *, *, #50110, .T. ) ;
#47049 = CARTESIAN_POINT ( 'NONE',  ( -6.792285115252133743, -9.804649428959608670, 34.18742332936588468 ) ) ;
#47050 = EDGE_LOOP ( 'NONE', ( #27258, #86645 ) ) ;
#47051 = B_SPLINE_CURVE_WITH_KNOTS ( 'NONE', 3,
 ( #33047, #82128, #41575, #47434, #55527, #47884 ),
 .UNSPECIFIED., .F., .F.,
 ( 4, 2, 4 ),
 ( 4.220987180333913380E-17, 0.0001954756301637125201, 0.0003909512603273828648 ),
 .UNSPECIFIED. ) ;
#47052 = ORIENTED_EDGE ( 'NONE', *, *, #61418, .T. ) ;
#47053 = CARTESIAN_POINT ( 'NONE',  ( 16.37662582282421653, -9.418065098278011860, 34.63729479722530158 ) ) ;
#47054 = CARTESIAN_POINT ( 'NONE',  ( -14.30769230769230660, -6.343179335718451384, 34.87096338111211935 ) ) ;
#47055 = CARTESIAN_POINT ( 'NONE',  ( -7.053686578281003428, -7.722926974430166069, 34.99546784045485737 ) ) ;
#47056 = CARTESIAN_POINT ( 'NONE',  ( 6.065255139512838234, -8.656820664281605460, 34.87096338111211224 ) ) ;
#47057 = DIRECTION ( 'NONE',  ( 0.000000000000000000, 0.000000000000000000, 1.000000000000000000 ) ) ;
#47058 = VERTEX_POINT ( 'NONE', #5705 ) ;
#47059 = EDGE_LOOP ( 'NONE', ( #32098, #82511, #86896, #57892 ) ) ;
#47060 = AXIS2_PLACEMENT_3D ( 'NONE', #85105, #65697, #9008 ) ;
#47061 = ORIENTED_EDGE ( 'NONE', *, *, #38780, .T. ) ;
#47062 = ORIENTED_EDGE ( 'NONE', *, *, #33358, .F. ) ;
#47063 = EDGE_CURVE ( 'NONE', #33682, #29234, #80741, .T. ) ;
#47064 = CARTESIAN_POINT ( 'NONE',  ( 5.869852790561782108, -2.619462340734462380, 30.83744416345203021 ) ) ;
#47065 = CARTESIAN_POINT ( 'NONE',  ( 0.4615384615384611200, -7.500000000000001776, 35.04278698407183867 ) ) ;
#47066 = VECTOR ( 'NONE', #75865, 999.9999999999998863 ) ;
#47067 = CARTESIAN_POINT ( 'NONE',  ( 16.21991348719623360, -5.471508081941601098, 34.59228464037088457 ) ) ;
#47068 = EDGE_CURVE ( 'NONE', #70411, #2304, #52796, .T. ) ;
#47069 = CARTESIAN_POINT ( 'NONE',  ( -15.36091644020745051, -11.47017969459904130, 32.78971311882034456 ) ) ;
#47070 = CARTESIAN_POINT ( 'NONE',  ( 17.99999999999987566, -5.219633306517616589, 34.19971097300220464 ) ) ;
#47071 = EDGE_CURVE ( 'NONE', #44439, #74721, #7660, .T. ) ;
#47072 = CARTESIAN_POINT ( 'NONE',  ( 14.08420736396836226, -12.44517049084099725, 30.48991314939691932 ) ) ;
#47073 = AXIS2_PLACEMENT_3D ( 'NONE', #22664, #64084, #6165 ) ;
#47074 = ORIENTED_EDGE ( 'NONE', *, *, #60093, .F. ) ;
#47075 = VERTEX_POINT ( 'NONE', #39063 ) ;
#47076 = ORIENTED_EDGE ( 'NONE', *, *, #42470, .F. ) ;
#47078 = ORIENTED_EDGE ( 'NONE', *, *, #66693, .T. ) ;
#47077 = FACE_OUTER_BOUND ( 'NONE', #30085, .T. ) ;
#47079 = DIRECTION ( 'NONE',  ( -0.000000000000000000, 0.5000000000000011102, -0.8660254037844381525 ) ) ;
#47080 = CARTESIAN_POINT ( 'NONE',  ( 6.792600214960459404, -7.276988635370452485, 34.74523720219453793 ) ) ;
#47081 = B_SPLINE_CURVE_WITH_KNOTS ( 'NONE', 3,
 ( #43233, #70710, #61719, #36, #54979, #20744, #62608, #62173, #27951, #918 ),
 .UNSPECIFIED., .F., .F.,
 ( 4, 2, 2, 2, 4 ),
 ( 0.0007817359430256262112, 0.0009771253907249911191, 0.001172514838424356136, 0.001367904286123721152, 0.001563293733823086168 ),
 .UNSPECIFIED. ) ;
#47082 = CARTESIAN_POINT ( 'NONE',  ( -2.651650429449565305, -4.848349570550461785, 22.75000000000000000 ) ) ;
#47083 = ORIENTED_EDGE ( 'NONE', *, *, #78507, .T. ) ;
#47084 = EDGE_CURVE ( 'NONE', #13666, #80199, #88153, .T. ) ;
#47085 = CARTESIAN_POINT ( 'NONE',  ( 8.096099255531889582, -4.176053281294515251, 33.81426240980091791 ) ) ;
#47086 = EDGE_LOOP ( 'NONE', ( #50662, #34320 ) ) ;
#47087 = CARTESIAN_POINT ( 'NONE',  ( -16.15384615384615330, -9.780366693483667717, 34.19971097300155094 ) ) ;
#47088 = FACE_BOUND ( 'NONE', #13213, .T. ) ;
#47089 = FACE_OUTER_BOUND ( 'NONE', #26197, .T. ) ;
#47090 = CARTESIAN_POINT ( 'NONE',  ( -17.07692307692307665, -11.11383981884818262, 36.00935417666054406 ) ) ;
#47091 = EDGE_LOOP ( 'NONE', ( #46619, #7983, #49455, #1060 ) ) ;
#47092 = EDGE_CURVE ( 'NONE', #34883, #32683, #16950, .T. ) ;
#47093 = DIRECTION ( 'NONE',  ( 0.000000000000000000, 0.4999999999999960032, -0.8660254037844410391 ) ) ;
#47094 = DIRECTION ( 'NONE',  ( -0.000000000000000000, -0.8660254037844397068, -0.4999999999999978906 ) ) ;
#47095 = CARTESIAN_POINT ( 'NONE',  ( -13.38461538461538325, -1.242168528481310874, 33.36296068462461051 ) ) ;
#47096 = VERTEX_POINT ( 'NONE', #6152 ) ;
#47097 = DIRECTION ( 'NONE',  ( -0.000000000000000000, 0.9396926207859093161, -0.3420201433256663259 ) ) ;
#47098 = CARTESIAN_POINT ( 'NONE',  ( 1.607626736228236375, -8.239487800360276282, 34.69522927552633718 ) ) ;
#47099 = DIRECTION ( 'NONE',  ( -0.000000000000000000, 1.000000000000000000, -0.000000000000000000 ) ) ;
#47100 = CARTESIAN_POINT ( 'NONE',  ( -2.176901866725356349, -9.084667340241226796, 34.75534355489798344 ) ) ;
#47101 = LINE ( 'NONE', #39930, #37173 ) ;
#47102 = EDGE_CURVE ( 'NONE', #40306, #73925, #33625, .T. ) ;
#47103 = FACE_BOUND ( 'NONE', #79800, .T. ) ;
#47105 = DIRECTION ( 'NONE',  ( 0.000000000000000000, 0.3420201433256610524, 0.9396926207859113145 ) ) ;
#47104 = CARTESIAN_POINT ( 'NONE',  ( 10.61538461538461675, -3.322132147404559976, 32.92929555188717927 ) ) ;
#47106 = CIRCLE ( 'NONE', #87395, 0.2500000000000002220 ) ;
#47107 = DIRECTION ( 'NONE',  ( 1.000000000000000000, 0.000000000000000000, 0.000000000000000000 ) ) ;
#47109 = CYLINDRICAL_SURFACE ( 'NONE', #36307, 0.2500000000000008882 ) ;
#47108 = DIRECTION ( 'NONE',  ( 1.000000000000000000, 0.000000000000000000, 0.000000000000000000 ) ) ;
#47110 = CARTESIAN_POINT ( 'NONE',  ( -8.703162418228330921, -3.513871655860379306, 32.76840700105978499 ) ) ;
#47111 = CARTESIAN_POINT ( 'NONE',  ( -1.077988221561460236, -10.27530806549876452, 17.10750670625848713 ) ) ;
#47113 = EDGE_CURVE ( 'NONE', #54572, #82999, #85031, .T. ) ;
#47112 = VERTEX_POINT ( 'NONE', #39507 ) ;
#47114 = CARTESIAN_POINT ( 'NONE',  ( -8.769230769230768274, -5.557115091759785130, 34.35708131394839171 ) ) ;
#47115 = ORIENTED_EDGE ( 'NONE', *, *, #26185, .F. ) ;
#47116 = CARTESIAN_POINT ( 'NONE',  ( -18.22348492456433178, -3.562934362175797176, 33.22335522853831691 ) ) ;
#47117 = ORIENTED_EDGE ( 'NONE', *, *, #15723, .T. ) ;
#47118 = CARTESIAN_POINT ( 'NONE',  ( 16.28437159207980045, -12.70449254468099198, 30.44128974285582956 ) ) ;
#47119 = CARTESIAN_POINT ( 'NONE',  ( -13.60748164767848323, -2.251424796025575770, 29.88072029997477230 ) ) ;
#47121 = VERTEX_POINT ( 'NONE', #10079 ) ;
#47120 = CARTESIAN_POINT ( 'NONE',  ( -5.076923076923199218, -9.528491918059723176, 34.59228464037033035 ) ) ;
#47122 = CARTESIAN_POINT ( 'NONE',  ( 17.01084069756293715, -12.62096338111211580, 30.90682066428152908 ) ) ;
#47123 = CARTESIAN_POINT ( 'NONE',  ( 18.25000000000141753, -7.500000000000154543, 35.00000000000007105 ) ) ;
#47124 = CARTESIAN_POINT ( 'NONE',  ( -2.694853999681210865, -4.891553140782108677, 27.49813170625849068 ) ) ;
#47125 = FACE_OUTER_BOUND ( 'NONE', #33988, .T. ) ;
#47126 = FACE_OUTER_BOUND ( 'NONE', #45519, .T. ) ;
#47127 = EDGE_CURVE ( 'NONE', #49729, #71435, #68709, .T. ) ;
#47128 = B_SPLINE_CURVE_WITH_KNOTS ( 'NONE', 3,
 ( #23898, #78851, #44610, #10851, #10408, #58573, #65337, #31102, #72541, #38321 ),
 .UNSPECIFIED., .F., .F.,
 ( 4, 2, 2, 2, 4 ),
 ( 0.000000000000000000, 0.0001954311564186864678, 0.0003908623128373729357, 0.0005862934692560594577, 0.0007817246256747458714 ),
 .UNSPECIFIED. ) ;
#47129 = CARTESIAN_POINT ( 'NONE',  ( -12.39547112818838492, -9.058645607665452459, 34.76329471203371924 ) ) ;
#47130 = DIRECTION ( 'NONE',  ( -0.000000000000000000, -0.9396926207859093161, -0.3420201433256663259 ) ) ;
#47131 = CARTESIAN_POINT ( 'NONE',  ( 2.438484115517092654, -2.729792928343269587, 31.24908615093345077 ) ) ;
#47132 = CARTESIAN_POINT ( 'NONE',  ( -11.31568199719312773, -10.11255958852956027, 34.01340905677048454 ) ) ;
#47133 = CARTESIAN_POINT ( 'NONE',  ( 0.06109907496451268821, -3.749999999999999556, 19.40811829374151287 ) ) ;
#47134 = AXIS2_PLACEMENT_3D ( 'NONE', #74481, #34372, #11901 ) ;
#47135 = CARTESIAN_POINT ( 'NONE',  ( 5.076923076922953193, -2.657715359629662988, 31.77849191805970364 ) ) ;
#47136 = ADVANCED_FACE ( 'NONE', ( #85748 ), #10530, .F. ) ;
#47137 = CARTESIAN_POINT ( 'NONE',  ( -8.899378738962470337, -3.069018819979302926, 32.56621877034667278 ) ) ;
#47138 = VERTEX_POINT ( 'NONE', #30353 ) ;
#47139 = CYLINDRICAL_SURFACE ( 'NONE', #18261, 0.2499999999999973355 ) ;
#47140 = DIRECTION ( 'NONE',  ( 0.000000000000000000, 0.8660254037844377084, 0.5000000000000015543 ) ) ;
#47141 = CARTESIAN_POINT ( 'NONE',  ( -0.06109907496450878162, -11.25000000000000000, 21.28311829374151287 ) ) ;
#47142 = FACE_OUTER_BOUND ( 'NONE', #50926, .T. ) ;
#47143 = CARTESIAN_POINT ( 'NONE',  ( -16.28399412357785536, -11.04286588640298561, 33.62463336215343901 ) ) ;
#47144 = ORIENTED_EDGE ( 'NONE', *, *, #31098, .F. ) ;
#47145 = DIRECTION ( 'NONE',  ( -0.000000000000000000, 0.1736481776669307198, -0.9848077530122080203 ) ) ;
#47146 = CARTESIAN_POINT ( 'NONE',  ( 2.980745993476266786, -3.711651800289232916, 33.01384336483936011 ) ) ;
#47148 = VERTEX_POINT ( 'NONE', #51480 ) ;
#47147 = CARTESIAN_POINT ( 'NONE',  ( 5.076923076923075762, -9.819645486525091727, 36.12317359536749706 ) ) ;
#47149 = CARTESIAN_POINT ( 'NONE',  ( 12.52760681254089725, -12.37446782046654192, 30.86335684631486842 ) ) ;
#47150 = CIRCLE ( 'NONE', #67282, 0.2500000000000002220 ) ;
#47151 = EDGE_CURVE ( 'NONE', #86521, #86086, #76408, .T. ) ;
#47152 = CARTESIAN_POINT ( 'NONE',  ( -15.10024379253559168, -12.15418822224088835, 32.17964115625579069 ) ) ;
#47153 = CARTESIAN_POINT ( 'NONE',  ( 14.30769230769262279, -2.255955759149395501, 30.00000000000324363 ) ) ;
#47154 = EDGE_CURVE ( 'NONE', #15980, #79283, #48483, .T. ) ;
#47155 = ORIENTED_EDGE ( 'NONE', *, *, #70006, .F. ) ;
#47156 = CARTESIAN_POINT ( 'NONE',  ( 3.007284306204897728, -2.612411019501189813, 31.66733052389439962 ) ) ;
#47157 = CARTESIAN_POINT ( 'NONE',  ( 6.857806477116148436, -5.219633306516282545, 34.19971097300152252 ) ) ;
#47158 = CARTESIAN_POINT ( 'NONE',  ( 1.318533005255250412, -2.833524468853757305, 32.15551576947924417 ) ) ;
#47159 = VERTEX_POINT ( 'NONE', #23588 ) ;
#47160 = EDGE_LOOP ( 'NONE', ( #23616, #77426 ) ) ;
#47161 = ORIENTED_EDGE ( 'NONE', *, *, #69552, .F. ) ;
#47162 = ORIENTED_EDGE ( 'NONE', *, *, #3762, .T. ) ;
#47163 = CIRCLE ( 'NONE', #14056, 4.000000000000000000 ) ;
#47164 = CARTESIAN_POINT ( 'NONE',  ( 5.076923076923075762, -12.10708131394839349, 31.69288490824020244 ) ) ;
#47165 = CARTESIAN_POINT ( 'NONE',  ( -2.084680956079456582, -5.667800583137508674, 34.40243808032445827 ) ) ;
#47166 = DIRECTION ( 'NONE',  ( -0.000000000000000000, -0.000000000000000000, -1.000000000000000000 ) ) ;
#47167 = CARTESIAN_POINT ( 'NONE',  ( 4.153846153846154188, -9.905515769479276145, 34.41647553114623292 ) ) ;
#47168 = AXIS2_PLACEMENT_3D ( 'NONE', #33462, #26699, #118 ) ;
#47169 = CARTESIAN_POINT ( 'NONE',  ( -2.307692307692305711, -1.215029322943914858, 32.30358669280327177 ) ) ;
#47170 = VERTEX_POINT ( 'NONE', #30789 ) ;
#47171 = EDGE_LOOP ( 'NONE', ( #13343, #17122 ) ) ;
#47172 = ORIENTED_EDGE ( 'NONE', *, *, #56571, .F. ) ;
#47174 = VERTEX_POINT ( 'NONE', #51039 ) ;
#47173 = CARTESIAN_POINT ( 'NONE',  ( -3.007393290071045833, -2.501478030877322567, 29.88021232661720816 ) ) ;
#47175 = DIRECTION ( 'NONE',  ( 1.000000000000000000, 0.000000000000000000, 0.000000000000000000 ) ) ;
#47176 = CARTESIAN_POINT ( 'NONE',  ( -10.68070862818892230, -7.749976730030849303, 34.74374725381503737 ) ) ;
#47177 = EDGE_CURVE ( 'NONE', #17613, #42225, #78634, .T. ) ;
#47178 = CARTESIAN_POINT ( 'NONE',  ( -19.50000000000000000, -3.499999999999999556, 29.75000000000000355 ) ) ;
#47179 = CARTESIAN_POINT ( 'NONE',  ( -15.00798968950081758, -9.332535724633409302, 34.40230450496446934 ) ) ;
#47180 = ADVANCED_FACE ( 'NONE', ( #44283 ), #71771, .F. ) ;
#47181 = EDGE_LOOP ( 'NONE', ( #60258, #28012 ) ) ;
#47182 = ORIENTED_EDGE ( 'NONE', *, *, #46169, .T. ) ;
#47183 = EDGE_LOOP ( 'NONE', ( #19558, #38505 ) ) ;
#47184 = CARTESIAN_POINT ( 'NONE',  ( -10.83831157429145975, -10.77366814457252175, 33.85459836347579454 ) ) ;
#47186 = ORIENTED_EDGE ( 'NONE', *, *, #35542, .F. ) ;
#47185 = CARTESIAN_POINT ( 'NONE',  ( 11.53846153846153832, -6.435427911321262684, 35.78748833219616898 ) ) ;
#47187 = EDGE_CURVE ( 'NONE', #33472, #58556, #14197, .T. ) ;
#47188 = FACE_OUTER_BOUND ( 'NONE', #7448, .T. ) ;
#47189 = CARTESIAN_POINT ( 'NONE',  ( -18.00000000000000000, -13.83693561022309915, 32.05645593858272235 ) ) ;
#47190 = EDGE_LOOP ( 'NONE', ( #31803, #25120 ) ) ;
#47191 = CARTESIAN_POINT ( 'NONE',  ( 16.15384615384603251, -11.67786785259630911, 32.92929555188603530 ) ) ;
#47192 = CARTESIAN_POINT ( 'NONE',  ( -3.931066612577743147, -5.114059244376869984, 34.14424750095245287 ) ) ;
#47193 = ADVANCED_FACE ( 'NONE', ( #81655 ), #75339, .F. ) ;
#47194 = CARTESIAN_POINT ( 'NONE',  ( 0.3313904918067657190, -9.504002272028875709, 34.60269587691767867 ) ) ;
#47195 = VECTOR ( 'NONE', #5667, 1000.000000000000000 ) ;
#47196 = FACE_BOUND ( 'NONE', #68805, .T. ) ;
#47197 = B_SPLINE_CURVE_WITH_KNOTS ( 'NONE', 3,
 ( #69958, #10369, #49250, #78815, #64849, #58098, #8271, #31523, #38281, #86489 ),
 .UNSPECIFIED., .F., .F.,
 ( 4, 2, 2, 2, 4 ),
 ( 0.0007817246256747481482, 0.0009771112852218909357, 0.001172497944769033832, 0.001367884604316176728, 0.001563271263863319407 ),
 .UNSPECIFIED. ) ;
#47198 = CARTESIAN_POINT ( 'NONE',  ( 10.68145296638705410, -9.780366693483667717, 34.19971097300155805 ) ) ;
#47199 = DIRECTION ( 'NONE',  ( -0.000000000000000000, 1.000000000000000000, -0.000000000000000000 ) ) ;
#47200 = CARTESIAN_POINT ( 'NONE',  ( 15.23076923076923173, -3.050289026998446396, 32.03036669348365706 ) ) ;
#47202 = DIRECTION ( 'NONE',  ( 0.000000000000000000, -6.938893903907222067E-15, 1.000000000000000000 ) ) ;
#47201 = CARTESIAN_POINT ( 'NONE',  ( 9.562160482869472844, -3.285722584762969856, 32.44110544564090759 ) ) ;
#47203 = ADVANCED_FACE ( 'NONE', ( #82098 ), #81214, .F. ) ;
#47204 = CARTESIAN_POINT ( 'NONE',  ( 0.3962680155776854285, -12.27809138561121394, 31.22303859784730307 ) ) ;
#47205 = CARTESIAN_POINT ( 'NONE',  ( 12.68431813051652313, -3.020022701398814569, 32.48759521482552515 ) ) ;
#47206 = ORIENTED_EDGE ( 'NONE', *, *, #10684, .F. ) ;
#47207 = VECTOR ( 'NONE', #10728, 1000.000000000000227 ) ;
#47208 = CARTESIAN_POINT ( 'NONE',  ( -15.23076923076922995, -11.35647404775217417, 33.31231777344666511 ) ) ;
#47209 = SURFACE_STYLE_FILL_AREA ( #19746 ) ;
#47210 = ORIENTED_EDGE ( 'NONE', *, *, #11258, .F. ) ;
#47211 = CARTESIAN_POINT ( 'NONE',  ( -15.23076923076922995, -1.466349020453238561, 30.81389545987213907 ) ) ;
#47212 = EDGE_CURVE ( 'NONE', #48528, #26836, #51655, .T. ) ;
#47213 = CARTESIAN_POINT ( 'NONE',  ( -15.36091644020745051, -2.619462340734462380, 30.83744416345203021 ) ) ;
#47214 = CARTESIAN_POINT ( 'NONE',  ( 9.626224281351811740, -2.721908614388770964, 31.22303859784723912 ) ) ;
#47215 = ORIENTED_EDGE ( 'NONE', *, *, #88857, .F. ) ;
#47216 = CARTESIAN_POINT ( 'NONE',  ( -9.692307692307814193, -9.528491918059723176, 34.59228464037033035 ) ) ;
#47217 = DIRECTION ( 'NONE',  ( -0.000000000000000000, 0.9396926207859092051, -0.3420201433256662704 ) ) ;
#47218 = FACE_BOUND ( 'NONE', #20345, .T. ) ;
#47220 = CARTESIAN_POINT ( 'NONE',  ( -10.61538461538461320, -13.20930481340135110, 34.54067556320372745 ) ) ;
#47219 = CARTESIAN_POINT ( 'NONE',  ( -14.55771553191376633, -4.175268141568685643, 33.81360843649122216 ) ) ;
#47221 = CARTESIAN_POINT ( 'NONE',  ( -13.38461538461550759, -5.094484230521993062, 34.41647553114689373 ) ) ;
#47222 = CARTESIAN_POINT ( 'NONE',  ( -5.207614543590635137, -8.999036380462719364, 34.52022231692819076 ) ) ;
#47224 = CARTESIAN_POINT ( 'NONE',  ( 2.307692307692309264, -10.67929555188718282, 33.92786785259544047 ) ) ;
#47223 = DIRECTION ( 'NONE',  ( 1.000000000000000000, 0.000000000000000000, 0.000000000000000000 ) ) ;
#47225 = CARTESIAN_POINT ( 'NONE',  ( 2.651650429449539104, -4.848349570550432475, 21.81250000000000000 ) ) ;
#47226 = ORIENTED_EDGE ( 'NONE', *, *, #26002, .F. ) ;
#47227 = EDGE_CURVE ( 'NONE', #8709, #68144, #66852, .T. ) ;
#47228 = EDGE_LOOP ( 'NONE', ( #46939, #38348, #44345, #56276 ) ) ;
#47229 = CARTESIAN_POINT ( 'NONE',  ( -20.00000000000000355, 10.00000000000000711, 13.00000000000000178 ) ) ;
#47230 = EDGE_CURVE ( 'NONE', #43122, #37045, #5549, .T. ) ;
#47231 = CARTESIAN_POINT ( 'NONE',  ( 16.40390046548447245, -6.567000820036036579, 34.66262288849541306 ) ) ;
#47232 = CARTESIAN_POINT ( 'NONE',  ( -2.307692307692305711, -7.500000000000001776, 35.04278698407183867 ) ) ;
#47233 = CARTESIAN_POINT ( 'NONE',  ( -0.7115384615384606759, -7.500000000000001776, 34.75000000000000000 ) ) ;
#47234 = CARTESIAN_POINT ( 'NONE',  ( 5.299935921016471596, -3.395485233115139057, 33.02377354290275946 ) ) ;
#47235 = CARTESIAN_POINT ( 'NONE',  ( -3.750000000000008438, -5.946699141100917352, 23.92187500000000355 ) ) ;
#47236 = CARTESIAN_POINT ( 'NONE',  ( -8.834500769787091201, -10.33852847137145048, 34.16647553114627556 ) ) ;
#47237 = CARTESIAN_POINT ( 'NONE',  ( 1.384615384615386802, -9.905515769479276145, 34.41647553114623292 ) ) ;
#47238 = AXIS2_PLACEMENT_3D ( 'NONE', #53928, #53480, #81862 ) ;
#47239 = CARTESIAN_POINT ( 'NONE',  ( 7.716005876422150855, -5.915902021225892149, 34.75552854090298638 ) ) ;
#47240 = CARTESIAN_POINT ( 'NONE',  ( -24.00000000000000000, 5.000000000000023093, 29.24999999999999645 ) ) ;
#47241 = CARTESIAN_POINT ( 'NONE',  ( 9.757563263583719504, -2.892918686051625166, 31.69288490824026638 ) ) ;
#47242 = VECTOR ( 'NONE', #67080, 1000.000000000000000 ) ;
#47243 = CARTESIAN_POINT ( 'NONE',  ( 8.703147358274886614, -12.10708131394839349, 31.69288490824020244 ) ) ;
#47244 = B_SPLINE_CURVE_WITH_KNOTS ( 'NONE', 3,
 ( #56888, #56456, #31073, #15920, #42068, #35296, #83943, #70864, #24314, #9166 ),
 .UNSPECIFIED., .F., .F.,
 ( 4, 2, 2, 2, 4 ),
 ( 0.0007817246256747474977, 0.0009771112852218911526, 0.001172497944769034699, 0.001367884604316178462, 0.001563271263863322009 ),
 .UNSPECIFIED. ) ;
#47245 = CARTESIAN_POINT ( 'NONE',  ( -0.2385256174450664235, -4.026326845037961455, 33.68677907613344047 ) ) ;
#47247 = EDGE_CURVE ( 'NONE', #77897, #18500, #6439, .T. ) ;
#47246 = CARTESIAN_POINT ( 'NONE',  ( -8.638705330997126453, -11.66157788607254098, 32.95092075102925833 ) ) ;
#47248 = EDGE_CURVE ( 'NONE', #17957, #34265, #58678, .T. ) ;
#47249 = CARTESIAN_POINT ( 'NONE',  ( -3.480745974817820887, -12.41104346484419452, 31.60698883733904196 ) ) ;
#47250 = ORIENTED_EDGE ( 'NONE', *, *, #47625, .T. ) ;
#47251 = CARTESIAN_POINT ( 'NONE',  ( -4.283993363284374745, -5.195881422630167279, 34.18770438780618548 ) ) ;
#47252 = CARTESIAN_POINT ( 'NONE',  ( -3.230769230769229949, -3.513871655860378418, 32.76840700105978499 ) ) ;
#47253 = CARTESIAN_POINT ( 'NONE',  ( 2.724691934501250135, -8.700186371490531201, 16.04874329374151287 ) ) ;
#47254 = CARTESIAN_POINT ( 'NONE',  ( -0.2115930521604175163, -10.92531984108285670, 33.72920026020278073 ) ) ;
#47255 = CARTESIAN_POINT ( 'NONE',  ( 6.000000000000001776, -9.819645486525091727, 36.12317359536749706 ) ) ;
#47256 = CARTESIAN_POINT ( 'NONE',  ( 10.36536137809165403, -5.851115903089112003, 34.47074536777953568 ) ) ;
#47258 = ORIENTED_EDGE ( 'NONE', *, *, #18171, .T. ) ;
#47257 = CARTESIAN_POINT ( 'NONE',  ( 10.36538461538461675, -7.500000000000001776, 35.00000000000000000 ) ) ;
#47259 = CARTESIAN_POINT ( 'NONE',  ( 1.944543648262996083, -5.555456351736983045, 24.31250000000000000 ) ) ;
#47260 = CARTESIAN_POINT ( 'NONE',  ( 3.453782074862625784, -8.282913670948747864, 34.94150082978203642 ) ) ;
#47261 = EDGE_CURVE ( 'NONE', #47404, #37079, #62522, .T. ) ;
#47262 = ORIENTED_EDGE ( 'NONE', *, *, #37356, .F. ) ;
#47263 = CARTESIAN_POINT ( 'NONE',  ( 11.60371667797437567, -9.528491918058460186, 34.59228464037086326 ) ) ;
#47264 = CARTESIAN_POINT ( 'NONE',  ( 0.3962680155776857061, -2.892918686051582533, 31.69288490824015270 ) ) ;
#47265 = VERTEX_POINT ( 'NONE', #27143 ) ;
#47266 = CARTESIAN_POINT ( 'NONE',  ( 0.4615384615384611200, -4.945431358278436385, 36.03766855953609394 ) ) ;
#47267 = EDGE_CURVE ( 'NONE', #14607, #53071, #1274, .T. ) ;
#47268 = ADVANCED_FACE ( 'NONE', ( #34337 ), #20392, .F. ) ;
#47269 = LINE ( 'NONE', #40965, #24975 ) ;
#47270 = CARTESIAN_POINT ( 'NONE',  ( -8.069080063669991532, -3.586966769969701208, 32.86292498521069660 ) ) ;
#47271 = ORIENTED_EDGE ( 'NONE', *, *, #88402, .T. ) ;
#47272 = VERTEX_POINT ( 'NONE', #1006 ) ;
#47273 = AXIS2_PLACEMENT_3D ( 'NONE', #34042, #13328, #18764 ) ;
#47274 = EDGE_CURVE ( 'NONE', #78089, #8848, #25841, .T. ) ;
#47275 = ORIENTED_EDGE ( 'NONE', *, *, #41030, .F. ) ;
#47276 = CARTESIAN_POINT ( 'NONE',  ( 7.596130621932389637, -9.356822207818508375, 34.66110646841856635 ) ) ;
#47277 = DIRECTION ( 'NONE',  ( 0.000000000000000000, 0.000000000000000000, 1.000000000000000000 ) ) ;
#47278 = CARTESIAN_POINT ( 'NONE',  ( 18.13052543823364360, -10.31582465632704704, 34.18122507451815295 ) ) ;
#47279 = CARTESIAN_POINT ( 'NONE',  ( -15.48079245499068612, -2.341070481393819236, 30.72580821765574299 ) ) ;
#47280 = CARTESIAN_POINT ( 'NONE',  ( -0.4615384615385826339, -12.27809138561165270, 31.22303859784587132 ) ) ;
#47281 = CARTESIAN_POINT ( 'NONE',  ( -3.007989561791163613, -4.989023458446561143, 34.36081565061822118 ) ) ;
#47282 = CARTESIAN_POINT ( 'NONE',  ( 13.44987095589141113, -3.300289026998473041, 32.46337939537591666 ) ) ;
#47283 = LINE ( 'NONE', #81534, #82339 ) ;
#47284 = ORIENTED_EDGE ( 'NONE', *, *, #10844, .F. ) ;
#47285 = ORIENTED_EDGE ( 'NONE', *, *, #85819, .T. ) ;
#47287 = VERTEX_POINT ( 'NONE', #76209 ) ;
#47286 = CARTESIAN_POINT ( 'NONE',  ( -2.307692307692305711, -12.09954503811598769, 35.62045528018868623 ) ) ;
#47288 = EDGE_CURVE ( 'NONE', #10737, #10260, #82797, .T. ) ;
#47289 = AXIS2_PLACEMENT_3D ( 'NONE', #23523, #78466, #44222 ) ;
#47290 = LINE ( 'NONE', #75222, #59367 ) ;
#47291 = CARTESIAN_POINT ( 'NONE',  ( 11.78851585009985392, -12.17597550085003810, 31.52189283813460463 ) ) ;
#47292 = EDGE_LOOP ( 'NONE', ( #10744, #2388, #74298, #58710 ) ) ;
#47293 = CARTESIAN_POINT ( 'NONE',  ( -12.23875879256039489, -11.60474049983371003, 33.02348890104160262 ) ) ;
#47294 = B_SPLINE_CURVE_WITH_KNOTS ( 'NONE', 3,
 ( #60706, #81440, #74679, #37213, #36776, #69678, #14746, #21939, #50718, #779 ),
 .UNSPECIFIED., .F., .F.,
 ( 4, 2, 2, 2, 4 ),
 ( 0.000000000000000000, 0.0001954339857564126514, 0.0003908679715128183098, 0.0005863019572692239681, 0.0007817359430256294638 ),
 .UNSPECIFIED. ) ;
#47295 = VECTOR ( 'NONE', #51693, 1000.000000000000000 ) ;
#47296 = ORIENTED_EDGE ( 'NONE', *, *, #73825, .T. ) ;
#47297 = CARTESIAN_POINT ( 'NONE',  ( 17.01165263096229907, -10.21337939537584383, 33.94971097300158647 ) ) ;
#47298 = ORIENTED_EDGE ( 'NONE', *, *, #5196, .F. ) ;
#47299 = VECTOR ( 'NONE', #26873, 1000.000000000000000 ) ;
#47300 = CARTESIAN_POINT ( 'NONE',  ( -18.00000000000012079, -9.528491918059723176, 34.59228464037033035 ) ) ;
#47301 = VERTEX_POINT ( 'NONE', #83877 ) ;
#47302 = AXIS2_PLACEMENT_3D ( 'NONE', #84899, #8795, #29949 ) ;
#47303 = CARTESIAN_POINT ( 'NONE',  ( -12.21148404162501144, -10.06805714834173493, 34.32951233291982618 ) ) ;
#47304 = CARTESIAN_POINT ( 'NONE',  ( 10.83816415665302380, -5.114059244376869984, 34.14424750095245287 ) ) ;
#47305 = FACE_BOUND ( 'NONE', #21911, .T. ) ;
#47306 = DIRECTION ( 'NONE',  ( 0.000000000000000000, 0.3420201433256641055, -0.9396926207859100932 ) ) ;
#47307 = PLANE ( 'NONE',  #57245 ) ;
#47308 = CARTESIAN_POINT ( 'NONE',  ( -1.634638608836841644, -2.341070481393820124, 30.72580821765574299 ) ) ;
#47309 = CARTESIAN_POINT ( 'NONE',  ( 1.384615384615264011, -12.51329471203414379, 31.30864560766407578 ) ) ;
#47310 = DIRECTION ( 'NONE',  ( -0.000000000000000000, 0.7660444431189791237, -0.6427876096865379196 ) ) ;
#47311 = LINE ( 'NONE', #40576, #62009 ) ;
#47312 = CARTESIAN_POINT ( 'NONE',  ( -10.36533030374629760, -4.235687564193447052, 33.53795663066793509 ) ) ;
#47313 = ORIENTED_EDGE ( 'NONE', *, *, #66135, .F. ) ;
#47314 = ORIENTED_EDGE ( 'NONE', *, *, #73658, .T. ) ;
#47316 = CARTESIAN_POINT ( 'NONE',  ( -18.00000000000000000, -9.905515769479279697, 34.41647553114623292 ) ) ;
#47315 = CARTESIAN_POINT ( 'NONE',  ( -5.299850035829923200, -11.98009711892699691, 32.48740034544075428 ) ) ;
#47317 = EDGE_CURVE ( 'NONE', #30720, #61793, #9716, .T. ) ;
#47318 = CARTESIAN_POINT ( 'NONE',  ( -4.088701373126520267, -7.750023224968867197, 34.99404313364389907 ) ) ;
#47319 = CARTESIAN_POINT ( 'NONE',  ( 3.480714749117372886, -10.76462480002816235, 33.53768742498949962 ) ) ;
#47320 = CARTESIAN_POINT ( 'NONE',  ( 8.834375549950401307, -7.750023224968867197, 34.99404313364389907 ) ) ;
#47321 = CARTESIAN_POINT ( 'NONE',  ( -13.38461538461538325, -2.721908614388771852, 31.22303859784724978 ) ) ;
#47322 = ORIENTED_EDGE ( 'NONE', *, *, #55597, .T. ) ;
#47323 = CARTESIAN_POINT ( 'NONE',  ( -5.999999999999998224, -1.790695186598648903, 34.54067556320373455 ) ) ;
#47324 = CARTESIAN_POINT ( 'NONE',  ( -4.854143535654667829, -2.600157965045225339, 30.74683119005207743 ) ) ;
#47325 = CARTESIAN_POINT ( 'NONE',  ( -14.30769230769242917, -12.51329471203414379, 31.30864560766407578 ) ) ;
#47326 = FACE_OUTER_BOUND ( 'NONE', #82583, .T. ) ;
#47327 = ORIENTED_EDGE ( 'NONE', *, *, #31684, .F. ) ;
#47328 = B_SPLINE_CURVE_WITH_KNOTS ( 'NONE', 3,
 ( #24026, #15181, #44737, #44281, #3759, #72215 ),
 .UNSPECIFIED., .F., .F.,
 ( 4, 2, 4 ),
 ( 0.000000000000000000, 0.0001954784845028914619, 0.0003909569690057829237 ),
 .UNSPECIFIED. ) ;
#47329 = AXIS2_PLACEMENT_3D ( 'NONE', #22737, #70935, #30829 ) ;
#47330 = VERTEX_POINT ( 'NONE', #82551 ) ;
#47331 = B_SPLINE_CURVE_WITH_KNOTS ( 'NONE', 3,
 ( #6956, #61890, #34427, #1087, #77627, #48821, #76296, #202, #34864, #83517 ),
 .UNSPECIFIED., .F., .F.,
 ( 4, 2, 2, 2, 4 ),
 ( 0.0007817246256747463051, 0.0009771112852218896347, 0.001172497944769033181, 0.001367884604316176728, 0.001563271263863320057 ),
 .UNSPECIFIED. ) ;
#47332 = ORIENTED_EDGE ( 'NONE', *, *, #9846, .F. ) ;
#47333 = DIRECTION ( 'NONE',  ( 0.000000000000000000, 0.3420201433256641055, -0.9396926207859100932 ) ) ;
#47334 = EDGE_CURVE ( 'NONE', #19302, #22650, #50553, .T. ) ;
#47335 = ORIENTED_EDGE ( 'NONE', *, *, #36300, .F. ) ;
#47336 = CYLINDRICAL_SURFACE ( 'NONE', #9359, 0.2500000000000002220 ) ;
#47337 = CARTESIAN_POINT ( 'NONE',  ( 4.153846153846154188, -2.499999999999998668, 29.75000000000001421 ) ) ;
#47339 = B_SPLINE_CURVE_WITH_KNOTS ( 'NONE', 3,
 ( #49591, #42405, #35188, #69864, #68973, #28894, #27987, #21675, #56351, #76622 ),
 .UNSPECIFIED., .F., .F.,
 ( 4, 2, 2, 2, 4 ),
 ( 0.000000000000000000, 0.0001954339857564053873, 0.0003908679715128107746, 0.0005863019572692161618, 0.0007817359430256215491 ),
 .UNSPECIFIED. ) ;
#47338 = DIRECTION ( 'NONE',  ( 0.000000000000000000, 0.1736481776669267785, -0.9848077530122087975 ) ) ;
#47340 = CARTESIAN_POINT ( 'NONE',  ( 9.692307692307572609, -8.613356846316285953, 34.62446782046622218 ) ) ;
#47341 = DIRECTION ( 'NONE',  ( 0.000000000000000000, 0.000000000000000000, -1.000000000000000000 ) ) ;
#47342 = VERTEX_POINT ( 'NONE', #14072 ) ;
#47343 = CARTESIAN_POINT ( 'NONE',  ( 3.230769230769546141, -2.255955759149395501, 30.00000000000324363 ) ) ;
#47345 = EDGE_LOOP ( 'NONE', ( #60728, #34370 ) ) ;
#47344 = CARTESIAN_POINT ( 'NONE',  ( -4.153846153846152411, -6.386643153685126251, 34.62446782046654192 ) ) ;
#47346 = DIRECTION ( 'NONE',  ( 0.000000000000000000, 0.9396926207859126468, 0.3420201433256571111 ) ) ;
#47347 = CARTESIAN_POINT ( 'NONE',  ( 8.992010438208829726, -12.47679350104403007, 31.42216943046555855 ) ) ;
#47348 = CARTESIAN_POINT ( 'NONE',  ( -11.66860950819323861, -11.04286588640298561, 33.62463336215343901 ) ) ;
#47349 = CARTESIAN_POINT ( 'NONE',  ( -2.530619266599154038, -12.64616026154729411, 30.79003144601913533 ) ) ;
#47350 = CARTESIAN_POINT ( 'NONE',  ( -8.638705330997124676, -8.630441415882550871, 34.87705825610312615 ) ) ;
#47351 = ADVANCED_FACE ( 'NONE', ( #41546 ), #14968, .F. ) ;
#47352 = CYLINDRICAL_SURFACE ( 'NONE', #55013, 0.2499999999999995559 ) ;
#47353 = DIRECTION ( 'NONE',  ( -0.000000000000000000, 0.9396926207859093161, -0.3420201433256663259 ) ) ;
#47354 = CARTESIAN_POINT ( 'NONE',  ( -1.901340078031369618, -5.512252781505359245, 21.75186829374151287 ) ) ;
#47355 = ORIENTED_EDGE ( 'NONE', *, *, #75205, .T. ) ;
#47356 = CARTESIAN_POINT ( 'NONE',  ( -17.06410256410256565, -7.500000000000000000, 29.75000000000000355 ) ) ;
#47357 = CARTESIAN_POINT ( 'NONE',  ( -14.17690186672535901, -3.338503747796866872, 32.95102852606553512 ) ) ;
#47358 = AXIS2_PLACEMENT_3D ( 'NONE', #25502, #4338, #33916 ) ;
#47359 =( LENGTH_UNIT ( ) NAMED_UNIT ( * ) SI_UNIT ( .MILLI., .METRE. ) );
#47360 = ORIENTED_EDGE ( 'NONE', *, *, #82321, .T. ) ;
#47361 = DIRECTION ( 'NONE',  ( 0.000000000000000000, 0.8660254037844377084, -0.5000000000000015543 ) ) ;
#47362 = CARTESIAN_POINT ( 'NONE',  ( -2.980823712421087901, -5.852078868378310261, 34.47109172314383585 ) ) ;
#47363 = CIRCLE ( 'NONE', #87635, 5.000000000000000888 ) ;
#47364 = CARTESIAN_POINT ( 'NONE',  ( -7.173100160369890510, -5.851115903089112003, 34.47074536777953568 ) ) ;
#47365 = CARTESIAN_POINT ( 'NONE',  ( -2.307692307692305711, -8.318370150425687726, 35.83090037661290239 ) ) ;
#47366 = CIRCLE ( 'NONE', #21514, 8.000000000000000000 ) ;
#47367 = CARTESIAN_POINT ( 'NONE',  ( 17.99999999999987566, -2.657715359629662544, 31.77849191805970364 ) ) ;
#47368 = EDGE_LOOP ( 'NONE', ( #55334, #25896 ) ) ;
#47370 = EDGE_CURVE ( 'NONE', #71718, #25852, #42441, .T. ) ;
#47369 = FACE_OUTER_BOUND ( 'NONE', #86864, .T. ) ;
#47371 = EDGE_CURVE ( 'NONE', #49175, #9891, #84322, .T. ) ;
#47372 = CARTESIAN_POINT ( 'NONE',  ( 9.692307692307695177, -6.189225973068211317, 35.74407628777942847 ) ) ;
#47373 = CARTESIAN_POINT ( 'NONE',  ( 5.207713517890025123, -12.35292014791297710, 31.75344720912887198 ) ) ;
#47374 = B_SPLINE_CURVE_WITH_KNOTS ( 'NONE', 3,
 ( #55861, #8130, #49104, #35599, #84243, #8572, #83799, #45892, #24738, #79242 ),
 .UNSPECIFIED., .F., .F.,
 ( 4, 2, 2, 2, 4 ),
 ( 0.0007817246256747458714, 0.0009771112852218889842, 0.001172497944769032097, 0.001367884604316175210, 0.001563271263863318323 ),
 .UNSPECIFIED. ) ;
#47375 = ORIENTED_EDGE ( 'NONE', *, *, #60564, .F. ) ;
#47376 = CARTESIAN_POINT ( 'NONE',  ( 20.00000000000000000, -4.000000000000000000, 29.75000000000000355 ) ) ;
#47377 = EDGE_LOOP ( 'NONE', ( #41818, #69674, #65586, #78027 ) ) ;
#47378 = CARTESIAN_POINT ( 'NONE',  ( 12.59206389977210527, -12.50538340440932394, 31.33453814440721885 ) ) ;
#47379 = SHAPE_REPRESENTATION_RELATIONSHIP ( 'NONE' , 'NONE' ,  #14956, #17033 ) ;
#47380 = CARTESIAN_POINT ( 'NONE',  ( 11.53846153846141576, -6.835583212225970762, 34.95778746994575670 ) ) ;
#47381 = EDGE_LOOP ( 'NONE', ( #20867, #48010, #57725, #25859 ) ) ;
#47382 = DIRECTION ( 'NONE',  ( -0.000000000000000000, 1.000000000000000000, -0.000000000000000000 ) ) ;
#47383 = CARTESIAN_POINT ( 'NONE',  ( -16.15384615384615330, -11.35647404775217417, 33.31231777344666511 ) ) ;
#47384 = CARTESIAN_POINT ( 'NONE',  ( 5.448717948717947124, -3.499999999999999556, 29.75000000000000355 ) ) ;
#47385 = LINE ( 'NONE', #541, #6218 ) ;
#47386 = LINE ( 'NONE', #21242, #78519 ) ;
#47387 = VERTEX_POINT ( 'NONE', #50065 ) ;
#47388 = FACE_BOUND ( 'NONE', #60008, .T. ) ;
#47389 = VERTEX_POINT ( 'NONE', #82979 ) ;
#47390 = DIRECTION ( 'NONE',  ( -0.000000000000000000, 1.000000000000000000, 3.491481338843133355E-15 ) ) ;
#47391 = AXIS2_PLACEMENT_3D ( 'NONE', #57755, #23516, #84359 ) ;
#47392 = CARTESIAN_POINT ( 'NONE',  ( -0.4615384615385826339, -8.613356846316285953, 34.62446782046622218 ) ) ;
#47393 = CARTESIAN_POINT ( 'NONE',  ( 5.010839665967194101, -11.69971097300155272, 32.46337939537587403 ) ) ;
#47394 = CARTESIAN_POINT ( 'NONE',  ( 3.164686851409094892, -11.35647404775217595, 33.31231777344666511 ) ) ;
#47395 = CARTESIAN_POINT ( 'NONE',  ( 14.37294744720514572, -8.656820664281605460, 34.87096338111211224 ) ) ;
#47396 = ORIENTED_EDGE ( 'NONE', *, *, #9810, .F. ) ;
#47397 = ORIENTED_EDGE ( 'NONE', *, *, #41064, .F. ) ;
#47398 = EDGE_LOOP ( 'NONE', ( #34058, #54608, #34085, #1643 ) ) ;
#47399 = ORIENTED_EDGE ( 'NONE', *, *, #55807, .T. ) ;
#47400 = CARTESIAN_POINT ( 'NONE',  ( -4.153846153846273204, -6.026961402154118908, 34.52809138561165270 ) ) ;
#47401 = CARTESIAN_POINT ( 'NONE',  ( -17.07692307692307665, -9.905515769479276145, 34.41647553114623292 ) ) ;
#47402 = CARTESIAN_POINT ( 'NONE',  ( 8.769230769230768274, -4.661471528628507777, 34.16647553114623292 ) ) ;
#47403 = CARTESIAN_POINT ( 'NONE',  ( 4.153846153846032507, -3.300289026999228881, 32.46337939537708905 ) ) ;
#47404 = VERTEX_POINT ( 'NONE', #55056 ) ;
#47405 = CARTESIAN_POINT ( 'NONE',  ( 17.75002326905764960, -9.943427161483782584, 34.11278801902876978 ) ) ;
#47406 = VECTOR ( 'NONE', #84964, 1000.000000000000227 ) ;
#47407 = CARTESIAN_POINT ( 'NONE',  ( 16.15384615384615330, -1.117168528481311540, 33.14645433367849847 ) ) ;
#47408 = CARTESIAN_POINT ( 'NONE',  ( -18.00000000104979492, -12.75000000000000355, 29.50000000010276935 ) ) ;
#47409 = CARTESIAN_POINT ( 'NONE',  ( -4.826868657009622865, -11.47946981652013498, 33.17500667209846910 ) ) ;
#47410 = ORIENTED_EDGE ( 'NONE', *, *, #13423, .T. ) ;
#47411 = VERTEX_POINT ( 'NONE', #7323 ) ;
#47412 = CIRCLE ( 'NONE', #43121, 0.5000000000000004441 ) ;
#47413 = ORIENTED_EDGE ( 'NONE', *, *, #48351, .F. ) ;
#47414 = CARTESIAN_POINT ( 'NONE',  ( -11.60454494941741999, -12.37446782046654192, 30.86335684631486487 ) ) ;
#47416 = CARTESIAN_POINT ( 'NONE',  ( -8.096177083446809419, -4.335965774309649134, 33.62209801155881905 ) ) ;
#47415 = FACE_OUTER_BOUND ( 'NONE', #27128, .T. ) ;
#47417 = ADVANCED_FACE ( 'NONE', ( #34782 ), #62248, .F. ) ;
#47418 = AXIS2_PLACEMENT_3D ( 'NONE', #43831, #69976, #50138 ) ;
#47419 = EDGE_CURVE ( 'NONE', #177, #84975, #22732, .T. ) ;
#47420 = CARTESIAN_POINT ( 'NONE',  ( -15.12820512820512953, -3.499999999999999556, 29.75000000000000355 ) ) ;
#47421 = CARTESIAN_POINT ( 'NONE',  ( 17.07692307692307665, -1.215029322943914858, 32.30358669280327177 ) ) ;
#47422 = FACE_BOUND ( 'NONE', #40250, .T. ) ;
#47423 = ORIENTED_EDGE ( 'NONE', *, *, #71947, .F. ) ;
#47424 = CARTESIAN_POINT ( 'NONE',  ( 17.01165263096229907, -6.879047030191174805, 34.71129190930000163 ) ) ;
#47425 = CARTESIAN_POINT ( 'NONE',  ( -3.453696189676079165, -3.395401636524185474, 33.02366814457250399 ) ) ;
#47426 = ORIENTED_EDGE ( 'NONE', *, *, #14039, .F. ) ;
#47427 = CARTESIAN_POINT ( 'NONE',  ( -11.53846153846165912, -12.46129190930018460, 30.37095296980731973 ) ) ;
#47428 = ORIENTED_EDGE ( 'NONE', *, *, #84200, .T. ) ;
#47429 = FACE_BOUND ( 'NONE', #48670, .T. ) ;
#47430 = CARTESIAN_POINT ( 'NONE',  ( 7.715462379486289990, -11.71456829005830080, 32.44064028649416542 ) ) ;
#47431 = EDGE_CURVE ( 'NONE', #57842, #44468, #63471, .T. ) ;
#47432 = CARTESIAN_POINT ( 'NONE',  ( -39.05038313613820122, -2.249999999999998668, 29.75000000000000355 ) ) ;
#47433 = VERTEX_POINT ( 'NONE', #5419 ) ;
#47434 = CARTESIAN_POINT ( 'NONE',  ( -7.976713759767205758, -2.254533558242300284, 29.97296025877828285 ) ) ;
#47435 = LINE ( 'NONE', #67723, #5900 ) ;
#47436 = DIRECTION ( 'NONE',  ( -0.000000000000000000, 0.6427876096865404731, -0.7660444431189770143 ) ) ;
#47437 = VERTEX_POINT ( 'NONE', #12620 ) ;
#47438 = EDGE_CURVE ( 'NONE', #2406, #58364, #70983, .T. ) ;
#47439 = CARTESIAN_POINT ( 'NONE',  ( 6.923076923076924238, -5.557115091759785130, 34.35708131394839171 ) ) ;
#47440 = FACE_OUTER_BOUND ( 'NONE', #13151, .T. ) ;
#47441 = CARTESIAN_POINT ( 'NONE',  ( 12.59206416330202494, -6.852161475712352789, 34.70806712695775786 ) ) ;
#47442 = CARTESIAN_POINT ( 'NONE',  ( -17.74994558008654622, -12.65882529074907126, 30.72640787790838601 ) ) ;
#47443 = ORIENTED_EDGE ( 'NONE', *, *, #74661, .F. ) ;
#47444 = CARTESIAN_POINT ( 'NONE',  ( 16.15384615384603251, -10.90142922262034020, 33.41473453929536674 ) ) ;
#47445 = DIRECTION ( 'NONE',  ( 0.000000000000000000, 0.000000000000000000, -1.000000000000000000 ) ) ;
#47446 = ORIENTED_EDGE ( 'NONE', *, *, #55113, .T. ) ;
#47447 = CARTESIAN_POINT ( 'NONE',  ( -8.519176457592454454, -10.66356715214248396, 33.62249196103329751 ) ) ;
#47448 = CARTESIAN_POINT ( 'NONE',  ( -4.219929564802034072, -2.538708090699994813, 30.37095296980875148 ) ) ;
#47449 = CARTESIAN_POINT ( 'NONE',  ( -13.38461538461538325, -13.87047571288749737, 32.06866353760679544 ) ) ;
#47450 = CARTESIAN_POINT ( 'NONE',  ( -11.78843826940389583, -8.303909089506435137, 34.68538101551103381 ) ) ;
#47451 = CYLINDRICAL_SURFACE ( 'NONE', #15716, 0.2500000000000012212 ) ;
#47452 = CARTESIAN_POINT ( 'NONE',  ( -13.13456096470193302, -3.435999193479609914, 33.07426656108010832 ) ) ;
#47454 = FACE_OUTER_BOUND ( 'NONE', #61055, .T. ) ;
#47453 = CARTESIAN_POINT ( 'NONE',  ( 6.222779541268410597, -11.89424750095246175, 32.13594075562311758 ) ) ;
#47455 = EDGE_CURVE ( 'NONE', #17031, #56000, #67794, .T. ) ;
#47456 = LINE ( 'NONE', #13243, #79509 ) ;
#47457 = AXIS2_PLACEMENT_3D ( 'NONE', #22971, #9901, #56323 ) ;
#47458 = CARTESIAN_POINT ( 'NONE',  ( -1.944543648263014957, -5.555456351737005249, 20.25000000000000000 ) ) ;
#47459 = VERTEX_POINT ( 'NONE', #6309 ) ;
#47460 = CARTESIAN_POINT ( 'NONE',  ( -18.00000000000000000, -8.973038597847269315, 34.52809138561121927 ) ) ;
#47461 = ORIENTED_EDGE ( 'NONE', *, *, #12170, .T. ) ;
#47462 = ORIENTED_EDGE ( 'NONE', *, *, #75227, .T. ) ;
#47463 = CARTESIAN_POINT ( 'NONE',  ( -16.15384615384615330, -13.53365097954675988, 30.81389545987213552 ) ) ;
#47464 = ORIENTED_EDGE ( 'NONE', *, *, #49867, .F. ) ;
#47465 = DIRECTION ( 'NONE',  ( -1.000000000000000000, 0.000000000000000000, 0.000000000000000000 ) ) ;
#47466 = CARTESIAN_POINT ( 'NONE',  ( -1.944543648263014957, -5.555456351737005249, 17.75000000000000355 ) ) ;
#47468 = B_SPLINE_CURVE_WITH_KNOTS ( 'NONE', 3,
 ( #54122, #81615, #19899, #46043, #73528, #66761, #13590, #62649, #75300, #83393 ),
 .UNSPECIFIED., .F., .F.,
 ( 4, 2, 2, 2, 4 ),
 ( 0.000000000000000000, 0.0001954311564186870371, 0.0003908623128373740741, 0.0005862934692560610840, 0.0007817246256747481482 ),
 .UNSPECIFIED. ) ;
#47467 = DIRECTION ( 'NONE',  ( -0.000000000000000000, 1.000000000000000000, -0.000000000000000000 ) ) ;
#47469 = DIRECTION ( 'NONE',  ( 0.000000000000000000, 0.3420201433256641055, -0.9396926207859100932 ) ) ;
#47470 = CARTESIAN_POINT ( 'NONE',  ( -2.241623956689868358, -6.386643153685127139, 34.62446782046654192 ) ) ;
#47471 = DIRECTION ( 'NONE',  ( 0.000000000000000000, 0.7660444431189807890, 0.6427876096865361433 ) ) ;
#47472 = CARTESIAN_POINT ( 'NONE',  ( 9.915320536401090123, -12.38742843783360748, 31.66772728687926985 ) ) ;
#47473 = LINE ( 'NONE', #39853, #9437 ) ;
#47474 = CARTESIAN_POINT ( 'NONE',  ( -3.750000000000008438, -5.946699141100917352, 25.17187500000000000 ) ) ;
#47475 = CARTESIAN_POINT ( 'NONE',  ( 10.83839745947800992, -12.38742843783360748, 31.66772728687926985 ) ) ;
#47477 = ADVANCED_FACE ( 'NONE', ( #46398 ), #68439, .F. ) ;
#47476 = DIRECTION ( 'NONE',  ( -0.000000000000000000, -0.9848077530122086864, -0.1736481776669273613 ) ) ;
#47478 = VECTOR ( 'NONE', #80712, 1000.000000000000114 ) ;
#47479 = EDGE_CURVE ( 'NONE', #7007, #21466, #73877, .T. ) ;
#47480 = CARTESIAN_POINT ( 'NONE',  ( -5.999999999999998224, -11.16473453929635440, 33.15142922261926373 ) ) ;
#47481 = VECTOR ( 'NONE', #22326, 1000.000000000000000 ) ;
#47482 = CIRCLE ( 'NONE', #20164, 0.2500000000000002220 ) ;
#47483 = ORIENTED_EDGE ( 'NONE', *, *, #77836, .T. ) ;
#47485 = EDGE_CURVE ( 'NONE', #14918, #28285, #14034, .T. ) ;
#47484 = EDGE_LOOP ( 'NONE', ( #17537, #62577 ) ) ;
#47486 = CARTESIAN_POINT ( 'NONE',  ( 6.699591979352976345, -2.599994579823202923, 30.74605699353653776 ) ) ;
#47487 = CARTESIAN_POINT ( 'NONE',  ( 5.326868595271216478, -9.272278438253401589, 34.42582936511637826 ) ) ;
#47488 = DIRECTION ( 'NONE',  ( -0.000000000000000000, 0.8660254037844397068, -0.4999999999999978906 ) ) ;
#47489 = CARTESIAN_POINT ( 'NONE',  ( -10.61538461538461320, -13.95598074871891292, 31.83374038241031911 ) ) ;
#47490 = EDGE_CURVE ( 'NONE', #72105, #8333, #26962, .T. ) ;
#47491 = VECTOR ( 'NONE', #66077, 1000.000000000000000 ) ;
#47492 = CARTESIAN_POINT ( 'NONE',  ( 8.639083559792549494, -4.460286881179643004, 33.72017969459903242 ) ) ;
#47493 = VECTOR ( 'NONE', #7988, 1000.000000000000000 ) ;
#47494 = CARTESIAN_POINT ( 'NONE',  ( -6.223484943723948781, -8.496056993536548418, 34.65000542017679663 ) ) ;
#47495 = CARTESIAN_POINT ( 'NONE',  ( -19.99999999999996803, 15.00000000000000711, 13.00000000000000178 ) ) ;
#47496 = VERTEX_POINT ( 'NONE', #35994 ) ;
#47497 = CARTESIAN_POINT ( 'NONE',  ( 1.134638653673031738, -4.943428324936578910, 34.04746400365624481 ) ) ;
#47498 = EDGE_LOOP ( 'NONE', ( #32532, #59945 ) ) ;
#47499 = ORIENTED_EDGE ( 'NONE', *, *, #74852, .F. ) ;
#47500 = CARTESIAN_POINT ( 'NONE',  ( 17.86930853333243618, -3.062553014421049991, 32.05460306192773601 ) ) ;
#47501 = CARTESIAN_POINT ( 'NONE',  ( 15.23076923076910916, -3.643525952248795718, 33.31231777344771672 ) ) ;
#47502 = CARTESIAN_POINT ( 'NONE',  ( -0.3954701105360232671, -6.386643153685128027, 34.62446782046654903 ) ) ;
#47503 = CARTESIAN_POINT ( 'NONE',  ( 19.50000000000000000, -7.500000000000000000, 29.75000000000000355 ) ) ;
#47504 = FACE_OUTER_BOUND ( 'NONE', #5160, .T. ) ;
#47505 = ORIENTED_EDGE ( 'NONE', *, *, #73101, .T. ) ;
#47506 = VERTEX_POINT ( 'NONE', #56693 ) ;
#47507 = EDGE_CURVE ( 'NONE', #89050, #65380, #41960, .T. ) ;
#47508 = ORIENTED_EDGE ( 'NONE', *, *, #58811, .F. ) ;
#47509 = ORIENTED_EDGE ( 'NONE', *, *, #41639, .F. ) ;
#47510 = CARTESIAN_POINT ( 'NONE',  ( -6.250023224221455287, -4.931416488878822335, 34.32920672191015399 ) ) ;
#47511 = CARTESIAN_POINT ( 'NONE',  ( -2.438382910802615378, -9.929715669179220328, 34.40415004197138416 ) ) ;
#47512 = VECTOR ( 'NONE', #45921, 1000.000000000000000 ) ;
#47513 = CARTESIAN_POINT ( 'NONE',  ( 14.08420738312797660, -2.612411019501189369, 31.66733052389439962 ) ) ;
#47514 = CARTESIAN_POINT ( 'NONE',  ( 11.53846153846141753, -6.879047030192662504, 34.71129190930017927 ) ) ;
#47515 = CARTESIAN_POINT ( 'NONE',  ( 17.93472955403921887, -5.219633306516282545, 34.19971097300152252 ) ) ;
#47516 = DIRECTION ( 'NONE',  ( 0.000000000000000000, 0.6427876096865368094, 0.7660444431189802339 ) ) ;
#47517 = ORIENTED_EDGE ( 'NONE', *, *, #86108, .F. ) ;
#47518 = ORIENTED_EDGE ( 'NONE', *, *, #12795, .T. ) ;
#47519 = ADVANCED_FACE ( 'NONE', ( #62992 ), #9400, .T. ) ;
#47520 = ORIENTED_EDGE ( 'NONE', *, *, #42900, .F. ) ;
#47522 = EDGE_LOOP ( 'NONE', ( #38702, #60680, #82921, #17140 ) ) ;
#47521 = CARTESIAN_POINT ( 'NONE',  ( 11.53846153846141753, -9.442884908241554243, 34.35708131394783038 ) ) ;
#47523 = CARTESIAN_POINT ( 'NONE',  ( 10.61538461538449596, -12.46129190930018460, 30.37095296980731973 ) ) ;
#47524 = CARTESIAN_POINT ( 'NONE',  ( 7.146039826638408421, -7.369474270740069777, 34.74850911626239736 ) ) ;
#47525 = CARTESIAN_POINT ( 'NONE',  ( -3.749999999999988454, -9.053300858899127945, 18.76562500000000000 ) ) ;
#47526 = ORIENTED_EDGE ( 'NONE', *, *, #2412, .T. ) ;
#47527 = B_SPLINE_CURVE_WITH_KNOTS ( 'NONE', 3,
 ( #23406, #78350, #51292, #17099, #73840, #82369, #61633, #60307, #19332, #80600 ),
 .UNSPECIFIED., .F., .F.,
 ( 4, 2, 2, 2, 4 ),
 ( 0.0007817359430256293554, 0.0009771253907249941549, 0.001172514838424358954, 0.001367904286123723537, 0.001563293733823095276 ),
 .UNSPECIFIED. ) ;
#47528 = DIRECTION ( 'NONE',  ( 1.000000000000000000, 0.000000000000000000, 0.000000000000000000 ) ) ;
#47529 = ORIENTED_EDGE ( 'NONE', *, *, #771, .F. ) ;
#47530 = CARTESIAN_POINT ( 'NONE',  ( 7.911409417429874580, -12.27809138561124414, 31.22303859784719648 ) ) ;
#47531 = B_SPLINE_CURVE_WITH_KNOTS ( 'NONE', 3,
 ( #41476, #68940, #34717, #7698, #62183, #35156, #41926, #490, #27960, #62618 ),
 .UNSPECIFIED., .F., .F.,
 ( 4, 2, 2, 2, 4 ),
 ( 0.0007817246256747453293, 0.0009771112852218889842, 0.001172497944769032531, 0.001367884604316176294, 0.001563271263863319840 ),
 .UNSPECIFIED. ) ;
#47532 = FACE_BOUND ( 'NONE', #73413, .T. ) ;
#47534 = CIRCLE ( 'NONE', #86467, 4.000000000000000000 ) ;
#47533 = CARTESIAN_POINT ( 'NONE',  ( -19.50000000000000000, -3.499999999999999556, 29.75000000000000355 ) ) ;
#47535 = VECTOR ( 'NONE', #35697, 1000.000000000000000 ) ;
#47536 = ADVANCED_FACE ( 'NONE', ( #63449 ), #42752, .F. ) ;
#47537 = DIRECTION ( 'NONE',  ( 0.000000000000000000, 0.000000000000000000, 1.000000000000000000 ) ) ;
#47538 = ORIENTED_EDGE ( 'NONE', *, *, #22145, .F. ) ;
#47539 = CARTESIAN_POINT ( 'NONE',  ( 8.519254025182180001, -12.01397095200674059, 32.43157075238190146 ) ) ;
#47540 = CARTESIAN_POINT ( 'NONE',  ( 6.923076923076924238, -11.91647553114624181, 32.58852847137148245 ) ) ;
#47541 = ADVANCED_FACE ( 'NONE', ( #2623 ), #1752, .F. ) ;
#47542 = CARTESIAN_POINT ( 'NONE',  ( -16.94639763868943660, -12.70449254468099198, 30.44128974285582956 ) ) ;
#47543 = VECTOR ( 'NONE', #5270, 1000.000000000000227 ) ;
#47544 = CARTESIAN_POINT ( 'NONE',  ( 0.5267940328144856688, -12.46129190930001052, 30.37095296980870174 ) ) ;
#47545 = ORIENTED_EDGE ( 'NONE', *, *, #19058, .T. ) ;
#47546 = VECTOR ( 'NONE', #1582, 1000.000000000000000 ) ;
#47547 = CARTESIAN_POINT ( 'NONE',  ( 16.22001529480881388, -7.250054483168842268, 34.74374881642865631 ) ) ;
#47548 = CYLINDRICAL_SURFACE ( 'NONE', #74215, 0.2499999999999994726 ) ;
#47549 = DIRECTION ( 'NONE',  ( -0.000000000000000000, 0.8660254037844397068, -0.4999999999999978906 ) ) ;
#47550 = DIRECTION ( 'NONE',  ( 0.000000000000000000, 0.6427876096865373645, -0.7660444431189797898 ) ) ;
#47551 = CARTESIAN_POINT ( 'NONE',  ( 9.019285189144222059, -10.06805714834173493, 34.32951233291982618 ) ) ;
#47552 = FACE_BOUND ( 'NONE', #7748, .T. ) ;
#47554 = CARTESIAN_POINT ( 'NONE',  ( -17.07692307692307665, -10.67929555188718282, 33.92786785259544047 ) ) ;
#47553 = DIRECTION ( 'NONE',  ( -2.891205793294679312E-16, 1.000000000000000000, 0.000000000000000000 ) ) ;
#47555 = EDGE_CURVE ( 'NONE', #38257, #80199, #31254, .T. ) ;
#47556 = CARTESIAN_POINT ( 'NONE',  ( 2.177544337960614307, -10.31621877034669588, 34.18098118002070152 ) ) ;
#47558 = CARTESIAN_POINT ( 'NONE',  ( 17.99999999999987566, -11.48612834414049644, 32.76840700105863391 ) ) ;
#47557 = DIRECTION ( 'NONE',  ( -0.000000000000000000, 0.9396926207859093161, -0.3420201433256663259 ) ) ;
#47559 = CARTESIAN_POINT ( 'NONE',  ( -5.143005456283213483, -12.34228464037088280, 31.77849191805838558 ) ) ;
#47560 = CARTESIAN_POINT ( 'NONE',  ( -1.077988221561460236, -10.27530806549876452, 18.35750670625849068 ) ) ;
#47561 = ORIENTED_EDGE ( 'NONE', *, *, #2281, .F. ) ;
#47562 = CARTESIAN_POINT ( 'NONE',  ( 2.544871794871792936, -7.500000000000000000, 29.75000000000000355 ) ) ;
#47563 = EDGE_LOOP ( 'NONE', ( #76483, #39294, #87995, #16162 ) ) ;
#47564 = EDGE_CURVE ( 'NONE', #46418, #6445, #43066, .T. ) ;
#47565 = LINE ( 'NONE', #26859, #33443 ) ;
#47566 = ORIENTED_EDGE ( 'NONE', *, *, #70539, .F. ) ;
#47567 = CARTESIAN_POINT ( 'NONE',  ( -4.087777802843715058, -12.10708131394839882, 31.69288490824020954 ) ) ;
#47569 = EDGE_CURVE ( 'NONE', #52382, #73792, #30134, .T. ) ;
#47568 = CARTESIAN_POINT ( 'NONE',  ( 14.24242230713598900, -4.320704448112771878, 33.92786785259540494 ) ) ;
#47571 = VERTEX_POINT ( 'NONE', #76531 ) ;
#47570 = CARTESIAN_POINT ( 'NONE',  ( -4.946397638689432164, -9.503571793651733657, 34.60286762892837942 ) ) ;
#47572 = DIRECTION ( 'NONE',  ( 0.000000000000000000, 0.000000000000000000, -1.000000000000000000 ) ) ;
#47573 = CARTESIAN_POINT ( 'NONE',  ( 2.724691934501235036, -6.299813628509441266, 20.38875670625849068 ) ) ;
#47574 = B_SPLINE_CURVE_WITH_KNOTS ( 'NONE', 3,
 ( #51730, #79234, #78330, #29720, #49975, #37795, #9440, #51273, #2663, #16631 ),
 .UNSPECIFIED., .F., .F.,
 ( 4, 2, 2, 2, 4 ),
 ( 0.000000000000000000, 0.0001954311564186865763, 0.0003908623128373731525, 0.0005862934692560596746, 0.0007817246256747463051 ),
 .UNSPECIFIED. ) ;
#47575 = CARTESIAN_POINT ( 'NONE',  ( -13.38461538461538325, -1.242168528481310874, 33.36296068462461051 ) ) ;
#47577 = CARTESIAN_POINT ( 'NONE',  ( -6.989159302437058408, -12.62096338111211580, 30.90682066428152197 ) ) ;
#47576 = B_SPLINE_CURVE_WITH_KNOTS ( 'NONE', 3,
 ( #7230, #21175, #82456, #54516, #20304, #48202, #75674, #6776, #6354, #28 ),
 .UNSPECIFIED., .F., .F.,
 ( 4, 2, 2, 2, 4 ),
 ( 0.0007817359430256359690, 0.0009771253907250036959, 0.001172514838424371314, 0.001367904286123738933, 0.001563293733823106768 ),
 .UNSPECIFIED. ) ;
#47578 = CARTESIAN_POINT ( 'NONE',  ( 7.846153846153725020, -11.94971097300221174, 32.03036669348237098 ) ) ;
#47579 = CARTESIAN_POINT ( 'NONE',  ( 1.134638640566794754, -4.818429247618089661, 34.26397095200675125 ) ) ;
#47580 = DIRECTION ( 'NONE',  ( 0.000000000000000000, 0.4999999999999960032, -0.8660254037844410391 ) ) ;
#47581 = DIRECTION ( 'NONE',  ( -0.000000000000000000, -0.8660254037844399289, -0.4999999999999980016 ) ) ;
#47582 = B_SPLINE_CURVE_WITH_KNOTS ( 'NONE', 3,
 ( #26920, #75115, #20162, #13396, #47176, #12958, #43964, #56157, #70110, #43086 ),
 .UNSPECIFIED., .F., .F.,
 ( 4, 2, 2, 2, 4 ),
 ( 0.000000000000000000, 0.0001954339881912776238, 0.0003908679763825552477, 0.0005863019645738329257, 0.0007817359527651104954 ),
 .UNSPECIFIED. ) ;
#47583 = CARTESIAN_POINT ( 'NONE',  ( -3.749999999999997780, -7.438900925035489387, 22.84561829374151642 ) ) ;
#47584 = B_SPLINE_CURVE_WITH_KNOTS ( 'NONE', 3,
 ( #16607, #36018, #44068, #71550, #63469, #16176, #77432, #9856, #37319, #51250 ),
 .UNSPECIFIED., .F., .F.,
 ( 4, 2, 2, 2, 4 ),
 ( 0.0007817359430256371616, 0.0009771253907250049969, 0.001172514838424373049, 0.001367904286123741101, 0.001563293733823108937 ),
 .UNSPECIFIED. ) ;
#47586 = EDGE_CURVE ( 'NONE', #15849, #54731, #70252, .T. ) ;
#47585 = CARTESIAN_POINT ( 'NONE',  ( 9.626983679503386071, -7.749976730030849303, 34.74374725381503737 ) ) ;
#47587 = ORIENTED_EDGE ( 'NONE', *, *, #2941, .F. ) ;
#47588 = AXIS2_PLACEMENT_3D ( 'NONE', #68593, #83456, #19957 ) ;
#47589 = CARTESIAN_POINT ( 'NONE',  ( -1.326923076923076872, -3.499999999999999556, 29.75000000000000355 ) ) ;
#47590 = CARTESIAN_POINT ( 'NONE',  ( -0.06109907496450878162, -11.25000000000000000, 25.03311829374151287 ) ) ;
#47591 = AXIS2_PLACEMENT_3D ( 'NONE', #6287, #34187, #61207 ) ;
#47592 = EDGE_CURVE ( 'NONE', #84519, #87581, #78737, .T. ) ;
#47593 = CARTESIAN_POINT ( 'NONE',  ( 2.057669083470851756, -4.931416488878823223, 34.32920672191015399 ) ) ;
#47594 = CARTESIAN_POINT ( 'NONE',  ( 5.326868486301119532, -6.653508905675592722, 34.93172785388651391 ) ) ;
#47595 = ORIENTED_EDGE ( 'NONE', *, *, #4314, .T. ) ;
#47596 = CARTESIAN_POINT ( 'NONE',  ( -7.846153846153844924, -8.318370150425687726, 35.83090037661290239 ) ) ;
#47597 = LINE ( 'NONE', #67873, #83391 ) ;
#47599 = ORIENTED_EDGE ( 'NONE', *, *, #79069, .T. ) ;
#47598 = CARTESIAN_POINT ( 'NONE',  ( 16.15384615384615330, -4.786620604624113540, 33.94971097300155094 ) ) ;
#47600 = CARTESIAN_POINT ( 'NONE',  ( -2.057692307690886846, -7.500000000000154543, 35.00000000000007105 ) ) ;
#47601 = ADVANCED_FACE ( 'NONE', ( #4408 ), #17487, .F. ) ;
#47602 = CARTESIAN_POINT ( 'NONE',  ( -15.09997878980228059, -11.93129842949671726, 32.56571108434900452 ) ) ;
#47603 = CARTESIAN_POINT ( 'NONE',  ( 9.626224281351815293, -11.16473453929635440, 33.15142922261925662 ) ) ;
#47604 = CARTESIAN_POINT ( 'NONE',  ( 4.853438133199127869, -4.386631170607603991, 33.66268669641500111 ) ) ;
#47605 = CARTESIAN_POINT ( 'NONE',  ( -13.63463862190834952, -11.86270091957321249, 32.19358267280087915 ) ) ;
#47607 = CARTESIAN_POINT ( 'NONE',  ( 0.000000000000000000, -11.00000000000000000, 29.75000000000000355 ) ) ;
#47606 = AXIS2_PLACEMENT_3D ( 'NONE', #78233, #73260, #4356 ) ;
#47608 = ORIENTED_EDGE ( 'NONE', *, *, #20923, .F. ) ;
#47609 = EDGE_LOOP ( 'NONE', ( #77303, #76180 ) ) ;
#47610 = EDGE_CURVE ( 'NONE', #16729, #71888, #75975, .T. ) ;
#47611 = ORIENTED_EDGE ( 'NONE', *, *, #1175, .T. ) ;
#47612 = ORIENTED_EDGE ( 'NONE', *, *, #10951, .F. ) ;
#47613 = AXIS2_PLACEMENT_3D ( 'NONE', #69963, #69521, #6934 ) ;
#47614 = VECTOR ( 'NONE', #32824, 1000.000000000000000 ) ;
#47615 = CARTESIAN_POINT ( 'NONE',  ( 5.299702618191482806, -12.24180327182771855, 31.33663988360758168 ) ) ;
#47616 = CARTESIAN_POINT ( 'NONE',  ( 19.50000000000000000, -3.499999999999999556, 29.75000000000000355 ) ) ;
#47617 = EDGE_CURVE ( 'NONE', #84921, #78012, #38193, .T. ) ;
#47618 = CARTESIAN_POINT ( 'NONE',  ( 9.758376043310132530, -4.786620604624113540, 33.94971097300155805 ) ) ;
#47619 = DIRECTION ( 'NONE',  ( 1.000000000000000000, 0.000000000000000000, 0.000000000000000000 ) ) ;
#47620 = CIRCLE ( 'NONE', #8793, 8.000000000000000000 ) ;
#47621 = CARTESIAN_POINT ( 'NONE',  ( -2.373775718648186484, -5.557115091759785130, 34.35708131394839171 ) ) ;
#47622 = CARTESIAN_POINT ( 'NONE',  ( 16.15384615384603251, -5.219633306517616589, 34.19971097300220464 ) ) ;
#47623 = VERTEX_POINT ( 'NONE', #10729 ) ;
#47624 = B_SPLINE_CURVE_WITH_KNOTS ( 'NONE', 3,
 ( #45102, #31140, #44197, #58612, #3230, #24380, #18093, #73030, #72579, #10886 ),
 .UNSPECIFIED., .F., .F.,
 ( 4, 2, 2, 2, 4 ),
 ( 0.000000000000000000, 0.0001954311564186871184, 0.0003908623128373742367, 0.0005862934692560614093, 0.0007817246256747484735 ),
 .UNSPECIFIED. ) ;
#47625 = EDGE_CURVE ( 'NONE', #79882, #36678, #38766, .T. ) ;
#47626 = ORIENTED_EDGE ( 'NONE', *, *, #61916, .F. ) ;
#47627 = EDGE_LOOP ( 'NONE', ( #58230, #21936, #77341, #47298 ) ) ;
#47629 = VERTEX_POINT ( 'NONE', #51683 ) ;
#47628 = DIRECTION ( 'NONE',  ( 0.000000000000000000, 0.000000000000000000, 1.000000000000000000 ) ) ;
#47630 = CARTESIAN_POINT ( 'NONE',  ( -1.515305987725693582, -2.845849958028613624, 32.17971566917920967 ) ) ;
#47631 = EDGE_CURVE ( 'NONE', #29384, #4984, #85065, .T. ) ;
#47632 = DIRECTION ( 'NONE',  ( -1.000000000000000000, 0.000000000000000000, -0.000000000000000000 ) ) ;
#47633 = EDGE_CURVE ( 'NONE', #34772, #58985, #36446, .T. ) ;
#47634 = VECTOR ( 'NONE', #83271, 1000.000000000000227 ) ;
#47635 = LINE ( 'NONE', #60252, #33544 ) ;
#47636 = FACE_OUTER_BOUND ( 'NONE', #31992, .T. ) ;
#47637 = EDGE_LOOP ( 'NONE', ( #30209, #35786 ) ) ;
#47638 = VERTEX_POINT ( 'NONE', #9834 ) ;
#47639 = EDGE_CURVE ( 'NONE', #71802, #62031, #37553, .T. ) ;
#47640 = EDGE_LOOP ( 'NONE', ( #77295, #61385, #23409, #54387 ) ) ;
#47641 = DIRECTION ( 'NONE',  ( -1.000000000000000000, -0.000000000000000000, -0.000000000000000000 ) ) ;
#47643 = ORIENTED_EDGE ( 'NONE', *, *, #58443, .F. ) ;
#47642 = DIRECTION ( 'NONE',  ( 0.000000000000000000, 0.8660254037844377084, 0.5000000000000015543 ) ) ;
#47644 = CARTESIAN_POINT ( 'NONE',  ( -2.307692307692305711, -8.120952969808772792, 34.71129190930000163 ) ) ;
#47645 = AXIS2_PLACEMENT_3D ( 'NONE', #50246, #48933, #28672 ) ;
#47646 = DIRECTION ( 'NONE',  ( -0.000000000000000000, -0.6427876096865404731, -0.7660444431189771253 ) ) ;
#47647 = ORIENTED_EDGE ( 'NONE', *, *, #40617, .F. ) ;
#47648 = CARTESIAN_POINT ( 'NONE',  ( 16.21991450484859953, -3.513871655860379306, 32.76840700105978499 ) ) ;
#47649 = CARTESIAN_POINT ( 'NONE',  ( 0.2115617174898694053, -9.234221910056348293, 34.70572697212741531 ) ) ;
#47650 = FACE_BOUND ( 'NONE', #38310, .T. ) ;
#47651 = DIRECTION ( 'NONE',  ( 0.000000000000000000, 0.7660444431189822323, -0.6427876096865344779 ) ) ;
#47652 = CARTESIAN_POINT ( 'NONE',  ( -6.130690603110307002, -12.35290016733513951, 31.75349464988449455 ) ) ;
#47653 = LINE ( 'NONE', #75137, #20728 ) ;
#47655 = CARTESIAN_POINT ( 'NONE',  ( 5.076923076923075762, -3.050289026998446396, 32.03036669348365706 ) ) ;
#47654 = CARTESIAN_POINT ( 'NONE',  ( -18.00000000000000711, -12.74702886152665471, 29.99985851721553587 ) ) ;
#47656 = DIRECTION ( 'NONE',  ( 0.000000000000000000, 0.1736481776669275834, 0.9848077530122086864 ) ) ;
#47657 = CYLINDRICAL_SURFACE ( 'NONE', #33287, 0.2500000000000008882 ) ;
#47658 = EDGE_LOOP ( 'NONE', ( #28139, #33974, #65394, #68529 ) ) ;
#47659 = CARTESIAN_POINT ( 'NONE',  ( 14.30769230769231015, -4.098570777380720287, 33.41473453929634729 ) ) ;
#47660 = CARTESIAN_POINT ( 'NONE',  ( 13.63461538461682210, -7.500000000000155431, 34.75000000000007105 ) ) ;
#47661 = EDGE_CURVE ( 'NONE', #46929, #21962, #8538, .T. ) ;
#47662 = ORIENTED_EDGE ( 'NONE', *, *, #1489, .F. ) ;
#47663 = CARTESIAN_POINT ( 'NONE',  ( 15.93036122928182330, -2.353723527008297012, 30.78948104536958752 ) ) ;
#47664 = CARTESIAN_POINT ( 'NONE',  ( -4.284536756956462966, -3.338472653186242756, 32.95098750199972670 ) ) ;
#47665 = ORIENTED_EDGE ( 'NONE', *, *, #50424, .T. ) ;
#47666 = CARTESIAN_POINT ( 'NONE',  ( 18.00000000000000000, -3.886160181151819604, 36.00935417666054406 ) ) ;
#47667 = CARTESIAN_POINT ( 'NONE',  ( -15.23076923076935252, -12.70778746994576025, 30.41441678777401236 ) ) ;
#47668 = FACE_BOUND ( 'NONE', #47484, .T. ) ;
#47670 = DIRECTION ( 'NONE',  ( 0.000000000000000000, 0.000000000000000000, -1.000000000000000000 ) ) ;
#47669 = CARTESIAN_POINT ( 'NONE',  ( -15.23076923076922995, -5.557115091759785130, 34.35708131394839171 ) ) ;
#47671 = CARTESIAN_POINT ( 'NONE',  ( 8.096208157792162297, -9.148310452688876993, 34.47095581063188519 ) ) ;
#47672 = VECTOR ( 'NONE', #18119, 1000.000000000000000 ) ;
#47673 = CARTESIAN_POINT ( 'NONE',  ( 0.000000000000000000, -11.00000000000000000, 29.65000000000000213 ) ) ;
#47674 = CARTESIAN_POINT ( 'NONE',  ( -10.36543920600657209, -11.56426240980093745, 33.07394671870546432 ) ) ;
#47675 = CARTESIAN_POINT ( 'NONE',  ( 3.749999999999999556, -7.438900925035446754, 15.46688170625848713 ) ) ;
#47676 = ORIENTED_EDGE ( 'NONE', *, *, #79009, .F. ) ;
#47677 = VECTOR ( 'NONE', #32032, 1000.000000000000000 ) ;
#47678 = ORIENTED_EDGE ( 'NONE', *, *, #32237, .F. ) ;
#47679 = CARTESIAN_POINT ( 'NONE',  ( 24.00000000000000000, -5.499999999999981348, 27.25000000000000000 ) ) ;
#47680 = DIRECTION ( 'NONE',  ( 0.000000000000000000, -1.000000000000000000, -0.000000000000000000 ) ) ;
#47681 = CARTESIAN_POINT ( 'NONE',  ( 7.173076923076985523, -7.434744860731433924, 35.00000000000000711 ) ) ;
#47682 = CARTESIAN_POINT ( 'NONE',  ( 0.000000000000000000, -11.00000000000000000, 29.75000000000000355 ) ) ;
#47683 = CYLINDRICAL_SURFACE ( 'NONE', #41404, 0.2499999999999994726 ) ;
#47684 = CARTESIAN_POINT ( 'NONE',  ( 3.775308065498768517, -8.992201783934554271, 18.04500670625848713 ) ) ;
#47685 = VECTOR ( 'NONE', #61796, 1000.000000000000114 ) ;
#47686 = CARTESIAN_POINT ( 'NONE',  ( -12.52762084089859407, -3.937682226553330445, 33.60647404775217240 ) ) ;
#47687 = CYLINDRICAL_SURFACE ( 'NONE', #35963, 0.2499999999999986955 ) ;
#47688 = CARTESIAN_POINT ( 'NONE',  ( -11.53846153846153655, -13.49023893513002648, 31.06009739812518688 ) ) ;
#47689 = CARTESIAN_POINT ( 'NONE',  ( 10.68145194873469173, -3.322132147404559976, 32.92929555188717927 ) ) ;
#47690 = DIRECTION ( 'NONE',  ( -0.000000000000000000, -0.9396926207859092051, -0.3420201433256662704 ) ) ;
#47691 = CARTESIAN_POINT ( 'NONE',  ( 13.31934493865461278, -4.481592998940162609, 33.73612834413957984 ) ) ;
#47692 = CARTESIAN_POINT ( 'NONE',  ( 5.934729554039226862, -12.27809138561121394, 31.22303859784730307 ) ) ;
#47693 = CARTESIAN_POINT ( 'NONE',  ( -3.230769230769229949, -2.292212530054420494, 30.41441678777542634 ) ) ;
#47694 = ADVANCED_FACE ( 'NONE', ( #4869 ), #71978, .F. ) ;
#47695 = CARTESIAN_POINT ( 'NONE',  ( 3.007284287045282944, -2.599994579823203367, 30.74605699353653776 ) ) ;
#47696 = ORIENTED_EDGE ( 'NONE', *, *, #54665, .F. ) ;
#47697 = CARTESIAN_POINT ( 'NONE',  ( -4.826868765284763718, -11.79725096376909299, 32.30694842903960762 ) ) ;
#47698 = CYLINDRICAL_SURFACE ( 'NONE', #41714, 0.2499999999999986955 ) ;
#47699 = CARTESIAN_POINT ( 'NONE',  ( 2.775308065498755195, -6.422011778438505125, 15.89249329374151820 ) ) ;
#47700 = ADVANCED_FACE ( 'NONE', ( #12944 ), #40435, .F. ) ;
#47701 = CARTESIAN_POINT ( 'NONE',  ( -0.2387587925603968930, -10.97394488606064122, 33.68653795673694873 ) ) ;
#47702 = PRESENTATION_STYLE_ASSIGNMENT (( #46378 ) ) ;
#47703 = FACE_OUTER_BOUND ( 'NONE', #54315, .T. ) ;
#47705 = ORIENTED_EDGE ( 'NONE', *, *, #44311, .F. ) ;
#47704 = CARTESIAN_POINT ( 'NONE',  ( -14.30769230769230660, -12.10708131394839349, 31.69288490824020244 ) ) ;
#47706 = CARTESIAN_POINT ( 'NONE',  ( 2.749999999999995115, -6.360912703473971419, 21.89062500000000355 ) ) ;
#47707 = CARTESIAN_POINT ( 'NONE',  ( -14.53117723225663660, -5.827078755546623690, 34.72654668319379567 ) ) ;
#47708 = EDGE_CURVE ( 'NONE', #52031, #55252, #46191, .T. ) ;
#47709 = VERTEX_POINT ( 'NONE', #26019 ) ;
#47710 = CARTESIAN_POINT ( 'NONE',  ( -8.769230769230768274, -10.51840700105979565, 33.73612834413961536 ) ) ;
#47711 = LINE ( 'NONE', #75196, #87490 ) ;
#47712 = ADVANCED_FACE ( 'NONE', ( #67010 ), #54813, .F. ) ;
#47713 = VERTEX_POINT ( 'NONE', #47616 ) ;
#47714 = AXIS2_PLACEMENT_3D ( 'NONE', #6554, #46648, #74568 ) ;
#47715 = CARTESIAN_POINT ( 'NONE',  ( 7.623227628637700093, -4.186968288167446595, 33.49512374952580274 ) ) ;
#47716 = B_SPLINE_CURVE_WITH_KNOTS ( 'NONE', 3,
 ( #1089, #69982, #64106, #1975, #57799, #50594, #64538, #8297, #36216, #83968 ),
 .UNSPECIFIED., .F., .F.,
 ( 4, 2, 2, 2, 4 ),
 ( 0.0007817359430256332585, 0.0009771253907250054306, 0.001172514838424370664, 0.001367904286123735897, 0.001563293733823100913 ),
 .UNSPECIFIED. ) ;
#47717 = CARTESIAN_POINT ( 'NONE',  ( 2.438482748659258625, -8.191423895709840863, 34.95447573519442130 ) ) ;
#47718 = CARTESIAN_POINT ( 'NONE',  ( 12.46153846153846168, -1.129524287112498415, 32.06866353760679544 ) ) ;
#47719 = ORIENTED_EDGE ( 'NONE', *, *, #44356, .T. ) ;
#47721 = VERTEX_POINT ( 'NONE', #18822 ) ;
#47720 = CIRCLE ( 'NONE', #43412, 1.999999999999998224 ) ;
#47722 = ADVANCED_FACE ( 'NONE', ( #39990 ), #87745, .F. ) ;
#47723 = CARTESIAN_POINT ( 'NONE',  ( 6.130525438233644486, -12.15418822224088657, 32.17964115625579069 ) ) ;
#47724 = ORIENTED_EDGE ( 'NONE', *, *, #24772, .T. ) ;
#47725 = CARTESIAN_POINT ( 'NONE',  ( -17.74994558008654622, -4.818054556918155207, 34.26375889529406749 ) ) ;
#47726 = CARTESIAN_POINT ( 'NONE',  ( 9.692307692307570832, -3.083524468854526912, 32.58852847137268327 ) ) ;
#47727 = CARTESIAN_POINT ( 'NONE',  ( -10.83886955910856109, -2.599994579823203367, 30.74605699353653776 ) ) ;
#47728 = CARTESIAN_POINT ( 'NONE',  ( -9.822999158975251888, -4.809359713505814149, 33.96456829005828837 ) ) ;
#47729 = DIRECTION ( 'NONE',  ( 0.000000000000000000, 0.4999999999999985567, 0.8660254037844395958 ) ) ;
#47730 = CARTESIAN_POINT ( 'NONE',  ( 1.254467414883690068, -2.373036134822905208, 30.88089517874951540 ) ) ;
#47731 = CARTESIAN_POINT ( 'NONE',  ( -12.46153846153846168, -6.386643153685126251, 34.62446782046654192 ) ) ;
#47732 = ORIENTED_EDGE ( 'NONE', *, *, #59918, .T. ) ;
#47733 = ORIENTED_EDGE ( 'NONE', *, *, #75188, .F. ) ;
#47735 = VERTEX_POINT ( 'NONE', #89071 ) ;
#47734 = CARTESIAN_POINT ( 'NONE',  ( -17.32694631421604115, -10.05641848906368097, 34.04755513067966177 ) ) ;
#47736 = EDGE_CURVE ( 'NONE', #38569, #45581, #54799, .T. ) ;
#47737 = AXIS2_PLACEMENT_3D ( 'NONE', #64698, #2997, #57950 ) ;
#47738 = AXIS2_PLACEMENT_3D ( 'NONE', #67677, #87527, #5984 ) ;
#47739 = CARTESIAN_POINT ( 'NONE',  ( -13.51509056969110745, -7.276987145209185215, 34.99546412871779211 ) ) ;
#47740 = CARTESIAN_POINT ( 'NONE',  ( 8.769230769230645706, -12.16647553114689728, 32.15551576947799362 ) ) ;
#47741 = EDGE_LOOP ( 'NONE', ( #25553, #56296 ) ) ;
#47742 = CARTESIAN_POINT ( 'NONE',  ( 14.55774672760575861, -12.01375889529407281, 32.43194544308182969 ) ) ;
#47743 = AXIS2_PLACEMENT_3D ( 'NONE', #84491, #22766, #8383 ) ;
#47744 = B_SPLINE_CURVE_WITH_KNOTS ( 'NONE', 3,
 ( #8773, #2007, #85761, #77217, #9218, #15528, #42994, #43439, #56942, #51492 ),
 .UNSPECIFIED., .F., .F.,
 ( 4, 2, 2, 2, 4 ),
 ( 0.0007817359430256318490, 0.0009771253907249984917, 0.001172514838424365026, 0.001367904286123731560, 0.001563293733823098311 ),
 .UNSPECIFIED. ) ;
#47745 = EDGE_CURVE ( 'NONE', #32791, #69549, #27832, .T. ) ;
#47746 = VERTEX_POINT ( 'NONE', #87295 ) ;
#47747 = CARTESIAN_POINT ( 'NONE',  ( -12.21153846153846168, -2.499999999999998668, 29.75000000000000355 ) ) ;
#47748 = ORIENTED_EDGE ( 'NONE', *, *, #65064, .T. ) ;
#47749 = DIRECTION ( 'NONE',  ( -1.000000000000000000, -0.000000000000000000, -0.000000000000000000 ) ) ;
#47750 = ORIENTED_EDGE ( 'NONE', *, *, #7835, .T. ) ;
#47751 = ADVANCED_FACE ( 'NONE', ( #25574 ), #19266, .T. ) ;
#47752 = CARTESIAN_POINT ( 'NONE',  ( -16.37677237136229991, -6.503392248772476236, 34.64988816332204635 ) ) ;
#47753 = CARTESIAN_POINT ( 'NONE',  ( 16.94623161025552704, -2.729777683071817229, 31.24903638046269450 ) ) ;
#47754 = FACE_BOUND ( 'NONE', #56444, .T. ) ;
#47755 = CARTESIAN_POINT ( 'NONE',  ( 2.307692307692186251, -2.379036618888197285, 30.90682066428292885 ) ) ;
#47756 = CARTESIAN_POINT ( 'NONE',  ( 18.00000000000000000, -2.708943851104267164, 35.45975837776705220 ) ) ;
#47757 = CARTESIAN_POINT ( 'NONE',  ( -15.90379173393269951, -4.818054556918155207, 34.26375889529406749 ) ) ;
#47758 = LINE ( 'NONE', #40135, #50278 ) ;
#47759 = CARTESIAN_POINT ( 'NONE',  ( -5.076923076923199218, -4.320704448113951379, 33.92786785259630022 ) ) ;
#47760 = CARTESIAN_POINT ( 'NONE',  ( -12.46153846153846168, -13.37000171582298513, 34.34916445242398453 ) ) ;
#47761 = DIRECTION ( 'NONE',  ( -0.000000000000000000, 0.9396926207859092051, -0.3420201433256662704 ) ) ;
#47762 = VERTEX_POINT ( 'NONE', #81417 ) ;
#47763 = EDGE_CURVE ( 'NONE', #955, #45222, #53028, .T. ) ;
#47764 = VERTEX_POINT ( 'NONE', #74657 ) ;
#47766 = CARTESIAN_POINT ( 'NONE',  ( -18.00000000000012079, -10.33852847137269926, 34.16647553114546554 ) ) ;
#47765 = CARTESIAN_POINT ( 'NONE',  ( 2.241608896736429823, -10.51840700105979387, 33.73612834413961536 ) ) ;
#47767 = VECTOR ( 'NONE', #61386, 999.9999999999998863 ) ;
#47768 = CARTESIAN_POINT ( 'NONE',  ( 7.173131234715237170, -6.567000820036038355, 34.66262288849541306 ) ) ;
#47769 = LINE ( 'NONE', #34252, #22120 ) ;
#47770 = EDGE_CURVE ( 'NONE', #84339, #77971, #60049, .T. ) ;
#47771 = CARTESIAN_POINT ( 'NONE',  ( -17.14219307747939069, -12.51329471203370325, 31.30864560766548976 ) ) ;
#47772 = DIRECTION ( 'NONE',  ( 0.000000000000000000, 1.000000000000000000, 0.000000000000000000 ) ) ;
#47773 = EDGE_CURVE ( 'NONE', #49979, #52323, #23515, .T. ) ;
#47774 = VERTEX_POINT ( 'NONE', #56143 ) ;
#47775 = CARTESIAN_POINT ( 'NONE',  ( -11.60454494941741999, -12.10708131394839349, 31.69288490824020244 ) ) ;
#47776 = CARTESIAN_POINT ( 'NONE',  ( 11.28846153846153832, -7.566083408709835645, 34.74999999999999289 ) ) ;
#47777 = CARTESIAN_POINT ( 'NONE',  ( -3.230769230769352962, -11.67786785259630911, 32.92929555188603530 ) ) ;
#47778 = DIRECTION ( 'NONE',  ( 0.000000000000000000, 1.000000000000000000, 0.000000000000000000 ) ) ;
#47779 = AXIS2_PLACEMENT_3D ( 'NONE', #10719, #65642, #66092 ) ;
#47780 = ORIENTED_EDGE ( 'NONE', *, *, #51996, .T. ) ;
#47781 = EDGE_CURVE ( 'NONE', #64679, #26488, #17259, .T. ) ;
#47782 = VERTEX_POINT ( 'NONE', #29564 ) ;
#47783 = ORIENTED_EDGE ( 'NONE', *, *, #76428, .T. ) ;
#47784 = LINE ( 'NONE', #74375, #70793 ) ;
#47785 = B_SPLINE_CURVE_WITH_KNOTS ( 'NONE', 3,
 ( #73897, #66235, #66690, #81546, #40123, #19833, #60816, #46417, #81992, #67583 ),
 .UNSPECIFIED., .F., .F.,
 ( 4, 2, 2, 2, 4 ),
 ( 0.0007817359430256390048, 0.0009771253907250078159, 0.001172514838424376735, 0.001367904286123745655, 0.001563293733823114574 ),
 .UNSPECIFIED. ) ;
#47786 = VERTEX_POINT ( 'NONE', #84078 ) ;
#47787 = CARTESIAN_POINT ( 'NONE',  ( -15.93083480223330817, -4.887748414852789658, 34.01359900205216746 ) ) ;
#47788 = CARTESIAN_POINT ( 'NONE',  ( 5.076923076923075762, -12.09954503811598769, 35.62045528018868623 ) ) ;
#47789 = CARTESIAN_POINT ( 'NONE',  ( -5.300408020647025431, -4.386631170607603991, 33.66268669641500111 ) ) ;
#47790 = CARTESIAN_POINT ( 'NONE',  ( -2.084680956079457470, -4.887748414852789658, 34.01359900205216746 ) ) ;
#47791 = CARTESIAN_POINT ( 'NONE',  ( -11.53846153846153655, -6.386643153685126251, 34.62446782046654192 ) ) ;
#47792 = EDGE_LOOP ( 'NONE', ( #84208, #88679 ) ) ;
#47793 = FACE_OUTER_BOUND ( 'NONE', #84582, .T. ) ;
#47795 = VERTEX_POINT ( 'NONE', #70096 ) ;
#47794 = CARTESIAN_POINT ( 'NONE',  ( -16.15384615384615330, -11.69971097300155272, 32.46337939537588113 ) ) ;
#47796 = CYLINDRICAL_SURFACE ( 'NONE', #23850, 0.2500000000000004996 ) ;
#47797 = CARTESIAN_POINT ( 'NONE',  ( -3.230769230769229949, -2.486705287966279876, 31.30864560766543647 ) ) ;
#47798 = CARTESIAN_POINT ( 'NONE',  ( 4.153846153846154188, -4.102666532097928531, 36.13435417666054406 ) ) ;
#47799 = CARTESIAN_POINT ( 'NONE',  ( -16.28445580905022894, -7.722926974430166069, 34.99546784045485737 ) ) ;
#47800 = CARTESIAN_POINT ( 'NONE',  ( -12.68446467905461006, -2.758268499246657068, 31.33685645148948140 ) ) ;
#47801 = CARTESIAN_POINT ( 'NONE',  ( 17.20697068317875988, -7.723484964179501588, 34.74522123443823318 ) ) ;
#47802 = CARTESIAN_POINT ( 'NONE',  ( -0.5916856709766811218, -12.45813303252208648, 30.39737893381572675 ) ) ;
#47803 = CARTESIAN_POINT ( 'NONE',  ( 1.987747218494642309, -5.598659921968629050, 22.06436829374151287 ) ) ;
#47804 = EDGE_LOOP ( 'NONE', ( #47360, #79993 ) ) ;
#47805 = LINE ( 'NONE', #88379, #46012 ) ;
#47806 = CARTESIAN_POINT ( 'NONE',  ( -14.05763788777885637, -3.435999193479609914, 33.07426656108010832 ) ) ;
#47807 = EDGE_CURVE ( 'NONE', #88674, #44538, #52941, .T. ) ;
#47808 = AXIS2_PLACEMENT_3D ( 'NONE', #70049, #2467, #15116 ) ;
#47809 = CARTESIAN_POINT ( 'NONE',  ( 9.915320536401090123, -10.77377354290276124, 33.85451476688484718 ) ) ;
#47810 = CARTESIAN_POINT ( 'NONE',  ( -13.25408968285182354, -8.586989748646452369, 34.63063291749215011 ) ) ;
#47811 = ORIENTED_EDGE ( 'NONE', *, *, #10281, .F. ) ;
#47812 = CARTESIAN_POINT ( 'NONE',  ( -12.46153846153858247, -11.94971097300221174, 32.03036669348237098 ) ) ;
#47813 = DIRECTION ( 'NONE',  ( 1.000000000000000000, 0.000000000000000000, 0.000000000000000000 ) ) ;
#47814 = AXIS2_PLACEMENT_3D ( 'NONE', #16036, #70978, #83171 ) ;
#47815 = CARTESIAN_POINT ( 'NONE',  ( 2.438217745925951085, -11.04252011169590020, 33.62494198852677130 ) ) ;
#47816 = DIRECTION ( 'NONE',  ( -0.000000000000000000, 0.1736481776669307198, -0.9848077530122080203 ) ) ;
#47817 = EDGE_CURVE ( 'NONE', #10982, #2406, #14272, .T. ) ;
#47818 = CARTESIAN_POINT ( 'NONE',  ( -14.53061926659915315, -2.889293201056495786, 32.26117774369186009 ) ) ;
#47819 = ORIENTED_EDGE ( 'NONE', *, *, #13702, .F. ) ;
#47820 = CARTESIAN_POINT ( 'NONE',  ( -15.23076923076922995, -2.721908614388771852, 31.22303859784724978 ) ) ;
#47821 = DIRECTION ( 'NONE',  ( 1.000000000000000000, -2.454804199071658828E-16, -2.454804199071659026E-15 ) ) ;
#47822 = DIRECTION ( 'NONE',  ( -0.000000000000000000, -0.1736481776669307198, -0.9848077530122080203 ) ) ;
#47823 = EDGE_LOOP ( 'NONE', ( #87737, #55265 ) ) ;
#47824 = EDGE_CURVE ( 'NONE', #45139, #14506, #34980, .T. ) ;
#47825 = CYLINDRICAL_SURFACE ( 'NONE', #55684, 0.2499999999999973355 ) ;
#47826 = ORIENTED_EDGE ( 'NONE', *, *, #39525, .F. ) ;
#47827 = CARTESIAN_POINT ( 'NONE',  ( -2.557715544985271983, -12.22074536777954989, 31.39888409691088356 ) ) ;
#47828 = CARTESIAN_POINT ( 'NONE',  ( 11.47237915910140771, -2.486705287966279432, 31.30864560766542937 ) ) ;
#47829 = ORIENTED_EDGE ( 'NONE', *, *, #65431, .F. ) ;
#47830 = CARTESIAN_POINT ( 'NONE',  ( -17.93393266664992325, -9.905515769479281474, 34.41647553114623292 ) ) ;
#47831 = FACE_OUTER_BOUND ( 'NONE', #3211, .T. ) ;
#47832 = CARTESIAN_POINT ( 'NONE',  ( 13.16168916709923664, -6.503392248772476236, 34.64988816332204635 ) ) ;
#47833 = EDGE_CURVE ( 'NONE', #3657, #66348, #63337, .T. ) ;
#47834 = CARTESIAN_POINT ( 'NONE',  ( 7.053602361310568725, -12.50538340440932217, 31.33453814440721885 ) ) ;
#47835 = CARTESIAN_POINT ( 'NONE',  ( -0.6850233861027926752, -11.60425143139329940, 33.02411095842164457 ) ) ;
#47836 = EDGE_LOOP ( 'NONE', ( #69230, #55725, #9852, #50375 ) ) ;
#47837 = FACE_BOUND ( 'NONE', #42642, .T. ) ;
#47838 = EDGE_LOOP ( 'NONE', ( #72646, #47115 ) ) ;
#47839 = DIRECTION ( 'NONE',  ( -0.000000000000000000, 0.7660444431189791237, -0.6427876096865379196 ) ) ;
#47840 = CARTESIAN_POINT ( 'NONE',  ( 18.06525513951284267, -6.835583212224605631, 34.95778746994559327 ) ) ;
#47841 = EDGE_CURVE ( 'NONE', #75643, #12463, #756, .T. ) ;
#47842 = CARTESIAN_POINT ( 'NONE',  ( -17.07692307692319744, -6.026961402154118908, 34.52809138561165270 ) ) ;
#47843 = CARTESIAN_POINT ( 'NONE',  ( -6.130691466667561151, -12.11776431015576172, 31.66791131148498906 ) ) ;
#47844 = ORIENTED_EDGE ( 'NONE', *, *, #35388, .F. ) ;
#47845 = EDGE_LOOP ( 'NONE', ( #2240, #68683 ) ) ;
#47846 = VERTEX_POINT ( 'NONE', #15163 ) ;
#47847 = CARTESIAN_POINT ( 'NONE',  ( -0.4615384615385826339, -3.300289026999228881, 32.46337939537708905 ) ) ;
#47848 = VERTEX_POINT ( 'NONE', #36323 ) ;
#47849 = ADVANCED_FACE ( 'NONE', ( #7521 ), #44720, .F. ) ;
#47850 = ADVANCED_FACE ( 'NONE', ( #55691 ), #7072, .F. ) ;
#47851 = CARTESIAN_POINT ( 'NONE',  ( -17.14219307747939425, -10.33852847137145048, 34.16647553114627556 ) ) ;
#47852 = CARTESIAN_POINT ( 'NONE',  ( -9.442307692307627676, -7.434744429011176159, 34.75000000000000711 ) ) ;
#47853 = CARTESIAN_POINT ( 'NONE',  ( 4.946232473812767871, -11.37499894934982514, 33.29245874905763003 ) ) ;
#47854 = VECTOR ( 'NONE', #56874, 1000.000000000000000 ) ;
#47855 = CARTESIAN_POINT ( 'NONE',  ( 11.47237812750565666, -2.538708090699994813, 30.37095296980875148 ) ) ;
#47856 = AXIS2_PLACEMENT_3D ( 'NONE', #56706, #76546, #8532 ) ;
#47857 = CARTESIAN_POINT ( 'NONE',  ( 1.553300858899129944, -11.24999999999998934, 24.70312500000000000 ) ) ;
#47858 = DIRECTION ( 'NONE',  ( -1.000000000000000000, -0.000000000000000000, 0.000000000000000000 ) ) ;
#47859 = CARTESIAN_POINT ( 'NONE',  ( -4.946397375159513388, -4.459921816937789885, 33.71989282347011851 ) ) ;
#47860 = CARTESIAN_POINT ( 'NONE',  ( -5.076923076923075762, -3.513871655860378418, 32.76840700105978499 ) ) ;
#47861 = VERTEX_POINT ( 'NONE', #63779 ) ;
#47862 = VERTEX_POINT ( 'NONE', #56587 ) ;
#47863 = EDGE_CURVE ( 'NONE', #57873, #5535, #17146, .T. ) ;
#47864 = VECTOR ( 'NONE', #35550, 1000.000000000000114 ) ;
#47865 = ORIENTED_EDGE ( 'NONE', *, *, #61928, .F. ) ;
#47866 = DIRECTION ( 'NONE',  ( 0.000000000000000000, 0.9848077530122072432, 0.1736481776669354937 ) ) ;
#47868 = CARTESIAN_POINT ( 'NONE',  ( -5.777220458731585850, -3.755027918224367767, 33.06320215134714857 ) ) ;
#47867 = CARTESIAN_POINT ( 'NONE',  ( 1.384615384615265343, -6.026961402154118908, 34.52809138561165270 ) ) ;
#47869 = B_SPLINE_CURVE_WITH_KNOTS ( 'NONE', 3,
 ( #59424, #1938, #86931, #15463, #70849, #15905, #4020, #22211, #86011, #63186 ),
 .UNSPECIFIED., .F., .F.,
 ( 4, 2, 2, 2, 4 ),
 ( 0.000000000000000000, 0.0001954311564186865221, 0.0003908623128373730441, 0.0005862934692560595662, 0.0007817246256747460882 ),
 .UNSPECIFIED. ) ;
#47870 = LINE ( 'NONE', #74913, #64343 ) ;
#47871 = CARTESIAN_POINT ( 'NONE',  ( -15.45425415533356173, -10.23692288466677880, 34.23039457007281072 ) ) ;
#47872 = ADVANCED_FACE ( 'NONE', ( #82742 ), #80760, .T. ) ;
#47873 = FACE_BOUND ( 'NONE', #57839, .T. ) ;
#47874 = DIRECTION ( 'NONE',  ( -0.000000000000000000, 1.000000000000000000, 3.491481338843133355E-15 ) ) ;
#47875 = VERTEX_POINT ( 'NONE', #81197 ) ;
#47876 = CARTESIAN_POINT ( 'NONE',  ( 8.096208266067295156, -2.318338780012835443, 30.59689888758630261 ) ) ;
#47877 = LINE ( 'NONE', #42021, #76391 ) ;
#47878 = CARTESIAN_POINT ( 'NONE',  ( 2.980792499826877329, -10.66389620160130036, 33.62221079203477103 ) ) ;
#47879 = ORIENTED_EDGE ( 'NONE', *, *, #70151, .T. ) ;
#47880 = CARTESIAN_POINT ( 'NONE',  ( -4.826868765284762830, -6.567000820036038355, 34.66262288849541306 ) ) ;
#47881 = ORIENTED_EDGE ( 'NONE', *, *, #67683, .F. ) ;
#47882 = FACE_BOUND ( 'NONE', #47823, .T. ) ;
#47883 = CARTESIAN_POINT ( 'NONE',  ( 9.692307692307695177, -5.557115091759785130, 34.35708131394839171 ) ) ;
#47884 = CARTESIAN_POINT ( 'NONE',  ( -7.846153846153530509, -2.255955759149395501, 30.00000000000324363 ) ) ;
#47885 = CARTESIAN_POINT ( 'NONE',  ( -12.59168643127015486, -12.15440758774515473, 32.17923288041532004 ) ) ;
#47886 = EDGE_LOOP ( 'NONE', ( #79457, #82825, #65025, #74488 ) ) ;
#47887 = CARTESIAN_POINT ( 'NONE',  ( 6.857806477116147548, -6.026961402152685388, 34.52809138561120506 ) ) ;
#47888 = CARTESIAN_POINT ( 'NONE',  ( -7.780086512803768173, -8.164416787775445883, 34.95778746994558617 ) ) ;
#47889 = DIRECTION ( 'NONE',  ( -0.000000000000000000, -0.9848077530122086864, -0.1736481776669273613 ) ) ;
#47890 = CARTESIAN_POINT ( 'NONE',  ( -20.00000000000000000, -11.50000000000000000, 28.25000000000000000 ) ) ;
#47891 = ORIENTED_EDGE ( 'NONE', *, *, #86622, .T. ) ;
#47892 = CARTESIAN_POINT ( 'NONE',  ( 13.38461538461526601, -6.026961402154118019, 34.52809138561165270 ) ) ;
#47894 = CARTESIAN_POINT ( 'NONE',  ( -15.48079246806219267, -4.335965774309649134, 33.62209801155881905 ) ) ;
#47893 = AXIS2_PLACEMENT_3D ( 'NONE', #17240, #84837, #70872 ) ;
#47897 = EDGE_LOOP ( 'NONE', ( #71351, #43178, #33457, #15894 ) ) ;
#47896 = AXIS2_PLACEMENT_3D ( 'NONE', #58365, #66922, #51596 ) ;
#47895 = CARTESIAN_POINT ( 'NONE',  ( 4.403900573759607084, -2.920487667080175154, 32.31805714834170828 ) ) ;
#47898 = CARTESIAN_POINT ( 'NONE',  ( 16.08776377448601735, -3.937682226553330445, 33.60647404775217240 ) ) ;
#47899 = CARTESIAN_POINT ( 'NONE',  ( 5.076923076923075762, -11.91647553114624181, 32.58852847137148245 ) ) ;
#47900 = CARTESIAN_POINT ( 'NONE',  ( -18.00000000000000000, 2.999999999999935163, 32.75000000000000000 ) ) ;
#47901 = CARTESIAN_POINT ( 'NONE',  ( -2.307692307692427391, -4.481592998941358097, 33.73612834414048933 ) ) ;
#47902 = CARTESIAN_POINT ( 'NONE',  ( -13.38461538461550759, -3.643525952248795718, 33.31231777344771672 ) ) ;
#47904 = CARTESIAN_POINT ( 'NONE',  ( -16.85414353565466072, -8.496831190052089866, 34.64984203495476578 ) ) ;
#47903 = LINE ( 'NONE', #42489, #73531 ) ;
#47905 = CARTESIAN_POINT ( 'NONE',  ( 16.15384615384615330, -13.75783147151868846, 33.36296068462461051 ) ) ;
#47906 = CARTESIAN_POINT ( 'NONE',  ( 1.139087296526029469, -10.24999999999999467, 20.95312500000000000 ) ) ;
#47907 = ORIENTED_EDGE ( 'NONE', *, *, #63770, .T. ) ;
#47908 = DIRECTION ( 'NONE',  ( 0.000000000000000000, 0.6427876096865368094, 0.7660444431189802339 ) ) ;
#47909 = VERTEX_POINT ( 'NONE', #31212 ) ;
#47910 = VERTEX_POINT ( 'NONE', #66340 ) ;
#47911 = CARTESIAN_POINT ( 'NONE',  ( -22.75000000000000000, -7.500000000000000000, 29.75000000000000355 ) ) ;
#47912 = ORIENTED_EDGE ( 'NONE', *, *, #28238, .T. ) ;
#47913 = LINE ( 'NONE', #6930, #11018 ) ;
#47914 = CARTESIAN_POINT ( 'NONE',  ( 2.749999999999995115, -6.360912703473971419, 20.64062500000000000 ) ) ;
#47915 = DIRECTION ( 'NONE',  ( 0.000000000000000000, -2.413528314402514090E-16, 1.000000000000000000 ) ) ;
#47916 = CARTESIAN_POINT ( 'NONE',  ( -7.976844449264153702, -8.191372820521381826, 34.95448215188424967 ) ) ;
#47917 = CARTESIAN_POINT ( 'NONE',  ( 5.999999999999880096, -3.300289026999228881, 32.46337939537708905 ) ) ;
#47918 = B_SPLINE_CURVE_WITH_KNOTS ( 'NONE', 3,
 ( #65240, #17060, #11649, #58930, #72443, #52617, #80100, #66593, #44963, #24247 ),
 .UNSPECIFIED., .F., .F.,
 ( 4, 2, 2, 2, 4 ),
 ( 0.000000000000000000, 0.0001954339857564078267, 0.0003908679715128156535, 0.0005863019572692235344, 0.0007817359430256313069 ),
 .UNSPECIFIED. ) ;
#47919 = CARTESIAN_POINT ( 'NONE',  ( -7.053767526187232129, -9.084618155246140248, 34.75535874321725771 ) ) ;
#47920 = CARTESIAN_POINT ( 'NONE',  ( 9.942362112221147186, -12.41089969410671223, 31.60739465890703670 ) ) ;
#47921 = CARTESIAN_POINT ( 'NONE',  ( 2.438218009455871194, -11.46989282347013095, 32.79007818306219946 ) ) ;
#47922 = B_SPLINE_CURVE_WITH_KNOTS ( 'NONE', 3,
 ( #34759, #61329, #62229, #6417, #538, #55473, #48714, #977, #28449, #63109 ),
 .UNSPECIFIED., .F., .F.,
 ( 4, 2, 2, 2, 4 ),
 ( 0.000000000000000000, 0.0001954339857564074473, 0.0003908679715128148945, 0.0005863019572692223418, 0.0007817359430256297891 ),
 .UNSPECIFIED. ) ;
#47923 = CARTESIAN_POINT ( 'NONE',  ( 6.699591998512590685, -12.47654668319379567, 31.42292124445336654 ) ) ;
#47924 = B_SPLINE_CURVE_WITH_KNOTS ( 'NONE', 3,
 ( #10108, #56080, #15990, #78561, #42576, #36699, #23182, #29944, #9239, #16426 ),
 .UNSPECIFIED., .F., .F.,
 ( 4, 2, 2, 2, 4 ),
 ( 0.0007817246256747455461, 0.0009771112852218885505, 0.001172497944769031446, 0.001367884604316174559, 0.001563271263863317455 ),
 .UNSPECIFIED. ) ;
#47925 = CARTESIAN_POINT ( 'NONE',  ( -0.6850234052624093462, -2.599994579823202923, 30.74605699353653776 ) ) ;
#47926 = CARTESIAN_POINT ( 'NONE',  ( 15.00728430620490350, -9.417330523894424488, 34.63758898049880486 ) ) ;
#47927 = CYLINDRICAL_SURFACE ( 'NONE', #60814, 0.2499999999999986955 ) ;
#47928 = AXIS2_PLACEMENT_3D ( 'NONE', #85433, #36365, #1688 ) ;
#47929 = VERTEX_POINT ( 'NONE', #4642 ) ;
#47930 = EDGE_LOOP ( 'NONE', ( #81036, #62120, #48409, #76133, #28233, #44045 ) ) ;
#47931 = CARTESIAN_POINT ( 'NONE',  ( 12.68455130563185662, -2.523321265292115534, 31.42251411153756990 ) ) ;
#47932 = FACE_OUTER_BOUND ( 'NONE', #36122, .T. ) ;
#47933 = LINE ( 'NONE', #88077, #26801 ) ;
#47934 = CARTESIAN_POINT ( 'NONE',  ( 5.749976762707036393, -5.851115903089112003, 34.47074536777953568 ) ) ;
#47935 = DIRECTION ( 'NONE',  ( -0.000000000000000000, 0.5000000000000011102, -0.8660254037844381525 ) ) ;
#47936 = FACE_OUTER_BOUND ( 'NONE', #51678, .T. ) ;
#47937 = CARTESIAN_POINT ( 'NONE',  ( -2.438382910802613157, -8.191372820521381826, 34.95448215188423546 ) ) ;
#47938 = ORIENTED_EDGE ( 'NONE', *, *, #8344, .T. ) ;
#47939 = CARTESIAN_POINT ( 'NONE',  ( -14.37377468705243899, -12.62096338111211580, 30.90682066428152908 ) ) ;
#47940 = EDGE_LOOP ( 'NONE', ( #10323, #50457, #18703, #21834 ) ) ;
#47941 = CARTESIAN_POINT ( 'NONE',  ( -8.769230769230892619, -5.094484230521993062, 34.41647553114689373 ) ) ;
#47942 = EDGE_CURVE ( 'NONE', #17127, #1706, #20355, .T. ) ;
#47943 = CARTESIAN_POINT ( 'NONE',  ( 15.29602437028207085, -3.643525952247864463, 33.31231777344670064 ) ) ;
#47944 = CARTESIAN_POINT ( 'NONE',  ( -6.673076923076987299, -7.565270000091922853, 34.99999999999999289 ) ) ;
#47945 = PRODUCT_DEFINITION ( 'UNKNOWN', '', #53350, #70807 ) ;
#47946 = CARTESIAN_POINT ( 'NONE',  ( -15.29685264172511161, -3.050289026998445951, 32.03036669348365706 ) ) ;
#47947 = B_SPLINE_CURVE_WITH_KNOTS ( 'NONE', 3,
 ( #65764, #78392, #32001, #72980, #80188, #64874, #66215, #10838, #37407, #59467 ),
 .UNSPECIFIED., .F., .F.,
 ( 4, 2, 2, 2, 4 ),
 ( 0.0007817359430256327164, 0.0009771253907249993591, 0.001172514838424366110, 0.001367904286123732861, 0.001563293733823099396 ),
 .UNSPECIFIED. ) ;
#47948 = CARTESIAN_POINT ( 'NONE',  ( -13.44988538517170618, -2.657715359629089225, 31.77849191805832874 ) ) ;
#47949 = EDGE_LOOP ( 'NONE', ( #8545, #37428, #57696, #70995 ) ) ;
#47950 = VECTOR ( 'NONE', #88217, 1000.000000000000114 ) ;
#47951 = AXIS2_PLACEMENT_3D ( 'NONE', #15064, #82646, #88526 ) ;
#47952 = ORIENTED_EDGE ( 'NONE', *, *, #65637, .F. ) ;
#47953 = ORIENTED_EDGE ( 'NONE', *, *, #40772, .F. ) ;
#47954 = VERTEX_POINT ( 'NONE', #65448 ) ;
#47955 = EDGE_CURVE ( 'NONE', #81222, #3726, #67238, .T. ) ;
#47956 = CARTESIAN_POINT ( 'NONE',  ( 17.14299041027315695, -9.905515769479276145, 34.41647553114623292 ) ) ;
#47957 = CARTESIAN_POINT ( 'NONE',  ( 7.846153846153846700, -3.513871655860378418, 32.76840700105978499 ) ) ;
#47958 = CARTESIAN_POINT ( 'NONE',  ( 4.376858997939548246, -11.98016756924215009, 32.48728574198911190 ) ) ;
#47959 = CARTESIAN_POINT ( 'NONE',  ( 14.17708265248822386, -7.722926974430166069, 34.99546784045485737 ) ) ;
#47960 = DIRECTION ( 'NONE',  ( 0.000000000000000000, -1.000000000000000000, 0.000000000000000000 ) ) ;
#47961 = CARTESIAN_POINT ( 'NONE',  ( -9.692307692307691624, -11.91647553114624181, 32.58852847137148245 ) ) ;
#47962 = ORIENTED_EDGE ( 'NONE', *, *, #54184, .T. ) ;
#47963 = ORIENTED_EDGE ( 'NONE', *, *, #54929, .T. ) ;
#47964 = VERTEX_POINT ( 'NONE', #19482 ) ;
#47966 = ORIENTED_EDGE ( 'NONE', *, *, #15736, .F. ) ;
#47965 = CARTESIAN_POINT ( 'NONE',  ( -9.692307692307691624, -1.044019251281081972, 31.83374038241031911 ) ) ;
#47967 = CARTESIAN_POINT ( 'NONE',  ( 9.626225312947561008, -8.164416787775445883, 34.95778746994557906 ) ) ;
#47968 = FACE_OUTER_BOUND ( 'NONE', #83862, .T. ) ;
#47969 = CARTESIAN_POINT ( 'NONE',  ( 3.749999999999992006, -5.946699141100872943, 20.64062500000000000 ) ) ;
#47970 = ADVANCED_FACE ( 'NONE', ( #12284 ), #32113, .F. ) ;
#47971 = EDGE_LOOP ( 'NONE', ( #62531, #31570 ) ) ;
#47972 = DIRECTION ( 'NONE',  ( 0.000000000000000000, 0.000000000000000000, -1.000000000000000000 ) ) ;
#47973 = ORIENTED_EDGE ( 'NONE', *, *, #69326, .F. ) ;
#47974 = CARTESIAN_POINT ( 'NONE',  ( 7.976679547917411739, -12.27024696741798948, 31.24895572276498257 ) ) ;
#47975 = EDGE_CURVE ( 'NONE', #47786, #17409, #61165, .T. ) ;
#47976 = FACE_BOUND ( 'NONE', #72069, .T. ) ;
#47977 = CARTESIAN_POINT ( 'NONE',  ( 17.07692307692307665, -8.564572088678739092, 35.78748833219616898 ) ) ;
#47978 = VECTOR ( 'NONE', #55061, 1000.000000000000000 ) ;
#47979 = EDGE_CURVE ( 'NONE', #26836, #48528, #72986, .T. ) ;
#47980 = CARTESIAN_POINT ( 'NONE',  ( 1.384615384615264011, -2.379036618888197285, 30.90682066428292885 ) ) ;
#47981 = ORIENTED_EDGE ( 'NONE', *, *, #35752, .F. ) ;
#47982 = CARTESIAN_POINT ( 'NONE',  ( 8.639082799499076870, -12.15440758774515473, 32.17923288041532004 ) ) ;
#47983 = CARTESIAN_POINT ( 'NONE',  ( 6.700149964170075023, -11.98009711892699691, 32.48740034544075428 ) ) ;
#47984 = CARTESIAN_POINT ( 'NONE',  ( -13.13461538461394973, -7.500000000000155431, 34.75000000000007105 ) ) ;
#47985 = CARTESIAN_POINT ( 'NONE',  ( -3.361459833879538728, -9.084618155246140248, 34.75535874321725771 ) ) ;
#47986 = ORIENTED_EDGE ( 'NONE', *, *, #36274, .F. ) ;
#47987 = CARTESIAN_POINT ( 'NONE',  ( -12.46153846153858424, -2.379036618888197729, 30.90682066428292885 ) ) ;
#47988 = CARTESIAN_POINT ( 'NONE',  ( 1.384615384615264011, -4.320704448113951379, 33.92786785259630022 ) ) ;
#47989 = CARTESIAN_POINT ( 'NONE',  ( -16.40384615384615330, -2.249999999999998668, 29.75000000000000355 ) ) ;
#47990 = CARTESIAN_POINT ( 'NONE',  ( -2.557669038634660108, -10.66389620160130036, 33.62221079203477103 ) ) ;
#47991 = CARTESIAN_POINT ( 'NONE',  ( -0.3314908552827783850, -7.723484964179500700, 34.74522123443823318 ) ) ;
#47992 = FACE_BOUND ( 'NONE', #10331, .T. ) ;
#47994 = CARTESIAN_POINT ( 'NONE',  ( 11.47319109250076430, -12.46129190929999986, 30.37095296980880832 ) ) ;
#47993 = CARTESIAN_POINT ( 'NONE',  ( 1.134615384615387246, -7.500000000000001776, 35.00000000000000000 ) ) ;
#47995 = CARTESIAN_POINT ( 'NONE',  ( -14.55771553191376277, -3.520140089381495585, 33.17453946501458262 ) ) ;
#47997 = CARTESIAN_POINT ( 'NONE',  ( -2.084679463598911653, -8.282913670948747864, 34.94150082978203642 ) ) ;
#47996 = CARTESIAN_POINT ( 'NONE',  ( -5.999999999999998224, -8.564572088678739092, 35.78748833219616898 ) ) ;
#47998 = CARTESIAN_POINT ( 'NONE',  ( -5.207071046654774271, -12.50552854090298993, 31.33409797877408920 ) ) ;
#47999 = CARTESIAN_POINT ( 'NONE',  ( 1.987747218494664292, -9.401340078031346081, 15.62313170625848890 ) ) ;
#48000 = ORIENTED_EDGE ( 'NONE', *, *, #6361, .F. ) ;
#48001 = B_SPLINE_CURVE_WITH_KNOTS ( 'NONE', 3,
 ( #66626, #45896, #11688, #13890, #70165, #75585, #43141, #8474, #7140, #21983 ),
 .UNSPECIFIED., .F., .F.,
 ( 4, 2, 2, 2, 4 ),
 ( 0.0007817359430256308733, 0.0009771253907249971907, 0.001172514838424363725, 0.001367904286123730259, 0.001563293733823096577 ),
 .UNSPECIFIED. ) ;
#48002 = CARTESIAN_POINT ( 'NONE',  ( 12.71148397988660328, -2.587454068350148351, 30.68340429815432202 ) ) ;
#48003 = EDGE_LOOP ( 'NONE', ( #7484, #44397, #38049, #52841 ) ) ;
#48004 = B_SPLINE_CURVE_WITH_KNOTS ( 'NONE', 3,
 ( #34912, #62376, #689, #28157, #55625, #83115, #21407, #48873, #42136, #7895 ),
 .UNSPECIFIED., .F., .F.,
 ( 4, 2, 2, 2, 4 ),
 ( 0.0007817246256747520513, 0.0009771112852218959231, 0.001172497944769039903, 0.001367884604316183883, 0.001563271263863327864 ),
 .UNSPECIFIED. ) ;
#48005 = CARTESIAN_POINT ( 'NONE',  ( -13.31854805126531005, -9.058645607665452459, 34.76329471203371924 ) ) ;
#48006 = VERTEX_POINT ( 'NONE', #51921 ) ;
#48007 = CARTESIAN_POINT ( 'NONE',  ( -12.46153846153846168, -8.564572088678739092, 35.78748833219616898 ) ) ;
#48008 = CARTESIAN_POINT ( 'NONE',  ( 14.30769230769218581, -4.320704448113951379, 33.92786785259630022 ) ) ;
#48010 = ORIENTED_EDGE ( 'NONE', *, *, #38884, .F. ) ;
#48009 = CYLINDRICAL_SURFACE ( 'NONE', #38062, 0.2500000000000012212 ) ;
#48011 = CARTESIAN_POINT ( 'NONE',  ( 18.00000000000000000, -5.471508081941601098, 34.59228464037088457 ) ) ;
#48012 = CARTESIAN_POINT ( 'NONE',  ( 1.987747218494664292, -9.401340078031346081, 20.62313170625849068 ) ) ;
#48013 = DIRECTION ( 'NONE',  ( 0.000000000000000000, 0.7660444431189822323, -0.6427876096865344779 ) ) ;
#48014 = DIRECTION ( 'NONE',  ( -1.000000000000000000, -0.000000000000000000, 0.000000000000000000 ) ) ;
#48015 = VECTOR ( 'NONE', #52849, 1000.000000000000227 ) ;
#48016 = CARTESIAN_POINT ( 'NONE',  ( 17.01083966596719677, -12.37446782046654192, 30.86335684631486487 ) ) ;
#48017 = CARTESIAN_POINT ( 'NONE',  ( 24.00000000000000000, 9.000000000000024869, 28.74999999999999645 ) ) ;
#48018 = CARTESIAN_POINT ( 'NONE',  ( 2.307692307692187583, -2.892918686052166066, 31.69288490824153470 ) ) ;
#48019 = LINE ( 'NONE', #14690, #8028 ) ;
#48020 = CARTESIAN_POINT ( 'NONE',  ( 1.614399933863618797, -3.775308065498751198, 24.48624329374151642 ) ) ;
#48021 = EDGE_CURVE ( 'NONE', #65186, #54833, #25353, .T. ) ;
#48022 = CARTESIAN_POINT ( 'NONE',  ( 11.53846153846153832, -1.509761064869970415, 31.06009739812519044 ) ) ;
#48023 = CARTESIAN_POINT ( 'NONE',  ( -4.153846153846274980, -3.083524468854526912, 32.58852847137268327 ) ) ;
#48024 = VERTEX_POINT ( 'NONE', #17717 ) ;
#48025 = DIRECTION ( 'NONE',  ( 0.000000000000000000, 0.000000000000000000, 1.000000000000000000 ) ) ;
#48026 = CARTESIAN_POINT ( 'NONE',  ( 1.492201783934598236, -11.27530806549875031, 23.70499329374151642 ) ) ;
#48027 = CARTESIAN_POINT ( 'NONE',  ( 2.177001704582000485, -4.684245665217971144, 34.18127051446801090 ) ) ;
#48028 = DIRECTION ( 'NONE',  ( -0.000000000000000000, 1.000000000000000000, -0.000000000000000000 ) ) ;
#48029 = VERTEX_POINT ( 'NONE', #87985 ) ;
#48030 = CARTESIAN_POINT ( 'NONE',  ( -17.74994568836168085, -2.779044189368095275, 31.39831045268884324 ) ) ;
#48031 = CARTESIAN_POINT ( 'NONE',  ( -14.55766903863466055, -11.28823185664190376, 33.01397839955799896 ) ) ;
#48033 = VERTEX_POINT ( 'NONE', #31670 ) ;
#48032 = DIRECTION ( 'NONE',  ( -0.000000000000000000, -0.6427876096865404731, -0.7660444431189771253 ) ) ;
#48034 = CARTESIAN_POINT ( 'NONE',  ( 6.673076923076925127, -2.499999999999998668, 29.75000000000000355 ) ) ;
#48035 = CARTESIAN_POINT ( 'NONE',  ( -15.16551409125639083, -12.16647553114626490, 32.15551576947920864 ) ) ;
#48036 = EDGE_CURVE ( 'NONE', #31874, #69663, #77289, .T. ) ;
#48037 = CARTESIAN_POINT ( 'NONE',  ( 15.93091993633000136, -9.086856451489516928, 34.49173150075333183 ) ) ;
#48038 = CARTESIAN_POINT ( 'NONE',  ( 3.100078627658925612, -2.494641256782728966, 31.33461815524612959 ) ) ;
#48039 = DIRECTION ( 'NONE',  ( 0.000000000000000000, -1.000000000000000000, 0.000000000000000000 ) ) ;
#48040 = AXIS2_PLACEMENT_3D ( 'NONE', #66705, #53175, #68470 ) ;
#48041 = VERTEX_POINT ( 'NONE', #27129 ) ;
#48042 = ORIENTED_EDGE ( 'NONE', *, *, #53224, .T. ) ;
#48043 = ORIENTED_EDGE ( 'NONE', *, *, #47633, .F. ) ;
#48044 = AXIS2_PLACEMENT_3D ( 'NONE', #10758, #60719, #66136 ) ;
#48045 = EDGE_CURVE ( 'NONE', #36328, #43306, #64338, .T. ) ;
#48046 = DIRECTION ( 'NONE',  ( 0.000000000000000000, 1.000000000000000000, 0.000000000000000000 ) ) ;
#48047 = CARTESIAN_POINT ( 'NONE',  ( 0.2380535178145129771, -2.599994579823202923, 30.74605699353653776 ) ) ;
#48048 = EDGE_CURVE ( 'NONE', #62255, #64011, #82965, .T. ) ;
#48049 = DIRECTION ( 'NONE',  ( 0.000000000000000000, 0.000000000000000000, 1.000000000000000000 ) ) ;
#48050 = CARTESIAN_POINT ( 'NONE',  ( 1.576923076923075762, -7.500000000000000000, 29.75000000000000355 ) ) ;
#48051 = CARTESIAN_POINT ( 'NONE',  ( 5.076923076923075762, -5.557115091759785130, 34.35708131394839171 ) ) ;
#48052 = VERTEX_POINT ( 'NONE', #62672 ) ;
#48053 = ORIENTED_EDGE ( 'NONE', *, *, #20665, .F. ) ;
#48055 = ORIENTED_EDGE ( 'NONE', *, *, #85615, .F. ) ;
#48054 = EDGE_CURVE ( 'NONE', #27738, #221, #48722, .T. ) ;
#48057 = ORIENTED_EDGE ( 'NONE', *, *, #7616, .F. ) ;
#48056 = CARTESIAN_POINT ( 'NONE',  ( -18.00000000000000000, -13.02631839243208667, 34.71348354719103924 ) ) ;
#48058 = DIRECTION ( 'NONE',  ( 0.000000000000000000, 0.000000000000000000, -1.000000000000000000 ) ) ;
#48059 = CARTESIAN_POINT ( 'NONE',  ( -11.97435897435897267, -3.499999999999999556, 29.75000000000000355 ) ) ;
#48060 = EDGE_CURVE ( 'NONE', #64638, #57873, #21247, .T. ) ;
#48061 = CARTESIAN_POINT ( 'NONE',  ( -13.19230769230769162, -3.499999999999999556, 29.75000000000000355 ) ) ;
#48062 = CYLINDRICAL_SURFACE ( 'NONE', #49662, 3.000000000000000000 ) ;
#48063 = ADVANCED_FACE ( 'NONE', ( #68554 ), #101, .F. ) ;
#48064 = ORIENTED_EDGE ( 'NONE', *, *, #73926, .F. ) ;
#48065 = VERTEX_POINT ( 'NONE', #76193 ) ;
#48066 = B_SPLINE_CURVE_WITH_KNOTS ( 'NONE', 3,
 ( #22692, #23137, #84857, #42534, #77638, #43418, #70890, #2411, #50604, #29906 ),
 .UNSPECIFIED., .F., .F.,
 ( 4, 2, 2, 2, 4 ),
 ( 0.000000000000000000, 0.0001954311564186861697, 0.0003908623128373723394, 0.0005862934692560584820, 0.0007817246256747446788 ),
 .UNSPECIFIED. ) ;
#48067 = CIRCLE ( 'NONE', #46666, 2.000000000000001776 ) ;
#48068 = EDGE_LOOP ( 'NONE', ( #2840, #881 ) ) ;
#48069 = CARTESIAN_POINT ( 'NONE',  ( 6.166666666666664298, -3.499999999999999556, 29.75000000000000355 ) ) ;
#48071 = ORIENTED_EDGE ( 'NONE', *, *, #43070, .T. ) ;
#48070 = CARTESIAN_POINT ( 'NONE',  ( 7.846153846153846700, -2.538708090699994813, 30.37095296980875503 ) ) ;
#48073 = B_SPLINE_CURVE_WITH_KNOTS ( 'NONE', 3,
 ( #64407, #77938, #69416, #15363, #28426, #43273, #14923, #36081, #55892, #28887 ),
 .UNSPECIFIED., .F., .F.,
 ( 4, 2, 2, 2, 4 ),
 ( 0.0007817246256747459798, 0.0009771112852218887673, 0.001172497944769031663, 0.001367884604316174559, 0.001563271263863317455 ),
 .UNSPECIFIED. ) ;
#48072 = CARTESIAN_POINT ( 'NONE',  ( 6.923076923076802558, -6.879047030192662504, 34.71129190930017927 ) ) ;
#48074 = LINE ( 'NONE', #783, #47950 ) ;
#48075 = EDGE_CURVE ( 'NONE', #65429, #79653, #75322, .T. ) ;
#48076 = VERTEX_POINT ( 'NONE', #67676 ) ;
#48077 = CARTESIAN_POINT ( 'NONE',  ( 14.16025641025641235, -7.500000000000000000, 29.75000000000000355 ) ) ;
#48078 = CYLINDRICAL_SURFACE ( 'NONE', #35322, 4.000000000000000000 ) ;
#48079 = VERTEX_POINT ( 'NONE', #13614 ) ;
#48080 = FACE_BOUND ( 'NONE', #39469, .T. ) ;
#48081 = CARTESIAN_POINT ( 'NONE',  ( 10.74617642320940369, -9.804649428959608670, 34.18742332936588468 ) ) ;
#48082 = DIRECTION ( 'NONE',  ( -0.000000000000000000, 1.000000000000000000, -0.000000000000000000 ) ) ;
#48083 = CARTESIAN_POINT ( 'NONE',  ( -0.4615384615384611200, -11.35647404775217417, 33.31231777344666511 ) ) ;
#48085 = CARTESIAN_POINT ( 'NONE',  ( -0.5276218724943415594, -12.10708131394839349, 31.69288490824020244 ) ) ;
#48084 = CARTESIAN_POINT ( 'NONE',  ( 9.626224281351813516, -3.050289026998445951, 32.03036669348365706 ) ) ;
#48086 = EDGE_CURVE ( 'NONE', #44728, #73862, #63034, .T. ) ;
#48087 = CARTESIAN_POINT ( 'NONE',  ( -3.007756386675835447, -3.395485233115138168, 33.02377354290276656 ) ) ;
#48088 = CARTESIAN_POINT ( 'NONE',  ( -3.931066484868087851, -11.60474049983371003, 33.02348890104160262 ) ) ;
#48089 = ORIENTED_EDGE ( 'NONE', *, *, #24855, .F. ) ;
#48090 = EDGE_CURVE ( 'NONE', #31586, #71975, #50057, .T. ) ;
#48091 = CARTESIAN_POINT ( 'NONE',  ( -8.069638770718176701, -6.716662450894489211, 34.94144148231605840 ) ) ;
#48092 = LINE ( 'NONE', #83225, #52153 ) ;
#48093 = VERTEX_POINT ( 'NONE', #20812 ) ;
#48094 = DIRECTION ( 'NONE',  ( 0.000000000000000000, 0.8660254037844377084, 0.5000000000000015543 ) ) ;
#48095 = LINE ( 'NONE', #62490, #83566 ) ;
#48096 = VERTEX_POINT ( 'NONE', #40213 ) ;
#48097 = CYLINDRICAL_SURFACE ( 'NONE', #44252, 0.2500000000000009437 ) ;
#48098 = CARTESIAN_POINT ( 'NONE',  ( -4.219116154402471786, -2.379036618887870436, 30.90682066428147934 ) ) ;
#48099 = CIRCLE ( 'NONE', #17955, 4.000000000000000000 ) ;
#48100 = FACE_BOUND ( 'NONE', #43480, .T. ) ;
#48102 = CARTESIAN_POINT ( 'NONE',  ( 15.45378058238208219, -12.15243808032445827, 31.58219941686247978 ) ) ;
#48101 = CARTESIAN_POINT ( 'NONE',  ( -14.55766905174089665, -4.075325502946081535, 33.72974371597206300 ) ) ;
#48103 = CARTESIAN_POINT ( 'NONE',  ( 2.177001704582002262, -6.369640206132550553, 34.87707690430378449 ) ) ;
#48104 = CARTESIAN_POINT ( 'NONE',  ( -2.307692307692305711, -3.669653830205710676, 35.88435417666054406 ) ) ;
#48106 = CARTESIAN_POINT ( 'NONE',  ( -8.638705067467203236, -12.27024696741798948, 31.24895572276497546 ) ) ;
#48105 = FILL_AREA_STYLE ('',( #67511 ) ) ;
#48107 = CYLINDRICAL_SURFACE ( 'NONE', #79255, 2.750000000000000000 ) ;
#48108 = CARTESIAN_POINT ( 'NONE',  ( 0.06109907496455496689, -11.24999999999999822, 15.77938170625848890 ) ) ;
#48109 = VERTEX_POINT ( 'NONE', #48278 ) ;
#48110 = AXIS2_PLACEMENT_3D ( 'NONE', #48050, #34546, #68335 ) ;
#48111 = ORIENTED_EDGE ( 'NONE', *, *, #65566, .F. ) ;
#48112 = VECTOR ( 'NONE', #37938, 999.9999999999998863 ) ;
#48113 = B_SPLINE_CURVE_WITH_KNOTS ( 'NONE', 3,
 ( #79165, #57998, #43598, #44921, #59332, #72397, #86389, #17912, #86840, #52569 ),
 .UNSPECIFIED., .F., .F.,
 ( 4, 2, 2, 2, 4 ),
 ( 0.0007817246256747473893, 0.0009771112852218900684, 0.001172497944769032747, 0.001367884604316175427, 0.001563271263863318106 ),
 .UNSPECIFIED. ) ;
#48114 = CARTESIAN_POINT ( 'NONE',  ( 15.90386940979756858, -9.234221910056350069, 34.70572697212741531 ) ) ;
#48115 = CARTESIAN_POINT ( 'NONE',  ( -15.36145983387953962, -5.496505350115501010, 34.60290016733514307 ) ) ;
#48116 = CARTESIAN_POINT ( 'NONE',  ( 14.30769230769218581, -9.528491918059723176, 34.59228464037033035 ) ) ;
#48117 = CARTESIAN_POINT ( 'NONE',  ( 6.700150705560775855, -12.15238873228292071, 31.58232369045353849 ) ) ;
#48118 = CARTESIAN_POINT ( 'NONE',  ( 5.142178216435913107, -3.643525952247864463, 33.31231777344670064 ) ) ;
#48119 = CARTESIAN_POINT ( 'NONE',  ( -0.06109907496455085213, -3.750000000000000888, 17.65438170625849068 ) ) ;
#48120 = CARTESIAN_POINT ( 'NONE',  ( -7.846153846153965716, -2.625532179533778709, 30.86335684631627174 ) ) ;
#48121 = CARTESIAN_POINT ( 'NONE',  ( -6.130147969731693181, -8.630895178749536711, 34.87696386517710323 ) ) ;
#48122 = CARTESIAN_POINT ( 'NONE',  ( 9.692307692307695177, -10.67929555188718282, 33.92786785259544047 ) ) ;
#48123 = PLANE ( 'NONE',  #53074 ) ;
#48124 = CARTESIAN_POINT ( 'NONE',  ( -15.23076923076935074, -11.48612834414049644, 32.76840700105863391 ) ) ;
#48125 = CARTESIAN_POINT ( 'NONE',  ( 16.21910172512217585, -5.219633306516380244, 34.19971097300157936 ) ) ;
#48126 = CARTESIAN_POINT ( 'NONE',  ( 5.749976762707035505, -12.22074536777954989, 31.39888409691088356 ) ) ;
#48127 = EDGE_CURVE ( 'NONE', #18188, #5178, #55923, .T. ) ;
#48128 = CARTESIAN_POINT ( 'NONE',  ( -3.360916440207451839, -8.587444163452046197, 34.63053765926554206 ) ) ;
#48129 = CARTESIAN_POINT ( 'NONE',  ( 12.59206416330202494, -2.882268652242222284, 31.66798894389554064 ) ) ;
#48130 = ORIENTED_EDGE ( 'NONE', *, *, #47586, .F. ) ;
#48131 = EDGE_CURVE ( 'NONE', #67886, #18976, #75749, .T. ) ;
#48132 = CARTESIAN_POINT ( 'NONE',  ( 2.084207383127978375, -3.562934362175799841, 33.22335522853832401 ) ) ;
#48133 = EDGE_CURVE ( 'NONE', #47148, #24566, #41532, .T. ) ;
#48134 = FACE_OUTER_BOUND ( 'NONE', #82850, .T. ) ;
#48135 = CARTESIAN_POINT ( 'NONE',  ( -1.901340078031369618, -5.512252781505359245, 19.25186829374151287 ) ) ;
#48136 = EDGE_CURVE ( 'NONE', #29630, #32571, #54141, .T. ) ;
#48137 = CARTESIAN_POINT ( 'NONE',  ( -9.822998295417999515, -10.70098750199973203, 33.91152734681376302 ) ) ;
#48138 = CARTESIAN_POINT ( 'NONE',  ( 15.23076923076923173, -13.87047571288749737, 32.06866353760679544 ) ) ;
#48139 = DIRECTION ( 'NONE',  ( 0.000000000000000000, 0.8660254037844377084, -0.5000000000000015543 ) ) ;
#48141 = ORIENTED_EDGE ( 'NONE', *, *, #40597, .F. ) ;
#48140 = CARTESIAN_POINT ( 'NONE',  ( -1.134561072977068985, -4.235687564193446164, 33.53795663066793509 ) ) ;
#48142 = CARTESIAN_POINT ( 'NONE',  ( 1.799775606325937360E-14, -10.25000000000000000, 26.03125000000000000 ) ) ;
#48143 = CARTESIAN_POINT ( 'NONE',  ( -9.561782254074046250, -5.915461855592780260, 34.75538340440931506 ) ) ;
#48144 = ORIENTED_EDGE ( 'NONE', *, *, #27521, .T. ) ;
#48145 = CARTESIAN_POINT ( 'NONE',  ( -16.08777780284371417, -9.780366693483667717, 34.19971097300155805 ) ) ;
#48146 = EDGE_CURVE ( 'NONE', #64222, #76630, #88855, .T. ) ;
#48147 = VECTOR ( 'NONE', #18569, 1000.000000000000000 ) ;
#48148 = CARTESIAN_POINT ( 'NONE',  ( 7.911299625485813891, -7.750023238201979581, 34.74374492549440419 ) ) ;
#48149 = EDGE_LOOP ( 'NONE', ( #72976, #24579, #75015, #75221 ) ) ;
#48150 = CARTESIAN_POINT ( 'NONE',  ( -7.846153846153844924, -6.343179335718451384, 34.87096338111211935 ) ) ;
#48151 = CARTESIAN_POINT ( 'NONE',  ( -15.48076923076922995, -7.433932668274256805, 35.00000000000000711 ) ) ;
#48152 = CARTESIAN_POINT ( 'NONE',  ( -14.98082371242109012, -12.43552623307873972, 30.55307653245132826 ) ) ;
#48153 = ORIENTED_EDGE ( 'NONE', *, *, #66914, .F. ) ;
#48154 = VERTEX_POINT ( 'NONE', #74884 ) ;
#48155 = LINE ( 'NONE', #32101, #44133 ) ;
#48156 = B_SPLINE_CURVE_WITH_KNOTS ( 'NONE', 3,
 ( #22768, #77718, #16026, #61002, #74085, #5176, #38975, #38521, #11045, #60557 ),
 .UNSPECIFIED., .F., .F.,
 ( 4, 2, 2, 2, 4 ),
 ( 0.000000000000000000, 0.0001954339857564076099, 0.0003908679715128152198, 0.0005863019572692228839, 0.0007817359430256304396 ),
 .UNSPECIFIED. ) ;
#48157 = VERTEX_POINT ( 'NONE', #6424 ) ;
#48158 = CARTESIAN_POINT ( 'NONE',  ( -7.846153846153844924, -2.292212530054420494, 30.41441678777542634 ) ) ;
#48159 = CARTESIAN_POINT ( 'NONE',  ( 5.326868486301119532, -4.932303261841489039, 34.32971442181322885 ) ) ;
#48160 = CARTESIAN_POINT ( 'NONE',  ( -10.74553182482283198, -2.619462340734462380, 30.83744416345203021 ) ) ;
#48161 = DIRECTION ( 'NONE',  ( 1.000000000000000000, -0.000000000000000000, 0.000000000000000000 ) ) ;
#48163 = EDGE_CURVE ( 'NONE', #40118, #85711, #28975, .T. ) ;
#48162 = DIRECTION ( 'NONE',  ( 1.000000000000000000, 0.000000000000000000, 0.000000000000000000 ) ) ;
#48164 = CARTESIAN_POINT ( 'NONE',  ( 1.384615384615386802, -2.292212530054420494, 30.41441678777542634 ) ) ;
#48165 = CARTESIAN_POINT ( 'NONE',  ( -20.00000000000000000, -3.499999999999999556, 28.25000000000000000 ) ) ;
#48166 = ORIENTED_EDGE ( 'NONE', *, *, #3444, .F. ) ;
#48167 = ORIENTED_EDGE ( 'NONE', *, *, #16817, .T. ) ;
#48169 = VERTEX_POINT ( 'NONE', #50050 ) ;
#48168 = LINE ( 'NONE', #47286, #64513 ) ;
#48170 = CARTESIAN_POINT ( 'NONE',  ( 7.716005876422147303, -2.647304123082328875, 31.75400227202885972 ) ) ;
#48171 = VECTOR ( 'NONE', #35061, 1000.000000000000000 ) ;
#48172 = ORIENTED_EDGE ( 'NONE', *, *, #17347, .T. ) ;
#48173 = B_SPLINE_CURVE_WITH_KNOTS ( 'NONE', 3,
 ( #10764, #36897, #3106, #57176, #72013, #77448, #49968, #10321, #31477, #37786 ),
 .UNSPECIFIED., .F., .F.,
 ( 4, 2, 2, 2, 4 ),
 ( 0.0007817359430256390048, 0.0009771253907250075990, 0.001172514838424376085, 0.001367904286123744571, 0.001563293733823113056 ),
 .UNSPECIFIED. ) ;
#48174 = DIRECTION ( 'NONE',  ( -0.000000000000000000, -0.7660444431189791237, -0.6427876096865379196 ) ) ;
#48175 = CARTESIAN_POINT ( 'NONE',  ( 12.59233026936324684, -3.062576670634119758, 32.05464942895959979 ) ) ;
#48176 = CIRCLE ( 'NONE', #38153, 0.2500000000000002220 ) ;
#48177 = ORIENTED_EDGE ( 'NONE', *, *, #34021, .F. ) ;
#48178 = CARTESIAN_POINT ( 'NONE',  ( 7.846153846153846700, -8.120952969808772792, 34.71129190930000163 ) ) ;
#48179 = B_SPLINE_CURVE_WITH_KNOTS ( 'NONE', 3,
 ( #78663, #84989, #16966, #24156, #3442, #71023, #30475, #65582, #30909, #23272 ),
 .UNSPECIFIED., .F., .F.,
 ( 4, 2, 2, 2, 4 ),
 ( 0.000000000000000000, 0.0001954311564186879857, 0.0003908623128373759715, 0.0005862934692560640114, 0.0007817246256747519429 ),
 .UNSPECIFIED. ) ;
#48180 = ORIENTED_EDGE ( 'NONE', *, *, #19530, .F. ) ;
#48181 = DIRECTION ( 'NONE',  ( 0.000000000000000000, -8.673617379884033500E-16, 1.000000000000000000 ) ) ;
#48182 = B_SPLINE_CURVE_WITH_KNOTS ( 'NONE', 3,
 ( #30044, #44871, #72349, #24158, #64697, #86340, #2996, #57063, #30478, #77779 ),
 .UNSPECIFIED., .F., .F.,
 ( 4, 2, 2, 2, 4 ),
 ( 0.000000000000000000, 0.0001954311564186881213, 0.0003908623128373762425, 0.0005862934692560643367, 0.0007817246256747524850 ),
 .UNSPECIFIED. ) ;
#48183 = ORIENTED_EDGE ( 'NONE', *, *, #88510, .T. ) ;
#48184 = CARTESIAN_POINT ( 'NONE',  ( -12.59222906464877134, -3.338472653186243644, 32.95098750199972670 ) ) ;
#48186 = ORIENTED_EDGE ( 'NONE', *, *, #83418, .F. ) ;
#48185 = EDGE_CURVE ( 'NONE', #1012, #40626, #23027, .T. ) ;
#48187 = EDGE_CURVE ( 'NONE', #19974, #61584, #45055, .T. ) ;
#48188 = CARTESIAN_POINT ( 'NONE',  ( -16.40382288478850725, -6.567427716900048118, 34.66269422305636283 ) ) ;
#48189 = CARTESIAN_POINT ( 'NONE',  ( 12.46153846153833911, -2.379036618888197729, 30.90682066428292885 ) ) ;
#48190 = FACE_BOUND ( 'NONE', #73898, .T. ) ;
#48191 = LINE ( 'NONE', #20292, #49928 ) ;
#48193 = EDGE_CURVE ( 'NONE', #35118, #49988, #16038, .T. ) ;
#48192 = CARTESIAN_POINT ( 'NONE',  ( -17.74994568836169151, -12.17597550085003633, 31.52189283813461884 ) ) ;
#48194 = CARTESIAN_POINT ( 'NONE',  ( 4.376625695114563008, -12.44528174975671853, 30.48912976160716681 ) ) ;
#48195 = CARTESIAN_POINT ( 'NONE',  ( 1.254467414883688070, -12.50552854090298993, 31.33409797877408920 ) ) ;
#48196 = CARTESIAN_POINT ( 'NONE',  ( -17.20761368003338632, -8.191372820521381826, 34.95448215188424967 ) ) ;
#48197 = CARTESIAN_POINT ( 'NONE',  ( -7.846153846153844924, -9.058645607665452459, 34.76329471203371924 ) ) ;
#48198 = EDGE_CURVE ( 'NONE', #42793, #25852, #34377, .T. ) ;
#48199 = CARTESIAN_POINT ( 'NONE',  ( 10.48523740594639619, -10.19110544564092002, 33.96427741523702792 ) ) ;
#48200 = EDGE_LOOP ( 'NONE', ( #75388, #38127, #4244, #86294 ) ) ;
#48201 = VERTEX_POINT ( 'NONE', #84309 ) ;
#48203 = CARTESIAN_POINT ( 'NONE',  ( -3.480792454990687013, -5.765609946408404518, 34.70566812827425451 ) ) ;
#48202 = CARTESIAN_POINT ( 'NONE',  ( -16.82686876528476105, -9.943054286541403997, 34.11300777759954883 ) ) ;
#48204 = ADVANCED_FACE ( 'NONE', ( #9084 ), #77972, .T. ) ;
#48205 = CARTESIAN_POINT ( 'NONE',  ( -9.469294848214296678, -12.38742843783360748, 31.66772728687926985 ) ) ;
#48206 = LINE ( 'NONE', #43228, #13503 ) ;
#48207 = CARTESIAN_POINT ( 'NONE',  ( 15.48071474911737333, -3.712312575010499494, 33.01462480002815170 ) ) ;
#48208 = CARTESIAN_POINT ( 'NONE',  ( -7.846153846153844924, -8.810774026931790459, 35.74407628777942847 ) ) ;
#48209 = ORIENTED_EDGE ( 'NONE', *, *, #32259, .T. ) ;
#48210 = CARTESIAN_POINT ( 'NONE',  ( 2.307692307692187583, -9.442884908241554243, 34.35708131394783038 ) ) ;
#48211 = DIRECTION ( 'NONE',  ( -0.000000000000000000, 0.6427876096865404731, -0.7660444431189771253 ) ) ;
#48212 = CARTESIAN_POINT ( 'NONE',  ( -9.019254006523736322, -12.22074536777954989, 31.39888409691088356 ) ) ;
#48213 = LINE ( 'NONE', #39709, #3614 ) ;
#48214 = ORIENTED_EDGE ( 'NONE', *, *, #72290, .T. ) ;
#48215 = EDGE_CURVE ( 'NONE', #82729, #39385, #36551, .T. ) ;
#48216 = ORIENTED_EDGE ( 'NONE', *, *, #20027, .T. ) ;
#48217 = ORIENTED_EDGE ( 'NONE', *, *, #69265, .T. ) ;
#48218 = DIRECTION ( 'NONE',  ( -0.000000000000000000, 0.9848077530122085754, -0.1736481776669273613 ) ) ;
#48219 = EDGE_CURVE ( 'NONE', #5646, #44546, #35669, .T. ) ;
#48220 = EDGE_LOOP ( 'NONE', ( #45716, #5868, #23555, #28607 ) ) ;
#48221 = CARTESIAN_POINT ( 'NONE',  ( -9.915233909823838232, -12.39988816332205701, 30.74660775122750778 ) ) ;
#48222 = CARTESIAN_POINT ( 'NONE',  ( -17.32689980786543060, -3.137211980971222225, 32.19342716148376837 ) ) ;
#48223 = CARTESIAN_POINT ( 'NONE',  ( -5.076923076923075762, -4.098570777380720287, 33.41473453929634729 ) ) ;
#48224 = CARTESIAN_POINT ( 'NONE',  ( 2.320192649118979489E-14, -11.25000000000000000, 14.78125000000000178 ) ) ;
#48225 = CARTESIAN_POINT ( 'NONE',  ( -11.31568199719312773, -6.760870238392817200, 34.69528174975672385 ) ) ;
#48226 = ORIENTED_EDGE ( 'NONE', *, *, #67985, .F. ) ;
#48227 = CARTESIAN_POINT ( 'NONE',  ( -17.78205128205128105, -3.499999999999999556, 29.75000000000000355 ) ) ;
#48229 = EDGE_LOOP ( 'NONE', ( #33975, #42894, #66222, #49848 ) ) ;
#48228 = FACE_OUTER_BOUND ( 'NONE', #59990, .T. ) ;
#48230 = PLANE ( 'NONE',  #58367 ) ;
#48231 = FACE_OUTER_BOUND ( 'NONE', #38176, .T. ) ;
#48232 = CARTESIAN_POINT ( 'NONE',  ( 3.230769230769231726, -10.05456864172156806, 36.03766855953608683 ) ) ;
#48233 = CARTESIAN_POINT ( 'NONE',  ( -18.03205128205128105, -4.000000000000000000, 29.75000000000000355 ) ) ;
#48234 = EDGE_CURVE ( 'NONE', #44313, #75481, #87055, .T. ) ;
#48236 = VECTOR ( 'NONE', #88351, 999.9999999999998863 ) ;
#48235 = FACE_OUTER_BOUND ( 'NONE', #80325, .T. ) ;
#48237 = CARTESIAN_POINT ( 'NONE',  ( 17.14206885625503674, -7.750023238201980469, 34.74374492549440419 ) ) ;
#48238 = CARTESIAN_POINT ( 'NONE',  ( 12.52760681254089725, -11.16473453929635440, 33.15142922261926373 ) ) ;
#48239 = CARTESIAN_POINT ( 'NONE',  ( -1.200186371490524317, -10.22469193450124791, 20.11124329374151642 ) ) ;
#48240 = ORIENTED_EDGE ( 'NONE', *, *, #13081, .T. ) ;
#48241 = EDGE_CURVE ( 'NONE', #14268, #61355, #50480, .T. ) ;
#48242 = CARTESIAN_POINT ( 'NONE',  ( 13.38461538461538680, -13.53365097954675988, 30.81389545987213552 ) ) ;
#48243 = CARTESIAN_POINT ( 'NONE',  ( 0.5276068125408990284, -3.050289026998446840, 32.03036669348366416 ) ) ;
#48244 = FACE_OUTER_BOUND ( 'NONE', #18659, .T. ) ;
#48245 = FILL_AREA_STYLE ('',( #20779 ) ) ;
#48246 = VERTEX_POINT ( 'NONE', #3634 ) ;
#48247 = LINE ( 'NONE', #53680, #36907 ) ;
#48248 = DIRECTION ( 'NONE',  ( -0.000000000000000000, -0.9396926207859093161, -0.3420201433256663259 ) ) ;
#48249 = B_SPLINE_CURVE_WITH_KNOTS ( 'NONE', 3,
 ( #41669, #27261, #61923, #236, #33585, #33131, #48410, #13304, #6991, #34462 ),
 .UNSPECIFIED., .F., .F.,
 ( 4, 2, 2, 2, 4 ),
 ( 0.0007817246256747485819, 0.0009771112852218918031, 0.001172497944769034916, 0.001367884604316178029, 0.001563271263863321358 ),
 .UNSPECIFIED. ) ;
#48250 = B_SPLINE_CURVE_WITH_KNOTS ( 'NONE', 3,
 ( #17744, #45197, #4673, #32146, #72675, #51047, #65910, #38909, #4220, #52396 ),
 .UNSPECIFIED., .F., .F.,
 ( 4, 2, 2, 2, 4 ),
 ( 0.000000000000000000, 0.0001954311564186863594, 0.0003908623128373727188, 0.0005862934692560590241, 0.0007817246256747454377 ),
 .UNSPECIFIED. ) ;
#48251 = CARTESIAN_POINT ( 'NONE',  ( -8.992157728137614825, -10.77366814457252175, 33.85459836347579454 ) ) ;
#48252 = ADVANCED_FACE ( 'NONE', ( #79757 ), #51348, .F. ) ;
#48253 = CYLINDRICAL_SURFACE ( 'NONE', #81687, 0.2500000000000008882 ) ;
#48254 = CARTESIAN_POINT ( 'NONE',  ( -17.07692307692307665, -2.292212530054420494, 30.41441678777542634 ) ) ;
#48255 = ORIENTED_EDGE ( 'NONE', *, *, #69309, .T. ) ;
#48256 = LINE ( 'NONE', #56353, #20390 ) ;
#48257 = EDGE_CURVE ( 'NONE', #14427, #30672, #14928, .T. ) ;
#48258 = CYLINDRICAL_SURFACE ( 'NONE', #42656, 0.2499999999999986955 ) ;
#48259 = CARTESIAN_POINT ( 'NONE',  ( -15.23076923076922995, -3.886160181151819604, 36.00935417666054406 ) ) ;
#48260 = ORIENTED_EDGE ( 'NONE', *, *, #76997, .F. ) ;
#48261 = FACE_OUTER_BOUND ( 'NONE', #31866, .T. ) ;
#48262 = EDGE_LOOP ( 'NONE', ( #53286, #16491 ) ) ;
#48263 = CARTESIAN_POINT ( 'NONE',  ( 13.91025641025641235, -7.500000000000000000, 29.75000000000000355 ) ) ;
#48264 = CARTESIAN_POINT ( 'NONE',  ( 11.53846153846153832, -6.343179335718451384, 34.87096338111211935 ) ) ;
#48265 = AXIS2_PLACEMENT_3D ( 'NONE', #39282, #39726, #80719 ) ;
#48266 = ORIENTED_EDGE ( 'NONE', *, *, #6475, .T. ) ;
#48267 = LINE ( 'NONE', #8183, #13132 ) ;
#48269 = ADVANCED_FACE ( 'NONE', ( #31562 ), #72098, .F. ) ;
#48268 = DIRECTION ( 'NONE',  ( -0.000000000000000000, -0.000000000000000000, -1.000000000000000000 ) ) ;
#48270 = CARTESIAN_POINT ( 'NONE',  ( -1.384615384615505151, -10.21337939537710326, 33.94971097300076224 ) ) ;
#48271 = AXIS2_PLACEMENT_3D ( 'NONE', #65971, #32637, #51105 ) ;
#48272 = EDGE_CURVE ( 'NONE', #61398, #10299, #50300, .T. ) ;
#48273 = CARTESIAN_POINT ( 'NONE',  ( 7.145856592054990131, -12.47679350104403007, 31.42216943046555855 ) ) ;
#48274 = PLANE ( 'NONE',  #15276 ) ;
#48275 = ORIENTED_EDGE ( 'NONE', *, *, #54939, .T. ) ;
#48276 = FACE_BOUND ( 'NONE', #81613, .T. ) ;
#48277 = EDGE_LOOP ( 'NONE', ( #619, #34556, #31909, #54620 ) ) ;
#48278 = CARTESIAN_POINT ( 'NONE',  ( 9.692307692307695177, -9.905515769479276145, 34.41647553114623292 ) ) ;
#48279 = B_SPLINE_CURVE_WITH_KNOTS ( 'NONE', 3,
 ( #85527, #58475, #73802, #23803, #39580, #45862, #12103, #4897, #51255, #24249 ),
 .UNSPECIFIED., .F., .F.,
 ( 4, 2, 2, 2, 4 ),
 ( 0.0007817359430256262112, 0.0009771253907249911191, 0.001172514838424356136, 0.001367904286123721152, 0.001563293733823086168 ),
 .UNSPECIFIED. ) ;
#48280 = B_SPLINE_CURVE_WITH_KNOTS ( 'NONE', 3,
 ( #69435, #70321, #41081, #14942, #42420, #69877, #8184, #28912, #56365, #68546 ),
 .UNSPECIFIED., .F., .F.,
 ( 4, 2, 2, 2, 4 ),
 ( 0.000000000000000000, 0.0001954339857564098054, 0.0003908679715128196108, 0.0005863019572692293891, 0.0007817359430256392216 ),
 .UNSPECIFIED. ) ;
#48281 = B_SPLINE_CURVE_WITH_KNOTS ( 'NONE', 3,
 ( #17574, #71609, #78816, #45475, #72502, #10812, #16670, #64850, #11255, #17117 ),
 .UNSPECIFIED., .F., .F.,
 ( 4, 2, 2, 2, 4 ),
 ( 0.0007817359430256388964, 0.0009771253907250073822, 0.001172514838424375868, 0.001367904286123744571, 0.001563293733823113056 ),
 .UNSPECIFIED. ) ;
#48282 = CARTESIAN_POINT ( 'NONE',  ( 18.00000000000000000, -6.343179335718451384, 34.87096338111211935 ) ) ;
#48283 = CARTESIAN_POINT ( 'NONE',  ( 8.835299120233207404, -3.513871655860379306, 32.76840700105978499 ) ) ;
#48284 = CYLINDRICAL_SURFACE ( 'NONE', #20858, 0.2499999999999979738 ) ;
#48285 = VERTEX_POINT ( 'NONE', #52710 ) ;
#48286 = ORIENTED_EDGE ( 'NONE', *, *, #6509, .F. ) ;
#48287 = EDGE_LOOP ( 'NONE', ( #33392, #58289 ) ) ;
#48288 = CARTESIAN_POINT ( 'NONE',  ( 13.44976116394735222, -7.750023238201979581, 34.74374492549440419 ) ) ;
#48289 = ORIENTED_EDGE ( 'NONE', *, *, #51590, .T. ) ;
#48290 = AXIS2_PLACEMENT_3D ( 'NONE', #5441, #81104, #60371 ) ;
#48291 = CARTESIAN_POINT ( 'NONE',  ( -17.32694630114453105, -10.18141759479407327, 34.26406193332782379 ) ) ;
#48292 = CARTESIAN_POINT ( 'NONE',  ( 1.607394925883796732, -3.755027918224367767, 33.06320215134714857 ) ) ;
#48293 = B_SPLINE_CURVE_WITH_KNOTS ( 'NONE', 3,
 ( #45144, #32085, #86604, #85259, #44689, #17233, #79388, #80280, #78485, #65854 ),
 .UNSPECIFIED., .F., .F.,
 ( 4, 2, 2, 2, 4 ),
 ( 0.000000000000000000, 0.0001954339857564078809, 0.0003908679715128157619, 0.0005863019572692236428, 0.0007817359430256315238 ),
 .UNSPECIFIED. ) ;
#48294 = CARTESIAN_POINT ( 'NONE',  ( -18.25002323729296450, -11.37209801155882261, 32.91403422569033665 ) ) ;
#48295 = CARTESIAN_POINT ( 'NONE',  ( 3.296836564119306701, -9.058645607665452459, 34.76329471203371924 ) ) ;
#48296 = CARTESIAN_POINT ( 'NONE',  ( -2.651650429449565305, -4.848349570550461785, 26.50000000000000355 ) ) ;
#48297 = CARTESIAN_POINT ( 'NONE',  ( -4.284406067459515022, -2.254533558242299396, 29.97296025877828285 ) ) ;
#48298 = CARTESIAN_POINT ( 'NONE',  ( 14.53047184896071542, -6.760870238392817200, 34.69528174975672385 ) ) ;
#48299 = CARTESIAN_POINT ( 'NONE',  ( -5.010855743572999010, -11.35647404775217595, 33.31231777344667222 ) ) ;
#48300 = ORIENTED_EDGE ( 'NONE', *, *, #6786, .T. ) ;
#48301 = EDGE_CURVE ( 'NONE', #41851, #5737, #80656, .T. ) ;
#48302 = VERTEX_POINT ( 'NONE', #18499 ) ;
#48303 = EDGE_LOOP ( 'NONE', ( #1105, #9158 ) ) ;
#48304 = DIRECTION ( 'NONE',  ( -0.000000000000000000, 0.3420201433256694901, -0.9396926207859082059 ) ) ;
#48306 = CARTESIAN_POINT ( 'NONE',  ( 17.07692307692307665, -1.367168528481310208, 33.57946703557072254 ) ) ;
#48305 = FACE_OUTER_BOUND ( 'NONE', #42023, .T. ) ;
#48307 = ADVANCED_FACE ( 'NONE', ( #86526 ), #45956, .T. ) ;
#48308 = CARTESIAN_POINT ( 'NONE',  ( 8.769230769230768274, -5.180354513474913603, 36.12317359536750416 ) ) ;
#48309 = CARTESIAN_POINT ( 'NONE',  ( -15.48079245499068435, -10.18141759479407327, 34.26406193332782379 ) ) ;
#48310 = FACE_BOUND ( 'NONE', #71537, .T. ) ;
#48311 = CARTESIAN_POINT ( 'NONE',  ( 12.22435897435897623, -11.50000000000000000, 29.75000000000000355 ) ) ;
#48312 = ORIENTED_EDGE ( 'NONE', *, *, #47592, .T. ) ;
#48313 = DIRECTION ( 'NONE',  ( -0.000000000000000000, -0.7660444431189791237, -0.6427876096865379196 ) ) ;
#48314 = CARTESIAN_POINT ( 'NONE',  ( -0.3310127597748971362, -9.417988943895561960, 34.36773134775778260 ) ) ;
#48315 = CARTESIAN_POINT ( 'NONE',  ( -12.46153846153858424, -4.320704448113951379, 33.92786785259630022 ) ) ;
#48316 = CARTESIAN_POINT ( 'NONE',  ( -3.454254155333560394, -3.562934362175799841, 33.22335522853832401 ) ) ;
#48317 = EDGE_LOOP ( 'NONE', ( #40865, #75464, #52845, #5699 ) ) ;
#48318 = EDGE_CURVE ( 'NONE', #16798, #22156, #82563, .T. ) ;
#48319 = CARTESIAN_POINT ( 'NONE',  ( -18.24997673094235751, -8.303909089506435137, 34.68538101551103381 ) ) ;
#48320 = ORIENTED_EDGE ( 'NONE', *, *, #11768, .T. ) ;
#48321 = FACE_BOUND ( 'NONE', #84290, .T. ) ;
#48322 = CARTESIAN_POINT ( 'NONE',  ( -17.07692307692319744, -6.835583212225970762, 34.95778746994575670 ) ) ;
#48323 = CIRCLE ( 'NONE', #35409, 4.000000000000000000 ) ;
#48324 = DIRECTION ( 'NONE',  ( 0.000000000000000000, 0.000000000000000000, -1.000000000000000000 ) ) ;
#48325 = DIRECTION ( 'NONE',  ( 1.000000000000000000, 0.000000000000000000, 0.000000000000000000 ) ) ;
#48326 = EDGE_LOOP ( 'NONE', ( #42904, #63803, #84721, #58720 ) ) ;
#48327 = CARTESIAN_POINT ( 'NONE',  ( -12.71151519248081740, -9.943427161483782584, 34.11278801902876978 ) ) ;
#48328 = CARTESIAN_POINT ( 'NONE',  ( -17.77722033102192967, -4.226511098958373402, 33.85474049983370293 ) ) ;
#48329 = LINE ( 'NONE', #12338, #43768 ) ;
#48330 = CARTESIAN_POINT ( 'NONE',  ( -4.854143407945009869, -5.827830569534416583, 34.72679350104403539 ) ) ;
#48331 = ORIENTED_EDGE ( 'NONE', *, *, #38503, .F. ) ;
#48332 = EDGE_CURVE ( 'NONE', #18497, #47795, #47128, .T. ) ;
#48333 = CARTESIAN_POINT ( 'NONE',  ( -12.33101275977489841, -3.285477652293413264, 32.44071101563363158 ) ) ;
#48334 = CARTESIAN_POINT ( 'NONE',  ( 4.087763774486017354, -9.905515769479276145, 34.41647553114623292 ) ) ;
#48336 = ORIENTED_EDGE ( 'NONE', *, *, #23867, .T. ) ;
#48335 = CARTESIAN_POINT ( 'NONE',  ( -8.769230769230768274, -3.513871655860378418, 32.76840700105978499 ) ) ;
#48337 = LINE ( 'NONE', #34825, #28167 ) ;
#48338 = CARTESIAN_POINT ( 'NONE',  ( -19.00000000000000000, -3.499999999999999556, 29.75000000000000355 ) ) ;
#48339 = CARTESIAN_POINT ( 'NONE',  ( -4.853911725310227077, -8.239487800360276282, 34.69522927552633718 ) ) ;
#48340 = CARTESIAN_POINT ( 'NONE',  ( 14.24242186173153435, -9.442884908240170461, 34.35708131394840592 ) ) ;
#48341 = DIRECTION ( 'NONE',  ( 1.000000000000000000, 0.000000000000000000, 0.000000000000000000 ) ) ;
#48343 = DIRECTION ( 'NONE',  ( -0.000000000000000000, 0.7660444431189791237, -0.6427876096865379196 ) ) ;
#48342 = CARTESIAN_POINT ( 'NONE',  ( -7.976301055592065481, -10.88202310037935661, 33.43294751532457099 ) ) ;
#48344 = CARTESIAN_POINT ( 'NONE',  ( 14.05766907039934210, -3.711651800289232028, 33.01384336483936011 ) ) ;
#48345 = CARTESIAN_POINT ( 'NONE',  ( -1.944543648263014957, -5.555456351737005249, 21.50000000000000000 ) ) ;
#48346 = ORIENTED_EDGE ( 'NONE', *, *, #10835, .T. ) ;
#48347 = EDGE_CURVE ( 'NONE', #88176, #66583, #81984, .T. ) ;
#48348 = CARTESIAN_POINT ( 'NONE',  ( -17.77722045873158763, -9.332535724633405749, 34.40230450496446224 ) ) ;
#48349 = ORIENTED_EDGE ( 'NONE', *, *, #66802, .T. ) ;
#48350 = ORIENTED_EDGE ( 'NONE', *, *, #65921, .T. ) ;
#48351 = EDGE_CURVE ( 'NONE', #3309, #29230, #48168, .T. ) ;
#48352 = CARTESIAN_POINT ( 'NONE',  ( -8.519176349317314489, -6.523592122091592671, 34.90882529074906415 ) ) ;
#48353 = ORIENTED_EDGE ( 'NONE', *, *, #33429, .F. ) ;
#48354 = FACE_OUTER_BOUND ( 'NONE', #84772, .T. ) ;
#48355 = CARTESIAN_POINT ( 'NONE',  ( -1.944543648262992530, -9.444543648263016067, 19.93750000000000000 ) ) ;
#48356 = CARTESIAN_POINT ( 'NONE',  ( 14.55774661933062042, -11.28795663066794575, 33.01431243580653785 ) ) ;
#48357 = DIRECTION ( 'NONE',  ( 0.000000000000000000, -6.938893903907222067E-15, 1.000000000000000000 ) ) ;
#48358 = CARTESIAN_POINT ( 'NONE',  ( 6.130791807824786943, -3.062576670634119758, 32.05464942895959979 ) ) ;
#48359 = CARTESIAN_POINT ( 'NONE',  ( 1.254467414883686960, -2.647304123082328875, 31.75400227202885262 ) ) ;
#48360 = LINE ( 'NONE', #75839, #17209 ) ;
#48361 = CARTESIAN_POINT ( 'NONE',  ( 2.438484115517096207, -11.18335022499818621, 33.13157742990016885 ) ) ;
#48362 = B_SPLINE_CURVE_WITH_KNOTS ( 'NONE', 3,
 ( #64797, #72452, #44081, #23810, #79667, #23376, #71123, #2217, #3550, #17969 ),
 .UNSPECIFIED., .F., .F.,
 ( 4, 2, 2, 2, 4 ),
 ( 0.000000000000000000, 0.0001954339857564080707, 0.0003908679715128161414, 0.0005863019572692241849, 0.0007817359430256322827 ),
 .UNSPECIFIED. ) ;
#48363 = CARTESIAN_POINT ( 'NONE',  ( -2.651650429449535551, -10.15165042944956753, 24.93750000000000000 ) ) ;
#48364 = VECTOR ( 'NONE', #24167, 1000.000000000000000 ) ;
#48365 = CARTESIAN_POINT ( 'NONE',  ( -1.384615384615383471, -6.435427911321262684, 35.78748833219616898 ) ) ;
#48366 = CARTESIAN_POINT ( 'NONE',  ( -2.177166869458665222, -3.068774925481847493, 32.56582465632704526 ) ) ;
#48367 = EDGE_CURVE ( 'NONE', #63956, #16211, #49199, .T. ) ;
#48368 = CARTESIAN_POINT ( 'NONE',  ( 18.00000000000000000, -13.87047571288749737, 32.06866353760679544 ) ) ;
#48369 = CARTESIAN_POINT ( 'NONE',  ( -7.846153846153844924, -8.120952969808772792, 34.71129190930000163 ) ) ;
#48370 = ORIENTED_EDGE ( 'NONE', *, *, #5734, .F. ) ;
#48371 = ORIENTED_EDGE ( 'NONE', *, *, #671, .F. ) ;
#48372 = CARTESIAN_POINT ( 'NONE',  ( 3.230769230769231726, -6.435427911321262684, 35.78748833219616898 ) ) ;
#48373 = DIRECTION ( 'NONE',  ( 0.000000000000000000, 0.000000000000000000, -1.000000000000000000 ) ) ;
#48374 = CARTESIAN_POINT ( 'NONE',  ( -6.923076923077045919, -12.16647553114689728, 32.15551576947799362 ) ) ;
#48375 = CARTESIAN_POINT ( 'NONE',  ( 9.758375025657770152, -11.91647553114624358, 32.58852847137148245 ) ) ;
#48376 = VECTOR ( 'NONE', #7504, 1000.000000000000000 ) ;
#48378 = ADVANCED_FACE ( 'NONE', ( #75220 ), #12630, .T. ) ;
#48377 = CARTESIAN_POINT ( 'NONE',  ( 12.23805351781451201, -9.331801661448606566, 34.40259984581193464 ) ) ;
#48379 = CARTESIAN_POINT ( 'NONE',  ( -6.130147209438218781, -8.587444163452046197, 34.63053765926554206 ) ) ;
#48380 = DIRECTION ( 'NONE',  ( 0.000000000000000000, 8.131516293641283255E-17, 1.000000000000000000 ) ) ;
#48381 = ADVANCED_FACE ( 'NONE', ( #55376 ), #13508, .F. ) ;
#48382 = EDGE_CURVE ( 'NONE', #74290, #59987, #31001, .T. ) ;
#48383 = EDGE_LOOP ( 'NONE', ( #10848, #49273 ) ) ;
#48384 = CARTESIAN_POINT ( 'NONE',  ( 0.7115927731767752729, -5.728107161865378494, 34.42597550085002922 ) ) ;
#48385 = ORIENTED_EDGE ( 'NONE', *, *, #84014, .T. ) ;
#48386 = EDGE_CURVE ( 'NONE', #14886, #28072, #29912, .T. ) ;
#48387 = CARTESIAN_POINT ( 'NONE',  ( 10.68145296638705410, -8.120952969808772792, 34.71129190929999453 ) ) ;
#48388 = CARTESIAN_POINT ( 'NONE',  ( -18.12834546407006542, -12.74539338292710511, 29.97517285561845668 ) ) ;
#48389 = VECTOR ( 'NONE', #77941, 1000.000000000000000 ) ;
#48390 = CARTESIAN_POINT ( 'NONE',  ( -6.673076923075503153, -7.500000000000154543, 35.00000000000007105 ) ) ;
#48391 = DIRECTION ( 'NONE',  ( -0.000000000000000000, -0.9396926207859093161, -0.3420201433256663259 ) ) ;
#48392 = DIRECTION ( 'NONE',  ( -0.000000000000000000, -0.000000000000000000, -1.000000000000000000 ) ) ;
#48393 = AXIS2_PLACEMENT_3D ( 'NONE', #17883, #4361, #79586 ) ;
#48394 = ORIENTED_EDGE ( 'NONE', *, *, #55386, .T. ) ;
#48395 = ORIENTED_EDGE ( 'NONE', *, *, #73930, .T. ) ;
#48396 = EDGE_LOOP ( 'NONE', ( #20031, #36956 ) ) ;
#48397 = VERTEX_POINT ( 'NONE', #60362 ) ;
#48398 = AXIS2_PLACEMENT_3D ( 'NONE', #79492, #4722, #18234 ) ;
#48399 = CARTESIAN_POINT ( 'NONE',  ( -6.000000000000119904, -11.48612834414049644, 32.76840700105863391 ) ) ;
#48400 = CARTESIAN_POINT ( 'NONE',  ( 5.011652630962299959, -10.90142922261923886, 33.41473453929638993 ) ) ;
#48401 = CARTESIAN_POINT ( 'NONE',  ( 15.90384615384613021, -2.249999999999998668, 29.81609741502487054 ) ) ;
#48402 = CARTESIAN_POINT ( 'NONE',  ( 16.81410256410256565, -7.500000000000000000, 29.75000000000000355 ) ) ;
#48403 = CARTESIAN_POINT ( 'NONE',  ( 8.096153846155266010, -7.500000000000154543, 35.00000000000007105 ) ) ;
#48404 = CARTESIAN_POINT ( 'NONE',  ( 14.30769230769218758, -12.46129190930018460, 30.37095296980731973 ) ) ;
#48405 = ORIENTED_EDGE ( 'NONE', *, *, #46540, .F. ) ;
#48406 = ORIENTED_EDGE ( 'NONE', *, *, #83652, .T. ) ;
#48407 = ORIENTED_EDGE ( 'NONE', *, *, #13585, .F. ) ;
#48409 = ORIENTED_EDGE ( 'NONE', *, *, #65091, .T. ) ;
#48408 = CYLINDRICAL_SURFACE ( 'NONE', #83314, 0.2499999999999986955 ) ;
#48410 = CARTESIAN_POINT ( 'NONE',  ( 17.29993592101647337, -10.77377354290276301, 33.85451476688484718 ) ) ;
#48411 = CARTESIAN_POINT ( 'NONE',  ( -5.076923076923197442, -11.48612834414049644, 32.76840700105863391 ) ) ;
#48412 = CARTESIAN_POINT ( 'NONE',  ( 2.651650429449569302, -10.15165042944953733, 19.62500000000000000 ) ) ;
#48413 = EDGE_LOOP ( 'NONE', ( #23398, #22361 ) ) ;
#48414 = ORIENTED_EDGE ( 'NONE', *, *, #4410, .F. ) ;
#48415 = DIRECTION ( 'NONE',  ( 0.000000000000000000, 0.8660254037844377084, -0.5000000000000015543 ) ) ;
#48416 = VERTEX_POINT ( 'NONE', #13946 ) ;
#48417 = FACE_BOUND ( 'NONE', #22792, .T. ) ;
#48418 = CARTESIAN_POINT ( 'NONE',  ( 5.010840697562940704, -4.661471528628507777, 34.16647553114621871 ) ) ;
#48419 = FACE_OUTER_BOUND ( 'NONE', #40246, .T. ) ;
#48420 = VERTEX_POINT ( 'NONE', #82423 ) ;
#48421 = DIRECTION ( 'NONE',  ( 1.000000000000000000, 0.000000000000000000, 0.000000000000000000 ) ) ;
#48422 = AXIS2_PLACEMENT_3D ( 'NONE', #52582, #81410, #80521 ) ;
#48423 = DIRECTION ( 'NONE',  ( -0.000000000000000000, -0.1736481776669307198, -0.9848077530122080203 ) ) ;
#48424 = CARTESIAN_POINT ( 'NONE',  ( 16.37662582282421653, -6.717445702608400460, 34.94155399931962336 ) ) ;
#48425 = CARTESIAN_POINT ( 'NONE',  ( -3.480745974817822219, -9.234221910056348293, 34.70572697212741531 ) ) ;
#48426 = ORIENTED_EDGE ( 'NONE', *, *, #79555, .F. ) ;
#48427 = CARTESIAN_POINT ( 'NONE',  ( 11.76147289007438523, -3.105924265160262543, 32.13625925475356127 ) ) ;
#48428 = CARTESIAN_POINT ( 'NONE',  ( -2.980769230769230393, -7.500000000000001776, 35.04278698407183867 ) ) ;
#48429 = CARTESIAN_POINT ( 'NONE',  ( -3.931066484868084299, -2.353885683473779800, 30.79025554430704759 ) ) ;
#48430 = CARTESIAN_POINT ( 'NONE',  ( -2.530618525208451874, -10.61292498521070549, 33.66303323003028680 ) ) ;
#48431 = CYLINDRICAL_SURFACE ( 'NONE', #64476, 4.000000000000000000 ) ;
#48432 = FACE_BOUND ( 'NONE', #25562, .T. ) ;
#48434 = CARTESIAN_POINT ( 'NONE',  ( -17.30040800148741553, -10.97335522853832579, 33.68706563782419749 ) ) ;
#48433 = CARTESIAN_POINT ( 'NONE',  ( 13.31853197365950514, -11.69971097300155272, 32.46337939537587403 ) ) ;
#48435 = DIRECTION ( 'NONE',  ( -1.000000000000000000, -0.000000000000000000, -0.000000000000000000 ) ) ;
#48437 = CARTESIAN_POINT ( 'NONE',  ( 15.29683758177167086, -9.780366693483667717, 34.19971097300155805 ) ) ;
#48436 = CARTESIAN_POINT ( 'NONE',  ( -8.519176457592456231, -11.79725096376909299, 32.30694842903960762 ) ) ;
#48438 = CYLINDRICAL_SURFACE ( 'NONE', #28998, 0.2500000000000009437 ) ;
#48439 = CARTESIAN_POINT ( 'NONE',  ( -1.901340078031346525, -9.487747218494661183, 18.43563170625848713 ) ) ;
#48440 = VERTEX_POINT ( 'NONE', #41426 ) ;
#48441 = B_SPLINE_CURVE_WITH_KNOTS ( 'NONE', 3,
 ( #70880, #43400, #72191, #59121, #10504, #78068, #30762, #57794, #9187, #15936 ),
 .UNSPECIFIED., .F., .F.,
 ( 4, 2, 2, 2, 4 ),
 ( 0.000000000000000000, 0.0001954311564186867389, 0.0003908623128373734778, 0.0005862934692560602167, 0.0007817246256747469556 ),
 .UNSPECIFIED. ) ;
#48442 = DIRECTION ( 'NONE',  ( 0.000000000000000000, -1.000000000000000000, 5.421010862427522170E-17 ) ) ;
#48443 = EDGE_LOOP ( 'NONE', ( #41763, #43786, #52572, #72855 ) ) ;
#48444 = EDGE_CURVE ( 'NONE', #50622, #21128, #6314, .T. ) ;
#48445 = FACE_OUTER_BOUND ( 'NONE', #32438, .T. ) ;
#48446 = VECTOR ( 'NONE', #20691, 1000.000000000000000 ) ;
#48447 = VERTEX_POINT ( 'NONE', #13066 ) ;
#48448 = DIRECTION ( 'NONE',  ( -0.000000000000000000, 0.1736481776669307198, -0.9848077530122080203 ) ) ;
#48449 = CARTESIAN_POINT ( 'NONE',  ( -8.096177083446809419, -10.05641848906368097, 34.04755513067966177 ) ) ;
#48450 = EDGE_LOOP ( 'NONE', ( #83938, #76247 ) ) ;
#48451 = CARTESIAN_POINT ( 'NONE',  ( 17.75000000000000355, -7.433932668274255917, 35.00000000000000711 ) ) ;
#48452 = CARTESIAN_POINT ( 'NONE',  ( -1.077988221561460236, -10.27530806549876452, 20.85750670625849068 ) ) ;
#48453 = CARTESIAN_POINT ( 'NONE',  ( -10.54931728203453822, -12.62096338111211757, 30.90682066428152908 ) ) ;
#48454 = DIRECTION ( 'NONE',  ( 0.000000000000000000, 0.9396926207859126468, 0.3420201433256571111 ) ) ;
#48455 = AXIS2_PLACEMENT_3D ( 'NONE', #65503, #37583, #31281 ) ;
#48456 = CARTESIAN_POINT ( 'NONE',  ( 12.39626801557768587, -2.892918686051582533, 31.69288490824015980 ) ) ;
#48457 = LINE ( 'NONE', #67415, #47299 ) ;
#48458 = CARTESIAN_POINT ( 'NONE',  ( -0.4615384615385826339, -4.481592998941358097, 33.73612834414048933 ) ) ;
#48459 = DIRECTION ( 'NONE',  ( -0.000000000000000000, 0.000000000000000000, 1.000000000000000000 ) ) ;
#48460 = CARTESIAN_POINT ( 'NONE',  ( 2.608446859217924629, -10.19485399968118422, 22.37686829374150932 ) ) ;
#48461 = CARTESIAN_POINT ( 'NONE',  ( -10.36533030374629938, -2.779044189368095275, 31.39831045268885745 ) ) ;
#48462 = CYLINDRICAL_SURFACE ( 'NONE', #54947, 0.2500000000000002220 ) ;
#48463 = EDGE_CURVE ( 'NONE', #32867, #314, #66444, .T. ) ;
#48464 = AXIS2_PLACEMENT_3D ( 'NONE', #75503, #28197, #55231 ) ;
#48465 = ORIENTED_EDGE ( 'NONE', *, *, #82065, .F. ) ;
#48466 = DIRECTION ( 'NONE',  ( 0.000000000000000000, 0.000000000000000000, 1.000000000000000000 ) ) ;
#48467 = CARTESIAN_POINT ( 'NONE',  ( 1.614399933863618797, -3.775308065498751198, 24.48624329374151642 ) ) ;
#48468 = CARTESIAN_POINT ( 'NONE',  ( -17.86947429823644029, -12.45806712695776319, 30.39783852428763566 ) ) ;
#48469 = LINE ( 'NONE', #69635, #25431 ) ;
#48470 = VERTEX_POINT ( 'NONE', #71095 ) ;
#48471 = CARTESIAN_POINT ( 'NONE',  ( -17.86920819217520773, -2.729792928343270919, 31.24908615093346498 ) ) ;
#48472 = CARTESIAN_POINT ( 'NONE',  ( -16.94613263595612906, -9.084667340241228572, 34.75534355489798344 ) ) ;
#48474 = ORIENTED_EDGE ( 'NONE', *, *, #58443, .T. ) ;
#48473 = CARTESIAN_POINT ( 'NONE',  ( 3.903822929624696236, -9.356822207818506598, 34.66110646841856635 ) ) ;
#48475 = DIRECTION ( 'NONE',  ( -0.000000000000000000, 0.9848077530122086864, -0.1736481776669273891 ) ) ;
#48476 = CARTESIAN_POINT ( 'NONE',  ( -1.607541602131529856, -10.61292498521070549, 33.66303323003028680 ) ) ;
#48477 = DIRECTION ( 'NONE',  ( -0.000000000000000000, -0.5000000000000009992, -0.8660254037844380415 ) ) ;
#48478 = CARTESIAN_POINT ( 'NONE',  ( -17.01085472592064463, -2.721908614388772740, 31.22303859784725333 ) ) ;
#48479 = DIRECTION ( 'NONE',  ( -0.000000000000000000, 0.9396926207859092051, -0.3420201433256662704 ) ) ;
#48480 = VECTOR ( 'NONE', #1076, 1000.000000000000227 ) ;
#48481 = ADVANCED_FACE ( 'NONE', ( #36438 ), #30117, .F. ) ;
#48482 = EDGE_CURVE ( 'NONE', #33581, #70917, #31482, .T. ) ;
#48483 = B_SPLINE_CURVE_WITH_KNOTS ( 'NONE', 3,
 ( #2861, #72217, #31236, #72665, #24473, #52387, #4662, #37099, #65468, #64559 ),
 .UNSPECIFIED., .F., .F.,
 ( 4, 2, 2, 2, 4 ),
 ( 0.000000000000000000, 0.0001954311564186876605, 0.0003908623128373753209, 0.0005862934692560629272, 0.0007817246256747506419 ),
 .UNSPECIFIED. ) ;
#48484 = B_SPLINE_CURVE_WITH_KNOTS ( 'NONE', 3,
 ( #64139, #36251, #63706, #56948, #2012, #682, #48866, #84443, #2442, #29934 ),
 .UNSPECIFIED., .F., .F.,
 ( 4, 2, 2, 2, 4 ),
 ( 0.000000000000000000, 0.0001954311584214072923, 0.0003908623168428145846, 0.0005862934752642218498, 0.0007817246336856291692 ),
 .UNSPECIFIED. ) ;
#48485 = EDGE_LOOP ( 'NONE', ( #59847, #26027 ) ) ;
#48486 = ORIENTED_EDGE ( 'NONE', *, *, #53430, .F. ) ;
#48487 = AXIS2_PLACEMENT_3D ( 'NONE', #65296, #9912, #51765 ) ;
#48488 = EDGE_LOOP ( 'NONE', ( #69329, #79138, #14, #8088 ) ) ;
#48489 = EDGE_CURVE ( 'NONE', #56373, #35616, #63892, .T. ) ;
#48490 = LINE ( 'NONE', #6629, #5505 ) ;
#48491 = DIRECTION ( 'NONE',  ( 1.000000000000000000, 0.000000000000000000, 0.000000000000000000 ) ) ;
#48492 = VECTOR ( 'NONE', #63881, 1000.000000000000000 ) ;
#48493 = CARTESIAN_POINT ( 'NONE',  ( 2.241608896736428047, -5.557115091759785130, 34.35708131394839171 ) ) ;
#48494 = CARTESIAN_POINT ( 'NONE',  ( -7.976301815885546098, -11.04286588640298561, 33.62463336215343901 ) ) ;
#48495 = ORIENTED_EDGE ( 'NONE', *, *, #33364, .F. ) ;
#48496 = CARTESIAN_POINT ( 'NONE',  ( 17.07692307692295586, -11.67786785259630911, 32.92929555188603530 ) ) ;
#48497 = EDGE_LOOP ( 'NONE', ( #7641, #64378, #87577, #49123 ) ) ;
#48498 = EDGE_LOOP ( 'NONE', ( #65831, #17728, #74020, #60493 ) ) ;
#48499 = VERTEX_POINT ( 'NONE', #83303 ) ;
#48501 = EDGE_LOOP ( 'NONE', ( #33032, #43090 ) ) ;
#48500 = CARTESIAN_POINT ( 'NONE',  ( -12.94230769230769162, -3.499999999999999556, 29.75000000000000355 ) ) ;
#48502 = CARTESIAN_POINT ( 'NONE',  ( 4.153846153846154188, -5.557115091759785130, 34.35708131394839171 ) ) ;
#48503 = CARTESIAN_POINT ( 'NONE',  ( 6.000000000000001776, -12.62096338111211580, 30.90682066428153263 ) ) ;
#48504 = AXIS2_PLACEMENT_3D ( 'NONE', #51716, #10756, #45416 ) ;
#48505 = DIRECTION ( 'NONE',  ( -0.000000000000000000, -0.3420201433256694901, -0.9396926207859082059 ) ) ;
#48506 = CARTESIAN_POINT ( 'NONE',  ( 14.55769230769237232, -7.434744860731433924, 35.00000000000000711 ) ) ;
#48507 = VERTEX_POINT ( 'NONE', #28806 ) ;
#48508 = ORIENTED_EDGE ( 'NONE', *, *, #28483, .T. ) ;
#48509 = ORIENTED_EDGE ( 'NONE', *, *, #34747, .F. ) ;
#48510 = CARTESIAN_POINT ( 'NONE',  ( -14.55769230769230660, -7.500000000000001776, 34.75000000000000000 ) ) ;
#48512 = VERTEX_POINT ( 'NONE', #64331 ) ;
#48511 = DIRECTION ( 'NONE',  ( -0.000000000000000000, -0.9848077530122085754, -0.1736481776669273613 ) ) ;
#48513 = CARTESIAN_POINT ( 'NONE',  ( -11.31568186948346977, -12.69155399931963046, 30.53255429739157734 ) ) ;
#48514 = DIRECTION ( 'NONE',  ( -0.000000000000000000, 0.1736481776669307198, -0.9848077530122080203 ) ) ;
#48515 = ORIENTED_EDGE ( 'NONE', *, *, #54439, .F. ) ;
#48516 = AXIS2_PLACEMENT_3D ( 'NONE', #57116, #411, #49911 ) ;
#48517 = CARTESIAN_POINT ( 'NONE',  ( -17.93393164899756087, -2.538708090699994813, 30.37095296980875858 ) ) ;
#48518 = CARTESIAN_POINT ( 'NONE',  ( 0.3962684609821413573, -9.528491918058357157, 34.59228464037090589 ) ) ;
#48519 = ORIENTED_EDGE ( 'NONE', *, *, #7479, .T. ) ;
#48520 = FACE_BOUND ( 'NONE', #63053, .T. ) ;
#48521 = CARTESIAN_POINT ( 'NONE',  ( -15.48079245499068612, -8.475808217655753651, 34.90892951860618609 ) ) ;
#48522 = CARTESIAN_POINT ( 'NONE',  ( -18.06527000055631405, -12.51329471203370325, 31.30864560766548976 ) ) ;
#48523 = CARTESIAN_POINT ( 'NONE',  ( 10.61538461538461675, -6.435427911321262684, 35.78748833219616898 ) ) ;
#48525 = CARTESIAN_POINT ( 'NONE',  ( -0.7115151924808156281, -12.17611988154120972, 31.52148481390971213 ) ) ;
#48524 = CARTESIAN_POINT ( 'NONE',  ( 16.15384615384615330, -9.780366693483667717, 34.19971097300155094 ) ) ;
#48526 = CARTESIAN_POINT ( 'NONE',  ( 1.384615384615386802, -12.37446782046654192, 30.86335684631486131 ) ) ;
#48527 = CARTESIAN_POINT ( 'NONE',  ( 14.53070515178570332, -2.308499170217967134, 30.53291367094873721 ) ) ;
#48528 = VERTEX_POINT ( 'NONE', #21589 ) ;
#48529 = CARTESIAN_POINT ( 'NONE',  ( -4.230769230769230838, -7.500000000000000000, 29.75000000000000355 ) ) ;
#48530 = SURFACE_STYLE_USAGE ( .BOTH. , #41350 ) ;
#48531 = VERTEX_POINT ( 'NONE', #70664 ) ;
#48532 = ADVANCED_FACE ( 'NONE', ( #49058 ), #50809, .F. ) ;
#48533 = CARTESIAN_POINT ( 'NONE',  ( 14.05766907039934210, -10.05641848906368097, 34.04755513067966177 ) ) ;
#48534 = CARTESIAN_POINT ( 'NONE',  ( -3.230769230769229949, -11.69971097300155272, 32.46337939537588113 ) ) ;
#48535 = ORIENTED_EDGE ( 'NONE', *, *, #33341, .F. ) ;
#48536 = CARTESIAN_POINT ( 'NONE',  ( -9.822998295418001291, -9.084618155246140248, 34.75535874321725771 ) ) ;
#48537 = LINE ( 'NONE', #36373, #52980 ) ;
#48538 = FACE_BOUND ( 'NONE', #56100, .T. ) ;
#48540 = CARTESIAN_POINT ( 'NONE',  ( 3.903869409797563250, -12.41104346484419452, 31.60698883733904196 ) ) ;
#48539 = CARTESIAN_POINT ( 'NONE',  ( -1.450697763975519194, -6.343179335718451384, 34.87096338111212646 ) ) ;
#48541 = CARTESIAN_POINT ( 'NONE',  ( -13.63463860883683942, -2.341070481393819236, 30.72580821765574299 ) ) ;
#48542 = CARTESIAN_POINT ( 'NONE',  ( 12.33084785842815911, -12.35290016733513951, 31.75349464988449455 ) ) ;
#48544 = DIRECTION ( 'NONE',  ( -0.000000000000000000, 0.5000000000000009992, -0.8660254037844380415 ) ) ;
#48543 = CARTESIAN_POINT ( 'NONE',  ( 0.000000000000000000, 0.000000000000000000, 0.000000000000000000 ) ) ;
#48545 = CARTESIAN_POINT ( 'NONE',  ( 0.4615384615384611200, -9.058645607665452459, 34.76329471203371924 ) ) ;
#48546 = VECTOR ( 'NONE', #62048, 999.9999999999998863 ) ;
#48547 = CARTESIAN_POINT ( 'NONE',  ( 3.749999999999999556, -7.438900925035446754, 16.71688170625848713 ) ) ;
#48548 = ORIENTED_EDGE ( 'NONE', *, *, #59065, .F. ) ;
#48549 = VERTEX_POINT ( 'NONE', #14848 ) ;
#48550 = EDGE_CURVE ( 'NONE', #62397, #7759, #8377, .T. ) ;
#48551 = CARTESIAN_POINT ( 'NONE',  ( -9.915792616872025178, -2.353723527008296568, 30.78948104536958752 ) ) ;
#48552 = AXIS2_PLACEMENT_3D ( 'NONE', #32742, #25545, #66074 ) ;
#48553 = DIRECTION ( 'NONE',  ( -0.000000000000000000, 1.000000000000000000, -0.000000000000000000 ) ) ;
#48554 = DIRECTION ( 'NONE',  ( 0.000000000000000000, 0.9848077530122072432, 0.1736481776669354937 ) ) ;
#48555 = CARTESIAN_POINT ( 'NONE',  ( -1.634592115557737424, -3.137211980971221781, 32.19342716148376837 ) ) ;
#48556 = EDGE_CURVE ( 'NONE', #8808, #51516, #69623, .T. ) ;
#48557 = CARTESIAN_POINT ( 'NONE',  ( -13.16183571563731824, -2.612705202774698421, 31.66806509827799943 ) ) ;
#48558 = CARTESIAN_POINT ( 'NONE',  ( -3.775308065498766297, -6.007798216065450170, 18.67000670625849068 ) ) ;
#48559 = DIRECTION ( 'NONE',  ( 0.000000000000000000, -1.000000000000000000, -8.673617379884033500E-16 ) ) ;
#48560 = DIRECTION ( 'NONE',  ( 0.000000000000000000, 0.9848077530122072432, -0.1736481776669354937 ) ) ;
#48561 = CARTESIAN_POINT ( 'NONE',  ( 9.561617089197390840, -10.70098750199973203, 33.91152734681376302 ) ) ;
#48562 = CARTESIAN_POINT ( 'NONE',  ( -4.854143407945009869, -2.353885683473779800, 30.79025554430704759 ) ) ;
#48563 = CARTESIAN_POINT ( 'NONE',  ( -1.634615384615383027, -7.500000000000001776, 35.00000000000000000 ) ) ;
#48564 = CARTESIAN_POINT ( 'NONE',  ( -4.854143407945009869, -6.717445702608402236, 34.94155399931962336 ) ) ;
#48565 = B_SPLINE_CURVE_WITH_KNOTS ( 'NONE', 3,
 ( #36043, #56305, #29288, #77025, #77462, #63043, #41915, #77898, #70708, #43666 ),
 .UNSPECIFIED., .F., .F.,
 ( 4, 2, 2, 2, 4 ),
 ( 0.000000000000000000, 0.0001954339857564069594, 0.0003908679715128139187, 0.0005863019572692209323, 0.0007817359430256278375 ),
 .UNSPECIFIED. ) ;
#48566 = LINE ( 'NONE', #19341, #10704 ) ;
#48567 = CARTESIAN_POINT ( 'NONE',  ( -14.30769230769242739, -3.300289026999228881, 32.46337939537708905 ) ) ;
#48568 = EDGE_CURVE ( 'NONE', #77057, #10775, #33103, .T. ) ;
#48569 = FACE_OUTER_BOUND ( 'NONE', #27069, .T. ) ;
#48570 = EDGE_LOOP ( 'NONE', ( #23917, #49829 ) ) ;
#48571 = CARTESIAN_POINT ( 'NONE',  ( -0.3954701105360229341, -3.513871655860379306, 32.76840700105978499 ) ) ;
#48572 = CARTESIAN_POINT ( 'NONE',  ( 0.5267940328144855577, -2.625532179533470512, 30.86335684631491105 ) ) ;
#48573 = CARTESIAN_POINT ( 'NONE',  ( -2.749999999999999112, -7.438900925035484057, 19.09561829374150932 ) ) ;
#48574 = EDGE_CURVE ( 'NONE', #75011, #7293, #22038, .T. ) ;
#48575 = CARTESIAN_POINT ( 'NONE',  ( -18.23784950573857344, 12.75000000000000711, 32.75000000000000000 ) ) ;
#48577 = DIRECTION ( 'NONE',  ( -0.000000000000000000, 0.8660254037844397068, -0.4999999999999978906 ) ) ;
#48576 = VECTOR ( 'NONE', #60058, 1000.000000000000000 ) ;
#48578 = EDGE_LOOP ( 'NONE', ( #15930, #64836, #45263, #7888, #83766, #36652 ) ) ;
#48579 = CARTESIAN_POINT ( 'NONE',  ( -16.40384615384615685, -2.499999999999999556, 29.81609845454691765 ) ) ;
#48581 = ORIENTED_EDGE ( 'NONE', *, *, #68557, .T. ) ;
#48580 = CARTESIAN_POINT ( 'NONE',  ( -14.43838377435986864, -12.11776431015576172, 31.66791131148498906 ) ) ;
#48582 = CARTESIAN_POINT ( 'NONE',  ( 9.823098133274644539, -12.62708834333097663, 30.88030960425257021 ) ) ;
#48583 = LINE ( 'NONE', #29226, #19594 ) ;
#48584 = B_SPLINE_CURVE_WITH_KNOTS ( 'NONE', 3,
 ( #68746, #61982, #83155, #82717, #20990, #48461, #76388, #21447, #16023, #30421 ),
 .UNSPECIFIED., .F., .F.,
 ( 4, 2, 2, 2, 4 ),
 ( 0.0007817359430256293554, 0.0009771253907249941549, 0.001172514838424358954, 0.001367904286123723537, 0.001563293733823095276 ),
 .UNSPECIFIED. ) ;
#48585 = ORIENTED_EDGE ( 'NONE', *, *, #28539, .F. ) ;
#48586 = DIRECTION ( 'NONE',  ( -0.000000000000000000, -0.8660254037844397068, -0.4999999999999978906 ) ) ;
#48587 = VECTOR ( 'NONE', #39617, 1000.000000000000227 ) ;
#48588 = CARTESIAN_POINT ( 'NONE',  ( 8.096153846153782752, -7.565270445406050648, 34.75000000000000000 ) ) ;
#48589 = ORIENTED_EDGE ( 'NONE', *, *, #17456, .F. ) ;
#48590 = CARTESIAN_POINT ( 'NONE',  ( -10.83831157429146508, -4.026226216239094491, 33.68668979543634379 ) ) ;
#48591 = DIRECTION ( 'NONE',  ( 1.000000000000000000, 0.000000000000000000, 0.000000000000000000 ) ) ;
#48592 = EDGE_CURVE ( 'NONE', #34081, #23012, #67438, .T. ) ;
#48593 = VECTOR ( 'NONE', #57449, 1000.000000000000227 ) ;
#48594 = CARTESIAN_POINT ( 'NONE',  ( 12.71148387091650278, -12.07971442181322352, 32.31769673815850297 ) ) ;
#48595 = ORIENTED_EDGE ( 'NONE', *, *, #33748, .F. ) ;
#48596 = EDGE_CURVE ( 'NONE', #45649, #46211, #38531, .T. ) ;
#48597 = VERTEX_POINT ( 'NONE', #9842 ) ;
#48598 = CARTESIAN_POINT ( 'NONE',  ( -6.700064078983528404, -8.282913670948747864, 34.94150082978203642 ) ) ;
#48599 = ORIENTED_EDGE ( 'NONE', *, *, #73154, .F. ) ;
#48600 = CARTESIAN_POINT ( 'NONE',  ( -5.999999999999998224, -13.53365097954675988, 30.81389545987213552 ) ) ;
#48601 = ADVANCED_FACE ( 'NONE', ( #80540 ), #65222, .F. ) ;
#48602 = CARTESIAN_POINT ( 'NONE',  ( -5.326899820971668476, -9.234221910056348293, 34.70572697212741531 ) ) ;
#48603 = CARTESIAN_POINT ( 'NONE',  ( -14.43838377435986864, -3.062553014421049546, 32.05460306192773601 ) ) ;
#48604 = EDGE_CURVE ( 'NONE', #70832, #34382, #23786, .T. ) ;
#48605 = CARTESIAN_POINT ( 'NONE',  ( -9.758391103263569732, -4.786620604624113540, 33.94971097300155805 ) ) ;
#48606 = CYLINDRICAL_SURFACE ( 'NONE', #11954, 0.2499999999999973355 ) ;
#48607 = LINE ( 'NONE', #8080, #6410 ) ;
#48608 = CARTESIAN_POINT ( 'NONE',  ( 15.45414517146741140, -2.501478030877322567, 29.88021232661721172 ) ) ;
#48609 = CIRCLE ( 'NONE', #5494, 4.000000000000000000 ) ;
#48610 = EDGE_LOOP ( 'NONE', ( #75453, #88039, #50352, #64529 ) ) ;
#48611 = ORIENTED_EDGE ( 'NONE', *, *, #19707, .T. ) ;
#48613 = EDGE_LOOP ( 'NONE', ( #74675, #66662, #70858, #28805 ) ) ;
#48612 = DIRECTION ( 'NONE',  ( 0.000000000000000000, -6.938893903907222067E-15, 1.000000000000000000 ) ) ;
#48614 = B_SPLINE_CURVE_WITH_KNOTS ( 'NONE', 3,
 ( #81204, #20382, #47843, #28466, #33454, #88417, #61792, #69001, #75326, #27133 ),
 .UNSPECIFIED., .F., .F.,
 ( 4, 2, 2, 2, 4 ),
 ( 0.000000000000000000, 0.0001954339857564081520, 0.0003908679715128163040, 0.0005863019572692244018, 0.0007817359430256326080 ),
 .UNSPECIFIED. ) ;
#48615 = AXIS2_PLACEMENT_3D ( 'NONE', #9759, #84552, #50727 ) ;
#48616 = CARTESIAN_POINT ( 'NONE',  ( 7.780883845597526438, -2.657715359629088780, 31.77849191805832874 ) ) ;
#48617 = ORIENTED_EDGE ( 'NONE', *, *, #61153, .T. ) ;
#48618 = VECTOR ( 'NONE', #22347, 1000.000000000000114 ) ;
#48619 = CYLINDRICAL_SURFACE ( 'NONE', #49282, 0.2500000000000009437 ) ;
#48620 = CARTESIAN_POINT ( 'NONE',  ( 5.326868595271218254, -3.712312575010499494, 33.01462480002815170 ) ) ;
#48621 = ORIENTED_EDGE ( 'NONE', *, *, #1829, .T. ) ;
#48622 = CARTESIAN_POINT ( 'NONE',  ( -24.00000000000000000, -9.499999999999982236, 27.74999999999999645 ) ) ;
#48623 = EDGE_LOOP ( 'NONE', ( #25323, #86093, #36339, #60704 ) ) ;
#48624 = ORIENTED_EDGE ( 'NONE', *, *, #77315, .T. ) ;
#48625 = CARTESIAN_POINT ( 'NONE',  ( 4.480769230769229061, -3.499999999999999556, 29.75000000000000355 ) ) ;
#48626 = EDGE_CURVE ( 'NONE', #21723, #83108, #41718, .T. ) ;
#48627 = ORIENTED_EDGE ( 'NONE', *, *, #20165, .F. ) ;
#48628 = CYLINDRICAL_SURFACE ( 'NONE', #87759, 0.2500000000000009437 ) ;
#48629 = CARTESIAN_POINT ( 'NONE',  ( 17.01165263096230262, -2.892918686051582533, 31.69288490824015980 ) ) ;
#48630 = FACE_BOUND ( 'NONE', #78973, .T. ) ;
#48631 = FACE_OUTER_BOUND ( 'NONE', #26902, .T. ) ;
#48632 = DIRECTION ( 'NONE',  ( 0.000000000000000000, 0.4999999999999960032, -0.8660254037844410391 ) ) ;
#48633 = CARTESIAN_POINT ( 'NONE',  ( 9.692307692307695177, -2.292212530054420494, 30.41441678777542634 ) ) ;
#48634 = CARTESIAN_POINT ( 'NONE',  ( 3.296836564119306701, -4.661471528628508665, 34.16647553114624003 ) ) ;
#48635 = AXIS2_PLACEMENT_3D ( 'NONE', #22302, #70041, #77242 ) ;
#48636 = CARTESIAN_POINT ( 'NONE',  ( 5.326977388561387805, -10.66356715214248396, 33.62249196103329751 ) ) ;
#48637 = CARTESIAN_POINT ( 'NONE',  ( 15.93036121012220541, -4.386631170607603991, 33.66268669641500111 ) ) ;
#48638 = EDGE_LOOP ( 'NONE', ( #20543, #32560 ) ) ;
#48639 = CYLINDRICAL_SURFACE ( 'NONE', #84974, 0.2500000000000008882 ) ;
#48640 = EDGE_LOOP ( 'NONE', ( #2880, #25929, #70874, #12260 ) ) ;
#48641 = EDGE_CURVE ( 'NONE', #58240, #22124, #57811, .T. ) ;
#48642 = ORIENTED_EDGE ( 'NONE', *, *, #87179, .T. ) ;
#48643 = EDGE_CURVE ( 'NONE', #31900, #75897, #86875, .T. ) ;
#48644 = VECTOR ( 'NONE', #10511, 999.9999999999998863 ) ;
#48646 = FACE_OUTER_BOUND ( 'NONE', #15739, .T. ) ;
#48645 = CARTESIAN_POINT ( 'NONE',  ( 2.307692307692309264, -2.833524468853757305, 32.15551576947925838 ) ) ;
#48647 = DIRECTION ( 'NONE',  ( -0.000000000000000000, -0.8660254037844397068, -0.4999999999999978906 ) ) ;
#48648 = DIRECTION ( 'NONE',  ( -0.000000000000000000, 0.9396926207859092051, -0.3420201433256662704 ) ) ;
#48649 = CYLINDRICAL_SURFACE ( 'NONE', #2734, 0.2499999999999986955 ) ;
#48650 = FACE_OUTER_BOUND ( 'NONE', #76126, .T. ) ;
#48651 = ORIENTED_EDGE ( 'NONE', *, *, #14055, .T. ) ;
#48652 = CARTESIAN_POINT ( 'NONE',  ( -5.076923076923199218, -5.941354392335915335, 34.76329471203413846 ) ) ;
#48653 = CARTESIAN_POINT ( 'NONE',  ( -6.249976730942353065, -6.567427716900047230, 34.66269422305636283 ) ) ;
#48654 = CARTESIAN_POINT ( 'NONE',  ( 17.07692307692307665, -3.937682226553329556, 33.60647404775216529 ) ) ;
#48655 = CARTESIAN_POINT ( 'NONE',  ( 15.29602437028207085, -12.51329471203373345, 31.30864560766537963 ) ) ;
#48656 = ORIENTED_EDGE ( 'NONE', *, *, #23028, .T. ) ;
#48657 = B_SPLINE_CURVE_WITH_KNOTS ( 'NONE', 3,
 ( #32370, #3551, #59836, #51265, #44974, #17525, #4444, #85536, #86446, #64798 ),
 .UNSPECIFIED., .F., .F.,
 ( 4, 2, 2, 2, 4 ),
 ( 0.0007817246256747515092, 0.0009771112852218961399, 0.001172497944769040771, 0.001367884604316185401, 0.001563271263863330032 ),
 .UNSPECIFIED. ) ;
#48658 = VERTEX_POINT ( 'NONE', #46296 ) ;
#48659 = B_SPLINE_CURVE_WITH_KNOTS ( 'NONE', 3,
 ( #72724, #80393, #87603, #25881, #86719, #5165, #4727, #17799, #32202, #40293 ),
 .UNSPECIFIED., .F., .F.,
 ( 4, 2, 2, 2, 4 ),
 ( 0.000000000000000000, 0.0001954311564186882568, 0.0003908623128373765136, 0.0005862934692560647703, 0.0007817246256747530271 ),
 .UNSPECIFIED. ) ;
#48660 = ORIENTED_EDGE ( 'NONE', *, *, #12414, .T. ) ;
#48661 = EDGE_CURVE ( 'NONE', #32595, #13908, #1989, .T. ) ;
#48662 = CARTESIAN_POINT ( 'NONE',  ( -6.988347369037697376, -8.613356846314824011, 34.62446782046655613 ) ) ;
#48663 = VERTEX_POINT ( 'NONE', #3520 ) ;
#48664 = CYLINDRICAL_SURFACE ( 'NONE', #71408, 0.2499999999999994726 ) ;
#48665 = CARTESIAN_POINT ( 'NONE',  ( 15.48082365068267841, -4.074993327901527351, 33.72946981652012255 ) ) ;
#48666 = CARTESIAN_POINT ( 'NONE',  ( 14.08476534878545827, -10.01117774369187252, 34.36070679894347535 ) ) ;
#48667 = EDGE_CURVE ( 'NONE', #58521, #42680, #58456, .T. ) ;
#48668 = CARTESIAN_POINT ( 'NONE',  ( 6.923076923076924238, -9.780366693483667717, 34.19971097300155094 ) ) ;
#48669 = CARTESIAN_POINT ( 'NONE',  ( 12.23861224402231151, -9.886141570436013382, 34.14413921362392301 ) ) ;
#48670 = EDGE_LOOP ( 'NONE', ( #28834, #47182 ) ) ;
#48671 = CARTESIAN_POINT ( 'NONE',  ( 4.284637961670941131, -4.118422570099827595, 33.43335022499816489 ) ) ;
#48673 = VERTEX_POINT ( 'NONE', #65659 ) ;
#48672 = DIRECTION ( 'NONE',  ( 0.000000000000000000, 0.000000000000000000, 1.000000000000000000 ) ) ;
#48674 = CARTESIAN_POINT ( 'NONE',  ( -3.480769230769229061, -2.499999999999998668, 29.75000000000000355 ) ) ;
#48675 = CARTESIAN_POINT ( 'NONE',  ( -8.519230769230832223, -7.565270000091922853, 34.99999999999999289 ) ) ;
#48676 = CARTESIAN_POINT ( 'NONE',  ( 16.94623161025551639, -3.530157926970578508, 32.79014554554150607 ) ) ;
#48677 = CARTESIAN_POINT ( 'NONE',  ( 4.153846153846154188, -6.189225973068211317, 35.74407628777942847 ) ) ;
#48678 = CARTESIAN_POINT ( 'NONE',  ( -12.59168567097668223, -2.882441371585227508, 31.66841991370172238 ) ) ;
#48679 = CARTESIAN_POINT ( 'NONE',  ( -0.3589743589743593088, -11.50000000000000000, 29.75000000000000355 ) ) ;
#48680 = ADVANCED_FACE ( 'NONE', ( #86421 ), #6204, .F. ) ;
#48681 = DIRECTION ( 'NONE',  ( -0.000000000000000000, -0.7660444431189791237, -0.6427876096865379196 ) ) ;
#48682 = CARTESIAN_POINT ( 'NONE',  ( -1.200186371490524317, -10.22469193450124791, 25.11124329374151642 ) ) ;
#48683 = ORIENTED_EDGE ( 'NONE', *, *, #48351, .T. ) ;
#48684 = AXIS2_PLACEMENT_3D ( 'NONE', #54753, #35370, #82239 ) ;
#48685 = CARTESIAN_POINT ( 'NONE',  ( -1.318547033612945896, -11.16473453929635440, 33.15142922261926373 ) ) ;
#48686 = CARTESIAN_POINT ( 'NONE',  ( -14.24162497434223340, -3.322132147404559976, 32.92929555188717927 ) ) ;
#48687 = CYLINDRICAL_SURFACE ( 'NONE', #57603, 0.2499999999999995559 ) ;
#48688 = CARTESIAN_POINT ( 'NONE',  ( 9.561617089197383734, -6.369640206132551441, 34.87707690430378449 ) ) ;
#48689 = VERTEX_POINT ( 'NONE', #13836 ) ;
#48690 = CARTESIAN_POINT ( 'NONE',  ( 0.2380535369741295093, -4.225889041578353655, 33.85425143139329407 ) ) ;
#48691 = CARTESIAN_POINT ( 'NONE',  ( -15.93083480223330817, -12.15243808032446005, 31.58219941686247978 ) ) ;
#48692 = B_SPLINE_CURVE_WITH_KNOTS ( 'NONE', 3,
 ( #5011, #31587, #80687, #46435, #52296, #38349, #4104, #79786, #12214, #86553 ),
 .UNSPECIFIED., .F., .F.,
 ( 4, 2, 2, 2, 4 ),
 ( 0.000000000000000000, 0.0001954311564186868473, 0.0003908623128373736946, 0.0005862934692560605419, 0.0007817246256747473893 ),
 .UNSPECIFIED. ) ;
#48693 = CARTESIAN_POINT ( 'NONE',  ( -0.5916864312701589634, -12.70455904226513866, 30.44083106164009322 ) ) ;
#48694 = CARTESIAN_POINT ( 'NONE',  ( -0.6850233861027944515, -10.97335522853832579, 33.68706563782419749 ) ) ;
#48695 = B_SPLINE_CURVE_WITH_KNOTS ( 'NONE', 3,
 ( #68450, #880, #28345, #41429, #80768, #69779, #8087, #48170, #48616, #76984 ),
 .UNSPECIFIED., .F., .F.,
 ( 4, 2, 2, 2, 4 ),
 ( 0.000000000000000000, 0.0001954311564186862239, 0.0003908623128373724478, 0.0005862934692560586988, 0.0007817246256747448956 ),
 .UNSPECIFIED. ) ;
#48696 = ORIENTED_EDGE ( 'NONE', *, *, #64020, .F. ) ;
#48697 = B_SPLINE_CURVE_WITH_KNOTS ( 'NONE', 3,
 ( #52123, #71505, #45364, #9813, #37277, #38621, #44467, #25552, #67869, #53909 ),
 .UNSPECIFIED., .F., .F.,
 ( 4, 2, 2, 2, 4 ),
 ( 0.000000000000000000, 0.0001954339857564099951, 0.0003908679715128199903, 0.0005863019572692300396, 0.0007817359430256399806 ),
 .UNSPECIFIED. ) ;
#48698 = B_SPLINE_CURVE_WITH_KNOTS ( 'NONE', 3,
 ( #26084, #77368, #42706, #70170, #76036, #84587, #41823, #15677, #35050, #21986 ),
 .UNSPECIFIED., .F., .F.,
 ( 4, 2, 2, 2, 4 ),
 ( 0.0007817359430256251270, 0.0009771253907249900349, 0.001172514838424354834, 0.001367904286123719851, 0.001563293733823084650 ),
 .UNSPECIFIED. ) ;
#48699 = CARTESIAN_POINT ( 'NONE',  ( 17.07692307692295586, -3.300289026999228437, 32.46337939537709616 ) ) ;
#48700 = EDGE_CURVE ( 'NONE', #7957, #4203, #77116, .T. ) ;
#48701 = CARTESIAN_POINT ( 'NONE',  ( -19.00000000000000000, -11.00000000000000000, 29.75000000000000355 ) ) ;
#48702 = CARTESIAN_POINT ( 'NONE',  ( 18.13052543823364360, -12.50538340440932394, 31.33453814440721885 ) ) ;
#48703 = ORIENTED_EDGE ( 'NONE', *, *, #44715, .F. ) ;
#48704 = CYLINDRICAL_SURFACE ( 'NONE', #72916, 0.2500000000000009437 ) ;
#48705 = ADVANCED_FACE ( 'NONE', ( #62021 ), #39562, .T. ) ;
#48706 = ORIENTED_EDGE ( 'NONE', *, *, #53449, .T. ) ;
#48707 = VECTOR ( 'NONE', #65730, 1000.000000000000227 ) ;
#48708 = FACE_OUTER_BOUND ( 'NONE', #66320, .T. ) ;
#48709 = CARTESIAN_POINT ( 'NONE',  ( 5.076923076923075762, -5.471508081941601098, 34.59228464037088457 ) ) ;
#48710 = EDGE_LOOP ( 'NONE', ( #42919, #46913, #16200, #26668 ) ) ;
#48711 = ADVANCED_FACE ( 'NONE', ( #34109 ), #81869, .F. ) ;
#48712 = CARTESIAN_POINT ( 'NONE',  ( -39.05038313613820122, -2.249999999999998668, 29.75000000000000355 ) ) ;
#48713 = CARTESIAN_POINT ( 'NONE',  ( 4.284636594813103549, -9.084667340241226796, 34.75534355489798344 ) ) ;
#48714 = CARTESIAN_POINT ( 'NONE',  ( -11.76194648218548622, -6.760086850603066466, 34.69517049084099369 ) ) ;
#48715 = AXIS2_PLACEMENT_3D ( 'NONE', #76540, #84197, #70221 ) ;
#48716 = VECTOR ( 'NONE', #55640, 1000.000000000000000 ) ;
#48717 = CARTESIAN_POINT ( 'NONE',  ( 11.40777093535123399, -12.35290016733513951, 31.75349464988449455 ) ) ;
#48718 = DIRECTION ( 'NONE',  ( 1.000000000000000000, 0.000000000000000000, 0.000000000000000000 ) ) ;
#48719 = ORIENTED_EDGE ( 'NONE', *, *, #6773, .F. ) ;
#48720 = FACE_BOUND ( 'NONE', #81537, .T. ) ;
#48721 = EDGE_LOOP ( 'NONE', ( #82650, #68562 ) ) ;
#48723 = EDGE_CURVE ( 'NONE', #52054, #15626, #67460, .T. ) ;
#48722 = LINE ( 'NONE', #27573, #41456 ) ;
#48724 = B_SPLINE_CURVE_WITH_KNOTS ( 'NONE', 3,
 ( #75860, #2842, #65446, #58241, #10509, #37078, #45169, #71751, #9192, #16376 ),
 .UNSPECIFIED., .F., .F.,
 ( 4, 2, 2, 2, 4 ),
 ( 0.000000000000000000, 0.0001954339857564079623, 0.0003908679715128159245, 0.0005863019572692238597, 0.0007817359430256318490 ),
 .UNSPECIFIED. ) ;
#48725 = CARTESIAN_POINT ( 'NONE',  ( -14.05763788777885281, -11.47946981652013498, 33.17500667209847620 ) ) ;
#48726 = EDGE_CURVE ( 'NONE', #18197, #22884, #63240, .T. ) ;
#48727 = LINE ( 'NONE', #61345, #50683 ) ;
#48728 = CARTESIAN_POINT ( 'NONE',  ( 16.82694634598072625, -2.564618984488975517, 30.55390908950641915 ) ) ;
#48729 = ORIENTED_EDGE ( 'NONE', *, *, #76538, .F. ) ;
#48730 = VERTEX_POINT ( 'NONE', #27354 ) ;
#48731 = ORIENTED_EDGE ( 'NONE', *, *, #81780, .T. ) ;
#48732 = B_SPLINE_CURVE_WITH_KNOTS ( 'NONE', 3,
 ( #53404, #67374, #88120, #56411, #62707, #7781, #70370, #22184, #35246, #70818 ),
 .UNSPECIFIED., .F., .F.,
 ( 4, 2, 2, 2, 4 ),
 ( 0.0007817246256747469556, 0.0009771112852218896347, 0.001172497944769032531, 0.001367884604316175427, 0.001563271263863318106 ),
 .UNSPECIFIED. ) ;
#48733 = CARTESIAN_POINT ( 'NONE',  ( -3.230769230769352962, -11.67786785259630911, 32.92929555188603530 ) ) ;
#48734 = ORIENTED_EDGE ( 'NONE', *, *, #54167, .F. ) ;
#48735 = EDGE_CURVE ( 'NONE', #44386, #4983, #35327, .T. ) ;
#48736 = CARTESIAN_POINT ( 'NONE',  ( -6.250023237292964495, -12.43535235679832596, 30.55408501211184813 ) ) ;
#48737 = VECTOR ( 'NONE', #68181, 1000.000000000000000 ) ;
#48738 = CARTESIAN_POINT ( 'NONE',  ( -13.38461538461550759, -8.656820664282941280, 34.87096338111179961 ) ) ;
#48739 = ADVANCED_FACE ( 'NONE', ( #34557 ), #33231, .F. ) ;
#48740 = CARTESIAN_POINT ( 'NONE',  ( 13.63466980452883881, -11.47946981652013498, 33.17500667209847620 ) ) ;
#48741 = CARTESIAN_POINT ( 'NONE',  ( 16.15384615384615330, -2.292212530054420494, 30.41441678777542634 ) ) ;
#48742 = EDGE_CURVE ( 'NONE', #26012, #83335, #21026, .T. ) ;
#48743 = PLANE ( 'NONE',  #7177 ) ;
#48744 = CARTESIAN_POINT ( 'NONE',  ( 3.930919194939305861, -2.523278758544489797, 31.42238647778637528 ) ) ;
#48745 = CARTESIAN_POINT ( 'NONE',  ( 17.07692307692295586, -2.625532179533778709, 30.86335684631627174 ) ) ;
#48746 = ORIENTED_EDGE ( 'NONE', *, *, #78057, .F. ) ;
#48747 = EDGE_LOOP ( 'NONE', ( #69614, #26569, #28003, #49097 ) ) ;
#48748 = VERTEX_POINT ( 'NONE', #60692 ) ;
#48750 = EDGE_CURVE ( 'NONE', #17603, #10737, #73784, .T. ) ;
#48749 = CARTESIAN_POINT ( 'NONE',  ( -27.00000000000000000, 0.7500000000000051070, 24.75000000000000000 ) ) ;
#48752 = LINE ( 'NONE', #42897, #86555 ) ;
#48751 = CARTESIAN_POINT ( 'NONE',  ( -3.230769230769229949, -9.905515769479276145, 34.41647553114623292 ) ) ;
#48753 = DIRECTION ( 'NONE',  ( 0.000000000000000000, 0.6427876096865373645, -0.7660444431189797898 ) ) ;
#48754 = CARTESIAN_POINT ( 'NONE',  ( 12.52679360105129724, -12.70778746994558439, 30.41441678777536595 ) ) ;
#48755 = CYLINDRICAL_SURFACE ( 'NONE', #44329, 0.2499999999999994726 ) ;
#48756 = DIRECTION ( 'NONE',  ( 0.000000000000000000, 0.9396926207859126468, -0.3420201433256571111 ) ) ;
#48757 = ORIENTED_EDGE ( 'NONE', *, *, #26033, .T. ) ;
#48758 = CARTESIAN_POINT ( 'NONE',  ( -5.076923076923075762, -13.78497067705608181, 32.30358669280327177 ) ) ;
#48759 = CARTESIAN_POINT ( 'NONE',  ( -7.134615384615385025, -3.499999999999999556, 29.75000000000000355 ) ) ;
#48760 = CARTESIAN_POINT ( 'NONE',  ( -1.384615384615383471, -2.721908614388771852, 31.22303859784724978 ) ) ;
#48761 = CARTESIAN_POINT ( 'NONE',  ( 3.296024370282069071, -11.67786785259547777, 32.92929555188713664 ) ) ;
#48762 = ORIENTED_EDGE ( 'NONE', *, *, #32713, .T. ) ;
#48763 = CARTESIAN_POINT ( 'NONE',  ( 18.06606835100243913, -12.37446782046654192, 30.86335684631486842 ) ) ;
#48764 = ORIENTED_EDGE ( 'NONE', *, *, #33667, .T. ) ;
#48765 = FACE_BOUND ( 'NONE', #11876, .T. ) ;
#48766 = CARTESIAN_POINT ( 'NONE',  ( -17.20761368003338987, -3.957541250942358424, 33.62499894934981626 ) ) ;
#48767 = AXIS2_PLACEMENT_3D ( 'NONE', #20482, #7418, #74544 ) ;
#48768 = CARTESIAN_POINT ( 'NONE',  ( 16.82694634598072625, -11.79746400365624659, 32.30657167506340954 ) ) ;
#48769 = DIRECTION ( 'NONE',  ( -0.000000000000000000, 1.000000000000000000, -0.000000000000000000 ) ) ;
#48770 = ORIENTED_EDGE ( 'NONE', *, *, #32008, .F. ) ;
#48771 = CARTESIAN_POINT ( 'NONE',  ( -12.68446467905460828, -9.886141570436013382, 34.14413921362392301 ) ) ;
#48772 = CARTESIAN_POINT ( 'NONE',  ( 4.826923076923076650, -7.500000000000001776, 34.75000000000000000 ) ) ;
#48773 = CARTESIAN_POINT ( 'NONE',  ( -16.15384615384627409, -12.46129190930018460, 30.37095296980731973 ) ) ;
#48774 = EDGE_CURVE ( 'NONE', #59465, #46553, #81437, .T. ) ;
#48775 = DIRECTION ( 'NONE',  ( -1.000000000000000000, -0.000000000000000000, 0.000000000000000000 ) ) ;
#48776 = ORIENTED_EDGE ( 'NONE', *, *, #15674, .F. ) ;
#48777 = VECTOR ( 'NONE', #57487, 1000.000000000000227 ) ;
#48778 = CARTESIAN_POINT ( 'NONE',  ( -4.853910232829682592, -4.762714258010880997, 34.23016756924214832 ) ) ;
#48779 = ORIENTED_EDGE ( 'NONE', *, *, #48932, .F. ) ;
#48780 = AXIS2_PLACEMENT_3D ( 'NONE', #87162, #24990, #58323 ) ;
#48782 = ORIENTED_EDGE ( 'NONE', *, *, #28763, .F. ) ;
#48781 = CARTESIAN_POINT ( 'NONE',  ( 16.40384615384622080, -7.434744860731433924, 35.00000000000000711 ) ) ;
#48783 = CARTESIAN_POINT ( 'NONE',  ( 9.442330961365341224, -3.627789207965226748, 32.91389620160131102 ) ) ;
#48784 = CARTESIAN_POINT ( 'NONE',  ( -4.284537620513710010, -2.729777683071817229, 31.24903638046268739 ) ) ;
#48785 = CARTESIAN_POINT ( 'NONE',  ( -3.480769230769229061, -7.500000000000001776, 35.00000000000000000 ) ) ;
#48786 = CARTESIAN_POINT ( 'NONE',  ( -17.75000000000000000, -2.499999999999999556, 29.75000000000000355 ) ) ;
#48787 = CARTESIAN_POINT ( 'NONE',  ( -13.16183571563731824, -3.563462043263030399, 33.22394488606062879 ) ) ;
#48789 = LINE ( 'NONE', #33517, #48955 ) ;
#48788 = CARTESIAN_POINT ( 'NONE',  ( 13.63456090296352841, -5.852078868378309373, 34.47109172314383585 ) ) ;
#48790 = FACE_OUTER_BOUND ( 'NONE', #47940, .T. ) ;
#48791 = CARTESIAN_POINT ( 'NONE',  ( 1.139087296526029469, -10.24999999999999467, 18.45312500000000355 ) ) ;
#48792 = ORIENTED_EDGE ( 'NONE', *, *, #16437, .T. ) ;
#48793 = PLANE ( 'NONE',  #3077 ) ;
#48794 = VERTEX_POINT ( 'NONE', #28690 ) ;
#48795 = VERTEX_POINT ( 'NONE', #63788 ) ;
#48796 = CARTESIAN_POINT ( 'NONE',  ( 3.165498784808455923, -5.219633306516282545, 34.19971097300152252 ) ) ;
#48797 = EDGE_LOOP ( 'NONE', ( #82541, #60479 ) ) ;
#48798 = CARTESIAN_POINT ( 'NONE',  ( 14.30769230769218758, -8.613356846316285953, 34.62446782046622218 ) ) ;
#48799 = UNCERTAINTY_MEASURE_WITH_UNIT (LENGTH_MEASURE( 1.000000000000000082E-05 ), #88673, 'distance_accuracy_value', 'NONE');
#48800 = CARTESIAN_POINT ( 'NONE',  ( -11.47239420511146513, -9.905515769479276145, 34.41647553114623292 ) ) ;
#48801 = CARTESIAN_POINT ( 'NONE',  ( -16.02332045208259359, -6.001044277235011215, 34.52024696741798948 ) ) ;
#48802 = CARTESIAN_POINT ( 'NONE',  ( -11.60373198442231413, -11.48612834413959582, 32.76840700105983473 ) ) ;
#48803 = CARTESIAN_POINT ( 'NONE',  ( 11.53846153846153832, -1.422936976036506707, 30.56769352161908415 ) ) ;
#48804 = CARTESIAN_POINT ( 'NONE',  ( 12.33084699487090674, -10.54014554554150607, 33.71984207302941883 ) ) ;
#48805 = CARTESIAN_POINT ( 'NONE',  ( 20.00000000000000000, -4.000000000000000000, 29.75000000000000355 ) ) ;
#48806 = CARTESIAN_POINT ( 'NONE',  ( 1.553300858899129944, -11.24999999999998934, 24.70312500000000000 ) ) ;
#48807 = CARTESIAN_POINT ( 'NONE',  ( 6.923076923076924238, -9.905515769479276145, 34.41647553114623292 ) ) ;
#48808 = CARTESIAN_POINT ( 'NONE',  ( 17.75002326905764605, -11.79746400365624659, 32.30657167506340954 ) ) ;
#48809 = CARTESIAN_POINT ( 'NONE',  ( 5.299702745901138989, -10.97394488606064122, 33.68653795673694873 ) ) ;
#48810 = VECTOR ( 'NONE', #6906, 1000.000000000000000 ) ;
#48811 = CARTESIAN_POINT ( 'NONE',  ( -9.822455662039390134, -11.66186481527757302, 32.95055677023626117 ) ) ;
#48812 = B_SPLINE_CURVE_WITH_KNOTS ( 'NONE', 3,
 ( #32282, #18322, #23727, #10236, #25521, #72808, #3461, #44888, #11116, #66047 ),
 .UNSPECIFIED., .F., .F.,
 ( 4, 2, 2, 2, 4 ),
 ( 0.000000000000000000, 0.0001954339857564076099, 0.0003908679715128152198, 0.0005863019572692228839, 0.0007817359430256304396 ),
 .UNSPECIFIED. ) ;
#48813 = ADVANCED_FACE ( 'NONE', ( #62452 ), #42648, .F. ) ;
#48814 = ORIENTED_EDGE ( 'NONE', *, *, #27945, .F. ) ;
#48815 = ORIENTED_EDGE ( 'NONE', *, *, #56091, .T. ) ;
#48816 = CARTESIAN_POINT ( 'NONE',  ( -18.06608237936013239, -2.486705287966280320, 31.30864560766542937 ) ) ;
#48817 = CARTESIAN_POINT ( 'NONE',  ( -14.30769230769230660, -1.629998284177014645, 34.34916445242399163 ) ) ;
#48818 = LINE ( 'NONE', #6952, #23892 ) ;
#48819 = DIRECTION ( 'NONE',  ( -0.000000000000000000, 1.000000000000000000, -0.000000000000000000 ) ) ;
#48820 = EDGE_CURVE ( 'NONE', #43614, #14333, #36765, .T. ) ;
#48821 = CARTESIAN_POINT ( 'NONE',  ( 9.942362112221147186, -11.47946981652013498, 33.17500667209847620 ) ) ;
#48822 = LINE ( 'NONE', #55140, #47014 ) ;
#48823 = EDGE_CURVE ( 'NONE', #11766, #83962, #766, .T. ) ;
#48824 = LINE ( 'NONE', #61448, #62372 ) ;
#48825 = B_SPLINE_CURVE_WITH_KNOTS ( 'NONE', 3,
 ( #48403, #75883, #21380, #56933, #34890, #14181, #63691, #1998, #41660, #29480 ),
 .UNSPECIFIED., .F., .F.,
 ( 4, 2, 2, 2, 4 ),
 ( 0.0007817246336856291692, 0.0009771112958940103739, 0.001172497958102391470, 0.001367884620310772566, 0.001563271282519153879 ),
 .UNSPECIFIED. ) ;
#48826 = VERTEX_POINT ( 'NONE', #28234 ) ;
#48827 = B_SPLINE_CURVE_WITH_KNOTS ( 'NONE', 3,
 ( #4849, #87281, #66549, #4396, #31880, #80514, #25559, #81844, #46717, #59337 ),
 .UNSPECIFIED., .F., .F.,
 ( 4, 2, 2, 2, 4 ),
 ( 0.0007817359430256372700, 0.0009771253907250054306, 0.001172514838424373700, 0.001367904286123741969, 0.001563293733823110021 ),
 .UNSPECIFIED. ) ;
#48828 = CARTESIAN_POINT ( 'NONE',  ( -13.44988583057615905, -10.21337939537584383, 33.94971097300158647 ) ) ;
#48829 = ORIENTED_EDGE ( 'NONE', *, *, #44859, .T. ) ;
#48830 = EDGE_CURVE ( 'NONE', #84649, #45729, #39665, .T. ) ;
#48831 = LINE ( 'NONE', #76305, #20419 ) ;
#48832 = CARTESIAN_POINT ( 'NONE',  ( 15.45354889974729318, -3.563462043263030399, 33.22394488606062879 ) ) ;
#48833 = CARTESIAN_POINT ( 'NONE',  ( 11.60452988946397745, -10.51840700105979565, 33.73612834413962247 ) ) ;
#48834 = CARTESIAN_POINT ( 'NONE',  ( 3.100621261037537213, -8.630895178749536711, 34.87696386517710323 ) ) ;
#48835 = CARTESIAN_POINT ( 'NONE',  ( -3.007342831854442622, -7.630147987733843173, 34.99859428049665411 ) ) ;
#48836 = VECTOR ( 'NONE', #87814, 1000.000000000000000 ) ;
#48837 = AXIS2_PLACEMENT_3D ( 'NONE', #42118, #62795, #69571 ) ;
#48838 = VERTEX_POINT ( 'NONE', #77308 ) ;
#48839 = VECTOR ( 'NONE', #5726, 1000.000000000000114 ) ;
#48840 = ORIENTED_EDGE ( 'NONE', *, *, #31373, .F. ) ;
#48841 = ORIENTED_EDGE ( 'NONE', *, *, #57622, .T. ) ;
#48842 = EDGE_LOOP ( 'NONE', ( #39340, #23518, #8451, #5956 ) ) ;
#48843 = DIRECTION ( 'NONE',  ( -0.000000000000000000, -0.7660444431189791237, -0.6427876096865379196 ) ) ;
#48844 = CARTESIAN_POINT ( 'NONE',  ( 4.946775867484856093, -10.88202310037935661, 33.43294751532457099 ) ) ;
#48845 = EDGE_CURVE ( 'NONE', #37408, #66547, #3085, .T. ) ;
#48846 = CARTESIAN_POINT ( 'NONE',  ( -14.87820512820512953, -7.500000000000000000, 33.75000000000000000 ) ) ;
#48847 = CARTESIAN_POINT ( 'NONE',  ( 16.82694633287448838, -10.06842814019191401, 34.32929386961144758 ) ) ;
#48848 = CARTESIAN_POINT ( 'NONE',  ( 2.544871794871792936, -7.500000000000000000, 29.75000000000000355 ) ) ;
#48849 = DIRECTION ( 'NONE',  ( -0.000000000000000000, -0.3420201433256694901, -0.9396926207859082059 ) ) ;
#48850 = ORIENTED_EDGE ( 'NONE', *, *, #11291, .T. ) ;
#48851 = ORIENTED_EDGE ( 'NONE', *, *, #82278, .F. ) ;
#48852 = EDGE_LOOP ( 'NONE', ( #87047, #43690, #71898, #72718 ) ) ;
#48855 = VERTEX_POINT ( 'NONE', #43082 ) ;
#48854 = EDGE_CURVE ( 'NONE', #87106, #63890, #13793, .T. ) ;
#48853 = CARTESIAN_POINT ( 'NONE',  ( 4.284636594813105326, -3.957578996910242619, 33.62503395064540257 ) ) ;
#48857 = CARTESIAN_POINT ( 'NONE',  ( -10.39260494640654819, -6.717445702608402236, 34.94155399931962336 ) ) ;
#48856 = CARTESIAN_POINT ( 'NONE',  ( -24.00000000000000000, 5.000000000000023093, 28.74999999999999645 ) ) ;
#48858 = CYLINDRICAL_SURFACE ( 'NONE', #17269, 0.2499999999999994726 ) ;
#48859 = B_SPLINE_CURVE_WITH_KNOTS ( 'NONE', 3,
 ( #40707, #26735, #7360, #5580, #81249, #19535, #34815, #34373, #19972, #61392 ),
 .UNSPECIFIED., .F., .F.,
 ( 4, 2, 2, 2, 4 ),
 ( 0.000000000000000000, 0.0001954339857564080707, 0.0003908679715128161414, 0.0005863019572692241849, 0.0007817359430256322827 ),
 .UNSPECIFIED. ) ;
#48860 = CARTESIAN_POINT ( 'NONE',  ( -1.929879867024197893E-14, -3.750000000000000000, 24.15625000000000000 ) ) ;
#48861 = ORIENTED_EDGE ( 'NONE', *, *, #1243, .T. ) ;
#48862 = EDGE_CURVE ( 'NONE', #74896, #19448, #22801, .T. ) ;
#48863 = ADVANCED_FACE ( 'NONE', ( #64223 ), #2521, .F. ) ;
#48864 = AXIS2_PLACEMENT_3D ( 'NONE', #67184, #31618, #40165 ) ;
#48865 = VERTEX_POINT ( 'NONE', #48500 ) ;
#48866 = CARTESIAN_POINT ( 'NONE',  ( 5.206970512173528576, -7.723484941389743952, 34.99544897038808955 ) ) ;
#48867 = ORIENTED_EDGE ( 'NONE', *, *, #81144, .F. ) ;
#48868 = FACE_BOUND ( 'NONE', #23168, .T. ) ;
#48869 = CARTESIAN_POINT ( 'NONE',  ( 3.296024370282069071, -2.657715359629131857, 31.77849191805844242 ) ) ;
#48870 = CARTESIAN_POINT ( 'NONE',  ( -13.91025641025641058, -7.500000000000000000, 33.75000000000000000 ) ) ;
#48871 = ORIENTED_EDGE ( 'NONE', *, *, #51244, .T. ) ;
#48872 = CARTESIAN_POINT ( 'NONE',  ( 0.5276057948885366500, -8.164416787775445883, 34.95778746994558617 ) ) ;
#48873 = CARTESIAN_POINT ( 'NONE',  ( -16.02305571287920571, -12.62708834333097663, 30.88030960425256310 ) ) ;
#48874 = DIRECTION ( 'NONE',  ( 1.000000000000000000, 0.000000000000000000, 0.000000000000000000 ) ) ;
#48875 = CARTESIAN_POINT ( 'NONE',  ( 0.4615384615383396616, -6.879047030192662504, 34.71129190930017927 ) ) ;
#48876 = CYLINDRICAL_SURFACE ( 'NONE', #13561, 0.2500000000000004996 ) ;
#48878 = ORIENTED_EDGE ( 'NONE', *, *, #26903, .T. ) ;
#48877 = EDGE_CURVE ( 'NONE', #55049, #9891, #42210, .T. ) ;
#48879 = CARTESIAN_POINT ( 'NONE',  ( -0.3963936808188295857, -7.750023224968865421, 34.99404313364389907 ) ) ;
#48880 = CARTESIAN_POINT ( 'NONE',  ( 1.384615384615386802, -3.937682226553329556, 33.60647404775216529 ) ) ;
#48881 = CARTESIAN_POINT ( 'NONE',  ( -6.223484943723947893, -5.912607949931405038, 34.49155766932282319 ) ) ;
#48882 = CYLINDRICAL_SURFACE ( 'NONE', #48635, 0.2500000000000009437 ) ;
#48883 = EDGE_CURVE ( 'NONE', #64502, #86296, #6634, .T. ) ;
#48885 = EDGE_CURVE ( 'NONE', #81622, #47387, #44259, .T. ) ;
#48884 = CARTESIAN_POINT ( 'NONE',  ( 12.22435897435897267, -7.500000000000000000, 29.75000000000000355 ) ) ;
#48886 = FACE_BOUND ( 'NONE', #67804, .T. ) ;
#48888 = CARTESIAN_POINT ( 'NONE',  ( 7.846153846153846700, -13.63283147151868846, 33.57946703557072254 ) ) ;
#48887 = CARTESIAN_POINT ( 'NONE',  ( 17.29993442853592711, -3.587049720035815348, 32.86302985866382897 ) ) ;
#48889 = CARTESIAN_POINT ( 'NONE',  ( 5.076923076922953193, -9.528491918059723176, 34.59228464037033035 ) ) ;
#48891 = CARTESIAN_POINT ( 'NONE',  ( -18.06608237936013239, -2.833524468853756861, 32.15551576947925838 ) ) ;
#48890 = CARTESIAN_POINT ( 'NONE',  ( 3.480769230769167333, -7.565270445406050648, 34.75000000000000000 ) ) ;
#48892 = CARTESIAN_POINT ( 'NONE',  ( -5.326899820971668476, -12.41104346484419452, 31.60698883733904196 ) ) ;
#48893 = CARTESIAN_POINT ( 'NONE',  ( -2.775308065498764964, -6.422011778438537988, 19.92000670625849068 ) ) ;
#48894 = EDGE_CURVE ( 'NONE', #44944, #24055, #10947, .T. ) ;
#48895 = EDGE_LOOP ( 'NONE', ( #86138, #8758 ) ) ;
#48896 = CARTESIAN_POINT ( 'NONE',  ( -2.498132331094908398, -4.694831472195803101, 14.00000000000000178 ) ) ;
#48897 = EDGE_LOOP ( 'NONE', ( #31452, #31445, #27661, #62989 ) ) ;
#48898 = AXIS2_PLACEMENT_3D ( 'NONE', #36376, #87682, #18767 ) ;
#48899 = CARTESIAN_POINT ( 'NONE',  ( -15.16551365949320562, -4.481592998940250538, 33.73612834413965089 ) ) ;
#48900 = VERTEX_POINT ( 'NONE', #38097 ) ;
#48901 = CARTESIAN_POINT ( 'NONE',  ( 1.653273178848927064E-15, -7.500000000000000000, 18.00000000000000355 ) ) ;
#48902 = CARTESIAN_POINT ( 'NONE',  ( -16.15384615384627409, -12.16647553114689728, 32.15551576947799362 ) ) ;
#48903 = ORIENTED_EDGE ( 'NONE', *, *, #32193, .T. ) ;
#48904 = CARTESIAN_POINT ( 'NONE',  ( -15.48074596171158390, -4.943428324936578910, 34.04746400365624481 ) ) ;
#48905 = CARTESIAN_POINT ( 'NONE',  ( -2.775308065498764964, -6.422011778438537988, 19.92000670625849068 ) ) ;
#48906 = B_SPLINE_CURVE_WITH_KNOTS ( 'NONE', 3,
 ( #64947, #59085, #79817, #37936, #52325, #3253, #45125, #18116, #65399, #9569 ),
 .UNSPECIFIED., .F., .F.,
 ( 4, 2, 2, 2, 4 ),
 ( 0.000000000000000000, 0.0001954311564186860613, 0.0003908623128373721225, 0.0005862934692560581567, 0.0007817246256747442451 ),
 .UNSPECIFIED. ) ;
#48907 = AXIS2_PLACEMENT_3D ( 'NONE', #41390, #68855, #55336 ) ;
#48908 = CARTESIAN_POINT ( 'NONE',  ( -10.61538461538461320, -12.62096338111211580, 30.90682066428153263 ) ) ;
#48909 = CARTESIAN_POINT ( 'NONE',  ( -5.207614543590635137, -4.809359713505814149, 33.96456829005828837 ) ) ;
#48910 = VECTOR ( 'NONE', #18966, 1000.000000000000000 ) ;
#48911 = CARTESIAN_POINT ( 'NONE',  ( -17.74999999976641973, -2.249999999999989786, 29.74999979494859303 ) ) ;
#48912 = DIRECTION ( 'NONE',  ( -0.000000000000000000, 0.5000000000000011102, -0.8660254037844380415 ) ) ;
#48913 = CARTESIAN_POINT ( 'NONE',  ( -5.076923076923075762, -4.945431358278436385, 36.03766855953609394 ) ) ;
#48914 = FACE_OUTER_BOUND ( 'NONE', #44703, .T. ) ;
#48915 = CARTESIAN_POINT ( 'NONE',  ( -1.614399933863613468, -11.22469193450124969, 22.61124329374151287 ) ) ;
#48916 = CARTESIAN_POINT ( 'NONE',  ( 11.53846153846141576, -5.941354392335915335, 34.76329471203413846 ) ) ;
#48917 = DIRECTION ( 'NONE',  ( -1.000000000000000000, -0.000000000000000000, -0.000000000000000000 ) ) ;
#48918 = VERTEX_POINT ( 'NONE', #18277 ) ;
#48919 = CARTESIAN_POINT ( 'NONE',  ( 2.307692307692309264, -9.584722331328613620, 36.20867863119891439 ) ) ;
#48920 = CARTESIAN_POINT ( 'NONE',  ( -3.775308065498748977, -8.992201783934593351, 22.76749329374151287 ) ) ;
#48921 = EDGE_CURVE ( 'NONE', #15863, #88652, #75399, .T. ) ;
#48922 = LINE ( 'NONE', #42618, #40407 ) ;
#48923 = CARTESIAN_POINT ( 'NONE',  ( -9.469296340694842939, -11.24521262558773493, 33.06293181088029343 ) ) ;
#48924 = ORIENTED_EDGE ( 'NONE', *, *, #36555, .T. ) ;
#48925 = CARTESIAN_POINT ( 'NONE',  ( 18.00000000000000000, -13.53365097954675988, 30.81389545987213552 ) ) ;
#48926 = CARTESIAN_POINT ( 'NONE',  ( -23.50000000000000000, 5.000000000000023093, 29.24999999999999645 ) ) ;
#48928 = VERTEX_POINT ( 'NONE', #11075 ) ;
#48927 = CARTESIAN_POINT ( 'NONE',  ( 2.242421861731534349, -2.892918686051582533, 31.69288490824015270 ) ) ;
#48929 = CARTESIAN_POINT ( 'NONE',  ( -5.326946314216043810, -5.851115903089112003, 34.47074536777953568 ) ) ;
#48930 = LINE ( 'NONE', #76403, #57898 ) ;
#48931 = CYLINDRICAL_SURFACE ( 'NONE', #8321, 0.2499999999999994726 ) ;
#48932 = EDGE_CURVE ( 'NONE', #74896, #78895, #23840, .T. ) ;
#48933 = DIRECTION ( 'NONE',  ( -0.000000000000000000, 0.6427876096865404731, -0.7660444431189770143 ) ) ;
#48934 = CARTESIAN_POINT ( 'NONE',  ( -15.23076923076922995, -13.20930481340135110, 34.54067556320372745 ) ) ;
#48935 = ORIENTED_EDGE ( 'NONE', *, *, #13976, .T. ) ;
#48936 = DIRECTION ( 'NONE',  ( 0.000000000000000000, 0.9848077530122072432, -0.1736481776669354937 ) ) ;
#48937 = ORIENTED_EDGE ( 'NONE', *, *, #70558, .F. ) ;
#48938 = VERTEX_POINT ( 'NONE', #38548 ) ;
#48939 = FACE_OUTER_BOUND ( 'NONE', #30169, .T. ) ;
#48940 = CARTESIAN_POINT ( 'NONE',  ( -4.153846153846152411, -5.415277668671390821, 36.20867863119892149 ) ) ;
#48941 = CARTESIAN_POINT ( 'NONE',  ( 19.99999999999996803, 15.00000000000000711, 13.00000000000000178 ) ) ;
#48942 = CARTESIAN_POINT ( 'NONE',  ( -19.50000000000000000, -3.499999999999999556, 29.75000000000000355 ) ) ;
#48944 = EDGE_CURVE ( 'NONE', #73852, #5633, #79977, .T. ) ;
#48943 = VERTEX_POINT ( 'NONE', #66002 ) ;
#48945 = CARTESIAN_POINT ( 'NONE',  ( 17.14299041027315695, -11.35647404775217595, 33.31231777344667222 ) ) ;
#48946 = ORIENTED_EDGE ( 'NONE', *, *, #57199, .F. ) ;
#48947 = ORIENTED_EDGE ( 'NONE', *, *, #20852, .T. ) ;
#48948 = VECTOR ( 'NONE', #77825, 1000.000000000000000 ) ;
#48949 = EDGE_LOOP ( 'NONE', ( #40969, #87992, #71336, #26819 ) ) ;
#48951 = ORIENTED_EDGE ( 'NONE', *, *, #8682, .T. ) ;
#48950 = CARTESIAN_POINT ( 'NONE',  ( -15.45425417449318140, -12.24155766932282496, 31.33739205006857986 ) ) ;
#48952 = CARTESIAN_POINT ( 'NONE',  ( -0.6844646790546093928, -4.887634598454295265, 34.01352882383564946 ) ) ;
#48953 = B_SPLINE_CURVE_WITH_KNOTS ( 'NONE', 3,
 ( #20973, #15566, #274, #27740, #61518, #49350 ),
 .UNSPECIFIED., .F., .F.,
 ( 4, 2, 4 ),
 ( 0.0003909569690057822190, 0.0005862646681846078733, 0.0007815723673634334193 ),
 .UNSPECIFIED. ) ;
#48954 = CARTESIAN_POINT ( 'NONE',  ( 15.23076923076923173, -2.499999999999998668, 29.75000000000001421 ) ) ;
#48955 = VECTOR ( 'NONE', #48343, 1000.000000000000227 ) ;
#48956 = VECTOR ( 'NONE', #63600, 1000.000000000000114 ) ;
#48957 = CARTESIAN_POINT ( 'NONE',  ( -9.757578138268467427, -8.613356846314824011, 34.62446782046655613 ) ) ;
#48958 = EDGE_CURVE ( 'NONE', #86398, #42183, #68844, .T. ) ;
#48959 = CARTESIAN_POINT ( 'NONE',  ( 2.307692307692309264, -10.89733346790207413, 36.13435417666054406 ) ) ;
#48960 = ORIENTED_EDGE ( 'NONE', *, *, #49208, .T. ) ;
#48961 = EDGE_CURVE ( 'NONE', #61992, #52419, #59701, .T. ) ;
#48962 = VECTOR ( 'NONE', #37263, 1000.000000000000000 ) ;
#48963 = VERTEX_POINT ( 'NONE', #9736 ) ;
#48964 = VECTOR ( 'NONE', #75907, 1000.000000000000000 ) ;
#48965 = ORIENTED_EDGE ( 'NONE', *, *, #19711, .F. ) ;
#48966 = CARTESIAN_POINT ( 'NONE',  ( -6.857009589726848375, -2.833524468853757750, 32.15551576947925838 ) ) ;
#48968 = ORIENTED_EDGE ( 'NONE', *, *, #37975, .F. ) ;
#48967 = CARTESIAN_POINT ( 'NONE',  ( 1.384615384615386802, -8.120952969808772792, 34.71129190930000163 ) ) ;
#48969 = STYLED_ITEM ( 'NONE', ( #88841 ), #17033 ) ;
#48970 = CARTESIAN_POINT ( 'NONE',  ( 2.144117459101453788E-15, 12.75000000000001066, 13.00000000000000178 ) ) ;
#48971 = CARTESIAN_POINT ( 'NONE',  ( -14.30769230769242739, -2.625532179533778709, 30.86335684631627174 ) ) ;
#48972 = ORIENTED_EDGE ( 'NONE', *, *, #60439, .T. ) ;
#48973 = EDGE_CURVE ( 'NONE', #63168, #18413, #56082, .T. ) ;
#48974 = DIRECTION ( 'NONE',  ( -1.000000000000000000, -0.000000000000000000, -0.000000000000000000 ) ) ;
#48975 = CARTESIAN_POINT ( 'NONE',  ( 9.692307692307695177, -8.164416787775445883, 34.95778746994557906 ) ) ;
#48976 = EDGE_LOOP ( 'NONE', ( #24491, #18142 ) ) ;
#48977 = FACE_BOUND ( 'NONE', #54065, .T. ) ;
#48978 = CARTESIAN_POINT ( 'NONE',  ( -11.76194646302586655, -11.60425143139329940, 33.02411095842164457 ) ) ;
#48979 = CARTESIAN_POINT ( 'NONE',  ( 8.769230769230768274, -1.790695186598648903, 34.54067556320373455 ) ) ;
#48980 = PLANE ( 'NONE',  #40866 ) ;
#48982 = DIRECTION ( 'NONE',  ( 0.000000000000000000, 0.7660444431189807890, 0.6427876096865361433 ) ) ;
#48981 = CARTESIAN_POINT ( 'NONE',  ( 8.096208266067295156, -10.82426656108012075, 33.81400080652039009 ) ) ;
#48983 = CARTESIAN_POINT ( 'NONE',  ( -3.164701897419155419, -3.322132147404559976, 32.92929555188717927 ) ) ;
#48984 = CARTESIAN_POINT ( 'NONE',  ( 18.22277954126840527, -2.847695495035524882, 31.58253572463339154 ) ) ;
#48985 = ORIENTED_EDGE ( 'NONE', *, *, #78684, .F. ) ;
#48986 = CARTESIAN_POINT ( 'NONE',  ( -7.976301815885541657, -6.809168938359901446, 34.95455904226513866 ) ) ;
#48987 = CARTESIAN_POINT ( 'NONE',  ( 5.076923076923075762, -9.780366693483667717, 34.19971097300155094 ) ) ;
#48988 = ORIENTED_EDGE ( 'NONE', *, *, #1561, .F. ) ;
#48989 = CARTESIAN_POINT ( 'NONE',  ( 8.769230769230768274, -11.11383981884818262, 36.00935417666054406 ) ) ;
#48990 = CARTESIAN_POINT ( 'NONE',  ( -4.219928533206287469, -3.322132147404559976, 32.92929555188719348 ) ) ;
#48991 = ORIENTED_EDGE ( 'NONE', *, *, #74577, .T. ) ;
#48992 = CARTESIAN_POINT ( 'NONE',  ( 11.47319153790521717, -10.33852847137145048, 34.16647553114627556 ) ) ;
#48993 = ADVANCED_FACE ( 'NONE', ( #87642 ), #27248, .F. ) ;
#48994 = CARTESIAN_POINT ( 'NONE',  ( 4.376625695114559456, -10.11255958852955672, 34.01340905677048454 ) ) ;
#48995 = FACE_BOUND ( 'NONE', #1201, .T. ) ;
#48997 = CARTESIAN_POINT ( 'NONE',  ( -17.01085472592063397, -12.37446782046654192, 30.86335684631486842 ) ) ;
#48996 = CARTESIAN_POINT ( 'NONE',  ( -1.384615384615383471, -6.343179335718451384, 34.87096338111211935 ) ) ;
#48998 = CARTESIAN_POINT ( 'NONE',  ( 3.296024802045254720, -8.613356846314928816, 34.62446782046653482 ) ) ;
#48999 = B_SPLINE_CURVE_WITH_KNOTS ( 'NONE', 3,
 ( #11264, #22995, #10378, #51321, #38737, #38293, #71179, #9482, #36947, #64410 ),
 .UNSPECIFIED., .F., .F.,
 ( 4, 2, 2, 2, 4 ),
 ( 0.000000000000000000, 0.0001954339857564073388, 0.0003908679715128146777, 0.0005863019572692220165, 0.0007817359430256293554 ),
 .UNSPECIFIED. ) ;
#49000 = CARTESIAN_POINT ( 'NONE',  ( 12.23805353697412812, -12.47654668319379567, 31.42292124445336654 ) ) ;
#49002 = CARTESIAN_POINT ( 'NONE',  ( -12.68502340526241312, -4.386631170607603991, 33.66268669641500111 ) ) ;
#49001 = DIRECTION ( 'NONE',  ( 0.000000000000000000, 0.1736481776669267785, -0.9848077530122087975 ) ) ;
#49003 = VECTOR ( 'NONE', #79488, 999.9999999999998863 ) ;
#49004 = CYLINDRICAL_SURFACE ( 'NONE', #53345, 0.2500000000000004996 ) ;
#49005 = CARTESIAN_POINT ( 'NONE',  ( -0.06109907496455085213, -3.750000000000000888, 17.65438170625849068 ) ) ;
#49006 = EDGE_LOOP ( 'NONE', ( #69807, #80276, #25390, #6827 ) ) ;
#49007 = ORIENTED_EDGE ( 'NONE', *, *, #35770, .T. ) ;
#49008 = CARTESIAN_POINT ( 'NONE',  ( -9.822455662039388358, -2.373036134822904319, 30.88089517874952250 ) ) ;
#49009 = CARTESIAN_POINT ( 'NONE',  ( 14.43821774592595197, -12.70449254468099198, 30.44128974285582956 ) ) ;
#49010 = CARTESIAN_POINT ( 'NONE',  ( 7.146040057343598484, -7.369474539155828730, 34.99858011523957657 ) ) ;
#49011 = DIRECTION ( 'NONE',  ( -0.000000000000000000, -0.9396926207859093161, -0.3420201433256663259 ) ) ;
#49012 = CARTESIAN_POINT ( 'NONE',  ( -13.38461538461538325, -2.486705287966279876, 31.30864560766543647 ) ) ;
#49013 = CARTESIAN_POINT ( 'NONE',  ( -2.608446859217889546, -10.19485399968121264, 15.93563170625849068 ) ) ;
#49014 = CARTESIAN_POINT ( 'NONE',  ( -17.07692307692307665, -9.819645486525091727, 36.12317359536749706 ) ) ;
#49015 = CARTESIAN_POINT ( 'NONE',  ( 4.088576153289833037, -12.16647553114622049, 32.15551576947930812 ) ) ;
#49016 = CARTESIAN_POINT ( 'NONE',  ( 6.249945409378045547, -4.176053281294514363, 33.81426240980091791 ) ) ;
#49017 = CARTESIAN_POINT ( 'NONE',  ( -18.00000000000000000, -2.724637637897661335, 35.44105525097462106 ) ) ;
#49018 = DIRECTION ( 'NONE',  ( -1.000000000000000000, -0.000000000000000000, 0.000000000000000000 ) ) ;
#49019 = CARTESIAN_POINT ( 'NONE',  ( 16.40379167219429490, -5.057305518903949526, 34.11320923018887896 ) ) ;
#49020 = FACE_OUTER_BOUND ( 'NONE', #76431, .T. ) ;
#49021 = CARTESIAN_POINT ( 'NONE',  ( 12.68455130563185662, -2.308499170217967134, 30.53291367094873721 ) ) ;
#49022 = AXIS2_PLACEMENT_3D ( 'NONE', #61172, #33278, #46339 ) ;
#49023 = DIRECTION ( 'NONE',  ( -0.000000000000000000, 0.9848077530122086864, -0.1736481776669273891 ) ) ;
#49024 = ORIENTED_EDGE ( 'NONE', *, *, #66033, .F. ) ;
#49025 = DIRECTION ( 'NONE',  ( 0.000000000000000000, 1.000000000000000000, 8.673617379884034486E-16 ) ) ;
#49026 = CARTESIAN_POINT ( 'NONE',  ( 6.166666666666664298, -3.499999999999999556, 29.75000000000000355 ) ) ;
#49027 = CARTESIAN_POINT ( 'NONE',  ( 1.077988221561497539, -10.27530806549875386, 21.20499329374151998 ) ) ;
#49028 = VECTOR ( 'NONE', #85546, 1000.000000000000114 ) ;
#49029 = CARTESIAN_POINT ( 'NONE',  ( 4.153846153846154188, -4.661471528628507777, 34.16647553114623292 ) ) ;
#49030 = LINE ( 'NONE', #70635, #64870 ) ;
#49031 = VERTEX_POINT ( 'NONE', #25919 ) ;
#49032 = CARTESIAN_POINT ( 'NONE',  ( -7.053224892808621860, -3.069018819979302926, 32.56621877034667278 ) ) ;
#49034 = ORIENTED_EDGE ( 'NONE', *, *, #12405, .T. ) ;
#49033 = CARTESIAN_POINT ( 'NONE',  ( -3.230769230769229949, -1.422936976036506707, 30.56769352161908415 ) ) ;
#49035 = DIRECTION ( 'NONE',  ( -0.000000000000000000, -0.000000000000000000, -1.000000000000000000 ) ) ;
#49036 = CARTESIAN_POINT ( 'NONE',  ( -9.692307692307691624, -5.471508081941601098, 34.59228464037088457 ) ) ;
#49037 = ORIENTED_EDGE ( 'NONE', *, *, #5391, .T. ) ;
#49038 = CARTESIAN_POINT ( 'NONE',  ( 14.30769230769231015, -1.790695186598648903, 34.54067556320373455 ) ) ;
#49039 = CARTESIAN_POINT ( 'NONE',  ( 10.74617505635156789, -10.70102852606553157, 33.91149625220312913 ) ) ;
#49040 = ORIENTED_EDGE ( 'NONE', *, *, #10635, .F. ) ;
#49041 = CARTESIAN_POINT ( 'NONE',  ( 7.384615384615385025, -7.500000000000000000, 33.75000000000000000 ) ) ;
#49042 = CARTESIAN_POINT ( 'NONE',  ( -11.66860950819323861, -12.50552854090298993, 31.33409797877408920 ) ) ;
#49043 = CARTESIAN_POINT ( 'NONE',  ( 9.758375025657768376, -6.343179335718452272, 34.87096338111212646 ) ) ;
#49044 = ORIENTED_EDGE ( 'NONE', *, *, #24899, .F. ) ;
#49045 = ORIENTED_EDGE ( 'NONE', *, *, #36587, .T. ) ;
#49046 = CARTESIAN_POINT ( 'NONE',  ( 15.45354877203763877, -10.81320215134717344, 33.49497208177562868 ) ) ;
#49047 = ORIENTED_EDGE ( 'NONE', *, *, #65645, .T. ) ;
#49048 = CYLINDRICAL_SURFACE ( 'NONE', #28554, 0.2500000000000009437 ) ;
#49049 = CARTESIAN_POINT ( 'NONE',  ( 12.71159277317677549, -9.148310452688876993, 34.47095581063188519 ) ) ;
#49050 = CARTESIAN_POINT ( 'NONE',  ( 13.60739505359345181, -3.563462043263030399, 33.22394488606062879 ) ) ;
#49051 = CARTESIAN_POINT ( 'NONE',  ( -2.438383774359865974, -5.582088688514999397, 34.36776431015576350 ) ) ;
#49052 = CARTESIAN_POINT ( 'NONE',  ( -4.376772371362299019, -6.503392248772476236, 34.64988816332204635 ) ) ;
#49053 = DIRECTION ( 'NONE',  ( 0.000000000000000000, 0.000000000000000000, -1.000000000000000000 ) ) ;
#49054 = CARTESIAN_POINT ( 'NONE',  ( -39.05038313613820122, -2.249999999999998668, 29.75000000000000355 ) ) ;
#49055 = AXIS2_PLACEMENT_3D ( 'NONE', #19370, #32442, #45503 ) ;
#49056 = ORIENTED_EDGE ( 'NONE', *, *, #40773, .T. ) ;
#49057 = ORIENTED_EDGE ( 'NONE', *, *, #74403, .T. ) ;
#49059 = ORIENTED_EDGE ( 'NONE', *, *, #64272, .T. ) ;
#49058 = FACE_OUTER_BOUND ( 'NONE', #55426, .T. ) ;
#49060 = LINE ( 'NONE', #15287, #68120 ) ;
#49061 = EDGE_CURVE ( 'NONE', #18312, #47848, #19604, .T. ) ;
#49062 = ORIENTED_EDGE ( 'NONE', *, *, #47261, .F. ) ;
#49063 = B_SPLINE_CURVE_WITH_KNOTS ( 'NONE', 3,
 ( #15442, #8686, #36162, #63611, #22624, #15886, #43349, #81472, #54419, #81915 ),
 .UNSPECIFIED., .F., .F.,
 ( 4, 2, 2, 2, 4 ),
 ( 0.0007817359430256315238, 0.0009771253907249980580, 0.001172514838424364592, 0.001367904286123731127, 0.001563293733823097661 ),
 .UNSPECIFIED. ) ;
#49064 = FACE_OUTER_BOUND ( 'NONE', #72658, .T. ) ;
#49065 = CARTESIAN_POINT ( 'NONE',  ( 6.673100179028331524, -9.234221910056348293, 34.70572697212741531 ) ) ;
#49067 = ORIENTED_EDGE ( 'NONE', *, *, #87837, .T. ) ;
#49066 = ADVANCED_FACE ( 'NONE', ( #75437 ), #52931, .F. ) ;
#49068 = CARTESIAN_POINT ( 'NONE',  ( 10.61538461538461675, -2.499999999999998668, 29.75000000000001421 ) ) ;
#49069 = VERTEX_POINT ( 'NONE', #66907 ) ;
#49071 = ORIENTED_EDGE ( 'NONE', *, *, #8344, .F. ) ;
#49070 = CARTESIAN_POINT ( 'NONE',  ( -4.284537620513712675, -5.582088688514999397, 34.36776431015576350 ) ) ;
#49072 = CARTESIAN_POINT ( 'NONE',  ( -12.46153846153846168, -12.29105614889573062, 35.45975837776705220 ) ) ;
#49073 = VERTEX_POINT ( 'NONE', #80883 ) ;
#49074 = AXIS2_PLACEMENT_3D ( 'NONE', #68718, #41692, #2030 ) ;
#49075 = ADVANCED_FACE ( 'NONE', ( #40329 ), #68674, .F. ) ;
#49076 = CARTESIAN_POINT ( 'NONE',  ( 15.29683758177167086, -3.050289026998446840, 32.03036669348366416 ) ) ;
#49077 = CARTESIAN_POINT ( 'NONE',  ( -8.899921372341074388, -11.93127051446799847, 32.56575433478202797 ) ) ;
#49078 = FACE_BOUND ( 'NONE', #43190, .T. ) ;
#49079 = DIRECTION ( 'NONE',  ( -0.000000000000000000, 0.8660254037844399289, -0.4999999999999980016 ) ) ;
#49080 = CARTESIAN_POINT ( 'NONE',  ( -17.77722045873158407, -12.24180327182771855, 31.33663988360758168 ) ) ;
#49081 = CIRCLE ( 'NONE', #21773, 0.2500000000000002220 ) ;
#49082 = CARTESIAN_POINT ( 'NONE',  ( 15.36155967173618286, -2.494656445102012565, 31.33466734024120015 ) ) ;
#49083 = DIRECTION ( 'NONE',  ( 1.000000000000000000, 0.000000000000000000, 0.000000000000000000 ) ) ;
#49084 = CARTESIAN_POINT ( 'NONE',  ( -17.29985003582992320, -8.282780595021769443, 34.94152052738834158 ) ) ;
#49085 = DIRECTION ( 'NONE',  ( -0.000000000000000000, -0.7660444431189791237, -0.6427876096865379196 ) ) ;
#49086 = ORIENTED_EDGE ( 'NONE', *, *, #34256, .T. ) ;
#49087 = CARTESIAN_POINT ( 'NONE',  ( -19.50000000000000000, -11.00000000000000000, 28.25000000000000000 ) ) ;
#49088 = ORIENTED_EDGE ( 'NONE', *, *, #83394, .T. ) ;
#49089 = VERTEX_POINT ( 'NONE', #82201 ) ;
#49090 = VECTOR ( 'NONE', #85468, 1000.000000000000227 ) ;
#49092 = CARTESIAN_POINT ( 'NONE',  ( 2.307692307692186251, -11.06231777344772027, 33.60647404775119895 ) ) ;
#49091 = DIRECTION ( 'NONE',  ( -0.000000000000000000, 0.8660254037844399289, -0.4999999999999980016 ) ) ;
#49093 = CARTESIAN_POINT ( 'NONE',  ( -12.68502340526241134, -2.599994579823203367, 30.74605699353653776 ) ) ;
#49094 = DIRECTION ( 'NONE',  ( -0.000000000000000000, -0.3420201433256694346, -0.9396926207859080948 ) ) ;
#49095 = FACE_OUTER_BOUND ( 'NONE', #83288, .T. ) ;
#49096 = LINE ( 'NONE', #48208, #56234 ) ;
#49097 = ORIENTED_EDGE ( 'NONE', *, *, #6766, .F. ) ;
#49098 = EDGE_CURVE ( 'NONE', #24353, #51788, #6100, .T. ) ;
#49099 = CARTESIAN_POINT ( 'NONE',  ( 1.384615384615386802, -9.584722331328613620, 36.20867863119891439 ) ) ;
#49100 = CARTESIAN_POINT ( 'NONE',  ( -6.066083410955878996, -6.386643153685125363, 34.62446782046654903 ) ) ;
#49101 = LINE ( 'NONE', #15771, #64668 ) ;
#49102 = EDGE_CURVE ( 'NONE', #59690, #16656, #74278, .T. ) ;
#49103 = CARTESIAN_POINT ( 'NONE',  ( -15.23076923076922995, -13.95598074871891292, 31.83374038241031911 ) ) ;
#49104 = CARTESIAN_POINT ( 'NONE',  ( 2.438217745925954194, -5.915461855592777596, 34.75538340440931506 ) ) ;
#49105 = ORIENTED_EDGE ( 'NONE', *, *, #11258, .T. ) ;
#49106 = B_SPLINE_CURVE_WITH_KNOTS ( 'NONE', 3,
 ( #86506, #79736, #24782, #52249, #24165, #8897, #36368, #37233, #44424, #85436 ),
 .UNSPECIFIED., .F., .F.,
 ( 4, 2, 2, 2, 4 ),
 ( 0.000000000000000000, 0.0001954311564186862239, 0.0003908623128373724478, 0.0005862934692560586988, 0.0007817246256747448956 ),
 .UNSPECIFIED. ) ;
#49107 = CARTESIAN_POINT ( 'NONE',  ( -4.826923076921656452, -7.500000000000154543, 35.00000000000007105 ) ) ;
#49108 = VERTEX_POINT ( 'NONE', #11974 ) ;
#49109 = EDGE_CURVE ( 'NONE', #45585, #30008, #12077, .T. ) ;
#49110 = VERTEX_POINT ( 'NONE', #60137 ) ;
#49111 = EDGE_CURVE ( 'NONE', #33529, #55035, #63572, .T. ) ;
#49112 = DIRECTION ( 'NONE',  ( -0.000000000000000000, 0.1736481776669307198, -0.9848077530122080203 ) ) ;
#49113 = ORIENTED_EDGE ( 'NONE', *, *, #655, .T. ) ;
#49114 = FACE_OUTER_BOUND ( 'NONE', #41129, .T. ) ;
#49115 = CARTESIAN_POINT ( 'NONE',  ( -17.30040802064702987, -3.236172620538810385, 32.36188796281389557 ) ) ;
#49116 = CARTESIAN_POINT ( 'NONE',  ( 14.05771556364371655, -10.06842814019191401, 34.32929386961144758 ) ) ;
#49117 = CARTESIAN_POINT ( 'NONE',  ( 2.307692307692309264, -9.905515769479276145, 34.41647553114623292 ) ) ;
#49118 = CARTESIAN_POINT ( 'NONE',  ( -16.82697755857493505, -12.22109172314383052, 31.39792113162168263 ) ) ;
#49119 = CARTESIAN_POINT ( 'NONE',  ( 8.769230769230768274, -6.386643153685126251, 34.62446782046654192 ) ) ;
#49120 = EDGE_LOOP ( 'NONE', ( #76665, #88749 ) ) ;
#49121 = CYLINDRICAL_SURFACE ( 'NONE', #84673, 0.2499999999999998890 ) ;
#49123 = ORIENTED_EDGE ( 'NONE', *, *, #58218, .F. ) ;
#49122 = FACE_OUTER_BOUND ( 'NONE', #41271, .T. ) ;
#49124 = CARTESIAN_POINT ( 'NONE',  ( -3.480769230769241052, -2.499999999999999556, 29.81609845454692120 ) ) ;
#49125 = FACE_OUTER_BOUND ( 'NONE', #50934, .T. ) ;
#49126 = CARTESIAN_POINT ( 'NONE',  ( 17.32686859527121825, -11.37275283266504111, 32.91324779482534524 ) ) ;
#49127 = CARTESIAN_POINT ( 'NONE',  ( -3.230769230769351186, -5.219633306517616589, 34.19971097300220464 ) ) ;
#49128 = CARTESIAN_POINT ( 'NONE',  ( -17.93393266664992325, -10.67929555188718282, 33.92786785259543336 ) ) ;
#49129 = DIRECTION ( 'NONE',  ( -0.000000000000000000, 0.6427876096865404731, -0.7660444431189770143 ) ) ;
#49130 = CARTESIAN_POINT ( 'NONE',  ( 18.00000000000000000, -1.367168528481310208, 33.57946703557072254 ) ) ;
#49131 = AXIS2_PLACEMENT_3D ( 'NONE', #36618, #57325, #16775 ) ;
#49132 = CARTESIAN_POINT ( 'NONE',  ( -2.775308065498752086, -8.577988221561495763, 24.01749329374151287 ) ) ;
#49133 = EDGE_LOOP ( 'NONE', ( #38347, #38925, #4185, #65517 ) ) ;
#49134 = CARTESIAN_POINT ( 'NONE',  ( -15.36091720050093024, -6.809168938359901446, 34.95455904226513866 ) ) ;
#49135 = CARTESIAN_POINT ( 'NONE',  ( 1.253924781505078689, -9.084618155246140248, 34.75535874321725771 ) ) ;
#49136 = B_SPLINE_CURVE_WITH_KNOTS ( 'NONE', 3,
 ( #26730, #19529, #83012, #69049, #75367, #54190, #82582, #34368, #7356, #76239 ),
 .UNSPECIFIED., .F., .F.,
 ( 4, 2, 2, 2, 4 ),
 ( 0.000000000000000000, 0.0001954311564186867389, 0.0003908623128373734778, 0.0005862934692560602167, 0.0007817246256747469556 ),
 .UNSPECIFIED. ) ;
#49137 = CARTESIAN_POINT ( 'NONE',  ( 7.911409417429874580, -2.625532179533470512, 30.86335684631491105 ) ) ;
#49138 = CARTESIAN_POINT ( 'NONE',  ( 13.38461538461538680, -2.499999999999998668, 29.50000000000001066 ) ) ;
#49139 = VERTEX_POINT ( 'NONE', #88102 ) ;
#49140 = CARTESIAN_POINT ( 'NONE',  ( -2.749999999999991562, -8.639087296526026805, 15.01562500000000178 ) ) ;
#49141 = CARTESIAN_POINT ( 'NONE',  ( 1.384615384615386802, -9.780366693483667717, 34.19971097300155094 ) ) ;
#49142 = CARTESIAN_POINT ( 'NONE',  ( -0.5268084620947806052, -12.70778746994557551, 30.41441678777548319 ) ) ;
#49143 = CARTESIAN_POINT ( 'NONE',  ( 2.980769230769232170, -7.500000000000001776, 35.04278698407183867 ) ) ;
#49144 = ORIENTED_EDGE ( 'NONE', *, *, #62026, .T. ) ;
#49145 = EDGE_CURVE ( 'NONE', #34884, #78839, #19563, .T. ) ;
#49146 = CARTESIAN_POINT ( 'NONE',  ( 6.066068351002440906, -5.557115091759786019, 34.35708131394839882 ) ) ;
#49147 = DIRECTION ( 'NONE',  ( -0.000000000000000000, 1.000000000000000000, -0.000000000000000000 ) ) ;
#49148 = CARTESIAN_POINT ( 'NONE',  ( 4.153846153846032507, -2.625532179533778709, 30.86335684631627174 ) ) ;
#49149 = ORIENTED_EDGE ( 'NONE', *, *, #73577, .T. ) ;
#49150 = CARTESIAN_POINT ( 'NONE',  ( -13.16183571563731647, -3.020022701398813236, 32.48759521482552515 ) ) ;
#49151 = VECTOR ( 'NONE', #20077, 1000.000000000000114 ) ;
#49152 = EDGE_LOOP ( 'NONE', ( #69005, #7856 ) ) ;
#49153 = CARTESIAN_POINT ( 'NONE',  ( -16.37733109757010652, -5.912607949931405038, 34.49155766932282319 ) ) ;
#49154 = DIRECTION ( 'NONE',  ( -0.000000000000000000, -0.5000000000000009992, -0.8660254037844380415 ) ) ;
#49155 = ORIENTED_EDGE ( 'NONE', *, *, #67473, .F. ) ;
#49156 = CARTESIAN_POINT ( 'NONE',  ( 10.86533002476265786, -11.56426240980093745, 33.07394671870546432 ) ) ;
#49157 = DIRECTION ( 'NONE',  ( -1.000000000000000000, 0.000000000000000000, 0.000000000000000000 ) ) ;
#49158 = CARTESIAN_POINT ( 'NONE',  ( 0.3954550505825801254, -4.098570777380720287, 33.41473453929635440 ) ) ;
#49159 = VECTOR ( 'NONE', #89165, 1000.000000000000227 ) ;
#49160 = EDGE_CURVE ( 'NONE', #7198, #31425, #54967, .T. ) ;
#49161 = CARTESIAN_POINT ( 'NONE',  ( 17.07692307692307665, -10.51840700105979565, 33.73612834413961536 ) ) ;
#49162 = CARTESIAN_POINT ( 'NONE',  ( -18.06608341095587278, -4.098570777380720287, 33.41473453929634019 ) ) ;
#49163 = B_SPLINE_CURVE_WITH_KNOTS ( 'NONE', 3,
 ( #56090, #68276, #68719, #27289, #264, #61954, #82242, #61071, #75473, #1147 ),
 .UNSPECIFIED., .F., .F.,
 ( 4, 2, 2, 2, 4 ),
 ( 0.000000000000000000, 0.0001954311564186887718, 0.0003908623128373775435, 0.0005862934692560662882, 0.0007817246256747550871 ),
 .UNSPECIFIED. ) ;
#49164 = B_SPLINE_CURVE_WITH_KNOTS ( 'NONE', 3,
 ( #19486, #47394, #21252, #27575, #46948, #6857, #54592, #82970, #13616, #26689 ),
 .UNSPECIFIED., .F., .F.,
 ( 4, 2, 2, 2, 4 ),
 ( 0.000000000000000000, 0.0001954311564186869557, 0.0003908623128373739115, 0.0005862934692560608672, 0.0007817246256747478229 ),
 .UNSPECIFIED. ) ;
#49165 = EDGE_LOOP ( 'NONE', ( #21587, #17560, #56832, #24355 ) ) ;
#49166 = ORIENTED_EDGE ( 'NONE', *, *, #66406, .F. ) ;
#49167 = FACE_BOUND ( 'NONE', #50136, .T. ) ;
#49168 = EDGE_LOOP ( 'NONE', ( #62842, #7655, #34347, #21098 ) ) ;
#49169 = CARTESIAN_POINT ( 'NONE',  ( 8.519207531937803779, -3.711651800289232028, 33.01384336483936011 ) ) ;
#49170 = EDGE_CURVE ( 'NONE', #88377, #41347, #62351, .T. ) ;
#49171 = FACE_OUTER_BOUND ( 'NONE', #33202, .T. ) ;
#49172 = CARTESIAN_POINT ( 'NONE',  ( 6.222779668978062340, -3.020022701398814569, 32.48759521482552515 ) ) ;
#49173 = CARTESIAN_POINT ( 'NONE',  ( 5.076923076922954969, -4.481592998941358097, 33.73612834414048933 ) ) ;
#49174 = EDGE_CURVE ( 'NONE', #2875, #53698, #61910, .T. ) ;
#49175 = VERTEX_POINT ( 'NONE', #56495 ) ;
#49176 = EDGE_LOOP ( 'NONE', ( #71256, #48946 ) ) ;
#49177 = EDGE_LOOP ( 'NONE', ( #46550, #43079, #86776, #41207 ) ) ;
#49178 = B_SPLINE_CURVE_WITH_KNOTS ( 'NONE', 3,
 ( #85907, #10692, #44450, #51646, #25539, #85462, #45352, #79148, #18337, #17449 ),
 .UNSPECIFIED., .F., .F.,
 ( 4, 2, 2, 2, 4 ),
 ( 0.0007817246256747469556, 0.0009771112852218902852, 0.001172497944769033615, 0.001367884604316176728, 0.001563271263863320057 ),
 .UNSPECIFIED. ) ;
#49179 = VECTOR ( 'NONE', #76344, 1000.000000000000000 ) ;
#49180 = CARTESIAN_POINT ( 'NONE',  ( -0.3310127597748959705, -3.285477652293412820, 32.44071101563363158 ) ) ;
#49181 = ORIENTED_EDGE ( 'NONE', *, *, #88466, .T. ) ;
#49182 = EDGE_CURVE ( 'NONE', #38219, #36959, #69562, .T. ) ;
#49183 = CARTESIAN_POINT ( 'NONE',  ( -13.38461538461538325, -1.790695186598648903, 34.54067556320373455 ) ) ;
#49184 = CARTESIAN_POINT ( 'NONE',  ( -6.673076923076923350, -2.249999999999998668, 29.75000000000000355 ) ) ;
#49185 = CARTESIAN_POINT ( 'NONE',  ( -18.22292695890684655, -6.459968553980840689, 34.89616026154728701 ) ) ;
#49186 = ORIENTED_EDGE ( 'NONE', *, *, #50596, .T. ) ;
#49187 = CARTESIAN_POINT ( 'NONE',  ( 13.13459214732242408, -10.76384336483936011, 33.53834819971076087 ) ) ;
#49188 = EDGE_CURVE ( 'NONE', #18436, #44265, #34548, .T. ) ;
#49189 = CARTESIAN_POINT ( 'NONE',  ( 20.00000000000000000, -7.500000000000000000, 29.75000000000000355 ) ) ;
#49190 = DIRECTION ( 'NONE',  ( -0.000000000000000000, 1.000000000000000000, 3.491481338843133355E-15 ) ) ;
#49191 = CARTESIAN_POINT ( 'NONE',  ( -11.76194648218548444, -3.236172620538810385, 32.36188796281390267 ) ) ;
#49192 = EDGE_LOOP ( 'NONE', ( #1177, #21371, #35454, #62564 ) ) ;
#49193 = ADVANCED_FACE ( 'NONE', ( #21820 ), #35332, .F. ) ;
#49194 = B_SPLINE_CURVE_WITH_KNOTS ( 'NONE', 3,
 ( #80344, #4676, #10989, #58270, #65020, #65480, #78544, #16848, #59163, #17748 ),
 .UNSPECIFIED., .F., .F.,
 ( 4, 2, 2, 2, 4 ),
 ( 0.0007817246256747524850, 0.0009771112852218967904, 0.001172497944769040987, 0.001367884604316185184, 0.001563271263863329381 ),
 .UNSPECIFIED. ) ;
#49195 = ORIENTED_EDGE ( 'NONE', *, *, #39995, .T. ) ;
#49196 = B_SPLINE_CURVE_WITH_KNOTS ( 'NONE', 3,
 ( #23259, #77326, #43098, #43534, #70574, #78208, #8877, #71443, #36346, #22819 ),
 .UNSPECIFIED., .F., .F.,
 ( 4, 2, 2, 2, 4 ),
 ( 0.000000000000000000, 0.0001954339857564093175, 0.0003908679715128186350, 0.0005863019572692279796, 0.0007817359430256372700 ),
 .UNSPECIFIED. ) ;
#49197 = ORIENTED_EDGE ( 'NONE', *, *, #13721, .F. ) ;
#49198 = CARTESIAN_POINT ( 'NONE',  ( 4.087763774486018242, -2.833524468853757305, 32.15551576947924417 ) ) ;
#49199 = B_SPLINE_CURVE_WITH_KNOTS ( 'NONE', 3,
 ( #21143, #33782, #75642, #74331, #41876, #47734, #33345, #27025, #20270, #87870 ),
 .UNSPECIFIED., .F., .F.,
 ( 4, 2, 2, 2, 4 ),
 ( 0.000000000000000000, 0.0001954339857564089923, 0.0003908679715128179845, 0.0005863019572692270039, 0.0007817359430256359690 ),
 .UNSPECIFIED. ) ;
#49200 = UNCERTAINTY_MEASURE_WITH_UNIT (LENGTH_MEASURE( 1.000000000000000082E-05 ), #55033, 'distance_accuracy_value', 'NONE');
#49202 = CARTESIAN_POINT ( 'NONE',  ( 10.86543892702292879, -6.567000820036036579, 34.66262288849541306 ) ) ;
#49201 = CARTESIAN_POINT ( 'NONE',  ( 12.46153846153833911, -6.879047030192662504, 34.71129190930017927 ) ) ;
#49203 = CARTESIAN_POINT ( 'NONE',  ( 11.40831356872984514, -2.373036134822904319, 30.88089517874952250 ) ) ;
#49204 = CARTESIAN_POINT ( 'NONE',  ( -6.923076923076922462, -3.513871655860378418, 32.76840700105978499 ) ) ;
#49205 = FACE_BOUND ( 'NONE', #58462, .T. ) ;
#49206 = CARTESIAN_POINT ( 'NONE',  ( -0.4615384615384611200, -5.180354513474913603, 36.12317359536750416 ) ) ;
#49207 = ORIENTED_EDGE ( 'NONE', *, *, #43182, .F. ) ;
#49208 = EDGE_CURVE ( 'NONE', #64959, #81167, #5528, .T. ) ;
#49209 = CARTESIAN_POINT ( 'NONE',  ( 17.32697738856138869, -10.66356715214248574, 33.62249196103329751 ) ) ;
#49210 = LINE ( 'NONE', #48759, #33021 ) ;
#49211 = DIRECTION ( 'NONE',  ( -0.000000000000000000, 0.8660254037844397068, -0.4999999999999978906 ) ) ;
#49212 = CARTESIAN_POINT ( 'NONE',  ( -19.00000000000000000, 16.99999999999999289, 23.75000000000000000 ) ) ;
#49213 = ORIENTED_EDGE ( 'NONE', *, *, #82110, .T. ) ;
#49214 = CARTESIAN_POINT ( 'NONE',  ( 6.066067333350078528, -10.67929555188718282, 33.92786785259544757 ) ) ;
#49215 = ORIENTED_EDGE ( 'NONE', *, *, #34417, .T. ) ;
#49216 = FACE_BOUND ( 'NONE', #66339, .T. ) ;
#49218 = AXIS2_PLACEMENT_3D ( 'NONE', #56645, #22414, #25075 ) ;
#49217 = CYLINDRICAL_SURFACE ( 'NONE', #84962, 0.2499999999999998890 ) ;
#49219 = VECTOR ( 'NONE', #37751, 1000.000000000000000 ) ;
#49220 = EDGE_CURVE ( 'NONE', #88554, #64611, #37735, .T. ) ;
#49221 = DIRECTION ( 'NONE',  ( -0.000000000000000000, 0.9396926207859093161, -0.3420201433256663259 ) ) ;
#49223 = ADVANCED_FACE ( 'NONE', ( #56926 ), #43424, .F. ) ;
#49222 = CARTESIAN_POINT ( 'NONE',  ( 14.24160889673642671, -11.69971097300155272, 32.46337939537587403 ) ) ;
#49224 = ORIENTED_EDGE ( 'NONE', *, *, #39432, .F. ) ;
#49225 = CARTESIAN_POINT ( 'NONE',  ( -14.30769230769230660, -12.37446782046654192, 30.86335684631486131 ) ) ;
#49226 = CARTESIAN_POINT ( 'NONE',  ( -3.230769230769229949, -2.292212530054420494, 30.41441678777542634 ) ) ;
#49227 = CARTESIAN_POINT ( 'NONE',  ( -14.98082382139118884, -10.18230066228895758, 34.26354781536631577 ) ) ;
#49228 = CARTESIAN_POINT ( 'NONE',  ( 0.000000000000000000, -11.00000000000000000, 29.75000000000000355 ) ) ;
#49229 = ORIENTED_EDGE ( 'NONE', *, *, #8313, .T. ) ;
#49230 = VECTOR ( 'NONE', #44367, 1000.000000000000000 ) ;
#49231 = FACE_OUTER_BOUND ( 'NONE', #56382, .T. ) ;
#49232 = ORIENTED_EDGE ( 'NONE', *, *, #55161, .T. ) ;
#49234 = ORIENTED_EDGE ( 'NONE', *, *, #44474, .F. ) ;
#49233 = CARTESIAN_POINT ( 'NONE',  ( 5.999999999999878320, -5.941354392335915335, 34.76329471203413846 ) ) ;
#49235 = CARTESIAN_POINT ( 'NONE',  ( 9.468822748583743731, -3.754499324213721234, 33.06261337010820256 ) ) ;
#49236 = CYLINDRICAL_SURFACE ( 'NONE', #12524, 0.2500000000000009437 ) ;
#49237 = CARTESIAN_POINT ( 'NONE',  ( 13.16168916709923487, -9.086856451489515152, 34.49173150075333183 ) ) ;
#49238 = CARTESIAN_POINT ( 'NONE',  ( -10.48485891362104994, -2.619367082507849442, 30.83698974864643461 ) ) ;
#49239 = CARTESIAN_POINT ( 'NONE',  ( -4.023320452082590037, -12.45806712695776319, 30.39783852428763922 ) ) ;
#49241 = CARTESIAN_POINT ( 'NONE',  ( 8.519254025182180001, -4.075325502946081535, 33.72974371597206300 ) ) ;
#49240 = CARTESIAN_POINT ( 'NONE',  ( -8.069080063669987979, -10.61292498521070549, 33.66303323003028680 ) ) ;
#49242 = CARTESIAN_POINT ( 'NONE',  ( -11.25641025641025550, -3.499999999999999556, 29.75000000000000355 ) ) ;
#49243 = B_SPLINE_CURVE_WITH_KNOTS ( 'NONE', 3,
 ( #33700, #34136, #62480, #795, #82338, #7111, #28260, #40903, #56183, #27387 ),
 .UNSPECIFIED., .F., .F.,
 ( 4, 2, 2, 2, 4 ),
 ( 0.000000000000000000, 0.0001954339857564091278, 0.0003908679715128182556, 0.0005863019572692274375, 0.0007817359430256365111 ),
 .UNSPECIFIED. ) ;
#49244 = CARTESIAN_POINT ( 'NONE',  ( 1.799775606325937360E-14, -10.25000000000000000, 26.03125000000000000 ) ) ;
#49245 = EDGE_LOOP ( 'NONE', ( #10456, #43201, #88541, #39753 ) ) ;
#49246 = DIRECTION ( 'NONE',  ( 0.000000000000000000, 0.000000000000000000, -1.000000000000000000 ) ) ;
#49247 = EDGE_LOOP ( 'NONE', ( #15510, #33128, #34146, #62581 ) ) ;
#49248 = EDGE_CURVE ( 'NONE', #89050, #42119, #50614, .T. ) ;
#49249 = ORIENTED_EDGE ( 'NONE', *, *, #77235, .T. ) ;
#49250 = CARTESIAN_POINT ( 'NONE',  ( -16.02332071561251325, -6.808710257144159783, 34.95449254468098843 ) ) ;
#49251 = ORIENTED_EDGE ( 'NONE', *, *, #75539, .T. ) ;
#49252 = LINE ( 'NONE', #37046, #77171 ) ;
#49253 = B_SPLINE_CURVE_WITH_KNOTS ( 'NONE', 3,
 ( #88304, #19815, #47278, #40102, #32885, #53143, #26574, #54030, #61671, #80647 ),
 .UNSPECIFIED., .F., .F.,
 ( 4, 2, 2, 2, 4 ),
 ( 0.0007817246256747470640, 0.0009771112852218898515, 0.001172497944769032747, 0.001367884604316175643, 0.001563271263863318539 ),
 .UNSPECIFIED. ) ;
#49254 = CARTESIAN_POINT ( 'NONE',  ( -2.057746789344163663, -6.696923467548660192, 34.68552623307873972 ) ) ;
#49255 = CARTESIAN_POINT ( 'NONE',  ( -6.923076923076922462, -9.058645607665452459, 34.76329471203371924 ) ) ;
#49256 = CARTESIAN_POINT ( 'NONE',  ( 10.68145194873469173, -6.343179335718452272, 34.87096338111212646 ) ) ;
#49257 = CARTESIAN_POINT ( 'NONE',  ( 1.384615384615386802, -1.790695186598648903, 34.54067556320373455 ) ) ;
#49258 = DIRECTION ( 'NONE',  ( -0.000000000000000000, -0.000000000000000000, 1.000000000000000000 ) ) ;
#49259 = DIRECTION ( 'NONE',  ( -0.000000000000000000, -0.1736481776669307198, -0.9848077530122080203 ) ) ;
#49260 = EDGE_CURVE ( 'NONE', #48900, #58457, #3426, .T. ) ;
#49261 = CARTESIAN_POINT ( 'NONE',  ( 6.792386319966614572, -9.929715669179216775, 34.40415004197138416 ) ) ;
#49262 = CARTESIAN_POINT ( 'NONE',  ( 1.384615384615386802, -5.180354513474913603, 36.12317359536750416 ) ) ;
#49263 = DIRECTION ( 'NONE',  ( 1.000000000000000000, 0.000000000000000000, 0.000000000000000000 ) ) ;
#49264 = CARTESIAN_POINT ( 'NONE',  ( 13.38461538461538680, -2.249999999999998668, 29.50000000000001421 ) ) ;
#49265 = EDGE_CURVE ( 'NONE', #8287, #20476, #64119, .T. ) ;
#49266 = EDGE_CURVE ( 'NONE', #8131, #68101, #45183, .T. ) ;
#49267 = ORIENTED_EDGE ( 'NONE', *, *, #7407, .F. ) ;
#49268 = ORIENTED_EDGE ( 'NONE', *, *, #64615, .F. ) ;
#49269 = CARTESIAN_POINT ( 'NONE',  ( 3.165499230212911019, -11.06231777344662781, 33.60647404775220082 ) ) ;
#49270 =( LENGTH_UNIT ( ) NAMED_UNIT ( * ) SI_UNIT ( .MILLI., .METRE. ) );
#49271 = DIRECTION ( 'NONE',  ( -1.000000000000000000, -0.000000000000000000, -0.000000000000000000 ) ) ;
#49272 = CARTESIAN_POINT ( 'NONE',  ( 0.4615384615384611200, -9.905515769479276145, 34.41647553114623292 ) ) ;
#49273 = ORIENTED_EDGE ( 'NONE', *, *, #87534, .F. ) ;
#49274 = CARTESIAN_POINT ( 'NONE',  ( -15.93106648486808119, -8.540255544307068902, 34.89611431652622286 ) ) ;
#49275 = CARTESIAN_POINT ( 'NONE',  ( 4.153846153846154188, -13.20930481340135110, 34.54067556320372745 ) ) ;
#49276 = ADVANCED_FACE ( 'NONE', ( #51476 ), #16389, .F. ) ;
#49277 = CARTESIAN_POINT ( 'NONE',  ( 9.019176287578908102, -4.336752205174649433, 33.62275283266504289 ) ) ;
#49278 = VERTEX_POINT ( 'NONE', #37094 ) ;
#49279 = CARTESIAN_POINT ( 'NONE',  ( -13.60810032833933469, -10.11188796281391511, 34.01382737946119050 ) ) ;
#49280 = ORIENTED_EDGE ( 'NONE', *, *, #61175, .F. ) ;
#49281 = DIRECTION ( 'NONE',  ( 0.000000000000000000, 0.000000000000000000, -1.000000000000000000 ) ) ;
#49282 = AXIS2_PLACEMENT_3D ( 'NONE', #67577, #41881, #74334 ) ;
#49283 = CARTESIAN_POINT ( 'NONE',  ( -2.307692307692305711, -13.78497067705608181, 32.30358669280327177 ) ) ;
#49284 = CARTESIAN_POINT ( 'NONE',  ( 12.39626801557768587, -8.613356846314824011, 34.62446782046655613 ) ) ;
#49285 = CARTESIAN_POINT ( 'NONE',  ( 3.164686851409094448, -8.164416787775445883, 34.95778746994557906 ) ) ;
#49286 = CARTESIAN_POINT ( 'NONE',  ( -18.00000000000000000, -12.34228464037088635, 31.77849191805839268 ) ) ;
#49287 = ADVANCED_FACE ( 'NONE', ( #30784 ), #52383, .F. ) ;
#49288 = EDGE_LOOP ( 'NONE', ( #72692, #66298, #85645, #75013 ) ) ;
#49289 = EDGE_CURVE ( 'NONE', #25149, #67006, #30239, .T. ) ;
#49290 = EDGE_LOOP ( 'NONE', ( #36719, #47907, #55504, #56611 ) ) ;
#49291 = EDGE_LOOP ( 'NONE', ( #40493, #73768 ) ) ;
#49292 = ORIENTED_EDGE ( 'NONE', *, *, #46483, .F. ) ;
#49293 = CARTESIAN_POINT ( 'NONE',  ( -6.130691466667556710, -11.18331474514187995, 33.13161551792790505 ) ) ;
#49294 = CARTESIAN_POINT ( 'NONE',  ( 13.38461538461538680, -9.780366693483667717, 34.19971097300155094 ) ) ;
#49295 = CARTESIAN_POINT ( 'NONE',  ( 17.20771488474786892, -4.118422570099827595, 33.43335022499816489 ) ) ;
#49296 = CARTESIAN_POINT ( 'NONE',  ( 11.31553532094538994, -12.15238873228292071, 31.58232369045353849 ) ) ;
#49297 = B_SPLINE_CURVE_WITH_KNOTS ( 'NONE', 3,
 ( #37442, #51374, #3656, #31129, #38346, #65800, #4100, #66252, #32922, #54513 ),
 .UNSPECIFIED., .F., .F.,
 ( 4, 2, 2, 2, 4 ),
 ( 0.000000000000000000, 0.0001954339857564077183, 0.0003908679715128154366, 0.0005863019572692231007, 0.0007817359430256308733 ),
 .UNSPECIFIED. ) ;
#49298 = CARTESIAN_POINT ( 'NONE',  ( -10.36538461538319389, -7.500000000000154543, 35.00000000000007105 ) ) ;
#49299 = DIRECTION ( 'NONE',  ( -1.000000000000000000, -0.000000000000000000, 0.000000000000000000 ) ) ;
#49300 = EDGE_LOOP ( 'NONE', ( #45561, #86074, #23378, #73485 ) ) ;
#49301 = VERTEX_POINT ( 'NONE', #24919 ) ;
#49302 = ORIENTED_EDGE ( 'NONE', *, *, #37463, .F. ) ;
#49304 = ORIENTED_EDGE ( 'NONE', *, *, #69002, .T. ) ;
#49303 = CARTESIAN_POINT ( 'NONE',  ( 12.71159277317677549, -8.303483539816731707, 34.68545999027711702 ) ) ;
#49305 = CIRCLE ( 'NONE', #85315, 0.2500000000000002220 ) ;
#49307 = CARTESIAN_POINT ( 'NONE',  ( -5.076923076923199218, -12.70778746994576025, 30.41441678777401236 ) ) ;
#49306 = CARTESIAN_POINT ( 'NONE',  ( -16.85414353565466072, -9.332535724633405749, 34.40230450496446224 ) ) ;
#49308 = DIRECTION ( 'NONE',  ( 1.000000000000000000, 0.000000000000000000, 0.000000000000000000 ) ) ;
#49309 = AXIS2_PLACEMENT_3D ( 'NONE', #78653, #17852, #45304 ) ;
#49310 = B_SPLINE_CURVE_WITH_KNOTS ( 'NONE', 3,
 ( #43939, #9709, #1637, #37178, #64641, #63765, #56574, #84064, #29552, #86738 ),
 .UNSPECIFIED., .F., .F.,
 ( 4, 2, 2, 2, 4 ),
 ( 0.000000000000000000, 0.0001954339857564063089, 0.0003908679715128126177, 0.0005863019572692189808, 0.0007817359430256252354 ),
 .UNSPECIFIED. ) ;
#49311 = CARTESIAN_POINT ( 'NONE',  ( -10.83831083290076158, -11.76352882383564769, 32.36236540154569497 ) ) ;
#49312 = EDGE_LOOP ( 'NONE', ( #33658, #82190 ) ) ;
#49313 = EDGE_CURVE ( 'NONE', #30501, #48096, #79872, .T. ) ;
#49314 = EDGE_CURVE ( 'NONE', #75229, #13394, #73112, .T. ) ;
#49315 = ORIENTED_EDGE ( 'NONE', *, *, #73936, .T. ) ;
#49316 = DIRECTION ( 'NONE',  ( 0.000000000000000000, -6.938893903907222067E-15, 1.000000000000000000 ) ) ;
#49318 = EDGE_CURVE ( 'NONE', #86922, #72884, #73322, .T. ) ;
#49317 = VERTEX_POINT ( 'NONE', #23146 ) ;
#49319 = FACE_BOUND ( 'NONE', #7120, .T. ) ;
#49320 = CARTESIAN_POINT ( 'NONE',  ( -2.084679463598912097, -4.762714258010882773, 34.23016756924214832 ) ) ;
#49321 = CARTESIAN_POINT ( 'NONE',  ( 5.198717948717946236, -3.499999999999999556, 29.75000000000000355 ) ) ;
#49322 = ORIENTED_EDGE ( 'NONE', *, *, #15954, .F. ) ;
#49323 = CARTESIAN_POINT ( 'NONE',  ( -39.05038313613820122, -2.249999999999998668, 29.75000000000000355 ) ) ;
#49325 = EDGE_CURVE ( 'NONE', #9234, #82350, #36773, .T. ) ;
#49324 = CARTESIAN_POINT ( 'NONE',  ( 11.28848479441294650, -6.524016743844655686, 34.90889640711025521 ) ) ;
#49326 = CARTESIAN_POINT ( 'NONE',  ( 10.55011416942384272, -2.892918686051582533, 31.69288490824015980 ) ) ;
#49327 = CARTESIAN_POINT ( 'NONE',  ( -15.36146069743678844, -6.413092428213692742, 34.63065189839063152 ) ) ;
#49328 = CARTESIAN_POINT ( 'NONE',  ( -4.153846153846274980, -5.094484230521993062, 34.41647553114689373 ) ) ;
#49329 = EDGE_LOOP ( 'NONE', ( #69853, #68781, #45482, #45928 ) ) ;
#49330 = EDGE_CURVE ( 'NONE', #86499, #22286, #39994, .T. ) ;
#49331 = CARTESIAN_POINT ( 'NONE',  ( -11.53846153846166089, -12.51329471203414379, 31.30864560766407578 ) ) ;
#49332 = LINE ( 'NONE', #35824, #38276 ) ;
#49333 = DIRECTION ( 'NONE',  ( 0.000000000000000000, 0.6427876096865373645, -0.7660444431189797898 ) ) ;
#49334 = CARTESIAN_POINT ( 'NONE',  ( 15.90382292962469890, -10.92453946501459328, 33.72985991061849376 ) ) ;
#49335 = FACE_OUTER_BOUND ( 'NONE', #69041, .T. ) ;
#49336 = FACE_BOUND ( 'NONE', #28049, .T. ) ;
#49337 = B_SPLINE_CURVE_WITH_KNOTS ( 'NONE', 3,
 ( #19820, #54934, #34665, #7195, #75216, #20267, #54482, #32890, #74325, #80651 ),
 .UNSPECIFIED., .F., .F.,
 ( 4, 2, 2, 2, 4 ),
 ( 0.000000000000000000, 0.0001954339857564083688, 0.0003908679715128167377, 0.0005863019572692250523, 0.0007817359430256334753 ),
 .UNSPECIFIED. ) ;
#49339 = CARTESIAN_POINT ( 'NONE',  ( -11.25641025641025550, -7.500000000000000000, 29.75000000000000355 ) ) ;
#49338 = CYLINDRICAL_SURFACE ( 'NONE', #10258, 0.2499999999999986955 ) ;
#49340 = CARTESIAN_POINT ( 'NONE',  ( 5.207448515156721136, -9.503571793651733657, 34.60286762892837942 ) ) ;
#49342 = CARTESIAN_POINT ( 'NONE',  ( -5.999999999999998224, -4.786620604624113540, 33.94971097300155094 ) ) ;
#49341 = CARTESIAN_POINT ( 'NONE',  ( 11.25641025641025550, -3.499999999999999556, 29.75000000000000355 ) ) ;
#49343 = EDGE_CURVE ( 'NONE', #23595, #37993, #66065, .T. ) ;
#49344 = CARTESIAN_POINT ( 'NONE',  ( 25.00000000000000711, -9.999999999999957367, 13.00000000000000178 ) ) ;
#49345 = CARTESIAN_POINT ( 'NONE',  ( 0.06109907496454976272, -10.25000000000000000, 24.52938170625849423 ) ) ;
#49346 = ORIENTED_EDGE ( 'NONE', *, *, #59911, .F. ) ;
#49347 = STYLED_ITEM ( 'NONE', ( #76013 ), #28293 ) ;
#49348 = CARTESIAN_POINT ( 'NONE',  ( 12.59233026936324684, -2.541949514083464479, 30.39797389878540557 ) ) ;
#49349 = ORIENTED_EDGE ( 'NONE', *, *, #69220, .T. ) ;
#49350 = CARTESIAN_POINT ( 'NONE',  ( 0.7115384615384606759, -2.499999999999998668, 29.75000000000000355 ) ) ;
#49351 = EDGE_CURVE ( 'NONE', #53313, #19610, #76514, .T. ) ;
#49352 = VERTEX_POINT ( 'NONE', #4657 ) ;
#49353 = CARTESIAN_POINT ( 'NONE',  ( 2.307692307692186251, -12.51329471203414379, 31.30864560766407578 ) ) ;
#49354 = CARTESIAN_POINT ( 'NONE',  ( -15.93106648486808119, -12.11081565061823717, 32.26097654155341843 ) ) ;
#49355 = ORIENTED_EDGE ( 'NONE', *, *, #26942, .T. ) ;
#49356 = CARTESIAN_POINT ( 'NONE',  ( -1.384615384615383471, -13.37000171582298513, 34.34916445242398453 ) ) ;
#49357 = CARTESIAN_POINT ( 'NONE',  ( 2.750000000000001332, -7.438900925035452083, 21.71688170625848713 ) ) ;
#49358 = CARTESIAN_POINT ( 'NONE',  ( 12.46153846153846168, -4.661471528628507777, 34.16647553114623292 ) ) ;
#49359 = CARTESIAN_POINT ( 'NONE',  ( -10.61538461538473577, -12.70778746994576025, 30.41441678777401236 ) ) ;
#49360 = CARTESIAN_POINT ( 'NONE',  ( 16.08857615328984281, -8.656820664281497102, 34.87096338111211935 ) ) ;
#49361 = CARTESIAN_POINT ( 'NONE',  ( 12.33139125210024112, -2.882441371585227508, 31.66841991370172238 ) ) ;
#49362 = CARTESIAN_POINT ( 'NONE',  ( 14.98076923076923173, -7.500000000000001776, 34.75000000000000000 ) ) ;
#49363 = DIRECTION ( 'NONE',  ( -1.000000000000000000, -0.000000000000000000, -0.000000000000000000 ) ) ;
#49364 = CARTESIAN_POINT ( 'NONE',  ( 3.750000000000001776, -7.561099074964511502, 24.72061829374150932 ) ) ;
#49365 = LINE ( 'NONE', #49798, #5998 ) ;
#49366 = CARTESIAN_POINT ( 'NONE',  ( -6.222926958906846551, -3.395401636524186362, 33.02366814457250399 ) ) ;
#49367 = CARTESIAN_POINT ( 'NONE',  ( 8.900022577055556994, -9.804649428959608670, 34.18742332936588468 ) ) ;
#49368 = CARTESIAN_POINT ( 'NONE',  ( -3.775308065498748977, -8.992201783934593351, 24.01749329374151287 ) ) ;
#49369 = ADVANCED_FACE ( 'NONE', ( #33459 ), #38896, .F. ) ;
#49370 = CARTESIAN_POINT ( 'NONE',  ( 6.250000000000000888, -2.249999999999998668, 29.75000000000000355 ) ) ;
#49371 = ORIENTED_EDGE ( 'NONE', *, *, #2822, .T. ) ;
#49372 = CARTESIAN_POINT ( 'NONE',  ( 9.692307692307570832, -2.657715359629662544, 31.77849191805970364 ) ) ;
#49373 = FACE_OUTER_BOUND ( 'NONE', #5426, .T. ) ;
#49374 = CARTESIAN_POINT ( 'NONE',  ( -11.53846153846153655, -1.790695186598648903, 34.54067556320373455 ) ) ;
#49375 = CARTESIAN_POINT ( 'NONE',  ( 10.61538461538461675, -2.249999999999998668, 29.50000000000001421 ) ) ;
#49376 = B_SPLINE_CURVE_WITH_KNOTS ( 'NONE', 3,
 ( #88845, #55910, #91, #21686, #49156, #22137, #69876, #83852, #42419, #70320 ),
 .UNSPECIFIED., .F., .F.,
 ( 4, 2, 2, 2, 4 ),
 ( 0.0007817246256747463051, 0.0009771112852218896347, 0.001172497944769033181, 0.001367884604316176728, 0.001563271263863320057 ),
 .UNSPECIFIED. ) ;
#49377 = B_SPLINE_CURVE_WITH_KNOTS ( 'NONE', 3,
 ( #28354, #82440, #48184, #41887, #42334, #75233, #68901, #69359, #76998, #15299 ),
 .UNSPECIFIED., .F., .F.,
 ( 4, 2, 2, 2, 4 ),
 ( 0.000000000000000000, 0.0001954311564186858715, 0.0003908623128373717431, 0.0005862934692560576146, 0.0007817246256747434861 ),
 .UNSPECIFIED. ) ;
#49378 = CARTESIAN_POINT ( 'NONE',  ( -3.230769230769351186, -5.219633306517616589, 34.19971097300220464 ) ) ;
#49379 = CARTESIAN_POINT ( 'NONE',  ( 7.053602361310567836, -12.15418822224088657, 32.17964115625579069 ) ) ;
#49380 = ADVANCED_FACE ( 'NONE', ( #35114 ), #73574, .T. ) ;
#49381 = VECTOR ( 'NONE', #84543, 1000.000000000000227 ) ;
#49382 = CARTESIAN_POINT ( 'NONE',  ( 8.546304551714625219, -10.61292498521070549, 33.66303323003028680 ) ) ;
#49383 = DIRECTION ( 'NONE',  ( -0.000000000000000000, -0.5000000000000009992, -0.8660254037844380415 ) ) ;
#49384 = EDGE_CURVE ( 'NONE', #85420, #14506, #46355, .T. ) ;
#49385 = VERTEX_POINT ( 'NONE', #74898 ) ;
#49386 = VERTEX_POINT ( 'NONE', #40668 ) ;
#49387 = ORIENTED_EDGE ( 'NONE', *, *, #52737, .T. ) ;
#49388 = CARTESIAN_POINT ( 'NONE',  ( 5.299702618191484582, -11.89424750095246175, 32.13594075562311758 ) ) ;
#49389 = DIRECTION ( 'NONE',  ( -0.000000000000000000, -0.3420201433256694346, -0.9396926207859080948 ) ) ;
#49390 = CARTESIAN_POINT ( 'NONE',  ( -8.992715693795103604, -2.353723527008296568, 30.78948104536958752 ) ) ;
#49391 = LINE ( 'NONE', #6632, #76642 ) ;
#49392 = DIRECTION ( 'NONE',  ( 0.000000000000000000, -1.000000000000000000, 0.000000000000000000 ) ) ;
#49393 = EDGE_CURVE ( 'NONE', #27552, #88462, #51752, .T. ) ;
#49394 = ORIENTED_EDGE ( 'NONE', *, *, #28483, .F. ) ;
#49395 = EDGE_CURVE ( 'NONE', #61816, #4310, #78564, .T. ) ;
#49396 = CARTESIAN_POINT ( 'NONE',  ( -18.22282669247899989, -7.369208160676171460, 34.74850200257122879 ) ) ;
#49397 = EDGE_LOOP ( 'NONE', ( #36363, #63244 ) ) ;
#49398 = ADVANCED_FACE ( 'NONE', ( #23360 ), #9853, .F. ) ;
#49399 = ORIENTED_EDGE ( 'NONE', *, *, #72574, .F. ) ;
#49400 = VECTOR ( 'NONE', #12400, 1000.000000000000000 ) ;
#49401 = ORIENTED_EDGE ( 'NONE', *, *, #24604, .F. ) ;
#49403 = VERTEX_POINT ( 'NONE', #63010 ) ;
#49402 = CARTESIAN_POINT ( 'NONE',  ( 8.519254025182178225, -12.41104346484419452, 31.60698883733904196 ) ) ;
#49404 = CARTESIAN_POINT ( 'NONE',  ( -4.854143407945007205, -12.47679350104403007, 31.42216943046555855 ) ) ;
#49405 = CARTESIAN_POINT ( 'NONE',  ( -16.21911659980693443, -4.481592998940161721, 33.73612834413957984 ) ) ;
#49406 = CIRCLE ( 'NONE', #58015, 0.2500000000000002220 ) ;
#49407 = B_SPLINE_CURVE_WITH_KNOTS ( 'NONE', 3,
 ( #86490, #24764, #72954, #66187, #39186, #81059, #5832, #59883, #26551, #80163 ),
 .UNSPECIFIED., .F., .F.,
 ( 4, 2, 2, 2, 4 ),
 ( 0.0007817246256747514008, 0.0009771112852218952725, 0.001172497944769039036, 0.001367884604316182799, 0.001563271263863326779 ),
 .UNSPECIFIED. ) ;
#49408 = LINE ( 'NONE', #2526, #36430 ) ;
#49409 = CARTESIAN_POINT ( 'NONE',  ( 14.05769230769230838, -7.500000000000001776, 35.00000000000000000 ) ) ;
#49410 = ORIENTED_EDGE ( 'NONE', *, *, #11166, .F. ) ;
#49411 = B_SPLINE_CURVE_WITH_KNOTS ( 'NONE', 3,
 ( #71283, #11369, #3271, #23540, #86153, #78934, #16354, #31187, #50997, #10031 ),
 .UNSPECIFIED., .F., .F.,
 ( 4, 2, 2, 2, 4 ),
 ( 0.0007817246256747450040, 0.0009771112852218872494, 0.001172497944769029278, 0.001367884604316171523, 0.001563271263863313769 ),
 .UNSPECIFIED. ) ;
#49412 = ORIENTED_EDGE ( 'NONE', *, *, #54590, .F. ) ;
#49413 = ORIENTED_EDGE ( 'NONE', *, *, #5592, .T. ) ;
#49414 = CARTESIAN_POINT ( 'NONE',  ( -9.561515884482904681, -5.582136614379148654, 34.36778462344220486 ) ) ;
#49416 = VERTEX_POINT ( 'NONE', #70677 ) ;
#49415 = CARTESIAN_POINT ( 'NONE',  ( 11.78851595837499566, -5.642605341092957971, 34.66089969410670335 ) ) ;
#49417 = CARTESIAN_POINT ( 'NONE',  ( -4.153846153846152411, -2.499999999999998668, 29.50000000000001066 ) ) ;
#49418 = DIRECTION ( 'NONE',  ( 1.000000000000000000, 0.000000000000000000, 0.000000000000000000 ) ) ;
#49419 = CARTESIAN_POINT ( 'NONE',  ( 7.173131234715236282, -11.79725096376909299, 32.30694842903960762 ) ) ;
#49420 = EDGE_LOOP ( 'NONE', ( #87216, #70055, #79912, #31683 ) ) ;
#49421 = LINE ( 'NONE', #15635, #78198 ) ;
#49422 = CARTESIAN_POINT ( 'NONE',  ( -15.23076923076935252, -12.51329471203414379, 31.30864560766407578 ) ) ;
#49423 = EDGE_LOOP ( 'NONE', ( #40166, #776, #22962, #10723 ) ) ;
#49424 = FACE_BOUND ( 'NONE', #58574, .T. ) ;
#49425 = CARTESIAN_POINT ( 'NONE',  ( 15.45378207486262667, -11.43677907613344757, 33.22367315496202167 ) ) ;
#49426 = CARTESIAN_POINT ( 'NONE',  ( -13.38461538461538325, -10.05456864172156806, 36.03766855953608683 ) ) ;
#49427 = FACE_OUTER_BOUND ( 'NONE', #12606, .T. ) ;
#49429 = CARTESIAN_POINT ( 'NONE',  ( -0.6844646790546066173, -12.15238873228291538, 31.58232369045354915 ) ) ;
#49428 = FACE_OUTER_BOUND ( 'NONE', #78954, .T. ) ;
#49430 = CARTESIAN_POINT ( 'NONE',  ( -12.46153846153846168, -13.87047571288749737, 32.06866353760679544 ) ) ;
#49431 = DIRECTION ( 'NONE',  ( 1.000000000000000000, 0.000000000000000000, 0.000000000000000000 ) ) ;
#49432 = ORIENTED_EDGE ( 'NONE', *, *, #67646, .T. ) ;
#49433 = CARTESIAN_POINT ( 'NONE',  ( 14.55763782604045176, -12.43552623307873972, 30.55307653245132826 ) ) ;
#49434 = CARTESIAN_POINT ( 'NONE',  ( -16.85391023282967993, -6.460100341425561332, 34.89618726649961644 ) ) ;
#49435 = ORIENTED_EDGE ( 'NONE', *, *, #54053, .T. ) ;
#49436 = AXIS2_PLACEMENT_3D ( 'NONE', #11774, #87909, #68480 ) ;
#49437 = ADVANCED_FACE ( 'NONE', ( #1770 ), #29696, .T. ) ;
#49438 = DIRECTION ( 'NONE',  ( 0.000000000000000000, 0.000000000000000000, -1.000000000000000000 ) ) ;
#49439 = DIRECTION ( 'NONE',  ( -0.000000000000000000, -0.000000000000000000, -1.000000000000000000 ) ) ;
#49440 = CARTESIAN_POINT ( 'NONE',  ( -7.846153846153844924, -10.67929555188718282, 33.92786785259544047 ) ) ;
#49441 = VERTEX_POINT ( 'NONE', #64781 ) ;
#49442 = CARTESIAN_POINT ( 'NONE',  ( -0.3307466537136760643, -12.38066358083363738, 30.83685684665853444 ) ) ;
#49443 = DIRECTION ( 'NONE',  ( 0.000000000000000000, 0.9396926207859126468, -0.3420201433256571111 ) ) ;
#49444 = FACE_BOUND ( 'NONE', #78192, .T. ) ;
#49446 = CARTESIAN_POINT ( 'NONE',  ( -3.903900635498011251, -8.433404298154334455, 34.66254593164985920 ) ) ;
#49445 = CARTESIAN_POINT ( 'NONE',  ( 8.769230769230768274, -8.120952969808772792, 34.71129190930000163 ) ) ;
#49447 = CARTESIAN_POINT ( 'NONE',  ( -16.02305434602136458, -2.541949514083464479, 30.39797389878540557 ) ) ;
#49449 = CYLINDRICAL_SURFACE ( 'NONE', #49218, 0.2499999999999997502 ) ;
#49448 = DIRECTION ( 'NONE',  ( -0.000000000000000000, -0.9848077530122085754, -0.1736481776669273613 ) ) ;
#49450 = EDGE_CURVE ( 'NONE', #54935, #82557, #67897, .T. ) ;
#49451 = CARTESIAN_POINT ( 'NONE',  ( -17.77722045873158763, -5.114059244376869984, 34.14424750095245287 ) ) ;
#49452 = CARTESIAN_POINT ( 'NONE',  ( 2.608446859217893099, -4.805146000318787358, 20.31063170625848713 ) ) ;
#49453 = ORIENTED_EDGE ( 'NONE', *, *, #16391, .T. ) ;
#49454 = B_SPLINE_CURVE_WITH_KNOTS ( 'NONE', 3,
 ( #69741, #84161, #35066, #76946, #13909, #22000, #15250, #76503, #28307, #83267 ),
 .UNSPECIFIED., .F., .F.,
 ( 4, 2, 2, 2, 4 ),
 ( 0.000000000000000000, 0.0001954311564186866034, 0.0003908623128373732067, 0.0005862934692560597830, 0.0007817246256747464135 ),
 .UNSPECIFIED. ) ;
#49455 = ORIENTED_EDGE ( 'NONE', *, *, #75759, .F. ) ;
#49456 = CARTESIAN_POINT ( 'NONE',  ( -9.561515884482904681, -11.71459661697925903, 32.44059661609676937 ) ) ;
#49457 = CARTESIAN_POINT ( 'NONE',  ( -12.39628332202562433, -6.835583212224610072, 34.95778746994559327 ) ) ;
#49458 = CARTESIAN_POINT ( 'NONE',  ( -9.692307692307812417, -9.442884908241554243, 34.35708131394783038 ) ) ;
#49459 = CARTESIAN_POINT ( 'NONE',  ( 8.638670855617402111, -2.254533558242300284, 29.97296025877827930 ) ) ;
#49460 = CARTESIAN_POINT ( 'NONE',  ( -17.01085472592063752, -6.386643153685127139, 34.62446782046654192 ) ) ;
#49461 = CARTESIAN_POINT ( 'NONE',  ( 0.06109907496455496689, -11.24999999999999822, 17.02938170625848713 ) ) ;
#49462 = CARTESIAN_POINT ( 'NONE',  ( 6.923076923076800782, -2.379036618888197729, 30.90682066428292885 ) ) ;
#49463 = CARTESIAN_POINT ( 'NONE',  ( -39.05038313613820122, -2.249999999999998668, 29.75000000000000355 ) ) ;
#49464 = EDGE_CURVE ( 'NONE', #8676, #36288, #79702, .T. ) ;
#49465 = FACE_OUTER_BOUND ( 'NONE', #71214, .T. ) ;
#49466 = DIRECTION ( 'NONE',  ( 0.000000000000000000, 0.000000000000000000, -1.000000000000000000 ) ) ;
#49467 = CARTESIAN_POINT ( 'NONE',  ( 5.326923076923075762, -2.499999999999998668, 29.75000000000000355 ) ) ;
#49468 = DIRECTION ( 'NONE',  ( -0.000000000000000000, 0.3420201433256694901, -0.9396926207859082059 ) ) ;
#49469 = CARTESIAN_POINT ( 'NONE',  ( -5.011667505647052323, -2.892918686051625166, 31.69288490824025928 ) ) ;
#49470 = AXIS2_PLACEMENT_3D ( 'NONE', #37399, #85596, #23873 ) ;
#49471 = CARTESIAN_POINT ( 'NONE',  ( 10.86538461538455458, -7.565270000091922853, 34.99999999999999289 ) ) ;
#49472 = CARTESIAN_POINT ( 'NONE',  ( 3.165498784808455479, -2.625532179533444754, 30.86335684631481513 ) ) ;
#49473 = ORIENTED_EDGE ( 'NONE', *, *, #37081, .F. ) ;
#49474 = CARTESIAN_POINT ( 'NONE',  ( -14.43838377435986686, -3.530157926970578952, 32.79014554554150607 ) ) ;
#49475 = CYLINDRICAL_SURFACE ( 'NONE', #61815, 0.2500000000000008882 ) ;
#49476 = CARTESIAN_POINT ( 'NONE',  ( 2.750000000000002665, -7.561099074964516831, 19.72061829374151287 ) ) ;
#49477 = EDGE_CURVE ( 'NONE', #1316, #20998, #16192, .T. ) ;
#49478 = VECTOR ( 'NONE', #68116, 999.9999999999998863 ) ;
#49479 = VECTOR ( 'NONE', #68363, 1000.000000000000000 ) ;
#49480 = CARTESIAN_POINT ( 'NONE',  ( 0.4615384615384611200, -3.322132147404559976, 32.92929555188717927 ) ) ;
#49481 = CARTESIAN_POINT ( 'NONE',  ( 16.15384615384615330, -4.102666532097928531, 36.13435417666054406 ) ) ;
#49482 = ORIENTED_EDGE ( 'NONE', *, *, #27409, .F. ) ;
#49483 = LINE ( 'NONE', #69747, #21211 ) ;
#49485 = ORIENTED_EDGE ( 'NONE', *, *, #39541, .T. ) ;
#49484 = DIRECTION ( 'NONE',  ( -0.000000000000000000, 0.9848077530122085754, -0.1736481776669273613 ) ) ;
#49486 = CARTESIAN_POINT ( 'NONE',  ( 2.307692307692623679, -2.255955759149395501, 30.00000000000324363 ) ) ;
#49487 = ADVANCED_FACE ( 'NONE', ( #77866 ), #14861, .F. ) ;
#49488 = CARTESIAN_POINT ( 'NONE',  ( -2.372962308248626417, -11.06231777344662781, 33.60647404775220082 ) ) ;
#49489 = VERTEX_POINT ( 'NONE', #30564 ) ;
#49490 = CARTESIAN_POINT ( 'NONE',  ( -13.38461538461538325, -3.513871655860378418, 32.76840700105978499 ) ) ;
#49491 = CARTESIAN_POINT ( 'NONE',  ( 10.68063975489745410, -11.06231777344671130, 33.60647404775212976 ) ) ;
#49492 = EDGE_LOOP ( 'NONE', ( #44528, #39290, #79856, #11707 ) ) ;
#49493 = B_SPLINE_CURVE_WITH_KNOTS ( 'NONE', 3,
 ( #67099, #81506, #39191, #19794, #45481, #80170, #45923, #24769, #52234, #79724 ),
 .UNSPECIFIED., .F., .F.,
 ( 4, 2, 2, 2, 4 ),
 ( 0.0007817359430256401974, 0.0009771253907250091169, 0.001172514838424378036, 0.001367904286123747173, 0.001563293733823116092 ),
 .UNSPECIFIED. ) ;
#49494 = DIRECTION ( 'NONE',  ( 1.000000000000000000, 0.000000000000000000, 0.000000000000000000 ) ) ;
#49495 = CARTESIAN_POINT ( 'NONE',  ( -16.08859058257013075, -3.300289026998475261, 32.46337939537591666 ) ) ;
#49496 = EDGE_CURVE ( 'NONE', #48689, #18273, #16173, .T. ) ;
#49497 = LINE ( 'NONE', #70650, #88774 ) ;
#49498 = ORIENTED_EDGE ( 'NONE', *, *, #74428, .F. ) ;
#49499 = ORIENTED_EDGE ( 'NONE', *, *, #44686, .T. ) ;
#49500 = CARTESIAN_POINT ( 'NONE',  ( 6.250054311638314708, -6.567000820036038355, 34.66262288849541306 ) ) ;
#49501 = EDGE_LOOP ( 'NONE', ( #49851, #82985, #53371, #45527, #13856, #49249 ) ) ;
#49502 = CARTESIAN_POINT ( 'NONE',  ( -1.253823576790598748, -2.541949514083463590, 30.39797389878540557 ) ) ;
#49503 = CARTESIAN_POINT ( 'NONE',  ( 2.438482748659261290, -11.37503395064541678, 33.29242100308974983 ) ) ;
#49504 = CARTESIAN_POINT ( 'NONE',  ( -7.596153846153780087, -7.434744429011175271, 34.75000000000000000 ) ) ;
#49505 = EDGE_CURVE ( 'NONE', #59888, #10587, #8718, .T. ) ;
#49506 = AXIS2_PLACEMENT_3D ( 'NONE', #27962, #22531, #57203 ) ;
#49507 = LINE ( 'NONE', #29679, #66518 ) ;
#49508 = ADVANCED_FACE ( 'NONE', ( #52610 ), #31457, .F. ) ;
#49509 = EDGE_CURVE ( 'NONE', #22240, #75095, #72437, .T. ) ;
#49510 = EDGE_LOOP ( 'NONE', ( #74049, #80930, #20834, #23332 ) ) ;
#49511 = ORIENTED_EDGE ( 'NONE', *, *, #36260, .F. ) ;
#49513 = ORIENTED_EDGE ( 'NONE', *, *, #81274, .T. ) ;
#49512 = DIRECTION ( 'NONE',  ( -0.000000000000000000, -0.8660254037844397068, -0.4999999999999978906 ) ) ;
#49514 = EDGE_CURVE ( 'NONE', #63322, #11864, #22575, .T. ) ;
#49515 = DIRECTION ( 'NONE',  ( -0.000000000000000000, 0.7660444431189791237, -0.6427876096865379196 ) ) ;
#49516 = ORIENTED_EDGE ( 'NONE', *, *, #28396, .F. ) ;
#49517 = CARTESIAN_POINT ( 'NONE',  ( 14.30769230769231015, -9.584722331328613620, 36.20867863119891439 ) ) ;
#49518 = FACE_OUTER_BOUND ( 'NONE', #88983, .T. ) ;
#49519 = VERTEX_POINT ( 'NONE', #59375 ) ;
#49520 = CARTESIAN_POINT ( 'NONE',  ( -12.23875892027004753, -5.913360116392397892, 34.49180327182771322 ) ) ;
#49521 = ORIENTED_EDGE ( 'NONE', *, *, #76637, .F. ) ;
#49523 = ORIENTED_EDGE ( 'NONE', *, *, #33188, .T. ) ;
#49522 = CARTESIAN_POINT ( 'NONE',  ( -8.546219417617919589, -8.239487800360276282, 34.69522927552633718 ) ) ;
#49524 = CARTESIAN_POINT ( 'NONE',  ( -10.86538461538461320, -7.500000000000001776, 34.75000000000000000 ) ) ;
#49525 = AXIS2_PLACEMENT_3D ( 'NONE', #27255, #53390, #46641 ) ;
#49526 = CARTESIAN_POINT ( 'NONE',  ( -5.326946314216043810, -10.05641848906368097, 34.04755513067966177 ) ) ;
#49527 = VERTEX_POINT ( 'NONE', #80093 ) ;
#49528 = DIRECTION ( 'NONE',  ( 0.000000000000000000, 1.000000000000000000, 0.000000000000000000 ) ) ;
#49529 = DIRECTION ( 'NONE',  ( -0.000000000000000000, 0.9396926207859093161, -0.3420201433256663259 ) ) ;
#49530 = FACE_BOUND ( 'NONE', #7549, .T. ) ;
#49531 = VECTOR ( 'NONE', #81089, 1000.000000000000000 ) ;
#49532 = CARTESIAN_POINT ( 'NONE',  ( -11.53846153846165912, -2.625532179533778709, 30.86335684631627174 ) ) ;
#49533 = CARTESIAN_POINT ( 'NONE',  ( -11.76194646302587010, -6.716662450894489211, 34.94144148231605840 ) ) ;
#49534 = VECTOR ( 'NONE', #81050, 1000.000000000000000 ) ;
#49535 = CARTESIAN_POINT ( 'NONE',  ( 9.562159722575998444, -11.66186481527757302, 32.95055677023626117 ) ) ;
#49536 = DIRECTION ( 'NONE',  ( -1.000000000000000000, -0.000000000000000000, -0.000000000000000000 ) ) ;
#49537 = CARTESIAN_POINT ( 'NONE',  ( -3.164700879766792152, -3.050289026998446840, 32.03036669348366416 ) ) ;
#49538 = CYLINDRICAL_SURFACE ( 'NONE', #11685, 0.2499999999999994726 ) ;
#49539 = ORIENTED_EDGE ( 'NONE', *, *, #18578, .F. ) ;
#49540 = CARTESIAN_POINT ( 'NONE',  ( -7.846153846153965716, -6.026961402154118019, 34.52809138561165270 ) ) ;
#49541 = ORIENTED_EDGE ( 'NONE', *, *, #47154, .F. ) ;
#49542 = VERTEX_POINT ( 'NONE', #51246 ) ;
#49544 = CARTESIAN_POINT ( 'NONE',  ( 16.21991450484859953, -12.10708131394839882, 31.69288490824020954 ) ) ;
#49543 = CARTESIAN_POINT ( 'NONE',  ( 14.43848411551709177, -3.530189275343204702, 32.79018710029569661 ) ) ;
#49545 = CARTESIAN_POINT ( 'NONE',  ( -9.442362282929648742, -12.45601412856602686, 31.48342859153981621 ) ) ;
#49546 = CARTESIAN_POINT ( 'NONE',  ( -8.769230769230890843, -2.892918686052166066, 31.69288490824153470 ) ) ;
#49547 = CARTESIAN_POINT ( 'NONE',  ( -12.21148404162500611, -2.544122305571458575, 31.48381861865057729 ) ) ;
#49548 = CARTESIAN_POINT ( 'NONE',  ( 9.822833394071260216, -2.619367082507849442, 30.83698974864643461 ) ) ;
#49549 = ORIENTED_EDGE ( 'NONE', *, *, #26395, .F. ) ;
#49550 = CARTESIAN_POINT ( 'NONE',  ( -6.923076923077045919, -3.643525952248796163, 33.31231777344771672 ) ) ;
#49551 = CARTESIAN_POINT ( 'NONE',  ( 1.449870955891411350, -12.27809138561124591, 31.22303859784720359 ) ) ;
#49552 = PLANE ( 'NONE',  #87661 ) ;
#49553 = CARTESIAN_POINT ( 'NONE',  ( 18.00000000000000000, -2.499999999999998668, 29.50000000000001066 ) ) ;
#49554 = DIRECTION ( 'NONE',  ( 1.000000000000000000, 0.000000000000000000, 0.000000000000000000 ) ) ;
#49555 = EDGE_LOOP ( 'NONE', ( #35652, #43277 ) ) ;
#49556 = CARTESIAN_POINT ( 'NONE',  ( 3.007284306204902613, -12.11044203135681840, 32.26167407432752299 ) ) ;
#49557 = VERTEX_POINT ( 'NONE', #39574 ) ;
#49558 = ORIENTED_EDGE ( 'NONE', *, *, #18951, .F. ) ;
#49559 = CARTESIAN_POINT ( 'NONE',  ( -7.173053654019277303, -8.303909089506435137, 34.68538101551103381 ) ) ;
#49560 = ORIENTED_EDGE ( 'NONE', *, *, #17347, .F. ) ;
#49561 = CARTESIAN_POINT ( 'NONE',  ( -1.318547033612945674, -8.120952969808772792, 34.71129190929999453 ) ) ;
#49562 = CARTESIAN_POINT ( 'NONE',  ( -17.29984929443921970, -3.105860786376062332, 32.13614157043599562 ) ) ;
#49563 = FACE_OUTER_BOUND ( 'NONE', #54806, .T. ) ;
#49564 = CARTESIAN_POINT ( 'NONE',  ( -8.638438961405983108, -10.54018710029568595, 33.71981072465678864 ) ) ;
#49565 = CARTESIAN_POINT ( 'NONE',  ( -16.15384615384615330, -8.164416787775445883, 34.95778746994557906 ) ) ;
#49566 = CARTESIAN_POINT ( 'NONE',  ( 0.6843181305165270123, -9.418065098278011860, 34.63729479722530158 ) ) ;
#49568 = EDGE_LOOP ( 'NONE', ( #53036, #70551, #51028, #73047 ) ) ;
#49567 = AXIS2_PLACEMENT_3D ( 'NONE', #65409, #31175, #11815 ) ;
#49569 = CARTESIAN_POINT ( 'NONE',  ( 3.903846153846155076, -7.566083408709834757, 34.74999999999999289 ) ) ;
#49571 = ORIENTED_EDGE ( 'NONE', *, *, #18954, .F. ) ;
#49570 = CARTESIAN_POINT ( 'NONE',  ( 17.77713373693690002, -2.251424796025574881, 29.88072029997477941 ) ) ;
#49572 = FACE_OUTER_BOUND ( 'NONE', #79034, .T. ) ;
#49573 = DIRECTION ( 'NONE',  ( -0.000000000000000000, -0.6427876096865404731, -0.7660444431189770143 ) ) ;
#49574 = DIRECTION ( 'NONE',  ( 0.000000000000000000, -6.938893903907222067E-15, 1.000000000000000000 ) ) ;
#49575 = CARTESIAN_POINT ( 'NONE',  ( 5.076923076922954969, -11.48612834414049644, 32.76840700105863391 ) ) ;
#49576 = LINE ( 'NONE', #20339, #31794 ) ;
#49577 = DIRECTION ( 'NONE',  ( 1.000000000000000000, 0.000000000000000000, 0.000000000000000000 ) ) ;
#49578 = CARTESIAN_POINT ( 'NONE',  ( 1.492201783934598236, -11.27530806549875031, 13.70499329374151287 ) ) ;
#49579 = VERTEX_POINT ( 'NONE', #4426 ) ;
#49580 = B_SPLINE_CURVE_WITH_KNOTS ( 'NONE', 3,
 ( #43745, #71207, #63571, #9511, #15403, #3197, #1875, #36978, #69889, #2741 ),
 .UNSPECIFIED., .F., .F.,
 ( 4, 2, 2, 2, 4 ),
 ( 0.0007817359430256294638, 0.0009771253907249948054, 0.001172514838424360255, 0.001367904286123725489, 0.001563293733823090939 ),
 .UNSPECIFIED. ) ;
#49581 = CARTESIAN_POINT ( 'NONE',  ( -3.230769230769352962, -6.835583212225970762, 34.95778746994575670 ) ) ;
#49582 = CARTESIAN_POINT ( 'NONE',  ( 4.376625822824220080, -10.97394488606064122, 33.68653795673696294 ) ) ;
#49583 = EDGE_CURVE ( 'NONE', #79249, #55049, #59819, .T. ) ;
#49584 = CARTESIAN_POINT ( 'NONE',  ( 0.3954550505825799589, -3.513871655860377086, 32.76840700105978499 ) ) ;
#49585 = CARTESIAN_POINT ( 'NONE',  ( -7.846153846153844924, -2.833524468853757305, 32.15551576947925838 ) ) ;
#49586 = ORIENTED_EDGE ( 'NONE', *, *, #23328, .T. ) ;
#49587 = CARTESIAN_POINT ( 'NONE',  ( 0.2115152373170042510, -4.175268141568690083, 33.81360843649122927 ) ) ;
#49588 = CARTESIAN_POINT ( 'NONE',  ( -3.296039676730006196, -10.90142922261923886, 33.41473453929638993 ) ) ;
#49589 = ORIENTED_EDGE ( 'NONE', *, *, #48641, .T. ) ;
#49590 = CARTESIAN_POINT ( 'NONE',  ( -0.4615384615385840772, -12.70778746994576025, 30.41441678777401236 ) ) ;
#49591 = CARTESIAN_POINT ( 'NONE',  ( -4.153846153846152411, -10.51840700105979565, 33.73612834413961536 ) ) ;
#49592 = ORIENTED_EDGE ( 'NONE', *, *, #63735, .T. ) ;
#49593 = CARTESIAN_POINT ( 'NONE',  ( 14.37376065869475106, -12.10708131394839704, 31.69288490824020954 ) ) ;
#49594 = CYLINDRICAL_SURFACE ( 'NONE', #76790, 0.2499999999999995559 ) ;
#49595 = AXIS2_PLACEMENT_3D ( 'NONE', #6890, #74465, #27606 ) ;
#49596 = EDGE_CURVE ( 'NONE', #55616, #18826, #47363, .T. ) ;
#49597 = CARTESIAN_POINT ( 'NONE',  ( -11.28846153846011902, -7.500000000000154543, 35.00000000000007105 ) ) ;
#49598 = CARTESIAN_POINT ( 'NONE',  ( 7.846153846153846700, -3.050289026998446396, 32.03036669348365706 ) ) ;
#49599 = ORIENTED_EDGE ( 'NONE', *, *, #40484, .F. ) ;
#49600 = CARTESIAN_POINT ( 'NONE',  ( -2.438382910802613601, -11.93127051446800024, 32.56575433478200665 ) ) ;
#49601 = VECTOR ( 'NONE', #75666, 1000.000000000000000 ) ;
#49602 = ORIENTED_EDGE ( 'NONE', *, *, #7616, .T. ) ;
#49603 = CARTESIAN_POINT ( 'NONE',  ( -6.793031760242145722, -2.504778602574660340, 29.97347330155780298 ) ) ;
#49604 = CARTESIAN_POINT ( 'NONE',  ( 0.5267936010512989098, -10.33852847137154107, 34.16647553114620450 ) ) ;
#49605 = EDGE_LOOP ( 'NONE', ( #59709, #37419 ) ) ;
#49606 = CARTESIAN_POINT ( 'NONE',  ( 16.15384615384615330, -1.790695186598648903, 34.54067556320373455 ) ) ;
#49607 = DIRECTION ( 'NONE',  ( 0.000000000000000000, 0.8660254037844377084, -0.5000000000000015543 ) ) ;
#49608 = LINE ( 'NONE', #7743, #49478 ) ;
#49609 = DIRECTION ( 'NONE',  ( 0.000000000000000000, 0.7660444431189807890, 0.6427876096865361433 ) ) ;
#49610 = CYLINDRICAL_SURFACE ( 'NONE', #22467, 0.2500000000000008882 ) ;
#49611 = EDGE_CURVE ( 'NONE', #20058, #51973, #59101, .T. ) ;
#49612 = ADVANCED_FACE ( 'NONE', ( #86878 ), #11189, .F. ) ;
#49613 = ORIENTED_EDGE ( 'NONE', *, *, #57453, .T. ) ;
#49614 = ORIENTED_EDGE ( 'NONE', *, *, #80852, .T. ) ;
#49615 = B_SPLINE_CURVE_WITH_KNOTS ( 'NONE', 3,
 ( #87563, #34361, #54625, #33488, #39805, #47880, #80351, #18648, #67272, #81235 ),
 .UNSPECIFIED., .F., .F.,
 ( 4, 2, 2, 2, 4 ),
 ( 0.0007817359430256308733, 0.0009771253907249971907, 0.001172514838424363725, 0.001367904286123730259, 0.001563293733823096577 ),
 .UNSPECIFIED. ) ;
#49616 = FACE_BOUND ( 'NONE', #23758, .T. ) ;
#49617 = ORIENTED_EDGE ( 'NONE', *, *, #11877, .F. ) ;
#49618 = CARTESIAN_POINT ( 'NONE',  ( -4.826923076923076650, -2.249999999999998668, 29.75000000000000355 ) ) ;
#49619 = CARTESIAN_POINT ( 'NONE',  ( 4.219914504848593317, -11.69971097300155272, 32.46337939537588113 ) ) ;
#49620 = CARTESIAN_POINT ( 'NONE',  ( -18.00000000000000000, -1.270656007487078965, 33.34651343095210052 ) ) ;
#49621 = LINE ( 'NONE', #42432, #36676 ) ;
#49622 = EDGE_CURVE ( 'NONE', #61355, #14268, #31182, .T. ) ;
#49623 = ORIENTED_EDGE ( 'NONE', *, *, #79759, .T. ) ;
#49624 = VECTOR ( 'NONE', #43795, 1000.000000000000227 ) ;
#49625 = ORIENTED_EDGE ( 'NONE', *, *, #88355, .T. ) ;
#49626 = ORIENTED_EDGE ( 'NONE', *, *, #66552, .T. ) ;
#49627 = CARTESIAN_POINT ( 'NONE',  ( -10.68146699474474914, -8.164416787775445883, 34.95778746994557906 ) ) ;
#49628 = ORIENTED_EDGE ( 'NONE', *, *, #22646, .F. ) ;
#49629 = CARTESIAN_POINT ( 'NONE',  ( 13.25446817517716980, -2.882441371585227508, 31.66841991370172238 ) ) ;
#49630 = CARTESIAN_POINT ( 'NONE',  ( 16.82694633287448838, -3.436278759898155677, 33.07459398097509506 ) ) ;
#49631 = CARTESIAN_POINT ( 'NONE',  ( -18.13069146666755671, -11.18331474514187640, 33.13161551792790505 ) ) ;
#49632 = ORIENTED_EDGE ( 'NONE', *, *, #56002, .F. ) ;
#49633 = CARTESIAN_POINT ( 'NONE',  ( -5.300408020647025431, -10.81261337010820256, 33.49550067578627477 ) ) ;
#49634 = DIRECTION ( 'NONE',  ( 0.000000000000000000, 0.9848077530122072432, 0.1736481776669354937 ) ) ;
#49635 = CARTESIAN_POINT ( 'NONE',  ( 3.903869409797563250, -2.544273027872574922, 31.48422191005632342 ) ) ;
#49636 = CARTESIAN_POINT ( 'NONE',  ( 10.61538461538461675, -12.62096338111211580, 30.90682066428153263 ) ) ;
#49637 = ORIENTED_EDGE ( 'NONE', *, *, #16892, .T. ) ;
#49638 = VERTEX_POINT ( 'NONE', #66120 ) ;
#49639 = ORIENTED_EDGE ( 'NONE', *, *, #25481, .T. ) ;
#49640 = CARTESIAN_POINT ( 'NONE',  ( 13.38461538461538680, -2.499999999999998668, 29.75000000000001421 ) ) ;
#49642 = CARTESIAN_POINT ( 'NONE',  ( 1.384615384615386802, -11.35647404775217417, 33.31231777344666511 ) ) ;
#49641 = LINE ( 'NONE', #78436, #50426 ) ;
#49643 = B_SPLINE_CURVE_WITH_KNOTS ( 'NONE', 3,
 ( #65901, #44738, #4208, #31693, #45641, #52386, #11413, #38900, #66358, #4661 ),
 .UNSPECIFIED., .F., .F.,
 ( 4, 2, 2, 2, 4 ),
 ( 0.000000000000000000, 0.0001954339857564080165, 0.0003908679715128160329, 0.0005863019572692240765, 0.0007817359430256320659 ),
 .UNSPECIFIED. ) ;
#49644 = DIRECTION ( 'NONE',  ( -0.000000000000000000, 0.8660254037844399289, -0.4999999999999980016 ) ) ;
#49645 = DIRECTION ( 'NONE',  ( -0.000000000000000000, 1.000000000000000000, 3.491481338843133355E-15 ) ) ;
#49646 = FACE_BOUND ( 'NONE', #28125, .T. ) ;
#49647 = CARTESIAN_POINT ( 'NONE',  ( 7.911409417429871027, -11.48612834413965977, 32.76840700105972815 ) ) ;
#49648 = VERTEX_POINT ( 'NONE', #79208 ) ;
#49649 = VECTOR ( 'NONE', #61622, 1000.000000000000000 ) ;
#49650 = CARTESIAN_POINT ( 'NONE',  ( -2.980823712421087901, -2.587454068350147907, 30.68340429815432202 ) ) ;
#49651 = CARTESIAN_POINT ( 'NONE',  ( -0.3307466537136744544, -8.999086150933472084, 34.52020707165672064 ) ) ;
#49652 = CARTESIAN_POINT ( 'NONE',  ( -17.07692307692307665, -11.69971097300155272, 32.46337939537588113 ) ) ;
#49653 = DIRECTION ( 'NONE',  ( -1.000000000000000000, -0.000000000000000000, 0.000000000000000000 ) ) ;
#49654 = ORIENTED_EDGE ( 'NONE', *, *, #29491, .F. ) ;
#49655 = CARTESIAN_POINT ( 'NONE',  ( 4.826899852701617810, -12.68155406624981119, 30.59749803192733708 ) ) ;
#49656 = ORIENTED_EDGE ( 'NONE', *, *, #82826, .F. ) ;
#49657 = FACE_BOUND ( 'NONE', #78463, .T. ) ;
#49658 = CARTESIAN_POINT ( 'NONE',  ( -17.29985003582992320, -4.026226216239093603, 33.68668979543632958 ) ) ;
#49659 = FACE_OUTER_BOUND ( 'NONE', #48610, .T. ) ;
#49660 = CARTESIAN_POINT ( 'NONE',  ( 12.39545505058258001, -12.10708131394839349, 31.69288490824020244 ) ) ;
#49661 = ORIENTED_EDGE ( 'NONE', *, *, #60237, .F. ) ;
#49662 = AXIS2_PLACEMENT_3D ( 'NONE', #339, #26481, #27803 ) ;
#49663 = CARTESIAN_POINT ( 'NONE',  ( -12.46153846153858247, -10.21337939537710326, 33.94971097300076224 ) ) ;
#49664 = CARTESIAN_POINT ( 'NONE',  ( 15.36155967173618286, -2.295524264805589354, 30.44142389570982488 ) ) ;
#49665 = CARTESIAN_POINT ( 'NONE',  ( -14.98071481085577972, -10.06805714834173493, 34.32951233291982618 ) ) ;
#49666 = CARTESIAN_POINT ( 'NONE',  ( -16.15384615384627409, -2.625532179533778709, 30.86335684631627174 ) ) ;
#49667 = ORIENTED_EDGE ( 'NONE', *, *, #70658, .T. ) ;
#49668 = EDGE_CURVE ( 'NONE', #80366, #71586, #68841, .T. ) ;
#49669 = CARTESIAN_POINT ( 'NONE',  ( -7.623374304885436104, -10.81320215134717344, 33.49497208177562868 ) ) ;
#49670 = ORIENTED_EDGE ( 'NONE', *, *, #24074, .T. ) ;
#49672 = ORIENTED_EDGE ( 'NONE', *, *, #40973, .F. ) ;
#49671 = DIRECTION ( 'NONE',  ( -0.000000000000000000, 0.7660444431189791237, -0.6427876096865379196 ) ) ;
#49673 = CARTESIAN_POINT ( 'NONE',  ( 3.453548772037639658, -2.600157965045225783, 30.74683119005207743 ) ) ;
#49674 = CARTESIAN_POINT ( 'NONE',  ( -6.700065571464072889, -11.76359900205217457, 32.36225158514719880 ) ) ;
#49675 = CARTESIAN_POINT ( 'NONE',  ( 13.31853197365950514, -8.973038597847271092, 34.52809138561120506 ) ) ;
#49676 = CARTESIAN_POINT ( 'NONE',  ( 12.46153846153833911, -4.481592998941358097, 33.73612834414048933 ) ) ;
#49678 = CARTESIAN_POINT ( 'NONE',  ( -20.00000000000000000, -7.500000000000000000, 29.75000000000000355 ) ) ;
#49677 = CARTESIAN_POINT ( 'NONE',  ( -3.165514091256391715, -4.320704448112861584, 33.92786785259548310 ) ) ;
#49679 = CARTESIAN_POINT ( 'NONE',  ( 12.52668424087042531, -7.750023238201979581, 34.74374492549440419 ) ) ;
#49680 = CARTESIAN_POINT ( 'NONE',  ( -2.749999999999998224, -7.500000000000015987, 22.59375000000000355 ) ) ;
#49681 = VERTEX_POINT ( 'NONE', #18840 ) ;
#49682 = CARTESIAN_POINT ( 'NONE',  ( -15.09997742294444478, -3.530189275343204702, 32.79018710029569661 ) ) ;
#49683 = CARTESIAN_POINT ( 'NONE',  ( -9.561517251340740486, -11.37503395064541678, 33.29242100308974273 ) ) ;
#49684 = ORIENTED_EDGE ( 'NONE', *, *, #2527, .T. ) ;
#49685 = ADVANCED_FACE ( 'NONE', ( #46307 ), #67916, .F. ) ;
#49686 = EDGE_LOOP ( 'NONE', ( #8610, #75978, #3780, #17940 ) ) ;
#49687 = ORIENTED_EDGE ( 'NONE', *, *, #16040, .F. ) ;
#49688 = LINE ( 'NONE', #56001, #62755 ) ;
#49689 = ADVANCED_FACE ( 'NONE', ( #27371 ), #54837, .F. ) ;
#49690 = CARTESIAN_POINT ( 'NONE',  ( 3.100077764101672795, -9.804603061927743113, 34.18744698557895845 ) ) ;
#49691 = VECTOR ( 'NONE', #20555, 1000.000000000000114 ) ;
#49692 = CARTESIAN_POINT ( 'NONE',  ( -2.307692307692305711, -1.509761064869970415, 31.06009739812519044 ) ) ;
#49693 = DIRECTION ( 'NONE',  ( -0.000000000000000000, -0.9848077530122086864, -0.1736481776669273613 ) ) ;
#49694 = CARTESIAN_POINT ( 'NONE',  ( -16.40386939113911779, -3.202444869320336895, 32.30641848906366675 ) ) ;
#49695 = CARTESIAN_POINT ( 'NONE',  ( 7.145856464345329506, -11.41317474335729187, 32.86274602512330034 ) ) ;
#49696 = CARTESIAN_POINT ( 'NONE',  ( 13.44980837291003795, -2.255955759149235629, 29.99999999999988987 ) ) ;
#49697 = B_SPLINE_CURVE_WITH_KNOTS ( 'NONE', 3,
 ( #16095, #79127, #66041, #23287, #24622, #37689, #50307, #78231, #78683, #17428 ),
 .UNSPECIFIED., .F., .F.,
 ( 4, 2, 2, 2, 4 ),
 ( 0.000000000000000000, 0.0001954339857564078809, 0.0003908679715128157619, 0.0005863019572692236428, 0.0007817359430256315238 ),
 .UNSPECIFIED. ) ;
#49698 = CARTESIAN_POINT ( 'NONE',  ( 16.15384615384615330, -11.33034616979429110, 35.88435417666054406 ) ) ;
#49699 = CARTESIAN_POINT ( 'NONE',  ( 11.28848480751918437, -10.66389620160130036, 33.62221079203477103 ) ) ;
#49700 = EDGE_CURVE ( 'NONE', #15714, #27642, #75993, .T. ) ;
#49701 = CARTESIAN_POINT ( 'NONE',  ( 2.177545098254086486, -3.817052484675422797, 33.13202310037935661 ) ) ;
#49702 = CARTESIAN_POINT ( 'NONE',  ( -3.262820512820514107, -3.499999999999999556, 29.75000000000000355 ) ) ;
#49703 = EDGE_CURVE ( 'NONE', #14282, #35719, #34121, .T. ) ;
#49704 = VERTEX_POINT ( 'NONE', #61141 ) ;
#49705 = ORIENTED_EDGE ( 'NONE', *, *, #8303, .F. ) ;
#49706 = CARTESIAN_POINT ( 'NONE',  ( 17.07692307692295586, -11.06231777344772027, 33.60647404775119895 ) ) ;
#49707 = CARTESIAN_POINT ( 'NONE',  ( 3.296024370282069071, -11.06231777344671130, 33.60647404775212976 ) ) ;
#49708 = CARTESIAN_POINT ( 'NONE',  ( 13.38461538461526601, -12.27809138561165270, 31.22303859784587132 ) ) ;
#49709 = VERTEX_POINT ( 'NONE', #19285 ) ;
#49710 = FACE_OUTER_BOUND ( 'NONE', #86172, .T. ) ;
#49711 = CARTESIAN_POINT ( 'NONE',  ( -12.71153846153846345, -7.433931650972299465, 34.75000000000000711 ) ) ;
#49712 = CARTESIAN_POINT ( 'NONE',  ( -8.835313148590904220, -9.058645607665454236, 34.76329471203372634 ) ) ;
#49713 = VECTOR ( 'NONE', #11569, 1000.000000000000114 ) ;
#49714 = EDGE_CURVE ( 'NONE', #86676, #46211, #40457, .T. ) ;
#49715 = ORIENTED_EDGE ( 'NONE', *, *, #38194, .F. ) ;
#49716 = CARTESIAN_POINT ( 'NONE',  ( 16.15384615384603251, -2.892918686052165622, 31.69288490824153470 ) ) ;
#49717 = ADVANCED_FACE ( 'NONE', ( #68796 ), #26487, .F. ) ;
#49718 = ORIENTED_EDGE ( 'NONE', *, *, #76773, .F. ) ;
#49719 = CARTESIAN_POINT ( 'NONE',  ( 16.28463659481310444, -9.084667340241228572, 34.75534355489798344 ) ) ;
#49720 = FACE_OUTER_BOUND ( 'NONE', #6239, .T. ) ;
#49721 = ADVANCED_FACE ( 'NONE', ( #88654 ), #5771, .F. ) ;
#49722 = CARTESIAN_POINT ( 'NONE',  ( 17.07692307692307665, -1.129524287112498415, 32.06866353760679544 ) ) ;
#49723 = ADVANCED_FACE ( 'NONE', ( #14294 ), #61587, .T. ) ;
#49724 = VECTOR ( 'NONE', #62472, 1000.000000000000000 ) ;
#49725 = CYLINDRICAL_SURFACE ( 'NONE', #10544, 0.2500000000000008882 ) ;
#49726 = CARTESIAN_POINT ( 'NONE',  ( 13.38461538461538680, -1.466349020453238561, 30.81389545987213907 ) ) ;
#49727 = EDGE_LOOP ( 'NONE', ( #72226, #14291 ) ) ;
#49728 = VERTEX_POINT ( 'NONE', #53948 ) ;
#49729 = VERTEX_POINT ( 'NONE', #13407 ) ;
#49730 = CARTESIAN_POINT ( 'NONE',  ( -10.68146699474474914, -12.34228464037088280, 31.77849191805838558 ) ) ;
#49731 = CARTESIAN_POINT ( 'NONE',  ( 16.02369818411445834, -5.915902021225892149, 34.75552854090298638 ) ) ;
#49732 = CARTESIAN_POINT ( 'NONE',  ( 0.4615384615384611200, -6.343179335718451384, 34.87096338111211935 ) ) ;
#49733 = B_SPLINE_CURVE_WITH_KNOTS ( 'NONE', 3,
 ( #30856, #58327, #65532, #85822, #24100, #3833, #31315, #58777, #24547, #25890 ),
 .UNSPECIFIED., .F., .F.,
 ( 4, 2, 2, 2, 4 ),
 ( 0.000000000000000000, 0.0001954311564186858715, 0.0003908623128373717431, 0.0005862934692560576146, 0.0007817246256747434861 ),
 .UNSPECIFIED. ) ;
#49734 = CARTESIAN_POINT ( 'NONE',  ( 11.28843830116857383, -12.22074536777954989, 31.39888409691088356 ) ) ;
#49735 = CARTESIAN_POINT ( 'NONE',  ( 4.219914504848592429, -6.386643153685127139, 34.62446782046654192 ) ) ;
#49736 = CARTESIAN_POINT ( 'NONE',  ( 14.37376065869474751, -9.780366693483667717, 34.19971097300155805 ) ) ;
#49737 = EDGE_LOOP ( 'NONE', ( #21021, #58735, #78607, #86146 ) ) ;
#49738 = VERTEX_POINT ( 'NONE', #48070 ) ;
#49739 = VECTOR ( 'NONE', #21002, 1000.000000000000000 ) ;
#49740 = ORIENTED_EDGE ( 'NONE', *, *, #56562, .T. ) ;
#49742 = VERTEX_POINT ( 'NONE', #34571 ) ;
#49741 = CARTESIAN_POINT ( 'NONE',  ( 3.903822916553188360, -2.823816976329321271, 31.52131813110797154 ) ) ;
#49744 = CARTESIAN_POINT ( 'NONE',  ( -8.638438961405981331, -11.18335022499818621, 33.13157742990016885 ) ) ;
#49743 = CARTESIAN_POINT ( 'NONE',  ( -9.692307692307691624, -8.973038597847269315, 34.52809138561121927 ) ) ;
#49745 = EDGE_CURVE ( 'NONE', #18725, #52344, #35006, .T. ) ;
#49746 = CARTESIAN_POINT ( 'NONE',  ( -3.749999999999997335, -7.500000000000021316, 23.84375000000000000 ) ) ;
#49747 = ORIENTED_EDGE ( 'NONE', *, *, #74571, .F. ) ;
#49748 = ORIENTED_EDGE ( 'NONE', *, *, #39859, .T. ) ;
#49749 = CARTESIAN_POINT ( 'NONE',  ( 13.60799132531357003, -2.501478030877322567, 29.88021232661721172 ) ) ;
#49750 = VERTEX_POINT ( 'NONE', #68353 ) ;
#49751 = FACE_BOUND ( 'NONE', #1756, .T. ) ;
#49752 = CARTESIAN_POINT ( 'NONE',  ( -5.933932666649923249, -2.833524468853757750, 32.15551576947925838 ) ) ;
#49753 = EDGE_CURVE ( 'NONE', #62900, #29059, #10768, .T. ) ;
#49754 = CARTESIAN_POINT ( 'NONE',  ( -8.769230769230892619, -12.16647553114689728, 32.15551576947799362 ) ) ;
#49755 = ORIENTED_EDGE ( 'NONE', *, *, #6301, .F. ) ;
#49756 = CARTESIAN_POINT ( 'NONE',  ( -14.98082371242109012, -5.057305518903948638, 34.11320923018887896 ) ) ;
#49757 = CARTESIAN_POINT ( 'NONE',  ( 11.53846153846141576, -6.835583212225970762, 34.95778746994575670 ) ) ;
#49758 = DIRECTION ( 'NONE',  ( 0.000000000000000000, 0.000000000000000000, -1.000000000000000000 ) ) ;
#49759 = CARTESIAN_POINT ( 'NONE',  ( -15.23076923076922995, -6.386643153685126251, 34.62446782046654192 ) ) ;
#49760 = CARTESIAN_POINT ( 'NONE',  ( 4.284637961670939355, -3.062576670634119758, 32.05464942895959979 ) ) ;
#49761 = EDGE_LOOP ( 'NONE', ( #10405, #26913 ) ) ;
#49762 = EDGE_CURVE ( 'NONE', #12856, #22911, #7094, .T. ) ;
#49763 = CARTESIAN_POINT ( 'NONE',  ( -7.146561866800870355, -11.41268669641500466, 32.86336882939237825 ) ) ;
#49764 = CARTESIAN_POINT ( 'NONE',  ( -8.096177070375304652, -12.07920672191015221, 32.31858351112116168 ) ) ;
#49765 = LINE ( 'NONE', #22301, #35546 ) ;
#49766 = DIRECTION ( 'NONE',  ( 0.000000000000000000, 1.000000000000000000, 0.000000000000000000 ) ) ;
#49767 = CARTESIAN_POINT ( 'NONE',  ( -14.98071491913091791, -11.79725096376909299, 32.30694842903960762 ) ) ;
#49768 = AXIS2_PLACEMENT_3D ( 'NONE', #39040, #80466, #44881 ) ;
#49769 = CARTESIAN_POINT ( 'NONE',  ( -13.38461538461538325, -12.34228464037088635, 31.77849191805839268 ) ) ;
#49771 = CARTESIAN_POINT ( 'NONE',  ( 11.76124107972994359, -4.387253974876679230, 33.66317474335728832 ) ) ;
#49770 = DIRECTION ( 'NONE',  ( 0.000000000000000000, 0.9396926207859126468, -0.3420201433256571111 ) ) ;
#49772 = CARTESIAN_POINT ( 'NONE',  ( 5.142178216435913107, -9.528491918058460186, 34.59228464037085615 ) ) ;
#49774 = FACE_OUTER_BOUND ( 'NONE', #82793, .T. ) ;
#49773 = CARTESIAN_POINT ( 'NONE',  ( -11.47320596718551755, -11.48612834413965977, 32.76840700105972815 ) ) ;
#49775 = CARTESIAN_POINT ( 'NONE',  ( 6.000000000000001776, -1.629998284177014645, 34.34916445242399163 ) ) ;
#49776 = B_SPLINE_CURVE_WITH_KNOTS ( 'NONE', 3,
 ( #70357, #77551, #64023, #35692, #77992, #55945, #2321, #71225, #8662, #2759 ),
 .UNSPECIFIED., .F., .F.,
 ( 4, 2, 2, 2, 4 ),
 ( 0.0007817246256747473893, 0.0009771112852218909357, 0.001172497944769034482, 0.001367884604316178246, 0.001563271263863321792 ),
 .UNSPECIFIED. ) ;
#49777 = CARTESIAN_POINT ( 'NONE',  ( 1.987747218494664292, -9.401340078031346081, 20.62313170625849068 ) ) ;
#49778 = ORIENTED_EDGE ( 'NONE', *, *, #79517, .F. ) ;
#49779 = CARTESIAN_POINT ( 'NONE',  ( -0.7781152905427543010, -3.838812988065675835, 13.99999999999999289 ) ) ;
#49780 = ORIENTED_EDGE ( 'NONE', *, *, #79416, .F. ) ;
#49781 = CARTESIAN_POINT ( 'NONE',  ( 6.000000000000001776, -4.102666532097928531, 36.13435417666054406 ) ) ;
#49782 = ADVANCED_FACE ( 'NONE', ( #74230 ), #33243, .F. ) ;
#49783 = ORIENTED_EDGE ( 'NONE', *, *, #46847, .F. ) ;
#49784 = CARTESIAN_POINT ( 'NONE',  ( -3.930834802233303282, -11.24521262558773671, 33.06293181088029343 ) ) ;
#49785 = LINE ( 'NONE', #1609, #7192 ) ;
#49787 = ORIENTED_EDGE ( 'NONE', *, *, #29265, .T. ) ;
#49786 = VECTOR ( 'NONE', #75561, 1000.000000000000000 ) ;
#49788 = CARTESIAN_POINT ( 'NONE',  ( -18.22348494372394967, -12.44517049084099725, 30.48991314939691932 ) ) ;
#49789 = CARTESIAN_POINT ( 'NONE',  ( -1.200186371490556958, -4.775308065498765409, 21.32625670625849423 ) ) ;
#49790 = CARTESIAN_POINT ( 'NONE',  ( -17.77698715590660328, -9.172514111537580561, 34.72667873470787470 ) ) ;
#49791 = EDGE_CURVE ( 'NONE', #58385, #46391, #47294, .T. ) ;
#49792 = CYLINDRICAL_SURFACE ( 'NONE', #70505, 0.2499999999999998890 ) ;
#49793 = CARTESIAN_POINT ( 'NONE',  ( 7.053868730901711182, -8.999086150933472084, 34.52020707165672064 ) ) ;
#49794 = CARTESIAN_POINT ( 'NONE',  ( 7.912222197156284054, -11.69971097300155272, 32.46337939537588113 ) ) ;
#49795 = DIRECTION ( 'NONE',  ( -0.000000000000000000, -0.3420201433256694901, -0.9396926207859082059 ) ) ;
#49796 = CARTESIAN_POINT ( 'NONE',  ( 5.011652630962299959, -8.613356846314824011, 34.62446782046655613 ) ) ;
#49797 = CARTESIAN_POINT ( 'NONE',  ( 2.651650429449539104, -4.848349570550432475, 18.06250000000000355 ) ) ;
#49798 = CARTESIAN_POINT ( 'NONE',  ( -9.320512820512821150, -3.499999999999999556, 29.75000000000000355 ) ) ;
#49799 = LINE ( 'NONE', #20991, #63559 ) ;
#49800 = LINE ( 'NONE', #48919, #53613 ) ;
#49801 = CARTESIAN_POINT ( 'NONE',  ( 3.749999999999992006, -5.946699141100872943, 18.14062500000000711 ) ) ;
#49802 = CARTESIAN_POINT ( 'NONE',  ( -14.08491276642389245, -10.81320215134717344, 33.49497208177562868 ) ) ;
#49803 = EDGE_LOOP ( 'NONE', ( #42351, #70665 ) ) ;
#49804 = AXIS2_PLACEMENT_3D ( 'NONE', #31639, #16782, #59099 ) ;
#49805 = CARTESIAN_POINT ( 'NONE',  ( -11.00641025641025550, -11.50000000000000000, 29.75000000000000355 ) ) ;
#49806 = CARTESIAN_POINT ( 'NONE',  ( 16.15384615384615330, -12.10708131394839349, 31.69288490824020244 ) ) ;
#49807 = CARTESIAN_POINT ( 'NONE',  ( 1.318531973659505807, -12.37446782046654192, 30.86335684631486487 ) ) ;
#49808 = CARTESIAN_POINT ( 'NONE',  ( 24.99999999999999645, -15.00000000000000000, 3.000000000000000000 ) ) ;
#49809 = CARTESIAN_POINT ( 'NONE',  ( 13.60762673622823549, -2.554770724473668153, 30.48948780036025852 ) ) ;
#49810 = B_SPLINE_CURVE_WITH_KNOTS ( 'NONE', 3,
 ( #48645, #34700, #12656, #27497, #27941, #74359, #88779, #40142, #82894, #87904 ),
 .UNSPECIFIED., .F., .F.,
 ( 4, 2, 2, 2, 4 ),
 ( 0.000000000000000000, 0.0001954311564186861697, 0.0003908623128373723394, 0.0005862934692560584820, 0.0007817246256747446788 ),
 .UNSPECIFIED. ) ;
#49811 = VECTOR ( 'NONE', #10607, 1000.000000000000000 ) ;
#49812 = CARTESIAN_POINT ( 'NONE',  ( 2.057669070399343436, -12.22074536777954989, 31.39888409691088356 ) ) ;
#49813 = LINE ( 'NONE', #64203, #31972 ) ;
#49814 = B_SPLINE_CURVE_WITH_KNOTS ( 'NONE', 3,
 ( #59311, #44445, #4371, #37255, #23738, #65610, #71485, #86817, #72374, #30507 ),
 .UNSPECIFIED., .F., .F.,
 ( 4, 2, 2, 2, 4 ),
 ( 0.000000000000000000, 0.0001954339857564054144, 0.0003908679715128108288, 0.0005863019572692162703, 0.0007817359430256216575 ),
 .UNSPECIFIED. ) ;
#49815 = EDGE_CURVE ( 'NONE', #79032, #32391, #64511, .T. ) ;
#49816 = ORIENTED_EDGE ( 'NONE', *, *, #72427, .T. ) ;
#49817 = EDGE_LOOP ( 'NONE', ( #15404, #22569, #38929, #36034 ) ) ;
#49818 = EDGE_CURVE ( 'NONE', #50723, #66717, #11905, .T. ) ;
#49819 = ORIENTED_EDGE ( 'NONE', *, *, #29160, .F. ) ;
#49820 = LINE ( 'NONE', #55690, #38409 ) ;
#49821 = CARTESIAN_POINT ( 'NONE',  ( -10.61538461538461320, -12.48256725967547354, 35.29906147534542527 ) ) ;
#49822 = DIRECTION ( 'NONE',  ( -0.000000000000000000, 0.3420201433256694901, -0.9396926207859082059 ) ) ;
#49823 = ADVANCED_FACE ( 'NONE', ( #2102 ), #29153, .F. ) ;
#49824 = CARTESIAN_POINT ( 'NONE',  ( -9.692307692307377209, -2.255955759149395501, 30.00000000000324363 ) ) ;
#49825 = DIRECTION ( 'NONE',  ( -0.000000000000000000, -0.000000000000000000, -1.000000000000000000 ) ) ;
#49826 = ORIENTED_EDGE ( 'NONE', *, *, #72075, .F. ) ;
#49827 = CARTESIAN_POINT ( 'NONE',  ( -17.20761454359064047, -4.118384482072086072, 33.43331474514187107 ) ) ;
#49828 = EDGE_LOOP ( 'NONE', ( #83935, #63681 ) ) ;
#49829 = ORIENTED_EDGE ( 'NONE', *, *, #29449, .F. ) ;
#49831 = ORIENTED_EDGE ( 'NONE', *, *, #11173, .F. ) ;
#49830 = CARTESIAN_POINT ( 'NONE',  ( 4.219913487196230939, -12.34228464037088813, 31.77849191805839268 ) ) ;
#49832 = CARTESIAN_POINT ( 'NONE',  ( 8.769230769230768274, -2.721908614388771852, 31.22303859784724978 ) ) ;
#49833 = EDGE_CURVE ( 'NONE', #65922, #75150, #53844, .T. ) ;
#49834 = FACE_OUTER_BOUND ( 'NONE', #44094, .T. ) ;
#49835 = EDGE_CURVE ( 'NONE', #85483, #61122, #35453, .T. ) ;
#49836 = CARTESIAN_POINT ( 'NONE',  ( -9.942330929600657896, -8.432397168068783699, 34.66272746175022945 ) ) ;
#49837 = FACE_OUTER_BOUND ( 'NONE', #32761, .T. ) ;
#49838 = ORIENTED_EDGE ( 'NONE', *, *, #46515, .T. ) ;
#49839 = VERTEX_POINT ( 'NONE', #56610 ) ;
#49840 = EDGE_LOOP ( 'NONE', ( #20623, #71248, #72454, #25671 ) ) ;
#49841 = CARTESIAN_POINT ( 'NONE',  ( -2.057637887778853703, -3.435999193479609470, 33.07426656108011542 ) ) ;
#49843 = ORIENTED_EDGE ( 'NONE', *, *, #23010, .F. ) ;
#49842 = CARTESIAN_POINT ( 'NONE',  ( -14.08491263871423982, -2.353885683473779800, 30.79025554430704403 ) ) ;
#49844 = CARTESIAN_POINT ( 'NONE',  ( -6.923076923077044142, -12.46129190930018460, 30.37095296980731973 ) ) ;
#49845 = CARTESIAN_POINT ( 'NONE',  ( -11.53846153846153655, -13.95598074871891292, 31.83374038241031911 ) ) ;
#49846 = EDGE_CURVE ( 'NONE', #44756, #53910, #51573, .T. ) ;
#49847 = CARTESIAN_POINT ( 'NONE',  ( 6.923076923076802558, -11.94971097300221174, 32.03036669348237098 ) ) ;
#49848 = ORIENTED_EDGE ( 'NONE', *, *, #19045, .F. ) ;
#49849 = DIRECTION ( 'NONE',  ( -0.000000000000000000, 0.7660444431189791237, -0.6427876096865379196 ) ) ;
#49850 = CARTESIAN_POINT ( 'NONE',  ( -15.10024379253558635, -12.50538340440932394, 31.33453814440721885 ) ) ;
#49851 = ORIENTED_EDGE ( 'NONE', *, *, #53227, .F. ) ;
#49852 = FACE_BOUND ( 'NONE', #75390, .T. ) ;
#49853 = EDGE_CURVE ( 'NONE', #79858, #82502, #4219, .T. ) ;
#49854 = CARTESIAN_POINT ( 'NONE',  ( 4.153846153846154188, -4.661471528628507777, 34.16647553114623292 ) ) ;
#49855 = LINE ( 'NONE', #20617, #38538 ) ;
#49856 = CARTESIAN_POINT ( 'NONE',  ( -1.384615384615383471, -7.500000000000001776, 35.04278698407183867 ) ) ;
#49858 = DIRECTION ( 'NONE',  ( -1.000000000000000000, -0.000000000000000000, -0.000000000000000000 ) ) ;
#49857 = CARTESIAN_POINT ( 'NONE',  ( 7.976679284387491187, -11.04252011169590020, 33.62494198852677130 ) ) ;
#49859 = AXIS2_PLACEMENT_3D ( 'NONE', #10942, #75204, #18593 ) ;
#49860 = CARTESIAN_POINT ( 'NONE',  ( -1.161602540521988969, -8.282913670948747864, 34.94150082978203642 ) ) ;
#49861 = CARTESIAN_POINT ( 'NONE',  ( -15.93106661257773560, -9.332535724633405749, 34.40230450496446224 ) ) ;
#49862 = ORIENTED_EDGE ( 'NONE', *, *, #79821, .F. ) ;
#49863 = FACE_OUTER_BOUND ( 'NONE', #19621, .T. ) ;
#49864 = CARTESIAN_POINT ( 'NONE',  ( -16.85414340794500276, -6.717445702608400460, 34.94155399931962336 ) ) ;
#49865 = VERTEX_POINT ( 'NONE', #16067 ) ;
#49866 = AXIS2_PLACEMENT_3D ( 'NONE', #38412, #80296, #87069 ) ;
#49867 = EDGE_CURVE ( 'NONE', #55616, #8684, #35902, .T. ) ;
#49868 = CARTESIAN_POINT ( 'NONE',  ( -16.15384615384627409, -12.70778746994576025, 30.41441678777401236 ) ) ;
#49869 = CARTESIAN_POINT ( 'NONE',  ( -16.15384615384615330, -9.058645607665452459, 34.76329471203371924 ) ) ;
#49870 = CARTESIAN_POINT ( 'NONE',  ( -4.087777802843712394, -2.538708090699994813, 30.37095296980875503 ) ) ;
#49871 = DIRECTION ( 'NONE',  ( 1.000000000000000000, 0.000000000000000000, 0.000000000000000000 ) ) ;
#49872 = CARTESIAN_POINT ( 'NONE',  ( 17.99999999999987566, -6.026961402154118908, 34.52809138561165270 ) ) ;
#49873 = LINE ( 'NONE', #56198, #61667 ) ;
#49874 = FACE_BOUND ( 'NONE', #79893, .T. ) ;
#49875 = EDGE_CURVE ( 'NONE', #31330, #53433, #69962, .T. ) ;
#49877 = DIRECTION ( 'NONE',  ( 1.000000000000000000, 0.000000000000000000, 0.000000000000000000 ) ) ;
#49876 = FACE_OUTER_BOUND ( 'NONE', #44828, .T. ) ;
#49878 = VECTOR ( 'NONE', #35842, 1000.000000000000000 ) ;
#49879 = DIRECTION ( 'NONE',  ( -0.000000000000000000, -0.1736481776669307198, -0.9848077530122080203 ) ) ;
#49881 = CARTESIAN_POINT ( 'NONE',  ( -15.10024352900566846, -6.852161475712352789, 34.70806712695775786 ) ) ;
#49880 = CARTESIAN_POINT ( 'NONE',  ( -6.792551484843280640, -11.04252011169590020, 33.62494198852677130 ) ) ;
#49882 = LINE ( 'NONE', #76481, #39016 ) ;
#49883 = CARTESIAN_POINT ( 'NONE',  ( -3.775308065498766297, -6.007798216065450170, 18.67000670625849068 ) ) ;
#49884 = ORIENTED_EDGE ( 'NONE', *, *, #46004, .T. ) ;
#49885 = VERTEX_POINT ( 'NONE', #2982 ) ;
#49886 = CARTESIAN_POINT ( 'NONE',  ( -9.692307692307814193, -2.379036618888197729, 30.90682066428292885 ) ) ;
#49887 = CARTESIAN_POINT ( 'NONE',  ( -0.4615384615385826339, -10.90142922262034020, 33.41473453929536674 ) ) ;
#49888 = CARTESIAN_POINT ( 'NONE',  ( 2.307692307692309264, -2.249999999999998668, 29.50000000000001421 ) ) ;
#49889 = CARTESIAN_POINT ( 'NONE',  ( -1.634638621908350187, -3.202444869320336451, 32.30641848906366675 ) ) ;
#49890 = CARTESIAN_POINT ( 'NONE',  ( -3.930833309752755245, -2.889357225399416418, 32.26129605718031002 ) ) ;
#49891 = CARTESIAN_POINT ( 'NONE',  ( -2.608446859217889546, -10.19485399968121264, 20.93563170625849068 ) ) ;
#49892 = EDGE_CURVE ( 'NONE', #67170, #62464, #78651, .T. ) ;
#49893 = CARTESIAN_POINT ( 'NONE',  ( 4.220015294808810324, -7.250054483168843156, 34.74374881642865631 ) ) ;
#49894 = CARTESIAN_POINT ( 'NONE',  ( -6.000000000000119904, -12.46129190930018460, 30.37095296980731973 ) ) ;
#49895 = EDGE_CURVE ( 'NONE', #34931, #21233, #65638, .T. ) ;
#49896 = DIRECTION ( 'NONE',  ( 0.000000000000000000, 0.6427876096865368094, 0.7660444431189802339 ) ) ;
#49897 = CARTESIAN_POINT ( 'NONE',  ( -1.515306851282942624, -12.38065189839062263, 30.83690757178629482 ) ) ;
#49898 = CARTESIAN_POINT ( 'NONE',  ( -3.296039231325550212, -4.320704448112771878, 33.92786785259540494 ) ) ;
#49899 = CARTESIAN_POINT ( 'NONE',  ( 3.930361210122205406, -10.81261337010820256, 33.49550067578627477 ) ) ;
#49900 = CYLINDRICAL_SURFACE ( 'NONE', #33296, 0.2500000000000004996 ) ;
#49901 = CARTESIAN_POINT ( 'NONE',  ( 14.24242186173153435, -6.879047030191174805, 34.71129190930000163 ) ) ;
#49902 = VERTEX_POINT ( 'NONE', #86320 ) ;
#49903 = DIRECTION ( 'NONE',  ( -0.000000000000000000, -0.1736481776669307198, -0.9848077530122080203 ) ) ;
#49904 = CARTESIAN_POINT ( 'NONE',  ( 0.7114839798866029463, -2.587454068350147462, 30.68340429815432202 ) ) ;
#49905 = CIRCLE ( 'NONE', #5300, 0.2500000000000002220 ) ;
#49906 = CARTESIAN_POINT ( 'NONE',  ( -0.06109907496451398579, -10.25000000000000178, 21.28311829374151287 ) ) ;
#49907 = B_SPLINE_CURVE_WITH_KNOTS ( 'NONE', 3,
 ( #41542, #49627, #77099, #15409, #42879, #69006, #7316, #34777, #2308, #2749 ),
 .UNSPECIFIED., .F., .F.,
 ( 4, 2, 2, 2, 4 ),
 ( 0.000000000000000000, 0.0001954311564186871184, 0.0003908623128373742367, 0.0005862934692560614093, 0.0007817246256747484735 ),
 .UNSPECIFIED. ) ;
#49908 = CARTESIAN_POINT ( 'NONE',  ( -2.372962308248625973, -5.094484230520674117, 34.41647553114621161 ) ) ;
#49909 = CARTESIAN_POINT ( 'NONE',  ( -15.90379173393269596, -2.544122305571458575, 31.48381861865057729 ) ) ;
#49910 = ORIENTED_EDGE ( 'NONE', *, *, #40594, .T. ) ;
#49911 = DIRECTION ( 'NONE',  ( 0.000000000000000000, -6.938893903907222067E-15, 1.000000000000000000 ) ) ;
#49913 = ORIENTED_EDGE ( 'NONE', *, *, #66537, .F. ) ;
#49912 = CARTESIAN_POINT ( 'NONE',  ( 1.576923076923075762, -7.500000000000000000, 29.75000000000000355 ) ) ;
#49914 = CARTESIAN_POINT ( 'NONE',  ( 9.692307692307570832, -12.70778746994576025, 30.41441678777401236 ) ) ;
#49915 = CARTESIAN_POINT ( 'NONE',  ( 12.52679360105129547, -5.941354392334607049, 34.76329471203374055 ) ) ;
#49916 = ORIENTED_EDGE ( 'NONE', *, *, #52677, .T. ) ;
#49917 = CARTESIAN_POINT ( 'NONE',  ( -5.076923076923075762, -11.16473453929635440, 33.15142922261926373 ) ) ;
#49918 = CARTESIAN_POINT ( 'NONE',  ( -13.44988583057615905, -3.300289026998414865, 32.46337939537583139 ) ) ;
#49919 = ORIENTED_EDGE ( 'NONE', *, *, #62359, .T. ) ;
#49920 = CARTESIAN_POINT ( 'NONE',  ( -11.53846153846153655, -4.098570777380720287, 33.41473453929634729 ) ) ;
#49921 = CARTESIAN_POINT ( 'NONE',  ( 15.23076923076923173, -13.37000171582298513, 34.34916445242398453 ) ) ;
#49922 = CARTESIAN_POINT ( 'NONE',  ( -3.230769230769352962, -12.16647553114689728, 32.15551576947799362 ) ) ;
#49923 = ORIENTED_EDGE ( 'NONE', *, *, #62521, .T. ) ;
#49924 = EDGE_LOOP ( 'NONE', ( #50575, #43780 ) ) ;
#49925 = B_SPLINE_CURVE_WITH_KNOTS ( 'NONE', 3,
 ( #11351, #46905, #12243, #25314, #24859, #46025, #74846, #4597, #40614, #67638 ),
 .UNSPECIFIED., .F., .F.,
 ( 4, 2, 2, 2, 4 ),
 ( 0.000000000000000000, 0.0001954311564186866034, 0.0003908623128373732067, 0.0005862934692560597830, 0.0007817246256747464135 ),
 .UNSPECIFIED. ) ;
#49926 = EDGE_CURVE ( 'NONE', #18170, #35531, #18287, .T. ) ;
#49927 = ORIENTED_EDGE ( 'NONE', *, *, #35056, .F. ) ;
#49928 = VECTOR ( 'NONE', #75238, 1000.000000000000114 ) ;
#49929 = CARTESIAN_POINT ( 'NONE',  ( 12.59233026936325217, -8.999086150933475636, 34.52020707165672775 ) ) ;
#49930 = DIRECTION ( 'NONE',  ( 0.000000000000000000, 0.000000000000000000, -1.000000000000000000 ) ) ;
#49931 = EDGE_CURVE ( 'NONE', #39557, #49527, #29135, .T. ) ;
#49932 = CARTESIAN_POINT ( 'NONE',  ( 15.23076923076910916, -12.16647553114689728, 32.15551576947799362 ) ) ;
#49933 = EDGE_CURVE ( 'NONE', #45473, #80310, #63407, .T. ) ;
#49934 = FACE_OUTER_BOUND ( 'NONE', #33624, .T. ) ;
#49935 = B_SPLINE_CURVE_WITH_KNOTS ( 'NONE', 3,
 ( #9367, #72378, #65177, #85461, #79147, #36825, #51195, #64282, #24643, #50764 ),
 .UNSPECIFIED., .F., .F.,
 ( 4, 2, 2, 2, 4 ),
 ( 0.000000000000000000, 0.0001954311564186860613, 0.0003908623128373721225, 0.0005862934692560581567, 0.0007817246256747442451 ),
 .UNSPECIFIED. ) ;
#49936 = ORIENTED_EDGE ( 'NONE', *, *, #995, .F. ) ;
#49937 = B_SPLINE_CURVE_WITH_KNOTS ( 'NONE', 3,
 ( #79171, #17472, #44926, #71511, #72402, #10714, #3052, #71078, #9820, #65636 ),
 .UNSPECIFIED., .F., .F.,
 ( 4, 2, 2, 2, 4 ),
 ( 0.000000000000000000, 0.0001954311584214072381, 0.0003908623168428144762, 0.0005862934752642217414, 0.0007817246336856289524 ),
 .UNSPECIFIED. ) ;
#49938 = EDGE_LOOP ( 'NONE', ( #75125, #66128 ) ) ;
#49940 = ORIENTED_EDGE ( 'NONE', *, *, #46445, .F. ) ;
#49939 = CARTESIAN_POINT ( 'NONE',  ( 4.284371592079798674, -8.630441415882550871, 34.87705825610312615 ) ) ;
#49941 = EDGE_CURVE ( 'NONE', #5224, #54359, #55912, .T. ) ;
#49942 = CARTESIAN_POINT ( 'NONE',  ( 16.21910129335899597, -8.656820664281605460, 34.87096338111211224 ) ) ;
#49943 = ORIENTED_EDGE ( 'NONE', *, *, #3674, .T. ) ;
#49944 = CARTESIAN_POINT ( 'NONE',  ( -16.15384615384627409, -5.094484230521993062, 34.41647553114689373 ) ) ;
#49945 = CARTESIAN_POINT ( 'NONE',  ( -8.769230769230768274, -12.62096338111211580, 30.90682066428153263 ) ) ;
#49946 = ORIENTED_EDGE ( 'NONE', *, *, #8764, .F. ) ;
#49947 = ORIENTED_EDGE ( 'NONE', *, *, #75162, .F. ) ;
#49949 = ORIENTED_EDGE ( 'NONE', *, *, #76216, .F. ) ;
#49948 = CARTESIAN_POINT ( 'NONE',  ( 9.822833130541342328, -8.630441415882550871, 34.87705825610312615 ) ) ;
#49950 = CYLINDRICAL_SURFACE ( 'NONE', #25831, 0.2500000000000004996 ) ;
#49951 = AXIS2_PLACEMENT_3D ( 'NONE', #85602, #23879, #10388 ) ;
#49952 = CARTESIAN_POINT ( 'NONE',  ( 14.17754433796061164, -5.915902021225889484, 34.75552854090298638 ) ) ;
#49953 = EDGE_LOOP ( 'NONE', ( #78434, #56042, #11747, #70233 ) ) ;
#49954 = CARTESIAN_POINT ( 'NONE',  ( 15.93091993633000847, -12.39988816332205701, 30.74660775122750778 ) ) ;
#49955 = CARTESIAN_POINT ( 'NONE',  ( -4.403846153846174616, -2.249999999999999112, 29.81609741502488120 ) ) ;
#49956 = CARTESIAN_POINT ( 'NONE',  ( 14.30769230769231015, -6.189225973068211317, 35.74407628777942847 ) ) ;
#49957 = FACE_BOUND ( 'NONE', #30556, .T. ) ;
#49958 = ADVANCED_FACE ( 'NONE', ( #59713 ), #73689, .F. ) ;
#49959 = CARTESIAN_POINT ( 'NONE',  ( -9.692307692307691624, -3.937682226553329556, 33.60647404775216529 ) ) ;
#49960 = DIRECTION ( 'NONE',  ( -0.000000000000000000, -0.6427876096865404731, -0.7660444431189770143 ) ) ;
#49961 = CARTESIAN_POINT ( 'NONE',  ( -15.23076923076935074, -10.90142922262034020, 33.41473453929536674 ) ) ;
#49963 = CARTESIAN_POINT ( 'NONE',  ( -5.776988648387150427, -2.758310577978207778, 31.33698337089303010 ) ) ;
#49962 = CARTESIAN_POINT ( 'NONE',  ( 12.21151523731700550, -3.520140089381495585, 33.17453946501458262 ) ) ;
#49964 = DIRECTION ( 'NONE',  ( -1.000000000000000000, -0.000000000000000000, 0.000000000000000000 ) ) ;
#49965 = DIRECTION ( 'NONE',  ( 0.000000000000000000, 0.9848077530122072432, 0.1736481776669354937 ) ) ;
#49966 = ORIENTED_EDGE ( 'NONE', *, *, #35336, .T. ) ;
#49967 = VECTOR ( 'NONE', #5058, 1000.000000000000000 ) ;
#49968 = CARTESIAN_POINT ( 'NONE',  ( -5.776988648387149539, -11.76359900205217457, 32.36225158514719880 ) ) ;
#49969 = EDGE_LOOP ( 'NONE', ( #44418, #39654, #67959, #84184 ) ) ;
#49970 = ORIENTED_EDGE ( 'NONE', *, *, #69778, .T. ) ;
#49971 = B_SPLINE_CURVE_WITH_KNOTS ( 'NONE', 3,
 ( #77435, #8546, #56719, #84650, #50391, #894, #70683, #8989, #9421, #15746 ),
 .UNSPECIFIED., .F., .F.,
 ( 4, 2, 2, 2, 4 ),
 ( 0.000000000000000000, 0.0001954311564186876334, 0.0003908623128373752667, 0.0005862934692560629272, 0.0007817246256747505334 ),
 .UNSPECIFIED. ) ;
#49973 = CARTESIAN_POINT ( 'NONE',  ( 11.53846153846153832, -13.87047571288749737, 32.06866353760679544 ) ) ;
#49972 = CARTESIAN_POINT ( 'NONE',  ( 7.846153846153725020, -6.879047030192662504, 34.71129190930017927 ) ) ;
#49974 = EDGE_CURVE ( 'NONE', #82483, #66781, #3266, .T. ) ;
#49975 = CARTESIAN_POINT ( 'NONE',  ( 13.13463864056679853, -11.47974371597207899, 33.17467449705390692 ) ) ;
#49976 = CARTESIAN_POINT ( 'NONE',  ( -13.38461538461538325, -2.486705287966279876, 31.30864560766543647 ) ) ;
#49977 = FACE_OUTER_BOUND ( 'NONE', #79725, .T. ) ;
#49978 = CARTESIAN_POINT ( 'NONE',  ( -2.531177232256638376, -11.60425143139329940, 33.02411095842164457 ) ) ;
#49979 = VERTEX_POINT ( 'NONE', #19613 ) ;
#49980 = CARTESIAN_POINT ( 'NONE',  ( -1.384615384615383471, -12.34228464037088635, 31.77849191805839268 ) ) ;
#49981 = ADVANCED_FACE ( 'NONE', ( #47077 ), #53845, .F. ) ;
#49982 = ADVANCED_FACE ( 'NONE', ( #68686 ), #20937, .F. ) ;
#49983 = CARTESIAN_POINT ( 'NONE',  ( -6.923076923076922462, -13.95598074871891292, 31.83374038241031911 ) ) ;
#49984 = DIRECTION ( 'NONE',  ( -0.000000000000000000, -0.3420201433256694901, -0.9396926207859082059 ) ) ;
#49985 = CARTESIAN_POINT ( 'NONE',  ( -11.53846153846123102, -2.506253911140614576, 30.00000000000323297 ) ) ;
#49986 = LINE ( 'NONE', #84685, #53510 ) ;
#49987 = CARTESIAN_POINT ( 'NONE',  ( -1.929879867024197893E-14, -3.750000000000000000, 15.40625000000000000 ) ) ;
#49988 = VERTEX_POINT ( 'NONE', #39462 ) ;
#49989 = ORIENTED_EDGE ( 'NONE', *, *, #54439, .T. ) ;
#49990 = AXIS2_PLACEMENT_3D ( 'NONE', #22285, #8780, #15091 ) ;
#49991 = DIRECTION ( 'NONE',  ( 0.000000000000000000, 0.9848077530122072432, 0.1736481776669354937 ) ) ;
#49992 = ORIENTED_EDGE ( 'NONE', *, *, #86135, .F. ) ;
#49993 = DIRECTION ( 'NONE',  ( 0.000000000000000000, 0.3420201433256610524, 0.9396926207859113145 ) ) ;
#49994 = CARTESIAN_POINT ( 'NONE',  ( -1.253824943648434331, -9.929761469519744921, 34.40412654351204225 ) ) ;
#49995 = CARTESIAN_POINT ( 'NONE',  ( 3.230769230769110045, -9.442884908241554243, 34.35708131394783038 ) ) ;
#49996 = CARTESIAN_POINT ( 'NONE',  ( -15.84615384615384670, -11.50000000000000000, 29.75000000000000355 ) ) ;
#49997 = CARTESIAN_POINT ( 'NONE',  ( -3.749999999999988454, -9.053300858899127945, 18.76562500000000000 ) ) ;
#49998 = EDGE_CURVE ( 'NONE', #4532, #66010, #75890, .T. ) ;
#49999 = CARTESIAN_POINT ( 'NONE',  ( 0.6845513056318561773, -9.172514111537584114, 34.72667873470787470 ) ) ;
#50000 = ORIENTED_EDGE ( 'NONE', *, *, #63165, .F. ) ;
#50001 = AXIS2_PLACEMENT_3D ( 'NONE', #12902, #40393, #19661 ) ;
#50002 = LINE ( 'NONE', #15791, #47242 ) ;
#50004 = ORIENTED_EDGE ( 'NONE', *, *, #21032, .F. ) ;
#50003 = CARTESIAN_POINT ( 'NONE',  ( -2.307692307692428724, -12.70778746994576025, 30.41441678777401236 ) ) ;
#50005 = CARTESIAN_POINT ( 'NONE',  ( -15.23076923076922995, -5.415277668671390821, 36.20867863119892149 ) ) ;
#50006 = CYLINDRICAL_SURFACE ( 'NONE', #83245, 0.2500000000000002220 ) ;
#50007 = EDGE_CURVE ( 'NONE', #41676, #1947, #67807, .T. ) ;
#50008 = EDGE_CURVE ( 'NONE', #24402, #50148, #35504, .T. ) ;
#50009 = CARTESIAN_POINT ( 'NONE',  ( -17.93474442872397390, -11.94971097300157936, 32.03036669348361443 ) ) ;
#50010 = CARTESIAN_POINT ( 'NONE',  ( 0.5276068125408994725, -2.721908614388772740, 31.22303859784725333 ) ) ;
#50011 = VECTOR ( 'NONE', #32751, 1000.000000000000000 ) ;
#50012 = FACE_OUTER_BOUND ( 'NONE', #14351, .T. ) ;
#50013 = CARTESIAN_POINT ( 'NONE',  ( -7.846153846153965716, -12.46129190930018460, 30.37095296980731973 ) ) ;
#50014 = CARTESIAN_POINT ( 'NONE',  ( -1.987747218494638313, -9.401340078031370950, 25.18936829374151642 ) ) ;
#50015 = VERTEX_POINT ( 'NONE', #234 ) ;
#50016 = ADVANCED_FACE ( 'NONE', ( #33129 ), #48408, .F. ) ;
#50017 = CARTESIAN_POINT ( 'NONE',  ( -16.85391172531022619, -10.61302985866384141, 33.66295027996417843 ) ) ;
#50018 = CARTESIAN_POINT ( 'NONE',  ( -17.30040800148741553, -4.988325925672468131, 34.36044203135681130 ) ) ;
#50019 = CARTESIAN_POINT ( 'NONE',  ( -1.139087296525992166, -10.25000000000000533, 19.85937500000000355 ) ) ;
#50020 = CARTESIAN_POINT ( 'NONE',  ( 0.2380535369741308138, -5.827078755546623690, 34.72654668319379567 ) ) ;
#50021 = CARTESIAN_POINT ( 'NONE',  ( -18.00000000000000000, -5.419720871348011393, 36.19647103217484130 ) ) ;
#50022 = ORIENTED_EDGE ( 'NONE', *, *, #28818, .F. ) ;
#50023 = CARTESIAN_POINT ( 'NONE',  ( 0.2115617174898685449, -4.075325502946085976, 33.72974371597207721 ) ) ;
#50024 = CARTESIAN_POINT ( 'NONE',  ( -15.90390063549801347, -12.22109172314383052, 31.39792113162168263 ) ) ;
#50025 = B_SPLINE_CURVE_WITH_KNOTS ( 'NONE', 3,
 ( #74387, #33406, #501, #27971, #21654, #14911, #76604, #34280, #48675, #77483 ),
 .UNSPECIFIED., .F., .F.,
 ( 4, 2, 2, 2, 4 ),
 ( 0.000000000000000000, 0.0001954311584214072923, 0.0003908623168428145846, 0.0005862934752642218498, 0.0007817246336856291692 ),
 .UNSPECIFIED. ) ;
#50026 = ORIENTED_EDGE ( 'NONE', *, *, #65965, .T. ) ;
#50027 = CARTESIAN_POINT ( 'NONE',  ( 9.942307692309114486, -7.500000000000154543, 35.00000000000007105 ) ) ;
#50028 = EDGE_LOOP ( 'NONE', ( #33572, #11616, #80122, #5913 ) ) ;
#50029 = AXIS2_PLACEMENT_3D ( 'NONE', #78560, #18660, #37574 ) ;
#50030 = CARTESIAN_POINT ( 'NONE',  ( 7.384615384615385025, -7.500000000000000000, 33.75000000000000000 ) ) ;
#50031 = CARTESIAN_POINT ( 'NONE',  ( 3.930919936330005360, -3.586966769969700763, 32.86292498521069660 ) ) ;
#50032 = CARTESIAN_POINT ( 'NONE',  ( -8.638705330997124676, -5.915461855592780260, 34.75538340440931506 ) ) ;
#50033 = FACE_OUTER_BOUND ( 'NONE', #46347, .T. ) ;
#50034 = ORIENTED_EDGE ( 'NONE', *, *, #19555, .T. ) ;
#50035 = CARTESIAN_POINT ( 'NONE',  ( -6.792551484843277976, -6.808710257144159783, 34.95449254468098843 ) ) ;
#50036 = EDGE_CURVE ( 'NONE', #763, #73158, #45223, .T. ) ;
#50037 = ORIENTED_EDGE ( 'NONE', *, *, #42602, .F. ) ;
#50038 = DIRECTION ( 'NONE',  ( -0.000000000000000000, 1.000000000000000000, -0.000000000000000000 ) ) ;
#50039 = FACE_OUTER_BOUND ( 'NONE', #67555, .T. ) ;
#50040 = ORIENTED_EDGE ( 'NONE', *, *, #63416, .F. ) ;
#50041 = CARTESIAN_POINT ( 'NONE',  ( 11.66925197942848769, -12.62708834333097663, 30.88030960425257021 ) ) ;
#50042 = CARTESIAN_POINT ( 'NONE',  ( 10.86533013373275836, -3.202959910592335646, 32.30730279482227019 ) ) ;
#50043 = DIRECTION ( 'NONE',  ( 0.000000000000000000, 0.8660254037844377084, -0.5000000000000015543 ) ) ;
#50044 = CARTESIAN_POINT ( 'NONE',  ( 13.60762822870878352, -11.98016756924215009, 32.48728574198911190 ) ) ;
#50045 = DIRECTION ( 'NONE',  ( 1.000000000000000000, 0.000000000000000000, 0.000000000000000000 ) ) ;
#50046 = VERTEX_POINT ( 'NONE', #6988 ) ;
#50047 = EDGE_LOOP ( 'NONE', ( #36757, #76674 ) ) ;
#50048 = FACE_BOUND ( 'NONE', #87952, .T. ) ;
#50049 = ORIENTED_EDGE ( 'NONE', *, *, #76854, .T. ) ;
#50050 = CARTESIAN_POINT ( 'NONE',  ( 12.21153846153846168, -2.249999999999998668, 29.75000000000000355 ) ) ;
#50051 = B_SPLINE_CURVE_WITH_KNOTS ( 'NONE', 3,
 ( #23493, #72126, #66261, #79789, #44642, #58608, #72573, #52742, #38353, #65806 ),
 .UNSPECIFIED., .F., .F.,
 ( 4, 2, 2, 2, 4 ),
 ( 0.0007817359430256332585, 0.0009771253907250054306, 0.001172514838424370664, 0.001367904286123735897, 0.001563293733823100913 ),
 .UNSPECIFIED. ) ;
#50052 = AXIS2_PLACEMENT_3D ( 'NONE', #44671, #24407, #18117 ) ;
#50053 = CARTESIAN_POINT ( 'NONE',  ( -14.17690186672535901, -11.37503395064541678, 33.29242100308974273 ) ) ;
#50054 = CARTESIAN_POINT ( 'NONE',  ( -2.307692307692427391, -2.625532179533779154, 30.86335684631627174 ) ) ;
#50055 = FACE_OUTER_BOUND ( 'NONE', #62258, .T. ) ;
#50056 = ORIENTED_EDGE ( 'NONE', *, *, #20911, .F. ) ;
#50057 = CIRCLE ( 'NONE', #38560, 0.2500000000000002220 ) ;
#50058 = EDGE_CURVE ( 'NONE', #36412, #47496, #88178, .T. ) ;
#50059 = ORIENTED_EDGE ( 'NONE', *, *, #60487, .F. ) ;
#50060 = ORIENTED_EDGE ( 'NONE', *, *, #18813, .T. ) ;
#50061 = CARTESIAN_POINT ( 'NONE',  ( 15.90386942290380290, -9.943427161483782584, 34.11278801902876978 ) ) ;
#50062 = VECTOR ( 'NONE', #77722, 1000.000000000000000 ) ;
#50063 = CARTESIAN_POINT ( 'NONE',  ( -2.307692307692305711, -1.129524287112498415, 32.06866353760679544 ) ) ;
#50064 = DIRECTION ( 'NONE',  ( -1.000000000000000000, -0.000000000000000000, -0.000000000000000000 ) ) ;
#50065 = CARTESIAN_POINT ( 'NONE',  ( 1.384615384615265343, -11.48612834414049644, 32.76840700105863391 ) ) ;
#50066 = ORIENTED_EDGE ( 'NONE', *, *, #42475, .T. ) ;
#50067 = CARTESIAN_POINT ( 'NONE',  ( 13.25446817517716980, -10.88202310037935661, 33.43294751532457099 ) ) ;
#50068 = CARTESIAN_POINT ( 'NONE',  ( 0.4615384615384611200, -11.69971097300155272, 32.46337939537588113 ) ) ;
#50069 = DIRECTION ( 'NONE',  ( -1.000000000000000000, -0.000000000000000000, -0.000000000000000000 ) ) ;
#50070 = LINE ( 'NONE', #16296, #3044 ) ;
#50071 = VERTEX_POINT ( 'NONE', #26378 ) ;
#50072 = EDGE_CURVE ( 'NONE', #3390, #17581, #67731, .T. ) ;
#50073 = EDGE_LOOP ( 'NONE', ( #5476, #51537, #63361, #42839 ) ) ;
#50074 = ORIENTED_EDGE ( 'NONE', *, *, #72300, .F. ) ;
#50076 = CARTESIAN_POINT ( 'NONE',  ( 10.83839596699746721, -6.503523203565941380, 34.64991518177335195 ) ) ;
#50075 = CARTESIAN_POINT ( 'NONE',  ( -7.976301055592065481, -6.852621066184266141, 34.70813303252209181 ) ) ;
#50077 = DIRECTION ( 'NONE',  ( -0.000000000000000000, -0.3420201433256694901, -0.9396926207859082059 ) ) ;
#50078 = CARTESIAN_POINT ( 'NONE',  ( -3.296039676730005308, -11.48612834413959582, 32.76840700105983473 ) ) ;
#50079 = FACE_BOUND ( 'NONE', #17496, .T. ) ;
#50080 = CARTESIAN_POINT ( 'NONE',  ( -11.66860950819323328, -2.373036134822904319, 30.88089517874952250 ) ) ;
#50081 = ORIENTED_EDGE ( 'NONE', *, *, #5439, .T. ) ;
#50082 = CARTESIAN_POINT ( 'NONE',  ( 17.20771488474786892, -10.54018710029568595, 33.71981072465678864 ) ) ;
#50083 = EDGE_CURVE ( 'NONE', #35424, #49441, #57023, .T. ) ;
#50084 = CARTESIAN_POINT ( 'NONE',  ( -0.4615384615385826339, -9.442884908241554243, 34.35708131394783038 ) ) ;
#50085 = DIRECTION ( 'NONE',  ( -0.000000000000000000, 0.7660444431189791237, -0.6427876096865379196 ) ) ;
#50086 = CYLINDRICAL_SURFACE ( 'NONE', #87039, 0.2499999999999973355 ) ;
#50087 = VERTEX_POINT ( 'NONE', #2004 ) ;
#50088 = CARTESIAN_POINT ( 'NONE',  ( 2.372947878968334035, -11.94971097300157403, 32.03036669348361443 ) ) ;
#50089 = AXIS2_PLACEMENT_3D ( 'NONE', #47323, #46883, #26618 ) ;
#50090 = VERTEX_POINT ( 'NONE', #70012 ) ;
#50091 = FACE_BOUND ( 'NONE', #41101, .T. ) ;
#50092 = CYLINDRICAL_SURFACE ( 'NONE', #70625, 0.2500000000000009437 ) ;
#50093 = DIRECTION ( 'NONE',  ( -0.000000000000000000, -0.000000000000000000, -1.000000000000000000 ) ) ;
#50094 = CARTESIAN_POINT ( 'NONE',  ( -3.007989689500820685, -8.496831190052096971, 34.64984203495476578 ) ) ;
#50095 = ORIENTED_EDGE ( 'NONE', *, *, #49313, .F. ) ;
#50096 = CARTESIAN_POINT ( 'NONE',  ( 5.326977388561388693, -3.136992222400443175, 32.19305428654138979 ) ) ;
#50097 = CARTESIAN_POINT ( 'NONE',  ( -14.37296275365308418, -4.481592998940162609, 33.73612834413957984 ) ) ;
#50098 = CARTESIAN_POINT ( 'NONE',  ( 12.22435897435897267, -7.500000000000000000, 33.75000000000000000 ) ) ;
#50099 = CARTESIAN_POINT ( 'NONE',  ( 6.130525701763568591, -3.816742781228458448, 33.13167719472716044 ) ) ;
#50100 = ORIENTED_EDGE ( 'NONE', *, *, #18066, .T. ) ;
#50101 = CARTESIAN_POINT ( 'NONE',  ( -7.780898274877821486, -10.90142922261932057, 33.41473453929631887 ) ) ;
#50102 = ORIENTED_EDGE ( 'NONE', *, *, #10966, .T. ) ;
#50104 = ORIENTED_EDGE ( 'NONE', *, *, #53622, .F. ) ;
#50103 = FACE_OUTER_BOUND ( 'NONE', #13514, .T. ) ;
#50105 = DIRECTION ( 'NONE',  ( -0.000000000000000000, 0.3420201433256694346, -0.9396926207859080948 ) ) ;
#50106 = FACE_OUTER_BOUND ( 'NONE', #19722, .T. ) ;
#50108 = B_SPLINE_CURVE_WITH_KNOTS ( 'NONE', 3,
 ( #13242, #19989, #69067, #88480, #75819, #13678, #68622, #28081, #82149, #74952 ),
 .UNSPECIFIED., .F., .F.,
 ( 4, 2, 2, 2, 4 ),
 ( 0.000000000000000000, 0.0001954311564186869286, 0.0003908623128373738573, 0.0005862934692560607588, 0.0007817246256747477145 ),
 .UNSPECIFIED. ) ;
#50107 = FACE_OUTER_BOUND ( 'NONE', #46569, .T. ) ;
#50109 = EDGE_CURVE ( 'NONE', #21924, #34293, #69133, .T. ) ;
#50110 = EDGE_CURVE ( 'NONE', #52382, #820, #1562, .T. ) ;
#50111 = CYLINDRICAL_SURFACE ( 'NONE', #20796, 0.2499999999999997502 ) ;
#50113 = CARTESIAN_POINT ( 'NONE',  ( 18.00000000000000000, -11.11383981884818262, 36.00935417666054406 ) ) ;
#50112 = FACE_OUTER_BOUND ( 'NONE', #29141, .T. ) ;
#50114 = LINE ( 'NONE', #15906, #19064 ) ;
#50115 = CARTESIAN_POINT ( 'NONE',  ( 2.749999999999995115, -6.360912703473971419, 25.64062500000000000 ) ) ;
#50116 = EDGE_LOOP ( 'NONE', ( #6006, #61477 ) ) ;
#50117 = CARTESIAN_POINT ( 'NONE',  ( 2.307692307692309264, -8.318370150425687726, 35.83090037661290239 ) ) ;
#50118 = DIRECTION ( 'NONE',  ( -0.000000000000000000, 0.3420201433256694901, -0.9396926207859082059 ) ) ;
#50119 = EDGE_LOOP ( 'NONE', ( #75245, #32156 ) ) ;
#50120 = AXIS2_PLACEMENT_3D ( 'NONE', #61194, #73847, #12145 ) ;
#50121 = VERTEX_POINT ( 'NONE', #29050 ) ;
#50122 = ORIENTED_EDGE ( 'NONE', *, *, #28751, .T. ) ;
#50123 = CYLINDRICAL_SURFACE ( 'NONE', #74287, 0.2500000000000002220 ) ;
#50124 = CARTESIAN_POINT ( 'NONE',  ( 4.153846153846154188, -12.29105614889573062, 35.45975837776705220 ) ) ;
#50126 = CARTESIAN_POINT ( 'NONE',  ( -5.448717948717947124, -4.000000000000000000, 29.75000000000000355 ) ) ;
#50125 = AXIS2_PLACEMENT_3D ( 'NONE', #87304, #72424, #25134 ) ;
#50127 = CARTESIAN_POINT ( 'NONE',  ( 8.769230769230645706, -11.67786785259630911, 32.92929555188603530 ) ) ;
#50128 = CARTESIAN_POINT ( 'NONE',  ( 8.703960323269992472, -11.48612834413959582, 32.76840700105983473 ) ) ;
#50129 = CARTESIAN_POINT ( 'NONE',  ( 7.173022441425066731, -11.37275283266503756, 32.91324779482534524 ) ) ;
#50130 = AXIS2_PLACEMENT_3D ( 'NONE', #9354, #64715, #71475 ) ;
#50131 = CARTESIAN_POINT ( 'NONE',  ( -4.153846153846273204, -3.835265460704628371, 33.15142922262033665 ) ) ;
#50132 = CARTESIAN_POINT ( 'NONE',  ( 3.164685819813350065, -6.386643153685125363, 34.62446782046654903 ) ) ;
#50133 = CARTESIAN_POINT ( 'NONE',  ( -1.449885830576159496, -6.879047030191174805, 34.71129190930000163 ) ) ;
#50134 = CARTESIAN_POINT ( 'NONE',  ( 12.46153846153833911, -11.94971097300221174, 32.03036669348237098 ) ) ;
#50135 = DIRECTION ( 'NONE',  ( -0.000000000000000000, -0.6427876096865404731, -0.7660444431189770143 ) ) ;
#50136 = EDGE_LOOP ( 'NONE', ( #28819, #15803 ) ) ;
#50137 = CARTESIAN_POINT ( 'NONE',  ( 0.5923302693632481741, -8.999086150933472084, 34.52020707165672064 ) ) ;
#50138 = DIRECTION ( 'NONE',  ( 0.000000000000000000, 0.4999999999999985567, 0.8660254037844395958 ) ) ;
#50139 = DIRECTION ( 'NONE',  ( -0.000000000000000000, -0.6427876096865404731, -0.7660444431189771253 ) ) ;
#50140 = FACE_OUTER_BOUND ( 'NONE', #75997, .T. ) ;
#50141 = ORIENTED_EDGE ( 'NONE', *, *, #62570, .T. ) ;
#50142 = CARTESIAN_POINT ( 'NONE',  ( -14.30769230769230660, -9.905515769479276145, 34.41647553114623292 ) ) ;
#50143 = CARTESIAN_POINT ( 'NONE',  ( 9.626225312947559232, -2.833524468853757305, 32.15551576947924417 ) ) ;
#50144 = B_SPLINE_CURVE_WITH_KNOTS ( 'NONE', 3,
 ( #19605, #12848, #13295, #61467, #21375, #6542, #34003, #48844, #48400, #75878 ),
 .UNSPECIFIED., .F., .F.,
 ( 4, 2, 2, 2, 4 ),
 ( 0.000000000000000000, 0.0001954339857564053873, 0.0003908679715128107746, 0.0005863019572692161618, 0.0007817359430256215491 ),
 .UNSPECIFIED. ) ;
#50145 = CARTESIAN_POINT ( 'NONE',  ( -8.769230769230768274, -9.058645607665452459, 34.76329471203371924 ) ) ;
#50146 = ORIENTED_EDGE ( 'NONE', *, *, #11981, .F. ) ;
#50147 = CARTESIAN_POINT ( 'NONE',  ( 7.716005876422150855, -11.66186481527757302, 32.95055677023626117 ) ) ;
#50148 = VERTEX_POINT ( 'NONE', #64130 ) ;
#50149 = FACE_OUTER_BOUND ( 'NONE', #71654, .T. ) ;
#50150 = CARTESIAN_POINT ( 'NONE',  ( 8.769230769230768274, -9.058645607665452459, 34.76329471203371924 ) ) ;
#50151 = CARTESIAN_POINT ( 'NONE',  ( 12.46153846153833911, -8.613356846316285953, 34.62446782046622218 ) ) ;
#50152 = CARTESIAN_POINT ( 'NONE',  ( 1.161130460051055913, -8.539481045369598178, 34.89627647299170832 ) ) ;
#50153 = CARTESIAN_POINT ( 'NONE',  ( -17.75005459062195712, -12.45601412856602686, 31.48342859153981621 ) ) ;
#50154 = ORIENTED_EDGE ( 'NONE', *, *, #35378, .T. ) ;
#50155 = EDGE_CURVE ( 'NONE', #78633, #35413, #78399, .T. ) ;
#50156 = ORIENTED_EDGE ( 'NONE', *, *, #34345, .T. ) ;
#50157 = ORIENTED_EDGE ( 'NONE', *, *, #12170, .F. ) ;
#50158 = CARTESIAN_POINT ( 'NONE',  ( -17.07692307692319744, -10.90142922262034020, 33.41473453929536674 ) ) ;
#50159 = CARTESIAN_POINT ( 'NONE',  ( -17.07692307692319744, -3.835265460704628815, 33.15142922262033665 ) ) ;
#50160 = CARTESIAN_POINT ( 'NONE',  ( -4.153846153846152411, -12.34228464037088635, 31.77849191805839268 ) ) ;
#50162 = EDGE_CURVE ( 'NONE', #10616, #43687, #3083, .T. ) ;
#50161 = CARTESIAN_POINT ( 'NONE',  ( -2.999999999999998224, -7.500000000000000000, 0.000000000000000000 ) ) ;
#50163 = B_SPLINE_CURVE_WITH_KNOTS ( 'NONE', 3,
 ( #12430, #5669, #8783, #82676, #83110, #76340, #36255, #61932, #49752, #62371 ),
 .UNSPECIFIED., .F., .F.,
 ( 4, 2, 2, 2, 4 ),
 ( 0.0007817246256747447872, 0.0009771112852218874663, 0.001172497944769030362, 0.001367884604316173258, 0.001563271263863315937 ),
 .UNSPECIFIED. ) ;
#50164 = CIRCLE ( 'NONE', #11360, 4.000000000000000000 ) ;
#50165 = CARTESIAN_POINT ( 'NONE',  ( 11.53846153846153832, -2.499999999999998668, 29.50000000000001066 ) ) ;
#50166 = LINE ( 'NONE', #77209, #85467 ) ;
#50167 = ORIENTED_EDGE ( 'NONE', *, *, #21347, .T. ) ;
#50168 = ADVANCED_FACE ( 'NONE', ( #29925 ), #57381, .F. ) ;
#50169 = B_SPLINE_CURVE_WITH_KNOTS ( 'NONE', 3,
 ( #22134, #36961, #973, #63104, #14939, #9495, #56796, #22571, #50474, #77959 ),
 .UNSPECIFIED., .F., .F.,
 ( 4, 2, 2, 2, 4 ),
 ( 0.0007817359527651090859, 0.0009771254036996478414, 0.001172514854634186705, 0.001367904305568725569, 0.001563293756503264433 ),
 .UNSPECIFIED. ) ;
#50170 = EDGE_LOOP ( 'NONE', ( #45319, #58141, #44103, #39119 ) ) ;
#50171 = ORIENTED_EDGE ( 'NONE', *, *, #8010, .T. ) ;
#50173 = EDGE_LOOP ( 'NONE', ( #34019, #30347 ) ) ;
#50172 = CARTESIAN_POINT ( 'NONE',  ( 4.088575707885378385, -2.892918686051582089, 31.69288490824015270 ) ) ;
#50175 = CARTESIAN_POINT ( 'NONE',  ( -8.546451227962361230, -11.41317474335729543, 32.86274602512330034 ) ) ;
#50174 = FACE_OUTER_BOUND ( 'NONE', #19119, .T. ) ;
#50176 = AXIS2_PLACEMENT_3D ( 'NONE', #21091, #75173, #69734 ) ;
#50177 = CARTESIAN_POINT ( 'NONE',  ( 2.320192649118979489E-14, -11.25000000000000000, 26.03125000000000000 ) ) ;
#50178 = EDGE_LOOP ( 'NONE', ( #69150, #78536 ) ) ;
#50179 = VECTOR ( 'NONE', #67735, 1000.000000000000227 ) ;
#50180 = EDGE_CURVE ( 'NONE', #58342, #17484, #14186, .T. ) ;
#50181 = EDGE_LOOP ( 'NONE', ( #416, #61572, #39681, #14275, #40651, #41187 ) ) ;
#50182 = CARTESIAN_POINT ( 'NONE',  ( 13.60762822870878352, -10.77377354290276124, 33.85451476688484718 ) ) ;
#50183 = EDGE_LOOP ( 'NONE', ( #4786, #66678, #30275, #30844 ) ) ;
#50184 = FACE_BOUND ( 'NONE', #50925, .T. ) ;
#50185 = CARTESIAN_POINT ( 'NONE',  ( 13.38461538461538680, -12.34228464037088635, 31.77849191805839268 ) ) ;
#50186 = CARTESIAN_POINT ( 'NONE',  ( 11.53846153846153832, -12.37446782046654192, 30.86335684631486131 ) ) ;
#50187 = ORIENTED_EDGE ( 'NONE', *, *, #17366, .T. ) ;
#50188 = CARTESIAN_POINT ( 'NONE',  ( 16.28437185560971656, -11.46989282347013095, 32.79007818306219946 ) ) ;
#50189 = CARTESIAN_POINT ( 'NONE',  ( 15.12820512820512953, -7.500000000000000000, 33.75000000000000000 ) ) ;
#50190 = FACE_OUTER_BOUND ( 'NONE', #35316, .T. ) ;
#50191 = CARTESIAN_POINT ( 'NONE',  ( -11.76138775597768671, -5.667676309546437530, 34.40238873228292249 ) ) ;
#50192 = CARTESIAN_POINT ( 'NONE',  ( -13.16160403300253634, -11.76359900205217457, 32.36225158514719880 ) ) ;
#50193 = CARTESIAN_POINT ( 'NONE',  ( -6.988347369037698265, -11.48612834413959582, 32.76840700105983473 ) ) ;
#50194 = CARTESIAN_POINT ( 'NONE',  ( -7.596208327805704208, -6.696923467548660192, 34.68552623307873972 ) ) ;
#50195 = PLANE ( 'NONE',  #22553 ) ;
#50196 = CARTESIAN_POINT ( 'NONE',  ( -0.5268084620947812713, -5.094484230520674117, 34.41647553114621161 ) ) ;
#50197 = CARTESIAN_POINT ( 'NONE',  ( -18.00000000000000000, -6.386643153685127139, 34.62446782046654192 ) ) ;
#50198 = ADVANCED_FACE ( 'NONE', ( #55610 ), #14633, .F. ) ;
#50199 = CARTESIAN_POINT ( 'NONE',  ( 8.068933515131908152, -3.020022701398814569, 32.48759521482552515 ) ) ;
#50201 = CARTESIAN_POINT ( 'NONE',  ( 6.988332494352947677, -3.300289026998475705, 32.46337939537591666 ) ) ;
#50200 = CARTESIAN_POINT ( 'NONE',  ( 13.38461538461526601, -11.94971097300221174, 32.03036669348237098 ) ) ;
#50202 = LINE ( 'NONE', #2905, #59804 ) ;
#50204 = CARTESIAN_POINT ( 'NONE',  ( -19.99999999999996803, 12.00000000000000711, 10.00000000000000178 ) ) ;
#50203 = CARTESIAN_POINT ( 'NONE',  ( -3.454254155333563503, -3.019605429927184836, 32.48692288466676814 ) ) ;
#50205 = EDGE_CURVE ( 'NONE', #59796, #18998, #35928, .T. ) ;
#50206 = CARTESIAN_POINT ( 'NONE',  ( -2.438382910802614933, -5.496505350115500121, 34.60290016733514307 ) ) ;
#50207 = VECTOR ( 'NONE', #64926, 1000.000000000000000 ) ;
#50208 = CARTESIAN_POINT ( 'NONE',  ( 2.775308065498768517, -8.577988221561467341, 24.29500670625849423 ) ) ;
#50209 = B_SPLINE_CURVE_WITH_KNOTS ( 'NONE', 3,
 ( #13155, #69427, #7734, #35193, #40636, #76629, #75302, #13594, #41071, #3170 ),
 .UNSPECIFIED., .F., .F.,
 ( 4, 2, 2, 2, 4 ),
 ( 0.0007817246336856291692, 0.0009771112958940105907, 0.001172497958102391904, 0.001367884620310773434, 0.001563271282519154747 ),
 .UNSPECIFIED. ) ;
#50210 = ORIENTED_EDGE ( 'NONE', *, *, #35607, .F. ) ;
#50211 = CARTESIAN_POINT ( 'NONE',  ( 2.705532133667545747, -5.066125464207517304, 14.00000000000000355 ) ) ;
#50212 = EDGE_LOOP ( 'NONE', ( #58157, #82083 ) ) ;
#50213 = CARTESIAN_POINT ( 'NONE',  ( -2.307692307692428724, -3.083524468854526912, 32.58852847137268327 ) ) ;
#50214 = EDGE_CURVE ( 'NONE', #87648, #13360, #45053, .T. ) ;
#50215 = EDGE_LOOP ( 'NONE', ( #26789, #66223, #24007, #72370 ) ) ;
#50216 = ADVANCED_FACE ( 'NONE', ( #11426 ), #38007, .F. ) ;
#50217 = CARTESIAN_POINT ( 'NONE',  ( -13.13466997523734037, -2.341251567377310217, 30.72681386836322659 ) ) ;
#50218 = ORIENTED_EDGE ( 'NONE', *, *, #15597, .F. ) ;
#50219 = DIRECTION ( 'NONE',  ( -0.000000000000000000, 0.7660444431189791237, -0.6427876096865379196 ) ) ;
#50220 = CARTESIAN_POINT ( 'NONE',  ( -1.987747218494660295, -5.598659921968651254, 22.49813170625848713 ) ) ;
#50221 = CARTESIAN_POINT ( 'NONE',  ( 17.20771488474786892, -8.147973898785416225, 34.70805048591653730 ) ) ;
#50222 = CARTESIAN_POINT ( 'NONE',  ( 7.146089767170319185, -10.01129605718032778, 34.36064277460058491 ) ) ;
#50223 = CARTESIAN_POINT ( 'NONE',  ( 17.75002325595141173, -2.318417181685854978, 30.59732222474233865 ) ) ;
#50224 = CARTESIAN_POINT ( 'NONE',  ( -16.21992853320628925, -9.905515769479276145, 34.41647553114623292 ) ) ;
#50225 = CARTESIAN_POINT ( 'NONE',  ( 6.923076923076924238, -7.500000000000001776, 35.04278698407183867 ) ) ;
#50226 = DIRECTION ( 'NONE',  ( 1.000000000000000000, 0.000000000000000000, 0.000000000000000000 ) ) ;
#50227 = CARTESIAN_POINT ( 'NONE',  ( -3.750000000000008438, -5.946699141100917352, 16.42187500000000000 ) ) ;
#50228 = CARTESIAN_POINT ( 'NONE',  ( 17.99999999999987566, -11.67786785259630911, 32.92929555188603530 ) ) ;
#50229 = CARTESIAN_POINT ( 'NONE',  ( -2.242437168179468365, -12.16647553114626490, 32.15551576947920864 ) ) ;
#50230 = CARTESIAN_POINT ( 'NONE',  ( 10.55011461482829560, -5.941354392334499579, 34.76329471203369792 ) ) ;
#50231 = CARTESIAN_POINT ( 'NONE',  ( -3.750000000000008438, -5.946699141100917352, 16.42187500000000000 ) ) ;
#50232 = B_SPLINE_CURVE_WITH_KNOTS ( 'NONE', 3,
 ( #33370, #19848, #25276, #12210, #53179, #52735 ),
 .UNSPECIFIED., .F., .F.,
 ( 4, 2, 4 ),
 ( 0.0003909512603273899664, 0.0005862562993132173919, 0.0007815613382990448717 ),
 .UNSPECIFIED. ) ;
#50233 = AXIS2_PLACEMENT_3D ( 'NONE', #65812, #4112, #24832 ) ;
#50234 = CARTESIAN_POINT ( 'NONE',  ( -1.944543648263014957, -5.555456351737005249, 26.50000000000000355 ) ) ;
#50235 = VECTOR ( 'NONE', #2311, 1000.000000000000000 ) ;
#50236 = ORIENTED_EDGE ( 'NONE', *, *, #20773, .F. ) ;
#50237 = CARTESIAN_POINT ( 'NONE',  ( 17.20771488474786892, -12.11778462344220841, 31.66786338562085135 ) ) ;
#50238 = CARTESIAN_POINT ( 'NONE',  ( 11.53846153846153832, -5.557115091759785130, 34.35708131394839171 ) ) ;
#50239 = CARTESIAN_POINT ( 'NONE',  ( 1.319345384059066983, -5.941354392334500467, 34.76329471203369792 ) ) ;
#50240 = CARTESIAN_POINT ( 'NONE',  ( 0.6089743589743582541, -3.499999999999999556, 29.75000000000000355 ) ) ;
#50241 = VECTOR ( 'NONE', #25533, 999.9999999999998863 ) ;
#50242 = CARTESIAN_POINT ( 'NONE',  ( 3.230769230769231726, -12.48256725967547354, 35.29906147534542527 ) ) ;
#50243 = VECTOR ( 'NONE', #71767, 1000.000000000000000 ) ;
#50244 = CARTESIAN_POINT ( 'NONE',  ( 7.846153846153723244, -3.083524468854526912, 32.58852847137268327 ) ) ;
#50245 = VECTOR ( 'NONE', #63539, 1000.000000000000000 ) ;
#50246 = CARTESIAN_POINT ( 'NONE',  ( -17.07692307692307665, -12.29105614889573062, 35.45975837776705220 ) ) ;
#50247 = EDGE_CURVE ( 'NONE', #87443, #43614, #1041, .T. ) ;
#50248 = EDGE_LOOP ( 'NONE', ( #12800, #14754, #71895, #50442 ) ) ;
#50249 = ORIENTED_EDGE ( 'NONE', *, *, #68714, .F. ) ;
#50250 = ORIENTED_EDGE ( 'NONE', *, *, #49314, .F. ) ;
#50251 = CARTESIAN_POINT ( 'NONE',  ( -6.700064078983529292, -5.582272713120727481, 34.63742843783360570 ) ) ;
#50252 = CARTESIAN_POINT ( 'NONE',  ( -6.700297381808511865, -4.387253974876676565, 33.66317474335728832 ) ) ;
#50253 = CARTESIAN_POINT ( 'NONE',  ( 16.28463796167093847, -2.729792928343269587, 31.24908615093345077 ) ) ;
#50254 = CARTESIAN_POINT ( 'NONE',  ( -13.13466986626724342, -9.272278438253398036, 34.42582936511637115 ) ) ;
#50255 = CARTESIAN_POINT ( 'NONE',  ( 17.86985203026830504, -9.504002272028873932, 34.60269587691767867 ) ) ;
#50256 = EDGE_CURVE ( 'NONE', #60579, #18944, #23596, .T. ) ;
#50257 = ORIENTED_EDGE ( 'NONE', *, *, #44201, .F. ) ;
#50258 = CYLINDRICAL_SURFACE ( 'NONE', #80873, 0.2499999999999979738 ) ;
#50259 = ORIENTED_EDGE ( 'NONE', *, *, #10967, .T. ) ;
#50260 = EDGE_LOOP ( 'NONE', ( #71267, #2866, #25364, #6446 ) ) ;
#50261 = CARTESIAN_POINT ( 'NONE',  ( -4.153846153846152411, -13.88283147151868846, 33.14645433367849847 ) ) ;
#50262 = CARTESIAN_POINT ( 'NONE',  ( 27.00000000000000000, -8.999999999999996447, 22.25000000000000000 ) ) ;
#50263 = FACE_OUTER_BOUND ( 'NONE', #34503, .T. ) ;
#50264 = EDGE_CURVE ( 'NONE', #13929, #32893, #30361, .T. ) ;
#50265 = CARTESIAN_POINT ( 'NONE',  ( 6.000000000000001776, -5.180354513474913603, 36.12317359536750416 ) ) ;
#50266 = CARTESIAN_POINT ( 'NONE',  ( -11.53846153846153655, -13.63283147151868846, 33.57946703557072254 ) ) ;
#50267 = ORIENTED_EDGE ( 'NONE', *, *, #14290, .F. ) ;
#50268 = EDGE_CURVE ( 'NONE', #88017, #87879, #48250, .T. ) ;
#50269 = EDGE_LOOP ( 'NONE', ( #54277, #11296, #1414, #143 ) ) ;
#50270 = CARTESIAN_POINT ( 'NONE',  ( 3.750000000000009770, -9.053300858899081760, 19.54687499999999645 ) ) ;
#50271 = EDGE_LOOP ( 'NONE', ( #69774, #62744, #38407, #71202 ) ) ;
#50273 = ORIENTED_EDGE ( 'NONE', *, *, #27038, .T. ) ;
#50272 = CARTESIAN_POINT ( 'NONE',  ( 11.76147438255493327, -5.582272713120729257, 34.63742843783360570 ) ) ;
#50274 = CARTESIAN_POINT ( 'NONE',  ( -6.923076923076922462, -12.37446782046654192, 30.86335684631486131 ) ) ;
#50275 = DIRECTION ( 'NONE',  ( -0.000000000000000000, 0.7660444431189791237, -0.6427876096865379196 ) ) ;
#50276 = CARTESIAN_POINT ( 'NONE',  ( -20.00000000000000355, -10.00000000000000533, 13.00000000000000178 ) ) ;
#50277 = VERTEX_POINT ( 'NONE', #31703 ) ;
#50278 = VECTOR ( 'NONE', #67595, 1000.000000000000000 ) ;
#50279 = ADVANCED_FACE ( 'NONE', ( #30796 ), #79886, .F. ) ;
#50280 = CARTESIAN_POINT ( 'NONE',  ( 15.10062202133100939, -10.88202310037935661, 33.43294751532457099 ) ) ;
#50281 = CARTESIAN_POINT ( 'NONE',  ( -14.30769230769242917, -8.656820664282941280, 34.87096338111179961 ) ) ;
#50282 = ORIENTED_EDGE ( 'NONE', *, *, #66365, .T. ) ;
#50283 = FACE_BOUND ( 'NONE', #83439, .T. ) ;
#50284 = DIRECTION ( 'NONE',  ( 0.000000000000000000, 0.000000000000000000, -1.000000000000000000 ) ) ;
#50285 = CARTESIAN_POINT ( 'NONE',  ( 10.83839596699746721, -9.086983370893049639, 34.49168942202179267 ) ) ;
#50286 = CARTESIAN_POINT ( 'NONE',  ( -15.23076923076922995, -2.833524468853757305, 32.15551576947925838 ) ) ;
#50289 = CARTESIAN_POINT ( 'NONE',  ( 4.826946345980720920, -3.137211980971221781, 32.19342716148376837 ) ) ;
#50288 = AXIS2_PLACEMENT_3D ( 'NONE', #5246, #17878, #33609 ) ;
#50287 = CARTESIAN_POINT ( 'NONE',  ( 4.153846153846154188, -11.69971097300155272, 32.46337939537588113 ) ) ;
#50290 = VECTOR ( 'NONE', #36244, 1000.000000000000227 ) ;
#50291 = EDGE_CURVE ( 'NONE', #37623, #23768, #82731, .T. ) ;
#50292 = CYLINDRICAL_SURFACE ( 'NONE', #33779, 0.2499999999999998890 ) ;
#50293 = LINE ( 'NONE', #2121, #17519 ) ;
#50294 = ORIENTED_EDGE ( 'NONE', *, *, #81563, .F. ) ;
#50295 = DIRECTION ( 'NONE',  ( -0.000000000000000000, 0.9848077530122085754, -0.1736481776669273613 ) ) ;
#50296 = EDGE_CURVE ( 'NONE', #47433, #15714, #16845, .T. ) ;
#50297 = B_SPLINE_CURVE_WITH_KNOTS ( 'NONE', 3,
 ( #63596, #77558, #15869, #2328, #51379, #73023, #37448, #24825, #3660, #32038 ),
 .UNSPECIFIED., .F., .F.,
 ( 4, 2, 2, 2, 4 ),
 ( 0.0007817246256747484735, 0.0009771112852218928873, 0.001172497944769037084, 0.001367884604316181498, 0.001563271263863325912 ),
 .UNSPECIFIED. ) ;
#50298 = VECTOR ( 'NONE', #41497, 1000.000000000000000 ) ;
#50299 = EDGE_LOOP ( 'NONE', ( #15348, #7305, #7719, #42864 ) ) ;
#50300 = B_SPLINE_CURVE_WITH_KNOTS ( 'NONE', 3,
 ( #87413, #53153, #59477, #11289, #11743, #39219, #66226, #25248, #85619, #65775 ),
 .UNSPECIFIED., .F., .F.,
 ( 4, 2, 2, 2, 4 ),
 ( 0.0007817359430256372700, 0.0009771253907250054306, 0.001172514838424373700, 0.001367904286123741969, 0.001563293733823110021 ),
 .UNSPECIFIED. ) ;
#50301 = AXIS2_PLACEMENT_3D ( 'NONE', #24555, #17360, #45266 ) ;
#50302 = CARTESIAN_POINT ( 'NONE',  ( -12.39547112818838670, -3.322132147404559976, 32.92929555188717927 ) ) ;
#50303 = CARTESIAN_POINT ( 'NONE',  ( 10.55011416942384272, -6.879047030191174805, 34.71129190930000163 ) ) ;
#50304 = CARTESIAN_POINT ( 'NONE',  ( -15.23076923076935252, -5.941354392335915335, 34.76329471203413846 ) ) ;
#50305 = CARTESIAN_POINT ( 'NONE',  ( -5.999999999999998224, -12.78798330534102767, 29.49999999999997868 ) ) ;
#50306 = CARTESIAN_POINT ( 'NONE',  ( 24.00000000000000000, -9.499999999999982236, 27.25000000000000000 ) ) ;
#50307 = CARTESIAN_POINT ( 'NONE',  ( 12.23805351781451201, -4.386631170607603991, 33.66268669641500111 ) ) ;
#50308 = ADVANCED_FACE ( 'NONE', ( #10086 ), #65017, .F. ) ;
#50309 = FACE_BOUND ( 'NONE', #12252, .T. ) ;
#50311 = DIRECTION ( 'NONE',  ( -0.000000000000000000, 0.3420201433256694901, -0.9396926207859082059 ) ) ;
#50310 = DIRECTION ( 'NONE',  ( -0.000000000000000000, 0.1736481776669307198, -0.9848077530122080203 ) ) ;
#50312 = CARTESIAN_POINT ( 'NONE',  ( 0.000000000000000000, -11.00000000000000000, 29.75000000000000355 ) ) ;
#50314 = CARTESIAN_POINT ( 'NONE',  ( -15.00775787915638126, -6.503523203565941380, 34.64991518177335195 ) ) ;
#50313 = CARTESIAN_POINT ( 'NONE',  ( -6.673131513698879580, -10.92531984108285670, 33.72920026020278073 ) ) ;
#50315 = FACE_OUTER_BOUND ( 'NONE', #76741, .T. ) ;
#50316 = CARTESIAN_POINT ( 'NONE',  ( -3.775308065498766297, -6.007798216065450170, 19.92000670625849068 ) ) ;
#50317 = ORIENTED_EDGE ( 'NONE', *, *, #81766, .T. ) ;
#50318 = EDGE_CURVE ( 'NONE', #66274, #42667, #54170, .T. ) ;
#50319 = EDGE_LOOP ( 'NONE', ( #13067, #76526, #33725, #37184 ) ) ;
#50320 = DIRECTION ( 'NONE',  ( 0.000000000000000000, 0.9396926207859126468, -0.3420201433256571111 ) ) ;
#50321 = EDGE_CURVE ( 'NONE', #4390, #76768, #84804, .T. ) ;
#50322 = CARTESIAN_POINT ( 'NONE',  ( -14.43783951713053249, -6.852621066184266141, 34.70813303252209181 ) ) ;
#50323 = DIRECTION ( 'NONE',  ( 0.000000000000000000, 1.000000000000000000, 0.000000000000000000 ) ) ;
#50324 = CARTESIAN_POINT ( 'NONE',  ( 8.546364506167671848, -2.251424796025575326, 29.88072029997477586 ) ) ;
#50325 = FACE_OUTER_BOUND ( 'NONE', #53954, .T. ) ;
#50326 = CARTESIAN_POINT ( 'NONE',  ( 3.724691934501232815, -5.885600066136343678, 22.88875670625849068 ) ) ;
#50327 = CARTESIAN_POINT ( 'NONE',  ( -1.161652250348709003, -7.369474539155830506, 34.99858011523957657 ) ) ;
#50328 = CARTESIAN_POINT ( 'NONE',  ( 18.22277954126840172, -3.236590943229497697, 32.36255958852954251 ) ) ;
#50329 = CARTESIAN_POINT ( 'NONE',  ( 3.480823650682684178, -4.074993327901525575, 33.72946981652012255 ) ) ;
#50330 = CARTESIAN_POINT ( 'NONE',  ( 10.36536139116316235, -6.652501968072648708, 34.93155406624980941 ) ) ;
#50331 = CARTESIAN_POINT ( 'NONE',  ( 2.531067793464728766, -2.251407671071270489, 29.88021292934942252 ) ) ;
#50332 = FACE_OUTER_BOUND ( 'NONE', #47091, .T. ) ;
#50333 = CARTESIAN_POINT ( 'NONE',  ( 10.68052939610424623, -7.750023224968867197, 34.99404313364389907 ) ) ;
#50334 = CARTESIAN_POINT ( 'NONE',  ( 7.846153846153846700, -6.386643153685126251, 34.62446782046654192 ) ) ;
#50335 = EDGE_CURVE ( 'NONE', #84739, #28583, #75348, .T. ) ;
#50336 = ORIENTED_EDGE ( 'NONE', *, *, #46379, .T. ) ;
#50337 = VECTOR ( 'NONE', #11242, 999.9999999999998863 ) ;
#50338 = CYLINDRICAL_SURFACE ( 'NONE', #39873, 0.2499999999999994726 ) ;
#50339 = CARTESIAN_POINT ( 'NONE',  ( -17.32689980786543060, -2.779195860258148798, 31.39871582349836743 ) ) ;
#50340 = CARTESIAN_POINT ( 'NONE',  ( 3.750000000000001776, -7.561099074964511502, 13.47061829374151465 ) ) ;
#50341 = B_SPLINE_CURVE_WITH_KNOTS ( 'NONE', 3,
 ( #20805, #13609, #47834, #48273, #75742, #67671, #26237, #87979, #5530, #61331 ),
 .UNSPECIFIED., .F., .F.,
 ( 4, 2, 2, 2, 4 ),
 ( 0.0007817246256747519429, 0.0009771112852218970073, 0.001172497944769042288, 0.001367884604316187353, 0.001563271263863332417 ),
 .UNSPECIFIED. ) ;
#50342 = CARTESIAN_POINT ( 'NONE',  ( 6.700149964170072359, -4.762599654559228846, 34.23009711892697737 ) ) ;
#50343 = CARTESIAN_POINT ( 'NONE',  ( 17.07692307692307665, -11.35647404775217417, 33.31231777344666511 ) ) ;
#50344 = ORIENTED_EDGE ( 'NONE', *, *, #20575, .T. ) ;
#50345 = EDGE_CURVE ( 'NONE', #14556, #76544, #16035, .T. ) ;
#50346 = CARTESIAN_POINT ( 'NONE',  ( -6.923076923076922462, -2.833524468853757305, 32.15551576947925838 ) ) ;
#50348 = ORIENTED_EDGE ( 'NONE', *, *, #2114, .T. ) ;
#50347 = LINE ( 'NONE', #17019, #888 ) ;
#50349 = CARTESIAN_POINT ( 'NONE',  ( 11.53846153846141576, -5.094484230521993062, 34.41647553114689373 ) ) ;
#50350 = CARTESIAN_POINT ( 'NONE',  ( 4.153846153846154188, -8.120952969808772792, 34.71129190930000163 ) ) ;
#50351 = B_SPLINE_CURVE_WITH_KNOTS ( 'NONE', 3,
 ( #8063, #61659, #35533, #21567, #35081, #1293, #62980, #15263, #28780, #62111 ),
 .UNSPECIFIED., .F., .F.,
 ( 4, 2, 2, 2, 4 ),
 ( 0.000000000000000000, 0.0001954311564186864949, 0.0003908623128373729899, 0.0005862934692560594577, 0.0007817246256747459798 ),
 .UNSPECIFIED. ) ;
#50352 = ORIENTED_EDGE ( 'NONE', *, *, #88185, .T. ) ;
#50353 = CARTESIAN_POINT ( 'NONE',  ( -13.38461538461550582, -2.625532179533778709, 30.86335684631627174 ) ) ;
#50354 = CARTESIAN_POINT ( 'NONE',  ( 8.899756470994333313, -5.195472089885680766, 34.18748526763464923 ) ) ;
#50355 = VERTEX_POINT ( 'NONE', #81665 ) ;
#50356 = FACE_OUTER_BOUND ( 'NONE', #18556, .T. ) ;
#50357 = EDGE_CURVE ( 'NONE', #58158, #345, #33475, .T. ) ;
#50358 = DIRECTION ( 'NONE',  ( 0.000000000000000000, 0.000000000000000000, -1.000000000000000000 ) ) ;
#50360 = CARTESIAN_POINT ( 'NONE',  ( 15.16468685140909400, -9.905515769479276145, 34.41647553114623292 ) ) ;
#50359 = VECTOR ( 'NONE', #84889, 1000.000000000000000 ) ;
#50361 = ORIENTED_EDGE ( 'NONE', *, *, #12922, .F. ) ;
#50362 = ORIENTED_EDGE ( 'NONE', *, *, #57103, .T. ) ;
#50363 = ADVANCED_FACE ( 'NONE', ( #20402 ), #61818, .F. ) ;
#50364 = ORIENTED_EDGE ( 'NONE', *, *, #84756, .T. ) ;
#50365 = AXIS2_PLACEMENT_3D ( 'NONE', #74616, #4375, #86821 ) ;
#50366 = VECTOR ( 'NONE', #25599, 1000.000000000000000 ) ;
#50367 = EDGE_CURVE ( 'NONE', #22025, #54188, #25771, .T. ) ;
#50368 = CARTESIAN_POINT ( 'NONE',  ( -18.24997673094235751, -3.627789207965225415, 32.91389620160128970 ) ) ;
#50369 = CARTESIAN_POINT ( 'NONE',  ( -5.749945580086545327, -5.642605341092957083, 34.66089969410670335 ) ) ;
#50370 = DIRECTION ( 'NONE',  ( -0.000000000000000000, 0.9848077530122086864, -0.1736481776669273891 ) ) ;
#50371 = AXIS2_PLACEMENT_3D ( 'NONE', #65915, #29930, #78545 ) ;
#50372 = EDGE_CURVE ( 'NONE', #65236, #74312, #12752, .T. ) ;
#50373 =( GEOMETRIC_REPRESENTATION_CONTEXT ( 3 ) GLOBAL_UNCERTAINTY_ASSIGNED_CONTEXT ( ( #62697 ) ) GLOBAL_UNIT_ASSIGNED_CONTEXT ( ( #39608, #38252, #52648 ) ) REPRESENTATION_CONTEXT ( 'NONE', 'WORKASPACE' ) );
#50374 = CARTESIAN_POINT ( 'NONE',  ( -2.307692307692305711, -9.905515769479276145, 34.41647553114623292 ) ) ;
#50375 = ORIENTED_EDGE ( 'NONE', *, *, #76740, .F. ) ;
#50376 = VERTEX_POINT ( 'NONE', #60047 ) ;
#50378 = EDGE_LOOP ( 'NONE', ( #32434, #69444, #5096, #51589 ) ) ;
#50377 = CARTESIAN_POINT ( 'NONE',  ( 4.403900573759605308, -8.346898887586323923, 34.93166121998716278 ) ) ;
#50379 = B_SPLINE_CURVE_WITH_KNOTS ( 'NONE', 3,
 ( #77691, #29518, #70498, #55202, #84468, #82696, #69607, #55641, #70942, #7913 ),
 .UNSPECIFIED., .F., .F.,
 ( 4, 2, 2, 2, 4 ),
 ( 0.000000000000000000, 0.0001954339857564053873, 0.0003908679715128107746, 0.0005863019572692161618, 0.0007817359430256215491 ),
 .UNSPECIFIED. ) ;
#50380 = CARTESIAN_POINT ( 'NONE',  ( 16.37662582282421653, -8.540255544307068902, 34.89611431652622286 ) ) ;
#50381 = CYLINDRICAL_SURFACE ( 'NONE', #82474, 0.2500000000000012212 ) ;
#50382 = CARTESIAN_POINT ( 'NONE',  ( 6.792928953345229282, -9.504002272028875709, 34.60269587691767867 ) ) ;
#50383 = ORIENTED_EDGE ( 'NONE', *, *, #5376, .F. ) ;
#50384 = EDGE_CURVE ( 'NONE', #5929, #15629, #8536, .T. ) ;
#50385 = VERTEX_POINT ( 'NONE', #26710 ) ;
#50387 = EDGE_LOOP ( 'NONE', ( #5401, #40417 ) ) ;
#50386 = CARTESIAN_POINT ( 'NONE',  ( 9.942253101685738059, -8.476813868363244353, 34.90874843262270133 ) ) ;
#50388 = DIRECTION ( 'NONE',  ( 0.000000000000000000, 0.000000000000000000, -1.000000000000000000 ) ) ;
#50389 = CARTESIAN_POINT ( 'NONE',  ( -4.230769230769230838, -7.500000000000000000, 29.75000000000000355 ) ) ;
#50390 = ORIENTED_EDGE ( 'NONE', *, *, #80136, .T. ) ;
#50391 = CARTESIAN_POINT ( 'NONE',  ( 14.98079248672064345, -2.318417181685855422, 30.59732222474233865 ) ) ;
#50392 = VECTOR ( 'NONE', #87705, 1000.000000000000227 ) ;
#50393 = CARTESIAN_POINT ( 'NONE',  ( -6.923076923077044142, -12.27809138561165270, 31.22303859784587132 ) ) ;
#50394 = DIRECTION ( 'NONE',  ( 0.000000000000000000, 0.1736481776669275834, 0.9848077530122086864 ) ) ;
#50395 = FACE_BOUND ( 'NONE', #8137, .T. ) ;
#50396 = CARTESIAN_POINT ( 'NONE',  ( 7.976679284387494739, -12.50538340440932394, 31.33453814440721885 ) ) ;
#50397 = CARTESIAN_POINT ( 'NONE',  ( 11.40777007179398161, -8.147922237126337563, 34.70805685702651999 ) ) ;
#50398 = CARTESIAN_POINT ( 'NONE',  ( 13.16168842570853670, -12.64616026154729411, 30.79003144601914244 ) ) ;
#50400 = CARTESIAN_POINT ( 'NONE',  ( 6.792385456409367528, -11.71456829005830080, 32.44064028649416542 ) ) ;
#50399 = CARTESIAN_POINT ( 'NONE',  ( -16.82697766754503377, -12.45601412856602686, 31.48342859153981621 ) ) ;
#50401 = CARTESIAN_POINT ( 'NONE',  ( -25.00000000000000000, -10.00000000000000533, 3.000000000000000000 ) ) ;
#50402 = CYLINDRICAL_SURFACE ( 'NONE', #77822, 0.2499999999999995559 ) ;
#50403 = ORIENTED_EDGE ( 'NONE', *, *, #7080, .T. ) ;
#50404 = CARTESIAN_POINT ( 'NONE',  ( 10.39245839786847014, -10.61292498521070549, 33.66303323003028680 ) ) ;
#50405 = EDGE_LOOP ( 'NONE', ( #66141, #32016, #65934, #50845 ) ) ;
#50406 = VERTEX_POINT ( 'NONE', #19509 ) ;
#50408 = CARTESIAN_POINT ( 'NONE',  ( 10.86543903529806876, -12.01375889529407281, 32.43194544308182969 ) ) ;
#50407 = CARTESIAN_POINT ( 'NONE',  ( 7.715462379486289990, -6.413092428213692742, 34.63065189839063152 ) ) ;
#50409 = CARTESIAN_POINT ( 'NONE',  ( 11.28848479441294650, -8.347322224742351082, 34.93158281831414769 ) ) ;
#50410 = LINE ( 'NONE', #87231, #71091 ) ;
#50411 = DIRECTION ( 'NONE',  ( 0.000000000000000000, 0.6427876096865373645, -0.7660444431189797898 ) ) ;
#50412 = CARTESIAN_POINT ( 'NONE',  ( 1.161130440891438242, -11.89387501736622710, 32.13663884655806413 ) ) ;
#50413 = EDGE_LOOP ( 'NONE', ( #25745, #88010, #66146, #49498 ) ) ;
#50414 = LINE ( 'NONE', #27950, #54397 ) ;
#50415 = ADVANCED_FACE ( 'NONE', ( #8668 ), #35237, .F. ) ;
#50416 = CARTESIAN_POINT ( 'NONE',  ( 0.3308478584281529522, -12.62707690430377383, 30.88035979386743435 ) ) ;
#50417 = CARTESIAN_POINT ( 'NONE',  ( -12.68502338610279345, -11.60425143139329940, 33.02411095842164457 ) ) ;
#50418 = AXIS2_PLACEMENT_3D ( 'NONE', #1247, #71038, #62496 ) ;
#50419 = LINE ( 'NONE', #7687, #15140 ) ;
#50420 = DIRECTION ( 'NONE',  ( -0.000000000000000000, 0.9848077530122085754, -0.1736481776669273613 ) ) ;
#50421 = VECTOR ( 'NONE', #9052, 1000.000000000000114 ) ;
#50422 = CARTESIAN_POINT ( 'NONE',  ( 1.553300858899129944, -11.24999999999998934, 15.95312500000000000 ) ) ;
#50423 = ORIENTED_EDGE ( 'NONE', *, *, #79079, .F. ) ;
#50424 = EDGE_CURVE ( 'NONE', #18739, #33177, #4217, .T. ) ;
#50425 = AXIS2_PLACEMENT_3D ( 'NONE', #86720, #45702, #87159 ) ;
#50426 = VECTOR ( 'NONE', #29387, 1000.000000000000000 ) ;
#50427 = ORIENTED_EDGE ( 'NONE', *, *, #19710, .T. ) ;
#50428 = CARTESIAN_POINT ( 'NONE',  ( -7.846153846153844924, -11.91647553114624181, 32.58852847137148245 ) ) ;
#50430 = ORIENTED_EDGE ( 'NONE', *, *, #24615, .T. ) ;
#50429 = EDGE_CURVE ( 'NONE', #83191, #17226, #27830, .T. ) ;
#50431 = CARTESIAN_POINT ( 'NONE',  ( 11.97435897435897267, -4.000000000000000000, 29.75000000000000355 ) ) ;
#50432 = CARTESIAN_POINT ( 'NONE',  ( -11.25641025641025195, -4.000000000000000000, 29.75000000000000355 ) ) ;
#50433 = DIRECTION ( 'NONE',  ( -0.000000000000000000, 1.000000000000000000, -0.000000000000000000 ) ) ;
#50434 = DIRECTION ( 'NONE',  ( -0.000000000000000000, -1.000000000000000000, -0.000000000000000000 ) ) ;
#50435 = CARTESIAN_POINT ( 'NONE',  ( 2.651650429449569302, -10.15165042944953733, 17.12500000000000000 ) ) ;
#50436 = AXIS2_PLACEMENT_3D ( 'NONE', #64800, #4908, #32372 ) ;
#50437 = DIRECTION ( 'NONE',  ( -0.000000000000000000, 0.6427876096865404731, -0.7660444431189770143 ) ) ;
#50438 = ORIENTED_EDGE ( 'NONE', *, *, #23238, .T. ) ;
#50439 = EDGE_CURVE ( 'NONE', #86419, #40595, #75778, .T. ) ;
#50440 = CARTESIAN_POINT ( 'NONE',  ( -12.46153846153846168, -10.51840700105979565, 33.73612834413961536 ) ) ;
#50442 = ORIENTED_EDGE ( 'NONE', *, *, #58212, .F. ) ;
#50441 = CARTESIAN_POINT ( 'NONE',  ( -2.242436736416281384, -10.90142922261932057, 33.41473453929631887 ) ) ;
#50443 = CARTESIAN_POINT ( 'NONE',  ( -13.45069879557126136, -11.16473453929635440, 33.15142922261925662 ) ) ;
#50444 = CARTESIAN_POINT ( 'NONE',  ( -12.23875892027004397, -3.755027918224367323, 33.06320215134714857 ) ) ;
#50445 = CARTESIAN_POINT ( 'NONE',  ( -17.93393164899756087, -11.69971097300155449, 32.46337939537587403 ) ) ;
#50446 = CARTESIAN_POINT ( 'NONE',  ( -0.6089743589743593644, -3.499999999999999556, 29.75000000000000355 ) ) ;
#50447 = CARTESIAN_POINT ( 'NONE',  ( 10.61538461538461675, -1.466349020453238561, 30.81389545987213907 ) ) ;
#50448 = PLANE ( 'NONE',  #71502 ) ;
#50449 = EDGE_CURVE ( 'NONE', #62741, #34985, #57979, .T. ) ;
#50450 = CARTESIAN_POINT ( 'NONE',  ( -2.724691934501246582, -6.299813628509474128, 25.42374329374151998 ) ) ;
#50451 = ORIENTED_EDGE ( 'NONE', *, *, #72418, .F. ) ;
#50452 = PLANE ( 'NONE',  #77708 ) ;
#50453 = CARTESIAN_POINT ( 'NONE',  ( 4.403791563224197070, -10.92531984108285670, 33.72920026020278073 ) ) ;
#50454 = CARTESIAN_POINT ( 'NONE',  ( -1.139087296525992166, -10.25000000000000533, 24.85937500000001421 ) ) ;
#50455 = CARTESIAN_POINT ( 'NONE',  ( -3.296039676730006196, -9.442884908240170461, 34.35708131394840592 ) ) ;
#50456 = CARTESIAN_POINT ( 'NONE',  ( -4.153846153846274980, -3.643525952248796163, 33.31231777344771672 ) ) ;
#50457 = ORIENTED_EDGE ( 'NONE', *, *, #9836, .T. ) ;
#50458 = CARTESIAN_POINT ( 'NONE',  ( 0.2386115026316108223, -4.026226216239096267, 33.68668979543633668 ) ) ;
#50459 = CARTESIAN_POINT ( 'NONE',  ( -10.61538461538461320, -13.78497067705608181, 32.30358669280327177 ) ) ;
#50460 = ORIENTED_EDGE ( 'NONE', *, *, #21421, .F. ) ;
#50461 = CARTESIAN_POINT ( 'NONE',  ( -9.692307692307691624, -13.53365097954675988, 30.81389545987213552 ) ) ;
#50462 = ORIENTED_EDGE ( 'NONE', *, *, #13938, .F. ) ;
#50463 = VECTOR ( 'NONE', #32875, 1000.000000000000000 ) ;
#50464 = LINE ( 'NONE', #37396, #26179 ) ;
#50465 = CARTESIAN_POINT ( 'NONE',  ( 4.153846153846154188, -3.513871655860378418, 32.76840700105978499 ) ) ;
#50466 = CARTESIAN_POINT ( 'NONE',  ( -8.703163435880695076, -5.471508081941601098, 34.59228464037088457 ) ) ;
#50467 = CARTESIAN_POINT ( 'NONE',  ( 16.15384615384615330, -2.292212530054420494, 30.41441678777542634 ) ) ;
#50469 = ORIENTED_EDGE ( 'NONE', *, *, #64186, .F. ) ;
#50468 = VECTOR ( 'NONE', #10705, 1000.000000000000114 ) ;
#50470 = CARTESIAN_POINT ( 'NONE',  ( 7.846153846153846700, -4.098570777380720287, 33.41473453929634729 ) ) ;
#50471 = EDGE_CURVE ( 'NONE', #26348, #16935, #28947, .T. ) ;
#50472 = VERTEX_POINT ( 'NONE', #82990 ) ;
#50473 = CARTESIAN_POINT ( 'NONE',  ( -14.30769230769230660, -12.09954503811598769, 35.62045528018868623 ) ) ;
#50474 = CARTESIAN_POINT ( 'NONE',  ( -4.403846153846152411, -7.433931650972300353, 34.75000000000000711 ) ) ;
#50475 = VERTEX_POINT ( 'NONE', #22175 ) ;
#50476 = CARTESIAN_POINT ( 'NONE',  ( 8.703148389870632329, -4.661471528628507777, 34.16647553114621871 ) ) ;
#50477 = CARTESIAN_POINT ( 'NONE',  ( -12.59222992820602371, -5.582088688514999397, 34.36776431015576350 ) ) ;
#50478 = CARTESIAN_POINT ( 'NONE',  ( -11.78843826940389050, -2.779195860258146578, 31.39871582349836032 ) ) ;
#50479 = EDGE_CURVE ( 'NONE', #80774, #148, #8615, .T. ) ;
#50480 = B_SPLINE_CURVE_WITH_KNOTS ( 'NONE', 3,
 ( #30666, #21697, #77092, #15397, #42868, #8642, #36114, #45064, #73447, #4073 ),
 .UNSPECIFIED., .F., .F.,
 ( 4, 2, 2, 2, 4 ),
 ( 0.0007817359430256390048, 0.0009771253907250078159, 0.001172514838424376735, 0.001367904286123745655, 0.001563293733823114574 ),
 .UNSPECIFIED. ) ;
#50481 = CARTESIAN_POINT ( 'NONE',  ( 9.692307692307695177, -12.29105614889573062, 35.45975837776705220 ) ) ;
#50482 = CARTESIAN_POINT ( 'NONE',  ( 13.38461538461538680, -13.53365097954675988, 30.81389545987213552 ) ) ;
#50483 = VERTEX_POINT ( 'NONE', #14082 ) ;
#50485 = ADVANCED_FACE ( 'NONE', ( #69027 ), #7335, .F. ) ;
#50484 = ORIENTED_EDGE ( 'NONE', *, *, #72442, .F. ) ;
#50486 = AXIS2_PLACEMENT_3D ( 'NONE', #22542, #77486, #63960 ) ;
#50487 = FACE_BOUND ( 'NONE', #77345, .T. ) ;
#50488 = ORIENTED_EDGE ( 'NONE', *, *, #4551, .T. ) ;
#50489 = CARTESIAN_POINT ( 'NONE',  ( -4.946878021003303871, -2.254550872974306674, 29.97347326024527447 ) ) ;
#50490 = VECTOR ( 'NONE', #66390, 1000.000000000000227 ) ;
#50491 = CARTESIAN_POINT ( 'NONE',  ( 17.86930939688969033, -5.496505350115500121, 34.60290016733514307 ) ) ;
#50492 = CARTESIAN_POINT ( 'NONE',  ( 0.6843181305165274564, -12.69155399931963046, 30.53255429739158444 ) ) ;
#50493 = EDGE_CURVE ( 'NONE', #3057, #64684, #55508, .T. ) ;
#50494 = AXIS2_PLACEMENT_3D ( 'NONE', #9356, #38145, #24632 ) ;
#50495 = ORIENTED_EDGE ( 'NONE', *, *, #5948, .F. ) ;
#50496 = ORIENTED_EDGE ( 'NONE', *, *, #1210, .T. ) ;
#50497 = CARTESIAN_POINT ( 'NONE',  ( 15.23076923076911093, -9.442884908241554243, 34.35708131394783038 ) ) ;
#50498 = ORIENTED_EDGE ( 'NONE', *, *, #13927, .F. ) ;
#50499 = CARTESIAN_POINT ( 'NONE',  ( -10.54931626438217585, -8.973038597847271092, 34.52809138561121216 ) ) ;
#50500 = EDGE_CURVE ( 'NONE', #84435, #71169, #33269, .T. ) ;
#50501 = EDGE_CURVE ( 'NONE', #88089, #77626, #5884, .T. ) ;
#50502 = LINE ( 'NONE', #77102, #8607 ) ;
#50503 = B_SPLINE_CURVE_WITH_KNOTS ( 'NONE', 3,
 ( #59488, #12200, #32023, #32913, #4999, #51822, #86539, #11304, #38782, #73904 ),
 .UNSPECIFIED., .F., .F.,
 ( 4, 2, 2, 2, 4 ),
 ( 0.0007817246256747447872, 0.0009771112852218876831, 0.001172497944769030579, 0.001367884604316173475, 0.001563271263863316371 ),
 .UNSPECIFIED. ) ;
#50504 = CARTESIAN_POINT ( 'NONE',  ( -2.307692307692428724, -12.51329471203414379, 31.30864560766407578 ) ) ;
#50505 = EDGE_CURVE ( 'NONE', #68329, #69454, #68030, .T. ) ;
#50506 = FACE_BOUND ( 'NONE', #40054, .T. ) ;
#50507 = EDGE_LOOP ( 'NONE', ( #9748, #44946 ) ) ;
#50508 = CYLINDRICAL_SURFACE ( 'NONE', #34219, 0.2500000000000009437 ) ;
#50509 = B_SPLINE_CURVE_WITH_KNOTS ( 'NONE', 3,
 ( #49581, #43269, #70743, #57223, #22987, #82933, #75714, #14019, #7270, #34736 ),
 .UNSPECIFIED., .F., .F.,
 ( 4, 2, 2, 2, 4 ),
 ( 0.0007817246256747469556, 0.0009771112852218902852, 0.001172497944769033615, 0.001367884604316176728, 0.001563271263863320057 ),
 .UNSPECIFIED. ) ;
#50510 = CYLINDRICAL_SURFACE ( 'NONE', #41898, 0.2499999999999979738 ) ;
#50511 = CARTESIAN_POINT ( 'NONE',  ( -14.53061852520845498, -9.086856451489515152, 34.49173150075333183 ) ) ;
#50512 = CARTESIAN_POINT ( 'NONE',  ( 10.61538461538461675, -3.886160181151819604, 36.00935417666054406 ) ) ;
#50513 = ORIENTED_EDGE ( 'NONE', *, *, #20344, .T. ) ;
#50514 = VERTEX_POINT ( 'NONE', #32908 ) ;
#50515 = ORIENTED_EDGE ( 'NONE', *, *, #35986, .F. ) ;
#50517 = CARTESIAN_POINT ( 'NONE',  ( 19.00000000000000000, 0.7500000000000059952, 24.75000000000000000 ) ) ;
#50516 = CARTESIAN_POINT ( 'NONE',  ( -7.846153846153965716, -6.879047030192662504, 34.71129190930017927 ) ) ;
#50518 = CARTESIAN_POINT ( 'NONE',  ( 16.15384615384615330, -5.557115091759785130, 34.35708131394839171 ) ) ;
#50519 = CARTESIAN_POINT ( 'NONE',  ( -3.296852641725110278, -11.16473453929635440, 33.15142922261925662 ) ) ;
#50520 = CARTESIAN_POINT ( 'NONE',  ( -9.692307692307691624, -3.886160181151819604, 36.00935417666054406 ) ) ;
#50521 = CARTESIAN_POINT ( 'NONE',  ( 14.17754433796061164, -3.069018819979302926, 32.56621877034667278 ) ) ;
#50522 = ORIENTED_EDGE ( 'NONE', *, *, #24074, .F. ) ;
#50523 = CARTESIAN_POINT ( 'NONE',  ( 11.53846153846141576, -5.094484230521993062, 34.41647553114689373 ) ) ;
#50524 = LINE ( 'NONE', #16744, #67560 ) ;
#50525 = CARTESIAN_POINT ( 'NONE',  ( -4.153846153846152411, -1.951392089020283160, 34.73218667398347748 ) ) ;
#50526 = CYLINDRICAL_SURFACE ( 'NONE', #58254, 0.2499999999999979738 ) ;
#50527 = AXIS2_PLACEMENT_3D ( 'NONE', #87594, #54215, #24976 ) ;
#50528 = ORIENTED_EDGE ( 'NONE', *, *, #82274, .T. ) ;
#50529 = FACE_OUTER_BOUND ( 'NONE', #71735, .T. ) ;
#50530 = B_SPLINE_CURVE_WITH_KNOTS ( 'NONE', 3,
 ( #44238, #4155, #10030, #3269, #23978, #59550, #86152, #52790, #79836, #30741 ),
 .UNSPECIFIED., .F., .F.,
 ( 4, 2, 2, 2, 4 ),
 ( 0.000000000000000000, 0.0001954311564186860071, 0.0003908623128373720141, 0.0005862934692560580483, 0.0007817246256747440282 ),
 .UNSPECIFIED. ) ;
#50531 = EDGE_LOOP ( 'NONE', ( #21754, #72400 ) ) ;
#50532 = FACE_BOUND ( 'NONE', #23102, .T. ) ;
#50533 = EDGE_CURVE ( 'NONE', #60787, #82557, #26595, .T. ) ;
#50534 = FACE_OUTER_BOUND ( 'NONE', #47018, .T. ) ;
#50535 = CARTESIAN_POINT ( 'NONE',  ( 18.13052543823364360, -12.70449254468099198, 30.44128974285582956 ) ) ;
#50536 = CARTESIAN_POINT ( 'NONE',  ( -11.47239318745909742, -11.69971097300155272, 32.46337939537588113 ) ) ;
#50537 = ORIENTED_EDGE ( 'NONE', *, *, #46509, .F. ) ;
#50538 = DIRECTION ( 'NONE',  ( -0.000000000000000000, -0.9396926207859092051, -0.3420201433256662704 ) ) ;
#50539 = CARTESIAN_POINT ( 'NONE',  ( -10.61538461538461320, -6.386643153685126251, 34.62446782046654192 ) ) ;
#50540 = CARTESIAN_POINT ( 'NONE',  ( -11.53846153846153655, -4.661471528628507777, 34.16647553114623292 ) ) ;
#50541 = CARTESIAN_POINT ( 'NONE',  ( 10.28846153846153832, -3.499999999999999556, 29.75000000000000355 ) ) ;
#50542 = VERTEX_POINT ( 'NONE', #39682 ) ;
#50543 = DIRECTION ( 'NONE',  ( -0.000000000000000000, -0.9396926207859093161, -0.3420201433256663259 ) ) ;
#50544 = ORIENTED_EDGE ( 'NONE', *, *, #15567, .T. ) ;
#50545 = EDGE_CURVE ( 'NONE', #43177, #52380, #7121, .T. ) ;
#50547 = EDGE_LOOP ( 'NONE', ( #35343, #44758 ) ) ;
#50546 = CARTESIAN_POINT ( 'NONE',  ( 13.51514082284903040, -8.630441415882550871, 34.87705825610312615 ) ) ;
#50548 = CARTESIAN_POINT ( 'NONE',  ( 7.716006636715626144, -10.88202310037936194, 33.43294751532457099 ) ) ;
#50549 = CARTESIAN_POINT ( 'NONE',  ( -17.07692307692307665, -2.708943851104267164, 35.45975837776705220 ) ) ;
#50550 = FACE_OUTER_BOUND ( 'NONE', #57003, .T. ) ;
#50551 = CARTESIAN_POINT ( 'NONE',  ( -12.71156168575991963, -10.92453946501458795, 33.72985991061850086 ) ) ;
#50552 = CARTESIAN_POINT ( 'NONE',  ( -6.923076923076922462, -9.819645486525091727, 36.12317359536749706 ) ) ;
#50553 = B_SPLINE_CURVE_WITH_KNOTS ( 'NONE', 3,
 ( #75766, #77104, #35227, #28476, #55939, #15413, #63583, #76664, #28030, #1885 ),
 .UNSPECIFIED., .F., .F.,
 ( 4, 2, 2, 2, 4 ),
 ( 0.000000000000000000, 0.0001954311564186888531, 0.0003908623128373777062, 0.0005862934692560666135, 0.0007817246256747554124 ),
 .UNSPECIFIED. ) ;
#50554 = B_SPLINE_CURVE_WITH_KNOTS ( 'NONE', 3,
 ( #42581, #29511, #63281, #57409, #78129, #36269, #50650, #1591, #43460, #37136 ),
 .UNSPECIFIED., .F., .F.,
 ( 4, 2, 2, 2, 4 ),
 ( 0.0007817246256747505334, 0.0009771112852218954894, 0.001172497944769040554, 0.001367884604316185618, 0.001563271263863330682 ),
 .UNSPECIFIED. ) ;
#50555 = CARTESIAN_POINT ( 'NONE',  ( -9.915792616872019849, -12.11044203135681840, 32.26167407432752299 ) ) ;
#50556 = B_SPLINE_CURVE_WITH_KNOTS ( 'NONE', 3,
 ( #59298, #58852, #3015, #18323, #45785, #86358, #79585, #44434, #17882, #45336 ),
 .UNSPECIFIED., .F., .F.,
 ( 4, 2, 2, 2, 4 ),
 ( 0.000000000000000000, 0.0001954311564186862781, 0.0003908623128373725562, 0.0005862934692560588072, 0.0007817246256747451124 ),
 .UNSPECIFIED. ) ;
#50557 = EDGE_CURVE ( 'NONE', #11880, #14834, #52721, .T. ) ;
#50558 = CARTESIAN_POINT ( 'NONE',  ( -1.944543648263014957, -5.555456351737005249, 26.50000000000000355 ) ) ;
#50559 = ORIENTED_EDGE ( 'NONE', *, *, #74213, .F. ) ;
#50560 = B_SPLINE_CURVE_WITH_KNOTS ( 'NONE', 3,
 ( #19221, #31851, #25532, #59309, #87251, #4821, #81373, #25969, #74163, #19657 ),
 .UNSPECIFIED., .F., .F.,
 ( 4, 2, 2, 2, 4 ),
 ( 0.000000000000000000, 0.0001954311564186879044, 0.0003908623128373758088, 0.0005862934692560636861, 0.0007817246256747516176 ),
 .UNSPECIFIED. ) ;
#50561 = CARTESIAN_POINT ( 'NONE',  ( -0.5268089074992370335, -6.026961402152685388, 34.52809138561120506 ) ) ;
#50562 = DIRECTION ( 'NONE',  ( -0.000000000000000000, -0.9848077530122086864, -0.1736481776669273613 ) ) ;
#50563 = ORIENTED_EDGE ( 'NONE', *, *, #16052, .T. ) ;
#50564 = ORIENTED_EDGE ( 'NONE', *, *, #19101, .F. ) ;
#50565 = ORIENTED_EDGE ( 'NONE', *, *, #61274, .F. ) ;
#50566 = CARTESIAN_POINT ( 'NONE',  ( -10.74553182482283198, -11.47017969459904130, 32.78971311882034456 ) ) ;
#50567 = DIRECTION ( 'NONE',  ( 1.000000000000000000, -0.000000000000000000, -0.000000000000000000 ) ) ;
#50568 = CARTESIAN_POINT ( 'NONE',  ( -5.999999999999998224, -12.62096338111211580, 30.90682066428153263 ) ) ;
#50569 = AXIS2_PLACEMENT_3D ( 'NONE', #77815, #1272, #56225 ) ;
#50570 = DIRECTION ( 'NONE',  ( -0.000000000000000000, -0.9848077530122085754, -0.1736481776669273613 ) ) ;
#50571 = DIRECTION ( 'NONE',  ( -0.000000000000000000, 0.9848077530122086864, -0.1736481776669273891 ) ) ;
#50572 = EDGE_CURVE ( 'NONE', #45405, #81436, #66237, .T. ) ;
#50573 = LINE ( 'NONE', #40631, #54271 ) ;
#50574 = DIRECTION ( 'NONE',  ( -0.000000000000000000, -0.5000000000000009992, -0.8660254037844380415 ) ) ;
#50575 = ORIENTED_EDGE ( 'NONE', *, *, #5336, .T. ) ;
#50576 = CARTESIAN_POINT ( 'NONE',  ( -0.4615384615384611200, -13.95598074871891292, 31.83374038241031911 ) ) ;
#50577 = CARTESIAN_POINT ( 'NONE',  ( -1.634592115557738090, -6.567427716900047230, 34.66269422305636283 ) ) ;
#50578 = CARTESIAN_POINT ( 'NONE',  ( -18.00000000000000000, -12.62096338111211580, 30.90682066428153263 ) ) ;
#50579 = CARTESIAN_POINT ( 'NONE',  ( 8.096099364501990081, -2.824170634883622633, 31.52227843825338738 ) ) ;
#50580 = ORIENTED_EDGE ( 'NONE', *, *, #46184, .T. ) ;
#50581 = LINE ( 'NONE', #2829, #65702 ) ;
#50582 = EDGE_CURVE ( 'NONE', #18632, #34976, #23514, .T. ) ;
#50583 = ORIENTED_EDGE ( 'NONE', *, *, #79306, .F. ) ;
#50584 = CARTESIAN_POINT ( 'NONE',  ( 8.992243613324166773, -2.889357225399416418, 32.26129605718031002 ) ) ;
#50585 = CARTESIAN_POINT ( 'NONE',  ( 3.230769230769108269, -11.06231777344772027, 33.60647404775119895 ) ) ;
#50586 = CARTESIAN_POINT ( 'NONE',  ( 1.384615384615264011, -11.67786785259630911, 32.92929555188603530 ) ) ;
#50587 = ORIENTED_EDGE ( 'NONE', *, *, #24131, .T. ) ;
#50588 = EDGE_CURVE ( 'NONE', #61992, #70675, #13955, .T. ) ;
#50589 = DIRECTION ( 'NONE',  ( 0.000000000000000000, 0.4999999999999985567, 0.8660254037844395958 ) ) ;
#50590 = B_SPLINE_CURVE_WITH_KNOTS ( 'NONE', 3,
 ( #371, #47214, #75570, #1241, #68377, #54865, #7570, #8012, #28732, #74708 ),
 .UNSPECIFIED., .F., .F.,
 ( 4, 2, 2, 2, 4 ),
 ( 0.000000000000000000, 0.0001954339857564073659, 0.0003908679715128147319, 0.0005863019572692221250, 0.0007817359430256294638 ),
 .UNSPECIFIED. ) ;
#50591 = CARTESIAN_POINT ( 'NONE',  ( -12.52729526405276772, -7.249945686854186278, 34.74374336980224598 ) ) ;
#50592 = B_SPLINE_CURVE_WITH_KNOTS ( 'NONE', 3,
 ( #20397, #11874, #87548, #88003, #61811, #66810, #53731, #34342, #39351, #13198 ),
 .UNSPECIFIED., .F., .F.,
 ( 4, 2, 2, 2, 4 ),
 ( 0.000000000000000000, 0.0001954339857564098054, 0.0003908679715128196108, 0.0005863019572692293891, 0.0007817359430256392216 ),
 .UNSPECIFIED. ) ;
#50593 = AXIS2_PLACEMENT_3D ( 'NONE', #2764, #45096, #10879 ) ;
#50594 = CARTESIAN_POINT ( 'NONE',  ( -2.980714919130916574, -12.17597550085003455, 31.52189283813461884 ) ) ;
#50595 = B_SPLINE_CURVE_WITH_KNOTS ( 'NONE', 3,
 ( #87367, #60312, #87821, #72941, #10801, #38270 ),
 .UNSPECIFIED., .F., .F.,
 ( 4, 2, 4 ),
 ( 0.0003909569690057415072, 0.0005862646681845472664, 0.0007815723673633529715 ),
 .UNSPECIFIED. ) ;
#50596 = EDGE_CURVE ( 'NONE', #41015, #62484, #26151, .T. ) ;
#50597 = ORIENTED_EDGE ( 'NONE', *, *, #66981, .T. ) ;
#50599 = EDGE_CURVE ( 'NONE', #83223, #22047, #37548, .T. ) ;
#50598 = CARTESIAN_POINT ( 'NONE',  ( -10.61538461538430589, -2.506253911140614576, 30.00000000000323297 ) ) ;
#50600 = ORIENTED_EDGE ( 'NONE', *, *, #37251, .T. ) ;
#50601 = AXIS2_PLACEMENT_3D ( 'NONE', #74518, #5173, #80400 ) ;
#50602 = DIRECTION ( 'NONE',  ( -0.000000000000000000, 0.3420201433256694346, -0.9396926207859080948 ) ) ;
#50603 = LINE ( 'NONE', #24012, #72994 ) ;
#50604 = CARTESIAN_POINT ( 'NONE',  ( -7.911423846710166075, -2.657715359629089225, 31.77849191805832874 ) ) ;
#50605 = CARTESIAN_POINT ( 'NONE',  ( -14.30769230769230660, -9.780366693483667717, 34.19971097300155094 ) ) ;
#50606 = CARTESIAN_POINT ( 'NONE',  ( 18.24994540937804643, -8.476813868363244353, 34.90874843262270133 ) ) ;
#50607 = EDGE_CURVE ( 'NONE', #38805, #57991, #25262, .T. ) ;
#50608 = VERTEX_POINT ( 'NONE', #73457 ) ;
#50609 = PRODUCT_DEFINITION_SHAPE ( 'NONE', 'NONE',  #35868 ) ;
#50610 = ADVANCED_FACE ( 'NONE', ( #34684 ), #63012, .F. ) ;
#50612 = EDGE_CURVE ( 'NONE', #81234, #51205, #455, .T. ) ;
#50611 = VERTEX_POINT ( 'NONE', #54500 ) ;
#50613 = EDGE_LOOP ( 'NONE', ( #27826, #57637, #87693, #47226 ) ) ;
#50614 = LINE ( 'NONE', #58699, #35870 ) ;
#50615 = DIRECTION ( 'NONE',  ( -0.000000000000000000, -0.000000000000000000, -1.000000000000000000 ) ) ;
#50616 = CARTESIAN_POINT ( 'NONE',  ( 17.29970261819148902, -4.387253974876675677, 33.66317474335728832 ) ) ;
#50617 = AXIS2_PLACEMENT_3D ( 'NONE', #16206, #21632, #36485 ) ;
#50618 = CARTESIAN_POINT ( 'NONE',  ( 0.3962684609821411907, -12.51329471203370325, 31.30864560766548976 ) ) ;
#50619 = CARTESIAN_POINT ( 'NONE',  ( -4.153846153846152411, -12.78798330534102945, 29.74999999999997868 ) ) ;
#50620 = CARTESIAN_POINT ( 'NONE',  ( 5.076923076923075762, -9.780366693483667717, 34.19971097300155094 ) ) ;
#50621 = ORIENTED_EDGE ( 'NONE', *, *, #20527, .T. ) ;
#50622 = VERTEX_POINT ( 'NONE', #7658 ) ;
#50623 = AXIS2_PLACEMENT_3D ( 'NONE', #23216, #2935, #52014 ) ;
#50624 = EDGE_LOOP ( 'NONE', ( #39962, #69578, #44302, #38665 ) ) ;
#50626 = ORIENTED_EDGE ( 'NONE', *, *, #56622, .T. ) ;
#50625 = DIRECTION ( 'NONE',  ( 0.000000000000000000, 0.000000000000000000, -1.000000000000000000 ) ) ;
#50628 = CARTESIAN_POINT ( 'NONE',  ( -8.519285250882626670, -11.37275283266504111, 32.91324779482534524 ) ) ;
#50627 = CARTESIAN_POINT ( 'NONE',  ( 0.5276068125408990284, -8.120952969808772792, 34.71129190929999453 ) ) ;
#50629 = B_SPLINE_CURVE_WITH_KNOTS ( 'NONE', 3,
 ( #27032, #87421, #67580, #20278, #66688, #47742, #80663, #19831, #75226, #33787 ),
 .UNSPECIFIED., .F., .F.,
 ( 4, 2, 2, 2, 4 ),
 ( 0.0007817246256747448956, 0.0009771112852218876831, 0.001172497944769030579, 0.001367884604316173475, 0.001563271263863316371 ),
 .UNSPECIFIED. ) ;
#50630 = CARTESIAN_POINT ( 'NONE',  ( -1.384615384615383471, -4.661471528628507777, 34.16647553114623292 ) ) ;
#50631 = CARTESIAN_POINT ( 'NONE',  ( -3.749999999999997335, -7.500000000000021316, 25.09374999999999645 ) ) ;
#50632 = ORIENTED_EDGE ( 'NONE', *, *, #25470, .T. ) ;
#50633 = EDGE_LOOP ( 'NONE', ( #78789, #35448, #38211, #88730, #41075 ) ) ;
#50634 = CARTESIAN_POINT ( 'NONE',  ( -17.93474486048716088, -3.083524468853784839, 32.58852847137153930 ) ) ;
#50635 = ORIENTED_EDGE ( 'NONE', *, *, #59028, .T. ) ;
#50636 = FACE_BOUND ( 'NONE', #37459, .T. ) ;
#50637 = CARTESIAN_POINT ( 'NONE',  ( 15.00728428704528561, -10.11188796281391511, 34.01382737946119050 ) ) ;
#50638 = DIRECTION ( 'NONE',  ( 0.000000000000000000, 0.9396926207859126468, 0.3420201433256571111 ) ) ;
#50639 = ORIENTED_EDGE ( 'NONE', *, *, #5316, .T. ) ;
#50640 = CARTESIAN_POINT ( 'NONE',  ( -15.23076923076922995, -4.786620604624113540, 33.94971097300155094 ) ) ;
#50641 = DIRECTION ( 'NONE',  ( -0.000000000000000000, 0.8660254037844399289, -0.4999999999999980016 ) ) ;
#50642 = CARTESIAN_POINT ( 'NONE',  ( 12.21153846153846168, -7.500000000000001776, 34.75000000000000000 ) ) ;
#50643 = CARTESIAN_POINT ( 'NONE',  ( 13.91025641025641235, -3.499999999999999556, 29.75000000000000355 ) ) ;
#50644 = CARTESIAN_POINT ( 'NONE',  ( -2.307692307692305711, -8.164416787775445883, 34.95778746994557906 ) ) ;
#50645 = CYLINDRICAL_SURFACE ( 'NONE', #44485, 0.2500000000000009437 ) ;
#50646 = AXIS2_PLACEMENT_3D ( 'NONE', #76238, #49221, #1479 ) ;
#50647 = CARTESIAN_POINT ( 'NONE',  ( 12.46153846153846168, -5.471508081941601098, 34.59228464037088457 ) ) ;
#50648 = CARTESIAN_POINT ( 'NONE',  ( 2.177001704582001818, -11.93127051446800024, 32.56575433478200665 ) ) ;
#50649 = DIRECTION ( 'NONE',  ( -1.000000000000000000, -0.000000000000000000, -0.000000000000000000 ) ) ;
#50650 = CARTESIAN_POINT ( 'NONE',  ( 13.60762822870878352, -2.308499170217967134, 30.53291367094873721 ) ) ;
#50651 = CARTESIAN_POINT ( 'NONE',  ( -12.46153846153846168, -2.499999999999998668, 29.75000000000001421 ) ) ;
#50652 = CARTESIAN_POINT ( 'NONE',  ( 8.834485908743602067, -4.320704448112861584, 33.92786785259548310 ) ) ;
#50654 = CARTESIAN_POINT ( 'NONE',  ( 11.60452988946397745, -4.098570777380720287, 33.41473453929635440 ) ) ;
#50653 = CARTESIAN_POINT ( 'NONE',  ( -13.38461538461550759, -4.320704448113951379, 33.92786785259630022 ) ) ;
#50655 = CYLINDRICAL_SURFACE ( 'NONE', #74148, 0.2499999999999995559 ) ;
#50657 = DIRECTION ( 'NONE',  ( -0.000000000000000000, 1.000000000000000000, 3.491481338843133355E-15 ) ) ;
#50656 = CARTESIAN_POINT ( 'NONE',  ( 4.023698184114459231, -5.915902021225892149, 34.75552854090298638 ) ) ;
#50658 = DIRECTION ( 'NONE',  ( -0.000000000000000000, 1.000000000000000000, 3.491481338843133355E-15 ) ) ;
#50659 = CARTESIAN_POINT ( 'NONE',  ( -1.987747218494660295, -5.598659921968651254, 24.99813170625849423 ) ) ;
#50660 = EDGE_LOOP ( 'NONE', ( #70695, #50156, #81578, #9687, #46502, #51947 ) ) ;
#50661 = CARTESIAN_POINT ( 'NONE',  ( 2.248691020740372082, -4.605660251581315201, 14.00000000000000355 ) ) ;
#50662 = ORIENTED_EDGE ( 'NONE', *, *, #29147, .T. ) ;
#50663 = CARTESIAN_POINT ( 'NONE',  ( -9.915792636031639518, -5.912607949931405926, 34.49155766932282319 ) ) ;
#50664 = VERTEX_POINT ( 'NONE', #6332 ) ;
#50665 = CARTESIAN_POINT ( 'NONE',  ( -3.903791842207838148, -11.28795663066794219, 33.01431243580653785 ) ) ;
#50666 = VERTEX_POINT ( 'NONE', #54952 ) ;
#50667 = FACE_OUTER_BOUND ( 'NONE', #62203, .T. ) ;
#50668 = CARTESIAN_POINT ( 'NONE',  ( 2.775308065498768517, -8.577988221561467341, 23.04500670625849068 ) ) ;
#50669 = CARTESIAN_POINT ( 'NONE',  ( -18.00000000000000000, -9.058645607665452459, 34.76329471203371924 ) ) ;
#50670 = DIRECTION ( 'NONE',  ( -0.000000000000000000, 1.000000000000000000, -0.000000000000000000 ) ) ;
#50671 = CARTESIAN_POINT ( 'NONE',  ( -5.299850035829926753, -2.889293201056495786, 32.26117774369186009 ) ) ;
#50672 = FACE_OUTER_BOUND ( 'NONE', #10102, .T. ) ;
#50673 = CARTESIAN_POINT ( 'NONE',  ( 14.98076923076922817, -7.566083408709835645, 34.74999999999999289 ) ) ;
#50674 = CARTESIAN_POINT ( 'NONE',  ( -14.24243716817946925, -5.094484230520773593, 34.41647553114626845 ) ) ;
#50675 = CARTESIAN_POINT ( 'NONE',  ( -2.608446859217920633, -4.805146000318815780, 25.50186829374151287 ) ) ;
#50676 = CARTESIAN_POINT ( 'NONE',  ( 18.13052543823364360, -11.66157788607254275, 32.95092075102925833 ) ) ;
#50677 = CARTESIAN_POINT ( 'NONE',  ( -15.16551365949320740, -2.625532179533470512, 30.86335684631491105 ) ) ;
#50678 = CARTESIAN_POINT ( 'NONE',  ( 10.36536139116315880, -5.765609946408404518, 34.70566812827425451 ) ) ;
#50679 = CARTESIAN_POINT ( 'NONE',  ( -1.553300858899081538, -11.25000000000000711, 17.35937500000000000 ) ) ;
#50680 = VECTOR ( 'NONE', #54104, 1000.000000000000114 ) ;
#50681 = ADVANCED_FACE ( 'NONE', ( #13959 ), #42774, .T. ) ;
#50682 = CARTESIAN_POINT ( 'NONE',  ( -14.17690049986752143, -10.54018710029568595, 33.71981072465678864 ) ) ;
#50683 = VECTOR ( 'NONE', #28019, 1000.000000000000000 ) ;
#50684 = ORIENTED_EDGE ( 'NONE', *, *, #3994, .F. ) ;
#50685 = CARTESIAN_POINT ( 'NONE',  ( 14.37376065869474751, -4.786620604624113540, 33.94971097300155805 ) ) ;
#50686 = CARTESIAN_POINT ( 'NONE',  ( -11.40793583669797506, -8.586989748646452369, 34.63063291749215011 ) ) ;
#50687 = CARTESIAN_POINT ( 'NONE',  ( 1.161130440891438687, -12.44517049084099725, 30.48991314939691932 ) ) ;
#50688 = CARTESIAN_POINT ( 'NONE',  ( 1.634615384615386580, -2.499999999999998668, 29.75000000000000355 ) ) ;
#50689 = DIRECTION ( 'NONE',  ( 1.000000000000000000, 0.000000000000000000, 0.000000000000000000 ) ) ;
#50690 = VECTOR ( 'NONE', #22243, 1000.000000000000227 ) ;
#50691 = CARTESIAN_POINT ( 'NONE',  ( 9.627037246346917598, -11.48612834413959582, 32.76840700105983473 ) ) ;
#50692 = ADVANCED_FACE ( 'NONE', ( #76554 ), #22051, .F. ) ;
#50693 = ORIENTED_EDGE ( 'NONE', *, *, #22646, .T. ) ;
#50694 = DIRECTION ( 'NONE',  ( 0.000000000000000000, 0.3420201433256610524, 0.9396926207859113145 ) ) ;
#50695 = EDGE_LOOP ( 'NONE', ( #76089, #68433, #69706, #60521 ) ) ;
#50696 = ORIENTED_EDGE ( 'NONE', *, *, #75181, .T. ) ;
#50697 = CARTESIAN_POINT ( 'NONE',  ( 14.98079249982687777, -6.567427716900048118, 34.66269422305636283 ) ) ;
#50698 = CARTESIAN_POINT ( 'NONE',  ( -11.53846153846153655, -11.35647404775217417, 33.31231777344666511 ) ) ;
#50699 = DIRECTION ( 'NONE',  ( -0.000000000000000000, -0.9396926207859092051, -0.3420201433256662704 ) ) ;
#50700 = CARTESIAN_POINT ( 'NONE',  ( 1.450683735617825709, -11.69971097300155272, 32.46337939537588113 ) ) ;
#50701 = LINE ( 'NONE', #70548, #32312 ) ;
#50702 = ORIENTED_EDGE ( 'NONE', *, *, #63653, .T. ) ;
#50703 = CYLINDRICAL_SURFACE ( 'NONE', #63675, 0.2499999999999986955 ) ;
#50704 = VECTOR ( 'NONE', #39288, 1000.000000000000000 ) ;
#50705 = ORIENTED_EDGE ( 'NONE', *, *, #77670, .T. ) ;
#50706 = EDGE_CURVE ( 'NONE', #1675, #76030, #14864, .T. ) ;
#50707 = ORIENTED_EDGE ( 'NONE', *, *, #41608, .F. ) ;
#50708 = CARTESIAN_POINT ( 'NONE',  ( -6.989159302437059296, -11.91647553114624181, 32.58852847137148245 ) ) ;
#50709 = CARTESIAN_POINT ( 'NONE',  ( 3.262820512820510999, -3.499999999999999556, 29.75000000000000355 ) ) ;
#50710 = DIRECTION ( 'NONE',  ( -0.000000000000000000, 1.000000000000000000, 3.491481338843133355E-15 ) ) ;
#50711 = EDGE_CURVE ( 'NONE', #33924, #25611, #19228, .T. ) ;
#50712 = CARTESIAN_POINT ( 'NONE',  ( -11.53846153846153655, -8.164416787775445883, 34.95778746994557906 ) ) ;
#50713 = DIRECTION ( 'NONE',  ( -0.000000000000000000, 1.000000000000000000, -0.000000000000000000 ) ) ;
#50714 = ORIENTED_EDGE ( 'NONE', *, *, #65991, .T. ) ;
#50715 = ORIENTED_EDGE ( 'NONE', *, *, #63468, .F. ) ;
#50716 = CARTESIAN_POINT ( 'NONE',  ( 3.750000000000000888, -7.499999999999978684, 23.21875000000000000 ) ) ;
#50717 = VERTEX_POINT ( 'NONE', #82876 ) ;
#50719 = ORIENTED_EDGE ( 'NONE', *, *, #83687, .T. ) ;
#50718 = CARTESIAN_POINT ( 'NONE',  ( -2.372962753653081514, -2.892918686051582533, 31.69288490824015270 ) ) ;
#50720 = CARTESIAN_POINT ( 'NONE',  ( 1.450683735617824599, -8.973038597847269315, 34.52809138561122637 ) ) ;
#50721 = CARTESIAN_POINT ( 'NONE',  ( 10.61538461538461675, -3.050289026998446396, 32.03036669348365706 ) ) ;
#50722 = CARTESIAN_POINT ( 'NONE',  ( -0.4615384615384611200, -9.058645607665452459, 34.76329471203371924 ) ) ;
#50723 = VERTEX_POINT ( 'NONE', #41439 ) ;
#50724 = DIRECTION ( 'NONE',  ( 0.000000000000000000, 0.6427876096865373645, -0.7660444431189797898 ) ) ;
#50725 = ORIENTED_EDGE ( 'NONE', *, *, #75539, .F. ) ;
#50726 = CARTESIAN_POINT ( 'NONE',  ( 17.07692307692307665, -2.538708090699994813, 30.37095296980875503 ) ) ;
#50727 = DIRECTION ( 'NONE',  ( 0.000000000000000000, 0.9396926207859126468, 0.3420201433256571111 ) ) ;
#50728 = PRESENTATION_LAYER_ASSIGNMENT (  '', '', ( #63737 ) ) ;
#50729 = CARTESIAN_POINT ( 'NONE',  ( -17.86947456176635640, -2.647132371071621026, 31.75357179365173010 ) ) ;
#50731 = CARTESIAN_POINT ( 'NONE',  ( 4.153846153846030731, -5.941354392335915335, 34.76329471203413846 ) ) ;
#50730 = CARTESIAN_POINT ( 'NONE',  ( 0.4615384615384611200, -11.35647404775217417, 33.31231777344666511 ) ) ;
#50732 = VECTOR ( 'NONE', #8766, 1000.000000000000227 ) ;
#50733 = CARTESIAN_POINT ( 'NONE',  ( 16.15384615384603251, -2.625532179533778709, 30.86335684631627174 ) ) ;
#50734 = CARTESIAN_POINT ( 'NONE',  ( -0.4615384615385840772, -12.70778746994576025, 30.41441678777401236 ) ) ;
#50735 = EDGE_LOOP ( 'NONE', ( #471, #10180, #38622, #32091 ) ) ;
#50736 = LINE ( 'NONE', #64252, #71981 ) ;
#50737 =( NAMED_UNIT ( * ) PLANE_ANGLE_UNIT ( ) SI_UNIT ( $, .RADIAN. ) );
#50738 = ORIENTED_EDGE ( 'NONE', *, *, #44442, .F. ) ;
#50739 = VECTOR ( 'NONE', #31334, 1000.000000000000227 ) ;
#50740 = B_SPLINE_CURVE_WITH_KNOTS ( 'NONE', 3,
 ( #61498, #59403, #27277, #48424, #86454, #82231, #17980, #41244, #86904, #52638 ),
 .UNSPECIFIED., .F., .F.,
 ( 4, 2, 2, 2, 4 ),
 ( 0.0007817246256747486903, 0.0009771112852218918031, 0.001172497944769034699, 0.001367884604316177595, 0.001563271263863320708 ),
 .UNSPECIFIED. ) ;
#50741 = B_SPLINE_CURVE_WITH_KNOTS ( 'NONE', 3,
 ( #31937, #65695, #23817, #64803, #80117, #10325, #85988, #31483, #9874, #45878 ),
 .UNSPECIFIED., .F., .F.,
 ( 4, 2, 2, 2, 4 ),
 ( 0.000000000000000000, 0.0001954339857564077183, 0.0003908679715128154366, 0.0005863019572692231007, 0.0007817359430256308733 ),
 .UNSPECIFIED. ) ;
#50742 = DIRECTION ( 'NONE',  ( -0.000000000000000000, -0.5000000000000009992, -0.8660254037844380415 ) ) ;
#50743 = CARTESIAN_POINT ( 'NONE',  ( 15.23076923076923173, -4.098570777380720287, 33.41473453929634729 ) ) ;
#50744 = CARTESIAN_POINT ( 'NONE',  ( 3.361607648781993696, -7.277220443632450575, 34.74524770363009196 ) ) ;
#50745 = LINE ( 'NONE', #50305, #10190 ) ;
#50746 = CARTESIAN_POINT ( 'NONE',  ( -0.4615384615384611200, -12.37446782046654192, 30.86335684631486131 ) ) ;
#50747 = CARTESIAN_POINT ( 'NONE',  ( -8.096153846153844924, -7.500000000000001776, 35.00000000000000000 ) ) ;
#50748 = FACE_BOUND ( 'NONE', #87968, .T. ) ;
#50750 = DIRECTION ( 'NONE',  ( 0.000000000000000000, -6.938893903907222067E-15, 1.000000000000000000 ) ) ;
#50749 = CARTESIAN_POINT ( 'NONE',  ( 13.13463864056679675, -2.318417181685855422, 30.59732222474233865 ) ) ;
#50751 = CARTESIAN_POINT ( 'NONE',  ( -6.792551221313359200, -10.88167719472716399, 33.43325721877153711 ) ) ;
#50753 = CARTESIAN_POINT ( 'NONE',  ( -14.05769230769237055, -7.565270000091922853, 34.99999999999999289 ) ) ;
#50752 = CARTESIAN_POINT ( 'NONE',  ( -4.946397638689432164, -10.31582465632705237, 34.18122507451815295 ) ) ;
#50754 = DIRECTION ( 'NONE',  ( 0.000000000000000000, 0.000000000000000000, 1.000000000000000000 ) ) ;
#50755 = CARTESIAN_POINT ( 'NONE',  ( 0.06109907496455496689, -11.24999999999999822, 18.27938170625849068 ) ) ;
#50756 = ORIENTED_EDGE ( 'NONE', *, *, #42757, .F. ) ;
#50757 = CARTESIAN_POINT ( 'NONE',  ( 15.93036122928182330, -9.417330523894424488, 34.63758898049880486 ) ) ;
#50758 = CARTESIAN_POINT ( 'NONE',  ( -14.30769230769230660, -6.386643153685126251, 34.62446782046654192 ) ) ;
#50759 = DIRECTION ( 'NONE',  ( -0.000000000000000000, 0.9848077530122086864, -0.1736481776669273891 ) ) ;
#50760 = CARTESIAN_POINT ( 'NONE',  ( -10.74607521849492464, -11.37499894934982692, 33.29245874905763003 ) ) ;
#50761 = CARTESIAN_POINT ( 'NONE',  ( 7.846153846153725020, -5.219633306517616589, 34.19971097300220464 ) ) ;
#50762 = CARTESIAN_POINT ( 'NONE',  ( -1.492201783934549164, -11.27530806549876807, 22.10750670625849068 ) ) ;
#50763 = EDGE_CURVE ( 'NONE', #32348, #18061, #49377, .T. ) ;
#50764 = CARTESIAN_POINT ( 'NONE',  ( -2.307692307692428724, -3.643525952248796163, 33.31231777344771672 ) ) ;
#50765 = LINE ( 'NONE', #64729, #1503 ) ;
#50766 = VECTOR ( 'NONE', #33089, 1000.000000000000000 ) ;
#50767 = CARTESIAN_POINT ( 'NONE',  ( 11.76188793737632743, -7.630147987733840509, 34.99859428049665411 ) ) ;
#50768 = CARTESIAN_POINT ( 'NONE',  ( 19.50000000000000000, -7.500000000000000000, 33.75000000000000000 ) ) ;
#50769 = CARTESIAN_POINT ( 'NONE',  ( 14.30769230769231015, -9.819645486525091727, 36.12317359536749706 ) ) ;
#50770 = CARTESIAN_POINT ( 'NONE',  ( 4.088575707885377497, -10.90142922261923886, 33.41473453929638993 ) ) ;
#50771 = CARTESIAN_POINT ( 'NONE',  ( -18.06527044596077047, -2.892918686051583421, 31.69288490824015270 ) ) ;
#50772 = CARTESIAN_POINT ( 'NONE',  ( 20.00000000000000000, -4.000000000000000000, 29.75000000000000355 ) ) ;
#50773 = EDGE_LOOP ( 'NONE', ( #83013, #62242, #19858, #66036 ) ) ;
#50774 = CARTESIAN_POINT ( 'NONE',  ( 17.32697749683652688, -12.65882529074907126, 30.72640787790838601 ) ) ;
#50775 = CARTESIAN_POINT ( 'NONE',  ( -6.000000000000121680, -2.657715359629662988, 31.77849191805970364 ) ) ;
#50776 = CARTESIAN_POINT ( 'NONE',  ( -3.724691934501248802, -5.885600066136383646, 15.42374329374151642 ) ) ;
#50777 = EDGE_CURVE ( 'NONE', #63664, #29143, #6757, .T. ) ;
#50778 = CARTESIAN_POINT ( 'NONE',  ( 6.988332062589762472, -11.06231777344671130, 33.60647404775212976 ) ) ;
#50779 = CARTESIAN_POINT ( 'NONE',  ( 3.453548772037640546, -11.89424750095246175, 32.13594075562311758 ) ) ;
#50780 = ORIENTED_EDGE ( 'NONE', *, *, #77427, .F. ) ;
#50781 = PLANE ( 'NONE',  #22686 ) ;
#50783 = ORIENTED_EDGE ( 'NONE', *, *, #64633, .T. ) ;
#50782 = CARTESIAN_POINT ( 'NONE',  ( -0.4615384615384611200, -3.513871655860378418, 32.76840700105978499 ) ) ;
#50784 = CARTESIAN_POINT ( 'NONE',  ( -3.903846153846152855, -2.249999999999998668, 29.75000000000000355 ) ) ;
#50785 = CARTESIAN_POINT ( 'NONE',  ( 23.00000000000000000, -9.499999999999982236, 27.25000000000000000 ) ) ;
#50786 = ADVANCED_FACE ( 'NONE', ( #13517 ), #55831, .F. ) ;
#50787 = FACE_OUTER_BOUND ( 'NONE', #68420, .T. ) ;
#50788 = FACE_OUTER_BOUND ( 'NONE', #77098, .T. ) ;
#50789 = ORIENTED_EDGE ( 'NONE', *, *, #35536, .T. ) ;
#50790 = CARTESIAN_POINT ( 'NONE',  ( -13.38461538461538325, -12.09954503811598769, 35.62045528018868623 ) ) ;
#50791 = CARTESIAN_POINT ( 'NONE',  ( 5.326923076923075762, -2.249999999999998668, 29.75000000000000355 ) ) ;
#50792 = AXIS2_PLACEMENT_3D ( 'NONE', #71761, #38435, #86642 ) ;
#50793 = CARTESIAN_POINT ( 'NONE',  ( -1.253823576790597194, -5.582136614379148654, 34.36778462344220486 ) ) ;
#50794 = EDGE_CURVE ( 'NONE', #20449, #45365, #71856, .T. ) ;
#50795 = EDGE_LOOP ( 'NONE', ( #84732, #82737, #49232, #89006 ) ) ;
#50796 = ORIENTED_EDGE ( 'NONE', *, *, #20634, .T. ) ;
#50797 = AXIS2_PLACEMENT_3D ( 'NONE', #23541, #50574, #50998 ) ;
#50798 = EDGE_LOOP ( 'NONE', ( #46295, #84521 ) ) ;
#50799 = ADVANCED_FACE ( 'NONE', ( #78304 ), #23362, .F. ) ;
#50800 = CARTESIAN_POINT ( 'NONE',  ( 3.296836564119307589, -2.292212530054420494, 30.41441678777542990 ) ) ;
#50801 = CARTESIAN_POINT ( 'NONE',  ( 9.823098133274648092, -3.957578996910242619, 33.62503395064540257 ) ) ;
#50802 = B_SPLINE_CURVE_WITH_KNOTS ( 'NONE', 3,
 ( #8829, #15583, #22334, #36301, #69630, #63315, #1625, #41285, #20558, #48916 ),
 .UNSPECIFIED., .F., .F.,
 ( 4, 2, 2, 2, 4 ),
 ( 0.000000000000000000, 0.0001954311564186862510, 0.0003908623128373725020, 0.0005862934692560588072, 0.0007817246256747450040 ),
 .UNSPECIFIED. ) ;
#50803 = DIRECTION ( 'NONE',  ( 1.000000000000000000, 0.000000000000000000, 0.000000000000000000 ) ) ;
#50804 = B_SPLINE_CURVE_WITH_KNOTS ( 'NONE', 3,
 ( #38672, #52623, #67487, #4902, #80107, #33258, #18408, #11657, #39133, #66599 ),
 .UNSPECIFIED., .F., .F.,
 ( 4, 2, 2, 2, 4 ),
 ( 0.000000000000000000, 0.0001954339857564078267, 0.0003908679715128156535, 0.0005863019572692235344, 0.0007817359430256313069 ),
 .UNSPECIFIED. ) ;
#50805 = LINE ( 'NONE', #45839, #298 ) ;
#50806 = EDGE_CURVE ( 'NONE', #56977, #51043, #84806, .T. ) ;
#50807 = ORIENTED_EDGE ( 'NONE', *, *, #60133, .F. ) ;
#50808 = ORIENTED_EDGE ( 'NONE', *, *, #63569, .T. ) ;
#50811 = ORIENTED_EDGE ( 'NONE', *, *, #80705, .F. ) ;
#50810 = EDGE_CURVE ( 'NONE', #29819, #61584, #58468, .T. ) ;
#50809 = CYLINDRICAL_SURFACE ( 'NONE', #48715, 0.2499999999999973355 ) ;
#50812 = CARTESIAN_POINT ( 'NONE',  ( 9.692307692307572609, -12.46129190930018460, 30.37095296980731973 ) ) ;
#50813 = EDGE_CURVE ( 'NONE', #5990, #5809, #57596, .T. ) ;
#50814 = EDGE_CURVE ( 'NONE', #45215, #6722, #71548, .T. ) ;
#50815 = CARTESIAN_POINT ( 'NONE',  ( 7.623226887246997485, -11.98009711892699691, 32.48740034544075428 ) ) ;
#50816 = CARTESIAN_POINT ( 'NONE',  ( -9.019230769230768274, -7.500000000000001776, 34.75000000000000000 ) ) ;
#50817 = ORIENTED_EDGE ( 'NONE', *, *, #12454, .F. ) ;
#50818 = EDGE_LOOP ( 'NONE', ( #57583, #29923, #60420, #23732 ) ) ;
#50820 = VERTEX_POINT ( 'NONE', #51249 ) ;
#50819 = CARTESIAN_POINT ( 'NONE',  ( -6.792285115252135519, -11.18335022499818621, 33.13157742990016885 ) ) ;
#50821 = DIRECTION ( 'NONE',  ( -0.000000000000000000, -0.9848077530122085754, -0.1736481776669273613 ) ) ;
#50822 = FACE_OUTER_BOUND ( 'NONE', #51286, .T. ) ;
#50823 = EDGE_LOOP ( 'NONE', ( #59273, #9257, #69883, #48703 ) ) ;
#50824 = CARTESIAN_POINT ( 'NONE',  ( 12.71159288145191368, -6.523592122091592671, 34.90882529074906415 ) ) ;
#50825 = CARTESIAN_POINT ( 'NONE',  ( 15.29683758177166908, -8.973038597847271092, 34.52809138561121216 ) ) ;
#50826 = CARTESIAN_POINT ( 'NONE',  ( 10.86533013373275836, -3.712312575010499494, 33.01462480002815170 ) ) ;
#50827 = FACE_BOUND ( 'NONE', #48287, .T. ) ;
#50828 = CARTESIAN_POINT ( 'NONE',  ( -9.442253272394237840, -4.074993327901527351, 33.72946981652012255 ) ) ;
#50829 = CARTESIAN_POINT ( 'NONE',  ( 7.846153846153846700, -1.129524287112498415, 32.06866353760679544 ) ) ;
#50830 = CARTESIAN_POINT ( 'NONE',  ( 13.38461538461526423, -12.70778746994576025, 30.41441678777401236 ) ) ;
#50832 = DIRECTION ( 'NONE',  ( -0.000000000000000000, -0.9848077530122086864, -0.1736481776669273613 ) ) ;
#50831 = CARTESIAN_POINT ( 'NONE',  ( 16.82689985270161870, -9.356822207818511927, 34.66110646841856635 ) ) ;
#50833 = CARTESIAN_POINT ( 'NONE',  ( -11.40766973063675493, -3.062576670634119758, 32.05464942895959979 ) ) ;
#50834 = CARTESIAN_POINT ( 'NONE',  ( 10.28846153846153832, -7.500000000000000000, 29.75000000000000355 ) ) ;
#50835 = ORIENTED_EDGE ( 'NONE', *, *, #16413, .T. ) ;
#50836 = DIRECTION ( 'NONE',  ( 0.000000000000000000, 0.3420201433256641055, -0.9396926207859100932 ) ) ;
#50837 = EDGE_LOOP ( 'NONE', ( #76789, #66001, #27430, #51006 ) ) ;
#50838 = ORIENTED_EDGE ( 'NONE', *, *, #36863, .T. ) ;
#50840 = CARTESIAN_POINT ( 'NONE',  ( 1.134638653673032183, -10.66389620160130036, 33.62221079203477103 ) ) ;
#50839 = CARTESIAN_POINT ( 'NONE',  ( 9.469441429244595199, -2.251424796025574881, 29.88072029997477230 ) ) ;
#50841 = CARTESIAN_POINT ( 'NONE',  ( -6.700297381808513641, -6.760870238392817200, 34.69528174975672385 ) ) ;
#50842 = CARTESIAN_POINT ( 'NONE',  ( -14.30769230769242739, -2.892918686052166066, 31.69288490824153470 ) ) ;
#50843 = CARTESIAN_POINT ( 'NONE',  ( 1.134638653673032405, -6.567427716900047230, 34.66269422305636283 ) ) ;
#50844 = CARTESIAN_POINT ( 'NONE',  ( -2.307692307692428724, -11.67786785259630911, 32.92929555188603530 ) ) ;
#50845 = ORIENTED_EDGE ( 'NONE', *, *, #67814, .F. ) ;
#50846 = ADVANCED_FACE ( 'NONE', ( #64342 ), #9855, .F. ) ;
#50847 = CARTESIAN_POINT ( 'NONE',  ( 18.13052543823364360, -2.647132371071621471, 31.75357179365173010 ) ) ;
#50848 = AXIS2_PLACEMENT_3D ( 'NONE', #77751, #8865, #51140 ) ;
#50849 = CARTESIAN_POINT ( 'NONE',  ( 15.10062126103753322, -11.04286588640298561, 33.62463336215343901 ) ) ;
#50850 = LINE ( 'NONE', #37347, #4260 ) ;
#50851 = DIRECTION ( 'NONE',  ( -0.000000000000000000, 0.5000000000000011102, -0.8660254037844380415 ) ) ;
#50852 = CARTESIAN_POINT ( 'NONE',  ( 15.23076923076923173, -2.708943851104267164, 35.45975837776705220 ) ) ;
#50853 = ADVANCED_FACE ( 'NONE', ( #77868 ), #49950, .F. ) ;
#50854 = CARTESIAN_POINT ( 'NONE',  ( 2.320192649118979489E-14, -11.25000000000000000, 17.28125000000000000 ) ) ;
#50855 = VERTEX_POINT ( 'NONE', #37318 ) ;
#50857 = EDGE_CURVE ( 'NONE', #76807, #77663, #79360, .T. ) ;
#50856 = ORIENTED_EDGE ( 'NONE', *, *, #36667, .T. ) ;
#50858 = AXIS2_PLACEMENT_3D ( 'NONE', #62335, #40757, #81301 ) ;
#50859 = CARTESIAN_POINT ( 'NONE',  ( -7.846153846153967493, -11.67786785259630911, 32.92929555188603530 ) ) ;
#50860 = EDGE_LOOP ( 'NONE', ( #37357, #11060, #56549, #47953 ) ) ;
#50861 = CARTESIAN_POINT ( 'NONE',  ( 12.46153846153846168, -7.500000000000001776, 35.04278698407183867 ) ) ;
#50862 = CARTESIAN_POINT ( 'NONE',  ( -12.21148414990014963, -9.943054286541403997, 34.11300777759954883 ) ) ;
#50863 = CARTESIAN_POINT ( 'NONE',  ( -16.15384615384615330, -2.721908614388771852, 31.22303859784724978 ) ) ;
#50864 = CARTESIAN_POINT ( 'NONE',  ( -1.384615384615383471, -6.435427911321262684, 35.78748833219616898 ) ) ;
#50865 = CARTESIAN_POINT ( 'NONE',  ( -3.750000000000008438, -5.946699141100917352, 16.42187500000000000 ) ) ;
#50866 = EDGE_CURVE ( 'NONE', #19392, #52736, #56713, .T. ) ;
#50867 = CYLINDRICAL_SURFACE ( 'NONE', #16, 0.2499999999999995559 ) ;
#50868 = EDGE_LOOP ( 'NONE', ( #10266, #79262 ) ) ;
#50869 = LINE ( 'NONE', #57649, #37197 ) ;
#50871 = VERTEX_POINT ( 'NONE', #10304 ) ;
#50870 = CARTESIAN_POINT ( 'NONE',  ( -1.254089682851819987, -9.417988943895561960, 34.36773134775778260 ) ) ;
#50872 = CARTESIAN_POINT ( 'NONE',  ( 3.007842271862382066, -12.38737895849757820, 31.66785238281580206 ) ) ;
#50873 = CARTESIAN_POINT ( 'NONE',  ( 6.923076923076924238, -13.20930481340135110, 34.54067556320372745 ) ) ;
#50874 = CARTESIAN_POINT ( 'NONE',  ( -3.480792468062195333, -5.056417327199099532, 34.11270091957320716 ) ) ;
#50875 = FACE_OUTER_BOUND ( 'NONE', #62593, .T. ) ;
#50876 = DIRECTION ( 'NONE',  ( -0.000000000000000000, -0.5000000000000009992, -0.8660254037844380415 ) ) ;
#50877 = CARTESIAN_POINT ( 'NONE',  ( 7.596177102105254875, -3.436278759898155677, 33.07459398097509506 ) ) ;
#50878 = CYLINDRICAL_SURFACE ( 'NONE', #57110, 0.2499999999999995559 ) ;
#50879 = CARTESIAN_POINT ( 'NONE',  ( 2.608446859217924629, -10.19485399968118422, 19.87686829374151287 ) ) ;
#50880 = ORIENTED_EDGE ( 'NONE', *, *, #45579, .F. ) ;
#50881 = CARTESIAN_POINT ( 'NONE',  ( -17.07692307692307665, -9.780366693483667717, 34.19971097300155094 ) ) ;
#50882 = DIRECTION ( 'NONE',  ( -0.000000000000000000, 1.000000000000000000, -0.000000000000000000 ) ) ;
#50883 = CARTESIAN_POINT ( 'NONE',  ( -1.253824943648432555, -3.338503747796865984, 32.95102852606552801 ) ) ;
#50884 = CARTESIAN_POINT ( 'NONE',  ( -1.139087296525992166, -10.25000000000000533, 26.10937500000001066 ) ) ;
#50885 = LINE ( 'NONE', #78373, #87873 ) ;
#50886 = CARTESIAN_POINT ( 'NONE',  ( 14.08476534878545827, -4.762599654559228846, 34.23009711892697737 ) ) ;
#50887 = EDGE_LOOP ( 'NONE', ( #60537, #8663, #59753, #81663 ) ) ;
#50888 = CARTESIAN_POINT ( 'NONE',  ( -2.750000000000006217, -6.360912703474006946, 16.42187500000000000 ) ) ;
#50889 = CARTESIAN_POINT ( 'NONE',  ( -1.254089946381742759, -12.50538340440932394, 31.33453814440721885 ) ) ;
#50890 = EDGE_CURVE ( 'NONE', #87401, #63245, #18110, .T. ) ;
#50891 = ORIENTED_EDGE ( 'NONE', *, *, #73596, .F. ) ;
#50892 = CARTESIAN_POINT ( 'NONE',  ( 6.856994543716787405, -6.343179335718451384, 34.87096338111212646 ) ) ;
#50893 = ORIENTED_EDGE ( 'NONE', *, *, #82548, .F. ) ;
#50894 = CARTESIAN_POINT ( 'NONE',  ( 14.55763782604044998, -12.22109172314383052, 31.39792113162168263 ) ) ;
#50895 = CARTESIAN_POINT ( 'NONE',  ( 3.007284306204900837, -4.225889041578354544, 33.85425143139329407 ) ) ;
#50896 = CARTESIAN_POINT ( 'NONE',  ( -8.519285359852727169, -5.766571408460171355, 34.70601412856602508 ) ) ;
#50897 = CARTESIAN_POINT ( 'NONE',  ( -12.33101302330481808, -11.04252011169590020, 33.62494198852677130 ) ) ;
#50898 = ORIENTED_EDGE ( 'NONE', *, *, #84404, .T. ) ;
#50899 = CARTESIAN_POINT ( 'NONE',  ( -13.13456096470193302, -2.920487667080175598, 32.31805714834170828 ) ) ;
#50900 = ORIENTED_EDGE ( 'NONE', *, *, #24997, .T. ) ;
#50901 = DIRECTION ( 'NONE',  ( 1.000000000000000000, 0.000000000000000000, 0.000000000000000000 ) ) ;
#50902 = LINE ( 'NONE', #57686, #87259 ) ;
#50903 = VERTEX_POINT ( 'NONE', #43204 ) ;
#50904 = CARTESIAN_POINT ( 'NONE',  ( 8.703960768674447124, -5.094484230520674117, 34.41647553114621161 ) ) ;
#50905 = CARTESIAN_POINT ( 'NONE',  ( -14.30769230769230660, -10.51840700105979565, 33.73612834413961536 ) ) ;
#50906 = CARTESIAN_POINT ( 'NONE',  ( -11.60454391782167427, -2.833524468853757305, 32.15551576947924417 ) ) ;
#50907 = CARTESIAN_POINT ( 'NONE',  ( 8.769230769230768274, -13.87047571288749737, 32.06866353760679544 ) ) ;
#50908 = CARTESIAN_POINT ( 'NONE',  ( -18.22348494372394967, -4.386631170607604879, 33.66268669641500111 ) ) ;
#50909 = B_SPLINE_CURVE_WITH_KNOTS ( 'NONE', 3,
 ( #82884, #34690, #35126, #42344, #41896, #41445, #56284, #83773, #68910, #15751 ),
 .UNSPECIFIED., .F., .F.,
 ( 4, 2, 2, 2, 4 ),
 ( 0.0007817359430256326080, 0.0009771253907250047801, 0.001172514838424369796, 0.001367904286123735030, 0.001563293733823100046 ),
 .UNSPECIFIED. ) ;
#50910 = AXIS2_PLACEMENT_3D ( 'NONE', #4319, #31802, #5210 ) ;
#50911 = EDGE_CURVE ( 'NONE', #44484, #78555, #70752, .T. ) ;
#50913 = ORIENTED_EDGE ( 'NONE', *, *, #21316, .T. ) ;
#50912 = EDGE_CURVE ( 'NONE', #24183, #73834, #40603, .T. ) ;
#50914 = ORIENTED_EDGE ( 'NONE', *, *, #78938, .T. ) ;
#50915 = FACE_BOUND ( 'NONE', #32599, .T. ) ;
#50916 = ORIENTED_EDGE ( 'NONE', *, *, #14671, .T. ) ;
#50917 = CARTESIAN_POINT ( 'NONE',  ( -0.3589743589743593088, -7.500000000000000000, 29.75000000000000355 ) ) ;
#50918 = VECTOR ( 'NONE', #54481, 1000.000000000000227 ) ;
#50919 = ADVANCED_FACE ( 'NONE', ( #32355 ), #18397, .F. ) ;
#50920 = AXIS2_PLACEMENT_3D ( 'NONE', #49856, #9760, #35917 ) ;
#50921 = EDGE_CURVE ( 'NONE', #29864, #955, #38888, .T. ) ;
#50922 = CARTESIAN_POINT ( 'NONE',  ( 17.75002325595141173, -5.643011162660950042, 34.66104346484419096 ) ) ;
#50923 = CYLINDRICAL_SURFACE ( 'NONE', #55384, 0.2499999999999994726 ) ;
#50924 = ORIENTED_EDGE ( 'NONE', *, *, #45271, .T. ) ;
#50925 = EDGE_LOOP ( 'NONE', ( #49602, #5027 ) ) ;
#50926 = EDGE_LOOP ( 'NONE', ( #27040, #5009, #76541, #8301 ) ) ;
#50927 = CARTESIAN_POINT ( 'NONE',  ( 3.296024802045255164, -5.219633306516380244, 34.19971097300157936 ) ) ;
#50928 = ORIENTED_EDGE ( 'NONE', *, *, #18080, .F. ) ;
#50929 = CARTESIAN_POINT ( 'NONE',  ( 16.02369894440793630, -10.19110544564092002, 33.96427741523702792 ) ) ;
#50930 = CARTESIAN_POINT ( 'NONE',  ( -4.826868765284761942, -4.943051570960391494, 34.04725096376909477 ) ) ;
#50931 = EDGE_CURVE ( 'NONE', #6445, #12293, #24703, .T. ) ;
#50932 = CARTESIAN_POINT ( 'NONE',  ( -12.33149340561869067, -2.254550872974305342, 29.97347326024527092 ) ) ;
#50933 = FACE_BOUND ( 'NONE', #64319, .T. ) ;
#50934 = EDGE_LOOP ( 'NONE', ( #46646, #12158, #77146, #53936, #21181 ) ) ;
#50935 = CARTESIAN_POINT ( 'NONE',  ( 13.13459216039392707, -10.92453946501458795, 33.72985991061850086 ) ) ;
#50936 = CARTESIAN_POINT ( 'NONE',  ( 4.946775107191381693, -3.625366637846544560, 33.29286588640298561 ) ) ;
#50937 = EDGE_CURVE ( 'NONE', #53938, #87198, #81442, .T. ) ;
#50938 = CARTESIAN_POINT ( 'NONE',  ( 8.900022577055551665, -3.062576670634119758, 32.05464942895959979 ) ) ;
#50939 = CARTESIAN_POINT ( 'NONE',  ( 11.53846153846153832, -8.120952969808772792, 34.71129190930000163 ) ) ;
#50940 = VERTEX_POINT ( 'NONE', #12097 ) ;
#50941 = PRODUCT_DEFINITION_CONTEXT ( 'detailed design', #22214, 'design' ) ;
#50942 = CARTESIAN_POINT ( 'NONE',  ( 9.442330961365341224, -2.564618984488975517, 30.55390908950641915 ) ) ;
#50943 = VERTEX_POINT ( 'NONE', #80998 ) ;
#50944 = ORIENTED_EDGE ( 'NONE', *, *, #82677, .T. ) ;
#50946 = CARTESIAN_POINT ( 'NONE',  ( 5.869308533332441513, -3.062553014421049546, 32.05460306192773601 ) ) ;
#50945 = LINE ( 'NONE', #9113, #28854 ) ;
#50947 = CARTESIAN_POINT ( 'NONE',  ( -18.75000000000000000, -3.499999999999999556, 29.75000000000000355 ) ) ;
#50948 = DIRECTION ( 'NONE',  ( 0.000000000000000000, -1.000000000000000000, 0.000000000000000000 ) ) ;
#50949 = CARTESIAN_POINT ( 'NONE',  ( 17.32692307692314415, -7.434744429011175271, 34.75000000000000711 ) ) ;
#50950 = CARTESIAN_POINT ( 'NONE',  ( -11.53846153846153655, -2.292212530054420494, 30.41441678777542634 ) ) ;
#50951 = VERTEX_POINT ( 'NONE', #44960 ) ;
#50952 = EDGE_CURVE ( 'NONE', #31437, #6751, #33098, .T. ) ;
#50953 = DIRECTION ( 'NONE',  ( -0.000000000000000000, 0.000000000000000000, 1.000000000000000000 ) ) ;
#50954 = CARTESIAN_POINT ( 'NONE',  ( 17.93472999944368240, -3.643525952247789856, 33.31231777344662959 ) ) ;
#50955 = CARTESIAN_POINT ( 'NONE',  ( 4.284637961670941131, -8.999086150933472084, 34.52020707165672064 ) ) ;
#50956 = CARTESIAN_POINT ( 'NONE',  ( 5.300350038784647388, -7.630147231320743018, 34.74852402298682819 ) ) ;
#50957 = VERTEX_POINT ( 'NONE', #46309 ) ;
#50958 = EDGE_CURVE ( 'NONE', #57723, #75758, #872, .T. ) ;
#50959 = ORIENTED_EDGE ( 'NONE', *, *, #24027, .T. ) ;
#50960 = FACE_BOUND ( 'NONE', #15422, .T. ) ;
#50961 = CARTESIAN_POINT ( 'NONE',  ( 7.846153846153725020, -2.892918686052165622, 31.69288490824153470 ) ) ;
#50962 = CARTESIAN_POINT ( 'NONE',  ( -3.007757879156381264, -8.239487800360276282, 34.69522927552633718 ) ) ;
#50963 = ORIENTED_EDGE ( 'NONE', *, *, #74087, .T. ) ;
#50964 = LINE ( 'NONE', #78454, #3546 ) ;
#50965 = LINE ( 'NONE', #9559, #84568 ) ;
#50966 = CARTESIAN_POINT ( 'NONE',  ( 15.90382291655318880, -8.432397168068783699, 34.66272746175022945 ) ) ;
#50967 = CARTESIAN_POINT ( 'NONE',  ( 4.153846153846154188, -5.471508081941601098, 34.59228464037088457 ) ) ;
#50968 = EDGE_LOOP ( 'NONE', ( #26821, #64052 ) ) ;
#50969 = EDGE_CURVE ( 'NONE', #32456, #85159, #28799, .T. ) ;
#50970 = CYLINDRICAL_SURFACE ( 'NONE', #8575, 0.2499999999999973355 ) ;
#50971 = ORIENTED_EDGE ( 'NONE', *, *, #3824, .T. ) ;
#50973 = ORIENTED_EDGE ( 'NONE', *, *, #46928, .T. ) ;
#50972 = LINE ( 'NONE', #22636, #49624 ) ;
#50974 = CARTESIAN_POINT ( 'NONE',  ( 11.60452988946397923, -6.386643153685127139, 34.62446782046654192 ) ) ;
#50975 = CARTESIAN_POINT ( 'NONE',  ( 15.16468581981334651, -2.721908614388770964, 31.22303859784723912 ) ) ;
#50976 = DIRECTION ( 'NONE',  ( 0.000000000000000000, 1.000000000000000000, 0.000000000000000000 ) ) ;
#50977 = CYLINDRICAL_SURFACE ( 'NONE', #86983, 0.2499999999999998890 ) ;
#50979 = AXIS2_PLACEMENT_3D ( 'NONE', #12110, #33701, #61157 ) ;
#50978 = DIRECTION ( 'NONE',  ( -0.000000000000000000, 1.000000000000000000, 3.491481338843133355E-15 ) ) ;
#50980 = EDGE_CURVE ( 'NONE', #42554, #17692, #41713, .T. ) ;
#50981 = DIRECTION ( 'NONE',  ( -0.000000000000000000, 0.6427876096865404731, -0.7660444431189771253 ) ) ;
#50982 = CARTESIAN_POINT ( 'NONE',  ( 2.724691934501250135, -8.700186371490531201, 14.79874329374151642 ) ) ;
#50983 = EDGE_LOOP ( 'NONE', ( #36679, #86017 ) ) ;
#50984 = VECTOR ( 'NONE', #49392, 1000.000000000000000 ) ;
#50985 = DIRECTION ( 'NONE',  ( -0.000000000000000000, -0.8660254037844399289, -0.4999999999999980016 ) ) ;
#50986 = CARTESIAN_POINT ( 'NONE',  ( 6.000000000000001776, -8.164416787775445883, 34.95778746994557906 ) ) ;
#50987 = VECTOR ( 'NONE', #13240, 1000.000000000000227 ) ;
#50988 = VERTEX_POINT ( 'NONE', #61589 ) ;
#50989 = ORIENTED_EDGE ( 'NONE', *, *, #43948, .T. ) ;
#50990 = CARTESIAN_POINT ( 'NONE',  ( 16.85399685940693004, -4.887634598454295265, 34.01352882383564946 ) ) ;
#50991 = DIRECTION ( 'NONE',  ( -1.734723475976813750E-16, 1.000000000000000000, -0.000000000000000000 ) ) ;
#50992 = ADVANCED_FACE ( 'NONE', ( #47188 ), #74681, .F. ) ;
#50993 = CARTESIAN_POINT ( 'NONE',  ( -17.29984929443921970, -9.086856451489516928, 34.49173150075333183 ) ) ;
#50994 = CARTESIAN_POINT ( 'NONE',  ( 5.076923076923075762, -2.249999999999998668, 29.50000000000001421 ) ) ;
#50995 = CARTESIAN_POINT ( 'NONE',  ( 8.769230769230768274, -11.35647404775217417, 33.31231777344666511 ) ) ;
#50996 = EDGE_CURVE ( 'NONE', #45323, #14249, #27374, .T. ) ;
#50997 = CARTESIAN_POINT ( 'NONE',  ( 16.21991348719623360, -3.322132147404559532, 32.92929555188717927 ) ) ;
#50998 = DIRECTION ( 'NONE',  ( 0.000000000000000000, 0.8660254037844377084, -0.5000000000000015543 ) ) ;
#50999 = EDGE_LOOP ( 'NONE', ( #59096, #74908, #65955, #76157 ) ) ;
#51000 = CARTESIAN_POINT ( 'NONE',  ( -11.53846153846153655, -2.708943851104267164, 35.45975837776705220 ) ) ;
#51001 = DIRECTION ( 'NONE',  ( -0.000000000000000000, 1.000000000000000000, -0.000000000000000000 ) ) ;
#51002 = CARTESIAN_POINT ( 'NONE',  ( -9.019253993452229778, -11.56360843649121684, 33.07473185843129926 ) ) ;
#51003 = FACE_OUTER_BOUND ( 'NONE', #4240, .T. ) ;
#51004 = EDGE_LOOP ( 'NONE', ( #51093, #72307 ) ) ;
#51005 = CARTESIAN_POINT ( 'NONE',  ( -17.07692307692276046, -2.255955759149395501, 30.00000000000324363 ) ) ;
#51006 = ORIENTED_EDGE ( 'NONE', *, *, #60998, .F. ) ;
#51007 = CARTESIAN_POINT ( 'NONE',  ( 0.4615384615384611200, -8.973038597847269315, 34.52809138561121927 ) ) ;
#51008 = DIRECTION ( 'NONE',  ( 0.000000000000000000, 0.000000000000000000, 1.000000000000000000 ) ) ;
#51009 = CARTESIAN_POINT ( 'NONE',  ( -15.23076923076922995, -1.509761064869970415, 31.06009739812519044 ) ) ;
#51010 = CYLINDRICAL_SURFACE ( 'NONE', #32647, 0.2499999999999994726 ) ;
#51011 = VERTEX_POINT ( 'NONE', #82326 ) ;
#51012 = DIRECTION ( 'NONE',  ( -0.000000000000000000, 0.8660254037844399289, -0.4999999999999980016 ) ) ;
#51013 = CARTESIAN_POINT ( 'NONE',  ( -10.48459280755982981, -10.54018710029568595, 33.71981072465678864 ) ) ;
#51014 = CARTESIAN_POINT ( 'NONE',  ( -10.83886953994894853, -12.69144148231606017, 30.53333754910549303 ) ) ;
#51015 = CIRCLE ( 'NONE', #30895, 4.000000000000000000 ) ;
#51016 = CARTESIAN_POINT ( 'NONE',  ( -9.469528023329624844, -3.563462043263030399, 33.22394488606062879 ) ) ;
#51017 = ORIENTED_EDGE ( 'NONE', *, *, #17283, .F. ) ;
#51018 = CARTESIAN_POINT ( 'NONE',  ( 12.46153846153833911, -10.90142922262034020, 33.41473453929536674 ) ) ;
#51019 = ORIENTED_EDGE ( 'NONE', *, *, #80713, .F. ) ;
#51020 = DIRECTION ( 'NONE',  ( 0.000000000000000000, 0.000000000000000000, 1.000000000000000000 ) ) ;
#51021 = EDGE_CURVE ( 'NONE', #58097, #25224, #27812, .T. ) ;
#51022 = LINE ( 'NONE', #16379, #36976 ) ;
#51023 = CARTESIAN_POINT ( 'NONE',  ( -6.222926217516146608, -2.554751324335733820, 30.48935550225260727 ) ) ;
#51024 = EDGE_CURVE ( 'NONE', #39385, #3, #58919, .T. ) ;
#51025 = CARTESIAN_POINT ( 'NONE',  ( -14.17716660592874689, -10.19071101563364756, 33.96452234770658407 ) ) ;
#51026 = CYLINDRICAL_SURFACE ( 'NONE', #50792, 0.2500000000000004996 ) ;
#51027 = ORIENTED_EDGE ( 'NONE', *, *, #58070, .F. ) ;
#51029 = EDGE_CURVE ( 'NONE', #49865, #20268, #57809, .T. ) ;
#51028 = ORIENTED_EDGE ( 'NONE', *, *, #16955, .T. ) ;
#51030 = B_SPLINE_CURVE_WITH_KNOTS ( 'NONE', 3,
 ( #3475, #10691, #50327, #2152, #57536, #38157, #65615, #71489, #57980, #16999 ),
 .UNSPECIFIED., .F., .F.,
 ( 4, 2, 2, 2, 4 ),
 ( 0.0007817246336856293861, 0.0009771112958940105907, 0.001172497958102391904, 0.001367884620310773217, 0.001563271282519154530 ),
 .UNSPECIFIED. ) ;
#51031 = ORIENTED_EDGE ( 'NONE', *, *, #68936, .F. ) ;
#51032 = ORIENTED_EDGE ( 'NONE', *, *, #59573, .F. ) ;
#51033 = VECTOR ( 'NONE', #17542, 1000.000000000000000 ) ;
#51034 = DIRECTION ( 'NONE',  ( -0.000000000000000000, 1.000000000000000000, -0.000000000000000000 ) ) ;
#51035 = CARTESIAN_POINT ( 'NONE',  ( 20.00000000000000000, -4.000000000000000000, 29.75000000000000355 ) ) ;
#51036 = EDGE_CURVE ( 'NONE', #27164, #7165, #14296, .T. ) ;
#51037 = CARTESIAN_POINT ( 'NONE',  ( 14.43853063817906524, -7.277220318596961057, 34.99547417642776992 ) ) ;
#51038 = CARTESIAN_POINT ( 'NONE',  ( -4.284536756956459413, -12.35290016733513951, 31.75349464988449455 ) ) ;
#51039 = CARTESIAN_POINT ( 'NONE',  ( 17.99999999999987566, -9.442884908241554243, 34.35708131394783038 ) ) ;
#51040 = LINE ( 'NONE', #45188, #28361 ) ;
#51041 = CARTESIAN_POINT ( 'NONE',  ( -17.86947429823644029, -10.19071101563364579, 33.96452234770658407 ) ) ;
#51042 = CARTESIAN_POINT ( 'NONE',  ( -4.500000000000000000, -7.499999999999999112, 13.00000000000000178 ) ) ;
#51043 = VERTEX_POINT ( 'NONE', #69243 ) ;
#51044 = ORIENTED_EDGE ( 'NONE', *, *, #9067, .F. ) ;
#51045 = EDGE_LOOP ( 'NONE', ( #59815, #929 ) ) ;
#51046 = EDGE_CURVE ( 'NONE', #2381, #84018, #78223, .T. ) ;
#51048 = ORIENTED_EDGE ( 'NONE', *, *, #75012, .F. ) ;
#51047 = CARTESIAN_POINT ( 'NONE',  ( 0.2115152373170022249, -12.07920672191015221, 32.31858351112116168 ) ) ;
#51050 = CARTESIAN_POINT ( 'NONE',  ( -16.15384615384627409, -10.21337939537710326, 33.94971097300076224 ) ) ;
#51049 = DIRECTION ( 'NONE',  ( -0.000000000000000000, -0.6427876096865404731, -0.7660444431189771253 ) ) ;
#51051 = CARTESIAN_POINT ( 'NONE',  ( -1.384615384615069056, -2.255955759149395501, 30.00000000000324363 ) ) ;
#51052 = DIRECTION ( 'NONE',  ( 0.000000000000000000, 0.6427876096865368094, 0.7660444431189802339 ) ) ;
#51053 = ORIENTED_EDGE ( 'NONE', *, *, #42763, .F. ) ;
#51054 = ORIENTED_EDGE ( 'NONE', *, *, #1086, .T. ) ;
#51055 = CARTESIAN_POINT ( 'NONE',  ( -17.07692307692307665, -11.35647404775217417, 33.31231777344666511 ) ) ;
#51056 = EDGE_CURVE ( 'NONE', #28593, #49579, #12680, .T. ) ;
#51057 = VERTEX_POINT ( 'NONE', #40893 ) ;
#51058 = FACE_BOUND ( 'NONE', #87091, .T. ) ;
#51059 = DIRECTION ( 'NONE',  ( 0.000000000000000000, 0.000000000000000000, -1.000000000000000000 ) ) ;
#51060 = CARTESIAN_POINT ( 'NONE',  ( 16.02315468717859659, -6.413092428213692742, 34.63065189839063152 ) ) ;
#51061 = ORIENTED_EDGE ( 'NONE', *, *, #48568, .F. ) ;
#51062 = CARTESIAN_POINT ( 'NONE',  ( 9.320512820512821150, -7.500000000000000000, 29.75000000000000355 ) ) ;
#51063 = EDGE_CURVE ( 'NONE', #84960, #25936, #21273, .T. ) ;
#51064 = CARTESIAN_POINT ( 'NONE',  ( 5.011653076366756387, -8.656820664281497102, 34.87096338111211935 ) ) ;
#51065 = FACE_OUTER_BOUND ( 'NONE', #20047, .T. ) ;
#51066 = ORIENTED_EDGE ( 'NONE', *, *, #19049, .F. ) ;
#51067 = CYLINDRICAL_SURFACE ( 'NONE', #50029, 0.2500000000000008882 ) ;
#51068 = CARTESIAN_POINT ( 'NONE',  ( 4.219101725122177626, -3.300289026998475705, 32.46337939537591666 ) ) ;
#51069 = ORIENTED_EDGE ( 'NONE', *, *, #73427, .F. ) ;
#51070 = B_SPLINE_CURVE_WITH_KNOTS ( 'NONE', 3,
 ( #55454, #40187, #82939, #46485, #60436, #87953, #26212, #60880, #29764, #2707 ),
 .UNSPECIFIED., .F., .F.,
 ( 4, 2, 2, 2, 4 ),
 ( 0.0007817246256747446788, 0.0009771112852218874663, 0.001172497944769030362, 0.001367884604316173258, 0.001563271263863315937 ),
 .UNSPECIFIED. ) ;
#51071 = B_SPLINE_CURVE_WITH_KNOTS ( 'NONE', 3,
 ( #47401, #82096, #81212, #20825, #20389, #48291, #40669, #61800, #47851, #33894 ),
 .UNSPECIFIED., .F., .F.,
 ( 4, 2, 2, 2, 4 ),
 ( 0.000000000000000000, 0.0001954311564186867660, 0.0003908623128373735320, 0.0005862934692560603251, 0.0007817246256747470640 ),
 .UNSPECIFIED. ) ;
#51072 = VECTOR ( 'NONE', #14455, 1000.000000000000114 ) ;
#51073 = DIRECTION ( 'NONE',  ( 1.000000000000000000, 0.000000000000000000, 0.000000000000000000 ) ) ;
#51074 = DIRECTION ( 'NONE',  ( 0.000000000000000000, 0.000000000000000000, -1.000000000000000000 ) ) ;
#51075 = CARTESIAN_POINT ( 'NONE',  ( -14.16025641025641058, -7.500000000000000000, 29.75000000000000355 ) ) ;
#51076 = CARTESIAN_POINT ( 'NONE',  ( -7.846153846153967493, -12.16647553114689728, 32.15551576947799362 ) ) ;
#51077 = DIRECTION ( 'NONE',  ( 0.000000000000000000, 8.673617379884033500E-16, -1.000000000000000000 ) ) ;
#51078 = CARTESIAN_POINT ( 'NONE',  ( -8.769230769230768274, -8.973038597847269315, 34.52809138561121927 ) ) ;
#51079 = CARTESIAN_POINT ( 'NONE',  ( 9.627037691751372250, -12.51329471203370325, 31.30864560766548976 ) ) ;
#51080 = CARTESIAN_POINT ( 'NONE',  ( 7.912221179503922563, -2.833524468853757750, 32.15551576947925838 ) ) ;
#51082 = CARTESIAN_POINT ( 'NONE',  ( 1.384615384615386802, -8.318370150425687726, 35.83090037661290239 ) ) ;
#51081 = CARTESIAN_POINT ( 'NONE',  ( 4.853438133199127869, -12.44517049084099725, 30.48991314939691932 ) ) ;
#51083 = ADVANCED_FACE ( 'NONE', ( #29156 ), #44403, .F. ) ;
#51084 = CARTESIAN_POINT ( 'NONE',  ( 8.519230769230770051, -2.499999999999999556, 29.81609845454691765 ) ) ;
#51086 = CARTESIAN_POINT ( 'NONE',  ( -8.704037780936115354, -2.255955759149235629, 29.99999999999988987 ) ) ;
#51085 = CARTESIAN_POINT ( 'NONE',  ( 12.33092880633437716, -7.722926974430166069, 34.99546784045485737 ) ) ;
#51087 = CARTESIAN_POINT ( 'NONE',  ( -2.530619266599154038, -5.582147617184174848, 34.63737895849758530 ) ) ;
#51088 = CARTESIAN_POINT ( 'NONE',  ( 1.200186371490561621, -10.22469193450123193, 23.20125670625849068 ) ) ;
#51089 = ORIENTED_EDGE ( 'NONE', *, *, #87488, .F. ) ;
#51090 = CARTESIAN_POINT ( 'NONE',  ( 3.392537894537152265, -7.689361227255397502, 14.00000000000201794 ) ) ;
#51091 = ORIENTED_EDGE ( 'NONE', *, *, #10622, .T. ) ;
#51092 = DIRECTION ( 'NONE',  ( 0.000000000000000000, 0.000000000000000000, -1.000000000000000000 ) ) ;
#51093 = ORIENTED_EDGE ( 'NONE', *, *, #48198, .T. ) ;
#51094 = CARTESIAN_POINT ( 'NONE',  ( 17.74997676270703550, -12.22074536777955345, 31.39888409691088356 ) ) ;
#51095 = EDGE_LOOP ( 'NONE', ( #21648, #52698, #30675, #42803 ) ) ;
#51096 = CARTESIAN_POINT ( 'NONE',  ( 5.869309396889695662, -10.70098750199973203, 33.91152734681376302 ) ) ;
#51097 = CARTESIAN_POINT ( 'NONE',  ( -0.06109907496454585613, -4.750000000000000000, 22.65438170625849068 ) ) ;
#51098 = DIRECTION ( 'NONE',  ( -0.000000000000000000, -0.9848077530122086864, -0.1736481776669273613 ) ) ;
#51099 = EDGE_CURVE ( 'NONE', #82533, #10196, #30463, .T. ) ;
#51100 = CARTESIAN_POINT ( 'NONE',  ( -5.076923076923197442, -2.892918686052165622, 31.69288490824153470 ) ) ;
#51101 = DIRECTION ( 'NONE',  ( 1.000000000000000000, 0.000000000000000000, 0.000000000000000000 ) ) ;
#51102 = CARTESIAN_POINT ( 'NONE',  ( -14.53117723225664015, -10.97335522853832579, 33.68706563782419749 ) ) ;
#51103 = CARTESIAN_POINT ( 'NONE',  ( -17.74999999976641973, -2.249999999999989786, 29.74999979494859303 ) ) ;
#51104 = CARTESIAN_POINT ( 'NONE',  ( -11.53846153846153655, -9.819645486525091727, 36.12317359536749706 ) ) ;
#51105 = DIRECTION ( 'NONE',  ( -1.000000000000000000, 0.000000000000000000, 0.000000000000000000 ) ) ;
#51106 = CARTESIAN_POINT ( 'NONE',  ( 2.320192649118979489E-14, -11.25000000000000000, 18.53125000000000000 ) ) ;
#51107 = EDGE_CURVE ( 'NONE', #87423, #64241, #2853, .T. ) ;
#51108 = EDGE_CURVE ( 'NONE', #87066, #33781, #65310, .T. ) ;
#51109 = VECTOR ( 'NONE', #26311, 1000.000000000000000 ) ;
#51110 = LINE ( 'NONE', #24099, #10365 ) ;
#51111 = CARTESIAN_POINT ( 'NONE',  ( -15.12820512820512953, -3.499999999999999556, 29.75000000000000355 ) ) ;
#51112 = CARTESIAN_POINT ( 'NONE',  ( 16.15384615384615330, -11.11383981884818262, 36.00935417666054406 ) ) ;
#51113 = CARTESIAN_POINT ( 'NONE',  ( 3.750000000000000888, -7.499999999999978684, 18.21875000000000000 ) ) ;
#51114 = ADVANCED_FACE ( 'NONE', ( #57934 ), #29591, .T. ) ;
#51115 = ORIENTED_EDGE ( 'NONE', *, *, #56336, .F. ) ;
#51116 = CARTESIAN_POINT ( 'NONE',  ( 0.000000000000000000, -11.00000000000000000, 29.75000000000000355 ) ) ;
#51117 = CARTESIAN_POINT ( 'NONE',  ( -11.53846153846165912, -8.613356846316285953, 34.62446782046622218 ) ) ;
#51118 = CARTESIAN_POINT ( 'NONE',  ( -3.230769230769229949, -13.53365097954675988, 30.81389545987213552 ) ) ;
#51119 = CARTESIAN_POINT ( 'NONE',  ( 18.00000000000000000, -10.51840700105979565, 33.73612834413961536 ) ) ;
#51120 = VECTOR ( 'NONE', #23474, 1000.000000000000000 ) ;
#51121 = CARTESIAN_POINT ( 'NONE',  ( 4.023155550735844521, -3.338472653186242756, 32.95098750199972670 ) ) ;
#51122 = CARTESIAN_POINT ( 'NONE',  ( 2.084766090176160436, -12.15238873228292071, 31.58232369045353849 ) ) ;
#51123 = EDGE_LOOP ( 'NONE', ( #49718, #63470, #67633, #43782 ) ) ;
#51124 = CARTESIAN_POINT ( 'NONE',  ( -14.30769230769230660, -1.242168528481310874, 33.36296068462461051 ) ) ;
#51125 = ORIENTED_EDGE ( 'NONE', *, *, #87665, .F. ) ;
#51126 = VERTEX_POINT ( 'NONE', #15191 ) ;
#51127 = LINE ( 'NONE', #79527, #50739 ) ;
#51128 = CARTESIAN_POINT ( 'NONE',  ( 5.142991427925514891, -11.69971097300155272, 32.46337939537588113 ) ) ;
#51129 = VECTOR ( 'NONE', #10468, 999.9999999999998863 ) ;
#51130 = DIRECTION ( 'NONE',  ( 0.000000000000000000, 0.6427876096865368094, 0.7660444431189802339 ) ) ;
#51131 = CARTESIAN_POINT ( 'NONE',  ( -13.25382357679059453, -8.999086150933475636, 34.52020707165672775 ) ) ;
#51132 = CARTESIAN_POINT ( 'NONE',  ( 10.83839745947800992, -10.01129605718032600, 34.36064277460058491 ) ) ;
#51133 = AXIS2_PLACEMENT_3D ( 'NONE', #12157, #31531, #53121 ) ;
#51134 = ORIENTED_EDGE ( 'NONE', *, *, #1103, .T. ) ;
#51135 = CARTESIAN_POINT ( 'NONE',  ( -6.857008572074484221, -5.557115091759786019, 34.35708131394839882 ) ) ;
#51136 = VERTEX_POINT ( 'NONE', #8431 ) ;
#51137 = VERTEX_POINT ( 'NONE', #50721 ) ;
#51138 = CARTESIAN_POINT ( 'NONE',  ( -3.931066484868086963, -12.11081565061823717, 32.26097654155341843 ) ) ;
#51139 = CYLINDRICAL_SURFACE ( 'NONE', #21505, 0.2499999999999994726 ) ;
#51140 = DIRECTION ( 'NONE',  ( 0.000000000000000000, 0.000000000000000000, 1.000000000000000000 ) ) ;
#51141 = LINE ( 'NONE', #48622, #38469 ) ;
#51142 = CARTESIAN_POINT ( 'NONE',  ( -11.60454391782167249, -8.164416787775445883, 34.95778746994557906 ) ) ;
#51143 = CARTESIAN_POINT ( 'NONE',  ( 17.77707378248385339, -8.239355502252617924, 34.69524867566427417 ) ) ;
#51144 = EDGE_LOOP ( 'NONE', ( #80292, #41837 ) ) ;
#51145 = ORIENTED_EDGE ( 'NONE', *, *, #34535, .T. ) ;
#51146 = CARTESIAN_POINT ( 'NONE',  ( 1.553300858899129944, -11.24999999999998934, 19.70312500000000355 ) ) ;
#51147 = ORIENTED_EDGE ( 'NONE', *, *, #84704, .F. ) ;
#51148 = ADVANCED_FACE ( 'NONE', ( #35905 ), #63805, .F. ) ;
#51150 = ORIENTED_EDGE ( 'NONE', *, *, #80913, .T. ) ;
#51149 = CARTESIAN_POINT ( 'NONE',  ( -12.59222992820602194, -11.18331474514187995, 33.13161551792790505 ) ) ;
#51151 = CARTESIAN_POINT ( 'NONE',  ( -7.053768389744481837, -12.38065189839062263, 30.83690757178629482 ) ) ;
#51152 = CARTESIAN_POINT ( 'NONE',  ( 6.066068351002440906, -12.37446782046654192, 30.86335684631486842 ) ) ;
#51153 = AXIS2_PLACEMENT_3D ( 'NONE', #17669, #37477, #3691 ) ;
#51154 = DIRECTION ( 'NONE',  ( -0.000000000000000000, -0.1736481776669307198, -0.9848077530122080203 ) ) ;
#51155 = ORIENTED_EDGE ( 'NONE', *, *, #2408, .T. ) ;
#51156 = CARTESIAN_POINT ( 'NONE',  ( 10.61538461538461675, -2.292212530054420494, 30.41441678777542634 ) ) ;
#51157 = VERTEX_POINT ( 'NONE', #57490 ) ;
#51158 = CARTESIAN_POINT ( 'NONE',  ( -8.899921372341079717, -4.684245665217972032, 34.18127051446801090 ) ) ;
#51159 = CYLINDRICAL_SURFACE ( 'NONE', #48615, 0.2499999999999986955 ) ;
#51160 = FACE_OUTER_BOUND ( 'NONE', #3654, .T. ) ;
#51162 = CARTESIAN_POINT ( 'NONE',  ( -10.83831157429146330, -5.582147617184174848, 34.63737895849758530 ) ) ;
#51161 = CARTESIAN_POINT ( 'NONE',  ( 1.384615384615386802, -2.486705287966279876, 31.30864560766543647 ) ) ;
#51163 = CARTESIAN_POINT ( 'NONE',  ( 20.00000000000000711, -9.999999999999994671, 0.000000000000000000 ) ) ;
#51164 = CARTESIAN_POINT ( 'NONE',  ( -0.2385256174450664512, -12.64618726649961289, 30.78989965857442712 ) ) ;
#51165 = ORIENTED_EDGE ( 'NONE', *, *, #3219, .T. ) ;
#51166 = EDGE_CURVE ( 'NONE', #51205, #85054, #31682, .T. ) ;
#51167 = DIRECTION ( 'NONE',  ( 0.000000000000000000, 0.9848077530122072432, -0.1736481776669354937 ) ) ;
#51168 = AXIS2_PLACEMENT_3D ( 'NONE', #26238, #40209, #33876 ) ;
#51169 = CARTESIAN_POINT ( 'NONE',  ( -6.250023224221458840, -11.56360843649121861, 33.07473185843129926 ) ) ;
#51170 = ORIENTED_EDGE ( 'NONE', *, *, #52585, .T. ) ;
#51171 = CARTESIAN_POINT ( 'NONE',  ( 7.173131234715239835, -2.779044189368096163, 31.39831045268886456 ) ) ;
#51172 = CARTESIAN_POINT ( 'NONE',  ( 15.48071474911737333, -4.336752205174649433, 33.62275283266504289 ) ) ;
#51173 = CARTESIAN_POINT ( 'NONE',  ( -15.93106661257773560, -10.81320215134717166, 33.49497208177562868 ) ) ;
#51174 = CARTESIAN_POINT ( 'NONE',  ( -7.715628407920204879, -11.04252011169590020, 33.62494198852677130 ) ) ;
#51175 = CARTESIAN_POINT ( 'NONE',  ( 8.096099255531889582, -6.653508905675592722, 34.93172785388651391 ) ) ;
#51176 = CARTESIAN_POINT ( 'NONE',  ( -17.07692307692307665, -13.75783147151868846, 33.36296068462461051 ) ) ;
#51177 = FACE_BOUND ( 'NONE', #54066, .T. ) ;
#51179 = DIRECTION ( 'NONE',  ( 0.000000000000000000, 0.9848077530122072432, -0.1736481776669354937 ) ) ;
#51178 = CARTESIAN_POINT ( 'NONE',  ( 12.23805353697412990, -10.23692288466677880, 34.23039457007281072 ) ) ;
#51180 = EDGE_CURVE ( 'NONE', #57194, #29384, #84102, .T. ) ;
#51181 = DIRECTION ( 'NONE',  ( 0.000000000000000000, 0.000000000000000000, -1.000000000000000000 ) ) ;
#51183 = FACE_OUTER_BOUND ( 'NONE', #20378, .T. ) ;
#51182 = CARTESIAN_POINT ( 'NONE',  ( -11.28846153846160050, -7.565270445406050648, 34.75000000000000000 ) ) ;
#51184 = DIRECTION ( 'NONE',  ( -0.000000000000000000, 0.7660444431189791237, -0.6427876096865379196 ) ) ;
#51185 = CARTESIAN_POINT ( 'NONE',  ( 8.992010310499177095, -10.81320215134717344, 33.49497208177562868 ) ) ;
#51186 = CARTESIAN_POINT ( 'NONE',  ( 2.608446859217893099, -4.805146000318787358, 19.06063170625849068 ) ) ;
#51187 = EDGE_LOOP ( 'NONE', ( #62020, #11006, #51891, #136 ) ) ;
#51188 = CARTESIAN_POINT ( 'NONE',  ( -4.377331097570100304, -11.89387501736622710, 32.13663884655806413 ) ) ;
#51189 = CARTESIAN_POINT ( 'NONE',  ( -14.53061852520844965, -6.503392248772476236, 34.64988816332204635 ) ) ;
#51190 = FACE_OUTER_BOUND ( 'NONE', #32382, .T. ) ;
#51191 = CARTESIAN_POINT ( 'NONE',  ( -10.86540783960607293, -11.56360843649121684, 33.07473185843129926 ) ) ;
#51192 = DIRECTION ( 'NONE',  ( 0.000000000000000000, 0.000000000000000000, 1.000000000000000000 ) ) ;
#51193 = CARTESIAN_POINT ( 'NONE',  ( -4.153846153846152411, -1.367168528481310208, 33.57946703557072254 ) ) ;
#51194 = CARTESIAN_POINT ( 'NONE',  ( -2.694853999681210865, -4.891553140782108677, 19.99813170625848713 ) ) ;
#51195 = CARTESIAN_POINT ( 'NONE',  ( -2.531177232256636600, -3.562934362175799841, 33.22335522853832401 ) ) ;
#51196 = CARTESIAN_POINT ( 'NONE',  ( -14.53061926659915315, -11.43668979543635089, 33.22377378376089752 ) ) ;
#51197 = DIRECTION ( 'NONE',  ( -0.000000000000000000, -0.9848077530122085754, -0.1736481776669273613 ) ) ;
#51198 = DIRECTION ( 'NONE',  ( 1.000000000000000000, 0.000000000000000000, 0.000000000000000000 ) ) ;
#51199 = CARTESIAN_POINT ( 'NONE',  ( 5.076923076923383071, -2.506253911140614576, 30.00000000000323297 ) ) ;
#51200 = CARTESIAN_POINT ( 'NONE',  ( 12.39626846098214230, -12.70778746994557551, 30.41441678777548319 ) ) ;
#51201 = EDGE_CURVE ( 'NONE', #17652, #5312, #9321, .T. ) ;
#51202 = EDGE_CURVE ( 'NONE', #5871, #48512, #49196, .T. ) ;
#51203 = LINE ( 'NONE', #64291, #72103 ) ;
#51204 = LINE ( 'NONE', #50772, #41372 ) ;
#51205 = VERTEX_POINT ( 'NONE', #71012 ) ;
#51206 = CARTESIAN_POINT ( 'NONE',  ( -17.07692307692307665, -13.49023893513002648, 31.06009739812518688 ) ) ;
#51207 = CARTESIAN_POINT ( 'NONE',  ( -1.634615384615383027, -2.249999999999998668, 29.75000000000000355 ) ) ;
#51208 = CARTESIAN_POINT ( 'NONE',  ( -3.724691934501248802, -5.885600066136383646, 14.17374329374151287 ) ) ;
#51209 = CARTESIAN_POINT ( 'NONE',  ( -2.307692307692428724, -5.094484230521993062, 34.41647553114689373 ) ) ;
#51210 = CARTESIAN_POINT ( 'NONE',  ( 13.38461538461538680, -6.189225973068211317, 35.74407628777942847 ) ) ;
#51211 = ORIENTED_EDGE ( 'NONE', *, *, #64002, .F. ) ;
#51212 = CARTESIAN_POINT ( 'NONE',  ( -16.15384615384627409, -4.320704448113951379, 33.92786785259630022 ) ) ;
#51213 = CARTESIAN_POINT ( 'NONE',  ( 9.692307692307572609, -11.48612834414049644, 32.76840700105863391 ) ) ;
#51215 = VERTEX_POINT ( 'NONE', #36779 ) ;
#51214 = DIRECTION ( 'NONE',  ( 0.000000000000000000, 0.000000000000000000, 1.000000000000000000 ) ) ;
#51216 = CARTESIAN_POINT ( 'NONE',  ( 6.923076923076924238, -3.050289026998446396, 32.03036669348365706 ) ) ;
#51217 = LINE ( 'NONE', #78271, #25374 ) ;
#51218 = CARTESIAN_POINT ( 'NONE',  ( -4.946397375159511611, -9.417988943895561960, 34.36773134775778260 ) ) ;
#51219 = CARTESIAN_POINT ( 'NONE',  ( -14.30769230769242739, -11.48612834414049644, 32.76840700105863391 ) ) ;
#51220 = ORIENTED_EDGE ( 'NONE', *, *, #21370, .T. ) ;
#51221 = CARTESIAN_POINT ( 'NONE',  ( -11.76194648218548622, -4.386631170607604879, 33.66268669641500111 ) ) ;
#51222 = CARTESIAN_POINT ( 'NONE',  ( -11.66902145207490094, -2.254533558242300284, 29.97296025877828285 ) ) ;
#51223 = VECTOR ( 'NONE', #76603, 1000.000000000000000 ) ;
#51224 = CARTESIAN_POINT ( 'NONE',  ( -1.134669866267241867, -5.852078868378310261, 34.47109172314383585 ) ) ;
#51225 = ORIENTED_EDGE ( 'NONE', *, *, #28144, .F. ) ;
#51226 = ORIENTED_EDGE ( 'NONE', *, *, #40652, .F. ) ;
#51227 = ORIENTED_EDGE ( 'NONE', *, *, #24010, .F. ) ;
#51228 = CYLINDRICAL_SURFACE ( 'NONE', #44287, 0.2500000000000004996 ) ;
#51229 = CARTESIAN_POINT ( 'NONE',  ( 6.065255139512838234, -2.379036618887895305, 30.90682066428159303 ) ) ;
#51230 = B_SPLINE_CURVE_WITH_KNOTS ( 'NONE', 3,
 ( #33926, #28062, #19091, #35716, #71246, #35258, #2782, #63166, #36594, #69930 ),
 .UNSPECIFIED., .F., .F.,
 ( 4, 2, 2, 2, 4 ),
 ( 0.000000000000000000, 0.0001954311564186865221, 0.0003908623128373730441, 0.0005862934692560595662, 0.0007817246256747460882 ),
 .UNSPECIFIED. ) ;
#51231 = AXIS2_PLACEMENT_3D ( 'NONE', #53457, #11601, #80959 ) ;
#51232 = CYLINDRICAL_SURFACE ( 'NONE', #17907, 0.2500000000000009437 ) ;
#51233 = CARTESIAN_POINT ( 'NONE',  ( -10.36543909703647159, -3.202959910592335646, 32.30730279482227019 ) ) ;
#51234 = ORIENTED_EDGE ( 'NONE', *, *, #13208, .T. ) ;
#51235 = ORIENTED_EDGE ( 'NONE', *, *, #73696, .T. ) ;
#51237 = ORIENTED_EDGE ( 'NONE', *, *, #65645, .F. ) ;
#51236 = CARTESIAN_POINT ( 'NONE',  ( 11.66898697669518192, -11.66157788607254098, 32.95092075102925833 ) ) ;
#51238 = DIRECTION ( 'NONE',  ( -0.000000000000000000, 0.1736481776669307198, -0.9848077530122080203 ) ) ;
#51239 = AXIS2_PLACEMENT_3D ( 'NONE', #39537, #33203, #60667 ) ;
#51240 = DIRECTION ( 'NONE',  ( -0.000000000000000000, 0.3420201433256694901, -0.9396926207859082059 ) ) ;
#51241 = CARTESIAN_POINT ( 'NONE',  ( -4.153846153846152411, -10.89733346790207413, 36.13435417666054406 ) ) ;
#51242 = ORIENTED_EDGE ( 'NONE', *, *, #11303, .F. ) ;
#51243 = ORIENTED_EDGE ( 'NONE', *, *, #6537, .T. ) ;
#51244 = EDGE_CURVE ( 'NONE', #49175, #8541, #64235, .T. ) ;
#51245 = VERTEX_POINT ( 'NONE', #9750 ) ;
#51247 = ORIENTED_EDGE ( 'NONE', *, *, #11183, .F. ) ;
#51246 = CARTESIAN_POINT ( 'NONE',  ( -16.15384615384627409, -2.657715359629662988, 31.77849191805970364 ) ) ;
#51248 = EDGE_CURVE ( 'NONE', #44876, #622, #37217, .T. ) ;
#51249 = CARTESIAN_POINT ( 'NONE',  ( -7.846153846153965716, -2.892918686052166066, 31.69288490824153470 ) ) ;
#51250 = CARTESIAN_POINT ( 'NONE',  ( -16.15384615384615330, -3.513871655860378418, 32.76840700105978499 ) ) ;
#51251 = ORIENTED_EDGE ( 'NONE', *, *, #46165, .T. ) ;
#51252 = VECTOR ( 'NONE', #71048, 1000.000000000000114 ) ;
#51253 = CARTESIAN_POINT ( 'NONE',  ( 12.59232890250540926, -6.369690395747422684, 34.87708834333098196 ) ) ;
#51254 = DIRECTION ( 'NONE',  ( 0.000000000000000000, 0.3420201433256641055, -0.9396926207859100932 ) ) ;
#51255 = CARTESIAN_POINT ( 'NONE',  ( -2.241623956689868358, -11.16473453929635440, 33.15142922261926373 ) ) ;
#51256 = FACE_BOUND ( 'NONE', #52140, .T. ) ;
#51257 = LINE ( 'NONE', #79662, #38432 ) ;
#51258 = CARTESIAN_POINT ( 'NONE',  ( 4.088576153289833925, -2.379036618887870436, 30.90682066428147934 ) ) ;
#51259 = EDGE_CURVE ( 'NONE', #44052, #44046, #4046, .T. ) ;
#51260 = CARTESIAN_POINT ( 'NONE',  ( -15.10024352900566846, -10.88167719472716399, 33.43325721877153711 ) ) ;
#51262 = CARTESIAN_POINT ( 'NONE',  ( 6.673100192134569397, -11.79746400365624659, 32.30657167506340954 ) ) ;
#51261 = CARTESIAN_POINT ( 'NONE',  ( 9.692307692307695177, -12.62096338111211580, 30.90682066428153263 ) ) ;
#51263 = B_SPLINE_CURVE_WITH_KNOTS ( 'NONE', 3,
 ( #1129, #83564, #42567, #21402, #75458, #15094 ),
 .UNSPECIFIED., .F., .F.,
 ( 4, 2, 4 ),
 ( 0.0003909569690057822732, 0.0005862646681846077649, 0.0007815723673634333108 ),
 .UNSPECIFIED. ) ;
#51264 = CARTESIAN_POINT ( 'NONE',  ( 8.639082799499075094, -9.504002272028875709, 34.60269587691767867 ) ) ;
#51265 = CARTESIAN_POINT ( 'NONE',  ( 1.607395053593452028, -2.353885683473779356, 30.79025554430704759 ) ) ;
#51266 = EDGE_LOOP ( 'NONE', ( #62943, #17332, #11442, #63693 ) ) ;
#51267 = CARTESIAN_POINT ( 'NONE',  ( -16.02305571287920216, -3.338503747796866872, 32.95102852606552801 ) ) ;
#51268 = EDGE_CURVE ( 'NONE', #33434, #82159, #56695, .T. ) ;
#51269 = EDGE_LOOP ( 'NONE', ( #49862, #84644, #29584, #47829 ) ) ;
#51270 = EDGE_LOOP ( 'NONE', ( #15777, #17084 ) ) ;
#51272 = CARTESIAN_POINT ( 'NONE',  ( 10.68145194873469173, -12.62096338111211757, 30.90682066428152908 ) ) ;
#51271 = DIRECTION ( 'NONE',  ( -0.000000000000000000, 0.8660254037844397068, -0.4999999999999978906 ) ) ;
#51273 = CARTESIAN_POINT ( 'NONE',  ( 13.25446741488368829, -11.66186481527757302, 32.95055677023626117 ) ) ;
#51274 = CARTESIAN_POINT ( 'NONE',  ( 2.557637717070352590, -2.341251567377310217, 30.72681386836322659 ) ) ;
#51275 = CARTESIAN_POINT ( 'NONE',  ( -2.557669051740896649, -11.47974371597207899, 33.17467449705390692 ) ) ;
#51276 = ORIENTED_EDGE ( 'NONE', *, *, #37856, .T. ) ;
#51277 = FACE_OUTER_BOUND ( 'NONE', #83100, .T. ) ;
#51278 = CARTESIAN_POINT ( 'NONE',  ( 6.699591979352973681, -3.754499324213721234, 33.06261337010820256 ) ) ;
#51279 = CARTESIAN_POINT ( 'NONE',  ( -1.384615384615506484, -10.33852847137269571, 34.16647553114546554 ) ) ;
#51280 = EDGE_CURVE ( 'NONE', #2315, #18545, #83442, .T. ) ;
#51281 = CARTESIAN_POINT ( 'NONE',  ( 10.68064018666064285, -4.481592998940250538, 33.73612834413965089 ) ) ;
#51282 = CARTESIAN_POINT ( 'NONE',  ( -15.00775638667583678, -10.77377354290276124, 33.85451476688484718 ) ) ;
#51283 = AXIS2_PLACEMENT_3D ( 'NONE', #45835, #80977, #33221 ) ;
#51284 = CARTESIAN_POINT ( 'NONE',  ( -2.651650429449565305, -4.848349570550461785, 19.00000000000000000 ) ) ;
#51285 = ORIENTED_EDGE ( 'NONE', *, *, #24713, .T. ) ;
#51286 = EDGE_LOOP ( 'NONE', ( #7771, #71738, #69242, #39844 ) ) ;
#51287 = CARTESIAN_POINT ( 'NONE',  ( -7.911423846710166075, -11.67786785259540849, 32.92929555188721480 ) ) ;
#51288 = ORIENTED_EDGE ( 'NONE', *, *, #38218, .T. ) ;
#51289 = CARTESIAN_POINT ( 'NONE',  ( 17.32686848630112308, -4.176053281294515251, 33.81426240980091791 ) ) ;
#51290 = CARTESIAN_POINT ( 'NONE',  ( 9.823099500132483897, -9.804649428959608670, 34.18742332936588468 ) ) ;
#51291 = CARTESIAN_POINT ( 'NONE',  ( -16.28399336328437386, -5.195881422630167279, 34.18770438780618548 ) ) ;
#51292 = CARTESIAN_POINT ( 'NONE',  ( -15.10024352900566669, -2.882268652242222284, 31.66798894389554064 ) ) ;
#51293 = CARTESIAN_POINT ( 'NONE',  ( 1.553300858899129944, -11.24999999999998934, 17.20312500000000000 ) ) ;
#51294 = FACE_OUTER_BOUND ( 'NONE', #33588, .T. ) ;
#51295 = ORIENTED_EDGE ( 'NONE', *, *, #10809, .T. ) ;
#51296 = CARTESIAN_POINT ( 'NONE',  ( -3.512820512820513663, -7.500000000000000000, 29.75000000000000355 ) ) ;
#51298 = ORIENTED_EDGE ( 'NONE', *, *, #72083, .T. ) ;
#51297 = CARTESIAN_POINT ( 'NONE',  ( 4.153846153846154188, -13.95598074871891292, 31.83374038241031911 ) ) ;
#51299 = CARTESIAN_POINT ( 'NONE',  ( -13.63463862190834952, -11.37209801155882971, 32.91403422569032955 ) ) ;
#51300 = CARTESIAN_POINT ( 'NONE',  ( 3.296837581771669523, -2.721908614388771852, 31.22303859784725333 ) ) ;
#51301 = CARTESIAN_POINT ( 'NONE',  ( -3.453595923248235167, -7.369208160676173236, 34.74850200257122879 ) ) ;
#51302 = CARTESIAN_POINT ( 'NONE',  ( 0.5267940328144850026, -2.892918686051626498, 31.69288490824025928 ) ) ;
#51303 = EDGE_CURVE ( 'NONE', #6050, #34465, #20170, .T. ) ;
#51304 = DIRECTION ( 'NONE',  ( -0.000000000000000000, 0.1736481776669307198, -0.9848077530122080203 ) ) ;
#51305 = DIRECTION ( 'NONE',  ( -0.000000000000000000, 0.1736481776669307198, -0.9848077530122080203 ) ) ;
#51306 = CARTESIAN_POINT ( 'NONE',  ( -11.28851612908349722, -2.986452184633680229, 32.43230066228895225 ) ) ;
#51307 = EDGE_CURVE ( 'NONE', #39142, #43722, #17067, .T. ) ;
#51308 = CARTESIAN_POINT ( 'NONE',  ( 1.492201783934598236, -11.27530806549875031, 16.20499329374151642 ) ) ;
#51309 = ORIENTED_EDGE ( 'NONE', *, *, #5316, .F. ) ;
#51310 = DIRECTION ( 'NONE',  ( -1.000000000000000000, 0.000000000000000000, 0.000000000000000000 ) ) ;
#51311 = CARTESIAN_POINT ( 'NONE',  ( -15.23076923076922995, -13.63283147151868846, 33.57946703557072254 ) ) ;
#51312 = CARTESIAN_POINT ( 'NONE',  ( 4.219913487196229163, -10.67929555188718282, 33.92786785259544757 ) ) ;
#51313 = CARTESIAN_POINT ( 'NONE',  ( -1.409462824231155764E-14, -4.749999999999999112, 22.90625000000000355 ) ) ;
#51314 = EDGE_CURVE ( 'NONE', #74101, #40454, #33195, .T. ) ;
#51315 = CARTESIAN_POINT ( 'NONE',  ( 0.3313912521002385092, -3.817052484675422797, 33.13202310037935661 ) ) ;
#51317 = CARTESIAN_POINT ( 'NONE',  ( 14.30769230769231015, -4.661471528628507777, 34.16647553114623292 ) ) ;
#51316 = AXIS2_PLACEMENT_3D ( 'NONE', #70040, #50649, #78128 ) ;
#51318 = EDGE_CURVE ( 'NONE', #48507, #21400, #56114, .T. ) ;
#51319 = VERTEX_POINT ( 'NONE', #18741 ) ;
#51320 = CARTESIAN_POINT ( 'NONE',  ( 2.750000000000001776, -7.499999999999984013, 19.46875000000000000 ) ) ;
#51321 = CARTESIAN_POINT ( 'NONE',  ( 3.007843013253082898, -9.086856451489515152, 34.49173150075333183 ) ) ;
#51322 = VERTEX_POINT ( 'NONE', #46207 ) ;
#51323 = VECTOR ( 'NONE', #22206, 1000.000000000000000 ) ;
#51324 = CARTESIAN_POINT ( 'NONE',  ( -2.749999999999998224, -7.500000000000000000, 18.00000000000000355 ) ) ;
#51325 = ORIENTED_EDGE ( 'NONE', *, *, #41655, .F. ) ;
#51326 = CARTESIAN_POINT ( 'NONE',  ( 14.43848411551709532, -12.11778462344221019, 31.66786338562085135 ) ) ;
#51327 = LINE ( 'NONE', #25228, #88324 ) ;
#51328 = CIRCLE ( 'NONE', #71473, 0.2500000000000002220 ) ;
#51329 = CARTESIAN_POINT ( 'NONE',  ( -1.514762594053604028, -4.460286881179644780, 33.72017969459903242 ) ) ;
#51330 = ORIENTED_EDGE ( 'NONE', *, *, #32693, .T. ) ;
#51331 = DIRECTION ( 'NONE',  ( -0.000000000000000000, -0.1736481776669307198, -0.9848077530122080203 ) ) ;
#51332 = ORIENTED_EDGE ( 'NONE', *, *, #19585, .F. ) ;
#51333 = DIRECTION ( 'NONE',  ( 0.000000000000000000, 0.6427876096865368094, 0.7660444431189802339 ) ) ;
#51334 = ORIENTED_EDGE ( 'NONE', *, *, #28878, .T. ) ;
#51335 = CARTESIAN_POINT ( 'NONE',  ( -17.93393266664992680, -11.91647553114624358, 32.58852847137147535 ) ) ;
#51336 = FACE_OUTER_BOUND ( 'NONE', #41139, .T. ) ;
#51337 = ORIENTED_EDGE ( 'NONE', *, *, #54583, .F. ) ;
#51338 = CARTESIAN_POINT ( 'NONE',  ( -39.05038313613820122, -2.249999999999999556, 27.25000000000000000 ) ) ;
#51339 = CARTESIAN_POINT ( 'NONE',  ( 4.153846153846154188, -8.318370150425687726, 35.83090037661290239 ) ) ;
#51340 = DIRECTION ( 'NONE',  ( 1.000000000000000000, 0.000000000000000000, 0.000000000000000000 ) ) ;
#51341 = CARTESIAN_POINT ( 'NONE',  ( 4.826946345980720920, -9.148715823498378086, 34.47080413974185120 ) ) ;
#51342 = CARTESIAN_POINT ( 'NONE',  ( -16.21992853320628925, -2.833524468853757305, 32.15551576947924417 ) ) ;
#51343 = EDGE_CURVE ( 'NONE', #54183, #66607, #74124, .T. ) ;
#51344 = VECTOR ( 'NONE', #20840, 1000.000000000000000 ) ;
#51345 = EDGE_LOOP ( 'NONE', ( #80717, #84917, #15913, #15730 ) ) ;
#51346 = ORIENTED_EDGE ( 'NONE', *, *, #84019, .F. ) ;
#51347 = ORIENTED_EDGE ( 'NONE', *, *, #38078, .T. ) ;
#51349 = ORIENTED_EDGE ( 'NONE', *, *, #18294, .F. ) ;
#51348 = CYLINDRICAL_SURFACE ( 'NONE', #15682, 0.2499999999999994726 ) ;
#51350 = AXIS2_PLACEMENT_3D ( 'NONE', #19170, #69127, #7433 ) ;
#51351 = VECTOR ( 'NONE', #2159, 999.9999999999998863 ) ;
#51352 = LINE ( 'NONE', #24348, #26262 ) ;
#51353 = LINE ( 'NONE', #10412, #87052 ) ;
#51354 = ORIENTED_EDGE ( 'NONE', *, *, #25004, .F. ) ;
#51355 = ADVANCED_FACE ( 'NONE', ( #79098 ), #67367, .F. ) ;
#51356 = ORIENTED_EDGE ( 'NONE', *, *, #78057, .T. ) ;
#51357 = ADVANCED_FACE ( 'NONE', ( #58820 ), #24596, .F. ) ;
#51358 = ORIENTED_EDGE ( 'NONE', *, *, #87174, .T. ) ;
#51359 = CARTESIAN_POINT ( 'NONE',  ( -11.53846153846153655, -9.780366693483667717, 34.19971097300155094 ) ) ;
#51360 = ORIENTED_EDGE ( 'NONE', *, *, #57103, .F. ) ;
#51361 = DIRECTION ( 'NONE',  ( 0.000000000000000000, 0.000000000000000000, 1.000000000000000000 ) ) ;
#51362 = B_SPLINE_CURVE_WITH_KNOTS ( 'NONE', 3,
 ( #61676, #68017, #6316, #53149, #60357, #12625, #68882, #18934, #27021, #26579 ),
 .UNSPECIFIED., .F., .F.,
 ( 4, 2, 2, 2, 4 ),
 ( 0.0007817246256747524850, 0.0009771112852218974409, 0.001172497944769042288, 0.001367884604316187136, 0.001563271263863332200 ),
 .UNSPECIFIED. ) ;
#51363 = CARTESIAN_POINT ( 'NONE',  ( 4.088576153289834814, -12.70778746994557551, 30.41441678777548319 ) ) ;
#51364 = CARTESIAN_POINT ( 'NONE',  ( 12.33084699487089964, -2.541943142973491554, 30.39792223712631980 ) ) ;
#51365 = FACE_BOUND ( 'NONE', #70200, .T. ) ;
#51366 = ORIENTED_EDGE ( 'NONE', *, *, #51389, .F. ) ;
#51367 = CARTESIAN_POINT ( 'NONE',  ( 12.59233026936325039, -5.582136614379148654, 34.36778462344220486 ) ) ;
#51368 = ADVANCED_FACE ( 'NONE', ( #72776 ), #82669, .F. ) ;
#51369 = CARTESIAN_POINT ( 'NONE',  ( 5.011653076366756387, -3.643525952247789412, 33.31231777344662959 ) ) ;
#51370 = AXIS2_PLACEMENT_3D ( 'NONE', #26599, #20726, #54058 ) ;
#51371 = DIRECTION ( 'NONE',  ( 0.000000000000000000, 0.000000000000000000, -1.000000000000000000 ) ) ;
#51372 = CARTESIAN_POINT ( 'NONE',  ( 7.846153846153725020, -10.90142922262034020, 33.41473453929536674 ) ) ;
#51373 = ORIENTED_EDGE ( 'NONE', *, *, #68142, .T. ) ;
#51374 = CARTESIAN_POINT ( 'NONE',  ( -6.989160334032802346, -6.386643153685125363, 34.62446782046654903 ) ) ;
#51375 = ADVANCED_FACE ( 'NONE', ( #47968 ), #6112, .T. ) ;
#51376 = ORIENTED_EDGE ( 'NONE', *, *, #15156, .T. ) ;
#51377 = VERTEX_POINT ( 'NONE', #54724 ) ;
#51379 = CARTESIAN_POINT ( 'NONE',  ( -9.442362282929646966, -8.476813868363244353, 34.90874843262270133 ) ) ;
#51378 = CARTESIAN_POINT ( 'NONE',  ( 5.750023255951410839, -12.01397095200673881, 32.43157075238190146 ) ) ;
#51380 = CARTESIAN_POINT ( 'NONE',  ( 8.769230769230768274, -13.49023893513002648, 31.06009739812518688 ) ) ;
#51381 = CARTESIAN_POINT ( 'NONE',  ( -19.50000000000000000, -11.50000000000000000, 29.75000000000000355 ) ) ;
#51382 = DIRECTION ( 'NONE',  ( -0.000000000000000000, -0.5000000000000009992, -0.8660254037844380415 ) ) ;
#51383 = CARTESIAN_POINT ( 'NONE',  ( -15.29603923132555110, -3.643525952247789412, 33.31231777344662959 ) ) ;
#51384 = ORIENTED_EDGE ( 'NONE', *, *, #55704, .F. ) ;
#51385 = CARTESIAN_POINT ( 'NONE',  ( 6.923076923076800782, -2.657715359629662988, 31.77849191805970364 ) ) ;
#51386 = AXIS2_PLACEMENT_3D ( 'NONE', #65418, #20241, #72619 ) ;
#51387 = CARTESIAN_POINT ( 'NONE',  ( 17.77707304109314279, -3.395401636524186362, 33.02366814457250399 ) ) ;
#51388 = FACE_OUTER_BOUND ( 'NONE', #53708, .T. ) ;
#51389 = EDGE_CURVE ( 'NONE', #74826, #41702, #51, .T. ) ;
#51390 = CARTESIAN_POINT ( 'NONE',  ( 13.31853197365950514, -12.37446782046654192, 30.86335684631486487 ) ) ;
#51391 = ORIENTED_EDGE ( 'NONE', *, *, #29547, .F. ) ;
#51392 = ORIENTED_EDGE ( 'NONE', *, *, #3824, .F. ) ;
#51393 = FACE_BOUND ( 'NONE', #69937, .T. ) ;
#51394 = ORIENTED_EDGE ( 'NONE', *, *, #38503, .T. ) ;
#51395 = FACE_OUTER_BOUND ( 'NONE', #26353, .T. ) ;
#51396 = CARTESIAN_POINT ( 'NONE',  ( -7.846153846153844924, -4.786620604624113540, 33.94971097300155094 ) ) ;
#51397 = ORIENTED_EDGE ( 'NONE', *, *, #66406, .T. ) ;
#51398 = EDGE_CURVE ( 'NONE', #1771, #77592, #54610, .T. ) ;
#51399 = CARTESIAN_POINT ( 'NONE',  ( -3.296852641725109834, -12.37446782046654192, 30.86335684631486487 ) ) ;
#51400 = CARTESIAN_POINT ( 'NONE',  ( -5.076923076923075762, -10.89733346790207413, 36.13435417666054406 ) ) ;
#51401 = DIRECTION ( 'NONE',  ( 0.000000000000000000, 0.6427876096865368094, 0.7660444431189802339 ) ) ;
#51402 = DIRECTION ( 'NONE',  ( -1.000000000000000000, 0.000000000000000000, 0.000000000000000000 ) ) ;
#51403 = VERTEX_POINT ( 'NONE', #34463 ) ;
#51404 = CARTESIAN_POINT ( 'NONE',  ( 7.173076923076923350, -2.249999999999998668, 29.75000000000000355 ) ) ;
#51405 = EDGE_LOOP ( 'NONE', ( #13931, #81180, #27817, #77190 ) ) ;
#51407 = ORIENTED_EDGE ( 'NONE', *, *, #87760, .F. ) ;
#51406 = CARTESIAN_POINT ( 'NONE',  ( 16.94677586748485965, -10.88202310037936194, 33.43294751532457099 ) ) ;
#51408 = CARTESIAN_POINT ( 'NONE',  ( 11.53846153846153832, -6.386643153685126251, 34.62446782046654192 ) ) ;
#51409 = CARTESIAN_POINT ( 'NONE',  ( 4.088575707885377497, -6.879047030191174805, 34.71129190930000163 ) ) ;
#51410 = CARTESIAN_POINT ( 'NONE',  ( 4.480769230769229061, -11.50000000000000000, 29.75000000000000355 ) ) ;
#51411 = AXIS2_PLACEMENT_3D ( 'NONE', #18422, #7005, #73363 ) ;
#51412 = CARTESIAN_POINT ( 'NONE',  ( 10.55011461482829738, -12.51329471203370325, 31.30864560766548976 ) ) ;
#51413 = DIRECTION ( 'NONE',  ( 0.000000000000000000, 0.000000000000000000, -1.000000000000000000 ) ) ;
#51414 = EDGE_CURVE ( 'NONE', #68029, #42856, #83617, .T. ) ;
#51415 = CARTESIAN_POINT ( 'NONE',  ( 5.299934428535925335, -12.39991518177334129, 30.74647679643404530 ) ) ;
#51416 = CARTESIAN_POINT ( 'NONE',  ( -1.200186371490524317, -10.22469193450124791, 15.11124329374151287 ) ) ;
#51417 = ORIENTED_EDGE ( 'NONE', *, *, #49853, .F. ) ;
#51418 = AXIS2_PLACEMENT_3D ( 'NONE', #56725, #899, #48632 ) ;
#51419 = CARTESIAN_POINT ( 'NONE',  ( 17.07692307692307665, -2.833524468853757305, 32.15551576947925838 ) ) ;
#51420 = CARTESIAN_POINT ( 'NONE',  ( -15.16551365949320029, -3.835265460703683349, 33.15142922261929925 ) ) ;
#51421 = CYLINDRICAL_SURFACE ( 'NONE', #62540, 0.2500000000000009437 ) ;
#51422 = ADVANCED_FACE ( 'NONE', ( #88113 ), #48858, .F. ) ;
#51423 = ORIENTED_EDGE ( 'NONE', *, *, #30049, .T. ) ;
#51424 = EDGE_CURVE ( 'NONE', #78537, #75330, #1916, .T. ) ;
#51425 = ORIENTED_EDGE ( 'NONE', *, *, #88361, .T. ) ;
#51426 = CARTESIAN_POINT ( 'NONE',  ( -15.23076923076922995, -13.53365097954675988, 30.81389545987213552 ) ) ;
#51427 = CARTESIAN_POINT ( 'NONE',  ( 7.780071466793711643, -6.343179335718451384, 34.87096338111212646 ) ) ;
#51428 = LINE ( 'NONE', #22223, #40431 ) ;
#51429 = DIRECTION ( 'NONE',  ( 0.000000000000000000, 0.000000000000000000, 1.000000000000000000 ) ) ;
#51430 = CARTESIAN_POINT ( 'NONE',  ( 16.08857615328984281, -10.33852847137145048, 34.16647553114627556 ) ) ;
#51431 = CARTESIAN_POINT ( 'NONE',  ( -6.923076923076922462, -6.435427911321262684, 35.78748833219616898 ) ) ;
#51432 = CARTESIAN_POINT ( 'NONE',  ( -14.98082382139119062, -8.476813868363244353, 34.90874843262270133 ) ) ;
#51433 = VERTEX_POINT ( 'NONE', #75451 ) ;
#51434 = CARTESIAN_POINT ( 'NONE',  ( -9.692307692307812417, -12.27809138561165270, 31.22303859784587132 ) ) ;
#51435 = CARTESIAN_POINT ( 'NONE',  ( -17.30040802064703342, -12.24155766932282496, 31.33739205006857986 ) ) ;
#51436 = CARTESIAN_POINT ( 'NONE',  ( -6.222878682428645725, -7.630691491037286056, 34.74850469731152458 ) ) ;
#51437 = ADVANCED_FACE ( 'NONE', ( #19616 ), #41670, .F. ) ;
#51438 = CARTESIAN_POINT ( 'NONE',  ( -6.166666666666667851, -7.500000000000000000, 29.75000000000000355 ) ) ;
#51439 = B_SPLINE_CURVE_WITH_KNOTS ( 'NONE', 3,
 ( #33694, #40897, #75999, #88221, #68359, #68803, #69249, #34577, #7102, #27816 ),
 .UNSPECIFIED., .F., .F.,
 ( 4, 2, 2, 2, 4 ),
 ( 0.0007817246256747459798, 0.0009771112852218896347, 0.001172497944769033398, 0.001367884604316177161, 0.001563271263863320708 ),
 .UNSPECIFIED. ) ;
#51440 = ORIENTED_EDGE ( 'NONE', *, *, #44800, .T. ) ;
#51441 = CARTESIAN_POINT ( 'NONE',  ( 13.63456090296352841, -6.696923467548660192, 34.68552623307873972 ) ) ;
#51442 = B_SPLINE_CURVE_WITH_KNOTS ( 'NONE', 3,
 ( #69550, #36654, #20915, #1541, #56033, #22690, #42972, #56914, #48387, #70445 ),
 .UNSPECIFIED., .F., .F.,
 ( 4, 2, 2, 2, 4 ),
 ( 0.0007817359430256318490, 0.0009771253907249984917, 0.001172514838424365026, 0.001367904286123731560, 0.001563293733823098311 ),
 .UNSPECIFIED. ) ;
#51443 = EDGE_LOOP ( 'NONE', ( #19380, #70843, #50344, #47062 ) ) ;
#51444 = VECTOR ( 'NONE', #42251, 1000.000000000000227 ) ;
#51445 = CARTESIAN_POINT ( 'NONE',  ( 0.5267940328144851136, -9.442884908240271713, 34.35708131394835618 ) ) ;
#51446 = CARTESIAN_POINT ( 'NONE',  ( 2.307692307692309264, -7.500000000000001776, 35.04278698407183867 ) ) ;
#51447 = ADVANCED_FACE ( 'NONE', ( #27702 ), #88989, .F. ) ;
#51448 = CARTESIAN_POINT ( 'NONE',  ( 6.923076923076924238, -1.466349020453238561, 30.81389545987213907 ) ) ;
#51449 = ORIENTED_EDGE ( 'NONE', *, *, #35378, .F. ) ;
#51450 = B_SPLINE_CURVE_WITH_KNOTS ( 'NONE', 3,
 ( #35980, #41405, #22015, #70199, #76066, #48148, #14365, #76962, #48588, #68866 ),
 .UNSPECIFIED., .F., .F.,
 ( 4, 2, 2, 2, 4 ),
 ( 0.000000000000000000, 0.0001954339881912759433, 0.0003908679763825518867, 0.0005863019645738304321, 0.0007817359527651089775 ),
 .UNSPECIFIED. ) ;
#51451 = CARTESIAN_POINT ( 'NONE',  ( -1.634638608836841867, -12.68155406624981119, 30.59749803192733708 ) ) ;
#51452 = CARTESIAN_POINT ( 'NONE',  ( -5.999999999999998224, -4.786620604624113540, 33.94971097300155094 ) ) ;
#51453 = LINE ( 'NONE', #39658, #81553 ) ;
#51454 = CIRCLE ( 'NONE', #25577, 0.2500000000000002220 ) ;
#51455 = DIRECTION ( 'NONE',  ( 0.000000000000000000, 0.3420201433256641055, -0.9396926207859100932 ) ) ;
#51456 = CARTESIAN_POINT ( 'NONE',  ( 3.230769230769231726, -2.833524468853757305, 32.15551576947925838 ) ) ;
#51457 = EDGE_CURVE ( 'NONE', #71885, #71376, #87949, .T. ) ;
#51458 = AXIS2_PLACEMENT_3D ( 'NONE', #71851, #65981, #10160 ) ;
#51459 = ORIENTED_EDGE ( 'NONE', *, *, #51926, .F. ) ;
#51460 = CARTESIAN_POINT ( 'NONE',  ( 16.21991348719623360, -9.905515769479276145, 34.41647553114623292 ) ) ;
#51461 = VERTEX_POINT ( 'NONE', #3217 ) ;
#51462 = ADVANCED_FACE ( 'NONE', ( #64911 ), #8329, .F. ) ;
#51463 = CARTESIAN_POINT ( 'NONE',  ( 4.946231610255514610, -12.11776431015576172, 31.66791131148498906 ) ) ;
#51464 = ADVANCED_FACE ( 'NONE', ( #31583 ), #15086, .T. ) ;
#51465 = CARTESIAN_POINT ( 'NONE',  ( -16.40382288478850725, -11.28823185664190376, 33.01397839955799896 ) ) ;
#51466 = CARTESIAN_POINT ( 'NONE',  ( -9.070512820512819374, -7.500000000000000000, 29.75000000000000355 ) ) ;
#51467 = CARTESIAN_POINT ( 'NONE',  ( -14.08491276642389423, -11.89424750095246175, 32.13594075562311758 ) ) ;
#51468 = CARTESIAN_POINT ( 'NONE',  ( 12.59233026936325039, -9.804649428959608670, 34.18742332936588468 ) ) ;
#51469 = VERTEX_POINT ( 'NONE', #17178 ) ;
#51470 = EDGE_CURVE ( 'NONE', #13621, #43102, #86094, .T. ) ;
#51471 = ORIENTED_EDGE ( 'NONE', *, *, #78853, .T. ) ;
#51472 = EDGE_LOOP ( 'NONE', ( #45513, #26829, #49571, #8113, #6909, #20879, #76270, #59840 ) ) ;
#51473 = ORIENTED_EDGE ( 'NONE', *, *, #28009, .T. ) ;
#51474 = ORIENTED_EDGE ( 'NONE', *, *, #46445, .T. ) ;
#51475 = B_SPLINE_CURVE_WITH_KNOTS ( 'NONE', 3,
 ( #77151, #49675, #34827, #49237, #606, #69503, #28077, #64066, #69945, #15457 ),
 .UNSPECIFIED., .F., .F.,
 ( 4, 2, 2, 2, 4 ),
 ( 0.000000000000000000, 0.0001954339857564073659, 0.0003908679715128147319, 0.0005863019572692221250, 0.0007817359430256294638 ),
 .UNSPECIFIED. ) ;
#51476 = FACE_OUTER_BOUND ( 'NONE', #15394, .T. ) ;
#51477 = CARTESIAN_POINT ( 'NONE',  ( -2.177166605928740672, -3.285477652293413264, 32.44071101563363158 ) ) ;
#51478 = DIRECTION ( 'NONE',  ( 0.000000000000000000, 0.6427876096865368094, 0.7660444431189802339 ) ) ;
#51479 = LINE ( 'NONE', #38445, #82530 ) ;
#51480 = CARTESIAN_POINT ( 'NONE',  ( -4.153846153846274980, -9.528491918059723176, 34.59228464037033035 ) ) ;
#51481 = CARTESIAN_POINT ( 'NONE',  ( -12.71156168575991785, -12.45566812827425451, 31.48439005359158926 ) ) ;
#51482 = CARTESIAN_POINT ( 'NONE',  ( 5.749976762707035505, -11.86270091957321249, 32.19358267280087915 ) ) ;
#51483 = CARTESIAN_POINT ( 'NONE',  ( -4.153846153846152411, -10.51840700105979565, 33.73612834413961536 ) ) ;
#51484 = CARTESIAN_POINT ( 'NONE',  ( 8.096208266067298709, -4.818054556918156983, 34.26375889529406749 ) ) ;
#51485 = AXIS2_PLACEMENT_3D ( 'NONE', #73670, #59245, #26356 ) ;
#51486 = ORIENTED_EDGE ( 'NONE', *, *, #36958, .T. ) ;
#51487 = EDGE_CURVE ( 'NONE', #84770, #37942, #86813, .T. ) ;
#51488 = ORIENTED_EDGE ( 'NONE', *, *, #17043, .F. ) ;
#51489 = ORIENTED_EDGE ( 'NONE', *, *, #25820, .F. ) ;
#51491 = ORIENTED_EDGE ( 'NONE', *, *, #79140, .T. ) ;
#51490 = CARTESIAN_POINT ( 'NONE',  ( 6.066067333350078528, -12.34228464037088813, 31.77849191805839268 ) ) ;
#51493 = CARTESIAN_POINT ( 'NONE',  ( 8.769230769230768274, -5.471508081941601098, 34.59228464037088457 ) ) ;
#51492 = CARTESIAN_POINT ( 'NONE',  ( 8.769230769230768274, -8.120952969808772792, 34.71129190930000163 ) ) ;
#51494 = CARTESIAN_POINT ( 'NONE',  ( 1.634560793993429462, -4.932303261841489039, 34.32971442181322885 ) ) ;
#51495 = CARTESIAN_POINT ( 'NONE',  ( -11.40767109749459074, -9.084667340241226796, 34.75534355489798344 ) ) ;
#51496 = ORIENTED_EDGE ( 'NONE', *, *, #38635, .T. ) ;
#51497 = ORIENTED_EDGE ( 'NONE', *, *, #49313, .T. ) ;
#51498 = CARTESIAN_POINT ( 'NONE',  ( -2.242498325908949486, -2.506253911140448043, 29.99999999999988631 ) ) ;
#51499 = VERTEX_POINT ( 'NONE', #86550 ) ;
#51500 = FACE_BOUND ( 'NONE', #36052, .T. ) ;
#51501 = CARTESIAN_POINT ( 'NONE',  ( 13.45068271796546178, -12.34228464037088813, 31.77849191805839268 ) ) ;
#51502 = AXIS2_PLACEMENT_3D ( 'NONE', #5680, #6131, #47550 ) ;
#51503 = FACE_OUTER_BOUND ( 'NONE', #15083, .T. ) ;
#51504 = ORIENTED_EDGE ( 'NONE', *, *, #49477, .T. ) ;
#51505 = CARTESIAN_POINT ( 'NONE',  ( 14.24160889673642671, -2.721908614388770964, 31.22303859784723912 ) ) ;
#51506 = CARTESIAN_POINT ( 'NONE',  ( 8.546402671595890510, -7.369209533119137845, 34.99857337881830688 ) ) ;
#51507 = CARTESIAN_POINT ( 'NONE',  ( -2.307692307692305711, -2.708943851104267164, 35.45975837776705220 ) ) ;
#51508 = ORIENTED_EDGE ( 'NONE', *, *, #55368, .T. ) ;
#51509 = CARTESIAN_POINT ( 'NONE',  ( -11.66860950819323328, -5.070767119584671079, 34.40440758774516183 ) ) ;
#51510 = CARTESIAN_POINT ( 'NONE',  ( 6.989144256427000990, -5.471508081941601098, 34.59228464037088457 ) ) ;
#51511 = EDGE_LOOP ( 'NONE', ( #63333, #49113, #7542, #7425, #53923 ) ) ;
#51512 = B_SPLINE_CURVE_WITH_KNOTS ( 'NONE', 3,
 ( #55839, #56289, #22499, #57170, #69800, #49962, #35129, #55399, #8108, #29710 ),
 .UNSPECIFIED., .F., .F.,
 ( 4, 2, 2, 2, 4 ),
 ( 0.000000000000000000, 0.0001954311564186858715, 0.0003908623128373717431, 0.0005862934692560576146, 0.0007817246256747434861 ),
 .UNSPECIFIED. ) ;
#51513 = AXIS2_PLACEMENT_3D ( 'NONE', #34767, #88411, #81638 ) ;
#51514 = CARTESIAN_POINT ( 'NONE',  ( 6.066166606591640864, -7.250054591869668386, 34.99404684341514127 ) ) ;
#51515 = DIRECTION ( 'NONE',  ( 0.000000000000000000, 0.7660444431189807890, 0.6427876096865361433 ) ) ;
#51516 = VERTEX_POINT ( 'NONE', #44186 ) ;
#51517 = CARTESIAN_POINT ( 'NONE',  ( -0.4615384615384611200, -8.318370150425687726, 35.83090037661290239 ) ) ;
#51518 = CARTESIAN_POINT ( 'NONE',  ( -12.39628289026243380, -2.625532179533470512, 30.86335684631491105 ) ) ;
#51519 = DIRECTION ( 'NONE',  ( 0.000000000000000000, 1.000000000000000000, 8.673617379884033500E-16 ) ) ;
#51520 = CARTESIAN_POINT ( 'NONE',  ( -10.55012904410859242, -6.026961402152789304, 34.52809138561124769 ) ) ;
#51521 = CARTESIAN_POINT ( 'NONE',  ( -8.769230769230768274, -12.78798330534102945, 29.74999999999997868 ) ) ;
#51522 = FACE_BOUND ( 'NONE', #75479, .T. ) ;
#51524 = DIRECTION ( 'NONE',  ( 0.000000000000000000, 0.000000000000000000, -1.000000000000000000 ) ) ;
#51523 = CARTESIAN_POINT ( 'NONE',  ( -1.514762594053602029, -2.882441371585227952, 31.66841991370172948 ) ) ;
#51525 = AXIS2_PLACEMENT_3D ( 'NONE', #60905, #52368, #11392 ) ;
#51526 = DIRECTION ( 'NONE',  ( -0.000000000000000000, 0.1736481776669307198, -0.9848077530122080203 ) ) ;
#51528 = CARTESIAN_POINT ( 'NONE',  ( 9.019285080869085647, -2.779044189368095719, 31.39831045268885745 ) ) ;
#51527 = DIRECTION ( 'NONE',  ( -0.000000000000000000, 0.7660444431189791237, -0.6427876096865379196 ) ) ;
#51529 = CARTESIAN_POINT ( 'NONE',  ( -1.139087296525992166, -10.25000000000000533, 14.85937500000000355 ) ) ;
#51530 = ORIENTED_EDGE ( 'NONE', *, *, #65218, .T. ) ;
#51531 = LINE ( 'NONE', #9683, #30350 ) ;
#51532 = ORIENTED_EDGE ( 'NONE', *, *, #48163, .F. ) ;
#51533 = EDGE_CURVE ( 'NONE', #49416, #19438, #24821, .T. ) ;
#51534 = ORIENTED_EDGE ( 'NONE', *, *, #49583, .T. ) ;
#51535 = CARTESIAN_POINT ( 'NONE',  ( 16.15384615384603251, -11.48612834414049644, 32.76840700105863391 ) ) ;
#51536 = EDGE_CURVE ( 'NONE', #47433, #74652, #72565, .T. ) ;
#51537 = ORIENTED_EDGE ( 'NONE', *, *, #27806, .F. ) ;
#51538 = CARTESIAN_POINT ( 'NONE',  ( -39.05038313613820122, -2.249999999999998668, 29.75000000000000355 ) ) ;
#51539 = CARTESIAN_POINT ( 'NONE',  ( 1.200186371490561621, -10.22469193450123193, 26.95125670625849068 ) ) ;
#51540 = CARTESIAN_POINT ( 'NONE',  ( -13.16160254052198830, -5.582272713120729257, 34.63742843783360570 ) ) ;
#51541 = CARTESIAN_POINT ( 'NONE',  ( -9.822455662039388358, -12.70455904226513866, 30.44083106164009322 ) ) ;
#51542 = DIRECTION ( 'NONE',  ( -0.000000000000000000, 1.000000000000000000, -0.000000000000000000 ) ) ;
#51543 = CARTESIAN_POINT ( 'NONE',  ( -14.37296230824862953, -11.06231777344662781, 33.60647404775220082 ) ) ;
#51544 = CARTESIAN_POINT ( 'NONE',  ( 14.30769230769231015, -6.386643153685126251, 34.62446782046654192 ) ) ;
#51545 = CARTESIAN_POINT ( 'NONE',  ( -12.46153846153846168, -13.04860791097971706, 34.73218667398347037 ) ) ;
#51546 = DIRECTION ( 'NONE',  ( 1.000000000000000000, -0.000000000000000000, -0.000000000000000000 ) ) ;
#51547 = EDGE_CURVE ( 'NONE', #51792, #30710, #7354, .T. ) ;
#51548 = CARTESIAN_POINT ( 'NONE',  ( -2.651650429449535551, -10.15165042944956753, 17.43750000000000000 ) ) ;
#51549 = CARTESIAN_POINT ( 'NONE',  ( 17.07692307692307665, -5.557115091759785130, 34.35708131394839171 ) ) ;
#51550 = CARTESIAN_POINT ( 'NONE',  ( 14.37376065869474751, -10.51840700105979565, 33.73612834413962247 ) ) ;
#51551 = ADVANCED_FACE ( 'NONE', ( #63260 ), #56063, .F. ) ;
#51552 = DIRECTION ( 'NONE',  ( -0.000000000000000000, 0.5000000000000011102, -0.8660254037844381525 ) ) ;
#51553 = AXIS2_PLACEMENT_3D ( 'NONE', #51176, #30922, #17875 ) ;
#51554 = EDGE_LOOP ( 'NONE', ( #3346, #5545 ) ) ;
#51555 = CARTESIAN_POINT ( 'NONE',  ( -13.44988538517170440, -6.835583212224499938, 34.95778746994557906 ) ) ;
#51556 = CARTESIAN_POINT ( 'NONE',  ( 11.53846153846141753, -3.835265460704628371, 33.15142922262033665 ) ) ;
#51557 = CARTESIAN_POINT ( 'NONE',  ( -2.307692307692305711, -2.292212530054420494, 30.41441678777542634 ) ) ;
#51558 = CARTESIAN_POINT ( 'NONE',  ( 1.634615384615389688, -2.499999999999999556, 29.81604066197450109 ) ) ;
#51559 = CARTESIAN_POINT ( 'NONE',  ( 15.36160764878199458, -7.277220443632450575, 34.74524770363009196 ) ) ;
#51560 = CARTESIAN_POINT ( 'NONE',  ( -2.980714810855777497, -5.642605341092957083, 34.66089969410670335 ) ) ;
#51561 = B_SPLINE_CURVE_WITH_KNOTS ( 'NONE', 3,
 ( #56413, #77126, #17190, #10888, #60397, #45552, #51849, #31142, #31597, #38808 ),
 .UNSPECIFIED., .F., .F.,
 ( 4, 2, 2, 2, 4 ),
 ( 0.000000000000000000, 0.0001954339857564092904, 0.0003908679715128185808, 0.0005863019572692278712, 0.0007817359430256371616 ),
 .UNSPECIFIED. ) ;
#51562 = ORIENTED_EDGE ( 'NONE', *, *, #62800, .T. ) ;
#51563 = DIRECTION ( 'NONE',  ( 0.000000000000000000, 0.6427876096865373645, -0.7660444431189797898 ) ) ;
#51564 = ORIENTED_EDGE ( 'NONE', *, *, #86161, .F. ) ;
#51565 = EDGE_CURVE ( 'NONE', #13394, #14834, #83554, .T. ) ;
#51566 = ORIENTED_EDGE ( 'NONE', *, *, #7791, .T. ) ;
#51567 = LINE ( 'NONE', #30439, #57956 ) ;
#51568 = AXIS2_PLACEMENT_3D ( 'NONE', #59086, #59534, #87036 ) ;
#51569 = CARTESIAN_POINT ( 'NONE',  ( 3.361561038594018225, -5.582136614379148654, 34.36778462344220486 ) ) ;
#51570 = CARTESIAN_POINT ( 'NONE',  ( -9.442362173959550020, -6.696923467548660192, 34.68552623307873972 ) ) ;
#51571 = CARTESIAN_POINT ( 'NONE',  ( 2.445221920924756368E-15, -13.25000000000000533, 13.00000000000000178 ) ) ;
#51572 = CARTESIAN_POINT ( 'NONE',  ( 5.869308533332444178, -2.729777683071817229, 31.24903638046268739 ) ) ;
#51573 = B_SPLINE_CURVE_WITH_KNOTS ( 'NONE', 3,
 ( #42224, #56167, #30026, #22816, #64232, #7985, #1217, #9318, #43094, #28701 ),
 .UNSPECIFIED., .F., .F.,
 ( 4, 2, 2, 2, 4 ),
 ( 0.0007817359430256257775, 0.0009771253907249911191, 0.001172514838424356352, 0.001367904286123721586, 0.001563293733823086819 ),
 .UNSPECIFIED. ) ;
#51574 = AXIS2_PLACEMENT_3D ( 'NONE', #74666, #53937, #329 ) ;
#51575 = EDGE_LOOP ( 'NONE', ( #18857, #56691 ) ) ;
#51576 = EDGE_CURVE ( 'NONE', #43597, #25676, #49297, .T. ) ;
#51577 = AXIS2_PLACEMENT_3D ( 'NONE', #16019, #64183, #43927 ) ;
#51578 = ORIENTED_EDGE ( 'NONE', *, *, #41605, .F. ) ;
#51579 = ORIENTED_EDGE ( 'NONE', *, *, #63537, .T. ) ;
#51580 = EDGE_CURVE ( 'NONE', #51322, #10219, #40699, .T. ) ;
#51581 = VECTOR ( 'NONE', #68818, 1000.000000000000000 ) ;
#51582 = EDGE_CURVE ( 'NONE', #76630, #39878, #50232, .T. ) ;
#51583 = CARTESIAN_POINT ( 'NONE',  ( 1.318531973659506251, -11.16473453929635440, 33.15142922261925662 ) ) ;
#51584 = CARTESIAN_POINT ( 'NONE',  ( 15.23076923076910916, -4.320704448113951379, 33.92786785259630022 ) ) ;
#51585 = FACE_OUTER_BOUND ( 'NONE', #68326, .T. ) ;
#51586 = CARTESIAN_POINT ( 'NONE',  ( -14.98071491913091791, -3.136992222400443175, 32.19305428654138979 ) ) ;
#51587 = CARTESIAN_POINT ( 'NONE',  ( -11.60373153901785948, -8.656820664281498878, 34.87096338111211935 ) ) ;
#51588 = CARTESIAN_POINT ( 'NONE',  ( -16.15384615384627409, -2.892918686052165622, 31.69288490824153470 ) ) ;
#51589 = ORIENTED_EDGE ( 'NONE', *, *, #29503, .F. ) ;
#51590 = EDGE_CURVE ( 'NONE', #75299, #68166, #24568, .T. ) ;
#51591 = ORIENTED_EDGE ( 'NONE', *, *, #38429, .T. ) ;
#51592 = CARTESIAN_POINT ( 'NONE',  ( -2.651650429449535551, -10.15165042944956753, 21.18750000000000000 ) ) ;
#51593 = VERTEX_POINT ( 'NONE', #20300 ) ;
#51595 = ORIENTED_EDGE ( 'NONE', *, *, #54730, .T. ) ;
#51594 = CARTESIAN_POINT ( 'NONE',  ( -10.61538461538473399, -11.94971097300221174, 32.03036669348237098 ) ) ;
#51596 = DIRECTION ( 'NONE',  ( -1.000000000000000000, 0.000000000000000000, 0.000000000000000000 ) ) ;
#51597 = DIRECTION ( 'NONE',  ( 1.000000000000000000, 0.000000000000000000, 0.000000000000000000 ) ) ;
#51598 = ADVANCED_FACE ( 'NONE', ( #26606 ), #45981, .F. ) ;
#51599 = ADVANCED_FACE ( 'NONE', ( #73018 ), #5897, .F. ) ;
#51600 = CARTESIAN_POINT ( 'NONE',  ( 2.651650429449539104, -4.848349570550432475, 16.81250000000000000 ) ) ;
#51601 = ORIENTED_EDGE ( 'NONE', *, *, #74131, .F. ) ;
#51602 = DIRECTION ( 'NONE',  ( -0.000000000000000000, 1.000000000000000000, 3.491481338843133355E-15 ) ) ;
#51603 = B_SPLINE_CURVE_WITH_KNOTS ( 'NONE', 3,
 ( #75542, #54832, #67469, #34565, #33237, #60701, #18835, #88208, #33681, #62028 ),
 .UNSPECIFIED., .F., .F.,
 ( 4, 2, 2, 2, 4 ),
 ( 0.0007817359430256303312, 0.0009771253907249965402, 0.001172514838424362641, 0.001367904286123728958, 0.001563293733823095059 ),
 .UNSPECIFIED. ) ;
#51604 = AXIS2_PLACEMENT_3D ( 'NONE', #38490, #60529, #32612 ) ;
#51605 = EDGE_LOOP ( 'NONE', ( #80340, #44998, #82261, #55183 ) ) ;
#51606 = ADVANCED_FACE ( 'NONE', ( #88775 ), #32034, .F. ) ;
#51607 = CARTESIAN_POINT ( 'NONE',  ( -2.307692307692305711, -12.10708131394839349, 31.69288490824020244 ) ) ;
#51608 = DIRECTION ( 'NONE',  ( -0.000000000000000000, 0.6427876096865404731, -0.7660444431189771253 ) ) ;
#51609 = B_SPLINE_CURVE_WITH_KNOTS ( 'NONE', 3,
 ( #72637, #10946, #4180, #58231, #30327, #44258, #5527, #6416, #66331, #53701 ),
 .UNSPECIFIED., .F., .F.,
 ( 4, 2, 2, 2, 4 ),
 ( 0.000000000000000000, 0.0001954339857564091278, 0.0003908679715128182556, 0.0005863019572692274375, 0.0007817359430256365111 ),
 .UNSPECIFIED. ) ;
#51610 = CARTESIAN_POINT ( 'NONE',  ( -15.23076923076935252, -3.083524468854526912, 32.58852847137268327 ) ) ;
#51612 = CARTESIAN_POINT ( 'NONE',  ( -6.792285115252136407, -2.541949514083464479, 30.39797389878540557 ) ) ;
#51611 = CARTESIAN_POINT ( 'NONE',  ( 10.74622303339737606, -7.277220443632450575, 34.74524770363009196 ) ) ;
#51613 = CARTESIAN_POINT ( 'NONE',  ( 8.639083559792549494, -6.001485441113819874, 34.52039167877662607 ) ) ;
#51614 = CARTESIAN_POINT ( 'NONE',  ( -3.361459833879537840, -8.191372820521381826, 34.95448215188423546 ) ) ;
#51615 = VERTEX_POINT ( 'NONE', #46872 ) ;
#51616 = CARTESIAN_POINT ( 'NONE',  ( -10.74553182482283198, -10.19110544564092002, 33.96427741523702792 ) ) ;
#51617 = CARTESIAN_POINT ( 'NONE',  ( -8.899378738962466784, -4.299443229763728169, 33.91186481527756058 ) ) ;
#51618 = ORIENTED_EDGE ( 'NONE', *, *, #56395, .F. ) ;
#51619 = CARTESIAN_POINT ( 'NONE',  ( -7.846153846153844924, -4.102666532097928531, 36.13435417666054406 ) ) ;
#51620 = CARTESIAN_POINT ( 'NONE',  ( 15.36129493253279676, -4.459921816937791661, 33.71989282347011851 ) ) ;
#51621 = CARTESIAN_POINT ( 'NONE',  ( 10.39189969082028675, -8.539481045369596401, 34.89627647299170832 ) ) ;
#51622 = DIRECTION ( 'NONE',  ( -0.000000000000000000, 0.1736481776669307198, -0.9848077530122080203 ) ) ;
#51623 = CARTESIAN_POINT ( 'NONE',  ( 7.716006636715626144, -8.587444163452046197, 34.63053765926554206 ) ) ;
#51624 = FACE_BOUND ( 'NONE', #56736, .T. ) ;
#51626 = DIRECTION ( 'NONE',  ( 0.000000000000000000, 0.000000000000000000, 1.000000000000000000 ) ) ;
#51625 = CARTESIAN_POINT ( 'NONE',  ( 5.207713517890025123, -5.496552790871117367, 34.60292014791297532 ) ) ;
#51627 = PLANE ( 'NONE',  #77053 ) ;
#51629 = CARTESIAN_POINT ( 'NONE',  ( 0.7114838709165041131, -2.986452184633680229, 32.43230066228895225 ) ) ;
#51628 = DIRECTION ( 'NONE',  ( -0.000000000000000000, 0.9396926207859093161, -0.3420201433256663259 ) ) ;
#51630 = CYLINDRICAL_SURFACE ( 'NONE', #64256, 0.2499999999999997502 ) ;
#51631 = CARTESIAN_POINT ( 'NONE',  ( -39.05038313613820122, 12.25000000000000711, 28.74999999999999645 ) ) ;
#51632 = CARTESIAN_POINT ( 'NONE',  ( -1.614399933863656544, -3.775308065498769405, 25.07625670625849423 ) ) ;
#51633 = EDGE_CURVE ( 'NONE', #15955, #21459, #88336, .T. ) ;
#51634 = ORIENTED_EDGE ( 'NONE', *, *, #26498, .F. ) ;
#51635 = VECTOR ( 'NONE', #13987, 1000.000000000000000 ) ;
#51636 = AXIS2_PLACEMENT_3D ( 'NONE', #78083, #63677, #15062 ) ;
#51637 = LINE ( 'NONE', #38600, #82377 ) ;
#51638 = CARTESIAN_POINT ( 'NONE',  ( -13.38461538461506883, -2.255955759149395501, 30.00000000000324363 ) ) ;
#51639 = DIRECTION ( 'NONE',  ( 0.000000000000000000, 0.1736481776669275834, 0.9848077530122086864 ) ) ;
#51640 = CARTESIAN_POINT ( 'NONE',  ( -0.1752029071980582831, -10.24545254656222149, 28.77370482994317058 ) ) ;
#51641 = CARTESIAN_POINT ( 'NONE',  ( -4.219116154402472674, -5.094484230520674117, 34.41647553114621161 ) ) ;
#51642 = CARTESIAN_POINT ( 'NONE',  ( -9.627052121031661969, -4.481592998940250538, 33.73612834413965089 ) ) ;
#51643 = CARTESIAN_POINT ( 'NONE',  ( 2.608446859217893099, -4.805146000318787358, 22.81063170625848713 ) ) ;
#51644 = EDGE_CURVE ( 'NONE', #58712, #3792, #65411, .T. ) ;
#51645 = CYLINDRICAL_SURFACE ( 'NONE', #87835, 0.2499999999999986955 ) ;
#51646 = CARTESIAN_POINT ( 'NONE',  ( -2.084912638714239375, -6.717445702608402236, 34.94155399931962336 ) ) ;
#51647 = AXIS2_PLACEMENT_3D ( 'NONE', #41776, #67476, #47642 ) ;
#51648 = CARTESIAN_POINT ( 'NONE',  ( 3.230769230769231726, -3.937682226553329556, 33.60647404775216529 ) ) ;
#51649 = DIRECTION ( 'NONE',  ( -0.000000000000000000, -0.000000000000000000, -1.000000000000000000 ) ) ;
#51650 = CARTESIAN_POINT ( 'NONE',  ( 8.545745825506822158, -10.11188796281391511, 34.01382737946119050 ) ) ;
#51651 = CARTESIAN_POINT ( 'NONE',  ( 3.903869422903799347, -10.66389620160130036, 33.62221079203477103 ) ) ;
#51652 = ADVANCED_FACE ( 'NONE', ( #27050 ), #82005, .F. ) ;
#51653 = VECTOR ( 'NONE', #14242, 1000.000000000000000 ) ;
#51654 = LINE ( 'NONE', #45357, #34760 ) ;
#51655 = B_SPLINE_CURVE_WITH_KNOTS ( 'NONE', 3,
 ( #25821, #73579, #47853, #13627, #74447, #53278, #11871, #61354, #60488, #74901 ),
 .UNSPECIFIED., .F., .F.,
 ( 4, 2, 2, 2, 4 ),
 ( 0.000000000000000000, 0.0001954311564186868744, 0.0003908623128373737488, 0.0005862934692560606504, 0.0007817246256747474977 ),
 .UNSPECIFIED. ) ;
#51656 = DIRECTION ( 'NONE',  ( 0.000000000000000000, 0.000000000000000000, -1.000000000000000000 ) ) ;
#51657 = ORIENTED_EDGE ( 'NONE', *, *, #51590, .F. ) ;
#51658 = EDGE_CURVE ( 'NONE', #15864, #51461, #39695, .T. ) ;
#51659 = CARTESIAN_POINT ( 'NONE',  ( -6.923076923076922462, -3.886160181151819604, 36.00935417666054406 ) ) ;
#51660 = CARTESIAN_POINT ( 'NONE',  ( 19.99999999999996803, 12.00000000000000711, 13.00000000000000178 ) ) ;
#51661 = CARTESIAN_POINT ( 'NONE',  ( 2.694853999681185108, -4.891553140782077591, 13.31436829374151287 ) ) ;
#51662 = CARTESIAN_POINT ( 'NONE',  ( -10.74553258511630993, -10.31621877034669588, 34.18098118002070152 ) ) ;
#51663 = CARTESIAN_POINT ( 'NONE',  ( 3.230769230769231726, -11.69971097300155272, 32.46337939537588113 ) ) ;
#51664 = ORIENTED_EDGE ( 'NONE', *, *, #81102, .F. ) ;
#51665 = CARTESIAN_POINT ( 'NONE',  ( 14.30769230769261569, -2.506253911140615021, 30.00000000000323297 ) ) ;
#51666 = DIRECTION ( 'NONE',  ( -0.000000000000000000, 0.7660444431189791237, -0.6427876096865379196 ) ) ;
#51668 = ORIENTED_EDGE ( 'NONE', *, *, #32979, .F. ) ;
#51667 = CYLINDRICAL_SURFACE ( 'NONE', #72758, 4.000000000000000000 ) ;
#51669 = CARTESIAN_POINT ( 'NONE',  ( -12.46153846153858424, -9.528491918059723176, 34.59228464037033035 ) ) ;
#51670 = DIRECTION ( 'NONE',  ( 0.000000000000000000, 0.9396926207859126468, 0.3420201433256571111 ) ) ;
#51671 = CARTESIAN_POINT ( 'NONE',  ( 14.30769230769218758, -4.481592998941358097, 33.73612834414048933 ) ) ;
#51673 = EDGE_CURVE ( 'NONE', #13144, #72929, #4146, .T. ) ;
#51672 = CARTESIAN_POINT ( 'NONE',  ( 8.900022577055556994, -4.809403383903225304, 33.96459661697924304 ) ) ;
#51674 = VERTEX_POINT ( 'NONE', #49087 ) ;
#51675 = CARTESIAN_POINT ( 'NONE',  ( 2.307692307692187583, -12.27809138561165270, 31.22303859784587132 ) ) ;
#51676 = CARTESIAN_POINT ( 'NONE',  ( -11.78846153846154543, -2.249999999999999556, 29.81609741502489541 ) ) ;
#51677 = CARTESIAN_POINT ( 'NONE',  ( -10.61538461538461320, -7.500000000000001776, 35.04278698407183867 ) ) ;
#51678 = EDGE_LOOP ( 'NONE', ( #56153, #75801, #56842, #8648 ) ) ;
#51679 = ORIENTED_EDGE ( 'NONE', *, *, #86075, .T. ) ;
#51680 = AXIS2_PLACEMENT_3D ( 'NONE', #41147, #15895, #70392 ) ;
#51681 = EDGE_LOOP ( 'NONE', ( #42570, #55373, #15296, #17769 ) ) ;
#51682 = CYLINDRICAL_SURFACE ( 'NONE', #24185, 0.2499999999999995559 ) ;
#51683 = CARTESIAN_POINT ( 'NONE',  ( 10.61538461538461675, -11.35647404775217417, 33.31231777344666511 ) ) ;
#51684 = EDGE_CURVE ( 'NONE', #82908, #69788, #8558, .T. ) ;
#51685 = EDGE_CURVE ( 'NONE', #42060, #45555, #76090, .T. ) ;
#51686 = CARTESIAN_POINT ( 'NONE',  ( 13.16168916709923664, -11.24512374952581872, 33.06303171183252942 ) ) ;
#51687 = CARTESIAN_POINT ( 'NONE',  ( -0.4615384615384611200, -9.819645486525091727, 36.12317359536749706 ) ) ;
#51688 = B_SPLINE_CURVE_WITH_KNOTS ( 'NONE', 3,
 ( #34651, #62119, #6728, #68000, #7178, #88296, #26568, #12167, #54024, #39652 ),
 .UNSPECIFIED., .F., .F.,
 ( 4, 2, 2, 2, 4 ),
 ( 0.000000000000000000, 0.0001954311564186877960, 0.0003908623128373755920, 0.0005862934692560633609, 0.0007817246256747511840 ),
 .UNSPECIFIED. ) ;
#51689 = B_SPLINE_CURVE_WITH_KNOTS ( 'NONE', 3,
 ( #78253, #76940, #1720, #42715, #63857, #70177, #2156, #29643, #49898, #78707 ),
 .UNSPECIFIED., .F., .F.,
 ( 4, 2, 2, 2, 4 ),
 ( 0.000000000000000000, 0.0001954311564186868202, 0.0003908623128373736404, 0.0005862934692560604335, 0.0007817246256747472808 ),
 .UNSPECIFIED. ) ;
#51690 = EDGE_LOOP ( 'NONE', ( #66842, #12698 ) ) ;
#51691 = EDGE_CURVE ( 'NONE', #69353, #60920, #34134, .T. ) ;
#51692 = EDGE_LOOP ( 'NONE', ( #34269, #16602 ) ) ;
#51694 = ORIENTED_EDGE ( 'NONE', *, *, #583, .F. ) ;
#51693 = DIRECTION ( 'NONE',  ( -0.000000000000000000, -0.1736481776669307198, -0.9848077530122080203 ) ) ;
#51695 = CARTESIAN_POINT ( 'NONE',  ( 7.596153846153846700, -7.500000000000001776, 34.75000000000000000 ) ) ;
#51696 = CARTESIAN_POINT ( 'NONE',  ( 16.21991348719623360, -8.164416787775445883, 34.95778746994558617 ) ) ;
#51697 = VECTOR ( 'NONE', #32563, 999.9999999999998863 ) ;
#51698 = CARTESIAN_POINT ( 'NONE',  ( -8.519176457592452678, -12.41262288849542017, 30.68299917996395010 ) ) ;
#51699 = DIRECTION ( 'NONE',  ( -0.000000000000000000, 0.5000000000000011102, -0.8660254037844380415 ) ) ;
#51700 = ORIENTED_EDGE ( 'NONE', *, *, #23884, .F. ) ;
#51701 = AXIS2_PLACEMENT_3D ( 'NONE', #71484, #50759, #51639 ) ;
#51702 = ORIENTED_EDGE ( 'NONE', *, *, #70344, .T. ) ;
#51703 = VECTOR ( 'NONE', #47749, 1000.000000000000000 ) ;
#51704 = ORIENTED_EDGE ( 'NONE', *, *, #26826, .F. ) ;
#51706 = EDGE_LOOP ( 'NONE', ( #40315, #66681 ) ) ;
#51705 = DIRECTION ( 'NONE',  ( -1.000000000000000000, 0.000000000000000000, -0.000000000000000000 ) ) ;
#51707 = CIRCLE ( 'NONE', #43064, 4.000000000000000000 ) ;
#51708 = CARTESIAN_POINT ( 'NONE',  ( -5.749945688361683516, -8.303483539816728154, 34.68545999027711702 ) ) ;
#51709 = ADVANCED_FACE ( 'NONE', ( #62594 ), #8112, .F. ) ;
#51710 = CARTESIAN_POINT ( 'NONE',  ( -13.63463862190834952, -6.695914987888146541, 34.68535235679833306 ) ) ;
#51711 = ORIENTED_EDGE ( 'NONE', *, *, #81891, .T. ) ;
#51712 = CARTESIAN_POINT ( 'NONE',  ( -23.50000000000000000, 16.99999999999999289, 30.36437827766147279 ) ) ;
#51713 = CARTESIAN_POINT ( 'NONE',  ( 17.07692307692295586, -4.320704448113951379, 33.92786785259630022 ) ) ;
#51714 = CARTESIAN_POINT ( 'NONE',  ( -5.934744860487159102, -3.643525952247864463, 33.31231777344670064 ) ) ;
#51715 = FACE_BOUND ( 'NONE', #19945, .T. ) ;
#51716 = CARTESIAN_POINT ( 'NONE',  ( -19.50000000000000000, -3.499999999999999556, 29.75000000000000355 ) ) ;
#51717 = CARTESIAN_POINT ( 'NONE',  ( -4.284537620513714451, -12.11776431015576172, 31.66791131148498906 ) ) ;
#51718 = CARTESIAN_POINT ( 'NONE',  ( 8.519254038288416098, -2.564618984488975517, 30.55390908950641915 ) ) ;
#51720 = CARTESIAN_POINT ( 'NONE',  ( 9.823099500132480344, -3.062576670634119758, 32.05464942895959979 ) ) ;
#51719 = CARTESIAN_POINT ( 'NONE',  ( 20.00000000000000711, -9.999999999999994671, 13.00000000000000178 ) ) ;
#51721 = CARTESIAN_POINT ( 'NONE',  ( 17.99999999999987566, -6.835583212225970762, 34.95778746994575670 ) ) ;
#51722 = CARTESIAN_POINT ( 'NONE',  ( -19.50000000000000000, -3.499999999999999556, 29.75000000000000355 ) ) ;
#51723 = ORIENTED_EDGE ( 'NONE', *, *, #61421, .T. ) ;
#51724 = CARTESIAN_POINT ( 'NONE',  ( 14.53111926955388000, -7.630147231320743018, 34.74852402298682819 ) ) ;
#51725 = CARTESIAN_POINT ( 'NONE',  ( -13.31854805126531005, -3.937682226553329556, 33.60647404775216529 ) ) ;
#51726 = ORIENTED_EDGE ( 'NONE', *, *, #35977, .T. ) ;
#51727 = VERTEX_POINT ( 'NONE', #49540 ) ;
#51729 = CARTESIAN_POINT ( 'NONE',  ( 15.23076923076923173, -2.833524468853757305, 32.15551576947925838 ) ) ;
#51728 = DIRECTION ( 'NONE',  ( 1.000000000000000000, 0.000000000000000000, 0.000000000000000000 ) ) ;
#51730 = CARTESIAN_POINT ( 'NONE',  ( 13.38461538461538680, -11.35647404775217417, 33.31231777344666511 ) ) ;
#51731 = CARTESIAN_POINT ( 'NONE',  ( -8.769230769230768274, -12.29105614889573062, 35.45975837776705220 ) ) ;
#51732 = CARTESIAN_POINT ( 'NONE',  ( -0.2114841499001479108, -11.79725096376909654, 32.30694842903960762 ) ) ;
#51733 = ORIENTED_EDGE ( 'NONE', *, *, #45747, .T. ) ;
#51734 = CARTESIAN_POINT ( 'NONE',  ( 17.07692307692307665, -1.790695186598648903, 34.54067556320373455 ) ) ;
#51735 = FACE_OUTER_BOUND ( 'NONE', #80703, .T. ) ;
#51736 = CARTESIAN_POINT ( 'NONE',  ( 7.623227628637697428, -5.667676309546437530, 34.40238873228292249 ) ) ;
#51737 = CARTESIAN_POINT ( 'NONE',  ( -12.46153846153846168, -11.16473453929635440, 33.15142922261926373 ) ) ;
#51738 = DIRECTION ( 'NONE',  ( -0.000000000000000000, 1.000000000000000000, -0.000000000000000000 ) ) ;
#51739 = AXIS2_PLACEMENT_3D ( 'NONE', #59972, #32062, #73502 ) ;
#51740 = CARTESIAN_POINT ( 'NONE',  ( 3.749999999999992006, -5.946699141100872943, 18.14062500000000711 ) ) ;
#51741 = ORIENTED_EDGE ( 'NONE', *, *, #6851, .T. ) ;
#51742 = ORIENTED_EDGE ( 'NONE', *, *, #15951, .F. ) ;
#51743 = SHAPE_REPRESENTATION ( 'BR-833', ( #74894, #4347, #83521, #5849, #84934, #54692, #1536, #46083, #7257, #15870, #17351, #66204, #56169 ), #24543 ) ;
#51744 = DIRECTION ( 'NONE',  ( -0.000000000000000000, 0.000000000000000000, 1.000000000000000000 ) ) ;
#51745 = ORIENTED_EDGE ( 'NONE', *, *, #11989, .F. ) ;
#51746 = DIRECTION ( 'NONE',  ( 1.000000000000000000, 0.000000000000000000, 0.000000000000000000 ) ) ;
#51747 = CARTESIAN_POINT ( 'NONE',  ( 17.93472999944367530, -11.67786785259541027, 32.92929555188721480 ) ) ;
#51748 = B_SPLINE_CURVE_WITH_KNOTS ( 'NONE', 3,
 ( #24879, #26223, #60889, #10932, #59555, #74409, #66314, #18137, #32525, #80740 ),
 .UNSPECIFIED., .F., .F.,
 ( 4, 2, 2, 2, 4 ),
 ( 0.000000000000000000, 0.0001954339857564054144, 0.0003908679715128108288, 0.0005863019572692162703, 0.0007817359430256216575 ),
 .UNSPECIFIED. ) ;
#51749 = CARTESIAN_POINT ( 'NONE',  ( 12.46153846153846168, -13.87047571288749737, 32.06866353760679544 ) ) ;
#51750 = CARTESIAN_POINT ( 'NONE',  ( 17.14308968351471663, -7.250054591869668386, 34.99404684341514127 ) ) ;
#51751 = CARTESIAN_POINT ( 'NONE',  ( 2.320192649118979489E-14, -11.25000000000000000, 18.53125000000000000 ) ) ;
#51752 = B_SPLINE_CURVE_WITH_KNOTS ( 'NONE', 3,
 ( #69357, #66800, #7654, #52832, #39783, #890, #62578, #83316, #11409, #80327 ),
 .UNSPECIFIED., .F., .F.,
 ( 4, 2, 2, 2, 4 ),
 ( 0.000000000000000000, 0.0001954339857564092904, 0.0003908679715128185808, 0.0005863019572692278712, 0.0007817359430256371616 ),
 .UNSPECIFIED. ) ;
#51753 = FACE_OUTER_BOUND ( 'NONE', #72735, .T. ) ;
#51754 = LINE ( 'NONE', #73389, #28766 ) ;
#51755 = ORIENTED_EDGE ( 'NONE', *, *, #82751, .F. ) ;
#51756 = DIRECTION ( 'NONE',  ( 0.000000000000000000, 0.4999999999999985567, 0.8660254037844395958 ) ) ;
#51758 = ORIENTED_EDGE ( 'NONE', *, *, #71630, .T. ) ;
#51757 = LINE ( 'NONE', #60758, #43894 ) ;
#51759 = FACE_OUTER_BOUND ( 'NONE', #12901, .T. ) ;
#51760 = CARTESIAN_POINT ( 'NONE',  ( -9.942284423250045577, -12.17611988154120972, 31.52148481390971213 ) ) ;
#51761 = DIRECTION ( 'NONE',  ( 0.000000000000000000, 0.6427876096865368094, 0.7660444431189802339 ) ) ;
#51762 = DIRECTION ( 'NONE',  ( 0.000000000000000000, 0.000000000000000000, -1.000000000000000000 ) ) ;
#51763 = CARTESIAN_POINT ( 'NONE',  ( -0.3310127597748993566, -11.46989282347013095, 32.79007818306219946 ) ) ;
#51764 = CARTESIAN_POINT ( 'NONE',  ( -4.376772371362300795, -9.086856451489516928, 34.49173150075333183 ) ) ;
#51765 = DIRECTION ( 'NONE',  ( -1.000000000000000000, 0.000000000000000000, -0.000000000000000000 ) ) ;
#51766 = CARTESIAN_POINT ( 'NONE',  ( -3.724691934501248802, -5.885600066136383646, 19.17374329374151642 ) ) ;
#51767 = ORIENTED_EDGE ( 'NONE', *, *, #19496, .F. ) ;
#51768 = CARTESIAN_POINT ( 'NONE',  ( 11.76147289007438701, -11.76359900205217635, 32.36225158514719880 ) ) ;
#51769 = CARTESIAN_POINT ( 'NONE',  ( 1.253923917947827205, -5.582088688514999397, 34.36776431015576350 ) ) ;
#51770 = CARTESIAN_POINT ( 'NONE',  ( 14.30769230769231015, -1.951392089020283160, 34.73218667398347748 ) ) ;
#51771 = CARTESIAN_POINT ( 'NONE',  ( 1.200186371490529202, -4.775308065498752974, 13.23624329374151465 ) ) ;
#51772 = AXIS2_PLACEMENT_3D ( 'NONE', #57383, #71785, #70469 ) ;
#51773 = CARTESIAN_POINT ( 'NONE',  ( 0.4615384615383382183, -5.941354392335915335, 34.76329471203413846 ) ) ;
#51774 = DIRECTION ( 'NONE',  ( 1.000000000000000000, 0.000000000000000000, 0.000000000000000000 ) ) ;
#51776 = VERTEX_POINT ( 'NONE', #469 ) ;
#51775 = CARTESIAN_POINT ( 'NONE',  ( -14.30769230769242739, -10.90142922262034020, 33.41473453929536674 ) ) ;
#51777 = CARTESIAN_POINT ( 'NONE',  ( 1.139087296525997051, -4.749999999999992895, 16.73437500000000000 ) ) ;
#51778 = CARTESIAN_POINT ( 'NONE',  ( -1.161602540521989635, -12.38742843783360748, 31.66772728687926985 ) ) ;
#51779 = VECTOR ( 'NONE', #53566, 1000.000000000000227 ) ;
#51780 = ORIENTED_EDGE ( 'NONE', *, *, #21717, .F. ) ;
#51781 = CYLINDRICAL_SURFACE ( 'NONE', #84584, 0.2500000000000008882 ) ;
#51782 = ORIENTED_EDGE ( 'NONE', *, *, #86278, .T. ) ;
#51783 = CARTESIAN_POINT ( 'NONE',  ( -13.13461538461396394, -7.500000000000154543, 35.00000000000007105 ) ) ;
#51784 = CARTESIAN_POINT ( 'NONE',  ( 3.230769230769110045, -10.21337939537710326, 33.94971097300076224 ) ) ;
#51785 = CARTESIAN_POINT ( 'NONE',  ( -0.3954711281883860896, -6.343179335718452272, 34.87096338111212646 ) ) ;
#51786 = EDGE_LOOP ( 'NONE', ( #35107, #77527, #45396, #70718 ) ) ;
#51787 = CARTESIAN_POINT ( 'NONE',  ( -0.5267883933125464546, -2.255955759149247619, 30.00000000000013856 ) ) ;
#51788 = VERTEX_POINT ( 'NONE', #28374 ) ;
#51789 = LINE ( 'NONE', #31544, #47007 ) ;
#51790 = B_SPLINE_CURVE_WITH_KNOTS ( 'NONE', 3,
 ( #37310, #39116, #64778, #30559, #58031, #40451, #53943, #61136, #39568, #87762 ),
 .UNSPECIFIED., .F., .F.,
 ( 4, 2, 2, 2, 4 ),
 ( 0.000000000000000000, 0.0001954311564186872268, 0.0003908623128373744536, 0.0005862934692560616261, 0.0007817246256747489071 ),
 .UNSPECIFIED. ) ;
#51791 = EDGE_CURVE ( 'NONE', #19576, #11048, #28905, .T. ) ;
#51792 = VERTEX_POINT ( 'NONE', #41452 ) ;
#51793 = DIRECTION ( 'NONE',  ( -0.000000000000000000, -0.7660444431189791237, -0.6427876096865379196 ) ) ;
#51794 = CARTESIAN_POINT ( 'NONE',  ( 10.61538461538449596, -4.481592998941358097, 33.73612834414048933 ) ) ;
#51795 = B_SPLINE_CURVE_WITH_KNOTS ( 'NONE', 3,
 ( #31503, #17998, #85124, #84692, #25191, #38706, #66167, #31956, #67074, #61184 ),
 .UNSPECIFIED., .F., .F.,
 ( 4, 2, 2, 2, 4 ),
 ( 0.0007817359430256390048, 0.0009771253907250078159, 0.001172514838424376735, 0.001367904286123745655, 0.001563293733823114574 ),
 .UNSPECIFIED. ) ;
#51796 = ORIENTED_EDGE ( 'NONE', *, *, #81305, .F. ) ;
#51797 = PRODUCT_RELATED_PRODUCT_CATEGORY ( 'part', '', ( #54864 ) ) ;
#51798 = LINE ( 'NONE', #72089, #24618 ) ;
#51799 = DIRECTION ( 'NONE',  ( 0.000000000000000000, 0.6427876096865373645, -0.7660444431189797898 ) ) ;
#51800 = CARTESIAN_POINT ( 'NONE',  ( -3.230769230769229949, -6.189225973068211317, 35.74407628777942847 ) ) ;
#51801 = CYLINDRICAL_SURFACE ( 'NONE', #59307, 0.2499999999999973355 ) ;
#51802 = CYLINDRICAL_SURFACE ( 'NONE', #57987, 0.2499999999999993616 ) ;
#51803 = ORIENTED_EDGE ( 'NONE', *, *, #13142, .F. ) ;
#51804 = VERTEX_POINT ( 'NONE', #68915 ) ;
#51805 = EDGE_CURVE ( 'NONE', #63541, #17157, #42350, .T. ) ;
#51806 = EDGE_LOOP ( 'NONE', ( #29781, #12417, #61696, #65569 ) ) ;
#51808 = EDGE_LOOP ( 'NONE', ( #24614, #2286, #84, #77845, #6862, #85928 ) ) ;
#51807 = CARTESIAN_POINT ( 'NONE',  ( -3.903791733932699515, -8.346898887586323923, 34.93166121998716278 ) ) ;
#51809 = DIRECTION ( 'NONE',  ( -0.000000000000000000, -0.9848077530122086864, -0.1736481776669273613 ) ) ;
#51810 = CARTESIAN_POINT ( 'NONE',  ( -10.61538461538461320, -8.973038597847269315, 34.52809138561121927 ) ) ;
#51811 = ORIENTED_EDGE ( 'NONE', *, *, #82535, .F. ) ;
#51812 = ORIENTED_EDGE ( 'NONE', *, *, #80536, .F. ) ;
#51813 = ORIENTED_EDGE ( 'NONE', *, *, #21616, .T. ) ;
#51814 = CARTESIAN_POINT ( 'NONE',  ( 16.94677586748485965, -4.460286881179643004, 33.72017969459903242 ) ) ;
#51815 = EDGE_LOOP ( 'NONE', ( #78618, #56772, #64719, #39354 ) ) ;
#51816 = CARTESIAN_POINT ( 'NONE',  ( 2.372947878968333146, -4.481592998940250538, 33.73612834413965089 ) ) ;
#51817 = ADVANCED_FACE ( 'NONE', ( #15314 ), #7227, .F. ) ;
#51818 = B_SPLINE_CURVE_WITH_KNOTS ( 'NONE', 3,
 ( #34037, #34918, #1588, #68710, #47547, #75913, #21854, #27281, #20522, #696 ),
 .UNSPECIFIED., .F., .F.,
 ( 4, 2, 2, 2, 4 ),
 ( 0.0007817359527651133143, 0.0009771254036996530456, 0.001172514854634192777, 0.001367904305568732291, 0.001563293756503272023 ),
 .UNSPECIFIED. ) ;
#51819 = B_SPLINE_CURVE_WITH_KNOTS ( 'NONE', 3,
 ( #71899, #72341, #24153, #18747, #31821, #45311, #25498, #80453, #73700, #52069 ),
 .UNSPECIFIED., .F., .F.,
 ( 4, 2, 2, 2, 4 ),
 ( 0.000000000000000000, 0.0001954311564186865763, 0.0003908623128373731525, 0.0005862934692560596746, 0.0007817246256747463051 ),
 .UNSPECIFIED. ) ;
#51820 = AXIS2_PLACEMENT_3D ( 'NONE', #25054, #18750, #74580 ) ;
#51821 = CARTESIAN_POINT ( 'NONE',  ( 17.07692307692307665, -11.16473453929635440, 33.15142922261926373 ) ) ;
#51822 = CARTESIAN_POINT ( 'NONE',  ( -11.28840711854808632, -12.01375889529407281, 32.43194544308182969 ) ) ;
#51823 = FACE_BOUND ( 'NONE', #45826, .T. ) ;
#51826 = VERTEX_POINT ( 'NONE', #27936 ) ;
#51825 = EDGE_CURVE ( 'NONE', #27494, #85233, #29277, .T. ) ;
#51824 = B_SPLINE_CURVE_WITH_KNOTS ( 'NONE', 3,
 ( #30281, #84799, #23080, #3682, #86121, #85229, #79806, #23509, #79356, #9558 ),
 .UNSPECIFIED., .F., .F.,
 ( 4, 2, 2, 2, 4 ),
 ( 0.000000000000000000, 0.0001954311564186872268, 0.0003908623128373744536, 0.0005862934692560616261, 0.0007817246256747489071 ),
 .UNSPECIFIED. ) ;
#51827 = DIRECTION ( 'NONE',  ( 1.000000000000000000, 0.000000000000000000, 0.000000000000000000 ) ) ;
#51828 = CARTESIAN_POINT ( 'NONE',  ( 12.52679403281448423, -6.026961402152789304, 34.52809138561124769 ) ) ;
#51829 = AXIS2_PLACEMENT_3D ( 'NONE', #41908, #53636, #81124 ) ;
#51830 = ADVANCED_FACE ( 'NONE', ( #82891 ), #48639, .F. ) ;
#51831 = CARTESIAN_POINT ( 'NONE',  ( 7.846153846153846700, -11.11383981884818262, 36.00935417666054406 ) ) ;
#51832 = DIRECTION ( 'NONE',  ( -0.000000000000000000, 0.9848077530122085754, -0.1736481776669273613 ) ) ;
#51833 = CYLINDRICAL_SURFACE ( 'NONE', #53387, 0.2500000000000004996 ) ;
#51834 = VERTEX_POINT ( 'NONE', #30581 ) ;
#51835 = CARTESIAN_POINT ( 'NONE',  ( -17.30040802064702987, -12.44517049084099725, 30.48991314939691932 ) ) ;
#51836 = ORIENTED_EDGE ( 'NONE', *, *, #42077, .T. ) ;
#51837 = VECTOR ( 'NONE', #9643, 1000.000000000000000 ) ;
#51838 = EDGE_LOOP ( 'NONE', ( #58176, #79926, #18140, #45930, #8949, #85664 ) ) ;
#51839 = VECTOR ( 'NONE', #14206, 1000.000000000000000 ) ;
#51841 = LINE ( 'NONE', #43770, #3071 ) ;
#51840 = CARTESIAN_POINT ( 'NONE',  ( 5.869852030268307708, -12.15440758774515473, 32.17923288041532004 ) ) ;
#51842 = DIRECTION ( 'NONE',  ( -0.000000000000000000, -0.7660444431189791237, -0.6427876096865379196 ) ) ;
#51843 = CARTESIAN_POINT ( 'NONE',  ( -13.60754234352223335, -2.889293201056495786, 32.26117774369186009 ) ) ;
#51844 = CARTESIAN_POINT ( 'NONE',  ( 1.515141086378947621, -10.19071101563364756, 33.96452234770658407 ) ) ;
#51845 = CARTESIAN_POINT ( 'NONE',  ( 14.05766908347085220, -2.985938066672154445, 32.43141759479405550 ) ) ;
#51846 = VERTEX_POINT ( 'NONE', #16622 ) ;
#51847 = CARTESIAN_POINT ( 'NONE',  ( 6.923076923076924238, -2.486705287966279876, 31.30864560766543647 ) ) ;
#51848 = CARTESIAN_POINT ( 'NONE',  ( -0.3954711281883869778, -3.322132147404560865, 32.92929555188719348 ) ) ;
#51849 = CARTESIAN_POINT ( 'NONE',  ( -1.608100328339333807, -3.754499324213721234, 33.06261337010820256 ) ) ;
#51850 = DIRECTION ( 'NONE',  ( 0.000000000000000000, 0.7660444431189822323, -0.6427876096865344779 ) ) ;
#51851 = ORIENTED_EDGE ( 'NONE', *, *, #34392, .F. ) ;
#51852 = ORIENTED_EDGE ( 'NONE', *, *, #19517, .F. ) ;
#51853 = FACE_BOUND ( 'NONE', #59015, .T. ) ;
#51854 = APPLICATION_PROTOCOL_DEFINITION ( 'draft international standard', 'automotive_design', 1998, #19322 ) ;
#51855 = ORIENTED_EDGE ( 'NONE', *, *, #20804, .F. ) ;
#51856 = CARTESIAN_POINT ( 'NONE',  ( -13.38461538461550759, -2.379036618888197729, 30.90682066428292885 ) ) ;
#51857 = CARTESIAN_POINT ( 'NONE',  ( -14.30769230769242739, -11.48612834414049644, 32.76840700105863391 ) ) ;
#51858 = ORIENTED_EDGE ( 'NONE', *, *, #32932, .F. ) ;
#51859 = DIRECTION ( 'NONE',  ( 0.000000000000000000, 0.000000000000000000, 1.000000000000000000 ) ) ;
#51860 = CARTESIAN_POINT ( 'NONE',  ( 6.673053685783957967, -10.76384336483936011, 33.53834819971076087 ) ) ;
#51861 = CARTESIAN_POINT ( 'NONE',  ( -8.703162418228330921, -6.386643153685127139, 34.62446782046654192 ) ) ;
#51862 = FACE_OUTER_BOUND ( 'NONE', #11497, .T. ) ;
#51863 = B_SPLINE_CURVE_WITH_KNOTS ( 'NONE', 3,
 ( #23011, #17596, #18483, #30648, #64869, #80184 ),
 .UNSPECIFIED., .F., .F.,
 ( 4, 2, 4 ),
 ( 4.220987180333913997E-17, 0.0001954756301637137399, 0.0003909512603273853043 ),
 .UNSPECIFIED. ) ;
#51864 = LINE ( 'NONE', #4131, #41747 ) ;
#51865 = EDGE_LOOP ( 'NONE', ( #67114, #39987, #49656, #56255, #30341, #3666, #36950, #81606, #25947, #62467, #34987, #81507, #27506, #56263, #14061, #73962, #19803, #40786, #58174, #15089, #39018, #53288, #64582, #9169, #58350, #27166, #54527, #53757, #37844, #4843, #53634, #43200, #45219, #32644, #2743, #74226, #24139, #10746, #75928, #52779, #64883, #41164, #56923, #9261, #7331, #47538, #71693, #2431, #86682, #7092, #25014, #58739, #57951, #45820, #33286, #42924, #53652, #352, #60233, #14787, #36490, #15617, #7854, #26226, #15079, #77960, #29562, #79206, #23347, #52179, #74778, #48535, #10642, #23402, #78860, #68288, #53135, #18679, #26266, #25751, #8397, #76325, #18385, #24334, #37344, #20569, #88182, #74956, #39435, #27995, #33127, #70652, #66164, #33788, #60012, #12988, #444, #8398, #63515, #49412, #85143, #34989, #56681, #45081, #55899, #82105, #80727, #74651, #43834, #12362, #54966, #73073, #87080, #45983, #42158, #24564, #9517, #43539, #27185, #20366, #87982, #87662, #52596, #54371 ) ) ;
#51867 = VERTEX_POINT ( 'NONE', #38235 ) ;
#51866 = CARTESIAN_POINT ( 'NONE',  ( 23.00000000000000000, -5.499999999999982236, 27.75000000000000000 ) ) ;
#51868 = DIRECTION ( 'NONE',  ( -0.000000000000000000, 0.5000000000000011102, -0.8660254037844380415 ) ) ;
#51869 = CARTESIAN_POINT ( 'NONE',  ( 15.00784227186237807, -4.762599654559228846, 34.23009711892697737 ) ) ;
#51870 = CARTESIAN_POINT ( 'NONE',  ( -3.230769230769229949, -8.564572088678739092, 35.78748833219616898 ) ) ;
#51871 = EDGE_CURVE ( 'NONE', #30893, #59397, #68600, .T. ) ;
#51872 = CARTESIAN_POINT ( 'NONE',  ( -10.83831157429146330, -3.395401636524185474, 33.02366814457250399 ) ) ;
#51873 = DIRECTION ( 'NONE',  ( 0.000000000000000000, -6.938893903907222067E-15, 1.000000000000000000 ) ) ;
#51874 = CARTESIAN_POINT ( 'NONE',  ( 12.23861150263161335, -5.582147617184174848, 34.63737895849758530 ) ) ;
#51875 = AXIS2_PLACEMENT_3D ( 'NONE', #69197, #62421, #82279 ) ;
#51876 = CARTESIAN_POINT ( 'NONE',  ( 1.987747218494642309, -5.598659921968629050, 17.06436829374151287 ) ) ;
#51877 = ORIENTED_EDGE ( 'NONE', *, *, #61408, .F. ) ;
#51878 = LINE ( 'NONE', #18123, #37312 ) ;
#51879 = CARTESIAN_POINT ( 'NONE',  ( 2.557746727605761272, -4.074993327901525575, 33.72946981652012255 ) ) ;
#51880 = DIRECTION ( 'NONE',  ( -1.000000000000000000, -2.891205793294678326E-16, 0.000000000000000000 ) ) ;
#51881 = VERTEX_POINT ( 'NONE', #31021 ) ;
#51882 = ORIENTED_EDGE ( 'NONE', *, *, #61888, .T. ) ;
#51883 = CARTESIAN_POINT ( 'NONE',  ( -5.999999999999998224, -12.62096338111211580, 30.90682066428153263 ) ) ;
#51884 = CARTESIAN_POINT ( 'NONE',  ( -14.08467946359890988, -2.523321265292115534, 31.42251411153756990 ) ) ;
#51885 = CYLINDRICAL_SURFACE ( 'NONE', #41841, 0.2500000000000009437 ) ;
#51886 = ADVANCED_FACE ( 'NONE', ( #70696 ), #17527, .F. ) ;
#51887 = DIRECTION ( 'NONE',  ( -0.000000000000000000, -0.9848077530122085754, -0.1736481776669273613 ) ) ;
#51888 = DIRECTION ( 'NONE',  ( 1.000000000000000000, 0.000000000000000000, 0.000000000000000000 ) ) ;
#51889 = DIRECTION ( 'NONE',  ( 1.000000000000000000, 0.000000000000000000, 0.000000000000000000 ) ) ;
#51890 = CARTESIAN_POINT ( 'NONE',  ( 5.869852790561781219, -8.587444163452046197, 34.63053765926554206 ) ) ;
#51891 = ORIENTED_EDGE ( 'NONE', *, *, #20514, .F. ) ;
#51892 = DIRECTION ( 'NONE',  ( -0.000000000000000000, -0.3420201433256694346, -0.9396926207859080948 ) ) ;
#51893 = CARTESIAN_POINT ( 'NONE',  ( -17.14300648787895653, -12.10708131394839349, 31.69288490824020244 ) ) ;
#51894 = VECTOR ( 'NONE', #72241, 1000.000000000000000 ) ;
#51895 = CARTESIAN_POINT ( 'NONE',  ( -3.230769230769229949, -9.058645607665452459, 34.76329471203371924 ) ) ;
#51896 = AXIS2_PLACEMENT_3D ( 'NONE', #83381, #83831, #71175 ) ;
#51897 = CARTESIAN_POINT ( 'NONE',  ( 17.07692307692307665, -8.973038597847269315, 34.52809138561121927 ) ) ;
#51898 = ORIENTED_EDGE ( 'NONE', *, *, #13978, .T. ) ;
#51899 = CARTESIAN_POINT ( 'NONE',  ( 13.60762673622823726, -6.503523203565941380, 34.64991518177335195 ) ) ;
#51900 = PRODUCT_RELATED_PRODUCT_CATEGORY ( 'part', '', ( #8899 ) ) ;
#51901 = AXIS2_PLACEMENT_3D ( 'NONE', #4272, #19564, #47026 ) ;
#51902 = VECTOR ( 'NONE', #33273, 999.9999999999998863 ) ;
#51903 = ADVANCED_FACE ( 'NONE', ( #22943 ), #17073, .F. ) ;
#51904 = ORIENTED_EDGE ( 'NONE', *, *, #49505, .F. ) ;
#51905 = CARTESIAN_POINT ( 'NONE',  ( 12.46153846153846168, -9.058645607665452459, 34.76329471203371924 ) ) ;
#51906 = CARTESIAN_POINT ( 'NONE',  ( 10.48523664565292179, -3.625366637846545892, 33.29286588640298561 ) ) ;
#51907 = CARTESIAN_POINT ( 'NONE',  ( 17.74997677577853850, -10.18141759479407327, 34.26406193332782379 ) ) ;
#51908 = ORIENTED_EDGE ( 'NONE', *, *, #28640, .T. ) ;
#51909 = EDGE_CURVE ( 'NONE', #17639, #8057, #48173, .T. ) ;
#51910 = CARTESIAN_POINT ( 'NONE',  ( -11.53846153846153655, -2.292212530054420494, 30.41441678777542634 ) ) ;
#51911 = CARTESIAN_POINT ( 'NONE',  ( 12.59206389977210705, -11.04252011169590020, 33.62494198852677130 ) ) ;
#51912 = CARTESIAN_POINT ( 'NONE',  ( -39.05038313613820122, -2.499999999999999556, 29.75000000000000355 ) ) ;
#51913 = AXIS2_PLACEMENT_3D ( 'NONE', #41366, #68830, #7136 ) ;
#51914 = DIRECTION ( 'NONE',  ( -0.000000000000000000, -0.9396926207859093161, -0.3420201433256663259 ) ) ;
#51915 = CARTESIAN_POINT ( 'NONE',  ( -2.980714919130914797, -12.41262288849542017, 30.68299917996395010 ) ) ;
#51916 = B_SPLINE_CURVE_WITH_KNOTS ( 'NONE', 3,
 ( #71685, #38357, #11325, #38806, #66718, #66266, #4570, #87014, #25286, #52748 ),
 .UNSPECIFIED., .F., .F.,
 ( 4, 2, 2, 2, 4 ),
 ( 0.000000000000000000, 0.0001954339857564074202, 0.0003908679715128148403, 0.0005863019572692222334, 0.0007817359430256296806 ),
 .UNSPECIFIED. ) ;
#51917 = ORIENTED_EDGE ( 'NONE', *, *, #3518, .F. ) ;
#51918 = EDGE_CURVE ( 'NONE', #18937, #5324, #13725, .T. ) ;
#51919 = CARTESIAN_POINT ( 'NONE',  ( 16.37685899793954292, -10.01129605718032423, 34.36064277460058491 ) ) ;
#51920 = ORIENTED_EDGE ( 'NONE', *, *, #3481, .T. ) ;
#51921 = CARTESIAN_POINT ( 'NONE',  ( -11.53846153846153655, -3.937682226553329556, 33.60647404775216529 ) ) ;
#51922 = CARTESIAN_POINT ( 'NONE',  ( -10.36538461538460965, -2.499999999999999556, 29.81604066197449754 ) ) ;
#51923 = ADVANCED_FACE ( 'NONE', ( #9871 ), #58485, .F. ) ;
#51924 = CARTESIAN_POINT ( 'NONE',  ( -0.4615384615385840772, -2.657715359629662544, 31.77849191805970364 ) ) ;
#51925 = CARTESIAN_POINT ( 'NONE',  ( 9.757562831820530747, -2.657715359629132301, 31.77849191805844242 ) ) ;
#51926 = EDGE_CURVE ( 'NONE', #57710, #5662, #81540, .T. ) ;
#51927 = DIRECTION ( 'NONE',  ( -0.000000000000000000, -0.8660254037844397068, -0.4999999999999978906 ) ) ;
#51928 = CARTESIAN_POINT ( 'NONE',  ( 15.23076923076923173, -11.69971097300155272, 32.46337939537588113 ) ) ;
#51929 = ORIENTED_EDGE ( 'NONE', *, *, #77180, .T. ) ;
#51930 = ORIENTED_EDGE ( 'NONE', *, *, #79510, .F. ) ;
#51931 = ORIENTED_EDGE ( 'NONE', *, *, #27866, .T. ) ;
#51932 = ORIENTED_EDGE ( 'NONE', *, *, #75105, .F. ) ;
#51933 = ORIENTED_EDGE ( 'NONE', *, *, #71141, .F. ) ;
#51934 = ADVANCED_FACE ( 'NONE', ( #37334 ), #23380, .F. ) ;
#51935 = CARTESIAN_POINT ( 'NONE',  ( -12.68440472460156521, -2.251424796025575326, 29.88072029997477586 ) ) ;
#51936 = CARTESIAN_POINT ( 'NONE',  ( -9.320512820512821150, -7.500000000000000000, 33.75000000000000000 ) ) ;
#51937 = AXIS2_PLACEMENT_3D ( 'NONE', #61304, #54553, #13578 ) ;
#51938 = CARTESIAN_POINT ( 'NONE',  ( -10.54931728203453822, -4.661471528628508665, 34.16647553114624003 ) ) ;
#51939 = CARTESIAN_POINT ( 'NONE',  ( -5.869208192175213945, -4.809403383903225304, 33.96459661697924304 ) ) ;
#51940 = CARTESIAN_POINT ( 'NONE',  ( -13.38461538461538325, -3.322132147404559976, 32.92929555188717927 ) ) ;
#51941 = CARTESIAN_POINT ( 'NONE',  ( -12.71151520558705350, -12.41104346484419452, 31.60698883733904196 ) ) ;
#51942 = EDGE_CURVE ( 'NONE', #20277, #12856, #32078, .T. ) ;
#51943 = LINE ( 'NONE', #23591, #66701 ) ;
#51944 = EDGE_CURVE ( 'NONE', #56137, #43657, #58860, .T. ) ;
#51945 = CARTESIAN_POINT ( 'NONE',  ( 17.07692307692339284, -2.255955759149395501, 30.00000000000324363 ) ) ;
#51946 = DIRECTION ( 'NONE',  ( 0.000000000000000000, 0.000000000000000000, -1.000000000000000000 ) ) ;
#51947 = ORIENTED_EDGE ( 'NONE', *, *, #87746, .F. ) ;
#51948 = ORIENTED_EDGE ( 'NONE', *, *, #29946, .F. ) ;
#51949 = ORIENTED_EDGE ( 'NONE', *, *, #61708, .T. ) ;
#51951 = VERTEX_POINT ( 'NONE', #53518 ) ;
#51950 = CARTESIAN_POINT ( 'NONE',  ( 0.2380535369741276219, -3.019605429927184836, 32.48692288466676814 ) ) ;
#51953 = DIRECTION ( 'NONE',  ( -0.000000000000000000, -0.1736481776669307198, -0.9848077530122080203 ) ) ;
#51952 = CARTESIAN_POINT ( 'NONE',  ( 7.716006636715626144, -3.285722584762969856, 32.44110544564090759 ) ) ;
#51954 = CARTESIAN_POINT ( 'NONE',  ( -1.254570328695612247, -2.254550872974306674, 29.97347326024527447 ) ) ;
#51955 = LINE ( 'NONE', #17751, #72435 ) ;
#51956 = FACE_BOUND ( 'NONE', #44634, .T. ) ;
#51957 = EDGE_LOOP ( 'NONE', ( #69043, #63573 ) ) ;
#51958 = AXIS2_PLACEMENT_3D ( 'NONE', #45685, #4710, #12792 ) ;
#51959 = ORIENTED_EDGE ( 'NONE', *, *, #68209, .F. ) ;
#51960 = DIRECTION ( 'NONE',  ( 1.000000000000000000, 0.000000000000000000, 0.000000000000000000 ) ) ;
#51961 = ORIENTED_EDGE ( 'NONE', *, *, #42519, .T. ) ;
#51962 = FACE_BOUND ( 'NONE', #62931, .T. ) ;
#51964 = AXIS2_PLACEMENT_3D ( 'NONE', #5006, #24819, #66250 ) ;
#51963 = CARTESIAN_POINT ( 'NONE',  ( 13.63456079399342791, -12.45601412856602686, 31.48342859153981621 ) ) ;
#51965 = DIRECTION ( 'NONE',  ( 0.000000000000000000, 0.8660254037844377084, -0.5000000000000015543 ) ) ;
#51966 = ORIENTED_EDGE ( 'NONE', *, *, #60778, .T. ) ;
#51967 = CARTESIAN_POINT ( 'NONE',  ( 14.30769230769218758, -2.892918686052165622, 31.69288490824153470 ) ) ;
#51968 = DIRECTION ( 'NONE',  ( 0.000000000000000000, 0.000000000000000000, -1.000000000000000000 ) ) ;
#51969 = CYLINDRICAL_SURFACE ( 'NONE', #40745, 0.2500000000000009437 ) ;
#51970 = ORIENTED_EDGE ( 'NONE', *, *, #88306, .T. ) ;
#51971 = CARTESIAN_POINT ( 'NONE',  ( 12.46153846153833911, -5.219633306517616589, 34.19971097300220464 ) ) ;
#51972 = CARTESIAN_POINT ( 'NONE',  ( 16.15384615384603251, -11.94971097300221174, 32.03036669348237098 ) ) ;
#51973 = VERTEX_POINT ( 'NONE', #24722 ) ;
#51974 = VECTOR ( 'NONE', #51361, 1000.000000000000000 ) ;
#51975 = CARTESIAN_POINT ( 'NONE',  ( 5.750000000000003553, -7.433932668274256805, 35.00000000000000711 ) ) ;
#51976 = PLANE ( 'NONE',  #72932 ) ;
#51977 = ORIENTED_EDGE ( 'NONE', *, *, #53523, .F. ) ;
#51978 = DIRECTION ( 'NONE',  ( -0.000000000000000000, -0.000000000000000000, -1.000000000000000000 ) ) ;
#51979 = CARTESIAN_POINT ( 'NONE',  ( 13.25392391794783009, -2.541943142973491554, 30.39792223712631980 ) ) ;
#51980 = DIRECTION ( 'NONE',  ( -0.000000000000000000, -0.6427876096865404731, -0.7660444431189770143 ) ) ;
#51981 = CARTESIAN_POINT ( 'NONE',  ( 15.23076923076923173, -12.62096338111211580, 30.90682066428153263 ) ) ;
#51982 = CARTESIAN_POINT ( 'NONE',  ( 9.626225312947559232, -12.34228464037088280, 31.77849191805838558 ) ) ;
#51983 = ADVANCED_FACE ( 'NONE', ( #74249 ), #81014, .F. ) ;
#51984 = CARTESIAN_POINT ( 'NONE',  ( -16.15384615384615330, -12.09954503811598769, 35.62045528018868623 ) ) ;
#51986 = CARTESIAN_POINT ( 'NONE',  ( -0.4615384615384611200, -11.69971097300155272, 32.46337939537588113 ) ) ;
#51985 = CARTESIAN_POINT ( 'NONE',  ( -1.634592115557736092, -2.779195860258146134, 31.39871582349836032 ) ) ;
#51987 = CARTESIAN_POINT ( 'NONE',  ( -0.4615384615385840772, -8.656820664282941280, 34.87096338111179961 ) ) ;
#51989 = CARTESIAN_POINT ( 'NONE',  ( -10.74553182482283198, -8.587444163452046197, 34.63053765926554206 ) ) ;
#51988 = CARTESIAN_POINT ( 'NONE',  ( -5.076923076923197442, -9.442884908241554243, 34.35708131394783038 ) ) ;
#51990 = EDGE_CURVE ( 'NONE', #10982, #25678, #20274, .T. ) ;
#51991 = CARTESIAN_POINT ( 'NONE',  ( 2.749999999999995115, -6.360912703473971419, 14.39062500000000178 ) ) ;
#51993 = EDGE_CURVE ( 'NONE', #54682, #88786, #40475, .T. ) ;
#51992 = VERTEX_POINT ( 'NONE', #26505 ) ;
#51994 = CARTESIAN_POINT ( 'NONE',  ( 0.4615384615383396616, -12.46129190930018460, 30.37095296980731973 ) ) ;
#51995 = ORIENTED_EDGE ( 'NONE', *, *, #44715, .T. ) ;
#51996 = EDGE_CURVE ( 'NONE', #39467, #8676, #33266, .T. ) ;
#51997 = ORIENTED_EDGE ( 'NONE', *, *, #3523, .F. ) ;
#51998 = CARTESIAN_POINT ( 'NONE',  ( -2.057746789344164107, -12.43552623307873972, 30.55307653245132826 ) ) ;
#51999 = ORIENTED_EDGE ( 'NONE', *, *, #69804, .F. ) ;
#52000 = CARTESIAN_POINT ( 'NONE',  ( -15.16551365949320740, -6.026961402152789304, 34.52809138561124769 ) ) ;
#52001 = CARTESIAN_POINT ( 'NONE',  ( 1.901340078031349856, -5.512252781505337929, 26.56063170625849068 ) ) ;
#52002 = CARTESIAN_POINT ( 'NONE',  ( 2.980792486720640344, -2.318417181685854533, 30.59732222474233865 ) ) ;
#52003 = CARTESIAN_POINT ( 'NONE',  ( 5.777073782483853392, -11.24512374952581872, 33.06303171183252942 ) ) ;
#52004 = DIRECTION ( 'NONE',  ( -0.000000000000000000, 1.000000000000000000, -0.000000000000000000 ) ) ;
#52005 = CARTESIAN_POINT ( 'NONE',  ( -12.46153846153858424, -4.320704448113951379, 33.92786785259630022 ) ) ;
#52006 = EDGE_CURVE ( 'NONE', #64208, #38006, #27762, .T. ) ;
#52007 = CARTESIAN_POINT ( 'NONE',  ( -10.36533019547116474, -3.435999193479609914, 33.07426656108010832 ) ) ;
#52008 = CARTESIAN_POINT ( 'NONE',  ( 20.00000000000000000, -4.000000000000000000, 29.75000000000000355 ) ) ;
#52009 = FACE_OUTER_BOUND ( 'NONE', #47059, .T. ) ;
#52010 = VECTOR ( 'NONE', #21405, 1000.000000000000000 ) ;
#52011 = CARTESIAN_POINT ( 'NONE',  ( -1.553300858899125059, -3.750000000000009326, 21.57812500000000355 ) ) ;
#52012 = B_SPLINE_CURVE_WITH_KNOTS ( 'NONE', 3,
 ( #23567, #21802, #84403, #51016, #71748, #57357, #78510, #70439, #29896, #16809 ),
 .UNSPECIFIED., .F., .F.,
 ( 4, 2, 2, 2, 4 ),
 ( 0.0007817246256747434861, 0.0009771112852218859484, 0.001172497944769028411, 0.001367884604316171090, 0.001563271263863313552 ),
 .UNSPECIFIED. ) ;
#52013 = LINE ( 'NONE', #64187, #30468 ) ;
#52014 = DIRECTION ( 'NONE',  ( 0.000000000000000000, 0.1736481776669275834, 0.9848077530122086864 ) ) ;
#52015 = B_SPLINE_CURVE_WITH_KNOTS ( 'NONE', 3,
 ( #70209, #62550, #35989, #63444, #863, #14832, #48598, #41413, #7181, #14375 ),
 .UNSPECIFIED., .F., .F.,
 ( 4, 2, 2, 2, 4 ),
 ( 0.0007817246256747491240, 0.0009771112852218931041, 0.001172497944769036867, 0.001367884604316180631, 0.001563271263863324611 ),
 .UNSPECIFIED. ) ;
#52016 = VECTOR ( 'NONE', #42177, 1000.000000000000000 ) ;
#52017 = CARTESIAN_POINT ( 'NONE',  ( 14.30769230769231015, -13.37000171582298513, 34.34916445242398453 ) ) ;
#52018 = B_SPLINE_CURVE_WITH_KNOTS ( 'NONE', 3,
 ( #81456, #4904, #53964, #18854, #67932, #32368, #60721, #4442, #31928, #87332 ),
 .UNSPECIFIED., .F., .F.,
 ( 4, 2, 2, 2, 4 ),
 ( 0.000000000000000000, 0.0001954311564186865492, 0.0003908623128373730983, 0.0005862934692560596746, 0.0007817246256747461966 ),
 .UNSPECIFIED. ) ;
#52019 = EDGE_LOOP ( 'NONE', ( #27804, #4222 ) ) ;
#52020 = EDGE_LOOP ( 'NONE', ( #78280, #1607, #19466, #85208 ) ) ;
#52021 = DIRECTION ( 'NONE',  ( 0.000000000000000000, 0.000000000000000000, 1.000000000000000000 ) ) ;
#52022 = LINE ( 'NONE', #38073, #84862 ) ;
#52023 = CARTESIAN_POINT ( 'NONE',  ( 1.326923076923075762, -3.499999999999999556, 29.75000000000000355 ) ) ;
#52024 = CARTESIAN_POINT ( 'NONE',  ( -15.93106661257773915, -12.44528174975671853, 30.48912976160715615 ) ) ;
#52025 = EDGE_CURVE ( 'NONE', #64833, #26559, #80419, .T. ) ;
#52026 = CARTESIAN_POINT ( 'NONE',  ( 17.14217821643591932, -12.51329471203373345, 31.30864560766537963 ) ) ;
#52027 = PLANE ( 'NONE',  #32758 ) ;
#52028 = EDGE_CURVE ( 'NONE', #8235, #18795, #15210, .T. ) ;
#52029 = EDGE_LOOP ( 'NONE', ( #24814, #79930 ) ) ;
#52030 = CARTESIAN_POINT ( 'NONE',  ( -10.83826413212219641, -7.630690623152299956, 34.99857592706774057 ) ) ;
#52031 = VERTEX_POINT ( 'NONE', #47659 ) ;
#52032 = EDGE_LOOP ( 'NONE', ( #71338, #14706, #45121, #14965 ) ) ;
#52033 = CARTESIAN_POINT ( 'NONE',  ( -5.869474298236436738, -6.001044277235011215, 34.52024696741798948 ) ) ;
#52034 = AXIS2_PLACEMENT_3D ( 'NONE', #29787, #8187, #62666 ) ;
#52035 = FACE_OUTER_BOUND ( 'NONE', #21274, .T. ) ;
#52036 = CARTESIAN_POINT ( 'NONE',  ( -10.61538461538461320, -4.102666532097928531, 36.13435417666054406 ) ) ;
#52037 = CARTESIAN_POINT ( 'NONE',  ( 1.254467414883689846, -11.66186481527757479, 32.95055677023626117 ) ) ;
#52038 = CARTESIAN_POINT ( 'NONE',  ( -2.176900499867520100, -11.71459661697925903, 32.44059661609676937 ) ) ;
#52039 = AXIS2_PLACEMENT_3D ( 'NONE', #3720, #85266, #1958 ) ;
#52040 = VERTEX_POINT ( 'NONE', #20624 ) ;
#52041 = ORIENTED_EDGE ( 'NONE', *, *, #10683, .F. ) ;
#52042 = B_SPLINE_CURVE_WITH_KNOTS ( 'NONE', 3,
 ( #30574, #85974, #31013, #52173, #22936, #84657, #65245, #79219, #11201, #44077 ),
 .UNSPECIFIED., .F., .F.,
 ( 4, 2, 2, 2, 4 ),
 ( 0.0007817359430256317406, 0.0009771253907249982749, 0.001172514838424365026, 0.001367904286123731560, 0.001563293733823098094 ),
 .UNSPECIFIED. ) ;
#52043 = ORIENTED_EDGE ( 'NONE', *, *, #42110, .T. ) ;
#52044 = EDGE_CURVE ( 'NONE', #34465, #6050, #35257, .T. ) ;
#52045 = EDGE_CURVE ( 'NONE', #77968, #79258, #14853, .T. ) ;
#52046 = CARTESIAN_POINT ( 'NONE',  ( -3.930833309752757909, -11.98016756924215009, 32.48728574198911190 ) ) ;
#52047 = CARTESIAN_POINT ( 'NONE',  ( 15.23076923076911093, -11.48612834414049644, 32.76840700105863391 ) ) ;
#52048 = CARTESIAN_POINT ( 'NONE',  ( -19.99999999999996447, -12.00000000000000355, 0.000000000000000000 ) ) ;
#52049 = EDGE_CURVE ( 'NONE', #5606, #51992, #30934, .T. ) ;
#52050 = CARTESIAN_POINT ( 'NONE',  ( -8.703163435880695076, -9.905515769479276145, 34.41647553114623292 ) ) ;
#52051 = CARTESIAN_POINT ( 'NONE',  ( 11.53846153846153832, -10.67929555188718282, 33.92786785259544047 ) ) ;
#52052 = EDGE_CURVE ( 'NONE', #79032, #75182, #54859, .T. ) ;
#52053 = CARTESIAN_POINT ( 'NONE',  ( 6.000000000000001776, -12.37446782046654192, 30.86335684631486131 ) ) ;
#52054 = VERTEX_POINT ( 'NONE', #88672 ) ;
#52055 = EDGE_LOOP ( 'NONE', ( #54039, #3531 ) ) ;
#52056 = CARTESIAN_POINT ( 'NONE',  ( -1.553300858899081538, -11.25000000000000711, 21.10937500000000711 ) ) ;
#52057 = VERTEX_POINT ( 'NONE', #41800 ) ;
#52059 = ORIENTED_EDGE ( 'NONE', *, *, #33145, .T. ) ;
#52058 = CARTESIAN_POINT ( 'NONE',  ( 2.438218009455871638, -12.45806712695776319, 30.39783852428763922 ) ) ;
#52060 = ADVANCED_FACE ( 'NONE', ( #34140 ), #40907, .F. ) ;
#52061 = CARTESIAN_POINT ( 'NONE',  ( 1.134638653673032849, -9.943427161483782584, 34.11278801902876978 ) ) ;
#52062 = CARTESIAN_POINT ( 'NONE',  ( -19.50000000000000000, -3.499999999999999556, 29.75000000000000355 ) ) ;
#52063 = AXIS2_PLACEMENT_3D ( 'NONE', #56316, #77034, #84248 ) ;
#52064 = CARTESIAN_POINT ( 'NONE',  ( -2.651650429449535551, -10.15165042944956753, 16.18750000000000000 ) ) ;
#52065 = ORIENTED_EDGE ( 'NONE', *, *, #39642, .F. ) ;
#52066 = ADVANCED_FACE ( 'NONE', ( #26953 ), #82788, .T. ) ;
#52067 = DIRECTION ( 'NONE',  ( 0.000000000000000000, 0.1736481776669267785, -0.9848077530122087975 ) ) ;
#52068 = VERTEX_POINT ( 'NONE', #61608 ) ;
#52069 = CARTESIAN_POINT ( 'NONE',  ( -13.38461538461550759, -11.67786785259630911, 32.92929555188603530 ) ) ;
#52070 = CARTESIAN_POINT ( 'NONE',  ( 19.50000000000000000, -11.50000000000000000, 29.75000000000000355 ) ) ;
#52071 = FACE_BOUND ( 'NONE', #69372, .T. ) ;
#52073 = CARTESIAN_POINT ( 'NONE',  ( -27.00000000000000000, 0.7500000000000052180, 31.75000000000000000 ) ) ;
#52072 = CARTESIAN_POINT ( 'NONE',  ( 5.750000000000002665, -7.500000000000001776, 34.75000000000000000 ) ) ;
#52074 = DIRECTION ( 'NONE',  ( -0.000000000000000000, 0.3420201433256694346, -0.9396926207859080948 ) ) ;
#52075 = CYLINDRICAL_SURFACE ( 'NONE', #33348, 0.2500000000000002220 ) ;
#52076 = ORIENTED_EDGE ( 'NONE', *, *, #87224, .F. ) ;
#52077 = ADVANCED_FACE ( 'NONE', ( #76012 ), #75565, .F. ) ;
#52078 = CARTESIAN_POINT ( 'NONE',  ( 11.47319153790521717, -11.67786785259540849, 32.92929555188721480 ) ) ;
#52079 = CARTESIAN_POINT ( 'NONE',  ( 8.899756470994335089, -6.852161475712352789, 34.70806712695775786 ) ) ;
#52080 = ORIENTED_EDGE ( 'NONE', *, *, #51280, .T. ) ;
#52081 = DIRECTION ( 'NONE',  ( -0.000000000000000000, -0.000000000000000000, -1.000000000000000000 ) ) ;
#52082 = CARTESIAN_POINT ( 'NONE',  ( -18.00000000000000000, -12.62096338111211580, 30.90682066428153263 ) ) ;
#52084 = CARTESIAN_POINT ( 'NONE',  ( 14.30769230769218581, -10.33852847137269571, 34.16647553114546554 ) ) ;
#52083 = PRODUCT_DEFINITION_SHAPE ( 'NONE', 'NONE',  #89186 ) ;
#52085 = B_SPLINE_CURVE_WITH_KNOTS ( 'NONE', 3,
 ( #67746, #59648, #60538, #6051, #39838, #60981, #80835, #88484, #39402, #52885 ),
 .UNSPECIFIED., .F., .F.,
 ( 4, 2, 2, 2, 4 ),
 ( 0.000000000000000000, 0.0001954311564186871184, 0.0003908623128373742367, 0.0005862934692560614093, 0.0007817246256747484735 ),
 .UNSPECIFIED. ) ;
#52086 = DIRECTION ( 'NONE',  ( 0.000000000000000000, 0.1736481776669267785, -0.9848077530122087975 ) ) ;
#52087 = CARTESIAN_POINT ( 'NONE',  ( 20.00000000000000000, -4.000000000000000000, 29.75000000000000355 ) ) ;
#52088 = EDGE_CURVE ( 'NONE', #59241, #24770, #71613, .T. ) ;
#52089 = FACE_BOUND ( 'NONE', #971, .T. ) ;
#52091 = CARTESIAN_POINT ( 'NONE',  ( 4.403900573759605308, -12.65882529074907126, 30.72640787790839312 ) ) ;
#52090 = CARTESIAN_POINT ( 'NONE',  ( 13.16113044089143891, -12.24155766932282496, 31.33739205006857986 ) ) ;
#52092 = DIRECTION ( 'NONE',  ( -1.000000000000000000, 0.000000000000000000, -0.000000000000000000 ) ) ;
#52094 = CARTESIAN_POINT ( 'NONE',  ( 9.915087233576098669, -4.387253974876679230, 33.66317474335728832 ) ) ;
#52093 = CARTESIAN_POINT ( 'NONE',  ( 18.06606835100243913, -11.16473453929635440, 33.15142922261926373 ) ) ;
#52095 = LINE ( 'NONE', #10678, #75723 ) ;
#52096 = DIRECTION ( 'NONE',  ( -0.000000000000000000, 0.3420201433256694346, -0.9396926207859080948 ) ) ;
#52097 = CARTESIAN_POINT ( 'NONE',  ( -3.749999999999996447, -7.561099074964554134, 26.09188170625848358 ) ) ;
#52098 = EDGE_CURVE ( 'NONE', #5312, #11434, #78167, .T. ) ;
#52099 = ORIENTED_EDGE ( 'NONE', *, *, #6846, .F. ) ;
#52100 = CIRCLE ( 'NONE', #83755, 0.2500000000000002220 ) ;
#52101 = CARTESIAN_POINT ( 'NONE',  ( 12.46153846153846168, -2.708943851104267164, 35.45975837776705220 ) ) ;
#52102 = CARTESIAN_POINT ( 'NONE',  ( -14.98076923076929567, -7.565270445406050648, 34.75000000000000000 ) ) ;
#52103 = CARTESIAN_POINT ( 'NONE',  ( -19.50000000000000000, -3.499999999999999556, 29.75000000000000355 ) ) ;
#52104 = CARTESIAN_POINT ( 'NONE',  ( 6.000000000000001776, -12.10708131394839349, 31.69288490824020244 ) ) ;
#52105 = DIRECTION ( 'NONE',  ( -2.891205793294678326E-16, 1.000000000000000000, -0.000000000000000000 ) ) ;
#52106 = CARTESIAN_POINT ( 'NONE',  ( 5.326977496836529546, -12.01375889529407281, 32.43194544308182969 ) ) ;
#52107 = CARTESIAN_POINT ( 'NONE',  ( 0.06109907496455496689, -11.24999999999999822, 24.52938170625849423 ) ) ;
#52108 = CARTESIAN_POINT ( 'NONE',  ( -15.48079245499068612, -12.68155406624981119, 30.59749803192733708 ) ) ;
#52109 = LINE ( 'NONE', #10252, #77734 ) ;
#52110 = EDGE_CURVE ( 'NONE', #84431, #51157, #40539, .T. ) ;
#52111 = CARTESIAN_POINT ( 'NONE',  ( 0.4330127018922180770, -4.784304877199946127, 29.50000000000000355 ) ) ;
#52112 = CARTESIAN_POINT ( 'NONE',  ( 5.207448515156722912, -12.70449254468099198, 30.44128974285582956 ) ) ;
#52113 = DIRECTION ( 'NONE',  ( -0.000000000000000000, 0.7660444431189791237, -0.6427876096865379196 ) ) ;
#52114 = DIRECTION ( 'NONE',  ( -0.000000000000000000, 0.8660254037844399289, -0.4999999999999980016 ) ) ;
#52115 = DIRECTION ( 'NONE',  ( 0.000000000000000000, 0.000000000000000000, 1.000000000000000000 ) ) ;
#52116 = EDGE_CURVE ( 'NONE', #33268, #74563, #50736, .T. ) ;
#52117 = CARTESIAN_POINT ( 'NONE',  ( -1.319360245102545681, -12.16647553114626490, 32.15551576947920864 ) ) ;
#52118 = ORIENTED_EDGE ( 'NONE', *, *, #46698, .T. ) ;
#52119 = CARTESIAN_POINT ( 'NONE',  ( 17.07692307692295586, -12.70778746994576025, 30.41441678777401236 ) ) ;
#52120 = DIRECTION ( 'NONE',  ( 0.000000000000000000, 0.3420201433256610524, 0.9396926207859113145 ) ) ;
#52121 = CARTESIAN_POINT ( 'NONE',  ( -3.775308065498748977, -8.992201783934593351, 20.26749329374151998 ) ) ;
#52122 = CARTESIAN_POINT ( 'NONE',  ( 2.241608896736428047, -4.098570777380720287, 33.41473453929634729 ) ) ;
#52123 = CARTESIAN_POINT ( 'NONE',  ( -5.076923076923075762, -2.538708090699994813, 30.37095296980875503 ) ) ;
#52124 = ORIENTED_EDGE ( 'NONE', *, *, #87743, .T. ) ;
#52125 = CARTESIAN_POINT ( 'NONE',  ( -6.673022503163469565, -10.06805714834173848, 34.32951233291982618 ) ) ;
#52126 = PLANE ( 'NONE',  #54565 ) ;
#52128 = VERTEX_POINT ( 'NONE', #37231 ) ;
#52127 = DIRECTION ( 'NONE',  ( 0.000000000000000000, 1.000000000000000000, -0.000000000000000000 ) ) ;
#52129 = CYLINDRICAL_SURFACE ( 'NONE', #21157, 0.2500000000000009437 ) ;
#52130 = CYLINDRICAL_SURFACE ( 'NONE', #42621, 0.2500000000000009437 ) ;
#52131 = ADVANCED_FACE ( 'NONE', ( #35924 ), #71028, .T. ) ;
#52132 = LINE ( 'NONE', #3054, #30562 ) ;
#52133 = CARTESIAN_POINT ( 'NONE',  ( -6.166666666666667851, -7.500000000000000000, 33.75000000000000000 ) ) ;
#52134 = EDGE_CURVE ( 'NONE', #373, #60933, #67328, .T. ) ;
#52135 = VERTEX_POINT ( 'NONE', #84117 ) ;
#52136 = AXIS2_PLACEMENT_3D ( 'NONE', #7586, #76486, #35047 ) ;
#52137 = DIRECTION ( 'NONE',  ( 0.000000000000000000, 0.9396926207859126468, 0.3420201433256571111 ) ) ;
#52138 = CARTESIAN_POINT ( 'NONE',  ( -12.71156168575992318, -2.588893531581426988, 31.60682220781847818 ) ) ;
#52139 = LINE ( 'NONE', #32330, #992 ) ;
#52140 = EDGE_LOOP ( 'NONE', ( #24404, #56067 ) ) ;
#52141 = ORIENTED_EDGE ( 'NONE', *, *, #8657, .T. ) ;
#52142 = ORIENTED_EDGE ( 'NONE', *, *, #67104, .T. ) ;
#52143 = CARTESIAN_POINT ( 'NONE',  ( 3.480714640147274608, -2.341251567377310217, 30.72681386836322659 ) ) ;
#52144 = CARTESIAN_POINT ( 'NONE',  ( 12.94230769230769340, -3.499999999999999556, 29.75000000000000355 ) ) ;
#52145 = CARTESIAN_POINT ( 'NONE',  ( -7.846153846153844924, -2.538708090699994813, 30.37095296980875503 ) ) ;
#52146 = CARTESIAN_POINT ( 'NONE',  ( -17.20707028636129721, -6.852621066184266141, 34.70813303252209181 ) ) ;
#52147 = ORIENTED_EDGE ( 'NONE', *, *, #50572, .T. ) ;
#52148 = EDGE_LOOP ( 'NONE', ( #69927, #85071, #67850, #60217, #17585, #65519 ) ) ;
#52150 = VERTEX_POINT ( 'NONE', #71460 ) ;
#52149 = CARTESIAN_POINT ( 'NONE',  ( 4.219913487196229163, -5.471508081941601098, 34.59228464037088457 ) ) ;
#52151 = CARTESIAN_POINT ( 'NONE',  ( -5.076923076923199218, -2.657715359629662988, 31.77849191805970364 ) ) ;
#52152 = CARTESIAN_POINT ( 'NONE',  ( 20.00000000000000000, -4.000000000000000000, 29.75000000000000355 ) ) ;
#52153 = VECTOR ( 'NONE', #801, 1000.000000000000000 ) ;
#52154 = CARTESIAN_POINT ( 'NONE',  ( 2.557746619330623528, -3.627508038966689163, 32.91356715214248396 ) ) ;
#52155 = CARTESIAN_POINT ( 'NONE',  ( 13.51540582558233794, -9.929761469519743144, 34.40412654351204225 ) ) ;
#52156 = ADVANCED_FACE ( 'NONE', ( #23712 ), #22398, .F. ) ;
#52157 = ORIENTED_EDGE ( 'NONE', *, *, #22436, .F. ) ;
#52158 = AXIS2_PLACEMENT_3D ( 'NONE', #4630, #53250, #19910 ) ;
#52159 = ORIENTED_EDGE ( 'NONE', *, *, #38982, .T. ) ;
#52160 = ORIENTED_EDGE ( 'NONE', *, *, #81885, .T. ) ;
#52162 = VERTEX_POINT ( 'NONE', #44419 ) ;
#52161 = CARTESIAN_POINT ( 'NONE',  ( 5.076923076923075762, -4.786620604624113540, 33.94971097300155094 ) ) ;
#52163 = ADVANCED_FACE ( 'NONE', ( #49863 ), #15650, .F. ) ;
#52164 = CARTESIAN_POINT ( 'NONE',  ( 18.13052543823364360, -12.15418822224088657, 32.17964115625579069 ) ) ;
#52165 = CARTESIAN_POINT ( 'NONE',  ( -0.2114840416250083899, -4.818054556918156983, 34.26375889529406749 ) ) ;
#52166 = ORIENTED_EDGE ( 'NONE', *, *, #41106, .F. ) ;
#52167 = CARTESIAN_POINT ( 'NONE',  ( -8.992715712954719720, -10.81261337010820256, 33.49550067578627477 ) ) ;
#52168 = FACE_OUTER_BOUND ( 'NONE', #29401, .T. ) ;
#52169 = ADVANCED_FACE ( 'NONE', ( #63825 ), #3449, .F. ) ;
#52170 = CARTESIAN_POINT ( 'NONE',  ( -16.82692307692164135, -7.500000000000155431, 34.75000000000007105 ) ) ;
#52171 = FACE_BOUND ( 'NONE', #60917, .T. ) ;
#52172 = CARTESIAN_POINT ( 'NONE',  ( -8.638440328263820689, -2.295524264805589354, 30.44142389570982488 ) ) ;
#52173 = CARTESIAN_POINT ( 'NONE',  ( 2.530471848960717640, -8.496831190052096971, 34.64984203495476578 ) ) ;
#52174 = CARTESIAN_POINT ( 'NONE',  ( 11.66925334628632882, -12.38066358083363738, 30.83685684665853444 ) ) ;
#52176 = CARTESIAN_POINT ( 'NONE',  ( -8.519176349317314489, -12.01375889529407281, 32.43194544308182969 ) ) ;
#52175 = DIRECTION ( 'NONE',  ( 0.000000000000000000, 0.8660254037844377084, -0.5000000000000015543 ) ) ;
#52177 = CARTESIAN_POINT ( 'NONE',  ( 13.38461538461538680, -4.098570777380720287, 33.41473453929634729 ) ) ;
#52178 = CARTESIAN_POINT ( 'NONE',  ( 5.076923076923075762, -2.538708090699994813, 30.37095296980875503 ) ) ;
#52179 = ORIENTED_EDGE ( 'NONE', *, *, #18714, .F. ) ;
#52180 = CARTESIAN_POINT ( 'NONE',  ( -15.00798956179116317, -11.60474049983371003, 33.02348890104160262 ) ) ;
#52181 = CARTESIAN_POINT ( 'NONE',  ( -7.715362038329061534, -2.541949514083464479, 30.39797389878540557 ) ) ;
#52182 = EDGE_LOOP ( 'NONE', ( #9754, #10322 ) ) ;
#52183 = ORIENTED_EDGE ( 'NONE', *, *, #29160, .T. ) ;
#52185 = CARTESIAN_POINT ( 'NONE',  ( 10.68145194873469173, -11.91647553114624358, 32.58852847137148245 ) ) ;
#52184 = CARTESIAN_POINT ( 'NONE',  ( -11.66915214157184444, -12.62707690430377383, 30.88035979386743435 ) ) ;
#52186 = EDGE_CURVE ( 'NONE', #6380, #15876, #84560, .T. ) ;
#52187 = VECTOR ( 'NONE', #17810, 1000.000000000000227 ) ;
#52188 = VECTOR ( 'NONE', #80446, 1000.000000000000000 ) ;
#52189 = CARTESIAN_POINT ( 'NONE',  ( 16.15384615384603251, -2.625532179533778709, 30.86335684631627174 ) ) ;
#52190 = CARTESIAN_POINT ( 'NONE',  ( 10.61538461538449418, -3.083524468854526912, 32.58852847137268327 ) ) ;
#52191 = CARTESIAN_POINT ( 'NONE',  ( -15.45359592324823517, -7.369208160676171460, 34.74850200257122879 ) ) ;
#52192 = ORIENTED_EDGE ( 'NONE', *, *, #75199, .F. ) ;
#52193 = CARTESIAN_POINT ( 'NONE',  ( 8.703148389870632329, -12.62096338111211580, 30.90682066428152908 ) ) ;
#52194 = CARTESIAN_POINT ( 'NONE',  ( 18.13079044096696180, -3.957578996910245284, 33.62503395064540257 ) ) ;
#52196 = CARTESIAN_POINT ( 'NONE',  ( 0.2380535369741288987, -12.69144148231606017, 30.53333754910549303 ) ) ;
#52195 = CARTESIAN_POINT ( 'NONE',  ( 11.78851595837499211, -2.920487667080175598, 32.31805714834170828 ) ) ;
#52197 = CARTESIAN_POINT ( 'NONE',  ( 17.14299142792551578, -6.386643153685127139, 34.62446782046654192 ) ) ;
#52198 = CARTESIAN_POINT ( 'NONE',  ( 17.99999999999987566, -6.879047030192662504, 34.71129190930017927 ) ) ;
#52200 = CARTESIAN_POINT ( 'NONE',  ( -15.10024379253558635, -11.04252011169590020, 33.62494198852677130 ) ) ;
#52199 =( NAMED_UNIT ( * ) PLANE_ANGLE_UNIT ( ) SI_UNIT ( $, .RADIAN. ) );
#52201 = CARTESIAN_POINT ( 'NONE',  ( -3.749999999999988454, -9.053300858899127945, 21.26562500000000000 ) ) ;
#52202 = ORIENTED_EDGE ( 'NONE', *, *, #67452, .F. ) ;
#52203 = EDGE_CURVE ( 'NONE', #22124, #58240, #84554, .T. ) ;
#52204 = ORIENTED_EDGE ( 'NONE', *, *, #10835, .F. ) ;
#52205 = CARTESIAN_POINT ( 'NONE',  ( -14.37296230824862775, -5.094484230520674117, 34.41647553114621161 ) ) ;
#52206 = ADVANCED_FACE ( 'NONE', ( #3888 ), #10661, .T. ) ;
#52207 = CARTESIAN_POINT ( 'NONE',  ( -17.74999999999856115, -7.500000000000155431, 34.75000000000007105 ) ) ;
#52208 = CARTESIAN_POINT ( 'NONE',  ( -12.39547011053602432, -9.780366693483667717, 34.19971097300155805 ) ) ;
#52209 = CARTESIAN_POINT ( 'NONE',  ( 14.43821800945586986, -2.882268652242222284, 31.66798894389554064 ) ) ;
#52210 = CARTESIAN_POINT ( 'NONE',  ( 17.01116964860974079, -7.249945578846654470, 34.99404164642496795 ) ) ;
#52211 = CARTESIAN_POINT ( 'NONE',  ( 1.553300858899087311, -3.749999999999992006, 21.73437500000000000 ) ) ;
#52212 = CARTESIAN_POINT ( 'NONE',  ( -6.923076923077045919, -3.083524468854526912, 32.58852847137268327 ) ) ;
#52213 = DIRECTION ( 'NONE',  ( -1.000000000000000000, -0.000000000000000000, 0.000000000000000000 ) ) ;
#52214 = CARTESIAN_POINT ( 'NONE',  ( -13.31844624365272800, -7.250054483168843156, 34.74374881642865631 ) ) ;
#52215 = CARTESIAN_POINT ( 'NONE',  ( 5.776515075435672664, -10.23692288466677880, 34.23039457007281072 ) ) ;
#52216 = CARTESIAN_POINT ( 'NONE',  ( 2.980746006547774218, -12.45566812827425096, 31.48439005359158926 ) ) ;
#52217 = B_SPLINE_CURVE_WITH_KNOTS ( 'NONE', 3,
 ( #21240, #54580, #41976, #82077, #22139, #33873, #8185, #68988, #93, #68547 ),
 .UNSPECIFIED., .F., .F.,
 ( 4, 2, 2, 2, 4 ),
 ( 0.000000000000000000, 0.0001954339857564075557, 0.0003908679715128151114, 0.0005863019572692226671, 0.0007817359430256302227 ),
 .UNSPECIFIED. ) ;
#52218 = CARTESIAN_POINT ( 'NONE',  ( 14.05766907039934210, -12.22074536777954989, 31.39888409691088356 ) ) ;
#52219 = DIRECTION ( 'NONE',  ( -0.000000000000000000, -0.3420201433256694901, -0.9396926207859080948 ) ) ;
#52220 = CARTESIAN_POINT ( 'NONE',  ( 6.988332062589762472, -2.379036618887895305, 30.90682066428159303 ) ) ;
#52222 = EDGE_CURVE ( 'NONE', #87108, #42300, #65226, .T. ) ;
#52221 = CARTESIAN_POINT ( 'NONE',  ( -0.3954701105360237667, -11.16473453929635440, 33.15142922261926373 ) ) ;
#52223 = CARTESIAN_POINT ( 'NONE',  ( -3.007757879156381708, -11.24521262558773671, 33.06293181088029343 ) ) ;
#52224 = CARTESIAN_POINT ( 'NONE',  ( -7.715362038329059757, -12.38066358083363738, 30.83685684665853444 ) ) ;
#52225 = ORIENTED_EDGE ( 'NONE', *, *, #17477, .F. ) ;
#52226 = CYLINDRICAL_SURFACE ( 'NONE', #34127, 0.2500000000000002220 ) ;
#52227 = CARTESIAN_POINT ( 'NONE',  ( -13.13466997523734037, -10.18230066228895758, 34.26354781536631577 ) ) ;
#52228 = DIRECTION ( 'NONE',  ( 0.000000000000000000, -1.000000000000000000, 0.000000000000000000 ) ) ;
#52229 = CARTESIAN_POINT ( 'NONE',  ( -1.987747218494638313, -9.401340078031370950, 13.93936829374151465 ) ) ;
#52230 = AXIS2_PLACEMENT_3D ( 'NONE', #42367, #63051, #33928 ) ;
#52231 = AXIS2_PLACEMENT_3D ( 'NONE', #74223, #12519, #67468 ) ;
#52232 = CARTESIAN_POINT ( 'NONE',  ( -18.13056059174191148, -2.504760397472873379, 29.97295953869786800 ) ) ;
#52233 = CARTESIAN_POINT ( 'NONE',  ( 11.53846153846153832, -11.69971097300155272, 32.46337939537588113 ) ) ;
#52235 = ORIENTED_EDGE ( 'NONE', *, *, #43114, .F. ) ;
#52234 = CARTESIAN_POINT ( 'NONE',  ( -0.3954701105360219349, -2.538708090699994813, 30.37095296980875503 ) ) ;
#52236 = CARTESIAN_POINT ( 'NONE',  ( 1.799775606325937360E-14, -10.25000000000000000, 21.03125000000000000 ) ) ;
#52237 = DIRECTION ( 'NONE',  ( -1.000000000000000000, 0.000000000000000000, 0.000000000000000000 ) ) ;
#52238 = ADVANCED_FACE ( 'NONE', ( #18756 ), #72794, .T. ) ;
#52239 = AXIS2_PLACEMENT_3D ( 'NONE', #16378, #38430, #10059 ) ;
#52240 = ORIENTED_EDGE ( 'NONE', *, *, #73615, .F. ) ;
#52241 = CARTESIAN_POINT ( 'NONE',  ( -4.377331078410483300, -8.539481045369598178, 34.89627647299170832 ) ) ;
#52242 = ORIENTED_EDGE ( 'NONE', *, *, #64148, .F. ) ;
#52243 = CARTESIAN_POINT ( 'NONE',  ( 3.007284306204899504, -4.988325925672468131, 34.36044203135681130 ) ) ;
#52244 = ADVANCED_FACE ( 'NONE', ( #11102 ), #4343, .F. ) ;
#52245 = EDGE_CURVE ( 'NONE', #8848, #75979, #66034, .T. ) ;
#52246 = CARTESIAN_POINT ( 'NONE',  ( -1.384615384615506484, -12.16647553114689728, 32.15551576947799362 ) ) ;
#52247 = CARTESIAN_POINT ( 'NONE',  ( 4.499999999999999112, 7.500000000000002665, 13.00000000000000178 ) ) ;
#52248 = ORIENTED_EDGE ( 'NONE', *, *, #34838, .T. ) ;
#52249 = CARTESIAN_POINT ( 'NONE',  ( 11.31553457955469000, -11.98009711892699514, 32.48740034544076138 ) ) ;
#52250 = ORIENTED_EDGE ( 'NONE', *, *, #86412, .T. ) ;
#52251 = CYLINDRICAL_SURFACE ( 'NONE', #61462, 0.2499999999999997502 ) ;
#52252 = EDGE_CURVE ( 'NONE', #69985, #78986, #31906, .T. ) ;
#52253 = EDGE_CURVE ( 'NONE', #19260, #46007, #12434, .T. ) ;
#52254 = ORIENTED_EDGE ( 'NONE', *, *, #10857, .T. ) ;
#52255 = DIRECTION ( 'NONE',  ( -0.000000000000000000, -0.6427876096865404731, -0.7660444431189771253 ) ) ;
#52256 = CYLINDRICAL_SURFACE ( 'NONE', #88740, 0.2499999999999986955 ) ;
#52257 = ORIENTED_EDGE ( 'NONE', *, *, #76324, .T. ) ;
#52258 = B_SPLINE_CURVE_WITH_KNOTS ( 'NONE', 3,
 ( #69605, #35831, #7911, #89016, #63287, #47995, #75474, #13772, #29084, #56538 ),
 .UNSPECIFIED., .F., .F.,
 ( 4, 2, 2, 2, 4 ),
 ( 0.000000000000000000, 0.0001954311564186858715, 0.0003908623128373717431, 0.0005862934692560576146, 0.0007817246256747434861 ),
 .UNSPECIFIED. ) ;
#52259 = B_SPLINE_CURVE_WITH_KNOTS ( 'NONE', 3,
 ( #5523, #64426, #29780, #56362, #36101, #57248, #35201, #8181, #42855, #70318 ),
 .UNSPECIFIED., .F., .F.,
 ( 4, 2, 2, 2, 4 ),
 ( 0.000000000000000000, 0.0001954339881912772715, 0.0003908679763825545429, 0.0005863019645738318415, 0.0007817359527651090859 ),
 .UNSPECIFIED. ) ;
#52260 = CARTESIAN_POINT ( 'NONE',  ( 10.61538461538461675, -12.78798330534102945, 29.74999999999997868 ) ) ;
#52261 = DIRECTION ( 'NONE',  ( -0.000000000000000000, 1.000000000000000000, 3.491481338843133355E-15 ) ) ;
#52262 = CARTESIAN_POINT ( 'NONE',  ( 11.53846153846141753, -11.94971097300221174, 32.03036669348237098 ) ) ;
#52263 = AXIS2_PLACEMENT_3D ( 'NONE', #63981, #9490, #64866 ) ;
#52264 = AXIS2_PLACEMENT_3D ( 'NONE', #47503, #83530, #81751 ) ;
#52265 = DIRECTION ( 'NONE',  ( 1.000000000000000000, 0.000000000000000000, -0.000000000000000000 ) ) ;
#52266 = CARTESIAN_POINT ( 'NONE',  ( -2.298097038856290464, -5.201902961143733961, 26.50000000000000355 ) ) ;
#52267 = ORIENTED_EDGE ( 'NONE', *, *, #6305, .T. ) ;
#52268 = ORIENTED_EDGE ( 'NONE', *, *, #9713, .F. ) ;
#52269 = ORIENTED_EDGE ( 'NONE', *, *, #27663, .T. ) ;
#52271 = ORIENTED_EDGE ( 'NONE', *, *, #10358, .F. ) ;
#52270 = CARTESIAN_POINT ( 'NONE',  ( 3.230769230769231726, -12.62096338111211580, 30.90682066428153263 ) ) ;
#52272 = DIRECTION ( 'NONE',  ( 0.000000000000000000, 0.6427876096865373645, -0.7660444431189797898 ) ) ;
#52273 = CARTESIAN_POINT ( 'NONE',  ( 1.515141086378948732, -2.882268652242222728, 31.66798894389554064 ) ) ;
#52274 = ORIENTED_EDGE ( 'NONE', *, *, #10849, .F. ) ;
#52275 = ORIENTED_EDGE ( 'NONE', *, *, #47479, .T. ) ;
#52276 = CARTESIAN_POINT ( 'NONE',  ( 3.296837581771669523, -4.786620604624113540, 33.94971097300155805 ) ) ;
#52277 = ORIENTED_EDGE ( 'NONE', *, *, #86764, .T. ) ;
#52278 = CARTESIAN_POINT ( 'NONE',  ( -12.71153846153846168, -7.566082377512564960, 35.00000000000000711 ) ) ;
#52279 = AXIS2_PLACEMENT_3D ( 'NONE', #33234, #67021, #66111 ) ;
#52280 = B_SPLINE_CURVE_WITH_KNOTS ( 'NONE', 3,
 ( #53714, #47840, #27131, #34325, #82537, #33884, #60472, #20813, #68999, #48282 ),
 .UNSPECIFIED., .F., .F.,
 ( 4, 2, 2, 2, 4 ),
 ( 0.0007817246256747486903, 0.0009771112852218918031, 0.001172497944769034699, 0.001367884604316177595, 0.001563271263863320708 ),
 .UNSPECIFIED. ) ;
#52281 = DIRECTION ( 'NONE',  ( 1.000000000000000000, 0.000000000000000000, 0.000000000000000000 ) ) ;
#52282 = B_SPLINE_CURVE_WITH_KNOTS ( 'NONE', 3,
 ( #46991, #21634, #15333, #70268, #74931, #8576, #49556, #33049, #26288, #53756 ),
 .UNSPECIFIED., .F., .F.,
 ( 4, 2, 2, 2, 4 ),
 ( 0.000000000000000000, 0.0001954311564186862781, 0.0003908623128373725562, 0.0005862934692560588072, 0.0007817246256747451124 ),
 .UNSPECIFIED. ) ;
#52283 = CARTESIAN_POINT ( 'NONE',  ( 0.4615384615383396616, -5.219633306517616589, 34.19971097300220464 ) ) ;
#52284 = FACE_BOUND ( 'NONE', #58518, .T. ) ;
#52285 = AXIS2_PLACEMENT_3D ( 'NONE', #88829, #53685, #54566 ) ;
#52286 = CARTESIAN_POINT ( 'NONE',  ( -6.065270445960775803, -6.026961402152685388, 34.52809138561120506 ) ) ;
#52287 = FACE_OUTER_BOUND ( 'NONE', #15009, .T. ) ;
#52288 = VECTOR ( 'NONE', #31921, 1000.000000000000000 ) ;
#52289 = CARTESIAN_POINT ( 'NONE',  ( -0.4615384615384611200, -1.422936976036506707, 30.56769352161908415 ) ) ;
#52290 = CARTESIAN_POINT ( 'NONE',  ( 2.177544337960613863, -8.630895178749536711, 34.87696386517710323 ) ) ;
#52291 = LINE ( 'NONE', #30690, #47677 ) ;
#52292 = VERTEX_POINT ( 'NONE', #45772 ) ;
#52293 = CARTESIAN_POINT ( 'NONE',  ( -17.29984929443922681, -12.39988816332205701, 30.74660775122750778 ) ) ;
#52294 = ORIENTED_EDGE ( 'NONE', *, *, #18193, .T. ) ;
#52295 = EDGE_LOOP ( 'NONE', ( #41674, #32006 ) ) ;
#52297 = CARTESIAN_POINT ( 'NONE',  ( 10.68064018666063930, -6.026961402152789304, 34.52809138561124769 ) ) ;
#52296 = CARTESIAN_POINT ( 'NONE',  ( -7.173053667125515176, -4.075325502946086864, 33.72974371597207721 ) ) ;
#52298 = CYLINDRICAL_SURFACE ( 'NONE', #67267, 0.2499999999999995559 ) ;
#52299 = DIRECTION ( 'NONE',  ( 1.000000000000000000, 0.000000000000000000, 0.000000000000000000 ) ) ;
#52300 = DIRECTION ( 'NONE',  ( 0.000000000000000000, 0.000000000000000000, -1.000000000000000000 ) ) ;
#52301 = CARTESIAN_POINT ( 'NONE',  ( 1.607628228708781748, -4.026326845037962343, 33.68677907613344047 ) ) ;
#52302 = VERTEX_POINT ( 'NONE', #11552 ) ;
#52303 = CARTESIAN_POINT ( 'NONE',  ( 13.91025641025641235, -3.499999999999999556, 29.75000000000000355 ) ) ;
#52304 = CARTESIAN_POINT ( 'NONE',  ( 3.164686851409095336, -9.058645607665454236, 34.76329471203372634 ) ) ;
#52305 = CARTESIAN_POINT ( 'NONE',  ( 2.530705151785704210, -12.64618726649961289, 30.78989965857442712 ) ) ;
#52306 = CARTESIAN_POINT ( 'NONE',  ( -4.153846153846273204, -3.835265460704628371, 33.15142922262033665 ) ) ;
#52307 = ORIENTED_EDGE ( 'NONE', *, *, #3092, .F. ) ;
#52308 = VERTEX_POINT ( 'NONE', #32697 ) ;
#52309 = ADVANCED_FACE ( 'NONE', ( #67380 ), #87671, .F. ) ;
#52310 = PRODUCT_CONTEXT ( 'NONE', #83770, 'mechanical' ) ;
#52311 = VERTEX_POINT ( 'NONE', #60610 ) ;
#52312 = FACE_OUTER_BOUND ( 'NONE', #23845, .T. ) ;
#52313 = CARTESIAN_POINT ( 'NONE',  ( -1.318548051265307386, -2.292212530054420494, 30.41441678777542990 ) ) ;
#52314 = VERTEX_POINT ( 'NONE', #88125 ) ;
#52315 = DIRECTION ( 'NONE',  ( -0.000000000000000000, 1.000000000000000000, -0.000000000000000000 ) ) ;
#52316 = CARTESIAN_POINT ( 'NONE',  ( 6.066067333350078528, -11.35647404775217595, 33.31231777344667222 ) ) ;
#52317 = CARTESIAN_POINT ( 'NONE',  ( -7.846153846153965716, -11.94971097300221174, 32.03036669348237098 ) ) ;
#52318 = CARTESIAN_POINT ( 'NONE',  ( 4.284636594813103549, -6.369690395747422684, 34.87708834333098196 ) ) ;
#52319 = CARTESIAN_POINT ( 'NONE',  ( -7.596153846153844924, -2.499999999999998668, 29.75000000000000355 ) ) ;
#52321 = ORIENTED_EDGE ( 'NONE', *, *, #75688, .F. ) ;
#52320 = AXIS2_PLACEMENT_3D ( 'NONE', #68921, #2227, #42799 ) ;
#52323 = VERTEX_POINT ( 'NONE', #26396 ) ;
#52322 = CARTESIAN_POINT ( 'NONE',  ( -7.715628144390285215, -10.19071101563364756, 33.96452234770658407 ) ) ;
#52324 = CARTESIAN_POINT ( 'NONE',  ( -7.623142494540994463, -9.086983370893049639, 34.49168942202179267 ) ) ;
#52325 = CARTESIAN_POINT ( 'NONE',  ( -12.71151520558705528, -2.920706130388546651, 32.31842814019191223 ) ) ;
#52326 = CARTESIAN_POINT ( 'NONE',  ( -2.307692307692305711, -1.951392089020283160, 34.73218667398347748 ) ) ;
#52327 = FACE_BOUND ( 'NONE', #72783, .T. ) ;
#52328 = CARTESIAN_POINT ( 'NONE',  ( -5.999999999999998224, -13.75783147151868846, 33.36296068462461051 ) ) ;
#52329 = EDGE_CURVE ( 'NONE', #28930, #10260, #53861, .T. ) ;
#52330 = CARTESIAN_POINT ( 'NONE',  ( 6.249945518348143381, -2.824170634883622188, 31.52227843825338738 ) ) ;
#52331 = CARTESIAN_POINT ( 'NONE',  ( -2.724691934501246582, -6.299813628509474128, 15.42374329374151642 ) ) ;
#52332 = ORIENTED_EDGE ( 'NONE', *, *, #14033, .F. ) ;
#52333 = CARTESIAN_POINT ( 'NONE',  ( -3.361460697436790657, -3.062553014421049991, 32.05460306192774311 ) ) ;
#52334 = CARTESIAN_POINT ( 'NONE',  ( 8.096153846155266010, -7.500000000000154543, 35.00000000000007105 ) ) ;
#52335 = DIRECTION ( 'NONE',  ( -0.000000000000000000, 0.3420201433256694346, -0.9396926207859080948 ) ) ;
#52336 = ORIENTED_EDGE ( 'NONE', *, *, #24694, .T. ) ;
#52337 = ORIENTED_EDGE ( 'NONE', *, *, #82879, .T. ) ;
#52338 = CARTESIAN_POINT ( 'NONE',  ( -8.769230769230892619, -5.941354392335915335, 34.76329471203413846 ) ) ;
#52339 = CARTESIAN_POINT ( 'NONE',  ( -7.780898706641007578, -5.941354392334607049, 34.76329471203374055 ) ) ;
#52340 = CARTESIAN_POINT ( 'NONE',  ( 13.38461538461538680, -3.513871655860378418, 32.76840700105978499 ) ) ;
#52341 = LINE ( 'NONE', #64966, #63178 ) ;
#52342 = CARTESIAN_POINT ( 'NONE',  ( 0.000000000000000000, -11.00000000000000000, 29.75000000000000355 ) ) ;
#52343 = CARTESIAN_POINT ( 'NONE',  ( 5.750023269057646935, -8.303909089506435137, 34.68538101551103381 ) ) ;
#52344 = VERTEX_POINT ( 'NONE', #54741 ) ;
#52346 = ADVANCED_FACE ( 'NONE', ( #33598 ), #83570, .F. ) ;
#52345 = DIRECTION ( 'NONE',  ( 0.000000000000000000, -6.938893903907222067E-15, 1.000000000000000000 ) ) ;
#52347 = EDGE_CURVE ( 'NONE', #38268, #46042, #20517, .T. ) ;
#52348 = VECTOR ( 'NONE', #30018, 1000.000000000000227 ) ;
#52349 = CARTESIAN_POINT ( 'NONE',  ( 7.173022332454967120, -6.653508905675592722, 34.93172785388651391 ) ) ;
#52350 = CARTESIAN_POINT ( 'NONE',  ( 3.903822929624696236, -8.475808217655753651, 34.90892951860618609 ) ) ;
#52351 = EDGE_LOOP ( 'NONE', ( #44929, #195, #42311, #14937 ) ) ;
#52352 = CARTESIAN_POINT ( 'NONE',  ( 12.59206416330202671, -3.816742781228458448, 33.13167719472716044 ) ) ;
#52353 = AXIS2_PLACEMENT_3D ( 'NONE', #79852, #59122, #87074 ) ;
#52354 = AXIS2_PLACEMENT_3D ( 'NONE', #76901, #15204, #83218 ) ;
#52355 = EDGE_LOOP ( 'NONE', ( #46642, #5302, #9292, #82342 ) ) ;
#52356 = EDGE_CURVE ( 'NONE', #327, #25620, #41681, .T. ) ;
#52357 = CARTESIAN_POINT ( 'NONE',  ( 9.692307692307695177, -6.435427911321262684, 35.78748833219616898 ) ) ;
#52358 = FACE_OUTER_BOUND ( 'NONE', #11742, .T. ) ;
#52359 = CARTESIAN_POINT ( 'NONE',  ( 13.91025641025641235, -11.50000000000000000, 29.75000000000000355 ) ) ;
#52360 = VERTEX_POINT ( 'NONE', #55184 ) ;
#52361 = EDGE_CURVE ( 'NONE', #74826, #31771, #82680, .T. ) ;
#52362 = LINE ( 'NONE', #45611, #41872 ) ;
#52363 = DIRECTION ( 'NONE',  ( 0.000000000000000000, 0.000000000000000000, 1.000000000000000000 ) ) ;
#52364 = FACE_OUTER_BOUND ( 'NONE', #44146, .T. ) ;
#52365 = CARTESIAN_POINT ( 'NONE',  ( -6.250023224221455287, -5.765609946408404518, 34.70566812827425451 ) ) ;
#52366 = CARTESIAN_POINT ( 'NONE',  ( -2.307692307692428724, -11.06231777344772027, 33.60647404775119895 ) ) ;
#52367 = ORIENTED_EDGE ( 'NONE', *, *, #10777, .F. ) ;
#52368 = DIRECTION ( 'NONE',  ( -0.000000000000000000, 1.000000000000000000, 3.491481338843133355E-15 ) ) ;
#52369 = ORIENTED_EDGE ( 'NONE', *, *, #70270, .T. ) ;
#52370 = CARTESIAN_POINT ( 'NONE',  ( -19.50000000000000000, -3.499999999999999556, 29.75000000000000355 ) ) ;
#52371 = CARTESIAN_POINT ( 'NONE',  ( -10.48533945254983557, -2.504778602574660340, 29.97347330155780654 ) ) ;
#52372 = DIRECTION ( 'NONE',  ( 0.000000000000000000, 0.000000000000000000, 1.000000000000000000 ) ) ;
#52373 = CARTESIAN_POINT ( 'NONE',  ( 7.623226887246994821, -12.38737895849757820, 31.66785238281580206 ) ) ;
#52374 = DIRECTION ( 'NONE',  ( -0.000000000000000000, -0.7660444431189791237, -0.6427876096865379196 ) ) ;
#52375 = CARTESIAN_POINT ( 'NONE',  ( 12.46153846153833911, -10.21337939537710326, 33.94971097300076224 ) ) ;
#52376 = ORIENTED_EDGE ( 'NONE', *, *, #45480, .T. ) ;
#52377 = B_SPLINE_CURVE_WITH_KNOTS ( 'NONE', 3,
 ( #33111, #41202, #33993, #75866, #215, #60576, #53822, #12837, #67786, #33565 ),
 .UNSPECIFIED., .F., .F.,
 ( 4, 2, 2, 2, 4 ),
 ( 0.000000000000000000, 0.0001954339857564072033, 0.0003908679715128144066, 0.0005863019572692215828, 0.0007817359430256288133 ),
 .UNSPECIFIED. ) ;
#52378 = VECTOR ( 'NONE', #61499, 1000.000000000000000 ) ;
#52379 = EDGE_LOOP ( 'NONE', ( #3605, #61717 ) ) ;
#52380 = VERTEX_POINT ( 'NONE', #20079 ) ;
#52381 = EDGE_LOOP ( 'NONE', ( #75246, #54193, #76265, #54112 ) ) ;
#52382 = VERTEX_POINT ( 'NONE', #34475 ) ;
#52383 = CYLINDRICAL_SURFACE ( 'NONE', #44451, 0.2499999999999973355 ) ;
#52384 = DIRECTION ( 'NONE',  ( 0.000000000000000000, 0.4999999999999960032, -0.8660254037844410391 ) ) ;
#52385 = CARTESIAN_POINT ( 'NONE',  ( 14.98074599347626368, -5.056417327199099532, 34.11270091957321426 ) ) ;
#52386 = CARTESIAN_POINT ( 'NONE',  ( -7.173100160369890510, -3.202444869320336451, 32.30641848906366675 ) ) ;
#52387 = CARTESIAN_POINT ( 'NONE',  ( 7.596130621932389637, -12.68155406624981119, 30.59749803192733708 ) ) ;
#52388 = DIRECTION ( 'NONE',  ( -0.000000000000000000, 1.000000000000000000, -0.000000000000000000 ) ) ;
#52389 = CYLINDRICAL_SURFACE ( 'NONE', #10515, 0.2499999999999994726 ) ;
#52390 = CARTESIAN_POINT ( 'NONE',  ( -17.74994568836168440, -6.567000820036036579, 34.66262288849541306 ) ) ;
#52391 = DIRECTION ( 'NONE',  ( -0.000000000000000000, -0.3420201433256694346, -0.9396926207859080948 ) ) ;
#52392 = ORIENTED_EDGE ( 'NONE', *, *, #76293, .T. ) ;
#52393 = EDGE_LOOP ( 'NONE', ( #82808, #19993, #5128, #61439 ) ) ;
#52394 = EDGE_CURVE ( 'NONE', #82761, #19526, #60928, .T. ) ;
#52395 = EDGE_LOOP ( 'NONE', ( #4971, #43056, #87384, #27071 ) ) ;
#52397 = VERTEX_POINT ( 'NONE', #75461 ) ;
#52396 = CARTESIAN_POINT ( 'NONE',  ( 0.4615384615383382183, -12.16647553114689728, 32.15551576947799362 ) ) ;
#52399 = CARTESIAN_POINT ( 'NONE',  ( -16.28399336328437386, -10.19110544564092002, 33.96427741523702792 ) ) ;
#52398 = CARTESIAN_POINT ( 'NONE',  ( 7.623227628637696540, -3.105860786376062332, 32.13614157043599562 ) ) ;
#52400 = CARTESIAN_POINT ( 'NONE',  ( -1.515305987725692471, -4.684245665217972032, 34.18127051446801090 ) ) ;
#52401 = CARTESIAN_POINT ( 'NONE',  ( -1.384615384615383471, -2.517432740324522911, 35.29906147534542527 ) ) ;
#52402 = FACE_BOUND ( 'NONE', #10868, .T. ) ;
#52403 = ORIENTED_EDGE ( 'NONE', *, *, #29640, .F. ) ;
#52404 = AXIS2_PLACEMENT_3D ( 'NONE', #86547, #85203, #71671 ) ;
#52405 = B_SPLINE_CURVE_WITH_KNOTS ( 'NONE', 3,
 ( #52366, #79855, #45615, #73093, #38873, #4636, #34319, #27122, #26678, #46938 ),
 .UNSPECIFIED., .F., .F.,
 ( 4, 2, 2, 2, 4 ),
 ( 0.0007817246256747459798, 0.0009771112852218887673, 0.001172497944769031663, 0.001367884604316174559, 0.001563271263863317455 ),
 .UNSPECIFIED. ) ;
#52406 = ORIENTED_EDGE ( 'NONE', *, *, #16955, .F. ) ;
#52407 = CARTESIAN_POINT ( 'NONE',  ( -2.557669038634660552, -12.41269422305637171, 30.68257228309993323 ) ) ;
#52408 = AXIS2_PLACEMENT_3D ( 'NONE', #75214, #19819, #55367 ) ;
#52409 = ORIENTED_EDGE ( 'NONE', *, *, #32354, .F. ) ;
#52410 = FACE_BOUND ( 'NONE', #29884, .T. ) ;
#52411 = CARTESIAN_POINT ( 'NONE',  ( 9.692307692307695177, -2.538708090699994813, 30.37095296980875503 ) ) ;
#52412 = EDGE_CURVE ( 'NONE', #85101, #53248, #13319, .T. ) ;
#52413 = B_SPLINE_CURVE_WITH_KNOTS ( 'NONE', 3,
 ( #36413, #48579, #63870, #84609, #35074, #62532 ),
 .UNSPECIFIED., .F., .F.,
 ( 4, 2, 4 ),
 ( 0.000000000000000000, 0.0001954784845028914076, 0.0003909569690057828153 ),
 .UNSPECIFIED. ) ;
#52414 = CARTESIAN_POINT ( 'NONE',  ( 15.23076923076923173, -6.343179335718451384, 34.87096338111211935 ) ) ;
#52415 = VERTEX_POINT ( 'NONE', #26837 ) ;
#52416 = CARTESIAN_POINT ( 'NONE',  ( 2.057715576749954423, -8.303909089506435137, 34.68538101551103381 ) ) ;
#52417 = CARTESIAN_POINT ( 'NONE',  ( -6.857009589726846599, -2.292212530054420494, 30.41441678777542990 ) ) ;
#52418 = DIRECTION ( 'NONE',  ( -0.000000000000000000, -0.6427876096865404731, -0.7660444431189770143 ) ) ;
#52419 = VERTEX_POINT ( 'NONE', #67824 ) ;
#52420 = B_SPLINE_CURVE_WITH_KNOTS ( 'NONE', 3,
 ( #29239, #76530, #56692, #69766, #84187, #868, #70656, #68877, #14382, #20696 ),
 .UNSPECIFIED., .F., .F.,
 ( 4, 2, 2, 2, 4 ),
 ( 0.000000000000000000, 0.0001954311564186879044, 0.0003908623128373758088, 0.0005862934692560636861, 0.0007817246256747516176 ),
 .UNSPECIFIED. ) ;
#52421 = EDGE_CURVE ( 'NONE', #53195, #40406, #5105, .T. ) ;
#52422 = CARTESIAN_POINT ( 'NONE',  ( 18.22342639891478910, -7.630147987733843173, 34.99859428049665411 ) ) ;
#52423 = CARTESIAN_POINT ( 'NONE',  ( -18.00000000000000000, -8.973038597847269315, 34.52809138561121927 ) ) ;
#52424 = VERTEX_POINT ( 'NONE', #74584 ) ;
#52425 = CARTESIAN_POINT ( 'NONE',  ( -2.372962753653081069, -11.48612834413959582, 32.76840700105983473 ) ) ;
#52426 = LINE ( 'NONE', #17316, #71433 ) ;
#52427 = ORIENTED_EDGE ( 'NONE', *, *, #84375, .T. ) ;
#52428 = FACE_OUTER_BOUND ( 'NONE', #85879, .T. ) ;
#52429 = DIRECTION ( 'NONE',  ( -0.000000000000000000, -0.6427876096865404731, -0.7660444431189770143 ) ) ;
#52430 = DIRECTION ( 'NONE',  ( 0.000000000000000000, 0.7660444431189822323, -0.6427876096865344779 ) ) ;
#52431 = DIRECTION ( 'NONE',  ( -0.000000000000000000, 0.9848077530122086864, -0.1736481776669273891 ) ) ;
#52432 = DIRECTION ( 'NONE',  ( 0.000000000000000000, 0.3420201433256641055, -0.9396926207859100932 ) ) ;
#52433 = CARTESIAN_POINT ( 'NONE',  ( -20.99999999999999645, -4.249999999999998224, 29.75000000000000355 ) ) ;
#52435 = CYLINDRICAL_SURFACE ( 'NONE', #18702, 0.2499999999999995559 ) ;
#52434 = CARTESIAN_POINT ( 'NONE',  ( -13.63459212866397507, -4.075325502946081535, 33.72974371597206300 ) ) ;
#52436 = ADVANCED_FACE ( 'NONE', ( #6566 ), #35360, .F. ) ;
#52437 = CARTESIAN_POINT ( 'NONE',  ( 8.992242120843618736, -12.15243808032445827, 31.58219941686247978 ) ) ;
#52439 = CARTESIAN_POINT ( 'NONE',  ( 12.39545608217832395, -4.661471528628507777, 34.16647553114621871 ) ) ;
#52438 = CARTESIAN_POINT ( 'NONE',  ( -9.692307692307691624, -13.04860791097971706, 34.73218667398347037 ) ) ;
#52440 = CARTESIAN_POINT ( 'NONE',  ( 1.901340078031349856, -5.512252781505337929, 25.31063170625848713 ) ) ;
#52441 = ORIENTED_EDGE ( 'NONE', *, *, #49762, .T. ) ;
#52442 = CARTESIAN_POINT ( 'NONE',  ( -9.692307692307691624, -8.164416787775445883, 34.95778746994557906 ) ) ;
#52443 = ORIENTED_EDGE ( 'NONE', *, *, #80319, .F. ) ;
#52444 = EDGE_CURVE ( 'NONE', #20922, #88377, #48004, .T. ) ;
#52445 = ORIENTED_EDGE ( 'NONE', *, *, #77944, .F. ) ;
#52446 = CARTESIAN_POINT ( 'NONE',  ( 13.13461538461538680, -2.249999999999998668, 29.75000000000000355 ) ) ;
#52447 = ORIENTED_EDGE ( 'NONE', *, *, #43858, .T. ) ;
#52448 = DIRECTION ( 'NONE',  ( 1.000000000000000000, 0.000000000000000000, 0.000000000000000000 ) ) ;
#52449 = CARTESIAN_POINT ( 'NONE',  ( 1.799775606325937360E-14, -10.25000000000000000, 17.28125000000000000 ) ) ;
#52450 = CARTESIAN_POINT ( 'NONE',  ( -17.77722045873159473, -5.913360116392396115, 34.49180327182771322 ) ) ;
#52451 = CARTESIAN_POINT ( 'NONE',  ( -8.769230769230890843, -3.300289026999228881, 32.46337939537708905 ) ) ;
#52452 = CARTESIAN_POINT ( 'NONE',  ( -7.623374304885435215, -5.913360116392397892, 34.49180327182771322 ) ) ;
#52453 = FACE_OUTER_BOUND ( 'NONE', #52967, .T. ) ;
#52454 = VECTOR ( 'NONE', #13346, 1000.000000000000000 ) ;
#52455 = CARTESIAN_POINT ( 'NONE',  ( -5.207613680033387205, -3.338472653186242756, 32.95098750199972670 ) ) ;
#52456 = LINE ( 'NONE', #80397, #9945 ) ;
#52457 = PLANE ( 'NONE',  #10858 ) ;
#52458 = CARTESIAN_POINT ( 'NONE',  ( -1.553300858899125059, -3.750000000000009326, 19.07812500000000000 ) ) ;
#52459 = CARTESIAN_POINT ( 'NONE',  ( 17.32697749683652688, -2.318338780012835443, 30.59689888758630616 ) ) ;
#52461 = ADVANCED_FACE ( 'NONE', ( #62815 ), #56077, .F. ) ;
#52460 = CARTESIAN_POINT ( 'NONE',  ( -14.55769230769230660, -2.499999999999998668, 29.75000000000000355 ) ) ;
#52462 = B_SPLINE_CURVE_WITH_KNOTS ( 'NONE', 3,
 ( #13253, #19561, #75397, #5609, #61426, #48356, #82162, #27647, #180, #33532 ),
 .UNSPECIFIED., .F., .F.,
 ( 4, 2, 2, 2, 4 ),
 ( 0.0007817359430256253438, 0.0009771253907249898181, 0.001172514838424354401, 0.001367904286123718983, 0.001563293733823083566 ),
 .UNSPECIFIED. ) ;
#52463 = EDGE_CURVE ( 'NONE', #7973, #3259, #35818, .T. ) ;
#52464 = B_SPLINE_CURVE_WITH_KNOTS ( 'NONE', 3,
 ( #88126, #33149, #33599, #74138, #89003, #53862, #26397, #61058, #54294, #34913 ),
 .UNSPECIFIED., .F., .F.,
 ( 4, 2, 2, 2, 4 ),
 ( 0.0007817359430256392216, 0.0009771253907250080327, 0.001172514838424376952, 0.001367904286123745872, 0.001563293733823114791 ),
 .UNSPECIFIED. ) ;
#52465 = CARTESIAN_POINT ( 'NONE',  ( 5.999999999999878320, -3.643525952248796163, 33.31231777344771672 ) ) ;
#52466 = ORIENTED_EDGE ( 'NONE', *, *, #45638, .F. ) ;
#52468 = EDGE_CURVE ( 'NONE', #84116, #6052, #60477, .T. ) ;
#52467 = ORIENTED_EDGE ( 'NONE', *, *, #29772, .F. ) ;
#52469 = CARTESIAN_POINT ( 'NONE',  ( 14.24160992833217421, -8.164416787775445883, 34.95778746994557906 ) ) ;
#52470 = CARTESIAN_POINT ( 'NONE',  ( 7.846153846153725020, -11.48612834414049644, 32.76840700105863391 ) ) ;
#52471 = CARTESIAN_POINT ( 'NONE',  ( 1.254467414883688292, -11.04286588640298561, 33.62463336215343901 ) ) ;
#52472 = CARTESIAN_POINT ( 'NONE',  ( -6.923076923077045919, -5.941354392335915335, 34.76329471203413846 ) ) ;
#52473 = EDGE_CURVE ( 'NONE', #39792, #21373, #2845, .T. ) ;
#52474 = CARTESIAN_POINT ( 'NONE',  ( 8.519254038288416098, -11.79746400365624659, 32.30657167506340954 ) ) ;
#52475 = DIRECTION ( 'NONE',  ( 0.000000000000000000, 0.9396926207859126468, 0.3420201433256571111 ) ) ;
#52476 = AXIS2_PLACEMENT_3D ( 'NONE', #62270, #52074, #55079 ) ;
#52477 = ORIENTED_EDGE ( 'NONE', *, *, #68083, .F. ) ;
#52478 = CARTESIAN_POINT ( 'NONE',  ( 17.93472955403921887, -12.46129190929999986, 30.37095296980880832 ) ) ;
#52479 = VERTEX_POINT ( 'NONE', #70927 ) ;
#52480 = ORIENTED_EDGE ( 'NONE', *, *, #83880, .F. ) ;
#52481 = CYLINDRICAL_SURFACE ( 'NONE', #30637, 0.2500000000000004996 ) ;
#52482 = AXIS2_PLACEMENT_3D ( 'NONE', #70722, #61730, #70276 ) ;
#52483 = CARTESIAN_POINT ( 'NONE',  ( 6.130838418012763746, -7.277220443632450575, 34.74524770363009196 ) ) ;
#52484 = LINE ( 'NONE', #58797, #27169 ) ;
#52485 = CIRCLE ( 'NONE', #63990, 0.2500000000000002220 ) ;
#52486 = CARTESIAN_POINT ( 'NONE',  ( 11.53846153846153832, -2.292212530054420494, 30.41441678777542634 ) ) ;
#52487 = CARTESIAN_POINT ( 'NONE',  ( -5.326946301144532825, -8.475808217655753651, 34.90892951860618609 ) ) ;
#52488 = ORIENTED_EDGE ( 'NONE', *, *, #50214, .T. ) ;
#52489 = ORIENTED_EDGE ( 'NONE', *, *, #72683, .T. ) ;
#52490 = EDGE_CURVE ( 'NONE', #7165, #3616, #82499, .T. ) ;
#52491 = EDGE_LOOP ( 'NONE', ( #16717, #65567, #89083, #31007 ) ) ;
#52492 = CARTESIAN_POINT ( 'NONE',  ( -6.923076923076922462, -11.91647553114624181, 32.58852847137148245 ) ) ;
#52493 = CARTESIAN_POINT ( 'NONE',  ( -5.076923076923197442, -4.481592998941358097, 33.73612834414048933 ) ) ;
#52494 = LINE ( 'NONE', #79542, #10627 ) ;
#52495 = DIRECTION ( 'NONE',  ( 0.000000000000000000, -8.673617379884033500E-16, 1.000000000000000000 ) ) ;
#52496 = DIRECTION ( 'NONE',  ( -0.000000000000000000, -0.5000000000000009992, -0.8660254037844380415 ) ) ;
#52497 = CARTESIAN_POINT ( 'NONE',  ( 5.750023269057646935, -12.41269422305637171, 30.68257228309993323 ) ) ;
#52498 = ORIENTED_EDGE ( 'NONE', *, *, #85811, .T. ) ;
#52499 = EDGE_CURVE ( 'NONE', #43224, #5405, #15807, .T. ) ;
#52500 = EDGE_LOOP ( 'NONE', ( #36467, #79616 ) ) ;
#52501 = CARTESIAN_POINT ( 'NONE',  ( -2.651650429449535551, -10.15165042944956753, 24.93750000000000000 ) ) ;
#52502 = ADVANCED_FACE ( 'NONE', ( #9659 ), #36696, .F. ) ;
#52503 = VECTOR ( 'NONE', #53502, 1000.000000000000000 ) ;
#52504 = ORIENTED_EDGE ( 'NONE', *, *, #65666, .F. ) ;
#52506 = ORIENTED_EDGE ( 'NONE', *, *, #15521, .T. ) ;
#52505 = CARTESIAN_POINT ( 'NONE',  ( -12.71156169883142617, -11.37209801155882971, 32.91403422569032955 ) ) ;
#52507 = CARTESIAN_POINT ( 'NONE',  ( -10.36533019547115941, -4.074993327901527351, 33.72946981652012255 ) ) ;
#52508 = CARTESIAN_POINT ( 'NONE',  ( 7.846153846154153122, -2.506253911140614576, 30.00000000000323297 ) ) ;
#52509 = CARTESIAN_POINT ( 'NONE',  ( -3.750000000000007550, -5.946699141100917352, 15.17187500000000000 ) ) ;
#52510 = ORIENTED_EDGE ( 'NONE', *, *, #56076, .T. ) ;
#52511 = CARTESIAN_POINT ( 'NONE',  ( -14.37296230824862775, -12.51329471203370325, 31.30864560766548976 ) ) ;
#52512 = ORIENTED_EDGE ( 'NONE', *, *, #63030, .T. ) ;
#52513 = CARTESIAN_POINT ( 'NONE',  ( 13.19230769230769340, -7.500000000000000000, 33.75000000000000000 ) ) ;
#52514 = CARTESIAN_POINT ( 'NONE',  ( 0.4615384615384611200, -11.35647404775217417, 33.31231777344666511 ) ) ;
#52515 = CARTESIAN_POINT ( 'NONE',  ( 7.716005876422150855, -4.299443229763728169, 33.91186481527756058 ) ) ;
#52517 = DIRECTION ( 'NONE',  ( -0.000000000000000000, 0.9848077530122085754, -0.1736481776669273613 ) ) ;
#52516 = CARTESIAN_POINT ( 'NONE',  ( -6.700297381808513641, -12.44528174975671853, 30.48912976160716681 ) ) ;
#52518 = EDGE_CURVE ( 'NONE', #22873, #1344, #65033, .T. ) ;
#52519 = CARTESIAN_POINT ( 'NONE',  ( -2.980823712421088345, -6.696923467548660192, 34.68552623307873972 ) ) ;
#52520 = DIRECTION ( 'NONE',  ( -0.000000000000000000, 0.9396926207859093161, -0.3420201433256663259 ) ) ;
#52521 = ORIENTED_EDGE ( 'NONE', *, *, #8186, .T. ) ;
#52522 = DIRECTION ( 'NONE',  ( -0.000000000000000000, 0.7660444431189791237, -0.6427876096865379196 ) ) ;
#52523 = CARTESIAN_POINT ( 'NONE',  ( 11.28846153846153832, -2.249999999999998668, 29.75000000000000355 ) ) ;
#52524 = EDGE_CURVE ( 'NONE', #71802, #7759, #36261, .T. ) ;
#52525 = CARTESIAN_POINT ( 'NONE',  ( 14.55774672760576394, -4.074993327901527351, 33.72946981652012255 ) ) ;
#52526 = ORIENTED_EDGE ( 'NONE', *, *, #54583, .T. ) ;
#52527 = CARTESIAN_POINT ( 'NONE',  ( 1.653273178848927064E-15, -7.500000000000000000, 0.000000000000000000 ) ) ;
#52528 = CARTESIAN_POINT ( 'NONE',  ( -14.98082382139119062, -5.766571408460171355, 34.70601412856602508 ) ) ;
#52529 = CARTESIAN_POINT ( 'NONE',  ( -19.50000000000000000, -11.50000000000000000, 29.75000000000000355 ) ) ;
#52530 = CARTESIAN_POINT ( 'NONE',  ( -9.692307692307812417, -2.625532179533778709, 30.86335684631627174 ) ) ;
#52531 = CIRCLE ( 'NONE', #9403, 0.2500000000000002220 ) ;
#52532 = FACE_BOUND ( 'NONE', #38741, .T. ) ;
#52534 = LINE ( 'NONE', #32280, #37382 ) ;
#52533 = CARTESIAN_POINT ( 'NONE',  ( 12.21156173059610772, -3.137211980971221781, 32.19342716148376837 ) ) ;
#52535 = EDGE_CURVE ( 'NONE', #85190, #88762, #20100, .T. ) ;
#52536 = CARTESIAN_POINT ( 'NONE',  ( -15.10024379253558635, -5.070358843744210198, 34.40418822224088302 ) ) ;
#52538 = CARTESIAN_POINT ( 'NONE',  ( -11.47320639894870276, -11.06231777344671130, 33.60647404775212976 ) ) ;
#52537 = CARTESIAN_POINT ( 'NONE',  ( 18.13079180782478872, -11.18335022499818621, 33.13157742990016885 ) ) ;
#52539 = DIRECTION ( 'NONE',  ( -0.000000000000000000, 1.000000000000000000, -0.000000000000000000 ) ) ;
#52540 = CARTESIAN_POINT ( 'NONE',  ( 6.000000000000001776, -4.661471528628507777, 34.16647553114623292 ) ) ;
#52541 = CARTESIAN_POINT ( 'NONE',  ( 3.724691934501232815, -5.885600066136343678, 26.63875670625848713 ) ) ;
#52542 = CARTESIAN_POINT ( 'NONE',  ( 10.61538461538449418, -12.16647553114689728, 32.15551576947799362 ) ) ;
#52543 = ORIENTED_EDGE ( 'NONE', *, *, #37911, .F. ) ;
#52544 = CARTESIAN_POINT ( 'NONE',  ( -9.692307692307691624, -1.129524287112498415, 32.06866353760679544 ) ) ;
#52545 = CARTESIAN_POINT ( 'NONE',  ( -15.16562345143726631, -7.750023238201979581, 34.74374492549440419 ) ) ;
#52546 = CARTESIAN_POINT ( 'NONE',  ( -3.230769230769229949, -3.050289026998446396, 32.03036669348365706 ) ) ;
#52548 = AXIS2_PLACEMENT_3D ( 'NONE', #63911, #22932, #50394 ) ;
#52547 = CARTESIAN_POINT ( 'NONE',  ( -19.50000000000000000, -11.50000000000000000, 29.75000000000000355 ) ) ;
#52549 = CARTESIAN_POINT ( 'NONE',  ( 16.94623247381277054, -12.62707690430377383, 30.88035979386743435 ) ) ;
#52550 = CARTESIAN_POINT ( 'NONE',  ( 1.384615384615386802, -11.91647553114624181, 32.58852847137148245 ) ) ;
#52551 = CARTESIAN_POINT ( 'NONE',  ( 1.987747218494664292, -9.401340078031346081, 15.62313170625848890 ) ) ;
#52552 = CARTESIAN_POINT ( 'NONE',  ( 14.30769230769218758, -10.90142922262034020, 33.41473453929536674 ) ) ;
#52553 = LINE ( 'NONE', #80038, #28822 ) ;
#52554 = DIRECTION ( 'NONE',  ( 0.000000000000000000, 1.000000000000000000, 0.000000000000000000 ) ) ;
#52555 = CARTESIAN_POINT ( 'NONE',  ( -0.5922290646487686772, -8.191372820521381826, 34.95448215188423546 ) ) ;
#52556 = CARTESIAN_POINT ( 'NONE',  ( 14.53070365930516239, -5.667800583137506010, 34.40243808032445827 ) ) ;
#52557 = CARTESIAN_POINT ( 'NONE',  ( -8.899377978668987055, -9.418419913701741919, 34.36755862841477693 ) ) ;
#52559 = EDGE_CURVE ( 'NONE', #38361, #4430, #59053, .T. ) ;
#52558 = CARTESIAN_POINT ( 'NONE',  ( -18.25002323729295739, -2.823816976329321271, 31.52131813110797154 ) ) ;
#52560 = LINE ( 'NONE', #4382, #24058 ) ;
#52561 = ORIENTED_EDGE ( 'NONE', *, *, #18382, .F. ) ;
#52562 = CARTESIAN_POINT ( 'NONE',  ( 2.307692307692309264, -10.67929555188718282, 33.92786785259544047 ) ) ;
#52563 = CARTESIAN_POINT ( 'NONE',  ( -11.53846153846153655, -8.810774026931790459, 35.74407628777942847 ) ) ;
#52564 = CARTESIAN_POINT ( 'NONE',  ( 3.724691934501251023, -9.114399933863618131, 19.79874329374151287 ) ) ;
#52565 = ADVANCED_FACE ( 'NONE', ( #70483 ), #4238, .F. ) ;
#52566 = CARTESIAN_POINT ( 'NONE',  ( 6.000000000000001776, -4.098570777380720287, 33.41473453929634729 ) ) ;
#52567 = CARTESIAN_POINT ( 'NONE',  ( 3.296837581771670411, -11.69971097300155272, 32.46337939537588113 ) ) ;
#52568 = EDGE_LOOP ( 'NONE', ( #12718, #16970 ) ) ;
#52569 = CARTESIAN_POINT ( 'NONE',  ( -18.00000000000000000, -6.343179335718452272, 34.87096338111211935 ) ) ;
#52570 = PLANE ( 'NONE',  #66070 ) ;
#52572 = ORIENTED_EDGE ( 'NONE', *, *, #28502, .T. ) ;
#52571 = CARTESIAN_POINT ( 'NONE',  ( 8.834485908743600291, -2.657715359629132301, 31.77849191805844242 ) ) ;
#52573 = CARTESIAN_POINT ( 'NONE',  ( 11.78851595837499211, -4.818054556918156983, 34.26375889529406749 ) ) ;
#52574 = CARTESIAN_POINT ( 'NONE',  ( -15.23076923076922995, -5.180354513474913603, 36.12317359536750416 ) ) ;
#52575 = EDGE_CURVE ( 'NONE', #77667, #10170, #45667, .T. ) ;
#52576 = CARTESIAN_POINT ( 'NONE',  ( -4.946131269098287930, -8.999086150933472084, 34.52020707165672064 ) ) ;
#52577 = VECTOR ( 'NONE', #79943, 1000.000000000000227 ) ;
#52578 = CARTESIAN_POINT ( 'NONE',  ( -11.66915214157184444, -2.494641256782728966, 31.33461815524612959 ) ) ;
#52579 = ORIENTED_EDGE ( 'NONE', *, *, #69279, .F. ) ;
#52580 = DIRECTION ( 'NONE',  ( -0.000000000000000000, 0.7660444431189791237, -0.6427876096865379196 ) ) ;
#52581 = CARTESIAN_POINT ( 'NONE',  ( -12.59168643127016374, -2.647304123082328875, 31.75400227202885972 ) ) ;
#52582 = CARTESIAN_POINT ( 'NONE',  ( 1.653273178848927064E-15, -7.500000000000000000, 14.00000000000000178 ) ) ;
#52583 = VERTEX_POINT ( 'NONE', #86684 ) ;
#52584 = VERTEX_POINT ( 'NONE', #86232 ) ;
#52585 = EDGE_CURVE ( 'NONE', #70755, #75080, #60066, .T. ) ;
#52586 = B_SPLINE_CURVE_WITH_KNOTS ( 'NONE', 3,
 ( #43210, #2210, #22057, #64348, #69794, #29705, #2646, #63475, #8103, #28823 ),
 .UNSPECIFIED., .F., .F.,
 ( 4, 2, 2, 2, 4 ),
 ( 0.000000000000000000, 0.0001954311564186880399, 0.0003908623128373760799, 0.0005862934692560641198, 0.0007817246256747521597 ),
 .UNSPECIFIED. ) ;
#52587 = ORIENTED_EDGE ( 'NONE', *, *, #2804, .T. ) ;
#52588 = CARTESIAN_POINT ( 'NONE',  ( -23.50000000000000000, -1.749999999999991340, 28.86437827766147279 ) ) ;
#52589 = CARTESIAN_POINT ( 'NONE',  ( -8.519285250882628446, -3.202959910592335646, 32.30730279482227019 ) ) ;
#52590 = EDGE_CURVE ( 'NONE', #12230, #88550, #39812, .T. ) ;
#52591 = B_SPLINE_CURVE_WITH_KNOTS ( 'NONE', 3,
 ( #14264, #34534, #69207, #48037, #76856, #27336, #68320, #54798, #34088, #61552 ),
 .UNSPECIFIED., .F., .F.,
 ( 4, 2, 2, 2, 4 ),
 ( 0.000000000000000000, 0.0001954339857564073388, 0.0003908679715128146777, 0.0005863019572692220165, 0.0007817359430256293554 ),
 .UNSPECIFIED. ) ;
#52592 = FACE_OUTER_BOUND ( 'NONE', #6360, .T. ) ;
#52593 = CARTESIAN_POINT ( 'NONE',  ( 4.826923076923076650, -7.500000000000001776, 34.75000000000000000 ) ) ;
#52594 = EDGE_CURVE ( 'NONE', #80969, #51215, #81370, .T. ) ;
#52595 = VECTOR ( 'NONE', #49439, 1000.000000000000000 ) ;
#52596 = ORIENTED_EDGE ( 'NONE', *, *, #5988, .F. ) ;
#52597 = VERTEX_POINT ( 'NONE', #12334 ) ;
#52599 = ORIENTED_EDGE ( 'NONE', *, *, #86362, .T. ) ;
#52598 = CARTESIAN_POINT ( 'NONE',  ( 11.53846153846153832, -11.35647404775217417, 33.31231777344666511 ) ) ;
#52600 = CARTESIAN_POINT ( 'NONE',  ( -4.230769230769230838, -3.499999999999999556, 29.75000000000000355 ) ) ;
#52601 = EDGE_CURVE ( 'NONE', #82878, #57615, #65929, .T. ) ;
#52602 = CARTESIAN_POINT ( 'NONE',  ( 18.00000000000000000, -2.486705287966279876, 31.30864560766543647 ) ) ;
#52603 = CARTESIAN_POINT ( 'NONE',  ( 1.607394925883795844, -10.81320215134717344, 33.49497208177562868 ) ) ;
#52604 = DIRECTION ( 'NONE',  ( 1.000000000000000000, 0.000000000000000000, 0.000000000000000000 ) ) ;
#52605 = AXIS2_PLACEMENT_3D ( 'NONE', #1224, #35912, #21495 ) ;
#52606 = ORIENTED_EDGE ( 'NONE', *, *, #5301, .F. ) ;
#52607 = VERTEX_POINT ( 'NONE', #11898 ) ;
#52608 = EDGE_CURVE ( 'NONE', #65351, #79454, #53431, .T. ) ;
#52609 = ORIENTED_EDGE ( 'NONE', *, *, #82508, .T. ) ;
#52611 = EDGE_LOOP ( 'NONE', ( #70556, #82949, #49322, #4403 ) ) ;
#52610 = FACE_OUTER_BOUND ( 'NONE', #14935, .T. ) ;
#52612 = DIRECTION ( 'NONE',  ( -0.000000000000000000, 0.7660444431189791237, -0.6427876096865379196 ) ) ;
#52613 = DIRECTION ( 'NONE',  ( -1.000000000000000000, -0.000000000000000000, -0.000000000000000000 ) ) ;
#52614 = ORIENTED_EDGE ( 'NONE', *, *, #46647, .F. ) ;
#52615 = EDGE_CURVE ( 'NONE', #59590, #13160, #60549, .T. ) ;
#52616 = B_SPLINE_CURVE_WITH_KNOTS ( 'NONE', 3,
 ( #74710, #20201, #34148, #83232, #26959, #68379, #82794, #55744, #48992, #33275 ),
 .UNSPECIFIED., .F., .F.,
 ( 4, 2, 2, 2, 4 ),
 ( 0.000000000000000000, 0.0001954311564186863052, 0.0003908623128373726104, 0.0005862934692560589156, 0.0007817246256747452209 ),
 .UNSPECIFIED. ) ;
#52617 = CARTESIAN_POINT ( 'NONE',  ( -13.63463862190834952, -4.335965774309648246, 33.62209801155881905 ) ) ;
#52618 = CARTESIAN_POINT ( 'NONE',  ( 15.23076923076923173, -4.102666532097928531, 36.13435417666054406 ) ) ;
#52619 = CARTESIAN_POINT ( 'NONE',  ( -5.999999999999998224, -13.57706302396349152, 30.56769352161908060 ) ) ;
#52620 = FACE_BOUND ( 'NONE', #10537, .T. ) ;
#52621 = CARTESIAN_POINT ( 'NONE',  ( -5.299850035829926753, -10.01117774369187252, 34.36070679894347535 ) ) ;
#52622 = CARTESIAN_POINT ( 'NONE',  ( 16.15384615384615330, -10.67929555188718282, 33.92786785259544047 ) ) ;
#52623 = CARTESIAN_POINT ( 'NONE',  ( -8.835314180186648159, -4.098570777380719399, 33.41473453929634729 ) ) ;
#52625 = CARTESIAN_POINT ( 'NONE',  ( 14.53070515178570865, -2.889357225399416418, 32.26129605718031002 ) ) ;
#52624 = CARTESIAN_POINT ( 'NONE',  ( 3.296836564119306257, -3.322132147404559976, 32.92929555188717927 ) ) ;
#52626 = AXIS2_PLACEMENT_3D ( 'NONE', #53103, #32849, #31964 ) ;
#52627 = LINE ( 'NONE', #67935, #38080 ) ;
#52628 = DIRECTION ( 'NONE',  ( -0.000000000000000000, 1.000000000000000000, -0.000000000000000000 ) ) ;
#52629 = ORIENTED_EDGE ( 'NONE', *, *, #4537, .T. ) ;
#52630 = CARTESIAN_POINT ( 'NONE',  ( -16.08767701288349627, -7.250054483168842268, 34.74374881642865631 ) ) ;
#52631 = CARTESIAN_POINT ( 'NONE',  ( 12.46153846153833911, -3.643525952248795718, 33.31231777344771672 ) ) ;
#52632 = VERTEX_POINT ( 'NONE', #72246 ) ;
#52633 = EDGE_CURVE ( 'NONE', #87267, #23252, #16911, .T. ) ;
#52634 = ORIENTED_EDGE ( 'NONE', *, *, #19522, .F. ) ;
#52635 = CIRCLE ( 'NONE', #64128, 0.2500000000000002220 ) ;
#52637 = CARTESIAN_POINT ( 'NONE',  ( -17.29984929443922681, -11.24512374952581872, 33.06303171183252942 ) ) ;
#52636 = CARTESIAN_POINT ( 'NONE',  ( -9.320512820512821150, -11.00000000000000000, 29.75000000000000355 ) ) ;
#52638 = CARTESIAN_POINT ( 'NONE',  ( 16.15384615384615330, -6.343179335718451384, 34.87096338111211935 ) ) ;
#52639 = CARTESIAN_POINT ( 'NONE',  ( 16.02315468717859304, -3.530157926970578508, 32.79014554554150607 ) ) ;
#52640 = CARTESIAN_POINT ( 'NONE',  ( 13.38461538461538680, -11.33034616979429110, 35.88435417666054406 ) ) ;
#52641 = VERTEX_POINT ( 'NONE', #52861 ) ;
#52642 = LINE ( 'NONE', #79681, #70188 ) ;
#52643 = CARTESIAN_POINT ( 'NONE',  ( 4.376625822824220080, -4.989023458446560255, 34.36081565061822118 ) ) ;
#52645 = LINE ( 'NONE', #80129, #44501 ) ;
#52644 = CARTESIAN_POINT ( 'NONE',  ( 2.307692307692309264, -1.509761064869970415, 31.06009739812519044 ) ) ;
#52646 = DIRECTION ( 'NONE',  ( 2.891205793294679312E-16, -1.000000000000000000, 0.000000000000000000 ) ) ;
#52647 = CARTESIAN_POINT ( 'NONE',  ( 2.530703659305157949, -4.887748414852789658, 34.01359900205216746 ) ) ;
#52649 = CARTESIAN_POINT ( 'NONE',  ( -17.07692307692307665, -2.486705287966279876, 31.30864560766543647 ) ) ;
#52648 =( NAMED_UNIT ( * ) SI_UNIT ( $, .STERADIAN. ) SOLID_ANGLE_UNIT ( ) );
#52650 = CARTESIAN_POINT ( 'NONE',  ( 2.320192649118979489E-14, -11.25000000000000000, 22.28125000000000355 ) ) ;
#52651 = VERTEX_POINT ( 'NONE', #5131 ) ;
#52652 = ORIENTED_EDGE ( 'NONE', *, *, #17418, .T. ) ;
#52653 = DIRECTION ( 'NONE',  ( 0.000000000000000000, 1.000000000000000000, 0.000000000000000000 ) ) ;
#52654 = CARTESIAN_POINT ( 'NONE',  ( -4.377331097570100304, -12.44517049084099725, 30.48991314939691932 ) ) ;
#52655 = PLANE ( 'NONE',  #79063 ) ;
#52656 = DIRECTION ( 'NONE',  ( -0.000000000000000000, -0.9396926207859093161, -0.3420201433256663259 ) ) ;
#52657 = DIRECTION ( 'NONE',  ( 0.000000000000000000, 0.9848077530122072432, -0.1736481776669354937 ) ) ;
#52658 = CARTESIAN_POINT ( 'NONE',  ( 2.320192649118979489E-14, -11.25000000000000000, 21.03125000000000000 ) ) ;
#52659 = B_SPLINE_CURVE_WITH_KNOTS ( 'NONE', 3,
 ( #53526, #45883, #39600, #80581, #4915, #79679, #32381, #18865, #81467, #31941 ),
 .UNSPECIFIED., .F., .F.,
 ( 4, 2, 2, 2, 4 ),
 ( 0.000000000000000000, 0.0001954311564186862781, 0.0003908623128373725562, 0.0005862934692560588072, 0.0007817246256747451124 ),
 .UNSPECIFIED. ) ;
#52660 = CARTESIAN_POINT ( 'NONE',  ( -1.634638608836840534, -4.175268141568689195, 33.81360843649122216 ) ) ;
#52661 = CARTESIAN_POINT ( 'NONE',  ( -13.63459211555773720, -8.303909089506435137, 34.68538101551103381 ) ) ;
#52662 = LINE ( 'NONE', #11697, #57385 ) ;
#52663 = CARTESIAN_POINT ( 'NONE',  ( -6.250000000000018652, -2.249999999999999112, 29.81609741502488120 ) ) ;
#52664 = CARTESIAN_POINT ( 'NONE',  ( 6.923076923076924238, -10.51840700105979565, 33.73612834413961536 ) ) ;
#52665 = CARTESIAN_POINT ( 'NONE',  ( 15.10062126103753855, -12.50552854090298638, 31.33409797877408920 ) ) ;
#52666 = CARTESIAN_POINT ( 'NONE',  ( 2.241608896736428491, -3.050289026998445951, 32.03036669348365706 ) ) ;
#52668 = AXIS2_PLACEMENT_3D ( 'NONE', #86130, #24405, #73050 ) ;
#52667 = CARTESIAN_POINT ( 'NONE',  ( 7.146089767170317408, -2.308499170217967134, 30.53291367094873721 ) ) ;
#52669 = CARTESIAN_POINT ( 'NONE',  ( -5.934744860487160878, -5.094484230520773593, 34.41647553114626845 ) ) ;
#52670 = CARTESIAN_POINT ( 'NONE',  ( -4.219929564802033184, -8.973038597847269315, 34.52809138561120506 ) ) ;
#52671 = CARTESIAN_POINT ( 'NONE',  ( -15.48074596171158390, -9.943427161483782584, 34.11278801902876978 ) ) ;
#52672 = ORIENTED_EDGE ( 'NONE', *, *, #76759, .T. ) ;
#52673 = CARTESIAN_POINT ( 'NONE',  ( 1.384615384615264011, -10.33852847137269571, 34.16647553114546554 ) ) ;
#52674 = FACE_OUTER_BOUND ( 'NONE', #86833, .T. ) ;
#52675 = CARTESIAN_POINT ( 'NONE',  ( -4.283994123577847368, -5.915902021225892149, 34.75552854090298638 ) ) ;
#52676 = CARTESIAN_POINT ( 'NONE',  ( 0.06109907496451789238, -4.749999999999998224, 18.15811829374151642 ) ) ;
#52677 = EDGE_CURVE ( 'NONE', #30150, #51499, #80686, .T. ) ;
#52678 = CARTESIAN_POINT ( 'NONE',  ( 4.153846153846154188, -9.780366693483667717, 34.19971097300155094 ) ) ;
#52679 = CARTESIAN_POINT ( 'NONE',  ( -3.512820512820513663, -7.500000000000000000, 33.75000000000000000 ) ) ;
#52681 = ORIENTED_EDGE ( 'NONE', *, *, #15670, .F. ) ;
#52680 = DIRECTION ( 'NONE',  ( 1.000000000000000000, 0.000000000000000000, 0.000000000000000000 ) ) ;
#52682 = CARTESIAN_POINT ( 'NONE',  ( 2.750000000000008438, -8.639087296525996607, 17.04687500000000000 ) ) ;
#52683 = CARTESIAN_POINT ( 'NONE',  ( 3.230769230769108269, -8.656820664282941280, 34.87096338111179961 ) ) ;
#52684 = ADVANCED_FACE ( 'NONE', ( #45217 ), #72694, .F. ) ;
#52685 = CIRCLE ( 'NONE', #59814, 4.000000000000000000 ) ;
#52686 = ORIENTED_EDGE ( 'NONE', *, *, #22456, .F. ) ;
#52687 = CARTESIAN_POINT ( 'NONE',  ( 17.99999999999987566, -9.442884908241554243, 34.35708131394783038 ) ) ;
#52688 = EDGE_CURVE ( 'NONE', #86305, #82221, #47435, .T. ) ;
#52689 = EDGE_LOOP ( 'NONE', ( #46736, #84874, #69589, #75112 ) ) ;
#52690 = CARTESIAN_POINT ( 'NONE',  ( -7.596208436775802930, -6.653508905675592722, 34.93172785388651391 ) ) ;
#52691 = CARTESIAN_POINT ( 'NONE',  ( 13.16168916709923664, -9.886141570436013382, 34.14413921362392301 ) ) ;
#52692 = LINE ( 'NONE', #52247, #32554 ) ;
#52693 = ORIENTED_EDGE ( 'NONE', *, *, #27313, .T. ) ;
#52694 = CARTESIAN_POINT ( 'NONE',  ( -10.54931626438217585, -12.37446782046654192, 30.86335684631486842 ) ) ;
#52695 = EDGE_LOOP ( 'NONE', ( #3076, #38626, #33324, #71805 ) ) ;
#52696 = EDGE_CURVE ( 'NONE', #70675, #41861, #13223, .T. ) ;
#52697 = CARTESIAN_POINT ( 'NONE',  ( -18.00000000000000000, -12.37446782046654192, 30.86335684631486131 ) ) ;
#52698 = ORIENTED_EDGE ( 'NONE', *, *, #52222, .T. ) ;
#52699 = CARTESIAN_POINT ( 'NONE',  ( -0.7115151924808151840, -3.137211980971221781, 32.19342716148376837 ) ) ;
#52700 = CARTESIAN_POINT ( 'NONE',  ( 0.4615384615384611200, -13.75783147151868846, 33.36296068462461051 ) ) ;
#52701 = CARTESIAN_POINT ( 'NONE',  ( 9.626224281351815293, -8.973038597847271092, 34.52809138561120506 ) ) ;
#52702 = DIRECTION ( 'NONE',  ( 0.000000000000000000, 0.7660444431189807890, 0.6427876096865361433 ) ) ;
#52703 = CARTESIAN_POINT ( 'NONE',  ( 14.30769230769231015, -2.249999999999998668, 29.75000000000001776 ) ) ;
#52704 = AXIS2_PLACEMENT_3D ( 'NONE', #31201, #32536, #44255 ) ;
#52705 = LINE ( 'NONE', #44602, #14700 ) ;
#52706 = B_SPLINE_CURVE_WITH_KNOTS ( 'NONE', 3,
 ( #65047, #51982, #37585, #29512, #3357, #79479, #36705, #38041, #51079, #36270 ),
 .UNSPECIFIED., .F., .F.,
 ( 4, 2, 2, 2, 4 ),
 ( 0.000000000000000000, 0.0001954311564186881213, 0.0003908623128373762425, 0.0005862934692560643367, 0.0007817246256747524850 ),
 .UNSPECIFIED. ) ;
#52707 = ORIENTED_EDGE ( 'NONE', *, *, #69652, .F. ) ;
#52708 = ORIENTED_EDGE ( 'NONE', *, *, #45934, .T. ) ;
#52709 = ORIENTED_EDGE ( 'NONE', *, *, #71444, .T. ) ;
#52711 = ORIENTED_EDGE ( 'NONE', *, *, #63555, .T. ) ;
#52710 = CARTESIAN_POINT ( 'NONE',  ( 17.75000000000000000, -7.500000000000001776, 35.00000000000000000 ) ) ;
#52712 = EDGE_CURVE ( 'NONE', #71861, #28699, #56245, .T. ) ;
#52713 = CYLINDRICAL_SURFACE ( 'NONE', #80933, 0.2499999999999998890 ) ;
#52714 = CARTESIAN_POINT ( 'NONE',  ( 9.692307692307570832, -5.941354392335915335, 34.76329471203413846 ) ) ;
#52715 = ORIENTED_EDGE ( 'NONE', *, *, #38520, .F. ) ;
#52716 = CARTESIAN_POINT ( 'NONE',  ( -0.7115384615384606759, -7.500000000000001776, 35.00000000000000000 ) ) ;
#52717 = EDGE_CURVE ( 'NONE', #42856, #68029, #23271, .T. ) ;
#52718 = ORIENTED_EDGE ( 'NONE', *, *, #39369, .T. ) ;
#52719 = CARTESIAN_POINT ( 'NONE',  ( -10.83886955910856464, -3.236172620538810385, 32.36188796281390267 ) ) ;
#52720 = ORIENTED_EDGE ( 'NONE', *, *, #64441, .F. ) ;
#52721 = LINE ( 'NONE', #60373, #70452 ) ;
#52722 = EDGE_CURVE ( 'NONE', #30240, #23926, #62015, .T. ) ;
#52723 = EDGE_CURVE ( 'NONE', #33268, #49750, #49136, .T. ) ;
#52724 = CARTESIAN_POINT ( 'NONE',  ( 3.930361229281821966, -12.69144148231606017, 30.53333754910549303 ) ) ;
#52725 = CYLINDRICAL_SURFACE ( 'NONE', #58335, 0.2499999999999995559 ) ;
#52726 = FACE_BOUND ( 'NONE', #46846, .T. ) ;
#52727 = CARTESIAN_POINT ( 'NONE',  ( -9.070512820512819374, -3.499999999999999556, 29.75000000000000355 ) ) ;
#52728 = CARTESIAN_POINT ( 'NONE',  ( 2.307692307692309264, -2.538708090699994813, 30.37095296980875503 ) ) ;
#52729 = DIRECTION ( 'NONE',  ( 1.000000000000000000, 0.000000000000000000, 0.000000000000000000 ) ) ;
#52730 = CARTESIAN_POINT ( 'NONE',  ( -14.05774678934416499, -5.852078868378309373, 34.47109172314383585 ) ) ;
#52731 = CARTESIAN_POINT ( 'NONE',  ( -6.000000000000119904, -5.219633306517616589, 34.19971097300220464 ) ) ;
#52732 = CARTESIAN_POINT ( 'NONE',  ( 4.000000000000001776, -7.499999999999999112, 13.50000000000000178 ) ) ;
#52733 = ORIENTED_EDGE ( 'NONE', *, *, #88331, .F. ) ;
#52734 = AXIS2_PLACEMENT_3D ( 'NONE', #11375, #17697, #78943 ) ;
#52735 = CARTESIAN_POINT ( 'NONE',  ( 1.634615384615386580, -2.249999999999998668, 29.75000000000000355 ) ) ;
#52736 = VERTEX_POINT ( 'NONE', #20856 ) ;
#52737 = EDGE_CURVE ( 'NONE', #496, #84195, #21705, .T. ) ;
#52738 = ORIENTED_EDGE ( 'NONE', *, *, #20807, .T. ) ;
#52740 = DIRECTION ( 'NONE',  ( 1.000000000000000000, 0.000000000000000000, 0.000000000000000000 ) ) ;
#52739 = CARTESIAN_POINT ( 'NONE',  ( 10.68145296638705233, -12.37446782046654192, 30.86335684631486842 ) ) ;
#52741 = CARTESIAN_POINT ( 'NONE',  ( -12.46153846153846168, -13.75783147151868846, 33.36296068462461051 ) ) ;
#52742 = CARTESIAN_POINT ( 'NONE',  ( -2.176900499867519212, -12.11778462344221019, 31.66786338562085135 ) ) ;
#52743 = EDGE_CURVE ( 'NONE', #62464, #75687, #41853, .T. ) ;
#52744 = CARTESIAN_POINT ( 'NONE',  ( 17.01116627440877238, -7.249945686854186278, 34.74374336980224598 ) ) ;
#52745 = CARTESIAN_POINT ( 'NONE',  ( -2.057637996053991003, -2.779044189368095719, 31.39831045268885745 ) ) ;
#52746 = EDGE_CURVE ( 'NONE', #50514, #3262, #17397, .T. ) ;
#52747 = EDGE_LOOP ( 'NONE', ( #45074, #19007 ) ) ;
#52748 = CARTESIAN_POINT ( 'NONE',  ( 17.07692307692295586, -6.026961402154118908, 34.52809138561165270 ) ) ;
#52749 = CARTESIAN_POINT ( 'NONE',  ( 15.23076923076910916, -4.320704448113951379, 33.92786785259630022 ) ) ;
#52750 = CARTESIAN_POINT ( 'NONE',  ( 10.39189969082028497, -3.019605429927184392, 32.48692288466676814 ) ) ;
#52751 = CARTESIAN_POINT ( 'NONE',  ( 10.86543892702293057, -11.79725096376909654, 32.30694842903959341 ) ) ;
#52752 = ORIENTED_EDGE ( 'NONE', *, *, #9513, .F. ) ;
#52753 = ADVANCED_FACE ( 'NONE', ( #34811 ), #27616, .F. ) ;
#52754 = ORIENTED_EDGE ( 'NONE', *, *, #44412, .T. ) ;
#52755 = APPLICATION_PROTOCOL_DEFINITION ( 'draft international standard', 'automotive_design', 1998, #13007 ) ;
#52756 = VERTEX_POINT ( 'NONE', #74930 ) ;
#52757 = CARTESIAN_POINT ( 'NONE',  ( -0.4615384615384611200, -4.098570777380720287, 33.41473453929634729 ) ) ;
#52758 = CARTESIAN_POINT ( 'NONE',  ( 4.853996118016225658, -2.889293201056495786, 32.26117774369186009 ) ) ;
#52759 = ORIENTED_EDGE ( 'NONE', *, *, #47151, .F. ) ;
#52760 = FACE_OUTER_BOUND ( 'NONE', #32112, .T. ) ;
#52761 = DIRECTION ( 'NONE',  ( 0.000000000000000000, 0.8660254037844377084, 0.5000000000000015543 ) ) ;
#52763 = B_SPLINE_CURVE_WITH_KNOTS ( 'NONE', 3,
 ( #19784, #45471, #60318, #13027, #26099, #40513, #72950, #80159, #11705, #40078 ),
 .UNSPECIFIED., .F., .F.,
 ( 4, 2, 2, 2, 4 ),
 ( 0.0007817246256747554124, 0.0009771112852218991757, 0.001172497944769043156, 0.001367884604316187136, 0.001563271263863330899 ),
 .UNSPECIFIED. ) ;
#52762 = CARTESIAN_POINT ( 'NONE',  ( 16.02315468717859659, -8.147922237126337563, 34.70805685702651999 ) ) ;
#52764 = CARTESIAN_POINT ( 'NONE',  ( 1.450682717965461999, -6.343179335718451384, 34.87096338111212646 ) ) ;
#52765 = CIRCLE ( 'NONE', #13942, 0.2500000000000002220 ) ;
#52766 = CARTESIAN_POINT ( 'NONE',  ( -13.38461538461538325, -12.78798330534103123, 29.99999999999997868 ) ) ;
#52767 = ORIENTED_EDGE ( 'NONE', *, *, #61774, .T. ) ;
#52769 = ORIENTED_EDGE ( 'NONE', *, *, #48075, .F. ) ;
#52768 = CARTESIAN_POINT ( 'NONE',  ( 0.2380535178145120334, -10.11188796281391511, 34.01382737946119050 ) ) ;
#52770 = CARTESIAN_POINT ( 'NONE',  ( 15.36156103859402045, -8.147973898785416225, 34.70805048591653730 ) ) ;
#52771 = CARTESIAN_POINT ( 'NONE',  ( -3.165514091256391715, -2.657715359629131857, 31.77849191805844242 ) ) ;
#52772 = CARTESIAN_POINT ( 'NONE',  ( -7.780898706641008467, -3.643525952247865352, 33.31231777344670064 ) ) ;
#52773 = CARTESIAN_POINT ( 'NONE',  ( 10.36536139116315525, -12.45566812827425451, 31.48439005359158926 ) ) ;
#52774 = DIRECTION ( 'NONE',  ( 0.000000000000000000, 0.4999999999999985567, 0.8660254037844395958 ) ) ;
#52775 = AXIS2_PLACEMENT_3D ( 'NONE', #47911, #1061, #61861 ) ;
#52776 = DIRECTION ( 'NONE',  ( 1.000000000000000000, 0.000000000000000000, 0.000000000000000000 ) ) ;
#52777 = FACE_OUTER_BOUND ( 'NONE', #35391, .T. ) ;
#52778 = CARTESIAN_POINT ( 'NONE',  ( -1.901340078031369618, -5.512252781505359245, 18.00186829374151287 ) ) ;
#52779 = ORIENTED_EDGE ( 'NONE', *, *, #10287, .F. ) ;
#52780 = DIRECTION ( 'NONE',  ( -0.000000000000000000, -0.6427876096865404731, -0.7660444431189771253 ) ) ;
#52781 = B_SPLINE_CURVE_WITH_KNOTS ( 'NONE', 3,
 ( #49362, #50673, #36729, #30418, #1618, #43046, #42173, #14688, #84932, #22330 ),
 .UNSPECIFIED., .F., .F.,
 ( 4, 2, 2, 2, 4 ),
 ( 0.000000000000000000, 0.0001954339881912775425, 0.0003908679763825550850, 0.0005863019645738326005, 0.0007817359527651101701 ),
 .UNSPECIFIED. ) ;
#52782 = FACE_OUTER_BOUND ( 'NONE', #5544, .T. ) ;
#52783 = CARTESIAN_POINT ( 'NONE',  ( -0.2385271099256122407, -4.887748414852793211, 34.01359900205216746 ) ) ;
#52784 = EDGE_CURVE ( 'NONE', #54472, #9433, #14104, .T. ) ;
#52785 = EDGE_LOOP ( 'NONE', ( #88084, #75933, #15280, #31086 ) ) ;
#52786 = ORIENTED_EDGE ( 'NONE', *, *, #30504, .F. ) ;
#52787 = CARTESIAN_POINT ( 'NONE',  ( -11.78843826940389583, -10.66389620160130036, 33.62221079203477103 ) ) ;
#52788 = CARTESIAN_POINT ( 'NONE',  ( 11.31497661389720832, -4.988325925672468131, 34.36044203135681130 ) ) ;
#52789 = DIRECTION ( 'NONE',  ( -1.000000000000000000, -0.000000000000000000, 0.000000000000000000 ) ) ;
#52790 = CARTESIAN_POINT ( 'NONE',  ( 13.25446741488369007, -3.069018819979302926, 32.56621877034667278 ) ) ;
#52791 = CARTESIAN_POINT ( 'NONE',  ( -18.03205128205128105, -3.499999999999999556, 29.75000000000000355 ) ) ;
#52792 = CARTESIAN_POINT ( 'NONE',  ( 5.934729554039225974, -8.613356846314824011, 34.62446782046655613 ) ) ;
#52793 = ORIENTED_EDGE ( 'NONE', *, *, #30119, .F. ) ;
#52794 = AXIS2_PLACEMENT_3D ( 'NONE', #27558, #7736, #67662 ) ;
#52795 = LINE ( 'NONE', #72624, #54922 ) ;
#52796 = B_SPLINE_CURVE_WITH_KNOTS ( 'NONE', 3,
 ( #60640, #47122, #52549, #25535, #74612, #53438, #59759, #61087, #80034, #80486 ),
 .UNSPECIFIED., .F., .F.,
 ( 4, 2, 2, 2, 4 ),
 ( 0.000000000000000000, 0.0001954311564186879857, 0.0003908623128373759715, 0.0005862934692560640114, 0.0007817246256747519429 ),
 .UNSPECIFIED. ) ;
#52797 = FACE_OUTER_BOUND ( 'NONE', #52395, .T. ) ;
#52798 = CARTESIAN_POINT ( 'NONE',  ( 4.023155550735846298, -8.191372820521381826, 34.95448215188423546 ) ) ;
#52799 = ORIENTED_EDGE ( 'NONE', *, *, #13391, .T. ) ;
#52800 = CARTESIAN_POINT ( 'NONE',  ( 16.08857615328983925, -12.51329471203370325, 31.30864560766548976 ) ) ;
#52801 = ORIENTED_EDGE ( 'NONE', *, *, #88970, .T. ) ;
#52802 = FACE_OUTER_BOUND ( 'NONE', #70806, .T. ) ;
#52803 = CARTESIAN_POINT ( 'NONE',  ( -0.4615384615384611200, -12.34228464037088635, 31.77849191805839268 ) ) ;
#52804 = CARTESIAN_POINT ( 'NONE',  ( 6.222779668978065004, -12.11081565061823717, 32.26097654155341843 ) ) ;
#52805 = ORIENTED_EDGE ( 'NONE', *, *, #10671, .T. ) ;
#52806 = CARTESIAN_POINT ( 'NONE',  ( 0.7114839798866027243, -4.336752205174647656, 33.62275283266504289 ) ) ;
#52807 = FACE_OUTER_BOUND ( 'NONE', #69687, .T. ) ;
#52808 = CARTESIAN_POINT ( 'NONE',  ( -9.758391103263571509, -2.538708090699994813, 30.37095296980875148 ) ) ;
#52809 = EDGE_CURVE ( 'NONE', #63742, #52150, #62278, .T. ) ;
#52810 = DIRECTION ( 'NONE',  ( -0.000000000000000000, -0.5000000000000009992, -0.8660254037844380415 ) ) ;
#52811 = CARTESIAN_POINT ( 'NONE',  ( 3.480823650682684622, -2.920487667080175154, 32.31805714834170828 ) ) ;
#52812 = ORIENTED_EDGE ( 'NONE', *, *, #57239, .F. ) ;
#52813 = FACE_OUTER_BOUND ( 'NONE', #66411, .T. ) ;
#52814 = ORIENTED_EDGE ( 'NONE', *, *, #68538, .T. ) ;
#52815 = CARTESIAN_POINT ( 'NONE',  ( 8.519254038288414321, -12.41269422305637171, 30.68257228309993323 ) ) ;
#52816 = DIRECTION ( 'NONE',  ( -0.000000000000000000, -0.7660444431189791237, -0.6427876096865379196 ) ) ;
#52817 = CARTESIAN_POINT ( 'NONE',  ( -11.53846153846153655, -5.557115091759785130, 34.35708131394839171 ) ) ;
#52818 = VECTOR ( 'NONE', #40899, 1000.000000000000000 ) ;
#52819 = CARTESIAN_POINT ( 'NONE',  ( -16.81410256410256565, -7.500000000000000000, 29.75000000000000355 ) ) ;
#52820 = EDGE_CURVE ( 'NONE', #2196, #25833, #54631, .T. ) ;
#52821 = CARTESIAN_POINT ( 'NONE',  ( 6.923076923076924238, -2.833524468853757305, 32.15551576947925838 ) ) ;
#52822 = DIRECTION ( 'NONE',  ( 1.000000000000000000, 0.000000000000000000, -0.000000000000000000 ) ) ;
#52823 = CARTESIAN_POINT ( 'NONE',  ( 15.16468581981335007, -11.69971097300155272, 32.46337939537587403 ) ) ;
#52824 = ADVANCED_FACE ( 'NONE', ( #21297 ), #74476, .F. ) ;
#52825 = ORIENTED_EDGE ( 'NONE', *, *, #72543, .F. ) ;
#52826 = ORIENTED_EDGE ( 'NONE', *, *, #72516, .F. ) ;
#52827 = ORIENTED_EDGE ( 'NONE', *, *, #32008, .T. ) ;
#52828 = B_SPLINE_CURVE_WITH_KNOTS ( 'NONE', 3,
 ( #24323, #79290, #11271, #17592, #3168, #23875, #45040, #72520, #53132, #4053 ),
 .UNSPECIFIED., .F., .F.,
 ( 4, 2, 2, 2, 4 ),
 ( 0.000000000000000000, 0.0001954311564186871726, 0.0003908623128373743452, 0.0005862934692560615177, 0.0007817246256747486903 ),
 .UNSPECIFIED. ) ;
#52829 = ORIENTED_EDGE ( 'NONE', *, *, #38163, .F. ) ;
#52830 = VERTEX_POINT ( 'NONE', #26287 ) ;
#52831 = EDGE_CURVE ( 'NONE', #41914, #49557, #41138, .T. ) ;
#52832 = CARTESIAN_POINT ( 'NONE',  ( -16.37677237136229991, -3.586966769969702540, 32.86292498521069660 ) ) ;
#52833 = CARTESIAN_POINT ( 'NONE',  ( -11.60454494941741999, -8.973038597847271092, 34.52809138561120506 ) ) ;
#52834 = CARTESIAN_POINT ( 'NONE',  ( -17.07692307692307665, -13.04860791097971706, 34.73218667398347037 ) ) ;
#52835 = CARTESIAN_POINT ( 'NONE',  ( -5.749945688361683516, -4.943051570960391494, 34.04725096376909477 ) ) ;
#52836 = CARTESIAN_POINT ( 'NONE',  ( -13.38461538461538325, -5.557115091759785130, 34.35708131394839171 ) ) ;
#52837 = CARTESIAN_POINT ( 'NONE',  ( -6.222926958906846551, -2.889293201056495786, 32.26117774369186009 ) ) ;
#52838 = CARTESIAN_POINT ( 'NONE',  ( -0.5268089074992379217, -11.94971097300153140, 32.03036669348370680 ) ) ;
#52839 = CARTESIAN_POINT ( 'NONE',  ( -4.023054346021365468, -10.54018710029568595, 33.71981072465678864 ) ) ;
#52840 = CARTESIAN_POINT ( 'NONE',  ( 0.2386122440223125696, -3.105860786376062332, 32.13614157043599562 ) ) ;
#52841 = ORIENTED_EDGE ( 'NONE', *, *, #38853, .F. ) ;
#52842 = EDGE_LOOP ( 'NONE', ( #73431, #87752, #10748, #83551 ) ) ;
#52843 = VERTEX_POINT ( 'NONE', #63167 ) ;
#52845 = ORIENTED_EDGE ( 'NONE', *, *, #9454, .F. ) ;
#52844 = CARTESIAN_POINT ( 'NONE',  ( -1.450698795571263577, -11.16473453929635440, 33.15142922261925662 ) ) ;
#52847 = CARTESIAN_POINT ( 'NONE',  ( 0.000000000000000000, -11.00000000000000000, 29.75000000000000355 ) ) ;
#52846 = DIRECTION ( 'NONE',  ( -0.000000000000000000, -0.9848077530122085754, -0.1736481776669273613 ) ) ;
#52848 = CARTESIAN_POINT ( 'NONE',  ( 11.53846153846141753, -3.835265460704628371, 33.15142922262033665 ) ) ;
#52849 = DIRECTION ( 'NONE',  ( -0.000000000000000000, -0.6427876096865404731, -0.7660444431189771253 ) ) ;
#52850 = EDGE_CURVE ( 'NONE', #65772, #21923, #56465, .T. ) ;
#52851 = FACE_BOUND ( 'NONE', #45207, .T. ) ;
#52852 = ORIENTED_EDGE ( 'NONE', *, *, #77415, .F. ) ;
#52853 = VERTEX_POINT ( 'NONE', #42472 ) ;
#52854 = CARTESIAN_POINT ( 'NONE',  ( 4.946232473812767871, -2.295517848115769421, 30.44137282052136939 ) ) ;
#52855 = VERTEX_POINT ( 'NONE', #29838 ) ;
#52856 = FACE_BOUND ( 'NONE', #13917, .T. ) ;
#52857 = CARTESIAN_POINT ( 'NONE',  ( 7.623227628637698317, -11.76352882383564769, 32.36236540154569497 ) ) ;
#52858 = DIRECTION ( 'NONE',  ( -0.000000000000000000, -0.000000000000000000, -1.000000000000000000 ) ) ;
#52859 = EDGE_LOOP ( 'NONE', ( #45070, #73674 ) ) ;
#52860 = DIRECTION ( 'NONE',  ( -1.000000000000000000, -0.000000000000000000, 0.000000000000000000 ) ) ;
#52861 = CARTESIAN_POINT ( 'NONE',  ( 11.97435897435897267, -11.00000000000000000, 29.75000000000000355 ) ) ;
#52862 = AXIS2_PLACEMENT_3D ( 'NONE', #83715, #89149, #69739 ) ;
#52863 = FACE_OUTER_BOUND ( 'NONE', #8647, .T. ) ;
#52864 = ORIENTED_EDGE ( 'NONE', *, *, #85186, .F. ) ;
#52865 = CARTESIAN_POINT ( 'NONE',  ( -6.923076923077044142, -2.892918686052165622, 31.69288490824153470 ) ) ;
#52866 = CARTESIAN_POINT ( 'NONE',  ( -2.980769230767794653, -7.500000000000155431, 34.75000000000007105 ) ) ;
#52867 = CARTESIAN_POINT ( 'NONE',  ( -0.4615384615384611200, -8.564572088678739092, 35.78748833219616898 ) ) ;
#52868 = ORIENTED_EDGE ( 'NONE', *, *, #35494, .F. ) ;
#52869 = CARTESIAN_POINT ( 'NONE',  ( -4.153846153846152411, -12.10708131394839349, 31.69288490824020244 ) ) ;
#52870 = CARTESIAN_POINT ( 'NONE',  ( -16.82697755857493149, -11.86320923018887541, 32.19269448109604781 ) ) ;
#52871 = ORIENTED_EDGE ( 'NONE', *, *, #76937, .F. ) ;
#52872 = CARTESIAN_POINT ( 'NONE',  ( 0.2380535178145126440, -9.331801661448606566, 34.40259984581193464 ) ) ;
#52873 = CARTESIAN_POINT ( 'NONE',  ( -12.46153846153846168, -2.538708090699994813, 30.37095296980875503 ) ) ;
#52875 = B_SPLINE_CURVE_WITH_KNOTS ( 'NONE', 3,
 ( #11564, #74594, #4807, #33606, #53871, #32707, #26847, #25514, #80468, #52971 ),
 .UNSPECIFIED., .F., .F.,
 ( 4, 2, 2, 2, 4 ),
 ( 0.0007817359430256320659, 0.0009771253907249989254, 0.001172514838424365676, 0.001367904286123732428, 0.001563293733823099179 ),
 .UNSPECIFIED. ) ;
#52874 = DIRECTION ( 'NONE',  ( -0.000000000000000000, -0.7660444431189791237, -0.6427876096865379196 ) ) ;
#52876 = CARTESIAN_POINT ( 'NONE',  ( 15.16468685140909400, -12.62096338111211580, 30.90682066428152908 ) ) ;
#52877 = CARTESIAN_POINT ( 'NONE',  ( -3.230769230769229949, -6.435427911321262684, 35.78748833219616898 ) ) ;
#52878 = DIRECTION ( 'NONE',  ( -0.000000000000000000, 0.6427876096865404731, -0.7660444431189771253 ) ) ;
#52880 = CARTESIAN_POINT ( 'NONE',  ( -19.50000000000000000, -3.499999999999999556, 29.75000000000000355 ) ) ;
#52879 = LINE ( 'NONE', #40279, #15976 ) ;
#52881 = CARTESIAN_POINT ( 'NONE',  ( 8.769230769230768274, -12.10708131394839349, 31.69288490824020244 ) ) ;
#52882 = CARTESIAN_POINT ( 'NONE',  ( 11.53846153846153832, -11.91647553114624181, 32.58852847137148245 ) ) ;
#52883 = CARTESIAN_POINT ( 'NONE',  ( -2.749999999999991562, -8.639087296526025028, 16.26562500000000000 ) ) ;
#52884 = VERTEX_POINT ( 'NONE', #69931 ) ;
#52885 = CARTESIAN_POINT ( 'NONE',  ( 5.076923076922953193, -6.835583212225970762, 34.95778746994575670 ) ) ;
#52886 = ORIENTED_EDGE ( 'NONE', *, *, #62398, .F. ) ;
#52887 = ORIENTED_EDGE ( 'NONE', *, *, #17513, .F. ) ;
#52888 = DIRECTION ( 'NONE',  ( 0.000000000000000000, 0.1736481776669275834, 0.9848077530122086864 ) ) ;
#52889 = VERTEX_POINT ( 'NONE', #9133 ) ;
#52890 = CARTESIAN_POINT ( 'NONE',  ( 17.75000000000000000, -7.500000000000001776, 34.75000000000000000 ) ) ;
#52891 = CARTESIAN_POINT ( 'NONE',  ( 2.749999999999995115, -6.360912703473971419, 14.39062500000000178 ) ) ;
#52892 = DIRECTION ( 'NONE',  ( 1.000000000000000000, 0.000000000000000000, 0.000000000000000000 ) ) ;
#52893 = CARTESIAN_POINT ( 'NONE',  ( -18.06527000055631760, -12.16647553114622049, 32.15551576947930812 ) ) ;
#52894 = CARTESIAN_POINT ( 'NONE',  ( -2.980823712421088789, -9.272278438253398036, 34.42582936511637826 ) ) ;
#52895 = DIRECTION ( 'NONE',  ( 0.000000000000000000, 0.000000000000000000, -1.000000000000000000 ) ) ;
#52897 = CARTESIAN_POINT ( 'NONE',  ( -5.207071046654769830, -3.625366637846544560, 33.29286588640298561 ) ) ;
#52896 = VECTOR ( 'NONE', #28752, 999.9999999999998863 ) ;
#52898 = CARTESIAN_POINT ( 'NONE',  ( -7.846153846153844924, -2.721908614388771852, 31.22303859784724978 ) ) ;
#52899 = LINE ( 'NONE', #80398, #52577 ) ;
#52900 = CARTESIAN_POINT ( 'NONE',  ( -2.651650429449535551, -10.15165042944956753, 19.93750000000000000 ) ) ;
#52901 = CARTESIAN_POINT ( 'NONE',  ( 5.299702745901138101, -3.020022701398814569, 32.48759521482552515 ) ) ;
#52902 = CARTESIAN_POINT ( 'NONE',  ( -4.284536756956460302, -11.93127051446800024, 32.56575433478200665 ) ) ;
#52903 = AXIS2_PLACEMENT_3D ( 'NONE', #88399, #54128, #17703 ) ;
#52904 = PLANE ( 'NONE',  #66610 ) ;
#52905 = EDGE_LOOP ( 'NONE', ( #21205, #16723, #5756, #69360 ) ) ;
#52906 = VERTEX_POINT ( 'NONE', #15444 ) ;
#52907 = CARTESIAN_POINT ( 'NONE',  ( -8.899377978668987055, -12.45813303252208648, 30.39737893381572675 ) ) ;
#52908 = CARTESIAN_POINT ( 'NONE',  ( -14.08468095607945791, -8.239487800360276282, 34.69522927552633718 ) ) ;
#52909 = CARTESIAN_POINT ( 'NONE',  ( -2.437840277424001556, -2.373036134822904319, 30.88089517874952250 ) ) ;
#52910 = CYLINDRICAL_SURFACE ( 'NONE', #64248, 0.2499999999999973355 ) ;
#52911 = CARTESIAN_POINT ( 'NONE',  ( 8.545745825506822158, -4.386631170607603991, 33.66268669641500111 ) ) ;
#52912 = FACE_OUTER_BOUND ( 'NONE', #7236, .T. ) ;
#52913 = AXIS2_PLACEMENT_3D ( 'NONE', #53658, #32495, #52761 ) ;
#52914 = EDGE_LOOP ( 'NONE', ( #88776, #53971 ) ) ;
#52915 = CARTESIAN_POINT ( 'NONE',  ( 1.134592147322421862, -5.056417327199099532, 34.11270091957321426 ) ) ;
#52916 = ORIENTED_EDGE ( 'NONE', *, *, #23547, .F. ) ;
#52917 = AXIS2_PLACEMENT_3D ( 'NONE', #10776, #2668, #85994 ) ;
#52918 = EDGE_LOOP ( 'NONE', ( #42980, #28643 ) ) ;
#52919 = CARTESIAN_POINT ( 'NONE',  ( -9.627052552794857831, -3.083524468853784839, 32.58852847137153930 ) ) ;
#52920 = EDGE_CURVE ( 'NONE', #67556, #56376, #73703, .T. ) ;
#52921 = DIRECTION ( 'NONE',  ( 0.000000000000000000, 0.000000000000000000, -1.000000000000000000 ) ) ;
#52922 = CARTESIAN_POINT ( 'NONE',  ( -4.219928533206288357, -12.62096338111211580, 30.90682066428152197 ) ) ;
#52923 = VECTOR ( 'NONE', #21462, 1000.000000000000000 ) ;
#52924 = EDGE_CURVE ( 'NONE', #47721, #31669, #83464, .T. ) ;
#52925 = CARTESIAN_POINT ( 'NONE',  ( 1.161688425708537808, -11.43668979543635089, 33.22377378376089752 ) ) ;
#52926 = CARTESIAN_POINT ( 'NONE',  ( 13.38461538461526423, -5.941354392335915335, 34.76329471203413846 ) ) ;
#52927 = ORIENTED_EDGE ( 'NONE', *, *, #57838, .T. ) ;
#52928 = EDGE_LOOP ( 'NONE', ( #58014, #36219 ) ) ;
#52929 = ORIENTED_EDGE ( 'NONE', *, *, #39422, .T. ) ;
#52930 = EDGE_CURVE ( 'NONE', #32624, #82469, #636, .T. ) ;
#52931 = CYLINDRICAL_SURFACE ( 'NONE', #35800, 0.2500000000000004996 ) ;
#52932 = CARTESIAN_POINT ( 'NONE',  ( -0.4615384615385840772, -10.33852847137269571, 34.16647553114546554 ) ) ;
#52933 = CARTESIAN_POINT ( 'NONE',  ( 4.403791563224197070, -3.520799739797213501, 33.17531984108286025 ) ) ;
#52934 = B_SPLINE_CURVE_WITH_KNOTS ( 'NONE', 3,
 ( #69400, #88807, #82919, #27524, #68076, #28869 ),
 .UNSPECIFIED., .F., .F.,
 ( 4, 2, 4 ),
 ( 0.000000000000000000, 0.0001954784845028902692, 0.0003909569690057805385 ),
 .UNSPECIFIED. ) ;
#52935 = CARTESIAN_POINT ( 'NONE',  ( 1.134592147322421862, -3.711651800289232028, 33.01384336483936011 ) ) ;
#52936 = VECTOR ( 'NONE', #70490, 1000.000000000000114 ) ;
#52937 = LINE ( 'NONE', #16944, #82599 ) ;
#52938 = ORIENTED_EDGE ( 'NONE', *, *, #67392, .T. ) ;
#52939 = ORIENTED_EDGE ( 'NONE', *, *, #55342, .F. ) ;
#52940 = CARTESIAN_POINT ( 'NONE',  ( 4.853438152358744873, -10.23692288466677880, 34.23039457007281072 ) ) ;
#52941 = CIRCLE ( 'NONE', #44317, 4.000000000000000000 ) ;
#52943 = ORIENTED_EDGE ( 'NONE', *, *, #3609, .T. ) ;
#52942 = CARTESIAN_POINT ( 'NONE',  ( -17.78205128205128105, -3.499999999999999556, 29.75000000000000355 ) ) ;
#52944 = CARTESIAN_POINT ( 'NONE',  ( -12.46153846153858424, -11.67786785259630911, 32.92929555188603530 ) ) ;
#52945 = CARTESIAN_POINT ( 'NONE',  ( 8.069529786852024600, -2.501478030877322567, 29.88021232661721172 ) ) ;
#52946 = CARTESIAN_POINT ( 'NONE',  ( -1.929879867024197893E-14, -3.750000000000000000, 14.15625000000000000 ) ) ;
#52947 = EDGE_CURVE ( 'NONE', #54362, #88546, #81200, .T. ) ;
#52948 = EDGE_LOOP ( 'NONE', ( #27268, #48240, #5533, #6491 ) ) ;
#52949 = VECTOR ( 'NONE', #36651, 999.9999999999998863 ) ;
#52950 = B_SPLINE_CURVE_WITH_KNOTS ( 'NONE', 3,
 ( #49331, #82686, #42141, #70038, #7902, #83576, #76808, #75037, #20955, #14660 ),
 .UNSPECIFIED., .F., .F.,
 ( 4, 2, 2, 2, 4 ),
 ( 0.0007817246256747530271, 0.0009771112852218978746, 0.001172497944769042939, 0.001367884604316188003, 0.001563271263863332851 ),
 .UNSPECIFIED. ) ;
#52951 = EDGE_CURVE ( 'NONE', #31266, #85917, #32862, .T. ) ;
#52952 = CARTESIAN_POINT ( 'NONE',  ( -9.692307692307691624, -12.78798330534103123, 29.99999999999997868 ) ) ;
#52953 = ORIENTED_EDGE ( 'NONE', *, *, #238, .F. ) ;
#52954 = CARTESIAN_POINT ( 'NONE',  ( 2.438484115517096207, -8.999086150933472084, 34.52020707165672064 ) ) ;
#52955 = DIRECTION ( 'NONE',  ( 0.000000000000000000, -1.000000000000000000, 5.102127870520020612E-17 ) ) ;
#52956 = B_SPLINE_CURVE_WITH_KNOTS ( 'NONE', 3,
 ( #27208, #82163, #47916, #626, #83046, #21332, #14578, #7826, #35291, #62748 ),
 .UNSPECIFIED., .F., .F.,
 ( 4, 2, 2, 2, 4 ),
 ( 0.000000000000000000, 0.0001954311564186871184, 0.0003908623128373742367, 0.0005862934692560614093, 0.0007817246256747484735 ),
 .UNSPECIFIED. ) ;
#52957 = FACE_BOUND ( 'NONE', #18482, .T. ) ;
#52959 = CARTESIAN_POINT ( 'NONE',  ( 10.61538461538461675, -10.67929555188718282, 33.92786785259544047 ) ) ;
#52958 = LINE ( 'NONE', #47533, #8730 ) ;
#52960 = EDGE_CURVE ( 'NONE', #27628, #49317, #57572, .T. ) ;
#52961 = DIRECTION ( 'NONE',  ( -0.000000000000000000, -0.000000000000000000, -1.000000000000000000 ) ) ;
#52962 = ORIENTED_EDGE ( 'NONE', *, *, #25012, .F. ) ;
#52963 = EDGE_CURVE ( 'NONE', #46553, #59465, #28558, .T. ) ;
#52964 = DIRECTION ( 'NONE',  ( -0.000000000000000000, -0.8660254037844399289, -0.4999999999999980016 ) ) ;
#52965 = CARTESIAN_POINT ( 'NONE',  ( 15.16549878480846125, -4.481592998940162609, 33.73612834413957984 ) ) ;
#52966 = CARTESIAN_POINT ( 'NONE',  ( 9.692307692307695177, -9.819645486525091727, 36.12317359536749706 ) ) ;
#52967 = EDGE_LOOP ( 'NONE', ( #42551, #76718, #21080, #23325 ) ) ;
#52968 = CARTESIAN_POINT ( 'NONE',  ( -18.06527000055631405, -12.70778746994557551, 30.41441678777548319 ) ) ;
#52969 = CYLINDRICAL_SURFACE ( 'NONE', #88639, 0.2499999999999994726 ) ;
#52970 = CARTESIAN_POINT ( 'NONE',  ( 14.55769230769231015, -2.249999999999998668, 29.75000000000000355 ) ) ;
#52971 = CARTESIAN_POINT ( 'NONE',  ( 7.846153846153846700, -3.050289026998446396, 32.03036669348365706 ) ) ;
#52972 = FACE_BOUND ( 'NONE', #76704, .T. ) ;
#52974 = CARTESIAN_POINT ( 'NONE',  ( -15.23076923076922995, -11.16473453929635440, 33.15142922261926373 ) ) ;
#52973 = CARTESIAN_POINT ( 'NONE',  ( 1.514662819865838062, -7.723484941389743952, 34.99544897038808955 ) ) ;
#52975 = CARTESIAN_POINT ( 'NONE',  ( -39.05038313613820122, -2.249999999999998668, 29.75000000000000355 ) ) ;
#52977 = FACE_OUTER_BOUND ( 'NONE', #44083, .T. ) ;
#52976 = CARTESIAN_POINT ( 'NONE',  ( -17.77698864838715309, -11.24521262558773493, 33.06293181088030053 ) ) ;
#52978 = FACE_OUTER_BOUND ( 'NONE', #57812, .T. ) ;
#52979 = CARTESIAN_POINT ( 'NONE',  ( 17.99999999999987566, -4.320704448113951379, 33.92786785259630022 ) ) ;
#52980 = VECTOR ( 'NONE', #42691, 1000.000000000000000 ) ;
#52981 = CARTESIAN_POINT ( 'NONE',  ( -3.724691934501229262, -9.114399933863657211, 27.26375670625849423 ) ) ;
#52982 = CARTESIAN_POINT ( 'NONE',  ( 10.36540787133602848, -12.01397095200674059, 32.43157075238190146 ) ) ;
#52983 = EDGE_LOOP ( 'NONE', ( #77854, #13080, #26973, #33027, #31051, #50914 ) ) ;
#52984 = CARTESIAN_POINT ( 'NONE',  ( 0.2386122440223136798, -6.503392248772476236, 34.64988816332204635 ) ) ;
#52985 = CARTESIAN_POINT ( 'NONE',  ( -4.153846153846273204, -12.27809138561165270, 31.22303859784587132 ) ) ;
#52986 = DIRECTION ( 'NONE',  ( 1.000000000000000000, 2.602085213965214586E-16, 0.000000000000000000 ) ) ;
#52987 = CARTESIAN_POINT ( 'NONE',  ( -2.307692307692305711, -11.69971097300155272, 32.46337939537588113 ) ) ;
#52988 = CARTESIAN_POINT ( 'NONE',  ( -10.39260494640654819, -12.11081565061824250, 32.26097654155340422 ) ) ;
#52989 = CARTESIAN_POINT ( 'NONE',  ( -12.68446542044531178, -6.459968553980841577, 34.89616026154728701 ) ) ;
#52990 = CARTESIAN_POINT ( 'NONE',  ( -3.775308065498766297, -6.007798216065450170, 27.42000670625849068 ) ) ;
#52991 = CARTESIAN_POINT ( 'NONE',  ( 2.307692307692187583, -11.94971097300221174, 32.03036669348237098 ) ) ;
#52992 = CARTESIAN_POINT ( 'NONE',  ( 8.638540166120462160, -2.494641256782728966, 31.33461815524612959 ) ) ;
#52993 = CARTESIAN_POINT ( 'NONE',  ( -12.23852561744506851, -9.172514111537584114, 34.72667873470787470 ) ) ;
#52994 = CARTESIAN_POINT ( 'NONE',  ( 5.076923076922953193, -9.528491918059723176, 34.59228464037033035 ) ) ;
#52995 = DIRECTION ( 'NONE',  ( -0.000000000000000000, -0.3420201433256694346, -0.9396926207859080948 ) ) ;
#52996 = CARTESIAN_POINT ( 'NONE',  ( -11.53846153846153655, -9.780366693483667717, 34.19971097300155094 ) ) ;
#52997 = B_SPLINE_CURVE_WITH_KNOTS ( 'NONE', 3,
 ( #36460, #21165, #63915, #29271, #63478, #63022, #49533, #20727, #62155, #2213 ),
 .UNSPECIFIED., .F., .F.,
 ( 4, 2, 2, 2, 4 ),
 ( 0.000000000000000000, 0.0001954311564186868744, 0.0003908623128373737488, 0.0005862934692560606504, 0.0007817246256747474977 ),
 .UNSPECIFIED. ) ;
#52998 = EDGE_CURVE ( 'NONE', #72857, #798, #38818, .T. ) ;
#52999 = CARTESIAN_POINT ( 'NONE',  ( 9.942307692307631228, -7.565270445406050648, 34.75000000000000000 ) ) ;
#53000 = CARTESIAN_POINT ( 'NONE',  ( -11.31568199719312773, -10.81320215134717344, 33.49497208177562868 ) ) ;
#53001 = VERTEX_POINT ( 'NONE', #32491 ) ;
#53002 = DIRECTION ( 'NONE',  ( 0.000000000000000000, 0.8660254037844377084, 0.5000000000000015543 ) ) ;
#53003 = CYLINDRICAL_SURFACE ( 'NONE', #22997, 0.2500000000000004996 ) ;
#53004 = CARTESIAN_POINT ( 'NONE',  ( -3.724691934501248802, -5.885600066136383646, 16.67374329374151998 ) ) ;
#53005 = CARTESIAN_POINT ( 'NONE',  ( 6.065255571276025215, -4.481592998940251427, 33.73612834413965089 ) ) ;
#53006 = CARTESIAN_POINT ( 'NONE',  ( 17.07692307692307665, -4.945431358278436385, 36.03766855953609394 ) ) ;
#53007 = ORIENTED_EDGE ( 'NONE', *, *, #48921, .T. ) ;
#53008 = CARTESIAN_POINT ( 'NONE',  ( 2.307692307692309264, -6.386643153685126251, 34.62446782046654192 ) ) ;
#53009 = DIRECTION ( 'NONE',  ( -0.000000000000000000, 1.000000000000000000, -0.000000000000000000 ) ) ;
#53011 = ORIENTED_EDGE ( 'NONE', *, *, #53808, .T. ) ;
#53010 = CARTESIAN_POINT ( 'NONE',  ( 7.912221179503920787, -2.486705287966279876, 31.30864560766543647 ) ) ;
#53012 = CARTESIAN_POINT ( 'NONE',  ( -9.822998295417999515, -11.37499894934982692, 33.29245874905763003 ) ) ;
#53013 = CARTESIAN_POINT ( 'NONE',  ( 4.023698944407932743, -8.587444163452046197, 34.63053765926554206 ) ) ;
#53014 = CARTESIAN_POINT ( 'NONE',  ( -17.20739826199879730, -7.276987145209182550, 34.99546412871779211 ) ) ;
#53015 = EDGE_CURVE ( 'NONE', #327, #85237, #84392, .T. ) ;
#53016 = CARTESIAN_POINT ( 'NONE',  ( -39.05038313613820122, -2.249999999999998668, 29.75000000000000355 ) ) ;
#53017 = ORIENTED_EDGE ( 'NONE', *, *, #30527, .F. ) ;
#53018 = AXIS2_PLACEMENT_3D ( 'NONE', #53559, #45465, #59432 ) ;
#53019 = DIRECTION ( 'NONE',  ( 0.000000000000000000, 0.7660444431189807890, 0.6427876096865361433 ) ) ;
#53020 = DIRECTION ( 'NONE',  ( -0.000000000000000000, -0.000000000000000000, 1.000000000000000000 ) ) ;
#53021 = VECTOR ( 'NONE', #9442, 1000.000000000000000 ) ;
#53022 = CARTESIAN_POINT ( 'NONE',  ( 8.545745844666440050, -3.562934362175799841, 33.22335522853832401 ) ) ;
#53023 = ORIENTED_EDGE ( 'NONE', *, *, #7468, .T. ) ;
#53024 = ORIENTED_EDGE ( 'NONE', *, *, #84053, .T. ) ;
#53025 = VERTEX_POINT ( 'NONE', #4123 ) ;
#53026 = EDGE_CURVE ( 'NONE', #45061, #63264, #37153, .T. ) ;
#53027 = CARTESIAN_POINT ( 'NONE',  ( -16.28453675695646652, -3.338472653186243200, 32.95098750199972670 ) ) ;
#53028 = LINE ( 'NONE', #80531, #80303 ) ;
#53029 = EDGE_CURVE ( 'NONE', #36439, #62255, #85496, .T. ) ;
#53030 = CARTESIAN_POINT ( 'NONE',  ( -9.442362282929646966, -12.68172785388650681, 30.59649109432439218 ) ) ;
#53031 = CARTESIAN_POINT ( 'NONE',  ( -17.01085472592063752, -4.786620604624113540, 33.94971097300155805 ) ) ;
#53032 = ORIENTED_EDGE ( 'NONE', *, *, #15459, .T. ) ;
#53033 = B_SPLINE_CURVE_WITH_KNOTS ( 'NONE', 3,
 ( #12106, #39583, #87781, #42673, #70133, #56624, #8444, #89104, #48522, #35916 ),
 .UNSPECIFIED., .F., .F.,
 ( 4, 2, 2, 2, 4 ),
 ( 0.000000000000000000, 0.0001954311564186883110, 0.0003908623128373766220, 0.0005862934692560648788, 0.0007817246256747532440 ),
 .UNSPECIFIED. ) ;
#53034 = ORIENTED_EDGE ( 'NONE', *, *, #18597, .F. ) ;
#53036 = ORIENTED_EDGE ( 'NONE', *, *, #21023, .F. ) ;
#53035 = EDGE_CURVE ( 'NONE', #7863, #1158, #44627, .T. ) ;
#53038 = ORIENTED_EDGE ( 'NONE', *, *, #37201, .T. ) ;
#53037 = CARTESIAN_POINT ( 'NONE',  ( 15.23076923076923173, -4.786620604624113540, 33.94971097300155094 ) ) ;
#53039 = CARTESIAN_POINT ( 'NONE',  ( -16.37733107841048863, -12.47654668319379567, 31.42292124445336654 ) ) ;
#53040 = AXIS2_PLACEMENT_3D ( 'NONE', #50651, #24515, #78130 ) ;
#53041 = CARTESIAN_POINT ( 'NONE',  ( 15.23076923076923173, -3.050289026998446396, 32.03036669348365706 ) ) ;
#53042 = EDGE_CURVE ( 'NONE', #60227, #28663, #44655, .T. ) ;
#53043 = LINE ( 'NONE', #58916, #72347 ) ;
#53044 = CARTESIAN_POINT ( 'NONE',  ( 13.63466980452883526, -10.06805714834173493, 34.32951233291982618 ) ) ;
#53045 = EDGE_CURVE ( 'NONE', #5642, #84975, #31151, .T. ) ;
#53046 = VERTEX_POINT ( 'NONE', #51857 ) ;
#53047 = ORIENTED_EDGE ( 'NONE', *, *, #34481, .T. ) ;
#53048 = ORIENTED_EDGE ( 'NONE', *, *, #38115, .T. ) ;
#53049 = CARTESIAN_POINT ( 'NONE',  ( -10.68065461594093435, -11.06231777344662781, 33.60647404775220082 ) ) ;
#53051 = ORIENTED_EDGE ( 'NONE', *, *, #11760, .F. ) ;
#53050 = CARTESIAN_POINT ( 'NONE',  ( 8.899756470994335089, -2.619367082507849442, 30.83698974864643461 ) ) ;
#53052 = CARTESIAN_POINT ( 'NONE',  ( 16.82694633287449193, -5.643011162660950042, 34.66104346484419096 ) ) ;
#53053 = DIRECTION ( 'NONE',  ( 0.000000000000000000, 0.000000000000000000, -1.000000000000000000 ) ) ;
#53054 = EDGE_CURVE ( 'NONE', #879, #80092, #79354, .T. ) ;
#53055 = CARTESIAN_POINT ( 'NONE',  ( 13.63461538461538680, -2.499999999999998668, 29.75000000000000355 ) ) ;
#53056 = FACE_OUTER_BOUND ( 'NONE', #13622, .T. ) ;
#53057 = CARTESIAN_POINT ( 'NONE',  ( 9.019176287578909879, -5.852078868378309373, 34.47109172314383585 ) ) ;
#53058 = FACE_BOUND ( 'NONE', #87926, .T. ) ;
#53059 = LINE ( 'NONE', #38670, #87381 ) ;
#53060 = DIRECTION ( 'NONE',  ( -0.000000000000000000, 0.6427876096865404731, -0.7660444431189771253 ) ) ;
#53061 = CARTESIAN_POINT ( 'NONE',  ( 11.60452988946397923, -12.37446782046654192, 30.86335684631486842 ) ) ;
#53063 = FACE_OUTER_BOUND ( 'NONE', #80071, .T. ) ;
#53062 = DIRECTION ( 'NONE',  ( -0.000000000000000000, 1.000000000000000000, -0.000000000000000000 ) ) ;
#53064 = VECTOR ( 'NONE', #17943, 1000.000000000000114 ) ;
#53065 = FACE_OUTER_BOUND ( 'NONE', #54911, .T. ) ;
#53066 = CARTESIAN_POINT ( 'NONE',  ( 7.173076923076926015, -2.499999999999999112, 29.81604066197450109 ) ) ;
#53067 = ORIENTED_EDGE ( 'NONE', *, *, #2973, .T. ) ;
#53068 = ADVANCED_FACE ( 'NONE', ( #83695 ), #48107, .T. ) ;
#53069 = DIRECTION ( 'NONE',  ( -0.000000000000000000, 0.7660444431189791237, -0.6427876096865379196 ) ) ;
#53070 = CARTESIAN_POINT ( 'NONE',  ( -13.25408994638174143, -4.299079248970732792, 33.91157788607253565 ) ) ;
#53071 = VERTEX_POINT ( 'NONE', #35942 ) ;
#53072 = ORIENTED_EDGE ( 'NONE', *, *, #7656, .T. ) ;
#53073 = CARTESIAN_POINT ( 'NONE',  ( -19.50000000000000000, -3.499999999999999556, 29.75000000000000355 ) ) ;
#53074 = AXIS2_PLACEMENT_3D ( 'NONE', #75596, #41381, #68846 ) ;
#53075 = CARTESIAN_POINT ( 'NONE',  ( 16.08857570788537572, -3.835265460703609186, 33.15142922261924241 ) ) ;
#53076 = DIRECTION ( 'NONE',  ( -0.000000000000000000, 1.000000000000000000, -0.000000000000000000 ) ) ;
#53077 = ORIENTED_EDGE ( 'NONE', *, *, #71798, .F. ) ;
#53078 = CARTESIAN_POINT ( 'NONE',  ( -1.944543648263015179, -5.555456351737005249, 14.00000000000000000 ) ) ;
#53079 = CARTESIAN_POINT ( 'NONE',  ( -1.384615384615505151, -11.94971097300221174, 32.03036669348237098 ) ) ;
#53081 = CARTESIAN_POINT ( 'NONE',  ( -1.384615384615506484, -12.51329471203414379, 31.30864560766407578 ) ) ;
#53080 = DIRECTION ( 'NONE',  ( -0.000000000000000000, -0.000000000000000000, -1.000000000000000000 ) ) ;
#53082 = CARTESIAN_POINT ( 'NONE',  ( 11.53846153846153832, -2.708943851104267164, 35.45975837776705220 ) ) ;
#53083 = DIRECTION ( 'NONE',  ( -1.000000000000000000, -0.000000000000000000, -0.000000000000000000 ) ) ;
#53085 = CARTESIAN_POINT ( 'NONE',  ( 7.846153846153846700, -6.681629849574314051, 35.83090037661290239 ) ) ;
#53084 = PRESENTATION_STYLE_ASSIGNMENT (( #87805 ) ) ;
#53086 = EDGE_CURVE ( 'NONE', #10442, #61210, #21530, .T. ) ;
#53087 = B_SPLINE_CURVE_WITH_KNOTS ( 'NONE', 3,
 ( #66182, #23419, #78364, #45019, #37826, #79268, #86024, #31518, #4493, #58983 ),
 .UNSPECIFIED., .F., .F.,
 ( 4, 2, 2, 2, 4 ),
 ( 0.000000000000000000, 0.0001954311564186871184, 0.0003908623128373742367, 0.0005862934692560614093, 0.0007817246256747484735 ),
 .UNSPECIFIED. ) ;
#53088 = CARTESIAN_POINT ( 'NONE',  ( 1.553300858899087311, -3.749999999999992006, 22.98437500000000000 ) ) ;
#53089 = EDGE_LOOP ( 'NONE', ( #39712, #60593 ) ) ;
#53090 = B_SPLINE_CURVE_WITH_KNOTS ( 'NONE', 3,
 ( #55933, #42437, #63126, #1441, #28931, #48288, #75761, #56387, #14066, #83872 ),
 .UNSPECIFIED., .F., .F.,
 ( 4, 2, 2, 2, 4 ),
 ( 0.000000000000000000, 0.0001954339881912775425, 0.0003908679763825550850, 0.0005863019645738326005, 0.0007817359527651101701 ),
 .UNSPECIFIED. ) ;
#53091 = ORIENTED_EDGE ( 'NONE', *, *, #51063, .F. ) ;
#53092 = CARTESIAN_POINT ( 'NONE',  ( 5.011653076366754611, -11.06231777344662781, 33.60647404775220082 ) ) ;
#53093 = EDGE_CURVE ( 'NONE', #24465, #10994, #40353, .T. ) ;
#53094 = CARTESIAN_POINT ( 'NONE',  ( 7.146088274689775588, -12.15243808032446005, 31.58219941686247978 ) ) ;
#53095 = FACE_OUTER_BOUND ( 'NONE', #3774, .T. ) ;
#53096 = DIRECTION ( 'NONE',  ( 1.000000000000000000, 0.000000000000000000, 0.000000000000000000 ) ) ;
#53097 = CARTESIAN_POINT ( 'NONE',  ( -3.480745961711583902, -5.728515186090277211, 34.42611988154120439 ) ) ;
#53098 = CARTESIAN_POINT ( 'NONE',  ( -3.749999999999997335, -7.500000000000021316, 22.59375000000000355 ) ) ;
#53099 = CYLINDRICAL_SURFACE ( 'NONE', #54678, 0.2499999999999994726 ) ;
#53100 = CYLINDRICAL_SURFACE ( 'NONE', #74794, 0.2500000000000012212 ) ;
#53101 = CARTESIAN_POINT ( 'NONE',  ( -13.60744207709438847, -7.369208160676171460, 34.74850200257122879 ) ) ;
#53102 = CARTESIAN_POINT ( 'NONE',  ( -12.46153846153846168, -1.951392089020283160, 34.73218667398347748 ) ) ;
#53103 = CARTESIAN_POINT ( 'NONE',  ( 16.09615384615384670, -7.500000000000000000, 29.75000000000000355 ) ) ;
#53104 = CARTESIAN_POINT ( 'NONE',  ( 13.45068271796546178, -2.486705287966280320, 31.30864560766543647 ) ) ;
#53105 = CARTESIAN_POINT ( 'NONE',  ( -18.00000000000012079, -12.16647553114689906, 32.15551576947799362 ) ) ;
#53106 = EDGE_CURVE ( 'NONE', #10700, #73496, #40438, .T. ) ;
#53107 = CARTESIAN_POINT ( 'NONE',  ( 7.912221179503920787, -8.164416787775445883, 34.95778746994558617 ) ) ;
#53108 = CARTESIAN_POINT ( 'NONE',  ( -6.700297254098854793, -3.563462043263029955, 33.22394488606062879 ) ) ;
#53109 = CARTESIAN_POINT ( 'NONE',  ( -15.45369544828537656, -9.886141570436013382, 34.14413921362392301 ) ) ;
#53110 = ORIENTED_EDGE ( 'NONE', *, *, #41889, .F. ) ;
#53111 = CIRCLE ( 'NONE', #83290, 5.000000000000000888 ) ;
#53112 = CARTESIAN_POINT ( 'NONE',  ( 8.900021210197715860, -4.684288915650983043, 34.18129842949671371 ) ) ;
#53113 = EDGE_CURVE ( 'NONE', #3961, #75689, #1252, .T. ) ;
#53114 = DIRECTION ( 'NONE',  ( 0.000000000000000000, 0.9396926207859126468, -0.3420201433256571111 ) ) ;
#53115 = CARTESIAN_POINT ( 'NONE',  ( 5.869852030268300602, -2.647304123082328875, 31.75400227202885262 ) ) ;
#53116 = CARTESIAN_POINT ( 'NONE',  ( -0.06109907496451398579, -10.25000000000000178, 15.03311829374151287 ) ) ;
#53117 = B_SPLINE_CURVE_WITH_KNOTS ( 'NONE', 3,
 ( #71263, #36610, #45129, #57319, #84817, #24409, #79371, #72603, #23093, #78034 ),
 .UNSPECIFIED., .F., .F.,
 ( 4, 2, 2, 2, 4 ),
 ( 0.000000000000000000, 0.0001954339857564073659, 0.0003908679715128147319, 0.0005863019572692221250, 0.0007817359430256294638 ),
 .UNSPECIFIED. ) ;
#53118 = ADVANCED_FACE ( 'NONE', ( #35491 ), #49004, .F. ) ;
#53119 = CARTESIAN_POINT ( 'NONE',  ( -20.74999999999999645, -7.500000000000000000, 32.75000000000000000 ) ) ;
#53120 = CARTESIAN_POINT ( 'NONE',  ( -17.75005448165186195, -10.76462480002816235, 33.53768742498949962 ) ) ;
#53122 = ORIENTED_EDGE ( 'NONE', *, *, #16286, .T. ) ;
#53121 = DIRECTION ( 'NONE',  ( 0.000000000000000000, 0.000000000000000000, -1.000000000000000000 ) ) ;
#53123 = CARTESIAN_POINT ( 'NONE',  ( 2.750000000000008438, -8.639087296525996607, 24.54687500000000000 ) ) ;
#53124 = DIRECTION ( 'NONE',  ( 0.000000000000000000, 0.000000000000000000, -1.000000000000000000 ) ) ;
#53125 = VERTEX_POINT ( 'NONE', #55753 ) ;
#53126 = EDGE_CURVE ( 'NONE', #20882, #13118, #32947, .T. ) ;
#53127 = CARTESIAN_POINT ( 'NONE',  ( -7.146561847641254239, -11.60425143139329940, 33.02411095842164457 ) ) ;
#53128 = ORIENTED_EDGE ( 'NONE', *, *, #41473, .T. ) ;
#53129 = CARTESIAN_POINT ( 'NONE',  ( 6.000000000000001776, -13.53365097954675988, 30.81389545987213552 ) ) ;
#53130 = CARTESIAN_POINT ( 'NONE',  ( -7.623374304885435215, -11.89424750095246175, 32.13594075562311758 ) ) ;
#53131 = B_SPLINE_CURVE_WITH_KNOTS ( 'NONE', 3,
 ( #18807, #38628, #39974, #86845, #12930, #53915, #33649, #45822, #47149, #67435 ),
 .UNSPECIFIED., .F., .F.,
 ( 4, 2, 2, 2, 4 ),
 ( 0.0007817359430256324996, 0.0009771253907249993591, 0.001172514838424366110, 0.001367904286123732861, 0.001563293733823099829 ),
 .UNSPECIFIED. ) ;
#53132 = CARTESIAN_POINT ( 'NONE',  ( 17.01165307636676260, -6.835583212224500826, 34.95778746994557906 ) ) ;
#53133 = ORIENTED_EDGE ( 'NONE', *, *, #51942, .F. ) ;
#53134 = CARTESIAN_POINT ( 'NONE',  ( 0.3962684609821410797, -5.094484230520674117, 34.41647553114621161 ) ) ;
#53135 = ORIENTED_EDGE ( 'NONE', *, *, #14678, .T. ) ;
#53136 = B_SPLINE_CURVE_WITH_KNOTS ( 'NONE', 3,
 ( #44523, #43217, #72009, #72451, #57612, #31016, #85978, #51720, #79223, #17522 ),
 .UNSPECIFIED., .F., .F.,
 ( 4, 2, 2, 2, 4 ),
 ( 0.0007817359430256322827, 0.0009771253907249989254, 0.001172514838424365676, 0.001367904286123732428, 0.001563293733823099179 ),
 .UNSPECIFIED. ) ;
#53137 = B_SPLINE_CURVE_WITH_KNOTS ( 'NONE', 3,
 ( #62736, #67740, #6045, #75382, #33515, #61852, #60972, #81704, #88478, #26747 ),
 .UNSPECIFIED., .F., .F.,
 ( 4, 2, 2, 2, 4 ),
 ( 0.000000000000000000, 0.0001954311564186862510, 0.0003908623128373725020, 0.0005862934692560588072, 0.0007817246256747450040 ),
 .UNSPECIFIED. ) ;
#53138 = VERTEX_POINT ( 'NONE', #48545 ) ;
#53139 = VECTOR ( 'NONE', #37914, 1000.000000000000000 ) ;
#53140 = VECTOR ( 'NONE', #12409, 1000.000000000000000 ) ;
#53141 = CARTESIAN_POINT ( 'NONE',  ( -0.4615384615384611200, -3.050289026998446396, 32.03036669348365706 ) ) ;
#53142 = CARTESIAN_POINT ( 'NONE',  ( -20.99999999999999645, -4.249999999999999112, 29.75000000000000355 ) ) ;
#53143 = CARTESIAN_POINT ( 'NONE',  ( 18.25005441991345734, -10.06805714834173138, 34.32951233291982618 ) ) ;
#53144 = CARTESIAN_POINT ( 'NONE',  ( 8.096153846155266010, -7.500000000000154543, 35.00000000000007105 ) ) ;
#53146 = EDGE_CURVE ( 'NONE', #48673, #13156, #49882, .T. ) ;
#53145 = CARTESIAN_POINT ( 'NONE',  ( -2.980714810855777497, -4.818054556918156983, 34.26375889529406749 ) ) ;
#53147 = CARTESIAN_POINT ( 'NONE',  ( -8.769230769230768274, -6.189225973068211317, 35.74407628777942847 ) ) ;
#53148 = VECTOR ( 'NONE', #17508, 1000.000000000000000 ) ;
#53149 = CARTESIAN_POINT ( 'NONE',  ( -0.2387587925603944505, -12.47679350104403007, 31.42216943046555855 ) ) ;
#53150 = ORIENTED_EDGE ( 'NONE', *, *, #73177, .T. ) ;
#53151 = ORIENTED_EDGE ( 'NONE', *, *, #64839, .T. ) ;
#53152 = ORIENTED_EDGE ( 'NONE', *, *, #75722, .F. ) ;
#53154 = ORIENTED_EDGE ( 'NONE', *, *, #11568, .T. ) ;
#53153 = CARTESIAN_POINT ( 'NONE',  ( 3.296024802045255608, -3.835265460703683349, 33.15142922261929925 ) ) ;
#53155 = CARTESIAN_POINT ( 'NONE',  ( -14.08467946359890988, -10.77377354290276124, 33.85451476688484718 ) ) ;
#53156 = CARTESIAN_POINT ( 'NONE',  ( -10.83886955910856464, -9.331801661448606566, 34.40259984581193464 ) ) ;
#53157 = ORIENTED_EDGE ( 'NONE', *, *, #73893, .T. ) ;
#53158 = CARTESIAN_POINT ( 'NONE',  ( 23.49999999999998934, 9.000000000000024869, 32.75000000000000000 ) ) ;
#53159 = B_SPLINE_CURVE_WITH_KNOTS ( 'NONE', 3,
 ( #1524, #23118, #71292, #85270, #77620, #76736, #9599, #15041, #29008, #56464 ),
 .UNSPECIFIED., .F., .F.,
 ( 4, 2, 2, 2, 4 ),
 ( 0.000000000000000000, 0.0001954311564186876876, 0.0003908623128373753751, 0.0005862934692560630356, 0.0007817246256747507503 ),
 .UNSPECIFIED. ) ;
#53160 = VERTEX_POINT ( 'NONE', #816 ) ;
#53161 = CARTESIAN_POINT ( 'NONE',  ( 17.07692307692307665, -9.780366693483667717, 34.19971097300155094 ) ) ;
#53162 = ORIENTED_EDGE ( 'NONE', *, *, #11411, .T. ) ;
#53163 = CARTESIAN_POINT ( 'NONE',  ( -18.22292695890684655, -9.172386477786394821, 34.72672124145550043 ) ) ;
#53164 = B_SPLINE_CURVE_WITH_KNOTS ( 'NONE', 3,
 ( #54636, #20861, #6472, #61840, #82135, #62283, #33932, #21301, #13664, #48773 ),
 .UNSPECIFIED., .F., .F.,
 ( 4, 2, 2, 2, 4 ),
 ( 0.000000000000000000, 0.0001954339857564082062, 0.0003908679715128164124, 0.0005863019572692246186, 0.0007817359430256328248 ),
 .UNSPECIFIED. ) ;
#53165 = EDGE_CURVE ( 'NONE', #72099, #7817, #47620, .T. ) ;
#53166 = DIRECTION ( 'NONE',  ( -0.000000000000000000, -0.7660444431189791237, -0.6427876096865379196 ) ) ;
#53167 = AXIS2_PLACEMENT_3D ( 'NONE', #29414, #85236, #16328 ) ;
#53168 = CARTESIAN_POINT ( 'NONE',  ( 4.153846153846468603, -2.255955759149395501, 30.00000000000324363 ) ) ;
#53169 = FACE_BOUND ( 'NONE', #66916, .T. ) ;
#53170 = CARTESIAN_POINT ( 'NONE',  ( 17.07692307692295586, -6.835583212225970762, 34.95778746994575670 ) ) ;
#53172 = EDGE_CURVE ( 'NONE', #21818, #43106, #88715, .T. ) ;
#53171 = CARTESIAN_POINT ( 'NONE',  ( 2.307692307692309264, -1.242168528481310874, 33.36296068462461051 ) ) ;
#53173 = CARTESIAN_POINT ( 'NONE',  ( 5.934749009838759193, -2.506253911140460477, 30.00000000000013856 ) ) ;
#53174 = LINE ( 'NONE', #54961, #22982 ) ;
#53175 = DIRECTION ( 'NONE',  ( -0.000000000000000000, 1.000000000000000000, 0.000000000000000000 ) ) ;
#53176 = CARTESIAN_POINT ( 'NONE',  ( 17.32686859527121825, -9.272278438253401589, 34.42582936511637826 ) ) ;
#53177 = ORIENTED_EDGE ( 'NONE', *, *, #62994, .T. ) ;
#53178 = EDGE_CURVE ( 'NONE', #38632, #8057, #75581, .T. ) ;
#53179 = CARTESIAN_POINT ( 'NONE',  ( 1.634615384615401013, -2.249999999999999112, 29.81603969181031033 ) ) ;
#53180 = ORIENTED_EDGE ( 'NONE', *, *, #60582, .F. ) ;
#53181 = ORIENTED_EDGE ( 'NONE', *, *, #22774, .T. ) ;
#53183 = CARTESIAN_POINT ( 'NONE',  ( -3.230769230769229949, -4.661471528628507777, 34.16647553114623292 ) ) ;
#53182 = CARTESIAN_POINT ( 'NONE',  ( -0.4615384615384611200, -8.973038597847269315, 34.52809138561121927 ) ) ;
#53184 = ADVANCED_FACE ( 'NONE', ( #1704 ), #26187, .T. ) ;
#53185 = CARTESIAN_POINT ( 'NONE',  ( -4.023798718595700485, -7.723484941389743952, 34.99544897038808955 ) ) ;
#53186 = CARTESIAN_POINT ( 'NONE',  ( -9.692307692307691624, -8.318370150425687726, 35.83090037661290239 ) ) ;
#53187 = CARTESIAN_POINT ( 'NONE',  ( 6.166666666666664298, -3.499999999999999556, 29.75000000000000355 ) ) ;
#53188 = CARTESIAN_POINT ( 'NONE',  ( -18.00000000000000000, -10.67929555188718282, 33.92786785259543336 ) ) ;
#53189 = EDGE_LOOP ( 'NONE', ( #46979, #69122 ) ) ;
#53190 = CARTESIAN_POINT ( 'NONE',  ( 2.242421861731533017, -9.442884908240170461, 34.35708131394840592 ) ) ;
#53191 = CARTESIAN_POINT ( 'NONE',  ( 11.40785117883701183, -7.722926236386453702, 34.74524107206102030 ) ) ;
#53192 = CARTESIAN_POINT ( 'NONE',  ( -14.53061852520844965, -8.239355502252617924, 34.69524867566427417 ) ) ;
#53193 = AXIS2_PLACEMENT_3D ( 'NONE', #72594, #10902, #2790 ) ;
#53194 = CYLINDRICAL_SURFACE ( 'NONE', #6524, 0.2500000000000008882 ) ;
#53195 = VERTEX_POINT ( 'NONE', #34607 ) ;
#53196 = ADVANCED_FACE ( 'NONE', ( #383 ), #2138, .F. ) ;
#53197 = ORIENTED_EDGE ( 'NONE', *, *, #40379, .T. ) ;
#53198 = B_SPLINE_CURVE_WITH_KNOTS ( 'NONE', 3,
 ( #7291, #533, #28001, #7738, #20367, #47827, #8180, #19906, #35200, #75308 ),
 .UNSPECIFIED., .F., .F.,
 ( 4, 2, 2, 2, 4 ),
 ( 0.000000000000000000, 0.0001954339857564083146, 0.0003908679715128166293, 0.0005863019572692249439, 0.0007817359430256332585 ),
 .UNSPECIFIED. ) ;
#53199 = AXIS2_PLACEMENT_3D ( 'NONE', #24625, #72805, #60623 ) ;
#53201 = AXIS2_PLACEMENT_3D ( 'NONE', #56061, #81889, #32803 ) ;
#53200 = APPLICATION_PROTOCOL_DEFINITION ( 'draft international standard', 'automotive_design', 1998, #80885 ) ;
#53202 = ORIENTED_EDGE ( 'NONE', *, *, #62389, .T. ) ;
#53203 = CARTESIAN_POINT ( 'NONE',  ( 0.6843180028068704956, -10.81320215134717344, 33.49497208177562868 ) ) ;
#53204 = CARTESIAN_POINT ( 'NONE',  ( -7.846153846153965716, -5.219633306517616589, 34.19971097300220464 ) ) ;
#53205 = ORIENTED_EDGE ( 'NONE', *, *, #70142, .T. ) ;
#53206 = DIRECTION ( 'NONE',  ( -0.000000000000000000, -0.6427876096865404731, -0.7660444431189770143 ) ) ;
#53207 = CARTESIAN_POINT ( 'NONE',  ( -5.076923076923075762, -2.721908614388771852, 31.22303859784724978 ) ) ;
#53208 = DIRECTION ( 'NONE',  ( -0.000000000000000000, 0.3420201433256694346, -0.9396926207859080948 ) ) ;
#53209 = CARTESIAN_POINT ( 'NONE',  ( -6.166666666666667851, -11.00000000000000000, 29.75000000000000355 ) ) ;
#53210 = AXIS2_PLACEMENT_3D ( 'NONE', #17223, #66299, #65843 ) ;
#53211 = CARTESIAN_POINT ( 'NONE',  ( -0.6850234052624084580, -11.41268669641500466, 32.86336882939237825 ) ) ;
#53212 = ORIENTED_EDGE ( 'NONE', *, *, #3737, .F. ) ;
#53213 = COLOUR_RGB ( '', 0.66274510, 0.83137255, 0.94901961) ;
#53215 = ORIENTED_EDGE ( 'NONE', *, *, #68904, .F. ) ;
#53214 = CARTESIAN_POINT ( 'NONE',  ( -7.623374304885437880, -10.11255958852956027, 34.01340905677048454 ) ) ;
#53216 = CARTESIAN_POINT ( 'NONE',  ( 4.153846153846032507, -3.300289026999228881, 32.46337939537708905 ) ) ;
#53217 = CYLINDRICAL_SURFACE ( 'NONE', #57069, 0.2499999999999973355 ) ;
#53218 = DIRECTION ( 'NONE',  ( -0.000000000000000000, -0.9848077530122086864, -0.1736481776669273613 ) ) ;
#53219 = LINE ( 'NONE', #38835, #12188 ) ;
#53220 = CARTESIAN_POINT ( 'NONE',  ( -4.087778820496076548, -4.661471528628508665, 34.16647553114624003 ) ) ;
#53221 = LINE ( 'NONE', #19005, #62231 ) ;
#53222 = CARTESIAN_POINT ( 'NONE',  ( 2.724691934501250135, -8.700186371490531201, 18.54874329374151642 ) ) ;
#53223 = ORIENTED_EDGE ( 'NONE', *, *, #15846, .F. ) ;
#53224 = EDGE_CURVE ( 'NONE', #10043, #328, #77989, .T. ) ;
#53225 = CARTESIAN_POINT ( 'NONE',  ( 15.23076923076911093, -8.613356846316285953, 34.62446782046622218 ) ) ;
#53226 = CARTESIAN_POINT ( 'NONE',  ( -9.692307692307812417, -8.613356846316285953, 34.62446782046622218 ) ) ;
#53227 = EDGE_CURVE ( 'NONE', #59485, #49728, #57527, .T. ) ;
#53228 = ORIENTED_EDGE ( 'NONE', *, *, #28972, .F. ) ;
#53229 = EDGE_LOOP ( 'NONE', ( #13163, #16222 ) ) ;
#53230 = CARTESIAN_POINT ( 'NONE',  ( 9.915087361285758405, -3.563462043263030399, 33.22394488606062879 ) ) ;
#53231 = CARTESIAN_POINT ( 'NONE',  ( -12.52762187249433978, -3.050289026998445951, 32.03036669348365706 ) ) ;
#53232 = CARTESIAN_POINT ( 'NONE',  ( 13.31853197365950514, -3.513871655860377086, 32.76840700105978499 ) ) ;
#53233 = CARTESIAN_POINT ( 'NONE',  ( -7.173053654019277303, -5.728515186090277211, 34.42611988154120439 ) ) ;
#53234 = ADVANCED_FACE ( 'NONE', ( #36381 ), #72368, .F. ) ;
#53235 = CARTESIAN_POINT ( 'NONE',  ( 7.145856464345329506, -5.913360116392398780, 34.49180327182771322 ) ) ;
#53236 = DIRECTION ( 'NONE',  ( -0.000000000000000000, -0.1736481776669307198, -0.9848077530122080203 ) ) ;
#53237 = ORIENTED_EDGE ( 'NONE', *, *, #27023, .T. ) ;
#53238 = CARTESIAN_POINT ( 'NONE',  ( 5.869308533332440625, -3.530157926970578508, 32.79014554554150607 ) ) ;
#53239 = EDGE_CURVE ( 'NONE', #6052, #76630, #41471, .T. ) ;
#53240 = DIRECTION ( 'NONE',  ( -0.000000000000000000, 0.8660254037844397068, -0.4999999999999978906 ) ) ;
#53241 = DIRECTION ( 'NONE',  ( 0.000000000000000000, 0.6427876096865368094, 0.7660444431189802339 ) ) ;
#53242 = EDGE_LOOP ( 'NONE', ( #38318, #51091 ) ) ;
#53243 = CARTESIAN_POINT ( 'NONE',  ( 13.38461538461526601, -6.879047030192662504, 34.71129190930017927 ) ) ;
#53244 = ORIENTED_EDGE ( 'NONE', *, *, #57901, .F. ) ;
#53245 = FACE_OUTER_BOUND ( 'NONE', #83668, .T. ) ;
#53246 = SURFACE_SIDE_STYLE ('',( #71740 ) ) ;
#53247 = CARTESIAN_POINT ( 'NONE',  ( -13.44993830010755609, -7.749976743299138882, 34.99404534957040624 ) ) ;
#53248 = VERTEX_POINT ( 'NONE', #10240 ) ;
#53249 = PLANE ( 'NONE',  #26046 ) ;
#53251 = ADVANCED_FACE ( 'NONE', ( #65163 ), #23294, .T. ) ;
#53250 = DIRECTION ( 'NONE',  ( -0.000000000000000000, 0.3420201433256694346, -0.9396926207859080948 ) ) ;
#53252 = CARTESIAN_POINT ( 'NONE',  ( -8.769230769230768274, -2.517432740324522911, 35.29906147534542527 ) ) ;
#53253 = CARTESIAN_POINT ( 'NONE',  ( -6.000000000000121680, -5.941354392335915335, 34.76329471203413846 ) ) ;
#53254 = CARTESIAN_POINT ( 'NONE',  ( -4.946397638689432164, -8.630441415882550871, 34.87705825610312615 ) ) ;
#53255 = ADVANCED_FACE ( 'NONE', ( #50315 ), #84578, .F. ) ;
#53256 = EDGE_CURVE ( 'NONE', #11627, #6016, #16104, .T. ) ;
#53257 = VERTEX_POINT ( 'NONE', #77799 ) ;
#53258 = AXIS2_PLACEMENT_3D ( 'NONE', #51719, #78318, #59389 ) ;
#53259 = CARTESIAN_POINT ( 'NONE',  ( -5.076923076923075762, -6.343179335718451384, 34.87096338111211935 ) ) ;
#53260 = ORIENTED_EDGE ( 'NONE', *, *, #75188, .T. ) ;
#53261 = CARTESIAN_POINT ( 'NONE',  ( -14.98082382139119062, -6.653508905675592722, 34.93172785388651391 ) ) ;
#53262 = ADVANCED_FACE ( 'NONE', ( #65603 ), #57969, .F. ) ;
#53263 = CARTESIAN_POINT ( 'NONE',  ( -10.55012947587177941, -10.33852847137154107, 34.16647553114620450 ) ) ;
#53264 = CARTESIAN_POINT ( 'NONE',  ( -14.30769230769242917, -10.33852847137269571, 34.16647553114546554 ) ) ;
#53265 = LINE ( 'NONE', #5985, #32971 ) ;
#53266 = CARTESIAN_POINT ( 'NONE',  ( 11.53846153846141576, -11.67786785259630911, 32.92929555188603530 ) ) ;
#53267 = CARTESIAN_POINT ( 'NONE',  ( -0.4615384615384611200, -13.78497067705608181, 32.30358669280327177 ) ) ;
#53268 = DIRECTION ( 'NONE',  ( 0.000000000000000000, 0.3420201433256641055, -0.9396926207859100932 ) ) ;
#53269 = VECTOR ( 'NONE', #32206, 1000.000000000000000 ) ;
#53270 = AXIS2_PLACEMENT_3D ( 'NONE', #6123, #50641, #29067 ) ;
#53271 = ORIENTED_EDGE ( 'NONE', *, *, #995, .T. ) ;
#53272 = ORIENTED_EDGE ( 'NONE', *, *, #24010, .T. ) ;
#53273 = VERTEX_POINT ( 'NONE', #9785 ) ;
#53274 = EDGE_LOOP ( 'NONE', ( #32424, #4836, #13289, #24207 ) ) ;
#53275 = CARTESIAN_POINT ( 'NONE',  ( 2.307692307692309264, -4.786620604624113540, 33.94971097300155094 ) ) ;
#53276 = CARTESIAN_POINT ( 'NONE',  ( -3.230769230769352962, -6.835583212225970762, 34.95778746994575670 ) ) ;
#53277 = DIRECTION ( 'NONE',  ( -0.000000000000000000, 1.000000000000000000, -0.000000000000000000 ) ) ;
#53278 = CARTESIAN_POINT ( 'NONE',  ( 4.826899852701616034, -11.56360843649121861, 33.07473185843129926 ) ) ;
#53279 = EDGE_CURVE ( 'NONE', #62427, #79550, #15667, .T. ) ;
#53280 = FACE_OUTER_BOUND ( 'NONE', #34575, .T. ) ;
#53281 = CARTESIAN_POINT ( 'NONE',  ( -0.7115151924808161832, -11.79746400365624659, 32.30657167506340954 ) ) ;
#53282 = CARTESIAN_POINT ( 'NONE',  ( -5.011667505647053211, -4.481592998940251427, 33.73612834413965089 ) ) ;
#53283 = DIRECTION ( 'NONE',  ( -0.000000000000000000, 0.6427876096865404731, -0.7660444431189771253 ) ) ;
#53284 = EDGE_LOOP ( 'NONE', ( #10300, #2010, #73421, #55271, #47962, #26588 ) ) ;
#53285 = ORIENTED_EDGE ( 'NONE', *, *, #36201, .T. ) ;
#53286 = ORIENTED_EDGE ( 'NONE', *, *, #54246, .T. ) ;
#53288 = ORIENTED_EDGE ( 'NONE', *, *, #20116, .F. ) ;
#53287 = CARTESIAN_POINT ( 'NONE',  ( -13.60810030917971858, -12.47654668319379567, 31.42292124445336654 ) ) ;
#53290 = LINE ( 'NONE', #576, #10289 ) ;
#53289 = DIRECTION ( 'NONE',  ( -0.000000000000000000, 0.9396926207859093161, -0.3420201433256663259 ) ) ;
#53291 = EDGE_CURVE ( 'NONE', #60920, #60370, #85896, .T. ) ;
#53292 = CARTESIAN_POINT ( 'NONE',  ( 11.25641025641025550, -7.500000000000000000, 29.75000000000000355 ) ) ;
#53293 = CARTESIAN_POINT ( 'NONE',  ( -8.992157728137618378, -6.459968553980841577, 34.89616026154728701 ) ) ;
#53294 = FACE_BOUND ( 'NONE', #10993, .T. ) ;
#53295 = ORIENTED_EDGE ( 'NONE', *, *, #48054, .F. ) ;
#53296 = B_SPLINE_CURVE_WITH_KNOTS ( 'NONE', 3,
 ( #16499, #10193, #64671, #57925, #85409, #71882, #80439, #66913, #13738, #81765 ),
 .UNSPECIFIED., .F., .F.,
 ( 4, 2, 2, 2, 4 ),
 ( 0.0007817359430256315238, 0.0009771253907249980580, 0.001172514838424364592, 0.001367904286123731127, 0.001563293733823097661 ),
 .UNSPECIFIED. ) ;
#53297 = AXIS2_PLACEMENT_3D ( 'NONE', #66193, #39636, #40083 ) ;
#53298 = ORIENTED_EDGE ( 'NONE', *, *, #68061, .T. ) ;
#53299 = EDGE_CURVE ( 'NONE', #29827, #16936, #2571, .T. ) ;
#53300 = CARTESIAN_POINT ( 'NONE',  ( 5.076923076923075762, -12.78798330534102767, 29.49999999999997868 ) ) ;
#53301 = ORIENTED_EDGE ( 'NONE', *, *, #28898, .T. ) ;
#53302 = FACE_BOUND ( 'NONE', #34916, .T. ) ;
#53303 = CARTESIAN_POINT ( 'NONE',  ( -10.74553258511631348, -3.069018819979302926, 32.56621877034667278 ) ) ;
#53304 = CARTESIAN_POINT ( 'NONE',  ( 15.10007862765892206, -6.369640206132551441, 34.87707690430378449 ) ) ;
#53305 = ORIENTED_EDGE ( 'NONE', *, *, #11488, .T. ) ;
#53306 = CARTESIAN_POINT ( 'NONE',  ( -2.307692307692305711, -1.466349020453238561, 30.81389545987213907 ) ) ;
#53307 = CARTESIAN_POINT ( 'NONE',  ( -1.634592128663975297, -8.347322224742351082, 34.93158281831414769 ) ) ;
#53308 = CARTESIAN_POINT ( 'NONE',  ( -2.108822856672541768, -5.366237147583038158, 13.71190574791610928 ) ) ;
#53309 = ORIENTED_EDGE ( 'NONE', *, *, #64218, .F. ) ;
#53310 = CARTESIAN_POINT ( 'NONE',  ( -7.846153846153844924, -8.164416787775445883, 34.95778746994557906 ) ) ;
#53311 = DIRECTION ( 'NONE',  ( 0.000000000000000000, 0.000000000000000000, -1.000000000000000000 ) ) ;
#53312 = CARTESIAN_POINT ( 'NONE',  ( 2.307692307692309264, -2.833524468853757305, 32.15551576947925838 ) ) ;
#53313 = VERTEX_POINT ( 'NONE', #37245 ) ;
#53314 = ADVANCED_FACE ( 'NONE', ( #64717 ), #24179, .T. ) ;
#53315 = CARTESIAN_POINT ( 'NONE',  ( -2.531177251416253604, -11.41268669641500466, 32.86336882939237825 ) ) ;
#53316 = CARTESIAN_POINT ( 'NONE',  ( -16.08777882049607655, -9.905515769479276145, 34.41647553114623292 ) ) ;
#53317 = ORIENTED_EDGE ( 'NONE', *, *, #47863, .T. ) ;
#53318 = CARTESIAN_POINT ( 'NONE',  ( 3.453548899747296730, -6.717445702608402236, 34.94155399931962336 ) ) ;
#53319 = LINE ( 'NONE', #71810, #3738 ) ;
#53320 = CARTESIAN_POINT ( 'NONE',  ( 5.869308533332443290, -8.999036380462719364, 34.52022231692819076 ) ) ;
#53321 = CARTESIAN_POINT ( 'NONE',  ( -5.010854725920638408, -8.120952969808772792, 34.71129190929999453 ) ) ;
#53322 = CARTESIAN_POINT ( 'NONE',  ( 8.769230769230645706, -4.320704448113951379, 33.92786785259630022 ) ) ;
#53323 = CARTESIAN_POINT ( 'NONE',  ( -1.384615384615383471, -13.49023893513002648, 31.06009739812518688 ) ) ;
#53325 = CARTESIAN_POINT ( 'NONE',  ( 9.942253101685738059, -4.932303261841489928, 34.32971442181322885 ) ) ;
#53324 = DIRECTION ( 'NONE',  ( 1.000000000000000000, -0.000000000000000000, -0.000000000000000000 ) ) ;
#53326 = AXIS2_PLACEMENT_3D ( 'NONE', #43563, #50310, #16097 ) ;
#53327 = CARTESIAN_POINT ( 'NONE',  ( 10.86533002476265963, -9.357781135181031829, 34.66075350412533851 ) ) ;
#53328 = CARTESIAN_POINT ( 'NONE',  ( 14.16025641025641235, -7.500000000000000000, 33.75000000000000000 ) ) ;
#53329 = CARTESIAN_POINT ( 'NONE',  ( 1.901340078031349856, -5.512252781505337929, 26.56063170625849068 ) ) ;
#53330 = VERTEX_POINT ( 'NONE', #17884 ) ;
#53331 = EDGE_CURVE ( 'NONE', #87991, #52162, #25525, .T. ) ;
#53332 = CARTESIAN_POINT ( 'NONE',  ( -12.59168567097668401, -8.587444163452046197, 34.63053765926554206 ) ) ;
#53333 = EDGE_LOOP ( 'NONE', ( #9524, #9160, #66814, #39022 ) ) ;
#53334 = VECTOR ( 'NONE', #43093, 1000.000000000000000 ) ;
#53335 = VECTOR ( 'NONE', #80121, 1000.000000000000114 ) ;
#53336 = ORIENTED_EDGE ( 'NONE', *, *, #58150, .F. ) ;
#53337 = EDGE_CURVE ( 'NONE', #73147, #26379, #54382, .T. ) ;
#53338 = CARTESIAN_POINT ( 'NONE',  ( -3.007989561791163613, -9.418065098278011860, 34.63729479722530158 ) ) ;
#53339 = ORIENTED_EDGE ( 'NONE', *, *, #214, .F. ) ;
#53340 = LINE ( 'NONE', #19123, #71423 ) ;
#53341 = CARTESIAN_POINT ( 'NONE',  ( 2.749999999999995115, -6.360912703473971419, 15.64062500000000178 ) ) ;
#53342 = CARTESIAN_POINT ( 'NONE',  ( -17.93474442872397390, -6.026961402152790193, 34.52809138561124769 ) ) ;
#53343 = CARTESIAN_POINT ( 'NONE',  ( 10.83839745947800992, -2.523321265292115534, 31.42251411153756990 ) ) ;
#53344 = CARTESIAN_POINT ( 'NONE',  ( -0.3954701105360234892, -5.557115091759786019, 34.35708131394839882 ) ) ;
#53345 = AXIS2_PLACEMENT_3D ( 'NONE', #56646, #84140, #62501 ) ;
#53346 = B_SPLINE_CURVE_WITH_KNOTS ( 'NONE', 3,
 ( #30785, #87542, #51477, #19060, #80328, #72213, #4659, #87094, #44735, #59148 ),
 .UNSPECIFIED., .F., .F.,
 ( 4, 2, 2, 2, 4 ),
 ( 0.0007817359430256327164, 0.0009771253907249993591, 0.001172514838424366110, 0.001367904286123732861, 0.001563293733823099396 ),
 .UNSPECIFIED. ) ;
#53347 = CARTESIAN_POINT ( 'NONE',  ( -18.03205128205128105, -3.499999999999999556, 29.75000000000000355 ) ) ;
#53348 = CARTESIAN_POINT ( 'NONE',  ( -15.29603923132555110, -5.094484230520674117, 34.41647553114621161 ) ) ;
#53349 = CARTESIAN_POINT ( 'NONE',  ( 13.38461538461526601, -9.442884908241554243, 34.35708131394783038 ) ) ;
#53350 = PRODUCT_DEFINITION_FORMATION_WITH_SPECIFIED_SOURCE ( 'ANY', '', #54864, .NOT_KNOWN. ) ;
#53351 = CARTESIAN_POINT ( 'NONE',  ( -2.651650429449565305, -4.848349570550461785, 22.75000000000000000 ) ) ;
#53352 = B_SPLINE_CURVE_WITH_KNOTS ( 'NONE', 3,
 ( #64211, #29563, #2511, #44378, #71866, #57463, #37638, #78184, #65099, #77737 ),
 .UNSPECIFIED., .F., .F.,
 ( 4, 2, 2, 2, 4 ),
 ( 0.000000000000000000, 0.0001954311564186879315, 0.0003908623128373758630, 0.0005862934692560637946, 0.0007817246256747517261 ),
 .UNSPECIFIED. ) ;
#53353 = B_SPLINE_CURVE_WITH_KNOTS ( 'NONE', 3,
 ( #27058, #54519, #82012, #31, #47319, #54973, #5467, #66714, #67605, #20307 ),
 .UNSPECIFIED., .F., .F.,
 ( 4, 2, 2, 2, 4 ),
 ( 0.0007817359430256219828, 0.0009771253907249863487, 0.001172514838424350498, 0.001367904286123714647, 0.001563293733823079013 ),
 .UNSPECIFIED. ) ;
#53354 = CARTESIAN_POINT ( 'NONE',  ( 17.32686848630112308, -2.341251567377310217, 30.72681386836322659 ) ) ;
#53355 = CARTESIAN_POINT ( 'NONE',  ( -10.55019162708995850, -2.255955759149236073, 29.99999999999988987 ) ) ;
#53356 = EDGE_CURVE ( 'NONE', #44478, #27810, #33973, .T. ) ;
#53357 = CARTESIAN_POINT ( 'NONE',  ( 11.53846153846153832, -3.050289026998446396, 32.03036669348365706 ) ) ;
#53358 = ORIENTED_EDGE ( 'NONE', *, *, #56925, .T. ) ;
#53359 = EDGE_LOOP ( 'NONE', ( #58139, #51397, #3220, #86647, #7313, #66881 ) ) ;
#53360 = CARTESIAN_POINT ( 'NONE',  ( 14.17754433796061875, -8.630895178749533159, 34.87696386517710323 ) ) ;
#53361 = DIRECTION ( 'NONE',  ( -1.000000000000000000, 0.000000000000000000, -0.000000000000000000 ) ) ;
#53362 = CARTESIAN_POINT ( 'NONE',  ( 9.692307692307695177, -10.89733346790207413, 36.13435417666054406 ) ) ;
#53363 = CARTESIAN_POINT ( 'NONE',  ( -7.173053667125516952, -5.643011162660950042, 34.66104346484419096 ) ) ;
#53365 = EDGE_CURVE ( 'NONE', #56098, #39942, #80476, .T. ) ;
#53364 = DIRECTION ( 'NONE',  ( -0.000000000000000000, 1.000000000000000000, 3.491481338843133355E-15 ) ) ;
#53366 = CARTESIAN_POINT ( 'NONE',  ( -16.37733109757010652, -9.331801661448606566, 34.40259984581193464 ) ) ;
#53367 = EDGE_CURVE ( 'NONE', #26351, #17177, #60629, .T. ) ;
#53368 = ADVANCED_FACE ( 'NONE', ( #66050 ), #32717, .F. ) ;
#53369 = EDGE_LOOP ( 'NONE', ( #55934, #64339, #56864, #83545 ) ) ;
#53370 = DIRECTION ( 'NONE',  ( -1.000000000000000000, -0.000000000000000000, -0.000000000000000000 ) ) ;
#53371 = ORIENTED_EDGE ( 'NONE', *, *, #83385, .F. ) ;
#53372 = VECTOR ( 'NONE', #4388, 1000.000000000000114 ) ;
#53373 = ORIENTED_EDGE ( 'NONE', *, *, #25027, .T. ) ;
#53374 = CARTESIAN_POINT ( 'NONE',  ( 5.076923076923075762, -12.78798330534103123, 29.99999999999997868 ) ) ;
#53375 = B_SPLINE_CURVE_WITH_KNOTS ( 'NONE', 3,
 ( #37564, #78553, #84447, #43883, #51963, #58280, #43447, #24053, #51501, #50185 ),
 .UNSPECIFIED., .F., .F.,
 ( 4, 2, 2, 2, 4 ),
 ( 0.0007817246256747524850, 0.0009771112852218972241, 0.001172497944769042072, 0.001367884604316186702, 0.001563271263863331550 ),
 .UNSPECIFIED. ) ;
#53376 = CARTESIAN_POINT ( 'NONE',  ( 5.750000000000002665, -7.500000000000001776, 34.75000000000000000 ) ) ;
#53377 = LINE ( 'NONE', #85840, #35862 ) ;
#53378 = CARTESIAN_POINT ( 'NONE',  ( 11.97435897435897623, -3.499999999999999556, 29.75000000000000355 ) ) ;
#53379 = LINE ( 'NONE', #68234, #53835 ) ;
#53380 = VERTEX_POINT ( 'NONE', #52979 ) ;
#53381 = ORIENTED_EDGE ( 'NONE', *, *, #42861, .T. ) ;
#53382 = EDGE_LOOP ( 'NONE', ( #76568, #7650, #63177, #62534 ) ) ;
#53383 = AXIS2_PLACEMENT_3D ( 'NONE', #3359, #58753, #86248 ) ;
#53384 = CARTESIAN_POINT ( 'NONE',  ( 5.933916589044118339, -2.538708090699994813, 30.37095296980875148 ) ) ;
#53385 = CARTESIAN_POINT ( 'NONE',  ( 10.48469401227430886, -11.37499894934982692, 33.29245874905763003 ) ) ;
#53386 = CARTESIAN_POINT ( 'NONE',  ( 4.376858997939549134, -3.395485233115139057, 33.02377354290275946 ) ) ;
#53387 = AXIS2_PLACEMENT_3D ( 'NONE', #37897, #25720, #24367 ) ;
#53388 = CARTESIAN_POINT ( 'NONE',  ( -8.546451100252701494, -10.23759521482555357, 34.22997729860117033 ) ) ;
#53389 = DIRECTION ( 'NONE',  ( -0.000000000000000000, 1.000000000000000000, -0.000000000000000000 ) ) ;
#53390 = DIRECTION ( 'NONE',  ( -0.000000000000000000, -0.9396926207859093161, -0.3420201433256663259 ) ) ;
#53391 = VERTEX_POINT ( 'NONE', #38594 ) ;
#53392 = ORIENTED_EDGE ( 'NONE', *, *, #44665, .F. ) ;
#53393 = VECTOR ( 'NONE', #81806, 1000.000000000000000 ) ;
#53395 = EDGE_LOOP ( 'NONE', ( #12191, #8836 ) ) ;
#53394 = CARTESIAN_POINT ( 'NONE',  ( -3.454254155333563503, -2.612411019501189813, 31.66733052389439962 ) ) ;
#53396 = CARTESIAN_POINT ( 'NONE',  ( 10.36536137809165403, -12.43535235679832596, 30.55408501211184813 ) ) ;
#53397 = CARTESIAN_POINT ( 'NONE',  ( 8.096153846153848477, -2.499999999999999112, 29.81604066197449754 ) ) ;
#53398 = CARTESIAN_POINT ( 'NONE',  ( 2.320192649118979489E-14, -11.25000000000000000, 14.78125000000000178 ) ) ;
#53399 = ORIENTED_EDGE ( 'NONE', *, *, #12070, .T. ) ;
#53400 = CARTESIAN_POINT ( 'NONE',  ( -1.384615384615506484, -11.67786785259630911, 32.92929555188603530 ) ) ;
#53401 = VERTEX_POINT ( 'NONE', #79587 ) ;
#53402 = B_SPLINE_CURVE_WITH_KNOTS ( 'NONE', 3,
 ( #63830, #35929, #84564, #65150, #22839, #16526, #9771, #1691, #64705, #49868 ),
 .UNSPECIFIED., .F., .F.,
 ( 4, 2, 2, 2, 4 ),
 ( 0.000000000000000000, 0.0001954311564186880128, 0.0003908623128373760257, 0.0005862934692560640114, 0.0007817246256747520513 ),
 .UNSPECIFIED. ) ;
#53403 = CARTESIAN_POINT ( 'NONE',  ( -4.000000000000002665, 7.500000000000000000, 14.00000000000000178 ) ) ;
#53404 = CARTESIAN_POINT ( 'NONE',  ( 17.07692307692295586, -12.16647553114689728, 32.15551576947799362 ) ) ;
#53405 = FACE_BOUND ( 'NONE', #1426, .T. ) ;
#53406 = CARTESIAN_POINT ( 'NONE',  ( -4.853911725310226188, -12.15243808032446005, 31.58219941686247978 ) ) ;
#53407 = CARTESIAN_POINT ( 'NONE',  ( 1.134615384615387246, -7.500000000000001776, 35.04278698407183867 ) ) ;
#53408 = ORIENTED_EDGE ( 'NONE', *, *, #83874, .F. ) ;
#53409 = DIRECTION ( 'NONE',  ( -0.000000000000000000, 0.9396926207859093161, -0.3420201433256663259 ) ) ;
#53410 = CARTESIAN_POINT ( 'NONE',  ( 8.835299120233207404, -6.386643153685127139, 34.62446782046654192 ) ) ;
#53411 = DIRECTION ( 'NONE',  ( -0.000000000000000000, 0.000000000000000000, 1.000000000000000000 ) ) ;
#53412 = ORIENTED_EDGE ( 'NONE', *, *, #29659, .T. ) ;
#53413 = AXIS2_PLACEMENT_3D ( 'NONE', #76573, #34701, #56738 ) ;
#53414 = CARTESIAN_POINT ( 'NONE',  ( -0.4615384615381544209, -2.506253911140615021, 30.00000000000323297 ) ) ;
#53415 = CARTESIAN_POINT ( 'NONE',  ( 14.43821774592595553, -10.31582465632705237, 34.18122507451815295 ) ) ;
#53416 = CARTESIAN_POINT ( 'NONE',  ( -4.153846153846152411, -2.292212530054420494, 30.41441678777542634 ) ) ;
#53417 = CARTESIAN_POINT ( 'NONE',  ( -16.40386937806761125, -12.07920672191015221, 32.31858351112116168 ) ) ;
#53418 = CARTESIAN_POINT ( 'NONE',  ( -19.00000000000000000, 1.250000000000007327, 31.75000000000000000 ) ) ;
#53419 = FACE_BOUND ( 'NONE', #43519, .T. ) ;
#53421 = CARTESIAN_POINT ( 'NONE',  ( 8.769230769230645706, -2.657715359629662544, 31.77849191805970364 ) ) ;
#53420 = CARTESIAN_POINT ( 'NONE',  ( 13.16113046005105858, -12.11044203135681840, 32.26167407432752299 ) ) ;
#53422 = CARTESIAN_POINT ( 'NONE',  ( 2.242422307135988557, -10.33852847137145048, 34.16647553114627556 ) ) ;
#53424 = CARTESIAN_POINT ( 'NONE',  ( 15.29602480204525250, -10.21337939537593620, 33.94971097300152252 ) ) ;
#53423 = CYLINDRICAL_SURFACE ( 'NONE', #54443, 0.2500000000000008882 ) ;
#53425 = CARTESIAN_POINT ( 'NONE',  ( 6.065255139512838234, -5.094484230520773593, 34.41647553114626845 ) ) ;
#53426 = CARTESIAN_POINT ( 'NONE',  ( 3.724691934501232815, -5.885600066136343678, 24.13875670625849068 ) ) ;
#53427 = ORIENTED_EDGE ( 'NONE', *, *, #44095, .F. ) ;
#53428 = CARTESIAN_POINT ( 'NONE',  ( -7.173053654019277303, -9.148715823498378086, 34.47080413974185120 ) ) ;
#53429 = ORIENTED_EDGE ( 'NONE', *, *, #61243, .T. ) ;
#53430 = EDGE_CURVE ( 'NONE', #24285, #6115, #60184, .T. ) ;
#53431 = B_SPLINE_CURVE_WITH_KNOTS ( 'NONE', 3,
 ( #18205, #38028, #46118, #67281, #73606, #87571, #80359, #65492, #52417, #3790 ),
 .UNSPECIFIED., .F., .F.,
 ( 4, 2, 2, 2, 4 ),
 ( 0.0007817246256747516176, 0.0009771112852218965736, 0.001172497944769041421, 0.001367884604316186269, 0.001563271263863331333 ),
 .UNSPECIFIED. ) ;
#53432 = CARTESIAN_POINT ( 'NONE',  ( 0.4615384615383396616, -6.879047030192662504, 34.71129190930017927 ) ) ;
#53433 = VERTEX_POINT ( 'NONE', #18772 ) ;
#53434 = CARTESIAN_POINT ( 'NONE',  ( 7.976944287120795174, -9.929761469519743144, 34.40412654351204225 ) ) ;
#53435 = LINE ( 'NONE', #60195, #86288 ) ;
#53437 = ORIENTED_EDGE ( 'NONE', *, *, #28885, .T. ) ;
#53436 = CARTESIAN_POINT ( 'NONE',  ( -2.372962753653081958, -11.94971097300153140, 32.03036669348370680 ) ) ;
#53438 = CARTESIAN_POINT ( 'NONE',  ( 16.82689985270161515, -12.68155406624981119, 30.59749803192733708 ) ) ;
#53439 = CARTESIAN_POINT ( 'NONE',  ( 1.161688425708538697, -11.98009711892699691, 32.48740034544075428 ) ) ;
#53440 = CARTESIAN_POINT ( 'NONE',  ( -2.694853999681210865, -4.891553140782108677, 24.99813170625849423 ) ) ;
#53441 = CARTESIAN_POINT ( 'NONE',  ( 14.05766907039934210, -10.76384336483936011, 33.53834819971076087 ) ) ;
#53442 = CARTESIAN_POINT ( 'NONE',  ( -12.46153846153858247, -12.27809138561165270, 31.22303859784587132 ) ) ;
#53443 = CARTESIAN_POINT ( 'NONE',  ( -12.33074802057151409, -9.084667340241226796, 34.75534355489798344 ) ) ;
#53444 = CARTESIAN_POINT ( 'NONE',  ( -14.30769230769242917, -6.835583212225970762, 34.95778746994575670 ) ) ;
#53445 = CARTESIAN_POINT ( 'NONE',  ( 7.173131234715237170, -4.235687564193446164, 33.53795663066793509 ) ) ;
#53446 = CARTESIAN_POINT ( 'NONE',  ( -11.53846153846165912, -10.21337939537710326, 33.94971097300076224 ) ) ;
#53447 = CARTESIAN_POINT ( 'NONE',  ( 3.724691934501251023, -9.114399933863618131, 19.79874329374151287 ) ) ;
#53448 = CARTESIAN_POINT ( 'NONE',  ( 14.08476609017615644, -5.667676309546437530, 34.40238873228292249 ) ) ;
#53449 = EDGE_CURVE ( 'NONE', #5201, #64026, #29673, .T. ) ;
#53450 = CARTESIAN_POINT ( 'NONE',  ( -1.254089946381740761, -12.15418822224088657, 32.17964115625579069 ) ) ;
#53451 = ORIENTED_EDGE ( 'NONE', *, *, #13894, .T. ) ;
#53452 = DIRECTION ( 'NONE',  ( -0.000000000000000000, 0.6427876096865404731, -0.7660444431189770143 ) ) ;
#53453 = CARTESIAN_POINT ( 'NONE',  ( 15.45378207486262667, -10.77377354290276124, 33.85451476688484718 ) ) ;
#53454 = CARTESIAN_POINT ( 'NONE',  ( -2.694853999681181556, -10.10844685921792241, 20.18936829374151287 ) ) ;
#53455 = VECTOR ( 'NONE', #64250, 1000.000000000000000 ) ;
#53456 = CARTESIAN_POINT ( 'NONE',  ( 2.057669070399344324, -4.335965774309649134, 33.62209801155881905 ) ) ;
#53457 = CARTESIAN_POINT ( 'NONE',  ( -13.38461538461538325, -3.886160181151819604, 36.00935417666054406 ) ) ;
#53458 = VERTEX_POINT ( 'NONE', #67396 ) ;
#53459 = CYLINDRICAL_SURFACE ( 'NONE', #83073, 0.2500000000000009437 ) ;
#53460 = CARTESIAN_POINT ( 'NONE',  ( -12.39628332202562433, -12.70778746994558439, 30.41441678777536595 ) ) ;
#53462 = EDGE_LOOP ( 'NONE', ( #67185, #81989 ) ) ;
#53461 = CARTESIAN_POINT ( 'NONE',  ( 11.60365452675619302, -2.255955759149235629, 29.99999999999988987 ) ) ;
#53463 = CARTESIAN_POINT ( 'NONE',  ( -13.13466986626724164, -11.37275283266504111, 32.91324779482534524 ) ) ;
#53464 = CARTESIAN_POINT ( 'NONE',  ( -2.557692307692305267, -7.500000000000001776, 35.00000000000000000 ) ) ;
#53465 = CARTESIAN_POINT ( 'NONE',  ( -11.00641025641025550, -3.499999999999999556, 29.75000000000000355 ) ) ;
#53466 = AXIS2_PLACEMENT_3D ( 'NONE', #32305, #66980, #5275 ) ;
#53467 = CARTESIAN_POINT ( 'NONE',  ( -16.40384615384615330, -7.500000000000001776, 35.00000000000000000 ) ) ;
#53468 = VERTEX_POINT ( 'NONE', #88583 ) ;
#53470 = LINE ( 'NONE', #10277, #34666 ) ;
#53469 = B_SPLINE_CURVE_WITH_KNOTS ( 'NONE', 3,
 ( #22847, #10674, #71039, #71920, #65598, #31384, #16535, #79130, #37692, #17431 ),
 .UNSPECIFIED., .F., .F.,
 ( 4, 2, 2, 2, 4 ),
 ( 0.0007817246336856291692, 0.0009771112958940105907, 0.001172497958102391904, 0.001367884620310773434, 0.001563271282519154747 ),
 .UNSPECIFIED. ) ;
#53471 = CARTESIAN_POINT ( 'NONE',  ( 6.923076923076802558, -5.219633306517616589, 34.19971097300220464 ) ) ;
#53472 = EDGE_CURVE ( 'NONE', #87090, #70251, #22004, .T. ) ;
#53473 = EDGE_CURVE ( 'NONE', #59229, #58032, #70335, .T. ) ;
#53474 = CARTESIAN_POINT ( 'NONE',  ( 8.638540166120458608, -3.338472653186243644, 32.95098750199972670 ) ) ;
#53475 = EDGE_LOOP ( 'NONE', ( #14909, #53162 ) ) ;
#53476 = EDGE_LOOP ( 'NONE', ( #80834, #36775, #76590, #28635 ) ) ;
#53477 = ORIENTED_EDGE ( 'NONE', *, *, #35459, .F. ) ;
#53478 = EDGE_CURVE ( 'NONE', #15316, #485, #12266, .T. ) ;
#53479 = CARTESIAN_POINT ( 'NONE',  ( 0.4615384615383396616, -8.613356846316285953, 34.62446782046622218 ) ) ;
#53480 = DIRECTION ( 'NONE',  ( -0.000000000000000000, -0.8660254037844399289, -0.4999999999999980016 ) ) ;
#53481 = CARTESIAN_POINT ( 'NONE',  ( 2.307692307692187583, -6.026961402154118908, 34.52809138561165270 ) ) ;
#53482 = CARTESIAN_POINT ( 'NONE',  ( -17.77703709643851226, -7.369474270740072441, 34.74850911626239736 ) ) ;
#53483 = AXIS2_PLACEMENT_3D ( 'NONE', #59178, #26286, #48324 ) ;
#53484 = ORIENTED_EDGE ( 'NONE', *, *, #13554, .T. ) ;
#53485 = VERTEX_POINT ( 'NONE', #75477 ) ;
#53486 = ORIENTED_EDGE ( 'NONE', *, *, #38296, .T. ) ;
#53488 = EDGE_LOOP ( 'NONE', ( #30129, #35668, #71447, #76985 ) ) ;
#53487 = CARTESIAN_POINT ( 'NONE',  ( -8.096177083446809419, -5.056417327199099532, 34.11270091957321426 ) ) ;
#53489 = DIRECTION ( 'NONE',  ( 0.000000000000000000, 0.9848077530122072432, 0.1736481776669354937 ) ) ;
#53490 = VECTOR ( 'NONE', #71730, 1000.000000000000114 ) ;
#53491 = DIRECTION ( 'NONE',  ( -0.000000000000000000, -0.000000000000000000, -1.000000000000000000 ) ) ;
#53492 = DIRECTION ( 'NONE',  ( 0.000000000000000000, 0.000000000000000000, 1.000000000000000000 ) ) ;
#53493 = DIRECTION ( 'NONE',  ( -0.000000000000000000, -0.3420201433256694346, -0.9396926207859080948 ) ) ;
#53494 = B_SPLINE_CURVE_WITH_KNOTS ( 'NONE', 3,
 ( #59055, #52297, #79787, #66259, #18083, #25280, #45543, #11318, #16302, #6355 ),
 .UNSPECIFIED., .F., .F.,
 ( 4, 2, 2, 2, 4 ),
 ( 0.0007817359430256297891, 0.0009771253907249958896, 0.001172514838424362207, 0.001367904286123728524, 0.001563293733823094625 ),
 .UNSPECIFIED. ) ;
#53495 = ORIENTED_EDGE ( 'NONE', *, *, #53093, .F. ) ;
#53496 = EDGE_LOOP ( 'NONE', ( #40862, #1218, #48762, #57122 ) ) ;
#53497 = ORIENTED_EDGE ( 'NONE', *, *, #15907, .T. ) ;
#53498 = CARTESIAN_POINT ( 'NONE',  ( -4.826923076921640465, -7.500000000000155431, 34.75000000000007105 ) ) ;
#53500 = EDGE_LOOP ( 'NONE', ( #35232, #46406 ) ) ;
#53499 = CARTESIAN_POINT ( 'NONE',  ( -10.36533019547115764, -2.544122305571458575, 31.48381861865057729 ) ) ;
#53501 = CARTESIAN_POINT ( 'NONE',  ( 2.057715563643719658, -2.544273027872574922, 31.48422191005632342 ) ) ;
#53502 = DIRECTION ( 'NONE',  ( 1.000000000000000000, 0.000000000000000000, 0.000000000000000000 ) ) ;
#53503 = ORIENTED_EDGE ( 'NONE', *, *, #8303, .T. ) ;
#53504 = CARTESIAN_POINT ( 'NONE',  ( -16.85391172531022619, -9.086983370893049639, 34.49168942202179267 ) ) ;
#53505 = CARTESIAN_POINT ( 'NONE',  ( 16.37685750545900376, -3.587049720035815348, 32.86302985866382897 ) ) ;
#53506 = DIRECTION ( 'NONE',  ( 0.000000000000000000, 0.000000000000000000, -1.000000000000000000 ) ) ;
#53507 = FACE_BOUND ( 'NONE', #24160, .T. ) ;
#53508 = CARTESIAN_POINT ( 'NONE',  ( -17.77698864838715309, -8.239487800360276282, 34.69522927552633718 ) ) ;
#53509 = CARTESIAN_POINT ( 'NONE',  ( -12.71156169883143150, -9.271318131107980420, 34.42618302367067429 ) ) ;
#53510 = VECTOR ( 'NONE', #22521, 1000.000000000000000 ) ;
#53511 = CARTESIAN_POINT ( 'NONE',  ( -10.61538461538473577, -11.06231777344772027, 33.60647404775119895 ) ) ;
#53513 = CARTESIAN_POINT ( 'NONE',  ( -5.076923076923075762, -1.242168528481310874, 33.36296068462461051 ) ) ;
#53512 = DIRECTION ( 'NONE',  ( 0.000000000000000000, 0.000000000000000000, -1.000000000000000000 ) ) ;
#53514 = VECTOR ( 'NONE', #83189, 1000.000000000000114 ) ;
#53515 = DIRECTION ( 'NONE',  ( 0.000000000000000000, 0.000000000000000000, -1.000000000000000000 ) ) ;
#53516 = CARTESIAN_POINT ( 'NONE',  ( -11.53846153846153655, -11.11383981884818262, 36.00935417666054406 ) ) ;
#53517 = EDGE_LOOP ( 'NONE', ( #78075, #7214, #48617, #57042 ) ) ;
#53518 = CARTESIAN_POINT ( 'NONE',  ( 16.15384615384646949, -2.255955759149395501, 30.00000000000324363 ) ) ;
#53519 = CARTESIAN_POINT ( 'NONE',  ( -13.60810030917971503, -9.417330523894424488, 34.63758898049880486 ) ) ;
#53520 = VERTEX_POINT ( 'NONE', #83591 ) ;
#53521 = ORIENTED_EDGE ( 'NONE', *, *, #23249, .F. ) ;
#53522 = CIRCLE ( 'NONE', #4670, 2.750000000000000000 ) ;
#53523 = EDGE_CURVE ( 'NONE', #19429, #29827, #20967, .T. ) ;
#53524 = CARTESIAN_POINT ( 'NONE',  ( 0.6843181305165264572, -8.540255544307065350, 34.89611431652622286 ) ) ;
#53525 = CARTESIAN_POINT ( 'NONE',  ( 16.15384615384603251, -2.379036618888197729, 30.90682066428292885 ) ) ;
#53526 = CARTESIAN_POINT ( 'NONE',  ( 12.46153846153846168, -10.67929555188718282, 33.92786785259544047 ) ) ;
#53527 = EDGE_LOOP ( 'NONE', ( #75191, #42647 ) ) ;
#53528 = DIRECTION ( 'NONE',  ( -1.000000000000000000, -0.000000000000000000, -0.000000000000000000 ) ) ;
#53529 = CYLINDRICAL_SURFACE ( 'NONE', #21362, 0.2500000000000002220 ) ;
#53530 = FACE_BOUND ( 'NONE', #66364, .T. ) ;
#53532 = CARTESIAN_POINT ( 'NONE',  ( 5.869852030268306819, -6.809168938359898782, 34.95455904226513866 ) ) ;
#53531 = CARTESIAN_POINT ( 'NONE',  ( -10.61538461538461320, -4.661471528628507777, 34.16647553114623292 ) ) ;
#53533 = CARTESIAN_POINT ( 'NONE',  ( -8.769230769230890843, -6.879047030192662504, 34.71129190930017927 ) ) ;
#53534 = CARTESIAN_POINT ( 'NONE',  ( 0.4615384615383382183, -5.094484230521993062, 34.41647553114689373 ) ) ;
#53536 = CYLINDRICAL_SURFACE ( 'NONE', #1760, 0.2499999999999994726 ) ;
#53535 = FILL_AREA_STYLE_COLOUR ( '', #87850 ) ;
#53537 = B_SPLINE_CURVE_WITH_KNOTS ( 'NONE', 3,
 ( #81192, #74424, #12726, #19915, #82527, #67672, #27569, #5976, #41085, #33445 ),
 .UNSPECIFIED., .F., .F.,
 ( 4, 2, 2, 2, 4 ),
 ( 0.000000000000000000, 0.0001954311564186865492, 0.0003908623128373730983, 0.0005862934692560596746, 0.0007817246256747461966 ),
 .UNSPECIFIED. ) ;
#53538 = CARTESIAN_POINT ( 'NONE',  ( -1.929879867024197893E-14, -3.750000000000000000, 24.15625000000000000 ) ) ;
#53539 = ORIENTED_EDGE ( 'NONE', *, *, #19160, .T. ) ;
#53540 = ORIENTED_EDGE ( 'NONE', *, *, #14187, .F. ) ;
#53541 = ADVANCED_FACE ( 'NONE', ( #56096 ), #42591, .F. ) ;
#53542 = B_SPLINE_CURVE_WITH_KNOTS ( 'NONE', 3,
 ( #21440, #56559, #14687, #83607, #42609, #84049, #22329, #35396, #13353, #70070 ),
 .UNSPECIFIED., .F., .F.,
 ( 4, 2, 2, 2, 4 ),
 ( 0.000000000000000000, 0.0001954339857564080707, 0.0003908679715128161414, 0.0005863019572692241849, 0.0007817359430256322827 ),
 .UNSPECIFIED. ) ;
#53543 = CARTESIAN_POINT ( 'NONE',  ( -12.21148404162501144, -5.642605341092957971, 34.66089969410670335 ) ) ;
#53544 = DIRECTION ( 'NONE',  ( -0.000000000000000000, -0.5000000000000009992, -0.8660254037844380415 ) ) ;
#53545 = DIRECTION ( 'NONE',  ( 1.000000000000000000, 0.000000000000000000, 0.000000000000000000 ) ) ;
#53547 = B_SPLINE_CURVE_WITH_KNOTS ( 'NONE', 3,
 ( #31777, #32654, #59235, #73660, #46616, #11955, #25006, #79959, #26345, #53810 ),
 .UNSPECIFIED., .F., .F.,
 ( 4, 2, 2, 2, 4 ),
 ( 0.0007817246256747447872, 0.0009771112852218874663, 0.001172497944769030362, 0.001367884604316173258, 0.001563271263863315937 ),
 .UNSPECIFIED. ) ;
#53546 = CYLINDRICAL_SURFACE ( 'NONE', #81282, 0.2499999999999973355 ) ;
#53548 = ADVANCED_FACE ( 'NONE', ( #8361 ), #48438, .F. ) ;
#53549 = DIRECTION ( 'NONE',  ( -0.000000000000000000, 0.5000000000000011102, -0.8660254037844381525 ) ) ;
#53550 = CARTESIAN_POINT ( 'NONE',  ( -1.553300858899125059, -3.750000000000009326, 20.32812500000000000 ) ) ;
#53551 = CARTESIAN_POINT ( 'NONE',  ( -7.623142494540996239, -8.239487800360276282, 34.69522927552633718 ) ) ;
#53552 = CARTESIAN_POINT ( 'NONE',  ( 1.634669696253701732, -4.943051570960395047, 34.04725096376909477 ) ) ;
#53553 = DIRECTION ( 'NONE',  ( -0.000000000000000000, -0.9396926207859092051, -0.3420201433256662704 ) ) ;
#53554 = CARTESIAN_POINT ( 'NONE',  ( 12.21151523731700372, -11.56360843649121861, 33.07473185843129926 ) ) ;
#53555 = CARTESIAN_POINT ( 'NONE',  ( -9.942284423250047354, -11.28823185664190376, 33.01397839955799896 ) ) ;
#53556 = CARTESIAN_POINT ( 'NONE',  ( 13.63466980452884236, -2.544122305571458575, 31.48381861865057729 ) ) ;
#53557 = CIRCLE ( 'NONE', #40647, 4.000000000000000000 ) ;
#53558 = CARTESIAN_POINT ( 'NONE',  ( 6.923076923076800782, -3.643525952248796163, 33.31231777344771672 ) ) ;
#53559 = CARTESIAN_POINT ( 'NONE',  ( 9.692307692307695177, -13.87047571288749737, 32.06866353760679544 ) ) ;
#53560 = CARTESIAN_POINT ( 'NONE',  ( -6.673131513698879580, -3.520799739797213501, 33.17531984108286025 ) ) ;
#53561 = EDGE_CURVE ( 'NONE', #88595, #71008, #709, .T. ) ;
#53562 = CARTESIAN_POINT ( 'NONE',  ( -15.36091644020745051, -8.587444163452046197, 34.63053765926554206 ) ) ;
#53563 = AXIS2_PLACEMENT_3D ( 'NONE', #28782, #49494, #29665 ) ;
#53564 = EDGE_LOOP ( 'NONE', ( #36099, #72459 ) ) ;
#53565 = CARTESIAN_POINT ( 'NONE',  ( -16.09615384615384670, -3.499999999999999556, 29.75000000000000355 ) ) ;
#53566 = DIRECTION ( 'NONE',  ( -0.000000000000000000, -0.8660254037844397068, -0.4999999999999978906 ) ) ;
#53567 = CARTESIAN_POINT ( 'NONE',  ( 1.077988221561497539, -10.27530806549875386, 18.70499329374151287 ) ) ;
#53568 = EDGE_CURVE ( 'NONE', #11900, #30370, #57394, .T. ) ;
#53569 = CARTESIAN_POINT ( 'NONE',  ( 13.45068373561782593, -4.786620604624113540, 33.94971097300155805 ) ) ;
#53570 = FACE_OUTER_BOUND ( 'NONE', #23551, .T. ) ;
#53571 = CYLINDRICAL_SURFACE ( 'NONE', #28414, 0.2500000000000012212 ) ;
#53573 = ORIENTED_EDGE ( 'NONE', *, *, #22708, .T. ) ;
#53572 = CARTESIAN_POINT ( 'NONE',  ( 5.207713517890028676, -3.957578996910242619, 33.62503395064540257 ) ) ;
#53574 = CARTESIAN_POINT ( 'NONE',  ( -2.749999999999998224, -7.500000000000015987, 25.09374999999999645 ) ) ;
#53575 = CARTESIAN_POINT ( 'NONE',  ( 7.846153846153846700, -11.16473453929635440, 33.15142922261926373 ) ) ;
#53576 = ORIENTED_EDGE ( 'NONE', *, *, #11331, .F. ) ;
#53577 = DIRECTION ( 'NONE',  ( 0.000000000000000000, 0.000000000000000000, -1.000000000000000000 ) ) ;
#53578 = CARTESIAN_POINT ( 'NONE',  ( 18.06525557127602610, -9.442884908240273489, 34.35708131394835618 ) ) ;
#53579 = VERTEX_POINT ( 'NONE', #61513 ) ;
#53580 = FACE_OUTER_BOUND ( 'NONE', #33029, .T. ) ;
#53581 = CARTESIAN_POINT ( 'NONE',  ( -7.596208327805705096, -11.86320923018887719, 32.19269448109603360 ) ) ;
#53582 = EDGE_CURVE ( 'NONE', #24932, #24126, #34907, .T. ) ;
#53583 = CARTESIAN_POINT ( 'NONE',  ( 3.230769230769231726, -5.180354513474913603, 36.12317359536750416 ) ) ;
#53584 = ORIENTED_EDGE ( 'NONE', *, *, #13046, .F. ) ;
#53585 = EDGE_CURVE ( 'NONE', #15450, #7242, #68724, .T. ) ;
#53586 = B_SPLINE_CURVE_WITH_KNOTS ( 'NONE', 3,
 ( #21212, #55884, #68512, #27534, #76608, #34732, #62199, #83371, #14463, #14915 ),
 .UNSPECIFIED., .F., .F.,
 ( 4, 2, 2, 2, 4 ),
 ( 0.000000000000000000, 0.0001954339857564091007, 0.0003908679715128182013, 0.0005863019572692273291, 0.0007817359430256364027 ),
 .UNSPECIFIED. ) ;
#53587 = ORIENTED_EDGE ( 'NONE', *, *, #60848, .T. ) ;
#53588 = B_SPLINE_CURVE_WITH_KNOTS ( 'NONE', 3,
 ( #25782, #80743, #46495, #73974, #53691, #81179, #19464, #46925, #74412, #62651 ),
 .UNSPECIFIED., .F., .F.,
 ( 4, 2, 2, 2, 4 ),
 ( 0.0007817246256747458714, 0.0009771112852218889842, 0.001172497944769032097, 0.001367884604316175210, 0.001563271263863318323 ),
 .UNSPECIFIED. ) ;
#53589 = VECTOR ( 'NONE', #1940, 1000.000000000000114 ) ;
#53590 = VERTEX_POINT ( 'NONE', #49344 ) ;
#53592 = DIRECTION ( 'NONE',  ( -0.000000000000000000, 0.000000000000000000, 1.000000000000000000 ) ) ;
#53591 = AXIS2_PLACEMENT_3D ( 'NONE', #31564, #66229, #78855 ) ;
#53593 = CARTESIAN_POINT ( 'NONE',  ( 6.923076923076924238, -11.35647404775217417, 33.31231777344666511 ) ) ;
#53594 = EDGE_CURVE ( 'NONE', #69885, #63787, #70051, .T. ) ;
#53595 = DIRECTION ( 'NONE',  ( -0.000000000000000000, 1.000000000000000000, -0.000000000000000000 ) ) ;
#53596 = CARTESIAN_POINT ( 'NONE',  ( -10.61538461538461320, -2.538708090699994813, 30.37095296980875503 ) ) ;
#53597 = EDGE_CURVE ( 'NONE', #88692, #19422, #30399, .T. ) ;
#53598 = CARTESIAN_POINT ( 'NONE',  ( -9.692307692307691624, -9.058645607665452459, 34.76329471203371924 ) ) ;
#53599 = CARTESIAN_POINT ( 'NONE',  ( 14.30769230769218758, -11.94971097300221174, 32.03036669348237098 ) ) ;
#53600 = CARTESIAN_POINT ( 'NONE',  ( 12.59233026936325039, -4.809403383903225304, 33.96459661697924304 ) ) ;
#53601 = AXIS2_PLACEMENT_3D ( 'NONE', #33872, #27117, #87974 ) ;
#53602 = CARTESIAN_POINT ( 'NONE',  ( 15.90386940979756858, -12.65889640711025521, 30.72598325615533454 ) ) ;
#53603 = ORIENTED_EDGE ( 'NONE', *, *, #23999, .T. ) ;
#53604 = ORIENTED_EDGE ( 'NONE', *, *, #84883, .T. ) ;
#53605 = ORIENTED_EDGE ( 'NONE', *, *, #84059, .T. ) ;
#53607 = VERTEX_POINT ( 'NONE', #84032 ) ;
#53606 = CARTESIAN_POINT ( 'NONE',  ( 18.13052543823364360, -9.503571793651730104, 34.60286762892837942 ) ) ;
#53608 = CARTESIAN_POINT ( 'NONE',  ( -8.546217925137375104, -10.77377354290276124, 33.85451476688484718 ) ) ;
#53609 = CARTESIAN_POINT ( 'NONE',  ( 6.000000000000001776, -9.905515769479276145, 34.41647553114623292 ) ) ;
#53610 = ORIENTED_EDGE ( 'NONE', *, *, #13385, .F. ) ;
#53611 = CARTESIAN_POINT ( 'NONE',  ( -14.17690049986751433, -4.118422570099831148, 33.43335022499816489 ) ) ;
#53612 = B_SPLINE_CURVE_WITH_KNOTS ( 'NONE', 3,
 ( #8553, #79665, #44971, #58048, #57611, #78767, #18409, #37329, #45867, #11203 ),
 .UNSPECIFIED., .F., .F.,
 ( 4, 2, 2, 2, 4 ),
 ( 0.0007817246256747476061, 0.0009771112852218896347, 0.001172497944769031880, 0.001367884604316173909, 0.001563271263863315937 ),
 .UNSPECIFIED. ) ;
#53613 = VECTOR ( 'NONE', #13361, 999.9999999999998863 ) ;
#53614 = EDGE_LOOP ( 'NONE', ( #43637, #32214 ) ) ;
#53615 = LINE ( 'NONE', #4995, #56908 ) ;
#53616 = VERTEX_POINT ( 'NONE', #56541 ) ;
#53617 = CIRCLE ( 'NONE', #26299, 4.000000000000000000 ) ;
#53618 = B_SPLINE_CURVE_WITH_KNOTS ( 'NONE', 3,
 ( #74636, #19684, #743, #13812, #54347, #48473, #68759, #302, #28207, #21458 ),
 .UNSPECIFIED., .F., .F.,
 ( 4, 2, 2, 2, 4 ),
 ( 0.000000000000000000, 0.0001954311564186868202, 0.0003908623128373736404, 0.0005862934692560604335, 0.0007817246256747472808 ),
 .UNSPECIFIED. ) ;
#53619 = CARTESIAN_POINT ( 'NONE',  ( -18.13014796973170206, -9.504002272028873932, 34.60269587691767867 ) ) ;
#53620 = EDGE_CURVE ( 'NONE', #10201, #33117, #39239, .T. ) ;
#53621 = CARTESIAN_POINT ( 'NONE',  ( -4.377331078410484189, -4.225889041578354544, 33.85425143139329407 ) ) ;
#53622 = EDGE_CURVE ( 'NONE', #57810, #86321, #44465, .T. ) ;
#53623 = CARTESIAN_POINT ( 'NONE',  ( -16.02305571287920571, -10.70102852606553157, 33.91149625220312913 ) ) ;
#53624 = FACE_BOUND ( 'NONE', #87809, .T. ) ;
#53625 = DIRECTION ( 'NONE',  ( 0.000000000000000000, 1.000000000000000000, 0.000000000000000000 ) ) ;
#53626 = CARTESIAN_POINT ( 'NONE',  ( 1.634615384616805889, -7.500000000000154543, 35.00000000000007105 ) ) ;
#53627 = EDGE_CURVE ( 'NONE', #44944, #54584, #37593, .T. ) ;
#53628 = DIRECTION ( 'NONE',  ( -0.000000000000000000, 0.6427876096865404731, -0.7660444431189771253 ) ) ;
#53629 = CARTESIAN_POINT ( 'NONE',  ( 3.480714640147273720, -4.932303261841488151, 34.32971442181322885 ) ) ;
#53630 = CARTESIAN_POINT ( 'NONE',  ( -17.07692307692319744, -2.379036618888197285, 30.90682066428292885 ) ) ;
#53631 = DIRECTION ( 'NONE',  ( -0.000000000000000000, -0.8660254037844397068, -0.4999999999999978906 ) ) ;
#53632 = CARTESIAN_POINT ( 'NONE',  ( -11.78848476268299628, -3.520140089381495585, 33.17453946501458262 ) ) ;
#53633 = EDGE_LOOP ( 'NONE', ( #62743, #3234, #21455, #51811 ) ) ;
#53634 = ORIENTED_EDGE ( 'NONE', *, *, #57046, .F. ) ;
#53635 = EDGE_CURVE ( 'NONE', #10850, #73234, #73538, .T. ) ;
#53637 = CARTESIAN_POINT ( 'NONE',  ( 15.23076923076923173, -3.886160181151819604, 36.00935417666054406 ) ) ;
#53636 = DIRECTION ( 'NONE',  ( -0.000000000000000000, 0.5000000000000011102, -0.8660254037844381525 ) ) ;
#53638 = CARTESIAN_POINT ( 'NONE',  ( 15.36129466900288065, -8.630441415882550871, 34.87705825610312615 ) ) ;
#53639 = LINE ( 'NONE', #81569, #25007 ) ;
#53640 = CARTESIAN_POINT ( 'NONE',  ( -3.230769230769229949, -2.499999999999998668, 29.50000000000001066 ) ) ;
#53641 = DIRECTION ( 'NONE',  ( -1.000000000000000000, -0.000000000000000000, -0.000000000000000000 ) ) ;
#53642 = VERTEX_POINT ( 'NONE', #22745 ) ;
#53643 = CARTESIAN_POINT ( 'NONE',  ( -5.299850035829923200, -5.582147617184174848, 34.63737895849758530 ) ) ;
#53644 = B_SPLINE_CURVE_WITH_KNOTS ( 'NONE', 3,
 ( #61127, #34104, #81865, #61569, #87299, #88637, #32775, #12509, #13831, #47622 ),
 .UNSPECIFIED., .F., .F.,
 ( 4, 2, 2, 2, 4 ),
 ( 0.000000000000000000, 0.0001954339857564071491, 0.0003908679715128142982, 0.0005863019572692214744, 0.0007817359430256285964 ),
 .UNSPECIFIED. ) ;
#53645 = CYLINDRICAL_SURFACE ( 'NONE', #37307, 8.000000000000000000 ) ;
#53646 = CARTESIAN_POINT ( 'NONE',  ( -6.923076923076922462, -12.29105614889573062, 35.45975837776705220 ) ) ;
#53647 = CARTESIAN_POINT ( 'NONE',  ( -7.173053667125516064, -6.524016743844655686, 34.90889640711025521 ) ) ;
#53648 = ORIENTED_EDGE ( 'NONE', *, *, #58686, .T. ) ;
#53649 = ORIENTED_EDGE ( 'NONE', *, *, #20266, .T. ) ;
#53650 = VECTOR ( 'NONE', #29942, 1000.000000000000114 ) ;
#53651 = PRODUCT_CONTEXT ( 'NONE', #56140, 'mechanical' ) ;
#53652 = ORIENTED_EDGE ( 'NONE', *, *, #65091, .F. ) ;
#53653 = AXIS2_PLACEMENT_3D ( 'NONE', #72223, #31239, #65470 ) ;
#53654 = CARTESIAN_POINT ( 'NONE',  ( 0.2115384615384615641, -7.500000000000001776, 34.75000000000000000 ) ) ;
#53655 = CARTESIAN_POINT ( 'NONE',  ( -14.17716686945866122, -5.915461855592780260, 34.75538340440931506 ) ) ;
#53656 = ORIENTED_EDGE ( 'NONE', *, *, #79636, .F. ) ;
#53657 = PLANE ( 'NONE',  #53907 ) ;
#53658 = CARTESIAN_POINT ( 'NONE',  ( 2.307692307692309264, -11.11383981884818262, 36.00935417666054406 ) ) ;
#53659 = DIRECTION ( 'NONE',  ( -0.000000000000000000, 1.000000000000000000, -0.000000000000000000 ) ) ;
#53660 = ADVANCED_FACE ( 'NONE', ( #77692 ), #29960, .F. ) ;
#53661 = CARTESIAN_POINT ( 'NONE',  ( 1.449870524128224814, -6.835583212224609184, 34.95778746994559327 ) ) ;
#53662 = CIRCLE ( 'NONE', #68014, 4.000000000000000000 ) ;
#53663 = CARTESIAN_POINT ( 'NONE',  ( -0.4615384615384611200, -11.16473453929635440, 33.15142922261926373 ) ) ;
#53664 = ORIENTED_EDGE ( 'NONE', *, *, #866, .T. ) ;
#53666 = VERTEX_POINT ( 'NONE', #16004 ) ;
#53665 = CARTESIAN_POINT ( 'NONE',  ( -0.3310130233048185211, -12.15418822224088657, 32.17964115625579069 ) ) ;
#53667 = LINE ( 'NONE', #12239, #21022 ) ;
#53668 = CARTESIAN_POINT ( 'NONE',  ( 16.02328556210422761, -2.504760397472873823, 29.97295953869789997 ) ) ;
#53669 = CARTESIAN_POINT ( 'NONE',  ( 1.254005024990858308, -7.722926236386453702, 34.74524107206102030 ) ) ;
#53670 = CARTESIAN_POINT ( 'NONE',  ( 8.899756207464411872, -12.15418822224088657, 32.17964115625579069 ) ) ;
#53671 = FACE_OUTER_BOUND ( 'NONE', #53274, .T. ) ;
#53672 = CARTESIAN_POINT ( 'NONE',  ( -5.076923076923199218, -11.06231777344772027, 33.60647404775119895 ) ) ;
#53673 = CARTESIAN_POINT ( 'NONE',  ( -14.30769230769230660, -12.37446782046654192, 30.86335684631486131 ) ) ;
#53674 = CARTESIAN_POINT ( 'NONE',  ( 1.987747218494642309, -5.598659921968629050, 19.56436829374151287 ) ) ;
#53675 = ORIENTED_EDGE ( 'NONE', *, *, #58823, .T. ) ;
#53676 = CARTESIAN_POINT ( 'NONE',  ( 15.16549878480845770, -8.613356846314824011, 34.62446782046655613 ) ) ;
#53677 = CARTESIAN_POINT ( 'NONE',  ( 7.780830930661671196, -7.749976743299137993, 34.99404534957040624 ) ) ;
#53678 = CARTESIAN_POINT ( 'NONE',  ( 20.74999999999999645, -12.50000000000000000, 27.25000000000000000 ) ) ;
#53679 = VERTEX_POINT ( 'NONE', #9254 ) ;
#53680 = CARTESIAN_POINT ( 'NONE',  ( -2.307692307692305711, -2.900454961884010974, 35.62045528018868623 ) ) ;
#53681 = CARTESIAN_POINT ( 'NONE',  ( 27.00000000000000000, -1.249999999999999778, 24.75000000000000000 ) ) ;
#53682 = CARTESIAN_POINT ( 'NONE',  ( -8.769230769230892619, -11.06231777344772027, 33.60647404775119895 ) ) ;
#53683 = AXIS2_PLACEMENT_3D ( 'NONE', #70386, #15446, #8691 ) ;
#53684 = CARTESIAN_POINT ( 'NONE',  ( 6.923076923076800782, -9.528491918059723176, 34.59228464037033035 ) ) ;
#53685 = DIRECTION ( 'NONE',  ( 1.000000000000000000, 0.000000000000000000, 0.000000000000000000 ) ) ;
#53686 = EDGE_LOOP ( 'NONE', ( #22810, #12419 ) ) ;
#53687 = CARTESIAN_POINT ( 'NONE',  ( 2.307692307692309264, -11.69971097300155272, 32.46337939537588113 ) ) ;
#53688 = EDGE_CURVE ( 'NONE', #62981, #53520, #78139, .T. ) ;
#53689 = EDGE_CURVE ( 'NONE', #47713, #87461, #41907, .T. ) ;
#53690 = CYLINDRICAL_SURFACE ( 'NONE', #58451, 4.000000000000000000 ) ;
#53691 = CARTESIAN_POINT ( 'NONE',  ( -2.057746898314263717, -5.766571408460171355, 34.70601412856602508 ) ) ;
#53692 = EDGE_LOOP ( 'NONE', ( #33760, #76871, #85738, #37849 ) ) ;
#53693 = DIRECTION ( 'NONE',  ( 0.000000000000000000, 0.7660444431189807890, 0.6427876096865361433 ) ) ;
#53694 = EDGE_CURVE ( 'NONE', #81733, #21693, #85326, .T. ) ;
#53695 = ORIENTED_EDGE ( 'NONE', *, *, #78372, .T. ) ;
#53696 = DIRECTION ( 'NONE',  ( -0.000000000000000000, -0.1736481776669307198, -0.9848077530122080203 ) ) ;
#53697 = CARTESIAN_POINT ( 'NONE',  ( 11.78851595837499211, -6.523592122091592671, 34.90882529074906415 ) ) ;
#53698 = VERTEX_POINT ( 'NONE', #75332 ) ;
#53699 = ADVANCED_FACE ( 'NONE', ( #7760 ), #41994, .F. ) ;
#53700 = CARTESIAN_POINT ( 'NONE',  ( 12.33139125210023934, -3.817052484675422797, 33.13202310037935661 ) ) ;
#53701 = CARTESIAN_POINT ( 'NONE',  ( 5.999999999999880096, -10.21337939537710326, 33.94971097300076224 ) ) ;
#53702 = LINE ( 'NONE', #25346, #81112 ) ;
#53703 = CARTESIAN_POINT ( 'NONE',  ( 11.28848479441294828, -12.41104346484419452, 31.60698883733904196 ) ) ;
#53704 = FACE_OUTER_BOUND ( 'NONE', #11334, .T. ) ;
#53705 = AXIS2_PLACEMENT_3D ( 'NONE', #86424, #24695, #47632 ) ;
#53706 = ORIENTED_EDGE ( 'NONE', *, *, #24046, .T. ) ;
#53707 = DIRECTION ( 'NONE',  ( 0.000000000000000000, 0.6427876096865373645, -0.7660444431189797898 ) ) ;
#53708 = EDGE_LOOP ( 'NONE', ( #54629, #28564, #64774, #36622 ) ) ;
#53710 = ADVANCED_FACE ( 'NONE', ( #36125 ), #999, .F. ) ;
#53709 = CARTESIAN_POINT ( 'NONE',  ( -2.557669051740895760, -2.544273027872574922, 31.48422191005632342 ) ) ;
#53711 = B_SPLINE_CURVE_WITH_KNOTS ( 'NONE', 3,
 ( #79301, #65767, #30656, #29344, #50042, #77519, #44153, #10842, #36965, #9498 ),
 .UNSPECIFIED., .F., .F.,
 ( 4, 2, 2, 2, 4 ),
 ( 0.0007817359430256322827, 0.0009771253907249989254, 0.001172514838424365676, 0.001367904286123732428, 0.001563293733823099179 ),
 .UNSPECIFIED. ) ;
#53712 = AXIS2_PLACEMENT_3D ( 'NONE', #57780, #49259, #15035 ) ;
#53713 = CARTESIAN_POINT ( 'NONE',  ( -10.61538461538461320, -9.905515769479276145, 34.41647553114623292 ) ) ;
#53714 = CARTESIAN_POINT ( 'NONE',  ( 17.99999999999987566, -6.835583212225970762, 34.95778746994575670 ) ) ;
#53715 = EDGE_CURVE ( 'NONE', #3961, #3690, #17701, .T. ) ;
#53716 = DIRECTION ( 'NONE',  ( -0.000000000000000000, 0.3420201433256694901, -0.9396926207859082059 ) ) ;
#53717 = CARTESIAN_POINT ( 'NONE',  ( 4.826923076923076650, -2.499999999999998668, 29.75000000000000355 ) ) ;
#53718 = B_SPLINE_CURVE_WITH_KNOTS ( 'NONE', 3,
 ( #52687, #53578, #81513, #86957, #46385, #81073, #4962, #5848, #25223, #19802 ),
 .UNSPECIFIED., .F., .F.,
 ( 4, 2, 2, 2, 4 ),
 ( 0.0007817359430256293554, 0.0009771253907249952391, 0.001172514838424361123, 0.001367904286123726790, 0.001563293733823092673 ),
 .UNSPECIFIED. ) ;
#53719 = ORIENTED_EDGE ( 'NONE', *, *, #26280, .T. ) ;
#53720 = ORIENTED_EDGE ( 'NONE', *, *, #85554, .F. ) ;
#53721 = VERTEX_POINT ( 'NONE', #22157 ) ;
#53722 = ORIENTED_EDGE ( 'NONE', *, *, #82859, .T. ) ;
#53723 = EDGE_CURVE ( 'NONE', #60966, #13706, #68564, .T. ) ;
#53724 = CARTESIAN_POINT ( 'NONE',  ( -5.299850035829926753, -4.026226216239095379, 33.68668979543632958 ) ) ;
#53725 = CARTESIAN_POINT ( 'NONE',  ( 16.21910129335899597, -11.06231777344670952, 33.60647404775212266 ) ) ;
#53726 = DIRECTION ( 'NONE',  ( 0.000000000000000000, 0.000000000000000000, 1.000000000000000000 ) ) ;
#53727 = EDGE_CURVE ( 'NONE', #35101, #22351, #82975, .T. ) ;
#53728 = CARTESIAN_POINT ( 'NONE',  ( -8.096130590202436750, -3.436278759898153901, 33.07459398097509506 ) ) ;
#53729 = CARTESIAN_POINT ( 'NONE',  ( 11.53846153846153832, -2.538708090699994813, 30.37095296980875503 ) ) ;
#53730 = DIRECTION ( 'NONE',  ( 0.000000000000000000, 0.000000000000000000, 1.000000000000000000 ) ) ;
#53731 = CARTESIAN_POINT ( 'NONE',  ( 17.77651505627605033, -2.599994579823202923, 30.74605699353653776 ) ) ;
#53732 = CARTESIAN_POINT ( 'NONE',  ( -8.703975629717932705, -3.083524468853784839, 32.58852847137153930 ) ) ;
#53733 = ORIENTED_EDGE ( 'NONE', *, *, #65204, .T. ) ;
#53734 = ORIENTED_EDGE ( 'NONE', *, *, #7623, .F. ) ;
#53735 = EDGE_LOOP ( 'NONE', ( #7228, #82865, #43854, #24370 ) ) ;
#53738 = ORIENTED_EDGE ( 'NONE', *, *, #62673, .F. ) ;
#53737 = EDGE_CURVE ( 'NONE', #23542, #13174, #14509, .T. ) ;
#53736 = CARTESIAN_POINT ( 'NONE',  ( 2.242421861731532573, -2.625532179533444754, 30.86335684631481513 ) ) ;
#53739 = AXIS2_PLACEMENT_3D ( 'NONE', #69032, #54618, #12759 ) ;
#53741 = CARTESIAN_POINT ( 'NONE',  ( 11.28846153846153832, -2.499999999999998668, 29.75000000000000355 ) ) ;
#53740 = DIRECTION ( 'NONE',  ( 0.000000000000000000, 0.000000000000000000, 1.000000000000000000 ) ) ;
#53742 = CARTESIAN_POINT ( 'NONE',  ( 5.326923076923075762, -2.499999999999998668, 29.75000000000000355 ) ) ;
#53743 = CARTESIAN_POINT ( 'NONE',  ( -9.942330929600657896, -6.695914987888146541, 34.68535235679833306 ) ) ;
#53744 = FACE_BOUND ( 'NONE', #67212, .T. ) ;
#53745 = ORIENTED_EDGE ( 'NONE', *, *, #22304, .F. ) ;
#53746 = ADVANCED_FACE ( 'NONE', ( #113 ), #28471, .F. ) ;
#53747 = ORIENTED_EDGE ( 'NONE', *, *, #36512, .T. ) ;
#53748 = CARTESIAN_POINT ( 'NONE',  ( 5.999999999999878320, -11.06231777344772027, 33.60647404775119895 ) ) ;
#53749 = ORIENTED_EDGE ( 'NONE', *, *, #57440, .F. ) ;
#53750 = FACE_BOUND ( 'NONE', #46890, .T. ) ;
#53751 = CARTESIAN_POINT ( 'NONE',  ( -10.61538461538473577, -3.083524468854526912, 32.58852847137268327 ) ) ;
#53752 = LINE ( 'NONE', #6025, #39079 ) ;
#53753 = ORIENTED_EDGE ( 'NONE', *, *, #63704, .T. ) ;
#53754 = LINE ( 'NONE', #6897, #37666 ) ;
#53755 = CARTESIAN_POINT ( 'NONE',  ( -12.71151520558704995, -12.01397095200674059, 32.43157075238190146 ) ) ;
#53756 = CARTESIAN_POINT ( 'NONE',  ( 3.230769230769108269, -12.16647553114689728, 32.15551576947799362 ) ) ;
#53757 = ORIENTED_EDGE ( 'NONE', *, *, #40548, .F. ) ;
#53758 = CARTESIAN_POINT ( 'NONE',  ( 6.792929713638703682, -6.001485441113818986, 34.52039167877662607 ) ) ;
#53759 = DIRECTION ( 'NONE',  ( 0.000000000000000000, 0.000000000000000000, 1.000000000000000000 ) ) ;
#53760 = CARTESIAN_POINT ( 'NONE',  ( -3.296852641725110278, -2.721908614388772296, 31.22303859784724622 ) ) ;
#53761 = EDGE_CURVE ( 'NONE', #79237, #41543, #53090, .T. ) ;
#53762 = CARTESIAN_POINT ( 'NONE',  ( -9.561781990544128362, -2.619367082507849442, 30.83698974864643461 ) ) ;
#53763 = ORIENTED_EDGE ( 'NONE', *, *, #47084, .F. ) ;
#53764 = EDGE_CURVE ( 'NONE', #72978, #77307, #49907, .T. ) ;
#53765 = DIRECTION ( 'NONE',  ( 0.000000000000000000, -1.000000000000000000, -1.084202172485503448E-16 ) ) ;
#53766 = DIRECTION ( 'NONE',  ( -0.000000000000000000, 0.6427876096865404731, -0.7660444431189771253 ) ) ;
#53767 = EDGE_LOOP ( 'NONE', ( #24045, #8413 ) ) ;
#53768 = CARTESIAN_POINT ( 'NONE',  ( 3.296024370282069071, -6.835583212224609184, 34.95778746994559327 ) ) ;
#53769 = DIRECTION ( 'NONE',  ( -0.000000000000000000, 0.6427876096865404731, -0.7660444431189771253 ) ) ;
#53770 = CARTESIAN_POINT ( 'NONE',  ( -8.096130590202434973, -12.41104346484419452, 31.60698883733904196 ) ) ;
#53771 = LINE ( 'NONE', #74492, #17014 ) ;
#53772 = CARTESIAN_POINT ( 'NONE',  ( -6.792238592590160273, -7.277220318596959281, 34.99547417642776992 ) ) ;
#53773 = DIRECTION ( 'NONE',  ( -0.000000000000000000, -0.1736481776669307198, -0.9848077530122080203 ) ) ;
#53776 = CARTESIAN_POINT ( 'NONE',  ( 8.546303810323914618, -2.889293201056495786, 32.26117774369186009 ) ) ;
#53775 = AXIS2_PLACEMENT_3D ( 'NONE', #41217, #61034, #88536 ) ;
#53774 = DIRECTION ( 'NONE',  ( 0.000000000000000000, 0.000000000000000000, 1.000000000000000000 ) ) ;
#53777 = CARTESIAN_POINT ( 'NONE',  ( -15.90390063549800992, -11.86320923018887541, 32.19269448109604781 ) ) ;
#53778 = CARTESIAN_POINT ( 'NONE',  ( -6.673131404728782634, -2.824170634883622188, 31.52227843825338738 ) ) ;
#53779 = CARTESIAN_POINT ( 'NONE',  ( -1.139087296526025916, -4.750000000000006217, 20.32812500000000000 ) ) ;
#53780 = EDGE_LOOP ( 'NONE', ( #907, #6926 ) ) ;
#53781 = AXIS2_PLACEMENT_3D ( 'NONE', #1186, #49383, #9609 ) ;
#53782 = DIRECTION ( 'NONE',  ( -0.000000000000000000, -0.6427876096865404731, -0.7660444431189771253 ) ) ;
#53783 = EDGE_LOOP ( 'NONE', ( #40155, #36926, #8425, #76822 ) ) ;
#53784 = ORIENTED_EDGE ( 'NONE', *, *, #77400, .F. ) ;
#53785 = CARTESIAN_POINT ( 'NONE',  ( -7.596208436775802930, -2.589246495874658383, 31.60778113518102828 ) ) ;
#53786 = ORIENTED_EDGE ( 'NONE', *, *, #43956, .T. ) ;
#53787 = CARTESIAN_POINT ( 'NONE',  ( -5.300408001487407539, -11.60425143139329940, 33.02411095842164457 ) ) ;
#53788 = CARTESIAN_POINT ( 'NONE',  ( 1.944543648262996083, -5.555456351736983045, 19.31250000000000000 ) ) ;
#53789 = CARTESIAN_POINT ( 'NONE',  ( -14.24243716817946925, -3.083524468853784839, 32.58852847137153930 ) ) ;
#53790 = CARTESIAN_POINT ( 'NONE',  ( 10.83816428436267465, -2.612705202774698421, 31.66806509827799943 ) ) ;
#53791 = CARTESIAN_POINT ( 'NONE',  ( 9.915320536401090123, -9.172514111537584114, 34.72667873470787470 ) ) ;
#53792 = CARTESIAN_POINT ( 'NONE',  ( -19.50000000000000000, -3.499999999999999556, 29.75000000000000355 ) ) ;
#53793 = CARTESIAN_POINT ( 'NONE',  ( -2.307692307692305711, -3.322132147404559976, 32.92929555188717927 ) ) ;
#53794 = LINE ( 'NONE', #81285, #5139 ) ;
#53795 = B_SPLINE_CURVE_WITH_KNOTS ( 'NONE', 3,
 ( #58743, #78567, #30823, #72254, #10564, #32606, #31728, #24067, #37579, #58293 ),
 .UNSPECIFIED., .F., .F.,
 ( 4, 2, 2, 2, 4 ),
 ( 0.0007817246256747460882, 0.0009771112852218900684, 0.001172497944769033832, 0.001367884604316177595, 0.001563271263863321575 ),
 .UNSPECIFIED. ) ;
#53796 = CARTESIAN_POINT ( 'NONE',  ( -1.384615384615383471, -8.973038597847269315, 34.52809138561121927 ) ) ;
#53797 = B_SPLINE_CURVE_WITH_KNOTS ( 'NONE', 3,
 ( #80626, #18908, #33316, #26558, #39639, #18469 ),
 .UNSPECIFIED., .F., .F.,
 ( 4, 2, 4 ),
 ( 0.000000000000000000, 0.2500000631573452425, 0.5000001263146904851 ),
 .UNSPECIFIED. ) ;
#53798 = CARTESIAN_POINT ( 'NONE',  ( 5.142990410273151625, -2.833524468853757750, 32.15551576947925838 ) ) ;
#53799 = CARTESIAN_POINT ( 'NONE',  ( -13.25408968285182176, -6.852161475712352789, 34.70806712695775786 ) ) ;
#53800 = FACE_OUTER_BOUND ( 'NONE', #60507, .T. ) ;
#53801 = EDGE_CURVE ( 'NONE', #52607, #41015, #37885, .T. ) ;
#53802 = ORIENTED_EDGE ( 'NONE', *, *, #83868, .F. ) ;
#53803 = EDGE_LOOP ( 'NONE', ( #87810, #43329 ) ) ;
#53804 = CARTESIAN_POINT ( 'NONE',  ( 6.792929713638703682, -2.619462340734462380, 30.83744416345203021 ) ) ;
#53805 = CARTESIAN_POINT ( 'NONE',  ( -16.15384615384615330, -12.78798330534102945, 29.74999999999997868 ) ) ;
#53806 = DIRECTION ( 'NONE',  ( -0.000000000000000000, -0.1736481776669307198, -0.9848077530122080203 ) ) ;
#53807 = CARTESIAN_POINT ( 'NONE',  ( -6.065270445960774914, -3.835265460703609186, 33.15142922261924241 ) ) ;
#53808 = EDGE_CURVE ( 'NONE', #29864, #80082, #70794, .T. ) ;
#53809 = DIRECTION ( 'NONE',  ( -0.000000000000000000, -0.000000000000000000, -1.000000000000000000 ) ) ;
#53810 = CARTESIAN_POINT ( 'NONE',  ( -5.076923076923075762, -2.833524468853757305, 32.15551576947925838 ) ) ;
#53811 = VECTOR ( 'NONE', #67382, 1000.000000000000000 ) ;
#53812 = ADVANCED_FACE ( 'NONE', ( #36983 ), #9094, .F. ) ;
#53813 = CARTESIAN_POINT ( 'NONE',  ( -2.530619266599154038, -8.282780595021769443, 34.94152052738834868 ) ) ;
#53814 = ORIENTED_EDGE ( 'NONE', *, *, #12302, .T. ) ;
#53815 = CARTESIAN_POINT ( 'NONE',  ( -4.946397375159514276, -12.45806712695776319, 30.39783852428763922 ) ) ;
#53816 = EDGE_LOOP ( 'NONE', ( #45011, #80666, #39769, #4819 ) ) ;
#53817 = EDGE_CURVE ( 'NONE', #84095, #54976, #66006, .T. ) ;
#53818 = ORIENTED_EDGE ( 'NONE', *, *, #50205, .F. ) ;
#53819 = FACE_OUTER_BOUND ( 'NONE', #74336, .T. ) ;
#53820 = CARTESIAN_POINT ( 'NONE',  ( 3.930361210122205406, -2.599994579823202923, 30.74605699353653776 ) ) ;
#53821 = ADVANCED_FACE ( 'NONE', ( #72552 ), #16718, .F. ) ;
#53822 = CARTESIAN_POINT ( 'NONE',  ( 14.08420736396836226, -5.113361153441934093, 34.14387501736622710 ) ) ;
#53823 = CARTESIAN_POINT ( 'NONE',  ( 1.134638640566795642, -11.47974371597208076, 33.17467449705390692 ) ) ;
#53824 = CARTESIAN_POINT ( 'NONE',  ( -13.60810030917972036, -2.612411019501189369, 31.66733052389439962 ) ) ;
#53826 = EDGE_CURVE ( 'NONE', #5010, #28697, #59650, .T. ) ;
#53825 = VERTEX_POINT ( 'NONE', #77541 ) ;
#53827 = ORIENTED_EDGE ( 'NONE', *, *, #53597, .T. ) ;
#53828 = ORIENTED_EDGE ( 'NONE', *, *, #48136, .T. ) ;
#53829 = EDGE_LOOP ( 'NONE', ( #65758, #23697, #75618, #45541 ) ) ;
#53830 = AXIS2_PLACEMENT_3D ( 'NONE', #6873, #60491, #82102 ) ;
#53831 = DIRECTION ( 'NONE',  ( 0.000000000000000000, 0.4999999999999960032, -0.8660254037844410391 ) ) ;
#53832 = CARTESIAN_POINT ( 'NONE',  ( 6.923076923076924238, -3.886160181151819604, 36.00935417666054406 ) ) ;
#53833 = EDGE_CURVE ( 'NONE', #60125, #79174, #41305, .T. ) ;
#53834 = DIRECTION ( 'NONE',  ( 0.000000000000000000, 0.000000000000000000, 1.000000000000000000 ) ) ;
#53835 = VECTOR ( 'NONE', #60578, 1000.000000000000000 ) ;
#53836 = VECTOR ( 'NONE', #72495, 1000.000000000000114 ) ;
#53837 = CARTESIAN_POINT ( 'NONE',  ( 16.40390046548447245, -9.943054286541403997, 34.11300777759954883 ) ) ;
#53838 =( NAMED_UNIT ( * ) PLANE_ANGLE_UNIT ( ) SI_UNIT ( $, .RADIAN. ) );
#53839 = EDGE_CURVE ( 'NONE', #19138, #65478, #87596, .T. ) ;
#53840 = CARTESIAN_POINT ( 'NONE',  ( -15.45369618967607828, -2.523278758544489797, 31.42238647778637528 ) ) ;
#53841 = VERTEX_POINT ( 'NONE', #22593 ) ;
#53842 = B_SPLINE_CURVE_WITH_KNOTS ( 'NONE', 3,
 ( #55900, #35644, #69424, #69866, #14478, #8171, #7282, #82512, #27991, #88833 ),
 .UNSPECIFIED., .F., .F.,
 ( 4, 2, 2, 2, 4 ),
 ( 0.0007817359430256294638, 0.0009771253907249948054, 0.001172514838424360255, 0.001367904286123725489, 0.001563293733823090939 ),
 .UNSPECIFIED. ) ;
#53843 = VERTEX_POINT ( 'NONE', #77980 ) ;
#53844 = B_SPLINE_CURVE_WITH_KNOTS ( 'NONE', 3,
 ( #48967, #15628, #28245, #76442, #63802, #77761, #84538, #36343, #43531, #29588 ),
 .UNSPECIFIED., .F., .F.,
 ( 4, 2, 2, 2, 4 ),
 ( 0.000000000000000000, 0.0001954339857564079623, 0.0003908679715128159245, 0.0005863019572692238597, 0.0007817359430256318490 ),
 .UNSPECIFIED. ) ;
#53846 = EDGE_LOOP ( 'NONE', ( #31228, #66085, #19216, #45403 ) ) ;
#53845 = CYLINDRICAL_SURFACE ( 'NONE', #80425, 0.2499999999999997502 ) ;
#53847 = CYLINDRICAL_SURFACE ( 'NONE', #14605, 0.2500000000000008882 ) ;
#53848 = CARTESIAN_POINT ( 'NONE',  ( -4.853911725310227077, -11.24521262558773671, 33.06293181088029343 ) ) ;
#53849 = CARTESIAN_POINT ( 'NONE',  ( -3.750000000000007550, -5.946699141100917352, 22.67187499999999645 ) ) ;
#53850 = EDGE_LOOP ( 'NONE', ( #40771, #50944, #65693, #19712 ) ) ;
#53851 = EDGE_CURVE ( 'NONE', #68800, #45914, #75751, .T. ) ;
#53852 = ADVANCED_FACE ( 'NONE', ( #26546 ), #61644, .F. ) ;
#53853 = CARTESIAN_POINT ( 'NONE',  ( 7.976679284387491187, -4.299079248970732792, 33.91157788607253565 ) ) ;
#53854 = EDGE_LOOP ( 'NONE', ( #15357, #14230, #52801, #84833 ) ) ;
#53855 = LINE ( 'NONE', #34469, #80167 ) ;
#53856 = CARTESIAN_POINT ( 'NONE',  ( 16.15384615384615330, -3.669653830205710676, 35.88435417666054406 ) ) ;
#53857 = CARTESIAN_POINT ( 'NONE',  ( 14.87820512820512953, -7.500000000000000000, 29.75000000000000355 ) ) ;
#53858 = CARTESIAN_POINT ( 'NONE',  ( -6.989160334032800570, -3.513871655860377086, 32.76840700105978499 ) ) ;
#53859 = CARTESIAN_POINT ( 'NONE',  ( 8.638539302563209787, -4.809359713505814149, 33.96456829005828837 ) ) ;
#53860 = ORIENTED_EDGE ( 'NONE', *, *, #4362, .F. ) ;
#53861 = LINE ( 'NONE', #81348, #80633 ) ;
#53862 = CARTESIAN_POINT ( 'NONE',  ( -14.05763799605399278, -2.564540009722895419, 30.55348353981670684 ) ) ;
#53863 = CARTESIAN_POINT ( 'NONE',  ( -6.416666666666667851, -3.499999999999999556, 29.75000000000000355 ) ) ;
#53865 = EDGE_LOOP ( 'NONE', ( #3202, #34841, #2912, #33644 ) ) ;
#53864 = EDGE_CURVE ( 'NONE', #43306, #12236, #67975, .T. ) ;
#53866 = CARTESIAN_POINT ( 'NONE',  ( 20.00000000000000000, -4.000000000000000000, 29.75000000000000355 ) ) ;
#53867 = CARTESIAN_POINT ( 'NONE',  ( 0.4615384615383396616, -2.892918686052166066, 31.69288490824153470 ) ) ;
#53868 = CARTESIAN_POINT ( 'NONE',  ( -12.59168567097668934, -12.27039167877662251, 31.24851455888617835 ) ) ;
#53869 = DIRECTION ( 'NONE',  ( -0.000000000000000000, 0.9848077530122085754, -0.1736481776669273613 ) ) ;
#53870 = EDGE_CURVE ( 'NONE', #7171, #53, #2677, .T. ) ;
#53872 = EDGE_CURVE ( 'NONE', #49709, #34790, #16565, .T. ) ;
#53871 = CARTESIAN_POINT ( 'NONE',  ( 8.096099364501988305, -3.202959910592335202, 32.30730279482227019 ) ) ;
#53873 = FACE_BOUND ( 'NONE', #61004, .T. ) ;
#53875 = CARTESIAN_POINT ( 'NONE',  ( 4.284636594813103549, -12.62708834333097663, 30.88030960425257021 ) ) ;
#53874 = CARTESIAN_POINT ( 'NONE',  ( 13.25446741488369540, -12.15440758774515473, 32.17923288041532004 ) ) ;
#53876 = CARTESIAN_POINT ( 'NONE',  ( 2.057669083470851756, -10.18141759479407327, 34.26406193332782379 ) ) ;
#53878 = CARTESIAN_POINT ( 'NONE',  ( 17.93391658904412012, -11.16473453929635440, 33.15142922261925662 ) ) ;
#53877 = CARTESIAN_POINT ( 'NONE',  ( -8.769230769230890843, -11.94971097300221174, 32.03036669348237098 ) ) ;
#53879 = CARTESIAN_POINT ( 'NONE',  ( -9.692307692307691624, -5.415277668671390821, 36.20867863119892149 ) ) ;
#53880 = CARTESIAN_POINT ( 'NONE',  ( 0.06109907496454976272, -10.25000000000000000, 17.02938170625848713 ) ) ;
#53881 = ADVANCED_FACE ( 'NONE', ( #67530 ), #82379, .F. ) ;
#53882 = VERTEX_POINT ( 'NONE', #13024 ) ;
#53883 = CARTESIAN_POINT ( 'NONE',  ( -12.39537185494681992, -7.250054591869670162, 34.99404684341514127 ) ) ;
#53884 = EDGE_LOOP ( 'NONE', ( #57619, #32233, #58428, #51782 ) ) ;
#53885 = CARTESIAN_POINT ( 'NONE',  ( -18.13069060311030611, -3.338472653186240091, 32.95098750199971960 ) ) ;
#53886 = VERTEX_POINT ( 'NONE', #47693 ) ;
#53887 = FACE_OUTER_BOUND ( 'NONE', #7842, .T. ) ;
#53888 = DIRECTION ( 'NONE',  ( -0.000000000000000000, -0.5000000000000009992, -0.8660254037844380415 ) ) ;
#53890 = ORIENTED_EDGE ( 'NONE', *, *, #78124, .F. ) ;
#53889 = CARTESIAN_POINT ( 'NONE',  ( 14.98076923076923173, -2.499999999999998668, 29.75000000000000355 ) ) ;
#53891 = CARTESIAN_POINT ( 'NONE',  ( -14.30769230769230660, -1.367168528481310208, 33.57946703557072254 ) ) ;
#53892 = CARTESIAN_POINT ( 'NONE',  ( -11.78848476268299628, -4.175268141568685643, 33.81360843649122216 ) ) ;
#53893 = CARTESIAN_POINT ( 'NONE',  ( -3.724691934501229262, -9.114399933863657211, 27.26375670625849423 ) ) ;
#53894 = CARTESIAN_POINT ( 'NONE',  ( 2.057715576749954423, -11.79746400365624659, 32.30657167506340954 ) ) ;
#53895 = CARTESIAN_POINT ( 'NONE',  ( -2.980769230769230393, -2.249999999999998668, 29.75000000000000355 ) ) ;
#53896 = CARTESIAN_POINT ( 'NONE',  ( 3.230769230769231726, -2.499999999999998668, 29.75000000000001421 ) ) ;
#53897 = CARTESIAN_POINT ( 'NONE',  ( 10.48469401227430886, -2.494641256782728966, 31.33461815524612959 ) ) ;
#53898 = CARTESIAN_POINT ( 'NONE',  ( -0.3310127597748976913, -4.459921816937789885, 33.71989282347011851 ) ) ;
#53899 = CARTESIAN_POINT ( 'NONE',  ( 9.469380733400843297, -3.395401636524185474, 33.02366814457250399 ) ) ;
#53900 = CARTESIAN_POINT ( 'NONE',  ( -0.06109907496450878162, -11.25000000000000000, 18.78311829374151287 ) ) ;
#53901 = CARTESIAN_POINT ( 'NONE',  ( -4.283994123577850921, -3.069018819979302926, 32.56621877034667278 ) ) ;
#53902 = CARTESIAN_POINT ( 'NONE',  ( -19.50000000000000000, -3.499999999999999556, 29.75000000000000355 ) ) ;
#53903 = VERTEX_POINT ( 'NONE', #40075 ) ;
#53904 = LINE ( 'NONE', #39963, #62855 ) ;
#53905 = FACE_OUTER_BOUND ( 'NONE', #1540, .T. ) ;
#53906 = CARTESIAN_POINT ( 'NONE',  ( 2.608446859217924629, -10.19485399968118422, 21.12686829374151287 ) ) ;
#53907 = AXIS2_PLACEMENT_3D ( 'NONE', #73941, #26189, #12676 ) ;
#53908 = CARTESIAN_POINT ( 'NONE',  ( 2.242422307135989890, -5.094484230520674117, 34.41647553114621161 ) ) ;
#53909 = CARTESIAN_POINT ( 'NONE',  ( -5.076923076923197442, -2.625532179533778709, 30.86335684631627174 ) ) ;
#53910 = VERTEX_POINT ( 'NONE', #88270 ) ;
#53911 = CARTESIAN_POINT ( 'NONE',  ( 14.30769230769231015, -9.780366693483667717, 34.19971097300155094 ) ) ;
#53912 = CARTESIAN_POINT ( 'NONE',  ( -16.85391023282967993, -9.172514111537580561, 34.72667873470787470 ) ) ;
#53914 = ORIENTED_EDGE ( 'NONE', *, *, #3448, .F. ) ;
#53913 = CARTESIAN_POINT ( 'NONE',  ( -17.14267987943738802, -7.249945686854186278, 34.74374336980224598 ) ) ;
#53915 = CARTESIAN_POINT ( 'NONE',  ( 12.71159277317677905, -12.41262288849542017, 30.68299917996395010 ) ) ;
#53916 = DIRECTION ( 'NONE',  ( -0.000000000000000000, 0.1736481776669307198, -0.9848077530122080203 ) ) ;
#53917 = CARTESIAN_POINT ( 'NONE',  ( -12.52762084089859407, -4.661471528628507777, 34.16647553114621871 ) ) ;
#53918 = ORIENTED_EDGE ( 'NONE', *, *, #46501, .T. ) ;
#53919 = CARTESIAN_POINT ( 'NONE',  ( 2.980792486720641676, -2.544273027872574922, 31.48422191005632342 ) ) ;
#53920 = CARTESIAN_POINT ( 'NONE',  ( 15.23076923076910916, -12.70778746994576025, 30.41441678777401236 ) ) ;
#53921 = B_SPLINE_CURVE_WITH_KNOTS ( 'NONE', 3,
 ( #7786, #52193, #60286, #29833, #57295, #17985, #31943, #45436, #87798, #84789 ),
 .UNSPECIFIED., .F., .F.,
 ( 4, 2, 2, 2, 4 ),
 ( 0.000000000000000000, 0.0001954311564186876876, 0.0003908623128373753751, 0.0005862934692560630356, 0.0007817246256747507503 ),
 .UNSPECIFIED. ) ;
#53922 = DIRECTION ( 'NONE',  ( -0.000000000000000000, -0.9848077530122086864, -0.1736481776669273613 ) ) ;
#53923 = ORIENTED_EDGE ( 'NONE', *, *, #26142, .T. ) ;
#53924 = ORIENTED_EDGE ( 'NONE', *, *, #21387, .T. ) ;
#53925 = ORIENTED_EDGE ( 'NONE', *, *, #54569, .T. ) ;
#53926 = ORIENTED_EDGE ( 'NONE', *, *, #14215, .T. ) ;
#53927 = CARTESIAN_POINT ( 'NONE',  ( 12.59206389977210705, -10.31582465632705237, 34.18122507451815295 ) ) ;
#53928 = CARTESIAN_POINT ( 'NONE',  ( 8.769230769230768274, -1.242168528481310874, 33.36296068462461051 ) ) ;
#53929 = CARTESIAN_POINT ( 'NONE',  ( -11.40793610022789650, -3.625058011473228703, 33.29252011169590020 ) ) ;
#53930 = DIRECTION ( 'NONE',  ( 0.000000000000000000, 1.000000000000000000, 0.000000000000000000 ) ) ;
#53931 = CIRCLE ( 'NONE', #42434, 6.614378277661474570 ) ;
#53932 = EDGE_CURVE ( 'NONE', #82469, #32624, #78948, .T. ) ;
#53933 = CARTESIAN_POINT ( 'NONE',  ( 5.299702618191482806, -5.913360116392398780, 34.49180327182771322 ) ) ;
#53934 = ORIENTED_EDGE ( 'NONE', *, *, #32395, .F. ) ;
#53935 = ORIENTED_EDGE ( 'NONE', *, *, #58792, .F. ) ;
#53936 = ORIENTED_EDGE ( 'NONE', *, *, #30402, .T. ) ;
#53938 = VERTEX_POINT ( 'NONE', #12148 ) ;
#53937 = DIRECTION ( 'NONE',  ( -0.000000000000000000, -0.3420201433256694901, -0.9396926207859082059 ) ) ;
#53939 = CARTESIAN_POINT ( 'NONE',  ( 0.6089743589743589203, -11.50000000000000000, 29.75000000000000355 ) ) ;
#53940 = CARTESIAN_POINT ( 'NONE',  ( 14.98074599347626368, -3.202444869320336451, 32.30641848906366675 ) ) ;
#53941 = CARTESIAN_POINT ( 'NONE',  ( 5.749976775778542937, -4.175268141568689195, 33.81360843649122216 ) ) ;
#53942 = EDGE_CURVE ( 'NONE', #37401, #50277, #7154, .T. ) ;
#53943 = CARTESIAN_POINT ( 'NONE',  ( 15.93036122928182330, -11.60425143139329940, 33.02411095842164457 ) ) ;
#53944 = ORIENTED_EDGE ( 'NONE', *, *, #68429, .T. ) ;
#53945 = VERTEX_POINT ( 'NONE', #73850 ) ;
#53946 = ORIENTED_EDGE ( 'NONE', *, *, #33136, .T. ) ;
#53947 = CARTESIAN_POINT ( 'NONE',  ( -9.627052121031667298, -6.026961402152789304, 34.52809138561124769 ) ) ;
#53949 = EDGE_LOOP ( 'NONE', ( #81434, #19459 ) ) ;
#53948 = CARTESIAN_POINT ( 'NONE',  ( 11.53846153846153832, -2.249999999999998668, 29.50000000000001421 ) ) ;
#53950 = CARTESIAN_POINT ( 'NONE',  ( -5.999999999999998224, -5.180354513474913603, 36.12317359536750416 ) ) ;
#53951 = B_SPLINE_CURVE_WITH_KNOTS ( 'NONE', 3,
 ( #17210, #2355, #50546, #23519, #64490, #72150, #78462, #17667, #36174, #78028 ),
 .UNSPECIFIED., .F., .F.,
 ( 4, 2, 2, 2, 4 ),
 ( 0.0007817246256747483650, 0.0009771112852218926705, 0.001172497944769037084, 0.001367884604316181498, 0.001563271263863325695 ),
 .UNSPECIFIED. ) ;
#53952 = VECTOR ( 'NONE', #74820, 1000.000000000000000 ) ;
#53953 = CARTESIAN_POINT ( 'NONE',  ( -0.4615384615385840772, -6.835583212225970762, 34.95778746994575670 ) ) ;
#53954 = EDGE_LOOP ( 'NONE', ( #3402, #65364, #13380, #53540 ) ) ;
#53955 = EDGE_CURVE ( 'NONE', #51834, #39901, #39629, .T. ) ;
#53956 = CARTESIAN_POINT ( 'NONE',  ( 18.00000000000000000, -13.37000171582298513, 34.34916445242398453 ) ) ;
#53957 = CARTESIAN_POINT ( 'NONE',  ( -17.07692307692307665, -12.78798330534102945, 29.74999999999997868 ) ) ;
#53958 = LINE ( 'NONE', #67924, #26706 ) ;
#53959 = FACE_BOUND ( 'NONE', #4929, .T. ) ;
#53960 = CARTESIAN_POINT ( 'NONE',  ( 20.00000000000000000, -4.000000000000000000, 29.75000000000000355 ) ) ;
#53961 = FACE_OUTER_BOUND ( 'NONE', #63357, .T. ) ;
#53962 = CARTESIAN_POINT ( 'NONE',  ( 11.53846153846153832, -12.37446782046654192, 30.86335684631486131 ) ) ;
#53964 = CARTESIAN_POINT ( 'NONE',  ( 6.792386319966619013, -10.70098750199973203, 33.91152734681376302 ) ) ;
#53963 = CARTESIAN_POINT ( 'NONE',  ( 0.2380535369741297591, -6.716662450894490100, 34.94144148231605840 ) ) ;
#53965 = CARTESIAN_POINT ( 'NONE',  ( -18.75000000000000000, -7.500000000000000000, 29.75000000000000355 ) ) ;
#53966 = CARTESIAN_POINT ( 'NONE',  ( -0.5268089074992371446, -3.835265460703609186, 33.15142922261924241 ) ) ;
#53967 = VERTEX_POINT ( 'NONE', #5826 ) ;
#53968 = CARTESIAN_POINT ( 'NONE',  ( -14.98082382139119062, -11.56426240980093745, 33.07394671870546432 ) ) ;
#53969 = AXIS2_PLACEMENT_3D ( 'NONE', #46745, #75118, #89089 ) ;
#53970 = CARTESIAN_POINT ( 'NONE',  ( 0.3308478584281538404, -10.70098750199973203, 33.91152734681376302 ) ) ;
#53971 = ORIENTED_EDGE ( 'NONE', *, *, #64272, .F. ) ;
#53972 = EDGE_LOOP ( 'NONE', ( #46703, #69790 ) ) ;
#53973 = CARTESIAN_POINT ( 'NONE',  ( 0.4615384615384611200, -8.164416787775445883, 34.95778746994557906 ) ) ;
#53974 = CARTESIAN_POINT ( 'NONE',  ( -13.60754234352223335, -4.762599654559228846, 34.23009711892697737 ) ) ;
#53975 = CARTESIAN_POINT ( 'NONE',  ( -11.78843828251013015, -10.06842814019191401, 34.32929386961144758 ) ) ;
#53976 = ORIENTED_EDGE ( 'NONE', *, *, #87891, .F. ) ;
#53978 = ADVANCED_FACE ( 'NONE', ( #33305 ), #49900, .F. ) ;
#53977 = LINE ( 'NONE', #81469, #11167 ) ;
#53979 = EDGE_CURVE ( 'NONE', #80426, #62209, #28366, .T. ) ;
#53980 = CARTESIAN_POINT ( 'NONE',  ( 6.700149964170072359, -8.282780595021769443, 34.94152052738834868 ) ) ;
#53981 = FACE_BOUND ( 'NONE', #53767, .T. ) ;
#53983 = DIRECTION ( 'NONE',  ( 1.000000000000000000, 0.000000000000000000, 0.000000000000000000 ) ) ;
#53982 = LINE ( 'NONE', #19757, #66238 ) ;
#53984 = CARTESIAN_POINT ( 'NONE',  ( 7.846153846153846700, -8.973038597847269315, 34.52809138561121927 ) ) ;
#53985 = CARTESIAN_POINT ( 'NONE',  ( 2.373760658694747061, -4.786620604624113540, 33.94971097300155805 ) ) ;
#53987 = CARTESIAN_POINT ( 'NONE',  ( 0.3308469948709015784, -5.582088688514999397, 34.36776431015576350 ) ) ;
#53986 =( NAMED_UNIT ( * ) SI_UNIT ( $, .STERADIAN. ) SOLID_ANGLE_UNIT ( ) );
#53988 = CARTESIAN_POINT ( 'NONE',  ( 3.750000000000000888, -7.499999999999978684, 19.46875000000000000 ) ) ;
#53989 = VERTEX_POINT ( 'NONE', #62959 ) ;
#53990 = ORIENTED_EDGE ( 'NONE', *, *, #81263, .T. ) ;
#53991 = CARTESIAN_POINT ( 'NONE',  ( 0.4615384615384611755, -12.48256725967547354, 35.29906147534542527 ) ) ;
#53992 = CARTESIAN_POINT ( 'NONE',  ( 16.15384615384603251, -6.879047030192662504, 34.71129190930017927 ) ) ;
#53993 = CARTESIAN_POINT ( 'NONE',  ( 13.38461538461538680, -1.129524287112498415, 32.06866353760679544 ) ) ;
#53994 = DIRECTION ( 'NONE',  ( -0.000000000000000000, 0.1736481776669307198, -0.9848077530122080203 ) ) ;
#53995 = CARTESIAN_POINT ( 'NONE',  ( -7.622778360381425422, -2.251407671071268712, 29.88021292934942252 ) ) ;
#53996 = CARTESIAN_POINT ( 'NONE',  ( -2.651650429449565305, -4.848349570550461785, 25.25000000000000000 ) ) ;
#53997 = LINE ( 'NONE', #40505, #23045 ) ;
#53998 = CARTESIAN_POINT ( 'NONE',  ( -6.223484924564328225, -8.539481045369598178, 34.89627647299170832 ) ) ;
#53999 = CARTESIAN_POINT ( 'NONE',  ( -4.946132635956127288, -2.295524264805589354, 30.44142389570982488 ) ) ;
#54000 = CARTESIAN_POINT ( 'NONE',  ( 10.74591005361826390, -3.625058011473228703, 33.29252011169590020 ) ) ;
#54001 = CARTESIAN_POINT ( 'NONE',  ( -6.000000000000119904, -2.892918686052165622, 31.69288490824153470 ) ) ;
#54002 = CARTESIAN_POINT ( 'NONE',  ( 15.16468685140909400, -12.34228464037088280, 31.77849191805838558 ) ) ;
#54003 = CARTESIAN_POINT ( 'NONE',  ( -0.3307480205715105370, -3.957578996910242619, 33.62503395064540257 ) ) ;
#54004 = CARTESIAN_POINT ( 'NONE',  ( -8.638440328263817136, -11.37503395064541678, 33.29242100308974273 ) ) ;
#54005 = CARTESIAN_POINT ( 'NONE',  ( -7.780085495151406683, -12.37446782046654192, 30.86335684631486842 ) ) ;
#54006 = EDGE_LOOP ( 'NONE', ( #28617, #303, #72468, #77906 ) ) ;
#54007 = CARTESIAN_POINT ( 'NONE',  ( -4.946131269098290595, -11.71459661697925903, 32.44059661609676937 ) ) ;
#54008 = CARTESIAN_POINT ( 'NONE',  ( 5.076923076923075762, -6.189225973068211317, 35.74407628777942847 ) ) ;
#54009 = CARTESIAN_POINT ( 'NONE',  ( -1.077988221561493543, -4.724691934501247914, 16.82999329374151287 ) ) ;
#54010 = CARTESIAN_POINT ( 'NONE',  ( -9.692307692307691624, -10.67929555188718282, 33.92786785259544047 ) ) ;
#54011 = DIRECTION ( 'NONE',  ( 0.000000000000000000, 0.1736481776669267785, -0.9848077530122087975 ) ) ;
#54013 = VERTEX_POINT ( 'NONE', #76942 ) ;
#54012 = CARTESIAN_POINT ( 'NONE',  ( 6.923076923076924238, -2.708943851104267164, 35.45975837776705220 ) ) ;
#54014 = CARTESIAN_POINT ( 'NONE',  ( -1.139087296526025250, -4.750000000000006217, 21.57812500000000355 ) ) ;
#54015 = CARTESIAN_POINT ( 'NONE',  ( -6.166666666666667851, -7.500000000000000000, 29.75000000000000355 ) ) ;
#54017 = ORIENTED_EDGE ( 'NONE', *, *, #87906, .F. ) ;
#54016 = B_SPLINE_CURVE_WITH_KNOTS ( 'NONE', 3,
 ( #10120, #5594, #31284, #4709, #33063, #81260, #66849, #60530, #79919, #39391 ),
 .UNSPECIFIED., .F., .F.,
 ( 4, 2, 2, 2, 4 ),
 ( 0.0007817246256747514008, 0.0009771112852218952725, 0.001172497944769039036, 0.001367884604316182799, 0.001563271263863326779 ),
 .UNSPECIFIED. ) ;
#54018 = CARTESIAN_POINT ( 'NONE',  ( -16.02332045208259359, -10.19071101563364401, 33.96452234770658407 ) ) ;
#54019 = CARTESIAN_POINT ( 'NONE',  ( -17.75005448165186195, -3.712312575010499494, 33.01462480002815880 ) ) ;
#54020 = ORIENTED_EDGE ( 'NONE', *, *, #16201, .T. ) ;
#54021 = DIRECTION ( 'NONE',  ( -0.000000000000000000, -0.7660444431189791237, -0.6427876096865379196 ) ) ;
#54022 = CARTESIAN_POINT ( 'NONE',  ( -15.36124441584495237, -7.276987145209185215, 34.99546412871779211 ) ) ;
#54023 = AXIS2_PLACEMENT_3D ( 'NONE', #34491, #61955, #16001 ) ;
#54024 = CARTESIAN_POINT ( 'NONE',  ( 2.242422307135989890, -12.70778746994557551, 30.41441678777548319 ) ) ;
#54025 = ORIENTED_EDGE ( 'NONE', *, *, #17480, .T. ) ;
#54026 = EDGE_LOOP ( 'NONE', ( #51226, #43033, #61237, #50451 ) ) ;
#54027 = ORIENTED_EDGE ( 'NONE', *, *, #28027, .F. ) ;
#54028 = CARTESIAN_POINT ( 'NONE',  ( -18.00000000000000000, -4.661471528628506000, 34.16647553114623292 ) ) ;
#54029 = CYLINDRICAL_SURFACE ( 'NONE', #72823, 0.2499999999999994726 ) ;
#54030 = CARTESIAN_POINT ( 'NONE',  ( 18.13079044096694759, -9.929761469519743144, 34.40412654351204225 ) ) ;
#54031 = CARTESIAN_POINT ( 'NONE',  ( -17.20707028636129721, -6.001485441113818986, 34.52039167877662607 ) ) ;
#54032 = DIRECTION ( 'NONE',  ( 0.000000000000000000, 0.7660444431189807890, 0.6427876096865361433 ) ) ;
#54033 = CARTESIAN_POINT ( 'NONE',  ( 9.942253101685738059, -10.18230066228895758, 34.26354781536631577 ) ) ;
#54034 = CARTESIAN_POINT ( 'NONE',  ( 1.384615384615264011, -2.379036618888197285, 30.90682066428292885 ) ) ;
#54035 = ADVANCED_FACE ( 'NONE', ( #14349 ), #84599, .F. ) ;
#54036 = CARTESIAN_POINT ( 'NONE',  ( 16.02369818411445479, -12.70455904226513866, 30.44083106164009322 ) ) ;
#54037 = EDGE_CURVE ( 'NONE', #17526, #4994, #36403, .T. ) ;
#54038 = EDGE_LOOP ( 'NONE', ( #72332, #12684, #50587, #17668 ) ) ;
#54039 = ORIENTED_EDGE ( 'NONE', *, *, #78853, .F. ) ;
#54041 = ORIENTED_EDGE ( 'NONE', *, *, #32699, .T. ) ;
#54040 = DIRECTION ( 'NONE',  ( 1.000000000000000000, 0.000000000000000000, 0.000000000000000000 ) ) ;
#54042 = EDGE_CURVE ( 'NONE', #56376, #67556, #58505, .T. ) ;
#54043 = VECTOR ( 'NONE', #50991, 1000.000000000000000 ) ;
#54044 = CARTESIAN_POINT ( 'NONE',  ( -8.352564102564102200, -4.000000000000000000, 29.75000000000000355 ) ) ;
#54045 = CARTESIAN_POINT ( 'NONE',  ( 12.52760681254089903, -3.050289026998446840, 32.03036669348366416 ) ) ;
#54047 = ORIENTED_EDGE ( 'NONE', *, *, #35494, .T. ) ;
#54046 = ADVANCED_FACE ( 'NONE', ( #28762 ), #15247, .F. ) ;
#54048 = CARTESIAN_POINT ( 'NONE',  ( -12.39547112818838670, -11.35647404775217595, 33.31231777344666511 ) ) ;
#54049 = ORIENTED_EDGE ( 'NONE', *, *, #48643, .T. ) ;
#54050 = CARTESIAN_POINT ( 'NONE',  ( 0.2115384615384616196, -2.499999999999998668, 29.75000000000000355 ) ) ;
#54051 = ORIENTED_EDGE ( 'NONE', *, *, #87230, .F. ) ;
#54052 = DIRECTION ( 'NONE',  ( -0.000000000000000000, 1.000000000000000000, -0.000000000000000000 ) ) ;
#54053 = EDGE_CURVE ( 'NONE', #45298, #38438, #22869, .T. ) ;
#54054 = CARTESIAN_POINT ( 'NONE',  ( -12.33101302330481985, -10.31582465632705237, 34.18122507451815295 ) ) ;
#54055 = CARTESIAN_POINT ( 'NONE',  ( -8.992156986746914882, -2.758268499246657068, 31.33685645148948140 ) ) ;
#54056 = FACE_BOUND ( 'NONE', #62133, .T. ) ;
#54057 = B_SPLINE_CURVE_WITH_KNOTS ( 'NONE', 3,
 ( #3810, #19877, #3362, #31290, #86252, #47343 ),
 .UNSPECIFIED., .F., .F.,
 ( 4, 2, 4 ),
 ( 4.220987180333913997E-17, 0.0001954756301637161793, 0.0003909512603273901832 ),
 .UNSPECIFIED. ) ;
#54058 = DIRECTION ( 'NONE',  ( 0.000000000000000000, 0.7660444431189822323, -0.6427876096865344779 ) ) ;
#54059 = CARTESIAN_POINT ( 'NONE',  ( 1.634615384615449862, -7.434744860731434812, 35.00000000000000711 ) ) ;
#54060 = CARTESIAN_POINT ( 'NONE',  ( -12.22435897435897267, -7.500000000000000000, 29.75000000000000355 ) ) ;
#54061 = CARTESIAN_POINT ( 'NONE',  ( 9.070512820512819374, -11.50000000000000000, 29.75000000000000355 ) ) ;
#54062 = CARTESIAN_POINT ( 'NONE',  ( 10.55006060258030942, -7.749976730030849303, 34.74374725381503737 ) ) ;
#54063 = CARTESIAN_POINT ( 'NONE',  ( 16.15384615384615330, -4.098570777380720287, 33.41473453929634729 ) ) ;
#54064 = CARTESIAN_POINT ( 'NONE',  ( -13.13461538461538325, -2.499999999999999556, 29.81604066197449754 ) ) ;
#54065 = EDGE_LOOP ( 'NONE', ( #44292, #6260 ) ) ;
#54066 = EDGE_LOOP ( 'NONE', ( #28888, #37490 ) ) ;
#54068 = LINE ( 'NONE', #13538, #76446 ) ;
#54067 = CARTESIAN_POINT ( 'NONE',  ( -5.076923076923075762, -11.91647553114624181, 32.58852847137148245 ) ) ;
#54069 = DIRECTION ( 'NONE',  ( -0.000000000000000000, 0.3420201433256694901, -0.9396926207859082059 ) ) ;
#54070 = CARTESIAN_POINT ( 'NONE',  ( 14.30769230769218581, -11.06231777344772027, 33.60647404775119895 ) ) ;
#54071 = CARTESIAN_POINT ( 'NONE',  ( 16.94677586748485965, -8.587444163452046197, 34.63053765926554206 ) ) ;
#54072 = CARTESIAN_POINT ( 'NONE',  ( -12.23852710992561121, -4.187068189119699468, 33.49521262558774026 ) ) ;
#54073 = ORIENTED_EDGE ( 'NONE', *, *, #64333, .F. ) ;
#54074 = VECTOR ( 'NONE', #5588, 1000.000000000000000 ) ;
#54075 = EDGE_CURVE ( 'NONE', #70832, #88089, #46728, .T. ) ;
#54076 = CARTESIAN_POINT ( 'NONE',  ( -6.000000000000121680, -8.656820664282941280, 34.87096338111179961 ) ) ;
#54077 = CARTESIAN_POINT ( 'NONE',  ( 11.28846153846153832, -7.500000000000001776, 34.75000000000000000 ) ) ;
#54078 = CARTESIAN_POINT ( 'NONE',  ( -8.899377978668994160, -12.27039167877662251, 31.24851455888617835 ) ) ;
#54079 = EDGE_CURVE ( 'NONE', #86419, #55273, #71063, .T. ) ;
#54080 = DIRECTION ( 'NONE',  ( -0.000000000000000000, -0.3420201433256694901, -0.9396926207859082059 ) ) ;
#54081 = VERTEX_POINT ( 'NONE', #82823 ) ;
#54082 = B_SPLINE_CURVE_WITH_KNOTS ( 'NONE', 3,
 ( #54063, #13972, #81560, #27049, #60830, #19847, #48637, #54512, #5454, #34695 ),
 .UNSPECIFIED., .F., .F.,
 ( 4, 2, 2, 2, 4 ),
 ( 0.000000000000000000, 0.0001954339857564078538, 0.0003908679715128157077, 0.0005863019572692235344, 0.0007817359430256314154 ),
 .UNSPECIFIED. ) ;
#54083 = ORIENTED_EDGE ( 'NONE', *, *, #2057, .F. ) ;
#54084 = ORIENTED_EDGE ( 'NONE', *, *, #37512, .F. ) ;
#54085 = EDGE_CURVE ( 'NONE', #80199, #38257, #15471, .T. ) ;
#54086 = CYLINDRICAL_SURFACE ( 'NONE', #80898, 0.2500000000000012212 ) ;
#54087 = ADVANCED_FACE ( 'NONE', ( #30952 ), #85030, .F. ) ;
#54088 = ORIENTED_EDGE ( 'NONE', *, *, #45591, .T. ) ;
#54089 = VECTOR ( 'NONE', #10650, 1000.000000000000000 ) ;
#54090 = FACE_OUTER_BOUND ( 'NONE', #80939, .T. ) ;
#54091 = CARTESIAN_POINT ( 'NONE',  ( 14.55763771707034948, -5.766571408460171355, 34.70601412856602508 ) ) ;
#54092 = CARTESIAN_POINT ( 'NONE',  ( 16.15384615384603251, -8.613356846316285953, 34.62446782046622218 ) ) ;
#54093 = CARTESIAN_POINT ( 'NONE',  ( 8.769230769230768274, -3.322132147404559976, 32.92929555188717927 ) ) ;
#54094 = CARTESIAN_POINT ( 'NONE',  ( -5.999999999999998224, -9.819645486525091727, 36.12317359536749706 ) ) ;
#54095 = ORIENTED_EDGE ( 'NONE', *, *, #67646, .F. ) ;
#54096 = CARTESIAN_POINT ( 'NONE',  ( 12.68496486045324900, -7.630147987733840509, 34.99859428049665411 ) ) ;
#54098 = ORIENTED_EDGE ( 'NONE', *, *, #56596, .T. ) ;
#54097 = CARTESIAN_POINT ( 'NONE',  ( -2.307692307692428724, -3.643525952248796163, 33.31231777344771672 ) ) ;
#54099 = FACE_OUTER_BOUND ( 'NONE', #77184, .T. ) ;
#54100 = DIRECTION ( 'NONE',  ( 0.000000000000000000, 0.6427876096865368094, 0.7660444431189802339 ) ) ;
#54101 = CARTESIAN_POINT ( 'NONE',  ( 16.15384615384603251, -3.835265460704628815, 33.15142922262033665 ) ) ;
#54102 = CARTESIAN_POINT ( 'NONE',  ( -2.307692307692305711, -12.62096338111211580, 30.90682066428153263 ) ) ;
#54103 = CARTESIAN_POINT ( 'NONE',  ( 2.557637717070350813, -2.589246495874657938, 31.60778113518102828 ) ) ;
#54104 = DIRECTION ( 'NONE',  ( -0.000000000000000000, -0.9396926207859092051, -0.3420201433256662704 ) ) ;
#54105 = FACE_OUTER_BOUND ( 'NONE', #70294, .T. ) ;
#54106 = CARTESIAN_POINT ( 'NONE',  ( 2.724691934501250135, -8.700186371490531201, 19.79874329374151287 ) ) ;
#54107 = ORIENTED_EDGE ( 'NONE', *, *, #65796, .F. ) ;
#54108 = FACE_OUTER_BOUND ( 'NONE', #28691, .T. ) ;
#54109 = CARTESIAN_POINT ( 'NONE',  ( -1.134669975237340589, -3.520799739797214389, 33.17531984108286025 ) ) ;
#54111 = ORIENTED_EDGE ( 'NONE', *, *, #49496, .T. ) ;
#54110 = AXIS2_PLACEMENT_3D ( 'NONE', #87493, #40188, #73964 ) ;
#54112 = ORIENTED_EDGE ( 'NONE', *, *, #5926, .F. ) ;
#54113 = CARTESIAN_POINT ( 'NONE',  ( -12.59168567097668401, -11.93770438780619259, 32.05411857736982029 ) ) ;
#54114 = DIRECTION ( 'NONE',  ( -0.000000000000000000, -0.7660444431189791237, -0.6427876096865379196 ) ) ;
#54115 = B_SPLINE_CURVE_WITH_KNOTS ( 'NONE', 3,
 ( #42898, #62700, #22179, #76223, #69031, #1464, #28952, #42014, #55071, #1017 ),
 .UNSPECIFIED., .F., .F.,
 ( 4, 2, 2, 2, 4 ),
 ( 0.0007817246256747463051, 0.0009771112852218887673, 0.001172497944769031446, 0.001367884604316173909, 0.001563271263863316371 ),
 .UNSPECIFIED. ) ;
#54116 = VECTOR ( 'NONE', #57007, 1000.000000000000000 ) ;
#54117 = DIRECTION ( 'NONE',  ( 0.000000000000000000, 0.9848077530122072432, 0.1736481776669354937 ) ) ;
#54118 = CARTESIAN_POINT ( 'NONE',  ( -4.153846153846152411, -11.69971097300155272, 32.46337939537588113 ) ) ;
#54119 = CARTESIAN_POINT ( 'NONE',  ( 17.77651507543566822, -2.612411019501191589, 31.66733052389440672 ) ) ;
#54120 = EDGE_LOOP ( 'NONE', ( #61767, #12871, #24086, #33239 ) ) ;
#54121 = ADVANCED_FACE ( 'NONE', ( #44025 ), #25096, .F. ) ;
#54122 = CARTESIAN_POINT ( 'NONE',  ( -16.15384615384615330, -6.343179335718451384, 34.87096338111211935 ) ) ;
#54123 = CARTESIAN_POINT ( 'NONE',  ( -14.53061852520845321, -2.758268499246657068, 31.33685645148948140 ) ) ;
#54124 = CARTESIAN_POINT ( 'NONE',  ( -16.15384615384627409, -2.379036618888197285, 30.90682066428292885 ) ) ;
#54125 = ORIENTED_EDGE ( 'NONE', *, *, #13667, .F. ) ;
#54126 = CARTESIAN_POINT ( 'NONE',  ( -16.94613263595612906, -11.93129842949672437, 32.56571108434900452 ) ) ;
#54127 = ORIENTED_EDGE ( 'NONE', *, *, #27013, .F. ) ;
#54128 = DIRECTION ( 'NONE',  ( -0.000000000000000000, -0.8660254037844399289, -0.4999999999999980016 ) ) ;
#54129 = CARTESIAN_POINT ( 'NONE',  ( 11.53846153846153832, -2.486705287966279876, 31.30864560766543647 ) ) ;
#54130 = VERTEX_POINT ( 'NONE', #44911 ) ;
#54131 = CARTESIAN_POINT ( 'NONE',  ( 0.4615384615384611200, -2.249999999999998668, 29.75000000000001776 ) ) ;
#54132 = CARTESIAN_POINT ( 'NONE',  ( -6.065270000556318486, -2.379036618887870436, 30.90682066428147934 ) ) ;
#54133 = CARTESIAN_POINT ( 'NONE',  ( 12.46153846153846168, -13.95598074871891292, 31.83374038241031911 ) ) ;
#54134 = EDGE_CURVE ( 'NONE', #69108, #88101, #3922, .T. ) ;
#54135 = DIRECTION ( 'NONE',  ( -0.000000000000000000, 0.3420201433256694901, -0.9396926207859082059 ) ) ;
#54136 = DIRECTION ( 'NONE',  ( -0.000000000000000000, -0.8660254037844397068, -0.4999999999999978906 ) ) ;
#54137 = AXIS2_PLACEMENT_3D ( 'NONE', #70954, #37159, #56988 ) ;
#54138 = ORIENTED_EDGE ( 'NONE', *, *, #39214, .F. ) ;
#54139 = DIRECTION ( 'NONE',  ( 0.000000000000000000, 0.3420201433256610524, 0.9396926207859113145 ) ) ;
#54140 = ORIENTED_EDGE ( 'NONE', *, *, #17869, .T. ) ;
#54141 = LINE ( 'NONE', #68996, #88939 ) ;
#54142 = FACE_OUTER_BOUND ( 'NONE', #17398, .T. ) ;
#54143 = B_SPLINE_CURVE_WITH_KNOTS ( 'NONE', 3,
 ( #30769, #85728, #84406, #78076, #43844, #30334, #51919, #24008, #51460, #84852 ),
 .UNSPECIFIED., .F., .F.,
 ( 4, 2, 2, 2, 4 ),
 ( 0.0007817246256747470640, 0.0009771112852218898515, 0.001172497944769032747, 0.001367884604316175643, 0.001563271263863318539 ),
 .UNSPECIFIED. ) ;
#54144 = EDGE_CURVE ( 'NONE', #71169, #40972, #51654, .T. ) ;
#54145 = CARTESIAN_POINT ( 'NONE',  ( -18.24997674404859183, -10.82459398097509862, 33.81372124010183455 ) ) ;
#54146 = AXIS2_PLACEMENT_3D ( 'NONE', #11828, #39307, #19025 ) ;
#54147 = CYLINDRICAL_SURFACE ( 'NONE', #57891, 0.2500000000000004996 ) ;
#54148 = CARTESIAN_POINT ( 'NONE',  ( 16.94623161025552349, -2.541943142973489334, 30.39792223712631980 ) ) ;
#54149 = EDGE_CURVE ( 'NONE', #24050, #40179, #70163, .T. ) ;
#54150 = ORIENTED_EDGE ( 'NONE', *, *, #60176, .F. ) ;
#54151 = ORIENTED_EDGE ( 'NONE', *, *, #13821, .T. ) ;
#54152 = ORIENTED_EDGE ( 'NONE', *, *, #60809, .T. ) ;
#54153 = ORIENTED_EDGE ( 'NONE', *, *, #13358, .T. ) ;
#54154 = CARTESIAN_POINT ( 'NONE',  ( -4.403822884788507253, -5.728515186090277211, 34.42611988154120439 ) ) ;
#54155 = EDGE_CURVE ( 'NONE', #3262, #37853, #11137, .T. ) ;
#54156 = CARTESIAN_POINT ( 'NONE',  ( 16.40390057375961064, -10.82426656108011720, 33.81400080652039009 ) ) ;
#54157 = CARTESIAN_POINT ( 'NONE',  ( -3.262820512820514107, -7.500000000000000000, 29.75000000000000355 ) ) ;
#54158 = CARTESIAN_POINT ( 'NONE',  ( -7.976844449264153702, -3.338472653186243644, 32.95098750199972670 ) ) ;
#54159 = ORIENTED_EDGE ( 'NONE', *, *, #5266, .T. ) ;
#54160 = CYLINDRICAL_SURFACE ( 'NONE', #31259, 0.2499999999999995559 ) ;
#54161 = EDGE_CURVE ( 'NONE', #38632, #72796, #72393, .T. ) ;
#54162 = CIRCLE ( 'NONE', #72874, 0.2500000000000002220 ) ;
#54163 = DIRECTION ( 'NONE',  ( -1.000000000000000000, -0.000000000000000000, -0.000000000000000000 ) ) ;
#54164 = CARTESIAN_POINT ( 'NONE',  ( -2.241623956689867914, -3.513871655860379306, 32.76840700105978499 ) ) ;
#54165 = CARTESIAN_POINT ( 'NONE',  ( -5.011667937410240192, -11.67786785259547777, 32.92929555188713664 ) ) ;
#54166 = ORIENTED_EDGE ( 'NONE', *, *, #54814, .T. ) ;
#54167 = EDGE_CURVE ( 'NONE', #69237, #85805, #24649, .T. ) ;
#54168 = ORIENTED_EDGE ( 'NONE', *, *, #32820, .F. ) ;
#54169 = ORIENTED_EDGE ( 'NONE', *, *, #30110, .F. ) ;
#54171 = ORIENTED_EDGE ( 'NONE', *, *, #26653, .F. ) ;
#54170 = LINE ( 'NONE', #5113, #33030 ) ;
#54173 = CARTESIAN_POINT ( 'NONE',  ( -8.352564102564102200, -3.499999999999999556, 29.75000000000000355 ) ) ;
#54172 = CARTESIAN_POINT ( 'NONE',  ( -4.153846153846152411, -3.886160181151819604, 36.00935417666054406 ) ) ;
#54174 = LINE ( 'NONE', #47420, #1051 ) ;
#54175 = CARTESIAN_POINT ( 'NONE',  ( 16.15384615384615330, -6.435427911321262684, 35.78748833219616898 ) ) ;
#54176 = FACE_BOUND ( 'NONE', #12082, .T. ) ;
#54177 = ORIENTED_EDGE ( 'NONE', *, *, #63895, .F. ) ;
#54178 = ADVANCED_FACE ( 'NONE', ( #3482 ), #3035, .T. ) ;
#54179 = CARTESIAN_POINT ( 'NONE',  ( 17.01083966596719677, -6.386643153685125363, 34.62446782046654903 ) ) ;
#54180 = DIRECTION ( 'NONE',  ( -0.000000000000000000, 0.5000000000000011102, -0.8660254037844381525 ) ) ;
#54181 = ORIENTED_EDGE ( 'NONE', *, *, #70562, .T. ) ;
#54182 = CARTESIAN_POINT ( 'NONE',  ( -10.61538461538461320, -2.249999999999998668, 29.50000000000001421 ) ) ;
#54184 = EDGE_CURVE ( 'NONE', #66121, #36550, #68108, .T. ) ;
#54183 = VERTEX_POINT ( 'NONE', #38613 ) ;
#54185 = FACE_BOUND ( 'NONE', #28944, .T. ) ;
#54186 = DIRECTION ( 'NONE',  ( -1.000000000000000000, -0.000000000000000000, -0.000000000000000000 ) ) ;
#54187 = CARTESIAN_POINT ( 'NONE',  ( 18.25005431163831204, -4.943051570960395047, 34.04725096376909477 ) ) ;
#54188 = VERTEX_POINT ( 'NONE', #30518 ) ;
#54189 = CARTESIAN_POINT ( 'NONE',  ( -12.23875892027004753, -8.496831190052096971, 34.64984203495476578 ) ) ;
#54191 = EDGE_CURVE ( 'NONE', #88099, #72117, #57989, .T. ) ;
#54190 = CARTESIAN_POINT ( 'NONE',  ( 16.82689985270161870, -12.07920672191015221, 32.31858351112116168 ) ) ;
#54192 = CARTESIAN_POINT ( 'NONE',  ( 1.134592147322420752, -3.202444869320336451, 32.30641848906366675 ) ) ;
#54193 = ORIENTED_EDGE ( 'NONE', *, *, #74155, .T. ) ;
#54194 = DIRECTION ( 'NONE',  ( -0.000000000000000000, 0.6427876096865404731, -0.7660444431189770143 ) ) ;
#54195 = CARTESIAN_POINT ( 'NONE',  ( 14.43848274865926129, -3.338503747796866872, 32.95102852606553512 ) ) ;
#54196 = CARTESIAN_POINT ( 'NONE',  ( 18.00000000000000000, -10.67929555188718282, 33.92786785259544047 ) ) ;
#54197 = CARTESIAN_POINT ( 'NONE',  ( -9.692307692307812417, -2.625532179533778709, 30.86335684631627174 ) ) ;
#54198 = ORIENTED_EDGE ( 'NONE', *, *, #78241, .T. ) ;
#54199 = CARTESIAN_POINT ( 'NONE',  ( -1.384615384615383471, -5.557115091759785130, 34.35708131394839171 ) ) ;
#54200 = DIRECTION ( 'NONE',  ( 1.000000000000000000, -0.000000000000000000, 0.000000000000000000 ) ) ;
#54201 = EDGE_LOOP ( 'NONE', ( #46629, #68349, #50462, #31341 ) ) ;
#54202 = CARTESIAN_POINT ( 'NONE',  ( 23.49999999999998934, 5.000000000000023093, 29.24999999999999645 ) ) ;
#54203 = CARTESIAN_POINT ( 'NONE',  ( 15.93091919493929964, -4.026226216239093603, 33.68668979543632958 ) ) ;
#54204 = CARTESIAN_POINT ( 'NONE',  ( -7.976301815885545210, -12.50552854090298993, 31.33409797877408920 ) ) ;
#54205 = CARTESIAN_POINT ( 'NONE',  ( 13.45068373561782415, -12.37446782046654192, 30.86335684631486842 ) ) ;
#54206 = CARTESIAN_POINT ( 'NONE',  ( 0.3308478584281552837, -2.494641256782729410, 31.33461815524612248 ) ) ;
#54207 = AXIS2_PLACEMENT_3D ( 'NONE', #18361, #85929, #79617 ) ;
#54208 = LINE ( 'NONE', #74950, #75441 ) ;
#54210 = DIRECTION ( 'NONE',  ( 1.000000000000000000, 0.000000000000000000, 0.000000000000000000 ) ) ;
#54209 = CARTESIAN_POINT ( 'NONE',  ( -5.076923076923197442, -10.21337939537710326, 33.94971097300076224 ) ) ;
#54211 = CYLINDRICAL_SURFACE ( 'NONE', #33464, 0.2500000000000009437 ) ;
#54212 = EDGE_CURVE ( 'NONE', #22195, #79858, #51203, .T. ) ;
#54213 = CARTESIAN_POINT ( 'NONE',  ( 2.749999999999995115, -6.360912703473971419, 16.89062500000000000 ) ) ;
#54214 = ORIENTED_EDGE ( 'NONE', *, *, #8557, .F. ) ;
#54215 = DIRECTION ( 'NONE',  ( -0.000000000000000000, -0.9396926207859093161, -0.3420201433256663259 ) ) ;
#54216 = ORIENTED_EDGE ( 'NONE', *, *, #36048, .F. ) ;
#54217 = EDGE_CURVE ( 'NONE', #27545, #38500, #43375, .T. ) ;
#54218 = ORIENTED_EDGE ( 'NONE', *, *, #87179, .F. ) ;
#54219 = CARTESIAN_POINT ( 'NONE',  ( 2.307692307692309264, -3.669653830205710676, 35.88435417666054406 ) ) ;
#54221 = ORIENTED_EDGE ( 'NONE', *, *, #25976, .T. ) ;
#54220 = VECTOR ( 'NONE', #53766, 1000.000000000000227 ) ;
#54222 = CARTESIAN_POINT ( 'NONE',  ( -4.153846153846274980, -2.657715359629662988, 31.77849191805970364 ) ) ;
#54223 = CARTESIAN_POINT ( 'NONE',  ( 1.139087296525997273, -4.749999999999992895, 21.73437500000000000 ) ) ;
#54224 = CARTESIAN_POINT ( 'NONE',  ( 13.63466969625370417, -2.779044189368095719, 31.39831045268885745 ) ) ;
#54225 = DIRECTION ( 'NONE',  ( -0.000000000000000000, 0.3420201433256694901, -0.9396926207859082059 ) ) ;
#54226 = CARTESIAN_POINT ( 'NONE',  ( -2.177166605928742893, -6.852161475712352789, 34.70806712695775786 ) ) ;
#54227 = CARTESIAN_POINT ( 'NONE',  ( -11.53846153846165912, -11.48612834414049644, 32.76840700105863391 ) ) ;
#54228 = CARTESIAN_POINT ( 'NONE',  ( -13.63463862190834952, -2.587272538249755893, 30.68239716806877837 ) ) ;
#54229 = LINE ( 'NONE', #6506, #15241 ) ;
#54230 = CARTESIAN_POINT ( 'NONE',  ( 1.553300858899087311, -3.749999999999992006, 24.23437500000000355 ) ) ;
#54231 = EDGE_CURVE ( 'NONE', #10613, #36751, #88606, .T. ) ;
#54232 = CARTESIAN_POINT ( 'NONE',  ( 5.142178216435912219, -3.083524468853784839, 32.58852847137153930 ) ) ;
#54233 = CARTESIAN_POINT ( 'NONE',  ( -14.53055772989594807, -2.501496062324912284, 29.88072118266895671 ) ) ;
#54234 = CARTESIAN_POINT ( 'NONE',  ( 5.750023255951411727, -11.47974371597207899, 33.17467449705390692 ) ) ;
#54235 = EDGE_CURVE ( 'NONE', #34985, #62741, #62655, .T. ) ;
#54236 = EDGE_CURVE ( 'NONE', #79333, #19438, #83091, .T. ) ;
#54237 = VERTEX_POINT ( 'NONE', #40404 ) ;
#54238 = ORIENTED_EDGE ( 'NONE', *, *, #4871, .F. ) ;
#54239 = AXIS2_PLACEMENT_3D ( 'NONE', #26944, #20186, #47651 ) ;
#54240 = CARTESIAN_POINT ( 'NONE',  ( -8.992156986746914882, -12.39988816332205701, 30.74660775122750778 ) ) ;
#54241 = CARTESIAN_POINT ( 'NONE',  ( 0.5923289025054093715, -11.93129842949671726, 32.56571108434900452 ) ) ;
#54242 = DIRECTION ( 'NONE',  ( 1.000000000000000000, 0.000000000000000000, 0.000000000000000000 ) ) ;
#54243 = CARTESIAN_POINT ( 'NONE',  ( -15.84615384615384670, -7.500000000000000000, 33.75000000000000000 ) ) ;
#54244 = CARTESIAN_POINT ( 'NONE',  ( 5.999999999999880096, -5.219633306517616589, 34.19971097300220464 ) ) ;
#54245 = CARTESIAN_POINT ( 'NONE',  ( -13.60754234352223158, -10.77366814457252175, 33.85459836347579454 ) ) ;
#54246 = EDGE_CURVE ( 'NONE', #75680, #42058, #65846, .T. ) ;
#54247 = PLANE ( 'NONE',  #12133 ) ;
#54248 = VERTEX_POINT ( 'NONE', #67419 ) ;
#54249 = CARTESIAN_POINT ( 'NONE',  ( 3.007842271862381622, -6.459968553980839800, 34.89616026154728701 ) ) ;
#54250 = VERTEX_POINT ( 'NONE', #18791 ) ;
#54251 = B_SPLINE_CURVE_WITH_KNOTS ( 'NONE', 3,
 ( #25313, #65401, #39284, #86133, #31166, #52773, #59981, #72155, #51412, #80263 ),
 .UNSPECIFIED., .F., .F.,
 ( 4, 2, 2, 2, 4 ),
 ( 0.000000000000000000, 0.0001954311564186881213, 0.0003908623128373762425, 0.0005862934692560643367, 0.0007817246256747524850 ),
 .UNSPECIFIED. ) ;
#54252 = ORIENTED_EDGE ( 'NONE', *, *, #6213, .T. ) ;
#54253 = CARTESIAN_POINT ( 'NONE',  ( 15.23076923076923173, -4.098570777380720287, 33.41473453929634729 ) ) ;
#54254 = CARTESIAN_POINT ( 'NONE',  ( 5.076923076922953193, -5.094484230521993062, 34.41647553114689373 ) ) ;
#54255 = CARTESIAN_POINT ( 'NONE',  ( -0.2114841499001470504, -6.567000820036036579, 34.66262288849542728 ) ) ;
#54256 = DIRECTION ( 'NONE',  ( -1.681660752236433198E-16, -1.000000000000000000, 5.102127870520020612E-17 ) ) ;
#54257 = DIRECTION ( 'NONE',  ( -0.000000000000000000, -0.1736481776669307198, -0.9848077530122080203 ) ) ;
#54258 = EDGE_CURVE ( 'NONE', #32578, #28537, #56285, .T. ) ;
#54259 = ORIENTED_EDGE ( 'NONE', *, *, #42062, .T. ) ;
#54260 = ORIENTED_EDGE ( 'NONE', *, *, #21917, .F. ) ;
#54261 = VECTOR ( 'NONE', #86967, 1000.000000000000000 ) ;
#54262 = ORIENTED_EDGE ( 'NONE', *, *, #56121, .T. ) ;
#54263 = EDGE_LOOP ( 'NONE', ( #88437, #29967, #7921, #89164, #85082 ) ) ;
#54264 = DIRECTION ( 'NONE',  ( -0.000000000000000000, -0.8660254037844399289, -0.4999999999999980016 ) ) ;
#54265 = CYLINDRICAL_SURFACE ( 'NONE', #31606, 0.2500000000000008882 ) ;
#54266 = AXIS2_PLACEMENT_3D ( 'NONE', #41884, #69786, #22045 ) ;
#54267 = CARTESIAN_POINT ( 'NONE',  ( 15.93097989078305687, -2.251424796025574881, 29.88072029997477230 ) ) ;
#54268 = CARTESIAN_POINT ( 'NONE',  ( 2.057669070399343880, -11.37209801155882971, 32.91403422569032955 ) ) ;
#54269 = CARTESIAN_POINT ( 'NONE',  ( -15.00775638667583678, -9.172514111537584114, 34.72667873470787470 ) ) ;
#54270 = CARTESIAN_POINT ( 'NONE',  ( 12.23861150263161157, -2.889293201056495786, 32.26117774369186009 ) ) ;
#54271 = VECTOR ( 'NONE', #61314, 1000.000000000000227 ) ;
#54272 = ORIENTED_EDGE ( 'NONE', *, *, #59237, .F. ) ;
#54273 = ORIENTED_EDGE ( 'NONE', *, *, #85686, .T. ) ;
#54274 = B_SPLINE_CURVE_WITH_KNOTS ( 'NONE', 3,
 ( #68905, #67143, #60374, #46862, #87886, #15, #5885, #27484, #33359, #40128 ),
 .UNSPECIFIED., .F., .F.,
 ( 4, 2, 2, 2, 4 ),
 ( 0.0007817359430256307648, 0.0009771253907249971907, 0.001172514838424363508, 0.001367904286123729826, 0.001563293733823096143 ),
 .UNSPECIFIED. ) ;
#54275 = ORIENTED_EDGE ( 'NONE', *, *, #47102, .T. ) ;
#54277 = ORIENTED_EDGE ( 'NONE', *, *, #43278, .F. ) ;
#54276 = DIRECTION ( 'NONE',  ( -0.000000000000000000, 0.6427876096865404731, -0.7660444431189771253 ) ) ;
#54278 = CARTESIAN_POINT ( 'NONE',  ( -9.915792636031639518, -5.113361153441934093, 34.14387501736622710 ) ) ;
#54279 = CARTESIAN_POINT ( 'NONE',  ( 6.700250230597919909, -7.369208160676172348, 34.74850200257122879 ) ) ;
#54280 = CARTESIAN_POINT ( 'NONE',  ( -3.750000000000007550, -5.946699141100917352, 18.92187500000000000 ) ) ;
#54281 = ORIENTED_EDGE ( 'NONE', *, *, #23734, .F. ) ;
#54282 = ADVANCED_FACE ( 'NONE', ( #59769 ), #11591, .F. ) ;
#54283 = CARTESIAN_POINT ( 'NONE',  ( -1.134560964701931240, -11.47946981652013498, 33.17500667209846910 ) ) ;
#54284 = ORIENTED_EDGE ( 'NONE', *, *, #44096, .F. ) ;
#54285 = CARTESIAN_POINT ( 'NONE',  ( 2.084207363968360927, -6.760086850603068243, 34.69517049084099369 ) ) ;
#54286 = EDGE_CURVE ( 'NONE', #61438, #2479, #32740, .T. ) ;
#54287 = FACE_BOUND ( 'NONE', #1904, .T. ) ;
#54288 = DIRECTION ( 'NONE',  ( -0.000000000000000000, 0.6427876096865404731, -0.7660444431189770143 ) ) ;
#54289 = AXIS2_PLACEMENT_3D ( 'NONE', #38585, #44882, #45778 ) ;
#54290 = CARTESIAN_POINT ( 'NONE',  ( 8.703960323269994248, -5.219633306516282545, 34.19971097300152962 ) ) ;
#54291 = ORIENTED_EDGE ( 'NONE', *, *, #80951, .T. ) ;
#54293 = EDGE_CURVE ( 'NONE', #70654, #61347, #42264, .T. ) ;
#54292 = CARTESIAN_POINT ( 'NONE',  ( -5.749999999999999112, -7.500000000000001776, 35.04278698407183867 ) ) ;
#54294 = CARTESIAN_POINT ( 'NONE',  ( -14.24162395668986747, -2.538708090699994813, 30.37095296980875503 ) ) ;
#54295 = CARTESIAN_POINT ( 'NONE',  ( -19.50000000000000000, -11.50000000000000000, 29.75000000000000355 ) ) ;
#54296 = CARTESIAN_POINT ( 'NONE',  ( -3.296039231325549768, -9.528491918058357157, 34.59228464037090589 ) ) ;
#54297 = ORIENTED_EDGE ( 'NONE', *, *, #21189, .F. ) ;
#54298 = ADVANCED_FACE ( 'NONE', ( #56999 ), #48462, .F. ) ;
#54299 = FACE_OUTER_BOUND ( 'NONE', #2761, .T. ) ;
#54301 = CARTESIAN_POINT ( 'NONE',  ( 1.254467414883690290, -4.299443229763728169, 33.91186481527756058 ) ) ;
#54300 = PRODUCT_DEFINITION_SHAPE ( 'NONE', 'NONE',  #89181 ) ;
#54302 = CARTESIAN_POINT ( 'NONE',  ( 4.376625822824220080, -11.60474049983371003, 33.02348890104160262 ) ) ;
#54303 = DIRECTION ( 'NONE',  ( -0.000000000000000000, 1.000000000000000000, -0.000000000000000000 ) ) ;
#54304 = CARTESIAN_POINT ( 'NONE',  ( 10.54930120442873154, -11.69971097300155272, 32.46337939537587403 ) ) ;
#54305 = FACE_BOUND ( 'NONE', #28472, .T. ) ;
#54307 = CARTESIAN_POINT ( 'NONE',  ( 8.769230769230768274, -3.886160181151819604, 36.00935417666054406 ) ) ;
#54306 = CARTESIAN_POINT ( 'NONE',  ( 13.13463864056679853, -12.01397095200674059, 32.43157075238190146 ) ) ;
#54308 = AXIS2_PLACEMENT_3D ( 'NONE', #56676, #77827, #69313 ) ;
#54309 = FACE_OUTER_BOUND ( 'NONE', #3321, .T. ) ;
#54311 = CARTESIAN_POINT ( 'NONE',  ( -0.7115384615384606759, -2.249999999999998668, 29.75000000000000355 ) ) ;
#54310 = CYLINDRICAL_SURFACE ( 'NONE', #58744, 0.2499999999999995559 ) ;
#54312 = EDGE_CURVE ( 'NONE', #38219, #37130, #46555, .T. ) ;
#54313 = DIRECTION ( 'NONE',  ( -0.000000000000000000, 0.9848077530122086864, -0.1736481776669273891 ) ) ;
#54314 = CARTESIAN_POINT ( 'NONE',  ( 1.987747218494664292, -9.401340078031346081, 19.37313170625848713 ) ) ;
#54315 = EDGE_LOOP ( 'NONE', ( #49747, #28344, #6440, #22718 ) ) ;
#54316 = CARTESIAN_POINT ( 'NONE',  ( -6.988347369037697376, -9.442884908240170461, 34.35708131394840592 ) ) ;
#54317 = VERTEX_POINT ( 'NONE', #76845 ) ;
#54318 = CARTESIAN_POINT ( 'NONE',  ( 0.4615384615384611200, -6.386643153685126251, 34.62446782046654192 ) ) ;
#54319 = ORIENTED_EDGE ( 'NONE', *, *, #449, .F. ) ;
#54320 = B_SPLINE_CURVE_WITH_KNOTS ( 'NONE', 3,
 ( #13077, #68028, #6330, #33789, #11298, #61246, #73455, #88758, #59484, #86990 ),
 .UNSPECIFIED., .F., .F.,
 ( 4, 2, 2, 2, 4 ),
 ( 0.0007817246256747484735, 0.0009771112852218915863, 0.001172497944769034916, 0.001367884604316178029, 0.001563271263863321141 ),
 .UNSPECIFIED. ) ;
#54321 = DIRECTION ( 'NONE',  ( -0.000000000000000000, -0.5000000000000009992, -0.8660254037844380415 ) ) ;
#54322 = FACE_OUTER_BOUND ( 'NONE', #18527, .T. ) ;
#54324 = ORIENTED_EDGE ( 'NONE', *, *, #66755, .T. ) ;
#54323 = CARTESIAN_POINT ( 'NONE',  ( -2.557715544985270206, -11.86270091957321249, 32.19358267280087915 ) ) ;
#54325 = CARTESIAN_POINT ( 'NONE',  ( 3.480823542407545101, -6.567000820036038355, 34.66262288849541306 ) ) ;
#54326 = PLANE ( 'NONE',  #26827 ) ;
#54327 = CARTESIAN_POINT ( 'NONE',  ( 1.077988221561464899, -4.724691934501233703, 20.23250670625849423 ) ) ;
#54328 = CARTESIAN_POINT ( 'NONE',  ( 2.241608896736427159, -11.69971097300155272, 32.46337939537587403 ) ) ;
#54329 = CARTESIAN_POINT ( 'NONE',  ( -6.988346923633240948, -12.70778746994557551, 30.41441678777548319 ) ) ;
#54330 = CARTESIAN_POINT ( 'NONE',  ( -24.99999999999999645, -19.99999999999999645, 0.000000000000000000 ) ) ;
#54331 = CARTESIAN_POINT ( 'NONE',  ( 4.153846153846032507, -11.94971097300221174, 32.03036669348237098 ) ) ;
#54332 = CARTESIAN_POINT ( 'NONE',  ( -1.253824943648433665, -6.369690395747424461, 34.87708834333098196 ) ) ;
#54333 = DIRECTION ( 'NONE',  ( 0.000000000000000000, 0.7660444431189807890, 0.6427876096865361433 ) ) ;
#54334 = CARTESIAN_POINT ( 'NONE',  ( 3.724691934501251023, -9.114399933863618131, 22.29874329374151642 ) ) ;
#54335 = VECTOR ( 'NONE', #55428, 1000.000000000000114 ) ;
#54336 = CARTESIAN_POINT ( 'NONE',  ( 3.007941133134353073, -7.369209533119137845, 34.99857337881830688 ) ) ;
#54337 = ORIENTED_EDGE ( 'NONE', *, *, #21446, .F. ) ;
#54338 = CARTESIAN_POINT ( 'NONE',  ( 17.07692307692307665, -12.62096338111211580, 30.90682066428153263 ) ) ;
#54339 = AXIS2_PLACEMENT_3D ( 'NONE', #61254, #74799, #5002 ) ;
#54340 = CARTESIAN_POINT ( 'NONE',  ( 3.750000000000001776, -7.561099074964511502, 24.72061829374150932 ) ) ;
#54341 = EDGE_CURVE ( 'NONE', #63622, #55385, #49799, .T. ) ;
#54342 = LINE ( 'NONE', #26445, #38991 ) ;
#54343 = DIRECTION ( 'NONE',  ( 1.000000000000000000, 1.845450506358306311E-16, 0.000000000000000000 ) ) ;
#54344 = EDGE_LOOP ( 'NONE', ( #42482, #35132, #37919, #80994 ) ) ;
#54345 = DIRECTION ( 'NONE',  ( -0.000000000000000000, 0.6427876096865404731, -0.7660444431189771253 ) ) ;
#54346 = CARTESIAN_POINT ( 'NONE',  ( 3.100622021331009392, -3.817052484675422797, 33.13202310037935661 ) ) ;
#54348 = ORIENTED_EDGE ( 'NONE', *, *, #8895, .T. ) ;
#54347 = CARTESIAN_POINT ( 'NONE',  ( 3.903869409797563250, -9.234221910056348293, 34.70572697212741531 ) ) ;
#54349 = DIRECTION ( 'NONE',  ( -0.000000000000000000, -0.3420201433256694901, -0.9396926207859082059 ) ) ;
#54350 = VECTOR ( 'NONE', #40529, 1000.000000000000227 ) ;
#54351 = CARTESIAN_POINT ( 'NONE',  ( 2.177000841024750333, -12.38065189839062263, 30.83690757178629482 ) ) ;
#54352 = CARTESIAN_POINT ( 'NONE',  ( 7.173022332454966232, -12.07971442181322352, 32.31769673815850297 ) ) ;
#54353 = EDGE_CURVE ( 'NONE', #26695, #23520, #70525, .T. ) ;
#54354 = VERTEX_POINT ( 'NONE', #69191 ) ;
#54355 = CARTESIAN_POINT ( 'NONE',  ( 2.177544337960612975, -4.299443229763728169, 33.91186481527756058 ) ) ;
#54356 = CARTESIAN_POINT ( 'NONE',  ( -18.13014720943822766, -12.27039167877662251, 31.24851455888617480 ) ) ;
#54357 = ADVANCED_FACE ( 'NONE', ( #21891 ), #15142, .F. ) ;
#54358 = CARTESIAN_POINT ( 'NONE',  ( 1.161130460051053470, -3.019605429927184836, 32.48692288466676814 ) ) ;
#54359 = VERTEX_POINT ( 'NONE', #34955 ) ;
#54360 = B_SPLINE_CURVE_WITH_KNOTS ( 'NONE', 3,
 ( #87735, #13819, #40424, #88184, #67443, #41302, #14266, #54801, #47157, #53471 ),
 .UNSPECIFIED., .F., .F.,
 ( 4, 2, 2, 2, 4 ),
 ( 0.000000000000000000, 0.0001954339857564070678, 0.0003908679715128141356, 0.0005863019572692211492, 0.0007817359430256282712 ),
 .UNSPECIFIED. ) ;
#54361 = VERTEX_POINT ( 'NONE', #68747 ) ;
#54362 = VERTEX_POINT ( 'NONE', #1172 ) ;
#54363 = ORIENTED_EDGE ( 'NONE', *, *, #84122, .F. ) ;
#54364 = AXIS2_PLACEMENT_3D ( 'NONE', #55987, #70846, #70400 ) ;
#54365 = CARTESIAN_POINT ( 'NONE',  ( -5.999999999999998224, -13.20930481340135110, 34.54067556320372745 ) ) ;
#54366 = CARTESIAN_POINT ( 'NONE',  ( -2.242436736416282272, -6.026961402152789304, 34.52809138561124769 ) ) ;
#54367 = CARTESIAN_POINT ( 'NONE',  ( -13.38461538461538325, -12.10708131394839349, 31.69288490824020244 ) ) ;
#54368 = DIRECTION ( 'NONE',  ( -0.000000000000000000, 0.8660254037844399289, -0.4999999999999980016 ) ) ;
#54369 = ADVANCED_FACE ( 'NONE', ( #29544 ), #77274, .F. ) ;
#54370 = DIRECTION ( 'NONE',  ( -0.000000000000000000, 0.9396926207859093161, -0.3420201433256663259 ) ) ;
#54371 = ORIENTED_EDGE ( 'NONE', *, *, #10333, .F. ) ;
#54372 = EDGE_CURVE ( 'NONE', #35493, #75936, #86602, .T. ) ;
#54373 = ADVANCED_FACE ( 'NONE', ( #43050 ), #15584, .F. ) ;
#54374 = EDGE_LOOP ( 'NONE', ( #271, #70543, #716, #15520 ) ) ;
#54375 = VECTOR ( 'NONE', #81623, 1000.000000000000000 ) ;
#54376 = ORIENTED_EDGE ( 'NONE', *, *, #44311, .T. ) ;
#54378 = ORIENTED_EDGE ( 'NONE', *, *, #52960, .T. ) ;
#54377 = CARTESIAN_POINT ( 'NONE',  ( -6.923076923076922462, -1.466349020453238561, 30.81389545987213907 ) ) ;
#54379 = CARTESIAN_POINT ( 'NONE',  ( -1.450697763975519861, -2.833524468853757305, 32.15551576947924417 ) ) ;
#54380 = EDGE_CURVE ( 'NONE', #3164, #70275, #35856, .T. ) ;
#54381 = CARTESIAN_POINT ( 'NONE',  ( 15.23076923076911093, -5.219633306517616589, 34.19971097300220464 ) ) ;
#54382 = B_SPLINE_CURVE_WITH_KNOTS ( 'NONE', 3,
 ( #33613, #12889, #11573, #59750, #31845, #86807, #45338, #19649, #47110, #46240 ),
 .UNSPECIFIED., .F., .F.,
 ( 4, 2, 2, 2, 4 ),
 ( 0.0007817359430256369448, 0.0009771253907250049969, 0.001172514838424373049, 0.001367904286123741101, 0.001563293733823109153 ),
 .UNSPECIFIED. ) ;
#54383 = CARTESIAN_POINT ( 'NONE',  ( 5.776515075435670887, -4.225889041578354544, 33.85425143139329407 ) ) ;
#54384 = DIRECTION ( 'NONE',  ( -0.000000000000000000, 0.5000000000000011102, -0.8660254037844380415 ) ) ;
#54385 = ORIENTED_EDGE ( 'NONE', *, *, #30456, .T. ) ;
#54386 = EDGE_LOOP ( 'NONE', ( #21058, #88732, #2181, #25592 ) ) ;
#54387 = ORIENTED_EDGE ( 'NONE', *, *, #78285, .F. ) ;
#54388 = CARTESIAN_POINT ( 'NONE',  ( 14.30769230769218581, -11.06231777344772027, 33.60647404775119895 ) ) ;
#54390 = ORIENTED_EDGE ( 'NONE', *, *, #12281, .T. ) ;
#54389 = DIRECTION ( 'NONE',  ( -0.000000000000000000, 0.000000000000000000, 1.000000000000000000 ) ) ;
#54391 = CARTESIAN_POINT ( 'NONE',  ( -2.057637996053990559, -8.303483539816728154, 34.68545999027711702 ) ) ;
#54392 = CARTESIAN_POINT ( 'NONE',  ( -17.30040800148741198, -3.562934362175799841, 33.22335522853832401 ) ) ;
#54393 = VERTEX_POINT ( 'NONE', #69631 ) ;
#54394 = CARTESIAN_POINT ( 'NONE',  ( 16.15384615384603251, -8.613356846316285953, 34.62446782046622218 ) ) ;
#54395 = CARTESIAN_POINT ( 'NONE',  ( -17.93474442872397390, -2.625532179533469623, 30.86335684631491105 ) ) ;
#54396 = DIRECTION ( 'NONE',  ( -0.000000000000000000, -0.7660444431189791237, -0.6427876096865379196 ) ) ;
#54397 = VECTOR ( 'NONE', #14429, 1000.000000000000227 ) ;
#54398 = FACE_BOUND ( 'NONE', #72022, .T. ) ;
#54399 = CYLINDRICAL_SURFACE ( 'NONE', #54239, 0.2499999999999979738 ) ;
#54400 = CARTESIAN_POINT ( 'NONE',  ( -1.134561072977070317, -11.79725096376909654, 32.30694842903960762 ) ) ;
#54401 = EDGE_CURVE ( 'NONE', #78771, #17034, #14334, .T. ) ;
#54402 = CARTESIAN_POINT ( 'NONE',  ( -12.46153846153846168, -1.509761064869970415, 31.06009739812519044 ) ) ;
#54404 = LINE ( 'NONE', #81899, #9483 ) ;
#54403 = CYLINDRICAL_SURFACE ( 'NONE', #5827, 0.2500000000000008882 ) ;
#54405 = CARTESIAN_POINT ( 'NONE',  ( 0.2386122440223155117, -12.15238873228291538, 31.58232369045354915 ) ) ;
#54406 = CARTESIAN_POINT ( 'NONE',  ( 12.59206389977210350, -3.068774925481848825, 32.56582465632704526 ) ) ;
#54407 = ORIENTED_EDGE ( 'NONE', *, *, #19183, .F. ) ;
#54408 = CARTESIAN_POINT ( 'NONE',  ( -18.06608341095587278, -10.51840700105979387, 33.73612834413961536 ) ) ;
#54409 = CARTESIAN_POINT ( 'NONE',  ( 0.4615384615383382183, -11.06231777344772027, 33.60647404775119895 ) ) ;
#54410 = ORIENTED_EDGE ( 'NONE', *, *, #69579, .F. ) ;
#54411 = ADVANCED_FACE ( 'NONE', ( #57887 ), #36735, .F. ) ;
#54412 = LINE ( 'NONE', #73819, #64522 ) ;
#54413 = DIRECTION ( 'NONE',  ( 0.000000000000000000, 0.000000000000000000, 1.000000000000000000 ) ) ;
#54414 = ORIENTED_EDGE ( 'NONE', *, *, #70782, .F. ) ;
#54415 = CARTESIAN_POINT ( 'NONE',  ( -16.02332045208259359, -11.46989282347013095, 32.79007818306219946 ) ) ;
#54416 = CARTESIAN_POINT ( 'NONE',  ( -4.377331078410483300, -9.417330523894424488, 34.63758898049880486 ) ) ;
#54417 = B_SPLINE_CURVE_WITH_KNOTS ( 'NONE', 3,
 ( #79982, #57480, #16943, #18281, #45749, #73228, #44394, #39010, #66469, #78199 ),
 .UNSPECIFIED., .F., .F.,
 ( 4, 2, 2, 2, 4 ),
 ( 0.000000000000000000, 0.0001954339881912772715, 0.0003908679763825545429, 0.0005863019645738318415, 0.0007817359527651090859 ),
 .UNSPECIFIED. ) ;
#54418 = FACE_BOUND ( 'NONE', #3019, .T. ) ;
#54420 = FACE_OUTER_BOUND ( 'NONE', #82200, .T. ) ;
#54419 = CARTESIAN_POINT ( 'NONE',  ( -17.01085472592063752, -4.098570777380720287, 33.41473453929635440 ) ) ;
#54421 = CARTESIAN_POINT ( 'NONE',  ( -13.63459212866397685, -2.318417181685855422, 30.59732222474233865 ) ) ;
#54422 = DIRECTION ( 'NONE',  ( 0.000000000000000000, 0.9396926207859126468, 0.3420201433256571111 ) ) ;
#54424 = CARTESIAN_POINT ( 'NONE',  ( 0.2115617305961066674, -5.728515186090277211, 34.42611988154120439 ) ) ;
#54423 = DIRECTION ( 'NONE',  ( 0.000000000000000000, 0.000000000000000000, 1.000000000000000000 ) ) ;
#54425 = ADVANCED_FACE ( 'NONE', ( #65976 ), #86730, .F. ) ;
#54426 = CARTESIAN_POINT ( 'NONE',  ( -1.492201783934549164, -11.27530806549876807, 17.10750670625848713 ) ) ;
#54427 = ORIENTED_EDGE ( 'NONE', *, *, #1808, .T. ) ;
#54428 = ORIENTED_EDGE ( 'NONE', *, *, #72781, .F. ) ;
#54429 = AXIS2_PLACEMENT_3D ( 'NONE', #77682, #49766, #15550 ) ;
#54430 = CARTESIAN_POINT ( 'NONE',  ( -9.758390071667825794, -2.486705287966279432, 31.30864560766542937 ) ) ;
#54431 = CARTESIAN_POINT ( 'NONE',  ( 16.28437185560972011, -6.852161475712351013, 34.70806712695775786 ) ) ;
#54432 = DIRECTION ( 'NONE',  ( -0.000000000000000000, 0.9396926207859092051, -0.3420201433256662704 ) ) ;
#54433 = CARTESIAN_POINT ( 'NONE',  ( 10.74591005361825680, -3.068774925481848825, 32.56582465632704526 ) ) ;
#54434 = FACE_OUTER_BOUND ( 'NONE', #7454, .T. ) ;
#54435 = CARTESIAN_POINT ( 'NONE',  ( 1.553300858899087311, -3.749999999999992006, 25.48437500000000000 ) ) ;
#54436 = CARTESIAN_POINT ( 'NONE',  ( -19.50000000000000000, -3.499999999999999556, 29.75000000000000355 ) ) ;
#54437 = CARTESIAN_POINT ( 'NONE',  ( -6.000000000000121680, -8.656820664282941280, 34.87096338111179961 ) ) ;
#54438 = VECTOR ( 'NONE', #69447, 999.9999999999998863 ) ;
#54439 = EDGE_CURVE ( 'NONE', #68982, #69859, #33641, .T. ) ;
#54440 = CARTESIAN_POINT ( 'NONE',  ( 17.93472999944368240, -4.320704448112772766, 33.92786785259540494 ) ) ;
#54441 = CARTESIAN_POINT ( 'NONE',  ( -1.449938300107559641, -7.749976743299137993, 34.99404534957040624 ) ) ;
#54442 = CARTESIAN_POINT ( 'NONE',  ( 9.915319043920542086, -2.758310577978208666, 31.33698337089302299 ) ) ;
#54443 = AXIS2_PLACEMENT_3D ( 'NONE', #41696, #47557, #75047 ) ;
#54444 = DIRECTION ( 'NONE',  ( 0.000000000000000000, 1.000000000000000000, 0.000000000000000000 ) ) ;
#54445 = CARTESIAN_POINT ( 'NONE',  ( -13.38461538461538325, -1.117168528481311540, 33.14645433367849847 ) ) ;
#54446 = CARTESIAN_POINT ( 'NONE',  ( 2.557692307693728129, -7.500000000000154543, 35.00000000000007105 ) ) ;
#54447 = CARTESIAN_POINT ( 'NONE',  ( -12.52678945169970604, -2.506253911140460922, 30.00000000000013856 ) ) ;
#54448 = ORIENTED_EDGE ( 'NONE', *, *, #64523, .F. ) ;
#54449 = CARTESIAN_POINT ( 'NONE',  ( 1.384615384615265343, -2.625532179533778709, 30.86335684631627174 ) ) ;
#54450 = CARTESIAN_POINT ( 'NONE',  ( -17.20761368003338276, -6.369640206132551441, 34.87707690430378449 ) ) ;
#54451 = CARTESIAN_POINT ( 'NONE',  ( -1.901340078031369618, -5.512252781505359245, 15.50186829374151287 ) ) ;
#54452 = FACE_BOUND ( 'NONE', #44616, .T. ) ;
#54453 = CARTESIAN_POINT ( 'NONE',  ( -17.77722045873158763, -10.81320215134717344, 33.49497208177562868 ) ) ;
#54454 = CARTESIAN_POINT ( 'NONE',  ( -11.40793610022789828, -5.070358843744210198, 34.40418822224088302 ) ) ;
#54456 = EDGE_LOOP ( 'NONE', ( #51125, #25764 ) ) ;
#54455 = CARTESIAN_POINT ( 'NONE',  ( 24.00000000000000000, -9.499999999999982236, 27.74999999999999645 ) ) ;
#54457 = CARTESIAN_POINT ( 'NONE',  ( 1.139087296525997051, -4.749999999999992895, 25.48437500000000000 ) ) ;
#54458 = EDGE_CURVE ( 'NONE', #78293, #36536, #64632, .T. ) ;
#54459 = CARTESIAN_POINT ( 'NONE',  ( 17.86985279056177944, -3.817052484675422797, 33.13202310037935661 ) ) ;
#54460 = B_SPLINE_CURVE_WITH_KNOTS ( 'NONE', 3,
 ( #11003, #18204, #46117, #25849, #60065, #79007, #10103, #85775, #45666, #24056 ),
 .UNSPECIFIED., .F., .F.,
 ( 4, 2, 2, 2, 4 ),
 ( 0.0007817246256747465219, 0.0009771112852218898515, 0.001172497944769033181, 0.001367884604316176294, 0.001563271263863319624 ),
 .UNSPECIFIED. ) ;
#54461 = ORIENTED_EDGE ( 'NONE', *, *, #4207, .F. ) ;
#54462 = CARTESIAN_POINT ( 'NONE',  ( -16.15384615384615330, -9.780366693483667717, 34.19971097300155094 ) ) ;
#54463 = CARTESIAN_POINT ( 'NONE',  ( -6.989159302437058408, -11.35647404775217595, 33.31231777344666511 ) ) ;
#54464 = ORIENTED_EDGE ( 'NONE', *, *, #51318, .T. ) ;
#54465 = CARTESIAN_POINT ( 'NONE',  ( 7.780883400193072674, -4.481592998940162609, 33.73612834413957984 ) ) ;
#54466 = B_SPLINE_CURVE_WITH_KNOTS ( 'NONE', 3,
 ( #49847, #16071, #36783, #62907, #9322, #49419, #2540, #70124, #21946, #71013 ),
 .UNSPECIFIED., .F., .F.,
 ( 4, 2, 2, 2, 4 ),
 ( 0.0007817359430256390048, 0.0009771253907250075990, 0.001172514838424376085, 0.001367904286123744571, 0.001563293733823113056 ),
 .UNSPECIFIED. ) ;
#54467 = CARTESIAN_POINT ( 'NONE',  ( -15.00780609650255570, -7.369474539155828730, 34.99858011523957657 ) ) ;
#54468 = EDGE_CURVE ( 'NONE', #60949, #33215, #9275, .T. ) ;
#54469 = DIRECTION ( 'NONE',  ( 0.000000000000000000, 0.3420201433256641055, -0.9396926207859100932 ) ) ;
#54470 = EDGE_CURVE ( 'NONE', #78525, #78212, #25013, .T. ) ;
#54471 = ORIENTED_EDGE ( 'NONE', *, *, #18602, .F. ) ;
#54472 = VERTEX_POINT ( 'NONE', #72288 ) ;
#54473 = CARTESIAN_POINT ( 'NONE',  ( -6.923076923076922462, -12.78798330534102945, 29.74999999999997868 ) ) ;
#54474 = AXIS2_PLACEMENT_3D ( 'NONE', #72918, #64370, #71576 ) ;
#54475 = ORIENTED_EDGE ( 'NONE', *, *, #28904, .T. ) ;
#54476 = CARTESIAN_POINT ( 'NONE',  ( -18.00000000000012079, -5.094484230521992174, 34.41647553114689373 ) ) ;
#54477 = DIRECTION ( 'NONE',  ( 0.000000000000000000, 0.3420201433256610524, 0.9396926207859113145 ) ) ;
#54478 = CARTESIAN_POINT ( 'NONE',  ( 9.561617089197383734, -9.084618155246140248, 34.75535874321725771 ) ) ;
#54479 = CARTESIAN_POINT ( 'NONE',  ( -2.307692307692305711, -5.557115091759785130, 34.35708131394839171 ) ) ;
#54480 = CARTESIAN_POINT ( 'NONE',  ( -0.3310130233048163562, -5.915461855592777596, 34.75538340440931506 ) ) ;
#54481 = DIRECTION ( 'NONE',  ( -0.000000000000000000, -0.8660254037844397068, -0.4999999999999978906 ) ) ;
#54482 = CARTESIAN_POINT ( 'NONE',  ( 10.39189967166066708, -12.24155766932282496, 31.33739205006857986 ) ) ;
#54483 = EDGE_CURVE ( 'NONE', #3281, #19723, #59224, .T. ) ;
#54484 = ORIENTED_EDGE ( 'NONE', *, *, #10311, .T. ) ;
#54485 = ORIENTED_EDGE ( 'NONE', *, *, #22053, .F. ) ;
#54487 = ORIENTED_EDGE ( 'NONE', *, *, #86603, .T. ) ;
#54486 = CARTESIAN_POINT ( 'NONE',  ( 6.923076923076924238, -12.62096338111211580, 30.90682066428153263 ) ) ;
#54488 = CIRCLE ( 'NONE', #47289, 3.249999999999999556 ) ;
#54489 = CARTESIAN_POINT ( 'NONE',  ( -13.63461538461538325, -7.500000000000001776, 35.00000000000000000 ) ) ;
#54490 = CARTESIAN_POINT ( 'NONE',  ( 12.46153846153846168, -3.050289026998446396, 32.03036669348365706 ) ) ;
#54491 = B_SPLINE_CURVE_WITH_KNOTS ( 'NONE', 3,
 ( #32770, #25573, #53027, #62011, #317, #62878, #56586, #75525, #28221, #1191 ),
 .UNSPECIFIED., .F., .F.,
 ( 4, 2, 2, 2, 4 ),
 ( 0.000000000000000000, 0.0001954311564186863052, 0.0003908623128373726104, 0.0005862934692560589156, 0.0007817246256747452209 ),
 .UNSPECIFIED. ) ;
#54492 = ORIENTED_EDGE ( 'NONE', *, *, #8617, .T. ) ;
#54493 = B_SPLINE_CURVE_WITH_KNOTS ( 'NONE', 3,
 ( #66326, #16801, #58672, #44705, #37970, #3728, #79847, #51906, #18592, #66771 ),
 .UNSPECIFIED., .F., .F.,
 ( 4, 2, 2, 2, 4 ),
 ( 0.000000000000000000, 0.0001954311564186858715, 0.0003908623128373717431, 0.0005862934692560576146, 0.0007817246256747434861 ),
 .UNSPECIFIED. ) ;
#54494 = DIRECTION ( 'NONE',  ( -1.000000000000000000, -1.734723475976813504E-16, 0.000000000000000000 ) ) ;
#54495 = AXIS2_PLACEMENT_3D ( 'NONE', #77418, #55816, #42761 ) ;
#54496 = ORIENTED_EDGE ( 'NONE', *, *, #26707, .F. ) ;
#54497 = CARTESIAN_POINT ( 'NONE',  ( -10.61538461538473399, -3.300289026999228881, 32.46337939537708905 ) ) ;
#54498 = ORIENTED_EDGE ( 'NONE', *, *, #35016, .T. ) ;
#54499 = CIRCLE ( 'NONE', #70325, 4.000000000000000000 ) ;
#54500 = CARTESIAN_POINT ( 'NONE',  ( 1.384615384615386802, -2.833524468853757305, 32.15551576947925838 ) ) ;
#54501 = B_SPLINE_CURVE_WITH_KNOTS ( 'NONE', 3,
 ( #80395, #73185, #11483, #18692, #68966, #34292, #32634, #60104, #61752, #21219 ),
 .UNSPECIFIED., .F., .F.,
 ( 4, 2, 2, 2, 4 ),
 ( 0.0007817246256747440282, 0.0009771112852218863821, 0.001172497944769028844, 0.001367884604316171307, 0.001563271263863313769 ),
 .UNSPECIFIED. ) ;
#54502 = EDGE_LOOP ( 'NONE', ( #10640, #17822, #27396, #81187 ) ) ;
#54503 = VECTOR ( 'NONE', #60616, 1000.000000000000000 ) ;
#54504 = CARTESIAN_POINT ( 'NONE',  ( -4.376773112753002515, -4.026226216239095379, 33.68668979543632958 ) ) ;
#54505 = CARTESIAN_POINT ( 'NONE',  ( 5.198717948717946236, -7.500000000000000000, 29.75000000000000355 ) ) ;
#54506 = FACE_BOUND ( 'NONE', #1318, .T. ) ;
#54507 = CARTESIAN_POINT ( 'NONE',  ( -14.55771553191376633, -9.356822207818506598, 34.66110646841856635 ) ) ;
#54508 = DIRECTION ( 'NONE',  ( 0.000000000000000000, 0.4999999999999960032, -0.8660254037844410391 ) ) ;
#54509 = CARTESIAN_POINT ( 'NONE',  ( 13.38461538461538680, -4.661471528628507777, 34.16647553114623292 ) ) ;
#54510 = CARTESIAN_POINT ( 'NONE',  ( -3.296852641725110722, -4.098570777380720287, 33.41473453929634729 ) ) ;
#54511 = DIRECTION ( 'NONE',  ( -0.000000000000000000, 0.6427876096865404731, -0.7660444431189770143 ) ) ;
#54512 = CARTESIAN_POINT ( 'NONE',  ( 16.02369894440793630, -4.460286881179643004, 33.72017969459903242 ) ) ;
#54513 = CARTESIAN_POINT ( 'NONE',  ( -6.923076923077044142, -6.879047030192662504, 34.71129190930017927 ) ) ;
#54514 = VERTEX_POINT ( 'NONE', #10601 ) ;
#54515 = EDGE_LOOP ( 'NONE', ( #74162, #22811, #63140, #24343 ) ) ;
#54517 = CARTESIAN_POINT ( 'NONE',  ( -18.22348492456433178, -10.23692288466677525, 34.23039457007281072 ) ) ;
#54516 = CARTESIAN_POINT ( 'NONE',  ( -16.85414353565466428, -10.11255958852955672, 34.01340905677048454 ) ) ;
#54518 = CARTESIAN_POINT ( 'NONE',  ( -4.376725670583738292, -7.630690623152302621, 34.99857592706774057 ) ) ;
#54519 = CARTESIAN_POINT ( 'NONE',  ( 3.296024802045254720, -10.90142922261932057, 33.41473453929631887 ) ) ;
#54520 = CARTESIAN_POINT ( 'NONE',  ( 16.82694634598072625, -8.303909089506435137, 34.68538101551103381 ) ) ;
#54521 = CARTESIAN_POINT ( 'NONE',  ( 13.45068373561782415, -11.16473453929635440, 33.15142922261926373 ) ) ;
#54522 = VERTEX_POINT ( 'NONE', #16466 ) ;
#54523 = CARTESIAN_POINT ( 'NONE',  ( -11.53846153846165912, -12.27809138561165270, 31.22303859784587132 ) ) ;
#54524 = CARTESIAN_POINT ( 'NONE',  ( -19.99999999999996803, 15.00000000000000711, 3.000000000000000000 ) ) ;
#54525 = CARTESIAN_POINT ( 'NONE',  ( 16.85343815235874487, -4.225889041578354544, 33.85425143139329407 ) ) ;
#54526 = CARTESIAN_POINT ( 'NONE',  ( -16.15384615384615330, -3.937682226553329556, 33.60647404775216529 ) ) ;
#54527 = ORIENTED_EDGE ( 'NONE', *, *, #47092, .F. ) ;
#54528 = AXIS2_PLACEMENT_3D ( 'NONE', #66847, #87586, #19985 ) ;
#54529 = B_SPLINE_CURVE_WITH_KNOTS ( 'NONE', 3,
 ( #47439, #86348, #40705, #45325, #58840, #19970, #74934, #53758, #47887, #68604 ),
 .UNSPECIFIED., .F., .F.,
 ( 4, 2, 2, 2, 4 ),
 ( 0.000000000000000000, 0.0001954339857564070678, 0.0003908679715128141356, 0.0005863019572692211492, 0.0007817359430256282712 ),
 .UNSPECIFIED. ) ;
#54530 = ORIENTED_EDGE ( 'NONE', *, *, #4182, .T. ) ;
#54531 = VERTEX_POINT ( 'NONE', #43932 ) ;
#54532 = CARTESIAN_POINT ( 'NONE',  ( -6.923076923076922462, -13.20930481340135110, 34.54067556320372745 ) ) ;
#54533 = ORIENTED_EDGE ( 'NONE', *, *, #2890, .F. ) ;
#54534 = CARTESIAN_POINT ( 'NONE',  ( -16.08859058257012720, -5.219633306516380244, 34.19971097300157936 ) ) ;
#54535 = CARTESIAN_POINT ( 'NONE',  ( -6.066082379360133281, -9.058645607665454236, 34.76329471203372634 ) ) ;
#54536 = CARTESIAN_POINT ( 'NONE',  ( 5.076923076923075762, -6.386643153685126251, 34.62446782046654192 ) ) ;
#54537 = CARTESIAN_POINT ( 'NONE',  ( 8.769230769230645706, -3.643525952248795718, 33.31231777344771672 ) ) ;
#54538 = CARTESIAN_POINT ( 'NONE',  ( 14.53070365930516061, -4.187068189119697692, 33.49521262558774026 ) ) ;
#54539 = ORIENTED_EDGE ( 'NONE', *, *, #72295, .F. ) ;
#54540 = LINE ( 'NONE', #27967, #73157 ) ;
#54542 = VERTEX_POINT ( 'NONE', #51111 ) ;
#54541 = CARTESIAN_POINT ( 'NONE',  ( -13.25382357679059453, -4.118422570099831148, 33.43335022499816489 ) ) ;
#54543 = CARTESIAN_POINT ( 'NONE',  ( -5.299850035829923200, -2.308479472611653094, 30.53278059502174457 ) ) ;
#54544 = CARTESIAN_POINT ( 'NONE',  ( -3.164701897419155419, -2.486705287966280320, 31.30864560766543647 ) ) ;
#54545 = CARTESIAN_POINT ( 'NONE',  ( -13.45069879557126136, -4.786620604624113540, 33.94971097300155805 ) ) ;
#54546 = CARTESIAN_POINT ( 'NONE',  ( 11.78840694783958298, -10.18230066228895758, 34.26354781536631577 ) ) ;
#54547 = DIRECTION ( 'NONE',  ( -0.000000000000000000, -0.5000000000000009992, -0.8660254037844380415 ) ) ;
#54548 = SURFACE_STYLE_FILL_AREA ( #61299 ) ;
#54549 = CARTESIAN_POINT ( 'NONE',  ( 12.46153846153833911, -11.48612834414049644, 32.76840700105863391 ) ) ;
#54550 = CARTESIAN_POINT ( 'NONE',  ( -2.775308065498752086, -8.577988221561495763, 22.76749329374151287 ) ) ;
#54551 = VERTEX_POINT ( 'NONE', #78602 ) ;
#54552 = DIRECTION ( 'NONE',  ( 0.000000000000000000, 0.000000000000000000, -1.000000000000000000 ) ) ;
#54553 = DIRECTION ( 'NONE',  ( -0.000000000000000000, -0.9396926207859093161, -0.3420201433256663259 ) ) ;
#54554 = ADVANCED_FACE ( 'NONE', ( #37617 ), #16906, .T. ) ;
#54555 = VECTOR ( 'NONE', #57291, 1000.000000000000000 ) ;
#54556 = VECTOR ( 'NONE', #80986, 1000.000000000000000 ) ;
#54557 = DIRECTION ( 'NONE',  ( -0.000000000000000000, 0.8660254037844399289, -0.4999999999999980016 ) ) ;
#54558 = SURFACE_SIDE_STYLE ('',( #6395 ) ) ;
#54559 = VERTEX_POINT ( 'NONE', #72733 ) ;
#54560 = CARTESIAN_POINT ( 'NONE',  ( -12.68502340526241312, -11.89387501736622710, 32.13663884655806413 ) ) ;
#54561 = CARTESIAN_POINT ( 'NONE',  ( -5.326946314216043810, -6.695914987888143877, 34.68535235679833306 ) ) ;
#54562 = VECTOR ( 'NONE', #89094, 1000.000000000000000 ) ;
#54563 = CARTESIAN_POINT ( 'NONE',  ( -10.61538461538473577, -2.379036618888197729, 30.90682066428292885 ) ) ;
#54564 = CARTESIAN_POINT ( 'NONE',  ( -4.826923076923073985, -2.499999999999999112, 29.81604066197450109 ) ) ;
#54565 = AXIS2_PLACEMENT_3D ( 'NONE', #79614, #11149, #38624 ) ;
#54566 = DIRECTION ( 'NONE',  ( 0.000000000000000000, 0.000000000000000000, -1.000000000000000000 ) ) ;
#54567 = ORIENTED_EDGE ( 'NONE', *, *, #48556, .F. ) ;
#54568 = CARTESIAN_POINT ( 'NONE',  ( 6.223011351612852238, -5.667800583137508674, 34.40243808032445827 ) ) ;
#54569 = EDGE_CURVE ( 'NONE', #65380, #89050, #49733, .T. ) ;
#54570 = DIRECTION ( 'NONE',  ( 0.000000000000000000, 0.9396926207859126468, -0.3420201433256571111 ) ) ;
#54571 = CARTESIAN_POINT ( 'NONE',  ( -14.30769230769230660, -6.189225973068211317, 35.74407628777942847 ) ) ;
#54572 = VERTEX_POINT ( 'NONE', #45710 ) ;
#54573 = DIRECTION ( 'NONE',  ( -1.000000000000000000, -0.000000000000000000, -0.000000000000000000 ) ) ;
#54574 = ORIENTED_EDGE ( 'NONE', *, *, #78457, .F. ) ;
#54575 = CARTESIAN_POINT ( 'NONE',  ( -16.15384615384627409, -6.026961402154118908, 34.52809138561165270 ) ) ;
#54576 = LINE ( 'NONE', #82073, #61312 ) ;
#54577 = ORIENTED_EDGE ( 'NONE', *, *, #85984, .F. ) ;
#54578 = CARTESIAN_POINT ( 'NONE',  ( -11.53846153846153655, -12.34228464037088635, 31.77849191805839268 ) ) ;
#54579 = FACE_OUTER_BOUND ( 'NONE', #29812, .T. ) ;
#54580 = CARTESIAN_POINT ( 'NONE',  ( 1.318531973659505807, -4.098570777380720287, 33.41473453929634729 ) ) ;
#54581 = CARTESIAN_POINT ( 'NONE',  ( -7.976844449264155479, -4.684245665217972032, 34.18127051446801090 ) ) ;
#54582 = DIRECTION ( 'NONE',  ( 0.000000000000000000, 0.9848077530122072432, 0.1736481776669354937 ) ) ;
#54583 = EDGE_CURVE ( 'NONE', #81438, #14205, #25446, .T. ) ;
#54584 = VERTEX_POINT ( 'NONE', #81289 ) ;
#54585 = FACE_BOUND ( 'NONE', #37562, .T. ) ;
#54586 = VERTEX_POINT ( 'NONE', #46167 ) ;
#54587 = CARTESIAN_POINT ( 'NONE',  ( -8.992157728137618378, -12.38737895849757820, 31.66785238281580206 ) ) ;
#54588 = VECTOR ( 'NONE', #35597, 1000.000000000000000 ) ;
#54589 = EDGE_CURVE ( 'NONE', #1870, #7785, #11491, .T. ) ;
#54590 = EDGE_CURVE ( 'NONE', #13908, #74567, #26147, .T. ) ;
#54591 = CARTESIAN_POINT ( 'NONE',  ( 18.13079180782478161, -12.11778462344220841, 31.66786338562085135 ) ) ;
#54592 = CARTESIAN_POINT ( 'NONE',  ( 3.007284306204899504, -11.60425143139329940, 33.02411095842164457 ) ) ;
#54593 = CARTESIAN_POINT ( 'NONE',  ( -11.31568199719312773, -2.600157965045224451, 30.74683119005207743 ) ) ;
#54594 = ORIENTED_EDGE ( 'NONE', *, *, #33487, .T. ) ;
#54595 = VERTEX_POINT ( 'NONE', #18248 ) ;
#54596 = ORIENTED_EDGE ( 'NONE', *, *, #70633, .T. ) ;
#54597 = B_SPLINE_CURVE_WITH_KNOTS ( 'NONE', 3,
 ( #40711, #83020, #33938, #68173, #21753, #21305, #48778, #76246, #42039, #27181 ),
 .UNSPECIFIED., .F., .F.,
 ( 4, 2, 2, 2, 4 ),
 ( 0.0007817246256747503166, 0.0009771112852218946220, 0.001172497944769039036, 0.001367884604316183233, 0.001563271263863327647 ),
 .UNSPECIFIED. ) ;
#54598 = ORIENTED_EDGE ( 'NONE', *, *, #10938, .F. ) ;
#54599 = CARTESIAN_POINT ( 'NONE',  ( -4.826977558574935934, -5.057305518903949526, 34.11320923018887896 ) ) ;
#54600 = CARTESIAN_POINT ( 'NONE',  ( 6.673076923076925127, -7.500000000000001776, 35.00000000000000000 ) ) ;
#54601 = CARTESIAN_POINT ( 'NONE',  ( -7.911423846710166075, -3.643525952247789412, 33.31231777344662959 ) ) ;
#54602 = CARTESIAN_POINT ( 'NONE',  ( 11.28843830116857383, -2.587272538249754117, 30.68239716806877837 ) ) ;
#54603 = AXIS2_PLACEMENT_3D ( 'NONE', #86651, #24920, #52384 ) ;
#54604 = CARTESIAN_POINT ( 'NONE',  ( 2.320192649118979489E-14, -11.25000000000000000, 26.03125000000000000 ) ) ;
#54605 = CARTESIAN_POINT ( 'NONE',  ( -19.00000000000000000, 8.999999999999994671, 31.75000000000000000 ) ) ;
#54606 = CYLINDRICAL_SURFACE ( 'NONE', #53830, 0.2499999999999973355 ) ;
#54607 = CARTESIAN_POINT ( 'NONE',  ( 11.28848480751918437, -9.943427161483782584, 34.11278801902876978 ) ) ;
#54608 = ORIENTED_EDGE ( 'NONE', *, *, #26817, .T. ) ;
#54609 = EDGE_LOOP ( 'NONE', ( #51449, #61180, #6184, #23842 ) ) ;
#54610 = B_SPLINE_CURVE_WITH_KNOTS ( 'NONE', 3,
 ( #13305, #55171, #47524, #33132, #69136, #12860, #47080, #54279, #21393, #60598 ),
 .UNSPECIFIED., .F., .F.,
 ( 4, 2, 2, 2, 4 ),
 ( 0.0007817359527651090859, 0.0009771254036996478414, 0.001172514854634186489, 0.001367904305568725136, 0.001563293756503263783 ),
 .UNSPECIFIED. ) ;
#54611 = VECTOR ( 'NONE', #45898, 1000.000000000000000 ) ;
#54612 = ORIENTED_EDGE ( 'NONE', *, *, #16558, .T. ) ;
#54613 = DIRECTION ( 'NONE',  ( -0.000000000000000000, -0.9396926207859092051, -0.3420201433256662704 ) ) ;
#54615 = CARTESIAN_POINT ( 'NONE',  ( -7.715363405186893786, -9.084667340241226796, 34.75534355489798344 ) ) ;
#54614 = CARTESIAN_POINT ( 'NONE',  ( 1.384615384615386802, -5.557115091759785130, 34.35708131394839171 ) ) ;
#54616 = EDGE_CURVE ( 'NONE', #49089, #69788, #40200, .T. ) ;
#54617 = CARTESIAN_POINT ( 'NONE',  ( -0.2114840416250090560, -2.318338780012835443, 30.59689888758630261 ) ) ;
#54618 = DIRECTION ( 'NONE',  ( -0.000000000000000000, -0.6427876096865404731, -0.7660444431189770143 ) ) ;
#54619 = FACE_BOUND ( 'NONE', #73595, .T. ) ;
#54620 = ORIENTED_EDGE ( 'NONE', *, *, #88036, .T. ) ;
#54621 = FACE_OUTER_BOUND ( 'NONE', #55259, .T. ) ;
#54622 = CARTESIAN_POINT ( 'NONE',  ( 16.94623161025552704, -6.413092428213692742, 34.63065189839063152 ) ) ;
#54623 = CARTESIAN_POINT ( 'NONE',  ( 3.230769230769231726, -10.51840700105979565, 33.73612834413961536 ) ) ;
#54624 = VERTEX_POINT ( 'NONE', #66432 ) ;
#54625 = CARTESIAN_POINT ( 'NONE',  ( -4.946397375159514276, -6.852161475712352789, 34.70806712695775786 ) ) ;
#54626 = EDGE_LOOP ( 'NONE', ( #38889, #12635 ) ) ;
#54627 = FACE_BOUND ( 'NONE', #35655, .T. ) ;
#54628 = CARTESIAN_POINT ( 'NONE',  ( -16.08865217206279752, -2.506253911140448043, 29.99999999999988631 ) ) ;
#54629 = ORIENTED_EDGE ( 'NONE', *, *, #21772, .F. ) ;
#54630 = CARTESIAN_POINT ( 'NONE',  ( -22.75000000000000000, -4.499999999999999112, 29.75000000000000355 ) ) ;
#54631 = LINE ( 'NONE', #593, #54817 ) ;
#54632 = CARTESIAN_POINT ( 'NONE',  ( -0.4615384615384611200, -2.292212530054420494, 30.41441678777542634 ) ) ;
#54633 = ORIENTED_EDGE ( 'NONE', *, *, #8506, .F. ) ;
#54634 = CARTESIAN_POINT ( 'NONE',  ( 6.857806477116148436, -10.21337939537584383, 33.94971097300158647 ) ) ;
#54635 = CARTESIAN_POINT ( 'NONE',  ( 14.05766908347085220, -11.56360843649121861, 33.07473185843129926 ) ) ;
#54636 = CARTESIAN_POINT ( 'NONE',  ( -16.15384615384615330, -12.37446782046654192, 30.86335684631486131 ) ) ;
#54637 = CARTESIAN_POINT ( 'NONE',  ( -8.096177083446812972, -2.823816976329319051, 31.52131813110795733 ) ) ;
#54638 = EDGE_LOOP ( 'NONE', ( #51733, #43092, #86125, #29308 ) ) ;
#54639 = EDGE_CURVE ( 'NONE', #39942, #69003, #39078, .T. ) ;
#54640 = LINE ( 'NONE', #82138, #61788 ) ;
#54641 = CARTESIAN_POINT ( 'NONE',  ( -15.36146069743678844, -4.118384482072085184, 33.43331474514187107 ) ) ;
#54643 = ORIENTED_EDGE ( 'NONE', *, *, #32527, .F. ) ;
#54642 = CARTESIAN_POINT ( 'NONE',  ( -3.230769230769351186, -12.27809138561165270, 31.22303859784587132 ) ) ;
#54644 = CARTESIAN_POINT ( 'NONE',  ( 2.557637717070353034, -10.18230066228895758, 34.26354781536631577 ) ) ;
#54645 = CARTESIAN_POINT ( 'NONE',  ( -4.283993363284372080, -2.619462340734462380, 30.83744416345203021 ) ) ;
#54646 = CARTESIAN_POINT ( 'NONE',  ( 5.777073782483852504, -9.086856451489516928, 34.49173150075333183 ) ) ;
#54647 = DIRECTION ( 'NONE',  ( 0.000000000000000000, 0.000000000000000000, 1.000000000000000000 ) ) ;
#54648 = LINE ( 'NONE', #41154, #67464 ) ;
#54649 = CARTESIAN_POINT ( 'NONE',  ( 9.942362003946010773, -9.148310452688876993, 34.47095581063188519 ) ) ;
#54651 = FACE_OUTER_BOUND ( 'NONE', #88800, .T. ) ;
#54650 = CARTESIAN_POINT ( 'NONE',  ( -7.976845312821404299, -10.54014554554150607, 33.71984207302941883 ) ) ;
#54652 = CARTESIAN_POINT ( 'NONE',  ( -6.792285115252139072, -2.729792928343270919, 31.24908615093345077 ) ) ;
#54653 = AXIS2_PLACEMENT_3D ( 'NONE', #45007, #59868, #46357 ) ;
#54654 = CARTESIAN_POINT ( 'NONE',  ( 2.750000000000001776, -7.499999999999984013, 20.71875000000000000 ) ) ;
#54655 = ORIENTED_EDGE ( 'NONE', *, *, #73718, .F. ) ;
#54656 = LINE ( 'NONE', #82608, #1627 ) ;
#54657 = ORIENTED_EDGE ( 'NONE', *, *, #21772, .T. ) ;
#54658 = EDGE_CURVE ( 'NONE', #60613, #51834, #60111, .T. ) ;
#54659 = EDGE_LOOP ( 'NONE', ( #20647, #70742 ) ) ;
#54660 = CARTESIAN_POINT ( 'NONE',  ( 3.007843013253082898, -4.887634598454295265, 34.01352882383564946 ) ) ;
#54661 = VERTEX_POINT ( 'NONE', #33540 ) ;
#54662 = CARTESIAN_POINT ( 'NONE',  ( 14.05771557674995442, -8.303909089506435137, 34.68538101551103381 ) ) ;
#54663 = CARTESIAN_POINT ( 'NONE',  ( -2.749999999999998224, -7.500000000000015987, 21.34375000000000000 ) ) ;
#54664 = CARTESIAN_POINT ( 'NONE',  ( 17.74997677577854205, -4.931416488878822335, 34.32920672191015399 ) ) ;
#54665 = EDGE_CURVE ( 'NONE', #3680, #16511, #24052, .T. ) ;
#54666 = DIRECTION ( 'NONE',  ( -0.000000000000000000, 0.1736481776669307198, -0.9848077530122080203 ) ) ;
#54667 = CARTESIAN_POINT ( 'NONE',  ( 6.000000000000001776, -11.11383981884818262, 36.00935417666054406 ) ) ;
#54668 = CARTESIAN_POINT ( 'NONE',  ( -7.173100147298381302, -9.356822207818506598, 34.66110646841856635 ) ) ;
#54669 = DIRECTION ( 'NONE',  ( 0.000000000000000000, 0.6427876096865373645, -0.7660444431189797898 ) ) ;
#54670 = DIRECTION ( 'NONE',  ( 0.000000000000000000, 0.000000000000000000, 1.000000000000000000 ) ) ;
#54671 = CARTESIAN_POINT ( 'NONE',  ( -3.749999999999997335, -7.500000000000021316, 25.09374999999999645 ) ) ;
#54672 = CARTESIAN_POINT ( 'NONE',  ( 10.36540788444226102, -2.564618984488975517, 30.55390908950641915 ) ) ;
#54673 = CARTESIAN_POINT ( 'NONE',  ( 17.77707378248385339, -11.76352882383564769, 32.36236540154569497 ) ) ;
#54674 = AXIS2_PLACEMENT_3D ( 'NONE', #21167, #1783, #69367 ) ;
#54675 = EDGE_CURVE ( 'NONE', #6751, #57920, #84221, .T. ) ;
#54676 = CARTESIAN_POINT ( 'NONE',  ( 5.777073041093150785, -11.43668979543635089, 33.22377378376089752 ) ) ;
#54677 = B_SPLINE_CURVE_WITH_KNOTS ( 'NONE', 3,
 ( #49806, #10161, #43058, #42623, #83621, #65085, #36742, #64196, #56130, #1636 ),
 .UNSPECIFIED., .F., .F.,
 ( 4, 2, 2, 2, 4 ),
 ( 0.000000000000000000, 0.0001954339857564084773, 0.0003908679715128169545, 0.0005863019572692254860, 0.0007817359430256339090 ),
 .UNSPECIFIED. ) ;
#54678 = AXIS2_PLACEMENT_3D ( 'NONE', #33734, #45904, #61188 ) ;
#54679 = AXIS2_PLACEMENT_3D ( 'NONE', #10752, #38220, #37774 ) ;
#54680 = EDGE_CURVE ( 'NONE', #78895, #74896, #18652, .T. ) ;
#54681 = ORIENTED_EDGE ( 'NONE', *, *, #78903, .T. ) ;
#54682 = VERTEX_POINT ( 'NONE', #67764 ) ;
#54683 = CARTESIAN_POINT ( 'NONE',  ( -18.00000000000000000, -2.486705287966279876, 31.30864560766543647 ) ) ;
#54684 = CARTESIAN_POINT ( 'NONE',  ( 0.5276057948885367610, -11.91647553114624358, 32.58852847137148245 ) ) ;
#54685 = LINE ( 'NONE', #6519, #19599 ) ;
#54686 = CARTESIAN_POINT ( 'NONE',  ( 9.822833130541338775, -12.15418822224088657, 32.17964115625579069 ) ) ;
#54687 = EDGE_CURVE ( 'NONE', #27674, #20836, #6068, .T. ) ;
#54688 = VECTOR ( 'NONE', #81394, 1000.000000000000114 ) ;
#54689 = CARTESIAN_POINT ( 'NONE',  ( 8.546304551714619890, -4.186968288167450147, 33.49512374952580274 ) ) ;
#54690 = AXIS2_PLACEMENT_3D ( 'NONE', #6555, #68690, #20504 ) ;
#54691 = CARTESIAN_POINT ( 'NONE',  ( -9.692307692307814193, -11.06231777344772027, 33.60647404775119895 ) ) ;
#54692 = AXIS2_PLACEMENT_3D ( 'NONE', #12564, #82802, #76026 ) ;
#54693 = CARTESIAN_POINT ( 'NONE',  ( 7.134615384615385025, -3.499999999999999556, 29.75000000000000355 ) ) ;
#54694 = EDGE_CURVE ( 'NONE', #74098, #58055, #7959, .T. ) ;
#54695 = VERTEX_POINT ( 'NONE', #41620 ) ;
#54696 = CARTESIAN_POINT ( 'NONE',  ( 1.319344938654611665, -5.219633306516282545, 34.19971097300152962 ) ) ;
#54697 = ORIENTED_EDGE ( 'NONE', *, *, #11480, .T. ) ;
#54698 = B_SPLINE_CURVE_WITH_KNOTS ( 'NONE', 3,
 ( #60655, #59772, #66076, #19675, #12048, #25099, #74627, #6167, #32744, #12481 ),
 .UNSPECIFIED., .F., .F.,
 ( 4, 2, 2, 2, 4 ),
 ( 0.000000000000000000, 0.0001954311584214072923, 0.0003908623168428145846, 0.0005862934752642218498, 0.0007817246336856291692 ),
 .UNSPECIFIED. ) ;
#54699 = CARTESIAN_POINT ( 'NONE',  ( 17.77707378248384629, -3.105860786376062332, 32.13614157043599562 ) ) ;
#54700 = CARTESIAN_POINT ( 'NONE',  ( -18.06870381900337108, -12.74406763069169202, 29.99950897402481687 ) ) ;
#54701 = EDGE_CURVE ( 'NONE', #59987, #24082, #1074, .T. ) ;
#54702 = CARTESIAN_POINT ( 'NONE',  ( -6.793029487826470536, -7.723484941389743952, 34.99544897038808955 ) ) ;
#54703 = ADVANCED_FACE ( 'NONE', ( #76733 ), #21787, .F. ) ;
#54704 = CARTESIAN_POINT ( 'NONE',  ( 3.165499230212911908, -8.656820664281497102, 34.87096338111211935 ) ) ;
#54705 = CARTESIAN_POINT ( 'NONE',  ( -13.45069776397551742, -2.486705287966279432, 31.30864560766542937 ) ) ;
#54706 = ORIENTED_EDGE ( 'NONE', *, *, #82743, .F. ) ;
#54707 = EDGE_LOOP ( 'NONE', ( #72832, #81412, #63345, #59271 ) ) ;
#54708 = ORIENTED_EDGE ( 'NONE', *, *, #18880, .F. ) ;
#54709 = ORIENTED_EDGE ( 'NONE', *, *, #23274, .F. ) ;
#54710 = CARTESIAN_POINT ( 'NONE',  ( 17.29993592101647337, -10.01129605718032423, 34.36064277460058491 ) ) ;
#54711 = CARTESIAN_POINT ( 'NONE',  ( -2.372962308248626417, -10.33852847137145048, 34.16647553114627556 ) ) ;
#54712 = VECTOR ( 'NONE', #42608, 1000.000000000000000 ) ;
#54713 = CARTESIAN_POINT ( 'NONE',  ( 16.15384615384615330, -5.471508081941601098, 34.59228464037088457 ) ) ;
#54714 = CARTESIAN_POINT ( 'NONE',  ( 14.05769230769230838, -7.500000000000001776, 35.00000000000000000 ) ) ;
#54715 = CARTESIAN_POINT ( 'NONE',  ( 18.00000000000000000, -2.833524468853757305, 32.15551576947925838 ) ) ;
#54716 = DIRECTION ( 'NONE',  ( -0.000000000000000000, 0.8660254037844397068, -0.4999999999999978906 ) ) ;
#54717 = VERTEX_POINT ( 'NONE', #69088 ) ;
#54718 = ORIENTED_EDGE ( 'NONE', *, *, #17708, .T. ) ;
#54719 = B_SPLINE_CURVE_WITH_KNOTS ( 'NONE', 3,
 ( #65795, #38339, #73013, #71670, #52730, #78428, #86999, #25271, #30688, #11309 ),
 .UNSPECIFIED., .F., .F.,
 ( 4, 2, 2, 2, 4 ),
 ( 0.0007817359430256297891, 0.0009771253907249961065, 0.001172514838424362424, 0.001367904286123728741, 0.001563293733823095059 ),
 .UNSPECIFIED. ) ;
#54720 = ORIENTED_EDGE ( 'NONE', *, *, #88799, .F. ) ;
#54722 = ORIENTED_EDGE ( 'NONE', *, *, #5164, .F. ) ;
#54721 = CARTESIAN_POINT ( 'NONE',  ( 11.47319109250076430, -9.442884908240170461, 34.35708131394840592 ) ) ;
#54723 = DIRECTION ( 'NONE',  ( 0.000000000000000000, 0.1736481776669267785, -0.9848077530122087975 ) ) ;
#54724 = CARTESIAN_POINT ( 'NONE',  ( -17.07692307692277112, -2.506253911140615021, 30.00000000000323297 ) ) ;
#54725 = EDGE_CURVE ( 'NONE', #30706, #79011, #79740, .T. ) ;
#54726 = CARTESIAN_POINT ( 'NONE',  ( -1.553300858899081760, -11.25000000000000888, 18.60937500000000355 ) ) ;
#54727 = ORIENTED_EDGE ( 'NONE', *, *, #65014, .T. ) ;
#54728 = VECTOR ( 'NONE', #72471, 999.9999999999998863 ) ;
#54729 = CARTESIAN_POINT ( 'NONE',  ( -1.161835715637319133, -2.612705202774697533, 31.66806509827799943 ) ) ;
#54730 = EDGE_CURVE ( 'NONE', #84238, #51881, #63610, .T. ) ;
#54731 = VERTEX_POINT ( 'NONE', #41180 ) ;
#54732 = EDGE_CURVE ( 'NONE', #71085, #30670, #25964, .T. ) ;
#54733 = CARTESIAN_POINT ( 'NONE',  ( 2.241608896736428047, -6.386643153685125363, 34.62446782046654903 ) ) ;
#54734 = FACE_BOUND ( 'NONE', #71832, .T. ) ;
#54736 = VECTOR ( 'NONE', #29152, 1000.000000000000000 ) ;
#54735 = CARTESIAN_POINT ( 'NONE',  ( -2.057746898314263273, -4.932303261841488151, 34.32971442181322885 ) ) ;
#54737 = AXIS2_PLACEMENT_3D ( 'NONE', #2224, #16628, #36900 ) ;
#54738 = EDGE_CURVE ( 'NONE', #20850, #82752, #59303, .T. ) ;
#54739 = DIRECTION ( 'NONE',  ( -1.000000000000000000, -0.000000000000000000, -0.000000000000000000 ) ) ;
#54740 = ORIENTED_EDGE ( 'NONE', *, *, #69907, .T. ) ;
#54741 = CARTESIAN_POINT ( 'NONE',  ( -10.86538461538461320, -2.499999999999998668, 29.75000000000000355 ) ) ;
#54742 = PRESENTATION_STYLE_ASSIGNMENT (( #82229 ) ) ;
#54743 = CARTESIAN_POINT ( 'NONE',  ( -0.4615384615381544209, -2.506253911140615021, 30.00000000000323297 ) ) ;
#54744 = CARTESIAN_POINT ( 'NONE',  ( 15.36155967173618286, -6.369690395747422684, 34.87708834333098196 ) ) ;
#54745 = ORIENTED_EDGE ( 'NONE', *, *, #26377, .T. ) ;
#54746 = VECTOR ( 'NONE', #31269, 1000.000000000000000 ) ;
#54747 = EDGE_CURVE ( 'NONE', #86296, #54717, #82625, .T. ) ;
#54748 = PRODUCT_DEFINITION_FORMATION_WITH_SPECIFIED_SOURCE ( 'ANY', '', #75728, .NOT_KNOWN. ) ;
#54749 = CARTESIAN_POINT ( 'NONE',  ( -0.2115384615370421995, -7.500000000000154543, 35.00000000000007105 ) ) ;
#54750 = CARTESIAN_POINT ( 'NONE',  ( 1.318533005255251744, -3.937682226553329556, 33.60647404775217240 ) ) ;
#54751 = CARTESIAN_POINT ( 'NONE',  ( 18.00000000000000000, -12.48256725967547354, 35.29906147534542527 ) ) ;
#54752 = DIRECTION ( 'NONE',  ( 0.000000000000000000, 0.4999999999999960032, -0.8660254037844410391 ) ) ;
#54753 = CARTESIAN_POINT ( 'NONE',  ( -20.99999999999999645, -4.249999999999998224, 27.25000000000000000 ) ) ;
#54754 = FACE_BOUND ( 'NONE', #56186, .T. ) ;
#54756 = CARTESIAN_POINT ( 'NONE',  ( -17.20761368003338632, -10.70098750199973203, 33.91152734681376302 ) ) ;
#54755 = CARTESIAN_POINT ( 'NONE',  ( 13.16168842570853492, -11.98009711892699514, 32.48740034544076138 ) ) ;
#54757 = CARTESIAN_POINT ( 'NONE',  ( -7.053224132515145683, -12.27039167877662251, 31.24851455888617835 ) ) ;
#54759 = CARTESIAN_POINT ( 'NONE',  ( 15.36129493253279499, -10.19071101563364756, 33.96452234770658407 ) ) ;
#54758 = CARTESIAN_POINT ( 'NONE',  ( 2.980769230769232170, -7.500000000000001776, 34.75000000000000000 ) ) ;
#54760 = CARTESIAN_POINT ( 'NONE',  ( -8.096130590202436750, -4.075325502946081535, 33.72974371597206300 ) ) ;
#54761 = CARTESIAN_POINT ( 'NONE',  ( 2.775308065498768517, -8.577988221561467341, 18.04500670625848713 ) ) ;
#54762 = ORIENTED_EDGE ( 'NONE', *, *, #32693, .F. ) ;
#54763 = CARTESIAN_POINT ( 'NONE',  ( -8.703061628268114802, -7.250054483168843156, 34.74374881642865631 ) ) ;
#54764 = ORIENTED_EDGE ( 'NONE', *, *, #18584, .T. ) ;
#54765 = DIRECTION ( 'NONE',  ( -0.000000000000000000, 1.000000000000000000, 3.491481338843133355E-15 ) ) ;
#54766 = ORIENTED_EDGE ( 'NONE', *, *, #47592, .F. ) ;
#54767 = CYLINDRICAL_SURFACE ( 'NONE', #8173, 0.2499999999999995559 ) ;
#54768 = CARTESIAN_POINT ( 'NONE',  ( -16.15384615384615330, -11.91647553114624181, 32.58852847137148245 ) ) ;
#54770 = ORIENTED_EDGE ( 'NONE', *, *, #50588, .F. ) ;
#54769 = DIRECTION ( 'NONE',  ( 0.000000000000000000, 0.000000000000000000, -1.000000000000000000 ) ) ;
#54771 = CARTESIAN_POINT ( 'NONE',  ( -15.36091644020745051, -5.195881422630166391, 34.18770438780619259 ) ) ;
#54772 = CARTESIAN_POINT ( 'NONE',  ( 2.750000000000001332, -7.438900925035452083, 17.96688170625848713 ) ) ;
#54773 = EDGE_CURVE ( 'NONE', #59060, #64127, #79393, .T. ) ;
#54774 = CARTESIAN_POINT ( 'NONE',  ( -15.48079245499068435, -9.356822207818506598, 34.66110646841856635 ) ) ;
#54775 = DIRECTION ( 'NONE',  ( -1.000000000000000000, -0.000000000000000000, 0.000000000000000000 ) ) ;
#54776 = CARTESIAN_POINT ( 'NONE',  ( 17.01165263096229907, -12.46129190929999986, 30.37095296980880832 ) ) ;
#54777 = LINE ( 'NONE', #69186, #7064 ) ;
#54778 = CARTESIAN_POINT ( 'NONE',  ( -0.3307466537136745655, -4.118422570099827595, 33.43335022499816489 ) ) ;
#54779 = DIRECTION ( 'NONE',  ( -0.000000000000000000, 0.6427876096865404731, -0.7660444431189770143 ) ) ;
#54780 = B_SPLINE_CURVE_WITH_KNOTS ( 'NONE', 3,
 ( #72473, #31034, #80130, #31947, #72921, #4005, #17088, #10781, #44541, #51279 ),
 .UNSPECIFIED., .F., .F.,
 ( 4, 2, 2, 2, 4 ),
 ( 0.000000000000000000, 0.0001954311564186864407, 0.0003908623128373728815, 0.0005862934692560593493, 0.0007817246256747457630 ),
 .UNSPECIFIED. ) ;
#54781 = CARTESIAN_POINT ( 'NONE',  ( -3.724691934501248802, -5.885600066136383646, 22.92374329374151998 ) ) ;
#54782 = CARTESIAN_POINT ( 'NONE',  ( -16.15384615384615330, -1.422936976036506707, 30.56769352161908415 ) ) ;
#54783 = CARTESIAN_POINT ( 'NONE',  ( -4.284536756956462078, -2.845849958028613624, 32.17971566917920967 ) ) ;
#54784 = VERTEX_POINT ( 'NONE', #23113 ) ;
#54785 = VECTOR ( 'NONE', #82387, 1000.000000000000227 ) ;
#54786 = CARTESIAN_POINT ( 'NONE',  ( 9.442307692307693401, -7.500000000000001776, 35.04278698407183867 ) ) ;
#54787 = CARTESIAN_POINT ( 'NONE',  ( -3.724691934501248802, -5.885600066136383646, 21.67374329374151287 ) ) ;
#54788 = CARTESIAN_POINT ( 'NONE',  ( -17.75005448165186195, -12.43552623307873972, 30.55307653245132826 ) ) ;
#54789 = CARTESIAN_POINT ( 'NONE',  ( 17.32686859527121825, -11.86320923018887541, 32.19269448109604781 ) ) ;
#54790 = VERTEX_POINT ( 'NONE', #29444 ) ;
#54791 = CARTESIAN_POINT ( 'NONE',  ( 1.607395053593451806, -8.540255544307065350, 34.89611431652622286 ) ) ;
#54792 = CARTESIAN_POINT ( 'NONE',  ( -19.50000000000000000, -11.50000000000000000, 29.75000000000000355 ) ) ;
#54794 = ORIENTED_EDGE ( 'NONE', *, *, #27771, .T. ) ;
#54793 = CARTESIAN_POINT ( 'NONE',  ( -5.076923076923197442, -6.026961402154118908, 34.52809138561165270 ) ) ;
#54795 = DIRECTION ( 'NONE',  ( -0.000000000000000000, -0.9396926207859092051, -0.3420201433256662704 ) ) ;
#54796 = B_SPLINE_CURVE_WITH_KNOTS ( 'NONE', 3,
 ( #12498, #88625, #75966, #67883, #19691, #34089, #82292, #7515, #81408, #34971 ),
 .UNSPECIFIED., .F., .F.,
 ( 4, 2, 2, 2, 4 ),
 ( 0.0007817246256747446788, 0.0009771112852218874663, 0.001172497944769030145, 0.001367884604316172825, 0.001563271263863315720 ),
 .UNSPECIFIED. ) ;
#54797 = CARTESIAN_POINT ( 'NONE',  ( 5.299886211189750895, -7.369474539155828730, 34.99858011523957657 ) ) ;
#54798 = CARTESIAN_POINT ( 'NONE',  ( 16.02369894440793630, -9.418419913701741919, 34.36755862841477693 ) ) ;
#54799 = B_SPLINE_CURVE_WITH_KNOTS ( 'NONE', 3,
 ( #27347, #67451, #26906, #82300, #20148, #20581, #48047, #59798, #88633, #75526 ),
 .UNSPECIFIED., .F., .F.,
 ( 4, 2, 2, 2, 4 ),
 ( 0.000000000000000000, 0.0001954339857564099680, 0.0003908679715128199361, 0.0005863019572692299312, 0.0007817359430256398721 ),
 .UNSPECIFIED. ) ;
#54800 = CARTESIAN_POINT ( 'NONE',  ( 2.057715563643716994, -4.075325502946086864, 33.72974371597207721 ) ) ;
#54801 = CARTESIAN_POINT ( 'NONE',  ( 6.792929713638702793, -5.195881422630167279, 34.18770438780618548 ) ) ;
#54802 = EDGE_CURVE ( 'NONE', #38366, #18924, #35713, .T. ) ;
#54803 = EDGE_CURVE ( 'NONE', #6878, #36243, #19016, .T. ) ;
#54804 = AXIS2_PLACEMENT_3D ( 'NONE', #83370, #41489, #68957 ) ;
#54805 = ORIENTED_EDGE ( 'NONE', *, *, #16887, .F. ) ;
#54806 = EDGE_LOOP ( 'NONE', ( #28150, #71984, #65494, #56410 ) ) ;
#54807 = ORIENTED_EDGE ( 'NONE', *, *, #82435, .F. ) ;
#54808 = ADVANCED_FACE ( 'NONE', ( #71731 ), #37058, .F. ) ;
#54809 = ORIENTED_EDGE ( 'NONE', *, *, #76660, .F. ) ;
#54810 = AXIS2_PLACEMENT_3D ( 'NONE', #4098, #31127, #65363 ) ;
#54811 = AXIS2_PLACEMENT_3D ( 'NONE', #86456, #67058, #24730 ) ;
#54812 = CARTESIAN_POINT ( 'NONE',  ( -13.44988583057615728, -3.835265460703609186, 33.15142922261924241 ) ) ;
#54813 = CYLINDRICAL_SURFACE ( 'NONE', #47238, 0.2500000000000004996 ) ;
#54814 = EDGE_CURVE ( 'NONE', #20693, #1437, #15286, .T. ) ;
#54815 = CARTESIAN_POINT ( 'NONE',  ( 2.307692307692309264, -5.557115091759785130, 34.35708131394839171 ) ) ;
#54816 = CARTESIAN_POINT ( 'NONE',  ( -16.94687564167263005, -7.723484941389743952, 34.99544897038808955 ) ) ;
#54817 = VECTOR ( 'NONE', #28063, 999.9999999999998863 ) ;
#54818 = EDGE_CURVE ( 'NONE', #11535, #20749, #72218, .T. ) ;
#54819 = CARTESIAN_POINT ( 'NONE',  ( -16.94613126909829148, -4.809403383903226192, 33.96459661697924304 ) ) ;
#54820 = ORIENTED_EDGE ( 'NONE', *, *, #4194, .T. ) ;
#54821 = ORIENTED_EDGE ( 'NONE', *, *, #48086, .F. ) ;
#54822 = VERTEX_POINT ( 'NONE', #71287 ) ;
#54824 = EDGE_LOOP ( 'NONE', ( #16258, #40889, #47410, #42262 ) ) ;
#54823 = CARTESIAN_POINT ( 'NONE',  ( -7.146003881983769901, -2.523278758544489797, 31.42238647778637528 ) ) ;
#54825 = FACE_OUTER_BOUND ( 'NONE', #86196, .T. ) ;
#54826 = EDGE_CURVE ( 'NONE', #7446, #45168, #70771, .T. ) ;
#54827 = B_SPLINE_CURVE_WITH_KNOTS ( 'NONE', 3,
 ( #63107, #20372, #82076, #6842, #7297, #55911, #62662, #48713, #83406, #1419 ),
 .UNSPECIFIED., .F., .F.,
 ( 4, 2, 2, 2, 4 ),
 ( 0.0007817246256747472808, 0.0009771112852218907189, 0.001172497944769034265, 0.001367884604316177595, 0.001563271263863321141 ),
 .UNSPECIFIED. ) ;
#54828 = DIRECTION ( 'NONE',  ( 0.000000000000000000, 0.7660444431189807890, 0.6427876096865361433 ) ) ;
#54829 = B_SPLINE_CURVE_WITH_KNOTS ( 'NONE', 3,
 ( #8049, #35518, #1278, #7161, #21554, #28768, #406, #22440, #15693, #55776 ),
 .UNSPECIFIED., .F., .F.,
 ( 4, 2, 2, 2, 4 ),
 ( 0.000000000000000000, 0.0001954311564186873623, 0.0003908623128373747246, 0.0005862934692560620598, 0.0007817246256747494492 ),
 .UNSPECIFIED. ) ;
#54830 = EDGE_CURVE ( 'NONE', #57014, #43002, #27093, .T. ) ;
#54831 = DIRECTION ( 'NONE',  ( -1.000000000000000000, -0.000000000000000000, 0.000000000000000000 ) ) ;
#54832 = CARTESIAN_POINT ( 'NONE',  ( -5.934744428723973897, -4.481592998940251427, 33.73612834413965089 ) ) ;
#54833 = VERTEX_POINT ( 'NONE', #2384 ) ;
#54834 = ORIENTED_EDGE ( 'NONE', *, *, #79424, .T. ) ;
#54835 = EDGE_LOOP ( 'NONE', ( #49410, #73545, #24238, #316 ) ) ;
#54836 = CARTESIAN_POINT ( 'NONE',  ( 14.37375964104238513, -10.67929555188718282, 33.92786785259544757 ) ) ;
#54838 = VERTEX_POINT ( 'NONE', #29879 ) ;
#54837 = CYLINDRICAL_SURFACE ( 'NONE', #58872, 0.2500000000000009437 ) ;
#54839 = CARTESIAN_POINT ( 'NONE',  ( -11.40767109749459074, -12.62708834333097663, 30.88030960425257021 ) ) ;
#54840 = VECTOR ( 'NONE', #48161, 1000.000000000000000 ) ;
#54841 = EDGE_CURVE ( 'NONE', #57687, #19139, #63652, .T. ) ;
#54842 = CARTESIAN_POINT ( 'NONE',  ( -0.6850233861027926752, -6.716662450894490100, 34.94144148231605840 ) ) ;
#54843 = ORIENTED_EDGE ( 'NONE', *, *, #34410, .F. ) ;
#54844 = AXIS2_PLACEMENT_3D ( 'NONE', #84372, #29862, #42938 ) ;
#54845 = PLANE ( 'NONE',  #71001 ) ;
#54846 = CARTESIAN_POINT ( 'NONE',  ( 4.480769230769229061, -7.500000000000000000, 29.75000000000000355 ) ) ;
#54847 = ORIENTED_EDGE ( 'NONE', *, *, #76555, .F. ) ;
#54848 = FACE_BOUND ( 'NONE', #72046, .T. ) ;
#54849 = EDGE_CURVE ( 'NONE', #38767, #39886, #16791, .T. ) ;
#54850 = B_SPLINE_CURVE_WITH_KNOTS ( 'NONE', 3,
 ( #88384, #81172, #13147, #19895, #53233, #47364, #39299, #80736, #19456, #46918 ),
 .UNSPECIFIED., .F., .F.,
 ( 4, 2, 2, 2, 4 ),
 ( 0.000000000000000000, 0.0001954339857564070678, 0.0003908679715128141356, 0.0005863019572692211492, 0.0007817359430256282712 ),
 .UNSPECIFIED. ) ;
#54851 = LINE ( 'NONE', #12981, #42750 ) ;
#54852 = CARTESIAN_POINT ( 'NONE',  ( 16.15384615384615330, -2.486705287966279876, 31.30864560766543647 ) ) ;
#54853 = CARTESIAN_POINT ( 'NONE',  ( 12.46153846153833911, -6.835583212225970762, 34.95778746994575670 ) ) ;
#54855 = CARTESIAN_POINT ( 'NONE',  ( 18.22277954126840172, -4.387253974876675677, 33.66317474335728832 ) ) ;
#54854 = CARTESIAN_POINT ( 'NONE',  ( -17.75000000000000711, -12.75000000000000178, 29.81919447696817116 ) ) ;
#54856 = CARTESIAN_POINT ( 'NONE',  ( -4.153846153846273204, -2.892918686052165622, 31.69288490824153470 ) ) ;
#54857 = LINE ( 'NONE', #82341, #1646 ) ;
#54858 = EDGE_LOOP ( 'NONE', ( #74891, #59591, #80090, #11446 ) ) ;
#54859 = LINE ( 'NONE', #364, #44637 ) ;
#54860 = CARTESIAN_POINT ( 'NONE',  ( -7.911404836315086619, -2.506253911140460922, 30.00000000000013856 ) ) ;
#54861 = EDGE_LOOP ( 'NONE', ( #56023, #25307, #82747, #73677 ) ) ;
#54862 = EDGE_CURVE ( 'NONE', #48928, #18617, #78606, .T. ) ;
#54863 = DIRECTION ( 'NONE',  ( -1.000000000000000000, 0.000000000000000000, -0.000000000000000000 ) ) ;
#54864 = PRODUCT ( 'spring', 'spring', '', ( #40156 ) ) ;
#54865 = CARTESIAN_POINT ( 'NONE',  ( 9.442284455014727129, -2.823816976329317274, 31.52131813110795733 ) ) ;
#54866 = ORIENTED_EDGE ( 'NONE', *, *, #25633, .T. ) ;
#54867 = DIRECTION ( 'NONE',  ( -0.000000000000000000, -0.5000000000000009992, -0.8660254037844380415 ) ) ;
#54868 = CARTESIAN_POINT ( 'NONE',  ( -7.053768389744483613, -9.804603061927743113, 34.18744698557895845 ) ) ;
#54869 = FACE_BOUND ( 'NONE', #61464, .T. ) ;
#54870 = ADVANCED_FACE ( 'NONE', ( #21115 ), #74754, .T. ) ;
#54872 = CARTESIAN_POINT ( 'NONE',  ( 3.930361229281820190, -12.47654668319379567, 31.42292124445336654 ) ) ;
#54871 = DIRECTION ( 'NONE',  ( 1.000000000000000000, 0.000000000000000000, 0.000000000000000000 ) ) ;
#54873 = CARTESIAN_POINT ( 'NONE',  ( -14.16025641025641058, -7.500000000000000000, 29.75000000000000355 ) ) ;
#54874 = CARTESIAN_POINT ( 'NONE',  ( 9.692307692307695177, -6.435427911321262684, 35.78748833219616898 ) ) ;
#54876 = LINE ( 'NONE', #6687, #31996 ) ;
#54875 = CARTESIAN_POINT ( 'NONE',  ( 0.000000000000000000, 15.00000000000000000, 0.000000000000000000 ) ) ;
#54877 = B_SPLINE_CURVE_WITH_KNOTS ( 'NONE', 3,
 ( #60743, #26526, #40491, #67955, #33721, #89129, #20641, #15226, #50753, #1251 ),
 .UNSPECIFIED., .F., .F.,
 ( 4, 2, 2, 2, 4 ),
 ( 0.000000000000000000, 0.0001954311584214072923, 0.0003908623168428145846, 0.0005862934752642218498, 0.0007817246336856291692 ),
 .UNSPECIFIED. ) ;
#54878 = CARTESIAN_POINT ( 'NONE',  ( 3.750000000000009770, -9.053300858899081760, 25.79687500000000355 ) ) ;
#54879 = ORIENTED_EDGE ( 'NONE', *, *, #50500, .T. ) ;
#54880 = B_SPLINE_CURVE_WITH_KNOTS ( 'NONE', 3,
 ( #39060, #79591, #47118, #74608, #80483, #40389, #67847, #18330, #17888, #46246 ),
 .UNSPECIFIED., .F., .F.,
 ( 4, 2, 2, 2, 4 ),
 ( 0.0007817246256747519429, 0.0009771112852218959231, 0.001172497944769039686, 0.001367884604316183667, 0.001563271263863327647 ),
 .UNSPECIFIED. ) ;
#54881 = AXIS2_PLACEMENT_3D ( 'NONE', #75029, #67378, #25942 ) ;
#54882 = ORIENTED_EDGE ( 'NONE', *, *, #14503, .T. ) ;
#54883 = LINE ( 'NONE', #67516, #76574 ) ;
#54884 = FACE_OUTER_BOUND ( 'NONE', #12132, .T. ) ;
#54885 = CARTESIAN_POINT ( 'NONE',  ( 14.37375964104238513, -9.058645607665452459, 34.76329471203371924 ) ) ;
#54886 = CARTESIAN_POINT ( 'NONE',  ( 10.83839745947801347, -2.889357225399416418, 32.26129605718031002 ) ) ;
#54887 = CARTESIAN_POINT ( 'NONE',  ( 5.207448515156721136, -3.625058011473227815, 33.29252011169590020 ) ) ;
#54888 = CARTESIAN_POINT ( 'NONE',  ( -2.694853999681210865, -4.891553140782108677, 16.24813170625848713 ) ) ;
#54889 = EDGE_CURVE ( 'NONE', #10626, #1790, #42093, .T. ) ;
#54890 = CARTESIAN_POINT ( 'NONE',  ( 14.30769230769231015, -5.471508081941601098, 34.59228464037088457 ) ) ;
#54891 = CARTESIAN_POINT ( 'NONE',  ( 5.933917620639865831, -2.833524468853757305, 32.15551576947924417 ) ) ;
#54892 = EDGE_CURVE ( 'NONE', #85253, #73759, #71098, .T. ) ;
#54893 = CARTESIAN_POINT ( 'NONE',  ( 6.130525438233648039, -4.299079248970732792, 33.91157788607253565 ) ) ;
#54894 = CARTESIAN_POINT ( 'NONE',  ( -4.853910232829682592, -2.308499170217967134, 30.53291367094873721 ) ) ;
#54895 = DIRECTION ( 'NONE',  ( -0.000000000000000000, -0.8660254037844397068, -0.4999999999999978906 ) ) ;
#54896 = CARTESIAN_POINT ( 'NONE',  ( 18.22301135161285046, -9.886259254753566594, 34.14407573483972413 ) ) ;
#54897 = CARTESIAN_POINT ( 'NONE',  ( 5.777073782483852504, -12.15238873228292071, 31.58232369045353849 ) ) ;
#54898 = CARTESIAN_POINT ( 'NONE',  ( -6.673022503163469565, -3.435999193479609914, 33.07426656108010832 ) ) ;
#54899 = DIRECTION ( 'NONE',  ( 0.000000000000000000, 0.1736481776669275834, 0.9848077530122086864 ) ) ;
#54900 = ORIENTED_EDGE ( 'NONE', *, *, #62979, .T. ) ;
#54901 = CARTESIAN_POINT ( 'NONE',  ( 3.930919936330005360, -4.887634598454295265, 34.01352882383564946 ) ) ;
#54902 = CARTESIAN_POINT ( 'NONE',  ( 0.5923302693632462868, -2.541949514083464479, 30.39797389878540557 ) ) ;
#54903 = CARTESIAN_POINT ( 'NONE',  ( -2.724691934501246582, -6.299813628509474128, 22.92374329374151998 ) ) ;
#54904 = DIRECTION ( 'NONE',  ( -0.000000000000000000, 0.000000000000000000, 1.000000000000000000 ) ) ;
#54905 = FACE_OUTER_BOUND ( 'NONE', #50887, .T. ) ;
#54906 = CYLINDRICAL_SURFACE ( 'NONE', #51386, 0.2499999999999994726 ) ;
#54908 = ORIENTED_EDGE ( 'NONE', *, *, #31627, .F. ) ;
#54907 = LINE ( 'NONE', #54455, #82872 ) ;
#54909 = CARTESIAN_POINT ( 'NONE',  ( 2.750000000000008438, -8.639087296525996607, 25.79687500000000355 ) ) ;
#54910 = CARTESIAN_POINT ( 'NONE',  ( 16.94677510719138169, -2.647304123082329763, 31.75400227202886683 ) ) ;
#54911 = EDGE_LOOP ( 'NONE', ( #85414, #25135, #84803, #7260 ) ) ;
#54912 = CARTESIAN_POINT ( 'NONE',  ( 6.000000000000001776, -13.49023893513002648, 31.06009739812518688 ) ) ;
#54913 = DIRECTION ( 'NONE',  ( -0.000000000000000000, 0.000000000000000000, 1.000000000000000000 ) ) ;
#54914 = B_SPLINE_CURVE_WITH_KNOTS ( 'NONE', 3,
 ( #5553, #6443, #33901, #46966, #60042, #75343, #41112, #26264, #54164, #33024 ),
 .UNSPECIFIED., .F., .F.,
 ( 4, 2, 2, 2, 4 ),
 ( 0.0007817359430256372700, 0.0009771253907250054306, 0.001172514838424373700, 0.001367904286123741969, 0.001563293733823110021 ),
 .UNSPECIFIED. ) ;
#54915 = VERTEX_POINT ( 'NONE', #47710 ) ;
#54917 = B_SPLINE_CURVE_WITH_KNOTS ( 'NONE', 3,
 ( #19258, #40426, #46724, #74202, #39983, #68325, #67885, #67445, #75092, #13377 ),
 .UNSPECIFIED., .F., .F.,
 ( 4, 2, 2, 2, 4 ),
 ( 0.0007817246256747484735, 0.0009771112852218928873, 0.001172497944769037084, 0.001367884604316181498, 0.001563271263863325912 ),
 .UNSPECIFIED. ) ;
#54916 = CIRCLE ( 'NONE', #20386, 4.000000000000000000 ) ;
#54918 = CARTESIAN_POINT ( 'NONE',  ( 14.24242186173153435, -2.625532179533445198, 30.86335684631481513 ) ) ;
#54919 = DIRECTION ( 'NONE',  ( -0.000000000000000000, 0.6427876096865404731, -0.7660444431189771253 ) ) ;
#54920 = CARTESIAN_POINT ( 'NONE',  ( -15.16551365949320562, -12.46129190930001052, 30.37095296980870174 ) ) ;
#54921 = EDGE_LOOP ( 'NONE', ( #39366, #86302, #10847, #22881 ) ) ;
#54923 = EDGE_LOOP ( 'NONE', ( #69370, #77838, #4405, #9019 ) ) ;
#54922 = VECTOR ( 'NONE', #33428, 1000.000000000000000 ) ;
#54924 = DIRECTION ( 'NONE',  ( -0.000000000000000000, 1.000000000000000000, 3.491481338843133355E-15 ) ) ;
#54925 = ORIENTED_EDGE ( 'NONE', *, *, #15921, .T. ) ;
#54926 = CARTESIAN_POINT ( 'NONE',  ( -7.976844449264155479, -2.295517848115769421, 30.44137282052137294 ) ) ;
#54927 = CARTESIAN_POINT ( 'NONE',  ( 12.46153846153846168, -8.973038597847269315, 34.52809138561121927 ) ) ;
#54928 = CARTESIAN_POINT ( 'NONE',  ( -17.32689980786543060, -5.728515186090277211, 34.42611988154120439 ) ) ;
#54929 = EDGE_CURVE ( 'NONE', #68374, #3616, #86609, .T. ) ;
#54930 = CARTESIAN_POINT ( 'NONE',  ( -2.307692307692427391, -6.026961402154118908, 34.52809138561165270 ) ) ;
#54931 = CYLINDRICAL_SURFACE ( 'NONE', #33473, 0.2500000000000009437 ) ;
#54932 = CARTESIAN_POINT ( 'NONE',  ( 1.319345384059066983, -2.379036618887870880, 30.90682066428147579 ) ) ;
#54933 = ADVANCED_FACE ( 'NONE', ( #13483 ), #13044, .F. ) ;
#54934 = CARTESIAN_POINT ( 'NONE',  ( 10.54930120442873687, -12.10708131394839349, 31.69288490824020244 ) ) ;
#54935 = VERTEX_POINT ( 'NONE', #31647 ) ;
#54936 = VERTEX_POINT ( 'NONE', #33757 ) ;
#54938 = ORIENTED_EDGE ( 'NONE', *, *, #36108, .F. ) ;
#54937 = CARTESIAN_POINT ( 'NONE',  ( -0.3310127597748961925, -12.27024696741798770, 31.24895572276497546 ) ) ;
#54939 = EDGE_CURVE ( 'NONE', #84958, #33781, #59109, .T. ) ;
#54940 = LINE ( 'NONE', #61682, #78133 ) ;
#54941 = VECTOR ( 'NONE', #51738, 1000.000000000000000 ) ;
#54942 = AXIS2_PLACEMENT_3D ( 'NONE', #64843, #86485, #45467 ) ;
#54943 = CARTESIAN_POINT ( 'NONE',  ( 10.48482470177125059, -2.254533558242299396, 29.97296025877828285 ) ) ;
#54944 = CARTESIAN_POINT ( 'NONE',  ( 11.53846153846153832, -12.10708131394839349, 31.69288490824020244 ) ) ;
#54945 = ORIENTED_EDGE ( 'NONE', *, *, #83067, .T. ) ;
#54946 = CARTESIAN_POINT ( 'NONE',  ( -12.33101275977489841, -6.001044277235009439, 34.52024696741798948 ) ) ;
#54947 = AXIS2_PLACEMENT_3D ( 'NONE', #291, #75951, #28195 ) ;
#54948 = ADVANCED_FACE ( 'NONE', ( #67994 ), #67547, .F. ) ;
#54949 = ORIENTED_EDGE ( 'NONE', *, *, #1303, .T. ) ;
#54950 = LINE ( 'NONE', #13957, #75622 ) ;
#54951 = VERTEX_POINT ( 'NONE', #5846 ) ;
#54952 = CARTESIAN_POINT ( 'NONE',  ( 7.846153846153846700, -9.780366693483667717, 34.19971097300155094 ) ) ;
#54953 = ORIENTED_EDGE ( 'NONE', *, *, #63224, .F. ) ;
#54954 = CARTESIAN_POINT ( 'NONE',  ( -8.835314180186648159, -4.786620604624113540, 33.94971097300155805 ) ) ;
#54955 = CARTESIAN_POINT ( 'NONE',  ( 22.00000000000001066, -9.999999999999957367, 13.00000000000000178 ) ) ;
#54956 = FACE_BOUND ( 'NONE', #35572, .T. ) ;
#54957 = EDGE_CURVE ( 'NONE', #87554, #76215, #67928, .T. ) ;
#54958 = DIRECTION ( 'NONE',  ( -0.000000000000000000, 1.000000000000000000, -0.000000000000000000 ) ) ;
#54959 = CARTESIAN_POINT ( 'NONE',  ( 15.90382292962469890, -3.520140089381496473, 33.17453946501458262 ) ) ;
#54960 = CARTESIAN_POINT ( 'NONE',  ( -16.15384615384615330, -4.661471528628507777, 34.16647553114623292 ) ) ;
#54961 = CARTESIAN_POINT ( 'NONE',  ( 17.07692307692307665, -13.95598074871891292, 31.83374038241031911 ) ) ;
#54962 = LINE ( 'NONE', #41901, #22262 ) ;
#54963 = DIRECTION ( 'NONE',  ( 0.000000000000000000, 0.000000000000000000, 1.000000000000000000 ) ) ;
#54964 = ADVANCED_FACE ( 'NONE', ( #75616 ), #83729, .T. ) ;
#54965 = CARTESIAN_POINT ( 'NONE',  ( -14.30769230769242739, -3.835265460704628371, 33.15142922262033665 ) ) ;
#54966 = ORIENTED_EDGE ( 'NONE', *, *, #87400, .F. ) ;
#54967 = B_SPLINE_CURVE_WITH_KNOTS ( 'NONE', 3,
 ( #76316, #49730, #84423, #14623, #42543, #7428, #63246, #27687, #223, #29037 ),
 .UNSPECIFIED., .F., .F.,
 ( 4, 2, 2, 2, 4 ),
 ( 0.000000000000000000, 0.0001954311564186882568, 0.0003908623128373765136, 0.0005862934692560647703, 0.0007817246256747530271 ),
 .UNSPECIFIED. ) ;
#54968 = EDGE_LOOP ( 'NONE', ( #39802, #16679, #20565, #69973, #72526, #9936, #9436, #46778 ) ) ;
#54970 = CARTESIAN_POINT ( 'NONE',  ( 8.069165197766697162, -9.886259254753566594, 34.14407573483972413 ) ) ;
#54969 = CARTESIAN_POINT ( 'NONE',  ( 17.07692307692307665, -12.48256725967547354, 35.29906147534542527 ) ) ;
#54971 = AXIS2_PLACEMENT_3D ( 'NONE', #86470, #80138, #18439 ) ;
#54972 = CARTESIAN_POINT ( 'NONE',  ( -12.46153846153858247, -2.625532179533778709, 30.86335684631627174 ) ) ;
#54973 = CARTESIAN_POINT ( 'NONE',  ( 3.480823542407545546, -10.66356715214248396, 33.62249196103329751 ) ) ;
#54974 = CARTESIAN_POINT ( 'NONE',  ( -17.30040800148741553, -12.47654668319379567, 31.42292124445336654 ) ) ;
#54975 = CARTESIAN_POINT ( 'NONE',  ( 9.757563263583721280, -2.625532179533470512, 30.86335684631491105 ) ) ;
#54976 = VERTEX_POINT ( 'NONE', #30097 ) ;
#54977 = CARTESIAN_POINT ( 'NONE',  ( -5.750054590621955342, -8.476813868363244353, 34.90874843262270133 ) ) ;
#54978 = EDGE_CURVE ( 'NONE', #32754, #4121, #2342, .T. ) ;
#54979 = CARTESIAN_POINT ( 'NONE',  ( 3.480714749117373330, -11.37275283266503756, 32.91324779482534524 ) ) ;
#54980 = CARTESIAN_POINT ( 'NONE',  ( -14.24162497434223162, -12.34228464037088813, 31.77849191805839268 ) ) ;
#54981 = CARTESIAN_POINT ( 'NONE',  ( 3.230769230769231726, -3.050289026998446396, 32.03036669348365706 ) ) ;
#54982 = ORIENTED_EDGE ( 'NONE', *, *, #81443, .T. ) ;
#54983 = ORIENTED_EDGE ( 'NONE', *, *, #83582, .F. ) ;
#54984 = ORIENTED_EDGE ( 'NONE', *, *, #35536, .F. ) ;
#54985 = DIRECTION ( 'NONE',  ( -0.000000000000000000, 0.7660444431189791237, -0.6427876096865379196 ) ) ;
#54986 = VERTEX_POINT ( 'NONE', #76516 ) ;
#54987 = CARTESIAN_POINT ( 'NONE',  ( -9.822454901745912181, -12.45813303252208648, 30.39737893381572675 ) ) ;
#54988 = CARTESIAN_POINT ( 'NONE',  ( -12.23875892027004930, -6.760870238392817200, 34.69528174975672385 ) ) ;
#54989 = CARTESIAN_POINT ( 'NONE',  ( 5.076923076922954969, -6.879047030192662504, 34.71129190930017927 ) ) ;
#54990 = CARTESIAN_POINT ( 'NONE',  ( -16.94613126909829148, -12.11778462344220841, 31.66786338562085135 ) ) ;
#54991 = ADVANCED_FACE ( 'NONE', ( #85051 ), #15705, .F. ) ;
#54992 = CARTESIAN_POINT ( 'NONE',  ( 9.915087233576102221, -5.913360116392397892, 34.49180327182771322 ) ) ;
#54993 = VERTEX_POINT ( 'NONE', #49490 ) ;
#54994 = DIRECTION ( 'NONE',  ( 1.000000000000000000, 8.673617379884044347E-16, 0.000000000000000000 ) ) ;
#54996 = ORIENTED_EDGE ( 'NONE', *, *, #22345, .F. ) ;
#54995 = CARTESIAN_POINT ( 'NONE',  ( -0.5916864312701560769, -5.915902021225892149, 34.75552854090298638 ) ) ;
#54997 = CARTESIAN_POINT ( 'NONE',  ( -5.143005456283213483, -2.292212530054419606, 30.41441678777542634 ) ) ;
#54998 = DIRECTION ( 'NONE',  ( 0.000000000000000000, -6.938893903907222067E-15, 1.000000000000000000 ) ) ;
#54999 = CARTESIAN_POINT ( 'NONE',  ( -11.53846153846153655, -10.67929555188718282, 33.92786785259544047 ) ) ;
#55000 = EDGE_CURVE ( 'NONE', #4543, #427, #69355, .T. ) ;
#55001 = EDGE_CURVE ( 'NONE', #77704, #56543, #4605, .T. ) ;
#55002 = CARTESIAN_POINT ( 'NONE',  ( 9.692307692307695177, -10.51840700105979565, 33.73612834413961536 ) ) ;
#55003 = CARTESIAN_POINT ( 'NONE',  ( -12.71156169883142795, -2.823816976329319051, 31.52131813110795733 ) ) ;
#55004 = CARTESIAN_POINT ( 'NONE',  ( 17.30035003878465005, -7.630147231320743018, 34.74852402298682819 ) ) ;
#55005 = CARTESIAN_POINT ( 'NONE',  ( 12.71159277317677549, -11.28795663066794575, 33.01431243580653785 ) ) ;
#55006 = CARTESIAN_POINT ( 'NONE',  ( 2.750000000000002665, -7.561099074964516831, 18.47061829374151287 ) ) ;
#55007 = EDGE_CURVE ( 'NONE', #72869, #25632, #14823, .T. ) ;
#55008 = ORIENTED_EDGE ( 'NONE', *, *, #56649, .T. ) ;
#55009 = B_SPLINE_CURVE_WITH_KNOTS ( 'NONE', 3,
 ( #17156, #37878, #31107, #65782, #24349, #4077, #41882, #40557, #61685, #53609 ),
 .UNSPECIFIED., .F., .F.,
 ( 4, 2, 2, 2, 4 ),
 ( 0.0007817246256747460882, 0.0009771112852218892010, 0.001172497944769032314, 0.001367884604316175210, 0.001563271263863318323 ),
 .UNSPECIFIED. ) ;
#55010 = ADVANCED_FACE ( 'NONE', ( #9387 ), #8505, .F. ) ;
#55011 = CARTESIAN_POINT ( 'NONE',  ( -15.23076923076935252, -12.16647553114689728, 32.15551576947799362 ) ) ;
#55012 = CARTESIAN_POINT ( 'NONE',  ( 1.319345384059066761, -9.528491918058357157, 34.59228464037090589 ) ) ;
#55013 = AXIS2_PLACEMENT_3D ( 'NONE', #32072, #80265, #87481 ) ;
#55014 = AXIS2_PLACEMENT_3D ( 'NONE', #69340, #21586, #63452 ) ;
#55015 = B_SPLINE_CURVE_WITH_KNOTS ( 'NONE', 3,
 ( #2242, #57202, #3130, #86472, #64383, #58968, #71588, #24287, #22967, #9458 ),
 .UNSPECIFIED., .F., .F.,
 ( 4, 2, 2, 2, 4 ),
 ( 0.0007817359430256296806, 0.0009771253907249958896, 0.001172514838424361990, 0.001367904286123728091, 0.001563293733823094408 ),
 .UNSPECIFIED. ) ;
#55016 = CARTESIAN_POINT ( 'NONE',  ( 9.757562831820530747, -11.06231777344671130, 33.60647404775212976 ) ) ;
#55017 = CARTESIAN_POINT ( 'NONE',  ( 6.923076923076800782, -3.643525952248796163, 33.31231777344771672 ) ) ;
#55018 = EDGE_LOOP ( 'NONE', ( #27454, #67717 ) ) ;
#55019 = FACE_OUTER_BOUND ( 'NONE', #73872, .T. ) ;
#55020 = CARTESIAN_POINT ( 'NONE',  ( -5.999999999999998224, -5.471508081941601098, 34.59228464037088457 ) ) ;
#55021 = CIRCLE ( 'NONE', #78025, 4.000000000000000000 ) ;
#55022 = CARTESIAN_POINT ( 'NONE',  ( -10.28846153846153832, -3.499999999999999556, 29.75000000000000355 ) ) ;
#55023 = CARTESIAN_POINT ( 'NONE',  ( -0.7115152055870523906, -10.82459398097509684, 33.81372124010185587 ) ) ;
#55024 = LINE ( 'NONE', #82510, #22086 ) ;
#55025 = ORIENTED_EDGE ( 'NONE', *, *, #83264, .T. ) ;
#55026 = CARTESIAN_POINT ( 'NONE',  ( 6.249945518348143381, -5.852078868378311149, 34.47109172314383585 ) ) ;
#55027 = CARTESIAN_POINT ( 'NONE',  ( -14.37296275365308418, -2.892918686051582977, 31.69288490824015980 ) ) ;
#55028 = FACE_OUTER_BOUND ( 'NONE', #34835, .T. ) ;
#55029 = ORIENTED_EDGE ( 'NONE', *, *, #30398, .F. ) ;
#55030 = CYLINDRICAL_SURFACE ( 'NONE', #52794, 0.2499999999999986955 ) ;
#55031 = ORIENTED_EDGE ( 'NONE', *, *, #43754, .F. ) ;
#55032 = CARTESIAN_POINT ( 'NONE',  ( 12.46153846153846168, -12.34228464037088635, 31.77849191805839268 ) ) ;
#55033 =( LENGTH_UNIT ( ) NAMED_UNIT ( * ) SI_UNIT ( .MILLI., .METRE. ) );
#55034 = CARTESIAN_POINT ( 'NONE',  ( 11.76147438255493327, -6.460100341425560444, 34.89618726649961644 ) ) ;
#55035 = VERTEX_POINT ( 'NONE', #29228 ) ;
#55036 = CARTESIAN_POINT ( 'NONE',  ( 3.512820512820510555, -3.499999999999999556, 29.75000000000000355 ) ) ;
#55037 = DIRECTION ( 'NONE',  ( 0.000000000000000000, 0.9396926207859126468, -0.3420201433256571111 ) ) ;
#55038 = CARTESIAN_POINT ( 'NONE',  ( -10.74553182482283198, -6.001485441113819874, 34.52039167877662607 ) ) ;
#55039 = VECTOR ( 'NONE', #5256, 1000.000000000000000 ) ;
#55040 = CARTESIAN_POINT ( 'NONE',  ( -8.069638770718176701, -4.988325925672468131, 34.36044203135681130 ) ) ;
#55041 = FACE_OUTER_BOUND ( 'NONE', #85386, .T. ) ;
#55042 = ORIENTED_EDGE ( 'NONE', *, *, #8416, .T. ) ;
#55043 = FACE_BOUND ( 'NONE', #56295, .T. ) ;
#55044 = ORIENTED_EDGE ( 'NONE', *, *, #83558, .T. ) ;
#55045 = CARTESIAN_POINT ( 'NONE',  ( -8.992715693795103604, -12.47654668319379567, 31.42292124445336654 ) ) ;
#55046 = FACE_OUTER_BOUND ( 'NONE', #88641, .T. ) ;
#55047 = CARTESIAN_POINT ( 'NONE',  ( 6.130525438233648039, -5.915461855592777596, 34.75538340440931506 ) ) ;
#55048 = CARTESIAN_POINT ( 'NONE',  ( 16.85399685940693004, -2.554751324335733376, 30.48935550225260727 ) ) ;
#55049 = VERTEX_POINT ( 'NONE', #42298 ) ;
#55050 = ORIENTED_EDGE ( 'NONE', *, *, #64218, .T. ) ;
#55051 = ORIENTED_EDGE ( 'NONE', *, *, #37624, .T. ) ;
#55052 = CARTESIAN_POINT ( 'NONE',  ( -2.980823821391187511, -11.56426240980093567, 33.07394671870546432 ) ) ;
#55053 = ORIENTED_EDGE ( 'NONE', *, *, #74196, .F. ) ;
#55054 = CARTESIAN_POINT ( 'NONE',  ( -6.416666666666667851, -3.499999999999999556, 29.75000000000000355 ) ) ;
#55055 = CARTESIAN_POINT ( 'NONE',  ( -9.469344788746207442, -7.369474270740069777, 34.74850911626239736 ) ) ;
#55056 = CARTESIAN_POINT ( 'NONE',  ( 4.153846153846154188, -3.050289026998446396, 32.03036669348365706 ) ) ;
#55057 = VECTOR ( 'NONE', #48423, 1000.000000000000000 ) ;
#55059 = EDGE_CURVE ( 'NONE', #59461, #33924, #84176, .T. ) ;
#55058 = DIRECTION ( 'NONE',  ( -0.000000000000000000, -0.1736481776669307198, -0.9848077530122080203 ) ) ;
#55060 = CARTESIAN_POINT ( 'NONE',  ( 3.749999999999992006, -5.946699141100872943, 24.39062500000000000 ) ) ;
#55061 = DIRECTION ( 'NONE',  ( 1.000000000000000000, 0.000000000000000000, 0.000000000000000000 ) ) ;
#55062 = CARTESIAN_POINT ( 'NONE',  ( 27.00000000000000000, -16.99999999999999289, 30.25000000000000000 ) ) ;
#55063 = DIRECTION ( 'NONE',  ( 0.000000000000000000, 0.9396926207859126468, 0.3420201433256571111 ) ) ;
#55064 = ORIENTED_EDGE ( 'NONE', *, *, #76972, .F. ) ;
#55065 = ORIENTED_EDGE ( 'NONE', *, *, #54161, .F. ) ;
#55066 = ORIENTED_EDGE ( 'NONE', *, *, #23002, .T. ) ;
#55067 = CARTESIAN_POINT ( 'NONE',  ( 3.230769230769231726, -9.584722331328613620, 36.20867863119891439 ) ) ;
#55069 = CARTESIAN_POINT ( 'NONE',  ( -7.846153846153965716, -4.481592998941358097, 33.73612834414048933 ) ) ;
#55068 = LINE ( 'NONE', #61819, #12960 ) ;
#55070 = B_SPLINE_CURVE_WITH_KNOTS ( 'NONE', 3,
 ( #43205, #80561, #46310, #45859, #4429, #52165, #87321, #85966, #86882, #67035 ),
 .UNSPECIFIED., .F., .F.,
 ( 4, 2, 2, 2, 4 ),
 ( 0.0007817246256747502082, 0.0009771112852218941883, 0.001172497944769038385, 0.001367884604316182365, 0.001563271263863326346 ),
 .UNSPECIFIED. ) ;
#55071 = CARTESIAN_POINT ( 'NONE',  ( -17.93393266664992680, -5.471508081941600210, 34.59228464037088457 ) ) ;
#55072 = CARTESIAN_POINT ( 'NONE',  ( -15.29685161012936589, -9.905515769479276145, 34.41647553114623292 ) ) ;
#55073 = FACE_BOUND ( 'NONE', #17851, .T. ) ;
#55074 = CARTESIAN_POINT ( 'NONE',  ( 16.28463796167094202, -3.062576670634119758, 32.05464942895959979 ) ) ;
#55075 = ORIENTED_EDGE ( 'NONE', *, *, #1489, .T. ) ;
#55076 = EDGE_CURVE ( 'NONE', #75330, #78537, #20708, .T. ) ;
#55077 = CARTESIAN_POINT ( 'NONE',  ( -18.00000000000012079, -5.219633306517615701, 34.19971097300220464 ) ) ;
#55078 = CARTESIAN_POINT ( 'NONE',  ( 16.85343813319912698, -6.760086850603066466, 34.69517049084099369 ) ) ;
#55079 = DIRECTION ( 'NONE',  ( 0.000000000000000000, 0.9396926207859126468, 0.3420201433256571111 ) ) ;
#55080 = ORIENTED_EDGE ( 'NONE', *, *, #4309, .F. ) ;
#55081 = CARTESIAN_POINT ( 'NONE',  ( -18.13069146666755671, -8.147922237126337563, 34.70805685702651999 ) ) ;
#55082 = ORIENTED_EDGE ( 'NONE', *, *, #64848, .F. ) ;
#55083 = FACE_BOUND ( 'NONE', #39217, .T. ) ;
#55084 = FACE_OUTER_BOUND ( 'NONE', #41803, .T. ) ;
#55085 = CARTESIAN_POINT ( 'NONE',  ( -4.153846153846152411, -13.04860791097971706, 34.73218667398347037 ) ) ;
#55086 = DIRECTION ( 'NONE',  ( 1.000000000000000000, 0.000000000000000000, 0.000000000000000000 ) ) ;
#55087 = VERTEX_POINT ( 'NONE', #71079 ) ;
#55088 = FACE_OUTER_BOUND ( 'NONE', #1213, .T. ) ;
#55089 = CARTESIAN_POINT ( 'NONE',  ( -17.07692307692307665, -9.905515769479276145, 34.41647553114623292 ) ) ;
#55090 = CARTESIAN_POINT ( 'NONE',  ( -1.384615384615505151, -3.835265460704628371, 33.15142922262033665 ) ) ;
#55091 = DIRECTION ( 'NONE',  ( -0.000000000000000000, -0.1736481776669307198, -0.9848077530122080203 ) ) ;
#55092 = ORIENTED_EDGE ( 'NONE', *, *, #85795, .F. ) ;
#55093 = CARTESIAN_POINT ( 'NONE',  ( 16.21991450484859243, -10.51840700105979565, 33.73612834413962247 ) ) ;
#55095 = CARTESIAN_POINT ( 'NONE',  ( 5.076923076923075762, -1.117168528481311540, 33.14645433367849847 ) ) ;
#55094 = CIRCLE ( 'NONE', #59401, 0.2500000000000002220 ) ;
#55098 = ORIENTED_EDGE ( 'NONE', *, *, #82653, .T. ) ;
#55097 = AXIS2_PLACEMENT_3D ( 'NONE', #71640, #5746, #37413 ) ;
#55096 = CARTESIAN_POINT ( 'NONE',  ( -12.46153846153846168, -9.905515769479276145, 34.41647553114623292 ) ) ;
#55099 = CARTESIAN_POINT ( 'NONE',  ( 6.000000000000001776, -2.292212530054420494, 30.41441678777542634 ) ) ;
#55100 = CARTESIAN_POINT ( 'NONE',  ( 5.999999999999880096, -9.442884908241554243, 34.35708131394783038 ) ) ;
#55101 = CARTESIAN_POINT ( 'NONE',  ( 16.21910129335899597, -12.16647553114626490, 32.15551576947920864 ) ) ;
#55102 = FACE_OUTER_BOUND ( 'NONE', #60921, .T. ) ;
#55103 = EDGE_CURVE ( 'NONE', #32391, #51245, #28779, .T. ) ;
#55104 = ADVANCED_FACE ( 'NONE', ( #50787 ), #56244, .T. ) ;
#55105 = DIRECTION ( 'NONE',  ( -0.000000000000000000, 0.9848077530122085754, -0.1736481776669273613 ) ) ;
#55107 = CARTESIAN_POINT ( 'NONE',  ( -2.530557729895944963, -2.501496062324912284, 29.88072118266895671 ) ) ;
#55106 = CARTESIAN_POINT ( 'NONE',  ( 3.230769230769231726, -12.37446782046654192, 30.86335684631486131 ) ) ;
#55108 = CARTESIAN_POINT ( 'NONE',  ( 7.912222197156284054, -4.098570777380720287, 33.41473453929635440 ) ) ;
#55109 = CARTESIAN_POINT ( 'NONE',  ( -2.749999999999991562, -8.639087296526025028, 21.26562500000000000 ) ) ;
#55110 = ORIENTED_EDGE ( 'NONE', *, *, #20454, .F. ) ;
#55111 = CARTESIAN_POINT ( 'NONE',  ( -17.77698864838715309, -9.086983370893047862, 34.49168942202179267 ) ) ;
#55112 = VERTEX_POINT ( 'NONE', #39089 ) ;
#55113 = EDGE_CURVE ( 'NONE', #60496, #10987, #44039, .T. ) ;
#55114 = ORIENTED_EDGE ( 'NONE', *, *, #78644, .T. ) ;
#55115 = CARTESIAN_POINT ( 'NONE',  ( -11.40767109749459074, -2.295524264805589354, 30.44142389570982488 ) ) ;
#55116 = EDGE_LOOP ( 'NONE', ( #60987, #46777, #39520, #35251 ) ) ;
#55117 = CARTESIAN_POINT ( 'NONE',  ( -4.284536756956458525, -2.494641256782728966, 31.33461815524612959 ) ) ;
#55118 = CARTESIAN_POINT ( 'NONE',  ( -2.749999999999991562, -8.639087296526025028, 20.01562500000000355 ) ) ;
#55119 = CARTESIAN_POINT ( 'NONE',  ( 12.21153846153846168, -7.500000000000001776, 35.00000000000000000 ) ) ;
#55120 = CARTESIAN_POINT ( 'NONE',  ( -12.46153846153846168, -12.78798330534102945, 29.74999999999997868 ) ) ;
#55121 = CARTESIAN_POINT ( 'NONE',  ( -15.90379184220783948, -5.728107161865375829, 34.42597550085002922 ) ) ;
#55122 = CARTESIAN_POINT ( 'NONE',  ( 22.75000000000000000, -10.50000000000000000, 29.75000000000000355 ) ) ;
#55123 = CARTESIAN_POINT ( 'NONE',  ( -23.50000000000000000, -9.499999999999982236, 27.25000000000000000 ) ) ;
#55124 = FACE_OUTER_BOUND ( 'NONE', #61691, .T. ) ;
#55125 = CARTESIAN_POINT ( 'NONE',  ( 6.857806922520603976, -12.51329471203370325, 31.30864560766548976 ) ) ;
#55126 = PLANE ( 'NONE',  #88071 ) ;
#55127 = CARTESIAN_POINT ( 'NONE',  ( -17.07692307692307665, -10.67929555188718282, 33.92786785259544047 ) ) ;
#55128 = CARTESIAN_POINT ( 'NONE',  ( -2.307692307692305711, -5.180354513474913603, 36.12317359536750416 ) ) ;
#55129 = CARTESIAN_POINT ( 'NONE',  ( -19.00000000000000000, -1.749999999999990674, 30.25000000000000000 ) ) ;
#55130 =( GEOMETRIC_REPRESENTATION_CONTEXT ( 3 ) GLOBAL_UNCERTAINTY_ASSIGNED_CONTEXT ( ( #83045 ) ) GLOBAL_UNIT_ASSIGNED_CONTEXT ( ( #75908, #5674, #61496 ) ) REPRESENTATION_CONTEXT ( 'NONE', 'WORKASPACE' ) );
#55131 = VECTOR ( 'NONE', #51240, 999.9999999999998863 ) ;
#55132 = ORIENTED_EDGE ( 'NONE', *, *, #1837, .T. ) ;
#55133 = ORIENTED_EDGE ( 'NONE', *, *, #18466, .T. ) ;
#55134 = CARTESIAN_POINT ( 'NONE',  ( -15.23076923076922995, -6.681629849574314051, 35.83090037661290239 ) ) ;
#55135 = DIRECTION ( 'NONE',  ( -0.000000000000000000, 1.000000000000000000, 3.491481338843133355E-15 ) ) ;
#55136 = CARTESIAN_POINT ( 'NONE',  ( -6.923076923076922462, -13.20930481340135110, 34.54067556320372745 ) ) ;
#55137 = CARTESIAN_POINT ( 'NONE',  ( 5.777073782483852504, -5.667676309546437530, 34.40238873228292249 ) ) ;
#55138 = B_SPLINE_CURVE_WITH_KNOTS ( 'NONE', 3,
 ( #3386, #70966, #85821, #3832, #31766, #16905, #45259, #79050, #4278, #78161 ),
 .UNSPECIFIED., .F., .F.,
 ( 4, 2, 2, 2, 4 ),
 ( 0.0007817359430256324996, 0.0009771253907249991422, 0.001172514838424365676, 0.001367904286123732428, 0.001563293733823098962 ),
 .UNSPECIFIED. ) ;
#55139 = CARTESIAN_POINT ( 'NONE',  ( 12.39545505058258001, -8.973038597847271092, 34.52809138561120506 ) ) ;
#55140 = CARTESIAN_POINT ( 'NONE',  ( 0.000000000000000000, -11.00000000000000000, 29.75000000000000355 ) ) ;
#55141 = CARTESIAN_POINT ( 'NONE',  ( 14.30769230769218758, -9.442884908241554243, 34.35708131394783038 ) ) ;
#55142 = ORIENTED_EDGE ( 'NONE', *, *, #73192, .F. ) ;
#55143 = CARTESIAN_POINT ( 'NONE',  ( 18.25005441991345378, -3.435999193479609026, 33.07426656108011542 ) ) ;
#55144 = ORIENTED_EDGE ( 'NONE', *, *, #64441, .T. ) ;
#55145 = CARTESIAN_POINT ( 'NONE',  ( -18.00000000000012079, -4.481592998941359873, 33.73612834414048933 ) ) ;
#55146 = DIRECTION ( 'NONE',  ( 0.000000000000000000, 0.1736481776669267785, -0.9848077530122087975 ) ) ;
#55147 = CARTESIAN_POINT ( 'NONE',  ( 17.07692307692307665, -2.249999999999998668, 29.75000000000001776 ) ) ;
#55148 = DIRECTION ( 'NONE',  ( 0.000000000000000000, 0.3420201433256641055, -0.9396926207859100932 ) ) ;
#55149 = CARTESIAN_POINT ( 'NONE',  ( -5.999999999999998224, -7.500000000000001776, 35.04278698407183867 ) ) ;
#55150 = ADVANCED_FACE ( 'NONE', ( #71512 ), #17919, .F. ) ;
#55151 = VERTEX_POINT ( 'NONE', #44927 ) ;
#55152 = VECTOR ( 'NONE', #348, 1000.000000000000114 ) ;
#55153 = VECTOR ( 'NONE', #8754, 1000.000000000000227 ) ;
#55154 = ORIENTED_EDGE ( 'NONE', *, *, #81780, .F. ) ;
#55155 = VERTEX_POINT ( 'NONE', #78273 ) ;
#55156 = ORIENTED_EDGE ( 'NONE', *, *, #22729, .T. ) ;
#55157 = CARTESIAN_POINT ( 'NONE',  ( 13.31934493865461278, -3.300289026998414865, 32.46337939537583139 ) ) ;
#55158 = CARTESIAN_POINT ( 'NONE',  ( -15.93106648486808119, -9.418065098278011860, 34.63729479722530158 ) ) ;
#55159 = CARTESIAN_POINT ( 'NONE',  ( 14.24160992833217243, -2.486705287966279432, 31.30864560766542937 ) ) ;
#55161 = EDGE_CURVE ( 'NONE', #16151, #30233, #3185, .T. ) ;
#55160 = CARTESIAN_POINT ( 'NONE',  ( 16.21991450484859953, -9.780366693483667717, 34.19971097300155805 ) ) ;
#55162 = CARTESIAN_POINT ( 'NONE',  ( 17.86985203026830504, -3.069018819979304702, 32.56621877034667278 ) ) ;
#55163 = CARTESIAN_POINT ( 'NONE',  ( 14.17700084102475344, -12.38065189839062263, 30.83690757178629482 ) ) ;
#55164 = ORIENTED_EDGE ( 'NONE', *, *, #20701, .T. ) ;
#55165 = EDGE_CURVE ( 'NONE', #7875, #73152, #14165, .T. ) ;
#55166 = ORIENTED_EDGE ( 'NONE', *, *, #19926, .F. ) ;
#55167 = EDGE_LOOP ( 'NONE', ( #25362, #46112 ) ) ;
#55169 = VERTEX_POINT ( 'NONE', #87283 ) ;
#55168 = CARTESIAN_POINT ( 'NONE',  ( 11.28843830116857383, -9.271318131107980420, 34.42618302367067429 ) ) ;
#55170 = CARTESIAN_POINT ( 'NONE',  ( 9.468822767743363400, -8.539481045369596401, 34.89627647299170832 ) ) ;
#55171 = CARTESIAN_POINT ( 'NONE',  ( 7.173076923076986411, -7.434744429011176159, 34.75000000000000711 ) ) ;
#55172 = CARTESIAN_POINT ( 'NONE',  ( 1.553300858899129722, -11.24999999999999112, 19.70312500000000355 ) ) ;
#55173 = ORIENTED_EDGE ( 'NONE', *, *, #9339, .T. ) ;
#55174 = VECTOR ( 'NONE', #10631, 1000.000000000000000 ) ;
#55175 = EDGE_CURVE ( 'NONE', #84371, #77885, #52132, .T. ) ;
#55176 = ORIENTED_EDGE ( 'NONE', *, *, #68396, .T. ) ;
#55177 = DIRECTION ( 'NONE',  ( -0.000000000000000000, 1.000000000000000000, -0.000000000000000000 ) ) ;
#55178 = VECTOR ( 'NONE', #2615, 1000.000000000000114 ) ;
#55179 = FACE_BOUND ( 'NONE', #38764, .T. ) ;
#55180 = CARTESIAN_POINT ( 'NONE',  ( -2.176901866725357237, -4.684288915650983043, 34.18129842949671371 ) ) ;
#55181 = EDGE_CURVE ( 'NONE', #14974, #37386, #31428, .T. ) ;
#55182 = DIRECTION ( 'NONE',  ( -1.000000000000000000, -0.000000000000000000, 0.000000000000000000 ) ) ;
#55183 = ORIENTED_EDGE ( 'NONE', *, *, #1623, .F. ) ;
#55184 = CARTESIAN_POINT ( 'NONE',  ( -3.230769230769229949, -10.67929555188718282, 33.92786785259544047 ) ) ;
#55185 = CARTESIAN_POINT ( 'NONE',  ( -5.076923076923199218, -9.528491918059723176, 34.59228464037033035 ) ) ;
#55186 = FACE_OUTER_BOUND ( 'NONE', #59022, .T. ) ;
#55187 = DIRECTION ( 'NONE',  ( -0.000000000000000000, 1.000000000000000000, 3.491481338843133355E-15 ) ) ;
#55188 = ORIENTED_EDGE ( 'NONE', *, *, #55970, .F. ) ;
#55189 = B_SPLINE_CURVE_WITH_KNOTS ( 'NONE', 3,
 ( #20887, #35747, #15029, #27209, #82164, #34405 ),
 .UNSPECIFIED., .F., .F.,
 ( 4, 2, 4 ),
 ( 4.220987180333913997E-17, 0.0001954756301637145801, 0.0003909512603273869848 ),
 .UNSPECIFIED. ) ;
#55190 = CARTESIAN_POINT ( 'NONE',  ( 6.222779541268409709, -8.496831190052096971, 34.64984203495476578 ) ) ;
#55191 = CARTESIAN_POINT ( 'NONE',  ( 1.319345384059067428, -4.320704448112771878, 33.92786785259540494 ) ) ;
#55192 = CARTESIAN_POINT ( 'NONE',  ( -12.52680890749923748, -12.27809138561121394, 31.22303859784730307 ) ) ;
#55193 = CARTESIAN_POINT ( 'NONE',  ( -39.05038313613820122, -2.249999999999998668, 29.75000000000000355 ) ) ;
#55194 = DIRECTION ( 'NONE',  ( -0.000000000000000000, 1.000000000000000000, 3.491481338843133355E-15 ) ) ;
#55195 = EDGE_CURVE ( 'NONE', #86900, #54833, #22771, .T. ) ;
#55196 = FACE_BOUND ( 'NONE', #7461, .T. ) ;
#55198 = CARTESIAN_POINT ( 'NONE',  ( 11.40777007179398339, -12.38065189839062263, 30.83690757178629482 ) ) ;
#55197 = CARTESIAN_POINT ( 'NONE',  ( 2.307692307692309264, -11.33034616979429110, 35.88435417666054406 ) ) ;
#55199 = B_SPLINE_CURVE_WITH_KNOTS ( 'NONE', 3,
 ( #5448, #38336, #66242, #3648, #73907, #87889, #87432, #32026, #86996, #67147 ),
 .UNSPECIFIED., .F., .F.,
 ( 4, 2, 2, 2, 4 ),
 ( 0.000000000000000000, 0.0001954339881912774070, 0.0003908679763825548140, 0.0005863019645738322752, 0.0007817359527651096280 ),
 .UNSPECIFIED. ) ;
#55200 = CARTESIAN_POINT ( 'NONE',  ( 5.142178216435913107, -2.379036618887895305, 30.90682066428159303 ) ) ;
#55202 = CARTESIAN_POINT ( 'NONE',  ( 5.777073782483853392, -10.61292498521070549, 33.66303323003028680 ) ) ;
#55201 = CARTESIAN_POINT ( 'NONE',  ( 3.165445217964922175, -7.749976730030849303, 34.74374725381503737 ) ) ;
#55203 = EDGE_CURVE ( 'NONE', #51403, #30568, #37736, .T. ) ;
#55204 = CARTESIAN_POINT ( 'NONE',  ( -7.976301815885541657, -4.299443229763728169, 33.91186481527756058 ) ) ;
#55205 = B_SPLINE_CURVE_WITH_KNOTS ( 'NONE', 3,
 ( #38229, #65687, #3986, #56730, #84224, #22500, #49963, #77443, #11659, #40028 ),
 .UNSPECIFIED., .F., .F.,
 ( 4, 2, 2, 2, 4 ),
 ( 0.0007817359430256294638, 0.0009771253907249974075, 0.001172514838424365460, 0.001367904286123733295, 0.001563293733823094191 ),
 .UNSPECIFIED. ) ;
#55206 = CARTESIAN_POINT ( 'NONE',  ( 0.06109907496454976272, -10.25000000000000000, 15.77938170625848890 ) ) ;
#55207 = ORIENTED_EDGE ( 'NONE', *, *, #75433, .T. ) ;
#55208 = LINE ( 'NONE', #15121, #10239 ) ;
#55209 = ORIENTED_EDGE ( 'NONE', *, *, #81722, .T. ) ;
#55210 = CARTESIAN_POINT ( 'NONE',  ( -13.16183571563731647, -10.97394488606064122, 33.68653795673694873 ) ) ;
#55211 = ADVANCED_FACE ( 'NONE', ( #38629 ), #66088, .F. ) ;
#55212 = ORIENTED_EDGE ( 'NONE', *, *, #29358, .F. ) ;
#55213 = ADVANCED_FACE ( 'NONE', ( #25113 ), #44476, .F. ) ;
#55214 = CARTESIAN_POINT ( 'NONE',  ( -11.31568186948346977, -6.717445702608402236, 34.94155399931962336 ) ) ;
#55215 = CARTESIAN_POINT ( 'NONE',  ( -18.00000000000012079, -2.625532179533778709, 30.86335684631627174 ) ) ;
#55217 = ORIENTED_EDGE ( 'NONE', *, *, #49464, .T. ) ;
#55216 = CARTESIAN_POINT ( 'NONE',  ( -9.469294848214294902, -11.43677907613344757, 33.22367315496202167 ) ) ;
#55218 = DIRECTION ( 'NONE',  ( -0.000000000000000000, 1.000000000000000000, -0.000000000000000000 ) ) ;
#55219 = CARTESIAN_POINT ( 'NONE',  ( -1.987747218494660295, -5.598659921968651254, 19.99813170625848713 ) ) ;
#55220 = CARTESIAN_POINT ( 'NONE',  ( -10.55012947587177941, -12.70778746994558439, 30.41441678777536595 ) ) ;
#55221 = CARTESIAN_POINT ( 'NONE',  ( -12.46153846153846168, -9.819645486525091727, 36.12317359536749706 ) ) ;
#55222 = AXIS2_PLACEMENT_3D ( 'NONE', #80346, #18192, #30801 ) ;
#55223 = CARTESIAN_POINT ( 'NONE',  ( 16.94677586748485965, -12.45813303252208648, 30.39737893381572675 ) ) ;
#55224 = CARTESIAN_POINT ( 'NONE',  ( 10.39189969082028497, -2.612411019501189369, 31.66733052389439962 ) ) ;
#55225 = CARTESIAN_POINT ( 'NONE',  ( 2.372947878968334035, -2.892918686051626498, 31.69288490824026638 ) ) ;
#55226 = CARTESIAN_POINT ( 'NONE',  ( -5.869474298236434961, -10.88167719472716399, 33.43325721877153711 ) ) ;
#55227 = CARTESIAN_POINT ( 'NONE',  ( -3.775308065498748977, -8.992201783934593351, 22.76749329374151287 ) ) ;
#55228 = LINE ( 'NONE', #84054, #67839 ) ;
#55229 = CARTESIAN_POINT ( 'NONE',  ( -6.065270000556318486, -3.643525952247789412, 33.31231777344662959 ) ) ;
#55230 = EDGE_LOOP ( 'NONE', ( #8073, #72414, #29352, #53976 ) ) ;
#55231 = DIRECTION ( 'NONE',  ( -1.000000000000000000, 0.000000000000000000, -0.000000000000000000 ) ) ;
#55232 = CARTESIAN_POINT ( 'NONE',  ( -2.608446859217920633, -4.805146000318815780, 23.00186829374151287 ) ) ;
#55233 = DIRECTION ( 'NONE',  ( -0.000000000000000000, 0.5000000000000011102, -0.8660254037844380415 ) ) ;
#55234 = CARTESIAN_POINT ( 'NONE',  ( -8.899378738962465007, -3.625366637846544116, 33.29286588640298561 ) ) ;
#55235 = ORIENTED_EDGE ( 'NONE', *, *, #47631, .F. ) ;
#55236 = CARTESIAN_POINT ( 'NONE',  ( 7.053124529332606585, -7.723484964179500700, 34.74522123443823318 ) ) ;
#55237 = CARTESIAN_POINT ( 'NONE',  ( -0.3954701105360226010, -9.780366693483669494, 34.19971097300155805 ) ) ;
#55239 = ORIENTED_EDGE ( 'NONE', *, *, #21952, .F. ) ;
#55238 = LINE ( 'NONE', #7947, #49739 ) ;
#55240 = CARTESIAN_POINT ( 'NONE',  ( -5.143006487878955646, -5.557115091759785130, 34.35708131394839171 ) ) ;
#55241 = CARTESIAN_POINT ( 'NONE',  ( 13.60739492588379385, -2.600157965045224895, 30.74683119005207743 ) ) ;
#55242 = B_SPLINE_CURVE_WITH_KNOTS ( 'NONE', 3,
 ( #68537, #5962, #20365, #81181, #55464, #6409, #75734, #54126, #33433, #14038 ),
 .UNSPECIFIED., .F., .F.,
 ( 4, 2, 2, 2, 4 ),
 ( 0.0007817246256747470640, 0.0009771112852218898515, 0.001172497944769032531, 0.001367884604316175427, 0.001563271263863318106 ),
 .UNSPECIFIED. ) ;
#55243 = CARTESIAN_POINT ( 'NONE',  ( -10.61538461538473577, -9.528491918059723176, 34.59228464037033035 ) ) ;
#55244 = CARTESIAN_POINT ( 'NONE',  ( -16.85414353565466783, -2.847695495035524438, 31.58253572463339154 ) ) ;
#55245 = B_SPLINE_CURVE_WITH_KNOTS ( 'NONE', 3,
 ( #9970, #24816, #37894, #79776, #59493, #23918, #65360, #37435, #79327, #66243 ),
 .UNSPECIFIED., .F., .F.,
 ( 4, 2, 2, 2, 4 ),
 ( 0.0007817359430256294638, 0.0009771253907249950223, 0.001172514838424360472, 0.001367904286123725922, 0.001563293733823091372 ),
 .UNSPECIFIED. ) ;
#55246 = ADVANCED_FACE ( 'NONE', ( #18363 ), #10273, .F. ) ;
#55247 = CARTESIAN_POINT ( 'NONE',  ( -13.63459211555773720, -11.79746400365624659, 32.30657167506340954 ) ) ;
#55248 = AXIS2_PLACEMENT_3D ( 'NONE', #13298, #80890, #19173 ) ;
#55249 = ORIENTED_EDGE ( 'NONE', *, *, #83558, .F. ) ;
#55250 = ORIENTED_EDGE ( 'NONE', *, *, #46634, .T. ) ;
#55251 = PRESENTATION_LAYER_ASSIGNMENT (  '', '', ( #25030 ) ) ;
#55252 = VERTEX_POINT ( 'NONE', #51671 ) ;
#55253 = CARTESIAN_POINT ( 'NONE',  ( 11.53846153846153832, -2.708943851104267164, 35.45975837776705220 ) ) ;
#55254 = DIRECTION ( 'NONE',  ( -0.000000000000000000, -0.3420201433256694346, -0.9396926207859080948 ) ) ;
#55255 = CARTESIAN_POINT ( 'NONE',  ( -7.846153846153844924, -12.78798330534103123, 29.99999999999997868 ) ) ;
#55256 = FACE_OUTER_BOUND ( 'NONE', #65863, .T. ) ;
#55257 = EDGE_CURVE ( 'NONE', #48006, #60933, #17474, .T. ) ;
#55258 = EDGE_CURVE ( 'NONE', #41455, #13933, #36815, .T. ) ;
#55259 = EDGE_LOOP ( 'NONE', ( #76303, #55948, #73241, #68685, #70800, #87901 ) ) ;
#55260 = CARTESIAN_POINT ( 'NONE',  ( -17.07692307692307665, -4.098570777380720287, 33.41473453929634729 ) ) ;
#55261 = EDGE_LOOP ( 'NONE', ( #5742, #82391 ) ) ;
#55262 = EDGE_LOOP ( 'NONE', ( #86858, #17832, #62279, #35678, #62760 ) ) ;
#55263 = ORIENTED_EDGE ( 'NONE', *, *, #77950, .T. ) ;
#55265 = ORIENTED_EDGE ( 'NONE', *, *, #8506, .T. ) ;
#55264 = CARTESIAN_POINT ( 'NONE',  ( -3.165575248985873280, -2.506253911140448043, 29.99999999999988631 ) ) ;
#55266 = PLANE ( 'NONE',  #14254 ) ;
#55267 = CARTESIAN_POINT ( 'NONE',  ( 5.869309396889694774, -12.62707690430377383, 30.88035979386743435 ) ) ;
#55268 = EDGE_CURVE ( 'NONE', #46752, #64747, #41134, .T. ) ;
#55269 = CARTESIAN_POINT ( 'NONE',  ( 6.000000000000001776, -1.129524287112498415, 32.06866353760679544 ) ) ;
#55270 = CARTESIAN_POINT ( 'NONE',  ( 15.23076923076923173, -8.164416787775445883, 34.95778746994557906 ) ) ;
#55271 = ORIENTED_EDGE ( 'NONE', *, *, #43823, .T. ) ;
#55272 = EDGE_CURVE ( 'NONE', #65911, #9598, #69045, .T. ) ;
#55273 = VERTEX_POINT ( 'NONE', #53465 ) ;
#55274 = VECTOR ( 'NONE', #56860, 999.9999999999998863 ) ;
#55275 = ORIENTED_EDGE ( 'NONE', *, *, #82150, .T. ) ;
#55276 = CARTESIAN_POINT ( 'NONE',  ( 4.153846153846154188, -2.900454961884010974, 35.62045528018868623 ) ) ;
#55278 = ORIENTED_EDGE ( 'NONE', *, *, #31527, .F. ) ;
#55277 = CARTESIAN_POINT ( 'NONE',  ( 8.769230769230768274, -7.500000000000001776, 35.04278698407183867 ) ) ;
#55279 = CARTESIAN_POINT ( 'NONE',  ( 6.856993512121044354, -6.386643153685125363, 34.62446782046654903 ) ) ;
#55280 = CARTESIAN_POINT ( 'NONE',  ( -0.7115616857599186273, -6.652501968072646932, 34.93155406624980941 ) ) ;
#55281 = ORIENTED_EDGE ( 'NONE', *, *, #22249, .F. ) ;
#55282 = ADVANCED_FACE ( 'NONE', ( #66999 ), #5291, .F. ) ;
#55283 = CARTESIAN_POINT ( 'NONE',  ( -17.74994568836168440, -2.564540009722896752, 30.55348353981672105 ) ) ;
#55284 = DIRECTION ( 'NONE',  ( 1.000000000000000000, 0.000000000000000000, 0.000000000000000000 ) ) ;
#55285 = ORIENTED_EDGE ( 'NONE', *, *, #55709, .F. ) ;
#55286 = FACE_BOUND ( 'NONE', #16398, .T. ) ;
#55287 = CARTESIAN_POINT ( 'NONE',  ( 10.68064018666063575, -10.21337939537593620, 33.94971097300152252 ) ) ;
#55288 = CARTESIAN_POINT ( 'NONE',  ( 16.08776377448601735, -2.486705287966279432, 31.30864560766543647 ) ) ;
#55289 = CARTESIAN_POINT ( 'NONE',  ( 3.480823542407545546, -9.148310452688873440, 34.47095581063188519 ) ) ;
#55291 = CARTESIAN_POINT ( 'NONE',  ( -8.769230769230768274, -7.500000000000001776, 35.04278698407183867 ) ) ;
#55290 = CARTESIAN_POINT ( 'NONE',  ( 7.846153846153846700, -10.67929555188718282, 33.92786785259544047 ) ) ;
#55292 = CYLINDRICAL_SURFACE ( 'NONE', #58195, 0.2499999999999998890 ) ;
#55293 = CARTESIAN_POINT ( 'NONE',  ( -4.377331078410485077, -10.97335522853832579, 33.68706563782419749 ) ) ;
#55294 = ORIENTED_EDGE ( 'NONE', *, *, #21133, .F. ) ;
#55295 = CARTESIAN_POINT ( 'NONE',  ( 14.43848411551709887, -12.38066358083363738, 30.83685684665853444 ) ) ;
#55296 = FACE_OUTER_BOUND ( 'NONE', #80700, .T. ) ;
#55297 = VERTEX_POINT ( 'NONE', #40854 ) ;
#55298 = CARTESIAN_POINT ( 'NONE',  ( 2.557692307693728129, -7.500000000000154543, 35.00000000000007105 ) ) ;
#55299 = CARTESIAN_POINT ( 'NONE',  ( -7.846153846153844924, -2.292212530054420494, 30.41441678777542634 ) ) ;
#55300 = EDGE_LOOP ( 'NONE', ( #42990, #74941, #51634, #44179, #2519 ) ) ;
#55301 = DIRECTION ( 'NONE',  ( 0.000000000000000000, 0.1736481776669275834, 0.9848077530122086864 ) ) ;
#55302 = CARTESIAN_POINT ( 'NONE',  ( 2.373759641042384683, -4.661471528628508665, 34.16647553114624003 ) ) ;
#55303 = CIRCLE ( 'NONE', #16479, 8.000000000000000000 ) ;
#55304 = EDGE_CURVE ( 'NONE', #16656, #33691, #88620, .T. ) ;
#55305 = FACE_BOUND ( 'NONE', #77547, .T. ) ;
#55307 = CARTESIAN_POINT ( 'NONE',  ( -6.923076923076922462, -1.215029322943914858, 32.30358669280327177 ) ) ;
#55306 = CARTESIAN_POINT ( 'NONE',  ( 6.792386319966614572, -3.957541250942359756, 33.62499894934981626 ) ) ;
#55308 = CARTESIAN_POINT ( 'NONE',  ( 10.48523740594639619, -8.587444163452046197, 34.63053765926554206 ) ) ;
#55309 = DIRECTION ( 'NONE',  ( -0.000000000000000000, -0.5000000000000009992, -0.8660254037844380415 ) ) ;
#55310 = CARTESIAN_POINT ( 'NONE',  ( 16.15384615384603251, -10.33852847137269571, 34.16647553114546554 ) ) ;
#55311 = CARTESIAN_POINT ( 'NONE',  ( -17.74994568836168440, -4.943051570960393271, 34.04725096376909477 ) ) ;
#55312 = CARTESIAN_POINT ( 'NONE',  ( -3.724691934501229262, -9.114399933863657211, 16.01375670625849068 ) ) ;
#55313 = ORIENTED_EDGE ( 'NONE', *, *, #3553, .T. ) ;
#55314 = VECTOR ( 'NONE', #26020, 1000.000000000000000 ) ;
#55315 = EDGE_CURVE ( 'NONE', #20998, #22047, #33205, .T. ) ;
#55316 = ORIENTED_EDGE ( 'NONE', *, *, #6293, .T. ) ;
#55317 = CARTESIAN_POINT ( 'NONE',  ( -9.822998295418001291, -2.295517848115769421, 30.44137282052137294 ) ) ;
#55318 = EDGE_CURVE ( 'NONE', #49527, #39557, #28199, .T. ) ;
#55319 = CARTESIAN_POINT ( 'NONE',  ( -0.4615384615384611200, -2.721908614388771852, 31.22303859784724978 ) ) ;
#55320 = CARTESIAN_POINT ( 'NONE',  ( 16.15384615384615330, -2.833524468853757305, 32.15551576947925838 ) ) ;
#55321 = CARTESIAN_POINT ( 'NONE',  ( 7.846153846153846700, -13.53365097954675988, 30.81389545987213552 ) ) ;
#55322 = CARTESIAN_POINT ( 'NONE',  ( 2.980792499826877773, -11.28823185664190376, 33.01397839955799896 ) ) ;
#55323 = CARTESIAN_POINT ( 'NONE',  ( -0.06109907496455085213, -3.750000000000000888, 16.40438170625849068 ) ) ;
#55324 = CARTESIAN_POINT ( 'NONE',  ( 4.403846153847589484, -7.500000000000155431, 34.75000000000007105 ) ) ;
#55325 = CYLINDRICAL_SURFACE ( 'NONE', #43157, 0.2499999999999995559 ) ;
#55326 = CARTESIAN_POINT ( 'NONE',  ( -5.999999999999998224, -6.681629849574314051, 35.83090037661290239 ) ) ;
#55327 = LINE ( 'NONE', #47688, #45880 ) ;
#55328 = LINE ( 'NONE', #1268, #71211 ) ;
#55329 = DIRECTION ( 'NONE',  ( -0.000000000000000000, -0.5000000000000009992, -0.8660254037844380415 ) ) ;
#55330 = CARTESIAN_POINT ( 'NONE',  ( -0.3962833220256233302, -4.320704448112861584, 33.92786785259548310 ) ) ;
#55331 = CARTESIAN_POINT ( 'NONE',  ( 10.36538461538461675, -7.566082377512564960, 35.00000000000000711 ) ) ;
#55332 = CARTESIAN_POINT ( 'NONE',  ( 2.980792499826876440, -2.564618984488975961, 30.55390908950641915 ) ) ;
#55333 = EDGE_CURVE ( 'NONE', #34697, #36124, #7789, .T. ) ;
#55334 = ORIENTED_EDGE ( 'NONE', *, *, #9022, .T. ) ;
#55335 = CARTESIAN_POINT ( 'NONE',  ( 2.177001704582000485, -3.338472653186242756, 32.95098750199972670 ) ) ;
#55336 = DIRECTION ( 'NONE',  ( -1.000000000000000000, 0.000000000000000000, -0.000000000000000000 ) ) ;
#55337 = B_SPLINE_CURVE_WITH_KNOTS ( 'NONE', 3,
 ( #18778, #61081, #46245, #12457, #6146, #39502 ),
 .UNSPECIFIED., .F., .F.,
 ( 4, 2, 4 ),
 ( 2.168404344971008868E-19, 0.0001954784845028926274, 0.0003909569690057850379 ),
 .UNSPECIFIED. ) ;
#55338 = CARTESIAN_POINT ( 'NONE',  ( -2.775308065498752086, -8.577988221561495763, 22.76749329374151287 ) ) ;
#55339 = CARTESIAN_POINT ( 'NONE',  ( 23.49999999999998934, 9.000000000000024869, 29.25000000000000000 ) ) ;
#55340 = DIRECTION ( 'NONE',  ( -1.000000000000000000, -0.000000000000000000, -0.000000000000000000 ) ) ;
#55341 = VERTEX_POINT ( 'NONE', #62867 ) ;
#55342 = EDGE_CURVE ( 'NONE', #65473, #47265, #13054, .T. ) ;
#55343 = FACE_OUTER_BOUND ( 'NONE', #31919, .T. ) ;
#55345 = ORIENTED_EDGE ( 'NONE', *, *, #56315, .F. ) ;
#55344 = CARTESIAN_POINT ( 'NONE',  ( -14.53117725141625449, -12.24155766932282496, 31.33739205006857986 ) ) ;
#55346 = DIRECTION ( 'NONE',  ( -0.000000000000000000, 0.7660444431189791237, -0.6427876096865379196 ) ) ;
#55347 = CARTESIAN_POINT ( 'NONE',  ( 12.46153846153833911, -5.941354392335915335, 34.76329471203413846 ) ) ;
#55348 = EDGE_LOOP ( 'NONE', ( #34202, #13404 ) ) ;
#55349 = CARTESIAN_POINT ( 'NONE',  ( 3.230769230769231726, -1.117168528481311540, 33.14645433367849847 ) ) ;
#55350 = DIRECTION ( 'NONE',  ( 0.000000000000000000, 0.000000000000000000, -1.000000000000000000 ) ) ;
#55351 = ORIENTED_EDGE ( 'NONE', *, *, #48661, .T. ) ;
#55352 = CARTESIAN_POINT ( 'NONE',  ( -7.780086512803769949, -6.343179335718451384, 34.87096338111212646 ) ) ;
#55353 = EDGE_CURVE ( 'NONE', #51205, #85537, #69642, .T. ) ;
#55354 = CARTESIAN_POINT ( 'NONE',  ( 8.703960768674447124, -6.835583212224499938, 34.95778746994557906 ) ) ;
#55355 = DIRECTION ( 'NONE',  ( -0.000000000000000000, 0.7660444431189791237, -0.6427876096865379196 ) ) ;
#55356 = ORIENTED_EDGE ( 'NONE', *, *, #15289, .F. ) ;
#55357 = ORIENTED_EDGE ( 'NONE', *, *, #11073, .T. ) ;
#55358 = CARTESIAN_POINT ( 'NONE',  ( 15.23076923076911093, -10.90142922262034020, 33.41473453929536674 ) ) ;
#55359 = ADVANCED_FACE ( 'NONE', ( #36745 ), #8393, .F. ) ;
#55360 = ORIENTED_EDGE ( 'NONE', *, *, #36491, .F. ) ;
#55361 = EDGE_CURVE ( 'NONE', #70706, #72614, #19423, .T. ) ;
#55362 = CARTESIAN_POINT ( 'NONE',  ( 3.453548899747295398, -12.11081565061823717, 32.26097654155341843 ) ) ;
#55363 = CARTESIAN_POINT ( 'NONE',  ( 12.71148397988660150, -9.272278438253398036, 34.42582936511637115 ) ) ;
#55364 = DIRECTION ( 'NONE',  ( -1.000000000000000000, 0.000000000000000000, 0.000000000000000000 ) ) ;
#55365 = CARTESIAN_POINT ( 'NONE',  ( -9.692307692307691624, -4.786620604624113540, 33.94971097300155094 ) ) ;
#55366 = CARTESIAN_POINT ( 'NONE',  ( -4.377331097570101193, -6.760086850603068243, 34.69517049084099369 ) ) ;
#55367 = DIRECTION ( 'NONE',  ( 0.000000000000000000, 0.8660254037844377084, -0.5000000000000015543 ) ) ;
#55368 = EDGE_CURVE ( 'NONE', #2477, #87198, #40971, .T. ) ;
#55369 = LINE ( 'NONE', #69772, #77957 ) ;
#55370 = B_SPLINE_CURVE_WITH_KNOTS ( 'NONE', 3,
 ( #67966, #81489, #88262, #12140, #67522, #66632, #19775, #5819, #47236, #74730 ),
 .UNSPECIFIED., .F., .F.,
 ( 4, 2, 2, 2, 4 ),
 ( 0.000000000000000000, 0.0001954311564186863323, 0.0003908623128373726646, 0.0005862934692560590241, 0.0007817246256747453293 ),
 .UNSPECIFIED. ) ;
#55371 = B_SPLINE_CURVE_WITH_KNOTS ( 'NONE', 3,
 ( #13197, #40677, #6442, #88873, #33900, #15747, #6872, #9859, #16179, #61809 ),
 .UNSPECIFIED., .F., .F.,
 ( 4, 2, 2, 2, 4 ),
 ( 0.000000000000000000, 0.0001954339857564070949, 0.0003908679715128141898, 0.0005863019572692212576, 0.0007817359430256283796 ),
 .UNSPECIFIED. ) ;
#55372 = VECTOR ( 'NONE', #20208, 1000.000000000000227 ) ;
#55374 = EDGE_CURVE ( 'NONE', #76058, #9375, #53522, .T. ) ;
#55373 = ORIENTED_EDGE ( 'NONE', *, *, #62802, .T. ) ;
#55375 = ORIENTED_EDGE ( 'NONE', *, *, #14604, .F. ) ;
#55377 = EDGE_LOOP ( 'NONE', ( #27805, #26317, #5916, #968 ) ) ;
#55376 = FACE_OUTER_BOUND ( 'NONE', #7046, .T. ) ;
#55378 = B_SPLINE_CURVE_WITH_KNOTS ( 'NONE', 3,
 ( #74943, #47002, #74490, #13236, #12787, #68178, #88474, #62292, #26743, #82143 ),
 .UNSPECIFIED., .F., .F.,
 ( 4, 2, 2, 2, 4 ),
 ( 0.0007817246336856289524, 0.0009771112958940101571, 0.001172497958102391253, 0.001367884620310772350, 0.001563271282519153446 ),
 .UNSPECIFIED. ) ;
#55379 = CARTESIAN_POINT ( 'NONE',  ( 16.15384615384603251, -6.879047030192662504, 34.71129190930017927 ) ) ;
#55380 = VECTOR ( 'NONE', #56003, 1000.000000000000000 ) ;
#55381 = ORIENTED_EDGE ( 'NONE', *, *, #11877, .T. ) ;
#55382 = CYLINDRICAL_SURFACE ( 'NONE', #16239, 0.2500000000000002220 ) ;
#55383 = CARTESIAN_POINT ( 'NONE',  ( 5.207448778686640800, -3.816742781228458448, 33.13167719472716044 ) ) ;
#55384 = AXIS2_PLACEMENT_3D ( 'NONE', #22589, #70787, #78410 ) ;
#55385 = VERTEX_POINT ( 'NONE', #41740 ) ;
#55386 = EDGE_CURVE ( 'NONE', #60358, #39836, #26919, .T. ) ;
#55387 = CARTESIAN_POINT ( 'NONE',  ( -9.822868284049613763, -2.504760397472875155, 29.97295953869789997 ) ) ;
#55388 = EDGE_LOOP ( 'NONE', ( #28155, #52332, #40210, #66211 ) ) ;
#55389 = DIRECTION ( 'NONE',  ( -0.000000000000000000, -0.000000000000000000, -1.000000000000000000 ) ) ;
#55390 = ORIENTED_EDGE ( 'NONE', *, *, #38859, .F. ) ;
#55391 = DIRECTION ( 'NONE',  ( -0.000000000000000000, 0.6427876096865404731, -0.7660444431189770143 ) ) ;
#55392 = EDGE_LOOP ( 'NONE', ( #14622, #88710, #7091, #153 ) ) ;
#55393 = CARTESIAN_POINT ( 'NONE',  ( -9.019254006523732770, -5.056417327199099532, 34.11270091957321426 ) ) ;
#55394 = CARTESIAN_POINT ( 'NONE',  ( -4.283994123577848256, -6.809168938359898782, 34.95455904226513866 ) ) ;
#55395 = FACE_BOUND ( 'NONE', #20610, .T. ) ;
#55396 = CARTESIAN_POINT ( 'NONE',  ( -17.77662405930182032, -2.501478030877322567, 29.88021232661720461 ) ) ;
#55397 = LINE ( 'NONE', #77007, #3980 ) ;
#55398 = CARTESIAN_POINT ( 'NONE',  ( 4.219914504848592429, -12.37446782046654192, 30.86335684631486842 ) ) ;
#55399 = CARTESIAN_POINT ( 'NONE',  ( 12.33139049180676672, -3.625366637846545892, 33.29286588640298561 ) ) ;
#55400 = CARTESIAN_POINT ( 'NONE',  ( 5.326868595271218254, -10.76462480002816235, 33.53768742498949962 ) ) ;
#55401 = CARTESIAN_POINT ( 'NONE',  ( -4.403869391139119571, -11.37209801155882971, 32.91403422569032955 ) ) ;
#55402 = CARTESIAN_POINT ( 'NONE',  ( 2.307692307692309264, -13.95598074871891292, 31.83374038241031911 ) ) ;
#55403 = ORIENTED_EDGE ( 'NONE', *, *, #27739, .T. ) ;
#55404 = ORIENTED_EDGE ( 'NONE', *, *, #14671, .F. ) ;
#55405 = VECTOR ( 'NONE', #37265, 1000.000000000000000 ) ;
#55407 = CARTESIAN_POINT ( 'NONE',  ( 16.37685750545900376, -12.15243808032446005, 31.58219941686247978 ) ) ;
#55406 = CARTESIAN_POINT ( 'NONE',  ( 24.00000000000000000, -5.499999999999981348, 27.75000000000000000 ) ) ;
#55408 = B_SPLINE_CURVE_WITH_KNOTS ( 'NONE', 3,
 ( #40646, #7298, #20373, #47832, #61777, #34314, #35659, #69436, #75313, #28007 ),
 .UNSPECIFIED., .F., .F.,
 ( 4, 2, 2, 2, 4 ),
 ( 0.000000000000000000, 0.0001954339857564074473, 0.0003908679715128148945, 0.0005863019572692223418, 0.0007817359430256297891 ),
 .UNSPECIFIED. ) ;
#55409 = CARTESIAN_POINT ( 'NONE',  ( -11.53846153846165912, -11.94971097300221174, 32.03036669348237098 ) ) ;
#55411 = B_SPLINE_CURVE_WITH_KNOTS ( 'NONE', 3,
 ( #9725, #70988, #85839, #58344, #23678, #65549, #50251, #57908, #22787, #10175 ),
 .UNSPECIFIED., .F., .F.,
 ( 4, 2, 2, 2, 4 ),
 ( 0.0007817246256747459798, 0.0009771112852218896347, 0.001172497944769033181, 0.001367884604316176728, 0.001563271263863320491 ),
 .UNSPECIFIED. ) ;
#55410 = CARTESIAN_POINT ( 'NONE',  ( 1.653273178848927064E-15, -7.500000000000000000, 29.50000000000000355 ) ) ;
#55412 = CARTESIAN_POINT ( 'NONE',  ( 1.515405825582337052, -10.70102852606553157, 33.91149625220312913 ) ) ;
#55413 = CARTESIAN_POINT ( 'NONE',  ( -12.23875879256039489, -4.989023458446560255, 34.36081565061822118 ) ) ;
#55415 = ORIENTED_EDGE ( 'NONE', *, *, #12406, .F. ) ;
#55414 = B_SPLINE_CURVE_WITH_KNOTS ( 'NONE', 3,
 ( #58737, #46564, #18661, #17768, #3348, #73610, #5135, #31725, #38931, #19097 ),
 .UNSPECIFIED., .F., .F.,
 ( 4, 2, 2, 2, 4 ),
 ( 0.000000000000000000, 0.0001954339857564071491, 0.0003908679715128142982, 0.0005863019572692214744, 0.0007817359430256285964 ),
 .UNSPECIFIED. ) ;
#55416 = LINE ( 'NONE', #21626, #9786 ) ;
#55417 = LINE ( 'NONE', #82902, #51635 ) ;
#55418 = CARTESIAN_POINT ( 'NONE',  ( -8.769230769230890843, -12.27809138561165270, 31.22303859784587132 ) ) ;
#55419 = DIRECTION ( 'NONE',  ( -0.000000000000000000, 1.000000000000000000, -0.000000000000000000 ) ) ;
#55420 = ORIENTED_EDGE ( 'NONE', *, *, #81166, .T. ) ;
#55421 = ORIENTED_EDGE ( 'NONE', *, *, #6964, .F. ) ;
#55422 = EDGE_CURVE ( 'NONE', #23361, #46498, #84502, .T. ) ;
#55423 = ORIENTED_EDGE ( 'NONE', *, *, #74142, .T. ) ;
#55424 = CARTESIAN_POINT ( 'NONE',  ( -9.469528151039281028, -12.44528174975671853, 30.48912976160716681 ) ) ;
#55426 = EDGE_LOOP ( 'NONE', ( #43173, #30694, #9870, #77539 ) ) ;
#55425 = EDGE_CURVE ( 'NONE', #22884, #45410, #66526, .T. ) ;
#55427 = CARTESIAN_POINT ( 'NONE',  ( -10.61538461538461320, -3.937682226553329556, 33.60647404775216529 ) ) ;
#55428 = DIRECTION ( 'NONE',  ( -0.000000000000000000, 0.9396926207859092051, -0.3420201433256662704 ) ) ;
#55429 = LINE ( 'NONE', #9459, #88364 ) ;
#55430 = CARTESIAN_POINT ( 'NONE',  ( -3.749999999999997335, -7.500000000000021316, 15.09375000000000000 ) ) ;
#55431 = CARTESIAN_POINT ( 'NONE',  ( 14.43821800945587519, -4.459921816937791661, 33.71989282347011851 ) ) ;
#55432 = ORIENTED_EDGE ( 'NONE', *, *, #20083, .T. ) ;
#55433 = EDGE_CURVE ( 'NONE', #31499, #63487, #48930, .T. ) ;
#55434 = CARTESIAN_POINT ( 'NONE',  ( 11.53846153846141753, -10.21337939537710326, 33.94971097300076224 ) ) ;
#55436 = ORIENTED_EDGE ( 'NONE', *, *, #78422, .T. ) ;
#55435 = LINE ( 'NONE', #76145, #81330 ) ;
#55437 = CARTESIAN_POINT ( 'NONE',  ( -39.05038313613820122, -2.249999999999998668, 29.75000000000000355 ) ) ;
#55438 = CARTESIAN_POINT ( 'NONE',  ( -10.36533030374629938, -3.627508038966690496, 32.91356715214248396 ) ) ;
#55439 = CARTESIAN_POINT ( 'NONE',  ( 0.4615384615384611200, -12.78798330534102945, 29.74999999999997868 ) ) ;
#55440 = CARTESIAN_POINT ( 'NONE',  ( -18.00000000000000000, -1.145656007487079631, 33.13000708000598848 ) ) ;
#55442 = VECTOR ( 'NONE', #3201, 1000.000000000000114 ) ;
#55441 = CARTESIAN_POINT ( 'NONE',  ( -9.757577692864010999, -12.51329471203370325, 31.30864560766548976 ) ) ;
#55443 = CARTESIAN_POINT ( 'NONE',  ( -3.454254155333563059, -10.97335522853832579, 33.68706563782419749 ) ) ;
#55444 = CARTESIAN_POINT ( 'NONE',  ( -3.099930900282468649, -7.277220318596959281, 34.99547417642776992 ) ) ;
#55445 = EDGE_CURVE ( 'NONE', #81881, #58148, #42190, .T. ) ;
#55446 = CARTESIAN_POINT ( 'NONE',  ( -0.06109907496451398579, -10.25000000000000178, 23.78311829374151998 ) ) ;
#55447 = EDGE_LOOP ( 'NONE', ( #75276, #30259, #56363, #40875 ) ) ;
#55448 = DIRECTION ( 'NONE',  ( -0.000000000000000000, -0.9848077530122086864, -0.1736481776669273613 ) ) ;
#55449 = LINE ( 'NONE', #21218, #24630 ) ;
#55450 = B_SPLINE_CURVE_WITH_KNOTS ( 'NONE', 3,
 ( #47993, #68275, #25517, #25956, #5684, #81359, #52973, #81801, #33608, #61507 ),
 .UNSPECIFIED., .F., .F.,
 ( 4, 2, 2, 2, 4 ),
 ( 0.000000000000000000, 0.0001954311584214073465, 0.0003908623168428146930, 0.0005862934752642220667, 0.0007817246336856293861 ),
 .UNSPECIFIED. ) ;
#55451 = FACE_OUTER_BOUND ( 'NONE', #48003, .T. ) ;
#55452 = DIRECTION ( 'NONE',  ( -0.000000000000000000, 0.1736481776669307198, -0.9848077530122080203 ) ) ;
#55453 = EDGE_LOOP ( 'NONE', ( #44510, #59771 ) ) ;
#55454 = CARTESIAN_POINT ( 'NONE',  ( 7.846153846153723244, -12.16647553114689728, 32.15551576947799362 ) ) ;
#55455 = CARTESIAN_POINT ( 'NONE',  ( -3.361460697436787104, -10.54014554554150607, 33.71984207302941883 ) ) ;
#55456 = AXIS2_PLACEMENT_3D ( 'NONE', #31010, #46314, #72445 ) ;
#55457 = CARTESIAN_POINT ( 'NONE',  ( 14.30769230769262279, -2.255955759149395501, 30.00000000000324363 ) ) ;
#55458 = DIRECTION ( 'NONE',  ( -0.000000000000000000, -0.9848077530122085754, -0.1736481776669273613 ) ) ;
#55459 = VERTEX_POINT ( 'NONE', #17364 ) ;
#55460 = CARTESIAN_POINT ( 'NONE',  ( 6.923076923076802558, -4.481592998941358097, 33.73612834414048933 ) ) ;
#55461 = CARTESIAN_POINT ( 'NONE',  ( 17.14299142792551578, -5.557115091759786019, 34.35708131394839882 ) ) ;
#55462 = LINE ( 'NONE', #83396, #20627 ) ;
#55463 = ORIENTED_EDGE ( 'NONE', *, *, #67995, .F. ) ;
#55464 = CARTESIAN_POINT ( 'NONE',  ( -16.82697766754503377, -12.07971442181321997, 32.31769673815850297 ) ) ;
#55465 = EDGE_CURVE ( 'NONE', #18250, #55647, #4291, .T. ) ;
#55466 = EDGE_LOOP ( 'NONE', ( #77784, #34778 ) ) ;
#55467 = CARTESIAN_POINT ( 'NONE',  ( 1.134615384615387468, -7.433931650972300353, 34.75000000000000711 ) ) ;
#55468 = CARTESIAN_POINT ( 'NONE',  ( 0.5920638997721054952, -10.31582465632705237, 34.18122507451815295 ) ) ;
#55469 = CIRCLE ( 'NONE', #78674, 4.000000000000000000 ) ;
#55470 = ORIENTED_EDGE ( 'NONE', *, *, #46861, .F. ) ;
#55471 = CARTESIAN_POINT ( 'NONE',  ( -18.00000000000000000, -9.905515769479279697, 34.41647553114623292 ) ) ;
#55472 = DIRECTION ( 'NONE',  ( 0.000000000000000000, 0.000000000000000000, -1.000000000000000000 ) ) ;
#55473 = CARTESIAN_POINT ( 'NONE',  ( -11.78848477575450282, -6.695914987888146541, 34.68535235679833306 ) ) ;
#55474 = AXIS2_PLACEMENT_3D ( 'NONE', #32866, #13038, #11261 ) ;
#55475 = EDGE_CURVE ( 'NONE', #79227, #61132, #29168, .T. ) ;
#55476 = CARTESIAN_POINT ( 'NONE',  ( 8.769230769230768274, -1.129524287112498415, 32.06866353760679544 ) ) ;
#55477 = DIRECTION ( 'NONE',  ( 0.000000000000000000, 0.000000000000000000, -1.000000000000000000 ) ) ;
#55478 = EDGE_CURVE ( 'NONE', #65424, #34542, #81811, .T. ) ;
#55479 = VERTEX_POINT ( 'NONE', #18257 ) ;
#55480 = EDGE_CURVE ( 'NONE', #6648, #4047, #88204, .T. ) ;
#55481 = FACE_BOUND ( 'NONE', #55830, .T. ) ;
#55482 = VERTEX_POINT ( 'NONE', #85831 ) ;
#55483 = CARTESIAN_POINT ( 'NONE',  ( -8.899378738962468560, -12.50552854090298993, 31.33409797877408920 ) ) ;
#55484 = CARTESIAN_POINT ( 'NONE',  ( -14.30769230769230660, -11.35647404775217417, 33.31231777344666511 ) ) ;
#55485 = FACE_OUTER_BOUND ( 'NONE', #66707, .T. ) ;
#55486 = CARTESIAN_POINT ( 'NONE',  ( -11.40766973063675493, -2.541949514083464479, 30.39797389878540557 ) ) ;
#55487 = ADVANCED_FACE ( 'NONE', ( #44821 ), #11054, .F. ) ;
#55488 = ORIENTED_EDGE ( 'NONE', *, *, #35617, .T. ) ;
#55489 = EDGE_LOOP ( 'NONE', ( #73653, #38545, #15697, #9881 ) ) ;
#55490 = ORIENTED_EDGE ( 'NONE', *, *, #71289, .T. ) ;
#55491 = CARTESIAN_POINT ( 'NONE',  ( -3.230769230769229949, -11.35647404775217417, 33.31231777344666511 ) ) ;
#55492 = EDGE_CURVE ( 'NONE', #62484, #47159, #64644, .T. ) ;
#55494 = ORIENTED_EDGE ( 'NONE', *, *, #60417, .T. ) ;
#55493 = EDGE_CURVE ( 'NONE', #34480, #84245, #21666, .T. ) ;
#55495 = CARTESIAN_POINT ( 'NONE',  ( 15.00784227186237807, -3.395401636524185474, 33.02366814457250399 ) ) ;
#55496 = CARTESIAN_POINT ( 'NONE',  ( -11.60454391782167249, -5.471508081941602875, 34.59228464037088457 ) ) ;
#55497 = EDGE_CURVE ( 'NONE', #86970, #5565, #38076, .T. ) ;
#55498 = B_SPLINE_CURVE_WITH_KNOTS ( 'NONE', 3,
 ( #69488, #7793, #28966, #56853, #48768, #77579, #70383, #56422, #14997, #42471 ),
 .UNSPECIFIED., .F., .F.,
 ( 4, 2, 2, 2, 4 ),
 ( 0.000000000000000000, 0.0001954339857564096699, 0.0003908679715128193398, 0.0005863019572692289554, 0.0007817359430256386795 ),
 .UNSPECIFIED. ) ;
#55499 = DIRECTION ( 'NONE',  ( 0.000000000000000000, -6.938893903907222067E-15, 1.000000000000000000 ) ) ;
#55500 = DIRECTION ( 'NONE',  ( -0.000000000000000000, 0.5000000000000011102, -0.8660254037844380415 ) ) ;
#55501 = FACE_OUTER_BOUND ( 'NONE', #55799, .T. ) ;
#55502 = DIRECTION ( 'NONE',  ( -0.000000000000000000, -0.000000000000000000, -1.000000000000000000 ) ) ;
#55503 = CARTESIAN_POINT ( 'NONE',  ( 7.846153846153846700, -4.661471528628507777, 34.16647553114623292 ) ) ;
#55504 = ORIENTED_EDGE ( 'NONE', *, *, #30433, .T. ) ;
#55505 = AXIS2_PLACEMENT_3D ( 'NONE', #68256, #25935, #12425 ) ;
#55506 = VERTEX_POINT ( 'NONE', #45269 ) ;
#55507 = ORIENTED_EDGE ( 'NONE', *, *, #74903, .T. ) ;
#55508 = LINE ( 'NONE', #48749, #20115 ) ;
#55510 = CARTESIAN_POINT ( 'NONE',  ( 10.54930223602447725, -2.292212530054419606, 30.41441678777542634 ) ) ;
#55509 = DIRECTION ( 'NONE',  ( 0.000000000000000000, 1.000000000000000000, 0.000000000000000000 ) ) ;
#55511 = CARTESIAN_POINT ( 'NONE',  ( 11.28843831424008393, -2.341070481393819236, 30.72580821765574299 ) ) ;
#55512 = CARTESIAN_POINT ( 'NONE',  ( -3.230769230769229949, -11.16473453929635440, 33.15142922261926373 ) ) ;
#55513 = FACE_BOUND ( 'NONE', #41469, .T. ) ;
#55514 = CYLINDRICAL_SURFACE ( 'NONE', #40356, 0.2499999999999986955 ) ;
#55515 = EDGE_LOOP ( 'NONE', ( #67913, #59142, #35087, #4415 ) ) ;
#55516 = CARTESIAN_POINT ( 'NONE',  ( -6.000000000000119904, -10.21337939537710326, 33.94971097300076224 ) ) ;
#55517 = LINE ( 'NONE', #28498, #80480 ) ;
#55518 = CARTESIAN_POINT ( 'NONE',  ( -1.319359813339360477, -2.892918686051626498, 31.69288490824025928 ) ) ;
#55519 = CARTESIAN_POINT ( 'NONE',  ( 6.923076923076800782, -9.528491918059723176, 34.59228464037033035 ) ) ;
#55520 = ORIENTED_EDGE ( 'NONE', *, *, #1894, .F. ) ;
#55521 = CARTESIAN_POINT ( 'NONE',  ( 18.06525557127602610, -12.46129190930001052, 30.37095296980869819 ) ) ;
#55522 = EDGE_LOOP ( 'NONE', ( #63125, #72388 ) ) ;
#55523 = FACE_BOUND ( 'NONE', #2977, .T. ) ;
#55524 = EDGE_CURVE ( 'NONE', #65891, #34882, #69987, .T. ) ;
#55525 = CYLINDRICAL_SURFACE ( 'NONE', #63415, 4.000000000000000000 ) ;
#55526 = VECTOR ( 'NONE', #76384, 1000.000000000000114 ) ;
#55527 = CARTESIAN_POINT ( 'NONE',  ( -7.911403777927930925, -2.255955759149247619, 30.00000000000013856 ) ) ;
#55528 = CARTESIAN_POINT ( 'NONE',  ( -12.71156168575991963, -12.07920672191015221, 32.31858351112116168 ) ) ;
#55529 = ORIENTED_EDGE ( 'NONE', *, *, #63223, .F. ) ;
#55530 = CARTESIAN_POINT ( 'NONE',  ( 11.66925197942848769, -10.70102852606553157, 33.91149625220312913 ) ) ;
#55531 = CARTESIAN_POINT ( 'NONE',  ( -14.55766903863466055, -4.236021600441997492, 33.53823185664189310 ) ) ;
#55532 = CARTESIAN_POINT ( 'NONE',  ( 18.22277966897806678, -10.97394488606063589, 33.68653795673696294 ) ) ;
#55533 = CARTESIAN_POINT ( 'NONE',  ( -4.826868657009623753, -5.642605341092957083, 34.66089969410670335 ) ) ;
#55534 = ORIENTED_EDGE ( 'NONE', *, *, #59719, .T. ) ;
#55535 = VECTOR ( 'NONE', #2168, 1000.000000000000114 ) ;
#55536 = CARTESIAN_POINT ( 'NONE',  ( -12.23852710992561299, -3.105924265160262543, 32.13625925475356127 ) ) ;
#55537 = ORIENTED_EDGE ( 'NONE', *, *, #60698, .F. ) ;
#55538 = EDGE_CURVE ( 'NONE', #54237, #62563, #25455, .T. ) ;
#55540 = ORIENTED_EDGE ( 'NONE', *, *, #48257, .F. ) ;
#55539 = CARTESIAN_POINT ( 'NONE',  ( 4.403791563224197070, -2.986452184633681117, 32.43230066228895225 ) ) ;
#55541 = CARTESIAN_POINT ( 'NONE',  ( 3.296024802045255164, -2.625532179533470512, 30.86335684631491105 ) ) ;
#55542 = CARTESIAN_POINT ( 'NONE',  ( -4.219929564802033184, -2.721908614388772740, 31.22303859784724622 ) ) ;
#55543 = CARTESIAN_POINT ( 'NONE',  ( 7.846153846153846700, -9.905515769479276145, 34.41647553114623292 ) ) ;
#55544 = CARTESIAN_POINT ( 'NONE',  ( 14.05766907039934210, -9.271318131107980420, 34.42618302367067429 ) ) ;
#55545 = CARTESIAN_POINT ( 'NONE',  ( -30.00000000000000000, 15.00000000000000355, 0.000000000000000000 ) ) ;
#55547 = CARTESIAN_POINT ( 'NONE',  ( 14.16025641025641235, -4.000000000000000000, 29.75000000000000355 ) ) ;
#55546 = CARTESIAN_POINT ( 'NONE',  ( 13.44987095589141290, -6.026961402152789304, 34.52809138561124769 ) ) ;
#55548 = CARTESIAN_POINT ( 'NONE',  ( 14.30769230769218758, -3.835265460704628371, 33.15142922262033665 ) ) ;
#55549 = CARTESIAN_POINT ( 'NONE',  ( -1.139087296525992166, -10.25000000000000533, 18.60937500000000355 ) ) ;
#55550 = ORIENTED_EDGE ( 'NONE', *, *, #78384, .T. ) ;
#55551 = FACE_OUTER_BOUND ( 'NONE', #78300, .T. ) ;
#55552 = ORIENTED_EDGE ( 'NONE', *, *, #8916, .F. ) ;
#55553 = ORIENTED_EDGE ( 'NONE', *, *, #36621, .F. ) ;
#55554 = CARTESIAN_POINT ( 'NONE',  ( -8.352564102564102200, -11.00000000000000000, 29.75000000000000355 ) ) ;
#55555 = ORIENTED_EDGE ( 'NONE', *, *, #84912, .F. ) ;
#55556 = DIRECTION ( 'NONE',  ( 0.000000000000000000, 0.000000000000000000, -1.000000000000000000 ) ) ;
#55557 = CARTESIAN_POINT ( 'NONE',  ( -11.40793610022789650, -10.31582465632705237, 34.18122507451815295 ) ) ;
#55558 = CARTESIAN_POINT ( 'NONE',  ( 3.165498784808455923, -8.613356846314824011, 34.62446782046655613 ) ) ;
#55559 = CARTESIAN_POINT ( 'NONE',  ( -0.4615384615384611200, -8.120952969808772792, 34.71129190930000163 ) ) ;
#55560 = CARTESIAN_POINT ( 'NONE',  ( 6.249945518348143381, -2.587454068350147462, 30.68340429815432202 ) ) ;
#55562 = ADVANCED_FACE ( 'NONE', ( #18710 ), #26343, .F. ) ;
#55561 = CARTESIAN_POINT ( 'NONE',  ( -16.37677237136229991, -3.105860786376062332, 32.13614157043599562 ) ) ;
#55563 = CARTESIAN_POINT ( 'NONE',  ( 16.02315468717859659, -11.71456829005830080, 32.44064028649416542 ) ) ;
#55564 = CARTESIAN_POINT ( 'NONE',  ( -5.999999999999998224, -1.422936976036506707, 30.56769352161908415 ) ) ;
#55565 = AXIS2_PLACEMENT_3D ( 'NONE', #74508, #20001, #47465 ) ;
#55566 = DIRECTION ( 'NONE',  ( -0.000000000000000000, 0.9848077530122086864, -0.1736481776669273891 ) ) ;
#55567 = CARTESIAN_POINT ( 'NONE',  ( 11.31497659473759043, -10.81261337010820256, 33.49550067578627477 ) ) ;
#55568 = CARTESIAN_POINT ( 'NONE',  ( 5.999999999999878320, -11.67786785259630911, 32.92929555188603530 ) ) ;
#55569 = CARTESIAN_POINT ( 'NONE',  ( -13.60810030917971680, -10.23692288466677880, 34.23039457007281072 ) ) ;
#55570 = ORIENTED_EDGE ( 'NONE', *, *, #33829, .T. ) ;
#55571 = ORIENTED_EDGE ( 'NONE', *, *, #89074, .F. ) ;
#55572 = DIRECTION ( 'NONE',  ( 0.000000000000000000, 0.9848077530122072432, -0.1736481776669354937 ) ) ;
#55573 = CARTESIAN_POINT ( 'NONE',  ( 1.607628228708782414, -3.395485233115138168, 33.02377354290276656 ) ) ;
#55574 = DIRECTION ( 'NONE',  ( -1.000000000000000000, 0.000000000000000000, -0.000000000000000000 ) ) ;
#55575 = CARTESIAN_POINT ( 'NONE',  ( 9.692307692307695177, -10.05456864172156806, 36.03766855953608683 ) ) ;
#55576 = EDGE_CURVE ( 'NONE', #17484, #68101, #59131, .T. ) ;
#55577 = VECTOR ( 'NONE', #36840, 1000.000000000000000 ) ;
#55578 = EDGE_CURVE ( 'NONE', #31488, #5024, #39869, .T. ) ;
#55579 = DIRECTION ( 'NONE',  ( -0.000000000000000000, -0.7660444431189791237, -0.6427876096865379196 ) ) ;
#55580 = DIRECTION ( 'NONE',  ( -0.000000000000000000, -0.1736481776669307198, -0.9848077530122080203 ) ) ;
#55581 = B_SPLINE_CURVE_WITH_KNOTS ( 'NONE', 3,
 ( #60641, #44901, #24641, #72376, #10689, #52106, #280, #26868, #41272, #82262 ),
 .UNSPECIFIED., .F., .F.,
 ( 4, 2, 2, 2, 4 ),
 ( 0.0007817246256747446788, 0.0009771112852218879000, 0.001172497944769031013, 0.001367884604316174126, 0.001563271263863317238 ),
 .UNSPECIFIED. ) ;
#55582 = B_SPLINE_CURVE_WITH_KNOTS ( 'NONE', 3,
 ( #39334, #47393, #82086, #106, #19485, #551, #13177, #27574, #26246, #34769 ),
 .UNSPECIFIED., .F., .F.,
 ( 4, 2, 2, 2, 4 ),
 ( 0.000000000000000000, 0.0001954339857564097512, 0.0003908679715128195024, 0.0005863019572692292807, 0.0007817359430256390048 ),
 .UNSPECIFIED. ) ;
#55583 = CARTESIAN_POINT ( 'NONE',  ( -2.373774687052440768, -8.164416787775445883, 34.95778746994557906 ) ) ;
#55584 = EDGE_CURVE ( 'NONE', #1538, #34578, #82183, .T. ) ;
#55585 = VERTEX_POINT ( 'NONE', #33551 ) ;
#55586 = DIRECTION ( 'NONE',  ( -1.000000000000000000, 0.000000000000000000, 0.000000000000000000 ) ) ;
#55587 = ORIENTED_EDGE ( 'NONE', *, *, #10156, .F. ) ;
#55588 = DIRECTION ( 'NONE',  ( 1.000000000000000000, 0.000000000000000000, 0.000000000000000000 ) ) ;
#55589 = CARTESIAN_POINT ( 'NONE',  ( 10.61538461538461675, -9.584722331328613620, 36.20867863119891439 ) ) ;
#55590 = AXIS2_PLACEMENT_3D ( 'NONE', #86394, #64307, #2171 ) ;
#55591 = CARTESIAN_POINT ( 'NONE',  ( 12.46153846153846168, -8.120952969808772792, 34.71129190930000163 ) ) ;
#55592 = DIRECTION ( 'NONE',  ( 0.000000000000000000, 0.3420201433256641055, -0.9396926207859100932 ) ) ;
#55593 = CARTESIAN_POINT ( 'NONE',  ( -3.296092146261405897, -7.749976743299137993, 34.99404534957040624 ) ) ;
#55594 = CIRCLE ( 'NONE', #6672, 2.000000000000001776 ) ;
#55595 = ORIENTED_EDGE ( 'NONE', *, *, #68089, .F. ) ;
#55596 = ORIENTED_EDGE ( 'NONE', *, *, #35542, .T. ) ;
#55597 = EDGE_CURVE ( 'NONE', #7139, #49175, #55021, .T. ) ;
#55598 = ORIENTED_EDGE ( 'NONE', *, *, #13820, .F. ) ;
#55599 = VERTEX_POINT ( 'NONE', #67337 ) ;
#55600 = AXIS2_PLACEMENT_3D ( 'NONE', #41821, #82810, #82366 ) ;
#55601 = CARTESIAN_POINT ( 'NONE',  ( -6.250023237292964495, -11.37209801155882971, 32.91403422569032955 ) ) ;
#55602 = CARTESIAN_POINT ( 'NONE',  ( 8.769230769230645706, -11.06231777344772027, 33.60647404775119895 ) ) ;
#55603 = CARTESIAN_POINT ( 'NONE',  ( 4.284636594813102661, -11.93129842949671726, 32.56571108434900452 ) ) ;
#55604 = CARTESIAN_POINT ( 'NONE',  ( 14.30769230769218758, -2.625532179533778709, 30.86335684631627174 ) ) ;
#55605 = CARTESIAN_POINT ( 'NONE',  ( -7.780086512803769949, -3.937682226553329556, 33.60647404775216529 ) ) ;
#55606 = CARTESIAN_POINT ( 'NONE',  ( 14.30769230769231015, -9.780366693483667717, 34.19971097300155094 ) ) ;
#55607 = EDGE_LOOP ( 'NONE', ( #35090, #53733, #76828, #28945 ) ) ;
#55608 = ORIENTED_EDGE ( 'NONE', *, *, #40521, .T. ) ;
#55609 = ORIENTED_EDGE ( 'NONE', *, *, #26580, .T. ) ;
#55611 = ORIENTED_EDGE ( 'NONE', *, *, #21670, .F. ) ;
#55610 = FACE_OUTER_BOUND ( 'NONE', #72696, .T. ) ;
#55612 = PLANE ( 'NONE',  #63521 ) ;
#55613 = CARTESIAN_POINT ( 'NONE',  ( -5.011667505647053211, -11.48612834413965977, 32.76840700105972815 ) ) ;
#55614 = CARTESIAN_POINT ( 'NONE',  ( -1.929879867024197893E-14, -3.750000000000000000, 22.90625000000000355 ) ) ;
#55615 = ORIENTED_EDGE ( 'NONE', *, *, #85294, .F. ) ;
#55616 = VERTEX_POINT ( 'NONE', #13271 ) ;
#55617 = FACE_OUTER_BOUND ( 'NONE', #84666, .T. ) ;
#55618 = AXIS2_PLACEMENT_3D ( 'NONE', #69543, #55580, #61447 ) ;
#55619 = ORIENTED_EDGE ( 'NONE', *, *, #75028, .T. ) ;
#55620 = FACE_BOUND ( 'NONE', #46873, .T. ) ;
#55621 = DIRECTION ( 'NONE',  ( -0.000000000000000000, 0.1736481776669307198, -0.9848077530122080203 ) ) ;
#55622 = CARTESIAN_POINT ( 'NONE',  ( -8.769230769230768274, -3.513871655860378418, 32.76840700105978499 ) ) ;
#55623 = VERTEX_POINT ( 'NONE', #20473 ) ;
#55624 = CARTESIAN_POINT ( 'NONE',  ( -6.923076923076922462, -4.786620604624113540, 33.94971097300155094 ) ) ;
#55625 = CARTESIAN_POINT ( 'NONE',  ( -15.90390074446811042, -12.68172785388650681, 30.59649109432439573 ) ) ;
#55626 = FACE_OUTER_BOUND ( 'NONE', #37576, .T. ) ;
#55627 = LINE ( 'NONE', #34914, #18398 ) ;
#55628 = CARTESIAN_POINT ( 'NONE',  ( -3.360917200500926239, -9.504002272028875709, 34.60269587691767867 ) ) ;
#55629 = ORIENTED_EDGE ( 'NONE', *, *, #79741, .T. ) ;
#55630 = CARTESIAN_POINT ( 'NONE',  ( -12.23875879256039489, -2.353885683473779800, 30.79025554430704403 ) ) ;
#55631 = CARTESIAN_POINT ( 'NONE',  ( -5.869474561766354626, -4.299079248970732792, 33.91157788607253565 ) ) ;
#55632 = DIRECTION ( 'NONE',  ( 0.000000000000000000, 0.000000000000000000, -1.000000000000000000 ) ) ;
#55633 = CARTESIAN_POINT ( 'NONE',  ( 22.75000000000000000, -4.499999999999999112, 29.75000000000000355 ) ) ;
#55634 = DIRECTION ( 'NONE',  ( -0.000000000000000000, -0.1736481776669307198, -0.9848077530122080203 ) ) ;
#55635 = FACE_BOUND ( 'NONE', #45669, .T. ) ;
#55637 = CARTESIAN_POINT ( 'NONE',  ( -7.846153846153844924, -7.500000000000001776, 35.04278698407183867 ) ) ;
#55636 = CARTESIAN_POINT ( 'NONE',  ( -8.769230769230460965, -2.506253911140614576, 30.00000000000323297 ) ) ;
#55638 = B_SPLINE_CURVE_WITH_KNOTS ( 'NONE', 3,
 ( #63748, #2482, #44348, #42606, #43041, #6702, #34174, #70514, #56110, #21882 ),
 .UNSPECIFIED., .F., .F.,
 ( 4, 2, 2, 2, 4 ),
 ( 0.0007817246256747484735, 0.0009771112852218920199, 0.001172497944769035783, 0.001367884604316179330, 0.001563271263863322876 ),
 .UNSPECIFIED. ) ;
#55639 = DIRECTION ( 'NONE',  ( -0.000000000000000000, -0.6427876096865404731, -0.7660444431189771253 ) ) ;
#55641 = CARTESIAN_POINT ( 'NONE',  ( 5.869852790561781219, -10.88202310037935661, 33.43294751532457099 ) ) ;
#55640 = DIRECTION ( 'NONE',  ( -0.000000000000000000, 1.000000000000000000, -0.000000000000000000 ) ) ;
#55642 = CARTESIAN_POINT ( 'NONE',  ( -7.912236225513978205, -3.937682226553330445, 33.60647404775217240 ) ) ;
#55643 = CARTESIAN_POINT ( 'NONE',  ( 2.724691934501235036, -6.299813628509441266, 16.63875670625849068 ) ) ;
#55644 = B_SPLINE_CURVE_WITH_KNOTS ( 'NONE', 3,
 ( #14036, #75732, #48702, #76177, #6407, #26665, #88392, #5960, #61766, #40197 ),
 .UNSPECIFIED., .F., .F.,
 ( 4, 2, 2, 2, 4 ),
 ( 0.0007817246256747521597, 0.0009771112852218961399, 0.001172497944769040337, 0.001367884604316184534, 0.001563271263863328514 ),
 .UNSPECIFIED. ) ;
#55645 = ORIENTED_EDGE ( 'NONE', *, *, #49835, .F. ) ;
#55646 = CARTESIAN_POINT ( 'NONE',  ( -6.923076923076922462, -2.900454961884010974, 35.62045528018868623 ) ) ;
#55647 = VERTEX_POINT ( 'NONE', #74094 ) ;
#55648 = LINE ( 'NONE', #68730, #56458 ) ;
#55649 = AXIS2_PLACEMENT_3D ( 'NONE', #15994, #29076, #69599 ) ;
#55650 = ORIENTED_EDGE ( 'NONE', *, *, #42973, .T. ) ;
#55651 = CARTESIAN_POINT ( 'NONE',  ( -18.00000000000000000, -2.499999999999999556, 29.74999999999998579 ) ) ;
#55652 = CARTESIAN_POINT ( 'NONE',  ( -15.90390074446811042, -12.07971442181321997, 32.31769673815850297 ) ) ;
#55653 = ORIENTED_EDGE ( 'NONE', *, *, #8635, .F. ) ;
#55654 = LINE ( 'NONE', #34063, #3805 ) ;
#55655 = CARTESIAN_POINT ( 'NONE',  ( -2.775308065498764964, -6.422011778438537988, 18.67000670625849068 ) ) ;
#55656 = CARTESIAN_POINT ( 'NONE',  ( -4.088653165551497715, -2.255955759149235629, 29.99999999999988631 ) ) ;
#55657 = CARTESIAN_POINT ( 'NONE',  ( -5.076923076923199218, -3.083524468854526912, 32.58852847137268327 ) ) ;
#55658 = VECTOR ( 'NONE', #6385, 999.9999999999998863 ) ;
#55659 = CARTESIAN_POINT ( 'NONE',  ( 12.39545505058258001, -2.721908614388770964, 31.22303859784723912 ) ) ;
#55660 = LINE ( 'NONE', #286, #68900 ) ;
#55661 = CARTESIAN_POINT ( 'NONE',  ( 11.53846153846153832, -1.242168528481310874, 33.36296068462461051 ) ) ;
#55662 = CARTESIAN_POINT ( 'NONE',  ( 11.78851585009985570, -3.627508038966690496, 32.91356715214248396 ) ) ;
#55663 = CARTESIAN_POINT ( 'NONE',  ( -3.724691934501248802, -5.885600066136383646, 21.67374329374151287 ) ) ;
#55664 = CARTESIAN_POINT ( 'NONE',  ( -9.758391103263571509, -3.513871655860377086, 32.76840700105978499 ) ) ;
#55665 = DIRECTION ( 'NONE',  ( -0.000000000000000000, 0.6427876096865404731, -0.7660444431189771253 ) ) ;
#55666 = AXIS2_PLACEMENT_3D ( 'NONE', #6927, #34399, #51310 ) ;
#55667 = ORIENTED_EDGE ( 'NONE', *, *, #37207, .T. ) ;
#55668 = DIRECTION ( 'NONE',  ( 1.000000000000000000, 0.000000000000000000, 0.000000000000000000 ) ) ;
#55669 = CARTESIAN_POINT ( 'NONE',  ( 0.06109907496451268821, -3.749999999999999556, 21.90811829374151642 ) ) ;
#55670 = ADVANCED_FACE ( 'NONE', ( #19583 ), #40754, .F. ) ;
#55671 = CARTESIAN_POINT ( 'NONE',  ( -16.15384615384615330, -12.34228464037088635, 31.77849191805839268 ) ) ;
#55672 = DIRECTION ( 'NONE',  ( -0.000000000000000000, -0.7660444431189791237, -0.6427876096865379196 ) ) ;
#55673 = ORIENTED_EDGE ( 'NONE', *, *, #74521, .T. ) ;
#55674 = DIRECTION ( 'NONE',  ( 0.000000000000000000, 0.000000000000000000, -1.000000000000000000 ) ) ;
#55675 = CARTESIAN_POINT ( 'NONE',  ( 3.230769230769110045, -3.835265460704628371, 33.15142922262033665 ) ) ;
#55677 = VERTEX_POINT ( 'NONE', #26785 ) ;
#55676 = CARTESIAN_POINT ( 'NONE',  ( 2.177000841024751221, -2.729777683071816785, 31.24903638046268739 ) ) ;
#55678 = CARTESIAN_POINT ( 'NONE',  ( -5.076923076923197442, -6.026961402154118908, 34.52809138561165270 ) ) ;
#55679 = ADVANCED_FACE ( 'NONE', ( #74532 ), #60120, .F. ) ;
#55680 = CARTESIAN_POINT ( 'NONE',  ( -16.15384615384627409, -10.90142922262034020, 33.41473453929536674 ) ) ;
#55681 = DIRECTION ( 'NONE',  ( 0.000000000000000000, 0.4999999999999985567, 0.8660254037844395958 ) ) ;
#55682 = CARTESIAN_POINT ( 'NONE',  ( 2.307692307692186251, -4.320704448113951379, 33.92786785259630022 ) ) ;
#55683 = CYLINDRICAL_SURFACE ( 'NONE', #19262, 0.2500000000000008882 ) ;
#55684 = AXIS2_PLACEMENT_3D ( 'NONE', #14482, #46927, #53693 ) ;
#55685 = EDGE_CURVE ( 'NONE', #24805, #1012, #33100, .T. ) ;
#55686 = ORIENTED_EDGE ( 'NONE', *, *, #6461, .F. ) ;
#55687 = CARTESIAN_POINT ( 'NONE',  ( 4.153846153846154188, -11.11383981884818262, 36.00935417666054406 ) ) ;
#55688 = ORIENTED_EDGE ( 'NONE', *, *, #42574, .F. ) ;
#55689 = ORIENTED_EDGE ( 'NONE', *, *, #34876, .F. ) ;
#55690 = CARTESIAN_POINT ( 'NONE',  ( 5.076923076923075762, -5.415277668671390821, 36.20867863119892149 ) ) ;
#55691 = FACE_OUTER_BOUND ( 'NONE', #71864, .T. ) ;
#55692 = VECTOR ( 'NONE', #42069, 1000.000000000000000 ) ;
#55693 = CARTESIAN_POINT ( 'NONE',  ( -2.307692307692305711, -9.819645486525091727, 36.12317359536749706 ) ) ;
#55694 = CARTESIAN_POINT ( 'NONE',  ( -17.01177829620344895, -7.750023224968867197, 34.99404313364389907 ) ) ;
#55695 = ORIENTED_EDGE ( 'NONE', *, *, #80829, .T. ) ;
#55696 = CARTESIAN_POINT ( 'NONE',  ( -18.25000000000000000, -7.433931650972299465, 34.75000000000000711 ) ) ;
#55697 = ORIENTED_EDGE ( 'NONE', *, *, #57988, .T. ) ;
#55698 = B_SPLINE_CURVE_WITH_KNOTS ( 'NONE', 3,
 ( #54077, #47776, #60396, #53191, #87456, #40588, #81132, #18978, #88789, #68486 ),
 .UNSPECIFIED., .F., .F.,
 ( 4, 2, 2, 2, 4 ),
 ( 0.000000000000000000, 0.0001954339881912775425, 0.0003908679763825550850, 0.0005863019645738326005, 0.0007817359527651101701 ),
 .UNSPECIFIED. ) ;
#55699 = EDGE_CURVE ( 'NONE', #37657, #48658, #12827, .T. ) ;
#55701 = ORIENTED_EDGE ( 'NONE', *, *, #53801, .F. ) ;
#55700 = B_SPLINE_CURVE_WITH_KNOTS ( 'NONE', 3,
 ( #6198, #46735, #59802, #4872, #74211, #33670, #73778, #5309, #75529, #26911 ),
 .UNSPECIFIED., .F., .F.,
 ( 4, 2, 2, 2, 4 ),
 ( 0.000000000000000000, 0.1250000000000000000, 0.2500000000000000000, 0.3750000000000000000, 0.5000000000000000000 ),
 .UNSPECIFIED. ) ;
#55702 = ORIENTED_EDGE ( 'NONE', *, *, #40247, .F. ) ;
#55705 = ORIENTED_EDGE ( 'NONE', *, *, #18193, .F. ) ;
#55704 = EDGE_CURVE ( 'NONE', #16132, #38188, #74982, .T. ) ;
#55703 = CARTESIAN_POINT ( 'NONE',  ( 4.219101293358989757, -12.51329471203373700, 31.30864560766537963 ) ) ;
#55706 = CARTESIAN_POINT ( 'NONE',  ( -0.5268089074992365894, -5.219633306516282545, 34.19971097300152962 ) ) ;
#55707 = EDGE_CURVE ( 'NONE', #19274, #16174, #61356, .T. ) ;
#55708 = FACE_OUTER_BOUND ( 'NONE', #72032, .T. ) ;
#55709 = EDGE_CURVE ( 'NONE', #49902, #83302, #33463, .T. ) ;
#55710 = CARTESIAN_POINT ( 'NONE',  ( -2.980823712421088789, -4.336752205174647656, 33.62275283266504289 ) ) ;
#55711 = CARTESIAN_POINT ( 'NONE',  ( 14.37385891428395013, -7.250054591869670162, 34.99404684341514127 ) ) ;
#55712 = EDGE_LOOP ( 'NONE', ( #8872, #24610, #66725, #18114 ) ) ;
#55713 = ORIENTED_EDGE ( 'NONE', *, *, #14158, .T. ) ;
#55714 = ORIENTED_EDGE ( 'NONE', *, *, #88082, .F. ) ;
#55715 = CARTESIAN_POINT ( 'NONE',  ( -6.673131513698878692, -2.986452184633680673, 32.43230066228895225 ) ) ;
#55717 = ORIENTED_EDGE ( 'NONE', *, *, #13585, .T. ) ;
#55716 = CARTESIAN_POINT ( 'NONE',  ( 11.53846153846141576, -5.941354392335915335, 34.76329471203413846 ) ) ;
#55718 = B_SPLINE_CURVE_WITH_KNOTS ( 'NONE', 3,
 ( #61174, #12562, #6682, #33280, #40488, #47671, #60740, #26521, #380, #53984 ),
 .UNSPECIFIED., .F., .F.,
 ( 4, 2, 2, 2, 4 ),
 ( 0.0007817359430256294638, 0.0009771253907249948054, 0.001172514838424360255, 0.001367904286123725489, 0.001563293733823090939 ),
 .UNSPECIFIED. ) ;
#55719 = CARTESIAN_POINT ( 'NONE',  ( 9.469381474791543241, -11.76352882383564769, 32.36236540154569497 ) ) ;
#55720 = CARTESIAN_POINT ( 'NONE',  ( -17.14300545628320904, -3.322132147404559976, 32.92929555188719348 ) ) ;
#55721 = ORIENTED_EDGE ( 'NONE', *, *, #9767, .T. ) ;
#55722 = VECTOR ( 'NONE', #44688, 999.9999999999998863 ) ;
#55723 = CYLINDRICAL_SURFACE ( 'NONE', #22088, 0.2499999999999986955 ) ;
#55724 = FACE_OUTER_BOUND ( 'NONE', #63590, .T. ) ;
#55725 = ORIENTED_EDGE ( 'NONE', *, *, #214, .T. ) ;
#55726 = FACE_BOUND ( 'NONE', #85939, .T. ) ;
#55727 = DIRECTION ( 'NONE',  ( -0.000000000000000000, -0.9848077530122086864, -0.1736481776669273613 ) ) ;
#55728 = LINE ( 'NONE', #27820, #75880 ) ;
#55729 = CYLINDRICAL_SURFACE ( 'NONE', #79694, 0.2499999999999995559 ) ;
#55731 = FACE_OUTER_BOUND ( 'NONE', #78381, .T. ) ;
#55730 = CARTESIAN_POINT ( 'NONE',  ( -6.793029316821241004, -7.723484964179500700, 34.74522123443823318 ) ) ;
#55732 = CARTESIAN_POINT ( 'NONE',  ( -3.007989561791163169, -3.563462043263030399, 33.22394488606062879 ) ) ;
#55733 = CARTESIAN_POINT ( 'NONE',  ( -2.437839517130528488, -3.817052484675422797, 33.13202310037935661 ) ) ;
#55734 = ORIENTED_EDGE ( 'NONE', *, *, #32741, .F. ) ;
#55735 = DIRECTION ( 'NONE',  ( -0.000000000000000000, -0.7660444431189791237, -0.6427876096865379196 ) ) ;
#55736 = B_SPLINE_CURVE_WITH_KNOTS ( 'NONE', 3,
 ( #24790, #80191, #67123, #74321, #65766, #60351, #4523, #87862, #12621, #26576 ),
 .UNSPECIFIED., .F., .F.,
 ( 4, 2, 2, 2, 4 ),
 ( 0.000000000000000000, 0.0001954311564186861968, 0.0003908623128373723936, 0.0005862934692560585904, 0.0007817246256747447872 ),
 .UNSPECIFIED. ) ;
#55737 = CARTESIAN_POINT ( 'NONE',  ( -8.096153846153846700, -2.499999999999999556, 29.81609845454691765 ) ) ;
#55738 = ORIENTED_EDGE ( 'NONE', *, *, #28211, .T. ) ;
#55739 = CARTESIAN_POINT ( 'NONE',  ( 14.08476609017615644, -9.886141570436013382, 34.14413921362392301 ) ) ;
#55740 = FACE_OUTER_BOUND ( 'NONE', #28916, .T. ) ;
#55741 = ORIENTED_EDGE ( 'NONE', *, *, #66533, .T. ) ;
#55742 = EDGE_CURVE ( 'NONE', #51126, #41438, #68655, .T. ) ;
#55743 = VECTOR ( 'NONE', #33035, 1000.000000000000114 ) ;
#55744 = CARTESIAN_POINT ( 'NONE',  ( 11.40831356872984514, -10.31621877034669588, 34.18098118002070152 ) ) ;
#55745 = CARTESIAN_POINT ( 'NONE',  ( 2.307692307692309264, -4.661471528628507777, 34.16647553114623292 ) ) ;
#55746 = FACE_BOUND ( 'NONE', #24981, .T. ) ;
#55748 = CARTESIAN_POINT ( 'NONE',  ( -17.07692307692319744, -12.46129190930018460, 30.37095296980731973 ) ) ;
#55747 = CARTESIAN_POINT ( 'NONE',  ( -2.307692307692305711, -6.386643153685126251, 34.62446782046654192 ) ) ;
#55749 = CARTESIAN_POINT ( 'NONE',  ( -6.923076923077044142, -9.442884908241554243, 34.35708131394783038 ) ) ;
#55750 = DIRECTION ( 'NONE',  ( -1.000000000000000000, 0.000000000000000000, -0.000000000000000000 ) ) ;
#55752 = CARTESIAN_POINT ( 'NONE',  ( -12.46153846153846168, -4.098570777380720287, 33.41473453929634729 ) ) ;
#55751 = SHAPE_REPRESENTATION_RELATIONSHIP ( 'NONE' , 'NONE' ,  #45449, #38570 ) ;
#55753 = CARTESIAN_POINT ( 'NONE',  ( 13.38461538461538680, -2.833524468853757305, 32.15551576947925838 ) ) ;
#55754 = CARTESIAN_POINT ( 'NONE',  ( -2.694853999681210865, -4.891553140782108677, 17.49813170625848713 ) ) ;
#55755 = EDGE_LOOP ( 'NONE', ( #65776, #51966 ) ) ;
#55756 = VERTEX_POINT ( 'NONE', #50142 ) ;
#55757 = CARTESIAN_POINT ( 'NONE',  ( 5.076923076923075762, -2.538708090699994813, 30.37095296980875503 ) ) ;
#55758 = VECTOR ( 'NONE', #43279, 1000.000000000000000 ) ;
#55759 = CARTESIAN_POINT ( 'NONE',  ( 14.53070515178570332, -12.64618726649961289, 30.78989965857442712 ) ) ;
#55760 = DIRECTION ( 'NONE',  ( 0.000000000000000000, 0.1736481776669267785, -0.9848077530122087975 ) ) ;
#55761 = CARTESIAN_POINT ( 'NONE',  ( -1.449885830576160162, -3.300289026998414865, 32.46337939537583139 ) ) ;
#55762 = CARTESIAN_POINT ( 'NONE',  ( -3.931066484868087851, -3.020022701398814124, 32.48759521482552515 ) ) ;
#55763 = CARTESIAN_POINT ( 'NONE',  ( 1.492201783934554493, -3.724691934501233703, 16.48250670625849423 ) ) ;
#55764 = EDGE_CURVE ( 'NONE', #25331, #39262, #47331, .T. ) ;
#55765 = CARTESIAN_POINT ( 'NONE',  ( 4.403846153846216360, -7.434744429011176159, 34.75000000000000711 ) ) ;
#55766 = DIRECTION ( 'NONE',  ( -0.000000000000000000, 0.6427876096865404731, -0.7660444431189770143 ) ) ;
#55767 = CARTESIAN_POINT ( 'NONE',  ( 9.442330948259105128, -10.82459398097509329, 33.81372124010185587 ) ) ;
#55768 = DIRECTION ( 'NONE',  ( -0.000000000000000000, -0.9848077530122086864, -0.1736481776669273613 ) ) ;
#55769 = CARTESIAN_POINT ( 'NONE',  ( 10.61538461538449418, -3.643525952248795718, 33.31231777344771672 ) ) ;
#55770 = CARTESIAN_POINT ( 'NONE',  ( 18.13079180782478872, -9.804649428959608670, 34.18742332936588468 ) ) ;
#55771 = CARTESIAN_POINT ( 'NONE',  ( 10.61538461538461675, -11.33034616979429110, 35.88435417666054406 ) ) ;
#55772 = CARTESIAN_POINT ( 'NONE',  ( -14.08468095607945969, -3.105924265160262543, 32.13625925475356127 ) ) ;
#55773 = DIRECTION ( 'NONE',  ( 1.000000000000000000, 0.000000000000000000, 0.000000000000000000 ) ) ;
#55774 = EDGE_LOOP ( 'NONE', ( #29834, #72688, #45035, #38392 ) ) ;
#55775 = CARTESIAN_POINT ( 'NONE',  ( 3.903822916553188804, -5.056417327199098644, 34.11270091957320716 ) ) ;
#55776 = CARTESIAN_POINT ( 'NONE',  ( 7.846153846153723244, -5.094484230521993062, 34.41647553114689373 ) ) ;
#55777 = CARTESIAN_POINT ( 'NONE',  ( 2.775308065498755195, -6.422011778438505125, 23.39249329374151642 ) ) ;
#55778 = EDGE_CURVE ( 'NONE', #5919, #25778, #10815, .T. ) ;
#55779 = B_SPLINE_CURVE_WITH_KNOTS ( 'NONE', 3,
 ( #18338, #59765, #25979, #33183, #81825, #81383, #52993, #53443, #47129, #45802 ),
 .UNSPECIFIED., .F., .F.,
 ( 4, 2, 2, 2, 4 ),
 ( 0.0007817246256747460882, 0.0009771112852218900684, 0.001172497944769033832, 0.001367884604316177595, 0.001563271263863321575 ),
 .UNSPECIFIED. ) ;
#55780 = CARTESIAN_POINT ( 'NONE',  ( -5.776987155906605942, -12.38742843783360748, 31.66772728687926985 ) ) ;
#55781 = DIRECTION ( 'NONE',  ( 0.000000000000000000, 0.000000000000000000, 1.000000000000000000 ) ) ;
#55782 = ORIENTED_EDGE ( 'NONE', *, *, #24656, .F. ) ;
#55783 = CARTESIAN_POINT ( 'NONE',  ( -12.46153846153846168, -2.538708090699994813, 30.37095296980875503 ) ) ;
#55785 = VERTEX_POINT ( 'NONE', #69103 ) ;
#55784 = CARTESIAN_POINT ( 'NONE',  ( -6.249999999999997335, -7.500000000000001776, 35.00000000000000000 ) ) ;
#55786 = CARTESIAN_POINT ( 'NONE',  ( 9.627056702146452594, -2.506253911140460922, 30.00000000000013856 ) ) ;
#55787 = CARTESIAN_POINT ( 'NONE',  ( 9.692307692307695177, -2.486705287966279876, 31.30864560766543647 ) ) ;
#55788 = B_SPLINE_CURVE_WITH_KNOTS ( 'NONE', 3,
 ( #27004, #54463, #81960, #45929, #87390, #25670, #53127, #80634, #29229, #83280 ),
 .UNSPECIFIED., .F., .F.,
 ( 4, 2, 2, 2, 4 ),
 ( 0.000000000000000000, 0.0001954311564186868744, 0.0003908623128373737488, 0.0005862934692560606504, 0.0007817246256747474977 ),
 .UNSPECIFIED. ) ;
#55789 = EDGE_CURVE ( 'NONE', #75410, #4576, #70437, .T. ) ;
#55790 = ORIENTED_EDGE ( 'NONE', *, *, #13042, .F. ) ;
#55791 = CARTESIAN_POINT ( 'NONE',  ( -13.13466986626724164, -2.587454068350147018, 30.68340429815432202 ) ) ;
#55792 = VECTOR ( 'NONE', #73738, 1000.000000000000227 ) ;
#55793 = CARTESIAN_POINT ( 'NONE',  ( 10.28846153846153832, -3.499999999999999556, 29.75000000000000355 ) ) ;
#55794 = ORIENTED_EDGE ( 'NONE', *, *, #45969, .F. ) ;
#55795 = CARTESIAN_POINT ( 'NONE',  ( 17.01083966596719677, -11.16473453929635440, 33.15142922261925662 ) ) ;
#55796 = CARTESIAN_POINT ( 'NONE',  ( 2.373759641042384683, -8.164416787775445883, 34.95778746994558617 ) ) ;
#55797 = CARTESIAN_POINT ( 'NONE',  ( 9.915087361285756629, -6.717445702608402236, 34.94155399931962336 ) ) ;
#55798 = EDGE_CURVE ( 'NONE', #15172, #73147, #28112, .T. ) ;
#55799 = EDGE_LOOP ( 'NONE', ( #43289, #68768, #64757, #85674 ) ) ;
#55800 = VERTEX_POINT ( 'NONE', #62768 ) ;
#55801 = CARTESIAN_POINT ( 'NONE',  ( 3.165499230212911908, -3.083524468853724443, 32.58852847137143272 ) ) ;
#55802 = VERTEX_POINT ( 'NONE', #42965 ) ;
#55803 = EDGE_CURVE ( 'NONE', #8424, #27342, #56024, .T. ) ;
#55804 = CARTESIAN_POINT ( 'NONE',  ( 3.230769230769108269, -12.16647553114689728, 32.15551576947799362 ) ) ;
#55805 = CARTESIAN_POINT ( 'NONE',  ( 15.23076923076910916, -12.70778746994576025, 30.41441678777401236 ) ) ;
#55806 = CARTESIAN_POINT ( 'NONE',  ( -14.53061852520844965, -3.105860786376062332, 32.13614157043599562 ) ) ;
#55807 = EDGE_CURVE ( 'NONE', #74851, #46484, #59315, .T. ) ;
#55808 = CARTESIAN_POINT ( 'NONE',  ( 18.03205128205128105, -4.000000000000000000, 29.75000000000000355 ) ) ;
#55809 = CARTESIAN_POINT ( 'NONE',  ( 15.16549878480846125, -6.879047030191174805, 34.71129190930000163 ) ) ;
#55810 = CARTESIAN_POINT ( 'NONE',  ( 0.5277050681301012069, -7.250054591869666609, 34.99404684341514127 ) ) ;
#55811 = DIRECTION ( 'NONE',  ( -0.000000000000000000, 0.9848077530122086864, -0.1736481776669273891 ) ) ;
#55812 = CIRCLE ( 'NONE', #42844, 2.999999999999999112 ) ;
#55813 = ADVANCED_FACE ( 'NONE', ( #21799 ), #76749, .F. ) ;
#55814 = ORIENTED_EDGE ( 'NONE', *, *, #64896, .F. ) ;
#55815 = EDGE_LOOP ( 'NONE', ( #56173, #69078, #5112, #48861, #2011, #43879 ) ) ;
#55817 = ORIENTED_EDGE ( 'NONE', *, *, #70968, .F. ) ;
#55816 = DIRECTION ( 'NONE',  ( 0.000000000000000000, -0.000000000000000000, -1.000000000000000000 ) ) ;
#55818 = VECTOR ( 'NONE', #51608, 1000.000000000000227 ) ;
#55819 = LINE ( 'NONE', #6748, #37886 ) ;
#55820 = ORIENTED_EDGE ( 'NONE', *, *, #38423, .T. ) ;
#55821 = EDGE_CURVE ( 'NONE', #26289, #5224, #36214, .T. ) ;
#55822 = ADVANCED_FACE ( 'NONE', ( #49710 ), #63666, .F. ) ;
#55823 = VECTOR ( 'NONE', #78506, 1000.000000000000000 ) ;
#55824 = CARTESIAN_POINT ( 'NONE',  ( 15.45414471654164856, -2.251407671071270489, 29.88021292934942963 ) ) ;
#55825 = CARTESIAN_POINT ( 'NONE',  ( -8.069638770718176701, -10.23692288466677880, 34.23039457007281072 ) ) ;
#55826 = ORIENTED_EDGE ( 'NONE', *, *, #21906, .T. ) ;
#55827 = LINE ( 'NONE', #7651, #6835 ) ;
#55828 = ORIENTED_EDGE ( 'NONE', *, *, #37875, .T. ) ;
#55830 = EDGE_LOOP ( 'NONE', ( #20154, #30213 ) ) ;
#55829 = CARTESIAN_POINT ( 'NONE',  ( -4.403869391139119571, -5.851115903089112003, 34.47074536777953568 ) ) ;
#55831 = CYLINDRICAL_SURFACE ( 'NONE', #15815, 0.2499999999999995559 ) ;
#55832 = ORIENTED_EDGE ( 'NONE', *, *, #2096, .T. ) ;
#55833 = CARTESIAN_POINT ( 'NONE',  ( 0.4615384615384611200, -5.557115091759785130, 34.35708131394839171 ) ) ;
#55834 = CARTESIAN_POINT ( 'NONE',  ( -4.219116154402471786, -6.835583212224499938, 34.95778746994557906 ) ) ;
#55835 = FACE_BOUND ( 'NONE', #40384, .T. ) ;
#55836 = CARTESIAN_POINT ( 'NONE',  ( 5.933917620639864943, -2.292212530054419606, 30.41441678777542634 ) ) ;
#55837 = CYLINDRICAL_SURFACE ( 'NONE', #16923, 0.2499999999999994726 ) ;
#55838 = CARTESIAN_POINT ( 'NONE',  ( 9.692307692307570832, -11.67786785259630911, 32.92929555188603530 ) ) ;
#55839 = CARTESIAN_POINT ( 'NONE',  ( 12.46153846153846168, -3.322132147404559976, 32.92929555188717927 ) ) ;
#55840 = CIRCLE ( 'NONE', #22722, 0.2500000000000002220 ) ;
#55841 = ADVANCED_FACE ( 'NONE', ( #31661 ), #17250, .F. ) ;
#55842 = CARTESIAN_POINT ( 'NONE',  ( 0.000000000000000000, -11.00000000000000000, 29.75000000000000355 ) ) ;
#55843 = CARTESIAN_POINT ( 'NONE',  ( -16.37677311275300340, -2.523278758544490685, 31.42238647778638239 ) ) ;
#55844 = ORIENTED_EDGE ( 'NONE', *, *, #81015, .T. ) ;
#55845 = CARTESIAN_POINT ( 'NONE',  ( 14.53047197667037516, -6.717445702608402236, 34.94155399931962336 ) ) ;
#55846 = ORIENTED_EDGE ( 'NONE', *, *, #28146, .T. ) ;
#55847 = ORIENTED_EDGE ( 'NONE', *, *, #17513, .T. ) ;
#55849 = CARTESIAN_POINT ( 'NONE',  ( -9.320512820512821150, -3.499999999999999556, 29.75000000000000355 ) ) ;
#55848 = CARTESIAN_POINT ( 'NONE',  ( 7.596130608860880429, -6.695914987888143877, 34.68535235679833306 ) ) ;
#55850 = DIRECTION ( 'NONE',  ( -0.000000000000000000, -0.3420201433256694346, -0.9396926207859080948 ) ) ;
#55851 = CARTESIAN_POINT ( 'NONE',  ( -17.01085574357299990, -9.905515769479276145, 34.41647553114623292 ) ) ;
#55852 = CARTESIAN_POINT ( 'NONE',  ( 14.30769230769218581, -5.941354392335915335, 34.76329471203413846 ) ) ;
#55853 = CARTESIAN_POINT ( 'NONE',  ( 13.63456090296352841, -11.37275283266504111, 32.91324779482534524 ) ) ;
#55854 = ORIENTED_EDGE ( 'NONE', *, *, #40277, .F. ) ;
#55855 = EDGE_CURVE ( 'NONE', #13051, #83441, #119, .T. ) ;
#55856 = CARTESIAN_POINT ( 'NONE',  ( 3.230769230769110045, -3.300289026999228881, 32.46337939537708905 ) ) ;
#55857 = AXIS2_PLACEMENT_3D ( 'NONE', #51124, #11061, #17368 ) ;
#55858 = PLANE ( 'NONE',  #81898 ) ;
#55859 = CARTESIAN_POINT ( 'NONE',  ( -39.05038313613820122, -2.499999999999999556, 29.75000000000000355 ) ) ;
#55860 = CARTESIAN_POINT ( 'NONE',  ( -8.769230769230768274, -2.708943851104267164, 35.45975837776705220 ) ) ;
#55861 = CARTESIAN_POINT ( 'NONE',  ( 2.307692307692186251, -5.941354392335915335, 34.76329471203413846 ) ) ;
#55862 = ORIENTED_EDGE ( 'NONE', *, *, #16793, .T. ) ;
#55863 = EDGE_CURVE ( 'NONE', #31586, #17756, #44708, .T. ) ;
#55864 = EDGE_LOOP ( 'NONE', ( #50928, #57160 ) ) ;
#55866 = EDGE_CURVE ( 'NONE', #3281, #18498, #48441, .T. ) ;
#55865 = ORIENTED_EDGE ( 'NONE', *, *, #29446, .T. ) ;
#55867 = CARTESIAN_POINT ( 'NONE',  ( -0.4615384615384611200, -11.33034616979429110, 35.88435417666054406 ) ) ;
#55868 = ORIENTED_EDGE ( 'NONE', *, *, #21437, .T. ) ;
#55869 = LINE ( 'NONE', #83356, #64205 ) ;
#55870 = CARTESIAN_POINT ( 'NONE',  ( 15.48071464014727106, -4.176053281294518804, 33.81426240980091791 ) ) ;
#55871 = CYLINDRICAL_SURFACE ( 'NONE', #79729, 0.2499999999999986955 ) ;
#55872 = CYLINDRICAL_SURFACE ( 'NONE', #25891, 4.000000000000000000 ) ;
#55873 = EDGE_CURVE ( 'NONE', #42788, #81338, #7630, .T. ) ;
#55874 = CARTESIAN_POINT ( 'NONE',  ( 12.33084699487090319, -9.804603061927743113, 34.18744698557895845 ) ) ;
#55875 = ORIENTED_EDGE ( 'NONE', *, *, #46089, .T. ) ;
#55876 = CARTESIAN_POINT ( 'NONE',  ( -6.000000000000119904, -3.835265460704628371, 33.15142922262033665 ) ) ;
#55878 = ORIENTED_EDGE ( 'NONE', *, *, #76712, .T. ) ;
#55877 = DIRECTION ( 'NONE',  ( -0.000000000000000000, 1.000000000000000000, -0.000000000000000000 ) ) ;
#55879 = FACE_OUTER_BOUND ( 'NONE', #31431, .T. ) ;
#55880 = CARTESIAN_POINT ( 'NONE',  ( 3.100622021331011169, -12.45813303252208648, 30.39737893381572675 ) ) ;
#55881 = DIRECTION ( 'NONE',  ( -0.000000000000000000, 1.000000000000000000, 3.491481338843133355E-15 ) ) ;
#55882 = CARTESIAN_POINT ( 'NONE',  ( 15.23076923076910916, -3.083524468854526912, 32.58852847137268327 ) ) ;
#55883 = CARTESIAN_POINT ( 'NONE',  ( -17.77698715590660328, -10.77377354290276301, 33.85451476688484718 ) ) ;
#55884 = CARTESIAN_POINT ( 'NONE',  ( 9.626224281351811740, -9.780366693483667717, 34.19971097300155805 ) ) ;
#55885 = CARTESIAN_POINT ( 'NONE',  ( 6.923076923076924238, -9.819645486525091727, 36.12317359536749706 ) ) ;
#55886 = CARTESIAN_POINT ( 'NONE',  ( -3.724691934501248802, -5.885600066136383646, 15.42374329374151642 ) ) ;
#55887 = ORIENTED_EDGE ( 'NONE', *, *, #28009, .F. ) ;
#55888 = AXIS2_PLACEMENT_3D ( 'NONE', #35935, #76915, #49443 ) ;
#55889 = CARTESIAN_POINT ( 'NONE',  ( -15.29685161012936412, -6.343179335718451384, 34.87096338111212646 ) ) ;
#55890 = CARTESIAN_POINT ( 'NONE',  ( -1.254089946381738763, -3.625058011473228259, 33.29252011169590020 ) ) ;
#55891 = CARTESIAN_POINT ( 'NONE',  ( 8.992010438208831502, -10.97394488606064122, 33.68653795673694873 ) ) ;
#55892 = CARTESIAN_POINT ( 'NONE',  ( -3.164701897419154530, -10.67929555188718282, 33.92786785259544757 ) ) ;
#55893 = ORIENTED_EDGE ( 'NONE', *, *, #37251, .F. ) ;
#55894 = CARTESIAN_POINT ( 'NONE',  ( 0.3954560821783256741, -3.937682226553328668, 33.60647404775217950 ) ) ;
#55895 = CARTESIAN_POINT ( 'NONE',  ( -2.530618525208454983, -3.105860786376062332, 32.13614157043598851 ) ) ;
#55896 = EDGE_CURVE ( 'NONE', #25338, #76825, #34881, .T. ) ;
#55897 = CARTESIAN_POINT ( 'NONE',  ( 1.384615384615386802, -8.973038597847269315, 34.52809138561121927 ) ) ;
#55898 = CARTESIAN_POINT ( 'NONE',  ( 14.05766907039934210, -3.202444869320336451, 32.30641848906366675 ) ) ;
#55899 = ORIENTED_EDGE ( 'NONE', *, *, #15177, .F. ) ;
#55900 = CARTESIAN_POINT ( 'NONE',  ( -12.46153846153858247, -9.442884908241554243, 34.35708131394783038 ) ) ;
#55901 = CARTESIAN_POINT ( 'NONE',  ( -0.5276208408985970655, -9.905515769479276145, 34.41647553114623292 ) ) ;
#55902 = CARTESIAN_POINT ( 'NONE',  ( 5.076923076923075762, -12.34228464037088635, 31.77849191805839268 ) ) ;
#55903 = ORIENTED_EDGE ( 'NONE', *, *, #37660, .F. ) ;
#55904 = CARTESIAN_POINT ( 'NONE',  ( -13.16160254052199008, -2.889357225399414197, 32.26129605718031002 ) ) ;
#55905 = EDGE_LOOP ( 'NONE', ( #40715, #80524, #78411, #59820 ) ) ;
#55906 = AXIS2_PLACEMENT_3D ( 'NONE', #86132, #73508, #32959 ) ;
#55907 = CARTESIAN_POINT ( 'NONE',  ( 1.653273178848927064E-15, -7.500000000000000000, 13.50000000000000178 ) ) ;
#55908 = CARTESIAN_POINT ( 'NONE',  ( 0.4615384615384611755, -13.88283147151868846, 33.14645433367849847 ) ) ;
#55909 = ORIENTED_EDGE ( 'NONE', *, *, #52490, .T. ) ;
#55910 = CARTESIAN_POINT ( 'NONE',  ( 10.68063975489745410, -11.67786785259547777, 32.92929555188713664 ) ) ;
#55911 = CARTESIAN_POINT ( 'NONE',  ( 4.403900573759605308, -9.233818618650603938, 34.70587769442853698 ) ) ;
#55912 = B_SPLINE_CURVE_WITH_KNOTS ( 'NONE', 3,
 ( #79988, #72773, #66015, #85415, #38561, #4324, #23696, #3429, #46204, #4779 ),
 .UNSPECIFIED., .F., .F.,
 ( 4, 2, 2, 2, 4 ),
 ( 0.0007817359430256320659, 0.0009771253907249987086, 0.001172514838424365460, 0.001367904286123731994, 0.001563293733823098745 ),
 .UNSPECIFIED. ) ;
#55913 = CARTESIAN_POINT ( 'NONE',  ( 0.4615384615384611200, -4.098570777380720287, 33.41473453929634729 ) ) ;
#55914 = DIRECTION ( 'NONE',  ( 0.000000000000000000, 8.131516293641283255E-17, 1.000000000000000000 ) ) ;
#55915 = FACE_OUTER_BOUND ( 'NONE', #8047, .T. ) ;
#55916 = ADVANCED_FACE ( 'NONE', ( #24892 ), #29892, .F. ) ;
#55917 = AXIS2_PLACEMENT_3D ( 'NONE', #32702, #39926, #18313 ) ;
#55919 = ORIENTED_EDGE ( 'NONE', *, *, #9216, .T. ) ;
#55918 = EDGE_CURVE ( 'NONE', #30358, #87048, #83760, .T. ) ;
#55920 = VERTEX_POINT ( 'NONE', #9608 ) ;
#55921 = FACE_BOUND ( 'NONE', #11971, .T. ) ;
#55922 = ORIENTED_EDGE ( 'NONE', *, *, #43966, .T. ) ;
#55923 = LINE ( 'NONE', #41985, #54438 ) ;
#55924 = EDGE_CURVE ( 'NONE', #19020, #88839, #2836, .T. ) ;
#55925 = CARTESIAN_POINT ( 'NONE',  ( 4.376857505459002873, -11.76359900205217457, 32.36225158514719880 ) ) ;
#55926 = EDGE_CURVE ( 'NONE', #65002, #82311, #38417, .T. ) ;
#55927 = CARTESIAN_POINT ( 'NONE',  ( 6.130790440966954691, -2.845873456487966635, 32.17976146951972538 ) ) ;
#55928 = CARTESIAN_POINT ( 'NONE',  ( 5.207448778686639912, -4.459921816937789885, 33.71989282347011851 ) ) ;
#55929 = ORIENTED_EDGE ( 'NONE', *, *, #73902, .F. ) ;
#55931 = EDGE_CURVE ( 'NONE', #22606, #40886, #51609, .T. ) ;
#55930 = EDGE_LOOP ( 'NONE', ( #73080, #64293, #55080, #21771 ) ) ;
#55932 = ORIENTED_EDGE ( 'NONE', *, *, #63943, .F. ) ;
#55933 = CARTESIAN_POINT ( 'NONE',  ( 13.13461538461538680, -7.500000000000001776, 34.75000000000000000 ) ) ;
#55934 = ORIENTED_EDGE ( 'NONE', *, *, #64510, .F. ) ;
#55935 = CARTESIAN_POINT ( 'NONE',  ( 10.61538461538461675, -2.292212530054420494, 30.41441678777542634 ) ) ;
#55936 = ADVANCED_FACE ( 'NONE', ( #52807 ), #39317, .F. ) ;
#55937 = B_SPLINE_CURVE_WITH_KNOTS ( 'NONE', 3,
 ( #11412, #87095, #33018, #60037, #74446, #18622, #80330, #87544, #67693, #25819 ),
 .UNSPECIFIED., .F., .F.,
 ( 4, 2, 2, 2, 4 ),
 ( 0.0007817359430256294638, 0.0009771253907249952391, 0.001172514838424361123, 0.001367904286123727007, 0.001563293733823092890 ),
 .UNSPECIFIED. ) ;
#55938 = CARTESIAN_POINT ( 'NONE',  ( 1.515407192440173745, -3.530189275343204702, 32.79018710029569661 ) ) ;
#55939 = CARTESIAN_POINT ( 'NONE',  ( -17.32689982097166492, -2.920706130388546651, 32.31842814019191223 ) ) ;
#55940 = CARTESIAN_POINT ( 'NONE',  ( 13.25392391794783187, -10.54014554554150607, 33.71984207302941883 ) ) ;
#55941 = B_SPLINE_CURVE_WITH_KNOTS ( 'NONE', 3,
 ( #61968, #69616, #20106, #82258, #7486, #7923, #21433, #14234, #47568, #48008 ),
 .UNSPECIFIED., .F., .F.,
 ( 4, 2, 2, 2, 4 ),
 ( 0.000000000000000000, 0.0001954311564186866034, 0.0003908623128373732067, 0.0005862934692560597830, 0.0007817246256747464135 ),
 .UNSPECIFIED. ) ;
#55942 = DIRECTION ( 'NONE',  ( 0.000000000000000000, 0.7660444431189822323, -0.6427876096865344779 ) ) ;
#55943 = EDGE_CURVE ( 'NONE', #4654, #75693, #11386, .T. ) ;
#55944 = CARTESIAN_POINT ( 'NONE',  ( 5.076923076923075762, -10.51840700105979565, 33.73612834413961536 ) ) ;
#55945 = CARTESIAN_POINT ( 'NONE',  ( 9.019285189144222059, -6.523592122091592671, 34.90882529074906415 ) ) ;
#55946 = ORIENTED_EDGE ( 'NONE', *, *, #26750, .T. ) ;
#55947 = B_SPLINE_CURVE_WITH_KNOTS ( 'NONE', 3,
 ( #67421, #59323, #44912, #86832, #25097, #69967, #57337, #56457, #70421, #7831 ),
 .UNSPECIFIED., .F., .F.,
 ( 4, 2, 2, 2, 4 ),
 ( 0.0007817246256747476061, 0.0009771112852218902852, 0.001172497944769033181, 0.001367884604316175860, 0.001563271263863318539 ),
 .UNSPECIFIED. ) ;
#55948 = ORIENTED_EDGE ( 'NONE', *, *, #31899, .F. ) ;
#55949 = ORIENTED_EDGE ( 'NONE', *, *, #81536, .F. ) ;
#55950 = DIRECTION ( 'NONE',  ( 0.000000000000000000, 0.9848077530122072432, -0.1736481776669354937 ) ) ;
#55952 = DIRECTION ( 'NONE',  ( -0.000000000000000000, -0.8660254037844397068, -0.4999999999999978906 ) ) ;
#55951 = CARTESIAN_POINT ( 'NONE',  ( -1.449885385171703733, -2.657715359629089225, 31.77849191805834295 ) ) ;
#55953 = DIRECTION ( 'NONE',  ( 0.000000000000000000, 0.9396926207859126468, -0.3420201433256571111 ) ) ;
#55954 = CARTESIAN_POINT ( 'NONE',  ( -8.769230769230892619, -6.835583212225970762, 34.95778746994575670 ) ) ;
#55955 = FACE_BOUND ( 'NONE', #30898, .T. ) ;
#55956 = CARTESIAN_POINT ( 'NONE',  ( 9.942362003946010773, -3.627508038966690496, 32.91356715214248396 ) ) ;
#55957 = ORIENTED_EDGE ( 'NONE', *, *, #48973, .T. ) ;
#55958 = CARTESIAN_POINT ( 'NONE',  ( -8.096153846153844924, -7.566082377512565849, 35.00000000000000711 ) ) ;
#55959 = CARTESIAN_POINT ( 'NONE',  ( 9.468822767743365176, -12.11044203135681840, 32.26167407432752299 ) ) ;
#55960 = CARTESIAN_POINT ( 'NONE',  ( -19.00000000000000000, -17.00000000000000000, 2.999999999999999112 ) ) ;
#55961 = CARTESIAN_POINT ( 'NONE',  ( 3.480823650682683734, -11.47946981652013498, 33.17500667209846910 ) ) ;
#55962 = EDGE_LOOP ( 'NONE', ( #37405, #4455 ) ) ;
#55963 = FACE_OUTER_BOUND ( 'NONE', #55447, .T. ) ;
#55964 = ADVANCED_FACE ( 'NONE', ( #32994 ), #74876, .F. ) ;
#55965 = VERTEX_POINT ( 'NONE', #38869 ) ;
#55966 = FACE_BOUND ( 'NONE', #81770, .T. ) ;
#55967 = CARTESIAN_POINT ( 'NONE',  ( -17.07692307692307665, -3.937682226553329556, 33.60647404775216529 ) ) ;
#55968 = AXIS2_PLACEMENT_3D ( 'NONE', #35749, #62750, #13695 ) ;
#55969 = VECTOR ( 'NONE', #21702, 1000.000000000000000 ) ;
#55970 = EDGE_CURVE ( 'NONE', #36014, #54362, #81630, .T. ) ;
#55971 = DIRECTION ( 'NONE',  ( 0.000000000000000000, 0.9848077530122072432, -0.1736481776669354937 ) ) ;
#55972 = CARTESIAN_POINT ( 'NONE',  ( -7.145903615555926791, -7.369208160676172348, 34.74850200257122879 ) ) ;
#55973 = EDGE_LOOP ( 'NONE', ( #2954, #23943, #38456, #12130 ) ) ;
#55974 = CARTESIAN_POINT ( 'NONE',  ( -14.43783951713053249, -12.45813303252208648, 30.39737893381572675 ) ) ;
#55975 = CARTESIAN_POINT ( 'NONE',  ( 15.36129466900287532, -2.372941743896879174, 30.88044141588253666 ) ) ;
#55976 = CARTESIAN_POINT ( 'NONE',  ( -7.173076923076921574, -2.499999999999998668, 29.75000000000000355 ) ) ;
#55977 = FACE_OUTER_BOUND ( 'NONE', #44217, .T. ) ;
#55978 = EDGE_LOOP ( 'NONE', ( #60790, #79349, #36366, #79205 ) ) ;
#55979 = VECTOR ( 'NONE', #87770, 1000.000000000000000 ) ;
#55980 = EDGE_CURVE ( 'NONE', #3730, #59070, #68697, .T. ) ;
#55981 = CARTESIAN_POINT ( 'NONE',  ( 13.25446817517716980, -6.001485441113819874, 34.52039167877662607 ) ) ;
#55982 = VERTEX_POINT ( 'NONE', #47383 ) ;
#55984 = EDGE_LOOP ( 'NONE', ( #13958, #26300, #53373, #54140, #70511 ) ) ;
#55983 = CARTESIAN_POINT ( 'NONE',  ( 4.284371592079796010, -3.068774925481847493, 32.56582465632704526 ) ) ;
#55985 = CARTESIAN_POINT ( 'NONE',  ( 3.480823542407545101, -2.564540009722895419, 30.55348353981670684 ) ) ;
#55986 = FACE_OUTER_BOUND ( 'NONE', #5556, .T. ) ;
#55987 = CARTESIAN_POINT ( 'NONE',  ( 16.15384615384615330, -11.11383981884818262, 36.00935417666054406 ) ) ;
#55988 = CARTESIAN_POINT ( 'NONE',  ( -13.25408968285181821, -3.816742781228458004, 33.13167719472716044 ) ) ;
#55989 = LINE ( 'NONE', #610, #25103 ) ;
#55991 = CARTESIAN_POINT ( 'NONE',  ( -2.372943297853547850, -2.506253911140460922, 30.00000000000013856 ) ) ;
#55990 = CARTESIAN_POINT ( 'NONE',  ( -5.933932666649925025, -6.343179335718452272, 34.87096338111212646 ) ) ;
#55992 = EDGE_CURVE ( 'NONE', #76544, #14556, #32189, .T. ) ;
#55993 = CARTESIAN_POINT ( 'NONE',  ( 14.08420736396835871, -3.754499324213721234, 33.06261337010820256 ) ) ;
#55994 = CARTESIAN_POINT ( 'NONE',  ( 1.944543648263018731, -9.444543648262994751, 25.87500000000000355 ) ) ;
#55995 = ORIENTED_EDGE ( 'NONE', *, *, #53026, .F. ) ;
#55996 = DIRECTION ( 'NONE',  ( -0.000000000000000000, 0.7660444431189791237, -0.6427876096865379196 ) ) ;
#55997 = ORIENTED_EDGE ( 'NONE', *, *, #85498, .F. ) ;
#55998 = ORIENTED_EDGE ( 'NONE', *, *, #6928, .F. ) ;
#55999 = CARTESIAN_POINT ( 'NONE',  ( 2.980792499826876440, -4.943428324936578910, 34.04746400365624481 ) ) ;
#56000 = VERTEX_POINT ( 'NONE', #18148 ) ;
#56001 = CARTESIAN_POINT ( 'NONE',  ( -8.769230769230768274, -13.88283147151868846, 33.14645433367849847 ) ) ;
#56002 = EDGE_CURVE ( 'NONE', #18112, #20214, #61204, .T. ) ;
#56003 = DIRECTION ( 'NONE',  ( -1.000000000000000000, -0.000000000000000000, 0.000000000000000000 ) ) ;
#56004 = CARTESIAN_POINT ( 'NONE',  ( -2.307692307692427391, -6.879047030192662504, 34.71129190930017927 ) ) ;
#56005 = CARTESIAN_POINT ( 'NONE',  ( -7.053224892808618307, -9.504002272028875709, 34.60269587691767867 ) ) ;
#56006 = CARTESIAN_POINT ( 'NONE',  ( 6.065255571276025215, -2.625532179533470512, 30.86335684631491105 ) ) ;
#56007 = CARTESIAN_POINT ( 'NONE',  ( 8.519254038288414321, -11.28823185664190376, 33.01397839955799896 ) ) ;
#56008 = ADVANCED_FACE ( 'NONE', ( #73548 ), #66777, .F. ) ;
#56009 = CARTESIAN_POINT ( 'NONE',  ( 16.02369894440793985, -11.93770438780619259, 32.05411857736982029 ) ) ;
#56010 = CARTESIAN_POINT ( 'NONE',  ( -8.102564102564102200, -3.499999999999999556, 29.75000000000000355 ) ) ;
#56011 = EDGE_CURVE ( 'NONE', #11473, #37767, #60090, .T. ) ;
#56012 = CARTESIAN_POINT ( 'NONE',  ( -0.7115151924808164052, -2.564618984488975961, 30.55390908950641915 ) ) ;
#56013 = CARTESIAN_POINT ( 'NONE',  ( 17.99999999999987566, -11.94971097300221174, 32.03036669348237098 ) ) ;
#56014 = CYLINDRICAL_SURFACE ( 'NONE', #68026, 0.2500000000000008882 ) ;
#56015 = AXIS2_PLACEMENT_3D ( 'NONE', #33718, #67509, #5361 ) ;
#56016 = CARTESIAN_POINT ( 'NONE',  ( -9.915234651214539952, -3.395401636524185474, 33.02366814457250399 ) ) ;
#56017 = ORIENTED_EDGE ( 'NONE', *, *, #16286, .F. ) ;
#56018 = ORIENTED_EDGE ( 'NONE', *, *, #55709, .T. ) ;
#56019 = CARTESIAN_POINT ( 'NONE',  ( -18.24997674404858827, -2.544273027872574922, 31.48422191005632342 ) ) ;
#56020 = CARTESIAN_POINT ( 'NONE',  ( -3.230769230769229949, -11.16473453929635440, 33.15142922261926373 ) ) ;
#56021 = CARTESIAN_POINT ( 'NONE',  ( 11.76147289007438701, -9.886259254753566594, 34.14407573483972413 ) ) ;
#56022 = CARTESIAN_POINT ( 'NONE',  ( 0.4615384615387756462, -2.255955759149395501, 30.00000000000324363 ) ) ;
#56023 = ORIENTED_EDGE ( 'NONE', *, *, #84001, .F. ) ;
#56024 = LINE ( 'NONE', #14602, #21904 ) ;
#56025 = CARTESIAN_POINT ( 'NONE',  ( -9.692307692307814193, -6.835583212225970762, 34.95778746994575670 ) ) ;
#56026 = B_SPLINE_CURVE_WITH_KNOTS ( 'NONE', 3,
 ( #66470, #38102, #73229, #51143, #10194, #65564, #66915, #3423, #31350, #80440 ),
 .UNSPECIFIED., .F., .F.,
 ( 4, 2, 2, 2, 4 ),
 ( 0.000000000000000000, 0.0001954339857564080165, 0.0003908679715128160329, 0.0005863019572692240765, 0.0007817359430256320659 ),
 .UNSPECIFIED. ) ;
#56027 = B_SPLINE_CURVE_WITH_KNOTS ( 'NONE', 3,
 ( #5736, #47158, #12067, #33213, #5297, #87736, #54358, #74649, #81855, #80973 ),
 .UNSPECIFIED., .F., .F.,
 ( 4, 2, 2, 2, 4 ),
 ( 0.000000000000000000, 0.0001954311564186862510, 0.0003908623128373725020, 0.0005862934692560588072, 0.0007817246256747450040 ),
 .UNSPECIFIED. ) ;
#56028 = CARTESIAN_POINT ( 'NONE',  ( -0.6089743589743593644, -7.500000000000000000, 29.75000000000000355 ) ) ;
#56029 = VERTEX_POINT ( 'NONE', #61776 ) ;
#56030 = CARTESIAN_POINT ( 'NONE',  ( 15.90386942290380290, -2.779195860258148798, 31.39871582349836743 ) ) ;
#56031 = ORIENTED_EDGE ( 'NONE', *, *, #14299, .F. ) ;
#56032 = CIRCLE ( 'NONE', #67557, 0.2500000000000002220 ) ;
#56033 = CARTESIAN_POINT ( 'NONE',  ( 10.86533013373275658, -8.433404298154334455, 34.66254593164985920 ) ) ;
#56034 = VECTOR ( 'NONE', #77464, 1000.000000000000114 ) ;
#56035 = VECTOR ( 'NONE', #22802, 1000.000000000000000 ) ;
#56036 = DIRECTION ( 'NONE',  ( 0.000000000000000000, 0.000000000000000000, -1.000000000000000000 ) ) ;
#56037 = FACE_OUTER_BOUND ( 'NONE', #51187, .T. ) ;
#56038 = CARTESIAN_POINT ( 'NONE',  ( 4.088576153289833925, -6.835583212224499938, 34.95778746994557906 ) ) ;
#56039 = CARTESIAN_POINT ( 'NONE',  ( -6.700297254098858346, -2.612705202774697533, 31.66806509827799943 ) ) ;
#56040 = AXIS2_PLACEMENT_3D ( 'NONE', #75587, #6693, #34165 ) ;
#56041 = AXIS2_PLACEMENT_3D ( 'NONE', #34791, #62259, #28040 ) ;
#56042 = ORIENTED_EDGE ( 'NONE', *, *, #56614, .T. ) ;
#56043 = EDGE_CURVE ( 'NONE', #33723, #6671, #54827, .T. ) ;
#56044 = VECTOR ( 'NONE', #38848, 999.9999999999998863 ) ;
#56045 = ORIENTED_EDGE ( 'NONE', *, *, #13293, .F. ) ;
#56046 = ORIENTED_EDGE ( 'NONE', *, *, #55272, .T. ) ;
#56047 = EDGE_LOOP ( 'NONE', ( #63436, #24224 ) ) ;
#56048 = CARTESIAN_POINT ( 'NONE',  ( -17.29984929443921970, -10.61292498521070549, 33.66303323003028680 ) ) ;
#56049 = CARTESIAN_POINT ( 'NONE',  ( 16.02315555073584719, -5.496505350115500121, 34.60290016733514307 ) ) ;
#56050 = ADVANCED_FACE ( 'NONE', ( #47831 ), #92, .F. ) ;
#56051 = CARTESIAN_POINT ( 'NONE',  ( -12.33074802057151409, -12.35292014791297710, 31.75344720912887198 ) ) ;
#56052 = CARTESIAN_POINT ( 'NONE',  ( 17.07692307692295586, -10.33852847137269571, 34.16647553114546554 ) ) ;
#56053 = CARTESIAN_POINT ( 'NONE',  ( -17.86920819217521483, -4.118422570099828484, 33.43335022499816489 ) ) ;
#56054 = LINE ( 'NONE', #64125, #76859 ) ;
#56055 = ORIENTED_EDGE ( 'NONE', *, *, #25495, .F. ) ;
#56056 = ORIENTED_EDGE ( 'NONE', *, *, #41723, .F. ) ;
#56057 = ORIENTED_EDGE ( 'NONE', *, *, #19648, .T. ) ;
#56058 = ADVANCED_FACE ( 'NONE', ( #54579 ), #68987, .F. ) ;
#56060 = EDGE_LOOP ( 'NONE', ( #75097, #79869 ) ) ;
#56059 = CARTESIAN_POINT ( 'NONE',  ( -3.230769230769351186, -10.90142922262034020, 33.41473453929536674 ) ) ;
#56062 = DIRECTION ( 'NONE',  ( 0.000000000000000000, 0.000000000000000000, -1.000000000000000000 ) ) ;
#56061 = CARTESIAN_POINT ( 'NONE',  ( 17.07692307692307665, -1.129524287112498415, 32.06866353760679544 ) ) ;
#56063 = CYLINDRICAL_SURFACE ( 'NONE', #14388, 0.2499999999999986955 ) ;
#56064 = CARTESIAN_POINT ( 'NONE',  ( -2.651650429449565305, -4.848349570550461785, 24.00000000000000000 ) ) ;
#56065 = VERTEX_POINT ( 'NONE', #14488 ) ;
#56066 = VECTOR ( 'NONE', #30610, 1000.000000000000000 ) ;
#56067 = ORIENTED_EDGE ( 'NONE', *, *, #79701, .F. ) ;
#56068 = DIRECTION ( 'NONE',  ( -0.000000000000000000, -0.8660254037844398178, -0.4999999999999980571 ) ) ;
#56069 = EDGE_CURVE ( 'NONE', #30238, #80750, #82956, .T. ) ;
#56070 = ORIENTED_EDGE ( 'NONE', *, *, #40173, .F. ) ;
#56071 = FACE_BOUND ( 'NONE', #30183, .T. ) ;
#56072 = CARTESIAN_POINT ( 'NONE',  ( -2.241624974342230292, -4.661471528628508665, 34.16647553114624003 ) ) ;
#56073 = LINE ( 'NONE', #49321, #76484 ) ;
#56074 = EDGE_LOOP ( 'NONE', ( #69560, #49989, #72628, #6219 ) ) ;
#56075 = CARTESIAN_POINT ( 'NONE',  ( 15.45373236503590952, -7.369474539155828730, 34.99858011523957657 ) ) ;
#56076 = EDGE_CURVE ( 'NONE', #66717, #50723, #77313, .T. ) ;
#56077 = CYLINDRICAL_SURFACE ( 'NONE', #53270, 0.2500000000000009437 ) ;
#56078 = CARTESIAN_POINT ( 'NONE',  ( -13.38461538461538325, -4.945431358278436385, 36.03766855953609394 ) ) ;
#56079 = CARTESIAN_POINT ( 'NONE',  ( 0.5923302693632480631, -6.413143153341454017, 34.63066358083362672 ) ) ;
#56080 = CARTESIAN_POINT ( 'NONE',  ( 1.449870524128223703, -2.657715359629131857, 31.77849191805844242 ) ) ;
#56081 = ORIENTED_EDGE ( 'NONE', *, *, #32617, .F. ) ;
#56082 = B_SPLINE_CURVE_WITH_KNOTS ( 'NONE', 3,
 ( #85403, #37202, #78636, #16939, #44389, #10185, #88533, #75003, #13294, #67796 ),
 .UNSPECIFIED., .F., .F.,
 ( 4, 2, 2, 2, 4 ),
 ( 0.0007817246256747530271, 0.0009771112852218974409, 0.001172497944769041638, 0.001367884604316185835, 0.001563271263863330249 ),
 .UNSPECIFIED. ) ;
#56083 = CARTESIAN_POINT ( 'NONE',  ( 11.66925334628632527, -3.062576670634119758, 32.05464942895959979 ) ) ;
#56084 = CARTESIAN_POINT ( 'NONE',  ( -7.780898274877819709, -6.879047030191282275, 34.71129190930002295 ) ) ;
#56085 = CARTESIAN_POINT ( 'NONE',  ( -7.846153846153844924, -13.88283147151868846, 33.14645433367849847 ) ) ;
#56086 = FACE_OUTER_BOUND ( 'NONE', #76557, .T. ) ;
#56087 = DIRECTION ( 'NONE',  ( 0.000000000000000000, 0.000000000000000000, 1.000000000000000000 ) ) ;
#56088 = FACE_BOUND ( 'NONE', #17092, .T. ) ;
#56090 = CARTESIAN_POINT ( 'NONE',  ( 17.07692307692307665, -2.833524468853757305, 32.15551576947925838 ) ) ;
#56089 = CARTESIAN_POINT ( 'NONE',  ( -6.857821783564083340, -12.70778746994558439, 30.41441678777537305 ) ) ;
#56091 = EDGE_CURVE ( 'NONE', #73152, #7875, #48280, .T. ) ;
#56092 = AXIS2_PLACEMENT_3D ( 'NONE', #49189, #43759, #9527 ) ;
#56093 = CARTESIAN_POINT ( 'NONE',  ( 11.76124120743959978, -12.11081565061823717, 32.26097654155341843 ) ) ;
#56095 = FACE_OUTER_BOUND ( 'NONE', #2237, .T. ) ;
#56094 = CARTESIAN_POINT ( 'NONE',  ( 4.087763774486018242, -5.471508081941601986, 34.59228464037088457 ) ) ;
#56096 = FACE_OUTER_BOUND ( 'NONE', #42823, .T. ) ;
#56097 = CARTESIAN_POINT ( 'NONE',  ( 1.077988221561464899, -4.724691934501233703, 22.73250670625849068 ) ) ;
#56098 = VERTEX_POINT ( 'NONE', #34313 ) ;
#56099 = CARTESIAN_POINT ( 'NONE',  ( -5.776987155906605942, -10.77377354290276301, 33.85451476688484718 ) ) ;
#56100 = EDGE_LOOP ( 'NONE', ( #64061, #10839 ) ) ;
#56101 = VECTOR ( 'NONE', #5685, 1000.000000000000000 ) ;
#56102 = VECTOR ( 'NONE', #81001, 1000.000000000000227 ) ;
#56103 = CARTESIAN_POINT ( 'NONE',  ( -13.13456096470193302, -9.233818618650603938, 34.70587769442853698 ) ) ;
#56104 = ORIENTED_EDGE ( 'NONE', *, *, #47274, .T. ) ;
#56105 = CARTESIAN_POINT ( 'NONE',  ( -11.47320596718551577, -2.892918686051626498, 31.69288490824026638 ) ) ;
#56106 = CARTESIAN_POINT ( 'NONE',  ( -15.90379173393269951, -12.01375889529407992, 32.43194544308182969 ) ) ;
#56107 = ORIENTED_EDGE ( 'NONE', *, *, #6200, .T. ) ;
#56108 = CYLINDRICAL_SURFACE ( 'NONE', #59929, 0.2499999999999994726 ) ;
#56109 = CARTESIAN_POINT ( 'NONE',  ( -1.077988221561460236, -10.27530806549876452, 17.10750670625848713 ) ) ;
#56110 = CARTESIAN_POINT ( 'NONE',  ( 6.066067333350075863, -6.343179335718452272, 34.87096338111212646 ) ) ;
#56111 = ADVANCED_FACE ( 'NONE', ( #82523 ), #20802, .F. ) ;
#56112 = CYLINDRICAL_SURFACE ( 'NONE', #80621, 0.2499999999999979738 ) ;
#56113 = DIRECTION ( 'NONE',  ( -0.000000000000000000, -0.000000000000000000, -1.000000000000000000 ) ) ;
#56114 = CIRCLE ( 'NONE', #24463, 4.000000000000000000 ) ;
#56115 = CARTESIAN_POINT ( 'NONE',  ( 16.82694634598072625, -12.41269422305637171, 30.68257228309993323 ) ) ;
#56116 = CARTESIAN_POINT ( 'NONE',  ( 12.22435897435897267, -11.00000000000000000, 29.75000000000000355 ) ) ;
#56117 = CARTESIAN_POINT ( 'NONE',  ( -14.17716686945866655, -5.070358843744210198, 34.40418822224088302 ) ) ;
#56118 =( GEOMETRIC_REPRESENTATION_CONTEXT ( 3 ) GLOBAL_UNCERTAINTY_ASSIGNED_CONTEXT ( ( #36528 ) ) GLOBAL_UNIT_ASSIGNED_CONTEXT ( ( #4174, #44254, #10500 ) ) REPRESENTATION_CONTEXT ( 'NONE', 'WORKASPACE' ) );
#56119 = CARTESIAN_POINT ( 'NONE',  ( -2.608446859217920633, -4.805146000318815780, 21.75186829374151287 ) ) ;
#56120 = ADVANCED_FACE ( 'NONE', ( #41975 ), #8632, .F. ) ;
#56121 = EDGE_CURVE ( 'NONE', #59958, #80080, #77082, .T. ) ;
#56122 = CARTESIAN_POINT ( 'NONE',  ( -18.06608237936013950, -11.35647404775217595, 33.31231777344666511 ) ) ;
#56123 = DIRECTION ( 'NONE',  ( -0.000000000000000000, -0.6427876096865404731, -0.7660444431189770143 ) ) ;
#56124 = CARTESIAN_POINT ( 'NONE',  ( 8.834486340506792601, -10.21337939537593620, 33.94971097300152252 ) ) ;
#56125 = CARTESIAN_POINT ( 'NONE',  ( -2.694853999681181556, -10.10844685921792241, 23.93936829374151642 ) ) ;
#56126 = EDGE_CURVE ( 'NONE', #58001, #58140, #537, .T. ) ;
#56127 = CARTESIAN_POINT ( 'NONE',  ( -14.24162395668986747, -10.51840700105979565, 33.73612834413962247 ) ) ;
#56128 = ORIENTED_EDGE ( 'NONE', *, *, #53627, .T. ) ;
#56129 = CARTESIAN_POINT ( 'NONE',  ( 6.988222702408889653, -7.750023238201980469, 34.74374492549440419 ) ) ;
#56130 = CARTESIAN_POINT ( 'NONE',  ( 16.08857570788537927, -12.27809138561121394, 31.22303859784730307 ) ) ;
#56131 = CARTESIAN_POINT ( 'NONE',  ( 1.134638653673032183, -12.41269422305637171, 30.68257228309993323 ) ) ;
#56132 = CARTESIAN_POINT ( 'NONE',  ( -14.43783951713052893, -11.93770438780619259, 32.05411857736982029 ) ) ;
#56133 = CARTESIAN_POINT ( 'NONE',  ( -16.15384615384615330, -10.51840700105979565, 33.73612834413961536 ) ) ;
#56134 = FACE_OUTER_BOUND ( 'NONE', #34117, .T. ) ;
#56135 = DIRECTION ( 'NONE',  ( 0.000000000000000000, 0.8660254037844377084, -0.5000000000000015543 ) ) ;
#56136 = CARTESIAN_POINT ( 'NONE',  ( -10.36543909703647337, -10.76462480002816235, 33.53768742498949962 ) ) ;
#56137 = VERTEX_POINT ( 'NONE', #28006 ) ;
#56138 = ORIENTED_EDGE ( 'NONE', *, *, #28891, .T. ) ;
#56139 = VECTOR ( 'NONE', #48014, 1000.000000000000000 ) ;
#56140 = APPLICATION_CONTEXT ( 'automotive_design' ) ;
#56141 = ORIENTED_EDGE ( 'NONE', *, *, #88466, .F. ) ;
#56142 = CARTESIAN_POINT ( 'NONE',  ( -13.38461538461538325, -2.708943851104267164, 35.45975837776705220 ) ) ;
#56143 = CARTESIAN_POINT ( 'NONE',  ( 1.384615384615386802, -11.35647404775217417, 33.31231777344666511 ) ) ;
#56144 = CARTESIAN_POINT ( 'NONE',  ( -15.23076923076922995, -10.67929555188718282, 33.92786785259544047 ) ) ;
#56145 = CARTESIAN_POINT ( 'NONE',  ( 3.230769230769231726, -5.471508081941601098, 34.59228464037088457 ) ) ;
#56146 = CARTESIAN_POINT ( 'NONE',  ( 13.16168842570853492, -8.282780595021769443, 34.94152052738834868 ) ) ;
#56147 = VERTEX_POINT ( 'NONE', #21239 ) ;
#56148 = CARTESIAN_POINT ( 'NONE',  ( -17.32689980786543060, -4.236021600441997492, 33.53823185664189310 ) ) ;
#56149 = ORIENTED_EDGE ( 'NONE', *, *, #59357, .T. ) ;
#56150 = ORIENTED_EDGE ( 'NONE', *, *, #41170, .T. ) ;
#56151 = B_SPLINE_CURVE_WITH_KNOTS ( 'NONE', 3,
 ( #42672, #77334, #76458, #16079, #15640, #43541, #35915, #57057, #43108, #29166 ),
 .UNSPECIFIED., .F., .F.,
 ( 4, 2, 2, 2, 4 ),
 ( 0.000000000000000000, 0.0001954339857564072033, 0.0003908679715128144066, 0.0005863019572692215828, 0.0007817359430256288133 ),
 .UNSPECIFIED. ) ;
#56152 = VECTOR ( 'NONE', #86336, 1000.000000000000000 ) ;
#56153 = ORIENTED_EDGE ( 'NONE', *, *, #32487, .F. ) ;
#56155 = EDGE_LOOP ( 'NONE', ( #82364, #985, #33672, #4866 ) ) ;
#56154 = DIRECTION ( 'NONE',  ( 1.000000000000000000, 0.000000000000000000, 0.000000000000000000 ) ) ;
#56156 = LINE ( 'NONE', #82755, #5696 ) ;
#56157 = CARTESIAN_POINT ( 'NONE',  ( -10.39195765352304512, -7.630147231320743018, 34.74852402298682819 ) ) ;
#56158 = VECTOR ( 'NONE', #2332, 1000.000000000000227 ) ;
#56159 = CARTESIAN_POINT ( 'NONE',  ( -8.102564102564102200, -7.500000000000000000, 29.75000000000000355 ) ) ;
#56160 = CARTESIAN_POINT ( 'NONE',  ( 14.05769230769231015, -7.433932668274256805, 35.00000000000000711 ) ) ;
#56161 = ORIENTED_EDGE ( 'NONE', *, *, #75753, .T. ) ;
#56162 = VECTOR ( 'NONE', #58322, 1000.000000000000000 ) ;
#56163 = ORIENTED_EDGE ( 'NONE', *, *, #22256, .F. ) ;
#56164 = AXIS2_PLACEMENT_3D ( 'NONE', #2123, #29608, #57066 ) ;
#56165 = ORIENTED_EDGE ( 'NONE', *, *, #86722, .T. ) ;
#56166 = CARTESIAN_POINT ( 'NONE',  ( -2.307692307692428724, -3.643525952248796163, 33.31231777344771672 ) ) ;
#56168 = ORIENTED_EDGE ( 'NONE', *, *, #16338, .F. ) ;
#56167 = CARTESIAN_POINT ( 'NONE',  ( 4.219101725122177626, -11.48612834413965977, 32.76840700105972815 ) ) ;
#56169 = AXIS2_PLACEMENT_3D ( 'NONE', #67954, #88689, #26967 ) ;
#56170 = LINE ( 'NONE', #84101, #9077 ) ;
#56171 = CARTESIAN_POINT ( 'NONE',  ( -2.176900499867520100, -8.147973898785416225, 34.70805048591653730 ) ) ;
#56172 = DIRECTION ( 'NONE',  ( -0.000000000000000000, -0.9396926207859092051, -0.3420201433256662704 ) ) ;
#56173 = ORIENTED_EDGE ( 'NONE', *, *, #84000, .F. ) ;
#56174 = CYLINDRICAL_SURFACE ( 'NONE', #43676, 0.2499999999999979738 ) ;
#56175 = CARTESIAN_POINT ( 'NONE',  ( -15.23076923076922995, -12.34228464037088635, 31.77849191805839268 ) ) ;
#56176 = VERTEX_POINT ( 'NONE', #38312 ) ;
#56177 = FACE_BOUND ( 'NONE', #19837, .T. ) ;
#56178 = CARTESIAN_POINT ( 'NONE',  ( -6.249999999999997335, -2.249999999999998668, 29.75000000000000355 ) ) ;
#56179 = DIRECTION ( 'NONE',  ( -0.000000000000000000, -0.7660444431189791237, -0.6427876096865379196 ) ) ;
#56180 = EDGE_CURVE ( 'NONE', #14452, #28219, #45052, .T. ) ;
#56181 = CARTESIAN_POINT ( 'NONE',  ( 3.361294932532796764, -9.417988943895561960, 34.36773134775778260 ) ) ;
#56183 = CARTESIAN_POINT ( 'NONE',  ( 5.011652630962299959, -10.21337939537584383, 33.94971097300158647 ) ) ;
#56182 = CARTESIAN_POINT ( 'NONE',  ( -17.07692307692307665, -1.215029322943914858, 32.30358669280327177 ) ) ;
#56184 = CARTESIAN_POINT ( 'NONE',  ( -3.903900635498011695, -2.824170634883622188, 31.52227843825338738 ) ) ;
#56185 = DIRECTION ( 'NONE',  ( 0.000000000000000000, 0.1736481776669267785, -0.9848077530122087975 ) ) ;
#56186 = EDGE_LOOP ( 'NONE', ( #25767, #78921 ) ) ;
#56187 = CARTESIAN_POINT ( 'NONE',  ( -2.531177232256637488, -4.225889041578354544, 33.85425143139329407 ) ) ;
#56188 = CARTESIAN_POINT ( 'NONE',  ( -2.939152317953646711E-15, 7.500000000000000000, 13.50000000000000178 ) ) ;
#56189 = ORIENTED_EDGE ( 'NONE', *, *, #66564, .T. ) ;
#56190 = B_SPLINE_CURVE_WITH_KNOTS ( 'NONE', 3,
 ( #83340, #7232, #474, #62601, #1794, #1350, #27943, #41459, #41910, #55409 ),
 .UNSPECIFIED., .F., .F.,
 ( 4, 2, 2, 2, 4 ),
 ( 0.000000000000000000, 0.0001954339857564097241, 0.0003908679715128194482, 0.0005863019572692291723, 0.0007817359430256388964 ),
 .UNSPECIFIED. ) ;
#56191 = B_SPLINE_CURVE_WITH_KNOTS ( 'NONE', 3,
 ( #56409, #49647, #135, #42456, #69918, #8675, #76683, #15430, #8227, #75784 ),
 .UNSPECIFIED., .F., .F.,
 ( 4, 2, 2, 2, 4 ),
 ( 0.0007817359430256256691, 0.0009771253907249902518, 0.001172514838424355051, 0.001367904286123719851, 0.001563293733823084434 ),
 .UNSPECIFIED. ) ;
#56192 = B_SPLINE_CURVE_WITH_KNOTS ( 'NONE', 3,
 ( #74185, #32315, #46269, #39968, #26446, #73758, #76396, #55234, #68755, #297 ),
 .UNSPECIFIED., .F., .F.,
 ( 4, 2, 2, 2, 4 ),
 ( 0.000000000000000000, 0.0001954311564186858715, 0.0003908623128373717431, 0.0005862934692560576146, 0.0007817246256747434861 ),
 .UNSPECIFIED. ) ;
#56193 = DIRECTION ( 'NONE',  ( -1.000000000000000000, -0.000000000000000000, -0.000000000000000000 ) ) ;
#56194 = CARTESIAN_POINT ( 'NONE',  ( -17.32692307692307665, -7.500000000000001776, 35.00000000000000000 ) ) ;
#56195 = CARTESIAN_POINT ( 'NONE',  ( 7.596153846153846700, -7.500000000000001776, 35.04278698407183867 ) ) ;
#56196 = ORIENTED_EDGE ( 'NONE', *, *, #40660, .T. ) ;
#56197 = CARTESIAN_POINT ( 'NONE',  ( -13.13466997523734214, -11.56426240980093745, 33.07394671870546432 ) ) ;
#56198 = CARTESIAN_POINT ( 'NONE',  ( -12.94230769230769162, -11.50000000000000000, 29.75000000000000355 ) ) ;
#56199 = FACE_BOUND ( 'NONE', #34094, .T. ) ;
#56201 = CARTESIAN_POINT ( 'NONE',  ( -3.930834802233302394, -8.239487800360276282, 34.69522927552633718 ) ) ;
#56200 = CARTESIAN_POINT ( 'NONE',  ( -1.514763354347079982, -6.809168938359898782, 34.95455904226513866 ) ) ;
#56202 = ADVANCED_FACE ( 'NONE', ( #15830 ), #78841, .T. ) ;
#56203 = CARTESIAN_POINT ( 'NONE',  ( -15.93106661257774270, -2.600157965045223563, 30.74683119005207033 ) ) ;
#56205 = CARTESIAN_POINT ( 'NONE',  ( -17.07692307692276046, -2.255955759149395501, 30.00000000000324363 ) ) ;
#56204 = CARTESIAN_POINT ( 'NONE',  ( -5.011667937410237528, -10.33852847137154107, 34.16647553114620450 ) ) ;
#56206 = DIRECTION ( 'NONE',  ( 5.997714145664496128E-17, 1.000000000000000000, -5.102127870520021228E-17 ) ) ;
#56207 = CARTESIAN_POINT ( 'NONE',  ( 3.750000000000000888, -7.499999999999978684, 24.46875000000000000 ) ) ;
#56208 = ORIENTED_EDGE ( 'NONE', *, *, #65273, .T. ) ;
#56209 = EDGE_LOOP ( 'NONE', ( #56608, #32035, #4142, #86144 ) ) ;
#56210 = CARTESIAN_POINT ( 'NONE',  ( -9.469528151039279251, -11.89424750095246175, 32.13594075562311758 ) ) ;
#56211 = CARTESIAN_POINT ( 'NONE',  ( -10.54931728203453822, -8.164416787775445883, 34.95778746994558617 ) ) ;
#56212 = CARTESIAN_POINT ( 'NONE',  ( 7.173076923078343548, -7.500000000000154543, 35.00000000000007105 ) ) ;
#56213 = CARTESIAN_POINT ( 'NONE',  ( -0.5916864312701606288, -3.069018819979302926, 32.56621877034667278 ) ) ;
#56214 = CARTESIAN_POINT ( 'NONE',  ( -16.21992956480203318, -12.10708131394839349, 31.69288490824020244 ) ) ;
#56215 = CARTESIAN_POINT ( 'NONE',  ( -3.724691934501229262, -9.114399933863657211, 16.01375670625849068 ) ) ;
#56216 = CARTESIAN_POINT ( 'NONE',  ( 0.4615384615383382183, -4.320704448113951379, 33.92786785259630022 ) ) ;
#56217 = DIRECTION ( 'NONE',  ( 0.000000000000000000, 0.9396926207859126468, -0.3420201433256571111 ) ) ;
#56218 = CARTESIAN_POINT ( 'NONE',  ( -17.14300648787895298, -4.786620604624113540, 33.94971097300155805 ) ) ;
#56219 = CARTESIAN_POINT ( 'NONE',  ( 18.00000000000000000, -8.164416787775445883, 34.95778746994557906 ) ) ;
#56220 = DIRECTION ( 'NONE',  ( -0.000000000000000000, 0.7660444431189791237, -0.6427876096865379196 ) ) ;
#56221 = DIRECTION ( 'NONE',  ( -1.000000000000000000, -0.000000000000000000, -0.000000000000000000 ) ) ;
#56222 = CARTESIAN_POINT ( 'NONE',  ( -5.776987155906604166, -11.43677907613344757, 33.22367315496201456 ) ) ;
#56223 = ADVANCED_FACE ( 'NONE', ( #70769 ), #86058, .F. ) ;
#56224 = EDGE_CURVE ( 'NONE', #12547, #70275, #39687, .T. ) ;
#56225 = DIRECTION ( 'NONE',  ( 0.000000000000000000, 0.9396926207859126468, -0.3420201433256571111 ) ) ;
#56226 = AXIS2_PLACEMENT_3D ( 'NONE', #69272, #82798, #21521 ) ;
#56227 = CARTESIAN_POINT ( 'NONE',  ( 3.100077764101672351, -2.541943142973489778, 30.39792223712631980 ) ) ;
#56228 = ORIENTED_EDGE ( 'NONE', *, *, #28936, .T. ) ;
#56229 = CARTESIAN_POINT ( 'NONE',  ( -14.30769230769230660, -3.513871655860378418, 32.76840700105978499 ) ) ;
#56230 = CARTESIAN_POINT ( 'NONE',  ( -5.076923076923075762, -3.322132147404559976, 32.92929555188717927 ) ) ;
#56231 = CARTESIAN_POINT ( 'NONE',  ( -1.077988221561493543, -4.724691934501247914, 19.32999329374151642 ) ) ;
#56232 = B_SPLINE_CURVE_WITH_KNOTS ( 'NONE', 3,
 ( #64920, #71234, #85653, #18533, #17185, #79790, #9539, #72575, #37005, #2767 ),
 .UNSPECIFIED., .F., .F.,
 ( 4, 2, 2, 2, 4 ),
 ( 0.000000000000000000, 0.0001954339857564080978, 0.0003908679715128161956, 0.0005863019572692242934, 0.0007817359430256323911 ),
 .UNSPECIFIED. ) ;
#56233 = VECTOR ( 'NONE', #86209, 999.9999999999998863 ) ;
#56234 = VECTOR ( 'NONE', #14426, 1000.000000000000000 ) ;
#56235 = CARTESIAN_POINT ( 'NONE',  ( 0.6845513056318562883, -3.395485233115138168, 33.02377354290275946 ) ) ;
#56236 = CARTESIAN_POINT ( 'NONE',  ( 16.85343815235874132, -11.60425143139329940, 33.02411095842164457 ) ) ;
#56237 = ORIENTED_EDGE ( 'NONE', *, *, #23064, .T. ) ;
#56238 = CARTESIAN_POINT ( 'NONE',  ( -9.942284436356281674, -5.643011162660950042, 34.66104346484419096 ) ) ;
#56240 = VERTEX_POINT ( 'NONE', #56800 ) ;
#56239 = CARTESIAN_POINT ( 'NONE',  ( -3.262820512820514107, -3.499999999999999556, 29.75000000000000355 ) ) ;
#56241 = CARTESIAN_POINT ( 'NONE',  ( 7.846153846153846700, -3.513871655860378418, 32.76840700105978499 ) ) ;
#56242 = CARTESIAN_POINT ( 'NONE',  ( -2.557715531913763662, -10.92453946501458439, 33.72985991061850086 ) ) ;
#56243 = ORIENTED_EDGE ( 'NONE', *, *, #47334, .F. ) ;
#56244 = CYLINDRICAL_SURFACE ( 'NONE', #6036, 4.000000000000000000 ) ;
#56245 = CIRCLE ( 'NONE', #15991, 4.000000000000000000 ) ;
#56246 = FACE_OUTER_BOUND ( 'NONE', #30546, .T. ) ;
#56247 = PRODUCT_DEFINITION_FORMATION_WITH_SPECIFIED_SOURCE ( 'ANY', '', #8899, .NOT_KNOWN. ) ;
#56248 = EDGE_LOOP ( 'NONE', ( #72670, #87397, #16525, #8651 ) ) ;
#56249 = CARTESIAN_POINT ( 'NONE',  ( 8.769230769230645706, -2.379036618888197729, 30.90682066428292885 ) ) ;
#56250 = CARTESIAN_POINT ( 'NONE',  ( -11.53846153846166089, -12.51329471203414379, 31.30864560766407578 ) ) ;
#56251 = CARTESIAN_POINT ( 'NONE',  ( -9.442307692307688072, -2.499999999999999556, 29.81604066197449754 ) ) ;
#56252 = ORIENTED_EDGE ( 'NONE', *, *, #24908, .T. ) ;
#56253 = EDGE_LOOP ( 'NONE', ( #61537, #11948, #45284, #31131 ) ) ;
#56254 = CARTESIAN_POINT ( 'NONE',  ( 6.066068351002440906, -6.386643153685127139, 34.62446782046654192 ) ) ;
#56255 = ORIENTED_EDGE ( 'NONE', *, *, #27874, .T. ) ;
#56256 = CARTESIAN_POINT ( 'NONE',  ( 5.142990410273151625, -4.661471528628508665, 34.16647553114624003 ) ) ;
#56257 = CARTESIAN_POINT ( 'NONE',  ( 13.63466980452883881, -3.435999193479609914, 33.07426656108010832 ) ) ;
#56258 = CARTESIAN_POINT ( 'NONE',  ( -4.403822884788506364, -6.567427716900047230, 34.66269422305636283 ) ) ;
#56259 = CARTESIAN_POINT ( 'NONE',  ( -4.153846153846152411, -12.62096338111211580, 30.90682066428153263 ) ) ;
#56260 = CARTESIAN_POINT ( 'NONE',  ( -17.07692307692307665, -5.180354513474913603, 36.12317359536750416 ) ) ;
#56261 = VECTOR ( 'NONE', #35418, 1000.000000000000000 ) ;
#56262 = ORIENTED_EDGE ( 'NONE', *, *, #74398, .T. ) ;
#56263 = ORIENTED_EDGE ( 'NONE', *, *, #28038, .T. ) ;
#56265 = ORIENTED_EDGE ( 'NONE', *, *, #51248, .F. ) ;
#56264 = CARTESIAN_POINT ( 'NONE',  ( 9.626224281351811740, -4.098570777380720287, 33.41473453929634729 ) ) ;
#56266 = VECTOR ( 'NONE', #44130, 999.9999999999998863 ) ;
#56267 = CARTESIAN_POINT ( 'NONE',  ( -9.442307692307691624, -2.499999999999998668, 29.75000000000000355 ) ) ;
#56268 = ORIENTED_EDGE ( 'NONE', *, *, #26522, .F. ) ;
#56269 = CARTESIAN_POINT ( 'NONE',  ( -17.93474442872397034, -3.300289026998476150, 32.46337939537591666 ) ) ;
#56270 = DIRECTION ( 'NONE',  ( 0.000000000000000000, -2.413528314402514090E-16, 1.000000000000000000 ) ) ;
#56271 = VERTEX_POINT ( 'NONE', #43728 ) ;
#56272 = DIRECTION ( 'NONE',  ( 0.000000000000000000, 0.9848077530122072432, -0.1736481776669354937 ) ) ;
#56273 = EDGE_CURVE ( 'NONE', #53485, #51137, #53711, .T. ) ;
#56274 = ORIENTED_EDGE ( 'NONE', *, *, #33823, .T. ) ;
#56276 = ORIENTED_EDGE ( 'NONE', *, *, #42871, .F. ) ;
#56275 = CARTESIAN_POINT ( 'NONE',  ( -6.857008572074484221, -11.16473453929635440, 33.15142922261926373 ) ) ;
#56277 = DIRECTION ( 'NONE',  ( 0.000000000000000000, 0.9848077530122072432, -0.1736481776669354937 ) ) ;
#56278 = ORIENTED_EDGE ( 'NONE', *, *, #62165, .F. ) ;
#56279 = CARTESIAN_POINT ( 'NONE',  ( 17.93472955403921887, -10.90142922261923886, 33.41473453929638993 ) ) ;
#56280 = DIRECTION ( 'NONE',  ( 0.000000000000000000, 0.3420201433256610524, 0.9396926207859113145 ) ) ;
#56281 = B_SPLINE_CURVE_WITH_KNOTS ( 'NONE', 3,
 ( #59715, #72335, #18740, #32684, #52061, #10645, #38110, #60152, #79553, #72775 ),
 .UNSPECIFIED., .F., .F.,
 ( 4, 2, 2, 2, 4 ),
 ( 0.000000000000000000, 0.0001954339857564091549, 0.0003908679715128183098, 0.0005863019572692274375, 0.0007817359430256366195 ),
 .UNSPECIFIED. ) ;
#56282 = FACE_BOUND ( 'NONE', #19090, .T. ) ;
#56283 = CARTESIAN_POINT ( 'NONE',  ( -11.78843826940389405, -2.564618984488975073, 30.55390908950641915 ) ) ;
#56284 = CARTESIAN_POINT ( 'NONE',  ( -6.700065571464072889, -12.15243808032446005, 31.58219941686247978 ) ) ;
#56285 = B_SPLINE_CURVE_WITH_KNOTS ( 'NONE', 3,
 ( #27321, #5716, #54783, #33189, #88163, #82273, #39518, #53901, #20559, #48023 ),
 .UNSPECIFIED., .F., .F.,
 ( 4, 2, 2, 2, 4 ),
 ( 0.000000000000000000, 0.0001954311564186861968, 0.0003908623128373723936, 0.0005862934692560585904, 0.0007817246256747447872 ),
 .UNSPECIFIED. ) ;
#56286 = VECTOR ( 'NONE', #74697, 1000.000000000000000 ) ;
#56287 = ADVANCED_FACE ( 'NONE', ( #9074 ), #63992, .F. ) ;
#56288 = CARTESIAN_POINT ( 'NONE',  ( 15.45354889974729318, -2.612705202774698421, 31.66806509827799943 ) ) ;
#56289 = CARTESIAN_POINT ( 'NONE',  ( 12.39545608217832395, -3.322132147404559532, 32.92929555188719348 ) ) ;
#56290 = CARTESIAN_POINT ( 'NONE',  ( 5.299702618191484582, -10.81320215134717344, 33.49497208177562868 ) ) ;
#56291 = CARTESIAN_POINT ( 'NONE',  ( -17.07692307692319744, -5.941354392335915335, 34.76329471203413846 ) ) ;
#56292 = EDGE_LOOP ( 'NONE', ( #29428, #53814 ) ) ;
#56293 = CARTESIAN_POINT ( 'NONE',  ( 10.55011416942384095, -10.21337939537584383, 33.94971097300158647 ) ) ;
#56294 = ADVANCED_FACE ( 'NONE', ( #37864 ), #9942, .F. ) ;
#56295 = EDGE_LOOP ( 'NONE', ( #19933, #33274 ) ) ;
#56296 = ORIENTED_EDGE ( 'NONE', *, *, #3699, .F. ) ;
#56297 = AXIS2_PLACEMENT_3D ( 'NONE', #84913, #37146, #2908 ) ;
#56299 = CARTESIAN_POINT ( 'NONE',  ( 7.976945653978634532, -9.804649428959608670, 34.18742332936588468 ) ) ;
#56298 = CARTESIAN_POINT ( 'NONE',  ( 14.55774661933062397, -3.627508038966690496, 32.91356715214248396 ) ) ;
#56300 = CARTESIAN_POINT ( 'NONE',  ( -18.00000000000000000, -6.436573248120765811, 35.78099280442780383 ) ) ;
#56301 = CARTESIAN_POINT ( 'NONE',  ( 7.976679284387491187, -3.625058011473228703, 33.29252011169590020 ) ) ;
#56302 = CARTESIAN_POINT ( 'NONE',  ( 1.634560793993430794, -10.92531984108285670, 33.72920026020278073 ) ) ;
#56303 = CARTESIAN_POINT ( 'NONE',  ( -12.46153846153846168, -4.661471528628507777, 34.16647553114623292 ) ) ;
#56304 = VERTEX_POINT ( 'NONE', #85171 ) ;
#56305 = CARTESIAN_POINT ( 'NONE',  ( -18.06608341095587278, -5.557115091759785130, 34.35708131394839171 ) ) ;
#56306 = CARTESIAN_POINT ( 'NONE',  ( -17.07692307692307665, -12.09954503811598769, 35.62045528018868623 ) ) ;
#56307 = CARTESIAN_POINT ( 'NONE',  ( -12.46153846153858424, -11.67786785259630911, 32.92929555188603530 ) ) ;
#56308 = EDGE_CURVE ( 'NONE', #25632, #15004, #17171, .T. ) ;
#56309 = CARTESIAN_POINT ( 'NONE',  ( -8.703163435880695076, -2.486705287966280320, 31.30864560766543647 ) ) ;
#56310 = CARTESIAN_POINT ( 'NONE',  ( -15.23076923076892264, -2.506253911140614576, 30.00000000000323297 ) ) ;
#56311 = ORIENTED_EDGE ( 'NONE', *, *, #4017, .F. ) ;
#56312 = CARTESIAN_POINT ( 'NONE',  ( -0.5268084620947809382, -2.379036618887870880, 30.90682066428147579 ) ) ;
#56313 = EDGE_LOOP ( 'NONE', ( #53152, #88991, #29969, #87917 ) ) ;
#56315 = EDGE_CURVE ( 'NONE', #10775, #28383, #2730, .T. ) ;
#56314 = EDGE_LOOP ( 'NONE', ( #38425, #78590, #59349, #76553 ) ) ;
#56316 = CARTESIAN_POINT ( 'NONE',  ( 17.07692307692307665, -13.75783147151868846, 33.36296068462461051 ) ) ;
#56317 = ORIENTED_EDGE ( 'NONE', *, *, #22671, .T. ) ;
#56318 = CARTESIAN_POINT ( 'NONE',  ( -1.134561072977068763, -8.303483539816728154, 34.68545999027711702 ) ) ;
#56319 = CARTESIAN_POINT ( 'NONE',  ( -1.384615384615506484, -10.33852847137269571, 34.16647553114546554 ) ) ;
#56320 = CARTESIAN_POINT ( 'NONE',  ( 14.17700170458200404, -9.929715669179220328, 34.40415004197138416 ) ) ;
#56321 = CARTESIAN_POINT ( 'NONE',  ( -5.076923076923199218, -3.643525952248796163, 33.31231777344771672 ) ) ;
#56322 = DIRECTION ( 'NONE',  ( 0.000000000000000000, 0.000000000000000000, 1.000000000000000000 ) ) ;
#56323 = DIRECTION ( 'NONE',  ( -1.000000000000000000, 0.000000000000000000, 0.000000000000000000 ) ) ;
#56324 = EDGE_LOOP ( 'NONE', ( #55404, #27244, #68313, #7243, #58579, #66376 ) ) ;
#56325 = CARTESIAN_POINT ( 'NONE',  ( -11.47229493186989657, -7.250054591869670162, 34.99404684341514127 ) ) ;
#56327 = ORIENTED_EDGE ( 'NONE', *, *, #81963, .T. ) ;
#56326 = CARTESIAN_POINT ( 'NONE',  ( -13.13466986626724342, -4.336752205174649433, 33.62275283266504289 ) ) ;
#56328 = DIRECTION ( 'NONE',  ( -0.000000000000000000, -0.8660254037844397068, -0.4999999999999978906 ) ) ;
#56329 = CARTESIAN_POINT ( 'NONE',  ( -10.48459280755982981, -3.530189275343204702, 32.79018710029569661 ) ) ;
#56330 = CARTESIAN_POINT ( 'NONE',  ( 16.82694634598072270, -3.627789207965226304, 32.91389620160131102 ) ) ;
#56331 = CARTESIAN_POINT ( 'NONE',  ( -17.75005448165186195, -11.86320923018887896, 32.19269448109603360 ) ) ;
#56332 = CARTESIAN_POINT ( 'NONE',  ( -2.057746898314262385, -2.341251567377310217, 30.72681386836322659 ) ) ;
#56333 = ADVANCED_FACE ( 'NONE', ( #17143 ), #44600, .F. ) ;
#56334 = CARTESIAN_POINT ( 'NONE',  ( 16.82692307692307665, -7.500000000000001776, 34.75000000000000000 ) ) ;
#56335 = LINE ( 'NONE', #9041, #20573 ) ;
#56336 = EDGE_CURVE ( 'NONE', #59263, #86041, #34418, .T. ) ;
#56337 = AXIS2_PLACEMENT_3D ( 'NONE', #21342, #69087, #14589 ) ;
#56338 = CARTESIAN_POINT ( 'NONE',  ( 2.694853999681185108, -4.891553140782077591, 13.31436829374151287 ) ) ;
#56339 = EDGE_LOOP ( 'NONE', ( #50236, #16592 ) ) ;
#56340 = CARTESIAN_POINT ( 'NONE',  ( -1.134561072977069651, -11.28795663066794219, 33.01431243580653785 ) ) ;
#56341 = CARTESIAN_POINT ( 'NONE',  ( -1.449885830576159274, -12.27809138561121394, 31.22303859784730307 ) ) ;
#56342 = EDGE_CURVE ( 'NONE', #43796, #75345, #5864, .T. ) ;
#56343 = CARTESIAN_POINT ( 'NONE',  ( 8.069165197766695385, -2.554770724473667709, 30.48948780036025852 ) ) ;
#56344 = CARTESIAN_POINT ( 'NONE',  ( 25.00000000000000355, 9.999999999999971578, 3.000000000000000000 ) ) ;
#56345 = EDGE_CURVE ( 'NONE', #1161, #48109, #27872, .T. ) ;
#56346 = ORIENTED_EDGE ( 'NONE', *, *, #52006, .F. ) ;
#56347 = LINE ( 'NONE', #77940, #67213 ) ;
#56348 = CARTESIAN_POINT ( 'NONE',  ( 6.000000000000001776, -4.098570777380720287, 33.41473453929634729 ) ) ;
#56349 = ORIENTED_EDGE ( 'NONE', *, *, #50582, .F. ) ;
#56350 = CARTESIAN_POINT ( 'NONE',  ( -3.262820512820514995, -4.000000000000000000, 29.75000000000000355 ) ) ;
#56351 = CARTESIAN_POINT ( 'NONE',  ( -4.219116599806928214, -10.90142922261923886, 33.41473453929638993 ) ) ;
#56352 = ORIENTED_EDGE ( 'NONE', *, *, #66072, .F. ) ;
#56353 = CARTESIAN_POINT ( 'NONE',  ( -39.05038313613820122, -2.249999999999998668, 29.75000000000000355 ) ) ;
#56354 = DIRECTION ( 'NONE',  ( -0.000000000000000000, -0.000000000000000000, -1.000000000000000000 ) ) ;
#56355 = CARTESIAN_POINT ( 'NONE',  ( -13.38461538461538325, -10.51840700105979565, 33.73612834413961536 ) ) ;
#56356 = CARTESIAN_POINT ( 'NONE',  ( -4.284536756956459413, -11.37499894934982514, 33.29245874905763003 ) ) ;
#56357 = EDGE_LOOP ( 'NONE', ( #34331, #45502 ) ) ;
#56358 = CARTESIAN_POINT ( 'NONE',  ( -6.857821783564084228, -6.835583212224609184, 34.95778746994559327 ) ) ;
#56359 = ORIENTED_EDGE ( 'NONE', *, *, #29881, .T. ) ;
#56361 = FACE_OUTER_BOUND ( 'NONE', #79181, .T. ) ;
#56360 = VECTOR ( 'NONE', #29347, 1000.000000000000000 ) ;
#56362 = CARTESIAN_POINT ( 'NONE',  ( 5.869389640375470840, -7.722926236386453702, 34.74524107206102030 ) ) ;
#56363 = ORIENTED_EDGE ( 'NONE', *, *, #72348, .F. ) ;
#56364 = DIRECTION ( 'NONE',  ( -0.000000000000000000, 1.000000000000000000, -0.000000000000000000 ) ) ;
#56365 = CARTESIAN_POINT ( 'NONE',  ( -8.834501215191544077, -2.625532179533444754, 30.86335684631481513 ) ) ;
#56366 = CARTESIAN_POINT ( 'NONE',  ( 4.230769230769229061, -3.499999999999999556, 29.75000000000000355 ) ) ;
#56367 = B_SPLINE_CURVE_WITH_KNOTS ( 'NONE', 3,
 ( #78724, #10713, #38177, #65635, #3937, #46275, #55569, #14592, #19250, #32321 ),
 .UNSPECIFIED., .F., .F.,
 ( 4, 2, 2, 2, 4 ),
 ( 0.000000000000000000, 0.0001954311564186863323, 0.0003908623128373726646, 0.0005862934692560590241, 0.0007817246256747453293 ),
 .UNSPECIFIED. ) ;
#56368 = B_SPLINE_CURVE_WITH_KNOTS ( 'NONE', 3,
 ( #12977, #60264, #7881, #49306, #28599, #14635, #53504, #15084, #1120, #40462 ),
 .UNSPECIFIED., .F., .F.,
 ( 4, 2, 2, 2, 4 ),
 ( 0.0007817359430256293554, 0.0009771253907249950223, 0.001172514838424360906, 0.001367904286123726790, 0.001563293733823092457 ),
 .UNSPECIFIED. ) ;
#56369 = CARTESIAN_POINT ( 'NONE',  ( -11.28851612908349722, -5.766571408460171355, 34.70601412856602508 ) ) ;
#56370 = CARTESIAN_POINT ( 'NONE',  ( -20.00000000000000000, -11.50000000000000000, 29.75000000000000355 ) ) ;
#56371 = B_SPLINE_CURVE_WITH_KNOTS ( 'NONE', 3,
 ( #40333, #67801, #46639, #74116, #12850, #12412, #61037, #26813, #20053, #40779 ),
 .UNSPECIFIED., .F., .F.,
 ( 4, 2, 2, 2, 4 ),
 ( 0.000000000000000000, 0.0001954311564186882026, 0.0003908623128373764051, 0.0005862934692560646619, 0.0007817246256747528103 ),
 .UNSPECIFIED. ) ;
#56372 = EDGE_CURVE ( 'NONE', #55677, #22548, #12622, .T. ) ;
#56373 = VERTEX_POINT ( 'NONE', #5421 ) ;
#56374 = EDGE_LOOP ( 'NONE', ( #54414, #24433 ) ) ;
#56375 = FACE_BOUND ( 'NONE', #7671, .T. ) ;
#56376 = VERTEX_POINT ( 'NONE', #53599 ) ;
#56377 = CARTESIAN_POINT ( 'NONE',  ( 8.519254038288416098, -3.627789207965226748, 32.91389620160131102 ) ) ;
#56378 = ADVANCED_FACE ( 'NONE', ( #60352 ), #73438, .F. ) ;
#56379 = CARTESIAN_POINT ( 'NONE',  ( -14.17716686945866655, -11.66157788607254098, 32.95092075102925833 ) ) ;
#56380 = CARTESIAN_POINT ( 'NONE',  ( 13.38461538461526601, -8.613356846316285953, 34.62446782046622218 ) ) ;
#56381 = CARTESIAN_POINT ( 'NONE',  ( -15.23076923076922995, -9.905515769479276145, 34.41647553114623292 ) ) ;
#56382 = EDGE_LOOP ( 'NONE', ( #40001, #4236, #9962, #63193 ) ) ;
#56383 = ADVANCED_FACE ( 'NONE', ( #19818 ), #40105, .F. ) ;
#56384 = ORIENTED_EDGE ( 'NONE', *, *, #40660, .F. ) ;
#56385 = ORIENTED_EDGE ( 'NONE', *, *, #35553, .F. ) ;
#56386 = AXIS2_PLACEMENT_3D ( 'NONE', #66276, #45112, #73494 ) ;
#56387 = CARTESIAN_POINT ( 'NONE',  ( 13.60804234647695843, -7.630147231320743018, 34.74852402298682819 ) ) ;
#56388 = VERTEX_POINT ( 'NONE', #32888 ) ;
#56389 = DIRECTION ( 'NONE',  ( 1.000000000000000000, -5.421010862427522170E-17, 2.602085213965210642E-15 ) ) ;
#56390 = AXIS2_PLACEMENT_3D ( 'NONE', #67442, #33210, #60675 ) ;
#56391 = CARTESIAN_POINT ( 'NONE',  ( -2.557715531913763662, -12.45566812827425096, 31.48439005359158926 ) ) ;
#56392 = CARTESIAN_POINT ( 'NONE',  ( -18.00000000000000000, -11.16473453929635440, 33.15142922261927083 ) ) ;
#56393 = ORIENTED_EDGE ( 'NONE', *, *, #20665, .T. ) ;
#56394 = CARTESIAN_POINT ( 'NONE',  ( -6.923076923076922462, -10.67929555188718282, 33.92786785259544047 ) ) ;
#56395 = EDGE_CURVE ( 'NONE', #73783, #15793, #11757, .T. ) ;
#56396 = CARTESIAN_POINT ( 'NONE',  ( -6.222926958906846551, -6.459968553980839800, 34.89616026154728701 ) ) ;
#56397 = DIRECTION ( 'NONE',  ( 0.000000000000000000, 0.000000000000000000, 1.000000000000000000 ) ) ;
#56398 = CARTESIAN_POINT ( 'NONE',  ( 9.692307692307570832, -11.67786785259630911, 32.92929555188603530 ) ) ;
#56399 = ORIENTED_EDGE ( 'NONE', *, *, #31470, .F. ) ;
#56400 = EDGE_CURVE ( 'NONE', #41883, #47389, #13061, .T. ) ;
#56401 = ORIENTED_EDGE ( 'NONE', *, *, #60568, .T. ) ;
#56402 = ORIENTED_EDGE ( 'NONE', *, *, #66459, .T. ) ;
#56403 = CARTESIAN_POINT ( 'NONE',  ( 4.023155550735844521, -2.845849958028613624, 32.17971566917920967 ) ) ;
#56405 = CARTESIAN_POINT ( 'NONE',  ( 17.07692307692307665, -1.117168528481311540, 33.14645433367849847 ) ) ;
#56404 = DIRECTION ( 'NONE',  ( 0.000000000000000000, 0.3420201433256610524, 0.9396926207859113145 ) ) ;
#56406 = CARTESIAN_POINT ( 'NONE',  ( 11.31553457955468645, -2.308479472611653094, 30.53278059502174457 ) ) ;
#56407 = CARTESIAN_POINT ( 'NONE',  ( -2.242437168179468365, -2.657715359629131857, 31.77849191805844242 ) ) ;
#56408 = FACE_BOUND ( 'NONE', #52928, .T. ) ;
#56409 = CARTESIAN_POINT ( 'NONE',  ( 7.846153846153725020, -11.48612834414049644, 32.76840700105863391 ) ) ;
#56410 = ORIENTED_EDGE ( 'NONE', *, *, #74669, .F. ) ;
#56411 = CARTESIAN_POINT ( 'NONE',  ( 17.29970274590113632, -12.11081565061823717, 32.26097654155341843 ) ) ;
#56412 = CARTESIAN_POINT ( 'NONE',  ( 8.769230769230768274, -4.786620604624113540, 33.94971097300155094 ) ) ;
#56413 = CARTESIAN_POINT ( 'NONE',  ( -1.384615384615383471, -3.513871655860378418, 32.76840700105978499 ) ) ;
#56414 = CARTESIAN_POINT ( 'NONE',  ( -10.03846153846153832, -3.499999999999999556, 29.75000000000000355 ) ) ;
#56415 = ORIENTED_EDGE ( 'NONE', *, *, #41064, .T. ) ;
#56416 = CARTESIAN_POINT ( 'NONE',  ( 2.373760658694747949, -11.69971097300155272, 32.46337939537588113 ) ) ;
#56417 = ORIENTED_EDGE ( 'NONE', *, *, #29407, .F. ) ;
#56418 = FACE_BOUND ( 'NONE', #19070, .T. ) ;
#56420 = VECTOR ( 'NONE', #75925, 1000.000000000000000 ) ;
#56419 = CARTESIAN_POINT ( 'NONE',  ( 13.13461538461538680, -2.499999999999998668, 29.75000000000000355 ) ) ;
#56421 = AXIS2_PLACEMENT_3D ( 'NONE', #35884, #63343, #22360 ) ;
#56422 = CARTESIAN_POINT ( 'NONE',  ( 16.94677586748486320, -11.93770438780619259, 32.05411857736982029 ) ) ;
#56423 = CARTESIAN_POINT ( 'NONE',  ( -11.28840722682322273, -11.79725096376909299, 32.30694842903960762 ) ) ;
#56424 = VERTEX_POINT ( 'NONE', #67124 ) ;
#56425 = CARTESIAN_POINT ( 'NONE',  ( 11.66898697669518192, -11.04252011169590020, 33.62494198852677130 ) ) ;
#56426 = CARTESIAN_POINT ( 'NONE',  ( -3.360917200500926239, -2.373036134822904319, 30.88089517874952250 ) ) ;
#56427 = CARTESIAN_POINT ( 'NONE',  ( 8.546303810323919947, -8.282780595021769443, 34.94152052738834868 ) ) ;
#56428 = CARTESIAN_POINT ( 'NONE',  ( 6.223011351612852238, -3.587049720035815348, 32.86302985866382897 ) ) ;
#56429 = ORIENTED_EDGE ( 'NONE', *, *, #34013, .T. ) ;
#56430 = VECTOR ( 'NONE', #52363, 1000.000000000000000 ) ;
#56431 = CARTESIAN_POINT ( 'NONE',  ( -3.930834802233303282, -6.503523203565942268, 34.64991518177335195 ) ) ;
#56432 = EDGE_LOOP ( 'NONE', ( #28843, #13887, #73307, #5925 ) ) ;
#56434 = EDGE_LOOP ( 'NONE', ( #7068, #49740 ) ) ;
#56433 = LINE ( 'NONE', #75810, #59778 ) ;
#56435 = CARTESIAN_POINT ( 'NONE',  ( 11.76124107972994537, -6.760870238392817200, 34.69528174975672385 ) ) ;
#56436 = CARTESIAN_POINT ( 'NONE',  ( -16.81410256410256565, -3.499999999999999556, 29.75000000000000355 ) ) ;
#56437 = CARTESIAN_POINT ( 'NONE',  ( -5.076923076923075762, -12.10708131394839349, 31.69288490824020244 ) ) ;
#56438 = FACE_OUTER_BOUND ( 'NONE', #49329, .T. ) ;
#56440 = CARTESIAN_POINT ( 'NONE',  ( 0.3962144487341521248, -7.749976730030849303, 34.74374725381503737 ) ) ;
#56439 = CARTESIAN_POINT ( 'NONE',  ( -5.749945580086545327, -6.523592122091591783, 34.90882529074906415 ) ) ;
#56441 = EDGE_CURVE ( 'NONE', #88317, #32595, #32003, .T. ) ;
#56442 = LINE ( 'NONE', #68623, #42094 ) ;
#56443 = CARTESIAN_POINT ( 'NONE',  ( -2.750000000000007105, -6.360912703474006946, 26.42187500000000000 ) ) ;
#56444 = EDGE_LOOP ( 'NONE', ( #75146, #51048 ) ) ;
#56445 = CARTESIAN_POINT ( 'NONE',  ( -15.16470087976679437, -3.513871655860379306, 32.76840700105978499 ) ) ;
#56446 = ORIENTED_EDGE ( 'NONE', *, *, #43494, .F. ) ;
#56447 = ADVANCED_FACE ( 'NONE', ( #72983 ), #11282, .F. ) ;
#56448 = EDGE_LOOP ( 'NONE', ( #62901, #60539, #83076, #87951 ) ) ;
#56449 = CARTESIAN_POINT ( 'NONE',  ( 11.66925334628632882, -11.71459661697925903, 32.44059661609676937 ) ) ;
#56450 = EDGE_CURVE ( 'NONE', #42680, #87653, #73007, .T. ) ;
#56451 = EDGE_LOOP ( 'NONE', ( #27332, #39814, #61270, #34228 ) ) ;
#56452 = DIRECTION ( 'NONE',  ( -0.000000000000000000, 0.3420201433256694901, -0.9396926207859082059 ) ) ;
#56453 = DIRECTION ( 'NONE',  ( 1.000000000000000000, 0.000000000000000000, 0.000000000000000000 ) ) ;
#56454 = LINE ( 'NONE', #77166, #16907 ) ;
#56455 = DIRECTION ( 'NONE',  ( -0.000000000000000000, -0.9848077530122086864, -0.1736481776669273613 ) ) ;
#56456 = CARTESIAN_POINT ( 'NONE',  ( -13.31936024510254413, -6.835583212224610072, 34.95778746994559327 ) ) ;
#56457 = CARTESIAN_POINT ( 'NONE',  ( 17.20771351789003489, -8.191423895709842640, 34.95447573519442130 ) ) ;
#56458 = VECTOR ( 'NONE', #7025, 1000.000000000000227 ) ;
#56459 = CARTESIAN_POINT ( 'NONE',  ( 16.15384615384603251, -10.90142922262034020, 33.41473453929536674 ) ) ;
#56460 = CARTESIAN_POINT ( 'NONE',  ( -6.923076923076922462, -13.53365097954675988, 30.81389545987213552 ) ) ;
#56461 = CARTESIAN_POINT ( 'NONE',  ( 15.10062126103753499, -9.504002272028875709, 34.60269587691767867 ) ) ;
#56462 = EDGE_CURVE ( 'NONE', #68993, #55800, #82756, .T. ) ;
#56463 = CARTESIAN_POINT ( 'NONE',  ( 7.976679547917408186, -2.882268652242222728, 31.66798894389554064 ) ) ;
#56464 = CARTESIAN_POINT ( 'NONE',  ( 7.846153846153723244, -2.379036618888197729, 30.90682066428292885 ) ) ;
#56465 = B_SPLINE_CURVE_WITH_KNOTS ( 'NONE', 3,
 ( #70831, #71247, #43785, #1480 ),
 .UNSPECIFIED., .F., .F.,
 ( 4, 4 ),
 ( 0.000000000000000000, 0.0004756990114773013145 ),
 .UNSPECIFIED. ) ;
#56466 = ORIENTED_EDGE ( 'NONE', *, *, #32641, .T. ) ;
#56467 = ORIENTED_EDGE ( 'NONE', *, *, #12708, .T. ) ;
#56468 = CYLINDRICAL_SURFACE ( 'NONE', #35684, 0.2500000000000009437 ) ;
#56469 =( NAMED_UNIT ( * ) PLANE_ANGLE_UNIT ( ) SI_UNIT ( $, .RADIAN. ) );
#56470 = CARTESIAN_POINT ( 'NONE',  ( -3.007989689500821129, -2.847695495035523550, 31.58253572463339154 ) ) ;
#56471 = ADVANCED_FACE ( 'NONE', ( #61230 ), #6312, .F. ) ;
#56472 = LINE ( 'NONE', #85718, #26860 ) ;
#56473 = EDGE_LOOP ( 'NONE', ( #57200, #20056 ) ) ;
#56474 = DIRECTION ( 'NONE',  ( 0.000000000000000000, 0.6427876096865368094, 0.7660444431189802339 ) ) ;
#56475 = CARTESIAN_POINT ( 'NONE',  ( -17.29984929443921970, -3.586966769969702540, 32.86292498521069660 ) ) ;
#56476 = CARTESIAN_POINT ( 'NONE',  ( 8.769230769230768274, -4.098570777380720287, 33.41473453929634729 ) ) ;
#56477 = EDGE_CURVE ( 'NONE', #38481, #69764, #40979, .T. ) ;
#56478 = ORIENTED_EDGE ( 'NONE', *, *, #42638, .T. ) ;
#56479 = CARTESIAN_POINT ( 'NONE',  ( 0.7114839798866030574, -5.852078868378310261, 34.47109172314383585 ) ) ;
#56480 = EDGE_LOOP ( 'NONE', ( #67663, #86711, #21947, #41288, #681 ) ) ;
#56481 = ADVANCED_FACE ( 'NONE', ( #7190 ), #78183, .F. ) ;
#56482 = CIRCLE ( 'NONE', #86732, 0.2500000000000002220 ) ;
#56483 = CARTESIAN_POINT ( 'NONE',  ( 13.16113046005105325, -12.47654668319379567, 31.42292124445336654 ) ) ;
#56484 = VECTOR ( 'NONE', #21593, 1000.000000000000227 ) ;
#56485 = CARTESIAN_POINT ( 'NONE',  ( -16.94613263595612551, -3.338503747796866872, 32.95102852606552801 ) ) ;
#56486 = DIRECTION ( 'NONE',  ( -0.000000000000000000, -0.9396926207859093161, -0.3420201433256663259 ) ) ;
#56487 = CARTESIAN_POINT ( 'NONE',  ( 1.161688425708537808, -8.282780595021769443, 34.94152052738834868 ) ) ;
#56488 = CARTESIAN_POINT ( 'NONE',  ( -17.93393266664992325, -12.34228464037088813, 31.77849191805839268 ) ) ;
#56489 = AXIS2_PLACEMENT_3D ( 'NONE', #28798, #81978, #41419 ) ;
#56490 = EDGE_LOOP ( 'NONE', ( #19921, #45147 ) ) ;
#56491 = ADVANCED_FACE ( 'NONE', ( #22030 ), #54931, .F. ) ;
#56492 = ORIENTED_EDGE ( 'NONE', *, *, #5941, .F. ) ;
#56493 = ORIENTED_EDGE ( 'NONE', *, *, #83979, .F. ) ;
#56494 = ADVANCED_FACE ( 'NONE', ( #61674 ), #69769, .F. ) ;
#56495 = CARTESIAN_POINT ( 'NONE',  ( 9.320512820512821150, -11.50000000000000000, 29.75000000000000355 ) ) ;
#56496 = B_SPLINE_CURVE_WITH_KNOTS ( 'NONE', 3,
 ( #34296, #53231, #27547, #68095, #67207, #13146, #40628, #5508, #67650, #32976 ),
 .UNSPECIFIED., .F., .F.,
 ( 4, 2, 2, 2, 4 ),
 ( 0.000000000000000000, 0.0001954339857564080707, 0.0003908679715128161414, 0.0005863019572692241849, 0.0007817359430256322827 ),
 .UNSPECIFIED. ) ;
#56497 = CARTESIAN_POINT ( 'NONE',  ( -2.939152317953646711E-15, 7.500000000000000000, 13.00000000000000178 ) ) ;
#56498 = CARTESIAN_POINT ( 'NONE',  ( 17.14217864819909920, -4.481592998940251427, 33.73612834413965089 ) ) ;
#56499 = CARTESIAN_POINT ( 'NONE',  ( 0.2115617174898697384, -12.41104346484419452, 31.60698883733904196 ) ) ;
#56500 = CARTESIAN_POINT ( 'NONE',  ( 17.75002325595140817, -2.920706130388546651, 32.31842814019191223 ) ) ;
#56501 = CARTESIAN_POINT ( 'NONE',  ( -7.846153846153844924, -5.180354513474913603, 36.12317359536750416 ) ) ;
#56502 = EDGE_LOOP ( 'NONE', ( #2443, #601, #39368, #84757 ) ) ;
#56503 = EDGE_CURVE ( 'NONE', #80445, #36228, #23553, .T. ) ;
#56504 = EDGE_LOOP ( 'NONE', ( #62551, #66584, #41262, #88628 ) ) ;
#56505 = ORIENTED_EDGE ( 'NONE', *, *, #77315, .F. ) ;
#56507 = VERTEX_POINT ( 'NONE', #21581 ) ;
#56506 = CARTESIAN_POINT ( 'NONE',  ( 12.59206416330202671, -8.586989748646452369, 34.63063291749215011 ) ) ;
#56508 = ADVANCED_FACE ( 'NONE', ( #7637 ), #48606, .F. ) ;
#56510 = CARTESIAN_POINT ( 'NONE',  ( 13.51514082284903218, -4.299079248970732792, 33.91157788607253565 ) ) ;
#56509 = CARTESIAN_POINT ( 'NONE',  ( -9.915233909823841785, -9.086856451489515152, 34.49173150075333183 ) ) ;
#56511 = AXIS2_PLACEMENT_3D ( 'NONE', #82493, #75283, #6390 ) ;
#56512 = CARTESIAN_POINT ( 'NONE',  ( -3.750000000000007550, -5.946699141100917352, 23.92187500000000355 ) ) ;
#56513 = ORIENTED_EDGE ( 'NONE', *, *, #13097, .T. ) ;
#56514 = VERTEX_POINT ( 'NONE', #6737 ) ;
#56515 = DIRECTION ( 'NONE',  ( 0.000000000000000000, 0.4999999999999960032, -0.8660254037844410391 ) ) ;
#56516 = VERTEX_POINT ( 'NONE', #42316 ) ;
#56517 = FACE_BOUND ( 'NONE', #29657, .T. ) ;
#56518 = CARTESIAN_POINT ( 'NONE',  ( 6.857806477116147548, -4.481592998940161721, 33.73612834413957984 ) ) ;
#56519 = CARTESIAN_POINT ( 'NONE',  ( -4.153846153846274980, -10.33852847137269571, 34.16647553114546554 ) ) ;
#56520 = ORIENTED_EDGE ( 'NONE', *, *, #61279, .F. ) ;
#56521 = CARTESIAN_POINT ( 'NONE',  ( 15.10029404569351286, -7.276987145209184327, 34.99546412871779211 ) ) ;
#56522 = CARTESIAN_POINT ( 'NONE',  ( 11.47319153790521717, -6.835583212224499938, 34.95778746994557906 ) ) ;
#56523 = CARTESIAN_POINT ( 'NONE',  ( 12.46153846153846168, -4.786620604624113540, 33.94971097300155094 ) ) ;
#56524 = CARTESIAN_POINT ( 'NONE',  ( 0.4615384615384611200, -6.386643153685126251, 34.62446782046654192 ) ) ;
#56525 = CARTESIAN_POINT ( 'NONE',  ( -16.94613126909828793, -2.541949514083464479, 30.39797389878540557 ) ) ;
#56526 = ORIENTED_EDGE ( 'NONE', *, *, #48894, .T. ) ;
#56527 = B_SPLINE_CURVE_WITH_KNOTS ( 'NONE', 3,
 ( #84612, #22885, #8944, #62975, #55786, #83276 ),
 .UNSPECIFIED., .F., .F.,
 ( 4, 2, 4 ),
 ( 0.000000000000000000, 0.0001954784845028902692, 0.0003909569690057805385 ),
 .UNSPECIFIED. ) ;
#56528 = CARTESIAN_POINT ( 'NONE',  ( 11.53846153846153832, -3.050289026998446396, 32.03036669348365706 ) ) ;
#56529 = CARTESIAN_POINT ( 'NONE',  ( 3.296024802045255164, -4.481592998940250538, 33.73612834413965089 ) ) ;
#56530 = CARTESIAN_POINT ( 'NONE',  ( -8.769230769230460965, -2.506253911140614576, 30.00000000000323297 ) ) ;
#56531 = CARTESIAN_POINT ( 'NONE',  ( -0.5922290646487701204, -4.684245665217972032, 34.18127051446801090 ) ) ;
#56532 = B_SPLINE_CURVE_WITH_KNOTS ( 'NONE', 3,
 ( #43071, #15603, #3405, #30877, #8852, #24118, #16044, #51569, #79075, #37191 ),
 .UNSPECIFIED., .F., .F.,
 ( 4, 2, 2, 2, 4 ),
 ( 0.0007817359430256283796, 0.0009771253907249941549, 0.001172514838424359822, 0.001367904286123725489, 0.001563293733823091156 ),
 .UNSPECIFIED. ) ;
#56533 = DIRECTION ( 'NONE',  ( -1.000000000000000000, -0.000000000000000000, -0.000000000000000000 ) ) ;
#56534 = B_SPLINE_CURVE_WITH_KNOTS ( 'NONE', 3,
 ( #36903, #64366, #57624, #30588, #85106, #52525, #58060, #16632, #44091, #71572 ),
 .UNSPECIFIED., .F., .F.,
 ( 4, 2, 2, 2, 4 ),
 ( 0.0007817246256747464135, 0.0009771112852218900684, 0.001172497944769033615, 0.001367884604316177161, 0.001563271263863320925 ),
 .UNSPECIFIED. ) ;
#56535 = CARTESIAN_POINT ( 'NONE',  ( 7.173076923078343548, -7.500000000000154543, 35.00000000000007105 ) ) ;
#56537 = CYLINDRICAL_SURFACE ( 'NONE', #66112, 0.2499999999999973355 ) ;
#56536 = CARTESIAN_POINT ( 'NONE',  ( 17.20744877868664346, -3.816742781228458448, 33.13167719472716044 ) ) ;
#56538 = CARTESIAN_POINT ( 'NONE',  ( -14.30769230769242917, -3.643525952248795718, 33.31231777344771672 ) ) ;
#56540 = CARTESIAN_POINT ( 'NONE',  ( 2.530471976670374712, -6.717445702608402236, 34.94155399931962336 ) ) ;
#56539 = CARTESIAN_POINT ( 'NONE',  ( 13.38461538461538680, -9.905515769479276145, 34.41647553114623292 ) ) ;
#56541 = CARTESIAN_POINT ( 'NONE',  ( -10.03846153846153832, -4.000000000000000000, 28.25000000000000000 ) ) ;
#56542 = CARTESIAN_POINT ( 'NONE',  ( -2.775308065498764964, -6.422011778438537988, 24.92000670625849068 ) ) ;
#56543 = VERTEX_POINT ( 'NONE', #8079 ) ;
#56544 = AXIS2_PLACEMENT_3D ( 'NONE', #51507, #65930, #79010 ) ;
#56545 = CARTESIAN_POINT ( 'NONE',  ( 12.52760681254089903, -2.538708090699994813, 30.37095296980875503 ) ) ;
#56546 = ORIENTED_EDGE ( 'NONE', *, *, #39924, .F. ) ;
#56547 = EDGE_CURVE ( 'NONE', #5737, #77395, #69468, .T. ) ;
#56548 = CARTESIAN_POINT ( 'NONE',  ( -13.13456096470193302, -10.82426656108012075, 33.81400080652039009 ) ) ;
#56549 = ORIENTED_EDGE ( 'NONE', *, *, #21139, .F. ) ;
#56550 = CARTESIAN_POINT ( 'NONE',  ( 16.15384615384615330, -12.37446782046654192, 30.86335684631486131 ) ) ;
#56551 = EDGE_CURVE ( 'NONE', #54237, #47138, #82417, .T. ) ;
#56552 = CARTESIAN_POINT ( 'NONE',  ( 4.826946332874485712, -12.01397095200673881, 32.43157075238190146 ) ) ;
#56553 = ORIENTED_EDGE ( 'NONE', *, *, #63724, .F. ) ;
#56554 = CARTESIAN_POINT ( 'NONE',  ( 5.749976775778544713, -10.92453946501458439, 33.72985991061850086 ) ) ;
#56555 = CARTESIAN_POINT ( 'NONE',  ( 1.077988221561464899, -4.724691934501233703, 23.98250670625849068 ) ) ;
#56556 = CARTESIAN_POINT ( 'NONE',  ( -5.076923076923075762, -6.435427911321262684, 35.78748833219616898 ) ) ;
#56557 = CARTESIAN_POINT ( 'NONE',  ( -3.903846153846138201, -2.249999999999999112, 29.81603969181031033 ) ) ;
#56558 = CARTESIAN_POINT ( 'NONE',  ( -14.98076923076781064, -7.500000000000154543, 35.00000000000007105 ) ) ;
#56559 = CARTESIAN_POINT ( 'NONE',  ( -5.143006487878956534, -12.37446782046654192, 30.86335684631486487 ) ) ;
#56560 = CARTESIAN_POINT ( 'NONE',  ( 11.47237812750565666, -2.721908614388770964, 31.22303859784723912 ) ) ;
#56561 = CARTESIAN_POINT ( 'NONE',  ( 4.946231610255517275, -8.147922237126337563, 34.70805685702651999 ) ) ;
#56562 = EDGE_CURVE ( 'NONE', #820, #77192, #43962, .T. ) ;
#56563 = CARTESIAN_POINT ( 'NONE',  ( 2.651650429449539104, -4.848349570550432475, 16.81250000000000000 ) ) ;
#56564 = CARTESIAN_POINT ( 'NONE',  ( -9.692307692307812417, -3.835265460704628371, 33.15142922262033665 ) ) ;
#56565 = CARTESIAN_POINT ( 'NONE',  ( -6.130690603110308778, -3.338472653186242756, 32.95098750199972670 ) ) ;
#56566 = ADVANCED_FACE ( 'NONE', ( #86297 ), #52481, .F. ) ;
#56567 = PLANE ( 'NONE',  #62287 ) ;
#56568 = CARTESIAN_POINT ( 'NONE',  ( 3.750000000000009770, -9.053300858899081760, 15.79687500000000178 ) ) ;
#56569 = CARTESIAN_POINT ( 'NONE',  ( 14.30769230769231015, -2.538708090699994813, 30.37095296980875503 ) ) ;
#56570 = ORIENTED_EDGE ( 'NONE', *, *, #55175, .F. ) ;
#56571 = EDGE_CURVE ( 'NONE', #4984, #53967, #51567, .T. ) ;
#56572 = CYLINDRICAL_SURFACE ( 'NONE', #45762, 0.2500000000000009437 ) ;
#56573 = DIRECTION ( 'NONE',  ( -0.000000000000000000, -0.9848077530122085754, -0.1736481776669273613 ) ) ;
#56574 = CARTESIAN_POINT ( 'NONE',  ( -8.992715712954716167, -11.41268669641500466, 32.86336882939237825 ) ) ;
#56575 = CARTESIAN_POINT ( 'NONE',  ( -7.596153846153909761, -7.565270445406050648, 34.75000000000000000 ) ) ;
#56576 = B_SPLINE_CURVE_WITH_KNOTS ( 'NONE', 3,
 ( #48709, #14485, #41971, #36538, #63988, #69432, #7739, #85166, #23883, #24788 ),
 .UNSPECIFIED., .F., .F.,
 ( 4, 2, 2, 2, 4 ),
 ( 0.000000000000000000, 0.0001954311564186864949, 0.0003908623128373729899, 0.0005862934692560594577, 0.0007817246256747459798 ),
 .UNSPECIFIED. ) ;
#56577 = CARTESIAN_POINT ( 'NONE',  ( 13.44987095589141468, -2.625532179533470512, 30.86335684631491105 ) ) ;
#56579 = EDGE_CURVE ( 'NONE', #57828, #54784, #65992, .T. ) ;
#56578 = CARTESIAN_POINT ( 'NONE',  ( -17.76215049426128445, -1.749999999999992450, 30.25000000000000000 ) ) ;
#56580 = VECTOR ( 'NONE', #7074, 1000.000000000000000 ) ;
#56581 = CARTESIAN_POINT ( 'NONE',  ( 11.53846153846153832, -8.164416787775445883, 34.95778746994557906 ) ) ;
#56582 = ORIENTED_EDGE ( 'NONE', *, *, #24461, .T. ) ;
#56583 = VERTEX_POINT ( 'NONE', #72309 ) ;
#56584 = EDGE_CURVE ( 'NONE', #25408, #5324, #51127, .T. ) ;
#56585 = ORIENTED_EDGE ( 'NONE', *, *, #67497, .T. ) ;
#56586 = CARTESIAN_POINT ( 'NONE',  ( -16.37733107841048152, -3.562934362175799841, 33.22335522853832401 ) ) ;
#56587 = CARTESIAN_POINT ( 'NONE',  ( -2.307692307691999289, -2.506253911140615021, 30.00000000000323297 ) ) ;
#56588 = CARTESIAN_POINT ( 'NONE',  ( -9.019207513279360100, -2.318417181685855422, 30.59732222474233865 ) ) ;
#56589 = CARTESIAN_POINT ( 'NONE',  ( 2.177545098254088707, -6.001485441113818986, 34.52039167877662607 ) ) ;
#56590 = CARTESIAN_POINT ( 'NONE',  ( 17.74997677577853850, -9.356822207818511927, 34.66110646841856635 ) ) ;
#56591 = ORIENTED_EDGE ( 'NONE', *, *, #70116, .T. ) ;
#56592 = LINE ( 'NONE', #62447, #53514 ) ;
#56593 = VERTEX_POINT ( 'NONE', #16926 ) ;
#56594 = ORIENTED_EDGE ( 'NONE', *, *, #76293, .F. ) ;
#56595 = B_SPLINE_CURVE_WITH_KNOTS ( 'NONE', 3,
 ( #21250, #42430, #56379, #1433, #79200, #48725, #72426, #50053, #65662, #55484 ),
 .UNSPECIFIED., .F., .F.,
 ( 4, 2, 2, 2, 4 ),
 ( 0.0007817246256747463051, 0.0009771112852218896347, 0.001172497944769032747, 0.001367884604316176077, 0.001563271263863319407 ),
 .UNSPECIFIED. ) ;
#56596 = EDGE_CURVE ( 'NONE', #73377, #10767, #69826, .T. ) ;
#56597 = EDGE_CURVE ( 'NONE', #17339, #39542, #25803, .T. ) ;
#56599 = ORIENTED_EDGE ( 'NONE', *, *, #74571, .T. ) ;
#56598 = CARTESIAN_POINT ( 'NONE',  ( 4.376625822824220080, -12.47679350104403007, 31.42216943046555855 ) ) ;
#56600 = DIRECTION ( 'NONE',  ( -0.000000000000000000, -0.000000000000000000, -1.000000000000000000 ) ) ;
#56601 = B_SPLINE_CURVE_WITH_KNOTS ( 'NONE', 3,
 ( #20180, #19729, #81445, #41782, #89098, #75551, #69683, #12975, #81887, #48971 ),
 .UNSPECIFIED., .F., .F.,
 ( 4, 2, 2, 2, 4 ),
 ( 0.000000000000000000, 0.0001954339857564098054, 0.0003908679715128196108, 0.0005863019572692293891, 0.0007817359430256392216 ),
 .UNSPECIFIED. ) ;
#56602 = DIRECTION ( 'NONE',  ( 1.000000000000000000, 0.000000000000000000, 0.000000000000000000 ) ) ;
#56603 = AXIS2_PLACEMENT_3D ( 'NONE', #5333, #18402, #4434 ) ;
#56604 = CARTESIAN_POINT ( 'NONE',  ( -9.692307692307812417, -8.613356846316285953, 34.62446782046622218 ) ) ;
#56605 = ORIENTED_EDGE ( 'NONE', *, *, #2631, .F. ) ;
#56606 = EDGE_CURVE ( 'NONE', #35354, #25404, #59243, .T. ) ;
#56607 = ORIENTED_EDGE ( 'NONE', *, *, #29128, .F. ) ;
#56608 = ORIENTED_EDGE ( 'NONE', *, *, #31520, .T. ) ;
#56609 = CARTESIAN_POINT ( 'NONE',  ( -9.469296340694841163, -5.667800583137506010, 34.40243808032445827 ) ) ;
#56611 = ORIENTED_EDGE ( 'NONE', *, *, #67558, .F. ) ;
#56610 = CARTESIAN_POINT ( 'NONE',  ( -0.4615384615384611200, -3.937682226553329556, 33.60647404775216529 ) ) ;
#56612 = CARTESIAN_POINT ( 'NONE',  ( 1.607394925883795844, -9.332535724633405749, 34.40230450496446224 ) ) ;
#56613 = DIRECTION ( 'NONE',  ( 0.000000000000000000, 0.000000000000000000, -1.000000000000000000 ) ) ;
#56614 = EDGE_CURVE ( 'NONE', #63009, #29939, #16057, .T. ) ;
#56615 = EDGE_CURVE ( 'NONE', #27341, #856, #53662, .T. ) ;
#56616 = CARTESIAN_POINT ( 'NONE',  ( -3.099977422944443894, -9.804649428959608670, 34.18742332936588468 ) ) ;
#56617 = ORIENTED_EDGE ( 'NONE', *, *, #43221, .F. ) ;
#56618 = LINE ( 'NONE', #76453, #33595 ) ;
#56619 = CARTESIAN_POINT ( 'NONE',  ( 15.10007862765892739, -2.494641256782728966, 31.33461815524612959 ) ) ;
#56620 = EDGE_LOOP ( 'NONE', ( #42496, #75777 ) ) ;
#56621 = FACE_BOUND ( 'NONE', #69192, .T. ) ;
#56622 = EDGE_CURVE ( 'NONE', #80708, #33767, #46185, .T. ) ;
#56623 = CARTESIAN_POINT ( 'NONE',  ( 13.38461538461538680, -11.16473453929635440, 33.15142922261926373 ) ) ;
#56624 = CARTESIAN_POINT ( 'NONE',  ( -18.25002322422145440, -12.45566812827425096, 31.48439005359158926 ) ) ;
#56625 = CYLINDRICAL_SURFACE ( 'NONE', #71118, 0.2499999999999997502 ) ;
#56627 = CARTESIAN_POINT ( 'NONE',  ( 15.00790296770613352, -2.251424796025574881, 29.88072029997477586 ) ) ;
#56626 = LINE ( 'NONE', #35467, #20156 ) ;
#56628 = LINE ( 'NONE', #61605, #19377 ) ;
#56629 = CARTESIAN_POINT ( 'NONE',  ( 14.37294744720514572, -2.379036618887895305, 30.90682066428158592 ) ) ;
#56630 = ORIENTED_EDGE ( 'NONE', *, *, #83250, .T. ) ;
#56631 = CARTESIAN_POINT ( 'NONE',  ( -11.31545018684868786, -12.15243808032446005, 31.58219941686247978 ) ) ;
#56632 = CARTESIAN_POINT ( 'NONE',  ( -5.999999999999998224, -11.35647404775217417, 33.31231777344666511 ) ) ;
#56633 = ORIENTED_EDGE ( 'NONE', *, *, #25983, .F. ) ;
#56634 = CARTESIAN_POINT ( 'NONE',  ( 6.923076923076802558, -2.892918686052165622, 31.69288490824153470 ) ) ;
#56635 = CARTESIAN_POINT ( 'NONE',  ( -14.30769230769230660, -9.058645607665452459, 34.76329471203371924 ) ) ;
#56636 = DIRECTION ( 'NONE',  ( 1.000000000000000000, 0.000000000000000000, 0.000000000000000000 ) ) ;
#56637 = DIRECTION ( 'NONE',  ( -0.000000000000000000, 1.000000000000000000, 3.491481338843133355E-15 ) ) ;
#56638 = DIRECTION ( 'NONE',  ( 0.000000000000000000, 0.4999999999999985567, 0.8660254037844395958 ) ) ;
#56639 = CARTESIAN_POINT ( 'NONE',  ( -4.403822897894745125, -2.318417181685854978, 30.59732222474233865 ) ) ;
#56640 = FACE_BOUND ( 'NONE', #69443, .T. ) ;
#56642 = CARTESIAN_POINT ( 'NONE',  ( -7.846153846153844924, -4.661471528628507777, 34.16647553114623292 ) ) ;
#56641 = CYLINDRICAL_SURFACE ( 'NONE', #53326, 0.2499999999999995559 ) ;
#56643 = CARTESIAN_POINT ( 'NONE',  ( -14.30769230769230660, -2.486705287966279876, 31.30864560766543647 ) ) ;
#56645 = CARTESIAN_POINT ( 'NONE',  ( 6.923076923076924238, -13.20930481340135110, 34.54067556320372745 ) ) ;
#56644 = CARTESIAN_POINT ( 'NONE',  ( -7.715628407920204879, -12.70449254468099198, 30.44128974285582956 ) ) ;
#56646 = CARTESIAN_POINT ( 'NONE',  ( 8.769230769230768274, -1.242168528481310874, 33.36296068462461051 ) ) ;
#56647 = CARTESIAN_POINT ( 'NONE',  ( -3.724691934501229262, -9.114399933863657211, 22.26375670625849068 ) ) ;
#56648 = EDGE_LOOP ( 'NONE', ( #23255, #36688, #16812, #61860 ) ) ;
#56649 = EDGE_CURVE ( 'NONE', #33013, #10290, #78425, .T. ) ;
#56650 = VERTEX_POINT ( 'NONE', #88521 ) ;
#56651 = CARTESIAN_POINT ( 'NONE',  ( -9.915234651214538175, -2.308479472611653094, 30.53278059502174457 ) ) ;
#56652 = CARTESIAN_POINT ( 'NONE',  ( -12.23852561744506673, -6.460100341425560444, 34.89618726649961644 ) ) ;
#56653 = FACE_OUTER_BOUND ( 'NONE', #1330, .T. ) ;
#56654 = FACE_OUTER_BOUND ( 'NONE', #51786, .T. ) ;
#56655 = CARTESIAN_POINT ( 'NONE',  ( -16.94613126909829148, -6.413143153341451352, 34.63066358083362672 ) ) ;
#56656 = CARTESIAN_POINT ( 'NONE',  ( -3.724691934501229262, -9.114399933863657211, 23.51375670625848713 ) ) ;
#56657 = CARTESIAN_POINT ( 'NONE',  ( 6.792928953345228393, -2.373036134822904319, 30.88089517874952250 ) ) ;
#56658 = FACE_OUTER_BOUND ( 'NONE', #27577, .T. ) ;
#56659 = CARTESIAN_POINT ( 'NONE',  ( 15.45378058238208219, -11.76359900205217635, 32.36225158514719880 ) ) ;
#56660 = CARTESIAN_POINT ( 'NONE',  ( 4.153846153846460609, -2.506253911140614576, 30.00000000000323297 ) ) ;
#56661 = FACE_OUTER_BOUND ( 'NONE', #76343, .T. ) ;
#56662 = CARTESIAN_POINT ( 'NONE',  ( -3.230769230769352962, -2.657715359629662544, 31.77849191805970364 ) ) ;
#56663 = B_SPLINE_CURVE_WITH_KNOTS ( 'NONE', 3,
 ( #55748, #34153, #63391, #13440, #35485, #82355, #62936, #21522, #48997, #76476 ),
 .UNSPECIFIED., .F., .F.,
 ( 4, 2, 2, 2, 4 ),
 ( 0.0007817359430256328248, 0.0009771253907249997928, 0.001172514838424366544, 0.001367904286123733295, 0.001563293733823100263 ),
 .UNSPECIFIED. ) ;
#56664 = B_SPLINE_CURVE_WITH_KNOTS ( 'NONE', 3,
 ( #38771, #44613, #18942, #11745, #72100, #66685, #53155, #80660, #86070, #37877 ),
 .UNSPECIFIED., .F., .F.,
 ( 4, 2, 2, 2, 4 ),
 ( 0.0007817246256747453293, 0.0009771112852218889842, 0.001172497944769032531, 0.001367884604316176294, 0.001563271263863319840 ),
 .UNSPECIFIED. ) ;
#56665 = CARTESIAN_POINT ( 'NONE',  ( 12.71159288145191013, -2.318338780012835443, 30.59689888758630261 ) ) ;
#56666 = CARTESIAN_POINT ( 'NONE',  ( 14.17754509825408960, -6.852621066184266141, 34.70813303252209181 ) ) ;
#56667 = ORIENTED_EDGE ( 'NONE', *, *, #36048, .T. ) ;
#56668 = CARTESIAN_POINT ( 'NONE',  ( -6.923076923076615152, -2.506253911140614576, 30.00000000000323297 ) ) ;
#56669 = DIRECTION ( 'NONE',  ( -0.000000000000000000, 0.9396926207859093161, -0.3420201433256663259 ) ) ;
#56670 = CARTESIAN_POINT ( 'NONE',  ( 0.06109907496451789238, -4.749999999999998224, 23.15811829374151642 ) ) ;
#56671 = VECTOR ( 'NONE', #85172, 1000.000000000000000 ) ;
#56672 = VECTOR ( 'NONE', #52810, 1000.000000000000000 ) ;
#56673 = CARTESIAN_POINT ( 'NONE',  ( 8.992606709928951503, -2.501478030877322567, 29.88021232661721172 ) ) ;
#56674 = CARTESIAN_POINT ( 'NONE',  ( 1.653273178848927064E-15, -7.500000000000000000, 14.00000000000000178 ) ) ;
#56675 = EDGE_LOOP ( 'NONE', ( #59808, #41337 ) ) ;
#56676 = CARTESIAN_POINT ( 'NONE',  ( 1.653273178848927064E-15, -7.500000000000000000, 13.50000000000000178 ) ) ;
#56678 = ORIENTED_EDGE ( 'NONE', *, *, #53585, .F. ) ;
#56677 = CARTESIAN_POINT ( 'NONE',  ( 1.384615384615386802, -5.415277668671390821, 36.20867863119892149 ) ) ;
#56679 = CARTESIAN_POINT ( 'NONE',  ( 9.942253101685738059, -12.68172785388650681, 30.59649109432439218 ) ) ;
#56680 = CARTESIAN_POINT ( 'NONE',  ( -4.946131269098288818, -9.804649428959608670, 34.18742332936588468 ) ) ;
#56681 = ORIENTED_EDGE ( 'NONE', *, *, #77235, .F. ) ;
#56682 = DIRECTION ( 'NONE',  ( 0.000000000000000000, -0.000000000000000000, -1.000000000000000000 ) ) ;
#56684 = EDGE_CURVE ( 'NONE', #46285, #55965, #85941, .T. ) ;
#56683 = CARTESIAN_POINT ( 'NONE',  ( -16.09615384615384670, -7.500000000000000000, 29.75000000000000355 ) ) ;
#56685 = ORIENTED_EDGE ( 'NONE', *, *, #61961, .F. ) ;
#56686 = CARTESIAN_POINT ( 'NONE',  ( -13.38461538461538325, -12.78798330534102767, 29.49999999999997868 ) ) ;
#56687 = CARTESIAN_POINT ( 'NONE',  ( -1.384615384615383471, -13.57706302396349152, 30.56769352161908060 ) ) ;
#56688 = CARTESIAN_POINT ( 'NONE',  ( 12.68455130563185662, -11.98016756924215009, 32.48728574198911190 ) ) ;
#56689 = VERTEX_POINT ( 'NONE', #54253 ) ;
#56690 = ORIENTED_EDGE ( 'NONE', *, *, #1001, .F. ) ;
#56691 = ORIENTED_EDGE ( 'NONE', *, *, #41393, .F. ) ;
#56692 = CARTESIAN_POINT ( 'NONE',  ( -7.053767526187231240, -2.295517848115769421, 30.44137282052136939 ) ) ;
#56693 = CARTESIAN_POINT ( 'NONE',  ( 17.07692307692295586, -11.94971097300221174, 32.03036669348237098 ) ) ;
#56694 = EDGE_CURVE ( 'NONE', #83315, #13183, #37596, .T. ) ;
#56695 = B_SPLINE_CURVE_WITH_KNOTS ( 'NONE', 3,
 ( #52508, #80897, #39906, #52945, #53397, #4327 ),
 .UNSPECIFIED., .F., .F.,
 ( 4, 2, 4 ),
 ( 0.0003909569690057824900, 0.0005862646681846072228, 0.0007815723673634320098 ),
 .UNSPECIFIED. ) ;
#56696 = LINE ( 'NONE', #57138, #84074 ) ;
#56697 = CARTESIAN_POINT ( 'NONE',  ( -17.32694631421604115, -6.695914987888146541, 34.68535235679833306 ) ) ;
#56698 = B_SPLINE_CURVE_WITH_KNOTS ( 'NONE', 3,
 ( #79723, #23431, #86494, #72959, #3156, #80168, #85587, #25217, #72064, #57666 ),
 .UNSPECIFIED., .F., .F.,
 ( 4, 2, 2, 2, 4 ),
 ( 0.000000000000000000, 0.0001954311564186878502, 0.0003908623128373757004, 0.0005862934692560635777, 0.0007817246256747514008 ),
 .UNSPECIFIED. ) ;
#56699 = VERTEX_POINT ( 'NONE', #55145 ) ;
#56700 = EDGE_CURVE ( 'NONE', #79283, #273, #26355, .T. ) ;
#56701 = ORIENTED_EDGE ( 'NONE', *, *, #66768, .F. ) ;
#56703 = ORIENTED_EDGE ( 'NONE', *, *, #74669, .T. ) ;
#56702 = CARTESIAN_POINT ( 'NONE',  ( -1.384615384615383471, -11.11383981884818262, 36.00935417666054406 ) ) ;
#56704 = CARTESIAN_POINT ( 'NONE',  ( 17.14217864819909920, -5.219633306516380244, 34.19971097300157936 ) ) ;
#56705 = ORIENTED_EDGE ( 'NONE', *, *, #74654, .T. ) ;
#56706 = CARTESIAN_POINT ( 'NONE',  ( 3.230769230769231726, -3.886160181151819604, 36.00935417666054406 ) ) ;
#56707 = CARTESIAN_POINT ( 'NONE',  ( 6.673053698855465399, -9.356822207818506598, 34.66110646841856635 ) ) ;
#56708 = ORIENTED_EDGE ( 'NONE', *, *, #35687, .T. ) ;
#56709 = CARTESIAN_POINT ( 'NONE',  ( 8.096099364501986528, -8.433404298154334455, 34.66254593164985920 ) ) ;
#56710 = EDGE_LOOP ( 'NONE', ( #55929, #79119, #59837, #67582 ) ) ;
#56712 = VERTEX_POINT ( 'NONE', #61454 ) ;
#56711 = CARTESIAN_POINT ( 'NONE',  ( -10.54931626438217585, -11.16473453929635440, 33.15142922261926373 ) ) ;
#56713 = LINE ( 'NONE', #79210, #14316 ) ;
#56714 = EDGE_CURVE ( 'NONE', #54514, #29911, #897, .T. ) ;
#56715 = ADVANCED_FACE ( 'NONE', ( #53819 ), #33108, .F. ) ;
#56716 = AXIS2_PLACEMENT_3D ( 'NONE', #73014, #44630, #2758 ) ;
#56717 = CARTESIAN_POINT ( 'NONE',  ( 14.05771556364371833, -5.643011162660950042, 34.66104346484419096 ) ) ;
#56718 = ORIENTED_EDGE ( 'NONE', *, *, #13712, .F. ) ;
#56719 = CARTESIAN_POINT ( 'NONE',  ( 15.10007862765892206, -2.295517848115769421, 30.44137282052137294 ) ) ;
#56720 = LINE ( 'NONE', #58041, #30687 ) ;
#56721 = DIRECTION ( 'NONE',  ( -1.000000000000000000, -0.000000000000000000, -0.000000000000000000 ) ) ;
#56722 = FACE_BOUND ( 'NONE', #23177, .T. ) ;
#56723 = VECTOR ( 'NONE', #45054, 1000.000000000000000 ) ;
#56724 = CARTESIAN_POINT ( 'NONE',  ( -8.703975629717932705, -2.379036618887895305, 30.90682066428158592 ) ) ;
#56725 = CARTESIAN_POINT ( 'NONE',  ( 12.46153846153846168, -1.242168528481310874, 33.36296068462461051 ) ) ;
#56726 = AXIS2_PLACEMENT_3D ( 'NONE', #32614, #31735, #73164 ) ;
#56727 = CARTESIAN_POINT ( 'NONE',  ( -5.999999999999998224, -9.905515769479276145, 34.41647553114623292 ) ) ;
#56728 = B_SPLINE_CURVE_WITH_KNOTS ( 'NONE', 3,
 ( #50346, #29655, #43164, #21560, #70637, #83723, #34637, #49032, #76509, #14816 ),
 .UNSPECIFIED., .F., .F.,
 ( 4, 2, 2, 2, 4 ),
 ( 0.000000000000000000, 0.0001954311564186861968, 0.0003908623128373723936, 0.0005862934692560585904, 0.0007817246256747447872 ),
 .UNSPECIFIED. ) ;
#56730 = CARTESIAN_POINT ( 'NONE',  ( -5.777220458731590291, -2.847695495035524882, 31.58253572463339509 ) ) ;
#56729 = LINE ( 'NONE', #63918, #11492 ) ;
#56731 = CARTESIAN_POINT ( 'NONE',  ( -4.853910232829680815, -4.026326845037961455, 33.68677907613344047 ) ) ;
#56732 = DIRECTION ( 'NONE',  ( -0.000000000000000000, 0.1736481776669307198, -0.9848077530122080203 ) ) ;
#56733 = ORIENTED_EDGE ( 'NONE', *, *, #23340, .T. ) ;
#56734 = CARTESIAN_POINT ( 'NONE',  ( -14.08491276642389245, -3.755027918224367323, 33.06320215134714857 ) ) ;
#56735 = EDGE_LOOP ( 'NONE', ( #34966, #54745, #29381, #60747 ) ) ;
#56736 = EDGE_LOOP ( 'NONE', ( #68503, #86964 ) ) ;
#56738 = DIRECTION ( 'NONE',  ( -1.000000000000000000, 0.000000000000000000, -0.000000000000000000 ) ) ;
#56737 = CARTESIAN_POINT ( 'NONE',  ( 14.53047184896071720, -3.755027918224367767, 33.06320215134714857 ) ) ;
#56739 = CARTESIAN_POINT ( 'NONE',  ( 25.00000000000000711, -9.999999999999957367, 13.00000000000000178 ) ) ;
#56740 = CARTESIAN_POINT ( 'NONE',  ( 8.096208266067295156, -3.435999193479609914, 33.07426656108010832 ) ) ;
#56741 = CARTESIAN_POINT ( 'NONE',  ( 8.769230769230768274, -8.318370150425687726, 35.83090037661290239 ) ) ;
#56742 = CARTESIAN_POINT ( 'NONE',  ( -0.3954701105360223234, -11.69971097300155272, 32.46337939537588113 ) ) ;
#56743 = ORIENTED_EDGE ( 'NONE', *, *, #33706, .T. ) ;
#56744 = CARTESIAN_POINT ( 'NONE',  ( 13.25392391794782654, -4.809359713505814149, 33.96456829005828837 ) ) ;
#56745 = CARTESIAN_POINT ( 'NONE',  ( 1.450683735617824599, -12.10708131394839704, 31.69288490824020954 ) ) ;
#56746 = DIRECTION ( 'NONE',  ( -0.000000000000000000, 0.9848077530122085754, -0.1736481776669273613 ) ) ;
#56747 = CARTESIAN_POINT ( 'NONE',  ( 15.48082365068268018, -12.41089969410671223, 31.60739465890703670 ) ) ;
#56748 = CARTESIAN_POINT ( 'NONE',  ( -15.48076923076922995, -2.499999999999999556, 29.81609845454691765 ) ) ;
#56749 = CARTESIAN_POINT ( 'NONE',  ( 3.750000000000000888, -7.499999999999978684, 15.71875000000000000 ) ) ;
#56750 = VERTEX_POINT ( 'NONE', #6965 ) ;
#56751 = ORIENTED_EDGE ( 'NONE', *, *, #19049, .T. ) ;
#56752 = CARTESIAN_POINT ( 'NONE',  ( -6.923076923077044142, -8.613356846316285953, 34.62446782046622218 ) ) ;
#56753 = EDGE_LOOP ( 'NONE', ( #46631, #39575, #15169, #53605 ) ) ;
#56754 = CARTESIAN_POINT ( 'NONE',  ( -10.61538461538473577, -2.657715359629662544, 31.77849191805970364 ) ) ;
#56755 = CARTESIAN_POINT ( 'NONE',  ( -1.134669975237340367, -10.18230066228895758, 34.26354781536631577 ) ) ;
#56756 = DIRECTION ( 'NONE',  ( -0.000000000000000000, -0.1736481776669307198, -0.9848077530122080203 ) ) ;
#56757 = CARTESIAN_POINT ( 'NONE',  ( -17.20707104665477516, -12.70455904226513866, 30.44083106164009322 ) ) ;
#56758 = CARTESIAN_POINT ( 'NONE',  ( -2.307692307692427391, -5.219633306517616589, 34.19971097300220464 ) ) ;
#56759 = CARTESIAN_POINT ( 'NONE',  ( 8.519207531937803779, -6.695914987888146541, 34.68535235679833306 ) ) ;
#56760 = VERTEX_POINT ( 'NONE', #61899 ) ;
#56761 = CARTESIAN_POINT ( 'NONE',  ( 13.38461538461538680, -2.538708090699994813, 30.37095296980875503 ) ) ;
#56763 = ORIENTED_EDGE ( 'NONE', *, *, #38744, .T. ) ;
#56762 = CARTESIAN_POINT ( 'NONE',  ( -2.084912766423896446, -10.81320215134717344, 33.49497208177562868 ) ) ;
#56764 = CARTESIAN_POINT ( 'NONE',  ( 3.007284287045283389, -12.44517049084099725, 30.48991314939691932 ) ) ;
#56765 = CARTESIAN_POINT ( 'NONE',  ( -0.6844654204453112234, -4.026226216239095379, 33.68668979543632958 ) ) ;
#56766 = CARTESIAN_POINT ( 'NONE',  ( -3.296852641725110722, -4.786620604624113540, 33.94971097300155805 ) ) ;
#56767 = CARTESIAN_POINT ( 'NONE',  ( 0.6843180028068698295, -2.847695495035523106, 31.58253572463339154 ) ) ;
#56768 = CARTESIAN_POINT ( 'NONE',  ( 10.61538461538461675, -8.564572088678739092, 35.78748833219616898 ) ) ;
#56769 = CARTESIAN_POINT ( 'NONE',  ( 15.23076923076923173, -11.16473453929635440, 33.15142922261926373 ) ) ;
#56770 = B_SPLINE_CURVE_WITH_KNOTS ( 'NONE', 3,
 ( #73056, #26647, #11353, #74847, #19885, #13136, #40615, #38837, #66295, #4598 ),
 .UNSPECIFIED., .F., .F.,
 ( 4, 2, 2, 2, 4 ),
 ( 0.0007817359430256392216, 0.0009771253907250078159, 0.001172514838424376302, 0.001367904286123745004, 0.001563293733823113490 ),
 .UNSPECIFIED. ) ;
#56771 = CARTESIAN_POINT ( 'NONE',  ( 1.200186371490529202, -4.775308065498752974, 24.48624329374151642 ) ) ;
#56772 = ORIENTED_EDGE ( 'NONE', *, *, #32410, .T. ) ;
#56773 = DIRECTION ( 'NONE',  ( -0.000000000000000000, 0.9396926207859093161, -0.3420201433256663259 ) ) ;
#56774 = CARTESIAN_POINT ( 'NONE',  ( 4.284636594813102661, -10.70102852606553157, 33.91149625220312913 ) ) ;
#56775 = CARTESIAN_POINT ( 'NONE',  ( -1.409462824231155764E-14, -4.749999999999999112, 21.65625000000000355 ) ) ;
#56776 = CARTESIAN_POINT ( 'NONE',  ( -13.60754160213153163, -12.39988816332205701, 30.74660775122750778 ) ) ;
#56777 = LINE ( 'NONE', #35636, #66317 ) ;
#56778 = ORIENTED_EDGE ( 'NONE', *, *, #21103, .F. ) ;
#56779 = CARTESIAN_POINT ( 'NONE',  ( 1.139087296526029469, -10.24999999999999289, 14.70312500000000355 ) ) ;
#56780 = CARTESIAN_POINT ( 'NONE',  ( -1.384615384615383471, -9.780366693483667717, 34.19971097300155094 ) ) ;
#56781 = ORIENTED_EDGE ( 'NONE', *, *, #8101, .T. ) ;
#56782 = CARTESIAN_POINT ( 'NONE',  ( 14.30769230769231015, -3.050289026998446396, 32.03036669348365706 ) ) ;
#56783 = EDGE_CURVE ( 'NONE', #32856, #69537, #82606, .T. ) ;
#56784 = EDGE_CURVE ( 'NONE', #15438, #34255, #32123, .T. ) ;
#56785 = ORIENTED_EDGE ( 'NONE', *, *, #8064, .F. ) ;
#56786 = CARTESIAN_POINT ( 'NONE',  ( 7.053602361310569613, -4.299079248970732792, 33.91157788607253565 ) ) ;
#56787 = CARTESIAN_POINT ( 'NONE',  ( -17.07692307692319744, -2.379036618888197285, 30.90682066428292885 ) ) ;
#56788 = AXIS2_PLACEMENT_3D ( 'NONE', #80680, #47310, #74802 ) ;
#56789 = CARTESIAN_POINT ( 'NONE',  ( -12.71156168575991785, -10.18141759479407327, 34.26406193332782379 ) ) ;
#56790 = CARTESIAN_POINT ( 'NONE',  ( -13.31936024510254413, -12.70778746994558439, 30.41441678777536595 ) ) ;
#56791 = EDGE_LOOP ( 'NONE', ( #50639, #56274, #81372, #2532, #54577, #70434, #57928, #42593 ) ) ;
#56792 = DIRECTION ( 'NONE',  ( -0.000000000000000000, 0.6427876096865404731, -0.7660444431189771253 ) ) ;
#56793 = EDGE_CURVE ( 'NONE', #21434, #83848, #64110, .T. ) ;
#56794 = ORIENTED_EDGE ( 'NONE', *, *, #48774, .T. ) ;
#56795 = CARTESIAN_POINT ( 'NONE',  ( 2.557692307692311928, -2.499999999999999556, 29.81604066197450109 ) ) ;
#56796 = CARTESIAN_POINT ( 'NONE',  ( -4.284322861962616358, -7.276988635370452485, 34.74523720219453793 ) ) ;
#56797 = ORIENTED_EDGE ( 'NONE', *, *, #25275, .T. ) ;
#56798 = EDGE_CURVE ( 'NONE', #74166, #85495, #19261, .T. ) ;
#56799 = CARTESIAN_POINT ( 'NONE',  ( 11.60452887181161508, -12.62096338111211757, 30.90682066428152908 ) ) ;
#56800 = CARTESIAN_POINT ( 'NONE',  ( -17.32692307692307665, -2.499999999999998668, 29.75000000000000355 ) ) ;
#56801 = CARTESIAN_POINT ( 'NONE',  ( 5.076923076923075762, -9.905515769479276145, 34.41647553114623292 ) ) ;
#56802 = CARTESIAN_POINT ( 'NONE',  ( -11.31568186948346977, -5.827830569534417471, 34.72679350104403539 ) ) ;
#56803 = DIRECTION ( 'NONE',  ( 1.734723475976812518E-16, -1.000000000000000000, 0.000000000000000000 ) ) ;
#56804 = EDGE_LOOP ( 'NONE', ( #1380, #330, #29755, #64436 ) ) ;
#56805 = EDGE_LOOP ( 'NONE', ( #13413, #84887 ) ) ;
#56806 = EDGE_CURVE ( 'NONE', #34885, #34676, #51442, .T. ) ;
#56807 = FACE_BOUND ( 'NONE', #83226, .T. ) ;
#56808 = EDGE_LOOP ( 'NONE', ( #16827, #24395 ) ) ;
#56809 = CARTESIAN_POINT ( 'NONE',  ( 0.000000000000000000, -11.00000000000000000, 29.75000000000000355 ) ) ;
#56810 = CARTESIAN_POINT ( 'NONE',  ( 8.769230769230768274, -8.564572088678739092, 35.78748833219616898 ) ) ;
#56811 = FACE_OUTER_BOUND ( 'NONE', #713, .T. ) ;
#56812 = CARTESIAN_POINT ( 'NONE',  ( 13.38461538461538680, -12.10708131394839349, 31.69288490824020244 ) ) ;
#56813 = ORIENTED_EDGE ( 'NONE', *, *, #87151, .T. ) ;
#56814 = VECTOR ( 'NONE', #52613, 1000.000000000000000 ) ;
#56815 = VERTEX_POINT ( 'NONE', #1095 ) ;
#56816 = VERTEX_POINT ( 'NONE', #8751 ) ;
#56817 = CARTESIAN_POINT ( 'NONE',  ( -10.61538461538461320, -8.973038597847269315, 34.52809138561121927 ) ) ;
#56818 = ORIENTED_EDGE ( 'NONE', *, *, #13462, .F. ) ;
#56819 = EDGE_CURVE ( 'NONE', #49579, #28593, #41748, .T. ) ;
#56820 = B_SPLINE_CURVE_WITH_KNOTS ( 'NONE', 3,
 ( #47731, #46403, #68445, #73883, #46843, #12179, #6741, #34212, #40108, #67127 ),
 .UNSPECIFIED., .F., .F.,
 ( 4, 2, 2, 2, 4 ),
 ( 0.000000000000000000, 0.0001954339857564074473, 0.0003908679715128148945, 0.0005863019572692223418, 0.0007817359430256297891 ),
 .UNSPECIFIED. ) ;
#56821 = CARTESIAN_POINT ( 'NONE',  ( 18.00000000000000000, -13.87047571288749737, 32.06866353760679544 ) ) ;
#56822 = ADVANCED_FACE ( 'NONE', ( #50149 ), #650, .F. ) ;
#56823 = CARTESIAN_POINT ( 'NONE',  ( -2.372962308248625529, -12.51329471203370325, 31.30864560766548976 ) ) ;
#56824 = DIRECTION ( 'NONE',  ( -0.000000000000000000, -0.7660444431189791237, -0.6427876096865379196 ) ) ;
#56825 = VERTEX_POINT ( 'NONE', #15059 ) ;
#56826 = CYLINDRICAL_SURFACE ( 'NONE', #88894, 0.2500000000000004996 ) ;
#56827 = EDGE_CURVE ( 'NONE', #73862, #85779, #82281, .T. ) ;
#56828 = CARTESIAN_POINT ( 'NONE',  ( 0.7114839798866037235, -11.86320923018887719, 32.19269448109604781 ) ) ;
#56829 = EDGE_CURVE ( 'NONE', #4690, #71093, #63229, .T. ) ;
#56830 = CARTESIAN_POINT ( 'NONE',  ( 14.37376065869474751, -6.386643153685127139, 34.62446782046654192 ) ) ;
#56831 = PLANE ( 'NONE',  #8784 ) ;
#56832 = ORIENTED_EDGE ( 'NONE', *, *, #47113, .F. ) ;
#56833 = ORIENTED_EDGE ( 'NONE', *, *, #41234, .T. ) ;
#56834 = ORIENTED_EDGE ( 'NONE', *, *, #45799, .T. ) ;
#56835 = CARTESIAN_POINT ( 'NONE',  ( -4.153846153846152411, -9.780366693483667717, 34.19971097300155094 ) ) ;
#56837 = LINE ( 'NONE', #56405, #75036 ) ;
#56836 = FACE_OUTER_BOUND ( 'NONE', #76203, .T. ) ;
#56838 = CARTESIAN_POINT ( 'NONE',  ( -39.05038313613820122, -2.249999999999998668, 29.75000000000000355 ) ) ;
#56839 = CARTESIAN_POINT ( 'NONE',  ( -6.857008572074484221, -3.513871655860379306, 32.76840700105978499 ) ) ;
#56840 = FACE_BOUND ( 'NONE', #24230, .T. ) ;
#56841 = CARTESIAN_POINT ( 'NONE',  ( -11.76138849736838488, -2.308479472611653094, 30.53278059502174457 ) ) ;
#56842 = ORIENTED_EDGE ( 'NONE', *, *, #12406, .T. ) ;
#56843 = CIRCLE ( 'NONE', #64035, 6.777720855862973792 ) ;
#56844 = CARTESIAN_POINT ( 'NONE',  ( -15.23076923076922995, -13.53365097954675988, 30.81389545987213552 ) ) ;
#56845 = CARTESIAN_POINT ( 'NONE',  ( -25.00000000000000000, -10.00000000000000533, 13.00000000000000178 ) ) ;
#56846 = CARTESIAN_POINT ( 'NONE',  ( 4.219914504848592429, -8.973038597847269315, 34.52809138561122637 ) ) ;
#56847 = CARTESIAN_POINT ( 'NONE',  ( -11.47320596718551045, -3.835265460703683349, 33.15142922261929925 ) ) ;
#56848 = EDGE_LOOP ( 'NONE', ( #52852, #51285, #63698, #86986 ) ) ;
#56849 = CARTESIAN_POINT ( 'NONE',  ( -19.50000000000000000, -11.50000000000000000, 29.75000000000000355 ) ) ;
#56850 = ORIENTED_EDGE ( 'NONE', *, *, #34339, .F. ) ;
#56851 = FACE_BOUND ( 'NONE', #68162, .T. ) ;
#56852 = LINE ( 'NONE', #52644, #34626 ) ;
#56853 = CARTESIAN_POINT ( 'NONE',  ( 16.85399685940693004, -11.76352882383564769, 32.36236540154569497 ) ) ;
#56854 = CARTESIAN_POINT ( 'NONE',  ( -11.53846153846165912, -11.94971097300221174, 32.03036669348237098 ) ) ;
#56855 = ORIENTED_EDGE ( 'NONE', *, *, #81824, .F. ) ;
#56856 = B_SPLINE_CURVE_WITH_KNOTS ( 'NONE', 3,
 ( #82857, #76533, #40978, #40545, #27462, #83297, #68442, #7636, #68879, #21580 ),
 .UNSPECIFIED., .F., .F.,
 ( 4, 2, 2, 2, 4 ),
 ( 0.0007817246256747474977, 0.0009771112852218909357, 0.001172497944769034482, 0.001367884604316178029, 0.001563271263863321575 ),
 .UNSPECIFIED. ) ;
#56857 = VECTOR ( 'NONE', #32013, 1000.000000000000000 ) ;
#56858 = CYLINDRICAL_SURFACE ( 'NONE', #3326, 0.2499999999999973355 ) ;
#56859 = CARTESIAN_POINT ( 'NONE',  ( 5.326923076923137934, -7.434744429011176159, 34.75000000000000711 ) ) ;
#56860 = DIRECTION ( 'NONE',  ( -0.000000000000000000, -0.9848077530122086864, -0.1736481776669273613 ) ) ;
#56861 = CARTESIAN_POINT ( 'NONE',  ( -4.946132635956127288, -5.496552790871117367, 34.60292014791297532 ) ) ;
#56862 = ORIENTED_EDGE ( 'NONE', *, *, #72584, .T. ) ;
#56863 = CARTESIAN_POINT ( 'NONE',  ( -9.942284436356285227, -2.920706130388546651, 32.31842814019191223 ) ) ;
#56864 = ORIENTED_EDGE ( 'NONE', *, *, #62429, .T. ) ;
#56866 = VERTEX_POINT ( 'NONE', #21363 ) ;
#56865 = CARTESIAN_POINT ( 'NONE',  ( 16.85343813319912698, -10.81261337010820256, 33.49550067578627477 ) ) ;
#56867 = CARTESIAN_POINT ( 'NONE',  ( 9.692307692307695177, -3.513871655860378418, 32.76840700105978499 ) ) ;
#56868 = DIRECTION ( 'NONE',  ( -0.000000000000000000, 0.5000000000000011102, -0.8660254037844381525 ) ) ;
#56869 = DIRECTION ( 'NONE',  ( -0.000000000000000000, -0.6427876096865404731, -0.7660444431189771253 ) ) ;
#56870 = EDGE_CURVE ( 'NONE', #36685, #83058, #48831, .T. ) ;
#56871 = DIRECTION ( 'NONE',  ( 0.000000000000000000, 1.000000000000000000, 0.000000000000000000 ) ) ;
#56873 = CARTESIAN_POINT ( 'NONE',  ( 1.576923076923075762, -7.500000000000000000, 29.75000000000000355 ) ) ;
#56872 = FACE_OUTER_BOUND ( 'NONE', #68047, .T. ) ;
#56874 = DIRECTION ( 'NONE',  ( -0.000000000000000000, 1.000000000000000000, -0.000000000000000000 ) ) ;
#56875 = CARTESIAN_POINT ( 'NONE',  ( 1.139087296525997273, -4.749999999999992895, 22.98437500000000000 ) ) ;
#56876 = ORIENTED_EDGE ( 'NONE', *, *, #83979, .T. ) ;
#56877 = CYLINDRICAL_SURFACE ( 'NONE', #54844, 0.2500000000000004996 ) ;
#56878 = CARTESIAN_POINT ( 'NONE',  ( -9.442362282929648742, -11.56426240980093745, 33.07394671870546432 ) ) ;
#56879 = EDGE_LOOP ( 'NONE', ( #87920, #61686 ) ) ;
#56880 = VERTEX_POINT ( 'NONE', #29465 ) ;
#56881 = VERTEX_POINT ( 'NONE', #42532 ) ;
#56882 = CARTESIAN_POINT ( 'NONE',  ( 16.82694634598072625, -4.943428324936578910, 34.04746400365624481 ) ) ;
#56883 = CARTESIAN_POINT ( 'NONE',  ( 3.164685819813350065, -9.780366693483667717, 34.19971097300155805 ) ) ;
#56884 = EDGE_CURVE ( 'NONE', #2315, #18504, #69988, .T. ) ;
#56885 = VECTOR ( 'NONE', #40954, 1000.000000000000227 ) ;
#56886 = DIRECTION ( 'NONE',  ( -1.000000000000000000, -0.000000000000000000, -0.000000000000000000 ) ) ;
#56887 = CARTESIAN_POINT ( 'NONE',  ( -19.99999999999996803, 15.00000000000000711, 13.00000000000000178 ) ) ;
#56888 = CARTESIAN_POINT ( 'NONE',  ( -13.38461538461550759, -6.835583212225970762, 34.95778746994575670 ) ) ;
#56889 = LINE ( 'NONE', #15922, #81627 ) ;
#56890 = CARTESIAN_POINT ( 'NONE',  ( 13.63461538461540457, -2.249999999999999112, 29.81603969181030322 ) ) ;
#56891 = CARTESIAN_POINT ( 'NONE',  ( 0.000000000000000000, -11.00000000000000000, 29.75000000000000355 ) ) ;
#56892 = DIRECTION ( 'NONE',  ( -0.000000000000000000, -0.5000000000000009992, -0.8660254037844380415 ) ) ;
#56893 = CARTESIAN_POINT ( 'NONE',  ( 2.084766090176160436, -3.586966769969700763, 32.86292498521069660 ) ) ;
#56894 = DIRECTION ( 'NONE',  ( -1.000000000000000000, -0.000000000000000000, 0.000000000000000000 ) ) ;
#56895 = ADVANCED_FACE ( 'NONE', ( #29028 ), #3297, .T. ) ;
#56896 = ORIENTED_EDGE ( 'NONE', *, *, #46647, .T. ) ;
#56897 = B_SPLINE_CURVE_WITH_KNOTS ( 'NONE', 3,
 ( #50775, #23318, #23754, #78261, #3927, #57109, #43593, #63865, #17460, #29649 ),
 .UNSPECIFIED., .F., .F.,
 ( 4, 2, 2, 2, 4 ),
 ( 0.0007817246256747457630, 0.0009771112852218887673, 0.001172497944769031880, 0.001367884604316174993, 0.001563271263863318106 ),
 .UNSPECIFIED. ) ;
#56898 = CARTESIAN_POINT ( 'NONE',  ( -17.20707104665477516, -2.647304123082328875, 31.75400227202885262 ) ) ;
#56899 =( LENGTH_UNIT ( ) NAMED_UNIT ( * ) SI_UNIT ( .MILLI., .METRE. ) );
#56900 = CARTESIAN_POINT ( 'NONE',  ( 3.453782074862625340, -10.77377354290276301, 33.85451476688484718 ) ) ;
#56901 = DIRECTION ( 'NONE',  ( 0.000000000000000000, 0.9848077530122072432, 0.1736481776669354937 ) ) ;
#56902 = ORIENTED_EDGE ( 'NONE', *, *, #9095, .T. ) ;
#56903 = B_SPLINE_CURVE_WITH_KNOTS ( 'NONE', 3,
 ( #70087, #47603, #2504, #84503, #22781, #85383, #79065, #8842, #50691, #23668 ),
 .UNSPECIFIED., .F., .F.,
 ( 4, 2, 2, 2, 4 ),
 ( 0.000000000000000000, 0.0001954339857564063360, 0.0003908679715128126719, 0.0005863019572692189808, 0.0007817359430256253438 ),
 .UNSPECIFIED. ) ;
#56904 = EDGE_CURVE ( 'NONE', #13379, #76411, #21418, .T. ) ;
#56905 = CARTESIAN_POINT ( 'NONE',  ( -5.999999999999998224, -1.367168528481310208, 33.57946703557072254 ) ) ;
#56906 = CARTESIAN_POINT ( 'NONE',  ( -12.33070004352569704, -7.277220443632450575, 34.74524770363009196 ) ) ;
#56907 = CARTESIAN_POINT ( 'NONE',  ( -8.899378738962465007, -9.504002272028875709, 34.60269587691767867 ) ) ;
#56908 = VECTOR ( 'NONE', #32905, 1000.000000000000227 ) ;
#56909 = ORIENTED_EDGE ( 'NONE', *, *, #16212, .F. ) ;
#56910 = ADVANCED_FACE ( 'NONE', ( #71755 ), #10514, .F. ) ;
#56911 = CARTESIAN_POINT ( 'NONE',  ( -13.51530685128294529, -9.804603061927743113, 34.18744698557895845 ) ) ;
#56912 = EDGE_LOOP ( 'NONE', ( #8627, #41886, #40461, #10549 ) ) ;
#56913 = B_SPLINE_CURVE_WITH_KNOTS ( 'NONE', 3,
 ( #27767, #82284, #19683, #75511, #21457, #47146, #26888, #54346, #40849, #55675 ),
 .UNSPECIFIED., .F., .F.,
 ( 4, 2, 2, 2, 4 ),
 ( 0.000000000000000000, 0.0001954339857564093175, 0.0003908679715128186350, 0.0005863019572692279796, 0.0007817359430256372700 ),
 .UNSPECIFIED. ) ;
#56914 = CARTESIAN_POINT ( 'NONE',  ( 10.74617642320940369, -8.147973898785416225, 34.70805048591653730 ) ) ;
#56915 = ADVANCED_FACE ( 'NONE', ( #58687 ), #37982, .F. ) ;
#56916 = DIRECTION ( 'NONE',  ( -0.000000000000000000, -0.7660444431189791237, -0.6427876096865379196 ) ) ;
#56917 = CYLINDRICAL_SURFACE ( 'NONE', #28662, 0.2499999999999997502 ) ;
#56918 = EDGE_CURVE ( 'NONE', #61846, #33850, #37421, .T. ) ;
#56919 = VECTOR ( 'NONE', #15636, 1000.000000000000000 ) ;
#56920 = CARTESIAN_POINT ( 'NONE',  ( -9.692307692307691624, -8.164416787775445883, 34.95778746994557906 ) ) ;
#56921 = CARTESIAN_POINT ( 'NONE',  ( 9.692307692307695177, -2.499999999999998668, 29.75000000000001421 ) ) ;
#56922 = ORIENTED_EDGE ( 'NONE', *, *, #82986, .F. ) ;
#56923 = ORIENTED_EDGE ( 'NONE', *, *, #34856, .F. ) ;
#56924 = ORIENTED_EDGE ( 'NONE', *, *, #36461, .F. ) ;
#56925 = EDGE_CURVE ( 'NONE', #50406, #59796, #57938, .T. ) ;
#56926 = FACE_OUTER_BOUND ( 'NONE', #72197, .T. ) ;
#56927 = CARTESIAN_POINT ( 'NONE',  ( 13.63456090296352841, -10.05730279482229683, 34.04704008940765902 ) ) ;
#56928 = B_SPLINE_CURVE_WITH_KNOTS ( 'NONE', 3,
 ( #39632, #13029, #33308, #40947, #60766, #6280, #26550, #33745, #26991, #54449 ),
 .UNSPECIFIED., .F., .F.,
 ( 4, 2, 2, 2, 4 ),
 ( 0.000000000000000000, 0.0001954339857564099680, 0.0003908679715128199361, 0.0005863019572692299312, 0.0007817359430256398721 ),
 .UNSPECIFIED. ) ;
#56929 = CARTESIAN_POINT ( 'NONE',  ( 17.32697738856138869, -4.235687564193445276, 33.53795663066793509 ) ) ;
#56930 = EDGE_CURVE ( 'NONE', #23513, #57142, #57804, .T. ) ;
#56931 = CARTESIAN_POINT ( 'NONE',  ( 14.30769230769218581, -2.657715359629662544, 31.77849191805970364 ) ) ;
#56932 = VECTOR ( 'NONE', #84827, 1000.000000000000227 ) ;
#56933 = CARTESIAN_POINT ( 'NONE',  ( 7.976992176640605337, -7.277220318596961057, 34.99547417642776992 ) ) ;
#56934 = ADVANCED_FACE ( 'NONE', ( #45622 ), #45172, .F. ) ;
#56935 = CARTESIAN_POINT ( 'NONE',  ( -2.307692307692305711, -12.78798330534102767, 29.49999999999997868 ) ) ;
#56936 = ORIENTED_EDGE ( 'NONE', *, *, #10012, .T. ) ;
#56937 = ORIENTED_EDGE ( 'NONE', *, *, #56714, .F. ) ;
#56938 = VECTOR ( 'NONE', #22883, 1000.000000000000000 ) ;
#56939 = VERTEX_POINT ( 'NONE', #72648 ) ;
#56941 = ORIENTED_EDGE ( 'NONE', *, *, #79384, .T. ) ;
#56940 = CARTESIAN_POINT ( 'NONE',  ( -5.999999999999998224, -5.415277668671390821, 36.20867863119892149 ) ) ;
#56943 = CARTESIAN_POINT ( 'NONE',  ( 14.30769230769218581, -5.094484230521993062, 34.41647553114689373 ) ) ;
#56942 = CARTESIAN_POINT ( 'NONE',  ( 8.835299120233207404, -8.120952969808772792, 34.71129190929999453 ) ) ;
#56944 = CARTESIAN_POINT ( 'NONE',  ( 3.749999999999992006, -5.946699141100872943, 25.64062500000000000 ) ) ;
#56945 = ORIENTED_EDGE ( 'NONE', *, *, #20485, .T. ) ;
#56946 = ADVANCED_FACE ( 'NONE', ( #10956 ), #71312, .F. ) ;
#56947 = EDGE_LOOP ( 'NONE', ( #39923, #53722, #69282, #53077 ) ) ;
#56948 = CARTESIAN_POINT ( 'NONE',  ( 4.946313421718993020, -7.722926974430166069, 34.99546784045485737 ) ) ;
#56949 = ORIENTED_EDGE ( 'NONE', *, *, #442, .F. ) ;
#56950 = FACE_BOUND ( 'NONE', #78345, .T. ) ;
#56951 = CARTESIAN_POINT ( 'NONE',  ( -8.102564102564102200, -7.500000000000000000, 29.75000000000000355 ) ) ;
#56952 = DIRECTION ( 'NONE',  ( -0.000000000000000000, -1.000000000000000000, -0.000000000000000000 ) ) ;
#56953 = ORIENTED_EDGE ( 'NONE', *, *, #5376, .T. ) ;
#56954 = ADVANCED_FACE ( 'NONE', ( #4191 ), #78080, .F. ) ;
#56955 = DIRECTION ( 'NONE',  ( 1.000000000000000000, 0.000000000000000000, 0.000000000000000000 ) ) ;
#56956 = DIRECTION ( 'NONE',  ( -0.000000000000000000, 1.000000000000000000, -0.000000000000000000 ) ) ;
#56957 = DIRECTION ( 'NONE',  ( 0.000000000000000000, -0.000000000000000000, 1.000000000000000000 ) ) ;
#56958 = CARTESIAN_POINT ( 'NONE',  ( 4.153846153846032507, -11.48612834414049644, 32.76840700105863391 ) ) ;
#56959 = CARTESIAN_POINT ( 'NONE',  ( -13.13456107297707121, -11.79725096376909299, 32.30694842903960762 ) ) ;
#56960 = B_SPLINE_CURVE_WITH_KNOTS ( 'NONE', 3,
 ( #63482, #1784, #29274, #84225, #22501, #77445, #30578, #50833, #3987, #31474 ),
 .UNSPECIFIED., .F., .F.,
 ( 4, 2, 2, 2, 4 ),
 ( 0.0007817359430256322827, 0.0009771253907249989254, 0.001172514838424365676, 0.001367904286123732428, 0.001563293733823098962 ),
 .UNSPECIFIED. ) ;
#56961 = CARTESIAN_POINT ( 'NONE',  ( 6.989144256426998325, -2.486705287966279876, 31.30864560766543647 ) ) ;
#56962 = CARTESIAN_POINT ( 'NONE',  ( -7.780085495151407571, -6.386643153685127139, 34.62446782046654192 ) ) ;
#56963 = CARTESIAN_POINT ( 'NONE',  ( 16.15384615384615330, -8.973038597847269315, 34.52809138561121927 ) ) ;
#56964 = B_SPLINE_CURVE_WITH_KNOTS ( 'NONE', 3,
 ( #16902, #31309, #39416, #5170, #79047, #17350, #18245, #25443, #66427, #3830 ),
 .UNSPECIFIED., .F., .F.,
 ( 4, 2, 2, 2, 4 ),
 ( 0.0007817359430256333669, 0.0009771253907250056474, 0.001172514838424371098, 0.001367904286123736331, 0.001563293733823101781 ),
 .UNSPECIFIED. ) ;
#56965 = CARTESIAN_POINT ( 'NONE',  ( 5.933916589044120116, -4.786620604624113540, 33.94971097300155805 ) ) ;
#56966 = CARTESIAN_POINT ( 'NONE',  ( -18.06527044596078113, -6.879047030191175693, 34.71129190930000163 ) ) ;
#56967 = EDGE_CURVE ( 'NONE', #74567, #58941, #70764, .T. ) ;
#56968 = CIRCLE ( 'NONE', #18153, 0.2500000000000002220 ) ;
#56969 = CARTESIAN_POINT ( 'NONE',  ( 6.222779541268408821, -10.11255958852956027, 34.01340905677048454 ) ) ;
#56971 = CARTESIAN_POINT ( 'NONE',  ( 11.53846153846153832, -4.098570777380720287, 33.41473453929634729 ) ) ;
#56970 = CARTESIAN_POINT ( 'NONE',  ( 13.25446817517716802, -11.93770438780619259, 32.05411857736982029 ) ) ;
#56972 = CARTESIAN_POINT ( 'NONE',  ( 8.546365347027130355, -2.501496062324912284, 29.88072118266895671 ) ) ;
#56974 = CARTESIAN_POINT ( 'NONE',  ( -19.50000000000000000, -3.499999999999999556, 29.75000000000000355 ) ) ;
#56973 = DIRECTION ( 'NONE',  ( -0.000000000000000000, 0.7660444431189791237, -0.6427876096865379196 ) ) ;
#56975 = CARTESIAN_POINT ( 'NONE',  ( 13.51466281986583873, -7.723484941389743952, 34.99544897038808955 ) ) ;
#56976 = CARTESIAN_POINT ( 'NONE',  ( -2.724691934501232371, -8.700186371490559623, 24.76375670625848713 ) ) ;
#56978 = EDGE_CURVE ( 'NONE', #3936, #13945, #44268, .T. ) ;
#56977 = VERTEX_POINT ( 'NONE', #78516 ) ;
#56979 = CARTESIAN_POINT ( 'NONE',  ( 3.443994336716911242, -7.367359615244446935, 14.00000000000001421 ) ) ;
#56980 = EDGE_LOOP ( 'NONE', ( #15741, #4637, #49399, #80759 ) ) ;
#56981 = EDGE_CURVE ( 'NONE', #46544, #55585, #21321, .T. ) ;
#56982 = CARTESIAN_POINT ( 'NONE',  ( -2.557715531913763218, -2.985938066672154445, 32.43141759479405550 ) ) ;
#56983 = VERTEX_POINT ( 'NONE', #74885 ) ;
#56984 = CARTESIAN_POINT ( 'NONE',  ( 15.93091993633000847, -11.24512374952581872, 33.06303171183252942 ) ) ;
#56985 = CARTESIAN_POINT ( 'NONE',  ( 5.010840697562939816, -11.91647553114624181, 32.58852847137148245 ) ) ;
#56987 = ORIENTED_EDGE ( 'NONE', *, *, #82044, .T. ) ;
#56986 = VECTOR ( 'NONE', #35920, 1000.000000000000000 ) ;
#56988 = DIRECTION ( 'NONE',  ( -1.000000000000000000, 0.000000000000000000, 0.000000000000000000 ) ) ;
#56989 = CARTESIAN_POINT ( 'NONE',  ( 1.901340078031349856, -5.512252781505337929, 24.06063170625849423 ) ) ;
#56990 = CARTESIAN_POINT ( 'NONE',  ( -17.86947456176635640, -9.503571793651730104, 34.60286762892837942 ) ) ;
#56991 = CARTESIAN_POINT ( 'NONE',  ( 13.60762822870878530, -2.889357225399416418, 32.26129605718031002 ) ) ;
#56992 = CARTESIAN_POINT ( 'NONE',  ( 17.93391762063986050, -2.292212530054419606, 30.41441678777542634 ) ) ;
#56993 = ADVANCED_FACE ( 'NONE', ( #5537 ), #46517, .F. ) ;
#56994 = CARTESIAN_POINT ( 'NONE',  ( -16.15384615384615330, -9.905515769479276145, 34.41647553114623292 ) ) ;
#56995 = FACE_OUTER_BOUND ( 'NONE', #53854, .T. ) ;
#56996 = DIRECTION ( 'NONE',  ( 0.000000000000000000, 0.1736481776669267785, -0.9848077530122087975 ) ) ;
#56997 = CARTESIAN_POINT ( 'NONE',  ( -1.553300858899081538, -11.25000000000000711, 14.85937500000000355 ) ) ;
#56998 = FACE_OUTER_BOUND ( 'NONE', #14631, .T. ) ;
#56999 = FACE_OUTER_BOUND ( 'NONE', #28594, .T. ) ;
#57000 = DIRECTION ( 'NONE',  ( -1.000000000000000000, -0.000000000000000000, -0.000000000000000000 ) ) ;
#57001 = CARTESIAN_POINT ( 'NONE',  ( 3.750000000000009770, -9.053300858899081760, 17.04687500000000000 ) ) ;
#57002 = CARTESIAN_POINT ( 'NONE',  ( -10.55012947587177941, -5.941354392334607049, 34.76329471203374055 ) ) ;
#57003 = EDGE_LOOP ( 'NONE', ( #2397, #84419, #80744, #82775 ) ) ;
#57004 = AXIS2_PLACEMENT_3D ( 'NONE', #66199, #75193, #68422 ) ;
#57005 = CARTESIAN_POINT ( 'NONE',  ( 14.30769230769231015, -4.786620604624113540, 33.94971097300155094 ) ) ;
#57006 = CARTESIAN_POINT ( 'NONE',  ( 12.21156171748986807, -8.347322224742351082, 34.93158281831414769 ) ) ;
#57007 = DIRECTION ( 'NONE',  ( 1.000000000000000000, 0.000000000000000000, 0.000000000000000000 ) ) ;
#57008 = CARTESIAN_POINT ( 'NONE',  ( 1.384615384615693667, -2.506253911140615021, 30.00000000000323297 ) ) ;
#57009 = ADVANCED_FACE ( 'NONE', ( #54142 ), #39330, .F. ) ;
#57010 = CARTESIAN_POINT ( 'NONE',  ( -3.230769230769229949, -4.786620604624113540, 33.94971097300155094 ) ) ;
#57011 = VECTOR ( 'NONE', #74316, 1000.000000000000227 ) ;
#57012 = CARTESIAN_POINT ( 'NONE',  ( 2.084207363968358706, -12.24155766932282496, 31.33739205006857986 ) ) ;
#57013 = CARTESIAN_POINT ( 'NONE',  ( 3.230769230769231726, -3.886160181151819604, 36.00935417666054406 ) ) ;
#57014 = VERTEX_POINT ( 'NONE', #47392 ) ;
#57015 = EDGE_LOOP ( 'NONE', ( #29860, #15498, #39106, #43327 ) ) ;
#57016 = ORIENTED_EDGE ( 'NONE', *, *, #49833, .F. ) ;
#57017 = VECTOR ( 'NONE', #42728, 1000.000000000000227 ) ;
#57018 = CARTESIAN_POINT ( 'NONE',  ( -11.28851612908349722, -11.56426240980093745, 33.07394671870546432 ) ) ;
#57019 = CARTESIAN_POINT ( 'NONE',  ( -4.023320452082588261, -3.285477652293412820, 32.44071101563363158 ) ) ;
#57020 = FACE_OUTER_BOUND ( 'NONE', #22581, .T. ) ;
#57021 = CARTESIAN_POINT ( 'NONE',  ( -2.999999999999998224, -7.500000000000000000, 10.00000000000000178 ) ) ;
#57022 = CARTESIAN_POINT ( 'NONE',  ( 18.00000000000000000, -4.786620604624113540, 33.94971097300155094 ) ) ;
#57023 = B_SPLINE_CURVE_WITH_KNOTS ( 'NONE', 3,
 ( #56059, #8771, #42555, #35801, #15969, #21388, #8325, #83992, #23158, #63256 ),
 .UNSPECIFIED., .F., .F.,
 ( 4, 2, 2, 2, 4 ),
 ( 0.0007817359430256219828, 0.0009771253907249863487, 0.001172514838424350498, 0.001367904286123714647, 0.001563293733823079013 ),
 .UNSPECIFIED. ) ;
#57024 = ORIENTED_EDGE ( 'NONE', *, *, #51926, .T. ) ;
#57025 = DIRECTION ( 'NONE',  ( -0.000000000000000000, -0.5000000000000009992, -0.8660254037844380415 ) ) ;
#57026 = ORIENTED_EDGE ( 'NONE', *, *, #36522, .F. ) ;
#57027 = VECTOR ( 'NONE', #80277, 1000.000000000000000 ) ;
#57028 = ORIENTED_EDGE ( 'NONE', *, *, #45385, .T. ) ;
#57029 = ADVANCED_FACE ( 'NONE', ( #87986 ), #73997, .T. ) ;
#57031 = ORIENTED_EDGE ( 'NONE', *, *, #12931, .T. ) ;
#57030 = CARTESIAN_POINT ( 'NONE',  ( 4.284636594813102661, -12.35292014791297710, 31.75344720912887198 ) ) ;
#57032 = CARTESIAN_POINT ( 'NONE',  ( 16.15384615384603251, -12.46129190930018460, 30.37095296980731973 ) ) ;
#57033 = LINE ( 'NONE', #22806, #30748 ) ;
#57034 = ADVANCED_FACE ( 'NONE', ( #81639 ), #32115, .F. ) ;
#57035 = CARTESIAN_POINT ( 'NONE',  ( 2.057692307692299938, -2.499999999999999556, 29.81609845454692120 ) ) ;
#57036 = EDGE_CURVE ( 'NONE', #83747, #4121, #33005, .T. ) ;
#57037 = CARTESIAN_POINT ( 'NONE',  ( -16.15384615384615330, -5.471508081941601098, 34.59228464037088457 ) ) ;
#57038 = AXIS2_PLACEMENT_3D ( 'NONE', #75731, #34303, #47821 ) ;
#57039 = ORIENTED_EDGE ( 'NONE', *, *, #69892, .F. ) ;
#57040 = ORIENTED_EDGE ( 'NONE', *, *, #15651, .F. ) ;
#57041 = CARTESIAN_POINT ( 'NONE',  ( -1.553300858899125059, -3.750000000000009326, 22.82812500000000355 ) ) ;
#57042 = ORIENTED_EDGE ( 'NONE', *, *, #16601, .F. ) ;
#57043 = CARTESIAN_POINT ( 'NONE',  ( -14.37301632049661571, -7.749976730030849303, 34.74374725381503737 ) ) ;
#57045 = VERTEX_POINT ( 'NONE', #33451 ) ;
#57044 = CARTESIAN_POINT ( 'NONE',  ( -14.24162497434223162, -2.292212530054420494, 30.41441678777542990 ) ) ;
#57046 = EDGE_CURVE ( 'NONE', #57920, #76633, #40755, .T. ) ;
#57047 = CARTESIAN_POINT ( 'NONE',  ( 0.000000000000000000, -11.00000000000000000, 29.75000000000000355 ) ) ;
#57048 = CARTESIAN_POINT ( 'NONE',  ( 6.249945518348142492, -12.43552623307873972, 30.55307653245132826 ) ) ;
#57049 = CARTESIAN_POINT ( 'NONE',  ( -0.2385256174450662570, -9.172514111537584114, 34.72667873470787470 ) ) ;
#57050 = ORIENTED_EDGE ( 'NONE', *, *, #55798, .T. ) ;
#57051 = DIRECTION ( 'NONE',  ( 0.000000000000000000, 0.9396926207859126468, -0.3420201433256571111 ) ) ;
#57052 = EDGE_CURVE ( 'NONE', #14174, #73862, #60910, .T. ) ;
#57053 = CARTESIAN_POINT ( 'NONE',  ( 17.06410256410256565, -3.499999999999999556, 29.75000000000000355 ) ) ;
#57054 = B_SPLINE_CURVE_WITH_KNOTS ( 'NONE', 3,
 ( #12304, #38444, #11870, #4206, #19498, #45639, #81213, #66804, #51938, #66357 ),
 .UNSPECIFIED., .F., .F.,
 ( 4, 2, 2, 2, 4 ),
 ( 0.0007817246256747484735, 0.0009771112852218922368, 0.001172497944769036217, 0.001367884604316180197, 0.001563271263863323960 ),
 .UNSPECIFIED. ) ;
#57055 = ORIENTED_EDGE ( 'NONE', *, *, #35727, .F. ) ;
#57056 = FACE_BOUND ( 'NONE', #88172, .T. ) ;
#57057 = CARTESIAN_POINT ( 'NONE',  ( 11.40831432902331954, -5.195881422630166391, 34.18770438780619259 ) ) ;
#57058 = FACE_OUTER_BOUND ( 'NONE', #64317, .T. ) ;
#57059 = CARTESIAN_POINT ( 'NONE',  ( -18.00000000000012079, -2.657715359629662988, 31.77849191805970364 ) ) ;
#57061 = CARTESIAN_POINT ( 'NONE',  ( -10.68065461594093435, -5.941354392334499579, 34.76329471203369792 ) ) ;
#57060 = CARTESIAN_POINT ( 'NONE',  ( -6.673076923076987299, -7.565270445406050648, 34.75000000000000000 ) ) ;
#57062 = AXIS2_PLACEMENT_3D ( 'NONE', #10163, #30864, #58334 ) ;
#57063 = CARTESIAN_POINT ( 'NONE',  ( -0.5916864312701598516, -12.50552854090298993, 31.33409797877408920 ) ) ;
#57064 = CARTESIAN_POINT ( 'NONE',  ( -16.15384615384627409, -9.442884908241554243, 34.35708131394783038 ) ) ;
#57065 = ORIENTED_EDGE ( 'NONE', *, *, #64014, .T. ) ;
#57066 = DIRECTION ( 'NONE',  ( 0.000000000000000000, 0.6427876096865373645, -0.7660444431189797898 ) ) ;
#57067 = CARTESIAN_POINT ( 'NONE',  ( -16.82686865700962286, -6.523592122091590895, 34.90882529074906415 ) ) ;
#57068 = ORIENTED_EDGE ( 'NONE', *, *, #40039, .T. ) ;
#57069 = AXIS2_PLACEMENT_3D ( 'NONE', #75278, #19000, #26199 ) ;
#57070 = DIRECTION ( 'NONE',  ( 0.000000000000000000, 0.000000000000000000, 1.000000000000000000 ) ) ;
#57071 = CARTESIAN_POINT ( 'NONE',  ( 10.36540788444226102, -6.567427716900048118, 34.66269422305636283 ) ) ;
#57072 = CARTESIAN_POINT ( 'NONE',  ( -3.930834802233304170, -2.554770724473668153, 30.48948780036025852 ) ) ;
#57073 = LINE ( 'NONE', #71467, #50490 ) ;
#57074 = CARTESIAN_POINT ( 'NONE',  ( -16.15384615384627409, -12.46129190930018460, 30.37095296980731973 ) ) ;
#57075 = CARTESIAN_POINT ( 'NONE',  ( -8.899922235898330314, -5.582088688514999397, 34.36776431015576350 ) ) ;
#57076 = FACE_BOUND ( 'NONE', #34804, .T. ) ;
#57078 = DIRECTION ( 'NONE',  ( -0.000000000000000000, 1.000000000000000000, 3.491481338843133355E-15 ) ) ;
#57077 = CARTESIAN_POINT ( 'NONE',  ( 6.856994543716788293, -3.937682226553329556, 33.60647404775217240 ) ) ;
#57079 = VECTOR ( 'NONE', #65187, 1000.000000000000000 ) ;
#57080 = CARTESIAN_POINT ( 'NONE',  ( -18.22348492456433178, -8.539481045369599954, 34.89627647299170832 ) ) ;
#57082 = CARTESIAN_POINT ( 'NONE',  ( -15.23076923076935074, -6.879047030192662504, 34.71129190930017927 ) ) ;
#57081 = CARTESIAN_POINT ( 'NONE',  ( 20.99999999999999645, -12.75000000000000178, 29.75000000000000355 ) ) ;
#57083 = CARTESIAN_POINT ( 'NONE',  ( 14.16025641025641235, -7.500000000000000000, 29.75000000000000355 ) ) ;
#57084 = CARTESIAN_POINT ( 'NONE',  ( -3.749999999999996447, -7.561099074964554134, 18.59188170625849068 ) ) ;
#57085 = EDGE_LOOP ( 'NONE', ( #64169, #2043, #2688, #5768 ) ) ;
#57086 = EDGE_CURVE ( 'NONE', #19283, #33070, #73977, .T. ) ;
#57087 = EDGE_LOOP ( 'NONE', ( #63883, #62040, #59478, #1821 ) ) ;
#57088 = CARTESIAN_POINT ( 'NONE',  ( -9.561781990544126586, -11.93748526763465279, 32.05452791011430946 ) ) ;
#57089 = CARTESIAN_POINT ( 'NONE',  ( -4.230769230769230838, -7.500000000000000000, 33.75000000000000000 ) ) ;
#57090 = CARTESIAN_POINT ( 'NONE',  ( -7.780959864370489143, -2.506253911140448487, 29.99999999999988631 ) ) ;
#57091 = CARTESIAN_POINT ( 'NONE',  ( -19.50000000000000000, -3.499999999999999556, 29.75000000000000355 ) ) ;
#57092 = CARTESIAN_POINT ( 'NONE',  ( -4.023055712879200385, -2.845873456487966635, 32.17976146951972538 ) ) ;
#57093 = CARTESIAN_POINT ( 'NONE',  ( -3.775308065498766297, -6.007798216065450170, 23.67000670625849779 ) ) ;
#57094 = CARTESIAN_POINT ( 'NONE',  ( -7.846153846153844924, -9.819645486525091727, 36.12317359536749706 ) ) ;
#57095 = CYLINDRICAL_SURFACE ( 'NONE', #84884, 0.2499999999999986955 ) ;
#57096 = EDGE_CURVE ( 'NONE', #33571, #25404, #14953, .T. ) ;
#57097 = CARTESIAN_POINT ( 'NONE',  ( 3.453782074862627560, -4.026326845037965008, 33.68677907613344047 ) ) ;
#57098 = CARTESIAN_POINT ( 'NONE',  ( 17.75000000000000000, -2.499999999999998668, 29.75000000000000355 ) ) ;
#57099 = CARTESIAN_POINT ( 'NONE',  ( 2.307692307692187583, -3.835265460704628371, 33.15142922262033665 ) ) ;
#57100 = CARTESIAN_POINT ( 'NONE',  ( 25.00000000000000355, 9.999999999999971578, 13.00000000000000178 ) ) ;
#57101 = AXIS2_PLACEMENT_3D ( 'NONE', #16362, #78061, #58225 ) ;
#57102 = DIRECTION ( 'NONE',  ( 0.000000000000000000, 0.9396926207859126468, -0.3420201433256571111 ) ) ;
#57103 = EDGE_CURVE ( 'NONE', #23768, #22173, #3591, .T. ) ;
#57104 = B_SPLINE_CURVE_WITH_KNOTS ( 'NONE', 3,
 ( #78700, #58408, #16996, #85457, #66060, #30071, #37706, #23740, #23303, #50761 ),
 .UNSPECIFIED., .F., .F.,
 ( 4, 2, 2, 2, 4 ),
 ( 0.000000000000000000, 0.0001954339857564072033, 0.0003908679715128144066, 0.0005863019572692215828, 0.0007817359430256288133 ),
 .UNSPECIFIED. ) ;
#57105 = B_SPLINE_CURVE_WITH_KNOTS ( 'NONE', 3,
 ( #12764, #74467, #33920, #13652, #19084, #6020, #66824, #61380, #68596, #13214 ),
 .UNSPECIFIED., .F., .F.,
 ( 4, 2, 2, 2, 4 ),
 ( 0.0007817246256747473893, 0.0009771112852218900684, 0.001172497944769032747, 0.001367884604316175643, 0.001563271263863318323 ),
 .UNSPECIFIED. ) ;
#57106 = DIRECTION ( 'NONE',  ( 0.000000000000000000, 1.000000000000000000, 0.000000000000000000 ) ) ;
#57107 = ORIENTED_EDGE ( 'NONE', *, *, #15552, .F. ) ;
#57108 = CARTESIAN_POINT ( 'NONE',  ( -8.519230769230768274, -2.499999999999998668, 29.75000000000000355 ) ) ;
#57109 = CARTESIAN_POINT ( 'NONE',  ( -5.749945580086543551, -2.544122305571457687, 31.48381861865059150 ) ) ;
#57110 = AXIS2_PLACEMENT_3D ( 'NONE', #78365, #42329, #56272 ) ;
#57111 = CARTESIAN_POINT ( 'NONE',  ( 2.775308065498755195, -6.422011778438505125, 24.64249329374151642 ) ) ;
#57112 = B_SPLINE_CURVE_WITH_KNOTS ( 'NONE', 3,
 ( #72933, #11689, #31955, #81483, #19770, #4931, #59419, #86925, #67517, #13012 ),
 .UNSPECIFIED., .F., .F.,
 ( 4, 2, 2, 2, 4 ),
 ( 0.0007817359527651101701, 0.0009771254036996489256, 0.001172514854634187790, 0.001367904305568726653, 0.001563293756503265517 ),
 .UNSPECIFIED. ) ;
#57113 = DIRECTION ( 'NONE',  ( -0.000000000000000000, 0.8660254037844397068, -0.4999999999999978906 ) ) ;
#57114 = CARTESIAN_POINT ( 'NONE',  ( 6.416666666666664298, -7.500000000000000000, 29.75000000000000355 ) ) ;
#57115 = VERTEX_POINT ( 'NONE', #59878 ) ;
#57116 = CARTESIAN_POINT ( 'NONE',  ( 15.23076923076923173, -12.78798330534102945, 29.74999999999997868 ) ) ;
#57118 = ORIENTED_EDGE ( 'NONE', *, *, #54293, .T. ) ;
#57117 = CARTESIAN_POINT ( 'NONE',  ( 22.75000000000000000, -7.500000000000000000, 29.75000000000000355 ) ) ;
#57119 = CARTESIAN_POINT ( 'NONE',  ( 7.173022441425065843, -3.712312575010499494, 33.01462480002815170 ) ) ;
#57120 = CARTESIAN_POINT ( 'NONE',  ( -13.38461538461538325, -9.780366693483667717, 34.19971097300155094 ) ) ;
#57121 = EDGE_CURVE ( 'NONE', #16656, #59690, #79399, .T. ) ;
#57122 = ORIENTED_EDGE ( 'NONE', *, *, #59251, .F. ) ;
#57123 = CARTESIAN_POINT ( 'NONE',  ( -5.326899807865431491, -11.28823185664190376, 33.01397839955799896 ) ) ;
#57124 = CARTESIAN_POINT ( 'NONE',  ( -17.07692307692319744, -3.300289026999228437, 32.46337939537709616 ) ) ;
#57125 = EDGE_LOOP ( 'NONE', ( #39810, #14718, #42198, #69399 ) ) ;
#57126 = CARTESIAN_POINT ( 'NONE',  ( -11.66860874789976066, -4.460286881179644780, 33.72017969459903242 ) ) ;
#57127 = EDGE_CURVE ( 'NONE', #13990, #44873, #45018, .T. ) ;
#57128 = EDGE_CURVE ( 'NONE', #82159, #56176, #79379, .T. ) ;
#57129 = DIRECTION ( 'NONE',  ( 0.000000000000000000, 0.000000000000000000, 1.000000000000000000 ) ) ;
#57130 = CARTESIAN_POINT ( 'NONE',  ( 12.59206389977210705, -12.15418822224088657, 32.17964115625579069 ) ) ;
#57131 = ORIENTED_EDGE ( 'NONE', *, *, #4646, .T. ) ;
#57132 = ORIENTED_EDGE ( 'NONE', *, *, #73926, .T. ) ;
#57133 = EDGE_CURVE ( 'NONE', #20836, #23257, #6340, .T. ) ;
#57134 = VERTEX_POINT ( 'NONE', #72948 ) ;
#57135 = AXIS2_PLACEMENT_3D ( 'NONE', #7220, #81555, #13967 ) ;
#57136 = CARTESIAN_POINT ( 'NONE',  ( 3.453782074862624896, -2.308499170217967134, 30.53291367094873721 ) ) ;
#57137 = CARTESIAN_POINT ( 'NONE',  ( -5.869474561766354626, -5.915461855592777596, 34.75538340440931506 ) ) ;
#57138 = CARTESIAN_POINT ( 'NONE',  ( 18.00000000000000000, -5.415277668671390821, 36.20867863119892149 ) ) ;
#57139 = B_SPLINE_CURVE_WITH_KNOTS ( 'NONE', 3,
 ( #36952, #84729, #57676, #16252, #23440, #43716, #50895, #78383, #16687, #44142 ),
 .UNSPECIFIED., .F., .F.,
 ( 4, 2, 2, 2, 4 ),
 ( 0.000000000000000000, 0.0001954311564186868202, 0.0003908623128373736404, 0.0005862934692560604335, 0.0007817246256747472808 ),
 .UNSPECIFIED. ) ;
#57140 = CARTESIAN_POINT ( 'NONE',  ( 3.007842271862380290, -10.01117774369187252, 34.36070679894347535 ) ) ;
#57141 = B_SPLINE_CURVE_WITH_KNOTS ( 'NONE', 3,
 ( #77508, #9489, #1851, #29334, #16688, #56789, #22565, #23007, #77951, #16253 ),
 .UNSPECIFIED., .F., .F.,
 ( 4, 2, 2, 2, 4 ),
 ( 0.000000000000000000, 0.0001954311564186863323, 0.0003908623128373726646, 0.0005862934692560590241, 0.0007817246256747453293 ),
 .UNSPECIFIED. ) ;
#57142 = VERTEX_POINT ( 'NONE', #11250 ) ;
#57143 = AXIS2_PLACEMENT_3D ( 'NONE', #21000, #43057, #55674 ) ;
#57144 = ORIENTED_EDGE ( 'NONE', *, *, #46527, .F. ) ;
#57146 = ORIENTED_EDGE ( 'NONE', *, *, #10210, .F. ) ;
#57145 = CARTESIAN_POINT ( 'NONE',  ( 24.00000000000000000, -5.499999999999981348, 27.75000000000000000 ) ) ;
#57147 = EDGE_CURVE ( 'NONE', #58077, #6775, #46050, .T. ) ;
#57148 = CARTESIAN_POINT ( 'NONE',  ( 17.14299142792551578, -4.786620604624113540, 33.94971097300155805 ) ) ;
#57149 = ORIENTED_EDGE ( 'NONE', *, *, #2045, .T. ) ;
#57150 = CARTESIAN_POINT ( 'NONE',  ( -17.86920819217521483, -3.062576670634121534, 32.05464942895958558 ) ) ;
#57151 = FACE_OUTER_BOUND ( 'NONE', #13210, .T. ) ;
#57152 = ORIENTED_EDGE ( 'NONE', *, *, #38614, .T. ) ;
#57153 = ORIENTED_EDGE ( 'NONE', *, *, #76457, .T. ) ;
#57155 = ORIENTED_EDGE ( 'NONE', *, *, #20804, .T. ) ;
#57154 = CARTESIAN_POINT ( 'NONE',  ( -12.33074665371367651, -4.809403383903225304, 33.96459661697924304 ) ) ;
#57156 = ADVANCED_FACE ( 'NONE', ( #3144 ), #39181, .F. ) ;
#57157 = CARTESIAN_POINT ( 'NONE',  ( 4.376857505459002873, -4.887748414852789658, 34.01359900205216746 ) ) ;
#57158 = AXIS2_PLACEMENT_3D ( 'NONE', #132, #49644, #69473 ) ;
#57159 = CARTESIAN_POINT ( 'NONE',  ( -11.53846153846153655, -3.050289026998446396, 32.03036669348365706 ) ) ;
#57160 = ORIENTED_EDGE ( 'NONE', *, *, #23330, .F. ) ;
#57161 = CARTESIAN_POINT ( 'NONE',  ( 15.48071474911737333, -3.202959910592335646, 32.30730279482227019 ) ) ;
#57162 = DIRECTION ( 'NONE',  ( 0.000000000000000000, 0.000000000000000000, -1.000000000000000000 ) ) ;
#57163 = EDGE_CURVE ( 'NONE', #77307, #9234, #30620, .T. ) ;
#57164 = CYLINDRICAL_SURFACE ( 'NONE', #3681, 0.2500000000000008882 ) ;
#57165 = AXIS2_PLACEMENT_3D ( 'NONE', #50829, #77877, #17964 ) ;
#57166 = FACE_BOUND ( 'NONE', #25219, .T. ) ;
#57167 = CARTESIAN_POINT ( 'NONE',  ( 8.069166690247241647, -12.38742843783360748, 31.66772728687926985 ) ) ;
#57168 = CARTESIAN_POINT ( 'NONE',  ( -2.307692307692305711, -12.37446782046654192, 30.86335684631486131 ) ) ;
#57169 = CARTESIAN_POINT ( 'NONE',  ( 8.703147358274884837, -2.538708090699994813, 30.37095296980875148 ) ) ;
#57171 = CARTESIAN_POINT ( 'NONE',  ( 6.856993512121042578, -11.69971097300155272, 32.46337939537587403 ) ) ;
#57170 = CARTESIAN_POINT ( 'NONE',  ( 12.23861150263161157, -3.395401636524185474, 33.02366814457250399 ) ) ;
#57172 = CARTESIAN_POINT ( 'NONE',  ( 11.28848480751918437, -11.28823185664190376, 33.01397839955799896 ) ) ;
#57173 = CARTESIAN_POINT ( 'NONE',  ( -16.21911615440246734, -2.657715359629089669, 31.77849191805834295 ) ) ;
#57174 = ORIENTED_EDGE ( 'NONE', *, *, #69548, .F. ) ;
#57175 = AXIS2_PLACEMENT_3D ( 'NONE', #72174, #78486, #51889 ) ;
#57176 = CARTESIAN_POINT ( 'NONE',  ( -5.777220458731589403, -11.89424750095246175, 32.13594075562311758 ) ) ;
#57177 = ORIENTED_EDGE ( 'NONE', *, *, #6944, .F. ) ;
#57178 = EDGE_LOOP ( 'NONE', ( #32701, #11834 ) ) ;
#57180 = CARTESIAN_POINT ( 'NONE',  ( -5.750054481651856619, -12.22109172314383052, 31.39792113162168263 ) ) ;
#57179 = CARTESIAN_POINT ( 'NONE',  ( 14.55763782604045353, -3.712312575010499494, 33.01462480002815170 ) ) ;
#57181 = EDGE_CURVE ( 'NONE', #12918, #48531, #78809, .T. ) ;
#57182 = B_SPLINE_CURVE_WITH_KNOTS ( 'NONE', 3,
 ( #5908, #87454, #68926, #53643, #33384, #67611, #7237, #59953, #35595, #48652 ),
 .UNSPECIFIED., .F., .F.,
 ( 4, 2, 2, 2, 4 ),
 ( 0.000000000000000000, 0.0001954311564186864949, 0.0003908623128373729899, 0.0005862934692560594577, 0.0007817246256747459798 ),
 .UNSPECIFIED. ) ;
#57183 = CARTESIAN_POINT ( 'NONE',  ( -5.934744428723973897, -6.879047030191282275, 34.71129190930002295 ) ) ;
#57184 = CARTESIAN_POINT ( 'NONE',  ( 7.846153846153846700, -11.11383981884818262, 36.00935417666054406 ) ) ;
#57185 = CARTESIAN_POINT ( 'NONE',  ( 1.449870524128225036, -11.06231777344671130, 33.60647404775212976 ) ) ;
#57186 = CARTESIAN_POINT ( 'NONE',  ( -4.087778820496077437, -3.322132147404559976, 32.92929555188717927 ) ) ;
#57187 = VERTEX_POINT ( 'NONE', #10362 ) ;
#57188 = CARTESIAN_POINT ( 'NONE',  ( 11.28848479441294650, -3.436278759898153901, 33.07459398097509506 ) ) ;
#57189 = CARTESIAN_POINT ( 'NONE',  ( 0.3313904918067634431, -12.70455904226513866, 30.44083106164009322 ) ) ;
#57190 = CARTESIAN_POINT ( 'NONE',  ( -5.076923076923075762, -13.49023893513002648, 31.06009739812518688 ) ) ;
#57191 = CARTESIAN_POINT ( 'NONE',  ( 11.53846153846153832, -12.78798330534102945, 29.74999999999997868 ) ) ;
#57192 = CARTESIAN_POINT ( 'NONE',  ( -15.45363465297287142, -2.501496062324912284, 29.88072118266895671 ) ) ;
#57193 = CARTESIAN_POINT ( 'NONE',  ( -2.651650429449535551, -10.15165042944956753, 17.43750000000000000 ) ) ;
#57194 = VERTEX_POINT ( 'NONE', #39762 ) ;
#57195 = EDGE_CURVE ( 'NONE', #34806, #84581, #27568, .T. ) ;
#57196 = ORIENTED_EDGE ( 'NONE', *, *, #22945, .F. ) ;
#57197 = VECTOR ( 'NONE', #24732, 1000.000000000000114 ) ;
#57198 = CARTESIAN_POINT ( 'NONE',  ( -9.692307692307812417, -12.46129190930018460, 30.37095296980731973 ) ) ;
#57199 = EDGE_CURVE ( 'NONE', #51136, #33889, #50341, .T. ) ;
#57200 = ORIENTED_EDGE ( 'NONE', *, *, #1976, .F. ) ;
#57201 = CARTESIAN_POINT ( 'NONE',  ( -6.989160334032804123, -2.538708090699994813, 30.37095296980875148 ) ) ;
#57202 = CARTESIAN_POINT ( 'NONE',  ( 18.06525557127601900, -6.026961402152790193, 34.52809138561124769 ) ) ;
#57203 = DIRECTION ( 'NONE',  ( 0.000000000000000000, -6.938893903907222067E-15, 1.000000000000000000 ) ) ;
#57204 = CARTESIAN_POINT ( 'NONE',  ( 2.438482748659258625, -9.929761469519744921, 34.40412654351204225 ) ) ;
#57205 = CARTESIAN_POINT ( 'NONE',  ( 3.749999999999992006, -5.946699141100872943, 19.39062500000000711 ) ) ;
#57206 = DIRECTION ( 'NONE',  ( -1.000000000000000000, -0.000000000000000000, -0.000000000000000000 ) ) ;
#57207 = VERTEX_POINT ( 'NONE', #68118 ) ;
#57208 = AXIS2_PLACEMENT_3D ( 'NONE', #45003, #18000, #25193 ) ;
#57209 = CYLINDRICAL_SURFACE ( 'NONE', #86080, 0.2500000000000012212 ) ;
#57211 = EDGE_LOOP ( 'NONE', ( #81666, #54530, #29549, #40530 ) ) ;
#57210 = CARTESIAN_POINT ( 'NONE',  ( -2.177166605928742005, -10.88167719472716399, 33.43325721877153711 ) ) ;
#57212 = CARTESIAN_POINT ( 'NONE',  ( -13.51476259405360558, -11.47017969459904130, 32.78971311882034456 ) ) ;
#57213 = CARTESIAN_POINT ( 'NONE',  ( -9.692307692307691624, -8.564572088678739092, 35.78748833219616898 ) ) ;
#57214 = CARTESIAN_POINT ( 'NONE',  ( 11.40831432902331954, -4.460286881179643004, 33.72017969459903242 ) ) ;
#57215 = LINE ( 'NONE', #50446, #39003 ) ;
#57216 = ADVANCED_FACE ( 'NONE', ( #67232 ), #88406, .F. ) ;
#57217 = VECTOR ( 'NONE', #26887, 1000.000000000000114 ) ;
#57218 = EDGE_CURVE ( 'NONE', #17825, #26012, #34237, .T. ) ;
#57219 = CARTESIAN_POINT ( 'NONE',  ( -3.480769230769229505, -7.433932668274255029, 35.00000000000000711 ) ) ;
#57220 = CARTESIAN_POINT ( 'NONE',  ( 15.48082354240754555, -11.28795663066794575, 33.01431243580653785 ) ) ;
#57221 = CARTESIAN_POINT ( 'NONE',  ( 2.775308065498755195, -6.422011778438505125, 23.39249329374151642 ) ) ;
#57222 = VERTEX_POINT ( 'NONE', #6418 ) ;
#57223 = CARTESIAN_POINT ( 'NONE',  ( -3.007989561791163613, -6.717445702608402236, 34.94155399931962336 ) ) ;
#57224 = CARTESIAN_POINT ( 'NONE',  ( 4.153846153846154188, -10.67929555188718282, 33.92786785259544047 ) ) ;
#57225 = CARTESIAN_POINT ( 'NONE',  ( 1.799775606325937360E-14, -10.25000000000000000, 23.53125000000000000 ) ) ;
#57226 = CARTESIAN_POINT ( 'NONE',  ( -16.02305571287920216, -11.37503395064541678, 33.29242100308974983 ) ) ;
#57227 = CARTESIAN_POINT ( 'NONE',  ( 2.438217745925951530, -12.15418822224088657, 32.17964115625579069 ) ) ;
#57228 = ORIENTED_EDGE ( 'NONE', *, *, #69144, .T. ) ;
#57229 = CARTESIAN_POINT ( 'NONE',  ( -1.944543648262992530, -9.444543648263016067, 16.18750000000000000 ) ) ;
#57230 = DIRECTION ( 'NONE',  ( -0.000000000000000000, 0.1736481776669307198, -0.9848077530122080203 ) ) ;
#57231 = EDGE_CURVE ( 'NONE', #88055, #26451, #61779, .T. ) ;
#57232 = ORIENTED_EDGE ( 'NONE', *, *, #23734, .T. ) ;
#57233 = DIRECTION ( 'NONE',  ( -0.000000000000000000, -0.9848077530122085754, -0.1736481776669273613 ) ) ;
#57234 = UNCERTAINTY_MEASURE_WITH_UNIT (LENGTH_MEASURE( 1.000000000000000082E-05 ), #25788, 'distance_accuracy_value', 'NONE');
#57235 = VERTEX_POINT ( 'NONE', #81632 ) ;
#57236 = VECTOR ( 'NONE', #8791, 1000.000000000000000 ) ;
#57237 = CARTESIAN_POINT ( 'NONE',  ( 17.99999999999987566, -6.879047030192662504, 34.71129190930017927 ) ) ;
#57238 = EDGE_CURVE ( 'NONE', #22716, #81377, #66465, .T. ) ;
#57239 = EDGE_CURVE ( 'NONE', #78895, #2854, #68990, .T. ) ;
#57240 = CARTESIAN_POINT ( 'NONE',  ( -17.20761368003338632, -2.295517848115768089, 30.44137282052136939 ) ) ;
#57241 = DIRECTION ( 'NONE',  ( -0.000000000000000000, -0.5000000000000009992, -0.8660254037844380415 ) ) ;
#57242 = CARTESIAN_POINT ( 'NONE',  ( 13.38461538461538680, -3.322132147404559976, 32.92929555188717927 ) ) ;
#57243 = ORIENTED_EDGE ( 'NONE', *, *, #1781, .T. ) ;
#57244 = CARTESIAN_POINT ( 'NONE',  ( -0.7115384615384606759, -2.499999999999998668, 29.75000000000000355 ) ) ;
#57245 = AXIS2_PLACEMENT_3D ( 'NONE', #6764, #40572, #11759 ) ;
#57246 = VERTEX_POINT ( 'NONE', #27121 ) ;
#57247 = CARTESIAN_POINT ( 'NONE',  ( -18.00000000000012079, -12.16647553114689906, 32.15551576947799362 ) ) ;
#57248 = CARTESIAN_POINT ( 'NONE',  ( 6.065145779331965414, -7.750023238201980469, 34.74374492549440419 ) ) ;
#57249 = B_SPLINE_CURVE_WITH_KNOTS ( 'NONE', 3,
 ( #69934, #2348, #55975, #83467, #69053, #42034, #22197, #49664, #36167, #28067 ),
 .UNSPECIFIED., .F., .F.,
 ( 4, 2, 2, 2, 4 ),
 ( 0.0007817246256747505334, 0.0009771112852218954894, 0.001172497944769040554, 0.001367884604316185618, 0.001563271263863330682 ),
 .UNSPECIFIED. ) ;
#57250 = ORIENTED_EDGE ( 'NONE', *, *, #24038, .T. ) ;
#57251 = LINE ( 'NONE', #70768, #73569 ) ;
#57252 = DIRECTION ( 'NONE',  ( -1.000000000000000000, 0.000000000000000000, -0.000000000000000000 ) ) ;
#57253 = CARTESIAN_POINT ( 'NONE',  ( -11.76194646302586833, -3.019605429927184836, 32.48692288466676814 ) ) ;
#57254 = CARTESIAN_POINT ( 'NONE',  ( 13.63456079399342791, -12.07971442181322352, 32.31769673815850297 ) ) ;
#57255 = CARTESIAN_POINT ( 'NONE',  ( -3.903900744468109529, -4.176053281294514363, 33.81426240980091791 ) ) ;
#57256 = ORIENTED_EDGE ( 'NONE', *, *, #50372, .F. ) ;
#57257 = ORIENTED_EDGE ( 'NONE', *, *, #58232, .T. ) ;
#57258 = FACE_BOUND ( 'NONE', #60782, .T. ) ;
#57259 = ORIENTED_EDGE ( 'NONE', *, *, #61916, .T. ) ;
#57260 = CARTESIAN_POINT ( 'NONE',  ( -8.519176457592452678, -4.235687564193447052, 33.53795663066793509 ) ) ;
#57261 = VECTOR ( 'NONE', #27284, 1000.000000000000227 ) ;
#57262 = CARTESIAN_POINT ( 'NONE',  ( 9.468822748583745508, -12.24155766932282496, 31.33739205006857986 ) ) ;
#57263 = CARTESIAN_POINT ( 'NONE',  ( 5.207714884747862705, -4.118422570099827595, 33.43335022499816489 ) ) ;
#57264 = ORIENTED_EDGE ( 'NONE', *, *, #49846, .F. ) ;
#57265 = VERTEX_POINT ( 'NONE', #13169 ) ;
#57266 = CARTESIAN_POINT ( 'NONE',  ( -1.384615384615505151, -11.94971097300221174, 32.03036669348237098 ) ) ;
#57267 = ORIENTED_EDGE ( 'NONE', *, *, #55181, .F. ) ;
#57268 = CARTESIAN_POINT ( 'NONE',  ( 2.530471848960718528, -4.387253974876676565, 33.66317474335728832 ) ) ;
#57269 = VECTOR ( 'NONE', #79953, 1000.000000000000000 ) ;
#57270 = B_SPLINE_CURVE_WITH_KNOTS ( 'NONE', 3,
 ( #62381, #6571, #41686, #35823, #13763, #8349, #48427, #56083, #61501, #56528 ),
 .UNSPECIFIED., .F., .F.,
 ( 4, 2, 2, 2, 4 ),
 ( 0.0007817359430256322827, 0.0009771253907249989254, 0.001172514838424365676, 0.001367904286123732428, 0.001563293733823099179 ),
 .UNSPECIFIED. ) ;
#57271 = CARTESIAN_POINT ( 'NONE',  ( 3.100077764101674127, -2.729777683071816785, 31.24903638046268739 ) ) ;
#57272 = LINE ( 'NONE', #23040, #51120 ) ;
#57273 = FACE_BOUND ( 'NONE', #7761, .T. ) ;
#57274 = ORIENTED_EDGE ( 'NONE', *, *, #38296, .F. ) ;
#57275 = CARTESIAN_POINT ( 'NONE',  ( -17.07692307692307665, -13.75783147151868846, 33.36296068462461051 ) ) ;
#57276 = CARTESIAN_POINT ( 'NONE',  ( 0.7115927731767742737, -11.79725096376909654, 32.30694842903960762 ) ) ;
#57277 = CARTESIAN_POINT ( 'NONE',  ( -17.74999994631756906, -12.75000000000001066, 29.68455032392686732 ) ) ;
#57278 = LINE ( 'NONE', #9107, #17463 ) ;
#57279 = EDGE_LOOP ( 'NONE', ( #86230, #67133, #78367 ) ) ;
#57280 = PRODUCT_DEFINITION_CONTEXT ( 'detailed design', #42340, 'design' ) ;
#57281 = ORIENTED_EDGE ( 'NONE', *, *, #74036, .T. ) ;
#57282 = ORIENTED_EDGE ( 'NONE', *, *, #4853, .F. ) ;
#57284 = CARTESIAN_POINT ( 'NONE',  ( 1.515140822849029734, -11.66157788607254275, 32.95092075102925833 ) ) ;
#57283 = DIRECTION ( 'NONE',  ( -0.000000000000000000, -0.6427876096865404731, -0.7660444431189770143 ) ) ;
#57285 = DIRECTION ( 'NONE',  ( -0.000000000000000000, 0.9848077530122085754, -0.1736481776669273613 ) ) ;
#57286 = CARTESIAN_POINT ( 'NONE',  ( 12.71148387091650278, -12.68172785388650681, 30.59649109432439218 ) ) ;
#57287 = DIRECTION ( 'NONE',  ( -0.000000000000000000, -0.7660444431189791237, -0.6427876096865379196 ) ) ;
#57288 = CYLINDRICAL_SURFACE ( 'NONE', #5835, 0.2500000000000009437 ) ;
#57289 = ORIENTED_EDGE ( 'NONE', *, *, #14217, .T. ) ;
#57290 = CYLINDRICAL_SURFACE ( 'NONE', #45788, 0.2500000000000009437 ) ;
#57291 = DIRECTION ( 'NONE',  ( -0.000000000000000000, 1.000000000000000000, -0.000000000000000000 ) ) ;
#57292 = CARTESIAN_POINT ( 'NONE',  ( 4.376857505459002873, -9.086983370893049639, 34.49168942202179267 ) ) ;
#57293 = FACE_OUTER_BOUND ( 'NONE', #23774, .T. ) ;
#57294 = VERTEX_POINT ( 'NONE', #7299 ) ;
#57295 = CARTESIAN_POINT ( 'NONE',  ( 8.519254025182178225, -12.65889640711025521, 30.72598325615533454 ) ) ;
#57296 = AXIS2_PLACEMENT_3D ( 'NONE', #21284, #17647, #9986 ) ;
#57297 = ORIENTED_EDGE ( 'NONE', *, *, #6661, .F. ) ;
#57298 = FACE_BOUND ( 'NONE', #70776, .T. ) ;
#57299 = CARTESIAN_POINT ( 'NONE',  ( -17.07692307692307665, -1.466349020453238561, 30.81389545987213907 ) ) ;
#57300 = ADVANCED_FACE ( 'NONE', ( #82078 ), #19914, .F. ) ;
#57301 = DIRECTION ( 'NONE',  ( -0.000000000000000000, 1.000000000000000000, -0.000000000000000000 ) ) ;
#57302 = CARTESIAN_POINT ( 'NONE',  ( 14.30769230769231015, -11.69971097300155272, 32.46337939537588113 ) ) ;
#57303 = EDGE_LOOP ( 'NONE', ( #54843, #18816, #13947, #44173, #14397 ) ) ;
#57304 = PRODUCT_RELATED_PRODUCT_CATEGORY ( 'part', '', ( #963 ) ) ;
#57305 = CARTESIAN_POINT ( 'NONE',  ( 5.299702618191484582, -3.236590943229499029, 32.36255958852954251 ) ) ;
#57306 = DIRECTION ( 'NONE',  ( 0.000000000000000000, 0.1736481776669267785, -0.9848077530122087975 ) ) ;
#57307 = CARTESIAN_POINT ( 'NONE',  ( -4.153846153846152411, -12.62096338111211580, 30.90682066428153263 ) ) ;
#57308 = CARTESIAN_POINT ( 'NONE',  ( -6.700297381808511865, -3.236590943229499029, 32.36255958852954251 ) ) ;
#57309 = ORIENTED_EDGE ( 'NONE', *, *, #55778, .F. ) ;
#57310 = B_SPLINE_CURVE_WITH_KNOTS ( 'NONE', 3,
 ( #22130, #22568, #49600, #64421, #83398, #69870, #9935, #16256, #28439, #23445 ),
 .UNSPECIFIED., .F., .F.,
 ( 4, 2, 2, 2, 4 ),
 ( 0.000000000000000000, 0.0001954311564186862781, 0.0003908623128373725562, 0.0005862934692560588072, 0.0007817246256747451124 ),
 .UNSPECIFIED. ) ;
#57311 = CARTESIAN_POINT ( 'NONE',  ( -7.780085495151408459, -10.51840700105979565, 33.73612834413962247 ) ) ;
#57312 = VERTEX_POINT ( 'NONE', #5975 ) ;
#57314 = ORIENTED_EDGE ( 'NONE', *, *, #76813, .T. ) ;
#57313 = DIRECTION ( 'NONE',  ( -1.000000000000000000, 0.000000000000000000, 0.000000000000000000 ) ) ;
#57315 = CARTESIAN_POINT ( 'NONE',  ( 9.692307692307572609, -3.835265460704628371, 33.15142922262033665 ) ) ;
#57316 = CARTESIAN_POINT ( 'NONE',  ( 3.903822916553187028, -6.695914987888143877, 34.68535235679833306 ) ) ;
#57317 = CARTESIAN_POINT ( 'NONE',  ( 7.780883845597525550, -10.33852847137145048, 34.16647553114627556 ) ) ;
#57318 = CARTESIAN_POINT ( 'NONE',  ( -12.21148414990014608, -2.779044189368095275, 31.39831045268885745 ) ) ;
#57320 = LINE ( 'NONE', #22644, #25941 ) ;
#57319 = CARTESIAN_POINT ( 'NONE',  ( -8.069080063669991532, -9.086856451489515152, 34.49173150075333183 ) ) ;
#57321 = EDGE_CURVE ( 'NONE', #8388, #43710, #47385, .T. ) ;
#57322 = CARTESIAN_POINT ( 'NONE',  ( -4.153846153846152411, -8.810774026931790459, 35.74407628777942847 ) ) ;
#57323 = CARTESIAN_POINT ( 'NONE',  ( 1.944543648262996083, -5.555456351736983045, 25.56250000000000355 ) ) ;
#57324 = ORIENTED_EDGE ( 'NONE', *, *, #23452, .F. ) ;
#57325 = DIRECTION ( 'NONE',  ( -0.000000000000000000, -0.5000000000000009992, -0.8660254037844380415 ) ) ;
#57326 = CARTESIAN_POINT ( 'NONE',  ( 5.776515075435672664, -8.539481045369598178, 34.89627647299170832 ) ) ;
#57327 = VERTEX_POINT ( 'NONE', #20374 ) ;
#57328 = VECTOR ( 'NONE', #85363, 1000.000000000000227 ) ;
#57329 = ORIENTED_EDGE ( 'NONE', *, *, #28922, .F. ) ;
#57330 = VERTEX_POINT ( 'NONE', #60902 ) ;
#57331 = CARTESIAN_POINT ( 'NONE',  ( 3.903869422903798903, -12.17611988154120972, 31.52148481390971213 ) ) ;
#57332 = CARTESIAN_POINT ( 'NONE',  ( -6.673076923076923350, -2.499999999999998668, 29.75000000000000355 ) ) ;
#57333 = CARTESIAN_POINT ( 'NONE',  ( 12.94230769230769340, -7.500000000000000000, 33.75000000000000000 ) ) ;
#57335 = CARTESIAN_POINT ( 'NONE',  ( 0.5915858967889124909, -7.723484941389743952, 34.99544897038808955 ) ) ;
#57334 = VECTOR ( 'NONE', #20158, 1000.000000000000000 ) ;
#57336 = CARTESIAN_POINT ( 'NONE',  ( -4.946397375159509835, -3.816742781228458448, 33.13167719472716044 ) ) ;
#57337 = CARTESIAN_POINT ( 'NONE',  ( 17.29993592101647693, -8.282913670948747864, 34.94150082978203642 ) ) ;
#57338 = DIRECTION ( 'NONE',  ( 0.000000000000000000, 0.9848077530122072432, 0.1736481776669354937 ) ) ;
#57339 = VERTEX_POINT ( 'NONE', #74878 ) ;
#57340 = CARTESIAN_POINT ( 'NONE',  ( 3.100622021331010725, -6.852621066184267029, 34.70813303252209181 ) ) ;
#57342 = EDGE_CURVE ( 'NONE', #29327, #20327, #28825, .T. ) ;
#57341 = CARTESIAN_POINT ( 'NONE',  ( -7.134615384615385025, -3.499999999999999556, 29.75000000000000355 ) ) ;
#57343 = CARTESIAN_POINT ( 'NONE',  ( 12.22435897435897267, -3.499999999999999556, 29.75000000000000355 ) ) ;
#57344 = CARTESIAN_POINT ( 'NONE',  ( 12.21151522424549896, -11.86270091957321249, 32.19358267280087915 ) ) ;
#57345 = VERTEX_POINT ( 'NONE', #84745 ) ;
#57346 = CARTESIAN_POINT ( 'NONE',  ( 3.480769230769230838, -7.500000000000001776, 35.04278698407183867 ) ) ;
#57347 = ADVANCED_FACE ( 'NONE', ( #77524 ), #63995, .F. ) ;
#57348 = B_SPLINE_CURVE_WITH_KNOTS ( 'NONE', 3,
 ( #42091, #69547, #35317, #8300, #34432, #55143, #36218, #20477, #63226, #27673 ),
 .UNSPECIFIED., .F., .F.,
 ( 4, 2, 2, 2, 4 ),
 ( 0.0007817246256747450040, 0.0009771112852218872494, 0.001172497944769029278, 0.001367884604316171523, 0.001563271263863313769 ),
 .UNSPECIFIED. ) ;
#57350 = EDGE_CURVE ( 'NONE', #67687, #55802, #67870, .T. ) ;
#57349 = ORIENTED_EDGE ( 'NONE', *, *, #71969, .T. ) ;
#57351 = CARTESIAN_POINT ( 'NONE',  ( -17.86947456176635640, -8.630441415882550871, 34.87705825610312615 ) ) ;
#57352 = DIRECTION ( 'NONE',  ( 1.000000000000000000, 1.734723475976812518E-16, -0.000000000000000000 ) ) ;
#57353 = CARTESIAN_POINT ( 'NONE',  ( 6.065255139512839122, -12.70778746994558439, 30.41441678777537305 ) ) ;
#57354 = VERTEX_POINT ( 'NONE', #49161 ) ;
#57355 = CARTESIAN_POINT ( 'NONE',  ( -39.05038313613820122, -2.499999999999999556, 29.75000000000000355 ) ) ;
#57356 = CARTESIAN_POINT ( 'NONE',  ( -17.32694631421604115, -3.711651800289232916, 33.01384336483936011 ) ) ;
#57357 = CARTESIAN_POINT ( 'NONE',  ( -9.442253272394241392, -3.435999193479609914, 33.07426656108010832 ) ) ;
#57358 = VERTEX_POINT ( 'NONE', #23456 ) ;
#57359 = CARTESIAN_POINT ( 'NONE',  ( 7.780883845597524662, -11.67786785259540849, 32.92929555188721480 ) ) ;
#57360 = EDGE_LOOP ( 'NONE', ( #15934, #31687, #54291, #42054 ) ) ;
#57361 = VECTOR ( 'NONE', #43020, 1000.000000000000227 ) ;
#57362 = CARTESIAN_POINT ( 'NONE',  ( 16.15384615384615330, -9.819645486525091727, 36.12317359536749706 ) ) ;
#57363 = CARTESIAN_POINT ( 'NONE',  ( -15.23076923076922995, -9.819645486525091727, 36.12317359536749706 ) ) ;
#57364 = CARTESIAN_POINT ( 'NONE',  ( 12.21151522424549896, -8.432397168068783699, 34.66272746175022945 ) ) ;
#57365 = CARTESIAN_POINT ( 'NONE',  ( 1.384615384615386802, -8.164416787775445883, 34.95778746994557906 ) ) ;
#57366 = DIRECTION ( 'NONE',  ( 0.000000000000000000, 0.9396926207859126468, -0.3420201433256571111 ) ) ;
#57367 = ORIENTED_EDGE ( 'NONE', *, *, #53864, .F. ) ;
#57368 = ORIENTED_EDGE ( 'NONE', *, *, #36663, .T. ) ;
#57369 = ORIENTED_EDGE ( 'NONE', *, *, #77903, .F. ) ;
#57370 = CARTESIAN_POINT ( 'NONE',  ( 12.68454981315131214, -11.76359900205217635, 32.36225158514719880 ) ) ;
#57371 = DIRECTION ( 'NONE',  ( 0.000000000000000000, 0.8660254037844377084, 0.5000000000000015543 ) ) ;
#57372 = CARTESIAN_POINT ( 'NONE',  ( -12.46153846153858424, -12.51329471203414379, 31.30864560766407578 ) ) ;
#57373 = CARTESIAN_POINT ( 'NONE',  ( -14.30769230769230660, -2.708943851104267164, 35.45975837776705220 ) ) ;
#57374 = CYLINDRICAL_SURFACE ( 'NONE', #53653, 0.2500000000000008882 ) ;
#57375 = CARTESIAN_POINT ( 'NONE',  ( 5.326868595271216478, -10.05730279482229683, 34.04704008940765902 ) ) ;
#57376 = ORIENTED_EDGE ( 'NONE', *, *, #37848, .F. ) ;
#57377 = EDGE_LOOP ( 'NONE', ( #40339, #74605 ) ) ;
#57378 = EDGE_CURVE ( 'NONE', #20400, #68350, #83857, .T. ) ;
#57379 = VERTEX_POINT ( 'NONE', #22140 ) ;
#57380 = AXIS2_PLACEMENT_3D ( 'NONE', #30897, #85859, #24143 ) ;
#57382 = ORIENTED_EDGE ( 'NONE', *, *, #49700, .T. ) ;
#57381 = PLANE ( 'NONE',  #80493 ) ;
#57384 = CARTESIAN_POINT ( 'NONE',  ( 13.91025641025641235, -7.500000000000000000, 33.75000000000000000 ) ) ;
#57383 = CARTESIAN_POINT ( 'NONE',  ( -11.53846153846153655, -1.129524287112498415, 32.06866353760679544 ) ) ;
#57385 = VECTOR ( 'NONE', #53553, 1000.000000000000114 ) ;
#57386 = CARTESIAN_POINT ( 'NONE',  ( -1.450697763975519194, -4.661471528628507777, 34.16647553114621871 ) ) ;
#57387 = CARTESIAN_POINT ( 'NONE',  ( -1.553300858899081760, -11.25000000000000888, 26.10937500000000355 ) ) ;
#57388 = ORIENTED_EDGE ( 'NONE', *, *, #87519, .F. ) ;
#57389 = VECTOR ( 'NONE', #12008, 1000.000000000000227 ) ;
#57390 = EDGE_LOOP ( 'NONE', ( #29850, #11147, #40565, #8334 ) ) ;
#57391 = CARTESIAN_POINT ( 'NONE',  ( -2.373775718648186928, -12.37446782046654192, 30.86335684631486487 ) ) ;
#57392 = ORIENTED_EDGE ( 'NONE', *, *, #29078, .F. ) ;
#57393 = FACE_BOUND ( 'NONE', #54626, .T. ) ;
#57394 = B_SPLINE_CURVE_WITH_KNOTS ( 'NONE', 3,
 ( #61958, #47559, #41260, #21425, #48892, #6585, #40817, #47998, #15117, #13335 ),
 .UNSPECIFIED., .F., .F.,
 ( 4, 2, 2, 2, 4 ),
 ( 0.000000000000000000, 0.0001954311564186879857, 0.0003908623128373759715, 0.0005862934692560640114, 0.0007817246256747519429 ),
 .UNSPECIFIED. ) ;
#57395 = CARTESIAN_POINT ( 'NONE',  ( 14.98074599347626368, -10.05641848906368097, 34.04755513067966177 ) ) ;
#57396 = EDGE_CURVE ( 'NONE', #65802, #7817, #8636, .T. ) ;
#57397 = CYLINDRICAL_SURFACE ( 'NONE', #31871, 0.2499999999999986955 ) ;
#57398 = ORIENTED_EDGE ( 'NONE', *, *, #65395, .T. ) ;
#57399 = CARTESIAN_POINT ( 'NONE',  ( -15.23076923076922995, -8.164416787775445883, 34.95778746994557906 ) ) ;
#57400 = CARTESIAN_POINT ( 'NONE',  ( 3.230769230769110045, -3.300289026999228881, 32.46337939537708905 ) ) ;
#57401 = CARTESIAN_POINT ( 'NONE',  ( -7.846153846153844924, -3.513871655860378418, 32.76840700105978499 ) ) ;
#57402 = ADVANCED_FACE ( 'NONE', ( #23020 ), #36106, .F. ) ;
#57403 = CARTESIAN_POINT ( 'NONE',  ( 4.087762742890272527, -11.16473453929635440, 33.15142922261925662 ) ) ;
#57404 = CARTESIAN_POINT ( 'NONE',  ( -16.94639737515951339, -2.619367082507847222, 30.83698974864643461 ) ) ;
#57405 = DIRECTION ( 'NONE',  ( -0.000000000000000000, 0.8660254037844399289, -0.4999999999999980016 ) ) ;
#57406 = LINE ( 'NONE', #51517, #15688 ) ;
#57407 = CARTESIAN_POINT ( 'NONE',  ( -7.623374304885435215, -6.760870238392817200, 34.69528174975672385 ) ) ;
#57408 = CARTESIAN_POINT ( 'NONE',  ( 16.37662569511456567, -9.332535724633405749, 34.40230450496446224 ) ) ;
#57409 = CARTESIAN_POINT ( 'NONE',  ( 13.60739505359345181, -2.353885683473779800, 30.79025554430704403 ) ) ;
#57410 = CARTESIAN_POINT ( 'NONE',  ( -5.999999999999998224, -11.69971097300155272, 32.46337939537588113 ) ) ;
#57411 = CARTESIAN_POINT ( 'NONE',  ( 6.066068351002442682, -9.780366693483667717, 34.19971097300155805 ) ) ;
#57413 = CARTESIAN_POINT ( 'NONE',  ( 7.846153846153846700, -1.215029322943914858, 32.30358669280327177 ) ) ;
#57412 = CARTESIAN_POINT ( 'NONE',  ( -13.51476335434707821, -4.299443229763728169, 33.91186481527756058 ) ) ;
#57414 = ADVANCED_FACE ( 'NONE', ( #21689 ), #77085, .F. ) ;
#57415 = LINE ( 'NONE', #84909, #85657 ) ;
#57417 = DIRECTION ( 'NONE',  ( 0.000000000000000000, 0.3420201433256610524, 0.9396926207859113145 ) ) ;
#57416 = DIRECTION ( 'NONE',  ( 0.000000000000000000, 0.7660444431189807890, 0.6427876096865361433 ) ) ;
#57418 = DIRECTION ( 'NONE',  ( -0.000000000000000000, 0.8660254037844399289, -0.4999999999999980016 ) ) ;
#57419 = CARTESIAN_POINT ( 'NONE',  ( 2.750000000000001332, -7.438900925035452083, 20.46688170625848713 ) ) ;
#57420 = ORIENTED_EDGE ( 'NONE', *, *, #83250, .F. ) ;
#57421 = B_SPLINE_CURVE_WITH_KNOTS ( 'NONE', 3,
 ( #4139, #26202, #73054, #12689, #59088, #87038 ),
 .UNSPECIFIED., .F., .F.,
 ( 4, 2, 4 ),
 ( 0.0003909512603273906169, 0.0005862562993132179340, 0.0007815613382990451970 ),
 .UNSPECIFIED. ) ;
#57422 = CARTESIAN_POINT ( 'NONE',  ( 0.2115152242454955145, -12.43535235679832596, 30.55408501211184813 ) ) ;
#57423 = ORIENTED_EDGE ( 'NONE', *, *, #12352, .F. ) ;
#57424 = ADVANCED_FACE ( 'NONE', ( #42862 ), #15390, .F. ) ;
#57425 = CARTESIAN_POINT ( 'NONE',  ( -9.915233909823841785, -5.667676309546437530, 34.40238873228292249 ) ) ;
#57426 = VERTEX_POINT ( 'NONE', #14491 ) ;
#57427 = CARTESIAN_POINT ( 'NONE',  ( 15.90382291655318880, -11.37209801155882793, 32.91403422569033665 ) ) ;
#57428 = ORIENTED_EDGE ( 'NONE', *, *, #82177, .T. ) ;
#57429 = CARTESIAN_POINT ( 'NONE',  ( -16.15384615384627409, -3.300289026999228437, 32.46337939537709616 ) ) ;
#57430 = CARTESIAN_POINT ( 'NONE',  ( 1.987747218494664292, -9.401340078031346081, 21.87313170625849068 ) ) ;
#57431 = CARTESIAN_POINT ( 'NONE',  ( -17.77722033102192967, -9.418065098278011860, 34.63729479722530158 ) ) ;
#57432 = CARTESIAN_POINT ( 'NONE',  ( -3.164701897419153642, -12.34228464037088813, 31.77849191805839268 ) ) ;
#57433 = CARTESIAN_POINT ( 'NONE',  ( 15.90386940979756858, -8.347322224742351082, 34.93158281831414769 ) ) ;
#57434 = CYLINDRICAL_SURFACE ( 'NONE', #80631, 2.000000000000001776 ) ;
#57435 = CARTESIAN_POINT ( 'NONE',  ( -13.63459212866397863, -8.347322224742351082, 34.93158281831414058 ) ) ;
#57436 = CARTESIAN_POINT ( 'NONE',  ( 4.853438133199127869, -8.496056993536548418, 34.65000542017679663 ) ) ;
#57437 = CARTESIAN_POINT ( 'NONE',  ( -2.651650429449565305, -4.848349570550461785, 17.75000000000000355 ) ) ;
#57438 = CARTESIAN_POINT ( 'NONE',  ( 1.161130440891440241, -2.847400154188068022, 31.58180166144859058 ) ) ;
#57440 = EDGE_CURVE ( 'NONE', #18050, #17526, #25733, .T. ) ;
#57439 = CARTESIAN_POINT ( 'NONE',  ( -2.057637887778852814, -12.01375889529407637, 32.43194544308182969 ) ) ;
#57441 = EDGE_CURVE ( 'NONE', #14948, #10893, #36967, .T. ) ;
#57442 = CYLINDRICAL_SURFACE ( 'NONE', #450, 0.2500000000000012212 ) ;
#57443 = CARTESIAN_POINT ( 'NONE',  ( -3.749999999999988454, -9.053300858899127945, 18.76562500000000000 ) ) ;
#57444 = B_SPLINE_CURVE_WITH_KNOTS ( 'NONE', 3,
 ( #70736, #56766, #2254, #9469, #77485, #50874, #1384, #28411, #78360, #49127 ),
 .UNSPECIFIED., .F., .F.,
 ( 4, 2, 2, 2, 4 ),
 ( 0.000000000000000000, 0.0001954339857564070949, 0.0003908679715128141898, 0.0005863019572692212576, 0.0007817359430256283796 ),
 .UNSPECIFIED. ) ;
#57445 = VECTOR ( 'NONE', #3883, 1000.000000000000000 ) ;
#57446 = DIRECTION ( 'NONE',  ( -1.000000000000000000, 0.000000000000000000, -0.000000000000000000 ) ) ;
#57447 = ORIENTED_EDGE ( 'NONE', *, *, #46319, .F. ) ;
#57448 = EDGE_CURVE ( 'NONE', #20488, #84107, #26680, .T. ) ;
#57449 = DIRECTION ( 'NONE',  ( -0.000000000000000000, -0.8660254037844397068, -0.4999999999999978906 ) ) ;
#57450 = CARTESIAN_POINT ( 'NONE',  ( -11.47239318745910097, -8.120952969808772792, 34.71129190929999453 ) ) ;
#57451 = CARTESIAN_POINT ( 'NONE',  ( -13.38461538461550582, -5.219633306517616589, 34.19971097300220464 ) ) ;
#57452 = CARTESIAN_POINT ( 'NONE',  ( 1.449809366398742361, -2.506253911140448043, 29.99999999999988631 ) ) ;
#57453 = EDGE_CURVE ( 'NONE', #40861, #9213, #87408, .T. ) ;
#57454 = VECTOR ( 'NONE', #12898, 1000.000000000000000 ) ;
#57455 = CARTESIAN_POINT ( 'NONE',  ( 15.16501242825492390, -7.249945686854186278, 34.74374336980224598 ) ) ;
#57456 = CARTESIAN_POINT ( 'NONE',  ( -14.55769230769230660, -2.249999999999998668, 29.75000000000000355 ) ) ;
#57457 = VECTOR ( 'NONE', #15478, 1000.000000000000114 ) ;
#57458 = CARTESIAN_POINT ( 'NONE',  ( 8.545745825506822158, -10.81261337010820256, 33.49550067578627477 ) ) ;
#57459 = EDGE_LOOP ( 'NONE', ( #19698, #39696 ) ) ;
#57460 = CARTESIAN_POINT ( 'NONE',  ( -1.319359813339360032, -10.21337939537593620, 33.94971097300152252 ) ) ;
#57461 = ORIENTED_EDGE ( 'NONE', *, *, #61298, .F. ) ;
#57462 = EDGE_LOOP ( 'NONE', ( #55403, #59417, #45980, #88287, #59254 ) ) ;
#57463 = CARTESIAN_POINT ( 'NONE',  ( -6.250023224221457063, -12.68155406624981119, 30.59749803192733708 ) ) ;
#57464 = LINE ( 'NONE', #76866, #61880 ) ;
#57465 = CARTESIAN_POINT ( 'NONE',  ( 15.23076923076923173, -8.564572088678739092, 35.78748833219616898 ) ) ;
#57466 = DIRECTION ( 'NONE',  ( 0.000000000000000000, -6.938893903907222067E-15, 1.000000000000000000 ) ) ;
#57467 = B_SPLINE_CURVE_WITH_KNOTS ( 'NONE', 3,
 ( #78947, #80290, #17242, #38858, #87507, #31196, #18141, #45600, #38408, #80745 ),
 .UNSPECIFIED., .F., .F.,
 ( 4, 2, 2, 2, 4 ),
 ( 0.0007817359430256369448, 0.0009771253907250049969, 0.001172514838424373266, 0.001367904286123741535, 0.001563293733823109587 ),
 .UNSPECIFIED. ) ;
#57468 = ORIENTED_EDGE ( 'NONE', *, *, #70274, .T. ) ;
#57469 = CARTESIAN_POINT ( 'NONE',  ( -14.08468095607945969, -12.15243808032446005, 31.58219941686247978 ) ) ;
#57470 = B_SPLINE_CURVE_WITH_KNOTS ( 'NONE', 3,
 ( #17933, #59354, #24227, #74209, #53030, #45388, #3955, #44941, #80533, #80979 ),
 .UNSPECIFIED., .F., .F.,
 ( 4, 2, 2, 2, 4 ),
 ( 0.0007817246256747507503, 0.0009771112852218957062, 0.001172497944769040771, 0.001367884604316185835, 0.001563271263863330682 ),
 .UNSPECIFIED. ) ;
#57471 = ORIENTED_EDGE ( 'NONE', *, *, #35774, .T. ) ;
#57472 = B_SPLINE_CURVE_WITH_KNOTS ( 'NONE', 3,
 ( #25032, #58356, #46198, #17390, #60140, #52935, #25480, #86762, #73227, #44393 ),
 .UNSPECIFIED., .F., .F.,
 ( 4, 2, 2, 2, 4 ),
 ( 0.000000000000000000, 0.0001954339857564092904, 0.0003908679715128185808, 0.0005863019572692278712, 0.0007817359430256371616 ),
 .UNSPECIFIED. ) ;
#57473 = EDGE_CURVE ( 'NONE', #51319, #48499, #43904, .T. ) ;
#57474 = ORIENTED_EDGE ( 'NONE', *, *, #88960, .T. ) ;
#57475 = DIRECTION ( 'NONE',  ( 0.000000000000000000, 0.1736481776669267785, -0.9848077530122087975 ) ) ;
#57476 = CARTESIAN_POINT ( 'NONE',  ( 14.30769230769231015, -11.11383981884818262, 36.00935417666054406 ) ) ;
#57477 = EDGE_CURVE ( 'NONE', #22156, #28775, #45950, .T. ) ;
#57478 = CARTESIAN_POINT ( 'NONE',  ( -16.28453762051371712, -4.118384482072086072, 33.43331474514187107 ) ) ;
#57479 = EDGE_CURVE ( 'NONE', #43220, #20800, #78016, .T. ) ;
#57480 = CARTESIAN_POINT ( 'NONE',  ( -4.403846153846151523, -7.566083408709834757, 34.74999999999999289 ) ) ;
#57481 = CARTESIAN_POINT ( 'NONE',  ( 7.846153846153846700, -12.62096338111211580, 30.90682066428153263 ) ) ;
#57482 = ORIENTED_EDGE ( 'NONE', *, *, #53035, .T. ) ;
#57483 = ORIENTED_EDGE ( 'NONE', *, *, #3655, .T. ) ;
#57484 = CARTESIAN_POINT ( 'NONE',  ( -1.929879867024197893E-14, -3.750000000000000000, 22.90625000000000355 ) ) ;
#57485 = EDGE_CURVE ( 'NONE', #5035, #55756, #71816, .T. ) ;
#57486 = ORIENTED_EDGE ( 'NONE', *, *, #43677, .F. ) ;
#57488 = ORIENTED_EDGE ( 'NONE', *, *, #51791, .F. ) ;
#57487 = DIRECTION ( 'NONE',  ( -0.000000000000000000, -0.7660444431189791237, -0.6427876096865379196 ) ) ;
#57489 = CARTESIAN_POINT ( 'NONE',  ( 1.515141086378950952, -9.417988943895561960, 34.36773134775778260 ) ) ;
#57490 = CARTESIAN_POINT ( 'NONE',  ( -10.61538461538473399, -10.21337939537710326, 33.94971097300076224 ) ) ;
#57491 = CARTESIAN_POINT ( 'NONE',  ( 2.307692307692186251, -9.528491918059723176, 34.59228464037033035 ) ) ;
#57492 = ORIENTED_EDGE ( 'NONE', *, *, #81956, .F. ) ;
#57493 = AXIS2_PLACEMENT_3D ( 'NONE', #30253, #69463, #7766 ) ;
#57494 = CARTESIAN_POINT ( 'NONE',  ( -15.23076923076935074, -3.835265460704628371, 33.15142922262033665 ) ) ;
#57495 = ORIENTED_EDGE ( 'NONE', *, *, #78010, .T. ) ;
#57496 = FACE_BOUND ( 'NONE', #59698, .T. ) ;
#57497 = CARTESIAN_POINT ( 'NONE',  ( 15.48071464014727283, -11.56426240980093745, 33.07394671870546432 ) ) ;
#57498 = CARTESIAN_POINT ( 'NONE',  ( -7.146003140593069958, -2.758268499246657957, 31.33685645148948140 ) ) ;
#57499 = CARTESIAN_POINT ( 'NONE',  ( 2.307692307692186251, -12.51329471203414379, 31.30864560766407578 ) ) ;
#57500 = B_SPLINE_CURVE_WITH_KNOTS ( 'NONE', 3,
 ( #53141, #18925, #58559, #32000, #52699, #80187, #60347, #73874, #18487, #4060 ),
 .UNSPECIFIED., .F., .F.,
 ( 4, 2, 2, 2, 4 ),
 ( 0.000000000000000000, 0.0001954339857564081249, 0.0003908679715128162498, 0.0005863019572692244018, 0.0007817359430256324996 ),
 .UNSPECIFIED. ) ;
#57503 = CYLINDRICAL_SURFACE ( 'NONE', #71316, 0.2499999999999994726 ) ;
#57502 = VECTOR ( 'NONE', #35374, 1000.000000000000227 ) ;
#57501 = CARTESIAN_POINT ( 'NONE',  ( -0.3962833220256231637, -11.67786785259547777, 32.92929555188713664 ) ) ;
#57504 = VECTOR ( 'NONE', #69573, 1000.000000000000000 ) ;
#57505 = CARTESIAN_POINT ( 'NONE',  ( 15.93091993633000847, -2.554751324335733376, 30.48935550225260727 ) ) ;
#57506 = CARTESIAN_POINT ( 'NONE',  ( 18.13079180782477096, -2.729792928343269587, 31.24908615093345077 ) ) ;
#57507 = EDGE_LOOP ( 'NONE', ( #9404, #30933, #1206, #71791 ) ) ;
#57508 = CARTESIAN_POINT ( 'NONE',  ( -11.40766973063674961, -12.11778462344220841, 31.66786338562085135 ) ) ;
#57509 = CARTESIAN_POINT ( 'NONE',  ( 4.946232473812766095, -3.957541250942359756, 33.62499894934981626 ) ) ;
#57510 = B_SPLINE_CURVE_WITH_KNOTS ( 'NONE', 3,
 ( #7711, #83819, #941, #63519, #29312, #22102, #56764, #55880, #15349, #84260 ),
 .UNSPECIFIED., .F., .F.,
 ( 4, 2, 2, 2, 4 ),
 ( 0.000000000000000000, 0.0001954339857564082062, 0.0003908679715128164124, 0.0005863019572692246186, 0.0007817359430256328248 ),
 .UNSPECIFIED. ) ;
#57511 = ADVANCED_FACE ( 'NONE', ( #71639 ), #51801, .F. ) ;
#57512 = VECTOR ( 'NONE', #82049, 1000.000000000000000 ) ;
#57513 = ORIENTED_EDGE ( 'NONE', *, *, #83071, .T. ) ;
#57514 = AXIS2_PLACEMENT_3D ( 'NONE', #22381, #1669, #56613 ) ;
#57515 = CARTESIAN_POINT ( 'NONE',  ( -9.692307692307691624, -3.669653830205710676, 35.88435417666054406 ) ) ;
#57516 = CARTESIAN_POINT ( 'NONE',  ( -18.13069060311030967, -12.62707690430377383, 30.88035979386743435 ) ) ;
#57517 = DIRECTION ( 'NONE',  ( -0.000000000000000000, 1.000000000000000000, -0.000000000000000000 ) ) ;
#57518 = FACE_OUTER_BOUND ( 'NONE', #32226, .T. ) ;
#57519 = CARTESIAN_POINT ( 'NONE',  ( 7.911408985666682270, -6.835583212224610072, 34.95778746994559327 ) ) ;
#57520 = CARTESIAN_POINT ( 'NONE',  ( -8.992715712954719720, -5.912607949931405926, 34.49155766932282319 ) ) ;
#57521 = FACE_BOUND ( 'NONE', #82863, .T. ) ;
#57523 = CARTESIAN_POINT ( 'NONE',  ( 1.384615384615386802, -2.538708090699994813, 30.37095296980875503 ) ) ;
#57522 = CARTESIAN_POINT ( 'NONE',  ( 9.942307692307695177, -2.499999999999998668, 29.75000000000000355 ) ) ;
#57524 = CARTESIAN_POINT ( 'NONE',  ( -18.22292695890684655, -8.282780595021769443, 34.94152052738834158 ) ) ;
#57526 = CARTESIAN_POINT ( 'NONE',  ( 7.053602624840485724, -12.45806712695776319, 30.39783852428763922 ) ) ;
#57525 = CARTESIAN_POINT ( 'NONE',  ( 5.999999999999880096, -6.879047030192662504, 34.71129190930017927 ) ) ;
#57527 = LINE ( 'NONE', #44891, #85052 ) ;
#57528 = CARTESIAN_POINT ( 'NONE',  ( -3.724691934501229262, -9.114399933863657211, 19.76375670625849423 ) ) ;
#57529 = ORIENTED_EDGE ( 'NONE', *, *, #17057, .T. ) ;
#57530 = CARTESIAN_POINT ( 'NONE',  ( -9.692307692307691624, -13.63283147151868846, 33.57946703557072254 ) ) ;
#57531 = CARTESIAN_POINT ( 'NONE',  ( -14.37377571864818293, -6.386643153685125363, 34.62446782046654903 ) ) ;
#57532 = CARTESIAN_POINT ( 'NONE',  ( 5.999999999999878320, -5.941354392335915335, 34.76329471203413846 ) ) ;
#57533 = CARTESIAN_POINT ( 'NONE',  ( 17.07692307692307665, -8.164416787775445883, 34.95778746994557906 ) ) ;
#57534 = CARTESIAN_POINT ( 'NONE',  ( 10.61538461538461675, -12.10708131394839349, 31.69288490824020244 ) ) ;
#57535 = CARTESIAN_POINT ( 'NONE',  ( -0.06109907496455085213, -3.750000000000000888, 21.40438170625849068 ) ) ;
#57536 = CARTESIAN_POINT ( 'NONE',  ( -1.318448778023743273, -7.250054591869667497, 34.99404684341514127 ) ) ;
#57537 = CARTESIAN_POINT ( 'NONE',  ( 12.46153846153846168, -7.500000000000001776, 35.04278698407183867 ) ) ;
#57538 = CARTESIAN_POINT ( 'NONE',  ( -16.85391172531022619, -5.667800583137506898, 34.40243808032445827 ) ) ;
#57539 = CARTESIAN_POINT ( 'NONE',  ( 10.39245765647776309, -6.459968553980841577, 34.89616026154728701 ) ) ;
#57540 = CARTESIAN_POINT ( 'NONE',  ( 5.142117058706431543, -2.506253911140448487, 29.99999999999988631 ) ) ;
#57541 = CARTESIAN_POINT ( 'NONE',  ( 2.544871794871792936, -3.499999999999999556, 29.75000000000000355 ) ) ;
#57543 = EDGE_CURVE ( 'NONE', #63049, #68522, #24794, .T. ) ;
#57542 = DIRECTION ( 'NONE',  ( 0.000000000000000000, 0.8660254037844377084, -0.5000000000000015543 ) ) ;
#57544 = EDGE_CURVE ( 'NONE', #87399, #26565, #52705, .T. ) ;
#57545 = CARTESIAN_POINT ( 'NONE',  ( 7.912222197156284054, -6.386643153685127139, 34.62446782046654192 ) ) ;
#57546 = ORIENTED_EDGE ( 'NONE', *, *, #63784, .F. ) ;
#57547 = AXIS2_PLACEMENT_3D ( 'NONE', #73046, #17665, #45119 ) ;
#57548 = LINE ( 'NONE', #30086, #83001 ) ;
#57549 = CARTESIAN_POINT ( 'NONE',  ( 6.923076923076924238, -4.786620604624113540, 33.94971097300155094 ) ) ;
#57550 = CARTESIAN_POINT ( 'NONE',  ( -3.749999999999997780, -7.438900925035489387, 15.34561829374151465 ) ) ;
#57551 = ADVANCED_FACE ( 'NONE', ( #23893 ), #38763, .F. ) ;
#57552 = CARTESIAN_POINT ( 'NONE',  ( 9.019230769230775380, -2.499999999999999556, 29.81604066197449754 ) ) ;
#57553 = DIRECTION ( 'NONE',  ( 0.000000000000000000, -0.000000000000000000, 1.000000000000000000 ) ) ;
#57554 = VERTEX_POINT ( 'NONE', #39215 ) ;
#57555 = CARTESIAN_POINT ( 'NONE',  ( 15.23076923076923173, -4.661471528628507777, 34.16647553114623292 ) ) ;
#57557 = EDGE_LOOP ( 'NONE', ( #62291, #43077 ) ) ;
#57556 = CARTESIAN_POINT ( 'NONE',  ( 4.153846153846032507, -6.026961402154118908, 34.52809138561165270 ) ) ;
#57558 = DIRECTION ( 'NONE',  ( 1.000000000000000000, 0.000000000000000000, 0.000000000000000000 ) ) ;
#57559 = DIRECTION ( 'NONE',  ( 0.000000000000000000, 0.9848077530122072432, -0.1736481776669354937 ) ) ;
#57560 = ADVANCED_FACE ( 'NONE', ( #45059 ), #66220, .F. ) ;
#57561 = CARTESIAN_POINT ( 'NONE',  ( -5.207070286361296318, -11.47017969459903952, 32.78971311882034456 ) ) ;
#57562 = CARTESIAN_POINT ( 'NONE',  ( -13.63459211555773720, -3.137211980971221781, 32.19342716148376837 ) ) ;
#57563 = EDGE_CURVE ( 'NONE', #34671, #50071, #52100, .T. ) ;
#57564 = ORIENTED_EDGE ( 'NONE', *, *, #76189, .T. ) ;
#57565 = CARTESIAN_POINT ( 'NONE',  ( -11.76138775597768138, -4.186968288167451036, 33.49512374952580274 ) ) ;
#57566 = CARTESIAN_POINT ( 'NONE',  ( 12.46153846153846168, -6.189225973068211317, 35.74407628777942847 ) ) ;
#57568 = CARTESIAN_POINT ( 'NONE',  ( -2.307692307692305711, -1.422936976036506707, 30.56769352161908415 ) ) ;
#57567 = VECTOR ( 'NONE', #31368, 999.9999999999998863 ) ;
#57569 = ORIENTED_EDGE ( 'NONE', *, *, #66552, .F. ) ;
#57570 = ORIENTED_EDGE ( 'NONE', *, *, #16892, .F. ) ;
#57571 = EDGE_CURVE ( 'NONE', #57617, #54951, #32005, .T. ) ;
#57573 = ORIENTED_EDGE ( 'NONE', *, *, #80658, .T. ) ;
#57572 = B_SPLINE_CURVE_WITH_KNOTS ( 'NONE', 3,
 ( #36164, #57748, #16753, #44208, #71695, #9997, #62718, #55972, #83910, #38368 ),
 .UNSPECIFIED., .F., .F.,
 ( 4, 2, 2, 2, 4 ),
 ( 0.0007817359527651090859, 0.0009771254036996478414, 0.001172514854634186489, 0.001367904305568725136, 0.001563293756503263783 ),
 .UNSPECIFIED. ) ;
#57574 = AXIS2_PLACEMENT_3D ( 'NONE', #29534, #51101, #58320 ) ;
#57575 = VECTOR ( 'NONE', #72016, 1000.000000000000000 ) ;
#57576 = CARTESIAN_POINT ( 'NONE',  ( -9.915792636031639518, -10.11188796281391511, 34.01382737946119050 ) ) ;
#57577 = DIRECTION ( 'NONE',  ( -0.000000000000000000, -0.7660444431189791237, -0.6427876096865379196 ) ) ;
#57578 = ADVANCED_FACE ( 'NONE', ( #59912 ), #37412, .F. ) ;
#57579 = DIRECTION ( 'NONE',  ( -0.000000000000000000, -0.3420201433256694346, -0.9396926207859080948 ) ) ;
#57580 = VECTOR ( 'NONE', #12809, 1000.000000000000000 ) ;
#57581 = DIRECTION ( 'NONE',  ( 0.000000000000000000, 0.000000000000000000, 1.000000000000000000 ) ) ;
#57582 = ADVANCED_FACE ( 'NONE', ( #20702 ), #61232, .F. ) ;
#57583 = ORIENTED_EDGE ( 'NONE', *, *, #4735, .F. ) ;
#57584 = ORIENTED_EDGE ( 'NONE', *, *, #75306, .F. ) ;
#57586 = EDGE_LOOP ( 'NONE', ( #85119, #82754, #83034, #42660 ) ) ;
#57585 = CARTESIAN_POINT ( 'NONE',  ( -2.084729173425631465, -7.369474539155830506, 34.99858011523957657 ) ) ;
#57587 = EDGE_CURVE ( 'NONE', #46688, #47170, #49337, .T. ) ;
#57588 = CARTESIAN_POINT ( 'NONE',  ( 17.32697738856138869, -4.943051570960395047, 34.04725096376909477 ) ) ;
#57589 = DIRECTION ( 'NONE',  ( 0.000000000000000000, 0.3420201433256641055, -0.9396926207859100932 ) ) ;
#57590 = CARTESIAN_POINT ( 'NONE',  ( -8.519285359852727169, -12.68172785388650681, 30.59649109432439218 ) ) ;
#57591 = EDGE_LOOP ( 'NONE', ( #71102, #20269 ) ) ;
#57592 = EDGE_CURVE ( 'NONE', #85237, #67642, #39666, .T. ) ;
#57593 = EDGE_LOOP ( 'NONE', ( #85497, #38363, #56149, #62796 ) ) ;
#57595 = ORIENTED_EDGE ( 'NONE', *, *, #66872, .F. ) ;
#57594 = CARTESIAN_POINT ( 'NONE',  ( 9.915087361285758405, -8.540255544307065350, 34.89611431652622286 ) ) ;
#57596 = LINE ( 'NONE', #3089, #66118 ) ;
#57597 = CARTESIAN_POINT ( 'NONE',  ( -18.23784950573860186, -1.749999999999998668, 28.00000000000000355 ) ) ;
#57598 = ORIENTED_EDGE ( 'NONE', *, *, #6917, .F. ) ;
#57599 = EDGE_CURVE ( 'NONE', #63565, #69312, #15998, .T. ) ;
#57600 = CARTESIAN_POINT ( 'NONE',  ( -8.899922235898326761, -10.54014554554150607, 33.71984207302941883 ) ) ;
#57601 = B_SPLINE_CURVE_WITH_KNOTS ( 'NONE', 3,
 ( #65309, #16681, #37388, #45033, #72511, #10822, #16244, #30636, #59449, #78377 ),
 .UNSPECIFIED., .F., .F.,
 ( 4, 2, 2, 2, 4 ),
 ( 0.000000000000000000, 0.0001954311564186866305, 0.0003908623128373732609, 0.0005862934692560598914, 0.0007817246256747465219 ),
 .UNSPECIFIED. ) ;
#57602 = AXIS2_PLACEMENT_3D ( 'NONE', #56674, #55781, #35970 ) ;
#57603 = AXIS2_PLACEMENT_3D ( 'NONE', #73643, #66871, #41949 ) ;
#57604 = CARTESIAN_POINT ( 'NONE',  ( 5.076923076923075762, -11.16473453929635440, 33.15142922261926373 ) ) ;
#57605 = CARTESIAN_POINT ( 'NONE',  ( 10.74591031714818357, -3.816742781228458448, 33.13167719472716044 ) ) ;
#57606 = FACE_BOUND ( 'NONE', #15007, .T. ) ;
#57607 = DIRECTION ( 'NONE',  ( -0.000000000000000000, 0.000000000000000000, 1.000000000000000000 ) ) ;
#57608 = FACE_OUTER_BOUND ( 'NONE', #6108, .T. ) ;
#57609 = B_SPLINE_CURVE_WITH_KNOTS ( 'NONE', 3,
 ( #73287, #40401, #5273, #17899, #88161, #12473, #81386, #4380, #5713, #39515 ),
 .UNSPECIFIED., .F., .F.,
 ( 4, 2, 2, 2, 4 ),
 ( 0.0007817246256747457630, 0.0009771112852218887673, 0.001172497944769031663, 0.001367884604316174559, 0.001563271263863317672 ),
 .UNSPECIFIED. ) ;
#57610 = FACE_OUTER_BOUND ( 'NONE', #50260, .T. ) ;
#57612 = CARTESIAN_POINT ( 'NONE',  ( 9.942253210655836781, -3.202959910592335646, 32.30730279482227019 ) ) ;
#57611 = CARTESIAN_POINT ( 'NONE',  ( 16.40379156322419973, -4.176053281294515251, 33.81426240980091791 ) ) ;
#57613 = CARTESIAN_POINT ( 'NONE',  ( 8.519254025182178225, -9.234221910056348293, 34.70572697212741531 ) ) ;
#57614 = CARTESIAN_POINT ( 'NONE',  ( 11.53846153846153832, -1.951392089020283160, 34.73218667398347748 ) ) ;
#57615 = VERTEX_POINT ( 'NONE', #48165 ) ;
#57616 = CARTESIAN_POINT ( 'NONE',  ( 14.24236829488800105, -7.749976730030849303, 34.74374725381503737 ) ) ;
#57617 = VERTEX_POINT ( 'NONE', #41421 ) ;
#57618 = EDGE_CURVE ( 'NONE', #53071, #64411, #47283, .T. ) ;
#57619 = ORIENTED_EDGE ( 'NONE', *, *, #54658, .F. ) ;
#57621 = CARTESIAN_POINT ( 'NONE',  ( 10.83816428436268176, -12.11081565061823717, 32.26097654155341843 ) ) ;
#57620 = CYLINDRICAL_SURFACE ( 'NONE', #77753, 0.2500000000000009437 ) ;
#57622 = EDGE_CURVE ( 'NONE', #64660, #71506, #51362, .T. ) ;
#57623 = CARTESIAN_POINT ( 'NONE',  ( 11.53846153846141576, -8.656820664282941280, 34.87096338111179961 ) ) ;
#57624 = CARTESIAN_POINT ( 'NONE',  ( 14.43821774592595553, -4.299079248970732792, 33.91157788607253565 ) ) ;
#57625 = CARTESIAN_POINT ( 'NONE',  ( 1.253923917947829203, -6.413092428213692742, 34.63065189839063152 ) ) ;
#57626 = CARTESIAN_POINT ( 'NONE',  ( -0.3310127597748964146, -11.93748526763465279, 32.05452791011430946 ) ) ;
#57627 = ORIENTED_EDGE ( 'NONE', *, *, #84593, .T. ) ;
#57628 = DIRECTION ( 'NONE',  ( -0.000000000000000000, 0.9396926207859092051, -0.3420201433256662704 ) ) ;
#57629 = CARTESIAN_POINT ( 'NONE',  ( 14.05766908347085042, -12.68155406624981119, 30.59749803192733708 ) ) ;
#57630 = CARTESIAN_POINT ( 'NONE',  ( -12.52762084089859584, -11.35647404775217595, 33.31231777344666511 ) ) ;
#57631 = DIRECTION ( 'NONE',  ( -0.000000000000000000, 0.7660444431189791237, -0.6427876096865379196 ) ) ;
#57632 = CARTESIAN_POINT ( 'NONE',  ( 13.60739505359345536, -5.827830569534417471, 34.72679350104403539 ) ) ;
#57633 = CARTESIAN_POINT ( 'NONE',  ( -2.651650429449535551, -10.15165042944956753, 16.18750000000000000 ) ) ;
#57634 = ORIENTED_EDGE ( 'NONE', *, *, #38260, .F. ) ;
#57635 = AXIS2_PLACEMENT_3D ( 'NONE', #6502, #33962, #62310 ) ;
#57636 = VECTOR ( 'NONE', #42479, 1000.000000000000227 ) ;
#57637 = ORIENTED_EDGE ( 'NONE', *, *, #30037, .T. ) ;
#57638 = DIRECTION ( 'NONE',  ( -0.000000000000000000, 1.000000000000000000, -0.000000000000000000 ) ) ;
#57639 = VERTEX_POINT ( 'NONE', #81981 ) ;
#57640 = DIRECTION ( 'NONE',  ( 0.000000000000000000, 0.3420201433256641055, -0.9396926207859100932 ) ) ;
#57641 = CARTESIAN_POINT ( 'NONE',  ( -13.38461538461538325, -4.102666532097928531, 36.13435417666054406 ) ) ;
#57642 = CARTESIAN_POINT ( 'NONE',  ( 4.088576153289833037, -11.06231777344662781, 33.60647404775220082 ) ) ;
#57643 = CARTESIAN_POINT ( 'NONE',  ( 5.934750068225916664, -2.255955759149247619, 30.00000000000013856 ) ) ;
#57644 = CARTESIAN_POINT ( 'NONE',  ( 3.750000000000009770, -9.053300858899081760, 18.29687500000000000 ) ) ;
#57645 = VECTOR ( 'NONE', #42031, 1000.000000000000000 ) ;
#57646 = B_SPLINE_CURVE_WITH_KNOTS ( 'NONE', 3,
 ( #33836, #54997, #67634, #54543, #74840, #14008, #46901, #27081, #40610, #73950 ),
 .UNSPECIFIED., .F., .F.,
 ( 4, 2, 2, 2, 4 ),
 ( 0.000000000000000000, 0.0001954311564186879044, 0.0003908623128373758088, 0.0005862934692560636861, 0.0007817246256747516176 ),
 .UNSPECIFIED. ) ;
#57647 = DIRECTION ( 'NONE',  ( -1.000000000000000000, 0.000000000000000000, 0.000000000000000000 ) ) ;
#57648 = ORIENTED_EDGE ( 'NONE', *, *, #88535, .F. ) ;
#57649 = CARTESIAN_POINT ( 'NONE',  ( -5.999999999999998224, -2.517432740324522911, 35.29906147534542527 ) ) ;
#57651 = ORIENTED_EDGE ( 'NONE', *, *, #55707, .F. ) ;
#57650 = CARTESIAN_POINT ( 'NONE',  ( -1.134561072977068763, -9.148310452688873440, 34.47095581063188519 ) ) ;
#57652 = CARTESIAN_POINT ( 'NONE',  ( -14.87820512820512953, -7.500000000000000000, 29.75000000000000355 ) ) ;
#57653 = CARTESIAN_POINT ( 'NONE',  ( -12.33074665371367651, -3.530189275343204702, 32.79018710029569661 ) ) ;
#57654 = B_SPLINE_CURVE_WITH_KNOTS ( 'NONE', 3,
 ( #73214, #67344, #61020, #81310, #65993, #80874, #53820, #86748, #88522, #79966 ),
 .UNSPECIFIED., .F., .F.,
 ( 4, 2, 2, 2, 4 ),
 ( 0.000000000000000000, 0.0001954339857564099951, 0.0003908679715128199903, 0.0005863019572692300396, 0.0007817359430256399806 ),
 .UNSPECIFIED. ) ;
#57656 = CARTESIAN_POINT ( 'NONE',  ( 11.47237812750565666, -4.098570777380720287, 33.41473453929634729 ) ) ;
#57655 = B_SPLINE_CURVE_WITH_KNOTS ( 'NONE', 3,
 ( #4697, #31274, #59629, #79907, #24506, #24062, #85781, #46122, #4242, #18209 ),
 .UNSPECIFIED., .F., .F.,
 ( 4, 2, 2, 2, 4 ),
 ( 0.000000000000000000, 0.0001954339857564083146, 0.0003908679715128166293, 0.0005863019572692249439, 0.0007817359430256332585 ),
 .UNSPECIFIED. ) ;
#57657 = CARTESIAN_POINT ( 'NONE',  ( 6.923076923076924238, -3.322132147404559976, 32.92929555188717927 ) ) ;
#57658 = DIRECTION ( 'NONE',  ( 0.000000000000000000, 0.9848077530122072432, -0.1736481776669354937 ) ) ;
#57659 = CARTESIAN_POINT ( 'NONE',  ( -11.31568186948346977, -3.020022701398813236, 32.48759521482552515 ) ) ;
#57660 = CARTESIAN_POINT ( 'NONE',  ( 1.614399933863618797, -3.775308065498751198, 15.73624329374151998 ) ) ;
#57661 = ORIENTED_EDGE ( 'NONE', *, *, #68893, .F. ) ;
#57662 = CARTESIAN_POINT ( 'NONE',  ( -13.13456096470193302, -10.06805714834173493, 34.32951233291982618 ) ) ;
#57663 = CARTESIAN_POINT ( 'NONE',  ( -13.60810032833933469, -9.331801661448606566, 34.40259984581193464 ) ) ;
#57664 = CARTESIAN_POINT ( 'NONE',  ( -1.409462824231155764E-14, -4.749999999999999112, 25.40625000000000000 ) ) ;
#57665 = CARTESIAN_POINT ( 'NONE',  ( -16.08859101433331062, -11.67786785259547777, 32.92929555188713664 ) ) ;
#57666 = CARTESIAN_POINT ( 'NONE',  ( 16.15384615384603251, -5.094484230521993062, 34.41647553114689373 ) ) ;
#57667 = ORIENTED_EDGE ( 'NONE', *, *, #25204, .F. ) ;
#57668 = DIRECTION ( 'NONE',  ( 0.000000000000000000, 0.8660254037844377084, -0.5000000000000015543 ) ) ;
#57669 = LINE ( 'NONE', #50459, #26797 ) ;
#57670 = EDGE_CURVE ( 'NONE', #10085, #66377, #56820, .T. ) ;
#57671 = ORIENTED_EDGE ( 'NONE', *, *, #70043, .T. ) ;
#57672 = CARTESIAN_POINT ( 'NONE',  ( -12.46153846153846168, -1.466349020453238561, 30.81389545987213907 ) ) ;
#57673 = EDGE_CURVE ( 'NONE', #62136, #29682, #33342, .T. ) ;
#57674 = ORIENTED_EDGE ( 'NONE', *, *, #14593, .T. ) ;
#57675 = CARTESIAN_POINT ( 'NONE',  ( 20.00000000000000000, -4.000000000000000000, 29.75000000000000355 ) ) ;
#57676 = CARTESIAN_POINT ( 'NONE',  ( 3.100078627658921615, -3.957541250942359756, 33.62499894934981626 ) ) ;
#57677 = CARTESIAN_POINT ( 'NONE',  ( -0.7115152055870533898, -10.06842814019191401, 34.32929386961144758 ) ) ;
#57678 = DIRECTION ( 'NONE',  ( -0.000000000000000000, 0.9848077530122086864, -0.1736481776669273891 ) ) ;
#57680 = ORIENTED_EDGE ( 'NONE', *, *, #5486, .T. ) ;
#57679 = AXIS2_PLACEMENT_3D ( 'NONE', #75077, #41291, #61105 ) ;
#57681 = ADVANCED_FACE ( 'NONE', ( #13943 ), #60801, .F. ) ;
#57682 = CARTESIAN_POINT ( 'NONE',  ( -13.31854805126531005, -2.833524468853757305, 32.15551576947925838 ) ) ;
#57683 = ORIENTED_EDGE ( 'NONE', *, *, #80522, .T. ) ;
#57684 = B_SPLINE_CURVE_WITH_KNOTS ( 'NONE', 3,
 ( #27271, #21845, #27709, #43006, #54735, #7452, #49320, #55180, #56072, #34908 ),
 .UNSPECIFIED., .F., .F.,
 ( 4, 2, 2, 2, 4 ),
 ( 0.0007817246256747499913, 0.0009771112852218944052, 0.001172497944769038819, 0.001367884604316183016, 0.001563271263863327430 ),
 .UNSPECIFIED. ) ;
#57685 = CYLINDRICAL_SURFACE ( 'NONE', #37075, 0.2499999999999986955 ) ;
#57686 = CARTESIAN_POINT ( 'NONE',  ( 6.000000000000001776, -13.57706302396349152, 30.56769352161908060 ) ) ;
#57687 = VERTEX_POINT ( 'NONE', #26132 ) ;
#57688 = B_SPLINE_CURVE_WITH_KNOTS ( 'NONE', 3,
 ( #79026, #9676, #24078, #23194, #64163, #37590, #65052, #78136, #2032, #17328 ),
 .UNSPECIFIED., .F., .F.,
 ( 4, 2, 2, 2, 4 ),
 ( 0.0007817246256747471724, 0.0009771112852218905021, 0.001172497944769033832, 0.001367884604316177161, 0.001563271263863320491 ),
 .UNSPECIFIED. ) ;
#57689 = PLANE ( 'NONE',  #5934 ) ;
#57690 = CARTESIAN_POINT ( 'NONE',  ( -12.52680890749923570, -6.026961402152685388, 34.52809138561120506 ) ) ;
#57691 = DIRECTION ( 'NONE',  ( -0.000000000000000000, -5.102127870520021228E-17, -1.000000000000000000 ) ) ;
#57692 = ADVANCED_FACE ( 'NONE', ( #88310 ), #15724, .F. ) ;
#57693 = CARTESIAN_POINT ( 'NONE',  ( 1.161688425708537808, -6.459968553980839800, 34.89616026154728701 ) ) ;
#57694 = CARTESIAN_POINT ( 'NONE',  ( -11.00641025641025550, -7.500000000000000000, 29.75000000000000355 ) ) ;
#57695 = B_SPLINE_CURVE_WITH_KNOTS ( 'NONE', 3,
 ( #85477, #22005, #35969, #50342, #17013, #43595, #36410, #44466, #35521, #37276 ),
 .UNSPECIFIED., .F., .F.,
 ( 4, 2, 2, 2, 4 ),
 ( 0.000000000000000000, 0.0001954311564186875792, 0.0003908623128373751583, 0.0005862934692560627103, 0.0007817246256747503166 ),
 .UNSPECIFIED. ) ;
#57696 = ORIENTED_EDGE ( 'NONE', *, *, #7047, .F. ) ;
#57697 = ORIENTED_EDGE ( 'NONE', *, *, #54236, .F. ) ;
#57698 = AXIS2_PLACEMENT_3D ( 'NONE', #38492, #16877, #10121 ) ;
#57699 = FACE_BOUND ( 'NONE', #14106, .T. ) ;
#57700 = ORIENTED_EDGE ( 'NONE', *, *, #29929, .T. ) ;
#57701 = CARTESIAN_POINT ( 'NONE',  ( -5.076923076922761346, -2.255955759149395501, 30.00000000000324363 ) ) ;
#57702 = EDGE_CURVE ( 'NONE', #25936, #8816, #55369, .T. ) ;
#57703 = AXIS2_PLACEMENT_3D ( 'NONE', #6349, #68043, #54963 ) ;
#57704 = EDGE_CURVE ( 'NONE', #45635, #66313, #68644, .T. ) ;
#57705 = CARTESIAN_POINT ( 'NONE',  ( 13.45068373561782593, -10.51840700105979565, 33.73612834413962247 ) ) ;
#57706 = CARTESIAN_POINT ( 'NONE',  ( -10.61538461538473577, -10.33852847137269571, 34.16647553114546554 ) ) ;
#57707 = VERTEX_POINT ( 'NONE', #50374 ) ;
#57708 = VECTOR ( 'NONE', #14964, 1000.000000000000000 ) ;
#57709 = VERTEX_POINT ( 'NONE', #76083 ) ;
#57710 = VERTEX_POINT ( 'NONE', #77851 ) ;
#57711 = CARTESIAN_POINT ( 'NONE',  ( 3.230769230769110045, -5.219633306517616589, 34.19971097300220464 ) ) ;
#57712 = VERTEX_POINT ( 'NONE', #43189 ) ;
#57713 = CARTESIAN_POINT ( 'NONE',  ( -4.153846153846152411, -5.180354513474913603, 36.12317359536750416 ) ) ;
#57714 = ADVANCED_FACE ( 'NONE', ( #16157 ), #7640, .F. ) ;
#57715 = CARTESIAN_POINT ( 'NONE',  ( 3.230769230769110045, -2.892918686052166066, 31.69288490824153470 ) ) ;
#57716 = CARTESIAN_POINT ( 'NONE',  ( -2.530619266599154038, -12.38737895849757820, 31.66785238281580206 ) ) ;
#57717 = FACE_BOUND ( 'NONE', #55864, .T. ) ;
#57718 = ORIENTED_EDGE ( 'NONE', *, *, #47017, .F. ) ;
#57719 = DIRECTION ( 'NONE',  ( -0.000000000000000000, 1.000000000000000000, -0.000000000000000000 ) ) ;
#57720 = CARTESIAN_POINT ( 'NONE',  ( -12.46153846153846168, -2.708943851104267164, 35.45975837776705220 ) ) ;
#57721 = CYLINDRICAL_SURFACE ( 'NONE', #52404, 0.2499999999999979738 ) ;
#57722 = CARTESIAN_POINT ( 'NONE',  ( 11.66898724022510514, -8.586989748646452369, 34.63063291749215011 ) ) ;
#57723 = VERTEX_POINT ( 'NONE', #84633 ) ;
#57724 = CARTESIAN_POINT ( 'NONE',  ( -17.32694631421604115, -12.43535235679832596, 30.55408501211184813 ) ) ;
#57725 = ORIENTED_EDGE ( 'NONE', *, *, #52850, .F. ) ;
#57726 = EDGE_CURVE ( 'NONE', #80807, #27135, #67529, .T. ) ;
#57727 = EDGE_LOOP ( 'NONE', ( #27353, #4070 ) ) ;
#57729 = LINE ( 'NONE', #71231, #64917 ) ;
#57728 = CARTESIAN_POINT ( 'NONE',  ( -18.00000000000000711, -2.252971138473345292, 29.99985851721553942 ) ) ;
#57730 = CIRCLE ( 'NONE', #67776, 1.999999999999998224 ) ;
#57731 = CARTESIAN_POINT ( 'NONE',  ( -8.638705330997124676, -12.50538340440932394, 31.33453814440721885 ) ) ;
#57732 = CARTESIAN_POINT ( 'NONE',  ( 16.15384615384615330, -5.415277668671390821, 36.20867863119892149 ) ) ;
#57733 = ADVANCED_FACE ( 'NONE', ( #49934 ), #70660, .F. ) ;
#57734 = CARTESIAN_POINT ( 'NONE',  ( -18.13014796973169851, -5.915902021225892149, 34.75552854090298638 ) ) ;
#57735 = DIRECTION ( 'NONE',  ( -0.000000000000000000, 0.6427876096865404731, -0.7660444431189770143 ) ) ;
#57736 = EDGE_CURVE ( 'NONE', #48416, #47272, #35100, .T. ) ;
#57737 = EDGE_LOOP ( 'NONE', ( #64486, #13491, #86551, #11253 ) ) ;
#57738 = CYLINDRICAL_SURFACE ( 'NONE', #57296, 4.000000000000000000 ) ;
#57739 = DIRECTION ( 'NONE',  ( -0.000000000000000000, 1.000000000000000000, -0.000000000000000000 ) ) ;
#57740 = CARTESIAN_POINT ( 'NONE',  ( -17.32694631421604115, -11.86270091957321071, 32.19358267280088626 ) ) ;
#57741 = CARTESIAN_POINT ( 'NONE',  ( 14.30769230769218581, -2.657715359629662544, 31.77849191805970364 ) ) ;
#57742 = VECTOR ( 'NONE', #4036, 1000.000000000000000 ) ;
#57743 = VERTEX_POINT ( 'NONE', #22032 ) ;
#57744 = EDGE_CURVE ( 'NONE', #43102, #6970, #49507, .T. ) ;
#57745 = EDGE_LOOP ( 'NONE', ( #11508, #44894, #23878, #77482 ) ) ;
#57746 = FACE_BOUND ( 'NONE', #20578, .T. ) ;
#57747 = DIRECTION ( 'NONE',  ( -1.000000000000000000, -0.000000000000000000, 0.000000000000000000 ) ) ;
#57748 = CARTESIAN_POINT ( 'NONE',  ( -6.673076923076859401, -7.434744429011176159, 34.75000000000000711 ) ) ;
#57749 = ORIENTED_EDGE ( 'NONE', *, *, #12411, .T. ) ;
#57750 = CARTESIAN_POINT ( 'NONE',  ( 0.000000000000000000, -11.00000000000000000, 29.75000000000000355 ) ) ;
#57751 = CARTESIAN_POINT ( 'NONE',  ( 5.999999999999878320, -11.67786785259630911, 32.92929555188603530 ) ) ;
#57752 = DIRECTION ( 'NONE',  ( -0.000000000000000000, 1.000000000000000000, -0.000000000000000000 ) ) ;
#57753 = CARTESIAN_POINT ( 'NONE',  ( -6.673022611438607754, -3.136992222400443175, 32.19305428654138979 ) ) ;
#57754 = ORIENTED_EDGE ( 'NONE', *, *, #47841, .F. ) ;
#57755 = CARTESIAN_POINT ( 'NONE',  ( 8.769230769230768274, -1.790695186598648903, 34.54067556320373455 ) ) ;
#57756 = EDGE_LOOP ( 'NONE', ( #68141, #86164 ) ) ;
#57758 = ORIENTED_EDGE ( 'NONE', *, *, #23029, .F. ) ;
#57757 = DIRECTION ( 'NONE',  ( 0.000000000000000000, 0.000000000000000000, 1.000000000000000000 ) ) ;
#57759 = CARTESIAN_POINT ( 'NONE',  ( 15.45378058238208041, -8.239487800360276282, 34.69522927552633718 ) ) ;
#57760 = CARTESIAN_POINT ( 'NONE',  ( -4.153846153846273204, -2.892918686052165622, 31.69288490824153470 ) ) ;
#57761 = LINE ( 'NONE', #32068, #1256 ) ;
#57762 = CYLINDRICAL_SURFACE ( 'NONE', #35198, 0.2499999999999986955 ) ;
#57763 = CARTESIAN_POINT ( 'NONE',  ( 13.38461538461538680, -5.557115091759785130, 34.35708131394839171 ) ) ;
#57764 = CARTESIAN_POINT ( 'NONE',  ( 14.16025641025641235, -3.499999999999999556, 29.75000000000000355 ) ) ;
#57765 = CARTESIAN_POINT ( 'NONE',  ( 2.750000000000008438, -8.639087296525996607, 23.29687500000000000 ) ) ;
#57766 = ORIENTED_EDGE ( 'NONE', *, *, #15929, .T. ) ;
#57767 = CARTESIAN_POINT ( 'NONE',  ( -0.6850234052624096792, -5.912607949931405926, 34.49155766932282319 ) ) ;
#57768 = FACE_OUTER_BOUND ( 'NONE', #31699, .T. ) ;
#57769 = VERTEX_POINT ( 'NONE', #70218 ) ;
#57770 = AXIS2_PLACEMENT_3D ( 'NONE', #60608, #54739, #47537 ) ;
#57771 = ORIENTED_EDGE ( 'NONE', *, *, #5196, .T. ) ;
#57772 = VERTEX_POINT ( 'NONE', #8966 ) ;
#57773 = DIRECTION ( 'NONE',  ( -0.000000000000000000, 0.8660254037844397068, -0.4999999999999978906 ) ) ;
#57774 = CARTESIAN_POINT ( 'NONE',  ( 12.68455130563185840, -4.026326845037962343, 33.68677907613344047 ) ) ;
#57775 = CARTESIAN_POINT ( 'NONE',  ( 3.165498784808455923, -10.21337939537584383, 33.94971097300158647 ) ) ;
#57776 = VECTOR ( 'NONE', #18897, 1000.000000000000000 ) ;
#57777 = DIRECTION ( 'NONE',  ( 0.000000000000000000, 0.1736481776669267785, -0.9848077530122087975 ) ) ;
#57778 = CARTESIAN_POINT ( 'NONE',  ( -17.07692307692307665, -2.900454961884010974, 35.62045528018868623 ) ) ;
#57779 = DIRECTION ( 'NONE',  ( -0.000000000000000000, 0.9396926207859093161, -0.3420201433256663259 ) ) ;
#57780 = CARTESIAN_POINT ( 'NONE',  ( 1.384615384615386802, -6.435427911321262684, 35.78748833219616898 ) ) ;
#57781 = ORIENTED_EDGE ( 'NONE', *, *, #58854, .F. ) ;
#57782 = DIRECTION ( 'NONE',  ( -0.000000000000000000, -0.6427876096865404731, -0.7660444431189770143 ) ) ;
#57783 = CARTESIAN_POINT ( 'NONE',  ( -0.2385271099256120464, -8.239487800360278058, 34.69522927552634428 ) ) ;
#57784 = CARTESIAN_POINT ( 'NONE',  ( -9.561781990544131915, -11.46989282347013095, 32.79007818306219946 ) ) ;
#57785 = CARTESIAN_POINT ( 'NONE',  ( 14.30769230769231015, -8.164416787775445883, 34.95778746994557906 ) ) ;
#57786 = EDGE_LOOP ( 'NONE', ( #939, #70407 ) ) ;
#57787 = CARTESIAN_POINT ( 'NONE',  ( 0.4615384615384611200, -9.905515769479276145, 34.41647553114623292 ) ) ;
#57788 = ORIENTED_EDGE ( 'NONE', *, *, #51576, .F. ) ;
#57789 = CARTESIAN_POINT ( 'NONE',  ( 0.7115927731767761610, -9.148310452688873440, 34.47095581063188519 ) ) ;
#57790 = CARTESIAN_POINT ( 'NONE',  ( -8.769230769230768274, -2.499999999999998668, 29.75000000000001421 ) ) ;
#57791 = LINE ( 'NONE', #29453, #41206 ) ;
#57792 = CARTESIAN_POINT ( 'NONE',  ( 12.59233026936324684, -10.54018710029568595, 33.71981072465678864 ) ) ;
#57793 = ORIENTED_EDGE ( 'NONE', *, *, #78408, .T. ) ;
#57794 = CARTESIAN_POINT ( 'NONE',  ( -2.437840277424001556, -6.809168938359898782, 34.95455904226513866 ) ) ;
#57795 = CARTESIAN_POINT ( 'NONE',  ( -16.15384615384615330, -8.318370150425687726, 35.83090037661290239 ) ) ;
#57796 = CARTESIAN_POINT ( 'NONE',  ( -18.00000000104979492, -12.75000000000000355, 29.50000000010276935 ) ) ;
#57797 = B_SPLINE_CURVE_WITH_KNOTS ( 'NONE', 3,
 ( #49119, #76598, #42380, #5924, #2246, #56759, #36500, #70281, #8143, #29307 ),
 .UNSPECIFIED., .F., .F.,
 ( 4, 2, 2, 2, 4 ),
 ( 0.000000000000000000, 0.0001954339857564074473, 0.0003908679715128148945, 0.0005863019572692223418, 0.0007817359430256297891 ),
 .UNSPECIFIED. ) ;
#57798 = VECTOR ( 'NONE', #52740, 1000.000000000000000 ) ;
#57799 = CARTESIAN_POINT ( 'NONE',  ( -2.980823712421088345, -12.22109172314383052, 31.39792113162168263 ) ) ;
#57800 = ORIENTED_EDGE ( 'NONE', *, *, #514, .T. ) ;
#57801 = CARTESIAN_POINT ( 'NONE',  ( -1.254089682851817988, -3.816742781228458448, 33.13167719472716044 ) ) ;
#57802 = ORIENTED_EDGE ( 'NONE', *, *, #41341, .F. ) ;
#57803 = CIRCLE ( 'NONE', #23265, 4.000000000000000000 ) ;
#57804 = LINE ( 'NONE', #31214, #29043 ) ;
#57805 = CARTESIAN_POINT ( 'NONE',  ( 7.145856592054986578, -3.020022701398814569, 32.48759521482552515 ) ) ;
#57806 = CARTESIAN_POINT ( 'NONE',  ( -1.515305987725692249, -9.084618155246140248, 34.75535874321725771 ) ) ;
#57807 = CARTESIAN_POINT ( 'NONE',  ( -14.05774678934416499, -10.05730279482229683, 34.04704008940765902 ) ) ;
#57808 = FACE_OUTER_BOUND ( 'NONE', #40430, .T. ) ;
#57809 = B_SPLINE_CURVE_WITH_KNOTS ( 'NONE', 3,
 ( #12974, #61143, #89097, #48513, #62906, #88656, #7096, #54839, #41779, #6653 ),
 .UNSPECIFIED., .F., .F.,
 ( 4, 2, 2, 2, 4 ),
 ( 0.0007817246256747507503, 0.0009771112852218957062, 0.001172497944769040771, 0.001367884604316185835, 0.001563271263863330682 ),
 .UNSPECIFIED. ) ;
#57810 = VERTEX_POINT ( 'NONE', #42756 ) ;
#57811 = B_SPLINE_CURVE_WITH_KNOTS ( 'NONE', 3,
 ( #45395, #45843, #51236, #44947, #59361, #66572, #37304, #4878, #10736, #52598 ),
 .UNSPECIFIED., .F., .F.,
 ( 4, 2, 2, 2, 4 ),
 ( 0.0007817246256747463051, 0.0009771112852218896347, 0.001172497944769033181, 0.001367884604316176728, 0.001563271263863320057 ),
 .UNSPECIFIED. ) ;
#57812 = EDGE_LOOP ( 'NONE', ( #55520, #54221, #27682, #52634 ) ) ;
#57813 = PRODUCT_DEFINITION_SHAPE ( 'NONE', 'NONE',  #79883 ) ;
#57814 = EDGE_LOOP ( 'NONE', ( #28485, #34894, #30582, #76872 ) ) ;
#57815 = ORIENTED_EDGE ( 'NONE', *, *, #22750, .F. ) ;
#57816 = ADVANCED_FACE ( 'NONE', ( #14390 ), #41870, .F. ) ;
#57817 = CARTESIAN_POINT ( 'NONE',  ( -10.54931626438217585, -8.120952969808772792, 34.71129190929999453 ) ) ;
#57818 = DIRECTION ( 'NONE',  ( 1.000000000000000000, 0.000000000000000000, 0.000000000000000000 ) ) ;
#57819 = CARTESIAN_POINT ( 'NONE',  ( -5.299749769402080979, -7.369208160676172348, 34.74850200257122879 ) ) ;
#57820 = CARTESIAN_POINT ( 'NONE',  ( -18.00000000000000000, -2.724637637897661335, 35.44105525097462106 ) ) ;
#57821 = CARTESIAN_POINT ( 'NONE',  ( -13.16160403300253634, -5.667800583137506010, 34.40243808032445827 ) ) ;
#57822 = CIRCLE ( 'NONE', #26208, 4.000000000000000000 ) ;
#57823 = CARTESIAN_POINT ( 'NONE',  ( -6.130147969731697621, -3.069018819979302926, 32.56621877034667278 ) ) ;
#57824 = VECTOR ( 'NONE', #79193, 1000.000000000000000 ) ;
#57825 = CARTESIAN_POINT ( 'NONE',  ( 5.999999999999880096, -11.94971097300221174, 32.03036669348237098 ) ) ;
#57826 = CARTESIAN_POINT ( 'NONE',  ( -17.77722045873158763, -6.760870238392815423, 34.69528174975672385 ) ) ;
#57827 = ORIENTED_EDGE ( 'NONE', *, *, #70420, .F. ) ;
#57828 = VERTEX_POINT ( 'NONE', #36435 ) ;
#57829 = VECTOR ( 'NONE', #48586, 1000.000000000000227 ) ;
#57830 = ORIENTED_EDGE ( 'NONE', *, *, #14227, .F. ) ;
#57832 = EDGE_LOOP ( 'NONE', ( #43303, #38104 ) ) ;
#57831 = DIRECTION ( 'NONE',  ( 0.000000000000000000, 0.000000000000000000, 1.000000000000000000 ) ) ;
#57834 = DIRECTION ( 'NONE',  ( 0.000000000000000000, 0.9396926207859126468, -0.3420201433256571111 ) ) ;
#57833 = CARTESIAN_POINT ( 'NONE',  ( 0.7114839798866022802, -8.433404298154336232, 34.66254593164985920 ) ) ;
#57835 = DIRECTION ( 'NONE',  ( -1.000000000000000000, -0.000000000000000000, -0.000000000000000000 ) ) ;
#57836 = EDGE_CURVE ( 'NONE', #35268, #32683, #84192, .T. ) ;
#57837 = CARTESIAN_POINT ( 'NONE',  ( 2.651650429449569302, -10.15165042944953733, 25.87500000000000355 ) ) ;
#57838 = EDGE_CURVE ( 'NONE', #35434, #57639, #1959, .T. ) ;
#57839 = EDGE_LOOP ( 'NONE', ( #70662, #71673 ) ) ;
#57840 = ORIENTED_EDGE ( 'NONE', *, *, #43902, .T. ) ;
#57841 = CARTESIAN_POINT ( 'NONE',  ( -2.557715544985270650, -12.43535235679832596, 30.55408501211184813 ) ) ;
#57842 = VERTEX_POINT ( 'NONE', #86863 ) ;
#57843 = FACE_BOUND ( 'NONE', #51957, .T. ) ;
#57844 = CARTESIAN_POINT ( 'NONE',  ( 0.6089743589743582541, -7.500000000000000000, 29.75000000000000355 ) ) ;
#57845 = DIRECTION ( 'NONE',  ( -0.000000000000000000, -0.5000000000000009992, -0.8660254037844380415 ) ) ;
#57846 = ORIENTED_EDGE ( 'NONE', *, *, #89142, .F. ) ;
#57847 = CARTESIAN_POINT ( 'NONE',  ( -15.23076923076935074, -5.219633306517616589, 34.19971097300220464 ) ) ;
#57848 = DIRECTION ( 'NONE',  ( -0.000000000000000000, -0.6427876096865404731, -0.7660444431189771253 ) ) ;
#57849 = CARTESIAN_POINT ( 'NONE',  ( 17.99999999999987566, -8.613356846316285953, 34.62446782046622218 ) ) ;
#57850 = EDGE_LOOP ( 'NONE', ( #68255, #66689 ) ) ;
#57851 = DIRECTION ( 'NONE',  ( -0.000000000000000000, -0.000000000000000000, -1.000000000000000000 ) ) ;
#57852 = FACE_OUTER_BOUND ( 'NONE', #82286, .T. ) ;
#57853 = ORIENTED_EDGE ( 'NONE', *, *, #84696, .T. ) ;
#57854 = CARTESIAN_POINT ( 'NONE',  ( -6.673022611438605978, -9.148310452688871663, 34.47095581063188519 ) ) ;
#57855 = VECTOR ( 'NONE', #12771, 1000.000000000000000 ) ;
#57856 = CARTESIAN_POINT ( 'NONE',  ( -6.989160334032800570, -11.16473453929635440, 33.15142922261925662 ) ) ;
#57857 = DIRECTION ( 'NONE',  ( -0.000000000000000000, 1.000000000000000000, 3.491481338843133355E-15 ) ) ;
#57858 = PLANE ( 'NONE',  #48455 ) ;
#57859 = CARTESIAN_POINT ( 'NONE',  ( -10.36533030374629938, -5.728107161865378494, 34.42597550085002922 ) ) ;
#57860 = CARTESIAN_POINT ( 'NONE',  ( -23.50000000000000000, 12.75000000000000355, 13.00000000000000178 ) ) ;
#57861 = CARTESIAN_POINT ( 'NONE',  ( 8.069166690247241647, -2.889357225399416418, 32.26129605718031002 ) ) ;
#57863 = CARTESIAN_POINT ( 'NONE',  ( 7.846153846153846700, -4.661471528628507777, 34.16647553114623292 ) ) ;
#57862 = CARTESIAN_POINT ( 'NONE',  ( -1.384615384615383471, -2.721908614388771852, 31.22303859784724978 ) ) ;
#57864 = DIRECTION ( 'NONE',  ( -0.000000000000000000, -0.3420201433256694346, -0.9396926207859080948 ) ) ;
#57866 = CARTESIAN_POINT ( 'NONE',  ( 5.076923076922953193, -2.657715359629662988, 31.77849191805970364 ) ) ;
#57865 = CARTESIAN_POINT ( 'NONE',  ( -15.23076923076935074, -11.94971097300221174, 32.03036669348237098 ) ) ;
#57867 = CARTESIAN_POINT ( 'NONE',  ( -5.869474298236438514, -12.45806712695776319, 30.39783852428763922 ) ) ;
#57868 = CARTESIAN_POINT ( 'NONE',  ( 2.724691934501235036, -6.299813628509441266, 22.88875670625849068 ) ) ;
#57869 = EDGE_LOOP ( 'NONE', ( #35944, #86779, #44508, #3799 ) ) ;
#57870 = CARTESIAN_POINT ( 'NONE',  ( 3.299694722263635693, -7.944920208824736818, 14.00000000000000178 ) ) ;
#57871 = EDGE_LOOP ( 'NONE', ( #48217, #6372, #27978, #14406 ) ) ;
#57872 = CARTESIAN_POINT ( 'NONE',  ( 9.442284455014730682, -6.695914987888146541, 34.68535235679833306 ) ) ;
#57873 = VERTEX_POINT ( 'NONE', #72420 ) ;
#57874 = CARTESIAN_POINT ( 'NONE',  ( -4.088590582570128973, -11.48612834413965977, 32.76840700105972815 ) ) ;
#57875 = ORIENTED_EDGE ( 'NONE', *, *, #78502, .F. ) ;
#57876 = CARTESIAN_POINT ( 'NONE',  ( -5.326923076923075762, -7.500000000000001776, 34.75000000000000000 ) ) ;
#57877 = CARTESIAN_POINT ( 'NONE',  ( -2.724691934501232371, -8.700186371490559623, 26.01375670625848713 ) ) ;
#57878 = CARTESIAN_POINT ( 'NONE',  ( 7.623226887246995709, -8.282780595021769443, 34.94152052738834868 ) ) ;
#57879 = CARTESIAN_POINT ( 'NONE',  ( 8.769230769230768274, -3.886160181151819604, 36.00935417666054406 ) ) ;
#57880 = CARTESIAN_POINT ( 'NONE',  ( 13.44987052412822059, -3.083524468853784839, 32.58852847137153930 ) ) ;
#57881 = LINE ( 'NONE', #71389, #63334 ) ;
#57882 = DIRECTION ( 'NONE',  ( 1.000000000000000000, 0.000000000000000000, 0.000000000000000000 ) ) ;
#57883 = CARTESIAN_POINT ( 'NONE',  ( 11.31553532094538994, -2.758268499246657068, 31.33685645148948140 ) ) ;
#57884 = CARTESIAN_POINT ( 'NONE',  ( 2.307692307692309264, -12.34228464037088635, 31.77849191805839268 ) ) ;
#57885 = CARTESIAN_POINT ( 'NONE',  ( -3.749999999999997335, -7.500000000000021316, 16.34375000000000000 ) ) ;
#57886 = CARTESIAN_POINT ( 'NONE',  ( -11.47239420511146157, -2.486705287966280320, 31.30864560766543647 ) ) ;
#57887 = FACE_OUTER_BOUND ( 'NONE', #17702, .T. ) ;
#57888 = CARTESIAN_POINT ( 'NONE',  ( 14.30769230769231015, -3.050289026998446396, 32.03036669348365706 ) ) ;
#57889 = CARTESIAN_POINT ( 'NONE',  ( 2.651650429449569302, -10.15165042944953733, 17.12500000000000000 ) ) ;
#57890 = VECTOR ( 'NONE', #42492, 1000.000000000000000 ) ;
#57891 = AXIS2_PLACEMENT_3D ( 'NONE', #81643, #68559, #34326 ) ;
#57892 = ORIENTED_EDGE ( 'NONE', *, *, #26244, .F. ) ;
#57893 = CARTESIAN_POINT ( 'NONE',  ( -2.939152317953646711E-15, 7.500000000000000000, 13.50000000000000178 ) ) ;
#57894 = CARTESIAN_POINT ( 'NONE',  ( 12.46153846153833911, -8.656820664282941280, 34.87096338111179961 ) ) ;
#57895 = CARTESIAN_POINT ( 'NONE',  ( 1.134638640566795420, -5.643011162660950042, 34.66104346484419096 ) ) ;
#57896 = LINE ( 'NONE', #79061, #45557 ) ;
#57897 = CARTESIAN_POINT ( 'NONE',  ( 15.10029252265276867, -7.276988635370452485, 34.74523720219453793 ) ) ;
#57898 = VECTOR ( 'NONE', #14708, 1000.000000000000000 ) ;
#57899 = ADVANCED_FACE ( 'NONE', ( #3956 ), #31443, .T. ) ;
#57900 = CARTESIAN_POINT ( 'NONE',  ( -3.230769230769352962, -5.941354392335915335, 34.76329471203413846 ) ) ;
#57901 = EDGE_CURVE ( 'NONE', #15863, #83740, #4411, .T. ) ;
#57902 = ORIENTED_EDGE ( 'NONE', *, *, #52499, .F. ) ;
#57903 = DIRECTION ( 'NONE',  ( -0.000000000000000000, 1.000000000000000000, -0.000000000000000000 ) ) ;
#57904 = ORIENTED_EDGE ( 'NONE', *, *, #76055, .T. ) ;
#57905 = ORIENTED_EDGE ( 'NONE', *, *, #59703, .T. ) ;
#57906 = DIRECTION ( 'NONE',  ( -0.000000000000000000, 1.000000000000000000, -0.000000000000000000 ) ) ;
#57907 = EDGE_CURVE ( 'NONE', #1726, #74923, #83644, .T. ) ;
#57908 = CARTESIAN_POINT ( 'NONE',  ( -6.792286482109972212, -5.496552790871117367, 34.60292014791297532 ) ) ;
#57909 = CARTESIAN_POINT ( 'NONE',  ( -8.899378738962466784, -2.373036134822904319, 30.88089517874952250 ) ) ;
#57910 = ADVANCED_FACE ( 'NONE', ( #37301 ), #24228, .F. ) ;
#57911 = DIRECTION ( 'NONE',  ( -1.000000000000000000, -1.845450506358306311E-16, 0.000000000000000000 ) ) ;
#57912 = CARTESIAN_POINT ( 'NONE',  ( 10.68063975489745232, -10.33852847137154107, 34.16647553114620450 ) ) ;
#57913 = B_SPLINE_CURVE_WITH_KNOTS ( 'NONE', 3,
 ( #43216, #62590, #2215, #84660, #902, #83775 ),
 .UNSPECIFIED., .F., .F.,
 ( 4, 2, 4 ),
 ( 0.0003909512603273874185, 0.0005862562993132133804, 0.0007815613382990393423 ),
 .UNSPECIFIED. ) ;
#57914 = ORIENTED_EDGE ( 'NONE', *, *, #32820, .T. ) ;
#57915 = AXIS2_PLACEMENT_3D ( 'NONE', #68535, #33862, #68105 ) ;
#57916 = B_SPLINE_CURVE_WITH_KNOTS ( 'NONE', 3,
 ( #52306, #45553, #72133, #79798, #59514, #3672, #2773, #73033, #65378, #11328 ),
 .UNSPECIFIED., .F., .F.,
 ( 4, 2, 2, 2, 4 ),
 ( 0.0007817359430256372700, 0.0009771253907250052138, 0.001172514838424373049, 0.001367904286123741101, 0.001563293733823108937 ),
 .UNSPECIFIED. ) ;
#57917 = DIRECTION ( 'NONE',  ( -0.000000000000000000, 0.3420201433256694346, -0.9396926207859080948 ) ) ;
#57918 = AXIS2_PLACEMENT_3D ( 'NONE', #31394, #58863, #16109 ) ;
#57919 = VERTEX_POINT ( 'NONE', #52593 ) ;
#57920 = VERTEX_POINT ( 'NONE', #80078 ) ;
#57921 = EDGE_CURVE ( 'NONE', #78112, #45549, #18380, .T. ) ;
#57922 = CARTESIAN_POINT ( 'NONE',  ( -4.153846153846152411, -11.91647553114624181, 32.58852847137148245 ) ) ;
#57923 = DIRECTION ( 'NONE',  ( 0.000000000000000000, 0.000000000000000000, 1.000000000000000000 ) ) ;
#57924 = CYLINDRICAL_SURFACE ( 'NONE', #6333, 0.2500000000000002220 ) ;
#57925 = CARTESIAN_POINT ( 'NONE',  ( -16.85414353565466783, -3.236590943229499473, 32.36255958852954251 ) ) ;
#57926 = DIRECTION ( 'NONE',  ( 0.000000000000000000, 0.000000000000000000, 1.000000000000000000 ) ) ;
#57927 = ORIENTED_EDGE ( 'NONE', *, *, #36088, .T. ) ;
#57928 = ORIENTED_EDGE ( 'NONE', *, *, #16116, .F. ) ;
#57929 = CARTESIAN_POINT ( 'NONE',  ( -3.749999999999988454, -9.053300858899127945, 23.76562499999999645 ) ) ;
#57930 = VERTEX_POINT ( 'NONE', #78290 ) ;
#57932 = ORIENTED_EDGE ( 'NONE', *, *, #85795, .T. ) ;
#57931 = CARTESIAN_POINT ( 'NONE',  ( 2.307692307692309264, -12.37446782046654192, 30.86335684631486131 ) ) ;
#57933 = CARTESIAN_POINT ( 'NONE',  ( -3.230769230768923084, -2.506253911140615021, 30.00000000000323297 ) ) ;
#57934 = FACE_OUTER_BOUND ( 'NONE', #39672, .T. ) ;
#57935 = CARTESIAN_POINT ( 'NONE',  ( 2.530471976670375600, -9.418065098278011860, 34.63729479722530158 ) ) ;
#57936 = EDGE_CURVE ( 'NONE', #34055, #23619, #50805, .T. ) ;
#57937 = ORIENTED_EDGE ( 'NONE', *, *, #24896, .T. ) ;
#57938 = B_SPLINE_CURVE_WITH_KNOTS ( 'NONE', 3,
 ( #66342, #24452, #52371, #85730, #51922, #79860 ),
 .UNSPECIFIED., .F., .F.,
 ( 4, 2, 4 ),
 ( 0.0003909569690057804843, 0.0005862646681846042955, 0.0007815723673634281067 ),
 .UNSPECIFIED. ) ;
#57939 = EDGE_CURVE ( 'NONE', #23981, #57246, #64314, .T. ) ;
#57940 = CARTESIAN_POINT ( 'NONE',  ( -14.30769230769242917, -12.51329471203414379, 31.30864560766407578 ) ) ;
#57941 = ORIENTED_EDGE ( 'NONE', *, *, #42620, .F. ) ;
#57942 = LINE ( 'NONE', #2991, #21193 ) ;
#57943 = CARTESIAN_POINT ( 'NONE',  ( 17.86930939688969033, -12.62707690430377383, 30.88035979386743435 ) ) ;
#57944 = COLOUR_RGB ( '', 0.08235294, 0.09019608, 0.10196078) ;
#57945 = CARTESIAN_POINT ( 'NONE',  ( -14.98071481085577972, -2.920487667080175598, 32.31805714834170828 ) ) ;
#57947 = CARTESIAN_POINT ( 'NONE',  ( 4.853996859406926490, -3.105860786376062332, 32.13614157043599562 ) ) ;
#57946 = CARTESIAN_POINT ( 'NONE',  ( -6.923076923077044142, -12.46129190930018460, 30.37095296980731973 ) ) ;
#57948 = EDGE_CURVE ( 'NONE', #40774, #62177, #17491, .T. ) ;
#57949 = CARTESIAN_POINT ( 'NONE',  ( 16.02315468717859659, -2.541943142973489334, 30.39792223712631980 ) ) ;
#57950 = DIRECTION ( 'NONE',  ( -1.000000000000000000, 0.000000000000000000, 0.000000000000000000 ) ) ;
#57951 = ORIENTED_EDGE ( 'NONE', *, *, #70901, .T. ) ;
#57952 = EDGE_CURVE ( 'NONE', #64392, #65658, #17936, .T. ) ;
#57953 = CARTESIAN_POINT ( 'NONE',  ( -11.40793583669797506, -4.459921816937791661, 33.71989282347011851 ) ) ;
#57954 = CARTESIAN_POINT ( 'NONE',  ( 4.946775107191379028, -4.299443229763728169, 33.91186481527756058 ) ) ;
#57955 = ORIENTED_EDGE ( 'NONE', *, *, #13821, .F. ) ;
#57956 = VECTOR ( 'NONE', #57906, 1000.000000000000000 ) ;
#57957 = LINE ( 'NONE', #51619, #70980 ) ;
#57958 = LINE ( 'NONE', #45326, #43001 ) ;
#57959 = CARTESIAN_POINT ( 'NONE',  ( -4.023320452082591814, -2.619367082507848554, 30.83698974864644171 ) ) ;
#57960 = LINE ( 'NONE', #5581, #70632 ) ;
#57961 = CARTESIAN_POINT ( 'NONE',  ( -13.38461538461550759, -11.67786785259630911, 32.92929555188603530 ) ) ;
#57962 = DIRECTION ( 'NONE',  ( 0.000000000000000000, 0.000000000000000000, -1.000000000000000000 ) ) ;
#57963 = FACE_BOUND ( 'NONE', #3263, .T. ) ;
#57965 = CARTESIAN_POINT ( 'NONE',  ( 17.75002325595140462, -10.82459398097509862, 33.81372124010183455 ) ) ;
#57964 = CARTESIAN_POINT ( 'NONE',  ( 12.46153846153846168, -9.905515769479276145, 34.41647553114623292 ) ) ;
#57966 = CARTESIAN_POINT ( 'NONE',  ( -18.13069060311030611, -8.191372820521383602, 34.95448215188424967 ) ) ;
#57968 = CARTESIAN_POINT ( 'NONE',  ( 9.942253210655836781, -4.336752205174649433, 33.62275283266504289 ) ) ;
#57967 = CARTESIAN_POINT ( 'NONE',  ( -6.923076923077045919, -11.06231777344772027, 33.60647404775119895 ) ) ;
#57969 = CYLINDRICAL_SURFACE ( 'NONE', #59123, 0.2499999999999986955 ) ;
#57970 = CARTESIAN_POINT ( 'NONE',  ( -1.492201783934549164, -11.27530806549876807, 22.10750670625849068 ) ) ;
#57971 = ORIENTED_EDGE ( 'NONE', *, *, #39432, .T. ) ;
#57972 = CARTESIAN_POINT ( 'NONE',  ( -4.376772371362298131, -11.76352882383564769, 32.36236540154569497 ) ) ;
#57973 = CARTESIAN_POINT ( 'NONE',  ( -4.853911725310228853, -3.105924265160262543, 32.13625925475356127 ) ) ;
#57974 = CYLINDRICAL_SURFACE ( 'NONE', #64643, 0.2499999999999994726 ) ;
#57975 = CARTESIAN_POINT ( 'NONE',  ( -0.5000075107691263065, -10.20416206785629498, 29.33696104038924446 ) ) ;
#57976 = CARTESIAN_POINT ( 'NONE',  ( -4.153846153846274980, -5.094484230521993062, 34.41647553114689373 ) ) ;
#57977 = CARTESIAN_POINT ( 'NONE',  ( -5.142174067084318345, -2.506253911140460477, 30.00000000000013856 ) ) ;
#57978 = CARTESIAN_POINT ( 'NONE',  ( -1.614399933863656544, -3.775308065498769405, 18.82625670625848713 ) ) ;
#57979 = B_SPLINE_CURVE_WITH_KNOTS ( 'NONE', 3,
 ( #42449, #21726, #42011, #63593, #41556, #35696, #69470, #1460, #21275, #27595 ),
 .UNSPECIFIED., .F., .F.,
 ( 4, 2, 2, 2, 4 ),
 ( 0.000000000000000000, 0.0001954311584214071026, 0.0003908623168428142051, 0.0005862934752642213077, 0.0007817246336856284103 ),
 .UNSPECIFIED. ) ;
#57980 = CARTESIAN_POINT ( 'NONE',  ( -1.634615384615383027, -7.433932668274255029, 35.00000000000000711 ) ) ;
#57981 = CARTESIAN_POINT ( 'NONE',  ( -18.00000000000000000, -3.322132147404558200, 32.92929555188717217 ) ) ;
#57982 = VECTOR ( 'NONE', #5516, 1000.000000000000114 ) ;
#57983 = CARTESIAN_POINT ( 'NONE',  ( -8.069080805060693251, -2.889293201056495786, 32.26117774369186009 ) ) ;
#57984 = DIRECTION ( 'NONE',  ( -0.000000000000000000, 0.8660254037844399289, -0.4999999999999980016 ) ) ;
#57985 = CARTESIAN_POINT ( 'NONE',  ( -2.307692307692428724, -2.657715359629662544, 31.77849191805970364 ) ) ;
#57986 = CARTESIAN_POINT ( 'NONE',  ( 12.39545608217832218, -12.62096338111211580, 30.90682066428152908 ) ) ;
#57987 = AXIS2_PLACEMENT_3D ( 'NONE', #79304, #47166, #74659 ) ;
#57988 = EDGE_CURVE ( 'NONE', #37091, #43657, #78740, .T. ) ;
#57989 = LINE ( 'NONE', #36832, #49090 ) ;
#57990 = CARTESIAN_POINT ( 'NONE',  ( 8.769230769230768274, -2.499999999999998668, 29.75000000000001421 ) ) ;
#57991 = VERTEX_POINT ( 'NONE', #3516 ) ;
#57992 = CARTESIAN_POINT ( 'NONE',  ( 15.00728430620490350, -11.60425143139329940, 33.02411095842164457 ) ) ;
#57993 = DIRECTION ( 'NONE',  ( -0.000000000000000000, -0.1736481776669307198, -0.9848077530122080203 ) ) ;
#57994 = CARTESIAN_POINT ( 'NONE',  ( 3.775308065498752086, -6.007798216065404873, 13.39249329374151642 ) ) ;
#57995 = CARTESIAN_POINT ( 'NONE',  ( -2.437840277424002888, -5.070767119584671967, 34.40440758774516183 ) ) ;
#57996 = LINE ( 'NONE', #51210, #55577 ) ;
#57997 = EDGE_LOOP ( 'NONE', ( #83421, #83792, #6469, #86607 ) ) ;
#57998 = CARTESIAN_POINT ( 'NONE',  ( -17.93474486048716088, -6.835583212224609184, 34.95778746994559327 ) ) ;
#57999 = CARTESIAN_POINT ( 'NONE',  ( 1.254468175177165801, -9.418419913701741919, 34.36755862841477693 ) ) ;
#58001 = VERTEX_POINT ( 'NONE', #10733 ) ;
#58000 = CARTESIAN_POINT ( 'NONE',  ( 3.930361210122205406, -5.912607949931405038, 34.49155766932282319 ) ) ;
#58002 = CARTESIAN_POINT ( 'NONE',  ( -14.30769230769230660, -3.050289026998446396, 32.03036669348365706 ) ) ;
#58003 = CARTESIAN_POINT ( 'NONE',  ( -2.307692307692428724, -12.70778746994576025, 30.41441678777401236 ) ) ;
#58004 = EDGE_CURVE ( 'NONE', #6887, #64930, #44491, .T. ) ;
#58005 = CARTESIAN_POINT ( 'NONE',  ( -5.011667505647053211, -9.442884908240271713, 34.35708131394835618 ) ) ;
#58006 = EDGE_CURVE ( 'NONE', #58570, #79428, #45391, .T. ) ;
#58007 = DIRECTION ( 'NONE',  ( -1.000000000000000000, -0.000000000000000000, 0.000000000000000000 ) ) ;
#58008 = VERTEX_POINT ( 'NONE', #18825 ) ;
#58009 = DIRECTION ( 'NONE',  ( -1.000000000000000000, -0.000000000000000000, -0.000000000000000000 ) ) ;
#58010 = CARTESIAN_POINT ( 'NONE',  ( -11.53846153846153655, -12.34228464037088635, 31.77849191805839268 ) ) ;
#58011 = AXIS2_PLACEMENT_3D ( 'NONE', #66792, #21591, #22040 ) ;
#58012 = CARTESIAN_POINT ( 'NONE',  ( 4.088575707885378385, -10.21337939537584383, 33.94971097300158647 ) ) ;
#58013 = ORIENTED_EDGE ( 'NONE', *, *, #47212, .F. ) ;
#58014 = ORIENTED_EDGE ( 'NONE', *, *, #58070, .T. ) ;
#58015 = AXIS2_PLACEMENT_3D ( 'NONE', #70203, #62983, #57129 ) ;
#58016 = ORIENTED_EDGE ( 'NONE', *, *, #59028, .F. ) ;
#58017 = VECTOR ( 'NONE', #32359, 999.9999999999998863 ) ;
#58018 = EDGE_CURVE ( 'NONE', #69663, #46391, #68338, .T. ) ;
#58019 = DIRECTION ( 'NONE',  ( -1.000000000000000000, 0.000000000000000000, -0.000000000000000000 ) ) ;
#58020 = CARTESIAN_POINT ( 'NONE',  ( 6.066067333350078528, -2.292212530054420494, 30.41441678777542990 ) ) ;
#58021 = EDGE_CURVE ( 'NONE', #22897, #4699, #40871, .T. ) ;
#58022 = DIRECTION ( 'NONE',  ( 0.000000000000000000, 0.1736481776669275834, 0.9848077530122086864 ) ) ;
#58023 = DIRECTION ( 'NONE',  ( -0.000000000000000000, 0.3420201433256694346, -0.9396926207859080948 ) ) ;
#58024 = ORIENTED_EDGE ( 'NONE', *, *, #66434, .F. ) ;
#58026 = ORIENTED_EDGE ( 'NONE', *, *, #58018, .F. ) ;
#58025 = EDGE_CURVE ( 'NONE', #50717, #44728, #26472, .T. ) ;
#58028 = EDGE_LOOP ( 'NONE', ( #73814, #1546, #66536, #32665 ) ) ;
#58027 = CARTESIAN_POINT ( 'NONE',  ( 10.68057760367926790, -2.255955759149235629, 29.99999999999988987 ) ) ;
#58029 = LINE ( 'NONE', #23788, #69721 ) ;
#58030 = DIRECTION ( 'NONE',  ( -0.000000000000000000, -0.6427876096865404731, -0.7660444431189770143 ) ) ;
#58031 = CARTESIAN_POINT ( 'NONE',  ( 15.90386940979756858, -11.47974371597207899, 33.17467449705390692 ) ) ;
#58032 = VERTEX_POINT ( 'NONE', #46290 ) ;
#58033 = VERTEX_POINT ( 'NONE', #33226 ) ;
#58035 = ORIENTED_EDGE ( 'NONE', *, *, #77740, .F. ) ;
#58034 = CARTESIAN_POINT ( 'NONE',  ( -8.703975197954745724, -8.613356846314928816, 34.62446782046653482 ) ) ;
#58036 = DIRECTION ( 'NONE',  ( -0.000000000000000000, 1.000000000000000000, -0.000000000000000000 ) ) ;
#58037 = CARTESIAN_POINT ( 'NONE',  ( 14.05766908347085220, -5.765609946408404518, 34.70566812827425451 ) ) ;
#58039 = VERTEX_POINT ( 'NONE', #19269 ) ;
#58038 = EDGE_CURVE ( 'NONE', #48024, #60048, #23471, .T. ) ;
#58040 = DIRECTION ( 'NONE',  ( 0.000000000000000000, 0.000000000000000000, 1.000000000000000000 ) ) ;
#58041 = CARTESIAN_POINT ( 'NONE',  ( 0.000000000000000000, -11.00000000000000000, 29.75000000000000355 ) ) ;
#58042 = DIRECTION ( 'NONE',  ( -0.000000000000000000, -0.6427876096865404731, -0.7660444431189771253 ) ) ;
#58043 = FACE_BOUND ( 'NONE', #41324, .T. ) ;
#58044 = CARTESIAN_POINT ( 'NONE',  ( 0.4615384615384611755, -6.681629849574314051, 35.83090037661290239 ) ) ;
#58046 = ADVANCED_FACE ( 'NONE', ( #32337 ), #80534, .F. ) ;
#58045 = CARTESIAN_POINT ( 'NONE',  ( -4.153846153846152411, -12.10708131394839349, 31.69288490824020244 ) ) ;
#58047 = CARTESIAN_POINT ( 'NONE',  ( -4.500000000000003553, 7.499999999999996447, 13.50000000000000178 ) ) ;
#58049 = CARTESIAN_POINT ( 'NONE',  ( -15.90379173393269596, -2.920487667080175154, 32.31805714834170828 ) ) ;
#58048 = CARTESIAN_POINT ( 'NONE',  ( 16.37662582282421653, -4.226511098958373402, 33.85474049983370293 ) ) ;
#58050 = CARTESIAN_POINT ( 'NONE',  ( 11.40831432902331777, -11.47017969459903952, 32.78971311882035167 ) ) ;
#58051 = FACE_OUTER_BOUND ( 'NONE', #15985, .T. ) ;
#58052 = ORIENTED_EDGE ( 'NONE', *, *, #12518, .F. ) ;
#58053 = EDGE_CURVE ( 'NONE', #3642, #46562, #6276, .T. ) ;
#58054 = CARTESIAN_POINT ( 'NONE',  ( 14.05769230769230838, -7.500000000000001776, 34.75000000000000000 ) ) ;
#58055 = VERTEX_POINT ( 'NONE', #6635 ) ;
#58056 = ORIENTED_EDGE ( 'NONE', *, *, #88088, .F. ) ;
#58058 = CARTESIAN_POINT ( 'NONE',  ( 10.83816428436268176, -12.69155399931963046, 30.53255429739157734 ) ) ;
#58057 = CARTESIAN_POINT ( 'NONE',  ( -0.4615384615385826339, -3.300289026999228881, 32.46337939537708905 ) ) ;
#58059 = CARTESIAN_POINT ( 'NONE',  ( -4.153846153846274980, -12.70778746994576025, 30.41441678777401236 ) ) ;
#58060 = CARTESIAN_POINT ( 'NONE',  ( 14.53070515178570510, -4.026326845037962343, 33.68677907613344047 ) ) ;
#58061 = CARTESIAN_POINT ( 'NONE',  ( -11.53846153846165912, -6.026961402154118019, 34.52809138561165270 ) ) ;
#58062 = LINE ( 'NONE', #43230, #49028 ) ;
#58063 = EDGE_LOOP ( 'NONE', ( #50066, #82213, #62913, #16764 ) ) ;
#58064 = LINE ( 'NONE', #38247, #22769 ) ;
#58065 = AXIS2_PLACEMENT_3D ( 'NONE', #15178, #50710, #42652 ) ;
#58066 = CARTESIAN_POINT ( 'NONE',  ( -14.98071491913091791, -9.943054286541403997, 34.11300777759954883 ) ) ;
#58067 = FACE_OUTER_BOUND ( 'NONE', #12891, .T. ) ;
#58068 = CARTESIAN_POINT ( 'NONE',  ( 0.3954560821783261182, -3.322132147404559976, 32.92929555188719348 ) ) ;
#58069 = PLANE ( 'NONE',  #13278 ) ;
#58070 = EDGE_CURVE ( 'NONE', #6072, #40774, #55700, .T. ) ;
#58071 = CARTESIAN_POINT ( 'NONE',  ( 2.320192649118979489E-14, -11.25000000000000000, 14.78125000000000178 ) ) ;
#58072 = ORIENTED_EDGE ( 'NONE', *, *, #71147, .F. ) ;
#58073 = VECTOR ( 'NONE', #37072, 1000.000000000000000 ) ;
#58074 = VERTEX_POINT ( 'NONE', #20153 ) ;
#58075 = CARTESIAN_POINT ( 'NONE',  ( 15.23076923076923173, -12.09954503811598769, 35.62045528018868623 ) ) ;
#58076 = EDGE_CURVE ( 'NONE', #70789, #58120, #53644, .T. ) ;
#58077 = VERTEX_POINT ( 'NONE', #60242 ) ;
#58078 = CARTESIAN_POINT ( 'NONE',  ( -4.153846153846273204, -4.481592998941358097, 33.73612834414048933 ) ) ;
#58079 = CARTESIAN_POINT ( 'NONE',  ( 17.74997677577853850, -11.56360843649121861, 33.07473185843129926 ) ) ;
#58080 = CARTESIAN_POINT ( 'NONE',  ( -16.37733109757010652, -5.113361153441931428, 34.14387501736621999 ) ) ;
#58081 = CARTESIAN_POINT ( 'NONE',  ( 13.63461538461538680, -7.500000000000001776, 35.04278698407183867 ) ) ;
#58082 = CARTESIAN_POINT ( 'NONE',  ( 1.553300858899087311, -3.749999999999992006, 16.73437500000000000 ) ) ;
#58083 = CARTESIAN_POINT ( 'NONE',  ( 0.4615384615384611200, -9.058645607665452459, 34.76329471203371924 ) ) ;
#58084 = ORIENTED_EDGE ( 'NONE', *, *, #1520, .F. ) ;
#58085 = CARTESIAN_POINT ( 'NONE',  ( -12.71156169883143150, -10.76384336483936011, 33.53834819971076087 ) ) ;
#58087 = ORIENTED_EDGE ( 'NONE', *, *, #65855, .F. ) ;
#58086 = CARTESIAN_POINT ( 'NONE',  ( -1.318547033612945896, -8.973038597847269315, 34.52809138561122637 ) ) ;
#58088 = CARTESIAN_POINT ( 'NONE',  ( -13.60754160213153163, -11.24512374952581872, 33.06303171183252942 ) ) ;
#58089 = DIRECTION ( 'NONE',  ( -0.000000000000000000, -0.8660254037844399289, -0.4999999999999980016 ) ) ;
#58090 = CARTESIAN_POINT ( 'NONE',  ( 2.307692307692187583, -3.300289026999228881, 32.46337939537708905 ) ) ;
#58091 = EDGE_CURVE ( 'NONE', #62177, #52057, #24599, .T. ) ;
#58092 = DIRECTION ( 'NONE',  ( -0.000000000000000000, 1.000000000000000000, -0.000000000000000000 ) ) ;
#58093 = CARTESIAN_POINT ( 'NONE',  ( -10.61538461538461320, -8.810774026931790459, 35.74407628777942847 ) ) ;
#58094 = CARTESIAN_POINT ( 'NONE',  ( -3.099977422944443006, -11.18335022499818621, 33.13157742990016885 ) ) ;
#58095 = CARTESIAN_POINT ( 'NONE',  ( 15.36129493253279499, -11.46989282347013095, 32.79007818306219946 ) ) ;
#58096 = CARTESIAN_POINT ( 'NONE',  ( -2.694853999681181556, -10.10844685921792241, 18.93936829374151287 ) ) ;
#58097 = VERTEX_POINT ( 'NONE', #1198 ) ;
#58098 = CARTESIAN_POINT ( 'NONE',  ( -15.90379173393269951, -6.523592122091590895, 34.90882529074906415 ) ) ;
#58099 = EDGE_CURVE ( 'NONE', #63192, #48024, #34550, .T. ) ;
#58100 = CARTESIAN_POINT ( 'NONE',  ( -12.68441714396711006, -7.630691491037285168, 34.74850469731152458 ) ) ;
#58101 = CARTESIAN_POINT ( 'NONE',  ( -17.32689982097166492, -4.818429247618091438, 34.26397095200675125 ) ) ;
#58102 = CARTESIAN_POINT ( 'NONE',  ( -1.901340078031369618, -5.512252781505359245, 13.00186829374151465 ) ) ;
#58103 = EDGE_CURVE ( 'NONE', #15420, #69076, #72947, .T. ) ;
#58104 = CARTESIAN_POINT ( 'NONE',  ( 0.4615384615384611200, -5.471508081941601098, 34.59228464037088457 ) ) ;
#58105 = DIRECTION ( 'NONE',  ( 0.000000000000000000, 0.000000000000000000, -1.000000000000000000 ) ) ;
#58106 = ORIENTED_EDGE ( 'NONE', *, *, #67215, .F. ) ;
#58107 = CARTESIAN_POINT ( 'NONE',  ( -2.749999999999998224, -7.500000000000015987, 16.34375000000000000 ) ) ;
#58108 = CARTESIAN_POINT ( 'NONE',  ( -5.198717948717948012, -11.00000000000000000, 29.75000000000000355 ) ) ;
#58109 = EDGE_LOOP ( 'NONE', ( #52506, #43919 ) ) ;
#58110 = ADVANCED_FACE ( 'NONE', ( #75977 ), #50258, .F. ) ;
#58111 = CARTESIAN_POINT ( 'NONE',  ( -27.00000000000000000, -1.249999999999999778, 24.75000000000000000 ) ) ;
#58112 = VERTEX_POINT ( 'NONE', #69223 ) ;
#58113 = CARTESIAN_POINT ( 'NONE',  ( 14.30769230769218758, -12.27809138561165270, 31.22303859784587132 ) ) ;
#58114 = CARTESIAN_POINT ( 'NONE',  ( 17.07692307692338218, -2.506253911140615021, 30.00000000000323297 ) ) ;
#58115 = DIRECTION ( 'NONE',  ( -0.000000000000000000, 2.546383084002652634E-16, 1.000000000000000000 ) ) ;
#58116 = ORIENTED_EDGE ( 'NONE', *, *, #25752, .F. ) ;
#58117 = CARTESIAN_POINT ( 'NONE',  ( -13.13466997523734037, -12.68172785388650681, 30.59649109432439218 ) ) ;
#58118 = ORIENTED_EDGE ( 'NONE', *, *, #61801, .F. ) ;
#58119 = CARTESIAN_POINT ( 'NONE',  ( -5.750054590621955342, -2.341251567377310217, 30.72681386836322659 ) ) ;
#58120 = VERTEX_POINT ( 'NONE', #77304 ) ;
#58121 = DIRECTION ( 'NONE',  ( -0.000000000000000000, 0.3420201433256694346, -0.9396926207859080948 ) ) ;
#58122 = CYLINDRICAL_SURFACE ( 'NONE', #22483, 0.2500000000000008882 ) ;
#58123 = EDGE_LOOP ( 'NONE', ( #30838, #78100, #62073, #59119 ) ) ;
#58124 = CARTESIAN_POINT ( 'NONE',  ( 16.15384615384615330, -3.937682226553329556, 33.60647404775216529 ) ) ;
#58126 = EDGE_CURVE ( 'NONE', #65231, #70653, #89079, .T. ) ;
#58125 = CARTESIAN_POINT ( 'NONE',  ( 11.53846153846153832, -1.790695186598648903, 34.54067556320373455 ) ) ;
#58127 = CARTESIAN_POINT ( 'NONE',  ( 19.00000000000000000, -7.500000000000000000, 33.75000000000000000 ) ) ;
#58128 = CARTESIAN_POINT ( 'NONE',  ( -5.076923076923075762, -2.499999999999998668, 29.75000000000001421 ) ) ;
#58129 = CARTESIAN_POINT ( 'NONE',  ( -13.16160254052199008, -11.98016756924215009, 32.48728574198911190 ) ) ;
#58130 = VERTEX_POINT ( 'NONE', #62017 ) ;
#58131 = ORIENTED_EDGE ( 'NONE', *, *, #80306, .F. ) ;
#58132 = ORIENTED_EDGE ( 'NONE', *, *, #37165, .T. ) ;
#58134 = ORIENTED_EDGE ( 'NONE', *, *, #34902, .F. ) ;
#58133 = CARTESIAN_POINT ( 'NONE',  ( 8.638539302563209787, -3.530157926970578952, 32.79014554554150607 ) ) ;
#58135 = AXIS2_PLACEMENT_3D ( 'NONE', #40980, #13062, #26578 ) ;
#58136 = AXIS2_PLACEMENT_3D ( 'NONE', #17672, #60424, #18560 ) ;
#58137 = CARTESIAN_POINT ( 'NONE',  ( -8.835314180186648159, -9.780366693483667717, 34.19971097300155805 ) ) ;
#58138 = CARTESIAN_POINT ( 'NONE',  ( 9.469380733400845074, -5.582147617184174848, 34.63737895849758530 ) ) ;
#58139 = ORIENTED_EDGE ( 'NONE', *, *, #80541, .F. ) ;
#58140 = VERTEX_POINT ( 'NONE', #7526 ) ;
#58141 = ORIENTED_EDGE ( 'NONE', *, *, #66192, .F. ) ;
#58142 = CARTESIAN_POINT ( 'NONE',  ( 3.361561038594017337, -4.809403383903226192, 33.96459661697924304 ) ) ;
#58143 = ORIENTED_EDGE ( 'NONE', *, *, #49509, .F. ) ;
#58144 = CARTESIAN_POINT ( 'NONE',  ( 11.76124107972994182, -11.41317474335729543, 32.86274602512330034 ) ) ;
#58145 = CARTESIAN_POINT ( 'NONE',  ( 16.82689985270161515, -12.45566812827425096, 31.48439005359158926 ) ) ;
#58146 = CARTESIAN_POINT ( 'NONE',  ( 14.30769230769218581, -12.16647553114689728, 32.15551576947799362 ) ) ;
#58147 = FACE_BOUND ( 'NONE', #24503, .T. ) ;
#58148 = VERTEX_POINT ( 'NONE', #28227 ) ;
#58150 = EDGE_CURVE ( 'NONE', #8365, #40118, #14728, .T. ) ;
#58149 = CARTESIAN_POINT ( 'NONE',  ( 12.46153846153833911, -6.026961402154118019, 34.52809138561165270 ) ) ;
#58151 = CARTESIAN_POINT ( 'NONE',  ( -17.07692307692307665, -2.249999999999998668, 29.75000000000001776 ) ) ;
#58152 = CARTESIAN_POINT ( 'NONE',  ( 8.769230769230768274, -3.050289026998446396, 32.03036669348365706 ) ) ;
#58153 = CARTESIAN_POINT ( 'NONE',  ( 17.29970261819148902, -9.332535724633405749, 34.40230450496446224 ) ) ;
#58154 = ORIENTED_EDGE ( 'NONE', *, *, #66473, .T. ) ;
#58155 = EDGE_CURVE ( 'NONE', #17681, #36898, #15170, .T. ) ;
#58156 = CARTESIAN_POINT ( 'NONE',  ( 9.942307692307695177, -7.500000000000001776, 35.04278698407183867 ) ) ;
#58157 = ORIENTED_EDGE ( 'NONE', *, *, #78957, .T. ) ;
#58158 = VERTEX_POINT ( 'NONE', #70103 ) ;
#58159 = AXIS2_PLACEMENT_3D ( 'NONE', #88908, #88032, #82586 ) ;
#58161 = CARTESIAN_POINT ( 'NONE',  ( -19.50000000000000000, -11.50000000000000000, 29.75000000000000355 ) ) ;
#58160 = DIRECTION ( 'NONE',  ( -1.000000000000000000, 0.000000000000000000, 0.000000000000000000 ) ) ;
#58162 = EDGE_CURVE ( 'NONE', #22613, #49527, #56592, .T. ) ;
#58163 = DIRECTION ( 'NONE',  ( -0.000000000000000000, -0.3420201433256694901, -0.9396926207859082059 ) ) ;
#58164 = DIRECTION ( 'NONE',  ( -1.000000000000000000, -0.000000000000000000, -0.000000000000000000 ) ) ;
#58165 = CARTESIAN_POINT ( 'NONE',  ( 16.82692307692307665, -7.500000000000001776, 34.75000000000000000 ) ) ;
#58166 = CARTESIAN_POINT ( 'NONE',  ( -15.36091720050092846, -3.625366637846544116, 33.29286588640298561 ) ) ;
#58167 = ORIENTED_EDGE ( 'NONE', *, *, #87315, .T. ) ;
#58168 = DIRECTION ( 'NONE',  ( 0.000000000000000000, 0.9396926207859126468, 0.3420201433256571111 ) ) ;
#58169 = CARTESIAN_POINT ( 'NONE',  ( 3.230769230769108269, -9.528491918059723176, 34.59228464037033035 ) ) ;
#58170 = CARTESIAN_POINT ( 'NONE',  ( 11.76142444202302961, -7.369474270740069777, 34.74850911626239736 ) ) ;
#58171 = CARTESIAN_POINT ( 'NONE',  ( 13.16113044089144068, -12.44517049084099725, 30.48991314939691932 ) ) ;
#58172 = ORIENTED_EDGE ( 'NONE', *, *, #20152, .F. ) ;
#58173 = EDGE_CURVE ( 'NONE', #85470, #7626, #84085, .T. ) ;
#58174 = ORIENTED_EDGE ( 'NONE', *, *, #78938, .F. ) ;
#58175 = FACE_BOUND ( 'NONE', #87414, .T. ) ;
#58176 = ORIENTED_EDGE ( 'NONE', *, *, #88949, .F. ) ;
#58177 = CARTESIAN_POINT ( 'NONE',  ( 18.06606733335007675, -12.62096338111211757, 30.90682066428152908 ) ) ;
#58178 = CARTESIAN_POINT ( 'NONE',  ( -13.38461538461538325, -10.51840700105979565, 33.73612834413961536 ) ) ;
#58179 = ORIENTED_EDGE ( 'NONE', *, *, #70191, .F. ) ;
#58180 = DIRECTION ( 'NONE',  ( 0.000000000000000000, 0.000000000000000000, 1.000000000000000000 ) ) ;
#58181 = CARTESIAN_POINT ( 'NONE',  ( 6.249945409378044658, -11.56426240980093745, 33.07394671870546432 ) ) ;
#58183 = B_SPLINE_CURVE_WITH_KNOTS ( 'NONE', 3,
 ( #5717, #80045, #4835, #53000, #86379, #60653, #88165, #45807, #11592, #46702 ),
 .UNSPECIFIED., .F., .F.,
 ( 4, 2, 2, 2, 4 ),
 ( 0.0007817359430256216575, 0.0009771253907249856981, 0.001172514838424349847, 0.001367904286123713779, 0.001563293733823077928 ),
 .UNSPECIFIED. ) ;
#58182 = CARTESIAN_POINT ( 'NONE',  ( -8.638438961405983108, -6.413143153341454017, 34.63066358083362672 ) ) ;
#58184 = CARTESIAN_POINT ( 'NONE',  ( -6.673131404728781746, -3.202959910592335202, 32.30730279482227019 ) ) ;
#58185 = ORIENTED_EDGE ( 'NONE', *, *, #23485, .T. ) ;
#58186 = CARTESIAN_POINT ( 'NONE',  ( -4.088590582570128973, -6.879047030191282275, 34.71129190930002295 ) ) ;
#58187 = ORIENTED_EDGE ( 'NONE', *, *, #66417, .F. ) ;
#58189 = VERTEX_POINT ( 'NONE', #35433 ) ;
#58188 = CARTESIAN_POINT ( 'NONE',  ( 16.82694634598072270, -10.66389620160130036, 33.62221079203477103 ) ) ;
#58190 = CARTESIAN_POINT ( 'NONE',  ( -7.780085495151407571, -8.973038597847271092, 34.52809138561121216 ) ) ;
#58191 = DIRECTION ( 'NONE',  ( 1.000000000000000000, 0.000000000000000000, 0.000000000000000000 ) ) ;
#58192 = CARTESIAN_POINT ( 'NONE',  ( 12.46153846153846168, -1.044019251281081972, 31.83374038241031911 ) ) ;
#58193 = CARTESIAN_POINT ( 'NONE',  ( -4.153846153846273204, -12.46129190930018460, 30.37095296980731973 ) ) ;
#58195 = AXIS2_PLACEMENT_3D ( 'NONE', #82784, #21056, #14310 ) ;
#58194 = CARTESIAN_POINT ( 'NONE',  ( 0.4615384615384611200, -12.78798330534103123, 29.99999999999997868 ) ) ;
#58196 = DIRECTION ( 'NONE',  ( 0.000000000000000000, 0.000000000000000000, -1.000000000000000000 ) ) ;
#58197 = CARTESIAN_POINT ( 'NONE',  ( -0.06109907496451398579, -10.25000000000000178, 16.28311829374151287 ) ) ;
#58198 = ORIENTED_EDGE ( 'NONE', *, *, #44725, .F. ) ;
#58199 = ADVANCED_FACE ( 'NONE', ( #83642 ), #8412, .F. ) ;
#58201 = VECTOR ( 'NONE', #54257, 1000.000000000000000 ) ;
#58200 = B_SPLINE_CURVE_WITH_KNOTS ( 'NONE', 3,
 ( #1953, #77611, #57336, #71282, #37052, #28547, #83496, #83942, #29438, #84830 ),
 .UNSPECIFIED., .F., .F.,
 ( 4, 2, 2, 2, 4 ),
 ( 0.0007817359430256372700, 0.0009771253907250052138, 0.001172514838424373266, 0.001367904286123741101, 0.001563293733823109153 ),
 .UNSPECIFIED. ) ;
#58202 = CARTESIAN_POINT ( 'NONE',  ( -15.10024352900566491, -3.816742781228458004, 33.13167719472716044 ) ) ;
#58203 = FACE_OUTER_BOUND ( 'NONE', #41351, .T. ) ;
#58204 = AXIS2_PLACEMENT_3D ( 'NONE', #60826, #12204, #32465 ) ;
#58205 = VERTEX_POINT ( 'NONE', #70550 ) ;
#58206 = VERTEX_POINT ( 'NONE', #8859 ) ;
#58207 = CARTESIAN_POINT ( 'NONE',  ( -11.66860874789975888, -10.88202310037935661, 33.43294751532457099 ) ) ;
#58208 = CARTESIAN_POINT ( 'NONE',  ( 7.596177102105253987, -6.524016743844655686, 34.90889640711025521 ) ) ;
#58209 = CARTESIAN_POINT ( 'NONE',  ( 6.250054311638314708, -11.28795663066794219, 33.01431243580653785 ) ) ;
#58210 = CARTESIAN_POINT ( 'NONE',  ( 9.468822748583747284, -12.44517049084099725, 30.48991314939691932 ) ) ;
#58211 = CARTESIAN_POINT ( 'NONE',  ( 6.923076923076924238, -9.584722331328613620, 36.20867863119891439 ) ) ;
#58212 = EDGE_CURVE ( 'NONE', #78414, #24781, #36329, .T. ) ;
#58213 = PLANE ( 'NONE',  #57175 ) ;
#58214 = FACE_OUTER_BOUND ( 'NONE', #57085, .T. ) ;
#58215 = EDGE_LOOP ( 'NONE', ( #14436, #59161 ) ) ;
#58216 = LINE ( 'NONE', #50576, #53490 ) ;
#58217 = CARTESIAN_POINT ( 'NONE',  ( -17.20753343654760315, -7.722926236386454590, 34.74524107206102030 ) ) ;
#58218 = EDGE_CURVE ( 'NONE', #25874, #77885, #70709, .T. ) ;
#58219 = EDGE_CURVE ( 'NONE', #3688, #6905, #32120, .T. ) ;
#58220 = B_SPLINE_CURVE_WITH_KNOTS ( 'NONE', 3,
 ( #62368, #57391, #22717, #21398, #52407, #57841, #30807, #65485, #3783, #31258 ),
 .UNSPECIFIED., .F., .F.,
 ( 4, 2, 2, 2, 4 ),
 ( 0.000000000000000000, 0.0001954339857564082062, 0.0003908679715128164124, 0.0005863019572692246186, 0.0007817359430256328248 ),
 .UNSPECIFIED. ) ;
#58221 = CARTESIAN_POINT ( 'NONE',  ( -5.869952393744314989, -7.723484964179500700, 34.74522123443823318 ) ) ;
#58222 = CARTESIAN_POINT ( 'NONE',  ( -24.00000000000000000, 0.000000000000000000, 0.000000000000000000 ) ) ;
#58223 = B_SPLINE_CURVE_WITH_KNOTS ( 'NONE', 3,
 ( #10218, #24159, #51614, #44872, #10659, #38126, #65585, #72791, #38577, #66031 ),
 .UNSPECIFIED., .F., .F.,
 ( 4, 2, 2, 2, 4 ),
 ( 0.000000000000000000, 0.0001954311564186873623, 0.0003908623128373747246, 0.0005862934692560620598, 0.0007817246256747494492 ),
 .UNSPECIFIED. ) ;
#58224 = ORIENTED_EDGE ( 'NONE', *, *, #37749, .T. ) ;
#58225 = DIRECTION ( 'NONE',  ( 0.000000000000000000, 0.000000000000000000, -1.000000000000000000 ) ) ;
#58226 = ORIENTED_EDGE ( 'NONE', *, *, #79560, .F. ) ;
#58227 = CARTESIAN_POINT ( 'NONE',  ( -17.30040800148741553, -2.612411019501189813, 31.66733052389439962 ) ) ;
#58228 = DIRECTION ( 'NONE',  ( -1.000000000000000000, 0.000000000000000000, -0.000000000000000000 ) ) ;
#58229 = CARTESIAN_POINT ( 'NONE',  ( 10.61538461538461675, -11.91647553114624181, 32.58852847137148245 ) ) ;
#58230 = ORIENTED_EDGE ( 'NONE', *, *, #88574, .F. ) ;
#58232 = EDGE_CURVE ( 'NONE', #56373, #53401, #67243, .T. ) ;
#58231 = CARTESIAN_POINT ( 'NONE',  ( 5.777073782483852504, -9.886141570436013382, 34.14413921362392301 ) ) ;
#58233 = DIRECTION ( 'NONE',  ( -0.000000000000000000, 0.7660444431189791237, -0.6427876096865379196 ) ) ;
#58234 = DIRECTION ( 'NONE',  ( -0.000000000000000000, 1.000000000000000000, -0.000000000000000000 ) ) ;
#58235 = VECTOR ( 'NONE', #72817, 1000.000000000000114 ) ;
#58236 = LINE ( 'NONE', #10949, #56672 ) ;
#58237 = DIRECTION ( 'NONE',  ( -0.000000000000000000, 0.3420201433256694346, -0.9396926207859080948 ) ) ;
#58238 = ADVANCED_FACE ( 'NONE', ( #16050 ), #50703, .F. ) ;
#58239 = EDGE_CURVE ( 'NONE', #43247, #2381, #43518, .T. ) ;
#58240 = VERTEX_POINT ( 'NONE', #53266 ) ;
#58241 = CARTESIAN_POINT ( 'NONE',  ( -0.6844646790546090598, -8.239355502252617924, 34.69524867566427417 ) ) ;
#58242 = EDGE_LOOP ( 'NONE', ( #45571, #72088, #8251, #65497 ) ) ;
#58243 = ADVANCED_FACE ( 'NONE', ( #9303 ), #25807, .T. ) ;
#58244 = CARTESIAN_POINT ( 'NONE',  ( 4.826899839630110378, -12.22074536777954989, 31.39888409691088356 ) ) ;
#58245 = CARTESIAN_POINT ( 'NONE',  ( 7.173022332454966232, -2.986452184633680673, 32.43230066228895225 ) ) ;
#58246 = CARTESIAN_POINT ( 'NONE',  ( 9.822833130541335223, -2.647132371071621471, 31.75357179365171589 ) ) ;
#58247 = CARTESIAN_POINT ( 'NONE',  ( 1.254467414883692067, -8.630895178749536711, 34.87696386517710323 ) ) ;
#58248 = CARTESIAN_POINT ( 'NONE',  ( 15.93036122928182330, -12.11044203135681840, 32.26167407432752299 ) ) ;
#58249 = VERTEX_POINT ( 'NONE', #52821 ) ;
#58250 = ORIENTED_EDGE ( 'NONE', *, *, #67088, .F. ) ;
#58251 = B_SPLINE_CURVE_WITH_KNOTS ( 'NONE', 3,
 ( #37726, #16568, #30090, #50779, #24206, #71072, #71954, #10265, #52567, #51663 ),
 .UNSPECIFIED., .F., .F.,
 ( 4, 2, 2, 2, 4 ),
 ( 0.0007817359430256392216, 0.0009771253907250073822, 0.001172514838424375651, 0.001367904286123743920, 0.001563293733823112189 ),
 .UNSPECIFIED. ) ;
#58252 = EDGE_LOOP ( 'NONE', ( #58035, #84811 ) ) ;
#58253 = EDGE_LOOP ( 'NONE', ( #44617, #7530 ) ) ;
#58254 = AXIS2_PLACEMENT_3D ( 'NONE', #78008, #16313, #51850 ) ;
#58255 = DIRECTION ( 'NONE',  ( 0.000000000000000000, 0.7660444431189807890, 0.6427876096865361433 ) ) ;
#58256 = CARTESIAN_POINT ( 'NONE',  ( -3.361459833879538284, -6.369640206132550553, 34.87707690430378449 ) ) ;
#58257 = CARTESIAN_POINT ( 'NONE',  ( -5.207399785039540596, -7.276988635370452485, 34.74523720219453793 ) ) ;
#58258 = CARTESIAN_POINT ( 'NONE',  ( -13.38461538461538325, -4.098570777380720287, 33.41473453929634729 ) ) ;
#58259 = DIRECTION ( 'NONE',  ( 0.000000000000000000, 0.000000000000000000, -1.000000000000000000 ) ) ;
#58260 = ADVANCED_FACE ( 'NONE', ( #80766 ), #23242, .F. ) ;
#58261 = CARTESIAN_POINT ( 'NONE',  ( 14.30769230769218758, -12.46129190930018460, 30.37095296980731973 ) ) ;
#58262 = CARTESIAN_POINT ( 'NONE',  ( -5.999999999999998224, -4.661471528628507777, 34.16647553114623292 ) ) ;
#58263 = CARTESIAN_POINT ( 'NONE',  ( -3.931066612577743147, -10.81320215134717344, 33.49497208177562868 ) ) ;
#58264 = ORIENTED_EDGE ( 'NONE', *, *, #44168, .T. ) ;
#58265 = ORIENTED_EDGE ( 'NONE', *, *, #6488, .T. ) ;
#58266 = ORIENTED_EDGE ( 'NONE', *, *, #2106, .F. ) ;
#58268 = ORIENTED_EDGE ( 'NONE', *, *, #4458, .T. ) ;
#58267 = CARTESIAN_POINT ( 'NONE',  ( 6.222779668978067669, -12.47679350104403007, 31.42216943046555855 ) ) ;
#58270 = CARTESIAN_POINT ( 'NONE',  ( -17.77722033102192967, -11.60474049983370470, 33.02348890104160262 ) ) ;
#58269 = CARTESIAN_POINT ( 'NONE',  ( 0.4615384615383396616, -8.613356846316285953, 34.62446782046622218 ) ) ;
#58271 = EDGE_CURVE ( 'NONE', #81602, #5877, #66403, .T. ) ;
#58272 = CYLINDRICAL_SURFACE ( 'NONE', #50371, 0.2499999999999994726 ) ;
#58273 = CARTESIAN_POINT ( 'NONE',  ( 5.076923076922953193, -6.835583212225970762, 34.95778746994575670 ) ) ;
#58274 = ORIENTED_EDGE ( 'NONE', *, *, #53449, .F. ) ;
#58275 = ORIENTED_EDGE ( 'NONE', *, *, #35386, .T. ) ;
#58276 = CARTESIAN_POINT ( 'NONE',  ( -2.307692307691999289, -2.506253911140615021, 30.00000000000323297 ) ) ;
#58277 = VERTEX_POINT ( 'NONE', #19050 ) ;
#58278 = FACE_BOUND ( 'NONE', #32874, .T. ) ;
#58279 = B_SPLINE_CURVE_WITH_KNOTS ( 'NONE', 3,
 ( #16198, #78778, #45433, #4453, #51274, #24270, #72020, #77895, #36904, #2665 ),
 .UNSPECIFIED., .F., .F.,
 ( 4, 2, 2, 2, 4 ),
 ( 0.0007817246256747516176, 0.0009771112852218965736, 0.001172497944769041638, 0.001367884604316186702, 0.001563271263863331550 ),
 .UNSPECIFIED. ) ;
#58280 = CARTESIAN_POINT ( 'NONE',  ( 13.63466980452883526, -12.41089969410671223, 31.60739465890703670 ) ) ;
#58281 = LINE ( 'NONE', #17305, #24714 ) ;
#58282 = ORIENTED_EDGE ( 'NONE', *, *, #50533, .T. ) ;
#58283 = CARTESIAN_POINT ( 'NONE',  ( 2.084766090176161324, -8.239355502252617924, 34.69524867566427417 ) ) ;
#58284 = DIRECTION ( 'NONE',  ( -0.000000000000000000, -0.5000000000000009992, -0.8660254037844380415 ) ) ;
#58285 = CARTESIAN_POINT ( 'NONE',  ( -18.22348492456433178, -4.225889041578354544, 33.85425143139329407 ) ) ;
#58286 = ORIENTED_EDGE ( 'NONE', *, *, #78682, .F. ) ;
#58287 = CARTESIAN_POINT ( 'NONE',  ( 12.33139125210024112, -5.195881422630166391, 34.18770438780619259 ) ) ;
#58288 = CARTESIAN_POINT ( 'NONE',  ( 7.596153846153846700, -2.249999999999998668, 29.75000000000000355 ) ) ;
#58289 = ORIENTED_EDGE ( 'NONE', *, *, #89105, .F. ) ;
#58290 = AXIS2_PLACEMENT_3D ( 'NONE', #44218, #24403, #57313 ) ;
#58291 = ADVANCED_FACE ( 'NONE', ( #16492 ), #46522, .F. ) ;
#58292 = CARTESIAN_POINT ( 'NONE',  ( 6.222963134266677798, -7.369474539155828730, 34.99858011523957657 ) ) ;
#58293 = CARTESIAN_POINT ( 'NONE',  ( -9.692307692307691624, -9.058645607665452459, 34.76329471203371924 ) ) ;
#58294 = ORIENTED_EDGE ( 'NONE', *, *, #18391, .F. ) ;
#58295 = CARTESIAN_POINT ( 'NONE',  ( 7.846153846153725020, -5.219633306517616589, 34.19971097300220464 ) ) ;
#58296 = CARTESIAN_POINT ( 'NONE',  ( -2.057692307692306599, -2.249999999999998668, 29.75000000000000355 ) ) ;
#58297 = FACE_OUTER_BOUND ( 'NONE', #30244, .T. ) ;
#58298 = CARTESIAN_POINT ( 'NONE',  ( 14.98074600654777377, -12.68155406624981119, 30.59749803192733708 ) ) ;
#58299 = CARTESIAN_POINT ( 'NONE',  ( 7.846153846153725020, -8.613356846316285953, 34.62446782046622218 ) ) ;
#58300 = CARTESIAN_POINT ( 'NONE',  ( 6.250054311638317373, -9.943054286541403997, 34.11300777759954883 ) ) ;
#58302 = CARTESIAN_POINT ( 'NONE',  ( 2.530703659305158837, -9.886259254753566594, 34.14407573483972413 ) ) ;
#58301 = CARTESIAN_POINT ( 'NONE',  ( -14.30769230769230660, -9.058645607665452459, 34.76329471203371924 ) ) ;
#58303 = CARTESIAN_POINT ( 'NONE',  ( -0.3307480205715115917, -8.191423895709840863, 34.95447573519442130 ) ) ;
#58305 = CARTESIAN_POINT ( 'NONE',  ( -8.769230769230455635, -2.255955759149395501, 30.00000000000324363 ) ) ;
#58304 = CARTESIAN_POINT ( 'NONE',  ( -15.45425417449318317, -11.89387501736622710, 32.13663884655806413 ) ) ;
#58306 = CARTESIAN_POINT ( 'NONE',  ( 1.944543648263018731, -9.444543648262994751, 14.62500000000000000 ) ) ;
#58307 = EDGE_LOOP ( 'NONE', ( #12331, #65558, #27, #80802 ) ) ;
#58308 = CARTESIAN_POINT ( 'NONE',  ( 18.06525557127601900, -11.94971097300157403, 32.03036669348361443 ) ) ;
#58309 = ORIENTED_EDGE ( 'NONE', *, *, #4243, .T. ) ;
#58310 = LINE ( 'NONE', #85357, #79472 ) ;
#58311 = ORIENTED_EDGE ( 'NONE', *, *, #87530, .F. ) ;
#58312 = EDGE_CURVE ( 'NONE', #60815, #35903, #85396, .T. ) ;
#58313 = CARTESIAN_POINT ( 'NONE',  ( -13.13456096470193302, -2.318338780012835443, 30.59689888758630261 ) ) ;
#58314 = ORIENTED_EDGE ( 'NONE', *, *, #77565, .T. ) ;
#58315 = CARTESIAN_POINT ( 'NONE',  ( 1.384615384615264011, -12.16647553114689728, 32.15551576947799362 ) ) ;
#58316 = CARTESIAN_POINT ( 'NONE',  ( -2.749999999999997780, -7.561099074964547917, 22.34188170625849068 ) ) ;
#58317 = CARTESIAN_POINT ( 'NONE',  ( -14.30769230769230660, -13.75783147151868846, 33.36296068462461051 ) ) ;
#58318 = EDGE_CURVE ( 'NONE', #25852, #42793, #39447, .T. ) ;
#58319 = CARTESIAN_POINT ( 'NONE',  ( -9.915792616872025178, -12.69144148231606017, 30.53333754910549303 ) ) ;
#58320 = DIRECTION ( 'NONE',  ( 0.000000000000000000, 0.000000000000000000, -1.000000000000000000 ) ) ;
#58321 = CARTESIAN_POINT ( 'NONE',  ( -12.46153846153846168, -3.937682226553329556, 33.60647404775216529 ) ) ;
#58322 = DIRECTION ( 'NONE',  ( -0.000000000000000000, 1.000000000000000000, -0.000000000000000000 ) ) ;
#58323 = DIRECTION ( 'NONE',  ( 0.000000000000000000, 0.7660444431189807890, 0.6427876096865361433 ) ) ;
#58324 = CARTESIAN_POINT ( 'NONE',  ( 0.000000000000000000, -11.00000000000000000, 29.75000000000000355 ) ) ;
#58325 = CARTESIAN_POINT ( 'NONE',  ( -1.929879867024197893E-14, -3.750000000000000000, 17.90625000000000000 ) ) ;
#58326 = CARTESIAN_POINT ( 'NONE',  ( 1.318531973659506251, -2.721908614388772296, 31.22303859784725688 ) ) ;
#58327 = CARTESIAN_POINT ( 'NONE',  ( 13.31853300525525086, -3.322132147404559532, 32.92929555188719348 ) ) ;
#58328 = ADVANCED_FACE ( 'NONE', ( #33886 ), #40658, .F. ) ;
#58329 = CARTESIAN_POINT ( 'NONE',  ( -13.38461538461550759, -11.06231777344772027, 33.60647404775119895 ) ) ;
#58330 = ORIENTED_EDGE ( 'NONE', *, *, #8671, .T. ) ;
#58331 = FACE_OUTER_BOUND ( 'NONE', #80259, .T. ) ;
#58332 = CARTESIAN_POINT ( 'NONE',  ( -17.32689980786543060, -8.303909089506435137, 34.68538101551103381 ) ) ;
#58333 = CARTESIAN_POINT ( 'NONE',  ( 1.253924781505079133, -10.70098750199973203, 33.91152734681376302 ) ) ;
#58334 = DIRECTION ( 'NONE',  ( 0.000000000000000000, 0.000000000000000000, 1.000000000000000000 ) ) ;
#58335 = AXIS2_PLACEMENT_3D ( 'NONE', #39685, #66240, #80216 ) ;
#58336 = CARTESIAN_POINT ( 'NONE',  ( 8.639083559792549494, -11.93770438780619259, 32.05411857736982029 ) ) ;
#58337 = CARTESIAN_POINT ( 'NONE',  ( -3.165514091256391715, -5.941354392334606160, 34.76329471203374055 ) ) ;
#58338 = EDGE_CURVE ( 'NONE', #30672, #85857, #6429, .T. ) ;
#58339 = ORIENTED_EDGE ( 'NONE', *, *, #7963, .T. ) ;
#58340 = CARTESIAN_POINT ( 'NONE',  ( -1.134561072977068319, -9.943054286541400444, 34.11300777759954883 ) ) ;
#58341 = ORIENTED_EDGE ( 'NONE', *, *, #75807, .F. ) ;
#58342 = VERTEX_POINT ( 'NONE', #62239 ) ;
#58343 = CARTESIAN_POINT ( 'NONE',  ( -9.469528023329624844, -3.020022701398813236, 32.48759521482552515 ) ) ;
#58344 = CARTESIAN_POINT ( 'NONE',  ( -6.700297254098854793, -5.827830569534416583, 34.72679350104403539 ) ) ;
#58345 = VECTOR ( 'NONE', #20660, 1000.000000000000114 ) ;
#58346 = CARTESIAN_POINT ( 'NONE',  ( -0.7115384615384606759, -7.433932668274254141, 35.00000000000001421 ) ) ;
#58347 = DIRECTION ( 'NONE',  ( 0.000000000000000000, 0.9848077530122072432, 0.1736481776669354937 ) ) ;
#58348 = CARTESIAN_POINT ( 'NONE',  ( -5.300408001487407539, -8.539481045369598178, 34.89627647299170832 ) ) ;
#58349 = ORIENTED_EDGE ( 'NONE', *, *, #49384, .F. ) ;
#58350 = ORIENTED_EDGE ( 'NONE', *, *, #64503, .F. ) ;
#58351 = VERTEX_POINT ( 'NONE', #41536 ) ;
#58352 = CARTESIAN_POINT ( 'NONE',  ( -7.146003881983769901, -11.98009711892699691, 32.48740034544075428 ) ) ;
#58353 = CARTESIAN_POINT ( 'NONE',  ( 8.546304551714621667, -2.758268499246657068, 31.33685645148948140 ) ) ;
#58354 = CARTESIAN_POINT ( 'NONE',  ( 8.834485908743602067, -5.941354392334607049, 34.76329471203374055 ) ) ;
#58355 = B_SPLINE_CURVE_WITH_KNOTS ( 'NONE', 3,
 ( #38495, #26638, #33402, #88366, #31741, #30834, #58304, #58757, #85798, #57865 ),
 .UNSPECIFIED., .F., .F.,
 ( 4, 2, 2, 2, 4 ),
 ( 0.000000000000000000, 0.0001954339857564097241, 0.0003908679715128194482, 0.0005863019572692291723, 0.0007817359430256388964 ),
 .UNSPECIFIED. ) ;
#58356 = CARTESIAN_POINT ( 'NONE',  ( 1.318531973659505585, -3.513871655860377086, 32.76840700105978499 ) ) ;
#58357 = CARTESIAN_POINT ( 'NONE',  ( 11.40831356872984337, -11.04286588640298561, 33.62463336215343901 ) ) ;
#58358 = FACE_OUTER_BOUND ( 'NONE', #1798, .T. ) ;
#58359 = EDGE_LOOP ( 'NONE', ( #77066, #22438, #33498, #9059, #10303 ) ) ;
#58360 = EDGE_LOOP ( 'NONE', ( #70579, #81716 ) ) ;
#58361 = CARTESIAN_POINT ( 'NONE',  ( 3.749999999999992006, -5.946699141100872943, 23.14062500000000000 ) ) ;
#58362 = ORIENTED_EDGE ( 'NONE', *, *, #85493, .F. ) ;
#58364 = VERTEX_POINT ( 'NONE', #47842 ) ;
#58363 = CARTESIAN_POINT ( 'NONE',  ( 2.557746619330623528, -12.41262288849542017, 30.68299917996395010 ) ) ;
#58365 = CARTESIAN_POINT ( 'NONE',  ( 1.384615384615386802, -7.500000000000001776, 35.04278698407183867 ) ) ;
#58366 = CARTESIAN_POINT ( 'NONE',  ( 9.692307692307695177, -13.20930481340135110, 34.54067556320372745 ) ) ;
#58367 = AXIS2_PLACEMENT_3D ( 'NONE', #6384, #75277, #74386 ) ;
#58368 = CARTESIAN_POINT ( 'NONE',  ( 2.320192649118979489E-14, -11.25000000000000000, 16.03125000000000000 ) ) ;
#58369 = ORIENTED_EDGE ( 'NONE', *, *, #10944, .T. ) ;
#58370 = B_SPLINE_CURVE_WITH_KNOTS ( 'NONE', 3,
 ( #82688, #20524, #88131, #259, #27721, #19202, #33604, #53868, #55192, #41688 ),
 .UNSPECIFIED., .F., .F.,
 ( 4, 2, 2, 2, 4 ),
 ( 0.000000000000000000, 0.0001954339857564083417, 0.0003908679715128166835, 0.0005863019572692250523, 0.0007817359430256333669 ),
 .UNSPECIFIED. ) ;
#58371 = CARTESIAN_POINT ( 'NONE',  ( -13.45069879557126313, -12.10708131394839349, 31.69288490824020244 ) ) ;
#58372 = ORIENTED_EDGE ( 'NONE', *, *, #86954, .T. ) ;
#58373 = CARTESIAN_POINT ( 'NONE',  ( -8.899378738962466784, -5.070767119584671079, 34.40440758774516183 ) ) ;
#58374 = CARTESIAN_POINT ( 'NONE',  ( 10.74591031714818357, -9.417988943895561960, 34.36773134775777550 ) ) ;
#58375 = B_SPLINE_CURVE_WITH_KNOTS ( 'NONE', 3,
 ( #13023, #33740, #61195, #16455, #71387, #43923, #2925, #9693, #85812, #30414 ),
 .UNSPECIFIED., .F., .F.,
 ( 4, 2, 2, 2, 4 ),
 ( 0.000000000000000000, 0.0001954339857564064444, 0.0003908679715128128888, 0.0005863019572692193060, 0.0007817359430256257775 ),
 .UNSPECIFIED. ) ;
#58376 = FACE_OUTER_BOUND ( 'NONE', #37820, .T. ) ;
#58378 = CARTESIAN_POINT ( 'NONE',  ( -6.700297381808513641, -2.600157965045225339, 30.74683119005207743 ) ) ;
#58377 = CARTESIAN_POINT ( 'NONE',  ( 10.83834751894610093, -7.369474270740069777, 34.74850911626239736 ) ) ;
#58379 = CARTESIAN_POINT ( 'NONE',  ( 8.519207531937803779, -5.851115903089112003, 34.47074536777953568 ) ) ;
#58380 = CARTESIAN_POINT ( 'NONE',  ( -22.75000000000000000, -10.50000000000000000, 27.25000000000000000 ) ) ;
#58381 = ORIENTED_EDGE ( 'NONE', *, *, #30456, .F. ) ;
#58382 = CARTESIAN_POINT ( 'NONE',  ( -11.47239318745910452, -12.10708131394839882, 31.69288490824020954 ) ) ;
#58383 = AXIS2_PLACEMENT_3D ( 'NONE', #61780, #48718, #55477 ) ;
#58384 = CARTESIAN_POINT ( 'NONE',  ( -8.992715693795101828, -4.225889041578353655, 33.85425143139329407 ) ) ;
#58385 = VERTEX_POINT ( 'NONE', #81203 ) ;
#58386 = CARTESIAN_POINT ( 'NONE',  ( -12.33101302330481808, -3.625058011473228703, 33.29252011169590020 ) ) ;
#58387 = CARTESIAN_POINT ( 'NONE',  ( 15.45354877203763522, -4.387253974876679230, 33.66317474335728832 ) ) ;
#58388 = CARTESIAN_POINT ( 'NONE',  ( -24.99999999999999645, 12.00000000000000711, 0.000000000000000000 ) ) ;
#58389 = FACE_OUTER_BOUND ( 'NONE', #34531, .T. ) ;
#58390 = CARTESIAN_POINT ( 'NONE',  ( -8.096153846153844924, -7.433932668274256805, 35.00000000000000711 ) ) ;
#58391 = FACE_BOUND ( 'NONE', #12953, .T. ) ;
#58393 = CARTESIAN_POINT ( 'NONE',  ( 17.93472999944368240, -11.06231777344662959, 33.60647404775220082 ) ) ;
#58392 = CARTESIAN_POINT ( 'NONE',  ( 13.31934538405906565, -2.379036618887870436, 30.90682066428147934 ) ) ;
#58394 = DIRECTION ( 'NONE',  ( -0.000000000000000000, -0.000000000000000000, -1.000000000000000000 ) ) ;
#58396 = CARTESIAN_POINT ( 'NONE',  ( 10.61538461538449418, -12.16647553114689728, 32.15551576947799362 ) ) ;
#58395 = CARTESIAN_POINT ( 'NONE',  ( -13.63461538461538325, -2.249999999999998668, 29.75000000000000355 ) ) ;
#58397 = CARTESIAN_POINT ( 'NONE',  ( 15.84615384615384670, -7.500000000000000000, 29.75000000000000355 ) ) ;
#58398 = CARTESIAN_POINT ( 'NONE',  ( -14.30769230769230660, -9.819645486525091727, 36.12317359536749706 ) ) ;
#58399 = CARTESIAN_POINT ( 'NONE',  ( 2.694853999681214862, -10.10844685921789043, 20.62313170625849068 ) ) ;
#58400 = VERTEX_POINT ( 'NONE', #60915 ) ;
#58401 = EDGE_CURVE ( 'NONE', #10136, #51826, #5986, .T. ) ;
#58402 = CARTESIAN_POINT ( 'NONE',  ( -8.069638789877794594, -11.41268669641500466, 32.86336882939237825 ) ) ;
#58403 = VECTOR ( 'NONE', #41062, 1000.000000000000000 ) ;
#58404 = CARTESIAN_POINT ( 'NONE',  ( -14.55771554498526932, -6.695914987888146541, 34.68535235679833306 ) ) ;
#58405 = CARTESIAN_POINT ( 'NONE',  ( -7.716108683319066408, -2.504778602574660340, 29.97347330155780298 ) ) ;
#58406 = CARTESIAN_POINT ( 'NONE',  ( -16.15384615384615330, -13.57706302396349152, 30.56769352161908060 ) ) ;
#58407 = ADVANCED_FACE ( 'NONE', ( #993 ), #12734, .T. ) ;
#58408 = CARTESIAN_POINT ( 'NONE',  ( 7.780070435197966816, -4.786620604624111763, 33.94971097300155805 ) ) ;
#58409 = PLANE ( 'NONE',  #35436 ) ;
#58410 = CARTESIAN_POINT ( 'NONE',  ( 3.749999999999999556, -7.438900925035446754, 20.46688170625848713 ) ) ;
#58411 = CARTESIAN_POINT ( 'NONE',  ( -11.47331675774190352, -7.750023224968867197, 34.99404313364389907 ) ) ;
#58412 = CARTESIAN_POINT ( 'NONE',  ( -14.53117723225663660, -11.60425143139329940, 33.02411095842164457 ) ) ;
#58413 = VECTOR ( 'NONE', #75854, 1000.000000000000114 ) ;
#58414 = CARTESIAN_POINT ( 'NONE',  ( 9.019230769230768274, -7.500000000000001776, 35.04278698407183867 ) ) ;
#58415 = CARTESIAN_POINT ( 'NONE',  ( 4.826946332874483048, -9.234221910056348293, 34.70572697212741531 ) ) ;
#58416 = CARTESIAN_POINT ( 'NONE',  ( 14.30769230769218758, -6.026961402154118019, 34.52809138561165270 ) ) ;
#58417 = CARTESIAN_POINT ( 'NONE',  ( 4.087762742890272527, -10.51840700105979387, 33.73612834413961536 ) ) ;
#58418 = B_SPLINE_CURVE_WITH_KNOTS ( 'NONE', 3,
 ( #68395, #27414, #54433, #13014, #40501, #34166, #54886, #67963, #75588, #87361 ),
 .UNSPECIFIED., .F., .F.,
 ( 4, 2, 2, 2, 4 ),
 ( 0.0007817246256747440282, 0.0009771112852218863821, 0.001172497944769028844, 0.001367884604316171307, 0.001563271263863313769 ),
 .UNSPECIFIED. ) ;
#58419 = CARTESIAN_POINT ( 'NONE',  ( -18.00000000000012079, -2.892918686052166066, 31.69288490824153470 ) ) ;
#58420 = EDGE_CURVE ( 'NONE', #3529, #38748, #48727, .T. ) ;
#58421 = DIRECTION ( 'NONE',  ( -0.000000000000000000, 0.1736481776669307198, -0.9848077530122080203 ) ) ;
#58422 = ORIENTED_EDGE ( 'NONE', *, *, #87170, .T. ) ;
#58423 = CARTESIAN_POINT ( 'NONE',  ( 15.16468685140909578, -11.35647404775217595, 33.31231777344666511 ) ) ;
#58424 = CARTESIAN_POINT ( 'NONE',  ( 6.989145274079363368, -4.786620604624113540, 33.94971097300155805 ) ) ;
#58425 = CARTESIAN_POINT ( 'NONE',  ( -1.492201783934593573, -3.724691934501250135, 13.07999329374151642 ) ) ;
#58426 = CARTESIAN_POINT ( 'NONE',  ( -10.74607521849492109, -2.494641256782728966, 31.33461815524612959 ) ) ;
#58427 = CARTESIAN_POINT ( 'NONE',  ( -17.07692307692319744, -5.941354392335915335, 34.76329471203413846 ) ) ;
#58428 = ORIENTED_EDGE ( 'NONE', *, *, #18270, .T. ) ;
#58429 = CARTESIAN_POINT ( 'NONE',  ( 1.607626736228236153, -4.187068189119697692, 33.49521262558774026 ) ) ;
#58430 = CARTESIAN_POINT ( 'NONE',  ( 1.253923917947828537, -8.999036380462717588, 34.52022231692819076 ) ) ;
#58432 = EDGE_LOOP ( 'NONE', ( #41991, #61607 ) ) ;
#58431 = LINE ( 'NONE', #29656, #67053 ) ;
#58433 = CARTESIAN_POINT ( 'NONE',  ( 11.76147438255493327, -4.762714258010881885, 34.23016756924214832 ) ) ;
#58434 = CARTESIAN_POINT ( 'NONE',  ( -13.16183584334697443, -10.11255958852956027, 34.01340905677048454 ) ) ;
#58435 = DIRECTION ( 'NONE',  ( 0.000000000000000000, 0.000000000000000000, 1.000000000000000000 ) ) ;
#58436 = CARTESIAN_POINT ( 'NONE',  ( -14.08468095607945969, -11.24521262558773493, 33.06293181088029343 ) ) ;
#58437 = EDGE_LOOP ( 'NONE', ( #24526, #54567 ) ) ;
#58438 = DIRECTION ( 'NONE',  ( -0.000000000000000000, 0.3420201433256694901, -0.9396926207859082059 ) ) ;
#58439 = CARTESIAN_POINT ( 'NONE',  ( 10.74617505635156789, -3.957578996910242619, 33.62503395064540257 ) ) ;
#58440 = ADVANCED_FACE ( 'NONE', ( #55485 ), #74888, .F. ) ;
#58441 = CARTESIAN_POINT ( 'NONE',  ( -1.161604033002533898, -5.667800583137508674, 34.40243808032445827 ) ) ;
#58442 = VERTEX_POINT ( 'NONE', #19928 ) ;
#58443 = EDGE_CURVE ( 'NONE', #23084, #14741, #49164, .T. ) ;
#58444 = ORIENTED_EDGE ( 'NONE', *, *, #70558, .T. ) ;
#58445 = EDGE_CURVE ( 'NONE', #35007, #8069, #7310, .T. ) ;
#58446 = VERTEX_POINT ( 'NONE', #28465 ) ;
#58447 = B_SPLINE_CURVE_WITH_KNOTS ( 'NONE', 3,
 ( #63671, #42530, #56911, #15500, #76302, #21359, #49279, #34869, #48828, #1093 ),
 .UNSPECIFIED., .F., .F.,
 ( 4, 2, 2, 2, 4 ),
 ( 0.000000000000000000, 0.0001954339857564090194, 0.0003908679715128180387, 0.0005863019572692270039, 0.0007817359430256360774 ),
 .UNSPECIFIED. ) ;
#58448 = ADVANCED_FACE ( 'NONE', ( #69450 ), #54147, .F. ) ;
#58449 = CARTESIAN_POINT ( 'NONE',  ( -5.300408001487407539, -9.417330523894424488, 34.63758898049880486 ) ) ;
#58450 = DIRECTION ( 'NONE',  ( 0.000000000000000000, 0.000000000000000000, 1.000000000000000000 ) ) ;
#58451 = AXIS2_PLACEMENT_3D ( 'NONE', #76176, #46924, #27104 ) ;
#58452 = CARTESIAN_POINT ( 'NONE',  ( 4.153846153846154188, -12.78798330534102945, 29.74999999999997868 ) ) ;
#58453 = CARTESIAN_POINT ( 'NONE',  ( 14.98074599347626901, -3.711651800289232028, 33.01384336483936011 ) ) ;
#58454 = ORIENTED_EDGE ( 'NONE', *, *, #18541, .F. ) ;
#58455 = ORIENTED_EDGE ( 'NONE', *, *, #10849, .T. ) ;
#58457 = VERTEX_POINT ( 'NONE', #88859 ) ;
#58456 = LINE ( 'NONE', #24231, #47295 ) ;
#58458 = CARTESIAN_POINT ( 'NONE',  ( -18.00000000000012079, -2.657715359629662988, 31.77849191805970364 ) ) ;
#58459 = CARTESIAN_POINT ( 'NONE',  ( -23.50000000000000000, -9.499999999999982236, 32.75000000000000000 ) ) ;
#58460 = CARTESIAN_POINT ( 'NONE',  ( 10.39245839786846837, -11.24512374952581872, 33.06303171183252942 ) ) ;
#58461 = CARTESIAN_POINT ( 'NONE',  ( 13.63456079399343146, -10.18230066228895758, 34.26354781536631577 ) ) ;
#58462 = EDGE_LOOP ( 'NONE', ( #28920, #17612 ) ) ;
#58463 = ORIENTED_EDGE ( 'NONE', *, *, #83633, .F. ) ;
#58464 = AXIS2_PLACEMENT_3D ( 'NONE', #71741, #11837, #58228 ) ;
#58465 = ORIENTED_EDGE ( 'NONE', *, *, #23379, .F. ) ;
#58467 = ORIENTED_EDGE ( 'NONE', *, *, #73665, .F. ) ;
#58466 = CARTESIAN_POINT ( 'NONE',  ( 15.16468581981334651, -2.538708090699994813, 30.37095296980875148 ) ) ;
#58468 = LINE ( 'NONE', #17056, #26022 ) ;
#58469 = EDGE_CURVE ( 'NONE', #27365, #74160, #39267, .T. ) ;
#58470 = CARTESIAN_POINT ( 'NONE',  ( 17.99999999999987566, -5.941354392335915335, 34.76329471203413846 ) ) ;
#58471 = VERTEX_POINT ( 'NONE', #68128 ) ;
#58472 = VECTOR ( 'NONE', #38959, 1000.000000000000114 ) ;
#58473 = CARTESIAN_POINT ( 'NONE',  ( 20.00000000000000000, -11.50000000000000000, 28.25000000000000000 ) ) ;
#58474 = CARTESIAN_POINT ( 'NONE',  ( -1.514762594053604916, -8.587444163452046197, 34.63053765926554206 ) ) ;
#58475 = CARTESIAN_POINT ( 'NONE',  ( -2.242436736416281828, -11.48612834413965977, 32.76840700105972815 ) ) ;
#58476 = FACE_BOUND ( 'NONE', #18774, .T. ) ;
#58477 = CARTESIAN_POINT ( 'NONE',  ( -8.769230769230768274, -2.292212530054420494, 30.41441678777542634 ) ) ;
#58478 = CARTESIAN_POINT ( 'NONE',  ( 11.53846153846153832, -8.120952969808772792, 34.71129190930000163 ) ) ;
#58479 = CARTESIAN_POINT ( 'NONE',  ( 8.546304551714618114, -2.554751324335735152, 30.48935550225260727 ) ) ;
#58481 = CARTESIAN_POINT ( 'NONE',  ( 4.153846153846030731, -2.379036618888197729, 30.90682066428292885 ) ) ;
#58480 = PLANE ( 'NONE',  #83502 ) ;
#58482 = CARTESIAN_POINT ( 'NONE',  ( 11.47237812750566022, -11.16473453929635440, 33.15142922261925662 ) ) ;
#58483 = DIRECTION ( 'NONE',  ( 0.000000000000000000, 0.000000000000000000, 1.000000000000000000 ) ) ;
#58484 = ORIENTED_EDGE ( 'NONE', *, *, #67436, .T. ) ;
#58485 = CYLINDRICAL_SURFACE ( 'NONE', #46079, 0.2500000000000002220 ) ;
#58486 = CARTESIAN_POINT ( 'NONE',  ( -13.38461538461550759, -9.528491918059723176, 34.59228464037033035 ) ) ;
#58487 = ORIENTED_EDGE ( 'NONE', *, *, #12885, .F. ) ;
#58488 = ORIENTED_EDGE ( 'NONE', *, *, #55000, .F. ) ;
#58489 = EDGE_CURVE ( 'NONE', #72151, #79461, #29880, .T. ) ;
#58491 = CARTESIAN_POINT ( 'NONE',  ( -5.999999999999998224, -12.10708131394839349, 31.69288490824020244 ) ) ;
#58490 = CARTESIAN_POINT ( 'NONE',  ( -39.05038313613820122, -2.249999999999998668, 29.75000000000000355 ) ) ;
#58492 = CARTESIAN_POINT ( 'NONE',  ( -6.792285115252135519, -6.413143153341454017, 34.63066358083362672 ) ) ;
#58493 = CARTESIAN_POINT ( 'NONE',  ( 14.53106779346472877, -2.251407671071270489, 29.88021292934943318 ) ) ;
#58494 = CARTESIAN_POINT ( 'NONE',  ( 18.00000000000000000, -13.78497067705608181, 32.30358669280327177 ) ) ;
#58495 = ORIENTED_EDGE ( 'NONE', *, *, #85298, .F. ) ;
#58496 = CIRCLE ( 'NONE', #54207, 4.000000000000000000 ) ;
#58497 = CARTESIAN_POINT ( 'NONE',  ( 18.25005441991345734, -4.074993327901525575, 33.72946981652012255 ) ) ;
#58498 = CARTESIAN_POINT ( 'NONE',  ( -7.846153846153844924, -3.669653830205710676, 35.88435417666054406 ) ) ;
#58499 = CARTESIAN_POINT ( 'NONE',  ( -15.23076923076922995, -12.78798330534103123, 29.99999999999997868 ) ) ;
#58500 = DIRECTION ( 'NONE',  ( -0.000000000000000000, 0.3420201433256694901, -0.9396926207859082059 ) ) ;
#58501 = DIRECTION ( 'NONE',  ( 0.000000000000000000, 0.000000000000000000, -1.000000000000000000 ) ) ;
#58502 = CIRCLE ( 'NONE', #83170, 4.000000000000000000 ) ;
#58503 = CARTESIAN_POINT ( 'NONE',  ( 1.553300858899129944, -11.24999999999998934, 17.20312500000000000 ) ) ;
#58504 = VERTEX_POINT ( 'NONE', #50054 ) ;
#58505 = B_SPLINE_CURVE_WITH_KNOTS ( 'NONE', 3,
 ( #7600, #15687, #27865, #402, #43154, #16123, #8931, #63861, #2158, #8489 ),
 .UNSPECIFIED., .F., .F.,
 ( 4, 2, 2, 2, 4 ),
 ( 0.0007817359430256388964, 0.0009771253907250073822, 0.001172514838424375868, 0.001367904286123744571, 0.001563293733823113056 ),
 .UNSPECIFIED. ) ;
#58506 = VERTEX_POINT ( 'NONE', #2302 ) ;
#58507 = EDGE_CURVE ( 'NONE', #26351, #23513, #60973, .T. ) ;
#58508 = FACE_OUTER_BOUND ( 'NONE', #805, .T. ) ;
#58509 = EDGE_LOOP ( 'NONE', ( #55029, #60513 ) ) ;
#58510 = VECTOR ( 'NONE', #26010, 1000.000000000000000 ) ;
#58511 = CARTESIAN_POINT ( 'NONE',  ( 17.29993592101647693, -4.026326845037969449, 33.68677907613345468 ) ) ;
#58512 = CARTESIAN_POINT ( 'NONE',  ( 9.758376043310132530, -9.780366693483667717, 34.19971097300155805 ) ) ;
#58513 = CARTESIAN_POINT ( 'NONE',  ( 14.37294787896833270, -2.892918686051625166, 31.69288490824026638 ) ) ;
#58514 = EDGE_CURVE ( 'NONE', #37333, #5428, #33064, .T. ) ;
#58515 = FACE_OUTER_BOUND ( 'NONE', #74484, .T. ) ;
#58516 = CARTESIAN_POINT ( 'NONE',  ( 3.750000000000000888, -7.499999999999978684, 16.96875000000000000 ) ) ;
#58517 = CARTESIAN_POINT ( 'NONE',  ( 1.384615384615386802, -4.786620604624113540, 33.94971097300155094 ) ) ;
#58518 = EDGE_LOOP ( 'NONE', ( #14456, #69175 ) ) ;
#58519 = CARTESIAN_POINT ( 'NONE',  ( 4.218991933178116938, -7.750023238201980469, 34.74374492549440419 ) ) ;
#58521 = VERTEX_POINT ( 'NONE', #83866 ) ;
#58520 = DIRECTION ( 'NONE',  ( 0.000000000000000000, 0.1736481776669267785, -0.9848077530122087975 ) ) ;
#58522 = DIRECTION ( 'NONE',  ( -1.000000000000000000, -0.000000000000000000, -0.000000000000000000 ) ) ;
#58523 = CARTESIAN_POINT ( 'NONE',  ( 14.08476609017615644, -12.15238873228292071, 31.58232369045353849 ) ) ;
#58524 = CARTESIAN_POINT ( 'NONE',  ( -7.134615384615385025, -11.50000000000000000, 29.75000000000000355 ) ) ;
#58525 = CARTESIAN_POINT ( 'NONE',  ( 7.846153846153846700, -13.75783147151868846, 33.36296068462461051 ) ) ;
#58526 = CARTESIAN_POINT ( 'NONE',  ( -6.000000000000121680, -5.094484230521993062, 34.41647553114689373 ) ) ;
#58527 = EDGE_CURVE ( 'NONE', #15410, #31669, #15835, .T. ) ;
#58528 = CARTESIAN_POINT ( 'NONE',  ( 7.846153846153846700, -3.322132147404559976, 32.92929555188717927 ) ) ;
#58529 = CARTESIAN_POINT ( 'NONE',  ( -7.146003140593070846, -4.887634598454295265, 34.01352882383564946 ) ) ;
#58530 = CARTESIAN_POINT ( 'NONE',  ( -3.724691934501248802, -5.885600066136383646, 20.42374329374152353 ) ) ;
#58531 = ORIENTED_EDGE ( 'NONE', *, *, #79555, .T. ) ;
#58532 = CARTESIAN_POINT ( 'NONE',  ( -4.403869391139117795, -5.056417327199099532, 34.11270091957320716 ) ) ;
#58533 = CARTESIAN_POINT ( 'NONE',  ( -12.33149085528277844, -7.723484964179501588, 34.74522123443823318 ) ) ;
#58534 = CARTESIAN_POINT ( 'NONE',  ( -4.377331078410482412, -5.827078755546623690, 34.72654668319379567 ) ) ;
#58535 = CARTESIAN_POINT ( 'NONE',  ( -1.944543648262992530, -9.444543648263016067, 26.18750000000000355 ) ) ;
#58536 = ADVANCED_FACE ( 'NONE', ( #56811 ), #8198, .F. ) ;
#58537 = LINE ( 'NONE', #30631, #17299 ) ;
#58539 = CARTESIAN_POINT ( 'NONE',  ( -17.29984929443922681, -2.554751324335733376, 30.48935550225260727 ) ) ;
#58538 = VECTOR ( 'NONE', #16916, 1000.000000000000000 ) ;
#58541 = ORIENTED_EDGE ( 'NONE', *, *, #39000, .F. ) ;
#58540 = DIRECTION ( 'NONE',  ( -0.000000000000000000, -0.7660444431189791237, -0.6427876096865379196 ) ) ;
#58542 = CARTESIAN_POINT ( 'NONE',  ( -2.750000000000006217, -6.360912703474006946, 20.17187500000000000 ) ) ;
#58543 = CARTESIAN_POINT ( 'NONE',  ( -20.00000000000000355, 10.00000000000000711, 13.00000000000000178 ) ) ;
#58544 = EDGE_CURVE ( 'NONE', #10963, #60703, #12642, .T. ) ;
#58545 = EDGE_LOOP ( 'NONE', ( #82074, #48508, #54088, #88638 ) ) ;
#58546 = CARTESIAN_POINT ( 'NONE',  ( 6.673100179028331524, -6.524016743844655686, 34.90889640711025521 ) ) ;
#58547 = ORIENTED_EDGE ( 'NONE', *, *, #49395, .F. ) ;
#58548 = B_SPLINE_CURVE_WITH_KNOTS ( 'NONE', 3,
 ( #46157, #5611, #18691, #52452, #74077, #39850, #11934, #38510, #32633, #73184 ),
 .UNSPECIFIED., .F., .F.,
 ( 4, 2, 2, 2, 4 ),
 ( 0.0007817359430256297891, 0.0009771253907249963233, 0.001172514838424362858, 0.001367904286123729175, 0.001563293733823095709 ),
 .UNSPECIFIED. ) ;
#58549 = PRODUCT_DEFINITION_SHAPE ( 'NONE', 'NONE',  #89182 ) ;
#58550 = CARTESIAN_POINT ( 'NONE',  ( -14.30769230769242917, -3.083524468854526912, 32.58852847137268327 ) ) ;
#58551 = CARTESIAN_POINT ( 'NONE',  ( -1.634638608836842089, -12.07920672191015221, 32.31858351112116168 ) ) ;
#58552 = EDGE_CURVE ( 'NONE', #2097, #77497, #29801, .T. ) ;
#58553 = CARTESIAN_POINT ( 'NONE',  ( -0.2385256174450664790, -6.460100341425560444, 34.89618726649961644 ) ) ;
#58554 = ORIENTED_EDGE ( 'NONE', *, *, #207, .F. ) ;
#58555 = CARTESIAN_POINT ( 'NONE',  ( -0.7115384615384854339, -2.249999999999999112, 29.81609741502488120 ) ) ;
#58556 = VERTEX_POINT ( 'NONE', #56380 ) ;
#58557 = CARTESIAN_POINT ( 'NONE',  ( -11.53846153846153655, -13.53365097954675988, 30.81389545987213552 ) ) ;
#58558 = ORIENTED_EDGE ( 'NONE', *, *, #75820, .F. ) ;
#58559 = CARTESIAN_POINT ( 'NONE',  ( -0.5922299282060219383, -3.062553014421049546, 32.05460306192773601 ) ) ;
#58560 = DIRECTION ( 'NONE',  ( 0.000000000000000000, 0.3420201433256610524, 0.9396926207859113145 ) ) ;
#58561 = ADVANCED_FACE ( 'NONE', ( #43311 ), #9088, .F. ) ;
#58562 = VERTEX_POINT ( 'NONE', #36977 ) ;
#58563 = ADVANCED_FACE ( 'NONE', ( #2740 ), #30236, .F. ) ;
#58564 = LINE ( 'NONE', #86057, #82185 ) ;
#58565 = DIRECTION ( 'NONE',  ( -0.000000000000000000, -0.5000000000000009992, -0.8660254037844380415 ) ) ;
#58566 = CARTESIAN_POINT ( 'NONE',  ( -11.78848477575450460, -2.823816976329319051, 31.52131813110795733 ) ) ;
#58567 = CARTESIAN_POINT ( 'NONE',  ( 13.38461538461538680, -11.91647553114624181, 32.58852847137148245 ) ) ;
#58568 = CARTESIAN_POINT ( 'NONE',  ( -8.096177070375304652, -12.68155406624981119, 30.59749803192733708 ) ) ;
#58569 = VECTOR ( 'NONE', #46877, 1000.000000000000000 ) ;
#58570 = VERTEX_POINT ( 'NONE', #12189 ) ;
#58571 = ORIENTED_EDGE ( 'NONE', *, *, #5205, .T. ) ;
#58572 = ORIENTED_EDGE ( 'NONE', *, *, #25118, .T. ) ;
#58574 = EDGE_LOOP ( 'NONE', ( #74756, #59509 ) ) ;
#58573 = CARTESIAN_POINT ( 'NONE',  ( 2.980746006547774218, -5.765609946408404518, 34.70566812827425451 ) ) ;
#58575 = AXIS2_PLACEMENT_3D ( 'NONE', #9633, #11415, #31695 ) ;
#58576 = ADVANCED_FACE ( 'NONE', ( #39674 ), #32012, .F. ) ;
#58577 = CARTESIAN_POINT ( 'NONE',  ( -11.53846153846166089, -2.379036618888197729, 30.90682066428292885 ) ) ;
#58578 = CARTESIAN_POINT ( 'NONE',  ( 9.442330948259103351, -5.643011162660950042, 34.66104346484419096 ) ) ;
#58579 = ORIENTED_EDGE ( 'NONE', *, *, #15343, .T. ) ;
#58580 = ORIENTED_EDGE ( 'NONE', *, *, #45472, .T. ) ;
#58581 = B_SPLINE_CURVE_WITH_KNOTS ( 'NONE', 3,
 ( #40732, #13251, #27645, #88059, #26320, #178, #53787, #75395, #7386, #67753 ),
 .UNSPECIFIED., .F., .F.,
 ( 4, 2, 2, 2, 4 ),
 ( 0.000000000000000000, 0.0001954311564186868744, 0.0003908623128373737488, 0.0005862934692560606504, 0.0007817246256747474977 ),
 .UNSPECIFIED. ) ;
#58582 = ORIENTED_EDGE ( 'NONE', *, *, #70331, .T. ) ;
#58583 = CARTESIAN_POINT ( 'NONE',  ( 17.07692307692295586, -4.481592998941358097, 33.73612834414048933 ) ) ;
#58584 = ORIENTED_EDGE ( 'NONE', *, *, #54773, .T. ) ;
#58585 = CARTESIAN_POINT ( 'NONE',  ( -9.070512820512819374, -7.500000000000000000, 33.75000000000000000 ) ) ;
#58586 = B_SPLINE_CURVE_WITH_KNOTS ( 'NONE', 3,
 ( #39275, #45564, #3245, #79808, #18108, #30716, #79358, #58182, #51861, #58627 ),
 .UNSPECIFIED., .F., .F.,
 ( 4, 2, 2, 2, 4 ),
 ( 0.0007817359430256297891, 0.0009771253907249958896, 0.001172514838424361990, 0.001367904286123728091, 0.001563293733823094191 ),
 .UNSPECIFIED. ) ;
#58587 = EDGE_CURVE ( 'NONE', #35011, #4267, #65262, .T. ) ;
#58588 = CARTESIAN_POINT ( 'NONE',  ( -7.846153846153844924, -2.538708090699994813, 30.37095296980875503 ) ) ;
#58589 = CARTESIAN_POINT ( 'NONE',  ( -9.942307692307693401, -7.433932668274256805, 35.00000000000000711 ) ) ;
#58590 = ADVANCED_FACE ( 'NONE', ( #18502 ), #52713, .F. ) ;
#58591 = FACE_BOUND ( 'NONE', #34118, .T. ) ;
#58592 = ORIENTED_EDGE ( 'NONE', *, *, #70727, .T. ) ;
#58593 = FACE_OUTER_BOUND ( 'NONE', #46033, .T. ) ;
#58594 = CARTESIAN_POINT ( 'NONE',  ( 12.71159277317677549, -5.728107161865378494, 34.42597550085002922 ) ) ;
#58595 = EDGE_CURVE ( 'NONE', #77057, #47782, #67134, .T. ) ;
#58596 = CARTESIAN_POINT ( 'NONE',  ( 4.153846153846032507, -8.613356846316285953, 34.62446782046622218 ) ) ;
#58597 = VECTOR ( 'NONE', #81783, 1000.000000000000000 ) ;
#58598 = DIRECTION ( 'NONE',  ( -0.000000000000000000, -0.1736481776669307198, -0.9848077530122080203 ) ) ;
#58599 = CARTESIAN_POINT ( 'NONE',  ( 8.068933387422253745, -10.81320215134717344, 33.49497208177562868 ) ) ;
#58600 = ORIENTED_EDGE ( 'NONE', *, *, #46962, .T. ) ;
#58601 = CARTESIAN_POINT ( 'NONE',  ( 20.00000000000000000, -4.000000000000000000, 29.75000000000000355 ) ) ;
#58602 = ORIENTED_EDGE ( 'NONE', *, *, #65140, .F. ) ;
#58603 = VERTEX_POINT ( 'NONE', #24803 ) ;
#58604 = EDGE_CURVE ( 'NONE', #72334, #26024, #80203, .T. ) ;
#58606 = CARTESIAN_POINT ( 'NONE',  ( 5.750023269057648712, -3.137211980971221781, 32.19342716148376837 ) ) ;
#58605 = FACE_OUTER_BOUND ( 'NONE', #85169, .T. ) ;
#58607 = LINE ( 'NONE', #31590, #38462 ) ;
#58608 = CARTESIAN_POINT ( 'NONE',  ( -2.057637996053991891, -12.17597550085003455, 31.52189283813461884 ) ) ;
#58609 = CARTESIAN_POINT ( 'NONE',  ( 17.14309221788574078, -7.250054483168842268, 34.74374881642865631 ) ) ;
#58610 = CARTESIAN_POINT ( 'NONE',  ( -15.45425415533356173, -3.562934362175800285, 33.22335522853832401 ) ) ;
#58611 = ORIENTED_EDGE ( 'NONE', *, *, #40958, .T. ) ;
#58612 = CARTESIAN_POINT ( 'NONE',  ( -5.299850035829924089, -6.459968553980839800, 34.89616026154728701 ) ) ;
#58613 = VECTOR ( 'NONE', #47145, 1000.000000000000000 ) ;
#58614 = CARTESIAN_POINT ( 'NONE',  ( 3.230769230769231726, -10.51840700105979565, 33.73612834413961536 ) ) ;
#58615 = PLANE ( 'NONE',  #17115 ) ;
#58616 = CARTESIAN_POINT ( 'NONE',  ( -13.38461538461538325, -12.62096338111211580, 30.90682066428153263 ) ) ;
#58617 = EDGE_LOOP ( 'NONE', ( #18947, #47483, #26816, #80641 ) ) ;
#58618 = ORIENTED_EDGE ( 'NONE', *, *, #28675, .F. ) ;
#58619 = FACE_BOUND ( 'NONE', #9720, .T. ) ;
#58620 = B_SPLINE_CURVE_WITH_KNOTS ( 'NONE', 3,
 ( #11949, #73199, #38978, #86736, #61006, #88506, #88075, #39426, #25897, #6073 ),
 .UNSPECIFIED., .F., .F.,
 ( 4, 2, 2, 2, 4 ),
 ( 0.0007817359430256369448, 0.0009771253907250049969, 0.001172514838424373049, 0.001367904286123741101, 0.001563293733823109153 ),
 .UNSPECIFIED. ) ;
#58621 = ORIENTED_EDGE ( 'NONE', *, *, #49266, .T. ) ;
#58622 = CARTESIAN_POINT ( 'NONE',  ( 11.66898697669518192, -12.50538340440932394, 31.33453814440721885 ) ) ;
#58623 = CARTESIAN_POINT ( 'NONE',  ( 19.99999999999996803, 15.00000000000000711, 13.00000000000000178 ) ) ;
#58624 = ORIENTED_EDGE ( 'NONE', *, *, #5177, .T. ) ;
#58625 = CARTESIAN_POINT ( 'NONE',  ( -7.846153846153844924, -2.499999999999998668, 29.75000000000001421 ) ) ;
#58626 = FACE_OUTER_BOUND ( 'NONE', #21496, .T. ) ;
#58627 = CARTESIAN_POINT ( 'NONE',  ( -8.769230769230768274, -6.386643153685126251, 34.62446782046654192 ) ) ;
#58628 = EDGE_CURVE ( 'NONE', #33723, #56881, #39222, .T. ) ;
#58629 = CARTESIAN_POINT ( 'NONE',  ( -6.857821351800897247, -3.300289026998475705, 32.46337939537591666 ) ) ;
#58630 = VERTEX_POINT ( 'NONE', #4076 ) ;
#58631 = ADVANCED_FACE ( 'NONE', ( #59920 ), #85623, .F. ) ;
#58632 = DIRECTION ( 'NONE',  ( -0.000000000000000000, -0.9396926207859092051, -0.3420201433256662704 ) ) ;
#58633 = ORIENTED_EDGE ( 'NONE', *, *, #16623, .F. ) ;
#58635 = EDGE_LOOP ( 'NONE', ( #27483, #88408 ) ) ;
#58634 = CARTESIAN_POINT ( 'NONE',  ( 17.07692307692295586, -10.90142922262034020, 33.41473453929536674 ) ) ;
#58636 = CARTESIAN_POINT ( 'NONE',  ( 15.45354877203763522, -8.496831190052093419, 34.64984203495476578 ) ) ;
#58637 = DIRECTION ( 'NONE',  ( -1.000000000000000000, -0.000000000000000000, 0.000000000000000000 ) ) ;
#58638 = CARTESIAN_POINT ( 'NONE',  ( -7.596099426240392916, -3.435999193479609470, 33.07426656108010832 ) ) ;
#58639 = VECTOR ( 'NONE', #82478, 1000.000000000000227 ) ;
#58640 = CARTESIAN_POINT ( 'NONE',  ( 0.4615384615383396616, -12.27809138561165270, 31.22303859784587132 ) ) ;
#58641 = CARTESIAN_POINT ( 'NONE',  ( -17.78205128205128105, -7.500000000000000000, 29.75000000000000355 ) ) ;
#58642 = CARTESIAN_POINT ( 'NONE',  ( -9.692307692307691624, -11.91647553114624181, 32.58852847137148245 ) ) ;
#58643 = CARTESIAN_POINT ( 'NONE',  ( -0.06109907496451398579, -10.25000000000000178, 15.03311829374151287 ) ) ;
#58644 = ORIENTED_EDGE ( 'NONE', *, *, #64173, .F. ) ;
#58645 = AXIS2_PLACEMENT_3D ( 'NONE', #6002, #19065, #12307 ) ;
#58646 = LINE ( 'NONE', #59093, #10068 ) ;
#58647 = DIRECTION ( 'NONE',  ( -0.000000000000000000, -0.7660444431189791237, -0.6427876096865379196 ) ) ;
#58648 = LINE ( 'NONE', #39293, #10732 ) ;
#58649 = ORIENTED_EDGE ( 'NONE', *, *, #5857, .F. ) ;
#58651 = VERTEX_POINT ( 'NONE', #58577 ) ;
#58650 = VECTOR ( 'NONE', #43943, 1000.000000000000000 ) ;
#58652 = DIRECTION ( 'NONE',  ( -0.000000000000000000, 1.000000000000000000, 3.491481338843133355E-15 ) ) ;
#58653 = CARTESIAN_POINT ( 'NONE',  ( 2.307692307692309264, -3.322132147404559976, 32.92929555188717927 ) ) ;
#58654 = CARTESIAN_POINT ( 'NONE',  ( 17.20744851515672025, -3.625058011473227815, 33.29252011169590020 ) ) ;
#58655 = DIRECTION ( 'NONE',  ( -0.000000000000000000, -0.9396926207859093161, -0.3420201433256663259 ) ) ;
#58656 = CARTESIAN_POINT ( 'NONE',  ( 15.48076923077065103, -7.500000000000154543, 35.00000000000007105 ) ) ;
#58657 = CARTESIAN_POINT ( 'NONE',  ( -17.07692307692307665, -11.35647404775217417, 33.31231777344666511 ) ) ;
#58658 = DIRECTION ( 'NONE',  ( 0.000000000000000000, 8.131516293641283255E-17, 1.000000000000000000 ) ) ;
#58659 = ORIENTED_EDGE ( 'NONE', *, *, #73409, .T. ) ;
#58660 = DIRECTION ( 'NONE',  ( 0.000000000000000000, 0.7660444431189822323, -0.6427876096865344779 ) ) ;
#58661 = CARTESIAN_POINT ( 'NONE',  ( -0.2114841499001464675, -8.303483539816728154, 34.68545999027710991 ) ) ;
#58662 = EDGE_CURVE ( 'NONE', #89067, #28242, #84598, .T. ) ;
#58663 = EDGE_CURVE ( 'NONE', #3164, #17506, #56664, .T. ) ;
#58664 = CARTESIAN_POINT ( 'NONE',  ( 4.283893589096606114, -7.723484941389743952, 34.99544897038808955 ) ) ;
#58665 = B_SPLINE_CURVE_WITH_KNOTS ( 'NONE', 3,
 ( #24443, #23565, #42194, #71302, #69645, #14713, #44260, #28673, #64536, #10948 ),
 .UNSPECIFIED., .F., .F.,
 ( 4, 2, 2, 2, 4 ),
 ( 0.000000000000000000, 0.0001954311564186876876, 0.0003908623128373753751, 0.0005862934692560630356, 0.0007817246256747507503 ),
 .UNSPECIFIED. ) ;
#58666 = CARTESIAN_POINT ( 'NONE',  ( 9.627037691751374027, -2.657715359629088780, 31.77849191805832874 ) ) ;
#58667 = ORIENTED_EDGE ( 'NONE', *, *, #47485, .T. ) ;
#58668 = CARTESIAN_POINT ( 'NONE',  ( 10.36536139116315880, -9.356822207818506598, 34.66110646841856635 ) ) ;
#58669 = EDGE_CURVE ( 'NONE', #51593, #84770, #51352, .T. ) ;
#58670 = ORIENTED_EDGE ( 'NONE', *, *, #15382, .F. ) ;
#58671 = CARTESIAN_POINT ( 'NONE',  ( -17.32689982097166492, -2.544273027872574922, 31.48422191005632342 ) ) ;
#58672 = CARTESIAN_POINT ( 'NONE',  ( 10.48469401227430708, -3.338472653186243644, 32.95098750199972670 ) ) ;
#58673 = CARTESIAN_POINT ( 'NONE',  ( 15.36155967173618286, -4.684288915650983043, 34.18129842949671371 ) ) ;
#58674 = VERTEX_POINT ( 'NONE', #79313 ) ;
#58675 = EDGE_CURVE ( 'NONE', #75329, #75936, #45067, .T. ) ;
#58676 = DIRECTION ( 'NONE',  ( 1.000000000000000000, 0.000000000000000000, 0.000000000000000000 ) ) ;
#58677 = CARTESIAN_POINT ( 'NONE',  ( -19.50000000000000000, -3.499999999999999556, 29.75000000000000355 ) ) ;
#58678 = CIRCLE ( 'NONE', #42876, 4.000000000000000000 ) ;
#58679 = EDGE_CURVE ( 'NONE', #58941, #32595, #23313, .T. ) ;
#58680 = CARTESIAN_POINT ( 'NONE',  ( 5.999999999999880096, -11.94971097300221174, 32.03036669348237098 ) ) ;
#58681 = CARTESIAN_POINT ( 'NONE',  ( -5.076923076923075762, -8.164416787775445883, 34.95778746994557906 ) ) ;
#58682 = ORIENTED_EDGE ( 'NONE', *, *, #60678, .T. ) ;
#58683 = CARTESIAN_POINT ( 'NONE',  ( -1.318547033612945230, -3.513871655860379306, 32.76840700105978499 ) ) ;
#58684 = ORIENTED_EDGE ( 'NONE', *, *, #85663, .F. ) ;
#58686 = EDGE_CURVE ( 'NONE', #19715, #14549, #36249, .T. ) ;
#58685 = CARTESIAN_POINT ( 'NONE',  ( 8.545745825506822158, -12.44517049084099725, 30.48991314939691932 ) ) ;
#58687 = FACE_OUTER_BOUND ( 'NONE', #71567, .T. ) ;
#58688 = CARTESIAN_POINT ( 'NONE',  ( -0.2385256174450663680, -2.523321265292116422, 31.42251411153756990 ) ) ;
#58689 = CARTESIAN_POINT ( 'NONE',  ( 0.4615384615384611755, -1.509761064869970415, 31.06009739812519044 ) ) ;
#58690 = EDGE_CURVE ( 'NONE', #53001, #48794, #34177, .T. ) ;
#58691 = CARTESIAN_POINT ( 'NONE',  ( -6.222926217516144831, -4.186968288167446595, 33.49512374952580274 ) ) ;
#58692 = FACE_OUTER_BOUND ( 'NONE', #36874, .T. ) ;
#58693 = EDGE_LOOP ( 'NONE', ( #53584, #49181, #25908, #18805 ) ) ;
#58694 = ORIENTED_EDGE ( 'NONE', *, *, #46456, .F. ) ;
#58695 = ORIENTED_EDGE ( 'NONE', *, *, #7622, .T. ) ;
#58696 = ORIENTED_EDGE ( 'NONE', *, *, #38683, .T. ) ;
#58698 = EDGE_CURVE ( 'NONE', #13749, #31351, #43733, .T. ) ;
#58697 = ORIENTED_EDGE ( 'NONE', *, *, #4062, .F. ) ;
#58699 = CARTESIAN_POINT ( 'NONE',  ( 13.38461538461538680, -1.951392089020283160, 34.73218667398347748 ) ) ;
#58700 = CARTESIAN_POINT ( 'NONE',  ( -1.384615384615383471, -12.37446782046654192, 30.86335684631486131 ) ) ;
#58701 = VECTOR ( 'NONE', #46213, 1000.000000000000000 ) ;
#58702 = CARTESIAN_POINT ( 'NONE',  ( 14.98079249982687777, -4.943428324936578910, 34.04746400365624481 ) ) ;
#58703 = EDGE_CURVE ( 'NONE', #49742, #6248, #47290, .T. ) ;
#58704 = CARTESIAN_POINT ( 'NONE',  ( -8.769230769230768274, -1.466349020453238561, 30.81389545987213907 ) ) ;
#58705 = CARTESIAN_POINT ( 'NONE',  ( -13.44988538517170440, -3.643525952247789412, 33.31231777344662959 ) ) ;
#58706 = DIRECTION ( 'NONE',  ( -0.000000000000000000, -0.5000000000000009992, -0.8660254037844380415 ) ) ;
#58707 = CARTESIAN_POINT ( 'NONE',  ( 5.869852790561781219, -11.93770438780619259, 32.05411857736982029 ) ) ;
#58708 = CARTESIAN_POINT ( 'NONE',  ( -5.326923076923075762, -2.249999999999998668, 29.75000000000000355 ) ) ;
#58709 = DIRECTION ( 'NONE',  ( -0.000000000000000000, 1.000000000000000000, -0.000000000000000000 ) ) ;
#58710 = ORIENTED_EDGE ( 'NONE', *, *, #15801, .F. ) ;
#58711 = ORIENTED_EDGE ( 'NONE', *, *, #73930, .F. ) ;
#58712 = VERTEX_POINT ( 'NONE', #82430 ) ;
#58715 = ORIENTED_EDGE ( 'NONE', *, *, #61591, .T. ) ;
#58714 = EDGE_CURVE ( 'NONE', #14193, #2419, #46851, .T. ) ;
#58713 = CARTESIAN_POINT ( 'NONE',  ( 1.576923076923075762, -3.499999999999999556, 29.75000000000000355 ) ) ;
#58717 = CARTESIAN_POINT ( 'NONE',  ( -17.07692307692307665, -4.098570777380720287, 33.41473453929634729 ) ) ;
#58716 = CARTESIAN_POINT ( 'NONE',  ( 7.846153846153846700, -3.050289026998446396, 32.03036669348365706 ) ) ;
#58718 = CYLINDRICAL_SURFACE ( 'NONE', #40362, 0.2499999999999986955 ) ;
#58719 = CARTESIAN_POINT ( 'NONE',  ( -11.53846153846153655, -9.058645607665452459, 34.76329471203371924 ) ) ;
#58720 = ORIENTED_EDGE ( 'NONE', *, *, #16793, .F. ) ;
#58721 = B_SPLINE_CURVE_WITH_KNOTS ( 'NONE', 3,
 ( #70113, #57035, #35897, #64226, #83651, #41769 ),
 .UNSPECIFIED., .F., .F.,
 ( 4, 2, 4 ),
 ( 0.000000000000000000, 0.0001954784845028924105, 0.0003909569690057848211 ),
 .UNSPECIFIED. ) ;
#58722 = EDGE_CURVE ( 'NONE', #18827, #78695, #6325, .T. ) ;
#58723 = B_SPLINE_CURVE_WITH_KNOTS ( 'NONE', 3,
 ( #81171, #60437, #46915, #81608, #33421, #73522 ),
 .UNSPECIFIED., .F., .F.,
 ( 4, 2, 4 ),
 ( 0.000000000000000000, 0.0001954784845028924105, 0.0003909569690057848211 ),
 .UNSPECIFIED. ) ;
#58724 = ORIENTED_EDGE ( 'NONE', *, *, #54803, .T. ) ;
#58725 = DIRECTION ( 'NONE',  ( 0.000000000000000000, 0.9396926207859126468, -0.3420201433256571111 ) ) ;
#58726 = VERTEX_POINT ( 'NONE', #54044 ) ;
#58727 = FACE_BOUND ( 'NONE', #21195, .T. ) ;
#58728 = CARTESIAN_POINT ( 'NONE',  ( -6.066083410955878108, -8.973038597847269315, 34.52809138561120506 ) ) ;
#58729 = VECTOR ( 'NONE', #8352, 1000.000000000000000 ) ;
#58730 = DIRECTION ( 'NONE',  ( 0.000000000000000000, 0.8660254037844377084, -0.5000000000000015543 ) ) ;
#58731 = EDGE_LOOP ( 'NONE', ( #87226, #68491, #52159, #71331 ) ) ;
#58732 = CARTESIAN_POINT ( 'NONE',  ( 14.08420736396836404, -2.847400154188068022, 31.58180166144859058 ) ) ;
#58733 = DIRECTION ( 'NONE',  ( 1.000000000000000000, 0.000000000000000000, 0.000000000000000000 ) ) ;
#58734 = CYLINDRICAL_SURFACE ( 'NONE', #29236, 0.2500000000000002220 ) ;
#58735 = ORIENTED_EDGE ( 'NONE', *, *, #84991, .T. ) ;
#58736 = CARTESIAN_POINT ( 'NONE',  ( 12.21156173059610772, -4.943428324936578910, 34.04746400365624481 ) ) ;
#58737 = CARTESIAN_POINT ( 'NONE',  ( -18.00000000000000000, -4.786620604624112651, 33.94971097300155094 ) ) ;
#58738 = ADVANCED_FACE ( 'NONE', ( #62141 ), #55382, .F. ) ;
#58739 = ORIENTED_EDGE ( 'NONE', *, *, #8682, .F. ) ;
#58740 = AXIS2_PLACEMENT_3D ( 'NONE', #64017, #21265, #15857 ) ;
#58741 = EDGE_CURVE ( 'NONE', #3368, #3730, #4742, .T. ) ;
#58742 = PLANE ( 'NONE',  #63209 ) ;
#58743 = CARTESIAN_POINT ( 'NONE',  ( -9.692307692307814193, -9.528491918059723176, 34.59228464037033035 ) ) ;
#58744 = AXIS2_PLACEMENT_3D ( 'NONE', #47996, #19211, #266 ) ;
#58745 = ORIENTED_EDGE ( 'NONE', *, *, #46579, .F. ) ;
#58746 = CARTESIAN_POINT ( 'NONE',  ( 6.923076923076924238, -2.486705287966279876, 31.30864560766543647 ) ) ;
#58747 = CARTESIAN_POINT ( 'NONE',  ( 15.84615384615384670, -3.499999999999999556, 29.75000000000000355 ) ) ;
#58748 = CARTESIAN_POINT ( 'NONE',  ( 16.15384615384615330, -2.833524468853757305, 32.15551576947925838 ) ) ;
#58749 = CARTESIAN_POINT ( 'NONE',  ( 16.02369818411445834, -11.04286588640298916, 33.62463336215343901 ) ) ;
#58751 = ADVANCED_FACE ( 'NONE', ( #21149 ), #48619, .F. ) ;
#58750 = DIRECTION ( 'NONE',  ( -0.000000000000000000, 0.1736481776669307198, -0.9848077530122080203 ) ) ;
#58752 = CARTESIAN_POINT ( 'NONE',  ( 6.792929713638702793, -9.418419913701741919, 34.36755862841477693 ) ) ;
#58754 = FACE_OUTER_BOUND ( 'NONE', #52393, .T. ) ;
#58753 = DIRECTION ( 'NONE',  ( -1.000000000000000000, 0.000000000000000000, 0.000000000000000000 ) ) ;
#58755 = AXIS2_PLACEMENT_3D ( 'NONE', #11321, #52300, #45547 ) ;
#58756 = CARTESIAN_POINT ( 'NONE',  ( 1.634669696253700621, -11.28795663066794219, 33.01431243580653785 ) ) ;
#58758 = CARTESIAN_POINT ( 'NONE',  ( 5.076923076923075762, -9.819645486525091727, 36.12317359536749706 ) ) ;
#58757 = CARTESIAN_POINT ( 'NONE',  ( -15.36091644020745051, -11.93770438780619259, 32.05411857736982029 ) ) ;
#58759 = CARTESIAN_POINT ( 'NONE',  ( -1.944543648263014957, -5.555456351737005249, 14.00000000000000000 ) ) ;
#58760 = VERTEX_POINT ( 'NONE', #12633 ) ;
#58761 = CARTESIAN_POINT ( 'NONE',  ( 3.311681672511759267, -7.920257152778357401, 14.00000000000000888 ) ) ;
#58762 = ORIENTED_EDGE ( 'NONE', *, *, #33037, .F. ) ;
#58763 = ORIENTED_EDGE ( 'NONE', *, *, #60300, .T. ) ;
#58764 = DIRECTION ( 'NONE',  ( 0.000000000000000000, -6.938893903907222067E-15, 1.000000000000000000 ) ) ;
#58765 = EDGE_LOOP ( 'NONE', ( #2798, #45303, #43436, #74807, #4530, #4744 ) ) ;
#58766 = LINE ( 'NONE', #51538, #31116 ) ;
#58767 = CARTESIAN_POINT ( 'NONE',  ( -1.139087296526025916, -4.750000000000006217, 16.57812500000000000 ) ) ;
#58768 = CARTESIAN_POINT ( 'NONE',  ( 3.100621261037536325, -2.373036134822904319, 30.88089517874952250 ) ) ;
#58769 = CARTESIAN_POINT ( 'NONE',  ( -5.933932666649922361, -11.35647404775217595, 33.31231777344667222 ) ) ;
#58770 = CARTESIAN_POINT ( 'NONE',  ( -5.933931648997561759, -8.973038597847269315, 34.52809138561122637 ) ) ;
#58771 = CARTESIAN_POINT ( 'NONE',  ( -4.153846153846273204, -12.46129190930018460, 30.37095296980731973 ) ) ;
#58772 = CARTESIAN_POINT ( 'NONE',  ( 15.23076923076923173, -8.164416787775445883, 34.95778746994557906 ) ) ;
#58773 = CARTESIAN_POINT ( 'NONE',  ( -10.74553182482283198, -4.460286881179643004, 33.72017969459903242 ) ) ;
#58774 = CARTESIAN_POINT ( 'NONE',  ( -2.999999999999998224, -7.500000000000000000, 14.00000000000000178 ) ) ;
#58775 = CARTESIAN_POINT ( 'NONE',  ( 3.750000000000009770, -9.053300858899081760, 20.79687500000000000 ) ) ;
#58776 = CARTESIAN_POINT ( 'NONE',  ( 18.24994540937804643, -11.56426240980093567, 33.07394671870546432 ) ) ;
#58777 = CARTESIAN_POINT ( 'NONE',  ( 13.25446741488369362, -3.625366637846545892, 33.29286588640298561 ) ) ;
#58778 = CARTESIAN_POINT ( 'NONE',  ( -0.4615384615385840772, -12.51329471203414379, 31.30864560766407578 ) ) ;
#58779 = VECTOR ( 'NONE', #64811, 1000.000000000000000 ) ;
#58780 = EDGE_LOOP ( 'NONE', ( #61351, #33092, #18032, #19908 ) ) ;
#58781 = ORIENTED_EDGE ( 'NONE', *, *, #48723, .T. ) ;
#58782 = DIRECTION ( 'NONE',  ( 0.000000000000000000, 0.9848077530122072432, -0.1736481776669354937 ) ) ;
#58783 = CARTESIAN_POINT ( 'NONE',  ( 7.846153846153846700, -1.129524287112498415, 32.06866353760679544 ) ) ;
#58784 = LINE ( 'NONE', #52023, #42628 ) ;
#58785 = CARTESIAN_POINT ( 'NONE',  ( 16.40384615384757439, -7.500000000000154543, 35.00000000000007105 ) ) ;
#58786 = DIRECTION ( 'NONE',  ( -1.000000000000000000, -0.000000000000000000, -0.000000000000000000 ) ) ;
#58787 = LINE ( 'NONE', #86290, #31337 ) ;
#58788 = EDGE_CURVE ( 'NONE', #24326, #45549, #19828, .T. ) ;
#58789 = ORIENTED_EDGE ( 'NONE', *, *, #2716, .F. ) ;
#58790 = CARTESIAN_POINT ( 'NONE',  ( 18.00000000000000000, -1.790695186598648903, 34.54067556320373455 ) ) ;
#58791 = VERTEX_POINT ( 'NONE', #23355 ) ;
#58792 = EDGE_CURVE ( 'NONE', #22135, #80981, #28810, .T. ) ;
#58793 = ORIENTED_EDGE ( 'NONE', *, *, #47479, .F. ) ;
#58794 = CARTESIAN_POINT ( 'NONE',  ( -6.000000000000119904, -6.026961402154118908, 34.52809138561165270 ) ) ;
#58795 = AXIS2_PLACEMENT_3D ( 'NONE', #73052, #50976, #37032 ) ;
#58796 = CARTESIAN_POINT ( 'NONE',  ( -11.31568186948346977, -11.60474049983371003, 33.02348890104160262 ) ) ;
#58797 = CARTESIAN_POINT ( 'NONE',  ( 14.55769230769231015, -7.500000000000001776, 35.04278698407183867 ) ) ;
#58798 = CARTESIAN_POINT ( 'NONE',  ( 0.4615384615383396616, -3.835265460704628371, 33.15142922262033665 ) ) ;
#58799 = CARTESIAN_POINT ( 'NONE',  ( -13.31854703361294767, -3.050289026998446840, 32.03036669348366416 ) ) ;
#58800 = AXIS2_PLACEMENT_3D ( 'NONE', #14734, #30015, #57475 ) ;
#58802 = EDGE_CURVE ( 'NONE', #4325, #10751, #35562, .T. ) ;
#58801 = ORIENTED_EDGE ( 'NONE', *, *, #60237, .T. ) ;
#58803 = EDGE_LOOP ( 'NONE', ( #55738, #46888 ) ) ;
#58804 = ORIENTED_EDGE ( 'NONE', *, *, #87197, .F. ) ;
#58805 = CARTESIAN_POINT ( 'NONE',  ( 12.68491440223663957, -2.501478030877322567, 29.88021232661721172 ) ) ;
#58806 = FACE_OUTER_BOUND ( 'NONE', #18743, .T. ) ;
#58807 = ADVANCED_FACE ( 'NONE', ( #49064 ), #1763, .F. ) ;
#58808 = CARTESIAN_POINT ( 'NONE',  ( 4.153846153846154188, -3.322132147404559976, 32.92929555188717927 ) ) ;
#58809 = LINE ( 'NONE', #72766, #35575 ) ;
#58810 = DIRECTION ( 'NONE',  ( -0.000000000000000000, 0.5000000000000011102, -0.8660254037844380415 ) ) ;
#58811 = EDGE_CURVE ( 'NONE', #57115, #59563, #73900, .T. ) ;
#58812 = CARTESIAN_POINT ( 'NONE',  ( 16.15384615384603251, -9.528491918059723176, 34.59228464037033035 ) ) ;
#58813 = EDGE_LOOP ( 'NONE', ( #72457, #127 ) ) ;
#58814 = EDGE_LOOP ( 'NONE', ( #22115, #48757, #61832, #12089 ) ) ;
#58815 = CARTESIAN_POINT ( 'NONE',  ( -2.651650429449535551, -10.15165042944956753, 19.93750000000000000 ) ) ;
#58816 = VERTEX_POINT ( 'NONE', #69351 ) ;
#58818 = EDGE_LOOP ( 'NONE', ( #57486, #73994, #77631, #31243 ) ) ;
#58817 = CARTESIAN_POINT ( 'NONE',  ( -12.52762187249433978, -11.16473453929635440, 33.15142922261925662 ) ) ;
#58819 = CARTESIAN_POINT ( 'NONE',  ( -10.36543920600657387, -4.176053281294518804, 33.81426240980091791 ) ) ;
#58820 = FACE_OUTER_BOUND ( 'NONE', #71743, .T. ) ;
#58821 = CARTESIAN_POINT ( 'NONE',  ( 3.750000000000009770, -9.053300858899081760, 17.04687500000000000 ) ) ;
#58822 = VERTEX_POINT ( 'NONE', #8974 ) ;
#58823 = EDGE_CURVE ( 'NONE', #80750, #54790, #84203, .T. ) ;
#58824 = B_SPLINE_CURVE_WITH_KNOTS ( 'NONE', 3,
 ( #56632, #84119, #22836, #16524, #43990, #51169, #35474, #62927, #1238, #28722 ),
 .UNSPECIFIED., .F., .F.,
 ( 4, 2, 2, 2, 4 ),
 ( 0.000000000000000000, 0.0001954311564186868744, 0.0003908623128373737488, 0.0005862934692560606504, 0.0007817246256747474977 ),
 .UNSPECIFIED. ) ;
#58825 = CARTESIAN_POINT ( 'NONE',  ( -14.43838291080261449, -12.35290016733513951, 31.75349464988449455 ) ) ;
#58826 = AXIS2_PLACEMENT_3D ( 'NONE', #34260, #41917, #62174 ) ;
#58827 = EDGE_LOOP ( 'NONE', ( #18810, #67630, #58455, #53427 ) ) ;
#58828 = PLANE ( 'NONE',  #88797 ) ;
#58829 = CARTESIAN_POINT ( 'NONE',  ( 10.61538461538461675, -8.973038597847269315, 34.52809138561121927 ) ) ;
#58830 = FACE_OUTER_BOUND ( 'NONE', #80322, .T. ) ;
#58832 = CARTESIAN_POINT ( 'NONE',  ( 19.50000000000000000, -7.500000000000000000, 29.75000000000000355 ) ) ;
#58831 = DIRECTION ( 'NONE',  ( -0.000000000000000000, 0.6427876096865404731, -0.7660444431189770143 ) ) ;
#58833 = CARTESIAN_POINT ( 'NONE',  ( 5.076923076923075762, -2.538708090699994813, 30.37095296980875503 ) ) ;
#58834 = CARTESIAN_POINT ( 'NONE',  ( -10.83886955910856464, -10.81261337010820256, 33.49550067578627477 ) ) ;
#58835 = ORIENTED_EDGE ( 'NONE', *, *, #82177, .F. ) ;
#58836 = CARTESIAN_POINT ( 'NONE',  ( 11.28848479441295005, -11.47974371597207899, 33.17467449705390692 ) ) ;
#58837 = CARTESIAN_POINT ( 'NONE',  ( 6.923076923076924238, -9.058645607665452459, 34.76329471203371924 ) ) ;
#58839 = EDGE_LOOP ( 'NONE', ( #40443, #3631 ) ) ;
#58838 = EDGE_CURVE ( 'NONE', #79443, #83509, #14854, .T. ) ;
#58840 = CARTESIAN_POINT ( 'NONE',  ( 6.673100192134570285, -5.728515186090277211, 34.42611988154120439 ) ) ;
#58841 = CARTESIAN_POINT ( 'NONE',  ( 12.23867303933482553, -2.501496062324912284, 29.88072118266895671 ) ) ;
#58842 = CARTESIAN_POINT ( 'NONE',  ( -15.10024379253558635, -5.915461855592780260, 34.75538340440931506 ) ) ;
#58843 = CARTESIAN_POINT ( 'NONE',  ( -13.31854805126530827, -11.35647404775217595, 33.31231777344666511 ) ) ;
#58844 = EDGE_CURVE ( 'NONE', #30667, #65648, #13591, .T. ) ;
#58846 = ADVANCED_FACE ( 'NONE', ( #69782 ), #63005, .F. ) ;
#58845 = LINE ( 'NONE', #3456, #15637 ) ;
#58847 = FACE_BOUND ( 'NONE', #87869, .T. ) ;
#58849 = DIRECTION ( 'NONE',  ( 0.000000000000000000, 0.9396926207859126468, -0.3420201433256571111 ) ) ;
#58848 = CARTESIAN_POINT ( 'NONE',  ( 13.16113046005105325, -2.353723527008296568, 30.78948104536958752 ) ) ;
#58850 = CARTESIAN_POINT ( 'NONE',  ( 16.15384615384615330, -3.050289026998446396, 32.03036669348365706 ) ) ;
#58852 = CARTESIAN_POINT ( 'NONE',  ( 14.24160992833217421, -10.67929555188718460, 33.92786785259543336 ) ) ;
#58851 = CARTESIAN_POINT ( 'NONE',  ( 1.318533005255250412, -12.62096338111211580, 30.90682066428152197 ) ) ;
#58853 = FACE_OUTER_BOUND ( 'NONE', #39122, .T. ) ;
#58854 = EDGE_CURVE ( 'NONE', #21870, #46711, #83481, .T. ) ;
#58855 = DIRECTION ( 'NONE',  ( 0.000000000000000000, 0.6427876096865373645, -0.7660444431189797898 ) ) ;
#58856 = CARTESIAN_POINT ( 'NONE',  ( -3.749999999999996447, -7.561099074964554134, 23.59188170625849068 ) ) ;
#58857 = EDGE_CURVE ( 'NONE', #45410, #30860, #16169, .T. ) ;
#58858 = B_SPLINE_CURVE_WITH_KNOTS ( 'NONE', 3,
 ( #43886, #62814, #69590, #8788, #36259, #16861 ),
 .UNSPECIFIED., .F., .F.,
 ( 4, 2, 4 ),
 ( 0.000000000000000000, 0.0001954784845028928442, 0.0003909569690057856884 ),
 .UNSPECIFIED. ) ;
#58859 = VERTEX_POINT ( 'NONE', #63460 ) ;
#58860 = B_SPLINE_CURVE_WITH_KNOTS ( 'NONE', 3,
 ( #6240, #74699, #33704, #81460, #86448, #39592, #79670, #66605, #87336, #25613 ),
 .UNSPECIFIED., .F., .F.,
 ( 4, 2, 2, 2, 4 ),
 ( 0.0007817359430256306564, 0.0009771253907249969738, 0.001172514838424363291, 0.001367904286123729826, 0.001563293733823096143 ),
 .UNSPECIFIED. ) ;
#58861 = VECTOR ( 'NONE', #87914, 1000.000000000000000 ) ;
#58862 = AXIS2_PLACEMENT_3D ( 'NONE', #9086, #28464, #77534 ) ;
#58863 = DIRECTION ( 'NONE',  ( -0.000000000000000000, 1.000000000000000000, 3.491481338843133355E-15 ) ) ;
#58864 = CARTESIAN_POINT ( 'NONE',  ( -4.219116599806928214, -3.300289026998414865, 32.46337939537583139 ) ) ;
#58865 = CARTESIAN_POINT ( 'NONE',  ( -7.596208436775802930, -11.56426240980093745, 33.07394671870546432 ) ) ;
#58866 = CARTESIAN_POINT ( 'NONE',  ( 16.94623247381277054, -8.191372820521381826, 34.95448215188423546 ) ) ;
#58867 = CARTESIAN_POINT ( 'NONE',  ( 6.856994543716788293, -12.62096338111211580, 30.90682066428152197 ) ) ;
#58868 = CARTESIAN_POINT ( 'NONE',  ( -11.53846153846153655, -3.937682226553329556, 33.60647404775216529 ) ) ;
#58869 = CARTESIAN_POINT ( 'NONE',  ( -2.608446859217889546, -10.19485399968121264, 27.18563170625849068 ) ) ;
#58870 = CARTESIAN_POINT ( 'NONE',  ( -15.45369618967607828, -12.64616026154729411, 30.79003144601914244 ) ) ;
#58871 = CARTESIAN_POINT ( 'NONE',  ( -14.37296230824862775, -11.67786785259540849, 32.92929555188721480 ) ) ;
#58872 = AXIS2_PLACEMENT_3D ( 'NONE', #21041, #6222, #7544 ) ;
#58873 = CARTESIAN_POINT ( 'NONE',  ( -7.780086512803768173, -9.905515769479276145, 34.41647553114623292 ) ) ;
#58874 = FACE_OUTER_BOUND ( 'NONE', #53517, .T. ) ;
#58875 = CARTESIAN_POINT ( 'NONE',  ( 14.53047184896071897, -5.913360116392397892, 34.49180327182771322 ) ) ;
#58876 = CARTESIAN_POINT ( 'NONE',  ( -11.28840722682322273, -9.943054286541403997, 34.11300777759954883 ) ) ;
#58877 = VECTOR ( 'NONE', #63088, 1000.000000000000114 ) ;
#58878 = CARTESIAN_POINT ( 'NONE',  ( -5.999999999999998224, -11.91647553114624181, 32.58852847137148245 ) ) ;
#58879 = CARTESIAN_POINT ( 'NONE',  ( -1.134669975237341477, -12.07971442181322352, 32.31769673815850297 ) ) ;
#58880 = ORIENTED_EDGE ( 'NONE', *, *, #36123, .F. ) ;
#58881 = DIRECTION ( 'NONE',  ( 0.000000000000000000, 0.8660254037844377084, 0.5000000000000015543 ) ) ;
#58882 = CARTESIAN_POINT ( 'NONE',  ( 7.053868730901709405, -4.809403383903225304, 33.96459661697924304 ) ) ;
#58883 = CARTESIAN_POINT ( 'NONE',  ( -2.724691934501246582, -6.299813628509474128, 24.17374329374151642 ) ) ;
#58884 = CARTESIAN_POINT ( 'NONE',  ( -10.86540783960607293, -2.588893531581426988, 31.60682220781847818 ) ) ;
#58885 = LINE ( 'NONE', #24659, #61344 ) ;
#58886 = ORIENTED_EDGE ( 'NONE', *, *, #73551, .T. ) ;
#58888 = AXIS2_PLACEMENT_3D ( 'NONE', #57114, #84607, #15696 ) ;
#58887 = CARTESIAN_POINT ( 'NONE',  ( -16.40382289789474513, -4.075325502946085976, 33.72974371597207721 ) ) ;
#58889 = DIRECTION ( 'NONE',  ( -0.000000000000000000, 0.5000000000000011102, -0.8660254037844380415 ) ) ;
#58891 = VERTEX_POINT ( 'NONE', #22480 ) ;
#58890 = CARTESIAN_POINT ( 'NONE',  ( 11.66850659438130755, -2.254550872974306674, 29.97347326024527092 ) ) ;
#58892 = DIRECTION ( 'NONE',  ( 0.000000000000000000, 0.4999999999999985567, 0.8660254037844395958 ) ) ;
#58893 = CARTESIAN_POINT ( 'NONE',  ( -12.46153846153846168, -8.164416787775445883, 34.95778746994557906 ) ) ;
#58894 = CARTESIAN_POINT ( 'NONE',  ( -5.076923076923075762, -8.973038597847269315, 34.52809138561121927 ) ) ;
#58895 = CARTESIAN_POINT ( 'NONE',  ( 8.992010310499175318, -5.114059244376869984, 34.14424750095245287 ) ) ;
#58896 = VERTEX_POINT ( 'NONE', #49944 ) ;
#58897 = CARTESIAN_POINT ( 'NONE',  ( 18.03205128205128105, -7.500000000000000000, 33.75000000000000000 ) ) ;
#58898 = CARTESIAN_POINT ( 'NONE',  ( -12.59222906464876779, -2.494641256782728966, 31.33461815524612959 ) ) ;
#58899 = LINE ( 'NONE', #71523, #13973 ) ;
#58900 = ORIENTED_EDGE ( 'NONE', *, *, #12444, .T. ) ;
#58901 = ORIENTED_EDGE ( 'NONE', *, *, #64148, .T. ) ;
#58902 = ORIENTED_EDGE ( 'NONE', *, *, #2428, .F. ) ;
#58903 = CARTESIAN_POINT ( 'NONE',  ( 3.480823650682684178, -2.318338780012835443, 30.59689888758630261 ) ) ;
#58904 = CARTESIAN_POINT ( 'NONE',  ( 6.222779668978068557, -2.353885683473779800, 30.79025554430704759 ) ) ;
#58905 = CARTESIAN_POINT ( 'NONE',  ( 2.530471848960717196, -5.913360116392399668, 34.49180327182771322 ) ) ;
#58906 = DIRECTION ( 'NONE',  ( -1.000000000000000000, -0.000000000000000000, -0.000000000000000000 ) ) ;
#58907 = ORIENTED_EDGE ( 'NONE', *, *, #7090, .F. ) ;
#58908 = ORIENTED_EDGE ( 'NONE', *, *, #29470, .F. ) ;
#58910 = ORIENTED_EDGE ( 'NONE', *, *, #71313, .F. ) ;
#58909 = CARTESIAN_POINT ( 'NONE',  ( 15.48071474911737333, -5.057305518903948638, 34.11320923018887896 ) ) ;
#58911 = CARTESIAN_POINT ( 'NONE',  ( -6.923076923077045919, -4.320704448113951379, 33.92786785259630022 ) ) ;
#58912 = CYLINDRICAL_SURFACE ( 'NONE', #12187, 0.2499999999999973355 ) ;
#58913 = ADVANCED_FACE ( 'NONE', ( #71100 ), #50381, .F. ) ;
#58914 = AXIS2_PLACEMENT_3D ( 'NONE', #11113, #11567, #86802 ) ;
#58915 = VECTOR ( 'NONE', #36766, 1000.000000000000000 ) ;
#58916 = CARTESIAN_POINT ( 'NONE',  ( -13.38461538461538325, -13.63283147151868846, 33.57946703557072254 ) ) ;
#58917 = DIRECTION ( 'NONE',  ( -0.000000000000000000, 1.000000000000000000, -0.000000000000000000 ) ) ;
#58918 = VERTEX_POINT ( 'NONE', #86870 ) ;
#58919 = B_SPLINE_CURVE_WITH_KNOTS ( 'NONE', 3,
 ( #62037, #55279, #346, #26932, #68798, #21043, #20177, #69681, #35456, #48072 ),
 .UNSPECIFIED., .F., .F.,
 ( 4, 2, 2, 2, 4 ),
 ( 0.000000000000000000, 0.0001954339857564077183, 0.0003908679715128154366, 0.0005863019572692231007, 0.0007817359430256308733 ),
 .UNSPECIFIED. ) ;
#58920 = VECTOR ( 'NONE', #39504, 1000.000000000000000 ) ;
#58921 = EDGE_LOOP ( 'NONE', ( #9765, #8539, #74357, #29354 ) ) ;
#58922 = AXIS2_PLACEMENT_3D ( 'NONE', #49640, #15424, #42895 ) ;
#58923 = VERTEX_POINT ( 'NONE', #64777 ) ;
#58925 = ORIENTED_EDGE ( 'NONE', *, *, #19806, .F. ) ;
#58924 = CARTESIAN_POINT ( 'NONE',  ( 14.98079249982687955, -2.564618984488975517, 30.55390908950641915 ) ) ;
#58926 = DIRECTION ( 'NONE',  ( 1.000000000000000000, 0.000000000000000000, 0.000000000000000000 ) ) ;
#58927 = CARTESIAN_POINT ( 'NONE',  ( 18.22301284409340028, -5.582272713120730145, 34.63742843783360570 ) ) ;
#58928 = VERTEX_POINT ( 'NONE', #32345 ) ;
#58929 = EDGE_CURVE ( 'NONE', #56388, #67048, #14714, .T. ) ;
#58930 = CARTESIAN_POINT ( 'NONE',  ( -13.60754160213153163, -4.186968288167449259, 33.49512374952580274 ) ) ;
#58931 = CARTESIAN_POINT ( 'NONE',  ( -1.384615384615505151, -8.613356846316285953, 34.62446782046622218 ) ) ;
#58932 = CARTESIAN_POINT ( 'NONE',  ( -5.999999999999998224, -3.322132147404559976, 32.92929555188717927 ) ) ;
#58933 = FACE_BOUND ( 'NONE', #42435, .T. ) ;
#58934 = CARTESIAN_POINT ( 'NONE',  ( -16.15384615384627409, -12.27809138561165270, 31.22303859784587132 ) ) ;
#58935 = CARTESIAN_POINT ( 'NONE',  ( 4.153846153846030731, -2.379036618888197729, 30.90682066428292885 ) ) ;
#58936 = CARTESIAN_POINT ( 'NONE',  ( -10.36533019547115941, -10.82426656108012075, 33.81400080652039009 ) ) ;
#58938 = CARTESIAN_POINT ( 'NONE',  ( -8.638705330997128229, -12.15418822224088835, 32.17964115625579069 ) ) ;
#58937 = CARTESIAN_POINT ( 'NONE',  ( 17.01165307636676260, -9.528491918058357157, 34.59228464037090589 ) ) ;
#58939 = CARTESIAN_POINT ( 'NONE',  ( 11.00641025641025550, -3.499999999999999556, 29.75000000000000355 ) ) ;
#58940 = CARTESIAN_POINT ( 'NONE',  ( 15.23076923076923173, -2.900454961884010974, 35.62045528018868623 ) ) ;
#58941 = VERTEX_POINT ( 'NONE', #25139 ) ;
#58942 = CARTESIAN_POINT ( 'NONE',  ( 10.61538461538449596, -10.90142922262034020, 33.41473453929536674 ) ) ;
#58943 = CARTESIAN_POINT ( 'NONE',  ( 12.46153846153846168, -1.422936976036506707, 30.56769352161908415 ) ) ;
#58944 = VERTEX_POINT ( 'NONE', #17946 ) ;
#58945 = ORIENTED_EDGE ( 'NONE', *, *, #7841, .T. ) ;
#58947 = CARTESIAN_POINT ( 'NONE',  ( 14.98079248672063990, -2.920706130388546651, 32.31842814019191223 ) ) ;
#58946 = CARTESIAN_POINT ( 'NONE',  ( -6.673022611438607754, -8.303483539816728154, 34.68545999027711702 ) ) ;
#58948 = DIRECTION ( 'NONE',  ( -0.000000000000000000, -0.3420201433256694901, -0.9396926207859082059 ) ) ;
#58949 = CARTESIAN_POINT ( 'NONE',  ( 9.692307692307695177, -13.87047571288749737, 32.06866353760679544 ) ) ;
#58950 = CARTESIAN_POINT ( 'NONE',  ( -11.60373153901785948, -10.33852847137145048, 34.16647553114627556 ) ) ;
#58951 = ORIENTED_EDGE ( 'NONE', *, *, #50866, .T. ) ;
#58953 = EDGE_CURVE ( 'NONE', #69595, #67905, #73749, .T. ) ;
#58952 = LINE ( 'NONE', #59407, #3952 ) ;
#58954 = EDGE_CURVE ( 'NONE', #62271, #48748, #53043, .T. ) ;
#58955 = CYLINDRICAL_SURFACE ( 'NONE', #73114, 0.2499999999999998890 ) ;
#58957 = CARTESIAN_POINT ( 'NONE',  ( -9.915233909823838232, -4.186968288167449259, 33.49512374952580274 ) ) ;
#58956 = CARTESIAN_POINT ( 'NONE',  ( 18.24994551834813805, -3.712312575010499494, 33.01462480002815170 ) ) ;
#58958 = CARTESIAN_POINT ( 'NONE',  ( 7.596130608860880429, -5.851115903089112003, 34.47074536777953568 ) ) ;
#58959 = CARTESIAN_POINT ( 'NONE',  ( 10.86543892702293412, -4.235687564193448829, 33.53795663066793509 ) ) ;
#58961 = CYLINDRICAL_SURFACE ( 'NONE', #46318, 0.2500000000000008882 ) ;
#58960 =( NAMED_UNIT ( * ) SI_UNIT ( $, .STERADIAN. ) SOLID_ANGLE_UNIT ( ) );
#58962 = CARTESIAN_POINT ( 'NONE',  ( -1.553300858899125059, -3.750000000000009326, 20.32812500000000000 ) ) ;
#58963 = ORIENTED_EDGE ( 'NONE', *, *, #936, .F. ) ;
#58964 = VERTEX_POINT ( 'NONE', #17500 ) ;
#58965 = B_SPLINE_CURVE_WITH_KNOTS ( 'NONE', 3,
 ( #56994, #50224, #70519, #44804, #72283, #64627, #43487, #8823, #85815, #29976 ),
 .UNSPECIFIED., .F., .F.,
 ( 4, 2, 2, 2, 4 ),
 ( 0.000000000000000000, 0.0001954311564186867660, 0.0003908623128373735320, 0.0005862934692560603251, 0.0007817246256747470640 ),
 .UNSPECIFIED. ) ;
#58966 = CARTESIAN_POINT ( 'NONE',  ( -14.37377468705243722, -4.661471528628507777, 34.16647553114621871 ) ) ;
#58967 = CARTESIAN_POINT ( 'NONE',  ( -17.77657303813842304, -7.630147231320743018, 34.74852402298682819 ) ) ;
#58968 = CARTESIAN_POINT ( 'NONE',  ( 18.25005431163831204, -5.728107161865375829, 34.42597550085002922 ) ) ;
#58969 = ADVANCED_FACE ( 'NONE', ( #45851 ), #31450, .F. ) ;
#58970 = CARTESIAN_POINT ( 'NONE',  ( 3.930361229281820190, -10.97335522853832579, 33.68706563782419749 ) ) ;
#58971 = CARTESIAN_POINT ( 'NONE',  ( 16.82692307692307665, -7.433932668274255917, 35.00000000000000711 ) ) ;
#58972 = CARTESIAN_POINT ( 'NONE',  ( -2.651650429449535551, -10.15165042944956753, 18.68750000000000000 ) ) ;
#58973 = CARTESIAN_POINT ( 'NONE',  ( 2.544871794871793824, -11.50000000000000000, 29.75000000000000355 ) ) ;
#58974 = LINE ( 'NONE', #86478, #10039 ) ;
#58975 = CARTESIAN_POINT ( 'NONE',  ( -8.769230769230768274, -12.62096338111211580, 30.90682066428153263 ) ) ;
#58976 = CARTESIAN_POINT ( 'NONE',  ( -6.065249931774084224, -2.255955759149247619, 30.00000000000013856 ) ) ;
#58977 = FACE_OUTER_BOUND ( 'NONE', #60032, .T. ) ;
#58978 = CARTESIAN_POINT ( 'NONE',  ( -12.46153846153846168, -3.513871655860378418, 32.76840700105978499 ) ) ;
#58979 = CARTESIAN_POINT ( 'NONE',  ( -12.71151520558705350, -8.347322224742351082, 34.93158281831414058 ) ) ;
#58980 = CARTESIAN_POINT ( 'NONE',  ( -3.100243529005665355, -11.93748526763465279, 32.05452791011430946 ) ) ;
#58981 = CARTESIAN_POINT ( 'NONE',  ( -0.2387589202700531599, -11.41317474335729187, 32.86274602512330034 ) ) ;
#58982 = AXIS2_PLACEMENT_3D ( 'NONE', #84223, #49083, #83328 ) ;
#58983 = CARTESIAN_POINT ( 'NONE',  ( 9.692307692307570832, -5.094484230521993062, 34.41647553114689373 ) ) ;
#58984 = CARTESIAN_POINT ( 'NONE',  ( -3.230769230769352962, -12.51329471203414379, 31.30864560766407578 ) ) ;
#58985 = VERTEX_POINT ( 'NONE', #71988 ) ;
#58986 = CARTESIAN_POINT ( 'NONE',  ( -16.15384615384627409, -9.528491918059723176, 34.59228464037033035 ) ) ;
#58987 = CARTESIAN_POINT ( 'NONE',  ( 2.980769230769232170, -2.499999999999998668, 29.75000000000000355 ) ) ;
#58988 = CARTESIAN_POINT ( 'NONE',  ( 13.16168842570853492, -6.459968553980841577, 34.89616026154728701 ) ) ;
#58989 = CARTESIAN_POINT ( 'NONE',  ( -2.750000000000007105, -6.360912703474006946, 22.67187500000000355 ) ) ;
#58990 = AXIS2_PLACEMENT_3D ( 'NONE', #13897, #68842, #48559 ) ;
#58991 = CIRCLE ( 'NONE', #7185, 0.2500000000000002220 ) ;
#58992 = CARTESIAN_POINT ( 'NONE',  ( 5.076923076923075762, -10.05456864172156806, 36.03766855953608683 ) ) ;
#58993 = CARTESIAN_POINT ( 'NONE',  ( 14.24242230713598900, -5.094484230520674117, 34.41647553114621161 ) ) ;
#58995 = ORIENTED_EDGE ( 'NONE', *, *, #66365, .F. ) ;
#58994 = FACE_OUTER_BOUND ( 'NONE', #68889, .T. ) ;
#58996 = CARTESIAN_POINT ( 'NONE',  ( 2.750000000000008438, -8.639087296525996607, 18.29687500000000000 ) ) ;
#58997 = CYLINDRICAL_SURFACE ( 'NONE', #77134, 5.000000000000000888 ) ;
#58998 = VECTOR ( 'NONE', #61648, 1000.000000000000000 ) ;
#58999 = ORIENTED_EDGE ( 'NONE', *, *, #7841, .F. ) ;
#59000 = AXIS2_PLACEMENT_3D ( 'NONE', #71893, #70123, #42665 ) ;
#59001 = CYLINDRICAL_SURFACE ( 'NONE', #1114, 0.2499999999999995559 ) ;
#59002 = STYLED_ITEM ( 'NONE', ( #73831 ), #63293 ) ;
#59003 = ORIENTED_EDGE ( 'NONE', *, *, #85067, .T. ) ;
#59004 = CARTESIAN_POINT ( 'NONE',  ( -18.06527044596078113, -11.94971097300153140, 32.03036669348370680 ) ) ;
#59005 = CARTESIAN_POINT ( 'NONE',  ( -7.780085495151404906, -11.69971097300155094, 32.46337939537588113 ) ) ;
#59006 = CARTESIAN_POINT ( 'NONE',  ( 15.45354877203764232, -2.847695495035523550, 31.58253572463339154 ) ) ;
#59007 = EDGE_LOOP ( 'NONE', ( #82684, #42745 ) ) ;
#59008 = CARTESIAN_POINT ( 'NONE',  ( -0.4615384615381466493, -2.255955759149395501, 30.00000000000324363 ) ) ;
#59009 = B_SPLINE_CURVE_WITH_KNOTS ( 'NONE', 3,
 ( #58305, #51086, #43909, #38047, #17330, #45689 ),
 .UNSPECIFIED., .F., .F.,
 ( 4, 2, 4 ),
 ( 0.0003909512603273816180, 0.0005862562993132069836, 0.0007815613382990322950 ),
 .UNSPECIFIED. ) ;
#59010 = ORIENTED_EDGE ( 'NONE', *, *, #47043, .T. ) ;
#59011 = PLANE ( 'NONE',  #49951 ) ;
#59012 = EDGE_LOOP ( 'NONE', ( #29839, #85515 ) ) ;
#59013 = PLANE ( 'NONE',  #83129 ) ;
#59014 = CARTESIAN_POINT ( 'NONE',  ( 0.5923302693632481741, -11.18335022499818621, 33.13157742990016885 ) ) ;
#59015 = EDGE_LOOP ( 'NONE', ( #33525, #87935 ) ) ;
#59016 = CARTESIAN_POINT ( 'NONE',  ( -10.61538461538461320, -13.88283147151868846, 33.14645433367849847 ) ) ;
#59017 = DIRECTION ( 'NONE',  ( 0.000000000000000000, 0.8660254037844377084, -0.5000000000000015543 ) ) ;
#59018 = DIRECTION ( 'NONE',  ( -0.000000000000000000, 1.000000000000000000, -0.000000000000000000 ) ) ;
#59019 = EDGE_CURVE ( 'NONE', #61347, #70654, #65092, .T. ) ;
#59020 = CARTESIAN_POINT ( 'NONE',  ( -5.999999999999998224, -12.29105614889573062, 35.45975837776705220 ) ) ;
#59021 = CARTESIAN_POINT ( 'NONE',  ( -13.16183571563731824, -12.11081565061824250, 32.26097654155340422 ) ) ;
#59022 = EDGE_LOOP ( 'NONE', ( #67187, #30684, #35839, #7524 ) ) ;
#59023 = ORIENTED_EDGE ( 'NONE', *, *, #23436, .F. ) ;
#59024 = EDGE_LOOP ( 'NONE', ( #62691, #53818, #74328, #61419, #23156, #81480 ) ) ;
#59026 = ORIENTED_EDGE ( 'NONE', *, *, #54849, .T. ) ;
#59025 = CARTESIAN_POINT ( 'NONE',  ( 3.230769230769231726, -12.78798330534102945, 29.74999999999997868 ) ) ;
#59027 =( REPRESENTATION_RELATIONSHIP ('NONE','NONE', #51743, #14956 ) REPRESENTATION_RELATIONSHIP_WITH_TRANSFORMATION ( #18100 )SHAPE_REPRESENTATION_RELATIONSHIP( ) );
#59028 = EDGE_CURVE ( 'NONE', #56098, #14112, #20595, .T. ) ;
#59029 = CARTESIAN_POINT ( 'NONE',  ( 5.076923076923075762, -13.63283147151868846, 33.57946703557072254 ) ) ;
#59030 = CARTESIAN_POINT ( 'NONE',  ( -10.68065506134539078, -9.442884908240170461, 34.35708131394840592 ) ) ;
#59032 = ORIENTED_EDGE ( 'NONE', *, *, #14517, .T. ) ;
#59031 = EDGE_CURVE ( 'NONE', #68235, #53721, #71542, .T. ) ;
#59033 = ORIENTED_EDGE ( 'NONE', *, *, #83874, .T. ) ;
#59034 = CARTESIAN_POINT ( 'NONE',  ( 13.38461538461526423, -5.941354392335915335, 34.76329471203413846 ) ) ;
#59035 = ORIENTED_EDGE ( 'NONE', *, *, #30467, .T. ) ;
#59036 = CARTESIAN_POINT ( 'NONE',  ( -18.24997674404858827, -9.234221910056350069, 34.70572697212741531 ) ) ;
#59037 = EDGE_CURVE ( 'NONE', #72270, #49557, #10404, .T. ) ;
#59038 = CARTESIAN_POINT ( 'NONE',  ( -11.76138775597768316, -3.586966769969701208, 32.86292498521069660 ) ) ;
#59039 = CARTESIAN_POINT ( 'NONE',  ( -9.561469361820931212, -7.277220318596961057, 34.99547417642776992 ) ) ;
#59040 = FACE_BOUND ( 'NONE', #83286, .T. ) ;
#59041 = ORIENTED_EDGE ( 'NONE', *, *, #14071, .T. ) ;
#59042 = CARTESIAN_POINT ( 'NONE',  ( 7.846153846153846700, -8.973038597847269315, 34.52809138561121927 ) ) ;
#59043 = CARTESIAN_POINT ( 'NONE',  ( -4.153846153846152411, -12.29105614889573062, 35.45975837776705220 ) ) ;
#59044 = VECTOR ( 'NONE', #65803, 1000.000000000000000 ) ;
#59045 = EDGE_CURVE ( 'NONE', #40306, #57930, #30803, .T. ) ;
#59046 = CYLINDRICAL_SURFACE ( 'NONE', #84851, 0.2500000000000009437 ) ;
#59047 = CARTESIAN_POINT ( 'NONE',  ( -19.50000000000000000, -3.499999999999999556, 29.75000000000000355 ) ) ;
#59048 = CARTESIAN_POINT ( 'NONE',  ( -1.515306851282943956, -2.541943142973489778, 30.39792223712631980 ) ) ;
#59049 = ORIENTED_EDGE ( 'NONE', *, *, #27419, .F. ) ;
#59050 = CARTESIAN_POINT ( 'NONE',  ( 9.469381474791543241, -2.554751324335735152, 30.48935550225260727 ) ) ;
#59051 = ORIENTED_EDGE ( 'NONE', *, *, #57543, .T. ) ;
#59052 = EDGE_LOOP ( 'NONE', ( #8269, #75851 ) ) ;
#59053 = CIRCLE ( 'NONE', #82089, 8.000000000000000000 ) ;
#59055 = CARTESIAN_POINT ( 'NONE',  ( 10.61538461538449596, -6.026961402154118019, 34.52809138561165270 ) ) ;
#59054 = CARTESIAN_POINT ( 'NONE',  ( 6.000000000000001776, -11.91647553114624181, 32.58852847137148245 ) ) ;
#59056 = DIRECTION ( 'NONE',  ( -0.000000000000000000, -1.000000000000000000, 3.491481338843133355E-15 ) ) ;
#59057 = CARTESIAN_POINT ( 'NONE',  ( -19.00000000000000000, 0.7500000000000041078, 31.75000000000000000 ) ) ;
#59058 = CARTESIAN_POINT ( 'NONE',  ( 1.384615384615386802, -9.780366693483667717, 34.19971097300155094 ) ) ;
#59059 = CARTESIAN_POINT ( 'NONE',  ( 1.607395053593452472, -4.226511098958374291, 33.85474049983370293 ) ) ;
#59060 = VERTEX_POINT ( 'NONE', #13841 ) ;
#59061 = EDGE_CURVE ( 'NONE', #10433, #31195, #37183, .T. ) ;
#59062 = PLANE ( 'NONE',  #35710 ) ;
#59063 = CARTESIAN_POINT ( 'NONE',  ( -11.76138775597768138, -9.886141570436013382, 34.14413921362392301 ) ) ;
#59064 = CARTESIAN_POINT ( 'NONE',  ( -14.30769230769199218, -2.255955759149395501, 30.00000000000324363 ) ) ;
#59065 = EDGE_CURVE ( 'NONE', #87793, #63742, #47635, .T. ) ;
#59066 = CARTESIAN_POINT ( 'NONE',  ( 10.68145296638705410, -11.69971097300155272, 32.46337939537588113 ) ) ;
#59067 = ORIENTED_EDGE ( 'NONE', *, *, #51691, .F. ) ;
#59068 = EDGE_LOOP ( 'NONE', ( #1300, #5478 ) ) ;
#59069 = FACE_BOUND ( 'NONE', #69954, .T. ) ;
#59070 = VERTEX_POINT ( 'NONE', #75541 ) ;
#59071 = ADVANCED_FACE ( 'NONE', ( #40450 ), #26480, .F. ) ;
#59072 = CARTESIAN_POINT ( 'NONE',  ( 7.780070435197967704, -2.721908614388772740, 31.22303859784724622 ) ) ;
#59074 = ADVANCED_FACE ( 'NONE', ( #81431 ), #33680, .F. ) ;
#59073 = CARTESIAN_POINT ( 'NONE',  ( 5.011653076366756387, -3.083524468853724443, 32.58852847137143272 ) ) ;
#59075 = ORIENTED_EDGE ( 'NONE', *, *, #4739, .F. ) ;
#59076 = CYLINDRICAL_SURFACE ( 'NONE', #82722, 0.2499999999999998890 ) ;
#59077 = CARTESIAN_POINT ( 'NONE',  ( -18.00000000000000000, -3.513871655860376197, 32.76840700105977788 ) ) ;
#59078 = CARTESIAN_POINT ( 'NONE',  ( 5.011652630962299959, -2.892918686051582089, 31.69288490824015270 ) ) ;
#59079 = DIRECTION ( 'NONE',  ( -0.000000000000000000, -0.5000000000000009992, -0.8660254037844380415 ) ) ;
#59080 = CARTESIAN_POINT ( 'NONE',  ( -11.47320596718551045, -9.442884908240273489, 34.35708131394835618 ) ) ;
#59081 = ORIENTED_EDGE ( 'NONE', *, *, #9513, .T. ) ;
#59083 = ORIENTED_EDGE ( 'NONE', *, *, #71660, .F. ) ;
#59082 = CARTESIAN_POINT ( 'NONE',  ( 0.4615384615384611200, -9.780366693483667717, 34.19971097300155094 ) ) ;
#59084 = CARTESIAN_POINT ( 'NONE',  ( -7.596099534515530216, -9.148310452688876993, 34.47095581063188519 ) ) ;
#59085 = CARTESIAN_POINT ( 'NONE',  ( -12.52762084089859407, -2.833524468853757305, 32.15551576947924417 ) ) ;
#59086 = CARTESIAN_POINT ( 'NONE',  ( 20.99999999999999645, -10.75000000000000000, 29.75000000000000355 ) ) ;
#59087 = CARTESIAN_POINT ( 'NONE',  ( -15.23076923076922995, -2.486705287966279876, 31.30864560766543647 ) ) ;
#59088 = CARTESIAN_POINT ( 'NONE',  ( -5.749999999999984013, -2.249999999999999112, 29.81603969181031033 ) ) ;
#59089 = CARTESIAN_POINT ( 'NONE',  ( 5.207714884747860928, -12.38066358083363738, 30.83685684665853444 ) ) ;
#59090 = AXIS2_PLACEMENT_3D ( 'NONE', #69480, #62709, #21738 ) ;
#59091 = CARTESIAN_POINT ( 'NONE',  ( -2.775308065498752086, -8.577988221561495763, 15.26749329374151465 ) ) ;
#59092 = EDGE_LOOP ( 'NONE', ( #11557, #75522, #38190, #21014 ) ) ;
#59093 = CARTESIAN_POINT ( 'NONE',  ( 23.49999999999998579, 0.000000000000000000, 28.86437827766148345 ) ) ;
#59094 = CARTESIAN_POINT ( 'NONE',  ( 2.438482748659259958, -3.957578996910244395, 33.62503395064540257 ) ) ;
#59095 = CARTESIAN_POINT ( 'NONE',  ( 6.000000000000309086, -2.506253911140614576, 30.00000000000323297 ) ) ;
#59096 = ORIENTED_EDGE ( 'NONE', *, *, #43840, .F. ) ;
#59097 = ORIENTED_EDGE ( 'NONE', *, *, #14110, .F. ) ;
#59098 = CARTESIAN_POINT ( 'NONE',  ( -1.384615384615076605, -2.506253911140615021, 30.00000000000323297 ) ) ;
#59099 = DIRECTION ( 'NONE',  ( 0.000000000000000000, 0.000000000000000000, -1.000000000000000000 ) ) ;
#59100 = B_SPLINE_CURVE_WITH_KNOTS ( 'NONE', 3,
 ( #61217, #82845, #21120, #48590, #13487, #42302, #14368, #21569, #7621, #35083 ),
 .UNSPECIFIED., .F., .F.,
 ( 4, 2, 2, 2, 4 ),
 ( 0.000000000000000000, 0.0001954311564186866305, 0.0003908623128373732609, 0.0005862934692560598914, 0.0007817246256747465219 ),
 .UNSPECIFIED. ) ;
#59101 = B_SPLINE_CURVE_WITH_KNOTS ( 'NONE', 3,
 ( #60260, #17952, #53050, #31003, #3530, #10747, #5326, #17054, #18395, #71993 ),
 .UNSPECIFIED., .F., .F.,
 ( 4, 2, 2, 2, 4 ),
 ( 0.0007817359430256390048, 0.0009771253907250078159, 0.001172514838424376735, 0.001367904286123745655, 0.001563293733823114574 ),
 .UNSPECIFIED. ) ;
#59102 = CARTESIAN_POINT ( 'NONE',  ( 17.32686848630112308, -3.520799739797213501, 33.17531984108286025 ) ) ;
#59103 = CARTESIAN_POINT ( 'NONE',  ( 9.019285189144223835, -11.47946981652013498, 33.17500667209847620 ) ) ;
#59104 = CARTESIAN_POINT ( 'NONE',  ( 17.86930939688968678, -11.93127051446800380, 32.56575433478200665 ) ) ;
#59105 = CARTESIAN_POINT ( 'NONE',  ( 5.777073782483853392, -8.239355502252617924, 34.69524867566427417 ) ) ;
#59106 = ORIENTED_EDGE ( 'NONE', *, *, #81549, .F. ) ;
#59107 = EDGE_CURVE ( 'NONE', #19283, #51157, #26923, .T. ) ;
#59108 = CARTESIAN_POINT ( 'NONE',  ( -2.980823821391186623, -12.68172785388650681, 30.59649109432439218 ) ) ;
#59109 = LINE ( 'NONE', #54912, #88035 ) ;
#59110 = VECTOR ( 'NONE', #69046, 1000.000000000000000 ) ;
#59111 = CYLINDRICAL_SURFACE ( 'NONE', #34030, 0.2499999999999986955 ) ;
#59112 = CARTESIAN_POINT ( 'NONE',  ( -3.230769230769351186, -11.94971097300221174, 32.03036669348237098 ) ) ;
#59113 = ORIENTED_EDGE ( 'NONE', *, *, #59795, .T. ) ;
#59114 = CARTESIAN_POINT ( 'NONE',  ( 10.61538461538449418, -9.528491918059723176, 34.59228464037033035 ) ) ;
#59115 = ORIENTED_EDGE ( 'NONE', *, *, #62528, .F. ) ;
#59116 = CARTESIAN_POINT ( 'NONE',  ( 13.63456090296352841, -3.712312575010499494, 33.01462480002815170 ) ) ;
#59117 = CARTESIAN_POINT ( 'NONE',  ( 16.40384615384615330, -2.249999999999998668, 29.75000000000000355 ) ) ;
#59118 = CARTESIAN_POINT ( 'NONE',  ( 17.77651507543566822, -10.23692288466677880, 34.23039457007281072 ) ) ;
#59119 = ORIENTED_EDGE ( 'NONE', *, *, #67690, .F. ) ;
#59120 = CARTESIAN_POINT ( 'NONE',  ( 8.769230769230768274, -10.51840700105979565, 33.73612834413961536 ) ) ;
#59121 = CARTESIAN_POINT ( 'NONE',  ( -2.530619266599154038, -6.459968553980839800, 34.89616026154728701 ) ) ;
#59122 = DIRECTION ( 'NONE',  ( 1.000000000000000000, 0.000000000000000000, 0.000000000000000000 ) ) ;
#59123 = AXIS2_PLACEMENT_3D ( 'NONE', #58398, #44007, #86360 ) ;
#59124 = EDGE_CURVE ( 'NONE', #26314, #62464, #4794, .T. ) ;
#59125 = CARTESIAN_POINT ( 'NONE',  ( -7.846153846153844924, -4.661471528628507777, 34.16647553114623292 ) ) ;
#59126 = CYLINDRICAL_SURFACE ( 'NONE', #77112, 0.2500000000000008882 ) ;
#59127 = ORIENTED_EDGE ( 'NONE', *, *, #40164, .F. ) ;
#59128 = CARTESIAN_POINT ( 'NONE',  ( 8.769230769230768274, -6.386643153685126251, 34.62446782046654192 ) ) ;
#59129 = VERTEX_POINT ( 'NONE', #48061 ) ;
#59130 = CARTESIAN_POINT ( 'NONE',  ( 8.638539302563209787, -12.38065189839062263, 30.83690757178629482 ) ) ;
#59131 = B_SPLINE_CURVE_WITH_KNOTS ( 'NONE', 3,
 ( #66888, #87181, #88958, #54689, #88079, #5186, #52911, #47492, #19145, #61010 ),
 .UNSPECIFIED., .F., .F.,
 ( 4, 2, 2, 2, 4 ),
 ( 0.000000000000000000, 0.0001954339857564078809, 0.0003908679715128157619, 0.0005863019572692236428, 0.0007817359430256315238 ),
 .UNSPECIFIED. ) ;
#59132 = CARTESIAN_POINT ( 'NONE',  ( -19.00000000000000000, 8.999999999999996447, 23.75000000000000000 ) ) ;
#59134 = EDGE_CURVE ( 'NONE', #45405, #86404, #85521, .T. ) ;
#59133 = CARTESIAN_POINT ( 'NONE',  ( -0.3954711281883865337, -2.486705287966280320, 31.30864560766543647 ) ) ;
#59135 = B_SPLINE_CURVE_WITH_KNOTS ( 'NONE', 3,
 ( #70184, #8493, #35965, #89154, #41839, #27870, #70629, #63421, #1728, #27432 ),
 .UNSPECIFIED., .F., .F.,
 ( 4, 2, 2, 2, 4 ),
 ( 0.0007817246256747450040, 0.0009771112852218881168, 0.001172497944769031230, 0.001367884604316174342, 0.001563271263863317455 ),
 .UNSPECIFIED. ) ;
#59136 = CARTESIAN_POINT ( 'NONE',  ( 7.596177102105255763, -12.41104346484419452, 31.60698883733904196 ) ) ;
#59137 = DIRECTION ( 'NONE',  ( -1.000000000000000000, -0.000000000000000000, -0.000000000000000000 ) ) ;
#59138 = CARTESIAN_POINT ( 'NONE',  ( -6.857009589726848375, -2.486705287966279876, 31.30864560766543647 ) ) ;
#59139 = EDGE_CURVE ( 'NONE', #3063, #10751, #46452, .T. ) ;
#59140 = ORIENTED_EDGE ( 'NONE', *, *, #11918, .T. ) ;
#59141 = EDGE_LOOP ( 'NONE', ( #581, #88504 ) ) ;
#59142 = ORIENTED_EDGE ( 'NONE', *, *, #26034, .T. ) ;
#59143 = VECTOR ( 'NONE', #61327, 1000.000000000000000 ) ;
#59144 = ORIENTED_EDGE ( 'NONE', *, *, #18090, .F. ) ;
#59145 = ORIENTED_EDGE ( 'NONE', *, *, #29124, .T. ) ;
#59146 = CARTESIAN_POINT ( 'NONE',  ( -1.134561072977070095, -3.136992222400443175, 32.19305428654138979 ) ) ;
#59147 = ADVANCED_FACE ( 'NONE', ( #19277 ), #46744, .F. ) ;
#59148 = CARTESIAN_POINT ( 'NONE',  ( -2.307692307692305711, -3.050289026998446396, 32.03036669348365706 ) ) ;
#59149 = AXIS2_PLACEMENT_3D ( 'NONE', #16236, #1833, #22550 ) ;
#59150 = CARTESIAN_POINT ( 'NONE',  ( -15.45369544828537656, -10.61292498521070549, 33.66303323003028680 ) ) ;
#59151 = DIRECTION ( 'NONE',  ( 0.000000000000000000, 0.000000000000000000, 1.000000000000000000 ) ) ;
#59152 = DIRECTION ( 'NONE',  ( 0.000000000000000000, 0.4999999999999960032, -0.8660254037844410391 ) ) ;
#59153 = CARTESIAN_POINT ( 'NONE',  ( -12.52762084089859762, -12.34228464037088280, 31.77849191805838558 ) ) ;
#59154 = DIRECTION ( 'NONE',  ( 0.000000000000000000, 0.3420201433256641055, -0.9396926207859100932 ) ) ;
#59155 = CARTESIAN_POINT ( 'NONE',  ( -7.596099534515531104, -3.136992222400443175, 32.19305428654138979 ) ) ;
#59156 = DIRECTION ( 'NONE',  ( -0.000000000000000000, -0.6427876096865404731, -0.7660444431189770143 ) ) ;
#59157 = VERTEX_POINT ( 'NONE', #5764 ) ;
#59158 = ORIENTED_EDGE ( 'NONE', *, *, #54957, .T. ) ;
#59159 = ORIENTED_EDGE ( 'NONE', *, *, #28518, .T. ) ;
#59161 = ORIENTED_EDGE ( 'NONE', *, *, #74949, .T. ) ;
#59160 = CARTESIAN_POINT ( 'NONE',  ( 0.2115152373170035849, -2.985938066672154445, 32.43141759479405550 ) ) ;
#59163 = CARTESIAN_POINT ( 'NONE',  ( -17.93393266664992680, -11.35647404775217240, 33.31231777344667222 ) ) ;
#59162 = CARTESIAN_POINT ( 'NONE',  ( 6.856994543716788293, -11.35647404775217595, 33.31231777344666511 ) ) ;
#59164 = DIRECTION ( 'NONE',  ( 0.000000000000000000, 0.9396926207859126468, 0.3420201433256571111 ) ) ;
#59165 = CARTESIAN_POINT ( 'NONE',  ( -14.55766903863466055, -9.943427161483782584, 34.11278801902876978 ) ) ;
#59166 = FACE_BOUND ( 'NONE', #21244, .T. ) ;
#59167 = EDGE_LOOP ( 'NONE', ( #100, #7610, #83164, #6923 ) ) ;
#59168 = EDGE_CURVE ( 'NONE', #13394, #13635, #45027, .T. ) ;
#59169 = VECTOR ( 'NONE', #74495, 1000.000000000000000 ) ;
#59170 = ORIENTED_EDGE ( 'NONE', *, *, #71313, .T. ) ;
#59171 = DIRECTION ( 'NONE',  ( -0.000000000000000000, -0.1736481776669307198, -0.9848077530122080203 ) ) ;
#59173 = EDGE_CURVE ( 'NONE', #24890, #26148, #63740, .T. ) ;
#59172 = VERTEX_POINT ( 'NONE', #88207 ) ;
#59174 = FACE_BOUND ( 'NONE', #36664, .T. ) ;
#59175 = CARTESIAN_POINT ( 'NONE',  ( -10.68146699474474914, -2.833524468853757305, 32.15551576947924417 ) ) ;
#59176 = CARTESIAN_POINT ( 'NONE',  ( 4.499999999999999112, 7.500000000000002665, 13.00000000000000178 ) ) ;
#59177 = VERTEX_POINT ( 'NONE', #76879 ) ;
#59178 = CARTESIAN_POINT ( 'NONE',  ( 18.03205128205128105, -7.500000000000000000, 29.75000000000000355 ) ) ;
#59180 = ADVANCED_FACE ( 'NONE', ( #2093 ), #30020, .F. ) ;
#59179 = CARTESIAN_POINT ( 'NONE',  ( 8.519230769230768274, -7.500000000000001776, 35.00000000000000000 ) ) ;
#59181 = CARTESIAN_POINT ( 'NONE',  ( -18.00000000000012079, -4.320704448113953156, 33.92786785259630022 ) ) ;
#59182 = VERTEX_POINT ( 'NONE', #77755 ) ;
#59183 = CARTESIAN_POINT ( 'NONE',  ( -9.442307692307691624, -7.500000000000001776, 35.04278698407183867 ) ) ;
#59184 = CARTESIAN_POINT ( 'NONE',  ( -14.43838377435986864, -5.582088688514999397, 34.36776431015576350 ) ) ;
#59185 = VERTEX_POINT ( 'NONE', #21932 ) ;
#59186 = VECTOR ( 'NONE', #61076, 1000.000000000000000 ) ;
#59187 = CARTESIAN_POINT ( 'NONE',  ( -1.450698795571263577, -5.557115091759785130, 34.35708131394839171 ) ) ;
#59188 = CARTESIAN_POINT ( 'NONE',  ( -13.63461538461538325, -7.500000000000001776, 34.75000000000000000 ) ) ;
#59189 = EDGE_LOOP ( 'NONE', ( #71128, #57282, #28582, #85924, #6226 ) ) ;
#59190 = CARTESIAN_POINT ( 'NONE',  ( -12.68446542044531000, -5.582147617184174848, 34.63737895849758530 ) ) ;
#59191 = CARTESIAN_POINT ( 'NONE',  ( -10.48459280755982803, -4.809403383903225304, 33.96459661697924304 ) ) ;
#59192 = CARTESIAN_POINT ( 'NONE',  ( -3.230769230769229949, -2.721908614388771852, 31.22303859784724978 ) ) ;
#59193 = CARTESIAN_POINT ( 'NONE',  ( 9.070512820512819374, -7.500000000000000000, 29.75000000000000355 ) ) ;
#59194 = FACE_OUTER_BOUND ( 'NONE', #77433, .T. ) ;
#59195 = CARTESIAN_POINT ( 'NONE',  ( -9.692307692307691624, -6.435427911321262684, 35.78748833219616898 ) ) ;
#59197 = DIRECTION ( 'NONE',  ( -0.000000000000000000, -0.6427876096865404731, -0.7660444431189770143 ) ) ;
#59196 = CARTESIAN_POINT ( 'NONE',  ( -13.60754234352223335, -4.026226216239094491, 33.68668979543634379 ) ) ;
#59198 = CARTESIAN_POINT ( 'NONE',  ( -3.360916440207450506, -2.619462340734462380, 30.83744416345203021 ) ) ;
#59200 = FACE_OUTER_BOUND ( 'NONE', #49510, .T. ) ;
#59199 = CARTESIAN_POINT ( 'NONE',  ( 0.7115384615384606759, -2.499999999999998668, 29.75000000000000355 ) ) ;
#59201 = EDGE_CURVE ( 'NONE', #6421, #33663, #63014, .T. ) ;
#59202 = CARTESIAN_POINT ( 'NONE',  ( -1.987747218494660295, -5.598659921968651254, 26.24813170625849068 ) ) ;
#59203 = EDGE_LOOP ( 'NONE', ( #83105, #59635, #87984, #29697 ) ) ;
#59204 = CARTESIAN_POINT ( 'NONE',  ( 2.307692307692309264, -2.517432740324522911, 35.29906147534542527 ) ) ;
#59205 = ORIENTED_EDGE ( 'NONE', *, *, #7197, .T. ) ;
#59206 = ADVANCED_FACE ( 'NONE', ( #21034 ), #77316, .T. ) ;
#59207 = VERTEX_POINT ( 'NONE', #84093 ) ;
#59208 = CARTESIAN_POINT ( 'NONE',  ( -3.100243792535585463, -9.503571793651733657, 34.60286762892837942 ) ) ;
#59209 = ORIENTED_EDGE ( 'NONE', *, *, #80541, .T. ) ;
#59210 = CARTESIAN_POINT ( 'NONE',  ( 17.74999999999999289, -7.566083408709835645, 34.74999999999999289 ) ) ;
#59211 = CARTESIAN_POINT ( 'NONE',  ( -1.139087296526025916, -4.750000000000006217, 15.32812500000000355 ) ) ;
#59212 = CARTESIAN_POINT ( 'NONE',  ( -13.25382494364843389, -5.496552790871120031, 34.60292014791297532 ) ) ;
#59213 = CARTESIAN_POINT ( 'NONE',  ( -8.992156986746916658, -3.105860786376062332, 32.13614157043599562 ) ) ;
#59214 = LINE ( 'NONE', #88494, #73467 ) ;
#59215 = LINE ( 'NONE', #79044, #44612 ) ;
#59216 = CARTESIAN_POINT ( 'NONE',  ( -7.846153846153844924, -8.564572088678739092, 35.78748833219616898 ) ) ;
#59217 = CARTESIAN_POINT ( 'NONE',  ( -10.61538461538461320, -4.098570777380720287, 33.41473453929634729 ) ) ;
#59218 = DIRECTION ( 'NONE',  ( -0.000000000000000000, -0.000000000000000000, -1.000000000000000000 ) ) ;
#59220 = B_SPLINE_CURVE_WITH_KNOTS ( 'NONE', 3,
 ( #78385, #55901, #30216, #28899, #57677, #44144, #8174, #84730, #7733, #84288 ),
 .UNSPECIFIED., .F., .F.,
 ( 4, 2, 2, 2, 4 ),
 ( 0.000000000000000000, 0.0001954311564186864407, 0.0003908623128373728815, 0.0005862934692560593493, 0.0007817246256747457630 ),
 .UNSPECIFIED. ) ;
#59219 = AXIS2_PLACEMENT_3D ( 'NONE', #20503, #13746, #41227 ) ;
#59221 = CARTESIAN_POINT ( 'NONE',  ( 3.749999999999992006, -5.946699141100872943, 21.89062500000000355 ) ) ;
#59222 = EDGE_CURVE ( 'NONE', #18025, #88852, #49408, .T. ) ;
#59223 = CARTESIAN_POINT ( 'NONE',  ( -0.5922299282060213832, -2.541943142973490666, 30.39792223712631980 ) ) ;
#59224 = LINE ( 'NONE', #44358, #64963 ) ;
#59225 = VECTOR ( 'NONE', #964, 1000.000000000000000 ) ;
#59226 = LINE ( 'NONE', #39858, #88181 ) ;
#59227 = EDGE_CURVE ( 'NONE', #46293, #54130, #26516, .T. ) ;
#59228 = ORIENTED_EDGE ( 'NONE', *, *, #7715, .T. ) ;
#59229 = VERTEX_POINT ( 'NONE', #14286 ) ;
#59230 = CARTESIAN_POINT ( 'NONE',  ( 6.000000000000001776, -13.75783147151868846, 33.36296068462461051 ) ) ;
#59231 = CARTESIAN_POINT ( 'NONE',  ( -14.05763799605399278, -8.303483539816728154, 34.68545999027711702 ) ) ;
#59232 = CARTESIAN_POINT ( 'NONE',  ( -4.480769230769230838, -3.499999999999999556, 29.75000000000000355 ) ) ;
#59233 = CARTESIAN_POINT ( 'NONE',  ( -6.223484943723949669, -3.754499324213721234, 33.06261337010820256 ) ) ;
#59234 = CARTESIAN_POINT ( 'NONE',  ( 15.29693837173189053, -7.250054483168843156, 34.74374881642865631 ) ) ;
#59235 = CARTESIAN_POINT ( 'NONE',  ( -4.946397638689434828, -3.068774925481847937, 32.56582465632704526 ) ) ;
#59236 = EDGE_CURVE ( 'NONE', #22041, #16132, #58721, .T. ) ;
#59237 = EDGE_CURVE ( 'NONE', #78849, #177, #69235, .T. ) ;
#59238 = ORIENTED_EDGE ( 'NONE', *, *, #77003, .F. ) ;
#59239 = CARTESIAN_POINT ( 'NONE',  ( -1.253823576790597638, -9.804649428959606894, 34.18742332936588468 ) ) ;
#59240 = ORIENTED_EDGE ( 'NONE', *, *, #49714, .F. ) ;
#59241 = VERTEX_POINT ( 'NONE', #36336 ) ;
#59242 = CIRCLE ( 'NONE', #70762, 4.000000000000000000 ) ;
#59243 = LINE ( 'NONE', #3403, #80992 ) ;
#59244 = AXIS2_PLACEMENT_3D ( 'NONE', #7857, #43416, #28118 ) ;
#59245 = DIRECTION ( 'NONE',  ( 0.000000000000000000, 0.000000000000000000, -1.000000000000000000 ) ) ;
#59246 = DIRECTION ( 'NONE',  ( -0.000000000000000000, -0.5000000000000009992, -0.8660254037844380415 ) ) ;
#59247 = CARTESIAN_POINT ( 'NONE',  ( 11.60452887181161508, -2.292212530054420494, 30.41441678777542990 ) ) ;
#59248 = CARTESIAN_POINT ( 'NONE',  ( -12.22435897435897267, -11.00000000000000000, 29.75000000000000355 ) ) ;
#59249 = ADVANCED_FACE ( 'NONE', ( #62458 ), #63354, .F. ) ;
#59250 = ORIENTED_EDGE ( 'NONE', *, *, #39995, .F. ) ;
#59251 = EDGE_CURVE ( 'NONE', #70013, #79114, #61907, .T. ) ;
#59252 = EDGE_LOOP ( 'NONE', ( #49086, #15213, #19744, #27741 ) ) ;
#59253 = B_SPLINE_CURVE_WITH_KNOTS ( 'NONE', 3,
 ( #10332, #86459, #79682, #52643, #11224, #30160, #80125, #18427, #37345, #36908 ),
 .UNSPECIFIED., .F., .F.,
 ( 4, 2, 2, 2, 4 ),
 ( 0.0007817246256747503166, 0.0009771112852218946220, 0.001172497944769039036, 0.001367884604316183233, 0.001563271263863327647 ),
 .UNSPECIFIED. ) ;
#59254 = ORIENTED_EDGE ( 'NONE', *, *, #49265, .T. ) ;
#59255 = CARTESIAN_POINT ( 'NONE',  ( -7.053224892808618307, -12.15440758774515473, 32.17923288041532004 ) ) ;
#59256 = DIRECTION ( 'NONE',  ( -0.000000000000000000, 0.000000000000000000, 1.000000000000000000 ) ) ;
#59257 = CARTESIAN_POINT ( 'NONE',  ( 4.403900573759607084, -3.435999193479609914, 33.07426656108010832 ) ) ;
#59258 = CARTESIAN_POINT ( 'NONE',  ( 2.177000841024751665, -11.18331474514187995, 33.13161551792790505 ) ) ;
#59259 = CARTESIAN_POINT ( 'NONE',  ( -4.219929564802034072, -8.120952969808774569, 34.71129190930000163 ) ) ;
#59260 = DIRECTION ( 'NONE',  ( -0.000000000000000000, -0.9848077530122086864, -0.1736481776669273613 ) ) ;
#59261 = ORIENTED_EDGE ( 'NONE', *, *, #35329, .F. ) ;
#59262 = B_SPLINE_CURVE_WITH_KNOTS ( 'NONE', 3,
 ( #18477, #46827, #80637, #5851, #79732, #66206, #52243, #74308, #5408, #45931 ),
 .UNSPECIFIED., .F., .F.,
 ( 4, 2, 2, 2, 4 ),
 ( 0.000000000000000000, 0.0001954311564186874978, 0.0003908623128373749957, 0.0005862934692560624935, 0.0007817246256747499913 ),
 .UNSPECIFIED. ) ;
#59263 = VERTEX_POINT ( 'NONE', #66008 ) ;
#59264 = CARTESIAN_POINT ( 'NONE',  ( 1.553300858899087311, -3.749999999999992006, 24.23437500000000355 ) ) ;
#59265 = ORIENTED_EDGE ( 'NONE', *, *, #8237, .F. ) ;
#59267 = ORIENTED_EDGE ( 'NONE', *, *, #36001, .F. ) ;
#59266 = CARTESIAN_POINT ( 'NONE',  ( -12.68446467905460828, -11.24512374952581872, 33.06303171183252942 ) ) ;
#59268 = CARTESIAN_POINT ( 'NONE',  ( -9.915234651214539952, -10.01117774369187252, 34.36070679894347535 ) ) ;
#59269 = CARTESIAN_POINT ( 'NONE',  ( -2.084679463598910321, -4.026326845037965008, 33.68677907613344047 ) ) ;
#59270 = CARTESIAN_POINT ( 'NONE',  ( 3.749999999999992006, -5.946699141100872943, 14.39062500000000000 ) ) ;
#59271 = ORIENTED_EDGE ( 'NONE', *, *, #27457, .F. ) ;
#59272 = CARTESIAN_POINT ( 'NONE',  ( -14.30769230769230660, -1.466349020453238561, 30.81389545987213907 ) ) ;
#59273 = ORIENTED_EDGE ( 'NONE', *, *, #37373, .T. ) ;
#59274 = CARTESIAN_POINT ( 'NONE',  ( 5.749976775778544713, -9.356822207818506598, 34.66110646841856635 ) ) ;
#59275 = CARTESIAN_POINT ( 'NONE',  ( -1.384615384615383471, -1.367168528481310208, 33.57946703557072254 ) ) ;
#59276 = ADVANCED_FACE ( 'NONE', ( #84968 ), #78643, .T. ) ;
#59277 = FACE_BOUND ( 'NONE', #11454, .T. ) ;
#59279 = CARTESIAN_POINT ( 'NONE',  ( 8.069166690247241647, -2.308499170217967134, 30.53291367094873721 ) ) ;
#59278 = CARTESIAN_POINT ( 'NONE',  ( 10.36538461538461675, -7.433931650972300353, 34.75000000000000711 ) ) ;
#59280 = DIRECTION ( 'NONE',  ( 1.000000000000000000, -9.483446719664426957E-15, 0.000000000000000000 ) ) ;
#59281 = CARTESIAN_POINT ( 'NONE',  ( 18.00000000000000000, -2.721908614388771852, 31.22303859784724978 ) ) ;
#59282 = ORIENTED_EDGE ( 'NONE', *, *, #18930, .T. ) ;
#59284 = EDGE_CURVE ( 'NONE', #76616, #38055, #65563, .T. ) ;
#59283 = CARTESIAN_POINT ( 'NONE',  ( 6.699591979352975457, -8.496056993536548418, 34.65000542017679663 ) ) ;
#59285 = DIRECTION ( 'NONE',  ( 1.000000000000000000, 0.000000000000000000, 0.000000000000000000 ) ) ;
#59286 = EDGE_LOOP ( 'NONE', ( #48867, #21174 ) ) ;
#59287 = EDGE_CURVE ( 'NONE', #28775, #24594, #42631, .T. ) ;
#59288 = CARTESIAN_POINT ( 'NONE',  ( -8.703163435880695076, -3.322132147404559976, 32.92929555188717927 ) ) ;
#59289 = DIRECTION ( 'NONE',  ( 0.000000000000000000, 0.3420201433256641055, -0.9396926207859100932 ) ) ;
#59290 = DIRECTION ( 'NONE',  ( -1.000000000000000000, 0.000000000000000000, 0.000000000000000000 ) ) ;
#59291 = DIRECTION ( 'NONE',  ( -0.000000000000000000, -0.9848077530122085754, -0.1736481776669273891 ) ) ;
#59292 = CYLINDRICAL_SURFACE ( 'NONE', #67397, 0.2499999999999994726 ) ;
#59293 = FACE_BOUND ( 'NONE', #84782, .T. ) ;
#59295 = DIRECTION ( 'NONE',  ( -0.000000000000000000, -0.000000000000000000, -1.000000000000000000 ) ) ;
#59294 = CARTESIAN_POINT ( 'NONE',  ( 17.99999999999987566, -6.026961402154118908, 34.52809138561165270 ) ) ;
#59296 = CARTESIAN_POINT ( 'NONE',  ( -4.153846153846152411, -1.509761064869970415, 31.06009739812519044 ) ) ;
#59298 = CARTESIAN_POINT ( 'NONE',  ( 14.30769230769231015, -10.67929555188718282, 33.92786785259544047 ) ) ;
#59297 = CARTESIAN_POINT ( 'NONE',  ( -11.40841393220585509, -7.723484964179501588, 34.74522123443823318 ) ) ;
#59299 = CARTESIAN_POINT ( 'NONE',  ( -3.903900744468109085, -10.92531984108285670, 33.72920026020278073 ) ) ;
#59300 = EDGE_CURVE ( 'NONE', #41958, #2122, #43965, .T. ) ;
#59301 = CARTESIAN_POINT ( 'NONE',  ( 6.130525438233646263, -5.070358843744210198, 34.40418822224088302 ) ) ;
#59302 = CARTESIAN_POINT ( 'NONE',  ( 2.608446859217893099, -4.805146000318787358, 25.31063170625848713 ) ) ;
#59303 = B_SPLINE_CURVE_WITH_KNOTS ( 'NONE', 3,
 ( #27216, #14590, #82171, #75407, #34412, #42073, #61875, #190, #27656, #55127 ),
 .UNSPECIFIED., .F., .F.,
 ( 4, 2, 2, 2, 4 ),
 ( 0.0007817246256747481482, 0.0009771112852218911526, 0.001172497944769034265, 0.001367884604316177161, 0.001563271263863320274 ),
 .UNSPECIFIED. ) ;
#59304 = VECTOR ( 'NONE', #24972, 1000.000000000000227 ) ;
#59305 = CARTESIAN_POINT ( 'NONE',  ( -8.703975197954745724, -6.026961402152789304, 34.52809138561124769 ) ) ;
#59306 = ORIENTED_EDGE ( 'NONE', *, *, #82946, .T. ) ;
#59307 = AXIS2_PLACEMENT_3D ( 'NONE', #59020, #10401, #25244 ) ;
#59308 = LINE ( 'NONE', #86814, #26236 ) ;
#59309 = CARTESIAN_POINT ( 'NONE',  ( 2.084765348785459604, -2.308479472611653094, 30.53278059502174457 ) ) ;
#59310 = DIRECTION ( 'NONE',  ( 0.000000000000000000, 0.000000000000000000, -1.000000000000000000 ) ) ;
#59311 = CARTESIAN_POINT ( 'NONE',  ( -9.692307692307691624, -10.51840700105979565, 33.73612834413961536 ) ) ;
#59312 = CARTESIAN_POINT ( 'NONE',  ( 10.83816415665302380, -12.24180327182771855, 31.33663988360758879 ) ) ;
#59313 = CARTESIAN_POINT ( 'NONE',  ( -11.53846153846166089, -4.320704448113951379, 33.92786785259630022 ) ) ;
#59314 = CARTESIAN_POINT ( 'NONE',  ( -1.200186371490556958, -4.775308065498765409, 15.07625670625849068 ) ) ;
#59315 = CIRCLE ( 'NONE', #17607, 4.000000000000000000 ) ;
#59316 = CARTESIAN_POINT ( 'NONE',  ( -5.999999999999998224, -6.435427911321262684, 35.78748833219616898 ) ) ;
#59317 = CARTESIAN_POINT ( 'NONE',  ( -14.30769230769242917, -11.67786785259630911, 32.92929555188603530 ) ) ;
#59318 = CARTESIAN_POINT ( 'NONE',  ( 8.096208157792160520, -11.79725096376909654, 32.30694842903959341 ) ) ;
#59319 = CARTESIAN_POINT ( 'NONE',  ( 9.692307692307695177, -3.937682226553329556, 33.60647404775216529 ) ) ;
#59320 = CARTESIAN_POINT ( 'NONE',  ( 14.55774661933062397, -5.728107161865378494, 34.42597550085002922 ) ) ;
#59321 = CARTESIAN_POINT ( 'NONE',  ( 9.626225312947559232, -3.322132147404559532, 32.92929555188719348 ) ) ;
#59322 = CARTESIAN_POINT ( 'NONE',  ( -6.065270000556321150, -12.16647553114622049, 32.15551576947930812 ) ) ;
#59323 = CARTESIAN_POINT ( 'NONE',  ( 17.14217821643591932, -8.656820664281605460, 34.87096338111211224 ) ) ;
#59324 = ORIENTED_EDGE ( 'NONE', *, *, #44827, .F. ) ;
#59325 = CARTESIAN_POINT ( 'NONE',  ( 16.15384615384615330, -4.661471528628507777, 34.16647553114623292 ) ) ;
#59326 = PLANE ( 'NONE',  #34510 ) ;
#59327 = CARTESIAN_POINT ( 'NONE',  ( 1.492201783934598236, -11.27530806549875031, 18.70499329374151287 ) ) ;
#59328 = EDGE_CURVE ( 'NONE', #42300, #87108, #9290, .T. ) ;
#59329 = CARTESIAN_POINT ( 'NONE',  ( 5.999999999999880096, -4.481592998941358097, 33.73612834414048933 ) ) ;
#59330 = PLANE ( 'NONE',  #74302 ) ;
#59331 = ORIENTED_EDGE ( 'NONE', *, *, #66253, .F. ) ;
#59332 = CARTESIAN_POINT ( 'NONE',  ( -17.75005459062195712, -6.653508905675592722, 34.93172785388651391 ) ) ;
#59333 = CARTESIAN_POINT ( 'NONE',  ( -16.94639763868943660, -9.503571793651730104, 34.60286762892837942 ) ) ;
#59335 = VERTEX_POINT ( 'NONE', #38101 ) ;
#59334 = CARTESIAN_POINT ( 'NONE',  ( 8.900021210197719412, -2.494656445102012565, 31.33466734024120015 ) ) ;
#59336 = CARTESIAN_POINT ( 'NONE',  ( -12.46153846153846168, -9.058645607665452459, 34.76329471203371924 ) ) ;
#59337 = CARTESIAN_POINT ( 'NONE',  ( -3.230769230769229949, -3.513871655860378418, 32.76840700105978499 ) ) ;
#59338 = CARTESIAN_POINT ( 'NONE',  ( -8.769230769230890843, -2.625532179533778709, 30.86335684631627174 ) ) ;
#59339 = CARTESIAN_POINT ( 'NONE',  ( 2.544871794871792936, -3.499999999999999556, 29.75000000000000355 ) ) ;
#59340 = EDGE_CURVE ( 'NONE', #2112, #62210, #1773, .T. ) ;
#59341 = ORIENTED_EDGE ( 'NONE', *, *, #36306, .F. ) ;
#59342 = CARTESIAN_POINT ( 'NONE',  ( 3.262820512820510999, -7.500000000000000000, 29.75000000000000355 ) ) ;
#59343 = DIRECTION ( 'NONE',  ( 1.000000000000000000, 0.000000000000000000, 0.000000000000000000 ) ) ;
#59344 = ADVANCED_FACE ( 'NONE', ( #45294 ), #79089, .F. ) ;
#59345 = EDGE_CURVE ( 'NONE', #48076, #66517, #54417, .T. ) ;
#59346 = B_SPLINE_CURVE_WITH_KNOTS ( 'NONE', 3,
 ( #38571, #46212, #51158, #11995, #78660, #37673, #3439, #58373, #85867, #38118 ),
 .UNSPECIFIED., .F., .F.,
 ( 4, 2, 2, 2, 4 ),
 ( 0.000000000000000000, 0.0001954311564186871184, 0.0003908623128373742367, 0.0005862934692560614093, 0.0007817246256747484735 ),
 .UNSPECIFIED. ) ;
#59347 = CYLINDRICAL_SURFACE ( 'NONE', #61422, 0.2500000000000002220 ) ;
#59348 = ORIENTED_EDGE ( 'NONE', *, *, #7321, .T. ) ;
#59349 = ORIENTED_EDGE ( 'NONE', *, *, #37752, .F. ) ;
#59350 = B_SPLINE_CURVE_WITH_KNOTS ( 'NONE', 3,
 ( #16322, #37021, #64482, #16755, #44211, #71697, #33826, #60410, #40160, #61284 ),
 .UNSPECIFIED., .F., .F.,
 ( 4, 2, 2, 2, 4 ),
 ( 0.000000000000000000, 0.0001954311564186869286, 0.0003908623128373738573, 0.0005862934692560607588, 0.0007817246256747477145 ),
 .UNSPECIFIED. ) ;
#59351 = ORIENTED_EDGE ( 'NONE', *, *, #30993, .F. ) ;
#59352 = FACE_OUTER_BOUND ( 'NONE', #85741, .T. ) ;
#59353 = CARTESIAN_POINT ( 'NONE',  ( 9.915320536401090123, -4.026326845037962343, 33.68677907613344047 ) ) ;
#59354 = CARTESIAN_POINT ( 'NONE',  ( -9.627052552794857831, -12.70778746994558439, 30.41441678777536595 ) ) ;
#59355 = EDGE_CURVE ( 'NONE', #3401, #6432, #53296, .T. ) ;
#59356 = CARTESIAN_POINT ( 'NONE',  ( -10.36533030374629938, -3.136992222400443175, 32.19305428654138979 ) ) ;
#59357 = EDGE_CURVE ( 'NONE', #34683, #4768, #68680, .T. ) ;
#59358 = EDGE_CURVE ( 'NONE', #54559, #65254, #12851, .T. ) ;
#59359 = ORIENTED_EDGE ( 'NONE', *, *, #38087, .F. ) ;
#59360 = ORIENTED_EDGE ( 'NONE', *, *, #42615, .F. ) ;
#59362 = ORIENTED_EDGE ( 'NONE', *, *, #79525, .T. ) ;
#59361 = CARTESIAN_POINT ( 'NONE',  ( 11.78840694783958298, -11.56426240980093745, 33.07394671870546432 ) ) ;
#59363 = LINE ( 'NONE', #67019, #53064 ) ;
#59364 = EDGE_CURVE ( 'NONE', #11346, #7995, #25482, .T. ) ;
#59365 = DIRECTION ( 'NONE',  ( 1.000000000000000000, 0.000000000000000000, 0.000000000000000000 ) ) ;
#59366 = AXIS2_PLACEMENT_3D ( 'NONE', #68187, #74954, #87146 ) ;
#59367 = VECTOR ( 'NONE', #32898, 1000.000000000000114 ) ;
#59368 = CARTESIAN_POINT ( 'NONE',  ( 10.54930120442873687, -11.16473453929635440, 33.15142922261925662 ) ) ;
#59369 = CARTESIAN_POINT ( 'NONE',  ( -13.38461538461538325, -11.11383981884818262, 36.00935417666054406 ) ) ;
#59370 = EDGE_LOOP ( 'NONE', ( #26360, #38681 ) ) ;
#59371 = EDGE_LOOP ( 'NONE', ( #31100, #67153 ) ) ;
#59372 = B_SPLINE_CURVE_WITH_KNOTS ( 'NONE', 3,
 ( #52189, #6568, #72912, #11216, #38687, #75462, #252, #45881, #4452, #34032 ),
 .UNSPECIFIED., .F., .F.,
 ( 4, 2, 2, 2, 4 ),
 ( 0.0007817359430256392216, 0.0009771253907250078159, 0.001172514838424376302, 0.001367904286123745004, 0.001563293733823113490 ),
 .UNSPECIFIED. ) ;
#59373 = B_SPLINE_CURVE_WITH_KNOTS ( 'NONE', 3,
 ( #34797, #62265, #14090, #41562, #69034, #55956, #28047, #83896, #42902, #62704 ),
 .UNSPECIFIED., .F., .F.,
 ( 4, 2, 2, 2, 4 ),
 ( 0.0007817359430256372700, 0.0009771253907250054306, 0.001172514838424373483, 0.001367904286123741535, 0.001563293733823109804 ),
 .UNSPECIFIED. ) ;
#59374 = EDGE_LOOP ( 'NONE', ( #64586, #69546, #49045, #46558 ) ) ;
#59376 = VERTEX_POINT ( 'NONE', #26372 ) ;
#59375 = CARTESIAN_POINT ( 'NONE',  ( 7.846153846153846700, -11.69971097300155272, 32.46337939537588113 ) ) ;
#59377 = CARTESIAN_POINT ( 'NONE',  ( 16.94677510719138169, -5.915902021225892149, 34.75552854090298638 ) ) ;
#59378 = B_SPLINE_CURVE_WITH_KNOTS ( 'NONE', 3,
 ( #63067, #69840, #27079, #28870, #56326, #88808, #22099, #54541, #33834, #82037 ),
 .UNSPECIFIED., .F., .F.,
 ( 4, 2, 2, 2, 4 ),
 ( 0.0007817359430256313069, 0.0009771253907249971907, 0.001172514838424363074, 0.001367904286123728958, 0.001563293733823094842 ),
 .UNSPECIFIED. ) ;
#59379 = CYLINDRICAL_SURFACE ( 'NONE', #76961, 4.000000000000000000 ) ;
#59380 = ORIENTED_EDGE ( 'NONE', *, *, #4651, .F. ) ;
#59381 = CARTESIAN_POINT ( 'NONE',  ( 6.673076923076925127, -2.499999999999998668, 29.75000000000000355 ) ) ;
#59382 = CARTESIAN_POINT ( 'NONE',  ( 0.4615384615384611200, -9.584722331328613620, 36.20867863119891439 ) ) ;
#59383 = CARTESIAN_POINT ( 'NONE',  ( 4.403791672194295792, -2.824170634883622188, 31.52227843825338738 ) ) ;
#59384 = FACE_BOUND ( 'NONE', #63998, .T. ) ;
#59385 = CARTESIAN_POINT ( 'NONE',  ( -5.207613680033385428, -9.929715669179216775, 34.40415004197138416 ) ) ;
#59386 = CARTESIAN_POINT ( 'NONE',  ( -12.68446467905461006, -9.086856451489515152, 34.49173150075333183 ) ) ;
#59387 = EDGE_CURVE ( 'NONE', #82473, #50376, #8172, .T. ) ;
#59388 = CARTESIAN_POINT ( 'NONE',  ( -7.912237257109728361, -12.10708131394839349, 31.69288490824020244 ) ) ;
#59390 = CARTESIAN_POINT ( 'NONE',  ( 15.23076923076910916, -10.33852847137269571, 34.16647553114546554 ) ) ;
#59389 = DIRECTION ( 'NONE',  ( -1.000000000000000000, 0.000000000000000000, 0.000000000000000000 ) ) ;
#59391 = DIRECTION ( 'NONE',  ( -0.000000000000000000, -0.9396926207859092051, -0.3420201433256662704 ) ) ;
#59392 = DIRECTION ( 'NONE',  ( -1.000000000000000000, -0.000000000000000000, -0.000000000000000000 ) ) ;
#59393 = ORIENTED_EDGE ( 'NONE', *, *, #21667, .F. ) ;
#59394 = CARTESIAN_POINT ( 'NONE',  ( -15.09997878980228059, -11.37503395064541678, 33.29242100308974273 ) ) ;
#59395 = CARTESIAN_POINT ( 'NONE',  ( 13.38461538461538680, -1.044019251281081972, 31.83374038241031911 ) ) ;
#59396 = ORIENTED_EDGE ( 'NONE', *, *, #21160, .T. ) ;
#59397 = VERTEX_POINT ( 'NONE', #6104 ) ;
#59398 = MANIFOLD_SOLID_BREP ( 'Boss-Extrude1', #44325 ) ;
#59400 = CARTESIAN_POINT ( 'NONE',  ( 0.6845513056318556222, -8.282913670948747864, 34.94150082978203642 ) ) ;
#59399 = CARTESIAN_POINT ( 'NONE',  ( -11.76138849736838488, -12.64616026154729411, 30.79003144601914244 ) ) ;
#59401 = AXIS2_PLACEMENT_3D ( 'NONE', #85268, #78059, #23549 ) ;
#59402 = VECTOR ( 'NONE', #74848, 1000.000000000000000 ) ;
#59403 = CARTESIAN_POINT ( 'NONE',  ( 16.21910129335899597, -6.835583212224605631, 34.95778746994559327 ) ) ;
#59404 = CARTESIAN_POINT ( 'NONE',  ( 16.15384615384615330, -3.513871655860378418, 32.76840700105978499 ) ) ;
#59405 = CARTESIAN_POINT ( 'NONE',  ( 12.22435897435897267, -3.499999999999999556, 29.75000000000000355 ) ) ;
#59406 = ORIENTED_EDGE ( 'NONE', *, *, #10571, .T. ) ;
#59407 = CARTESIAN_POINT ( 'NONE',  ( -19.00000000000000000, 16.99999999999999289, 31.75000000000000000 ) ) ;
#59408 = CARTESIAN_POINT ( 'NONE',  ( 18.06525513951284267, -4.320704448112858032, 33.92786785259548310 ) ) ;
#59410 = CARTESIAN_POINT ( 'NONE',  ( -9.692307692307812417, -4.481592998941358097, 33.73612834414048933 ) ) ;
#59409 = CARTESIAN_POINT ( 'NONE',  ( 18.25005431163831204, -3.627508038966690496, 32.91356715214248396 ) ) ;
#59411 = CYLINDRICAL_SURFACE ( 'NONE', #64609, 0.2499999999999979738 ) ;
#59412 = CARTESIAN_POINT ( 'NONE',  ( 0.3308478584281517865, -3.338472653186242756, 32.95098750199972670 ) ) ;
#59414 = DIRECTION ( 'NONE',  ( -0.000000000000000000, -0.1736481776669307198, -0.9848077530122080203 ) ) ;
#59413 = SURFACE_STYLE_FILL_AREA ( #72923 ) ;
#59415 = CARTESIAN_POINT ( 'NONE',  ( -2.651650429449535551, -10.15165042944956753, 23.68750000000000000 ) ) ;
#59416 = ORIENTED_EDGE ( 'NONE', *, *, #68097, .F. ) ;
#59417 = ORIENTED_EDGE ( 'NONE', *, *, #64405, .T. ) ;
#59418 = CARTESIAN_POINT ( 'NONE',  ( -8.096130590202434973, -11.47974371597208076, 33.17467449705390692 ) ) ;
#59419 = CARTESIAN_POINT ( 'NONE',  ( 12.33106175342199862, -7.276988635370452485, 34.74523720219453793 ) ) ;
#59420 = CARTESIAN_POINT ( 'NONE',  ( 16.37685899793955357, -2.889357225399416418, 32.26129605718031002 ) ) ;
#59421 = CYLINDRICAL_SURFACE ( 'NONE', #40961, 0.2500000000000012212 ) ;
#59422 = CARTESIAN_POINT ( 'NONE',  ( 2.373861448654965844, -7.250054483168843156, 34.74374881642865631 ) ) ;
#59423 = CARTESIAN_POINT ( 'NONE',  ( 1.553300858899129944, -11.24999999999998934, 24.70312500000000000 ) ) ;
#59424 = CARTESIAN_POINT ( 'NONE',  ( -11.53846153846153655, -9.058645607665452459, 34.76329471203371924 ) ) ;
#59425 = LINE ( 'NONE', #60310, #64737 ) ;
#59426 = EDGE_CURVE ( 'NONE', #31091, #9304, #70538, .T. ) ;
#59427 = CYLINDRICAL_SURFACE ( 'NONE', #4158, 0.2499999999999994726 ) ;
#59428 = CARTESIAN_POINT ( 'NONE',  ( 5.750023255951409951, -10.06842814019191401, 34.32929386961144758 ) ) ;
#59429 = CARTESIAN_POINT ( 'NONE',  ( -9.822454901745910405, -11.47017969459904130, 32.78971311882034456 ) ) ;
#59430 = CARTESIAN_POINT ( 'NONE',  ( 1.384615384615386802, -8.973038597847269315, 34.52809138561121927 ) ) ;
#59431 = CARTESIAN_POINT ( 'NONE',  ( 2.307692307692309264, -3.050289026998446396, 32.03036669348365706 ) ) ;
#59432 = DIRECTION ( 'NONE',  ( 0.000000000000000000, 0.3420201433256610524, 0.9396926207859113145 ) ) ;
#59433 = CARTESIAN_POINT ( 'NONE',  ( -0.2114841499001473835, -11.28795663066794219, 33.01431243580653785 ) ) ;
#59434 = CARTESIAN_POINT ( 'NONE',  ( 11.53846153846153832, -6.386643153685126251, 34.62446782046654192 ) ) ;
#59435 = CARTESIAN_POINT ( 'NONE',  ( -3.296039231325549768, -12.51329471203370325, 31.30864560766548976 ) ) ;
#59436 = ORIENTED_EDGE ( 'NONE', *, *, #84082, .T. ) ;
#59437 = DIRECTION ( 'NONE',  ( -1.000000000000000000, 0.000000000000000000, 0.000000000000000000 ) ) ;
#59438 = CARTESIAN_POINT ( 'NONE',  ( -13.31854805126531005, -9.905515769479276145, 34.41647553114623292 ) ) ;
#59439 = CARTESIAN_POINT ( 'NONE',  ( 13.38461538461526423, -6.835583212225970762, 34.95778746994575670 ) ) ;
#59440 = CARTESIAN_POINT ( 'NONE',  ( 2.724691934501250135, -8.700186371490531201, 14.79874329374151642 ) ) ;
#59441 = AXIS2_PLACEMENT_3D ( 'NONE', #64701, #30483, #71461 ) ;
#59442 = VECTOR ( 'NONE', #87203, 1000.000000000000000 ) ;
#59443 = CARTESIAN_POINT ( 'NONE',  ( 5.076923076922953193, -10.33852847137269571, 34.16647553114546554 ) ) ;
#59444 = CARTESIAN_POINT ( 'NONE',  ( -17.32694631421604115, -2.587272538249754117, 30.68239716806877837 ) ) ;
#59446 = ORIENTED_EDGE ( 'NONE', *, *, #8723, .F. ) ;
#59445 = CARTESIAN_POINT ( 'NONE',  ( 10.36538461538461853, -7.433932668274256805, 35.00000000000000711 ) ) ;
#59447 = CARTESIAN_POINT ( 'NONE',  ( -2.749999999999991562, -8.639087296526026805, 17.51562500000000000 ) ) ;
#59448 = EDGE_CURVE ( 'NONE', #1012, #36253, #75009, .T. ) ;
#59449 = CARTESIAN_POINT ( 'NONE',  ( -15.29603923132555110, -4.320704448112771878, 33.92786785259540494 ) ) ;
#59450 = B_SPLINE_CURVE_WITH_KNOTS ( 'NONE', 3,
 ( #48807, #62315, #49261, #13699, #6941, #76732, #42510, #34411, #632, #28102 ),
 .UNSPECIFIED., .F., .F.,
 ( 4, 2, 2, 2, 4 ),
 ( 0.000000000000000000, 0.0001954311564186865221, 0.0003908623128373730441, 0.0005862934692560595662, 0.0007817246256747460882 ),
 .UNSPECIFIED. ) ;
#59451 = EDGE_CURVE ( 'NONE', #1878, #19254, #88980, .T. ) ;
#59452 = VECTOR ( 'NONE', #72051, 1000.000000000000000 ) ;
#59454 = VERTEX_POINT ( 'NONE', #80889 ) ;
#59453 = B_SPLINE_CURVE_WITH_KNOTS ( 'NONE', 3,
 ( #86335, #18749, #11998, #31367, #73244, #24605, #45767, #52515, #25939, #46214 ),
 .UNSPECIFIED., .F., .F.,
 ( 4, 2, 2, 2, 4 ),
 ( 0.000000000000000000, 0.0001954311564186866305, 0.0003908623128373732609, 0.0005862934692560598914, 0.0007817246256747465219 ),
 .UNSPECIFIED. ) ;
#59455 = CARTESIAN_POINT ( 'NONE',  ( -12.46153846153846168, -1.117168528481311540, 33.14645433367849847 ) ) ;
#59456 = ORIENTED_EDGE ( 'NONE', *, *, #27138, .F. ) ;
#59457 = CARTESIAN_POINT ( 'NONE',  ( -18.13069146666756382, -11.71456829005830436, 32.44064028649417253 ) ) ;
#59458 = CARTESIAN_POINT ( 'NONE',  ( -1.449885385171704399, -12.16647553114622049, 32.15551576947930812 ) ) ;
#59459 = EDGE_CURVE ( 'NONE', #4299, #31229, #25391, .T. ) ;
#59460 = CARTESIAN_POINT ( 'NONE',  ( 15.23076923076911093, -2.892918686052165622, 31.69288490824153470 ) ) ;
#59461 = VERTEX_POINT ( 'NONE', #49298 ) ;
#59462 = DIRECTION ( 'NONE',  ( 0.000000000000000000, 0.6427876096865373645, -0.7660444431189797898 ) ) ;
#59463 = ORIENTED_EDGE ( 'NONE', *, *, #29492, .T. ) ;
#59464 = FACE_OUTER_BOUND ( 'NONE', #70182, .T. ) ;
#59465 = VERTEX_POINT ( 'NONE', #228 ) ;
#59466 = LINE ( 'NONE', #32883, #41409 ) ;
#59467 = CARTESIAN_POINT ( 'NONE',  ( 2.307692307692309264, -3.050289026998446396, 32.03036669348365706 ) ) ;
#59468 = CARTESIAN_POINT ( 'NONE',  ( -19.50000000000000000, -11.50000000000000000, 29.75000000000000355 ) ) ;
#59469 = CARTESIAN_POINT ( 'NONE',  ( 9.823098133274644539, -9.929761469519743144, 34.40412654351204225 ) ) ;
#59470 = CARTESIAN_POINT ( 'NONE',  ( 0.4615384615384611200, -2.292212530054420494, 30.41441678777542634 ) ) ;
#59471 = AXIS2_PLACEMENT_3D ( 'NONE', #85292, #29031, #30774 ) ;
#59472 = CARTESIAN_POINT ( 'NONE',  ( -5.076923076923075762, -13.88283147151868846, 33.14645433367849847 ) ) ;
#59473 = EDGE_CURVE ( 'NONE', #63264, #65067, #69128, .T. ) ;
#59474 = EDGE_LOOP ( 'NONE', ( #15531, #84394, #68884, #83923, #87902 ) ) ;
#59475 = EDGE_LOOP ( 'NONE', ( #19272, #85655, #65890, #26757 ) ) ;
#59476 = EDGE_LOOP ( 'NONE', ( #29735, #37445 ) ) ;
#59478 = ORIENTED_EDGE ( 'NONE', *, *, #51547, .F. ) ;
#59477 = CARTESIAN_POINT ( 'NONE',  ( 3.361294932532797208, -3.816742781228458448, 33.13167719472716044 ) ) ;
#59479 = DIRECTION ( 'NONE',  ( -0.000000000000000000, -0.7660444431189791237, -0.6427876096865379196 ) ) ;
#59480 = DIRECTION ( 'NONE',  ( -0.000000000000000000, 0.8660254037844399289, -0.4999999999999980016 ) ) ;
#59481 = VERTEX_POINT ( 'NONE', #15077 ) ;
#59482 = CARTESIAN_POINT ( 'NONE',  ( 15.36129466900287532, -9.503571793651731880, 34.60286762892837942 ) ) ;
#59483 = ORIENTED_EDGE ( 'NONE', *, *, #26822, .T. ) ;
#59484 = CARTESIAN_POINT ( 'NONE',  ( 17.14299041027315695, -9.058645607665452459, 34.76329471203371924 ) ) ;
#59485 = VERTEX_POINT ( 'NONE', #50165 ) ;
#59486 = CARTESIAN_POINT ( 'NONE',  ( 9.692307692307695177, -8.120952969808772792, 34.71129190930000163 ) ) ;
#59487 = CARTESIAN_POINT ( 'NONE',  ( -3.230769230769229949, -12.48256725967547354, 35.29906147534542527 ) ) ;
#59488 = CARTESIAN_POINT ( 'NONE',  ( -11.53846153846166089, -12.16647553114689728, 32.15551576947799362 ) ) ;
#59489 = FACE_BOUND ( 'NONE', #27390, .T. ) ;
#59491 = VECTOR ( 'NONE', #6940, 999.9999999999998863 ) ;
#59490 = B_SPLINE_CURVE_WITH_KNOTS ( 'NONE', 3,
 ( #19342, #67085, #38275, #72946, #25206, #4944, #5387, #80157, #18896, #32852 ),
 .UNSPECIFIED., .F., .F.,
 ( 4, 2, 2, 2, 4 ),
 ( 0.000000000000000000, 0.0001954339857564080707, 0.0003908679715128161414, 0.0005863019572692241849, 0.0007817359430256322827 ),
 .UNSPECIFIED. ) ;
#59492 = CARTESIAN_POINT ( 'NONE',  ( -6.166666666666667851, -7.500000000000000000, 29.75000000000000355 ) ) ;
#59493 = CARTESIAN_POINT ( 'NONE',  ( 13.63456090296352841, -9.272278438253398036, 34.42582936511637115 ) ) ;
#59494 = AXIS2_PLACEMENT_3D ( 'NONE', #2863, #30356, #24475 ) ;
#59495 = CARTESIAN_POINT ( 'NONE',  ( -1.384615384615383471, -2.292212530054420494, 30.41441678777542634 ) ) ;
#59496 = DIRECTION ( 'NONE',  ( 0.000000000000000000, 0.000000000000000000, 1.000000000000000000 ) ) ;
#59497 = PLANE ( 'NONE',  #78255 ) ;
#59498 = CARTESIAN_POINT ( 'NONE',  ( 8.096208157792160520, -10.66356715214248396, 33.62249196103329751 ) ) ;
#59499 = ORIENTED_EDGE ( 'NONE', *, *, #13382, .T. ) ;
#59500 = CARTESIAN_POINT ( 'NONE',  ( -10.36543909703647337, -4.336752205174649433, 33.62275283266504289 ) ) ;
#59501 = ORIENTED_EDGE ( 'NONE', *, *, #14490, .F. ) ;
#59502 = VERTEX_POINT ( 'NONE', #21826 ) ;
#59504 = CARTESIAN_POINT ( 'NONE',  ( -1.514763354347078206, -5.915902021225892149, 34.75552854090298638 ) ) ;
#59503 = CARTESIAN_POINT ( 'NONE',  ( 10.74617642320940369, -12.38066358083363738, 30.83685684665853444 ) ) ;
#59505 = CYLINDRICAL_SURFACE ( 'NONE', #85912, 0.2499999999999995559 ) ;
#59506 = CARTESIAN_POINT ( 'NONE',  ( -4.088590582570126308, -4.481592998940251427, 33.73612834413965089 ) ) ;
#59507 = DIRECTION ( 'NONE',  ( 0.000000000000000000, 1.000000000000000000, -0.000000000000000000 ) ) ;
#59508 = CARTESIAN_POINT ( 'NONE',  ( -15.45369544828538011, -3.586966769969701208, 32.86292498521069660 ) ) ;
#59509 = ORIENTED_EDGE ( 'NONE', *, *, #19631, .F. ) ;
#59510 = B_SPLINE_CURVE_WITH_KNOTS ( 'NONE', 3,
 ( #8744, #70882, #35773, #2402, #49277, #28568, #84849, #37521, #23129, #56476 ),
 .UNSPECIFIED., .F., .F.,
 ( 4, 2, 2, 2, 4 ),
 ( 0.0007817359430256315238, 0.0009771253907249976244, 0.001172514838424363508, 0.001367904286123729392, 0.001563293733823095492 ),
 .UNSPECIFIED. ) ;
#59511 = DIRECTION ( 'NONE',  ( 0.000000000000000000, 0.6427876096865373645, -0.7660444431189797898 ) ) ;
#59512 = CARTESIAN_POINT ( 'NONE',  ( 0.6845498131513109152, -9.886259254753564818, 34.14407573483972413 ) ) ;
#59513 = CARTESIAN_POINT ( 'NONE',  ( 10.54930223602447903, -2.833524468853757305, 32.15551576947924417 ) ) ;
#59514 = CARTESIAN_POINT ( 'NONE',  ( -3.903900635498010363, -3.712312575010499494, 33.01462480002815170 ) ) ;
#59515 = EDGE_LOOP ( 'NONE', ( #22821, #77733, #71, #21617 ) ) ;
#59516 = B_SPLINE_CURVE_WITH_KNOTS ( 'NONE', 3,
 ( #32812, #5341, #45868, #25608, #66138, #87784, #26057, #81010, #59832, #80571 ),
 .UNSPECIFIED., .F., .F.,
 ( 4, 2, 2, 2, 4 ),
 ( 0.000000000000000000, 0.0001954339857564080165, 0.0003908679715128160329, 0.0005863019572692240765, 0.0007817359430256320659 ),
 .UNSPECIFIED. ) ;
#59517 = ORIENTED_EDGE ( 'NONE', *, *, #20701, .F. ) ;
#59518 = ORIENTED_EDGE ( 'NONE', *, *, #69647, .F. ) ;
#59519 = CARTESIAN_POINT ( 'NONE',  ( 7.623227628637697428, -2.758268499246657957, 31.33685645148948140 ) ) ;
#59520 = CARTESIAN_POINT ( 'NONE',  ( -6.222828097634878652, -7.369209533119140509, 34.99857337881830688 ) ) ;
#59521 = EDGE_LOOP ( 'NONE', ( #39227, #5407, #21633, #19280 ) ) ;
#59522 = CARTESIAN_POINT ( 'NONE',  ( 3.164686851409094004, -12.62096338111211580, 30.90682066428152197 ) ) ;
#59523 = LINE ( 'NONE', #33397, #71622 ) ;
#59524 = CARTESIAN_POINT ( 'NONE',  ( 4.853438133199130533, -2.847400154188068022, 31.58180166144859058 ) ) ;
#59525 = CARTESIAN_POINT ( 'NONE',  ( 1.634560793993429906, -6.653508905675590945, 34.93172785388651391 ) ) ;
#59526 = DIRECTION ( 'NONE',  ( 0.000000000000000000, 0.3420201433256641055, -0.9396926207859100932 ) ) ;
#59528 = ORIENTED_EDGE ( 'NONE', *, *, #46014, .T. ) ;
#59527 = VECTOR ( 'NONE', #7777, 999.9999999999998863 ) ;
#59530 = VERTEX_POINT ( 'NONE', #61915 ) ;
#59529 = CARTESIAN_POINT ( 'NONE',  ( -0.2115930521604189873, -12.07971442181321997, 32.31769673815850297 ) ) ;
#59531 = CARTESIAN_POINT ( 'NONE',  ( -5.076923076923197442, -5.219633306517616589, 34.19971097300220464 ) ) ;
#59532 = EDGE_CURVE ( 'NONE', #24126, #24932, #21069, .T. ) ;
#59533 = CARTESIAN_POINT ( 'NONE',  ( 13.38461538461526423, -8.656820664282941280, 34.87096338111179961 ) ) ;
#59534 = DIRECTION ( 'NONE',  ( -0.000000000000000000, 0.000000000000000000, 1.000000000000000000 ) ) ;
#59535 = CARTESIAN_POINT ( 'NONE',  ( -23.50000000000000000, 1.674711738930281374E-15, 32.75000000000000000 ) ) ;
#59536 = CARTESIAN_POINT ( 'NONE',  ( -4.153846153846274980, -5.094484230521993062, 34.41647553114689373 ) ) ;
#59537 = CARTESIAN_POINT ( 'NONE',  ( -8.546451100252703270, -9.418065098278013636, 34.63729479722530158 ) ) ;
#59538 = CARTESIAN_POINT ( 'NONE',  ( -1.987747218494638313, -9.401340078031370950, 16.43936829374151287 ) ) ;
#59539 = ORIENTED_EDGE ( 'NONE', *, *, #11863, .F. ) ;
#59540 = CARTESIAN_POINT ( 'NONE',  ( 4.853438152358745761, -12.11044203135681840, 32.26167407432752299 ) ) ;
#59541 = CYLINDRICAL_SURFACE ( 'NONE', #76452, 0.2499999999999998890 ) ;
#59542 = CARTESIAN_POINT ( 'NONE',  ( -0.4615384615385826339, -5.219633306517616589, 34.19971097300220464 ) ) ;
#59543 = EDGE_CURVE ( 'NONE', #60046, #39792, #29044, .T. ) ;
#59544 = ORIENTED_EDGE ( 'NONE', *, *, #58714, .T. ) ;
#59545 = ORIENTED_EDGE ( 'NONE', *, *, #63895, .T. ) ;
#59546 = CARTESIAN_POINT ( 'NONE',  ( -8.834500769787091201, -5.941354392334499579, 34.76329471203369792 ) ) ;
#59547 = CARTESIAN_POINT ( 'NONE',  ( 11.28843831424008926, -4.931416488878822335, 34.32920672191015399 ) ) ;
#59548 = EDGE_CURVE ( 'NONE', #56699, #39535, #16588, .T. ) ;
#59549 = DIRECTION ( 'NONE',  ( -1.000000000000000000, -0.000000000000000000, 0.000000000000000000 ) ) ;
#59550 = CARTESIAN_POINT ( 'NONE',  ( 13.13459216039393240, -2.985938066672154445, 32.43141759479405550 ) ) ;
#59551 = FACE_OUTER_BOUND ( 'NONE', #35153, .T. ) ;
#59552 = CARTESIAN_POINT ( 'NONE',  ( 10.28846153846153832, -11.50000000000000000, 29.75000000000000355 ) ) ;
#59553 = ORIENTED_EDGE ( 'NONE', *, *, #5423, .F. ) ;
#59554 = B_SPLINE_CURVE_WITH_KNOTS ( 'NONE', 3,
 ( #83433, #23043, #15859, #42002, #42442, #63135, #62687, #15415, #64019, #21716 ),
 .UNSPECIFIED., .F., .F.,
 ( 4, 2, 2, 2, 4 ),
 ( 0.0007817359430256294638, 0.0009771253907249950223, 0.001172514838424360472, 0.001367904286123725922, 0.001563293733823091372 ),
 .UNSPECIFIED. ) ;
#59555 = CARTESIAN_POINT ( 'NONE',  ( 9.442330961365339448, -10.66389620160130036, 33.62221079203477103 ) ) ;
#59556 = EDGE_CURVE ( 'NONE', #44733, #24141, #25227, .T. ) ;
#59557 = CARTESIAN_POINT ( 'NONE',  ( -9.070512820512819374, -11.50000000000000000, 29.75000000000000355 ) ) ;
#59558 = DIRECTION ( 'NONE',  ( -0.000000000000000000, -0.9396926207859093161, -0.3420201433256663259 ) ) ;
#59559 = EDGE_LOOP ( 'NONE', ( #4876, #79538 ) ) ;
#59560 = CARTESIAN_POINT ( 'NONE',  ( 16.02315555073584363, -12.35290016733513951, 31.75349464988449455 ) ) ;
#59561 = VECTOR ( 'NONE', #51340, 1000.000000000000000 ) ;
#59562 = AXIS2_PLACEMENT_3D ( 'NONE', #67043, #32810, #4440 ) ;
#59563 = VERTEX_POINT ( 'NONE', #36236 ) ;
#59564 = CARTESIAN_POINT ( 'NONE',  ( -0.2114841499001482161, -2.779044189368093498, 31.39831045268884324 ) ) ;
#59565 = FACE_OUTER_BOUND ( 'NONE', #50818, .T. ) ;
#59566 = CARTESIAN_POINT ( 'NONE',  ( -16.15384615384615330, -7.500000000000001776, 35.04278698407183867 ) ) ;
#59567 = EDGE_LOOP ( 'NONE', ( #37656, #18760, #20213, #84202 ) ) ;
#59568 = CARTESIAN_POINT ( 'NONE',  ( 0.6845498131513103601, -4.187068189119697692, 33.49521262558774026 ) ) ;
#59569 = CARTESIAN_POINT ( 'NONE',  ( -11.40766973063675493, -12.38066358083363738, 30.83685684665853444 ) ) ;
#59570 = DIRECTION ( 'NONE',  ( 0.000000000000000000, 0.6427876096865368094, 0.7660444431189802339 ) ) ;
#59571 = CARTESIAN_POINT ( 'NONE',  ( -7.596208436775802930, -4.932303261841489928, 34.32971442181322885 ) ) ;
#59572 = CARTESIAN_POINT ( 'NONE',  ( -4.946397638689433940, -11.04252011169590020, 33.62494198852677130 ) ) ;
#59573 = EDGE_CURVE ( 'NONE', #14985, #8100, #48825, .T. ) ;
#59574 = ORIENTED_EDGE ( 'NONE', *, *, #73987, .F. ) ;
#59575 = CARTESIAN_POINT ( 'NONE',  ( -18.23784950573857344, 12.75000000000000888, 13.00000000000000178 ) ) ;
#59576 = ADVANCED_FACE ( 'NONE', ( #7873 ), #28134, .T. ) ;
#59577 = ORIENTED_EDGE ( 'NONE', *, *, #25004, .T. ) ;
#59578 = CARTESIAN_POINT ( 'NONE',  ( 5.299935921016471596, -11.43677907613344757, 33.22367315496201456 ) ) ;
#59579 = DIRECTION ( 'NONE',  ( -0.000000000000000000, 0.3420201433256694346, -0.9396926207859080948 ) ) ;
#59580 = CYLINDRICAL_SURFACE ( 'NONE', #65777, 0.2500000000000009437 ) ;
#59581 = EDGE_CURVE ( 'NONE', #485, #15316, #29540, .T. ) ;
#59582 = CARTESIAN_POINT ( 'NONE',  ( 9.692307692307695177, -2.486705287966279876, 31.30864560766543647 ) ) ;
#59583 = ADVANCED_FACE ( 'NONE', ( #16396 ), #57374, .F. ) ;
#59584 = CARTESIAN_POINT ( 'NONE',  ( 1.384615384615386802, -9.819645486525091727, 36.12317359536749706 ) ) ;
#59585 = LINE ( 'NONE', #31679, #45058 ) ;
#59586 = CARTESIAN_POINT ( 'NONE',  ( -14.05769230769230660, -7.500000000000001776, 35.04278698407183867 ) ) ;
#59587 = EDGE_LOOP ( 'NONE', ( #81320, #56667, #69512, #51349 ) ) ;
#59588 = VECTOR ( 'NONE', #47889, 999.9999999999998863 ) ;
#59589 = ORIENTED_EDGE ( 'NONE', *, *, #10172, .T. ) ;
#59590 = VERTEX_POINT ( 'NONE', #29920 ) ;
#59591 = ORIENTED_EDGE ( 'NONE', *, *, #83418, .T. ) ;
#59592 = ORIENTED_EDGE ( 'NONE', *, *, #84625, .F. ) ;
#59593 = CARTESIAN_POINT ( 'NONE',  ( -5.143005456283212595, -3.937682226553329556, 33.60647404775217240 ) ) ;
#59594 = CARTESIAN_POINT ( 'NONE',  ( -3.296039231325549768, -6.835583212224499938, 34.95778746994557906 ) ) ;
#59595 = CARTESIAN_POINT ( 'NONE',  ( -2.438302667316833983, -7.722926236386453702, 34.74524107206102030 ) ) ;
#59596 = CARTESIAN_POINT ( 'NONE',  ( -4.153846153846152411, -2.900454961884010974, 35.62045528018868623 ) ) ;
#59597 = CARTESIAN_POINT ( 'NONE',  ( 13.25446817517716980, -8.587444163452046197, 34.63053765926554206 ) ) ;
#59598 = CARTESIAN_POINT ( 'NONE',  ( 19.00000000000000000, -1.249999999999999112, 32.75000000000000000 ) ) ;
#59599 = CARTESIAN_POINT ( 'NONE',  ( -5.142193522883852452, -8.613356846314824011, 34.62446782046655613 ) ) ;
#59600 = CARTESIAN_POINT ( 'NONE',  ( -5.299789339986176628, -2.251424796025575770, 29.88072029997477586 ) ) ;
#59601 = CARTESIAN_POINT ( 'NONE',  ( 18.03205128205128105, -7.500000000000000000, 29.75000000000000355 ) ) ;
#59602 = ORIENTED_EDGE ( 'NONE', *, *, #87946, .T. ) ;
#59603 = VERTEX_POINT ( 'NONE', #23153 ) ;
#59604 = ORIENTED_EDGE ( 'NONE', *, *, #76660, .T. ) ;
#59606 = EDGE_LOOP ( 'NONE', ( #78461, #3562 ) ) ;
#59605 = CARTESIAN_POINT ( 'NONE',  ( -5.999999999999998224, -1.242168528481310874, 33.36296068462461051 ) ) ;
#59608 = CARTESIAN_POINT ( 'NONE',  ( -16.40386939113911779, -10.05641848906368097, 34.04755513067966177 ) ) ;
#59607 = CARTESIAN_POINT ( 'NONE',  ( -15.93106661257773560, -6.760870238392814535, 34.69528174975672385 ) ) ;
#59609 = EDGE_CURVE ( 'NONE', #36772, #60982, #65904, .T. ) ;
#59610 = DIRECTION ( 'NONE',  ( -0.000000000000000000, -0.9396926207859093161, -0.3420201433256663259 ) ) ;
#59611 = CARTESIAN_POINT ( 'NONE',  ( 7.146088274689772923, -2.554770724473668153, 30.48948780036025852 ) ) ;
#59612 = FACE_BOUND ( 'NONE', #3189, .T. ) ;
#59613 = ORIENTED_EDGE ( 'NONE', *, *, #44168, .F. ) ;
#59614 = VECTOR ( 'NONE', #19742, 1000.000000000000000 ) ;
#59615 = B_SPLINE_CURVE_WITH_KNOTS ( 'NONE', 3,
 ( #84742, #77083, #44154, #15389, #42860, #9499 ),
 .UNSPECIFIED., .F., .F.,
 ( 4, 2, 4 ),
 ( 0.0003909569690057856884, 0.0005862646681846128607, 0.0007815723673634400329 ),
 .UNSPECIFIED. ) ;
#59616 = VERTEX_POINT ( 'NONE', #24032 ) ;
#59617 = CARTESIAN_POINT ( 'NONE',  ( 3.999999999999997335, 7.500000000000000888, 14.00000000000000178 ) ) ;
#59618 = ORIENTED_EDGE ( 'NONE', *, *, #5208, .F. ) ;
#59619 = FACE_BOUND ( 'NONE', #10884, .T. ) ;
#59620 = CARTESIAN_POINT ( 'NONE',  ( -30.00000000000000000, -15.00000000000000000, 3.000000000000000000 ) ) ;
#59621 = AXIS2_PLACEMENT_3D ( 'NONE', #80455, #25500, #79563 ) ;
#59622 = CARTESIAN_POINT ( 'NONE',  ( -13.45069879557126313, -10.51840700105979387, 33.73612834413961536 ) ) ;
#59623 = ORIENTED_EDGE ( 'NONE', *, *, #5994, .T. ) ;
#59624 = DIRECTION ( 'NONE',  ( -0.000000000000000000, 0.5000000000000009992, -0.8660254037844380415 ) ) ;
#59625 = CARTESIAN_POINT ( 'NONE',  ( -19.50000000000000000, -3.499999999999999556, 29.75000000000000355 ) ) ;
#59626 = CARTESIAN_POINT ( 'NONE',  ( -5.142245992415251266, -7.749976743299137993, 34.99404534957040624 ) ) ;
#59627 = ORIENTED_EDGE ( 'NONE', *, *, #26214, .T. ) ;
#59628 = DIRECTION ( 'NONE',  ( -0.000000000000000000, 0.6427876096865404731, -0.7660444431189770143 ) ) ;
#59629 = CARTESIAN_POINT ( 'NONE',  ( 3.100077764101669686, -12.11776431015576172, 31.66791131148498906 ) ) ;
#59630 = FACE_OUTER_BOUND ( 'NONE', #75981, .T. ) ;
#59631 = ORIENTED_EDGE ( 'NONE', *, *, #25033, .T. ) ;
#59632 = EDGE_CURVE ( 'NONE', #79092, #54595, #10979, .T. ) ;
#59633 = LINE ( 'NONE', #38936, #35892 ) ;
#59634 = CARTESIAN_POINT ( 'NONE',  ( -16.85414353565466428, -11.89424750095246175, 32.13594075562311758 ) ) ;
#59635 = ORIENTED_EDGE ( 'NONE', *, *, #20596, .T. ) ;
#59636 = CARTESIAN_POINT ( 'NONE',  ( -17.32689982097166492, -12.65889640711025521, 30.72598325615533454 ) ) ;
#59637 = CARTESIAN_POINT ( 'NONE',  ( 13.25446817517716447, -2.619462340734462380, 30.83744416345203021 ) ) ;
#59638 = CARTESIAN_POINT ( 'NONE',  ( -2.372962753653082402, -2.625532179533444754, 30.86335684631481513 ) ) ;
#59639 = DIRECTION ( 'NONE',  ( -0.000000000000000000, -0.7660444431189791237, -0.6427876096865379196 ) ) ;
#59640 = FACE_OUTER_BOUND ( 'NONE', #20249, .T. ) ;
#59641 = CARTESIAN_POINT ( 'NONE',  ( -16.15384615384615330, -1.509761064869970415, 31.06009739812519044 ) ) ;
#59643 = CARTESIAN_POINT ( 'NONE',  ( -8.769230769230768274, -6.435427911321262684, 35.78748833219616898 ) ) ;
#59642 = CARTESIAN_POINT ( 'NONE',  ( 20.00000000000000711, -9.999999999999994671, 10.00000000000000178 ) ) ;
#59644 = DIRECTION ( 'NONE',  ( -1.000000000000000000, -0.000000000000000000, -0.000000000000000000 ) ) ;
#59645 = FACE_OUTER_BOUND ( 'NONE', #5114, .T. ) ;
#59646 = CARTESIAN_POINT ( 'NONE',  ( 1.987747218494664292, -9.401340078031346081, 26.87313170625849423 ) ) ;
#59647 = ORIENTED_EDGE ( 'NONE', *, *, #51533, .F. ) ;
#59648 = CARTESIAN_POINT ( 'NONE',  ( 5.010840697562940704, -6.343179335718451384, 34.87096338111212646 ) ) ;
#59649 = ORIENTED_EDGE ( 'NONE', *, *, #34560, .F. ) ;
#59650 = B_SPLINE_CURVE_WITH_KNOTS ( 'NONE', 3,
 ( #24356, #51816, #44174, #57268, #15850, #3643, #9518, #44620, #71659, #9964 ),
 .UNSPECIFIED., .F., .F.,
 ( 4, 2, 2, 2, 4 ),
 ( 0.0007817359430256304396, 0.0009771253907249963233, 0.001172514838424362424, 0.001367904286123728524, 0.001563293733823094408 ),
 .UNSPECIFIED. ) ;
#59651 = ADVANCED_FACE ( 'NONE', ( #10533 ), #31696, .F. ) ;
#59652 = ORIENTED_EDGE ( 'NONE', *, *, #18699, .F. ) ;
#59653 = CARTESIAN_POINT ( 'NONE',  ( -16.85414340794500276, -4.226511098958372514, 33.85474049983370293 ) ) ;
#59654 = VERTEX_POINT ( 'NONE', #43864 ) ;
#59655 = LINE ( 'NONE', #67311, #25417 ) ;
#59656 = CARTESIAN_POINT ( 'NONE',  ( -1.987747218494660295, -5.598659921968651254, 27.49813170625849068 ) ) ;
#59657 = SPHERICAL_SURFACE ( 'NONE', #76091, 8.000000000000000000 ) ;
#59658 = EDGE_CURVE ( 'NONE', #62474, #60580, #1624, .T. ) ;
#59659 = CARTESIAN_POINT ( 'NONE',  ( 10.86533002476265786, -2.589246495874658383, 31.60778113518102828 ) ) ;
#59660 = CARTESIAN_POINT ( 'NONE',  ( -0.2387589202700531044, -5.913360116392399668, 34.49180327182771322 ) ) ;
#59661 = CARTESIAN_POINT ( 'NONE',  ( -14.30769230769230660, -10.67929555188718282, 33.92786785259544047 ) ) ;
#59662 = AXIS2_PLACEMENT_3D ( 'NONE', #51749, #17999, #10347 ) ;
#59663 = LINE ( 'NONE', #72727, #83308 ) ;
#59664 = CARTESIAN_POINT ( 'NONE',  ( 0.4615384615384611200, -11.91647553114624181, 32.58852847137148245 ) ) ;
#59665 = CARTESIAN_POINT ( 'NONE',  ( 16.15384615384615330, -6.343179335718451384, 34.87096338111211935 ) ) ;
#59666 = CARTESIAN_POINT ( 'NONE',  ( -1.553300858899125059, -3.750000000000009326, 20.32812500000000000 ) ) ;
#59667 = CARTESIAN_POINT ( 'NONE',  ( 5.076923076922953193, -3.083524468854526912, 32.58852847137268327 ) ) ;
#59668 = CARTESIAN_POINT ( 'NONE',  ( -10.36538461538460254, -2.249999999999999112, 29.81603969181031388 ) ) ;
#59669 = ADVANCED_FACE ( 'NONE', ( #84870 ), #52389, .F. ) ;
#59671 = VECTOR ( 'NONE', #55340, 1000.000000000000000 ) ;
#59670 = DIRECTION ( 'NONE',  ( -0.000000000000000000, 0.000000000000000000, 1.000000000000000000 ) ) ;
#59672 = B_SPLINE_CURVE_WITH_KNOTS ( 'NONE', 3,
 ( #944, #15354, #68084, #8152, #62197, #77052, #61744, #507, #55441, #6388 ),
 .UNSPECIFIED., .F., .F.,
 ( 4, 2, 2, 2, 4 ),
 ( 0.000000000000000000, 0.0001954311564186882568, 0.0003908623128373765136, 0.0005862934692560647703, 0.0007817246256747530271 ),
 .UNSPECIFIED. ) ;
#59673 = ADVANCED_FACE ( 'NONE', ( #70904 ), #9634, .F. ) ;
#59674 = ORIENTED_EDGE ( 'NONE', *, *, #79521, .F. ) ;
#59675 = EDGE_LOOP ( 'NONE', ( #51562, #61842, #43913, #15966 ) ) ;
#59676 = CARTESIAN_POINT ( 'NONE',  ( -9.019254006523732770, -12.43535235679832596, 30.55408501211184813 ) ) ;
#59677 = CARTESIAN_POINT ( 'NONE',  ( 7.622668902429899696, -11.41268669641500466, 32.86336882939237825 ) ) ;
#59678 = DIRECTION ( 'NONE',  ( -0.000000000000000000, -0.5000000000000009992, -0.8660254037844380415 ) ) ;
#59679 = CARTESIAN_POINT ( 'NONE',  ( -5.076923076923199218, -10.33852847137269571, 34.16647553114546554 ) ) ;
#59680 = EDGE_CURVE ( 'NONE', #11769, #17756, #60853, .T. ) ;
#59681 = CARTESIAN_POINT ( 'NONE',  ( 14.08420738312797837, -3.562934362175799841, 33.22335522853832401 ) ) ;
#59682 = CARTESIAN_POINT ( 'NONE',  ( -9.942330916529147800, -6.652501968072648708, 34.93155406624980941 ) ) ;
#59683 = B_SPLINE_CURVE_WITH_KNOTS ( 'NONE', 3,
 ( #68138, #39788, #74449, #11418, #46964, #87099, #40231, #18628, #59599, #19501 ),
 .UNSPECIFIED., .F., .F.,
 ( 4, 2, 2, 2, 4 ),
 ( 0.000000000000000000, 0.0001954339857564079894, 0.0003908679715128159787, 0.0005863019572692239681, 0.0007817359430256319575 ),
 .UNSPECIFIED. ) ;
#59684 = AXIS2_PLACEMENT_3D ( 'NONE', #13003, #26076, #39159 ) ;
#59685 = EDGE_CURVE ( 'NONE', #86793, #1879, #51943, .T. ) ;
#59686 = ORIENTED_EDGE ( 'NONE', *, *, #50256, .T. ) ;
#59687 = CARTESIAN_POINT ( 'NONE',  ( -4.826977558574935045, -12.43552623307873972, 30.55307653245132826 ) ) ;
#59688 = ORIENTED_EDGE ( 'NONE', *, *, #15278, .F. ) ;
#59689 = ADVANCED_FACE ( 'NONE', ( #64124 ), #38449, .F. ) ;
#59690 = VERTEX_POINT ( 'NONE', #58262 ) ;
#59691 = CARTESIAN_POINT ( 'NONE',  ( 7.715463243043540587, -10.70098750199973203, 33.91152734681376302 ) ) ;
#59692 = CARTESIAN_POINT ( 'NONE',  ( -25.00000000000000355, 9.999999999999971578, 13.00000000000000178 ) ) ;
#59693 = CARTESIAN_POINT ( 'NONE',  ( 9.822833394071260216, -12.27024696741798770, 31.24895572276497546 ) ) ;
#59694 = EDGE_CURVE ( 'NONE', #23339, #53520, #23143, .T. ) ;
#59695 = VECTOR ( 'NONE', #72101, 1000.000000000000114 ) ;
#59696 = CARTESIAN_POINT ( 'NONE',  ( 1.318533005255250412, -11.35647404775217595, 33.31231777344666511 ) ) ;
#59697 = CARTESIAN_POINT ( 'NONE',  ( -13.25408968285182354, -3.285477652293413264, 32.44071101563363158 ) ) ;
#59698 = EDGE_LOOP ( 'NONE', ( #62873, #85250 ) ) ;
#59699 = ORIENTED_EDGE ( 'NONE', *, *, #21387, .F. ) ;
#59700 = EDGE_LOOP ( 'NONE', ( #59723, #55846, #52443, #87614 ) ) ;
#59701 = LINE ( 'NONE', #23246, #77452 ) ;
#59702 = DIRECTION ( 'NONE',  ( 1.000000000000000000, 0.000000000000000000, 0.000000000000000000 ) ) ;
#59703 = EDGE_CURVE ( 'NONE', #18976, #54695, #59683, .T. ) ;
#59704 = DIRECTION ( 'NONE',  ( -0.000000000000000000, 0.8660254037844399289, -0.4999999999999980016 ) ) ;
#59705 = LINE ( 'NONE', #87202, #8267 ) ;
#59706 = EDGE_CURVE ( 'NONE', #29522, #5877, #82101, .T. ) ;
#59707 = CARTESIAN_POINT ( 'NONE',  ( -2.749999999999998224, -7.500000000000000000, 11.00000000000000178 ) ) ;
#59708 = ORIENTED_EDGE ( 'NONE', *, *, #2273, .T. ) ;
#59709 = ORIENTED_EDGE ( 'NONE', *, *, #41274, .F. ) ;
#59710 = CARTESIAN_POINT ( 'NONE',  ( 0.5920641633020259365, -11.93748526763465279, 32.05452791011430946 ) ) ;
#59711 = B_SPLINE_CURVE_WITH_KNOTS ( 'NONE', 3,
 ( #7320, #28028, #6867, #55495, #68134, #82549, #27583, #12741, #60923, #14512 ),
 .UNSPECIFIED., .F., .F.,
 ( 4, 2, 2, 2, 4 ),
 ( 0.000000000000000000, 0.0001954311564186858715, 0.0003908623128373717431, 0.0005862934692560576146, 0.0007817246256747434861 ),
 .UNSPECIFIED. ) ;
#59712 = AXIS2_PLACEMENT_3D ( 'NONE', #21651, #76601, #14908 ) ;
#59714 = ORIENTED_EDGE ( 'NONE', *, *, #9949, .T. ) ;
#59713 = FACE_OUTER_BOUND ( 'NONE', #59203, .T. ) ;
#59715 = CARTESIAN_POINT ( 'NONE',  ( 1.384615384615386802, -9.780366693483667717, 34.19971097300155094 ) ) ;
#59716 = CARTESIAN_POINT ( 'NONE',  ( -2.057637887778853703, -4.074993327901525575, 33.72946981652012255 ) ) ;
#59717 = B_SPLINE_CURVE_WITH_KNOTS ( 'NONE', 3,
 ( #59470, #79749, #31553, #39664, #67568, #18933, #72985, #88309, #86975, #66673 ),
 .UNSPECIFIED., .F., .F.,
 ( 4, 2, 2, 2, 4 ),
 ( 0.000000000000000000, 0.0001954311564186878502, 0.0003908623128373757004, 0.0005862934692560635777, 0.0007817246256747514008 ),
 .UNSPECIFIED. ) ;
#59718 = B_SPLINE_CURVE_WITH_KNOTS ( 'NONE', 3,
 ( #79269, #43697, #29753, #57659, #51306, #9042, #36511, #38279, #77488, #84710 ),
 .UNSPECIFIED., .F., .F.,
 ( 4, 2, 2, 2, 4 ),
 ( 0.0007817246256747442451, 0.0009771112852218865989, 0.001172497944769029061, 0.001367884604316171523, 0.001563271263863313986 ),
 .UNSPECIFIED. ) ;
#59719 = EDGE_CURVE ( 'NONE', #427, #82221, #63793, .T. ) ;
#59720 = DIRECTION ( 'NONE',  ( -0.000000000000000000, -0.000000000000000000, -1.000000000000000000 ) ) ;
#59721 = ORIENTED_EDGE ( 'NONE', *, *, #17567, .F. ) ;
#59722 = CARTESIAN_POINT ( 'NONE',  ( -14.53117723225664015, -12.47654668319379567, 31.42292124445336654 ) ) ;
#59723 = ORIENTED_EDGE ( 'NONE', *, *, #51580, .T. ) ;
#59724 = EDGE_CURVE ( 'NONE', #48246, #13160, #12746, .T. ) ;
#59725 = CARTESIAN_POINT ( 'NONE',  ( 2.750000000000001776, -7.500000000000000000, 21.00000000000000000 ) ) ;
#59726 = DIRECTION ( 'NONE',  ( -0.000000000000000000, -0.8660254037844397068, -0.4999999999999978906 ) ) ;
#59727 = FACE_BOUND ( 'NONE', #27035, .T. ) ;
#59729 = CARTESIAN_POINT ( 'NONE',  ( 9.320512820512821150, -3.499999999999999556, 29.75000000000000355 ) ) ;
#59728 = CARTESIAN_POINT ( 'NONE',  ( 1.326923076923075762, -7.500000000000000000, 29.75000000000000355 ) ) ;
#59730 = ADVANCED_FACE ( 'NONE', ( #67696 ), #88002, .F. ) ;
#59731 = DIRECTION ( 'NONE',  ( 0.000000000000000000, 0.8660254037844377084, 0.5000000000000015543 ) ) ;
#59732 = ORIENTED_EDGE ( 'NONE', *, *, #67361, .F. ) ;
#59733 = DIRECTION ( 'NONE',  ( -1.734723475976812518E-16, 1.000000000000000000, 0.000000000000000000 ) ) ;
#59734 = CARTESIAN_POINT ( 'NONE',  ( 0.02645256023170453746, -4.500116625257376768, 13.72411352175840626 ) ) ;
#59735 = FACE_OUTER_BOUND ( 'NONE', #74536, .T. ) ;
#59736 = VERTEX_POINT ( 'NONE', #73581 ) ;
#59737 = ADVANCED_FACE ( 'NONE', ( #11873 ), #6003, .F. ) ;
#59738 = CARTESIAN_POINT ( 'NONE',  ( 17.07692307692307665, -12.10708131394839349, 31.69288490824020244 ) ) ;
#59739 = CARTESIAN_POINT ( 'NONE',  ( 10.39245765647776665, -8.282780595021769443, 34.94152052738834868 ) ) ;
#59740 = CARTESIAN_POINT ( 'NONE',  ( 16.82692307692307665, -7.500000000000001776, 34.75000000000000000 ) ) ;
#59741 = CARTESIAN_POINT ( 'NONE',  ( 10.61538461538461675, -11.69971097300155272, 32.46337939537588113 ) ) ;
#59742 = AXIS2_PLACEMENT_3D ( 'NONE', #77466, #920, #28387 ) ;
#59743 = FACE_BOUND ( 'NONE', #43706, .T. ) ;
#59745 = CARTESIAN_POINT ( 'NONE',  ( 20.00000000000000000, -4.000000000000000000, 29.75000000000000355 ) ) ;
#59744 = CARTESIAN_POINT ( 'NONE',  ( -7.053224892808621860, -12.50552854090298993, 31.33409797877408920 ) ) ;
#59746 = CARTESIAN_POINT ( 'NONE',  ( 3.230769230769108269, -12.16647553114689728, 32.15551576947799362 ) ) ;
#59748 = CARTESIAN_POINT ( 'NONE',  ( -11.31568186948346977, -10.97394488606064122, 33.68653795673694873 ) ) ;
#59747 = CARTESIAN_POINT ( 'NONE',  ( -11.76134022089018671, -7.630691491037285168, 34.74850469731152458 ) ) ;
#59749 = CARTESIAN_POINT ( 'NONE',  ( -4.023055712879203938, -10.70102852606553157, 33.91149625220312913 ) ) ;
#59750 = CARTESIAN_POINT ( 'NONE',  ( -8.546451227962355901, -3.755027918224367323, 33.06320215134714857 ) ) ;
#59751 = CARTESIAN_POINT ( 'NONE',  ( 0.06109907496455496689, -11.24999999999999822, 27.02938170625848358 ) ) ;
#59752 = CARTESIAN_POINT ( 'NONE',  ( -6.989160334032801458, -8.973038597847269315, 34.52809138561120506 ) ) ;
#59753 = ORIENTED_EDGE ( 'NONE', *, *, #43966, .F. ) ;
#59754 = DIRECTION ( 'NONE',  ( 0.000000000000000000, 0.000000000000000000, 1.000000000000000000 ) ) ;
#59755 = CYLINDRICAL_SURFACE ( 'NONE', #34074, 0.2500000000000004996 ) ;
#59756 = CARTESIAN_POINT ( 'NONE',  ( -1.253823576790597860, -10.54018710029568595, 33.71981072465678864 ) ) ;
#59758 = AXIS2_PLACEMENT_3D ( 'NONE', #74687, #87778, #13415 ) ;
#59757 = DIRECTION ( 'NONE',  ( 0.000000000000000000, 0.000000000000000000, -1.000000000000000000 ) ) ;
#59759 = CARTESIAN_POINT ( 'NONE',  ( 16.85343815235874132, -12.69144148231606017, 30.53333754910549303 ) ) ;
#59760 = DIRECTION ( 'NONE',  ( 0.000000000000000000, 0.3420201433256641055, -0.9396926207859100932 ) ) ;
#59761 = CARTESIAN_POINT ( 'NONE',  ( -2.724691934501232371, -8.700186371490559623, 16.01375670625849068 ) ) ;
#59762 = EDGE_CURVE ( 'NONE', #66117, #72102, #13474, .T. ) ;
#59763 = CARTESIAN_POINT ( 'NONE',  ( 15.16468685140909400, -11.91647553114624181, 32.58852847137148245 ) ) ;
#59764 = DIRECTION ( 'NONE',  ( -0.000000000000000000, -0.6427876096865404731, -0.7660444431189770143 ) ) ;
#59765 = CARTESIAN_POINT ( 'NONE',  ( -12.39628332202562433, -9.528491918058460186, 34.59228464037086326 ) ) ;
#59766 = CARTESIAN_POINT ( 'NONE',  ( 4.853438152358744873, -9.417330523894424488, 34.63758898049880486 ) ) ;
#59767 = LINE ( 'NONE', #66068, #46855 ) ;
#59768 = CARTESIAN_POINT ( 'NONE',  ( 9.442330948259101575, -3.436278759898153901, 33.07459398097509506 ) ) ;
#59769 = FACE_OUTER_BOUND ( 'NONE', #55515, .T. ) ;
#59770 = CARTESIAN_POINT ( 'NONE',  ( 7.911408985666682270, -9.528491918058460186, 34.59228464037086326 ) ) ;
#59771 = ORIENTED_EDGE ( 'NONE', *, *, #13576, .T. ) ;
#59772 = CARTESIAN_POINT ( 'NONE',  ( 6.673076923076926015, -7.566082377512563184, 35.00000000000000711 ) ) ;
#59773 = CARTESIAN_POINT ( 'NONE',  ( 9.019285080869082094, -11.28795663066794575, 33.01431243580653785 ) ) ;
#59774 = CARTESIAN_POINT ( 'NONE',  ( -1.614399933863613468, -11.22469193450124969, 21.36124329374151642 ) ) ;
#59775 = CARTESIAN_POINT ( 'NONE',  ( -10.68146699474474914, -9.905515769479276145, 34.41647553114623292 ) ) ;
#59776 = CARTESIAN_POINT ( 'NONE',  ( -16.40386937806761836, -10.92453946501458439, 33.72985991061850086 ) ) ;
#59777 = ORIENTED_EDGE ( 'NONE', *, *, #76165, .T. ) ;
#59778 = VECTOR ( 'NONE', #42927, 999.9999999999998863 ) ;
#59779 = DIRECTION ( 'NONE',  ( 0.000000000000000000, 0.000000000000000000, -1.000000000000000000 ) ) ;
#59780 = CARTESIAN_POINT ( 'NONE',  ( -12.33074802057151409, -12.62708834333097663, 30.88030960425257021 ) ) ;
#59782 = ORIENTED_EDGE ( 'NONE', *, *, #45977, .T. ) ;
#59781 = CARTESIAN_POINT ( 'NONE',  ( 11.53846153846185274, -2.255955759149395501, 30.00000000000324363 ) ) ;
#59783 = CARTESIAN_POINT ( 'NONE',  ( -9.758390071667827570, -11.35647404775217595, 33.31231777344666511 ) ) ;
#59784 = CARTESIAN_POINT ( 'NONE',  ( -2.242547526972674010, -7.750023224968865421, 34.99404313364389907 ) ) ;
#59785 = CARTESIAN_POINT ( 'NONE',  ( -8.638438961405986660, -2.541949514083464479, 30.39797389878540557 ) ) ;
#59786 = VECTOR ( 'NONE', #31762, 1000.000000000000000 ) ;
#59787 = CARTESIAN_POINT ( 'NONE',  ( -11.53846153846166089, -2.657715359629662544, 31.77849191805970364 ) ) ;
#59788 = ORIENTED_EDGE ( 'NONE', *, *, #19763, .F. ) ;
#59789 = CARTESIAN_POINT ( 'NONE',  ( -19.99999999999996447, -15.00000000000000533, 3.000000000000000000 ) ) ;
#59790 = DIRECTION ( 'NONE',  ( -0.000000000000000000, 1.000000000000000000, 3.491481338843133355E-15 ) ) ;
#59791 = ADVANCED_FACE ( 'NONE', ( #60041 ), #26701, .T. ) ;
#59792 = CARTESIAN_POINT ( 'NONE',  ( 8.546303810323914618, -3.395401636524185474, 33.02366814457250399 ) ) ;
#59793 = ORIENTED_EDGE ( 'NONE', *, *, #24851, .F. ) ;
#59794 = EDGE_LOOP ( 'NONE', ( #55044, #6099, #73947, #61039 ) ) ;
#59795 = EDGE_CURVE ( 'NONE', #19537, #73867, #25824, .T. ) ;
#59796 = VERTEX_POINT ( 'NONE', #67254 ) ;
#59797 = CARTESIAN_POINT ( 'NONE',  ( 5.142991427925514003, -12.10708131394839882, 31.69288490824020954 ) ) ;
#59798 = CARTESIAN_POINT ( 'NONE',  ( 0.3313912521002409517, -2.619462340734462380, 30.83744416345203021 ) ) ;
#59799 = ADVANCED_FACE ( 'NONE', ( #46536 ), #66361, .F. ) ;
#59800 = CARTESIAN_POINT ( 'NONE',  ( -12.71156169883142617, -3.711651800289232028, 33.01384336483936011 ) ) ;
#59801 = EDGE_CURVE ( 'NONE', #39037, #49681, #34998, .T. ) ;
#59802 = CARTESIAN_POINT ( 'NONE',  ( -18.22520792652332844, -7.371819721847150397, 34.99865929289143196 ) ) ;
#59803 = EDGE_LOOP ( 'NONE', ( #29732, #41625, #6107, #64981 ) ) ;
#59804 = VECTOR ( 'NONE', #3361, 1000.000000000000227 ) ;
#59805 = VERTEX_POINT ( 'NONE', #81658 ) ;
#59806 = EDGE_LOOP ( 'NONE', ( #79673, #50259 ) ) ;
#59808 = ORIENTED_EDGE ( 'NONE', *, *, #10639, .F. ) ;
#59807 = DIRECTION ( 'NONE',  ( 0.000000000000000000, 0.000000000000000000, 1.000000000000000000 ) ) ;
#59809 = CARTESIAN_POINT ( 'NONE',  ( -5.207071046654776048, -2.647304123082328875, 31.75400227202885262 ) ) ;
#59810 = EDGE_CURVE ( 'NONE', #31984, #69894, #55371, .T. ) ;
#59811 = CARTESIAN_POINT ( 'NONE',  ( -3.296039231325550212, -5.094484230520674117, 34.41647553114621161 ) ) ;
#59812 = CARTESIAN_POINT ( 'NONE',  ( 1.515407192440172413, -10.54018710029568595, 33.71981072465678864 ) ) ;
#59813 = CARTESIAN_POINT ( 'NONE',  ( -13.16160403300253634, -12.39991518177334129, 30.74647679643404530 ) ) ;
#59814 = AXIS2_PLACEMENT_3D ( 'NONE', #67815, #47528, #47972 ) ;
#59815 = ORIENTED_EDGE ( 'NONE', *, *, #52723, .F. ) ;
#59816 = VERTEX_POINT ( 'NONE', #68575 ) ;
#59817 = EDGE_LOOP ( 'NONE', ( #38302, #44135 ) ) ;
#59818 = CARTESIAN_POINT ( 'NONE',  ( -5.011777297591113012, -7.750023238201980469, 34.74374492549440419 ) ) ;
#59820 = ORIENTED_EDGE ( 'NONE', *, *, #82307, .F. ) ;
#59819 = LINE ( 'NONE', #67031, #67499 ) ;
#59821 = CARTESIAN_POINT ( 'NONE',  ( 3.007284287045282500, -11.89387501736622710, 32.13663884655806413 ) ) ;
#59822 = LINE ( 'NONE', #39124, #52503 ) ;
#59823 = CARTESIAN_POINT ( 'NONE',  ( 16.28437185560972011, -8.586989748646450593, 34.63063291749215011 ) ) ;
#59824 = CARTESIAN_POINT ( 'NONE',  ( -13.38461538461507594, -2.506253911140614576, 30.00000000000323297 ) ) ;
#59825 = CARTESIAN_POINT ( 'NONE',  ( -1.326923076923076206, -11.50000000000000000, 29.75000000000000355 ) ) ;
#59826 = FACE_BOUND ( 'NONE', #67990, .T. ) ;
#59827 = EDGE_CURVE ( 'NONE', #74119, #87173, #61743, .T. ) ;
#59828 = DIRECTION ( 'NONE',  ( -0.000000000000000000, 0.3420201433256694901, -0.9396926207859082059 ) ) ;
#59829 = CARTESIAN_POINT ( 'NONE',  ( 8.769230769230768274, -2.708943851104267164, 35.45975837776705220 ) ) ;
#59830 = DIRECTION ( 'NONE',  ( -0.000000000000000000, 1.000000000000000000, 3.491481338843133355E-15 ) ) ;
#59832 = CARTESIAN_POINT ( 'NONE',  ( -5.142193522883852452, -3.300289026998414865, 32.46337939537583139 ) ) ;
#59831 = CARTESIAN_POINT ( 'NONE',  ( 9.692307692307572609, -3.300289026999228881, 32.46337939537708905 ) ) ;
#59833 = EDGE_CURVE ( 'NONE', #32893, #87104, #56720, .T. ) ;
#59834 = VECTOR ( 'NONE', #50567, 1000.000000000000000 ) ;
#59835 = CARTESIAN_POINT ( 'NONE',  ( 20.00000000000000711, -9.999999999999994671, 13.00000000000000178 ) ) ;
#59836 = CARTESIAN_POINT ( 'NONE',  ( 1.515140822849031954, -2.372941743896878286, 30.88044141588254377 ) ) ;
#59837 = ORIENTED_EDGE ( 'NONE', *, *, #48131, .T. ) ;
#59838 = CARTESIAN_POINT ( 'NONE',  ( -15.16551409125639260, -11.67786785259547777, 32.92929555188713664 ) ) ;
#59839 = DIRECTION ( 'NONE',  ( 0.000000000000000000, 0.8660254037844377084, -0.5000000000000015543 ) ) ;
#59840 = ORIENTED_EDGE ( 'NONE', *, *, #88340, .T. ) ;
#59841 = EDGE_LOOP ( 'NONE', ( #48111, #7583 ) ) ;
#59842 = VECTOR ( 'NONE', #43832, 1000.000000000000000 ) ;
#59843 = CARTESIAN_POINT ( 'NONE',  ( -17.32694631421604115, -11.37209801155882793, 32.91403422569033665 ) ) ;
#59844 = EDGE_CURVE ( 'NONE', #61826, #313, #67193, .T. ) ;
#59845 = CARTESIAN_POINT ( 'NONE',  ( -14.43838377435986864, -4.809359713505814149, 33.96456829005828837 ) ) ;
#59846 = CARTESIAN_POINT ( 'NONE',  ( -11.53846153846153655, -5.415277668671390821, 36.20867863119892149 ) ) ;
#59847 = ORIENTED_EDGE ( 'NONE', *, *, #20634, .F. ) ;
#59848 = CYLINDRICAL_SURFACE ( 'NONE', #74504, 0.2499999999999998890 ) ;
#59849 = CARTESIAN_POINT ( 'NONE',  ( -6.923076923076922462, -9.780366693483667717, 34.19971097300155094 ) ) ;
#59850 = EDGE_CURVE ( 'NONE', #28389, #20358, #22931, .T. ) ;
#59852 = DIRECTION ( 'NONE',  ( 0.000000000000000000, 0.3420201433256610524, 0.9396926207859113145 ) ) ;
#59851 = CARTESIAN_POINT ( 'NONE',  ( 4.480769230769229061, -7.500000000000000000, 33.75000000000000000 ) ) ;
#59853 = CARTESIAN_POINT ( 'NONE',  ( -12.68446467905460828, -4.887634598454295265, 34.01352882383564946 ) ) ;
#59854 = B_SPLINE_CURVE_WITH_KNOTS ( 'NONE', 3,
 ( #75472, #13330, #66504, #39932, #87681, #40812, #60622, #59744, #88135, #20529 ),
 .UNSPECIFIED., .F., .F.,
 ( 4, 2, 2, 2, 4 ),
 ( 0.000000000000000000, 0.0001954311564186879857, 0.0003908623128373759715, 0.0005862934692560640114, 0.0007817246256747519429 ),
 .UNSPECIFIED. ) ;
#59855 = CARTESIAN_POINT ( 'NONE',  ( 0.5267936010512997980, -5.094484230520773593, 34.41647553114626845 ) ) ;
#59856 = CARTESIAN_POINT ( 'NONE',  ( -15.16470189741915675, -10.67929555188718282, 33.92786785259544757 ) ) ;
#59857 = CARTESIAN_POINT ( 'NONE',  ( 3.749999999999992006, -5.946699141100872943, 23.14062500000000000 ) ) ;
#59858 = ORIENTED_EDGE ( 'NONE', *, *, #77924, .T. ) ;
#59859 = VERTEX_POINT ( 'NONE', #50393 ) ;
#59860 = DIRECTION ( 'NONE',  ( -1.000000000000000000, -0.000000000000000000, -0.000000000000000000 ) ) ;
#59861 = CARTESIAN_POINT ( 'NONE',  ( 7.173131234715240723, -12.17597550085003633, 31.52189283813461884 ) ) ;
#59862 = CARTESIAN_POINT ( 'NONE',  ( 16.40390057375960708, -2.920487667080175154, 32.31805714834170828 ) ) ;
#59863 = CARTESIAN_POINT ( 'NONE',  ( -0.5920151696549253995, -7.276988635370452485, 34.74523720219453793 ) ) ;
#59864 = LINE ( 'NONE', #34167, #48587 ) ;
#59865 = CARTESIAN_POINT ( 'NONE',  ( -2.651650429449535551, -10.15165042944956753, 24.93750000000000000 ) ) ;
#59866 = EDGE_CURVE ( 'NONE', #35777, #45661, #26347, .T. ) ;
#59867 = CARTESIAN_POINT ( 'NONE',  ( 0.7115384615383971711, -7.565270445406050648, 34.75000000000000000 ) ) ;
#59868 = DIRECTION ( 'NONE',  ( -0.000000000000000000, 0.9848077530122086864, -0.1736481776669273891 ) ) ;
#59869 = CARTESIAN_POINT ( 'NONE',  ( -13.45037218712969462, -7.249945686854186278, 34.74374336980224598 ) ) ;
#59870 = CARTESIAN_POINT ( 'NONE',  ( 12.39626846098214052, -11.67786785259540849, 32.92929555188721480 ) ) ;
#59871 = CARTESIAN_POINT ( 'NONE',  ( -6.222926217516145719, -2.758268499246657957, 31.33685645148948140 ) ) ;
#59872 = CARTESIAN_POINT ( 'NONE',  ( 13.60739505359344825, -2.612705202774698421, 31.66806509827799943 ) ) ;
#59873 = ADVANCED_FACE ( 'NONE', ( #77873 ), #9422, .F. ) ;
#59874 = EDGE_CURVE ( 'NONE', #26509, #79445, #44073, .T. ) ;
#59875 = CARTESIAN_POINT ( 'NONE',  ( 2.084766090176159992, -3.105860786376062332, 32.13614157043598851 ) ) ;
#59877 = VECTOR ( 'NONE', #35367, 1000.000000000000114 ) ;
#59876 = CARTESIAN_POINT ( 'NONE',  ( -9.692307692307691624, -3.322132147404559976, 32.92929555188717927 ) ) ;
#59878 = CARTESIAN_POINT ( 'NONE',  ( 15.23076923076954614, -2.255955759149395501, 30.00000000000324363 ) ) ;
#59879 = CARTESIAN_POINT ( 'NONE',  ( -7.846153846153965716, -12.46129190930018460, 30.37095296980731973 ) ) ;
#59880 = VERTEX_POINT ( 'NONE', #85087 ) ;
#59881 = EDGE_CURVE ( 'NONE', #87104, #47433, #78310, .T. ) ;
#59882 = CARTESIAN_POINT ( 'NONE',  ( 2.307692307692309264, -2.900454961884010974, 35.62045528018868623 ) ) ;
#59883 = CARTESIAN_POINT ( 'NONE',  ( 18.13079044096694759, -4.684288915650984819, 34.18129842949671371 ) ) ;
#59884 = CARTESIAN_POINT ( 'NONE',  ( -4.500000000000003553, 7.499999999999996447, 13.00000000000000178 ) ) ;
#59885 = CARTESIAN_POINT ( 'NONE',  ( 1.077988221561497539, -10.27530806549875386, 14.95499329374151642 ) ) ;
#59886 = DIRECTION ( 'NONE',  ( 0.000000000000000000, 0.9396926207859126468, 0.3420201433256571111 ) ) ;
#59888 = VERTEX_POINT ( 'NONE', #84215 ) ;
#59887 = CARTESIAN_POINT ( 'NONE',  ( -39.05038313613820122, -2.499999999999999556, 29.75000000000000355 ) ) ;
#59889 = CARTESIAN_POINT ( 'NONE',  ( 1.944543648263018731, -9.444543648262994751, 23.37500000000000000 ) ) ;
#59890 = FACE_OUTER_BOUND ( 'NONE', #52905, .T. ) ;
#59891 = B_SPLINE_CURVE_WITH_KNOTS ( 'NONE', 3,
 ( #71679, #9980, #50946, #31588, #58606, #9536, #64916, #23930, #37002, #65804 ),
 .UNSPECIFIED., .F., .F.,
 ( 4, 2, 2, 2, 4 ),
 ( 0.000000000000000000, 0.0001954339857564080165, 0.0003908679715128160329, 0.0005863019572692240765, 0.0007817359430256320659 ),
 .UNSPECIFIED. ) ;
#59892 = VECTOR ( 'NONE', #18479, 1000.000000000000000 ) ;
#59893 = EDGE_LOOP ( 'NONE', ( #9217, #68193, #76684, #56570 ) ) ;
#59894 = CARTESIAN_POINT ( 'NONE',  ( -9.692307692307691624, -13.57706302396349152, 30.56769352161908060 ) ) ;
#59895 = ORIENTED_EDGE ( 'NONE', *, *, #81264, .T. ) ;
#59896 = DIRECTION ( 'NONE',  ( 0.000000000000000000, 0.1736481776669267785, -0.9848077530122087975 ) ) ;
#59897 = CARTESIAN_POINT ( 'NONE',  ( 13.38461538461526601, -10.21337939537710326, 33.94971097300076224 ) ) ;
#59898 = LINE ( 'NONE', #86046, #67154 ) ;
#59899 = VERTEX_POINT ( 'NONE', #71553 ) ;
#59900 = CARTESIAN_POINT ( 'NONE',  ( -10.36543909703647159, -12.43552623307873972, 30.55307653245132826 ) ) ;
#59901 = ORIENTED_EDGE ( 'NONE', *, *, #46089, .F. ) ;
#59902 = EDGE_CURVE ( 'NONE', #22022, #66369, #87622, .T. ) ;
#59903 = ORIENTED_EDGE ( 'NONE', *, *, #69002, .F. ) ;
#59904 = DIRECTION ( 'NONE',  ( -0.000000000000000000, 0.5000000000000011102, -0.8660254037844380415 ) ) ;
#59905 = DIRECTION ( 'NONE',  ( 0.000000000000000000, 0.1736481776669267785, -0.9848077530122087975 ) ) ;
#59906 = CYLINDRICAL_SURFACE ( 'NONE', #63004, 0.2499999999999994726 ) ;
#59907 = CARTESIAN_POINT ( 'NONE',  ( 9.562160482869472844, -9.418419913701741919, 34.36755862841477693 ) ) ;
#59908 = CARTESIAN_POINT ( 'NONE',  ( -2.980823821391187955, -4.932303261841488151, 34.32971442181322885 ) ) ;
#59909 = DIRECTION ( 'NONE',  ( -0.000000000000000000, 1.000000000000000000, -0.000000000000000000 ) ) ;
#59910 = AXIS2_PLACEMENT_3D ( 'NONE', #70432, #57352, #84397 ) ;
#59911 = EDGE_CURVE ( 'NONE', #8847, #34885, #2209, .T. ) ;
#59912 = FACE_OUTER_BOUND ( 'NONE', #36229, .T. ) ;
#59913 = EDGE_LOOP ( 'NONE', ( #46794, #52147, #31328, #17154 ) ) ;
#59914 = ORIENTED_EDGE ( 'NONE', *, *, #56884, .T. ) ;
#59915 = ORIENTED_EDGE ( 'NONE', *, *, #6420, .F. ) ;
#59917 = ORIENTED_EDGE ( 'NONE', *, *, #18918, .T. ) ;
#59916 = CARTESIAN_POINT ( 'NONE',  ( -4.023320715612507925, -8.630441415882550871, 34.87705825610312615 ) ) ;
#59918 = EDGE_CURVE ( 'NONE', #53138, #22316, #79658, .T. ) ;
#59919 = B_SPLINE_CURVE_WITH_KNOTS ( 'NONE', 3,
 ( #23107, #37051, #37495, #2816, #30740, #30308, #58210, #85701, #23977, #17232 ),
 .UNSPECIFIED., .F., .F.,
 ( 4, 2, 2, 2, 4 ),
 ( 0.000000000000000000, 0.0001954339857564081249, 0.0003908679715128162498, 0.0005863019572692244018, 0.0007817359430256324996 ),
 .UNSPECIFIED. ) ;
#59920 = FACE_OUTER_BOUND ( 'NONE', #82703, .T. ) ;
#59921 = CARTESIAN_POINT ( 'NONE',  ( 3.230769230769231726, -11.33034616979429110, 35.88435417666054406 ) ) ;
#59922 = EDGE_LOOP ( 'NONE', ( #86664, #40879, #9155, #87102 ) ) ;
#59923 = CARTESIAN_POINT ( 'NONE',  ( -14.24162395668986925, -4.098570777380720287, 33.41473453929635440 ) ) ;
#59924 = EDGE_CURVE ( 'NONE', #84701, #35616, #39127, .T. ) ;
#59925 = EDGE_LOOP ( 'NONE', ( #72928, #51243 ) ) ;
#59926 = CARTESIAN_POINT ( 'NONE',  ( 0.2386730393348221735, -2.501496062324912284, 29.88072118266895671 ) ) ;
#59927 = ORIENTED_EDGE ( 'NONE', *, *, #68323, .T. ) ;
#59928 = DIRECTION ( 'NONE',  ( -0.000000000000000000, -0.000000000000000000, -1.000000000000000000 ) ) ;
#59929 = AXIS2_PLACEMENT_3D ( 'NONE', #62405, #74613, #21435 ) ;
#59930 = CARTESIAN_POINT ( 'NONE',  ( -11.78843826940389583, -3.627789207965226748, 32.91389620160131102 ) ) ;
#59931 = CARTESIAN_POINT ( 'NONE',  ( 4.023286240232789801, -2.254533558242299396, 29.97296025877828285 ) ) ;
#59932 = FACE_BOUND ( 'NONE', #15335, .T. ) ;
#59933 = EDGE_CURVE ( 'NONE', #45617, #31900, #73345, .T. ) ;
#59934 = CARTESIAN_POINT ( 'NONE',  ( -17.07692307692307665, -11.35647404775217417, 33.31231777344666511 ) ) ;
#59935 = CARTESIAN_POINT ( 'NONE',  ( -13.38461538461538325, -2.900454961884010974, 35.62045528018868623 ) ) ;
#59936 = CARTESIAN_POINT ( 'NONE',  ( 5.869439408258079638, -2.504760397472873823, 29.97295953869789997 ) ) ;
#59937 = FACE_OUTER_BOUND ( 'NONE', #43443, .T. ) ;
#59938 = CARTESIAN_POINT ( 'NONE',  ( 24.00000000000000000, -5.499999999999981348, 27.75000000000000000 ) ) ;
#59939 = CARTESIAN_POINT ( 'NONE',  ( 8.096099364501986528, -10.76462480002816235, 33.53768742498949962 ) ) ;
#59940 = ORIENTED_EDGE ( 'NONE', *, *, #54085, .F. ) ;
#59941 = EDGE_CURVE ( 'NONE', #48029, #61382, #10308, .T. ) ;
#59942 = CIRCLE ( 'NONE', #44108, 0.2500000000000002220 ) ;
#59943 = CARTESIAN_POINT ( 'NONE',  ( 10.61538461538461675, -9.780366693483667717, 34.19971097300155094 ) ) ;
#59944 = EDGE_LOOP ( 'NONE', ( #53763, #55114, #31701, #59940 ) ) ;
#59945 = ORIENTED_EDGE ( 'NONE', *, *, #43455, .T. ) ;
#59947 = CARTESIAN_POINT ( 'NONE',  ( 2.307692307692187583, -10.90142922262034020, 33.41473453929536674 ) ) ;
#59946 = CARTESIAN_POINT ( 'NONE',  ( 10.83839596699746721, -12.39991518177334129, 30.74647679643404530 ) ) ;
#59948 = CARTESIAN_POINT ( 'NONE',  ( 15.23076923076910916, -8.656820664282941280, 34.87096338111179961 ) ) ;
#59949 = LINE ( 'NONE', #82459, #1990 ) ;
#59950 = CARTESIAN_POINT ( 'NONE',  ( 13.38461538461538680, -13.78497067705608181, 32.30358669280327177 ) ) ;
#59951 = CARTESIAN_POINT ( 'NONE',  ( 1.449870524128224591, -4.320704448112861584, 33.92786785259548310 ) ) ;
#59952 = ORIENTED_EDGE ( 'NONE', *, *, #74524, .F. ) ;
#59953 = CARTESIAN_POINT ( 'NONE',  ( -5.207071046654771607, -5.915902021225892149, 34.75552854090298638 ) ) ;
#59954 = ADVANCED_FACE ( 'NONE', ( #67037 ), #24248, .F. ) ;
#59955 = CARTESIAN_POINT ( 'NONE',  ( -5.076923076923075762, -2.538708090699994813, 30.37095296980875503 ) ) ;
#59956 = CARTESIAN_POINT ( 'NONE',  ( -14.05769230769229772, -2.249999999999999112, 29.81603969181032099 ) ) ;
#59957 = LINE ( 'NONE', #13548, #53952 ) ;
#59958 = VERTEX_POINT ( 'NONE', #38667 ) ;
#59959 = B_SPLINE_CURVE_WITH_KNOTS ( 'NONE', 3,
 ( #67218, #19026, #26225, #38406, #65862, #12711, #31650, #39752, #25334, #59112 ),
 .UNSPECIFIED., .F., .F.,
 ( 4, 2, 2, 2, 4 ),
 ( 0.000000000000000000, 0.0001954339857564098054, 0.0003908679715128196108, 0.0005863019572692293891, 0.0007817359430256392216 ),
 .UNSPECIFIED. ) ;
#59960 = ORIENTED_EDGE ( 'NONE', *, *, #57571, .T. ) ;
#59961 = APPLICATION_PROTOCOL_DEFINITION ( 'draft international standard', 'automotive_design', 1998, #83770 ) ;
#59962 = EDGE_LOOP ( 'NONE', ( #47566, #41774 ) ) ;
#59963 = CARTESIAN_POINT ( 'NONE',  ( 15.45354877203763522, -6.760870238392817200, 34.69528174975672385 ) ) ;
#59964 = CARTESIAN_POINT ( 'NONE',  ( -7.596099534515531104, -4.943051570960392382, 34.04725096376909477 ) ) ;
#59965 = ORIENTED_EDGE ( 'NONE', *, *, #86772, .F. ) ;
#59966 = DIRECTION ( 'NONE',  ( -0.000000000000000000, -0.7660444431189791237, -0.6427876096865379196 ) ) ;
#59967 = CARTESIAN_POINT ( 'NONE',  ( -6.000000000000121680, -9.528491918059723176, 34.59228464037033035 ) ) ;
#59968 = CARTESIAN_POINT ( 'NONE',  ( 16.08776274289027342, -8.120952969808774569, 34.71129190930000163 ) ) ;
#59969 = CARTESIAN_POINT ( 'NONE',  ( -2.557669038634660996, -8.303909089506435137, 34.68538101551103381 ) ) ;
#59970 = ADVANCED_FACE ( 'NONE', ( #44964 ), #66130, .T. ) ;
#59971 = AXIS2_PLACEMENT_3D ( 'NONE', #15011, #56868, #76709 ) ;
#59972 = CARTESIAN_POINT ( 'NONE',  ( 5.076923076923075762, -13.87047571288749737, 32.06866353760679544 ) ) ;
#59973 = ORIENTED_EDGE ( 'NONE', *, *, #26120, .F. ) ;
#59975 = ORIENTED_EDGE ( 'NONE', *, *, #35675, .T. ) ;
#59974 = CARTESIAN_POINT ( 'NONE',  ( -7.780898274877820597, -10.21337939537593620, 33.94971097300152252 ) ) ;
#59976 = CYLINDRICAL_SURFACE ( 'NONE', #82847, 0.2499999999999997502 ) ;
#59977 = CARTESIAN_POINT ( 'NONE',  ( 16.08859516368491072, -2.506253911140460477, 30.00000000000013856 ) ) ;
#59978 = CARTESIAN_POINT ( 'NONE',  ( -11.76194646302586833, -10.97335522853832579, 33.68706563782419749 ) ) ;
#59979 = ADVANCED_FACE ( 'NONE', ( #53056 ), #80101, .F. ) ;
#59980 = EDGE_CURVE ( 'NONE', #7315, #75299, #30642, .T. ) ;
#59981 = CARTESIAN_POINT ( 'NONE',  ( 10.39189969082028497, -12.47654668319379567, 31.42292124445336654 ) ) ;
#59982 = CARTESIAN_POINT ( 'NONE',  ( -13.38461538461538325, -5.557115091759785130, 34.35708131394839171 ) ) ;
#59983 = VECTOR ( 'NONE', #49025, 1000.000000000000000 ) ;
#59984 = CARTESIAN_POINT ( 'NONE',  ( -5.207071046654775159, -11.04286588640298561, 33.62463336215343901 ) ) ;
#59985 = DIRECTION ( 'NONE',  ( 1.000000000000000000, 0.000000000000000000, 0.000000000000000000 ) ) ;
#59986 = CARTESIAN_POINT ( 'NONE',  ( 1.077988221561497539, -10.27530806549875386, 16.20499329374151642 ) ) ;
#59987 = VERTEX_POINT ( 'NONE', #85526 ) ;
#59988 = CARTESIAN_POINT ( 'NONE',  ( 11.60452988946397923, -2.721908614388771852, 31.22303859784725333 ) ) ;
#59989 = CARTESIAN_POINT ( 'NONE',  ( 17.06410256410256565, -7.500000000000000000, 29.75000000000000355 ) ) ;
#59990 = EDGE_LOOP ( 'NONE', ( #41060, #83508, #76528, #75568 ) ) ;
#59991 = ORIENTED_EDGE ( 'NONE', *, *, #65701, .T. ) ;
#59992 = CARTESIAN_POINT ( 'NONE',  ( -5.750054590621955342, -12.68172785388650681, 30.59649109432439573 ) ) ;
#59993 = CARTESIAN_POINT ( 'NONE',  ( -3.007989689500822017, -5.913360116392399668, 34.49180327182771322 ) ) ;
#59994 = CARTESIAN_POINT ( 'NONE',  ( -0.2115384615384583999, -2.499999999999999556, 29.81604066197450109 ) ) ;
#59995 = B_SPLINE_CURVE_WITH_KNOTS ( 'NONE', 3,
 ( #57946, #85426, #23707, #52516, #32265, #67820, #33143, #46215, #45768, #66933 ),
 .UNSPECIFIED., .F., .F.,
 ( 4, 2, 2, 2, 4 ),
 ( 0.0007817359430256322827, 0.0009771253907249989254, 0.001172514838424365676, 0.001367904286123732428, 0.001563293733823098962 ),
 .UNSPECIFIED. ) ;
#59996 = CARTESIAN_POINT ( 'NONE',  ( 10.83816428436268176, -4.989023458446560255, 34.36081565061822118 ) ) ;
#59997 = B_SPLINE_CURVE_WITH_KNOTS ( 'NONE', 3,
 ( #79346, #37458, #17650, #65814, #4114, #52751, #85220, #31599, #59066, #64927 ),
 .UNSPECIFIED., .F., .F.,
 ( 4, 2, 2, 2, 4 ),
 ( 0.0007817359430256388964, 0.0009771253907250073822, 0.001172514838424375868, 0.001367904286123744571, 0.001563293733823113056 ),
 .UNSPECIFIED. ) ;
#59998 = LINE ( 'NONE', #12704, #3939 ) ;
#59999 = LINE ( 'NONE', #25777, #82536 ) ;
#60000 = ORIENTED_EDGE ( 'NONE', *, *, #9547, .T. ) ;
#60001 = AXIS2_PLACEMENT_3D ( 'NONE', #88394, #26667, #88837 ) ;
#60002 = DIRECTION ( 'NONE',  ( 0.000000000000000000, 0.1736481776669275834, 0.9848077530122086864 ) ) ;
#60003 = CARTESIAN_POINT ( 'NONE',  ( -22.00000000000000711, 9.999999999999971578, 10.00000000000000178 ) ) ;
#60004 = CARTESIAN_POINT ( 'NONE',  ( 5.076923076923075762, -11.33034616979429110, 35.88435417666054406 ) ) ;
#60005 = ORIENTED_EDGE ( 'NONE', *, *, #81286, .F. ) ;
#60006 = CARTESIAN_POINT ( 'NONE',  ( 12.52760681254089903, -3.513871655860379306, 32.76840700105978499 ) ) ;
#60007 = VECTOR ( 'NONE', #27236, 1000.000000000000114 ) ;
#60008 = EDGE_LOOP ( 'NONE', ( #23117, #65746 ) ) ;
#60009 = LINE ( 'NONE', #73542, #74520 ) ;
#60010 = CARTESIAN_POINT ( 'NONE',  ( -13.13461538461544542, -7.565270000091922853, 34.99999999999999289 ) ) ;
#60011 = CARTESIAN_POINT ( 'NONE',  ( 18.00000000000000000, -1.129524287112498415, 32.06866353760679544 ) ) ;
#60012 = ORIENTED_EDGE ( 'NONE', *, *, #16208, .T. ) ;
#60013 = VECTOR ( 'NONE', #67652, 1000.000000000000000 ) ;
#60014 = CARTESIAN_POINT ( 'NONE',  ( 12.23805351781451201, -3.754499324213721234, 33.06261337010820256 ) ) ;
#60015 = CARTESIAN_POINT ( 'NONE',  ( -6.250023224221455287, -2.341070481393820124, 30.72580821765574299 ) ) ;
#60016 = CARTESIAN_POINT ( 'NONE',  ( -9.822999158975251888, -2.541943142973491554, 30.39792223712631980 ) ) ;
#60017 = CARTESIAN_POINT ( 'NONE',  ( -7.623141002060451754, -4.762714258010881885, 34.23016756924214832 ) ) ;
#60018 = DIRECTION ( 'NONE',  ( 1.000000000000000000, 0.000000000000000000, 0.000000000000000000 ) ) ;
#60019 = ORIENTED_EDGE ( 'NONE', *, *, #1432, .T. ) ;
#60020 = FACE_BOUND ( 'NONE', #67747, .T. ) ;
#60021 = EDGE_LOOP ( 'NONE', ( #22747, #31582, #77510, #55998 ) ) ;
#60022 = CARTESIAN_POINT ( 'NONE',  ( -2.307692307692305711, -2.486705287966279876, 31.30864560766543647 ) ) ;
#60023 = CARTESIAN_POINT ( 'NONE',  ( 9.692307692307695177, -5.180354513474913603, 36.12317359536750416 ) ) ;
#60024 = CARTESIAN_POINT ( 'NONE',  ( -3.361379590393758221, -7.722926236386453702, 34.74524107206102030 ) ) ;
#60025 = CIRCLE ( 'NONE', #18305, 0.2500000000000002220 ) ;
#60026 = CARTESIAN_POINT ( 'NONE',  ( 4.230769230769229061, -3.499999999999999556, 29.75000000000000355 ) ) ;
#60027 = CARTESIAN_POINT ( 'NONE',  ( 8.992242120843616959, -3.587049720035815348, 32.86302985866382897 ) ) ;
#60028 = LINE ( 'NONE', #17723, #17749 ) ;
#60029 = CARTESIAN_POINT ( 'NONE',  ( 0.000000000000000000, -11.00000000000000000, 29.75000000000000355 ) ) ;
#60030 = ORIENTED_EDGE ( 'NONE', *, *, #82981, .T. ) ;
#60031 = ORIENTED_EDGE ( 'NONE', *, *, #80880, .T. ) ;
#60032 = EDGE_LOOP ( 'NONE', ( #39195, #23322, #84292, #865 ) ) ;
#60033 = VERTEX_POINT ( 'NONE', #18847 ) ;
#60034 = AXIS2_PLACEMENT_3D ( 'NONE', #15256, #62972, #1733 ) ;
#60035 = CARTESIAN_POINT ( 'NONE',  ( -10.55012904410859242, -11.48612834413965977, 32.76840700105972815 ) ) ;
#60036 = CARTESIAN_POINT ( 'NONE',  ( -1.384615384615505151, -12.46129190930018460, 30.37095296980731973 ) ) ;
#60037 = CARTESIAN_POINT ( 'NONE',  ( -3.931066612577743147, -9.332535724633407526, 34.40230450496446224 ) ) ;
#60038 = CARTESIAN_POINT ( 'NONE',  ( 3.903869422903800679, -3.137211980971221781, 32.19342716148376837 ) ) ;
#60040 = EDGE_CURVE ( 'NONE', #21841, #18937, #39579, .T. ) ;
#60039 = FACE_OUTER_BOUND ( 'NONE', #19747, .T. ) ;
#60041 = FACE_OUTER_BOUND ( 'NONE', #48317, .T. ) ;
#60042 = CARTESIAN_POINT ( 'NONE',  ( -2.057746789344164107, -3.712312575010499938, 33.01462480002815170 ) ) ;
#60043 = FACE_OUTER_BOUND ( 'NONE', #61837, .T. ) ;
#60044 = VERTEX_POINT ( 'NONE', #37775 ) ;
#60045 = ORIENTED_EDGE ( 'NONE', *, *, #48347, .T. ) ;
#60046 = VERTEX_POINT ( 'NONE', #23802 ) ;
#60048 = VERTEX_POINT ( 'NONE', #3539 ) ;
#60047 = CARTESIAN_POINT ( 'NONE',  ( -15.23076923076922995, -9.058645607665452459, 34.76329471203371924 ) ) ;
#60049 = B_SPLINE_CURVE_WITH_KNOTS ( 'NONE', 3,
 ( #5304, #46731, #74207, #50252, #28680, #76865, #41753, #8404, #62012, #8853 ),
 .UNSPECIFIED., .F., .F.,
 ( 4, 2, 2, 2, 4 ),
 ( 0.0007817359430256303312, 0.0009771253907249965402, 0.001172514838424362641, 0.001367904286123728958, 0.001563293733823095059 ),
 .UNSPECIFIED. ) ;
#60051 = CARTESIAN_POINT ( 'NONE',  ( 0.000000000000000000, -4.000000000000000000, 28.75000000000000000 ) ) ;
#60050 = CARTESIAN_POINT ( 'NONE',  ( 7.596177115211491859, -3.137211980971221781, 32.19342716148376837 ) ) ;
#60052 = CARTESIAN_POINT ( 'NONE',  ( 6.000000000000001776, -5.415277668671390821, 36.20867863119892149 ) ) ;
#60053 = CARTESIAN_POINT ( 'NONE',  ( -8.769230769230768274, -6.343179335718451384, 34.87096338111211935 ) ) ;
#60054 = FACE_BOUND ( 'NONE', #17765, .T. ) ;
#60055 = ORIENTED_EDGE ( 'NONE', *, *, #44827, .T. ) ;
#60056 = EDGE_CURVE ( 'NONE', #22892, #60384, #10230, .T. ) ;
#60057 = ORIENTED_EDGE ( 'NONE', *, *, #82400, .F. ) ;
#60058 = DIRECTION ( 'NONE',  ( -0.000000000000000000, 1.000000000000000000, -0.000000000000000000 ) ) ;
#60059 = VECTOR ( 'NONE', #55500, 1000.000000000000114 ) ;
#60060 = VERTEX_POINT ( 'NONE', #51713 ) ;
#60061 = FACE_BOUND ( 'NONE', #71087, .T. ) ;
#60062 = CARTESIAN_POINT ( 'NONE',  ( 7.596177115211490971, -11.79746400365624659, 32.30657167506340954 ) ) ;
#60063 = CARTESIAN_POINT ( 'NONE',  ( 18.00000000000000000, -4.786620604624113540, 33.94971097300155094 ) ) ;
#60064 = ORIENTED_EDGE ( 'NONE', *, *, #67545, .T. ) ;
#60065 = CARTESIAN_POINT ( 'NONE',  ( -1.134669975237340811, -5.766571408460172243, 34.70601412856602508 ) ) ;
#60066 = LINE ( 'NONE', #79008, #1587 ) ;
#60067 = CARTESIAN_POINT ( 'NONE',  ( -0.6850233861027925641, -2.353723527008297012, 30.78948104536958397 ) ) ;
#60068 = ORIENTED_EDGE ( 'NONE', *, *, #41100, .T. ) ;
#60069 = CARTESIAN_POINT ( 'NONE',  ( 14.53070515178570510, -3.395485233115139057, 33.02377354290275946 ) ) ;
#60070 = CARTESIAN_POINT ( 'NONE',  ( 7.145856592054988354, -5.827830569534416583, 34.72679350104403539 ) ) ;
#60071 = CARTESIAN_POINT ( 'NONE',  ( -9.692307692307691624, -2.538708090699994813, 30.37095296980875503 ) ) ;
#60072 = EDGE_LOOP ( 'NONE', ( #88487, #14160 ) ) ;
#60073 = CARTESIAN_POINT ( 'NONE',  ( 2.530705151785703766, -12.38742843783360748, 31.66772728687926985 ) ) ;
#60074 = FACE_OUTER_BOUND ( 'NONE', #45924, .T. ) ;
#60075 = VERTEX_POINT ( 'NONE', #79215 ) ;
#60076 = CARTESIAN_POINT ( 'NONE',  ( 0.3954550505825807916, -8.973038597847271092, 34.52809138561120506 ) ) ;
#60077 = CARTESIAN_POINT ( 'NONE',  ( -7.846153846153530509, -2.255955759149395501, 30.00000000000324363 ) ) ;
#60078 = LINE ( 'NONE', #46572, #62659 ) ;
#60079 = CARTESIAN_POINT ( 'NONE',  ( 15.23076923076923173, -1.951392089020283160, 34.73218667398347748 ) ) ;
#60080 = FACE_OUTER_BOUND ( 'NONE', #83761, .T. ) ;
#60081 = ADVANCED_FACE ( 'NONE', ( #11196 ), #72444, .F. ) ;
#60082 = ADVANCED_FACE ( 'NONE', ( #52168 ), #17960, .F. ) ;
#60083 = LINE ( 'NONE', #51984, #7821 ) ;
#60085 = DIRECTION ( 'NONE',  ( 1.000000000000000000, 0.000000000000000000, 0.000000000000000000 ) ) ;
#60084 = CARTESIAN_POINT ( 'NONE',  ( 14.30769230769261569, -2.506253911140615021, 30.00000000000323297 ) ) ;
#60086 = CARTESIAN_POINT ( 'NONE',  ( 10.61538461538461675, -9.058645607665452459, 34.76329471203371924 ) ) ;
#60087 = DIRECTION ( 'NONE',  ( -0.000000000000000000, 0.9848077530122085754, -0.1736481776669273613 ) ) ;
#60088 = CARTESIAN_POINT ( 'NONE',  ( -0.06109907496454585613, -4.750000000000000000, 26.40438170625848713 ) ) ;
#60089 = EDGE_LOOP ( 'NONE', ( #43347, #71765, #59777, #63703 ) ) ;
#60090 = B_SPLINE_CURVE_WITH_KNOTS ( 'NONE', 3,
 ( #12721, #40206, #12275, #67668, #26674, #60015, #87516, #5970, #54132, #67228 ),
 .UNSPECIFIED., .F., .F.,
 ( 4, 2, 2, 2, 4 ),
 ( 0.000000000000000000, 0.0001954311564186879044, 0.0003908623128373758088, 0.0005862934692560636861, 0.0007817246256747516176 ),
 .UNSPECIFIED. ) ;
#60091 = DIRECTION ( 'NONE',  ( 0.000000000000000000, 0.000000000000000000, -1.000000000000000000 ) ) ;
#60092 = ORIENTED_EDGE ( 'NONE', *, *, #77936, .T. ) ;
#60093 = EDGE_CURVE ( 'NONE', #20476, #24943, #81448, .T. ) ;
#60094 = B_SPLINE_CURVE_WITH_KNOTS ( 'NONE', 3,
 ( #7148, #79150, #11132, #2587, #22864, #50329, #57097, #16119, #63855, #51648 ),
 .UNSPECIFIED., .F., .F.,
 ( 4, 2, 2, 2, 4 ),
 ( 0.0007817246256747472808, 0.0009771112852218905021, 0.001172497944769033832, 0.001367884604316177161, 0.001563271263863320274 ),
 .UNSPECIFIED. ) ;
#60095 = AXIS2_PLACEMENT_3D ( 'NONE', #33041, #75361, #46110 ) ;
#60096 = ORIENTED_EDGE ( 'NONE', *, *, #60146, .F. ) ;
#60097 = CARTESIAN_POINT ( 'NONE',  ( -7.780086512803770837, -2.486705287966280320, 31.30864560766543647 ) ) ;
#60098 = EDGE_LOOP ( 'NONE', ( #27940, #38828 ) ) ;
#60099 = CARTESIAN_POINT ( 'NONE',  ( -5.749945580086545327, -10.06805714834173848, 34.32951233291982618 ) ) ;
#60100 = CARTESIAN_POINT ( 'NONE',  ( -1.139087296526025916, -4.750000000000006217, 14.07812500000000178 ) ) ;
#60101 = CARTESIAN_POINT ( 'NONE',  ( 12.68450159580513592, -7.369474539155828730, 34.99858011523957657 ) ) ;
#60102 = DIRECTION ( 'NONE',  ( -0.000000000000000000, 0.8660254037844397068, -0.4999999999999978906 ) ) ;
#60103 = CARTESIAN_POINT ( 'NONE',  ( -0.2385271099256116856, -5.667800583137508674, 34.40243808032445827 ) ) ;
#60104 = CARTESIAN_POINT ( 'NONE',  ( 9.823098133274648092, -2.845873456487966635, 32.17976146951972538 ) ) ;
#60106 = CARTESIAN_POINT ( 'NONE',  ( -4.826977667545034656, -2.589246495874657938, 31.60778113518102828 ) ) ;
#60105 = VECTOR ( 'NONE', #43251, 1000.000000000000000 ) ;
#60107 = CARTESIAN_POINT ( 'NONE',  ( 0.7115928814519137946, -5.642605341092957083, 34.66089969410670335 ) ) ;
#60108 = CARTESIAN_POINT ( 'NONE',  ( -14.30769230769230660, -4.661471528628507777, 34.16647553114623292 ) ) ;
#60109 = CARTESIAN_POINT ( 'NONE',  ( 2.320192649118979489E-14, -11.25000000000000000, 22.28125000000000355 ) ) ;
#60110 = DIRECTION ( 'NONE',  ( -0.000000000000000000, 1.000000000000000000, -0.000000000000000000 ) ) ;
#60111 = LINE ( 'NONE', #88501, #82290 ) ;
#60112 = VECTOR ( 'NONE', #7186, 1000.000000000000227 ) ;
#60113 = CARTESIAN_POINT ( 'NONE',  ( -17.07692307692307665, -13.53365097954675988, 30.81389545987213552 ) ) ;
#60114 = VERTEX_POINT ( 'NONE', #61148 ) ;
#60115 = EDGE_LOOP ( 'NONE', ( #14595, #71583, #62105, #34009 ) ) ;
#60116 = CARTESIAN_POINT ( 'NONE',  ( 14.08420738312797837, -8.539481045369596401, 34.89627647299170832 ) ) ;
#60117 = DIRECTION ( 'NONE',  ( -0.000000000000000000, -0.8660254037844399289, -0.4999999999999980016 ) ) ;
#60118 = DIRECTION ( 'NONE',  ( -0.000000000000000000, 0.1736481776669307198, -0.9848077530122080203 ) ) ;
#60119 = CARTESIAN_POINT ( 'NONE',  ( -6.130147209438219669, -3.817052484675422797, 33.13202310037935661 ) ) ;
#60120 = PLANE ( 'NONE',  #13285 ) ;
#60121 = CARTESIAN_POINT ( 'NONE',  ( -0.4615384615384611200, -6.386643153685126251, 34.62446782046654192 ) ) ;
#60122 = AXIS2_PLACEMENT_3D ( 'NONE', #83117, #1584, #84895 ) ;
#60123 = ORIENTED_EDGE ( 'NONE', *, *, #12544, .T. ) ;
#60124 = CARTESIAN_POINT ( 'NONE',  ( 3.230769230769231726, -6.343179335718451384, 34.87096338111211935 ) ) ;
#60125 = VERTEX_POINT ( 'NONE', #75130 ) ;
#60126 = B_SPLINE_CURVE_WITH_KNOTS ( 'NONE', 3,
 ( #46705, #18796, #26442, #61102, #46264, #19240, #73293, #67423, #4385, #59325 ),
 .UNSPECIFIED., .F., .F.,
 ( 4, 2, 2, 2, 4 ),
 ( 0.0007817246256747514008, 0.0009771112852218952725, 0.001172497944769039036, 0.001367884604316182799, 0.001563271263863326779 ),
 .UNSPECIFIED. ) ;
#60127 = ORIENTED_EDGE ( 'NONE', *, *, #29678, .T. ) ;
#60128 = CARTESIAN_POINT ( 'NONE',  ( 5.207714884747862705, -8.147973898785416225, 34.70805048591653730 ) ) ;
#60129 = CARTESIAN_POINT ( 'NONE',  ( 5.750000000000002665, -7.433931650972300353, 34.75000000000000711 ) ) ;
#60130 = CARTESIAN_POINT ( 'NONE',  ( -0.6843665591733403275, -7.369209533119137845, 34.99857337881830688 ) ) ;
#60131 = CARTESIAN_POINT ( 'NONE',  ( 3.903846153846154632, -7.500000000000001776, 35.00000000000000000 ) ) ;
#60132 = CARTESIAN_POINT ( 'NONE',  ( -5.326899820971668476, -8.347322224742351082, 34.93158281831414769 ) ) ;
#60133 = EDGE_CURVE ( 'NONE', #72521, #51846, #41330, .T. ) ;
#60134 = VERTEX_POINT ( 'NONE', #82773 ) ;
#60135 = ORIENTED_EDGE ( 'NONE', *, *, #75215, .T. ) ;
#60136 = ORIENTED_EDGE ( 'NONE', *, *, #13651, .T. ) ;
#60137 = CARTESIAN_POINT ( 'NONE',  ( -12.46153846153846168, -11.69971097300155272, 32.46337939537588113 ) ) ;
#60138 = CARTESIAN_POINT ( 'NONE',  ( 10.55011461482829560, -11.67786785259540849, 32.92929555188721480 ) ) ;
#60139 = CARTESIAN_POINT ( 'NONE',  ( 16.40390057375960708, -5.642605341092955307, 34.66089969410670335 ) ) ;
#60141 = EDGE_CURVE ( 'NONE', #37287, #6173, #73571, .T. ) ;
#60140 = CARTESIAN_POINT ( 'NONE',  ( 1.134638653673031961, -3.627789207965226748, 32.91389620160131102 ) ) ;
#60142 = VECTOR ( 'NONE', #61067, 1000.000000000000000 ) ;
#60143 =( LENGTH_UNIT ( ) NAMED_UNIT ( * ) SI_UNIT ( .MILLI., .METRE. ) );
#60144 = FACE_OUTER_BOUND ( 'NONE', #49840, .T. ) ;
#60145 = EDGE_LOOP ( 'NONE', ( #6527, #79320 ) ) ;
#60146 = EDGE_CURVE ( 'NONE', #38304, #37932, #22033, .T. ) ;
#60147 = ORIENTED_EDGE ( 'NONE', *, *, #24880, .F. ) ;
#60148 = CARTESIAN_POINT ( 'NONE',  ( -2.651650429449535551, -10.15165042944956753, 26.18750000000000355 ) ) ;
#60149 = VECTOR ( 'NONE', #49389, 1000.000000000000114 ) ;
#60151 = ORIENTED_EDGE ( 'NONE', *, *, #84784, .T. ) ;
#60150 = CARTESIAN_POINT ( 'NONE',  ( -3.360917200500930235, -2.647304123082328875, 31.75400227202885262 ) ) ;
#60152 = CARTESIAN_POINT ( 'NONE',  ( 1.254468175177163358, -10.19110544564091825, 33.96427741523702792 ) ) ;
#60153 = CARTESIAN_POINT ( 'NONE',  ( -7.173076923076921574, -2.249999999999998668, 29.75000000000000355 ) ) ;
#60154 = B_SPLINE_CURVE_WITH_KNOTS ( 'NONE', 3,
 ( #9698, #50674, #56117, #16461, #76841, #64629, #42611, #38970, #44806, #60108 ),
 .UNSPECIFIED., .F., .F.,
 ( 4, 2, 2, 2, 4 ),
 ( 0.0007817246256747484735, 0.0009771112852218922368, 0.001172497944769036217, 0.001367884604316180197, 0.001563271263863323960 ),
 .UNSPECIFIED. ) ;
#60155 = CARTESIAN_POINT ( 'NONE',  ( 1.553300858899129722, -11.24999999999999112, 14.70312500000000355 ) ) ;
#60156 = EDGE_LOOP ( 'NONE', ( #46465, #32166 ) ) ;
#60157 = EDGE_CURVE ( 'NONE', #78012, #72078, #70369, .T. ) ;
#60158 = CARTESIAN_POINT ( 'NONE',  ( -1.161602540521988747, -11.43677907613345113, 33.22367315496201456 ) ) ;
#60159 = ORIENTED_EDGE ( 'NONE', *, *, #38910, .F. ) ;
#60160 = CARTESIAN_POINT ( 'NONE',  ( 13.38461538461526423, -11.06231777344772027, 33.60647404775119895 ) ) ;
#60161 = CARTESIAN_POINT ( 'NONE',  ( 9.692307692307572609, -9.442884908241554243, 34.35708131394783038 ) ) ;
#60162 = FACE_BOUND ( 'NONE', #83878, .T. ) ;
#60163 = CARTESIAN_POINT ( 'NONE',  ( -5.011667505647051435, -12.27809138561124591, 31.22303859784720359 ) ) ;
#60164 = ADVANCED_FACE ( 'NONE', ( #34128 ), #54845, .T. ) ;
#60165 = CARTESIAN_POINT ( 'NONE',  ( 17.07692307692295586, -3.083524468854526912, 32.58852847137268327 ) ) ;
#60166 = ORIENTED_EDGE ( 'NONE', *, *, #58954, .F. ) ;
#60167 = CARTESIAN_POINT ( 'NONE',  ( -11.28851612908349722, -8.476813868363244353, 34.90874843262270133 ) ) ;
#60168 = CARTESIAN_POINT ( 'NONE',  ( 9.019176287578909879, -6.696923467548660192, 34.68552623307873972 ) ) ;
#60169 = CARTESIAN_POINT ( 'NONE',  ( 1.384615384615386802, -11.91647553114624181, 32.58852847137148245 ) ) ;
#60170 = ORIENTED_EDGE ( 'NONE', *, *, #3154, .F. ) ;
#60171 = DIRECTION ( 'NONE',  ( -0.000000000000000000, -0.000000000000000000, 1.000000000000000000 ) ) ;
#60172 = CARTESIAN_POINT ( 'NONE',  ( -16.15384615384615330, -2.249999999999998668, 29.50000000000001421 ) ) ;
#60173 = DIRECTION ( 'NONE',  ( 0.000000000000000000, 1.835858764360065031E-15, 1.000000000000000000 ) ) ;
#60174 = CARTESIAN_POINT ( 'NONE',  ( -16.37677311275300340, -11.98009711892700224, 32.48740034544074007 ) ) ;
#60175 = CARTESIAN_POINT ( 'NONE',  ( -12.46153846153846168, -2.721908614388771852, 31.22303859784724978 ) ) ;
#60176 = EDGE_CURVE ( 'NONE', #17409, #47786, #84420, .T. ) ;
#60177 = FACE_BOUND ( 'NONE', #77889, .T. ) ;
#60179 = CARTESIAN_POINT ( 'NONE',  ( -5.448717948717948012, -7.500000000000000000, 29.75000000000000355 ) ) ;
#60178 = CARTESIAN_POINT ( 'NONE',  ( 13.13459216039392530, -12.07920672191015221, 32.31858351112116168 ) ) ;
#60180 = DIRECTION ( 'NONE',  ( 1.000000000000000000, 0.000000000000000000, 0.000000000000000000 ) ) ;
#60182 = CARTESIAN_POINT ( 'NONE',  ( -0.4615384615385826339, -12.46129190930018460, 30.37095296980731973 ) ) ;
#60181 = CARTESIAN_POINT ( 'NONE',  ( -5.869208192175211281, -9.804649428959608670, 34.18742332936588468 ) ) ;
#60183 = ADVANCED_FACE ( 'NONE', ( #75998 ), #14300, .F. ) ;
#60184 = LINE ( 'NONE', #4363, #10274 ) ;
#60185 = VECTOR ( 'NONE', #55194, 1000.000000000000000 ) ;
#60186 = CARTESIAN_POINT ( 'NONE',  ( -1.200186371490556958, -4.775308065498765409, 15.07625670625849068 ) ) ;
#60187 = ORIENTED_EDGE ( 'NONE', *, *, #68499, .F. ) ;
#60188 = CARTESIAN_POINT ( 'NONE',  ( 10.55011461482829560, -12.16647553114622049, 32.15551576947930812 ) ) ;
#60189 = EDGE_LOOP ( 'NONE', ( #340, #35219, #56936, #33711 ) ) ;
#60190 = CARTESIAN_POINT ( 'NONE',  ( -8.769230769230768274, -13.75783147151868846, 33.36296068462461051 ) ) ;
#60191 = EDGE_CURVE ( 'NONE', #16008, #28285, #49421, .T. ) ;
#60192 = ORIENTED_EDGE ( 'NONE', *, *, #51056, .T. ) ;
#60193 = EDGE_CURVE ( 'NONE', #35799, #19030, #85371, .T. ) ;
#60194 = CARTESIAN_POINT ( 'NONE',  ( 7.623227628637698317, -9.086856451489516928, 34.49173150075333183 ) ) ;
#60195 = CARTESIAN_POINT ( 'NONE',  ( 13.38461538461538680, -1.215029322943914858, 32.30358669280327177 ) ) ;
#60197 = ORIENTED_EDGE ( 'NONE', *, *, #34316, .T. ) ;
#60196 = CYLINDRICAL_SURFACE ( 'NONE', #17935, 0.2499999999999994726 ) ;
#60198 = CARTESIAN_POINT ( 'NONE',  ( -16.21992956480203674, -2.538708090699995257, 30.37095296980875148 ) ) ;
#60199 = CARTESIAN_POINT ( 'NONE',  ( -11.60454391782167249, -3.937682226553330445, 33.60647404775217240 ) ) ;
#60200 = CARTESIAN_POINT ( 'NONE',  ( 0.06109907496455496689, -11.24999999999999822, 25.77938170625848713 ) ) ;
#60201 = CARTESIAN_POINT ( 'NONE',  ( 2.084766090176161324, -11.76352882383564769, 32.36236540154569497 ) ) ;
#60202 = DIRECTION ( 'NONE',  ( -0.000000000000000000, -0.3420201433256694901, -0.9396926207859082059 ) ) ;
#60203 = CARTESIAN_POINT ( 'NONE',  ( -6.923076923076922462, -9.584722331328613620, 36.20867863119891439 ) ) ;
#60204 = CARTESIAN_POINT ( 'NONE',  ( 15.23076923076911093, -6.879047030192662504, 34.71129190930017927 ) ) ;
#60205 = CARTESIAN_POINT ( 'NONE',  ( -6.988347369037697376, -4.481592998940161721, 33.73612834413957984 ) ) ;
#60206 = DIRECTION ( 'NONE',  ( -1.000000000000000000, -2.602085213965214586E-16, 0.000000000000000000 ) ) ;
#60207 = B_SPLINE_CURVE_WITH_KNOTS ( 'NONE', 3,
 ( #14120, #28078, #55988, #162, #33946, #7371, #61403, #27632, #74947, #41593 ),
 .UNSPECIFIED., .F., .F.,
 ( 4, 2, 2, 2, 4 ),
 ( 0.0007817359430256369448, 0.0009771253907250049969, 0.001172514838424373049, 0.001367904286123741101, 0.001563293733823109153 ),
 .UNSPECIFIED. ) ;
#60208 = CARTESIAN_POINT ( 'NONE',  ( 3.724691934501251023, -9.114399933863618131, 16.04874329374151287 ) ) ;
#60209 = CARTESIAN_POINT ( 'NONE',  ( -19.00000000000000000, -1.249999999999999334, 32.75000000000000000 ) ) ;
#60210 = CARTESIAN_POINT ( 'NONE',  ( -1.384615384615506484, -12.16647553114689728, 32.15551576947799362 ) ) ;
#60211 = ORIENTED_EDGE ( 'NONE', *, *, #62802, .F. ) ;
#60212 = CYLINDRICAL_SURFACE ( 'NONE', #77276, 0.2499999999999994726 ) ;
#60213 = FACE_OUTER_BOUND ( 'NONE', #63068, .T. ) ;
#60214 = CARTESIAN_POINT ( 'NONE',  ( 3.750000000000001776, -7.561099074964511502, 19.72061829374151287 ) ) ;
#60215 = CARTESIAN_POINT ( 'NONE',  ( 14.30769230769231015, -1.629998284177014645, 34.34916445242399163 ) ) ;
#60216 = CARTESIAN_POINT ( 'NONE',  ( 2.445221920924756368E-15, -13.25000000000000355, 32.75000000000000000 ) ) ;
#60217 = ORIENTED_EDGE ( 'NONE', *, *, #28948, .T. ) ;
#60218 = CARTESIAN_POINT ( 'NONE',  ( -0.4615384615384611200, -2.249999999999998668, 29.50000000000001421 ) ) ;
#60219 = CARTESIAN_POINT ( 'NONE',  ( 9.692307692307695177, -12.62096338111211580, 30.90682066428153263 ) ) ;
#60221 = EDGE_LOOP ( 'NONE', ( #7564, #23337, #63377, #9414 ) ) ;
#60220 = CARTESIAN_POINT ( 'NONE',  ( 7.846153846153723244, -2.657715359629662544, 31.77849191805970364 ) ) ;
#60222 = CARTESIAN_POINT ( 'NONE',  ( -7.976845312821407852, -8.147922237126337563, 34.70805685702651999 ) ) ;
#60223 = CARTESIAN_POINT ( 'NONE',  ( 4.403846153846153300, -2.499999999999998668, 29.75000000000000355 ) ) ;
#60224 = DIRECTION ( 'NONE',  ( -0.000000000000000000, -0.6427876096865404731, -0.7660444431189771253 ) ) ;
#60225 = VECTOR ( 'NONE', #12083, 1000.000000000000000 ) ;
#60226 = CARTESIAN_POINT ( 'NONE',  ( 13.38461538461538680, -5.180354513474913603, 36.12317359536750416 ) ) ;
#60227 = VERTEX_POINT ( 'NONE', #22385 ) ;
#60228 = VECTOR ( 'NONE', #23633, 1000.000000000000000 ) ;
#60229 = CARTESIAN_POINT ( 'NONE',  ( 7.146452408849343740, -2.251407671071270489, 29.88021292934942252 ) ) ;
#60230 = EDGE_CURVE ( 'NONE', #86240, #22218, #56618, .T. ) ;
#60231 = VECTOR ( 'NONE', #37234, 1000.000000000000000 ) ;
#60232 = CARTESIAN_POINT ( 'NONE',  ( 8.703148389870632329, -3.322132147404559532, 32.92929555188719348 ) ) ;
#60233 = ORIENTED_EDGE ( 'NONE', *, *, #609, .T. ) ;
#60234 = ORIENTED_EDGE ( 'NONE', *, *, #36717, .T. ) ;
#60235 = EDGE_CURVE ( 'NONE', #35516, #48302, #63811, .T. ) ;
#60236 = ORIENTED_EDGE ( 'NONE', *, *, #8114, .T. ) ;
#60237 = EDGE_CURVE ( 'NONE', #45764, #39096, #3667, .T. ) ;
#60238 = CARTESIAN_POINT ( 'NONE',  ( 0.2115152242454957365, -8.432397168068783699, 34.66272746175022945 ) ) ;
#60239 = CARTESIAN_POINT ( 'NONE',  ( 14.05766907039934210, -4.335965774309649134, 33.62209801155881905 ) ) ;
#60240 = DIRECTION ( 'NONE',  ( 0.000000000000000000, 0.9396926207859126468, -0.3420201433256571111 ) ) ;
#60241 = ADVANCED_FACE ( 'NONE', ( #8881 ), #36349, .F. ) ;
#60242 = CARTESIAN_POINT ( 'NONE',  ( -5.999999999999998224, -9.780366693483667717, 34.19971097300155094 ) ) ;
#60243 = ORIENTED_EDGE ( 'NONE', *, *, #21898, .T. ) ;
#60244 = EDGE_LOOP ( 'NONE', ( #45179, #34294 ) ) ;
#60245 = ORIENTED_EDGE ( 'NONE', *, *, #42519, .F. ) ;
#60247 = ORIENTED_EDGE ( 'NONE', *, *, #53042, .F. ) ;
#60246 = CARTESIAN_POINT ( 'NONE',  ( -7.976845312821407852, -4.809359713505814149, 33.96456829005828837 ) ) ;
#60248 = CARTESIAN_POINT ( 'NONE',  ( -8.102564102564102200, -3.499999999999999556, 29.75000000000000355 ) ) ;
#60249 = B_SPLINE_CURVE_WITH_KNOTS ( 'NONE', 3,
 ( #36987, #16287, #50932, #15412, #71218, #8653 ),
 .UNSPECIFIED., .F., .F.,
 ( 4, 2, 4 ),
 ( 0.0003909512603273706676, 0.0005862562993131958163, 0.0007815613382990209109 ),
 .UNSPECIFIED. ) ;
#60250 = AXIS2_PLACEMENT_3D ( 'NONE', #42461, #35706, #28959 ) ;
#60251 = CARTESIAN_POINT ( 'NONE',  ( 12.59232890250541281, -11.37503395064541678, 33.29242100308974273 ) ) ;
#60252 = CARTESIAN_POINT ( 'NONE',  ( 0.000000000000000000, -11.00000000000000000, 29.75000000000000355 ) ) ;
#60253 = CARTESIAN_POINT ( 'NONE',  ( -4.403846153846151523, -7.500000000000001776, 35.00000000000000000 ) ) ;
#60254 = ORIENTED_EDGE ( 'NONE', *, *, #51918, .F. ) ;
#60255 = B_SPLINE_CURVE_WITH_KNOTS ( 'NONE', 3,
 ( #10380, #84726, #37393, #24775, #30211, #72515, #52241, #3162, #9485, #30639 ),
 .UNSPECIFIED., .F., .F.,
 ( 4, 2, 2, 2, 4 ),
 ( 0.000000000000000000, 0.0001954311564186872810, 0.0003908623128373745620, 0.0005862934692560618430, 0.0007817246256747491240 ),
 .UNSPECIFIED. ) ;
#60256 = ADVANCED_FACE ( 'NONE', ( #2110 ), #55723, .F. ) ;
#60257 = EDGE_LOOP ( 'NONE', ( #8400, #3239 ) ) ;
#60258 = ORIENTED_EDGE ( 'NONE', *, *, #3206, .T. ) ;
#60259 = CARTESIAN_POINT ( 'NONE',  ( -15.12820512820512953, -7.500000000000000000, 33.75000000000000000 ) ) ;
#60261 = VERTEX_POINT ( 'NONE', #786 ) ;
#60260 = CARTESIAN_POINT ( 'NONE',  ( 8.769230769230647482, -2.625532179533778709, 30.86335684631627174 ) ) ;
#60262 = CARTESIAN_POINT ( 'NONE',  ( 2.084765348785460937, -2.523278758544489353, 31.42238647778637528 ) ) ;
#60263 = CARTESIAN_POINT ( 'NONE',  ( 12.33139125210024112, -11.47017969459903952, 32.78971311882035167 ) ) ;
#60264 = CARTESIAN_POINT ( 'NONE',  ( -17.01166750564705055, -9.442884908240273489, 34.35708131394835618 ) ) ;
#60265 = CARTESIAN_POINT ( 'NONE',  ( 16.40379167219429846, -3.712312575010499494, 33.01462480002815170 ) ) ;
#60266 = DIRECTION ( 'NONE',  ( -1.000000000000000000, -0.000000000000000000, -0.000000000000000000 ) ) ;
#60267 = FACE_BOUND ( 'NONE', #34139, .T. ) ;
#60268 = CARTESIAN_POINT ( 'NONE',  ( -8.703163435880695076, -2.292212530054420494, 30.41441678777542990 ) ) ;
#60269 = LINE ( 'NONE', #61152, #28440 ) ;
#60270 = CARTESIAN_POINT ( 'NONE',  ( -8.069638789877792817, -12.24155766932282496, 31.33739205006857986 ) ) ;
#60272 = CARTESIAN_POINT ( 'NONE',  ( 14.37375964104238335, -2.833524468853757750, 32.15551576947925838 ) ) ;
#60271 = DIRECTION ( 'NONE',  ( -0.000000000000000000, -0.000000000000000000, -1.000000000000000000 ) ) ;
#60273 = CIRCLE ( 'NONE', #68890, 4.000000000000000000 ) ;
#60274 = LINE ( 'NONE', #74246, #68303 ) ;
#60275 = CARTESIAN_POINT ( 'NONE',  ( 12.59232890250541814, -2.845873456487966635, 32.17976146951972538 ) ) ;
#60276 = EDGE_LOOP ( 'NONE', ( #46551, #23316, #68735, #20681, #75861, #55490 ) ) ;
#60277 = CARTESIAN_POINT ( 'NONE',  ( -16.21960295636046823, -7.249945686854186278, 34.74374336980224598 ) ) ;
#60278 = CARTESIAN_POINT ( 'NONE',  ( -13.16160254052198830, -4.026326845037962343, 33.68677907613344047 ) ) ;
#60279 = EDGE_LOOP ( 'NONE', ( #58999, #35810, #65333, #8115, #51354, #70105 ) ) ;
#60280 = ORIENTED_EDGE ( 'NONE', *, *, #88681, .T. ) ;
#60281 = CARTESIAN_POINT ( 'NONE',  ( -17.14300648787895298, -11.16473453929635440, 33.15142922261925662 ) ) ;
#60282 = VECTOR ( 'NONE', #48912, 1000.000000000000114 ) ;
#60283 = CARTESIAN_POINT ( 'NONE',  ( 16.02369818411445834, -2.373036134822905208, 30.88089517874952250 ) ) ;
#60284 = CARTESIAN_POINT ( 'NONE',  ( -2.307692307692305711, -11.35647404775217417, 33.31231777344666511 ) ) ;
#60285 = ORIENTED_EDGE ( 'NONE', *, *, #26257, .T. ) ;
#60286 = CARTESIAN_POINT ( 'NONE',  ( 8.638540166120462160, -12.62707690430377383, 30.88035979386743435 ) ) ;
#60287 = CARTESIAN_POINT ( 'NONE',  ( 6.673100179028331524, -8.347322224742351082, 34.93158281831414769 ) ) ;
#60288 = EDGE_CURVE ( 'NONE', #76927, #20882, #28707, .T. ) ;
#60289 = EDGE_CURVE ( 'NONE', #22236, #1002, #21948, .T. ) ;
#60290 = B_SPLINE_CURVE_WITH_KNOTS ( 'NONE', 3,
 ( #71051, #44446, #72818, #59312, #64724, #24189, #3024, #77806, #2581, #57534 ),
 .UNSPECIFIED., .F., .F.,
 ( 4, 2, 2, 2, 4 ),
 ( 0.0007817359430256334753, 0.0009771253907250058643, 0.001172514838424371098, 0.001367904286123736764, 0.001563293733823101998 ),
 .UNSPECIFIED. ) ;
#60292 = FACE_OUTER_BOUND ( 'NONE', #22248, .T. ) ;
#60291 = CARTESIAN_POINT ( 'NONE',  ( -15.29603967673000575, -6.026961402152685388, 34.52809138561120506 ) ) ;
#60294 = CARTESIAN_POINT ( 'NONE',  ( -8.835314180186648159, -6.386643153685125363, 34.62446782046654903 ) ) ;
#60293 = B_SPLINE_CURVE_WITH_KNOTS ( 'NONE', 3,
 ( #25937, #54733, #26832, #82222, #74578, #6560, #54285, #67817, #46656, #81342 ),
 .UNSPECIFIED., .F., .F.,
 ( 4, 2, 2, 2, 4 ),
 ( 0.000000000000000000, 0.0001954339857564076641, 0.0003908679715128153282, 0.0005863019572692229923, 0.0007817359430256306564 ),
 .UNSPECIFIED. ) ;
#60295 = CARTESIAN_POINT ( 'NONE',  ( -5.326899807865431491, -9.148715823498378086, 34.47080413974185120 ) ) ;
#60296 = CARTESIAN_POINT ( 'NONE',  ( -10.39260494640654819, -11.60474049983371003, 33.02348890104160262 ) ) ;
#60297 = B_SPLINE_CURVE_WITH_KNOTS ( 'NONE', 3,
 ( #57064, #70587, #63823, #49861, #70139, #9336, #42242, #22396, #35922, #41798 ),
 .UNSPECIFIED., .F., .F.,
 ( 4, 2, 2, 2, 4 ),
 ( 0.0007817359430256293554, 0.0009771253907249950223, 0.001172514838424360906, 0.001367904286123726790, 0.001563293733823092457 ),
 .UNSPECIFIED. ) ;
#60298 = CARTESIAN_POINT ( 'NONE',  ( -2.651650429449565305, -4.848349570550461785, 24.00000000000000000 ) ) ;
#60299 = ORIENTED_EDGE ( 'NONE', *, *, #1363, .T. ) ;
#60300 = EDGE_CURVE ( 'NONE', #57554, #62076, #16074, .T. ) ;
#60301 = ORIENTED_EDGE ( 'NONE', *, *, #20827, .F. ) ;
#60302 = CARTESIAN_POINT ( 'NONE',  ( 4.826946332874485712, -10.82459398097509684, 33.81372124010185587 ) ) ;
#60303 = ADVANCED_FACE ( 'NONE', ( #1223 ), #56174, .F. ) ;
#60304 = CARTESIAN_POINT ( 'NONE',  ( 7.173022441425064955, -12.22109172314383052, 31.39792113162168263 ) ) ;
#60305 = CARTESIAN_POINT ( 'NONE',  ( -4.480769230769230838, -3.499999999999999556, 29.75000000000000355 ) ) ;
#60306 = CARTESIAN_POINT ( 'NONE',  ( -9.692307692307814193, -8.656820664282941280, 34.87096338111179961 ) ) ;
#60307 = CARTESIAN_POINT ( 'NONE',  ( -15.09997742294444834, -2.729792928343269587, 31.24908615093345077 ) ) ;
#60308 = CARTESIAN_POINT ( 'NONE',  ( -3.749999999999997335, -7.500000000000021316, 25.09374999999999645 ) ) ;
#60309 = CARTESIAN_POINT ( 'NONE',  ( -16.15384615384615330, -2.721908614388771852, 31.22303859784724978 ) ) ;
#60310 = CARTESIAN_POINT ( 'NONE',  ( 0.000000000000000000, -11.00000000000000000, 29.75000000000000355 ) ) ;
#60311 = CARTESIAN_POINT ( 'NONE',  ( -13.25377696660261861, -7.277220443632450575, 34.74524770363009196 ) ) ;
#60312 = CARTESIAN_POINT ( 'NONE',  ( -18.06519398178334868, -12.49374608885955062, 29.99999999999984723 ) ) ;
#60313 = LINE ( 'NONE', #45462, #61238 ) ;
#60314 = CARTESIAN_POINT ( 'NONE',  ( 8.769230769230768274, -12.10708131394839349, 31.69288490824020244 ) ) ;
#60315 = CARTESIAN_POINT ( 'NONE',  ( 5.999999999999880096, -12.27809138561165270, 31.22303859784587132 ) ) ;
#60316 = CARTESIAN_POINT ( 'NONE',  ( 7.976679284387491187, -8.630441415882550871, 34.87705825610312615 ) ) ;
#60317 = CARTESIAN_POINT ( 'NONE',  ( -3.480792468062195333, -8.432397168068783699, 34.66272746175022945 ) ) ;
#60318 = CARTESIAN_POINT ( 'NONE',  ( -16.94639763868943660, -3.068774925481847937, 32.56582465632704526 ) ) ;
#60319 = EDGE_CURVE ( 'NONE', #67219, #43247, #12297, .T. ) ;
#60320 = ORIENTED_EDGE ( 'NONE', *, *, #19926, .T. ) ;
#60321 = DIRECTION ( 'NONE',  ( -0.000000000000000000, 0.1736481776669307198, -0.9848077530122080203 ) ) ;
#60322 = CYLINDRICAL_SURFACE ( 'NONE', #40311, 0.2499999999999995559 ) ;
#60323 = CARTESIAN_POINT ( 'NONE',  ( 2.724691934501250135, -8.700186371490531201, 17.29874329374151642 ) ) ;
#60324 = CARTESIAN_POINT ( 'NONE',  ( 5.299935921016469820, -10.01129605718032778, 34.36064277460058491 ) ) ;
#60325 = DIRECTION ( 'NONE',  ( -0.000000000000000000, 0.9396926207859093161, -0.3420201433256663259 ) ) ;
#60326 = EDGE_CURVE ( 'NONE', #45410, #82411, #12072, .T. ) ;
#60327 = DIRECTION ( 'NONE',  ( 0.000000000000000000, 0.1736481776669267785, -0.9848077530122087975 ) ) ;
#60329 = ORIENTED_EDGE ( 'NONE', *, *, #46655, .F. ) ;
#60328 = CYLINDRICAL_SURFACE ( 'NONE', #77016, 0.2499999999999979738 ) ;
#60330 = CARTESIAN_POINT ( 'NONE',  ( -1.409462824231155764E-14, -4.749999999999999112, 21.65625000000000355 ) ) ;
#60331 = LINE ( 'NONE', #61212, #62777 ) ;
#60332 = ORIENTED_EDGE ( 'NONE', *, *, #2536, .T. ) ;
#60333 = CARTESIAN_POINT ( 'NONE',  ( -18.00000000000012079, -3.835265460704626150, 33.15142922262032954 ) ) ;
#60334 = B_SPLINE_CURVE_WITH_KNOTS ( 'NONE', 3,
 ( #10980, #79880, #18629, #58263, #46095, #38450, #85753, #52839, #2864, #51483 ),
 .UNSPECIFIED., .F., .F.,
 ( 4, 2, 2, 2, 4 ),
 ( 0.0007817359430256215491, 0.0009771253907249856981, 0.001172514838424349847, 0.001367904286123713779, 0.001563293733823077928 ),
 .UNSPECIFIED. ) ;
#60335 = ORIENTED_EDGE ( 'NONE', *, *, #61999, .T. ) ;
#60336 = B_SPLINE_CURVE_WITH_KNOTS ( 'NONE', 3,
 ( #66531, #74174, #72383, #19234, #12039, #18340, #24647, #5272, #3479, #30949 ),
 .UNSPECIFIED., .F., .F.,
 ( 4, 2, 2, 2, 4 ),
 ( 0.000000000000000000, 0.0001954339857564065257, 0.0003908679715128130514, 0.0005863019572692196313, 0.0007817359430256261028 ),
 .UNSPECIFIED. ) ;
#60337 = CARTESIAN_POINT ( 'NONE',  ( -7.780898706641009355, -6.835583212224610072, 34.95778746994559327 ) ) ;
#60338 = ADVANCED_FACE ( 'NONE', ( #7853 ), #82186, .F. ) ;
#60339 = CARTESIAN_POINT ( 'NONE',  ( -11.78846153846153832, -2.249999999999998668, 29.75000000000000355 ) ) ;
#60340 = CARTESIAN_POINT ( 'NONE',  ( -8.096177083446805867, -3.711651800289232028, 33.01384336483936011 ) ) ;
#60341 = ORIENTED_EDGE ( 'NONE', *, *, #56547, .F. ) ;
#60342 = EDGE_LOOP ( 'NONE', ( #65513, #80985 ) ) ;
#60343 = ADVANCED_FACE ( 'NONE', ( #12829 ), #14159, .F. ) ;
#60344 = VERTEX_POINT ( 'NONE', #20475 ) ;
#60345 = CIRCLE ( 'NONE', #21503, 0.4999999999999994449 ) ;
#60346 = VECTOR ( 'NONE', #21930, 1000.000000000000000 ) ;
#60347 = CARTESIAN_POINT ( 'NONE',  ( -0.6850234052624102343, -3.236172620538810385, 32.36188796281390267 ) ) ;
#60348 = CARTESIAN_POINT ( 'NONE',  ( -0.2115929431903195990, -10.76462480002816235, 33.53768742498949962 ) ) ;
#60349 = CARTESIAN_POINT ( 'NONE',  ( 0.4615384615384611200, -1.790695186598648903, 34.54067556320373455 ) ) ;
#60350 = DIRECTION ( 'NONE',  ( 0.000000000000000000, 0.4999999999999960032, -0.8660254037844410391 ) ) ;
#60351 = CARTESIAN_POINT ( 'NONE',  ( -10.86540783960606760, -12.07920672191015221, 32.31858351112116168 ) ) ;
#60352 = FACE_OUTER_BOUND ( 'NONE', #48623, .T. ) ;
#60353 = CARTESIAN_POINT ( 'NONE',  ( 20.00000000000000000, -4.000000000000000000, 29.75000000000000355 ) ) ;
#60354 = AXIS2_PLACEMENT_3D ( 'NONE', #66628, #5372, #88696 ) ;
#60355 = VECTOR ( 'NONE', #54613, 1000.000000000000114 ) ;
#60356 = EDGE_CURVE ( 'NONE', #2085, #34232, #82637, .T. ) ;
#60357 = CARTESIAN_POINT ( 'NONE',  ( -0.2115930521604184877, -12.45601412856602863, 31.48342859153981621 ) ) ;
#60358 = VERTEX_POINT ( 'NONE', #19586 ) ;
#60360 = EDGE_CURVE ( 'NONE', #66580, #87401, #48824, .T. ) ;
#60359 = ORIENTED_EDGE ( 'NONE', *, *, #78616, .T. ) ;
#60361 = VERTEX_POINT ( 'NONE', #55141 ) ;
#60363 = ORIENTED_EDGE ( 'NONE', *, *, #43494, .T. ) ;
#60362 = CARTESIAN_POINT ( 'NONE',  ( 1.384615384615264011, -5.941354392335915335, 34.76329471203413846 ) ) ;
#60364 = CARTESIAN_POINT ( 'NONE',  ( -8.638440328263820689, -10.70102852606553157, 33.91149625220312913 ) ) ;
#60365 = CARTESIAN_POINT ( 'NONE',  ( 12.68454981315131036, -3.105924265160262543, 32.13625925475356127 ) ) ;
#60366 = ORIENTED_EDGE ( 'NONE', *, *, #86603, .F. ) ;
#60367 = EDGE_CURVE ( 'NONE', #3726, #31481, #23609, .T. ) ;
#60368 = FACE_OUTER_BOUND ( 'NONE', #74907, .T. ) ;
#60369 = EDGE_CURVE ( 'NONE', #73822, #5646, #73909, .T. ) ;
#60370 = VERTEX_POINT ( 'NONE', #76299 ) ;
#60371 = DIRECTION ( 'NONE',  ( 0.000000000000000000, 0.9396926207859126468, -0.3420201433256571111 ) ) ;
#60372 = VERTEX_POINT ( 'NONE', #6523 ) ;
#60373 = CARTESIAN_POINT ( 'NONE',  ( 8.102564102564102200, -3.499999999999999556, 29.75000000000000355 ) ) ;
#60374 = CARTESIAN_POINT ( 'NONE',  ( 1.515141086378949842, -6.852161475712352789, 34.70806712695775786 ) ) ;
#60375 = AXIS2_PLACEMENT_3D ( 'NONE', #77478, #50437, #16652 ) ;
#60376 = CARTESIAN_POINT ( 'NONE',  ( -15.90379173393269951, -10.82426656108011720, 33.81400080652039009 ) ) ;
#60377 = FACE_BOUND ( 'NONE', #81714, .T. ) ;
#60378 = DIRECTION ( 'NONE',  ( 0.000000000000000000, 0.000000000000000000, -1.000000000000000000 ) ) ;
#60379 = CARTESIAN_POINT ( 'NONE',  ( -19.99999999999996447, -15.00000000000000533, 13.00000000000000178 ) ) ;
#60380 = CARTESIAN_POINT ( 'NONE',  ( 13.51514082284902862, -5.070358843744210198, 34.40418822224088302 ) ) ;
#60381 = CARTESIAN_POINT ( 'NONE',  ( 3.361294669002876212, -5.070358843744209310, 34.40418822224088302 ) ) ;
#60382 = CARTESIAN_POINT ( 'NONE',  ( 7.846153846153846700, -12.29105614889573062, 35.45975837776705220 ) ) ;
#60383 = LINE ( 'NONE', #87897, #73539 ) ;
#60384 = VERTEX_POINT ( 'NONE', #20026 ) ;
#60385 = DIRECTION ( 'NONE',  ( -0.000000000000000000, -0.9848077530122085754, -0.1736481776669273613 ) ) ;
#60386 = ORIENTED_EDGE ( 'NONE', *, *, #33552, .T. ) ;
#60387 = VERTEX_POINT ( 'NONE', #47046 ) ;
#60389 = DIRECTION ( 'NONE',  ( 0.000000000000000000, 0.1736481776669267785, -0.9848077530122087975 ) ) ;
#60388 = DIRECTION ( 'NONE',  ( -0.000000000000000000, 0.9848077530122086864, -0.1736481776669273891 ) ) ;
#60390 = FACE_OUTER_BOUND ( 'NONE', #51095, .T. ) ;
#60391 = CARTESIAN_POINT ( 'NONE',  ( -4.087778820496076548, -9.058645607665452459, 34.76329471203371924 ) ) ;
#60392 = DIRECTION ( 'NONE',  ( -0.000000000000000000, 1.000000000000000000, -0.000000000000000000 ) ) ;
#60393 = CARTESIAN_POINT ( 'NONE',  ( -2.084912766423897335, -2.847695495035523550, 31.58253572463339154 ) ) ;
#60394 = ORIENTED_EDGE ( 'NONE', *, *, #89007, .T. ) ;
#60395 = CARTESIAN_POINT ( 'NONE',  ( 17.07692307692307665, -3.050289026998446396, 32.03036669348365706 ) ) ;
#60396 = CARTESIAN_POINT ( 'NONE',  ( 11.31558285603289349, -7.630691491037285168, 34.74850469731152458 ) ) ;
#60397 = CARTESIAN_POINT ( 'NONE',  ( -1.634592115557738312, -3.627789207965226748, 32.91389620160131102 ) ) ;
#60398 = CARTESIAN_POINT ( 'NONE',  ( -15.93106648486808119, -4.226511098958372514, 33.85474049983370293 ) ) ;
#60399 = ORIENTED_EDGE ( 'NONE', *, *, #38467, .T. ) ;
#60400 = ORIENTED_EDGE ( 'NONE', *, *, #61975, .T. ) ;
#60401 = EDGE_CURVE ( 'NONE', #6010, #45845, #14606, .T. ) ;
#60402 = VECTOR ( 'NONE', #16878, 1000.000000000000000 ) ;
#60404 = CIRCLE ( 'NONE', #11496, 0.2500000000000002220 ) ;
#60403 = SHAPE_DEFINITION_REPRESENTATION ( #50609, #45449 ) ;
#60405 = ORIENTED_EDGE ( 'NONE', *, *, #64548, .T. ) ;
#60406 = CARTESIAN_POINT ( 'NONE',  ( 0.5267940328144853357, -10.90142922261932057, 33.41473453929631887 ) ) ;
#60407 = CARTESIAN_POINT ( 'NONE',  ( -18.00000000000012079, -5.219633306517615701, 34.19971097300220464 ) ) ;
#60409 = VERTEX_POINT ( 'NONE', #33985 ) ;
#60408 = EDGE_CURVE ( 'NONE', #85626, #45, #42088, .T. ) ;
#60410 = CARTESIAN_POINT ( 'NONE',  ( 4.023698184114456566, -11.66186481527757479, 32.95055677023626117 ) ) ;
#60411 = CARTESIAN_POINT ( 'NONE',  ( -5.076923076923197442, -2.892918686052165622, 31.69288490824153470 ) ) ;
#60412 = CARTESIAN_POINT ( 'NONE',  ( 3.361559671736181976, -5.496552790871119143, 34.60292014791297532 ) ) ;
#60413 = CARTESIAN_POINT ( 'NONE',  ( 1.607395053593452028, -6.717445702608402236, 34.94155399931962336 ) ) ;
#60414 = VECTOR ( 'NONE', #78654, 1000.000000000000000 ) ;
#60415 = CARTESIAN_POINT ( 'NONE',  ( -11.31545018684868964, -9.086983370893049639, 34.49168942202179267 ) ) ;
#60416 = EDGE_LOOP ( 'NONE', ( #78479, #26617, #54083, #52274 ) ) ;
#60417 = EDGE_CURVE ( 'NONE', #35014, #17254, #68658, .T. ) ;
#60418 = PRESENTATION_LAYER_ASSIGNMENT (  '', '', ( #14389 ) ) ;
#60420 = ORIENTED_EDGE ( 'NONE', *, *, #26628, .T. ) ;
#60419 = CARTESIAN_POINT ( 'NONE',  ( -18.00000000000000000, -13.83693561022309915, 32.05645593858272235 ) ) ;
#60421 = DIRECTION ( 'NONE',  ( -0.000000000000000000, 0.000000000000000000, 1.000000000000000000 ) ) ;
#60422 = CARTESIAN_POINT ( 'NONE',  ( -2.307692307692305711, -8.973038597847269315, 34.52809138561121927 ) ) ;
#60423 = CARTESIAN_POINT ( 'NONE',  ( 1.161736702186739745, -7.630691491037286056, 34.74850469731152458 ) ) ;
#60424 = DIRECTION ( 'NONE',  ( -1.000000000000000000, -0.000000000000000000, -0.000000000000000000 ) ) ;
#60425 = CARTESIAN_POINT ( 'NONE',  ( 2.557746727605763049, -2.544122305571458575, 31.48381861865057729 ) ) ;
#60426 = CARTESIAN_POINT ( 'NONE',  ( -5.143005456283212595, -10.67929555188718460, 33.92786785259543336 ) ) ;
#60427 = CARTESIAN_POINT ( 'NONE',  ( -0.7115151924808159611, -12.41269422305637171, 30.68257228309993323 ) ) ;
#60428 = EDGE_CURVE ( 'NONE', #22275, #78937, #7410, .T. ) ;
#60429 = CARTESIAN_POINT ( 'NONE',  ( 0.06109907496451789238, -4.749999999999998224, 19.40811829374151287 ) ) ;
#60430 = VERTEX_POINT ( 'NONE', #33555 ) ;
#60431 = CARTESIAN_POINT ( 'NONE',  ( -7.173100147298380413, -10.92453946501458439, 33.72985991061850086 ) ) ;
#60432 = LINE ( 'NONE', #40182, #16025 ) ;
#60433 = ADVANCED_FACE ( 'NONE', ( #88514 ), #54247, .T. ) ;
#60434 = LINE ( 'NONE', #53678, #34801 ) ;
#60435 = VERTEX_POINT ( 'NONE', #61894 ) ;
#60436 = CARTESIAN_POINT ( 'NONE',  ( 8.096099255531887806, -12.07971442181321997, 32.31769673815850297 ) ) ;
#60437 = CARTESIAN_POINT ( 'NONE',  ( 2.980769230769221956, -2.499999999999999556, 29.81609845454692120 ) ) ;
#60438 = CARTESIAN_POINT ( 'NONE',  ( 10.68063975489745410, -5.094484230520773593, 34.41647553114626845 ) ) ;
#60439 = EDGE_CURVE ( 'NONE', #50355, #52314, #35907, .T. ) ;
#60440 = CARTESIAN_POINT ( 'NONE',  ( -16.15384615384615330, -3.050289026998446396, 32.03036669348365706 ) ) ;
#60441 = CARTESIAN_POINT ( 'NONE',  ( 17.75002325595141173, -2.544273027872574477, 31.48422191005632698 ) ) ;
#60442 = ORIENTED_EDGE ( 'NONE', *, *, #36642, .F. ) ;
#60443 = CARTESIAN_POINT ( 'NONE',  ( 5.999999999999880096, -3.835265460704628371, 33.15142922262033665 ) ) ;
#60444 = CARTESIAN_POINT ( 'NONE',  ( 17.32697738856138869, -5.728107161865375829, 34.42597550085002922 ) ) ;
#60445 = DIRECTION ( 'NONE',  ( 0.000000000000000000, 0.000000000000000000, 1.000000000000000000 ) ) ;
#60447 = ORIENTED_EDGE ( 'NONE', *, *, #44870, .F. ) ;
#60446 = AXIS2_PLACEMENT_3D ( 'NONE', #68296, #81823, #61974 ) ;
#60448 = CARTESIAN_POINT ( 'NONE',  ( 12.39626846098214230, -2.657715359629088780, 31.77849191805832874 ) ) ;
#60449 = EDGE_CURVE ( 'NONE', #23968, #86388, #52012, .T. ) ;
#60450 = B_SPLINE_CURVE_WITH_KNOTS ( 'NONE', 3,
 ( #86933, #73390, #62516, #48562, #42276, #13455, #54894, #53999, #88264, #7596 ),
 .UNSPECIFIED., .F., .F.,
 ( 4, 2, 2, 2, 4 ),
 ( 0.0007817246256747516176, 0.0009771112852218965736, 0.001172497944769041421, 0.001367884604316186269, 0.001563271263863331333 ),
 .UNSPECIFIED. ) ;
#60451 = EDGE_LOOP ( 'NONE', ( #59903, #25812 ) ) ;
#60452 = FACE_OUTER_BOUND ( 'NONE', #15858, .T. ) ;
#60453 =( NAMED_UNIT ( * ) PLANE_ANGLE_UNIT ( ) SI_UNIT ( $, .RADIAN. ) );
#60454 = CARTESIAN_POINT ( 'NONE',  ( -1.384615384615383471, -13.20930481340135110, 34.54067556320372745 ) ) ;
#60455 = ORIENTED_EDGE ( 'NONE', *, *, #47071, .F. ) ;
#60456 = ADVANCED_FACE ( 'NONE', ( #36648 ), #44264, .F. ) ;
#60457 = CARTESIAN_POINT ( 'NONE',  ( 0.4615384615384611200, -4.098570777380720287, 33.41473453929634729 ) ) ;
#60458 = CARTESIAN_POINT ( 'NONE',  ( -11.53846153846153655, -13.88283147151868846, 33.14645433367849847 ) ) ;
#60459 = LINE ( 'NONE', #47384, #84004 ) ;
#60460 = CARTESIAN_POINT ( 'NONE',  ( -7.846153846153844924, -4.661471528628507777, 34.16647553114623292 ) ) ;
#60461 = CARTESIAN_POINT ( 'NONE',  ( -0.5916864312701586304, -11.66186481527757479, 32.95055677023626117 ) ) ;
#60462 = EDGE_CURVE ( 'NONE', #88588, #34081, #83522, .T. ) ;
#60463 = ORIENTED_EDGE ( 'NONE', *, *, #40838, .F. ) ;
#60464 = B_SPLINE_CURVE_WITH_KNOTS ( 'NONE', 3,
 ( #62047, #19295, #40024, #81894, #26496, #26053, #81452, #13418, #19736, #14304 ),
 .UNSPECIFIED., .F., .F.,
 ( 4, 2, 2, 2, 4 ),
 ( 0.000000000000000000, 0.0001954339857564091278, 0.0003908679715128182556, 0.0005863019572692274375, 0.0007817359430256365111 ),
 .UNSPECIFIED. ) ;
#60465 = VECTOR ( 'NONE', #45314, 1000.000000000000114 ) ;
#60466 = FACE_OUTER_BOUND ( 'NONE', #62678, .T. ) ;
#60467 = ORIENTED_EDGE ( 'NONE', *, *, #87282, .F. ) ;
#60468 = CARTESIAN_POINT ( 'NONE',  ( 5.207448515156718472, -11.66157788607254275, 32.95092075102925833 ) ) ;
#60469 = CARTESIAN_POINT ( 'NONE',  ( -10.48459417441766561, -9.929761469519743144, 34.40412654351204225 ) ) ;
#60470 = VECTOR ( 'NONE', #66171, 999.9999999999998863 ) ;
#60471 = AXIS2_PLACEMENT_3D ( 'NONE', #15164, #71416, #51130 ) ;
#60472 = CARTESIAN_POINT ( 'NONE',  ( 18.22301284409339672, -6.460100341425561332, 34.89618726649961644 ) ) ;
#60473 = CARTESIAN_POINT ( 'NONE',  ( -6.923076923076922462, -5.557115091759785130, 34.35708131394839171 ) ) ;
#60474 = DIRECTION ( 'NONE',  ( -0.000000000000000000, 1.000000000000000000, 3.491481338843133355E-15 ) ) ;
#60475 = AXIS2_PLACEMENT_3D ( 'NONE', #24042, #10545, #38914 ) ;
#60476 = EDGE_CURVE ( 'NONE', #63332, #18616, #35070, .T. ) ;
#60477 = CIRCLE ( 'NONE', #15937, 0.2500000000000002220 ) ;
#60478 = EDGE_LOOP ( 'NONE', ( #80789, #61738 ) ) ;
#60479 = ORIENTED_EDGE ( 'NONE', *, *, #24561, .F. ) ;
#60480 = ORIENTED_EDGE ( 'NONE', *, *, #40650, .F. ) ;
#60481 = EDGE_CURVE ( 'NONE', #68101, #17484, #59510, .T. ) ;
#60483 = VERTEX_POINT ( 'NONE', #22247 ) ;
#60482 = EDGE_CURVE ( 'NONE', #72207, #64027, #47716, .T. ) ;
#60484 = DIRECTION ( 'NONE',  ( -0.000000000000000000, 0.000000000000000000, 1.000000000000000000 ) ) ;
#60485 = CARTESIAN_POINT ( 'NONE',  ( -6.130691466667556710, -12.38065189839062263, 30.83690757178629482 ) ) ;
#60486 = CARTESIAN_POINT ( 'NONE',  ( -15.48074596171158390, -10.66389620160130036, 33.62221079203477103 ) ) ;
#60487 = EDGE_CURVE ( 'NONE', #14315, #23009, #84264, .T. ) ;
#60488 = CARTESIAN_POINT ( 'NONE',  ( 5.011653076366756387, -11.67786785259541027, 32.92929555188721480 ) ) ;
#60489 = CARTESIAN_POINT ( 'NONE',  ( 3.361559671736181976, -9.084667340241226796, 34.75534355489798344 ) ) ;
#60490 = CARTESIAN_POINT ( 'NONE',  ( -0.5922299282060186076, -11.71456829005830080, 32.44064028649416542 ) ) ;
#60491 = DIRECTION ( 'NONE',  ( -0.000000000000000000, 0.6427876096865404731, -0.7660444431189770143 ) ) ;
#60492 = LINE ( 'NONE', #72225, #5891 ) ;
#60493 = ORIENTED_EDGE ( 'NONE', *, *, #6214, .F. ) ;
#60494 = EDGE_LOOP ( 'NONE', ( #53157, #87300 ) ) ;
#60495 = B_SPLINE_CURVE_WITH_KNOTS ( 'NONE', 3,
 ( #29282, #75249, #7678, #75676, #34703, #68920, #49093, #35139, #62167, #54972 ),
 .UNSPECIFIED., .F., .F.,
 ( 4, 2, 2, 2, 4 ),
 ( 0.000000000000000000, 0.0001954339857564098054, 0.0003908679715128196108, 0.0005863019572692293891, 0.0007817359430256392216 ),
 .UNSPECIFIED. ) ;
#60496 = VERTEX_POINT ( 'NONE', #71304 ) ;
#60498 = ORIENTED_EDGE ( 'NONE', *, *, #81873, .T. ) ;
#60497 = CARTESIAN_POINT ( 'NONE',  ( -1.634592115557738090, -11.28823185664190376, 33.01397839955799896 ) ) ;
#60500 = CARTESIAN_POINT ( 'NONE',  ( -7.846153846153844924, -9.058645607665452459, 34.76329471203371924 ) ) ;
#60499 = DIRECTION ( 'NONE',  ( -0.000000000000000000, 1.000000000000000000, -0.000000000000000000 ) ) ;
#60501 = B_SPLINE_CURVE_WITH_KNOTS ( 'NONE', 3,
 ( #58427, #64743, #43596, #23321, #86838, #3491, #85043, #3046, #72395, #2601 ),
 .UNSPECIFIED., .F., .F.,
 ( 4, 2, 2, 2, 4 ),
 ( 0.0007817246256747470640, 0.0009771112852218896347, 0.001172497944769032314, 0.001367884604316174993, 0.001563271263863317455 ),
 .UNSPECIFIED. ) ;
#60502 = B_SPLINE_CURVE_WITH_KNOTS ( 'NONE', 3,
 ( #59082, #32500, #46466, #12237, #45570, #25753, #52768, #86580, #80258, #88367 ),
 .UNSPECIFIED., .F., .F.,
 ( 4, 2, 2, 2, 4 ),
 ( 0.000000000000000000, 0.0001954339857564091549, 0.0003908679715128183098, 0.0005863019572692274375, 0.0007817359430256366195 ),
 .UNSPECIFIED. ) ;
#60503 = CARTESIAN_POINT ( 'NONE',  ( 11.47319109250076608, -3.835265460703609186, 33.15142922261924241 ) ) ;
#60504 = DIRECTION ( 'NONE',  ( -0.000000000000000000, 0.1736481776669307198, -0.9848077530122080203 ) ) ;
#60505 = FACE_BOUND ( 'NONE', #50119, .T. ) ;
#60506 = ORIENTED_EDGE ( 'NONE', *, *, #70971, .T. ) ;
#60507 = EDGE_LOOP ( 'NONE', ( #22749, #60779, #9905, #21154 ) ) ;
#60508 = DIRECTION ( 'NONE',  ( -0.000000000000000000, -0.000000000000000000, -1.000000000000000000 ) ) ;
#60509 = ORIENTED_EDGE ( 'NONE', *, *, #2107, .T. ) ;
#60510 = FACE_BOUND ( 'NONE', #62285, .T. ) ;
#60511 = CARTESIAN_POINT ( 'NONE',  ( 9.823098133274648092, -5.496552790871120031, 34.60292014791297532 ) ) ;
#60512 = CARTESIAN_POINT ( 'NONE',  ( 0.4615384615384611200, -7.500000000000001776, 35.04278698407183867 ) ) ;
#60513 = ORIENTED_EDGE ( 'NONE', *, *, #29287, .F. ) ;
#60514 = CARTESIAN_POINT ( 'NONE',  ( -23.00000000000000000, -4.249999999999998224, 27.25000000000000000 ) ) ;
#60515 = CARTESIAN_POINT ( 'NONE',  ( 9.019230769230832223, -7.434744860731433924, 35.00000000000000711 ) ) ;
#60516 = CARTESIAN_POINT ( 'NONE',  ( -4.853496678008289322, -7.630147987733840509, 34.99859428049665411 ) ) ;
#60517 = ORIENTED_EDGE ( 'NONE', *, *, #44940, .T. ) ;
#60518 = DIRECTION ( 'NONE',  ( -0.000000000000000000, -0.9848077530122085754, -0.1736481776669273613 ) ) ;
#60519 = CARTESIAN_POINT ( 'NONE',  ( 16.15384615384615330, -1.629998284177014645, 34.34916445242399163 ) ) ;
#60520 = DIRECTION ( 'NONE',  ( -0.000000000000000000, 0.6427876096865404731, -0.7660444431189771253 ) ) ;
#60521 = ORIENTED_EDGE ( 'NONE', *, *, #60157, .F. ) ;
#60522 = CARTESIAN_POINT ( 'NONE',  ( 13.38461538461538680, -6.435427911321262684, 35.78748833219616898 ) ) ;
#60523 = CARTESIAN_POINT ( 'NONE',  ( -15.90379173393269951, -10.06805714834173138, 34.32951233291982618 ) ) ;
#60524 = EDGE_LOOP ( 'NONE', ( #81254, #22013 ) ) ;
#60525 = DIRECTION ( 'NONE',  ( 0.000000000000000000, 0.3420201433256610524, 0.9396926207859113145 ) ) ;
#60526 = CARTESIAN_POINT ( 'NONE',  ( -0.4615384615384611200, -13.53365097954675988, 30.81389545987213552 ) ) ;
#60527 = CARTESIAN_POINT ( 'NONE',  ( -8.069080805060693251, -12.38737895849757820, 31.66785238281580206 ) ) ;
#60528 = CARTESIAN_POINT ( 'NONE',  ( -0.2115384615370257404, -7.500000000000155431, 34.75000000000007105 ) ) ;
#60529 = DIRECTION ( 'NONE',  ( -0.000000000000000000, -0.000000000000000000, -1.000000000000000000 ) ) ;
#60530 = CARTESIAN_POINT ( 'NONE',  ( 17.20771351789002424, -4.684288915650984819, 34.18129842949671371 ) ) ;
#60532 = DIRECTION ( 'NONE',  ( -1.000000000000000000, -0.000000000000000000, -0.000000000000000000 ) ) ;
#60531 = CARTESIAN_POINT ( 'NONE',  ( 0.5920638997721034968, -11.66157788607254275, 32.95092075102925833 ) ) ;
#60533 = VECTOR ( 'NONE', #13000, 1000.000000000000227 ) ;
#60534 = CARTESIAN_POINT ( 'NONE',  ( -16.15384615384615330, -11.69971097300155272, 32.46337939537588113 ) ) ;
#60535 = LINE ( 'NONE', #6048, #43543 ) ;
#60536 = CARTESIAN_POINT ( 'NONE',  ( 2.750000000000001776, -7.499999999999984013, 19.46875000000000000 ) ) ;
#60537 = ORIENTED_EDGE ( 'NONE', *, *, #87309, .T. ) ;
#60538 = CARTESIAN_POINT ( 'NONE',  ( 4.946232473812769648, -6.369640206132550553, 34.87707690430378449 ) ) ;
#60539 = ORIENTED_EDGE ( 'NONE', *, *, #71147, .T. ) ;
#60540 = CIRCLE ( 'NONE', #21699, 4.000000000000000000 ) ;
#60541 = ORIENTED_EDGE ( 'NONE', *, *, #27797, .F. ) ;
#60542 = CARTESIAN_POINT ( 'NONE',  ( -3.099978789802280144, -9.084667340241226796, 34.75534355489798344 ) ) ;
#60543 = ORIENTED_EDGE ( 'NONE', *, *, #27334, .T. ) ;
#60544 = CARTESIAN_POINT ( 'NONE',  ( -14.30769230769230660, -13.57706302396349152, 30.56769352161908060 ) ) ;
#60545 = CARTESIAN_POINT ( 'NONE',  ( 1.944543648263018731, -9.444543648262994751, 14.62500000000000000 ) ) ;
#60546 = CARTESIAN_POINT ( 'NONE',  ( 17.77707304109314634, -4.762599654559227069, 34.23009711892697737 ) ) ;
#60547 = CARTESIAN_POINT ( 'NONE',  ( -18.25002322422145440, -12.07920672191015754, 32.31858351112115457 ) ) ;
#60548 = CARTESIAN_POINT ( 'NONE',  ( -0.4615384615384611200, -5.557115091759785130, 34.35708131394839171 ) ) ;
#60549 = CIRCLE ( 'NONE', #18824, 4.000000000000000000 ) ;
#60550 = LINE ( 'NONE', #53792, #7253 ) ;
#60551 = CARTESIAN_POINT ( 'NONE',  ( 9.692307692307695177, -1.117168528481311540, 33.14645433367849847 ) ) ;
#60553 = ADVANCED_FACE ( 'NONE', ( #9612 ), #37074, .F. ) ;
#60552 = FACE_OUTER_BOUND ( 'NONE', #7054, .T. ) ;
#60554 = CARTESIAN_POINT ( 'NONE',  ( -3.749999999999997335, -7.500000000000021316, 20.09375000000000000 ) ) ;
#60555 = CARTESIAN_POINT ( 'NONE',  ( 10.61538461538461675, -12.34228464037088635, 31.77849191805839268 ) ) ;
#60556 = CARTESIAN_POINT ( 'NONE',  ( -17.86920955903304886, -2.295524264805589354, 30.44142389570983198 ) ) ;
#60557 = CARTESIAN_POINT ( 'NONE',  ( -2.307692307692427391, -4.481592998941358097, 33.73612834414048933 ) ) ;
#60558 = VERTEX_POINT ( 'NONE', #24894 ) ;
#60559 = VERTEX_POINT ( 'NONE', #5077 ) ;
#60560 = CARTESIAN_POINT ( 'NONE',  ( 14.05766908347085042, -8.475808217655753651, 34.90892951860618609 ) ) ;
#60561 = DIRECTION ( 'NONE',  ( -0.000000000000000000, -0.7660444431189791237, -0.6427876096865379196 ) ) ;
#60562 = CARTESIAN_POINT ( 'NONE',  ( -19.50000000000000000, -3.499999999999999556, 29.75000000000000355 ) ) ;
#60563 = DIRECTION ( 'NONE',  ( 0.000000000000000000, 0.1736481776669267785, -0.9848077530122087975 ) ) ;
#60564 = EDGE_CURVE ( 'NONE', #17125, #76030, #73092, .T. ) ;
#60565 = CARTESIAN_POINT ( 'NONE',  ( 14.30769230769218581, -3.643525952248795718, 33.31231777344771672 ) ) ;
#60566 = CARTESIAN_POINT ( 'NONE',  ( -39.05038313613820122, -12.50000000000000000, 29.75000000000000355 ) ) ;
#60567 = VECTOR ( 'NONE', #40104, 1000.000000000000227 ) ;
#60568 = EDGE_CURVE ( 'NONE', #44606, #31297, #30765, .T. ) ;
#60569 = ORIENTED_EDGE ( 'NONE', *, *, #82301, .F. ) ;
#60570 = CARTESIAN_POINT ( 'NONE',  ( 1.161130440891438020, -5.113361153441934093, 34.14387501736622710 ) ) ;
#60571 = ORIENTED_EDGE ( 'NONE', *, *, #51457, .T. ) ;
#60572 = VECTOR ( 'NONE', #27092, 1000.000000000000000 ) ;
#60573 = ORIENTED_EDGE ( 'NONE', *, *, #55742, .F. ) ;
#60574 = CARTESIAN_POINT ( 'NONE',  ( 5.299702618191483694, -8.496831190052096971, 34.64984203495476578 ) ) ;
#60575 = CARTESIAN_POINT ( 'NONE',  ( -2.557669051740897537, -9.234221910056348293, 34.70572697212741531 ) ) ;
#60576 = CARTESIAN_POINT ( 'NONE',  ( 14.05766907039934210, -5.056417327199099532, 34.11270091957321426 ) ) ;
#60577 = CARTESIAN_POINT ( 'NONE',  ( -23.50000000000000000, 1.674711738930281374E-15, 28.74999999999999645 ) ) ;
#60578 = DIRECTION ( 'NONE',  ( -0.000000000000000000, -0.5000000000000009992, -0.8660254037844380415 ) ) ;
#60579 = VERTEX_POINT ( 'NONE', #79411 ) ;
#60580 = VERTEX_POINT ( 'NONE', #58680 ) ;
#60581 = EDGE_CURVE ( 'NONE', #27068, #20882, #4183, .T. ) ;
#60582 = EDGE_CURVE ( 'NONE', #81377, #22716, #39105, .T. ) ;
#60583 = ORIENTED_EDGE ( 'NONE', *, *, #4318, .T. ) ;
#60584 = EDGE_LOOP ( 'NONE', ( #40887, #73940, #42115, #5109 ) ) ;
#60585 = AXIS2_PLACEMENT_3D ( 'NONE', #50552, #10016, #31167 ) ;
#60586 = CARTESIAN_POINT ( 'NONE',  ( 5.934729554039225974, -2.625532179533445198, 30.86335684631481513 ) ) ;
#60587 = DIRECTION ( 'NONE',  ( -0.000000000000000000, 1.000000000000000000, -0.000000000000000000 ) ) ;
#60588 = CARTESIAN_POINT ( 'NONE',  ( 15.90384615384615330, -2.249999999999998668, 29.75000000000000355 ) ) ;
#60589 = AXIS2_PLACEMENT_3D ( 'NONE', #3988, #18412, #44082 ) ;
#60590 = CARTESIAN_POINT ( 'NONE',  ( -15.48079246806219267, -11.37209801155882971, 32.91403422569032955 ) ) ;
#60591 = CARTESIAN_POINT ( 'NONE',  ( 12.23805353697412812, -3.019605429927184392, 32.48692288466676814 ) ) ;
#60592 = ORIENTED_EDGE ( 'NONE', *, *, #3523, .T. ) ;
#60593 = ORIENTED_EDGE ( 'NONE', *, *, #29659, .F. ) ;
#60594 = AXIS2_PLACEMENT_3D ( 'NONE', #78710, #52115, #72829 ) ;
#60596 = VERTEX_POINT ( 'NONE', #72642 ) ;
#60595 = CARTESIAN_POINT ( 'NONE',  ( 17.20771488474786892, -12.38066358083363738, 30.83685684665853444 ) ) ;
#60597 = DIRECTION ( 'NONE',  ( -0.000000000000000000, -0.9848077530122085754, -0.1736481776669273613 ) ) ;
#60598 = CARTESIAN_POINT ( 'NONE',  ( 6.673076923076925127, -7.500000000000001776, 34.75000000000000000 ) ) ;
#60599 = CARTESIAN_POINT ( 'NONE',  ( 3.750000000000009770, -9.053300858899081760, 22.04687500000000000 ) ) ;
#60600 = ORIENTED_EDGE ( 'NONE', *, *, #24683, .T. ) ;
#60601 = CARTESIAN_POINT ( 'NONE',  ( 7.911408985666682270, -4.320704448112861584, 33.92786785259548310 ) ) ;
#60602 = VERTEX_POINT ( 'NONE', #66779 ) ;
#60603 = CARTESIAN_POINT ( 'NONE',  ( -12.94230769230769162, -3.499999999999999556, 29.75000000000000355 ) ) ;
#60604 = CARTESIAN_POINT ( 'NONE',  ( 14.30769230769218581, -12.51329471203414379, 31.30864560766407578 ) ) ;
#60605 = B_SPLINE_CURVE_WITH_KNOTS ( 'NONE', 3,
 ( #57967, #36811, #49880, #22849, #50313, #29192, #1702, #44005, #3014, #42697 ),
 .UNSPECIFIED., .F., .F.,
 ( 4, 2, 2, 2, 4 ),
 ( 0.0007817246256747461966, 0.0009771112852218892010, 0.001172497944769032314, 0.001367884604316175427, 0.001563271263863318323 ),
 .UNSPECIFIED. ) ;
#60606 = CARTESIAN_POINT ( 'NONE',  ( -2.557692307692305267, -2.249999999999998668, 29.75000000000000355 ) ) ;
#60607 = DIRECTION ( 'NONE',  ( 1.000000000000000000, 0.000000000000000000, 0.000000000000000000 ) ) ;
#60608 = CARTESIAN_POINT ( 'NONE',  ( 2.544871794871792936, -7.500000000000000000, 29.75000000000000355 ) ) ;
#60609 = VERTEX_POINT ( 'NONE', #25347 ) ;
#60610 = CARTESIAN_POINT ( 'NONE',  ( 23.49999999999998579, -13.25000000000000178, 13.00000000000000178 ) ) ;
#60611 = DIRECTION ( 'NONE',  ( 1.000000000000000000, 0.000000000000000000, 0.000000000000000000 ) ) ;
#60612 = DIRECTION ( 'NONE',  ( -0.000000000000000000, -0.9848077530122086864, -0.1736481776669273613 ) ) ;
#60613 = VERTEX_POINT ( 'NONE', #25795 ) ;
#60614 = B_SPLINE_CURVE_WITH_KNOTS ( 'NONE', 3,
 ( #25977, #73281, #88599, #25538, #61090, #53441, #38607, #4827, #33628, #52552 ),
 .UNSPECIFIED., .F., .F.,
 ( 4, 2, 2, 2, 4 ),
 ( 0.000000000000000000, 0.0001954339857564054144, 0.0003908679715128108288, 0.0005863019572692162703, 0.0007817359430256216575 ),
 .UNSPECIFIED. ) ;
#60615 = AXIS2_PLACEMENT_3D ( 'NONE', #53637, #12657, #5902 ) ;
#60616 = DIRECTION ( 'NONE',  ( -0.000000000000000000, 0.5000000000000009992, -0.8660254037844380415 ) ) ;
#60617 = CARTESIAN_POINT ( 'NONE',  ( -3.930833309752758797, -10.01129605718032778, 34.36064277460058491 ) ) ;
#60618 = CARTESIAN_POINT ( 'NONE',  ( -16.28440606745951413, -2.254533558242299396, 29.97296025877828640 ) ) ;
#60619 = FACE_OUTER_BOUND ( 'NONE', #20502, .T. ) ;
#60620 = DIRECTION ( 'NONE',  ( -0.000000000000000000, 1.000000000000000000, 3.491481338843133355E-15 ) ) ;
#60621 = FACE_BOUND ( 'NONE', #75611, .T. ) ;
#60623 = DIRECTION ( 'NONE',  ( 1.000000000000000000, 0.000000000000000000, 0.000000000000000000 ) ) ;
#60622 = CARTESIAN_POINT ( 'NONE',  ( -7.146561847641256016, -12.47654668319379567, 31.42292124445336654 ) ) ;
#60624 = B_SPLINE_CURVE_WITH_KNOTS ( 'NONE', 3,
 ( #89176, #31658, #11839, #20257, #39314, #37971, #6731, #58673, #27456, #32537 ),
 .UNSPECIFIED., .F., .F.,
 ( 4, 2, 2, 2, 4 ),
 ( 0.0007817246256747484735, 0.0009771112852218931041, 0.001172497944769037735, 0.001367884604316182365, 0.001563271263863326996 ),
 .UNSPECIFIED. ) ;
#60625 = CARTESIAN_POINT ( 'NONE',  ( -15.09997878980228059, -4.684288915650983043, 34.18129842949671371 ) ) ;
#60627 = CARTESIAN_POINT ( 'NONE',  ( -9.692307692307691624, -10.51840700105979565, 33.73612834413961536 ) ) ;
#60626 = CARTESIAN_POINT ( 'NONE',  ( -8.519285250882624894, -11.86320923018887541, 32.19269448109604781 ) ) ;
#60628 = AXIS2_PLACEMENT_3D ( 'NONE', #76159, #7271, #13141 ) ;
#60629 = LINE ( 'NONE', #11119, #79316 ) ;
#60630 = CARTESIAN_POINT ( 'NONE',  ( 1.492201783934554493, -3.724691934501233703, 23.98250670625849068 ) ) ;
#60631 = ORIENTED_EDGE ( 'NONE', *, *, #10967, .F. ) ;
#60632 = CARTESIAN_POINT ( 'NONE',  ( -12.71153846153846345, -7.433932668274256805, 35.00000000000000711 ) ) ;
#60633 = ORIENTED_EDGE ( 'NONE', *, *, #70817, .T. ) ;
#60634 = CARTESIAN_POINT ( 'NONE',  ( 0.3962680155776852065, -6.879047030191174805, 34.71129190930000163 ) ) ;
#60635 = ORIENTED_EDGE ( 'NONE', *, *, #68694, .T. ) ;
#60636 = CARTESIAN_POINT ( 'NONE',  ( 7.912221179503920787, -9.905515769479276145, 34.41647553114623292 ) ) ;
#60637 = CARTESIAN_POINT ( 'NONE',  ( 2.307692307692186251, -12.16647553114689728, 32.15551576947799362 ) ) ;
#60639 = VERTEX_POINT ( 'NONE', #85724 ) ;
#60638 = LINE ( 'NONE', #52547, #33758 ) ;
#60640 = CARTESIAN_POINT ( 'NONE',  ( 17.07692307692307665, -12.62096338111211580, 30.90682066428153263 ) ) ;
#60641 = CARTESIAN_POINT ( 'NONE',  ( 5.076923076922953193, -12.16647553114689728, 32.15551576947799362 ) ) ;
#60642 = CARTESIAN_POINT ( 'NONE',  ( -1.614399933863656544, -3.775308065498769405, 23.82625670625849068 ) ) ;
#60643 = ADVANCED_FACE ( 'NONE', ( #86627 ), #17252, .F. ) ;
#60644 = CARTESIAN_POINT ( 'NONE',  ( 4.153846153846154188, -10.51840700105979565, 33.73612834413961536 ) ) ;
#60645 = CARTESIAN_POINT ( 'NONE',  ( 4.853996859406927378, -4.887634598454295265, 34.01352882383564946 ) ) ;
#60646 = CARTESIAN_POINT ( 'NONE',  ( 7.976679547917413515, -11.93748526763465279, 32.05452791011430946 ) ) ;
#60647 = DIRECTION ( 'NONE',  ( -1.000000000000000000, -0.000000000000000000, 0.000000000000000000 ) ) ;
#60648 = CARTESIAN_POINT ( 'NONE',  ( -1.161602540521988747, -6.460100341425561332, 34.89618726649961644 ) ) ;
#60649 = DIRECTION ( 'NONE',  ( -2.602085213965214586E-16, 1.000000000000000000, 0.000000000000000000 ) ) ;
#60650 = EDGE_CURVE ( 'NONE', #15793, #39836, #58236, .T. ) ;
#60651 = CARTESIAN_POINT ( 'NONE',  ( 3.775308065498752086, -6.007798216065404873, 18.39249329374151642 ) ) ;
#60652 = CARTESIAN_POINT ( 'NONE',  ( 2.980769230769232170, -7.433932668274255029, 35.00000000000000711 ) ) ;
#60653 = CARTESIAN_POINT ( 'NONE',  ( -11.28840722682322628, -10.66356715214248396, 33.62249196103329751 ) ) ;
#60654 = EDGE_LOOP ( 'NONE', ( #23050, #44771, #7627, #6790 ) ) ;
#60655 = CARTESIAN_POINT ( 'NONE',  ( 6.673076923076925127, -7.500000000000001776, 35.00000000000000000 ) ) ;
#60656 = FACE_OUTER_BOUND ( 'NONE', #83547, .T. ) ;
#60657 = CARTESIAN_POINT ( 'NONE',  ( 3.775308065498752086, -6.007798216065404873, 19.64249329374151642 ) ) ;
#60658 = AXIS2_PLACEMENT_3D ( 'NONE', #62923, #84558, #56185 ) ;
#60659 = EDGE_CURVE ( 'NONE', #73792, #52382, #87388, .T. ) ;
#60660 = DIRECTION ( 'NONE',  ( -0.000000000000000000, 0.9848077530122086864, -0.1736481776669273891 ) ) ;
#60661 = CARTESIAN_POINT ( 'NONE',  ( 5.207713517890026012, -6.369690395747422684, 34.87708834333098196 ) ) ;
#60662 = ORIENTED_EDGE ( 'NONE', *, *, #88611, .T. ) ;
#60663 = LINE ( 'NONE', #81399, #57217 ) ;
#60664 = CARTESIAN_POINT ( 'NONE',  ( 9.562159722575998444, -12.70455904226513866, 30.44083106164009322 ) ) ;
#60666 = ORIENTED_EDGE ( 'NONE', *, *, #75764, .T. ) ;
#60665 = CARTESIAN_POINT ( 'NONE',  ( 19.50000000000000000, -11.00000000000000000, 28.25000000000000000 ) ) ;
#60667 = DIRECTION ( 'NONE',  ( 0.000000000000000000, 0.000000000000000000, 1.000000000000000000 ) ) ;
#60668 = EDGE_CURVE ( 'NONE', #49648, #32624, #80755, .T. ) ;
#60669 = CARTESIAN_POINT ( 'NONE',  ( 15.23076923076910916, -5.941354392335915335, 34.76329471203413846 ) ) ;
#60670 = VECTOR ( 'NONE', #37502, 1000.000000000000000 ) ;
#60671 = B_SPLINE_CURVE_WITH_KNOTS ( 'NONE', 3,
 ( #48369, #25558, #60222, #80965, #46716, #75848, #69092, #7399, #34855, #30319 ),
 .UNSPECIFIED., .F., .F.,
 ( 4, 2, 2, 2, 4 ),
 ( 0.000000000000000000, 0.0001954339857564078809, 0.0003908679715128157619, 0.0005863019572692236428, 0.0007817359430256315238 ),
 .UNSPECIFIED. ) ;
#60672 = B_SPLINE_CURVE_WITH_KNOTS ( 'NONE', 3,
 ( #59381, #86884, #73344, #78759, #10307, #3538 ),
 .UNSPECIFIED., .F., .F.,
 ( 4, 2, 4 ),
 ( 0.000000000000000000, 0.0001954784845028908113, 0.0003909569690057816227 ),
 .UNSPECIFIED. ) ;
#60673 = LINE ( 'NONE', #18809, #14105 ) ;
#60674 = VERTEX_POINT ( 'NONE', #18599 ) ;
#60675 = DIRECTION ( 'NONE',  ( 0.000000000000000000, 0.7660444431189822323, -0.6427876096865344779 ) ) ;
#60676 = CARTESIAN_POINT ( 'NONE',  ( -13.45069879557126669, -11.69971097300155272, 32.46337939537587403 ) ) ;
#60677 = DIRECTION ( 'NONE',  ( -0.000000000000000000, 1.000000000000000000, -0.000000000000000000 ) ) ;
#60678 = EDGE_CURVE ( 'NONE', #32941, #57045, #35848, .T. ) ;
#60679 = ORIENTED_EDGE ( 'NONE', *, *, #32625, .T. ) ;
#60680 = ORIENTED_EDGE ( 'NONE', *, *, #25204, .T. ) ;
#60681 = EDGE_LOOP ( 'NONE', ( #7705, #386 ) ) ;
#60682 = EDGE_LOOP ( 'NONE', ( #37302, #54324, #10435, #62731 ) ) ;
#60683 = CARTESIAN_POINT ( 'NONE',  ( -9.822454901745910405, -2.882441371585227508, 31.66841991370172238 ) ) ;
#60684 = CARTESIAN_POINT ( 'NONE',  ( -2.057637996053991447, -5.728107161865378494, 34.42597550085002922 ) ) ;
#60685 = CARTESIAN_POINT ( 'NONE',  ( -7.911423846710166075, -12.70778746994557551, 30.41441678777548319 ) ) ;
#60686 = CARTESIAN_POINT ( 'NONE',  ( 9.320512820512821150, -4.000000000000000000, 28.25000000000000000 ) ) ;
#60687 = CARTESIAN_POINT ( 'NONE',  ( -16.82697755857493505, -5.057305518903949526, 34.11320923018887896 ) ) ;
#60688 = ORIENTED_EDGE ( 'NONE', *, *, #23816, .T. ) ;
#60689 = ADVANCED_FACE ( 'NONE', ( #65876 ), #43215, .F. ) ;
#60690 = EDGE_LOOP ( 'NONE', ( #15507, #7205 ) ) ;
#60691 = ORIENTED_EDGE ( 'NONE', *, *, #13046, .T. ) ;
#60694 = VERTEX_POINT ( 'NONE', #29709 ) ;
#60693 = EDGE_CURVE ( 'NONE', #43000, #42649, #23373, .T. ) ;
#60692 = CARTESIAN_POINT ( 'NONE',  ( -13.38461538461538325, -11.69971097300155272, 32.46337939537588113 ) ) ;
#60695 = FACE_OUTER_BOUND ( 'NONE', #29803, .T. ) ;
#60696 = LINE ( 'NONE', #88205, #83949 ) ;
#60697 = EDGE_CURVE ( 'NONE', #16683, #32754, #3984, .T. ) ;
#60698 = EDGE_CURVE ( 'NONE', #51973, #20058, #20680, .T. ) ;
#60699 = B_SPLINE_CURVE_WITH_KNOTS ( 'NONE', 3,
 ( #54050, #32457, #59926, #39680, #27034, #45965 ),
 .UNSPECIFIED., .F., .F.,
 ( 4, 2, 4 ),
 ( 1.084202172485504434E-19, 0.0001954784845028911637, 0.0003909569690057822190 ),
 .UNSPECIFIED. ) ;
#60700 = DIRECTION ( 'NONE',  ( 1.000000000000000000, 0.000000000000000000, 0.000000000000000000 ) ) ;
#60701 = CARTESIAN_POINT ( 'NONE',  ( -5.749945688361685292, -4.235687564193446164, 33.53795663066793509 ) ) ;
#60702 = ORIENTED_EDGE ( 'NONE', *, *, #86940, .T. ) ;
#60703 = VERTEX_POINT ( 'NONE', #37328 ) ;
#60704 = ORIENTED_EDGE ( 'NONE', *, *, #80829, .F. ) ;
#60705 = CARTESIAN_POINT ( 'NONE',  ( 14.53070515178570332, -10.77377354290276124, 33.85451476688484718 ) ) ;
#60707 = VERTEX_POINT ( 'NONE', #56727 ) ;
#60706 = CARTESIAN_POINT ( 'NONE',  ( -2.307692307692305711, -2.721908614388771852, 31.22303859784724978 ) ) ;
#60708 = CARTESIAN_POINT ( 'NONE',  ( 3.100622021331010725, -11.93770438780619259, 32.05411857736982029 ) ) ;
#60709 = B_SPLINE_CURVE_WITH_KNOTS ( 'NONE', 3,
 ( #738, #19679, #26884, #14253, #67427, #41732, #28200, #40845, #68311, #55671 ),
 .UNSPECIFIED., .F., .F.,
 ( 4, 2, 2, 2, 4 ),
 ( 0.0007817246256747525934, 0.0009771112852218970073, 0.001172497944769041204, 0.001367884604316185401, 0.001563271263863329815 ),
 .UNSPECIFIED. ) ;
#60710 = FACE_OUTER_BOUND ( 'NONE', #47627, .T. ) ;
#60711 = ORIENTED_EDGE ( 'NONE', *, *, #6420, .T. ) ;
#60712 = CARTESIAN_POINT ( 'NONE',  ( -11.28840711854808632, -4.074993327901527351, 33.72946981652012255 ) ) ;
#60713 = CARTESIAN_POINT ( 'NONE',  ( 8.900022577055556994, -12.38066358083363738, 30.83685684665853444 ) ) ;
#60714 = CARTESIAN_POINT ( 'NONE',  ( 0.2115152373170033906, -9.356822207818506598, 34.66110646841856635 ) ) ;
#60715 = FACE_BOUND ( 'NONE', #45647, .T. ) ;
#60716 = CARTESIAN_POINT ( 'NONE',  ( -15.45425415533356350, -8.539481045369596401, 34.89627647299170832 ) ) ;
#60717 = CARTESIAN_POINT ( 'NONE',  ( -1.253823576790597638, -11.71459661697925903, 32.44059661609676937 ) ) ;
#60718 = AXIS2_PLACEMENT_3D ( 'NONE', #72809, #44889, #37695 ) ;
#60719 = DIRECTION ( 'NONE',  ( -0.000000000000000000, -0.8660254037844399289, -0.4999999999999980016 ) ) ;
#60721 = CARTESIAN_POINT ( 'NONE',  ( 6.699591998512590685, -10.97335522853832579, 33.68706563782419749 ) ) ;
#60720 = DIRECTION ( 'NONE',  ( -0.000000000000000000, 0.3420201433256694901, -0.9396926207859082059 ) ) ;
#60722 = VECTOR ( 'NONE', #72864, 1000.000000000000000 ) ;
#60723 = DIRECTION ( 'NONE',  ( 0.000000000000000000, 0.000000000000000000, 1.000000000000000000 ) ) ;
#60724 = DIRECTION ( 'NONE',  ( 0.000000000000000000, 0.8660254037844377084, 0.5000000000000015543 ) ) ;
#60725 = ORIENTED_EDGE ( 'NONE', *, *, #64523, .T. ) ;
#60726 = CARTESIAN_POINT ( 'NONE',  ( -16.37667284632515674, -7.369208160676171460, 34.74850200257122879 ) ) ;
#60727 = DIRECTION ( 'NONE',  ( 0.000000000000000000, 0.1736481776669275834, 0.9848077530122086864 ) ) ;
#60728 = ORIENTED_EDGE ( 'NONE', *, *, #88529, .T. ) ;
#60729 = VERTEX_POINT ( 'NONE', #15752 ) ;
#60730 = CYLINDRICAL_SURFACE ( 'NONE', #69376, 0.2499999999999997502 ) ;
#60731 = CARTESIAN_POINT ( 'NONE',  ( 16.08857615328984281, -2.379036618887870436, 30.90682066428148644 ) ) ;
#60732 = CARTESIAN_POINT ( 'NONE',  ( -14.98076923076916778, -7.434744429011176159, 34.75000000000000711 ) ) ;
#60733 = ORIENTED_EDGE ( 'NONE', *, *, #31684, .T. ) ;
#60734 = EDGE_CURVE ( 'NONE', #8309, #68985, #22498, .T. ) ;
#60735 = CARTESIAN_POINT ( 'NONE',  ( -15.90379184220783948, -11.28795663066794575, 33.01431243580653785 ) ) ;
#60736 = CARTESIAN_POINT ( 'NONE',  ( 3.512820512820510555, -7.500000000000000000, 33.75000000000000000 ) ) ;
#60737 = FACE_BOUND ( 'NONE', #25350, .T. ) ;
#60739 = CARTESIAN_POINT ( 'NONE',  ( 5.934729999443682402, -6.835583212224499938, 34.95778746994557906 ) ) ;
#60738 = CARTESIAN_POINT ( 'NONE',  ( -14.53117723225664015, -4.225889041578353655, 33.85425143139329407 ) ) ;
#60740 = CARTESIAN_POINT ( 'NONE',  ( 8.069165197766697162, -9.086983370893049639, 34.49168942202179267 ) ) ;
#60741 = CARTESIAN_POINT ( 'NONE',  ( 2.438484115517094430, -4.809403383903226192, 33.96459661697924304 ) ) ;
#60743 = CARTESIAN_POINT ( 'NONE',  ( -14.55769230769230660, -7.500000000000001776, 35.00000000000000000 ) ) ;
#60742 = DIRECTION ( 'NONE',  ( 1.000000000000000000, 0.000000000000000000, 0.000000000000000000 ) ) ;
#60744 =( REPRESENTATION_RELATIONSHIP ('NONE','NONE', #51743, #11000 ) REPRESENTATION_RELATIONSHIP_WITH_TRANSFORMATION ( #31605 )SHAPE_REPRESENTATION_RELATIONSHIP( ) );
#60745 = CARTESIAN_POINT ( 'NONE',  ( 1.553300858899129944, -11.24999999999998934, 22.20312500000000000 ) ) ;
#60746 = ORIENTED_EDGE ( 'NONE', *, *, #82400, .T. ) ;
#60747 = ORIENTED_EDGE ( 'NONE', *, *, #1187, .F. ) ;
#60748 = CARTESIAN_POINT ( 'NONE',  ( 4.946232473812770536, -10.70098750199973203, 33.91152734681376302 ) ) ;
#60749 = CARTESIAN_POINT ( 'NONE',  ( -4.219929564802033184, -12.37446782046654192, 30.86335684631486487 ) ) ;
#60750 = FACE_OUTER_BOUND ( 'NONE', #13633, .T. ) ;
#60751 = CARTESIAN_POINT ( 'NONE',  ( 17.07692307692339284, -2.255955759149395501, 30.00000000000324363 ) ) ;
#60752 = CARTESIAN_POINT ( 'NONE',  ( 5.076923076923075762, -1.466349020453238561, 30.81389545987213907 ) ) ;
#60753 = CARTESIAN_POINT ( 'NONE',  ( -3.749999999999988454, -9.053300858899127945, 23.76562499999999645 ) ) ;
#60754 = EDGE_CURVE ( 'NONE', #73212, #52584, #72007, .T. ) ;
#60755 = CARTESIAN_POINT ( 'NONE',  ( -1.515305987725693138, -3.957541250942359756, 33.62499894934981626 ) ) ;
#60756 = FACE_OUTER_BOUND ( 'NONE', #61735, .T. ) ;
#60757 = LINE ( 'NONE', #79705, #77523 ) ;
#60758 = CARTESIAN_POINT ( 'NONE',  ( -0.4615384615384611200, -13.63283147151868846, 33.57946703557072254 ) ) ;
#60759 = CARTESIAN_POINT ( 'NONE',  ( -6.250023237292966272, -2.823816976329319495, 31.52131813110795733 ) ) ;
#60760 = FACE_OUTER_BOUND ( 'NONE', #56074, .T. ) ;
#60761 = AXIS2_PLACEMENT_3D ( 'NONE', #41820, #70610, #20648 ) ;
#60762 = DIRECTION ( 'NONE',  ( 1.000000000000000000, 0.000000000000000000, 0.000000000000000000 ) ) ;
#60763 = CARTESIAN_POINT ( 'NONE',  ( -6.923076923077045919, -3.643525952248796163, 33.31231777344771672 ) ) ;
#60764 = CARTESIAN_POINT ( 'NONE',  ( -7.780898274877819709, -12.46129190930001052, 30.37095296980870174 ) ) ;
#60765 = ORIENTED_EDGE ( 'NONE', *, *, #57563, .T. ) ;
#60766 = CARTESIAN_POINT ( 'NONE',  ( 1.134638653673031738, -2.564618984488975961, 30.55390908950641915 ) ) ;
#60767 = CARTESIAN_POINT ( 'NONE',  ( -17.29985003582992320, -6.459968553980840689, 34.89616026154728701 ) ) ;
#60768 = B_SPLINE_CURVE_WITH_KNOTS ( 'NONE', 3,
 ( #54318, #33619, #67402, #52984, #80482, #32723, #45792, #18329, #60634, #53432 ),
 .UNSPECIFIED., .F., .F.,
 ( 4, 2, 2, 2, 4 ),
 ( 0.000000000000000000, 0.0001954339857564076099, 0.0003908679715128152198, 0.0005863019572692228839, 0.0007817359430256304396 ),
 .UNSPECIFIED. ) ;
#60769 = CARTESIAN_POINT ( 'NONE',  ( 2.775308065498755195, -6.422011778438505125, 14.64249329374151110 ) ) ;
#60770 = EDGE_CURVE ( 'NONE', #72857, #37303, #81957, .T. ) ;
#60771 = CARTESIAN_POINT ( 'NONE',  ( -27.00000000000000000, 0.7500000000000061062, 23.75000000000000000 ) ) ;
#60772 = CYLINDRICAL_SURFACE ( 'NONE', #41242, 0.2500000000000008882 ) ;
#60773 = LINE ( 'NONE', #5839, #6866 ) ;
#60775 = ORIENTED_EDGE ( 'NONE', *, *, #54293, .F. ) ;
#60774 = CARTESIAN_POINT ( 'NONE',  ( 20.74999999999998224, -12.50000000000000000, 27.25000000000000000 ) ) ;
#60776 = CARTESIAN_POINT ( 'NONE',  ( 1.944543648262996083, -5.555456351736983045, 21.81250000000000000 ) ) ;
#60777 = CARTESIAN_POINT ( 'NONE',  ( -14.37377468705243722, -5.471508081941602875, 34.59228464037088457 ) ) ;
#60778 = EDGE_CURVE ( 'NONE', #275, #62404, #29306, .T. ) ;
#60779 = ORIENTED_EDGE ( 'NONE', *, *, #34103, .T. ) ;
#60780 = CARTESIAN_POINT ( 'NONE',  ( -11.28846153846152589, -2.249999999999999112, 29.81603969181031744 ) ) ;
#60781 = CARTESIAN_POINT ( 'NONE',  ( -2.307692307692305711, -2.538708090699994813, 30.37095296980875503 ) ) ;
#60782 = EDGE_LOOP ( 'NONE', ( #87639, #52886 ) ) ;
#60783 = CARTESIAN_POINT ( 'NONE',  ( 14.08420736396836226, -2.599994579823202923, 30.74605699353653776 ) ) ;
#60784 = DIRECTION ( 'NONE',  ( -1.000000000000000000, -0.000000000000000000, -0.000000000000000000 ) ) ;
#60785 = CARTESIAN_POINT ( 'NONE',  ( -20.74999999999999289, -7.500000000000000000, 29.75000000000000355 ) ) ;
#60786 = ADVANCED_FACE ( 'NONE', ( #71120 ), #36891, .F. ) ;
#60787 = VERTEX_POINT ( 'NONE', #2650 ) ;
#60788 = ORIENTED_EDGE ( 'NONE', *, *, #32069, .T. ) ;
#60789 = VECTOR ( 'NONE', #61745, 1000.000000000000000 ) ;
#60790 = ORIENTED_EDGE ( 'NONE', *, *, #55943, .F. ) ;
#60791 = ADVANCED_FACE ( 'NONE', ( #57610 ), #64794, .F. ) ;
#60792 = CARTESIAN_POINT ( 'NONE',  ( -8.096130590202436750, -2.318417181685855422, 30.59732222474233865 ) ) ;
#60793 = CARTESIAN_POINT ( 'NONE',  ( -0.3962828902624368488, -10.90142922261932057, 33.41473453929631887 ) ) ;
#60794 = CARTESIAN_POINT ( 'NONE',  ( 9.562159722575998444, -3.069018819979302926, 32.56621877034667278 ) ) ;
#60795 = CARTESIAN_POINT ( 'NONE',  ( -17.32694631421604115, -5.851115903089112003, 34.47074536777953568 ) ) ;
#60796 = ADVANCED_FACE ( 'NONE', ( #31014 ), #72449, .F. ) ;
#60797 = CARTESIAN_POINT ( 'NONE',  ( 9.692307692307572609, -9.442884908241554243, 34.35708131394783038 ) ) ;
#60798 = CARTESIAN_POINT ( 'NONE',  ( 6.988332062589762472, -8.656820664281605460, 34.87096338111211224 ) ) ;
#60799 = LINE ( 'NONE', #79302, #56723 ) ;
#60800 = VECTOR ( 'NONE', #30226, 1000.000000000000000 ) ;
#60801 = CYLINDRICAL_SURFACE ( 'NONE', #1762, 0.2500000000000002220 ) ;
#60802 = ADVANCED_FACE ( 'NONE', ( #19739 ), #32366, .F. ) ;
#60803 = ORIENTED_EDGE ( 'NONE', *, *, #83293, .F. ) ;
#60804 = B_SPLINE_CURVE_WITH_KNOTS ( 'NONE', 3,
 ( #7039, #51427, #37950, #25326, #58208, #44685, #86600, #87050, #80278, #64508 ),
 .UNSPECIFIED., .F., .F.,
 ( 4, 2, 2, 2, 4 ),
 ( 0.000000000000000000, 0.0001954311564186869015, 0.0003908623128373738030, 0.0005862934692560607588, 0.0007817246256747476061 ),
 .UNSPECIFIED. ) ;
#60805 = EDGE_LOOP ( 'NONE', ( #82486, #18830, #4879, #54428 ) ) ;
#60807 = ORIENTED_EDGE ( 'NONE', *, *, #83019, .T. ) ;
#60806 = CARTESIAN_POINT ( 'NONE',  ( 7.145856592054990131, -12.69155399931963046, 30.53255429739158444 ) ) ;
#60808 = EDGE_CURVE ( 'NONE', #64117, #44046, #86442, .T. ) ;
#60809 = EDGE_CURVE ( 'NONE', #3657, #69245, #4560, .T. ) ;
#60810 = CARTESIAN_POINT ( 'NONE',  ( -8.519285359852727169, -10.92531984108285670, 33.72920026020278073 ) ) ;
#60811 = CARTESIAN_POINT ( 'NONE',  ( 12.59206416330202494, -3.285477652293413264, 32.44071101563363158 ) ) ;
#60812 = EDGE_LOOP ( 'NONE', ( #1765, #22622 ) ) ;
#60813 = CARTESIAN_POINT ( 'NONE',  ( -14.05774678934416499, -4.336752205174649433, 33.62275283266504289 ) ) ;
#60814 = AXIS2_PLACEMENT_3D ( 'NONE', #9175, #83950, #29883 ) ;
#60815 = VERTEX_POINT ( 'NONE', #19297 ) ;
#60816 = CARTESIAN_POINT ( 'NONE',  ( 11.76147289007438523, -2.554770724473668153, 30.48948780036025852 ) ) ;
#60817 = EDGE_LOOP ( 'NONE', ( #43635, #51591, #37700, #70359 ) ) ;
#60818 = AXIS2_PLACEMENT_3D ( 'NONE', #84709, #21660, #77487 ) ;
#60819 = CARTESIAN_POINT ( 'NONE',  ( -18.13069060311030967, -9.084618155246140248, 34.75535874321725771 ) ) ;
#60820 = CARTESIAN_POINT ( 'NONE',  ( -12.33074802057151409, -9.929761469519743144, 34.40412654351204225 ) ) ;
#60821 = EDGE_CURVE ( 'NONE', #59736, #26488, #45389, .T. ) ;
#60822 = CARTESIAN_POINT ( 'NONE',  ( 10.86543892702293057, -4.943051570960394159, 34.04725096376909477 ) ) ;
#60823 = FACE_BOUND ( 'NONE', #82095, .T. ) ;
#60824 = DIRECTION ( 'NONE',  ( 0.000000000000000000, 0.4999999999999985567, 0.8660254037844395958 ) ) ;
#60825 = CARTESIAN_POINT ( 'NONE',  ( -7.846153846153844924, -4.945431358278436385, 36.03766855953609394 ) ) ;
#60826 = CARTESIAN_POINT ( 'NONE',  ( -4.230769230769230838, -7.500000000000000000, 29.75000000000000355 ) ) ;
#60827 = CARTESIAN_POINT ( 'NONE',  ( -5.749999999999999112, -2.499999999999998668, 29.75000000000000355 ) ) ;
#60828 = ADVANCED_FACE ( 'NONE', ( #87330 ), #80569, .F. ) ;
#60829 = CARTESIAN_POINT ( 'NONE',  ( 10.86538461538605205, -7.500000000000155431, 34.75000000000007105 ) ) ;
#60830 = CARTESIAN_POINT ( 'NONE',  ( 15.90386942290380290, -4.236021600441997492, 33.53823185664189310 ) ) ;
#60831 = CARTESIAN_POINT ( 'NONE',  ( -11.66915214157184622, -3.338472653186243644, 32.95098750199972670 ) ) ;
#60832 = ORIENTED_EDGE ( 'NONE', *, *, #54286, .T. ) ;
#60833 = VERTEX_POINT ( 'NONE', #47200 ) ;
#60835 = CARTESIAN_POINT ( 'NONE',  ( -14.05774678934416499, -12.43552623307873972, 30.55307653245132826 ) ) ;
#60834 = DIRECTION ( 'NONE',  ( -0.000000000000000000, 0.6427876096865404731, -0.7660444431189771253 ) ) ;
#60836 = LINE ( 'NONE', #74810, #11136 ) ;
#60838 = B_SPLINE_CURVE_WITH_KNOTS ( 'NONE', 3,
 ( #23575, #15503, #43848, #57805, #58245, #43417, #36221, #64111, #63676, #2409 ),
 .UNSPECIFIED., .F., .F.,
 ( 4, 2, 2, 2, 4 ),
 ( 0.0007817246256747447872, 0.0009771112852218874663, 0.001172497944769030362, 0.001367884604316173258, 0.001563271263863315937 ),
 .UNSPECIFIED. ) ;
#60837 = CARTESIAN_POINT ( 'NONE',  ( -4.088591014333315066, -9.528491918058460186, 34.59228464037085615 ) ) ;
#60839 = DIRECTION ( 'NONE',  ( 0.000000000000000000, -1.000000000000000000, 0.000000000000000000 ) ) ;
#60840 = CARTESIAN_POINT ( 'NONE',  ( 1.634560793993430350, -4.176053281294515251, 33.81426240980091791 ) ) ;
#60841 = VERTEX_POINT ( 'NONE', #12983 ) ;
#60842 = ADVANCED_FACE ( 'NONE', ( #31926 ), #74242, .F. ) ;
#60843 = CARTESIAN_POINT ( 'NONE',  ( -13.38461538461538325, -1.951392089020283160, 34.73218667398347748 ) ) ;
#60844 = PLANE ( 'NONE',  #73271 ) ;
#60845 = CARTESIAN_POINT ( 'NONE',  ( 16.85399611801622655, -4.026226216239093603, 33.68668979543632958 ) ) ;
#60846 = CARTESIAN_POINT ( 'NONE',  ( -7.146003881983771677, -6.459968553980839800, 34.89616026154728701 ) ) ;
#60847 = ORIENTED_EDGE ( 'NONE', *, *, #66974, .T. ) ;
#60848 = EDGE_CURVE ( 'NONE', #81591, #36076, #79865, .T. ) ;
#60849 = ORIENTED_EDGE ( 'NONE', *, *, #88439, .F. ) ;
#60850 = ITEM_DEFINED_TRANSFORMATION ( 'NONE', 'NONE', #17351,  #83448 ) ;
#60852 = EDGE_CURVE ( 'NONE', #85711, #40118, #50804, .T. ) ;
#60851 = ORIENTED_EDGE ( 'NONE', *, *, #83977, .T. ) ;
#60853 = CIRCLE ( 'NONE', #59494, 0.2500000000000002220 ) ;
#60854 = CARTESIAN_POINT ( 'NONE',  ( 15.29683758177167086, -6.386643153685127139, 34.62446782046654192 ) ) ;
#60855 = ORIENTED_EDGE ( 'NONE', *, *, #10671, .F. ) ;
#60856 = LINE ( 'NONE', #19871, #5048 ) ;
#60857 = DIRECTION ( 'NONE',  ( -0.000000000000000000, 1.000000000000000000, -0.000000000000000000 ) ) ;
#60858 = CARTESIAN_POINT ( 'NONE',  ( -5.299849294439221481, -4.186968288167446595, 33.49512374952580274 ) ) ;
#60859 = CARTESIAN_POINT ( 'NONE',  ( 11.53846153846153832, -1.215029322943914858, 32.30358669280327177 ) ) ;
#60860 = VECTOR ( 'NONE', #19925, 1000.000000000000000 ) ;
#60861 = EDGE_CURVE ( 'NONE', #76945, #84175, #73806, .T. ) ;
#60862 = CARTESIAN_POINT ( 'NONE',  ( -1.384615384615383471, -8.564572088678739092, 35.78748833219616898 ) ) ;
#60863 = ORIENTED_EDGE ( 'NONE', *, *, #14535, .T. ) ;
#60864 = CARTESIAN_POINT ( 'NONE',  ( 22.75000000000000000, -4.499999999999999112, 27.25000000000000000 ) ) ;
#60866 = ORIENTED_EDGE ( 'NONE', *, *, #54818, .F. ) ;
#60865 = CARTESIAN_POINT ( 'NONE',  ( -0.2387587925603967820, -12.11081565061823717, 32.26097654155341843 ) ) ;
#60867 = CARTESIAN_POINT ( 'NONE',  ( -4.000000000000002665, 7.500000000000000000, 13.50000000000000178 ) ) ;
#60868 = CARTESIAN_POINT ( 'NONE',  ( 16.15384615384645883, -2.506253911140615021, 30.00000000000323297 ) ) ;
#60869 = CARTESIAN_POINT ( 'NONE',  ( 1.634615384615323075, -7.565270445406050648, 34.75000000000000000 ) ) ;
#60870 = DIRECTION ( 'NONE',  ( -0.000000000000000000, -0.1736481776669307198, -0.9848077530122080203 ) ) ;
#60871 = CARTESIAN_POINT ( 'NONE',  ( -6.000000000000121680, -11.06231777344772027, 33.60647404775119895 ) ) ;
#60872 = CARTESIAN_POINT ( 'NONE',  ( -8.769230769230768274, -9.058645607665452459, 34.76329471203371924 ) ) ;
#60873 = CARTESIAN_POINT ( 'NONE',  ( -0.5922299282060203840, -12.38065189839062263, 30.83690757178629482 ) ) ;
#60874 = CARTESIAN_POINT ( 'NONE',  ( 2.724691934501250135, -8.700186371490531201, 21.04874329374151642 ) ) ;
#60875 = ORIENTED_EDGE ( 'NONE', *, *, #13069, .F. ) ;
#60876 = DIRECTION ( 'NONE',  ( 1.000000000000000000, 0.000000000000000000, 0.000000000000000000 ) ) ;
#60877 = CARTESIAN_POINT ( 'NONE',  ( 12.59206389977210705, -5.070358843744210198, 34.40418822224088302 ) ) ;
#60878 = ORIENTED_EDGE ( 'NONE', *, *, #24995, .F. ) ;
#60879 = VERTEX_POINT ( 'NONE', #61154 ) ;
#60880 = CARTESIAN_POINT ( 'NONE',  ( 7.976944287120795174, -11.93129842949671726, 32.56571108434900452 ) ) ;
#60881 = CARTESIAN_POINT ( 'NONE',  ( -3.230769230769351186, -6.026961402154118908, 34.52809138561165270 ) ) ;
#60882 = B_SPLINE_CURVE_WITH_KNOTS ( 'NONE', 3,
 ( #63179, #62730, #55983, #42483, #55539, #47895, #34381, #7804, #1492, #28978 ),
 .UNSPECIFIED., .F., .F.,
 ( 4, 2, 2, 2, 4 ),
 ( 0.0007817246256747448956, 0.0009771112852218876831, 0.001172497944769030362, 0.001367884604316173258, 0.001563271263863315937 ),
 .UNSPECIFIED. ) ;
#60883 = EDGE_CURVE ( 'NONE', #45658, #36243, #88666, .T. ) ;
#60884 = DIRECTION ( 'NONE',  ( 0.000000000000000000, 0.000000000000000000, -1.000000000000000000 ) ) ;
#60885 = CARTESIAN_POINT ( 'NONE',  ( -5.076923076922769340, -2.506253911140614576, 30.00000000000323297 ) ) ;
#60886 = CIRCLE ( 'NONE', #32151, 0.2500000000000002220 ) ;
#60887 = CARTESIAN_POINT ( 'NONE',  ( 0.7115928814519132395, -2.318338780012835443, 30.59689888758630261 ) ) ;
#60888 = ORIENTED_EDGE ( 'NONE', *, *, #71630, .F. ) ;
#60889 = CARTESIAN_POINT ( 'NONE',  ( 9.561616225640134914, -10.54014554554150607, 33.71984207302941883 ) ) ;
#60890 = CARTESIAN_POINT ( 'NONE',  ( 17.29970261819148902, -5.913360116392396115, 34.49180327182771322 ) ) ;
#60891 = FACE_OUTER_BOUND ( 'NONE', #11377, .T. ) ;
#60892 = ORIENTED_EDGE ( 'NONE', *, *, #64573, .T. ) ;
#60893 = LINE ( 'NONE', #13596, #9644 ) ;
#60894 = ORIENTED_EDGE ( 'NONE', *, *, #44686, .F. ) ;
#60895 = DIRECTION ( 'NONE',  ( -1.000000000000000000, 0.000000000000000000, -0.000000000000000000 ) ) ;
#60896 = SHAPE_REPRESENTATION_RELATIONSHIP ( 'NONE' , 'NONE' ,  #11000, #37432 ) ;
#60897 = DIRECTION ( 'NONE',  ( 0.000000000000000000, 0.6427876096865368094, 0.7660444431189802339 ) ) ;
#60898 = VERTEX_POINT ( 'NONE', #28258 ) ;
#60899 = CARTESIAN_POINT ( 'NONE',  ( 3.230769230769110045, -12.27809138561165270, 31.22303859784587132 ) ) ;
#60900 = CARTESIAN_POINT ( 'NONE',  ( -11.53846153846165912, -12.46129190930018460, 30.37095296980731973 ) ) ;
#60901 = CARTESIAN_POINT ( 'NONE',  ( -9.942330929600657896, -2.587272538249755893, 30.68239716806877837 ) ) ;
#60902 = CARTESIAN_POINT ( 'NONE',  ( 2.307692307692186251, -4.320704448113951379, 33.92786785259630022 ) ) ;
#60903 = DIRECTION ( 'NONE',  ( -0.000000000000000000, 0.1736481776669307198, -0.9848077530122080203 ) ) ;
#60904 = ORIENTED_EDGE ( 'NONE', *, *, #72083, .F. ) ;
#60905 = CARTESIAN_POINT ( 'NONE',  ( 2.307692307692309264, -12.78798330534102945, 29.74999999999997868 ) ) ;
#60906 = ORIENTED_EDGE ( 'NONE', *, *, #17840, .F. ) ;
#60907 = B_SPLINE_CURVE_WITH_KNOTS ( 'NONE', 3,
 ( #6826, #5955, #82060, #34299, #60441, #81612, #54119, #77, #87958, #47367 ),
 .UNSPECIFIED., .F., .F.,
 ( 4, 2, 2, 2, 4 ),
 ( 0.000000000000000000, 0.0001954311564186867389, 0.0003908623128373734778, 0.0005862934692560602167, 0.0007817246256747469556 ),
 .UNSPECIFIED. ) ;
#60908 = CARTESIAN_POINT ( 'NONE',  ( 6.923076923076924238, -1.044019251281081972, 31.83374038241031911 ) ) ;
#60909 = CIRCLE ( 'NONE', #46516, 0.2500000000000002220 ) ;
#60910 = LINE ( 'NONE', #26686, #43430 ) ;
#60911 = ADVANCED_FACE ( 'NONE', ( #21052 ), #55729, .F. ) ;
#60912 = VECTOR ( 'NONE', #84546, 1000.000000000000227 ) ;
#60913 = CARTESIAN_POINT ( 'NONE',  ( -18.06608237936013239, -10.67929555188718460, 33.92786785259543336 ) ) ;
#60914 = ADVANCED_FACE ( 'NONE', ( #49427 ), #8000, .F. ) ;
#60915 = CARTESIAN_POINT ( 'NONE',  ( 5.999999999999878320, -12.70778746994576025, 30.41441678777401236 ) ) ;
#60916 = CARTESIAN_POINT ( 'NONE',  ( 7.173131234715239835, -9.943054286541403997, 34.11300777759954883 ) ) ;
#60917 = EDGE_LOOP ( 'NONE', ( #59359, #8915 ) ) ;
#60919 = ADVANCED_FACE ( 'NONE', ( #357 ), #48980, .F. ) ;
#60918 = EDGE_LOOP ( 'NONE', ( #40768, #18460, #6403, #30783 ) ) ;
#60920 = VERTEX_POINT ( 'NONE', #20188 ) ;
#60921 = EDGE_LOOP ( 'NONE', ( #34628, #20060, #14856, #64193 ) ) ;
#60922 = DIRECTION ( 'NONE',  ( -1.000000000000000000, -0.000000000000000000, -0.000000000000000000 ) ) ;
#60923 = CARTESIAN_POINT ( 'NONE',  ( 15.16549923021291058, -3.643525952247789412, 33.31231777344662959 ) ) ;
#60924 = EDGE_CURVE ( 'NONE', #20422, #71376, #47653, .T. ) ;
#60925 = CARTESIAN_POINT ( 'NONE',  ( -11.53846153846153655, -5.471508081941601098, 34.59228464037088457 ) ) ;
#60926 = CARTESIAN_POINT ( 'NONE',  ( -7.912236225513978205, -3.322132147404559532, 32.92929555188719348 ) ) ;
#60927 = CARTESIAN_POINT ( 'NONE',  ( -5.326899807865431491, -10.66389620160130036, 33.62221079203477103 ) ) ;
#60928 = B_SPLINE_CURVE_WITH_KNOTS ( 'NONE', 3,
 ( #250, #27275, #81789, #76345, #47539, #61057, #75031, #47982, #14652, #69591 ),
 .UNSPECIFIED., .F., .F.,
 ( 4, 2, 2, 2, 4 ),
 ( 0.000000000000000000, 0.0001954311564186862239, 0.0003908623128373724478, 0.0005862934692560586988, 0.0007817246256747448956 ),
 .UNSPECIFIED. ) ;
#60929 = CARTESIAN_POINT ( 'NONE',  ( 4.153846153846154188, -2.499999999999998668, 29.75000000000001421 ) ) ;
#60930 = CARTESIAN_POINT ( 'NONE',  ( -5.010854725920638408, -4.098570777380720287, 33.41473453929635440 ) ) ;
#60931 = CARTESIAN_POINT ( 'NONE',  ( -4.826977667545033768, -11.56426240980093745, 33.07394671870546432 ) ) ;
#60932 = EDGE_LOOP ( 'NONE', ( #41304, #28678 ) ) ;
#60933 = VERTEX_POINT ( 'NONE', #42674 ) ;
#60934 = ORIENTED_EDGE ( 'NONE', *, *, #5496, .F. ) ;
#60936 = EDGE_LOOP ( 'NONE', ( #31537, #69051, #42457, #69865, #81415, #29763 ) ) ;
#60935 = CARTESIAN_POINT ( 'NONE',  ( 2.177000841024749889, -2.541943142973489778, 30.39792223712631980 ) ) ;
#60937 = AXIS2_PLACEMENT_3D ( 'NONE', #57184, #84675, #21178 ) ;
#60939 = CARTESIAN_POINT ( 'NONE',  ( -8.069638789877792817, -4.386631170607604879, 33.66268669641500111 ) ) ;
#60938 = DIRECTION ( 'NONE',  ( 0.000000000000000000, 0.1736481776669267785, -0.9848077530122087975 ) ) ;
#60940 = FACE_OUTER_BOUND ( 'NONE', #31566, .T. ) ;
#60941 = CARTESIAN_POINT ( 'NONE',  ( -10.74607608205217346, -3.530157926970578952, 32.79014554554150607 ) ) ;
#60942 = FACE_BOUND ( 'NONE', #24328, .T. ) ;
#60943 = EDGE_LOOP ( 'NONE', ( #88651, #72351, #78751, #20863 ) ) ;
#60944 = CARTESIAN_POINT ( 'NONE',  ( 16.82694634598072625, -6.567427716900048118, 34.66269422305636283 ) ) ;
#60945 = CARTESIAN_POINT ( 'NONE',  ( -3.164700879766791708, -6.386643153685127139, 34.62446782046654192 ) ) ;
#60946 = ORIENTED_EDGE ( 'NONE', *, *, #61348, .F. ) ;
#60947 = CARTESIAN_POINT ( 'NONE',  ( 5.010840697562938928, -2.292212530054419606, 30.41441678777542634 ) ) ;
#60948 = EDGE_CURVE ( 'NONE', #43471, #34591, #83068, .T. ) ;
#60949 = VERTEX_POINT ( 'NONE', #62478 ) ;
#60950 = FACE_BOUND ( 'NONE', #89133, .T. ) ;
#60951 = CARTESIAN_POINT ( 'NONE',  ( -9.692307692307691624, -2.292212530054420494, 30.41441678777542634 ) ) ;
#60952 = CARTESIAN_POINT ( 'NONE',  ( 18.13079180782478872, -4.809403383903225304, 33.96459661697925014 ) ) ;
#60953 = VERTEX_POINT ( 'NONE', #48083 ) ;
#60954 = CYLINDRICAL_SURFACE ( 'NONE', #41993, 0.2500000000000009437 ) ;
#60955 = DIRECTION ( 'NONE',  ( -0.000000000000000000, -0.000000000000000000, -1.000000000000000000 ) ) ;
#60956 = CARTESIAN_POINT ( 'NONE',  ( -0.5922290646487694543, -2.295517848115769421, 30.44137282052137294 ) ) ;
#60957 = ORIENTED_EDGE ( 'NONE', *, *, #52575, .T. ) ;
#60958 = CYLINDRICAL_SURFACE ( 'NONE', #82506, 0.2500000000000008882 ) ;
#60959 = LINE ( 'NONE', #74935, #11192 ) ;
#60960 = CARTESIAN_POINT ( 'NONE',  ( -3.360916440207447398, -2.882441371585227508, 31.66841991370171527 ) ) ;
#60961 = CARTESIAN_POINT ( 'NONE',  ( -7.846153846153965716, -2.892918686052166066, 31.69288490824153470 ) ) ;
#60962 = ORIENTED_EDGE ( 'NONE', *, *, #53694, .F. ) ;
#60963 = EDGE_CURVE ( 'NONE', #423, #34521, #76460, .T. ) ;
#60964 = CARTESIAN_POINT ( 'NONE',  ( 12.52673144983311637, -2.255955759149235629, 29.99999999999988987 ) ) ;
#60965 = DIRECTION ( 'NONE',  ( 0.000000000000000000, 0.4999999999999960032, -0.8660254037844410391 ) ) ;
#60966 = VERTEX_POINT ( 'NONE', #793 ) ;
#60967 = CARTESIAN_POINT ( 'NONE',  ( -4.826977667545032880, -3.520799739797213501, 33.17531984108286025 ) ) ;
#60968 = CARTESIAN_POINT ( 'NONE',  ( -4.403869391139117795, -2.587272538249754117, 30.68239716806877837 ) ) ;
#60969 = CARTESIAN_POINT ( 'NONE',  ( -8.096177070375301099, -12.45566812827425096, 31.48439005359158926 ) ) ;
#60970 = CARTESIAN_POINT ( 'NONE',  ( 13.63456090296352841, -12.43552623307873972, 30.55307653245132826 ) ) ;
#60971 = CARTESIAN_POINT ( 'NONE',  ( -6.673076923076859401, -7.434744860731433924, 35.00000000000000711 ) ) ;
#60972 = CARTESIAN_POINT ( 'NONE',  ( 15.00728430620490350, -5.827078755546623690, 34.72654668319379567 ) ) ;
#60973 = B_SPLINE_CURVE_WITH_KNOTS ( 'NONE', 3,
 ( #70786, #37422, #63570, #49172, #84311, #1874, #63121, #55927, #83419, #15844 ),
 .UNSPECIFIED., .F., .F.,
 ( 4, 2, 2, 2, 4 ),
 ( 0.0007817246256747447872, 0.0009771112852218874663, 0.001172497944769030362, 0.001367884604316173258, 0.001563271263863315937 ),
 .UNSPECIFIED. ) ;
#60975 = CARTESIAN_POINT ( 'NONE',  ( 16.15384615384615330, -5.557115091759785130, 34.35708131394839171 ) ) ;
#60974 = CARTESIAN_POINT ( 'NONE',  ( 6.249945518348144269, -11.86320923018887541, 32.19269448109604781 ) ) ;
#60976 = EDGE_CURVE ( 'NONE', #19826, #53468, #69693, .T. ) ;
#60977 = CARTESIAN_POINT ( 'NONE',  ( -2.939152317953646711E-15, 7.500000000000000000, 13.50000000000000178 ) ) ;
#60978 = CARTESIAN_POINT ( 'NONE',  ( 1.944543648263018731, -9.444543648262994751, 18.37500000000000355 ) ) ;
#60979 = EDGE_LOOP ( 'NONE', ( #22044, #11947 ) ) ;
#60980 = AXIS2_PLACEMENT_3D ( 'NONE', #14048, #41522, #83407 ) ;
#60981 = CARTESIAN_POINT ( 'NONE',  ( 4.826899852701618698, -6.652501968072646932, 34.93155406624980941 ) ) ;
#60982 = VERTEX_POINT ( 'NONE', #62917 ) ;
#60983 = AXIS2_PLACEMENT_3D ( 'NONE', #35466, #61602, #1231 ) ;
#60984 = SHAPE_REPRESENTATION ( 'Dual Reciprocating Inner Cutter Blades', ( #83448 ), #70522 ) ;
#60985 = ORIENTED_EDGE ( 'NONE', *, *, #33667, .F. ) ;
#60986 = CARTESIAN_POINT ( 'NONE',  ( -11.53846153846166089, -2.379036618888197729, 30.90682066428292885 ) ) ;
#60987 = ORIENTED_EDGE ( 'NONE', *, *, #59358, .F. ) ;
#60988 = CARTESIAN_POINT ( 'NONE',  ( -4.403822897894741573, -2.544273027872574922, 31.48422191005632342 ) ) ;
#60989 = CARTESIAN_POINT ( 'NONE',  ( 1.139087296525997273, -4.749999999999992895, 17.98437500000000000 ) ) ;
#60990 = CARTESIAN_POINT ( 'NONE',  ( 12.23871036390358569, -7.369209533119137845, 34.99857337881830688 ) ) ;
#60991 = EDGE_CURVE ( 'NONE', #55273, #75823, #33664, .T. ) ;
#60992 = CARTESIAN_POINT ( 'NONE',  ( 5.776515056276056548, -11.41268669641500466, 32.86336882939237825 ) ) ;
#60993 = CARTESIAN_POINT ( 'NONE',  ( 0.000000000000000000, -11.00000000000000000, 29.75000000000000355 ) ) ;
#60994 = FACE_OUTER_BOUND ( 'NONE', #43387, .T. ) ;
#60995 = CARTESIAN_POINT ( 'NONE',  ( -13.60754160213153163, -2.554751324335734708, 30.48935550225260727 ) ) ;
#60996 = DIRECTION ( 'NONE',  ( -1.000000000000000000, -0.000000000000000000, -0.000000000000000000 ) ) ;
#60997 = CARTESIAN_POINT ( 'NONE',  ( -2.651650429449565305, -4.848349570550461785, 24.00000000000000000 ) ) ;
#60998 = EDGE_CURVE ( 'NONE', #67793, #16935, #74438, .T. ) ;
#60999 = ADVANCED_FACE ( 'NONE', ( #68809 ), #7108, .F. ) ;
#61000 = CARTESIAN_POINT ( 'NONE',  ( -0.5276218724943432248, -2.538708090699994813, 30.37095296980875148 ) ) ;
#61001 = CARTESIAN_POINT ( 'NONE',  ( -14.37294329785354918, -2.506253911140460922, 30.00000000000013856 ) ) ;
#61002 = CARTESIAN_POINT ( 'NONE',  ( -2.530618525208451874, -4.186968288167446595, 33.49512374952580274 ) ) ;
#61003 = ADVANCED_FACE ( 'NONE', ( #64691 ), #22829, .F. ) ;
#61004 = EDGE_LOOP ( 'NONE', ( #32524, #76723 ) ) ;
#61005 = ORIENTED_EDGE ( 'NONE', *, *, #52784, .T. ) ;
#61006 = CARTESIAN_POINT ( 'NONE',  ( -9.442362173959550020, -3.712312575010499049, 33.01462480002815170 ) ) ;
#61007 = FACE_OUTER_BOUND ( 'NONE', #35632, .T. ) ;
#61008 = CARTESIAN_POINT ( 'NONE',  ( 17.07692307692307665, -2.249999999999998668, 29.75000000000001776 ) ) ;
#61009 = CARTESIAN_POINT ( 'NONE',  ( -16.02305434602136458, -12.38066358083363738, 30.83685684665853444 ) ) ;
#61010 = CARTESIAN_POINT ( 'NONE',  ( 8.769230769230647482, -4.481592998941358097, 33.73612834414048933 ) ) ;
#61011 = CARTESIAN_POINT ( 'NONE',  ( -6.000000000000119904, -8.613356846316285953, 34.62446782046622218 ) ) ;
#61012 = AXIS2_PLACEMENT_3D ( 'NONE', #31155, #80253, #44659 ) ;
#61013 = CARTESIAN_POINT ( 'NONE',  ( -2.531177232256637044, -8.539481045369598178, 34.89627647299170832 ) ) ;
#61014 = ORIENTED_EDGE ( 'NONE', *, *, #25633, .F. ) ;
#61015 = CARTESIAN_POINT ( 'NONE',  ( -6.792551221313363641, -10.19071101563364756, 33.96452234770658407 ) ) ;
#61016 = ORIENTED_EDGE ( 'NONE', *, *, #42552, .F. ) ;
#61018 = ADVANCED_FACE ( 'NONE', ( #51160 ), #1680, .F. ) ;
#61017 = ORIENTED_EDGE ( 'NONE', *, *, #1946, .F. ) ;
#61019 = CARTESIAN_POINT ( 'NONE',  ( 16.28437159207980045, -9.503571793651730104, 34.60286762892837942 ) ) ;
#61020 = CARTESIAN_POINT ( 'NONE',  ( 4.023154687178593925, -2.541943142973490666, 30.39792223712631980 ) ) ;
#61021 = CARTESIAN_POINT ( 'NONE',  ( -0.4615384615385826339, -6.879047030192662504, 34.71129190930017927 ) ) ;
#61022 = CARTESIAN_POINT ( 'NONE',  ( 5.076923076923075762, -1.129524287112498415, 32.06866353760679544 ) ) ;
#61023 = CARTESIAN_POINT ( 'NONE',  ( -7.846153846153965716, -9.442884908241554243, 34.35708131394783038 ) ) ;
#61024 = EDGE_CURVE ( 'NONE', #85855, #36501, #84191, .T. ) ;
#61025 = ORIENTED_EDGE ( 'NONE', *, *, #58587, .T. ) ;
#61026 = ADVANCED_FACE ( 'NONE', ( #71022 ), #65137, .F. ) ;
#61027 = ORIENTED_EDGE ( 'NONE', *, *, #55257, .F. ) ;
#61028 = ORIENTED_EDGE ( 'NONE', *, *, #23669, .F. ) ;
#61029 = ORIENTED_EDGE ( 'NONE', *, *, #4202, .F. ) ;
#61030 = VECTOR ( 'NONE', #72224, 1000.000000000000227 ) ;
#61031 = CARTESIAN_POINT ( 'NONE',  ( 17.07692307692295586, -10.33852847137269571, 34.16647553114546554 ) ) ;
#61032 = FACE_OUTER_BOUND ( 'NONE', #15269, .T. ) ;
#61033 = EDGE_CURVE ( 'NONE', #29561, #45384, #64245, .T. ) ;
#61034 = DIRECTION ( 'NONE',  ( 1.000000000000000000, 0.000000000000000000, 0.000000000000000000 ) ) ;
#61035 = VECTOR ( 'NONE', #15167, 1000.000000000000000 ) ;
#61036 = VECTOR ( 'NONE', #5825, 1000.000000000000000 ) ;
#61037 = CARTESIAN_POINT ( 'NONE',  ( -16.37733107841048508, -2.353723527008297012, 30.78948104536958752 ) ) ;
#61038 = CARTESIAN_POINT ( 'NONE',  ( -10.48459280755982981, -12.11778462344220841, 31.66786338562085135 ) ) ;
#61039 = ORIENTED_EDGE ( 'NONE', *, *, #23589, .F. ) ;
#61040 = ORIENTED_EDGE ( 'NONE', *, *, #31225, .T. ) ;
#61041 = ORIENTED_EDGE ( 'NONE', *, *, #11342, .T. ) ;
#61042 = ADVANCED_FACE ( 'NONE', ( #78662 ), #56625, .F. ) ;
#61044 = ORIENTED_EDGE ( 'NONE', *, *, #55425, .T. ) ;
#61043 = CARTESIAN_POINT ( 'NONE',  ( -10.39237326377176274, -11.76359900205217457, 32.36225158514719880 ) ) ;
#61045 = CARTESIAN_POINT ( 'NONE',  ( 9.561617089197390840, -8.191372820521381826, 34.95448215188423546 ) ) ;
#61046 = CARTESIAN_POINT ( 'NONE',  ( -10.61538461538461320, -7.500000000000001776, 35.04278698407183867 ) ) ;
#61047 = CARTESIAN_POINT ( 'NONE',  ( -3.749999999999997335, -7.500000000000021316, 18.84375000000000000 ) ) ;
#61048 = VERTEX_POINT ( 'NONE', #22392 ) ;
#61049 = CARTESIAN_POINT ( 'NONE',  ( -1.384615384615383471, -2.486705287966279876, 31.30864560766543647 ) ) ;
#61050 = ORIENTED_EDGE ( 'NONE', *, *, #50321, .F. ) ;
#61051 = CYLINDRICAL_SURFACE ( 'NONE', #35670, 0.2499999999999995559 ) ;
#61052 = FACE_BOUND ( 'NONE', #10891, .T. ) ;
#61053 = CYLINDRICAL_SURFACE ( 'NONE', #51820, 8.000000000000000000 ) ;
#61054 = FACE_OUTER_BOUND ( 'NONE', #9119, .T. ) ;
#61055 = EDGE_LOOP ( 'NONE', ( #17337, #69792, #22785, #37547 ) ) ;
#61056 = EDGE_CURVE ( 'NONE', #69885, #63541, #11105, .T. ) ;
#61057 = CARTESIAN_POINT ( 'NONE',  ( 8.519207545009310323, -12.07920672191015221, 32.31858351112116168 ) ) ;
#61058 = CARTESIAN_POINT ( 'NONE',  ( -14.17690049986752321, -2.541949514083464479, 30.39797389878540557 ) ) ;
#61059 = EDGE_CURVE ( 'NONE', #74128, #70315, #10213, .T. ) ;
#61060 = CARTESIAN_POINT ( 'NONE',  ( -13.60749406704403519, -7.630691491037285168, 34.74850469731152458 ) ) ;
#61061 = DIRECTION ( 'NONE',  ( -0.000000000000000000, -0.8660254037844399289, -0.4999999999999980016 ) ) ;
#61062 = ORIENTED_EDGE ( 'NONE', *, *, #70101, .F. ) ;
#61063 = VECTOR ( 'NONE', #35949, 1000.000000000000114 ) ;
#61064 = CARTESIAN_POINT ( 'NONE',  ( -18.13014796973170206, -12.70455904226513866, 30.44083106164009322 ) ) ;
#61065 = CARTESIAN_POINT ( 'NONE',  ( -5.750054590621955342, -4.176053281294514363, 33.81426240980091791 ) ) ;
#61066 = LINE ( 'NONE', #56085, #68574 ) ;
#61067 = DIRECTION ( 'NONE',  ( -0.000000000000000000, 0.1736481776669307198, -0.9848077530122080203 ) ) ;
#61068 = CARTESIAN_POINT ( 'NONE',  ( -1.384615384615383471, -2.499999999999998668, 29.75000000000001421 ) ) ;
#61069 = FACE_BOUND ( 'NONE', #3496, .T. ) ;
#61071 = CARTESIAN_POINT ( 'NONE',  ( 16.94677510719138169, -3.069018819979304702, 32.56621877034667278 ) ) ;
#61070 = FACE_OUTER_BOUND ( 'NONE', #38639, .T. ) ;
#61072 = ADVANCED_FACE ( 'NONE', ( #58376 ), #37225, .F. ) ;
#61073 = CARTESIAN_POINT ( 'NONE',  ( 1.653273178848927064E-15, -7.500000000000000000, 18.00000000000000355 ) ) ;
#61075 = CARTESIAN_POINT ( 'NONE',  ( -11.40767109749459074, -10.70102852606553157, 33.91149625220312913 ) ) ;
#61074 = FACE_OUTER_BOUND ( 'NONE', #2103, .T. ) ;
#61076 = DIRECTION ( 'NONE',  ( 1.000000000000000000, 0.000000000000000000, 0.000000000000000000 ) ) ;
#61077 = CARTESIAN_POINT ( 'NONE',  ( -0.06109907496454585613, -4.750000000000000000, 18.90438170625848713 ) ) ;
#61078 = EDGE_LOOP ( 'NONE', ( #16107, #80682 ) ) ;
#61079 = DIRECTION ( 'NONE',  ( 0.000000000000000000, 0.000000000000000000, -1.000000000000000000 ) ) ;
#61080 = ORIENTED_EDGE ( 'NONE', *, *, #3845, .T. ) ;
#61081 = CARTESIAN_POINT ( 'NONE',  ( 1.134615384615377698, -2.499999999999999556, 29.81609845454692120 ) ) ;
#61082 = ORIENTED_EDGE ( 'NONE', *, *, #48272, .T. ) ;
#61083 = CARTESIAN_POINT ( 'NONE',  ( -11.53846153846153655, -2.721908614388771852, 31.22303859784724978 ) ) ;
#61084 = CARTESIAN_POINT ( 'NONE',  ( -18.13014720943822056, -2.619462340734461048, 30.83744416345203021 ) ) ;
#61086 = ORIENTED_EDGE ( 'NONE', *, *, #2448, .F. ) ;
#61085 = CARTESIAN_POINT ( 'NONE',  ( 18.00000000000000000, -2.249999999999998668, 29.50000000000001421 ) ) ;
#61087 = CARTESIAN_POINT ( 'NONE',  ( 16.94677510719138169, -12.70455904226513866, 30.44083106164009322 ) ) ;
#61088 = CARTESIAN_POINT ( 'NONE',  ( -9.822918051932216343, -7.722926236386453702, 34.74524107206102030 ) ) ;
#61089 = CARTESIAN_POINT ( 'NONE',  ( -1.200186371490556958, -4.775308065498765409, 20.07625670625849068 ) ) ;
#61090 = CARTESIAN_POINT ( 'NONE',  ( 14.05771557674995620, -10.66389620160130036, 33.62221079203477103 ) ) ;
#61091 = CARTESIAN_POINT ( 'NONE',  ( 4.946775867484854317, -5.195881422630167279, 34.18770438780618548 ) ) ;
#61092 = CARTESIAN_POINT ( 'NONE',  ( -4.946397638689433940, -12.15418822224088657, 32.17964115625579069 ) ) ;
#61093 = CARTESIAN_POINT ( 'NONE',  ( 3.230769230769231726, -10.89733346790207413, 36.13435417666054406 ) ) ;
#61094 = DIRECTION ( 'NONE',  ( -0.000000000000000000, -0.8660254037844399289, -0.4999999999999980016 ) ) ;
#61095 = CARTESIAN_POINT ( 'NONE',  ( -5.934744428723972121, -10.90142922261932057, 33.41473453929631887 ) ) ;
#61096 = CARTESIAN_POINT ( 'NONE',  ( 2.608446859217924629, -10.19485399968118422, 24.87686829374151642 ) ) ;
#61097 = EDGE_CURVE ( 'NONE', #79197, #84840, #77628, .T. ) ;
#61098 = CIRCLE ( 'NONE', #74030, 4.000000000000000000 ) ;
#61099 = CARTESIAN_POINT ( 'NONE',  ( -14.98076923076922995, -7.500000000000001776, 35.04278698407183867 ) ) ;
#61100 = LINE ( 'NONE', #48805, #21171 ) ;
#61101 = ORIENTED_EDGE ( 'NONE', *, *, #81425, .T. ) ;
#61102 = CARTESIAN_POINT ( 'NONE',  ( 16.37662582282421653, -4.989023458446561143, 34.36081565061822118 ) ) ;
#61103 = CARTESIAN_POINT ( 'NONE',  ( 1.492201783934598236, -11.27530806549875031, 19.95499329374151642 ) ) ;
#61104 = AXIS2_PLACEMENT_3D ( 'NONE', #58625, #45115, #51859 ) ;
#61105 = DIRECTION ( 'NONE',  ( 0.000000000000000000, 0.000000000000000000, 1.000000000000000000 ) ) ;
#61106 = FACE_OUTER_BOUND ( 'NONE', #77089, .T. ) ;
#61107 = EDGE_LOOP ( 'NONE', ( #42499, #48706, #7179, #54150 ) ) ;
#61108 = PLANE ( 'NONE',  #44198 ) ;
#61109 = LINE ( 'NONE', #54792, #84809 ) ;
#61111 = ORIENTED_EDGE ( 'NONE', *, *, #40514, .T. ) ;
#61110 = CARTESIAN_POINT ( 'NONE',  ( 2.057715576749954867, -2.779195860258149242, 31.39871582349837453 ) ) ;
#61112 = FACE_OUTER_BOUND ( 'NONE', #6626, .T. ) ;
#61113 = CARTESIAN_POINT ( 'NONE',  ( 15.45354889974729495, -5.827830569534417471, 34.72679350104403539 ) ) ;
#61114 = LINE ( 'NONE', #34969, #74477 ) ;
#61115 = ORIENTED_EDGE ( 'NONE', *, *, #71775, .F. ) ;
#61116 = CARTESIAN_POINT ( 'NONE',  ( 3.230769230769108269, -2.657715359629662544, 31.77849191805970364 ) ) ;
#61117 = CARTESIAN_POINT ( 'NONE',  ( -9.942307692307691624, -2.499999999999998668, 29.75000000000000355 ) ) ;
#61118 = CARTESIAN_POINT ( 'NONE',  ( 8.639082799499075094, -3.625366637846545892, 33.29286588640298561 ) ) ;
#61119 = ORIENTED_EDGE ( 'NONE', *, *, #667, .T. ) ;
#61120 = EDGE_LOOP ( 'NONE', ( #84635, #29057 ) ) ;
#61121 = ORIENTED_EDGE ( 'NONE', *, *, #35386, .F. ) ;
#61122 = VERTEX_POINT ( 'NONE', #71453 ) ;
#61123 = CARTESIAN_POINT ( 'NONE',  ( -9.692307692307812417, -2.892918686052166066, 31.69288490824153470 ) ) ;
#61124 = CARTESIAN_POINT ( 'NONE',  ( 14.17754509825408960, -4.460286881179643004, 33.72017969459903242 ) ) ;
#61125 = CARTESIAN_POINT ( 'NONE',  ( -11.31568186948346977, -3.563462043263030399, 33.22394488606062879 ) ) ;
#61126 = CARTESIAN_POINT ( 'NONE',  ( 11.53846153846153832, -2.499999999999998668, 29.75000000000001421 ) ) ;
#61127 = CARTESIAN_POINT ( 'NONE',  ( 16.15384615384615330, -4.786620604624113540, 33.94971097300155094 ) ) ;
#61128 = ORIENTED_EDGE ( 'NONE', *, *, #43677, .T. ) ;
#61129 = VERTEX_POINT ( 'NONE', #11545 ) ;
#61130 = EDGE_LOOP ( 'NONE', ( #41538, #74045, #16248, #55893 ) ) ;
#61132 = VERTEX_POINT ( 'NONE', #66932 ) ;
#61131 = CARTESIAN_POINT ( 'NONE',  ( -16.15384615384615330, -6.189225973068211317, 35.74407628777942847 ) ) ;
#61133 = CARTESIAN_POINT ( 'NONE',  ( -4.853910232829682592, -12.38742843783360748, 31.66772728687926985 ) ) ;
#61134 = CARTESIAN_POINT ( 'NONE',  ( -3.360917200500922686, -12.15440758774515473, 32.17923288041532004 ) ) ;
#61135 = DIRECTION ( 'NONE',  ( -1.000000000000000000, 0.000000000000000000, -0.000000000000000000 ) ) ;
#61136 = CARTESIAN_POINT ( 'NONE',  ( 16.02369818411446190, -11.66186481527757479, 32.95055677023626117 ) ) ;
#61137 = ORIENTED_EDGE ( 'NONE', *, *, #76662, .F. ) ;
#61138 = ORIENTED_EDGE ( 'NONE', *, *, #38778, .T. ) ;
#61139 = ORIENTED_EDGE ( 'NONE', *, *, #40838, .T. ) ;
#61140 = CARTESIAN_POINT ( 'NONE',  ( 10.74617642320940369, -10.54018710029568595, 33.71981072465678864 ) ) ;
#61142 = ORIENTED_EDGE ( 'NONE', *, *, #87847, .T. ) ;
#61141 = CARTESIAN_POINT ( 'NONE',  ( -10.03846153846153832, -7.500000000000000000, 33.75000000000000000 ) ) ;
#61143 = CARTESIAN_POINT ( 'NONE',  ( -11.47320639894870276, -12.70778746994558439, 30.41441678777536595 ) ) ;
#61144 = AXIS2_PLACEMENT_3D ( 'NONE', #21526, #22412, #55750 ) ;
#61145 = CARTESIAN_POINT ( 'NONE',  ( -17.07692307692319744, -3.643525952248796163, 33.31231777344771672 ) ) ;
#61146 = ORIENTED_EDGE ( 'NONE', *, *, #31815, .T. ) ;
#61147 = CARTESIAN_POINT ( 'NONE',  ( 1.384615384615386802, -11.11383981884818262, 36.00935417666054406 ) ) ;
#61148 = CARTESIAN_POINT ( 'NONE',  ( -6.923076923076922462, -12.37446782046654192, 30.86335684631486131 ) ) ;
#61149 = CARTESIAN_POINT ( 'NONE',  ( -17.07692307692319744, -11.06231777344772027, 33.60647404775119895 ) ) ;
#61150 = FACE_BOUND ( 'NONE', #36338, .T. ) ;
#61151 = CARTESIAN_POINT ( 'NONE',  ( 10.86543892702293057, -9.943054286541403997, 34.11300777759954883 ) ) ;
#61152 = CARTESIAN_POINT ( 'NONE',  ( 10.28846153846153832, -3.499999999999999556, 29.75000000000000355 ) ) ;
#61153 = EDGE_CURVE ( 'NONE', #3259, #42959, #13599, .T. ) ;
#61154 = CARTESIAN_POINT ( 'NONE',  ( -9.942307692307691624, -7.500000000000001776, 34.75000000000000000 ) ) ;
#61156 = FACE_OUTER_BOUND ( 'NONE', #87313, .T. ) ;
#61155 = CARTESIAN_POINT ( 'NONE',  ( 9.627037246346917598, -3.300289026998414865, 32.46337939537583139 ) ) ;
#61157 = DIRECTION ( 'NONE',  ( 0.000000000000000000, 0.9848077530122072432, -0.1736481776669354937 ) ) ;
#61158 = CARTESIAN_POINT ( 'NONE',  ( -11.53846153846153655, -1.466349020453238561, 30.81389545987213907 ) ) ;
#61159 = ORIENTED_EDGE ( 'NONE', *, *, #45103, .F. ) ;
#61160 = CARTESIAN_POINT ( 'NONE',  ( 14.30769230769231015, -12.37446782046654192, 30.86335684631486131 ) ) ;
#61161 = B_SPLINE_CURVE_WITH_KNOTS ( 'NONE', 3,
 ( #28005, #14046, #34312, #75311, #13604, #82522, #7296, #20801, #41520, #62227 ),
 .UNSPECIFIED., .F., .F.,
 ( 4, 2, 2, 2, 4 ),
 ( 0.000000000000000000, 0.0001954339857564082333, 0.0003908679715128164666, 0.0005863019572692247270, 0.0007817359430256329332 ),
 .UNSPECIFIED. ) ;
#61162 = CIRCLE ( 'NONE', #12314, 0.2500000000000002220 ) ;
#61163 = ORIENTED_EDGE ( 'NONE', *, *, #69296, .T. ) ;
#61164 = PLANE ( 'NONE',  #85191 ) ;
#61165 = B_SPLINE_CURVE_WITH_KNOTS ( 'NONE', 3,
 ( #5536, #73557, #59130, #24901, #52815, #73995, #58685, #45620, #11853, #39770 ),
 .UNSPECIFIED., .F., .F.,
 ( 4, 2, 2, 2, 4 ),
 ( 0.000000000000000000, 0.0001954339857564081249, 0.0003908679715128162498, 0.0005863019572692244018, 0.0007817359430256324996 ),
 .UNSPECIFIED. ) ;
#61166 = CARTESIAN_POINT ( 'NONE',  ( -14.43783951713053249, -5.195881422630166391, 34.18770438780619259 ) ) ;
#61167 = FACE_OUTER_BOUND ( 'NONE', #11344, .T. ) ;
#61168 = VERTEX_POINT ( 'NONE', #25053 ) ;
#61169 = CARTESIAN_POINT ( 'NONE',  ( -5.448717948717948012, -3.499999999999999556, 29.75000000000000355 ) ) ;
#61170 = CARTESIAN_POINT ( 'NONE',  ( -4.153846153846274980, -9.528491918059723176, 34.59228464037033035 ) ) ;
#61171 = FACE_BOUND ( 'NONE', #23641, .T. ) ;
#61173 = CYLINDRICAL_SURFACE ( 'NONE', #14308, 0.2499999999999993616 ) ;
#61172 = CARTESIAN_POINT ( 'NONE',  ( -4.153846153846152411, -2.499999999999998668, 29.75000000000001421 ) ) ;
#61174 = CARTESIAN_POINT ( 'NONE',  ( 7.846153846153725020, -9.442884908241554243, 34.35708131394783038 ) ) ;
#61175 = EDGE_CURVE ( 'NONE', #34461, #46042, #26390, .T. ) ;
#61176 = CARTESIAN_POINT ( 'NONE',  ( -5.300408020647025431, -9.331801661448606566, 34.40259984581193464 ) ) ;
#61178 = DIRECTION ( 'NONE',  ( 0.000000000000000000, 0.000000000000000000, -1.000000000000000000 ) ) ;
#61177 = CARTESIAN_POINT ( 'NONE',  ( -4.577262028924688101E-15, 14.50000000000000533, 1.499999999999997780 ) ) ;
#61179 = CARTESIAN_POINT ( 'NONE',  ( 3.775308065498768517, -8.992201783934554271, 16.79500670625849068 ) ) ;
#61180 = ORIENTED_EDGE ( 'NONE', *, *, #7492, .T. ) ;
#61181 = ORIENTED_EDGE ( 'NONE', *, *, #52052, .F. ) ;
#61182 = DIRECTION ( 'NONE',  ( -0.000000000000000000, 0.7660444431189791237, -0.6427876096865379196 ) ) ;
#61183 = CARTESIAN_POINT ( 'NONE',  ( -17.86920955903305597, -3.338503747796863319, 32.95102852606552801 ) ) ;
#61184 = CARTESIAN_POINT ( 'NONE',  ( 10.61538461538461675, -2.538708090699994813, 30.37095296980875503 ) ) ;
#61185 = CARTESIAN_POINT ( 'NONE',  ( 6.792929713638700129, -12.27039167877662251, 31.24851455888617835 ) ) ;
#61186 = FACE_OUTER_BOUND ( 'NONE', #88314, .T. ) ;
#61187 = CARTESIAN_POINT ( 'NONE',  ( -1.553300858899081538, -11.25000000000000711, 26.10937500000001066 ) ) ;
#61188 = DIRECTION ( 'NONE',  ( 0.000000000000000000, 0.8660254037844377084, 0.5000000000000015543 ) ) ;
#61189 = CYLINDRICAL_SURFACE ( 'NONE', #24432, 0.2499999999999997502 ) ;
#61190 = AXIS2_PLACEMENT_3D ( 'NONE', #21442, #34515, #12910 ) ;
#61191 = CARTESIAN_POINT ( 'NONE',  ( 7.846153846153723244, -3.643525952248796163, 33.31231777344771672 ) ) ;
#61192 = DIRECTION ( 'NONE',  ( -0.000000000000000000, -0.7660444431189791237, -0.6427876096865379196 ) ) ;
#61193 = CARTESIAN_POINT ( 'NONE',  ( 9.942362003946008997, -2.779044189368095719, 31.39831045268885745 ) ) ;
#61194 = CARTESIAN_POINT ( 'NONE',  ( 7.846153846153846700, -2.499999999999998668, 29.75000000000001421 ) ) ;
#61195 = CARTESIAN_POINT ( 'NONE',  ( 6.792385456409367528, -11.18331474514187995, 33.13161551792790505 ) ) ;
#61196 = EDGE_CURVE ( 'NONE', #77096, #39874, #59453, .T. ) ;
#61197 = DIRECTION ( 'NONE',  ( 0.000000000000000000, 0.6427876096865373645, -0.7660444431189797898 ) ) ;
#61198 = CARTESIAN_POINT ( 'NONE',  ( 12.46153846153833911, -2.892918686052165622, 31.69288490824153470 ) ) ;
#61199 = ORIENTED_EDGE ( 'NONE', *, *, #37757, .T. ) ;
#61200 = CARTESIAN_POINT ( 'NONE',  ( 9.019176178608811156, -4.932303261841489928, 34.32971442181322885 ) ) ;
#61201 = LINE ( 'NONE', #54008, #69024 ) ;
#61202 = CARTESIAN_POINT ( 'NONE',  ( -2.724691934501246582, -6.299813628509474128, 17.92374329374151287 ) ) ;
#61203 = EDGE_CURVE ( 'NONE', #69402, #38647, #17490, .T. ) ;
#61204 = B_SPLINE_CURVE_WITH_KNOTS ( 'NONE', 3,
 ( #46935, #87073, #80752, #80301, #45612, #73088, #33439, #39760, #18596, #46059 ),
 .UNSPECIFIED., .F., .F.,
 ( 4, 2, 2, 2, 4 ),
 ( 0.0007817246256747459798, 0.0009771112852218896347, 0.001172497944769033398, 0.001367884604316177161, 0.001563271263863320708 ),
 .UNSPECIFIED. ) ;
#61205 = ADVANCED_FACE ( 'NONE', ( #58830 ), #66490, .F. ) ;
#61206 = CARTESIAN_POINT ( 'NONE',  ( -9.692307692307814193, -11.06231777344772027, 33.60647404775119895 ) ) ;
#61207 = DIRECTION ( 'NONE',  ( 0.000000000000000000, 0.8660254037844377084, 0.5000000000000015543 ) ) ;
#61208 = CARTESIAN_POINT ( 'NONE',  ( 10.61538461538449596, -6.026961402154118019, 34.52809138561165270 ) ) ;
#61210 = VERTEX_POINT ( 'NONE', #60606 ) ;
#61209 = LINE ( 'NONE', #41847, #69879 ) ;
#61211 = CARTESIAN_POINT ( 'NONE',  ( -1.944543648262992530, -9.444543648263016067, 23.68750000000000000 ) ) ;
#61212 = CARTESIAN_POINT ( 'NONE',  ( -16.15384615384615330, -4.102666532097928531, 36.13435417666054406 ) ) ;
#61213 = VERTEX_POINT ( 'NONE', #32691 ) ;
#61214 = CARTESIAN_POINT ( 'NONE',  ( -16.02305434602136458, -9.804649428959608670, 34.18742332936588468 ) ) ;
#61215 = CARTESIAN_POINT ( 'NONE',  ( 0.3313912521002425060, -2.882441371585227508, 31.66841991370171527 ) ) ;
#61216 = EDGE_LOOP ( 'NONE', ( #60803, #4056, #50362, #20734 ) ) ;
#61217 = CARTESIAN_POINT ( 'NONE',  ( -10.61538461538461320, -3.937682226553329556, 33.60647404775216529 ) ) ;
#61218 = CARTESIAN_POINT ( 'NONE',  ( 8.545745844666436497, -6.716662450894489211, 34.94144148231605840 ) ) ;
#61219 = AXIS2_PLACEMENT_3D ( 'NONE', #20282, #57517, #16092 ) ;
#61220 = CARTESIAN_POINT ( 'NONE',  ( 15.23076923076923173, -2.721908614388771852, 31.22303859784724978 ) ) ;
#61221 = ORIENTED_EDGE ( 'NONE', *, *, #48318, .F. ) ;
#61222 = ORIENTED_EDGE ( 'NONE', *, *, #80077, .T. ) ;
#61223 = ORIENTED_EDGE ( 'NONE', *, *, #62683, .F. ) ;
#61224 = CARTESIAN_POINT ( 'NONE',  ( -15.16470189741915320, -3.937682226553329556, 33.60647404775216529 ) ) ;
#61225 = CARTESIAN_POINT ( 'NONE',  ( -0.4615384615384611200, -10.51840700105979565, 33.73612834413961536 ) ) ;
#61226 = DIRECTION ( 'NONE',  ( 0.000000000000000000, 0.8660254037844377084, 0.5000000000000015543 ) ) ;
#61227 = CARTESIAN_POINT ( 'NONE',  ( 9.627037691751374027, -9.528491918058357157, 34.59228464037090589 ) ) ;
#61228 = VECTOR ( 'NONE', #9423, 1000.000000000000227 ) ;
#61229 = CARTESIAN_POINT ( 'NONE',  ( -2.531177251416254492, -5.912607949931405038, 34.49155766932282319 ) ) ;
#61230 = FACE_OUTER_BOUND ( 'NONE', #4470, .T. ) ;
#61231 = LINE ( 'NONE', #88739, #26529 ) ;
#61232 = CYLINDRICAL_SURFACE ( 'NONE', #70829, 0.2499999999999994726 ) ;
#61233 = ADVANCED_FACE ( 'NONE', ( #60162, #52957, #87666, #4791, #53405, #80906, #32264, #19189, #88121, #59727, #52071, #3881, #72344, #10654, #74132, #12429, #38121, #17860, #65581, #45313, #72786, #11096, #38573, #66027, #4336, #31823, #59277, #86783, #56071, #68698, #48868, #61490, #21401, #47088, #75026, #28151, #75901, #27708, #75457, #20946, #14202, #76339, #7889, #35355, #88997, #41677, #83109, #82675, #6119, #74579, #40352, #62370, #55179, #14647, #69145, #55620, #7451, #42130, #27270, #13314, #48417, #69584, #33593, #54734, #245, #40795, #34906, #13753, #62809, #41235, #1128, #61052, #684, #28608, #19626, #6999, #12867, #67819, #34471, #88557, #26833, #54287, #81784, #20074, #47532, #82223, #68259, #61931, #6561, #20512, #34025, #47976, #15981, #2881, #71348, #77668, #84888, #71794, #22719, #35813, #42566, #9654, #29497, #44304, #43446, #36691, #2015, #30810, #70921, #23607, #36254, #85325, #21844, #49751, #30373, #50636, #2444, #50184, #23171, #78115, #9230, #10099, #37563, #63708, #16416, #57843, #57393, #70027, #64142, #43882, #37118, #29936, #65028, #29062, #3339, #83563, #63267, #49319, #64583, #51058, #1574, #78552, #16857, #76796, #15093, #8337, #56517, #77226, #84007, #8782, #22287, #15536, #43005, #70478, #56950, #84446, #65487, #32591, #53302, #65923, #87565, #73600, #39807, #17303, #67275, #74037, #18200, #32159, #38922, #39370, #12328, #44761, #59619, #24051, #5570, #72240, #52856, #85770, #51500, #11893, #66827, #72689, #58278, #3785, #73139, #10552, #86679, #17757, #31263, #60061, #80803, #4233, #25845, #19086, #58727, #38471, #46113, #79003, #38022, #86226, #24495, #5125, #18651, #45662, #51962, #46554, #87119, #79458, #45211, #10998, #80353, #31716, #25397, #59174, #24944, #11439, #52410, #79898, #66380, #4687, #6022, #34807, #13217, #88454, #6895, #27167, #28059, #47429, #62274, #88022, #74924, #40696, #54185, #14544, #27610, #7352, #33922, #21293, #61383, #74471, #81238, #20851, #68160, #83009, #54627, #75363, #6463, #69485, #82124, #590, #88897, #55523, #60510, #26724, #41571, #144, #41133, #20417, #34364, #55083, #47882, #48765, #76236, #13654, #82579, #42026, #61833, #19523, #26282, #53750, #75796, #68598, #33043, #46984, #12766, #67718, #48321, #14101, #40253, #33491, #60950, #69044, #81681, #19962, #8239, #36161, #50091, #16318, #57298, #84347, #62714, #43783, #36592, #76692, #83461, #7788, #2341, #28506, #64044, #1030, #63163, #63609, #83906, #55966, #14995, #49657, #84791, #9552, #77131, #1477, #71245, #42468, #44205, #69928, #29835, #70378, #23075, #50960, #1914, #85223, #2776, #37017, #21743, #15441, #42915, #28964, #78449, #50532, #64478, #8685, #49216, #35712, #15884, #29402, #56851, #16750, #35254, #56418, #22191, #22623, #77576, #43348, #30277, #57746, #70826, #9130, #23504, #78013, #40485, #10450, #44652, #40045, #53530, #9992, #72137, #81914, #86568, #38364, #71692, #81027, #58175, #67949, #79350, #12999, #6252, #17195, #51853, #60737, #54418, #3237, #37462, #64932, #30708, #33277, #23942, #72586, #17653, #24837, #85665, #26518, #61171, #19756, #20203, #51393, #67506, #19316, #46785, #4119, #81471, #88244, #65818, #74262, #88684, #10892, #78898, #37920, #65383, #33715, #47218, #31603, #59069, #45110, #3676, #12559, #26961, #24388, #74712, #31147, #58619, #86113, #5800, #53981, #14324, #48995, #42253, #62495, #29188, #82353, #35936, #56640, #34151, #55305, #809, #61618, #1246, #63389, #28276, #83234, #7129, #84133, #76474, #8016, #21520, #35483, #82796, #8463, #41809, #55746, #21070, #47668, #7574, #20635, #69710, #48538, #14776, #1697, #69271, #75154, #42692, #62064, #62934, #28736, #15220, #13438, #40917, #76020, #56199, #27840, #68381, #35035, #83689, #89123, #6679, #21973, #49444, #27399, #376, #76917, #70152, #54869, #48100, #75575, #13877, #41358, #68824, #34598, #84571, #31382, #37239, #78232, #22409, #85007, #22845, #57521, #44001, #58847, #37690, #3896, #70599, #49874, #57076, #77354, #15661, #71918, #63837, #23288, #30056, #64711, #8904, #65156, #10672, #58391, #51177, #2132, #36374, #43131, #16980, #29620, #78685, #50309, #77792, #3010, #30923, #85887, #16096, #43562, #71037, #44429, #50748, #10231, #65596, #16533, #17429, #36807, #24172, #9350, #64265, #30492, #2565, #3457, #38138, #57963, #85443, #71470, #9778, #51624, #79128, #23723, #44884, #72361, #47103, #39490, #5683, #33159, #4355, #33607, #59293, #80921, #59743, #53419, #40373, #80469, #74595, #81358, #11565, #19207, #32708, #53873, #12882, #67833, #39045, #60621, #87237, #79580, #72803, #31838, #26406, #5244, #39931, #19642, #11111, #66503, #66950, #80016, #60177, #18765, #6133, #46231, #86353, #38587, #46672, #12013, #66042, #67389, #24623, #87680, #25955, #45780, #52089, #74149, #12445, #88134, #17876, #32278, #45331, #73719, #86800, #4808, #25070, #52532, #18317, #73259, #52972, #25516, #55635, #75918, #42584, #6577, #49336, #70044, #13329, #8354, #42147, #28168, #40811, #75471, #13769, #7907, #7013, #28626, #89013, #54754, #20089, #41252, #61069, #68274, #14218, #47552, #262, #20528, #34044, #35372, #56088, #68717, #1145, #83583, #88576, #75043, #83126, #69164, #34923, #14665, #76814, #41691, #7469, #47992, #26848, #702, #21417, #62386, #48886, #34487, #21859, #55196, #76357, #61952, #54305, #20961, #15111, #27724, #62825, #69602, #81800, #82691, #61506, #27287, #48432, #82240, #71366, #3358, #24075, #51522, #77684, #43462, #72261, #84906, #65049, #15997, #37586, #63283, #2029 ), #85343, .F. ) ;
#61234 = ORIENTED_EDGE ( 'NONE', *, *, #36357, .F. ) ;
#61235 = ORIENTED_EDGE ( 'NONE', *, *, #61460, .F. ) ;
#61237 = ORIENTED_EDGE ( 'NONE', *, *, #75042, .T. ) ;
#61236 = CARTESIAN_POINT ( 'NONE',  ( -0.2114841499001473557, -12.17597550085003455, 31.52189283813461884 ) ) ;
#61238 = VECTOR ( 'NONE', #25648, 1000.000000000000000 ) ;
#61239 = CARTESIAN_POINT ( 'NONE',  ( -5.999999999999998224, -12.78798330534102945, 29.74999999999997868 ) ) ;
#61240 = CARTESIAN_POINT ( 'NONE',  ( 2.307692307692309264, -1.129524287112498415, 32.06866353760679544 ) ) ;
#61241 = ORIENTED_EDGE ( 'NONE', *, *, #78640, .T. ) ;
#61242 = CARTESIAN_POINT ( 'NONE',  ( 15.29602437028206907, -9.528491918058460186, 34.59228464037086326 ) ) ;
#61243 = EDGE_CURVE ( 'NONE', #8131, #58342, #66943, .T. ) ;
#61244 = AXIS2_PLACEMENT_3D ( 'NONE', #60562, #69101, #55574 ) ;
#61245 = VERTEX_POINT ( 'NONE', #29081 ) ;
#61246 = CARTESIAN_POINT ( 'NONE',  ( 17.32697749683652688, -9.233818618650598609, 34.70587769442853698 ) ) ;
#61247 = ORIENTED_EDGE ( 'NONE', *, *, #76329, .F. ) ;
#61248 = CARTESIAN_POINT ( 'NONE',  ( -10.74586132350107981, -7.276988635370452485, 34.74523720219453793 ) ) ;
#61249 = VERTEX_POINT ( 'NONE', #56535 ) ;
#61250 = CARTESIAN_POINT ( 'NONE',  ( -12.21159305216042057, -10.18230066228895758, 34.26354781536631577 ) ) ;
#61251 = CARTESIAN_POINT ( 'NONE',  ( 12.33139049180676672, -2.373036134822904319, 30.88089517874952250 ) ) ;
#61252 = FACE_BOUND ( 'NONE', #78088, .T. ) ;
#61253 = CARTESIAN_POINT ( 'NONE',  ( 5.934729999443682402, -2.379036618887870436, 30.90682066428147934 ) ) ;
#61254 = CARTESIAN_POINT ( 'NONE',  ( -8.769230769230768274, -11.11383981884818262, 36.00935417666054406 ) ) ;
#61255 = EDGE_CURVE ( 'NONE', #76768, #4390, #46525, .T. ) ;
#61256 = LINE ( 'NONE', #33365, #75505 ) ;
#61257 = CARTESIAN_POINT ( 'NONE',  ( -13.38461538461538325, -2.292212530054420494, 30.41441678777542634 ) ) ;
#61258 = FACE_OUTER_BOUND ( 'NONE', #69177, .T. ) ;
#61259 = CARTESIAN_POINT ( 'NONE',  ( -13.13461538461538325, -2.499999999999998668, 29.75000000000000355 ) ) ;
#61260 = EDGE_CURVE ( 'NONE', #40886, #22606, #9977, .T. ) ;
#61261 = ORIENTED_EDGE ( 'NONE', *, *, #15711, .T. ) ;
#61262 = VERTEX_POINT ( 'NONE', #84463 ) ;
#61264 = CARTESIAN_POINT ( 'NONE',  ( 2.557637826040450424, -10.76462480002816235, 33.53768742498949962 ) ) ;
#61263 = LINE ( 'NONE', #54969, #18753 ) ;
#61265 = B_SPLINE_CURVE_WITH_KNOTS ( 'NONE', 3,
 ( #22705, #77652, #43432, #36674, #57375, #2429, #29921, #84871, #23154, #50620 ),
 .UNSPECIFIED., .F., .F.,
 ( 4, 2, 2, 2, 4 ),
 ( 0.0007817359430256365111, 0.0009771253907250043464, 0.001172514838424372399, 0.001367904286123740234, 0.001563293733823108069 ),
 .UNSPECIFIED. ) ;
#61266 = CARTESIAN_POINT ( 'NONE',  ( 3.100078627658922503, -3.338472653186242756, 32.95098750199972670 ) ) ;
#61267 = DIRECTION ( 'NONE',  ( -0.000000000000000000, 0.1736481776669307198, -0.9848077530122080203 ) ) ;
#61268 = CARTESIAN_POINT ( 'NONE',  ( 6.923076923076800782, -5.094484230521993062, 34.41647553114689373 ) ) ;
#61269 = CARTESIAN_POINT ( 'NONE',  ( -12.39628332202562433, -5.094484230520773593, 34.41647553114626845 ) ) ;
#61270 = ORIENTED_EDGE ( 'NONE', *, *, #15242, .F. ) ;
#61271 = CARTESIAN_POINT ( 'NONE',  ( -11.78843826940389405, -12.17611988154120972, 31.52148481390971213 ) ) ;
#61272 = CARTESIAN_POINT ( 'NONE',  ( 14.98079248672064345, -4.075325502946081535, 33.72974371597206300 ) ) ;
#61273 = PLANE ( 'NONE',  #86183 ) ;
#61274 = EDGE_CURVE ( 'NONE', #3673, #41031, #86268, .T. ) ;
#61275 = CARTESIAN_POINT ( 'NONE',  ( 13.19230769230769340, -7.500000000000000000, 29.75000000000000355 ) ) ;
#61276 = ORIENTED_EDGE ( 'NONE', *, *, #22871, .F. ) ;
#61277 = ORIENTED_EDGE ( 'NONE', *, *, #4526, .T. ) ;
#61279 = EDGE_CURVE ( 'NONE', #63347, #41758, #16876, .T. ) ;
#61278 = ORIENTED_EDGE ( 'NONE', *, *, #46259, .F. ) ;
#61280 = CARTESIAN_POINT ( 'NONE',  ( 16.15384615384615330, -2.499999999999998668, 29.50000000000001066 ) ) ;
#61281 = ORIENTED_EDGE ( 'NONE', *, *, #70350, .F. ) ;
#61282 = EDGE_CURVE ( 'NONE', #12918, #41880, #54016, .T. ) ;
#61283 = VECTOR ( 'NONE', #56803, 1000.000000000000000 ) ;
#61284 = CARTESIAN_POINT ( 'NONE',  ( 4.153846153846030731, -11.67786785259630911, 32.92929555188603530 ) ) ;
#61285 = CARTESIAN_POINT ( 'NONE',  ( 15.16549878480845770, -9.442884908240170461, 34.35708131394840592 ) ) ;
#61286 = CARTESIAN_POINT ( 'NONE',  ( 3.480823650682683734, -5.642605341092957083, 34.66089969410670335 ) ) ;
#61287 = CARTESIAN_POINT ( 'NONE',  ( 1.384615384615386802, -6.343179335718451384, 34.87096338111211935 ) ) ;
#61288 = CARTESIAN_POINT ( 'NONE',  ( -11.53846153846165912, -6.879047030192662504, 34.71129190930017927 ) ) ;
#61289 = ORIENTED_EDGE ( 'NONE', *, *, #3834, .F. ) ;
#61290 = CARTESIAN_POINT ( 'NONE',  ( 4.376857505459002873, -4.187068189119697692, 33.49521262558774026 ) ) ;
#61292 = ORIENTED_EDGE ( 'NONE', *, *, #11963, .T. ) ;
#61291 = DIRECTION ( 'NONE',  ( 1.000000000000000000, 0.000000000000000000, 0.000000000000000000 ) ) ;
#61293 = CARTESIAN_POINT ( 'NONE',  ( -6.923076923077045919, -5.941354392335915335, 34.76329471203413846 ) ) ;
#61294 = CARTESIAN_POINT ( 'NONE',  ( -3.230769230769352962, -2.657715359629662544, 31.77849191805970364 ) ) ;
#61295 = CARTESIAN_POINT ( 'NONE',  ( -10.86538461538461320, -7.500000000000001776, 35.00000000000000000 ) ) ;
#61296 = DIRECTION ( 'NONE',  ( 0.000000000000000000, 0.000000000000000000, 1.000000000000000000 ) ) ;
#61297 = DIRECTION ( 'NONE',  ( -0.000000000000000000, 0.8660254037844397068, -0.4999999999999978906 ) ) ;
#61298 = EDGE_CURVE ( 'NONE', #71149, #53698, #13182, .T. ) ;
#61299 = FILL_AREA_STYLE ('',( #81160 ) ) ;
#61300 = CARTESIAN_POINT ( 'NONE',  ( 12.68431800280686517, -11.41317474335729543, 32.86274602512330034 ) ) ;
#61301 = CARTESIAN_POINT ( 'NONE',  ( -1.200186371490524317, -10.22469193450124791, 21.36124329374151642 ) ) ;
#61302 = ORIENTED_EDGE ( 'NONE', *, *, #40439, .T. ) ;
#61303 = CARTESIAN_POINT ( 'NONE',  ( -13.38461538461538325, -8.120952969808772792, 34.71129190930000163 ) ) ;
#61304 = CARTESIAN_POINT ( 'NONE',  ( -15.23076923076922995, -1.129524287112498415, 32.06866353760679544 ) ) ;
#61305 = ADVANCED_FACE ( 'NONE', ( #24516 ), #38944, .T. ) ;
#61307 = EDGE_LOOP ( 'NONE', ( #44188, #61660 ) ) ;
#61306 = AXIS2_PLACEMENT_3D ( 'NONE', #73304, #11608, #39088 ) ;
#61308 = EDGE_CURVE ( 'NONE', #82157, #70706, #60083, .T. ) ;
#61309 = ORIENTED_EDGE ( 'NONE', *, *, #46415, .F. ) ;
#61310 = CARTESIAN_POINT ( 'NONE',  ( 9.692307692307572609, -2.625532179533778709, 30.86335684631627174 ) ) ;
#61311 = CARTESIAN_POINT ( 'NONE',  ( -5.299849294439222369, -6.503392248772476236, 34.64988816332204635 ) ) ;
#61312 = VECTOR ( 'NONE', #26231, 1000.000000000000000 ) ;
#61313 = CARTESIAN_POINT ( 'NONE',  ( -10.86536135943320502, -2.318417181685855422, 30.59732222474233865 ) ) ;
#61314 = DIRECTION ( 'NONE',  ( -0.000000000000000000, -0.6427876096865404731, -0.7660444431189771253 ) ) ;
#61315 = CARTESIAN_POINT ( 'NONE',  ( -14.37296230824862953, -3.083524468853724443, 32.58852847137143272 ) ) ;
#61316 = VERTEX_POINT ( 'NONE', #88045 ) ;
#61317 = CARTESIAN_POINT ( 'NONE',  ( 12.46153846153877609, -2.255955759149395501, 30.00000000000324363 ) ) ;
#61318 = CARTESIAN_POINT ( 'NONE',  ( -12.46153846153846168, -5.180354513474913603, 36.12317359536750416 ) ) ;
#61319 = CARTESIAN_POINT ( 'NONE',  ( 1.634615384615386580, -2.499999999999998668, 29.75000000000000355 ) ) ;
#61320 = ORIENTED_EDGE ( 'NONE', *, *, #35663, .F. ) ;
#61321 = CARTESIAN_POINT ( 'NONE',  ( -4.153846153846152411, -3.937682226553329556, 33.60647404775216529 ) ) ;
#61322 = ORIENTED_EDGE ( 'NONE', *, *, #66349, .T. ) ;
#61323 = CARTESIAN_POINT ( 'NONE',  ( -16.37677237136229991, -5.667676309546437530, 34.40238873228292249 ) ) ;
#61324 =( NAMED_UNIT ( * ) SI_UNIT ( $, .STERADIAN. ) SOLID_ANGLE_UNIT ( ) );
#61325 = CARTESIAN_POINT ( 'NONE',  ( -5.776987155906605054, -11.98016756924215009, 32.48728574198911190 ) ) ;
#61326 = ORIENTED_EDGE ( 'NONE', *, *, #14276, .T. ) ;
#61327 = DIRECTION ( 'NONE',  ( -0.000000000000000000, 1.000000000000000000, -0.000000000000000000 ) ) ;
#61328 = DIRECTION ( 'NONE',  ( -0.000000000000000000, 0.8660254037844397068, -0.4999999999999978906 ) ) ;
#61329 = CARTESIAN_POINT ( 'NONE',  ( -11.60454494941741999, -6.386643153685125363, 34.62446782046654903 ) ) ;
#61330 = EDGE_CURVE ( 'NONE', #82159, #72717, #74059, .T. ) ;
#61331 = CARTESIAN_POINT ( 'NONE',  ( 6.923076923076924238, -12.34228464037088635, 31.77849191805839268 ) ) ;
#61332 = CARTESIAN_POINT ( 'NONE',  ( 18.00000000000000000, -8.564572088678739092, 35.78748833219616898 ) ) ;
#61333 = EDGE_CURVE ( 'NONE', #75057, #16191, #41097, .T. ) ;
#61334 = VECTOR ( 'NONE', #83602, 1000.000000000000227 ) ;
#61335 = ORIENTED_EDGE ( 'NONE', *, *, #84358, .F. ) ;
#61336 = FACE_BOUND ( 'NONE', #5718, .T. ) ;
#61337 = ORIENTED_EDGE ( 'NONE', *, *, #45977, .F. ) ;
#61338 = CARTESIAN_POINT ( 'NONE',  ( -8.519285250882628446, -4.336752205174649433, 33.62275283266504289 ) ) ;
#61339 = ADVANCED_FACE ( 'NONE', ( #66402 ), #11019, .F. ) ;
#61340 = ADVANCED_FACE ( 'NONE', ( #19546 ), #25419, .T. ) ;
#61341 = DIRECTION ( 'NONE',  ( 0.000000000000000000, 0.9396926207859126468, -0.3420201433256571111 ) ) ;
#61342 = ADVANCED_FACE ( 'NONE', ( #5148 ), #38042, .F. ) ;
#61343 = CARTESIAN_POINT ( 'NONE',  ( -18.22292695890684655, -10.77366814457252175, 33.85459836347580875 ) ) ;
#61344 = VECTOR ( 'NONE', #57553, 1000.000000000000000 ) ;
#61345 = CARTESIAN_POINT ( 'NONE',  ( -6.166666666666667851, -7.500000000000000000, 33.75000000000000000 ) ) ;
#61346 = CARTESIAN_POINT ( 'NONE',  ( -11.40793583669797506, -2.619367082507849442, 30.83698974864643461 ) ) ;
#61347 = VERTEX_POINT ( 'NONE', #80377 ) ;
#61348 = EDGE_CURVE ( 'NONE', #65223, #82999, #86700, .T. ) ;
#61349 = ORIENTED_EDGE ( 'NONE', *, *, #7910, .T. ) ;
#61350 = ORIENTED_EDGE ( 'NONE', *, *, #71103, .F. ) ;
#61351 = ORIENTED_EDGE ( 'NONE', *, *, #58021, .F. ) ;
#61352 = CARTESIAN_POINT ( 'NONE',  ( -5.011667505647053211, -5.219633306516380244, 34.19971097300157936 ) ) ;
#61353 = CARTESIAN_POINT ( 'NONE',  ( -16.94687791408830080, -2.504778602574659896, 29.97347330155780654 ) ) ;
#61354 = CARTESIAN_POINT ( 'NONE',  ( 4.946775107191379028, -11.66186481527757479, 32.95055677023626117 ) ) ;
#61355 = VERTEX_POINT ( 'NONE', #67298 ) ;
#61356 = B_SPLINE_CURVE_WITH_KNOTS ( 'NONE', 3,
 ( #54244, #40312, #67774, #81740, #20024, #6521, #22679, #84401, #63218, #8295 ),
 .UNSPECIFIED., .F., .F.,
 ( 4, 2, 2, 2, 4 ),
 ( 0.0007817359430256282712, 0.0009771253907249945886, 0.001172514838424360689, 0.001367904286123726790, 0.001563293733823093107 ),
 .UNSPECIFIED. ) ;
#61357 = CARTESIAN_POINT ( 'NONE',  ( -13.38461538461538325, -6.435427911321262684, 35.78748833219616898 ) ) ;
#61358 = CARTESIAN_POINT ( 'NONE',  ( -2.307692307692305711, -13.20930481340135110, 34.54067556320372745 ) ) ;
#61359 = DIRECTION ( 'NONE',  ( 0.000000000000000000, 0.7660444431189822323, -0.6427876096865344779 ) ) ;
#61360 = CARTESIAN_POINT ( 'NONE',  ( 11.53846153846153832, -9.780366693483667717, 34.19971097300155094 ) ) ;
#61361 = VERTEX_POINT ( 'NONE', #87141 ) ;
#61362 = B_SPLINE_CURVE_WITH_KNOTS ( 'NONE', 3,
 ( #34379, #61844, #86487, #4494, #81055, #74289, #12588, #53562, #18459, #31519 ),
 .UNSPECIFIED., .F., .F.,
 ( 4, 2, 2, 2, 4 ),
 ( 0.000000000000000000, 0.0001954339857564078538, 0.0003908679715128157077, 0.0005863019572692235344, 0.0007817359430256314154 ),
 .UNSPECIFIED. ) ;
#61363 = EDGE_CURVE ( 'NONE', #10767, #34572, #24966, .T. ) ;
#61364 = VERTEX_POINT ( 'NONE', #11460 ) ;
#61365 = AXIS2_PLACEMENT_3D ( 'NONE', #52700, #44597, #85605 ) ;
#61366 = ORIENTED_EDGE ( 'NONE', *, *, #26554, .F. ) ;
#61367 = DIRECTION ( 'NONE',  ( -0.000000000000000000, -0.1736481776669307198, -0.9848077530122080203 ) ) ;
#61368 = EDGE_CURVE ( 'NONE', #13051, #27912, #25865, .T. ) ;
#61370 = CARTESIAN_POINT ( 'NONE',  ( -7.623141002060451754, -9.172514111537584114, 34.72667873470787470 ) ) ;
#61369 = CARTESIAN_POINT ( 'NONE',  ( -1.450697763975518528, -2.486705287966279876, 31.30864560766542937 ) ) ;
#61371 = CARTESIAN_POINT ( 'NONE',  ( 16.08852214104184242, -7.749976730030849303, 34.74374725381503737 ) ) ;
#61372 = CARTESIAN_POINT ( 'NONE',  ( -9.915792636031639518, -6.760086850603066466, 34.69517049084099369 ) ) ;
#61373 = FACE_BOUND ( 'NONE', #43156, .T. ) ;
#61374 = ORIENTED_EDGE ( 'NONE', *, *, #15790, .T. ) ;
#61375 = VECTOR ( 'NONE', #48553, 1000.000000000000000 ) ;
#61376 = CARTESIAN_POINT ( 'NONE',  ( 15.23076923076923173, -2.721908614388771852, 31.22303859784724978 ) ) ;
#61377 = CARTESIAN_POINT ( 'NONE',  ( 17.07692307692295586, -6.879047030192662504, 34.71129190930017927 ) ) ;
#61378 = CYLINDRICAL_SURFACE ( 'NONE', #49595, 0.2499999999999994726 ) ;
#61379 = VERTEX_POINT ( 'NONE', #13676 ) ;
#61380 = CARTESIAN_POINT ( 'NONE',  ( 17.20771351789003489, -5.496552790871120031, 34.60292014791297532 ) ) ;
#61381 = B_SPLINE_CURVE_WITH_KNOTS ( 'NONE', 3,
 ( #10694, #38160, #52112, #39513, #39069, #86374, #38610, #30947, #46255, #65618 ),
 .UNSPECIFIED., .F., .F.,
 ( 4, 2, 2, 2, 4 ),
 ( 0.0007817246256747517261, 0.0009771112852218961399, 0.001172497944769040771, 0.001367884604316185401, 0.001563271263863329815 ),
 .UNSPECIFIED. ) ;
#61382 = VERTEX_POINT ( 'NONE', #27633 ) ;
#61383 = FACE_BOUND ( 'NONE', #43476, .T. ) ;
#61384 = CARTESIAN_POINT ( 'NONE',  ( 9.626224281351813516, -5.557115091759785130, 34.35708131394839171 ) ) ;
#61385 = ORIENTED_EDGE ( 'NONE', *, *, #6508, .T. ) ;
#61386 = DIRECTION ( 'NONE',  ( -0.000000000000000000, -0.9848077530122086864, -0.1736481776669273613 ) ) ;
#61387 = CARTESIAN_POINT ( 'NONE',  ( -12.59222906464876779, -11.93127051446799847, 32.56575433478202797 ) ) ;
#61388 = CARTESIAN_POINT ( 'NONE',  ( 1.161689167099237752, -3.105860786376062332, 32.13614157043599562 ) ) ;
#61389 = ORIENTED_EDGE ( 'NONE', *, *, #55433, .F. ) ;
#61390 = CARTESIAN_POINT ( 'NONE',  ( -8.769230769230892619, -3.643525952248795718, 33.31231777344771672 ) ) ;
#61391 = FACE_OUTER_BOUND ( 'NONE', #35789, .T. ) ;
#61392 = CARTESIAN_POINT ( 'NONE',  ( 6.923076923076802558, -12.46129190930018460, 30.37095296980731973 ) ) ;
#61393 = CARTESIAN_POINT ( 'NONE',  ( 2.438217745925950641, -3.068774925481847493, 32.56582465632704526 ) ) ;
#61394 = VERTEX_POINT ( 'NONE', #6914 ) ;
#61395 = CARTESIAN_POINT ( 'NONE',  ( 13.38461538461538680, -5.557115091759785130, 34.35708131394839171 ) ) ;
#61396 = CARTESIAN_POINT ( 'NONE',  ( 2.438482748659259958, -3.338503747796865984, 32.95102852606552801 ) ) ;
#61398 = VERTEX_POINT ( 'NONE', #75817 ) ;
#61397 = CARTESIAN_POINT ( 'NONE',  ( -8.899377978668990608, -3.817052484675422797, 33.13202310037935661 ) ) ;
#61399 = CARTESIAN_POINT ( 'NONE',  ( 5.076923076923075762, -5.557115091759785130, 34.35708131394839171 ) ) ;
#61400 = CARTESIAN_POINT ( 'NONE',  ( 15.90382292962469890, -4.175268141568689195, 33.81360843649122216 ) ) ;
#61401 = CARTESIAN_POINT ( 'NONE',  ( 6.000000000000001776, -8.973038597847269315, 34.52809138561121927 ) ) ;
#61402 = CARTESIAN_POINT ( 'NONE',  ( 13.51514108637895006, -12.45806712695776319, 30.39783852428763922 ) ) ;
#61403 = CARTESIAN_POINT ( 'NONE',  ( -13.16160403300253634, -3.587049720035815348, 32.86302985866382897 ) ) ;
#61404 = VECTOR ( 'NONE', #54573, 1000.000000000000000 ) ;
#61405 = CARTESIAN_POINT ( 'NONE',  ( -12.46153846153846168, -10.67929555188718282, 33.92786785259544047 ) ) ;
#61407 = CARTESIAN_POINT ( 'NONE',  ( -16.85391172531022619, -8.239487800360276282, 34.69522927552633718 ) ) ;
#61406 = CARTESIAN_POINT ( 'NONE',  ( -1.450698795571263577, -4.786620604624113540, 33.94971097300155805 ) ) ;
#61408 = EDGE_CURVE ( 'NONE', #25915, #22155, #163, .T. ) ;
#61409 = EDGE_CURVE ( 'NONE', #41880, #12918, #16595, .T. ) ;
#61410 = B_SPLINE_CURVE_WITH_KNOTS ( 'NONE', 3,
 ( #22425, #77369, #13895, #21538, #42708, #76490, #83251, #56655, #49460, #1713 ),
 .UNSPECIFIED., .F., .F.,
 ( 4, 2, 2, 2, 4 ),
 ( 0.0007817359430256301143, 0.0009771253907249963233, 0.001172514838424362641, 0.001367904286123728958, 0.001563293733823095059 ),
 .UNSPECIFIED. ) ;
#61411 = CYLINDRICAL_SURFACE ( 'NONE', #59366, 0.2499999999999995559 ) ;
#61412 = CARTESIAN_POINT ( 'NONE',  ( -1.409462824231155764E-14, -4.749999999999999112, 20.40625000000000000 ) ) ;
#61413 = ORIENTED_EDGE ( 'NONE', *, *, #58802, .F. ) ;
#61414 = VECTOR ( 'NONE', #71415, 1000.000000000000227 ) ;
#61415 = B_SPLINE_CURVE_WITH_KNOTS ( 'NONE', 3,
 ( #14871, #13969, #82001, #8107, #464, #68468, #35579, #49535, #76111, #55838 ),
 .UNSPECIFIED., .F., .F.,
 ( 4, 2, 2, 2, 4 ),
 ( 0.000000000000000000, 0.0001954311564186865763, 0.0003908623128373731525, 0.0005862934692560596746, 0.0007817246256747463051 ),
 .UNSPECIFIED. ) ;
#61416 = CARTESIAN_POINT ( 'NONE',  ( -8.769230769230890843, -12.27809138561165270, 31.22303859784587132 ) ) ;
#61417 = VERTEX_POINT ( 'NONE', #55545 ) ;
#61418 = EDGE_CURVE ( 'NONE', #6801, #27837, #86510, .T. ) ;
#61419 = ORIENTED_EDGE ( 'NONE', *, *, #70181, .T. ) ;
#61420 = CYLINDRICAL_SURFACE ( 'NONE', #55666, 5.000000000000000888 ) ;
#61421 = EDGE_CURVE ( 'NONE', #81196, #86663, #55989, .T. ) ;
#61423 = VERTEX_POINT ( 'NONE', #14121 ) ;
#61422 = AXIS2_PLACEMENT_3D ( 'NONE', #51677, #17482, #44933 ) ;
#61424 = DIRECTION ( 'NONE',  ( 1.000000000000000000, 0.000000000000000000, 0.000000000000000000 ) ) ;
#61425 = CARTESIAN_POINT ( 'NONE',  ( 1.139087296526029469, -10.24999999999999467, 19.70312500000000355 ) ) ;
#61426 = CARTESIAN_POINT ( 'NONE',  ( 14.55763782604045176, -11.37275283266504111, 32.91324779482534524 ) ) ;
#61427 = LINE ( 'NONE', #68201, #72613 ) ;
#61428 = CARTESIAN_POINT ( 'NONE',  ( 3.007284287045282500, -8.496056993536548418, 34.65000542017679663 ) ) ;
#61429 = DIRECTION ( 'NONE',  ( 0.000000000000000000, 1.000000000000000000, 0.000000000000000000 ) ) ;
#61430 = CARTESIAN_POINT ( 'NONE',  ( -11.53846153846165912, -11.48612834414049644, 32.76840700105863391 ) ) ;
#61431 = DIRECTION ( 'NONE',  ( -0.000000000000000000, 0.1736481776669307198, -0.9848077530122080203 ) ) ;
#61432 = EDGE_CURVE ( 'NONE', #42225, #17613, #1632, .T. ) ;
#61433 = LINE ( 'NONE', #20011, #42214 ) ;
#61434 = CYLINDRICAL_SURFACE ( 'NONE', #34780, 0.2499999999999995559 ) ;
#61435 = CARTESIAN_POINT ( 'NONE',  ( -17.75005459062195712, -2.341251567377310217, 30.72681386836322659 ) ) ;
#61436 = EDGE_CURVE ( 'NONE', #62595, #52583, #14563, .T. ) ;
#61437 = DIRECTION ( 'NONE',  ( 0.000000000000000000, 0.000000000000000000, -1.000000000000000000 ) ) ;
#61438 = VERTEX_POINT ( 'NONE', #69505 ) ;
#61439 = ORIENTED_EDGE ( 'NONE', *, *, #46965, .T. ) ;
#61440 = CARTESIAN_POINT ( 'NONE',  ( -17.86943940825808852, -12.49523960252712484, 29.97295953869786800 ) ) ;
#61441 = CARTESIAN_POINT ( 'NONE',  ( 0.4615384615384611200, -11.91647553114624181, 32.58852847137148245 ) ) ;
#61442 = DIRECTION ( 'NONE',  ( 0.000000000000000000, 0.6427876096865368094, 0.7660444431189802339 ) ) ;
#61443 = EDGE_CURVE ( 'NONE', #11769, #52068, #88920, .T. ) ;
#61444 = DIRECTION ( 'NONE',  ( 0.000000000000000000, 0.7660444431189807890, 0.6427876096865361433 ) ) ;
#61445 = CARTESIAN_POINT ( 'NONE',  ( 14.24242230713598900, -3.643525952247789412, 33.31231777344662959 ) ) ;
#61446 = B_SPLINE_CURVE_WITH_KNOTS ( 'NONE', 3,
 ( #9443, #84677, #65259, #36040, #17083, #3116, #79236, #8566, #63495, #77460 ),
 .UNSPECIFIED., .F., .F.,
 ( 4, 2, 2, 2, 4 ),
 ( 0.0007817246256747463051, 0.0009771112852218896347, 0.001172497944769033181, 0.001367884604316176728, 0.001563271263863320057 ),
 .UNSPECIFIED. ) ;
#61447 = DIRECTION ( 'NONE',  ( 0.000000000000000000, 0.9848077530122072432, -0.1736481776669354937 ) ) ;
#61448 = CARTESIAN_POINT ( 'NONE',  ( -0.4615384615384611200, -12.09954503811598769, 35.62045528018868623 ) ) ;
#61449 = EDGE_CURVE ( 'NONE', #64747, #46752, #53137, .T. ) ;
#61450 = ORIENTED_EDGE ( 'NONE', *, *, #16167, .F. ) ;
#61451 = DIRECTION ( 'NONE',  ( -0.000000000000000000, -0.9848077530122086864, -0.1736481776669273891 ) ) ;
#61452 = ORIENTED_EDGE ( 'NONE', *, *, #11703, .T. ) ;
#61453 = EDGE_CURVE ( 'NONE', #51043, #86240, #54208, .T. ) ;
#61454 = CARTESIAN_POINT ( 'NONE',  ( 5.076923076922953193, -11.06231777344772027, 33.60647404775119895 ) ) ;
#61455 = CARTESIAN_POINT ( 'NONE',  ( -18.25000000000001066, -12.75000000000000178, 29.81889780837731152 ) ) ;
#61456 = CARTESIAN_POINT ( 'NONE',  ( -4.153846153846152411, -11.91647553114624181, 32.58852847137148245 ) ) ;
#61457 = CARTESIAN_POINT ( 'NONE',  ( 2.144117459101453788E-15, 12.75000000000001243, 32.75000000000000000 ) ) ;
#61458 = CARTESIAN_POINT ( 'NONE',  ( -12.46153846153846168, -12.10708131394839349, 31.69288490824020244 ) ) ;
#61459 = ORIENTED_EDGE ( 'NONE', *, *, #34619, .T. ) ;
#61460 = EDGE_CURVE ( 'NONE', #63896, #64886, #72428, .T. ) ;
#61461 = EDGE_LOOP ( 'NONE', ( #36694, #64653, #44975, #74642 ) ) ;
#61462 = AXIS2_PLACEMENT_3D ( 'NONE', #38305, #3619, #51333 ) ;
#61463 = EDGE_LOOP ( 'NONE', ( #68257, #44460 ) ) ;
#61464 = EDGE_LOOP ( 'NONE', ( #29586, #24229 ) ) ;
#61465 = EDGE_CURVE ( 'NONE', #861, #63608, #69654, .T. ) ;
#61466 = CARTESIAN_POINT ( 'NONE',  ( 17.14217821643591932, -10.33852847137154107, 34.16647553114620450 ) ) ;
#61467 = CARTESIAN_POINT ( 'NONE',  ( 4.853996859406927378, -10.61292498521070549, 33.66303323003028680 ) ) ;
#61468 = AXIS2_PLACEMENT_3D ( 'NONE', #68231, #8304, #55146 ) ;
#61469 = CARTESIAN_POINT ( 'NONE',  ( -3.296852641725110722, -9.780366693483667717, 34.19971097300155805 ) ) ;
#61470 = B_SPLINE_CURVE_WITH_KNOTS ( 'NONE', 3,
 ( #59404, #80120, #52639, #19308, #40910, #5352, #39599, #18423, #53075, #12554 ),
 .UNSPECIFIED., .F., .F.,
 ( 4, 2, 2, 2, 4 ),
 ( 0.000000000000000000, 0.0001954339857564093717, 0.0003908679715128187434, 0.0005863019572692280881, 0.0007817359430256374869 ),
 .UNSPECIFIED. ) ;
#61471 = CARTESIAN_POINT ( 'NONE',  ( -15.45369544828537656, -11.24512374952581872, 33.06303171183252942 ) ) ;
#61472 = SURFACE_STYLE_FILL_AREA ( #73683 ) ;
#61473 = CARTESIAN_POINT ( 'NONE',  ( -15.48074597481781822, -2.544273027872575366, 31.48422191005632342 ) ) ;
#61474 = VECTOR ( 'NONE', #18346, 1000.000000000000000 ) ;
#61475 = ORIENTED_EDGE ( 'NONE', *, *, #34606, .F. ) ;
#61476 = ADVANCED_FACE ( 'NONE', ( #16336 ), #50111, .F. ) ;
#61477 = ORIENTED_EDGE ( 'NONE', *, *, #71839, .T. ) ;
#61478 = ORIENTED_EDGE ( 'NONE', *, *, #82885, .T. ) ;
#61480 = ORIENTED_EDGE ( 'NONE', *, *, #20852, .F. ) ;
#61479 = DIRECTION ( 'NONE',  ( -0.000000000000000000, 0.6427876096865404731, -0.7660444431189770143 ) ) ;
#61481 = ADVANCED_FACE ( 'NONE', ( #64067 ), #57762, .F. ) ;
#61482 = CARTESIAN_POINT ( 'NONE',  ( -8.769230769230892619, -3.643525952248795718, 33.31231777344771672 ) ) ;
#61483 = CARTESIAN_POINT ( 'NONE',  ( -12.33101302330482341, -12.15418822224088835, 32.17964115625579069 ) ) ;
#61484 = B_SPLINE_CURVE_WITH_KNOTS ( 'NONE', 3,
 ( #59849, #32827, #54868, #88243, #46338, #18868, #26071, #26515, #39603, #73826 ),
 .UNSPECIFIED., .F., .F.,
 ( 4, 2, 2, 2, 4 ),
 ( 0.000000000000000000, 0.0001954339857564091278, 0.0003908679715128182556, 0.0005863019572692274375, 0.0007817359430256365111 ),
 .UNSPECIFIED. ) ;
#61485 = CARTESIAN_POINT ( 'NONE',  ( 3.749999999999992006, -5.946699141100872943, 18.14062500000000355 ) ) ;
#61486 = ORIENTED_EDGE ( 'NONE', *, *, #31527, .T. ) ;
#61487 = CARTESIAN_POINT ( 'NONE',  ( -3.165513659493205623, -12.46129190930001052, 30.37095296980870174 ) ) ;
#61488 = ORIENTED_EDGE ( 'NONE', *, *, #17655, .F. ) ;
#61489 = CARTESIAN_POINT ( 'NONE',  ( -19.50000000000000000, -3.499999999999999556, 29.75000000000000355 ) ) ;
#61490 = FACE_BOUND ( 'NONE', #77645, .T. ) ;
#61491 = DIRECTION ( 'NONE',  ( 0.000000000000000000, -6.938893903907222067E-15, 1.000000000000000000 ) ) ;
#61492 = AXIS2_PLACEMENT_3D ( 'NONE', #36372, #2130, #2563 ) ;
#61493 = CARTESIAN_POINT ( 'NONE',  ( 8.703147358274890166, -4.786620604624113540, 33.94971097300155805 ) ) ;
#61494 = ORIENTED_EDGE ( 'NONE', *, *, #36232, .F. ) ;
#61495 = CARTESIAN_POINT ( 'NONE',  ( -9.757577692864012775, -5.094484230520674117, 34.41647553114621161 ) ) ;
#61496 =( NAMED_UNIT ( * ) SI_UNIT ( $, .STERADIAN. ) SOLID_ANGLE_UNIT ( ) );
#61497 = B_SPLINE_CURVE_WITH_KNOTS ( 'NONE', 3,
 ( #67321, #81728, #38973, #20012, #73649, #12813, #47475, #81288, #74973, #60555 ),
 .UNSPECIFIED., .F., .F.,
 ( 4, 2, 2, 2, 4 ),
 ( 0.0007817246256747524850, 0.0009771112852218972241, 0.001172497944769042072, 0.001367884604316186702, 0.001563271263863331550 ),
 .UNSPECIFIED. ) ;
#61498 = CARTESIAN_POINT ( 'NONE',  ( 16.15384615384603251, -6.835583212225970762, 34.95778746994575670 ) ) ;
#61499 = DIRECTION ( 'NONE',  ( -1.000000000000000000, -0.000000000000000000, 0.000000000000000000 ) ) ;
#61500 = VERTEX_POINT ( 'NONE', #69948 ) ;
#61501 = CARTESIAN_POINT ( 'NONE',  ( 11.60452988946397745, -3.050289026998446840, 32.03036669348366416 ) ) ;
#61502 = CARTESIAN_POINT ( 'NONE',  ( -7.623374304885434327, -11.41317474335729543, 32.86274602512330034 ) ) ;
#61503 = CARTESIAN_POINT ( 'NONE',  ( -16.21909608562023664, -2.255955759149247175, 30.00000000000014211 ) ) ;
#61504 = DIRECTION ( 'NONE',  ( 0.000000000000000000, 0.000000000000000000, -1.000000000000000000 ) ) ;
#61505 = DIRECTION ( 'NONE',  ( 0.000000000000000000, 0.7660444431189822323, -0.6427876096865344779 ) ) ;
#61506 = FACE_BOUND ( 'NONE', #11081, .T. ) ;
#61508 = CARTESIAN_POINT ( 'NONE',  ( -17.32689982097166492, -10.82459398097509684, 33.81372124010185587 ) ) ;
#61507 = CARTESIAN_POINT ( 'NONE',  ( 1.634615384616805889, -7.500000000000154543, 35.00000000000007105 ) ) ;
#61509 = AXIS2_PLACEMENT_3D ( 'NONE', #44237, #8720, #64514 ) ;
#61510 = CARTESIAN_POINT ( 'NONE',  ( 5.326868486301119532, -2.341251567377310217, 30.72681386836322659 ) ) ;
#61512 = CARTESIAN_POINT ( 'NONE',  ( 15.23076923076911093, -10.21337939537710326, 33.94971097300076224 ) ) ;
#61511 = DIRECTION ( 'NONE',  ( -0.000000000000000000, -0.1736481776669307198, -0.9848077530122080203 ) ) ;
#61513 = CARTESIAN_POINT ( 'NONE',  ( 5.999999999999878320, -8.656820664282941280, 34.87096338111179961 ) ) ;
#61514 = CARTESIAN_POINT ( 'NONE',  ( 1.077988221561464899, -4.724691934501233703, 16.48250670625849423 ) ) ;
#61515 = ORIENTED_EDGE ( 'NONE', *, *, #48386, .T. ) ;
#61516 = CARTESIAN_POINT ( 'NONE',  ( 1.384615384615265343, -12.27809138561165270, 31.22303859784587132 ) ) ;
#61517 = ORIENTED_EDGE ( 'NONE', *, *, #53337, .F. ) ;
#61518 = CARTESIAN_POINT ( 'NONE',  ( 0.7115384615384637845, -2.499999999999999556, 29.81604066197450109 ) ) ;
#61519 = ORIENTED_EDGE ( 'NONE', *, *, #22803, .T. ) ;
#61520 = CARTESIAN_POINT ( 'NONE',  ( 12.46153846153846168, -13.53365097954675988, 30.81389545987213552 ) ) ;
#61521 = EDGE_CURVE ( 'NONE', #51057, #7803, #64931, .T. ) ;
#61522 = CARTESIAN_POINT ( 'NONE',  ( -14.30769230769230660, -3.937682226553329556, 33.60647404775216529 ) ) ;
#61524 = EDGE_LOOP ( 'NONE', ( #82844, #413, #45276, #22523 ) ) ;
#61523 = DIRECTION ( 'NONE',  ( 1.000000000000000000, 0.000000000000000000, 0.000000000000000000 ) ) ;
#61525 = CARTESIAN_POINT ( 'NONE',  ( 18.25000000000006395, -7.434744860731433924, 35.00000000000000711 ) ) ;
#61526 = CARTESIAN_POINT ( 'NONE',  ( 2.750000000000001332, -7.438900925035452083, 20.46688170625848713 ) ) ;
#61527 = CARTESIAN_POINT ( 'NONE',  ( 12.71153846153846168, -2.499999999999998668, 29.75000000000000355 ) ) ;
#61528 = CARTESIAN_POINT ( 'NONE',  ( 4.853438133199127869, -5.113361153441932316, 34.14387501736621999 ) ) ;
#61529 = PLANE ( 'NONE',  #61889 ) ;
#61530 = CARTESIAN_POINT ( 'NONE',  ( 10.39245765647776309, -2.523278758544489797, 31.42238647778637528 ) ) ;
#61531 = CARTESIAN_POINT ( 'NONE',  ( -12.21159305216042057, -8.476813868363244353, 34.90874843262270133 ) ) ;
#61532 = CARTESIAN_POINT ( 'NONE',  ( -14.87820512820512953, -3.499999999999999556, 29.75000000000000355 ) ) ;
#61533 = ADVANCED_FACE ( 'NONE', ( #56438 ), #50977, .F. ) ;
#61534 = CARTESIAN_POINT ( 'NONE',  ( 0.06109907496451268821, -3.749999999999999556, 20.65811829374151287 ) ) ;
#61535 = CARTESIAN_POINT ( 'NONE',  ( 5.776515075435668223, -2.612411019501189813, 31.66733052389439962 ) ) ;
#61536 = CARTESIAN_POINT ( 'NONE',  ( 14.17700084102474989, -5.582088688514999397, 34.36776431015576350 ) ) ;
#61537 = ORIENTED_EDGE ( 'NONE', *, *, #41274, .T. ) ;
#61538 = EDGE_CURVE ( 'NONE', #62944, #10070, #7999, .T. ) ;
#61539 = CARTESIAN_POINT ( 'NONE',  ( -18.00000000000000000, -12.46687347288208159, 35.28035834855298702 ) ) ;
#61540 = B_SPLINE_CURVE_WITH_KNOTS ( 'NONE', 3,
 ( #81863, #34101, #20150, #89072, #69658, #7964, #82744, #40869, #47618, #62013 ),
 .UNSPECIFIED., .F., .F.,
 ( 4, 2, 2, 2, 4 ),
 ( 0.0007817359430256288133, 0.0009771253907249948054, 0.001172514838424360689, 0.001367904286123726573, 0.001563293733823092457 ),
 .UNSPECIFIED. ) ;
#61541 = CARTESIAN_POINT ( 'NONE',  ( -2.608446859217920633, -4.805146000318815780, 25.50186829374151287 ) ) ;
#61542 = CARTESIAN_POINT ( 'NONE',  ( -11.53846153846153655, -12.10708131394839349, 31.69288490824020244 ) ) ;
#61543 = CARTESIAN_POINT ( 'NONE',  ( -16.37677311275299985, -10.77366814457252175, 33.85459836347579454 ) ) ;
#61544 = EDGE_LOOP ( 'NONE', ( #88745, #28789, #72748, #48627 ) ) ;
#61545 = CARTESIAN_POINT ( 'NONE',  ( -6.923076923076922462, -6.386643153685126251, 34.62446782046654192 ) ) ;
#61546 = CARTESIAN_POINT ( 'NONE',  ( 16.37685899793955357, -2.523321265292116866, 31.42251411153756990 ) ) ;
#61548 = ORIENTED_EDGE ( 'NONE', *, *, #82132, .F. ) ;
#61547 = CARTESIAN_POINT ( 'NONE',  ( -17.01075393596041962, -7.250054483168842268, 34.74374881642865631 ) ) ;
#61549 = DIRECTION ( 'NONE',  ( -0.000000000000000000, -0.8660254037844399289, -0.4999999999999980016 ) ) ;
#61550 = AXIS2_PLACEMENT_3D ( 'NONE', #13817, #75088, #75965 ) ;
#61551 = CARTESIAN_POINT ( 'NONE',  ( 15.29602437028207085, -5.941354392334607049, 34.76329471203374055 ) ) ;
#61553 = EDGE_CURVE ( 'NONE', #2810, #10613, #12306, .T. ) ;
#61552 = CARTESIAN_POINT ( 'NONE',  ( 16.15384615384603251, -9.442884908241554243, 34.35708131394783038 ) ) ;
#61554 = CARTESIAN_POINT ( 'NONE',  ( 4.826899839630110378, -4.335965774309649134, 33.62209801155881905 ) ) ;
#61555 = FACE_OUTER_BOUND ( 'NONE', #3942, .T. ) ;
#61556 = CARTESIAN_POINT ( 'NONE',  ( 8.769230769230768274, -6.189225973068211317, 35.74407628777942847 ) ) ;
#61557 = VERTEX_POINT ( 'NONE', #3255 ) ;
#61558 = ORIENTED_EDGE ( 'NONE', *, *, #27988, .F. ) ;
#61559 = ORIENTED_EDGE ( 'NONE', *, *, #21341, .F. ) ;
#61560 = EDGE_CURVE ( 'NONE', #10726, #28342, #9129, .T. ) ;
#61561 = ORIENTED_EDGE ( 'NONE', *, *, #72434, .T. ) ;
#61562 = CIRCLE ( 'NONE', #80293, 4.000000000000000000 ) ;
#61563 = CARTESIAN_POINT ( 'NONE',  ( -5.198717948717948012, -11.50000000000000000, 29.75000000000000355 ) ) ;
#61564 = CARTESIAN_POINT ( 'NONE',  ( 20.00000000000000355, 10.00000000000000533, 13.00000000000000178 ) ) ;
#61565 = EDGE_CURVE ( 'NONE', #10638, #22672, #5039, .T. ) ;
#61566 = CARTESIAN_POINT ( 'NONE',  ( 25.00000000000000355, 9.999999999999971578, 3.000000000000000000 ) ) ;
#61567 = DIRECTION ( 'NONE',  ( -1.000000000000000000, 0.000000000000000000, -0.000000000000000000 ) ) ;
#61568 = VECTOR ( 'NONE', #20828, 1000.000000000000000 ) ;
#61569 = CARTESIAN_POINT ( 'NONE',  ( 15.93091993633000847, -4.887634598454295265, 34.01352882383564946 ) ) ;
#61570 = VERTEX_POINT ( 'NONE', #58640 ) ;
#61571 = CLOSED_SHELL ( 'NONE', ( #29021, #8123, #64879, #72068, #21945, #43758, #82758, #21399, #23546, #28045, #22779, #62403, #38079, #50279, #49066, #44772, #6081, #39011, #78515, #9838, #65211, #40559, #70379, #38796, #55964, #80781, #82516, #28862, #22767, #30883, #64528, #78949, #88992, #58440, #20704, #42516, #63668, #85161, #22543, #27636, #10111, #30664, #56910, #35565, #77662, #49982, #66279, #2946, #29252, #10022, #78153, #14658, #84438, #54808, #55936, #37650, #63080, #23372, #33238, #81444, #56008, #18664, #36303, #74776, #74303, #39840, #1000, #26776, #34078, #71530, #7919, #621, #43406, #31215, #5238, #49487, #29080, #28796, #69596, #18898, #37323, #65286, #21765, #67784, #57582, #18927, #73562, #55010, #9827, #27364, #31070, #85272, #1722, #57560, #55813, #21525, #6953, #18493, #19385, #72744, #9240, #3511, #22208, #40697, #25392, #36056, #33235, #31313, #20822, #62963, #67911, #73436, #18292, #15221, #56954, #29845, #29090, #65827, #59799, #60802, #41146, #68115, #6160, #7536, #22563, #18993, #19168, #51148, #15897, #1939, #9112, #6514, #608, #13107, #17766, #84456, #49721, #76392, #51422, #30355, #60643, #3186, #8952, #3743, #34668, #26548, #57714, #3951, #20063, #76878, #62880, #18039, #15201, #66302, #52156, #33440, #25290, #12098, #10223, #38113, #60303, #49717, #32025, #39917, #45713, #17141, #66221, #14697, #66927, #86274, #77312, #10799, #44298, #57009, #15352, #47351, #53978, #80679, #75540, #74728, #22805, #49782, #81225, #72903, #85825, #85248, #10143, #37902, #45834, #43062, #64137, #44303, #62094, #8177, #53118, #9509, #6310, #2964, #31763, #42747, #27499, #10444, #43912, #3330, #75614, #66305, #83539, #33541, #86660, #41208, #56120, #88996, #74535, #38754, #58969, #43246, #84393, #87864, #69947, #31790, #78281, #86849, #14155, #45404, #51437, #83952, #39333, #44250, #76257, #17215, #4245, #6959, #70957, #58260, #21113, #44967, #2661, #43944, #73360, #63141, #76668, #83426, #34334, #73461, #15421, #59180, #70314, #59071, #39565, #53710, #75879, #71909, #55213, #56058, #9621, #30980, #54991, #63697, #70865, #83077, #79971, #66906, #74503, #45560, #60338, #39154, #68286, #12496, #49223, #46704, #83359, #10649, #59583, #72512, #5447, #35276, #41362, #63511, #77766, #10187, #34441, #27800, #30545, #59954, #12363, #45244, #82957, #43268, #30721, #18462, #16469, #19428, #61866, #2205, #21295, #77228, #2440, #46624, #44000, #86145, #14477, #69255, #43081, #83006, #6753, #13802, #48269, #71426, #86649, #38255, #37049, #28266, #76624, #64766, #40357, #85731, #10177, #8896, #29901, #32873, #47477, #77778, #60842, #57347, #71264, #70089, #3396, #54948, #10400, #31333, #34324, #5767, #23621, #34852, #29027, #15327, #2461, #83841, #60796, #11849, #66294, #15851, #48381, #26685, #46602, #71777, #55246, #40967, #15061, #64047, #26354, #27254, #81206, #10434, #52753, #11222, #3597, #4171, #77247, #74201, #78147, #15838, #21263, #74281, #50198, #7431, #57910, #21892, #20762, #34768, #55487, #34641, #26607, #88751, #51652, #75314, #26330, #21547, #66905, #70050, #71070, #67979, #71644, #9189, #74109, #9705, #82906, #49287, #13188, #40639, #87301, #87209, #57300, #39318, #14322, #43101, #17307, #40836, #80324, #17950, #35145, #57733, #18524, #14148, #74031, #38787, #43703, #64840, #40977, #9597, #49075, #76823, #28784, #16309, #47268, #43214, #46111, #89156, #16129, #22929, #40758, #77782, #53196, #40005, #43790, #65010, #81628, #51598, #24171, #62665, #82890, #86433, #15719, #79629, #65724, #19575, #60241, #76152, #26631, #33655, #7702, #5918, #50992, #53812, #81168, #40046, #37063, #88164, #86382, #3002, #59673, #22526, #62895, #30787, #20325, #81849, #73399, #40023, #64315, #21661, #71891, #50846, #51886, #62990, #44299, #87061, #81316, #39981, #28788, #31238, #40913, #40753, #17927, #44753, #10962, #86658, #67331, #57511, #50415, #58291, #68305, #7891, #15005, #1044, #47417, #67617, #67709, #60082, #41954, #53660, #71176, #13157, #85962, #20004, #62925, #8687, #2676, #39260, #64253, #243, #67879, #10818, #38482, #86790, #20686, #8422, #35524, #47694, #72157, #42802, #23852, #10789, #48252, #56508, #28355, #32968, #63718, #88052, #30106, #53255, #10415, #33424, #76300, #21638, #52309, #17450, #33656, #311, #68532, #27710, #72463, #88019, #23264, #41790, #7028, #61881, #56566, #84773, #34669, #56946, #40983, #36009, #26140, #81986, #50485, #3078, #7277, #21873, #45609, #51462, #4352, #30753, #45321, #51903, #45849, #84905, #46234, #4752, #3650, #51447, #86545, #12477, #12197, #31676, #67600, #9028, #49685, #9520, #60791, #51551, #52502, #37215, #50853, #34149, #72249, #17256, #70202, #78038, #66848, #43613, #14396, #38992, #32768, #29018, #64202, #84153, #319, #27247, #74255, #80857, #78533, #70939, #33527, #25904, #50692, #69116, #34043, #87449, #61476, #77832, #36227, #55211, #347, #50610, #13190, #10192, #48739, #31516, #5829, #5880, #51934, #40860, #36469, #37788, #34552, #32119, #22271, #20645, #6551, #25691, #19695, #31847, #5700, #947, #708, #26679, #67072, #79927, #24014, #37734, #46328, #32110, #8045, #78529, #51817, #55670, #54357, #76826, #49958, #84182, #20262, #36867, #54121, #9247, #53234, #61533, #27130, #21129, #21609, #36573, #81063, #43991, #46732, #6876, #4875, #16811, #36195, #14921, #84680, #74485, #65213, #46755, #35430, #56993, #34470, #1200, #47136, #75022, #20544, #55841, #52077, #86063, #74214, #25699, #18511, #69787, #33989, #494, #12388, #5231, #67259, #73684, #48993, #23775, #89078, #57681, #56934, #5810, #67581, #64769, #23739, #55282, #32347, #87950, #32896, #38730, #36780, #40338, #16605, #45627, #19750, #32942, #60183, #12815, #79378, #76311, #75921, #87339, #6189, #61869, #39584, #50363, #32909, #46607, #24906, #4086, #7539, #27697, #65884, #31145, #39365, #87659, #3796, #61233, #28674, #45293, #36377, #19550, #71021, #54964, #84031, #76647, #58631, #84304, #69036, #3627, #72848, #27098, #57034, #71173, #66809, #7977, #3923, #17381, #39742, #32360, #22891, #58561, #77174, #59147, #34126, #85034, #72567, #6743, #28337, #16802, #34328, #57692, #9526, #14443, #26295, #3037, #56378, #44370, #81876, #7696, #71825, #77931, #62036, #48863, #19268, #85224, #31460, #49193, #81333, #34981, #82993, #84275, #49398, #28933, #68693, #63810, #51368, #5083, #12968, #56111, #17382, #16059, #32179, #73208, #24169, #12568, #53541, #22813, #37724, #82064, #42113, #53746, #44493, #37908, #29897, #58751, #84492, #7944, #2399, #63317, #5593, #15023, #44793, #65146, #41177, #56050, #7877, #42645, #74965, #86969, #53262, #11706, #26622, #45045, #31303, #16566, #81762, #37316, #4569, #80291, #23901, #67938, #42282, #83526, #59979, #14093, #63017, #154, #30178, #10091, #4178, #80893, #72324, #45515, #62327, #3072, #83444, #7288, #42134, #79149, #44936, #1085, #5188, #54087, #10657, #63549, #10548, #65330, #38935, #39479, #41597, #26153, #12991, #86537, #13313, #58590, #58199, #66569, #45297, #54046, #50786, #76889, #25916, #39472, #87961, #66959, #49981, #80139, #47193, #63994, #62908, #14511, #8077, #7482, #58448, #21926, #43328, #15124, #83616, #1866, #55562, #72052, #3782, #83574, #22487, #24573, #64327, #1723, #7412, #13178, #28729, #77320, #12205, #17392, #26601, #43414, #61339, #52060, #72887, #78178, #8551, #19891, #28261, #39232, #21304, #26193, #8071, #32429, #9207, #34221, #62449, #64622, #10708, #61481, #26940, #45602, #6000, #9930, #35009, #36771, #31883, #81659, #28357, #56822, #70596, #85511, #58110, #20904, #5079, #6712, #29039, #71814, #29346, #23235, #4090, #42912, #58328, #41198, #75284, #89170, #66775, #23054, #75098, #48680, #26933, #80198, #83036, #77676, #76881, #14196, #14441, #33290, #9420, #27996, #35515, #17363, #16733, #2883, #71874, #11781, #58738, #15193, #60828, #7063, #50216, #60553, #29394, #50919, #23954, #76258, #81550, #6971, #9732, #35099, #4345, #86089, #46451, #30679, #87391, #67111, #12608, #36557, #24796, #37398, #15781, #39376, #78496, #11712, #21808, #88295, #21376, #6179, #65118, #9103, #23888, #12615, #73711, #14058, #62811, #80299, #47601, #333, #5305, #85548, #18777, #56447, #74431, #8051, #53368, #43384, #72640, #1355, #47849, #58846, #6704, #29983, #72793, #22418, #63382, #43285, #83908, #39485, #8195, #15516, #50308, #74997, #12874, #70909, #59249, #59689, #53852, #75591, #7097, #88930, #23245, #43012, #65627, #80178, #59344, #57156, #13484, #60081, #59669, #47722, #25195, #2715, #59737, #78378, #61018, #37482, #54298, #63688, #20995, #65438, #77306, #25524, #16639, #60343, #46630, #65741, #48481, #30043, #24383, #53548, #30113, #40003, #45206, #61026, #13469, #43297, #51599, #39165, #61913, #14618, #41957, #81940, #32667, #31814, #24686, #82830, #50016, #36623, #78998, #84996, #17833, #75506, #12609, #84006, #11551, #24004, #58536, #74559, #56333, #35886, #43892, #32236, #14715, #13608, #37070, #35218, #25576, #75624, #4088, #79794, #51709, #61205, #79135, #70217, #42126, #46139, #18364, #54703, #20439, #42219, #80817, #70137, #58238, #88298, #46643, #77408, #52163, #18342, #45189, #69836, #54373, #25428, #6077, #19574, #61342, #9700, #71222, #57424, #25679, #32600, #20224, #64326, #42379, #68555, #47006, #72505, #62542, #49612, #63775, #10975, #47180, #62299, #58807, #1375, #15063, #68031, #37180, #47536, #51083, #57816, #72034, #11793, #42065, #75364, #13826, #26111, #57578, #58563, #52565, #9500, #74948, #46720, #17918, #24494, #71883, #40874, #88888, #978, #4030, #80602, #26934, #1321, #36109, #69208, #42910, #88390, #2041, #18885, #83399, #54035, #75338, #34397, #55150, #17792, #27554, #33908, #63277, #52461, #28856, #35277, #67336, #40131, #62137, #8044, #86186, #68432, #3434, #87899, #80028, #64298, #24391, #72751, #337, #13722, #1399, #77042, #73205, #46425, #85876, #74917, #70324, #62868, #83429, #12310, #79765, #15769, #56915, #54369, #60999, #88448, #17979, #65404, #27226, #10828, #53821, #12081, #78073, #81134, #85179, #11240, #4289, #6249, #65024, #14068, #76284, #48063, #66856, #65898, #3777, #68103, #79053, #86316, #2141, #52346, #87540, #51606, #60786, #6500, #47712, #57216, #23037, #39268, #21200, #49823, #62596, #79195, #15214, #21124, #58576, #56491, #57414, #41729, #33369, #61003, #9311, #13870, #52244, #38866, #71744, #73035, #35089, #57402, #31747, #32777, #66014, #54411, #51355, #808, #86377, #77133, #15054, #17931, #36545, #52169, #12358, #73881, #43262, #31355, #60911, #56715, #2593, #56223, #24379, #13467, #14177, #44681, #8710, #7325, #24797, #5603, #4534, #56294, #69771, #59651, #54425, #60256, #16536, #85656, #29404, #79363, #28016, #67537, #25637, #31186, #22996, #32642, #26783, #50799, #17323, #53881, #71962, #1367, #89086, #48711, #8225, #86799, #52824, #5968, #42304, #63544, #77849, #66462, #563, #10216, #63190, #79810, #22870, #72265, #15945, #82538, #63594, #23396, #26369, #9948, #47203, #71756, #36736, #41446, #38180, #49689, #78305, #17533, #42005, #54282, #25129, #12198, #76315, #75521, #37994, #16674, #83580, #44262, #79597, #85174, #68566, #74531, #2777, #87307, #58046, #60689, #21925, #51830, #26793, #45569, #80089, #58913, #15852, #23502, #41754, #56383, #73311, #83626, #69086, #80640, #68726, #64652, #323, #75049, #43577, #40348, #81739, #76966, #928, #72953, #30293, #19924, #29159, #35028, #64667, #88831, #83404, #72779, #61042, #10727, #10036, #18126, #62785, #79625, #32861, #7295, #56494, #80801, #3568, #77963, #4301, #56471, #46747, #84550, #38738, #11463, #65306, #16903, #44823, #51923, #39558, #39820, #40844, #27658, #14702, #75058, #76957, #7594, #18259, #48532, #8961, #1581, #44452, #77533, #82225, #16454, #80194, #78049, #70655, #29006, #66887, #1403, #60914, #41742, #7629, #54178, #68938, #71549, #79289, #61340, #27231, #37220, #46368, #72242, #3973, #64910, #59970, #23770, #17026, #56202 ) ) ;
#61572 = ORIENTED_EDGE ( 'NONE', *, *, #88949, .T. ) ;
#61573 = ADVANCED_FACE ( 'NONE', ( #86587 ), #46024, .T. ) ;
#61574 = ORIENTED_EDGE ( 'NONE', *, *, #65771, .T. ) ;
#61576 = EDGE_LOOP ( 'NONE', ( #87856, #29164 ) ) ;
#61575 = CARTESIAN_POINT ( 'NONE',  ( -12.46153846153846168, -3.886160181151819604, 36.00935417666054406 ) ) ;
#61577 = CARTESIAN_POINT ( 'NONE',  ( -1.608100309179717025, -3.019605429927184836, 32.48692288466676814 ) ) ;
#61578 = B_SPLINE_CURVE_WITH_KNOTS ( 'NONE', 3,
 ( #30255, #9973, #57722, #62690, #85204, #36138, #15862, #1010, #23483, #50939 ),
 .UNSPECIFIED., .F., .F.,
 ( 4, 2, 2, 2, 4 ),
 ( 0.0007817359430256318490, 0.0009771253907249984917, 0.001172514838424365026, 0.001367904286123731560, 0.001563293733823098311 ),
 .UNSPECIFIED. ) ;
#61579 = CARTESIAN_POINT ( 'NONE',  ( -3.480792454990688789, -12.07920672191015221, 32.31858351112116168 ) ) ;
#61580 = CARTESIAN_POINT ( 'NONE',  ( 6.923076923076924238, -4.661471528628507777, 34.16647553114623292 ) ) ;
#61581 = CYLINDRICAL_SURFACE ( 'NONE', #53969, 0.2499999999999986955 ) ;
#61582 = EDGE_LOOP ( 'NONE', ( #29689, #67750, #39341, #71274 ) ) ;
#61583 = EDGE_CURVE ( 'NONE', #61584, #19974, #38147, .T. ) ;
#61584 = VERTEX_POINT ( 'NONE', #32505 ) ;
#61585 = ORIENTED_EDGE ( 'NONE', *, *, #69200, .T. ) ;
#61586 = CARTESIAN_POINT ( 'NONE',  ( -4.853496115061506799, -7.630147231320743018, 34.74852402298682819 ) ) ;
#61588 = ORIENTED_EDGE ( 'NONE', *, *, #27948, .T. ) ;
#61587 = PLANE ( 'NONE',  #31554 ) ;
#61589 = CARTESIAN_POINT ( 'NONE',  ( 4.153846153846154188, -8.973038597847269315, 34.52809138561121927 ) ) ;
#61590 = EDGE_CURVE ( 'NONE', #51043, #61382, #53219, .T. ) ;
#61591 = EDGE_CURVE ( 'NONE', #77888, #4198, #54251, .T. ) ;
#61592 = CARTESIAN_POINT ( 'NONE',  ( -17.20707104665477161, -3.625366637846545448, 33.29286588640298561 ) ) ;
#61593 = VERTEX_POINT ( 'NONE', #59087 ) ;
#61594 = CARTESIAN_POINT ( 'NONE',  ( -19.50000000000000000, -3.499999999999999556, 29.75000000000000355 ) ) ;
#61595 = CARTESIAN_POINT ( 'NONE',  ( 0.4615384615384611200, -9.058645607665452459, 34.76329471203371924 ) ) ;
#61596 = EDGE_CURVE ( 'NONE', #70222, #12394, #70377, .T. ) ;
#61597 = AXIS2_PLACEMENT_3D ( 'NONE', #43232, #36479, #34708 ) ;
#61598 = FACE_BOUND ( 'NONE', #29747, .T. ) ;
#61599 = EDGE_CURVE ( 'NONE', #28595, #67660, #28424, .T. ) ;
#61600 = CARTESIAN_POINT ( 'NONE',  ( -15.29685161012936767, -8.164416787775445883, 34.95778746994557906 ) ) ;
#61601 = CARTESIAN_POINT ( 'NONE',  ( 0.4615384615384611200, -6.343179335718451384, 34.87096338111211935 ) ) ;
#61602 = DIRECTION ( 'NONE',  ( 1.000000000000000000, 0.000000000000000000, 0.000000000000000000 ) ) ;
#61604 = CARTESIAN_POINT ( 'NONE',  ( 18.06525557127601900, -4.481592998940251427, 33.73612834413965089 ) ) ;
#61603 = CYLINDRICAL_SURFACE ( 'NONE', #25934, 0.5000000000000004441 ) ;
#61605 = CARTESIAN_POINT ( 'NONE',  ( 2.307692307692309264, -8.810774026931790459, 35.74407628777942847 ) ) ;
#61606 = CARTESIAN_POINT ( 'NONE',  ( -3.903791733932698182, -11.47946981652013498, 33.17500667209846910 ) ) ;
#61607 = ORIENTED_EDGE ( 'NONE', *, *, #77019, .T. ) ;
#61608 = CARTESIAN_POINT ( 'NONE',  ( -8.769230769230768274, -2.249999999999998668, 29.50000000000001421 ) ) ;
#61609 = DIRECTION ( 'NONE',  ( 0.000000000000000000, -1.000000000000000000, 0.000000000000000000 ) ) ;
#61610 = ORIENTED_EDGE ( 'NONE', *, *, #56714, .T. ) ;
#61611 = B_SPLINE_CURVE_WITH_KNOTS ( 'NONE', 3,
 ( #68038, #20, #80674, #33363, #33798, #54959, #19399, #12203, #46866, #74350 ),
 .UNSPECIFIED., .F., .F.,
 ( 4, 2, 2, 2, 4 ),
 ( 0.000000000000000000, 0.0001954311564186862510, 0.0003908623128373725020, 0.0005862934692560588072, 0.0007817246256747450040 ),
 .UNSPECIFIED. ) ;
#61612 = CARTESIAN_POINT ( 'NONE',  ( 14.05771557674995442, -9.943427161483782584, 34.11278801902876978 ) ) ;
#61613 = CARTESIAN_POINT ( 'NONE',  ( -7.596099426240392027, -2.318338780012835443, 30.59689888758630261 ) ) ;
#61615 = EDGE_LOOP ( 'NONE', ( #10907, #11865, #43811, #9024, #32420, #86689 ) ) ;
#61614 = B_SPLINE_CURVE_WITH_KNOTS ( 'NONE', 3,
 ( #826, #29634, #50324, #49459, #76489, #43144 ),
 .UNSPECIFIED., .F., .F.,
 ( 4, 2, 4 ),
 ( 3.879202041849148443E-17, 0.0001954756301637101349, 0.0003909512603273815096 ),
 .UNSPECIFIED. ) ;
#61616 = CARTESIAN_POINT ( 'NONE',  ( -16.08859058257013430, -11.48612834413965977, 32.76840700105972815 ) ) ;
#61617 = DIRECTION ( 'NONE',  ( 1.000000000000000000, 0.000000000000000000, 0.000000000000000000 ) ) ;
#61618 = FACE_BOUND ( 'NONE', #70885, .T. ) ;
#61620 = CARTESIAN_POINT ( 'NONE',  ( 15.48071474911736978, -12.22109172314383052, 31.39792113162168263 ) ) ;
#61619 = CARTESIAN_POINT ( 'NONE',  ( -18.13014720943822056, -3.285722584762971632, 32.44110544564090759 ) ) ;
#61621 = CARTESIAN_POINT ( 'NONE',  ( 2.057669083470851756, -6.652501968072646932, 34.93155406624980941 ) ) ;
#61622 = DIRECTION ( 'NONE',  ( 1.000000000000000000, 0.000000000000000000, 0.000000000000000000 ) ) ;
#61624 = CARTESIAN_POINT ( 'NONE',  ( 2.307692307692186251, -11.06231777344772027, 33.60647404775119895 ) ) ;
#61623 = DIRECTION ( 'NONE',  ( 0.000000000000000000, 0.000000000000000000, 1.000000000000000000 ) ) ;
#61625 = CARTESIAN_POINT ( 'NONE',  ( -1.492201783934549164, -11.27530806549876807, 15.85750670625849068 ) ) ;
#61626 = EDGE_LOOP ( 'NONE', ( #68078, #71870, #22699, #28991 ) ) ;
#61627 = ORIENTED_EDGE ( 'NONE', *, *, #69225, .F. ) ;
#61628 = CIRCLE ( 'NONE', #11292, 4.000000000000000000 ) ;
#61629 = CARTESIAN_POINT ( 'NONE',  ( -12.39628332202562433, -5.941354392334607049, 34.76329471203374055 ) ) ;
#61630 = DIRECTION ( 'NONE',  ( 0.000000000000000000, 0.1736481776669275834, 0.9848077530122086864 ) ) ;
#61631 = CARTESIAN_POINT ( 'NONE',  ( -4.153846153846152411, -12.34228464037088635, 31.77849191805839268 ) ) ;
#61632 = CARTESIAN_POINT ( 'NONE',  ( -0.2115384615370257404, -7.500000000000155431, 34.75000000000007105 ) ) ;
#61633 = CARTESIAN_POINT ( 'NONE',  ( -15.00775787915638482, -2.758310577978207778, 31.33698337089302299 ) ) ;
#61634 = CARTESIAN_POINT ( 'NONE',  ( 3.750000000000000888, -7.499999999999978684, 25.71875000000000000 ) ) ;
#61635 = CARTESIAN_POINT ( 'NONE',  ( -1.607542343522233796, -4.026226216239095379, 33.68668979543632958 ) ) ;
#61636 = CARTESIAN_POINT ( 'NONE',  ( 1.384615384615264011, -10.33852847137269571, 34.16647553114546554 ) ) ;
#61637 = VECTOR ( 'NONE', #9306, 1000.000000000000227 ) ;
#61638 = CARTESIAN_POINT ( 'NONE',  ( 4.153846153846154188, -1.422936976036506707, 30.56769352161908415 ) ) ;
#61639 = CARTESIAN_POINT ( 'NONE',  ( 27.00000000000000000, 9.000000000000001776, 3.000000000000000444 ) ) ;
#61640 = CARTESIAN_POINT ( 'NONE',  ( 20.00000000000000000, -7.500000000000000000, 29.75000000000000355 ) ) ;
#61641 = VECTOR ( 'NONE', #86704, 1000.000000000000000 ) ;
#61642 = CARTESIAN_POINT ( 'NONE',  ( 7.780071466793711643, -8.164416787775445883, 34.95778746994557906 ) ) ;
#61643 = CARTESIAN_POINT ( 'NONE',  ( -4.826923076923076650, -7.500000000000001776, 35.04278698407183867 ) ) ;
#61644 = CYLINDRICAL_SURFACE ( 'NONE', #69221, 0.2500000000000008882 ) ;
#61645 = CARTESIAN_POINT ( 'NONE',  ( 3.230769230769231726, -13.53365097954675988, 30.81389545987213552 ) ) ;
#61646 = ORIENTED_EDGE ( 'NONE', *, *, #19631, .T. ) ;
#61647 = CARTESIAN_POINT ( 'NONE',  ( 8.899756207464411872, -5.070358843744210198, 34.40418822224088302 ) ) ;
#61648 = DIRECTION ( 'NONE',  ( -0.000000000000000000, -0.000000000000000000, -1.000000000000000000 ) ) ;
#61649 = CARTESIAN_POINT ( 'NONE',  ( -1.077988221561493543, -4.724691934501247914, 21.82999329374151642 ) ) ;
#61650 = CARTESIAN_POINT ( 'NONE',  ( -9.757577692864012775, -11.06231777344662781, 33.60647404775220082 ) ) ;
#61651 = CARTESIAN_POINT ( 'NONE',  ( -17.86920819217521483, -10.54018710029568595, 33.71981072465678864 ) ) ;
#61652 = FACE_OUTER_BOUND ( 'NONE', #66236, .T. ) ;
#61654 = EDGE_LOOP ( 'NONE', ( #82572, #29294, #86668, #80739, #70393, #5543, #15952, #34712, #14289, #19468, #78019, #17044, #16711, #80777, #18989, #61349 ) ) ;
#61653 = CARTESIAN_POINT ( 'NONE',  ( -1.254089682851819987, -4.459921816937788996, 33.71989282347011851 ) ) ;
#61655 = CARTESIAN_POINT ( 'NONE',  ( 2.750000000000001776, -7.499999999999984013, 24.46875000000000000 ) ) ;
#61656 = CARTESIAN_POINT ( 'NONE',  ( 16.82694633287448838, -2.544273027872574477, 31.48422191005632698 ) ) ;
#61657 = ORIENTED_EDGE ( 'NONE', *, *, #52028, .F. ) ;
#61658 = CARTESIAN_POINT ( 'NONE',  ( -11.53846153846122391, -2.255955759149395501, 30.00000000000324363 ) ) ;
#61659 = CARTESIAN_POINT ( 'NONE',  ( 13.31853300525525086, -9.058645607665454236, 34.76329471203372634 ) ) ;
#61660 = ORIENTED_EDGE ( 'NONE', *, *, #35094, .F. ) ;
#61661 = CARTESIAN_POINT ( 'NONE',  ( -17.78205128205128105, -11.50000000000000000, 29.75000000000000355 ) ) ;
#61662 = CARTESIAN_POINT ( 'NONE',  ( -7.780085495151404906, -2.538708090699994813, 30.37095296980875503 ) ) ;
#61663 = CARTESIAN_POINT ( 'NONE',  ( 2.307692307692309264, -1.215029322943914858, 32.30358669280327177 ) ) ;
#61664 = ORIENTED_EDGE ( 'NONE', *, *, #27988, .T. ) ;
#61665 = EDGE_LOOP ( 'NONE', ( #23357, #72085 ) ) ;
#61666 = CYLINDRICAL_SURFACE ( 'NONE', #49859, 0.2500000000000002220 ) ;
#61667 = VECTOR ( 'NONE', #21972, 1000.000000000000000 ) ;
#61668 = ADVANCED_FACE ( 'NONE', ( #52327, #79822, #73053 ), #66292, .F. ) ;
#61669 = ORIENTED_EDGE ( 'NONE', *, *, #11173, .T. ) ;
#61670 = CARTESIAN_POINT ( 'NONE',  ( -15.23076923076935252, -4.320704448113951379, 33.92786785259630022 ) ) ;
#61671 = CARTESIAN_POINT ( 'NONE',  ( 18.06606733335007675, -9.905515769479276145, 34.41647553114623292 ) ) ;
#61672 = CARTESIAN_POINT ( 'NONE',  ( 9.468822767743363400, -9.417330523894424488, 34.63758898049880486 ) ) ;
#61673 = CYLINDRICAL_SURFACE ( 'NONE', #16021, 0.2499999999999995559 ) ;
#61674 = FACE_OUTER_BOUND ( 'NONE', #50299, .T. ) ;
#61675 = CARTESIAN_POINT ( 'NONE',  ( 13.60762673622823549, -3.105924265160262543, 32.13625925475356127 ) ) ;
#61676 = CARTESIAN_POINT ( 'NONE',  ( -0.4615384615385840772, -12.51329471203414379, 31.30864560766407578 ) ) ;
#61677 = ORIENTED_EDGE ( 'NONE', *, *, #69226, .F. ) ;
#61678 = EDGE_CURVE ( 'NONE', #11687, #23012, #27531, .T. ) ;
#61679 = EDGE_LOOP ( 'NONE', ( #82874, #65623, #88152, #41232 ) ) ;
#61681 = EDGE_LOOP ( 'NONE', ( #71065, #8681, #37872, #15610 ) ) ;
#61680 = CARTESIAN_POINT ( 'NONE',  ( 7.173022332454968009, -12.68172785388650681, 30.59649109432439573 ) ) ;
#61682 = CARTESIAN_POINT ( 'NONE',  ( -19.00000000000000000, -16.99999999999999289, 30.25000000000000000 ) ) ;
#61683 = AXIS2_PLACEMENT_3D ( 'NONE', #56810, #15843, #64003 ) ;
#61684 = CARTESIAN_POINT ( 'NONE',  ( 11.76147438255493327, -3.395485233115139057, 33.02377354290275946 ) ) ;
#61685 = CARTESIAN_POINT ( 'NONE',  ( 6.066067333350078528, -9.905515769479277921, 34.41647553114623292 ) ) ;
#61686 = ORIENTED_EDGE ( 'NONE', *, *, #41708, .F. ) ;
#61687 = CARTESIAN_POINT ( 'NONE',  ( 8.069165197766697162, -8.239487800360276282, 34.69522927552633718 ) ) ;
#61688 = AXIS2_PLACEMENT_3D ( 'NONE', #47185, #20605, #12971 ) ;
#61689 = ORIENTED_EDGE ( 'NONE', *, *, #88080, .T. ) ;
#61690 = CARTESIAN_POINT ( 'NONE',  ( -24.00000000000000000, 9.000000000000024869, 29.25000000000000000 ) ) ;
#61691 = EDGE_LOOP ( 'NONE', ( #3342, #12453, #19701, #67620, #76485, #61159 ) ) ;
#61692 = VECTOR ( 'NONE', #61977, 1000.000000000000000 ) ;
#61693 = CARTESIAN_POINT ( 'NONE',  ( -14.08467946359891165, -11.98016756924215009, 32.48728574198911190 ) ) ;
#61694 = EDGE_CURVE ( 'NONE', #49073, #15199, #7713, .T. ) ;
#61695 = EDGE_CURVE ( 'NONE', #19526, #82761, #76757, .T. ) ;
#61696 = ORIENTED_EDGE ( 'NONE', *, *, #58445, .T. ) ;
#61697 = CARTESIAN_POINT ( 'NONE',  ( -12.39628332202562433, -10.33852847137154107, 34.16647553114620450 ) ) ;
#61698 = CARTESIAN_POINT ( 'NONE',  ( -9.019207500173122227, -2.779195860258146578, 31.39871582349836032 ) ) ;
#61699 = FACE_BOUND ( 'NONE', #23157, .T. ) ;
#61700 = CARTESIAN_POINT ( 'NONE',  ( -14.55766905174089665, -9.234221910056348293, 34.70572697212741531 ) ) ;
#61701 = DIRECTION ( 'NONE',  ( 0.000000000000000000, 0.9848077530122072432, 0.1736481776669354937 ) ) ;
#61702 = CARTESIAN_POINT ( 'NONE',  ( 9.561617089197387287, -2.295517848115769421, 30.44137282052137294 ) ) ;
#61704 = EDGE_CURVE ( 'NONE', #21602, #65648, #68510, .T. ) ;
#61703 = CARTESIAN_POINT ( 'NONE',  ( 10.54930223602447903, -9.905515769479276145, 34.41647553114623292 ) ) ;
#61705 = LINE ( 'NONE', #55842, #9349 ) ;
#61706 = DIRECTION ( 'NONE',  ( -0.000000000000000000, 0.5000000000000011102, -0.8660254037844380415 ) ) ;
#61707 = CARTESIAN_POINT ( 'NONE',  ( -6.250000000000007994, -2.499999999999999556, 29.81609845454692120 ) ) ;
#61708 = EDGE_CURVE ( 'NONE', #30802, #77995, #37016, .T. ) ;
#61709 = ORIENTED_EDGE ( 'NONE', *, *, #75225, .F. ) ;
#61710 = ORIENTED_EDGE ( 'NONE', *, *, #56614, .F. ) ;
#61712 = FACE_OUTER_BOUND ( 'NONE', #85592, .T. ) ;
#61711 = CYLINDRICAL_SURFACE ( 'NONE', #1525, 0.2500000000000009437 ) ;
#61713 = CARTESIAN_POINT ( 'NONE',  ( -9.626240358957616650, -12.34228464037088813, 31.77849191805839268 ) ) ;
#61714 = CARTESIAN_POINT ( 'NONE',  ( -3.903900744468109529, -9.357781135181031829, 34.66075350412533851 ) ) ;
#61715 = FACE_OUTER_BOUND ( 'NONE', #3466, .T. ) ;
#61716 = LINE ( 'NONE', #33, #7307 ) ;
#61717 = ORIENTED_EDGE ( 'NONE', *, *, #73658, .F. ) ;
#61718 = CARTESIAN_POINT ( 'NONE',  ( 2.057715576749954867, -9.148715823498378086, 34.47080413974185120 ) ) ;
#61719 = CARTESIAN_POINT ( 'NONE',  ( 3.361294932532793656, -11.46989282347013095, 32.79007818306219946 ) ) ;
#61720 = FACE_OUTER_BOUND ( 'NONE', #88021, .T. ) ;
#61721 = CARTESIAN_POINT ( 'NONE',  ( -7.146561847641254239, -6.716662450894490100, 34.94144148231605840 ) ) ;
#61722 = ORIENTED_EDGE ( 'NONE', *, *, #29568, .T. ) ;
#61723 = AXIS2_PLACEMENT_3D ( 'NONE', #14562, #21312, #69064 ) ;
#61724 = ORIENTED_EDGE ( 'NONE', *, *, #57670, .F. ) ;
#61725 = B_SPLINE_CURVE_WITH_KNOTS ( 'NONE', 3,
 ( #14122, #69506, #1499, #62737, #28984, #56439, #82598, #1053, #55990, #83482 ),
 .UNSPECIFIED., .F., .F.,
 ( 4, 2, 2, 2, 4 ),
 ( 0.0007817246256747484735, 0.0009771112852218920199, 0.001172497944769035783, 0.001367884604316179330, 0.001563271263863322876 ),
 .UNSPECIFIED. ) ;
#61726 = CONTEXT_DEPENDENT_SHAPE_REPRESENTATION ( #62437, #86646 ) ;
#61727 = VERTEX_POINT ( 'NONE', #19442 ) ;
#61728 = CARTESIAN_POINT ( 'NONE',  ( 0.2387117690594567077, -7.369208160676172348, 34.74850200257122879 ) ) ;
#61729 = ORIENTED_EDGE ( 'NONE', *, *, #82547, .T. ) ;
#61730 = DIRECTION ( 'NONE',  ( -0.000000000000000000, 0.3420201433256694346, -0.9396926207859080948 ) ) ;
#61731 = DIRECTION ( 'NONE',  ( 0.000000000000000000, 0.000000000000000000, -1.000000000000000000 ) ) ;
#61732 = CARTESIAN_POINT ( 'NONE',  ( 4.853438133199126980, -6.760086850603068243, 34.69517049084099369 ) ) ;
#61733 = LINE ( 'NONE', #15342, #5753 ) ;
#61734 = CARTESIAN_POINT ( 'NONE',  ( 12.46153846153846168, -9.780366693483667717, 34.19971097300155094 ) ) ;
#61735 = EDGE_LOOP ( 'NONE', ( #27807, #30401, #63298, #15157, #80836, #40110, #78387, #75460, #51486, #82673, #12833, #9615, #57700, #32234, #11232, #69752, #78179, #70569, #66839, #56953, #72229, #24510, #71701, #41297, #59051, #9080, #67305, #49523, #26562, #41472, #62221, #70908, #11178, #78393, #87116, #26425, #75231, #66145, #87207, #58314, #26420, #38335, #46433, #84972, #61813, #19785, #53603, #72237, #2160, #4764, #19425, #56630, #14859, #76913, #47061, #41519, #70428, #36918, #61138, #55494, #54025, #60405, #34497, #29072, #30979, #75266, #29415, #70115, #39315, #6983, #72590, #68247, #31744, #40605, #21913, #46968, #82091, #41103, #68106, #51170, #18587, #56797, #4674, #19795, #75093, #55875, #48209, #25123, #60127, #46665, #73811, #54385, #65197, #26890, #51813 ) ) ;
#61736 = CARTESIAN_POINT ( 'NONE',  ( 18.00000000000000000, -1.044019251281081972, 31.83374038241031911 ) ) ;
#61738 = ORIENTED_EDGE ( 'NONE', *, *, #36881, .T. ) ;
#61737 = CARTESIAN_POINT ( 'NONE',  ( 6.000000000000001776, -13.04860791097971706, 34.73218667398347037 ) ) ;
#61739 = DIRECTION ( 'NONE',  ( 0.000000000000000000, -1.000000000000000000, 0.000000000000000000 ) ) ;
#61740 = CARTESIAN_POINT ( 'NONE',  ( -10.61538461538473399, -3.835265460704628371, 33.15142922262033665 ) ) ;
#61741 = CARTESIAN_POINT ( 'NONE',  ( -13.44988583057615905, -5.219633306516282545, 34.19971097300152962 ) ) ;
#61742 = CARTESIAN_POINT ( 'NONE',  ( 8.835298102580845025, -11.91647553114624358, 32.58852847137148245 ) ) ;
#61743 = B_SPLINE_CURVE_WITH_KNOTS ( 'NONE', 3,
 ( #75342, #49955, #20396, #48297, #41111, #71112 ),
 .UNSPECIFIED., .F., .F.,
 ( 4, 2, 4 ),
 ( 4.220987180333914613E-17, 0.0001954756301637170196, 0.0003909512603273918637 ),
 .UNSPECIFIED. ) ;
#61744 = CARTESIAN_POINT ( 'NONE',  ( -9.915792616872026954, -12.47654668319379567, 31.42292124445336654 ) ) ;
#61745 = DIRECTION ( 'NONE',  ( -1.000000000000000000, -0.000000000000000000, -0.000000000000000000 ) ) ;
#61746 = CARTESIAN_POINT ( 'NONE',  ( -0.5916864312701615169, -2.647304123082328875, 31.75400227202885262 ) ) ;
#61747 = CARTESIAN_POINT ( 'NONE',  ( -1.901340078031369618, -5.512252781505359245, 23.00186829374151287 ) ) ;
#61748 = EDGE_LOOP ( 'NONE', ( #67730, #687, #45240, #74018, #78308, #51019 ) ) ;
#61749 = CARTESIAN_POINT ( 'NONE',  ( 5.076923076923075762, -3.322132147404559976, 32.92929555188717927 ) ) ;
#61750 = CARTESIAN_POINT ( 'NONE',  ( 0.5923302693632463978, -3.062576670634119758, 32.05464942895959979 ) ) ;
#61751 = AXIS2_PLACEMENT_3D ( 'NONE', #44992, #31493, #71138 ) ;
#61752 = CARTESIAN_POINT ( 'NONE',  ( 9.758375025657770152, -2.833524468853757750, 32.15551576947925838 ) ) ;
#61753 = ORIENTED_EDGE ( 'NONE', *, *, #30547, .F. ) ;
#61754 = DIRECTION ( 'NONE',  ( 1.000000000000000000, 0.000000000000000000, 0.000000000000000000 ) ) ;
#61755 = CARTESIAN_POINT ( 'NONE',  ( 4.230769230769229061, -4.000000000000000000, 29.75000000000000355 ) ) ;
#61756 = AXIS2_PLACEMENT_3D ( 'NONE', #86366, #53888, #46247 ) ;
#61757 = EDGE_CURVE ( 'NONE', #80981, #64802, #44499, .T. ) ;
#61758 = AXIS2_PLACEMENT_3D ( 'NONE', #76102, #88760, #75657 ) ;
#61759 = LINE ( 'NONE', #12257, #77590 ) ;
#61760 = CARTESIAN_POINT ( 'NONE',  ( -0.4615384615385840772, -11.06231777344772027, 33.60647404775119895 ) ) ;
#61761 = VECTOR ( 'NONE', #56455, 999.9999999999998863 ) ;
#61762 = CARTESIAN_POINT ( 'NONE',  ( -14.30769230769242917, -3.083524468854526912, 32.58852847137268327 ) ) ;
#61763 = ORIENTED_EDGE ( 'NONE', *, *, #43683, .T. ) ;
#61764 = CARTESIAN_POINT ( 'NONE',  ( -15.29685264172511161, -2.721908614388770964, 31.22303859784723912 ) ) ;
#61765 = CARTESIAN_POINT ( 'NONE',  ( 3.453548772037640546, -12.24180327182771855, 31.33663988360758168 ) ) ;
#61766 = CARTESIAN_POINT ( 'NONE',  ( 18.06606733335007675, -12.34228464037088813, 31.77849191805839268 ) ) ;
#61767 = ORIENTED_EDGE ( 'NONE', *, *, #39859, .F. ) ;
#61768 = CARTESIAN_POINT ( 'NONE',  ( -8.992058866865649591, -7.369209533119140509, 34.99857337881830688 ) ) ;
#61769 = EDGE_CURVE ( 'NONE', #38026, #59454, #69254, .T. ) ;
#61770 = ORIENTED_EDGE ( 'NONE', *, *, #1281, .F. ) ;
#61771 = CARTESIAN_POINT ( 'NONE',  ( 12.68431813051652313, -12.47679350104403007, 31.42216943046555855 ) ) ;
#61772 = CARTESIAN_POINT ( 'NONE',  ( 11.47319153790521717, -2.657715359629088780, 31.77849191805832874 ) ) ;
#61773 = VERTEX_POINT ( 'NONE', #48233 ) ;
#61774 = EDGE_CURVE ( 'NONE', #37061, #73584, #68956, .T. ) ;
#61775 = CARTESIAN_POINT ( 'NONE',  ( -17.75005459062195712, -10.18230066228896646, 34.26354781536631577 ) ) ;
#61776 = CARTESIAN_POINT ( 'NONE',  ( 11.53846153846141753, -4.481592998941358097, 33.73612834414048933 ) ) ;
#61777 = CARTESIAN_POINT ( 'NONE',  ( 13.13463865367303285, -6.567427716900048118, 34.66269422305636283 ) ) ;
#61778 = B_SPLINE_CURVE_WITH_KNOTS ( 'NONE', 3,
 ( #87997, #53725, #19497, #88425, #26697, #54156, #81652, #74899, #19935, #13191 ),
 .UNSPECIFIED., .F., .F.,
 ( 4, 2, 2, 2, 4 ),
 ( 0.0007817246256747485819, 0.0009771112852218918031, 0.001172497944769034916, 0.001367884604316178029, 0.001563271263863321358 ),
 .UNSPECIFIED. ) ;
#61779 = LINE ( 'NONE', #26677, #16108 ) ;
#61780 = CARTESIAN_POINT ( 'NONE',  ( 9.070512820512819374, -7.500000000000000000, 29.75000000000000355 ) ) ;
#61781 = B_SPLINE_CURVE_WITH_KNOTS ( 'NONE', 3,
 ( #72220, #39349, #71772, #4210, #10080, #66806, #86205, #79438, #38000, #17736 ),
 .UNSPECIFIED., .F., .F.,
 ( 4, 2, 2, 2, 4 ),
 ( 0.0007817359430256285964, 0.0009771253907249943717, 0.001172514838424360039, 0.001367904286123725706, 0.001563293733823091372 ),
 .UNSPECIFIED. ) ;
#61782 = B_SPLINE_CURVE_WITH_KNOTS ( 'NONE', 3,
 ( #29842, #84355, #70388, #15892, #64484, #29411, #2789, #8249, #14552, #22198 ),
 .UNSPECIFIED., .F., .F.,
 ( 4, 2, 2, 2, 4 ),
 ( 0.000000000000000000, 0.0001954311564186876334, 0.0003908623128373752667, 0.0005862934692560629272, 0.0007817246256747505334 ),
 .UNSPECIFIED. ) ;
#61783 = ORIENTED_EDGE ( 'NONE', *, *, #28570, .T. ) ;
#61784 = EDGE_CURVE ( 'NONE', #3322, #24141, #26644, .T. ) ;
#61785 = FACE_BOUND ( 'NONE', #66865, .T. ) ;
#61786 = ORIENTED_EDGE ( 'NONE', *, *, #18530, .F. ) ;
#61787 = CARTESIAN_POINT ( 'NONE',  ( -9.019207513279360100, -12.41104346484419452, 31.60698883733904196 ) ) ;
#61788 = VECTOR ( 'NONE', #20429, 1000.000000000000114 ) ;
#61789 = EDGE_CURVE ( 'NONE', #49742, #74216, #4817, .T. ) ;
#61790 = CARTESIAN_POINT ( 'NONE',  ( 18.06606835100244268, -12.10708131394839882, 31.69288490824020954 ) ) ;
#61791 = DIRECTION ( 'NONE',  ( 0.000000000000000000, 1.000000000000000000, 0.000000000000000000 ) ) ;
#61792 = CARTESIAN_POINT ( 'NONE',  ( -6.223484943723949669, -12.24155766932282496, 31.33739205006857986 ) ) ;
#61793 = VERTEX_POINT ( 'NONE', #9908 ) ;
#61794 = ORIENTED_EDGE ( 'NONE', *, *, #1475, .F. ) ;
#61795 = ORIENTED_EDGE ( 'NONE', *, *, #25008, .T. ) ;
#61796 = DIRECTION ( 'NONE',  ( -0.000000000000000000, -0.9396926207859092051, -0.3420201433256662704 ) ) ;
#61797 = ORIENTED_EDGE ( 'NONE', *, *, #29058, .F. ) ;
#61798 = EDGE_CURVE ( 'NONE', #39836, #60358, #57444, .T. ) ;
#61799 = VECTOR ( 'NONE', #41009, 1000.000000000000000 ) ;
#61800 = CARTESIAN_POINT ( 'NONE',  ( -17.20707104665477161, -10.31621877034669588, 34.18098118002070152 ) ) ;
#61801 = EDGE_CURVE ( 'NONE', #40219, #85070, #5947, .T. ) ;
#61802 = FACE_OUTER_BOUND ( 'NONE', #2636, .T. ) ;
#61803 = CARTESIAN_POINT ( 'NONE',  ( -2.307692307692305711, -12.78798330534102945, 29.74999999999997868 ) ) ;
#61804 = CARTESIAN_POINT ( 'NONE',  ( -13.63461538461538325, -7.500000000000001776, 35.04278698407183867 ) ) ;
#61805 = AXIS2_PLACEMENT_3D ( 'NONE', #84465, #59197, #39832 ) ;
#61806 = CIRCLE ( 'NONE', #82025, 0.2500000000000002220 ) ;
#61807 = EDGE_CURVE ( 'NONE', #70953, #68235, #31602, .T. ) ;
#61808 = CARTESIAN_POINT ( 'NONE',  ( 2.651650429449569302, -10.15165042944953733, 25.87500000000000355 ) ) ;
#61809 = CARTESIAN_POINT ( 'NONE',  ( -2.307692307692427391, -5.219633306517616589, 34.19971097300220464 ) ) ;
#61810 = EDGE_CURVE ( 'NONE', #69536, #32821, #84274, .T. ) ;
#61811 = CARTESIAN_POINT ( 'NONE',  ( 17.75002326905764605, -2.564618984488975517, 30.55390908950641915 ) ) ;
#61812 = CARTESIAN_POINT ( 'NONE',  ( -8.546217925137375104, -2.889357225399414197, 32.26129605718031002 ) ) ;
#61813 = ORIENTED_EDGE ( 'NONE', *, *, #53126, .T. ) ;
#61814 = ORIENTED_EDGE ( 'NONE', *, *, #83855, .F. ) ;
#61815 = AXIS2_PLACEMENT_3D ( 'NONE', #36407, #56669, #76947 ) ;
#61816 = VERTEX_POINT ( 'NONE', #70289 ) ;
#61817 = VECTOR ( 'NONE', #66815, 1000.000000000000000 ) ;
#61818 = CYLINDRICAL_SURFACE ( 'NONE', #74775, 0.2499999999999995559 ) ;
#61820 = CARTESIAN_POINT ( 'NONE',  ( -6.000000000000119904, -3.835265460704628371, 33.15142922262033665 ) ) ;
#61819 = CARTESIAN_POINT ( 'NONE',  ( 1.384615384615386802, -10.05456864172156806, 36.03766855953608683 ) ) ;
#61821 = B_SPLINE_CURVE_WITH_KNOTS ( 'NONE', 3,
 ( #34054, #21871, #42157, #75480, #7480, #14229, #89024, #712, #82251, #61516 ),
 .UNSPECIFIED., .F., .F.,
 ( 4, 2, 2, 2, 4 ),
 ( 0.000000000000000000, 0.0001954339857564058210, 0.0003908679715128116419, 0.0005863019572692174629, 0.0007817359430256232838 ),
 .UNSPECIFIED. ) ;
#61822 = DIRECTION ( 'NONE',  ( -1.000000000000000000, 0.000000000000000000, 0.000000000000000000 ) ) ;
#61823 = CARTESIAN_POINT ( 'NONE',  ( -9.758391103263569732, -6.386643153685125363, 34.62446782046654903 ) ) ;
#61824 = FACE_BOUND ( 'NONE', #22340, .T. ) ;
#61825 = CARTESIAN_POINT ( 'NONE',  ( -7.053224892808616531, -3.625366637846544560, 33.29286588640298561 ) ) ;
#61826 = VERTEX_POINT ( 'NONE', #49575 ) ;
#61827 = DIRECTION ( 'NONE',  ( 0.000000000000000000, 0.9848077530122072432, 0.1736481776669354937 ) ) ;
#61828 = CARTESIAN_POINT ( 'NONE',  ( -9.692307692307691624, -13.88283147151868846, 33.14645433367849847 ) ) ;
#61829 = CARTESIAN_POINT ( 'NONE',  ( -1.384615384615383471, -3.322132147404559976, 32.92929555188717927 ) ) ;
#61830 = VERTEX_POINT ( 'NONE', #63522 ) ;
#61831 = FACE_OUTER_BOUND ( 'NONE', #73613, .T. ) ;
#61832 = ORIENTED_EDGE ( 'NONE', *, *, #15460, .T. ) ;
#61833 = FACE_BOUND ( 'NONE', #9453, .T. ) ;
#61834 = FACE_OUTER_BOUND ( 'NONE', #38774, .T. ) ;
#61835 = CARTESIAN_POINT ( 'NONE',  ( -9.320512820512821150, -1.926643599941765039, 29.65000000000000213 ) ) ;
#61836 = DIRECTION ( 'NONE',  ( 0.000000000000000000, 0.000000000000000000, -1.000000000000000000 ) ) ;
#61837 = EDGE_LOOP ( 'NONE', ( #76721, #50597, #41116, #35604 ) ) ;
#61838 = CYLINDRICAL_SURFACE ( 'NONE', #86824, 0.2499999999999973355 ) ;
#61839 = CARTESIAN_POINT ( 'NONE',  ( 14.53047197667037338, -3.563462043263030399, 33.22394488606062879 ) ) ;
#61840 = CARTESIAN_POINT ( 'NONE',  ( -16.37677237136229991, -12.39988816332205701, 30.74660775122750778 ) ) ;
#61841 = CARTESIAN_POINT ( 'NONE',  ( -7.053768389744480061, -10.54014554554150607, 33.71984207302941883 ) ) ;
#61842 = ORIENTED_EDGE ( 'NONE', *, *, #37138, .T. ) ;
#61843 = CARTESIAN_POINT ( 'NONE',  ( 16.28437185560972011, -10.88167719472716399, 33.43325721877153711 ) ) ;
#61844 = CARTESIAN_POINT ( 'NONE',  ( -15.29685264172511161, -8.120952969808774569, 34.71129190930000163 ) ) ;
#61846 = VERTEX_POINT ( 'NONE', #36933 ) ;
#61845 = CYLINDRICAL_SURFACE ( 'NONE', #62847, 0.2500000000000009437 ) ;
#61847 = DIRECTION ( 'NONE',  ( -0.000000000000000000, 0.6427876096865404731, -0.7660444431189771253 ) ) ;
#61848 = CARTESIAN_POINT ( 'NONE',  ( -14.30769230769230660, -2.486705287966279876, 31.30864560766543647 ) ) ;
#61849 = CARTESIAN_POINT ( 'NONE',  ( 16.28437159207980045, -12.15418822224088657, 32.17964115625579069 ) ) ;
#61850 = CARTESIAN_POINT ( 'NONE',  ( -10.48459280755983158, -2.541949514083464479, 30.39797389878540557 ) ) ;
#61851 = EDGE_CURVE ( 'NONE', #31297, #56029, #63818, .T. ) ;
#61852 = CARTESIAN_POINT ( 'NONE',  ( 14.98074600654777733, -5.765609946408404518, 34.70566812827425451 ) ) ;
#61854 = FACE_OUTER_BOUND ( 'NONE', #78972, .T. ) ;
#61853 = CARTESIAN_POINT ( 'NONE',  ( 8.769230769230768274, -13.20930481340135110, 34.54067556320372745 ) ) ;
#61855 = DIRECTION ( 'NONE',  ( -0.000000000000000000, 1.000000000000000000, -0.000000000000000000 ) ) ;
#61856 = CARTESIAN_POINT ( 'NONE',  ( 1.944543648262996083, -5.555456351736983045, 19.31250000000000000 ) ) ;
#61857 = ORIENTED_EDGE ( 'NONE', *, *, #25203, .F. ) ;
#61858 = DIRECTION ( 'NONE',  ( -1.000000000000000000, -0.000000000000000000, 0.000000000000000000 ) ) ;
#61859 = ORIENTED_EDGE ( 'NONE', *, *, #24456, .F. ) ;
#61860 = ORIENTED_EDGE ( 'NONE', *, *, #34410, .T. ) ;
#61861 = DIRECTION ( 'NONE',  ( 0.000000000000000000, 0.000000000000000000, 1.000000000000000000 ) ) ;
#61862 = ORIENTED_EDGE ( 'NONE', *, *, #76670, .T. ) ;
#61863 = CARTESIAN_POINT ( 'NONE',  ( -4.219928533206287469, -2.486705287966279432, 31.30864560766542937 ) ) ;
#61864 = CARTESIAN_POINT ( 'NONE',  ( -1.944543648263014957, -5.555456351737005249, 19.00000000000000000 ) ) ;
#61865 = CARTESIAN_POINT ( 'NONE',  ( 17.86930939688969033, -4.684245665217972032, 34.18127051446801090 ) ) ;
#61866 = ADVANCED_FACE ( 'NONE', ( #77923 ), #16228, .F. ) ;
#61867 = CARTESIAN_POINT ( 'NONE',  ( -11.53846153846153655, -9.905515769479276145, 34.41647553114623292 ) ) ;
#61868 = CARTESIAN_POINT ( 'NONE',  ( 6.130525701763568591, -3.285477652293412820, 32.44071101563363158 ) ) ;
#61869 = ADVANCED_FACE ( 'NONE', ( #30618 ), #45910, .F. ) ;
#61870 = CARTESIAN_POINT ( 'NONE',  ( 1.161130460051053248, -2.612411019501189813, 31.66733052389439962 ) ) ;
#61871 = CARTESIAN_POINT ( 'NONE',  ( 9.915087361285756629, -12.47679350104403007, 31.42216943046555855 ) ) ;
#61872 = CARTESIAN_POINT ( 'NONE',  ( -11.66915300512910214, -4.809359713505814149, 33.96456829005828837 ) ) ;
#61873 = CARTESIAN_POINT ( 'NONE',  ( -3.750000000000008438, -5.946699141100917352, 26.42187500000000000 ) ) ;
#61874 = CARTESIAN_POINT ( 'NONE',  ( 10.39189967166066708, -2.599994579823202923, 30.74605699353653776 ) ) ;
#61875 = CARTESIAN_POINT ( 'NONE',  ( -16.85391023282967993, -10.77377354290276301, 33.85451476688484718 ) ) ;
#61876 = VECTOR ( 'NONE', #69257, 1000.000000000000114 ) ;
#61877 = DIRECTION ( 'NONE',  ( -0.000000000000000000, 0.7660444431189791237, -0.6427876096865379196 ) ) ;
#61878 = CARTESIAN_POINT ( 'NONE',  ( -13.16183584334697798, -11.41317474335729543, 32.86274602512330034 ) ) ;
#61879 = AXIS2_PLACEMENT_3D ( 'NONE', #6487, #21763, #20442 ) ;
#61880 = VECTOR ( 'NONE', #16488, 1000.000000000000000 ) ;
#61882 = VERTEX_POINT ( 'NONE', #31967 ) ;
#61881 = ADVANCED_FACE ( 'NONE', ( #24757 ), #4490, .F. ) ;
#61883 = ORIENTED_EDGE ( 'NONE', *, *, #40597, .T. ) ;
#61884 = CARTESIAN_POINT ( 'NONE',  ( -18.00000000000030553, -12.49374608885938542, 30.00000000000319744 ) ) ;
#61885 = CARTESIAN_POINT ( 'NONE',  ( 11.78846153846295763, -7.500000000000154543, 35.00000000000007105 ) ) ;
#61886 = CARTESIAN_POINT ( 'NONE',  ( -18.00000000000000000, -12.27536236210233866, 35.44105525097462106 ) ) ;
#61887 = CARTESIAN_POINT ( 'NONE',  ( 3.230769230769231726, -2.499999999999998668, 29.50000000000001066 ) ) ;
#61888 = EDGE_CURVE ( 'NONE', #57222, #26954, #43415, .T. ) ;
#61889 = AXIS2_PLACEMENT_3D ( 'NONE', #82266, #89037, #28649 ) ;
#61890 = CARTESIAN_POINT ( 'NONE',  ( 9.757562831820530747, -11.67786785259547777, 32.92929555188713664 ) ) ;
#61891 = VECTOR ( 'NONE', #44633, 1000.000000000000000 ) ;
#61892 = CARTESIAN_POINT ( 'NONE',  ( -9.469294848214296678, -10.77377354290276124, 33.85451476688484718 ) ) ;
#61893 = COLOUR_RGB ( '', 0.40784314, 0.44705882, 0.49803922) ;
#61894 = CARTESIAN_POINT ( 'NONE',  ( 6.923076923076924238, -4.786620604624113540, 33.94971097300155094 ) ) ;
#61895 = ORIENTED_EDGE ( 'NONE', *, *, #13976, .F. ) ;
#61896 = EDGE_CURVE ( 'NONE', #67262, #10170, #14377, .T. ) ;
#61897 = CARTESIAN_POINT ( 'NONE',  ( 12.46153846153876898, -2.506253911140615021, 30.00000000000323297 ) ) ;
#61898 = ORIENTED_EDGE ( 'NONE', *, *, #54184, .F. ) ;
#61899 = CARTESIAN_POINT ( 'NONE',  ( -2.307692307692427391, -6.879047030192662504, 34.71129190930017927 ) ) ;
#61900 = CARTESIAN_POINT ( 'NONE',  ( -5.076923076923197442, -2.625532179533778709, 30.86335684631627174 ) ) ;
#61901 = CARTESIAN_POINT ( 'NONE',  ( 11.78851585009985214, -10.66356715214248752, 33.62249196103329751 ) ) ;
#61902 = CARTESIAN_POINT ( 'NONE',  ( 4.023698184114458343, -6.809168938359898782, 34.95455904226513866 ) ) ;
#61903 = FACE_OUTER_BOUND ( 'NONE', #14621, .T. ) ;
#61904 = ORIENTED_EDGE ( 'NONE', *, *, #28301, .F. ) ;
#61905 = EDGE_LOOP ( 'NONE', ( #80441, #86119, #34551, #16210 ) ) ;
#61906 = ORIENTED_EDGE ( 'NONE', *, *, #72529, .F. ) ;
#61908 = VERTEX_POINT ( 'NONE', #37823 ) ;
#61907 = B_SPLINE_CURVE_WITH_KNOTS ( 'NONE', 3,
 ( #772, #9310, #7537, #28239, #55710, #21483, #76434, #14738, #69671, #35444 ),
 .UNSPECIFIED., .F., .F.,
 ( 4, 2, 2, 2, 4 ),
 ( 0.0007817359430256304396, 0.0009771253907249963233, 0.001172514838424362424, 0.001367904286123728524, 0.001563293733823094408 ),
 .UNSPECIFIED. ) ;
#61909 = EDGE_CURVE ( 'NONE', #57687, #65753, #25650, .T. ) ;
#61910 = LINE ( 'NONE', #77647, #42991 ) ;
#61911 = CARTESIAN_POINT ( 'NONE',  ( -16.02305571287920571, -9.084667340241228572, 34.75534355489798344 ) ) ;
#61912 = CARTESIAN_POINT ( 'NONE',  ( -3.296039676730006196, -10.21337939537584383, 33.94971097300158647 ) ) ;
#61913 = ADVANCED_FACE ( 'NONE', ( #11248 ), #86937, .F. ) ;
#61914 = LINE ( 'NONE', #82205, #25478 ) ;
#61915 = CARTESIAN_POINT ( 'NONE',  ( -5.999999999999998224, -11.35647404775217417, 33.31231777344666511 ) ) ;
#61916 = EDGE_CURVE ( 'NONE', #30008, #31103, #79711, .T. ) ;
#61917 = CARTESIAN_POINT ( 'NONE',  ( 12.39545608217832395, -2.833524468853757305, 32.15551576947924417 ) ) ;
#61918 = ORIENTED_EDGE ( 'NONE', *, *, #46933, .F. ) ;
#61919 = ORIENTED_EDGE ( 'NONE', *, *, #10905, .T. ) ;
#61920 = ORIENTED_EDGE ( 'NONE', *, *, #19799, .F. ) ;
#61922 = ORIENTED_EDGE ( 'NONE', *, *, #70162, .T. ) ;
#61921 = CARTESIAN_POINT ( 'NONE',  ( 17.32697738856138869, -12.41262288849542017, 30.68299917996395010 ) ) ;
#61923 = CARTESIAN_POINT ( 'NONE',  ( 17.20744851515672025, -11.04252011169589842, 33.62494198852677840 ) ) ;
#61924 = CARTESIAN_POINT ( 'NONE',  ( -4.826868765284762830, -11.28795663066794219, 33.01431243580653785 ) ) ;
#61925 = CARTESIAN_POINT ( 'NONE',  ( 2.651650429449539104, -4.848349570550432475, 20.56250000000000000 ) ) ;
#61926 = ORIENTED_EDGE ( 'NONE', *, *, #85811, .F. ) ;
#61927 = VECTOR ( 'NONE', #38139, 1000.000000000000114 ) ;
#61928 = EDGE_CURVE ( 'NONE', #74382, #55112, #8959, .T. ) ;
#61929 = VERTEX_POINT ( 'NONE', #4943 ) ;
#61930 = LINE ( 'NONE', #33591, #58597 ) ;
#61931 = FACE_BOUND ( 'NONE', #66570, .T. ) ;
#61933 = VECTOR ( 'NONE', #80845, 1000.000000000000000 ) ;
#61932 = CARTESIAN_POINT ( 'NONE',  ( -5.869209559033045309, -2.845873456487966635, 32.17976146951972538 ) ) ;
#61934 = AXIS2_PLACEMENT_3D ( 'NONE', #36143, #57283, #23057 ) ;
#61935 = CARTESIAN_POINT ( 'NONE',  ( 13.38461538461538680, -6.435427911321262684, 35.78748833219616898 ) ) ;
#61936 = VERTEX_POINT ( 'NONE', #53105 ) ;
#61937 = EDGE_CURVE ( 'NONE', #81881, #59129, #86483, .T. ) ;
#61938 = CARTESIAN_POINT ( 'NONE',  ( 11.53846153846153832, -12.78798330534103123, 29.99999999999997868 ) ) ;
#61939 = CARTESIAN_POINT ( 'NONE',  ( 6.857806922520602200, -12.16647553114622049, 32.15551576947930812 ) ) ;
#61940 = CARTESIAN_POINT ( 'NONE',  ( -17.07692307692307665, -12.62096338111211580, 30.90682066428153263 ) ) ;
#61941 = CARTESIAN_POINT ( 'NONE',  ( 12.46153846153846168, -11.69971097300155272, 32.46337939537588113 ) ) ;
#61942 = ORIENTED_EDGE ( 'NONE', *, *, #31373, .T. ) ;
#61943 = VECTOR ( 'NONE', #21615, 1000.000000000000114 ) ;
#61944 = CARTESIAN_POINT ( 'NONE',  ( -24.99999999999999645, -19.99999999999999645, 3.000000000000000000 ) ) ;
#61945 = CARTESIAN_POINT ( 'NONE',  ( -3.931066484868084299, -10.23759521482555357, 34.22997729860117033 ) ) ;
#61946 = CARTESIAN_POINT ( 'NONE',  ( 17.20744877868663281, -10.19071101563364401, 33.96452234770658407 ) ) ;
#61947 = CARTESIAN_POINT ( 'NONE',  ( -2.531177251416254936, -10.81261337010820256, 33.49550067578627477 ) ) ;
#61948 = B_SPLINE_CURVE_WITH_KNOTS ( 'NONE', 3,
 ( #22984, #16665, #23854, #17569, #2698, #84267, #37375, #22546, #30194, #50013 ),
 .UNSPECIFIED., .F., .F.,
 ( 4, 2, 2, 2, 4 ),
 ( 0.000000000000000000, 0.0001954339857564081791, 0.0003908679715128163582, 0.0005863019572692245102, 0.0007817359430256327164 ),
 .UNSPECIFIED. ) ;
#61949 = CYLINDRICAL_SURFACE ( 'NONE', #9845, 0.2499999999999979738 ) ;
#61950 = B_SPLINE_CURVE_WITH_KNOTS ( 'NONE', 3,
 ( #76806, #36264, #30383, #43891, #8792, #56959, #50192, #16867, #64151, #77678 ),
 .UNSPECIFIED., .F., .F.,
 ( 4, 2, 2, 2, 4 ),
 ( 0.0007817359430256388964, 0.0009771253907250075990, 0.001172514838424376085, 0.001367904286123744571, 0.001563293733823113273 ),
 .UNSPECIFIED. ) ;
#61951 = EDGE_CURVE ( 'NONE', #13845, #53903, #38024, .T. ) ;
#61952 = FACE_BOUND ( 'NONE', #43512, .T. ) ;
#61954 = CARTESIAN_POINT ( 'NONE',  ( 16.82689985270161870, -2.985938066672154889, 32.43141759479405550 ) ) ;
#61953 = CARTESIAN_POINT ( 'NONE',  ( -6.792551484843276199, -12.70449254468099198, 30.44128974285582956 ) ) ;
#61955 = DIRECTION ( 'NONE',  ( -0.000000000000000000, 0.3420201433256694346, -0.9396926207859080948 ) ) ;
#61957 = CARTESIAN_POINT ( 'NONE',  ( -2.307692307692428724, -8.656820664282941280, 34.87096338111179961 ) ) ;
#61956 = FACE_OUTER_BOUND ( 'NONE', #46609, .T. ) ;
#61958 = CARTESIAN_POINT ( 'NONE',  ( -5.076923076923075762, -12.34228464037088635, 31.77849191805839268 ) ) ;
#61959 = CARTESIAN_POINT ( 'NONE',  ( -1.200186371490556958, -4.775308065498765409, 18.82625670625848713 ) ) ;
#61961 = EDGE_CURVE ( 'NONE', #47861, #78029, #64759, .T. ) ;
#61960 = ORIENTED_EDGE ( 'NONE', *, *, #67001, .T. ) ;
#61962 = CARTESIAN_POINT ( 'NONE',  ( -5.999999999999998224, -10.67929555188718282, 33.92786785259544047 ) ) ;
#61963 = VERTEX_POINT ( 'NONE', #40511 ) ;
#61964 = EDGE_CURVE ( 'NONE', #55273, #16936, #87824, .T. ) ;
#61965 = CARTESIAN_POINT ( 'NONE',  ( -13.31936024510254413, -11.06231777344671130, 33.60647404775212976 ) ) ;
#61966 = ORIENTED_EDGE ( 'NONE', *, *, #18276, .T. ) ;
#61967 = CARTESIAN_POINT ( 'NONE',  ( -11.40793583669797684, -2.882268652242222284, 31.66798894389554064 ) ) ;
#61968 = CARTESIAN_POINT ( 'NONE',  ( 14.30769230769231015, -3.937682226553329556, 33.60647404775216529 ) ) ;
#61970 = ORIENTED_EDGE ( 'NONE', *, *, #9611, .F. ) ;
#61969 = CARTESIAN_POINT ( 'NONE',  ( 5.933917620639864943, -8.164416787775445883, 34.95778746994557906 ) ) ;
#61971 = CARTESIAN_POINT ( 'NONE',  ( -15.23076923076922995, -4.786620604624113540, 33.94971097300155094 ) ) ;
#61972 = CARTESIAN_POINT ( 'NONE',  ( 1.901340078031349856, -5.512252781505337929, 17.81063170625849068 ) ) ;
#61973 = CARTESIAN_POINT ( 'NONE',  ( -15.45425415533356173, -9.417330523894424488, 34.63758898049880486 ) ) ;
#61974 = DIRECTION ( 'NONE',  ( 0.000000000000000000, 0.4999999999999985567, 0.8660254037844395958 ) ) ;
#61975 = EDGE_CURVE ( 'NONE', #20924, #84442, #48566, .T. ) ;
#61976 = CARTESIAN_POINT ( 'NONE',  ( 12.23861224402230974, -2.758268499246657068, 31.33685645148948140 ) ) ;
#61977 = DIRECTION ( 'NONE',  ( -0.000000000000000000, 0.1736481776669307198, -0.9848077530122080203 ) ) ;
#61978 = CARTESIAN_POINT ( 'NONE',  ( -12.39547112818838492, -8.164416787775445883, 34.95778746994558617 ) ) ;
#61979 = LINE ( 'NONE', #7496, #62716 ) ;
#61980 = AXIS2_PLACEMENT_3D ( 'NONE', #19255, #3943, #52137 ) ;
#61981 = CARTESIAN_POINT ( 'NONE',  ( 3.750000000000001776, -7.561099074964511502, 20.97061829374151642 ) ) ;
#61982 = CARTESIAN_POINT ( 'NONE',  ( -10.55012904410859420, -2.892918686051626498, 31.69288490824026638 ) ) ;
#61983 = CARTESIAN_POINT ( 'NONE',  ( 10.68064018666063575, -11.48612834413965977, 32.76840700105972815 ) ) ;
#61984 = EDGE_CURVE ( 'NONE', #68144, #8709, #4643, .T. ) ;
#61985 = EDGE_LOOP ( 'NONE', ( #82441, #41577 ) ) ;
#61986 = VECTOR ( 'NONE', #57446, 1000.000000000000000 ) ;
#61987 = CARTESIAN_POINT ( 'NONE',  ( 8.992242120843618736, -9.886259254753566594, 34.14407573483972413 ) ) ;
#61988 = CARTESIAN_POINT ( 'NONE',  ( -3.749999999999997780, -7.438900925035489387, 22.84561829374151642 ) ) ;
#61989 = B_SPLINE_CURVE_WITH_KNOTS ( 'NONE', 3,
 ( #20889, #88940, #20008, #7828, #68638, #21334, #61870, #48359, #28546, #33963 ),
 .UNSPECIFIED., .F., .F.,
 ( 4, 2, 2, 2, 4 ),
 ( 0.000000000000000000, 0.0001954311564186863865, 0.0003908623128373727731, 0.0005862934692560591325, 0.0007817246256747455461 ),
 .UNSPECIFIED. ) ;
#61990 = CARTESIAN_POINT ( 'NONE',  ( -17.74994568836168440, -12.41262288849542017, 30.68299917996395010 ) ) ;
#61991 = LINE ( 'NONE', #739, #12435 ) ;
#61992 = VERTEX_POINT ( 'NONE', #26096 ) ;
#61993 = CARTESIAN_POINT ( 'NONE',  ( 6.792466563452393302, -7.722926236386453702, 34.74524107206102030 ) ) ;
#61994 = CARTESIAN_POINT ( 'NONE',  ( -0.3962828902624376815, -10.21337939537593442, 33.94971097300152252 ) ) ;
#61996 = ORIENTED_EDGE ( 'NONE', *, *, #61097, .T. ) ;
#61995 = CARTESIAN_POINT ( 'NONE',  ( 2.307692307692187583, -2.892918686052166066, 31.69288490824153470 ) ) ;
#61997 = CARTESIAN_POINT ( 'NONE',  ( -5.326899807865430603, -5.728515186090277211, 34.42611988154120439 ) ) ;
#61998 = B_SPLINE_CURVE_WITH_KNOTS ( 'NONE', 3,
 ( #813, #63392, #69715, #56203, #84136, #21976, #77357, #49447, #76920, #1701 ),
 .UNSPECIFIED., .F., .F.,
 ( 4, 2, 2, 2, 4 ),
 ( 0.0007817359430256395469, 0.0009771253907250080327, 0.001172514838424376735, 0.001367904286123745438, 0.001563293733823113924 ),
 .UNSPECIFIED. ) ;
#61999 = EDGE_CURVE ( 'NONE', #32338, #49839, #73406, .T. ) ;
#62000 = CARTESIAN_POINT ( 'NONE',  ( 4.946447891847356004, -7.276987145209185215, 34.99546412871779211 ) ) ;
#62001 = DIRECTION ( 'NONE',  ( 1.000000000000000000, -0.000000000000000000, -0.000000000000000000 ) ) ;
#62002 = CARTESIAN_POINT ( 'NONE',  ( -17.07692307692319744, -2.892918686052165622, 31.69288490824153470 ) ) ;
#62003 = B_SPLINE_CURVE_WITH_KNOTS ( 'NONE', 3,
 ( #81948, #21104, #20672, #47701, #47254, #74746, #76056, #14355, #81503, #41843 ),
 .UNSPECIFIED., .F., .F.,
 ( 4, 2, 2, 2, 4 ),
 ( 0.0007817246256747460882, 0.0009771112852218887673, 0.001172497944769031663, 0.001367884604316174559, 0.001563271263863317238 ),
 .UNSPECIFIED. ) ;
#62004 = CARTESIAN_POINT ( 'NONE',  ( -13.44988583057616083, -11.94971097300153140, 32.03036669348370680 ) ) ;
#62005 = AXIS2_PLACEMENT_3D ( 'NONE', #52328, #32071, #52774 ) ;
#62006 = ORIENTED_EDGE ( 'NONE', *, *, #57948, .T. ) ;
#62007 = ORIENTED_EDGE ( 'NONE', *, *, #667, .F. ) ;
#62008 = ORIENTED_EDGE ( 'NONE', *, *, #4164, .F. ) ;
#62009 = VECTOR ( 'NONE', #68471, 1000.000000000000000 ) ;
#62010 = VECTOR ( 'NONE', #15893, 1000.000000000000000 ) ;
#62011 = CARTESIAN_POINT ( 'NONE',  ( -16.37677311275300340, -3.395401636524186362, 33.02366814457250399 ) ) ;
#62012 = CARTESIAN_POINT ( 'NONE',  ( -6.857008572074484221, -4.098570777380720287, 33.41473453929635440 ) ) ;
#62013 = CARTESIAN_POINT ( 'NONE',  ( 9.692307692307695177, -4.786620604624113540, 33.94971097300155094 ) ) ;
#62014 = CARTESIAN_POINT ( 'NONE',  ( 11.53846153846141576, -10.33852847137269571, 34.16647553114546554 ) ) ;
#62015 = CIRCLE ( 'NONE', #13099, 0.2500000000000002220 ) ;
#62016 = VERTEX_POINT ( 'NONE', #74738 ) ;
#62017 = CARTESIAN_POINT ( 'NONE',  ( 15.23076923076923173, -9.780366693483667717, 34.19971097300155094 ) ) ;
#62018 = ORIENTED_EDGE ( 'NONE', *, *, #67818, .T. ) ;
#62019 = VERTEX_POINT ( 'NONE', #13461 ) ;
#62020 = ORIENTED_EDGE ( 'NONE', *, *, #74137, .T. ) ;
#62022 = ORIENTED_EDGE ( 'NONE', *, *, #5351, .F. ) ;
#62021 = FACE_OUTER_BOUND ( 'NONE', #52355, .T. ) ;
#62023 = CARTESIAN_POINT ( 'NONE',  ( 6.000000000000001776, -10.89733346790207413, 36.13435417666054406 ) ) ;
#62024 = B_SPLINE_CURVE_WITH_KNOTS ( 'NONE', 3,
 ( #72079, #25232, #80182, #86965, #31542, #11727, #3617, #25677, #53134, #80642 ),
 .UNSPECIFIED., .F., .F.,
 ( 4, 2, 2, 2, 4 ),
 ( 0.000000000000000000, 0.0001954311564186875520, 0.0003908623128373751041, 0.0005862934692560627103, 0.0007817246256747502082 ),
 .UNSPECIFIED. ) ;
#62025 = DIRECTION ( 'NONE',  ( -0.000000000000000000, 0.7660444431189791237, -0.6427876096865379196 ) ) ;
#62026 = EDGE_CURVE ( 'NONE', #10, #49638, #32550, .T. ) ;
#62027 = CARTESIAN_POINT ( 'NONE',  ( 5.934729999443682402, -4.320704448112771878, 33.92786785259540494 ) ) ;
#62028 = CARTESIAN_POINT ( 'NONE',  ( -5.999999999999998224, -4.098570777380720287, 33.41473453929634729 ) ) ;
#62029 = EDGE_CURVE ( 'NONE', #84688, #21487, #32851, .T. ) ;
#62030 = VERTEX_POINT ( 'NONE', #75599 ) ;
#62031 = VERTEX_POINT ( 'NONE', #67528 ) ;
#62032 = ORIENTED_EDGE ( 'NONE', *, *, #15087, .F. ) ;
#62033 = CARTESIAN_POINT ( 'NONE',  ( -9.442362173959550020, -5.852078868378309373, 34.47109172314383585 ) ) ;
#62035 = EDGE_LOOP ( 'NONE', ( #86038, #5855, #88453, #2870 ) ) ;
#62034 = DIRECTION ( 'NONE',  ( -0.000000000000000000, 0.7660444431189791237, -0.6427876096865379196 ) ) ;
#62036 = ADVANCED_FACE ( 'NONE', ( #20229 ), #33303, .F. ) ;
#62037 = CARTESIAN_POINT ( 'NONE',  ( 6.923076923076924238, -6.386643153685126251, 34.62446782046654192 ) ) ;
#62038 = CIRCLE ( 'NONE', #30344, 0.2500000000000002220 ) ;
#62039 = FACE_OUTER_BOUND ( 'NONE', #56480, .T. ) ;
#62040 = ORIENTED_EDGE ( 'NONE', *, *, #70420, .T. ) ;
#62041 = VECTOR ( 'NONE', #9156, 1000.000000000000000 ) ;
#62042 = CARTESIAN_POINT ( 'NONE',  ( 8.769230769230768274, -12.37446782046654192, 30.86335684631486131 ) ) ;
#62043 = EDGE_CURVE ( 'NONE', #76426, #14630, #6275, .T. ) ;
#62044 = DIRECTION ( 'NONE',  ( -0.000000000000000000, -0.9396926207859092051, -0.3420201433256662704 ) ) ;
#62045 = EDGE_LOOP ( 'NONE', ( #16826, #70376, #8508, #24850 ) ) ;
#62046 = FACE_BOUND ( 'NONE', #20516, .T. ) ;
#62047 = CARTESIAN_POINT ( 'NONE',  ( -0.4615384615384611200, -9.780366693483667717, 34.19971097300155094 ) ) ;
#62048 = DIRECTION ( 'NONE',  ( -0.000000000000000000, -0.9848077530122086864, -0.1736481776669273613 ) ) ;
#62049 = CARTESIAN_POINT ( 'NONE',  ( 6.923076923076924238, -11.11383981884818262, 36.00935417666054406 ) ) ;
#62051 = CARTESIAN_POINT ( 'NONE',  ( -0.4615384615385826339, -12.27809138561165270, 31.22303859784587132 ) ) ;
#62050 = CARTESIAN_POINT ( 'NONE',  ( -14.30769230769230660, -12.29105614889573062, 35.45975837776705220 ) ) ;
#62052 = CARTESIAN_POINT ( 'NONE',  ( -4.853911725310227077, -10.61302985866383963, 33.66295027996417843 ) ) ;
#62053 = CARTESIAN_POINT ( 'NONE',  ( 13.38461538461569411, -2.506253911140615021, 30.00000000000323297 ) ) ;
#62054 = ORIENTED_EDGE ( 'NONE', *, *, #19375, .T. ) ;
#62055 = CARTESIAN_POINT ( 'NONE',  ( -2.372962308248625529, -4.320704448112771878, 33.92786785259540494 ) ) ;
#62056 = CARTESIAN_POINT ( 'NONE',  ( -8.096153846153844924, -2.499999999999998668, 29.75000000000000355 ) ) ;
#62057 = ORIENTED_EDGE ( 'NONE', *, *, #19204, .F. ) ;
#62058 = B_SPLINE_CURVE_WITH_KNOTS ( 'NONE', 3,
 ( #72188, #5070, #25789, #17705, #53247, #78952, #24438, #65435, #60010, #18144 ),
 .UNSPECIFIED., .F., .F.,
 ( 4, 2, 2, 2, 4 ),
 ( 0.000000000000000000, 0.0001954311584214072923, 0.0003908623168428145846, 0.0005862934752642218498, 0.0007817246336856291692 ),
 .UNSPECIFIED. ) ;
#62059 = CARTESIAN_POINT ( 'NONE',  ( 5.448717948717947124, -7.500000000000000000, 29.75000000000000355 ) ) ;
#62060 = CARTESIAN_POINT ( 'NONE',  ( 13.38461538461538680, -1.129524287112498415, 32.06866353760679544 ) ) ;
#62061 = ORIENTED_EDGE ( 'NONE', *, *, #77878, .F. ) ;
#62062 = CARTESIAN_POINT ( 'NONE',  ( -9.757577692864012775, -9.528491918058357157, 34.59228464037090589 ) ) ;
#62063 = CARTESIAN_POINT ( 'NONE',  ( 2.307692307692186251, -5.094484230521993062, 34.41647553114689373 ) ) ;
#62064 = FACE_BOUND ( 'NONE', #18746, .T. ) ;
#62066 = CARTESIAN_POINT ( 'NONE',  ( 15.48082354240754732, -12.17597550085003810, 31.52189283813460463 ) ) ;
#62065 = LINE ( 'NONE', #40047, #24580 ) ;
#62067 = CARTESIAN_POINT ( 'NONE',  ( -8.769230769230768274, -6.386643153685126251, 34.62446782046654192 ) ) ;
#62068 = CARTESIAN_POINT ( 'NONE',  ( 1.515140822849032398, -12.70449254468099198, 30.44128974285582956 ) ) ;
#62070 = CARTESIAN_POINT ( 'NONE',  ( 2.294871794871793380, -11.00000000000000000, 29.75000000000000355 ) ) ;
#62069 = DIRECTION ( 'NONE',  ( 1.000000000000000000, 0.000000000000000000, 0.000000000000000000 ) ) ;
#62071 = CARTESIAN_POINT ( 'NONE',  ( -14.08467946359890988, -5.582272713120729257, 34.63742843783360570 ) ) ;
#62072 = CARTESIAN_POINT ( 'NONE',  ( 3.724691934501232815, -5.885600066136343678, 15.38875670625848890 ) ) ;
#62073 = ORIENTED_EDGE ( 'NONE', *, *, #72925, .F. ) ;
#62074 = EDGE_CURVE ( 'NONE', #39806, #88852, #58375, .T. ) ;
#62075 = VECTOR ( 'NONE', #26393, 1000.000000000000000 ) ;
#62076 = VERTEX_POINT ( 'NONE', #72280 ) ;
#62077 = DIRECTION ( 'NONE',  ( 0.000000000000000000, 0.3420201433256641055, -0.9396926207859100932 ) ) ;
#62078 = CARTESIAN_POINT ( 'NONE',  ( -15.23076923076935252, -5.941354392335915335, 34.76329471203413846 ) ) ;
#62079 = CARTESIAN_POINT ( 'NONE',  ( -9.469528151039281028, -9.332535724633409302, 34.40230450496446934 ) ) ;
#62080 = CARTESIAN_POINT ( 'NONE',  ( -8.992157728137614825, -8.282780595021769443, 34.94152052738834158 ) ) ;
#62081 = DIRECTION ( 'NONE',  ( -1.000000000000000000, -0.000000000000000000, -0.000000000000000000 ) ) ;
#62082 = CARTESIAN_POINT ( 'NONE',  ( -1.492201783934549164, -11.27530806549876807, 18.35750670625849068 ) ) ;
#62083 = AXIS2_PLACEMENT_3D ( 'NONE', #4381, #65621, #16559 ) ;
#62084 = DIRECTION ( 'NONE',  ( 1.000000000000000000, 0.000000000000000000, 0.000000000000000000 ) ) ;
#62085 = CARTESIAN_POINT ( 'NONE',  ( 16.15384615384615330, -13.20930481340135110, 34.54067556320372745 ) ) ;
#62086 = EDGE_CURVE ( 'NONE', #3191, #59530, #30473, .T. ) ;
#62087 = CARTESIAN_POINT ( 'NONE',  ( 6.222779668978068557, -4.226511098958374291, 33.85474049983370293 ) ) ;
#62088 = CARTESIAN_POINT ( 'NONE',  ( 17.77707304109314279, -4.026226216239093603, 33.68668979543632958 ) ) ;
#62089 = CARTESIAN_POINT ( 'NONE',  ( -1.254567949364932211, -7.723484941389743952, 34.99544897038808955 ) ) ;
#62090 = CARTESIAN_POINT ( 'NONE',  ( 5.076923076923075762, -4.102666532097928531, 36.13435417666054406 ) ) ;
#62091 = CARTESIAN_POINT ( 'NONE',  ( -0.4615384615384611200, -3.937682226553329556, 33.60647404775216529 ) ) ;
#62093 = EDGE_CURVE ( 'NONE', #37921, #68993, #86267, .T. ) ;
#62092 = CARTESIAN_POINT ( 'NONE',  ( 15.23076923076923173, -13.78497067705608181, 32.30358669280327177 ) ) ;
#62094 = ADVANCED_FACE ( 'NONE', ( #49020 ), #23649, .F. ) ;
#62095 = DIRECTION ( 'NONE',  ( 1.000000000000000000, 0.000000000000000000, 0.000000000000000000 ) ) ;
#62096 = ORIENTED_EDGE ( 'NONE', *, *, #9223, .F. ) ;
#62097 = CARTESIAN_POINT ( 'NONE',  ( 4.088575707885377497, -5.219633306516282545, 34.19971097300152252 ) ) ;
#62098 = CARTESIAN_POINT ( 'NONE',  ( 6.923076923076800782, -11.06231777344772027, 33.60647404775119895 ) ) ;
#62099 = CARTESIAN_POINT ( 'NONE',  ( -1.200186371490524317, -10.22469193450124791, 20.11124329374151642 ) ) ;
#62100 = FACE_BOUND ( 'NONE', #37281, .T. ) ;
#62101 = CARTESIAN_POINT ( 'NONE',  ( -16.15384615384615330, -5.180354513474913603, 36.12317359536750416 ) ) ;
#62102 = ORIENTED_EDGE ( 'NONE', *, *, #54730, .F. ) ;
#62103 = CARTESIAN_POINT ( 'NONE',  ( -13.38461538461550582, -11.94971097300221174, 32.03036669348237098 ) ) ;
#62105 = ORIENTED_EDGE ( 'NONE', *, *, #32772, .T. ) ;
#62104 = CARTESIAN_POINT ( 'NONE',  ( -14.37377571864818293, -12.10708131394839349, 31.69288490824020244 ) ) ;
#62106 = CARTESIAN_POINT ( 'NONE',  ( 9.758375025657770152, -12.62096338111211757, 30.90682066428152908 ) ) ;
#62107 = CARTESIAN_POINT ( 'NONE',  ( 12.71159288145191724, -5.642605341092957971, 34.66089969410670335 ) ) ;
#62108 = EDGE_CURVE ( 'NONE', #85233, #25506, #67020, .T. ) ;
#62109 = EDGE_LOOP ( 'NONE', ( #63441, #32053, #23941, #11882 ) ) ;
#62110 = CARTESIAN_POINT ( 'NONE',  ( 11.97435897435897267, -7.500000000000000000, 29.75000000000000355 ) ) ;
#62111 = CARTESIAN_POINT ( 'NONE',  ( 13.38461538461526423, -9.528491918059723176, 34.59228464037033035 ) ) ;
#62112 = B_SPLINE_CURVE_WITH_KNOTS ( 'NONE', 3,
 ( #27964, #68502, #55431, #33831, #62623, #27076, #54538, #34274, #13560, #41042 ),
 .UNSPECIFIED., .F., .F.,
 ( 4, 2, 2, 2, 4 ),
 ( 0.0007817359430256315238, 0.0009771253907249976244, 0.001172514838424363508, 0.001367904286123729392, 0.001563293733823095492 ),
 .UNSPECIFIED. ) ;
#62113 = ORIENTED_EDGE ( 'NONE', *, *, #31738, .F. ) ;
#62114 = AXIS2_PLACEMENT_3D ( 'NONE', #73591, #18639, #37555 ) ;
#62115 = CARTESIAN_POINT ( 'NONE',  ( 16.82694634598072625, -11.28823185664190376, 33.01397839955799896 ) ) ;
#62116 = EDGE_CURVE ( 'NONE', #88566, #32155, #10058, .T. ) ;
#62117 = EDGE_CURVE ( 'NONE', #49489, #44980, #77696, .T. ) ;
#62118 = CARTESIAN_POINT ( 'NONE',  ( -15.29652265908256048, -7.249945578846652694, 34.99404164642496795 ) ) ;
#62119 = CARTESIAN_POINT ( 'NONE',  ( 2.241609928332172430, -12.62096338111211580, 30.90682066428152197 ) ) ;
#62120 = ORIENTED_EDGE ( 'NONE', *, *, #33109, .T. ) ;
#62121 = VERTEX_POINT ( 'NONE', #38059 ) ;
#62122 = CARTESIAN_POINT ( 'NONE',  ( -10.36543920600657209, -2.341251567377310217, 30.72681386836322659 ) ) ;
#62123 = EDGE_CURVE ( 'NONE', #22049, #72929, #28300, .T. ) ;
#62124 = ORIENTED_EDGE ( 'NONE', *, *, #47955, .F. ) ;
#62125 = CARTESIAN_POINT ( 'NONE',  ( -15.10024379253558457, -4.299079248970732792, 33.91157788607253565 ) ) ;
#62126 = CARTESIAN_POINT ( 'NONE',  ( -1.134669866267241867, -2.587454068350147907, 30.68340429815432202 ) ) ;
#62127 = DIRECTION ( 'NONE',  ( -0.000000000000000000, -0.000000000000000000, -1.000000000000000000 ) ) ;
#62128 = B_SPLINE_CURVE_WITH_KNOTS ( 'NONE', 3,
 ( #24934, #79449, #78992, #10089, #85762, #59608, #73129, #52399, #23599, #51050 ),
 .UNSPECIFIED., .F., .F.,
 ( 4, 2, 2, 2, 4 ),
 ( 0.000000000000000000, 0.0001954339857564089923, 0.0003908679715128179845, 0.0005863019572692270039, 0.0007817359430256359690 ),
 .UNSPECIFIED. ) ;
#62129 = DIRECTION ( 'NONE',  ( 0.000000000000000000, 0.9396926207859126468, -0.3420201433256571111 ) ) ;
#62130 = CARTESIAN_POINT ( 'NONE',  ( -4.219116599806928214, -6.879047030191174805, 34.71129190930000163 ) ) ;
#62131 = CARTESIAN_POINT ( 'NONE',  ( 1.253924781505078911, -2.295517848115769421, 30.44137282052137294 ) ) ;
#62132 = CARTESIAN_POINT ( 'NONE',  ( 15.93091919493930320, -12.64616026154729411, 30.79003144601914244 ) ) ;
#62133 = EDGE_LOOP ( 'NONE', ( #76885, #43031 ) ) ;
#62134 = ORIENTED_EDGE ( 'NONE', *, *, #49170, .T. ) ;
#62136 = VERTEX_POINT ( 'NONE', #69737 ) ;
#62135 = CARTESIAN_POINT ( 'NONE',  ( -23.50000000000000000, 1.674711738930281374E-15, 27.25000000000000000 ) ) ;
#62137 = ADVANCED_FACE ( 'NONE', ( #78154 ), #35511, .F. ) ;
#62138 = CARTESIAN_POINT ( 'NONE',  ( 16.85399611801622655, -2.308479472611653094, 30.53278059502174457 ) ) ;
#62139 = ORIENTED_EDGE ( 'NONE', *, *, #39857, .F. ) ;
#62140 = VECTOR ( 'NONE', #79303, 1000.000000000000114 ) ;
#62141 = FACE_OUTER_BOUND ( 'NONE', #9990, .T. ) ;
#62142 = CARTESIAN_POINT ( 'NONE',  ( 14.30769230769218581, -6.835583212225970762, 34.95778746994575670 ) ) ;
#62143 = ORIENTED_EDGE ( 'NONE', *, *, #22053, .T. ) ;
#62144 = FACE_OUTER_BOUND ( 'NONE', #31064, .T. ) ;
#62145 = AXIS2_PLACEMENT_3D ( 'NONE', #81729, #26333, #4737 ) ;
#62146 = ORIENTED_EDGE ( 'NONE', *, *, #30730, .F. ) ;
#62147 = CARTESIAN_POINT ( 'NONE',  ( -12.21153846153845990, -2.499999999999999556, 29.81604066197449754 ) ) ;
#62148 = ORIENTED_EDGE ( 'NONE', *, *, #55896, .F. ) ;
#62149 = CARTESIAN_POINT ( 'NONE',  ( -11.53846153846153655, -6.435427911321262684, 35.78748833219616898 ) ) ;
#62150 = ORIENTED_EDGE ( 'NONE', *, *, #26712, .T. ) ;
#62151 = CARTESIAN_POINT ( 'NONE',  ( -4.153846153846274980, -4.320704448113951379, 33.92786785259630022 ) ) ;
#62152 = CARTESIAN_POINT ( 'NONE',  ( -8.899922235898324985, -2.729777683071817229, 31.24903638046269450 ) ) ;
#62153 = FACE_BOUND ( 'NONE', #47171, .T. ) ;
#62154 = CARTESIAN_POINT ( 'NONE',  ( 5.777073041093152561, -2.308479472611653094, 30.53278059502174457 ) ) ;
#62155 = CARTESIAN_POINT ( 'NONE',  ( -11.60373153901785948, -6.835583212224499938, 34.95778746994557906 ) ) ;
#62156 = CARTESIAN_POINT ( 'NONE',  ( -16.02305571287920571, -4.684288915650984819, 34.18129842949671371 ) ) ;
#62157 = CARTESIAN_POINT ( 'NONE',  ( -0.3954711281883858676, -2.833524468853757750, 32.15551576947925838 ) ) ;
#62158 = CARTESIAN_POINT ( 'NONE',  ( -2.980823712421087901, -3.202959910592335202, 32.30730279482227019 ) ) ;
#62159 = CARTESIAN_POINT ( 'NONE',  ( -4.377331097570100304, -11.41268669641500466, 32.86336882939237825 ) ) ;
#62160 = CARTESIAN_POINT ( 'NONE',  ( -14.05763799605399278, -3.627508038966690496, 32.91356715214248396 ) ) ;
#62161 = VERTEX_POINT ( 'NONE', #66869 ) ;
#62162 = ORIENTED_EDGE ( 'NONE', *, *, #51993, .T. ) ;
#62164 = CARTESIAN_POINT ( 'NONE',  ( 14.98079249982687955, -12.17611988154120972, 31.52148481390971213 ) ) ;
#62163 = DIRECTION ( 'NONE',  ( -0.000000000000000000, -0.000000000000000000, 1.000000000000000000 ) ) ;
#62165 = EDGE_CURVE ( 'NONE', #88652, #81428, #26324, .T. ) ;
#62166 = VECTOR ( 'NONE', #46559, 1000.000000000000000 ) ;
#62167 = CARTESIAN_POINT ( 'NONE',  ( -12.52680890749923570, -2.625532179533444754, 30.86335684631481513 ) ) ;
#62168 = CARTESIAN_POINT ( 'NONE',  ( -8.769230769230768274, -10.89733346790207413, 36.13435417666054406 ) ) ;
#62169 = CARTESIAN_POINT ( 'NONE',  ( 15.48082354240754555, -3.627508038966690496, 32.91356715214248396 ) ) ;
#62170 = DIRECTION ( 'NONE',  ( -1.000000000000000000, -0.000000000000000000, -0.000000000000000000 ) ) ;
#62171 = ORIENTED_EDGE ( 'NONE', *, *, #33556, .F. ) ;
#62172 = CYLINDRICAL_SURFACE ( 'NONE', #61597, 0.2499999999999986955 ) ;
#62173 = CARTESIAN_POINT ( 'NONE',  ( 3.361561038594018225, -11.18335022499818621, 33.13157742990016885 ) ) ;
#62174 = DIRECTION ( 'NONE',  ( 0.000000000000000000, 0.3420201433256610524, 0.9396926207859113145 ) ) ;
#62175 = LINE ( 'NONE', #49103, #7935 ) ;
#62176 = VECTOR ( 'NONE', #52580, 1000.000000000000227 ) ;
#62177 = VERTEX_POINT ( 'NONE', #66422 ) ;
#62178 = ORIENTED_EDGE ( 'NONE', *, *, #68149, .T. ) ;
#62179 = EDGE_LOOP ( 'NONE', ( #62781, #46330, #60386, #86752 ) ) ;
#62180 = DIRECTION ( 'NONE',  ( -0.000000000000000000, -0.000000000000000000, -1.000000000000000000 ) ) ;
#62181 = EDGE_CURVE ( 'NONE', #11993, #27559, #48659, .T. ) ;
#62182 = ORIENTED_EDGE ( 'NONE', *, *, #45066, .T. ) ;
#62183 = CARTESIAN_POINT ( 'NONE',  ( -9.442362282929646966, -10.18230066228895758, 34.26354781536631577 ) ) ;
#62184 = DIRECTION ( 'NONE',  ( 0.000000000000000000, 0.000000000000000000, 1.000000000000000000 ) ) ;
#62185 = LINE ( 'NONE', #5484, #19357 ) ;
#62186 = CARTESIAN_POINT ( 'NONE',  ( -3.749999999999988454, -9.053300858899127945, 15.01562500000000178 ) ) ;
#62187 = EDGE_CURVE ( 'NONE', #56825, #35354, #7840, .T. ) ;
#62188 = CARTESIAN_POINT ( 'NONE',  ( -11.31545018684868786, -6.503523203565941380, 34.64991518177335195 ) ) ;
#62189 = ORIENTED_EDGE ( 'NONE', *, *, #77412, .F. ) ;
#62190 = CARTESIAN_POINT ( 'NONE',  ( 4.219914504848592429, -4.098570777380720287, 33.41473453929635440 ) ) ;
#62192 = ORIENTED_EDGE ( 'NONE', *, *, #10334, .F. ) ;
#62191 = CARTESIAN_POINT ( 'NONE',  ( -1.576923076923076872, -7.500000000000000000, 29.75000000000000355 ) ) ;
#62193 = CARTESIAN_POINT ( 'NONE',  ( 17.78205128205128105, -7.500000000000000000, 29.75000000000000355 ) ) ;
#62194 = CARTESIAN_POINT ( 'NONE',  ( -10.39260507411620260, -3.755027918224367323, 33.06320215134714857 ) ) ;
#62195 = FACE_OUTER_BOUND ( 'NONE', #52148, .T. ) ;
#62196 = CARTESIAN_POINT ( 'NONE',  ( 9.758376043310132530, -10.51840700105979565, 33.73612834413962247 ) ) ;
#62197 = CARTESIAN_POINT ( 'NONE',  ( -9.942284436356281674, -12.41104346484419452, 31.60698883733904196 ) ) ;
#62198 = EDGE_CURVE ( 'NONE', #35844, #61936, #41185, .T. ) ;
#62199 = CARTESIAN_POINT ( 'NONE',  ( 9.468822748583747284, -10.11188796281391511, 34.01382737946119050 ) ) ;
#62200 = CARTESIAN_POINT ( 'NONE',  ( -0.4615384615385840772, -2.657715359629662544, 31.77849191805970364 ) ) ;
#62201 = B_SPLINE_CURVE_WITH_KNOTS ( 'NONE', 3,
 ( #80832, #74063, #47011, #19115, #53778, #5598, #27196, #54652, #82151, #40724 ),
 .UNSPECIFIED., .F., .F.,
 ( 4, 2, 2, 2, 4 ),
 ( 0.0007817359430256294638, 0.0009771253907249974075, 0.001172514838424365460, 0.001367904286123733295, 0.001563293733823094191 ),
 .UNSPECIFIED. ) ;
#62202 = CARTESIAN_POINT ( 'NONE',  ( -1.987747218494638313, -9.401340078031370950, 20.18936829374151287 ) ) ;
#62203 = EDGE_LOOP ( 'NONE', ( #65849, #85416, #74507, #66990 ) ) ;
#62204 = LINE ( 'NONE', #27979, #66200 ) ;
#62205 = CARTESIAN_POINT ( 'NONE',  ( 0.7115927731767749398, -3.136992222400443175, 32.19305428654138979 ) ) ;
#62206 = MECHANICAL_DESIGN_GEOMETRIC_PRESENTATION_REPRESENTATION (  '', ( #27675 ), #1835 ) ;
#62207 = VECTOR ( 'NONE', #552, 1000.000000000000227 ) ;
#62208 = DIRECTION ( 'NONE',  ( -0.000000000000000000, 0.6427876096865404731, -0.7660444431189770143 ) ) ;
#62209 = VERTEX_POINT ( 'NONE', #11481 ) ;
#62210 = VERTEX_POINT ( 'NONE', #11933 ) ;
#62211 = CARTESIAN_POINT ( 'NONE',  ( 2.084864210057430167, -7.369209533119137845, 34.99857337881830688 ) ) ;
#62212 = CARTESIAN_POINT ( 'NONE',  ( -3.296852641725108501, -10.51840700105979387, 33.73612834413961536 ) ) ;
#62213 = VECTOR ( 'NONE', #24442, 1000.000000000000000 ) ;
#62214 = CARTESIAN_POINT ( 'NONE',  ( 8.769230769230768274, -1.044019251281081972, 31.83374038241031911 ) ) ;
#62215 = CARTESIAN_POINT ( 'NONE',  ( 14.24160889673642849, -3.050289026998445951, 32.03036669348365706 ) ) ;
#62216 = ORIENTED_EDGE ( 'NONE', *, *, #45903, .F. ) ;
#62217 = CARTESIAN_POINT ( 'NONE',  ( -15.23076923076935074, -2.892918686052166066, 31.69288490824153470 ) ) ;
#62218 = EDGE_CURVE ( 'NONE', #21962, #46929, #2549, .T. ) ;
#62219 = CARTESIAN_POINT ( 'NONE',  ( 3.230769230769231726, -12.10708131394839349, 31.69288490824020244 ) ) ;
#62220 = CARTESIAN_POINT ( 'NONE',  ( 24.00000000000000000, -9.499999999999982236, 27.25000000000000000 ) ) ;
#62221 = ORIENTED_EDGE ( 'NONE', *, *, #81321, .T. ) ;
#62222 = CARTESIAN_POINT ( 'NONE',  ( 11.25641025641025550, -7.500000000000000000, 29.75000000000000355 ) ) ;
#62223 = ORIENTED_EDGE ( 'NONE', *, *, #69729, .T. ) ;
#62224 = LINE ( 'NONE', #82952, #68782 ) ;
#62225 = CARTESIAN_POINT ( 'NONE',  ( 15.12820512820512953, -3.499999999999999556, 29.75000000000000355 ) ) ;
#62226 = ORIENTED_EDGE ( 'NONE', *, *, #48234, .T. ) ;
#62227 = CARTESIAN_POINT ( 'NONE',  ( 7.846153846153725020, -12.27809138561165270, 31.22303859784587132 ) ) ;
#62228 = CARTESIAN_POINT ( 'NONE',  ( -14.55771553191376277, -2.341070481393819236, 30.72580821765574299 ) ) ;
#62229 = CARTESIAN_POINT ( 'NONE',  ( -11.66915300512910214, -6.413092428213692742, 34.63065189839063152 ) ) ;
#62230 = B_SPLINE_CURVE_WITH_KNOTS ( 'NONE', 3,
 ( #74801, #54510, #75667, #13970, #41448, #68912, #80678, #18962, #46427, #12206 ),
 .UNSPECIFIED., .F., .F.,
 ( 4, 2, 2, 2, 4 ),
 ( 0.000000000000000000, 0.0001954339857564076099, 0.0003908679715128152198, 0.0005863019572692228839, 0.0007817359430256304396 ),
 .UNSPECIFIED. ) ;
#62231 = VECTOR ( 'NONE', #36718, 1000.000000000000000 ) ;
#62232 = DIRECTION ( 'NONE',  ( 0.000000000000000000, 0.4999999999999960032, -0.8660254037844410391 ) ) ;
#62233 = DIRECTION ( 'NONE',  ( -0.000000000000000000, 1.000000000000000000, -0.000000000000000000 ) ) ;
#62234 = ORIENTED_EDGE ( 'NONE', *, *, #50180, .T. ) ;
#62235 = FACE_BOUND ( 'NONE', #77642, .T. ) ;
#62236 = ORIENTED_EDGE ( 'NONE', *, *, #13069, .T. ) ;
#62237 = DIRECTION ( 'NONE',  ( 0.000000000000000000, 0.000000000000000000, -1.000000000000000000 ) ) ;
#62238 = CARTESIAN_POINT ( 'NONE',  ( -12.46153846153846168, -1.129524287112498415, 32.06866353760679544 ) ) ;
#62239 = CARTESIAN_POINT ( 'NONE',  ( 8.769230769230768274, -3.937682226553329556, 33.60647404775216529 ) ) ;
#62240 = CARTESIAN_POINT ( 'NONE',  ( -11.28840722682322628, -2.564540009722895419, 30.55348353981670684 ) ) ;
#62241 = ORIENTED_EDGE ( 'NONE', *, *, #32323, .F. ) ;
#62242 = ORIENTED_EDGE ( 'NONE', *, *, #32277, .T. ) ;
#62243 = ORIENTED_EDGE ( 'NONE', *, *, #14252, .F. ) ;
#62244 = DIRECTION ( 'NONE',  ( 1.000000000000000000, 0.000000000000000000, 0.000000000000000000 ) ) ;
#62245 = ORIENTED_EDGE ( 'NONE', *, *, #80843, .T. ) ;
#62246 = CARTESIAN_POINT ( 'NONE',  ( -13.38461538461550582, -3.300289026999228881, 32.46337939537708905 ) ) ;
#62247 = CARTESIAN_POINT ( 'NONE',  ( 13.38461538461538680, -9.058645607665452459, 34.76329471203371924 ) ) ;
#62248 = CYLINDRICAL_SURFACE ( 'NONE', #17024, 0.2499999999999979738 ) ;
#62249 = DIRECTION ( 'NONE',  ( 0.000000000000000000, 0.4999999999999985567, 0.8660254037844395958 ) ) ;
#62250 = AXIS2_PLACEMENT_3D ( 'NONE', #18389, #58030, #44953 ) ;
#62251 = CARTESIAN_POINT ( 'NONE',  ( -1.553300858899125059, -3.750000000000009326, 25.32812500000000711 ) ) ;
#62252 = CARTESIAN_POINT ( 'NONE',  ( 15.29602480204525605, -9.442884908240273489, 34.35708131394835618 ) ) ;
#62253 = CARTESIAN_POINT ( 'NONE',  ( -18.25000000000000355, -7.500000000000000000, 35.00000000000000000 ) ) ;
#62254 = CARTESIAN_POINT ( 'NONE',  ( 11.40831432902331954, -10.19110544564092002, 33.96427741523702792 ) ) ;
#62255 = VERTEX_POINT ( 'NONE', #79938 ) ;
#62256 = ORIENTED_EDGE ( 'NONE', *, *, #81144, .T. ) ;
#62257 = VECTOR ( 'NONE', #33990, 1000.000000000000114 ) ;
#62258 = EDGE_LOOP ( 'NONE', ( #58286, #76240, #17948, #62143 ) ) ;
#62259 = DIRECTION ( 'NONE',  ( -0.000000000000000000, 0.7660444431189791237, -0.6427876096865379196 ) ) ;
#62261 = DIRECTION ( 'NONE',  ( 1.000000000000000000, 0.000000000000000000, 0.000000000000000000 ) ) ;
#62260 = CYLINDRICAL_SURFACE ( 'NONE', #30252, 0.2499999999999995559 ) ;
#62262 = DIRECTION ( 'NONE',  ( -0.000000000000000000, -0.7660444431189791237, -0.6427876096865379196 ) ) ;
#62263 = CARTESIAN_POINT ( 'NONE',  ( -6.792285115252135519, -3.530189275343204702, 32.79018710029569661 ) ) ;
#62264 = FACE_BOUND ( 'NONE', #79766, .T. ) ;
#62265 = CARTESIAN_POINT ( 'NONE',  ( 9.757563263583719504, -3.835265460703683349, 33.15142922261929925 ) ) ;
#62266 = VERTEX_POINT ( 'NONE', #74512 ) ;
#62267 = CYLINDRICAL_SURFACE ( 'NONE', #83160, 0.2499999999999979738 ) ;
#62268 = CARTESIAN_POINT ( 'NONE',  ( 0.4615384615384611200, -9.780366693483667717, 34.19971097300155094 ) ) ;
#62269 = DIRECTION ( 'NONE',  ( 0.000000000000000000, 0.7660444431189807890, 0.6427876096865361433 ) ) ;
#62270 = CARTESIAN_POINT ( 'NONE',  ( 1.384615384615386802, -9.819645486525091727, 36.12317359536749706 ) ) ;
#62271 = VERTEX_POINT ( 'NONE', #12807 ) ;
#62272 = CARTESIAN_POINT ( 'NONE',  ( 18.25005431163831204, -12.41262288849542017, 30.68299917996395010 ) ) ;
#62273 = ORIENTED_EDGE ( 'NONE', *, *, #34632, .T. ) ;
#62274 = FACE_BOUND ( 'NONE', #28137, .T. ) ;
#62275 = DIRECTION ( 'NONE',  ( 0.000000000000000000, 0.6427876096865373645, -0.7660444431189797898 ) ) ;
#62276 = EDGE_CURVE ( 'NONE', #71689, #88631, #83137, .T. ) ;
#62277 = CARTESIAN_POINT ( 'NONE',  ( -12.46153846153846168, -8.120952969808772792, 34.71129190930000163 ) ) ;
#62278 = LINE ( 'NONE', #7794, #2979 ) ;
#62279 = ORIENTED_EDGE ( 'NONE', *, *, #13025, .F. ) ;
#62280 = EDGE_CURVE ( 'NONE', #21769, #5919, #45251, .T. ) ;
#62281 = CARTESIAN_POINT ( 'NONE',  ( 5.076923076922954969, -3.300289026999228881, 32.46337939537708905 ) ) ;
#62282 = CARTESIAN_POINT ( 'NONE',  ( -3.296039231325549768, -2.379036618887870880, 30.90682066428147934 ) ) ;
#62283 = CARTESIAN_POINT ( 'NONE',  ( -16.40386939113911779, -12.43535235679832596, 30.55408501211184813 ) ) ;
#62284 = CARTESIAN_POINT ( 'NONE',  ( -13.38461538461538325, -12.48256725967547354, 35.29906147534542527 ) ) ;
#62285 = EDGE_LOOP ( 'NONE', ( #13291, #44171 ) ) ;
#62286 = CARTESIAN_POINT ( 'NONE',  ( -7.846153846153967493, -10.33852847137269571, 34.16647553114546554 ) ) ;
#62288 = CARTESIAN_POINT ( 'NONE',  ( -15.93106648486808119, -10.23759521482555357, 34.22997729860117033 ) ) ;
#62287 = AXIS2_PLACEMENT_3D ( 'NONE', #41289, #40842, #84056 ) ;
#62291 = ORIENTED_EDGE ( 'NONE', *, *, #79797, .F. ) ;
#62290 = VECTOR ( 'NONE', #49577, 1000.000000000000000 ) ;
#62289 = DIRECTION ( 'NONE',  ( 0.000000000000000000, 0.4999999999999985567, 0.8660254037844395958 ) ) ;
#62292 = CARTESIAN_POINT ( 'NONE',  ( 9.469479594672815637, -7.369209533119137845, 34.99857337881830688 ) ) ;
#62293 = CARTESIAN_POINT ( 'NONE',  ( -4.153846153846152411, -2.721908614388771852, 31.22303859784724978 ) ) ;
#62294 = CARTESIAN_POINT ( 'NONE',  ( 5.011653076366757276, -2.657715359629089225, 31.77849191805834295 ) ) ;
#62295 = CARTESIAN_POINT ( 'NONE',  ( 5.448717948717947124, -4.000000000000000000, 29.75000000000000355 ) ) ;
#62296 = CARTESIAN_POINT ( 'NONE',  ( 9.757563263583717728, -9.442884908240273489, 34.35708131394835618 ) ) ;
#62298 = FACE_OUTER_BOUND ( 'NONE', #8940, .T. ) ;
#62297 = DIRECTION ( 'NONE',  ( -0.000000000000000000, 0.7660444431189791237, -0.6427876096865379196 ) ) ;
#62299 = ADVANCED_FACE ( 'NONE', ( #14136 ), #82618, .F. ) ;
#62300 = LINE ( 'NONE', #83032, #3238 ) ;
#62301 = CARTESIAN_POINT ( 'NONE',  ( 1.139087296525997273, -4.749999999999992895, 20.48437500000000000 ) ) ;
#62302 = ORIENTED_EDGE ( 'NONE', *, *, #82787, .T. ) ;
#62303 = CARTESIAN_POINT ( 'NONE',  ( -17.32692307692307665, -2.249999999999998668, 29.75000000000000355 ) ) ;
#62304 = ORIENTED_EDGE ( 'NONE', *, *, #45057, .F. ) ;
#62305 = ORIENTED_EDGE ( 'NONE', *, *, #24779, .T. ) ;
#62306 = CARTESIAN_POINT ( 'NONE',  ( -11.28851612908349722, -2.341251567377310217, 30.72681386836322659 ) ) ;
#62307 = EDGE_LOOP ( 'NONE', ( #47665, #86549, #49062, #13944 ) ) ;
#62308 = DIRECTION ( 'NONE',  ( -0.000000000000000000, -0.5000000000000009992, -0.8660254037844380415 ) ) ;
#62309 = CARTESIAN_POINT ( 'NONE',  ( -8.352564102564102200, -3.499999999999999556, 29.75000000000000355 ) ) ;
#62310 = DIRECTION ( 'NONE',  ( 0.000000000000000000, 0.9396926207859126468, 0.3420201433256571111 ) ) ;
#62311 = CARTESIAN_POINT ( 'NONE',  ( -11.78848477575450282, -11.37209801155882971, 32.91403422569032955 ) ) ;
#62312 = CARTESIAN_POINT ( 'NONE',  ( -18.75000000000000000, -7.500000000000000000, 29.75000000000000355 ) ) ;
#62313 = CARTESIAN_POINT ( 'NONE',  ( 2.307692307692309264, -9.780366693483667717, 34.19971097300155094 ) ) ;
#62314 = CARTESIAN_POINT ( 'NONE',  ( -4.403869391139116907, -3.711651800289232916, 33.01384336483936011 ) ) ;
#62315 = CARTESIAN_POINT ( 'NONE',  ( 6.856994543716788293, -9.905515769479276145, 34.41647553114623292 ) ) ;
#62317 = ADVANCED_FACE ( 'NONE', ( #41171 ), #34404, .T. ) ;
#62316 = CARTESIAN_POINT ( 'NONE',  ( 11.31553532094539172, -10.61292498521070549, 33.66303323003028680 ) ) ;
#62318 = VECTOR ( 'NONE', #87533, 1000.000000000000000 ) ;
#62319 = EDGE_CURVE ( 'NONE', #27068, #32893, #7388, .T. ) ;
#62320 = CARTESIAN_POINT ( 'NONE',  ( -6.416666666666667851, -7.500000000000000000, 29.75000000000000355 ) ) ;
#62321 = B_SPLINE_CURVE_WITH_KNOTS ( 'NONE', 3,
 ( #86652, #5102, #5548, #59595, #73115, #12743, #79434, #31692, #46959, #72663 ),
 .UNSPECIFIED., .F., .F.,
 ( 4, 2, 2, 2, 4 ),
 ( 0.000000000000000000, 0.0001954339881912774070, 0.0003908679763825548140, 0.0005863019645738322752, 0.0007817359527651096280 ),
 .UNSPECIFIED. ) ;
#62322 = CARTESIAN_POINT ( 'NONE',  ( -13.16160403300253634, -11.24521262558773493, 33.06293181088029343 ) ) ;
#62323 = CIRCLE ( 'NONE', #6283, 4.000000000000000000 ) ;
#62324 = VECTOR ( 'NONE', #5106, 1000.000000000000114 ) ;
#62325 = ORIENTED_EDGE ( 'NONE', *, *, #47773, .T. ) ;
#62327 = ADVANCED_FACE ( 'NONE', ( #28543 ), #68636, .F. ) ;
#62326 = EDGE_LOOP ( 'NONE', ( #83168, #55064 ) ) ;
#62328 = CARTESIAN_POINT ( 'NONE',  ( -18.06527000055631760, -2.657715359629089669, 31.77849191805835005 ) ) ;
#62329 = CARTESIAN_POINT ( 'NONE',  ( 1.449870524128224591, -3.643525952247864463, 33.31231777344670064 ) ) ;
#62330 = DIRECTION ( 'NONE',  ( -0.000000000000000000, 1.000000000000000000, 3.491481338843133355E-15 ) ) ;
#62331 = CARTESIAN_POINT ( 'NONE',  ( -5.076923076923075762, -2.517432740324522911, 35.29906147534542527 ) ) ;
#62332 = EDGE_CURVE ( 'NONE', #12780, #31146, #1065, .T. ) ;
#62333 = CARTESIAN_POINT ( 'NONE',  ( 12.33084699487090674, -8.999036380462717588, 34.52022231692819076 ) ) ;
#62334 = CARTESIAN_POINT ( 'NONE',  ( -6.250023237292963607, -8.432397168068783699, 34.66272746175022945 ) ) ;
#62335 = CARTESIAN_POINT ( 'NONE',  ( -1.384615384615383471, -5.180354513474913603, 36.12317359536750416 ) ) ;
#62336 = ORIENTED_EDGE ( 'NONE', *, *, #15597, .T. ) ;
#62337 = CARTESIAN_POINT ( 'NONE',  ( 16.08857570788537572, -2.892918686051582533, 31.69288490824015980 ) ) ;
#62338 = ORIENTED_EDGE ( 'NONE', *, *, #44581, .T. ) ;
#62339 = CARTESIAN_POINT ( 'NONE',  ( 9.915319043920545639, -11.76359900205217635, 32.36225158514719880 ) ) ;
#62340 = CARTESIAN_POINT ( 'NONE',  ( 6.923076923076800782, -6.835583212225970762, 34.95778746994575670 ) ) ;
#62341 = CARTESIAN_POINT ( 'NONE',  ( -0.2387589202700526325, -6.760870238392817200, 34.69528174975673096 ) ) ;
#62342 = DIRECTION ( 'NONE',  ( -0.000000000000000000, -0.9396926207859093161, -0.3420201433256663259 ) ) ;
#62343 = CARTESIAN_POINT ( 'NONE',  ( -13.60754234352223335, -2.523278758544489797, 31.42238647778637528 ) ) ;
#62344 = ORIENTED_EDGE ( 'NONE', *, *, #85734, .F. ) ;
#62345 = CIRCLE ( 'NONE', #22046, 0.2500000000000002220 ) ;
#62346 = AXIS2_PLACEMENT_3D ( 'NONE', #61022, #62342, #55148 ) ;
#62347 = ORIENTED_EDGE ( 'NONE', *, *, #79035, .F. ) ;
#62348 = EDGE_CURVE ( 'NONE', #34190, #14282, #335, .T. ) ;
#62349 = ORIENTED_EDGE ( 'NONE', *, *, #29526, .F. ) ;
#62350 = EDGE_LOOP ( 'NONE', ( #73634, #41264 ) ) ;
#62351 = LINE ( 'NONE', #34886, #24265 ) ;
#62352 = CARTESIAN_POINT ( 'NONE',  ( 7.623227628637698317, -3.586966769969700763, 32.86292498521069660 ) ) ;
#62353 = LINE ( 'NONE', #28131, #63860 ) ;
#62354 = CARTESIAN_POINT ( 'NONE',  ( 2.177545098254091371, -11.47017969459903952, 32.78971311882034456 ) ) ;
#62355 = CARTESIAN_POINT ( 'NONE',  ( 4.403791672194296680, -6.696923467548660192, 34.68552623307873972 ) ) ;
#62356 = DIRECTION ( 'NONE',  ( -0.000000000000000000, 0.3420201433256694901, -0.9396926207859082059 ) ) ;
#62357 = EDGE_LOOP ( 'NONE', ( #20049, #82531 ) ) ;
#62358 = ORIENTED_EDGE ( 'NONE', *, *, #49818, .T. ) ;
#62359 = EDGE_CURVE ( 'NONE', #71793, #5237, #61427, .T. ) ;
#62360 = ORIENTED_EDGE ( 'NONE', *, *, #86022, .F. ) ;
#62362 = ORIENTED_EDGE ( 'NONE', *, *, #1445, .T. ) ;
#62361 = CARTESIAN_POINT ( 'NONE',  ( 4.284371592079798674, -4.299079248970732792, 33.91157788607253565 ) ) ;
#62363 = CARTESIAN_POINT ( 'NONE',  ( 10.36540788444226102, -12.41269422305637171, 30.68257228309993323 ) ) ;
#62364 = CARTESIAN_POINT ( 'NONE',  ( -2.242436736416281384, -9.442884908240271713, 34.35708131394835618 ) ) ;
#62365 = CARTESIAN_POINT ( 'NONE',  ( 3.750000000000000888, -7.499999999999978684, 18.21875000000000000 ) ) ;
#62366 = ORIENTED_EDGE ( 'NONE', *, *, #7182, .F. ) ;
#62367 = ORIENTED_EDGE ( 'NONE', *, *, #49514, .T. ) ;
#62368 = CARTESIAN_POINT ( 'NONE',  ( -2.307692307692305711, -12.37446782046654192, 30.86335684631486131 ) ) ;
#62369 = VERTEX_POINT ( 'NONE', #182 ) ;
#62370 = FACE_BOUND ( 'NONE', #141, .T. ) ;
#62371 = CARTESIAN_POINT ( 'NONE',  ( -5.999999999999998224, -2.833524468853757305, 32.15551576947925838 ) ) ;
#62372 = VECTOR ( 'NONE', #27229, 1000.000000000000227 ) ;
#62373 = EDGE_CURVE ( 'NONE', #61417, #34053, #28094, .T. ) ;
#62374 = CARTESIAN_POINT ( 'NONE',  ( -8.102564102564102200, -7.500000000000000000, 33.75000000000000000 ) ) ;
#62375 = VERTEX_POINT ( 'NONE', #62309 ) ;
#62376 = CARTESIAN_POINT ( 'NONE',  ( -16.08859101433330707, -12.70778746994558439, 30.41441678777537305 ) ) ;
#62377 = EDGE_CURVE ( 'NONE', #54531, #59736, #40735, .T. ) ;
#62378 = CARTESIAN_POINT ( 'NONE',  ( -10.03846153846153832, -7.500000000000000000, 29.75000000000000355 ) ) ;
#62379 = CARTESIAN_POINT ( 'NONE',  ( -1.134615384613964384, -7.500000000000154543, 35.00000000000007105 ) ) ;
#62380 = ORIENTED_EDGE ( 'NONE', *, *, #2536, .F. ) ;
#62381 = CARTESIAN_POINT ( 'NONE',  ( 11.53846153846141753, -3.300289026999228881, 32.46337939537708905 ) ) ;
#62382 = CARTESIAN_POINT ( 'NONE',  ( -5.869209559033047974, -3.957578996910242619, 33.62503395064540257 ) ) ;
#62383 = CARTESIAN_POINT ( 'NONE',  ( 0.4615384615384611200, -11.69971097300155272, 32.46337939537588113 ) ) ;
#62384 = DIRECTION ( 'NONE',  ( 0.000000000000000000, 0.000000000000000000, 1.000000000000000000 ) ) ;
#62385 = CARTESIAN_POINT ( 'NONE',  ( -0.2115384615385252354, -7.565270445406050648, 34.75000000000000000 ) ) ;
#62386 = FACE_BOUND ( 'NONE', #11840, .T. ) ;
#62388 = CARTESIAN_POINT ( 'NONE',  ( -4.153846153845845102, -2.506253911140614576, 30.00000000000323297 ) ) ;
#62387 = LINE ( 'NONE', #703, #20361 ) ;
#62389 = EDGE_CURVE ( 'NONE', #51433, #47287, #52956, .T. ) ;
#62390 = CARTESIAN_POINT ( 'NONE',  ( -6.989160334032800570, -12.10708131394839349, 31.69288490824020244 ) ) ;
#62392 = CARTESIAN_POINT ( 'NONE',  ( 8.992010310499178871, -2.847695495035523550, 31.58253572463339154 ) ) ;
#62391 = CARTESIAN_POINT ( 'NONE',  ( -10.61538461538461320, -6.189225973068211317, 35.74407628777942847 ) ) ;
#62393 = CARTESIAN_POINT ( 'NONE',  ( -18.13069146666756382, -9.804603061927748442, 34.18744698557895845 ) ) ;
#62394 = CARTESIAN_POINT ( 'NONE',  ( 0.06109907496454976272, -10.25000000000000000, 19.52938170625848713 ) ) ;
#62395 = ORIENTED_EDGE ( 'NONE', *, *, #3737, .T. ) ;
#62396 = CARTESIAN_POINT ( 'NONE',  ( -9.019230769230770051, -7.433931650972299465, 34.75000000000000711 ) ) ;
#62397 = VERTEX_POINT ( 'NONE', #75398 ) ;
#62398 = EDGE_CURVE ( 'NONE', #86296, #64502, #78819, .T. ) ;
#62399 = CARTESIAN_POINT ( 'NONE',  ( 3.230769230769231726, -6.681629849574314051, 35.83090037661290239 ) ) ;
#62400 = ORIENTED_EDGE ( 'NONE', *, *, #60040, .T. ) ;
#62401 = CARTESIAN_POINT ( 'NONE',  ( 17.77707378248384629, -12.15238873228291716, 31.58232369045353849 ) ) ;
#62403 = ADVANCED_FACE ( 'NONE', ( #87894 ), #26158, .F. ) ;
#62402 = CARTESIAN_POINT ( 'NONE',  ( -18.06608341095587278, -2.538708090699994813, 30.37095296980875503 ) ) ;
#62404 = VERTEX_POINT ( 'NONE', #67593 ) ;
#62405 = CARTESIAN_POINT ( 'NONE',  ( 14.30769230769231015, -11.11383981884818262, 36.00935417666054406 ) ) ;
#62406 = CARTESIAN_POINT ( 'NONE',  ( -2.724691934501232371, -8.700186371490559623, 18.51375670625849068 ) ) ;
#62407 = CARTESIAN_POINT ( 'NONE',  ( 4.153846153846032507, -9.442884908241554243, 34.35708131394783038 ) ) ;
#62408 = CARTESIAN_POINT ( 'NONE',  ( -5.207071046654774271, -3.069018819979302926, 32.56621877034667278 ) ) ;
#62409 = VECTOR ( 'NONE', #49645, 1000.000000000000000 ) ;
#62410 = FACE_OUTER_BOUND ( 'NONE', #85952, .T. ) ;
#62411 = CARTESIAN_POINT ( 'NONE',  ( -17.07692307692307665, -12.34228464037088635, 31.77849191805839268 ) ) ;
#62412 = FACE_OUTER_BOUND ( 'NONE', #60189, .T. ) ;
#62413 = LINE ( 'NONE', #41722, #20999 ) ;
#62414 = CARTESIAN_POINT ( 'NONE',  ( -2.694853999681181556, -10.10844685921792241, 23.93936829374151642 ) ) ;
#62415 = CARTESIAN_POINT ( 'NONE',  ( -18.22292695890684655, -11.43668979543635089, 33.22377378376089752 ) ) ;
#62417 = EDGE_CURVE ( 'NONE', #71459, #70755, #73012, .T. ) ;
#62416 = DIRECTION ( 'NONE',  ( 0.000000000000000000, 0.7660444431189822323, -0.6427876096865344779 ) ) ;
#62418 = VERTEX_POINT ( 'NONE', #66702 ) ;
#62419 = CARTESIAN_POINT ( 'NONE',  ( 24.99999999999999645, 20.00000000000000355, 3.000000000000000000 ) ) ;
#62420 = CARTESIAN_POINT ( 'NONE',  ( -2.608446859217920633, -4.805146000318815780, 21.75186829374151287 ) ) ;
#62421 = DIRECTION ( 'NONE',  ( 1.000000000000000000, 0.000000000000000000, 0.000000000000000000 ) ) ;
#62422 = CARTESIAN_POINT ( 'NONE',  ( -8.899378738962466784, -11.66186481527757302, 32.95055677023626117 ) ) ;
#62423 = ORIENTED_EDGE ( 'NONE', *, *, #89130, .T. ) ;
#62424 = CARTESIAN_POINT ( 'NONE',  ( 12.46153846153846168, -8.164416787775445883, 34.95778746994557906 ) ) ;
#62425 = CARTESIAN_POINT ( 'NONE',  ( -17.07692307692307665, -9.058645607665452459, 34.76329471203371924 ) ) ;
#62427 = VERTEX_POINT ( 'NONE', #80677 ) ;
#62426 = CARTESIAN_POINT ( 'NONE',  ( -17.29974976940208364, -7.369208160676171460, 34.74850200257122879 ) ) ;
#62428 = CARTESIAN_POINT ( 'NONE',  ( 7.846153846153846700, -1.242168528481310874, 33.36296068462461051 ) ) ;
#62429 = EDGE_CURVE ( 'NONE', #82187, #59241, #61256, .T. ) ;
#62430 = CARTESIAN_POINT ( 'NONE',  ( 13.38461538461526601, -2.625532179533778709, 30.86335684631627174 ) ) ;
#62431 = CARTESIAN_POINT ( 'NONE',  ( 3.230769230769231726, -3.050289026998446396, 32.03036669348365706 ) ) ;
#62432 = CARTESIAN_POINT ( 'NONE',  ( 5.076923076923075762, -4.098570777380720287, 33.41473453929634729 ) ) ;
#62433 = DIRECTION ( 'NONE',  ( -0.000000000000000000, 0.1736481776669307198, -0.9848077530122080203 ) ) ;
#62434 = VECTOR ( 'NONE', #20055, 1000.000000000000000 ) ;
#62435 = ORIENTED_EDGE ( 'NONE', *, *, #50980, .F. ) ;
#62436 = ORIENTED_EDGE ( 'NONE', *, *, #84193, .T. ) ;
#62437 =( REPRESENTATION_RELATIONSHIP ('NONE','NONE', #51743, #60984 ) REPRESENTATION_RELATIONSHIP_WITH_TRANSFORMATION ( #60850 )SHAPE_REPRESENTATION_RELATIONSHIP( ) );
#62438 = CIRCLE ( 'NONE', #617, 5.000000000000000888 ) ;
#62439 = ORIENTED_EDGE ( 'NONE', *, *, #87629, .T. ) ;
#62440 = VECTOR ( 'NONE', #30575, 999.9999999999998863 ) ;
#62441 = LINE ( 'NONE', #14271, #35718 ) ;
#62442 = CARTESIAN_POINT ( 'NONE',  ( -4.088590582570128973, -3.300289026998475705, 32.46337939537591666 ) ) ;
#62443 = ADVANCED_FACE ( 'NONE', ( #39241 ), #38788, .F. ) ;
#62444 = CARTESIAN_POINT ( 'NONE',  ( -3.230769230769229949, -12.78798330534103123, 29.99999999999997868 ) ) ;
#62445 = CARTESIAN_POINT ( 'NONE',  ( 17.07692307692307665, -5.180354513474913603, 36.12317359536750416 ) ) ;
#62446 = ORIENTED_EDGE ( 'NONE', *, *, #67467, .F. ) ;
#62447 = CARTESIAN_POINT ( 'NONE',  ( 2.307692307692309264, -13.49023893513002648, 31.06009739812518688 ) ) ;
#62448 = VERTEX_POINT ( 'NONE', #11308 ) ;
#62449 = ADVANCED_FACE ( 'NONE', ( #5450 ), #32028, .F. ) ;
#62450 = ORIENTED_EDGE ( 'NONE', *, *, #52722, .T. ) ;
#62451 = EDGE_LOOP ( 'NONE', ( #37104, #70853, #68609, #61450 ) ) ;
#62453 = ORIENTED_EDGE ( 'NONE', *, *, #28301, .T. ) ;
#62452 = FACE_OUTER_BOUND ( 'NONE', #82069, .T. ) ;
#62454 = CARTESIAN_POINT ( 'NONE',  ( -3.230769230769351186, -2.625532179533779154, 30.86335684631627174 ) ) ;
#62455 = ADVANCED_FACE ( 'NONE', ( #19400 ), #74351, .F. ) ;
#62456 = CYLINDRICAL_SURFACE ( 'NONE', #65206, 0.2499999999999997502 ) ;
#62457 = ADVANCED_FACE ( 'NONE', ( #25270 ), #19843, .T. ) ;
#62458 = FACE_OUTER_BOUND ( 'NONE', #40429, .T. ) ;
#62459 = CARTESIAN_POINT ( 'NONE',  ( -4.826923076921640465, -7.500000000000155431, 34.75000000000007105 ) ) ;
#62460 = ORIENTED_EDGE ( 'NONE', *, *, #35714, .T. ) ;
#62461 = EDGE_LOOP ( 'NONE', ( #51959, #71619, #64506, #9872 ) ) ;
#62462 = EDGE_CURVE ( 'NONE', #62255, #36439, #5759, .T. ) ;
#62463 = AXIS2_PLACEMENT_3D ( 'NONE', #66731, #37470, #24846 ) ;
#62464 = VERTEX_POINT ( 'NONE', #40573 ) ;
#62465 = CARTESIAN_POINT ( 'NONE',  ( -1.384615384615383471, -12.78798330534103123, 29.99999999999997868 ) ) ;
#62467 = ORIENTED_EDGE ( 'NONE', *, *, #73094, .F. ) ;
#62466 = CARTESIAN_POINT ( 'NONE',  ( -10.39260494640654819, -2.612705202774698421, 31.66806509827799943 ) ) ;
#62468 = CARTESIAN_POINT ( 'NONE',  ( -2.241623956689867914, -8.120952969808772792, 34.71129190929999453 ) ) ;
#62469 = DIRECTION ( 'NONE',  ( 0.000000000000000000, 0.000000000000000000, -1.000000000000000000 ) ) ;
#62470 = VERTEX_POINT ( 'NONE', #88770 ) ;
#62471 = CARTESIAN_POINT ( 'NONE',  ( 20.00000000000000000, -4.000000000000000000, 29.75000000000000355 ) ) ;
#62472 = DIRECTION ( 'NONE',  ( -0.000000000000000000, 1.000000000000000000, -0.000000000000000000 ) ) ;
#62473 = B_SPLINE_CURVE_WITH_KNOTS ( 'NONE', 3,
 ( #69352, #16598, #9411, #7649, #35109, #62572, #55825, #10741, #72876, #11637 ),
 .UNSPECIFIED., .F., .F.,
 ( 4, 2, 2, 2, 4 ),
 ( 0.000000000000000000, 0.0001954311564186863323, 0.0003908623128373726646, 0.0005862934692560590241, 0.0007817246256747453293 ),
 .UNSPECIFIED. ) ;
#62474 = VERTEX_POINT ( 'NONE', #80220 ) ;
#62475 = FACE_BOUND ( 'NONE', #3279, .T. ) ;
#62476 = CARTESIAN_POINT ( 'NONE',  ( -18.00000000000012079, -8.613356846316285953, 34.62446782046622218 ) ) ;
#62477 = CARTESIAN_POINT ( 'NONE',  ( 13.60762822870878352, -6.460100341425560444, 34.89618726649961644 ) ) ;
#62478 = CARTESIAN_POINT ( 'NONE',  ( -4.500000000000000000, -7.499999999999999112, 13.50000000000000178 ) ) ;
#62480 = CARTESIAN_POINT ( 'NONE',  ( 4.946231610255516387, -9.804603061927743113, 34.18744698557895845 ) ) ;
#62479 = FACE_OUTER_BOUND ( 'NONE', #53846, .T. ) ;
#62481 = B_SPLINE_CURVE_WITH_KNOTS ( 'NONE', 3,
 ( #15128, #62402, #42163, #1160, #42601, #8369, #83143, #61084, #28642, #55215 ),
 .UNSPECIFIED., .F., .F.,
 ( 4, 2, 2, 2, 4 ),
 ( 0.000000000000000000, 0.0001954339857564088296, 0.0003908679715128176592, 0.0005863019572692264618, 0.0007817359430256353185 ),
 .UNSPECIFIED. ) ;
#62482 = DIRECTION ( 'NONE',  ( -0.000000000000000000, 0.9396926207859093161, -0.3420201433256663259 ) ) ;
#62483 = CARTESIAN_POINT ( 'NONE',  ( -2.531177251416255825, -3.754499324213721234, 33.06261337010820256 ) ) ;
#62484 = VERTEX_POINT ( 'NONE', #18519 ) ;
#62485 = CARTESIAN_POINT ( 'NONE',  ( 0.4615384615384611755, -1.951392089020283160, 34.73218667398347748 ) ) ;
#62486 = CARTESIAN_POINT ( 'NONE',  ( 13.13461538461538680, -7.500000000000001776, 34.75000000000000000 ) ) ;
#62487 = EDGE_CURVE ( 'NONE', #71584, #70102, #3509, .T. ) ;
#62488 = VERTEX_POINT ( 'NONE', #34692 ) ;
#62489 = DIRECTION ( 'NONE',  ( 0.000000000000000000, 0.4999999999999960032, -0.8660254037844410391 ) ) ;
#62490 = CARTESIAN_POINT ( 'NONE',  ( 5.076923076923075762, -13.78497067705608181, 32.30358669280327177 ) ) ;
#62491 = ORIENTED_EDGE ( 'NONE', *, *, #52784, .F. ) ;
#62492 = CARTESIAN_POINT ( 'NONE',  ( 10.61538461538461675, -13.53365097954675988, 30.81389545987213552 ) ) ;
#62493 = CARTESIAN_POINT ( 'NONE',  ( 2.557746727605762160, -4.818054556918156983, 34.26375889529406749 ) ) ;
#62494 = VECTOR ( 'NONE', #1342, 999.9999999999998863 ) ;
#62495 = FACE_BOUND ( 'NONE', #82609, .T. ) ;
#62497 = DIRECTION ( 'NONE',  ( -0.000000000000000000, 0.8660254037844397068, -0.4999999999999978906 ) ) ;
#62496 = DIRECTION ( 'NONE',  ( 0.000000000000000000, 0.1736481776669275834, 0.9848077530122086864 ) ) ;
#62498 = CARTESIAN_POINT ( 'NONE',  ( 11.53846153846153832, -13.20930481340135110, 34.54067556320372745 ) ) ;
#62499 = CARTESIAN_POINT ( 'NONE',  ( -15.36091644020745051, -9.418419913701741919, 34.36755862841477693 ) ) ;
#62500 = CARTESIAN_POINT ( 'NONE',  ( -15.16551365949320562, -6.879047030191282275, 34.71129190930002295 ) ) ;
#62501 = DIRECTION ( 'NONE',  ( 0.000000000000000000, 0.4999999999999960032, -0.8660254037844410391 ) ) ;
#62502 = CARTESIAN_POINT ( 'NONE',  ( -0.06109907496455085213, -3.750000000000000888, 15.15438170625848890 ) ) ;
#62503 = EDGE_LOOP ( 'NONE', ( #37076, #65274, #57680, #71983 ) ) ;
#62504 = VECTOR ( 'NONE', #20593, 1000.000000000000000 ) ;
#62505 = VERTEX_POINT ( 'NONE', #34240 ) ;
#62506 = VECTOR ( 'NONE', #39915, 1000.000000000000000 ) ;
#62507 = CARTESIAN_POINT ( 'NONE',  ( 6.923076923076924238, -1.129524287112498415, 32.06866353760679544 ) ) ;
#62508 = CARTESIAN_POINT ( 'NONE',  ( -17.07692307692307665, -3.513871655860378418, 32.76840700105978499 ) ) ;
#62509 = CARTESIAN_POINT ( 'NONE',  ( 14.53047197667037338, -9.418065098278013636, 34.63729479722530158 ) ) ;
#62510 = PLANE ( 'NONE',  #78353 ) ;
#62511 = CARTESIAN_POINT ( 'NONE',  ( -13.25382494364843389, -2.494656445102012565, 31.33466734024120015 ) ) ;
#62512 = CARTESIAN_POINT ( 'NONE',  ( 1.614399933863660985, -11.22469193450123193, 15.70125670625848890 ) ) ;
#62513 = DIRECTION ( 'NONE',  ( 0.000000000000000000, 1.000000000000000000, -8.673617379884028076E-17 ) ) ;
#62514 = CARTESIAN_POINT ( 'NONE',  ( 2.242442375918224151, -2.255955759149247619, 30.00000000000013856 ) ) ;
#62515 = LINE ( 'NONE', #55326, #21645 ) ;
#62516 = CARTESIAN_POINT ( 'NONE',  ( -4.946397638689432164, -2.372941743896878286, 30.88044141588254377 ) ) ;
#62517 = CARTESIAN_POINT ( 'NONE',  ( -15.16470087976679615, -11.16473453929635440, 33.15142922261926373 ) ) ;
#62518 = DIRECTION ( 'NONE',  ( 0.000000000000000000, 0.000000000000000000, 1.000000000000000000 ) ) ;
#62519 = CARTESIAN_POINT ( 'NONE',  ( 9.822833394071256663, -11.46989282347013095, 32.79007818306219946 ) ) ;
#62520 = CARTESIAN_POINT ( 'NONE',  ( -14.08491276642389423, -3.236590943229499029, 32.36255958852954251 ) ) ;
#62521 = EDGE_CURVE ( 'NONE', #72856, #13730, #17577, .T. ) ;
#62522 = B_SPLINE_CURVE_WITH_KNOTS ( 'NONE', 3,
 ( #39348, #46534, #12305, #66805, #60038, #32565, #39786, #41108, #87545, #47403 ),
 .UNSPECIFIED., .F., .F.,
 ( 4, 2, 2, 2, 4 ),
 ( 0.000000000000000000, 0.0001954339857564080165, 0.0003908679715128160329, 0.0005863019572692240765, 0.0007817359430256320659 ),
 .UNSPECIFIED. ) ;
#62523 = CARTESIAN_POINT ( 'NONE',  ( -13.38461538461550582, -3.835265460704628371, 33.15142922262033665 ) ) ;
#62524 = ORIENTED_EDGE ( 'NONE', *, *, #88551, .F. ) ;
#62525 = CYLINDRICAL_SURFACE ( 'NONE', #3899, 0.2499999999999995559 ) ;
#62526 = CARTESIAN_POINT ( 'NONE',  ( -17.07692307692307665, -6.681629849574314051, 35.83090037661290239 ) ) ;
#62527 = CARTESIAN_POINT ( 'NONE',  ( 1.077988221561497539, -10.27530806549875386, 22.45499329374151287 ) ) ;
#62528 = EDGE_CURVE ( 'NONE', #85539, #18924, #42345, .T. ) ;
#62529 = CARTESIAN_POINT ( 'NONE',  ( -5.750054590621955342, -12.45601412856602863, 31.48342859153981621 ) ) ;
#62530 = CARTESIAN_POINT ( 'NONE',  ( -18.00000000000000000, -10.51840700105979387, 33.73612834413961536 ) ) ;
#62531 = ORIENTED_EDGE ( 'NONE', *, *, #32903, .T. ) ;
#62532 = CARTESIAN_POINT ( 'NONE',  ( -16.15384615384584777, -2.506253911140615021, 30.00000000000323297 ) ) ;
#62534 = ORIENTED_EDGE ( 'NONE', *, *, #52134, .F. ) ;
#62533 = CARTESIAN_POINT ( 'NONE',  ( -1.384615384615505151, -4.481592998941358097, 33.73612834414048933 ) ) ;
#62535 = CARTESIAN_POINT ( 'NONE',  ( 9.692307692307695177, -12.62096338111211580, 30.90682066428153263 ) ) ;
#62536 = CARTESIAN_POINT ( 'NONE',  ( 12.68431813051652313, -5.827830569534417471, 34.72679350104403539 ) ) ;
#62537 = EDGE_CURVE ( 'NONE', #58896, #80991, #70025, .T. ) ;
#62538 = ORIENTED_EDGE ( 'NONE', *, *, #1322, .T. ) ;
#62539 = CARTESIAN_POINT ( 'NONE',  ( -39.05038313613820122, -12.75000000000000178, 29.75000000000000355 ) ) ;
#62540 = AXIS2_PLACEMENT_3D ( 'NONE', #31633, #87046, #86141 ) ;
#62541 = PLANE ( 'NONE',  #27028 ) ;
#62542 = ADVANCED_FACE ( 'NONE', ( #41008 ), #83327, .F. ) ;
#62543 = ORIENTED_EDGE ( 'NONE', *, *, #81392, .F. ) ;
#62544 = CARTESIAN_POINT ( 'NONE',  ( 23.49999999999998934, -5.499999999999981348, 27.25000000000000000 ) ) ;
#62545 = CARTESIAN_POINT ( 'NONE',  ( -15.48076923076922995, -7.500000000000001776, 35.00000000000000000 ) ) ;
#62546 = LINE ( 'NONE', #7625, #87358 ) ;
#62547 = ORIENTED_EDGE ( 'NONE', *, *, #42683, .T. ) ;
#62548 = ORIENTED_EDGE ( 'NONE', *, *, #67902, .F. ) ;
#62549 = EDGE_CURVE ( 'NONE', #39262, #25331, #61415, .T. ) ;
#62550 = CARTESIAN_POINT ( 'NONE',  ( -6.857821783564084228, -8.656820664281605460, 34.87096338111211224 ) ) ;
#62551 = ORIENTED_EDGE ( 'NONE', *, *, #6990, .F. ) ;
#62552 = CARTESIAN_POINT ( 'NONE',  ( 3.230769230769231726, -11.91647553114624181, 32.58852847137148245 ) ) ;
#62553 = CARTESIAN_POINT ( 'NONE',  ( 12.52760681254089725, -8.973038597847271092, 34.52809138561121216 ) ) ;
#62554 = CARTESIAN_POINT ( 'NONE',  ( 2.557637717070352146, -11.56426240980093567, 33.07394671870546432 ) ) ;
#62555 = CARTESIAN_POINT ( 'NONE',  ( -2.372962753653081958, -6.026961402152685388, 34.52809138561120506 ) ) ;
#62556 = CARTESIAN_POINT ( 'NONE',  ( 2.544871794871792936, -3.499999999999999556, 29.75000000000000355 ) ) ;
#62557 = CARTESIAN_POINT ( 'NONE',  ( 0.7115384615385238476, -7.434744860731433036, 35.00000000000000000 ) ) ;
#62558 = B_SPLINE_CURVE_WITH_KNOTS ( 'NONE', 3,
 ( #6778, #20738, #82011, #76575, #49545, #77020, #48205, #14423, #61713, #68479 ),
 .UNSPECIFIED., .F., .F.,
 ( 4, 2, 2, 2, 4 ),
 ( 0.0007817246256747530271, 0.0009771112852218978746, 0.001172497944769042939, 0.001367884604316188003, 0.001563271263863332851 ),
 .UNSPECIFIED. ) ;
#62559 = B_SPLINE_CURVE_WITH_KNOTS ( 'NONE', 3,
 ( #68054, #5906, #32478, #60393, #33382, #52745, #73924, #87911, #45990, #81129 ),
 .UNSPECIFIED., .F., .F.,
 ( 4, 2, 2, 2, 4 ),
 ( 0.0007817359430256294638, 0.0009771253907249937212, 0.001172514838424358087, 0.001367904286123722453, 0.001563293733823093758 ),
 .UNSPECIFIED. ) ;
#62560 = DIRECTION ( 'NONE',  ( -0.000000000000000000, 1.000000000000000000, 3.491481338843133355E-15 ) ) ;
#62561 = B_SPLINE_CURVE_WITH_KNOTS ( 'NONE', 3,
 ( #966, #70758, #64418, #77073, #69867, #15378, #36532, #35192, #28436, #15820 ),
 .UNSPECIFIED., .F., .F.,
 ( 4, 2, 2, 2, 4 ),
 ( 0.0007817359430256282712, 0.0009771253907249939381, 0.001172514838424359388, 0.001367904286123725055, 0.001563293733823090722 ),
 .UNSPECIFIED. ) ;
#62562 = B_SPLINE_CURVE_WITH_KNOTS ( 'NONE', 3,
 ( #74838, #75703, #83364, #35619, #14006, #41045, #68077, #41483, #41933, #6382 ),
 .UNSPECIFIED., .F., .F.,
 ( 4, 2, 2, 2, 4 ),
 ( 0.0007817359430256388964, 0.0009771253907250075990, 0.001172514838424376085, 0.001367904286123744571, 0.001563293733823113273 ),
 .UNSPECIFIED. ) ;
#62563 = VERTEX_POINT ( 'NONE', #6767 ) ;
#62564 = ORIENTED_EDGE ( 'NONE', *, *, #47035, .T. ) ;
#62566 = ORIENTED_EDGE ( 'NONE', *, *, #50493, .T. ) ;
#62565 = CARTESIAN_POINT ( 'NONE',  ( 9.562160482869472844, -4.460286881179643004, 33.72017969459903242 ) ) ;
#62567 = EDGE_CURVE ( 'NONE', #51593, #67601, #74348, .T. ) ;
#62568 = CARTESIAN_POINT ( 'NONE',  ( -18.25000000000000000, -7.500000000000001776, 35.00000000000000000 ) ) ;
#62569 = EDGE_LOOP ( 'NONE', ( #4102, #37727, #7862, #9689 ) ) ;
#62570 = EDGE_CURVE ( 'NONE', #69653, #30568, #24885, .T. ) ;
#62571 = CARTESIAN_POINT ( 'NONE',  ( -18.00000000000000000, -3.050289026998447284, 32.03036669348365706 ) ) ;
#62572 = CARTESIAN_POINT ( 'NONE',  ( -8.096177070375302876, -10.18141759479407327, 34.26406193332782379 ) ) ;
#62573 = AXIS2_PLACEMENT_3D ( 'NONE', #85956, #44060, #25588 ) ;
#62574 = EDGE_LOOP ( 'NONE', ( #77033, #64481 ) ) ;
#62575 = DIRECTION ( 'NONE',  ( -0.000000000000000000, -0.7660444431189791237, -0.6427876096865379196 ) ) ;
#62576 = EDGE_CURVE ( 'NONE', #58816, #50855, #41899, .T. ) ;
#62577 = ORIENTED_EDGE ( 'NONE', *, *, #88235, .T. ) ;
#62579 = EDGE_LOOP ( 'NONE', ( #1442, #2745, #89069, #47662 ) ) ;
#62578 = CARTESIAN_POINT ( 'NONE',  ( -16.37733109757010652, -3.754499324213721234, 33.06261337010820256 ) ) ;
#62580 = CARTESIAN_POINT ( 'NONE',  ( -10.86538461538461320, -7.433931650972299465, 34.75000000000000711 ) ) ;
#62581 = ORIENTED_EDGE ( 'NONE', *, *, #19900, .F. ) ;
#62582 = EDGE_CURVE ( 'NONE', #59899, #87868, #86166, .T. ) ;
#62583 = DIRECTION ( 'NONE',  ( -0.000000000000000000, 0.9396926207859092051, -0.3420201433256662704 ) ) ;
#62584 = CARTESIAN_POINT ( 'NONE',  ( 10.61538461538449596, -5.219633306517616589, 34.19971097300220464 ) ) ;
#62585 = FACE_BOUND ( 'NONE', #73474, .T. ) ;
#62586 = FACE_OUTER_BOUND ( 'NONE', #4367, .T. ) ;
#62587 = FACE_OUTER_BOUND ( 'NONE', #35027, .T. ) ;
#62588 = B_SPLINE_CURVE_WITH_KNOTS ( 'NONE', 3,
 ( #63831, #3892, #36369, #43994, #3453, #9772, #16527, #79124, #71914, #24166 ),
 .UNSPECIFIED., .F., .F.,
 ( 4, 2, 2, 2, 4 ),
 ( 0.0007817359430256282712, 0.0009771253907249941549, 0.001172514838424359822, 0.001367904286123725489, 0.001563293733823091372 ),
 .UNSPECIFIED. ) ;
#62589 = CARTESIAN_POINT ( 'NONE',  ( 15.48082365068268551, -2.544122305571458575, 31.48381861865057729 ) ) ;
#62590 = CARTESIAN_POINT ( 'NONE',  ( 0.5267314498331145955, -2.255955759149235629, 29.99999999999988631 ) ) ;
#62591 = CARTESIAN_POINT ( 'NONE',  ( -3.230769230769229949, -3.050289026998446396, 32.03036669348365706 ) ) ;
#62592 = CARTESIAN_POINT ( 'NONE',  ( 2.307692307692309264, -11.11383981884818262, 36.00935417666054406 ) ) ;
#62593 = EDGE_LOOP ( 'NONE', ( #10131, #8649, #16072, #60906, #68614, #4495, #57028 ) ) ;
#62594 = FACE_OUTER_BOUND ( 'NONE', #68473, .T. ) ;
#62595 = VERTEX_POINT ( 'NONE', #23947 ) ;
#62596 = ADVANCED_FACE ( 'NONE', ( #37468 ), #24844, .F. ) ;
#62597 = EDGE_LOOP ( 'NONE', ( #77114, #31635 ) ) ;
#62599 = CARTESIAN_POINT ( 'NONE',  ( 16.40390046548447245, -12.17597550085003633, 31.52189283813461884 ) ) ;
#62598 = CARTESIAN_POINT ( 'NONE',  ( -1.319360245102545015, -5.094484230520773593, 34.41647553114626845 ) ) ;
#62600 = EDGE_CURVE ( 'NONE', #67350, #9817, #15075, .T. ) ;
#62601 = CARTESIAN_POINT ( 'NONE',  ( -11.76138775597768671, -11.76352882383564769, 32.36236540154569497 ) ) ;
#62602 = CARTESIAN_POINT ( 'NONE',  ( -16.85391023282967993, -10.01129605718032423, 34.36064277460058491 ) ) ;
#62603 = CARTESIAN_POINT ( 'NONE',  ( 15.45354877203763877, -3.755027918224367767, 33.06320215134714857 ) ) ;
#62604 = LINE ( 'NONE', #77023, #73468 ) ;
#62605 = EDGE_CURVE ( 'NONE', #58964, #51776, #10899, .T. ) ;
#62606 = ORIENTED_EDGE ( 'NONE', *, *, #11437, .T. ) ;
#62607 = DIRECTION ( 'NONE',  ( -0.000000000000000000, -0.1736481776669307198, -0.9848077530122080203 ) ) ;
#62608 = CARTESIAN_POINT ( 'NONE',  ( 3.453780582382079967, -11.24521262558773671, 33.06293181088029343 ) ) ;
#62609 = CARTESIAN_POINT ( 'NONE',  ( -3.361459833879538728, -11.37499894934982514, 33.29245874905763003 ) ) ;
#62610 = DIRECTION ( 'NONE',  ( 1.000000000000000000, 2.559449574374560688E-16, -2.559449574374560589E-15 ) ) ;
#62611 = CARTESIAN_POINT ( 'NONE',  ( -10.61538461538473399, -6.026961402154118019, 34.52809138561165270 ) ) ;
#62612 = ORIENTED_EDGE ( 'NONE', *, *, #9339, .F. ) ;
#62613 = EDGE_CURVE ( 'NONE', #11687, #52584, #38086, .T. ) ;
#62614 = VERTEX_POINT ( 'NONE', #24396 ) ;
#62615 = EDGE_LOOP ( 'NONE', ( #16854, #12629 ) ) ;
#62616 = CARTESIAN_POINT ( 'NONE',  ( -6.923076923076922462, -8.120952969808772792, 34.71129190930000163 ) ) ;
#62617 = ORIENTED_EDGE ( 'NONE', *, *, #76165, .F. ) ;
#62618 = CARTESIAN_POINT ( 'NONE',  ( -9.692307692307691624, -9.905515769479276145, 34.41647553114623292 ) ) ;
#62619 = CARTESIAN_POINT ( 'NONE',  ( -17.07692307692307665, -3.050289026998446396, 32.03036669348365706 ) ) ;
#62620 = B_SPLINE_CURVE_WITH_KNOTS ( 'NONE', 3,
 ( #50228, #9274, #50676, #17353, #58776, #78601, #44808, #72287, #87609, #25889 ),
 .UNSPECIFIED., .F., .F.,
 ( 4, 2, 2, 2, 4 ),
 ( 0.0007817246256747489071, 0.0009771112852218922368, 0.001172497944769035350, 0.001367884604316178679, 0.001563271263863322009 ),
 .UNSPECIFIED. ) ;
#62621 = CARTESIAN_POINT ( 'NONE',  ( 18.00000000000000000, -8.973038597847269315, 34.52809138561121927 ) ) ;
#62622 = CARTESIAN_POINT ( 'NONE',  ( -2.057746789344164995, -5.057305518903949526, 34.11320923018887896 ) ) ;
#62623 = CARTESIAN_POINT ( 'NONE',  ( 14.55763782604044998, -4.336752205174649433, 33.62275283266504289 ) ) ;
#62624 = VERTEX_POINT ( 'NONE', #85670 ) ;
#62625 = CARTESIAN_POINT ( 'NONE',  ( 4.153846153846032507, -4.481592998941358097, 33.73612834414048933 ) ) ;
#62627 = VERTEX_POINT ( 'NONE', #4585 ) ;
#62626 = CARTESIAN_POINT ( 'NONE',  ( -0.6844654204453102242, -5.582147617184174848, 34.63737895849758530 ) ) ;
#62628 = CARTESIAN_POINT ( 'NONE',  ( -9.469296340694841163, -4.187068189119699468, 33.49521262558774026 ) ) ;
#62629 = DIRECTION ( 'NONE',  ( -0.000000000000000000, 0.9848077530122086864, -0.1736481776669273891 ) ) ;
#62630 = CARTESIAN_POINT ( 'NONE',  ( -17.14219307747939425, -12.16647553114622049, 32.15551576947930812 ) ) ;
#62631 = CARTESIAN_POINT ( 'NONE',  ( 6.249945409378045547, -9.357781135181031829, 34.66075350412533851 ) ) ;
#62632 = DIRECTION ( 'NONE',  ( -0.000000000000000000, 1.000000000000000000, -0.000000000000000000 ) ) ;
#62633 = CARTESIAN_POINT ( 'NONE',  ( -3.480792454990688789, -10.92453946501458439, 33.72985991061850086 ) ) ;
#62634 = LINE ( 'NONE', #49130, #14863 ) ;
#62635 = CARTESIAN_POINT ( 'NONE',  ( 3.724691934501251023, -9.114399933863618131, 13.54874329374151465 ) ) ;
#62636 = ORIENTED_EDGE ( 'NONE', *, *, #30057, .T. ) ;
#62637 = CARTESIAN_POINT ( 'NONE',  ( -4.946084746436313573, -7.277220318596959281, 34.99547417642776992 ) ) ;
#62638 = CARTESIAN_POINT ( 'NONE',  ( 12.68455130563185662, -4.762714258010881885, 34.23016756924214832 ) ) ;
#62639 = DIRECTION ( 'NONE',  ( -0.000000000000000000, -0.7660444431189791237, -0.6427876096865379196 ) ) ;
#62640 = FACE_OUTER_BOUND ( 'NONE', #53884, .T. ) ;
#62641 = ORIENTED_EDGE ( 'NONE', *, *, #31804, .T. ) ;
#62642 = DIRECTION ( 'NONE',  ( -0.000000000000000000, -0.5000000000000009992, -0.8660254037844380415 ) ) ;
#62643 = CARTESIAN_POINT ( 'NONE',  ( -16.09615384615384670, -4.000000000000000000, 29.75000000000000355 ) ) ;
#62644 = VECTOR ( 'NONE', #46210, 1000.000000000000000 ) ;
#62645 = CARTESIAN_POINT ( 'NONE',  ( -1.384615384615383471, -6.386643153685126251, 34.62446782046654192 ) ) ;
#62646 = CARTESIAN_POINT ( 'NONE',  ( 14.17700084102474989, -3.062553014421049546, 32.05460306192773601 ) ) ;
#62647 = EDGE_CURVE ( 'NONE', #71008, #41980, #1280, .T. ) ;
#62648 = ORIENTED_EDGE ( 'NONE', *, *, #34899, .F. ) ;
#62649 = CARTESIAN_POINT ( 'NONE',  ( -16.28399412357784826, -6.809168938359901446, 34.95455904226513866 ) ) ;
#62650 = LINE ( 'NONE', #2718, #87228 ) ;
#62651 = CARTESIAN_POINT ( 'NONE',  ( -2.307692307692305711, -5.471508081941601098, 34.59228464037088457 ) ) ;
#62652 = EDGE_LOOP ( 'NONE', ( #38322, #40609, #6847, #83139 ) ) ;
#62653 = EDGE_CURVE ( 'NONE', #55982, #5477, #51824, .T. ) ;
#62654 = FACE_OUTER_BOUND ( 'NONE', #6110, .T. ) ;
#62655 = B_SPLINE_CURVE_WITH_KNOTS ( 'NONE', 3,
 ( #68304, #12914, #80499, #74177, #46260, #66534, #6607, #54336, #60652, #73750 ),
 .UNSPECIFIED., .F., .F.,
 ( 4, 2, 2, 2, 4 ),
 ( 0.0007817246336856284103, 0.0009771112958940092897, 0.001172497958102390169, 0.001367884620310771265, 0.001563271282519152145 ),
 .UNSPECIFIED. ) ;
#62656 = ORIENTED_EDGE ( 'NONE', *, *, #62165, .T. ) ;
#62657 = DIRECTION ( 'NONE',  ( 1.000000000000000000, 0.000000000000000000, 0.000000000000000000 ) ) ;
#62658 = CARTESIAN_POINT ( 'NONE',  ( -10.86540785267758125, -2.823816976329319051, 31.52131813110795733 ) ) ;
#62659 = VECTOR ( 'NONE', #74491, 1000.000000000000000 ) ;
#62660 = ORIENTED_EDGE ( 'NONE', *, *, #13104, .F. ) ;
#62661 = FACE_OUTER_BOUND ( 'NONE', #28329, .T. ) ;
#62662 = CARTESIAN_POINT ( 'NONE',  ( 4.376858997939548246, -9.172514111537584114, 34.72667873470787470 ) ) ;
#62663 = CARTESIAN_POINT ( 'NONE',  ( -10.74607608205217346, -5.582088688514999397, 34.36776431015576350 ) ) ;
#62664 = VECTOR ( 'NONE', #31861, 1000.000000000000227 ) ;
#62665 = ADVANCED_FACE ( 'NONE', ( #17661 ), #59076, .F. ) ;
#62666 = DIRECTION ( 'NONE',  ( 0.000000000000000000, 0.1736481776669267785, -0.9848077530122087975 ) ) ;
#62667 = LINE ( 'NONE', #981, #19582 ) ;
#62668 = VERTEX_POINT ( 'NONE', #38820 ) ;
#62669 = EDGE_LOOP ( 'NONE', ( #6294, #13408 ) ) ;
#62670 = FACE_BOUND ( 'NONE', #20925, .T. ) ;
#62671 = ORIENTED_EDGE ( 'NONE', *, *, #31751, .F. ) ;
#62672 = CARTESIAN_POINT ( 'NONE',  ( -16.81410256410256565, -3.499999999999999556, 29.75000000000000355 ) ) ;
#62673 = EDGE_CURVE ( 'NONE', #74204, #61048, #50964, .T. ) ;
#62674 = CARTESIAN_POINT ( 'NONE',  ( 6.923076923077238654, -2.255955759149395501, 30.00000000000324363 ) ) ;
#62675 = EDGE_CURVE ( 'NONE', #66285, #65590, #59350, .T. ) ;
#62676 = DIRECTION ( 'NONE',  ( 0.000000000000000000, 0.000000000000000000, 1.000000000000000000 ) ) ;
#62677 = LINE ( 'NONE', #19487, #66675 ) ;
#62678 = EDGE_LOOP ( 'NONE', ( #55673, #15383, #66115, #76571, #20898, #47811, #76076, #68462, #41246, #72340, #31203, #7770, #47508, #40097, #26858, #73252, #15024, #56678, #53228, #16361, #47608, #13116, #16621, #4669, #8202, #33401, #25036, #21153, #76087, #85430, #50807, #64369, #69411, #18817, #59416, #35340, #10717, #77865, #69838, #8512, #63127, #1242, #77036, #52614, #82739, #41314, #50004, #33648, #30770, #25568, #30299, #74698, #75571, #29629, #33683, #13565, #7022, #45966, #33106, #43980, #52480, #8655, #65366, #65879, #8958, #72813, #82092, #24762, #38769, #61898, #69882, #13309, #75976, #67734, #85807, #73597, #45842, #84981, #25041, #18199, #17831, #9002, #77556, #70856, #38071, #17192, #65483, #39295, #81664, #4161, #73932, #74110, #16388, #56349, #77867, #75502, #8054, #84751, #24018, #46384, #52403, #42079, #76312, #86450, #78719, #16125, #68553, #41555, #7787, #7824, #49473, #75548, #24959, #64077, #48414, #47733, #30372, #71294, #52715, #70121, #68756, #40328, #63891, #41515, #69373, #37414, #8414 ) ) ;
#62679 = ORIENTED_EDGE ( 'NONE', *, *, #59980, .T. ) ;
#62680 = ORIENTED_EDGE ( 'NONE', *, *, #24545, .T. ) ;
#62681 = CARTESIAN_POINT ( 'NONE',  ( -0.3307466537136761753, -3.062576670634119758, 32.05464942895959979 ) ) ;
#62682 = ORIENTED_EDGE ( 'NONE', *, *, #31916, .F. ) ;
#62683 = EDGE_CURVE ( 'NONE', #10877, #87392, #87467, .T. ) ;
#62684 = CARTESIAN_POINT ( 'NONE',  ( 0.4615384615383382183, -10.33852847137269571, 34.16647553114546554 ) ) ;
#62685 = CARTESIAN_POINT ( 'NONE',  ( -6.923076923076607159, -2.255955759149395501, 30.00000000000324363 ) ) ;
#62686 = CARTESIAN_POINT ( 'NONE',  ( 13.51514082284902862, -11.66157788607254098, 32.95092075102925833 ) ) ;
#62687 = CARTESIAN_POINT ( 'NONE',  ( 8.992242120843618736, -9.086983370893049639, 34.49168942202179267 ) ) ;
#62688 = FACE_OUTER_BOUND ( 'NONE', #14573, .T. ) ;
#62689 = LINE ( 'NONE', #35691, #66762 ) ;
#62690 = CARTESIAN_POINT ( 'NONE',  ( 11.76124107972994359, -8.496831190052093419, 34.64984203495476578 ) ) ;
#62691 = ORIENTED_EDGE ( 'NONE', *, *, #29609, .F. ) ;
#62692 = AXIS2_PLACEMENT_3D ( 'NONE', #59272, #30904, #52067 ) ;
#62693 = ORIENTED_EDGE ( 'NONE', *, *, #75688, .T. ) ;
#62694 = EDGE_CURVE ( 'NONE', #23520, #58603, #5920, .T. ) ;
#62695 = ORIENTED_EDGE ( 'NONE', *, *, #11925, .F. ) ;
#62696 = CARTESIAN_POINT ( 'NONE',  ( -5.999999999999998224, -6.435427911321262684, 35.78748833219616898 ) ) ;
#62697 = UNCERTAINTY_MEASURE_WITH_UNIT (LENGTH_MEASURE( 1.000000000000000082E-05 ), #39608, 'distance_accuracy_value', 'NONE');
#62699 = CARTESIAN_POINT ( 'NONE',  ( -13.51476259405360203, -6.001485441113819874, 34.52039167877662607 ) ) ;
#62698 = CARTESIAN_POINT ( 'NONE',  ( -11.25641025641025550, -7.500000000000000000, 29.75000000000000355 ) ) ;
#62700 = CARTESIAN_POINT ( 'NONE',  ( -17.93474486048716088, -5.941354392334603496, 34.76329471203374055 ) ) ;
#62701 = CARTESIAN_POINT ( 'NONE',  ( -6.792551221313355647, -3.816742781228458448, 33.13167719472716044 ) ) ;
#62702 = EDGE_CURVE ( 'NONE', #2541, #41728, #37807, .T. ) ;
#62703 = DIRECTION ( 'NONE',  ( 0.000000000000000000, 0.000000000000000000, -1.000000000000000000 ) ) ;
#62704 = CARTESIAN_POINT ( 'NONE',  ( 9.692307692307695177, -3.513871655860378418, 32.76840700105978499 ) ) ;
#62705 = ADVANCED_FACE ( 'NONE', ( #52760 ), #53657, .F. ) ;
#62706 = ORIENTED_EDGE ( 'NONE', *, *, #74069, .F. ) ;
#62707 = CARTESIAN_POINT ( 'NONE',  ( 17.32686848630112308, -12.07971442181321997, 32.31769673815850297 ) ) ;
#62708 = CARTESIAN_POINT ( 'NONE',  ( -0.4615384615384611200, -8.973038597847269315, 34.52809138561121927 ) ) ;
#62709 = DIRECTION ( 'NONE',  ( -0.000000000000000000, 0.8660254037844399289, -0.4999999999999980016 ) ) ;
#62710 = CARTESIAN_POINT ( 'NONE',  ( 6.923076923076924238, -9.058645607665452459, 34.76329471203371924 ) ) ;
#62711 = VERTEX_POINT ( 'NONE', #87026 ) ;
#62712 = CYLINDRICAL_SURFACE ( 'NONE', #2525, 0.2499999999999986955 ) ;
#62713 = VERTEX_POINT ( 'NONE', #39273 ) ;
#62714 = FACE_BOUND ( 'NONE', #11174, .T. ) ;
#62715 = CARTESIAN_POINT ( 'NONE',  ( -15.90384615384615330, -2.499999999999998668, 29.75000000000000355 ) ) ;
#62716 = VECTOR ( 'NONE', #23105, 1000.000000000000000 ) ;
#62717 = CARTESIAN_POINT ( 'NONE',  ( 4.219913487196228274, -2.486705287966279876, 31.30864560766543647 ) ) ;
#62718 = CARTESIAN_POINT ( 'NONE',  ( -7.053553631193387297, -7.276988635370452485, 34.74523720219453793 ) ) ;
#62719 = EDGE_LOOP ( 'NONE', ( #15323, #86282, #67842, #5287 ) ) ;
#62720 = CARTESIAN_POINT ( 'NONE',  ( -12.59168567097668401, -10.19110544564092002, 33.96427741523702792 ) ) ;
#62721 = CARTESIAN_POINT ( 'NONE',  ( -3.480792454990687013, -2.341070481393819236, 30.72580821765574299 ) ) ;
#62722 = DIRECTION ( 'NONE',  ( -1.000000000000000000, -0.000000000000000000, -0.000000000000000000 ) ) ;
#62723 = DIRECTION ( 'NONE',  ( 0.000000000000000000, 0.6427876096865373645, -0.7660444431189797898 ) ) ;
#62724 = ORIENTED_EDGE ( 'NONE', *, *, #18276, .F. ) ;
#62725 = B_SPLINE_CURVE_WITH_KNOTS ( 'NONE', 3,
 ( #11886, #88014, #26274, #19078, #61371, #88883, #68150, #5562, #80345, #46104 ),
 .UNSPECIFIED., .F., .F.,
 ( 4, 2, 2, 2, 4 ),
 ( 0.000000000000000000, 0.0001954339881912783286, 0.0003908679763825566571, 0.0005863019645738349857, 0.0007817359527651133143 ),
 .UNSPECIFIED. ) ;
#62726 = AXIS2_PLACEMENT_3D ( 'NONE', #55136, #88508, #61442 ) ;
#62727 = CARTESIAN_POINT ( 'NONE',  ( 12.71153846153847766, -2.249999999999999112, 29.81603969181029967 ) ) ;
#62728 = EDGE_LOOP ( 'NONE', ( #31148, #89132, #71027, #2855, #32095 ) ) ;
#62729 = B_SPLINE_CURVE_WITH_KNOTS ( 'NONE', 3,
 ( #18387, #46743, #31449, #79645, #45848, #4882, #73329, #32344, #59811, #12517 ),
 .UNSPECIFIED., .F., .F.,
 ( 4, 2, 2, 2, 4 ),
 ( 0.000000000000000000, 0.0001954311564186874978, 0.0003908623128373749957, 0.0005862934692560624935, 0.0007817246256747499913 ),
 .UNSPECIFIED. ) ;
#62731 = ORIENTED_EDGE ( 'NONE', *, *, #20149, .F. ) ;
#62730 = CARTESIAN_POINT ( 'NONE',  ( 4.219101293358991533, -3.083524468853784839, 32.58852847137153930 ) ) ;
#62732 = CARTESIAN_POINT ( 'NONE',  ( 17.32692307692449418, -7.500000000000154543, 35.00000000000007105 ) ) ;
#62733 = CARTESIAN_POINT ( 'NONE',  ( -4.283993363284368527, -2.882441371585227063, 31.66841991370171527 ) ) ;
#62734 = CARTESIAN_POINT ( 'NONE',  ( -18.00000000000000000, -12.75000000000000711, 29.49999999999997868 ) ) ;
#62735 = DIRECTION ( 'NONE',  ( 1.000000000000000000, 0.000000000000000000, 0.000000000000000000 ) ) ;
#62736 = CARTESIAN_POINT ( 'NONE',  ( 15.23076923076923173, -5.471508081941601098, 34.59228464037088457 ) ) ;
#62738 = CARTESIAN_POINT ( 'NONE',  ( 16.40379167219429490, -5.852078868378311149, 34.47109172314383585 ) ) ;
#62737 = CARTESIAN_POINT ( 'NONE',  ( -5.777220331021931443, -6.717445702608402236, 34.94155399931962336 ) ) ;
#62739 = CARTESIAN_POINT ( 'NONE',  ( -18.00000000000000000, -12.50000000000000000, 29.74999999999997868 ) ) ;
#62740 = CARTESIAN_POINT ( 'NONE',  ( -2.750000000000007105, -6.360912703474006946, 22.67187500000000355 ) ) ;
#62741 = VERTEX_POINT ( 'NONE', #73497 ) ;
#62742 = CARTESIAN_POINT ( 'NONE',  ( -17.86920819217521483, -8.999086150933472084, 34.52020707165672064 ) ) ;
#62743 = ORIENTED_EDGE ( 'NONE', *, *, #70715, .T. ) ;
#62744 = ORIENTED_EDGE ( 'NONE', *, *, #69652, .T. ) ;
#62745 = DIRECTION ( 'NONE',  ( 0.000000000000000000, 1.000000000000000000, 0.000000000000000000 ) ) ;
#62746 = VERTEX_POINT ( 'NONE', #5482 ) ;
#62747 = CARTESIAN_POINT ( 'NONE',  ( -5.934744860487158213, -12.70778746994558439, 30.41441678777537305 ) ) ;
#62748 = CARTESIAN_POINT ( 'NONE',  ( -7.846153846153967493, -8.656820664282941280, 34.87096338111179961 ) ) ;
#62749 = CARTESIAN_POINT ( 'NONE',  ( 6.250054311638314708, -3.136992222400443175, 32.19305428654138979 ) ) ;
#62750 = DIRECTION ( 'NONE',  ( -0.000000000000000000, -0.7660444431189791237, -0.6427876096865379196 ) ) ;
#62751 = CARTESIAN_POINT ( 'NONE',  ( 6.223011351612851350, -2.554770724473668153, 30.48948780036025852 ) ) ;
#62752 = CARTESIAN_POINT ( 'NONE',  ( 8.638539302563209787, -11.18331474514187995, 33.13161551792790505 ) ) ;
#62753 = CARTESIAN_POINT ( 'NONE',  ( 16.08776274289027697, -11.69971097300155272, 32.46337939537587403 ) ) ;
#62754 = CARTESIAN_POINT ( 'NONE',  ( 6.856994543716784740, -12.34228464037088280, 31.77849191805838558 ) ) ;
#62755 = VECTOR ( 'NONE', #43378, 1000.000000000000227 ) ;
#62756 = DIRECTION ( 'NONE',  ( -0.000000000000000000, -0.1736481776669307198, -0.9848077530122080203 ) ) ;
#62757 = CARTESIAN_POINT ( 'NONE',  ( -2.057637887778853258, -2.920487667080175154, 32.31805714834170828 ) ) ;
#62758 = CARTESIAN_POINT ( 'NONE',  ( 6.000000000000001776, -11.35647404775217417, 33.31231777344666511 ) ) ;
#62759 = CARTESIAN_POINT ( 'NONE',  ( 11.78840705680968171, -5.057305518903948638, 34.11320923018887896 ) ) ;
#62760 = ORIENTED_EDGE ( 'NONE', *, *, #64924, .F. ) ;
#62761 = ORIENTED_EDGE ( 'NONE', *, *, #19951, .F. ) ;
#62762 = DIRECTION ( 'NONE',  ( -0.000000000000000000, -0.1736481776669307198, -0.9848077530122080203 ) ) ;
#62763 = CARTESIAN_POINT ( 'NONE',  ( 0.000000000000000000, 0.000000000000000000, 0.000000000000000000 ) ) ;
#62764 = CARTESIAN_POINT ( 'NONE',  ( -3.007757879156382153, -2.758310577978208666, 31.33698337089302299 ) ) ;
#62765 = DIRECTION ( 'NONE',  ( -0.000000000000000000, -0.6427876096865404731, -0.7660444431189771253 ) ) ;
#62766 = EDGE_LOOP ( 'NONE', ( #1154, #57376 ) ) ;
#62767 = VECTOR ( 'NONE', #48028, 1000.000000000000000 ) ;
#62768 = CARTESIAN_POINT ( 'NONE',  ( -4.153846153846273204, -6.879047030192662504, 34.71129190930017927 ) ) ;
#62769 = CARTESIAN_POINT ( 'NONE',  ( -9.626240358957616650, -10.67929555188718282, 33.92786785259544757 ) ) ;
#62770 = DIRECTION ( 'NONE',  ( -0.000000000000000000, -0.5000000000000009992, -0.8660254037844380415 ) ) ;
#62771 = ORIENTED_EDGE ( 'NONE', *, *, #79541, .T. ) ;
#62772 = CARTESIAN_POINT ( 'NONE',  ( -14.55771553191376277, -12.68155406624981119, 30.59749803192733708 ) ) ;
#62773 = EDGE_LOOP ( 'NONE', ( #53946, #3138, #4996, #84863 ) ) ;
#62774 = CARTESIAN_POINT ( 'NONE',  ( 16.15384615384615330, -9.058645607665452459, 34.76329471203371924 ) ) ;
#62775 = ADVANCED_FACE ( 'NONE', ( #81145 ), #19430, .T. ) ;
#62776 = CARTESIAN_POINT ( 'NONE',  ( 4.284684484332913712, -7.277220318596959281, 34.99547417642776992 ) ) ;
#62777 = VECTOR ( 'NONE', #87844, 1000.000000000000000 ) ;
#62778 = LINE ( 'NONE', #28578, #8531 ) ;
#62779 = CARTESIAN_POINT ( 'NONE',  ( 27.00000000000000000, 0.7500000000000052180, 31.75000000000000000 ) ) ;
#62780 = CARTESIAN_POINT ( 'NONE',  ( -6.857821783564084228, -2.657715359629131857, 31.77849191805844242 ) ) ;
#62781 = ORIENTED_EDGE ( 'NONE', *, *, #26914, .F. ) ;
#62782 = ORIENTED_EDGE ( 'NONE', *, *, #86108, .T. ) ;
#62783 = VERTEX_POINT ( 'NONE', #81583 ) ;
#62784 = ORIENTED_EDGE ( 'NONE', *, *, #1993, .T. ) ;
#62785 = ADVANCED_FACE ( 'NONE', ( #41036 ), #47336, .F. ) ;
#62786 = CARTESIAN_POINT ( 'NONE',  ( -5.999999999999998224, -11.16473453929635440, 33.15142922261926373 ) ) ;
#62787 = CYLINDRICAL_SURFACE ( 'NONE', #70446, 0.2499999999999995837 ) ;
#62788 = CARTESIAN_POINT ( 'NONE',  ( -12.23875879256039667, -12.47679350104403007, 31.42216943046555855 ) ) ;
#62789 = CARTESIAN_POINT ( 'NONE',  ( -16.15384615384627409, -11.67786785259630911, 32.92929555188603530 ) ) ;
#62790 = CARTESIAN_POINT ( 'NONE',  ( 16.15384615384615330, -2.900454961884010974, 35.62045528018868623 ) ) ;
#62791 = CARTESIAN_POINT ( 'NONE',  ( 14.55774661933062575, -9.943054286541403997, 34.11300777759954883 ) ) ;
#62792 = ORIENTED_EDGE ( 'NONE', *, *, #40514, .F. ) ;
#62793 = ORIENTED_EDGE ( 'NONE', *, *, #20541, .T. ) ;
#62794 = ORIENTED_EDGE ( 'NONE', *, *, #88523, .F. ) ;
#62796 = ORIENTED_EDGE ( 'NONE', *, *, #75872, .F. ) ;
#62795 = DIRECTION ( 'NONE',  ( -0.000000000000000000, 0.7660444431189791237, -0.6427876096865379196 ) ) ;
#62798 = CARTESIAN_POINT ( 'NONE',  ( 13.60762822870878530, -4.026326845037962343, 33.68677907613344047 ) ) ;
#62797 = CARTESIAN_POINT ( 'NONE',  ( 16.37685750545900376, -8.239487800360276282, 34.69522927552633718 ) ) ;
#62799 = CARTESIAN_POINT ( 'NONE',  ( 9.627037246346919375, -2.625532179533445198, 30.86335684631481513 ) ) ;
#62800 = EDGE_CURVE ( 'NONE', #30672, #14427, #18515, .T. ) ;
#62801 = CARTESIAN_POINT ( 'NONE',  ( 13.51540719244017374, -8.147973898785416225, 34.70805048591653730 ) ) ;
#62802 = EDGE_CURVE ( 'NONE', #81013, #46051, #60856, .T. ) ;
#62803 = ORIENTED_EDGE ( 'NONE', *, *, #17005, .T. ) ;
#62804 = ORIENTED_EDGE ( 'NONE', *, *, #87452, .F. ) ;
#62806 = B_SPLINE_CURVE_WITH_KNOTS ( 'NONE', 3,
 ( #58528, #4031, #85578, #17568, #50877, #79714, #23853, #72949, #72053, #24303 ),
 .UNSPECIFIED., .F., .F.,
 ( 4, 2, 2, 2, 4 ),
 ( 0.000000000000000000, 0.0001954311564186858986, 0.0003908623128373717973, 0.0005862934692560577230, 0.0007817246256747435946 ),
 .UNSPECIFIED. ) ;
#62805 = CARTESIAN_POINT ( 'NONE',  ( 3.903869409797561474, -4.075325502946086864, 33.72974371597207721 ) ) ;
#62807 = AXIS2_PLACEMENT_3D ( 'NONE', #15273, #35993, #75631 ) ;
#62808 = EDGE_LOOP ( 'NONE', ( #73143, #5517, #47963, #80201 ) ) ;
#62809 = FACE_BOUND ( 'NONE', #81095, .T. ) ;
#62810 = CARTESIAN_POINT ( 'NONE',  ( 4.826899852701619587, -4.931416488878822335, 34.32920672191015399 ) ) ;
#62811 = ADVANCED_FACE ( 'NONE', ( #26632 ), #40599, .F. ) ;
#62812 = DIRECTION ( 'NONE',  ( 0.000000000000000000, 1.000000000000000000, -8.673617379884028076E-17 ) ) ;
#62813 = EDGE_LOOP ( 'NONE', ( #79548, #58372 ) ) ;
#62814 = CARTESIAN_POINT ( 'NONE',  ( -4.403846153846163070, -2.499999999999999556, 29.81609845454692120 ) ) ;
#62815 = FACE_OUTER_BOUND ( 'NONE', #55377, .T. ) ;
#62816 = DIRECTION ( 'NONE',  ( 1.000000000000000000, 0.000000000000000000, 0.000000000000000000 ) ) ;
#62817 = DIRECTION ( 'NONE',  ( 0.000000000000000000, 0.9396926207859126468, -0.3420201433256571111 ) ) ;
#62818 = CARTESIAN_POINT ( 'NONE',  ( -17.01085472592063397, -2.538708090699994813, 30.37095296980875503 ) ) ;
#62819 = ORIENTED_EDGE ( 'NONE', *, *, #44983, .F. ) ;
#62820 = CARTESIAN_POINT ( 'NONE',  ( 5.999999999999880096, -8.613356846316285953, 34.62446782046622218 ) ) ;
#62821 = CARTESIAN_POINT ( 'NONE',  ( 3.230769230769110045, -4.481592998941358097, 33.73612834414048933 ) ) ;
#62822 = FACE_OUTER_BOUND ( 'NONE', #39676, .T. ) ;
#62823 = LINE ( 'NONE', #21857, #8402 ) ;
#62824 = CARTESIAN_POINT ( 'NONE',  ( -15.16551365949320562, -11.94971097300157403, 32.03036669348361443 ) ) ;
#62825 = FACE_BOUND ( 'NONE', #10763, .T. ) ;
#62827 = CARTESIAN_POINT ( 'NONE',  ( -3.512820512820514995, -3.499999999999999556, 29.75000000000000355 ) ) ;
#62826 = CARTESIAN_POINT ( 'NONE',  ( 5.010839665967195877, -11.16473453929635440, 33.15142922261925662 ) ) ;
#62828 = CARTESIAN_POINT ( 'NONE',  ( 11.66898697669518548, -12.15418822224088657, 32.17964115625579069 ) ) ;
#62830 = CARTESIAN_POINT ( 'NONE',  ( -18.25002322422145085, -2.985938066672159330, 32.43141759479405550 ) ) ;
#62829 = CARTESIAN_POINT ( 'NONE',  ( -11.53846153846165912, -11.48612834414049644, 32.76840700105863391 ) ) ;
#62831 = CARTESIAN_POINT ( 'NONE',  ( -39.05038313613820122, -2.249999999999998668, 29.75000000000000355 ) ) ;
#62832 = CARTESIAN_POINT ( 'NONE',  ( -1.200186371490556958, -4.775308065498765409, 22.57625670625848713 ) ) ;
#62833 = ORIENTED_EDGE ( 'NONE', *, *, #46126, .T. ) ;
#62834 = B_SPLINE_CURVE_WITH_KNOTS ( 'NONE', 3,
 ( #17780, #45234, #23630, #85344, #65946, #86701, #51081, #36707, #2463, #24967 ),
 .UNSPECIFIED., .F., .F.,
 ( 4, 2, 2, 2, 4 ),
 ( 0.000000000000000000, 0.0001954339857564080707, 0.0003908679715128161414, 0.0005863019572692241849, 0.0007817359430256322827 ),
 .UNSPECIFIED. ) ;
#62835 = LINE ( 'NONE', #55646, #69193 ) ;
#62836 = ORIENTED_EDGE ( 'NONE', *, *, #15271, .F. ) ;
#62837 = LINE ( 'NONE', #62399, #17625 ) ;
#62838 = AXIS2_PLACEMENT_3D ( 'NONE', #60011, #65436, #45607 ) ;
#62839 = ORIENTED_EDGE ( 'NONE', *, *, #26025, .T. ) ;
#62840 = CARTESIAN_POINT ( 'NONE',  ( -11.31568199719312418, -2.847695495035523550, 31.58253572463339154 ) ) ;
#62841 = FACE_OUTER_BOUND ( 'NONE', #24688, .T. ) ;
#62842 = ORIENTED_EDGE ( 'NONE', *, *, #55866, .T. ) ;
#62843 = CARTESIAN_POINT ( 'NONE',  ( -9.442307692307755573, -7.565270445406050648, 34.75000000000000000 ) ) ;
#62844 = CARTESIAN_POINT ( 'NONE',  ( -1.200186371490556958, -4.775308065498765409, 16.32625670625849068 ) ) ;
#62845 = LINE ( 'NONE', #76379, #47481 ) ;
#62846 = CARTESIAN_POINT ( 'NONE',  ( 16.15384615384603251, -8.656820664282941280, 34.87096338111179961 ) ) ;
#62847 = AXIS2_PLACEMENT_3D ( 'NONE', #70396, #35728, #62289 ) ;
#62848 = CARTESIAN_POINT ( 'NONE',  ( 10.61538461538461675, -13.37000171582298513, 34.34916445242398453 ) ) ;
#62849 = CARTESIAN_POINT ( 'NONE',  ( 11.28843830116857383, -2.823816976329317274, 31.52131813110795733 ) ) ;
#62850 = LINE ( 'NONE', #69627, #2223 ) ;
#62851 = CARTESIAN_POINT ( 'NONE',  ( 14.30769230769231015, -1.242168528481310874, 33.36296068462461051 ) ) ;
#62852 = CARTESIAN_POINT ( 'NONE',  ( 2.694853999681185108, -4.891553140782077591, 24.56436829374151287 ) ) ;
#62853 = CARTESIAN_POINT ( 'NONE',  ( -15.23076923076922995, -11.35647404775217417, 33.31231777344666511 ) ) ;
#62854 = CARTESIAN_POINT ( 'NONE',  ( 10.86543892702293057, -11.28795663066794575, 33.01431243580653785 ) ) ;
#62855 = VECTOR ( 'NONE', #80502, 1000.000000000000000 ) ;
#62856 = B_SPLINE_CURVE_WITH_KNOTS ( 'NONE', 3,
 ( #5183, #32651, #87618, #52024, #66441, #6076, #25003, #61009, #19581, #25454 ),
 .UNSPECIFIED., .F., .F.,
 ( 4, 2, 2, 2, 4 ),
 ( 0.0007817359430256328248, 0.0009771253907249997928, 0.001172514838424366544, 0.001367904286123733295, 0.001563293733823100263 ),
 .UNSPECIFIED. ) ;
#62857 = CARTESIAN_POINT ( 'NONE',  ( -13.38461538461550759, -12.70778746994576025, 30.41441678777401236 ) ) ;
#62858 = B_SPLINE_CURVE_WITH_KNOTS ( 'NONE', 3,
 ( #65044, #3354, #51979, #65502, #30826, #72704, #11014, #59637, #79475, #16872 ),
 .UNSPECIFIED., .F., .F.,
 ( 4, 2, 2, 2, 4 ),
 ( 0.000000000000000000, 0.0001954339857564097512, 0.0003908679715128195024, 0.0005863019572692292807, 0.0007817359430256390048 ),
 .UNSPECIFIED. ) ;
#62859 = CARTESIAN_POINT ( 'NONE',  ( 1.614399933863618797, -3.775308065498751198, 23.23624329374151642 ) ) ;
#62860 = CARTESIAN_POINT ( 'NONE',  ( 5.999999999999880096, -4.481592998941358097, 33.73612834414048933 ) ) ;
#62861 = CARTESIAN_POINT ( 'NONE',  ( -15.84615384615384670, -3.499999999999999556, 29.75000000000000355 ) ) ;
#62862 = ORIENTED_EDGE ( 'NONE', *, *, #11789, .F. ) ;
#62863 = CARTESIAN_POINT ( 'NONE',  ( 6.673076923076925127, -7.566083408709834757, 34.74999999999999289 ) ) ;
#62864 = CARTESIAN_POINT ( 'NONE',  ( 1.134615384615387246, -7.500000000000001776, 35.00000000000000000 ) ) ;
#62865 = CARTESIAN_POINT ( 'NONE',  ( -16.82692307692164135, -7.500000000000155431, 34.75000000000007105 ) ) ;
#62866 = CARTESIAN_POINT ( 'NONE',  ( -14.55771554498526932, -11.86270091957321249, 32.19358267280087915 ) ) ;
#62867 = CARTESIAN_POINT ( 'NONE',  ( 9.692307692307570832, -12.16647553114689728, 32.15551576947799362 ) ) ;
#62868 = ADVANCED_FACE ( 'NONE', ( #54090 ), #67179, .F. ) ;
#62869 = LINE ( 'NONE', #68764, #64428 ) ;
#62870 = DIRECTION ( 'NONE',  ( 1.000000000000000000, 0.000000000000000000, 0.000000000000000000 ) ) ;
#62871 = CYLINDRICAL_SURFACE ( 'NONE', #37965, 0.2499999999999997502 ) ;
#62872 = VECTOR ( 'NONE', #48647, 1000.000000000000227 ) ;
#62873 = ORIENTED_EDGE ( 'NONE', *, *, #82463, .F. ) ;
#62874 = ORIENTED_EDGE ( 'NONE', *, *, #1948, .T. ) ;
#62875 = VECTOR ( 'NONE', #30622, 1000.000000000000000 ) ;
#62876 = ORIENTED_EDGE ( 'NONE', *, *, #27684, .F. ) ;
#62877 = ADVANCED_FACE ( 'NONE', ( #32949 ), #8138, .F. ) ;
#62878 = CARTESIAN_POINT ( 'NONE',  ( -16.40386937806761125, -3.520140089381496473, 33.17453946501458262 ) ) ;
#62879 = CARTESIAN_POINT ( 'NONE',  ( -4.153846153846152411, -3.050289026998446396, 32.03036669348365706 ) ) ;
#62880 = ADVANCED_FACE ( 'NONE', ( #76593 ), #27517, .F. ) ;
#62881 = CARTESIAN_POINT ( 'NONE',  ( 2.177000841024750333, -5.582088688514999397, 34.36776431015576350 ) ) ;
#62882 = DIRECTION ( 'NONE',  ( 1.000000000000000000, 0.000000000000000000, 0.000000000000000000 ) ) ;
#62883 = B_SPLINE_CURVE_WITH_KNOTS ( 'NONE', 3,
 ( #3977, #39126, #85086, #4895, #16609, #50824, #23366, #51253, #44072, #31008 ),
 .UNSPECIFIED., .F., .F.,
 ( 4, 2, 2, 2, 4 ),
 ( 0.0007817246256747473893, 0.0009771112852218909357, 0.001172497944769034482, 0.001367884604316178246, 0.001563271263863321792 ),
 .UNSPECIFIED. ) ;
#62884 = ORIENTED_EDGE ( 'NONE', *, *, #8086, .T. ) ;
#62885 = CARTESIAN_POINT ( 'NONE',  ( 17.29970274590113632, -11.60474049983370648, 33.02348890104160262 ) ) ;
#62886 = ORIENTED_EDGE ( 'NONE', *, *, #85621, .T. ) ;
#62887 = B_SPLINE_CURVE_WITH_KNOTS ( 'NONE', 3,
 ( #39456, #65562, #66912, #53388, #5207, #17842, #38552, #37653, #52050, #65113 ),
 .UNSPECIFIED., .F., .F.,
 ( 4, 2, 2, 2, 4 ),
 ( 0.0007817246256747453293, 0.0009771112852218889842, 0.001172497944769032531, 0.001367884604316176294, 0.001563271263863319840 ),
 .UNSPECIFIED. ) ;
#62888 = VERTEX_POINT ( 'NONE', #22091 ) ;
#62890 = ORIENTED_EDGE ( 'NONE', *, *, #66072, .T. ) ;
#62889 = EDGE_CURVE ( 'NONE', #60384, #22892, #4471, .T. ) ;
#62892 = ORIENTED_EDGE ( 'NONE', *, *, #37619, .T. ) ;
#62891 = CARTESIAN_POINT ( 'NONE',  ( 13.31853300525525086, -4.661471528628507777, 34.16647553114621871 ) ) ;
#62893 = LINE ( 'NONE', #7084, #15732 ) ;
#62894 = CARTESIAN_POINT ( 'NONE',  ( 6.066067333350076751, -2.486705287966279876, 31.30864560766543647 ) ) ;
#62895 = ADVANCED_FACE ( 'NONE', ( #63058 ), #15338, .F. ) ;
#62896 = AXIS2_PLACEMENT_3D ( 'NONE', #28363, #13525, #88768 ) ;
#62897 = CARTESIAN_POINT ( 'NONE',  ( -9.822999158975251888, -8.147922237126337563, 34.70805685702651999 ) ) ;
#62898 = CARTESIAN_POINT ( 'NONE',  ( 10.61538461538461675, -13.20930481340135110, 34.54067556320372745 ) ) ;
#62899 = ORIENTED_EDGE ( 'NONE', *, *, #85997, .F. ) ;
#62900 = VERTEX_POINT ( 'NONE', #56754 ) ;
#62901 = ORIENTED_EDGE ( 'NONE', *, *, #76854, .F. ) ;
#62902 = CARTESIAN_POINT ( 'NONE',  ( -14.55769230769230305, -7.566083408709835645, 34.74999999999999289 ) ) ;
#62904 = ORIENTED_EDGE ( 'NONE', *, *, #3108, .T. ) ;
#62903 = CARTESIAN_POINT ( 'NONE',  ( 11.60371667797437567, -5.941354392334607049, 34.76329471203374055 ) ) ;
#62905 = CARTESIAN_POINT ( 'NONE',  ( -6.988347369037698265, -12.46129190929999986, 30.37095296980880832 ) ) ;
#62906 = CARTESIAN_POINT ( 'NONE',  ( -11.28851612908349722, -12.68172785388650681, 30.59649109432439218 ) ) ;
#62907 = CARTESIAN_POINT ( 'NONE',  ( 7.145856464345331283, -11.89424750095246175, 32.13594075562311758 ) ) ;
#62908 = ADVANCED_FACE ( 'NONE', ( #34270 ), #82913, .F. ) ;
#62909 = VERTEX_POINT ( 'NONE', #63508 ) ;
#62910 = EDGE_CURVE ( 'NONE', #68389, #72129, #13086, .T. ) ;
#62911 = CARTESIAN_POINT ( 'NONE',  ( 9.692307692307695177, -1.951392089020283160, 34.73218667398347748 ) ) ;
#62912 = CARTESIAN_POINT ( 'NONE',  ( 2.294871794871793824, -4.000000000000000000, 29.75000000000000355 ) ) ;
#62913 = ORIENTED_EDGE ( 'NONE', *, *, #33870, .F. ) ;
#62914 = FACE_BOUND ( 'NONE', #61576, .T. ) ;
#62915 = DIRECTION ( 'NONE',  ( -1.000000000000000000, 0.000000000000000000, 0.000000000000000000 ) ) ;
#62916 = CARTESIAN_POINT ( 'NONE',  ( 13.51540582558234149, -6.369690395747422684, 34.87708834333098196 ) ) ;
#62917 = CARTESIAN_POINT ( 'NONE',  ( -23.00000000000000000, -9.499999999999982236, 27.74999999999999645 ) ) ;
#62918 = B_SPLINE_CURVE_WITH_KNOTS ( 'NONE', 3,
 ( #34082, #74187, #33645, #27329, #18802, #39083, #66544, #25996, #39532, #4844 ),
 .UNSPECIFIED., .F., .F.,
 ( 4, 2, 2, 2, 4 ),
 ( 0.0007817359430256319575, 0.0009771253907249984917, 0.001172514838424365026, 0.001367904286123731343, 0.001563293733823097878 ),
 .UNSPECIFIED. ) ;
#62920 = LINE ( 'NONE', #1233, #2323 ) ;
#62919 = LINE ( 'NONE', #8446, #61876 ) ;
#62921 = EDGE_CURVE ( 'NONE', #59502, #79391, #47531, .T. ) ;
#62922 = LINE ( 'NONE', #34137, #9291 ) ;
#62923 = CARTESIAN_POINT ( 'NONE',  ( 4.153846153846154188, -1.466349020453238561, 30.81389545987213907 ) ) ;
#62924 = VERTEX_POINT ( 'NONE', #55427 ) ;
#62925 = ADVANCED_FACE ( 'NONE', ( #21196 ), #48664, .F. ) ;
#62926 = CARTESIAN_POINT ( 'NONE',  ( 14.37376065869474751, -12.37446782046654192, 30.86335684631486842 ) ) ;
#62927 = CARTESIAN_POINT ( 'NONE',  ( -6.130147969731695845, -11.66186481527757479, 32.95055677023626117 ) ) ;
#62928 = VERTEX_POINT ( 'NONE', #930 ) ;
#62929 = FACE_OUTER_BOUND ( 'NONE', #85938, .T. ) ;
#62930 = CARTESIAN_POINT ( 'NONE',  ( -18.00000000000000000, -1.459774944578025924, 30.56119799385072611 ) ) ;
#62931 = EDGE_LOOP ( 'NONE', ( #80115, #36141 ) ) ;
#62932 = CARTESIAN_POINT ( 'NONE',  ( -13.25408994638174320, -11.66157788607254098, 32.95092075102925833 ) ) ;
#62933 = CARTESIAN_POINT ( 'NONE',  ( 4.403791672194294016, -10.05730279482229683, 34.04704008940765902 ) ) ;
#62934 = FACE_BOUND ( 'NONE', #3585, .T. ) ;
#62936 = CARTESIAN_POINT ( 'NONE',  ( -16.85391172531022619, -12.39991518177334129, 30.74647679643404530 ) ) ;
#62935 = CARTESIAN_POINT ( 'NONE',  ( 20.00000000000000000, -4.000000000000000000, 29.75000000000000355 ) ) ;
#62937 = CARTESIAN_POINT ( 'NONE',  ( 1.634669804528839476, -12.65882529074907126, 30.72640787790839312 ) ) ;
#62939 = CARTESIAN_POINT ( 'NONE',  ( 7.173022441425065843, -12.43552623307873972, 30.55307653245132826 ) ) ;
#62938 = CARTESIAN_POINT ( 'NONE',  ( -2.980823712421087013, -11.86320923018887719, 32.19269448109604781 ) ) ;
#62940 = DIRECTION ( 'NONE',  ( 0.000000000000000000, 0.000000000000000000, 1.000000000000000000 ) ) ;
#62941 = AXIS2_PLACEMENT_3D ( 'NONE', #70688, #69365, #7666 ) ;
#62942 = CARTESIAN_POINT ( 'NONE',  ( 3.750000000000009770, -9.053300858899081760, 24.54687500000000000 ) ) ;
#62943 = ORIENTED_EDGE ( 'NONE', *, *, #47824, .F. ) ;
#62944 = VERTEX_POINT ( 'NONE', #28398 ) ;
#62945 = CARTESIAN_POINT ( 'NONE',  ( -9.942284436356281674, -2.318417181685855422, 30.59732222474233865 ) ) ;
#62946 = CARTESIAN_POINT ( 'NONE',  ( -10.39260494640654642, -8.540255544307065350, 34.89611431652622286 ) ) ;
#62947 = CARTESIAN_POINT ( 'NONE',  ( 14.43848274865925774, -9.084667340241226796, 34.75534355489798344 ) ) ;
#62948 = CARTESIAN_POINT ( 'NONE',  ( -8.834500769787091201, -8.656820664281498878, 34.87096338111211935 ) ) ;
#62949 = CARTESIAN_POINT ( 'NONE',  ( 20.00000000000000000, -11.50000000000000000, 29.75000000000000355 ) ) ;
#62950 = CARTESIAN_POINT ( 'NONE',  ( -1.553300858899125059, -3.750000000000009326, 25.32812500000000711 ) ) ;
#62951 = CARTESIAN_POINT ( 'NONE',  ( 0.4615384615384611200, -3.937682226553329556, 33.60647404775216529 ) ) ;
#62952 = LINE ( 'NONE', #63409, #34541 ) ;
#62953 = DIRECTION ( 'NONE',  ( -0.000000000000000000, -0.6427876096865404731, -0.7660444431189771253 ) ) ;
#62954 = CARTESIAN_POINT ( 'NONE',  ( 17.93472999944368240, -8.656820664281497102, 34.87096338111211935 ) ) ;
#62955 = FACE_OUTER_BOUND ( 'NONE', #34420, .T. ) ;
#62956 = CARTESIAN_POINT ( 'NONE',  ( 18.22277954126840172, -10.11255958852955672, 34.01340905677048454 ) ) ;
#62957 = CARTESIAN_POINT ( 'NONE',  ( 6.000000000000001776, -2.708943851104267164, 35.45975837776705220 ) ) ;
#62958 = EDGE_CURVE ( 'NONE', #11362, #49139, #55869, .T. ) ;
#62959 = CARTESIAN_POINT ( 'NONE',  ( 15.23076923076923173, -3.937682226553329556, 33.60647404775216529 ) ) ;
#62960 = CARTESIAN_POINT ( 'NONE',  ( 11.53846153846153832, -10.67929555188718282, 33.92786785259544047 ) ) ;
#62961 = B_SPLINE_CURVE_WITH_KNOTS ( 'NONE', 3,
 ( #74250, #12549, #44977, #65692, #3991, #31479, #24723, #52181, #61662, #88728 ),
 .UNSPECIFIED., .F., .F.,
 ( 4, 2, 2, 2, 4 ),
 ( 0.0007817359430256392216, 0.0009771253907250082495, 0.001172514838424377169, 0.001367904286123746305, 0.001563293733823115225 ),
 .UNSPECIFIED. ) ;
#62962 = EDGE_LOOP ( 'NONE', ( #37643, #39425, #77263, #24242 ) ) ;
#62963 = ADVANCED_FACE ( 'NONE', ( #49114 ), #78794, .F. ) ;
#62965 = CARTESIAN_POINT ( 'NONE',  ( 2.057669083470853089, -3.520140089381496473, 33.17453946501458262 ) ) ;
#62964 = B_SPLINE_CURVE_WITH_KNOTS ( 'NONE', 3,
 ( #55512, #50519, #29390, #69474, #69916, #36580, #14982, #1018, #50078, #83894 ),
 .UNSPECIFIED., .F., .F.,
 ( 4, 2, 2, 2, 4 ),
 ( 0.000000000000000000, 0.0001954339857564065528, 0.0003908679715128131056, 0.0005863019572692196313, 0.0007817359430256262112 ),
 .UNSPECIFIED. ) ;
#62966 = CARTESIAN_POINT ( 'NONE',  ( 18.25000000000000000, -2.499999999999998668, 29.75000000000000355 ) ) ;
#62967 = CARTESIAN_POINT ( 'NONE',  ( 1.901340078031373171, -9.487747218494639867, 21.12686829374151287 ) ) ;
#62968 = EDGE_CURVE ( 'NONE', #77757, #30410, #36495, .T. ) ;
#62969 = CYLINDRICAL_SURFACE ( 'NONE', #5874, 0.2499999999999998890 ) ;
#62970 = DIRECTION ( 'NONE',  ( -0.000000000000000000, 1.000000000000000000, -0.000000000000000000 ) ) ;
#62971 = ORIENTED_EDGE ( 'NONE', *, *, #24561, .T. ) ;
#62972 = DIRECTION ( 'NONE',  ( 1.000000000000000000, 0.000000000000000000, 0.000000000000000000 ) ) ;
#62974 = VERTEX_POINT ( 'NONE', #72036 ) ;
#62973 = CARTESIAN_POINT ( 'NONE',  ( -9.442362173959551797, -5.057305518903948638, 34.11320923018887896 ) ) ;
#62975 = CARTESIAN_POINT ( 'NONE',  ( 9.561747100565771262, -2.504760397472875155, 29.97295953869789997 ) ) ;
#62976 = CARTESIAN_POINT ( 'NONE',  ( 12.46153846153846168, -5.471508081941601098, 34.59228464037088457 ) ) ;
#62977 = ORIENTED_EDGE ( 'NONE', *, *, #17742, .T. ) ;
#62978 = CARTESIAN_POINT ( 'NONE',  ( -5.207614543590632472, -11.18331474514187995, 33.13161551792790505 ) ) ;
#62979 = EDGE_CURVE ( 'NONE', #60060, #23103, #77532, .T. ) ;
#62980 = CARTESIAN_POINT ( 'NONE',  ( 13.16113046005105858, -9.417330523894424488, 34.63758898049880486 ) ) ;
#62981 = VERTEX_POINT ( 'NONE', #3575 ) ;
#62982 = CARTESIAN_POINT ( 'NONE',  ( 7.846153846153846700, -5.180354513474913603, 36.12317359536750416 ) ) ;
#62983 = DIRECTION ( 'NONE',  ( 0.000000000000000000, 1.000000000000000000, 0.000000000000000000 ) ) ;
#62984 = AXIS2_PLACEMENT_3D ( 'NONE', #74416, #73981, #26229 ) ;
#62985 = CARTESIAN_POINT ( 'NONE',  ( -9.692307692307384315, -2.506253911140614576, 30.00000000000323297 ) ) ;
#62986 = ORIENTED_EDGE ( 'NONE', *, *, #27373, .T. ) ;
#62987 = EDGE_LOOP ( 'NONE', ( #5665, #88054, #7333, #73097 ) ) ;
#62988 = CARTESIAN_POINT ( 'NONE',  ( -10.39260494640654819, -2.353885683473779800, 30.79025554430704403 ) ) ;
#62989 = ORIENTED_EDGE ( 'NONE', *, *, #1872, .F. ) ;
#62990 = ADVANCED_FACE ( 'NONE', ( #65279 ), #2241, .F. ) ;
#62991 = CARTESIAN_POINT ( 'NONE',  ( 5.207713517890025123, -4.684288915650984819, 34.18129842949671371 ) ) ;
#62992 = FACE_OUTER_BOUND ( 'NONE', #78301, .T. ) ;
#62994 = EDGE_CURVE ( 'NONE', #2791, #33014, #70001, .T. ) ;
#62993 = DIRECTION ( 'NONE',  ( -0.000000000000000000, 0.000000000000000000, 1.000000000000000000 ) ) ;
#62995 = CARTESIAN_POINT ( 'NONE',  ( 1.134592160393928628, -2.341070481393820124, 30.72580821765574299 ) ) ;
#62996 = CARTESIAN_POINT ( 'NONE',  ( 3.230769230769108269, -10.33852847137269571, 34.16647553114546554 ) ) ;
#62997 = VERTEX_POINT ( 'NONE', #58078 ) ;
#62998 = EDGE_LOOP ( 'NONE', ( #61895, #44607 ) ) ;
#63000 = ORIENTED_EDGE ( 'NONE', *, *, #51046, .F. ) ;
#62999 = CARTESIAN_POINT ( 'NONE',  ( -1.254567778359700680, -7.723484964179500700, 34.74522123443823318 ) ) ;
#63001 = VECTOR ( 'NONE', #15877, 1000.000000000000000 ) ;
#63002 = CARTESIAN_POINT ( 'NONE',  ( 16.85343815235874132, -2.353723527008297012, 30.78948104536958752 ) ) ;
#63003 = VERTEX_POINT ( 'NONE', #36920 ) ;
#63004 = AXIS2_PLACEMENT_3D ( 'NONE', #46837, #68438, #61226 ) ;
#63005 = CYLINDRICAL_SURFACE ( 'NONE', #82412, 0.2499999999999993616 ) ;
#63006 = CARTESIAN_POINT ( 'NONE',  ( 5.076923076923075762, -3.513871655860378418, 32.76840700105978499 ) ) ;
#63007 = ORIENTED_EDGE ( 'NONE', *, *, #2822, .F. ) ;
#63008 = CARTESIAN_POINT ( 'NONE',  ( 7.911409417429871027, -8.613356846314928816, 34.62446782046653482 ) ) ;
#63009 = VERTEX_POINT ( 'NONE', #86471 ) ;
#63011 = ORIENTED_EDGE ( 'NONE', *, *, #11939, .F. ) ;
#63010 = CARTESIAN_POINT ( 'NONE',  ( -14.30769230769242917, -5.094484230521993062, 34.41647553114689373 ) ) ;
#63012 = CYLINDRICAL_SURFACE ( 'NONE', #64645, 0.2499999999999973355 ) ;
#63013 = B_SPLINE_CURVE_WITH_KNOTS ( 'NONE', 3,
 ( #88246, #74264, #81029, #4921, #67063, #25180, #40048, #53532, #60739, #12125 ),
 .UNSPECIFIED., .F., .F.,
 ( 4, 2, 2, 2, 4 ),
 ( 0.000000000000000000, 0.0001954311564186871184, 0.0003908623128373742367, 0.0005862934692560614093, 0.0007817246256747484735 ),
 .UNSPECIFIED. ) ;
#63014 = B_SPLINE_CURVE_WITH_KNOTS ( 'NONE', 3,
 ( #28695, #84531, #62897, #1211, #8423, #49836, #1661, #82759, #48957, #56604 ),
 .UNSPECIFIED., .F., .F.,
 ( 4, 2, 2, 2, 4 ),
 ( 0.000000000000000000, 0.0001954339857564078809, 0.0003908679715128157619, 0.0005863019572692236428, 0.0007817359430256315238 ),
 .UNSPECIFIED. ) ;
#63016 = VERTEX_POINT ( 'NONE', #37811 ) ;
#63015 = EDGE_CURVE ( 'NONE', #65460, #86922, #31169, .T. ) ;
#63017 = ADVANCED_FACE ( 'NONE', ( #63946 ), #9025, .F. ) ;
#63018 = CARTESIAN_POINT ( 'NONE',  ( 6.923076923076924238, -13.95598074871891292, 31.83374038241031911 ) ) ;
#63019 = LINE ( 'NONE', #70685, #61228 ) ;
#63020 = FACE_BOUND ( 'NONE', #38919, .T. ) ;
#63021 = FACE_OUTER_BOUND ( 'NONE', #4049, .T. ) ;
#63023 = EDGE_CURVE ( 'NONE', #15955, #12463, #16647, .T. ) ;
#63022 = CARTESIAN_POINT ( 'NONE',  ( -11.78848476268299628, -6.652501968072648708, 34.93155406624980941 ) ) ;
#63024 = CARTESIAN_POINT ( 'NONE',  ( 9.469380733400845074, -2.308479472611653094, 30.53278059502174457 ) ) ;
#63025 = CARTESIAN_POINT ( 'NONE',  ( -0.2115930521604183767, -2.986452184633680229, 32.43230066228893804 ) ) ;
#63026 = AXIS2_PLACEMENT_3D ( 'NONE', #51870, #38834, #78916 ) ;
#63027 = CARTESIAN_POINT ( 'NONE',  ( -3.007757879156382153, -3.105924265160262543, 32.13625925475356127 ) ) ;
#63028 = CARTESIAN_POINT ( 'NONE',  ( -16.40382288478850725, -8.303909089506435137, 34.68538101551103381 ) ) ;
#63029 = EDGE_LOOP ( 'NONE', ( #51235, #27954, #57758, #64553 ) ) ;
#63030 = EDGE_CURVE ( 'NONE', #52057, #62177, #41005, .T. ) ;
#63031 = CARTESIAN_POINT ( 'NONE',  ( -14.30769230769230660, -13.20930481340135110, 34.54067556320372745 ) ) ;
#63032 = EDGE_LOOP ( 'NONE', ( #24297, #70453, #61763, #22084 ) ) ;
#63033 = ORIENTED_EDGE ( 'NONE', *, *, #38191, .T. ) ;
#63034 = CIRCLE ( 'NONE', #31429, 4.000000000000000000 ) ;
#63036 = CARTESIAN_POINT ( 'NONE',  ( 15.23076923076911093, -12.27809138561165270, 31.22303859784587132 ) ) ;
#63035 = FACE_OUTER_BOUND ( 'NONE', #18383, .T. ) ;
#63037 = VECTOR ( 'NONE', #18456, 1000.000000000000114 ) ;
#63038 = CYLINDRICAL_SURFACE ( 'NONE', #74408, 0.2500000000000004996 ) ;
#63039 = CARTESIAN_POINT ( 'NONE',  ( -10.61538461538461320, -11.69971097300155272, 32.46337939537588113 ) ) ;
#63040 = CARTESIAN_POINT ( 'NONE',  ( 1.607395053593450918, -10.97394488606064122, 33.68653795673694873 ) ) ;
#63041 = CARTESIAN_POINT ( 'NONE',  ( 9.692307692307572609, -2.625532179533778709, 30.86335684631627174 ) ) ;
#63042 = ORIENTED_EDGE ( 'NONE', *, *, #72553, .F. ) ;
#63043 = CARTESIAN_POINT ( 'NONE',  ( -18.25002323729296450, -5.851115903089110226, 34.47074536777953568 ) ) ;
#63044 = AXIS2_PLACEMENT_3D ( 'NONE', #81636, #40653, #13173 ) ;
#63045 = CARTESIAN_POINT ( 'NONE',  ( -14.37296230824862775, -10.33852847137145048, 34.16647553114627556 ) ) ;
#63046 = CARTESIAN_POINT ( 'NONE',  ( -12.71156168575992318, -11.56360843649121684, 33.07473185843129926 ) ) ;
#63047 = CARTESIAN_POINT ( 'NONE',  ( -8.703975629717932705, -2.657715359629131857, 31.77849191805844242 ) ) ;
#63048 = FACE_OUTER_BOUND ( 'NONE', #56980, .T. ) ;
#63049 = VERTEX_POINT ( 'NONE', #50431 ) ;
#63050 = EDGE_CURVE ( 'NONE', #78447, #40455, #2390, .T. ) ;
#63051 = DIRECTION ( 'NONE',  ( -0.000000000000000000, 0.9396926207859093161, -0.3420201433256663259 ) ) ;
#63052 = ORIENTED_EDGE ( 'NONE', *, *, #47248, .T. ) ;
#63053 = EDGE_LOOP ( 'NONE', ( #43734, #29493 ) ) ;
#63054 = CARTESIAN_POINT ( 'NONE',  ( -5.999999999999998224, -3.937682226553329556, 33.60647404775216529 ) ) ;
#63055 = EDGE_CURVE ( 'NONE', #28342, #10726, #79774, .T. ) ;
#63056 = ORIENTED_EDGE ( 'NONE', *, *, #47736, .T. ) ;
#63057 = B_SPLINE_CURVE_WITH_KNOTS ( 'NONE', 3,
 ( #17532, #16195, #31026, #3558, #50840, #30585, #9875, #78776, #10771, #72462 ),
 .UNSPECIFIED., .F., .F.,
 ( 4, 2, 2, 2, 4 ),
 ( 0.000000000000000000, 0.0001954339857564054686, 0.0003908679715128109372, 0.0005863019572692163787, 0.0007817359430256218744 ),
 .UNSPECIFIED. ) ;
#63058 = FACE_OUTER_BOUND ( 'NONE', #22451, .T. ) ;
#63059 = CARTESIAN_POINT ( 'NONE',  ( 0.000000000000000000, -4.000000000000000000, 29.75000000000000355 ) ) ;
#63060 = DIRECTION ( 'NONE',  ( -0.000000000000000000, -0.3420201433256694901, -0.9396926207859082059 ) ) ;
#63061 = CARTESIAN_POINT ( 'NONE',  ( 7.846153846153723244, -6.835583212225970762, 34.95778746994575670 ) ) ;
#63062 = DIRECTION ( 'NONE',  ( 0.000000000000000000, -6.938893903907222067E-15, 1.000000000000000000 ) ) ;
#63064 = CARTESIAN_POINT ( 'NONE',  ( 0.7115928814519135726, -9.233818618650603938, 34.70587769442853698 ) ) ;
#63063 = B_SPLINE_CURVE_WITH_KNOTS ( 'NONE', 3,
 ( #57032, #42650, #16940, #15618, #8864, #44390, #71877, #3417, #85848, #23247 ),
 .UNSPECIFIED., .F., .F.,
 ( 4, 2, 2, 2, 4 ),
 ( 0.0007817359430256323911, 0.0009771253907249991422, 0.001172514838424365893, 0.001367904286123732644, 0.001563293733823099396 ),
 .UNSPECIFIED. ) ;
#63065 = ORIENTED_EDGE ( 'NONE', *, *, #29870, .F. ) ;
#63066 = CARTESIAN_POINT ( 'NONE',  ( 5.999999999999880096, -12.46129190930018460, 30.37095296980731973 ) ) ;
#63068 = EDGE_LOOP ( 'NONE', ( #37335, #28000, #31262, #2812 ) ) ;
#63067 = CARTESIAN_POINT ( 'NONE',  ( -13.38461538461550582, -4.481592998941358097, 33.73612834414048933 ) ) ;
#63069 = CARTESIAN_POINT ( 'NONE',  ( -5.076923076922769340, -2.506253911140614576, 30.00000000000323297 ) ) ;
#63070 = CARTESIAN_POINT ( 'NONE',  ( -5.076923076923075762, -13.95598074871891292, 31.83374038241031911 ) ) ;
#63071 = CARTESIAN_POINT ( 'NONE',  ( 17.01165263096229907, -3.835265460703609186, 33.15142922261924241 ) ) ;
#63072 = CARTESIAN_POINT ( 'NONE',  ( 15.48071464014727461, -2.986452184633680673, 32.43230066228895225 ) ) ;
#63073 = EDGE_CURVE ( 'NONE', #83315, #72489, #33291, .T. ) ;
#63074 = CARTESIAN_POINT ( 'NONE',  ( -2.242437168179467033, -2.379036618887895305, 30.90682066428159303 ) ) ;
#63075 = LINE ( 'NONE', #28877, #68003 ) ;
#63076 = DIRECTION ( 'NONE',  ( -0.000000000000000000, 1.000000000000000000, 3.491481338843133355E-15 ) ) ;
#63077 = CARTESIAN_POINT ( 'NONE',  ( -1.200186371490524317, -10.22469193450124791, 23.86124329374151998 ) ) ;
#63078 = ORIENTED_EDGE ( 'NONE', *, *, #49611, .T. ) ;
#63079 = AXIS2_PLACEMENT_3D ( 'NONE', #34150, #61617, #69270 ) ;
#63080 = ADVANCED_FACE ( 'NONE', ( #81039 ), #4477, .F. ) ;
#63081 = CARTESIAN_POINT ( 'NONE',  ( -16.82697755857493505, -10.76462480002816413, 33.53768742498949962 ) ) ;
#63082 = CARTESIAN_POINT ( 'NONE',  ( -17.14219307747939069, -5.094484230520675894, 34.41647553114621161 ) ) ;
#63083 = CARTESIAN_POINT ( 'NONE',  ( 7.976945653978632755, -2.541949514083463590, 30.39797389878540557 ) ) ;
#63084 = CARTESIAN_POINT ( 'NONE',  ( -7.715363405186889345, -2.845873456487966635, 32.17976146951973249 ) ) ;
#63085 = ORIENTED_EDGE ( 'NONE', *, *, #27938, .T. ) ;
#63086 = CARTESIAN_POINT ( 'NONE',  ( 2.750000000000008438, -8.639087296525996607, 14.54687500000000000 ) ) ;
#63087 = CARTESIAN_POINT ( 'NONE',  ( -5.207070286361298095, -6.852621066184267029, 34.70813303252209181 ) ) ;
#63088 = DIRECTION ( 'NONE',  ( -0.000000000000000000, -0.9396926207859092051, -0.3420201433256662704 ) ) ;
#63089 = EDGE_CURVE ( 'NONE', #31532, #8324, #67984, .T. ) ;
#63090 = CARTESIAN_POINT ( 'NONE',  ( -9.692307692307691624, -12.78798330534102767, 29.49999999999997868 ) ) ;
#63091 = ORIENTED_EDGE ( 'NONE', *, *, #41668, .F. ) ;
#63092 = CARTESIAN_POINT ( 'NONE',  ( -23.00000000000000000, -5.499999999999981348, 27.75000000000000000 ) ) ;
#63093 = CARTESIAN_POINT ( 'NONE',  ( -5.999999999999690914, -2.506253911140614576, 30.00000000000323297 ) ) ;
#63094 = EDGE_CURVE ( 'NONE', #26115, #28684, #57112, .T. ) ;
#63095 = CARTESIAN_POINT ( 'NONE',  ( 3.230769230769231726, -2.249999999999998668, 29.75000000000001776 ) ) ;
#63096 = DIRECTION ( 'NONE',  ( -0.000000000000000000, 0.8660254037844397068, -0.4999999999999978906 ) ) ;
#63097 = B_SPLINE_CURVE_WITH_KNOTS ( 'NONE', 3,
 ( #50084, #20845, #48314, #14988, #14094, #22185, #69922, #49651, #75787, #62708 ),
 .UNSPECIFIED., .F., .F.,
 ( 4, 2, 2, 2, 4 ),
 ( 0.0007817359430256294638, 0.0009771253907249952391, 0.001172514838424361123, 0.001367904286123726790, 0.001563293733823092673 ),
 .UNSPECIFIED. ) ;
#63098 = ORIENTED_EDGE ( 'NONE', *, *, #8218, .F. ) ;
#63099 = CARTESIAN_POINT ( 'NONE',  ( -6.700064078983528404, -6.460100341425561332, 34.89618726649961644 ) ) ;
#63100 = ORIENTED_EDGE ( 'NONE', *, *, #17584, .F. ) ;
#63101 = B_SPLINE_CURVE_WITH_KNOTS ( 'NONE', 3,
 ( #74748, #67097, #54454, #5399, #87840, #13037, #75189, #19350, #13477, #6716 ),
 .UNSPECIFIED., .F., .F.,
 ( 4, 2, 2, 2, 4 ),
 ( 0.0007817246256747484735, 0.0009771112852218922368, 0.001172497944769036217, 0.001367884604316180197, 0.001563271263863323960 ),
 .UNSPECIFIED. ) ;
#63102 = VECTOR ( 'NONE', #3693, 1000.000000000000227 ) ;
#63103 = CARTESIAN_POINT ( 'NONE',  ( 1.384615384615386802, -12.34228464037088635, 31.77849191805839268 ) ) ;
#63104 = CARTESIAN_POINT ( 'NONE',  ( -4.023007735833388665, -7.277220443632450575, 34.74524770363009196 ) ) ;
#63105 = ORIENTED_EDGE ( 'NONE', *, *, #82408, .T. ) ;
#63106 = CYLINDRICAL_SURFACE ( 'NONE', #80721, 0.2500000000000009437 ) ;
#63108 = EDGE_CURVE ( 'NONE', #36685, #10416, #65714, .T. ) ;
#63107 = CARTESIAN_POINT ( 'NONE',  ( 4.153846153846030731, -9.528491918059723176, 34.59228464037033035 ) ) ;
#63109 = CARTESIAN_POINT ( 'NONE',  ( -11.53846153846165912, -6.879047030192662504, 34.71129190930017927 ) ) ;
#63110 = AXIS2_PLACEMENT_3D ( 'NONE', #4769, #66463, #71876 ) ;
#63111 = EDGE_CURVE ( 'NONE', #18498, #56760, #25190, .T. ) ;
#63112 = VECTOR ( 'NONE', #78158, 1000.000000000000114 ) ;
#63113 = DIRECTION ( 'NONE',  ( -0.000000000000000000, -0.1736481776669307198, -0.9848077530122080203 ) ) ;
#63114 = CARTESIAN_POINT ( 'NONE',  ( 3.230769230769231726, -12.37446782046654192, 30.86335684631486131 ) ) ;
#63115 = ORIENTED_EDGE ( 'NONE', *, *, #5799, .T. ) ;
#63116 = ORIENTED_EDGE ( 'NONE', *, *, #34999, .T. ) ;
#63117 = FACE_BOUND ( 'NONE', #36344, .T. ) ;
#63118 = EDGE_LOOP ( 'NONE', ( #59714, #54594, #25432, #88793 ) ) ;
#63119 = CARTESIAN_POINT ( 'NONE',  ( 15.16549878480845770, -12.46129190929999986, 30.37095296980880832 ) ) ;
#63120 = CARTESIAN_POINT ( 'NONE',  ( 6.673076923076925127, -2.249999999999998668, 29.75000000000000355 ) ) ;
#63121 = CARTESIAN_POINT ( 'NONE',  ( 6.223012844093399387, -2.889357225399416862, 32.26129605718031002 ) ) ;
#63122 = CARTESIAN_POINT ( 'NONE',  ( -17.07692307692307665, -2.833524468853757305, 32.15551576947925838 ) ) ;
#63123 = ORIENTED_EDGE ( 'NONE', *, *, #26438, .T. ) ;
#63124 = ORIENTED_EDGE ( 'NONE', *, *, #82460, .T. ) ;
#63125 = ORIENTED_EDGE ( 'NONE', *, *, #15856, .F. ) ;
#63126 = CARTESIAN_POINT ( 'NONE',  ( 13.16173670218674374, -7.630691491037285168, 34.74850469731152458 ) ) ;
#63127 = ORIENTED_EDGE ( 'NONE', *, *, #79220, .F. ) ;
#63128 = B_SPLINE_CURVE_WITH_KNOTS ( 'NONE', 3,
 ( #32200, #32631, #60101, #67755, #26765, #82616, #12806, #60990, #20455, #55119 ),
 .UNSPECIFIED., .F., .F.,
 ( 4, 2, 2, 2, 4 ),
 ( 0.0007817246336856289524, 0.0009771112958940101571, 0.001172497958102391253, 0.001367884620310772350, 0.001563271282519153446 ),
 .UNSPECIFIED. ) ;
#63129 = CARTESIAN_POINT ( 'NONE',  ( 13.16113044089144068, -2.847400154188068022, 31.58180166144859058 ) ) ;
#63130 = AXIS2_PLACEMENT_3D ( 'NONE', #2336, #63604, #36586 ) ;
#63131 = CARTESIAN_POINT ( 'NONE',  ( 16.94677510719138169, -3.625366637846545448, 33.29286588640298561 ) ) ;
#63132 = B_SPLINE_CURVE_WITH_KNOTS ( 'NONE', 3,
 ( #31085, #58555, #86048, #24325, #51787, #59008 ),
 .UNSPECIFIED., .F., .F.,
 ( 4, 2, 4 ),
 ( 4.224605973302673136E-17, 0.0001954756301637175888, 0.0003909512603273928937 ),
 .UNSPECIFIED. ) ;
#63133 = CARTESIAN_POINT ( 'NONE',  ( -18.25002322422145440, -6.652501968072647820, 34.93155406624980941 ) ) ;
#63134 = ORIENTED_EDGE ( 'NONE', *, *, #61243, .F. ) ;
#63136 = EDGE_CURVE ( 'NONE', #27202, #53025, #9892, .T. ) ;
#63135 = CARTESIAN_POINT ( 'NONE',  ( 9.019285080869083870, -9.148310452688876993, 34.47095581063188519 ) ) ;
#63137 = CARTESIAN_POINT ( 'NONE',  ( -15.09997878980228059, -3.338503747796866872, 32.95102852606553512 ) ) ;
#63138 = DIRECTION ( 'NONE',  ( -1.000000000000000000, -0.000000000000000000, -0.000000000000000000 ) ) ;
#63139 = CARTESIAN_POINT ( 'NONE',  ( -11.60373198442231590, -3.300289026998414865, 32.46337939537583139 ) ) ;
#63140 = ORIENTED_EDGE ( 'NONE', *, *, #72074, .T. ) ;
#63141 = ADVANCED_FACE ( 'NONE', ( #5371 ), #87813, .F. ) ;
#63142 = B_SPLINE_CURVE_WITH_KNOTS ( 'NONE', 3,
 ( #10595, #3380, #31758, #16899, #64626, #23651, #45253, #17345, #11038, #72726 ),
 .UNSPECIFIED., .F., .F.,
 ( 4, 2, 2, 2, 4 ),
 ( 0.000000000000000000, 0.0001954311564186864407, 0.0003908623128373728815, 0.0005862934692560593493, 0.0007817246256747457630 ),
 .UNSPECIFIED. ) ;
#63143 = ORIENTED_EDGE ( 'NONE', *, *, #58507, .T. ) ;
#63144 = ORIENTED_EDGE ( 'NONE', *, *, #38418, .T. ) ;
#63145 = DIRECTION ( 'NONE',  ( -1.000000000000000000, -0.000000000000000000, -0.000000000000000000 ) ) ;
#63147 = CARTESIAN_POINT ( 'NONE',  ( 10.61538461538449418, -2.379036618888197729, 30.90682066428292885 ) ) ;
#63146 = CARTESIAN_POINT ( 'NONE',  ( -7.846153846153844924, -6.386643153685126251, 34.62446782046654192 ) ) ;
#63148 = EDGE_CURVE ( 'NONE', #77307, #72978, #82967, .T. ) ;
#63149 = LINE ( 'NONE', #51380, #26958 ) ;
#63150 = CARTESIAN_POINT ( 'NONE',  ( 12.68455130563185662, -12.64618726649961289, 30.78989965857442712 ) ) ;
#63151 = FACE_BOUND ( 'NONE', #78836, .T. ) ;
#63152 = CARTESIAN_POINT ( 'NONE',  ( 8.519254025182180001, -10.82459398097509329, 33.81372124010185587 ) ) ;
#63153 = EDGE_LOOP ( 'NONE', ( #22190, #22838 ) ) ;
#63154 = CARTESIAN_POINT ( 'NONE',  ( -19.50000000000000000, -3.499999999999999556, 29.75000000000000355 ) ) ;
#63155 = CARTESIAN_POINT ( 'NONE',  ( 9.692307692307695177, -8.120952969808772792, 34.71129190930000163 ) ) ;
#63156 = CARTESIAN_POINT ( 'NONE',  ( 17.06410256410256565, -7.500000000000000000, 33.75000000000000000 ) ) ;
#63157 = DIRECTION ( 'NONE',  ( -0.000000000000000000, -0.1736481776669307198, -0.9848077530122080203 ) ) ;
#63158 = ORIENTED_EDGE ( 'NONE', *, *, #64025, .T. ) ;
#63159 = EDGE_CURVE ( 'NONE', #25471, #43749, #21082, .T. ) ;
#63160 = CARTESIAN_POINT ( 'NONE',  ( 6.065255139512840898, -11.06231777344671130, 33.60647404775212976 ) ) ;
#63161 = B_SPLINE_CURVE_WITH_KNOTS ( 'NONE', 3,
 ( #75366, #67280, #67722, #26729, #5575, #68601, #74041, #69048, #146, #88027 ),
 .UNSPECIFIED., .F., .F.,
 ( 4, 2, 2, 2, 4 ),
 ( 0.0007817359527651090859, 0.0009771254036996478414, 0.001172514854634186489, 0.001367904305568725136, 0.001563293756503263783 ),
 .UNSPECIFIED. ) ;
#63162 = ORIENTED_EDGE ( 'NONE', *, *, #85858, .F. ) ;
#63163 = FACE_BOUND ( 'NONE', #76301, .T. ) ;
#63164 = DIRECTION ( 'NONE',  ( -1.000000000000000000, -0.000000000000000000, -0.000000000000000000 ) ) ;
#63165 = EDGE_CURVE ( 'NONE', #64018, #88485, #45290, .T. ) ;
#63166 = CARTESIAN_POINT ( 'NONE',  ( -7.053224892808618307, -10.31621877034669588, 34.18098118002070152 ) ) ;
#63167 = CARTESIAN_POINT ( 'NONE',  ( 12.46153846153846168, -5.557115091759785130, 34.35708131394839171 ) ) ;
#63168 = VERTEX_POINT ( 'NONE', #28288 ) ;
#63169 = CARTESIAN_POINT ( 'NONE',  ( -14.43838377435986864, -12.38065189839062263, 30.83690757178629482 ) ) ;
#63170 = CARTESIAN_POINT ( 'NONE',  ( -6.000000000000121680, -9.528491918059723176, 34.59228464037033035 ) ) ;
#63171 = CYLINDRICAL_SURFACE ( 'NONE', #61012, 0.2500000000000009437 ) ;
#63172 = LINE ( 'NONE', #49228, #18819 ) ;
#63173 = ORIENTED_EDGE ( 'NONE', *, *, #22544, .F. ) ;
#63174 = VECTOR ( 'NONE', #51034, 1000.000000000000000 ) ;
#63175 = ADVANCED_FACE ( 'NONE', ( #54884 ), #13448, .F. ) ;
#63176 = CARTESIAN_POINT ( 'NONE',  ( -2.749999999999998224, -7.500000000000000000, 21.00000000000000000 ) ) ;
#63177 = ORIENTED_EDGE ( 'NONE', *, *, #55257, .T. ) ;
#63178 = VECTOR ( 'NONE', #73524, 1000.000000000000000 ) ;
#63180 = VERTEX_POINT ( 'NONE', #62508 ) ;
#63179 = CARTESIAN_POINT ( 'NONE',  ( 4.153846153846030731, -3.083524468854526912, 32.58852847137268327 ) ) ;
#63181 = CARTESIAN_POINT ( 'NONE',  ( 11.60371710973756620, -6.879047030191282275, 34.71129190930002295 ) ) ;
#63182 = CARTESIAN_POINT ( 'NONE',  ( -13.38461538461538325, -4.786620604624113540, 33.94971097300155094 ) ) ;
#63183 = DIRECTION ( 'NONE',  ( 0.000000000000000000, 0.8660254037844377084, 0.5000000000000015543 ) ) ;
#63184 = CARTESIAN_POINT ( 'NONE',  ( -12.46153846153858424, -11.06231777344772027, 33.60647404775119895 ) ) ;
#63186 = CARTESIAN_POINT ( 'NONE',  ( -11.53846153846166089, -9.528491918059723176, 34.59228464037033035 ) ) ;
#63185 = CARTESIAN_POINT ( 'NONE',  ( -8.096177083446809419, -10.76384336483936011, 33.53834819971076087 ) ) ;
#63187 = CARTESIAN_POINT ( 'NONE',  ( 7.846153846153846700, -4.098570777380720287, 33.41473453929634729 ) ) ;
#63188 = CARTESIAN_POINT ( 'NONE',  ( -2.750000000000007105, -6.360912703474006946, 25.17187500000000000 ) ) ;
#63189 = ORIENTED_EDGE ( 'NONE', *, *, #67981, .T. ) ;
#63190 = ADVANCED_FACE ( 'NONE', ( #35947 ), #40930, .F. ) ;
#63191 = CARTESIAN_POINT ( 'NONE',  ( -16.28399412357785536, -5.070767119584671079, 34.40440758774516183 ) ) ;
#63192 = VERTEX_POINT ( 'NONE', #20650 ) ;
#63193 = ORIENTED_EDGE ( 'NONE', *, *, #44843, .F. ) ;
#63194 = EDGE_CURVE ( 'NONE', #60729, #74862, #19624, .T. ) ;
#63195 = CARTESIAN_POINT ( 'NONE',  ( -16.21992853320628925, -9.058645607665454236, 34.76329471203372634 ) ) ;
#63196 = ORIENTED_EDGE ( 'NONE', *, *, #84001, .T. ) ;
#63197 = CARTESIAN_POINT ( 'NONE',  ( 10.83839745947800992, -8.282913670948747864, 34.94150082978203642 ) ) ;
#63198 = CARTESIAN_POINT ( 'NONE',  ( 6.065255571276024327, -3.300289026998475705, 32.46337939537591666 ) ) ;
#63199 = CARTESIAN_POINT ( 'NONE',  ( -11.78843826940389583, -11.28823185664190376, 33.01397839955799896 ) ) ;
#63200 = DIRECTION ( 'NONE',  ( 0.000000000000000000, 0.1736481776669275834, 0.9848077530122086864 ) ) ;
#63201 = CARTESIAN_POINT ( 'NONE',  ( -10.61538461538461320, -3.322132147404559976, 32.92929555188717927 ) ) ;
#63202 = CARTESIAN_POINT ( 'NONE',  ( 6.923076923076924238, -11.16473453929635440, 33.15142922261926373 ) ) ;
#63203 = CARTESIAN_POINT ( 'NONE',  ( -15.23076923076935252, -8.656820664282941280, 34.87096338111179961 ) ) ;
#63204 = FACE_OUTER_BOUND ( 'NONE', #20414, .T. ) ;
#63205 = CARTESIAN_POINT ( 'NONE',  ( -2.084679463598908544, -2.889357225399416862, 32.26129605718031002 ) ) ;
#63206 = EDGE_CURVE ( 'NONE', #72231, #41905, #75305, .T. ) ;
#63207 = EDGE_CURVE ( 'NONE', #68579, #74314, #46267, .T. ) ;
#63208 = CARTESIAN_POINT ( 'NONE',  ( 13.38461538461538680, -3.669653830205710676, 35.88435417666054406 ) ) ;
#63209 = AXIS2_PLACEMENT_3D ( 'NONE', #8019, #51073, #71359 ) ;
#63210 = CARTESIAN_POINT ( 'NONE',  ( 9.692307692307695177, -2.249999999999998668, 29.50000000000001421 ) ) ;
#63211 = EDGE_LOOP ( 'NONE', ( #70809, #57488 ) ) ;
#63212 = ORIENTED_EDGE ( 'NONE', *, *, #55000, .T. ) ;
#63213 = CARTESIAN_POINT ( 'NONE',  ( 12.52760579488853665, -2.486705287966280320, 31.30864560766543647 ) ) ;
#63214 = SURFACE_SIDE_STYLE ('',( #76744 ) ) ;
#63215 = CARTESIAN_POINT ( 'NONE',  ( 3.480714640147274608, -10.92531984108285670, 33.72920026020278073 ) ) ;
#63216 = CARTESIAN_POINT ( 'NONE',  ( 12.46153846153833911, -10.90142922262034020, 33.41473453929536674 ) ) ;
#63217 = EDGE_LOOP ( 'NONE', ( #64462, #64059, #40221, #61920 ) ) ;
#63219 = EDGE_CURVE ( 'NONE', #42018, #62448, #30068, .T. ) ;
#63218 = CARTESIAN_POINT ( 'NONE',  ( 6.066068351002440906, -4.786620604624113540, 33.94971097300155805 ) ) ;
#63220 = CARTESIAN_POINT ( 'NONE',  ( -10.74607521849492109, -12.62707690430377383, 30.88035979386743435 ) ) ;
#63221 = B_SPLINE_CURVE_WITH_KNOTS ( 'NONE', 3,
 ( #45224, #39383, #66393, #46567, #25409, #73616, #60073, #74051, #67290, #46998 ),
 .UNSPECIFIED., .F., .F.,
 ( 4, 2, 2, 2, 4 ),
 ( 0.0007817246256747528103, 0.0009771112852218980915, 0.001172497944769043156, 0.001367884604316188437, 0.001563271263863333718 ),
 .UNSPECIFIED. ) ;
#63222 = CARTESIAN_POINT ( 'NONE',  ( -12.39628289026243557, -10.90142922261932057, 33.41473453929631887 ) ) ;
#63223 = EDGE_CURVE ( 'NONE', #52323, #49979, #170, .T. ) ;
#63224 = EDGE_CURVE ( 'NONE', #2856, #86167, #38770, .T. ) ;
#63225 = ORIENTED_EDGE ( 'NONE', *, *, #36519, .F. ) ;
#63226 = CARTESIAN_POINT ( 'NONE',  ( 18.06606733335007675, -3.322132147404559532, 32.92929555188717927 ) ) ;
#63227 = ORIENTED_EDGE ( 'NONE', *, *, #41158, .T. ) ;
#63228 = ADVANCED_FACE ( 'NONE', ( #44443 ), #78243, .T. ) ;
#63229 = LINE ( 'NONE', #83078, #4607 ) ;
#63230 = VECTOR ( 'NONE', #28170, 1000.000000000000114 ) ;
#63231 = VECTOR ( 'NONE', #60587, 1000.000000000000000 ) ;
#63232 = CARTESIAN_POINT ( 'NONE',  ( 15.36129466900288065, -3.625058011473228703, 33.29252011169590020 ) ) ;
#63233 = CARTESIAN_POINT ( 'NONE',  ( -1.634638608836841200, -9.356822207818506598, 34.66110646841856635 ) ) ;
#63234 = B_SPLINE_CURVE_WITH_KNOTS ( 'NONE', 3,
 ( #42558, #70913, #16405, #50175, #50628, #2008, #78106, #49744, #63259, #70470 ),
 .UNSPECIFIED., .F., .F.,
 ( 4, 2, 2, 2, 4 ),
 ( 0.0007817359430256252354, 0.0009771253907249898181, 0.001172514838424354401, 0.001367904286123718983, 0.001563293733823083566 ),
 .UNSPECIFIED. ) ;
#63235 = CARTESIAN_POINT ( 'NONE',  ( -9.915792616872025178, -8.539481045369596401, 34.89627647299170832 ) ) ;
#63236 = FACE_OUTER_BOUND ( 'NONE', #81462, .T. ) ;
#63237 = CIRCLE ( 'NONE', #24400, 0.5000000000000004441 ) ;
#63238 = VECTOR ( 'NONE', #71783, 1000.000000000000000 ) ;
#63239 = EDGE_LOOP ( 'NONE', ( #69785, #114, #28371, #36583 ) ) ;
#63240 = B_SPLINE_CURVE_WITH_KNOTS ( 'NONE', 3,
 ( #88642, #55264, #81427, #47173, #32781, #5755 ),
 .UNSPECIFIED., .F., .F.,
 ( 4, 2, 4 ),
 ( 0.0003909569690057860679, 0.0005862646681846136196, 0.0007815723673634411171 ),
 .UNSPECIFIED. ) ;
#63241 = CIRCLE ( 'NONE', #25836, 5.250000000000000888 ) ;
#63242 = VERTEX_POINT ( 'NONE', #37253 ) ;
#63243 = B_SPLINE_CURVE_WITH_KNOTS ( 'NONE', 3,
 ( #18023, #17121, #44577, #45479, #37385, #10375, #37838, #66651, #78374, #64854 ),
 .UNSPECIFIED., .F., .F.,
 ( 4, 2, 2, 2, 4 ),
 ( 0.000000000000000000, 0.0001954311564186863052, 0.0003908623128373726104, 0.0005862934692560589156, 0.0007817246256747452209 ),
 .UNSPECIFIED. ) ;
#63244 = ORIENTED_EDGE ( 'NONE', *, *, #63941, .F. ) ;
#63245 = VERTEX_POINT ( 'NONE', #49887 ) ;
#63246 = CARTESIAN_POINT ( 'NONE',  ( -10.83886953994894853, -12.47654668319379567, 31.42292124445336654 ) ) ;
#63247 = CARTESIAN_POINT ( 'NONE',  ( -12.59168643127016196, -12.70455904226513866, 30.44083106164009322 ) ) ;
#63248 = CARTESIAN_POINT ( 'NONE',  ( 17.07692307692295586, -4.481592998941358097, 33.73612834414048933 ) ) ;
#63249 = EDGE_CURVE ( 'NONE', #2005, #81618, #78474, .T. ) ;
#63250 = CARTESIAN_POINT ( 'NONE',  ( 0.4615384615384611200, -12.34228464037088635, 31.77849191805839268 ) ) ;
#63251 = CARTESIAN_POINT ( 'NONE',  ( 17.99999999999987566, -3.083524468854526912, 32.58852847137268327 ) ) ;
#63252 = DIRECTION ( 'NONE',  ( -0.000000000000000000, 1.000000000000000000, -0.000000000000000000 ) ) ;
#63253 = ORIENTED_EDGE ( 'NONE', *, *, #55353, .F. ) ;
#63254 = ORIENTED_EDGE ( 'NONE', *, *, #61196, .T. ) ;
#63255 = EDGE_LOOP ( 'NONE', ( #50563, #73059, #62671, #21019 ) ) ;
#63257 = ORIENTED_EDGE ( 'NONE', *, *, #30603, .F. ) ;
#63256 = CARTESIAN_POINT ( 'NONE',  ( -3.230769230769229949, -10.51840700105979565, 33.73612834413961536 ) ) ;
#63259 = CARTESIAN_POINT ( 'NONE',  ( -8.703162418228332697, -11.16473453929635440, 33.15142922261926373 ) ) ;
#63258 = DIRECTION ( 'NONE',  ( 0.000000000000000000, 0.4999999999999985567, 0.8660254037844395958 ) ) ;
#63260 = FACE_OUTER_BOUND ( 'NONE', #42928, .T. ) ;
#63261 = CARTESIAN_POINT ( 'NONE',  ( 2.651650429449539104, -4.848349570550432475, 24.31250000000000000 ) ) ;
#63262 = ORIENTED_EDGE ( 'NONE', *, *, #62117, .T. ) ;
#63263 = B_SPLINE_CURVE_WITH_KNOTS ( 'NONE', 3,
 ( #70239, #8547, #36022, #85088, #1777, #29268, #22494, #77437, #15748, #8991 ),
 .UNSPECIFIED., .F., .F.,
 ( 4, 2, 2, 2, 4 ),
 ( 0.000000000000000000, 0.0001954311564186864949, 0.0003908623128373729899, 0.0005862934692560594577, 0.0007817246256747459798 ),
 .UNSPECIFIED. ) ;
#63264 = VERTEX_POINT ( 'NONE', #37703 ) ;
#63265 = CARTESIAN_POINT ( 'NONE',  ( -17.86947456176635640, -3.068774925481849269, 32.56582465632704526 ) ) ;
#63266 = ORIENTED_EDGE ( 'NONE', *, *, #19822, .T. ) ;
#63267 = FACE_BOUND ( 'NONE', #36127, .T. ) ;
#63268 = CARTESIAN_POINT ( 'NONE',  ( -6.000000000000121680, -4.320704448113951379, 33.92786785259630022 ) ) ;
#63269 = CARTESIAN_POINT ( 'NONE',  ( 7.976944287120798727, -5.496552790871120031, 34.60292014791297532 ) ) ;
#63270 = ORIENTED_EDGE ( 'NONE', *, *, #2639, .F. ) ;
#63271 = CARTESIAN_POINT ( 'NONE',  ( 16.37662569511456212, -11.41317474335729543, 32.86274602512330034 ) ) ;
#63272 = CARTESIAN_POINT ( 'NONE',  ( 11.40831356872984514, -6.809168938359901446, 34.95455904226513866 ) ) ;
#63273 = LINE ( 'NONE', #70484, #14833 ) ;
#63274 = DIRECTION ( 'NONE',  ( 1.000000000000000000, 0.000000000000000000, 0.000000000000000000 ) ) ;
#63275 = CARTESIAN_POINT ( 'NONE',  ( 7.846153846153725020, -2.625532179533779154, 30.86335684631627174 ) ) ;
#63276 = ORIENTED_EDGE ( 'NONE', *, *, #10896, .F. ) ;
#63277 = ADVANCED_FACE ( 'NONE', ( #16110 ), #2578, .F. ) ;
#63278 = CARTESIAN_POINT ( 'NONE',  ( -0.6844179782760478892, -7.630690623152301733, 34.99857592706774057 ) ) ;
#63279 = DIRECTION ( 'NONE',  ( -0.000000000000000000, -0.6427876096865404731, -0.7660444431189771253 ) ) ;
#63280 = FACE_OUTER_BOUND ( 'NONE', #16250, .T. ) ;
#63281 = CARTESIAN_POINT ( 'NONE',  ( 13.51514082284903040, -2.372941743896879174, 30.88044141588253666 ) ) ;
#63282 = CARTESIAN_POINT ( 'NONE',  ( 15.23076923076923173, -2.708943851104267164, 35.45975837776705220 ) ) ;
#63283 = FACE_BOUND ( 'NONE', #19656, .T. ) ;
#63285 = CARTESIAN_POINT ( 'NONE',  ( 7.146088274689772923, -3.105924265160262543, 32.13625925475356127 ) ) ;
#63284 = CARTESIAN_POINT ( 'NONE',  ( 5.011652630962300847, -11.48612834413959582, 32.76840700105983473 ) ) ;
#63286 = VECTOR ( 'NONE', #45118, 1000.000000000000000 ) ;
#63287 = CARTESIAN_POINT ( 'NONE',  ( -14.55766905174090020, -3.436278759898153901, 33.07459398097509506 ) ) ;
#63289 = CARTESIAN_POINT ( 'NONE',  ( 15.23076923076923173, -9.780366693483667717, 34.19971097300155094 ) ) ;
#63288 = CARTESIAN_POINT ( 'NONE',  ( -1.944543648263014957, -5.555456351737005249, 14.00000000000000000 ) ) ;
#63290 = CARTESIAN_POINT ( 'NONE',  ( -10.68065461594093435, -6.835583212224499938, 34.95778746994557906 ) ) ;
#63291 = CARTESIAN_POINT ( 'NONE',  ( -2.775308065498764964, -6.422011778438537988, 22.42000670625849068 ) ) ;
#63292 = EDGE_LOOP ( 'NONE', ( #70732, #46858, #13247, #2299 ) ) ;
#63293 = ADVANCED_BREP_SHAPE_REPRESENTATION ( '', ( #307, #83448 ), #14453 ) ;
#63294 = CARTESIAN_POINT ( 'NONE',  ( 16.15384615384615330, -3.322132147404559976, 32.92929555188717927 ) ) ;
#63295 = ORIENTED_EDGE ( 'NONE', *, *, #11973, .F. ) ;
#63296 = AXIS2_PLACEMENT_3D ( 'NONE', #25384, #52846, #60938 ) ;
#63297 = CARTESIAN_POINT ( 'NONE',  ( -13.16183571563731647, -9.418065098278013636, 34.63729479722530158 ) ) ;
#63298 = ORIENTED_EDGE ( 'NONE', *, *, #16220, .F. ) ;
#63299 = EDGE_CURVE ( 'NONE', #18589, #69653, #43574, .T. ) ;
#63300 = CARTESIAN_POINT ( 'NONE',  ( -1.384615384615506484, -4.320704448113951379, 33.92786785259630022 ) ) ;
#63301 = CARTESIAN_POINT ( 'NONE',  ( 4.826899852701617810, -12.07920672191015221, 32.31858351112116168 ) ) ;
#63302 = EDGE_LOOP ( 'NONE', ( #35458, #64118, #1886, #54448 ) ) ;
#63303 = CARTESIAN_POINT ( 'NONE',  ( -8.096177083446811196, -5.851115903089112003, 34.47074536777953568 ) ) ;
#63304 = CARTESIAN_POINT ( 'NONE',  ( -2.775308065498764964, -6.422011778438537988, 21.17000670625848713 ) ) ;
#63305 = DIRECTION ( 'NONE',  ( -0.000000000000000000, -0.8660254037844397068, -0.4999999999999978906 ) ) ;
#63306 = CIRCLE ( 'NONE', #14387, 0.2500000000000002220 ) ;
#63307 = CARTESIAN_POINT ( 'NONE',  ( -9.320512820512821150, -7.500000000000000000, 29.75000000000000355 ) ) ;
#63308 = CYLINDRICAL_SURFACE ( 'NONE', #11595, 0.2499999999999994726 ) ;
#63309 = VECTOR ( 'NONE', #2986, 1000.000000000000227 ) ;
#63310 = CARTESIAN_POINT ( 'NONE',  ( -15.12820512820512953, -3.499999999999999556, 29.75000000000000355 ) ) ;
#63311 = CARTESIAN_POINT ( 'NONE',  ( -5.076923076923075762, -1.044019251281081972, 31.83374038241031911 ) ) ;
#63312 = CARTESIAN_POINT ( 'NONE',  ( -14.16025641025641235, -4.000000000000000000, 29.75000000000000355 ) ) ;
#63313 = VECTOR ( 'NONE', #29014, 1000.000000000000000 ) ;
#63314 = CARTESIAN_POINT ( 'NONE',  ( 1.553300858899129944, -11.24999999999998934, 18.45312500000000355 ) ) ;
#63315 = CARTESIAN_POINT ( 'NONE',  ( 11.28843831424008393, -5.765609946408404518, 34.70566812827425451 ) ) ;
#63316 = CARTESIAN_POINT ( 'NONE',  ( 14.43821800945587519, -10.88167719472716399, 33.43325721877153711 ) ) ;
#63317 = ADVANCED_FACE ( 'NONE', ( #65170 ), #9362, .F. ) ;
#63318 = B_SPLINE_CURVE_WITH_KNOTS ( 'NONE', 3,
 ( #8264, #42052, #22647, #1502, #21317, #613, #15464, #167, #55108, #63187 ),
 .UNSPECIFIED., .F., .F.,
 ( 4, 2, 2, 2, 4 ),
 ( 0.0007817359430256304396, 0.0009771253907249961065, 0.001172514838424361773, 0.001367904286123727440, 0.001563293733823093107 ),
 .UNSPECIFIED. ) ;
#63319 = CYLINDRICAL_SURFACE ( 'NONE', #3270, 0.2499999999999994726 ) ;
#63320 = CARTESIAN_POINT ( 'NONE',  ( -3.724691934501248802, -5.885600066136383646, 24.17374329374151642 ) ) ;
#63321 = CARTESIAN_POINT ( 'NONE',  ( 0.4615384615384611200, -2.708943851104267164, 35.45975837776705220 ) ) ;
#63322 = VERTEX_POINT ( 'NONE', #51638 ) ;
#63323 = CARTESIAN_POINT ( 'NONE',  ( 1.384615384615264011, -8.656820664282941280, 34.87096338111179961 ) ) ;
#63324 = DIRECTION ( 'NONE',  ( -1.000000000000000000, -0.000000000000000000, -0.000000000000000000 ) ) ;
#63325 = DIRECTION ( 'NONE',  ( -0.000000000000000000, 0.9848077530122085754, -0.1736481776669273613 ) ) ;
#63326 = CARTESIAN_POINT ( 'NONE',  ( 8.519254025182178225, -5.643011162660950042, 34.66104346484419096 ) ) ;
#63327 = CARTESIAN_POINT ( 'NONE',  ( -16.37733109757010652, -10.81261337010820256, 33.49550067578627477 ) ) ;
#63328 = CARTESIAN_POINT ( 'NONE',  ( -12.46153846153846168, -6.681629849574314051, 35.83090037661290239 ) ) ;
#63329 = FACE_OUTER_BOUND ( 'NONE', #10280, .T. ) ;
#63330 = EDGE_CURVE ( 'NONE', #20258, #45665, #18353, .T. ) ;
#63331 = EDGE_CURVE ( 'NONE', #75513, #47058, #67798, .T. ) ;
#63332 = VERTEX_POINT ( 'NONE', #66057 ) ;
#63333 = ORIENTED_EDGE ( 'NONE', *, *, #50777, .T. ) ;
#63334 = VECTOR ( 'NONE', #31306, 1000.000000000000227 ) ;
#63335 = ORIENTED_EDGE ( 'NONE', *, *, #9004, .F. ) ;
#63336 = DIRECTION ( 'NONE',  ( -0.000000000000000000, 1.000000000000000000, -0.000000000000000000 ) ) ;
#63337 = LINE ( 'NONE', #49821, #40066 ) ;
#63338 = CARTESIAN_POINT ( 'NONE',  ( 16.15384615384615330, -2.721908614388771852, 31.22303859784724978 ) ) ;
#63339 = DIRECTION ( 'NONE',  ( 1.734723475976812518E-16, -1.000000000000000000, 0.000000000000000000 ) ) ;
#63340 = CARTESIAN_POINT ( 'NONE',  ( 10.86543903529806876, -10.06805714834173493, 34.32951233291982618 ) ) ;
#63341 = B_SPLINE_CURVE_WITH_KNOTS ( 'NONE', 3,
 ( #64021, #35690, #8212, #56396, #84767, #36993, #2318, #28479, #22599, #15860 ),
 .UNSPECIFIED., .F., .F.,
 ( 4, 2, 2, 2, 4 ),
 ( 0.000000000000000000, 0.0001954311564186871184, 0.0003908623128373742367, 0.0005862934692560614093, 0.0007817246256747484735 ),
 .UNSPECIFIED. ) ;
#63342 = VERTEX_POINT ( 'NONE', #45344 ) ;
#63343 = DIRECTION ( 'NONE',  ( -0.000000000000000000, -0.8660254037844399289, -0.4999999999999980016 ) ) ;
#63344 = ORIENTED_EDGE ( 'NONE', *, *, #3949, .T. ) ;
#63345 = ORIENTED_EDGE ( 'NONE', *, *, #88535, .T. ) ;
#63346 = VECTOR ( 'NONE', #75027, 1000.000000000000227 ) ;
#63347 = VERTEX_POINT ( 'NONE', #32291 ) ;
#63349 = ORIENTED_EDGE ( 'NONE', *, *, #62116, .F. ) ;
#63348 = DIRECTION ( 'NONE',  ( 0.000000000000000000, 0.000000000000000000, -1.000000000000000000 ) ) ;
#63350 = CYLINDRICAL_SURFACE ( 'NONE', #4282, 0.2500000000000008882 ) ;
#63351 = CARTESIAN_POINT ( 'NONE',  ( -10.74553182482283198, -5.195881422630166391, 34.18770438780619259 ) ) ;
#63352 = AXIS2_PLACEMENT_3D ( 'NONE', #42051, #88922, #67742 ) ;
#63353 = VECTOR ( 'NONE', #77891, 1000.000000000000000 ) ;
#63354 = CYLINDRICAL_SURFACE ( 'NONE', #9104, 0.2499999999999997502 ) ;
#63355 = EDGE_LOOP ( 'NONE', ( #52369, #20078 ) ) ;
#63356 = AXIS2_PLACEMENT_3D ( 'NONE', #41614, #68203, #69082 ) ;
#63357 = EDGE_LOOP ( 'NONE', ( #12832, #17788, #23612, #25380 ) ) ;
#63358 = ORIENTED_EDGE ( 'NONE', *, *, #64546, .T. ) ;
#63359 = CARTESIAN_POINT ( 'NONE',  ( -9.692307692307691624, -5.557115091759785130, 34.35708131394839171 ) ) ;
#63361 = ORIENTED_EDGE ( 'NONE', *, *, #16712, .T. ) ;
#63360 = CARTESIAN_POINT ( 'NONE',  ( 11.66925197942849302, -5.496552790871120031, 34.60292014791297532 ) ) ;
#63362 = CARTESIAN_POINT ( 'NONE',  ( -7.053224132515141243, -12.45813303252208648, 30.39737893381572675 ) ) ;
#63363 = CARTESIAN_POINT ( 'NONE',  ( 11.53846153846153832, -7.500000000000001776, 35.04278698407183867 ) ) ;
#63364 = CARTESIAN_POINT ( 'NONE',  ( 2.557637717070352590, -9.357781135181031829, 34.66075350412533851 ) ) ;
#63365 = EDGE_LOOP ( 'NONE', ( #27352, #21397, #81093, #61859 ) ) ;
#63366 = CARTESIAN_POINT ( 'NONE',  ( -11.47320596718551933, -5.219633306516380244, 34.19971097300157936 ) ) ;
#63367 = CARTESIAN_POINT ( 'NONE',  ( -14.16025641025641058, -3.499999999999999556, 29.75000000000000355 ) ) ;
#63368 = ORIENTED_EDGE ( 'NONE', *, *, #88415, .F. ) ;
#63369 = FACE_BOUND ( 'NONE', #21383, .T. ) ;
#63370 = CARTESIAN_POINT ( 'NONE',  ( -18.00000000000000000, -1.812984705146277520, 34.52197243641129631 ) ) ;
#63371 = CARTESIAN_POINT ( 'NONE',  ( -13.13461538461538325, -7.500000000000001776, 35.04278698407183867 ) ) ;
#63372 = DIRECTION ( 'NONE',  ( -1.000000000000000000, -0.000000000000000000, -0.000000000000000000 ) ) ;
#63374 = LINE ( 'NONE', #65139, #32493 ) ;
#63373 = DIRECTION ( 'NONE',  ( -0.000000000000000000, -0.9396926207859092051, -0.3420201433256662704 ) ) ;
#63375 = CARTESIAN_POINT ( 'NONE',  ( 15.23076923076923173, -1.242168528481310874, 33.36296068462461051 ) ) ;
#63376 = CARTESIAN_POINT ( 'NONE',  ( -2.530618525208453651, -3.586966769969700763, 32.86292498521069660 ) ) ;
#63377 = ORIENTED_EDGE ( 'NONE', *, *, #88070, .F. ) ;
#63378 = CARTESIAN_POINT ( 'NONE',  ( -11.53846153846165912, -4.481592998941358097, 33.73612834414048933 ) ) ;
#63379 = FACE_OUTER_BOUND ( 'NONE', #48488, .T. ) ;
#63380 = ORIENTED_EDGE ( 'NONE', *, *, #38205, .F. ) ;
#63381 = EDGE_CURVE ( 'NONE', #30821, #36751, #31260, .T. ) ;
#63382 = ADVANCED_FACE ( 'NONE', ( #53887 ), #59755, .F. ) ;
#63383 = LINE ( 'NONE', #57515, #7728 ) ;
#63384 = CARTESIAN_POINT ( 'NONE',  ( -14.05774689831426372, -9.357781135181031829, 34.66075350412533851 ) ) ;
#63385 = CARTESIAN_POINT ( 'NONE',  ( 3.007942538290226508, -7.369208160676173236, 34.74850200257122879 ) ) ;
#63386 = CARTESIAN_POINT ( 'NONE',  ( 2.307692307692309264, -5.471508081941601098, 34.59228464037088457 ) ) ;
#63387 = DIRECTION ( 'NONE',  ( -1.000000000000000000, -0.000000000000000000, 0.000000000000000000 ) ) ;
#63388 = CARTESIAN_POINT ( 'NONE',  ( -8.835314180186649935, -5.557115091759785130, 34.35708131394839171 ) ) ;
#63389 = FACE_BOUND ( 'NONE', #68459, .T. ) ;
#63391 = CARTESIAN_POINT ( 'NONE',  ( -16.94639737515951694, -12.45806712695776319, 30.39783852428763566 ) ) ;
#63390 = LINE ( 'NONE', #62935, #17383 ) ;
#63392 = CARTESIAN_POINT ( 'NONE',  ( -16.08859058257013075, -2.625532179533469623, 30.86335684631491105 ) ) ;
#63394 = CARTESIAN_POINT ( 'NONE',  ( -12.52762187249434156, -4.098570777380719399, 33.41473453929634729 ) ) ;
#63393 = CARTESIAN_POINT ( 'NONE',  ( -5.010855743573000787, -9.905515769479277921, 34.41647553114623292 ) ) ;
#63395 = AXIS2_PLACEMENT_3D ( 'NONE', #34802, #27605, #27162 ) ;
#63396 = CARTESIAN_POINT ( 'NONE',  ( -17.93393164899756087, -4.786620604624112651, 33.94971097300155805 ) ) ;
#63397 = CARTESIAN_POINT ( 'NONE',  ( 1.614399933863660985, -11.22469193450123193, 18.20125670625849068 ) ) ;
#63398 = ORIENTED_EDGE ( 'NONE', *, *, #12493, .F. ) ;
#63399 = EDGE_LOOP ( 'NONE', ( #27617, #82938, #58697, #63899 ) ) ;
#63400 = EDGE_CURVE ( 'NONE', #74750, #75555, #50560, .T. ) ;
#63401 = LINE ( 'NONE', #83700, #3203 ) ;
#63402 = CARTESIAN_POINT ( 'NONE',  ( -12.21159305216042057, -6.653508905675592722, 34.93172785388651391 ) ) ;
#63403 = CARTESIAN_POINT ( 'NONE',  ( 14.43821774592595197, -9.503571793651731880, 34.60286762892837942 ) ) ;
#63404 = DIRECTION ( 'NONE',  ( 0.000000000000000000, 0.1736481776669275834, 0.9848077530122086864 ) ) ;
#63405 = CARTESIAN_POINT ( 'NONE',  ( -13.31854805126531005, -2.486705287966280320, 31.30864560766543647 ) ) ;
#63406 = CARTESIAN_POINT ( 'NONE',  ( 1.492201783934554493, -3.724691934501233703, 18.98250670625849068 ) ) ;
#63407 = B_SPLINE_CURVE_WITH_KNOTS ( 'NONE', 3,
 ( #73233, #45302, #17399, #64678, #24593, #10200, #30460, #66476, #79551, #65123 ),
 .UNSPECIFIED., .F., .F.,
 ( 4, 2, 2, 2, 4 ),
 ( 0.000000000000000000, 0.0001954311564186862781, 0.0003908623128373725562, 0.0005862934692560588072, 0.0007817246256747451124 ),
 .UNSPECIFIED. ) ;
#63408 = CARTESIAN_POINT ( 'NONE',  ( 4.023369445729690241, -7.276988635370452485, 34.74523720219453793 ) ) ;
#63409 = CARTESIAN_POINT ( 'NONE',  ( 11.53846153846153832, -1.367168528481310208, 33.57946703557072254 ) ) ;
#63410 = CARTESIAN_POINT ( 'NONE',  ( 17.07692307692307665, -2.499999999999998668, 29.75000000000001421 ) ) ;
#63411 = CARTESIAN_POINT ( 'NONE',  ( 15.23076923076923173, -3.322132147404559976, 32.92929555188717927 ) ) ;
#63412 = LINE ( 'NONE', #64288, #55405 ) ;
#63413 = CARTESIAN_POINT ( 'NONE',  ( -4.826868657009622865, -6.523592122091591783, 34.90882529074906415 ) ) ;
#63414 = DIRECTION ( 'NONE',  ( 0.000000000000000000, 0.4999999999999960032, -0.8660254037844410391 ) ) ;
#63415 = AXIS2_PLACEMENT_3D ( 'NONE', #28965, #22192, #83010 ) ;
#63416 = EDGE_CURVE ( 'NONE', #69312, #63565, #54880, .T. ) ;
#63417 = CARTESIAN_POINT ( 'NONE',  ( 14.08476609017615644, -6.503392248772476236, 34.64988816332204635 ) ) ;
#63418 = AXIS2_PLACEMENT_3D ( 'NONE', #77061, #76615, #42400 ) ;
#63419 = ORIENTED_EDGE ( 'NONE', *, *, #60754, .T. ) ;
#63420 = CARTESIAN_POINT ( 'NONE',  ( 2.241609928332174206, -3.322132147404559976, 32.92929555188719348 ) ) ;
#63421 = CARTESIAN_POINT ( 'NONE',  ( 10.74617505635156789, -5.496552790871120031, 34.60292014791297532 ) ) ;
#63422 = CARTESIAN_POINT ( 'NONE',  ( 2.750000000000002665, -7.561099074964516831, 22.22061829374151287 ) ) ;
#63423 = AXIS2_PLACEMENT_3D ( 'NONE', #26041, #74229, #66585 ) ;
#63424 = AXIS2_PLACEMENT_3D ( 'NONE', #35142, #42359, #21624 ) ;
#63425 = CARTESIAN_POINT ( 'NONE',  ( 8.834424751014125832, -2.506253911140448043, 29.99999999999988631 ) ) ;
#63426 = CARTESIAN_POINT ( 'NONE',  ( -16.08859101433330707, -2.657715359629131857, 31.77849191805844242 ) ) ;
#63427 = ORIENTED_EDGE ( 'NONE', *, *, #16028, .T. ) ;
#63428 = CARTESIAN_POINT ( 'NONE',  ( -9.692307692307691624, -5.180354513474913603, 36.12317359536750416 ) ) ;
#63430 = VERTEX_POINT ( 'NONE', #86815 ) ;
#63429 = DIRECTION ( 'NONE',  ( -0.000000000000000000, -0.5000000000000009992, -0.8660254037844380415 ) ) ;
#63431 = CARTESIAN_POINT ( 'NONE',  ( 7.145856464345333059, -3.755027918224367767, 33.06320215134714857 ) ) ;
#63432 = CARTESIAN_POINT ( 'NONE',  ( -4.826868765284761054, -9.943054286541403997, 34.11300777759954883 ) ) ;
#63433 = ORIENTED_EDGE ( 'NONE', *, *, #75862, .T. ) ;
#63434 = CARTESIAN_POINT ( 'NONE',  ( -5.326899807865430603, -12.17611988154120972, 31.52148481390971213 ) ) ;
#63435 = CARTESIAN_POINT ( 'NONE',  ( 10.86533002476265963, -10.92531984108285670, 33.72920026020278073 ) ) ;
#63436 = ORIENTED_EDGE ( 'NONE', *, *, #43863, .F. ) ;
#63437 = CARTESIAN_POINT ( 'NONE',  ( 8.899756207464411872, -2.372941743896879174, 30.88044141588253666 ) ) ;
#63438 = FACE_OUTER_BOUND ( 'NONE', #8005, .T. ) ;
#63439 = EDGE_CURVE ( 'NONE', #30233, #52641, #80031, .T. ) ;
#63440 = FACE_OUTER_BOUND ( 'NONE', #42746, .T. ) ;
#63441 = ORIENTED_EDGE ( 'NONE', *, *, #10205, .F. ) ;
#63442 = EDGE_CURVE ( 'NONE', #80730, #11720, #33621, .T. ) ;
#63443 = ORIENTED_EDGE ( 'NONE', *, *, #77262, .F. ) ;
#63444 = CARTESIAN_POINT ( 'NONE',  ( -6.700297254098854793, -8.540255544307065350, 34.89611431652622286 ) ) ;
#63445 = EDGE_LOOP ( 'NONE', ( #9646, #43163, #3781, #75888 ) ) ;
#63446 = EDGE_CURVE ( 'NONE', #27850, #9213, #1109, .T. ) ;
#63447 = B_SPLINE_CURVE_WITH_KNOTS ( 'NONE', 3,
 ( #47252, #73403, #11709, #74744, #87833, #46814, #13470, #80618, #40948, #26102 ),
 .UNSPECIFIED., .F., .F.,
 ( 4, 2, 2, 2, 4 ),
 ( 0.000000000000000000, 0.0001954339857564093175, 0.0003908679715128186350, 0.0005863019572692279796, 0.0007817359430256372700 ),
 .UNSPECIFIED. ) ;
#63448 = CARTESIAN_POINT ( 'NONE',  ( 12.59206416330202671, -9.417988943895561960, 34.36773134775777550 ) ) ;
#63449 = FACE_OUTER_BOUND ( 'NONE', #87636, .T. ) ;
#63450 = EDGE_CURVE ( 'NONE', #1602, #3325, #82807, .T. ) ;
#63451 = PLANE ( 'NONE',  #3488 ) ;
#63452 = DIRECTION ( 'NONE',  ( 0.000000000000000000, 0.1736481776669275834, 0.9848077530122086864 ) ) ;
#63453 = AXIS2_PLACEMENT_3D ( 'NONE', #80648, #81530, #18931 ) ;
#63454 = EDGE_LOOP ( 'NONE', ( #32009, #32686, #78870, #27937 ) ) ;
#63455 = ORIENTED_EDGE ( 'NONE', *, *, #86640, .F. ) ;
#63457 = VERTEX_POINT ( 'NONE', #75059 ) ;
#63456 = CARTESIAN_POINT ( 'NONE',  ( -2.530520405327184807, -7.369209533119137845, 34.99857337881830688 ) ) ;
#63458 = CARTESIAN_POINT ( 'NONE',  ( 16.21904013562951263, -2.506253911140448043, 29.99999999999988631 ) ) ;
#63459 = EDGE_LOOP ( 'NONE', ( #55436, #15097, #26681, #78987 ) ) ;
#63460 = CARTESIAN_POINT ( 'NONE',  ( -18.00000000000000000, -5.471508081941599322, 34.59228464037088457 ) ) ;
#63461 = CARTESIAN_POINT ( 'NONE',  ( 10.36538461538461675, -2.499999999999998668, 29.75000000000000355 ) ) ;
#63462 = ORIENTED_EDGE ( 'NONE', *, *, #24560, .T. ) ;
#63463 = CARTESIAN_POINT ( 'NONE',  ( 8.068933387422255521, -8.496831190052093419, 34.64984203495476578 ) ) ;
#63464 = ORIENTED_EDGE ( 'NONE', *, *, #33015, .T. ) ;
#63466 = ORIENTED_EDGE ( 'NONE', *, *, #1090, .F. ) ;
#63465 = CARTESIAN_POINT ( 'NONE',  ( -6.673022611438608642, -11.28795663066794219, 33.01431243580653785 ) ) ;
#63467 = DIRECTION ( 'NONE',  ( 1.000000000000000000, 0.000000000000000000, 0.000000000000000000 ) ) ;
#63468 = EDGE_CURVE ( 'NONE', #51615, #65753, #68289, .T. ) ;
#63469 = CARTESIAN_POINT ( 'NONE',  ( -15.90390063549801347, -3.712312575010499494, 33.01462480002815170 ) ) ;
#63470 = ORIENTED_EDGE ( 'NONE', *, *, #31288, .T. ) ;
#63471 = B_SPLINE_CURVE_WITH_KNOTS ( 'NONE', 3,
 ( #33773, #67122, #13059, #7188, #74320, #34658, #81528, #34208, #32886, #430 ),
 .UNSPECIFIED., .F., .F.,
 ( 4, 2, 2, 2, 4 ),
 ( 0.000000000000000000, 0.0001954311564186869286, 0.0003908623128373738573, 0.0005862934692560607588, 0.0007817246256747477145 ),
 .UNSPECIFIED. ) ;
#63472 = B_SPLINE_CURVE_WITH_KNOTS ( 'NONE', 3,
 ( #28056, #21741, #82577, #70375, #77573, #49655, #76690, #14993, #77129, #42911 ),
 .UNSPECIFIED., .F., .F.,
 ( 4, 2, 2, 2, 4 ),
 ( 0.000000000000000000, 0.0001954311564186879315, 0.0003908623128373758630, 0.0005862934692560637946, 0.0007817246256747517261 ),
 .UNSPECIFIED. ) ;
#63473 = AXIS2_PLACEMENT_3D ( 'NONE', #61853, #62297, #27634 ) ;
#63474 = CARTESIAN_POINT ( 'NONE',  ( 16.08857570788537572, -12.46129190929999986, 30.37095296980880832 ) ) ;
#63475 = CARTESIAN_POINT ( 'NONE',  ( 17.86985203026830149, -12.50552854090298638, 31.33409797877408920 ) ) ;
#63476 = FACE_BOUND ( 'NONE', #52029, .T. ) ;
#63477 = CARTESIAN_POINT ( 'NONE',  ( -9.692307692307814193, -4.320704448113951379, 33.92786785259630022 ) ) ;
#63478 = CARTESIAN_POINT ( 'NONE',  ( -11.78843828251013015, -6.524016743844655686, 34.90889640711025521 ) ) ;
#63479 = VECTOR ( 'NONE', #68914, 1000.000000000000227 ) ;
#63480 = CARTESIAN_POINT ( 'NONE',  ( 15.23076923076910916, -2.657715359629662544, 31.77849191805970364 ) ) ;
#63481 = LINE ( 'NONE', #27933, #28847 ) ;
#63482 = CARTESIAN_POINT ( 'NONE',  ( -11.53846153846165912, -3.300289026999228881, 32.46337939537708905 ) ) ;
#63483 = CARTESIAN_POINT ( 'NONE',  ( -16.28399412357785536, -2.647304123082328875, 31.75400227202885262 ) ) ;
#63484 = EDGE_LOOP ( 'NONE', ( #59652, #4074, #6319, #24592, #32393, #70541, #17170 ) ) ;
#63485 = CARTESIAN_POINT ( 'NONE',  ( 10.39189967166066708, -10.11188796281391511, 34.01382737946119050 ) ) ;
#63486 = EDGE_LOOP ( 'NONE', ( #20330, #74070, #64126, #61017 ) ) ;
#63487 = VERTEX_POINT ( 'NONE', #35389 ) ;
#63488 = VECTOR ( 'NONE', #22435, 1000.000000000000114 ) ;
#63489 = EDGE_CURVE ( 'NONE', #63457, #86663, #72889, .T. ) ;
#63491 = CARTESIAN_POINT ( 'NONE',  ( 16.37662569511455857, -12.24180327182771855, 31.33663988360758168 ) ) ;
#63490 = CARTESIAN_POINT ( 'NONE',  ( -5.207071046654769830, -12.15440758774515473, 32.17923288041532004 ) ) ;
#63492 = LINE ( 'NONE', #21177, #62872 ) ;
#63493 = CARTESIAN_POINT ( 'NONE',  ( -15.23076923076922995, -1.422936976036506707, 30.56769352161908415 ) ) ;
#63494 = CARTESIAN_POINT ( 'NONE',  ( -10.39260494640654819, -12.47679350104403007, 31.42216943046555855 ) ) ;
#63495 = CARTESIAN_POINT ( 'NONE',  ( 14.37375964104238513, -11.35647404775217595, 33.31231777344666511 ) ) ;
#63496 = ORIENTED_EDGE ( 'NONE', *, *, #33312, .F. ) ;
#63497 = CARTESIAN_POINT ( 'NONE',  ( 13.13459214732242408, -5.056417327199099532, 34.11270091957321426 ) ) ;
#63498 = CARTESIAN_POINT ( 'NONE',  ( 0.4615384615384611200, -8.973038597847269315, 34.52809138561121927 ) ) ;
#63499 = CARTESIAN_POINT ( 'NONE',  ( -12.71151520558705172, -11.47974371597208076, 33.17467449705390692 ) ) ;
#63500 = CARTESIAN_POINT ( 'NONE',  ( -16.82692307692165556, -7.500000000000154543, 35.00000000000007105 ) ) ;
#63501 = CYLINDRICAL_SURFACE ( 'NONE', #4606, 0.2500000000000002220 ) ;
#63502 = CARTESIAN_POINT ( 'NONE',  ( 2.320192649118979489E-14, -11.25000000000000000, 18.53125000000000000 ) ) ;
#63503 = ORIENTED_EDGE ( 'NONE', *, *, #33980, .F. ) ;
#63504 = ORIENTED_EDGE ( 'NONE', *, *, #23061, .F. ) ;
#63505 = EDGE_CURVE ( 'NONE', #41484, #36333, #41268, .T. ) ;
#63506 = DIRECTION ( 'NONE',  ( -1.000000000000000000, 0.000000000000000000, -0.000000000000000000 ) ) ;
#63507 = EDGE_LOOP ( 'NONE', ( #79651, #31352, #76701, #58339, #53706, #48951 ) ) ;
#63508 = CARTESIAN_POINT ( 'NONE',  ( 16.15384615384603251, -11.06231777344772027, 33.60647404775119895 ) ) ;
#63509 = CARTESIAN_POINT ( 'NONE',  ( 8.769230769230768274, -13.78497067705608181, 32.30358669280327177 ) ) ;
#63510 = LINE ( 'NONE', #76140, #26484 ) ;
#63511 = ADVANCED_FACE ( 'NONE', ( #68732 ), #54767, .F. ) ;
#63512 = DIRECTION ( 'NONE',  ( -0.000000000000000000, -0.9396926207859092051, -0.3420201433256662704 ) ) ;
#63513 = CARTESIAN_POINT ( 'NONE',  ( 3.749999999999992006, -5.946699141100872943, 14.39062500000000178 ) ) ;
#63514 = DIRECTION ( 'NONE',  ( -0.000000000000000000, 0.1736481776669307198, -0.9848077530122080203 ) ) ;
#63515 = ORIENTED_EDGE ( 'NONE', *, *, #56967, .F. ) ;
#63516 = DIRECTION ( 'NONE',  ( -0.000000000000000000, -0.9396926207859093161, -0.3420201433256663259 ) ) ;
#63518 = ORIENTED_EDGE ( 'NONE', *, *, #28620, .F. ) ;
#63517 = CARTESIAN_POINT ( 'NONE',  ( -1.319359813339359366, -9.442884908240271713, 34.35708131394835618 ) ) ;
#63519 = CARTESIAN_POINT ( 'NONE',  ( 3.007843013253082454, -12.39988816332205701, 30.74660775122750778 ) ) ;
#63520 = CARTESIAN_POINT ( 'NONE',  ( -0.6850233861027927862, -4.225889041578354544, 33.85425143139329407 ) ) ;
#63521 = AXIS2_PLACEMENT_3D ( 'NONE', #21837, #76785, #1565 ) ;
#63522 = CARTESIAN_POINT ( 'NONE',  ( 2.544871794871792936, -7.500000000000000000, 33.75000000000000000 ) ) ;
#63523 = CARTESIAN_POINT ( 'NONE',  ( 6.856994543716787405, -3.322132147404559976, 32.92929555188719348 ) ) ;
#63524 = ADVANCED_FACE ( 'NONE', ( #83142 ), #34939, .T. ) ;
#63525 = DIRECTION ( 'NONE',  ( 0.000000000000000000, -1.000000000000000000, 5.421010862427522170E-17 ) ) ;
#63526 = CARTESIAN_POINT ( 'NONE',  ( 0.06109907496451268821, -3.749999999999999556, 14.40811829374151110 ) ) ;
#63527 = ORIENTED_EDGE ( 'NONE', *, *, #50424, .F. ) ;
#63528 = CARTESIAN_POINT ( 'NONE',  ( -1.161835843346975539, -11.41317474335729187, 32.86274602512330034 ) ) ;
#63529 = CARTESIAN_POINT ( 'NONE',  ( -1.134560964701930796, -3.435999193479609470, 33.07426656108011542 ) ) ;
#63530 = CARTESIAN_POINT ( 'NONE',  ( -1.139087296526025916, -4.750000000000006217, 17.82812500000000000 ) ) ;
#63531 = EDGE_CURVE ( 'NONE', #998, #47096, #41966, .T. ) ;
#63532 = CARTESIAN_POINT ( 'NONE',  ( 0.2115152373170033073, -5.765609946408404518, 34.70566812827425451 ) ) ;
#63533 = CARTESIAN_POINT ( 'NONE',  ( -7.715628407920204879, -3.068774925481847493, 32.56582465632704526 ) ) ;
#63534 = EDGE_LOOP ( 'NONE', ( #30303, #80308 ) ) ;
#63535 = CARTESIAN_POINT ( 'NONE',  ( 2.750000000000001776, -7.499999999999984013, 15.71875000000000000 ) ) ;
#63536 = CARTESIAN_POINT ( 'NONE',  ( -2.307692307692427391, -3.300289026999228881, 32.46337939537708905 ) ) ;
#63537 = EDGE_CURVE ( 'NONE', #65576, #46336, #28641, .T. ) ;
#63538 = EDGE_LOOP ( 'NONE', ( #76570, #25049, #35437, #77859 ) ) ;
#63539 = DIRECTION ( 'NONE',  ( 1.000000000000000000, 0.000000000000000000, 0.000000000000000000 ) ) ;
#63540 = CYLINDRICAL_SURFACE ( 'NONE', #28445, 0.2499999999999986955 ) ;
#63541 = VERTEX_POINT ( 'NONE', #49353 ) ;
#63542 = DIRECTION ( 'NONE',  ( 0.000000000000000000, 0.000000000000000000, 1.000000000000000000 ) ) ;
#63543 = CARTESIAN_POINT ( 'NONE',  ( 4.153846153846032507, -3.835265460704628371, 33.15142922262033665 ) ) ;
#63544 = ADVANCED_FACE ( 'NONE', ( #76830 ), #13344, .F. ) ;
#63545 = CARTESIAN_POINT ( 'NONE',  ( 8.769230769230768274, -12.78798330534103123, 29.99999999999997868 ) ) ;
#63546 = LINE ( 'NONE', #14934, #63769 ) ;
#63547 = EDGE_LOOP ( 'NONE', ( #33986, #76979, #18186 ) ) ;
#63548 = CARTESIAN_POINT ( 'NONE',  ( 7.846153846153846700, -8.164416787775445883, 34.95778746994557906 ) ) ;
#63549 = ADVANCED_FACE ( 'NONE', ( #20545 ), #82704, .F. ) ;
#63550 = AXIS2_PLACEMENT_3D ( 'NONE', #25058, #52520, #44417 ) ;
#63551 = ORIENTED_EDGE ( 'NONE', *, *, #57127, .F. ) ;
#63552 = CARTESIAN_POINT ( 'NONE',  ( 12.21156171748987163, -12.01397095200674059, 32.43157075238190146 ) ) ;
#63553 = CARTESIAN_POINT ( 'NONE',  ( -10.83831083290075981, -2.758268499246657068, 31.33685645148948140 ) ) ;
#63554 = ORIENTED_EDGE ( 'NONE', *, *, #43191, .F. ) ;
#63555 = EDGE_CURVE ( 'NONE', #54624, #38474, #10853, .T. ) ;
#63556 = CARTESIAN_POINT ( 'NONE',  ( -5.749945688361685292, -11.28795663066794219, 33.01431243580653785 ) ) ;
#63557 = CARTESIAN_POINT ( 'NONE',  ( -17.06410256410256565, -3.499999999999999556, 29.75000000000000355 ) ) ;
#63558 = CYLINDRICAL_SURFACE ( 'NONE', #9228, 0.2499999999999994726 ) ;
#63559 = VECTOR ( 'NONE', #70076, 1000.000000000000227 ) ;
#63560 = DIRECTION ( 'NONE',  ( 0.000000000000000000, 0.3420201433256610524, 0.9396926207859113145 ) ) ;
#63561 = LINE ( 'NONE', #84301, #61283 ) ;
#63562 = ORIENTED_EDGE ( 'NONE', *, *, #12424, .F. ) ;
#63563 = EDGE_LOOP ( 'NONE', ( #89076, #996 ) ) ;
#63564 = FACE_BOUND ( 'NONE', #15431, .T. ) ;
#63565 = VERTEX_POINT ( 'NONE', #44344 ) ;
#63567 = EDGE_CURVE ( 'NONE', #16683, #83747, #34452, .T. ) ;
#63566 = CARTESIAN_POINT ( 'NONE',  ( 15.00728428704528561, -12.44517049084099725, 30.48991314939691932 ) ) ;
#63568 = CARTESIAN_POINT ( 'NONE',  ( -20.74999999999999645, -4.499999999999999112, 29.75000000000000355 ) ) ;
#63569 = EDGE_CURVE ( 'NONE', #19556, #23382, #24087, .T. ) ;
#63570 = CARTESIAN_POINT ( 'NONE',  ( 6.130525438233644486, -3.068774925481847937, 32.56582465632704526 ) ) ;
#63571 = CARTESIAN_POINT ( 'NONE',  ( -14.17716660592874689, -9.417988943895561960, 34.36773134775777550 ) ) ;
#63572 = B_SPLINE_CURVE_WITH_KNOTS ( 'NONE', 3,
 ( #34449, #53384, #19166, #74113, #12407, #39891, #33120, #47064, #60586, #81322 ),
 .UNSPECIFIED., .F., .F.,
 ( 4, 2, 2, 2, 4 ),
 ( 0.000000000000000000, 0.0001954339857564099951, 0.0003908679715128199903, 0.0005863019572692300396, 0.0007817359430256399806 ),
 .UNSPECIFIED. ) ;
#63573 = ORIENTED_EDGE ( 'NONE', *, *, #25311, .T. ) ;
#63574 = ORIENTED_EDGE ( 'NONE', *, *, #59866, .T. ) ;
#63575 = VERTEX_POINT ( 'NONE', #16449 ) ;
#63576 = AXIS2_PLACEMENT_3D ( 'NONE', #85120, #51744, #78792 ) ;
#63577 = CARTESIAN_POINT ( 'NONE',  ( -2.939152317953646711E-15, 7.500000000000000000, 0.000000000000000000 ) ) ;
#63578 = VERTEX_POINT ( 'NONE', #79037 ) ;
#63579 = EDGE_CURVE ( 'NONE', #46007, #69974, #22652, .T. ) ;
#63580 = CARTESIAN_POINT ( 'NONE',  ( 13.13459214732242053, -2.823816976329317274, 31.52131813110795733 ) ) ;
#63581 = CARTESIAN_POINT ( 'NONE',  ( -2.531177232256638820, -12.47654668319379567, 31.42292124445336654 ) ) ;
#63582 = EDGE_CURVE ( 'NONE', #84853, #63945, #9722, .T. ) ;
#63583 = CARTESIAN_POINT ( 'NONE',  ( -17.30040800148741198, -3.019605429927187501, 32.48692288466676814 ) ) ;
#63584 = ORIENTED_EDGE ( 'NONE', *, *, #77344, .F. ) ;
#63585 = CARTESIAN_POINT ( 'NONE',  ( -8.546217925137373328, -4.026326845037962343, 33.68677907613344047 ) ) ;
#63586 = EDGE_CURVE ( 'NONE', #30665, #18168, #67130, .T. ) ;
#63587 = DIRECTION ( 'NONE',  ( -1.000000000000000000, 0.000000000000000000, -0.000000000000000000 ) ) ;
#63588 = CARTESIAN_POINT ( 'NONE',  ( -17.74989548036563036, -7.568793089027813004, 35.00000000000000711 ) ) ;
#63589 = PLANE ( 'NONE',  #31798 ) ;
#63590 = EDGE_LOOP ( 'NONE', ( #83548, #34062, #12, #34681 ) ) ;
#63591 = ORIENTED_EDGE ( 'NONE', *, *, #39750, .T. ) ;
#63592 = EDGE_LOOP ( 'NONE', ( #86978, #22419 ) ) ;
#63594 = ADVANCED_FACE ( 'NONE', ( #44795 ), #2478, .F. ) ;
#63593 = CARTESIAN_POINT ( 'NONE',  ( 3.100159575565149428, -7.722926974430166069, 34.99546784045485737 ) ) ;
#63596 = CARTESIAN_POINT ( 'NONE',  ( -9.692307692307814193, -8.656820664282941280, 34.87096338111179961 ) ) ;
#63595 = CYLINDRICAL_SURFACE ( 'NONE', #66245, 4.000000000000000000 ) ;
#63597 = CYLINDRICAL_SURFACE ( 'NONE', #87409, 0.2499999999999986955 ) ;
#63598 = LINE ( 'NONE', #82996, #62409 ) ;
#63599 = FACE_BOUND ( 'NONE', #65455, .T. ) ;
#63600 = DIRECTION ( 'NONE',  ( -0.000000000000000000, 0.9396926207859092051, -0.3420201433256662704 ) ) ;
#63601 = VERTEX_POINT ( 'NONE', #65066 ) ;
#63602 = CARTESIAN_POINT ( 'NONE',  ( -2.544871794871794268, -3.499999999999999556, 29.75000000000000355 ) ) ;
#63603 = CARTESIAN_POINT ( 'NONE',  ( 19.00000000000000000, -8.999999999999996447, 22.25000000000000000 ) ) ;
#63604 = DIRECTION ( 'NONE',  ( -0.000000000000000000, 0.3420201433256694346, -0.9396926207859080948 ) ) ;
#63605 = CARTESIAN_POINT ( 'NONE',  ( -11.40793583669797151, -3.816742781228458004, 33.13167719472716044 ) ) ;
#63606 = EDGE_LOOP ( 'NONE', ( #5850, #71850 ) ) ;
#63607 = DIRECTION ( 'NONE',  ( 0.000000000000000000, 0.000000000000000000, 1.000000000000000000 ) ) ;
#63608 = VERTEX_POINT ( 'NONE', #84040 ) ;
#63609 = FACE_BOUND ( 'NONE', #60690, .T. ) ;
#63610 = B_SPLINE_CURVE_WITH_KNOTS ( 'NONE', 3,
 ( #42511, #76282, #48366, #35757, #34851, #62757, #63205, #633, #69528, #1522 ),
 .UNSPECIFIED., .F., .F.,
 ( 4, 2, 2, 2, 4 ),
 ( 0.0007817246256747446788, 0.0009771112852218872494, 0.001172497944769029929, 0.001367884604316172391, 0.001563271263863315070 ),
 .UNSPECIFIED. ) ;
#63612 = VECTOR ( 'NONE', #69278, 1000.000000000000000 ) ;
#63611 = CARTESIAN_POINT ( 'NONE',  ( -16.85414353565466072, -4.387253974876675677, 33.66317474335728832 ) ) ;
#63613 = B_SPLINE_CURVE_WITH_KNOTS ( 'NONE', 3,
 ( #17097, #3576, #9897, #23404, #72037, #50862, #36496, #44551, #52208, #10346 ),
 .UNSPECIFIED., .F., .F.,
 ( 4, 2, 2, 2, 4 ),
 ( 0.0007817359430256360774, 0.0009771253907250041296, 0.001172514838424371965, 0.001367904286123740017, 0.001563293733823108069 ),
 .UNSPECIFIED. ) ;
#63614 = CARTESIAN_POINT ( 'NONE',  ( 14.30769230769231015, -1.044019251281081972, 31.83374038241031911 ) ) ;
#63615 = CARTESIAN_POINT ( 'NONE',  ( 14.05771557674995442, -11.79746400365624659, 32.30657167506340954 ) ) ;
#63616 = ORIENTED_EDGE ( 'NONE', *, *, #44942, .T. ) ;
#63617 = CARTESIAN_POINT ( 'NONE',  ( 11.78851595837499211, -10.82426656108012075, 33.81400080652039009 ) ) ;
#63618 = CARTESIAN_POINT ( 'NONE',  ( -18.00000000000000000, -3.937682226553330445, 33.60647404775216529 ) ) ;
#63619 = CARTESIAN_POINT ( 'NONE',  ( -10.61538461538461320, -1.422936976036506707, 30.56769352161908415 ) ) ;
#63620 = EDGE_CURVE ( 'NONE', #67687, #15943, #3372, .T. ) ;
#63621 = CARTESIAN_POINT ( 'NONE',  ( -5.076923076923199218, -5.941354392335915335, 34.76329471203413846 ) ) ;
#63622 = VERTEX_POINT ( 'NONE', #63300 ) ;
#63623 = VECTOR ( 'NONE', #66442, 1000.000000000000000 ) ;
#63624 = FACE_OUTER_BOUND ( 'NONE', #71597, .T. ) ;
#63625 = ORIENTED_EDGE ( 'NONE', *, *, #85635, .T. ) ;
#63627 = ORIENTED_EDGE ( 'NONE', *, *, #16714, .T. ) ;
#63626 = CARTESIAN_POINT ( 'NONE',  ( 13.63456090296352485, -12.22109172314383052, 31.39792113162168263 ) ) ;
#63628 = CARTESIAN_POINT ( 'NONE',  ( 11.76147289007438701, -6.503523203565941380, 34.64991518177335195 ) ) ;
#63629 = CARTESIAN_POINT ( 'NONE',  ( -10.68065506134539078, -12.46129190929999986, 30.37095296980880832 ) ) ;
#63630 = CYLINDRICAL_SURFACE ( 'NONE', #81764, 0.2499999999999994726 ) ;
#63631 = DIRECTION ( 'NONE',  ( -0.000000000000000000, -0.3420201433256694901, -0.9396926207859082059 ) ) ;
#63633 = CARTESIAN_POINT ( 'NONE',  ( 18.00000000000000000, -4.661471528628507777, 34.16647553114623292 ) ) ;
#63632 = CARTESIAN_POINT ( 'NONE',  ( 9.019230769230784261, -2.249999999999997780, 29.81603969181030322 ) ) ;
#63634 = CARTESIAN_POINT ( 'NONE',  ( 12.23865977910981506, -7.630691491037285168, 34.74850469731152458 ) ) ;
#63635 = CARTESIAN_POINT ( 'NONE',  ( 2.749999999999995115, -6.360912703473971419, 23.14062500000000000 ) ) ;
#63636 =( REPRESENTATION_RELATIONSHIP ('NONE','NONE', #51743, #11527 ) REPRESENTATION_RELATIONSHIP_WITH_TRANSFORMATION ( #86114 )SHAPE_REPRESENTATION_RELATIONSHIP( ) );
#63637 = VERTEX_POINT ( 'NONE', #56550 ) ;
#63638 = CARTESIAN_POINT ( 'NONE',  ( -0.5916856709766816769, -6.001485441113819874, 34.52039167877662607 ) ) ;
#63639 = DIRECTION ( 'NONE',  ( -0.000000000000000000, 1.000000000000000000, -0.000000000000000000 ) ) ;
#63640 = ORIENTED_EDGE ( 'NONE', *, *, #27657, .F. ) ;
#63641 = ORIENTED_EDGE ( 'NONE', *, *, #73537, .F. ) ;
#63642 = ORIENTED_EDGE ( 'NONE', *, *, #20116, .T. ) ;
#63643 = CARTESIAN_POINT ( 'NONE',  ( 16.94677586748485965, -5.195881422630167279, 34.18770438780618548 ) ) ;
#63644 = DIRECTION ( 'NONE',  ( 0.000000000000000000, 0.7660444431189807890, 0.6427876096865361433 ) ) ;
#63645 = CARTESIAN_POINT ( 'NONE',  ( 0.7115384615398802071, -7.500000000000154543, 35.00000000000007105 ) ) ;
#63646 = CARTESIAN_POINT ( 'NONE',  ( 10.61538461538461675, -6.343179335718451384, 34.87096338111211935 ) ) ;
#63647 = CARTESIAN_POINT ( 'NONE',  ( -9.019207513279360100, -2.544273027872575366, 31.48422191005632342 ) ) ;
#63648 = CARTESIAN_POINT ( 'NONE',  ( 20.74999999999999645, -2.499999999999999556, 29.75000000000000355 ) ) ;
#63649 = CIRCLE ( 'NONE', #24809, 4.000000000000000000 ) ;
#63650 = CYLINDRICAL_SURFACE ( 'NONE', #36489, 0.2499999999999995559 ) ;
#63651 = CARTESIAN_POINT ( 'NONE',  ( -8.769230769230892619, -2.379036618888197729, 30.90682066428292885 ) ) ;
#63652 = LINE ( 'NONE', #57341, #41977 ) ;
#63653 = EDGE_CURVE ( 'NONE', #56750, #32572, #70509, .T. ) ;
#63654 = B_SPLINE_CURVE_WITH_KNOTS ( 'NONE', 3,
 ( #13451, #18886, #5817, #53995, #20653, #33294 ),
 .UNSPECIFIED., .F., .F.,
 ( 4, 2, 4 ),
 ( 0.0003909512603273828648, 0.0005862562993132068752, 0.0007815613382990308855 ),
 .UNSPECIFIED. ) ;
#63655 = B_SPLINE_CURVE_WITH_KNOTS ( 'NONE', 3,
 ( #62476, #89103, #69252, #67926, #35017, #6231, #53508, #88664, #81005, #46764 ),
 .UNSPECIFIED., .F., .F.,
 ( 4, 2, 2, 2, 4 ),
 ( 0.0007817359430256328248, 0.0009771253907249995759, 0.001172514838424366327, 0.001367904286123732861, 0.001563293733823099612 ),
 .UNSPECIFIED. ) ;
#63656 = FACE_OUTER_BOUND ( 'NONE', #3772, .T. ) ;
#63657 = B_SPLINE_CURVE_WITH_KNOTS ( 'NONE', 3,
 ( #5786, #34138, #54406, #47205, #40905, #5344, #12987, #60275, #75563, #40032 ),
 .UNSPECIFIED., .F., .F.,
 ( 4, 2, 2, 2, 4 ),
 ( 0.0007817246256747440282, 0.0009771112852218863821, 0.001172497944769028844, 0.001367884604316171307, 0.001563271263863313769 ),
 .UNSPECIFIED. ) ;
#63658 = FACE_OUTER_BOUND ( 'NONE', #24725, .T. ) ;
#63659 = EDGE_CURVE ( 'NONE', #33070, #84431, #63743, .T. ) ;
#63660 = ORIENTED_EDGE ( 'NONE', *, *, #75116, .T. ) ;
#63661 = CARTESIAN_POINT ( 'NONE',  ( 15.10062202133100939, -11.47017969459903952, 32.78971311882035167 ) ) ;
#63662 = CARTESIAN_POINT ( 'NONE',  ( -2.307692307692305711, -8.973038597847269315, 34.52809138561121927 ) ) ;
#63663 = CARTESIAN_POINT ( 'NONE',  ( 12.68454981315131214, -10.61302985866384141, 33.66295027996417843 ) ) ;
#63664 = VERTEX_POINT ( 'NONE', #22753 ) ;
#63665 = EDGE_CURVE ( 'NONE', #74089, #41980, #19121, .T. ) ;
#63666 = PLANE ( 'NONE',  #67942 ) ;
#63667 = CARTESIAN_POINT ( 'NONE',  ( -17.07692307692319744, -3.835265460704628815, 33.15142922262033665 ) ) ;
#63668 = ADVANCED_FACE ( 'NONE', ( #25430 ), #66416, .F. ) ;
#63669 = CARTESIAN_POINT ( 'NONE',  ( -12.39547011053602432, -10.51840700105979565, 33.73612834413962247 ) ) ;
#63670 = EDGE_LOOP ( 'NONE', ( #57914, #679 ) ) ;
#63671 = CARTESIAN_POINT ( 'NONE',  ( -13.38461538461538325, -9.780366693483667717, 34.19971097300155094 ) ) ;
#63672 = ORIENTED_EDGE ( 'NONE', *, *, #58091, .T. ) ;
#63673 = EDGE_CURVE ( 'NONE', #41990, #6248, #66684, .T. ) ;
#63674 = CARTESIAN_POINT ( 'NONE',  ( 9.942253210655835005, -11.86320923018887719, 32.19269448109604070 ) ) ;
#63675 = AXIS2_PLACEMENT_3D ( 'NONE', #59584, #57917, #70993 ) ;
#63676 = CARTESIAN_POINT ( 'NONE',  ( 6.989144256426999213, -2.833524468853757750, 32.15551576947925838 ) ) ;
#63677 = DIRECTION ( 'NONE',  ( -0.000000000000000000, 1.000000000000000000, -0.000000000000000000 ) ) ;
#63678 = CARTESIAN_POINT ( 'NONE',  ( -12.46153846153846168, -3.937682226553329556, 33.60647404775216529 ) ) ;
#63679 = CARTESIAN_POINT ( 'NONE',  ( 1.384615384615386802, -13.53365097954675988, 30.81389545987213552 ) ) ;
#63680 = B_SPLINE_CURVE_WITH_KNOTS ( 'NONE', 3,
 ( #85102, #77453, #78327, #56737, #57179, #56298, #84232, #49543, #15317, #42794 ),
 .UNSPECIFIED., .F., .F.,
 ( 4, 2, 2, 2, 4 ),
 ( 0.0007817359430256372700, 0.0009771253907250054306, 0.001172514838424373483, 0.001367904286123741535, 0.001563293733823109804 ),
 .UNSPECIFIED. ) ;
#63681 = ORIENTED_EDGE ( 'NONE', *, *, #24896, .F. ) ;
#63682 = B_SPLINE_CURVE_WITH_KNOTS ( 'NONE', 3,
 ( #45151, #18585, #51436, #10934, #73076, #79395, #58221, #37960, #12262, #79841 ),
 .UNSPECIFIED., .F., .F.,
 ( 4, 2, 2, 2, 4 ),
 ( 0.000000000000000000, 0.0001954339881912772715, 0.0003908679763825545429, 0.0005863019645738318415, 0.0007817359527651090859 ),
 .UNSPECIFIED. ) ;
#63683 = B_SPLINE_CURVE_WITH_KNOTS ( 'NONE', 3,
 ( #81590, #11800, #4133, #39279, #66736, #18113, #38376, #65830, #81152, #5034 ),
 .UNSPECIFIED., .F., .F.,
 ( 4, 2, 2, 2, 4 ),
 ( 0.0007817246256747504250, 0.0009771112852218954894, 0.001172497944769040554, 0.001367884604316185401, 0.001563271263863330466 ),
 .UNSPECIFIED. ) ;
#63684 = EDGE_LOOP ( 'NONE', ( #29806, #20507 ) ) ;
#63685 = ORIENTED_EDGE ( 'NONE', *, *, #11488, .F. ) ;
#63686 = DIRECTION ( 'NONE',  ( 0.000000000000000000, 0.3420201433256641055, -0.9396926207859100932 ) ) ;
#63687 = CARTESIAN_POINT ( 'NONE',  ( 16.15384615384603251, -5.941354392335915335, 34.76329471203413846 ) ) ;
#63688 = ADVANCED_FACE ( 'NONE', ( #73636 ), #73178, .F. ) ;
#63689 = CARTESIAN_POINT ( 'NONE',  ( -4.377331078410485077, -12.47654668319379567, 31.42292124445336654 ) ) ;
#63690 = CARTESIAN_POINT ( 'NONE',  ( 11.40777007179397984, -12.11776431015576172, 31.66791131148498906 ) ) ;
#63691 = CARTESIAN_POINT ( 'NONE',  ( 7.715678661078126943, -7.276987145209185215, 34.99546412871779211 ) ) ;
#63692 = CARTESIAN_POINT ( 'NONE',  ( 17.99999999999987566, -12.46129190930018460, 30.37095296980731973 ) ) ;
#63693 = ORIENTED_EDGE ( 'NONE', *, *, #13412, .F. ) ;
#63694 = VERTEX_POINT ( 'NONE', #52446 ) ;
#63695 = VERTEX_POINT ( 'NONE', #5605 ) ;
#63698 = ORIENTED_EDGE ( 'NONE', *, *, #5566, .T. ) ;
#63697 = ADVANCED_FACE ( 'NONE', ( #19557 ), #80388, .F. ) ;
#63696 = CARTESIAN_POINT ( 'NONE',  ( 12.52760681254089903, -8.120952969808772792, 34.71129190929999453 ) ) ;
#63699 = AXIS2_PLACEMENT_3D ( 'NONE', #35404, #55668, #293 ) ;
#63701 = CARTESIAN_POINT ( 'NONE',  ( -10.39237177129122003, -6.460100341425560444, 34.89618726649961644 ) ) ;
#63700 = CARTESIAN_POINT ( 'NONE',  ( -9.758391103263571509, -8.973038597847271092, 34.52809138561120506 ) ) ;
#63702 = CARTESIAN_POINT ( 'NONE',  ( 3.750000000000000888, -7.499999999999978684, 23.21875000000000000 ) ) ;
#63703 = ORIENTED_EDGE ( 'NONE', *, *, #27715, .T. ) ;
#63704 = EDGE_CURVE ( 'NONE', #54661, #85662, #5433, .T. ) ;
#63705 = ORIENTED_EDGE ( 'NONE', *, *, #45844, .T. ) ;
#63706 = CARTESIAN_POINT ( 'NONE',  ( 4.854043560185492545, -7.630690623152302621, 34.99857592706774057 ) ) ;
#63707 = ORIENTED_EDGE ( 'NONE', *, *, #36863, .F. ) ;
#63708 = FACE_BOUND ( 'NONE', #53686, .T. ) ;
#63709 = B_SPLINE_CURVE_WITH_KNOTS ( 'NONE', 3,
 ( #370, #76910, #82348, #35930, #63384, #70146, #8458, #1692, #29182, #56635 ),
 .UNSPECIFIED., .F., .F.,
 ( 4, 2, 2, 2, 4 ),
 ( 0.0007817246256747460882, 0.0009771112852218900684, 0.001172497944769033832, 0.001367884604316177595, 0.001563271263863321575 ),
 .UNSPECIFIED. ) ;
#63710 = CARTESIAN_POINT ( 'NONE',  ( -19.00000000000000000, -8.999999999999996447, 22.25000000000000000 ) ) ;
#63711 = FACE_OUTER_BOUND ( 'NONE', #52689, .T. ) ;
#63712 = VERTEX_POINT ( 'NONE', #45696 ) ;
#63713 = CARTESIAN_POINT ( 'NONE',  ( 15.48076923077065103, -7.500000000000154543, 35.00000000000007105 ) ) ;
#63714 = CARTESIAN_POINT ( 'NONE',  ( 3.296024802045256941, -3.300289026998474817, 32.46337939537591666 ) ) ;
#63715 = DIRECTION ( 'NONE',  ( 1.000000000000000000, 0.000000000000000000, 0.000000000000000000 ) ) ;
#63716 = CARTESIAN_POINT ( 'NONE',  ( -11.53846153846153655, -5.557115091759785130, 34.35708131394839171 ) ) ;
#63717 = CARTESIAN_POINT ( 'NONE',  ( 4.219914504848592429, -3.050289026998446840, 32.03036669348366416 ) ) ;
#63718 = ADVANCED_FACE ( 'NONE', ( #3818 ), #46150, .F. ) ;
#63719 = CARTESIAN_POINT ( 'NONE',  ( 4.153846153846154188, -4.098570777380720287, 33.41473453929634729 ) ) ;
#63720 = CARTESIAN_POINT ( 'NONE',  ( -7.846153846153965716, -6.879047030192662504, 34.71129190930017927 ) ) ;
#63722 = B_SPLINE_CURVE_WITH_KNOTS ( 'NONE', 3,
 ( #52514, #79998, #11095, #25052, #19187, #80454, #12428, #46657, #41564, #38572 ),
 .UNSPECIFIED., .F., .F.,
 ( 4, 2, 2, 2, 4 ),
 ( 0.000000000000000000, 0.0001954311564186867931, 0.0003908623128373735862, 0.0005862934692560603251, 0.0007817246256747473893 ),
 .UNSPECIFIED. ) ;
#63721 = CYLINDRICAL_SURFACE ( 'NONE', #51316, 4.000000000000000000 ) ;
#63723 = DIRECTION ( 'NONE',  ( 0.000000000000000000, 0.000000000000000000, -1.000000000000000000 ) ) ;
#63724 = EDGE_CURVE ( 'NONE', #25656, #22888, #64581, .T. ) ;
#63726 = EDGE_CURVE ( 'NONE', #17306, #879, #28086, .T. ) ;
#63725 = CARTESIAN_POINT ( 'NONE',  ( -18.22348494372394967, -6.760086850603067354, 34.69517049084099369 ) ) ;
#63727 = CARTESIAN_POINT ( 'NONE',  ( 8.900021210197719412, -3.957578996910242619, 33.62503395064540257 ) ) ;
#63729 = CARTESIAN_POINT ( 'NONE',  ( 11.53846153846141753, -4.481592998941358097, 33.73612834414048933 ) ) ;
#63728 = CARTESIAN_POINT ( 'NONE',  ( 17.14299142792552288, -3.513871655860379306, 32.76840700105978499 ) ) ;
#63730 = CARTESIAN_POINT ( 'NONE',  ( 1.384615384615386802, -11.16473453929635440, 33.15142922261926373 ) ) ;
#63732 = CARTESIAN_POINT ( 'NONE',  ( 8.834486340506794377, -2.892918686051625166, 31.69288490824026638 ) ) ;
#63731 = LINE ( 'NONE', #49341, #48716 ) ;
#63733 = CARTESIAN_POINT ( 'NONE',  ( 13.13461538461538325, -7.566082377512564960, 35.00000000000000711 ) ) ;
#63734 = CARTESIAN_POINT ( 'NONE',  ( -1.200186371490556958, -4.775308065498765409, 23.82625670625849068 ) ) ;
#63735 = EDGE_CURVE ( 'NONE', #58651, #14505, #7664, .T. ) ;
#63736 = ORIENTED_EDGE ( 'NONE', *, *, #2573, .F. ) ;
#63737 = STYLED_ITEM ( 'NONE', ( #54742 ), #28450 ) ;
#63738 = CARTESIAN_POINT ( 'NONE',  ( 3.446590374638324406, -6.824229032706653264, 14.00000000000008349 ) ) ;
#63739 = ORIENTED_EDGE ( 'NONE', *, *, #64682, .F. ) ;
#63740 = CIRCLE ( 'NONE', #27801, 4.000000000000000000 ) ;
#63741 = CARTESIAN_POINT ( 'NONE',  ( 9.469381474791545017, -6.503392248772476236, 34.64988816332204635 ) ) ;
#63742 = VERTEX_POINT ( 'NONE', #21775 ) ;
#63743 = LINE ( 'NONE', #2044, #2364 ) ;
#63744 = CARTESIAN_POINT ( 'NONE',  ( 17.14299041027315695, -2.833524468853757750, 32.15551576947925838 ) ) ;
#63745 = VERTEX_POINT ( 'NONE', #55554 ) ;
#63746 = CARTESIAN_POINT ( 'NONE',  ( -6.130147209438219669, -11.93770438780619259, 32.05411857736982029 ) ) ;
#63747 = CARTESIAN_POINT ( 'NONE',  ( -1.987747218494660295, -5.598659921968651254, 23.74813170625849068 ) ) ;
#63748 = CARTESIAN_POINT ( 'NONE',  ( 5.999999999999878320, -6.835583212225970762, 34.95778746994575670 ) ) ;
#63749 = VECTOR ( 'NONE', #83527, 1000.000000000000000 ) ;
#63750 = DIRECTION ( 'NONE',  ( 0.000000000000000000, 0.000000000000000000, 1.000000000000000000 ) ) ;
#63751 = CARTESIAN_POINT ( 'NONE',  ( 18.00000000000000000, -2.292212530054420494, 30.41441678777542634 ) ) ;
#63752 = CARTESIAN_POINT ( 'NONE',  ( 15.00728430620490172, -8.539481045369596401, 34.89627647299170832 ) ) ;
#63753 = CARTESIAN_POINT ( 'NONE',  ( 11.47319109250076430, -2.892918686051582533, 31.69288490824015980 ) ) ;
#63754 = CARTESIAN_POINT ( 'NONE',  ( -13.51530598772569114, -11.93127051446799847, 32.56575433478202797 ) ) ;
#63755 = CARTESIAN_POINT ( 'NONE',  ( 3.749999999999992006, -5.946699141100872943, 14.39062500000000178 ) ) ;
#63756 = CARTESIAN_POINT ( 'NONE',  ( -9.915233909823841785, -3.586966769969701208, 32.86292498521069660 ) ) ;
#63757 = CARTESIAN_POINT ( 'NONE',  ( 10.68145296638705410, -11.16473453929635440, 33.15142922261926373 ) ) ;
#63758 = LINE ( 'NONE', #16467, #75228 ) ;
#63759 = CARTESIAN_POINT ( 'NONE',  ( -2.651650429449565305, -4.848349570550461785, 16.50000000000000000 ) ) ;
#63760 = EDGE_CURVE ( 'NONE', #13945, #36896, #76415, .T. ) ;
#63761 = CARTESIAN_POINT ( 'NONE',  ( 19.00000000000000000, -11.00000000000000000, 29.75000000000000355 ) ) ;
#63762 = ORIENTED_EDGE ( 'NONE', *, *, #46483, .T. ) ;
#63763 = LINE ( 'NONE', #300, #2493 ) ;
#63764 = CARTESIAN_POINT ( 'NONE',  ( 12.33084785842815378, -8.191372820521381826, 34.95448215188423546 ) ) ;
#63765 = CARTESIAN_POINT ( 'NONE',  ( -9.019254006523732770, -11.37209801155882971, 32.91403422569032955 ) ) ;
#63766 = DIRECTION ( 'NONE',  ( -1.000000000000000000, 0.000000000000000000, 0.000000000000000000 ) ) ;
#63767 = CARTESIAN_POINT ( 'NONE',  ( -16.21911659980693443, -10.90142922261923886, 33.41473453929638993 ) ) ;
#63768 = CARTESIAN_POINT ( 'NONE',  ( -8.992156986746914882, -8.239355502252617924, 34.69524867566427417 ) ) ;
#63769 = VECTOR ( 'NONE', #51331, 1000.000000000000000 ) ;
#63770 = EDGE_CURVE ( 'NONE', #5574, #61908, #3337, .T. ) ;
#63771 = VECTOR ( 'NONE', #16821, 1000.000000000000227 ) ;
#63772 = CARTESIAN_POINT ( 'NONE',  ( -8.769230769230768274, -1.117168528481311540, 33.14645433367849847 ) ) ;
#63773 = EDGE_LOOP ( 'NONE', ( #57570, #61234 ) ) ;
#63774 = ORIENTED_EDGE ( 'NONE', *, *, #43191, .T. ) ;
#63775 = ADVANCED_FACE ( 'NONE', ( #67751 ), #14131, .F. ) ;
#63776 = B_SPLINE_CURVE_WITH_KNOTS ( 'NONE', 3,
 ( #15606, #22356, #30442, #23239, #71417, #65101, #30005, #9299, #50700, #79077 ),
 .UNSPECIFIED., .F., .F.,
 ( 4, 2, 2, 2, 4 ),
 ( 0.0007817359430256391132, 0.0009771253907250075990, 0.001172514838424375868, 0.001367904286123744354, 0.001563293733823112840 ),
 .UNSPECIFIED. ) ;
#63777 = ORIENTED_EDGE ( 'NONE', *, *, #86960, .T. ) ;
#63778 = CYLINDRICAL_SURFACE ( 'NONE', #84444, 5.000000000000000888 ) ;
#63779 = CARTESIAN_POINT ( 'NONE',  ( -3.230769230769229949, -9.905515769479276145, 34.41647553114623292 ) ) ;
#63780 = CARTESIAN_POINT ( 'NONE',  ( -5.076923076923075762, -13.53365097954675988, 30.81389545987213552 ) ) ;
#63781 = CARTESIAN_POINT ( 'NONE',  ( -6.066083410955878108, -3.050289026998445951, 32.03036669348365706 ) ) ;
#63782 = DIRECTION ( 'NONE',  ( -0.000000000000000000, 1.000000000000000000, 3.491481338843133355E-15 ) ) ;
#63784 = EDGE_CURVE ( 'NONE', #74008, #56240, #51328, .T. ) ;
#63783 = ORIENTED_EDGE ( 'NONE', *, *, #78582, .T. ) ;
#63785 = CARTESIAN_POINT ( 'NONE',  ( 17.07692307692307665, -9.584722331328613620, 36.20867863119891439 ) ) ;
#63786 = VERTEX_POINT ( 'NONE', #13687 ) ;
#63787 = VERTEX_POINT ( 'NONE', #82158 ) ;
#63789 = ORIENTED_EDGE ( 'NONE', *, *, #48060, .F. ) ;
#63788 = CARTESIAN_POINT ( 'NONE',  ( -4.153846153846152411, -8.973038597847269315, 34.52809138561121927 ) ) ;
#63790 = LINE ( 'NONE', #29579, #56035 ) ;
#63791 = CARTESIAN_POINT ( 'NONE',  ( -10.61538461538473399, -5.219633306517616589, 34.19971097300220464 ) ) ;
#63792 = VECTOR ( 'NONE', #60784, 1000.000000000000000 ) ;
#63793 = CIRCLE ( 'NONE', #75323, 4.000000000000000000 ) ;
#63794 = CARTESIAN_POINT ( 'NONE',  ( -3.230769230769229949, -13.20930481340135110, 34.54067556320372745 ) ) ;
#63795 = EDGE_CURVE ( 'NONE', #16341, #72329, #24023, .T. ) ;
#63796 = FACE_OUTER_BOUND ( 'NONE', #63902, .T. ) ;
#63797 = ORIENTED_EDGE ( 'NONE', *, *, #74221, .T. ) ;
#63798 = ORIENTED_EDGE ( 'NONE', *, *, #64812, .T. ) ;
#63799 = CARTESIAN_POINT ( 'NONE',  ( 3.749999999999992006, -5.946699141100872943, 19.39062500000000711 ) ) ;
#63800 = ORIENTED_EDGE ( 'NONE', *, *, #47975, .T. ) ;
#63801 = CARTESIAN_POINT ( 'NONE',  ( -2.084912638714238486, -3.563462043263030399, 33.22394488606062879 ) ) ;
#63803 = ORIENTED_EDGE ( 'NONE', *, *, #67069, .T. ) ;
#63802 = CARTESIAN_POINT ( 'NONE',  ( 1.134638653673032183, -8.303909089506435137, 34.68538101551103381 ) ) ;
#63804 = DIRECTION ( 'NONE',  ( -0.000000000000000000, 1.000000000000000000, -0.000000000000000000 ) ) ;
#63805 = CYLINDRICAL_SURFACE ( 'NONE', #20172, 0.2500000000000002220 ) ;
#63806 = FACE_OUTER_BOUND ( 'NONE', #3768, .T. ) ;
#63807 = EDGE_LOOP ( 'NONE', ( #44374, #89095 ) ) ;
#63808 = EDGE_CURVE ( 'NONE', #78559, #53313, #68630, .T. ) ;
#63809 = B_SPLINE_CURVE_WITH_KNOTS ( 'NONE', 3,
 ( #66328, #13492, #40970, #31202, #24439, #51907, #59118, #24889, #73085, #11383 ),
 .UNSPECIFIED., .F., .F.,
 ( 4, 2, 2, 2, 4 ),
 ( 0.000000000000000000, 0.0001954311564186867660, 0.0003908623128373735320, 0.0005862934692560603251, 0.0007817246256747470640 ),
 .UNSPECIFIED. ) ;
#63810 = ADVANCED_FACE ( 'NONE', ( #28540 ), #34840, .F. ) ;
#63811 = LINE ( 'NONE', #69685, #76739 ) ;
#63812 = CARTESIAN_POINT ( 'NONE',  ( 4.854056813859977559, -2.251424796025575770, 29.88072029997477586 ) ) ;
#63813 = B_SPLINE_CURVE_WITH_KNOTS ( 'NONE', 3,
 ( #59390, #18410, #66601, #12542, #33260, #67045, #67490, #5784, #73352, #12109 ),
 .UNSPECIFIED., .F., .F.,
 ( 4, 2, 2, 2, 4 ),
 ( 0.0007817246256747452209, 0.0009771112852218887673, 0.001172497944769032531, 0.001367884604316176294, 0.001563271263863319840 ),
 .UNSPECIFIED. ) ;
#63814 = ORIENTED_EDGE ( 'NONE', *, *, #30197, .T. ) ;
#63815 = FACE_BOUND ( 'NONE', #4538, .T. ) ;
#63816 = DIRECTION ( 'NONE',  ( 0.000000000000000000, -1.000000000000000000, 0.000000000000000000 ) ) ;
#63817 = CARTESIAN_POINT ( 'NONE',  ( -6.923076923077044142, -2.892918686052165622, 31.69288490824153470 ) ) ;
#63818 = B_SPLINE_CURVE_WITH_KNOTS ( 'NONE', 3,
 ( #8595, #57656, #36072, #22541, #2694, #63959, #29750, #57214, #30190, #22979 ),
 .UNSPECIFIED., .F., .F.,
 ( 4, 2, 2, 2, 4 ),
 ( 0.000000000000000000, 0.0001954339857564078809, 0.0003908679715128157619, 0.0005863019572692236428, 0.0007817359430256315238 ),
 .UNSPECIFIED. ) ;
#63819 = DIRECTION ( 'NONE',  ( 0.000000000000000000, 0.3420201433256610524, 0.9396926207859113145 ) ) ;
#63821 = CARTESIAN_POINT ( 'NONE',  ( -6.673131404728780858, -2.587454068350147462, 30.68340429815432202 ) ) ;
#63820 = DIRECTION ( 'NONE',  ( 0.000000000000000000, 0.7660444431189807890, 0.6427876096865361433 ) ) ;
#63822 = CARTESIAN_POINT ( 'NONE',  ( -8.769230769230768274, -11.16473453929635440, 33.15142922261926373 ) ) ;
#63823 = CARTESIAN_POINT ( 'NONE',  ( -16.02332045208259359, -9.417988943895561960, 34.36773134775778260 ) ) ;
#63824 = ORIENTED_EDGE ( 'NONE', *, *, #4128, .F. ) ;
#63825 = FACE_OUTER_BOUND ( 'NONE', #72423, .T. ) ;
#63826 = CYLINDRICAL_SURFACE ( 'NONE', #78079, 0.2499999999999995559 ) ;
#63828 = ORIENTED_EDGE ( 'NONE', *, *, #31634, .F. ) ;
#63827 = ADVANCED_FACE ( 'NONE', ( #68196 ), #6495, .F. ) ;
#63829 = VECTOR ( 'NONE', #37451, 1000.000000000000114 ) ;
#63830 = CARTESIAN_POINT ( 'NONE',  ( -16.15384615384615330, -12.62096338111211580, 30.90682066428153263 ) ) ;
#63831 = CARTESIAN_POINT ( 'NONE',  ( -5.076923076923197442, -6.026961402154118908, 34.52809138561165270 ) ) ;
#63832 = CARTESIAN_POINT ( 'NONE',  ( 3.480769230769294786, -7.434744429011176159, 34.75000000000000711 ) ) ;
#63833 = CARTESIAN_POINT ( 'NONE',  ( 2.177544337960614307, -5.915902021225892149, 34.75552854090298638 ) ) ;
#63834 = CARTESIAN_POINT ( 'NONE',  ( -10.36543920600657209, -2.986452184633680229, 32.43230066228895225 ) ) ;
#63835 = ADVANCED_FACE ( 'NONE', ( #33956 ), #61420, .T. ) ;
#63836 = CARTESIAN_POINT ( 'NONE',  ( -5.076923076923075762, -2.538708090699994813, 30.37095296980875503 ) ) ;
#63837 = FACE_BOUND ( 'NONE', #44362, .T. ) ;
#63839 = CARTESIAN_POINT ( 'NONE',  ( 1.515407192440171968, -2.541949514083463590, 30.39797389878540557 ) ) ;
#63838 = CARTESIAN_POINT ( 'NONE',  ( 11.53846153846153832, -6.343179335718451384, 34.87096338111211935 ) ) ;
#63840 = FACE_OUTER_BOUND ( 'NONE', #81315, .T. ) ;
#63842 = CARTESIAN_POINT ( 'NONE',  ( -12.59168567097668401, -4.460286881179643004, 33.72017969459903242 ) ) ;
#63841 = CARTESIAN_POINT ( 'NONE',  ( -7.846153846153967493, -12.70778746994576025, 30.41441678777401236 ) ) ;
#63843 = CARTESIAN_POINT ( 'NONE',  ( 8.899756470994335089, -10.88167719472716399, 33.43325721877153711 ) ) ;
#63844 = CARTESIAN_POINT ( 'NONE',  ( 3.724691934501232815, -5.885600066136343678, 17.88875670625848713 ) ) ;
#63845 = ORIENTED_EDGE ( 'NONE', *, *, #56806, .F. ) ;
#63846 = ORIENTED_EDGE ( 'NONE', *, *, #38194, .T. ) ;
#63847 = DIRECTION ( 'NONE',  ( 0.000000000000000000, 0.000000000000000000, -1.000000000000000000 ) ) ;
#63848 = CARTESIAN_POINT ( 'NONE',  ( -4.219929564802031408, -3.050289026998445951, 32.03036669348365706 ) ) ;
#63849 = CARTESIAN_POINT ( 'NONE',  ( -8.769230769230768274, -12.78798330534102945, 29.74999999999997868 ) ) ;
#63850 = CARTESIAN_POINT ( 'NONE',  ( -0.6844654204453105573, -2.889293201056495786, 32.26117774369186009 ) ) ;
#63851 = CARTESIAN_POINT ( 'NONE',  ( 3.100622021331013833, -11.47017969459903952, 32.78971311882034456 ) ) ;
#63852 = CARTESIAN_POINT ( 'NONE',  ( -1.492201783934549164, -11.27530806549876807, 23.35750670625849423 ) ) ;
#63853 = CARTESIAN_POINT ( 'NONE',  ( -8.519285250882631999, -2.824170634883621744, 31.52227843825338738 ) ) ;
#63854 = LINE ( 'NONE', #35506, #44544 ) ;
#63855 = CARTESIAN_POINT ( 'NONE',  ( 3.296836564119306257, -3.937682226553329556, 33.60647404775216529 ) ) ;
#63856 = CARTESIAN_POINT ( 'NONE',  ( -1.634638621908349077, -12.43535235679832596, 30.55408501211184813 ) ) ;
#63857 = CARTESIAN_POINT ( 'NONE',  ( -3.480745974817822663, -4.075325502946086864, 33.72974371597207721 ) ) ;
#63858 = CYLINDRICAL_SURFACE ( 'NONE', #31017, 0.2499999999999994726 ) ;
#63859 = B_SPLINE_CURVE_WITH_KNOTS ( 'NONE', 3,
 ( #85563, #72484, #24745, #11691, #17098, #64827, #58080, #51291, #38263, #72038 ),
 .UNSPECIFIED., .F., .F.,
 ( 4, 2, 2, 2, 4 ),
 ( 0.000000000000000000, 0.0001954339857564071491, 0.0003908679715128142982, 0.0005863019572692214744, 0.0007817359430256285964 ),
 .UNSPECIFIED. ) ;
#63860 = VECTOR ( 'NONE', #69126, 1000.000000000000227 ) ;
#63861 = CARTESIAN_POINT ( 'NONE',  ( 14.43848411551709709, -11.71459661697925903, 32.44059661609676937 ) ) ;
#63862 = LINE ( 'NONE', #85033, #51351 ) ;
#63863 = ORIENTED_EDGE ( 'NONE', *, *, #65114, .T. ) ;
#63864 = CARTESIAN_POINT ( 'NONE',  ( -7.846153846153844924, -2.249999999999998668, 29.50000000000001421 ) ) ;
#63865 = CARTESIAN_POINT ( 'NONE',  ( -5.869209559033048862, -2.494656445102013453, 31.33466734024120015 ) ) ;
#63866 = CARTESIAN_POINT ( 'NONE',  ( -1.614399933863613468, -11.22469193450124969, 15.11124329374151287 ) ) ;
#63867 = CARTESIAN_POINT ( 'NONE',  ( 0.7114838709165042241, -3.520799739797213945, 33.17531984108286025 ) ) ;
#63868 = CARTESIAN_POINT ( 'NONE',  ( -15.93106648486808119, -2.612705202774696200, 31.66806509827799943 ) ) ;
#63869 = ORIENTED_EDGE ( 'NONE', *, *, #18055, .T. ) ;
#63870 = CARTESIAN_POINT ( 'NONE',  ( -16.37671157604979300, -2.501496062324912284, 29.88072118266895671 ) ) ;
#63872 = ORIENTED_EDGE ( 'NONE', *, *, #18021, .F. ) ;
#63871 = DIRECTION ( 'NONE',  ( 0.000000000000000000, -6.938893903907222067E-15, 1.000000000000000000 ) ) ;
#63873 = CARTESIAN_POINT ( 'NONE',  ( 7.053602624840491053, -3.816742781228458448, 33.13167719472716044 ) ) ;
#63874 = FACE_OUTER_BOUND ( 'NONE', #349, .T. ) ;
#63875 = ORIENTED_EDGE ( 'NONE', *, *, #75421, .F. ) ;
#63876 = DIRECTION ( 'NONE',  ( 0.000000000000000000, 0.000000000000000000, -1.000000000000000000 ) ) ;
#63877 = CARTESIAN_POINT ( 'NONE',  ( 9.019285080869083870, -4.943051570960394159, 34.04725096376909477 ) ) ;
#63878 = ORIENTED_EDGE ( 'NONE', *, *, #81549, .T. ) ;
#63879 = CARTESIAN_POINT ( 'NONE',  ( -12.46153846153846168, -2.292212530054420494, 30.41441678777542634 ) ) ;
#63880 = DIRECTION ( 'NONE',  ( 1.000000000000000000, 0.000000000000000000, 0.000000000000000000 ) ) ;
#63881 = DIRECTION ( 'NONE',  ( -0.000000000000000000, 1.000000000000000000, -0.000000000000000000 ) ) ;
#63882 = EDGE_LOOP ( 'NONE', ( #76115, #50580 ) ) ;
#63883 = ORIENTED_EDGE ( 'NONE', *, *, #46475, .T. ) ;
#63884 = ORIENTED_EDGE ( 'NONE', *, *, #84638, .T. ) ;
#63885 = DIRECTION ( 'NONE',  ( 0.000000000000000000, 0.4999999999999960032, -0.8660254037844410391 ) ) ;
#63886 = CARTESIAN_POINT ( 'NONE',  ( 2.372947447205147942, -11.67786785259547777, 32.92929555188713664 ) ) ;
#63887 = CARTESIAN_POINT ( 'NONE',  ( 3.262820512820510999, -7.500000000000000000, 29.75000000000000355 ) ) ;
#63888 = AXIS2_PLACEMENT_3D ( 'NONE', #52966, #77894, #25509 ) ;
#63889 = CARTESIAN_POINT ( 'NONE',  ( -17.30040802064702987, -6.760086850603066466, 34.69517049084099369 ) ) ;
#63890 = VERTEX_POINT ( 'NONE', #1509 ) ;
#63891 = ORIENTED_EDGE ( 'NONE', *, *, #20694, .F. ) ;
#63893 = ORIENTED_EDGE ( 'NONE', *, *, #24636, .F. ) ;
#63892 = LINE ( 'NONE', #57145, #38630 ) ;
#63894 = CARTESIAN_POINT ( 'NONE',  ( 12.71159288145191724, -11.47946981652013498, 33.17500667209847620 ) ) ;
#63895 = EDGE_CURVE ( 'NONE', #47746, #221, #79435, .T. ) ;
#63896 = VERTEX_POINT ( 'NONE', #44570 ) ;
#63897 = DIRECTION ( 'NONE',  ( 0.000000000000000000, 1.000000000000000000, 0.000000000000000000 ) ) ;
#63898 = CARTESIAN_POINT ( 'NONE',  ( 7.912222197156284054, -4.786620604624113540, 33.94971097300155805 ) ) ;
#63899 = ORIENTED_EDGE ( 'NONE', *, *, #73577, .F. ) ;
#63900 = ORIENTED_EDGE ( 'NONE', *, *, #37718, .F. ) ;
#63902 = EDGE_LOOP ( 'NONE', ( #53925, #84749, #30531, #13299 ) ) ;
#63901 = CARTESIAN_POINT ( 'NONE',  ( -12.46153846153846168, -4.786620604624113540, 33.94971097300155094 ) ) ;
#63903 = CARTESIAN_POINT ( 'NONE',  ( 4.403791672194294904, -5.057305518903949526, 34.11320923018887896 ) ) ;
#63904 = VECTOR ( 'NONE', #46428, 1000.000000000000227 ) ;
#63905 = CARTESIAN_POINT ( 'NONE',  ( -5.300408020647026319, -10.11188796281391511, 34.01382737946119050 ) ) ;
#63906 = ORIENTED_EDGE ( 'NONE', *, *, #52809, .T. ) ;
#63907 = ADVANCED_FACE ( 'NONE', ( #85582 ), #17573, .F. ) ;
#63908 = CARTESIAN_POINT ( 'NONE',  ( 15.36156103859402045, -3.062576670634119758, 32.05464942895959979 ) ) ;
#63909 = B_SPLINE_CURVE_WITH_KNOTS ( 'NONE', 3,
 ( #55913, #49158, #76640, #1420, #28913, #1862, #63993, #65329, #70322, #2290 ),
 .UNSPECIFIED., .F., .F.,
 ( 4, 2, 2, 2, 4 ),
 ( 0.000000000000000000, 0.0001954339857564076912, 0.0003908679715128153282, 0.0005863019572692228839, 0.0007817359430256304396 ),
 .UNSPECIFIED. ) ;
#63910 = CARTESIAN_POINT ( 'NONE',  ( -14.24162497434223162, -12.62096338111211757, 30.90682066428152908 ) ) ;
#63911 = CARTESIAN_POINT ( 'NONE',  ( -13.38461538461538325, -13.53365097954675988, 30.81389545987213552 ) ) ;
#63912 = FACE_BOUND ( 'NONE', #83203, .T. ) ;
#63913 = VECTOR ( 'NONE', #4067, 1000.000000000000000 ) ;
#63914 = CARTESIAN_POINT ( 'NONE',  ( -8.546451100252703270, -2.353885683473779800, 30.79025554430704403 ) ) ;
#63915 = CARTESIAN_POINT ( 'NONE',  ( -11.66915214157184977, -6.369640206132551441, 34.87707690430378449 ) ) ;
#63916 = AXIS2_PLACEMENT_3D ( 'NONE', #45684, #17779, #10572 ) ;
#63917 = DIRECTION ( 'NONE',  ( -0.000000000000000000, 1.000000000000000000, 3.491481338843133355E-15 ) ) ;
#63919 = CARTESIAN_POINT ( 'NONE',  ( 4.219913487196230939, -2.292212530054420494, 30.41441678777542990 ) ) ;
#63918 = CARTESIAN_POINT ( 'NONE',  ( 20.00000000000000000, -4.000000000000000000, 29.75000000000000355 ) ) ;
#63920 = CARTESIAN_POINT ( 'NONE',  ( -19.00000000000000000, -9.000000000000001776, 2.999999999999999112 ) ) ;
#63921 = CARTESIAN_POINT ( 'NONE',  ( -7.846153846153844924, -11.33034616979429110, 35.88435417666054406 ) ) ;
#63922 = ORIENTED_EDGE ( 'NONE', *, *, #66275, .F. ) ;
#63923 = DIRECTION ( 'NONE',  ( -0.000000000000000000, -0.9396926207859093161, -0.3420201433256663259 ) ) ;
#63924 = ORIENTED_EDGE ( 'NONE', *, *, #51314, .F. ) ;
#63925 = VERTEX_POINT ( 'NONE', #42498 ) ;
#63927 = CARTESIAN_POINT ( 'NONE',  ( -3.360917200500924906, -5.915902021225892149, 34.75552854090298638 ) ) ;
#63926 = CARTESIAN_POINT ( 'NONE',  ( -8.769230769230768274, -8.810774026931790459, 35.74407628777942847 ) ) ;
#63928 = CARTESIAN_POINT ( 'NONE',  ( 2.307692307692187583, -2.625532179533779154, 30.86335684631627174 ) ) ;
#63929 = CARTESIAN_POINT ( 'NONE',  ( 8.069166690247241647, -3.395485233115139057, 33.02377354290275946 ) ) ;
#63930 = CARTESIAN_POINT ( 'NONE',  ( -12.23875879256039667, -2.612705202774698421, 31.66806509827799943 ) ) ;
#63931 = LINE ( 'NONE', #58494, #1577 ) ;
#63932 = EDGE_LOOP ( 'NONE', ( #78668, #6625 ) ) ;
#63933 = ADVANCED_FACE ( 'NONE', ( #4034 ), #72952, .T. ) ;
#63934 = FACE_OUTER_BOUND ( 'NONE', #34431, .T. ) ;
#63935 = CARTESIAN_POINT ( 'NONE',  ( -15.23076923076922995, -9.780366693483667717, 34.19971097300155094 ) ) ;
#63936 = DIRECTION ( 'NONE',  ( 1.000000000000000000, 0.000000000000000000, 0.000000000000000000 ) ) ;
#63937 = CARTESIAN_POINT ( 'NONE',  ( 15.23076923076923173, -12.34228464037088635, 31.77849191805839268 ) ) ;
#63938 = DIRECTION ( 'NONE',  ( 0.000000000000000000, -6.938893903907222067E-15, 1.000000000000000000 ) ) ;
#63939 = CARTESIAN_POINT ( 'NONE',  ( 3.750000000000000888, -7.499999999999978684, 18.21875000000000000 ) ) ;
#63940 = ORIENTED_EDGE ( 'NONE', *, *, #63808, .F. ) ;
#63941 = EDGE_CURVE ( 'NONE', #57554, #52054, #47197, .T. ) ;
#63942 = ORIENTED_EDGE ( 'NONE', *, *, #17477, .T. ) ;
#63943 = EDGE_CURVE ( 'NONE', #45833, #71793, #11812, .T. ) ;
#63944 = CARTESIAN_POINT ( 'NONE',  ( -6.222926958906846551, -4.026226216239095379, 33.68668979543632958 ) ) ;
#63945 = VERTEX_POINT ( 'NONE', #24308 ) ;
#63946 = FACE_OUTER_BOUND ( 'NONE', #29017, .T. ) ;
#63947 = LINE ( 'NONE', #45453, #3974 ) ;
#63948 = DIRECTION ( 'NONE',  ( -0.000000000000000000, 1.000000000000000000, -0.000000000000000000 ) ) ;
#63949 = CARTESIAN_POINT ( 'NONE',  ( -4.853910232829680815, -3.395485233115139057, 33.02377354290275946 ) ) ;
#63950 = CARTESIAN_POINT ( 'NONE',  ( -1.553300858899081538, -11.25000000000000711, 16.10937500000000355 ) ) ;
#63951 = CARTESIAN_POINT ( 'NONE',  ( 0.5920638997721058283, -9.503571793651733657, 34.60286762892837942 ) ) ;
#63953 = ORIENTED_EDGE ( 'NONE', *, *, #63207, .T. ) ;
#63952 = AXIS2_PLACEMENT_3D ( 'NONE', #40933, #12137, #12575 ) ;
#63954 = CARTESIAN_POINT ( 'NONE',  ( -12.71151519248081563, -10.66389620160130036, 33.62221079203477103 ) ) ;
#63956 = VERTEX_POINT ( 'NONE', #50881 ) ;
#63955 = CARTESIAN_POINT ( 'NONE',  ( -2.176900499867520544, -10.54018710029568595, 33.71981072465678864 ) ) ;
#63957 = CARTESIAN_POINT ( 'NONE',  ( 3.164686851409094004, -12.34228464037088280, 31.77849191805838558 ) ) ;
#63958 = CARTESIAN_POINT ( 'NONE',  ( -17.14300545628321615, -11.91647553114624181, 32.58852847137148245 ) ) ;
#63959 = CARTESIAN_POINT ( 'NONE',  ( 11.28843830116857383, -4.335965774309649134, 33.62209801155881905 ) ) ;
#63960 = DIRECTION ( 'NONE',  ( 0.000000000000000000, 0.9848077530122072432, 0.1736481776669354937 ) ) ;
#63961 = DIRECTION ( 'NONE',  ( 0.000000000000000000, 0.9396926207859126468, 0.3420201433256571111 ) ) ;
#63962 = CARTESIAN_POINT ( 'NONE',  ( -6.988347369037697376, -5.219633306516282545, 34.19971097300152252 ) ) ;
#63963 = CARTESIAN_POINT ( 'NONE',  ( 3.724691934501251023, -9.114399933863618131, 14.79874329374151642 ) ) ;
#63964 = EDGE_LOOP ( 'NONE', ( #29495, #66379 ) ) ;
#63965 = CARTESIAN_POINT ( 'NONE',  ( -12.46153846153846168, -13.87047571288749737, 32.06866353760679544 ) ) ;
#63966 = CARTESIAN_POINT ( 'NONE',  ( -1.608100328339334029, -12.24155766932282496, 31.33739205006857986 ) ) ;
#63967 = CARTESIAN_POINT ( 'NONE',  ( 2.750000000000008438, -8.639087296525996607, 23.29687500000000000 ) ) ;
#63968 = CARTESIAN_POINT ( 'NONE',  ( -3.454254174493178731, -9.331801661448606566, 34.40259984581193464 ) ) ;
#63969 = CARTESIAN_POINT ( 'NONE',  ( 9.562159722575998444, -6.809168938359901446, 34.95455904226513866 ) ) ;
#63970 = ORIENTED_EDGE ( 'NONE', *, *, #18021, .T. ) ;
#63971 = CARTESIAN_POINT ( 'NONE',  ( 1.139087296525997051, -4.749999999999992895, 15.48437499999999822 ) ) ;
#63972 = LINE ( 'NONE', #14926, #21055 ) ;
#63973 = ORIENTED_EDGE ( 'NONE', *, *, #37752, .T. ) ;
#63974 = CARTESIAN_POINT ( 'NONE',  ( -18.00000000000012079, -5.094484230521992174, 34.41647553114689373 ) ) ;
#63975 = EDGE_LOOP ( 'NONE', ( #33476, #64377, #50544, #33846 ) ) ;
#63976 = ADVANCED_FACE ( 'NONE', ( #86944 ), #79718, .T. ) ;
#63977 = CARTESIAN_POINT ( 'NONE',  ( 17.74997676270703550, -6.695914987888146541, 34.68535235679833306 ) ) ;
#63978 = CARTESIAN_POINT ( 'NONE',  ( -17.32694630114453105, -2.341070481393820124, 30.72580821765574299 ) ) ;
#63979 = AXIS2_PLACEMENT_3D ( 'NONE', #49430, #62482, #84114 ) ;
#63980 = CARTESIAN_POINT ( 'NONE',  ( -8.769230769230892619, -5.941354392335915335, 34.76329471203413846 ) ) ;
#63981 = CARTESIAN_POINT ( 'NONE',  ( 9.320512820512821150, -7.500000000000000000, 29.75000000000000355 ) ) ;
#63982 = ORIENTED_EDGE ( 'NONE', *, *, #76449, .F. ) ;
#63983 = CARTESIAN_POINT ( 'NONE',  ( -3.230769230769229949, -2.292212530054420494, 30.41441678777542634 ) ) ;
#63984 = B_SPLINE_CURVE_WITH_KNOTS ( 'NONE', 3,
 ( #18007, #50443, #16657, #58088, #23846, #51299, #70733, #57212, #31055, #9036 ),
 .UNSPECIFIED., .F., .F.,
 ( 4, 2, 2, 2, 4 ),
 ( 0.000000000000000000, 0.0001954339857564063089, 0.0003908679715128126177, 0.0005863019572692189808, 0.0007817359430256252354 ),
 .UNSPECIFIED. ) ;
#63985 = AXIS2_PLACEMENT_3D ( 'NONE', #42814, #8583, #49993 ) ;
#63986 = EDGE_LOOP ( 'NONE', ( #70717, #35471, #35539, #79406 ) ) ;
#63987 = CARTESIAN_POINT ( 'NONE',  ( 20.00000000000000000, -3.499999999999999556, 28.25000000000000000 ) ) ;
#63988 = CARTESIAN_POINT ( 'NONE',  ( 4.826946332874483936, -5.643011162660950042, 34.66104346484419096 ) ) ;
#63989 = ORIENTED_EDGE ( 'NONE', *, *, #30188, .T. ) ;
#63990 = AXIS2_PLACEMENT_3D ( 'NONE', #73576, #24471, #38898 ) ;
#63991 = CARTESIAN_POINT ( 'NONE',  ( 11.66898697669518548, -12.70449254468099198, 30.44128974285582956 ) ) ;
#63992 = PLANE ( 'NONE',  #82419 ) ;
#63993 = CARTESIAN_POINT ( 'NONE',  ( 0.2380535178145126718, -4.386631170607604879, 33.66268669641500111 ) ) ;
#63994 = ADVANCED_FACE ( 'NONE', ( #65300 ), #52226, .F. ) ;
#63995 = CYLINDRICAL_SURFACE ( 'NONE', #52034, 0.2500000000000008882 ) ;
#63996 = CARTESIAN_POINT ( 'NONE',  ( -4.826923076921640465, -7.500000000000155431, 34.75000000000007105 ) ) ;
#63997 = VERTEX_POINT ( 'NONE', #9916 ) ;
#63998 = EDGE_LOOP ( 'NONE', ( #47520, #6638 ) ) ;
#63999 = FACE_BOUND ( 'NONE', #44750, .T. ) ;
#64000 = ORIENTED_EDGE ( 'NONE', *, *, #4410, .T. ) ;
#64001 = CARTESIAN_POINT ( 'NONE',  ( 6.923076923076924238, -6.189225973068211317, 35.74407628777942847 ) ) ;
#64002 = EDGE_CURVE ( 'NONE', #37932, #38304, #64423, .T. ) ;
#64003 = DIRECTION ( 'NONE',  ( 0.000000000000000000, 0.9848077530122072432, 0.1736481776669354937 ) ) ;
#64004 = DIRECTION ( 'NONE',  ( 0.000000000000000000, 0.4999999999999960032, -0.8660254037844410391 ) ) ;
#64005 = DIRECTION ( 'NONE',  ( 1.000000000000000000, 0.000000000000000000, 0.000000000000000000 ) ) ;
#64006 = EDGE_CURVE ( 'NONE', #65220, #30240, #29773, .T. ) ;
#64007 = ORIENTED_EDGE ( 'NONE', *, *, #47267, .F. ) ;
#64008 = CIRCLE ( 'NONE', #20888, 4.000000000000000000 ) ;
#64009 = VERTEX_POINT ( 'NONE', #52673 ) ;
#64010 = CARTESIAN_POINT ( 'NONE',  ( 16.85343813319912698, -4.386631170607603991, 33.66268669641500111 ) ) ;
#64011 = VERTEX_POINT ( 'NONE', #4948 ) ;
#64012 = CARTESIAN_POINT ( 'NONE',  ( -24.00000000000000000, -5.499999999999981348, 27.75000000000000000 ) ) ;
#64013 = B_SPLINE_CURVE_WITH_KNOTS ( 'NONE', 3,
 ( #68665, #61455, #88966, #48388, #54700, #1096 ),
 .UNSPECIFIED., .F., .F.,
 ( 4, 2, 4 ),
 ( 0.000000000000000000, 0.2500000000000000000, 0.5000000000000000000 ),
 .UNSPECIFIED. ) ;
#64014 = EDGE_CURVE ( 'NONE', #74179, #73852, #81500, .T. ) ;
#64015 = CARTESIAN_POINT ( 'NONE',  ( 2.980792499826877773, -2.779195860258149242, 31.39871582349837453 ) ) ;
#64016 = DIRECTION ( 'NONE',  ( -0.000000000000000000, 0.7660444431189791237, -0.6427876096865379196 ) ) ;
#64017 = CARTESIAN_POINT ( 'NONE',  ( 9.692307692307695177, -1.129524287112498415, 32.06866353760679544 ) ) ;
#64018 = VERTEX_POINT ( 'NONE', #81058 ) ;
#64019 = CARTESIAN_POINT ( 'NONE',  ( 8.835299120233205628, -8.973038597847271092, 34.52809138561121216 ) ) ;
#64020 = EDGE_CURVE ( 'NONE', #57330, #5010, #32413, .T. ) ;
#64021 = CARTESIAN_POINT ( 'NONE',  ( -5.999999999999998224, -6.343179335718451384, 34.87096338111211935 ) ) ;
#64022 = CYLINDRICAL_SURFACE ( 'NONE', #4919, 0.2500000000000008882 ) ;
#64023 = CARTESIAN_POINT ( 'NONE',  ( 8.899756207464411872, -6.808710257144161559, 34.95449254468098843 ) ) ;
#64024 = ORIENTED_EDGE ( 'NONE', *, *, #66590, .T. ) ;
#64025 = EDGE_CURVE ( 'NONE', #55155, #20155, #71928, .T. ) ;
#64026 = VERTEX_POINT ( 'NONE', #67091 ) ;
#64027 = VERTEX_POINT ( 'NONE', #88274 ) ;
#64029 = CARTESIAN_POINT ( 'NONE',  ( 10.48523664565292002, -2.373036134822904319, 30.88089517874952250 ) ) ;
#64028 = CARTESIAN_POINT ( 'NONE',  ( -13.91025641025641058, -7.500000000000000000, 29.75000000000000355 ) ) ;
#64030 = CARTESIAN_POINT ( 'NONE',  ( -15.90384615384615330, -7.500000000000001776, 35.04278698407183867 ) ) ;
#64031 = CARTESIAN_POINT ( 'NONE',  ( 12.59232890250541281, -12.62708834333097663, 30.88030960425257021 ) ) ;
#64032 = FACE_BOUND ( 'NONE', #44645, .T. ) ;
#64033 = CARTESIAN_POINT ( 'NONE',  ( -15.29685161012936412, -3.322132147404559532, 32.92929555188719348 ) ) ;
#64034 = ORIENTED_EDGE ( 'NONE', *, *, #30257, .T. ) ;
#64035 = AXIS2_PLACEMENT_3D ( 'NONE', #29729, #483, #62610 ) ;
#64036 = EDGE_CURVE ( 'NONE', #40036, #10299, #66644, .T. ) ;
#64037 = CARTESIAN_POINT ( 'NONE',  ( -3.099977422944443450, -2.541949514083463590, 30.39797389878540557 ) ) ;
#64038 = CARTESIAN_POINT ( 'NONE',  ( 9.442330948259105128, -12.01397095200674059, 32.43157075238190146 ) ) ;
#64039 = CARTESIAN_POINT ( 'NONE',  ( -17.07692307692319744, -11.94971097300221174, 32.03036669348237098 ) ) ;
#64040 = CARTESIAN_POINT ( 'NONE',  ( -11.47239318745910097, -3.513871655860379306, 32.76840700105978499 ) ) ;
#64041 = ORIENTED_EDGE ( 'NONE', *, *, #10368, .T. ) ;
#64042 = CARTESIAN_POINT ( 'NONE',  ( 2.307692307692309264, -11.69971097300155272, 32.46337939537588113 ) ) ;
#64043 = ORIENTED_EDGE ( 'NONE', *, *, #48885, .T. ) ;
#64044 = FACE_BOUND ( 'NONE', #52859, .T. ) ;
#64045 = CARTESIAN_POINT ( 'NONE',  ( 11.53846153846153832, -2.833524468853757305, 32.15551576947925838 ) ) ;
#64046 = B_SPLINE_CURVE_WITH_KNOTS ( 'NONE', 3,
 ( #48996, #48539, #69712, #9351, #28277, #36808, #2133, #56200, #8464, #29621 ),
 .UNSPECIFIED., .F., .F.,
 ( 4, 2, 2, 2, 4 ),
 ( 0.000000000000000000, 0.0001954311564186867931, 0.0003908623128373735862, 0.0005862934692560603251, 0.0007817246256747471724 ),
 .UNSPECIFIED. ) ;
#64047 = ADVANCED_FACE ( 'NONE', ( #75183 ), #40080, .F. ) ;
#64048 = CARTESIAN_POINT ( 'NONE',  ( 4.153846153846030731, -2.657715359629662988, 31.77849191805970364 ) ) ;
#64050 = EDGE_CURVE ( 'NONE', #54951, #13992, #42913, .T. ) ;
#64049 = CARTESIAN_POINT ( 'NONE',  ( 14.24242186173153257, -11.94971097300153140, 32.03036669348370680 ) ) ;
#64051 = B_SPLINE_CURVE_WITH_KNOTS ( 'NONE', 3,
 ( #2135, #71041, #57966, #57524, #9353, #72364, #57080, #65599, #84575, #77795 ),
 .UNSPECIFIED., .F., .F.,
 ( 4, 2, 2, 2, 4 ),
 ( 0.000000000000000000, 0.0001954311564186868473, 0.0003908623128373736946, 0.0005862934692560605419, 0.0007817246256747473893 ),
 .UNSPECIFIED. ) ;
#64052 = ORIENTED_EDGE ( 'NONE', *, *, #11293, .F. ) ;
#64053 = AXIS2_PLACEMENT_3D ( 'NONE', #57053, #84106, #77331 ) ;
#64055 = CARTESIAN_POINT ( 'NONE',  ( 5.207714884747860928, -3.062576670634119758, 32.05464942895959979 ) ) ;
#64054 = B_SPLINE_CURVE_WITH_KNOTS ( 'NONE', 3,
 ( #47380, #7292, #40203, #26670, #68541, #53697, #55034, #19032, #40642, #48264 ),
 .UNSPECIFIED., .F., .F.,
 ( 4, 2, 2, 2, 4 ),
 ( 0.0007817246256747473893, 0.0009771112852218909357, 0.001172497944769034482, 0.001367884604316178246, 0.001563271263863321792 ),
 .UNSPECIFIED. ) ;
#64056 = CARTESIAN_POINT ( 'NONE',  ( 4.826923076923077538, -7.433931650972300353, 34.75000000000000711 ) ) ;
#64057 = CARTESIAN_POINT ( 'NONE',  ( -10.61538461538473399, -3.835265460704628371, 33.15142922262033665 ) ) ;
#64058 = CARTESIAN_POINT ( 'NONE',  ( -6.923076923076922462, -3.050289026998446396, 32.03036669348365706 ) ) ;
#64059 = ORIENTED_EDGE ( 'NONE', *, *, #55926, .T. ) ;
#64060 = FACE_OUTER_BOUND ( 'NONE', #39163, .T. ) ;
#64061 = ORIENTED_EDGE ( 'NONE', *, *, #19183, .T. ) ;
#64063 = EDGE_LOOP ( 'NONE', ( #2354, #83731, #74788, #13369 ) ) ;
#64062 = CARTESIAN_POINT ( 'NONE',  ( 13.60739492588379385, -12.24180327182771855, 31.33663988360758879 ) ) ;
#64064 = CARTESIAN_POINT ( 'NONE',  ( 3.296837581771671299, -2.538708090699994813, 30.37095296980875503 ) ) ;
#64065 = CARTESIAN_POINT ( 'NONE',  ( -6.857821351800897247, -11.94971097300157403, 32.03036669348361443 ) ) ;
#64066 = CARTESIAN_POINT ( 'NONE',  ( 13.25446817517716980, -9.418419913701741919, 34.36755862841477693 ) ) ;
#64067 = FACE_OUTER_BOUND ( 'NONE', #38470, .T. ) ;
#64069 = CARTESIAN_POINT ( 'NONE',  ( 11.53846153846141753, -8.613356846316285953, 34.62446782046622218 ) ) ;
#64068 = CYLINDRICAL_SURFACE ( 'NONE', #60585, 0.2499999999999986955 ) ;
#64070 = LINE ( 'NONE', #65403, #44952 ) ;
#64071 = CARTESIAN_POINT ( 'NONE',  ( -1.139087296525992166, -10.25000000000000533, 24.85937500000001421 ) ) ;
#64072 = ORIENTED_EDGE ( 'NONE', *, *, #87775, .F. ) ;
#64073 = DIRECTION ( 'NONE',  ( 0.000000000000000000, 0.3420201433256641055, -0.9396926207859100932 ) ) ;
#64074 = LINE ( 'NONE', #10021, #43839 ) ;
#64075 = VERTEX_POINT ( 'NONE', #26101 ) ;
#64076 = EDGE_LOOP ( 'NONE', ( #13782, #69349, #84951, #45340, #83981, #37443 ) ) ;
#64077 = ORIENTED_EDGE ( 'NONE', *, *, #28038, .F. ) ;
#64078 = CARTESIAN_POINT ( 'NONE',  ( -10.68146802634049308, -11.16473453929635440, 33.15142922261925662 ) ) ;
#64079 = CARTESIAN_POINT ( 'NONE',  ( 3.007843013253082454, -9.886141570436013382, 34.14413921362392301 ) ) ;
#64080 = AXIS2_PLACEMENT_3D ( 'NONE', #73646, #10151, #79503 ) ;
#64081 = CARTESIAN_POINT ( 'NONE',  ( 0.3309288063343787667, -7.722926974430166069, 34.99546784045485737 ) ) ;
#64082 = CARTESIAN_POINT ( 'NONE',  ( 10.86543903529806876, -6.523592122091592671, 34.90882529074906415 ) ) ;
#64083 = CARTESIAN_POINT ( 'NONE',  ( -16.40382288478850725, -3.137211980971222225, 32.19342716148376837 ) ) ;
#64084 = DIRECTION ( 'NONE',  ( -0.000000000000000000, 0.5000000000000011102, -0.8660254037844381525 ) ) ;
#64085 = DIRECTION ( 'NONE',  ( -1.000000000000000000, 0.000000000000000000, 0.000000000000000000 ) ) ;
#64086 = ORIENTED_EDGE ( 'NONE', *, *, #69152, .F. ) ;
#64087 = EDGE_CURVE ( 'NONE', #10994, #84179, #46371, .T. ) ;
#64088 = DIRECTION ( 'NONE',  ( -1.000000000000000000, -0.000000000000000000, -0.000000000000000000 ) ) ;
#64089 = DIRECTION ( 'NONE',  ( 0.000000000000000000, 0.000000000000000000, -1.000000000000000000 ) ) ;
#64090 = B_SPLINE_CURVE_WITH_KNOTS ( 'NONE', 3,
 ( #52631, #11665, #31934, #45426, #18859, #39141, #67495, #11210, #80576, #4909 ),
 .UNSPECIFIED., .F., .F.,
 ( 4, 2, 2, 2, 4 ),
 ( 0.0007817246256747434861, 0.0009771112852218861652, 0.001172497944769028844, 0.001367884604316171740, 0.001563271263863314419 ),
 .UNSPECIFIED. ) ;
#64091 = CYLINDRICAL_SURFACE ( 'NONE', #78104, 0.2499999999999997502 ) ;
#64092 = EDGE_CURVE ( 'NONE', #67350, #64228, #74291, .T. ) ;
#64093 = ORIENTED_EDGE ( 'NONE', *, *, #22035, .T. ) ;
#64094 = CARTESIAN_POINT ( 'NONE',  ( 19.99999999999997158, -14.99999999999999467, 13.00000000000000178 ) ) ;
#64095 = B_SPLINE_CURVE_WITH_KNOTS ( 'NONE', 3,
 ( #78001, #56407, #22180, #2330, #28493, #77561, #42899, #15428, #1901, #84779 ),
 .UNSPECIFIED., .F., .F.,
 ( 4, 2, 2, 2, 4 ),
 ( 0.0007817246256747455461, 0.0009771112852218883336, 0.001172497944769031230, 0.001367884604316174126, 0.001563271263863317022 ),
 .UNSPECIFIED. ) ;
#64096 = EDGE_CURVE ( 'NONE', #15414, #67575, #56928, .T. ) ;
#64097 = EDGE_CURVE ( 'NONE', #21125, #81602, #81945, .T. ) ;
#64098 = EDGE_LOOP ( 'NONE', ( #10523, #43376 ) ) ;
#64099 = CARTESIAN_POINT ( 'NONE',  ( 12.39545608217832395, -9.058645607665454236, 34.76329471203372634 ) ) ;
#64100 = CARTESIAN_POINT ( 'NONE',  ( 3.361559671736181976, -10.70102852606553157, 33.91149625220312913 ) ) ;
#64101 = DIRECTION ( 'NONE',  ( 0.000000000000000000, 0.1736481776669267785, -0.9848077530122087975 ) ) ;
#64102 = ORIENTED_EDGE ( 'NONE', *, *, #17589, .T. ) ;
#64103 = CARTESIAN_POINT ( 'NONE',  ( 12.68431813051652668, -10.97394488606064122, 33.68653795673694873 ) ) ;
#64104 = LINE ( 'NONE', #37073, #12699 ) ;
#64105 = EDGE_CURVE ( 'NONE', #25692, #7689, #49454, .T. ) ;
#64106 = CARTESIAN_POINT ( 'NONE',  ( -3.100243529005665355, -12.27024696741798770, 31.24895572276497546 ) ) ;
#64107 = EDGE_LOOP ( 'NONE', ( #86746, #70053 ) ) ;
#64108 = CARTESIAN_POINT ( 'NONE',  ( -3.148799926473854982E-16, -1.749999999999995559, 32.75000000000000000 ) ) ;
#64109 = EDGE_LOOP ( 'NONE', ( #64043, #55488 ) ) ;
#64110 = LINE ( 'NONE', #82642, #37843 ) ;
#64111 = CARTESIAN_POINT ( 'NONE',  ( 7.053867364043877153, -2.845873456487966635, 32.17976146951972538 ) ) ;
#64112 = CARTESIAN_POINT ( 'NONE',  ( -5.999999999999998224, -2.538708090699994813, 30.37095296980875503 ) ) ;
#64113 = FACE_OUTER_BOUND ( 'NONE', #57125, .T. ) ;
#64114 = CARTESIAN_POINT ( 'NONE',  ( -17.86920955903305597, -12.35292014791297710, 31.75344720912887198 ) ) ;
#64115 = EDGE_CURVE ( 'NONE', #45555, #42060, #45134, .T. ) ;
#64116 = ORIENTED_EDGE ( 'NONE', *, *, #67467, .T. ) ;
#64117 = VERTEX_POINT ( 'NONE', #56668 ) ;
#64118 = ORIENTED_EDGE ( 'NONE', *, *, #58552, .T. ) ;
#64119 = LINE ( 'NONE', #23584, #50243 ) ;
#64120 = FACE_OUTER_BOUND ( 'NONE', #30103, .T. ) ;
#64121 = CARTESIAN_POINT ( 'NONE',  ( -4.403869378067610363, -12.45566812827425096, 31.48439005359158926 ) ) ;
#64122 = CARTESIAN_POINT ( 'NONE',  ( -24.00000000000000000, 5.000000000000023093, 29.24999999999999645 ) ) ;
#64123 = VECTOR ( 'NONE', #66636, 1000.000000000000114 ) ;
#64124 = FACE_OUTER_BOUND ( 'NONE', #30459, .T. ) ;
#64125 = CARTESIAN_POINT ( 'NONE',  ( 8.769230769230768274, -11.33034616979429110, 35.88435417666054406 ) ) ;
#64126 = ORIENTED_EDGE ( 'NONE', *, *, #67277, .F. ) ;
#64127 = VERTEX_POINT ( 'NONE', #8492 ) ;
#64128 = AXIS2_PLACEMENT_3D ( 'NONE', #61008, #26782, #81737 ) ;
#64129 = EDGE_LOOP ( 'NONE', ( #33191, #11069 ) ) ;
#64131 = ORIENTED_EDGE ( 'NONE', *, *, #12709, .T. ) ;
#64130 = CARTESIAN_POINT ( 'NONE',  ( 11.53846153846141753, -9.442884908241554243, 34.35708131394783038 ) ) ;
#64133 = CARTESIAN_POINT ( 'NONE',  ( -5.207071046654772495, -12.70455904226513866, 30.44083106164009322 ) ) ;
#64132 = CARTESIAN_POINT ( 'NONE',  ( -6.000000000000121680, -12.70778746994576025, 30.41441678777401236 ) ) ;
#64134 = CARTESIAN_POINT ( 'NONE',  ( 13.60762673622823549, -8.239487800360276282, 34.69522927552633718 ) ) ;
#64135 = EDGE_LOOP ( 'NONE', ( #32471, #86064, #44619, #1094 ) ) ;
#64136 = EDGE_CURVE ( 'NONE', #73637, #20256, #17222, .T. ) ;
#64137 = ADVANCED_FACE ( 'NONE', ( #41389 ), #62525, .F. ) ;
#64138 = ORIENTED_EDGE ( 'NONE', *, *, #48045, .T. ) ;
#64139 = CARTESIAN_POINT ( 'NONE',  ( 4.826923076923076650, -7.500000000000001776, 35.00000000000000000 ) ) ;
#64141 = EDGE_CURVE ( 'NONE', #45062, #86240, #15434, .T. ) ;
#64140 = ORIENTED_EDGE ( 'NONE', *, *, #84118, .F. ) ;
#64142 = FACE_BOUND ( 'NONE', #35184, .T. ) ;
#64143 = CARTESIAN_POINT ( 'NONE',  ( 3.453548899747295842, -2.612705202774697533, 31.66806509827799943 ) ) ;
#64144 = CARTESIAN_POINT ( 'NONE',  ( -3.903791842207839480, -11.79725096376909654, 32.30694842903960762 ) ) ;
#64145 = EDGE_LOOP ( 'NONE', ( #13777, #61918 ) ) ;
#64146 = CARTESIAN_POINT ( 'NONE',  ( -14.17716686945866122, -8.630441415882550871, 34.87705825610312615 ) ) ;
#64148 = EDGE_CURVE ( 'NONE', #78555, #44484, #22475, .T. ) ;
#64147 = DIRECTION ( 'NONE',  ( 0.000000000000000000, 0.8660254037844377084, -0.5000000000000015543 ) ) ;
#64149 = CARTESIAN_POINT ( 'NONE',  ( 1.318533005255251744, -3.322132147404559976, 32.92929555188719348 ) ) ;
#64150 = CARTESIAN_POINT ( 'NONE',  ( -11.66860874789975888, -6.001485441113819874, 34.52039167877662607 ) ) ;
#64151 = CARTESIAN_POINT ( 'NONE',  ( -13.31854703361294590, -11.69971097300155272, 32.46337939537588113 ) ) ;
#64152 = CARTESIAN_POINT ( 'NONE',  ( -6.700297381808512753, -9.332535724633407526, 34.40230450496446224 ) ) ;
#64153 = EDGE_CURVE ( 'NONE', #22567, #70591, #75133, .T. ) ;
#64154 = CARTESIAN_POINT ( 'NONE',  ( -15.23076923076922995, -5.557115091759785130, 34.35708131394839171 ) ) ;
#64155 = DIRECTION ( 'NONE',  ( 0.000000000000000000, 0.000000000000000000, -1.000000000000000000 ) ) ;
#64156 = CARTESIAN_POINT ( 'NONE',  ( -6.130691466667558487, -5.582088688514999397, 34.36776431015576350 ) ) ;
#64157 = PLANE ( 'NONE',  #31419 ) ;
#64158 = CYLINDRICAL_SURFACE ( 'NONE', #31522, 0.2499999999999998890 ) ;
#64159 = VECTOR ( 'NONE', #35730, 1000.000000000000114 ) ;
#64160 = CARTESIAN_POINT ( 'NONE',  ( -13.16183571563731824, -12.47679350104403007, 31.42216943046555855 ) ) ;
#64162 = LINE ( 'NONE', #85794, #44574 ) ;
#64161 = CARTESIAN_POINT ( 'NONE',  ( -17.07692307692307665, -3.937682226553329556, 33.60647404775216529 ) ) ;
#64163 = CARTESIAN_POINT ( 'NONE',  ( -1.134669975237340367, -9.357781135181031829, 34.66075350412533851 ) ) ;
#64165 = CARTESIAN_POINT ( 'NONE',  ( -18.00000000000012079, -3.083524468854528244, 32.58852847137268327 ) ) ;
#64164 = CYLINDRICAL_SURFACE ( 'NONE', #77456, 0.2499999999999973355 ) ;
#64166 = EDGE_CURVE ( 'NONE', #88839, #423, #841, .T. ) ;
#64167 = CARTESIAN_POINT ( 'NONE',  ( -2.372962308248625529, -5.941354392334500467, 34.76329471203369792 ) ) ;
#64168 = CARTESIAN_POINT ( 'NONE',  ( -2.749999999999997780, -7.561099074964547917, 23.59188170625849068 ) ) ;
#64169 = ORIENTED_EDGE ( 'NONE', *, *, #22877, .F. ) ;
#64170 = CARTESIAN_POINT ( 'NONE',  ( 18.25005431163831560, -11.79725096376909299, 32.30694842903960762 ) ) ;
#64171 = ORIENTED_EDGE ( 'NONE', *, *, #43484, .T. ) ;
#64172 = CARTESIAN_POINT ( 'NONE',  ( -2.373774687052442545, -2.833524468853757305, 32.15551576947924417 ) ) ;
#64173 = EDGE_CURVE ( 'NONE', #1510, #47623, #3175, .T. ) ;
#64174 = ORIENTED_EDGE ( 'NONE', *, *, #47625, .F. ) ;
#64175 = CARTESIAN_POINT ( 'NONE',  ( -13.16183571563731647, -2.353885683473779800, 30.79025554430704403 ) ) ;
#64176 = ORIENTED_EDGE ( 'NONE', *, *, #75872, .T. ) ;
#64177 = CARTESIAN_POINT ( 'NONE',  ( -6.065270445960775803, -11.94971097300153140, 32.03036669348370680 ) ) ;
#64178 = CARTESIAN_POINT ( 'NONE',  ( 2.775308065498768517, -8.577988221561467341, 21.79500670625849068 ) ) ;
#64179 = CARTESIAN_POINT ( 'NONE',  ( -6.000000000000119904, -4.481592998941358097, 33.73612834414048933 ) ) ;
#64180 = CARTESIAN_POINT ( 'NONE',  ( -3.007756386675836779, -12.38742843783360748, 31.66772728687926985 ) ) ;
#64181 = CARTESIAN_POINT ( 'NONE',  ( 6.923076923076924238, -8.973038597847269315, 34.52809138561121927 ) ) ;
#64182 = DIRECTION ( 'NONE',  ( 0.000000000000000000, 0.1736481776669275834, 0.9848077530122086864 ) ) ;
#64183 = DIRECTION ( 'NONE',  ( 0.000000000000000000, 0.000000000000000000, -1.000000000000000000 ) ) ;
#64184 = CARTESIAN_POINT ( 'NONE',  ( -13.44988538517170440, -12.16647553114622049, 32.15551576947930812 ) ) ;
#64185 = CARTESIAN_POINT ( 'NONE',  ( 1.553300858899129944, -11.24999999999998934, 17.20312500000000000 ) ) ;
#64186 = EDGE_CURVE ( 'NONE', #53590, #17102, #57548, .T. ) ;
#64187 = CARTESIAN_POINT ( 'NONE',  ( -23.50000000000000000, 6.011520428872295955E-15, 27.75000000000000355 ) ) ;
#64188 = CARTESIAN_POINT ( 'NONE',  ( -2.084679463598912097, -11.98016756924214832, 32.48728574198911190 ) ) ;
#64189 = CARTESIAN_POINT ( 'NONE',  ( -23.00000000000000000, -7.500000000000000000, 29.75000000000000355 ) ) ;
#64190 = CARTESIAN_POINT ( 'NONE',  ( 2.320192649118979489E-14, -11.25000000000000000, 17.28125000000000000 ) ) ;
#64191 = EDGE_CURVE ( 'NONE', #4986, #74135, #85471, .T. ) ;
#64192 = CARTESIAN_POINT ( 'NONE',  ( -10.36533019547115941, -5.642605341092957971, 34.66089969410670335 ) ) ;
#64193 = ORIENTED_EDGE ( 'NONE', *, *, #67377, .F. ) ;
#64194 = AXIS2_PLACEMENT_3D ( 'NONE', #28777, #14821, #28318 ) ;
#64195 = FACE_OUTER_BOUND ( 'NONE', #51815, .T. ) ;
#64196 = CARTESIAN_POINT ( 'NONE',  ( 16.02369894440793274, -12.27039167877662251, 31.24851455888617835 ) ) ;
#64197 = CARTESIAN_POINT ( 'NONE',  ( 1.161689167099238418, -12.39988816332205701, 30.74660775122750778 ) ) ;
#64198 = DIRECTION ( 'NONE',  ( -0.000000000000000000, -0.000000000000000000, -1.000000000000000000 ) ) ;
#64199 = CARTESIAN_POINT ( 'NONE',  ( -1.384615384615383471, -10.51840700105979565, 33.73612834413961536 ) ) ;
#64200 = VECTOR ( 'NONE', #69873, 1000.000000000000227 ) ;
#64201 = CARTESIAN_POINT ( 'NONE',  ( -8.769230769230768274, -8.120952969808772792, 34.71129190930000163 ) ) ;
#64202 = ADVANCED_FACE ( 'NONE', ( #84602 ), #11140, .F. ) ;
#64203 = CARTESIAN_POINT ( 'NONE',  ( 17.06410256410256565, -3.499999999999999556, 29.75000000000000355 ) ) ;
#64204 = EDGE_CURVE ( 'NONE', #42820, #51792, #79158, .T. ) ;
#64205 = VECTOR ( 'NONE', #21641, 1000.000000000000227 ) ;
#64206 = EDGE_LOOP ( 'NONE', ( #28014, #88560, #45021, #44055 ) ) ;
#64207 = CARTESIAN_POINT ( 'NONE',  ( -10.74599427058869416, -7.722926974430166069, 34.99546784045485737 ) ) ;
#64208 = VERTEX_POINT ( 'NONE', #44028 ) ;
#64209 = EDGE_LOOP ( 'NONE', ( #44338, #15779, #49149, #64565 ) ) ;
#64210 = B_SPLINE_CURVE_WITH_KNOTS ( 'NONE', 3,
 ( #4688, #80354, #33492, #81239, #81682, #39371, #87566, #4234, #31717, #60951 ),
 .UNSPECIFIED., .F., .F.,
 ( 4, 2, 2, 2, 4 ),
 ( 0.0007817246256747504250, 0.0009771112852218954894, 0.001172497944769040554, 0.001367884604316185401, 0.001563271263863330466 ),
 .UNSPECIFIED. ) ;
#64211 = CARTESIAN_POINT ( 'NONE',  ( -5.999999999999998224, -12.62096338111211580, 30.90682066428153263 ) ) ;
#64212 = CARTESIAN_POINT ( 'NONE',  ( 16.21910172512217940, -2.892918686051626498, 31.69288490824026638 ) ) ;
#64213 = B_SPLINE_CURVE_WITH_KNOTS ( 'NONE', 3,
 ( #24003, #81527, #74768, #80189, #18490, #45944, #73435, #39210, #4974, #32441 ),
 .UNSPECIFIED., .F., .F.,
 ( 4, 2, 2, 2, 4 ),
 ( 0.0007817359430256297891, 0.0009771253907249958896, 0.001172514838424361990, 0.001367904286123728091, 0.001563293733823094191 ),
 .UNSPECIFIED. ) ;
#64214 = CARTESIAN_POINT ( 'NONE',  ( -13.16160403300253279, -9.086983370893049639, 34.49168942202179267 ) ) ;
#64215 = CARTESIAN_POINT ( 'NONE',  ( 17.74997676270703550, -9.271318131107980420, 34.42618302367067429 ) ) ;
#64216 = EDGE_CURVE ( 'NONE', #22286, #79691, #44461, .T. ) ;
#64217 = VERTEX_POINT ( 'NONE', #44915 ) ;
#64218 = EDGE_CURVE ( 'NONE', #79996, #80137, #29648, .T. ) ;
#64219 = CARTESIAN_POINT ( 'NONE',  ( -6.673131404728780858, -5.852078868378311149, 34.47109172314383585 ) ) ;
#64220 = VERTEX_POINT ( 'NONE', #24653 ) ;
#64221 = AXIS2_PLACEMENT_3D ( 'NONE', #29970, #16013, #8817 ) ;
#64222 = VERTEX_POINT ( 'NONE', #78713 ) ;
#64223 = FACE_OUTER_BOUND ( 'NONE', #6839, .T. ) ;
#64224 = PLANE ( 'NONE',  #68965 ) ;
#64225 = CARTESIAN_POINT ( 'NONE',  ( -16.15384615384615330, -4.098570777380720287, 33.41473453929634729 ) ) ;
#64226 = CARTESIAN_POINT ( 'NONE',  ( 2.177131715950388458, -2.504760397472875155, 29.97295953869789997 ) ) ;
#64227 = CARTESIAN_POINT ( 'NONE',  ( 3.230769230769231726, -6.386643153685126251, 34.62446782046654192 ) ) ;
#64228 = VERTEX_POINT ( 'NONE', #63864 ) ;
#64229 = ORIENTED_EDGE ( 'NONE', *, *, #52850, .T. ) ;
#64230 = CARTESIAN_POINT ( 'NONE',  ( 2.320192649118979489E-14, -11.25000000000000000, 22.28125000000000355 ) ) ;
#64231 = VERTEX_POINT ( 'NONE', #57108 ) ;
#64233 = ORIENTED_EDGE ( 'NONE', *, *, #23436, .T. ) ;
#64232 = CARTESIAN_POINT ( 'NONE',  ( 4.403791672194295792, -11.37275283266503756, 32.91324779482534524 ) ) ;
#64234 = CARTESIAN_POINT ( 'NONE',  ( -14.87820512820512953, -4.000000000000000000, 29.75000000000000355 ) ) ;
#64235 = LINE ( 'NONE', #2538, #7193 ) ;
#64236 = CARTESIAN_POINT ( 'NONE',  ( 9.692307692307695177, -4.945431358278436385, 36.03766855953609394 ) ) ;
#64237 = EDGE_LOOP ( 'NONE', ( #56265, #59604, #51995, #71309 ) ) ;
#64238 = B_SPLINE_CURVE_WITH_KNOTS ( 'NONE', 3,
 ( #24119, #38089, #59693, #38996, #46187, #11964, #45734, #72311, #39441, #80875 ),
 .UNSPECIFIED., .F., .F.,
 ( 4, 2, 2, 2, 4 ),
 ( 0.0007817359430256334753, 0.0009771253907250058643, 0.001172514838424371098, 0.001367904286123736764, 0.001563293733823101998 ),
 .UNSPECIFIED. ) ;
#64239 = CARTESIAN_POINT ( 'NONE',  ( -11.31545018684868786, -4.887748414852792322, 34.01359900205216746 ) ) ;
#64240 = LINE ( 'NONE', #21949, #16599 ) ;
#64241 = VERTEX_POINT ( 'NONE', #22874 ) ;
#64242 = FACE_BOUND ( 'NONE', #88410, .T. ) ;
#64243 = CARTESIAN_POINT ( 'NONE',  ( 15.29602437028207085, -11.67786785259547777, 32.92929555188713664 ) ) ;
#64244 = CARTESIAN_POINT ( 'NONE',  ( -17.07692307692307665, -6.189225973068211317, 35.74407628777942847 ) ) ;
#64245 = LINE ( 'NONE', #9332, #84009 ) ;
#64247 = FACE_OUTER_BOUND ( 'NONE', #27393, .T. ) ;
#64246 = CARTESIAN_POINT ( 'NONE',  ( 6.000000000000001776, -10.05456864172156806, 36.03766855953608683 ) ) ;
#64248 = AXIS2_PLACEMENT_3D ( 'NONE', #68653, #28563, #61444 ) ;
#64249 = CARTESIAN_POINT ( 'NONE',  ( 5.076923076922954969, -2.625532179533778709, 30.86335684631627174 ) ) ;
#64250 = DIRECTION ( 'NONE',  ( 0.000000000000000000, 0.000000000000000000, -1.000000000000000000 ) ) ;
#64251 = ORIENTED_EDGE ( 'NONE', *, *, #35737, .F. ) ;
#64253 = ADVANCED_FACE ( 'NONE', ( #17010 ), #50338, .F. ) ;
#64252 = CARTESIAN_POINT ( 'NONE',  ( 17.07692307692307665, -13.63283147151868846, 33.57946703557072254 ) ) ;
#64254 = CARTESIAN_POINT ( 'NONE',  ( -16.94613263595612906, -6.369690395747424461, 34.87708834333098196 ) ) ;
#64255 = ORIENTED_EDGE ( 'NONE', *, *, #1175, .F. ) ;
#64256 = AXIS2_PLACEMENT_3D ( 'NONE', #24629, #51184, #23729 ) ;
#64257 = EDGE_CURVE ( 'NONE', #71435, #9433, #72389, .T. ) ;
#64258 = CARTESIAN_POINT ( 'NONE',  ( 20.00000000000000355, 10.00000000000000533, 10.00000000000000178 ) ) ;
#64259 = CARTESIAN_POINT ( 'NONE',  ( 16.85399611801622655, -10.77366814457252175, 33.85459836347580875 ) ) ;
#64261 = CARTESIAN_POINT ( 'NONE',  ( -15.16551409125639260, -5.941354392334607049, 34.76329471203374055 ) ) ;
#64260 = PRODUCT_DEFINITION_SHAPE ( 'NONE', 'NONE',  #45194 ) ;
#64262 = CARTESIAN_POINT ( 'NONE',  ( -7.780086512803768173, -10.67929555188718282, 33.92786785259544757 ) ) ;
#64263 = CYLINDRICAL_SURFACE ( 'NONE', #61492, 0.2499999999999998890 ) ;
#64264 = CARTESIAN_POINT ( 'NONE',  ( -8.834501215191545853, -6.026961402152685388, 34.52809138561120506 ) ) ;
#64265 = FACE_BOUND ( 'NONE', #64519, .T. ) ;
#64267 = LINE ( 'NONE', #30494, #86280 ) ;
#64266 = CARTESIAN_POINT ( 'NONE',  ( -2.531177251416254492, -6.760086850603068243, 34.69517049084099369 ) ) ;
#64268 = AXIS2_PLACEMENT_3D ( 'NONE', #37830, #44128, #31974 ) ;
#64269 = FACE_OUTER_BOUND ( 'NONE', #47228, .T. ) ;
#64271 = LINE ( 'NONE', #9355, #63612 ) ;
#64270 = DIRECTION ( 'NONE',  ( -1.000000000000000000, -0.000000000000000000, -0.000000000000000000 ) ) ;
#64272 = EDGE_CURVE ( 'NONE', #8206, #68769, #67643, .T. ) ;
#64273 = DIRECTION ( 'NONE',  ( -0.000000000000000000, 1.000000000000000000, 3.491481338843133355E-15 ) ) ;
#64274 = CARTESIAN_POINT ( 'NONE',  ( -0.06109907496455085213, -3.750000000000000888, 20.15438170625849068 ) ) ;
#64275 = ORIENTED_EDGE ( 'NONE', *, *, #77455, .F. ) ;
#64276 = LINE ( 'NONE', #85453, #32019 ) ;
#64277 = DIRECTION ( 'NONE',  ( -0.000000000000000000, -0.9848077530122085754, -0.1736481776669273613 ) ) ;
#64278 = CARTESIAN_POINT ( 'NONE',  ( -9.561515884482904681, -8.999086150933475636, 34.52020707165672775 ) ) ;
#64279 = CARTESIAN_POINT ( 'NONE',  ( -20.74999999999999645, -12.50000000000000000, 29.75000000000000355 ) ) ;
#64280 = CYLINDRICAL_SURFACE ( 'NONE', #19851, 0.2500000000000008882 ) ;
#64281 = CARTESIAN_POINT ( 'NONE',  ( -2.694853999681210865, -4.891553140782108677, 22.49813170625848713 ) ) ;
#64282 = CARTESIAN_POINT ( 'NONE',  ( -2.437840277424000224, -3.625366637846545448, 33.29286588640298561 ) ) ;
#64283 = CARTESIAN_POINT ( 'NONE',  ( -11.53846153846166089, -3.643525952248795718, 33.31231777344771672 ) ) ;
#64284 = EDGE_CURVE ( 'NONE', #2304, #70411, #38597, .T. ) ;
#64285 = CARTESIAN_POINT ( 'NONE',  ( -7.846153846153844924, -2.833524468853757305, 32.15551576947925838 ) ) ;
#64287 = B_SPLINE_CURVE_WITH_KNOTS ( 'NONE', 3,
 ( #61829, #45317, #139, #72790, #11099, #69040, #38576, #4340, #81676, #31826 ),
 .UNSPECIFIED., .F., .F.,
 ( 4, 2, 2, 2, 4 ),
 ( 0.000000000000000000, 0.0001954311564186861426, 0.0003908623128373722852, 0.0005862934692560583735, 0.0007817246256747445703 ),
 .UNSPECIFIED. ) ;
#64286 = CARTESIAN_POINT ( 'NONE',  ( -0.4615384615385840772, -2.657715359629662544, 31.77849191805970364 ) ) ;
#64288 = CARTESIAN_POINT ( 'NONE',  ( -19.50000000000000000, -11.50000000000000000, 29.75000000000000355 ) ) ;
#64289 = CARTESIAN_POINT ( 'NONE',  ( 12.21156171748987163, -12.65889640711025521, 30.72598325615533454 ) ) ;
#64290 = B_SPLINE_CURVE_WITH_KNOTS ( 'NONE', 3,
 ( #71075, #85482, #10269, #70638, #43599, #8500, #58000, #65196, #37280, #57556 ),
 .UNSPECIFIED., .F., .F.,
 ( 4, 2, 2, 2, 4 ),
 ( 0.000000000000000000, 0.0001954339857564070678, 0.0003908679715128141356, 0.0005863019572692211492, 0.0007817359430256282712 ),
 .UNSPECIFIED. ) ;
#64291 = CARTESIAN_POINT ( 'NONE',  ( 22.00000000000001066, -14.99999999999999112, 0.000000000000000000 ) ) ;
#64292 = CARTESIAN_POINT ( 'NONE',  ( 25.00000000000000355, 9.999999999999971578, 13.00000000000000178 ) ) ;
#64293 = ORIENTED_EDGE ( 'NONE', *, *, #5948, .T. ) ;
#64294 = CARTESIAN_POINT ( 'NONE',  ( 3.230769230769231726, -12.34228464037088635, 31.77849191805839268 ) ) ;
#64295 = CARTESIAN_POINT ( 'NONE',  ( -1.515175298228748080, -2.254533558242299396, 29.97296025877828285 ) ) ;
#64296 = CIRCLE ( 'NONE', #77294, 0.2500000000000002220 ) ;
#64297 = CARTESIAN_POINT ( 'NONE',  ( 1.077988221561497539, -10.27530806549875386, 24.95499329374151287 ) ) ;
#64298 = ADVANCED_FACE ( 'NONE', ( #31868 ), #47139, .F. ) ;
#64299 = CARTESIAN_POINT ( 'NONE',  ( -2.557669051740897537, -4.818429247618089661, 34.26397095200675125 ) ) ;
#64300 = DIRECTION ( 'NONE',  ( 1.000000000000000000, 0.000000000000000000, 0.000000000000000000 ) ) ;
#64301 = ORIENTED_EDGE ( 'NONE', *, *, #71995, .F. ) ;
#64302 = CARTESIAN_POINT ( 'NONE',  ( -16.28399412357784826, -4.299443229763728169, 33.91186481527756058 ) ) ;
#64304 = ORIENTED_EDGE ( 'NONE', *, *, #82211, .F. ) ;
#64303 = CARTESIAN_POINT ( 'NONE',  ( 12.39545505058258001, -5.557115091759785130, 34.35708131394839171 ) ) ;
#64305 = DIRECTION ( 'NONE',  ( -0.000000000000000000, 1.000000000000000000, -0.000000000000000000 ) ) ;
#64306 = EDGE_CURVE ( 'NONE', #77909, #46953, #53904, .T. ) ;
#64307 = DIRECTION ( 'NONE',  ( -0.000000000000000000, -0.5000000000000009992, -0.8660254037844380415 ) ) ;
#64308 = AXIS2_PLACEMENT_3D ( 'NONE', #6038, #74940, #60965 ) ;
#64309 = CARTESIAN_POINT ( 'NONE',  ( 11.53846153846153832, -4.945431358278436385, 36.03766855953609394 ) ) ;
#64310 = FACE_OUTER_BOUND ( 'NONE', #53829, .T. ) ;
#64311 = VERTEX_POINT ( 'NONE', #47589 ) ;
#64312 = CARTESIAN_POINT ( 'NONE',  ( -11.78848477575450282, -4.335965774309649134, 33.62209801155881905 ) ) ;
#64313 = CARTESIAN_POINT ( 'NONE',  ( 5.206968132842848540, -2.254550872974306674, 29.97347326024527447 ) ) ;
#64314 = B_SPLINE_CURVE_WITH_KNOTS ( 'NONE', 3,
 ( #71982, #24684, #73323, #10288, #11626, #58453, #39103, #16587, #71533, #79637 ),
 .UNSPECIFIED., .F., .F.,
 ( 4, 2, 2, 2, 4 ),
 ( 0.000000000000000000, 0.0001954339857564093175, 0.0003908679715128186350, 0.0005863019572692279796, 0.0007817359430256372700 ),
 .UNSPECIFIED. ) ;
#64315 = ADVANCED_FACE ( 'NONE', ( #33192 ), #60212, .F. ) ;
#64316 = DIRECTION ( 'NONE',  ( -1.000000000000000000, 0.000000000000000000, -0.000000000000000000 ) ) ;
#64317 = EDGE_LOOP ( 'NONE', ( #87154, #34247, #39446, #5222, #69561, #14128 ) ) ;
#64318 = EDGE_LOOP ( 'NONE', ( #4320, #37738 ) ) ;
#64319 = EDGE_LOOP ( 'NONE', ( #16949, #5158 ) ) ;
#64320 = VECTOR ( 'NONE', #75898, 1000.000000000000000 ) ;
#64321 = CARTESIAN_POINT ( 'NONE',  ( -9.942284423250047354, -9.943427161483782584, 34.11278801902876978 ) ) ;
#64322 = CARTESIAN_POINT ( 'NONE',  ( 13.45068271796546178, -3.322132147404559976, 32.92929555188717927 ) ) ;
#64323 = CARTESIAN_POINT ( 'NONE',  ( -4.088591014333314178, -12.70778746994558439, 30.41441678777537305 ) ) ;
#64324 = EDGE_CURVE ( 'NONE', #11896, #50121, #60126, .T. ) ;
#64325 = CARTESIAN_POINT ( 'NONE',  ( 3.230769230769231726, -9.905515769479276145, 34.41647553114623292 ) ) ;
#64326 = ADVANCED_FACE ( 'NONE', ( #26882 ), #81393, .F. ) ;
#64327 = ADVANCED_FACE ( 'NONE', ( #88167 ), #74180, .F. ) ;
#64328 = ORIENTED_EDGE ( 'NONE', *, *, #74064, .T. ) ;
#64329 = CIRCLE ( 'NONE', #60034, 4.000000000000000000 ) ;
#64330 = ORIENTED_EDGE ( 'NONE', *, *, #53172, .T. ) ;
#64332 = EDGE_LOOP ( 'NONE', ( #67342, #87768, #66568, #46682 ) ) ;
#64331 = CARTESIAN_POINT ( 'NONE',  ( 5.076923076922954969, -3.835265460704628371, 33.15142922262033665 ) ) ;
#64333 = EDGE_CURVE ( 'NONE', #20169, #61249, #54698, .T. ) ;
#64334 = CARTESIAN_POINT ( 'NONE',  ( 5.076923076923075762, -1.215029322943914858, 32.30358669280327177 ) ) ;
#64335 = CARTESIAN_POINT ( 'NONE',  ( 7.622668921589517588, -12.11044203135681840, 32.26167407432752299 ) ) ;
#64336 = CARTESIAN_POINT ( 'NONE',  ( 14.30769230769231015, -1.215029322943914858, 32.30358669280327177 ) ) ;
#64337 = EDGE_LOOP ( 'NONE', ( #23458, #1527 ) ) ;
#64338 = B_SPLINE_CURVE_WITH_KNOTS ( 'NONE', 3,
 ( #7306, #20379, #33450, #54587, #61787, #14054, #55045, #55483, #35212, #12731 ),
 .UNSPECIFIED., .F., .F.,
 ( 4, 2, 2, 2, 4 ),
 ( 0.000000000000000000, 0.0001954311564186882568, 0.0003908623128373765136, 0.0005862934692560647703, 0.0007817246256747530271 ),
 .UNSPECIFIED. ) ;
#64339 = ORIENTED_EDGE ( 'NONE', *, *, #86184, .T. ) ;
#64341 = EDGE_LOOP ( 'NONE', ( #56107, #85100, #65130, #6929 ) ) ;
#64340 = DIRECTION ( 'NONE',  ( 0.000000000000000000, 0.8660254037844377084, 0.5000000000000015543 ) ) ;
#64342 = FACE_OUTER_BOUND ( 'NONE', #47377, .T. ) ;
#64343 = VECTOR ( 'NONE', #12758, 1000.000000000000000 ) ;
#64344 = CARTESIAN_POINT ( 'NONE',  ( -5.143006487878958310, -9.780366693483667717, 34.19971097300155805 ) ) ;
#64345 = ORIENTED_EDGE ( 'NONE', *, *, #35769, .T. ) ;
#64346 = CARTESIAN_POINT ( 'NONE',  ( 17.86930853333243618, -10.54014554554151140, 33.71984207302941883 ) ) ;
#64347 = DIRECTION ( 'NONE',  ( -1.000000000000000000, 0.000000000000000000, -0.000000000000000000 ) ) ;
#64348 = CARTESIAN_POINT ( 'NONE',  ( 17.77707304109314634, -12.38737895849757820, 31.66785238281580206 ) ) ;
#64349 = VECTOR ( 'NONE', #76900, 999.9999999999998863 ) ;
#64350 = FACE_BOUND ( 'NONE', #47838, .T. ) ;
#64351 = CARTESIAN_POINT ( 'NONE',  ( 7.846153846153846700, -12.34228464037088635, 31.77849191805839268 ) ) ;
#64352 = CARTESIAN_POINT ( 'NONE',  ( 4.153846153846154188, -2.292212530054420494, 30.41441678777542634 ) ) ;
#64353 = DIRECTION ( 'NONE',  ( 0.000000000000000000, 0.7660444431189822323, -0.6427876096865344779 ) ) ;
#64355 = CARTESIAN_POINT ( 'NONE',  ( -16.15384615384615330, -2.833524468853757305, 32.15551576947925838 ) ) ;
#64354 = CARTESIAN_POINT ( 'NONE',  ( 5.076923076923075762, -12.62096338111211580, 30.90682066428153263 ) ) ;
#64356 = CARTESIAN_POINT ( 'NONE',  ( 17.86985203026830504, -6.809168938359901446, 34.95455904226513866 ) ) ;
#64357 = FACE_OUTER_BOUND ( 'NONE', #21360, .T. ) ;
#64358 = VERTEX_POINT ( 'NONE', #12919 ) ;
#64359 = CIRCLE ( 'NONE', #80202, 0.2500000000000002220 ) ;
#64360 = CARTESIAN_POINT ( 'NONE',  ( -16.15384615384615330, -3.322132147404559976, 32.92929555188717927 ) ) ;
#64361 = ORIENTED_EDGE ( 'NONE', *, *, #4419, .T. ) ;
#64362 = ORIENTED_EDGE ( 'NONE', *, *, #32794, .F. ) ;
#64364 = CARTESIAN_POINT ( 'NONE',  ( -19.50000000000000000, -11.50000000000000000, 29.75000000000000355 ) ) ;
#64363 = CARTESIAN_POINT ( 'NONE',  ( -1.161602540521989857, -4.762714258010882773, 34.23016756924214832 ) ) ;
#64365 = CARTESIAN_POINT ( 'NONE',  ( -5.999999999999998224, -6.386643153685126251, 34.62446782046654192 ) ) ;
#64366 = CARTESIAN_POINT ( 'NONE',  ( 14.37294744720514572, -4.320704448112861584, 33.92786785259548310 ) ) ;
#64367 = CARTESIAN_POINT ( 'NONE',  ( 1.318531973659506029, -6.386643153685125363, 34.62446782046654903 ) ) ;
#64368 = CARTESIAN_POINT ( 'NONE',  ( 1.254468175177164913, -11.93770438780619259, 32.05411857736982029 ) ) ;
#64369 = ORIENTED_EDGE ( 'NONE', *, *, #81657, .F. ) ;
#64370 = DIRECTION ( 'NONE',  ( -0.000000000000000000, -0.000000000000000000, -1.000000000000000000 ) ) ;
#64371 = CARTESIAN_POINT ( 'NONE',  ( 6.673053685783957967, -3.711651800289232916, 33.01384336483936011 ) ) ;
#64372 = CARTESIAN_POINT ( 'NONE',  ( -12.68446542044531000, -11.43668979543635089, 33.22377378376089752 ) ) ;
#64373 = CARTESIAN_POINT ( 'NONE',  ( -12.46153846153846168, -9.584722331328613620, 36.20867863119891439 ) ) ;
#64374 = CARTESIAN_POINT ( 'NONE',  ( -11.76132696066517802, -2.501496062324912284, 29.88072118266895671 ) ) ;
#64375 = B_SPLINE_CURVE_WITH_KNOTS ( 'NONE', 3,
 ( #14409, #82881, #47753, #7218, #19839, #35121, #27042, #5886, #48629, #76106 ),
 .UNSPECIFIED., .F., .F.,
 ( 4, 2, 2, 2, 4 ),
 ( 0.000000000000000000, 0.0001954339857564086670, 0.0003908679715128173340, 0.0005863019572692260281, 0.0007817359430256346680 ),
 .UNSPECIFIED. ) ;
#64376 = CARTESIAN_POINT ( 'NONE',  ( 1.553300858899129944, -11.24999999999998934, 18.45312500000000355 ) ) ;
#64377 = ORIENTED_EDGE ( 'NONE', *, *, #15956, .T. ) ;
#64378 = ORIENTED_EDGE ( 'NONE', *, *, #4583, .T. ) ;
#64379 = VECTOR ( 'NONE', #38920, 1000.000000000000000 ) ;
#64380 = DIRECTION ( 'NONE',  ( 0.000000000000000000, 1.000000000000000000, -0.000000000000000000 ) ) ;
#64381 = ORIENTED_EDGE ( 'NONE', *, *, #24529, .T. ) ;
#64382 = CARTESIAN_POINT ( 'NONE',  ( -7.146561866800870355, -2.599994579823202923, 30.74605699353653776 ) ) ;
#64383 = CARTESIAN_POINT ( 'NONE',  ( 18.24994551834813805, -5.852078868378311149, 34.47109172314383585 ) ) ;
#64385 = B_SPLINE_CURVE_WITH_KNOTS ( 'NONE', 3,
 ( #57900, #58337, #37631, #30866, #24110, #51560, #17365, #44822, #1640, #38530 ),
 .UNSPECIFIED., .F., .F.,
 ( 4, 2, 2, 2, 4 ),
 ( 0.0007817246256747458714, 0.0009771112852218889842, 0.001172497944769032097, 0.001367884604316175210, 0.001563271263863318323 ),
 .UNSPECIFIED. ) ;
#64384 = CARTESIAN_POINT ( 'NONE',  ( 4.153846153846154188, -10.67929555188718282, 33.92786785259544047 ) ) ;
#64386 = CARTESIAN_POINT ( 'NONE',  ( 2.177215599575844873, -7.276988635370450709, 34.74523720219453793 ) ) ;
#64387 = CARTESIAN_POINT ( 'NONE',  ( 2.651650429449569302, -10.15165042944953733, 19.62500000000000000 ) ) ;
#64388 = CYLINDRICAL_SURFACE ( 'NONE', #47457, 0.2500000000000002220 ) ;
#64389 = ORIENTED_EDGE ( 'NONE', *, *, #69448, .F. ) ;
#64390 = LINE ( 'NONE', #30181, #87580 ) ;
#64392 = VERTEX_POINT ( 'NONE', #52562 ) ;
#64391 = CARTESIAN_POINT ( 'NONE',  ( 11.53846153846153832, -10.05456864172156806, 36.03766855953608683 ) ) ;
#64393 = CARTESIAN_POINT ( 'NONE',  ( -9.757630607799864464, -7.749976743299138882, 34.99404534957040624 ) ) ;
#64394 = CARTESIAN_POINT ( 'NONE',  ( -12.21159294319032007, -3.712312575010499049, 33.01462480002815170 ) ) ;
#64395 = DIRECTION ( 'NONE',  ( -0.000000000000000000, 0.7660444431189791237, -0.6427876096865379196 ) ) ;
#64396 = CARTESIAN_POINT ( 'NONE',  ( 11.53846153846153832, -8.164416787775445883, 34.95778746994557906 ) ) ;
#64397 = AXIS2_PLACEMENT_3D ( 'NONE', #10940, #45604, #38411 ) ;
#64398 = CARTESIAN_POINT ( 'NONE',  ( -12.71156169883143150, -12.43535235679832596, 30.55408501211184813 ) ) ;
#64399 = CARTESIAN_POINT ( 'NONE',  ( 0.000000000000000000, -11.00000000000000000, 29.25000000000000000 ) ) ;
#64400 = CARTESIAN_POINT ( 'NONE',  ( 0.06109907496451268821, -3.749999999999999556, 18.15811829374151642 ) ) ;
#64401 = VERTEX_POINT ( 'NONE', #33639 ) ;
#64402 = FACE_OUTER_BOUND ( 'NONE', #68378, .T. ) ;
#64403 = CARTESIAN_POINT ( 'NONE',  ( -1.318548051265309384, -3.322132147404559976, 32.92929555188717927 ) ) ;
#64404 = CARTESIAN_POINT ( 'NONE',  ( 2.750000000000001776, -7.499999999999984013, 24.46875000000000000 ) ) ;
#64405 = EDGE_CURVE ( 'NONE', #29561, #78266, #72972, .T. ) ;
#64406 = CARTESIAN_POINT ( 'NONE',  ( -15.90390074446811042, -11.56426240980093567, 33.07394671870546432 ) ) ;
#64407 = CARTESIAN_POINT ( 'NONE',  ( -3.230769230769352962, -11.06231777344772027, 33.60647404775119895 ) ) ;
#64408 = ORIENTED_EDGE ( 'NONE', *, *, #83767, .F. ) ;
#64409 = CARTESIAN_POINT ( 'NONE',  ( 2.749999999999995115, -6.360912703473971419, 15.64062500000000178 ) ) ;
#64410 = CARTESIAN_POINT ( 'NONE',  ( 3.230769230769110045, -9.442884908241554243, 34.35708131394783038 ) ) ;
#64411 = VERTEX_POINT ( 'NONE', #80047 ) ;
#64412 = FACE_OUTER_BOUND ( 'NONE', #38342, .T. ) ;
#64413 = ORIENTED_EDGE ( 'NONE', *, *, #17813, .F. ) ;
#64414 = VECTOR ( 'NONE', #80252, 1000.000000000000227 ) ;
#64415 = DIRECTION ( 'NONE',  ( -0.000000000000000000, -0.6427876096865404731, -0.7660444431189771253 ) ) ;
#64416 = CARTESIAN_POINT ( 'NONE',  ( -17.14219307747939425, -2.379036618887870880, 30.90682066428148644 ) ) ;
#64417 = EDGE_CURVE ( 'NONE', #75871, #62121, #26792, .T. ) ;
#64418 = CARTESIAN_POINT ( 'NONE',  ( 7.976679547917409963, -6.001044277235011215, 34.52024696741798948 ) ) ;
#64419 = CARTESIAN_POINT ( 'NONE',  ( -4.376773112753000738, -11.43668979543635089, 33.22377378376089752 ) ) ;
#64420 = VERTEX_POINT ( 'NONE', #87268 ) ;
#64421 = CARTESIAN_POINT ( 'NONE',  ( -2.530619266599153150, -11.98009711892699691, 32.48740034544075428 ) ) ;
#64422 = VECTOR ( 'NONE', #40587, 1000.000000000000227 ) ;
#64423 = B_SPLINE_CURVE_WITH_KNOTS ( 'NONE', 3,
 ( #76722, #17116, #37378, #3596, #31065, #58532, #86029, #47251, #18901, #34181 ),
 .UNSPECIFIED., .F., .F.,
 ( 4, 2, 2, 2, 4 ),
 ( 0.000000000000000000, 0.0001954339857564070678, 0.0003908679715128141356, 0.0005863019572692211492, 0.0007817359430256282712 ),
 .UNSPECIFIED. ) ;
#64424 = VERTEX_POINT ( 'NONE', #25547 ) ;
#64425 = LINE ( 'NONE', #43292, #88947 ) ;
#64426 = CARTESIAN_POINT ( 'NONE',  ( 5.750000000000003553, -7.566083408709834757, 34.74999999999999289 ) ) ;
#64427 = VERTEX_POINT ( 'NONE', #62857 ) ;
#64428 = VECTOR ( 'NONE', #62001, 1000.000000000000000 ) ;
#64429 = CARTESIAN_POINT ( 'NONE',  ( 5.076923076923075762, -8.318370150425687726, 35.83090037661290239 ) ) ;
#64430 = CARTESIAN_POINT ( 'NONE',  ( -14.53117725141625627, -10.81261337010820256, 33.49550067578627477 ) ) ;
#64431 = CARTESIAN_POINT ( 'NONE',  ( -24.00000000000000000, 5.000000000000023093, 29.24999999999999645 ) ) ;
#64432 = CARTESIAN_POINT ( 'NONE',  ( 13.51514082284903040, -12.15418822224088657, 32.17964115625579069 ) ) ;
#64433 = CARTESIAN_POINT ( 'NONE',  ( -18.13069146666756382, -4.118384482072086072, 33.43331474514187818 ) ) ;
#64434 = EDGE_CURVE ( 'NONE', #60949, #31499, #38441, .T. ) ;
#64435 = EDGE_CURVE ( 'NONE', #9551, #68708, #69194, .T. ) ;
#64436 = ORIENTED_EDGE ( 'NONE', *, *, #77936, .F. ) ;
#64437 = VERTEX_POINT ( 'NONE', #75953 ) ;
#64438 = FACE_BOUND ( 'NONE', #51270, .T. ) ;
#64439 = EDGE_LOOP ( 'NONE', ( #38436, #13645, #45935, #70269 ) ) ;
#64440 = CARTESIAN_POINT ( 'NONE',  ( 8.545745825506818605, -3.754499324213721234, 33.06261337010820256 ) ) ;
#64441 = EDGE_CURVE ( 'NONE', #3688, #64945, #1023, .T. ) ;
#64442 = AXIS2_PLACEMENT_3D ( 'NONE', #80375, #52431, #24514 ) ;
#64443 = DIRECTION ( 'NONE',  ( -0.000000000000000000, -0.8660254037844397068, -0.4999999999999978906 ) ) ;
#64444 = CARTESIAN_POINT ( 'NONE',  ( -2.084912638714238931, -10.23759521482555357, 34.22997729860117033 ) ) ;
#64445 = VERTEX_POINT ( 'NONE', #20561 ) ;
#64446 = ORIENTED_EDGE ( 'NONE', *, *, #66862, .F. ) ;
#64447 = CARTESIAN_POINT ( 'NONE',  ( 9.692307692307570832, -5.941354392335915335, 34.76329471203413846 ) ) ;
#64448 = B_SPLINE_CURVE_WITH_KNOTS ( 'NONE', 3,
 ( #82888, #7669, #35130, #56290, #55400, #48636, #28830, #76113, #69801, #14415 ),
 .UNSPECIFIED., .F., .F.,
 ( 4, 2, 2, 2, 4 ),
 ( 0.0007817359430256215491, 0.0009771253907249856981, 0.001172514838424349847, 0.001367904286123713779, 0.001563293733823077928 ),
 .UNSPECIFIED. ) ;
#64449 = ORIENTED_EDGE ( 'NONE', *, *, #26926, .T. ) ;
#64450 = B_SPLINE_CURVE_WITH_KNOTS ( 'NONE', 3,
 ( #48018, #55225, #75495, #27753, #13796, #7495, #41280, #47131, #14243, #74621 ),
 .UNSPECIFIED., .F., .F.,
 ( 4, 2, 2, 2, 4 ),
 ( 0.0007817359430256294638, 0.0009771253907249937212, 0.001172514838424358087, 0.001367904286123722453, 0.001563293733823093758 ),
 .UNSPECIFIED. ) ;
#64451 = DIRECTION ( 'NONE',  ( -0.000000000000000000, -0.3420201433256694901, -0.9396926207859082059 ) ) ;
#64452 = DIRECTION ( 'NONE',  ( -0.000000000000000000, 0.7660444431189791237, -0.6427876096865379196 ) ) ;
#64453 = CARTESIAN_POINT ( 'NONE',  ( 16.85399611801622655, -3.395401636524186362, 33.02366814457250399 ) ) ;
#64454 = FACE_BOUND ( 'NONE', #27033, .T. ) ;
#64455 = EDGE_LOOP ( 'NONE', ( #42542, #79672 ) ) ;
#64456 = DIRECTION ( 'NONE',  ( -0.000000000000000000, 0.5000000000000011102, -0.8660254037844380415 ) ) ;
#64457 = CYLINDRICAL_SURFACE ( 'NONE', #56092, 4.000000000000000000 ) ;
#64458 = CARTESIAN_POINT ( 'NONE',  ( 7.846153846154153122, -2.506253911140614576, 30.00000000000323297 ) ) ;
#64459 = CYLINDRICAL_SURFACE ( 'NONE', #173, 0.2499999999999994726 ) ;
#64460 = EDGE_LOOP ( 'NONE', ( #43179, #46170 ) ) ;
#64461 = UNCERTAINTY_MEASURE_WITH_UNIT (LENGTH_MEASURE( 1.000000000000000082E-05 ), #82359, 'distance_accuracy_value', 'NONE');
#64462 = ORIENTED_EDGE ( 'NONE', *, *, #87379, .T. ) ;
#64463 = ORIENTED_EDGE ( 'NONE', *, *, #85198, .T. ) ;
#64465 = CARTESIAN_POINT ( 'NONE',  ( -3.230769230769229949, -12.78798330534102945, 29.74999999999997868 ) ) ;
#64464 = CARTESIAN_POINT ( 'NONE',  ( 20.00000000000000000, -4.000000000000000000, 29.75000000000000355 ) ) ;
#64466 = DIRECTION ( 'NONE',  ( -0.000000000000000000, -0.000000000000000000, -1.000000000000000000 ) ) ;
#64467 = LINE ( 'NONE', #45098, #78225 ) ;
#64468 = CARTESIAN_POINT ( 'NONE',  ( -18.13069060311031322, -5.496505350115500121, 34.60290016733514307 ) ) ;
#64469 = CARTESIAN_POINT ( 'NONE',  ( -11.76194646302587010, -2.353723527008296568, 30.78948104536958752 ) ) ;
#64470 = VERTEX_POINT ( 'NONE', #62419 ) ;
#64471 = CARTESIAN_POINT ( 'NONE',  ( -39.05038313613820122, -2.499999999999999556, 29.75000000000000355 ) ) ;
#64472 = CARTESIAN_POINT ( 'NONE',  ( -0.2385256174450659516, -3.395485233115138168, 33.02377354290276656 ) ) ;
#64473 = CARTESIAN_POINT ( 'NONE',  ( 4.153846153846154188, -8.973038597847269315, 34.52809138561121927 ) ) ;
#64474 = CARTESIAN_POINT ( 'NONE',  ( -13.38461538461550759, -12.70778746994576025, 30.41441678777401236 ) ) ;
#64475 = ORIENTED_EDGE ( 'NONE', *, *, #69668, .T. ) ;
#64476 = AXIS2_PLACEMENT_3D ( 'NONE', #48884, #56533, #77243 ) ;
#64477 = VERTEX_POINT ( 'NONE', #734 ) ;
#64478 = FACE_BOUND ( 'NONE', #80225, .T. ) ;
#64479 = FACE_OUTER_BOUND ( 'NONE', #54861, .T. ) ;
#64480 = CARTESIAN_POINT ( 'NONE',  ( 12.21151522424549718, -12.22074536777954989, 31.39888409691088356 ) ) ;
#64481 = ORIENTED_EDGE ( 'NONE', *, *, #51644, .T. ) ;
#64482 = CARTESIAN_POINT ( 'NONE',  ( 4.023155550735845409, -11.37499894934982514, 33.29245874905763003 ) ) ;
#64483 = CARTESIAN_POINT ( 'NONE',  ( 6.250054419913455561, -11.47946981652013498, 33.17500667209846910 ) ) ;
#64484 = CARTESIAN_POINT ( 'NONE',  ( 8.519254025182178225, -2.318417181685855422, 30.59732222474233865 ) ) ;
#64485 = LINE ( 'NONE', #50541, #63286 ) ;
#64486 = ORIENTED_EDGE ( 'NONE', *, *, #26545, .F. ) ;
#64487 = ADVANCED_FACE ( 'NONE', ( #20993 ), #83159, .F. ) ;
#64488 = CARTESIAN_POINT ( 'NONE',  ( -9.692307692307814193, -3.083524468854526912, 32.58852847137268327 ) ) ;
#64489 = ORIENTED_EDGE ( 'NONE', *, *, #47177, .F. ) ;
#64491 = ORIENTED_EDGE ( 'NONE', *, *, #82386, .T. ) ;
#64490 = CARTESIAN_POINT ( 'NONE',  ( 13.63456079399343146, -8.476813868363244353, 34.90874843262270133 ) ) ;
#64492 = CARTESIAN_POINT ( 'NONE',  ( 7.780883400193070898, -10.90142922261923886, 33.41473453929638993 ) ) ;
#64493 = CARTESIAN_POINT ( 'NONE',  ( 15.00728428704528383, -2.847400154188068022, 31.58180166144859058 ) ) ;
#64494 = CARTESIAN_POINT ( 'NONE',  ( -7.846153846153844924, -3.322132147404559976, 32.92929555188717927 ) ) ;
#64495 = CARTESIAN_POINT ( 'NONE',  ( 12.71148397988660150, -4.336752205174649433, 33.62275283266504289 ) ) ;
#64496 = CARTESIAN_POINT ( 'NONE',  ( -14.30769230769242917, -8.656820664282941280, 34.87096338111179961 ) ) ;
#64497 = CARTESIAN_POINT ( 'NONE',  ( 6.065255571276026103, -2.892918686051625166, 31.69288490824025928 ) ) ;
#64498 = CARTESIAN_POINT ( 'NONE',  ( -1.139087296525992166, -10.25000000000000533, 26.10937500000001066 ) ) ;
#64499 = EDGE_LOOP ( 'NONE', ( #58580, #51961, #1, #82007 ) ) ;
#64500 = CARTESIAN_POINT ( 'NONE',  ( 5.999999999999878320, -10.33852847137269571, 34.16647553114546554 ) ) ;
#64501 = CARTESIAN_POINT ( 'NONE',  ( 5.869309396889695662, -8.191372820521381826, 34.95448215188423546 ) ) ;
#64502 = VERTEX_POINT ( 'NONE', #89045 ) ;
#64503 = EDGE_CURVE ( 'NONE', #35268, #65460, #85891, .T. ) ;
#64504 = AXIS2_PLACEMENT_3D ( 'NONE', #41487, #68953, #7263 ) ;
#64505 = ORIENTED_EDGE ( 'NONE', *, *, #83864, .F. ) ;
#64506 = ORIENTED_EDGE ( 'NONE', *, *, #36861, .T. ) ;
#64507 = DIRECTION ( 'NONE',  ( 1.000000000000000000, 0.000000000000000000, 0.000000000000000000 ) ) ;
#64508 = CARTESIAN_POINT ( 'NONE',  ( 7.846153846153723244, -6.835583212225970762, 34.95778746994575670 ) ) ;
#64509 = B_SPLINE_CURVE_WITH_KNOTS ( 'NONE', 3,
 ( #38868, #80300, #73547, #39316, #5526, #32993, #32104, #5073, #66776, #81629 ),
 .UNSPECIFIED., .F., .F.,
 ( 4, 2, 2, 2, 4 ),
 ( 0.0007817246256747484735, 0.0009771112852218922368, 0.001172497944769036217, 0.001367884604316180197, 0.001563271263863323960 ),
 .UNSPECIFIED. ) ;
#64510 = EDGE_CURVE ( 'NONE', #42382, #24770, #1173, .T. ) ;
#64511 = B_SPLINE_CURVE_WITH_KNOTS ( 'NONE', 3,
 ( #55716, #62903, #84099, #23256, #22377, #49415, #50272, #63360, #9747, #78205 ),
 .UNSPECIFIED., .F., .F.,
 ( 4, 2, 2, 2, 4 ),
 ( 0.0007817246256747450040, 0.0009771112852218881168, 0.001172497944769031230, 0.001367884604316174342, 0.001563271263863317455 ),
 .UNSPECIFIED. ) ;
#64512 = CARTESIAN_POINT ( 'NONE',  ( 6.249945518348143381, -11.37275283266503756, 32.91324779482534524 ) ) ;
#64514 = DIRECTION ( 'NONE',  ( 0.000000000000000000, -0.000000000000000000, 1.000000000000000000 ) ) ;
#64513 = VECTOR ( 'NONE', #40986, 1000.000000000000227 ) ;
#64515 = CARTESIAN_POINT ( 'NONE',  ( -16.15384615384615330, -12.62096338111211580, 30.90682066428153263 ) ) ;
#64516 = DIRECTION ( 'NONE',  ( -1.000000000000000000, -0.000000000000000000, 0.000000000000000000 ) ) ;
#64517 = AXIS2_PLACEMENT_3D ( 'NONE', #78690, #51628, #38142 ) ;
#64518 = CARTESIAN_POINT ( 'NONE',  ( 5.869390344795919923, -7.722926974430166069, 34.99546784045485737 ) ) ;
#64519 = EDGE_LOOP ( 'NONE', ( #7509, #28331 ) ) ;
#64520 = LINE ( 'NONE', #2820, #72134 ) ;
#64521 = CARTESIAN_POINT ( 'NONE',  ( 3.512820512820510555, -7.500000000000000000, 29.75000000000000355 ) ) ;
#64522 = VECTOR ( 'NONE', #32380, 1000.000000000000000 ) ;
#64523 = EDGE_CURVE ( 'NONE', #33427, #68692, #34076, .T. ) ;
#64524 = DIRECTION ( 'NONE',  ( 0.000000000000000000, 0.4999999999999985567, 0.8660254037844395958 ) ) ;
#64525 = FACE_OUTER_BOUND ( 'NONE', #80770, .T. ) ;
#64526 = ORIENTED_EDGE ( 'NONE', *, *, #36001, .T. ) ;
#64527 = CARTESIAN_POINT ( 'NONE',  ( -17.32692307692308376, -2.250000000000000000, 29.81609741502490607 ) ) ;
#64528 = ADVANCED_FACE ( 'NONE', ( #27324 ), #63319, .F. ) ;
#64529 = ORIENTED_EDGE ( 'NONE', *, *, #56684, .F. ) ;
#64530 = CARTESIAN_POINT ( 'NONE',  ( -17.14300545628320904, -2.486705287966280320, 31.30864560766543647 ) ) ;
#64531 = CARTESIAN_POINT ( 'NONE',  ( -10.03846153846153832, -1.926643599941765039, 29.65000000000000213 ) ) ;
#64532 = CARTESIAN_POINT ( 'NONE',  ( 3.453548899747295398, -10.97394488606064122, 33.68653795673694873 ) ) ;
#64533 = CARTESIAN_POINT ( 'NONE',  ( 6.223012844093396723, -12.64618726649961289, 30.78989965857442712 ) ) ;
#64534 = ORIENTED_EDGE ( 'NONE', *, *, #70661, .T. ) ;
#64535 = CARTESIAN_POINT ( 'NONE',  ( -1.515305987725692027, -12.62707690430377383, 30.88035979386743435 ) ) ;
#64536 = CARTESIAN_POINT ( 'NONE',  ( 10.55011461482829738, -12.70778746994557551, 30.41441678777548319 ) ) ;
#64537 = CARTESIAN_POINT ( 'NONE',  ( -12.71153846153846168, -7.500000000000001776, 34.75000000000000000 ) ) ;
#64538 = CARTESIAN_POINT ( 'NONE',  ( -3.007757879156380376, -12.15243808032445827, 31.58219941686247978 ) ) ;
#64539 = ADVANCED_FACE ( 'NONE', ( #70078 ), #56567, .T. ) ;
#64540 = ORIENTED_EDGE ( 'NONE', *, *, #7844, .T. ) ;
#64541 = CARTESIAN_POINT ( 'NONE',  ( -1.576923076923076872, -7.500000000000000000, 33.75000000000000000 ) ) ;
#64542 = EDGE_CURVE ( 'NONE', #39901, #48658, #7652, .T. ) ;
#64543 = ORIENTED_EDGE ( 'NONE', *, *, #53178, .F. ) ;
#64544 = CARTESIAN_POINT ( 'NONE',  ( 6.923076923076924238, -6.435427911321262684, 35.78748833219616898 ) ) ;
#64545 = CARTESIAN_POINT ( 'NONE',  ( -3.454254174493180507, -12.24155766932282496, 31.33739205006857986 ) ) ;
#64546 = EDGE_CURVE ( 'NONE', #64975, #535, #49800, .T. ) ;
#64547 = CARTESIAN_POINT ( 'NONE',  ( -6.000000000000119904, -2.625532179533778709, 30.86335684631627174 ) ) ;
#64548 = EDGE_CURVE ( 'NONE', #47272, #13621, #76393, .T. ) ;
#64549 = CARTESIAN_POINT ( 'NONE',  ( -14.08468095607945791, -9.886259254753566594, 34.14407573483972413 ) ) ;
#64550 = CARTESIAN_POINT ( 'NONE',  ( -17.77698715590660328, -12.38742843783360925, 31.66772728687926985 ) ) ;
#64551 = EDGE_LOOP ( 'NONE', ( #37881, #51898, #83860, #22901 ) ) ;
#64552 = ORIENTED_EDGE ( 'NONE', *, *, #77035, .T. ) ;
#64553 = ORIENTED_EDGE ( 'NONE', *, *, #47781, .F. ) ;
#64554 = CARTESIAN_POINT ( 'NONE',  ( -1.384615384615383471, -12.29105614889573062, 35.45975837776705220 ) ) ;
#64555 = CARTESIAN_POINT ( 'NONE',  ( 11.28848479441294828, -9.234221910056348293, 34.70572697212741531 ) ) ;
#64556 = CARTESIAN_POINT ( 'NONE',  ( -4.023055712879203938, -6.369690395747422684, 34.87708834333098196 ) ) ;
#64557 = CARTESIAN_POINT ( 'NONE',  ( 15.23076923076923173, -1.215029322943914858, 32.30358669280327177 ) ) ;
#64558 = B_SPLINE_CURVE_WITH_KNOTS ( 'NONE', 3,
 ( #84487, #22762, #2488, #43488, #57435, #23212, #71391, #37167, #64628, #2931 ),
 .UNSPECIFIED., .F., .F.,
 ( 4, 2, 2, 2, 4 ),
 ( 0.000000000000000000, 0.0001954311564186871184, 0.0003908623128373742367, 0.0005862934692560614093, 0.0007817246256747484735 ),
 .UNSPECIFIED. ) ;
#64559 = CARTESIAN_POINT ( 'NONE',  ( 7.846153846153723244, -12.70778746994576025, 30.41441678777401236 ) ) ;
#64560 = CARTESIAN_POINT ( 'NONE',  ( 11.47237812750566022, -12.10708131394839349, 31.69288490824020244 ) ) ;
#64561 = AXIS2_PLACEMENT_3D ( 'NONE', #34438, #40764, #39882 ) ;
#64562 = DIRECTION ( 'NONE',  ( -0.000000000000000000, 1.000000000000000000, 3.491481338843133355E-15 ) ) ;
#64563 = CARTESIAN_POINT ( 'NONE',  ( 16.82692307692306244, -2.249999999999998668, 29.81609741502487410 ) ) ;
#64564 = VERTEX_POINT ( 'NONE', #34957 ) ;
#64565 = ORIENTED_EDGE ( 'NONE', *, *, #80002, .F. ) ;
#64566 = ORIENTED_EDGE ( 'NONE', *, *, #27874, .F. ) ;
#64567 = VECTOR ( 'NONE', #20059, 1000.000000000000114 ) ;
#64569 = ORIENTED_EDGE ( 'NONE', *, *, #12454, .T. ) ;
#64568 = CARTESIAN_POINT ( 'NONE',  ( 6.000000000000001776, -12.34228464037088635, 31.77849191805839268 ) ) ;
#64571 = CARTESIAN_POINT ( 'NONE',  ( -10.61538461538461320, -6.343179335718451384, 34.87096338111211935 ) ) ;
#64570 = CARTESIAN_POINT ( 'NONE',  ( -10.61538461538461320, -11.35647404775217417, 33.31231777344666511 ) ) ;
#64572 = AXIS2_PLACEMENT_3D ( 'NONE', #5821, #24751, #24295 ) ;
#64573 = EDGE_CURVE ( 'NONE', #38795, #79333, #82276, .T. ) ;
#64574 = CARTESIAN_POINT ( 'NONE',  ( 1.384615384615264011, -5.094484230521993062, 34.41647553114689373 ) ) ;
#64575 = CARTESIAN_POINT ( 'NONE',  ( 1.553300858899086867, -3.749999999999992006, 25.48437500000000000 ) ) ;
#64576 = ORIENTED_EDGE ( 'NONE', *, *, #41106, .T. ) ;
#64577 = AXIS2_PLACEMENT_3D ( 'NONE', #45900, #37361, #30176 ) ;
#64578 = B_SPLINE_CURVE_WITH_KNOTS ( 'NONE', 3,
 ( #43444, #83106, #83561, #49749, #77223, #15534 ),
 .UNSPECIFIED., .F., .F.,
 ( 4, 2, 4 ),
 ( 0.0003909569690057776653, 0.0005862646681846002839, 0.0007815723673634227941 ),
 .UNSPECIFIED. ) ;
#64579 = ORIENTED_EDGE ( 'NONE', *, *, #12816, .F. ) ;
#64580 = CARTESIAN_POINT ( 'NONE',  ( -11.66860950819323151, -12.15440758774515473, 32.17923288041532004 ) ) ;
#64581 = B_SPLINE_CURVE_WITH_KNOTS ( 'NONE', 3,
 ( #31298, #5159, #12365, #72719, #53785, #32627, #4266, #11030, #60097, #25876 ),
 .UNSPECIFIED., .F., .F.,
 ( 4, 2, 2, 2, 4 ),
 ( 0.0007817246256747446788, 0.0009771112852218874663, 0.001172497944769030362, 0.001367884604316173258, 0.001563271263863315937 ),
 .UNSPECIFIED. ) ;
#64582 = ORIENTED_EDGE ( 'NONE', *, *, #22668, .T. ) ;
#64583 = FACE_BOUND ( 'NONE', #29804, .T. ) ;
#64584 = CARTESIAN_POINT ( 'NONE',  ( 3.296836564119305812, -2.486705287966280320, 31.30864560766543647 ) ) ;
#64585 = CARTESIAN_POINT ( 'NONE',  ( -14.55771553191376277, -6.652501968072648708, 34.93155406624980941 ) ) ;
#64586 = ORIENTED_EDGE ( 'NONE', *, *, #80249, .F. ) ;
#64587 = CARTESIAN_POINT ( 'NONE',  ( -15.00775787915638126, -4.887748414852792322, 34.01359900205216746 ) ) ;
#64588 = CARTESIAN_POINT ( 'NONE',  ( 4.946232473812769648, -8.191372820521381826, 34.95448215188423546 ) ) ;
#64589 = CARTESIAN_POINT ( 'NONE',  ( 10.54930120442873864, -2.721908614388770964, 31.22303859784723912 ) ) ;
#64590 = ORIENTED_EDGE ( 'NONE', *, *, #78093, .F. ) ;
#64591 = DIRECTION ( 'NONE',  ( -0.000000000000000000, 1.000000000000000000, -0.000000000000000000 ) ) ;
#64592 = CARTESIAN_POINT ( 'NONE',  ( -16.85414353565466783, -2.600157965045223563, 30.74683119005207033 ) ) ;
#64593 = EDGE_CURVE ( 'NONE', #60344, #86735, #11634, .T. ) ;
#64594 = ORIENTED_EDGE ( 'NONE', *, *, #17674, .F. ) ;
#64595 = EDGE_CURVE ( 'NONE', #6322, #7995, #14695, .T. ) ;
#64596 = CARTESIAN_POINT ( 'NONE',  ( 3.453548772037639214, -8.496831190052096971, 34.64984203495476578 ) ) ;
#64597 = DIRECTION ( 'NONE',  ( -0.000000000000000000, -0.1736481776669307198, -0.9848077530122080203 ) ) ;
#64598 = CARTESIAN_POINT ( 'NONE',  ( 2.307692307692186251, -12.16647553114689728, 32.15551576947799362 ) ) ;
#64599 = CARTESIAN_POINT ( 'NONE',  ( 15.90382292962469535, -2.985938066672154889, 32.43141759479405550 ) ) ;
#64600 = FACE_OUTER_BOUND ( 'NONE', #6732, .T. ) ;
#64601 = DIRECTION ( 'NONE',  ( -0.000000000000000000, 1.000000000000000000, 3.491481338843133355E-15 ) ) ;
#64602 = CARTESIAN_POINT ( 'NONE',  ( 7.976679284387489410, -3.068774925481848825, 32.56582465632704526 ) ) ;
#64604 = CARTESIAN_POINT ( 'NONE',  ( 2.438218009455871638, -10.19071101563364401, 33.96452234770658407 ) ) ;
#64603 = DIRECTION ( 'NONE',  ( -0.000000000000000000, -0.1736481776669307198, -0.9848077530122080203 ) ) ;
#64605 = CARTESIAN_POINT ( 'NONE',  ( 8.769230769231075584, -2.506253911140615021, 30.00000000000323297 ) ) ;
#64607 = CARTESIAN_POINT ( 'NONE',  ( 6.000000000000001776, -11.91647553114624181, 32.58852847137148245 ) ) ;
#64606 = CARTESIAN_POINT ( 'NONE',  ( -2.557692307692305267, -7.500000000000001776, 35.04278698407183867 ) ) ;
#64608 = DIRECTION ( 'NONE',  ( -0.000000000000000000, 0.9396926207859092051, -0.3420201433256662704 ) ) ;
#64609 = AXIS2_PLACEMENT_3D ( 'NONE', #53082, #38250, #30595 ) ;
#64610 = CARTESIAN_POINT ( 'NONE',  ( -1.077988221561460236, -10.27530806549876452, 20.85750670625849068 ) ) ;
#64611 = VERTEX_POINT ( 'NONE', #85824 ) ;
#64612 = CARTESIAN_POINT ( 'NONE',  ( 3.460919881479461502, -7.042993046541733193, 14.00000000000001421 ) ) ;
#64613 = EDGE_LOOP ( 'NONE', ( #27662, #12550 ) ) ;
#64614 = CARTESIAN_POINT ( 'NONE',  ( -2.437840277424005553, -3.069018819979302926, 32.56621877034667278 ) ) ;
#64615 = EDGE_CURVE ( 'NONE', #54731, #58097, #38069, .T. ) ;
#64616 = EDGE_LOOP ( 'NONE', ( #59518, #79908, #42632, #43 ) ) ;
#64617 = DIRECTION ( 'NONE',  ( -0.000000000000000000, -0.5000000000000009992, -0.8660254037844380415 ) ) ;
#64618 = ORIENTED_EDGE ( 'NONE', *, *, #40063, .T. ) ;
#64619 = CARTESIAN_POINT ( 'NONE',  ( 5.869852030268300602, -11.04286588640298561, 33.62463336215343901 ) ) ;
#64620 = CARTESIAN_POINT ( 'NONE',  ( 0.06109907496454976272, -10.25000000000000000, 25.77938170625848713 ) ) ;
#64621 = CARTESIAN_POINT ( 'NONE',  ( 7.716005876422151744, -8.630895178749533159, 34.87696386517710323 ) ) ;
#64622 = ADVANCED_FACE ( 'NONE', ( #72291 ), #57442, .F. ) ;
#64623 = CARTESIAN_POINT ( 'NONE',  ( -4.854143535654667829, -2.847695495035524882, 31.58253572463339509 ) ) ;
#64624 = B_SPLINE_CURVE_WITH_KNOTS ( 'NONE', 3,
 ( #37022, #2788, #85230, #16756, #72144, #51860, #38821, #10900, #10000, #23081 ),
 .UNSPECIFIED., .F., .F.,
 ( 4, 2, 2, 2, 4 ),
 ( 0.000000000000000000, 0.0001954339857564053873, 0.0003908679715128107746, 0.0005863019572692161618, 0.0007817359430256215491 ),
 .UNSPECIFIED. ) ;
#64625 = CARTESIAN_POINT ( 'NONE',  ( -18.00000000000012079, -12.51329471203414379, 31.30864560766407578 ) ) ;
#64626 = CARTESIAN_POINT ( 'NONE',  ( -6.249976744048588273, -2.544273027872574922, 31.48422191005632342 ) ) ;
#64627 = CARTESIAN_POINT ( 'NONE',  ( -16.40386937806761125, -10.18141759479407327, 34.26406193332782379 ) ) ;
#64628 = CARTESIAN_POINT ( 'NONE',  ( -13.44988538517170440, -8.656820664281498878, 34.87096338111211935 ) ) ;
#64629 = CARTESIAN_POINT ( 'NONE',  ( -14.05763788777885281, -4.818054556918156983, 34.26375889529406749 ) ) ;
#64630 = CARTESIAN_POINT ( 'NONE',  ( -1.553300858899125059, -3.750000000000009326, 16.57812500000000000 ) ) ;
#64631 = CYLINDRICAL_SURFACE ( 'NONE', #79347, 0.2500000000000002220 ) ;
#64632 = LINE ( 'NONE', #43493, #75087 ) ;
#64633 = EDGE_CURVE ( 'NONE', #34232, #88674, #63758, .T. ) ;
#64634 = CYLINDRICAL_SURFACE ( 'NONE', #29206, 0.2499999999999994726 ) ;
#64635 = CARTESIAN_POINT ( 'NONE',  ( 3.750000000000000888, -7.499999999999978684, 16.96875000000000000 ) ) ;
#64636 = AXIS2_PLACEMENT_3D ( 'NONE', #72346, #46216, #10656 ) ;
#64637 = VECTOR ( 'NONE', #28692, 1000.000000000000114 ) ;
#64638 = VERTEX_POINT ( 'NONE', #43495 ) ;
#64639 = LINE ( 'NONE', #3838, #81730 ) ;
#64640 = CARTESIAN_POINT ( 'NONE',  ( -6.923076923077045919, -11.06231777344772027, 33.60647404775119895 ) ) ;
#64641 = CARTESIAN_POINT ( 'NONE',  ( -9.019207500173124004, -11.28823185664190376, 33.01397839955799896 ) ) ;
#64642 = CARTESIAN_POINT ( 'NONE',  ( 16.08852323835397513, -7.749976743299138882, 34.99404534957040624 ) ) ;
#64643 = AXIS2_PLACEMENT_3D ( 'NONE', #65609, #23737, #30937 ) ;
#64644 = LINE ( 'NONE', #29993, #75147 ) ;
#64645 = AXIS2_PLACEMENT_3D ( 'NONE', #49072, #55391, #68460 ) ;
#64646 = CARTESIAN_POINT ( 'NONE',  ( -14.30769230769242917, -4.320704448113951379, 33.92786785259630022 ) ) ;
#64647 = AXIS2_PLACEMENT_3D ( 'NONE', #17018, #44470, #66545 ) ;
#64648 = EDGE_CURVE ( 'NONE', #7426, #9090, #33168, .T. ) ;
#64649 = EDGE_LOOP ( 'NONE', ( #66020, #17358, #28074, #17008 ) ) ;
#64650 = CARTESIAN_POINT ( 'NONE',  ( 4.153846153846032507, -11.48612834414049644, 32.76840700105863391 ) ) ;
#64651 = ORIENTED_EDGE ( 'NONE', *, *, #16746, .F. ) ;
#64652 = ADVANCED_FACE ( 'NONE', ( #31317 ), #3388, .F. ) ;
#64653 = ORIENTED_EDGE ( 'NONE', *, *, #29626, .T. ) ;
#64654 = CARTESIAN_POINT ( 'NONE',  ( -5.869208192175211281, -5.582136614379148654, 34.36778462344220486 ) ) ;
#64655 = DIRECTION ( 'NONE',  ( -1.000000000000000000, 0.000000000000000000, 0.000000000000000000 ) ) ;
#64656 = CARTESIAN_POINT ( 'NONE',  ( -15.36145983387954139, -10.70098750199973203, 33.91152734681376302 ) ) ;
#64657 = EDGE_CURVE ( 'NONE', #60044, #52756, #69689, .T. ) ;
#64658 = LINE ( 'NONE', #51571, #40770 ) ;
#64659 = CARTESIAN_POINT ( 'NONE',  ( 17.77707378248384629, -9.086856451489516928, 34.49173150075333183 ) ) ;
#64660 = VERTEX_POINT ( 'NONE', #58778 ) ;
#64661 = CARTESIAN_POINT ( 'NONE',  ( -14.17716660592874156, -12.27024696741798948, 31.24895572276497546 ) ) ;
#64662 = EDGE_LOOP ( 'NONE', ( #24886, #49511 ) ) ;
#64663 = B_SPLINE_CURVE_WITH_KNOTS ( 'NONE', 3,
 ( #54076, #13109, #68485, #6362, #54977, #12664, #74815, #13986, #80696, #32937 ),
 .UNSPECIFIED., .F., .F.,
 ( 4, 2, 2, 2, 4 ),
 ( 0.0007817246256747491240, 0.0009771112852218931041, 0.001172497944769036867, 0.001367884604316180631, 0.001563271263863324611 ),
 .UNSPECIFIED. ) ;
#64664 = ORIENTED_EDGE ( 'NONE', *, *, #56967, .T. ) ;
#64665 = CARTESIAN_POINT ( 'NONE',  ( 1.161130440891439797, -11.41268669641500466, 32.86336882939237825 ) ) ;
#64666 = CYLINDRICAL_SURFACE ( 'NONE', #38815, 0.2499999999999993616 ) ;
#64667 = ADVANCED_FACE ( 'NONE', ( #24549 ), #64634, .F. ) ;
#64668 = VECTOR ( 'NONE', #23393, 1000.000000000000000 ) ;
#64669 = DIRECTION ( 'NONE',  ( -0.000000000000000000, -0.9848077530122086864, -0.1736481776669273613 ) ) ;
#64670 = EDGE_CURVE ( 'NONE', #38977, #33880, #72871, .T. ) ;
#64671 = CARTESIAN_POINT ( 'NONE',  ( -16.94639737515951339, -3.285477652293413264, 32.44071101563363158 ) ) ;
#64672 = DIRECTION ( 'NONE',  ( -0.000000000000000000, -0.9396926207859092051, -0.3420201433256662704 ) ) ;
#64673 = ORIENTED_EDGE ( 'NONE', *, *, #60191, .T. ) ;
#64674 = B_SPLINE_CURVE_WITH_KNOTS ( 'NONE', 3,
 ( #64851, #2702, #85584, #30199, #29757, #29320, #57663, #8158, #15360, #78370 ),
 .UNSPECIFIED., .F., .F.,
 ( 4, 2, 2, 2, 4 ),
 ( 0.000000000000000000, 0.0001954339857564073659, 0.0003908679715128147319, 0.0005863019572692221250, 0.0007817359430256294638 ),
 .UNSPECIFIED. ) ;
#64675 = VERTEX_POINT ( 'NONE', #58329 ) ;
#64676 = CARTESIAN_POINT ( 'NONE',  ( 2.320192649118979489E-14, -11.25000000000000000, 23.53125000000000000 ) ) ;
#64677 = ORIENTED_EDGE ( 'NONE', *, *, #36292, .T. ) ;
#64679 = VERTEX_POINT ( 'NONE', #17355 ) ;
#64678 = CARTESIAN_POINT ( 'NONE',  ( -13.60754234352223335, -5.582147617184174848, 34.63737895849758530 ) ) ;
#64680 = LINE ( 'NONE', #36345, #43587 ) ;
#64681 = CARTESIAN_POINT ( 'NONE',  ( 6.000000000000001776, -12.48256725967547354, 35.29906147534542527 ) ) ;
#64682 = EDGE_CURVE ( 'NONE', #81662, #45538, #4765, .T. ) ;
#64683 = DIRECTION ( 'NONE',  ( -0.000000000000000000, 0.3420201433256694901, -0.9396926207859082059 ) ) ;
#64684 = VERTEX_POINT ( 'NONE', #8833 ) ;
#64685 = VECTOR ( 'NONE', #27075, 1000.000000000000000 ) ;
#64686 = DIRECTION ( 'NONE',  ( 0.000000000000000000, 0.1736481776669275834, 0.9848077530122086864 ) ) ;
#64687 = ORIENTED_EDGE ( 'NONE', *, *, #83593, .F. ) ;
#64688 = EDGE_CURVE ( 'NONE', #15080, #8255, #48156, .T. ) ;
#64689 = CARTESIAN_POINT ( 'NONE',  ( 2.557637826040449980, -9.272278438253398036, 34.42582936511637826 ) ) ;
#64690 = DIRECTION ( 'NONE',  ( 0.000000000000000000, 0.000000000000000000, -1.000000000000000000 ) ) ;
#64691 = FACE_OUTER_BOUND ( 'NONE', #71890, .T. ) ;
#64694 = CARTESIAN_POINT ( 'NONE',  ( 4.826899839630109490, -3.202444869320336451, 32.30641848906366675 ) ) ;
#64693 = AXIS2_PLACEMENT_3D ( 'NONE', #54307, #20091, #69604 ) ;
#64692 = LINE ( 'NONE', #30041, #56152 ) ;
#64695 = AXIS2_PLACEMENT_3D ( 'NONE', #39796, #53740, #81226 ) ;
#64696 = EDGE_CURVE ( 'NONE', #53579, #32375, #47034, .T. ) ;
#64697 = CARTESIAN_POINT ( 'NONE',  ( -0.7115152055870525016, -12.41104346484419452, 31.60698883733904196 ) ) ;
#64698 = CARTESIAN_POINT ( 'NONE',  ( -9.692307692307691624, -7.500000000000001776, 35.04278698407183867 ) ) ;
#64699 = ORIENTED_EDGE ( 'NONE', *, *, #32784, .T. ) ;
#64700 = CARTESIAN_POINT ( 'NONE',  ( -10.83886955910856464, -10.11188796281391511, 34.01382737946119050 ) ) ;
#64701 = CARTESIAN_POINT ( 'NONE',  ( -24.99999999999999645, -15.00000000000000000, 3.000000000000000000 ) ) ;
#64702 = AXIS2_PLACEMENT_3D ( 'NONE', #47356, #60876, #39734 ) ;
#64703 = ORIENTED_EDGE ( 'NONE', *, *, #31598, .F. ) ;
#64704 = EDGE_CURVE ( 'NONE', #88692, #85285, #41791, .T. ) ;
#64705 = CARTESIAN_POINT ( 'NONE',  ( -16.21911615440246734, -12.70778746994557551, 30.41441678777548319 ) ) ;
#64706 = CARTESIAN_POINT ( 'NONE',  ( 16.82689985270161870, -10.92453946501459328, 33.72985991061849376 ) ) ;
#64707 = CARTESIAN_POINT ( 'NONE',  ( 16.08776377448601735, -6.343179335718451384, 34.87096338111212646 ) ) ;
#64708 = CARTESIAN_POINT ( 'NONE',  ( -7.623374177175779032, -10.97394488606064122, 33.68653795673694873 ) ) ;
#64709 = CARTESIAN_POINT ( 'NONE',  ( -0.3310127597748990236, -12.45806712695776319, 30.39783852428763922 ) ) ;
#64710 = CARTESIAN_POINT ( 'NONE',  ( 7.715462379486287325, -8.147922237126337563, 34.70805685702651999 ) ) ;
#64711 = FACE_BOUND ( 'NONE', #74370, .T. ) ;
#64713 = CYLINDRICAL_SURFACE ( 'NONE', #38813, 0.2499999999999986955 ) ;
#64712 = CARTESIAN_POINT ( 'NONE',  ( 5.299702745901139878, -5.827830569534416583, 34.72679350104403539 ) ) ;
#64714 = CARTESIAN_POINT ( 'NONE',  ( 15.12820512820512953, -7.500000000000000000, 29.75000000000000355 ) ) ;
#64716 = FACE_OUTER_BOUND ( 'NONE', #65555, .T. ) ;
#64715 = DIRECTION ( 'NONE',  ( -0.000000000000000000, -0.9848077530122085754, -0.1736481776669273613 ) ) ;
#64717 = FACE_OUTER_BOUND ( 'NONE', #81327, .T. ) ;
#64718 = CARTESIAN_POINT ( 'NONE',  ( -0.06109907496455085213, -3.750000000000000888, 21.40438170625849068 ) ) ;
#64719 = ORIENTED_EDGE ( 'NONE', *, *, #17285, .T. ) ;
#64720 = DIRECTION ( 'NONE',  ( -0.000000000000000000, 0.9848077530122086864, -0.1736481776669273891 ) ) ;
#64721 = CARTESIAN_POINT ( 'NONE',  ( -5.076923076923075762, -3.050289026998446396, 32.03036669348365706 ) ) ;
#64722 = CARTESIAN_POINT ( 'NONE',  ( -0.6844654204453108903, -3.395401636524185474, 33.02366814457250399 ) ) ;
#64723 = CARTESIAN_POINT ( 'NONE',  ( 0.4761625575576028391, -10.20882035374011565, 29.07450979259063928 ) ) ;
#64724 = CARTESIAN_POINT ( 'NONE',  ( 10.86533013373275836, -12.22109172314383052, 31.39792113162168263 ) ) ;
#64725 = LINE ( 'NONE', #21206, #28229 ) ;
#64726 = CARTESIAN_POINT ( 'NONE',  ( 0.06109907496455496689, -11.24999999999999822, 20.77938170625848713 ) ) ;
#64727 = EDGE_CURVE ( 'NONE', #64009, #32057, #45261, .T. ) ;
#64728 = CARTESIAN_POINT ( 'NONE',  ( -8.638705067467206788, -2.882268652242222284, 31.66798894389554064 ) ) ;
#64729 = CARTESIAN_POINT ( 'NONE',  ( -2.544871794871794268, -3.499999999999999556, 29.75000000000000355 ) ) ;
#64730 = CARTESIAN_POINT ( 'NONE',  ( -17.01085472592063752, -5.557115091759786019, 34.35708131394839882 ) ) ;
#64731 = CARTESIAN_POINT ( 'NONE',  ( 17.74997677577853850, -8.475808217655753651, 34.90892951860618609 ) ) ;
#64732 = DIRECTION ( 'NONE',  ( -1.000000000000000000, -0.000000000000000000, -0.000000000000000000 ) ) ;
#64733 = CARTESIAN_POINT ( 'NONE',  ( 4.023154687178598365, -10.54014554554150607, 33.71984207302941883 ) ) ;
#64734 = CARTESIAN_POINT ( 'NONE',  ( -6.130147969731692292, -12.15440758774515473, 32.17923288041532004 ) ) ;
#64735 = CARTESIAN_POINT ( 'NONE',  ( 17.14299041027315695, -2.486705287966280320, 31.30864560766543647 ) ) ;
#64736 = ORIENTED_EDGE ( 'NONE', *, *, #43963, .T. ) ;
#64737 = VECTOR ( 'NONE', #52213, 1000.000000000000000 ) ;
#64738 = CARTESIAN_POINT ( 'NONE',  ( 17.14217821643591932, -12.70778746994558439, 30.41441678777537305 ) ) ;
#64739 = CARTESIAN_POINT ( 'NONE',  ( 6.988332494352946789, -5.219633306516380244, 34.19971097300157936 ) ) ;
#64740 = CARTESIAN_POINT ( 'NONE',  ( 1.492201783934598236, -11.27530806549875031, 16.20499329374151642 ) ) ;
#64741 = B_SPLINE_CURVE_WITH_KNOTS ( 'NONE', 3,
 ( #27860, #37264, #44022, #57539, #30078, #50330, #71492, #22865, #16120, #8928 ),
 .UNSPECIFIED., .F., .F.,
 ( 4, 2, 2, 2, 4 ),
 ( 0.000000000000000000, 0.0001954311564186868473, 0.0003908623128373736946, 0.0005862934692560605419, 0.0007817246256747473893 ),
 .UNSPECIFIED. ) ;
#64742 = CARTESIAN_POINT ( 'NONE',  ( 7.146089767170319185, -10.77377354290276301, 33.85451476688484718 ) ) ;
#64743 = CARTESIAN_POINT ( 'NONE',  ( -17.01166793741023042, -5.941354392334603496, 34.76329471203374055 ) ) ;
#64744 = EDGE_LOOP ( 'NONE', ( #80026, #23899, #48385, #16795 ) ) ;
#64745 = CARTESIAN_POINT ( 'NONE',  ( -6.857009589726848375, -9.905515769479277921, 34.41647553114623292 ) ) ;
#64747 = VERTEX_POINT ( 'NONE', #31769 ) ;
#64746 = LINE ( 'NONE', #30964, #22429 ) ;
#64748 = CARTESIAN_POINT ( 'NONE',  ( 11.78840694783958298, -4.932303261841489928, 34.32971442181322885 ) ) ;
#64749 = FACE_OUTER_BOUND ( 'NONE', #13613, .T. ) ;
#64750 = CARTESIAN_POINT ( 'NONE',  ( -8.519285250882626670, -2.587454068350147018, 30.68340429815432202 ) ) ;
#64751 = DIRECTION ( 'NONE',  ( -0.000000000000000000, -0.5000000000000009992, -0.8660254037844380415 ) ) ;
#64752 = ORIENTED_EDGE ( 'NONE', *, *, #5063, .F. ) ;
#64753 = LINE ( 'NONE', #22894, #15953 ) ;
#64754 = CARTESIAN_POINT ( 'NONE',  ( -15.90390063549801347, -3.202959910592335202, 32.30730279482227019 ) ) ;
#64756 = CARTESIAN_POINT ( 'NONE',  ( -11.53846153846153655, -6.386643153685126251, 34.62446782046654192 ) ) ;
#64755 = VECTOR ( 'NONE', #5783, 1000.000000000000000 ) ;
#64757 = ORIENTED_EDGE ( 'NONE', *, *, #69921, .T. ) ;
#64758 = EDGE_LOOP ( 'NONE', ( #76200, #88987, #33351, #28832 ) ) ;
#64759 = B_SPLINE_CURVE_WITH_KNOTS ( 'NONE', 3,
 ( #37370, #64841, #27424, #88706, #68406, #7152, #81495, #40943, #34624, #19782 ),
 .UNSPECIFIED., .F., .F.,
 ( 4, 2, 2, 2, 4 ),
 ( 0.000000000000000000, 0.0001954311564186865492, 0.0003908623128373730983, 0.0005862934692560596746, 0.0007817246256747461966 ),
 .UNSPECIFIED. ) ;
#64760 = EDGE_CURVE ( 'NONE', #7820, #29336, #11493, .T. ) ;
#64761 = ORIENTED_EDGE ( 'NONE', *, *, #10581, .F. ) ;
#64762 = CIRCLE ( 'NONE', #83506, 4.000000000000000000 ) ;
#64763 = VECTOR ( 'NONE', #49822, 999.9999999999998863 ) ;
#64764 = DIRECTION ( 'NONE',  ( 0.000000000000000000, 0.000000000000000000, -1.000000000000000000 ) ) ;
#64765 = CARTESIAN_POINT ( 'NONE',  ( 6.250054419913455561, -2.318338780012835443, 30.59689888758630261 ) ) ;
#64766 = ADVANCED_FACE ( 'NONE', ( #53800 ), #72734, .F. ) ;
#64767 = CARTESIAN_POINT ( 'NONE',  ( 17.07692307692307665, -1.422936976036506707, 30.56769352161908415 ) ) ;
#64768 = AXIS2_PLACEMENT_3D ( 'NONE', #48529, #28721, #68370 ) ;
#64769 = ADVANCED_FACE ( 'NONE', ( #4281 ), #5618, .F. ) ;
#64770 = CARTESIAN_POINT ( 'NONE',  ( -6.923076923076922462, -13.63283147151868846, 33.57946703557072254 ) ) ;
#64771 = ORIENTED_EDGE ( 'NONE', *, *, #5740, .T. ) ;
#64772 = VERTEX_POINT ( 'NONE', #12380 ) ;
#64774 = ORIENTED_EDGE ( 'NONE', *, *, #39423, .T. ) ;
#64773 = CARTESIAN_POINT ( 'NONE',  ( 4.403791563224197070, -5.766571408460171355, 34.70601412856602508 ) ) ;
#64775 = ADVANCED_FACE ( 'NONE', ( #19573 ), #52904, .F. ) ;
#64776 = DIRECTION ( 'NONE',  ( -0.000000000000000000, 0.9848077530122086864, -0.1736481776669273891 ) ) ;
#64777 = CARTESIAN_POINT ( 'NONE',  ( -17.07692307692319744, -8.613356846316285953, 34.62446782046622218 ) ) ;
#64778 = CARTESIAN_POINT ( 'NONE',  ( 16.02315555073584363, -11.37499894934982514, 33.29245874905763003 ) ) ;
#64779 = ORIENTED_EDGE ( 'NONE', *, *, #19024, .F. ) ;
#64780 = ORIENTED_EDGE ( 'NONE', *, *, #19997, .T. ) ;
#64782 = ORIENTED_EDGE ( 'NONE', *, *, #43455, .F. ) ;
#64781 = CARTESIAN_POINT ( 'NONE',  ( -3.230769230769229949, -10.51840700105979565, 33.73612834413961536 ) ) ;
#64783 = B_SPLINE_CURVE_WITH_KNOTS ( 'NONE', 3,
 ( #34996, #770, #28237, #21482, #68346, #14737, #69669, #81430, #62894, #19718 ),
 .UNSPECIFIED., .F., .F.,
 ( 4, 2, 2, 2, 4 ),
 ( 0.0007817246256747457630, 0.0009771112852218887673, 0.001172497944769031880, 0.001367884604316174993, 0.001563271263863318106 ),
 .UNSPECIFIED. ) ;
#64784 = CARTESIAN_POINT ( 'NONE',  ( -14.30769230769230660, -11.91647553114624181, 32.58852847137148245 ) ) ;
#64785 = CARTESIAN_POINT ( 'NONE',  ( -9.692307692307691624, -2.249999999999998668, 29.75000000000001776 ) ) ;
#64786 = ORIENTED_EDGE ( 'NONE', *, *, #6475, .F. ) ;
#64787 = CARTESIAN_POINT ( 'NONE',  ( -6.416666666666667851, -4.000000000000000000, 29.75000000000000355 ) ) ;
#64788 = CARTESIAN_POINT ( 'NONE',  ( -14.05763788777885637, -12.65882529074907126, 30.72640787790839312 ) ) ;
#64789 = LINE ( 'NONE', #49956, #66967 ) ;
#64790 = FACE_BOUND ( 'NONE', #56339, .T. ) ;
#64791 = EDGE_CURVE ( 'NONE', #49542, #19289, #59226, .T. ) ;
#64792 = CARTESIAN_POINT ( 'NONE',  ( 7.976944287120795174, -12.35292014791297710, 31.75344720912887198 ) ) ;
#64793 = CARTESIAN_POINT ( 'NONE',  ( 3.903822929624695792, -2.341070481393820124, 30.72580821765574299 ) ) ;
#64794 = CYLINDRICAL_SURFACE ( 'NONE', #76798, 0.2499999999999995559 ) ;
#64796 = CARTESIAN_POINT ( 'NONE',  ( -0.4615384615384611200, -11.11383981884818262, 36.00935417666054406 ) ) ;
#64795 = FACE_OUTER_BOUND ( 'NONE', #65018, .T. ) ;
#64797 = CARTESIAN_POINT ( 'NONE',  ( -7.846153846153844924, -3.050289026998446396, 32.03036669348365706 ) ) ;
#64798 = CARTESIAN_POINT ( 'NONE',  ( 1.384615384615386802, -2.292212530054420494, 30.41441678777542634 ) ) ;
#64799 = VERTEX_POINT ( 'NONE', #45712 ) ;
#64800 = CARTESIAN_POINT ( 'NONE',  ( -12.46153846153846168, -2.708943851104267164, 35.45975837776705220 ) ) ;
#64801 = ORIENTED_EDGE ( 'NONE', *, *, #28372, .F. ) ;
#64802 = VERTEX_POINT ( 'NONE', #32212 ) ;
#64804 = CARTESIAN_POINT ( 'NONE',  ( 15.16468685140909400, -2.833524468853757305, 32.15551576947924417 ) ) ;
#64803 = CARTESIAN_POINT ( 'NONE',  ( 5.777073782483853392, -6.503392248772476236, 34.64988816332204635 ) ) ;
#64805 = EDGE_CURVE ( 'NONE', #1878, #75410, #46608, .T. ) ;
#64806 = CARTESIAN_POINT ( 'NONE',  ( -11.53846153846153655, -10.51840700105979565, 33.73612834413961536 ) ) ;
#64807 = CARTESIAN_POINT ( 'NONE',  ( -14.05763799605399100, -2.779044189368095275, 31.39831045268885745 ) ) ;
#64808 = DIRECTION ( 'NONE',  ( 0.000000000000000000, 0.000000000000000000, -1.000000000000000000 ) ) ;
#64809 = CARTESIAN_POINT ( 'NONE',  ( -0.2387589202700515223, -11.89424750095246175, 32.13594075562311758 ) ) ;
#64810 = ORIENTED_EDGE ( 'NONE', *, *, #23529, .F. ) ;
#64811 = DIRECTION ( 'NONE',  ( -0.000000000000000000, 1.000000000000000000, -0.000000000000000000 ) ) ;
#64812 = EDGE_CURVE ( 'NONE', #35909, #20857, #87171, .T. ) ;
#64813 = EDGE_CURVE ( 'NONE', #28639, #41851, #4117, .T. ) ;
#64814 = CARTESIAN_POINT ( 'NONE',  ( 6.673100192134568509, -3.627789207965226748, 32.91389620160131102 ) ) ;
#64815 = CARTESIAN_POINT ( 'NONE',  ( 17.29993442853592711, -6.503523203565941380, 34.64991518177335195 ) ) ;
#64816 = LINE ( 'NONE', #86914, #51033 ) ;
#64817 = CARTESIAN_POINT ( 'NONE',  ( -7.846153846153844924, -13.57706302396349152, 30.56769352161908060 ) ) ;
#64818 = CARTESIAN_POINT ( 'NONE',  ( 3.750000000000009770, -9.053300858899081760, 14.54687500000000178 ) ) ;
#64819 = ORIENTED_EDGE ( 'NONE', *, *, #19082, .F. ) ;
#64820 = VECTOR ( 'NONE', #52391, 1000.000000000000114 ) ;
#64821 = VECTOR ( 'NONE', #18534, 1000.000000000000114 ) ;
#64822 = ORIENTED_EDGE ( 'NONE', *, *, #53239, .T. ) ;
#64823 = CARTESIAN_POINT ( 'NONE',  ( 14.30769230769218581, -12.51329471203414379, 31.30864560766407578 ) ) ;
#64824 = ORIENTED_EDGE ( 'NONE', *, *, #72289, .F. ) ;
#64825 = CARTESIAN_POINT ( 'NONE',  ( -4.153846153846152411, -12.37446782046654192, 30.86335684631486131 ) ) ;
#64826 = DIRECTION ( 'NONE',  ( -0.000000000000000000, 1.000000000000000000, 3.491481338843133355E-15 ) ) ;
#64827 = CARTESIAN_POINT ( 'NONE',  ( -16.40386939113911779, -5.056417327199097755, 34.11270091957320716 ) ) ;
#64828 = CARTESIAN_POINT ( 'NONE',  ( 5.869440086386637390, -2.254533558242299396, 29.97296025877828285 ) ) ;
#64829 = CARTESIAN_POINT ( 'NONE',  ( -2.651650429449565305, -4.848349570550461785, 20.25000000000000000 ) ) ;
#64830 = EDGE_CURVE ( 'NONE', #21320, #16624, #11944, .T. ) ;
#64831 = VECTOR ( 'NONE', #19092, 1000.000000000000000 ) ;
#64832 = DIRECTION ( 'NONE',  ( 0.000000000000000000, 0.9848077530122072432, 0.1736481776669354937 ) ) ;
#64833 = VERTEX_POINT ( 'NONE', #53357 ) ;
#64834 = DIRECTION ( 'NONE',  ( -0.000000000000000000, 1.000000000000000000, -0.000000000000000000 ) ) ;
#64836 = ORIENTED_EDGE ( 'NONE', *, *, #37866, .T. ) ;
#64835 = CARTESIAN_POINT ( 'NONE',  ( -2.241624974342230292, -12.62096338111211757, 30.90682066428152908 ) ) ;
#64837 = CARTESIAN_POINT ( 'NONE',  ( -17.07692307692307665, -6.343179335718451384, 34.87096338111211935 ) ) ;
#64838 = CARTESIAN_POINT ( 'NONE',  ( 14.30769230769231015, -12.10708131394839349, 31.69288490824020244 ) ) ;
#64839 = EDGE_CURVE ( 'NONE', #43442, #12296, #87919, .T. ) ;
#64840 = ADVANCED_FACE ( 'NONE', ( #81731 ), #41182, .F. ) ;
#64841 = CARTESIAN_POINT ( 'NONE',  ( -3.296851610129365451, -9.905515769479276145, 34.41647553114623292 ) ) ;
#64842 = CARTESIAN_POINT ( 'NONE',  ( -12.94230769230769162, -11.50000000000000000, 29.75000000000000355 ) ) ;
#64843 = CARTESIAN_POINT ( 'NONE',  ( 7.846153846153846700, -2.499999999999998668, 29.75000000000001421 ) ) ;
#64844 = CARTESIAN_POINT ( 'NONE',  ( -4.153846153846273204, -9.442884908241554243, 34.35708131394783038 ) ) ;
#64845 = CARTESIAN_POINT ( 'NONE',  ( -6.923076923076922462, -4.786620604624113540, 33.94971097300155094 ) ) ;
#64846 = CARTESIAN_POINT ( 'NONE',  ( -2.608446859217920633, -4.805146000318815780, 18.00186829374151287 ) ) ;
#64847 = ORIENTED_EDGE ( 'NONE', *, *, #72228, .T. ) ;
#64848 = EDGE_CURVE ( 'NONE', #11070, #48730, #37460, .T. ) ;
#64849 = CARTESIAN_POINT ( 'NONE',  ( -15.90390074446811042, -6.653508905675593610, 34.93172785388651391 ) ) ;
#64850 = CARTESIAN_POINT ( 'NONE',  ( 8.900022577055556994, -11.71459661697925903, 32.44059661609676937 ) ) ;
#64851 = CARTESIAN_POINT ( 'NONE',  ( -13.38461538461538325, -8.973038597847269315, 34.52809138561121927 ) ) ;
#64852 = CARTESIAN_POINT ( 'NONE',  ( 2.749999999999995115, -6.360912703473971419, 25.64062500000000000 ) ) ;
#64853 = LINE ( 'NONE', #3155, #69125 ) ;
#64854 = CARTESIAN_POINT ( 'NONE',  ( 8.769230769230645706, -10.33852847137269571, 34.16647553114546554 ) ) ;
#64855 = ORIENTED_EDGE ( 'NONE', *, *, #65167, .F. ) ;
#64856 = CARTESIAN_POINT ( 'NONE',  ( 2.750000000000008438, -8.639087296525996607, 19.54687500000000000 ) ) ;
#64857 = CARTESIAN_POINT ( 'NONE',  ( -1.450698795571264466, -9.780366693483667717, 34.19971097300155805 ) ) ;
#64858 = EDGE_LOOP ( 'NONE', ( #85948, #8513 ) ) ;
#64859 = CARTESIAN_POINT ( 'NONE',  ( 6.699591998512592461, -6.716662450894490100, 34.94144148231605840 ) ) ;
#64860 = ORIENTED_EDGE ( 'NONE', *, *, #43695, .T. ) ;
#64861 = VECTOR ( 'NONE', #4179, 1000.000000000000000 ) ;
#64862 = CARTESIAN_POINT ( 'NONE',  ( 12.46153846153846168, -2.721908614388771852, 31.22303859784724978 ) ) ;
#64863 = DIRECTION ( 'NONE',  ( -1.000000000000000000, 0.000000000000000000, 0.000000000000000000 ) ) ;
#64864 = CARTESIAN_POINT ( 'NONE',  ( -0.2387587925603952832, -6.717445702608402236, 34.94155399931962336 ) ) ;
#64865 = ORIENTED_EDGE ( 'NONE', *, *, #76130, .F. ) ;
#64866 = DIRECTION ( 'NONE',  ( 0.000000000000000000, 0.000000000000000000, -1.000000000000000000 ) ) ;
#64868 = ORIENTED_EDGE ( 'NONE', *, *, #7950, .T. ) ;
#64867 = VECTOR ( 'NONE', #34079, 1000.000000000000000 ) ;
#64869 = CARTESIAN_POINT ( 'NONE',  ( 13.31936545284130169, -2.255955759149247619, 30.00000000000013856 ) ) ;
#64870 = VECTOR ( 'NONE', #48577, 1000.000000000000227 ) ;
#64871 = EDGE_CURVE ( 'NONE', #47629, #61347, #21345, .T. ) ;
#64872 = VERTEX_POINT ( 'NONE', #28555 ) ;
#64873 = DIRECTION ( 'NONE',  ( 0.000000000000000000, 0.000000000000000000, -1.000000000000000000 ) ) ;
#64874 = CARTESIAN_POINT ( 'NONE',  ( 2.557746619330623528, -3.136992222400443175, 32.19305428654138979 ) ) ;
#64875 = ORIENTED_EDGE ( 'NONE', *, *, #42512, .F. ) ;
#64876 = CARTESIAN_POINT ( 'NONE',  ( -6.223484924564331777, -10.97335522853832579, 33.68706563782419749 ) ) ;
#64877 = CARTESIAN_POINT ( 'NONE',  ( -12.71156169883143150, -5.851115903089112003, 34.47074536777953568 ) ) ;
#64878 = DIRECTION ( 'NONE',  ( -0.000000000000000000, -0.9396926207859093161, -0.3420201433256663259 ) ) ;
#64879 = ADVANCED_FACE ( 'NONE', ( #192 ), #56014, .F. ) ;
#64880 = CARTESIAN_POINT ( 'NONE',  ( 4.826899839630111266, -9.271318131107980420, 34.42618302367067429 ) ) ;
#64881 = LINE ( 'NONE', #79752, #27775 ) ;
#64882 = ORIENTED_EDGE ( 'NONE', *, *, #16825, .T. ) ;
#64883 = ORIENTED_EDGE ( 'NONE', *, *, #81712, .T. ) ;
#64884 = CIRCLE ( 'NONE', #44757, 8.000000000000000000 ) ;
#64885 = FACE_BOUND ( 'NONE', #8577, .T. ) ;
#64886 = VERTEX_POINT ( 'NONE', #27659 ) ;
#64888 = ORIENTED_EDGE ( 'NONE', *, *, #69648, .T. ) ;
#64887 = CARTESIAN_POINT ( 'NONE',  ( -7.976301815885541657, -5.915902021225889484, 34.75552854090298638 ) ) ;
#64889 = B_SPLINE_CURVE_WITH_KNOTS ( 'NONE', 3,
 ( #72093, #85612, #53929, #61125, #31097, #88634, #78845, #72536, #45060, #33224 ),
 .UNSPECIFIED., .F., .F.,
 ( 4, 2, 2, 2, 4 ),
 ( 0.0007817246256747434861, 0.0009771112852218859484, 0.001172497944769028411, 0.001367884604316171090, 0.001563271263863313552 ),
 .UNSPECIFIED. ) ;
#64890 = AXIS2_PLACEMENT_3D ( 'NONE', #45871, #73354, #11661 ) ;
#64891 = CARTESIAN_POINT ( 'NONE',  ( 13.60762673622823549, -10.61302985866384141, 33.66295027996417843 ) ) ;
#64892 = CARTESIAN_POINT ( 'NONE',  ( 0.4615384615384611200, -12.62096338111211580, 30.90682066428153263 ) ) ;
#64893 = EDGE_LOOP ( 'NONE', ( #61025, #50838 ) ) ;
#64894 = AXIS2_PLACEMENT_3D ( 'NONE', #63577, #557, #62244 ) ;
#64895 = ORIENTED_EDGE ( 'NONE', *, *, #5838, .F. ) ;
#64896 = EDGE_CURVE ( 'NONE', #56712, #78354, #78296, .T. ) ;
#64897 = ORIENTED_EDGE ( 'NONE', *, *, #72331, .F. ) ;
#64898 = LINE ( 'NONE', #36559, #3668 ) ;
#64899 = ORIENTED_EDGE ( 'NONE', *, *, #68375, .F. ) ;
#64900 = CARTESIAN_POINT ( 'NONE',  ( 11.78840705680968348, -11.37275283266504111, 32.91324779482534524 ) ) ;
#64901 = DIRECTION ( 'NONE',  ( 0.000000000000000000, 0.6427876096865373645, -0.7660444431189797898 ) ) ;
#64902 = CARTESIAN_POINT ( 'NONE',  ( -2.373774687052442989, -12.34228464037088280, 31.77849191805838558 ) ) ;
#64903 = FACE_BOUND ( 'NONE', #80976, .T. ) ;
#64904 = VERTEX_POINT ( 'NONE', #76285 ) ;
#64905 = LINE ( 'NONE', #10425, #87415 ) ;
#64906 = DIRECTION ( 'NONE',  ( -0.000000000000000000, 0.5000000000000011102, -0.8660254037844381525 ) ) ;
#64907 = CARTESIAN_POINT ( 'NONE',  ( 2.307692307692186251, -8.656820664282941280, 34.87096338111179961 ) ) ;
#64908 = CARTESIAN_POINT ( 'NONE',  ( -1.384615384615383471, -2.538708090699994813, 30.37095296980875503 ) ) ;
#64909 = ORIENTED_EDGE ( 'NONE', *, *, #68429, .F. ) ;
#64910 = ADVANCED_FACE ( 'NONE', ( #14146 ), #20466, .T. ) ;
#64911 = FACE_OUTER_BOUND ( 'NONE', #3003, .T. ) ;
#64912 = ORIENTED_EDGE ( 'NONE', *, *, #88303, .F. ) ;
#64913 = EDGE_CURVE ( 'NONE', #79882, #55035, #42514, .T. ) ;
#64914 = ORIENTED_EDGE ( 'NONE', *, *, #80015, .T. ) ;
#64916 = CARTESIAN_POINT ( 'NONE',  ( 5.776515056276054771, -3.236172620538810385, 32.36188796281390267 ) ) ;
#64915 = CARTESIAN_POINT ( 'NONE',  ( -7.912237257109724808, -6.386643153685125363, 34.62446782046654903 ) ) ;
#64917 = VECTOR ( 'NONE', #85211, 1000.000000000000000 ) ;
#64918 = CARTESIAN_POINT ( 'NONE',  ( -8.703975629717929152, -12.51329471203373700, 31.30864560766537963 ) ) ;
#64919 = CARTESIAN_POINT ( 'NONE',  ( -13.51530598772569469, -2.845849958028613624, 32.17971566917920967 ) ) ;
#64920 = CARTESIAN_POINT ( 'NONE',  ( 7.846153846153846700, -12.37446782046654192, 30.86335684631486131 ) ) ;
#64921 = CARTESIAN_POINT ( 'NONE',  ( -2.372962753653082402, -10.21337939537584383, 33.94971097300158647 ) ) ;
#64922 = ORIENTED_EDGE ( 'NONE', *, *, #37093, .F. ) ;
#64923 = CARTESIAN_POINT ( 'NONE',  ( -5.999999999999998224, -8.564572088678739092, 35.78748833219616898 ) ) ;
#64924 = EDGE_CURVE ( 'NONE', #38748, #72142, #73817, .T. ) ;
#64925 = CARTESIAN_POINT ( 'NONE',  ( -11.78848477575450282, -10.05641848906368097, 34.04755513067966177 ) ) ;
#64926 = DIRECTION ( 'NONE',  ( -0.000000000000000000, 1.000000000000000000, 3.491481338843133355E-15 ) ) ;
#64927 = CARTESIAN_POINT ( 'NONE',  ( 10.61538461538461675, -11.69971097300155272, 32.46337939537588113 ) ) ;
#64928 = VECTOR ( 'NONE', #11357, 1000.000000000000227 ) ;
#64929 = ORIENTED_EDGE ( 'NONE', *, *, #79170, .T. ) ;
#64930 = VERTEX_POINT ( 'NONE', #28104 ) ;
#64932 = FACE_BOUND ( 'NONE', #47050, .T. ) ;
#64931 = B_SPLINE_CURVE_WITH_KNOTS ( 'NONE', 3,
 ( #36609, #15903, #37480, #35733, #8261, #57318, #1936, #37035, #71710, #29422 ),
 .UNSPECIFIED., .F., .F.,
 ( 4, 2, 2, 2, 4 ),
 ( 0.0007817359430256293554, 0.0009771253907249941549, 0.001172514838424358954, 0.001367904286123723537, 0.001563293733823095276 ),
 .UNSPECIFIED. ) ;
#64933 = ORIENTED_EDGE ( 'NONE', *, *, #48444, .T. ) ;
#64934 = CARTESIAN_POINT ( 'NONE',  ( -18.00000000000000711, -2.252971138473345292, 29.99985851721553942 ) ) ;
#64935 = CARTESIAN_POINT ( 'NONE',  ( 4.826899852701618698, -2.985938066672154445, 32.43141759479405550 ) ) ;
#64936 = ORIENTED_EDGE ( 'NONE', *, *, #36653, .F. ) ;
#64937 = CARTESIAN_POINT ( 'NONE',  ( 8.769230769230768274, -11.11383981884818262, 36.00935417666054406 ) ) ;
#64938 = CARTESIAN_POINT ( 'NONE',  ( -2.084680956079457026, -4.187068189119697692, 33.49521262558774026 ) ) ;
#64939 = CARTESIAN_POINT ( 'NONE',  ( -7.912237257109724808, -11.69971097300155272, 32.46337939537587403 ) ) ;
#64940 = CARTESIAN_POINT ( 'NONE',  ( -1.161835715637317579, -4.226511098958374291, 33.85474049983370293 ) ) ;
#64941 = ORIENTED_EDGE ( 'NONE', *, *, #39224, .F. ) ;
#64942 = CARTESIAN_POINT ( 'NONE',  ( 4.153846153846154188, -1.129524287112498415, 32.06866353760679544 ) ) ;
#64943 = ORIENTED_EDGE ( 'NONE', *, *, #1452, .T. ) ;
#64945 = VERTEX_POINT ( 'NONE', #68210 ) ;
#64944 = CARTESIAN_POINT ( 'NONE',  ( 17.01083966596719321, -10.51840700105979565, 33.73612834413961536 ) ) ;
#64946 = CARTESIAN_POINT ( 'NONE',  ( -7.846153846153965716, -9.442884908241554243, 34.35708131394783038 ) ) ;
#64947 = CARTESIAN_POINT ( 'NONE',  ( -12.46153846153846168, -2.833524468853757305, 32.15551576947925838 ) ) ;
#64948 = LINE ( 'NONE', #79369, #15602 ) ;
#64949 = EDGE_CURVE ( 'NONE', #64502, #60134, #7837, .T. ) ;
#64950 = CARTESIAN_POINT ( 'NONE',  ( 12.59233026936325217, -4.118422570099828484, 33.43335022499816489 ) ) ;
#64951 = LINE ( 'NONE', #3256, #26075 ) ;
#64952 = LINE ( 'NONE', #57322, #14758 ) ;
#64953 = CARTESIAN_POINT ( 'NONE',  ( -1.987747218494638313, -9.401340078031370950, 13.93936829374151465 ) ) ;
#64954 = VERTEX_POINT ( 'NONE', #88948 ) ;
#64955 = CARTESIAN_POINT ( 'NONE',  ( -0.7115616988314271696, -5.851115903089112003, 34.47074536777953568 ) ) ;
#64956 = CARTESIAN_POINT ( 'NONE',  ( 5.934729999443682402, -8.656820664281497102, 34.87096338111211935 ) ) ;
#64957 = AXIS2_PLACEMENT_3D ( 'NONE', #29499, #62812, #82678 ) ;
#64958 = ORIENTED_EDGE ( 'NONE', *, *, #43185, .T. ) ;
#64959 = VERTEX_POINT ( 'NONE', #47480 ) ;
#64960 = FACE_OUTER_BOUND ( 'NONE', #36650, .T. ) ;
#64961 = DIRECTION ( 'NONE',  ( -1.734723475976813750E-16, 1.000000000000000000, -0.000000000000000000 ) ) ;
#64962 = CARTESIAN_POINT ( 'NONE',  ( 10.28846153846153832, -3.499999999999999556, 29.75000000000000355 ) ) ;
#64963 = VECTOR ( 'NONE', #10155, 1000.000000000000000 ) ;
#64964 = B_SPLINE_CURVE_WITH_KNOTS ( 'NONE', 3,
 ( #10088, #37554, #65019, #3327, #30798, #26272, #73590, #87109, #67263, #5560 ),
 .UNSPECIFIED., .F., .F.,
 ( 4, 2, 2, 2, 4 ),
 ( 0.0007817359430256386795, 0.0009771253907250069485, 0.001172514838424375217, 0.001367904286123743486, 0.001563293733823111755 ),
 .UNSPECIFIED. ) ;
#64965 = FACE_OUTER_BOUND ( 'NONE', #21288, .T. ) ;
#64966 = CARTESIAN_POINT ( 'NONE',  ( 0.000000000000000000, -11.00000000000000000, 29.75000000000000355 ) ) ;
#64967 = CARTESIAN_POINT ( 'NONE',  ( 17.86985203026830504, -12.15440758774515473, 32.17923288041532004 ) ) ;
#64968 = B_SPLINE_CURVE_WITH_KNOTS ( 'NONE', 3,
 ( #7421, #40323, #1545, #71318, #50153, #15065, #64550, #64114, #56488, #49286 ),
 .UNSPECIFIED., .F., .F.,
 ( 4, 2, 2, 2, 4 ),
 ( 0.0007817246256747532440, 0.0009771112852218978746, 0.001172497944769042288, 0.001367884604316186702, 0.001563271263863331333 ),
 .UNSPECIFIED. ) ;
#64969 = DIRECTION ( 'NONE',  ( 0.000000000000000000, 0.000000000000000000, -1.000000000000000000 ) ) ;
#64970 = ORIENTED_EDGE ( 'NONE', *, *, #48215, .T. ) ;
#64971 = CARTESIAN_POINT ( 'NONE',  ( 6.130525701763565927, -10.88167719472716399, 33.43325721877153711 ) ) ;
#64972 = CARTESIAN_POINT ( 'NONE',  ( -1.607541602131530967, -6.503392248772476236, 34.64988816332204635 ) ) ;
#64973 = CARTESIAN_POINT ( 'NONE',  ( 3.903846153846154632, -7.566082377512563184, 35.00000000000000711 ) ) ;
#64974 = CARTESIAN_POINT ( 'NONE',  ( 12.21156173059610772, -11.79746400365624659, 32.30657167506340954 ) ) ;
#64975 = VERTEX_POINT ( 'NONE', #26777 ) ;
#64976 = CARTESIAN_POINT ( 'NONE',  ( -5.999999999999998224, -11.91647553114624181, 32.58852847137148245 ) ) ;
#64977 = ORIENTED_EDGE ( 'NONE', *, *, #33829, .F. ) ;
#64978 = CARTESIAN_POINT ( 'NONE',  ( -17.93393266664992680, -8.164416787775447659, 34.95778746994558617 ) ) ;
#64979 = CARTESIAN_POINT ( 'NONE',  ( -1.607541602131531633, -9.086856451489515152, 34.49173150075333183 ) ) ;
#64980 = CARTESIAN_POINT ( 'NONE',  ( 3.903846153846154632, -7.500000000000001776, 34.75000000000000000 ) ) ;
#64981 = ORIENTED_EDGE ( 'NONE', *, *, #48021, .F. ) ;
#64982 = CARTESIAN_POINT ( 'NONE',  ( -1.450697763975519639, -12.62096338111211580, 30.90682066428152197 ) ) ;
#64983 = CARTESIAN_POINT ( 'NONE',  ( 5.076923076923075762, -8.120952969808772792, 34.71129190930000163 ) ) ;
#64984 = CARTESIAN_POINT ( 'NONE',  ( -17.20761454359064047, -3.530157926970578508, 32.79014554554150607 ) ) ;
#64985 = CARTESIAN_POINT ( 'NONE',  ( -7.715628407920200438, -5.070358843744210198, 34.40418822224088302 ) ) ;
#64986 = CARTESIAN_POINT ( 'NONE',  ( -5.076923076923199218, -8.656820664282941280, 34.87096338111179961 ) ) ;
#64987 = ORIENTED_EDGE ( 'NONE', *, *, #45015, .F. ) ;
#64988 = CARTESIAN_POINT ( 'NONE',  ( 7.623226887246995709, -11.43668979543635089, 33.22377378376089752 ) ) ;
#64989 = EDGE_LOOP ( 'NONE', ( #13869, #17925, #85389, #18036, #41848, #70037 ) ) ;
#64990 = AXIS2_PLACEMENT_3D ( 'NONE', #12261, #11827, #65859 ) ;
#64991 = DIRECTION ( 'NONE',  ( 0.000000000000000000, 0.000000000000000000, 1.000000000000000000 ) ) ;
#64992 = B_SPLINE_CURVE_WITH_KNOTS ( 'NONE', 3,
 ( #80748, #39312, #18143, #32534, #59116, #66770, #5965, #87510, #46930, #19031 ),
 .UNSPECIFIED., .F., .F.,
 ( 4, 2, 2, 2, 4 ),
 ( 0.0007817359430256372700, 0.0009771253907250054306, 0.001172514838424373483, 0.001367904286123741535, 0.001563293733823109804 ),
 .UNSPECIFIED. ) ;
#64993 = CARTESIAN_POINT ( 'NONE',  ( 2.307692307692309264, -1.951392089020283160, 34.73218667398347748 ) ) ;
#64994 = CARTESIAN_POINT ( 'NONE',  ( 9.915087361285756629, -2.612705202774698421, 31.66806509827799943 ) ) ;
#64995 = B_SPLINE_CURVE_WITH_KNOTS ( 'NONE', 3,
 ( #87676, #45777, #17425, #11562, #11108, #25512, #32274, #79577, #38584, #73256 ),
 .UNSPECIFIED., .F., .F.,
 ( 4, 2, 2, 2, 4 ),
 ( 0.000000000000000000, 0.0001954339857564053873, 0.0003908679715128107746, 0.0005863019572692161618, 0.0007817359430256215491 ),
 .UNSPECIFIED. ) ;
#64996 = CARTESIAN_POINT ( 'NONE',  ( -9.915234651214539952, -8.282780595021769443, 34.94152052738834158 ) ) ;
#64997 = CARTESIAN_POINT ( 'NONE',  ( 15.00728428704528561, -11.89387501736622710, 32.13663884655806413 ) ) ;
#64998 = ORIENTED_EDGE ( 'NONE', *, *, #46376, .F. ) ;
#64999 = ORIENTED_EDGE ( 'NONE', *, *, #76538, .T. ) ;
#65000 = PRODUCT_DEFINITION_SHAPE ( 'NONE', 'NONE',  #89192 ) ;
#65001 = ORIENTED_EDGE ( 'NONE', *, *, #39404, .F. ) ;
#65002 = VERTEX_POINT ( 'NONE', #75408 ) ;
#65003 = CARTESIAN_POINT ( 'NONE',  ( 12.59233026936325039, -11.71459661697925903, 32.44059661609676937 ) ) ;
#65004 = CARTESIAN_POINT ( 'NONE',  ( 13.60739492588379385, -10.11255958852956027, 34.01340905677048454 ) ) ;
#65005 = CARTESIAN_POINT ( 'NONE',  ( -4.946084658910312903, -7.277220443632450575, 34.74524770363009196 ) ) ;
#65006 = DIRECTION ( 'NONE',  ( -0.000000000000000000, 0.8660254037844397068, -0.4999999999999978906 ) ) ;
#65007 = CARTESIAN_POINT ( 'NONE',  ( -13.16183584334697265, -5.913360116392397892, 34.49180327182771322 ) ) ;
#65008 = VECTOR ( 'NONE', #30597, 1000.000000000000227 ) ;
#65010 = ADVANCED_FACE ( 'NONE', ( #33970 ), #47927, .F. ) ;
#65009 = CARTESIAN_POINT ( 'NONE',  ( 8.545745825506822158, -9.331801661448606566, 34.40259984581193464 ) ) ;
#65011 = DIRECTION ( 'NONE',  ( -0.000000000000000000, -0.9396926207859093161, -0.3420201433256663259 ) ) ;
#65012 = CARTESIAN_POINT ( 'NONE',  ( -7.846153846153965716, -3.300289026999228881, 32.46337939537708905 ) ) ;
#65013 = ORIENTED_EDGE ( 'NONE', *, *, #39404, .T. ) ;
#65014 = EDGE_CURVE ( 'NONE', #67905, #69595, #27734, .T. ) ;
#65015 = ORIENTED_EDGE ( 'NONE', *, *, #28412, .T. ) ;
#65016 = ORIENTED_EDGE ( 'NONE', *, *, #51108, .F. ) ;
#65018 = EDGE_LOOP ( 'NONE', ( #71752, #22583, #70023, #80882 ) ) ;
#65017 = CYLINDRICAL_SURFACE ( 'NONE', #38826, 0.2499999999999994726 ) ;
#65020 = CARTESIAN_POINT ( 'NONE',  ( -17.75005459062195712, -11.56426240980093567, 33.07394671870546432 ) ) ;
#65019 = CARTESIAN_POINT ( 'NONE',  ( 16.28437185560972011, -11.93748526763465279, 32.05452791011430946 ) ) ;
#65021 = CARTESIAN_POINT ( 'NONE',  ( -1.134615384615383915, -2.249999999999998668, 29.75000000000000355 ) ) ;
#65022 = CARTESIAN_POINT ( 'NONE',  ( 9.692307692307695177, -13.20930481340135110, 34.54067556320372745 ) ) ;
#65023 = ORIENTED_EDGE ( 'NONE', *, *, #26876, .F. ) ;
#65024 = ADVANCED_FACE ( 'NONE', ( #63656 ), #10038, .F. ) ;
#65025 = ORIENTED_EDGE ( 'NONE', *, *, #65816, .F. ) ;
#65026 = LINE ( 'NONE', #10097, #15488 ) ;
#65027 = ORIENTED_EDGE ( 'NONE', *, *, #16677, .T. ) ;
#65028 = FACE_BOUND ( 'NONE', #63882, .T. ) ;
#65029 = DIRECTION ( 'NONE',  ( -1.000000000000000000, -0.000000000000000000, -0.000000000000000000 ) ) ;
#65030 = CARTESIAN_POINT ( 'NONE',  ( 16.08857570788537572, -6.879047030191174805, 34.71129190930000163 ) ) ;
#65031 = EDGE_LOOP ( 'NONE', ( #53177, #27623, #50513 ) ) ;
#65032 = CARTESIAN_POINT ( 'NONE',  ( 17.86930853333243974, -2.729777683071817229, 31.24903638046269450 ) ) ;
#65033 = LINE ( 'NONE', #22293, #21646 ) ;
#65034 = CARTESIAN_POINT ( 'NONE',  ( 2.084207383127976598, -11.60425143139329940, 33.02411095842164457 ) ) ;
#65035 = EDGE_LOOP ( 'NONE', ( #86181, #60197, #6331, #76084 ) ) ;
#65036 = CARTESIAN_POINT ( 'NONE',  ( -11.78843828251013015, -4.818429247618089661, 34.26397095200675125 ) ) ;
#65037 = DIRECTION ( 'NONE',  ( 0.000000000000000000, 0.4999999999999960032, -0.8660254037844410391 ) ) ;
#65038 = EDGE_LOOP ( 'NONE', ( #70924, #64449, #22375, #56031 ) ) ;
#65039 = DIRECTION ( 'NONE',  ( 0.000000000000000000, 0.1736481776669275834, 0.9848077530122086864 ) ) ;
#65040 = CARTESIAN_POINT ( 'NONE',  ( 10.61538461538449596, -11.94971097300221174, 32.03036669348237098 ) ) ;
#65042 = ORIENTED_EDGE ( 'NONE', *, *, #47370, .F. ) ;
#65041 = AXIS2_PLACEMENT_3D ( 'NONE', #60190, #11577, #39059 ) ;
#65043 = CARTESIAN_POINT ( 'NONE',  ( 3.512820512820510555, -7.500000000000000000, 29.75000000000000355 ) ) ;
#65044 = CARTESIAN_POINT ( 'NONE',  ( 13.38461538461538680, -2.538708090699994813, 30.37095296980875503 ) ) ;
#65045 = CARTESIAN_POINT ( 'NONE',  ( 6.923076923076924238, -3.937682226553329556, 33.60647404775216529 ) ) ;
#65046 = CARTESIAN_POINT ( 'NONE',  ( 8.096153846155281997, -7.500000000000155431, 34.75000000000007105 ) ) ;
#65047 = CARTESIAN_POINT ( 'NONE',  ( 9.692307692307695177, -12.34228464037088635, 31.77849191805839268 ) ) ;
#65048 = EDGE_CURVE ( 'NONE', #67006, #25149, #65381, .T. ) ;
#65049 = FACE_BOUND ( 'NONE', #88843, .T. ) ;
#65051 = CARTESIAN_POINT ( 'NONE',  ( 7.053602624840490165, -3.285477652293412820, 32.44071101563363158 ) ) ;
#65050 = CARTESIAN_POINT ( 'NONE',  ( 3.512820512820510555, -7.500000000000000000, 29.75000000000000355 ) ) ;
#65052 = CARTESIAN_POINT ( 'NONE',  ( -1.161602540521988525, -9.172514111537584114, 34.72667873470787470 ) ) ;
#65054 = CARTESIAN_POINT ( 'NONE',  ( 9.019176287578909879, -2.824170634883621744, 31.52227843825338738 ) ) ;
#65053 = CARTESIAN_POINT ( 'NONE',  ( -18.00000000000000000, -4.949874560955057845, 36.02546096051201374 ) ) ;
#65055 = EDGE_CURVE ( 'NONE', #61936, #69536, #78944, .T. ) ;
#65056 = CARTESIAN_POINT ( 'NONE',  ( 13.16173586787780359, -7.630690623152299956, 34.99857592706774057 ) ) ;
#65057 = CARTESIAN_POINT ( 'NONE',  ( 2.750000000000001776, -7.499999999999984013, 14.46875000000000000 ) ) ;
#65058 = ORIENTED_EDGE ( 'NONE', *, *, #32395, .T. ) ;
#65059 = B_SPLINE_CURVE_WITH_KNOTS ( 'NONE', 3,
 ( #16888, #29965, #43916, #57425, #84919, #23202, #50663, #71378, #9685, #13137 ),
 .UNSPECIFIED., .F., .F.,
 ( 4, 2, 2, 2, 4 ),
 ( 0.000000000000000000, 0.0001954339857564074473, 0.0003908679715128148945, 0.0005863019572692223418, 0.0007817359430256297891 ),
 .UNSPECIFIED. ) ;
#65060 = ADVANCED_FACE ( 'NONE', ( #64525 ), #30750, .F. ) ;
#65061 = CARTESIAN_POINT ( 'NONE',  ( -0.4615384615384611200, -10.05456864172156806, 36.03766855953608683 ) ) ;
#65062 = ORIENTED_EDGE ( 'NONE', *, *, #42893, .T. ) ;
#65063 = CARTESIAN_POINT ( 'NONE',  ( -19.99999999999996447, -12.00000000000000355, 10.00000000000000178 ) ) ;
#65064 = EDGE_CURVE ( 'NONE', #57769, #77586, #28882, .T. ) ;
#65065 = VERTEX_POINT ( 'NONE', #57785 ) ;
#65066 = CARTESIAN_POINT ( 'NONE',  ( 1.384615384615265343, -5.219633306517616589, 34.19971097300220464 ) ) ;
#65067 = VERTEX_POINT ( 'NONE', #2386 ) ;
#65068 = CARTESIAN_POINT ( 'NONE',  ( -18.00000000000000000, -12.37446782046654192, 30.86335684631486131 ) ) ;
#65069 = CARTESIAN_POINT ( 'NONE',  ( 1.987747218494664292, -9.401340078031346081, 23.12313170625848713 ) ) ;
#65070 = CARTESIAN_POINT ( 'NONE',  ( -17.77698864838715309, -5.667800583137508674, 34.40243808032445827 ) ) ;
#65071 = CARTESIAN_POINT ( 'NONE',  ( -9.942284436356281674, -12.65889640711025521, 30.72598325615533454 ) ) ;
#65072 = CARTESIAN_POINT ( 'NONE',  ( -16.15384615384615330, -2.249999999999998668, 29.75000000000001776 ) ) ;
#65073 = CARTESIAN_POINT ( 'NONE',  ( 17.86985203026830504, -2.373036134822905208, 30.88089517874952250 ) ) ;
#65074 = CARTESIAN_POINT ( 'NONE',  ( -19.50000000000000000, -3.499999999999999556, 29.75000000000000355 ) ) ;
#65075 = DIRECTION ( 'NONE',  ( 1.000000000000000000, 0.000000000000000000, 0.000000000000000000 ) ) ;
#65076 = CARTESIAN_POINT ( 'NONE',  ( 5.999999999999880096, -4.481592998941358097, 33.73612834414048933 ) ) ;
#65077 = CARTESIAN_POINT ( 'NONE',  ( 3.750000000000000888, -7.499999999999978684, 16.96875000000000000 ) ) ;
#65078 = LINE ( 'NONE', #10154, #18981 ) ;
#65079 = CARTESIAN_POINT ( 'NONE',  ( 19.00000000000000000, -9.000000000000001776, 2.291744775602387568E-15 ) ) ;
#65080 = CARTESIAN_POINT ( 'NONE',  ( 14.53070365930516061, -3.105924265160262543, 32.13625925475356127 ) ) ;
#65081 = CARTESIAN_POINT ( 'NONE',  ( 2.651650429449539104, -4.848349570550432475, 15.56250000000000000 ) ) ;
#65082 = VECTOR ( 'NONE', #25696, 1000.000000000000227 ) ;
#65083 = ORIENTED_EDGE ( 'NONE', *, *, #55707, .T. ) ;
#65084 = CARTESIAN_POINT ( 'NONE',  ( -13.38461538461538325, -6.343179335718451384, 34.87096338111211935 ) ) ;
#65085 = CARTESIAN_POINT ( 'NONE',  ( 15.90382291655318880, -12.22074536777955345, 31.39888409691088356 ) ) ;
#65086 = CARTESIAN_POINT ( 'NONE',  ( 9.915319043920545639, -6.503523203565941380, 34.64991518177335195 ) ) ;
#65087 = CARTESIAN_POINT ( 'NONE',  ( 18.22277954126840172, -10.81320215134717166, 33.49497208177562868 ) ) ;
#65088 = CARTESIAN_POINT ( 'NONE',  ( 20.00000000000000000, -4.000000000000000000, 29.75000000000000355 ) ) ;
#65089 = VECTOR ( 'NONE', #12177, 1000.000000000000114 ) ;
#65090 = CARTESIAN_POINT ( 'NONE',  ( 2.242421861731533905, -12.27809138561121394, 31.22303859784730307 ) ) ;
#65091 = EDGE_CURVE ( 'NONE', #16329, #61210, #55094, .T. ) ;
#65092 = B_SPLINE_CURVE_WITH_KNOTS ( 'NONE', 3,
 ( #73332, #59368, #72430, #58460, #39115, #37309, #66578, #3524, #4884, #85513 ),
 .UNSPECIFIED., .F., .F.,
 ( 4, 2, 2, 2, 4 ),
 ( 0.000000000000000000, 0.0001954339857564063360, 0.0003908679715128126719, 0.0005863019572692189808, 0.0007817359430256253438 ),
 .UNSPECIFIED. ) ;
#65093 = VERTEX_POINT ( 'NONE', #8731 ) ;
#65094 = B_SPLINE_CURVE_WITH_KNOTS ( 'NONE', 3,
 ( #84174, #7170, #35976, #42295, #68863, #63432, #77393, #56680, #15260, #34642 ),
 .UNSPECIFIED., .F., .F.,
 ( 4, 2, 2, 2, 4 ),
 ( 0.0007817359430256365111, 0.0009771253907250043464, 0.001172514838424372399, 0.001367904286123740234, 0.001563293733823108069 ),
 .UNSPECIFIED. ) ;
#65095 = CARTESIAN_POINT ( 'NONE',  ( 7.780883845597524662, -3.083524468853724887, 32.58852847137143272 ) ) ;
#65096 = VERTEX_POINT ( 'NONE', #23988 ) ;
#65097 = ORIENTED_EDGE ( 'NONE', *, *, #11656, .T. ) ;
#65098 = DIRECTION ( 'NONE',  ( 1.000000000000000000, -0.000000000000000000, -0.000000000000000000 ) ) ;
#65099 = CARTESIAN_POINT ( 'NONE',  ( -6.065270000556318486, -12.70778746994557551, 30.41441678777548319 ) ) ;
#65100 = LINE ( 'NONE', #31336, #77578 ) ;
#65101 = CARTESIAN_POINT ( 'NONE',  ( 1.634669696253700399, -11.79725096376909654, 32.30694842903960762 ) ) ;
#65102 = CARTESIAN_POINT ( 'NONE',  ( -13.38461538461538325, -3.050289026998446396, 32.03036669348365706 ) ) ;
#65103 = ADVANCED_FACE ( 'NONE', ( #51003 ), #84390, .T. ) ;
#65104 = ORIENTED_EDGE ( 'NONE', *, *, #74326, .T. ) ;
#65105 = VECTOR ( 'NONE', #88502, 1000.000000000000000 ) ;
#65106 = CARTESIAN_POINT ( 'NONE',  ( 9.019176287578909879, -3.712312575010499494, 33.01462480002815170 ) ) ;
#65107 = CIRCLE ( 'NONE', #55097, 0.2500000000000002220 ) ;
#65108 = EDGE_LOOP ( 'NONE', ( #9221, #45210, #57788, #84608 ) ) ;
#65109 = ORIENTED_EDGE ( 'NONE', *, *, #70964, .F. ) ;
#65110 = CARTESIAN_POINT ( 'NONE',  ( 1.134638653673032405, -11.28823185664190376, 33.01397839955799896 ) ) ;
#65111 = DIRECTION ( 'NONE',  ( 0.000000000000000000, 0.8660254037844377084, 0.5000000000000015543 ) ) ;
#65112 = LINE ( 'NONE', #84965, #70996 ) ;
#65114 = EDGE_CURVE ( 'NONE', #8219, #16365, #78493, .T. ) ;
#65113 = CARTESIAN_POINT ( 'NONE',  ( -8.769230769230768274, -9.905515769479276145, 34.41647553114623292 ) ) ;
#65115 = CARTESIAN_POINT ( 'NONE',  ( -4.376772371362299019, -8.239355502252617924, 34.69524867566427417 ) ) ;
#65116 = LINE ( 'NONE', #85410, #88389 ) ;
#65117 = EDGE_LOOP ( 'NONE', ( #31364, #65715 ) ) ;
#65118 = ADVANCED_FACE ( 'NONE', ( #36637 ), #64091, .F. ) ;
#65119 = ORIENTED_EDGE ( 'NONE', *, *, #6786, .F. ) ;
#65120 = CARTESIAN_POINT ( 'NONE',  ( 3.750000000000009770, -9.053300858899081760, 20.79687500000000000 ) ) ;
#65121 = B_SPLINE_CURVE_WITH_KNOTS ( 'NONE', 3,
 ( #27546, #88382, #40627, #41504, #74857, #73963, #54560, #54113, #68523, #47812 ),
 .UNSPECIFIED., .F., .F.,
 ( 4, 2, 2, 2, 4 ),
 ( 0.000000000000000000, 0.0001954339857564097241, 0.0003908679715128194482, 0.0005863019572692291723, 0.0007817359430256388964 ),
 .UNSPECIFIED. ) ;
#65122 = EDGE_LOOP ( 'NONE', ( #4756, #27538 ) ) ;
#65124 = ORIENTED_EDGE ( 'NONE', *, *, #3444, .T. ) ;
#65123 = CARTESIAN_POINT ( 'NONE',  ( -13.38461538461550759, -5.941354392335915335, 34.76329471203413846 ) ) ;
#65125 = CARTESIAN_POINT ( 'NONE',  ( -10.48485917715096960, -4.299079248970732792, 33.91157788607253565 ) ) ;
#65126 = CARTESIAN_POINT ( 'NONE',  ( 6.130791807824786943, -12.38066358083363738, 30.83685684665853444 ) ) ;
#65127 = B_SPLINE_CURVE_WITH_KNOTS ( 'NONE', 3,
 ( #35425, #83635, #21914, #49388, #76864, #15162, #85391, #86298, #51128, #16927 ),
 .UNSPECIFIED., .F., .F.,
 ( 4, 2, 2, 2, 4 ),
 ( 0.0007817359430256390048, 0.0009771253907250075990, 0.001172514838424376085, 0.001367904286123744571, 0.001563293733823113056 ),
 .UNSPECIFIED. ) ;
#65128 = B_SPLINE_CURVE_WITH_KNOTS ( 'NONE', 3,
 ( #1585, #29070, #57404, #64592, #71357, #43014, #71804, #56525, #62818, #85335 ),
 .UNSPECIFIED., .F., .F.,
 ( 4, 2, 2, 2, 4 ),
 ( 0.0007817359430256395469, 0.0009771253907250080327, 0.001172514838424376735, 0.001367904286123745438, 0.001563293733823113924 ),
 .UNSPECIFIED. ) ;
#65129 = CARTESIAN_POINT ( 'NONE',  ( 2.651650429449539104, -4.848349570550432475, 15.56250000000000000 ) ) ;
#65130 = ORIENTED_EDGE ( 'NONE', *, *, #30188, .F. ) ;
#65131 = EDGE_CURVE ( 'NONE', #32626, #63712, #49305, .T. ) ;
#65132 = CARTESIAN_POINT ( 'NONE',  ( 10.74591005361826035, -2.372941743896879174, 30.88044141588253666 ) ) ;
#65133 = VERTEX_POINT ( 'NONE', #4168 ) ;
#65134 = CARTESIAN_POINT ( 'NONE',  ( 5.750023255951409951, -9.234221910056348293, 34.70572697212741531 ) ) ;
#65135 = FACE_OUTER_BOUND ( 'NONE', #47640, .T. ) ;
#65136 = VECTOR ( 'NONE', #30380, 1000.000000000000227 ) ;
#65137 = CYLINDRICAL_SURFACE ( 'NONE', #50920, 0.2499999999999995837 ) ;
#65139 = CARTESIAN_POINT ( 'NONE',  ( -9.692307692307691624, -10.05456864172156806, 36.03766855953608683 ) ) ;
#65138 = CARTESIAN_POINT ( 'NONE',  ( -2.307692307692428724, -3.083524468854526912, 32.58852847137268327 ) ) ;
#65140 = EDGE_CURVE ( 'NONE', #74204, #43756, #89022, .T. ) ;
#65141 =( GEOMETRIC_REPRESENTATION_CONTEXT ( 3 ) GLOBAL_UNCERTAINTY_ASSIGNED_CONTEXT ( ( #77946 ) ) GLOBAL_UNIT_ASSIGNED_CONTEXT ( ( #60143, #53838, #40780 ) ) REPRESENTATION_CONTEXT ( 'NONE', 'WORKASPACE' ) );
#65142 = CARTESIAN_POINT ( 'NONE',  ( 8.638539302563209787, -5.582088688514999397, 34.36776431015576350 ) ) ;
#65143 = CARTESIAN_POINT ( 'NONE',  ( -10.74553182482283198, -10.88202310037935661, 33.43294751532457099 ) ) ;
#65144 = ORIENTED_EDGE ( 'NONE', *, *, #28836, .F. ) ;
#65145 = CARTESIAN_POINT ( 'NONE',  ( -11.28840722682322628, -4.235687564193445276, 33.53795663066793509 ) ) ;
#65146 = ADVANCED_FACE ( 'NONE', ( #65428 ), #87505, .F. ) ;
#65147 = CARTESIAN_POINT ( 'NONE',  ( 9.019285080869080318, -6.567000820036036579, 34.66262288849541306 ) ) ;
#65148 = ORIENTED_EDGE ( 'NONE', *, *, #54589, .F. ) ;
#65149 = AXIS2_PLACEMENT_3D ( 'NONE', #9616, #2844, #30336 ) ;
#65150 = CARTESIAN_POINT ( 'NONE',  ( -16.37677311275299985, -12.64616026154729411, 30.79003144601914244 ) ) ;
#65151 = CARTESIAN_POINT ( 'NONE',  ( -16.15384615384615330, -11.69971097300155272, 32.46337939537588113 ) ) ;
#65152 = CARTESIAN_POINT ( 'NONE',  ( 5.076923076923075762, -12.78798330534102945, 29.74999999999997868 ) ) ;
#65153 = CARTESIAN_POINT ( 'NONE',  ( -16.15384615384627409, -12.16647553114689728, 32.15551576947799362 ) ) ;
#65154 = CARTESIAN_POINT ( 'NONE',  ( -7.623190711887172455, -7.369474539155828730, 34.99858011523957657 ) ) ;
#65155 = EDGE_CURVE ( 'NONE', #24781, #22672, #36353, .T. ) ;
#65156 = FACE_BOUND ( 'NONE', #65858, .T. ) ;
#65158 = CARTESIAN_POINT ( 'NONE',  ( 1.634560902963529072, -2.587454068350147907, 30.68340429815432202 ) ) ;
#65157 = CARTESIAN_POINT ( 'NONE',  ( 5.142990410273152513, -5.471508081941601098, 34.59228464037088457 ) ) ;
#65159 = DIRECTION ( 'NONE',  ( -0.000000000000000000, 0.9848077530122086864, -0.1736481776669273891 ) ) ;
#65161 = LINE ( 'NONE', #71476, #33417 ) ;
#65160 = CARTESIAN_POINT ( 'NONE',  ( -11.66907189808606482, -7.722926236386453702, 34.74524107206102030 ) ) ;
#65162 = CARTESIAN_POINT ( 'NONE',  ( 12.39626801557768587, -12.46129190929999986, 30.37095296980880832 ) ) ;
#65163 = FACE_OUTER_BOUND ( 'NONE', #11047, .T. ) ;
#65164 = CARTESIAN_POINT ( 'NONE',  ( -3.775308065498766297, -6.007798216065450170, 22.42000670625849068 ) ) ;
#65165 = ORIENTED_EDGE ( 'NONE', *, *, #38871, .T. ) ;
#65166 = FACE_OUTER_BOUND ( 'NONE', #85599, .T. ) ;
#65167 = EDGE_CURVE ( 'NONE', #82613, #34578, #59959, .T. ) ;
#65168 = EDGE_CURVE ( 'NONE', #10775, #77057, #8442, .T. ) ;
#65169 = B_SPLINE_CURVE_WITH_KNOTS ( 'NONE', 3,
 ( #84466, #22742, #71819, #10124, #53777, #32183, #31740, #73168, #86703, #60534 ),
 .UNSPECIFIED., .F., .F.,
 ( 4, 2, 2, 2, 4 ),
 ( 0.0007817359430256384627, 0.0009771253907250067317, 0.001172514838424375001, 0.001367904286123743270, 0.001563293733823111539 ),
 .UNSPECIFIED. ) ;
#65170 = FACE_OUTER_BOUND ( 'NONE', #68551, .T. ) ;
#65171 = CARTESIAN_POINT ( 'NONE',  ( -7.846153846153537614, -2.506253911140614576, 30.00000000000323297 ) ) ;
#65172 = CARTESIAN_POINT ( 'NONE',  ( 16.82694633287449193, -8.347322224742351082, 34.93158281831414769 ) ) ;
#65173 = CARTESIAN_POINT ( 'NONE',  ( 6.673053698855465399, -12.68155406624981119, 30.59749803192733708 ) ) ;
#65174 = DIRECTION ( 'NONE',  ( 0.000000000000000000, 0.000000000000000000, -1.000000000000000000 ) ) ;
#65175 = CARTESIAN_POINT ( 'NONE',  ( 3.724691934501232815, -5.885600066136343678, 21.63875670625848713 ) ) ;
#65176 = B_SPLINE_CURVE_WITH_KNOTS ( 'NONE', 3,
 ( #46931, #20369, #82520, #81625, #68984, #87971, #61325, #88842, #27113, #75309 ),
 .UNSPECIFIED., .F., .F.,
 ( 4, 2, 2, 2, 4 ),
 ( 0.0007817246256747446788, 0.0009771112852218879000, 0.001172497944769031013, 0.001367884604316174126, 0.001563271263863317238 ),
 .UNSPECIFIED. ) ;
#65177 = CARTESIAN_POINT ( 'NONE',  ( -2.438382910802615822, -3.338472653186242756, 32.95098750199972670 ) ) ;
#65178 = CARTESIAN_POINT ( 'NONE',  ( 0.5923302693632473970, -3.530189275343204702, 32.79018710029569661 ) ) ;
#65179 = AXIS2_PLACEMENT_3D ( 'NONE', #13411, #40460, #62469 ) ;
#65180 = CARTESIAN_POINT ( 'NONE',  ( -16.82697755857493505, -5.852078868378312038, 34.47109172314383585 ) ) ;
#65181 = CARTESIAN_POINT ( 'NONE',  ( 5.010840697562940704, -9.058645607665454236, 34.76329471203372634 ) ) ;
#65182 = DIRECTION ( 'NONE',  ( 0.000000000000000000, 0.000000000000000000, 1.000000000000000000 ) ) ;
#65183 = CARTESIAN_POINT ( 'NONE',  ( 10.61538461538492406, -2.506253911140615021, 30.00000000000323297 ) ) ;
#65184 = DIRECTION ( 'NONE',  ( -0.000000000000000000, -0.9848077530122086864, -0.1736481776669273613 ) ) ;
#65185 = CARTESIAN_POINT ( 'NONE',  ( 14.24160889673642849, -6.386643153685125363, 34.62446782046654903 ) ) ;
#65186 = VERTEX_POINT ( 'NONE', #32529 ) ;
#65187 = DIRECTION ( 'NONE',  ( -0.000000000000000000, 1.000000000000000000, -0.000000000000000000 ) ) ;
#65188 = CARTESIAN_POINT ( 'NONE',  ( -1.384615384615069056, -2.255955759149395501, 30.00000000000324363 ) ) ;
#65189 = CARTESIAN_POINT ( 'NONE',  ( -2.775308065498752086, -8.577988221561495763, 24.01749329374151287 ) ) ;
#65190 = CARTESIAN_POINT ( 'NONE',  ( -10.83886953994894675, -10.23692288466677880, 34.23039457007281072 ) ) ;
#65191 = FACE_OUTER_BOUND ( 'NONE', #13549, .T. ) ;
#65192 = ORIENTED_EDGE ( 'NONE', *, *, #66124, .F. ) ;
#65193 = EDGE_CURVE ( 'NONE', #52884, #41653, #5065, .T. ) ;
#65194 = CARTESIAN_POINT ( 'NONE',  ( -18.22348494372394967, -9.331801661448606566, 34.40259984581193464 ) ) ;
#65195 = CARTESIAN_POINT ( 'NONE',  ( -1.134561072977069429, -6.567000820036038355, 34.66262288849541306 ) ) ;
#65197 = ORIENTED_EDGE ( 'NONE', *, *, #71669, .F. ) ;
#65196 = CARTESIAN_POINT ( 'NONE',  ( 4.023698944407932743, -6.001485441113818986, 34.52039167877662607 ) ) ;
#65198 = FACE_OUTER_BOUND ( 'NONE', #53850, .T. ) ;
#65199 = DIRECTION ( 'NONE',  ( -0.000000000000000000, 0.3420201433256694346, -0.9396926207859080948 ) ) ;
#65200 = CARTESIAN_POINT ( 'NONE',  ( 0.4615384615384611200, -13.20930481340135110, 34.54067556320372745 ) ) ;
#65201 = CARTESIAN_POINT ( 'NONE',  ( -15.48076923076922995, -2.249999999999998668, 29.75000000000000355 ) ) ;
#65202 = ORIENTED_EDGE ( 'NONE', *, *, #23669, .T. ) ;
#65203 = CARTESIAN_POINT ( 'NONE',  ( 2.530703659305159725, -12.15243808032445827, 31.58219941686247978 ) ) ;
#65204 = EDGE_CURVE ( 'NONE', #86321, #57810, #53588, .T. ) ;
#65205 = CARTESIAN_POINT ( 'NONE',  ( 10.83816428436268353, -4.226511098958373402, 33.85474049983370293 ) ) ;
#65206 = AXIS2_PLACEMENT_3D ( 'NONE', #83197, #62025, #42213 ) ;
#65207 = LINE ( 'NONE', #18369, #12506 ) ;
#65208 = EDGE_LOOP ( 'NONE', ( #22478, #64505, #2307, #34288 ) ) ;
#65209 = EDGE_LOOP ( 'NONE', ( #46085, #79805, #55697, #13225 ) ) ;
#65210 = B_SPLINE_CURVE_WITH_KNOTS ( 'NONE', 3,
 ( #24617, #6470, #88906, #31377, #6031, #31832, #46993, #19533, #54634, #75369 ),
 .UNSPECIFIED., .F., .F.,
 ( 4, 2, 2, 2, 4 ),
 ( 0.000000000000000000, 0.0001954339857564091278, 0.0003908679715128182556, 0.0005863019572692274375, 0.0007817359430256365111 ),
 .UNSPECIFIED. ) ;
#65211 = ADVANCED_FACE ( 'NONE', ( #55028 ), #27556, .F. ) ;
#65212 = ORIENTED_EDGE ( 'NONE', *, *, #46037, .F. ) ;
#65213 = ADVANCED_FACE ( 'NONE', ( #60891 ), #7284, .F. ) ;
#65214 = AXIS2_PLACEMENT_3D ( 'NONE', #3978, #86437, #24708 ) ;
#65215 = DIRECTION ( 'NONE',  ( -0.000000000000000000, -0.1736481776669307198, -0.9848077530122080203 ) ) ;
#65216 = CARTESIAN_POINT ( 'NONE',  ( 9.692307692307695177, -3.937682226553329556, 33.60647404775216529 ) ) ;
#65217 = CARTESIAN_POINT ( 'NONE',  ( 2.373760658694747061, -5.557115091759786019, 34.35708131394839882 ) ) ;
#65218 = EDGE_CURVE ( 'NONE', #82401, #57426, #55644, .T. ) ;
#65219 = CARTESIAN_POINT ( 'NONE',  ( 2.307692307692309264, -6.189225973068211317, 35.74407628777942847 ) ) ;
#65220 = VERTEX_POINT ( 'NONE', #61319 ) ;
#65221 = ORIENTED_EDGE ( 'NONE', *, *, #17848, .T. ) ;
#65223 = VERTEX_POINT ( 'NONE', #54124 ) ;
#65222 = CYLINDRICAL_SURFACE ( 'NONE', #50125, 1.999999999999998224 ) ;
#65224 = B_SPLINE_CURVE_WITH_KNOTS ( 'NONE', 3,
 ( #10894, #45558, #24841, #65385, #85667, #64934 ),
 .UNSPECIFIED., .F., .F.,
 ( 4, 2, 4 ),
 ( 0.000000000000000000, 0.2499999999999978906, 0.4999999999999957812 ),
 .UNSPECIFIED. ) ;
#65225 = CARTESIAN_POINT ( 'NONE',  ( 9.915087233576103998, -12.44528174975671853, 30.48912976160716681 ) ) ;
#65226 = B_SPLINE_CURVE_WITH_KNOTS ( 'NONE', 3,
 ( #4797, #79571, #5234, #33148, #60167, #46663, #17867, #66495, #80006, #45320 ),
 .UNSPECIFIED., .F., .F.,
 ( 4, 2, 2, 2, 4 ),
 ( 0.0007817246256747484735, 0.0009771112852218928873, 0.001172497944769037084, 0.001367884604316181498, 0.001563271263863325912 ),
 .UNSPECIFIED. ) ;
#65227 = CARTESIAN_POINT ( 'NONE',  ( -8.703162418228330921, -12.37446782046654192, 30.86335684631486842 ) ) ;
#65228 = CARTESIAN_POINT ( 'NONE',  ( 13.51514082284903218, -10.31582465632705237, 34.18122507451815295 ) ) ;
#65229 = ORIENTED_EDGE ( 'NONE', *, *, #69921, .F. ) ;
#65230 = EDGE_CURVE ( 'NONE', #50666, #56147, #24550, .T. ) ;
#65231 = VERTEX_POINT ( 'NONE', #67658 ) ;
#65232 = EDGE_CURVE ( 'NONE', #59481, #4425, #66513, .T. ) ;
#65233 = VECTOR ( 'NONE', #7340, 1000.000000000000114 ) ;
#65234 = ORIENTED_EDGE ( 'NONE', *, *, #33504, .T. ) ;
#65236 = VERTEX_POINT ( 'NONE', #62220 ) ;
#65235 = CARTESIAN_POINT ( 'NONE',  ( -13.13461538461537259, -2.249999999999999112, 29.81603969181032454 ) ) ;
#65237 = CARTESIAN_POINT ( 'NONE',  ( -0.6844646790546077275, -10.61292498521070549, 33.66303323003028680 ) ) ;
#65238 = FACE_OUTER_BOUND ( 'NONE', #9902, .T. ) ;
#65239 = ORIENTED_EDGE ( 'NONE', *, *, #84572, .T. ) ;
#65240 = CARTESIAN_POINT ( 'NONE',  ( -13.38461538461538325, -4.098570777380720287, 33.41473453929634729 ) ) ;
#65241 = DIRECTION ( 'NONE',  ( -0.000000000000000000, -0.1736481776669307198, -0.9848077530122080203 ) ) ;
#65242 = CARTESIAN_POINT ( 'NONE',  ( -6.000000000000121680, -3.643525952248796163, 33.31231777344771672 ) ) ;
#65243 = FACE_BOUND ( 'NONE', #89177, .T. ) ;
#65244 = CARTESIAN_POINT ( 'NONE',  ( 15.00784301325307979, -5.667676309546437530, 34.40238873228292249 ) ) ;
#65245 = CARTESIAN_POINT ( 'NONE',  ( 2.530703659305157949, -8.239487800360276282, 34.69522927552633718 ) ) ;
#65246 = CARTESIAN_POINT ( 'NONE',  ( 13.25446741488368829, -12.70455904226513866, 30.44083106164009322 ) ) ;
#65248 = DIRECTION ( 'NONE',  ( 0.000000000000000000, 0.8660254037844377084, 0.5000000000000015543 ) ) ;
#65247 = CYLINDRICAL_SURFACE ( 'NONE', #53258, 5.000000000000000888 ) ;
#65249 = CARTESIAN_POINT ( 'NONE',  ( 17.77651507543566822, -6.716662450894490988, 34.94144148231605840 ) ) ;
#65250 = DIRECTION ( 'NONE',  ( 1.000000000000000000, 0.000000000000000000, 0.000000000000000000 ) ) ;
#65251 = ORIENTED_EDGE ( 'NONE', *, *, #37149, .F. ) ;
#65252 = CARTESIAN_POINT ( 'NONE',  ( 10.54930120442873331, -10.51840700105979387, 33.73612834413961536 ) ) ;
#65253 = ORIENTED_EDGE ( 'NONE', *, *, #38015, .F. ) ;
#65254 = VERTEX_POINT ( 'NONE', #49148 ) ;
#65256 = CARTESIAN_POINT ( 'NONE',  ( 10.61538461538461675, -12.62096338111211580, 30.90682066428153263 ) ) ;
#65255 = CARTESIAN_POINT ( 'NONE',  ( -2.307692307692305711, -1.044019251281081972, 31.83374038241031911 ) ) ;
#65257 = CARTESIAN_POINT ( 'NONE',  ( -5.933931648997561759, -6.386643153685127139, 34.62446782046654192 ) ) ;
#65258 = DIRECTION ( 'NONE',  ( 1.000000000000000000, 0.000000000000000000, 0.000000000000000000 ) ) ;
#65259 = CARTESIAN_POINT ( 'NONE',  ( 14.43821774592595197, -11.66157788607254098, 32.95092075102925833 ) ) ;
#65260 = ORIENTED_EDGE ( 'NONE', *, *, #62605, .F. ) ;
#65261 = DIRECTION ( 'NONE',  ( 1.000000000000000000, 0.000000000000000000, 0.000000000000000000 ) ) ;
#65262 = B_SPLINE_CURVE_WITH_KNOTS ( 'NONE', 3,
 ( #4990, #58137, #25251, #3636, #65781, #32451, #10854, #38323, #72996, #86984 ),
 .UNSPECIFIED., .F., .F.,
 ( 4, 2, 2, 2, 4 ),
 ( 0.000000000000000000, 0.0001954339857564090194, 0.0003908679715128180387, 0.0005863019572692270039, 0.0007817359430256360774 ),
 .UNSPECIFIED. ) ;
#65263 = VECTOR ( 'NONE', #56602, 1000.000000000000000 ) ;
#65264 = EDGE_CURVE ( 'NONE', #46286, #2856, #967, .T. ) ;
#65265 = EDGE_CURVE ( 'NONE', #25396, #31453, #82, .T. ) ;
#65266 = CARTESIAN_POINT ( 'NONE',  ( 0.2115152373170028632, -12.68155406624981119, 30.59749803192733708 ) ) ;
#65267 = DIRECTION ( 'NONE',  ( 0.000000000000000000, 0.9848077530122072432, 0.1736481776669354937 ) ) ;
#65268 = CARTESIAN_POINT ( 'NONE',  ( 0.3962684609821410242, -3.643525952247789412, 33.31231777344662959 ) ) ;
#65270 = DIRECTION ( 'NONE',  ( 0.000000000000000000, 0.7660444431189822323, -0.6427876096865344779 ) ) ;
#65269 = DIRECTION ( 'NONE',  ( 1.000000000000000000, 0.000000000000000000, 0.000000000000000000 ) ) ;
#65271 = CARTESIAN_POINT ( 'NONE',  ( 3.750000000000009770, -9.053300858899081760, 15.79687500000000178 ) ) ;
#65272 = ORIENTED_EDGE ( 'NONE', *, *, #36986, .F. ) ;
#65273 = EDGE_CURVE ( 'NONE', #24805, #6496, #55462, .T. ) ;
#65274 = ORIENTED_EDGE ( 'NONE', *, *, #56069, .F. ) ;
#65275 = AXIS2_PLACEMENT_3D ( 'NONE', #74692, #17966, #81454 ) ;
#65276 = CARTESIAN_POINT ( 'NONE',  ( -14.30769230769242917, -5.094484230521993062, 34.41647553114689373 ) ) ;
#65278 = ORIENTED_EDGE ( 'NONE', *, *, #25018, .T. ) ;
#65277 = EDGE_CURVE ( 'NONE', #72566, #26386, #50209, .T. ) ;
#65279 = FACE_OUTER_BOUND ( 'NONE', #55230, .T. ) ;
#65280 = CARTESIAN_POINT ( 'NONE',  ( -19.50000000000000000, -11.00000000000000000, 29.75000000000000355 ) ) ;
#65281 = CARTESIAN_POINT ( 'NONE',  ( 4.023155550735848074, -10.70098750199973203, 33.91152734681376302 ) ) ;
#65282 = CARTESIAN_POINT ( 'NONE',  ( 3.230769230769231726, -12.29105614889573062, 35.45975837776705220 ) ) ;
#65283 = CARTESIAN_POINT ( 'NONE',  ( -1.553300858899125059, -3.750000000000009326, 16.57812500000000000 ) ) ;
#65284 = CARTESIAN_POINT ( 'NONE',  ( -13.51476259405360203, -8.587444163452046197, 34.63053765926554206 ) ) ;
#65285 = EDGE_LOOP ( 'NONE', ( #7986, #48642, #24830, #85434 ) ) ;
#65286 = ADVANCED_FACE ( 'NONE', ( #1410 ), #42411, .F. ) ;
#65287 = FACE_OUTER_BOUND ( 'NONE', #18041, .T. ) ;
#65289 = ORIENTED_EDGE ( 'NONE', *, *, #78573, .T. ) ;
#65288 = CARTESIAN_POINT ( 'NONE',  ( -1.384615384615505151, -9.442884908241554243, 34.35708131394783038 ) ) ;
#65290 = CARTESIAN_POINT ( 'NONE',  ( -9.468881293392906073, -7.630147987733840509, 34.99859428049665411 ) ) ;
#65291 = CARTESIAN_POINT ( 'NONE',  ( 3.361561038594015116, -2.729792928343269587, 31.24908615093345077 ) ) ;
#65292 = DIRECTION ( 'NONE',  ( -1.000000000000000000, -0.000000000000000000, -0.000000000000000000 ) ) ;
#65293 = FACE_OUTER_BOUND ( 'NONE', #4624, .T. ) ;
#65294 = CARTESIAN_POINT ( 'NONE',  ( 10.61538461538449596, -2.892918686052165622, 31.69288490824153470 ) ) ;
#65295 = CARTESIAN_POINT ( 'NONE',  ( -3.230769230769351186, -11.48612834414049644, 32.76840700105863391 ) ) ;
#65296 = CARTESIAN_POINT ( 'NONE',  ( -19.50000000000000000, -3.499999999999999556, 29.75000000000000355 ) ) ;
#65297 = EDGE_CURVE ( 'NONE', #76436, #25676, #63546, .T. ) ;
#65298 = CARTESIAN_POINT ( 'NONE',  ( -1.614399933863613468, -11.22469193450124969, 18.86124329374151287 ) ) ;
#65299 = ORIENTED_EDGE ( 'NONE', *, *, #3736, .T. ) ;
#65300 = FACE_OUTER_BOUND ( 'NONE', #20717, .T. ) ;
#65301 = CARTESIAN_POINT ( 'NONE',  ( -12.71153846153846168, -7.500000000000001776, 34.75000000000000000 ) ) ;
#65302 = CARTESIAN_POINT ( 'NONE',  ( 20.00000000000000000, -11.50000000000000000, 28.25000000000000000 ) ) ;
#65303 = CARTESIAN_POINT ( 'NONE',  ( 1.139087296526029469, -10.24999999999999467, 25.95312500000000000 ) ) ;
#65304 = CARTESIAN_POINT ( 'NONE',  ( -15.93106648486808119, -11.60474049983370648, 33.02348890104160262 ) ) ;
#65305 = CARTESIAN_POINT ( 'NONE',  ( 2.307692307692309264, -11.91647553114624181, 32.58852847137148245 ) ) ;
#65306 = ADVANCED_FACE ( 'NONE', ( #83845 ), #85600, .F. ) ;
#65307 = ORIENTED_EDGE ( 'NONE', *, *, #27918, .F. ) ;
#65308 = CARTESIAN_POINT ( 'NONE',  ( 2.749999999999995115, -6.360912703473971419, 20.64062500000000000 ) ) ;
#65309 = CARTESIAN_POINT ( 'NONE',  ( -15.23076923076922995, -3.937682226553329556, 33.60647404775216529 ) ) ;
#65310 = B_SPLINE_CURVE_WITH_KNOTS ( 'NONE', 3,
 ( #16954, #77764, #15631, #43975, #57048, #3432, #10204, #65126, #51152, #83662 ),
 .UNSPECIFIED., .F., .F.,
 ( 4, 2, 2, 2, 4 ),
 ( 0.0007817359430256322827, 0.0009771253907249989254, 0.001172514838424365676, 0.001367904286123732428, 0.001563293733823098962 ),
 .UNSPECIFIED. ) ;
#65311 = ORIENTED_EDGE ( 'NONE', *, *, #31104, .F. ) ;
#65312 = VECTOR ( 'NONE', #60612, 999.9999999999998863 ) ;
#65313 = DIRECTION ( 'NONE',  ( 0.000000000000000000, 0.9848077530122072432, 0.1736481776669354937 ) ) ;
#65314 = ORIENTED_EDGE ( 'NONE', *, *, #23798, .T. ) ;
#65315 = LINE ( 'NONE', #84728, #80901 ) ;
#65316 = CARTESIAN_POINT ( 'NONE',  ( -1.634592128663974187, -12.01397095200673881, 32.43157075238190146 ) ) ;
#65317 = CARTESIAN_POINT ( 'NONE',  ( -1.607541602131530745, -4.186968288167446595, 33.49512374952580274 ) ) ;
#65318 = ORIENTED_EDGE ( 'NONE', *, *, #46259, .T. ) ;
#65319 = CARTESIAN_POINT ( 'NONE',  ( -10.61538461538461320, -12.37446782046654192, 30.86335684631486131 ) ) ;
#65320 = ORIENTED_EDGE ( 'NONE', *, *, #3770, .F. ) ;
#65321 = CARTESIAN_POINT ( 'NONE',  ( -18.00000000000000000, -12.10708131394839349, 31.69288490824020244 ) ) ;
#65322 = EDGE_CURVE ( 'NONE', #66893, #67169, #42848, .T. ) ;
#65323 = ORIENTED_EDGE ( 'NONE', *, *, #19505, .F. ) ;
#65324 = FACE_OUTER_BOUND ( 'NONE', #43408, .T. ) ;
#65325 = CARTESIAN_POINT ( 'NONE',  ( 0.4615384615384611200, -11.16473453929635440, 33.15142922261926373 ) ) ;
#65326 = VERTEX_POINT ( 'NONE', #49598 ) ;
#65327 = CARTESIAN_POINT ( 'NONE',  ( -5.869474298236436738, -11.46989282347013095, 32.79007818306219946 ) ) ;
#65328 = CARTESIAN_POINT ( 'NONE',  ( -24.00000000000000000, 0.000000000000000000, 0.000000000000000000 ) ) ;
#65329 = CARTESIAN_POINT ( 'NONE',  ( 0.3313912521002408407, -4.460286881179643892, 33.72017969459903952 ) ) ;
#65330 = ADVANCED_FACE ( 'NONE', ( #8624 ), #28900, .F. ) ;
#65331 = DIRECTION ( 'NONE',  ( 0.000000000000000000, 0.000000000000000000, 1.000000000000000000 ) ) ;
#65332 = CARTESIAN_POINT ( 'NONE',  ( -7.976844449264153702, -12.62707690430377383, 30.88035979386743435 ) ) ;
#65333 = ORIENTED_EDGE ( 'NONE', *, *, #52743, .T. ) ;
#65335 = EDGE_CURVE ( 'NONE', #23814, #50087, #36955, .T. ) ;
#65334 = ORIENTED_EDGE ( 'NONE', *, *, #39444, .T. ) ;
#65336 = ORIENTED_EDGE ( 'NONE', *, *, #75899, .F. ) ;
#65338 = VERTEX_POINT ( 'NONE', #71626 ) ;
#65337 = CARTESIAN_POINT ( 'NONE',  ( 3.007284306204901281, -5.827078755546623690, 34.72654668319379567 ) ) ;
#65339 =( REPRESENTATION_RELATIONSHIP ('NONE','NONE', #51743, #45449 ) REPRESENTATION_RELATIONSHIP_WITH_TRANSFORMATION ( #7692 )SHAPE_REPRESENTATION_RELATIONSHIP( ) );
#65340 = AXIS2_PLACEMENT_3D ( 'NONE', #29241, #77413, #36433 ) ;
#65341 = VECTOR ( 'NONE', #72708, 1000.000000000000000 ) ;
#65342 = B_SPLINE_CURVE_WITH_KNOTS ( 'NONE', 3,
 ( #21542, #14344, #54893, #62087, #49016, #22431, #76495, #21090, #14800, #70175 ),
 .UNSPECIFIED., .F., .F.,
 ( 4, 2, 2, 2, 4 ),
 ( 0.0007817246256747473893, 0.0009771112852218905021, 0.001172497944769033615, 0.001367884604316176944, 0.001563271263863320057 ),
 .UNSPECIFIED. ) ;
#65343 = CARTESIAN_POINT ( 'NONE',  ( 8.769230769230768274, -13.20930481340135110, 34.54067556320372745 ) ) ;
#65344 = CYLINDRICAL_SURFACE ( 'NONE', #75515, 0.2500000000000009437 ) ;
#65345 = VERTEX_POINT ( 'NONE', #77509 ) ;
#65346 = EDGE_CURVE ( 'NONE', #64886, #63896, #1884, .T. ) ;
#65347 = ORIENTED_EDGE ( 'NONE', *, *, #49318, .T. ) ;
#65348 = EDGE_CURVE ( 'NONE', #64427, #83601, #31890, .T. ) ;
#65349 = ORIENTED_EDGE ( 'NONE', *, *, #19806, .T. ) ;
#65350 = CARTESIAN_POINT ( 'NONE',  ( 15.23076923076923173, -10.51840700105979565, 33.73612834413961536 ) ) ;
#65351 = VERTEX_POINT ( 'NONE', #84731 ) ;
#65352 = DIRECTION ( 'NONE',  ( 0.000000000000000000, 0.9396926207859126468, -0.3420201433256571111 ) ) ;
#65353 = ADVANCED_FACE ( 'NONE', ( #50033 ), #15821, .T. ) ;
#65354 = CARTESIAN_POINT ( 'NONE',  ( 17.07692307692307665, -2.833524468853757305, 32.15551576947925838 ) ) ;
#65355 = CARTESIAN_POINT ( 'NONE',  ( 0.2115152242454959031, -5.056417327199099532, 34.11270091957321426 ) ) ;
#65356 = B_SPLINE_CURVE_WITH_KNOTS ( 'NONE', 3,
 ( #68651, #6074, #40308, #41628, #76291, #33095, #40750, #88507, #88076, #67333 ),
 .UNSPECIFIED., .F., .F.,
 ( 4, 2, 2, 2, 4 ),
 ( 0.0007817246256747448956, 0.0009771112852218876831, 0.001172497944769030579, 0.001367884604316173475, 0.001563271263863316371 ),
 .UNSPECIFIED. ) ;
#65357 = FACE_BOUND ( 'NONE', #19033, .T. ) ;
#65358 = ORIENTED_EDGE ( 'NONE', *, *, #17708, .F. ) ;
#65359 = CARTESIAN_POINT ( 'NONE',  ( -8.102564102564102200, -11.00000000000000000, 29.75000000000000355 ) ) ;
#65360 = CARTESIAN_POINT ( 'NONE',  ( 13.60762673622823726, -9.086983370893049639, 34.49168942202179267 ) ) ;
#65361 = DIRECTION ( 'NONE',  ( 0.000000000000000000, 0.9848077530122072432, -0.1736481776669354937 ) ) ;
#65362 = CARTESIAN_POINT ( 'NONE',  ( -13.38461538461538325, -2.721908614388771852, 31.22303859784724978 ) ) ;
#65363 = DIRECTION ( 'NONE',  ( 1.000000000000000000, 2.559449574374558716E-16, -5.118899148749117234E-15 ) ) ;
#65364 = ORIENTED_EDGE ( 'NONE', *, *, #9294, .T. ) ;
#65365 = DIRECTION ( 'NONE',  ( -1.000000000000000000, -0.000000000000000000, 0.000000000000000000 ) ) ;
#65366 = ORIENTED_EDGE ( 'NONE', *, *, #33984, .F. ) ;
#65367 = ORIENTED_EDGE ( 'NONE', *, *, #77275, .T. ) ;
#65369 = CARTESIAN_POINT ( 'NONE',  ( -1.384615384615506484, -5.941354392335915335, 34.76329471203413846 ) ) ;
#65368 = CARTESIAN_POINT ( 'NONE',  ( -0.7115151924808159611, -9.148715823498378086, 34.47080413974185120 ) ) ;
#65370 = DIRECTION ( 'NONE',  ( -0.000000000000000000, -0.1736481776669307198, -0.9848077530122080203 ) ) ;
#65371 = DIRECTION ( 'NONE',  ( -5.471219261342662483E-14, -1.000000000000000000, 0.000000000000000000 ) ) ;
#65372 = DIRECTION ( 'NONE',  ( -0.000000000000000000, -0.9848077530122086864, -0.1736481776669273613 ) ) ;
#65373 = CARTESIAN_POINT ( 'NONE',  ( -12.21148414990014963, -4.235687564193447052, 33.53795663066793509 ) ) ;
#65374 = ORIENTED_EDGE ( 'NONE', *, *, #70616, .T. ) ;
#65375 = CARTESIAN_POINT ( 'NONE',  ( 6.673053698855461846, -2.588893531581426544, 31.60682220781847818 ) ) ;
#65376 = CARTESIAN_POINT ( 'NONE',  ( -0.3307480205715102595, -3.338503747796865095, 32.95102852606552801 ) ) ;
#65377 = CARTESIAN_POINT ( 'NONE',  ( -16.81410256410256565, -7.500000000000000000, 29.75000000000000355 ) ) ;
#65378 = CARTESIAN_POINT ( 'NONE',  ( -4.087777802843714170, -3.513871655860379306, 32.76840700105978499 ) ) ;
#65379 = B_SPLINE_CURVE_WITH_KNOTS ( 'NONE', 3,
 ( #24410, #44225, #44674, #51874, #17675, #71712, #9574, #30729, #37037, #10017 ),
 .UNSPECIFIED., .F., .F.,
 ( 4, 2, 2, 2, 4 ),
 ( 0.000000000000000000, 0.0001954311564186862510, 0.0003908623128373725020, 0.0005862934692560588072, 0.0007817246256747450040 ),
 .UNSPECIFIED. ) ;
#65380 = VERTEX_POINT ( 'NONE', #57242 ) ;
#65381 = B_SPLINE_CURVE_WITH_KNOTS ( 'NONE', 3,
 ( #43825, #77618, #77175, #15484, #64974, #57344, #16360, #37961, #70425, #50134 ),
 .UNSPECIFIED., .F., .F.,
 ( 4, 2, 2, 2, 4 ),
 ( 0.000000000000000000, 0.0001954339857564097241, 0.0003908679715128194482, 0.0005863019572692291723, 0.0007817359430256388964 ),
 .UNSPECIFIED. ) ;
#65382 = ORIENTED_EDGE ( 'NONE', *, *, #65852, .F. ) ;
#65383 = FACE_BOUND ( 'NONE', #26135, .T. ) ;
#65384 = ORIENTED_EDGE ( 'NONE', *, *, #25664, .T. ) ;
#65385 = CARTESIAN_POINT ( 'NONE',  ( -17.87165453592967879, -2.254606617072892671, 29.97517285561840339 ) ) ;
#65386 = CARTESIAN_POINT ( 'NONE',  ( -1.319360245102545681, -2.379036618887895305, 30.90682066428159303 ) ) ;
#65387 = ORIENTED_EDGE ( 'NONE', *, *, #72458, .F. ) ;
#65388 = CARTESIAN_POINT ( 'NONE',  ( -3.453695448285377445, -12.39988816332205701, 30.74660775122750778 ) ) ;
#65389 = CARTESIAN_POINT ( 'NONE',  ( 15.23076923076910916, -3.083524468854526912, 32.58852847137268327 ) ) ;
#65390 = CARTESIAN_POINT ( 'NONE',  ( 15.90386942290380290, -8.303909089506435137, 34.68538101551103381 ) ) ;
#65391 = CARTESIAN_POINT ( 'NONE',  ( 4.376625822824220080, -6.717445702608402236, 34.94155399931962336 ) ) ;
#65392 = VERTEX_POINT ( 'NONE', #50467 ) ;
#65393 = CARTESIAN_POINT ( 'NONE',  ( -3.903900635498010807, -6.696923467548660192, 34.68552623307873972 ) ) ;
#65394 = ORIENTED_EDGE ( 'NONE', *, *, #57592, .T. ) ;
#65395 = EDGE_CURVE ( 'NONE', #10508, #6055, #9397, .T. ) ;
#65397 = ORIENTED_EDGE ( 'NONE', *, *, #46940, .T. ) ;
#65396 = CYLINDRICAL_SURFACE ( 'NONE', #58290, 5.000000000000000888 ) ;
#65398 = CARTESIAN_POINT ( 'NONE',  ( -8.769230769230768274, -9.780366693483667717, 34.19971097300155094 ) ) ;
#65399 = CARTESIAN_POINT ( 'NONE',  ( -12.52680846209478460, -3.083524468853724443, 32.58852847137143272 ) ) ;
#65400 = CYLINDRICAL_SURFACE ( 'NONE', #55906, 0.2500000000000002220 ) ;
#65401 = CARTESIAN_POINT ( 'NONE',  ( 10.54930223602447903, -12.34228464037088280, 31.77849191805838558 ) ) ;
#65402 = CARTESIAN_POINT ( 'NONE',  ( -19.50000000000000000, -3.499999999999999556, 29.75000000000000355 ) ) ;
#65403 = CARTESIAN_POINT ( 'NONE',  ( 4.153846153846154188, -9.584722331328613620, 36.20867863119891439 ) ) ;
#65404 = ADVANCED_FACE ( 'NONE', ( #38747 ), #18481, .F. ) ;
#65405 = CARTESIAN_POINT ( 'NONE',  ( -1.901340078031369618, -5.512252781505359245, 14.25186829374151465 ) ) ;
#65406 = ORIENTED_EDGE ( 'NONE', *, *, #38853, .T. ) ;
#65407 = DIRECTION ( 'NONE',  ( -0.000000000000000000, 0.9396926207859092051, -0.3420201433256662704 ) ) ;
#65408 = CARTESIAN_POINT ( 'NONE',  ( -18.00000000000000000, -6.190371309867714444, 35.73758076001107042 ) ) ;
#65409 = CARTESIAN_POINT ( 'NONE',  ( -19.00000000000000000, 8.999999999999996447, 23.75000000000000000 ) ) ;
#65410 = VECTOR ( 'NONE', #71250, 1000.000000000000000 ) ;
#65411 = B_SPLINE_CURVE_WITH_KNOTS ( 'NONE', 3,
 ( #40577, #68045, #81562, #11767, #59500, #47312, #46431, #74805, #73915, #13095 ),
 .UNSPECIFIED., .F., .F.,
 ( 4, 2, 2, 2, 4 ),
 ( 0.0007817359430256313069, 0.0009771253907249971907, 0.001172514838424363074, 0.001367904286123728958, 0.001563293733823094842 ),
 .UNSPECIFIED. ) ;
#65412 = ORIENTED_EDGE ( 'NONE', *, *, #84715, .T. ) ;
#65413 = ORIENTED_EDGE ( 'NONE', *, *, #39982, .T. ) ;
#65414 = CARTESIAN_POINT ( 'NONE',  ( -1.607480806819022945, -2.501496062324912284, 29.88072118266895671 ) ) ;
#65415 = CARTESIAN_POINT ( 'NONE',  ( 11.53846153846141576, -5.094484230521993062, 34.41647553114689373 ) ) ;
#65416 = CARTESIAN_POINT ( 'NONE',  ( 17.29970274590113632, -3.563462043263029955, 33.22394488606062879 ) ) ;
#65417 = B_SPLINE_CURVE_WITH_KNOTS ( 'NONE', 3,
 ( #11084, #79987, #32250, #75769, #80443, #45754 ),
 .UNSPECIFIED., .F., .F.,
 ( 4, 2, 4 ),
 ( 0.0003909569690057805385, 0.0005862646681846044039, 0.0007815723673634283235 ),
 .UNSPECIFIED. ) ;
#65418 = CARTESIAN_POINT ( 'NONE',  ( 10.61538461538461675, -3.886160181151819604, 36.00935417666054406 ) ) ;
#65419 = CARTESIAN_POINT ( 'NONE',  ( 15.93036122928182330, -10.23692288466677880, 34.23039457007281072 ) ) ;
#65420 = EDGE_CURVE ( 'NONE', #8287, #26079, #39202, .T. ) ;
#65421 = B_SPLINE_CURVE_WITH_KNOTS ( 'NONE', 3,
 ( #54623, #40692, #6458, #33918, #47878, #27163, #82119, #75359, #13649, #29831 ),
 .UNSPECIFIED., .F., .F.,
 ( 4, 2, 2, 2, 4 ),
 ( 0.000000000000000000, 0.0001954339857564054957, 0.0003908679715128109914, 0.0005863019572692164871, 0.0007817359430256219828 ),
 .UNSPECIFIED. ) ;
#65422 = CARTESIAN_POINT ( 'NONE',  ( -16.85414340794500276, -11.60474049983370648, 33.02348890104160262 ) ) ;
#65423 = CARTESIAN_POINT ( 'NONE',  ( -7.146561866800870355, -11.89387501736622710, 32.13663884655806413 ) ) ;
#65424 = VERTEX_POINT ( 'NONE', #66210 ) ;
#65425 = DIRECTION ( 'NONE',  ( -1.000000000000000000, -0.000000000000000000, 0.000000000000000000 ) ) ;
#65426 = CARTESIAN_POINT ( 'NONE',  ( -0.2115929431903199320, -8.433404298154338008, 34.66254593164986630 ) ) ;
#65427 = CARTESIAN_POINT ( 'NONE',  ( 7.053867364043874488, -6.369690395747422684, 34.87708834333098196 ) ) ;
#65428 = FACE_OUTER_BOUND ( 'NONE', #25249, .T. ) ;
#65429 = VERTEX_POINT ( 'NONE', #32435 ) ;
#65430 = CARTESIAN_POINT ( 'NONE',  ( 12.33139049180676139, -2.647304123082328875, 31.75400227202885972 ) ) ;
#65431 = EDGE_CURVE ( 'NONE', #64420, #47909, #10512, .T. ) ;
#65432 = EDGE_LOOP ( 'NONE', ( #82867, #16840 ) ) ;
#65433 = CARTESIAN_POINT ( 'NONE',  ( 9.019285189144218506, -2.920487667080175598, 32.31805714834170828 ) ) ;
#65434 =( NAMED_UNIT ( * ) PLANE_ANGLE_UNIT ( ) SI_UNIT ( $, .RADIAN. ) );
#65435 = CARTESIAN_POINT ( 'NONE',  ( -13.16118898570059947, -7.630147987733840509, 34.99859428049665411 ) ) ;
#65436 = DIRECTION ( 'NONE',  ( -0.000000000000000000, -0.9396926207859093161, -0.3420201433256663259 ) ) ;
#65437 = EDGE_LOOP ( 'NONE', ( #13250, #61588, #58172, #78488 ) ) ;
#65438 = ADVANCED_FACE ( 'NONE', ( #18922 ), #45494, .F. ) ;
#65439 = CARTESIAN_POINT ( 'NONE',  ( -1.384615384615383471, -12.62096338111211580, 30.90682066428153263 ) ) ;
#65440 = DIRECTION ( 'NONE',  ( -0.000000000000000000, -0.9848077530122085754, -0.1736481776669273613 ) ) ;
#65441 = AXIS2_PLACEMENT_3D ( 'NONE', #64785, #3090, #10305 ) ;
#65442 = CARTESIAN_POINT ( 'NONE',  ( 9.019230769230704325, -7.565270445406050648, 34.75000000000000000 ) ) ;
#65443 = CARTESIAN_POINT ( 'NONE',  ( -19.50000000000000000, -11.50000000000000000, 29.75000000000000355 ) ) ;
#65444 = EDGE_CURVE ( 'NONE', #27705, #56750, #62024, .T. ) ;
#65445 = EDGE_LOOP ( 'NONE', ( #4148, #81539, #85085, #1579 ) ) ;
#65446 = CARTESIAN_POINT ( 'NONE',  ( -0.5922299282060203840, -8.147922237126337563, 34.70805685702651999 ) ) ;
#65447 = EDGE_LOOP ( 'NONE', ( #74562, #19943, #29413, #3947 ) ) ;
#65448 = CARTESIAN_POINT ( 'NONE',  ( 2.307692307692186251, -12.70778746994576025, 30.41441678777401236 ) ) ;
#65449 = CARTESIAN_POINT ( 'NONE',  ( -9.442362173959551797, -12.22109172314383052, 31.39792113162168263 ) ) ;
#65450 = CARTESIAN_POINT ( 'NONE',  ( -13.51476259405360558, -2.882441371585227508, 31.66841991370172238 ) ) ;
#65451 = CARTESIAN_POINT ( 'NONE',  ( 7.780071466793708979, -12.34228464037088280, 31.77849191805838558 ) ) ;
#65452 = LINE ( 'NONE', #24909, #75297 ) ;
#65453 = CARTESIAN_POINT ( 'NONE',  ( 16.15384615384615330, -11.91647553114624181, 32.58852847137148245 ) ) ;
#65454 = EDGE_CURVE ( 'NONE', #32893, #13118, #17132, .T. ) ;
#65455 = EDGE_LOOP ( 'NONE', ( #15122, #47696 ) ) ;
#65456 = ORIENTED_EDGE ( 'NONE', *, *, #7387, .T. ) ;
#65457 = ORIENTED_EDGE ( 'NONE', *, *, #72789, .F. ) ;
#65458 = EDGE_CURVE ( 'NONE', #27369, #75057, #63132, .T. ) ;
#65460 = VERTEX_POINT ( 'NONE', #72522 ) ;
#65459 = EDGE_CURVE ( 'NONE', #79307, #36536, #79292, .T. ) ;
#65461 = ORIENTED_EDGE ( 'NONE', *, *, #39912, .F. ) ;
#65462 = VECTOR ( 'NONE', #85552, 1000.000000000000000 ) ;
#65463 = CARTESIAN_POINT ( 'NONE',  ( -10.61538461538473399, -8.613356846316285953, 34.62446782046622218 ) ) ;
#65464 = CARTESIAN_POINT ( 'NONE',  ( -3.453696189676077832, -6.459968553980839800, 34.89616026154728701 ) ) ;
#65465 = CARTESIAN_POINT ( 'NONE',  ( -4.153846153846152411, -6.343179335718451384, 34.87096338111211935 ) ) ;
#65466 = EDGE_CURVE ( 'NONE', #27738, #39506, #49106, .T. ) ;
#65467 = CARTESIAN_POINT ( 'NONE',  ( -6.000000000000119904, -5.219633306517616589, 34.19971097300220464 ) ) ;
#65468 = CARTESIAN_POINT ( 'NONE',  ( 7.780883845597526438, -12.70778746994557551, 30.41441678777548319 ) ) ;
#65469 = CARTESIAN_POINT ( 'NONE',  ( -16.09615384615384670, -3.499999999999999556, 29.75000000000000355 ) ) ;
#65470 = DIRECTION ( 'NONE',  ( 0.000000000000000000, 0.3420201433256610524, 0.9396926207859113145 ) ) ;
#65471 = CARTESIAN_POINT ( 'NONE',  ( -17.86920819217521483, -6.413143153341454017, 34.63066358083362672 ) ) ;
#65472 = CARTESIAN_POINT ( 'NONE',  ( -4.219929564802034072, -9.780366693483667717, 34.19971097300155805 ) ) ;
#65473 = VERTEX_POINT ( 'NONE', #43993 ) ;
#65474 = AXIS2_PLACEMENT_3D ( 'NONE', #62898, #76435, #51478 ) ;
#65475 = EDGE_LOOP ( 'NONE', ( #73666, #49919, #53212, #34375 ) ) ;
#65476 = ORIENTED_EDGE ( 'NONE', *, *, #73728, .F. ) ;
#65478 = VERTEX_POINT ( 'NONE', #70145 ) ;
#65477 = CARTESIAN_POINT ( 'NONE',  ( 0.2115617174898691832, -2.920706130388546651, 32.31842814019191223 ) ) ;
#65480 = CARTESIAN_POINT ( 'NONE',  ( -17.74994558008654622, -11.47946981652013321, 33.17500667209846910 ) ) ;
#65479 = CARTESIAN_POINT ( 'NONE',  ( 3.230769230769231726, -5.415277668671390821, 36.20867863119892149 ) ) ;
#65481 = CARTESIAN_POINT ( 'NONE',  ( -1.514763354347081092, -5.070767119584671967, 34.40440758774516183 ) ) ;
#65482 = CARTESIAN_POINT ( 'NONE',  ( -11.31544869436814338, -9.172514111537584114, 34.72667873470787470 ) ) ;
#65483 = ORIENTED_EDGE ( 'NONE', *, *, #81712, .F. ) ;
#65484 = ORIENTED_EDGE ( 'NONE', *, *, #12855, .T. ) ;
#65485 = CARTESIAN_POINT ( 'NONE',  ( -2.437839517130525824, -12.45813303252208648, 30.39737893381572675 ) ) ;
#65486 = ORIENTED_EDGE ( 'NONE', *, *, #87282, .T. ) ;
#65487 = FACE_BOUND ( 'NONE', #72878, .T. ) ;
#65488 = CARTESIAN_POINT ( 'NONE',  ( 15.23076923076923173, -9.780366693483667717, 34.19971097300155094 ) ) ;
#65489 = CARTESIAN_POINT ( 'NONE',  ( 16.15384615384615330, -6.386643153685126251, 34.62446782046654192 ) ) ;
#65490 = VERTEX_POINT ( 'NONE', #85000 ) ;
#65491 = CARTESIAN_POINT ( 'NONE',  ( 14.05771557674995798, -2.779195860258146578, 31.39871582349836032 ) ) ;
#65492 = CARTESIAN_POINT ( 'NONE',  ( -6.792286482109973988, -2.295524264805589354, 30.44142389570982488 ) ) ;
#65493 = CARTESIAN_POINT ( 'NONE',  ( -9.692307692307691624, -13.49023893513002648, 31.06009739812518688 ) ) ;
#65494 = ORIENTED_EDGE ( 'NONE', *, *, #54246, .F. ) ;
#65495 = CARTESIAN_POINT ( 'NONE',  ( 18.25000000000141753, -7.500000000000154543, 35.00000000000007105 ) ) ;
#65496 = DIRECTION ( 'NONE',  ( -0.000000000000000000, 1.000000000000000000, 3.491481338843133355E-15 ) ) ;
#65497 = ORIENTED_EDGE ( 'NONE', *, *, #51398, .F. ) ;
#65498 = CARTESIAN_POINT ( 'NONE',  ( 3.230769230769110045, -8.613356846316285953, 34.62446782046622218 ) ) ;
#65499 = LINE ( 'NONE', #5141, #45610 ) ;
#65500 = EDGE_LOOP ( 'NONE', ( #33869, #81858, #12941, #88458 ) ) ;
#65501 = CARTESIAN_POINT ( 'NONE',  ( 7.173022332454966232, -2.589246495874657938, 31.60778113518102828 ) ) ;
#65502 = CARTESIAN_POINT ( 'NONE',  ( 13.16168916709923664, -2.554751324335735152, 30.48935550225260727 ) ) ;
#65503 = CARTESIAN_POINT ( 'NONE',  ( -0.3589743589743593088, -7.500000000000000000, 29.75000000000000355 ) ) ;
#65504 = CARTESIAN_POINT ( 'NONE',  ( 7.715677138037380978, -7.276988635370448932, 34.74523720219453793 ) ) ;
#65505 = FACE_OUTER_BOUND ( 'NONE', #30437, .T. ) ;
#65506 = CARTESIAN_POINT ( 'NONE',  ( 6.857806477116148436, -9.442884908240170461, 34.35708131394840592 ) ) ;
#65508 = LINE ( 'NONE', #86702, #5761 ) ;
#65507 = CARTESIAN_POINT ( 'NONE',  ( -8.769230769230455635, -2.255955759149395501, 30.00000000000324363 ) ) ;
#65509 = CARTESIAN_POINT ( 'NONE',  ( 1.384615384615265343, -11.48612834414049644, 32.76840700105863391 ) ) ;
#65511 = CARTESIAN_POINT ( 'NONE',  ( -10.68065506134539078, -8.613356846314824011, 34.62446782046655613 ) ) ;
#65510 = CARTESIAN_POINT ( 'NONE',  ( 3.480769230769230838, -2.499999999999998668, 29.75000000000000355 ) ) ;
#65512 = CARTESIAN_POINT ( 'NONE',  ( -2.749999999999997780, -7.561099074964547917, 26.09188170625848358 ) ) ;
#65513 = ORIENTED_EDGE ( 'NONE', *, *, #87657, .F. ) ;
#65514 = CARTESIAN_POINT ( 'NONE',  ( 17.99999999999987566, -11.94971097300221174, 32.03036669348237098 ) ) ;
#65515 = VERTEX_POINT ( 'NONE', #16090 ) ;
#65516 = B_SPLINE_CURVE_WITH_KNOTS ( 'NONE', 3,
 ( #35067, #48572, #13910, #84162, #49904, #34630, #77383, #54902, #82384, #7606 ),
 .UNSPECIFIED., .F., .F.,
 ( 4, 2, 2, 2, 4 ),
 ( 0.0007817359430256398721, 0.0009771253907250084664, 0.001172514838424377169, 0.001367904286123745872, 0.001563293733823114574 ),
 .UNSPECIFIED. ) ;
#65517 = ORIENTED_EDGE ( 'NONE', *, *, #28306, .F. ) ;
#65518 = CARTESIAN_POINT ( 'NONE',  ( -2.057637996053991447, -12.41262288849542017, 30.68299917996395010 ) ) ;
#65519 = ORIENTED_EDGE ( 'NONE', *, *, #35893, .F. ) ;
#65520 = LINE ( 'NONE', #4268, #39764 ) ;
#65521 = CARTESIAN_POINT ( 'NONE',  ( 2.750000000000008438, -8.639087296525996607, 17.04687500000000000 ) ) ;
#65522 = CARTESIAN_POINT ( 'NONE',  ( -15.23076923076935074, -4.481592998941358097, 33.73612834414048933 ) ) ;
#65523 = CARTESIAN_POINT ( 'NONE',  ( -6.000000000000121680, -11.67786785259630911, 32.92929555188603530 ) ) ;
#65524 = CARTESIAN_POINT ( 'NONE',  ( -5.749945688361683516, -9.148310452688871663, 34.47095581063188519 ) ) ;
#65525 = CARTESIAN_POINT ( 'NONE',  ( -14.37377468705243899, -10.67929555188718460, 33.92786785259543336 ) ) ;
#65526 = CYLINDRICAL_SURFACE ( 'NONE', #67684, 0.2500000000000009437 ) ;
#65527 = CARTESIAN_POINT ( 'NONE',  ( -7.780898274877821486, -2.892918686051624722, 31.69288490824025928 ) ) ;
#65528 = CYLINDRICAL_SURFACE ( 'NONE', #64080, 0.2499999999999995837 ) ;
#65529 = CARTESIAN_POINT ( 'NONE',  ( -3.749999999999988454, -9.053300858899127945, 20.01562500000000355 ) ) ;
#65530 = VECTOR ( 'NONE', #73000, 1000.000000000000227 ) ;
#65531 = DIRECTION ( 'NONE',  ( -0.000000000000000000, 1.000000000000000000, 3.491481338843133355E-15 ) ) ;
#65532 = CARTESIAN_POINT ( 'NONE',  ( 13.25392478150507891, -3.338472653186243644, 32.95098750199972670 ) ) ;
#65533 = CARTESIAN_POINT ( 'NONE',  ( 14.37294787896833270, -3.300289026998473041, 32.46337939537591666 ) ) ;
#65534 = EDGE_CURVE ( 'NONE', #5535, #57873, #88856, .T. ) ;
#65535 = ORIENTED_EDGE ( 'NONE', *, *, #442, .T. ) ;
#65536 = ORIENTED_EDGE ( 'NONE', *, *, #80652, .F. ) ;
#65537 = CARTESIAN_POINT ( 'NONE',  ( 0.4615384615384611200, -6.435427911321262684, 35.78748833219616898 ) ) ;
#65538 = CARTESIAN_POINT ( 'NONE',  ( 7.780070435197966816, -11.16473453929635440, 33.15142922261925662 ) ) ;
#65539 = CARTESIAN_POINT ( 'NONE',  ( 20.00000000000000000, -4.000000000000000000, 29.75000000000000355 ) ) ;
#65540 = CARTESIAN_POINT ( 'NONE',  ( 0.3589743589743582541, -11.00000000000000000, 29.75000000000000355 ) ) ;
#65541 = CARTESIAN_POINT ( 'NONE',  ( 14.17700170458200404, -3.338472653186243644, 32.95098750199972670 ) ) ;
#65542 = DIRECTION ( 'NONE',  ( 0.000000000000000000, 0.1736481776669267785, -0.9848077530122087975 ) ) ;
#65543 = ADVANCED_FACE ( 'NONE', ( #8457 ), #79123, .T. ) ;
#65544 = EDGE_LOOP ( 'NONE', ( #53047, #21012, #8082, #77461 ) ) ;
#65545 = CARTESIAN_POINT ( 'NONE',  ( -1.134669866267242755, -10.05730279482229683, 34.04704008940765902 ) ) ;
#65546 = ORIENTED_EDGE ( 'NONE', *, *, #36721, .F. ) ;
#65547 = ORIENTED_EDGE ( 'NONE', *, *, #13104, .T. ) ;
#65548 = CARTESIAN_POINT ( 'NONE',  ( 7.622668921589514035, -10.97335522853832579, 33.68706563782419749 ) ) ;
#65549 = CARTESIAN_POINT ( 'NONE',  ( -6.673022503163469565, -5.642605341092957083, 34.66089969410670335 ) ) ;
#65550 = CARTESIAN_POINT ( 'NONE',  ( -9.442253380669381357, -6.567000820036036579, 34.66262288849541306 ) ) ;
#65551 = CARTESIAN_POINT ( 'NONE',  ( -6.222926217516147496, -3.105860786376062332, 32.13614157043599562 ) ) ;
#65552 = CARTESIAN_POINT ( 'NONE',  ( -13.13466986626724164, -3.202959910592335646, 32.30730279482227019 ) ) ;
#65553 = AXIS2_PLACEMENT_3D ( 'NONE', #4954, #86950, #32419 ) ;
#65554 = EDGE_LOOP ( 'NONE', ( #57971, #68227, #14773, #67352 ) ) ;
#65555 = EDGE_LOOP ( 'NONE', ( #27516, #76860, #40927, #12969, #69541 ) ) ;
#65556 = EDGE_CURVE ( 'NONE', #53195, #82297, #63383, .T. ) ;
#65557 = EDGE_CURVE ( 'NONE', #67458, #2192, #81020, .T. ) ;
#65558 = ORIENTED_EDGE ( 'NONE', *, *, #82910, .T. ) ;
#65559 = CARTESIAN_POINT ( 'NONE',  ( 13.13459216039393240, -4.931416488878822335, 34.32920672191015399 ) ) ;
#65560 = CARTESIAN_POINT ( 'NONE',  ( -16.15384615384627409, -9.528491918059723176, 34.59228464037033035 ) ) ;
#65561 = CARTESIAN_POINT ( 'NONE',  ( 9.692307692307695177, -11.16473453929635440, 33.15142922261926373 ) ) ;
#65562 = CARTESIAN_POINT ( 'NONE',  ( -8.703975629717932705, -10.33852847137154107, 34.16647553114620450 ) ) ;
#65563 = LINE ( 'NONE', #72326, #39331 ) ;
#65564 = CARTESIAN_POINT ( 'NONE',  ( 17.74997676270703550, -8.432397168068783699, 34.66272746175022945 ) ) ;
#65565 = ORIENTED_EDGE ( 'NONE', *, *, #25917, .F. ) ;
#65566 = EDGE_CURVE ( 'NONE', #88377, #20922, #53402, .T. ) ;
#65567 = ORIENTED_EDGE ( 'NONE', *, *, #70060, .T. ) ;
#65568 = CARTESIAN_POINT ( 'NONE',  ( -1.553300858899125059, -3.750000000000009326, 20.32812500000000000 ) ) ;
#65569 = ORIENTED_EDGE ( 'NONE', *, *, #78241, .F. ) ;
#65571 = ORIENTED_EDGE ( 'NONE', *, *, #15634, .T. ) ;
#65570 = CARTESIAN_POINT ( 'NONE',  ( 15.36156103859402222, -5.582136614379148654, 34.36778462344220486 ) ) ;
#65572 = CARTESIAN_POINT ( 'NONE',  ( -10.61538461538473577, -4.320704448113951379, 33.92786785259630022 ) ) ;
#65573 = DIRECTION ( 'NONE',  ( -0.000000000000000000, -0.3420201433256694346, -0.9396926207859080948 ) ) ;
#65574 = VECTOR ( 'NONE', #25067, 1000.000000000000000 ) ;
#65575 = CARTESIAN_POINT ( 'NONE',  ( 1.553300858899129722, -11.24999999999999112, 15.95312499999999822 ) ) ;
#65576 = VERTEX_POINT ( 'NONE', #77347 ) ;
#65577 = CARTESIAN_POINT ( 'NONE',  ( 10.83816428436268176, -2.353885683473779800, 30.79025554430704403 ) ) ;
#65578 = EDGE_LOOP ( 'NONE', ( #30407, #62243 ) ) ;
#65579 = DIRECTION ( 'NONE',  ( -0.000000000000000000, 0.9848077530122086864, -0.1736481776669273891 ) ) ;
#65580 = DIRECTION ( 'NONE',  ( -0.000000000000000000, 0.9848077530122086864, -0.1736481776669273891 ) ) ;
#65581 = FACE_BOUND ( 'NONE', #77743, .T. ) ;
#65583 = CARTESIAN_POINT ( 'NONE',  ( 8.068933515131908152, -2.353885683473779800, 30.79025554430704403 ) ) ;
#65582 = CARTESIAN_POINT ( 'NONE',  ( 5.869852030268303267, -12.50552854090298993, 31.33409797877408920 ) ) ;
#65584 = CARTESIAN_POINT ( 'NONE',  ( -3.230769230769229949, -3.322132147404559976, 32.92929555188717927 ) ) ;
#65585 = CARTESIAN_POINT ( 'NONE',  ( -3.454254155333561283, -8.539481045369598178, 34.89627647299170832 ) ) ;
#65586 = ORIENTED_EDGE ( 'NONE', *, *, #74511, .F. ) ;
#65587 = CARTESIAN_POINT ( 'NONE',  ( 11.28843831424007860, -11.56360843649121861, 33.07473185843129926 ) ) ;
#65588 = AXIS2_PLACEMENT_3D ( 'NONE', #57694, #14492, #85176 ) ;
#65589 = SURFACE_SIDE_STYLE ('',( #38130 ) ) ;
#65590 = VERTEX_POINT ( 'NONE', #30485 ) ;
#65591 = CARTESIAN_POINT ( 'NONE',  ( -12.46153846153846168, -9.780366693483667717, 34.19971097300155094 ) ) ;
#65592 = CARTESIAN_POINT ( 'NONE',  ( 12.46153846153876898, -2.506253911140615021, 30.00000000000323297 ) ) ;
#65593 = FACE_OUTER_BOUND ( 'NONE', #3447, .T. ) ;
#65594 = CARTESIAN_POINT ( 'NONE',  ( 11.31497659473759043, -5.912607949931405926, 34.49155766932282319 ) ) ;
#65595 = CYLINDRICAL_SURFACE ( 'NONE', #51553, 0.2500000000000009437 ) ;
#65596 = FACE_BOUND ( 'NONE', #15022, .T. ) ;
#65598 = CARTESIAN_POINT ( 'NONE',  ( -10.54921800879297322, -7.250054591869670162, 34.99404684341514127 ) ) ;
#65597 = CARTESIAN_POINT ( 'NONE',  ( 18.00000000000000000, -12.37446782046654192, 30.86335684631486131 ) ) ;
#65599 = CARTESIAN_POINT ( 'NONE',  ( -18.13014796973169851, -8.630895178749536711, 34.87696386517710323 ) ) ;
#65601 = CARTESIAN_POINT ( 'NONE',  ( 0.7115928814519136836, -2.920487667080175154, 32.31805714834170828 ) ) ;
#65600 = CARTESIAN_POINT ( 'NONE',  ( 18.22301135161285046, -11.24521262558773493, 33.06293181088029343 ) ) ;
#65602 = CARTESIAN_POINT ( 'NONE',  ( 0.4615384615387678746, -2.506253911140615021, 30.00000000000323297 ) ) ;
#65603 = FACE_OUTER_BOUND ( 'NONE', #39694, .T. ) ;
#65604 = CARTESIAN_POINT ( 'NONE',  ( 3.749999999999999556, -7.438900925035446754, 24.21688170625849068 ) ) ;
#65605 = ORIENTED_EDGE ( 'NONE', *, *, #43118, .T. ) ;
#65606 = DIRECTION ( 'NONE',  ( -0.000000000000000000, -0.6427876096865404731, -0.7660444431189770143 ) ) ;
#65607 = AXIS2_PLACEMENT_3D ( 'NONE', #3938, #30096, #57559 ) ;
#65608 = CARTESIAN_POINT ( 'NONE',  ( 8.096099255531889582, -10.18230066228896114, 34.26354781536631577 ) ) ;
#65609 = CARTESIAN_POINT ( 'NONE',  ( -2.307692307692305711, -3.886160181151819604, 36.00935417666054406 ) ) ;
#65610 = CARTESIAN_POINT ( 'NONE',  ( -9.942330929600657896, -10.76384336483936011, 33.53834819971076087 ) ) ;
#65611 = DIRECTION ( 'NONE',  ( 1.000000000000000000, 0.000000000000000000, 0.000000000000000000 ) ) ;
#65612 = CYLINDRICAL_SURFACE ( 'NONE', #72853, 2.000000000000001776 ) ;
#65613 = CARTESIAN_POINT ( 'NONE',  ( -0.06109907496454585613, -4.750000000000000000, 15.15438170625848890 ) ) ;
#65614 = EDGE_CURVE ( 'NONE', #81377, #46553, #57957, .T. ) ;
#65615 = CARTESIAN_POINT ( 'NONE',  ( -1.515090569691102562, -7.276987145209184327, 34.99546412871779211 ) ) ;
#65616 = CARTESIAN_POINT ( 'NONE',  ( 0.5920641633020268246, -3.816742781228458448, 33.13167719472716044 ) ) ;
#65617 = CARTESIAN_POINT ( 'NONE',  ( 11.40785188325745558, -7.722926974430166069, 34.99546784045485737 ) ) ;
#65618 = CARTESIAN_POINT ( 'NONE',  ( 5.076923076923075762, -12.62096338111211580, 30.90682066428153263 ) ) ;
#65619 = CARTESIAN_POINT ( 'NONE',  ( 8.546304551714619890, -9.886141570436013382, 34.14413921362392301 ) ) ;
#65620 = CARTESIAN_POINT ( 'NONE',  ( 4.153846153846154188, -10.51840700105979565, 33.73612834413961536 ) ) ;
#65621 = DIRECTION ( 'NONE',  ( -0.000000000000000000, 0.6427876096865404731, -0.7660444431189770143 ) ) ;
#65622 = CARTESIAN_POINT ( 'NONE',  ( 7.912221179503920787, -9.058645607665452459, 34.76329471203371924 ) ) ;
#65623 = ORIENTED_EDGE ( 'NONE', *, *, #77415, .T. ) ;
#65624 = CARTESIAN_POINT ( 'NONE',  ( 3.453548899747294953, -12.47679350104403007, 31.42216943046555855 ) ) ;
#65625 = CARTESIAN_POINT ( 'NONE',  ( 14.30769230769218758, -6.026961402154118019, 34.52809138561165270 ) ) ;
#65626 = CARTESIAN_POINT ( 'NONE',  ( -2.749999999999999112, -7.438900925035484057, 24.09561829374151287 ) ) ;
#65627 = ADVANCED_FACE ( 'NONE', ( #29181 ), #10224, .F. ) ;
#65628 = LINE ( 'NONE', #72394, #50468 ) ;
#65629 = LINE ( 'NONE', #3931, #21036 ) ;
#65630 = VERTEX_POINT ( 'NONE', #15654 ) ;
#65631 = CARTESIAN_POINT ( 'NONE',  ( -6.923076923077045919, -10.33852847137269571, 34.16647553114546554 ) ) ;
#65632 = CARTESIAN_POINT ( 'NONE',  ( -12.46153846153858424, -12.70778746994576025, 30.41441678777401236 ) ) ;
#65634 = ORIENTED_EDGE ( 'NONE', *, *, #35774, .F. ) ;
#65633 = CARTESIAN_POINT ( 'NONE',  ( 11.53846153846153832, -2.833524468853757305, 32.15551576947925838 ) ) ;
#65635 = CARTESIAN_POINT ( 'NONE',  ( -13.60754234352223335, -10.01117774369187252, 34.36070679894347535 ) ) ;
#65636 = CARTESIAN_POINT ( 'NONE',  ( 17.32692307692449418, -7.500000000000154543, 35.00000000000007105 ) ) ;
#65637 = EDGE_CURVE ( 'NONE', #18061, #32348, #5086, .T. ) ;
#65638 = B_SPLINE_CURVE_WITH_KNOTS ( 'NONE', 3,
 ( #80444, #58817, #51149, #59266, #87210, #52505, #39017, #71889, #31356, #10643 ),
 .UNSPECIFIED., .F., .F.,
 ( 4, 2, 2, 2, 4 ),
 ( 0.000000000000000000, 0.0001954339857564063089, 0.0003908679715128126177, 0.0005863019572692189808, 0.0007817359430256252354 ),
 .UNSPECIFIED. ) ;
#65639 = CARTESIAN_POINT ( 'NONE',  ( -8.546451227962355901, -2.600157965045224451, 30.74683119005207743 ) ) ;
#65640 = CARTESIAN_POINT ( 'NONE',  ( -14.17690049986751966, -11.18335022499818621, 33.13157742990016885 ) ) ;
#65641 = ORIENTED_EDGE ( 'NONE', *, *, #40883, .F. ) ;
#65642 = DIRECTION ( 'NONE',  ( -0.000000000000000000, -0.3420201433256694901, -0.9396926207859082059 ) ) ;
#65643 = CARTESIAN_POINT ( 'NONE',  ( 1.653273178848927064E-15, -7.500000000000000000, 0.000000000000000000 ) ) ;
#65644 = DIRECTION ( 'NONE',  ( -0.000000000000000000, 1.000000000000000000, -0.000000000000000000 ) ) ;
#65645 = EDGE_CURVE ( 'NONE', #78266, #30104, #43556, .T. ) ;
#65646 = ORIENTED_EDGE ( 'NONE', *, *, #81933, .F. ) ;
#65647 = ORIENTED_EDGE ( 'NONE', *, *, #71932, .F. ) ;
#65648 = VERTEX_POINT ( 'NONE', #72798 ) ;
#65649 = EDGE_CURVE ( 'NONE', #15172, #41806, #85637, .T. ) ;
#65650 = CARTESIAN_POINT ( 'NONE',  ( -9.758391103263573285, -2.721908614388770964, 31.22303859784723912 ) ) ;
#65651 = CARTESIAN_POINT ( 'NONE',  ( 16.15384615384615330, -1.951392089020283160, 34.73218667398347748 ) ) ;
#65652 = AXIS2_PLACEMENT_3D ( 'NONE', #85478, #9380, #66080 ) ;
#65653 = CARTESIAN_POINT ( 'NONE',  ( -5.999999999999998224, -13.78497067705608181, 32.30358669280327177 ) ) ;
#65654 = CARTESIAN_POINT ( 'NONE',  ( 3.230769230769231726, -12.78798330534103123, 29.99999999999997868 ) ) ;
#65655 = EDGE_CURVE ( 'NONE', #4047, #40157, #13226, .T. ) ;
#65656 = ORIENTED_EDGE ( 'NONE', *, *, #87641, .F. ) ;
#65657 = VECTOR ( 'NONE', #19792, 1000.000000000000000 ) ;
#65658 = VERTEX_POINT ( 'NONE', #79575 ) ;
#65661 = ORIENTED_EDGE ( 'NONE', *, *, #70651, .T. ) ;
#65660 = ADVANCED_FACE ( 'NONE', ( #82133 ), #41140, .F. ) ;
#65659 = CARTESIAN_POINT ( 'NONE',  ( -18.00000000000012079, -8.656820664282943056, 34.87096338111179961 ) ) ;
#65662 = CARTESIAN_POINT ( 'NONE',  ( -14.24162497434223162, -11.35647404775217595, 33.31231777344666511 ) ) ;
#65663 = PLANE ( 'NONE',  #53705 ) ;
#65664 = EDGE_CURVE ( 'NONE', #36550, #16329, #62345, .T. ) ;
#65665 = AXIS2_PLACEMENT_3D ( 'NONE', #45083, #74349, #39688 ) ;
#65666 = EDGE_CURVE ( 'NONE', #71441, #23412, #54529, .T. ) ;
#65667 = CARTESIAN_POINT ( 'NONE',  ( 1.384615384615386802, -10.51840700105979565, 33.73612834413961536 ) ) ;
#65668 = CYLINDRICAL_SURFACE ( 'NONE', #46775, 0.2499999999999994726 ) ;
#65669 = ORIENTED_EDGE ( 'NONE', *, *, #5798, .T. ) ;
#65670 = ORIENTED_EDGE ( 'NONE', *, *, #7098, .T. ) ;
#65671 = AXIS2_PLACEMENT_3D ( 'NONE', #42962, #29889, #21794 ) ;
#65672 = ORIENTED_EDGE ( 'NONE', *, *, #77434, .T. ) ;
#65674 = ORIENTED_EDGE ( 'NONE', *, *, #44589, .T. ) ;
#65673 = CARTESIAN_POINT ( 'NONE',  ( 5.326868595271217366, -5.057305518903949526, 34.11320923018887896 ) ) ;
#65675 = CARTESIAN_POINT ( 'NONE',  ( 2.980792499826877329, -11.79746400365624659, 32.30657167506340954 ) ) ;
#65676 = CARTESIAN_POINT ( 'NONE',  ( 18.24994540937804643, -5.766571408460170467, 34.70601412856602508 ) ) ;
#65677 = EDGE_LOOP ( 'NONE', ( #26711, #60170, #79231, #24785, #77575 ) ) ;
#65678 = VECTOR ( 'NONE', #11578, 1000.000000000000000 ) ;
#65679 = CARTESIAN_POINT ( 'NONE',  ( -8.835314180186646382, -10.51840700105979387, 33.73612834413961536 ) ) ;
#65680 = CARTESIAN_POINT ( 'NONE',  ( 10.61538461538461675, -8.810774026931790459, 35.74407628777942847 ) ) ;
#65681 = CARTESIAN_POINT ( 'NONE',  ( -6.923076923076922462, -12.78798330534102945, 29.74999999999997868 ) ) ;
#65682 = FACE_BOUND ( 'NONE', #87344, .T. ) ;
#65683 = CARTESIAN_POINT ( 'NONE',  ( -15.23076923076922995, -8.164416787775445883, 34.95778746994557906 ) ) ;
#65684 = CARTESIAN_POINT ( 'NONE',  ( 9.561830984191230343, -7.276988635370452485, 34.74523720219453793 ) ) ;
#65685 = CARTESIAN_POINT ( 'NONE',  ( -9.692307692307691624, -12.48256725967547354, 35.29906147534542527 ) ) ;
#65687 = CARTESIAN_POINT ( 'NONE',  ( -5.934744428723975673, -2.892918686051625166, 31.69288490824025928 ) ) ;
#65686 = CARTESIAN_POINT ( 'NONE',  ( 3.296024370282069516, -3.643525952247864463, 33.31231777344670064 ) ) ;
#65688 = CARTESIAN_POINT ( 'NONE',  ( 6.923076923076924238, -12.34228464037088635, 31.77849191805839268 ) ) ;
#65689 = PLANE ( 'NONE',  #60589 ) ;
#65690 = ORIENTED_EDGE ( 'NONE', *, *, #58595, .F. ) ;
#65691 = CARTESIAN_POINT ( 'NONE',  ( -16.08859101433330707, -3.643525952247864019, 33.31231777344670064 ) ) ;
#65692 = CARTESIAN_POINT ( 'NONE',  ( -7.623374304885434327, -2.600157965045225339, 30.74683119005207743 ) ) ;
#65693 = ORIENTED_EDGE ( 'NONE', *, *, #23928, .F. ) ;
#65694 = ORIENTED_EDGE ( 'NONE', *, *, #61896, .F. ) ;
#65696 = CARTESIAN_POINT ( 'NONE',  ( 10.61538461538461675, -11.91647553114624181, 32.58852847137148245 ) ) ;
#65695 = CARTESIAN_POINT ( 'NONE',  ( 5.933916589044120116, -6.386643153685125363, 34.62446782046654903 ) ) ;
#65697 = DIRECTION ( 'NONE',  ( 1.000000000000000000, 0.000000000000000000, 0.000000000000000000 ) ) ;
#65698 = CARTESIAN_POINT ( 'NONE',  ( -17.07692307692307665, -1.790695186598648903, 34.54067556320373455 ) ) ;
#65699 = CARTESIAN_POINT ( 'NONE',  ( 19.99999999999996803, 12.00000000000000711, 0.000000000000000000 ) ) ;
#65700 = ORIENTED_EDGE ( 'NONE', *, *, #42726, .F. ) ;
#65701 = EDGE_CURVE ( 'NONE', #83312, #4579, #65210, .T. ) ;
#65702 = VECTOR ( 'NONE', #37062, 1000.000000000000227 ) ;
#65703 = CARTESIAN_POINT ( 'NONE',  ( -18.00000000000000000, -13.92244064605451648, 31.82153278338624602 ) ) ;
#65704 = LINE ( 'NONE', #31490, #30034 ) ;
#65706 = CARTESIAN_POINT ( 'NONE',  ( 14.30769230769218581, -12.70778746994576025, 30.41441678777401236 ) ) ;
#65705 = LINE ( 'NONE', #36593, #2966 ) ;
#65708 = LINE ( 'NONE', #58499, #81944 ) ;
#65707 = B_SPLINE_CURVE_WITH_KNOTS ( 'NONE', 3,
 ( #51055, #79000, #38468, #72238, #65920, #45659, #71792, #78113, #38019, #66378 ),
 .UNSPECIFIED., .F., .F.,
 ( 4, 2, 2, 2, 4 ),
 ( 0.000000000000000000, 0.0001954311564186872268, 0.0003908623128373744536, 0.0005862934692560616261, 0.0007817246256747489071 ),
 .UNSPECIFIED. ) ;
#65709 = LINE ( 'NONE', #2671, #20910 ) ;
#65710 = DIRECTION ( 'NONE',  ( -0.000000000000000000, -0.7660444431189791237, -0.6427876096865379196 ) ) ;
#65711 = AXIS2_PLACEMENT_3D ( 'NONE', #80530, #20147, #39100 ) ;
#65712 = CARTESIAN_POINT ( 'NONE',  ( -2.651650429449565305, -4.848349570550461785, 20.25000000000000000 ) ) ;
#65713 = ORIENTED_EDGE ( 'NONE', *, *, #32269, .T. ) ;
#65714 = B_SPLINE_CURVE_WITH_KNOTS ( 'NONE', 3,
 ( #20216, #39167, #11235, #40499, #39614, #46796, #33728, #61183, #26082, #66166 ),
 .UNSPECIFIED., .F., .F.,
 ( 4, 2, 2, 2, 4 ),
 ( 0.0007817246256747459798, 0.0009771112852218885505, 0.001172497944769031013, 0.001367884604316173475, 0.001563271263863315937 ),
 .UNSPECIFIED. ) ;
#65716 = EDGE_CURVE ( 'NONE', #60483, #78849, #86794, .T. ) ;
#65715 = ORIENTED_EDGE ( 'NONE', *, *, #72984, .T. ) ;
#65717 = CARTESIAN_POINT ( 'NONE',  ( 14.05766908347085042, -12.45566812827425451, 31.48439005359158926 ) ) ;
#65718 = VECTOR ( 'NONE', #47445, 1000.000000000000000 ) ;
#65719 = DIRECTION ( 'NONE',  ( -0.000000000000000000, 1.000000000000000000, -0.000000000000000000 ) ) ;
#65720 = LINE ( 'NONE', #57641, #71857 ) ;
#65721 = CARTESIAN_POINT ( 'NONE',  ( 3.230769230769231726, -4.098570777380720287, 33.41473453929634729 ) ) ;
#65722 = CARTESIAN_POINT ( 'NONE',  ( 17.20776140740982996, -7.277220318596959281, 34.99547417642776992 ) ) ;
#65723 = CARTESIAN_POINT ( 'NONE',  ( -1.553300858899081538, -11.25000000000000711, 18.60937500000000355 ) ) ;
#65724 = ADVANCED_FACE ( 'NONE', ( #33499 ), #60958, .F. ) ;
#65725 = DIRECTION ( 'NONE',  ( 0.000000000000000000, 0.8660254037844377084, 0.5000000000000015543 ) ) ;
#65726 = CARTESIAN_POINT ( 'NONE',  ( -20.75000000000000355, -2.499999999999999556, 27.25000000000000000 ) ) ;
#65727 = CARTESIAN_POINT ( 'NONE',  ( 16.85343813319912343, -12.24155766932282496, 31.33739205006857986 ) ) ;
#65728 = LINE ( 'NONE', #17559, #15168 ) ;
#65729 = CYLINDRICAL_SURFACE ( 'NONE', #68451, 0.2499999999999994726 ) ;
#65730 = DIRECTION ( 'NONE',  ( -0.000000000000000000, 0.7660444431189791237, -0.6427876096865379196 ) ) ;
#65731 = DIRECTION ( 'NONE',  ( -0.000000000000000000, -0.9396926207859093161, -0.3420201433256663259 ) ) ;
#65732 = CARTESIAN_POINT ( 'NONE',  ( 5.076923076923075762, -13.95598074871891292, 31.83374038241031911 ) ) ;
#65733 = CARTESIAN_POINT ( 'NONE',  ( 10.61538461538461675, -2.721908614388771852, 31.22303859784724978 ) ) ;
#65734 = CARTESIAN_POINT ( 'NONE',  ( -3.230769230769229949, -11.16473453929635440, 33.15142922261926373 ) ) ;
#65735 = CARTESIAN_POINT ( 'NONE',  ( -7.053224132515143907, -5.195881422630167279, 34.18770438780618548 ) ) ;
#65736 = EDGE_LOOP ( 'NONE', ( #54982, #61374 ) ) ;
#65737 = CARTESIAN_POINT ( 'NONE',  ( -16.28399412357784826, -9.504002272028873932, 34.60269587691767867 ) ) ;
#65738 = CARTESIAN_POINT ( 'NONE',  ( 1.161689167099238418, -5.667676309546437530, 34.40238873228292249 ) ) ;
#65739 = CYLINDRICAL_SURFACE ( 'NONE', #80780, 0.2500000000000012212 ) ;
#65740 = CARTESIAN_POINT ( 'NONE',  ( -1.139087296526025916, -4.750000000000006217, 24.07812500000000355 ) ) ;
#65741 = ADVANCED_FACE ( 'NONE', ( #34371 ), #61838, .F. ) ;
#65742 = CARTESIAN_POINT ( 'NONE',  ( -14.24243673641628050, -5.219633306516380244, 34.19971097300157936 ) ) ;
#65744 = CARTESIAN_POINT ( 'NONE',  ( 14.08420738312797837, -4.988325925672468131, 34.36044203135681130 ) ) ;
#65743 = AXIS2_PLACEMENT_3D ( 'NONE', #7997, #63816, #50284 ) ;
#65746 = ORIENTED_EDGE ( 'NONE', *, *, #84084, .F. ) ;
#65745 = CARTESIAN_POINT ( 'NONE',  ( 5.142990410273151625, -3.937682226553329556, 33.60647404775216529 ) ) ;
#65747 = CARTESIAN_POINT ( 'NONE',  ( -2.750000000000006217, -6.360912703474006946, 18.92187500000000000 ) ) ;
#65748 = CARTESIAN_POINT ( 'NONE',  ( -12.46153846153815437, -2.506253911140614576, 30.00000000000323297 ) ) ;
#65749 = ADVANCED_FACE ( 'NONE', ( #55088 ), #82584, .T. ) ;
#65750 = ORIENTED_EDGE ( 'NONE', *, *, #7814, .T. ) ;
#65751 = DIRECTION ( 'NONE',  ( -0.000000000000000000, 0.1736481776669307198, -0.9848077530122080203 ) ) ;
#65752 = B_SPLINE_CURVE_WITH_KNOTS ( 'NONE', 3,
 ( #50465, #71185, #3166, #50031, #28897, #2717, #72076, #9488, #30215, #63543 ),
 .UNSPECIFIED., .F., .F.,
 ( 4, 2, 2, 2, 4 ),
 ( 0.000000000000000000, 0.0001954339857564092633, 0.0003908679715128185266, 0.0005863019572692277628, 0.0007817359430256370532 ),
 .UNSPECIFIED. ) ;
#65753 = VERTEX_POINT ( 'NONE', #38132 ) ;
#65754 = LINE ( 'NONE', #72518, #20465 ) ;
#65755 = CARTESIAN_POINT ( 'NONE',  ( 2.980769230769232170, -2.249999999999998668, 29.75000000000000355 ) ) ;
#65756 = VECTOR ( 'NONE', #3926, 1000.000000000000227 ) ;
#65757 = CARTESIAN_POINT ( 'NONE',  ( 4.153846153846154188, -7.500000000000001776, 35.04278698407183867 ) ) ;
#65758 = ORIENTED_EDGE ( 'NONE', *, *, #83753, .T. ) ;
#65759 = CARTESIAN_POINT ( 'NONE',  ( -10.48485891362105171, -12.45806712695776319, 30.39783852428763922 ) ) ;
#65760 = ORIENTED_EDGE ( 'NONE', *, *, #19426, .F. ) ;
#65761 = CARTESIAN_POINT ( 'NONE',  ( 18.03205128205128105, -11.50000000000000000, 29.75000000000000355 ) ) ;
#65762 = ORIENTED_EDGE ( 'NONE', *, *, #82173, .F. ) ;
#65763 = CARTESIAN_POINT ( 'NONE',  ( 13.60762673622823726, -11.76359900205217635, 32.36225158514719880 ) ) ;
#65764 = CARTESIAN_POINT ( 'NONE',  ( 2.307692307692187583, -3.300289026999228881, 32.46337939537708905 ) ) ;
#65765 = ORIENTED_EDGE ( 'NONE', *, *, #11072, .T. ) ;
#65766 = CARTESIAN_POINT ( 'NONE',  ( -10.86536135943320502, -12.01397095200674059, 32.43157075238190146 ) ) ;
#65767 = CARTESIAN_POINT ( 'NONE',  ( 10.68064018666064108, -3.300289026998473041, 32.46337939537591666 ) ) ;
#65768 = LINE ( 'NONE', #25686, #36617 ) ;
#65769 = DIRECTION ( 'NONE',  ( -0.000000000000000000, 0.8660254037844399289, -0.4999999999999980016 ) ) ;
#65770 = CARTESIAN_POINT ( 'NONE',  ( 11.25641025641025550, -3.499999999999999556, 29.75000000000000355 ) ) ;
#65771 = EDGE_CURVE ( 'NONE', #86292, #18500, #18016, .T. ) ;
#65772 = VERTEX_POINT ( 'NONE', #34813 ) ;
#65773 = ORIENTED_EDGE ( 'NONE', *, *, #75090, .T. ) ;
#65774 = ORIENTED_EDGE ( 'NONE', *, *, #42740, .F. ) ;
#65776 = ORIENTED_EDGE ( 'NONE', *, *, #20152, .T. ) ;
#65775 = CARTESIAN_POINT ( 'NONE',  ( 3.230769230769231726, -3.513871655860378418, 32.76840700105978499 ) ) ;
#65777 = AXIS2_PLACEMENT_3D ( 'NONE', #87083, #39332, #12288 ) ;
#65778 = EDGE_CURVE ( 'NONE', #15288, #75095, #36447, .T. ) ;
#65779 = EDGE_CURVE ( 'NONE', #17845, #55623, #44789, .T. ) ;
#65780 = AXIS2_PLACEMENT_3D ( 'NONE', #70626, #51656, #37271 ) ;
#65781 = CARTESIAN_POINT ( 'NONE',  ( -9.019207500173124004, -9.943427161483782584, 34.11278801902876978 ) ) ;
#65782 = CARTESIAN_POINT ( 'NONE',  ( 6.222779668978068557, -10.23759521482555357, 34.22997729860117033 ) ) ;
#65783 = ORIENTED_EDGE ( 'NONE', *, *, #56798, .F. ) ;
#65784 = ORIENTED_EDGE ( 'NONE', *, *, #66192, .T. ) ;
#65785 = CARTESIAN_POINT ( 'NONE',  ( -0.4615384615384611200, -5.415277668671390821, 36.20867863119892149 ) ) ;
#65786 = ORIENTED_EDGE ( 'NONE', *, *, #24427, .F. ) ;
#65787 = CARTESIAN_POINT ( 'NONE',  ( -10.48459280755982626, -8.999086150933475636, 34.52020707165672775 ) ) ;
#65788 = CARTESIAN_POINT ( 'NONE',  ( -7.911424292114618950, -2.625532179533444754, 30.86335684631481513 ) ) ;
#65789 = EDGE_CURVE ( 'NONE', #62210, #2112, #73853, .T. ) ;
#65790 = CARTESIAN_POINT ( 'NONE',  ( 12.33139125210024112, -2.619462340734462380, 30.83744416345203021 ) ) ;
#65791 = FACE_BOUND ( 'NONE', #53089, .T. ) ;
#65792 = ORIENTED_EDGE ( 'NONE', *, *, #15133, .T. ) ;
#65793 = LINE ( 'NONE', #11758, #83060 ) ;
#65794 = DIRECTION ( 'NONE',  ( -0.000000000000000000, 0.6427876096865404731, -0.7660444431189770143 ) ) ;
#65795 = CARTESIAN_POINT ( 'NONE',  ( -14.30769230769242739, -6.026961402154118019, 34.52809138561165270 ) ) ;
#65796 = EDGE_CURVE ( 'NONE', #65067, #56939, #8286, .T. ) ;
#65797 = CARTESIAN_POINT ( 'NONE',  ( 2.307692307692309264, -8.164416787775445883, 34.95778746994557906 ) ) ;
#65798 = FACE_OUTER_BOUND ( 'NONE', #279, .T. ) ;
#65799 = ORIENTED_EDGE ( 'NONE', *, *, #216, .F. ) ;
#65800 = CARTESIAN_POINT ( 'NONE',  ( -7.173100160369890510, -6.695914987888143877, 34.68535235679833306 ) ) ;
#65801 = ORIENTED_EDGE ( 'NONE', *, *, #72545, .T. ) ;
#65802 = VERTEX_POINT ( 'NONE', #42476 ) ;
#65804 = CARTESIAN_POINT ( 'NONE',  ( 5.999999999999880096, -3.300289026999228881, 32.46337939537708905 ) ) ;
#65803 = DIRECTION ( 'NONE',  ( -0.000000000000000000, -0.1736481776669307198, -0.9848077530122080203 ) ) ;
#65805 = CARTESIAN_POINT ( 'NONE',  ( -8.546451100252705047, -12.47679350104403007, 31.42216943046555855 ) ) ;
#65806 = CARTESIAN_POINT ( 'NONE',  ( -2.307692307692305711, -12.10708131394839349, 31.69288490824020244 ) ) ;
#65807 = CARTESIAN_POINT ( 'NONE',  ( 1.634669696253702176, -9.943054286541400444, 34.11300777759954883 ) ) ;
#65808 = CARTESIAN_POINT ( 'NONE',  ( 14.24242230713598900, -3.083524468853724443, 32.58852847137143272 ) ) ;
#65809 = ORIENTED_EDGE ( 'NONE', *, *, #71040, .T. ) ;
#65810 = ADVANCED_FACE ( 'NONE', ( #83913 ), #77139, .T. ) ;
#65811 = DIRECTION ( 'NONE',  ( -0.000000000000000000, -0.7660444431189791237, -0.6427876096865379196 ) ) ;
#65812 = CARTESIAN_POINT ( 'NONE',  ( 13.38461538461538680, -3.886160181151819604, 36.00935417666054406 ) ) ;
#65813 = FACE_OUTER_BOUND ( 'NONE', #82954, .T. ) ;
#65814 = CARTESIAN_POINT ( 'NONE',  ( 10.83816415665302202, -11.89424750095246175, 32.13594075562310337 ) ) ;
#65815 = ORIENTED_EDGE ( 'NONE', *, *, #66571, .F. ) ;
#65816 = EDGE_CURVE ( 'NONE', #56815, #42102, #20071, .T. ) ;
#65817 = ORIENTED_EDGE ( 'NONE', *, *, #16779, .T. ) ;
#65818 = FACE_BOUND ( 'NONE', #88253, .T. ) ;
#65819 = ORIENTED_EDGE ( 'NONE', *, *, #82345, .F. ) ;
#65820 = CARTESIAN_POINT ( 'NONE',  ( 7.715462379486289102, -2.729777683071817229, 31.24903638046268739 ) ) ;
#65821 = CARTESIAN_POINT ( 'NONE',  ( -5.933833393408360024, -7.250054591869668386, 34.99404684341514127 ) ) ;
#65822 = ORIENTED_EDGE ( 'NONE', *, *, #37262, .F. ) ;
#65823 = CARTESIAN_POINT ( 'NONE',  ( -7.780085495151407571, -4.098570777380720287, 33.41473453929635440 ) ) ;
#65824 = LINE ( 'NONE', #51400, #41423 ) ;
#65825 = PLANE ( 'NONE',  #62463 ) ;
#65826 = DIRECTION ( 'NONE',  ( 0.000000000000000000, 0.000000000000000000, 1.000000000000000000 ) ) ;
#65827 = ADVANCED_FACE ( 'NONE', ( #1920 ), #56858, .F. ) ;
#65828 = CARTESIAN_POINT ( 'NONE',  ( -0.5916856709766792344, -11.47017969459903952, 32.78971311882034456 ) ) ;
#65829 = VERTEX_POINT ( 'NONE', #14750 ) ;
#65831 = ORIENTED_EDGE ( 'NONE', *, *, #34103, .F. ) ;
#65830 = CARTESIAN_POINT ( 'NONE',  ( -15.09997878980228414, -2.295524264805589354, 30.44142389570982488 ) ) ;
#65832 = CARTESIAN_POINT ( 'NONE',  ( -7.596208327805705096, -9.272278438253398036, 34.42582936511637115 ) ) ;
#65833 = CARTESIAN_POINT ( 'NONE',  ( 15.23076923076923173, -2.721908614388771852, 31.22303859784724978 ) ) ;
#65834 = CARTESIAN_POINT ( 'NONE',  ( -6.923076923076922462, -5.557115091759785130, 34.35708131394839171 ) ) ;
#65835 = CIRCLE ( 'NONE', #16977, 0.2500000000000002220 ) ;
#65836 = CARTESIAN_POINT ( 'NONE',  ( 18.24994551834813805, -8.433404298154332679, 34.66254593164985920 ) ) ;
#65837 = DIRECTION ( 'NONE',  ( -1.000000000000000000, 0.000000000000000000, -0.000000000000000000 ) ) ;
#65838 = EDGE_CURVE ( 'NONE', #57810, #69549, #48074, .T. ) ;
#65839 = CARTESIAN_POINT ( 'NONE',  ( 5.326868595271218254, -12.43552623307873972, 30.55307653245132826 ) ) ;
#65840 = CARTESIAN_POINT ( 'NONE',  ( 1.901340078031373171, -9.487747218494639867, 13.62686829374151642 ) ) ;
#65841 = EDGE_LOOP ( 'NONE', ( #45307, #27607 ) ) ;
#65842 = AXIS2_PLACEMENT_3D ( 'NONE', #28364, #22497, #8994 ) ;
#65843 = DIRECTION ( 'NONE',  ( 1.000000000000000000, 0.000000000000000000, 0.000000000000000000 ) ) ;
#65844 = CARTESIAN_POINT ( 'NONE',  ( 2.307692307692186251, -4.320704448113951379, 33.92786785259630022 ) ) ;
#65845 = CARTESIAN_POINT ( 'NONE',  ( 11.25641025641025550, -4.000000000000000000, 29.75000000000000355 ) ) ;
#65846 = B_SPLINE_CURVE_WITH_KNOTS ( 'NONE', 3,
 ( #25985, #20123, #61536, #53448, #81389, #12044, #75072, #4834, #39072, #40840 ),
 .UNSPECIFIED., .F., .F.,
 ( 4, 2, 2, 2, 4 ),
 ( 0.000000000000000000, 0.0001954339857564074473, 0.0003908679715128148945, 0.0005863019572692223418, 0.0007817359430256297891 ),
 .UNSPECIFIED. ) ;
#65847 = ORIENTED_EDGE ( 'NONE', *, *, #17590, .T. ) ;
#65849 = ORIENTED_EDGE ( 'NONE', *, *, #42568, .F. ) ;
#65848 = AXIS2_PLACEMENT_3D ( 'NONE', #67996, #88725, #38740 ) ;
#65850 = CARTESIAN_POINT ( 'NONE',  ( -1.634615384615383027, -2.499999999999998668, 29.75000000000000355 ) ) ;
#65851 = LINE ( 'NONE', #24871, #54043 ) ;
#65852 = EDGE_CURVE ( 'NONE', #58944, #17200, #56601, .T. ) ;
#65853 = CARTESIAN_POINT ( 'NONE',  ( 16.15384615384615330, -1.422936976036506707, 30.56769352161908415 ) ) ;
#65854 = CARTESIAN_POINT ( 'NONE',  ( 10.61538461538449596, -4.481592998941358097, 33.73612834414048933 ) ) ;
#65855 = EDGE_CURVE ( 'NONE', #83084, #39482, #36208, .T. ) ;
#65856 = CARTESIAN_POINT ( 'NONE',  ( -5.198717948717948012, -3.499999999999999556, 29.75000000000000355 ) ) ;
#65857 = DIRECTION ( 'NONE',  ( 0.000000000000000000, 0.000000000000000000, 1.000000000000000000 ) ) ;
#65858 = EDGE_LOOP ( 'NONE', ( #34248, #14558 ) ) ;
#65859 = DIRECTION ( 'NONE',  ( 0.000000000000000000, 0.9848077530122072432, -0.1736481776669354937 ) ) ;
#65860 = CARTESIAN_POINT ( 'NONE',  ( 8.703147358274890166, -8.120952969808774569, 34.71129190930000163 ) ) ;
#65861 = CYLINDRICAL_SURFACE ( 'NONE', #52734, 0.2500000000000004996 ) ;
#65862 = CARTESIAN_POINT ( 'NONE',  ( -3.480745961711584791, -11.79746400365624659, 32.30657167506340954 ) ) ;
#65863 = EDGE_LOOP ( 'NONE', ( #6596, #44815, #69746, #48371 ) ) ;
#65864 = CARTESIAN_POINT ( 'NONE',  ( 12.21156171748987163, -2.544273027872575366, 31.48422191005632342 ) ) ;
#65865 = B_SPLINE_CURVE_WITH_KNOTS ( 'NONE', 3,
 ( #58975, #17558, #18005, #45460, #72940, #11244, #38713, #4486, #31962, #45906 ),
 .UNSPECIFIED., .F., .F.,
 ( 4, 2, 2, 2, 4 ),
 ( 0.000000000000000000, 0.0001954311564186876876, 0.0003908623128373753751, 0.0005862934692560630356, 0.0007817246256747507503 ),
 .UNSPECIFIED. ) ;
#65866 = ORIENTED_EDGE ( 'NONE', *, *, #61056, .T. ) ;
#65867 = AXIS2_PLACEMENT_3D ( 'NONE', #68713, #7011, #12880 ) ;
#65868 = CARTESIAN_POINT ( 'NONE',  ( 1.634615384616822320, -7.500000000000155431, 34.75000000000007105 ) ) ;
#65869 = CARTESIAN_POINT ( 'NONE',  ( 16.21903914214080800, -2.255955759149236073, 29.99999999999988276 ) ) ;
#65870 = DIRECTION ( 'NONE',  ( -0.000000000000000000, -0.000000000000000000, -1.000000000000000000 ) ) ;
#65871 = ORIENTED_EDGE ( 'NONE', *, *, #50501, .T. ) ;
#65872 = CARTESIAN_POINT ( 'NONE',  ( -11.53846153846153655, -13.20930481340135110, 34.54067556320372745 ) ) ;
#65873 = DIRECTION ( 'NONE',  ( -0.7071067811865510144, 0.7071067811865440200, 0.000000000000000000 ) ) ;
#65874 = DIRECTION ( 'NONE',  ( -0.000000000000000000, 0.7660444431189791237, -0.6427876096865379196 ) ) ;
#65875 = VECTOR ( 'NONE', #46943, 999.9999999999998863 ) ;
#65876 = FACE_OUTER_BOUND ( 'NONE', #37661, .T. ) ;
#65877 = CARTESIAN_POINT ( 'NONE',  ( 3.480714640147274164, -2.986452184633681117, 32.43230066228895225 ) ) ;
#65878 = VECTOR ( 'NONE', #23013, 1000.000000000000227 ) ;
#65879 = ORIENTED_EDGE ( 'NONE', *, *, #61333, .F. ) ;
#65880 = DIRECTION ( 'NONE',  ( -1.000000000000000000, 1.799314243699348838E-16, 0.000000000000000000 ) ) ;
#65881 = ORIENTED_EDGE ( 'NONE', *, *, #247, .F. ) ;
#65882 = CARTESIAN_POINT ( 'NONE',  ( 27.00000000000000000, 16.99999999999999645, 23.75000000000000355 ) ) ;
#65883 = CARTESIAN_POINT ( 'NONE',  ( 4.853996859406927378, -12.15238873228292071, 31.58232369045353849 ) ) ;
#65884 = ADVANCED_FACE ( 'NONE', ( #7099 ), #6654, .F. ) ;
#65885 = CARTESIAN_POINT ( 'NONE',  ( 7.846153846153846700, -11.35647404775217417, 33.31231777344666511 ) ) ;
#65886 = DIRECTION ( 'NONE',  ( -1.000000000000000000, -0.000000000000000000, -0.000000000000000000 ) ) ;
#65887 = EDGE_CURVE ( 'NONE', #34465, #15080, #42229, .T. ) ;
#65888 = DIRECTION ( 'NONE',  ( 0.000000000000000000, 1.000000000000000000, 0.000000000000000000 ) ) ;
#65889 = CARTESIAN_POINT ( 'NONE',  ( 15.16549878480845415, -11.94971097300153140, 32.03036669348370680 ) ) ;
#65890 = ORIENTED_EDGE ( 'NONE', *, *, #61368, .T. ) ;
#65892 = EDGE_CURVE ( 'NONE', #47638, #52597, #41331, .T. ) ;
#65891 = VERTEX_POINT ( 'NONE', #76450 ) ;
#65893 = EDGE_LOOP ( 'NONE', ( #49007, #32469 ) ) ;
#65894 = ORIENTED_EDGE ( 'NONE', *, *, #39153, .F. ) ;
#65895 = VERTEX_POINT ( 'NONE', #20609 ) ;
#65896 = CARTESIAN_POINT ( 'NONE',  ( -1.161604033002535230, -3.105924265160262099, 32.13625925475356127 ) ) ;
#65897 = CARTESIAN_POINT ( 'NONE',  ( -1.254089682851821097, -12.45806712695776319, 30.39783852428763922 ) ) ;
#65898 = ADVANCED_FACE ( 'NONE', ( #60710 ), #27813, .F. ) ;
#65899 = AXIS2_PLACEMENT_3D ( 'NONE', #11544, #25499, #52955 ) ;
#65900 = CARTESIAN_POINT ( 'NONE',  ( -15.29603967673000575, -10.90142922261923886, 33.41473453929638993 ) ) ;
#65901 = CARTESIAN_POINT ( 'NONE',  ( -6.923076923076922462, -3.050289026998446396, 32.03036669348365706 ) ) ;
#65902 = DIRECTION ( 'NONE',  ( -0.000000000000000000, 1.000000000000000000, 3.491481338843133355E-15 ) ) ;
#65903 = CARTESIAN_POINT ( 'NONE',  ( -12.52680846209478283, -12.51329471203370325, 31.30864560766548976 ) ) ;
#65904 = LINE ( 'NONE', #3765, #17720 ) ;
#65905 = DIRECTION ( 'NONE',  ( -1.000000000000000000, -0.000000000000000000, -0.000000000000000000 ) ) ;
#65906 = CARTESIAN_POINT ( 'NONE',  ( 0.3308469948709003572, -3.062553014421049546, 32.05460306192773601 ) ) ;
#65907 = ORIENTED_EDGE ( 'NONE', *, *, #18303, .T. ) ;
#65908 = EDGE_LOOP ( 'NONE', ( #84186, #12226, #76094, #16824 ) ) ;
#65909 = VERTEX_POINT ( 'NONE', #68799 ) ;
#65911 = VERTEX_POINT ( 'NONE', #26490 ) ;
#65910 = CARTESIAN_POINT ( 'NONE',  ( 0.2380535369741321461, -12.11044203135681840, 32.26167407432752299 ) ) ;
#65913 = CARTESIAN_POINT ( 'NONE',  ( 18.22337548577241861, -2.251407671071268712, 29.88021292934942963 ) ) ;
#65912 = CARTESIAN_POINT ( 'NONE',  ( 6.923076923076924238, -11.35647404775217417, 33.31231777344666511 ) ) ;
#65914 = B_SPLINE_CURVE_WITH_KNOTS ( 'NONE', 3,
 ( #7201, #4, #12292, #75645, #40989, #82866, #1317, #28808, #443, #13948 ),
 .UNSPECIFIED., .F., .F.,
 ( 4, 2, 2, 2, 4 ),
 ( 0.000000000000000000, 0.0001954311564186875792, 0.0003908623128373751583, 0.0005862934692560627103, 0.0007817246256747503166 ),
 .UNSPECIFIED. ) ;
#65915 = CARTESIAN_POINT ( 'NONE',  ( -13.38461538461538325, -3.886160181151819604, 36.00935417666054406 ) ) ;
#65916 = CARTESIAN_POINT ( 'NONE',  ( 7.053868730901709405, -2.541949514083464479, 30.39797389878540557 ) ) ;
#65917 = FACE_BOUND ( 'NONE', #19491, .T. ) ;
#65918 = ORIENTED_EDGE ( 'NONE', *, *, #46375, .F. ) ;
#65919 = ORIENTED_EDGE ( 'NONE', *, *, #43835, .T. ) ;
#65920 = CARTESIAN_POINT ( 'NONE',  ( -17.32689982097166492, -11.47974371597207899, 33.17467449705390692 ) ) ;
#65921 = EDGE_CURVE ( 'NONE', #34858, #2073, #69244, .T. ) ;
#65922 = VERTEX_POINT ( 'NONE', #68356 ) ;
#65923 = FACE_BOUND ( 'NONE', #6676, .T. ) ;
#65924 = DIRECTION ( 'NONE',  ( -0.000000000000000000, 0.1736481776669307198, -0.9848077530122080203 ) ) ;
#65925 = AXIS2_PLACEMENT_3D ( 'NONE', #26200, #20334, #41049 ) ;
#65926 = CARTESIAN_POINT ( 'NONE',  ( -4.023054346021367245, -11.71459661697925903, 32.44059661609676937 ) ) ;
#65927 = ORIENTED_EDGE ( 'NONE', *, *, #87169, .F. ) ;
#65928 = CARTESIAN_POINT ( 'NONE',  ( 2.307692307692187583, -8.613356846316285953, 34.62446782046622218 ) ) ;
#65929 = LINE ( 'NONE', #18657, #64831 ) ;
#65930 = DIRECTION ( 'NONE',  ( -0.000000000000000000, -0.6427876096865404731, -0.7660444431189770143 ) ) ;
#65931 = ORIENTED_EDGE ( 'NONE', *, *, #55165, .T. ) ;
#65932 = CARTESIAN_POINT ( 'NONE',  ( -11.60454391782167427, -4.661471528628507777, 34.16647553114621871 ) ) ;
#65933 = CARTESIAN_POINT ( 'NONE',  ( -14.30769230769230660, -5.557115091759785130, 34.35708131394839171 ) ) ;
#65934 = ORIENTED_EDGE ( 'NONE', *, *, #31168, .F. ) ;
#65935 = AXIS2_PLACEMENT_3D ( 'NONE', #88305, #88736, #60350 ) ;
#65936 = ADVANCED_FACE ( 'NONE', ( #62039 ), #82327, .T. ) ;
#65937 = CARTESIAN_POINT ( 'NONE',  ( -2.557715544985271983, -11.37209801155882971, 32.91403422569032955 ) ) ;
#65938 = DIRECTION ( 'NONE',  ( -0.000000000000000000, 0.6427876096865404731, -0.7660444431189770143 ) ) ;
#65939 = ORIENTED_EDGE ( 'NONE', *, *, #66537, .T. ) ;
#65940 = CARTESIAN_POINT ( 'NONE',  ( 18.13079180782478872, -6.413143153341454017, 34.63066358083362672 ) ) ;
#65941 = CARTESIAN_POINT ( 'NONE',  ( -12.46153846153858247, -2.625532179533778709, 30.86335684631627174 ) ) ;
#65942 = CARTESIAN_POINT ( 'NONE',  ( -2.307692307692427391, -2.625532179533779154, 30.86335684631627174 ) ) ;
#65943 = CARTESIAN_POINT ( 'NONE',  ( 5.076923076923075762, -1.951392089020283160, 34.73218667398347748 ) ) ;
#65944 = CARTESIAN_POINT ( 'NONE',  ( -16.02332045208259359, -4.459921816937789885, 33.71989282347011851 ) ) ;
#65945 = CARTESIAN_POINT ( 'NONE',  ( -0.3314934056186895073, -2.254550872974307119, 29.97347326024527447 ) ) ;
#65947 = CARTESIAN_POINT ( 'NONE',  ( -16.94639737515951339, -8.586989748646450593, 34.63063291749215011 ) ) ;
#65946 = CARTESIAN_POINT ( 'NONE',  ( 4.826946345980720920, -12.41269422305637171, 30.68257228309993323 ) ) ;
#65948 = EDGE_CURVE ( 'NONE', #65909, #40661, #6209, .T. ) ;
#65949 = VECTOR ( 'NONE', #7413, 1000.000000000000114 ) ;
#65950 = EDGE_CURVE ( 'NONE', #84284, #81366, #33690, .T. ) ;
#65951 = CARTESIAN_POINT ( 'NONE',  ( 17.07692307692307665, -4.098570777380720287, 33.41473453929634729 ) ) ;
#65953 = DIRECTION ( 'NONE',  ( 0.000000000000000000, 1.000000000000000000, 0.000000000000000000 ) ) ;
#65952 = CARTESIAN_POINT ( 'NONE',  ( 3.454145171467415398, -2.501478030877322567, 29.88021232661720816 ) ) ;
#65954 = CARTESIAN_POINT ( 'NONE',  ( -1.409462824231155764E-14, -4.749999999999999112, 14.15625000000000000 ) ) ;
#65955 = ORIENTED_EDGE ( 'NONE', *, *, #10786, .T. ) ;
#65956 = DIRECTION ( 'NONE',  ( -1.000000000000000000, 0.000000000000000000, -0.000000000000000000 ) ) ;
#65957 = EDGE_LOOP ( 'NONE', ( #82395, #404 ) ) ;
#65958 = B_SPLINE_CURVE_WITH_KNOTS ( 'NONE', 3,
 ( #78961, #71308, #57801, #85286, #17257, #44717, #23571, #23131, #58683, #15944 ),
 .UNSPECIFIED., .F., .F.,
 ( 4, 2, 2, 2, 4 ),
 ( 0.0007817359430256371616, 0.0009771253907250052138, 0.001172514838424373266, 0.001367904286123741318, 0.001563293733823109370 ),
 .UNSPECIFIED. ) ;
#65959 = ORIENTED_EDGE ( 'NONE', *, *, #88306, .F. ) ;
#65960 = CARTESIAN_POINT ( 'NONE',  ( -3.230769230769352962, -9.528491918059723176, 34.59228464037033035 ) ) ;
#65961 = ORIENTED_EDGE ( 'NONE', *, *, #925, .F. ) ;
#65962 = CARTESIAN_POINT ( 'NONE',  ( 17.77712131757136049, -7.630691491037286056, 34.74850469731152458 ) ) ;
#65963 = CARTESIAN_POINT ( 'NONE',  ( 0.06109907496454976272, -10.25000000000000000, 27.02938170625848358 ) ) ;
#65964 = CYLINDRICAL_SURFACE ( 'NONE', #67428, 0.2500000000000009437 ) ;
#65965 = EDGE_CURVE ( 'NONE', #19849, #33151, #54466, .T. ) ;
#65966 = CARTESIAN_POINT ( 'NONE',  ( -18.22292695890684655, -11.98009711892699691, 32.48740034544075428 ) ) ;
#65967 = CARTESIAN_POINT ( 'NONE',  ( 9.915087361285756629, -9.418065098278013636, 34.63729479722530158 ) ) ;
#65968 = FACE_OUTER_BOUND ( 'NONE', #41906, .T. ) ;
#65969 = DIRECTION ( 'NONE',  ( -0.000000000000000000, 0.6427876096865404731, -0.7660444431189771253 ) ) ;
#65970 = CYLINDRICAL_SURFACE ( 'NONE', #71787, 0.2499999999999986955 ) ;
#65971 = CARTESIAN_POINT ( 'NONE',  ( -1.384615384615383471, -7.500000000000001776, 35.04278698407183867 ) ) ;
#65972 = CARTESIAN_POINT ( 'NONE',  ( 2.651650429449539104, -4.848349570550432475, 19.31250000000000000 ) ) ;
#65973 = EDGE_CURVE ( 'NONE', #42127, #29932, #36347, .T. ) ;
#65974 = ADVANCED_FACE ( 'NONE', ( #63806 ), #30031, .T. ) ;
#65975 = CARTESIAN_POINT ( 'NONE',  ( 1.254468175177168465, -2.882441371585227952, 31.66841991370172948 ) ) ;
#65976 = FACE_OUTER_BOUND ( 'NONE', #72509, .T. ) ;
#65977 = CARTESIAN_POINT ( 'NONE',  ( 2.307692307692309264, -8.564572088678739092, 35.78748833219616898 ) ) ;
#65978 = EDGE_CURVE ( 'NONE', #25175, #64975, #74897, .T. ) ;
#65979 = ORIENTED_EDGE ( 'NONE', *, *, #63249, .F. ) ;
#65980 = EDGE_LOOP ( 'NONE', ( #48729, #22853, #54410, #50626, #61722, #52376 ) ) ;
#65981 = DIRECTION ( 'NONE',  ( 0.000000000000000000, 0.000000000000000000, -1.000000000000000000 ) ) ;
#65982 = CARTESIAN_POINT ( 'NONE',  ( -17.14219352288385778, -8.613356846314824011, 34.62446782046655613 ) ) ;
#65983 = CARTESIAN_POINT ( 'NONE',  ( 11.53846153846153832, -10.51840700105979565, 33.73612834413961536 ) ) ;
#65984 = LINE ( 'NONE', #38527, #41266 ) ;
#65985 = CARTESIAN_POINT ( 'NONE',  ( 4.153846153846154188, -3.322132147404559976, 32.92929555188717927 ) ) ;
#65986 = FACE_OUTER_BOUND ( 'NONE', #29221, .T. ) ;
#65987 = ORIENTED_EDGE ( 'NONE', *, *, #312, .T. ) ;
#65988 = CARTESIAN_POINT ( 'NONE',  ( 7.715463243043537034, -2.845849958028613624, 32.17971566917920967 ) ) ;
#65989 = ORIENTED_EDGE ( 'NONE', *, *, #41874, .T. ) ;
#65991 = EDGE_CURVE ( 'NONE', #84238, #32965, #70575, .T. ) ;
#65990 = ORIENTED_EDGE ( 'NONE', *, *, #53093, .T. ) ;
#65992 = LINE ( 'NONE', #23676, #26268 ) ;
#65993 = CARTESIAN_POINT ( 'NONE',  ( 3.903869422903798458, -2.564618984488975961, 30.55390908950641915 ) ) ;
#65994 = DIRECTION ( 'NONE',  ( -1.000000000000000000, -0.000000000000000000, -0.000000000000000000 ) ) ;
#65995 = DIRECTION ( 'NONE',  ( 0.000000000000000000, 0.9848077530122072432, -0.1736481776669354937 ) ) ;
#65996 = CARTESIAN_POINT ( 'NONE',  ( -5.207071046654770718, -8.630895178749536711, 34.87696386517710323 ) ) ;
#65997 = VECTOR ( 'NONE', #89082, 1000.000000000000114 ) ;
#65998 = ORIENTED_EDGE ( 'NONE', *, *, #9062, .F. ) ;
#65999 = AXIS2_PLACEMENT_3D ( 'NONE', #14801, #26540, #14345 ) ;
#66000 = ORIENTED_EDGE ( 'NONE', *, *, #42735, .F. ) ;
#66001 = ORIENTED_EDGE ( 'NONE', *, *, #5748, .T. ) ;
#66002 = CARTESIAN_POINT ( 'NONE',  ( -15.12820512820512953, -11.00000000000000000, 29.75000000000000355 ) ) ;
#66003 = CARTESIAN_POINT ( 'NONE',  ( 13.19230769230769340, -3.499999999999999556, 29.75000000000000355 ) ) ;
#66004 = B_SPLINE_CURVE_WITH_KNOTS ( 'NONE', 3,
 ( #26470, #3630, #10846, #59021, #44603, #67453, #58129, #26909, #9947, #38317 ),
 .UNSPECIFIED., .F., .F.,
 ( 4, 2, 2, 2, 4 ),
 ( 0.0007817246256747447872, 0.0009771112852218876831, 0.001172497944769030579, 0.001367884604316173475, 0.001563271263863316371 ),
 .UNSPECIFIED. ) ;
#66005 = CARTESIAN_POINT ( 'NONE',  ( -14.87820512820512953, -7.500000000000000000, 29.75000000000000355 ) ) ;
#66006 = B_SPLINE_CURVE_WITH_KNOTS ( 'NONE', 3,
 ( #36561, #29807, #45075, #30245, #50061, #85192, #23470, #50929, #17162, #78417 ),
 .UNSPECIFIED., .F., .F.,
 ( 4, 2, 2, 2, 4 ),
 ( 0.000000000000000000, 0.0001954339857564091278, 0.0003908679715128182556, 0.0005863019572692274375, 0.0007817359430256365111 ),
 .UNSPECIFIED. ) ;
#66007 = CARTESIAN_POINT ( 'NONE',  ( 10.39189969082028675, -4.988325925672468131, 34.36044203135681130 ) ) ;
#66008 = CARTESIAN_POINT ( 'NONE',  ( 6.923076923076800782, -8.656820664282941280, 34.87096338111179961 ) ) ;
#66009 = CARTESIAN_POINT ( 'NONE',  ( 5.869308533332443290, -12.38065189839062263, 30.83690757178629482 ) ) ;
#66010 = VERTEX_POINT ( 'NONE', #23700 ) ;
#66011 = ORIENTED_EDGE ( 'NONE', *, *, #23985, .T. ) ;
#66012 = CYLINDRICAL_SURFACE ( 'NONE', #45996, 0.2499999999999994726 ) ;
#66013 = ORIENTED_EDGE ( 'NONE', *, *, #31118, .T. ) ;
#66014 = ADVANCED_FACE ( 'NONE', ( #84980 ), #8878, .F. ) ;
#66016 = ORIENTED_EDGE ( 'NONE', *, *, #65666, .T. ) ;
#66015 = CARTESIAN_POINT ( 'NONE',  ( -5.869474298236434073, -3.285477652293412820, 32.44071101563363158 ) ) ;
#66017 = CARTESIAN_POINT ( 'NONE',  ( 8.769230769230645706, -2.379036618888197729, 30.90682066428292885 ) ) ;
#66018 = CARTESIAN_POINT ( 'NONE',  ( -7.145943186140023329, -2.251424796025575770, 29.88072029997477586 ) ) ;
#66019 = CARTESIAN_POINT ( 'NONE',  ( 2.651650429449539104, -4.848349570550432475, 14.31250000000000000 ) ) ;
#66020 = ORIENTED_EDGE ( 'NONE', *, *, #17401, .F. ) ;
#66021 = LINE ( 'NONE', #52952, #54089 ) ;
#66022 = CIRCLE ( 'NONE', #24307, 2.000000000000001776 ) ;
#66023 = ORIENTED_EDGE ( 'NONE', *, *, #28746, .T. ) ;
#66024 = CARTESIAN_POINT ( 'NONE',  ( 7.846153846154160227, -2.255955759149395501, 30.00000000000324363 ) ) ;
#66025 = CYLINDRICAL_SURFACE ( 'NONE', #27090, 0.2499999999999998890 ) ;
#66026 = B_SPLINE_CURVE_WITH_KNOTS ( 'NONE', 3,
 ( #88373, #73954, #39729, #5498, #54103, #60425, #27974, #62, #41940, #7265 ),
 .UNSPECIFIED., .F., .F.,
 ( 4, 2, 2, 2, 4 ),
 ( 0.0007817246256747455461, 0.0009771112852218883336, 0.001172497944769031230, 0.001367884604316174126, 0.001563271263863317022 ),
 .UNSPECIFIED. ) ;
#66027 = FACE_BOUND ( 'NONE', #63592, .T. ) ;
#66029 = CARTESIAN_POINT ( 'NONE',  ( 7.976679284387489410, -2.372941743896879174, 30.88044141588253666 ) ) ;
#66028 = CARTESIAN_POINT ( 'NONE',  ( -0.4615384615384611200, -11.35647404775217417, 33.31231777344666511 ) ) ;
#66030 = FACE_OUTER_BOUND ( 'NONE', #50271, .T. ) ;
#66031 = CARTESIAN_POINT ( 'NONE',  ( -3.230769230769352962, -8.656820664282941280, 34.87096338111179961 ) ) ;
#66032 = ORIENTED_EDGE ( 'NONE', *, *, #6162, .F. ) ;
#66033 = EDGE_CURVE ( 'NONE', #5283, #86522, #15632, .T. ) ;
#66034 = LINE ( 'NONE', #38129, #28866 ) ;
#66035 = CARTESIAN_POINT ( 'NONE',  ( 8.769230769230768274, -6.386643153685126251, 34.62446782046654192 ) ) ;
#66036 = ORIENTED_EDGE ( 'NONE', *, *, #79281, .F. ) ;
#66037 = CARTESIAN_POINT ( 'NONE',  ( -8.519285359852727169, -3.520799739797214389, 33.17531984108286025 ) ) ;
#66038 = LINE ( 'NONE', #12439, #9883 ) ;
#66039 = CARTESIAN_POINT ( 'NONE',  ( -15.23076923076922995, -11.11383981884818262, 36.00935417666054406 ) ) ;
#66040 = DIRECTION ( 'NONE',  ( -0.000000000000000000, -0.000000000000000000, -1.000000000000000000 ) ) ;
#66041 = CARTESIAN_POINT ( 'NONE',  ( 12.33084699487090319, -4.118384482072086072, 33.43331474514187107 ) ) ;
#66042 = FACE_BOUND ( 'NONE', #7, .T. ) ;
#66044 = CARTESIAN_POINT ( 'NONE',  ( 0.000000000000000000, -11.00000000000000000, 29.75000000000000355 ) ) ;
#66043 = CYLINDRICAL_SURFACE ( 'NONE', #47606, 0.2500000000000002220 ) ;
#66045 = EDGE_CURVE ( 'NONE', #34824, #2196, #26464, .T. ) ;
#66046 = CARTESIAN_POINT ( 'NONE',  ( -3.230769230769229949, -10.89733346790207413, 36.13435417666054406 ) ) ;
#66048 = DIRECTION ( 'NONE',  ( -0.000000000000000000, -0.3420201433256694901, -0.9396926207859082059 ) ) ;
#66047 = CARTESIAN_POINT ( 'NONE',  ( 3.230769230769110045, -4.481592998941358097, 33.73612834414048933 ) ) ;
#66049 = CARTESIAN_POINT ( 'NONE',  ( 15.93091993633000136, -10.61292498521070549, 33.66303323003028680 ) ) ;
#66050 = FACE_OUTER_BOUND ( 'NONE', #60682, .T. ) ;
#66051 = B_SPLINE_CURVE_WITH_KNOTS ( 'NONE', 3,
 ( #75914, #7009, #5678, #61945, #33603, #40368, #60617, #14212, #68270, #69160 ),
 .UNSPECIFIED., .F., .F.,
 ( 4, 2, 2, 2, 4 ),
 ( 0.0007817246256747460882, 0.0009771112852218892010, 0.001172497944769032314, 0.001367884604316175210, 0.001563271263863318323 ),
 .UNSPECIFIED. ) ;
#66052 = CARTESIAN_POINT ( 'NONE',  ( 2.694853999681214862, -10.10844685921789043, 24.37313170625848713 ) ) ;
#66053 = EDGE_LOOP ( 'NONE', ( #73568, #17740, #35209, #69391, #40800, #67029, #79493, #12528 ) ) ;
#66054 = VECTOR ( 'NONE', #70154, 1000.000000000000000 ) ;
#66055 = AXIS2_PLACEMENT_3D ( 'NONE', #62238, #19048, #87987 ) ;
#66056 = CARTESIAN_POINT ( 'NONE',  ( -4.153846153846152411, -11.69971097300155272, 32.46337939537588113 ) ) ;
#66057 = CARTESIAN_POINT ( 'NONE',  ( 3.000000000000001776, -7.500000000000000000, 10.00000000000000178 ) ) ;
#66058 = CARTESIAN_POINT ( 'NONE',  ( -1.254089682851819987, -10.88167719472716399, 33.43325721877153711 ) ) ;
#66059 = CARTESIAN_POINT ( 'NONE',  ( 0.5001402707344744236, -10.20413752056454193, 29.33712102935293942 ) ) ;
#66060 = CARTESIAN_POINT ( 'NONE',  ( 7.596177115211490083, -4.943428324936578910, 34.04746400365624481 ) ) ;
#66061 = CYLINDRICAL_SURFACE ( 'NONE', #5220, 0.2500000000000012212 ) ;
#66062 = CARTESIAN_POINT ( 'NONE',  ( -3.775308065498766297, -6.007798216065450170, 26.17000670625849068 ) ) ;
#66063 = CARTESIAN_POINT ( 'NONE',  ( 2.242421861731533017, -11.94971097300153140, 32.03036669348370680 ) ) ;
#66064 = CARTESIAN_POINT ( 'NONE',  ( 8.703148389870632329, -2.486705287966279432, 31.30864560766542937 ) ) ;
#66065 = CIRCLE ( 'NONE', #20044, 2.000000000000001776 ) ;
#66066 = CARTESIAN_POINT ( 'NONE',  ( -0.3892027609374598685, -4.777324899857646301, 28.92434864502810399 ) ) ;
#66067 = CARTESIAN_POINT ( 'NONE',  ( -5.076923076923075762, -4.786620604624113540, 33.94971097300155094 ) ) ;
#66068 = CARTESIAN_POINT ( 'NONE',  ( -3.230769230769229949, -13.04860791097971706, 34.73218667398347037 ) ) ;
#66069 = CARTESIAN_POINT ( 'NONE',  ( -11.47239318745909742, -9.780366693483667717, 34.19971097300155805 ) ) ;
#66070 = AXIS2_PLACEMENT_3D ( 'NONE', #19247, #12488, #39971 ) ;
#66071 = EDGE_CURVE ( 'NONE', #10540, #2738, #16510, .T. ) ;
#66072 = EDGE_CURVE ( 'NONE', #19388, #2266, #86615, .T. ) ;
#66073 = CARTESIAN_POINT ( 'NONE',  ( -2.307692307691991296, -2.255955759149395501, 30.00000000000324363 ) ) ;
#66074 = DIRECTION ( 'NONE',  ( 0.000000000000000000, 1.084202172485504434E-16, -1.000000000000000000 ) ) ;
#66075 = ORIENTED_EDGE ( 'NONE', *, *, #37618, .T. ) ;
#66076 = CARTESIAN_POINT ( 'NONE',  ( 6.700197406339339246, -7.630690623152302621, 34.99857592706774057 ) ) ;
#66077 = DIRECTION ( 'NONE',  ( -0.000000000000000000, 2.546383084002652634E-16, 1.000000000000000000 ) ) ;
#66078 = CARTESIAN_POINT ( 'NONE',  ( 2.694853999681185108, -4.891553140782077591, 17.06436829374151287 ) ) ;
#66079 = CARTESIAN_POINT ( 'NONE',  ( -10.61538461538461320, -9.905515769479276145, 34.41647553114623292 ) ) ;
#66080 = DIRECTION ( 'NONE',  ( 0.000000000000000000, 0.9396926207859126468, 0.3420201433256571111 ) ) ;
#66081 = ORIENTED_EDGE ( 'NONE', *, *, #74403, .F. ) ;
#66082 = DIRECTION ( 'NONE',  ( 0.000000000000000000, 0.000000000000000000, -1.000000000000000000 ) ) ;
#66083 = CARTESIAN_POINT ( 'NONE',  ( -11.97435897435897267, -11.00000000000000000, 29.75000000000000355 ) ) ;
#66085 = ORIENTED_EDGE ( 'NONE', *, *, #76135, .T. ) ;
#66084 = CARTESIAN_POINT ( 'NONE',  ( -7.780086512803768173, -12.34228464037088813, 31.77849191805839268 ) ) ;
#66086 = DIRECTION ( 'NONE',  ( 0.000000000000000000, 0.000000000000000000, 1.000000000000000000 ) ) ;
#66087 = CYLINDRICAL_SURFACE ( 'NONE', #28262, 0.2499999999999994726 ) ;
#66088 = CYLINDRICAL_SURFACE ( 'NONE', #42038, 0.2499999999999995559 ) ;
#66089 = B_SPLINE_CURVE_WITH_KNOTS ( 'NONE', 3,
 ( #13083, #54954, #20288, #27925, #46420, #55393, #39683, #12199, #73903, #12643 ),
 .UNSPECIFIED., .F., .F.,
 ( 4, 2, 2, 2, 4 ),
 ( 0.000000000000000000, 0.0001954339857564071762, 0.0003908679715128143524, 0.0005863019572692215828, 0.0007817359430256287049 ),
 .UNSPECIFIED. ) ;
#66090 = DIRECTION ( 'NONE',  ( -0.000000000000000000, 1.000000000000000000, -0.000000000000000000 ) ) ;
#66091 = EDGE_LOOP ( 'NONE', ( #57232, #24318, #68670, #13493 ) ) ;
#66092 = DIRECTION ( 'NONE',  ( 0.000000000000000000, 0.9396926207859126468, -0.3420201433256571111 ) ) ;
#66093 = B_SPLINE_CURVE_WITH_KNOTS ( 'NONE', 3,
 ( #85749, #4664, #87098, #78532, #79877, #16835, #72666, #24474, #78981, #17282 ),
 .UNSPECIFIED., .F., .F.,
 ( 4, 2, 2, 2, 4 ),
 ( 0.000000000000000000, 0.0001954339857564070949, 0.0003908679715128141898, 0.0005863019572692212576, 0.0007817359430256283796 ),
 .UNSPECIFIED. ) ;
#66094 = B_SPLINE_CURVE_WITH_KNOTS ( 'NONE', 3,
 ( #48223, #33828, #20757, #60858, #13558, #67181, #47789, #68498, #13121, #74831 ),
 .UNSPECIFIED., .F., .F.,
 ( 4, 2, 2, 2, 4 ),
 ( 0.000000000000000000, 0.0001954339857564075828, 0.0003908679715128151656, 0.0005863019572692227755, 0.0007817359430256303312 ),
 .UNSPECIFIED. ) ;
#66095 = CARTESIAN_POINT ( 'NONE',  ( -12.46153846153858424, -2.657715359629662544, 31.77849191805970364 ) ) ;
#66096 = FACE_OUTER_BOUND ( 'NONE', #37272, .T. ) ;
#66097 = ORIENTED_EDGE ( 'NONE', *, *, #1993, .F. ) ;
#66098 = VERTEX_POINT ( 'NONE', #44860 ) ;
#66099 = VECTOR ( 'NONE', #52646, 1000.000000000000000 ) ;
#66100 = EDGE_LOOP ( 'NONE', ( #17483, #43140 ) ) ;
#66101 = DIRECTION ( 'NONE',  ( 0.000000000000000000, 0.6427876096865368094, 0.7660444431189802339 ) ) ;
#66102 = CARTESIAN_POINT ( 'NONE',  ( 9.757562831820530747, -4.320704448112861584, 33.92786785259548310 ) ) ;
#66103 = CARTESIAN_POINT ( 'NONE',  ( -12.59222992820602194, -3.530157926970578952, 32.79014554554150607 ) ) ;
#66104 = CARTESIAN_POINT ( 'NONE',  ( -17.14219352288385778, -6.879047030191174805, 34.71129190930000163 ) ) ;
#66105 = VERTEX_POINT ( 'NONE', #30901 ) ;
#66106 = VECTOR ( 'NONE', #20730, 1000.000000000000000 ) ;
#66107 = VERTEX_POINT ( 'NONE', #73237 ) ;
#66109 = ORIENTED_EDGE ( 'NONE', *, *, #83072, .F. ) ;
#66108 = CARTESIAN_POINT ( 'NONE',  ( -1.161835843346975317, -5.114059244376869984, 34.14424750095245287 ) ) ;
#66110 = CARTESIAN_POINT ( 'NONE',  ( -6.857821783564084228, -4.320704448112861584, 33.92786785259548310 ) ) ;
#66111 = DIRECTION ( 'NONE',  ( 0.000000000000000000, 0.4999999999999985567, 0.8660254037844395958 ) ) ;
#66112 = AXIS2_PLACEMENT_3D ( 'NONE', #15555, #2902, #22307 ) ;
#66113 = CARTESIAN_POINT ( 'NONE',  ( 1.384615384615265343, -10.90142922262034020, 33.41473453929536674 ) ) ;
#66114 = CARTESIAN_POINT ( 'NONE',  ( 6.000000000000001776, -2.249999999999998668, 29.75000000000001776 ) ) ;
#66115 = ORIENTED_EDGE ( 'NONE', *, *, #26646, .F. ) ;
#66116 = B_SPLINE_CURVE_WITH_KNOTS ( 'NONE', 3,
 ( #61401, #41152, #53320, #54646, #88475, #80823, #13673, #74944, #13237, #55100 ),
 .UNSPECIFIED., .F., .F.,
 ( 4, 2, 2, 2, 4 ),
 ( 0.000000000000000000, 0.0001954339857564073659, 0.0003908679715128147319, 0.0005863019572692221250, 0.0007817359430256294638 ),
 .UNSPECIFIED. ) ;
#66117 = VERTEX_POINT ( 'NONE', #66925 ) ;
#66118 = VECTOR ( 'NONE', #58036, 1000.000000000000000 ) ;
#66119 = ORIENTED_EDGE ( 'NONE', *, *, #85300, .F. ) ;
#66121 = VERTEX_POINT ( 'NONE', #38565 ) ;
#66120 = CARTESIAN_POINT ( 'NONE',  ( 6.923076923076924238, -3.322132147404559976, 32.92929555188717927 ) ) ;
#66122 = EDGE_CURVE ( 'NONE', #46484, #26148, #71894, .T. ) ;
#66123 = PRESENTATION_LAYER_ASSIGNMENT (  '', '', ( #80559 ) ) ;
#66124 = EDGE_CURVE ( 'NONE', #10850, #79237, #10206, .T. ) ;
#66125 = DIRECTION ( 'NONE',  ( -0.000000000000000000, -0.9848077530122086864, -0.1736481776669273613 ) ) ;
#66126 = B_SPLINE_CURVE_WITH_KNOTS ( 'NONE', 3,
 ( #20098, #59305, #45790, #87689, #11575, #6143, #46243, #81812, #39057, #47114 ),
 .UNSPECIFIED., .F., .F.,
 ( 4, 2, 2, 2, 4 ),
 ( 0.0007817359430256297891, 0.0009771253907249961065, 0.001172514838424362424, 0.001367904286123728741, 0.001563293733823095059 ),
 .UNSPECIFIED. ) ;
#66127 = CARTESIAN_POINT ( 'NONE',  ( 12.23861224402231151, -11.24512374952581872, 33.06303171183252942 ) ) ;
#66128 = ORIENTED_EDGE ( 'NONE', *, *, #51414, .F. ) ;
#66129 = CARTESIAN_POINT ( 'NONE',  ( -10.03846153846153832, -11.00000000000000000, 29.25000000000000000 ) ) ;
#66130 = PLANE ( 'NONE',  #56603 ) ;
#66131 = CARTESIAN_POINT ( 'NONE',  ( 4.284371855609716562, -2.882268652242224505, 31.66798894389554064 ) ) ;
#66132 = FACE_BOUND ( 'NONE', #56357, .T. ) ;
#66133 = LINE ( 'NONE', #86889, #12595 ) ;
#66134 = CARTESIAN_POINT ( 'NONE',  ( 11.47319109250076430, -8.613356846314824011, 34.62446782046655613 ) ) ;
#66135 = EDGE_CURVE ( 'NONE', #25338, #58074, #42057, .T. ) ;
#66136 = DIRECTION ( 'NONE',  ( 0.000000000000000000, 0.4999999999999960032, -0.8660254037844410391 ) ) ;
#66138 = CARTESIAN_POINT ( 'NONE',  ( -5.326899807865430603, -3.137211980971221781, 32.19342716148376837 ) ) ;
#66137 = CARTESIAN_POINT ( 'NONE',  ( 16.85343815235874132, -9.417330523894424488, 34.63758898049880486 ) ) ;
#66139 = CYLINDRICAL_SURFACE ( 'NONE', #46700, 0.2500000000000009437 ) ;
#66140 = CARTESIAN_POINT ( 'NONE',  ( -6.923076923077044142, -6.026961402154118908, 34.52809138561165270 ) ) ;
#66141 = ORIENTED_EDGE ( 'NONE', *, *, #12821, .T. ) ;
#66142 = DIRECTION ( 'NONE',  ( -0.000000000000000000, 1.000000000000000000, -0.000000000000000000 ) ) ;
#66143 = EDGE_CURVE ( 'NONE', #58556, #33472, #39399, .T. ) ;
#66144 = DIRECTION ( 'NONE',  ( -0.000000000000000000, -0.1736481776669307198, -0.9848077530122080203 ) ) ;
#66145 = ORIENTED_EDGE ( 'NONE', *, *, #65420, .T. ) ;
#66146 = ORIENTED_EDGE ( 'NONE', *, *, #72289, .T. ) ;
#66148 = CARTESIAN_POINT ( 'NONE',  ( 7.846153846153846700, -12.62096338111211580, 30.90682066428153263 ) ) ;
#66147 = LINE ( 'NONE', #18420, #57575 ) ;
#66149 = CARTESIAN_POINT ( 'NONE',  ( -16.82686865700962286, -12.65882529074907126, 30.72640787790838601 ) ) ;
#66150 = CARTESIAN_POINT ( 'NONE',  ( 14.37288529598696307, -2.255955759149235629, 29.99999999999988987 ) ) ;
#66151 = CARTESIAN_POINT ( 'NONE',  ( 15.23076923076923173, -10.05456864172156806, 36.03766855953608683 ) ) ;
#66152 = EDGE_LOOP ( 'NONE', ( #58381, #51276, #66000, #29150 ) ) ;
#66153 = LINE ( 'NONE', #65703, #57197 ) ;
#66154 = DIRECTION ( 'NONE',  ( 0.000000000000000000, 0.6427876096865373645, -0.7660444431189797898 ) ) ;
#66156 = CARTESIAN_POINT ( 'NONE',  ( 12.46153846153846168, -2.708943851104267164, 35.45975837776705220 ) ) ;
#66155 = CARTESIAN_POINT ( 'NONE',  ( 18.13052570176356681, -3.816742781228458448, 33.13167719472716044 ) ) ;
#66157 = DIRECTION ( 'NONE',  ( 0.000000000000000000, 0.8660254037844377084, 0.5000000000000015543 ) ) ;
#66158 = EDGE_CURVE ( 'NONE', #66781, #82483, #77973, .T. ) ;
#66159 = DIRECTION ( 'NONE',  ( 0.000000000000000000, -2.546383084002652634E-16, -1.000000000000000000 ) ) ;
#66160 = CYLINDRICAL_SURFACE ( 'NONE', #6086, 0.2499999999999995559 ) ;
#66161 = AXIS2_PLACEMENT_3D ( 'NONE', #60862, #19875, #52 ) ;
#66162 = CARTESIAN_POINT ( 'NONE',  ( -2.651650429449535551, -10.15165042944956753, 21.18750000000000000 ) ) ;
#66163 = ORIENTED_EDGE ( 'NONE', *, *, #57592, .F. ) ;
#66164 = ORIENTED_EDGE ( 'NONE', *, *, #55918, .F. ) ;
#66165 = CARTESIAN_POINT ( 'NONE',  ( -8.069080805060693251, -11.43668979543635089, 33.22377378376089752 ) ) ;
#66166 = CARTESIAN_POINT ( 'NONE',  ( -18.00000000000000000, -3.322132147404558200, 32.92929555188717217 ) ) ;
#66167 = CARTESIAN_POINT ( 'NONE',  ( 10.83839596699746544, -2.554770724473668153, 30.48948780036025852 ) ) ;
#66168 = CARTESIAN_POINT ( 'NONE',  ( -14.30769230769230660, -6.386643153685126251, 34.62446782046654192 ) ) ;
#66169 = CARTESIAN_POINT ( 'NONE',  ( 17.29988621118975800, -7.369474539155830506, 34.99858011523957657 ) ) ;
#66170 = CARTESIAN_POINT ( 'NONE',  ( 3.750000000000009770, -9.053300858899081760, 24.54687500000000000 ) ) ;
#66171 = DIRECTION ( 'NONE',  ( -0.000000000000000000, 0.3420201433256694901, -0.9396926207859082059 ) ) ;
#66172 = DIRECTION ( 'NONE',  ( -0.000000000000000000, -0.9396926207859093161, -0.3420201433256663259 ) ) ;
#66173 = PLANE ( 'NONE',  #64572 ) ;
#66174 = CARTESIAN_POINT ( 'NONE',  ( -2.307692307692305711, -5.415277668671390821, 36.20867863119892149 ) ) ;
#66175 = CYLINDRICAL_SURFACE ( 'NONE', #85693, 0.2500000000000012212 ) ;
#66176 = DIRECTION ( 'NONE',  ( 0.000000000000000000, 0.4999999999999960032, -0.8660254037844410391 ) ) ;
#66177 = CARTESIAN_POINT ( 'NONE',  ( -12.52680846209478460, -8.656820664281498878, 34.87096338111211935 ) ) ;
#66178 = CARTESIAN_POINT ( 'NONE',  ( 8.096208266067295156, -8.346898887586323923, 34.93166121998716278 ) ) ;
#66179 = EDGE_CURVE ( 'NONE', #74977, #33753, #18956, .T. ) ;
#66180 = CARTESIAN_POINT ( 'NONE',  ( -6.065270445960774914, -10.21337939537584383, 33.94971097300158647 ) ) ;
#66181 = AXIS2_PLACEMENT_3D ( 'NONE', #32692, #18301, #80456 ) ;
#66182 = CARTESIAN_POINT ( 'NONE',  ( 9.692307692307695177, -4.661471528628507777, 34.16647553114623292 ) ) ;
#66183 = CARTESIAN_POINT ( 'NONE',  ( -3.480792454990687901, -12.45566812827425096, 31.48439005359158926 ) ) ;
#66184 = EDGE_CURVE ( 'NONE', #37534, #31340, #7159, .T. ) ;
#66185 = ORIENTED_EDGE ( 'NONE', *, *, #39750, .F. ) ;
#66186 = CARTESIAN_POINT ( 'NONE',  ( -16.37677311275299985, -9.172386477786394821, 34.72672124145550043 ) ) ;
#66187 = CARTESIAN_POINT ( 'NONE',  ( 18.22277966897806678, -4.989023458446561143, 34.36081565061822118 ) ) ;
#66188 = CARTESIAN_POINT ( 'NONE',  ( -4.153846153846152411, -5.471508081941601098, 34.59228464037088457 ) ) ;
#66189 = CARTESIAN_POINT ( 'NONE',  ( -2.775308065498752086, -8.577988221561495763, 15.26749329374151465 ) ) ;
#66190 = CIRCLE ( 'NONE', #77699, 0.2500000000000002220 ) ;
#66191 = VECTOR ( 'NONE', #37109, 1000.000000000000000 ) ;
#66192 = EDGE_CURVE ( 'NONE', #37853, #9873, #72235, .T. ) ;
#66193 = CARTESIAN_POINT ( 'NONE',  ( 3.230769230769231726, -1.790695186598648903, 34.54067556320373455 ) ) ;
#66194 = CYLINDRICAL_SURFACE ( 'NONE', #3412, 0.2500000000000012212 ) ;
#66195 = EDGE_CURVE ( 'NONE', #19174, #42436, #42563, .T. ) ;
#66197 = VERTEX_POINT ( 'NONE', #39362 ) ;
#66196 = CARTESIAN_POINT ( 'NONE',  ( 5.076923076923075762, -3.937682226553329556, 33.60647404775216529 ) ) ;
#66198 = CARTESIAN_POINT ( 'NONE',  ( 2.750000000000001776, -7.499999999999984013, 16.96875000000000000 ) ) ;
#66199 = CARTESIAN_POINT ( 'NONE',  ( -24.99999999999999645, -15.00000000000000000, 3.000000000000000000 ) ) ;
#66200 = VECTOR ( 'NONE', #55448, 999.9999999999998863 ) ;
#66201 = ORIENTED_EDGE ( 'NONE', *, *, #51024, .T. ) ;
#66202 = VECTOR ( 'NONE', #23699, 1000.000000000000114 ) ;
#66203 = CARTESIAN_POINT ( 'NONE',  ( -18.00000000000000000, -3.513871655860376197, 32.76840700105977788 ) ) ;
#66204 = AXIS2_PLACEMENT_3D ( 'NONE', #814, #88249, #81476 ) ;
#66205 = VERTEX_POINT ( 'NONE', #10093 ) ;
#66206 = CARTESIAN_POINT ( 'NONE',  ( 2.980746006547774218, -4.931416488878823223, 34.32920672191015399 ) ) ;
#66207 = DIRECTION ( 'NONE',  ( 0.000000000000000000, 1.000000000000000000, 8.673617379884033500E-16 ) ) ;
#66208 = FACE_OUTER_BOUND ( 'NONE', #48220, .T. ) ;
#66209 = ORIENTED_EDGE ( 'NONE', *, *, #29680, .T. ) ;
#66210 = CARTESIAN_POINT ( 'NONE',  ( 8.769230769230768274, -11.69971097300155272, 32.46337939537588113 ) ) ;
#66211 = ORIENTED_EDGE ( 'NONE', *, *, #16138, .F. ) ;
#66212 = CARTESIAN_POINT ( 'NONE',  ( 11.40831432902331599, -3.817052484675422797, 33.13202310037935661 ) ) ;
#66213 = ORIENTED_EDGE ( 'NONE', *, *, #34843, .F. ) ;
#66214 = CARTESIAN_POINT ( 'NONE',  ( 13.44987095589141113, -11.94971097300157403, 32.03036669348361443 ) ) ;
#66215 = CARTESIAN_POINT ( 'NONE',  ( 2.530703659305157505, -3.105924265160262543, 32.13625925475356127 ) ) ;
#66216 = ORIENTED_EDGE ( 'NONE', *, *, #21341, .T. ) ;
#66217 = DIRECTION ( 'NONE',  ( 1.000000000000000000, 0.000000000000000000, 0.000000000000000000 ) ) ;
#66218 = CARTESIAN_POINT ( 'NONE',  ( 7.173022332454967120, -8.476813868363244353, 34.90874843262270133 ) ) ;
#66219 = CARTESIAN_POINT ( 'NONE',  ( 11.53846153846153832, -11.69971097300155272, 32.46337939537588113 ) ) ;
#66220 = CYLINDRICAL_SURFACE ( 'NONE', #69350, 0.2500000000000009437 ) ;
#66221 = ADVANCED_FACE ( 'NONE', ( #31252 ), #44755, .F. ) ;
#66222 = ORIENTED_EDGE ( 'NONE', *, *, #43206, .T. ) ;
#66223 = ORIENTED_EDGE ( 'NONE', *, *, #42003, .F. ) ;
#66224 = B_SPLINE_CURVE_WITH_KNOTS ( 'NONE', 3,
 ( #73864, #60777, #5403, #88722, #20245, #67544, #47707, #32869, #74752, #6720 ),
 .UNSPECIFIED., .F., .F.,
 ( 4, 2, 2, 2, 4 ),
 ( 0.000000000000000000, 0.0001954311564186862781, 0.0003908623128373725562, 0.0005862934692560588072, 0.0007817246256747451124 ),
 .UNSPECIFIED. ) ;
#66225 = VERTEX_POINT ( 'NONE', #24486 ) ;
#66227 = ORIENTED_EDGE ( 'NONE', *, *, #70021, .T. ) ;
#66226 = CARTESIAN_POINT ( 'NONE',  ( 3.453780582382080411, -3.587049720035815348, 32.86302985866382897 ) ) ;
#66228 = CIRCLE ( 'NONE', #4384, 0.2500000000000002220 ) ;
#66229 = DIRECTION ( 'NONE',  ( -0.000000000000000000, -1.000000000000000000, 3.491481338843133355E-15 ) ) ;
#66230 = CARTESIAN_POINT ( 'NONE',  ( 1.607394925883795844, -2.847695495035523106, 31.58253572463339154 ) ) ;
#66231 = ORIENTED_EDGE ( 'NONE', *, *, #86420, .T. ) ;
#66232 = FACE_OUTER_BOUND ( 'NONE', #70368, .T. ) ;
#66233 = EDGE_CURVE ( 'NONE', #38114, #30359, #37931, .T. ) ;
#66234 = EDGE_LOOP ( 'NONE', ( #75961, #76994, #54262, #23201 ) ) ;
#66235 = CARTESIAN_POINT ( 'NONE',  ( 11.60371710973756620, -2.625532179533470512, 30.86335684631491105 ) ) ;
#66236 = EDGE_LOOP ( 'NONE', ( #35648, #34028, #43449, #63225 ) ) ;
#66237 = LINE ( 'NONE', #81107, #76170 ) ;
#66238 = VECTOR ( 'NONE', #27400, 1000.000000000000000 ) ;
#66239 = CARTESIAN_POINT ( 'NONE',  ( -7.846153846153965716, -2.625532179533778709, 30.86335684631627174 ) ) ;
#66240 = DIRECTION ( 'NONE',  ( -0.000000000000000000, -0.1736481776669307198, -0.9848077530122080203 ) ) ;
#66241 = FACE_BOUND ( 'NONE', #83355, .T. ) ;
#66242 = CARTESIAN_POINT ( 'NONE',  ( 2.084813625263661763, -7.630691491037286056, 34.74850469731152458 ) ) ;
#66243 = CARTESIAN_POINT ( 'NONE',  ( 13.38461538461538680, -8.973038597847269315, 34.52809138561121927 ) ) ;
#66244 = CIRCLE ( 'NONE', #51901, 8.000000000000000000 ) ;
#66245 = AXIS2_PLACEMENT_3D ( 'NONE', #64028, #8221, #37001 ) ;
#66246 = EDGE_CURVE ( 'NONE', #78733, #66604, #51955, .T. ) ;
#66247 = CARTESIAN_POINT ( 'NONE',  ( 13.63466980452883881, -4.818054556918156983, 34.26375889529406749 ) ) ;
#66248 = DIRECTION ( 'NONE',  ( 0.000000000000000000, 0.8660254037844377084, 0.5000000000000015543 ) ) ;
#66249 = DIRECTION ( 'NONE',  ( -0.000000000000000000, 0.7660444431189791237, -0.6427876096865379196 ) ) ;
#66250 = DIRECTION ( 'NONE',  ( 0.000000000000000000, 0.6427876096865373645, -0.7660444431189797898 ) ) ;
#66251 = EDGE_LOOP ( 'NONE', ( #71449, #64552, #59732, #77105 ) ) ;
#66252 = CARTESIAN_POINT ( 'NONE',  ( -7.053224132515142131, -6.852621066184267029, 34.70813303252209181 ) ) ;
#66253 = EDGE_CURVE ( 'NONE', #69827, #88074, #45202, .T. ) ;
#66254 = ORIENTED_EDGE ( 'NONE', *, *, #9256, .F. ) ;
#66255 = ORIENTED_EDGE ( 'NONE', *, *, #39991, .T. ) ;
#66256 = AXIS2_PLACEMENT_3D ( 'NONE', #69262, #89113, #8006 ) ;
#66257 = B_SPLINE_CURVE_WITH_KNOTS ( 'NONE', 3,
 ( #14683, #7926, #28644, #61088, #35392, #34942, #19662, #75063, #62843, #89032 ),
 .UNSPECIFIED., .F., .F.,
 ( 4, 2, 2, 2, 4 ),
 ( 0.000000000000000000, 0.0001954339881912776238, 0.0003908679763825552477, 0.0005863019645738329257, 0.0007817359527651104954 ),
 .UNSPECIFIED. ) ;
#66259 = CARTESIAN_POINT ( 'NONE',  ( 10.83816415665302380, -5.913360116392397892, 34.49180327182771322 ) ) ;
#66258 = CARTESIAN_POINT ( 'NONE',  ( 5.776515075435673552, -12.11044203135681840, 32.26167407432752299 ) ) ;
#66260 = CARTESIAN_POINT ( 'NONE',  ( -3.930419754931365972, -7.630147987733840509, 34.99859428049665411 ) ) ;
#66261 = CARTESIAN_POINT ( 'NONE',  ( -2.177166605928741117, -12.27024696741798770, 31.24895572276497546 ) ) ;
#66262 = PLANE ( 'NONE',  #5532 ) ;
#66263 = CARTESIAN_POINT ( 'NONE',  ( -15.29685264172511161, -3.513871655860377086, 32.76840700105978499 ) ) ;
#66265 = ORIENTED_EDGE ( 'NONE', *, *, #39559, .F. ) ;
#66264 = B_SPLINE_CURVE_WITH_KNOTS ( 'NONE', 3,
 ( #8224, #48754, #35700, #42454, #57286, #76224, #63150, #64031, #70813, #1465 ),
 .UNSPECIFIED., .F., .F.,
 ( 4, 2, 2, 2, 4 ),
 ( 0.0007817246256747507503, 0.0009771112852218959231, 0.001172497944769040987, 0.001367884604316186052, 0.001563271263863331116 ),
 .UNSPECIFIED. ) ;
#66266 = CARTESIAN_POINT ( 'NONE',  ( 16.82689983963011926, -5.851115903089112003, 34.47074536777953568 ) ) ;
#66267 = CARTESIAN_POINT ( 'NONE',  ( 18.00000000000000000, -3.322132147404559976, 32.92929555188717927 ) ) ;
#66268 = CARTESIAN_POINT ( 'NONE',  ( 2.557637717070352590, -12.68172785388650681, 30.59649109432439218 ) ) ;
#66269 = EDGE_CURVE ( 'NONE', #65254, #50483, #17838, .T. ) ;
#66270 = CARTESIAN_POINT ( 'NONE',  ( 4.854044394494430037, -7.630691491037286056, 34.74850469731152458 ) ) ;
#66271 = ORIENTED_EDGE ( 'NONE', *, *, #70345, .T. ) ;
#66272 = ORIENTED_EDGE ( 'NONE', *, *, #38226, .F. ) ;
#66273 = APPLICATION_PROTOCOL_DEFINITION ( 'draft international standard', 'automotive_design', 1998, #31413 ) ;
#66275 = EDGE_CURVE ( 'NONE', #8133, #29891, #87741, .T. ) ;
#66274 = VERTEX_POINT ( 'NONE', #58273 ) ;
#66276 = CARTESIAN_POINT ( 'NONE',  ( -1.384615384615383471, -3.886160181151819604, 36.00935417666054406 ) ) ;
#66277 = CARTESIAN_POINT ( 'NONE',  ( -13.13466986626724342, -10.76462480002816235, 33.53768742498949962 ) ) ;
#66278 = ORIENTED_EDGE ( 'NONE', *, *, #42408, .F. ) ;
#66279 = ADVANCED_FACE ( 'NONE', ( #26716 ), #74914, .F. ) ;
#66280 = CARTESIAN_POINT ( 'NONE',  ( -7.596208327805704208, -4.336752205174649433, 33.62275283266504289 ) ) ;
#66281 = CARTESIAN_POINT ( 'NONE',  ( -2.057746789344164551, -4.336752205174647656, 33.62275283266504289 ) ) ;
#66282 = CARTESIAN_POINT ( 'NONE',  ( 0.6845498131513105822, -12.15243808032445827, 31.58219941686247978 ) ) ;
#66283 = CARTESIAN_POINT ( 'NONE',  ( 14.05769230769230838, -7.500000000000001776, 34.75000000000000000 ) ) ;
#66284 = CARTESIAN_POINT ( 'NONE',  ( -11.40793583669797506, -9.417988943895561960, 34.36773134775777550 ) ) ;
#66285 = VERTEX_POINT ( 'NONE', #75782 ) ;
#66287 = ORIENTED_EDGE ( 'NONE', *, *, #17243, .F. ) ;
#66286 = CARTESIAN_POINT ( 'NONE',  ( -7.596099534515528440, -9.943054286541403997, 34.11300777759954883 ) ) ;
#66288 = CARTESIAN_POINT ( 'NONE',  ( -7.715362038329057981, -8.999086150933475636, 34.52020707165672775 ) ) ;
#66289 = CARTESIAN_POINT ( 'NONE',  ( 0.2115384615384615641, -7.500000000000001776, 35.00000000000000000 ) ) ;
#66290 = CYLINDRICAL_SURFACE ( 'NONE', #63026, 0.2499999999999995559 ) ;
#66291 = AXIS2_PLACEMENT_3D ( 'NONE', #59342, #80519, #18811 ) ;
#66292 = PLANE ( 'NONE',  #82658 ) ;
#66293 = CARTESIAN_POINT ( 'NONE',  ( -8.546217925137375104, -8.282913670948747864, 34.94150082978203642 ) ) ;
#66294 = ADVANCED_FACE ( 'NONE', ( #133 ), #19514, .F. ) ;
#66295 = CARTESIAN_POINT ( 'NONE',  ( 18.06606835100244268, -2.538708090699994813, 30.37095296980875503 ) ) ;
#66296 = VECTOR ( 'NONE', #8052, 1000.000000000000227 ) ;
#66297 = CARTESIAN_POINT ( 'NONE',  ( 2.750000000000002665, -7.561099074964516831, 14.72061829374151465 ) ) ;
#66298 = ORIENTED_EDGE ( 'NONE', *, *, #67683, .T. ) ;
#66299 = DIRECTION ( 'NONE',  ( 0.000000000000000000, 0.000000000000000000, 1.000000000000000000 ) ) ;
#66300 = CARTESIAN_POINT ( 'NONE',  ( -19.00000000000000000, -11.50000000000000000, 29.75000000000000355 ) ) ;
#66301 = CARTESIAN_POINT ( 'NONE',  ( -12.46153846153858424, -6.835583212225970762, 34.95778746994575670 ) ) ;
#66302 = ADVANCED_FACE ( 'NONE', ( #46977 ), #19079, .F. ) ;
#66303 = B_SPLINE_CURVE_WITH_KNOTS ( 'NONE', 3,
 ( #23211, #44352, #16459, #84931, #24095, #51103 ),
 .UNSPECIFIED., .F., .F.,
 ( 4, 2, 4 ),
 ( 0.5000001263146904851, 0.7500000631573452425, 1.000000000000000000 ),
 .UNSPECIFIED. ) ;
#66304 = VERTEX_POINT ( 'NONE', #12322 ) ;
#66305 = ADVANCED_FACE ( 'NONE', ( #82113 ), #67268, .F. ) ;
#66306 = ORIENTED_EDGE ( 'NONE', *, *, #74615, .T. ) ;
#66307 = CARTESIAN_POINT ( 'NONE',  ( 9.915320536401090123, -3.395485233115139057, 33.02377354290275946 ) ) ;
#66308 = CARTESIAN_POINT ( 'NONE',  ( -14.08491263871424160, -2.612705202774698421, 31.66806509827799943 ) ) ;
#66309 = CARTESIAN_POINT ( 'NONE',  ( 0.000000000000000000, -11.00000000000000000, 29.75000000000000355 ) ) ;
#66310 = DIRECTION ( 'NONE',  ( -0.000000000000000000, 1.000000000000000000, 1.084202172485503448E-16 ) ) ;
#66311 = CARTESIAN_POINT ( 'NONE',  ( 17.77707304109313924, -11.98009711892700224, 32.48740034544074007 ) ) ;
#66312 = DIRECTION ( 'NONE',  ( 0.000000000000000000, 0.8660254037844377084, 0.5000000000000015543 ) ) ;
#66313 = VERTEX_POINT ( 'NONE', #20406 ) ;
#66314 = CARTESIAN_POINT ( 'NONE',  ( 9.468822748583747284, -10.81261337010820256, 33.49550067578627477 ) ) ;
#66315 = AXIS2_PLACEMENT_3D ( 'NONE', #6809, #34283, #35627 ) ;
#66316 = CARTESIAN_POINT ( 'NONE',  ( -2.057637996053990115, -9.943054286541407549, 34.11300777759954883 ) ) ;
#66318 = EDGE_CURVE ( 'NONE', #19392, #37313, #9226, .T. ) ;
#66317 = VECTOR ( 'NONE', #14470, 1000.000000000000000 ) ;
#66319 = CARTESIAN_POINT ( 'NONE',  ( 16.82689983963011926, -9.271318131107980420, 34.42618302367067429 ) ) ;
#66320 = EDGE_LOOP ( 'NONE', ( #57827, #63591, #77490, #34788 ) ) ;
#66321 = CARTESIAN_POINT ( 'NONE',  ( 10.48469401227430708, -9.084618155246140248, 34.75535874321725771 ) ) ;
#66322 = VECTOR ( 'NONE', #71563, 1000.000000000000227 ) ;
#66323 = VECTOR ( 'NONE', #73151, 1000.000000000000000 ) ;
#66324 = ORIENTED_EDGE ( 'NONE', *, *, #9715, .T. ) ;
#66325 = CARTESIAN_POINT ( 'NONE',  ( 1.450784525578043382, -7.250054483168843156, 34.74374881642865631 ) ) ;
#66326 = CARTESIAN_POINT ( 'NONE',  ( 10.61538461538461675, -3.322132147404559976, 32.92929555188717927 ) ) ;
#66327 = EDGE_CURVE ( 'NONE', #54986, #75871, #14088, .T. ) ;
#66328 = CARTESIAN_POINT ( 'NONE',  ( 18.00000000000000000, -9.905515769479276145, 34.41647553114623292 ) ) ;
#66329 = ORIENTED_EDGE ( 'NONE', *, *, #10859, .T. ) ;
#66330 = CARTESIAN_POINT ( 'NONE',  ( 12.21156173059610772, -3.627789207965226748, 32.91389620160131102 ) ) ;
#66331 = CARTESIAN_POINT ( 'NONE',  ( 5.934729554039226862, -10.21337939537584383, 33.94971097300158647 ) ) ;
#66332 = DIRECTION ( 'NONE',  ( -1.000000000000000000, -0.000000000000000000, -0.000000000000000000 ) ) ;
#66333 = VECTOR ( 'NONE', #12229, 999.9999999999998863 ) ;
#66334 = CARTESIAN_POINT ( 'NONE',  ( -6.065270000556318486, -5.941354392334500467, 34.76329471203369792 ) ) ;
#66335 = CARTESIAN_POINT ( 'NONE',  ( -3.164700879766791708, -12.37446782046654192, 30.86335684631486842 ) ) ;
#66336 = EDGE_CURVE ( 'NONE', #73822, #55802, #67708, .T. ) ;
#66337 = ORIENTED_EDGE ( 'NONE', *, *, #80623, .T. ) ;
#66338 = CARTESIAN_POINT ( 'NONE',  ( -3.931066484868084299, -12.47679350104403007, 31.42216943046555855 ) ) ;
#66339 = EDGE_LOOP ( 'NONE', ( #8135, #85059 ) ) ;
#66340 = CARTESIAN_POINT ( 'NONE',  ( 11.28846153846153832, -7.500000000000001776, 34.75000000000000000 ) ) ;
#66341 = EDGE_CURVE ( 'NONE', #78622, #67447, #14643, .T. ) ;
#66342 = CARTESIAN_POINT ( 'NONE',  ( -10.61538461538430589, -2.506253911140614576, 30.00000000000323297 ) ) ;
#66343 = EDGE_CURVE ( 'NONE', #61908, #5574, #10339, .T. ) ;
#66344 = CARTESIAN_POINT ( 'NONE',  ( -13.38461538461550582, -2.892918686052166066, 31.69288490824153470 ) ) ;
#66345 = CYLINDRICAL_SURFACE ( 'NONE', #40184, 4.000000000000000000 ) ;
#66346 = CYLINDRICAL_SURFACE ( 'NONE', #27834, 0.2500000000000002220 ) ;
#66347 = DIRECTION ( 'NONE',  ( 0.000000000000000000, 0.000000000000000000, 1.000000000000000000 ) ) ;
#66348 = VERTEX_POINT ( 'NONE', #15873 ) ;
#66349 = EDGE_CURVE ( 'NONE', #89174, #75689, #62964, .T. ) ;
#66350 = ORIENTED_EDGE ( 'NONE', *, *, #43427, .T. ) ;
#66351 = ORIENTED_EDGE ( 'NONE', *, *, #29295, .F. ) ;
#66352 = ORIENTED_EDGE ( 'NONE', *, *, #86324, .T. ) ;
#66353 = ORIENTED_EDGE ( 'NONE', *, *, #51990, .F. ) ;
#66354 = CARTESIAN_POINT ( 'NONE',  ( 20.74999999999999645, -4.499999999999999112, 27.25000000000000000 ) ) ;
#66355 = CARTESIAN_POINT ( 'NONE',  ( -11.60373198442231590, -9.442884908240170461, 34.35708131394840592 ) ) ;
#66356 = AXIS2_PLACEMENT_3D ( 'NONE', #11923, #40285, #32191 ) ;
#66357 = CARTESIAN_POINT ( 'NONE',  ( -10.61538461538461320, -4.661471528628507777, 34.16647553114623292 ) ) ;
#66358 = CARTESIAN_POINT ( 'NONE',  ( -6.988347369037697376, -3.300289026998414865, 32.46337939537583139 ) ) ;
#66359 = CARTESIAN_POINT ( 'NONE',  ( -13.31854703361294590, -5.557115091759786019, 34.35708131394839882 ) ) ;
#66360 = CARTESIAN_POINT ( 'NONE',  ( -12.59168643127016196, -12.50552854090298993, 31.33409797877408920 ) ) ;
#66361 = CYLINDRICAL_SURFACE ( 'NONE', #86859, 0.2499999999999995559 ) ;
#66362 = CARTESIAN_POINT ( 'NONE',  ( 9.442284468086239002, -10.18141759479407327, 34.26406193332782379 ) ) ;
#66363 = CARTESIAN_POINT ( 'NONE',  ( 8.068933515131909928, -4.989023458446560255, 34.36081565061822118 ) ) ;
#66364 = EDGE_LOOP ( 'NONE', ( #19602, #87466 ) ) ;
#66365 = EDGE_CURVE ( 'NONE', #25943, #34857, #34795, .T. ) ;
#66366 = ORIENTED_EDGE ( 'NONE', *, *, #13930, .T. ) ;
#66367 = ORIENTED_EDGE ( 'NONE', *, *, #30539, .T. ) ;
#66369 = VERTEX_POINT ( 'NONE', #9116 ) ;
#66368 = CARTESIAN_POINT ( 'NONE',  ( 11.78840694783958121, -2.589246495874658383, 31.60778113518102828 ) ) ;
#66371 = CYLINDRICAL_SURFACE ( 'NONE', #62114, 0.2499999999999994726 ) ;
#66370 = CARTESIAN_POINT ( 'NONE',  ( -16.08777780284371772, -6.386643153685127139, 34.62446782046654192 ) ) ;
#66372 = B_SPLINE_CURVE_WITH_KNOTS ( 'NONE', 3,
 ( #30324, #37067, #35766, #56470, #8292, #35308, #62764, #22238, #83960, #78499 ),
 .UNSPECIFIED., .F., .F.,
 ( 4, 2, 2, 2, 4 ),
 ( 0.0007817359430256294638, 0.0009771253907249937212, 0.001172514838424358087, 0.001367904286123722453, 0.001563293733823093758 ),
 .UNSPECIFIED. ) ;
#66373 = FACE_OUTER_BOUND ( 'NONE', #54026, .T. ) ;
#66374 = CARTESIAN_POINT ( 'NONE',  ( -14.53061852520844965, -9.886141570436013382, 34.14413921362392301 ) ) ;
#66375 = FACE_BOUND ( 'NONE', #71949, .T. ) ;
#66376 = ORIENTED_EDGE ( 'NONE', *, *, #10333, .T. ) ;
#66377 = VERTEX_POINT ( 'NONE', #36147 ) ;
#66378 = CARTESIAN_POINT ( 'NONE',  ( -17.07692307692319744, -11.67786785259630911, 32.92929555188603530 ) ) ;
#66379 = ORIENTED_EDGE ( 'NONE', *, *, #79384, .F. ) ;
#66380 = FACE_BOUND ( 'NONE', #16086, .T. ) ;
#66381 = CARTESIAN_POINT ( 'NONE',  ( 9.942362112221147186, -5.642605341092957971, 34.66089969410670335 ) ) ;
#66382 = CARTESIAN_POINT ( 'NONE',  ( 3.512820512820511443, -4.000000000000000000, 29.75000000000000355 ) ) ;
#66383 = ORIENTED_EDGE ( 'NONE', *, *, #77213, .F. ) ;
#66384 = CARTESIAN_POINT ( 'NONE',  ( -14.98082371242108835, -12.22109172314383052, 31.39792113162168263 ) ) ;
#66385 = CARTESIAN_POINT ( 'NONE',  ( -1.608100309179714582, -8.539481045369598178, 34.89627647299170832 ) ) ;
#66386 = CARTESIAN_POINT ( 'NONE',  ( 2.084765348785460048, -11.43668979543635089, 33.22377378376089752 ) ) ;
#66387 = ORIENTED_EDGE ( 'NONE', *, *, #55699, .F. ) ;
#66388 = CARTESIAN_POINT ( 'NONE',  ( 12.23861224402231151, -4.887634598454295265, 34.01352882383564946 ) ) ;
#66389 = CARTESIAN_POINT ( 'NONE',  ( -14.30769230769242739, -6.026961402154118019, 34.52809138561165270 ) ) ;
#66390 = DIRECTION ( 'NONE',  ( -0.000000000000000000, 0.8660254037844397068, -0.4999999999999978906 ) ) ;
#66391 = ORIENTED_EDGE ( 'NONE', *, *, #33742, .F. ) ;
#66392 = VECTOR ( 'NONE', #34050, 1000.000000000000114 ) ;
#66393 = CARTESIAN_POINT ( 'NONE',  ( 2.438217745925951085, -12.50538340440932217, 31.33453814440721885 ) ) ;
#66394 = CARTESIAN_POINT ( 'NONE',  ( -16.94639737515951339, -11.93748526763465279, 32.05452791011430946 ) ) ;
#66395 = ORIENTED_EDGE ( 'NONE', *, *, #83228, .F. ) ;
#66396 = CARTESIAN_POINT ( 'NONE',  ( 0.4615384615384611200, -8.973038597847269315, 34.52809138561121927 ) ) ;
#66397 = CARTESIAN_POINT ( 'NONE',  ( 14.30769230769231015, -8.120952969808772792, 34.71129190930000163 ) ) ;
#66398 = CARTESIAN_POINT ( 'NONE',  ( -2.531177251416254492, -2.599994579823203367, 30.74605699353653776 ) ) ;
#66400 = B_SPLINE_CURVE_WITH_KNOTS ( 'NONE', 3,
 ( #46884, #32482, #20313, #46443, #82018, #74367, #59512, #25734, #27064, #73487 ),
 .UNSPECIFIED., .F., .F.,
 ( 4, 2, 2, 2, 4 ),
 ( 0.0007817359430256366195, 0.0009771253907250045632, 0.001172514838424372615, 0.001367904286123740668, 0.001563293733823108720 ),
 .UNSPECIFIED. ) ;
#66399 = CARTESIAN_POINT ( 'NONE',  ( -8.703162418228332697, -8.973038597847271092, 34.52809138561121216 ) ) ;
#66401 = CARTESIAN_POINT ( 'NONE',  ( -7.173076923076921574, -7.500000000000001776, 35.00000000000000000 ) ) ;
#66402 = FACE_OUTER_BOUND ( 'NONE', #24575, .T. ) ;
#66403 = B_SPLINE_CURVE_WITH_KNOTS ( 'NONE', 3,
 ( #11859, #5540, #64661, #33008, #10181, #39335, #57469, #66790, #78189, #5092 ),
 .UNSPECIFIED., .F., .F.,
 ( 4, 2, 2, 2, 4 ),
 ( 0.0007817359430256333669, 0.0009771253907250056474, 0.001172514838424370881, 0.001367904286123736331, 0.001563293733823101564 ),
 .UNSPECIFIED. ) ;
#66405 = CARTESIAN_POINT ( 'NONE',  ( 8.703960768674447124, -3.083524468853724443, 32.58852847137143272 ) ) ;
#66404 = CARTESIAN_POINT ( 'NONE',  ( 0.5267936010512991318, -11.67786785259547777, 32.92929555188713664 ) ) ;
#66406 = EDGE_CURVE ( 'NONE', #33660, #12785, #63598, .T. ) ;
#66407 = CARTESIAN_POINT ( 'NONE',  ( -11.97435897435897267, -11.50000000000000000, 29.75000000000000355 ) ) ;
#66409 = CARTESIAN_POINT ( 'NONE',  ( 12.39626846098214230, -5.094484230520674117, 34.41647553114621161 ) ) ;
#66408 = CARTESIAN_POINT ( 'NONE',  ( -14.98071481085577972, -2.544122305571458575, 31.48381861865057729 ) ) ;
#66410 = CARTESIAN_POINT ( 'NONE',  ( 1.139087296526029469, -10.24999999999999467, 15.95312500000000000 ) ) ;
#66411 = EDGE_LOOP ( 'NONE', ( #71242, #25669, #72167, #60366 ) ) ;
#66412 = CARTESIAN_POINT ( 'NONE',  ( -12.59222992820602194, -8.147922237126337563, 34.70805685702651999 ) ) ;
#66413 = ORIENTED_EDGE ( 'NONE', *, *, #56441, .F. ) ;
#66414 = EDGE_CURVE ( 'NONE', #13929, #14132, #77120, .T. ) ;
#66415 = ORIENTED_EDGE ( 'NONE', *, *, #66246, .T. ) ;
#66416 = CYLINDRICAL_SURFACE ( 'NONE', #13881, 0.2500000000000002220 ) ;
#66417 = EDGE_CURVE ( 'NONE', #38481, #36016, #66264, .T. ) ;
#66418 = ORIENTED_EDGE ( 'NONE', *, *, #48367, .F. ) ;
#66419 = CARTESIAN_POINT ( 'NONE',  ( 18.13004760625567968, -7.723484964179501588, 34.74522123443823318 ) ) ;
#66420 = CARTESIAN_POINT ( 'NONE',  ( -2.749999999999998224, -7.500000000000015987, 16.34375000000000000 ) ) ;
#66421 = CARTESIAN_POINT ( 'NONE',  ( -18.00000000000000000, -4.661471528628506000, 34.16647553114623292 ) ) ;
#66422 = CARTESIAN_POINT ( 'NONE',  ( -17.74999999999856115, -7.500000000000155431, 34.75000000000007105 ) ) ;
#66423 = CARTESIAN_POINT ( 'NONE',  ( 9.758375025657770152, -9.058645607665452459, 34.76329471203371924 ) ) ;
#66424 = CARTESIAN_POINT ( 'NONE',  ( 16.15384615384615330, -13.75783147151868846, 33.36296068462461051 ) ) ;
#66425 = LINE ( 'NONE', #79501, #53269 ) ;
#66426 = LINE ( 'NONE', #37612, #37267 ) ;
#66427 = CARTESIAN_POINT ( 'NONE',  ( -7.780085495151409347, -12.10708131394839882, 31.69288490824020954 ) ) ;
#66428 = EDGE_CURVE ( 'NONE', #69663, #31874, #64095, .T. ) ;
#66429 = VECTOR ( 'NONE', #77998, 1000.000000000000227 ) ;
#66430 = CARTESIAN_POINT ( 'NONE',  ( -3.749999999999988454, -9.053300858899127945, 23.76562499999999645 ) ) ;
#66431 = CARTESIAN_POINT ( 'NONE',  ( 17.14217821643591932, -2.379036618887895305, 30.90682066428158592 ) ) ;
#66432 = CARTESIAN_POINT ( 'NONE',  ( 18.00000000000000000, -12.10708131394839349, 31.69288490824020244 ) ) ;
#66433 = AXIS2_PLACEMENT_3D ( 'NONE', #36092, #16251, #1849 ) ;
#66434 = EDGE_CURVE ( 'NONE', #68701, #59603, #25337, .T. ) ;
#66435 = CARTESIAN_POINT ( 'NONE',  ( 5.448717948717947124, -3.499999999999999556, 29.75000000000000355 ) ) ;
#66436 = ORIENTED_EDGE ( 'NONE', *, *, #67215, .T. ) ;
#66437 = ORIENTED_EDGE ( 'NONE', *, *, #48234, .F. ) ;
#66438 = CARTESIAN_POINT ( 'NONE',  ( -11.31568199719312773, -5.913360116392397892, 34.49180327182771322 ) ) ;
#66439 = CARTESIAN_POINT ( 'NONE',  ( -14.17716660592874689, -8.586989748646452369, 34.63063291749215011 ) ) ;
#66440 = DIRECTION ( 'NONE',  ( -0.000000000000000000, 1.000000000000000000, -0.000000000000000000 ) ) ;
#66441 = CARTESIAN_POINT ( 'NONE',  ( -15.90390063549801347, -12.43552623307873972, 30.55307653245132826 ) ) ;
#66442 = DIRECTION ( 'NONE',  ( -1.000000000000000000, -0.000000000000000000, 0.000000000000000000 ) ) ;
#66443 = CARTESIAN_POINT ( 'NONE',  ( -0.5922299282060191628, -6.413092428213692742, 34.63065189839063152 ) ) ;
#66444 = B_SPLINE_CURVE_WITH_KNOTS ( 'NONE', 3,
 ( #6321, #34672, #27908, #43193, #43626, #16161, #62999, #15282, #8969, #29249 ),
 .UNSPECIFIED., .F., .F.,
 ( 4, 2, 2, 2, 4 ),
 ( 0.000000000000000000, 0.0001954339881912774612, 0.0003908679763825549224, 0.0005863019645738323836, 0.0007817359527651098448 ),
 .UNSPECIFIED. ) ;
#66445 = VERTEX_POINT ( 'NONE', #28044 ) ;
#66446 = CARTESIAN_POINT ( 'NONE',  ( 3.100621261037536325, -6.809168938359898782, 34.95455904226513866 ) ) ;
#66447 = EDGE_LOOP ( 'NONE', ( #10242, #52141, #29365, #10387 ) ) ;
#66448 = EDGE_CURVE ( 'NONE', #38559, #47058, #84336, .T. ) ;
#66449 = ORIENTED_EDGE ( 'NONE', *, *, #20750, .T. ) ;
#66450 = AXIS2_PLACEMENT_3D ( 'NONE', #8468, #35941, #84138 ) ;
#66451 = CARTESIAN_POINT ( 'NONE',  ( -5.999999999999998224, -5.557115091759785130, 34.35708131394839171 ) ) ;
#66452 = AXIS2_PLACEMENT_3D ( 'NONE', #34761, #40208, #62232 ) ;
#66453 = CARTESIAN_POINT ( 'NONE',  ( -24.99999999999999645, -19.99999999999999645, 3.000000000000000000 ) ) ;
#66454 = CARTESIAN_POINT ( 'NONE',  ( -9.561515884482904681, -6.413143153341454017, 34.63066358083362672 ) ) ;
#66455 = LINE ( 'NONE', #38543, #1930 ) ;
#66456 = CARTESIAN_POINT ( 'NONE',  ( 13.25446741488368829, -5.915902021225889484, 34.75552854090298638 ) ) ;
#66457 = AXIS2_PLACEMENT_3D ( 'NONE', #62110, #417, #53577 ) ;
#66458 = ORIENTED_EDGE ( 'NONE', *, *, #71272, .F. ) ;
#66459 = EDGE_CURVE ( 'NONE', #9541, #11982, #35241, .T. ) ;
#66460 = ORIENTED_EDGE ( 'NONE', *, *, #83911, .F. ) ;
#66461 = VERTEX_POINT ( 'NONE', #76681 ) ;
#66462 = ADVANCED_FACE ( 'NONE', ( #24375 ), #25282, .F. ) ;
#66463 = DIRECTION ( 'NONE',  ( 0.000000000000000000, 1.000000000000000000, 0.000000000000000000 ) ) ;
#66464 = CARTESIAN_POINT ( 'NONE',  ( 5.448717948717947124, -3.499999999999999556, 29.75000000000000355 ) ) ;
#66465 = B_SPLINE_CURVE_WITH_KNOTS ( 'NONE', 3,
 ( #60460, #19477, #54581, #46937, #74423, #94, #55040, #82526, #14049, #41525 ),
 .UNSPECIFIED., .F., .F.,
 ( 4, 2, 2, 2, 4 ),
 ( 0.000000000000000000, 0.0001954311564186871184, 0.0003908623128373742367, 0.0005862934692560614093, 0.0007817246256747484735 ),
 .UNSPECIFIED. ) ;
#66466 = DIRECTION ( 'NONE',  ( -0.000000000000000000, 0.1736481776669307198, -0.9848077530122080203 ) ) ;
#66467 = DIRECTION ( 'NONE',  ( 0.000000000000000000, -1.000000000000000000, -8.673617379884033500E-16 ) ) ;
#66468 = B_SPLINE_CURVE_WITH_KNOTS ( 'NONE', 3,
 ( #51051, #17296, #51954, #73131, #72680, #65021 ),
 .UNSPECIFIED., .F., .F.,
 ( 4, 2, 4 ),
 ( 0.0003909512603273872016, 0.0005862562993132132720, 0.0007815613382990393423 ),
 .UNSPECIFIED. ) ;
#66469 = CARTESIAN_POINT ( 'NONE',  ( -3.903846153846215472, -7.565270445406050648, 34.75000000000000000 ) ) ;
#66470 = CARTESIAN_POINT ( 'NONE',  ( 18.00000000000000000, -8.120952969808772792, 34.71129190930000163 ) ) ;
#66471 = ORIENTED_EDGE ( 'NONE', *, *, #65534, .F. ) ;
#66472 = B_SPLINE_CURVE_WITH_KNOTS ( 'NONE', 3,
 ( #3941, #85488, #23331, #22453, #57562, #78274, #71515, #9823, #49918, #85053 ),
 .UNSPECIFIED., .F., .F.,
 ( 4, 2, 2, 2, 4 ),
 ( 0.000000000000000000, 0.0001954339857564080707, 0.0003908679715128161414, 0.0005863019572692241849, 0.0007817359430256322827 ),
 .UNSPECIFIED. ) ;
#66473 = EDGE_CURVE ( 'NONE', #76426, #30118, #4925, .T. ) ;
#66474 = ORIENTED_EDGE ( 'NONE', *, *, #83296, .T. ) ;
#66475 = CARTESIAN_POINT ( 'NONE',  ( 0.4615384615383396616, -11.94971097300221174, 32.03036669348237098 ) ) ;
#66477 = ORIENTED_EDGE ( 'NONE', *, *, #17507, .T. ) ;
#66476 = CARTESIAN_POINT ( 'NONE',  ( -13.51476335434708353, -5.915902021225889484, 34.75552854090298638 ) ) ;
#66478 = CYLINDRICAL_SURFACE ( 'NONE', #47896, 0.2499999999999995837 ) ;
#66479 = CARTESIAN_POINT ( 'NONE',  ( -6.923076923076607159, -2.255955759149395501, 30.00000000000324363 ) ) ;
#66480 = ADVANCED_FACE ( 'NONE', ( #30266 ), #31135, .T. ) ;
#66481 = EDGE_CURVE ( 'NONE', #12502, #71930, #64467, .T. ) ;
#66482 = CARTESIAN_POINT ( 'NONE',  ( -1.553300858899081760, -11.25000000000000888, 16.10937500000000355 ) ) ;
#66483 = VERTEX_POINT ( 'NONE', #10881 ) ;
#66484 = CARTESIAN_POINT ( 'NONE',  ( 10.86543903529806876, -2.318338780012835443, 30.59689888758630261 ) ) ;
#66485 = ORIENTED_EDGE ( 'NONE', *, *, #35443, .T. ) ;
#66486 = EDGE_CURVE ( 'NONE', #67767, #68629, #66734, .T. ) ;
#66487 = B_SPLINE_CURVE_WITH_KNOTS ( 'NONE', 3,
 ( #18254, #65538, #79059, #66884, #73655, #87176, #59677, #79954, #39427, #52470 ),
 .UNSPECIFIED., .F., .F.,
 ( 4, 2, 2, 2, 4 ),
 ( 0.000000000000000000, 0.0001954339857564064173, 0.0003908679715128128345, 0.0005863019572692191976, 0.0007817359430256256691 ),
 .UNSPECIFIED. ) ;
#66488 = CARTESIAN_POINT ( 'NONE',  ( 15.12820512820512953, -7.500000000000000000, 29.75000000000000355 ) ) ;
#66489 = FACE_OUTER_BOUND ( 'NONE', #18543, .T. ) ;
#66490 = CYLINDRICAL_SURFACE ( 'NONE', #59621, 0.2500000000000008882 ) ;
#66492 = CYLINDRICAL_SURFACE ( 'NONE', #47358, 0.2499999999999995559 ) ;
#66491 = FACE_OUTER_BOUND ( 'NONE', #54006, .T. ) ;
#66493 = CARTESIAN_POINT ( 'NONE',  ( 0.4615384615384611200, -11.11383981884818262, 36.00935417666054406 ) ) ;
#66494 = EDGE_LOOP ( 'NONE', ( #71621, #54809 ) ) ;
#66495 = CARTESIAN_POINT ( 'NONE',  ( -11.40767109749459074, -8.191423895709840863, 34.95447573519442130 ) ) ;
#66496 = CARTESIAN_POINT ( 'NONE',  ( 11.40790162484817216, -2.254533558242299396, 29.97296025877828285 ) ) ;
#66497 = DIRECTION ( 'NONE',  ( 1.000000000000000000, 0.000000000000000000, 0.000000000000000000 ) ) ;
#66498 = ORIENTED_EDGE ( 'NONE', *, *, #87240, .F. ) ;
#66499 = CARTESIAN_POINT ( 'NONE',  ( -9.469528023329623068, -4.989023458446560255, 34.36081565061822118 ) ) ;
#66500 = CARTESIAN_POINT ( 'NONE',  ( 14.55763771707035303, -10.18230066228895758, 34.26354781536631577 ) ) ;
#66501 = CARTESIAN_POINT ( 'NONE',  ( 11.28848480751918437, -5.728515186090277211, 34.42611988154120439 ) ) ;
#66502 = CARTESIAN_POINT ( 'NONE',  ( 9.019176178608812933, -10.18230066228895758, 34.26354781536631577 ) ) ;
#66503 = FACE_BOUND ( 'NONE', #75409, .T. ) ;
#66505 = LINE ( 'NONE', #25072, #33090 ) ;
#66504 = CARTESIAN_POINT ( 'NONE',  ( -7.053767526187231240, -12.35290016733513951, 31.75349464988449455 ) ) ;
#66506 = B_SPLINE_CURVE_WITH_KNOTS ( 'NONE', 3,
 ( #74388, #54545, #33407, #60, #18559, #46023, #39283, #11804, #61741, #73952 ),
 .UNSPECIFIED., .F., .F.,
 ( 4, 2, 2, 2, 4 ),
 ( 0.000000000000000000, 0.0001954339857564071762, 0.0003908679715128143524, 0.0005863019572692215828, 0.0007817359430256287049 ),
 .UNSPECIFIED. ) ;
#66507 = LINE ( 'NONE', #33610, #39650 ) ;
#66509 = CARTESIAN_POINT ( 'NONE',  ( 2.307692307692186251, -5.094484230521993062, 34.41647553114689373 ) ) ;
#66508 = CARTESIAN_POINT ( 'NONE',  ( 1.161130460051055024, -12.69144148231606017, 30.53333754910549303 ) ) ;
#66510 = CARTESIAN_POINT ( 'NONE',  ( 16.15384615384603251, -10.90142922262034020, 33.41473453929536674 ) ) ;
#66511 = CARTESIAN_POINT ( 'NONE',  ( 13.31934538405906565, -2.657715359629088780, 31.77849191805832874 ) ) ;
#66512 = CARTESIAN_POINT ( 'NONE',  ( 1.614399933863660985, -11.22469193450123193, 24.45125670625849423 ) ) ;
#66513 = B_SPLINE_CURVE_WITH_KNOTS ( 'NONE', 3,
 ( #19902, #6831, #41512, #68979, #74866, #82514, #82067, #47373, #20363, #55902 ),
 .UNSPECIFIED., .F., .F.,
 ( 4, 2, 2, 2, 4 ),
 ( 0.0007817246256747519429, 0.0009771112852218970073, 0.001172497944769042288, 0.001367884604316187353, 0.001563271263863332417 ),
 .UNSPECIFIED. ) ;
#66514 = EDGE_CURVE ( 'NONE', #32981, #76146, #50051, .T. ) ;
#66515 = VECTOR ( 'NONE', #50981, 1000.000000000000227 ) ;
#66516 = CARTESIAN_POINT ( 'NONE',  ( 1.384615384615386802, -1.790695186598648903, 34.54067556320373455 ) ) ;
#66517 = VERTEX_POINT ( 'NONE', #10439 ) ;
#66518 = VECTOR ( 'NONE', #83300, 1000.000000000000000 ) ;
#66519 = DIRECTION ( 'NONE',  ( 1.000000000000000000, 0.000000000000000000, 0.000000000000000000 ) ) ;
#66520 = CARTESIAN_POINT ( 'NONE',  ( -4.023320452082587373, -12.27024696741798770, 31.24895572276497546 ) ) ;
#66521 = DIRECTION ( 'NONE',  ( -0.000000000000000000, -0.9396926207859092051, -0.3420201433256662704 ) ) ;
#66522 = DIRECTION ( 'NONE',  ( -1.000000000000000000, -0.000000000000000000, -0.000000000000000000 ) ) ;
#66523 = CARTESIAN_POINT ( 'NONE',  ( 6.000000000000001776, -2.517432740324522911, 35.29906147534542527 ) ) ;
#66524 = CARTESIAN_POINT ( 'NONE',  ( -12.46153846153846168, -6.343179335718451384, 34.87096338111211935 ) ) ;
#66525 = CARTESIAN_POINT ( 'NONE',  ( -1.901340078031346525, -9.487747218494661183, 15.93563170625849068 ) ) ;
#66526 = CIRCLE ( 'NONE', #47814, 0.2500000000000002220 ) ;
#66527 = CARTESIAN_POINT ( 'NONE',  ( 15.23076923076923173, -11.91647553114624181, 32.58852847137148245 ) ) ;
#66528 = CYLINDRICAL_SURFACE ( 'NONE', #27406, 0.2499999999999979738 ) ;
#66529 = CARTESIAN_POINT ( 'NONE',  ( 17.07692307692307665, -12.78798330534103123, 29.99999999999997868 ) ) ;
#66530 = CARTESIAN_POINT ( 'NONE',  ( 4.826899852701619587, -9.356822207818506598, 34.66110646841856635 ) ) ;
#66531 = CARTESIAN_POINT ( 'NONE',  ( 0.4615384615384611200, -11.16473453929635440, 33.15142922261926373 ) ) ;
#66532 = CARTESIAN_POINT ( 'NONE',  ( 12.46153846153846168, -13.75783147151868846, 33.36296068462461051 ) ) ;
#66533 = EDGE_CURVE ( 'NONE', #66936, #16713, #18532, .T. ) ;
#66534 = CARTESIAN_POINT ( 'NONE',  ( 3.165015802455898974, -7.249945578846654470, 34.99404164642496795 ) ) ;
#66535 = DIRECTION ( 'NONE',  ( 0.000000000000000000, 0.8660254037844377084, 0.5000000000000015543 ) ) ;
#66536 = ORIENTED_EDGE ( 'NONE', *, *, #39897, .F. ) ;
#66537 = EDGE_CURVE ( 'NONE', #43796, #28699, #4107, .T. ) ;
#66538 = CARTESIAN_POINT ( 'NONE',  ( 17.14299142792551578, -2.721908614388772296, 31.22303859784725333 ) ) ;
#66539 = CYLINDRICAL_SURFACE ( 'NONE', #31681, 0.2500000000000004996 ) ;
#66540 = CARTESIAN_POINT ( 'NONE',  ( 3.724691934501251023, -9.114399933863618131, 21.04874329374151642 ) ) ;
#66541 = CARTESIAN_POINT ( 'NONE',  ( -15.16557624247457348, -2.255955759149234741, 29.99999999999988631 ) ) ;
#66542 = CARTESIAN_POINT ( 'NONE',  ( -16.21911615440246734, -11.06231777344663136, 33.60647404775220082 ) ) ;
#66543 = ORIENTED_EDGE ( 'NONE', *, *, #37205, .T. ) ;
#66544 = CARTESIAN_POINT ( 'NONE',  ( 7.146088274689774700, -8.239487800360276282, 34.69522927552633718 ) ) ;
#66545 = DIRECTION ( 'NONE',  ( 0.000000000000000000, 0.000000000000000000, 1.000000000000000000 ) ) ;
#66547 = VERTEX_POINT ( 'NONE', #31591 ) ;
#66546 = CARTESIAN_POINT ( 'NONE',  ( 11.78846153846155431, -2.249999999999999112, 29.81603969181029967 ) ) ;
#66548 = CARTESIAN_POINT ( 'NONE',  ( -9.758390071667825794, -3.322132147404559532, 32.92929555188719348 ) ) ;
#66549 = CARTESIAN_POINT ( 'NONE',  ( -3.100243529005665355, -3.816742781228458448, 33.13167719472716044 ) ) ;
#66550 = CARTESIAN_POINT ( 'NONE',  ( -8.703975197954740395, -2.625532179533470512, 30.86335684631491105 ) ) ;
#66552 = EDGE_CURVE ( 'NONE', #7817, #38892, #85213, .T. ) ;
#66551 = CARTESIAN_POINT ( 'NONE',  ( -16.28432133892187395, -7.276987145209182550, 34.99546412871779211 ) ) ;
#66553 = VERTEX_POINT ( 'NONE', #3224 ) ;
#66554 = B_SPLINE_CURVE_WITH_KNOTS ( 'NONE', 3,
 ( #59781, #53461, #58890, #31877, #66546, #4846 ),
 .UNSPECIFIED., .F., .F.,
 ( 4, 2, 4 ),
 ( 0.0003909512603273880690, 0.0005862562993132132720, 0.0007815613382990384750 ),
 .UNSPECIFIED. ) ;
#66555 = LINE ( 'NONE', #32328, #82313 ) ;
#66556 = DIRECTION ( 'NONE',  ( 1.000000000000000000, 0.000000000000000000, 0.000000000000000000 ) ) ;
#66557 = CARTESIAN_POINT ( 'NONE',  ( 14.98079248672063990, -10.06842814019191401, 34.32929386961144758 ) ) ;
#66558 = ORIENTED_EDGE ( 'NONE', *, *, #71450, .F. ) ;
#66559 = ORIENTED_EDGE ( 'NONE', *, *, #71381, .F. ) ;
#66560 = EDGE_CURVE ( 'NONE', #64311, #47437, #27904, .T. ) ;
#66561 = VERTEX_POINT ( 'NONE', #11320 ) ;
#66562 = CARTESIAN_POINT ( 'NONE',  ( 12.52679360105129724, -10.33852847137154107, 34.16647553114620450 ) ) ;
#66563 = CARTESIAN_POINT ( 'NONE',  ( 9.915087361285760181, -4.226511098958373402, 33.85474049983370293 ) ) ;
#66564 = EDGE_CURVE ( 'NONE', #62997, #39886, #16810, .T. ) ;
#66565 = CARTESIAN_POINT ( 'NONE',  ( 13.31934493865461455, -11.48612834413959582, 32.76840700105983473 ) ) ;
#66566 = CARTESIAN_POINT ( 'NONE',  ( -17.07692307692319744, -5.219633306517616589, 34.19971097300220464 ) ) ;
#66567 = ORIENTED_EDGE ( 'NONE', *, *, #65131, .F. ) ;
#66568 = ORIENTED_EDGE ( 'NONE', *, *, #40372, .T. ) ;
#66569 = ADVANCED_FACE ( 'NONE', ( #9982 ), #12217, .F. ) ;
#66570 = EDGE_LOOP ( 'NONE', ( #73887, #65674 ) ) ;
#66571 = EDGE_CURVE ( 'NONE', #12150, #6421, #87448, .T. ) ;
#66573 = ORIENTED_EDGE ( 'NONE', *, *, #80871, .T. ) ;
#66572 = CARTESIAN_POINT ( 'NONE',  ( 11.78851595837499566, -11.47946981652013498, 33.17500667209847620 ) ) ;
#66574 = CARTESIAN_POINT ( 'NONE',  ( -16.21911615440246734, -12.51329471203370325, 31.30864560766548976 ) ) ;
#66575 = DIRECTION ( 'NONE',  ( 0.000000000000000000, -6.938893903907222067E-15, 1.000000000000000000 ) ) ;
#66576 = AXIS2_PLACEMENT_3D ( 'NONE', #21408, #15543, #28614 ) ;
#66577 = AXIS2_PLACEMENT_3D ( 'NONE', #37196, #30009, #46075 ) ;
#66578 = CARTESIAN_POINT ( 'NONE',  ( 10.39189967166066708, -11.41268669641499756, 32.86336882939238535 ) ) ;
#66579 = CARTESIAN_POINT ( 'NONE',  ( -1.384615384615383471, -12.62096338111211580, 30.90682066428153263 ) ) ;
#66580 = VERTEX_POINT ( 'NONE', #26170 ) ;
#66581 = EDGE_CURVE ( 'NONE', #46498, #22155, #53353, .T. ) ;
#66582 = AXIS2_PLACEMENT_3D ( 'NONE', #58125, #84741, #51799 ) ;
#66583 = VERTEX_POINT ( 'NONE', #39701 ) ;
#66584 = ORIENTED_EDGE ( 'NONE', *, *, #81321, .F. ) ;
#66585 = DIRECTION ( 'NONE',  ( 0.000000000000000000, 0.9396926207859126468, 0.3420201433256571111 ) ) ;
#66587 = ORIENTED_EDGE ( 'NONE', *, *, #7865, .F. ) ;
#66586 = CARTESIAN_POINT ( 'NONE',  ( -13.16123989884296286, -2.251407671071268712, 29.88021292934942963 ) ) ;
#66588 = B_SPLINE_CURVE_WITH_KNOTS ( 'NONE', 3,
 ( #82467, #68928, #40152, #88350, #82019, #48212, #67613, #54078, #7239, #55418 ),
 .UNSPECIFIED., .F., .F.,
 ( 4, 2, 2, 2, 4 ),
 ( 0.000000000000000000, 0.0001954339857564083417, 0.0003908679715128166835, 0.0005863019572692250523, 0.0007817359430256333669 ),
 .UNSPECIFIED. ) ;
#66589 = CARTESIAN_POINT ( 'NONE',  ( -10.86538461538462563, -2.249999999999999556, 29.81609741502489541 ) ) ;
#66590 = EDGE_CURVE ( 'NONE', #30707, #53458, #47769, .T. ) ;
#66591 = EDGE_CURVE ( 'NONE', #64427, #80479, #12660, .T. ) ;
#66592 = FACE_OUTER_BOUND ( 'NONE', #18167, .T. ) ;
#66593 = CARTESIAN_POINT ( 'NONE',  ( -13.51476259405360381, -4.460286881179643004, 33.72017969459903242 ) ) ;
#66594 = DIRECTION ( 'NONE',  ( -0.000000000000000000, 0.6427876096865404731, -0.7660444431189771253 ) ) ;
#66595 = CARTESIAN_POINT ( 'NONE',  ( 10.61538461538461675, -8.318370150425687726, 35.83090037661290239 ) ) ;
#66596 = FACE_BOUND ( 'NONE', #51144, .T. ) ;
#66597 = CARTESIAN_POINT ( 'NONE',  ( -0.5276218724943423366, -4.098570777380720287, 33.41473453929634729 ) ) ;
#66598 = CARTESIAN_POINT ( 'NONE',  ( -12.59168567097668401, -9.418419913701741919, 34.36755862841477693 ) ) ;
#66599 = CARTESIAN_POINT ( 'NONE',  ( -8.769230769230890843, -4.481592998941358097, 33.73612834414048933 ) ) ;
#66601 = CARTESIAN_POINT ( 'NONE',  ( 15.36129466900287888, -10.31582465632705237, 34.18122507451815295 ) ) ;
#66600 = FACE_OUTER_BOUND ( 'NONE', #82699, .T. ) ;
#66602 = CARTESIAN_POINT ( 'NONE',  ( 0.2115617305961068617, -12.17611988154120972, 31.52148481390971213 ) ) ;
#66603 = CARTESIAN_POINT ( 'NONE',  ( 12.46153846153833911, -9.442884908241554243, 34.35708131394783038 ) ) ;
#66604 = VERTEX_POINT ( 'NONE', #80691 ) ;
#66605 = CARTESIAN_POINT ( 'NONE',  ( 2.438484115517096651, -6.413143153341454017, 34.63066358083362672 ) ) ;
#66606 = DIRECTION ( 'NONE',  ( -0.000000000000000000, -0.9848077530122086864, -0.1736481776669273613 ) ) ;
#66607 = VERTEX_POINT ( 'NONE', #13541 ) ;
#66608 = ORIENTED_EDGE ( 'NONE', *, *, #73890, .T. ) ;
#66609 = CARTESIAN_POINT ( 'NONE',  ( 0.5920638997721051622, -8.630441415882550871, 34.87705825610312615 ) ) ;
#66610 = AXIS2_PLACEMENT_3D ( 'NONE', #66435, #59670, #86731 ) ;
#66611 = AXIS2_PLACEMENT_3D ( 'NONE', #30193, #1387, #57658 ) ;
#66612 = CARTESIAN_POINT ( 'NONE',  ( -0.5920990532803821482, -2.504760397472875155, 29.97295953869789997 ) ) ;
#66613 = CARTESIAN_POINT ( 'NONE',  ( -11.53846153846165912, -5.219633306517616589, 34.19971097300220464 ) ) ;
#66614 = CARTESIAN_POINT ( 'NONE',  ( -11.53846153846166089, -10.33852847137269571, 34.16647553114546554 ) ) ;
#66615 = VERTEX_POINT ( 'NONE', #81127 ) ;
#66616 = CARTESIAN_POINT ( 'NONE',  ( 14.30769230769231015, -8.973038597847269315, 34.52809138561121927 ) ) ;
#66617 = DIRECTION ( 'NONE',  ( 0.000000000000000000, 0.000000000000000000, 1.000000000000000000 ) ) ;
#66619 = DIRECTION ( 'NONE',  ( -1.000000000000000000, 0.000000000000000000, 0.000000000000000000 ) ) ;
#66618 = CARTESIAN_POINT ( 'NONE',  ( 18.22277954126840172, -3.755027918224367767, 33.06320215134714857 ) ) ;
#66620 = LINE ( 'NONE', #4922, #89152 ) ;
#66621 = DIRECTION ( 'NONE',  ( -0.000000000000000000, 0.3420201433256694346, -0.9396926207859080948 ) ) ;
#66622 = CARTESIAN_POINT ( 'NONE',  ( -16.85391023282967637, -2.523321265292116866, 31.42251411153756990 ) ) ;
#66623 = CARTESIAN_POINT ( 'NONE',  ( 2.320192649118979489E-14, -11.25000000000000000, 21.03125000000000000 ) ) ;
#66624 = ORIENTED_EDGE ( 'NONE', *, *, #59201, .T. ) ;
#66625 = ORIENTED_EDGE ( 'NONE', *, *, #61937, .F. ) ;
#66626 = CARTESIAN_POINT ( 'NONE',  ( 5.076923076922954969, -6.879047030192662504, 34.71129190930017927 ) ) ;
#66627 = DIRECTION ( 'NONE',  ( 0.000000000000000000, 0.3420201433256610524, 0.9396926207859113145 ) ) ;
#66628 = CARTESIAN_POINT ( 'NONE',  ( -3.230769230769229949, -9.819645486525091727, 36.12317359536749706 ) ) ;
#66629 = CARTESIAN_POINT ( 'NONE',  ( 6.699591979352973681, -12.24155766932282496, 31.33739205006857986 ) ) ;
#66630 = CARTESIAN_POINT ( 'NONE',  ( 5.326868486301119532, -3.520799739797213501, 33.17531984108286025 ) ) ;
#66631 = CARTESIAN_POINT ( 'NONE',  ( -1.553300858899081538, -11.25000000000000711, 22.35937500000000711 ) ) ;
#66632 = CARTESIAN_POINT ( 'NONE',  ( -9.019253993452226226, -10.18141759479407327, 34.26406193332782379 ) ) ;
#66633 = CARTESIAN_POINT ( 'NONE',  ( -17.07692307692307665, -4.661471528628507777, 34.16647553114623292 ) ) ;
#66634 = CARTESIAN_POINT ( 'NONE',  ( -1.384615384615383471, -3.886160181151819604, 36.00935417666054406 ) ) ;
#66635 = CARTESIAN_POINT ( 'NONE',  ( -19.50000000000000000, -3.499999999999999556, 29.75000000000000355 ) ) ;
#66636 = DIRECTION ( 'NONE',  ( -0.000000000000000000, -0.9396926207859092051, -0.3420201433256662704 ) ) ;
#66637 = CARTESIAN_POINT ( 'NONE',  ( 15.16549923021291235, -12.51329471203370325, 31.30864560766548976 ) ) ;
#66638 = CARTESIAN_POINT ( 'NONE',  ( -3.480769230769229061, -7.500000000000001776, 34.75000000000000000 ) ) ;
#66639 = CARTESIAN_POINT ( 'NONE',  ( 7.053867364043874488, -2.295524264805589354, 30.44142389570982488 ) ) ;
#66640 = CARTESIAN_POINT ( 'NONE',  ( -2.307692307692305711, -5.180354513474913603, 36.12317359536750416 ) ) ;
#66641 = LINE ( 'NONE', #4946, #1062 ) ;
#66642 = ORIENTED_EDGE ( 'NONE', *, *, #40114, .F. ) ;
#66643 = B_SPLINE_CURVE_WITH_KNOTS ( 'NONE', 3,
 ( #78978, #48506, #1212, #51037, #55711, #28696, #21933, #83200, #56160, #49409 ),
 .UNSPECIFIED., .F., .F.,
 ( 4, 2, 2, 2, 4 ),
 ( 0.0007817246336856289524, 0.0009771112958940101571, 0.001172497958102391253, 0.001367884620310772350, 0.001563271282519153446 ),
 .UNSPECIFIED. ) ;
#66644 = LINE ( 'NONE', #88711, #8231 ) ;
#66645 = DIRECTION ( 'NONE',  ( 0.000000000000000000, 0.000000000000000000, -1.000000000000000000 ) ) ;
#66646 = CARTESIAN_POINT ( 'NONE',  ( -4.403822897894745125, -5.643011162660950042, 34.66104346484419096 ) ) ;
#66647 = CARTESIAN_POINT ( 'NONE',  ( -1.901340078031369618, -5.512252781505359245, 14.25186829374151465 ) ) ;
#66648 = AXIS2_PLACEMENT_3D ( 'NONE', #31188, #87499, #58658 ) ;
#66649 = B_SPLINE_CURVE_WITH_KNOTS ( 'NONE', 3,
 ( #3151, #45024, #85583, #72059, #52227, #57662, #10370, #3598, #59438, #37831 ),
 .UNSPECIFIED., .F., .F.,
 ( 4, 2, 2, 2, 4 ),
 ( 0.0007817246256747453293, 0.0009771112852218889842, 0.001172497944769032531, 0.001367884604316176294, 0.001563271263863319840 ),
 .UNSPECIFIED. ) ;
#66650 = CARTESIAN_POINT ( 'NONE',  ( 13.63456090296352841, -5.057305518903948638, 34.11320923018887896 ) ) ;
#66651 = CARTESIAN_POINT ( 'NONE',  ( 8.639082799499075094, -10.31621877034669588, 34.18098118002070152 ) ) ;
#66653 = VERTEX_POINT ( 'NONE', #54070 ) ;
#66652 = CARTESIAN_POINT ( 'NONE',  ( 17.07692307692307665, -12.62096338111211580, 30.90682066428153263 ) ) ;
#66654 = CARTESIAN_POINT ( 'NONE',  ( 1.139087296525997051, -4.749999999999992895, 19.23437500000000000 ) ) ;
#66655 = CARTESIAN_POINT ( 'NONE',  ( 17.86930853333243618, -3.530157926970578508, 32.79014554554150607 ) ) ;
#66656 = EDGE_LOOP ( 'NONE', ( #15909, #88520 ) ) ;
#66657 = CARTESIAN_POINT ( 'NONE',  ( -17.93474442872397034, -3.835265460703682017, 33.15142922261929925 ) ) ;
#66658 = EDGE_LOOP ( 'NONE', ( #4947, #53408 ) ) ;
#66659 = FACE_OUTER_BOUND ( 'NONE', #58765, .T. ) ;
#66660 = CARTESIAN_POINT ( 'NONE',  ( -15.29685161012936589, -2.833524468853757305, 32.15551576947924417 ) ) ;
#66661 = CARTESIAN_POINT ( 'NONE',  ( -15.23076923076891553, -2.255955759149395501, 30.00000000000324363 ) ) ;
#66662 = ORIENTED_EDGE ( 'NONE', *, *, #66560, .F. ) ;
#66663 = CARTESIAN_POINT ( 'NONE',  ( -10.39260507411620438, -12.44528174975671853, 30.48912976160716681 ) ) ;
#66664 = VERTEX_POINT ( 'NONE', #75250 ) ;
#66665 = LINE ( 'NONE', #10834, #35512 ) ;
#66666 = ADVANCED_FACE ( 'NONE', ( #88344 ), #68052, .T. ) ;
#66667 = EDGE_LOOP ( 'NONE', ( #25063, #73772, #61857, #23887 ) ) ;
#66668 = CARTESIAN_POINT ( 'NONE',  ( 2.242422307135989890, -9.528491918058357157, 34.59228464037090589 ) ) ;
#66669 = CARTESIAN_POINT ( 'NONE',  ( 12.59233026936325039, -12.11778462344221019, 31.66786338562085135 ) ) ;
#66670 = CARTESIAN_POINT ( 'NONE',  ( -23.50000000000000000, -13.25000000000001066, 13.00000000000000888 ) ) ;
#66671 = CARTESIAN_POINT ( 'NONE',  ( -10.61538461538461320, -2.538708090699994813, 30.37095296980875503 ) ) ;
#66672 = CARTESIAN_POINT ( 'NONE',  ( 9.915087361285761958, -10.23759521482555357, 34.22997729860117033 ) ) ;
#66673 = CARTESIAN_POINT ( 'NONE',  ( 0.4615384615383382183, -2.379036618888197285, 30.90682066428292885 ) ) ;
#66674 = AXIS2_PLACEMENT_3D ( 'NONE', #68167, #52081, #40261 ) ;
#66675 = VECTOR ( 'NONE', #13617, 1000.000000000000000 ) ;
#66676 = CARTESIAN_POINT ( 'NONE',  ( 18.00000000000000000, -2.499999999999998668, 29.75000000000001421 ) ) ;
#66677 = VERTEX_POINT ( 'NONE', #26614 ) ;
#66678 = ORIENTED_EDGE ( 'NONE', *, *, #74300, .T. ) ;
#66679 = B_SPLINE_CURVE_WITH_KNOTS ( 'NONE', 3,
 ( #5796, #61616, #54415, #27397, #81912, #60735, #13875, #26514, #40482, #374 ),
 .UNSPECIFIED., .F., .F.,
 ( 4, 2, 2, 2, 4 ),
 ( 0.0007817359430256251270, 0.0009771253907249900349, 0.001172514838424354834, 0.001367904286123719851, 0.001563293733823084650 ),
 .UNSPECIFIED. ) ;
#66680 = EDGE_CURVE ( 'NONE', #86970, #20358, #53639, .T. ) ;
#66681 = ORIENTED_EDGE ( 'NONE', *, *, #78093, .T. ) ;
#66683 = ORIENTED_EDGE ( 'NONE', *, *, #54892, .T. ) ;
#66682 = CARTESIAN_POINT ( 'NONE',  ( 1.653273178848927064E-15, -7.500000000000000000, 14.00000000000000178 ) ) ;
#66684 = B_SPLINE_CURVE_WITH_KNOTS ( 'NONE', 3,
 ( #46591, #80838, #38504, #24531, #51998, #65518, #32196, #10588, #11475, #24980 ),
 .UNSPECIFIED., .F., .F.,
 ( 4, 2, 2, 2, 4 ),
 ( 0.0007817359430256328248, 0.0009771253907249995759, 0.001172514838424366327, 0.001367904286123733078, 0.001563293733823099829 ),
 .UNSPECIFIED. ) ;
#66685 = CARTESIAN_POINT ( 'NONE',  ( -14.05763788777885637, -10.82426656108012075, 33.81400080652039009 ) ) ;
#66686 = LINE ( 'NONE', #59921, #59695 ) ;
#66687 = EDGE_LOOP ( 'NONE', ( #56228, #70609, #78549, #12627 ) ) ;
#66688 = CARTESIAN_POINT ( 'NONE',  ( 14.55763771707034948, -12.07971442181322352, 32.31769673815850297 ) ) ;
#66689 = ORIENTED_EDGE ( 'NONE', *, *, #40936, .T. ) ;
#66690 = CARTESIAN_POINT ( 'NONE',  ( 11.66898724022510159, -2.619367082507849442, 30.83698974864643461 ) ) ;
#66691 = VERTEX_POINT ( 'NONE', #39252 ) ;
#66692 = CARTESIAN_POINT ( 'NONE',  ( -9.442307692307679190, -2.249999999999999112, 29.81603969181031033 ) ) ;
#66693 = EDGE_CURVE ( 'NONE', #82761, #65424, #59949, .T. ) ;
#66694 = VECTOR ( 'NONE', #70460, 1000.000000000000000 ) ;
#66695 = CARTESIAN_POINT ( 'NONE',  ( -8.096177083446809419, -2.587272538249755893, 30.68239716806877837 ) ) ;
#66696 = CARTESIAN_POINT ( 'NONE',  ( -9.442307692306272315, -7.500000000000154543, 35.00000000000007105 ) ) ;
#66697 = FACE_BOUND ( 'NONE', #14554, .T. ) ;
#66698 = AXIS2_PLACEMENT_3D ( 'NONE', #13587, #19897, #26220 ) ;
#66699 = PLANE ( 'NONE',  #19791 ) ;
#66700 = CARTESIAN_POINT ( 'NONE',  ( 1.161787286980507705, -7.369209533119137845, 34.99857337881830688 ) ) ;
#66701 = VECTOR ( 'NONE', #10081, 1000.000000000000114 ) ;
#66702 = CARTESIAN_POINT ( 'NONE',  ( -14.30769230769242917, -4.320704448113951379, 33.92786785259630022 ) ) ;
#66703 = EDGE_CURVE ( 'NONE', #45365, #20449, #36128, .T. ) ;
#66704 = CYLINDRICAL_SURFACE ( 'NONE', #24448, 0.2499999999999995559 ) ;
#66705 = CARTESIAN_POINT ( 'NONE',  ( 19.00000000000000000, -8.999999999999996447, 22.25000000000000000 ) ) ;
#66706 = CARTESIAN_POINT ( 'NONE',  ( 10.61538461538449418, -11.06231777344772027, 33.60647404775119895 ) ) ;
#66707 = EDGE_LOOP ( 'NONE', ( #53649, #55025, #14878, #50095 ) ) ;
#66708 = DIRECTION ( 'NONE',  ( 0.000000000000000000, 0.4999999999999960032, -0.8660254037844410391 ) ) ;
#66709 = EDGE_LOOP ( 'NONE', ( #2325, #55540 ) ) ;
#66710 = ORIENTED_EDGE ( 'NONE', *, *, #86211, .F. ) ;
#66712 = CARTESIAN_POINT ( 'NONE',  ( -14.17716660592874689, -12.45806712695776319, 30.39783852428763922 ) ) ;
#66711 = CARTESIAN_POINT ( 'NONE',  ( -0.6850234052624096792, -9.331801661448606566, 34.40259984581193464 ) ) ;
#66713 = CARTESIAN_POINT ( 'NONE',  ( -3.230769230769229949, -5.180354513474913603, 36.12317359536750416 ) ) ;
#66714 = CARTESIAN_POINT ( 'NONE',  ( 3.361561038594017337, -10.54018710029568595, 33.71981072465678864 ) ) ;
#66715 = CARTESIAN_POINT ( 'NONE',  ( 16.85399685940693004, -8.239355502252617924, 34.69524867566427417 ) ) ;
#66716 = CARTESIAN_POINT ( 'NONE',  ( -12.46153846153846168, -4.098570777380720287, 33.41473453929634729 ) ) ;
#66717 = VERTEX_POINT ( 'NONE', #32930 ) ;
#66718 = CARTESIAN_POINT ( 'NONE',  ( 16.82694634598072270, -5.728515186090277211, 34.42611988154120439 ) ) ;
#66719 = CARTESIAN_POINT ( 'NONE',  ( -5.010854725920637520, -2.538708090699994813, 30.37095296980875503 ) ) ;
#66720 = CARTESIAN_POINT ( 'NONE',  ( 10.39245765647776309, -2.889293201056495786, 32.26117774369186009 ) ) ;
#66721 = CARTESIAN_POINT ( 'NONE',  ( -16.08859101433330707, -4.320704448112858032, 33.92786785259548310 ) ) ;
#66722 = ORIENTED_EDGE ( 'NONE', *, *, #14287, .F. ) ;
#66723 = ORIENTED_EDGE ( 'NONE', *, *, #80323, .T. ) ;
#66724 = ITEM_DEFINED_TRANSFORMATION ( 'NONE', 'NONE', #5849,  #83448 ) ;
#66725 = ORIENTED_EDGE ( 'NONE', *, *, #55181, .T. ) ;
#66726 = CARTESIAN_POINT ( 'NONE',  ( 18.13079044096694759, -12.62708834333097663, 30.88030960425256310 ) ) ;
#66727 = CARTESIAN_POINT ( 'NONE',  ( 4.946232473812766983, -2.845849958028613624, 32.17971566917920967 ) ) ;
#66728 = EDGE_LOOP ( 'NONE', ( #27759, #83333 ) ) ;
#66729 = DIRECTION ( 'NONE',  ( 0.000000000000000000, 0.000000000000000000, 1.000000000000000000 ) ) ;
#66730 = CARTESIAN_POINT ( 'NONE',  ( -6.130690603110307890, -9.084618155246140248, 34.75535874321725771 ) ) ;
#66731 = CARTESIAN_POINT ( 'NONE',  ( 9.320512820512821150, -1.926643599941765039, 29.65000000000000213 ) ) ;
#66732 = CARTESIAN_POINT ( 'NONE',  ( -2.530618525208452763, -8.239355502252617924, 34.69524867566427417 ) ) ;
#66733 = CARTESIAN_POINT ( 'NONE',  ( -0.4615384615385826339, -2.625532179533779598, 30.86335684631627174 ) ) ;
#66735 = ORIENTED_EDGE ( 'NONE', *, *, #15698, .F. ) ;
#66734 = CIRCLE ( 'NONE', #35098, 4.755951259987790891 ) ;
#66737 = ORIENTED_EDGE ( 'NONE', *, *, #48596, .T. ) ;
#66736 = CARTESIAN_POINT ( 'NONE',  ( -14.98082382139119062, -2.341251567377310217, 30.72681386836322659 ) ) ;
#66738 = CARTESIAN_POINT ( 'NONE',  ( -8.769230769230890843, -10.21337939537710326, 33.94971097300076224 ) ) ;
#66739 = DIRECTION ( 'NONE',  ( -0.000000000000000000, -0.000000000000000000, -1.000000000000000000 ) ) ;
#66740 = CARTESIAN_POINT ( 'NONE',  ( 9.070512820512819374, -7.500000000000000000, 33.75000000000000000 ) ) ;
#66741 = CARTESIAN_POINT ( 'NONE',  ( 18.13052570176355971, -8.586989748646450593, 34.63063291749215011 ) ) ;
#66742 = CARTESIAN_POINT ( 'NONE',  ( -3.931066484868086075, -4.989023458446560255, 34.36081565061822118 ) ) ;
#66743 = CARTESIAN_POINT ( 'NONE',  ( -5.299850035829924977, -10.77366814457252175, 33.85459836347579454 ) ) ;
#66744 = DIRECTION ( 'NONE',  ( -0.000000000000000000, 0.5000000000000011102, -0.8660254037844381525 ) ) ;
#66745 = CARTESIAN_POINT ( 'NONE',  ( -1.987747218494638313, -9.401340078031370950, 15.18936829374151465 ) ) ;
#66746 = ORIENTED_EDGE ( 'NONE', *, *, #33748, .T. ) ;
#66747 = DIRECTION ( 'NONE',  ( 0.000000000000000000, 0.1736481776669275834, 0.9848077530122086864 ) ) ;
#66748 = CARTESIAN_POINT ( 'NONE',  ( 8.096153846153782752, -7.565270000091922853, 34.99999999999999289 ) ) ;
#66749 = CARTESIAN_POINT ( 'NONE',  ( -11.53846153846165912, -9.442884908241554243, 34.35708131394783038 ) ) ;
#66750 = ORIENTED_EDGE ( 'NONE', *, *, #11680, .T. ) ;
#66751 = ORIENTED_EDGE ( 'NONE', *, *, #12041, .F. ) ;
#66752 = CARTESIAN_POINT ( 'NONE',  ( -8.769230769230768274, -5.471508081941601098, 34.59228464037088457 ) ) ;
#66753 = CARTESIAN_POINT ( 'NONE',  ( 11.47319153790521717, -12.70778746994557551, 30.41441678777548319 ) ) ;
#66754 = CARTESIAN_POINT ( 'NONE',  ( -0.5916864312701568540, -9.504002272028875709, 34.60269587691767867 ) ) ;
#66755 = EDGE_CURVE ( 'NONE', #47148, #43255, #71521, .T. ) ;
#66756 = CARTESIAN_POINT ( 'NONE',  ( -10.83886953994894853, -2.353723527008296568, 30.78948104536958752 ) ) ;
#66757 = FACE_OUTER_BOUND ( 'NONE', #73111, .T. ) ;
#66758 = DIRECTION ( 'NONE',  ( -0.000000000000000000, -0.7660444431189791237, -0.6427876096865379196 ) ) ;
#66759 = B_SPLINE_CURVE_WITH_KNOTS ( 'NONE', 3,
 ( #47005, #12790, #54206, #40275, #4253, #33514, #67297, #73625, #39828, #5591 ),
 .UNSPECIFIED., .F., .F.,
 ( 4, 2, 2, 2, 4 ),
 ( 0.000000000000000000, 0.0001954311564186863594, 0.0003908623128373726104, 0.0005862934692560589156, 0.0007817246256747452209 ),
 .UNSPECIFIED. ) ;
#66760 = EDGE_LOOP ( 'NONE', ( #10481, #7385, #9649, #21740 ) ) ;
#66761 = CARTESIAN_POINT ( 'NONE',  ( -16.40386937806761125, -6.652501968072647820, 34.93155406624980941 ) ) ;
#66762 = VECTOR ( 'NONE', #63138, 1000.000000000000000 ) ;
#66763 = LINE ( 'NONE', #60003, #23924 ) ;
#66764 = CARTESIAN_POINT ( 'NONE',  ( 4.153846153846030731, -8.656820664282941280, 34.87096338111179961 ) ) ;
#66765 = ORIENTED_EDGE ( 'NONE', *, *, #21316, .F. ) ;
#66766 = CARTESIAN_POINT ( 'NONE',  ( 12.68454981315131036, -3.587049720035815348, 32.86302985866382897 ) ) ;
#66767 = AXIS2_PLACEMENT_3D ( 'NONE', #5735, #48039, #33211 ) ;
#66768 = EDGE_CURVE ( 'NONE', #87399, #51804, #34988, .T. ) ;
#66769 = ORIENTED_EDGE ( 'NONE', *, *, #23330, .T. ) ;
#66770 = CARTESIAN_POINT ( 'NONE',  ( 13.63466969625370062, -3.627508038966690496, 32.91356715214248396 ) ) ;
#66771 = CARTESIAN_POINT ( 'NONE',  ( 10.61538461538449418, -3.643525952248795718, 33.31231777344771672 ) ) ;
#66772 = DIRECTION ( 'NONE',  ( -1.000000000000000000, 0.000000000000000000, 0.000000000000000000 ) ) ;
#66773 = ORIENTED_EDGE ( 'NONE', *, *, #10586, .F. ) ;
#66774 = B_SPLINE_CURVE_WITH_KNOTS ( 'NONE', 3,
 ( #40195, #87059, #53238, #19022, #31646, #11373, #46922, #38852, #25779, #60443 ),
 .UNSPECIFIED., .F., .F.,
 ( 4, 2, 2, 2, 4 ),
 ( 0.000000000000000000, 0.0001954339857564093175, 0.0003908679715128186350, 0.0005863019572692279796, 0.0007817359430256372700 ),
 .UNSPECIFIED. ) ;
#66775 = ADVANCED_FACE ( 'NONE', ( #7233 ), #35591, .F. ) ;
#66776 = CARTESIAN_POINT ( 'NONE',  ( -13.31854805126531005, -4.661471528628508665, 34.16647553114624003 ) ) ;
#66777 = CYLINDRICAL_SURFACE ( 'NONE', #14769, 0.2499999999999986955 ) ;
#66778 = DIRECTION ( 'NONE',  ( 0.000000000000000000, 0.9848077530122072432, 0.1736481776669354937 ) ) ;
#66779 = CARTESIAN_POINT ( 'NONE',  ( -17.07692307692319744, -12.51329471203414379, 31.30864560766407578 ) ) ;
#66780 = CARTESIAN_POINT ( 'NONE',  ( -4.946132635956126400, -8.191423895709842640, 34.95447573519442130 ) ) ;
#66781 = VERTEX_POINT ( 'NONE', #63039 ) ;
#66782 = EDGE_CURVE ( 'NONE', #72551, #85757, #48206, .T. ) ;
#66783 = DIRECTION ( 'NONE',  ( -1.000000000000000000, -0.000000000000000000, -0.000000000000000000 ) ) ;
#66784 = ORIENTED_EDGE ( 'NONE', *, *, #9186, .T. ) ;
#66785 = CARTESIAN_POINT ( 'NONE',  ( 5.076923076922953193, -11.67786785259630911, 32.92929555188603530 ) ) ;
#66786 = DIRECTION ( 'NONE',  ( 1.000000000000000000, 0.000000000000000000, 0.000000000000000000 ) ) ;
#66787 = EDGE_CURVE ( 'NONE', #85159, #61364, #76576, .T. ) ;
#66788 = CARTESIAN_POINT ( 'NONE',  ( -11.78846153846153832, -7.500000000000001776, 35.00000000000000000 ) ) ;
#66789 = CARTESIAN_POINT ( 'NONE',  ( -11.97435897435897267, -7.500000000000000000, 29.75000000000000355 ) ) ;
#66790 = CARTESIAN_POINT ( 'NONE',  ( -14.17690049986752143, -12.11778462344220841, 31.66786338562085135 ) ) ;
#66791 = CARTESIAN_POINT ( 'NONE',  ( -7.134615384615385025, -11.00000000000000000, 29.75000000000000355 ) ) ;
#66792 = CARTESIAN_POINT ( 'NONE',  ( -19.99999999999996447, -15.00000000000000533, 13.00000000000000178 ) ) ;
#66793 = ORIENTED_EDGE ( 'NONE', *, *, #11994, .F. ) ;
#66794 = VECTOR ( 'NONE', #83118, 999.9999999999998863 ) ;
#66795 = ORIENTED_EDGE ( 'NONE', *, *, #11265, .F. ) ;
#66796 = ORIENTED_EDGE ( 'NONE', *, *, #59801, .T. ) ;
#66797 = EDGE_LOOP ( 'NONE', ( #51247, #447 ) ) ;
#66798 = ORIENTED_EDGE ( 'NONE', *, *, #32787, .F. ) ;
#66799 = EDGE_CURVE ( 'NONE', #72105, #78212, #21622, .T. ) ;
#66800 = CARTESIAN_POINT ( 'NONE',  ( -16.21992956480203318, -3.513871655860377086, 32.76840700105978499 ) ) ;
#66801 = CARTESIAN_POINT ( 'NONE',  ( -22.00000000000000355, -10.00000000000000533, 13.00000000000000178 ) ) ;
#66802 = EDGE_CURVE ( 'NONE', #19490, #35011, #84235, .T. ) ;
#66803 = B_SPLINE_CURVE_WITH_KNOTS ( 'NONE', 3,
 ( #70338, #29802, #21704, #64444, #43312, #8645, #28926, #29361, #23464, #30237 ),
 .UNSPECIFIED., .F., .F.,
 ( 4, 2, 2, 2, 4 ),
 ( 0.0007817246256747461966, 0.0009771112852218892010, 0.001172497944769032314, 0.001367884604316175427, 0.001563271263863318323 ),
 .UNSPECIFIED. ) ;
#66804 = CARTESIAN_POINT ( 'NONE',  ( -10.48459417441766561, -4.684288915650983043, 34.18129842949671371 ) ) ;
#66805 = CARTESIAN_POINT ( 'NONE',  ( 3.930919936330004472, -3.105860786376062332, 32.13614157043599562 ) ) ;
#66806 = CARTESIAN_POINT ( 'NONE',  ( 0.7115927731767758280, -4.943051570960395047, 34.04725096376909477 ) ) ;
#66807 = ADVANCED_FACE ( 'NONE', ( #77021 ), #70257, .T. ) ;
#66808 = DIRECTION ( 'NONE',  ( 1.000000000000000000, 0.000000000000000000, 0.000000000000000000 ) ) ;
#66809 = ADVANCED_FACE ( 'NONE', ( #14883 ), #83789, .F. ) ;
#66810 = CARTESIAN_POINT ( 'NONE',  ( 17.74997676270703550, -2.587272538249754117, 30.68239716806877837 ) ) ;
#66811 = CARTESIAN_POINT ( 'NONE',  ( 6.923076923076924238, -1.422936976036506707, 30.56769352161908415 ) ) ;
#66812 = VERTEX_POINT ( 'NONE', #75677 ) ;
#66813 = ORIENTED_EDGE ( 'NONE', *, *, #22721, .F. ) ;
#66814 = ORIENTED_EDGE ( 'NONE', *, *, #57473, .F. ) ;
#66816 = ORIENTED_EDGE ( 'NONE', *, *, #25976, .F. ) ;
#66815 = DIRECTION ( 'NONE',  ( -1.000000000000000000, -0.000000000000000000, -0.000000000000000000 ) ) ;
#66818 = CARTESIAN_POINT ( 'NONE',  ( -5.749945688361685292, -3.627508038966690496, 32.91356715214248396 ) ) ;
#66817 = CARTESIAN_POINT ( 'NONE',  ( 6.792928953345226617, -11.66186481527757479, 32.95055677023626117 ) ) ;
#66819 = DIRECTION ( 'NONE',  ( 0.000000000000000000, 0.000000000000000000, -1.000000000000000000 ) ) ;
#66820 = CARTESIAN_POINT ( 'NONE',  ( -11.47320639894870276, -9.528491918058460186, 34.59228464037086326 ) ) ;
#66821 = FACE_BOUND ( 'NONE', #112, .T. ) ;
#66822 = VERTEX_POINT ( 'NONE', #49546 ) ;
#66823 = ORIENTED_EDGE ( 'NONE', *, *, #88647, .T. ) ;
#66824 = CARTESIAN_POINT ( 'NONE',  ( 17.29993592101647693, -5.582272713120730145, 34.63742843783360570 ) ) ;
#66825 = AXIS2_PLACEMENT_3D ( 'NONE', #43622, #50803, #71532 ) ;
#66826 = EDGE_LOOP ( 'NONE', ( #14969, #3658, #51309, #52043 ) ) ;
#66827 = FACE_BOUND ( 'NONE', #60145, .T. ) ;
#66828 = CARTESIAN_POINT ( 'NONE',  ( -10.83886953994894675, -3.019605429927184836, 32.48692288466676814 ) ) ;
#66829 = VECTOR ( 'NONE', #60870, 1000.000000000000000 ) ;
#66830 = DIRECTION ( 'NONE',  ( -0.000000000000000000, -0.9396926207859093161, -0.3420201433256663259 ) ) ;
#66831 = ORIENTED_EDGE ( 'NONE', *, *, #18294, .T. ) ;
#66832 = LINE ( 'NONE', #3789, #44858 ) ;
#66833 = CARTESIAN_POINT ( 'NONE',  ( -1.449885385171703067, -8.656820664281497102, 34.87096338111211935 ) ) ;
#66834 = LINE ( 'NONE', #65493, #22024 ) ;
#66835 = VERTEX_POINT ( 'NONE', #49976 ) ;
#66836 = CARTESIAN_POINT ( 'NONE',  ( 9.320512820512821150, -4.000000000000000000, 29.25000000000000000 ) ) ;
#66837 = CARTESIAN_POINT ( 'NONE',  ( -14.43783951713053249, -6.001485441113819874, 34.52039167877662607 ) ) ;
#66838 = CARTESIAN_POINT ( 'NONE',  ( 11.53846153846153832, -3.669653830205710676, 35.88435417666054406 ) ) ;
#66839 = ORIENTED_EDGE ( 'NONE', *, *, #75843, .T. ) ;
#66840 = FACE_OUTER_BOUND ( 'NONE', #74217, .T. ) ;
#66841 = CARTESIAN_POINT ( 'NONE',  ( -7.384615384615385025, -11.00000000000000000, 29.75000000000000355 ) ) ;
#66842 = ORIENTED_EDGE ( 'NONE', *, *, #76373, .T. ) ;
#66843 = CARTESIAN_POINT ( 'NONE',  ( 8.769230769230645706, -11.67786785259630911, 32.92929555188603530 ) ) ;
#66844 = CARTESIAN_POINT ( 'NONE',  ( -12.33101275977489841, -2.619367082507849442, 30.83698974864643461 ) ) ;
#66845 = CARTESIAN_POINT ( 'NONE',  ( -14.53117723225664371, -2.612411019501189369, 31.66733052389439962 ) ) ;
#66846 = CARTESIAN_POINT ( 'NONE',  ( -12.46153846153846168, -5.415277668671390821, 36.20867863119892149 ) ) ;
#66847 = CARTESIAN_POINT ( 'NONE',  ( 13.38461538461538680, -2.249999999999998668, 29.75000000000001776 ) ) ;
#66848 = ADVANCED_FACE ( 'NONE', ( #15764 ), #70703, .F. ) ;
#66849 = CARTESIAN_POINT ( 'NONE',  ( 17.29993592101647337, -4.762714258010882773, 34.23016756924214832 ) ) ;
#66851 = FACE_OUTER_BOUND ( 'NONE', #79291, .T. ) ;
#66850 = CARTESIAN_POINT ( 'NONE',  ( -1.515306851282941958, -4.809359713505814149, 33.96456829005828837 ) ) ;
#66852 = B_SPLINE_CURVE_WITH_KNOTS ( 'NONE', 3,
 ( #19499, #12744, #46960, #6001, #68136, #5103, #80783, #68571, #27586, #33897 ),
 .UNSPECIFIED., .F., .F.,
 ( 4, 2, 2, 2, 4 ),
 ( 0.0007817359430256326080, 0.0009771253907250047801, 0.001172514838424369796, 0.001367904286123735030, 0.001563293733823100046 ),
 .UNSPECIFIED. ) ;
#66853 = B_SPLINE_CURVE_WITH_KNOTS ( 'NONE', 3,
 ( #22827, #69691, #83670, #9758, #28256, #70581, #84551, #1677, #37223, #21953 ),
 .UNSPECIFIED., .F., .F.,
 ( 4, 2, 2, 2, 4 ),
 ( 0.000000000000000000, 0.0001954311564186871184, 0.0003908623128373742367, 0.0005862934692560614093, 0.0007817246256747484735 ),
 .UNSPECIFIED. ) ;
#66854 = CARTESIAN_POINT ( 'NONE',  ( -39.05038313613820122, -2.249999999999998668, 29.75000000000000355 ) ) ;
#66855 = DIRECTION ( 'NONE',  ( -0.000000000000000000, 1.000000000000000000, -0.000000000000000000 ) ) ;
#66856 = ADVANCED_FACE ( 'NONE', ( #29721 ), #82897, .F. ) ;
#66857 = B_SPLINE_CURVE_WITH_KNOTS ( 'NONE', 3,
 ( #23710, #2554, #31371, #73247, #30045, #85874, #58834, #65143, #23276, #24609 ),
 .UNSPECIFIED., .F., .F.,
 ( 4, 2, 2, 2, 4 ),
 ( 0.000000000000000000, 0.0001954339857564054144, 0.0003908679715128108288, 0.0005863019572692162703, 0.0007817359430256216575 ),
 .UNSPECIFIED. ) ;
#66858 = CARTESIAN_POINT ( 'NONE',  ( 2.775308065498768517, -8.577988221561467341, 26.79500670625849423 ) ) ;
#66859 = ORIENTED_EDGE ( 'NONE', *, *, #53764, .T. ) ;
#66860 = CYLINDRICAL_SURFACE ( 'NONE', #20342, 0.2499999999999993616 ) ;
#66861 = EDGE_LOOP ( 'NONE', ( #56924, #53339 ) ) ;
#66862 = EDGE_CURVE ( 'NONE', #25698, #36076, #14424, .T. ) ;
#66863 = ORIENTED_EDGE ( 'NONE', *, *, #42003, .T. ) ;
#66864 = DIRECTION ( 'NONE',  ( -0.000000000000000000, 0.9848077530122086864, -0.1736481776669273891 ) ) ;
#66865 = EDGE_LOOP ( 'NONE', ( #20427, #21427 ) ) ;
#66866 = CARTESIAN_POINT ( 'NONE',  ( -6.000000000000121680, -10.33852847137269571, 34.16647553114546554 ) ) ;
#66867 = CARTESIAN_POINT ( 'NONE',  ( 1.139087296525997273, -4.749999999999992895, 15.48437500000000178 ) ) ;
#66868 = CARTESIAN_POINT ( 'NONE',  ( -13.13466997523734214, -5.766571408460171355, 34.70601412856602508 ) ) ;
#66869 = CARTESIAN_POINT ( 'NONE',  ( -16.82692307692307665, -2.499999999999998668, 29.75000000000000355 ) ) ;
#66870 = LINE ( 'NONE', #5166, #61933 ) ;
#66871 = DIRECTION ( 'NONE',  ( -0.000000000000000000, 0.1736481776669307198, -0.9848077530122080203 ) ) ;
#66872 = EDGE_CURVE ( 'NONE', #42322, #40124, #73781, .T. ) ;
#66873 = VECTOR ( 'NONE', #3023, 1000.000000000000114 ) ;
#66874 = CARTESIAN_POINT ( 'NONE',  ( -10.48459417441766206, -3.338503747796866872, 32.95102852606553512 ) ) ;
#66875 = DIRECTION ( 'NONE',  ( -0.000000000000000000, 1.000000000000000000, -0.000000000000000000 ) ) ;
#66876 = CARTESIAN_POINT ( 'NONE',  ( 5.750023269057646935, -4.236021600441998380, 33.53823185664189310 ) ) ;
#66877 = CARTESIAN_POINT ( 'NONE',  ( 2.651650429449539104, -4.848349570550432475, 20.56250000000000000 ) ) ;
#66878 = DIRECTION ( 'NONE',  ( -0.000000000000000000, -0.5000000000000009992, -0.8660254037844380415 ) ) ;
#66879 = CARTESIAN_POINT ( 'NONE',  ( -17.86947456176635640, -2.372941743896879174, 30.88044141588254377 ) ) ;
#66880 = CARTESIAN_POINT ( 'NONE',  ( 0.000000000000000000, -11.00000000000000000, 29.75000000000000355 ) ) ;
#66881 = ORIENTED_EDGE ( 'NONE', *, *, #85686, .F. ) ;
#66882 = ORIENTED_EDGE ( 'NONE', *, *, #36085, .F. ) ;
#66883 = DIRECTION ( 'NONE',  ( 0.000000000000000000, 0.4999999999999985567, 0.8660254037844395958 ) ) ;
#66884 = CARTESIAN_POINT ( 'NONE',  ( 7.623227628637697428, -11.24512374952581872, 33.06303171183252942 ) ) ;
#66885 = CARTESIAN_POINT ( 'NONE',  ( 16.40379156322419973, -12.45601412856602686, 31.48342859153981621 ) ) ;
#66886 = DIRECTION ( 'NONE',  ( -0.000000000000000000, -0.3420201433256694346, -0.9396926207859080948 ) ) ;
#66887 = ADVANCED_FACE ( 'NONE', ( #2664 ), #39481, .F. ) ;
#66888 = CARTESIAN_POINT ( 'NONE',  ( 8.769230769230768274, -4.098570777380720287, 33.41473453929634729 ) ) ;
#66889 = CARTESIAN_POINT ( 'NONE',  ( -9.915792616872025178, -6.716662450894489211, 34.94144148231605840 ) ) ;
#66890 = AXIS2_PLACEMENT_3D ( 'NONE', #61275, #6787, #88792 ) ;
#66891 = EDGE_LOOP ( 'NONE', ( #68595, #40326, #67136, #57297 ) ) ;
#66892 = CARTESIAN_POINT ( 'NONE',  ( 16.02315468717859659, -2.729777683071817229, 31.24903638046269450 ) ) ;
#66893 = VERTEX_POINT ( 'NONE', #60169 ) ;
#66894 = ORIENTED_EDGE ( 'NONE', *, *, #87731, .F. ) ;
#66895 = CARTESIAN_POINT ( 'NONE',  ( 16.21910129335899597, -9.528491918058456633, 34.59228464037085615 ) ) ;
#66896 = AXIS2_PLACEMENT_3D ( 'NONE', #20456, #74967, #47469 ) ;
#66897 = CARTESIAN_POINT ( 'NONE',  ( -4.230769230769230838, -3.499999999999999556, 29.75000000000000355 ) ) ;
#66898 = CARTESIAN_POINT ( 'NONE',  ( -0.7115384615384606759, -7.500000000000001776, 35.00000000000000000 ) ) ;
#66899 = CIRCLE ( 'NONE', #28065, 0.2500000000000002220 ) ;
#66900 = CARTESIAN_POINT ( 'NONE',  ( 11.78840694783958476, -2.341251567377310217, 30.72681386836322659 ) ) ;
#66901 = CARTESIAN_POINT ( 'NONE',  ( -5.076923076923199218, -8.656820664282941280, 34.87096338111179961 ) ) ;
#66902 = ORIENTED_EDGE ( 'NONE', *, *, #48332, .F. ) ;
#66903 = ORIENTED_EDGE ( 'NONE', *, *, #82454, .T. ) ;
#66904 = VERTEX_POINT ( 'NONE', #33150 ) ;
#66905 = ADVANCED_FACE ( 'NONE', ( #18759 ), #45774, .F. ) ;
#66906 = ADVANCED_FACE ( 'NONE', ( #30156 ), #66941, .F. ) ;
#66907 = CARTESIAN_POINT ( 'NONE',  ( 0.4615384615384611200, -4.098570777380720287, 33.41473453929634729 ) ) ;
#66908 = CARTESIAN_POINT ( 'NONE',  ( 10.61538461538461675, -11.35647404775217417, 33.31231777344666511 ) ) ;
#66909 = CARTESIAN_POINT ( 'NONE',  ( -27.00000000000000000, -1.249999999999999112, 32.75000000000000000 ) ) ;
#66910 = EDGE_CURVE ( 'NONE', #14505, #48663, #12006, .T. ) ;
#66911 = B_SPLINE_CURVE_WITH_KNOTS ( 'NONE', 3,
 ( #32933, #57185, #21623, #63040, #56302, #29722, #14425, #55412, #75678, #77459 ),
 .UNSPECIFIED., .F., .F.,
 ( 4, 2, 2, 2, 4 ),
 ( 0.0007817246256747461966, 0.0009771112852218889842, 0.001172497944769031880, 0.001367884604316174776, 0.001563271263863317672 ),
 .UNSPECIFIED. ) ;
#66912 = CARTESIAN_POINT ( 'NONE',  ( -8.638705330997126453, -10.31582465632705237, 34.18122507451815295 ) ) ;
#66913 = CARTESIAN_POINT ( 'NONE',  ( -16.94613126909829504, -3.062576670634119758, 32.05464942895959979 ) ) ;
#66914 = EDGE_CURVE ( 'NONE', #37313, #41563, #50410, .T. ) ;
#66915 = CARTESIAN_POINT ( 'NONE',  ( 17.77651505627605033, -8.496056993536548418, 34.65000542017679663 ) ) ;
#66916 = EDGE_LOOP ( 'NONE', ( #28772, #36834 ) ) ;
#66917 = ORIENTED_EDGE ( 'NONE', *, *, #81522, .F. ) ;
#66918 = CARTESIAN_POINT ( 'NONE',  ( -1.929879867024197893E-14, -3.750000000000000000, 24.15625000000000000 ) ) ;
#66919 = VECTOR ( 'NONE', #13127, 1000.000000000000227 ) ;
#66921 = EDGE_LOOP ( 'NONE', ( #9093, #27686 ) ) ;
#66920 = CARTESIAN_POINT ( 'NONE',  ( 11.31553532094538994, -9.086856451489515152, 34.49173150075333183 ) ) ;
#66922 = DIRECTION ( 'NONE',  ( -0.000000000000000000, -0.000000000000000000, -1.000000000000000000 ) ) ;
#66923 = CARTESIAN_POINT ( 'NONE',  ( -2.176901866725355461, -3.957578996910244395, 33.62503395064540257 ) ) ;
#66924 = B_SPLINE_CURVE_WITH_KNOTS ( 'NONE', 3,
 ( #87329, #25605, #80568, #59386, #74691, #53509, #46317, #66598, #12539, #67927 ),
 .UNSPECIFIED., .F., .F.,
 ( 4, 2, 2, 2, 4 ),
 ( 0.000000000000000000, 0.0001954339857564073659, 0.0003908679715128147319, 0.0005863019572692221250, 0.0007817359430256294638 ),
 .UNSPECIFIED. ) ;
#66925 = CARTESIAN_POINT ( 'NONE',  ( 4.153846153846154188, -2.499999999999998668, 29.50000000000001066 ) ) ;
#66926 = EDGE_LOOP ( 'NONE', ( #54770, #49617 ) ) ;
#66927 = ADVANCED_FACE ( 'NONE', ( #59735 ), #32271, .F. ) ;
#66928 = CARTESIAN_POINT ( 'NONE',  ( 3.360814286689004504, -2.254550872974306674, 29.97347326024527447 ) ) ;
#66929 = VERTEX_POINT ( 'NONE', #37341 ) ;
#66930 = DIRECTION ( 'NONE',  ( 0.000000000000000000, 0.9848077530122072432, -0.1736481776669354937 ) ) ;
#66931 = DIRECTION ( 'NONE',  ( 0.000000000000000000, 0.3420201433256641055, -0.9396926207859100932 ) ) ;
#66932 = CARTESIAN_POINT ( 'NONE',  ( 17.07692307692307665, -12.34228464037088635, 31.77849191805839268 ) ) ;
#66934 = FACE_OUTER_BOUND ( 'NONE', #52020, .T. ) ;
#66933 = CARTESIAN_POINT ( 'NONE',  ( -6.923076923076922462, -12.37446782046654192, 30.86335684631486131 ) ) ;
#66935 = CYLINDRICAL_SURFACE ( 'NONE', #18941, 0.2499999999999979738 ) ;
#66936 = VERTEX_POINT ( 'NONE', #4800 ) ;
#66937 = EDGE_CURVE ( 'NONE', #45196, #22351, #40442, .T. ) ;
#66938 = CARTESIAN_POINT ( 'NONE',  ( 9.692307692307695177, -1.242168528481310874, 33.36296068462461051 ) ) ;
#66939 = CARTESIAN_POINT ( 'NONE',  ( -18.75000000000000000, -3.499999999999999556, 29.75000000000000355 ) ) ;
#66940 = B_SPLINE_CURVE_WITH_KNOTS ( 'NONE', 3,
 ( #37170, #11043, #84936, #38067, #38516, #22765, #9701, #86276, #57886, #23215 ),
 .UNSPECIFIED., .F., .F.,
 ( 4, 2, 2, 2, 4 ),
 ( 0.0007817246256747446788, 0.0009771112852218874663, 0.001172497944769030145, 0.001367884604316172825, 0.001563271263863315720 ),
 .UNSPECIFIED. ) ;
#66941 = CYLINDRICAL_SURFACE ( 'NONE', #2053, 0.2499999999999973355 ) ;
#66942 = ORIENTED_EDGE ( 'NONE', *, *, #38313, .T. ) ;
#66943 = B_SPLINE_CURVE_WITH_KNOTS ( 'NONE', 3,
 ( #70492, #50652, #9248, #1593, #36706, #79023, #44781, #63727, #8800, #35828 ),
 .UNSPECIFIED., .F., .F.,
 ( 4, 2, 2, 2, 4 ),
 ( 0.0007817246256747464135, 0.0009771112852218900684, 0.001172497944769033615, 0.001367884604316177161, 0.001563271263863320925 ),
 .UNSPECIFIED. ) ;
#66944 = DIRECTION ( 'NONE',  ( -0.000000000000000000, -0.9848077530122086864, -0.1736481776669273613 ) ) ;
#66945 = CARTESIAN_POINT ( 'NONE',  ( 10.48523664565292002, -8.630895178749533159, 34.87696386517710323 ) ) ;
#66946 = DIRECTION ( 'NONE',  ( -1.000000000000000000, -0.000000000000000000, -0.000000000000000000 ) ) ;
#66947 = CARTESIAN_POINT ( 'NONE',  ( -0.6844171439671091761, -7.630691491037286056, 34.74850469731152458 ) ) ;
#66948 = EDGE_CURVE ( 'NONE', #70315, #68861, #48067, .T. ) ;
#66949 = VECTOR ( 'NONE', #47107, 1000.000000000000000 ) ;
#66950 = FACE_BOUND ( 'NONE', #47368, .T. ) ;
#66952 = DIRECTION ( 'NONE',  ( 0.000000000000000000, 0.1736481776669275834, 0.9848077530122086864 ) ) ;
#66951 = CARTESIAN_POINT ( 'NONE',  ( -4.153846153846152411, -5.557115091759785130, 34.35708131394839171 ) ) ;
#66953 = CARTESIAN_POINT ( 'NONE',  ( 2.084207383127978819, -10.23692288466677880, 34.23039457007281072 ) ) ;
#66955 = CARTESIAN_POINT ( 'NONE',  ( -9.469296340694842939, -10.61302985866383963, 33.66295027996417843 ) ) ;
#66954 = CARTESIAN_POINT ( 'NONE',  ( -17.86920819217521483, -11.18335022499818265, 33.13157742990017596 ) ) ;
#66956 = CARTESIAN_POINT ( 'NONE',  ( -39.05038313613820122, -2.499999999999999556, 29.75000000000000355 ) ) ;
#66957 = CARTESIAN_POINT ( 'NONE',  ( 1.492201783934554493, -3.724691934501233703, 26.48250670625848713 ) ) ;
#66959 = ADVANCED_FACE ( 'NONE', ( #19196 ), #39922, .F. ) ;
#66958 = ORIENTED_EDGE ( 'NONE', *, *, #43640, .T. ) ;
#66960 = CARTESIAN_POINT ( 'NONE',  ( 10.39245765647776487, -11.98009711892699514, 32.48740034544076138 ) ) ;
#66961 = ORIENTED_EDGE ( 'NONE', *, *, #70111, .F. ) ;
#66962 = LINE ( 'NONE', #88589, #55039 ) ;
#66963 = ORIENTED_EDGE ( 'NONE', *, *, #8118, .T. ) ;
#66964 = CARTESIAN_POINT ( 'NONE',  ( -3.903900635498009919, -12.22109172314383052, 31.39792113162168263 ) ) ;
#66965 = DIRECTION ( 'NONE',  ( -0.000000000000000000, 1.000000000000000000, -0.000000000000000000 ) ) ;
#66968 = ORIENTED_EDGE ( 'NONE', *, *, #38351, .F. ) ;
#66967 = VECTOR ( 'NONE', #9860, 1000.000000000000000 ) ;
#66966 = LINE ( 'NONE', #67849, #82685 ) ;
#66969 = CARTESIAN_POINT ( 'NONE',  ( -16.15384615384615330, -2.538708090699994813, 30.37095296980875503 ) ) ;
#66970 = CARTESIAN_POINT ( 'NONE',  ( 6.066067333350077639, -3.322132147404559976, 32.92929555188717927 ) ) ;
#66971 = CARTESIAN_POINT ( 'NONE',  ( -2.608446859217889546, -10.19485399968121264, 24.68563170625849068 ) ) ;
#66972 = CARTESIAN_POINT ( 'NONE',  ( 15.16549923021291413, -12.16647553114622049, 32.15551576947930812 ) ) ;
#66973 = CARTESIAN_POINT ( 'NONE',  ( -14.30769230769230660, -11.35647404775217417, 33.31231777344666511 ) ) ;
#66974 = EDGE_CURVE ( 'NONE', #23956, #64904, #74140, .T. ) ;
#66975 = CARTESIAN_POINT ( 'NONE',  ( 6.923076923076924238, -1.117168528481311540, 33.14645433367849847 ) ) ;
#66976 = CARTESIAN_POINT ( 'NONE',  ( 5.999999999999878320, -12.51329471203414379, 31.30864560766407578 ) ) ;
#66977 = CARTESIAN_POINT ( 'NONE',  ( 7.053602624840489277, -4.459921816937789885, 33.71989282347011851 ) ) ;
#66978 = LINE ( 'NONE', #26436, #69874 ) ;
#66979 = CARTESIAN_POINT ( 'NONE',  ( -3.775308065498748977, -8.992201783934593351, 16.51749329374151642 ) ) ;
#66980 = DIRECTION ( 'NONE',  ( -0.000000000000000000, -0.9848077530122085754, -0.1736481776669273613 ) ) ;
#66981 = EDGE_CURVE ( 'NONE', #57772, #25798, #56534, .T. ) ;
#66982 = CARTESIAN_POINT ( 'NONE',  ( 14.30769230769231015, -1.509761064869970415, 31.06009739812519044 ) ) ;
#66983 = VERTEX_POINT ( 'NONE', #9878 ) ;
#66984 = CARTESIAN_POINT ( 'NONE',  ( 5.448717948717947124, -7.500000000000000000, 29.75000000000000355 ) ) ;
#66985 = DIRECTION ( 'NONE',  ( 0.000000000000000000, 0.000000000000000000, 1.000000000000000000 ) ) ;
#66986 = B_SPLINE_CURVE_WITH_KNOTS ( 'NONE', 3,
 ( #57365, #77639, #43850, #56487, #22257, #71317, #50152, #58247, #15949, #43419 ),
 .UNSPECIFIED., .F., .F.,
 ( 4, 2, 2, 2, 4 ),
 ( 0.000000000000000000, 0.0001954311564186874436, 0.0003908623128373748873, 0.0005862934692560622767, 0.0007817246256747497745 ),
 .UNSPECIFIED. ) ;
#66987 = CARTESIAN_POINT ( 'NONE',  ( 1.614399933863618797, -3.775308065498751198, 18.23624329374151642 ) ) ;
#66988 = CARTESIAN_POINT ( 'NONE',  ( 0.6089743589743582541, -7.500000000000000000, 33.75000000000000000 ) ) ;
#66989 = CARTESIAN_POINT ( 'NONE',  ( -16.37733107841048863, -10.97335522853832579, 33.68706563782419749 ) ) ;
#66990 = ORIENTED_EDGE ( 'NONE', *, *, #68044, .T. ) ;
#66991 = VECTOR ( 'NONE', #1495, 1000.000000000000000 ) ;
#66992 = LINE ( 'NONE', #47596, #58613 ) ;
#66993 = CARTESIAN_POINT ( 'NONE',  ( 9.442284468086237226, -12.68155406624981119, 30.59749803192733708 ) ) ;
#66995 = EDGE_LOOP ( 'NONE', ( #21830, #75109, #57257, #58444 ) ) ;
#66994 = CARTESIAN_POINT ( 'NONE',  ( 4.853996118016225658, -12.38737895849757820, 31.66785238281580206 ) ) ;
#66996 = CARTESIAN_POINT ( 'NONE',  ( 11.66898724022510514, -5.195472089885680766, 34.18748526763464923 ) ) ;
#66997 = DIRECTION ( 'NONE',  ( 0.000000000000000000, 0.9396926207859126468, -0.3420201433256571111 ) ) ;
#66998 = EDGE_CURVE ( 'NONE', #48416, #74021, #85544, .T. ) ;
#66999 = FACE_OUTER_BOUND ( 'NONE', #18437, .T. ) ;
#67000 = CARTESIAN_POINT ( 'NONE',  ( 11.66925334628632882, -8.999086150933475636, 34.52020707165672775 ) ) ;
#67001 = EDGE_CURVE ( 'NONE', #33434, #76071, #41684, .T. ) ;
#67002 = ORIENTED_EDGE ( 'NONE', *, *, #35179, .T. ) ;
#67003 = DIRECTION ( 'NONE',  ( -0.000000000000000000, -0.9396926207859092051, -0.3420201433256662704 ) ) ;
#67004 = CARTESIAN_POINT ( 'NONE',  ( -15.48074597481782178, -11.47974371597208076, 33.17467449705390692 ) ) ;
#67005 = DIRECTION ( 'NONE',  ( -0.000000000000000000, -0.000000000000000000, -1.000000000000000000 ) ) ;
#67006 = VERTEX_POINT ( 'NONE', #61941 ) ;
#67007 = ORIENTED_EDGE ( 'NONE', *, *, #77635, .F. ) ;
#67008 = ORIENTED_EDGE ( 'NONE', *, *, #38982, .F. ) ;
#67009 = CARTESIAN_POINT ( 'NONE',  ( -3.230769230769229949, -12.09954503811598769, 35.62045528018868623 ) ) ;
#67010 = FACE_OUTER_BOUND ( 'NONE', #83903, .T. ) ;
#67011 = LINE ( 'NONE', #5307, #40926 ) ;
#67012 = CARTESIAN_POINT ( 'NONE',  ( 14.30769230769231015, -13.87047571288749737, 32.06866353760679544 ) ) ;
#67013 = EDGE_LOOP ( 'NONE', ( #40236, #27572, #68340, #71344 ) ) ;
#67014 = AXIS2_PLACEMENT_3D ( 'NONE', #73160, #69061, #33059 ) ;
#67015 = VERTEX_POINT ( 'NONE', #14208 ) ;
#67016 = ORIENTED_EDGE ( 'NONE', *, *, #73315, .T. ) ;
#67018 = ORIENTED_EDGE ( 'NONE', *, *, #55896, .T. ) ;
#67017 = CARTESIAN_POINT ( 'NONE',  ( -7.053767526187229464, -2.494641256782728966, 31.33461815524612959 ) ) ;
#67019 = CARTESIAN_POINT ( 'NONE',  ( 18.00000000000000000, -13.49023893513002648, 31.06009739812518688 ) ) ;
#67020 = B_SPLINE_CURVE_WITH_KNOTS ( 'NONE', 3,
 ( #51100, #49469, #17343, #64623, #7599, #3825, #71836, #42279, #21996, #44801 ),
 .UNSPECIFIED., .F., .F.,
 ( 4, 2, 2, 2, 4 ),
 ( 0.0007817359430256294638, 0.0009771253907249974075, 0.001172514838424365460, 0.001367904286123733295, 0.001563293733823094191 ),
 .UNSPECIFIED. ) ;
#67021 = DIRECTION ( 'NONE',  ( -0.000000000000000000, 0.8660254037844399289, -0.4999999999999980016 ) ) ;
#67022 = EDGE_CURVE ( 'NONE', #72142, #32479, #82683, .T. ) ;
#67023 = CARTESIAN_POINT ( 'NONE',  ( 7.173131342990377135, -4.818054556918156095, 34.26375889529406749 ) ) ;
#67024 = DIRECTION ( 'NONE',  ( -0.000000000000000000, -0.9396926207859093161, -0.3420201433256663259 ) ) ;
#67025 = EDGE_CURVE ( 'NONE', #79443, #35898, #44714, .T. ) ;
#67026 = VECTOR ( 'NONE', #4785, 1000.000000000000000 ) ;
#67027 = VERTEX_POINT ( 'NONE', #14656 ) ;
#67028 = EDGE_LOOP ( 'NONE', ( #68062, #83202, #37474, #57065 ) ) ;
#67029 = ORIENTED_EDGE ( 'NONE', *, *, #44990, .T. ) ;
#67030 = CARTESIAN_POINT ( 'NONE',  ( 14.55763771707035303, -10.92531984108285670, 33.72920026020278073 ) ) ;
#67032 = EDGE_LOOP ( 'NONE', ( #11277, #20589 ) ) ;
#67031 = CARTESIAN_POINT ( 'NONE',  ( 0.000000000000000000, -11.00000000000000000, 29.75000000000000355 ) ) ;
#67033 = EDGE_CURVE ( 'NONE', #88230, #51973, #7006, .T. ) ;
#67034 = CARTESIAN_POINT ( 'NONE',  ( -10.74594452899797936, -2.254533558242300284, 29.97296025877828285 ) ) ;
#67035 = CARTESIAN_POINT ( 'NONE',  ( -0.4615384615384611200, -4.661471528628507777, 34.16647553114623292 ) ) ;
#67036 = LINE ( 'NONE', #53956, #56102 ) ;
#67037 = FACE_OUTER_BOUND ( 'NONE', #34218, .T. ) ;
#67038 = EDGE_CURVE ( 'NONE', #11273, #28791, #67825, .T. ) ;
#67039 = LINE ( 'NONE', #52619, #23791 ) ;
#67040 = FACE_BOUND ( 'NONE', #35561, .T. ) ;
#67041 = CARTESIAN_POINT ( 'NONE',  ( -0.6850234052624097902, -4.386631170607604879, 33.66268669641500111 ) ) ;
#67042 = DIRECTION ( 'NONE',  ( -0.000000000000000000, 0.000000000000000000, 1.000000000000000000 ) ) ;
#67043 = CARTESIAN_POINT ( 'NONE',  ( -5.999999999999998224, -2.708943851104267164, 35.45975837776705220 ) ) ;
#67045 = CARTESIAN_POINT ( 'NONE',  ( 15.48082365068268018, -10.06805714834173493, 34.32951233291982618 ) ) ;
#67044 = CARTESIAN_POINT ( 'NONE',  ( 12.94230769230769340, -7.500000000000000000, 29.75000000000000355 ) ) ;
#67046 = CARTESIAN_POINT ( 'NONE',  ( -4.403846153846151523, -7.500000000000001776, 35.00000000000000000 ) ) ;
#67047 = DIRECTION ( 'NONE',  ( -0.000000000000000000, -0.9848077530122085754, -0.1736481776669273613 ) ) ;
#67048 = VERTEX_POINT ( 'NONE', #253 ) ;
#67049 = CARTESIAN_POINT ( 'NONE',  ( 12.22435897435897267, -3.499999999999999556, 29.75000000000000355 ) ) ;
#67050 = DIRECTION ( 'NONE',  ( 0.000000000000000000, 0.8660254037844377084, 0.5000000000000015543 ) ) ;
#67051 = ORIENTED_EDGE ( 'NONE', *, *, #66782, .T. ) ;
#67052 = ORIENTED_EDGE ( 'NONE', *, *, #11437, .F. ) ;
#67053 = VECTOR ( 'NONE', #70193, 1000.000000000000227 ) ;
#67054 = CARTESIAN_POINT ( 'NONE',  ( -6.923076923077044142, -5.219633306517616589, 34.19971097300220464 ) ) ;
#67055 = EDGE_CURVE ( 'NONE', #40219, #26904, #6569, .T. ) ;
#67056 = B_SPLINE_CURVE_WITH_KNOTS ( 'NONE', 3,
 ( #29813, #1449, #84324, #28031, #36134, #16291, #63585, #69013, #28939, #1887 ),
 .UNSPECIFIED., .F., .F.,
 ( 4, 2, 2, 2, 4 ),
 ( 0.0007817246256747465219, 0.0009771112852218900684, 0.001172497944769033615, 0.001367884604316177378, 0.001563271263863320925 ),
 .UNSPECIFIED. ) ;
#67057 = DIRECTION ( 'NONE',  ( 0.000000000000000000, 0.3420201433256610524, 0.9396926207859113145 ) ) ;
#67058 = DIRECTION ( 'NONE',  ( -0.000000000000000000, 0.5000000000000011102, -0.8660254037844381525 ) ) ;
#67059 = ORIENTED_EDGE ( 'NONE', *, *, #37154, .T. ) ;
#67060 = CARTESIAN_POINT ( 'NONE',  ( 13.38461538461526601, -2.892918686052165622, 31.69288490824153470 ) ) ;
#67061 = CARTESIAN_POINT ( 'NONE',  ( 6.923076923076924238, -13.78497067705608181, 32.30358669280327177 ) ) ;
#67063 = CARTESIAN_POINT ( 'NONE',  ( 5.750023255951410839, -6.524016743844655686, 34.90889640711025521 ) ) ;
#67062 = LINE ( 'NONE', #67950, #38948 ) ;
#67064 = CARTESIAN_POINT ( 'NONE',  ( -17.78205128205128105, -3.499999999999999556, 29.75000000000000355 ) ) ;
#67065 = CARTESIAN_POINT ( 'NONE',  ( 0.5920638997721049401, -5.070358843744209310, 34.40418822224088302 ) ) ;
#67066 = CARTESIAN_POINT ( 'NONE',  ( -10.55012947587177941, -11.67786785259547777, 32.92929555188713664 ) ) ;
#67067 = CARTESIAN_POINT ( 'NONE',  ( 1.553300858899129944, -11.24999999999998934, 19.70312500000000355 ) ) ;
#67068 = ORIENTED_EDGE ( 'NONE', *, *, #24063, .T. ) ;
#67069 = EDGE_CURVE ( 'NONE', #20099, #58521, #27505, .T. ) ;
#67070 = VERTEX_POINT ( 'NONE', #62379 ) ;
#67071 = DIRECTION ( 'NONE',  ( -1.000000000000000000, 0.000000000000000000, 0.000000000000000000 ) ) ;
#67072 = ADVANCED_FACE ( 'NONE', ( #82232 ), #48876, .F. ) ;
#67073 = CARTESIAN_POINT ( 'NONE',  ( 6.923076923076924238, -12.10708131394839349, 31.69288490824020244 ) ) ;
#67074 = CARTESIAN_POINT ( 'NONE',  ( 10.68145296638705410, -2.538708090699994813, 30.37095296980875503 ) ) ;
#67075 = DIRECTION ( 'NONE',  ( 0.000000000000000000, 0.000000000000000000, -1.000000000000000000 ) ) ;
#67076 = CARTESIAN_POINT ( 'NONE',  ( -3.454254174493178287, -5.912607949931405038, 34.49155766932282319 ) ) ;
#67077 = CARTESIAN_POINT ( 'NONE',  ( 3.749999999999992006, -5.946699141100872943, 24.39062500000000000 ) ) ;
#67078 = DIRECTION ( 'NONE',  ( -0.000000000000000000, 0.1736481776669307198, -0.9848077530122080203 ) ) ;
#67079 = CARTESIAN_POINT ( 'NONE',  ( 14.05766908347085042, -6.652501968072648708, 34.93155406624980941 ) ) ;
#67080 = DIRECTION ( 'NONE',  ( -0.000000000000000000, 1.000000000000000000, 3.491481338843133355E-15 ) ) ;
#67081 = CARTESIAN_POINT ( 'NONE',  ( 12.33139049180676494, -11.66186481527757302, 32.95055677023626117 ) ) ;
#67082 = CARTESIAN_POINT ( 'NONE',  ( 9.823099500132478568, -2.729792928343269587, 31.24908615093345077 ) ) ;
#67083 = CARTESIAN_POINT ( 'NONE',  ( 8.639083559792545941, -12.27039167877662251, 31.24851455888617835 ) ) ;
#67084 = CARTESIAN_POINT ( 'NONE',  ( 5.869308533332440625, -12.11776431015576172, 31.66791131148498906 ) ) ;
#67086 = VECTOR ( 'NONE', #50219, 1000.000000000000227 ) ;
#67085 = CARTESIAN_POINT ( 'NONE',  ( 4.087762742890272527, -12.37446782046654192, 30.86335684631486487 ) ) ;
#67088 = EDGE_CURVE ( 'NONE', #879, #17306, #12511, .T. ) ;
#67087 = CARTESIAN_POINT ( 'NONE',  ( -0.6089743589743593644, -3.499999999999999556, 29.75000000000000355 ) ) ;
#67089 = CARTESIAN_POINT ( 'NONE',  ( -7.596099534515530216, -12.41262288849542017, 30.68299917996395010 ) ) ;
#67090 = ORIENTED_EDGE ( 'NONE', *, *, #74654, .F. ) ;
#67091 = CARTESIAN_POINT ( 'NONE',  ( 8.769230769230768274, -12.62096338111211580, 30.90682066428153263 ) ) ;
#67092 = CARTESIAN_POINT ( 'NONE',  ( -17.14300545628320904, -6.343179335718451384, 34.87096338111212646 ) ) ;
#67093 = CARTESIAN_POINT ( 'NONE',  ( 6.000000000000001776, -2.486705287966279876, 31.30864560766543647 ) ) ;
#67094 = CARTESIAN_POINT ( 'NONE',  ( -1.077988221561493543, -4.724691934501247914, 15.57999329374151110 ) ) ;
#67095 = B_SPLINE_CURVE_WITH_KNOTS ( 'NONE', 3,
 ( #77632, #79415, #17715, #43410, #70884, #50598 ),
 .UNSPECIFIED., .F., .F.,
 ( 4, 2, 4 ),
 ( 0.000000000000000000, 0.0001954784845028902421, 0.0003909569690057804843 ),
 .UNSPECIFIED. ) ;
#67096 = CARTESIAN_POINT ( 'NONE',  ( 5.299702745901139878, -10.23759521482555357, 34.22997729860117033 ) ) ;
#67097 = CARTESIAN_POINT ( 'NONE',  ( -11.47320639894870276, -5.094484230520773593, 34.41647553114626845 ) ) ;
#67098 = B_SPLINE_CURVE_WITH_KNOTS ( 'NONE', 3,
 ( #24070, #39387, #44777, #80373, #38487, #87137, #24512, #17319, #38940, #66397 ),
 .UNSPECIFIED., .F., .F.,
 ( 4, 2, 2, 2, 4 ),
 ( 0.0007817359430256318490, 0.0009771253907249984917, 0.001172514838424365026, 0.001367904286123731560, 0.001563293733823098311 ),
 .UNSPECIFIED. ) ;
#67100 = ORIENTED_EDGE ( 'NONE', *, *, #44105, .F. ) ;
#67099 = CARTESIAN_POINT ( 'NONE',  ( -0.4615384615385826339, -2.625532179533779598, 30.86335684631627174 ) ) ;
#67101 = CARTESIAN_POINT ( 'NONE',  ( 1.944543648263018731, -9.444543648262994751, 24.62500000000000000 ) ) ;
#67102 = CARTESIAN_POINT ( 'NONE',  ( -20.75000000000000355, -12.50000000000000000, 27.25000000000000000 ) ) ;
#67103 = AXIS2_PLACEMENT_3D ( 'NONE', #19680, #5282, #74632 ) ;
#67104 = EDGE_CURVE ( 'NONE', #14267, #53679, #14587, .T. ) ;
#67105 = VERTEX_POINT ( 'NONE', #49328 ) ;
#67106 = CARTESIAN_POINT ( 'NONE',  ( 0.4615384615384611200, -2.721908614388771852, 31.22303859784724978 ) ) ;
#67107 = EDGE_LOOP ( 'NONE', ( #60332, #38400, #22068, #6745 ) ) ;
#67108 = B_SPLINE_CURVE_WITH_KNOTS ( 'NONE', 3,
 ( #53226, #18568, #46481, #46911, #10918, #87948, #45583, #11814, #39292, #38389 ),
 .UNSPECIFIED., .F., .F.,
 ( 4, 2, 2, 2, 4 ),
 ( 0.0007817359430256315238, 0.0009771253907249980580, 0.001172514838424364592, 0.001367904286123730910, 0.001563293733823097444 ),
 .UNSPECIFIED. ) ;
#67109 = DIRECTION ( 'NONE',  ( -0.000000000000000000, 1.000000000000000000, 3.491481338843133355E-15 ) ) ;
#67110 = EDGE_CURVE ( 'NONE', #11909, #72772, #2892, .T. ) ;
#67111 = ADVANCED_FACE ( 'NONE', ( #57852 ), #37129, .F. ) ;
#67112 = CARTESIAN_POINT ( 'NONE',  ( -7.846153846153965716, -11.94971097300221174, 32.03036669348237098 ) ) ;
#67113 = DIRECTION ( 'NONE',  ( 0.000000000000000000, 0.000000000000000000, -1.000000000000000000 ) ) ;
#67114 = ORIENTED_EDGE ( 'NONE', *, *, #26646, .T. ) ;
#67115 = ORIENTED_EDGE ( 'NONE', *, *, #16666, .F. ) ;
#67116 = EDGE_CURVE ( 'NONE', #43361, #48748, #61950, .T. ) ;
#67117 = ORIENTED_EDGE ( 'NONE', *, *, #49762, .F. ) ;
#67118 = CARTESIAN_POINT ( 'NONE',  ( -16.02305571287920216, -2.295524264805590686, 30.44142389570982488 ) ) ;
#67119 = CARTESIAN_POINT ( 'NONE',  ( 7.146089767170319185, -11.43677907613344757, 33.22367315496201456 ) ) ;
#67120 = VECTOR ( 'NONE', #72963, 1000.000000000000000 ) ;
#67121 = CYLINDRICAL_SURFACE ( 'NONE', #85849, 0.2499999999999994726 ) ;
#67122 = CARTESIAN_POINT ( 'NONE',  ( -1.450697763975519416, -11.35647404775217595, 33.31231777344666511 ) ) ;
#67123 = CARTESIAN_POINT ( 'NONE',  ( -10.74607521849492109, -11.93127051446799847, 32.56575433478202797 ) ) ;
#67124 = CARTESIAN_POINT ( 'NONE',  ( -6.923076923076922462, -8.973038597847269315, 34.52809138561121927 ) ) ;
#67125 = CARTESIAN_POINT ( 'NONE',  ( 12.52679403281448600, -5.219633306516380244, 34.19971097300157936 ) ) ;
#67126 = VECTOR ( 'NONE', #73084, 1000.000000000000227 ) ;
#67127 = CARTESIAN_POINT ( 'NONE',  ( -12.46153846153858247, -6.879047030192662504, 34.71129190930017927 ) ) ;
#67128 = ORIENTED_EDGE ( 'NONE', *, *, #79566, .F. ) ;
#67129 = VERTEX_POINT ( 'NONE', #70930 ) ;
#67130 = CIRCLE ( 'NONE', #23965, 0.2500000000000002220 ) ;
#67131 = VERTEX_POINT ( 'NONE', #21852 ) ;
#67133 = ORIENTED_EDGE ( 'NONE', *, *, #11973, .T. ) ;
#67132 = CARTESIAN_POINT ( 'NONE',  ( -3.930833309752757021, -8.282913670948747864, 34.94150082978203642 ) ) ;
#67134 = LINE ( 'NONE', #4535, #29173 ) ;
#67135 = LINE ( 'NONE', #23903, #15152 ) ;
#67136 = ORIENTED_EDGE ( 'NONE', *, *, #57838, .F. ) ;
#67137 = CARTESIAN_POINT ( 'NONE',  ( 15.36155967173618286, -9.084667340241226796, 34.75534355489798344 ) ) ;
#67138 = EDGE_LOOP ( 'NONE', ( #39563, #66415, #64752, #35086 ) ) ;
#67139 = CARTESIAN_POINT ( 'NONE',  ( -10.74553182482283198, -3.285722584762969856, 32.44110544564090759 ) ) ;
#67140 = ORIENTED_EDGE ( 'NONE', *, *, #70707, .F. ) ;
#67141 = CARTESIAN_POINT ( 'NONE',  ( 10.86538461538461675, -7.500000000000001776, 35.04278698407183867 ) ) ;
#67142 = CIRCLE ( 'NONE', #32668, 0.2500000000000002220 ) ;
#67143 = CARTESIAN_POINT ( 'NONE',  ( 1.449870955891410684, -6.879047030191282275, 34.71129190930002295 ) ) ;
#67144 = CARTESIAN_POINT ( 'NONE',  ( 0.3308469948709023556, -4.809359713505814149, 33.96456829005828837 ) ) ;
#67145 = B_SPLINE_CURVE_WITH_KNOTS ( 'NONE', 3,
 ( #86364, #37250, #72814, #36818, #3909, #30067, #58402, #30935, #24635, #71482 ),
 .UNSPECIFIED., .F., .F.,
 ( 4, 2, 2, 2, 4 ),
 ( 0.000000000000000000, 0.0001954339857564063089, 0.0003908679715128126177, 0.0005863019572692189808, 0.0007817359430256252354 ),
 .UNSPECIFIED. ) ;
#67146 = FACE_BOUND ( 'NONE', #72274, .T. ) ;
#67147 = CARTESIAN_POINT ( 'NONE',  ( 2.557692307693744560, -7.500000000000155431, 34.75000000000007105 ) ) ;
#67148 = DIRECTION ( 'NONE',  ( -0.000000000000000000, 1.000000000000000000, -0.000000000000000000 ) ) ;
#67149 = CARTESIAN_POINT ( 'NONE',  ( 5.777134577796363857, -2.501496062324911840, 29.88072118266895671 ) ) ;
#67150 = CARTESIAN_POINT ( 'NONE',  ( -13.38461538461550582, -12.27809138561165270, 31.22303859784587132 ) ) ;
#67151 = CARTESIAN_POINT ( 'NONE',  ( 10.36538461538461675, -7.500000000000001776, 34.75000000000000000 ) ) ;
#67152 = CARTESIAN_POINT ( 'NONE',  ( 0.4615384615384611200, -13.20930481340135110, 34.54067556320372745 ) ) ;
#67153 = ORIENTED_EDGE ( 'NONE', *, *, #36123, .T. ) ;
#67154 = VECTOR ( 'NONE', #72973, 1000.000000000000000 ) ;
#67155 = CARTESIAN_POINT ( 'NONE',  ( -3.230769230769229949, -1.129524287112498415, 32.06866353760679544 ) ) ;
#67156 = EDGE_LOOP ( 'NONE', ( #76869, #79756, #27052, #86879 ) ) ;
#67157 = VERTEX_POINT ( 'NONE', #15102 ) ;
#67159 = CARTESIAN_POINT ( 'NONE',  ( -5.999999999999998224, -8.318370150425687726, 35.83090037661290239 ) ) ;
#67158 = CARTESIAN_POINT ( 'NONE',  ( 5.933917620639864943, -11.91647553114624181, 32.58852847137148245 ) ) ;
#67160 = CARTESIAN_POINT ( 'NONE',  ( 2.057692307692309708, -7.500000000000001776, 35.04278698407183867 ) ) ;
#67161 = CARTESIAN_POINT ( 'NONE',  ( -14.37377468705243899, -11.91647553114624181, 32.58852847137148245 ) ) ;
#67162 = CARTESIAN_POINT ( 'NONE',  ( -17.29985003582992320, -12.38737895849757820, 31.66785238281580206 ) ) ;
#67163 = CARTESIAN_POINT ( 'NONE',  ( -13.38461538461550582, -2.892918686052166066, 31.69288490824153470 ) ) ;
#67164 = ORIENTED_EDGE ( 'NONE', *, *, #29798, .T. ) ;
#67165 = CARTESIAN_POINT ( 'NONE',  ( -8.096153846153844924, -7.500000000000001776, 35.00000000000000000 ) ) ;
#67166 = CARTESIAN_POINT ( 'NONE',  ( 15.10062126103753855, -4.299443229763728169, 33.91186481527756058 ) ) ;
#67167 = CARTESIAN_POINT ( 'NONE',  ( -14.53117725141625627, -8.496056993536548418, 34.65000542017679663 ) ) ;
#67168 = CARTESIAN_POINT ( 'NONE',  ( -6.989159302437059296, -6.343179335718451384, 34.87096338111212646 ) ) ;
#67169 = VERTEX_POINT ( 'NONE', #84455 ) ;
#67170 = VERTEX_POINT ( 'NONE', #2023 ) ;
#67171 = B_SPLINE_CURVE_WITH_KNOTS ( 'NONE', 3,
 ( #7811, #49677, #28528, #15462, #42933, #7374, #69949, #70402, #8704, #34388 ),
 .UNSPECIFIED., .F., .F.,
 ( 4, 2, 2, 2, 4 ),
 ( 0.0007817246256747472808, 0.0009771112852218905021, 0.001172497944769033832, 0.001367884604316177161, 0.001563271263863320274 ),
 .UNSPECIFIED. ) ;
#67172 = ITEM_DEFINED_TRANSFORMATION ( 'NONE', 'NONE', #83521,  #83448 ) ;
#67173 = ORIENTED_EDGE ( 'NONE', *, *, #34013, .F. ) ;
#67174 = VECTOR ( 'NONE', #68217, 1000.000000000000114 ) ;
#67175 = CARTESIAN_POINT ( 'NONE',  ( 20.00000000000000711, -9.999999999999994671, 3.000000000000000000 ) ) ;
#67176 = DIRECTION ( 'NONE',  ( -1.000000000000000000, -0.000000000000000000, -0.000000000000000000 ) ) ;
#67177 = EDGE_CURVE ( 'NONE', #88629, #84284, #47924, .T. ) ;
#67178 = VERTEX_POINT ( 'NONE', #63275 ) ;
#67179 = CYLINDRICAL_SURFACE ( 'NONE', #88456, 0.2499999999999998890 ) ;
#67180 = CARTESIAN_POINT ( 'NONE',  ( 14.55774672760576394, -5.642605341092957971, 34.66089969410670335 ) ) ;
#67181 = CARTESIAN_POINT ( 'NONE',  ( -5.326946314216042033, -4.335965774309649134, 33.62209801155881905 ) ) ;
#67182 = CARTESIAN_POINT ( 'NONE',  ( 9.019285189144222059, -3.435999193479609914, 33.07426656108010832 ) ) ;
#67183 = CIRCLE ( 'NONE', #74245, 4.000000000000000000 ) ;
#67184 = CARTESIAN_POINT ( 'NONE',  ( -20.00000000000000355, 10.00000000000000711, 13.00000000000000178 ) ) ;
#67185 = ORIENTED_EDGE ( 'NONE', *, *, #21630, .T. ) ;
#67187 = ORIENTED_EDGE ( 'NONE', *, *, #61449, .T. ) ;
#67186 = CARTESIAN_POINT ( 'NONE',  ( -7.780085495151405794, -9.780366693483667717, 34.19971097300155805 ) ) ;
#67188 = CARTESIAN_POINT ( 'NONE',  ( 13.38461538461538680, -3.937682226553329556, 33.60647404775216529 ) ) ;
#67189 = CARTESIAN_POINT ( 'NONE',  ( 8.899756207464413649, -12.50538340440932394, 31.33453814440721885 ) ) ;
#67191 = B_SPLINE_CURVE_WITH_KNOTS ( 'NONE', 3,
 ( #44449, #3916, #31402, #58870, #86371, #52108, #79598, #77808, #17894, #45351 ),
 .UNSPECIFIED., .F., .F.,
 ( 4, 2, 2, 2, 4 ),
 ( 0.000000000000000000, 0.0001954311564186876876, 0.0003908623128373753751, 0.0005862934692560630356, 0.0007817246256747507503 ),
 .UNSPECIFIED. ) ;
#67190 = DIRECTION ( 'NONE',  ( -0.000000000000000000, -0.5000000000000009992, -0.8660254037844380415 ) ) ;
#67192 = CARTESIAN_POINT ( 'NONE',  ( 18.00000000000000000, -8.120952969808772792, 34.71129190930000163 ) ) ;
#67193 = B_SPLINE_CURVE_WITH_KNOTS ( 'NONE', 3,
 ( #34341, #77436, #122, #22492, #29267, #2644, #84652, #29704, #30137, #57604 ),
 .UNSPECIFIED., .F., .F.,
 ( 4, 2, 2, 2, 4 ),
 ( 0.0007817359430256257775, 0.0009771253907249911191, 0.001172514838424356352, 0.001367904286123721586, 0.001563293733823086819 ),
 .UNSPECIFIED. ) ;
#67194 = DIRECTION ( 'NONE',  ( 0.000000000000000000, 0.1736481776669275834, 0.9848077530122086864 ) ) ;
#67195 = EDGE_CURVE ( 'NONE', #13888, #87291, #65128, .T. ) ;
#67196 = AXIS2_PLACEMENT_3D ( 'NONE', #6054, #7384, #69077 ) ;
#67197 = PRESENTATION_STYLE_ASSIGNMENT (( #19445 ) ) ;
#67198 = B_SPLINE_CURVE_WITH_KNOTS ( 'NONE', 3,
 ( #37628, #10608, #85381, #2069, #2501, #77285, #37179, #44366, #23226, #31324 ),
 .UNSPECIFIED., .F., .F.,
 ( 4, 2, 2, 2, 4 ),
 ( 0.0007817359430256294638, 0.0009771253907249974075, 0.001172514838424365460, 0.001367904286123733295, 0.001563293733823094191 ),
 .UNSPECIFIED. ) ;
#67199 = CARTESIAN_POINT ( 'NONE',  ( -0.7115152055870509473, -2.544273027872575366, 31.48422191005632342 ) ) ;
#67200 = CARTESIAN_POINT ( 'NONE',  ( 2.750000000000002665, -7.561099074964516831, 20.97061829374151642 ) ) ;
#67201 = ORIENTED_EDGE ( 'NONE', *, *, #57163, .F. ) ;
#67202 = CARTESIAN_POINT ( 'NONE',  ( 11.53846153846153832, -2.721908614388771852, 31.22303859784724978 ) ) ;
#67203 = CARTESIAN_POINT ( 'NONE',  ( 2.557637717070352590, -4.176053281294514363, 33.81426240980091791 ) ) ;
#67204 = CARTESIAN_POINT ( 'NONE',  ( 16.09615384615384670, -11.50000000000000000, 29.75000000000000355 ) ) ;
#67205 = ORIENTED_EDGE ( 'NONE', *, *, #2680, .T. ) ;
#67206 = CARTESIAN_POINT ( 'NONE',  ( 2.530655441958984397, -7.369474539155830506, 34.99858011523957657 ) ) ;
#67207 = CARTESIAN_POINT ( 'NONE',  ( -12.71151519248081740, -3.137211980971221781, 32.19342716148376837 ) ) ;
#67208 = CARTESIAN_POINT ( 'NONE',  ( -0.4615384615384611200, -9.058645607665452459, 34.76329471203371924 ) ) ;
#67209 = CARTESIAN_POINT ( 'NONE',  ( -9.019207513279360100, -10.82459398097509329, 33.81372124010185587 ) ) ;
#67210 = DIRECTION ( 'NONE',  ( -1.000000000000000000, 0.000000000000000000, -0.000000000000000000 ) ) ;
#67211 = CARTESIAN_POINT ( 'NONE',  ( 0.5267936010512991318, -2.379036618887895305, 30.90682066428159303 ) ) ;
#67212 = EDGE_LOOP ( 'NONE', ( #85154, #58908 ) ) ;
#67213 = VECTOR ( 'NONE', #76167, 1000.000000000000000 ) ;
#67215 = EDGE_CURVE ( 'NONE', #82495, #76951, #9665, .T. ) ;
#67214 = CARTESIAN_POINT ( 'NONE',  ( -3.100243792535588128, -12.70449254468099198, 30.44128974285582956 ) ) ;
#67216 = EDGE_CURVE ( 'NONE', #37079, #47404, #82403, .T. ) ;
#67217 = CARTESIAN_POINT ( 'NONE',  ( 7.145856592054988354, -6.717445702608402236, 34.94155399931962336 ) ) ;
#67218 = CARTESIAN_POINT ( 'NONE',  ( -3.230769230769229949, -11.69971097300155272, 32.46337939537588113 ) ) ;
#67219 = VERTEX_POINT ( 'NONE', #50644 ) ;
#67220 = CARTESIAN_POINT ( 'NONE',  ( 12.52679403281448423, -3.835265460703683349, 33.15142922261929925 ) ) ;
#67221 = AXIS2_PLACEMENT_3D ( 'NONE', #57373, #84868, #78094 ) ;
#67222 = ORIENTED_EDGE ( 'NONE', *, *, #10470, .F. ) ;
#67223 = PLANE ( 'NONE',  #8357 ) ;
#67224 = FILL_AREA_STYLE_COLOUR ( '', #44640 ) ;
#67225 = CARTESIAN_POINT ( 'NONE',  ( 22.00000000000001066, -9.999999999999957367, 10.00000000000000178 ) ) ;
#67226 = VERTEX_POINT ( 'NONE', #22731 ) ;
#67227 = CARTESIAN_POINT ( 'NONE',  ( 0.5276068125408992504, -4.098570777380720287, 33.41473453929635440 ) ) ;
#67228 = CARTESIAN_POINT ( 'NONE',  ( -6.000000000000121680, -2.379036618888197729, 30.90682066428292885 ) ) ;
#67229 = CYLINDRICAL_SURFACE ( 'NONE', #88328, 0.2499999999999997502 ) ;
#67230 = B_SPLINE_CURVE_WITH_KNOTS ( 'NONE', 3,
 ( #36083, #55894, #77063, #50458, #50023, #49587, #48690, #29325, #28889, #43275 ),
 .UNSPECIFIED., .F., .F.,
 ( 4, 2, 2, 2, 4 ),
 ( 0.000000000000000000, 0.0001954311564186869557, 0.0003908623128373738030, 0.0005862934692560607588, 0.0007817246256747476061 ),
 .UNSPECIFIED. ) ;
#67231 = B_SPLINE_CURVE_WITH_KNOTS ( 'NONE', 3,
 ( #44515, #65679, #57600, #25150, #78309, #45860, #52167, #9858, #31464, #24707 ),
 .UNSPECIFIED., .F., .F.,
 ( 4, 2, 2, 2, 4 ),
 ( 0.000000000000000000, 0.0001954339857564054144, 0.0003908679715128108288, 0.0005863019572692162703, 0.0007817359430256216575 ),
 .UNSPECIFIED. ) ;
#67232 = FACE_OUTER_BOUND ( 'NONE', #54707, .T. ) ;
#67233 = CARTESIAN_POINT ( 'NONE',  ( -0.5268084620947819374, -11.67786785259541027, 32.92929555188721480 ) ) ;
#67234 = B_SPLINE_CURVE_WITH_KNOTS ( 'NONE', 3,
 ( #8093, #68455, #54946, #49520, #35566, #1326, #76993, #13954, #21596, #6752 ),
 .UNSPECIFIED., .F., .F.,
 ( 4, 2, 2, 2, 4 ),
 ( 0.0007817359430256297891, 0.0009771253907249961065, 0.001172514838424362424, 0.001367904286123728741, 0.001563293733823095059 ),
 .UNSPECIFIED. ) ;
#67235 = EDGE_LOOP ( 'NONE', ( #18207, #55313, #25141, #33652 ) ) ;
#67236 = CARTESIAN_POINT ( 'NONE',  ( -3.903791733932700847, -12.41089969410671223, 31.60739465890703670 ) ) ;
#67237 = ORIENTED_EDGE ( 'NONE', *, *, #66135, .T. ) ;
#67238 = LINE ( 'NONE', #65882, #83187 ) ;
#67239 = CARTESIAN_POINT ( 'NONE',  ( -10.39237177129122003, -10.01129605718032600, 34.36064277460058491 ) ) ;
#67240 = CARTESIAN_POINT ( 'NONE',  ( -13.60754160213152808, -2.758268499246657068, 31.33685645148948140 ) ) ;
#67241 = VECTOR ( 'NONE', #40794, 1000.000000000000000 ) ;
#67242 = CARTESIAN_POINT ( 'NONE',  ( 6.250054311638317373, -9.148310452688871663, 34.47095581063188519 ) ) ;
#67243 = LINE ( 'NONE', #30446, #75208 ) ;
#67244 = FACE_OUTER_BOUND ( 'NONE', #70895, .T. ) ;
#67245 = ORIENTED_EDGE ( 'NONE', *, *, #72348, .T. ) ;
#67246 = EDGE_LOOP ( 'NONE', ( #77077, #74340, #8312, #19072 ) ) ;
#67247 = ORIENTED_EDGE ( 'NONE', *, *, #59473, .F. ) ;
#67248 = ORIENTED_EDGE ( 'NONE', *, *, #4526, .F. ) ;
#67249 = CARTESIAN_POINT ( 'NONE',  ( -10.48459280755982626, -11.18335022499818621, 33.13157742990016885 ) ) ;
#67250 = CARTESIAN_POINT ( 'NONE',  ( -3.230769230769229949, -6.343179335718451384, 34.87096338111211935 ) ) ;
#67251 = CARTESIAN_POINT ( 'NONE',  ( -15.36146069743679021, -10.54014554554150607, 33.71984207302941883 ) ) ;
#67252 = DIRECTION ( 'NONE',  ( -0.000000000000000000, 0.9396926207859093161, -0.3420201433256663259 ) ) ;
#67253 = CARTESIAN_POINT ( 'NONE',  ( 17.77707378248384629, -9.886141570436013382, 34.14413921362392301 ) ) ;
#67254 = CARTESIAN_POINT ( 'NONE',  ( -10.36538461538461320, -2.499999999999998668, 29.75000000000000355 ) ) ;
#67255 = DIRECTION ( 'NONE',  ( 0.000000000000000000, 1.000000000000000000, -2.546383084002652634E-16 ) ) ;
#67256 = CARTESIAN_POINT ( 'NONE',  ( 6.923076923076802558, -12.46129190930018460, 30.37095296980731973 ) ) ;
#67257 = ORIENTED_EDGE ( 'NONE', *, *, #44833, .F. ) ;
#67258 = EDGE_LOOP ( 'NONE', ( #37892, #79885, #8147, #71204 ) ) ;
#67259 = ADVANCED_FACE ( 'NONE', ( #43454 ), #2454, .F. ) ;
#67260 = ORIENTED_EDGE ( 'NONE', *, *, #72534, .T. ) ;
#67262 = VERTEX_POINT ( 'NONE', #52866 ) ;
#67261 = CARTESIAN_POINT ( 'NONE',  ( 2.241608896736426271, -2.538708090699994813, 30.37095296980875148 ) ) ;
#67264 = CARTESIAN_POINT ( 'NONE',  ( -7.596099426240392027, -9.233818618650603938, 34.70587769442853698 ) ) ;
#67263 = CARTESIAN_POINT ( 'NONE',  ( 16.21991450484859953, -11.69971097300155272, 32.46337939537588113 ) ) ;
#67265 = EDGE_CURVE ( 'NONE', #9623, #83736, #30820, .T. ) ;
#67266 = CARTESIAN_POINT ( 'NONE',  ( 12.46153846153833911, -8.656820664282941280, 34.87096338111179961 ) ) ;
#67267 = AXIS2_PLACEMENT_3D ( 'NONE', #85212, #65370, #78884 ) ;
#67268 = CYLINDRICAL_SURFACE ( 'NONE', #40832, 0.2499999999999995559 ) ;
#67269 = FACE_BOUND ( 'NONE', #60451, .T. ) ;
#67270 = ORIENTED_EDGE ( 'NONE', *, *, #73799, .F. ) ;
#67271 = VERTEX_POINT ( 'NONE', #52423 ) ;
#67272 = CARTESIAN_POINT ( 'NONE',  ( -5.010854725920638408, -6.386643153685127139, 34.62446782046654192 ) ) ;
#67273 = AXIS2_PLACEMENT_3D ( 'NONE', #13419, #67042, #19737 ) ;
#67274 = ORIENTED_EDGE ( 'NONE', *, *, #45903, .T. ) ;
#67275 = FACE_BOUND ( 'NONE', #478, .T. ) ;
#67276 = CARTESIAN_POINT ( 'NONE',  ( 9.822833130541342328, -5.915461855592780260, 34.75538340440931506 ) ) ;
#67277 = EDGE_CURVE ( 'NONE', #43616, #14619, #57655, .T. ) ;
#67278 = CARTESIAN_POINT ( 'NONE',  ( -13.63459211555773720, -10.66389620160130036, 33.62221079203477103 ) ) ;
#67279 = ORIENTED_EDGE ( 'NONE', *, *, #60056, .T. ) ;
#67280 = CARTESIAN_POINT ( 'NONE',  ( -5.749999999999936051, -7.434744429011176159, 34.75000000000000711 ) ) ;
#67281 = CARTESIAN_POINT ( 'NONE',  ( -6.700297254098854793, -2.353885683473779800, 30.79025554430704759 ) ) ;
#67282 = AXIS2_PLACEMENT_3D ( 'NONE', #17920, #45375, #72849 ) ;
#67283 = CARTESIAN_POINT ( 'NONE',  ( 2.651650429449539104, -4.848349570550432475, 14.31250000000000000 ) ) ;
#67284 = ORIENTED_EDGE ( 'NONE', *, *, #55863, .F. ) ;
#67285 = EDGE_CURVE ( 'NONE', #68032, #10589, #69675, .T. ) ;
#67286 = FACE_OUTER_BOUND ( 'NONE', #38547, .T. ) ;
#67287 = CARTESIAN_POINT ( 'NONE',  ( 17.99999999999987566, -11.06231777344772027, 33.60647404775119895 ) ) ;
#67288 = CARTESIAN_POINT ( 'NONE',  ( 2.530471976670372491, -3.020022701398814124, 32.48759521482552515 ) ) ;
#67289 = ORIENTED_EDGE ( 'NONE', *, *, #81140, .T. ) ;
#67290 = CARTESIAN_POINT ( 'NONE',  ( 2.373759641042385571, -12.34228464037088813, 31.77849191805839268 ) ) ;
#67291 = CYLINDRICAL_SURFACE ( 'NONE', #64308, 0.2500000000000004996 ) ;
#67292 = ORIENTED_EDGE ( 'NONE', *, *, #11058, .T. ) ;
#67293 = CARTESIAN_POINT ( 'NONE',  ( -12.68502338610279168, -5.827078755546623690, 34.72654668319379567 ) ) ;
#67294 = LINE ( 'NONE', #7367, #54074 ) ;
#67295 = CARTESIAN_POINT ( 'NONE',  ( 0.4615384615384611200, -10.67929555188718282, 33.92786785259544047 ) ) ;
#67296 = CARTESIAN_POINT ( 'NONE',  ( -5.011667505647054099, -8.613356846314928816, 34.62446782046653482 ) ) ;
#67297 = CARTESIAN_POINT ( 'NONE',  ( 0.2380535369741272611, -2.612411019501190701, 31.66733052389439962 ) ) ;
#67298 = CARTESIAN_POINT ( 'NONE',  ( 15.23076923076923173, -2.538708090699994813, 30.37095296980875503 ) ) ;
#67300 = CARTESIAN_POINT ( 'NONE',  ( -15.48079246806219267, -12.43535235679832596, 30.55408501211184813 ) ) ;
#67299 = CARTESIAN_POINT ( 'NONE',  ( 14.17713171595038446, -2.504760397472875155, 29.97295953869789997 ) ) ;
#67301 = EDGE_CURVE ( 'NONE', #3308, #6564, #23190, .T. ) ;
#67302 = CARTESIAN_POINT ( 'NONE',  ( -3.230769230769229949, -2.538708090699994813, 30.37095296980875503 ) ) ;
#67303 = CARTESIAN_POINT ( 'NONE',  ( -12.46153846153858247, -11.48612834414049644, 32.76840700105863391 ) ) ;
#67304 = CARTESIAN_POINT ( 'NONE',  ( 2.749999999999995115, -6.360912703473971419, 18.14062500000000711 ) ) ;
#67305 = ORIENTED_EDGE ( 'NONE', *, *, #2890, .T. ) ;
#67306 = CARTESIAN_POINT ( 'NONE',  ( -12.46153846153846168, -8.120952969808772792, 34.71129190930000163 ) ) ;
#67307 = ORIENTED_EDGE ( 'NONE', *, *, #41617, .F. ) ;
#67308 = ORIENTED_EDGE ( 'NONE', *, *, #77542, .T. ) ;
#67309 = CARTESIAN_POINT ( 'NONE',  ( -3.007756386675835447, -9.172514111537584114, 34.72667873470787470 ) ) ;
#67310 = VERTEX_POINT ( 'NONE', #38480 ) ;
#67311 = CARTESIAN_POINT ( 'NONE',  ( -19.50000000000000000, -11.50000000000000000, 29.75000000000000355 ) ) ;
#67312 = CARTESIAN_POINT ( 'NONE',  ( -1.139087296525992166, -10.25000000000000533, 16.10937500000000355 ) ) ;
#67313 = CARTESIAN_POINT ( 'NONE',  ( 13.44987095589141113, -2.892918686051625166, 31.69288490824026638 ) ) ;
#67314 = DIRECTION ( 'NONE',  ( -0.000000000000000000, -0.6427876096865404731, -0.7660444431189770143 ) ) ;
#67315 = CARTESIAN_POINT ( 'NONE',  ( 9.692307692307570832, -9.528491918059723176, 34.59228464037033035 ) ) ;
#67317 = CARTESIAN_POINT ( 'NONE',  ( -10.48485917715096782, -3.625058011473228703, 33.29252011169590020 ) ) ;
#67316 = VECTOR ( 'NONE', #12031, 1000.000000000000227 ) ;
#67318 = DIRECTION ( 'NONE',  ( 0.000000000000000000, 0.3420201433256641055, -0.9396926207859100932 ) ) ;
#67319 = CARTESIAN_POINT ( 'NONE',  ( 2.241608896736428047, -9.780366693483667717, 34.19971097300155805 ) ) ;
#67320 = CARTESIAN_POINT ( 'NONE',  ( 2.651650429449569302, -10.15165042944953733, 23.37500000000000000 ) ) ;
#67321 = CARTESIAN_POINT ( 'NONE',  ( 10.61538461538449418, -12.51329471203414379, 31.30864560766407578 ) ) ;
#67323 = EDGE_CURVE ( 'NONE', #43106, #21818, #55414, .T. ) ;
#67322 = CARTESIAN_POINT ( 'NONE',  ( -4.219116154402474450, -12.16647553114622049, 32.15551576947930812 ) ) ;
#67324 = AXIS2_PLACEMENT_3D ( 'NONE', #18253, #74978, #80860 ) ;
#67325 = EDGE_CURVE ( 'NONE', #84179, #37632, #21121, .T. ) ;
#67326 = CARTESIAN_POINT ( 'NONE',  ( 5.776515075435673552, -3.562934362175799841, 33.22335522853832401 ) ) ;
#67327 = B_SPLINE_CURVE_WITH_KNOTS ( 'NONE', 3,
 ( #44106, #71585, #9894, #66165, #59418, #79248, #79695, #17996, #51287, #50859 ),
 .UNSPECIFIED., .F., .F.,
 ( 4, 2, 2, 2, 4 ),
 ( 0.000000000000000000, 0.0001954311564186865763, 0.0003908623128373731525, 0.0005862934692560596746, 0.0007817246256747463051 ),
 .UNSPECIFIED. ) ;
#67328 = B_SPLINE_CURVE_WITH_KNOTS ( 'NONE', 3,
 ( #63378, #29178, #57953, #8893, #9338, #65145, #36798, #2556, #16523, #85432 ),
 .UNSPECIFIED., .F., .F.,
 ( 4, 2, 2, 2, 4 ),
 ( 0.0007817359430256313069, 0.0009771253907249971907, 0.001172514838424363291, 0.001367904286123729392, 0.001563293733823095276 ),
 .UNSPECIFIED. ) ;
#67329 = ORIENTED_EDGE ( 'NONE', *, *, #76632, .F. ) ;
#67331 = ADVANCED_FACE ( 'NONE', ( #25854 ), #80813, .F. ) ;
#67330 = VERTEX_POINT ( 'NONE', #58288 ) ;
#67332 = CARTESIAN_POINT ( 'NONE',  ( 14.30769230769218581, -8.656820664282941280, 34.87096338111179961 ) ) ;
#67333 = CARTESIAN_POINT ( 'NONE',  ( 15.23076923076923173, -11.91647553114624181, 32.58852847137148245 ) ) ;
#67334 = FACE_OUTER_BOUND ( 'NONE', #19245, .T. ) ;
#67335 = CARTESIAN_POINT ( 'NONE',  ( -6.222926217516147496, -3.586966769969700763, 32.86292498521069660 ) ) ;
#67336 = ADVANCED_FACE ( 'NONE', ( #72251 ), #10561, .F. ) ;
#67337 = CARTESIAN_POINT ( 'NONE',  ( -9.692307692307812417, -4.481592998941358097, 33.73612834414048933 ) ) ;
#67338 = DIRECTION ( 'NONE',  ( 0.000000000000000000, 0.9396926207859126468, 0.3420201433256571111 ) ) ;
#67339 = ORIENTED_EDGE ( 'NONE', *, *, #71393, .F. ) ;
#67340 = CARTESIAN_POINT ( 'NONE',  ( 1.161689167099238418, -4.887634598454295265, 34.01352882383564946 ) ) ;
#67341 = VERTEX_POINT ( 'NONE', #51972 ) ;
#67342 = ORIENTED_EDGE ( 'NONE', *, *, #9072, .F. ) ;
#67343 = CARTESIAN_POINT ( 'NONE',  ( 17.74997676270703550, -3.202444869320336451, 32.30641848906366675 ) ) ;
#67344 = CARTESIAN_POINT ( 'NONE',  ( 4.087762742890270751, -2.538708090699994813, 30.37095296980875148 ) ) ;
#67345 = CARTESIAN_POINT ( 'NONE',  ( 11.53846153846153832, -10.51840700105979565, 33.73612834413961536 ) ) ;
#67346 = VECTOR ( 'NONE', #43951, 1000.000000000000000 ) ;
#67347 = CARTESIAN_POINT ( 'NONE',  ( 19.50000000000000000, -11.00000000000000000, 29.25000000000000000 ) ) ;
#67348 = CYLINDRICAL_SURFACE ( 'NONE', #85345, 0.2499999999999993616 ) ;
#67349 = ORIENTED_EDGE ( 'NONE', *, *, #24867, .T. ) ;
#67350 = VERTEX_POINT ( 'NONE', #75371 ) ;
#67351 = EDGE_CURVE ( 'NONE', #48154, #19870, #45683, .T. ) ;
#67352 = ORIENTED_EDGE ( 'NONE', *, *, #70116, .F. ) ;
#67353 = VERTEX_POINT ( 'NONE', #55090 ) ;
#67354 = CARTESIAN_POINT ( 'NONE',  ( 17.29970274590113632, -10.23759521482555357, 34.22997729860117033 ) ) ;
#67355 = CARTESIAN_POINT ( 'NONE',  ( 10.36536139116315880, -11.56360843649121861, 33.07473185843129926 ) ) ;
#67356 = CARTESIAN_POINT ( 'NONE',  ( 4.219101293358989757, -3.643525952247864463, 33.31231777344670064 ) ) ;
#67357 = CARTESIAN_POINT ( 'NONE',  ( 2.057715576749955311, -11.28823185664190376, 33.01397839955799896 ) ) ;
#67358 = DIRECTION ( 'NONE',  ( -0.000000000000000000, -0.9848077530122086864, -0.1736481776669273613 ) ) ;
#67359 = CARTESIAN_POINT ( 'NONE',  ( -4.153846153846152411, -10.51840700105979565, 33.73612834413961536 ) ) ;
#67360 = VERTEX_POINT ( 'NONE', #13228 ) ;
#67361 = EDGE_CURVE ( 'NONE', #24082, #25133, #48859, .T. ) ;
#67362 = ORIENTED_EDGE ( 'NONE', *, *, #12444, .F. ) ;
#67363 = EDGE_CURVE ( 'NONE', #84614, #64470, #29386, .T. ) ;
#67365 = EDGE_LOOP ( 'NONE', ( #54041, #74839 ) ) ;
#67364 = CARTESIAN_POINT ( 'NONE',  ( -3.480745974817819555, -2.544273027872574922, 31.48422191005632342 ) ) ;
#67366 = CARTESIAN_POINT ( 'NONE',  ( -9.757578138268467427, -5.219633306516282545, 34.19971097300152962 ) ) ;
#67367 = CYLINDRICAL_SURFACE ( 'NONE', #73418, 0.2499999999999997502 ) ;
#67368 = CARTESIAN_POINT ( 'NONE',  ( 1.553300858899129722, -11.24999999999999112, 22.20312500000000000 ) ) ;
#67369 = EDGE_LOOP ( 'NONE', ( #41226, #68342, #6223, #32645 ) ) ;
#67370 = AXIS2_PLACEMENT_3D ( 'NONE', #64108, #29900, #65880 ) ;
#67371 = CARTESIAN_POINT ( 'NONE',  ( -3.230769230769351186, -12.46129190930018460, 30.37095296980731973 ) ) ;
#67372 = ORIENTED_EDGE ( 'NONE', *, *, #51343, .T. ) ;
#67373 = CARTESIAN_POINT ( 'NONE',  ( 8.096099364501988305, -12.22109172314383230, 31.39792113162168263 ) ) ;
#67374 = CARTESIAN_POINT ( 'NONE',  ( 17.14217821643591932, -12.16647553114626490, 32.15551576947920864 ) ) ;
#67375 = CARTESIAN_POINT ( 'NONE',  ( -12.39628289026243557, -12.46129190930001052, 30.37095296980870174 ) ) ;
#67376 = CARTESIAN_POINT ( 'NONE',  ( -7.146561866800873020, -3.754499324213721234, 33.06261337010820256 ) ) ;
#67377 = EDGE_CURVE ( 'NONE', #52302, #70228, #28457, .T. ) ;
#67378 = DIRECTION ( 'NONE',  ( -0.000000000000000000, 1.000000000000000000, -0.000000000000000000 ) ) ;
#67379 = EDGE_LOOP ( 'NONE', ( #54847, #52868 ) ) ;
#67380 = FACE_OUTER_BOUND ( 'NONE', #37027, .T. ) ;
#67381 = EDGE_CURVE ( 'NONE', #42328, #72479, #68169, .T. ) ;
#67382 = DIRECTION ( 'NONE',  ( 1.000000000000000000, 0.000000000000000000, 0.000000000000000000 ) ) ;
#67383 = ORIENTED_EDGE ( 'NONE', *, *, #45022, .T. ) ;
#67384 = FACE_OUTER_BOUND ( 'NONE', #4718, .T. ) ;
#67385 = CARTESIAN_POINT ( 'NONE',  ( -7.623142494540996239, -11.24521262558773493, 33.06293181088029343 ) ) ;
#67386 = CARTESIAN_POINT ( 'NONE',  ( 17.07692307692295586, -10.21337939537710326, 33.94971097300076224 ) ) ;
#67387 = LINE ( 'NONE', #20087, #32838 ) ;
#67388 = CARTESIAN_POINT ( 'NONE',  ( -0.3963926822064974820, -7.750023238201980469, 34.74374492549440419 ) ) ;
#67389 = FACE_BOUND ( 'NONE', #30276, .T. ) ;
#67391 = CARTESIAN_POINT ( 'NONE',  ( 4.153846153846154188, -12.62096338111211580, 30.90682066428153263 ) ) ;
#67390 = CARTESIAN_POINT ( 'NONE',  ( 5.934729999443681514, -5.094484230520674117, 34.41647553114621161 ) ) ;
#67392 = EDGE_CURVE ( 'NONE', #41347, #76970, #53164, .T. ) ;
#67393 = CARTESIAN_POINT ( 'NONE',  ( -9.561517251340744039, -11.93129842949671726, 32.56571108434900452 ) ) ;
#67395 = DIRECTION ( 'NONE',  ( -0.000000000000000000, -0.9848077530122085754, -0.1736481776669273613 ) ) ;
#67394 = CARTESIAN_POINT ( 'NONE',  ( 14.87820512820512953, -7.500000000000000000, 29.75000000000000355 ) ) ;
#67396 = CARTESIAN_POINT ( 'NONE',  ( 15.23076923076911093, -11.94971097300221174, 32.03036669348237098 ) ) ;
#67397 = AXIS2_PLACEMENT_3D ( 'NONE', #26405, #5243, #88573 ) ;
#67398 = CARTESIAN_POINT ( 'NONE',  ( 3.749999999999999556, -7.438900925035446754, 25.46688170625849423 ) ) ;
#67399 = ORIENTED_EDGE ( 'NONE', *, *, #33015, .F. ) ;
#67400 = CARTESIAN_POINT ( 'NONE',  ( -7.146003140593069958, -9.086856451489516928, 34.49173150075333183 ) ) ;
#67401 = ORIENTED_EDGE ( 'NONE', *, *, #5641, .T. ) ;
#67402 = CARTESIAN_POINT ( 'NONE',  ( 0.3308469948709031883, -6.413092428213692742, 34.63065189839063152 ) ) ;
#67403 = ORIENTED_EDGE ( 'NONE', *, *, #28940, .T. ) ;
#67404 = CARTESIAN_POINT ( 'NONE',  ( 7.780883400193070898, -9.442884908240170461, 34.35708131394840592 ) ) ;
#67406 = EDGE_CURVE ( 'NONE', #763, #72305, #48329, .T. ) ;
#67405 = DIRECTION ( 'NONE',  ( -0.000000000000000000, -0.9396926207859092051, -0.3420201433256662704 ) ) ;
#67408 = ORIENTED_EDGE ( 'NONE', *, *, #75753, .F. ) ;
#67407 = CARTESIAN_POINT ( 'NONE',  ( -5.011667937410237528, -9.528491918058460186, 34.59228464037085615 ) ) ;
#67409 = CARTESIAN_POINT ( 'NONE',  ( -10.61538461538473577, -12.16647553114689728, 32.15551576947799362 ) ) ;
#67410 = CARTESIAN_POINT ( 'NONE',  ( 1.134638640566796086, -12.01397095200673881, 32.43157075238190146 ) ) ;
#67411 = CARTESIAN_POINT ( 'NONE',  ( 3.749999999999999556, -7.438900925035446754, 24.21688170625849068 ) ) ;
#67412 = CARTESIAN_POINT ( 'NONE',  ( 8.769230769230647482, -5.219633306517616589, 34.19971097300220464 ) ) ;
#67413 = LINE ( 'NONE', #82265, #56139 ) ;
#67414 = CARTESIAN_POINT ( 'NONE',  ( 7.911409417429869251, -11.94971097300157403, 32.03036669348361443 ) ) ;
#67415 = CARTESIAN_POINT ( 'NONE',  ( -19.50000000000000000, -3.499999999999999556, 29.75000000000000355 ) ) ;
#67416 = CARTESIAN_POINT ( 'NONE',  ( -16.15384615384615330, -2.499999999999998668, 29.75000000000001421 ) ) ;
#67417 = CARTESIAN_POINT ( 'NONE',  ( -8.992715712954719720, -9.331801661448606566, 34.40259984581193464 ) ) ;
#67418 = CARTESIAN_POINT ( 'NONE',  ( -2.694853999681181556, -10.10844685921792241, 16.43936829374151287 ) ) ;
#67420 = EDGE_CURVE ( 'NONE', #11924, #72078, #41142, .T. ) ;
#67419 = CARTESIAN_POINT ( 'NONE',  ( 14.30769230769231015, -9.905515769479276145, 34.41647553114623292 ) ) ;
#67421 = CARTESIAN_POINT ( 'NONE',  ( 17.07692307692295586, -8.656820664282941280, 34.87096338111179961 ) ) ;
#67422 = ORIENTED_EDGE ( 'NONE', *, *, #11963, .F. ) ;
#67423 = CARTESIAN_POINT ( 'NONE',  ( 16.28463659481310444, -4.684288915650984819, 34.18129842949671371 ) ) ;
#67424 = DIRECTION ( 'NONE',  ( -0.000000000000000000, 0.5000000000000011102, -0.8660254037844381525 ) ) ;
#67425 = CARTESIAN_POINT ( 'NONE',  ( -3.775308065498748977, -8.992201783934593351, 17.76749329374151287 ) ) ;
#67426 = EDGE_CURVE ( 'NONE', #72305, #35045, #11220, .T. ) ;
#67427 = CARTESIAN_POINT ( 'NONE',  ( -15.90390074446811042, -12.45601412856602686, 31.48342859153981621 ) ) ;
#67429 = CARTESIAN_POINT ( 'NONE',  ( -16.40382289789473802, -10.82459398097509684, 33.81372124010185587 ) ) ;
#67428 = AXIS2_PLACEMENT_3D ( 'NONE', #58317, #38058, #18239 ) ;
#67430 = ORIENTED_EDGE ( 'NONE', *, *, #60861, .T. ) ;
#67431 = CARTESIAN_POINT ( 'NONE',  ( 7.846153846153846700, -4.786620604624113540, 33.94971097300155094 ) ) ;
#67432 = CARTESIAN_POINT ( 'NONE',  ( 18.00000000000000000, -4.945431358278436385, 36.03766855953609394 ) ) ;
#67434 = VERTEX_POINT ( 'NONE', #50540 ) ;
#67433 = CARTESIAN_POINT ( 'NONE',  ( 8.096208266067300485, -2.544122305571458131, 31.48381861865057729 ) ) ;
#67435 = CARTESIAN_POINT ( 'NONE',  ( 12.46153846153846168, -12.37446782046654192, 30.86335684631486131 ) ) ;
#67436 = EDGE_CURVE ( 'NONE', #37313, #19392, #32764, .T. ) ;
#67437 = CARTESIAN_POINT ( 'NONE',  ( 4.826923076923076650, -7.433932668274256805, 35.00000000000000711 ) ) ;
#67438 = CIRCLE ( 'NONE', #34317, 0.2500000000000002220 ) ;
#67439 = CARTESIAN_POINT ( 'NONE',  ( -11.60373153901786125, -2.657715359629089225, 31.77849191805832874 ) ) ;
#67440 = VERTEX_POINT ( 'NONE', #23082 ) ;
#67441 = AXIS2_PLACEMENT_3D ( 'NONE', #10353, #29745, #8590 ) ;
#67442 = CARTESIAN_POINT ( 'NONE',  ( -1.384615384615383471, -2.708943851104267164, 35.45975837776705220 ) ) ;
#67443 = CARTESIAN_POINT ( 'NONE',  ( 6.673100192134568509, -4.943428324936578910, 34.04746400365624481 ) ) ;
#67444 = AXIS2_PLACEMENT_3D ( 'NONE', #37581, #2895, #23624 ) ;
#67445 = CARTESIAN_POINT ( 'NONE',  ( -13.25382494364843389, -8.191423895709840863, 34.95447573519442130 ) ) ;
#67446 = VERTEX_POINT ( 'NONE', #9560 ) ;
#67447 = VERTEX_POINT ( 'NONE', #64057 ) ;
#67448 = EDGE_CURVE ( 'NONE', #52128, #50940, #1922, .T. ) ;
#67449 = ORIENTED_EDGE ( 'NONE', *, *, #49188, .F. ) ;
#67450 = CYLINDRICAL_SURFACE ( 'NONE', #78639, 0.2499999999999997502 ) ;
#67451 = CARTESIAN_POINT ( 'NONE',  ( 0.3954550505825790707, -2.538708090699994813, 30.37095296980875148 ) ) ;
#67452 = EDGE_CURVE ( 'NONE', #33780, #16151, #42478, .T. ) ;
#67453 = CARTESIAN_POINT ( 'NONE',  ( -13.13456096470193302, -12.01375889529407281, 32.43194544308182969 ) ) ;
#67454 = CARTESIAN_POINT ( 'NONE',  ( -7.846153846153844924, -10.67929555188718282, 33.92786785259544047 ) ) ;
#67455 = CARTESIAN_POINT ( 'NONE',  ( -7.846153846153844924, -12.48256725967547354, 35.29906147534542527 ) ) ;
#67456 = ORIENTED_EDGE ( 'NONE', *, *, #45524, .F. ) ;
#67457 = EDGE_CURVE ( 'NONE', #81768, #26583, #76787, .T. ) ;
#67458 = VERTEX_POINT ( 'NONE', #16324 ) ;
#67459 = ORIENTED_EDGE ( 'NONE', *, *, #14517, .F. ) ;
#67461 = ORIENTED_EDGE ( 'NONE', *, *, #63331, .F. ) ;
#67460 = LINE ( 'NONE', #61131, #57334 ) ;
#67462 = B_SPLINE_CURVE_WITH_KNOTS ( 'NONE', 3,
 ( #7457, #26839, #690, #69153, #41243, #28158, #6567, #81349, #34031, #20518 ),
 .UNSPECIFIED., .F., .F.,
 ( 4, 2, 2, 2, 4 ),
 ( 0.0007817246256747483650, 0.0009771112852218926705, 0.001172497944769037084, 0.001367884604316181498, 0.001563271263863325695 ),
 .UNSPECIFIED. ) ;
#67463 = CYLINDRICAL_SURFACE ( 'NONE', #70382, 0.2499999999999995559 ) ;
#67464 = VECTOR ( 'NONE', #82146, 1000.000000000000000 ) ;
#67465 = EDGE_CURVE ( 'NONE', #88230, #18284, #61782, .T. ) ;
#67466 = DIRECTION ( 'NONE',  ( -0.000000000000000000, 0.6427876096865404731, -0.7660444431189770143 ) ) ;
#67467 = EDGE_CURVE ( 'NONE', #45953, #35283, #21750, .T. ) ;
#67468 = DIRECTION ( 'NONE',  ( 0.000000000000000000, 0.3420201433256641055, -0.9396926207859100932 ) ) ;
#67469 = CARTESIAN_POINT ( 'NONE',  ( -5.869474298236435850, -4.459921816937789885, 33.71989282347011851 ) ) ;
#67470 = ORIENTED_EDGE ( 'NONE', *, *, #89173, .F. ) ;
#67471 = B_SPLINE_CURVE_WITH_KNOTS ( 'NONE', 3,
 ( #66973, #73743, #25090, #51196, #5268, #30945, #58412, #38608, #58871, #59317 ),
 .UNSPECIFIED., .F., .F.,
 ( 4, 2, 2, 2, 4 ),
 ( 0.000000000000000000, 0.0001954311564186865763, 0.0003908623128373731525, 0.0005862934692560596746, 0.0007817246256747463051 ),
 .UNSPECIFIED. ) ;
#67472 = ORIENTED_EDGE ( 'NONE', *, *, #1243, .F. ) ;
#67473 = EDGE_CURVE ( 'NONE', #40783, #14918, #8693, .T. ) ;
#67474 = ORIENTED_EDGE ( 'NONE', *, *, #19312, .F. ) ;
#67475 = CARTESIAN_POINT ( 'NONE',  ( -7.846153846153844924, -3.937682226553329556, 33.60647404775216529 ) ) ;
#67477 = ORIENTED_EDGE ( 'NONE', *, *, #80257, .F. ) ;
#67476 = DIRECTION ( 'NONE',  ( -0.000000000000000000, 0.5000000000000011102, -0.8660254037844381525 ) ) ;
#67478 = CARTESIAN_POINT ( 'NONE',  ( 4.153846153846154188, -4.786620604624113540, 33.94971097300155094 ) ) ;
#67479 = DIRECTION ( 'NONE',  ( 1.000000000000000000, 0.000000000000000000, 0.000000000000000000 ) ) ;
#67480 = ORIENTED_EDGE ( 'NONE', *, *, #19763, .T. ) ;
#67481 = CARTESIAN_POINT ( 'NONE',  ( -11.31568186948346622, -4.226511098958373402, 33.85474049983370293 ) ) ;
#67482 = CARTESIAN_POINT ( 'NONE',  ( 16.15384615384615330, -3.513871655860378418, 32.76840700105978499 ) ) ;
#67483 = CARTESIAN_POINT ( 'NONE',  ( -0.4615384615385826339, -11.48612834414049644, 32.76840700105863391 ) ) ;
#67484 = FACE_BOUND ( 'NONE', #88241, .T. ) ;
#67485 = CARTESIAN_POINT ( 'NONE',  ( -15.36091720050093024, -8.630895178749533159, 34.87696386517710323 ) ) ;
#67486 = CYLINDRICAL_SURFACE ( 'NONE', #37040, 0.2499999999999979738 ) ;
#67487 = CARTESIAN_POINT ( 'NONE',  ( -8.899922235898328537, -4.118384482072085184, 33.43331474514187107 ) ) ;
#67490 = CARTESIAN_POINT ( 'NONE',  ( 15.45378207486262667, -10.01129605718032600, 34.36064277460058491 ) ) ;
#67489 = VECTOR ( 'NONE', #185, 1000.000000000000000 ) ;
#67488 = CARTESIAN_POINT ( 'NONE',  ( -7.053687282701448069, -7.722926236386453702, 34.74524107206102030 ) ) ;
#67491 = CARTESIAN_POINT ( 'NONE',  ( -4.284321338921872169, -7.276987145209185215, 34.99546412871779211 ) ) ;
#67492 = CARTESIAN_POINT ( 'NONE',  ( 5.076923076923075762, -11.69971097300155272, 32.46337939537588113 ) ) ;
#67493 = VERTEX_POINT ( 'NONE', #57307 ) ;
#67494 = CARTESIAN_POINT ( 'NONE',  ( -14.98071481085577972, -11.47946981652013498, 33.17500667209847620 ) ) ;
#67495 = CARTESIAN_POINT ( 'NONE',  ( 12.68455130563185662, -3.395485233115139057, 33.02377354290275946 ) ) ;
#67496 = ORIENTED_EDGE ( 'NONE', *, *, #33799, .T. ) ;
#67497 = EDGE_CURVE ( 'NONE', #69896, #28781, #12351, .T. ) ;
#67498 = ORIENTED_EDGE ( 'NONE', *, *, #63055, .T. ) ;
#67499 = VECTOR ( 'NONE', #79652, 1000.000000000000000 ) ;
#67500 = CARTESIAN_POINT ( 'NONE',  ( 0.7114838709165038910, -8.476813868363244353, 34.90874843262270133 ) ) ;
#67501 = CARTESIAN_POINT ( 'NONE',  ( -13.63459212866397685, -4.818429247618089661, 34.26397095200675125 ) ) ;
#67502 = CARTESIAN_POINT ( 'NONE',  ( -11.78848476268299628, -10.18141759479407327, 34.26406193332782379 ) ) ;
#67503 = ORIENTED_EDGE ( 'NONE', *, *, #3518, .T. ) ;
#67504 = CARTESIAN_POINT ( 'NONE',  ( -9.942284436356281674, -9.234221910056348293, 34.70572697212741531 ) ) ;
#67505 = CARTESIAN_POINT ( 'NONE',  ( -4.153846153846152411, -9.058645607665452459, 34.76329471203371924 ) ) ;
#67506 = FACE_BOUND ( 'NONE', #53780, .T. ) ;
#67508 = CARTESIAN_POINT ( 'NONE',  ( -19.50000000000000000, -11.50000000000000000, 29.75000000000000355 ) ) ;
#67507 = CARTESIAN_POINT ( 'NONE',  ( -15.36146069743679199, -5.582088688514999397, 34.36776431015576350 ) ) ;
#67509 = DIRECTION ( 'NONE',  ( 0.000000000000000000, 1.000000000000000000, 0.000000000000000000 ) ) ;
#67510 = CARTESIAN_POINT ( 'NONE',  ( 2.438218009455872082, -5.195472089885680766, 34.18748526763464923 ) ) ;
#67512 = CARTESIAN_POINT ( 'NONE',  ( -10.36533019547115941, -11.47946981652013498, 33.17500667209847620 ) ) ;
#67511 = FILL_AREA_STYLE_COLOUR ( '', #21649 ) ;
#67513 = CARTESIAN_POINT ( 'NONE',  ( 3.750000000000009770, -9.053300858899081760, 19.54687499999999645 ) ) ;
#67514 = VERTEX_POINT ( 'NONE', #55976 ) ;
#67515 = VERTEX_POINT ( 'NONE', #69493 ) ;
#67516 = CARTESIAN_POINT ( 'NONE',  ( -15.23076923076922995, -13.88283147151868846, 33.14645433367849847 ) ) ;
#67517 = CARTESIAN_POINT ( 'NONE',  ( 12.21153846153846168, -7.433931650972300353, 34.75000000000000711 ) ) ;
#67518 = CARTESIAN_POINT ( 'NONE',  ( 4.153846153846030731, -10.33852847137269571, 34.16647553114546554 ) ) ;
#67519 = LINE ( 'NONE', #81928, #13620 ) ;
#67520 = CARTESIAN_POINT ( 'NONE',  ( -9.692307692307691624, -2.249999999999998668, 29.50000000000001421 ) ) ;
#67521 = CARTESIAN_POINT ( 'NONE',  ( 2.651650429449539104, -4.848349570550432475, 23.06250000000000000 ) ) ;
#67522 = CARTESIAN_POINT ( 'NONE',  ( -9.019207513279361876, -10.06842814019191401, 34.32929386961144758 ) ) ;
#67523 = CARTESIAN_POINT ( 'NONE',  ( -5.999999999999998224, -8.164416787775445883, 34.95778746994557906 ) ) ;
#67524 = DIRECTION ( 'NONE',  ( -0.000000000000000000, 0.8660254037844399289, -0.4999999999999980016 ) ) ;
#67525 = CARTESIAN_POINT ( 'NONE',  ( 13.31934538405906743, -10.33852847137145048, 34.16647553114627556 ) ) ;
#67526 = LINE ( 'NONE', #4941, #22421 ) ;
#67527 = CARTESIAN_POINT ( 'NONE',  ( 15.84615384615384670, -4.000000000000000000, 29.75000000000000355 ) ) ;
#67528 = CARTESIAN_POINT ( 'NONE',  ( 9.692307692307695177, -3.937682226553329556, 33.60647404775216529 ) ) ;
#67529 = B_SPLINE_CURVE_WITH_KNOTS ( 'NONE', 3,
 ( #35554, #21138, #71092, #48608, #8081, #9402 ),
 .UNSPECIFIED., .F., .F.,
 ( 4, 2, 4 ),
 ( 0.0003909569690057776653, 0.0005862646681846002839, 0.0007815723673634227941 ),
 .UNSPECIFIED. ) ;
#67530 = FACE_OUTER_BOUND ( 'NONE', #10897, .T. ) ;
#67531 = DIRECTION ( 'NONE',  ( -0.000000000000000000, -0.000000000000000000, -1.000000000000000000 ) ) ;
#67532 = VERTEX_POINT ( 'NONE', #76699 ) ;
#67533 = VECTOR ( 'NONE', #12342, 1000.000000000000227 ) ;
#67534 = CARTESIAN_POINT ( 'NONE',  ( -4.854143535654665165, -11.89424750095246175, 32.13594075562311758 ) ) ;
#67535 = FACE_OUTER_BOUND ( 'NONE', #87514, .T. ) ;
#67536 = CARTESIAN_POINT ( 'NONE',  ( -1.901340078031369618, -5.512252781505359245, 16.75186829374151287 ) ) ;
#67537 = ADVANCED_FACE ( 'NONE', ( #35722 ), #63171, .F. ) ;
#67538 = CARTESIAN_POINT ( 'NONE',  ( 13.44987095589141113, -5.219633306516380244, 34.19971097300157936 ) ) ;
#67539 = DIRECTION ( 'NONE',  ( -0.000000000000000000, -0.1736481776669307198, -0.9848077530122080203 ) ) ;
#67540 = CARTESIAN_POINT ( 'NONE',  ( 4.153846153846154188, -1.466349020453238561, 30.81389545987213907 ) ) ;
#67542 = EDGE_LOOP ( 'NONE', ( #65961, #76691, #35189, #54177 ) ) ;
#67541 = CARTESIAN_POINT ( 'NONE',  ( 10.86538461538468070, -7.434744860731433924, 35.00000000000000711 ) ) ;
#67543 = CARTESIAN_POINT ( 'NONE',  ( 1.799775606325937360E-14, -10.25000000000000000, 23.53125000000000000 ) ) ;
#67544 = CARTESIAN_POINT ( 'NONE',  ( -14.55771553191376633, -5.765609946408404518, 34.70566812827425451 ) ) ;
#67545 = EDGE_CURVE ( 'NONE', #13172, #36624, #17778, .T. ) ;
#67546 = ORIENTED_EDGE ( 'NONE', *, *, #71450, .T. ) ;
#67547 = CYLINDRICAL_SURFACE ( 'NONE', #39144, 0.2500000000000009437 ) ;
#67548 = DIRECTION ( 'NONE',  ( -0.000000000000000000, 0.9848077530122085754, -0.1736481776669273613 ) ) ;
#67549 = ADVANCED_FACE ( 'NONE', ( #72145 ), #65825, .T. ) ;
#67550 = B_SPLINE_CURVE_WITH_KNOTS ( 'NONE', 3,
 ( #84807, #78026, #43358, #23085, #56863, #83918, #70840, #8696, #9141, #64488 ),
 .UNSPECIFIED., .F., .F.,
 ( 4, 2, 2, 2, 4 ),
 ( 0.000000000000000000, 0.0001954311564186860613, 0.0003908623128373721225, 0.0005862934692560581567, 0.0007817246256747442451 ),
 .UNSPECIFIED. ) ;
#67551 = ORIENTED_EDGE ( 'NONE', *, *, #65277, .F. ) ;
#67552 = FACE_OUTER_BOUND ( 'NONE', #82951, .T. ) ;
#67553 = CARTESIAN_POINT ( 'NONE',  ( 8.769230769230768274, -6.343179335718451384, 34.87096338111211935 ) ) ;
#67554 = CYLINDRICAL_SURFACE ( 'NONE', #24000, 0.2499999999999997502 ) ;
#67555 = EDGE_LOOP ( 'NONE', ( #70985, #3507, #1236, #8988 ) ) ;
#67556 = VERTEX_POINT ( 'NONE', #17203 ) ;
#67558 = EDGE_CURVE ( 'NONE', #82155, #10320, #58586, .T. ) ;
#67557 = AXIS2_PLACEMENT_3D ( 'NONE', #31529, #4501, #78821 ) ;
#67559 = ORIENTED_EDGE ( 'NONE', *, *, #85554, .T. ) ;
#67560 = VECTOR ( 'NONE', #10445, 1000.000000000000114 ) ;
#67561 = AXIS2_PLACEMENT_3D ( 'NONE', #18173, #45637, #73113 ) ;
#67562 = CARTESIAN_POINT ( 'NONE',  ( 13.38461538461538680, -11.69971097300155272, 32.46337939537588113 ) ) ;
#67563 = CARTESIAN_POINT ( 'NONE',  ( 7.173131342990377135, -11.47946981652013498, 33.17500667209846910 ) ) ;
#67564 = CARTESIAN_POINT ( 'NONE',  ( -18.00000000000000000, -11.10434399251292881, 35.99290692298802696 ) ) ;
#67565 = CARTESIAN_POINT ( 'NONE',  ( 9.442330948259103351, -9.234221910056348293, 34.70572697212741531 ) ) ;
#67566 = CYLINDRICAL_SURFACE ( 'NONE', #34729, 0.2500000000000002220 ) ;
#67567 = CARTESIAN_POINT ( 'NONE',  ( -3.099978789802282364, -4.684288915650983043, 34.18129842949671371 ) ) ;
#67568 = CARTESIAN_POINT ( 'NONE',  ( 0.2115617174898694330, -2.318417181685854533, 30.59732222474233865 ) ) ;
#67569 = AXIS2_PLACEMENT_3D ( 'NONE', #63849, #10245, #10686 ) ;
#67570 = DIRECTION ( 'NONE',  ( -0.000000000000000000, -0.000000000000000000, -1.000000000000000000 ) ) ;
#67571 = EDGE_LOOP ( 'NONE', ( #14897, #64673, #84089, #49155 ) ) ;
#67572 = ORIENTED_EDGE ( 'NONE', *, *, #80404, .F. ) ;
#67573 = EDGE_LOOP ( 'NONE', ( #3869, #51504, #10852, #24634 ) ) ;
#67575 = VERTEX_POINT ( 'NONE', #10001 ) ;
#67574 = CARTESIAN_POINT ( 'NONE',  ( -14.87820512820512953, -7.500000000000000000, 29.75000000000000355 ) ) ;
#67576 = EDGE_CURVE ( 'NONE', #12730, #64872, #3718, .T. ) ;
#67577 = CARTESIAN_POINT ( 'NONE',  ( -15.23076923076922995, -13.75783147151868846, 33.36296068462461051 ) ) ;
#67578 = CARTESIAN_POINT ( 'NONE',  ( 16.15384615384615330, -2.833524468853757305, 32.15551576947925838 ) ) ;
#67579 = ORIENTED_EDGE ( 'NONE', *, *, #55524, .T. ) ;
#67580 = CARTESIAN_POINT ( 'NONE',  ( 14.43821774592595197, -12.15418822224088657, 32.17964115625579069 ) ) ;
#67581 = ADVANCED_FACE ( 'NONE', ( #78456 ), #4127, .F. ) ;
#67582 = ORIENTED_EDGE ( 'NONE', *, *, #77646, .F. ) ;
#67583 = CARTESIAN_POINT ( 'NONE',  ( 11.53846153846153832, -2.538708090699994813, 30.37095296980875503 ) ) ;
#67584 = ORIENTED_EDGE ( 'NONE', *, *, #26398, .F. ) ;
#67585 = CARTESIAN_POINT ( 'NONE',  ( -18.06527000055631405, -9.528491918058357157, 34.59228464037090589 ) ) ;
#67586 = EDGE_CURVE ( 'NONE', #61570, #61361, #4858, .T. ) ;
#67587 = EDGE_CURVE ( 'NONE', #1344, #67131, #86536, .T. ) ;
#67588 = CARTESIAN_POINT ( 'NONE',  ( -6.923076923077045919, -5.094484230521993062, 34.41647553114689373 ) ) ;
#67589 = CARTESIAN_POINT ( 'NONE',  ( 12.39545608217832218, -2.292212530054419606, 30.41441678777542634 ) ) ;
#67590 = FACE_BOUND ( 'NONE', #52500, .T. ) ;
#67591 = CARTESIAN_POINT ( 'NONE',  ( -14.43838291080261627, -9.084618155246140248, 34.75535874321725771 ) ) ;
#67592 = DIRECTION ( 'NONE',  ( 1.000000000000000000, 2.602085213965214586E-16, 0.000000000000000000 ) ) ;
#67593 = CARTESIAN_POINT ( 'NONE',  ( -15.23076923076922995, -10.51840700105979565, 33.73612834413961536 ) ) ;
#67594 = B_SPLINE_CURVE_WITH_KNOTS ( 'NONE', 3,
 ( #75942, #76839, #14241, #8378, #41719, #83149 ),
 .UNSPECIFIED., .F., .F.,
 ( 4, 2, 4 ),
 ( 0.0003909512603273914300, 0.0005862562993132194519, 0.0007815613382990475822 ),
 .UNSPECIFIED. ) ;
#67595 = DIRECTION ( 'NONE',  ( 1.000000000000000000, 0.000000000000000000, 0.000000000000000000 ) ) ;
#67596 = CARTESIAN_POINT ( 'NONE',  ( -18.75000000000000000, -7.500000000000000000, 29.75000000000000355 ) ) ;
#67597 = CYLINDRICAL_SURFACE ( 'NONE', #57703, 4.000000000000000000 ) ;
#67598 = CARTESIAN_POINT ( 'NONE',  ( -0.4615384615384611200, -2.708943851104267164, 35.45975837776705220 ) ) ;
#67599 = ORIENTED_EDGE ( 'NONE', *, *, #28940, .F. ) ;
#67600 = ADVANCED_FACE ( 'NONE', ( #25748 ), #40162, .F. ) ;
#67601 = VERTEX_POINT ( 'NONE', #19873 ) ;
#67603 = CYLINDRICAL_SURFACE ( 'NONE', #17492, 0.2500000000000008882 ) ;
#67602 = CARTESIAN_POINT ( 'NONE',  ( 12.46153846153846168, -13.04860791097971706, 34.73218667398347037 ) ) ;
#67604 = CARTESIAN_POINT ( 'NONE',  ( 15.29683656411930848, -8.164416787775445883, 34.95778746994558617 ) ) ;
#67605 = CARTESIAN_POINT ( 'NONE',  ( 3.296837581771668635, -10.51840700105979565, 33.73612834413962247 ) ) ;
#67606 = EDGE_CURVE ( 'NONE', #12551, #6115, #88803, .T. ) ;
#67607 = CARTESIAN_POINT ( 'NONE',  ( -17.20761368003338632, -12.35290016733513951, 31.75349464988449455 ) ) ;
#67608 = CARTESIAN_POINT ( 'NONE',  ( 8.352564102564102200, -3.499999999999999556, 29.75000000000000355 ) ) ;
#67609 = EDGE_CURVE ( 'NONE', #47795, #18497, #9170, .T. ) ;
#67610 = ORIENTED_EDGE ( 'NONE', *, *, #70971, .F. ) ;
#67611 = CARTESIAN_POINT ( 'NONE',  ( -5.326946301144534601, -5.765609946408404518, 34.70566812827425451 ) ) ;
#67612 = CARTESIAN_POINT ( 'NONE',  ( -25.00000000000000355, 9.999999999999971578, 13.00000000000000178 ) ) ;
#67613 = CARTESIAN_POINT ( 'NONE',  ( -8.992715712954719720, -12.24155766932282496, 31.33739205006857986 ) ) ;
#67614 = AXIS2_PLACEMENT_3D ( 'NONE', #42923, #20862, #62723 ) ;
#67615 = CARTESIAN_POINT ( 'NONE',  ( -0.4615384615384611200, -5.180354513474913603, 36.12317359536750416 ) ) ;
#67616 = ORIENTED_EDGE ( 'NONE', *, *, #10532, .F. ) ;
#67617 = ADVANCED_FACE ( 'NONE', ( #39719 ), #19432, .F. ) ;
#67618 = VERTEX_POINT ( 'NONE', #41038 ) ;
#67619 = VECTOR ( 'NONE', #58040, 1000.000000000000000 ) ;
#67620 = ORIENTED_EDGE ( 'NONE', *, *, #50952, .T. ) ;
#67621 = CARTESIAN_POINT ( 'NONE',  ( 0.5277076025011177007, -7.250054483168842268, 34.74374881642865631 ) ) ;
#67622 = EDGE_LOOP ( 'NONE', ( #88233, #16507, #72540, #72720 ) ) ;
#67623 = CARTESIAN_POINT ( 'NONE',  ( -16.15384615384615330, -4.786620604624113540, 33.94971097300155094 ) ) ;
#67624 = CARTESIAN_POINT ( 'NONE',  ( -5.142193522883851564, -2.892918686051582089, 31.69288490824015270 ) ) ;
#67625 = CARTESIAN_POINT ( 'NONE',  ( 3.230769230769231726, -5.471508081941601098, 34.59228464037088457 ) ) ;
#67626 = CARTESIAN_POINT ( 'NONE',  ( -2.307692307692427391, -8.613356846316285953, 34.62446782046622218 ) ) ;
#67627 = VECTOR ( 'NONE', #79273, 1000.000000000000227 ) ;
#67628 = VECTOR ( 'NONE', #14876, 1000.000000000000000 ) ;
#67629 = CYLINDRICAL_SURFACE ( 'NONE', #51739, 0.2500000000000008882 ) ;
#67630 = ORIENTED_EDGE ( 'NONE', *, *, #29071, .T. ) ;
#67631 = COLOUR_RGB ( '', 0.08235294, 0.09019608, 0.10196078) ;
#67633 = ORIENTED_EDGE ( 'NONE', *, *, #67891, .T. ) ;
#67632 = CARTESIAN_POINT ( 'NONE',  ( -0.3307480205715130350, -11.93129842949671726, 32.56571108434900452 ) ) ;
#67634 = CARTESIAN_POINT ( 'NONE',  ( -5.207613680033385428, -2.295517848115769421, 30.44137282052136939 ) ) ;
#67635 = CARTESIAN_POINT ( 'NONE',  ( 9.019285189144222059, -12.41089969410671223, 31.60739465890703670 ) ) ;
#67636 = CARTESIAN_POINT ( 'NONE',  ( -11.60454391782167249, -10.67929555188718460, 33.92786785259543336 ) ) ;
#67637 = CARTESIAN_POINT ( 'NONE',  ( -16.02379871859570670, -7.723484941389743952, 34.99544897038808955 ) ) ;
#67638 = CARTESIAN_POINT ( 'NONE',  ( 13.38461538461526423, -4.320704448113951379, 33.92786785259630022 ) ) ;
#67639 = CARTESIAN_POINT ( 'NONE',  ( -5.326899820971668476, -10.82459398097509684, 33.81372124010185587 ) ) ;
#67640 = CARTESIAN_POINT ( 'NONE',  ( -0.4615384615384611200, -2.486705287966279876, 31.30864560766543647 ) ) ;
#67641 = CARTESIAN_POINT ( 'NONE',  ( -0.06109907496451398579, -10.25000000000000178, 20.03311829374151287 ) ) ;
#67642 = VERTEX_POINT ( 'NONE', #46895 ) ;
#67643 = B_SPLINE_CURVE_WITH_KNOTS ( 'NONE', 3,
 ( #3485, #10701, #38167, #65624, #2596, #43592, #71066, #36835, #23753, #64294 ),
 .UNSPECIFIED., .F., .F.,
 ( 4, 2, 2, 2, 4 ),
 ( 0.0007817246256747528103, 0.0009771112852218980915, 0.001172497944769043156, 0.001367884604316188437, 0.001563271263863333718 ),
 .UNSPECIFIED. ) ;
#67644 = PLANE ( 'NONE',  #27366 ) ;
#67645 = DIRECTION ( 'NONE',  ( -0.000000000000000000, -0.3420201433256694346, -0.9396926207859080948 ) ) ;
#67646 = EDGE_CURVE ( 'NONE', #54317, #79691, #66094, .T. ) ;
#67647 = EDGE_LOOP ( 'NONE', ( #55878, #23895, #58684, #16446 ) ) ;
#67648 = EDGE_LOOP ( 'NONE', ( #24974, #51997 ) ) ;
#67649 = DIRECTION ( 'NONE',  ( 0.000000000000000000, 1.000000000000000000, 8.673617379884034486E-16 ) ) ;
#67650 = CARTESIAN_POINT ( 'NONE',  ( -12.52680890749923570, -3.300289026998414865, 32.46337939537583139 ) ) ;
#67651 = CARTESIAN_POINT ( 'NONE',  ( 10.68145194873469173, -4.661471528628508665, 34.16647553114624003 ) ) ;
#67652 = DIRECTION ( 'NONE',  ( -0.000000000000000000, 1.000000000000000000, -0.000000000000000000 ) ) ;
#67653 = EDGE_CURVE ( 'NONE', #66313, #45635, #27339, .T. ) ;
#67654 = CARTESIAN_POINT ( 'NONE',  ( -14.55771553191376633, -2.985938066672154445, 32.43141759479405550 ) ) ;
#67655 = EDGE_LOOP ( 'NONE', ( #50146, #65412, #83632, #52268 ) ) ;
#67656 = FACE_OUTER_BOUND ( 'NONE', #1078, .T. ) ;
#67657 = CARTESIAN_POINT ( 'NONE',  ( -5.076923076923075762, -1.509761064869970415, 31.06009739812519044 ) ) ;
#67658 = CARTESIAN_POINT ( 'NONE',  ( 17.07692307692295586, -11.67786785259630911, 32.92929555188603530 ) ) ;
#67660 = VERTEX_POINT ( 'NONE', #6798 ) ;
#67659 = AXIS2_PLACEMENT_3D ( 'NONE', #29205, #37260, #15240 ) ;
#67661 = EDGE_CURVE ( 'NONE', #82873, #42667, #19836, .T. ) ;
#67662 = DIRECTION ( 'NONE',  ( 0.000000000000000000, 0.9396926207859126468, 0.3420201433256571111 ) ) ;
#67663 = ORIENTED_EDGE ( 'NONE', *, *, #21877, .T. ) ;
#67664 = CARTESIAN_POINT ( 'NONE',  ( -0.2385271099256129623, -2.758310577978207334, 31.33698337089303010 ) ) ;
#67665 = FACE_OUTER_BOUND ( 'NONE', #14471, .T. ) ;
#67666 = ORIENTED_EDGE ( 'NONE', *, *, #13053, .T. ) ;
#67667 = CARTESIAN_POINT ( 'NONE',  ( 0.5923302693632478411, -4.118422570099827595, 33.43335022499816489 ) ) ;
#67668 = CARTESIAN_POINT ( 'NONE',  ( -6.222926958906846551, -2.308479472611653094, 30.53278059502174457 ) ) ;
#67669 = CARTESIAN_POINT ( 'NONE',  ( -6.857821783564084228, -12.51329471203373700, 31.30864560766537963 ) ) ;
#67670 = EDGE_CURVE ( 'NONE', #65590, #44756, #82479, .T. ) ;
#67671 = CARTESIAN_POINT ( 'NONE',  ( 7.173131342990377135, -12.41089969410671223, 31.60739465890703670 ) ) ;
#67672 = CARTESIAN_POINT ( 'NONE',  ( -1.634638608836842089, -10.92453946501458439, 33.72985991061850086 ) ) ;
#67673 = ORIENTED_EDGE ( 'NONE', *, *, #38090, .F. ) ;
#67674 = FACE_BOUND ( 'NONE', #69025, .T. ) ;
#67675 = ORIENTED_EDGE ( 'NONE', *, *, #55342, .T. ) ;
#67676 = CARTESIAN_POINT ( 'NONE',  ( -4.403846153846151523, -7.500000000000001776, 34.75000000000000000 ) ) ;
#67677 = CARTESIAN_POINT ( 'NONE',  ( -10.61538461538461320, -2.249999999999998668, 29.75000000000001776 ) ) ;
#67678 = CIRCLE ( 'NONE', #71976, 8.000000000000000000 ) ;
#67679 = CARTESIAN_POINT ( 'NONE',  ( -18.00000000000000000, -10.67929555188718282, 33.92786785259543336 ) ) ;
#67680 = EDGE_CURVE ( 'NONE', #47848, #11498, #62185, .T. ) ;
#67681 = CARTESIAN_POINT ( 'NONE',  ( 17.07692307692307665, -1.790695186598648903, 34.54067556320373455 ) ) ;
#67682 = CARTESIAN_POINT ( 'NONE',  ( 5.326923076923075762, -2.249999999999998668, 29.75000000000000355 ) ) ;
#67683 = EDGE_CURVE ( 'NONE', #20327, #82892, #63510, .T. ) ;
#67684 = AXIS2_PLACEMENT_3D ( 'NONE', #84486, #30851, #64182 ) ;
#67685 = AXIS2_PLACEMENT_3D ( 'NONE', #66938, #52964, #47093 ) ;
#67686 = EDGE_LOOP ( 'NONE', ( #78975, #55721 ) ) ;
#67687 = VERTEX_POINT ( 'NONE', #28400 ) ;
#67688 = ORIENTED_EDGE ( 'NONE', *, *, #76937, .T. ) ;
#67689 = ORIENTED_EDGE ( 'NONE', *, *, #4966, .T. ) ;
#67690 = EDGE_CURVE ( 'NONE', #75887, #79557, #70278, .T. ) ;
#67691 = CARTESIAN_POINT ( 'NONE',  ( -7.134615384615385025, -3.499999999999999556, 29.75000000000000355 ) ) ;
#67692 = CARTESIAN_POINT ( 'NONE',  ( -6.249976730942353953, -12.41269422305637171, 30.68257228309993323 ) ) ;
#67693 = CARTESIAN_POINT ( 'NONE',  ( -4.087777802843714170, -8.973038597847269315, 34.52809138561122637 ) ) ;
#67694 = CARTESIAN_POINT ( 'NONE',  ( -8.096177070375302876, -3.520140089381495585, 33.17453946501458262 ) ) ;
#67695 = CARTESIAN_POINT ( 'NONE',  ( 11.40831432902331954, -2.619462340734462380, 30.83744416345203021 ) ) ;
#67696 = FACE_OUTER_BOUND ( 'NONE', #8144, .T. ) ;
#67697 = CARTESIAN_POINT ( 'NONE',  ( 20.00000000000000000, -4.000000000000000000, 29.75000000000000355 ) ) ;
#67698 = CARTESIAN_POINT ( 'NONE',  ( -5.076923076923199218, -11.67786785259630911, 32.92929555188603530 ) ) ;
#67699 = ORIENTED_EDGE ( 'NONE', *, *, #16028, .F. ) ;
#67700 = ORIENTED_EDGE ( 'NONE', *, *, #2608, .F. ) ;
#67701 = VERTEX_POINT ( 'NONE', #62621 ) ;
#67703 = VERTEX_POINT ( 'NONE', #21198 ) ;
#67702 = CARTESIAN_POINT ( 'NONE',  ( -11.60373198442231590, -12.46129190929999986, 30.37095296980880832 ) ) ;
#67705 = DIRECTION ( 'NONE',  ( -0.000000000000000000, 0.6427876096865404731, -0.7660444431189770143 ) ) ;
#67704 = CARTESIAN_POINT ( 'NONE',  ( -3.165514091256391271, -10.33852847137154107, 34.16647553114620450 ) ) ;
#67706 = B_SPLINE_CURVE_WITH_KNOTS ( 'NONE', 3,
 ( #25735, #18538, #45995, #53192, #80698, #18979, #67167, #26177, #41466, #33386 ),
 .UNSPECIFIED., .F., .F.,
 ( 4, 2, 2, 2, 4 ),
 ( 0.000000000000000000, 0.0001954339857564078809, 0.0003908679715128157619, 0.0005863019572692236428, 0.0007817359430256315238 ),
 .UNSPECIFIED. ) ;
#67707 = CARTESIAN_POINT ( 'NONE',  ( -0.4615384615385840772, -2.379036618888197285, 30.90682066428292885 ) ) ;
#67708 = LINE ( 'NONE', #6014, #30778 ) ;
#67709 = ADVANCED_FACE ( 'NONE', ( #16217 ), #42376, .F. ) ;
#67710 = FACE_BOUND ( 'NONE', #62350, .T. ) ;
#67711 = ORIENTED_EDGE ( 'NONE', *, *, #61984, .T. ) ;
#67712 = PLANE ( 'NONE',  #34674 ) ;
#67713 = FACE_OUTER_BOUND ( 'NONE', #57871, .T. ) ;
#67714 = CIRCLE ( 'NONE', #51875, 4.000000000000000000 ) ;
#67715 = VERTEX_POINT ( 'NONE', #71152 ) ;
#67716 = CARTESIAN_POINT ( 'NONE',  ( 6.000000000000001776, -9.905515769479276145, 34.41647553114623292 ) ) ;
#67717 = ORIENTED_EDGE ( 'NONE', *, *, #57485, .F. ) ;
#67718 = FACE_BOUND ( 'NONE', #69072, .T. ) ;
#67719 = CARTESIAN_POINT ( 'NONE',  ( 7.846153846153846700, -11.69971097300155272, 32.46337939537588113 ) ) ;
#67720 = CARTESIAN_POINT ( 'NONE',  ( 15.16468685140909400, -6.343179335718451384, 34.87096338111212646 ) ) ;
#67721 = ORIENTED_EDGE ( 'NONE', *, *, #7073, .F. ) ;
#67722 = CARTESIAN_POINT ( 'NONE',  ( -5.777037096438515817, -7.369474270740069777, 34.74850911626239736 ) ) ;
#67723 = CARTESIAN_POINT ( 'NONE',  ( -19.50000000000000000, -11.50000000000000000, 29.75000000000000355 ) ) ;
#67724 = CARTESIAN_POINT ( 'NONE',  ( 1.254468175177166467, -3.285722584762969856, 32.44110544564090759 ) ) ;
#67725 = ORIENTED_EDGE ( 'NONE', *, *, #55007, .F. ) ;
#67726 = DIRECTION ( 'NONE',  ( 0.000000000000000000, 0.000000000000000000, 1.000000000000000000 ) ) ;
#67727 = CARTESIAN_POINT ( 'NONE',  ( -7.846153846153967493, -8.656820664282941280, 34.87096338111179961 ) ) ;
#67728 = CARTESIAN_POINT ( 'NONE',  ( 18.25005441991345734, -10.82426656108011720, 33.81400080652039009 ) ) ;
#67729 = CARTESIAN_POINT ( 'NONE',  ( -7.976845312821404299, -2.729777683071817229, 31.24903638046269450 ) ) ;
#67730 = ORIENTED_EDGE ( 'NONE', *, *, #34592, .F. ) ;
#67731 = B_SPLINE_CURVE_WITH_KNOTS ( 'NONE', 3,
 ( #83549, #43437, #56506, #7441, #21833, #49303, #76782, #36242, #63696, #15082 ),
 .UNSPECIFIED., .F., .F.,
 ( 4, 2, 2, 2, 4 ),
 ( 0.0007817359430256318490, 0.0009771253907249984917, 0.001172514838424365026, 0.001367904286123731560, 0.001563293733823098311 ),
 .UNSPECIFIED. ) ;
#67732 = CARTESIAN_POINT ( 'NONE',  ( -2.307692307692305711, -11.16473453929635440, 33.15142922261926373 ) ) ;
#67733 = CARTESIAN_POINT ( 'NONE',  ( 23.49999999999998934, -5.499999999999981348, 32.75000000000000000 ) ) ;
#67734 = ORIENTED_EDGE ( 'NONE', *, *, #49220, .F. ) ;
#67735 = DIRECTION ( 'NONE',  ( -0.000000000000000000, -0.8660254037844397068, -0.4999999999999978906 ) ) ;
#67736 = DIRECTION ( 'NONE',  ( -1.734723475976813504E-16, 1.000000000000000000, 0.000000000000000000 ) ) ;
#67737 = CARTESIAN_POINT ( 'NONE',  ( -13.38461538461550582, -5.219633306517616589, 34.19971097300220464 ) ) ;
#67738 = CARTESIAN_POINT ( 'NONE',  ( -4.826868765284761942, -8.303483539816728154, 34.68545999027711702 ) ) ;
#67739 = DIRECTION ( 'NONE',  ( -0.000000000000000000, -0.3420201433256694346, -0.9396926207859080948 ) ) ;
#67740 = CARTESIAN_POINT ( 'NONE',  ( 15.16468685140909400, -5.471508081941602875, 34.59228464037088457 ) ) ;
#67742 = DIRECTION ( 'NONE',  ( 0.000000000000000000, 0.4999999999999985567, 0.8660254037844395958 ) ) ;
#67741 = CARTESIAN_POINT ( 'NONE',  ( 0.2115384615384615641, -7.500000000000001776, 34.75000000000000000 ) ) ;
#67743 = DIRECTION ( 'NONE',  ( 0.000000000000000000, 0.6427876096865373645, -0.7660444431189797898 ) ) ;
#67744 = CARTESIAN_POINT ( 'NONE',  ( -1.139087296525992166, -10.25000000000000533, 19.85937500000000355 ) ) ;
#67745 = ORIENTED_EDGE ( 'NONE', *, *, #8844, .F. ) ;
#67746 = CARTESIAN_POINT ( 'NONE',  ( 5.076923076923075762, -6.343179335718451384, 34.87096338111211935 ) ) ;
#67747 = EDGE_LOOP ( 'NONE', ( #87855, #86005 ) ) ;
#67748 = VECTOR ( 'NONE', #87101, 1000.000000000000227 ) ;
#67749 = VECTOR ( 'NONE', #45434, 1000.000000000000000 ) ;
#67750 = ORIENTED_EDGE ( 'NONE', *, *, #25064, .F. ) ;
#67751 = FACE_OUTER_BOUND ( 'NONE', #25528, .T. ) ;
#67752 = ORIENTED_EDGE ( 'NONE', *, *, #19460, .T. ) ;
#67753 = CARTESIAN_POINT ( 'NONE',  ( -5.076923076923199218, -11.67786785259630911, 32.92929555188603530 ) ) ;
#67754 = CARTESIAN_POINT ( 'NONE',  ( -2.750000000000007105, -6.360912703474006946, 17.67187500000000355 ) ) ;
#67755 = CARTESIAN_POINT ( 'NONE',  ( 12.59237679202522031, -7.277220318596961057, 34.99547417642776992 ) ) ;
#67756 = CARTESIAN_POINT ( 'NONE',  ( -9.019207500173124004, -3.137211980971221781, 32.19342716148376837 ) ) ;
#67757 = CARTESIAN_POINT ( 'NONE',  ( -3.165513659493205623, -9.442884908240271713, 34.35708131394835618 ) ) ;
#67758 = VECTOR ( 'NONE', #22627, 1000.000000000000114 ) ;
#67759 = CARTESIAN_POINT ( 'NONE',  ( -5.076923076923199218, -2.657715359629662988, 31.77849191805970364 ) ) ;
#67760 = CARTESIAN_POINT ( 'NONE',  ( -7.846153846153537614, -2.506253911140614576, 30.00000000000323297 ) ) ;
#67761 = DIRECTION ( 'NONE',  ( 0.000000000000000000, 0.000000000000000000, -1.000000000000000000 ) ) ;
#67762 = CARTESIAN_POINT ( 'NONE',  ( 6.792928953345224841, -12.50552854090298993, 31.33409797877408920 ) ) ;
#67763 = CARTESIAN_POINT ( 'NONE',  ( 1.384615384615265343, -12.27809138561165270, 31.22303859784587132 ) ) ;
#67764 = CARTESIAN_POINT ( 'NONE',  ( -11.97435897435897267, -11.50000000000000000, 29.75000000000000355 ) ) ;
#67765 = CARTESIAN_POINT ( 'NONE',  ( 1.384615384615386802, -11.33034616979429110, 35.88435417666054406 ) ) ;
#67766 = ORIENTED_EDGE ( 'NONE', *, *, #25211, .T. ) ;
#67767 = VERTEX_POINT ( 'NONE', #8140 ) ;
#67768 = B_SPLINE_CURVE_WITH_KNOTS ( 'NONE', 3,
 ( #48902, #68290, #6593, #49354, #55652, #56106, #83600, #27305, #13784, #54768 ),
 .UNSPECIFIED., .F., .F.,
 ( 4, 2, 2, 2, 4 ),
 ( 0.0007817246256747470640, 0.0009771112852218898515, 0.001172497944769032531, 0.001367884604316175427, 0.001563271263863318106 ),
 .UNSPECIFIED. ) ;
#67769 = CARTESIAN_POINT ( 'NONE',  ( -8.899922235898328537, -12.38065189839062263, 30.83690757178629482 ) ) ;
#67770 = CARTESIAN_POINT ( 'NONE',  ( 0.4615384615384611200, -11.69971097300155272, 32.46337939537588113 ) ) ;
#67771 = CYLINDRICAL_SURFACE ( 'NONE', #45429, 0.2499999999999973355 ) ;
#67772 = CARTESIAN_POINT ( 'NONE',  ( 6.250000000000017764, -2.249999999999999112, 29.81603969181031033 ) ) ;
#67773 = B_SPLINE_CURVE_WITH_KNOTS ( 'NONE', 3,
 ( #70306, #27550, #82943, #8618, #36089, #29329, #84283, #21226, #34298, #50027 ),
 .UNSPECIFIED., .F., .F.,
 ( 4, 2, 2, 2, 4 ),
 ( 0.000000000000000000, 0.0001954311584214072381, 0.0003908623168428144762, 0.0005862934752642217414, 0.0007817246336856289524 ),
 .UNSPECIFIED. ) ;
#67774 = CARTESIAN_POINT ( 'NONE',  ( 6.130525701763564150, -5.195472089885680766, 34.18748526763464923 ) ) ;
#67775 = FACE_OUTER_BOUND ( 'NONE', #68068, .T. ) ;
#67776 = AXIS2_PLACEMENT_3D ( 'NONE', #25792, #80751, #46934 ) ;
#67777 = DIRECTION ( 'NONE',  ( -1.000000000000000000, -0.000000000000000000, -0.000000000000000000 ) ) ;
#67778 = EDGE_LOOP ( 'NONE', ( #44664, #1919, #20017, #73230 ) ) ;
#67779 = DIRECTION ( 'NONE',  ( 0.000000000000000000, 0.000000000000000000, -1.000000000000000000 ) ) ;
#67780 = ORIENTED_EDGE ( 'NONE', *, *, #53942, .F. ) ;
#67781 = AXIS2_PLACEMENT_3D ( 'NONE', #12361, #5155, #4717 ) ;
#67782 = ORIENTED_EDGE ( 'NONE', *, *, #35859, .T. ) ;
#67783 = CARTESIAN_POINT ( 'NONE',  ( -8.546217925137376881, -4.762714258010881885, 34.23016756924214832 ) ) ;
#67784 = ADVANCED_FACE ( 'NONE', ( #49563 ), #55871, .F. ) ;
#67785 = CARTESIAN_POINT ( 'NONE',  ( -2.373774687052442545, -9.058645607665454236, 34.76329471203372634 ) ) ;
#67786 = CARTESIAN_POINT ( 'NONE',  ( 14.24242186173153435, -5.219633306516282545, 34.19971097300152962 ) ) ;
#67787 = PRODUCT_RELATED_PRODUCT_CATEGORY ( 'part', '', ( #75728 ) ) ;
#67788 = CARTESIAN_POINT ( 'NONE',  ( 3.100078627658924280, -8.191372820521381826, 34.95448215188423546 ) ) ;
#67789 = CARTESIAN_POINT ( 'NONE',  ( 5.749976762707035505, -2.823816976329319495, 31.52131813110795733 ) ) ;
#67790 = ORIENTED_EDGE ( 'NONE', *, *, #42597, .F. ) ;
#67791 = ORIENTED_EDGE ( 'NONE', *, *, #47507, .F. ) ;
#67792 = ORIENTED_EDGE ( 'NONE', *, *, #74010, .F. ) ;
#67793 = VERTEX_POINT ( 'NONE', #49995 ) ;
#67794 = B_SPLINE_CURVE_WITH_KNOTS ( 'NONE', 3,
 ( #6735, #26575, #54478, #27900, #67565, #81976, #61672, #75211, #61227, #18929 ),
 .UNSPECIFIED., .F., .F.,
 ( 4, 2, 2, 2, 4 ),
 ( 0.000000000000000000, 0.0001954311564186864949, 0.0003908623128373729899, 0.0005862934692560594577, 0.0007817246256747459798 ),
 .UNSPECIFIED. ) ;
#67795 = EDGE_CURVE ( 'NONE', #73790, #30150, #43682, .T. ) ;
#67796 = CARTESIAN_POINT ( 'NONE',  ( 18.00000000000000000, -2.292212530054420494, 30.41441678777542634 ) ) ;
#67797 = CARTESIAN_POINT ( 'NONE',  ( 7.780883400193072674, -3.835265460703609186, 33.15142922261924241 ) ) ;
#67798 = B_SPLINE_CURVE_WITH_KNOTS ( 'NONE', 3,
 ( #12027, #12897, #72815, #60194, #46685, #80936, #5259, #39945, #67404, #5701 ),
 .UNSPECIFIED., .F., .F.,
 ( 4, 2, 2, 2, 4 ),
 ( 0.000000000000000000, 0.0001954339857564073659, 0.0003908679715128147319, 0.0005863019572692221250, 0.0007817359430256294638 ),
 .UNSPECIFIED. ) ;
#67799 = FACE_OUTER_BOUND ( 'NONE', #8411, .T. ) ;
#67800 = AXIS2_PLACEMENT_3D ( 'NONE', #53516, #12546, #60724 ) ;
#67801 = CARTESIAN_POINT ( 'NONE',  ( -16.21992853320628925, -2.292212530054420050, 30.41441678777542634 ) ) ;
#67802 = FILL_AREA_STYLE_COLOUR ( '', #24904 ) ;
#67803 = CARTESIAN_POINT ( 'NONE',  ( 12.21151523731700550, -2.985938066672154445, 32.43141759479405550 ) ) ;
#67804 = EDGE_LOOP ( 'NONE', ( #75347, #1949 ) ) ;
#67805 = ORIENTED_EDGE ( 'NONE', *, *, #2586, .T. ) ;
#67806 = VERTEX_POINT ( 'NONE', #83358 ) ;
#67808 = EDGE_LOOP ( 'NONE', ( #63982, #63270 ) ) ;
#67807 = LINE ( 'NONE', #47965, #64567 ) ;
#67809 = FACE_OUTER_BOUND ( 'NONE', #23074, .T. ) ;
#67810 = DIRECTION ( 'NONE',  ( 0.000000000000000000, 0.8660254037844377084, -0.5000000000000015543 ) ) ;
#67811 = CARTESIAN_POINT ( 'NONE',  ( 1.553300858899086867, -3.749999999999992006, 20.48437500000000000 ) ) ;
#67812 = EDGE_CURVE ( 'NONE', #26079, #85537, #55429, .T. ) ;
#67813 = VERTEX_POINT ( 'NONE', #36922 ) ;
#67814 = EDGE_CURVE ( 'NONE', #73573, #12391, #29303, .T. ) ;
#67815 = CARTESIAN_POINT ( 'NONE',  ( -4.480769230769230838, -7.500000000000000000, 29.75000000000000355 ) ) ;
#67816 = EDGE_LOOP ( 'NONE', ( #66387, #26571, #28124, #21706 ) ) ;
#67817 = CARTESIAN_POINT ( 'NONE',  ( 2.177545098254088707, -6.852621066184267029, 34.70813303252209181 ) ) ;
#67818 = EDGE_CURVE ( 'NONE', #54248, #28816, #29575, .T. ) ;
#67819 = FACE_BOUND ( 'NONE', #53972, .T. ) ;
#67820 = CARTESIAN_POINT ( 'NONE',  ( -6.673022611438608642, -12.41262288849542017, 30.68299917996395010 ) ) ;
#67821 = EDGE_CURVE ( 'NONE', #75335, #76807, #43250, .T. ) ;
#67822 = LINE ( 'NONE', #32695, #49151 ) ;
#67823 = ORIENTED_EDGE ( 'NONE', *, *, #88056, .T. ) ;
#67824 = CARTESIAN_POINT ( 'NONE',  ( -12.71153846153846168, -7.500000000000001776, 34.75000000000000000 ) ) ;
#67825 = LINE ( 'NONE', #12875, #66794 ) ;
#67826 = ORIENTED_EDGE ( 'NONE', *, *, #55493, .F. ) ;
#67827 = VECTOR ( 'NONE', #7231, 1000.000000000000000 ) ;
#67828 = CARTESIAN_POINT ( 'NONE',  ( 1.384615384615386802, -1.129524287112498415, 32.06866353760679544 ) ) ;
#67829 = CARTESIAN_POINT ( 'NONE',  ( -5.934744860487159102, -4.320704448112861584, 33.92786785259548310 ) ) ;
#67830 = CARTESIAN_POINT ( 'NONE',  ( 7.384615384615385025, -4.000000000000000000, 29.75000000000000355 ) ) ;
#67831 = CARTESIAN_POINT ( 'NONE',  ( -2.307692307692428724, -9.528491918059723176, 34.59228464037033035 ) ) ;
#67832 = CARTESIAN_POINT ( 'NONE',  ( 10.48523740594639619, -11.93770438780619259, 32.05411857736982029 ) ) ;
#67833 = FACE_BOUND ( 'NONE', #74005, .T. ) ;
#67835 = LINE ( 'NONE', #46674, #73330 ) ;
#67834 = FACE_OUTER_BOUND ( 'NONE', #57507, .T. ) ;
#67836 = CARTESIAN_POINT ( 'NONE',  ( 2.307692307692309264, -4.102666532097928531, 36.13435417666054406 ) ) ;
#67838 = CARTESIAN_POINT ( 'NONE',  ( -2.057746898314263273, -12.45601412856602686, 31.48342859153981621 ) ) ;
#67837 = LINE ( 'NONE', #5687, #19913 ) ;
#67839 = VECTOR ( 'NONE', #7498, 1000.000000000000227 ) ;
#67840 = CARTESIAN_POINT ( 'NONE',  ( 8.992010438208831502, -12.69155399931963046, 30.53255429739157734 ) ) ;
#67841 = CARTESIAN_POINT ( 'NONE',  ( -2.724691934501232371, -8.700186371490559623, 16.01375670625849068 ) ) ;
#67842 = ORIENTED_EDGE ( 'NONE', *, *, #50890, .F. ) ;
#67843 = CARTESIAN_POINT ( 'NONE',  ( 18.00000000000000000, -9.905515769479276145, 34.41647553114623292 ) ) ;
#67844 = ORIENTED_EDGE ( 'NONE', *, *, #59284, .F. ) ;
#67845 = CARTESIAN_POINT ( 'NONE',  ( -1.384615384615383471, -10.05456864172156806, 36.03766855953608683 ) ) ;
#67846 = ORIENTED_EDGE ( 'NONE', *, *, #37356, .T. ) ;
#67847 = CARTESIAN_POINT ( 'NONE',  ( 16.37685899793954292, -12.64618726649961289, 30.78989965857442712 ) ) ;
#67848 = CARTESIAN_POINT ( 'NONE',  ( -7.384615384615385025, -7.500000000000000000, 29.75000000000000355 ) ) ;
#67850 = ORIENTED_EDGE ( 'NONE', *, *, #14640, .T. ) ;
#67849 = CARTESIAN_POINT ( 'NONE',  ( -6.166666666666667851, -11.50000000000000000, 29.75000000000000355 ) ) ;
#67851 = CARTESIAN_POINT ( 'NONE',  ( -10.39237177129122003, -11.98016756924215009, 32.48728574198911190 ) ) ;
#67852 = CARTESIAN_POINT ( 'NONE',  ( 6.000000000000001776, -10.67929555188718282, 33.92786785259544047 ) ) ;
#67853 = CARTESIAN_POINT ( 'NONE',  ( -1.901340078031346525, -9.487747218494661183, 19.68563170625849068 ) ) ;
#67854 = CARTESIAN_POINT ( 'NONE',  ( 4.403791672194295792, -10.76462480002816235, 33.53768742498949962 ) ) ;
#67855 = CARTESIAN_POINT ( 'NONE',  ( 8.703960768674448900, -2.657715359629088780, 31.77849191805832874 ) ) ;
#67856 = CARTESIAN_POINT ( 'NONE',  ( -0.3253212748352862782, -4.768255367016290158, 28.86040964833806299 ) ) ;
#67857 = CARTESIAN_POINT ( 'NONE',  ( 1.318533005255250634, -4.661471528628507777, 34.16647553114621871 ) ) ;
#67858 = CARTESIAN_POINT ( 'NONE',  ( -0.3954701105360229896, -4.098570777380720287, 33.41473453929635440 ) ) ;
#67859 = CARTESIAN_POINT ( 'NONE',  ( 9.692307692307695177, -3.322132147404559976, 32.92929555188717927 ) ) ;
#67860 = CARTESIAN_POINT ( 'NONE',  ( 2.694853999681185108, -4.891553140782077591, 20.81436829374151287 ) ) ;
#67861 = EDGE_CURVE ( 'NONE', #34265, #3876, #9027, .T. ) ;
#67862 = CARTESIAN_POINT ( 'NONE',  ( 5.299935921016470708, -2.523321265292115090, 31.42251411153756280 ) ) ;
#67863 = CARTESIAN_POINT ( 'NONE',  ( 7.146088274689773812, -11.24521262558773671, 33.06293181088029343 ) ) ;
#67864 = ORIENTED_EDGE ( 'NONE', *, *, #49833, .T. ) ;
#67865 = DIRECTION ( 'NONE',  ( -0.000000000000000000, 0.9396926207859093161, -0.3420201433256663259 ) ) ;
#67866 = DIRECTION ( 'NONE',  ( -1.000000000000000000, 0.000000000000000000, -0.000000000000000000 ) ) ;
#67867 = CARTESIAN_POINT ( 'NONE',  ( -2.694853999681181556, -10.10844685921792241, 18.93936829374151287 ) ) ;
#67868 = CARTESIAN_POINT ( 'NONE',  ( -17.93393164899756087, -12.37446782046654192, 30.86335684631486842 ) ) ;
#67869 = CARTESIAN_POINT ( 'NONE',  ( -5.142193522883852452, -2.625532179533445198, 30.86335684631481513 ) ) ;
#67870 = CIRCLE ( 'NONE', #14842, 8.000000000000000000 ) ;
#67871 = ORIENTED_EDGE ( 'NONE', *, *, #14850, .T. ) ;
#67872 = CARTESIAN_POINT ( 'NONE',  ( -5.448717948717948012, -3.499999999999999556, 29.75000000000000355 ) ) ;
#67873 = CARTESIAN_POINT ( 'NONE',  ( 20.00000000000000000, -11.00000000000000000, 28.25000000000000000 ) ) ;
#67875 = ORIENTED_EDGE ( 'NONE', *, *, #15778, .T. ) ;
#67874 = CARTESIAN_POINT ( 'NONE',  ( 1.384615384615386802, -5.471508081941601098, 34.59228464037088457 ) ) ;
#67876 = DIRECTION ( 'NONE',  ( -0.000000000000000000, -0.5000000000000009992, -0.8660254037844380415 ) ) ;
#67877 = CARTESIAN_POINT ( 'NONE',  ( 4.854094979288197997, -7.369209533119140509, 34.99857337881830688 ) ) ;
#67878 = VECTOR ( 'NONE', #56892, 1000.000000000000000 ) ;
#67879 = ADVANCED_FACE ( 'NONE', ( #69396 ), #7700, .F. ) ;
#67880 = CARTESIAN_POINT ( 'NONE',  ( -12.71156168575991785, -4.931416488878822335, 34.32920672191015399 ) ) ;
#67881 = VERTEX_POINT ( 'NONE', #29739 ) ;
#67882 = B_SPLINE_CURVE_WITH_KNOTS ( 'NONE', 3,
 ( #79238, #78783, #50847, #17085, #86909, #44539, #4459, #45887, #25177, #30592 ),
 .UNSPECIFIED., .F., .F.,
 ( 4, 2, 2, 2, 4 ),
 ( 0.0007817246256747469556, 0.0009771112852218889842, 0.001172497944769031013, 0.001367884604316173041, 0.001563271263863315070 ),
 .UNSPECIFIED. ) ;
#67883 = CARTESIAN_POINT ( 'NONE',  ( -9.469528023329626620, -2.612705202774698421, 31.66806509827799943 ) ) ;
#67884 = DIRECTION ( 'NONE',  ( 0.000000000000000000, 0.9848077530122072432, 0.1736481776669354937 ) ) ;
#67885 = CARTESIAN_POINT ( 'NONE',  ( -13.16160254052199008, -8.282913670948747864, 34.94150082978203642 ) ) ;
#67886 = VERTEX_POINT ( 'NONE', #22968 ) ;
#67887 = ORIENTED_EDGE ( 'NONE', *, *, #62319, .T. ) ;
#67888 = ORIENTED_EDGE ( 'NONE', *, *, #55333, .T. ) ;
#67889 = PRODUCT_RELATED_PRODUCT_CATEGORY ( 'part', '', ( #6674 ) ) ;
#67890 = VERTEX_POINT ( 'NONE', #77912 ) ;
#67891 = EDGE_CURVE ( 'NONE', #81961, #38938, #35158, .T. ) ;
#67892 = CARTESIAN_POINT ( 'NONE',  ( 5.299934428535926223, -12.15243808032446005, 31.58219941686247978 ) ) ;
#67893 = CARTESIAN_POINT ( 'NONE',  ( 14.17700084102475344, -4.118384482072086072, 33.43331474514187107 ) ) ;
#67894 = EDGE_CURVE ( 'NONE', #86167, #2856, #84302, .T. ) ;
#67895 = CARTESIAN_POINT ( 'NONE',  ( -16.28453675695647007, -2.845849958028613624, 32.17971566917920967 ) ) ;
#67896 = FACE_OUTER_BOUND ( 'NONE', #31994, .T. ) ;
#67897 = B_SPLINE_CURVE_WITH_KNOTS ( 'NONE', 3,
 ( #29259, #71105, #22485, #8981, #78302, #83762, #36449, #57154, #85517, #63901 ),
 .UNSPECIFIED., .F., .F.,
 ( 4, 2, 2, 2, 4 ),
 ( 0.0007817359430256287049, 0.0009771253907249945886, 0.001172514838424360255, 0.001367904286123725922, 0.001563293733823091806 ),
 .UNSPECIFIED. ) ;
#67898 = CARTESIAN_POINT ( 'NONE',  ( 5.142991427925513115, -5.557115091759786019, 34.35708131394839882 ) ) ;
#67899 = AXIS2_PLACEMENT_3D ( 'NONE', #16213, #49112, #49991 ) ;
#67900 = ORIENTED_EDGE ( 'NONE', *, *, #50384, .T. ) ;
#67901 = ORIENTED_EDGE ( 'NONE', *, *, #16116, .T. ) ;
#67903 = VERTEX_POINT ( 'NONE', #73384 ) ;
#67902 = EDGE_CURVE ( 'NONE', #85628, #26549, #3577, .T. ) ;
#67905 = VERTEX_POINT ( 'NONE', #25192 ) ;
#67904 = CARTESIAN_POINT ( 'NONE',  ( -6.923076923076922462, -2.486705287966279876, 31.30864560766543647 ) ) ;
#67906 = CARTESIAN_POINT ( 'NONE',  ( -5.076923076923199218, -12.51329471203414379, 31.30864560766407578 ) ) ;
#67907 = CYLINDRICAL_SURFACE ( 'NONE', #88269, 0.2499999999999973355 ) ;
#67908 = EDGE_CURVE ( 'NONE', #41728, #2541, #63859, .T. ) ;
#67909 = DIRECTION ( 'NONE',  ( 0.000000000000000000, 0.000000000000000000, -1.000000000000000000 ) ) ;
#67910 = DIRECTION ( 'NONE',  ( -0.000000000000000000, 0.9848077530122086864, -0.1736481776669273891 ) ) ;
#67911 = ADVANCED_FACE ( 'NONE', ( #45002 ), #79698, .F. ) ;
#67912 = ORIENTED_EDGE ( 'NONE', *, *, #26803, .F. ) ;
#67913 = ORIENTED_EDGE ( 'NONE', *, *, #2471, .F. ) ;
#67914 = VERTEX_POINT ( 'NONE', #65721 ) ;
#67915 = CARTESIAN_POINT ( 'NONE',  ( -16.15384615384615330, -8.120952969808772792, 34.71129190930000163 ) ) ;
#67917 = ORIENTED_EDGE ( 'NONE', *, *, #26377, .F. ) ;
#67916 = CYLINDRICAL_SURFACE ( 'NONE', #51647, 0.2499999999999994726 ) ;
#67918 = CARTESIAN_POINT ( 'NONE',  ( 9.562160482869472844, -11.93770438780619259, 32.05411857736982029 ) ) ;
#67919 = CARTESIAN_POINT ( 'NONE',  ( -17.20761368003338987, -3.338472653186243200, 32.95098750199972670 ) ) ;
#67920 = EDGE_CURVE ( 'NONE', #80449, #81210, #543, .T. ) ;
#67921 = EDGE_LOOP ( 'NONE', ( #55008, #788 ) ) ;
#67922 = CARTESIAN_POINT ( 'NONE',  ( 20.00000000000000000, -4.000000000000000000, 29.75000000000000355 ) ) ;
#67923 = CARTESIAN_POINT ( 'NONE',  ( -18.00000000000000000, -2.538708090699994813, 30.37095296980875858 ) ) ;
#67924 = CARTESIAN_POINT ( 'NONE',  ( 20.00000000000000000, -4.000000000000000000, 29.75000000000000355 ) ) ;
#67925 = FACE_BOUND ( 'NONE', #44764, .T. ) ;
#67926 = CARTESIAN_POINT ( 'NONE',  ( -17.77722045873158763, -8.496831190052089866, 34.64984203495476578 ) ) ;
#67927 = CARTESIAN_POINT ( 'NONE',  ( -12.46153846153858247, -9.442884908241554243, 34.35708131394783038 ) ) ;
#67928 = B_SPLINE_CURVE_WITH_KNOTS ( 'NONE', 3,
 ( #33321, #26563, #54018, #82396, #27003, #6295, #20682, #61214, #48145, #54462 ),
 .UNSPECIFIED., .F., .F.,
 ( 4, 2, 2, 2, 4 ),
 ( 0.0007817359430256359690, 0.0009771253907250036959, 0.001172514838424371314, 0.001367904286123738933, 0.001563293733823106768 ),
 .UNSPECIFIED. ) ;
#67929 = AXIS2_PLACEMENT_3D ( 'NONE', #80591, #37804, #58501 ) ;
#67930 = CARTESIAN_POINT ( 'NONE',  ( 11.76124107972994537, -12.44528174975671853, 30.48912976160716681 ) ) ;
#67932 = CARTESIAN_POINT ( 'NONE',  ( 6.673100179028333301, -10.82459398097509684, 33.81372124010185587 ) ) ;
#67931 = PLANE ( 'NONE',  #2903 ) ;
#67933 = AXIS2_PLACEMENT_3D ( 'NONE', #9946, #25688, #16701 ) ;
#67934 = EDGE_CURVE ( 'NONE', #13671, #19193, #74551, .T. ) ;
#67935 = CARTESIAN_POINT ( 'NONE',  ( -0.4615384615384611200, -1.044019251281081972, 31.83374038241031911 ) ) ;
#67936 = CARTESIAN_POINT ( 'NONE',  ( 7.146452863775108355, -2.501478030877322567, 29.88021232661720816 ) ) ;
#67937 = ORIENTED_EDGE ( 'NONE', *, *, #68657, .T. ) ;
#67938 = ADVANCED_FACE ( 'NONE', ( #11237 ), #59421, .F. ) ;
#67939 = CARTESIAN_POINT ( 'NONE',  ( -15.16470189741915320, -11.35647404775217595, 33.31231777344666511 ) ) ;
#67940 = CARTESIAN_POINT ( 'NONE',  ( 0.3313904918067619998, -11.04286588640298561, 33.62463336215343901 ) ) ;
#67941 = ORIENTED_EDGE ( 'NONE', *, *, #55368, .F. ) ;
#67942 = AXIS2_PLACEMENT_3D ( 'NONE', #29456, #86624, #71745 ) ;
#67943 = CARTESIAN_POINT ( 'NONE',  ( 11.97435897435897267, -7.500000000000000000, 33.75000000000000000 ) ) ;
#67944 = CARTESIAN_POINT ( 'NONE',  ( -15.45369544828537833, -2.554751324335734708, 30.48935550225260727 ) ) ;
#67945 = CARTESIAN_POINT ( 'NONE',  ( 19.00000000000000000, 8.999999999999996447, 23.75000000000000000 ) ) ;
#67946 = ORIENTED_EDGE ( 'NONE', *, *, #32699, .F. ) ;
#67947 = FACE_OUTER_BOUND ( 'NONE', #56451, .T. ) ;
#67948 = CARTESIAN_POINT ( 'NONE',  ( 6.857806922520603976, -8.656820664281497102, 34.87096338111211935 ) ) ;
#67949 = FACE_BOUND ( 'NONE', #69957, .T. ) ;
#67951 = CARTESIAN_POINT ( 'NONE',  ( -16.82692307692306954, -2.249999999999999112, 29.81603969181033165 ) ) ;
#67950 = CARTESIAN_POINT ( 'NONE',  ( -14.30769230769230660, -13.49023893513002648, 31.06009739812518688 ) ) ;
#67952 = LINE ( 'NONE', #67064, #77619 ) ;
#67953 = CARTESIAN_POINT ( 'NONE',  ( 0.4615384615384611200, -4.661471528628507777, 34.16647553114623292 ) ) ;
#67955 = CARTESIAN_POINT ( 'NONE',  ( -14.43830196289638579, -7.722926974430166069, 34.99546784045485737 ) ) ;
#67954 = CARTESIAN_POINT ( 'NONE',  ( 0.000000000000000000, 0.000000000000000000, 0.000000000000000000 ) ) ;
#67956 = CARTESIAN_POINT ( 'NONE',  ( 1.553300858899087311, -3.749999999999992006, 25.48437500000000000 ) ) ;
#67957 = ORIENTED_EDGE ( 'NONE', *, *, #52110, .T. ) ;
#67958 = B_SPLINE_CURVE_WITH_KNOTS ( 'NONE', 3,
 ( #25199, #4939, #87820, #12142, #33299, #31509, #65727, #39174, #40068, #10800 ),
 .UNSPECIFIED., .F., .F.,
 ( 4, 2, 2, 2, 4 ),
 ( 0.000000000000000000, 0.0001954339857564084773, 0.0003908679715128169545, 0.0005863019572692254860, 0.0007817359430256339090 ),
 .UNSPECIFIED. ) ;
#67959 = ORIENTED_EDGE ( 'NONE', *, *, #2312, .T. ) ;
#67960 = CARTESIAN_POINT ( 'NONE',  ( 4.826899852701617810, -10.92453946501458439, 33.72985991061850086 ) ) ;
#67961 = CARTESIAN_POINT ( 'NONE',  ( -4.403822884788507253, -12.41269422305637171, 30.68257228309993323 ) ) ;
#67962 = CARTESIAN_POINT ( 'NONE',  ( 16.37662582282421297, -3.020022701398814569, 32.48759521482552515 ) ) ;
#67963 = CARTESIAN_POINT ( 'NONE',  ( 10.74617505635157144, -2.845873456487966635, 32.17976146951972538 ) ) ;
#67964 = CARTESIAN_POINT ( 'NONE',  ( -3.480792468062196221, -5.851115903089112003, 34.47074536777953568 ) ) ;
#67965 = CARTESIAN_POINT ( 'NONE',  ( -2.651650429449565305, -4.848349570550461785, 21.50000000000000000 ) ) ;
#67966 = CARTESIAN_POINT ( 'NONE',  ( -8.769230769230768274, -9.905515769479276145, 34.41647553114623292 ) ) ;
#67967 = CARTESIAN_POINT ( 'NONE',  ( 1.253924781505077801, -9.929715669179220328, 34.40415004197138416 ) ) ;
#67968 = CARTESIAN_POINT ( 'NONE',  ( 17.74997677577854560, -4.175268141568689195, 33.81360843649122216 ) ) ;
#67969 = CARTESIAN_POINT ( 'NONE',  ( -14.98082371242109012, -11.37275283266504111, 32.91324779482534524 ) ) ;
#67970 = CARTESIAN_POINT ( 'NONE',  ( -9.692307692307691624, -11.16473453929635440, 33.15142922261926373 ) ) ;
#67971 = CARTESIAN_POINT ( 'NONE',  ( 8.546304551714618114, -12.15238873228292071, 31.58232369045353849 ) ) ;
#67972 = VECTOR ( 'NONE', #84583, 1000.000000000000000 ) ;
#67973 = CARTESIAN_POINT ( 'NONE',  ( 6.000000000000001776, -12.10708131394839349, 31.69288490824020244 ) ) ;
#67974 = EDGE_CURVE ( 'NONE', #23594, #19289, #29421, .T. ) ;
#67975 = LINE ( 'NONE', #6277, #27567 ) ;
#67976 = B_SPLINE_CURVE_WITH_KNOTS ( 'NONE', 3,
 ( #23838, #86009, #44112, #64828, #57643, #85126 ),
 .UNSPECIFIED., .F., .F.,
 ( 4, 2, 4 ),
 ( 4.220987180333914613E-17, 0.0001954756301637177243, 0.0003909512603273932732 ),
 .UNSPECIFIED. ) ;
#67977 = CARTESIAN_POINT ( 'NONE',  ( -3.454254155333563059, -12.47654668319379567, 31.42292124445336654 ) ) ;
#67978 = EDGE_LOOP ( 'NONE', ( #68767, #1991, #12438, #39139 ) ) ;
#67979 = ADVANCED_FACE ( 'NONE', ( #37360 ), #3131, .F. ) ;
#67980 = CARTESIAN_POINT ( 'NONE',  ( -14.30769230769230660, -4.945431358278436385, 36.03766855953609394 ) ) ;
#67981 = EDGE_CURVE ( 'NONE', #20157, #39109, #67519, .T. ) ;
#67982 = CARTESIAN_POINT ( 'NONE',  ( -9.320512820512821150, -1.926643599941765039, 29.65000000000000213 ) ) ;
#67983 = CARTESIAN_POINT ( 'NONE',  ( -2.749999999999999112, -7.438900925035484057, 17.84561829374150932 ) ) ;
#67984 = B_SPLINE_CURVE_WITH_KNOTS ( 'NONE', 3,
 ( #53992, #25638, #54431, #73382, #81926, #47231, #73837, #19329, #74723, #40058 ),
 .UNSPECIFIED., .F., .F.,
 ( 4, 2, 2, 2, 4 ),
 ( 0.0007817359430256301143, 0.0009771253907249963233, 0.001172514838424362641, 0.001367904286123728958, 0.001563293733823095276 ),
 .UNSPECIFIED. ) ;
#67985 = EDGE_CURVE ( 'NONE', #66983, #7925, #20218, .T. ) ;
#67986 = CARTESIAN_POINT ( 'NONE',  ( 3.903822929624696680, -4.931416488878822335, 34.32920672191015399 ) ) ;
#67987 = CYLINDRICAL_SURFACE ( 'NONE', #71434, 0.2499999999999995559 ) ;
#67988 = DIRECTION ( 'NONE',  ( 0.000000000000000000, 0.1736481776669267785, -0.9848077530122087975 ) ) ;
#67990 = EDGE_LOOP ( 'NONE', ( #36980, #38690 ) ) ;
#67989 = CARTESIAN_POINT ( 'NONE',  ( -14.30769230769242739, -12.27809138561165270, 31.22303859784587132 ) ) ;
#67991 = CARTESIAN_POINT ( 'NONE',  ( 1.139087296526029469, -10.24999999999999289, 23.45312500000000000 ) ) ;
#67992 = CARTESIAN_POINT ( 'NONE',  ( 3.296024370282069071, -8.656820664281605460, 34.87096338111211224 ) ) ;
#67993 = ORIENTED_EDGE ( 'NONE', *, *, #27039, .F. ) ;
#67994 = FACE_OUTER_BOUND ( 'NONE', #71676, .T. ) ;
#67995 = EDGE_CURVE ( 'NONE', #19429, #21320, #46798, .T. ) ;
#67996 = CARTESIAN_POINT ( 'NONE',  ( 11.53846153846153832, -1.790695186598648903, 34.54067556320373455 ) ) ;
#67997 = ORIENTED_EDGE ( 'NONE', *, *, #71965, .T. ) ;
#67998 = CARTESIAN_POINT ( 'NONE',  ( 7.622668902429897919, -4.386631170607603991, 33.66268669641500111 ) ) ;
#67999 = CARTESIAN_POINT ( 'NONE',  ( -16.08870037451418966, -7.750023238201980469, 34.74374492549440419 ) ) ;
#68000 = CARTESIAN_POINT ( 'NONE',  ( 2.084765348785459604, -12.64616026154729411, 30.79003144601913533 ) ) ;
#68001 = ORIENTED_EDGE ( 'NONE', *, *, #10052, .F. ) ;
#68002 = VERTEX_POINT ( 'NONE', #82368 ) ;
#68003 = VECTOR ( 'NONE', #13572, 1000.000000000000227 ) ;
#68004 = EDGE_LOOP ( 'NONE', ( #78210, #45427 ) ) ;
#68006 = CARTESIAN_POINT ( 'NONE',  ( -8.096177070375304652, -2.341070481393819236, 30.72580821765574299 ) ) ;
#68005 = VECTOR ( 'NONE', #87085, 1000.000000000000000 ) ;
#68007 = FACE_OUTER_BOUND ( 'NONE', #7968, .T. ) ;
#68008 = DIRECTION ( 'NONE',  ( 1.000000000000000000, -0.000000000000000000, -0.000000000000000000 ) ) ;
#68009 = CARTESIAN_POINT ( 'NONE',  ( -17.14219352288385778, -6.026961402152685388, 34.52809138561120506 ) ) ;
#68010 = DIRECTION ( 'NONE',  ( -0.000000000000000000, -0.3420201433256694901, -0.9396926207859082059 ) ) ;
#68012 = EDGE_CURVE ( 'NONE', #53025, #27202, #78847, .T. ) ;
#68011 = CARTESIAN_POINT ( 'NONE',  ( 20.74999999999999645, -4.500000000000000000, 29.75000000000000355 ) ) ;
#68013 = CARTESIAN_POINT ( 'NONE',  ( 17.07692307692307665, -3.322132147404559976, 32.92929555188717927 ) ) ;
#68014 = AXIS2_PLACEMENT_3D ( 'NONE', #38994, #11513, #87187 ) ;
#68015 = B_SPLINE_CURVE_WITH_KNOTS ( 'NONE', 3,
 ( #67727, #19096, #39379, #27176, #88031, #40706, #81248, #6032, #47888, #53310 ),
 .UNSPECIFIED., .F., .F.,
 ( 4, 2, 2, 2, 4 ),
 ( 0.0007817246256747484735, 0.0009771112852218926705, 0.001172497944769037084, 0.001367884604316181498, 0.001563271263863325695 ),
 .UNSPECIFIED. ) ;
#68016 = EDGE_CURVE ( 'NONE', #65133, #62019, #42335, .T. ) ;
#68017 = CARTESIAN_POINT ( 'NONE',  ( -0.3962833220256225530, -12.51329471203373700, 31.30864560766537963 ) ) ;
#68018 = EDGE_LOOP ( 'NONE', ( #67018, #11850, #38386, #47313 ) ) ;
#68019 = ORIENTED_EDGE ( 'NONE', *, *, #41888, .F. ) ;
#68021 = EDGE_LOOP ( 'NONE', ( #23927, #67752 ) ) ;
#68020 = CARTESIAN_POINT ( 'NONE',  ( 18.00000000000000000, -9.058645607665452459, 34.76329471203371924 ) ) ;
#68022 = CARTESIAN_POINT ( 'NONE',  ( -13.45036881292871556, -7.249945578846652694, 34.99404164642496795 ) ) ;
#68023 = CARTESIAN_POINT ( 'NONE',  ( 12.46153846153833911, -3.300289026999228881, 32.46337939537708905 ) ) ;
#68024 = ORIENTED_EDGE ( 'NONE', *, *, #17276, .T. ) ;
#68025 = CARTESIAN_POINT ( 'NONE',  ( -14.30769230769230660, -4.098570777380720287, 33.41473453929634729 ) ) ;
#68026 = AXIS2_PLACEMENT_3D ( 'NONE', #48368, #20015, #82174 ) ;
#68027 = EDGE_LOOP ( 'NONE', ( #30795, #88273, #40793, #65320, #65786 ) ) ;
#68028 = CARTESIAN_POINT ( 'NONE',  ( 17.14217821643591932, -9.528491918058456633, 34.59228464037085615 ) ) ;
#68029 = VERTEX_POINT ( 'NONE', #87815 ) ;
#68030 = LINE ( 'NONE', #39231, #30126 ) ;
#68032 = VERTEX_POINT ( 'NONE', #4933 ) ;
#68031 = ADVANCED_FACE ( 'NONE', ( #88697 ), #53546, .F. ) ;
#68033 = EDGE_CURVE ( 'NONE', #77653, #43710, #8985, .T. ) ;
#68034 = CARTESIAN_POINT ( 'NONE',  ( -16.28399336328437386, -6.852621066184266141, 34.70813303252209181 ) ) ;
#68035 = CARTESIAN_POINT ( 'NONE',  ( 12.21156171748987163, -2.318417181685855422, 30.59732222474233865 ) ) ;
#68036 = FACE_BOUND ( 'NONE', #16482, .T. ) ;
#68037 = CARTESIAN_POINT ( 'NONE',  ( 0.4615384615384611200, -13.75783147151868846, 33.36296068462461051 ) ) ;
#68039 = EDGE_CURVE ( 'NONE', #45648, #37486, #58418, .T. ) ;
#68038 = CARTESIAN_POINT ( 'NONE',  ( 16.15384615384615330, -3.322132147404559976, 32.92929555188717927 ) ) ;
#68040 = CARTESIAN_POINT ( 'NONE',  ( 18.00000000000000000, -5.180354513474913603, 36.12317359536750416 ) ) ;
#68041 = CARTESIAN_POINT ( 'NONE',  ( 10.39245765647776309, -10.01117774369187252, 34.36070679894347535 ) ) ;
#68042 = DIRECTION ( 'NONE',  ( -0.000000000000000000, 0.6427876096865404731, -0.7660444431189771253 ) ) ;
#68043 = DIRECTION ( 'NONE',  ( -1.000000000000000000, -0.000000000000000000, -0.000000000000000000 ) ) ;
#68044 = EDGE_CURVE ( 'NONE', #3756, #7644, #51015, .T. ) ;
#68045 = CARTESIAN_POINT ( 'NONE',  ( -10.55012904410858532, -4.481592998940250538, 33.73612834413965089 ) ) ;
#68046 = ORIENTED_EDGE ( 'NONE', *, *, #20111, .T. ) ;
#68047 = EDGE_LOOP ( 'NONE', ( #71994, #53181, #18938, #59360 ) ) ;
#68049 = CARTESIAN_POINT ( 'NONE',  ( -18.22292695890684655, -10.01117774369187252, 34.36070679894347535 ) ) ;
#68048 = LINE ( 'NONE', #55406, #70561 ) ;
#68050 = EDGE_CURVE ( 'NONE', #77161, #38977, #80599, .T. ) ;
#68051 = CARTESIAN_POINT ( 'NONE',  ( -3.903846153846215472, -7.565270000091922853, 34.99999999999999289 ) ) ;
#68052 = CYLINDRICAL_SURFACE ( 'NONE', #81090, 4.000000000000000000 ) ;
#68053 = DIRECTION ( 'NONE',  ( 0.000000000000000000, 0.000000000000000000, 1.000000000000000000 ) ) ;
#68054 = CARTESIAN_POINT ( 'NONE',  ( -2.307692307692427391, -2.892918686052166066, 31.69288490824153470 ) ) ;
#68055 = ORIENTED_EDGE ( 'NONE', *, *, #45490, .F. ) ;
#68056 = CARTESIAN_POINT ( 'NONE',  ( 2.084766090176160436, -9.086856451489515152, 34.49173150075333183 ) ) ;
#68057 = CARTESIAN_POINT ( 'NONE',  ( 14.05771557674995442, -11.28823185664190376, 33.01397839955799896 ) ) ;
#68058 = CARTESIAN_POINT ( 'NONE',  ( -3.453696189676077832, -11.43668979543635089, 33.22377378376089752 ) ) ;
#68059 = CARTESIAN_POINT ( 'NONE',  ( -16.02305571287919861, -3.957578996910245284, 33.62503395064540257 ) ) ;
#68060 = VERTEX_POINT ( 'NONE', #60306 ) ;
#68061 = EDGE_CURVE ( 'NONE', #45177, #62016, #48698, .T. ) ;
#68062 = ORIENTED_EDGE ( 'NONE', *, *, #87924, .F. ) ;
#68063 = CONTEXT_DEPENDENT_SHAPE_REPRESENTATION ( #28533, #32703 ) ;
#68064 = ORIENTED_EDGE ( 'NONE', *, *, #12709, .F. ) ;
#68065 = AXIS2_PLACEMENT_3D ( 'NONE', #74673, #60700, #67909 ) ;
#68066 = CARTESIAN_POINT ( 'NONE',  ( 10.54930223602447903, -3.937682226553330445, 33.60647404775217240 ) ) ;
#68067 = ADVANCED_FACE ( 'NONE', ( #7589 ), #62510, .F. ) ;
#68068 = EDGE_LOOP ( 'NONE', ( #1440, #57256, #2965, #23297 ) ) ;
#68069 = CARTESIAN_POINT ( 'NONE',  ( 4.403846153846153300, -7.500000000000001776, 35.04278698407183867 ) ) ;
#68070 = LINE ( 'NONE', #26190, #87478 ) ;
#68071 = CARTESIAN_POINT ( 'NONE',  ( 3.480714640147274608, -10.18230066228895758, 34.26354781536631577 ) ) ;
#68072 = CARTESIAN_POINT ( 'NONE',  ( 1.515405825582336607, -6.369690395747424461, 34.87708834333098196 ) ) ;
#68073 = AXIS2_PLACEMENT_3D ( 'NONE', #66640, #37825, #71602 ) ;
#68074 = DIRECTION ( 'NONE',  ( -0.000000000000000000, 0.3420201433256694346, -0.9396926207859080948 ) ) ;
#68075 = EDGE_LOOP ( 'NONE', ( #51225, #75207 ) ) ;
#68076 = CARTESIAN_POINT ( 'NONE',  ( 11.47321054830029752, -2.506253911140460922, 30.00000000000013856 ) ) ;
#68078 = ORIENTED_EDGE ( 'NONE', *, *, #74069, .T. ) ;
#68077 = CARTESIAN_POINT ( 'NONE',  ( -12.23852710992561121, -11.76359900205217457, 32.36225158514719880 ) ) ;
#68079 = CARTESIAN_POINT ( 'NONE',  ( -16.15384615384615330, -11.91647553114624181, 32.58852847137148245 ) ) ;
#68080 = CARTESIAN_POINT ( 'NONE',  ( -2.372962753653081958, -9.442884908240170461, 34.35708131394840592 ) ) ;
#68081 = LINE ( 'NONE', #25757, #6980 ) ;
#68082 = DIRECTION ( 'NONE',  ( 1.000000000000000000, 0.000000000000000000, 0.000000000000000000 ) ) ;
#68083 = EDGE_CURVE ( 'NONE', #58457, #48900, #82062, .T. ) ;
#68084 = CARTESIAN_POINT ( 'NONE',  ( -9.822998295417995962, -12.35290016733513951, 31.75349464988449455 ) ) ;
#68085 = FACE_OUTER_BOUND ( 'NONE', #17745, .T. ) ;
#68086 = CARTESIAN_POINT ( 'NONE',  ( -10.61538461538461320, -1.629998284177014645, 34.34916445242399163 ) ) ;
#68087 = CARTESIAN_POINT ( 'NONE',  ( 1.077988221561497539, -10.27530806549875386, 22.45499329374151287 ) ) ;
#68088 = EDGE_LOOP ( 'NONE', ( #12404, #47076 ) ) ;
#68089 = EDGE_CURVE ( 'NONE', #22486, #12820, #1712, .T. ) ;
#68090 = CARTESIAN_POINT ( 'NONE',  ( 14.98079249982687777, -8.303909089506435137, 34.68538101551103381 ) ) ;
#68091 = CARTESIAN_POINT ( 'NONE',  ( 1.254467414883691401, -9.504002272028875709, 34.60269587691767867 ) ) ;
#68092 = ORIENTED_EDGE ( 'NONE', *, *, #71828, .F. ) ;
#68093 = EDGE_LOOP ( 'NONE', ( #80792, #37645 ) ) ;
#68094 = CARTESIAN_POINT ( 'NONE',  ( -5.934744428723973897, -2.625532179533470512, 30.86335684631491105 ) ) ;
#68095 = CARTESIAN_POINT ( 'NONE',  ( -12.68446467905460473, -3.105860786376062332, 32.13614157043599562 ) ) ;
#68096 = CARTESIAN_POINT ( 'NONE',  ( -8.899378738962470337, -11.04286588640298561, 33.62463336215343901 ) ) ;
#68097 = EDGE_CURVE ( 'NONE', #87048, #74753, #61614, .T. ) ;
#68098 = CYLINDRICAL_SURFACE ( 'NONE', #9661, 0.2500000000000009437 ) ;
#68099 = VECTOR ( 'NONE', #59137, 1000.000000000000000 ) ;
#68100 = CARTESIAN_POINT ( 'NONE',  ( 0.5920638997721057173, -2.372941743896879174, 30.88044141588254377 ) ) ;
#68101 = VERTEX_POINT ( 'NONE', #83249 ) ;
#68102 = CARTESIAN_POINT ( 'NONE',  ( 17.07692307692307665, -3.050289026998446396, 32.03036669348365706 ) ) ;
#68103 = ADVANCED_FACE ( 'NONE', ( #1260 ), #8477, .F. ) ;
#68104 = CARTESIAN_POINT ( 'NONE',  ( -14.43783951713052716, -2.882441371585227508, 31.66841991370172238 ) ) ;
#68105 = DIRECTION ( 'NONE',  ( 0.000000000000000000, 0.3420201433256610524, 0.9396926207859113145 ) ) ;
#68106 = ORIENTED_EDGE ( 'NONE', *, *, #62417, .T. ) ;
#68107 = CARTESIAN_POINT ( 'NONE',  ( -8.703064162639128298, -7.250054591869670162, 34.99404684341514127 ) ) ;
#68108 = B_SPLINE_CURVE_WITH_KNOTS ( 'NONE', 3,
 ( #66073, #86830, #80044, #18344, #45806, #73289 ),
 .UNSPECIFIED., .F., .F.,
 ( 4, 2, 4 ),
 ( 0.0003909512603273928395, 0.0005862562993132216203, 0.0007815613382990504012 ),
 .UNSPECIFIED. ) ;
#68109 = VERTEX_POINT ( 'NONE', #29201 ) ;
#68110 = DIRECTION ( 'NONE',  ( -0.000000000000000000, 1.000000000000000000, -0.000000000000000000 ) ) ;
#68111 = CARTESIAN_POINT ( 'NONE',  ( 11.40831356872983982, -2.647304123082328875, 31.75400227202885972 ) ) ;
#68112 = ORIENTED_EDGE ( 'NONE', *, *, #48862, .T. ) ;
#68113 = CYLINDRICAL_SURFACE ( 'NONE', #7338, 0.2500000000000012212 ) ;
#68115 = ADVANCED_FACE ( 'NONE', ( #56654 ), #83703, .F. ) ;
#68114 = CARTESIAN_POINT ( 'NONE',  ( -11.28840722682322628, -12.41262288849542017, 30.68299917996395010 ) ) ;
#68116 = DIRECTION ( 'NONE',  ( -0.000000000000000000, -0.9848077530122086864, -0.1736481776669273613 ) ) ;
#68117 = EDGE_CURVE ( 'NONE', #24060, #87089, #69120, .T. ) ;
#68118 = CARTESIAN_POINT ( 'NONE',  ( 16.09615384615384670, -3.499999999999999556, 29.75000000000000355 ) ) ;
#68119 = CARTESIAN_POINT ( 'NONE',  ( -0.6844654204453102242, -11.43668979543635089, 33.22377378376089752 ) ) ;
#68120 = VECTOR ( 'NONE', #5094, 1000.000000000000000 ) ;
#68121 = ORIENTED_EDGE ( 'NONE', *, *, #58053, .F. ) ;
#68122 = CARTESIAN_POINT ( 'NONE',  ( -3.930833309752758797, -12.38742843783360748, 31.66772728687926985 ) ) ;
#68123 = ORIENTED_EDGE ( 'NONE', *, *, #42638, .F. ) ;
#68124 = CARTESIAN_POINT ( 'NONE',  ( -8.638705067467205012, -4.459921816937791661, 33.71989282347011851 ) ) ;
#68125 = AXIS2_PLACEMENT_3D ( 'NONE', #73526, #10930, #3715 ) ;
#68126 = DIRECTION ( 'NONE',  ( -0.000000000000000000, -0.3420201433256694901, -0.9396926207859082059 ) ) ;
#68127 = CARTESIAN_POINT ( 'NONE',  ( 18.06525557127602255, -12.27809138561124591, 31.22303859784720359 ) ) ;
#68128 = CARTESIAN_POINT ( 'NONE',  ( -20.75000000000000000, -12.50000000000000000, 29.75000000000000355 ) ) ;
#68129 = CARTESIAN_POINT ( 'NONE',  ( 17.07692307692295586, -2.625532179533778709, 30.86335684631627174 ) ) ;
#68130 = ORIENTED_EDGE ( 'NONE', *, *, #59933, .F. ) ;
#68131 = ORIENTED_EDGE ( 'NONE', *, *, #53833, .T. ) ;
#68132 = ORIENTED_EDGE ( 'NONE', *, *, #67795, .F. ) ;
#68133 = ORIENTED_EDGE ( 'NONE', *, *, #51536, .F. ) ;
#68134 = CARTESIAN_POINT ( 'NONE',  ( 14.98079248672063990, -3.436278759898153901, 33.07459398097509506 ) ) ;
#68135 = CARTESIAN_POINT ( 'NONE',  ( 1.634560902963529294, -3.712312575010499938, 33.01462480002815170 ) ) ;
#68136 = CARTESIAN_POINT ( 'NONE',  ( 6.249945518348142492, -12.22109172314383052, 31.39792113162168263 ) ) ;
#68137 = CARTESIAN_POINT ( 'NONE',  ( 17.74997676270703550, -10.05641848906368097, 34.04755513067966177 ) ) ;
#68138 = CARTESIAN_POINT ( 'NONE',  ( -5.076923076923075762, -8.120952969808772792, 34.71129190930000163 ) ) ;
#68139 = FACE_OUTER_BOUND ( 'NONE', #1789, .T. ) ;
#68140 = CARTESIAN_POINT ( 'NONE',  ( -5.299849294439222369, -3.586966769969700763, 32.86292498521069660 ) ) ;
#68141 = ORIENTED_EDGE ( 'NONE', *, *, #62549, .F. ) ;
#68142 = EDGE_CURVE ( 'NONE', #75030, #603, #71341, .T. ) ;
#68143 = ORIENTED_EDGE ( 'NONE', *, *, #48272, .F. ) ;
#68144 = VERTEX_POINT ( 'NONE', #52104 ) ;
#68145 = CARTESIAN_POINT ( 'NONE',  ( -18.00000000000000000, -8.563426751879235965, 35.78099280442780383 ) ) ;
#68146 = VECTOR ( 'NONE', #59720, 1000.000000000000000 ) ;
#68148 = CARTESIAN_POINT ( 'NONE',  ( -7.780898706641007578, -9.528491918058460186, 34.59228464037086326 ) ) ;
#68147 = CARTESIAN_POINT ( 'NONE',  ( -20.75000000000000000, -2.499999999999999556, 29.75000000000000355 ) ) ;
#68149 = EDGE_CURVE ( 'NONE', #13706, #42649, #49814, .T. ) ;
#68150 = CARTESIAN_POINT ( 'NONE',  ( 16.28389376010183653, -7.723484964179501588, 34.74522123443823318 ) ) ;
#68151 = CARTESIAN_POINT ( 'NONE',  ( -10.68146802634049486, -3.513871655860377086, 32.76840700105978499 ) ) ;
#68152 = FACE_BOUND ( 'NONE', #75830, .T. ) ;
#68153 = ORIENTED_EDGE ( 'NONE', *, *, #52963, .F. ) ;
#68154 = CARTESIAN_POINT ( 'NONE',  ( -1.161604033002535230, -2.758310577978207334, 31.33698337089302299 ) ) ;
#68155 = CARTESIAN_POINT ( 'NONE',  ( -3.230769230769351186, -6.879047030192662504, 34.71129190930017927 ) ) ;
#68156 = ORIENTED_EDGE ( 'NONE', *, *, #27138, .T. ) ;
#68157 = EDGE_CURVE ( 'NONE', #14741, #48597, #31398, .T. ) ;
#68158 = LINE ( 'NONE', #46552, #45694 ) ;
#68159 = ORIENTED_EDGE ( 'NONE', *, *, #20498, .T. ) ;
#68160 = FACE_BOUND ( 'NONE', #37635, .T. ) ;
#68161 = LINE ( 'NONE', #83907, #59110 ) ;
#68162 = EDGE_LOOP ( 'NONE', ( #9071, #85875 ) ) ;
#68163 = CARTESIAN_POINT ( 'NONE',  ( -12.39547011053602432, -8.120952969808772792, 34.71129190929999453 ) ) ;
#68164 = DIRECTION ( 'NONE',  ( 0.000000000000000000, 0.000000000000000000, -1.000000000000000000 ) ) ;
#68165 = DIRECTION ( 'NONE',  ( 0.000000000000000000, 0.7660444431189807890, 0.6427876096865361433 ) ) ;
#68166 = VERTEX_POINT ( 'NONE', #79593 ) ;
#68167 = CARTESIAN_POINT ( 'NONE',  ( 20.00000000000000355, 10.00000000000000533, 13.00000000000000178 ) ) ;
#68168 = DIRECTION ( 'NONE',  ( -0.000000000000000000, -0.000000000000000000, 1.000000000000000000 ) ) ;
#68169 = LINE ( 'NONE', #20425, #59588 ) ;
#68170 = CARTESIAN_POINT ( 'NONE',  ( -7.912237257109724808, -2.721908614388770964, 31.22303859784723912 ) ) ;
#68171 = EDGE_LOOP ( 'NONE', ( #47647, #172 ) ) ;
#68172 = EDGE_CURVE ( 'NONE', #20922, #76970, #16995, .T. ) ;
#68173 = CARTESIAN_POINT ( 'NONE',  ( -4.854143407945010757, -4.989023458446560255, 34.36081565061822118 ) ) ;
#68174 = CARTESIAN_POINT ( 'NONE',  ( 2.307692307692186251, -3.643525952248796163, 33.31231777344771672 ) ) ;
#68176 = VERTEX_POINT ( 'NONE', #3471 ) ;
#68175 = CARTESIAN_POINT ( 'NONE',  ( 1.607628228708781748, -2.889357225399415086, 32.26129605718031002 ) ) ;
#68177 = CARTESIAN_POINT ( 'NONE',  ( -13.38461538461538325, -1.629998284177014645, 34.34916445242399163 ) ) ;
#68178 = CARTESIAN_POINT ( 'NONE',  ( 9.626554263994364646, -7.249945578846651806, 34.99404164642496795 ) ) ;
#68179 = CARTESIAN_POINT ( 'NONE',  ( -13.13466986626724342, -5.057305518903948638, 34.11320923018887896 ) ) ;
#68180 = CARTESIAN_POINT ( 'NONE',  ( 13.44987095589141113, -12.46129190930001052, 30.37095296980870174 ) ) ;
#68181 = DIRECTION ( 'NONE',  ( -0.000000000000000000, -0.000000000000000000, -1.000000000000000000 ) ) ;
#68182 = CARTESIAN_POINT ( 'NONE',  ( 16.82694633287449193, -4.818429247618089661, 34.26397095200675125 ) ) ;
#68183 = COLOUR_RGB ( '', 0.31764706, 0.68627451, 0.89019608) ;
#68186 = CARTESIAN_POINT ( 'NONE',  ( -16.94613126909829148, -8.147973898785416225, 34.70805048591653730 ) ) ;
#68185 = CIRCLE ( 'NONE', #73901, 4.500000000000001776 ) ;
#68184 = CARTESIAN_POINT ( 'NONE',  ( 5.076923076922953193, -5.941354392335915335, 34.76329471203413846 ) ) ;
#68187 = CARTESIAN_POINT ( 'NONE',  ( -8.769230769230768274, -8.564572088678739092, 35.78748833219616898 ) ) ;
#68188 = CARTESIAN_POINT ( 'NONE',  ( -2.750000000000007105, -6.360912703474006946, 20.17187500000000000 ) ) ;
#68189 = VERTEX_POINT ( 'NONE', #43576 ) ;
#68190 = EDGE_CURVE ( 'NONE', #88311, #2791, #83175, .T. ) ;
#68191 = CIRCLE ( 'NONE', #66767, 8.000000000000000000 ) ;
#68192 = CYLINDRICAL_SURFACE ( 'NONE', #70666, 0.2499999999999997502 ) ;
#68193 = ORIENTED_EDGE ( 'NONE', *, *, #13372, .T. ) ;
#68194 = EDGE_LOOP ( 'NONE', ( #32778, #85689, #42337, #9193 ) ) ;
#68195 = EDGE_CURVE ( 'NONE', #15069, #18273, #68268, .T. ) ;
#68196 = FACE_OUTER_BOUND ( 'NONE', #40387, .T. ) ;
#68197 = ORIENTED_EDGE ( 'NONE', *, *, #2075, .F. ) ;
#68198 = CARTESIAN_POINT ( 'NONE',  ( 1.634560793993429240, -12.07971442181322352, 32.31769673815850297 ) ) ;
#68199 = CARTESIAN_POINT ( 'NONE',  ( -1.139087296525992166, -10.25000000000000533, 21.10937500000000711 ) ) ;
#68200 = CARTESIAN_POINT ( 'NONE',  ( 17.93391762063986050, -4.661471528628507777, 34.16647553114621871 ) ) ;
#68201 = CARTESIAN_POINT ( 'NONE',  ( -16.15384615384615330, -10.05456864172156806, 36.03766855953608683 ) ) ;
#68202 = CARTESIAN_POINT ( 'NONE',  ( -16.08859058257012720, -6.026961402152789304, 34.52809138561124769 ) ) ;
#68203 = DIRECTION ( 'NONE',  ( 0.000000000000000000, 1.000000000000000000, 0.000000000000000000 ) ) ;
#68204 = CARTESIAN_POINT ( 'NONE',  ( -13.60810032833933292, -2.599994579823203367, 30.74605699353653776 ) ) ;
#68205 = CARTESIAN_POINT ( 'NONE',  ( 2.530471848960717196, -11.41317474335729187, 32.86274602512330034 ) ) ;
#68206 = CARTESIAN_POINT ( 'NONE',  ( -3.750000000000008438, -5.946699141100917352, 23.92187500000000355 ) ) ;
#68207 = CARTESIAN_POINT ( 'NONE',  ( 16.09615384615384670, -3.499999999999999556, 29.75000000000000355 ) ) ;
#68208 = CARTESIAN_POINT ( 'NONE',  ( -13.38461538461538325, -6.386643153685126251, 34.62446782046654192 ) ) ;
#68209 = EDGE_CURVE ( 'NONE', #28816, #28226, #37705, .T. ) ;
#68210 = CARTESIAN_POINT ( 'NONE',  ( -18.23784950573860186, -1.749999999999998668, 30.25000000000000000 ) ) ;
#68211 = B_SPLINE_CURVE_WITH_KNOTS ( 'NONE', 3,
 ( #16799, #30757, #57351, #44253, #9602, #70875, #71739, #10044, #64978, #78951 ),
 .UNSPECIFIED., .F., .F.,
 ( 4, 2, 2, 2, 4 ),
 ( 0.0007817246256747473893, 0.0009771112852218900684, 0.001172497944769032964, 0.001367884604316175860, 0.001563271263863318539 ),
 .UNSPECIFIED. ) ;
#68212 = ORIENTED_EDGE ( 'NONE', *, *, #57952, .T. ) ;
#68213 = ORIENTED_EDGE ( 'NONE', *, *, #20280, .F. ) ;
#68214 = CARTESIAN_POINT ( 'NONE',  ( -15.16551365949320562, -8.613356846314928816, 34.62446782046653482 ) ) ;
#68215 = CARTESIAN_POINT ( 'NONE',  ( 0.7115928814519144607, -12.01375889529407637, 32.43194544308182969 ) ) ;
#68216 = CARTESIAN_POINT ( 'NONE',  ( -19.50000000000000000, -11.50000000000000000, 29.75000000000000355 ) ) ;
#68217 = DIRECTION ( 'NONE',  ( -0.000000000000000000, 0.9396926207859092051, -0.3420201433256662704 ) ) ;
#68219 = EDGE_CURVE ( 'NONE', #74128, #58471, #17444, .T. ) ;
#68218 = DIRECTION ( 'NONE',  ( 0.000000000000000000, 0.000000000000000000, -1.000000000000000000 ) ) ;
#68220 = CARTESIAN_POINT ( 'NONE',  ( 3.230769230769231726, -4.661471528628507777, 34.16647553114623292 ) ) ;
#68221 = DIRECTION ( 'NONE',  ( 0.000000000000000000, 0.000000000000000000, -1.000000000000000000 ) ) ;
#68222 = B_SPLINE_CURVE_WITH_KNOTS ( 'NONE', 3,
 ( #20538, #68728, #7023, #42595, #34498, #21428, #56099, #14675, #69174, #61962 ),
 .UNSPECIFIED., .F., .F.,
 ( 4, 2, 2, 2, 4 ),
 ( 0.0007817246256747461966, 0.0009771112852218892010, 0.001172497944769032314, 0.001367884604316175427, 0.001563271263863318323 ),
 .UNSPECIFIED. ) ;
#68223 = EDGE_CURVE ( 'NONE', #4955, #84646, #25095, .T. ) ;
#68224 = EDGE_CURVE ( 'NONE', #80982, #27279, #73443, .T. ) ;
#68225 = ORIENTED_EDGE ( 'NONE', *, *, #45952, .T. ) ;
#68226 = DIRECTION ( 'NONE',  ( 0.000000000000000000, 0.8660254037844377084, -0.5000000000000015543 ) ) ;
#68227 = ORIENTED_EDGE ( 'NONE', *, *, #42740, .T. ) ;
#68228 = EDGE_CURVE ( 'NONE', #28534, #65186, #7864, .T. ) ;
#68229 = EDGE_CURVE ( 'NONE', #54682, #75345, #60638, .T. ) ;
#68230 = CARTESIAN_POINT ( 'NONE',  ( -14.37344911020661620, -7.249945686854186278, 34.74374336980224598 ) ) ;
#68231 = CARTESIAN_POINT ( 'NONE',  ( -9.692307692307691624, -1.466349020453238561, 30.81389545987213907 ) ) ;
#68232 = CARTESIAN_POINT ( 'NONE',  ( 25.00000000000000355, 9.999999999999971578, 13.00000000000000178 ) ) ;
#68233 = CARTESIAN_POINT ( 'NONE',  ( 3.007842271862381622, -8.282780595021769443, 34.94152052738834868 ) ) ;
#68234 = CARTESIAN_POINT ( 'NONE',  ( -17.07692307692307665, -3.669653830205710676, 35.88435417666054406 ) ) ;
#68235 = VERTEX_POINT ( 'NONE', #39947 ) ;
#68236 = ORIENTED_EDGE ( 'NONE', *, *, #59918, .F. ) ;
#68237 = ORIENTED_EDGE ( 'NONE', *, *, #58527, .T. ) ;
#68238 = VERTEX_POINT ( 'NONE', #61085 ) ;
#68239 = AXIS2_PLACEMENT_3D ( 'NONE', #9211, #8320, #83988 ) ;
#68240 = CARTESIAN_POINT ( 'NONE',  ( -6.223484924564330001, -4.988325925672468131, 34.36044203135681130 ) ) ;
#68241 = CARTESIAN_POINT ( 'NONE',  ( -16.02332071561251325, -9.503571793651730104, 34.60286762892837942 ) ) ;
#68242 = CARTESIAN_POINT ( 'NONE',  ( 14.17700170458200581, -2.494641256782728966, 31.33461815524612959 ) ) ;
#68243 = AXIS2_PLACEMENT_3D ( 'NONE', #53857, #5228, #87221 ) ;
#68244 = CARTESIAN_POINT ( 'NONE',  ( 2.084207363968361815, -11.41268669641500466, 32.86336882939237825 ) ) ;
#68245 = CARTESIAN_POINT ( 'NONE',  ( 17.86930853333243974, -4.809359713505814149, 33.96456829005828837 ) ) ;
#68246 = CARTESIAN_POINT ( 'NONE',  ( -10.39237326377176274, -12.15243808032446005, 31.58219941686247978 ) ) ;
#68247 = ORIENTED_EDGE ( 'NONE', *, *, #71305, .T. ) ;
#68248 = EDGE_LOOP ( 'NONE', ( #52686, #54574 ) ) ;
#68249 = ORIENTED_EDGE ( 'NONE', *, *, #55165, .F. ) ;
#68251 = EDGE_LOOP ( 'NONE', ( #55263, #44651 ) ) ;
#68250 = CARTESIAN_POINT ( 'NONE',  ( 11.31497659473759043, -9.331801661448606566, 34.40259984581193464 ) ) ;
#68252 = CARTESIAN_POINT ( 'NONE',  ( 18.03205128205128105, -7.500000000000000000, 29.75000000000000355 ) ) ;
#68253 = CARTESIAN_POINT ( 'NONE',  ( -12.23852561744506673, -11.98016756924215009, 32.48728574198911190 ) ) ;
#68254 = CARTESIAN_POINT ( 'NONE',  ( -3.750000000000007550, -5.946699141100917352, 21.42187500000000000 ) ) ;
#68255 = ORIENTED_EDGE ( 'NONE', *, *, #80910, .T. ) ;
#68256 = CARTESIAN_POINT ( 'NONE',  ( 8.769230769230768274, -6.435427911321262684, 35.78748833219616898 ) ) ;
#68257 = ORIENTED_EDGE ( 'NONE', *, *, #42333, .T. ) ;
#68258 = CARTESIAN_POINT ( 'NONE',  ( 8.069165197766697162, -12.15243808032445827, 31.58219941686247978 ) ) ;
#68259 = FACE_BOUND ( 'NONE', #49803, .T. ) ;
#68260 = CARTESIAN_POINT ( 'NONE',  ( -4.826977558574935934, -12.22109172314383052, 31.39792113162168263 ) ) ;
#68261 = CARTESIAN_POINT ( 'NONE',  ( 8.519207531937803779, -5.056417327199099532, 34.11270091957321426 ) ) ;
#68262 = ORIENTED_EDGE ( 'NONE', *, *, #68050, .T. ) ;
#68263 = CARTESIAN_POINT ( 'NONE',  ( -9.942284436356285227, -4.818429247618089661, 34.26397095200675125 ) ) ;
#68264 = CARTESIAN_POINT ( 'NONE',  ( -9.019230769230768274, -2.249999999999998668, 29.75000000000000355 ) ) ;
#68265 = CARTESIAN_POINT ( 'NONE',  ( -13.13461538461544897, -7.565270445406050648, 34.75000000000000000 ) ) ;
#68266 = CARTESIAN_POINT ( 'NONE',  ( 14.08420738312798015, -9.417330523894424488, 34.63758898049880486 ) ) ;
#68267 = ORIENTED_EDGE ( 'NONE', *, *, #31233, .T. ) ;
#68268 = CIRCLE ( 'NONE', #39555, 2.000000000000001776 ) ;
#68269 = CARTESIAN_POINT ( 'NONE',  ( -0.7115384615384606759, -7.500000000000001776, 35.00000000000000000 ) ) ;
#68270 = CARTESIAN_POINT ( 'NONE',  ( -4.087778820496077437, -9.905515769479277921, 34.41647553114623292 ) ) ;
#68271 = CARTESIAN_POINT ( 'NONE',  ( 17.07692307692307665, -9.780366693483667717, 34.19971097300155094 ) ) ;
#68272 = FACE_OUTER_BOUND ( 'NONE', #9021, .T. ) ;
#68273 = CARTESIAN_POINT ( 'NONE',  ( -10.61538461538461320, -8.318370150425687726, 35.83090037661290239 ) ) ;
#68274 = FACE_BOUND ( 'NONE', #39572, .T. ) ;
#68276 = CARTESIAN_POINT ( 'NONE',  ( 17.01084069756293715, -2.833524468853757305, 32.15551576947924417 ) ) ;
#68275 = CARTESIAN_POINT ( 'NONE',  ( 1.134615384615387246, -7.566082377512563184, 35.00000000000000711 ) ) ;
#68277 = CARTESIAN_POINT ( 'NONE',  ( -5.999999999999998224, -2.249999999999998668, 29.50000000000001421 ) ) ;
#68279 = CARTESIAN_POINT ( 'NONE',  ( -9.469528151039277475, -10.81320215134717344, 33.49497208177562868 ) ) ;
#68278 = CARTESIAN_POINT ( 'NONE',  ( -8.703975197954745724, -11.94971097300157403, 32.03036669348361443 ) ) ;
#68280 = CARTESIAN_POINT ( 'NONE',  ( -7.846153846153844924, -3.937682226553329556, 33.60647404775216529 ) ) ;
#68281 = CARTESIAN_POINT ( 'NONE',  ( -2.775308065498764964, -6.422011778438537988, 17.42000670625848713 ) ) ;
#68282 = ORIENTED_EDGE ( 'NONE', *, *, #11310, .T. ) ;
#68283 = B_SPLINE_CURVE_WITH_KNOTS ( 'NONE', 3,
 ( #27085, #13571, #69848, #47800, #21210, #55003, #69407, #48678, #82043, #76151 ),
 .UNSPECIFIED., .F., .F.,
 ( 4, 2, 2, 2, 4 ),
 ( 0.000000000000000000, 0.0001954339857564073388, 0.0003908679715128146777, 0.0005863019572692220165, 0.0007817359430256293554 ),
 .UNSPECIFIED. ) ;
#68284 = CARTESIAN_POINT ( 'NONE',  ( 0.5140118631390264703, -3.794621124119502031, 14.00000000000000178 ) ) ;
#68285 = ORIENTED_EDGE ( 'NONE', *, *, #55304, .T. ) ;
#68286 = ADVANCED_FACE ( 'NONE', ( #33176 ), #88151, .F. ) ;
#68287 = CARTESIAN_POINT ( 'NONE',  ( -18.25002322422145085, -3.520140089381496917, 33.17453946501457551 ) ) ;
#68288 = ORIENTED_EDGE ( 'NONE', *, *, #1182, .F. ) ;
#68289 = LINE ( 'NONE', #34504, #26879 ) ;
#68290 = CARTESIAN_POINT ( 'NONE',  ( -16.08859101433330707, -12.16647553114626490, 32.15551576947920864 ) ) ;
#68292 = ORIENTED_EDGE ( 'NONE', *, *, #37549, .T. ) ;
#68291 = CARTESIAN_POINT ( 'NONE',  ( -4.853910232829680815, -9.172514111537584114, 34.72667873470787470 ) ) ;
#68293 = CARTESIAN_POINT ( 'NONE',  ( -15.45369544828537656, -4.887634598454295265, 34.01352882383564946 ) ) ;
#68294 = CARTESIAN_POINT ( 'NONE',  ( -2.749999999999997780, -7.561099074964547917, 18.59188170625849068 ) ) ;
#68295 = CARTESIAN_POINT ( 'NONE',  ( -10.48485917715097138, -12.70449254468099198, 30.44128974285582956 ) ) ;
#68296 = CARTESIAN_POINT ( 'NONE',  ( 7.846153846153846700, -13.75783147151868846, 33.36296068462461051 ) ) ;
#68297 = CARTESIAN_POINT ( 'NONE',  ( -5.076923076923075762, -12.37446782046654192, 30.86335684631486131 ) ) ;
#68298 = CARTESIAN_POINT ( 'NONE',  ( 3.903822916553188804, -11.86270091957321249, 32.19358267280087915 ) ) ;
#68299 = CYLINDRICAL_SURFACE ( 'NONE', #13742, 0.2500000000000004996 ) ;
#68300 = DIRECTION ( 'NONE',  ( -0.000000000000000000, 0.1736481776669307198, -0.9848077530122080203 ) ) ;
#68301 = B_SPLINE_CURVE_WITH_KNOTS ( 'NONE', 3,
 ( #35830, #50201, #65051, #70494, #30394, #3360, #63285, #17326, #77686, #44783 ),
 .UNSPECIFIED., .F., .F.,
 ( 4, 2, 2, 2, 4 ),
 ( 0.0007817359430256320659, 0.0009771253907249987086, 0.001172514838424365460, 0.001367904286123731994, 0.001563293733823098745 ),
 .UNSPECIFIED. ) ;
#68302 = CARTESIAN_POINT ( 'NONE',  ( 1.614399933863618797, -3.775308065498751198, 23.23624329374151642 ) ) ;
#68303 = VECTOR ( 'NONE', #25161, 1000.000000000000000 ) ;
#68304 = CARTESIAN_POINT ( 'NONE',  ( 3.480769230770650147, -7.500000000000154543, 35.00000000000007105 ) ) ;
#68305 = ADVANCED_FACE ( 'NONE', ( #39062 ), #60196, .F. ) ;
#68306 = B_SPLINE_CURVE_WITH_KNOTS ( 'NONE', 3,
 ( #18131, #86148, #23535, #71721, #38394, #59547, #52788, #9583, #10483, #65415 ),
 .UNSPECIFIED., .F., .F.,
 ( 4, 2, 2, 2, 4 ),
 ( 0.000000000000000000, 0.0001954311564186871184, 0.0003908623128373742367, 0.0005862934692560614093, 0.0007817246256747484735 ),
 .UNSPECIFIED. ) ;
#68307 = ORIENTED_EDGE ( 'NONE', *, *, #47127, .F. ) ;
#68308 = DIRECTION ( 'NONE',  ( -0.000000000000000000, -0.000000000000000000, -1.000000000000000000 ) ) ;
#68309 = CARTESIAN_POINT ( 'NONE',  ( -1.492201783934593573, -3.724691934501250135, 23.07999329374151998 ) ) ;
#68310 = AXIS2_PLACEMENT_3D ( 'NONE', #41384, #88268, #68850 ) ;
#68311 = CARTESIAN_POINT ( 'NONE',  ( -16.08777882049607655, -12.34228464037088813, 31.77849191805839268 ) ) ;
#68312 = CARTESIAN_POINT ( 'NONE',  ( 17.29970261819148902, -11.89424750095246175, 32.13594075562311758 ) ) ;
#68313 = ORIENTED_EDGE ( 'NONE', *, *, #64813, .F. ) ;
#68314 = DIRECTION ( 'NONE',  ( 0.000000000000000000, -6.938893903907222067E-15, 1.000000000000000000 ) ) ;
#68315 = CARTESIAN_POINT ( 'NONE',  ( 6.923076923076802558, -11.48612834414049644, 32.76840700105863391 ) ) ;
#68317 = ORIENTED_EDGE ( 'NONE', *, *, #40594, .F. ) ;
#68316 = DIRECTION ( 'NONE',  ( 0.000000000000000000, 0.000000000000000000, 1.000000000000000000 ) ) ;
#68318 = CARTESIAN_POINT ( 'NONE',  ( 8.545745844666438273, -5.827078755546623690, 34.72654668319379567 ) ) ;
#68319 = CARTESIAN_POINT ( 'NONE',  ( 2.242421861731532573, -12.46129190929999986, 30.37095296980880832 ) ) ;
#68320 = CARTESIAN_POINT ( 'NONE',  ( 15.93036121012220541, -9.331801661448606566, 34.40259984581193464 ) ) ;
#68321 = CARTESIAN_POINT ( 'NONE',  ( 15.23076923076911093, -2.625532179533778709, 30.86335684631627174 ) ) ;
#68322 = CARTESIAN_POINT ( 'NONE',  ( -13.51530685128294174, -11.71456829005830080, 32.44064028649416542 ) ) ;
#68323 = EDGE_CURVE ( 'NONE', #18936, #36238, #45512, .T. ) ;
#68324 = EDGE_CURVE ( 'NONE', #36427, #23390, #53931, .T. ) ;
#68325 = CARTESIAN_POINT ( 'NONE',  ( -13.13456096470193302, -8.346898887586323923, 34.93166121998716278 ) ) ;
#68326 = EDGE_LOOP ( 'NONE', ( #39704, #20787, #57471, #3890 ) ) ;
#68327 = ORIENTED_EDGE ( 'NONE', *, *, #48257, .T. ) ;
#68328 = EDGE_LOOP ( 'NONE', ( #40579, #15454 ) ) ;
#68329 = VERTEX_POINT ( 'NONE', #80485 ) ;
#68330 = EDGE_CURVE ( 'NONE', #84875, #72142, #66966, .T. ) ;
#68331 = CARTESIAN_POINT ( 'NONE',  ( -13.51476259405360558, -3.817052484675422797, 33.13202310037935661 ) ) ;
#68332 = CARTESIAN_POINT ( 'NONE',  ( 14.08476609017615644, -4.186968288167450147, 33.49512374952580274 ) ) ;
#68333 = ADVANCED_FACE ( 'NONE', ( #5261 ), #32293, .F. ) ;
#68334 = CARTESIAN_POINT ( 'NONE',  ( 4.153846153846030731, -12.70778746994576025, 30.41441678777401236 ) ) ;
#68335 = DIRECTION ( 'NONE',  ( 0.000000000000000000, 0.000000000000000000, 1.000000000000000000 ) ) ;
#68336 = B_SPLINE_CURVE_WITH_KNOTS ( 'NONE', 3,
 ( #37430, #4998, #37889, #59038, #59930, #30681, #73004, #31572, #80669, #86993 ),
 .UNSPECIFIED., .F., .F.,
 ( 4, 2, 2, 2, 4 ),
 ( 0.000000000000000000, 0.0001954339857564092362, 0.0003908679715128184724, 0.0005863019572692276544, 0.0007817359430256369448 ),
 .UNSPECIFIED. ) ;
#68337 = VECTOR ( 'NONE', #70285, 1000.000000000000227 ) ;
#68338 = LINE ( 'NONE', #47169, #19010 ) ;
#68339 = B_SPLINE_CURVE_WITH_KNOTS ( 'NONE', 3,
 ( #12623, #25242, #38314, #18047, #10843, #46401, #73439, #86518, #11737, #87407 ),
 .UNSPECIFIED., .F., .F.,
 ( 4, 2, 2, 2, 4 ),
 ( 0.0007817246256747461966, 0.0009771112852218889842, 0.001172497944769031880, 0.001367884604316174776, 0.001563271263863317672 ),
 .UNSPECIFIED. ) ;
#68340 = ORIENTED_EDGE ( 'NONE', *, *, #18625, .T. ) ;
#68341 = ORIENTED_EDGE ( 'NONE', *, *, #79189, .F. ) ;
#68342 = ORIENTED_EDGE ( 'NONE', *, *, #82182, .T. ) ;
#68344 = ORIENTED_EDGE ( 'NONE', *, *, #6097, .F. ) ;
#68343 = CARTESIAN_POINT ( 'NONE',  ( -7.173100147298383078, -2.588893531581426544, 31.60682220781847818 ) ) ;
#68345 = CARTESIAN_POINT ( 'NONE',  ( -5.076923076923075762, -12.34228464037088635, 31.77849191805839268 ) ) ;
#68346 = CARTESIAN_POINT ( 'NONE',  ( 6.249945409378044658, -2.589246495874657938, 31.60778113518102828 ) ) ;
#68347 = CARTESIAN_POINT ( 'NONE',  ( -12.46153846153846168, -12.10708131394839349, 31.69288490824020244 ) ) ;
#68348 = DIRECTION ( 'NONE',  ( -1.000000000000000000, -0.000000000000000000, 0.000000000000000000 ) ) ;
#68349 = ORIENTED_EDGE ( 'NONE', *, *, #2471, .T. ) ;
#68350 = VERTEX_POINT ( 'NONE', #25534 ) ;
#68351 = ORIENTED_EDGE ( 'NONE', *, *, #17549, .T. ) ;
#68352 = CARTESIAN_POINT ( 'NONE',  ( -5.207533436547604921, -7.722926236386453702, 34.74524107206102030 ) ) ;
#68354 = ORIENTED_EDGE ( 'NONE', *, *, #66459, .F. ) ;
#68353 = CARTESIAN_POINT ( 'NONE',  ( 17.07692307692295586, -12.16647553114689728, 32.15551576947799362 ) ) ;
#68355 = CARTESIAN_POINT ( 'NONE',  ( 13.13461538461538858, -2.499999999999999556, 29.81609845454691765 ) ) ;
#68356 = CARTESIAN_POINT ( 'NONE',  ( 1.384615384615386802, -8.120952969808772792, 34.71129190930000163 ) ) ;
#68357 = VERTEX_POINT ( 'NONE', #74165 ) ;
#68358 = CARTESIAN_POINT ( 'NONE',  ( 16.15384615384603251, -3.835265460704628815, 33.15142922262033665 ) ) ;
#68359 = CARTESIAN_POINT ( 'NONE',  ( 12.71148387091650278, -9.357781135181031829, 34.66075350412533851 ) ) ;
#68360 = FACE_BOUND ( 'NONE', #85452, .T. ) ;
#68361 = LINE ( 'NONE', #27383, #71527 ) ;
#68362 = CARTESIAN_POINT ( 'NONE',  ( -6.066082379360135945, -12.34228464037088280, 31.77849191805838558 ) ) ;
#68363 = DIRECTION ( 'NONE',  ( 0.000000000000000000, 0.000000000000000000, -1.000000000000000000 ) ) ;
#68364 = B_SPLINE_CURVE_WITH_KNOTS ( 'NONE', 3,
 ( #63323, #75510, #21456, #54791, #82726, #35864, #8837, #42184, #68757, #69201 ),
 .UNSPECIFIED., .F., .F.,
 ( 4, 2, 2, 2, 4 ),
 ( 0.0007817246256747497745, 0.0009771112852218937547, 0.001172497944769037518, 0.001367884604316181498, 0.001563271263863325478 ),
 .UNSPECIFIED. ) ;
#68366 = DIRECTION ( 'NONE',  ( -1.000000000000000000, 0.000000000000000000, 0.000000000000000000 ) ) ;
#68365 = CARTESIAN_POINT ( 'NONE',  ( 0.7115384615398802071, -7.500000000000154543, 35.00000000000007105 ) ) ;
#68367 = CARTESIAN_POINT ( 'NONE',  ( -4.023054346021369021, -2.729792928343270919, 31.24908615093345077 ) ) ;
#68368 = CARTESIAN_POINT ( 'NONE',  ( -4.023320715612509701, -11.66157788607254275, 32.95092075102925833 ) ) ;
#68369 = ORIENTED_EDGE ( 'NONE', *, *, #35874, .F. ) ;
#68370 = DIRECTION ( 'NONE',  ( 0.000000000000000000, 0.000000000000000000, -1.000000000000000000 ) ) ;
#68371 = AXIS2_PLACEMENT_3D ( 'NONE', #14288, #41770, #21484 ) ;
#68372 = CARTESIAN_POINT ( 'NONE',  ( 13.63461538461544897, -7.434744429011176159, 34.75000000000000711 ) ) ;
#68373 = B_SPLINE_CURVE_WITH_KNOTS ( 'NONE', 3,
 ( #46054, #65869, #30758, #85717, #4175, #59117 ),
 .UNSPECIFIED., .F., .F.,
 ( 4, 2, 4 ),
 ( 0.0003909512603273990194, 0.0005862562993132244393, 0.0007815613382990498591 ),
 .UNSPECIFIED. ) ;
#68374 = VERTEX_POINT ( 'NONE', #12462 ) ;
#68375 = EDGE_CURVE ( 'NONE', #43958, #80807, #77731, .T. ) ;
#68376 = CARTESIAN_POINT ( 'NONE',  ( -15.48074596171158213, -2.564618984488975073, 30.55390908950641915 ) ) ;
#68377 = CARTESIAN_POINT ( 'NONE',  ( 9.442330961365341224, -2.779195860258146578, 31.39871582349836032 ) ) ;
#68378 = EDGE_LOOP ( 'NONE', ( #84331, #63863, #6459, #32308, #31702, #26936 ) ) ;
#68379 = CARTESIAN_POINT ( 'NONE',  ( 11.28843831424008570, -10.18141759479407327, 34.26406193332782379 ) ) ;
#68380 = CYLINDRICAL_SURFACE ( 'NONE', #83213, 0.2500000000000009437 ) ;
#68381 = FACE_BOUND ( 'NONE', #50212, .T. ) ;
#68383 = CARTESIAN_POINT ( 'NONE',  ( 4.023155550735846298, -12.35290016733513951, 31.75349464988449455 ) ) ;
#68382 = CARTESIAN_POINT ( 'NONE',  ( -14.43838291080261627, -3.957541250942358424, 33.62499894934981626 ) ) ;
#68384 = CARTESIAN_POINT ( 'NONE',  ( 2.242422307135989890, -6.835583212224499938, 34.95778746994557906 ) ) ;
#68385 = CARTESIAN_POINT ( 'NONE',  ( 2.557637826040450424, -5.057305518903949526, 34.11320923018887896 ) ) ;
#68387 = CARTESIAN_POINT ( 'NONE',  ( 2.177001704582002262, -10.70098750199973203, 33.91152734681376302 ) ) ;
#68386 = DIRECTION ( 'NONE',  ( 0.000000000000000000, 0.000000000000000000, 1.000000000000000000 ) ) ;
#68388 = CARTESIAN_POINT ( 'NONE',  ( -2.694853999681210865, -4.891553140782108677, 16.24813170625848713 ) ) ;
#68389 = VERTEX_POINT ( 'NONE', #6150 ) ;
#68390 = ORIENTED_EDGE ( 'NONE', *, *, #74524, .T. ) ;
#68391 = EDGE_CURVE ( 'NONE', #23252, #60384, #20107, .T. ) ;
#68392 = CARTESIAN_POINT ( 'NONE',  ( -12.46153846153858424, -5.941354392335915335, 34.76329471203413846 ) ) ;
#68393 = CARTESIAN_POINT ( 'NONE',  ( -10.55012947587177941, -8.656820664281605460, 34.87096338111211224 ) ) ;
#68394 = CARTESIAN_POINT ( 'NONE',  ( 6.989243529668563326, -7.250054591869668386, 34.99404684341514127 ) ) ;
#68395 = CARTESIAN_POINT ( 'NONE',  ( 10.61538461538449418, -3.083524468854526912, 32.58852847137268327 ) ) ;
#68396 = EDGE_CURVE ( 'NONE', #43877, #52607, #27306, .T. ) ;
#68397 = CARTESIAN_POINT ( 'NONE',  ( 5.076923076922953193, -3.643525952248796163, 33.31231777344771672 ) ) ;
#68398 = CARTESIAN_POINT ( 'NONE',  ( -3.749999999999996447, -7.561099074964554134, 17.34188170625849068 ) ) ;
#68399 = DIRECTION ( 'NONE',  ( 1.000000000000000000, 0.000000000000000000, 0.000000000000000000 ) ) ;
#68400 = CARTESIAN_POINT ( 'NONE',  ( 1.134592160393929516, -10.18141759479407327, 34.26406193332782379 ) ) ;
#68401 = VECTOR ( 'NONE', #21887, 1000.000000000000227 ) ;
#68402 = CARTESIAN_POINT ( 'NONE',  ( 7.715463243043539698, -5.496505350115500121, 34.60290016733514307 ) ) ;
#68403 = LINE ( 'NONE', #76044, #26676 ) ;
#68404 = CARTESIAN_POINT ( 'NONE',  ( 0.000000000000000000, -11.00000000000000000, 29.75000000000000355 ) ) ;
#68405 = DIRECTION ( 'NONE',  ( 1.000000000000000000, 0.000000000000000000, 0.000000000000000000 ) ) ;
#68406 = CARTESIAN_POINT ( 'NONE',  ( -3.480745974817821775, -10.06842814019191401, 34.32929386961144758 ) ) ;
#68407 = CARTESIAN_POINT ( 'NONE',  ( -3.454254174493179175, -8.496056993536548418, 34.65000542017679663 ) ) ;
#68408 = EDGE_CURVE ( 'NONE', #70248, #53579, #1497, .T. ) ;
#68409 = CARTESIAN_POINT ( 'NONE',  ( 12.68431800280687050, -2.847695495035523550, 31.58253572463339154 ) ) ;
#68410 = B_SPLINE_CURVE_WITH_KNOTS ( 'NONE', 3,
 ( #70868, #36203, #77170, #78052, #9168, #37498 ),
 .UNSPECIFIED., .F., .F.,
 ( 4, 2, 4 ),
 ( 4.221881728299276106E-17, 0.0001954756301637148241, 0.0003909512603273874185 ),
 .UNSPECIFIED. ) ;
#68411 = EDGE_LOOP ( 'NONE', ( #58185, #30977, #21326, #31332 ) ) ;
#68412 = CARTESIAN_POINT ( 'NONE',  ( -14.30769230769230660, -13.95598074871891292, 31.83374038241031911 ) ) ;
#68413 = CARTESIAN_POINT ( 'NONE',  ( -4.153846153846152411, -1.117168528481311540, 33.14645433367849847 ) ) ;
#68414 = CARTESIAN_POINT ( 'NONE',  ( 1.077988221561497539, -10.27530806549875386, 19.95499329374151642 ) ) ;
#68415 = EDGE_CURVE ( 'NONE', #34333, #23619, #37042, .T. ) ;
#68416 = CARTESIAN_POINT ( 'NONE',  ( -9.822455662039393687, -11.04286588640298561, 33.62463336215343901 ) ) ;
#68417 = CARTESIAN_POINT ( 'NONE',  ( -5.749999999998578915, -7.500000000000154543, 35.00000000000007105 ) ) ;
#68418 = CARTESIAN_POINT ( 'NONE',  ( -3.230769230769229949, -1.129524287112498415, 32.06866353760679544 ) ) ;
#68420 = EDGE_LOOP ( 'NONE', ( #65565, #80181, #43725, #12168 ) ) ;
#68419 = CARTESIAN_POINT ( 'NONE',  ( -14.37296275365308240, -12.27809138561121394, 31.22303859784730307 ) ) ;
#68421 = CARTESIAN_POINT ( 'NONE',  ( -1.139087296526025250, -4.750000000000006217, 24.07812500000000711 ) ) ;
#68422 = DIRECTION ( 'NONE',  ( -1.000000000000000000, 0.000000000000000000, 0.000000000000000000 ) ) ;
#68423 = EDGE_LOOP ( 'NONE', ( #77128, #60000 ) ) ;
#68424 = CARTESIAN_POINT ( 'NONE',  ( -11.28846153846153655, -2.249999999999998668, 29.75000000000000355 ) ) ;
#68425 = PLANE ( 'NONE',  #15519 ) ;
#68426 = ORIENTED_EDGE ( 'NONE', *, *, #39774, .T. ) ;
#68427 = CARTESIAN_POINT ( 'NONE',  ( 1.576923076923076428, -11.50000000000000000, 29.75000000000000355 ) ) ;
#68428 = CARTESIAN_POINT ( 'NONE',  ( 2.557746727605762160, -8.346898887586323923, 34.93166121998716278 ) ) ;
#68429 = EDGE_CURVE ( 'NONE', #50723, #17200, #64074, .T. ) ;
#68430 = DIRECTION ( 'NONE',  ( 1.000000000000000000, 0.000000000000000000, 0.000000000000000000 ) ) ;
#68431 = ORIENTED_EDGE ( 'NONE', *, *, #31168, .T. ) ;
#68432 = ADVANCED_FACE ( 'NONE', ( #85252 ), #48009, .F. ) ;
#68433 = ORIENTED_EDGE ( 'NONE', *, *, #2614, .T. ) ;
#68434 = CARTESIAN_POINT ( 'NONE',  ( 3.007842271862381178, -2.889293201056495786, 32.26117774369186009 ) ) ;
#68435 = EDGE_LOOP ( 'NONE', ( #17367, #12515 ) ) ;
#68436 = CARTESIAN_POINT ( 'NONE',  ( 3.480714640147273720, -12.07971442181321997, 32.31769673815850297 ) ) ;
#68437 = EDGE_CURVE ( 'NONE', #3673, #31209, #43373, .T. ) ;
#68438 = DIRECTION ( 'NONE',  ( -0.000000000000000000, 0.5000000000000011102, -0.8660254037844381525 ) ) ;
#68439 = CYLINDRICAL_SURFACE ( 'NONE', #65935, 0.2500000000000004996 ) ;
#68440 = EDGE_CURVE ( 'NONE', #48065, #51319, #75486, .T. ) ;
#68441 = AXIS2_PLACEMENT_3D ( 'NONE', #81892, #6657, #82774 ) ;
#68442 = CARTESIAN_POINT ( 'NONE',  ( -6.700064078983527516, -11.43677907613344757, 33.22367315496201456 ) ) ;
#68443 = CARTESIAN_POINT ( 'NONE',  ( -7.846153846153844924, -12.29105614889573062, 35.45975837776705220 ) ) ;
#68444 = CARTESIAN_POINT ( 'NONE',  ( 13.51540719244017374, -3.062576670634119758, 32.05464942895959979 ) ) ;
#68445 = CARTESIAN_POINT ( 'NONE',  ( -12.59222992820602194, -6.413092428213692742, 34.63065189839063152 ) ) ;
#68446 = VERTEX_POINT ( 'NONE', #78476 ) ;
#68447 = ORIENTED_EDGE ( 'NONE', *, *, #25418, .F. ) ;
#68449 = ORIENTED_EDGE ( 'NONE', *, *, #70968, .T. ) ;
#68448 = CARTESIAN_POINT ( 'NONE',  ( 6.923076923076800782, -12.70778746994576025, 30.41441678777401236 ) ) ;
#68450 = CARTESIAN_POINT ( 'NONE',  ( 7.846153846153846700, -2.486705287966279876, 31.30864560766543647 ) ) ;
#68451 = AXIS2_PLACEMENT_3D ( 'NONE', #22976, #85573, #79263 ) ;
#68452 = CARTESIAN_POINT ( 'NONE',  ( -8.769230769230892619, -11.06231777344772027, 33.60647404775119895 ) ) ;
#68453 = CARTESIAN_POINT ( 'NONE',  ( 11.60371710973756620, -12.27809138561124591, 31.22303859784720359 ) ) ;
#68454 = ORIENTED_EDGE ( 'NONE', *, *, #1561, .T. ) ;
#68455 = CARTESIAN_POINT ( 'NONE',  ( -12.39628289026243557, -6.026961402152789304, 34.52809138561124769 ) ) ;
#68456 = CIRCLE ( 'NONE', #38315, 2.000000000000001776 ) ;
#68457 = ORIENTED_EDGE ( 'NONE', *, *, #62123, .F. ) ;
#68458 = CYLINDRICAL_SURFACE ( 'NONE', #16589, 0.2500000000000002220 ) ;
#68459 = EDGE_LOOP ( 'NONE', ( #56252, #88468 ) ) ;
#68460 = DIRECTION ( 'NONE',  ( 0.000000000000000000, 0.7660444431189807890, 0.6427876096865361433 ) ) ;
#68461 = EDGE_CURVE ( 'NONE', #87211, #68522, #43808, .T. ) ;
#68462 = ORIENTED_EDGE ( 'NONE', *, *, #33145, .F. ) ;
#68463 = CARTESIAN_POINT ( 'NONE',  ( -4.283994123577849145, -4.299443229763728169, 33.91186481527756058 ) ) ;
#68464 = CARTESIAN_POINT ( 'NONE',  ( -8.835314180186649935, -2.721908614388770964, 31.22303859784723912 ) ) ;
#68465 = FACE_BOUND ( 'NONE', #76100, .T. ) ;
#68466 = CARTESIAN_POINT ( 'NONE',  ( -0.4615384615385826339, -5.219633306517616589, 34.19971097300220464 ) ) ;
#68467 = DIRECTION ( 'NONE',  ( -0.000000000000000000, -0.3420201433256694346, -0.9396926207859080948 ) ) ;
#68468 = CARTESIAN_POINT ( 'NONE',  ( 9.442284468086237226, -11.56360843649121861, 33.07473185843129926 ) ) ;
#68469 = CARTESIAN_POINT ( 'NONE',  ( -3.262820512820514107, -7.500000000000000000, 33.75000000000000000 ) ) ;
#68470 = DIRECTION ( 'NONE',  ( 0.000000000000000000, 0.000000000000000000, -1.000000000000000000 ) ) ;
#68471 = DIRECTION ( 'NONE',  ( 1.000000000000000000, 0.000000000000000000, 0.000000000000000000 ) ) ;
#68472 = CARTESIAN_POINT ( 'NONE',  ( 14.37375964104238335, -6.343179335718452272, 34.87096338111212646 ) ) ;
#68473 = EDGE_LOOP ( 'NONE', ( #45394, #87846, #67090, #30520, #86648, #42010 ) ) ;
#68474 = ADVANCED_FACE ( 'NONE', ( #57768 ), #42939, .F. ) ;
#68475 = ORIENTED_EDGE ( 'NONE', *, *, #24115, .T. ) ;
#68476 = EDGE_CURVE ( 'NONE', #73234, #10850, #372, .T. ) ;
#68478 = DIRECTION ( 'NONE',  ( -1.000000000000000000, 0.000000000000000000, 0.000000000000000000 ) ) ;
#68477 = CARTESIAN_POINT ( 'NONE',  ( 15.23076923076923173, -13.53365097954675988, 30.81389545987213552 ) ) ;
#68479 = CARTESIAN_POINT ( 'NONE',  ( -9.692307692307691624, -12.34228464037088635, 31.77849191805839268 ) ) ;
#68480 = DIRECTION ( 'NONE',  ( 0.000000000000000000, 0.3420201433256641055, -0.9396926207859100932 ) ) ;
#68481 = CARTESIAN_POINT ( 'NONE',  ( -17.14300545628321260, -12.34228464037088280, 31.77849191805838558 ) ) ;
#68482 = CARTESIAN_POINT ( 'NONE',  ( 11.53846153846153832, -10.89733346790207413, 36.13435417666054406 ) ) ;
#68483 = EDGE_LOOP ( 'NONE', ( #76227, #57482 ) ) ;
#68484 = VECTOR ( 'NONE', #78914, 1000.000000000000000 ) ;
#68485 = CARTESIAN_POINT ( 'NONE',  ( -5.869474561766354626, -8.630441415882550871, 34.87705825610312615 ) ) ;
#68486 = CARTESIAN_POINT ( 'NONE',  ( 11.78846153846297362, -7.500000000000155431, 34.75000000000007105 ) ) ;
#68487 = CARTESIAN_POINT ( 'NONE',  ( 16.94623247381276343, -3.957541250942358424, 33.62499894934981626 ) ) ;
#68488 = PLANE ( 'NONE',  #66890 ) ;
#68489 = EDGE_LOOP ( 'NONE', ( #82298, #53067, #44595, #65384, #56778, #52606 ) ) ;
#68490 = ORIENTED_EDGE ( 'NONE', *, *, #191, .F. ) ;
#68491 = ORIENTED_EDGE ( 'NONE', *, *, #68707, .T. ) ;
#68492 = EDGE_CURVE ( 'NONE', #69035, #81618, #29863, .T. ) ;
#68493 = CARTESIAN_POINT ( 'NONE',  ( 15.45378058238208219, -6.503523203565941380, 34.64991518177335195 ) ) ;
#68494 = ORIENTED_EDGE ( 'NONE', *, *, #88423, .F. ) ;
#68495 = VECTOR ( 'NONE', #78664, 1000.000000000000000 ) ;
#68496 = CARTESIAN_POINT ( 'NONE',  ( -15.93106661257773560, -5.114059244376869096, 34.14424750095245287 ) ) ;
#68497 = CARTESIAN_POINT ( 'NONE',  ( -6.250023224221455287, -9.356822207818506598, 34.66110646841856635 ) ) ;
#68498 = CARTESIAN_POINT ( 'NONE',  ( -5.207070286361298095, -4.460286881179643004, 33.72017969459903242 ) ) ;
#68499 = EDGE_CURVE ( 'NONE', #57235, #1867, #87502, .T. ) ;
#68500 = CARTESIAN_POINT ( 'NONE',  ( -2.241623956689868358, -4.786620604624113540, 33.94971097300155805 ) ) ;
#68501 = B_SPLINE_CURVE_WITH_KNOTS ( 'NONE', 3,
 ( #22756, #21880, #2480, #2048, #16451, #84925, #70512, #63746, #64177, #3374 ),
 .UNSPECIFIED., .F., .F.,
 ( 4, 2, 2, 2, 4 ),
 ( 0.000000000000000000, 0.0001954339857564097512, 0.0003908679715128195024, 0.0005863019572692292807, 0.0007817359430256390048 ),
 .UNSPECIFIED. ) ;
#68502 = CARTESIAN_POINT ( 'NONE',  ( 14.37294787896833448, -4.481592998940250538, 33.73612834413965089 ) ) ;
#68503 = ORIENTED_EDGE ( 'NONE', *, *, #26181, .T. ) ;
#68504 = DIRECTION ( 'NONE',  ( -1.000000000000000000, -0.000000000000000000, -0.000000000000000000 ) ) ;
#68506 = ORIENTED_EDGE ( 'NONE', *, *, #10052, .T. ) ;
#68505 = CYLINDRICAL_SURFACE ( 'NONE', #18004, 0.2499999999999986955 ) ;
#68507 = CARTESIAN_POINT ( 'NONE',  ( -4.153846153846152411, -1.242168528481310874, 33.36296068462461051 ) ) ;
#68508 = CARTESIAN_POINT ( 'NONE',  ( 15.90384615384615330, -2.499999999999998668, 29.75000000000000355 ) ) ;
#68509 = DIRECTION ( 'NONE',  ( -0.000000000000000000, -0.000000000000000000, -1.000000000000000000 ) ) ;
#68510 = LINE ( 'NONE', #55440, #16486 ) ;
#68511 = CARTESIAN_POINT ( 'NONE',  ( -14.30769230769242739, -6.879047030192662504, 34.71129190930017927 ) ) ;
#68512 = CARTESIAN_POINT ( 'NONE',  ( 9.561616225640136690, -9.804603061927743113, 34.18744698557895845 ) ) ;
#68513 = EDGE_CURVE ( 'NONE', #55920, #13845, #84373, .T. ) ;
#68514 = CARTESIAN_POINT ( 'NONE',  ( -0.4615384615385826339, -12.46129190930018460, 30.37095296980731973 ) ) ;
#68515 = CARTESIAN_POINT ( 'NONE',  ( -1.077988221561493543, -4.724691934501247914, 21.82999329374151642 ) ) ;
#68516 = ORIENTED_EDGE ( 'NONE', *, *, #6713, .T. ) ;
#68517 = LINE ( 'NONE', #20776, #30208 ) ;
#68518 = CARTESIAN_POINT ( 'NONE',  ( 0.6843180028068713838, -3.236590943229497697, 32.36255958852954251 ) ) ;
#68519 = CARTESIAN_POINT ( 'NONE',  ( 9.823098133274644539, -10.70102852606553157, 33.91149625220312913 ) ) ;
#68521 = EDGE_LOOP ( 'NONE', ( #13688, #38860, #10862, #36514 ) ) ;
#68520 = AXIS2_PLACEMENT_3D ( 'NONE', #34192, #53124, #25221 ) ;
#68522 = VERTEX_POINT ( 'NONE', #65845 ) ;
#68523 = CARTESIAN_POINT ( 'NONE',  ( -12.52680890749923925, -11.94971097300153140, 32.03036669348370680 ) ) ;
#68524 = CARTESIAN_POINT ( 'NONE',  ( 11.40777093535123221, -12.62707690430377383, 30.88035979386743435 ) ) ;
#68525 = VECTOR ( 'NONE', #69977, 1000.000000000000114 ) ;
#68526 = CARTESIAN_POINT ( 'NONE',  ( 2.557746727605760384, -10.82426656108011720, 33.81400080652039009 ) ) ;
#68527 = LINE ( 'NONE', #32522, #11154 ) ;
#68528 = CARTESIAN_POINT ( 'NONE',  ( -14.53117723225663838, -3.019605429927184836, 32.48692288466676814 ) ) ;
#68529 = ORIENTED_EDGE ( 'NONE', *, *, #16413, .F. ) ;
#68530 = PRODUCT_DEFINITION_SHAPE ( 'NONE', 'NONE',  #25379 ) ;
#68531 = CARTESIAN_POINT ( 'NONE',  ( 5.999999999999880096, -6.026961402154118908, 34.52809138561165270 ) ) ;
#68532 = ADVANCED_FACE ( 'NONE', ( #58203 ), #24415, .F. ) ;
#68533 = AXIS2_PLACEMENT_3D ( 'NONE', #48901, #28181, #7485 ) ;
#68534 = FACE_OUTER_BOUND ( 'NONE', #53735, .T. ) ;
#68535 = CARTESIAN_POINT ( 'NONE',  ( 17.07692307692307665, -13.87047571288749737, 32.06866353760679544 ) ) ;
#68536 = ORIENTED_EDGE ( 'NONE', *, *, #14725, .T. ) ;
#68537 = CARTESIAN_POINT ( 'NONE',  ( -17.07692307692319744, -12.16647553114689728, 32.15551576947799362 ) ) ;
#68538 = EDGE_CURVE ( 'NONE', #47848, #78478, #46032, .T. ) ;
#68539 = VERTEX_POINT ( 'NONE', #32513 ) ;
#68540 = CARTESIAN_POINT ( 'NONE',  ( 12.46153846153833911, -12.51329471203414379, 31.30864560766407578 ) ) ;
#68541 = CARTESIAN_POINT ( 'NONE',  ( 11.78840694783958298, -6.653508905675592722, 34.93172785388651391 ) ) ;
#68542 = EDGE_LOOP ( 'NONE', ( #57281, #46084, #88994, #12639, #45737, #33997, #20468, #13266 ) ) ;
#68543 = EDGE_CURVE ( 'NONE', #70102, #83933, #78680, .T. ) ;
#68544 = B_SPLINE_CURVE_WITH_KNOTS ( 'NONE', 3,
 ( #2184, #44487, #29675, #37298, #52143, #58903, #57136, #71977, #50800, #23341 ),
 .UNSPECIFIED., .F., .F.,
 ( 4, 2, 2, 2, 4 ),
 ( 0.0007817246256747516176, 0.0009771112852218965736, 0.001172497944769041638, 0.001367884604316186702, 0.001563271263863331550 ),
 .UNSPECIFIED. ) ;
#68545 = CARTESIAN_POINT ( 'NONE',  ( 18.00000000000000000, -1.242168528481310874, 33.36296068462461051 ) ) ;
#68546 = CARTESIAN_POINT ( 'NONE',  ( -8.769230769230890843, -2.625532179533778709, 30.86335684631627174 ) ) ;
#68547 = CARTESIAN_POINT ( 'NONE',  ( 1.384615384615265343, -4.481592998941358097, 33.73612834414048933 ) ) ;
#68548 = CARTESIAN_POINT ( 'NONE',  ( 11.47319153790522073, -12.51329471203370325, 31.30864560766548976 ) ) ;
#68549 = CARTESIAN_POINT ( 'NONE',  ( 3.453548772037640546, -12.44528174975671853, 30.48912976160716681 ) ) ;
#68550 = AXIS2_PLACEMENT_3D ( 'NONE', #4610, #32081, #25325 ) ;
#68551 = EDGE_LOOP ( 'NONE', ( #64909, #62358, #11474, #18128 ) ) ;
#68552 = FACE_BOUND ( 'NONE', #79552, .T. ) ;
#68553 = ORIENTED_EDGE ( 'NONE', *, *, #41158, .F. ) ;
#68555 = ADVANCED_FACE ( 'NONE', ( #4145 ), #51421, .F. ) ;
#68554 = FACE_OUTER_BOUND ( 'NONE', #4072, .T. ) ;
#68556 = CARTESIAN_POINT ( 'NONE',  ( 17.99999999999987566, -12.27809138561165270, 31.22303859784587132 ) ) ;
#68557 = EDGE_CURVE ( 'NONE', #75533, #27477, #82994, .T. ) ;
#68558 = CIRCLE ( 'NONE', #36919, 4.000000000000000000 ) ;
#68559 = DIRECTION ( 'NONE',  ( -0.000000000000000000, -0.8660254037844399289, -0.4999999999999980016 ) ) ;
#68560 = CARTESIAN_POINT ( 'NONE',  ( 14.30769230769231015, -2.721908614388771852, 31.22303859784724978 ) ) ;
#68561 = ORIENTED_EDGE ( 'NONE', *, *, #84542, .T. ) ;
#68562 = ORIENTED_EDGE ( 'NONE', *, *, #36151, .T. ) ;
#68563 = ORIENTED_EDGE ( 'NONE', *, *, #1439, .F. ) ;
#68564 = LINE ( 'NONE', #1880, #87977 ) ;
#68565 = VERTEX_POINT ( 'NONE', #3702 ) ;
#68566 = ADVANCED_FACE ( 'NONE', ( #10919 ), #86594, .F. ) ;
#68567 = CARTESIAN_POINT ( 'NONE',  ( 8.102564102564102200, -7.500000000000000000, 33.75000000000000000 ) ) ;
#68568 = B_SPLINE_CURVE_WITH_KNOTS ( 'NONE', 3,
 ( #47660, #68372, #14314, #35026, #34590, #41801, #69263, #75145, #7566, #62486 ),
 .UNSPECIFIED., .F., .F.,
 ( 4, 2, 2, 2, 4 ),
 ( 0.0007817359527651101701, 0.0009771254036996489256, 0.001172514854634187790, 0.001367904305568726653, 0.001563293756503265517 ),
 .UNSPECIFIED. ) ;
#68569 = CYLINDRICAL_SURFACE ( 'NONE', #19506, 0.2499999999999986955 ) ;
#68570 = ADVANCED_FACE ( 'NONE', ( #80273 ), #11358, .F. ) ;
#68571 = CARTESIAN_POINT ( 'NONE',  ( 6.130791807824788719, -12.11778462344220841, 31.66786338562085135 ) ) ;
#68572 = PLANE ( 'NONE',  #81620 ) ;
#68573 = CARTESIAN_POINT ( 'NONE',  ( 5.076923076923075762, -3.886160181151819604, 36.00935417666054406 ) ) ;
#68574 = VECTOR ( 'NONE', #28623, 1000.000000000000227 ) ;
#68575 = CARTESIAN_POINT ( 'NONE',  ( -4.153846153846152411, -5.471508081941601098, 34.59228464037088457 ) ) ;
#68576 = CARTESIAN_POINT ( 'NONE',  ( 15.23076923076923173, -13.20930481340135110, 34.54067556320372745 ) ) ;
#68577 = CARTESIAN_POINT ( 'NONE',  ( 17.20744877868664346, -2.619367082507847666, 30.83698974864643461 ) ) ;
#68578 = EDGE_LOOP ( 'NONE', ( #68064, #26504 ) ) ;
#68579 = VERTEX_POINT ( 'NONE', #66301 ) ;
#68580 = ORIENTED_EDGE ( 'NONE', *, *, #44242, .T. ) ;
#68582 = EDGE_CURVE ( 'NONE', #70011, #68729, #19407, .T. ) ;
#68581 = CARTESIAN_POINT ( 'NONE',  ( -13.63463860883684120, -12.45566812827425451, 31.48439005359158926 ) ) ;
#68584 = LINE ( 'NONE', #5116, #13186 ) ;
#68583 = CARTESIAN_POINT ( 'NONE',  ( 0.4615384615384611200, -6.435427911321262684, 35.78748833219616898 ) ) ;
#68585 = CARTESIAN_POINT ( 'NONE',  ( 1.384615384615264011, -12.51329471203414379, 31.30864560766407578 ) ) ;
#68586 = DIRECTION ( 'NONE',  ( -0.000000000000000000, -0.1736481776669307198, -0.9848077530122080203 ) ) ;
#68587 = FACE_BOUND ( 'NONE', #9405, .T. ) ;
#68588 = CARTESIAN_POINT ( 'NONE',  ( -7.173053667125516064, -3.436278759898155677, 33.07459398097509506 ) ) ;
#68589 = ORIENTED_EDGE ( 'NONE', *, *, #44498, .F. ) ;
#68590 = EDGE_CURVE ( 'NONE', #81222, #56866, #69754, .T. ) ;
#68591 = AXIS2_PLACEMENT_3D ( 'NONE', #35857, #48025, #6609 ) ;
#68592 = DIRECTION ( 'NONE',  ( -0.000000000000000000, -0.5000000000000009992, -0.8660254037844380415 ) ) ;
#68593 = CARTESIAN_POINT ( 'NONE',  ( -6.923076923076922462, -7.500000000000001776, 35.04278698407183867 ) ) ;
#68594 = CARTESIAN_POINT ( 'NONE',  ( -3.361459833879539616, -3.338472653186242756, 32.95098750199972670 ) ) ;
#68595 = ORIENTED_EDGE ( 'NONE', *, *, #41749, .T. ) ;
#68596 = CARTESIAN_POINT ( 'NONE',  ( 17.14299041027315695, -5.471508081941601098, 34.59228464037088457 ) ) ;
#68597 = EDGE_LOOP ( 'NONE', ( #40873, #29136 ) ) ;
#68598 = FACE_BOUND ( 'NONE', #48895, .T. ) ;
#68599 = DIRECTION ( 'NONE',  ( 0.000000000000000000, 0.6427876096865373645, -0.7660444431189797898 ) ) ;
#68600 = B_SPLINE_CURVE_WITH_KNOTS ( 'NONE', 3,
 ( #3990, #65691, #44527, #78772, #23813, #2220, #43655, #51267, #9434, #64360 ),
 .UNSPECIFIED., .F., .F.,
 ( 4, 2, 2, 2, 4 ),
 ( 0.0007817246256747452209, 0.0009771112852218879000, 0.001172497944769030362, 0.001367884604316172825, 0.001563271263863315504 ),
 .UNSPECIFIED. ) ;
#68601 = CARTESIAN_POINT ( 'NONE',  ( -6.065756802514307822, -7.249945686854186278, 34.74374336980224598 ) ) ;
#68602 = CARTESIAN_POINT ( 'NONE',  ( 0.4615384615384611200, -3.886160181151819604, 36.00935417666054406 ) ) ;
#68603 = EDGE_LOOP ( 'NONE', ( #85729, #67292 ) ) ;
#68604 = CARTESIAN_POINT ( 'NONE',  ( 6.923076923076802558, -6.026961402154118908, 34.52809138561165270 ) ) ;
#68605 = CARTESIAN_POINT ( 'NONE',  ( 20.00000000000000000, -7.500000000000000000, 33.75000000000000000 ) ) ;
#68606 = CARTESIAN_POINT ( 'NONE',  ( 18.22301284409339672, -10.77377354290276301, 33.85451476688484718 ) ) ;
#68607 = EDGE_CURVE ( 'NONE', #28603, #8219, #58648, .T. ) ;
#68608 = CARTESIAN_POINT ( 'NONE',  ( 2.307692307692186251, -3.083524468854526912, 32.58852847137268327 ) ) ;
#68609 = ORIENTED_EDGE ( 'NONE', *, *, #1208, .T. ) ;
#68610 = DIRECTION ( 'NONE',  ( -0.000000000000000000, -0.6427876096865404731, -0.7660444431189770143 ) ) ;
#68611 = CARTESIAN_POINT ( 'NONE',  ( 2.530705151785704654, -3.395485233115138168, 33.02377354290276656 ) ) ;
#68612 = B_SPLINE_CURVE_WITH_KNOTS ( 'NONE', 3,
 ( #68155, #74919, #86787, #25057, #52519, #19518, #33485, #13212, #60945, #88450 ),
 .UNSPECIFIED., .F., .F.,
 ( 4, 2, 2, 2, 4 ),
 ( 0.0007817359430256306564, 0.0009771253907249969738, 0.001172514838424363291, 0.001367904286123729826, 0.001563293733823096143 ),
 .UNSPECIFIED. ) ;
#68614 = ORIENTED_EDGE ( 'NONE', *, *, #46501, .F. ) ;
#68613 = CARTESIAN_POINT ( 'NONE',  ( -8.992156986746916658, -3.586966769969701208, 32.86292498521069660 ) ) ;
#68615 = DIRECTION ( 'NONE',  ( 0.000000000000000000, 0.1736481776669275834, 0.9848077530122086864 ) ) ;
#68616 = LINE ( 'NONE', #6911, #35552 ) ;
#68617 = CARTESIAN_POINT ( 'NONE',  ( 13.38461538461538680, -12.37446782046654192, 30.86335684631486131 ) ) ;
#68618 = CYLINDRICAL_SURFACE ( 'NONE', #61723, 0.2499999999999995559 ) ;
#68619 = VECTOR ( 'NONE', #77176, 999.9999999999998863 ) ;
#68620 = CARTESIAN_POINT ( 'NONE',  ( -13.25382494364843389, -3.338503747796866872, 32.95102852606553512 ) ) ;
#68622 = CARTESIAN_POINT ( 'NONE',  ( -16.37733107841048508, -8.539481045369598178, 34.89627647299170832 ) ) ;
#68621 = CARTESIAN_POINT ( 'NONE',  ( -7.846153846153965716, -10.90142922262034020, 33.41473453929536674 ) ) ;
#68623 = CARTESIAN_POINT ( 'NONE',  ( 2.544871794871792936, -3.499999999999999556, 29.75000000000000355 ) ) ;
#68624 = CARTESIAN_POINT ( 'NONE',  ( -2.749999999999998224, -7.500000000000015987, 18.84375000000000000 ) ) ;
#68625 = ORIENTED_EDGE ( 'NONE', *, *, #71723, .F. ) ;
#68626 = AXIS2_PLACEMENT_3D ( 'NONE', #34875, #56036, #20036 ) ;
#68627 = FACE_OUTER_BOUND ( 'NONE', #9463, .T. ) ;
#68628 = VERTEX_POINT ( 'NONE', #66749 ) ;
#68629 = VERTEX_POINT ( 'NONE', #57597 ) ;
#68630 = LINE ( 'NONE', #54219, #32655 ) ;
#68632 = EDGE_LOOP ( 'NONE', ( #45522, #87058 ) ) ;
#68631 = AXIS2_PLACEMENT_3D ( 'NONE', #53583, #46830, #82848 ) ;
#68633 = CARTESIAN_POINT ( 'NONE',  ( 14.17754509825408960, -8.587444163452046197, 34.63053765926554206 ) ) ;
#68634 = CARTESIAN_POINT ( 'NONE',  ( -1.944543648262992530, -9.444543648263016067, 22.43750000000000000 ) ) ;
#68635 = CARTESIAN_POINT ( 'NONE',  ( 13.38461538461538680, -2.721908614388771852, 31.22303859784724978 ) ) ;
#68636 = CYLINDRICAL_SURFACE ( 'NONE', #2143, 0.2500000000000002220 ) ;
#68637 = FACE_OUTER_BOUND ( 'NONE', #60943, .T. ) ;
#68638 = CARTESIAN_POINT ( 'NONE',  ( 1.134638640566797196, -2.544273027872574922, 31.48422191005632342 ) ) ;
#68639 = DIRECTION ( 'NONE',  ( -0.000000000000000000, -0.7660444431189791237, -0.6427876096865379196 ) ) ;
#68640 = CARTESIAN_POINT ( 'NONE',  ( 2.307692307692187583, -10.21337939537710326, 33.94971097300076224 ) ) ;
#68641 = CARTESIAN_POINT ( 'NONE',  ( 3.750000000000000888, -7.499999999999978684, 24.46875000000000000 ) ) ;
#68642 = DIRECTION ( 'NONE',  ( 0.000000000000000000, 0.1736481776669275834, 0.9848077530122086864 ) ) ;
#68643 = DIRECTION ( 'NONE',  ( -0.000000000000000000, -0.3420201433256694901, -0.9396926207859082059 ) ) ;
#68644 = B_SPLINE_CURVE_WITH_KNOTS ( 'NONE', 3,
 ( #64325, #35999, #1310, #57140, #77414, #2188, #82861, #22469, #875, #62996 ),
 .UNSPECIFIED., .F., .F.,
 ( 4, 2, 2, 2, 4 ),
 ( 0.000000000000000000, 0.0001954311564186865492, 0.0003908623128373730983, 0.0005862934692560596746, 0.0007817246256747461966 ),
 .UNSPECIFIED. ) ;
#68645 = CARTESIAN_POINT ( 'NONE',  ( 14.53106824839049160, -2.501478030877322567, 29.88021232661721172 ) ) ;
#68646 = CARTESIAN_POINT ( 'NONE',  ( -9.757577692864012775, -11.67786785259540849, 32.92929555188721480 ) ) ;
#68647 = EDGE_CURVE ( 'NONE', #46832, #48838, #23766, .T. ) ;
#68648 = ORIENTED_EDGE ( 'NONE', *, *, #60367, .F. ) ;
#68649 = ORIENTED_EDGE ( 'NONE', *, *, #18267, .F. ) ;
#68650 = CARTESIAN_POINT ( 'NONE',  ( -18.13069060311030611, -2.494641256782729855, 31.33461815524612959 ) ) ;
#68651 = CARTESIAN_POINT ( 'NONE',  ( 15.23076923076910916, -12.16647553114689728, 32.15551576947799362 ) ) ;
#68652 = LINE ( 'NONE', #26341, #77144 ) ;
#68653 = CARTESIAN_POINT ( 'NONE',  ( 15.23076923076923173, -12.29105614889573062, 35.45975837776705220 ) ) ;
#68654 = ADVANCED_FACE ( 'NONE', ( #65238 ), #1774, .T. ) ;
#68655 = LINE ( 'NONE', #21354, #23358 ) ;
#68656 = CARTESIAN_POINT ( 'NONE',  ( -9.469528023329624844, -10.97394488606064122, 33.68653795673694873 ) ) ;
#68657 = EDGE_CURVE ( 'NONE', #1046, #85754, #75499, .T. ) ;
#68658 = LINE ( 'NONE', #6958, #30755 ) ;
#68659 = AXIS2_PLACEMENT_3D ( 'NONE', #67540, #51887, #60327 ) ;
#68660 = VERTEX_POINT ( 'NONE', #85084 ) ;
#68661 = CARTESIAN_POINT ( 'NONE',  ( -14.55766905174089665, -12.65889640711025521, 30.72598325615533454 ) ) ;
#68662 = VERTEX_POINT ( 'NONE', #42775 ) ;
#68663 = EDGE_CURVE ( 'NONE', #78118, #88590, #5629, .T. ) ;
#68664 = CARTESIAN_POINT ( 'NONE',  ( 5.326977388561390470, -8.303483539816728154, 34.68545999027711702 ) ) ;
#68665 = CARTESIAN_POINT ( 'NONE',  ( -18.25000000000000000, -12.75000000000000888, 29.74999999999997868 ) ) ;
#68666 = CARTESIAN_POINT ( 'NONE',  ( -6.988399838569097966, -7.749976743299137993, 34.99404534957040624 ) ) ;
#68667 = CARTESIAN_POINT ( 'NONE',  ( -15.45425417449318317, -3.236172620538810385, 32.36188796281390267 ) ) ;
#68668 = CARTESIAN_POINT ( 'NONE',  ( 3.512820512820510555, -7.500000000000000000, 29.75000000000000355 ) ) ;
#68669 = ORIENTED_EDGE ( 'NONE', *, *, #34115, .T. ) ;
#68670 = ORIENTED_EDGE ( 'NONE', *, *, #27210, .F. ) ;
#68671 = AXIS2_PLACEMENT_3D ( 'NONE', #36579, #10880, #38352 ) ;
#68672 = ORIENTED_EDGE ( 'NONE', *, *, #39991, .F. ) ;
#68673 = ORIENTED_EDGE ( 'NONE', *, *, #25267, .T. ) ;
#68674 = CYLINDRICAL_SURFACE ( 'NONE', #8483, 0.2500000000000004996 ) ;
#68675 = CARTESIAN_POINT ( 'NONE',  ( 7.846153846153725020, -3.835265460704628371, 33.15142922262033665 ) ) ;
#68676 = AXIS2_PLACEMENT_3D ( 'NONE', #1230, #76459, #7556 ) ;
#68677 = EDGE_CURVE ( 'NONE', #23762, #45514, #84129, .T. ) ;
#68678 = DIRECTION ( 'NONE',  ( -1.000000000000000000, -0.000000000000000000, -0.000000000000000000 ) ) ;
#68679 = CARTESIAN_POINT ( 'NONE',  ( 16.40379167219429846, -10.05730279482229683, 34.04704008940765902 ) ) ;
#68680 = LINE ( 'NONE', #32675, #59442 ) ;
#68681 = CARTESIAN_POINT ( 'NONE',  ( 16.15384615384615330, -13.88283147151868846, 33.14645433367849847 ) ) ;
#68682 = AXIS2_PLACEMENT_3D ( 'NONE', #81611, #87957, #46040 ) ;
#68683 = ORIENTED_EDGE ( 'NONE', *, *, #20649, .T. ) ;
#68684 = ORIENTED_EDGE ( 'NONE', *, *, #73101, .F. ) ;
#68685 = ORIENTED_EDGE ( 'NONE', *, *, #87296, .T. ) ;
#68688 = ORIENTED_EDGE ( 'NONE', *, *, #36763, .F. ) ;
#68687 = ADVANCED_FACE ( 'NONE', ( #44513 ), #70236, .T. ) ;
#68686 = FACE_OUTER_BOUND ( 'NONE', #30723, .T. ) ;
#68689 = CYLINDRICAL_SURFACE ( 'NONE', #47714, 0.2499999999999986955 ) ;
#68690 = DIRECTION ( 'NONE',  ( -0.000000000000000000, 0.5000000000000011102, -0.8660254037844381525 ) ) ;
#68691 = CARTESIAN_POINT ( 'NONE',  ( -1.553300858899125059, -3.750000000000009326, 21.57812500000000355 ) ) ;
#68692 = VERTEX_POINT ( 'NONE', #57159 ) ;
#68693 = ADVANCED_FACE ( 'NONE', ( #50822 ), #70681, .F. ) ;
#68694 = EDGE_CURVE ( 'NONE', #88462, #27552, #47584, .T. ) ;
#68695 = ORIENTED_EDGE ( 'NONE', *, *, #55374, .T. ) ;
#68696 = CARTESIAN_POINT ( 'NONE',  ( -13.38461538461550582, -4.481592998941358097, 33.73612834414048933 ) ) ;
#68697 = B_SPLINE_CURVE_WITH_KNOTS ( 'NONE', 3,
 ( #40645, #88846, #19036, #73986, #46504, #26234 ),
 .UNSPECIFIED., .F., .F.,
 ( 4, 2, 4 ),
 ( 2.110382192020081086E-17, 0.0001954756301636924353, 0.0003909512603273637287 ),
 .UNSPECIFIED. ) ;
#68698 = FACE_BOUND ( 'NONE', #61985, .T. ) ;
#68699 = CARTESIAN_POINT ( 'NONE',  ( -5.076923076923075762, -4.661471528628507777, 34.16647553114623292 ) ) ;
#68700 = CARTESIAN_POINT ( 'NONE',  ( -4.219928533206287469, -9.905515769479276145, 34.41647553114623292 ) ) ;
#68701 = VERTEX_POINT ( 'NONE', #15744 ) ;
#68702 = CARTESIAN_POINT ( 'NONE',  ( 7.846153846153846700, -7.500000000000001776, 35.04278698407183867 ) ) ;
#68703 = CARTESIAN_POINT ( 'NONE',  ( 6.699591998512594238, -12.11044203135681840, 32.26167407432752299 ) ) ;
#68704 = B_SPLINE_CURVE_WITH_KNOTS ( 'NONE', 3,
 ( #26004, #46279, #86848, #74641, #39091, #38631, #66551, #4852, #5292, #53467 ),
 .UNSPECIFIED., .F., .F.,
 ( 4, 2, 2, 2, 4 ),
 ( 0.0007817246336856291692, 0.0009771112958940103739, 0.001172497958102391470, 0.001367884620310772566, 0.001563271282519153663 ),
 .UNSPECIFIED. ) ;
#68705 = FACE_OUTER_BOUND ( 'NONE', #12942, .T. ) ;
#68706 = CARTESIAN_POINT ( 'NONE',  ( 14.24160992833217065, -9.058645607665454236, 34.76329471203372634 ) ) ;
#68708 = VERTEX_POINT ( 'NONE', #17509 ) ;
#68707 = EDGE_CURVE ( 'NONE', #4668, #75052, #55070, .T. ) ;
#68709 = CIRCLE ( 'NONE', #28468, 4.000000000000000000 ) ;
#68710 = CARTESIAN_POINT ( 'NONE',  ( 16.28468457185891438, -7.277220443632451463, 34.74524770363009196 ) ) ;
#68711 = DIRECTION ( 'NONE',  ( 0.000000000000000000, 0.8660254037844377084, 0.5000000000000015543 ) ) ;
#68712 = CARTESIAN_POINT ( 'NONE',  ( 4.403791563224196182, -11.56426240980093745, 33.07394671870546432 ) ) ;
#68713 = CARTESIAN_POINT ( 'NONE',  ( 9.692307692307695177, -11.11383981884818262, 36.00935417666054406 ) ) ;
#68714 = EDGE_CURVE ( 'NONE', #44505, #58148, #59822, .T. ) ;
#68716 = EDGE_CURVE ( 'NONE', #40595, #21236, #79655, .T. ) ;
#68715 = CARTESIAN_POINT ( 'NONE',  ( -15.16470087976679082, -11.69971097300155272, 32.46337939537588113 ) ) ;
#68717 = FACE_BOUND ( 'NONE', #20193, .T. ) ;
#68719 = CARTESIAN_POINT ( 'NONE',  ( 16.94623247381276343, -2.845849958028613624, 32.17971566917920967 ) ) ;
#68718 = CARTESIAN_POINT ( 'NONE',  ( -7.846153846153844924, -1.466349020453238561, 30.81389545987213907 ) ) ;
#68720 = VECTOR ( 'NONE', #36640, 1000.000000000000227 ) ;
#68721 = CARTESIAN_POINT ( 'NONE',  ( 5.207713517890025123, -9.084667340241226796, 34.75534355489798344 ) ) ;
#68723 = CARTESIAN_POINT ( 'NONE',  ( -2.307692307692305711, -12.34228464037088635, 31.77849191805839268 ) ) ;
#68722 = CARTESIAN_POINT ( 'NONE',  ( -5.933931648997559982, -9.780366693483667717, 34.19971097300155805 ) ) ;
#68724 = LINE ( 'NONE', #62831, #39090 ) ;
#68725 = CARTESIAN_POINT ( 'NONE',  ( -1.077988221561460236, -10.27530806549876452, 15.85750670625849068 ) ) ;
#68726 = ADVANCED_FACE ( 'NONE', ( #66592 ), #17956, .F. ) ;
#68727 = VERTEX_POINT ( 'NONE', #74233 ) ;
#68728 = CARTESIAN_POINT ( 'NONE',  ( -5.934744860487159102, -11.06231777344671130, 33.60647404775212976 ) ) ;
#68729 = VERTEX_POINT ( 'NONE', #31918 ) ;
#68730 = CARTESIAN_POINT ( 'NONE',  ( -1.384615384615383471, -12.48256725967547354, 35.29906147534542527 ) ) ;
#68731 = ORIENTED_EDGE ( 'NONE', *, *, #51414, .T. ) ;
#68732 = FACE_OUTER_BOUND ( 'NONE', #75704, .T. ) ;
#68733 = FACE_OUTER_BOUND ( 'NONE', #63217, .T. ) ;
#68735 = ORIENTED_EDGE ( 'NONE', *, *, #83977, .F. ) ;
#68734 = CARTESIAN_POINT ( 'NONE',  ( -9.627052552794857831, -11.67786785259547777, 32.92929555188713664 ) ) ;
#68736 = CARTESIAN_POINT ( 'NONE',  ( 17.86952481492428291, -7.276987145209182550, 34.99546412871779211 ) ) ;
#68737 = CARTESIAN_POINT ( 'NONE',  ( -2.749999999999997780, -7.561099074964547917, 19.84188170625848713 ) ) ;
#68738 = CARTESIAN_POINT ( 'NONE',  ( -15.36145983387954139, -9.084618155246140248, 34.75535874321725771 ) ) ;
#68739 = CARTESIAN_POINT ( 'NONE',  ( 23.00000000000000000, -4.249999999999998224, 29.75000000000000355 ) ) ;
#68740 = CARTESIAN_POINT ( 'NONE',  ( -9.320512820512821150, -7.500000000000000000, 29.75000000000000355 ) ) ;
#68741 = CARTESIAN_POINT ( 'NONE',  ( 8.769230769230768274, -9.584722331328613620, 36.20867863119891439 ) ) ;
#68742 = CARTESIAN_POINT ( 'NONE',  ( -12.46153846153858424, -8.656820664282941280, 34.87096338111179961 ) ) ;
#68743 = CARTESIAN_POINT ( 'NONE',  ( -6.923076923076922462, -2.249999999999998668, 29.50000000000001421 ) ) ;
#68744 = CARTESIAN_POINT ( 'NONE',  ( -3.749999999999997780, -7.438900925035489387, 24.09561829374151287 ) ) ;
#68745 = AXIS2_PLACEMENT_3D ( 'NONE', #28615, #22295, #83572 ) ;
#68746 = CARTESIAN_POINT ( 'NONE',  ( -10.61538461538473399, -2.892918686052166066, 31.69288490824153470 ) ) ;
#68747 = CARTESIAN_POINT ( 'NONE',  ( -11.53846153846165912, -6.879047030192662504, 34.71129190930017927 ) ) ;
#68748 = B_SPLINE_CURVE_WITH_KNOTS ( 'NONE', 3,
 ( #24168, #4806, #73715, #60174, #12011, #53417, #16978, #10228, #37688, #65153 ),
 .UNSPECIFIED., .F., .F.,
 ( 4, 2, 2, 2, 4 ),
 ( 0.000000000000000000, 0.0001954311564186867660, 0.0003908623128373735320, 0.0005862934692560603251, 0.0007817246256747470640 ),
 .UNSPECIFIED. ) ;
#68749 = ORIENTED_EDGE ( 'NONE', *, *, #52608, .F. ) ;
#68750 = CARTESIAN_POINT ( 'NONE',  ( 8.992010310499175318, -10.11255958852956027, 34.01340905677048454 ) ) ;
#68751 = AXIS2_PLACEMENT_3D ( 'NONE', #30039, #65580, #17859 ) ;
#68752 = CARTESIAN_POINT ( 'NONE',  ( 2.651650429449539104, -4.848349570550432475, 14.31250000000000000 ) ) ;
#68753 = EDGE_CURVE ( 'NONE', #69788, #49089, #38987, .T. ) ;
#68754 = CARTESIAN_POINT ( 'NONE',  ( 6.923076923076924238, -2.292212530054420494, 30.41441678777542634 ) ) ;
#68755 = CARTESIAN_POINT ( 'NONE',  ( -8.834500769787091201, -3.643525952247789412, 33.31231777344662959 ) ) ;
#68756 = ORIENTED_EDGE ( 'NONE', *, *, #16666, .T. ) ;
#68757 = CARTESIAN_POINT ( 'NONE',  ( 1.450682717965462443, -8.164416787775445883, 34.95778746994558617 ) ) ;
#68758 = CARTESIAN_POINT ( 'NONE',  ( 24.00000000000000000, -5.499999999999981348, 27.25000000000000000 ) ) ;
#68760 = EDGE_LOOP ( 'NONE', ( #2296, #25926, #60341, #25968 ) ) ;
#68759 = CARTESIAN_POINT ( 'NONE',  ( 3.930361229281822855, -9.417330523894424488, 34.63758898049880486 ) ) ;
#68761 = CARTESIAN_POINT ( 'NONE',  ( -8.096153846153843148, -7.566083408709834757, 34.74999999999999289 ) ) ;
#68762 = AXIS2_PLACEMENT_3D ( 'NONE', #69755, #7173, #83730 ) ;
#68763 = CARTESIAN_POINT ( 'NONE',  ( -17.01075647033143667, -7.250054591869668386, 34.99404684341514127 ) ) ;
#68764 = CARTESIAN_POINT ( 'NONE',  ( 27.00000000000000000, 12.75000000000000711, 30.81664701255127881 ) ) ;
#68765 = CARTESIAN_POINT ( 'NONE',  ( 10.61538461538461675, -1.951392089020283160, 34.73218667398347748 ) ) ;
#68766 = DIRECTION ( 'NONE',  ( -0.000000000000000000, 0.1736481776669307198, -0.9848077530122080203 ) ) ;
#68767 = ORIENTED_EDGE ( 'NONE', *, *, #48883, .T. ) ;
#68768 = ORIENTED_EDGE ( 'NONE', *, *, #56783, .T. ) ;
#68769 = VERTEX_POINT ( 'NONE', #39577 ) ;
#68770 = AXIS2_PLACEMENT_3D ( 'NONE', #80467, #59291, #52086 ) ;
#68771 = DIRECTION ( 'NONE',  ( -0.000000000000000000, -0.6427876096865404731, -0.7660444431189770143 ) ) ;
#68772 = CARTESIAN_POINT ( 'NONE',  ( -2.307692307692305711, -5.557115091759785130, 34.35708131394839171 ) ) ;
#68773 = LINE ( 'NONE', #62444, #6185 ) ;
#68774 = CARTESIAN_POINT ( 'NONE',  ( -8.069638770718178478, -10.97335522853832579, 33.68706563782419749 ) ) ;
#68775 = B_SPLINE_CURVE_WITH_KNOTS ( 'NONE', 3,
 ( #69936, #15003, #61841, #76244, #43356, #34816, #70836, #8694, #35265, #8250 ),
 .UNSPECIFIED., .F., .F.,
 ( 4, 2, 2, 2, 4 ),
 ( 0.000000000000000000, 0.0001954339857564053873, 0.0003908679715128107746, 0.0005863019572692161618, 0.0007817359430256215491 ),
 .UNSPECIFIED. ) ;
#68776 = VECTOR ( 'NONE', #62127, 1000.000000000000000 ) ;
#68777 = ADVANCED_FACE ( 'NONE', ( #5330 ), #59379, .T. ) ;
#68778 = B_SPLINE_CURVE_WITH_KNOTS ( 'NONE', 3,
 ( #84768, #42444, #14972, #48298, #15418, #42006, #21268, #41550, #56830, #28480 ),
 .UNSPECIFIED., .F., .F.,
 ( 4, 2, 2, 2, 4 ),
 ( 0.0007817359430256297891, 0.0009771253907249958896, 0.001172514838424361990, 0.001367904286123728091, 0.001563293733823094191 ),
 .UNSPECIFIED. ) ;
#68779 = CARTESIAN_POINT ( 'NONE',  ( 17.07692307692307665, -11.35647404775217417, 33.31231777344666511 ) ) ;
#68780 = ORIENTED_EDGE ( 'NONE', *, *, #15433, .F. ) ;
#68781 = ORIENTED_EDGE ( 'NONE', *, *, #22016, .T. ) ;
#68782 = VECTOR ( 'NONE', #972, 1000.000000000000000 ) ;
#68783 = ORIENTED_EDGE ( 'NONE', *, *, #27322, .F. ) ;
#68785 = EDGE_LOOP ( 'NONE', ( #83836, #81398, #7805, #58925 ) ) ;
#68784 = DIRECTION ( 'NONE',  ( -1.000000000000000000, -0.000000000000000000, -0.000000000000000000 ) ) ;
#68786 = CARTESIAN_POINT ( 'NONE',  ( -3.230769230769229949, -2.249999999999998668, 29.75000000000001776 ) ) ;
#68787 = FACE_BOUND ( 'NONE', #5413, .T. ) ;
#68788 = CARTESIAN_POINT ( 'NONE',  ( -10.61538461538461320, -11.33034616979429110, 35.88435417666054406 ) ) ;
#68789 = EDGE_CURVE ( 'NONE', #18370, #81105, #64008, .T. ) ;
#68790 = LINE ( 'NONE', #12088, #84205 ) ;
#68791 = EDGE_LOOP ( 'NONE', ( #33012, #36121 ) ) ;
#68792 = EDGE_CURVE ( 'NONE', #64437, #46179, #46472, .T. ) ;
#68793 = ORIENTED_EDGE ( 'NONE', *, *, #25591, .F. ) ;
#68794 = ORIENTED_EDGE ( 'NONE', *, *, #63223, .T. ) ;
#68795 = CARTESIAN_POINT ( 'NONE',  ( -11.00641025641025550, -3.499999999999999556, 29.75000000000000355 ) ) ;
#68797 = ORIENTED_EDGE ( 'NONE', *, *, #11368, .F. ) ;
#68796 = FACE_OUTER_BOUND ( 'NONE', #14493, .T. ) ;
#68798 = CARTESIAN_POINT ( 'NONE',  ( 6.673100192134570285, -6.567427716900047230, 34.66269422305636283 ) ) ;
#68799 = CARTESIAN_POINT ( 'NONE',  ( -0.4615384615384611200, -6.343179335718451384, 34.87096338111211935 ) ) ;
#68800 = VERTEX_POINT ( 'NONE', #87774 ) ;
#68801 = EDGE_CURVE ( 'NONE', #51776, #85035, #19288, .T. ) ;
#68802 = CARTESIAN_POINT ( 'NONE',  ( -3.930834802233303282, -4.887748414852792322, 34.01359900205216746 ) ) ;
#68803 = CARTESIAN_POINT ( 'NONE',  ( 12.71159288145191013, -9.233818618650603938, 34.70587769442853698 ) ) ;
#68804 = VECTOR ( 'NONE', #72130, 1000.000000000000000 ) ;
#68805 = EDGE_LOOP ( 'NONE', ( #19724, #7822 ) ) ;
#68806 = FACE_BOUND ( 'NONE', #25009, .T. ) ;
#68807 = CARTESIAN_POINT ( 'NONE',  ( -15.48074597481782178, -8.347322224742351082, 34.93158281831414058 ) ) ;
#68808 = CARTESIAN_POINT ( 'NONE',  ( 15.90382292962469535, -2.588893531581426100, 31.60682220781849239 ) ) ;
#68809 = FACE_OUTER_BOUND ( 'NONE', #31299, .T. ) ;
#68811 = PLANE ( 'NONE',  #82856 ) ;
#68810 = DIRECTION ( 'NONE',  ( 0.000000000000000000, 0.7660444431189807890, 0.6427876096865361433 ) ) ;
#68812 = FACE_OUTER_BOUND ( 'NONE', #27523, .T. ) ;
#68813 = LINE ( 'NONE', #77340, #73602 ) ;
#68814 = EDGE_LOOP ( 'NONE', ( #26460, #70030, #29151, #35724 ) ) ;
#68815 = CARTESIAN_POINT ( 'NONE',  ( -7.911423846710166075, -6.835583212224499938, 34.95778746994557906 ) ) ;
#68816 = CARTESIAN_POINT ( 'NONE',  ( 0.4615384615384611200, -10.67929555188718282, 33.92786785259544047 ) ) ;
#68817 = ORIENTED_EDGE ( 'NONE', *, *, #44206, .F. ) ;
#68818 = DIRECTION ( 'NONE',  ( -1.000000000000000000, -0.000000000000000000, -0.000000000000000000 ) ) ;
#68819 = CARTESIAN_POINT ( 'NONE',  ( 10.61538461538461675, -8.164416787775445883, 34.95778746994557906 ) ) ;
#68820 = ORIENTED_EDGE ( 'NONE', *, *, #29613, .F. ) ;
#68821 = CARTESIAN_POINT ( 'NONE',  ( -12.46153846153858424, -2.379036618888197729, 30.90682066428292885 ) ) ;
#68822 = EDGE_CURVE ( 'NONE', #5428, #37333, #15374, .T. ) ;
#68823 = CYLINDRICAL_SURFACE ( 'NONE', #71690, 0.2499999999999998890 ) ;
#68824 = FACE_BOUND ( 'NONE', #39997, .T. ) ;
#68826 = CARTESIAN_POINT ( 'NONE',  ( 8.102564102564102200, -11.50000000000000000, 29.75000000000000355 ) ) ;
#68825 = CARTESIAN_POINT ( 'NONE',  ( -18.25002323729296805, -3.202444869320337784, 32.30641848906366675 ) ) ;
#68827 = CARTESIAN_POINT ( 'NONE',  ( 10.39189967166066708, -8.496056993536548418, 34.65000542017679663 ) ) ;
#68828 = CYLINDRICAL_SURFACE ( 'NONE', #23722, 0.2499999999999995559 ) ;
#68829 = CARTESIAN_POINT ( 'NONE',  ( -8.769230769230890843, -12.27809138561165270, 31.22303859784587132 ) ) ;
#68830 = DIRECTION ( 'NONE',  ( 0.000000000000000000, 8.673617379884033500E-16, -1.000000000000000000 ) ) ;
#68831 = CARTESIAN_POINT ( 'NONE',  ( 3.749999999999992006, -5.946699141100872943, 24.39062500000000000 ) ) ;
#68832 = ORIENTED_EDGE ( 'NONE', *, *, #6428, .F. ) ;
#68833 = VERTEX_POINT ( 'NONE', #51866 ) ;
#68834 = AXIS2_PLACEMENT_3D ( 'NONE', #40510, #26543, #26986 ) ;
#68835 = CARTESIAN_POINT ( 'NONE',  ( -4.153846153846152411, -9.780366693483667717, 34.19971097300155094 ) ) ;
#68836 = CARTESIAN_POINT ( 'NONE',  ( -15.45369618967607828, -5.582147617184174848, 34.63737895849758530 ) ) ;
#68837 = DIRECTION ( 'NONE',  ( -0.000000000000000000, 0.9396926207859093161, -0.3420201433256663259 ) ) ;
#68838 = CARTESIAN_POINT ( 'NONE',  ( -8.769230769230768274, -8.164416787775445883, 34.95778746994557906 ) ) ;
#68839 = CARTESIAN_POINT ( 'NONE',  ( -13.25408994638174498, -2.647132371071621471, 31.75357179365171589 ) ) ;
#68840 = CARTESIAN_POINT ( 'NONE',  ( 3.724691934501232815, -5.885600066136343678, 17.88875670625848713 ) ) ;
#68841 = B_SPLINE_CURVE_WITH_KNOTS ( 'NONE', 3,
 ( #11643, #38213, #39121, #32352, #65673, #3970, #80557, #87318, #25595, #52161 ),
 .UNSPECIFIED., .F., .F.,
 ( 4, 2, 2, 2, 4 ),
 ( 0.0007817359430256282712, 0.0009771253907249945886, 0.001172514838424360689, 0.001367904286123726790, 0.001563293733823093107 ),
 .UNSPECIFIED. ) ;
#68842 = DIRECTION ( 'NONE',  ( 0.000000000000000000, -8.673617379884033500E-16, 1.000000000000000000 ) ) ;
#68843 = PLANE ( 'NONE',  #31651 ) ;
#68844 = CIRCLE ( 'NONE', #63110, 0.2500000000000002220 ) ;
#68845 = CARTESIAN_POINT ( 'NONE',  ( 6.923076923076924238, -2.538708090699994813, 30.37095296980875503 ) ) ;
#68846 = DIRECTION ( 'NONE',  ( 1.000000000000000000, 0.000000000000000000, 0.000000000000000000 ) ) ;
#68847 = CARTESIAN_POINT ( 'NONE',  ( 10.61538461538461675, -3.322132147404559976, 32.92929555188717927 ) ) ;
#68848 = CARTESIAN_POINT ( 'NONE',  ( 5.142178216435913107, -8.656820664281605460, 34.87096338111211224 ) ) ;
#68849 = VECTOR ( 'NONE', #1598, 1000.000000000000000 ) ;
#68850 = DIRECTION ( 'NONE',  ( 0.000000000000000000, -6.938893903907222067E-15, 1.000000000000000000 ) ) ;
#68851 = CARTESIAN_POINT ( 'NONE',  ( -8.546217925137373328, -11.43677907613344757, 33.22367315496202167 ) ) ;
#68852 = CARTESIAN_POINT ( 'NONE',  ( 12.52760681254090080, -2.721908614388771852, 31.22303859784725333 ) ) ;
#68853 = ORIENTED_EDGE ( 'NONE', *, *, #13912, .T. ) ;
#68854 = DIRECTION ( 'NONE',  ( 0.000000000000000000, 0.9848077530122072432, -0.1736481776669354937 ) ) ;
#68855 = DIRECTION ( 'NONE',  ( 0.000000000000000000, 0.000000000000000000, -1.000000000000000000 ) ) ;
#68856 = CARTESIAN_POINT ( 'NONE',  ( 2.724691934501250135, -8.700186371490531201, 23.54874329374151642 ) ) ;
#68857 = CARTESIAN_POINT ( 'NONE',  ( -9.758390071667827570, -10.67929555188718460, 33.92786785259543336 ) ) ;
#68858 = CARTESIAN_POINT ( 'NONE',  ( -18.00000000000012079, -10.21337939537710504, 33.94971097300076224 ) ) ;
#68859 = FACE_OUTER_BOUND ( 'NONE', #12120, .T. ) ;
#68861 = VERTEX_POINT ( 'NONE', #86128 ) ;
#68860 = CARTESIAN_POINT ( 'NONE',  ( 7.623227628637697428, -2.554751324335733820, 30.48935550225260727 ) ) ;
#68862 = CARTESIAN_POINT ( 'NONE',  ( 2.750000000000008438, -8.639087296525996607, 22.04687500000000000 ) ) ;
#68863 = CARTESIAN_POINT ( 'NONE',  ( -4.826977558574935934, -10.05730279482229683, 34.04704008940765902 ) ) ;
#68864 = ORIENTED_EDGE ( 'NONE', *, *, #43333, .F. ) ;
#68865 = CARTESIAN_POINT ( 'NONE',  ( 11.76147438255493149, -9.172514111537584114, 34.72667873470787470 ) ) ;
#68866 = CARTESIAN_POINT ( 'NONE',  ( 8.096153846155281997, -7.500000000000155431, 34.75000000000007105 ) ) ;
#68867 = ORIENTED_EDGE ( 'NONE', *, *, #79450, .T. ) ;
#68868 = CARTESIAN_POINT ( 'NONE',  ( 7.596130608860880429, -4.335965774309649134, 33.62209801155881905 ) ) ;
#68869 = CARTESIAN_POINT ( 'NONE',  ( 8.519254025182176449, -6.524016743844655686, 34.90889640711025521 ) ) ;
#68870 = CARTESIAN_POINT ( 'NONE',  ( -15.00775787915638304, -12.39991518177334129, 30.74647679643404530 ) ) ;
#68871 = EDGE_LOOP ( 'NONE', ( #70753, #85274 ) ) ;
#68872 = ORIENTED_EDGE ( 'NONE', *, *, #66782, .F. ) ;
#68873 = CARTESIAN_POINT ( 'NONE',  ( 15.36156103859402045, -10.54018710029568595, 33.71981072465678864 ) ) ;
#68874 = VECTOR ( 'NONE', #55634, 1000.000000000000000 ) ;
#68875 = ORIENTED_EDGE ( 'NONE', *, *, #36881, .F. ) ;
#68876 = CARTESIAN_POINT ( 'NONE',  ( 7.780071466793711643, -9.058645607665454236, 34.76329471203372634 ) ) ;
#68877 = CARTESIAN_POINT ( 'NONE',  ( -7.053224892808619195, -2.373036134822904319, 30.88089517874952250 ) ) ;
#68878 = DIRECTION ( 'NONE',  ( 0.000000000000000000, 0.000000000000000000, 1.000000000000000000 ) ) ;
#68879 = CARTESIAN_POINT ( 'NONE',  ( -6.857009589726846599, -11.35647404775217595, 33.31231777344667222 ) ) ;
#68880 = CARTESIAN_POINT ( 'NONE',  ( -0.2387587925603955330, -5.827830569534416583, 34.72679350104403539 ) ) ;
#68881 = CARTESIAN_POINT ( 'NONE',  ( -2.372942239466390824, -2.255955759149247619, 30.00000000000013856 ) ) ;
#68882 = CARTESIAN_POINT ( 'NONE',  ( -0.2385256174450668676, -12.38742843783360748, 31.66772728687926985 ) ) ;
#68883 = ORIENTED_EDGE ( 'NONE', *, *, #42792, .F. ) ;
#68884 = ORIENTED_EDGE ( 'NONE', *, *, #45812, .T. ) ;
#68886 = ORIENTED_EDGE ( 'NONE', *, *, #73500, .F. ) ;
#68885 = CARTESIAN_POINT ( 'NONE',  ( 18.22277966897806678, -9.418065098278011860, 34.63729479722530158 ) ) ;
#68887 = CARTESIAN_POINT ( 'NONE',  ( 17.07692307692307665, -2.292212530054420494, 30.41441678777542634 ) ) ;
#68888 = EDGE_CURVE ( 'NONE', #32448, #19849, #50972, .T. ) ;
#68889 = EDGE_LOOP ( 'NONE', ( #840, #35695, #862, #45982 ) ) ;
#68890 = AXIS2_PLACEMENT_3D ( 'NONE', #51466, #18611, #73561 ) ;
#68891 = CARTESIAN_POINT ( 'NONE',  ( 9.692307692307695177, -1.629998284177014645, 34.34916445242399163 ) ) ;
#68892 = DIRECTION ( 'NONE',  ( 1.000000000000000000, 0.000000000000000000, 0.000000000000000000 ) ) ;
#68894 = ORIENTED_EDGE ( 'NONE', *, *, #19900, .T. ) ;
#68893 = EDGE_CURVE ( 'NONE', #72630, #58205, #53951, .T. ) ;
#68895 = DIRECTION ( 'NONE',  ( -0.000000000000000000, 0.9396926207859093161, -0.3420201433256663259 ) ) ;
#68896 = VECTOR ( 'NONE', #75547, 1000.000000000000000 ) ;
#68897 = ORIENTED_EDGE ( 'NONE', *, *, #9600, .F. ) ;
#68898 = DIRECTION ( 'NONE',  ( -1.000000000000000000, 0.000000000000000000, 0.000000000000000000 ) ) ;
#68899 = VERTEX_POINT ( 'NONE', #10465 ) ;
#68900 = VECTOR ( 'NONE', #33184, 1000.000000000000000 ) ;
#68901 = CARTESIAN_POINT ( 'NONE',  ( -12.68502338610279168, -3.562934362175800285, 33.22335522853832401 ) ) ;
#68902 = ORIENTED_EDGE ( 'NONE', *, *, #83019, .F. ) ;
#68903 = AXIS2_PLACEMENT_3D ( 'NONE', #52527, #60171, #87675 ) ;
#68904 = EDGE_CURVE ( 'NONE', #74960, #19286, #71183, .T. ) ;
#68905 = CARTESIAN_POINT ( 'NONE',  ( 1.384615384615265343, -6.879047030192662504, 34.71129190930017927 ) ) ;
#68906 = B_SPLINE_CURVE_WITH_KNOTS ( 'NONE', 3,
 ( #30813, #70923, #45214, #72691, #38025, #64144, #3787, #65926, #16859, #37121 ),
 .UNSPECIFIED., .F., .F.,
 ( 4, 2, 2, 2, 4 ),
 ( 0.0007817359430256390048, 0.0009771253907250075990, 0.001172514838424376085, 0.001367904286123744571, 0.001563293733823113056 ),
 .UNSPECIFIED. ) ;
#68907 = LINE ( 'NONE', #28359, #30998 ) ;
#68908 = FACE_BOUND ( 'NONE', #48570, .T. ) ;
#68909 = CYLINDRICAL_SURFACE ( 'NONE', #51370, 0.2499999999999979738 ) ;
#68910 = CARTESIAN_POINT ( 'NONE',  ( -6.857008572074485997, -12.10708131394839882, 31.69288490824020954 ) ) ;
#68911 = CARTESIAN_POINT ( 'NONE',  ( 4.284637961670939355, -12.38066358083363738, 30.83685684665853444 ) ) ;
#68912 = CARTESIAN_POINT ( 'NONE',  ( -3.480792468062195333, -4.335965774309649134, 33.62209801155881905 ) ) ;
#68913 = DIRECTION ( 'NONE',  ( -0.000000000000000000, 1.000000000000000000, -5.102127870520020612E-17 ) ) ;
#68914 = DIRECTION ( 'NONE',  ( -0.000000000000000000, 0.7660444431189791237, -0.6427876096865379196 ) ) ;
#68915 = CARTESIAN_POINT ( 'NONE',  ( 7.846153846153846700, -3.322132147404559976, 32.92929555188717927 ) ) ;
#68916 = EDGE_LOOP ( 'NONE', ( #57830, #85766 ) ) ;
#68917 = ORIENTED_EDGE ( 'NONE', *, *, #8407, .T. ) ;
#68919 = PLANE ( 'NONE',  #53413 ) ;
#68918 = DIRECTION ( 'NONE',  ( 0.000000000000000000, 0.1736481776669275834, 0.9848077530122086864 ) ) ;
#68920 = CARTESIAN_POINT ( 'NONE',  ( -12.71156169883142617, -2.587272538249755893, 30.68239716806877837 ) ) ;
#68921 = CARTESIAN_POINT ( 'NONE',  ( -7.846153846153844924, -13.87047571288749737, 32.06866353760679544 ) ) ;
#68922 = CARTESIAN_POINT ( 'NONE',  ( -23.00000000000000000, -4.249999999999998224, 29.75000000000000355 ) ) ;
#68923 = LINE ( 'NONE', #71574, #40432 ) ;
#68924 = VERTEX_POINT ( 'NONE', #3250 ) ;
#68925 = ADVANCED_FACE ( 'NONE', ( #37933 ), #65396, .T. ) ;
#68926 = CARTESIAN_POINT ( 'NONE',  ( -5.207613680033383652, -5.496505350115500121, 34.60290016733514307 ) ) ;
#68927 = CARTESIAN_POINT ( 'NONE',  ( -19.50000000000000000, -3.499999999999999556, 29.75000000000000355 ) ) ;
#68928 = CARTESIAN_POINT ( 'NONE',  ( -8.835314180186649935, -12.10708131394839349, 31.69288490824020244 ) ) ;
#68929 = ADVANCED_FACE ( 'NONE', ( #85679 ), #71704, .F. ) ;
#68930 = CARTESIAN_POINT ( 'NONE',  ( 3.007284287045282944, -3.236172620538810385, 32.36188796281390267 ) ) ;
#68931 = ORIENTED_EDGE ( 'NONE', *, *, #78288, .T. ) ;
#68932 = CIRCLE ( 'NONE', #25738, 0.2500000000000002220 ) ;
#68933 = ORIENTED_EDGE ( 'NONE', *, *, #21066, .F. ) ;
#68934 = CONTEXT_DEPENDENT_SHAPE_REPRESENTATION ( #23900, #44880 ) ;
#68935 = EDGE_LOOP ( 'NONE', ( #21358, #83699, #16150, #26585, #19919, #23800, #61452, #33418 ) ) ;
#68936 = EDGE_CURVE ( 'NONE', #5642, #76954, #10009, .T. ) ;
#68937 = CARTESIAN_POINT ( 'NONE',  ( 15.29602480204525605, -6.879047030191282275, 34.71129190930002295 ) ) ;
#68938 = ADVANCED_FACE ( 'NONE', ( #50103 ), #16330, .F. ) ;
#68939 = ORIENTED_EDGE ( 'NONE', *, *, #1290, .T. ) ;
#68940 = CARTESIAN_POINT ( 'NONE',  ( -9.627052552794857831, -10.33852847137154107, 34.16647553114620450 ) ) ;
#68941 = CARTESIAN_POINT ( 'NONE',  ( -17.20707028636129721, -3.285722584762970744, 32.44110544564090048 ) ) ;
#68942 = DIRECTION ( 'NONE',  ( -0.000000000000000000, 0.7660444431189791237, -0.6427876096865379196 ) ) ;
#68943 = CARTESIAN_POINT ( 'NONE',  ( -2.651650429449535551, -10.15165042944956753, 14.93750000000000000 ) ) ;
#68944 = B_SPLINE_CURVE_WITH_KNOTS ( 'NONE', 3,
 ( #69154, #32379, #61060, #79677, #25172, #13321, #20080, #40803, #68265, #47984 ),
 .UNSPECIFIED., .F., .F.,
 ( 4, 2, 2, 2, 4 ),
 ( 0.000000000000000000, 0.0001954339881912776238, 0.0003908679763825552477, 0.0005863019645738329257, 0.0007817359527651104954 ),
 .UNSPECIFIED. ) ;
#68945 = CARTESIAN_POINT ( 'NONE',  ( -11.28840722682322273, -6.567000820036036579, 34.66262288849541306 ) ) ;
#68946 = ORIENTED_EDGE ( 'NONE', *, *, #66862, .T. ) ;
#68948 = B_SPLINE_CURVE_WITH_KNOTS ( 'NONE', 3,
 ( #86045, #66660, #31990, #45039, #86962, #18478, #73423, #19361, #11724, #46828 ),
 .UNSPECIFIED., .F., .F.,
 ( 4, 2, 2, 2, 4 ),
 ( 0.000000000000000000, 0.0001954311564186860613, 0.0003908623128373721225, 0.0005862934692560581567, 0.0007817246256747442451 ),
 .UNSPECIFIED. ) ;
#68947 = CARTESIAN_POINT ( 'NONE',  ( 4.219039142140807996, -2.255955759149235629, 29.99999999999988631 ) ) ;
#68950 = ORIENTED_EDGE ( 'NONE', *, *, #4618, .T. ) ;
#68949 = DIRECTION ( 'NONE',  ( 0.000000000000000000, 0.9396926207859126468, 0.3420201433256571111 ) ) ;
#68951 = CARTESIAN_POINT ( 'NONE',  ( -16.94613263595612551, -8.191423895709842640, 34.95447573519442130 ) ) ;
#68952 = DIRECTION ( 'NONE',  ( 0.000000000000000000, 0.000000000000000000, -1.000000000000000000 ) ) ;
#68953 = DIRECTION ( 'NONE',  ( 1.000000000000000000, 0.000000000000000000, 0.000000000000000000 ) ) ;
#68954 = B_SPLINE_CURVE_WITH_KNOTS ( 'NONE', 3,
 ( #9829, #17924, #3061, #38187, #85937, #39095, #24221, #30541, #58012, #38637 ),
 .UNSPECIFIED., .F., .F.,
 ( 4, 2, 2, 2, 4 ),
 ( 0.000000000000000000, 0.0001954339857564091820, 0.0003908679715128183640, 0.0005863019572692275460, 0.0007817359430256367279 ),
 .UNSPECIFIED. ) ;
#68955 = B_SPLINE_CURVE_WITH_KNOTS ( 'NONE', 3,
 ( #51199, #57540, #15245, #36830, #30079, #49467 ),
 .UNSPECIFIED., .F., .F.,
 ( 4, 2, 4 ),
 ( 0.0003909569690057842790, 0.0005862646681846108007, 0.0007815723673634373224 ),
 .UNSPECIFIED. ) ;
#68956 = LINE ( 'NONE', #7264, #665 ) ;
#68957 = DIRECTION ( 'NONE',  ( 0.000000000000000000, 0.000000000000000000, -1.000000000000000000 ) ) ;
#68958 = CARTESIAN_POINT ( 'NONE',  ( -3.230769230769229949, -10.67929555188718282, 33.92786785259544047 ) ) ;
#68959 = DIRECTION ( 'NONE',  ( 0.000000000000000000, 0.3420201433256610524, 0.9396926207859113145 ) ) ;
#68960 = CARTESIAN_POINT ( 'NONE',  ( -2.775308065498752086, -8.577988221561495763, 19.01749329374151287 ) ) ;
#68961 = ORIENTED_EDGE ( 'NONE', *, *, #23061, .T. ) ;
#68962 = CARTESIAN_POINT ( 'NONE',  ( -15.48074597481782178, -6.524016743844655686, 34.90889640711025521 ) ) ;
#68963 = CARTESIAN_POINT ( 'NONE',  ( -24.00000000000000000, -9.499999999999982236, 27.25000000000000000 ) ) ;
#68964 = AXIS2_PLACEMENT_3D ( 'NONE', #63603, #584, #8232 ) ;
#68965 = AXIS2_PLACEMENT_3D ( 'NONE', #29144, #77310, #9737 ) ;
#68966 = CARTESIAN_POINT ( 'NONE',  ( 9.942253101685738059, -2.986452184633680673, 32.43230066228895225 ) ) ;
#68967 = EDGE_LOOP ( 'NONE', ( #46526, #58659, #68894, #85377 ) ) ;
#68968 = ORIENTED_EDGE ( 'NONE', *, *, #55863, .T. ) ;
#68969 = CARTESIAN_POINT ( 'NONE',  ( -5.869474298236436738, -2.619367082507848554, 30.83698974864644171 ) ) ;
#68970 = CARTESIAN_POINT ( 'NONE',  ( -16.02332045208259359, -12.27024696741798770, 31.24895572276497546 ) ) ;
#68971 = AXIS2_PLACEMENT_3D ( 'NONE', #44067, #63467, #50388 ) ;
#68972 = CARTESIAN_POINT ( 'NONE',  ( -9.070512820512819374, -3.499999999999999556, 29.75000000000000355 ) ) ;
#68973 = CARTESIAN_POINT ( 'NONE',  ( -4.403822884788508141, -10.66389620160130036, 33.62221079203477103 ) ) ;
#68974 = LINE ( 'NONE', #41508, #76738 ) ;
#68975 = ORIENTED_EDGE ( 'NONE', *, *, #63224, .T. ) ;
#68976 = EDGE_CURVE ( 'NONE', #57354, #41209, #1311, .T. ) ;
#68977 = CARTESIAN_POINT ( 'NONE',  ( 12.23867219847536170, -2.251424796025574881, 29.88072029997477230 ) ) ;
#68978 = CARTESIAN_POINT ( 'NONE',  ( 3.453780582382081743, -12.15243808032445827, 31.58219941686247978 ) ) ;
#68979 = CARTESIAN_POINT ( 'NONE',  ( 5.299702745901141654, -12.47679350104403007, 31.42216943046555855 ) ) ;
#68980 = ORIENTED_EDGE ( 'NONE', *, *, #30140, .F. ) ;
#68981 = LINE ( 'NONE', #47376, #61404 ) ;
#68982 = VERTEX_POINT ( 'NONE', #44666 ) ;
#68983 = CARTESIAN_POINT ( 'NONE',  ( -19.50000000000000000, -3.499999999999999556, 29.75000000000000355 ) ) ;
#68984 = CARTESIAN_POINT ( 'NONE',  ( -5.750054590621957118, -12.07971442181322352, 32.31769673815850297 ) ) ;
#68985 = VERTEX_POINT ( 'NONE', #79364 ) ;
#68986 = DIRECTION ( 'NONE',  ( -0.000000000000000000, 1.000000000000000000, 3.491481338843133355E-15 ) ) ;
#68987 = CYLINDRICAL_SURFACE ( 'NONE', #85295, 0.2499999999999993616 ) ;
#68988 = CARTESIAN_POINT ( 'NONE',  ( 1.254468175177166689, -4.460286881179644780, 33.72017969459903242 ) ) ;
#68989 = ADVANCED_FACE ( 'NONE', ( #77591 ), #43360, .T. ) ;
#68990 = LINE ( 'NONE', #12725, #40555 ) ;
#68991 = CARTESIAN_POINT ( 'NONE',  ( 3.453780582382079523, -12.39991518177334129, 30.74647679643404530 ) ) ;
#68992 = B_SPLINE_CURVE_WITH_KNOTS ( 'NONE', 3,
 ( #7683, #84239, #22517, #35144, #57188, #76580, #83345, #14887, #69816, #8126 ),
 .UNSPECIFIED., .F., .F.,
 ( 4, 2, 2, 2, 4 ),
 ( 0.000000000000000000, 0.0001954311564186858715, 0.0003908623128373717431, 0.0005862934692560576146, 0.0007817246256747434861 ),
 .UNSPECIFIED. ) ;
#68993 = VERTEX_POINT ( 'NONE', #47344 ) ;
#68994 = FACE_BOUND ( 'NONE', #56675, .T. ) ;
#68995 = ORIENTED_EDGE ( 'NONE', *, *, #26907, .T. ) ;
#68996 = CARTESIAN_POINT ( 'NONE',  ( -15.84615384615384670, -3.499999999999999556, 29.75000000000000355 ) ) ;
#68997 = CIRCLE ( 'NONE', #53167, 4.000000000000000000 ) ;
#68998 = ADVANCED_FACE ( 'NONE', ( #80716 ), #46018, .T. ) ;
#68999 = CARTESIAN_POINT ( 'NONE',  ( 18.06606733335007675, -6.343179335718452272, 34.87096338111212646 ) ) ;
#69000 = DIRECTION ( 'NONE',  ( 0.000000000000000000, 0.6427876096865373645, -0.7660444431189797898 ) ) ;
#69001 = CARTESIAN_POINT ( 'NONE',  ( -6.130147209438221445, -12.27039167877662251, 31.24851455888617835 ) ) ;
#69002 = EDGE_CURVE ( 'NONE', #13933, #41455, #24916, .T. ) ;
#69003 = VERTEX_POINT ( 'NONE', #10906 ) ;
#69004 = VERTEX_POINT ( 'NONE', #54097 ) ;
#69005 = ORIENTED_EDGE ( 'NONE', *, *, #38422, .T. ) ;
#69006 = CARTESIAN_POINT ( 'NONE',  ( -10.86540783960607115, -8.475808217655753651, 34.90892951860618609 ) ) ;
#69007 = ORIENTED_EDGE ( 'NONE', *, *, #24124, .T. ) ;
#69008 = AXIS2_PLACEMENT_3D ( 'NONE', #51831, #64906, #66248 ) ;
#69009 = EDGE_CURVE ( 'NONE', #8333, #72105, #63683, .T. ) ;
#69010 = DIRECTION ( 'NONE',  ( 0.000000000000000000, 0.4999999999999985567, 0.8660254037844395958 ) ) ;
#69011 = CARTESIAN_POINT ( 'NONE',  ( 1.450683735617825265, -3.513871655860379306, 32.76840700105978499 ) ) ;
#69012 = CARTESIAN_POINT ( 'NONE',  ( -18.13014796973169851, -6.809168938359903223, 34.95455904226513866 ) ) ;
#69013 = CARTESIAN_POINT ( 'NONE',  ( -8.638440328263817136, -3.957578996910242619, 33.62503395064540257 ) ) ;
#69014 = CIRCLE ( 'NONE', #80546, 2.000000000000001776 ) ;
#69015 = CIRCLE ( 'NONE', #34501, 4.000000000000000000 ) ;
#69016 = EDGE_CURVE ( 'NONE', #22109, #45697, #60502, .T. ) ;
#69017 = DIRECTION ( 'NONE',  ( -0.000000000000000000, -0.5000000000000009992, -0.8660254037844380415 ) ) ;
#69018 = CARTESIAN_POINT ( 'NONE',  ( -14.24243716817946925, -12.70778746994558439, 30.41441678777536595 ) ) ;
#69019 = CARTESIAN_POINT ( 'NONE',  ( 3.930361229281820190, -2.612411019501189813, 31.66733052389439962 ) ) ;
#69020 = CARTESIAN_POINT ( 'NONE',  ( -5.326946314216042033, -3.711651800289232916, 33.01384336483936011 ) ) ;
#69021 = EDGE_LOOP ( 'NONE', ( #4110, #69484, #21490, #21682 ) ) ;
#69022 = EDGE_CURVE ( 'NONE', #20097, #44863, #17426, .T. ) ;
#69023 = EDGE_LOOP ( 'NONE', ( #20707, #64345 ) ) ;
#69024 = VECTOR ( 'NONE', #19787, 1000.000000000000000 ) ;
#69025 = EDGE_LOOP ( 'NONE', ( #39601, #83453 ) ) ;
#69026 = VECTOR ( 'NONE', #65365, 1000.000000000000000 ) ;
#69027 = FACE_OUTER_BOUND ( 'NONE', #34275, .T. ) ;
#69029 = CARTESIAN_POINT ( 'NONE',  ( 1.607395053593451140, -11.60474049983370648, 33.02348890104160262 ) ) ;
#69028 = CARTESIAN_POINT ( 'NONE',  ( -1.514763354347083535, -2.647304123082328875, 31.75400227202885262 ) ) ;
#69030 =( GEOMETRIC_REPRESENTATION_CONTEXT ( 3 ) GLOBAL_UNCERTAINTY_ASSIGNED_CONTEXT ( ( #43713 ) ) GLOBAL_UNIT_ASSIGNED_CONTEXT ( ( #56899, #42081, #77623 ) ) REPRESENTATION_CONTEXT ( 'NONE', 'WORKASPACE' ) );
#69031 = CARTESIAN_POINT ( 'NONE',  ( -17.75005459062195712, -5.766571408460170467, 34.70601412856602508 ) ) ;
#69032 = CARTESIAN_POINT ( 'NONE',  ( 1.384615384615386802, -2.708943851104267164, 35.45975837776705220 ) ) ;
#69033 = FACE_BOUND ( 'NONE', #37013, .T. ) ;
#69034 = CARTESIAN_POINT ( 'NONE',  ( 9.942253210655836781, -3.712312575010499494, 33.01462480002815170 ) ) ;
#69035 = VERTEX_POINT ( 'NONE', #5489 ) ;
#69036 = ADVANCED_FACE ( 'NONE', ( #32955 ), #11345, .F. ) ;
#69037 = CARTESIAN_POINT ( 'NONE',  ( -10.61538461538429878, -2.255955759149395501, 30.00000000000324363 ) ) ;
#69038 = DIRECTION ( 'NONE',  ( 0.000000000000000000, 0.6427876096865368094, 0.7660444431189802339 ) ) ;
#69039 = CARTESIAN_POINT ( 'NONE',  ( -13.19230769230769162, -7.500000000000000000, 29.75000000000000355 ) ) ;
#69040 = CARTESIAN_POINT ( 'NONE',  ( -1.634638608836840534, -3.520140089381497361, 33.17453946501458262 ) ) ;
#69041 = EDGE_LOOP ( 'NONE', ( #9746, #22986, #49516, #33118 ) ) ;
#69042 = CARTESIAN_POINT ( 'NONE',  ( -18.13014720943822056, -8.587444163452046197, 34.63053765926554206 ) ) ;
#69043 = ORIENTED_EDGE ( 'NONE', *, *, #6268, .T. ) ;
#69044 = FACE_BOUND ( 'NONE', #37489, .T. ) ;
#69045 = B_SPLINE_CURVE_WITH_KNOTS ( 'NONE', 3,
 ( #26453, #12932, #54797, #87730, #40419, #6181, #62000, #67877, #67437, #73766 ),
 .UNSPECIFIED., .F., .F.,
 ( 4, 2, 2, 2, 4 ),
 ( 0.0007817246336856291692, 0.0009771112958940103739, 0.001172497958102391470, 0.001367884620310772566, 0.001563271282519153879 ),
 .UNSPECIFIED. ) ;
#69046 = DIRECTION ( 'NONE',  ( -0.000000000000000000, 1.000000000000000000, -0.000000000000000000 ) ) ;
#69047 = B_SPLINE_CURVE_WITH_KNOTS ( 'NONE', 3,
 ( #32397, #13013, #40500, #67962, #6264, #59862, #59420, #8476, #7142, #55320 ),
 .UNSPECIFIED., .F., .F.,
 ( 4, 2, 2, 2, 4 ),
 ( 0.0007817246256747550871, 0.0009771112852218989588, 0.001172497944769042939, 0.001367884604316186702, 0.001563271263863330682 ),
 .UNSPECIFIED. ) ;
#69048 = CARTESIAN_POINT ( 'NONE',  ( -6.222826692479002553, -7.369208160676172348, 34.74850200257122879 ) ) ;
#69050 = EDGE_CURVE ( 'NONE', #62981, #88144, #79820, .T. ) ;
#69049 = CARTESIAN_POINT ( 'NONE',  ( 16.85399611801622299, -11.98009711892700224, 32.48740034544074007 ) ) ;
#69051 = ORIENTED_EDGE ( 'NONE', *, *, #50479, .F. ) ;
#69052 = CARTESIAN_POINT ( 'NONE',  ( 11.76124120743960333, -10.97394488606064122, 33.68653795673694873 ) ) ;
#69053 = CARTESIAN_POINT ( 'NONE',  ( 15.48071464014727283, -2.341251567377310217, 30.72681386836322659 ) ) ;
#69054 = CARTESIAN_POINT ( 'NONE',  ( -3.361460697436787104, -2.729777683071816785, 31.24903638046268739 ) ) ;
#69055 = CARTESIAN_POINT ( 'NONE',  ( 6.249945518348143381, -3.712312575010499494, 33.01462480002815170 ) ) ;
#69056 = EDGE_LOOP ( 'NONE', ( #30693, #51423, #81647, #42319 ) ) ;
#69057 = CARTESIAN_POINT ( 'NONE',  ( 13.31934493865461278, -6.026961402152685388, 34.52809138561120506 ) ) ;
#69058 = CARTESIAN_POINT ( 'NONE',  ( 2.438217745925954194, -3.625058011473228259, 33.29252011169590020 ) ) ;
#69060 = ORIENTED_EDGE ( 'NONE', *, *, #80951, .F. ) ;
#69059 = CARTESIAN_POINT ( 'NONE',  ( -6.416666666666667851, -11.50000000000000000, 29.75000000000000355 ) ) ;
#69061 = DIRECTION ( 'NONE',  ( -0.000000000000000000, -0.000000000000000000, -1.000000000000000000 ) ) ;
#69062 = CARTESIAN_POINT ( 'NONE',  ( -10.83831083290076158, -12.39988816332205701, 30.74660775122750778 ) ) ;
#69063 = CARTESIAN_POINT ( 'NONE',  ( 4.946232473812771424, -2.494641256782728966, 31.33461815524612959 ) ) ;
#69064 = DIRECTION ( 'NONE',  ( 0.000000000000000000, 0.9848077530122072432, -0.1736481776669354937 ) ) ;
#69065 = CARTESIAN_POINT ( 'NONE',  ( 16.85343815235874132, -4.988325925672468131, 34.36044203135681130 ) ) ;
#69067 = CARTESIAN_POINT ( 'NONE',  ( -16.28453675695646652, -8.191372820521381826, 34.95448215188424967 ) ) ;
#69066 = CARTESIAN_POINT ( 'NONE',  ( 8.992606255003186888, -2.251407671071268712, 29.88021292934942963 ) ) ;
#69068 = LINE ( 'NONE', #28987, #21955 ) ;
#69069 = EDGE_CURVE ( 'NONE', #11070, #71689, #34277, .T. ) ;
#69070 = VECTOR ( 'NONE', #18995, 999.9999999999998863 ) ;
#69071 = CARTESIAN_POINT ( 'NONE',  ( -1.944543648263014957, -5.555456351737005249, 17.75000000000000355 ) ) ;
#69072 = EDGE_LOOP ( 'NONE', ( #42221, #6759 ) ) ;
#69073 = CARTESIAN_POINT ( 'NONE',  ( 17.86985279056177944, -4.460286881179643004, 33.72017969459903242 ) ) ;
#69074 = ORIENTED_EDGE ( 'NONE', *, *, #71759, .F. ) ;
#69075 = ADVANCED_FACE ( 'NONE', ( #498 ), #27525, .F. ) ;
#69076 = VERTEX_POINT ( 'NONE', #8146 ) ;
#69077 = DIRECTION ( 'NONE',  ( 0.000000000000000000, 0.7660444431189822323, -0.6427876096865344779 ) ) ;
#69078 = ORIENTED_EDGE ( 'NONE', *, *, #61465, .F. ) ;
#69079 = DIRECTION ( 'NONE',  ( 0.000000000000000000, 0.9848077530122072432, -0.1736481776669354937 ) ) ;
#69080 = DIRECTION ( 'NONE',  ( -0.000000000000000000, 1.000000000000000000, 3.491481338843133355E-15 ) ) ;
#69081 = CARTESIAN_POINT ( 'NONE',  ( 7.846153846153846700, -2.292212530054420494, 30.41441678777542634 ) ) ;
#69082 = DIRECTION ( 'NONE',  ( 0.000000000000000000, 0.000000000000000000, 1.000000000000000000 ) ) ;
#69083 = LINE ( 'NONE', #48803, #86219 ) ;
#69084 = CARTESIAN_POINT ( 'NONE',  ( -11.76194648218548622, -5.113361153441934093, 34.14387501736622710 ) ) ;
#69085 = CARTESIAN_POINT ( 'NONE',  ( -4.376772371362300795, -3.586966769969700763, 32.86292498521069660 ) ) ;
#69086 = ADVANCED_FACE ( 'NONE', ( #48228 ), #68505, .F. ) ;
#69087 = DIRECTION ( 'NONE',  ( -0.000000000000000000, -0.9848077530122085754, -0.1736481776669273613 ) ) ;
#69088 = CARTESIAN_POINT ( 'NONE',  ( 13.38461538461526601, -5.219633306517616589, 34.19971097300220464 ) ) ;
#69089 = B_SPLINE_CURVE_WITH_KNOTS ( 'NONE', 3,
 ( #16963, #17858, #18298, #72784, #64689, #87219, #23704, #52954, #86780, #44410 ),
 .UNSPECIFIED., .F., .F.,
 ( 4, 2, 2, 2, 4 ),
 ( 0.0007817359430256293554, 0.0009771253907249952391, 0.001172514838424361123, 0.001367904286123727007, 0.001563293733823092890 ),
 .UNSPECIFIED. ) ;
#69090 = CIRCLE ( 'NONE', #58982, 4.000000000000000000 ) ;
#69091 = CARTESIAN_POINT ( 'NONE',  ( 5.142178216435913107, -11.06231777344671130, 33.60647404775212976 ) ) ;
#69092 = CARTESIAN_POINT ( 'NONE',  ( -8.069638789877792817, -8.496056993536548418, 34.65000542017679663 ) ) ;
#69093 = EDGE_CURVE ( 'NONE', #36228, #80445, #3533, .T. ) ;
#69094 = AXIS2_PLACEMENT_3D ( 'NONE', #59316, #25089, #80037 ) ;
#69095 = VECTOR ( 'NONE', #41557, 1000.000000000000000 ) ;
#69096 = EDGE_CURVE ( 'NONE', #68565, #67330, #36700, .T. ) ;
#69097 = ORIENTED_EDGE ( 'NONE', *, *, #46026, .F. ) ;
#69098 = ORIENTED_EDGE ( 'NONE', *, *, #19694, .F. ) ;
#69099 = CYLINDRICAL_SURFACE ( 'NONE', #38567, 0.2499999999999995559 ) ;
#69100 = CARTESIAN_POINT ( 'NONE',  ( 16.15384615384615330, -12.48256725967547354, 35.29906147534542527 ) ) ;
#69101 = DIRECTION ( 'NONE',  ( 0.000000000000000000, 0.000000000000000000, -1.000000000000000000 ) ) ;
#69102 = CARTESIAN_POINT ( 'NONE',  ( -11.40762312044877014, -7.277220443632450575, 34.74524770363009196 ) ) ;
#69103 = CARTESIAN_POINT ( 'NONE',  ( -10.03846153846153832, -4.000000000000000000, 29.65000000000000213 ) ) ;
#69104 = CARTESIAN_POINT ( 'NONE',  ( -6.222926217516146608, -8.239355502252617924, 34.69524867566427417 ) ) ;
#69105 = EDGE_CURVE ( 'NONE', #12728, #49110, #62562, .T. ) ;
#69106 = MECHANICAL_DESIGN_GEOMETRIC_PRESENTATION_REPRESENTATION (  '', ( #59002 ), #13047 ) ;
#69107 = CARTESIAN_POINT ( 'NONE',  ( -2.372962308248625529, -8.656820664281497102, 34.87096338111211935 ) ) ;
#69108 = VERTEX_POINT ( 'NONE', #7259 ) ;
#69109 = CARTESIAN_POINT ( 'NONE',  ( -14.30769230769230660, -12.62096338111211580, 30.90682066428153263 ) ) ;
#69110 = ORIENTED_EDGE ( 'NONE', *, *, #75319, .F. ) ;
#69111 = CARTESIAN_POINT ( 'NONE',  ( 13.25392478150508069, -12.35290016733513951, 31.75349464988449455 ) ) ;
#69112 = PLANE ( 'NONE',  #68626 ) ;
#69113 = CARTESIAN_POINT ( 'NONE',  ( -6.699650524162136023, -7.630147987733840509, 34.99859428049665411 ) ) ;
#69114 = FACE_OUTER_BOUND ( 'NONE', #88109, .T. ) ;
#69115 = DIRECTION ( 'NONE',  ( -1.000000000000000000, 0.000000000000000000, 0.000000000000000000 ) ) ;
#69116 = ADVANCED_FACE ( 'NONE', ( #49122 ), #21204, .F. ) ;
#69117 = ORIENTED_EDGE ( 'NONE', *, *, #85614, .F. ) ;
#69118 = VERTEX_POINT ( 'NONE', #20329 ) ;
#69119 = B_SPLINE_CURVE_WITH_KNOTS ( 'NONE', 3,
 ( #83879, #22598, #29376, #43322, #70801, #2316, #7324, #34783, #82980, #48741 ),
 .UNSPECIFIED., .F., .F.,
 ( 4, 2, 2, 2, 4 ),
 ( 0.0007817246256747530271, 0.0009771112852218974409, 0.001172497944769041638, 0.001367884604316185835, 0.001563271263863330249 ),
 .UNSPECIFIED. ) ;
#69120 = B_SPLINE_CURVE_WITH_KNOTS ( 'NONE', 3,
 ( #70613, #36388, #42269, #63850, #27854, #2148, #41375, #56213, #69726, #8031 ),
 .UNSPECIFIED., .F., .F.,
 ( 4, 2, 2, 2, 4 ),
 ( 0.000000000000000000, 0.0001954311564186863323, 0.0003908623128373726646, 0.0005862934692560590241, 0.0007817246256747453293 ),
 .UNSPECIFIED. ) ;
#69121 = EDGE_LOOP ( 'NONE', ( #86629, #24416, #49936, #31849 ) ) ;
#69122 = ORIENTED_EDGE ( 'NONE', *, *, #40533, .T. ) ;
#69123 = CARTESIAN_POINT ( 'NONE',  ( 5.076923076923075762, -2.708943851104267164, 35.45975837776705220 ) ) ;
#69124 = CARTESIAN_POINT ( 'NONE',  ( 7.715462379486285549, -3.530157926970578508, 32.79014554554150607 ) ) ;
#69125 = VECTOR ( 'NONE', #8608, 1000.000000000000227 ) ;
#69126 = DIRECTION ( 'NONE',  ( -0.000000000000000000, 0.6427876096865404731, -0.7660444431189771253 ) ) ;
#69127 = DIRECTION ( 'NONE',  ( -0.000000000000000000, 0.7660444431189791237, -0.6427876096865379196 ) ) ;
#69128 = LINE ( 'NONE', #34455, #50732 ) ;
#69129 = CARTESIAN_POINT ( 'NONE',  ( -15.45425415533356528, -2.612411019501189369, 31.66733052389439962 ) ) ;
#69130 = VERTEX_POINT ( 'NONE', #42384 ) ;
#69131 = ORIENTED_EDGE ( 'NONE', *, *, #25687, .F. ) ;
#69132 = EDGE_LOOP ( 'NONE', ( #21828, #40260, #24699, #43654 ) ) ;
#69134 = ORIENTED_EDGE ( 'NONE', *, *, #41622, .F. ) ;
#69133 = LINE ( 'NONE', #70467, #71782 ) ;
#69135 = CYLINDRICAL_SURFACE ( 'NONE', #59219, 0.2500000000000009437 ) ;
#69136 = CARTESIAN_POINT ( 'NONE',  ( 6.989246064039581263, -7.250054483168843156, 34.74374881642865631 ) ) ;
#69137 = CARTESIAN_POINT ( 'NONE',  ( 2.320192649118979489E-14, -11.25000000000000000, 19.78125000000000000 ) ) ;
#69138 = ORIENTED_EDGE ( 'NONE', *, *, #38720, .T. ) ;
#69139 = EDGE_CURVE ( 'NONE', #22888, #4743, #34724, .T. ) ;
#69140 = VECTOR ( 'NONE', #46673, 1000.000000000000227 ) ;
#69141 = ORIENTED_EDGE ( 'NONE', *, *, #74844, .T. ) ;
#69142 = FACE_OUTER_BOUND ( 'NONE', #79380, .T. ) ;
#69144 = EDGE_CURVE ( 'NONE', #28039, #39612, #55435, .T. ) ;
#69143 = ORIENTED_EDGE ( 'NONE', *, *, #74682, .T. ) ;
#69145 = FACE_BOUND ( 'NONE', #26807, .T. ) ;
#69147 = AXIS2_PLACEMENT_3D ( 'NONE', #50124, #84828, #63644 ) ;
#69146 = CARTESIAN_POINT ( 'NONE',  ( 6.699591979352975457, -4.386631170607603991, 33.66268669641500111 ) ) ;
#69148 = AXIS2_PLACEMENT_3D ( 'NONE', #34374, #77142, #598 ) ;
#69149 = CYLINDRICAL_SURFACE ( 'NONE', #8914, 0.2499999999999995559 ) ;
#69150 = ORIENTED_EDGE ( 'NONE', *, *, #42770, .F. ) ;
#69152 = EDGE_CURVE ( 'NONE', #76205, #32515, #59378, .T. ) ;
#69151 = CARTESIAN_POINT ( 'NONE',  ( -9.822998295418001291, -4.684245665217972032, 34.18127051446801090 ) ) ;
#69153 = CARTESIAN_POINT ( 'NONE',  ( 8.992010438208831502, -8.540255544307065350, 34.89611431652622286 ) ) ;
#69154 = CARTESIAN_POINT ( 'NONE',  ( -13.63461538461538325, -7.500000000000001776, 34.75000000000000000 ) ) ;
#69155 = DIRECTION ( 'NONE',  ( -0.000000000000000000, 1.000000000000000000, -0.000000000000000000 ) ) ;
#69156 = ORIENTED_EDGE ( 'NONE', *, *, #80072, .F. ) ;
#69157 = AXIS2_PLACEMENT_3D ( 'NONE', #68602, #81686, #20421 ) ;
#69158 = EDGE_CURVE ( 'NONE', #45937, #64075, #88443, .T. ) ;
#69159 = CARTESIAN_POINT ( 'NONE',  ( 12.46153846153833911, -11.48612834414049644, 32.76840700105863391 ) ) ;
#69160 = CARTESIAN_POINT ( 'NONE',  ( -4.153846153846152411, -9.905515769479276145, 34.41647553114623292 ) ) ;
#69161 = FACE_OUTER_BOUND ( 'NONE', #57015, .T. ) ;
#69162 = CARTESIAN_POINT ( 'NONE',  ( -2.241624974342230292, -9.058645607665452459, 34.76329471203371924 ) ) ;
#69163 = FACE_OUTER_BOUND ( 'NONE', #84185, .T. ) ;
#69164 = FACE_BOUND ( 'NONE', #20751, .T. ) ;
#69166 = CARTESIAN_POINT ( 'NONE',  ( -17.29985003582992320, -10.77366814457252175, 33.85459836347579454 ) ) ;
#69165 = CARTESIAN_POINT ( 'NONE',  ( 4.826946345980721809, -11.28823185664190376, 33.01397839955799896 ) ) ;
#69167 = CARTESIAN_POINT ( 'NONE',  ( 5.076923076922953193, -2.379036618888197729, 30.90682066428292885 ) ) ;
#69169 = CARTESIAN_POINT ( 'NONE',  ( 2.557637717070352590, -6.653508905675590945, 34.93172785388651391 ) ) ;
#69168 = CARTESIAN_POINT ( 'NONE',  ( -1.384615384615383471, -4.661471528628507777, 34.16647553114623292 ) ) ;
#69170 = EDGE_CURVE ( 'NONE', #87106, #5632, #85571, .T. ) ;
#69171 = CARTESIAN_POINT ( 'NONE',  ( -18.06527044596078113, -10.21337939537584560, 33.94971097300158647 ) ) ;
#69172 = CARTESIAN_POINT ( 'NONE',  ( 1.901340078031349856, -5.512252781505337929, 16.56063170625848713 ) ) ;
#69173 = ORIENTED_EDGE ( 'NONE', *, *, #24273, .F. ) ;
#69174 = CARTESIAN_POINT ( 'NONE',  ( -5.933932666649923249, -10.67929555188718282, 33.92786785259544757 ) ) ;
#69175 = ORIENTED_EDGE ( 'NONE', *, *, #44181, .F. ) ;
#69176 = CARTESIAN_POINT ( 'NONE',  ( -15.16470087976679260, -4.098570777380720287, 33.41473453929635440 ) ) ;
#69177 = EDGE_LOOP ( 'NONE', ( #76649, #59396, #52738, #62862 ) ) ;
#69178 = CARTESIAN_POINT ( 'NONE',  ( -11.40793610022789828, -6.808710257144161559, 34.95449254468098843 ) ) ;
#69179 = CARTESIAN_POINT ( 'NONE',  ( -7.911424292114620727, -10.21337939537584383, 33.94971097300158647 ) ) ;
#69180 = ORIENTED_EDGE ( 'NONE', *, *, #37717, .T. ) ;
#69181 = DIRECTION ( 'NONE',  ( -0.000000000000000000, 0.8660254037844397068, -0.4999999999999978906 ) ) ;
#69182 = CARTESIAN_POINT ( 'NONE',  ( -0.06109907496454585613, -4.750000000000000000, 17.65438170625849068 ) ) ;
#69183 = CARTESIAN_POINT ( 'NONE',  ( 4.087762742890273415, -8.973038597847269315, 34.52809138561120506 ) ) ;
#69184 = CARTESIAN_POINT ( 'NONE',  ( -7.053224892808620083, -12.70455904226513866, 30.44083106164009322 ) ) ;
#69185 = LINE ( 'NONE', #62848, #23053 ) ;
#69186 = CARTESIAN_POINT ( 'NONE',  ( -17.07692307692307665, -1.367168528481310208, 33.57946703557072254 ) ) ;
#69187 = CARTESIAN_POINT ( 'NONE',  ( -1.134669975237340589, -6.653508905675590945, 34.93172785388651391 ) ) ;
#69188 = CARTESIAN_POINT ( 'NONE',  ( -5.999999999999998224, -10.51840700105979565, 33.73612834413961536 ) ) ;
#69189 = CARTESIAN_POINT ( 'NONE',  ( -3.775308065498748977, -8.992201783934593351, 25.26749329374151642 ) ) ;
#69190 = CARTESIAN_POINT ( 'NONE',  ( -9.692307692307691624, -3.513871655860378418, 32.76840700105978499 ) ) ;
#69191 = CARTESIAN_POINT ( 'NONE',  ( 1.384615384615265343, -11.94971097300221174, 32.03036669348237098 ) ) ;
#69192 = EDGE_LOOP ( 'NONE', ( #81547, #53749 ) ) ;
#69193 = VECTOR ( 'NONE', #28636, 1000.000000000000227 ) ;
#69194 = LINE ( 'NONE', #22336, #87323 ) ;
#69195 = CARTESIAN_POINT ( 'NONE',  ( 2.320192649118979489E-14, -11.25000000000000000, 14.78125000000000178 ) ) ;
#69196 = EDGE_CURVE ( 'NONE', #24412, #28929, #29246, .T. ) ;
#69197 = CARTESIAN_POINT ( 'NONE',  ( -17.06410256410256565, -7.500000000000000000, 29.75000000000000355 ) ) ;
#69198 = LINE ( 'NONE', #28201, #48376 ) ;
#69199 = EDGE_LOOP ( 'NONE', ( #50900, #18425 ) ) ;
#69200 = EDGE_CURVE ( 'NONE', #74216, #49742, #4511, .T. ) ;
#69201 = CARTESIAN_POINT ( 'NONE',  ( 1.384615384615386802, -8.164416787775445883, 34.95778746994557906 ) ) ;
#69202 = CARTESIAN_POINT ( 'NONE',  ( 16.28437159207980045, -2.647132371071621471, 31.75357179365173010 ) ) ;
#69204 = ORIENTED_EDGE ( 'NONE', *, *, #17818, .F. ) ;
#69203 = CARTESIAN_POINT ( 'NONE',  ( -16.94608465891031557, -7.277220443632451463, 34.74524770363009196 ) ) ;
#69205 = CYLINDRICAL_SURFACE ( 'NONE', #45501, 0.2500000000000004996 ) ;
#69206 = CARTESIAN_POINT ( 'NONE',  ( -16.21992956480203318, -10.51840700105979565, 33.73612834413961536 ) ) ;
#69207 = CARTESIAN_POINT ( 'NONE',  ( 16.02315468717859304, -8.999036380462719364, 34.52022231692819076 ) ) ;
#69208 = ADVANCED_FACE ( 'NONE', ( #17104 ), #44559, .F. ) ;
#69209 = CARTESIAN_POINT ( 'NONE',  ( 0.4615384615383396616, -12.46129190930018460, 30.37095296980731973 ) ) ;
#69210 = FACE_OUTER_BOUND ( 'NONE', #70108, .T. ) ;
#69211 = EDGE_CURVE ( 'NONE', #87523, #8641, #77481, .T. ) ;
#69212 = ORIENTED_EDGE ( 'NONE', *, *, #658, .F. ) ;
#69213 = ORIENTED_EDGE ( 'NONE', *, *, #28539, .T. ) ;
#69214 = ORIENTED_EDGE ( 'NONE', *, *, #28878, .F. ) ;
#69215 = VECTOR ( 'NONE', #72011, 1000.000000000000227 ) ;
#69216 = DIRECTION ( 'NONE',  ( -0.000000000000000000, 1.000000000000000000, -0.000000000000000000 ) ) ;
#69217 = CARTESIAN_POINT ( 'NONE',  ( -4.087777802843713282, -3.050289026998446840, 32.03036669348366416 ) ) ;
#69218 = CYLINDRICAL_SURFACE ( 'NONE', #44984, 0.2499999999999986955 ) ;
#69219 = DIRECTION ( 'NONE',  ( 0.000000000000000000, 0.4999999999999985567, 0.8660254037844395958 ) ) ;
#69220 = EDGE_CURVE ( 'NONE', #35285, #43192, #35625, .T. ) ;
#69221 = AXIS2_PLACEMENT_3D ( 'NONE', #13905, #87827, #6705 ) ;
#69222 = ORIENTED_EDGE ( 'NONE', *, *, #49098, .T. ) ;
#69223 = CARTESIAN_POINT ( 'NONE',  ( -12.46153846153858424, -5.094484230521993062, 34.41647553114689373 ) ) ;
#69224 = ORIENTED_EDGE ( 'NONE', *, *, #62181, .F. ) ;
#69225 = EDGE_CURVE ( 'NONE', #48928, #50148, #78356, .T. ) ;
#69226 = EDGE_CURVE ( 'NONE', #62924, #3792, #77046, .T. ) ;
#69227 = ORIENTED_EDGE ( 'NONE', *, *, #2360, .F. ) ;
#69228 = ORIENTED_EDGE ( 'NONE', *, *, #53955, .F. ) ;
#69230 = ORIENTED_EDGE ( 'NONE', *, *, #82677, .F. ) ;
#69229 = CARTESIAN_POINT ( 'NONE',  ( 8.638540166120463937, -12.35290016733513951, 31.75349464988449455 ) ) ;
#69231 = CARTESIAN_POINT ( 'NONE',  ( -0.6850234052624097902, -5.113361153441934093, 34.14387501736622710 ) ) ;
#69232 = EDGE_CURVE ( 'NONE', #74248, #29230, #12010, .T. ) ;
#69233 = CARTESIAN_POINT ( 'NONE',  ( -3.480745974817820887, -12.01397095200673881, 32.43157075238190146 ) ) ;
#69234 = B_SPLINE_CURVE_WITH_KNOTS ( 'NONE', 3,
 ( #79584, #25074, #80473, #10676, #45784, #37694, #16984, #79132, #18769, #44433 ),
 .UNSPECIFIED., .F., .F.,
 ( 4, 2, 2, 2, 4 ),
 ( 0.0007817359430256232838, 0.0009771253907249928539, 0.001172514838424355485, 0.001367904286123718116, 0.001563293733823080747 ),
 .UNSPECIFIED. ) ;
#69235 = LINE ( 'NONE', #22808, #6212 ) ;
#69236 = CARTESIAN_POINT ( 'NONE',  ( 1.384615384615386802, -4.786620604624113540, 33.94971097300155094 ) ) ;
#69237 = VERTEX_POINT ( 'NONE', #22974 ) ;
#69238 = ORIENTED_EDGE ( 'NONE', *, *, #56547, .T. ) ;
#69239 = EDGE_LOOP ( 'NONE', ( #5519, #17976 ) ) ;
#69240 = CARTESIAN_POINT ( 'NONE',  ( -14.05769230769237055, -7.565270445406050648, 34.75000000000000000 ) ) ;
#69242 = ORIENTED_EDGE ( 'NONE', *, *, #81799, .T. ) ;
#69241 = DIRECTION ( 'NONE',  ( 1.000000000000000000, 0.000000000000000000, 0.000000000000000000 ) ) ;
#69243 = CARTESIAN_POINT ( 'NONE',  ( -2.294871794871793824, -11.50000000000000000, 29.75000000000000355 ) ) ;
#69244 = LINE ( 'NONE', #35010, #69558 ) ;
#69245 = VERTEX_POINT ( 'NONE', #16224 ) ;
#69246 = B_SPLINE_CURVE_WITH_KNOTS ( 'NONE', 3,
 ( #71405, #9710, #71854, #65087, #30430, #29992, #2945, #36314, #3394, #51119 ),
 .UNSPECIFIED., .F., .F.,
 ( 4, 2, 2, 2, 4 ),
 ( 0.0007817359430256221996, 0.0009771253907249863487, 0.001172514838424350498, 0.001367904286123714647, 0.001563293733823078796 ),
 .UNSPECIFIED. ) ;
#69247 = AXIS2_PLACEMENT_3D ( 'NONE', #23530, #50985, #15468 ) ;
#69248 = CARTESIAN_POINT ( 'NONE',  ( -4.153846153846273204, -5.219633306517616589, 34.19971097300220464 ) ) ;
#69249 = CARTESIAN_POINT ( 'NONE',  ( 12.68455130563185662, -9.172514111537584114, 34.72667873470787470 ) ) ;
#69250 = ORIENTED_EDGE ( 'NONE', *, *, #27313, .F. ) ;
#69251 = FACE_BOUND ( 'NONE', #15058, .T. ) ;
#69252 = CARTESIAN_POINT ( 'NONE',  ( -17.86947429823644029, -8.586989748646450593, 34.63063291749215011 ) ) ;
#69253 = CARTESIAN_POINT ( 'NONE',  ( -24.00000000000000000, -5.499999999999981348, 27.75000000000000000 ) ) ;
#69254 = B_SPLINE_CURVE_WITH_KNOTS ( 'NONE', 3,
 ( #14461, #40174, #82490, #47799, #21209, #75280, #67637, #41939, #20769, #33408 ),
 .UNSPECIFIED., .F., .F.,
 ( 4, 2, 2, 2, 4 ),
 ( 0.000000000000000000, 0.0001954311584214072923, 0.0003908623168428145846, 0.0005862934752642218498, 0.0007817246336856291692 ),
 .UNSPECIFIED. ) ;
#69255 = ADVANCED_FACE ( 'NONE', ( #71158 ), #2690, .F. ) ;
#69256 = CARTESIAN_POINT ( 'NONE',  ( 3.230769230769231726, -8.973038597847269315, 34.52809138561121927 ) ) ;
#69258 = CARTESIAN_POINT ( 'NONE',  ( 0.000000000000000000, -11.00000000000000000, 29.75000000000000355 ) ) ;
#69257 = DIRECTION ( 'NONE',  ( -0.000000000000000000, 0.5000000000000011102, -0.8660254037844380415 ) ) ;
#69259 = DIRECTION ( 'NONE',  ( -0.000000000000000000, 0.1736481776669307198, -0.9848077530122080203 ) ) ;
#69260 = CARTESIAN_POINT ( 'NONE',  ( 0.7115384615384606759, -2.249999999999998668, 29.75000000000000355 ) ) ;
#69261 = EDGE_LOOP ( 'NONE', ( #66567, #675, #35438, #65347, #6431, #38070 ) ) ;
#69262 = CARTESIAN_POINT ( 'NONE',  ( -16.15384615384615330, -13.20930481340135110, 34.54067556320372745 ) ) ;
#69263 = CARTESIAN_POINT ( 'NONE',  ( 13.25413867649892552, -7.276988635370452485, 34.74523720219453793 ) ) ;
#69264 = EDGE_LOOP ( 'NONE', ( #14994, #48972 ) ) ;
#69265 = EDGE_CURVE ( 'NONE', #76524, #12327, #14065, .T. ) ;
#69266 = CARTESIAN_POINT ( 'NONE',  ( 8.638539302563209787, -3.062553014421049546, 32.05460306192773601 ) ) ;
#69267 = CARTESIAN_POINT ( 'NONE',  ( -4.403869378067608586, -3.520140089381497361, 33.17453946501458262 ) ) ;
#69268 = ORIENTED_EDGE ( 'NONE', *, *, #34369, .T. ) ;
#69269 = FACE_OUTER_BOUND ( 'NONE', #45182, .T. ) ;
#69270 = DIRECTION ( 'NONE',  ( 0.000000000000000000, 0.000000000000000000, -1.000000000000000000 ) ) ;
#69271 = FACE_BOUND ( 'NONE', #41014, .T. ) ;
#69273 = CARTESIAN_POINT ( 'NONE',  ( 4.153846153846154188, -12.34228464037088635, 31.77849191805839268 ) ) ;
#69272 = CARTESIAN_POINT ( 'NONE',  ( 7.846153846153846700, -2.708943851104267164, 35.45975837776705220 ) ) ;
#69274 = FACE_OUTER_BOUND ( 'NONE', #19905, .T. ) ;
#69275 = VECTOR ( 'NONE', #5504, 1000.000000000000000 ) ;
#69276 = PLANE ( 'NONE',  #61144 ) ;
#69278 = DIRECTION ( 'NONE',  ( -1.000000000000000000, -0.000000000000000000, -0.000000000000000000 ) ) ;
#69277 = DIRECTION ( 'NONE',  ( 1.000000000000000000, 0.000000000000000000, 0.000000000000000000 ) ) ;
#69279 = EDGE_CURVE ( 'NONE', #71146, #52853, #206, .T. ) ;
#69280 = DIRECTION ( 'NONE',  ( -0.000000000000000000, 0.8660254037844397068, -0.4999999999999978906 ) ) ;
#69281 = CARTESIAN_POINT ( 'NONE',  ( -0.06109907496455085213, -3.750000000000000888, 16.40438170625849068 ) ) ;
#69282 = ORIENTED_EDGE ( 'NONE', *, *, #75265, .T. ) ;
#69283 = VECTOR ( 'NONE', #87669, 1000.000000000000227 ) ;
#69284 = ORIENTED_EDGE ( 'NONE', *, *, #28238, .F. ) ;
#69285 = CARTESIAN_POINT ( 'NONE',  ( -23.00000000000000000, -9.499999999999982236, 27.74999999999999645 ) ) ;
#69286 = CARTESIAN_POINT ( 'NONE',  ( -0.7115616988314267255, -2.823816976329320827, 31.52131813110797154 ) ) ;
#69287 = CARTESIAN_POINT ( 'NONE',  ( 1.607628228708781748, -9.172514111537584114, 34.72667873470787470 ) ) ;
#69288 = CARTESIAN_POINT ( 'NONE',  ( -1.514762594053604250, -3.285722584762969856, 32.44110544564090759 ) ) ;
#69289 = CARTESIAN_POINT ( 'NONE',  ( -9.692307692307814193, -12.51329471203414379, 31.30864560766407578 ) ) ;
#69290 = CARTESIAN_POINT ( 'NONE',  ( -3.749999999999988454, -9.053300858899127945, 26.26562500000000000 ) ) ;
#69291 = VECTOR ( 'NONE', #16140, 1000.000000000000114 ) ;
#69292 = B_SPLINE_CURVE_WITH_KNOTS ( 'NONE', 3,
 ( #41624, #66548, #20897, #56016, #18806, #6946, #34416, #87728, #83504, #21790 ),
 .UNSPECIFIED., .F., .F.,
 ( 4, 2, 2, 2, 4 ),
 ( 0.000000000000000000, 0.0001954311564186858715, 0.0003908623128373717431, 0.0005862934692560576146, 0.0007817246256747434861 ),
 .UNSPECIFIED. ) ;
#69293 = CYLINDRICAL_SURFACE ( 'NONE', #82024, 0.2499999999999986955 ) ;
#69295 = CARTESIAN_POINT ( 'NONE',  ( 1.254467414883691401, -10.31621877034669588, 34.18098118002070152 ) ) ;
#69294 = B_SPLINE_CURVE_WITH_KNOTS ( 'NONE', 3,
 ( #42120, #33251, #46311, #67481, #12101, #60712, #21836, #76784, #88219, #2871 ),
 .UNSPECIFIED., .F., .F.,
 ( 4, 2, 2, 2, 4 ),
 ( 0.0007817246256747465219, 0.0009771112852218900684, 0.001172497944769033615, 0.001367884604316177378, 0.001563271263863320925 ),
 .UNSPECIFIED. ) ;
#69296 = EDGE_CURVE ( 'NONE', #18061, #86451, #80608, .T. ) ;
#69297 = CARTESIAN_POINT ( 'NONE',  ( -17.30040802064702987, -5.113361153441931428, 34.14387501736621999 ) ) ;
#69298 = CARTESIAN_POINT ( 'NONE',  ( 7.780071466793711643, -5.471508081941601986, 34.59228464037088457 ) ) ;
#69299 = DIRECTION ( 'NONE',  ( 0.000000000000000000, 0.000000000000000000, -1.000000000000000000 ) ) ;
#69300 = LINE ( 'NONE', #76498, #19527 ) ;
#69301 = B_SPLINE_CURVE_WITH_KNOTS ( 'NONE', 3,
 ( #67454, #88195, #26471, #13830, #82745, #20151, #68774, #48494, #21018, #40870 ),
 .UNSPECIFIED., .F., .F.,
 ( 4, 2, 2, 2, 4 ),
 ( 0.000000000000000000, 0.0001954311564186863323, 0.0003908623128373726646, 0.0005862934692560590241, 0.0007817246256747453293 ),
 .UNSPECIFIED. ) ;
#69302 = CARTESIAN_POINT ( 'NONE',  ( -9.915234651214539952, -12.64616026154729411, 30.79003144601914244 ) ) ;
#69303 = CARTESIAN_POINT ( 'NONE',  ( 10.86538461538603606, -7.500000000000154543, 35.00000000000007105 ) ) ;
#69304 = CARTESIAN_POINT ( 'NONE',  ( -12.46153846153815437, -2.506253911140614576, 30.00000000000323297 ) ) ;
#69305 = ORIENTED_EDGE ( 'NONE', *, *, #53942, .T. ) ;
#69306 = CARTESIAN_POINT ( 'NONE',  ( -0.2385271099256121019, -3.587049720035815348, 32.86302985866382897 ) ) ;
#69307 = CARTESIAN_POINT ( 'NONE',  ( -0.4615384615384611200, -9.905515769479276145, 34.41647553114623292 ) ) ;
#69308 = CARTESIAN_POINT ( 'NONE',  ( 2.750000000000002665, -7.561099074964516831, 23.47061829374151642 ) ) ;
#69309 = EDGE_CURVE ( 'NONE', #8757, #29571, #50595, .T. ) ;
#69310 = CARTESIAN_POINT ( 'NONE',  ( -6.000000000000121680, -12.51329471203414379, 31.30864560766407578 ) ) ;
#69311 = CARTESIAN_POINT ( 'NONE',  ( -16.09615384615384670, -7.500000000000000000, 33.75000000000000000 ) ) ;
#69312 = VERTEX_POINT ( 'NONE', #26092 ) ;
#69313 = DIRECTION ( 'NONE',  ( -1.000000000000000000, 0.000000000000000000, 0.000000000000000000 ) ) ;
#69315 = VERTEX_POINT ( 'NONE', #11245 ) ;
#69314 = CARTESIAN_POINT ( 'NONE',  ( -14.55766903863466055, -12.17611988154120972, 31.52148481390971213 ) ) ;
#69316 = CARTESIAN_POINT ( 'NONE',  ( 6.923076923076802558, -3.835265460704628371, 33.15142922262033665 ) ) ;
#69317 = EDGE_CURVE ( 'NONE', #86321, #32791, #38714, .T. ) ;
#69318 = CARTESIAN_POINT ( 'NONE',  ( 12.68455130563185840, -5.582272713120729257, 34.63742843783360570 ) ) ;
#69319 = ORIENTED_EDGE ( 'NONE', *, *, #23441, .T. ) ;
#69320 = CARTESIAN_POINT ( 'NONE',  ( 5.076923076923075762, -13.20930481340135110, 34.54067556320372745 ) ) ;
#69321 = DIRECTION ( 'NONE',  ( 1.000000000000000000, 0.000000000000000000, 0.000000000000000000 ) ) ;
#69322 = ORIENTED_EDGE ( 'NONE', *, *, #8517, .F. ) ;
#69323 = CIRCLE ( 'NONE', #41938, 8.000000000000000000 ) ;
#69324 = CARTESIAN_POINT ( 'NONE',  ( 14.05771557674995265, -2.564618984488975517, 30.55390908950641915 ) ) ;
#69325 = CARTESIAN_POINT ( 'NONE',  ( 7.846153846153846700, -12.34228464037088635, 31.77849191805839268 ) ) ;
#69326 = EDGE_CURVE ( 'NONE', #86793, #47021, #78511, .T. ) ;
#69327 = CARTESIAN_POINT ( 'NONE',  ( 10.03846153846153832, -3.499999999999999556, 29.75000000000000355 ) ) ;
#69328 = ORIENTED_EDGE ( 'NONE', *, *, #68142, .F. ) ;
#69329 = ORIENTED_EDGE ( 'NONE', *, *, #87668, .F. ) ;
#69330 = CARTESIAN_POINT ( 'NONE',  ( 2.980746006547773330, -2.985938066672154445, 32.43141759479405550 ) ) ;
#69331 = ORIENTED_EDGE ( 'NONE', *, *, #56584, .F. ) ;
#69332 = DIRECTION ( 'NONE',  ( -0.000000000000000000, 0.9848077530122086864, -0.1736481776669273891 ) ) ;
#69333 = CARTESIAN_POINT ( 'NONE',  ( 15.29683656411930848, -12.62096338111211757, 30.90682066428152908 ) ) ;
#69334 = CARTESIAN_POINT ( 'NONE',  ( 8.352564102564102200, -7.500000000000000000, 29.75000000000000355 ) ) ;
#69335 = B_SPLINE_CURVE_WITH_KNOTS ( 'NONE', 3,
 ( #71915, #63832, #29183, #50744, #43995, #2128, #70147, #63385, #1693, #84566 ),
 .UNSPECIFIED., .F., .F.,
 ( 4, 2, 2, 2, 4 ),
 ( 0.0007817359527651096280, 0.0009771254036996484919, 0.001172514854634187573, 0.001367904305568726653, 0.001563293756503265517 ),
 .UNSPECIFIED. ) ;
#69336 = FACE_OUTER_BOUND ( 'NONE', #39339, .T. ) ;
#69337 = DIRECTION ( 'NONE',  ( 0.000000000000000000, 0.7660444431189807890, 0.6427876096865361433 ) ) ;
#69338 = CARTESIAN_POINT ( 'NONE',  ( 0.7115384615398802071, -7.500000000000154543, 35.00000000000007105 ) ) ;
#69339 = EDGE_CURVE ( 'NONE', #88144, #23339, #51757, .T. ) ;
#69340 = CARTESIAN_POINT ( 'NONE',  ( 3.230769230769231726, -13.53365097954675988, 30.81389545987213552 ) ) ;
#69341 = EDGE_CURVE ( 'NONE', #75936, #60370, #25888, .T. ) ;
#69342 = EDGE_CURVE ( 'NONE', #75886, #88472, #65728, .T. ) ;
#69343 = ORIENTED_EDGE ( 'NONE', *, *, #13606, .T. ) ;
#69344 = ORIENTED_EDGE ( 'NONE', *, *, #19098, .F. ) ;
#69346 = ORIENTED_EDGE ( 'NONE', *, *, #42587, .T. ) ;
#69345 = CARTESIAN_POINT ( 'NONE',  ( -0.2385271099256117133, -12.15243808032445827, 31.58219941686247978 ) ) ;
#69347 = CARTESIAN_POINT ( 'NONE',  ( 17.07692307692295586, -2.379036618888197729, 30.90682066428292885 ) ) ;
#69348 = CIRCLE ( 'NONE', #29113, 2.000000000000001776 ) ;
#69349 = ORIENTED_EDGE ( 'NONE', *, *, #42587, .F. ) ;
#69350 = AXIS2_PLACEMENT_3D ( 'NONE', #4527, #65769, #4068 ) ;
#69351 = CARTESIAN_POINT ( 'NONE',  ( -13.91025641025641058, -11.00000000000000000, 29.75000000000000355 ) ) ;
#69352 = CARTESIAN_POINT ( 'NONE',  ( -7.846153846153844924, -9.905515769479276145, 34.41647553114623292 ) ) ;
#69353 = VERTEX_POINT ( 'NONE', #86480 ) ;
#69354 = CARTESIAN_POINT ( 'NONE',  ( -9.692307692307384315, -2.506253911140614576, 30.00000000000323297 ) ) ;
#69355 = CIRCLE ( 'NONE', #30511, 4.000000000000000000 ) ;
#69356 = ORIENTED_EDGE ( 'NONE', *, *, #74797, .F. ) ;
#69358 = ORIENTED_EDGE ( 'NONE', *, *, #62549, .T. ) ;
#69357 = CARTESIAN_POINT ( 'NONE',  ( -16.15384615384615330, -3.513871655860378418, 32.76840700105978499 ) ) ;
#69359 = CARTESIAN_POINT ( 'NONE',  ( -12.59168643127015841, -3.625366637846544116, 33.29286588640298561 ) ) ;
#69360 = ORIENTED_EDGE ( 'NONE', *, *, #87170, .F. ) ;
#69361 = CARTESIAN_POINT ( 'NONE',  ( 17.74997676270703550, -10.76384336483936011, 33.53834819971076087 ) ) ;
#69362 = CARTESIAN_POINT ( 'NONE',  ( -8.834501215191544077, -2.892918686051582977, 31.69288490824015980 ) ) ;
#69363 = FACE_BOUND ( 'NONE', #9100, .T. ) ;
#69364 = LINE ( 'NONE', #27487, #22600 ) ;
#69365 = DIRECTION ( 'NONE',  ( -1.000000000000000000, -0.000000000000000000, -0.000000000000000000 ) ) ;
#69366 = CARTESIAN_POINT ( 'NONE',  ( 0.000000000000000000, -11.00000000000000000, 29.75000000000000355 ) ) ;
#69367 = DIRECTION ( 'NONE',  ( 0.000000000000000000, 0.3420201433256641055, -0.9396926207859100932 ) ) ;
#69368 = CARTESIAN_POINT ( 'NONE',  ( -17.14219307747939425, -8.656820664281497102, 34.87096338111211935 ) ) ;
#69369 = CARTESIAN_POINT ( 'NONE',  ( 10.36536139116315525, -10.92453946501458795, 33.72985991061850086 ) ) ;
#69370 = ORIENTED_EDGE ( 'NONE', *, *, #63665, .F. ) ;
#69371 = CARTESIAN_POINT ( 'NONE',  ( -14.24243673641627339, -3.835265460703683349, 33.15142922261929925 ) ) ;
#69372 = EDGE_LOOP ( 'NONE', ( #12750, #61883 ) ) ;
#69373 = ORIENTED_EDGE ( 'NONE', *, *, #86095, .T. ) ;
#69375 = CARTESIAN_POINT ( 'NONE',  ( 13.38461538461538680, -1.242168528481310874, 33.36296068462461051 ) ) ;
#69374 = CARTESIAN_POINT ( 'NONE',  ( 6.923076923076802558, -5.219633306517616589, 34.19971097300220464 ) ) ;
#69376 = AXIS2_PLACEMENT_3D ( 'NONE', #88236, #25617, #42135 ) ;
#69377 = CARTESIAN_POINT ( 'NONE',  ( 2.307692307692187583, -12.46129190930018460, 30.37095296980731973 ) ) ;
#69378 = CARTESIAN_POINT ( 'NONE',  ( -16.94639763868943660, -10.31582465632704704, 34.18122507451815295 ) ) ;
#69379 = CARTESIAN_POINT ( 'NONE',  ( -10.54931728203453822, -12.34228464037088813, 31.77849191805839268 ) ) ;
#69380 = CARTESIAN_POINT ( 'NONE',  ( 13.38461538461526601, -11.48612834414049644, 32.76840700105863391 ) ) ;
#69381 = EDGE_LOOP ( 'NONE', ( #76659, #41475, #35974, #76655 ) ) ;
#69382 = CARTESIAN_POINT ( 'NONE',  ( 13.16113044089144068, -5.113361153441934093, 34.14387501736622710 ) ) ;
#69383 = LINE ( 'NONE', #49983, #56034 ) ;
#69384 = CARTESIAN_POINT ( 'NONE',  ( 17.01165307636676260, -4.320704448112772766, 33.92786785259540494 ) ) ;
#69385 = CARTESIAN_POINT ( 'NONE',  ( 6.166666666666664298, -4.000000000000000000, 29.75000000000000355 ) ) ;
#69386 = LINE ( 'NONE', #35149, #80805 ) ;
#69387 = AXIS2_PLACEMENT_3D ( 'NONE', #40094, #67109, #18916 ) ;
#69388 = EDGE_LOOP ( 'NONE', ( #76958, #70333, #9893, #60147 ) ) ;
#69389 = ORIENTED_EDGE ( 'NONE', *, *, #63249, .T. ) ;
#69390 = CONTEXT_DEPENDENT_SHAPE_REPRESENTATION ( #65339, #65000 ) ;
#69391 = ORIENTED_EDGE ( 'NONE', *, *, #73530, .T. ) ;
#69392 = CARTESIAN_POINT ( 'NONE',  ( -6.130690603110309667, -3.957541250942359756, 33.62499894934981626 ) ) ;
#69393 = ORIENTED_EDGE ( 'NONE', *, *, #936, .T. ) ;
#69394 = DIRECTION ( 'NONE',  ( 0.000000000000000000, 0.8660254037844377084, 0.5000000000000015543 ) ) ;
#69395 = CARTESIAN_POINT ( 'NONE',  ( -12.39547011053602432, -6.386643153685127139, 34.62446782046654192 ) ) ;
#69396 = FACE_OUTER_BOUND ( 'NONE', #85222, .T. ) ;
#69397 = CARTESIAN_POINT ( 'NONE',  ( 2.651650429449539104, -4.848349570550432475, 14.31250000000000000 ) ) ;
#69398 = CARTESIAN_POINT ( 'NONE',  ( 12.21151522424549896, -10.05641848906368097, 34.04755513067966177 ) ) ;
#69399 = ORIENTED_EDGE ( 'NONE', *, *, #29382, .F. ) ;
#69400 = CARTESIAN_POINT ( 'NONE',  ( 11.28846153846153832, -2.499999999999998668, 29.75000000000000355 ) ) ;
#69402 = VERTEX_POINT ( 'NONE', #80151 ) ;
#69401 = CARTESIAN_POINT ( 'NONE',  ( -0.6850233861027916760, -5.827078755546623690, 34.72654668319379567 ) ) ;
#69403 = CARTESIAN_POINT ( 'NONE',  ( 2.307692307692309264, -6.343179335718451384, 34.87096338111211935 ) ) ;
#69404 = CARTESIAN_POINT ( 'NONE',  ( -17.07692307692307665, -8.120952969808772792, 34.71129190930000163 ) ) ;
#69405 = CARTESIAN_POINT ( 'NONE',  ( 16.85399685940691938, -3.586966769969702540, 32.86292498521069660 ) ) ;
#69406 = CARTESIAN_POINT ( 'NONE',  ( 8.900021210197715860, -11.93129842949671726, 32.56571108434900452 ) ) ;
#69407 = CARTESIAN_POINT ( 'NONE',  ( -12.68502340526240957, -2.847400154188067578, 31.58180166144859058 ) ) ;
#69408 = CARTESIAN_POINT ( 'NONE',  ( 18.00000000000000000, -12.29105614889573062, 35.45975837776705220 ) ) ;
#69409 = CARTESIAN_POINT ( 'NONE',  ( -12.59168567097668401, -12.45813303252208648, 30.39737893381572675 ) ) ;
#69410 = CARTESIAN_POINT ( 'NONE',  ( 3.750000000000001776, -7.561099074964511502, 14.72061829374151465 ) ) ;
#69411 = ORIENTED_EDGE ( 'NONE', *, *, #16208, .F. ) ;
#69412 = DIRECTION ( 'NONE',  ( -0.000000000000000000, 0.9848077530122085754, -0.1736481776669273613 ) ) ;
#69413 = DIRECTION ( 'NONE',  ( -1.000000000000000000, -0.000000000000000000, -0.000000000000000000 ) ) ;
#69414 = ADVANCED_FACE ( 'NONE', ( #73391 ), #11698, .F. ) ;
#69415 = DIRECTION ( 'NONE',  ( 0.000000000000000000, 0.7660444431189807890, 0.6427876096865361433 ) ) ;
#69416 = CARTESIAN_POINT ( 'NONE',  ( -3.100243792535588128, -11.04252011169590020, 33.62494198852677130 ) ) ;
#69417 = ORIENTED_EDGE ( 'NONE', *, *, #18090, .T. ) ;
#69418 = CARTESIAN_POINT ( 'NONE',  ( -9.692307692307691624, -3.513871655860378418, 32.76840700105978499 ) ) ;
#69419 = CARTESIAN_POINT ( 'NONE',  ( -16.08859058257012720, -12.27809138561124591, 31.22303859784720359 ) ) ;
#69420 = VECTOR ( 'NONE', #85487, 1000.000000000000000 ) ;
#69421 = CARTESIAN_POINT ( 'NONE',  ( -0.6850233861027934523, -12.69144148231606017, 30.53333754910549303 ) ) ;
#69422 = CARTESIAN_POINT ( 'NONE',  ( 14.08476609017615644, -3.105860786376062332, 32.13614157043599562 ) ) ;
#69423 = ORIENTED_EDGE ( 'NONE', *, *, #58025, .F. ) ;
#69424 = CARTESIAN_POINT ( 'NONE',  ( -12.33101275977490197, -9.417988943895561960, 34.36773134775777550 ) ) ;
#69425 = EDGE_CURVE ( 'NONE', #69684, #7426, #68403, .T. ) ;
#69426 = DIRECTION ( 'NONE',  ( 0.000000000000000000, 0.8660254037844377084, -0.5000000000000015543 ) ) ;
#69427 = CARTESIAN_POINT ( 'NONE',  ( -14.05769230769224265, -7.434744860731433924, 35.00000000000000711 ) ) ;
#69428 = ORIENTED_EDGE ( 'NONE', *, *, #34021, .T. ) ;
#69429 = FACE_OUTER_BOUND ( 'NONE', #36069, .T. ) ;
#69430 = EDGE_LOOP ( 'NONE', ( #16778, #62693, #42265, #68249 ) ) ;
#69431 = DIRECTION ( 'NONE',  ( 1.000000000000000000, 0.000000000000000000, 0.000000000000000000 ) ) ;
#69432 = CARTESIAN_POINT ( 'NONE',  ( 4.826899852701619587, -5.765609946408404518, 34.70566812827425451 ) ) ;
#69433 = EDGE_LOOP ( 'NONE', ( #1747, #67257, #50783, #42480 ) ) ;
#69434 = LINE ( 'NONE', #20371, #79286 ) ;
#69435 = CARTESIAN_POINT ( 'NONE',  ( -8.769230769230768274, -2.538708090699994813, 30.37095296980875503 ) ) ;
#69436 = CARTESIAN_POINT ( 'NONE',  ( 13.25446817517716447, -6.852621066184266141, 34.70813303252209181 ) ) ;
#69437 = VECTOR ( 'NONE', #18701, 1000.000000000000227 ) ;
#69438 = AXIS2_PLACEMENT_3D ( 'NONE', #10243, #45341, #79139 ) ;
#69439 = CARTESIAN_POINT ( 'NONE',  ( 19.00000000000000000, -1.250000000000000000, 22.25000000000000000 ) ) ;
#69440 = CARTESIAN_POINT ( 'NONE',  ( -18.00000000000000000, -2.833524468853757305, 32.15551576947926549 ) ) ;
#69441 = EDGE_CURVE ( 'NONE', #74870, #38427, #69735, .T. ) ;
#69442 = EDGE_CURVE ( 'NONE', #2529, #85483, #5465, .T. ) ;
#69443 = EDGE_LOOP ( 'NONE', ( #42448, #34756 ) ) ;
#69444 = ORIENTED_EDGE ( 'NONE', *, *, #20584, .T. ) ;
#69445 = FACE_BOUND ( 'NONE', #25278, .T. ) ;
#69446 = ORIENTED_EDGE ( 'NONE', *, *, #11144, .T. ) ;
#69447 = DIRECTION ( 'NONE',  ( -0.000000000000000000, -0.9848077530122086864, -0.1736481776669273613 ) ) ;
#69448 = EDGE_CURVE ( 'NONE', #9433, #13174, #21544, .T. ) ;
#69449 = CARTESIAN_POINT ( 'NONE',  ( -5.076923076923075762, -11.91647553114624181, 32.58852847137148245 ) ) ;
#69450 = FACE_OUTER_BOUND ( 'NONE', #65500, .T. ) ;
#69451 = CARTESIAN_POINT ( 'NONE',  ( 6.923076923076924238, -9.780366693483667717, 34.19971097300155094 ) ) ;
#69452 = ORIENTED_EDGE ( 'NONE', *, *, #6860, .T. ) ;
#69453 = EDGE_LOOP ( 'NONE', ( #88823, #11956 ) ) ;
#69454 = VERTEX_POINT ( 'NONE', #81935 ) ;
#69455 = CARTESIAN_POINT ( 'NONE',  ( 2.544871794871792936, -3.499999999999999556, 29.75000000000000355 ) ) ;
#69456 = ORIENTED_EDGE ( 'NONE', *, *, #45283, .T. ) ;
#69457 = CARTESIAN_POINT ( 'NONE',  ( -5.198717948717948012, -3.499999999999999556, 29.75000000000000355 ) ) ;
#69458 = CARTESIAN_POINT ( 'NONE',  ( -9.442307692306256328, -7.500000000000155431, 34.75000000000007105 ) ) ;
#69459 = CARTESIAN_POINT ( 'NONE',  ( -18.00000000000012079, -11.48612834414049644, 32.76840700105863391 ) ) ;
#69460 = VECTOR ( 'NONE', #76908, 1000.000000000000000 ) ;
#69461 = CARTESIAN_POINT ( 'NONE',  ( -1.161652481053898844, -7.369474270740069777, 34.74850911626239736 ) ) ;
#69462 = VECTOR ( 'NONE', #53389, 1000.000000000000000 ) ;
#69463 = DIRECTION ( 'NONE',  ( 0.000000000000000000, 1.000000000000000000, 0.000000000000000000 ) ) ;
#69464 = CARTESIAN_POINT ( 'NONE',  ( -14.30769230769230660, -4.661471528628507777, 34.16647553114623292 ) ) ;
#69465 = CARTESIAN_POINT ( 'NONE',  ( -5.076923076923197442, -3.835265460704628371, 33.15142922262033665 ) ) ;
#69466 = VERTEX_POINT ( 'NONE', #61639 ) ;
#69467 = EDGE_LOOP ( 'NONE', ( #35841, #8567, #46056, #1377, #67472, #50210 ) ) ;
#69468 = CIRCLE ( 'NONE', #70894, 2.000000000000001776 ) ;
#69469 = EDGE_LOOP ( 'NONE', ( #53935, #48346, #65406, #44494 ) ) ;
#69470 = CARTESIAN_POINT ( 'NONE',  ( 3.360816666019682764, -7.723484941389743952, 34.99544897038808955 ) ) ;
#69472 = CARTESIAN_POINT ( 'NONE',  ( 10.48469401227430886, -2.295517848115769421, 30.44137282052137294 ) ) ;
#69471 = DIRECTION ( 'NONE',  ( 0.000000000000000000, 0.9848077530122072432, -0.1736481776669354937 ) ) ;
#69473 = DIRECTION ( 'NONE',  ( 0.000000000000000000, 0.4999999999999985567, 0.8660254037844395958 ) ) ;
#69474 = CARTESIAN_POINT ( 'NONE',  ( -3.453695448285377445, -11.24512374952581872, 33.06303171183252942 ) ) ;
#69475 = FACE_BOUND ( 'NONE', #20383, .T. ) ;
#69476 = CARTESIAN_POINT ( 'NONE',  ( 16.15384615384603251, -3.300289026999228437, 32.46337939537709616 ) ) ;
#69477 = ORIENTED_EDGE ( 'NONE', *, *, #17759, .F. ) ;
#69478 = CARTESIAN_POINT ( 'NONE',  ( -7.911476761646023093, -7.749976743299138882, 34.99404534957040624 ) ) ;
#69479 = CARTESIAN_POINT ( 'NONE',  ( 9.442284468086237226, -12.07920672191015221, 32.31858351112116168 ) ) ;
#69480 = CARTESIAN_POINT ( 'NONE',  ( 3.230769230769231726, -13.75783147151868846, 33.36296068462461051 ) ) ;
#69481 = CARTESIAN_POINT ( 'NONE',  ( 5.076923076923075762, -12.29105614889573062, 35.45975837776705220 ) ) ;
#69482 = ORIENTED_EDGE ( 'NONE', *, *, #86809, .T. ) ;
#69483 = CARTESIAN_POINT ( 'NONE',  ( 2.557637826040451756, -11.86320923018887719, 32.19269448109604781 ) ) ;
#69484 = ORIENTED_EDGE ( 'NONE', *, *, #15509, .T. ) ;
#69485 = FACE_BOUND ( 'NONE', #59817, .T. ) ;
#69486 = CARTESIAN_POINT ( 'NONE',  ( 3.512820512820510555, -7.500000000000000000, 33.75000000000000000 ) ) ;
#69487 = B_SPLINE_CURVE_WITH_KNOTS ( 'NONE', 3,
 ( #22675, #77622, #36210, #10499, #37968, #37066, #15931, #63661, #23994, #84842 ),
 .UNSPECIFIED., .F., .F.,
 ( 4, 2, 2, 2, 4 ),
 ( 0.000000000000000000, 0.0001954339857564063360, 0.0003908679715128126719, 0.0005863019572692189808, 0.0007817359430256253438 ),
 .UNSPECIFIED. ) ;
#69488 = CARTESIAN_POINT ( 'NONE',  ( 17.07692307692307665, -11.69971097300155272, 32.46337939537588113 ) ) ;
#69489 = CARTESIAN_POINT ( 'NONE',  ( -12.46153846153858424, -12.16647553114689728, 32.15551576947799362 ) ) ;
#69490 = ORIENTED_EDGE ( 'NONE', *, *, #62921, .T. ) ;
#69491 = DIRECTION ( 'NONE',  ( -0.000000000000000000, 0.6427876096865404731, -0.7660444431189770143 ) ) ;
#69492 = CARTESIAN_POINT ( 'NONE',  ( -17.93393266664992325, -3.937682226553330445, 33.60647404775216529 ) ) ;
#69493 = CARTESIAN_POINT ( 'NONE',  ( 3.230769230769231726, -11.16473453929635440, 33.15142922261926373 ) ) ;
#69494 = CARTESIAN_POINT ( 'NONE',  ( -17.86920955903305597, -12.62708834333097663, 30.88030960425256310 ) ) ;
#69495 = EDGE_LOOP ( 'NONE', ( #80643, #1084, #45841, #63295, #67237, #81499 ) ) ;
#69496 = EDGE_CURVE ( 'NONE', #78547, #42406, #13901, .T. ) ;
#69497 = LINE ( 'NONE', #1490, #2827 ) ;
#69498 = ORIENTED_EDGE ( 'NONE', *, *, #3173, .T. ) ;
#69500 = ORIENTED_EDGE ( 'NONE', *, *, #74949, .F. ) ;
#69499 = CARTESIAN_POINT ( 'NONE',  ( 16.02337096877043621, -7.276987145209182550, 34.99546412871779211 ) ) ;
#69501 = CARTESIAN_POINT ( 'NONE',  ( -18.13049666469081700, -12.75000000000001066, 29.52694327409752262 ) ) ;
#69502 = CARTESIAN_POINT ( 'NONE',  ( -4.403869391139119571, -2.823816976329319495, 31.52131813110795733 ) ) ;
#69503 = CARTESIAN_POINT ( 'NONE',  ( 13.13459214732242408, -9.271318131107980420, 34.42618302367067429 ) ) ;
#69504 = CARTESIAN_POINT ( 'NONE',  ( -4.500000000000003553, 7.499999999999996447, 13.50000000000000178 ) ) ;
#69505 = CARTESIAN_POINT ( 'NONE',  ( -19.00000000000000000, 0.7500000000000051070, 32.75000000000000000 ) ) ;
#69507 = CARTESIAN_POINT ( 'NONE',  ( 16.21910172512217585, -6.026961402152790193, 34.52809138561124769 ) ) ;
#69506 = CARTESIAN_POINT ( 'NONE',  ( -5.934744860487159102, -6.835583212224609184, 34.95778746994559327 ) ) ;
#69508 = CARTESIAN_POINT ( 'NONE',  ( 12.68496542340003508, -7.630147231320743018, 34.74852402298682819 ) ) ;
#69509 = CARTESIAN_POINT ( 'NONE',  ( -1.409462824231155764E-14, -4.749999999999999112, 25.40625000000000000 ) ) ;
#69510 = EDGE_LOOP ( 'NONE', ( #9718, #6627 ) ) ;
#69511 = CYLINDRICAL_SURFACE ( 'NONE', #33252, 0.2499999999999998890 ) ;
#69512 = ORIENTED_EDGE ( 'NONE', *, *, #8745, .T. ) ;
#69513 = EDGE_CURVE ( 'NONE', #18739, #47404, #41382, .T. ) ;
#69514 = ORIENTED_EDGE ( 'NONE', *, *, #8728, .F. ) ;
#69515 = CARTESIAN_POINT ( 'NONE',  ( -17.07692307692307665, -2.499999999999998668, 29.75000000000001421 ) ) ;
#69516 = ORIENTED_EDGE ( 'NONE', *, *, #87775, .T. ) ;
#69517 = DIRECTION ( 'NONE',  ( 0.000000000000000000, 0.1736481776669267785, -0.9848077530122087975 ) ) ;
#69519 = EDGE_CURVE ( 'NONE', #6010, #3726, #6503, .T. ) ;
#69518 = UNCERTAINTY_MEASURE_WITH_UNIT (LENGTH_MEASURE( 1.000000000000000082E-05 ), #80625, 'distance_accuracy_value', 'NONE');
#69520 = CARTESIAN_POINT ( 'NONE',  ( -11.31568186948346622, -10.23759521482555357, 34.22997729860117033 ) ) ;
#69521 = DIRECTION ( 'NONE',  ( -0.000000000000000000, 0.3420201433256694346, -0.9396926207859080948 ) ) ;
#69522 = CARTESIAN_POINT ( 'NONE',  ( -7.173053667125516064, -9.234221910056348293, 34.70572697212741531 ) ) ;
#69523 = CARTESIAN_POINT ( 'NONE',  ( -5.076923076923075762, -5.415277668671390821, 36.20867863119892149 ) ) ;
#69524 = CARTESIAN_POINT ( 'NONE',  ( -8.769230769230768274, -2.486705287966279876, 31.30864560766543647 ) ) ;
#69525 = PLANE ( 'NONE',  #9727 ) ;
#69526 = CARTESIAN_POINT ( 'NONE',  ( 3.750000000000000888, -7.499999999999978684, 25.71875000000000000 ) ) ;
#69527 = CARTESIAN_POINT ( 'NONE',  ( -8.769230769230768274, -4.661471528628507777, 34.16647553114623292 ) ) ;
#69528 = CARTESIAN_POINT ( 'NONE',  ( -2.241624974342230292, -2.833524468853757750, 32.15551576947925838 ) ) ;
#69529 = B_SPLINE_CURVE_WITH_KNOTS ( 'NONE', 3,
 ( #6967, #26357, #6532, #47055, #68666, #76307, #54702, #69113, #47944, #48390 ),
 .UNSPECIFIED., .F., .F.,
 ( 4, 2, 2, 2, 4 ),
 ( 0.000000000000000000, 0.0001954311584214072923, 0.0003908623168428145846, 0.0005862934752642218498, 0.0007817246336856291692 ),
 .UNSPECIFIED. ) ;
#69530 = ADVANCED_FACE ( 'NONE', ( #19779 ), #34622, .F. ) ;
#69531 = DIRECTION ( 'NONE',  ( 0.000000000000000000, 0.000000000000000000, -1.000000000000000000 ) ) ;
#69532 = CARTESIAN_POINT ( 'NONE',  ( -1.634615384615383027, -2.499999999999998668, 29.75000000000000355 ) ) ;
#69533 = VECTOR ( 'NONE', #16787, 999.9999999999998863 ) ;
#69534 = EDGE_CURVE ( 'NONE', #53330, #67070, #32427, .T. ) ;
#69535 = AXIS2_PLACEMENT_3D ( 'NONE', #61358, #33467, #39350 ) ;
#69536 = VERTEX_POINT ( 'NONE', #40508 ) ;
#69537 = VERTEX_POINT ( 'NONE', #35059 ) ;
#69538 = CARTESIAN_POINT ( 'NONE',  ( 3.100621261037532772, -11.04286588640298561, 33.62463336215343901 ) ) ;
#69539 = CARTESIAN_POINT ( 'NONE',  ( 20.00000000000000000, -4.000000000000000000, 29.75000000000000355 ) ) ;
#69540 = CARTESIAN_POINT ( 'NONE',  ( -11.78846153846153832, -7.500000000000001776, 34.75000000000000000 ) ) ;
#69541 = ORIENTED_EDGE ( 'NONE', *, *, #79306, .T. ) ;
#69542 = DIRECTION ( 'NONE',  ( 1.000000000000000000, 0.000000000000000000, 0.000000000000000000 ) ) ;
#69543 = CARTESIAN_POINT ( 'NONE',  ( -18.00000000000000000, -6.436573248120765811, 35.78099280442780383 ) ) ;
#69544 = CARTESIAN_POINT ( 'NONE',  ( -2.437840277424001112, -8.630895178749536711, 34.87696386517710323 ) ) ;
#69545 = EDGE_CURVE ( 'NONE', #17317, #22911, #79638, .T. ) ;
#69546 = ORIENTED_EDGE ( 'NONE', *, *, #64548, .F. ) ;
#69547 = CARTESIAN_POINT ( 'NONE',  ( 18.06525513951284267, -3.643525952247864019, 33.31231777344670064 ) ) ;
#69548 = EDGE_CURVE ( 'NONE', #32348, #23528, #42277, .T. ) ;
#69549 = VERTEX_POINT ( 'NONE', #26984 ) ;
#69550 = CARTESIAN_POINT ( 'NONE',  ( 10.61538461538449596, -8.613356846316285953, 34.62446782046622218 ) ) ;
#69551 = DIRECTION ( 'NONE',  ( -0.000000000000000000, 1.000000000000000000, -0.000000000000000000 ) ) ;
#69552 = EDGE_CURVE ( 'NONE', #18312, #64241, #55328, .T. ) ;
#69553 = CARTESIAN_POINT ( 'NONE',  ( -1.634592128663975297, -9.234221910056348293, 34.70572697212741531 ) ) ;
#69554 = EDGE_CURVE ( 'NONE', #1510, #87031, #28758, .T. ) ;
#69555 = CARTESIAN_POINT ( 'NONE',  ( 3.930361229281821966, -6.716662450894490100, 34.94144148231605840 ) ) ;
#69556 = CARTESIAN_POINT ( 'NONE',  ( -2.980769230769293454, -7.565270000091922853, 34.99999999999999289 ) ) ;
#69557 = ORIENTED_EDGE ( 'NONE', *, *, #83227, .F. ) ;
#69558 = VECTOR ( 'NONE', #83209, 1000.000000000000000 ) ;
#69559 = ORIENTED_EDGE ( 'NONE', *, *, #27337, .T. ) ;
#69560 = ORIENTED_EDGE ( 'NONE', *, *, #17231, .F. ) ;
#69561 = ORIENTED_EDGE ( 'NONE', *, *, #42720, .T. ) ;
#69562 = LINE ( 'NONE', #661, #41523 ) ;
#69563 = CARTESIAN_POINT ( 'NONE',  ( -2.530619266599156258, -10.01117774369187252, 34.36070679894347535 ) ) ;
#69564 = DIRECTION ( 'NONE',  ( 0.000000000000000000, 0.7660444431189822323, -0.6427876096865344779 ) ) ;
#69565 = CARTESIAN_POINT ( 'NONE',  ( -17.06410256410256565, -3.499999999999999556, 29.75000000000000355 ) ) ;
#69566 = CARTESIAN_POINT ( 'NONE',  ( 4.153846153846032507, -6.879047030192662504, 34.71129190930017927 ) ) ;
#69567 = CARTESIAN_POINT ( 'NONE',  ( 14.30769230769218758, -10.21337939537710326, 33.94971097300076224 ) ) ;
#69568 = ORIENTED_EDGE ( 'NONE', *, *, #37683, .F. ) ;
#69569 = ORIENTED_EDGE ( 'NONE', *, *, #33136, .F. ) ;
#69570 = ORIENTED_EDGE ( 'NONE', *, *, #17135, .F. ) ;
#69572 = ORIENTED_EDGE ( 'NONE', *, *, #9194, .T. ) ;
#69571 = DIRECTION ( 'NONE',  ( 0.000000000000000000, 0.6427876096865368094, 0.7660444431189802339 ) ) ;
#69574 = CARTESIAN_POINT ( 'NONE',  ( -5.143005456283213483, -12.62096338111211580, 30.90682066428152197 ) ) ;
#69573 = DIRECTION ( 'NONE',  ( -1.000000000000000000, -0.000000000000000000, -0.000000000000000000 ) ) ;
#69575 = DIRECTION ( 'NONE',  ( 0.000000000000000000, 0.000000000000000000, 1.000000000000000000 ) ) ;
#69576 = ADVANCED_FACE ( 'NONE', ( #56661 ), #83711, .F. ) ;
#69577 = CARTESIAN_POINT ( 'NONE',  ( 1.553300858899129722, -11.24999999999999112, 24.70312500000000000 ) ) ;
#69578 = ORIENTED_EDGE ( 'NONE', *, *, #14074, .F. ) ;
#69579 = EDGE_CURVE ( 'NONE', #80708, #39037, #68955, .T. ) ;
#69580 = ORIENTED_EDGE ( 'NONE', *, *, #63073, .F. ) ;
#69581 = CARTESIAN_POINT ( 'NONE',  ( -18.00000000000012079, -3.083524468854528244, 32.58852847137268327 ) ) ;
#69582 = VECTOR ( 'NONE', #66332, 1000.000000000000000 ) ;
#69583 = EDGE_LOOP ( 'NONE', ( #13445, #11163 ) ) ;
#69584 = FACE_BOUND ( 'NONE', #73175, .T. ) ;
#69585 = CARTESIAN_POINT ( 'NONE',  ( 5.076923076923075762, -4.661471528628507777, 34.16647553114623292 ) ) ;
#69586 = EDGE_CURVE ( 'NONE', #61963, #12929, #63412, .T. ) ;
#69587 = VECTOR ( 'NONE', #63917, 1000.000000000000000 ) ;
#69588 = CARTESIAN_POINT ( 'NONE',  ( -19.00000000000000000, -8.999999999999998224, 22.25000000000000000 ) ) ;
#69589 = ORIENTED_EDGE ( 'NONE', *, *, #583, .T. ) ;
#69590 = CARTESIAN_POINT ( 'NONE',  ( -4.376711576049792995, -2.501496062324911840, 29.88072118266895671 ) ) ;
#69591 = CARTESIAN_POINT ( 'NONE',  ( 8.769230769230645706, -12.16647553114689728, 32.15551576947799362 ) ) ;
#69592 = CARTESIAN_POINT ( 'NONE',  ( -1.384615384615383471, -10.67929555188718282, 33.92786785259544047 ) ) ;
#69593 = CARTESIAN_POINT ( 'NONE',  ( 4.023698944407935407, -11.47017969459903952, 32.78971311882034456 ) ) ;
#69594 = CARTESIAN_POINT ( 'NONE',  ( 8.769230769230768274, -1.422936976036506707, 30.56769352161908415 ) ) ;
#69595 = VERTEX_POINT ( 'NONE', #57099 ) ;
#69596 = ADVANCED_FACE ( 'NONE', ( #43151 ), #84156, .F. ) ;
#69597 = CARTESIAN_POINT ( 'NONE',  ( 6.000000000000001776, -8.120952969808772792, 34.71129190930000163 ) ) ;
#69598 = DIRECTION ( 'NONE',  ( 0.000000000000000000, -6.938893903907222067E-15, 1.000000000000000000 ) ) ;
#69599 = DIRECTION ( 'NONE',  ( 0.000000000000000000, 0.6427876096865368094, 0.7660444431189802339 ) ) ;
#69600 = CARTESIAN_POINT ( 'NONE',  ( 15.90386940979756503, -10.82459398097509862, 33.81372124010183455 ) ) ;
#69601 = CYLINDRICAL_SURFACE ( 'NONE', #27141, 0.2500000000000012212 ) ;
#69602 = FACE_BOUND ( 'NONE', #43679, .T. ) ;
#69604 = DIRECTION ( 'NONE',  ( 0.000000000000000000, 0.8660254037844377084, -0.5000000000000015543 ) ) ;
#69603 = CARTESIAN_POINT ( 'NONE',  ( 17.29970261819148902, -3.755027918224367767, 33.06320215134714857 ) ) ;
#69605 = CARTESIAN_POINT ( 'NONE',  ( -14.30769230769230660, -3.322132147404559976, 32.92929555188717927 ) ) ;
#69607 = CARTESIAN_POINT ( 'NONE',  ( 5.776515056276054771, -10.81261337010820256, 33.49550067578627477 ) ) ;
#69606 = CARTESIAN_POINT ( 'NONE',  ( -11.40793583669797506, -11.46989282347013095, 32.79007818306219946 ) ) ;
#69608 = DIRECTION ( 'NONE',  ( -0.000000000000000000, -0.5000000000000009992, -0.8660254037844380415 ) ) ;
#69609 = CARTESIAN_POINT ( 'NONE',  ( 1.901340078031349856, -5.512252781505337929, 17.81063170625849068 ) ) ;
#69610 = ORIENTED_EDGE ( 'NONE', *, *, #45739, .T. ) ;
#69611 = CARTESIAN_POINT ( 'NONE',  ( -8.519230769229334754, -7.500000000000155431, 34.75000000000007105 ) ) ;
#69612 = ORIENTED_EDGE ( 'NONE', *, *, #81758, .F. ) ;
#69613 = CARTESIAN_POINT ( 'NONE',  ( -11.53846153846153655, -5.471508081941601098, 34.59228464037088457 ) ) ;
#69614 = ORIENTED_EDGE ( 'NONE', *, *, #238, .T. ) ;
#69615 = CARTESIAN_POINT ( 'NONE',  ( -3.903791842207838592, -12.17597550085003633, 31.52189283813461884 ) ) ;
#69616 = CARTESIAN_POINT ( 'NONE',  ( 14.24160992833217065, -3.937682226553330445, 33.60647404775217240 ) ) ;
#69617 = EDGE_LOOP ( 'NONE', ( #14924, #1406, #14373, #37972, #36488 ) ) ;
#69618 = CARTESIAN_POINT ( 'NONE',  ( -19.50000000000000000, -3.499999999999999556, 29.75000000000000355 ) ) ;
#69619 = CARTESIAN_POINT ( 'NONE',  ( 1.200186371490561621, -10.22469193450123193, 16.95125670625848713 ) ) ;
#69620 = EDGE_CURVE ( 'NONE', #48440, #74923, #44455, .T. ) ;
#69621 = CARTESIAN_POINT ( 'NONE',  ( -10.36543920600657209, -12.68172785388650681, 30.59649109432439218 ) ) ;
#69622 = FACE_OUTER_BOUND ( 'NONE', #79963, .T. ) ;
#69623 = B_SPLINE_CURVE_WITH_KNOTS ( 'NONE', 3,
 ( #44054, #85072, #57585, #36004, #23350, #15727, #69776, #63456, #1757, #22472 ),
 .UNSPECIFIED., .F., .F.,
 ( 4, 2, 2, 2, 4 ),
 ( 0.0007817246336856284103, 0.0009771112958940092897, 0.001172497958102390169, 0.001367884620310771265, 0.001563271282519152145 ),
 .UNSPECIFIED. ) ;
#69624 = VECTOR ( 'NONE', #44296, 1000.000000000000000 ) ;
#69625 = FACE_OUTER_BOUND ( 'NONE', #54502, .T. ) ;
#69626 = LINE ( 'NONE', #70961, #80427 ) ;
#69627 = CARTESIAN_POINT ( 'NONE',  ( 16.15384615384615330, -9.584722331328613620, 36.20867863119891439 ) ) ;
#69628 = DIRECTION ( 'NONE',  ( -0.000000000000000000, -0.7660444431189791237, -0.6427876096865379196 ) ) ;
#69629 = CARTESIAN_POINT ( 'NONE',  ( 1.492201783934598236, -11.27530806549875031, 24.95499329374151287 ) ) ;
#69630 = CARTESIAN_POINT ( 'NONE',  ( 11.28848479441294828, -5.643011162660950042, 34.66104346484419096 ) ) ;
#69631 = CARTESIAN_POINT ( 'NONE',  ( 17.99999999999987566, -4.481592998941358097, 33.73612834414048933 ) ) ;
#69632 = CARTESIAN_POINT ( 'NONE',  ( -18.00000000000000000, 2.999999999999935163, 30.25000000000000000 ) ) ;
#69633 = CARTESIAN_POINT ( 'NONE',  ( 0.06109907496451268821, -3.749999999999999556, 23.15811829374151642 ) ) ;
#69634 = CARTESIAN_POINT ( 'NONE',  ( -10.36543920600657209, -5.766571408460171355, 34.70601412856602508 ) ) ;
#69635 = CARTESIAN_POINT ( 'NONE',  ( 1.384615384615386802, -1.951392089020283160, 34.73218667398347748 ) ) ;
#69636 = ORIENTED_EDGE ( 'NONE', *, *, #53224, .F. ) ;
#69637 = CARTESIAN_POINT ( 'NONE',  ( -17.77698864838714243, -2.758310577978209110, 31.33698337089303010 ) ) ;
#69638 = FACE_OUTER_BOUND ( 'NONE', #33998, .T. ) ;
#69640 = ORIENTED_EDGE ( 'NONE', *, *, #74511, .T. ) ;
#69639 = DIRECTION ( 'NONE',  ( -0.000000000000000000, 0.000000000000000000, 1.000000000000000000 ) ) ;
#69641 = CARTESIAN_POINT ( 'NONE',  ( -14.43838377435986686, -11.71456829005830080, 32.44064028649416542 ) ) ;
#69642 = LINE ( 'NONE', #22346, #10399 ) ;
#69643 = DIRECTION ( 'NONE',  ( 0.000000000000000000, -6.938893903907222067E-15, 1.000000000000000000 ) ) ;
#69644 = LINE ( 'NONE', #7953, #56261 ) ;
#69645 = CARTESIAN_POINT ( 'NONE',  ( 10.36540787133602670, -12.65889640711025521, 30.72598325615533454 ) ) ;
#69646 = VECTOR ( 'NONE', #50069, 1000.000000000000000 ) ;
#69647 = EDGE_CURVE ( 'NONE', #67129, #21924, #8486, .T. ) ;
#69648 = EDGE_CURVE ( 'NONE', #7735, #62030, #51689, .T. ) ;
#69649 = ORIENTED_EDGE ( 'NONE', *, *, #52110, .F. ) ;
#69650 = CARTESIAN_POINT ( 'NONE',  ( -0.2387589202700516056, -10.81320215134717344, 33.49497208177562868 ) ) ;
#69651 = ORIENTED_EDGE ( 'NONE', *, *, #32681, .T. ) ;
#69652 = EDGE_CURVE ( 'NONE', #63192, #10084, #15192, .T. ) ;
#69653 = VERTEX_POINT ( 'NONE', #30516 ) ;
#69654 = CIRCLE ( 'NONE', #23677, 0.2500000000000002220 ) ;
#69655 = CARTESIAN_POINT ( 'NONE',  ( -13.60810032833933469, -3.754499324213721234, 33.06261337010820256 ) ) ;
#69656 = CARTESIAN_POINT ( 'NONE',  ( -3.931066612577741370, -3.236590943229499029, 32.36255958852953540 ) ) ;
#69657 = EDGE_CURVE ( 'NONE', #38188, #68176, #30187, .T. ) ;
#69658 = CARTESIAN_POINT ( 'NONE',  ( 9.942253210655836781, -5.057305518903948638, 34.11320923018887896 ) ) ;
#69659 = CARTESIAN_POINT ( 'NONE',  ( 13.38461538461538680, -8.164416787775445883, 34.95778746994557906 ) ) ;
#69660 = ORIENTED_EDGE ( 'NONE', *, *, #15104, .F. ) ;
#69661 = CARTESIAN_POINT ( 'NONE',  ( 17.29993592101647693, -11.43677907613345113, 33.22367315496201456 ) ) ;
#69662 = ORIENTED_EDGE ( 'NONE', *, *, #69552, .T. ) ;
#69663 = VERTEX_POINT ( 'NONE', #57985 ) ;
#69664 = VERTEX_POINT ( 'NONE', #85465 ) ;
#69666 = ORIENTED_EDGE ( 'NONE', *, *, #83336, .T. ) ;
#69665 = CARTESIAN_POINT ( 'NONE',  ( 0.000000000000000000, -11.00000000000000000, 29.75000000000000355 ) ) ;
#69667 = CARTESIAN_POINT ( 'NONE',  ( -6.923076923076922462, -2.292212530054420494, 30.41441678777542634 ) ) ;
#69668 = EDGE_CURVE ( 'NONE', #14315, #75360, #17003, .T. ) ;
#69669 = CARTESIAN_POINT ( 'NONE',  ( 6.223012844093396723, -2.523321265292115090, 31.42251411153756280 ) ) ;
#69670 = ADVANCED_FACE ( 'NONE', ( #62955 ), #86375, .F. ) ;
#69671 = CARTESIAN_POINT ( 'NONE',  ( -3.164700879766792152, -4.098570777380720287, 33.41473453929635440 ) ) ;
#69672 = DIRECTION ( 'NONE',  ( -0.000000000000000000, 1.000000000000000000, -0.000000000000000000 ) ) ;
#69673 = ORIENTED_EDGE ( 'NONE', *, *, #19172, .F. ) ;
#69674 = ORIENTED_EDGE ( 'NONE', *, *, #88254, .T. ) ;
#69675 = CIRCLE ( 'NONE', #84048, 2.000000000000001776 ) ;
#69676 = ORIENTED_EDGE ( 'NONE', *, *, #85703, .T. ) ;
#69677 = CARTESIAN_POINT ( 'NONE',  ( -9.626239341305252495, -5.557115091759786019, 34.35708131394839882 ) ) ;
#69679 = VERTEX_POINT ( 'NONE', #24196 ) ;
#69678 = CARTESIAN_POINT ( 'NONE',  ( -2.557715544985270650, -2.823816976329320827, 31.52131813110797154 ) ) ;
#69680 = CARTESIAN_POINT ( 'NONE',  ( -7.146003140593069958, -12.39988816332205701, 30.74660775122750778 ) ) ;
#69681 = CARTESIAN_POINT ( 'NONE',  ( 6.792929713638703682, -6.852621066184267029, 34.70813303252209181 ) ) ;
#69682 = EDGE_CURVE ( 'NONE', #50475, #26485, #60336, .T. ) ;
#69683 = CARTESIAN_POINT ( 'NONE',  ( -14.53117725141625094, -2.599994579823203367, 30.74605699353653776 ) ) ;
#69684 = VERTEX_POINT ( 'NONE', #4379 ) ;
#69685 = CARTESIAN_POINT ( 'NONE',  ( -14.30769230769230660, -8.318370150425687726, 35.83090037661290239 ) ) ;
#69686 = CARTESIAN_POINT ( 'NONE',  ( 14.16025641025641235, -3.499999999999999556, 29.75000000000000355 ) ) ;
#69687 = EDGE_LOOP ( 'NONE', ( #26528, #28917, #66942, #13506, #52076, #12501 ) ) ;
#69688 = FACE_BOUND ( 'NONE', #43068, .T. ) ;
#69689 = B_SPLINE_CURVE_WITH_KNOTS ( 'NONE', 3,
 ( #70969, #86279, #71847, #23218, #37172, #50678, #84493, #79052, #50230, #9703 ),
 .UNSPECIFIED., .F., .F.,
 ( 4, 2, 2, 2, 4 ),
 ( 0.000000000000000000, 0.0001954311564186862510, 0.0003908623128373725020, 0.0005862934692560588072, 0.0007817246256747450040 ),
 .UNSPECIFIED. ) ;
#69690 = EDGE_CURVE ( 'NONE', #3690, #89174, #59767, .T. ) ;
#69691 = CARTESIAN_POINT ( 'NONE',  ( -10.68146699474474914, -4.661471528628507777, 34.16647553114621871 ) ) ;
#69692 = CARTESIAN_POINT ( 'NONE',  ( 13.44987052412822059, -6.835583212224610072, 34.95778746994559327 ) ) ;
#69693 = LINE ( 'NONE', #6662, #10633 ) ;
#69695 = FACE_OUTER_BOUND ( 'NONE', #88128, .T. ) ;
#69694 = CARTESIAN_POINT ( 'NONE',  ( -13.38461538461538325, -2.249999999999998668, 29.50000000000001421 ) ) ;
#69696 = CARTESIAN_POINT ( 'NONE',  ( 14.30769230769231015, -12.34228464037088635, 31.77849191805839268 ) ) ;
#69697 = CARTESIAN_POINT ( 'NONE',  ( -2.373775718648187816, -3.513871655860377086, 32.76840700105978499 ) ) ;
#69698 = EDGE_LOOP ( 'NONE', ( #51417, #30553, #34095, #66863 ) ) ;
#69699 = DIRECTION ( 'NONE',  ( 0.000000000000000000, 0.7660444431189807890, 0.6427876096865361433 ) ) ;
#69700 = CARTESIAN_POINT ( 'NONE',  ( 2.307692307692309264, -13.53365097954675988, 30.81389545987213552 ) ) ;
#69701 = B_SPLINE_CURVE_WITH_KNOTS ( 'NONE', 3,
 ( #35615, #83813, #63951, #49566, #9462, #63064, #49999, #29743, #23408, #58083 ),
 .UNSPECIFIED., .F., .F.,
 ( 4, 2, 2, 2, 4 ),
 ( 0.0007817246256747472808, 0.0009771112852218907189, 0.001172497944769034265, 0.001367884604316177595, 0.001563271263863321141 ),
 .UNSPECIFIED. ) ;
#69702 = ORIENTED_EDGE ( 'NONE', *, *, #67038, .T. ) ;
#69703 = EDGE_CURVE ( 'NONE', #77971, #84339, #9752, .T. ) ;
#69704 = FACE_OUTER_BOUND ( 'NONE', #79455, .T. ) ;
#69705 = CARTESIAN_POINT ( 'NONE',  ( -4.377331078410482412, -3.562934362175799841, 33.22335522853832401 ) ) ;
#69706 = ORIENTED_EDGE ( 'NONE', *, *, #67420, .T. ) ;
#69707 = CARTESIAN_POINT ( 'NONE',  ( 8.096208266067295156, -6.523592122091591783, 34.90882529074906415 ) ) ;
#69708 = CARTESIAN_POINT ( 'NONE',  ( -4.284536756956461190, -2.295517848115769421, 30.44137282052136939 ) ) ;
#69709 = AXIS2_PLACEMENT_3D ( 'NONE', #51163, #71025, #29604 ) ;
#69710 = FACE_BOUND ( 'NONE', #70457, .T. ) ;
#69711 = EDGE_CURVE ( 'NONE', #2618, #71762, #4832, .T. ) ;
#69713 = DIRECTION ( 'NONE',  ( -0.000000000000000000, -0.9396926207859092051, -0.3420201433256662704 ) ) ;
#69712 = CARTESIAN_POINT ( 'NONE',  ( -1.515305987725691139, -6.369640206132550553, 34.87707690430378449 ) ) ;
#69714 = CARTESIAN_POINT ( 'NONE',  ( -6.857008572074484221, -8.973038597847269315, 34.52809138561122637 ) ) ;
#69715 = CARTESIAN_POINT ( 'NONE',  ( -16.02332045208259004, -2.619367082507847222, 30.83698974864643461 ) ) ;
#69717 = CARTESIAN_POINT ( 'NONE',  ( -12.52680890749923570, -4.481592998940162609, 33.73612834413957984 ) ) ;
#69716 = CARTESIAN_POINT ( 'NONE',  ( -5.076923076923075762, -9.905515769479276145, 34.41647553114623292 ) ) ;
#69718 = CARTESIAN_POINT ( 'NONE',  ( -14.24162497434223340, -5.471508081941601098, 34.59228464037088457 ) ) ;
#69719 = CARTESIAN_POINT ( 'NONE',  ( 3.749999999999992006, -5.946699141100872943, 25.64062500000000000 ) ) ;
#69720 = ORIENTED_EDGE ( 'NONE', *, *, #82345, .T. ) ;
#69721 = VECTOR ( 'NONE', #51238, 1000.000000000000000 ) ;
#69722 = ORIENTED_EDGE ( 'NONE', *, *, #82454, .F. ) ;
#69723 = CARTESIAN_POINT ( 'NONE',  ( 16.08776377448601735, -9.058645607665454236, 34.76329471203372634 ) ) ;
#69724 = CARTESIAN_POINT ( 'NONE',  ( -12.46153846153858424, -6.835583212225970762, 34.95778746994575670 ) ) ;
#69725 = CARTESIAN_POINT ( 'NONE',  ( -7.846153846153844924, -13.37000171582298513, 34.34916445242398453 ) ) ;
#69726 = CARTESIAN_POINT ( 'NONE',  ( -0.5268084620947811603, -3.083524468853724443, 32.58852847137143272 ) ) ;
#69727 = CARTESIAN_POINT ( 'NONE',  ( -1.134615384615383915, -7.500000000000001776, 35.04278698407183867 ) ) ;
#69728 = CARTESIAN_POINT ( 'NONE',  ( -0.06109907496455085213, -3.750000000000000888, 15.15438170625848890 ) ) ;
#69729 = EDGE_CURVE ( 'NONE', #64747, #53433, #25093, .T. ) ;
#69730 = DIRECTION ( 'NONE',  ( 0.000000000000000000, 0.000000000000000000, -1.000000000000000000 ) ) ;
#69731 = CARTESIAN_POINT ( 'NONE',  ( 4.153846153846154188, -11.91647553114624181, 32.58852847137148245 ) ) ;
#69732 = EDGE_CURVE ( 'NONE', #42058, #75680, #43099, .T. ) ;
#69733 = CARTESIAN_POINT ( 'NONE',  ( 9.442284468086237226, -10.92453946501458795, 33.72985991061850086 ) ) ;
#69734 = DIRECTION ( 'NONE',  ( 0.000000000000000000, -6.938893903907222067E-15, 1.000000000000000000 ) ) ;
#69735 = LINE ( 'NONE', #41830, #84177 ) ;
#69736 = LINE ( 'NONE', #68404, #882 ) ;
#69737 = CARTESIAN_POINT ( 'NONE',  ( -6.000000000000121680, -12.51329471203414379, 31.30864560766407578 ) ) ;
#69738 = CARTESIAN_POINT ( 'NONE',  ( 10.36538461538461675, -7.500000000000001776, 35.00000000000000000 ) ) ;
#69739 = DIRECTION ( 'NONE',  ( 0.000000000000000000, 0.3420201433256610524, 0.9396926207859113145 ) ) ;
#69740 = ORIENTED_EDGE ( 'NONE', *, *, #13780, .F. ) ;
#69741 = CARTESIAN_POINT ( 'NONE',  ( 12.46153846153846168, -3.937682226553329556, 33.60647404775216529 ) ) ;
#69742 = CARTESIAN_POINT ( 'NONE',  ( -12.21153846153702638, -7.500000000000155431, 34.75000000000007105 ) ) ;
#69743 = CARTESIAN_POINT ( 'NONE',  ( -1.901340078031369618, -5.512252781505359245, 21.75186829374151287 ) ) ;
#69744 = CARTESIAN_POINT ( 'NONE',  ( 3.903869409797562806, -4.818429247618089661, 34.26397095200675125 ) ) ;
#69745 = FACE_OUTER_BOUND ( 'NONE', #76217, .T. ) ;
#69746 = ORIENTED_EDGE ( 'NONE', *, *, #6984, .F. ) ;
#69747 = CARTESIAN_POINT ( 'NONE',  ( -6.923076923076922462, -10.89733346790207413, 36.13435417666054406 ) ) ;
#69749 = ORIENTED_EDGE ( 'NONE', *, *, #73675, .T. ) ;
#69748 = CARTESIAN_POINT ( 'NONE',  ( -9.469296340694841163, -4.887748414852792322, 34.01359900205216746 ) ) ;
#69750 = DIRECTION ( 'NONE',  ( -0.000000000000000000, 0.6427876096865404731, -0.7660444431189771253 ) ) ;
#69751 = CARTESIAN_POINT ( 'NONE',  ( -9.442253272394237840, -5.642605341092957971, 34.66089969410670335 ) ) ;
#69752 = ORIENTED_EDGE ( 'NONE', *, *, #69946, .T. ) ;
#69753 = DIRECTION ( 'NONE',  ( -0.000000000000000000, -0.000000000000000000, -1.000000000000000000 ) ) ;
#69754 = CIRCLE ( 'NONE', #49567, 8.000000000000000000 ) ;
#69755 = CARTESIAN_POINT ( 'NONE',  ( -2.939152317953646711E-15, 7.500000000000000000, 0.000000000000000000 ) ) ;
#69756 = ORIENTED_EDGE ( 'NONE', *, *, #86362, .F. ) ;
#69757 = CARTESIAN_POINT ( 'NONE',  ( -15.23076923076922995, -4.661471528628507777, 34.16647553114623292 ) ) ;
#69758 = CARTESIAN_POINT ( 'NONE',  ( -11.78848476268299450, -12.45566812827425451, 31.48439005359158926 ) ) ;
#69759 = DIRECTION ( 'NONE',  ( 0.000000000000000000, 0.000000000000000000, 1.000000000000000000 ) ) ;
#69760 = ORIENTED_EDGE ( 'NONE', *, *, #59340, .F. ) ;
#69761 = ORIENTED_EDGE ( 'NONE', *, *, #30612, .T. ) ;
#69762 = CARTESIAN_POINT ( 'NONE',  ( 6.223011351612852238, -6.503523203565942268, 34.64991518177335195 ) ) ;
#69763 = EDGE_CURVE ( 'NONE', #86735, #60344, #22685, .T. ) ;
#69764 = VERTEX_POINT ( 'NONE', #38161 ) ;
#69765 = CARTESIAN_POINT ( 'NONE',  ( 7.846153846153846700, -2.833524468853757305, 32.15551576947925838 ) ) ;
#69766 = CARTESIAN_POINT ( 'NONE',  ( -7.146003881983771677, -2.308479472611653094, 30.53278059502174457 ) ) ;
#69767 = DIRECTION ( 'NONE',  ( -1.000000000000000000, -0.000000000000000000, 0.000000000000000000 ) ) ;
#69768 = EDGE_CURVE ( 'NONE', #13588, #363, #38800, .T. ) ;
#69769 = CYLINDRICAL_SURFACE ( 'NONE', #56489, 0.2500000000000004996 ) ;
#69770 = CARTESIAN_POINT ( 'NONE',  ( 17.07692307692307665, -1.044019251281081972, 31.83374038241031911 ) ) ;
#69771 = ADVANCED_FACE ( 'NONE', ( #83151 ), #68299, .F. ) ;
#69772 = CARTESIAN_POINT ( 'NONE',  ( 13.38461538461538680, -12.78798330534103123, 29.99999999999997868 ) ) ;
#69773 = B_SPLINE_CURVE_WITH_KNOTS ( 'NONE', 3,
 ( #78337, #57630, #36045, #64372, #63499, #63046, #50417, #29728, #28846, #56307 ),
 .UNSPECIFIED., .F., .F.,
 ( 4, 2, 2, 2, 4 ),
 ( 0.000000000000000000, 0.0001954311564186865763, 0.0003908623128373731525, 0.0005862934692560596746, 0.0007817246256747463051 ),
 .UNSPECIFIED. ) ;
#69774 = ORIENTED_EDGE ( 'NONE', *, *, #58099, .F. ) ;
#69775 = ORIENTED_EDGE ( 'NONE', *, *, #79918, .T. ) ;
#69777 = ORIENTED_EDGE ( 'NONE', *, *, #33763, .T. ) ;
#69776 = CARTESIAN_POINT ( 'NONE',  ( -2.438167492768025024, -7.276987145209184327, 34.99546412871779211 ) ) ;
#69778 = EDGE_CURVE ( 'NONE', #4584, #58033, #82714, .T. ) ;
#69779 = CARTESIAN_POINT ( 'NONE',  ( 7.596130621932386973, -2.588893531581426988, 31.60682220781847818 ) ) ;
#69780 = ORIENTED_EDGE ( 'NONE', *, *, #17439, .F. ) ;
#69781 = EDGE_CURVE ( 'NONE', #45658, #54250, #38181, .T. ) ;
#69782 = FACE_OUTER_BOUND ( 'NONE', #7571, .T. ) ;
#69783 = CARTESIAN_POINT ( 'NONE',  ( 8.068933387422255521, -5.114059244376869984, 34.14424750095245287 ) ) ;
#69784 = VECTOR ( 'NONE', #79647, 1000.000000000000000 ) ;
#69785 = ORIENTED_EDGE ( 'NONE', *, *, #38663, .T. ) ;
#69786 = DIRECTION ( 'NONE',  ( 0.000000000000000000, 1.000000000000000000, 0.000000000000000000 ) ) ;
#69787 = ADVANCED_FACE ( 'NONE', ( #6603 ), #33185, .F. ) ;
#69788 = VERTEX_POINT ( 'NONE', #12472 ) ;
#69790 = ORIENTED_EDGE ( 'NONE', *, *, #33358, .T. ) ;
#69789 = DIRECTION ( 'NONE',  ( -0.000000000000000000, -0.000000000000000000, -1.000000000000000000 ) ) ;
#69791 = CARTESIAN_POINT ( 'NONE',  ( -14.30769230769242917, -12.16647553114689728, 32.15551576947799362 ) ) ;
#69792 = ORIENTED_EDGE ( 'NONE', *, *, #71393, .T. ) ;
#69793 = CARTESIAN_POINT ( 'NONE',  ( 17.86985279056177944, -10.88202310037936194, 33.43294751532457099 ) ) ;
#69794 = CARTESIAN_POINT ( 'NONE',  ( 17.75002325595141173, -12.41104346484419452, 31.60698883733904196 ) ) ;
#69795 = FACE_BOUND ( 'NONE', #10555, .T. ) ;
#69796 = EDGE_CURVE ( 'NONE', #85539, #33270, #83787, .T. ) ;
#69797 = CARTESIAN_POINT ( 'NONE',  ( -11.60454494941742176, -2.538708090699994813, 30.37095296980875148 ) ) ;
#69798 = CARTESIAN_POINT ( 'NONE',  ( -18.00000000000000000, -3.895656007487076078, 35.99290692298802696 ) ) ;
#69799 = CARTESIAN_POINT ( 'NONE',  ( -16.08859101433330707, -5.094484230520771817, 34.41647553114626845 ) ) ;
#69800 = CARTESIAN_POINT ( 'NONE',  ( 12.21156171748986985, -3.436278759898153901, 33.07459398097509506 ) ) ;
#69801 = CARTESIAN_POINT ( 'NONE',  ( 5.142991427925513115, -10.51840700105979565, 33.73612834413962247 ) ) ;
#69802 = CARTESIAN_POINT ( 'NONE',  ( -39.05038313613820122, -2.499999999999999556, 29.75000000000000355 ) ) ;
#69803 = ORIENTED_EDGE ( 'NONE', *, *, #72074, .F. ) ;
#69804 = EDGE_CURVE ( 'NONE', #55112, #74382, #10718, .T. ) ;
#69805 = CARTESIAN_POINT ( 'NONE',  ( 10.36540788444226102, -9.943427161483782584, 34.11278801902876978 ) ) ;
#69806 = EDGE_LOOP ( 'NONE', ( #14081, #58132, #55529, #74327 ) ) ;
#69807 = ORIENTED_EDGE ( 'NONE', *, *, #63194, .T. ) ;
#69808 = AXIS2_PLACEMENT_3D ( 'NONE', #37475, #57757, #3689 ) ;
#69810 = DIRECTION ( 'NONE',  ( -0.000000000000000000, 0.9396926207859093161, -0.3420201433256663259 ) ) ;
#69809 = CARTESIAN_POINT ( 'NONE',  ( 7.622668902429897919, -6.760086850603068243, 34.69517049084099369 ) ) ;
#69811 = DIRECTION ( 'NONE',  ( 0.000000000000000000, 0.4999999999999960032, -0.8660254037844410391 ) ) ;
#69812 = DIRECTION ( 'NONE',  ( 0.000000000000000000, 0.000000000000000000, 1.000000000000000000 ) ) ;
#69813 = CARTESIAN_POINT ( 'NONE',  ( -10.36543920600657209, -12.45601412856602686, 31.48342859153981621 ) ) ;
#69814 = CARTESIAN_POINT ( 'NONE',  ( -12.33101302330481808, -5.070358843744210198, 34.40418822224088302 ) ) ;
#69815 = ORIENTED_EDGE ( 'NONE', *, *, #72413, .F. ) ;
#69816 = CARTESIAN_POINT ( 'NONE',  ( 11.47319153790521717, -3.643525952247789412, 33.31231777344662959 ) ) ;
#69817 = EDGE_CURVE ( 'NONE', #71873, #16707, #11848, .T. ) ;
#69818 = EDGE_CURVE ( 'NONE', #1987, #59805, #64450, .T. ) ;
#69819 = CARTESIAN_POINT ( 'NONE',  ( -6.130691466667556710, -6.413092428213692742, 34.63065189839063152 ) ) ;
#69820 = CARTESIAN_POINT ( 'NONE',  ( -10.48459280755982803, -9.804649428959608670, 34.18742332936588468 ) ) ;
#69821 = CARTESIAN_POINT ( 'NONE',  ( -12.46153846153858424, -9.528491918059723176, 34.59228464037033035 ) ) ;
#69822 = DIRECTION ( 'NONE',  ( -1.000000000000000000, -0.000000000000000000, -0.000000000000000000 ) ) ;
#69823 = ORIENTED_EDGE ( 'NONE', *, *, #59881, .T. ) ;
#69824 = FACE_OUTER_BOUND ( 'NONE', #1115, .T. ) ;
#69825 = ORIENTED_EDGE ( 'NONE', *, *, #80127, .T. ) ;
#69826 = B_SPLINE_CURVE_WITH_KNOTS ( 'NONE', 3,
 ( #17826, #79965, #59691, #78623, #24567, #44376, #65548, #4758, #25463, #38540 ),
 .UNSPECIFIED., .F., .F.,
 ( 4, 2, 2, 2, 4 ),
 ( 0.000000000000000000, 0.0001954311564186863323, 0.0003908623128373726646, 0.0005862934692560590241, 0.0007817246256747453293 ),
 .UNSPECIFIED. ) ;
#69827 = VERTEX_POINT ( 'NONE', #41721 ) ;
#69828 = B_SPLINE_CURVE_WITH_KNOTS ( 'NONE', 3,
 ( #77492, #55889, #15804, #28883, #68962, #83376, #21664, #49134, #8602, #36077 ),
 .UNSPECIFIED., .F., .F.,
 ( 4, 2, 2, 2, 4 ),
 ( 0.000000000000000000, 0.0001954311564186868744, 0.0003908623128373737488, 0.0005862934692560606504, 0.0007817246256747474977 ),
 .UNSPECIFIED. ) ;
#69829 = CARTESIAN_POINT ( 'NONE',  ( -6.130147969731695845, -4.299443229763728169, 33.91186481527756058 ) ) ;
#69830 = ORIENTED_EDGE ( 'NONE', *, *, #55992, .F. ) ;
#69831 = CARTESIAN_POINT ( 'NONE',  ( -1.253823576790597638, -8.147973898785416225, 34.70805048591653730 ) ) ;
#69832 = FACE_OUTER_BOUND ( 'NONE', #87132, .T. ) ;
#69833 = CARTESIAN_POINT ( 'NONE',  ( 6.000000000000001776, -1.044019251281081972, 31.83374038241031911 ) ) ;
#69834 = CARTESIAN_POINT ( 'NONE',  ( 3.230769230769110045, -10.90142922262034020, 33.41473453929536674 ) ) ;
#69835 = CARTESIAN_POINT ( 'NONE',  ( 5.076923076923075762, -12.78798330534102945, 29.74999999999997868 ) ) ;
#69836 = ADVANCED_FACE ( 'NONE', ( #62412 ), #6159, .F. ) ;
#69837 = CARTESIAN_POINT ( 'NONE',  ( -16.82692307692307665, -2.249999999999998668, 29.75000000000000355 ) ) ;
#69838 = ORIENTED_EDGE ( 'NONE', *, *, #22314, .F. ) ;
#69839 = DIRECTION ( 'NONE',  ( 0.000000000000000000, 0.6427876096865373645, -0.7660444431189797898 ) ) ;
#69841 = ORIENTED_EDGE ( 'NONE', *, *, #83520, .T. ) ;
#69840 = CARTESIAN_POINT ( 'NONE',  ( -13.31935981333935537, -4.481592998940250538, 33.73612834413965089 ) ) ;
#69842 = DIRECTION ( 'NONE',  ( -0.000000000000000000, 1.000000000000000000, -0.000000000000000000 ) ) ;
#69843 = CARTESIAN_POINT ( 'NONE',  ( -10.39237326377176451, -3.587049720035815348, 32.86302985866382897 ) ) ;
#69844 = CYLINDRICAL_SURFACE ( 'NONE', #87567, 0.2500000000000002220 ) ;
#69845 = EDGE_CURVE ( 'NONE', #35739, #88674, #7932, .T. ) ;
#69846 = EDGE_CURVE ( 'NONE', #58822, #73958, #43047, .T. ) ;
#69847 = CARTESIAN_POINT ( 'NONE',  ( -2.307692307692428724, -12.70778746994576025, 30.41441678777401236 ) ) ;
#69849 = AXIS2_PLACEMENT_3D ( 'NONE', #3013, #45334, #30495 ) ;
#69848 = CARTESIAN_POINT ( 'NONE',  ( -12.59222992820601661, -2.729777683071817229, 31.24903638046269450 ) ) ;
#69850 = FACE_OUTER_BOUND ( 'NONE', #67028, .T. ) ;
#69851 = CARTESIAN_POINT ( 'NONE',  ( -5.999999999999998224, -13.20930481340135110, 34.54067556320372745 ) ) ;
#69852 = CARTESIAN_POINT ( 'NONE',  ( -2.694853999681181556, -10.10844685921792241, 13.93936829374151465 ) ) ;
#69853 = ORIENTED_EDGE ( 'NONE', *, *, #35497, .T. ) ;
#69854 = EDGE_CURVE ( 'NONE', #29911, #54514, #15036, .T. ) ;
#69855 = CARTESIAN_POINT ( 'NONE',  ( -1.254089682851821985, -11.46989282347013095, 32.79007818306219946 ) ) ;
#69856 = CARTESIAN_POINT ( 'NONE',  ( 15.23076923076910916, -3.643525952248795718, 33.31231777344771672 ) ) ;
#69857 = CARTESIAN_POINT ( 'NONE',  ( 7.976679547917409963, -2.619367082507848998, 30.83698974864644171 ) ) ;
#69858 = CARTESIAN_POINT ( 'NONE',  ( -7.780086512803769061, -2.833524468853757750, 32.15551576947925838 ) ) ;
#69859 = VERTEX_POINT ( 'NONE', #70962 ) ;
#69860 = CARTESIAN_POINT ( 'NONE',  ( -1.944543648263014957, -5.555456351737005249, 15.25000000000000000 ) ) ;
#69861 = LINE ( 'NONE', #1843, #953 ) ;
#69862 = AXIS2_PLACEMENT_3D ( 'NONE', #84763, #29373, #78421 ) ;
#69863 = CARTESIAN_POINT ( 'NONE',  ( -0.5276208408985972875, -12.62096338111211580, 30.90682066428152197 ) ) ;
#69864 = CARTESIAN_POINT ( 'NONE',  ( -4.376772371362299019, -10.61292498521070549, 33.66303323003028680 ) ) ;
#69865 = ORIENTED_EDGE ( 'NONE', *, *, #57702, .T. ) ;
#69866 = CARTESIAN_POINT ( 'NONE',  ( -12.23875892027004753, -9.332535724633409302, 34.40230450496446934 ) ) ;
#69867 = CARTESIAN_POINT ( 'NONE',  ( 8.096099364501986528, -5.852078868378312038, 34.47109172314383585 ) ) ;
#69868 = CARTESIAN_POINT ( 'NONE',  ( 14.30769230769231015, -12.29105614889573062, 35.45975837776705220 ) ) ;
#69869 = ORIENTED_EDGE ( 'NONE', *, *, #42997, .F. ) ;
#69870 = CARTESIAN_POINT ( 'NONE',  ( -2.557715531913763662, -12.07920672191015221, 32.31858351112116168 ) ) ;
#69871 = ORIENTED_EDGE ( 'NONE', *, *, #42215, .F. ) ;
#69872 = CARTESIAN_POINT ( 'NONE',  ( -16.15384615384615330, -5.557115091759785130, 34.35708131394839171 ) ) ;
#69873 = DIRECTION ( 'NONE',  ( -0.000000000000000000, 0.8660254037844397068, -0.4999999999999978906 ) ) ;
#69874 = VECTOR ( 'NONE', #86376, 1000.000000000000000 ) ;
#69875 = ORIENTED_EDGE ( 'NONE', *, *, #53472, .T. ) ;
#69876 = CARTESIAN_POINT ( 'NONE',  ( 10.83839745947801170, -11.43677907613344757, 33.22367315496202167 ) ) ;
#69877 = CARTESIAN_POINT ( 'NONE',  ( -9.019254006523732770, -2.587272538249755893, 30.68239716806877837 ) ) ;
#69878 = CARTESIAN_POINT ( 'NONE',  ( -6.700297254098854793, -12.47679350104403007, 31.42216943046555855 ) ) ;
#69879 = VECTOR ( 'NONE', #76510, 1000.000000000000000 ) ;
#69880 = CARTESIAN_POINT ( 'NONE',  ( -11.53846153846153655, -5.471508081941601098, 34.59228464037088457 ) ) ;
#69881 = CARTESIAN_POINT ( 'NONE',  ( -18.06527044596078113, -4.481592998940164385, 33.73612834413957984 ) ) ;
#69882 = ORIENTED_EDGE ( 'NONE', *, *, #30600, .F. ) ;
#69883 = ORIENTED_EDGE ( 'NONE', *, *, #27426, .F. ) ;
#69884 = FACE_BOUND ( 'NONE', #50178, .T. ) ;
#69885 = VERTEX_POINT ( 'NONE', #57884 ) ;
#69886 = CARTESIAN_POINT ( 'NONE',  ( -8.546219417617917813, -4.187068189119699468, 33.49521262558774026 ) ) ;
#69887 = LINE ( 'NONE', #29799, #5636 ) ;
#69888 = CARTESIAN_POINT ( 'NONE',  ( 9.627037246346921151, -12.27809138561121394, 31.22303859784730307 ) ) ;
#69889 = CARTESIAN_POINT ( 'NONE',  ( -14.24162395668986925, -8.973038597847271092, 34.52809138561121216 ) ) ;
#69890 = B_SPLINE_CURVE_WITH_KNOTS ( 'NONE', 3,
 ( #88467, #88033, #81250, #26736, #19973, #47442, #74937, #69494, #22199, #22632 ),
 .UNSPECIFIED., .F., .F.,
 ( 4, 2, 2, 2, 4 ),
 ( 0.0007817246256747517261, 0.0009771112852218957062, 0.001172497944769039686, 0.001367884604316183667, 0.001563271263863327647 ),
 .UNSPECIFIED. ) ;
#69891 = ORIENTED_EDGE ( 'NONE', *, *, #55789, .F. ) ;
#69892 = EDGE_CURVE ( 'NONE', #32510, #2169, #2056, .T. ) ;
#69893 = ORIENTED_EDGE ( 'NONE', *, *, #54732, .T. ) ;
#69894 = VERTEX_POINT ( 'NONE', #2932 ) ;
#69895 = CARTESIAN_POINT ( 'NONE',  ( -0.2114841499001473557, -3.136992222400443175, 32.19305428654138979 ) ) ;
#69896 = VERTEX_POINT ( 'NONE', #15138 ) ;
#69897 = VECTOR ( 'NONE', #82236, 1000.000000000000000 ) ;
#69898 = CARTESIAN_POINT ( 'NONE',  ( 3.100622021331012501, -2.882441371585227508, 31.66841991370171527 ) ) ;
#69899 = CARTESIAN_POINT ( 'NONE',  ( 1.384615384615386802, -3.513871655860378418, 32.76840700105978499 ) ) ;
#69900 = CARTESIAN_POINT ( 'NONE',  ( -18.22348494372394967, -11.41268669641500111, 32.86336882939238535 ) ) ;
#69901 = ORIENTED_EDGE ( 'NONE', *, *, #66143, .T. ) ;
#69902 = FACE_OUTER_BOUND ( 'NONE', #42250, .T. ) ;
#69903 = CARTESIAN_POINT ( 'NONE',  ( 6.923076923076924238, -1.242168528481310874, 33.36296068462461051 ) ) ;
#69904 = FACE_OUTER_BOUND ( 'NONE', #32014, .T. ) ;
#69905 = CARTESIAN_POINT ( 'NONE',  ( -11.78848477575450460, -3.202444869320336451, 32.30641848906366675 ) ) ;
#69906 = ORIENTED_EDGE ( 'NONE', *, *, #29526, .T. ) ;
#69907 = EDGE_CURVE ( 'NONE', #11752, #1726, #29978, .T. ) ;
#69908 = VECTOR ( 'NONE', #49858, 1000.000000000000000 ) ;
#69909 = VERTEX_POINT ( 'NONE', #63312 ) ;
#69910 = EDGE_LOOP ( 'NONE', ( #81579, #22200, #17372, #8025 ) ) ;
#69911 = CARTESIAN_POINT ( 'NONE',  ( 4.153846153846154188, -2.833524468853757305, 32.15551576947925838 ) ) ;
#69912 = UNCERTAINTY_MEASURE_WITH_UNIT (LENGTH_MEASURE( 1.000000000000000082E-05 ), #73083, 'distance_accuracy_value', 'NONE');
#69914 = CARTESIAN_POINT ( 'NONE',  ( 11.53846153846153832, -1.117168528481311540, 33.14645433367849847 ) ) ;
#69913 = LINE ( 'NONE', #44189, #47535 ) ;
#69915 = CARTESIAN_POINT ( 'NONE',  ( 11.28848479441294828, -2.318417181685855422, 30.59732222474233865 ) ) ;
#69916 = CARTESIAN_POINT ( 'NONE',  ( -3.480745961711583902, -11.28823185664190376, 33.01397839955799896 ) ) ;
#69917 = FACE_BOUND ( 'NONE', #85760, .T. ) ;
#69918 = CARTESIAN_POINT ( 'NONE',  ( 8.096099364501990081, -11.37275283266504111, 32.91324779482534524 ) ) ;
#69919 = ORIENTED_EDGE ( 'NONE', *, *, #21795, .F. ) ;
#69920 = CARTESIAN_POINT ( 'NONE',  ( 17.14217864819909920, -10.90142922261932057, 33.41473453929631887 ) ) ;
#69921 = EDGE_CURVE ( 'NONE', #69537, #12402, #62850, .T. ) ;
#69922 = CARTESIAN_POINT ( 'NONE',  ( -0.2385271099256112415, -9.086983370893047862, 34.49168942202179267 ) ) ;
#69923 = CARTESIAN_POINT ( 'NONE',  ( 4.153846153846032507, -9.442884908241554243, 34.35708131394783038 ) ) ;
#69924 = FACE_OUTER_BOUND ( 'NONE', #26100, .T. ) ;
#69925 = ORIENTED_EDGE ( 'NONE', *, *, #65838, .F. ) ;
#69926 = CARTESIAN_POINT ( 'NONE',  ( 2.307692307692187583, -11.94971097300221174, 32.03036669348237098 ) ) ;
#69927 = ORIENTED_EDGE ( 'NONE', *, *, #81121, .F. ) ;
#69928 = FACE_BOUND ( 'NONE', #31621, .T. ) ;
#69929 = CARTESIAN_POINT ( 'NONE',  ( 16.15384615384603251, -3.643525952248796163, 33.31231777344771672 ) ) ;
#69930 = CARTESIAN_POINT ( 'NONE',  ( -6.923076923077045919, -10.33852847137269571, 34.16647553114546554 ) ) ;
#69931 = CARTESIAN_POINT ( 'NONE',  ( 5.076923076922953193, -10.33852847137269571, 34.16647553114546554 ) ) ;
#69932 = VERTEX_POINT ( 'NONE', #15580 ) ;
#69933 = CARTESIAN_POINT ( 'NONE',  ( 0.2115152242454954312, -10.76384336483936011, 33.53834819971076087 ) ) ;
#69934 = CARTESIAN_POINT ( 'NONE',  ( 15.23076923076910916, -2.379036618888197729, 30.90682066428292885 ) ) ;
#69935 = CARTESIAN_POINT ( 'NONE',  ( 8.519254025182176449, -8.347322224742351082, 34.93158281831414769 ) ) ;
#69936 = CARTESIAN_POINT ( 'NONE',  ( -6.923076923076922462, -10.51840700105979565, 33.73612834413961536 ) ) ;
#69937 = EDGE_LOOP ( 'NONE', ( #34735, #21045 ) ) ;
#69938 = VECTOR ( 'NONE', #68316, 1000.000000000000000 ) ;
#69939 = CYLINDRICAL_SURFACE ( 'NONE', #28693, 0.2499999999999979738 ) ;
#69940 = ORIENTED_EDGE ( 'NONE', *, *, #45022, .F. ) ;
#69942 = VERTEX_POINT ( 'NONE', #84933 ) ;
#69941 = CARTESIAN_POINT ( 'NONE',  ( 17.07692307692295586, -12.27809138561165270, 31.22303859784587132 ) ) ;
#69943 = CARTESIAN_POINT ( 'NONE',  ( -18.00000000104979492, -12.75000000000000355, 29.50000000010276935 ) ) ;
#69944 = CARTESIAN_POINT ( 'NONE',  ( -1.608100309179716803, -12.47654668319379567, 31.42292124445336654 ) ) ;
#69945 = CARTESIAN_POINT ( 'NONE',  ( 13.31934493865461278, -9.442884908240170461, 34.35708131394840592 ) ) ;
#69946 = EDGE_CURVE ( 'NONE', #17400, #78293, #29106, .T. ) ;
#69947 = ADVANCED_FACE ( 'NONE', ( #78159 ), #70072, .F. ) ;
#69948 = CARTESIAN_POINT ( 'NONE',  ( 9.692307692307570832, -5.094484230521993062, 34.41647553114689373 ) ) ;
#69950 = CARTESIAN_POINT ( 'NONE',  ( 0.2115384615384615641, -7.500000000000001776, 34.75000000000000000 ) ) ;
#69949 = CARTESIAN_POINT ( 'NONE',  ( -3.007756386675834559, -4.026326845037965008, 33.68677907613344047 ) ) ;
#69951 = CARTESIAN_POINT ( 'NONE',  ( 14.17700084102474811, -3.530157926970578952, 32.79014554554150607 ) ) ;
#69952 = CARTESIAN_POINT ( 'NONE',  ( -1.944543648263014957, -5.555456351737005249, 25.25000000000000000 ) ) ;
#69953 =( REPRESENTATION_RELATIONSHIP ('NONE','NONE', #51743, #11527 ) REPRESENTATION_RELATIONSHIP_WITH_TRANSFORMATION ( #67172 )SHAPE_REPRESENTATION_RELATIONSHIP( ) );
#69954 = EDGE_LOOP ( 'NONE', ( #32974, #12761 ) ) ;
#69955 = CARTESIAN_POINT ( 'NONE',  ( -17.93474442872397034, -9.442884908240273489, 34.35708131394837039 ) ) ;
#69956 = EDGE_LOOP ( 'NONE', ( #81924, #42330, #40010, #61960, #23772, #81081 ) ) ;
#69957 = EDGE_LOOP ( 'NONE', ( #46370, #61222 ) ) ;
#69958 = CARTESIAN_POINT ( 'NONE',  ( -16.15384615384627409, -6.835583212225970762, 34.95778746994575670 ) ) ;
#69959 = EDGE_LOOP ( 'NONE', ( #64140, #66784, #76707, #19824 ) ) ;
#69960 = CARTESIAN_POINT ( 'NONE',  ( -6.000000000000121680, -2.379036618888197729, 30.90682066428292885 ) ) ;
#69961 = B_SPLINE_CURVE_WITH_KNOTS ( 'NONE', 3,
 ( #68531, #41959, #35190, #21677, #55026, #6829, #54568, #76627, #49146, #14032 ),
 .UNSPECIFIED., .F., .F.,
 ( 4, 2, 2, 2, 4 ),
 ( 0.0007817359430256282712, 0.0009771253907249941549, 0.001172514838424359822, 0.001367904286123725489, 0.001563293733823091372 ),
 .UNSPECIFIED. ) ;
#69962 = B_SPLINE_CURVE_WITH_KNOTS ( 'NONE', 3,
 ( #70120, #25040, #11534, #16951, #3870, #44853, #44400, #65570, #72333, #45756 ),
 .UNSPECIFIED., .F., .F.,
 ( 4, 2, 2, 2, 4 ),
 ( 0.0007817359430256297891, 0.0009771253907249958896, 0.001172514838424362207, 0.001367904286123728524, 0.001563293733823094625 ),
 .UNSPECIFIED. ) ;
#69963 = CARTESIAN_POINT ( 'NONE',  ( 10.61538461538461675, -9.819645486525091727, 36.12317359536749706 ) ) ;
#69964 = CARTESIAN_POINT ( 'NONE',  ( -11.60454494941741999, -11.16473453929635440, 33.15142922261925662 ) ) ;
#69965 = CARTESIAN_POINT ( 'NONE',  ( 1.384615384615386802, -13.53365097954675988, 30.81389545987213552 ) ) ;
#69966 = CARTESIAN_POINT ( 'NONE',  ( 12.46153846153846168, -10.51840700105979565, 33.73612834413961536 ) ) ;
#69967 = CARTESIAN_POINT ( 'NONE',  ( 17.32697749683652688, -8.346898887586322147, 34.93166121998716278 ) ) ;
#69968 = DIRECTION ( 'NONE',  ( -0.000000000000000000, 0.1736481776669307198, -0.9848077530122080203 ) ) ;
#69969 = CARTESIAN_POINT ( 'NONE',  ( 2.307692307692309264, -9.780366693483667717, 34.19971097300155094 ) ) ;
#69970 = CARTESIAN_POINT ( 'NONE',  ( 17.93391658904411656, -11.69971097300155272, 32.46337939537587403 ) ) ;
#69971 = DIRECTION ( 'NONE',  ( -0.000000000000000000, -0.5000000000000009992, -0.8660254037844380415 ) ) ;
#69972 = LINE ( 'NONE', #1963, #68619 ) ;
#69973 = ORIENTED_EDGE ( 'NONE', *, *, #66948, .T. ) ;
#69974 = VERTEX_POINT ( 'NONE', #23213 ) ;
#69975 = CARTESIAN_POINT ( 'NONE',  ( 3.230769230769108269, -11.06231777344772027, 33.60647404775119895 ) ) ;
#69976 = DIRECTION ( 'NONE',  ( -0.000000000000000000, 0.8660254037844399289, -0.4999999999999980016 ) ) ;
#69977 = DIRECTION ( 'NONE',  ( -0.000000000000000000, 0.5000000000000011102, -0.8660254037844380415 ) ) ;
#69978 = CARTESIAN_POINT ( 'NONE',  ( -2.307692307692305711, -2.499999999999998668, 29.75000000000001421 ) ) ;
#69979 = ORIENTED_EDGE ( 'NONE', *, *, #14033, .T. ) ;
#69980 = CARTESIAN_POINT ( 'NONE',  ( -15.90379173393269596, -8.346898887586322147, 34.93166121998716278 ) ) ;
#69981 = CARTESIAN_POINT ( 'NONE',  ( -13.51476335434708353, -11.04286588640298561, 33.62463336215343901 ) ) ;
#69982 = CARTESIAN_POINT ( 'NONE',  ( -3.165513659493205623, -12.27809138561124591, 31.22303859784720359 ) ) ;
#69983 = ORIENTED_EDGE ( 'NONE', *, *, #31649, .T. ) ;
#69984 = CARTESIAN_POINT ( 'NONE',  ( 0.5267940328144853357, -6.026961402152789304, 34.52809138561124769 ) ) ;
#69985 = VERTEX_POINT ( 'NONE', #29538 ) ;
#69986 = B_SPLINE_CURVE_WITH_KNOTS ( 'NONE', 3,
 ( #27476, #20276, #6, #46852, #75223, #21150, #87877, #74335, #12634, #13511 ),
 .UNSPECIFIED., .F., .F.,
 ( 4, 2, 2, 2, 4 ),
 ( 0.000000000000000000, 0.0001954339857564072033, 0.0003908679715128144066, 0.0005863019572692215828, 0.0007817359430256288133 ),
 .UNSPECIFIED. ) ;
#69987 = B_SPLINE_CURVE_WITH_KNOTS ( 'NONE', 3,
 ( #85382, #16917, #65541, #3842, #46176, #11953, #59681, #33982, #61445, #60565 ),
 .UNSPECIFIED., .F., .F.,
 ( 4, 2, 2, 2, 4 ),
 ( 0.000000000000000000, 0.0001954311564186858715, 0.0003908623128373717431, 0.0005862934692560576146, 0.0007817246256747434861 ),
 .UNSPECIFIED. ) ;
#69988 = LINE ( 'NONE', #35779, #63749 ) ;
#69989 = LINE ( 'NONE', #26796, #78715 ) ;
#69990 = AXIS2_PLACEMENT_3D ( 'NONE', #49808, #8840, #63766 ) ;
#69991 = CYLINDRICAL_SURFACE ( 'NONE', #41574, 4.755951259985877755 ) ;
#69992 = CARTESIAN_POINT ( 'NONE',  ( -14.08468095607945969, -11.76359900205217457, 32.36225158514719880 ) ) ;
#69993 = CARTESIAN_POINT ( 'NONE',  ( 17.99999999999987566, -8.656820664282941280, 34.87096338111179961 ) ) ;
#69994 = B_SPLINE_CURVE_WITH_KNOTS ( 'NONE', 3,
 ( #59879, #60764, #26547, #86942, #79715, #67089, #5389, #52224, #54005, #73400 ),
 .UNSPECIFIED., .F., .F.,
 ( 4, 2, 2, 2, 4 ),
 ( 0.0007817359430256327164, 0.0009771253907249995759, 0.001172514838424366544, 0.001367904286123733295, 0.001563293733823100263 ),
 .UNSPECIFIED. ) ;
#69995 = ORIENTED_EDGE ( 'NONE', *, *, #42513, .T. ) ;
#69996 = EDGE_CURVE ( 'NONE', #52292, #38569, #8825, .T. ) ;
#69997 = ORIENTED_EDGE ( 'NONE', *, *, #33731, .T. ) ;
#69998 = EDGE_CURVE ( 'NONE', #62271, #66561, #3204, .T. ) ;
#69999 = VERTEX_POINT ( 'NONE', #23655 ) ;
#70000 = ORIENTED_EDGE ( 'NONE', *, *, #83557, .T. ) ;
#70001 = CIRCLE ( 'NONE', #78617, 2.750000000000000000 ) ;
#70002 = CARTESIAN_POINT ( 'NONE',  ( -6.130147209438217004, -11.47017969459903952, 32.78971311882034456 ) ) ;
#70003 = CARTESIAN_POINT ( 'NONE',  ( -16.82686876528476105, -3.627508038966690496, 32.91356715214248396 ) ) ;
#70004 = CARTESIAN_POINT ( 'NONE',  ( -12.39547112818838492, -12.34228464037088813, 31.77849191805839268 ) ) ;
#70006 = EDGE_CURVE ( 'NONE', #49403, #33332, #60154, .T. ) ;
#70005 = CARTESIAN_POINT ( 'NONE',  ( -2.241624974342229848, -11.35647404775217595, 33.31231777344667222 ) ) ;
#70007 = CARTESIAN_POINT ( 'NONE',  ( -17.75005448165186195, -4.336752205174650321, 33.62275283266504289 ) ) ;
#70008 = FACE_OUTER_BOUND ( 'NONE', #39782, .T. ) ;
#70009 = ORIENTED_EDGE ( 'NONE', *, *, #87442, .F. ) ;
#70010 = ORIENTED_EDGE ( 'NONE', *, *, #82498, .T. ) ;
#70011 = VERTEX_POINT ( 'NONE', #58774 ) ;
#70013 = VERTEX_POINT ( 'NONE', #87607 ) ;
#70012 = CARTESIAN_POINT ( 'NONE',  ( 15.12820512820512953, -4.000000000000000000, 29.75000000000000355 ) ) ;
#70015 = CARTESIAN_POINT ( 'NONE',  ( -10.54931728203453822, -6.343179335718452272, 34.87096338111212646 ) ) ;
#70014 = LINE ( 'NONE', #87776, #50366 ) ;
#70016 = CARTESIAN_POINT ( 'NONE',  ( 9.468822748583747284, -2.599994579823202923, 30.74605699353653776 ) ) ;
#70017 = AXIS2_PLACEMENT_3D ( 'NONE', #3497, #71510, #30095 ) ;
#70018 = CARTESIAN_POINT ( 'NONE',  ( 13.38461538461538680, -8.120952969808772792, 34.71129190930000163 ) ) ;
#70019 = ORIENTED_EDGE ( 'NONE', *, *, #11480, .F. ) ;
#70020 = B_SPLINE_CURVE_WITH_KNOTS ( 'NONE', 3,
 ( #82813, #56214, #21987, #84588, #70171, #28291, #7144, #14340, #8478, #2150 ),
 .UNSPECIFIED., .F., .F.,
 ( 4, 2, 2, 2, 4 ),
 ( 0.000000000000000000, 0.0001954339857564084502, 0.0003908679715128169003, 0.0005863019572692253776, 0.0007817359430256338006 ),
 .UNSPECIFIED. ) ;
#70021 = EDGE_CURVE ( 'NONE', #36076, #81591, #56964, .T. ) ;
#70022 = B_SPLINE_CURVE_WITH_KNOTS ( 'NONE', 3,
 ( #40473, #20622, #25610, #67936, #53066, #26059 ),
 .UNSPECIFIED., .F., .F.,
 ( 4, 2, 4 ),
 ( 0.0003909569690057816227, 0.0005862646681846067891, 0.0007815723673634319014 ),
 .UNSPECIFIED. ) ;
#70023 = ORIENTED_EDGE ( 'NONE', *, *, #60650, .T. ) ;
#70024 = CARTESIAN_POINT ( 'NONE',  ( -7.846153846153844924, -12.78798330534102945, 29.74999999999997868 ) ) ;
#70025 = B_SPLINE_CURVE_WITH_KNOTS ( 'NONE', 3,
 ( #1339, #69799, #21166, #7222, #77008, #47757, #20295, #62156, #42784, #54960 ),
 .UNSPECIFIED., .F., .F.,
 ( 4, 2, 2, 2, 4 ),
 ( 0.0007817246256747514008, 0.0009771112852218952725, 0.001172497944769039253, 0.001367884604316183233, 0.001563271263863327213 ),
 .UNSPECIFIED. ) ;
#70026 = ORIENTED_EDGE ( 'NONE', *, *, #85193, .F. ) ;
#70027 = FACE_BOUND ( 'NONE', #71244, .T. ) ;
#70028 = CARTESIAN_POINT ( 'NONE',  ( -6.923076923076922462, -13.04860791097971706, 34.73218667398347037 ) ) ;
#70029 = CARTESIAN_POINT ( 'NONE',  ( 0.4615384615383396616, -11.48612834414049644, 32.76840700105863391 ) ) ;
#70030 = ORIENTED_EDGE ( 'NONE', *, *, #59168, .F. ) ;
#70031 = CARTESIAN_POINT ( 'NONE',  ( 15.00794113313435219, -7.369209533119137845, 34.99857337881830688 ) ) ;
#70032 = CARTESIAN_POINT ( 'NONE',  ( 16.15384615384603251, -4.481592998941358097, 33.73612834414048933 ) ) ;
#70033 = VECTOR ( 'NONE', #19362, 1000.000000000000227 ) ;
#70034 = CARTESIAN_POINT ( 'NONE',  ( -1.384615384615383471, -4.102666532097928531, 36.13435417666054406 ) ) ;
#70035 = CARTESIAN_POINT ( 'NONE',  ( 4.023154687178596589, -11.18331474514187995, 33.13161551792790505 ) ) ;
#70036 = CARTESIAN_POINT ( 'NONE',  ( 4.376857505459001096, -3.105924265160262543, 32.13625925475356127 ) ) ;
#70037 = ORIENTED_EDGE ( 'NONE', *, *, #85460, .F. ) ;
#70038 = CARTESIAN_POINT ( 'NONE',  ( -11.31568186948347154, -12.47679350104403007, 31.42216943046555855 ) ) ;
#70039 = CARTESIAN_POINT ( 'NONE',  ( -23.50000000000000000, -8.999999999999996447, 28.86437827766147279 ) ) ;
#70040 = CARTESIAN_POINT ( 'NONE',  ( -17.78205128205128105, -7.500000000000000000, 29.75000000000000355 ) ) ;
#70041 = DIRECTION ( 'NONE',  ( -0.000000000000000000, 0.8660254037844399289, -0.4999999999999980016 ) ) ;
#70042 = FACE_OUTER_BOUND ( 'NONE', #50795, .T. ) ;
#70043 = EDGE_CURVE ( 'NONE', #28560, #65473, #52899, .T. ) ;
#70044 = FACE_BOUND ( 'NONE', #71177, .T. ) ;
#70046 = CARTESIAN_POINT ( 'NONE',  ( 11.53846153846153832, -12.37446782046654192, 30.86335684631486131 ) ) ;
#70045 = CARTESIAN_POINT ( 'NONE',  ( 17.32697738856138869, -3.627508038966690496, 32.91356715214248396 ) ) ;
#70047 = CARTESIAN_POINT ( 'NONE',  ( 11.66925197942848769, -11.93129842949671726, 32.56571108434900452 ) ) ;
#70049 = CARTESIAN_POINT ( 'NONE',  ( 19.00000000000000000, -7.500000000000000000, 29.75000000000000355 ) ) ;
#70048 = CARTESIAN_POINT ( 'NONE',  ( -3.360917200500929791, -3.069018819979302926, 32.56621877034667278 ) ) ;
#70050 = ADVANCED_FACE ( 'NONE', ( #4732 ), #87163, .F. ) ;
#70051 = LINE ( 'NONE', #29520, #70699 ) ;
#70052 = CARTESIAN_POINT ( 'NONE',  ( -1.901340078031346525, -9.487747218494661183, 22.18563170625848713 ) ) ;
#70053 = ORIENTED_EDGE ( 'NONE', *, *, #83416, .T. ) ;
#70054 = CARTESIAN_POINT ( 'NONE',  ( -1.980058552680825423, -4.310325471588868140, 13.99999999999999289 ) ) ;
#70055 = ORIENTED_EDGE ( 'NONE', *, *, #58239, .T. ) ;
#70056 = CARTESIAN_POINT ( 'NONE',  ( -13.25382494364843389, -10.70102852606553157, 33.91149625220312913 ) ) ;
#70057 = EDGE_CURVE ( 'NONE', #80983, #2346, #86273, .T. ) ;
#70058 = VECTOR ( 'NONE', #15750, 1000.000000000000000 ) ;
#70059 = EDGE_LOOP ( 'NONE', ( #29091, #47399, #80815, #53828, #14818 ) ) ;
#70060 = EDGE_CURVE ( 'NONE', #41484, #45738, #45167, .T. ) ;
#70061 = CARTESIAN_POINT ( 'NONE',  ( 0.4615384615384611755, -1.215029322943914858, 32.30358669280327177 ) ) ;
#70062 = DIRECTION ( 'NONE',  ( -0.000000000000000000, -0.5000000000000009992, -0.8660254037844380415 ) ) ;
#70063 = VERTEX_POINT ( 'NONE', #59665 ) ;
#70064 = CARTESIAN_POINT ( 'NONE',  ( -8.096130577096198877, -5.728515186090277211, 34.42611988154120439 ) ) ;
#70065 = CARTESIAN_POINT ( 'NONE',  ( -1.987747218494660295, -5.598659921968651254, 24.99813170625849423 ) ) ;
#70066 = CARTESIAN_POINT ( 'NONE',  ( 6.166666666666664298, -11.00000000000000000, 29.75000000000000355 ) ) ;
#70067 = B_SPLINE_CURVE_WITH_KNOTS ( 'NONE', 3,
 ( #36474, #57183, #77457, #17534, #44985, #44090, #22950, #15763, #65257, #64365 ),
 .UNSPECIFIED., .F., .F.,
 ( 4, 2, 2, 2, 4 ),
 ( 0.0007817359430256308733, 0.0009771253907249971907, 0.001172514838424363725, 0.001367904286123730259, 0.001563293733823096577 ),
 .UNSPECIFIED. ) ;
#70068 = CARTESIAN_POINT ( 'NONE',  ( 1.384615384615264011, -12.51329471203414379, 31.30864560766407578 ) ) ;
#70069 = CARTESIAN_POINT ( 'NONE',  ( 7.146088274689774700, -9.086983370893049639, 34.49168942202179267 ) ) ;
#70070 = CARTESIAN_POINT ( 'NONE',  ( -5.076923076923197442, -12.46129190930018460, 30.37095296980731973 ) ) ;
#70071 = LINE ( 'NONE', #63311, #63112 ) ;
#70072 = CYLINDRICAL_SURFACE ( 'NONE', #28138, 0.2500000000000008882 ) ;
#70073 = B_SPLINE_CURVE_WITH_KNOTS ( 'NONE', 3,
 ( #31797, #67356, #31346, #25479, #52933, #59257, #53386, #25921, #45745, #58808 ),
 .UNSPECIFIED., .F., .F.,
 ( 4, 2, 2, 2, 4 ),
 ( 0.0007817246256747444619, 0.0009771112852218868158, 0.001172497944769029061, 0.001367884604316171523, 0.001563271263863313769 ),
 .UNSPECIFIED. ) ;
#70074 = CARTESIAN_POINT ( 'NONE',  ( 3.750000000000009770, -9.053300858899081760, 18.29687500000000000 ) ) ;
#70075 = CARTESIAN_POINT ( 'NONE',  ( -11.97435897435897267, -7.500000000000000000, 29.75000000000000355 ) ) ;
#70076 = DIRECTION ( 'NONE',  ( -0.000000000000000000, -0.6427876096865404731, -0.7660444431189771253 ) ) ;
#70077 = AXIS2_PLACEMENT_3D ( 'NONE', #73402, #80162, #46813 ) ;
#70078 = FACE_OUTER_BOUND ( 'NONE', #16427, .T. ) ;
#70079 = CARTESIAN_POINT ( 'NONE',  ( 3.775308065498752086, -6.007798216065404873, 24.64249329374151642 ) ) ;
#70080 = DIRECTION ( 'NONE',  ( -0.000000000000000000, -0.1736481776669307198, -0.9848077530122080203 ) ) ;
#70081 = ORIENTED_EDGE ( 'NONE', *, *, #59680, .F. ) ;
#70082 = DIRECTION ( 'NONE',  ( -0.000000000000000000, -0.3420201433256694346, -0.9396926207859080948 ) ) ;
#70083 = CARTESIAN_POINT ( 'NONE',  ( -3.230769230769352962, -5.941354392335915335, 34.76329471203413846 ) ) ;
#70084 = DIRECTION ( 'NONE',  ( 0.000000000000000000, 0.6427876096865373645, -0.7660444431189797898 ) ) ;
#70085 = DIRECTION ( 'NONE',  ( 0.000000000000000000, 0.1736481776669275834, 0.9848077530122086864 ) ) ;
#70086 = DIRECTION ( 'NONE',  ( 0.000000000000000000, 0.000000000000000000, -1.000000000000000000 ) ) ;
#70087 = CARTESIAN_POINT ( 'NONE',  ( 9.692307692307695177, -11.16473453929635440, 33.15142922261926373 ) ) ;
#70088 = CYLINDRICAL_SURFACE ( 'NONE', #47645, 0.2499999999999973355 ) ;
#70089 = ADVANCED_FACE ( 'NONE', ( #52009 ), #65528, .F. ) ;
#70090 = VECTOR ( 'NONE', #64466, 1000.000000000000000 ) ;
#70091 = ORIENTED_EDGE ( 'NONE', *, *, #31671, .T. ) ;
#70092 = ORIENTED_EDGE ( 'NONE', *, *, #63555, .F. ) ;
#70093 = VECTOR ( 'NONE', #88429, 1000.000000000000000 ) ;
#70094 = VERTEX_POINT ( 'NONE', #11486 ) ;
#70095 = CARTESIAN_POINT ( 'NONE',  ( -13.63459211555773720, -3.627789207965226748, 32.91389620160131102 ) ) ;
#70096 = CARTESIAN_POINT ( 'NONE',  ( 3.230769230769108269, -5.941354392335915335, 34.76329471203413846 ) ) ;
#70097 = CARTESIAN_POINT ( 'NONE',  ( 6.673053698855467175, -2.985938066672154445, 32.43141759479405550 ) ) ;
#70098 = VECTOR ( 'NONE', #8933, 1000.000000000000000 ) ;
#70099 = DIRECTION ( 'NONE',  ( -0.000000000000000000, 0.3420201433256694346, -0.9396926207859080948 ) ) ;
#70100 = CARTESIAN_POINT ( 'NONE',  ( 13.13463864056679498, -8.347322224742351082, 34.93158281831414769 ) ) ;
#70101 = EDGE_CURVE ( 'NONE', #73925, #11539, #71967, .T. ) ;
#70102 = VERTEX_POINT ( 'NONE', #38514 ) ;
#70103 = CARTESIAN_POINT ( 'NONE',  ( -9.320512820512821150, -4.000000000000000000, 28.25000000000000000 ) ) ;
#70104 = ORIENTED_EDGE ( 'NONE', *, *, #85504, .T. ) ;
#70105 = ORIENTED_EDGE ( 'NONE', *, *, #37861, .F. ) ;
#70106 = VERTEX_POINT ( 'NONE', #3383 ) ;
#70108 = EDGE_LOOP ( 'NONE', ( #43294, #22129, #52441, #86319 ) ) ;
#70107 = CARTESIAN_POINT ( 'NONE',  ( -15.29685264172511161, -12.10708131394839349, 31.69288490824020244 ) ) ;
#70109 = CARTESIAN_POINT ( 'NONE',  ( 2.307692307692309264, -1.629998284177014645, 34.34916445242399163 ) ) ;
#70110 = CARTESIAN_POINT ( 'NONE',  ( -10.36538461538467715, -7.565270445406050648, 34.75000000000000000 ) ) ;
#70111 = EDGE_CURVE ( 'NONE', #4346, #42531, #30853, .T. ) ;
#70112 = AXIS2_PLACEMENT_3D ( 'NONE', #45532, #24815, #4549 ) ;
#70113 = CARTESIAN_POINT ( 'NONE',  ( 2.057692307692309708, -2.499999999999998668, 29.75000000000000355 ) ) ;
#70114 = CARTESIAN_POINT ( 'NONE',  ( -4.826923076923014477, -7.434744429011176159, 34.75000000000000711 ) ) ;
#70115 = ORIENTED_EDGE ( 'NONE', *, *, #33357, .T. ) ;
#70116 = EDGE_CURVE ( 'NONE', #19898, #48076, #85817, .T. ) ;
#70117 = ORIENTED_EDGE ( 'NONE', *, *, #69817, .F. ) ;
#70118 = VERTEX_POINT ( 'NONE', #86726 ) ;
#70119 = CARTESIAN_POINT ( 'NONE',  ( -14.43830266731683132, -7.722926236386453702, 34.74524107206102030 ) ) ;
#70121 = ORIENTED_EDGE ( 'NONE', *, *, #30369, .F. ) ;
#70120 = CARTESIAN_POINT ( 'NONE',  ( 15.23076923076911093, -6.026961402154118019, 34.52809138561165270 ) ) ;
#70122 = CARTESIAN_POINT ( 'NONE',  ( 1.634560902963527740, -9.272278438253398036, 34.42582936511637826 ) ) ;
#70123 = DIRECTION ( 'NONE',  ( -0.000000000000000000, 0.3420201433256694346, -0.9396926207859080948 ) ) ;
#70124 = CARTESIAN_POINT ( 'NONE',  ( 7.053868730901712070, -11.71459661697925903, 32.44059661609676937 ) ) ;
#70125 = ORIENTED_EDGE ( 'NONE', *, *, #69317, .T. ) ;
#70126 = AXIS2_PLACEMENT_3D ( 'NONE', #22661, #50570, #57777 ) ;
#70127 = ADVANCED_FACE ( 'NONE', ( #24991 ), #52457, .F. ) ;
#70128 = CARTESIAN_POINT ( 'NONE',  ( -11.31568199719312773, -5.114059244376869984, 34.14424750095245287 ) ) ;
#70129 = DIRECTION ( 'NONE',  ( 1.000000000000000000, 0.000000000000000000, 0.000000000000000000 ) ) ;
#70130 = EDGE_LOOP ( 'NONE', ( #43853, #81402, #9444, #41995 ) ) ;
#70131 = FACE_BOUND ( 'NONE', #20048, .T. ) ;
#70132 = DIRECTION ( 'NONE',  ( -0.000000000000000000, -0.7660444431189792347, -0.6427876096865379196 ) ) ;
#70133 = CARTESIAN_POINT ( 'NONE',  ( -18.24997674404858827, -12.41104346484419452, 31.60698883733904196 ) ) ;
#70134 = DIRECTION ( 'NONE',  ( 0.000000000000000000, 0.8660254037844377084, 0.5000000000000015543 ) ) ;
#70136 = CARTESIAN_POINT ( 'NONE',  ( -6.923076923076922462, -2.538708090699994813, 30.37095296980875503 ) ) ;
#70135 = DIRECTION ( 'NONE',  ( -0.000000000000000000, 1.000000000000000000, 3.491481338843133355E-15 ) ) ;
#70137 = ADVANCED_FACE ( 'NONE', ( #19130 ), #40297, .F. ) ;
#70138 = CARTESIAN_POINT ( 'NONE',  ( -4.946131269098289707, -10.54018710029568595, 33.71981072465678864 ) ) ;
#70139 = CARTESIAN_POINT ( 'NONE',  ( -15.90390063549801347, -9.272278438253401589, 34.42582936511637826 ) ) ;
#70140 = VERTEX_POINT ( 'NONE', #27652 ) ;
#70141 = CARTESIAN_POINT ( 'NONE',  ( -2.307692307692305711, -3.937682226553329556, 33.60647404775216529 ) ) ;
#70142 = EDGE_CURVE ( 'NONE', #37962, #4784, #54229, .T. ) ;
#70143 = FACE_OUTER_BOUND ( 'NONE', #31811, .T. ) ;
#70144 = EDGE_LOOP ( 'NONE', ( #23349, #7081, #82325, #87500 ) ) ;
#70145 = CARTESIAN_POINT ( 'NONE',  ( -10.61538461538461320, -8.973038597847269315, 34.52809138561121927 ) ) ;
#70146 = CARTESIAN_POINT ( 'NONE',  ( -14.05763788777885637, -9.233818618650603938, 34.70587769442853698 ) ) ;
#70147 = CARTESIAN_POINT ( 'NONE',  ( 3.100292522652767335, -7.276988635370450709, 34.74523720219453793 ) ) ;
#70148 = CARTESIAN_POINT ( 'NONE',  ( 20.00000000000000000, -4.000000000000000000, 29.75000000000000355 ) ) ;
#70149 = CARTESIAN_POINT ( 'NONE',  ( 17.86985279056177944, -6.001485441113818986, 34.52039167877662607 ) ) ;
#70150 = CARTESIAN_POINT ( 'NONE',  ( -8.769230769230768274, -5.557115091759785130, 34.35708131394839171 ) ) ;
#70151 = EDGE_CURVE ( 'NONE', #48865, #59129, #13258, .T. ) ;
#70152 = FACE_BOUND ( 'NONE', #32607, .T. ) ;
#70154 = DIRECTION ( 'NONE',  ( -0.000000000000000000, 1.000000000000000000, -0.000000000000000000 ) ) ;
#70153 = CYLINDRICAL_SURFACE ( 'NONE', #98, 0.2499999999999998890 ) ;
#70155 = CARTESIAN_POINT ( 'NONE',  ( 1.634560793993430350, -12.68172785388650681, 30.59649109432439573 ) ) ;
#70157 = CARTESIAN_POINT ( 'NONE',  ( 7.715593254411924562, -2.504760397472875155, 29.97295953869789997 ) ) ;
#70156 = CARTESIAN_POINT ( 'NONE',  ( -17.86947429823644029, -11.46989282347012740, 32.79007818306219946 ) ) ;
#70158 = DIRECTION ( 'NONE',  ( -0.000000000000000000, -0.000000000000000000, -1.000000000000000000 ) ) ;
#70159 = VECTOR ( 'NONE', #40900, 1000.000000000000227 ) ;
#70160 = CARTESIAN_POINT ( 'NONE',  ( -2.608446859217889546, -10.19485399968121264, 19.68563170625849068 ) ) ;
#70161 = ORIENTED_EDGE ( 'NONE', *, *, #24880, .T. ) ;
#70162 = EDGE_CURVE ( 'NONE', #81839, #12293, #77402, .T. ) ;
#70163 = B_SPLINE_CURVE_WITH_KNOTS ( 'NONE', 3,
 ( #44458, #79154, #31410, #10698, #17900, #52558, #30082, #24198, #50771, #58419 ),
 .UNSPECIFIED., .F., .F.,
 ( 4, 2, 2, 2, 4 ),
 ( 0.000000000000000000, 0.0001954339857564132749, 0.0003908679715128195566, 0.0005863019572692258112, 0.0007817359430256319575 ),
 .UNSPECIFIED. ) ;
#70164 = ORIENTED_EDGE ( 'NONE', *, *, #68195, .F. ) ;
#70165 = CARTESIAN_POINT ( 'NONE',  ( 5.326868595271218254, -6.696923467548660192, 34.68552623307873972 ) ) ;
#70166 = ADVANCED_FACE ( 'NONE', ( #60552 ), #33965, .T. ) ;
#70167 = VECTOR ( 'NONE', #2271, 1000.000000000000227 ) ;
#70168 = CARTESIAN_POINT ( 'NONE',  ( -15.29685161012936412, -5.471508081941602875, 34.59228464037088457 ) ) ;
#70169 = CARTESIAN_POINT ( 'NONE',  ( 14.37294744720514572, -9.528491918058460186, 34.59228464037086326 ) ) ;
#70170 = CARTESIAN_POINT ( 'NONE',  ( -16.85414353565466428, -11.41317474335729543, 32.86274602512330034 ) ) ;
#70171 = CARTESIAN_POINT ( 'NONE',  ( -16.40382288478850725, -12.17611988154120795, 31.52148481390971213 ) ) ;
#70172 = CARTESIAN_POINT ( 'NONE',  ( -3.775308065498766297, -6.007798216065450170, 16.17000670625848713 ) ) ;
#70173 = DIRECTION ( 'NONE',  ( -0.000000000000000000, 0.3420201433256694346, -0.9396926207859080948 ) ) ;
#70174 = CYLINDRICAL_SURFACE ( 'NONE', #46047, 0.2500000000000004996 ) ;
#70175 = CARTESIAN_POINT ( 'NONE',  ( 6.000000000000001776, -3.937682226553329556, 33.60647404775216529 ) ) ;
#70176 = CARTESIAN_POINT ( 'NONE',  ( -3.165514091256391715, -12.16647553114626490, 32.15551576947920864 ) ) ;
#70177 = CARTESIAN_POINT ( 'NONE',  ( -3.480792454990686124, -4.175268141568689195, 33.81360843649122216 ) ) ;
#70178 = CARTESIAN_POINT ( 'NONE',  ( 16.37685750545900376, -4.887748414852792322, 34.01359900205217457 ) ) ;
#70179 = CARTESIAN_POINT ( 'NONE',  ( 12.52760579488853665, -2.292212530054420494, 30.41441678777542990 ) ) ;
#70180 = DIRECTION ( 'NONE',  ( -1.000000000000000000, -0.000000000000000000, -0.000000000000000000 ) ) ;
#70181 = EDGE_CURVE ( 'NONE', #50406, #6751, #47473, .T. ) ;
#70182 = EDGE_LOOP ( 'NONE', ( #6408, #47938, #88108, #20949 ) ) ;
#70183 = CARTESIAN_POINT ( 'NONE',  ( -14.37296275365308240, -3.835265460703609186, 33.15142922261924241 ) ) ;
#70184 = CARTESIAN_POINT ( 'NONE',  ( 10.61538461538449418, -5.941354392335915335, 34.76329471203413846 ) ) ;
#70185 = CARTESIAN_POINT ( 'NONE',  ( -0.06109907496451398579, -10.25000000000000178, 22.53311829374151642 ) ) ;
#70186 = B_SPLINE_CURVE_WITH_KNOTS ( 'NONE', 3,
 ( #63841, #42258, #56644, #77796, #2136, #83693, #35489, #85011, #2569, #16101 ),
 .UNSPECIFIED., .F., .F.,
 ( 4, 2, 2, 2, 4 ),
 ( 0.0007817246256747509671, 0.0009771112852218959231, 0.001172497944769040987, 0.001367884604316185835, 0.001563271263863330899 ),
 .UNSPECIFIED. ) ;
#70187 = CARTESIAN_POINT ( 'NONE',  ( 0.6843181305165275674, -3.563462043263030399, 33.22394488606062879 ) ) ;
#70189 = CARTESIAN_POINT ( 'NONE',  ( 4.153846153846032507, -10.21337939537710326, 33.94971097300076224 ) ) ;
#70188 = VECTOR ( 'NONE', #18867, 1000.000000000000227 ) ;
#70190 = ORIENTED_EDGE ( 'NONE', *, *, #81140, .F. ) ;
#70191 = EDGE_CURVE ( 'NONE', #13277, #2439, #16143, .T. ) ;
#70192 = CARTESIAN_POINT ( 'NONE',  ( -9.915792616872023402, -5.827078755546623690, 34.72654668319379567 ) ) ;
#70194 = VERTEX_POINT ( 'NONE', #53349 ) ;
#70193 = DIRECTION ( 'NONE',  ( -0.000000000000000000, -0.8660254037844397068, -0.4999999999999978906 ) ) ;
#70195 = CARTESIAN_POINT ( 'NONE',  ( 9.942362112221147186, -12.65882529074907126, 30.72640787790839312 ) ) ;
#70196 = CARTESIAN_POINT ( 'NONE',  ( -22.75000000000000000, -7.500000000000000000, 29.75000000000000355 ) ) ;
#70197 = ORIENTED_EDGE ( 'NONE', *, *, #64097, .T. ) ;
#70198 = CARTESIAN_POINT ( 'NONE',  ( -5.207070286361299871, -12.27039167877662251, 31.24851455888617835 ) ) ;
#70199 = CARTESIAN_POINT ( 'NONE',  ( 7.715543486529319317, -7.722926236386456367, 34.74524107206103452 ) ) ;
#70200 = EDGE_LOOP ( 'NONE', ( #5007, #72598 ) ) ;
#70201 = LINE ( 'NONE', #50790, #1748 ) ;
#70202 = ADVANCED_FACE ( 'NONE', ( #55124 ), #47030, .F. ) ;
#70203 = CARTESIAN_POINT ( 'NONE',  ( 16.15384615384615330, -2.499999999999998668, 29.75000000000001421 ) ) ;
#70204 = AXIS2_PLACEMENT_3D ( 'NONE', #34754, #28907, #13161 ) ;
#70205 = B_SPLINE_CURVE_WITH_KNOTS ( 'NONE', 3,
 ( #6480, #22969, #9460, #88915, #19981, #47447, #43684, #49564, #16218, #22094 ),
 .UNSPECIFIED., .F., .F.,
 ( 4, 2, 2, 2, 4 ),
 ( 0.0007817359430256216575, 0.0009771253907249856981, 0.001172514838424349847, 0.001367904286123713779, 0.001563293733823077928 ),
 .UNSPECIFIED. ) ;
#70206 = CARTESIAN_POINT ( 'NONE',  ( 9.822833130541338775, -6.808710257144161559, 34.95449254468098843 ) ) ;
#70207 = ORIENTED_EDGE ( 'NONE', *, *, #68492, .F. ) ;
#70208 = ORIENTED_EDGE ( 'NONE', *, *, #10164, .F. ) ;
#70209 = CARTESIAN_POINT ( 'NONE',  ( -6.923076923077045919, -8.656820664282941280, 34.87096338111179961 ) ) ;
#70210 = B_SPLINE_CURVE_WITH_KNOTS ( 'NONE', 3,
 ( #19403, #46871, #1343, #23377, #1785, #69369, #43653, #71124, #36466, #35131 ),
 .UNSPECIFIED., .F., .F.,
 ( 4, 2, 2, 2, 4 ),
 ( 0.000000000000000000, 0.0001954311564186862781, 0.0003908623128373725562, 0.0005862934692560588072, 0.0007817246256747451124 ),
 .UNSPECIFIED. ) ;
#70211 = EDGE_CURVE ( 'NONE', #39096, #45764, #12950, .T. ) ;
#70212 = ORIENTED_EDGE ( 'NONE', *, *, #7073, .T. ) ;
#70213 = EDGE_CURVE ( 'NONE', #5990, #19429, #53794, .T. ) ;
#70214 = CARTESIAN_POINT ( 'NONE',  ( 5.076923076922953193, -5.094484230521993062, 34.41647553114689373 ) ) ;
#70215 = CARTESIAN_POINT ( 'NONE',  ( 13.38461538461538680, -3.322132147404559976, 32.92929555188717927 ) ) ;
#70216 = FACE_OUTER_BOUND ( 'NONE', #17149, .T. ) ;
#70217 = ADVANCED_FACE ( 'NONE', ( #33537 ), #26770, .F. ) ;
#70218 = CARTESIAN_POINT ( 'NONE',  ( 7.846153846153725020, -2.892918686052165622, 31.69288490824153470 ) ) ;
#70219 = ORIENTED_EDGE ( 'NONE', *, *, #60487, .T. ) ;
#70220 = ORIENTED_EDGE ( 'NONE', *, *, #5379, .F. ) ;
#70222 = VERTEX_POINT ( 'NONE', #63201 ) ;
#70221 = DIRECTION ( 'NONE',  ( 0.000000000000000000, 0.7660444431189807890, 0.6427876096865361433 ) ) ;
#70223 = VECTOR ( 'NONE', #30907, 1000.000000000000227 ) ;
#70224 = CARTESIAN_POINT ( 'NONE',  ( 16.37722209454433653, -2.501478030877322567, 29.88021232661721172 ) ) ;
#70225 = ORIENTED_EDGE ( 'NONE', *, *, #40029, .F. ) ;
#70226 = CARTESIAN_POINT ( 'NONE',  ( 7.846153846153723244, -12.16647553114689728, 32.15551576947799362 ) ) ;
#70227 = LINE ( 'NONE', #64336, #19455 ) ;
#70228 = VERTEX_POINT ( 'NONE', #84383 ) ;
#70229 = ADVANCED_FACE ( 'NONE', ( #43383 ), #10819, .F. ) ;
#70230 = DIRECTION ( 'NONE',  ( 0.000000000000000000, 0.3420201433256610524, 0.9396926207859113145 ) ) ;
#70231 = EDGE_LOOP ( 'NONE', ( #8516, #3073 ) ) ;
#70233 = ORIENTED_EDGE ( 'NONE', *, *, #67586, .F. ) ;
#70232 = CARTESIAN_POINT ( 'NONE',  ( -8.703162418228330921, -8.120952969808772792, 34.71129190929999453 ) ) ;
#70234 = B_SPLINE_CURVE_WITH_KNOTS ( 'NONE', 3,
 ( #86190, #16822, #11861, #45626, #37987, #85737, #10067, #73106, #39337, #11402 ),
 .UNSPECIFIED., .F., .F.,
 ( 4, 2, 2, 2, 4 ),
 ( 0.000000000000000000, 0.0001954339857564079623, 0.0003908679715128159245, 0.0005863019572692238597, 0.0007817359430256318490 ),
 .UNSPECIFIED. ) ;
#70235 = DIRECTION ( 'NONE',  ( -0.000000000000000000, 0.5000000000000011102, -0.8660254037844380415 ) ) ;
#70236 = CYLINDRICAL_SURFACE ( 'NONE', #74120, 4.000000000000000000 ) ;
#70237 = ORIENTED_EDGE ( 'NONE', *, *, #45902, .T. ) ;
#70238 = CARTESIAN_POINT ( 'NONE',  ( 4.153846153846154188, -13.75783147151868846, 33.36296068462461051 ) ) ;
#70239 = CARTESIAN_POINT ( 'NONE',  ( 6.923076923076924238, -5.471508081941601098, 34.59228464037088457 ) ) ;
#70240 = FACE_BOUND ( 'NONE', #66709, .T. ) ;
#70241 = CARTESIAN_POINT ( 'NONE',  ( -8.352564102564102200, -7.500000000000000000, 29.75000000000000355 ) ) ;
#70242 = DIRECTION ( 'NONE',  ( 1.000000000000000000, 0.000000000000000000, 0.000000000000000000 ) ) ;
#70243 = CARTESIAN_POINT ( 'NONE',  ( 9.626225312947553903, -2.292212530054419606, 30.41441678777542634 ) ) ;
#70244 = CARTESIAN_POINT ( 'NONE',  ( -17.01085574357299990, -12.34228464037088813, 31.77849191805839268 ) ) ;
#70245 = VECTOR ( 'NONE', #59639, 1000.000000000000227 ) ;
#70246 = CARTESIAN_POINT ( 'NONE',  ( -3.099977422944445671, -3.062576670634119758, 32.05464942895959979 ) ) ;
#70247 = CARTESIAN_POINT ( 'NONE',  ( 11.53846153846153832, -13.20930481340135110, 34.54067556320372745 ) ) ;
#70248 = VERTEX_POINT ( 'NONE', #22227 ) ;
#70249 = CARTESIAN_POINT ( 'NONE',  ( -14.30769230769230660, -3.513871655860378418, 32.76840700105978499 ) ) ;
#70250 = ORIENTED_EDGE ( 'NONE', *, *, #79544, .F. ) ;
#70251 = VERTEX_POINT ( 'NONE', #8278 ) ;
#70252 = CIRCLE ( 'NONE', #29947, 6.614378277661484340 ) ;
#70254 = CARTESIAN_POINT ( 'NONE',  ( -3.480745974817821775, -5.643011162660950042, 34.66104346484419096 ) ) ;
#70253 = CARTESIAN_POINT ( 'NONE',  ( -5.076923076923199218, -12.16647553114689728, 32.15551576947799362 ) ) ;
#70255 = CIRCLE ( 'NONE', #31432, 4.000000000000000000 ) ;
#70256 = CARTESIAN_POINT ( 'NONE',  ( 15.23076923076923173, -8.164416787775445883, 34.95778746994557906 ) ) ;
#70257 = PLANE ( 'NONE',  #73946 ) ;
#70258 = CARTESIAN_POINT ( 'NONE',  ( 0.4615384615383396616, -2.625532179533779154, 30.86335684631627174 ) ) ;
#70259 = CARTESIAN_POINT ( 'NONE',  ( -4.088591014333315066, -3.643525952247864463, 33.31231777344670064 ) ) ;
#70260 = EDGE_LOOP ( 'NONE', ( #27455, #66831 ) ) ;
#70261 = FACE_OUTER_BOUND ( 'NONE', #53284, .T. ) ;
#70262 = AXIS2_PLACEMENT_3D ( 'NONE', #78513, #37979, #31668 ) ;
#70263 = EDGE_CURVE ( 'NONE', #2917, #37415, #76280, .T. ) ;
#70264 = CARTESIAN_POINT ( 'NONE',  ( -14.43784027742400156, -10.31621877034669588, 34.18098118002070152 ) ) ;
#70265 = CARTESIAN_POINT ( 'NONE',  ( -10.54931626438217585, -9.780366693483667717, 34.19971097300155805 ) ) ;
#70266 = CARTESIAN_POINT ( 'NONE',  ( 3.165498784808455923, -3.300289026998414865, 32.46337939537583139 ) ) ;
#70267 = CARTESIAN_POINT ( 'NONE',  ( 13.63466980452883881, -5.642605341092957971, 34.66089969410670335 ) ) ;
#70268 = CARTESIAN_POINT ( 'NONE',  ( 3.007842271862383399, -11.98009711892699691, 32.48740034544075428 ) ) ;
#70269 = ORIENTED_EDGE ( 'NONE', *, *, #69768, .F. ) ;
#70270 = EDGE_CURVE ( 'NONE', #14815, #53666, #19340, .T. ) ;
#70271 = B_SPLINE_CURVE_WITH_KNOTS ( 'NONE', 3,
 ( #38354, #50949, #78440, #44193, #58609, #52744, #72127, #10440, #9983, #58165 ),
 .UNSPECIFIED., .F., .F.,
 ( 4, 2, 2, 2, 4 ),
 ( 0.0007817359527651133143, 0.0009771254036996530456, 0.001172514854634192777, 0.001367904305568732291, 0.001563293756503272023 ),
 .UNSPECIFIED. ) ;
#70272 = ORIENTED_EDGE ( 'NONE', *, *, #38404, .F. ) ;
#70273 = PLANE ( 'NONE',  #26168 ) ;
#70275 = VERTEX_POINT ( 'NONE', #51775 ) ;
#70274 = EDGE_CURVE ( 'NONE', #84739, #29700, #35435, .T. ) ;
#70276 = DIRECTION ( 'NONE',  ( 0.000000000000000000, 0.9396926207859126468, 0.3420201433256571111 ) ) ;
#70277 = DIRECTION ( 'NONE',  ( 0.000000000000000000, 0.4999999999999985567, 0.8660254037844395958 ) ) ;
#70278 = LINE ( 'NONE', #14902, #42381 ) ;
#70279 = CARTESIAN_POINT ( 'NONE',  ( -5.076923076923075762, -3.322132147404559976, 32.92929555188717927 ) ) ;
#70280 = CARTESIAN_POINT ( 'NONE',  ( -17.32689982097166492, -9.234221910056350069, 34.70572697212741531 ) ) ;
#70281 = CARTESIAN_POINT ( 'NONE',  ( 8.639083559792549494, -6.852621066184266141, 34.70813303252209181 ) ) ;
#70282 = ORIENTED_EDGE ( 'NONE', *, *, #72896, .F. ) ;
#70283 = EDGE_CURVE ( 'NONE', #25143, #45049, #31114, .T. ) ;
#70284 = DIRECTION ( 'NONE',  ( -0.000000000000000000, -0.6427876096865404731, -0.7660444431189771253 ) ) ;
#70286 = ORIENTED_EDGE ( 'NONE', *, *, #33394, .F. ) ;
#70285 = DIRECTION ( 'NONE',  ( -0.000000000000000000, -0.6427876096865404731, -0.7660444431189771253 ) ) ;
#70287 = DIRECTION ( 'NONE',  ( -0.000000000000000000, 0.1736481776669307198, -0.9848077530122080203 ) ) ;
#70288 = CARTESIAN_POINT ( 'NONE',  ( -17.20707104665477161, -12.15440758774515473, 32.17923288041532004 ) ) ;
#70289 = CARTESIAN_POINT ( 'NONE',  ( -10.61538461538473399, -11.48612834414049644, 32.76840700105863391 ) ) ;
#70290 = CARTESIAN_POINT ( 'NONE',  ( 0.4615384615383396616, -2.892918686052166066, 31.69288490824153470 ) ) ;
#70291 = CARTESIAN_POINT ( 'NONE',  ( -19.00000000000000000, 9.000000000000001776, 2.999999999999999112 ) ) ;
#70292 = EDGE_CURVE ( 'NONE', #2182, #82908, #47244, .T. ) ;
#70293 = CARTESIAN_POINT ( 'NONE',  ( -3.749999999999997780, -7.438900925035489387, 14.09561829374151642 ) ) ;
#70294 = EDGE_LOOP ( 'NONE', ( #42140, #48841, #9515, #88623 ) ) ;
#70295 = AXIS2_PLACEMENT_3D ( 'NONE', #61068, #88133, #73258 ) ;
#70296 = FACE_OUTER_BOUND ( 'NONE', #75021, .T. ) ;
#70297 = CARTESIAN_POINT ( 'NONE',  ( -4.153846153846152411, -9.584722331328613620, 36.20867863119891439 ) ) ;
#70298 = CARTESIAN_POINT ( 'NONE',  ( -1.944543648262992530, -9.444543648263016067, 18.68750000000000000 ) ) ;
#70299 = CARTESIAN_POINT ( 'NONE',  ( 13.13461538461538680, -7.500000000000001776, 35.00000000000000000 ) ) ;
#70300 = CARTESIAN_POINT ( 'NONE',  ( -7.623374177175779920, -3.020022701398814124, 32.48759521482552515 ) ) ;
#70301 = ORIENTED_EDGE ( 'NONE', *, *, #89047, .T. ) ;
#70302 = CARTESIAN_POINT ( 'NONE',  ( 1.139087296526029469, -10.24999999999999289, 15.95312499999999822 ) ) ;
#70303 = CARTESIAN_POINT ( 'NONE',  ( 11.31553457955468645, -4.026226216239094491, 33.68668979543634379 ) ) ;
#70304 = ORIENTED_EDGE ( 'NONE', *, *, #8448, .F. ) ;
#70305 = CARTESIAN_POINT ( 'NONE',  ( -1.161835843346974428, -6.760870238392817200, 34.69528174975672385 ) ) ;
#70306 = CARTESIAN_POINT ( 'NONE',  ( 9.442307692307693401, -7.500000000000001776, 35.00000000000000000 ) ) ;
#70307 = ORIENTED_EDGE ( 'NONE', *, *, #49351, .T. ) ;
#70308 = DIRECTION ( 'NONE',  ( -0.000000000000000000, 0.1736481776669307198, -0.9848077530122080203 ) ) ;
#70309 = DIRECTION ( 'NONE',  ( -1.000000000000000000, -0.000000000000000000, -0.000000000000000000 ) ) ;
#70310 = CARTESIAN_POINT ( 'NONE',  ( -8.546451100252703270, -5.827830569534417471, 34.72679350104403539 ) ) ;
#70311 = CARTESIAN_POINT ( 'NONE',  ( -13.16160254052199008, -12.64618726649961289, 30.78989965857442712 ) ) ;
#70312 = ORIENTED_EDGE ( 'NONE', *, *, #85376, .F. ) ;
#70313 = CARTESIAN_POINT ( 'NONE',  ( -3.099978789802282364, -2.295524264805589354, 30.44142389570982488 ) ) ;
#70314 = ADVANCED_FACE ( 'NONE', ( #79278 ), #5400, .F. ) ;
#70315 = VERTEX_POINT ( 'NONE', #60774 ) ;
#70316 = CIRCLE ( 'NONE', #58795, 0.2500000000000002220 ) ;
#70317 = CARTESIAN_POINT ( 'NONE',  ( 4.153846153846032507, -5.219633306517616589, 34.19971097300220464 ) ) ;
#70318 = CARTESIAN_POINT ( 'NONE',  ( 6.250000000001437961, -7.500000000000155431, 34.75000000000007105 ) ) ;
#70319 = EDGE_LOOP ( 'NONE', ( #82974, #11423, #54697, #66917 ) ) ;
#70320 = CARTESIAN_POINT ( 'NONE',  ( 10.61538461538461675, -11.35647404775217417, 33.31231777344666511 ) ) ;
#70321 = CARTESIAN_POINT ( 'NONE',  ( -8.835314180186649935, -2.538708090699994813, 30.37095296980875148 ) ) ;
#70322 = CARTESIAN_POINT ( 'NONE',  ( 0.3962680155776846513, -4.481592998940160832, 33.73612834413957984 ) ) ;
#70323 = AXIS2_PLACEMENT_3D ( 'NONE', #50917, #9954, #8193 ) ;
#70324 = ADVANCED_FACE ( 'NONE', ( #11716 ), #60328, .F. ) ;
#70325 = AXIS2_PLACEMENT_3D ( 'NONE', #7037, #26434, #75494 ) ;
#70326 = DIRECTION ( 'NONE',  ( -0.000000000000000000, 0.6427876096865404731, -0.7660444431189770143 ) ) ;
#70327 = CARTESIAN_POINT ( 'NONE',  ( 3.480769230769230838, -2.249999999999998668, 29.75000000000000355 ) ) ;
#70328 = AXIS2_PLACEMENT_3D ( 'NONE', #51075, #43016, #30825 ) ;
#70329 = VERTEX_POINT ( 'NONE', #87841 ) ;
#70331 = EDGE_CURVE ( 'NONE', #52128, #16142, #84902, .T. ) ;
#70330 = VERTEX_POINT ( 'NONE', #73412 ) ;
#70332 = FACE_BOUND ( 'NONE', #63211, .T. ) ;
#70333 = ORIENTED_EDGE ( 'NONE', *, *, #59222, .T. ) ;
#70334 = CARTESIAN_POINT ( 'NONE',  ( 19.00000000000000000, 0.7500000000000051070, 32.75000000000000000 ) ) ;
#70335 = B_SPLINE_CURVE_WITH_KNOTS ( 'NONE', 3,
 ( #75050, #35379, #82697, #41698, #76363, #269, #35834, #76820, #63290, #34929 ),
 .UNSPECIFIED., .F., .F.,
 ( 4, 2, 2, 2, 4 ),
 ( 0.000000000000000000, 0.0001954311564186868744, 0.0003908623128373737488, 0.0005862934692560606504, 0.0007817246256747474977 ),
 .UNSPECIFIED. ) ;
#70336 = CARTESIAN_POINT ( 'NONE',  ( 7.846153846153723244, -12.70778746994576025, 30.41441678777401236 ) ) ;
#70337 = CARTESIAN_POINT ( 'NONE',  ( 9.692307692307695177, -12.10708131394839349, 31.69288490824020244 ) ) ;
#70338 = CARTESIAN_POINT ( 'NONE',  ( -2.307692307692428724, -10.33852847137269571, 34.16647553114546554 ) ) ;
#70339 = EDGE_CURVE ( 'NONE', #88089, #70832, #79477, .T. ) ;
#70340 = EDGE_LOOP ( 'NONE', ( #12220, #83832 ) ) ;
#70341 = ORIENTED_EDGE ( 'NONE', *, *, #64812, .F. ) ;
#70342 = EDGE_LOOP ( 'NONE', ( #71411, #54198 ) ) ;
#70343 = CARTESIAN_POINT ( 'NONE',  ( -2.980714810855777053, -11.47946981652013498, 33.17500667209846910 ) ) ;
#70344 = EDGE_CURVE ( 'NONE', #49728, #49386, #88543, .T. ) ;
#70346 = VERTEX_POINT ( 'NONE', #46819 ) ;
#70345 = EDGE_CURVE ( 'NONE', #54542, #24890, #39678, .T. ) ;
#70347 = LINE ( 'NONE', #30247, #45941 ) ;
#70348 = VECTOR ( 'NONE', #76583, 1000.000000000000114 ) ;
#70349 = CARTESIAN_POINT ( 'NONE',  ( -15.23076923076935252, -11.67786785259630911, 32.92929555188603530 ) ) ;
#70350 = EDGE_CURVE ( 'NONE', #8229, #56240, #25218, .T. ) ;
#70351 = CARTESIAN_POINT ( 'NONE',  ( 13.51540582558233972, -11.37503395064541678, 33.29242100308974273 ) ) ;
#70352 = ORIENTED_EDGE ( 'NONE', *, *, #85284, .F. ) ;
#70353 = B_SPLINE_CURVE_WITH_KNOTS ( 'NONE', 3,
 ( #38945, #66404, #60531, #27193, #6046, #46576, #19547, #47009, #25866, #80827 ),
 .UNSPECIFIED., .F., .F.,
 ( 4, 2, 2, 2, 4 ),
 ( 0.0007817246256747473893, 0.0009771112852218907189, 0.001172497944769034049, 0.001367884604316177378, 0.001563271263863320708 ),
 .UNSPECIFIED. ) ;
#70354 = CARTESIAN_POINT ( 'NONE',  ( 13.13463865367303463, -10.66389620160130036, 33.62221079203477103 ) ) ;
#70355 = CARTESIAN_POINT ( 'NONE',  ( -19.50000000000000000, -3.499999999999999556, 29.75000000000000355 ) ) ;
#70356 = CARTESIAN_POINT ( 'NONE',  ( 4.088576153289834814, -2.657715359629089225, 31.77849191805834295 ) ) ;
#70357 = CARTESIAN_POINT ( 'NONE',  ( 8.769230769230645706, -6.835583212225970762, 34.95778746994575670 ) ) ;
#70358 = ORIENTED_EDGE ( 'NONE', *, *, #1312, .T. ) ;
#70359 = ORIENTED_EDGE ( 'NONE', *, *, #2937, .F. ) ;
#70360 = ORIENTED_EDGE ( 'NONE', *, *, #847, .T. ) ;
#70361 = CARTESIAN_POINT ( 'NONE',  ( -4.153846153846273204, -10.21337939537710326, 33.94971097300076224 ) ) ;
#70363 = CARTESIAN_POINT ( 'NONE',  ( 10.61538461538461675, -6.386643153685126251, 34.62446782046654192 ) ) ;
#70362 = CARTESIAN_POINT ( 'NONE',  ( 12.23805351781451201, -6.760086850603066466, 34.69517049084099369 ) ) ;
#70364 = LINE ( 'NONE', #56838, #51344 ) ;
#70365 = CARTESIAN_POINT ( 'NONE',  ( -6.700065571464073777, -3.587049720035815348, 32.86302985866382897 ) ) ;
#70366 = FACE_BOUND ( 'NONE', #84790, .T. ) ;
#70367 = CARTESIAN_POINT ( 'NONE',  ( 8.769230769230768274, -10.67929555188718282, 33.92786785259544047 ) ) ;
#70368 = EDGE_LOOP ( 'NONE', ( #51741, #27685, #59952, #58793 ) ) ;
#70369 = B_SPLINE_CURVE_WITH_KNOTS ( 'NONE', 3,
 ( #68358, #88661, #7101, #6656, #60265, #6228, #53505, #20182, #47648, #67482 ),
 .UNSPECIFIED., .F., .F.,
 ( 4, 2, 2, 2, 4 ),
 ( 0.0007817359430256374869, 0.0009771253907250054306, 0.001172514838424373266, 0.001367904286123741101, 0.001563293733823109153 ),
 .UNSPECIFIED. ) ;
#70370 = CARTESIAN_POINT ( 'NONE',  ( 17.29993592101647337, -11.98016756924215187, 32.48728574198911190 ) ) ;
#70371 = DIRECTION ( 'NONE',  ( -0.000000000000000000, -0.9396926207859092051, -0.3420201433256662704 ) ) ;
#70372 = CARTESIAN_POINT ( 'NONE',  ( 11.47270473594723228, -7.249945686854186278, 34.74374336980224598 ) ) ;
#70373 = DIRECTION ( 'NONE',  ( 1.000000000000000000, 0.000000000000000000, 0.000000000000000000 ) ) ;
#70374 = ORIENTED_EDGE ( 'NONE', *, *, #393, .T. ) ;
#70375 = CARTESIAN_POINT ( 'NONE',  ( 4.853996118016226546, -12.64616026154729411, 30.79003144601913533 ) ) ;
#70376 = ORIENTED_EDGE ( 'NONE', *, *, #86120, .T. ) ;
#70378 = FACE_BOUND ( 'NONE', #12364, .T. ) ;
#70377 = B_SPLINE_CURVE_WITH_KNOTS ( 'NONE', 3,
 ( #32070, #19002, #73953, #51872, #24408, #79370, #78917, #45575, #11350, #72602 ),
 .UNSPECIFIED., .F., .F.,
 ( 4, 2, 2, 2, 4 ),
 ( 0.000000000000000000, 0.0001954311564186858715, 0.0003908623128373717431, 0.0005862934692560576146, 0.0007817246256747434861 ),
 .UNSPECIFIED. ) ;
#70379 = ADVANCED_FACE ( 'NONE', ( #58994 ), #25665, .F. ) ;
#70380 = CARTESIAN_POINT ( 'NONE',  ( 5.076923076922954969, -6.026961402154118908, 34.52809138561165270 ) ) ;
#70381 = AXIS2_PLACEMENT_3D ( 'NONE', #58832, #18302, #41126 ) ;
#70382 = AXIS2_PLACEMENT_3D ( 'NONE', #88202, #11179, #53489 ) ;
#70383 = CARTESIAN_POINT ( 'NONE',  ( 16.85343813319913053, -11.89387501736623420, 32.13663884655804992 ) ) ;
#70384 = CARTESIAN_POINT ( 'NONE',  ( 14.05766907039934210, -11.86270091957321249, 32.19358267280087915 ) ) ;
#70385 = ORIENTED_EDGE ( 'NONE', *, *, #81758, .T. ) ;
#70386 = CARTESIAN_POINT ( 'NONE',  ( 0.6089743589743582541, -7.500000000000000000, 29.75000000000000355 ) ) ;
#70387 = CARTESIAN_POINT ( 'NONE',  ( -3.361459833879538284, -2.295517848115769421, 30.44137282052137294 ) ) ;
#70388 = CARTESIAN_POINT ( 'NONE',  ( 8.638540166120460384, -2.295517848115769421, 30.44137282052137294 ) ) ;
#70389 = CARTESIAN_POINT ( 'NONE',  ( -3.999999999999998224, -7.500000000000000000, 13.50000000000000178 ) ) ;
#70390 = ORIENTED_EDGE ( 'NONE', *, *, #86250, .T. ) ;
#70391 = VECTOR ( 'NONE', #33687, 1000.000000000000114 ) ;
#70392 = DIRECTION ( 'NONE',  ( 0.000000000000000000, 0.8660254037844377084, 0.5000000000000015543 ) ) ;
#70393 = ORIENTED_EDGE ( 'NONE', *, *, #16956, .F. ) ;
#70394 = EDGE_CURVE ( 'NONE', #8812, #19730, #53797, .T. ) ;
#70395 = VECTOR ( 'NONE', #28430, 1000.000000000000000 ) ;
#70397 = ORIENTED_EDGE ( 'NONE', *, *, #52134, .T. ) ;
#70396 = CARTESIAN_POINT ( 'NONE',  ( 18.00000000000000000, -13.75783147151868846, 33.36296068462461051 ) ) ;
#70398 = CARTESIAN_POINT ( 'NONE',  ( 11.78840705680968171, -6.696923467548660192, 34.68552623307873972 ) ) ;
#70399 = CARTESIAN_POINT ( 'NONE',  ( -10.86540785267757947, -12.43535235679832596, 30.55408501211184813 ) ) ;
#70400 = DIRECTION ( 'NONE',  ( 0.000000000000000000, 0.8660254037844377084, 0.5000000000000015543 ) ) ;
#70401 = CARTESIAN_POINT ( 'NONE',  ( -15.48076923076922995, -7.566082377512564960, 35.00000000000000711 ) ) ;
#70403 = CARTESIAN_POINT ( 'NONE',  ( 8.703960768674447124, -4.320704448112771878, 33.92786785259540494 ) ) ;
#70402 = CARTESIAN_POINT ( 'NONE',  ( -3.099978789802278811, -3.957578996910244395, 33.62503395064540257 ) ) ;
#70404 = DIRECTION ( 'NONE',  ( -0.000000000000000000, -0.3420201433256694901, -0.9396926207859082059 ) ) ;
#70405 = EDGE_CURVE ( 'NONE', #9565, #3410, #49493, .T. ) ;
#70406 = CARTESIAN_POINT ( 'NONE',  ( 1.944543648263018731, -9.444543648262994751, 22.12500000000000000 ) ) ;
#70407 = ORIENTED_EDGE ( 'NONE', *, *, #18440, .F. ) ;
#70408 = CYLINDRICAL_SURFACE ( 'NONE', #85074, 0.2500000000000012212 ) ;
#70409 = DIRECTION ( 'NONE',  ( 0.000000000000000000, 1.000000000000000000, 0.000000000000000000 ) ) ;
#70410 = ORIENTED_EDGE ( 'NONE', *, *, #27443, .F. ) ;
#70411 = VERTEX_POINT ( 'NONE', #66652 ) ;
#70412 = EDGE_LOOP ( 'NONE', ( #80135, #27831 ) ) ;
#70413 = CARTESIAN_POINT ( 'NONE',  ( 10.61538461538449418, -8.656820664282941280, 34.87096338111179961 ) ) ;
#70414 = DIRECTION ( 'NONE',  ( 0.000000000000000000, 0.000000000000000000, -1.000000000000000000 ) ) ;
#70415 = B_SPLINE_CURVE_WITH_KNOTS ( 'NONE', 3,
 ( #15381, #29337, #77954, #49150, #71189, #50899, #55904, #77076, #57682, #44147 ),
 .UNSPECIFIED., .F., .F.,
 ( 4, 2, 2, 2, 4 ),
 ( 0.0007817246256747442451, 0.0009771112852218865989, 0.001172497944769029061, 0.001367884604316171523, 0.001563271263863313986 ),
 .UNSPECIFIED. ) ;
#70416 = B_SPLINE_CURVE_WITH_KNOTS ( 'NONE', 3,
 ( #24811, #4087, #24358, #17627, #17164, #58145, #79770, #44621, #10421, #72555 ),
 .UNSPECIFIED., .F., .F.,
 ( 4, 2, 2, 2, 4 ),
 ( 0.000000000000000000, 0.0001954311564186880399, 0.0003908623128373760799, 0.0005862934692560641198, 0.0007817246256747521597 ),
 .UNSPECIFIED. ) ;
#70417 = CARTESIAN_POINT ( 'NONE',  ( -19.50000000000000000, -11.50000000000000000, 29.75000000000000355 ) ) ;
#70418 = DIRECTION ( 'NONE',  ( -0.000000000000000000, 0.1736481776669307198, -0.9848077530122080203 ) ) ;
#70420 = EDGE_CURVE ( 'NONE', #84034, #30710, #35526, .T. ) ;
#70419 = CARTESIAN_POINT ( 'NONE',  ( -8.992157728137614825, -2.523278758544489797, 31.42238647778637528 ) ) ;
#70421 = CARTESIAN_POINT ( 'NONE',  ( 17.14299041027315695, -8.164416787775445883, 34.95778746994558617 ) ) ;
#70422 = CARTESIAN_POINT ( 'NONE',  ( 5.934677084507826272, -7.749976743299137993, 34.99404534957040624 ) ) ;
#70423 = CARTESIAN_POINT ( 'NONE',  ( 6.000000000000001776, -12.78798330534103123, 29.99999999999997868 ) ) ;
#70424 = CARTESIAN_POINT ( 'NONE',  ( 17.93472955403922242, -11.94971097300153140, 32.03036669348370680 ) ) ;
#70425 = CARTESIAN_POINT ( 'NONE',  ( 12.39626801557768410, -11.94971097300153140, 32.03036669348370680 ) ) ;
#70426 = VECTOR ( 'NONE', #18871, 999.9999999999998863 ) ;
#70427 = CARTESIAN_POINT ( 'NONE',  ( -14.16025641025641058, -7.500000000000000000, 33.75000000000000000 ) ) ;
#70428 = ORIENTED_EDGE ( 'NONE', *, *, #82243, .T. ) ;
#70429 = ORIENTED_EDGE ( 'NONE', *, *, #74410, .T. ) ;
#70430 = CARTESIAN_POINT ( 'NONE',  ( 8.900021210197722965, -2.845873456487966635, 32.17976146951972538 ) ) ;
#70431 = CARTESIAN_POINT ( 'NONE',  ( -16.08865316555149860, -2.255955759149234741, 29.99999999999988276 ) ) ;
#70432 = CARTESIAN_POINT ( 'NONE',  ( -22.00000000000000711, 9.999999999999971578, 13.00000000000000178 ) ) ;
#70433 = CARTESIAN_POINT ( 'NONE',  ( -2.530519000171310484, -7.369208160676173236, 34.74850200257122879 ) ) ;
#70434 = ORIENTED_EDGE ( 'NONE', *, *, #11968, .T. ) ;
#70435 = EDGE_CURVE ( 'NONE', #67458, #79858, #61209, .T. ) ;
#70436 = EDGE_CURVE ( 'NONE', #5877, #81602, #41832, .T. ) ;
#70437 = LINE ( 'NONE', #7408, #76550 ) ;
#70438 = CARTESIAN_POINT ( 'NONE',  ( -17.14219352288385778, -3.835265460703609186, 33.15142922261924241 ) ) ;
#70439 = CARTESIAN_POINT ( 'NONE',  ( -9.561517251340742263, -3.338503747796866872, 32.95102852606553512 ) ) ;
#70440 = EDGE_CURVE ( 'NONE', #11287, #82297, #7369, .T. ) ;
#70441 = ORIENTED_EDGE ( 'NONE', *, *, #79894, .F. ) ;
#70443 = EDGE_CURVE ( 'NONE', #35844, #32821, #28774, .T. ) ;
#70442 = CARTESIAN_POINT ( 'NONE',  ( 0.5923302693632478411, -5.582136614379148654, 34.36778462344220486 ) ) ;
#70444 = ORIENTED_EDGE ( 'NONE', *, *, #23564, .F. ) ;
#70445 = CARTESIAN_POINT ( 'NONE',  ( 10.61538461538461675, -8.120952969808772792, 34.71129190930000163 ) ) ;
#70446 = AXIS2_PLACEMENT_3D ( 'NONE', #47065, #26810, #33575 ) ;
#70447 = CARTESIAN_POINT ( 'NONE',  ( -3.360916440207453615, -12.27039167877662251, 31.24851455888617835 ) ) ;
#70448 = CARTESIAN_POINT ( 'NONE',  ( -15.23076923076922995, -1.215029322943914858, 32.30358669280327177 ) ) ;
#70449 = CARTESIAN_POINT ( 'NONE',  ( -9.757577692864012775, -8.656820664281498878, 34.87096338111211935 ) ) ;
#70450 = DIRECTION ( 'NONE',  ( -0.000000000000000000, -0.9848077530122085754, -0.1736481776669273613 ) ) ;
#70451 = VECTOR ( 'NONE', #66965, 1000.000000000000000 ) ;
#70452 = VECTOR ( 'NONE', #18510, 1000.000000000000000 ) ;
#70453 = ORIENTED_EDGE ( 'NONE', *, *, #38274, .F. ) ;
#70454 = B_SPLINE_CURVE_WITH_KNOTS ( 'NONE', 3,
 ( #32288, #59752, #33616, #67400, #53428, #12455, #26857, #87247, #54316, #18775 ),
 .UNSPECIFIED., .F., .F.,
 ( 4, 2, 2, 2, 4 ),
 ( 0.000000000000000000, 0.0001954339857564073659, 0.0003908679715128147319, 0.0005863019572692221250, 0.0007817359430256294638 ),
 .UNSPECIFIED. ) ;
#70455 = EDGE_CURVE ( 'NONE', #86919, #23926, #7612, .T. ) ;
#70456 = ORIENTED_EDGE ( 'NONE', *, *, #31478, .F. ) ;
#70457 = EDGE_LOOP ( 'NONE', ( #77097, #50835 ) ) ;
#70458 = CARTESIAN_POINT ( 'NONE',  ( 13.25446817517716980, -3.285722584762969856, 32.44110544564090759 ) ) ;
#70459 = CARTESIAN_POINT ( 'NONE',  ( 13.44987095589141113, -10.21337939537593620, 33.94971097300152252 ) ) ;
#70460 = DIRECTION ( 'NONE',  ( -0.000000000000000000, 1.000000000000000000, -0.000000000000000000 ) ) ;
#70461 = CARTESIAN_POINT ( 'NONE',  ( -2.242437168179467477, -11.67786785259547777, 32.92929555188713664 ) ) ;
#70462 = CARTESIAN_POINT ( 'NONE',  ( 4.376625695114563008, -6.760870238392817200, 34.69528174975672385 ) ) ;
#70463 = CARTESIAN_POINT ( 'NONE',  ( 2.750000000000001776, -7.500000000000000000, 29.50000000000000355 ) ) ;
#70464 = ORIENTED_EDGE ( 'NONE', *, *, #57939, .T. ) ;
#70465 = VERTEX_POINT ( 'NONE', #56239 ) ;
#70466 = ORIENTED_EDGE ( 'NONE', *, *, #6851, .F. ) ;
#70468 = ORIENTED_EDGE ( 'NONE', *, *, #4957, .F. ) ;
#70467 = CARTESIAN_POINT ( 'NONE',  ( 9.320512820512821150, -3.499999999999999556, 29.75000000000000355 ) ) ;
#70470 = CARTESIAN_POINT ( 'NONE',  ( -8.769230769230768274, -11.16473453929635440, 33.15142922261926373 ) ) ;
#70469 = DIRECTION ( 'NONE',  ( 0.000000000000000000, 0.3420201433256641055, -0.9396926207859100932 ) ) ;
#70471 = CARTESIAN_POINT ( 'NONE',  ( 1.553300858899086867, -3.749999999999992006, 24.23437500000000355 ) ) ;
#70472 = EDGE_LOOP ( 'NONE', ( #233, #1655 ) ) ;
#70473 = B_SPLINE_CURVE_WITH_KNOTS ( 'NONE', 3,
 ( #45164, #83629, #16807, #72192, #751, #72638, #37518, #10049, #3287, #44709 ),
 .UNSPECIFIED., .F., .F.,
 ( 4, 2, 2, 2, 4 ),
 ( 0.000000000000000000, 0.0001954339857564093175, 0.0003908679715128186350, 0.0005863019572692279796, 0.0007817359430256372700 ),
 .UNSPECIFIED. ) ;
#70474 = VECTOR ( 'NONE', #26982, 1000.000000000000000 ) ;
#70475 = EDGE_LOOP ( 'NONE', ( #72774, #62344 ) ) ;
#70476 = CARTESIAN_POINT ( 'NONE',  ( 12.46153846153846168, -2.538708090699994813, 30.37095296980875503 ) ) ;
#70477 = ORIENTED_EDGE ( 'NONE', *, *, #43766, .T. ) ;
#70478 = FACE_BOUND ( 'NONE', #21981, .T. ) ;
#70479 = FACE_OUTER_BOUND ( 'NONE', #32895, .T. ) ;
#70480 = DIRECTION ( 'NONE',  ( 0.000000000000000000, 0.9848077530122072432, -0.1736481776669354937 ) ) ;
#70481 = VERTEX_POINT ( 'NONE', #82390 ) ;
#70482 = LINE ( 'NONE', #49323, #76520 ) ;
#70483 = FACE_OUTER_BOUND ( 'NONE', #2920, .T. ) ;
#70484 = CARTESIAN_POINT ( 'NONE',  ( -1.384615384615383471, -5.415277668671390821, 36.20867863119892149 ) ) ;
#70485 = CARTESIAN_POINT ( 'NONE',  ( -15.45425417449318317, -6.760086850603066466, 34.69517049084099369 ) ) ;
#70486 = CARTESIAN_POINT ( 'NONE',  ( 4.153846153846032507, -3.300289026999228881, 32.46337939537708905 ) ) ;
#70487 = LINE ( 'NONE', #72256, #74647 ) ;
#70488 = CARTESIAN_POINT ( 'NONE',  ( 16.15384615384615330, -1.215029322943914858, 32.30358669280327177 ) ) ;
#70489 = CARTESIAN_POINT ( 'NONE',  ( 16.21910172512217585, -9.442884908240273489, 34.35708131394835618 ) ) ;
#70490 = DIRECTION ( 'NONE',  ( -0.000000000000000000, 0.9396926207859092051, -0.3420201433256662704 ) ) ;
#70491 = LINE ( 'NONE', #75917, #80329 ) ;
#70492 = CARTESIAN_POINT ( 'NONE',  ( 8.769230769230645706, -4.320704448113951379, 33.92786785259630022 ) ) ;
#70494 = CARTESIAN_POINT ( 'NONE',  ( 7.145856464345332171, -3.236590943229499029, 32.36255958852954251 ) ) ;
#70493 = FACE_OUTER_BOUND ( 'NONE', #51266, .T. ) ;
#70495 = AXIS2_PLACEMENT_3D ( 'NONE', #20947, #14203, #8338 ) ;
#70496 = CARTESIAN_POINT ( 'NONE',  ( 1.607626736228236153, -11.24521262558773671, 33.06293181088029343 ) ) ;
#70498 = CARTESIAN_POINT ( 'NONE',  ( 5.869308533332445066, -10.54014554554150607, 33.71984207302941883 ) ) ;
#70497 = CARTESIAN_POINT ( 'NONE',  ( -11.31568199719312773, -11.41317474335729543, 32.86274602512330034 ) ) ;
#70499 = CARTESIAN_POINT ( 'NONE',  ( 12.46153846153846168, -12.78798330534103123, 29.99999999999997868 ) ) ;
#70500 = CARTESIAN_POINT ( 'NONE',  ( 0.06109907496454976272, -10.25000000000000000, 23.27938170625849068 ) ) ;
#70501 = ORIENTED_EDGE ( 'NONE', *, *, #52608, .T. ) ;
#70502 = B_SPLINE_CURVE_WITH_KNOTS ( 'NONE', 3,
 ( #12673, #75692, #87923, #41474, #67621, #75264, #5917, #61728, #26186, #53654 ),
 .UNSPECIFIED., .F., .F.,
 ( 4, 2, 2, 2, 4 ),
 ( 0.0007817359527651098448, 0.0009771254036996487088, 0.001172514854634187573, 0.001367904305568726437, 0.001563293756503265301 ),
 .UNSPECIFIED. ) ;
#70503 = CARTESIAN_POINT ( 'NONE',  ( -4.023320715612507925, -5.915461855592777596, 34.75538340440931506 ) ) ;
#70504 = ORIENTED_EDGE ( 'NONE', *, *, #40121, .F. ) ;
#70505 = AXIS2_PLACEMENT_3D ( 'NONE', #82710, #35394, #42169 ) ;
#70506 = AXIS2_PLACEMENT_3D ( 'NONE', #79657, #37321, #23801 ) ;
#70507 = CARTESIAN_POINT ( 'NONE',  ( -15.00775787915638304, -4.187068189119696804, 33.49521262558774026 ) ) ;
#70508 = ORIENTED_EDGE ( 'NONE', *, *, #28048, .F. ) ;
#70509 = LINE ( 'NONE', #8814, #41213 ) ;
#70510 = CARTESIAN_POINT ( 'NONE',  ( 14.17754433796061875, -2.373036134822904319, 30.88089517874952250 ) ) ;
#70511 = ORIENTED_EDGE ( 'NONE', *, *, #54079, .T. ) ;
#70512 = CARTESIAN_POINT ( 'NONE',  ( -6.223484943723947893, -11.89387501736622710, 32.13663884655806413 ) ) ;
#70513 = CARTESIAN_POINT ( 'NONE',  ( 1.077988221561464899, -4.724691934501233703, 22.73250670625849068 ) ) ;
#70514 = CARTESIAN_POINT ( 'NONE',  ( 6.130790440966952026, -6.369690395747422684, 34.87708834333098196 ) ) ;
#70515 = AXIS2_PLACEMENT_3D ( 'NONE', #19241, #67424, #47140 ) ;
#70516 = CARTESIAN_POINT ( 'NONE',  ( -7.846153846153967493, -4.320704448113951379, 33.92786785259630022 ) ) ;
#70517 = CARTESIAN_POINT ( 'NONE',  ( -5.300408001487409315, -3.019605429927184836, 32.48692288466676814 ) ) ;
#70518 = AXIS2_PLACEMENT_3D ( 'NONE', #31813, #39465, #32256 ) ;
#70519 = CARTESIAN_POINT ( 'NONE',  ( -16.28453675695646652, -9.929715669179216775, 34.40415004197138416 ) ) ;
#70520 = DIRECTION ( 'NONE',  ( 0.000000000000000000, 0.9396926207859126468, -0.3420201433256571111 ) ) ;
#70521 = DIRECTION ( 'NONE',  ( -0.000000000000000000, 0.9396926207859093161, -0.3420201433256663259 ) ) ;
#70522 =( GEOMETRIC_REPRESENTATION_CONTEXT ( 3 ) GLOBAL_UNCERTAINTY_ASSIGNED_CONTEXT ( ( #49200 ) ) GLOBAL_UNIT_ASSIGNED_CONTEXT ( ( #55033, #27561, #61324 ) ) REPRESENTATION_CONTEXT ( 'NONE', 'WORKASPACE' ) );
#70523 = CARTESIAN_POINT ( 'NONE',  ( -2.651650429449565305, -4.848349570550461785, 14.00000000000000000 ) ) ;
#70524 = CARTESIAN_POINT ( 'NONE',  ( -18.13014796973170206, -11.66186481527757124, 32.95055677023626117 ) ) ;
#70525 = LINE ( 'NONE', #21448, #11822 ) ;
#70526 = CARTESIAN_POINT ( 'NONE',  ( 13.63456090296352841, -4.336752205174649433, 33.62275283266504289 ) ) ;
#70527 = CARTESIAN_POINT ( 'NONE',  ( -3.749999999999988454, -9.053300858899127945, 17.51562500000000000 ) ) ;
#70528 = EDGE_CURVE ( 'NONE', #53886, #81564, #83724, .T. ) ;
#70529 = DIRECTION ( 'NONE',  ( 0.7071067811865510144, -0.7071067811865441310, 0.000000000000000000 ) ) ;
#70530 = ORIENTED_EDGE ( 'NONE', *, *, #86178, .F. ) ;
#70531 = CARTESIAN_POINT ( 'NONE',  ( 7.173076923076860290, -7.565270445406050648, 34.75000000000000000 ) ) ;
#70532 = CYLINDRICAL_SURFACE ( 'NONE', #40242, 0.2500000000000008882 ) ;
#70533 = CYLINDRICAL_SURFACE ( 'NONE', #8094, 0.2499999999999998890 ) ;
#70534 = CARTESIAN_POINT ( 'NONE',  ( 1.514660547450164874, -2.504778602574659896, 29.97347330155780298 ) ) ;
#70535 = CARTESIAN_POINT ( 'NONE',  ( -3.007757879156381708, -4.887748414852789658, 34.01359900205216746 ) ) ;
#70536 = CARTESIAN_POINT ( 'NONE',  ( -9.692307692307814193, -12.16647553114689728, 32.15551576947799362 ) ) ;
#70537 = CARTESIAN_POINT ( 'NONE',  ( 8.638539302563215116, -10.54014554554150607, 33.71984207302941883 ) ) ;
#70538 = B_SPLINE_CURVE_WITH_KNOTS ( 'NONE', 3,
 ( #20054, #39457, #68245, #5209, #5652, #19608, #74560, #87646, #47515, #47070 ),
 .UNSPECIFIED., .F., .F.,
 ( 4, 2, 2, 2, 4 ),
 ( 0.000000000000000000, 0.0001954339857564071491, 0.0003908679715128142982, 0.0005863019572692214744, 0.0007817359430256285964 ),
 .UNSPECIFIED. ) ;
#70539 = EDGE_CURVE ( 'NONE', #85237, #327, #4160, .T. ) ;
#70540 = ORIENTED_EDGE ( 'NONE', *, *, #2061, .F. ) ;
#70541 = ORIENTED_EDGE ( 'NONE', *, *, #80765, .F. ) ;
#70542 = AXIS2_PLACEMENT_3D ( 'NONE', #18906, #19349, #59886 ) ;
#70543 = ORIENTED_EDGE ( 'NONE', *, *, #76773, .T. ) ;
#70544 = CARTESIAN_POINT ( 'NONE',  ( -5.076923076923075762, -5.471508081941601098, 34.59228464037088457 ) ) ;
#70545 = CARTESIAN_POINT ( 'NONE',  ( 6.792929713638705458, -2.882441371585227063, 31.66841991370171527 ) ) ;
#70546 = CARTESIAN_POINT ( 'NONE',  ( -15.29603923132555288, -11.06231777344662781, 33.60647404775220082 ) ) ;
#70547 = CARTESIAN_POINT ( 'NONE',  ( -6.065270445960775803, -3.300289026998414865, 32.46337939537583139 ) ) ;
#70548 = CARTESIAN_POINT ( 'NONE',  ( -39.05038313613820122, -2.499999999999999556, 29.75000000000000355 ) ) ;
#70549 = ORIENTED_EDGE ( 'NONE', *, *, #55422, .F. ) ;
#70550 = CARTESIAN_POINT ( 'NONE',  ( 13.38461538461538680, -8.164416787775445883, 34.95778746994557906 ) ) ;
#70551 = ORIENTED_EDGE ( 'NONE', *, *, #42171, .T. ) ;
#70552 = EDGE_CURVE ( 'NONE', #55385, #88074, #17080, .T. ) ;
#70553 = ORIENTED_EDGE ( 'NONE', *, *, #47230, .F. ) ;
#70554 = AXIS2_PLACEMENT_3D ( 'NONE', #57299, #73369, #17987 ) ;
#70556 = ORIENTED_EDGE ( 'NONE', *, *, #71119, .T. ) ;
#70555 = CARTESIAN_POINT ( 'NONE',  ( 8.545745844666434721, -12.47654668319379567, 31.42292124445336654 ) ) ;
#70557 = DIRECTION ( 'NONE',  ( 0.000000000000000000, 0.1736481776669267785, -0.9848077530122087975 ) ) ;
#70558 = EDGE_CURVE ( 'NONE', #53401, #84701, #54907, .T. ) ;
#70559 = CYLINDRICAL_SURFACE ( 'NONE', #58065, 0.2500000000000002220 ) ;
#70560 = AXIS2_PLACEMENT_3D ( 'NONE', #17344, #44802, #72281 ) ;
#70561 = VECTOR ( 'NONE', #62163, 1000.000000000000000 ) ;
#70562 = EDGE_CURVE ( 'NONE', #49738, #67178, #9589, .T. ) ;
#70563 = CARTESIAN_POINT ( 'NONE',  ( 4.087762742890272527, -4.098570777380720287, 33.41473453929634729 ) ) ;
#70564 = CARTESIAN_POINT ( 'NONE',  ( -16.08777882049607655, -5.471508081941601098, 34.59228464037088457 ) ) ;
#70565 = EDGE_LOOP ( 'NONE', ( #2190, #342 ) ) ;
#70566 = ORIENTED_EDGE ( 'NONE', *, *, #39667, .F. ) ;
#70567 = AXIS2_PLACEMENT_3D ( 'NONE', #2450, #58284, #64147 ) ;
#70568 = B_SPLINE_CURVE_WITH_KNOTS ( 'NONE', 3,
 ( #65560, #31345, #68241, #55158, #88976, #83088, #14624, #61911, #76317, #27249 ),
 .UNSPECIFIED., .F., .F.,
 ( 4, 2, 2, 2, 4 ),
 ( 0.0007817246256747481482, 0.0009771112852218911526, 0.001172497944769034049, 0.001367884604316176944, 0.001563271263863319840 ),
 .UNSPECIFIED. ) ;
#70569 = ORIENTED_EDGE ( 'NONE', *, *, #26104, .T. ) ;
#70570 = LINE ( 'NONE', #62465, #54736 ) ;
#70572 = ORIENTED_EDGE ( 'NONE', *, *, #25531, .F. ) ;
#70571 = CARTESIAN_POINT ( 'NONE',  ( 20.00000000000000355, 10.00000000000000533, 0.000000000000000000 ) ) ;
#70573 = FACE_OUTER_BOUND ( 'NONE', #43015, .T. ) ;
#70574 = CARTESIAN_POINT ( 'NONE',  ( 4.826946345980720032, -3.627789207965226748, 32.91389620160131102 ) ) ;
#70575 = LINE ( 'NONE', #9753, #49381 ) ;
#70576 = ORIENTED_EDGE ( 'NONE', *, *, #9686, .F. ) ;
#70577 = DIRECTION ( 'NONE',  ( -0.000000000000000000, 1.000000000000000000, -0.000000000000000000 ) ) ;
#70578 = CARTESIAN_POINT ( 'NONE',  ( 15.00784227186237985, -2.523278758544489797, 31.42238647778637528 ) ) ;
#70579 = ORIENTED_EDGE ( 'NONE', *, *, #36721, .T. ) ;
#70580 = FACE_BOUND ( 'NONE', #74909, .T. ) ;
#70581 = CARTESIAN_POINT ( 'NONE',  ( -10.86540783960607115, -4.931416488878822335, 34.32920672191015399 ) ) ;
#70582 = CARTESIAN_POINT ( 'NONE',  ( 17.86985203026830149, -12.70455904226513866, 30.44083106164009322 ) ) ;
#70583 = CARTESIAN_POINT ( 'NONE',  ( 2.242422307135989445, -12.51329471203370325, 31.30864560766548976 ) ) ;
#70585 = CARTESIAN_POINT ( 'NONE',  ( -10.74607521849492464, -5.496505350115501010, 34.60290016733514307 ) ) ;
#70584 = LINE ( 'NONE', #42675, #13026 ) ;
#70586 = CARTESIAN_POINT ( 'NONE',  ( 8.769230769230768274, -5.557115091759785130, 34.35708131394839171 ) ) ;
#70587 = CARTESIAN_POINT ( 'NONE',  ( -16.08859058257012720, -9.442884908240273489, 34.35708131394835618 ) ) ;
#70588 = EDGE_LOOP ( 'NONE', ( #86515, #49831 ) ) ;
#70589 = DIRECTION ( 'NONE',  ( 0.000000000000000000, 0.000000000000000000, -1.000000000000000000 ) ) ;
#70590 = CARTESIAN_POINT ( 'NONE',  ( 4.826946332874483936, -4.075325502946086864, 33.72974371597207721 ) ) ;
#70591 = VERTEX_POINT ( 'NONE', #50782 ) ;
#70592 = CARTESIAN_POINT ( 'NONE',  ( -12.46153846153846168, -3.322132147404559976, 32.92929555188717927 ) ) ;
#70593 = CARTESIAN_POINT ( 'NONE',  ( 14.30769230769231015, -9.780366693483667717, 34.19971097300155094 ) ) ;
#70594 = CARTESIAN_POINT ( 'NONE',  ( -16.08859058257012720, -10.90142922261932057, 33.41473453929631887 ) ) ;
#70595 = CARTESIAN_POINT ( 'NONE',  ( -17.07692307692307665, -10.67929555188718282, 33.92786785259544047 ) ) ;
#70596 = ADVANCED_FACE ( 'NONE', ( #36843 ), #9816, .F. ) ;
#70597 = CARTESIAN_POINT ( 'NONE',  ( 0.000000000000000000, -11.00000000000000000, 29.75000000000000355 ) ) ;
#70598 = CARTESIAN_POINT ( 'NONE',  ( 2.557637717070351702, -4.932303261841488151, 34.32971442181322885 ) ) ;
#70599 = FACE_BOUND ( 'NONE', #14639, .T. ) ;
#70601 = CARTESIAN_POINT ( 'NONE',  ( 15.23076923076923173, -2.499999999999998668, 29.75000000000001421 ) ) ;
#70600 = FACE_OUTER_BOUND ( 'NONE', #61681, .T. ) ;
#70602 = FACE_OUTER_BOUND ( 'NONE', #32986, .T. ) ;
#70604 = CARTESIAN_POINT ( 'NONE',  ( -6.923076923077044142, -5.219633306517616589, 34.19971097300220464 ) ) ;
#70603 = FACE_OUTER_BOUND ( 'NONE', #24344, .T. ) ;
#70605 = AXIS2_PLACEMENT_3D ( 'NONE', #71953, #78717, #1282 ) ;
#70606 = CARTESIAN_POINT ( 'NONE',  ( 1.134615384615366374, -2.249999999999999112, 29.81609741502488120 ) ) ;
#70607 = CARTESIAN_POINT ( 'NONE',  ( 3.724691934501232815, -5.885600066136343678, 20.38875670625849068 ) ) ;
#70608 = ORIENTED_EDGE ( 'NONE', *, *, #10844, .T. ) ;
#70609 = ORIENTED_EDGE ( 'NONE', *, *, #80583, .T. ) ;
#70610 = DIRECTION ( 'NONE',  ( -0.000000000000000000, -0.9848077530122085754, -0.1736481776669273613 ) ) ;
#70611 = CARTESIAN_POINT ( 'NONE',  ( -4.283993363284373856, -3.285722584762969856, 32.44110544564090759 ) ) ;
#70612 = CARTESIAN_POINT ( 'NONE',  ( -7.596099426240391139, -11.47946981652013498, 33.17500667209846910 ) ) ;
#70613 = CARTESIAN_POINT ( 'NONE',  ( -0.4615384615384611200, -2.833524468853757305, 32.15551576947925838 ) ) ;
#70614 = CARTESIAN_POINT ( 'NONE',  ( 12.46153846153846168, -2.499999999999998668, 29.75000000000001421 ) ) ;
#70615 = CARTESIAN_POINT ( 'NONE',  ( -3.775308065498766297, -6.007798216065450170, 21.17000670625848713 ) ) ;
#70616 = EDGE_CURVE ( 'NONE', #52843, #74684, #25709, .T. ) ;
#70617 = CARTESIAN_POINT ( 'NONE',  ( -11.76134105519912154, -7.630690623152299956, 34.99857592706774057 ) ) ;
#70618 = CARTESIAN_POINT ( 'NONE',  ( 18.00000000000000000, -3.050289026998446396, 32.03036669348365706 ) ) ;
#70619 = CARTESIAN_POINT ( 'NONE',  ( -17.20761454359063691, -4.809359713505814149, 33.96456829005828837 ) ) ;
#70620 = CARTESIAN_POINT ( 'NONE',  ( -1.514762594053604028, -12.45813303252208648, 30.39737893381572675 ) ) ;
#70621 = DIRECTION ( 'NONE',  ( -0.000000000000000000, -0.8660254037844397068, -0.4999999999999978906 ) ) ;
#70622 = DIRECTION ( 'NONE',  ( -0.000000000000000000, 0.7660444431189791237, -0.6427876096865379196 ) ) ;
#70623 = B_SPLINE_CURVE_WITH_KNOTS ( 'NONE', 3,
 ( #59443, #80166, #26105, #67096, #4952, #32863, #60324, #87838, #33749, #20239 ),
 .UNSPECIFIED., .F., .F.,
 ( 4, 2, 2, 2, 4 ),
 ( 0.0007817246256747460882, 0.0009771112852218892010, 0.001172497944769032314, 0.001367884604316175210, 0.001563271263863318323 ),
 .UNSPECIFIED. ) ;
#70624 = CARTESIAN_POINT ( 'NONE',  ( 12.46153846153846168, -2.292212530054420494, 30.41441678777542634 ) ) ;
#70625 = AXIS2_PLACEMENT_3D ( 'NONE', #2343, #80128, #79685 ) ;
#70626 = CARTESIAN_POINT ( 'NONE',  ( -19.50000000000000000, -3.499999999999999556, 29.75000000000000355 ) ) ;
#70627 = ORIENTED_EDGE ( 'NONE', *, *, #33037, .T. ) ;
#70628 = CARTESIAN_POINT ( 'NONE',  ( 2.057715563643716550, -3.436278759898155233, 33.07459398097509506 ) ) ;
#70629 = CARTESIAN_POINT ( 'NONE',  ( 10.83839745947801170, -5.582272713120729257, 34.63742843783360570 ) ) ;
#70630 = CARTESIAN_POINT ( 'NONE',  ( 2.750000000000002665, -7.561099074964516831, 24.72061829374150932 ) ) ;
#70631 = AXIS2_PLACEMENT_3D ( 'NONE', #74906, #21269, #75344 ) ;
#70632 = VECTOR ( 'NONE', #41143, 1000.000000000000000 ) ;
#70633 = EDGE_CURVE ( 'NONE', #27791, #2893, #58431, .T. ) ;
#70634 = DIRECTION ( 'NONE',  ( 0.000000000000000000, 0.6427876096865373645, -0.7660444431189797898 ) ) ;
#70635 = CARTESIAN_POINT ( 'NONE',  ( 3.230769230769231726, -13.88283147151868846, 33.14645433367849847 ) ) ;
#70636 = EDGE_LOOP ( 'NONE', ( #65866, #43344, #38440, #10139 ) ) ;
#70637 = CARTESIAN_POINT ( 'NONE',  ( -7.173053667125516064, -2.920706130388546651, 32.31842814019191223 ) ) ;
#70639 = ORIENTED_EDGE ( 'NONE', *, *, #18969, .F. ) ;
#70638 = CARTESIAN_POINT ( 'NONE',  ( 3.930919936330004472, -5.667676309546437530, 34.40238873228292249 ) ) ;
#70640 = CARTESIAN_POINT ( 'NONE',  ( -5.999999999999998224, -3.322132147404559976, 32.92929555188717927 ) ) ;
#70641 = CARTESIAN_POINT ( 'NONE',  ( 16.82689985270161870, -2.588893531581426100, 31.60682220781849239 ) ) ;
#70642 = EDGE_CURVE ( 'NONE', #15672, #49031, #64290, .T. ) ;
#70643 = EDGE_LOOP ( 'NONE', ( #30526, #55790 ) ) ;
#70644 = CARTESIAN_POINT ( 'NONE',  ( -13.31935981333935537, -2.625532179533470512, 30.86335684631491105 ) ) ;
#70645 = VECTOR ( 'NONE', #64273, 1000.000000000000000 ) ;
#70646 = CARTESIAN_POINT ( 'NONE',  ( 7.846153846153846700, -13.53365097954675988, 30.81389545987213552 ) ) ;
#70647 = EDGE_LOOP ( 'NONE', ( #5430, #18986, #32795, #83594 ) ) ;
#70648 = CARTESIAN_POINT ( 'NONE',  ( -11.60373198442231413, -4.481592998940162609, 33.73612834413957984 ) ) ;
#70649 = PLANE ( 'NONE',  #71000 ) ;
#70650 = CARTESIAN_POINT ( 'NONE',  ( 5.448717948717947124, -3.499999999999999556, 29.75000000000000355 ) ) ;
#70651 = EDGE_CURVE ( 'NONE', #48397, #41602, #85047, .T. ) ;
#70652 = ORIENTED_EDGE ( 'NONE', *, *, #3514, .T. ) ;
#70653 = VERTEX_POINT ( 'NONE', #16571 ) ;
#70654 = VERTEX_POINT ( 'NONE', #71508 ) ;
#70655 = ADVANCED_FACE ( 'NONE', ( #3049 ), #15257, .F. ) ;
#70656 = CARTESIAN_POINT ( 'NONE',  ( -7.146561847641254239, -2.353723527008295680, 30.78948104536958752 ) ) ;
#70657 = CARTESIAN_POINT ( 'NONE',  ( -15.29603923132555110, -2.379036618887870436, 30.90682066428147934 ) ) ;
#70658 = EDGE_CURVE ( 'NONE', #10983, #67914, #64746, .T. ) ;
#70659 = CARTESIAN_POINT ( 'NONE',  ( -3.230769230769352962, -8.656820664282941280, 34.87096338111179961 ) ) ;
#70660 = CYLINDRICAL_SURFACE ( 'NONE', #8973, 0.2500000000000009437 ) ;
#70661 = EDGE_CURVE ( 'NONE', #43749, #78293, #35973, .T. ) ;
#70662 = ORIENTED_EDGE ( 'NONE', *, *, #32935, .F. ) ;
#70663 = ORIENTED_EDGE ( 'NONE', *, *, #86954, .F. ) ;
#70665 = ORIENTED_EDGE ( 'NONE', *, *, #68904, .T. ) ;
#70664 = CARTESIAN_POINT ( 'NONE',  ( 17.07692307692295586, -5.219633306517616589, 34.19971097300220464 ) ) ;
#70666 = AXIS2_PLACEMENT_3D ( 'NONE', #20446, #55996, #47908 ) ;
#70667 = B_SPLINE_CURVE_WITH_KNOTS ( 'NONE', 3,
 ( #38475, #37569, #87124, #73144, #66384, #87570, #38027, #30815, #79462, #11897 ),
 .UNSPECIFIED., .F., .F.,
 ( 4, 2, 2, 2, 4 ),
 ( 0.0007817359430256333669, 0.0009771253907250056474, 0.001172514838424370881, 0.001367904286123736331, 0.001563293733823101564 ),
 .UNSPECIFIED. ) ;
#70668 = CYLINDRICAL_SURFACE ( 'NONE', #7871, 0.2500000000000009437 ) ;
#70669 = ORIENTED_EDGE ( 'NONE', *, *, #59980, .F. ) ;
#70670 = EDGE_CURVE ( 'NONE', #3335, #88199, #50347, .T. ) ;
#70671 = ADVANCED_FACE ( 'NONE', ( #1734 ), #51667, .T. ) ;
#70672 = CARTESIAN_POINT ( 'NONE',  ( 15.29596221906388287, -2.255955759149235629, 29.99999999999988987 ) ) ;
#70673 = CARTESIAN_POINT ( 'NONE',  ( 7.846153846153725020, -5.219633306517616589, 34.19971097300220464 ) ) ;
#70674 = ORIENTED_EDGE ( 'NONE', *, *, #18391, .T. ) ;
#70675 = VERTEX_POINT ( 'NONE', #44471 ) ;
#70676 = B_SPLINE_CURVE_WITH_KNOTS ( 'NONE', 3,
 ( #23826, #51281, #79241, #38251, #31496, #58959, #86463, #79688, #45443, #72922 ),
 .UNSPECIFIED., .F., .F.,
 ( 4, 2, 2, 2, 4 ),
 ( 0.0007817359430256315238, 0.0009771253907249976244, 0.001172514838424363508, 0.001367904286123729392, 0.001563293733823095492 ),
 .UNSPECIFIED. ) ;
#70678 = VERTEX_POINT ( 'NONE', #29223 ) ;
#70677 = CARTESIAN_POINT ( 'NONE',  ( 9.942307692309114486, -7.500000000000154543, 35.00000000000007105 ) ) ;
#70679 = B_SPLINE_CURVE_WITH_KNOTS ( 'NONE', 3,
 ( #48374, #34861, #6075, #88955, #33096, #20902, #28110, #199, #27224, #41190 ),
 .UNSPECIFIED., .F., .F.,
 ( 4, 2, 2, 2, 4 ),
 ( 0.0007817246256747446788, 0.0009771112852218879000, 0.001172497944769031013, 0.001367884604316174126, 0.001563271263863317238 ),
 .UNSPECIFIED. ) ;
#70680 = CARTESIAN_POINT ( 'NONE',  ( 4.153846153846032507, -5.219633306517616589, 34.19971097300220464 ) ) ;
#70681 = CYLINDRICAL_SURFACE ( 'NONE', #19476, 0.2499999999999986955 ) ;
#70682 = ORIENTED_EDGE ( 'NONE', *, *, #49330, .F. ) ;
#70683 = CARTESIAN_POINT ( 'NONE',  ( 15.00728430620490172, -2.353723527008296568, 30.78948104536958752 ) ) ;
#70684 = CARTESIAN_POINT ( 'NONE',  ( 15.23076923076911093, -9.442884908241554243, 34.35708131394783038 ) ) ;
#70685 = CARTESIAN_POINT ( 'NONE',  ( 8.769230769230768274, -12.48256725967547354, 35.29906147534542527 ) ) ;
#70686 = FACE_BOUND ( 'NONE', #7960, .T. ) ;
#70687 = CARTESIAN_POINT ( 'NONE',  ( -8.638705330997126453, -2.372941743896879174, 30.88044141588253666 ) ) ;
#70688 = CARTESIAN_POINT ( 'NONE',  ( 13.19230769230769340, -7.500000000000000000, 29.75000000000000355 ) ) ;
#70689 = VECTOR ( 'NONE', #19964, 1000.000000000000000 ) ;
#70690 = CARTESIAN_POINT ( 'NONE',  ( 8.769230769230768274, -2.538708090699994813, 30.37095296980875503 ) ) ;
#70692 = CARTESIAN_POINT ( 'NONE',  ( -16.15384615384627409, -3.083524468854526912, 32.58852847137268327 ) ) ;
#70691 = CARTESIAN_POINT ( 'NONE',  ( -9.692307692307691624, -12.34228464037088635, 31.77849191805839268 ) ) ;
#70693 = CARTESIAN_POINT ( 'NONE',  ( -5.010855743573002563, -3.937682226553329556, 33.60647404775216529 ) ) ;
#70694 = FACE_OUTER_BOUND ( 'NONE', #5213, .T. ) ;
#70695 = ORIENTED_EDGE ( 'NONE', *, *, #51021, .T. ) ;
#70696 = FACE_OUTER_BOUND ( 'NONE', #78858, .T. ) ;
#70697 = EDGE_LOOP ( 'NONE', ( #45376, #4590 ) ) ;
#70698 = EDGE_LOOP ( 'NONE', ( #88148, #10712, #41098, #55734 ) ) ;
#70699 = VECTOR ( 'NONE', #64608, 1000.000000000000114 ) ;
#70701 = CARTESIAN_POINT ( 'NONE',  ( 16.15384615384603251, -12.27809138561165270, 31.22303859784587132 ) ) ;
#70700 = CARTESIAN_POINT ( 'NONE',  ( 1.384615384615386802, -11.16473453929635440, 33.15142922261926373 ) ) ;
#70702 = CARTESIAN_POINT ( 'NONE',  ( 11.28843831424008926, -8.475808217655753651, 34.90892951860618609 ) ) ;
#70703 = CYLINDRICAL_SURFACE ( 'NONE', #75349, 0.2500000000000008882 ) ;
#70704 = CARTESIAN_POINT ( 'NONE',  ( -10.48459417441766561, -12.35292014791297710, 31.75344720912887198 ) ) ;
#70705 = CARTESIAN_POINT ( 'NONE',  ( -4.023055712879200385, -3.338503747796866872, 32.95102852606553512 ) ) ;
#70706 = VERTEX_POINT ( 'NONE', #84170 ) ;
#70707 = EDGE_CURVE ( 'NONE', #25698, #55151, #80429, .T. ) ;
#70708 = CARTESIAN_POINT ( 'NONE',  ( -18.06527044596078113, -6.026961402152683611, 34.52809138561120506 ) ) ;
#70709 = B_SPLINE_CURVE_WITH_KNOTS ( 'NONE', 3,
 ( #39777, #87988, #73563, #12290, #64219, #74001, #18612, #84959, #51135, #60473 ),
 .UNSPECIFIED., .F., .F.,
 ( 4, 2, 2, 2, 4 ),
 ( 0.0007817359430256282712, 0.0009771253907249941549, 0.001172514838424359822, 0.001367904286123725489, 0.001563293733823091372 ),
 .UNSPECIFIED. ) ;
#70710 = CARTESIAN_POINT ( 'NONE',  ( 3.296024802045255164, -11.48612834413965977, 32.76840700105972815 ) ) ;
#70711 = CARTESIAN_POINT ( 'NONE',  ( 17.07692307692295586, -6.879047030192662504, 34.71129190930017927 ) ) ;
#70712 = CARTESIAN_POINT ( 'NONE',  ( -8.546451100252703270, -2.612705202774698421, 31.66806509827799943 ) ) ;
#70713 = LINE ( 'NONE', #9888, #16106 ) ;
#70714 = EDGE_CURVE ( 'NONE', #53248, #60559, #66554, .T. ) ;
#70715 = EDGE_CURVE ( 'NONE', #4425, #59481, #76101, .T. ) ;
#70716 = CARTESIAN_POINT ( 'NONE',  ( 3.750000000000000888, -7.499999999999978684, 16.96875000000000000 ) ) ;
#70717 = ORIENTED_EDGE ( 'NONE', *, *, #18455, .T. ) ;
#70719 = EDGE_CURVE ( 'NONE', #78911, #88008, #32090, .T. ) ;
#70718 = ORIENTED_EDGE ( 'NONE', *, *, #77908, .F. ) ;
#70720 = CARTESIAN_POINT ( 'NONE',  ( -7.715628407920203102, -12.15418822224088657, 32.17964115625579069 ) ) ;
#70721 = ORIENTED_EDGE ( 'NONE', *, *, #34763, .T. ) ;
#70722 = CARTESIAN_POINT ( 'NONE',  ( 10.61538461538461675, -9.819645486525091727, 36.12317359536749706 ) ) ;
#70723 = DIRECTION ( 'NONE',  ( -0.000000000000000000, 1.000000000000000000, -0.000000000000000000 ) ) ;
#70724 = CARTESIAN_POINT ( 'NONE',  ( 4.230769230769229061, -3.499999999999999556, 29.75000000000000355 ) ) ;
#70725 = CARTESIAN_POINT ( 'NONE',  ( -0.4615384615384611200, -11.91647553114624181, 32.58852847137148245 ) ) ;
#70726 = CARTESIAN_POINT ( 'NONE',  ( -2.651650429449565305, -4.848349570550461785, 19.00000000000000000 ) ) ;
#70727 = EDGE_CURVE ( 'NONE', #62488, #62470, #39598, .T. ) ;
#70728 = CARTESIAN_POINT ( 'NONE',  ( 14.30769230769231015, -6.343179335718451384, 34.87096338111211935 ) ) ;
#70729 = VERTEX_POINT ( 'NONE', #60665 ) ;
#70730 = CARTESIAN_POINT ( 'NONE',  ( -12.68446467905460473, -10.61292498521070549, 33.66303323003028680 ) ) ;
#70732 = ORIENTED_EDGE ( 'NONE', *, *, #45014, .T. ) ;
#70731 = DIRECTION ( 'NONE',  ( -0.000000000000000000, 1.000000000000000000, 3.491481338843133355E-15 ) ) ;
#70733 = CARTESIAN_POINT ( 'NONE',  ( -13.60810032833933292, -11.41268669641500466, 32.86336882939237825 ) ) ;
#70734 = DIRECTION ( 'NONE',  ( -0.000000000000000000, -0.000000000000000000, -1.000000000000000000 ) ) ;
#70735 = AXIS2_PLACEMENT_3D ( 'NONE', #18190, #24484, #57834 ) ;
#70736 = CARTESIAN_POINT ( 'NONE',  ( -3.230769230769229949, -4.786620604624113540, 33.94971097300155094 ) ) ;
#70737 = CARTESIAN_POINT ( 'NONE',  ( 6.673053698855467175, -3.520140089381497361, 33.17453946501458262 ) ) ;
#70738 = CARTESIAN_POINT ( 'NONE',  ( -3.453597328404108602, -7.369209533119137845, 34.99857337881830688 ) ) ;
#70739 = CARTESIAN_POINT ( 'NONE',  ( 15.48071474911737511, -11.37275283266504111, 32.91324779482534524 ) ) ;
#70740 = VECTOR ( 'NONE', #79, 1000.000000000000000 ) ;
#70741 = CARTESIAN_POINT ( 'NONE',  ( 3.775308065498752086, -6.007798216065404873, 14.64249329374151110 ) ) ;
#70742 = ORIENTED_EDGE ( 'NONE', *, *, #73136, .F. ) ;
#70743 = CARTESIAN_POINT ( 'NONE',  ( -3.100243792535585907, -6.808710257144159783, 34.95449254468098843 ) ) ;
#70744 = CARTESIAN_POINT ( 'NONE',  ( 4.403900573759606196, -10.82426656108011720, 33.81400080652039009 ) ) ;
#70745 = CARTESIAN_POINT ( 'NONE',  ( -1.944543648263014957, -5.555456351737005249, 20.25000000000000000 ) ) ;
#70746 = CARTESIAN_POINT ( 'NONE',  ( 0.3954560821783252300, -5.471508081941601986, 34.59228464037088457 ) ) ;
#70747 = CARTESIAN_POINT ( 'NONE',  ( -16.15384615384615330, -13.78497067705608181, 32.30358669280327177 ) ) ;
#70748 = ORIENTED_EDGE ( 'NONE', *, *, #81885, .F. ) ;
#70749 = CARTESIAN_POINT ( 'NONE',  ( 1.944543648262996083, -5.555456351736983045, 14.31250000000000000 ) ) ;
#70750 = CARTESIAN_POINT ( 'NONE',  ( -3.360916440207450062, -10.88202310037936194, 33.43294751532457099 ) ) ;
#70751 = EDGE_CURVE ( 'NONE', #22972, #35664, #982, .T. ) ;
#70752 = B_SPLINE_CURVE_WITH_KNOTS ( 'NONE', 3,
 ( #70680, #8983, #36880, #36452, #63903, #2204, #57157, #84647, #22926, #67478 ),
 .UNSPECIFIED., .F., .F.,
 ( 4, 2, 2, 2, 4 ),
 ( 0.0007817359430256280543, 0.0009771253907249941549, 0.001172514838424360472, 0.001367904286123726790, 0.001563293733823092890 ),
 .UNSPECIFIED. ) ;
#70753 = ORIENTED_EDGE ( 'NONE', *, *, #4682, .F. ) ;
#70754 = CARTESIAN_POINT ( 'NONE',  ( -0.7115616857599195155, -10.92453946501458439, 33.72985991061850086 ) ) ;
#70755 = VERTEX_POINT ( 'NONE', #86391 ) ;
#70756 = CARTESIAN_POINT ( 'NONE',  ( 17.93391658904412012, -6.386643153685125363, 34.62446782046654903 ) ) ;
#70757 = CARTESIAN_POINT ( 'NONE',  ( 10.61538461538493117, -2.255955759149395501, 30.00000000000324363 ) ) ;
#70758 = CARTESIAN_POINT ( 'NONE',  ( 7.911409417429871027, -6.026961402152789304, 34.52809138561124769 ) ) ;
#70759 = CARTESIAN_POINT ( 'NONE',  ( 17.07692307692307665, -13.20930481340135110, 34.54067556320372745 ) ) ;
#70760 = VERTEX_POINT ( 'NONE', #80055 ) ;
#70761 = CARTESIAN_POINT ( 'NONE',  ( -2.980823821391186623, -2.341251567377310217, 30.72681386836322659 ) ) ;
#70762 = AXIS2_PLACEMENT_3D ( 'NONE', #86681, #24947, #77671 ) ;
#70763 = ORIENTED_EDGE ( 'NONE', *, *, #79878, .T. ) ;
#70765 = CARTESIAN_POINT ( 'NONE',  ( 12.46153846153846168, -11.91647553114624181, 32.58852847137148245 ) ) ;
#70764 = CIRCLE ( 'NONE', #17725, 0.2500000000000002220 ) ;
#70766 = CARTESIAN_POINT ( 'NONE',  ( 0.7114838709165044461, -10.18230066228895758, 34.26354781536631577 ) ) ;
#70767 = ORIENTED_EDGE ( 'NONE', *, *, #12299, .F. ) ;
#70768 = CARTESIAN_POINT ( 'NONE',  ( -16.15384615384615330, -13.63283147151868846, 33.57946703557072254 ) ) ;
#70769 = FACE_OUTER_BOUND ( 'NONE', #84735, .T. ) ;
#70770 = CARTESIAN_POINT ( 'NONE',  ( -11.60373198442231413, -2.892918686051582977, 31.69288490824015980 ) ) ;
#70771 = CIRCLE ( 'NONE', #16115, 4.000000000000000000 ) ;
#70772 = CARTESIAN_POINT ( 'NONE',  ( 1.134592160393929294, -6.652501968072646932, 34.93155406624980941 ) ) ;
#70773 = CARTESIAN_POINT ( 'NONE',  ( -3.903791733932699515, -4.074993327901525575, 33.72946981652012255 ) ) ;
#70774 = EDGE_CURVE ( 'NONE', #4149, #8013, #24663, .T. ) ;
#70776 = EDGE_LOOP ( 'NONE', ( #46308, #11288 ) ) ;
#70775 = EDGE_CURVE ( 'NONE', #26164, #79365, #78538, .T. ) ;
#70777 = VERTEX_POINT ( 'NONE', #45819 ) ;
#70778 = FACE_BOUND ( 'NONE', #74456, .T. ) ;
#70779 = ORIENTED_EDGE ( 'NONE', *, *, #15284, .F. ) ;
#70780 = CARTESIAN_POINT ( 'NONE',  ( -8.769230769230768274, -4.098570777380720287, 33.41473453929634729 ) ) ;
#70781 = B_SPLINE_CURVE_WITH_KNOTS ( 'NONE', 3,
 ( #47655, #75139, #37227, #57947, #50289, #64694, #2119, #17414, #16083, #2995 ),
 .UNSPECIFIED., .F., .F.,
 ( 4, 2, 2, 2, 4 ),
 ( 0.000000000000000000, 0.0001954339857564080165, 0.0003908679715128160329, 0.0005863019572692240765, 0.0007817359430256320659 ),
 .UNSPECIFIED. ) ;
#70782 = EDGE_CURVE ( 'NONE', #6671, #33723, #53618, .T. ) ;
#70783 = B_SPLINE_CURVE_WITH_KNOTS ( 'NONE', 3,
 ( #11586, #80945, #61092, #19232, #80494, #74172, #12908, #4830, #88601, #26872 ),
 .UNSPECIFIED., .F., .F.,
 ( 4, 2, 2, 2, 4 ),
 ( 0.0007817246256747446788, 0.0009771112852218879000, 0.001172497944769031013, 0.001367884604316174126, 0.001563271263863317238 ),
 .UNSPECIFIED. ) ;
#70784 = CARTESIAN_POINT ( 'NONE',  ( -7.846153846153967493, -6.835583212225970762, 34.95778746994575670 ) ) ;
#70785 = EDGE_CURVE ( 'NONE', #59805, #1987, #3034, .T. ) ;
#70786 = CARTESIAN_POINT ( 'NONE',  ( 5.999999999999878320, -3.083524468854526912, 32.58852847137268327 ) ) ;
#70787 = DIRECTION ( 'NONE',  ( -0.000000000000000000, 0.5000000000000011102, -0.8660254037844381525 ) ) ;
#70788 = ORIENTED_EDGE ( 'NONE', *, *, #86411, .F. ) ;
#70790 = EDGE_CURVE ( 'NONE', #7689, #62944, #75960, .T. ) ;
#70789 = VERTEX_POINT ( 'NONE', #47598 ) ;
#70791 = CARTESIAN_POINT ( 'NONE',  ( 16.94623161025551639, -4.118384482072086072, 33.43331474514187107 ) ) ;
#70792 = ORIENTED_EDGE ( 'NONE', *, *, #47863, .F. ) ;
#70793 = VECTOR ( 'NONE', #48218, 1000.000000000000114 ) ;
#70794 = LINE ( 'NONE', #58585, #17475 ) ;
#70795 = CARTESIAN_POINT ( 'NONE',  ( 13.13463865367303640, -2.779195860258146578, 31.39871582349836032 ) ) ;
#70796 = AXIS2_PLACEMENT_3D ( 'NONE', #42630, #17709, #29995 ) ;
#70797 = EDGE_CURVE ( 'NONE', #22972, #79057, #41296, .T. ) ;
#70798 = DIRECTION ( 'NONE',  ( 0.000000000000000000, 0.6427876096865368094, 0.7660444431189802339 ) ) ;
#70799 = DIRECTION ( 'NONE',  ( -0.000000000000000000, 1.000000000000000000, 3.491481338843133355E-15 ) ) ;
#70800 = ORIENTED_EDGE ( 'NONE', *, *, #58811, .T. ) ;
#70801 = CARTESIAN_POINT ( 'NONE',  ( 16.40379156322419973, -2.341251567377310217, 30.72681386836322659 ) ) ;
#70802 = CARTESIAN_POINT ( 'NONE',  ( -15.23076923076922995, -3.322132147404559976, 32.92929555188717927 ) ) ;
#70803 = ADVANCED_FACE ( 'NONE', ( #75083 ), #7508, .F. ) ;
#70804 = CARTESIAN_POINT ( 'NONE',  ( -17.87165453593004827, -7.725172855618575696, 34.99539338292708379 ) ) ;
#70805 = CARTESIAN_POINT ( 'NONE',  ( -1.134560964701931018, -2.920487667080174710, 32.31805714834170828 ) ) ;
#70806 = EDGE_LOOP ( 'NONE', ( #50250, #32371, #84755, #14657 ) ) ;
#70807 = PRODUCT_DEFINITION_CONTEXT ( 'detailed design', #26811, 'design' ) ;
#70808 = ORIENTED_EDGE ( 'NONE', *, *, #24501, .F. ) ;
#70809 = ORIENTED_EDGE ( 'NONE', *, *, #9949, .F. ) ;
#70811 = CARTESIAN_POINT ( 'NONE',  ( 2.307692307692187583, -2.625532179533779154, 30.86335684631627174 ) ) ;
#70810 = CYLINDRICAL_SURFACE ( 'NONE', #61934, 0.2499999999999979738 ) ;
#70812 = CARTESIAN_POINT ( 'NONE',  ( 15.93091993633000136, -5.667676309546437530, 34.40238873228292249 ) ) ;
#70813 = CARTESIAN_POINT ( 'NONE',  ( 12.52760579488853665, -12.62096338111211757, 30.90682066428152908 ) ) ;
#70814 = CARTESIAN_POINT ( 'NONE',  ( -7.846153846153844924, -1.629998284177014645, 34.34916445242399163 ) ) ;
#70815 = CARTESIAN_POINT ( 'NONE',  ( -2.437839517130528044, -10.19110544564092002, 33.96427741523702792 ) ) ;
#70816 = ORIENTED_EDGE ( 'NONE', *, *, #68408, .F. ) ;
#70817 = EDGE_CURVE ( 'NONE', #86112, #81662, #27768, .T. ) ;
#70818 = CARTESIAN_POINT ( 'NONE',  ( 17.07692307692307665, -11.91647553114624181, 32.58852847137148245 ) ) ;
#70819 = CARTESIAN_POINT ( 'NONE',  ( 9.561617089197390840, -11.93127051446799847, 32.56575433478202797 ) ) ;
#70820 = CARTESIAN_POINT ( 'NONE',  ( 11.28846153846153832, -7.433931650972300353, 34.75000000000000711 ) ) ;
#70821 = CARTESIAN_POINT ( 'NONE',  ( -11.28840722682322628, -3.627508038966690496, 32.91356715214248396 ) ) ;
#70822 = EDGE_LOOP ( 'NONE', ( #15209, #21389 ) ) ;
#70823 = CARTESIAN_POINT ( 'NONE',  ( 2.438218009455874302, -11.93748526763465279, 32.05452791011430946 ) ) ;
#70824 = EDGE_CURVE ( 'NONE', #4668, #75533, #55238, .T. ) ;
#70825 = VERTEX_POINT ( 'NONE', #54793 ) ;
#70826 = FACE_BOUND ( 'NONE', #58432, .T. ) ;
#70828 = CIRCLE ( 'NONE', #67929, 4.000000000000000000 ) ;
#70827 = CARTESIAN_POINT ( 'NONE',  ( 4.826946345980721809, -5.728515186090277211, 34.42611988154120439 ) ) ;
#70829 = AXIS2_PLACEMENT_3D ( 'NONE', #74777, #13063, #19374 ) ;
#70830 = CYLINDRICAL_SURFACE ( 'NONE', #73693, 0.2500000000000004996 ) ;
#70831 = CARTESIAN_POINT ( 'NONE',  ( -18.23784950573857344, 12.75000000000000711, 30.81664701255125394 ) ) ;
#70832 = VERTEX_POINT ( 'NONE', #6176 ) ;
#70833 = CARTESIAN_POINT ( 'NONE',  ( -12.59222992820602371, -9.804603061927743113, 34.18744698557895845 ) ) ;
#70834 = CARTESIAN_POINT ( 'NONE',  ( 4.946446368806611815, -7.276988635370452485, 34.74523720219453793 ) ) ;
#70835 = CARTESIAN_POINT ( 'NONE',  ( -9.942330929600657896, -3.202444869320336451, 32.30641848906366675 ) ) ;
#70836 = CARTESIAN_POINT ( 'NONE',  ( -7.146561866800870355, -10.81261337010820256, 33.49550067578627477 ) ) ;
#70837 = ORIENTED_EDGE ( 'NONE', *, *, #28675, .T. ) ;
#70838 = VECTOR ( 'NONE', #60224, 1000.000000000000227 ) ;
#70839 = EDGE_CURVE ( 'NONE', #32871, #3063, #40850, .T. ) ;
#70840 = CARTESIAN_POINT ( 'NONE',  ( -9.915792616872025178, -3.019605429927184836, 32.48692288466676814 ) ) ;
#70841 = ORIENTED_EDGE ( 'NONE', *, *, #15165, .F. ) ;
#70843 = ORIENTED_EDGE ( 'NONE', *, *, #51791, .T. ) ;
#70842 = CARTESIAN_POINT ( 'NONE',  ( -15.84615384615384670, -7.500000000000000000, 29.75000000000000355 ) ) ;
#70844 = CARTESIAN_POINT ( 'NONE',  ( 7.846153846153725020, -10.90142922262034020, 33.41473453929536674 ) ) ;
#70845 = CARTESIAN_POINT ( 'NONE',  ( -6.923076923076922462, -11.69971097300155272, 32.46337939537588113 ) ) ;
#70846 = DIRECTION ( 'NONE',  ( -0.000000000000000000, 0.5000000000000011102, -0.8660254037844381525 ) ) ;
#70847 = CARTESIAN_POINT ( 'NONE',  ( 12.68454981315131214, -4.187068189119697692, 33.49521262558774026 ) ) ;
#70849 = CARTESIAN_POINT ( 'NONE',  ( -11.78843828251013015, -9.234221910056348293, 34.70572697212741531 ) ) ;
#70848 = CARTESIAN_POINT ( 'NONE',  ( 27.00000000000000000, 17.00000000000000000, 2.999999999999999112 ) ) ;
#70850 = EDGE_CURVE ( 'NONE', #63664, #74128, #68456, .T. ) ;
#70851 = PLANE ( 'NONE',  #4740 ) ;
#70852 = CARTESIAN_POINT ( 'NONE',  ( 1.799775606325937360E-14, -10.25000000000000000, 23.53125000000000000 ) ) ;
#70853 = ORIENTED_EDGE ( 'NONE', *, *, #80528, .T. ) ;
#70854 = CARTESIAN_POINT ( 'NONE',  ( 16.15384615384615330, -8.973038597847269315, 34.52809138561121927 ) ) ;
#70855 = CARTESIAN_POINT ( 'NONE',  ( 13.13461538461538680, -7.500000000000001776, 35.00000000000000000 ) ) ;
#70856 = ORIENTED_EDGE ( 'NONE', *, *, #58675, .F. ) ;
#70857 = ORIENTED_EDGE ( 'NONE', *, *, #14187, .T. ) ;
#70858 = ORIENTED_EDGE ( 'NONE', *, *, #45840, .T. ) ;
#70859 = CARTESIAN_POINT ( 'NONE',  ( 4.153846153846154188, -12.10708131394839349, 31.69288490824020244 ) ) ;
#70860 = EDGE_CURVE ( 'NONE', #20749, #11535, #72911, .T. ) ;
#70861 = CARTESIAN_POINT ( 'NONE',  ( -4.854143407945007205, -12.69155399931963046, 30.53255429739158444 ) ) ;
#70862 = CARTESIAN_POINT ( 'NONE',  ( 0.2115384615384615363, -7.566082377512563184, 35.00000000000000711 ) ) ;
#70863 = FACE_OUTER_BOUND ( 'NONE', #56710, .T. ) ;
#70864 = CARTESIAN_POINT ( 'NONE',  ( -13.25382494364843389, -6.369690395747422684, 34.87708834333098196 ) ) ;
#70865 = ADVANCED_FACE ( 'NONE', ( #27331 ), #82285, .F. ) ;
#70866 = CARTESIAN_POINT ( 'NONE',  ( -8.992715693795101828, -3.019605429927184836, 32.48692288466676814 ) ) ;
#70867 = AXIS2_PLACEMENT_3D ( 'NONE', #85804, #59985, #51092 ) ;
#70868 = CARTESIAN_POINT ( 'NONE',  ( 0.2115384615384616196, -2.249999999999998668, 29.75000000000000355 ) ) ;
#70869 = ORIENTED_EDGE ( 'NONE', *, *, #55103, .F. ) ;
#70870 = CARTESIAN_POINT ( 'NONE',  ( 6.222779541268410597, -10.81320215134717344, 33.49497208177562868 ) ) ;
#70871 = CARTESIAN_POINT ( 'NONE',  ( -17.29980175935171616, -7.630691491037286056, 34.74850469731152458 ) ) ;
#70872 = DIRECTION ( 'NONE',  ( 0.000000000000000000, 0.8660254037844377084, -0.5000000000000015543 ) ) ;
#70873 = LINE ( 'NONE', #8732, #39829 ) ;
#70874 = ORIENTED_EDGE ( 'NONE', *, *, #16316, .F. ) ;
#70875 = CARTESIAN_POINT ( 'NONE',  ( -17.74994558008654622, -8.346898887586322147, 34.93166121998716278 ) ) ;
#70876 = FILL_AREA_STYLE_COLOUR ( '', #67631 ) ;
#70877 = LINE ( 'NONE', #51009, #81533 ) ;
#70878 = CARTESIAN_POINT ( 'NONE',  ( 5.999999999999878320, -12.70778746994576025, 30.41441678777401236 ) ) ;
#70879 = ORIENTED_EDGE ( 'NONE', *, *, #75334, .F. ) ;
#70880 = CARTESIAN_POINT ( 'NONE',  ( -2.307692307692305711, -6.343179335718451384, 34.87096338111211935 ) ) ;
#70881 = CARTESIAN_POINT ( 'NONE',  ( -12.23857555797697927, -7.369474270740069777, 34.74850911626239736 ) ) ;
#70882 = CARTESIAN_POINT ( 'NONE',  ( 8.834486340506797930, -4.481592998940250538, 33.73612834413965089 ) ) ;
#70883 = VERTEX_POINT ( 'NONE', #40416 ) ;
#70884 = CARTESIAN_POINT ( 'NONE',  ( -10.68063560554585578, -2.506253911140460922, 30.00000000000013856 ) ) ;
#70885 = EDGE_LOOP ( 'NONE', ( #35381, #56189 ) ) ;
#70886 = CIRCLE ( 'NONE', #82410, 4.000000000000000000 ) ;
#70887 = CARTESIAN_POINT ( 'NONE',  ( 13.16168842570853670, -12.38737895849757820, 31.66785238281580206 ) ) ;
#70888 = AXIS2_PLACEMENT_3D ( 'NONE', #23463, #9956, #52272 ) ;
#70889 = CARTESIAN_POINT ( 'NONE',  ( 8.992243613324164997, -9.172514111537584114, 34.72667873470787470 ) ) ;
#70890 = CARTESIAN_POINT ( 'NONE',  ( -8.069638770718178478, -2.612411019501189369, 31.66733052389439962 ) ) ;
#70891 = EDGE_CURVE ( 'NONE', #30065, #48397, #36400, .T. ) ;
#70892 = CARTESIAN_POINT ( 'NONE',  ( -14.17690049986752321, -11.71459661697925903, 32.44059661609676937 ) ) ;
#70893 = CARTESIAN_POINT ( 'NONE',  ( -3.480769230769229061, -7.566082377512563184, 35.00000000000000711 ) ) ;
#70894 = AXIS2_PLACEMENT_3D ( 'NONE', #68011, #34210, #41855 ) ;
#70895 = EDGE_LOOP ( 'NONE', ( #32988, #33546, #6166, #21565, #19959, #44913 ) ) ;
#70896 = EDGE_CURVE ( 'NONE', #70330, #31113, #30012, .T. ) ;
#70897 = EDGE_LOOP ( 'NONE', ( #49267, #86001 ) ) ;
#70898 = ORIENTED_EDGE ( 'NONE', *, *, #55465, .F. ) ;
#70899 = CARTESIAN_POINT ( 'NONE',  ( -16.15384615384615330, -1.129524287112498415, 32.06866353760679544 ) ) ;
#70900 = CARTESIAN_POINT ( 'NONE',  ( -16.82697755857493149, -3.712312575010499494, 33.01462480002815170 ) ) ;
#70901 = EDGE_CURVE ( 'NONE', #38328, #88554, #83622, .T. ) ;
#70902 = CARTESIAN_POINT ( 'NONE',  ( 0.6843181305165266792, -6.717445702608402236, 34.94155399931962336 ) ) ;
#70903 = CARTESIAN_POINT ( 'NONE',  ( 0.2115152373170028910, -12.45566812827425096, 31.48439005359158926 ) ) ;
#70904 = FACE_OUTER_BOUND ( 'NONE', #48578, .T. ) ;
#70905 = CARTESIAN_POINT ( 'NONE',  ( -17.07692307692307665, -1.466349020453238561, 30.81389545987213907 ) ) ;
#70906 = EDGE_LOOP ( 'NONE', ( #17440, #64174 ) ) ;
#70907 = ORIENTED_EDGE ( 'NONE', *, *, #21168, .F. ) ;
#70908 = ORIENTED_EDGE ( 'NONE', *, *, #87789, .T. ) ;
#70909 = ADVANCED_FACE ( 'NONE', ( #23665 ), #10162, .F. ) ;
#70911 = EDGE_LOOP ( 'NONE', ( #43955, #57177, #65461, #4561, #14862 ) ) ;
#70910 = CARTESIAN_POINT ( 'NONE',  ( 4.403900573759605308, -4.074993327901525575, 33.72946981652012255 ) ) ;
#70913 = CARTESIAN_POINT ( 'NONE',  ( -8.703975197954743948, -11.48612834413965977, 32.76840700105972815 ) ) ;
#70912 = CARTESIAN_POINT ( 'NONE',  ( -9.915792636031639518, -9.331801661448606566, 34.40259984581193464 ) ) ;
#70914 = VECTOR ( 'NONE', #78207, 1000.000000000000000 ) ;
#70915 = CARTESIAN_POINT ( 'NONE',  ( 2.651650429449569302, -10.15165042944953733, 23.37500000000000000 ) ) ;
#70916 = EDGE_LOOP ( 'NONE', ( #17772, #56327, #18686, #30625 ) ) ;
#70917 = VERTEX_POINT ( 'NONE', #22343 ) ;
#70918 = CARTESIAN_POINT ( 'NONE',  ( -18.00000000000000000, -2.833524468853757305, 32.15551576947926549 ) ) ;
#70919 = EDGE_CURVE ( 'NONE', #21459, #82878, #36743, .T. ) ;
#70920 = ORIENTED_EDGE ( 'NONE', *, *, #42726, .T. ) ;
#70921 = FACE_BOUND ( 'NONE', #41667, .T. ) ;
#70922 = CARTESIAN_POINT ( 'NONE',  ( 15.10007776410167502, -9.804603061927743113, 34.18744698557895845 ) ) ;
#70923 = CARTESIAN_POINT ( 'NONE',  ( -4.088590582570127197, -11.94971097300157403, 32.03036669348361443 ) ) ;
#70924 = ORIENTED_EDGE ( 'NONE', *, *, #84190, .F. ) ;
#70925 = CARTESIAN_POINT ( 'NONE',  ( 16.28463796167094557, -11.18335022499818621, 33.13157742990016885 ) ) ;
#70926 = EDGE_CURVE ( 'NONE', #34160, #18655, #85845, .T. ) ;
#70927 = CARTESIAN_POINT ( 'NONE',  ( 0.3589743589743586982, -3.499999999999999556, 29.75000000000000355 ) ) ;
#70928 = CARTESIAN_POINT ( 'NONE',  ( 10.61538461538461675, -2.721908614388771852, 31.22303859784724978 ) ) ;
#70929 = CARTESIAN_POINT ( 'NONE',  ( -11.76194648218548444, -5.912607949931405926, 34.49155766932282319 ) ) ;
#70930 = CARTESIAN_POINT ( 'NONE',  ( 9.320512820512821150, -4.000000000000000000, 29.75000000000000355 ) ) ;
#70931 = CARTESIAN_POINT ( 'NONE',  ( -6.923076923076922462, -11.16473453929635440, 33.15142922261926373 ) ) ;
#70932 = CARTESIAN_POINT ( 'NONE',  ( 3.480714749117372442, -4.336752205174647656, 33.62275283266504289 ) ) ;
#70933 = FACE_OUTER_BOUND ( 'NONE', #36012, .T. ) ;
#70934 = DIRECTION ( 'NONE',  ( -0.000000000000000000, 0.5000000000000011102, -0.8660254037844380415 ) ) ;
#70935 = DIRECTION ( 'NONE',  ( -0.000000000000000000, 0.9396926207859093161, -0.3420201433256663259 ) ) ;
#70936 = DIRECTION ( 'NONE',  ( 1.000000000000000000, 0.000000000000000000, 0.000000000000000000 ) ) ;
#70938 = LINE ( 'NONE', #57413, #43112 ) ;
#70937 = CARTESIAN_POINT ( 'NONE',  ( 4.403791672194295792, -12.22109172314383052, 31.39792113162168263 ) ) ;
#70939 = ADVANCED_FACE ( 'NONE', ( #84500 ), #70533, .F. ) ;
#70940 = CARTESIAN_POINT ( 'NONE',  ( 13.38461538461538680, -3.513871655860378418, 32.76840700105978499 ) ) ;
#70942 = CARTESIAN_POINT ( 'NONE',  ( 5.934729554039225974, -10.90142922261923886, 33.41473453929638993 ) ) ;
#70941 = FACE_OUTER_BOUND ( 'NONE', #24320, .T. ) ;
#70943 = DIRECTION ( 'NONE',  ( -0.000000000000000000, 0.8660254037844397068, -0.4999999999999978906 ) ) ;
#70944 = CARTESIAN_POINT ( 'NONE',  ( 1.901340078031349856, -5.512252781505337929, 21.56063170625849068 ) ) ;
#70945 = ORIENTED_EDGE ( 'NONE', *, *, #44932, .F. ) ;
#70946 = AXIS2_PLACEMENT_3D ( 'NONE', #80912, #59285, #11554 ) ;
#70947 = CARTESIAN_POINT ( 'NONE',  ( 2.410688644434096695, -4.750108984206948826, 14.00000000000000533 ) ) ;
#70948 = VERTEX_POINT ( 'NONE', #57451 ) ;
#70949 = VECTOR ( 'NONE', #47960, 1000.000000000000000 ) ;
#70950 = CYLINDRICAL_SURFACE ( 'NONE', #11908, 0.2499999999999995559 ) ;
#70951 = ORIENTED_EDGE ( 'NONE', *, *, #15660, .T. ) ;
#70952 = CARTESIAN_POINT ( 'NONE',  ( 14.16025641025641235, -3.499999999999999556, 29.75000000000000355 ) ) ;
#70953 = VERTEX_POINT ( 'NONE', #71853 ) ;
#70954 = CARTESIAN_POINT ( 'NONE',  ( -2.307692307692305711, -7.500000000000001776, 35.04278698407183867 ) ) ;
#70955 = CARTESIAN_POINT ( 'NONE',  ( 2.775308065498768517, -8.577988221561467341, 25.54500670625849779 ) ) ;
#70956 = CARTESIAN_POINT ( 'NONE',  ( 7.622668921589514923, -8.539481045369596401, 34.89627647299170832 ) ) ;
#70957 = ADVANCED_FACE ( 'NONE', ( #78172 ), #76852, .F. ) ;
#70958 = CARTESIAN_POINT ( 'NONE',  ( 7.053602361310569613, -10.31582465632705237, 34.18122507451815295 ) ) ;
#70959 = CARTESIAN_POINT ( 'NONE',  ( -5.076923076923197442, -5.219633306517616589, 34.19971097300220464 ) ) ;
#70960 = CARTESIAN_POINT ( 'NONE',  ( 14.98079248672063990, -8.347322224742351082, 34.93158281831414769 ) ) ;
#70961 = CARTESIAN_POINT ( 'NONE',  ( -8.769230769230768274, -13.78497067705608181, 32.30358669280327177 ) ) ;
#70962 = CARTESIAN_POINT ( 'NONE',  ( -2.307692307692305711, -11.91647553114624181, 32.58852847137148245 ) ) ;
#70963 = CARTESIAN_POINT ( 'NONE',  ( -2.651650429449535551, -10.15165042944956753, 16.18750000000000000 ) ) ;
#70964 = EDGE_CURVE ( 'NONE', #70411, #47496, #35866, .T. ) ;
#70965 = EDGE_CURVE ( 'NONE', #34216, #8288, #49310, .T. ) ;
#70966 = CARTESIAN_POINT ( 'NONE',  ( 1.449870955891411128, -3.300289026998475705, 32.46337939537591666 ) ) ;
#70967 = DIRECTION ( 'NONE',  ( -0.000000000000000000, 1.000000000000000000, -0.000000000000000000 ) ) ;
#70968 = EDGE_CURVE ( 'NONE', #58674, #58923, #80409, .T. ) ;
#70969 = CARTESIAN_POINT ( 'NONE',  ( 10.61538461538461675, -5.471508081941601098, 34.59228464037088457 ) ) ;
#70970 = CARTESIAN_POINT ( 'NONE',  ( 1.553300858899087311, -3.749999999999992006, 15.48437500000000178 ) ) ;
#70971 = EDGE_CURVE ( 'NONE', #87104, #17208, #58784, .T. ) ;
#70972 = CARTESIAN_POINT ( 'NONE',  ( 3.230769230769110045, -6.026961402154118908, 34.52809138561165270 ) ) ;
#70973 = ORIENTED_EDGE ( 'NONE', *, *, #36483, .T. ) ;
#70974 = DIRECTION ( 'NONE',  ( -1.000000000000000000, 0.000000000000000000, 0.000000000000000000 ) ) ;
#70975 = CARTESIAN_POINT ( 'NONE',  ( 12.21151523731700550, -8.475808217655753651, 34.90892951860618609 ) ) ;
#70976 = CARTESIAN_POINT ( 'NONE',  ( 9.942362003946008997, -6.567000820036036579, 34.66262288849541306 ) ) ;
#70977 = CARTESIAN_POINT ( 'NONE',  ( 15.10015957556514721, -7.722926974430166069, 34.99546784045485737 ) ) ;
#70978 = DIRECTION ( 'NONE',  ( 0.000000000000000000, 1.000000000000000000, 0.000000000000000000 ) ) ;
#70979 = CARTESIAN_POINT ( 'NONE',  ( -17.78205128205128105, -7.500000000000000000, 33.75000000000000000 ) ) ;
#70980 = VECTOR ( 'NONE', #50742, 1000.000000000000000 ) ;
#70981 = AXIS2_PLACEMENT_3D ( 'NONE', #4761, #87633, #65995 ) ;
#70982 = CARTESIAN_POINT ( 'NONE',  ( -6.923076923076922462, -6.435427911321262684, 35.78748833219616898 ) ) ;
#70983 = B_SPLINE_CURVE_WITH_KNOTS ( 'NONE', 3,
 ( #13937, #40544, #81086, #12175, #54928, #60795, #13497, #54031, #68009, #20697 ),
 .UNSPECIFIED., .F., .F.,
 ( 4, 2, 2, 2, 4 ),
 ( 0.000000000000000000, 0.0001954339857564075015, 0.0003908679715128150029, 0.0005863019572692224502, 0.0007817359430256300059 ),
 .UNSPECIFIED. ) ;
#70984 = B_SPLINE_CURVE_WITH_KNOTS ( 'NONE', 3,
 ( #19754, #20632, #48536, #75573, #67504, #35033, #88242, #21518, #62062, #47216 ),
 .UNSPECIFIED., .F., .F.,
 ( 4, 2, 2, 2, 4 ),
 ( 0.000000000000000000, 0.0001954311564186865221, 0.0003908623128373730441, 0.0005862934692560595662, 0.0007817246256747460882 ),
 .UNSPECIFIED. ) ;
#70985 = ORIENTED_EDGE ( 'NONE', *, *, #84705, .F. ) ;
#70986 = ORIENTED_EDGE ( 'NONE', *, *, #51166, .T. ) ;
#70987 = VERTEX_POINT ( 'NONE', #38980 ) ;
#70988 = CARTESIAN_POINT ( 'NONE',  ( -6.857821783564084228, -5.941354392334606160, 34.76329471203374055 ) ) ;
#70989 = CARTESIAN_POINT ( 'NONE',  ( -8.834500769787091201, -2.379036618887870436, 30.90682066428147934 ) ) ;
#70990 = FACE_OUTER_BOUND ( 'NONE', #65447, .T. ) ;
#70991 = CARTESIAN_POINT ( 'NONE',  ( 17.93472999944368240, -9.528491918058357157, 34.59228464037090589 ) ) ;
#70992 = EDGE_LOOP ( 'NONE', ( #8270, #61783, #22524, #70808 ) ) ;
#70993 = DIRECTION ( 'NONE',  ( 0.000000000000000000, 0.9396926207859126468, 0.3420201433256571111 ) ) ;
#70994 = ORIENTED_EDGE ( 'NONE', *, *, #2804, .F. ) ;
#70995 = ORIENTED_EDGE ( 'NONE', *, *, #64546, .F. ) ;
#70996 = VECTOR ( 'NONE', #3418, 1000.000000000000114 ) ;
#70997 = CARTESIAN_POINT ( 'NONE',  ( -15.29603967673000398, -12.27809138561121394, 31.22303859784730307 ) ) ;
#70998 = DIRECTION ( 'NONE',  ( -0.000000000000000000, 1.000000000000000000, -0.000000000000000000 ) ) ;
#70999 = PLANE ( 'NONE',  #37959 ) ;
#71000 = AXIS2_PLACEMENT_3D ( 'NONE', #3060, #30101, #9826 ) ;
#71001 = AXIS2_PLACEMENT_3D ( 'NONE', #48077, #34576, #26050 ) ;
#71002 = CARTESIAN_POINT ( 'NONE',  ( 4.023154687178597477, -4.118384482072085184, 33.43331474514187107 ) ) ;
#71003 = PLANE ( 'NONE',  #46829 ) ;
#71004 = ORIENTED_EDGE ( 'NONE', *, *, #49351, .F. ) ;
#71005 = EDGE_LOOP ( 'NONE', ( #66351, #35462, #21270, #5979 ) ) ;
#71006 = CARTESIAN_POINT ( 'NONE',  ( -1.929879867024197893E-14, -3.750000000000000000, 21.65625000000000355 ) ) ;
#71007 = B_SPLINE_CURVE_WITH_KNOTS ( 'NONE', 3,
 ( #79809, #58629, #71253, #57308, #58184, #57753, #23512, #3685, #24399, #64058 ),
 .UNSPECIFIED., .F., .F.,
 ( 4, 2, 2, 2, 4 ),
 ( 0.0007817359430256320659, 0.0009771253907249987086, 0.001172514838424365460, 0.001367904286123731994, 0.001563293733823098745 ),
 .UNSPECIFIED. ) ;
#71008 = VERTEX_POINT ( 'NONE', #31323 ) ;
#71010 = ORIENTED_EDGE ( 'NONE', *, *, #76518, .F. ) ;
#71009 = CARTESIAN_POINT ( 'NONE',  ( -14.30769230769242917, -2.379036618888197729, 30.90682066428292885 ) ) ;
#71011 = CARTESIAN_POINT ( 'NONE',  ( -7.173100160369888734, -12.43535235679832596, 30.55408501211184813 ) ) ;
#71012 = CARTESIAN_POINT ( 'NONE',  ( 4.480769230769229061, -3.499999999999999556, 29.75000000000000355 ) ) ;
#71013 = CARTESIAN_POINT ( 'NONE',  ( 6.923076923076924238, -11.69971097300155272, 32.46337939537588113 ) ) ;
#71014 = ORIENTED_EDGE ( 'NONE', *, *, #23573, .T. ) ;
#71015 = CARTESIAN_POINT ( 'NONE',  ( -4.153846153846152411, -13.20930481340135110, 34.54067556320372745 ) ) ;
#71016 = CARTESIAN_POINT ( 'NONE',  ( 4.826923076923076650, -2.249999999999998668, 29.75000000000000355 ) ) ;
#71017 = ORIENTED_EDGE ( 'NONE', *, *, #68396, .F. ) ;
#71018 = FACE_BOUND ( 'NONE', #64858, .T. ) ;
#71019 = DIRECTION ( 'NONE',  ( -0.000000000000000000, -1.000000000000000000, -8.673617379884033500E-16 ) ) ;
#71020 = CARTESIAN_POINT ( 'NONE',  ( 17.93472999944368240, -12.70778746994557551, 30.41441678777548319 ) ) ;
#71021 = ADVANCED_FACE ( 'NONE', ( #73201 ), #86286, .T. ) ;
#71022 = FACE_OUTER_BOUND ( 'NONE', #33685, .T. ) ;
#71024 = CARTESIAN_POINT ( 'NONE',  ( 9.692307692307695177, -4.102666532097928531, 36.13435417666054406 ) ) ;
#71023 = CARTESIAN_POINT ( 'NONE',  ( 5.749976775778544713, -12.45566812827425096, 31.48439005359158926 ) ) ;
#71025 = DIRECTION ( 'NONE',  ( 0.000000000000000000, 0.000000000000000000, 1.000000000000000000 ) ) ;
#71026 = DIRECTION ( 'NONE',  ( -1.000000000000000000, -0.000000000000000000, -0.000000000000000000 ) ) ;
#71027 = ORIENTED_EDGE ( 'NONE', *, *, #83072, .T. ) ;
#71028 = PLANE ( 'NONE',  #76297 ) ;
#71029 = DIRECTION ( 'NONE',  ( -0.000000000000000000, -0.1736481776669307198, -0.9848077530122080203 ) ) ;
#71030 = EDGE_LOOP ( 'NONE', ( #51933, #66710 ) ) ;
#71031 = CARTESIAN_POINT ( 'NONE',  ( 7.145856464345333059, -2.847695495035524882, 31.58253572463339509 ) ) ;
#71032 = CARTESIAN_POINT ( 'NONE',  ( -18.06608237936013595, -12.62096338111211580, 30.90682066428152908 ) ) ;
#71033 = CARTESIAN_POINT ( 'NONE',  ( 16.02315555073584719, -6.369640206132551441, 34.87707690430378449 ) ) ;
#71034 = CARTESIAN_POINT ( 'NONE',  ( 16.15384615384603251, -2.892918686052165622, 31.69288490824153470 ) ) ;
#71035 = LINE ( 'NONE', #42690, #6855 ) ;
#71036 = CARTESIAN_POINT ( 'NONE',  ( 7.596130608860880429, -8.432397168068783699, 34.66272746175022945 ) ) ;
#71037 = FACE_BOUND ( 'NONE', #1127, .T. ) ;
#71039 = CARTESIAN_POINT ( 'NONE',  ( -10.39242148111793895, -7.369474539155828730, 34.99858011523957657 ) ) ;
#71038 = DIRECTION ( 'NONE',  ( -0.000000000000000000, 0.9848077530122086864, -0.1736481776669273891 ) ) ;
#71040 = EDGE_CURVE ( 'NONE', #67434, #39096, #3393, .T. ) ;
#71041 = CARTESIAN_POINT ( 'NONE',  ( -18.06608237936013239, -8.164416787775447659, 34.95778746994557906 ) ) ;
#71043 = CARTESIAN_POINT ( 'NONE',  ( -15.09997742294444478, -6.413143153341454017, 34.63066358083362672 ) ) ;
#71042 = DIRECTION ( 'NONE',  ( -0.000000000000000000, -0.000000000000000000, 1.000000000000000000 ) ) ;
#71044 = DIRECTION ( 'NONE',  ( -0.000000000000000000, 1.000000000000000000, 3.491481338843133355E-15 ) ) ;
#71045 = CARTESIAN_POINT ( 'NONE',  ( -3.749999999999996447, -7.561099074964554134, 21.09188170625849068 ) ) ;
#71046 = ORIENTED_EDGE ( 'NONE', *, *, #5336, .F. ) ;
#71047 = CARTESIAN_POINT ( 'NONE',  ( -4.403869391139118683, -11.86270091957321249, 32.19358267280087915 ) ) ;
#71048 = DIRECTION ( 'NONE',  ( -0.000000000000000000, 0.9848077530122085754, -0.1736481776669273613 ) ) ;
#71049 = CYLINDRICAL_SURFACE ( 'NONE', #51701, 0.2500000000000009437 ) ;
#71050 = CARTESIAN_POINT ( 'NONE',  ( -0.4999924855028897164, -10.20416484602898954, 29.16295261168903252 ) ) ;
#71051 = CARTESIAN_POINT ( 'NONE',  ( 10.61538461538449596, -12.27809138561165270, 31.22303859784587132 ) ) ;
#71052 = CARTESIAN_POINT ( 'NONE',  ( -3.724691934501229262, -9.114399933863657211, 22.26375670625849068 ) ) ;
#71053 = CARTESIAN_POINT ( 'NONE',  ( -11.31503513954675100, -7.630147987733840509, 34.99859428049665411 ) ) ;
#71054 = DIRECTION ( 'NONE',  ( 1.000000000000000000, 0.000000000000000000, 0.000000000000000000 ) ) ;
#71055 = CARTESIAN_POINT ( 'NONE',  ( -17.07692307692319744, -6.026961402154118908, 34.52809138561165270 ) ) ;
#71056 = CARTESIAN_POINT ( 'NONE',  ( 13.38461538461538680, -6.343179335718451384, 34.87096338111211935 ) ) ;
#71057 = CARTESIAN_POINT ( 'NONE',  ( -16.85414340794500276, -4.989023458446560255, 34.36081565061822118 ) ) ;
#71058 = DIRECTION ( 'NONE',  ( -1.000000000000000000, -1.734723475976813504E-16, 0.000000000000000000 ) ) ;
#71059 = B_SPLINE_CURVE_WITH_KNOTS ( 'NONE', 3,
 ( #81798, #46230, #5681, #20088, #66502, #47551, #39489, #40371, #75041, #19641 ),
 .UNSPECIFIED., .F., .F.,
 ( 4, 2, 2, 2, 4 ),
 ( 0.0007817246256747452209, 0.0009771112852218887673, 0.001172497944769032531, 0.001367884604316176294, 0.001563271263863319840 ),
 .UNSPECIFIED. ) ;
#71060 = EDGE_CURVE ( 'NONE', #1686, #59958, #1934, .T. ) ;
#71061 = EDGE_CURVE ( 'NONE', #23619, #17400, #39428, .T. ) ;
#71062 = VECTOR ( 'NONE', #65905, 1000.000000000000000 ) ;
#71063 = LINE ( 'NONE', #76500, #4540 ) ;
#71064 = DIRECTION ( 'NONE',  ( -0.000000000000000000, 0.9848077530122085754, -0.1736481776669273613 ) ) ;
#71065 = ORIENTED_EDGE ( 'NONE', *, *, #24956, .F. ) ;
#71066 = CARTESIAN_POINT ( 'NONE',  ( 3.453782074862625784, -12.38742843783360748, 31.66772728687926985 ) ) ;
#71067 = CARTESIAN_POINT ( 'NONE',  ( -17.14219352288385068, -2.892918686051582089, 31.69288490824015980 ) ) ;
#71068 = CARTESIAN_POINT ( 'NONE',  ( 1.901340078031373171, -9.487747218494639867, 24.87686829374151642 ) ) ;
#71069 = VECTOR ( 'NONE', #59909, 1000.000000000000000 ) ;
#71070 = ADVANCED_FACE ( 'NONE', ( #38074 ), #79515, .F. ) ;
#71071 = CARTESIAN_POINT ( 'NONE',  ( -9.692307692307812417, -5.219633306517616589, 34.19971097300220464 ) ) ;
#71072 = CARTESIAN_POINT ( 'NONE',  ( 3.480823542407543769, -11.79725096376909654, 32.30694842903960762 ) ) ;
#71073 = EDGE_LOOP ( 'NONE', ( #18836, #33891 ) ) ;
#71074 = CARTESIAN_POINT ( 'NONE',  ( -16.28453675695646652, -3.957541250942358424, 33.62499894934981626 ) ) ;
#71076 = EDGE_LOOP ( 'NONE', ( #31831, #77745 ) ) ;
#71075 = CARTESIAN_POINT ( 'NONE',  ( 4.153846153846154188, -5.557115091759785130, 34.35708131394839171 ) ) ;
#71077 = CARTESIAN_POINT ( 'NONE',  ( 6.989145274079363368, -3.513871655860379306, 32.76840700105978499 ) ) ;
#71078 = CARTESIAN_POINT ( 'NONE',  ( 17.30034947583786220, -7.630147987733843173, 34.99859428049665411 ) ) ;
#71079 = CARTESIAN_POINT ( 'NONE',  ( 6.923076923076924238, -3.050289026998446396, 32.03036669348365706 ) ) ;
#71080 = CARTESIAN_POINT ( 'NONE',  ( -15.23076923076891553, -2.255955759149395501, 30.00000000000324363 ) ) ;
#71081 = EDGE_LOOP ( 'NONE', ( #4448, #38955, #4413, #46633 ) ) ;
#71082 = CARTESIAN_POINT ( 'NONE',  ( 8.900021210197715860, -2.295524264805589354, 30.44142389570982488 ) ) ;
#71083 = CARTESIAN_POINT ( 'NONE',  ( -11.66915214157184444, -12.35290016733513951, 31.75349464988449455 ) ) ;
#71084 = LINE ( 'NONE', #57568, #26908 ) ;
#71085 = VERTEX_POINT ( 'NONE', #65983 ) ;
#71086 = ORIENTED_EDGE ( 'NONE', *, *, #54372, .T. ) ;
#71087 = EDGE_LOOP ( 'NONE', ( #78431, #56478 ) ) ;
#71088 = PLANE ( 'NONE',  #74546 ) ;
#71089 = CARTESIAN_POINT ( 'NONE',  ( 13.51514082284903040, -3.625058011473228703, 33.29252011169590020 ) ) ;
#71090 = CARTESIAN_POINT ( 'NONE',  ( -3.165514091256390827, -8.656820664281605460, 34.87096338111211224 ) ) ;
#71091 = VECTOR ( 'NONE', #39035, 1000.000000000000114 ) ;
#71092 = CARTESIAN_POINT ( 'NONE',  ( 15.36081439360400935, -2.504778602574659896, 29.97347330155780654 ) ) ;
#71093 = VERTEX_POINT ( 'NONE', #59232 ) ;
#71094 = ORIENTED_EDGE ( 'NONE', *, *, #85486, .F. ) ;
#71096 = ORIENTED_EDGE ( 'NONE', *, *, #22167, .F. ) ;
#71095 = CARTESIAN_POINT ( 'NONE',  ( -1.384615384615383471, -2.833524468853757305, 32.15551576947925838 ) ) ;
#71097 = B_SPLINE_CURVE_WITH_KNOTS ( 'NONE', 3,
 ( #33887, #41537, #61346, #54593, #5987, #62240, #82088, #55486, #82971, #21253 ),
 .UNSPECIFIED., .F., .F.,
 ( 4, 2, 2, 2, 4 ),
 ( 0.0007817359430256392216, 0.0009771253907250080327, 0.001172514838424376952, 0.001367904286123745872, 0.001563293733823114791 ),
 .UNSPECIFIED. ) ;
#71098 = B_SPLINE_CURVE_WITH_KNOTS ( 'NONE', 3,
 ( #38403, #65860, #88724, #81512, #46824, #34644, #12604, #26113, #40091, #19801 ),
 .UNSPECIFIED., .F., .F.,
 ( 4, 2, 2, 2, 4 ),
 ( 0.000000000000000000, 0.0001954339857564079623, 0.0003908679715128159245, 0.0005863019572692238597, 0.0007817359430256318490 ),
 .UNSPECIFIED. ) ;
#71099 = CARTESIAN_POINT ( 'NONE',  ( 16.28389131668093270, -2.504778602574659896, 29.97347330155780654 ) ) ;
#71100 = FACE_OUTER_BOUND ( 'NONE', #21756, .T. ) ;
#71101 = DIRECTION ( 'NONE',  ( 0.000000000000000000, 0.000000000000000000, 1.000000000000000000 ) ) ;
#71102 = ORIENTED_EDGE ( 'NONE', *, *, #39525, .T. ) ;
#71103 = EDGE_CURVE ( 'NONE', #40474, #9375, #44818, .T. ) ;
#71104 = ORIENTED_EDGE ( 'NONE', *, *, #68172, .T. ) ;
#71106 = ORIENTED_EDGE ( 'NONE', *, *, #31612, .T. ) ;
#71105 = CARTESIAN_POINT ( 'NONE',  ( -12.39628289026243557, -5.219633306516380244, 34.19971097300157936 ) ) ;
#71107 = CARTESIAN_POINT ( 'NONE',  ( -10.61538461538461320, -1.242168528481310874, 33.36296068462461051 ) ) ;
#71108 = AXIS2_PLACEMENT_3D ( 'NONE', #63375, #76009, #83675 ) ;
#71109 = CARTESIAN_POINT ( 'NONE',  ( -10.86540783960607293, -9.356822207818506598, 34.66110646841856635 ) ) ;
#71110 = EDGE_LOOP ( 'NONE', ( #8666, #51391, #16912, #80900 ) ) ;
#71111 = LINE ( 'NONE', #63018, #42 ) ;
#71112 = CARTESIAN_POINT ( 'NONE',  ( -4.153846153845837108, -2.255955759149395501, 30.00000000000324363 ) ) ;
#71113 = CARTESIAN_POINT ( 'NONE',  ( -9.019207513279360100, -12.01397095200674059, 32.43157075238190146 ) ) ;
#71114 = FACE_BOUND ( 'NONE', #86405, .T. ) ;
#71115 = AXIS2_PLACEMENT_3D ( 'NONE', #89073, #27349, #82303 ) ;
#71116 = CARTESIAN_POINT ( 'NONE',  ( -9.469528023329623068, -4.226511098958373402, 33.85474049983370293 ) ) ;
#71117 = CARTESIAN_POINT ( 'NONE',  ( -4.403822884788507253, -12.17611988154120972, 31.52148481390971213 ) ) ;
#71118 = AXIS2_PLACEMENT_3D ( 'NONE', #29170, #84111, #2550 ) ;
#71119 = EDGE_CURVE ( 'NONE', #76747, #88972, #45951, .T. ) ;
#71120 = FACE_OUTER_BOUND ( 'NONE', #10106, .T. ) ;
#71122 = DIRECTION ( 'NONE',  ( -1.000000000000000000, -0.000000000000000000, -0.000000000000000000 ) ) ;
#71121 = CARTESIAN_POINT ( 'NONE',  ( 2.307692307692187583, -11.94971097300221174, 32.03036669348237098 ) ) ;
#71123 = CARTESIAN_POINT ( 'NONE',  ( -8.069638789877792817, -3.236172620538810385, 32.36188796281390267 ) ) ;
#71124 = CARTESIAN_POINT ( 'NONE',  ( 10.48523664565291647, -11.04286588640298561, 33.62463336215343901 ) ) ;
#71125 = ORIENTED_EDGE ( 'NONE', *, *, #53106, .F. ) ;
#71126 = CARTESIAN_POINT ( 'NONE',  ( 14.43773991394799339, -7.723484964179501588, 34.74522123443823318 ) ) ;
#71127 = EDGE_CURVE ( 'NONE', #48109, #54822, #4747, .T. ) ;
#71128 = ORIENTED_EDGE ( 'NONE', *, *, #13316, .F. ) ;
#71129 = EDGE_LOOP ( 'NONE', ( #40037, #7229, #41433, #6821 ) ) ;
#71131 = CARTESIAN_POINT ( 'NONE',  ( -14.30769230769230660, -4.102666532097928531, 36.13435417666054406 ) ) ;
#71130 = CARTESIAN_POINT ( 'NONE',  ( -6.166666666666667851, -3.499999999999999556, 29.75000000000000355 ) ) ;
#71132 = CARTESIAN_POINT ( 'NONE',  ( 2.557746619330623083, -2.564540009722895419, 30.55348353981670684 ) ) ;
#71133 = CARTESIAN_POINT ( 'NONE',  ( -14.24162395668986747, -2.721908614388772296, 31.22303859784725333 ) ) ;
#71134 = CARTESIAN_POINT ( 'NONE',  ( 1.384615384615386802, -6.386643153685126251, 34.62446782046654192 ) ) ;
#71135 = LINE ( 'NONE', #44093, #17389 ) ;
#71136 = ORIENTED_EDGE ( 'NONE', *, *, #41435, .T. ) ;
#71137 = CARTESIAN_POINT ( 'NONE',  ( 13.25446817517716980, -5.195881422630166391, 34.18770438780619259 ) ) ;
#71138 = DIRECTION ( 'NONE',  ( 0.000000000000000000, 0.6427876096865373645, -0.7660444431189797898 ) ) ;
#71140 = CARTESIAN_POINT ( 'NONE',  ( -18.00000000000030553, -12.49374608885938542, 30.00000000000319744 ) ) ;
#71139 = B_SPLINE_CURVE_WITH_KNOTS ( 'NONE', 3,
 ( #33696, #55287, #76003, #6659, #41792, #61151, #13858, #48081, #47198, #74690 ),
 .UNSPECIFIED., .F., .F.,
 ( 4, 2, 2, 2, 4 ),
 ( 0.0007817359430256364027, 0.0009771253907250043464, 0.001172514838424372399, 0.001367904286123740234, 0.001563293733823108286 ),
 .UNSPECIFIED. ) ;
#71141 = EDGE_CURVE ( 'NONE', #37467, #48549, #83627, .T. ) ;
#71142 = CARTESIAN_POINT ( 'NONE',  ( -11.53846153846153655, -2.249999999999998668, 29.50000000000001421 ) ) ;
#71143 = FACE_OUTER_BOUND ( 'NONE', #6782, .T. ) ;
#71144 = CARTESIAN_POINT ( 'NONE',  ( -1.929879867024197893E-14, -3.750000000000000000, 17.90625000000000000 ) ) ;
#71145 = ORIENTED_EDGE ( 'NONE', *, *, #51318, .F. ) ;
#71147 = EDGE_CURVE ( 'NONE', #33955, #22635, #7405, .T. ) ;
#71146 = VERTEX_POINT ( 'NONE', #11951 ) ;
#71148 = FACE_OUTER_BOUND ( 'NONE', #30457, .T. ) ;
#71149 = VERTEX_POINT ( 'NONE', #33978 ) ;
#71150 = DIRECTION ( 'NONE',  ( 0.000000000000000000, 0.8660254037844377084, 0.5000000000000015543 ) ) ;
#71151 = CARTESIAN_POINT ( 'NONE',  ( 13.38461538461526423, -2.379036618888197729, 30.90682066428292885 ) ) ;
#71152 = CARTESIAN_POINT ( 'NONE',  ( -6.923076923077044142, -9.442884908241554243, 34.35708131394783038 ) ) ;
#71153 = DIRECTION ( 'NONE',  ( 1.000000000000000000, 0.000000000000000000, 0.000000000000000000 ) ) ;
#71154 = CARTESIAN_POINT ( 'NONE',  ( -1.553300858899125059, -3.750000000000009326, 19.07812500000000000 ) ) ;
#71155 = DIRECTION ( 'NONE',  ( -0.000000000000000000, -0.3420201433256694346, -0.9396926207859080948 ) ) ;
#71156 = ORIENTED_EDGE ( 'NONE', *, *, #77535, .T. ) ;
#71157 = CARTESIAN_POINT ( 'NONE',  ( 4.088522141041845082, -7.749976730030849303, 34.74374725381503737 ) ) ;
#71159 = ORIENTED_EDGE ( 'NONE', *, *, #46070, .T. ) ;
#71158 = FACE_OUTER_BOUND ( 'NONE', #35962, .T. ) ;
#71160 = CARTESIAN_POINT ( 'NONE',  ( 15.23076923076923173, -2.249999999999998668, 29.75000000000001776 ) ) ;
#71161 = DIRECTION ( 'NONE',  ( -0.000000000000000000, 0.7660444431189791237, -0.6427876096865379196 ) ) ;
#71162 = CARTESIAN_POINT ( 'NONE',  ( 6.065255139512838234, -9.528491918058460186, 34.59228464037085615 ) ) ;
#71163 = CYLINDRICAL_SURFACE ( 'NONE', #50486, 0.2499999999999995559 ) ;
#71164 = EDGE_CURVE ( 'NONE', #71551, #83423, #54685, .T. ) ;
#71165 = CARTESIAN_POINT ( 'NONE',  ( -12.46153846153846168, -12.37446782046654192, 30.86335684631486131 ) ) ;
#71166 = CARTESIAN_POINT ( 'NONE',  ( -6.923076923077044142, -5.219633306517616589, 34.19971097300220464 ) ) ;
#71167 = EDGE_CURVE ( 'NONE', #9998, #37993, #47933, .T. ) ;
#71168 = CARTESIAN_POINT ( 'NONE',  ( 2.775308065498755195, -6.422011778438505125, 24.64249329374151642 ) ) ;
#71169 = VERTEX_POINT ( 'NONE', #82180 ) ;
#71170 = CARTESIAN_POINT ( 'NONE',  ( 5.076923076922954969, -10.21337939537710326, 33.94971097300076224 ) ) ;
#71171 = DIRECTION ( 'NONE',  ( -0.000000000000000000, -0.000000000000000000, -1.000000000000000000 ) ) ;
#71172 = CARTESIAN_POINT ( 'NONE',  ( 1.139087296525997273, -4.749999999999992895, 25.48437500000000000 ) ) ;
#71173 = ADVANCED_FACE ( 'NONE', ( #76292 ), #67771, .F. ) ;
#71174 = CARTESIAN_POINT ( 'NONE',  ( -13.63459211555773720, -12.41269422305637171, 30.68257228309993323 ) ) ;
#71175 = DIRECTION ( 'NONE',  ( 1.000000000000000000, 0.000000000000000000, 0.000000000000000000 ) ) ;
#71176 = ADVANCED_FACE ( 'NONE', ( #67334 ), #75413, .F. ) ;
#71177 = EDGE_LOOP ( 'NONE', ( #43352, #86873 ) ) ;
#71178 = CARTESIAN_POINT ( 'NONE',  ( -1.944543648263015179, -5.555456351737005249, 14.00000000000000000 ) ) ;
#71179 = CARTESIAN_POINT ( 'NONE',  ( 3.007284287045282944, -9.331801661448606566, 34.40259984581193464 ) ) ;
#71180 = ORIENTED_EDGE ( 'NONE', *, *, #28793, .F. ) ;
#71181 = FACE_OUTER_BOUND ( 'NONE', #82542, .T. ) ;
#71182 = ORIENTED_EDGE ( 'NONE', *, *, #65649, .F. ) ;
#71183 = B_SPLINE_CURVE_WITH_KNOTS ( 'NONE', 3,
 ( #85239, #23958, #1929, #64062, #63626, #9566, #84361, #37028, #71257, #29849 ),
 .UNSPECIFIED., .F., .F.,
 ( 4, 2, 2, 2, 4 ),
 ( 0.0007817359430256334753, 0.0009771253907250058643, 0.001172514838424371098, 0.001367904286123736764, 0.001563293733823101998 ),
 .UNSPECIFIED. ) ;
#71184 = DIRECTION ( 'NONE',  ( -0.000000000000000000, 0.5000000000000011102, -0.8660254037844380415 ) ) ;
#71185 = CARTESIAN_POINT ( 'NONE',  ( 4.087762742890271639, -3.513871655860377086, 32.76840700105978499 ) ) ;
#71186 = CARTESIAN_POINT ( 'NONE',  ( -1.450698795571264021, -4.098570777380720287, 33.41473453929634729 ) ) ;
#71187 = CARTESIAN_POINT ( 'NONE',  ( -13.31854805126531005, -12.62096338111211757, 30.90682066428152908 ) ) ;
#71188 = ORIENTED_EDGE ( 'NONE', *, *, #80871, .F. ) ;
#71189 = CARTESIAN_POINT ( 'NONE',  ( -13.13466997523734037, -2.986452184633680229, 32.43230066228895225 ) ) ;
#71190 = AXIS2_PLACEMENT_3D ( 'NONE', #75835, #20886, #6501 ) ;
#71191 = ORIENTED_EDGE ( 'NONE', *, *, #60948, .F. ) ;
#71192 = CARTESIAN_POINT ( 'NONE',  ( 2.557692307692308376, -2.499999999999998668, 29.75000000000000355 ) ) ;
#71193 = LINE ( 'NONE', #55908, #64200 ) ;
#71194 = EDGE_LOOP ( 'NONE', ( #75806, #7893, #31447, #75673 ) ) ;
#71195 = DIRECTION ( 'NONE',  ( -0.000000000000000000, -0.6427876096865404731, -0.7660444431189771253 ) ) ;
#71196 = CARTESIAN_POINT ( 'NONE',  ( -14.55766903863466055, -10.66389620160130036, 33.62221079203477103 ) ) ;
#71197 = CARTESIAN_POINT ( 'NONE',  ( -11.66915300512909326, -2.729777683071817229, 31.24903638046269450 ) ) ;
#71198 = CARTESIAN_POINT ( 'NONE',  ( 2.307692307692309264, -12.29105614889573062, 35.45975837776705220 ) ) ;
#71199 = DIRECTION ( 'NONE',  ( -0.000000000000000000, 1.000000000000000000, 3.491481338843133355E-15 ) ) ;
#71200 = EDGE_CURVE ( 'NONE', #88652, #15863, #70679, .T. ) ;
#71201 = ORIENTED_EDGE ( 'NONE', *, *, #27126, .T. ) ;
#71202 = ORIENTED_EDGE ( 'NONE', *, *, #58038, .F. ) ;
#71203 = FACE_BOUND ( 'NONE', #83840, .T. ) ;
#71204 = ORIENTED_EDGE ( 'NONE', *, *, #54978, .F. ) ;
#71205 = CARTESIAN_POINT ( 'NONE',  ( -8.703162418228332697, -4.098570777380720287, 33.41473453929635440 ) ) ;
#71206 = CARTESIAN_POINT ( 'NONE',  ( 13.38461538461526601, -10.90142922262034020, 33.41473453929536674 ) ) ;
#71207 = CARTESIAN_POINT ( 'NONE',  ( -14.24243673641628050, -9.442884908240273489, 34.35708131394835618 ) ) ;
#71208 = EDGE_CURVE ( 'NONE', #19526, #34542, #68652, .T. ) ;
#71209 = ORIENTED_EDGE ( 'NONE', *, *, #7938, .T. ) ;
#71210 = EDGE_CURVE ( 'NONE', #40661, #32458, #48818, .T. ) ;
#71211 = VECTOR ( 'NONE', #64732, 1000.000000000000000 ) ;
#71212 = EDGE_LOOP ( 'NONE', ( #63685, #84418, #69138, #18860 ) ) ;
#71213 = CARTESIAN_POINT ( 'NONE',  ( 3.230769230769231726, -4.786620604624113540, 33.94971097300155094 ) ) ;
#71214 = EDGE_LOOP ( 'NONE', ( #13276, #32879, #23671, #12182 ) ) ;
#71215 = B_SPLINE_CURVE_WITH_KNOTS ( 'NONE', 3,
 ( #81573, #19416, #5471, #68056, #61718, #35, #20743, #27507, #53190, #48210 ),
 .UNSPECIFIED., .F., .F.,
 ( 4, 2, 2, 2, 4 ),
 ( 0.000000000000000000, 0.0001954339857564073388, 0.0003908679715128146777, 0.0005863019572692220165, 0.0007817359430256293554 ),
 .UNSPECIFIED. ) ;
#71216 = CARTESIAN_POINT ( 'NONE',  ( 2.084812790954723383, -7.630690623152302621, 34.99857592706774057 ) ) ;
#71217 = CYLINDRICAL_SURFACE ( 'NONE', #41642, 0.2500000000000012212 ) ;
#71218 = CARTESIAN_POINT ( 'NONE',  ( -12.21153846153845279, -2.249999999999999112, 29.81603969181031744 ) ) ;
#71219 = FACE_BOUND ( 'NONE', #16581, .T. ) ;
#71220 = ORIENTED_EDGE ( 'NONE', *, *, #1840, .T. ) ;
#71221 = DIRECTION ( 'NONE',  ( -1.000000000000000000, -0.000000000000000000, 0.000000000000000000 ) ) ;
#71222 = ADVANCED_FACE ( 'NONE', ( #34425 ), #27666, .F. ) ;
#71223 = CARTESIAN_POINT ( 'NONE',  ( 13.38461538461538680, -13.37000171582298513, 34.34916445242398453 ) ) ;
#71224 = FACE_OUTER_BOUND ( 'NONE', #26901, .T. ) ;
#71225 = CARTESIAN_POINT ( 'NONE',  ( 8.900021210197715860, -6.369690395747422684, 34.87708834333098196 ) ) ;
#71226 = ORIENTED_EDGE ( 'NONE', *, *, #25486, .F. ) ;
#71227 = EDGE_CURVE ( 'NONE', #27467, #87554, #81296, .T. ) ;
#71228 = ORIENTED_EDGE ( 'NONE', *, *, #76965, .F. ) ;
#71229 = ORIENTED_EDGE ( 'NONE', *, *, #24347, .F. ) ;
#71231 = CARTESIAN_POINT ( 'NONE',  ( -11.25641025641025550, -3.499999999999999556, 29.75000000000000355 ) ) ;
#71230 = LINE ( 'NONE', #64464, #21636 ) ;
#71232 = CARTESIAN_POINT ( 'NONE',  ( -10.68065506134538722, -12.27809138561121394, 31.22303859784730307 ) ) ;
#71233 = CARTESIAN_POINT ( 'NONE',  ( 7.846153846153846700, -10.05456864172156806, 36.03766855953608683 ) ) ;
#71234 = CARTESIAN_POINT ( 'NONE',  ( 7.780070435197965928, -12.37446782046654192, 30.86335684631486487 ) ) ;
#71235 = FACE_OUTER_BOUND ( 'NONE', #6550, .T. ) ;
#71236 = ORIENTED_EDGE ( 'NONE', *, *, #53113, .T. ) ;
#71237 = CARTESIAN_POINT ( 'NONE',  ( -3.230769230769229949, -2.538708090699994813, 30.37095296980875503 ) ) ;
#71238 = CARTESIAN_POINT ( 'NONE',  ( 2.980792486720640344, -9.234221910056348293, 34.70572697212741531 ) ) ;
#71239 = CARTESIAN_POINT ( 'NONE',  ( -17.20761454359064047, -11.71456829005830080, 32.44064028649416542 ) ) ;
#71240 = ADVANCED_FACE ( 'NONE', ( #47041 ), #41629, .F. ) ;
#71241 = CARTESIAN_POINT ( 'NONE',  ( 3.453782074862626228, -11.43677907613345113, 33.22367315496201456 ) ) ;
#71242 = ORIENTED_EDGE ( 'NONE', *, *, #81891, .F. ) ;
#71243 = LINE ( 'NONE', #4001, #75903 ) ;
#71244 = EDGE_LOOP ( 'NONE', ( #69893, #36041 ) ) ;
#71245 = FACE_BOUND ( 'NONE', #9358, .T. ) ;
#71246 = CARTESIAN_POINT ( 'NONE',  ( -7.173053667125515176, -10.06842814019191401, 34.32929386961144758 ) ) ;
#71247 = CARTESIAN_POINT ( 'NONE',  ( -18.07928316857947237, 12.74206001580630598, 30.82086045927834661 ) ) ;
#71248 = ORIENTED_EDGE ( 'NONE', *, *, #52329, .T. ) ;
#71249 = VECTOR ( 'NONE', #74900, 1000.000000000000000 ) ;
#71250 = DIRECTION ( 'NONE',  ( -1.000000000000000000, -0.000000000000000000, 0.000000000000000000 ) ) ;
#71251 = CARTESIAN_POINT ( 'NONE',  ( 6.130790440966954691, -11.37503395064541678, 33.29242100308974983 ) ) ;
#71252 = CARTESIAN_POINT ( 'NONE',  ( -15.23076923076922995, -9.905515769479276145, 34.41647553114623292 ) ) ;
#71253 = CARTESIAN_POINT ( 'NONE',  ( -6.792551221313358312, -3.285477652293412820, 32.44071101563363158 ) ) ;
#71254 = EDGE_LOOP ( 'NONE', ( #59973, #6617 ) ) ;
#71255 = CARTESIAN_POINT ( 'NONE',  ( -19.00000000000000000, 8.999999999999998224, 23.75000000000000000 ) ) ;
#71256 = ORIENTED_EDGE ( 'NONE', *, *, #28936, .F. ) ;
#71258 = ORIENTED_EDGE ( 'NONE', *, *, #74459, .T. ) ;
#71257 = CARTESIAN_POINT ( 'NONE',  ( 13.45068373561782771, -12.10708131394839704, 31.69288490824020954 ) ) ;
#71259 = CARTESIAN_POINT ( 'NONE',  ( 3.361294932532794100, -2.619367082507848998, 30.83698974864644171 ) ) ;
#71260 = CARTESIAN_POINT ( 'NONE',  ( 14.98079249982688133, -2.779195860258146578, 31.39871582349836032 ) ) ;
#71261 = LINE ( 'NONE', #52326, #24205 ) ;
#71262 = CARTESIAN_POINT ( 'NONE',  ( 12.59206416330202494, -4.459921816937791661, 33.71989282347011851 ) ) ;
#71263 = CARTESIAN_POINT ( 'NONE',  ( -7.846153846153844924, -8.973038597847269315, 34.52809138561121927 ) ) ;
#71264 = ADVANCED_FACE ( 'NONE', ( #83063 ), #74980, .F. ) ;
#71265 = CARTESIAN_POINT ( 'NONE',  ( 23.00000000000000000, -10.75000000000000000, 29.75000000000000355 ) ) ;
#71266 = CARTESIAN_POINT ( 'NONE',  ( -2.749999999999991562, -8.639087296526025028, 23.76562499999999645 ) ) ;
#71267 = ORIENTED_EDGE ( 'NONE', *, *, #53473, .T. ) ;
#71268 = B_SPLINE_CURVE_WITH_KNOTS ( 'NONE', 3,
 ( #85393, #16930, #36755, #23680, #50254, #77741, #64214, #51131, #16046, #3408 ),
 .UNSPECIFIED., .F., .F.,
 ( 4, 2, 2, 2, 4 ),
 ( 0.0007817359430256294638, 0.0009771253907249948054, 0.001172514838424360255, 0.001367904286123725489, 0.001563293733823090939 ),
 .UNSPECIFIED. ) ;
#71269 = DIRECTION ( 'NONE',  ( -0.000000000000000000, -0.9396926207859093161, -0.3420201433256663259 ) ) ;
#71270 = CARTESIAN_POINT ( 'NONE',  ( 11.25641025641025550, -3.499999999999999556, 29.75000000000000355 ) ) ;
#71271 = ORIENTED_EDGE ( 'NONE', *, *, #87975, .F. ) ;
#71272 = EDGE_CURVE ( 'NONE', #34255, #30233, #74529, .T. ) ;
#71274 = ORIENTED_EDGE ( 'NONE', *, *, #48086, .T. ) ;
#71273 = VECTOR ( 'NONE', #42387, 1000.000000000000114 ) ;
#71275 = EDGE_CURVE ( 'NONE', #75229, #34232, #40309, .T. ) ;
#71276 = EDGE_LOOP ( 'NONE', ( #51932, #62008 ) ) ;
#71277 = CARTESIAN_POINT ( 'NONE',  ( 4.153846153846032507, -12.27809138561165270, 31.22303859784587132 ) ) ;
#71278 = CARTESIAN_POINT ( 'NONE',  ( 2.999999999999997335, 7.500000000000000000, 10.00000000000000178 ) ) ;
#71279 = CARTESIAN_POINT ( 'NONE',  ( -17.30040802064702987, -9.331801661448606566, 34.40259984581193464 ) ) ;
#71280 = VECTOR ( 'NONE', #42174, 1000.000000000000000 ) ;
#71281 = CARTESIAN_POINT ( 'NONE',  ( 0.7115384615383975042, -7.565270000091922853, 34.99999999999999289 ) ) ;
#71282 = CARTESIAN_POINT ( 'NONE',  ( -4.854143535654666053, -3.755027918224367767, 33.06320215134714857 ) ) ;
#71283 = CARTESIAN_POINT ( 'NONE',  ( 16.15384615384603251, -3.643525952248796163, 33.31231777344771672 ) ) ;
#71284 = FACE_OUTER_BOUND ( 'NONE', #13823, .T. ) ;
#71285 = ORIENTED_EDGE ( 'NONE', *, *, #62910, .F. ) ;
#71286 = CARTESIAN_POINT ( 'NONE',  ( -4.023054346021365468, -5.582136614379148654, 34.36778462344220486 ) ) ;
#71287 = CARTESIAN_POINT ( 'NONE',  ( 9.692307692307695177, -9.780366693483667717, 34.19971097300155094 ) ) ;
#71288 = LINE ( 'NONE', #75508, #3819 ) ;
#71289 = EDGE_CURVE ( 'NONE', #62019, #53607, #52635, .T. ) ;
#71290 = CARTESIAN_POINT ( 'NONE',  ( 8.069165197766695385, -2.758310577978207334, 31.33698337089303010 ) ) ;
#71291 = ORIENTED_EDGE ( 'NONE', *, *, #67576, .T. ) ;
#71292 = CARTESIAN_POINT ( 'NONE',  ( 7.715463243043538810, -2.295517848115769421, 30.44137282052136939 ) ) ;
#71293 = B_SPLINE_CURVE_WITH_KNOTS ( 'NONE', 3,
 ( #33164, #34492, #20532, #14222, #74599, #26852, #25959, #60181, #68722, #6137 ),
 .UNSPECIFIED., .F., .F.,
 ( 4, 2, 2, 2, 4 ),
 ( 0.0007817359430256365111, 0.0009771253907250043464, 0.001172514838424372399, 0.001367904286123740234, 0.001563293733823108069 ),
 .UNSPECIFIED. ) ;
#71294 = ORIENTED_EDGE ( 'NONE', *, *, #22493, .F. ) ;
#71295 = CARTESIAN_POINT ( 'NONE',  ( 0.7114839798866020582, -9.272278438253398036, 34.42582936511637826 ) ) ;
#71296 =( NAMED_UNIT ( * ) SI_UNIT ( $, .STERADIAN. ) SOLID_ANGLE_UNIT ( ) );
#71297 = CARTESIAN_POINT ( 'NONE',  ( 11.60371710973756265, -10.21337939537593620, 33.94971097300152252 ) ) ;
#71298 = EDGE_CURVE ( 'NONE', #15704, #17995, #23123, .T. ) ;
#71299 = CYLINDRICAL_SURFACE ( 'NONE', #87310, 0.2499999999999995559 ) ;
#71300 = ORIENTED_EDGE ( 'NONE', *, *, #77275, .F. ) ;
#71301 = DIRECTION ( 'NONE',  ( 0.000000000000000000, 0.000000000000000000, 1.000000000000000000 ) ) ;
#71302 = CARTESIAN_POINT ( 'NONE',  ( 10.39245765647776309, -12.64616026154729411, 30.79003144601914244 ) ) ;
#71303 = CARTESIAN_POINT ( 'NONE',  ( -12.21153846153839595, -7.434744429011176159, 34.75000000000000711 ) ) ;
#71304 = CARTESIAN_POINT ( 'NONE',  ( 17.07692307692307665, -6.343179335718451384, 34.87096338111211935 ) ) ;
#71305 = EDGE_CURVE ( 'NONE', #5154, #5809, #15932, .T. ) ;
#71306 = AXIS2_PLACEMENT_3D ( 'NONE', #24626, #51181, #52092 ) ;
#71307 = EDGE_LOOP ( 'NONE', ( #42518, #5277 ) ) ;
#71308 = CARTESIAN_POINT ( 'NONE',  ( -1.319359813339358256, -3.835265460703683349, 33.15142922261929925 ) ) ;
#71309 = ORIENTED_EDGE ( 'NONE', *, *, #13308, .F. ) ;
#71310 = B_SPLINE_CURVE_WITH_KNOTS ( 'NONE', 3,
 ( #73583, #65472, #44745, #3767, #79441, #31698, #38003, #31241, #72669, #45192 ),
 .UNSPECIFIED., .F., .F.,
 ( 4, 2, 2, 2, 4 ),
 ( 0.000000000000000000, 0.0001954339857564091278, 0.0003908679715128182556, 0.0005863019572692274375, 0.0007817359430256365111 ),
 .UNSPECIFIED. ) ;
#71311 = EDGE_CURVE ( 'NONE', #87033, #25963, #35273, .T. ) ;
#71312 = CYLINDRICAL_SURFACE ( 'NONE', #52239, 0.2500000000000008882 ) ;
#71313 = EDGE_CURVE ( 'NONE', #34697, #20749, #78065, .T. ) ;
#71314 = CARTESIAN_POINT ( 'NONE',  ( -27.00000000000000000, 16.99999999999999289, 23.75000000000000000 ) ) ;
#71315 = FACE_OUTER_BOUND ( 'NONE', #47381, .T. ) ;
#71316 = AXIS2_PLACEMENT_3D ( 'NONE', #8889, #24157, #2552 ) ;
#71317 = CARTESIAN_POINT ( 'NONE',  ( 1.134592160393929072, -8.475808217655753651, 34.90892951860618609 ) ) ;
#71318 = CARTESIAN_POINT ( 'NONE',  ( -17.77722033102192967, -12.47679350104403007, 31.42216943046555855 ) ) ;
#71319 = ORIENTED_EDGE ( 'NONE', *, *, #74210, .F. ) ;
#71320 = EDGE_CURVE ( 'NONE', #8333, #78525, #70877, .T. ) ;
#71321 = ORIENTED_EDGE ( 'NONE', *, *, #24672, .F. ) ;
#71322 = ORIENTED_EDGE ( 'NONE', *, *, #12708, .F. ) ;
#71323 = EDGE_CURVE ( 'NONE', #82116, #61213, #15047, .T. ) ;
#71324 = CARTESIAN_POINT ( 'NONE',  ( -19.99999999999996447, -15.00000000000000533, 13.00000000000000178 ) ) ;
#71325 = CARTESIAN_POINT ( 'NONE',  ( 11.40777093535123043, -9.084618155246140248, 34.75535874321725771 ) ) ;
#71326 = CARTESIAN_POINT ( 'NONE',  ( 17.32686859527121470, -4.336752205174650321, 33.62275283266504289 ) ) ;
#71327 = CARTESIAN_POINT ( 'NONE',  ( -13.13466986626724164, -5.852078868378309373, 34.47109172314383585 ) ) ;
#71328 = CYLINDRICAL_SURFACE ( 'NONE', #58575, 0.2500000000000008882 ) ;
#71329 = CARTESIAN_POINT ( 'NONE',  ( 5.869308533332444178, -11.71456829005830080, 32.44064028649416542 ) ) ;
#71330 = CARTESIAN_POINT ( 'NONE',  ( 14.43848411551709709, -9.804649428959608670, 34.18742332936588468 ) ) ;
#71331 = ORIENTED_EDGE ( 'NONE', *, *, #68557, .F. ) ;
#71332 = EDGE_CURVE ( 'NONE', #4198, #47170, #9183, .T. ) ;
#71333 = ORIENTED_EDGE ( 'NONE', *, *, #11829, .F. ) ;
#71334 = B_SPLINE_CURVE_WITH_KNOTS ( 'NONE', 3,
 ( #10497, #17700, #66321, #32096, #4623, #58668, #11378, #37963, #19028, #59114 ),
 .UNSPECIFIED., .F., .F.,
 ( 4, 2, 2, 2, 4 ),
 ( 0.000000000000000000, 0.0001954311564186864949, 0.0003908623128373729899, 0.0005862934692560594577, 0.0007817246256747459798 ),
 .UNSPECIFIED. ) ;
#71335 = AXIS2_PLACEMENT_3D ( 'NONE', #80862, #74092, #4287 ) ;
#71336 = ORIENTED_EDGE ( 'NONE', *, *, #18608, .F. ) ;
#71338 = ORIENTED_EDGE ( 'NONE', *, *, #73530, .F. ) ;
#71337 = CARTESIAN_POINT ( 'NONE',  ( 6.130525438233648039, -12.50538340440932217, 31.33453814440721885 ) ) ;
#71340 = CARTESIAN_POINT ( 'NONE',  ( -5.326899820971668476, -12.65889640711025521, 30.72598325615533454 ) ) ;
#71339 = LINE ( 'NONE', #9641, #66191 ) ;
#71341 = B_SPLINE_CURVE_WITH_KNOTS ( 'NONE', 3,
 ( #68838, #7143, #34614, #62080, #390, #35501, #21084, #14339, #62948, #77805 ),
 .UNSPECIFIED., .F., .F.,
 ( 4, 2, 2, 2, 4 ),
 ( 0.000000000000000000, 0.0001954311564186871184, 0.0003908623128373742367, 0.0005862934692560614093, 0.0007817246256747484735 ),
 .UNSPECIFIED. ) ;
#71342 = CARTESIAN_POINT ( 'NONE',  ( 9.019230769230832223, -7.434744429011176159, 34.75000000000000711 ) ) ;
#71343 = CARTESIAN_POINT ( 'NONE',  ( 3.750000000000009770, -9.053300858899081760, 25.79687500000000355 ) ) ;
#71344 = ORIENTED_EDGE ( 'NONE', *, *, #15275, .F. ) ;
#71345 = ORIENTED_EDGE ( 'NONE', *, *, #2969, .T. ) ;
#71346 = CARTESIAN_POINT ( 'NONE',  ( -2.057692307692303046, -2.499999999999999556, 29.81604066197450109 ) ) ;
#71347 = ORIENTED_EDGE ( 'NONE', *, *, #3112, .T. ) ;
#71348 = FACE_BOUND ( 'NONE', #9927, .T. ) ;
#71349 = DIRECTION ( 'NONE',  ( -0.000000000000000000, -0.5000000000000009992, -0.8660254037844380415 ) ) ;
#71350 = CARTESIAN_POINT ( 'NONE',  ( -14.53117723225663838, -6.716662450894489211, 34.94144148231605840 ) ) ;
#71351 = ORIENTED_EDGE ( 'NONE', *, *, #13640, .F. ) ;
#71352 = CARTESIAN_POINT ( 'NONE',  ( -14.30769230769242917, -8.656820664282941280, 34.87096338111179961 ) ) ;
#71353 = CARTESIAN_POINT ( 'NONE',  ( 5.076923076922953193, -8.656820664282941280, 34.87096338111179961 ) ) ;
#71354 = CARTESIAN_POINT ( 'NONE',  ( 1.134592160393929738, -3.520140089381497361, 33.17453946501458262 ) ) ;
#71355 = EDGE_LOOP ( 'NONE', ( #58341, #44556 ) ) ;
#71356 = CARTESIAN_POINT ( 'NONE',  ( 12.33084699487090319, -4.809359713505814149, 33.96456829005828837 ) ) ;
#71357 = CARTESIAN_POINT ( 'NONE',  ( -16.82697755857493149, -2.587454068350149239, 30.68340429815432557 ) ) ;
#71358 = ORIENTED_EDGE ( 'NONE', *, *, #19136, .T. ) ;
#71359 = DIRECTION ( 'NONE',  ( 0.000000000000000000, 0.000000000000000000, -1.000000000000000000 ) ) ;
#71360 = DIRECTION ( 'NONE',  ( 0.000000000000000000, -1.000000000000000000, 0.000000000000000000 ) ) ;
#71361 = FACE_OUTER_BOUND ( 'NONE', #69261, .T. ) ;
#71362 = CARTESIAN_POINT ( 'NONE',  ( -2.557715544985270206, -2.587272538249755449, 30.68239716806877837 ) ) ;
#71363 = DIRECTION ( 'NONE',  ( -0.000000000000000000, -0.000000000000000000, -1.000000000000000000 ) ) ;
#71364 = CARTESIAN_POINT ( 'NONE',  ( -18.06608341095587633, -6.386643153685126251, 34.62446782046654903 ) ) ;
#71365 = VECTOR ( 'NONE', #12685, 999.9999999999998863 ) ;
#71366 = FACE_BOUND ( 'NONE', #6177, .T. ) ;
#71368 = DIRECTION ( 'NONE',  ( 1.000000000000000000, 0.000000000000000000, 0.000000000000000000 ) ) ;
#71367 = CARTESIAN_POINT ( 'NONE',  ( 4.499999999999999112, 7.500000000000002665, 13.50000000000000178 ) ) ;
#71369 = CARTESIAN_POINT ( 'NONE',  ( -0.3310130233048174109, -8.630441415882550871, 34.87705825610312615 ) ) ;
#71371 = CARTESIAN_POINT ( 'NONE',  ( 8.769230769230768274, -2.721908614388771852, 31.22303859784724978 ) ) ;
#71370 = CARTESIAN_POINT ( 'NONE',  ( 4.153846153846154188, -5.471508081941601098, 34.59228464037088457 ) ) ;
#71372 = CARTESIAN_POINT ( 'NONE',  ( 13.60804178353017768, -7.630147987733840509, 34.99859428049665411 ) ) ;
#71373 = CARTESIAN_POINT ( 'NONE',  ( -2.724691934501232371, -8.700186371490559623, 21.01375670625849068 ) ) ;
#71374 = ORIENTED_EDGE ( 'NONE', *, *, #81274, .F. ) ;
#71375 = CARTESIAN_POINT ( 'NONE',  ( 3.163032119165662515, -5.792891488981608994, 14.00000000000015099 ) ) ;
#71376 = VERTEX_POINT ( 'NONE', #63662 ) ;
#71377 = EDGE_CURVE ( 'NONE', #35045, #72305, #66372, .T. ) ;
#71378 = CARTESIAN_POINT ( 'NONE',  ( -9.822454901745912181, -6.001485441113819874, 34.52039167877662607 ) ) ;
#71379 = ORIENTED_EDGE ( 'NONE', *, *, #27533, .T. ) ;
#71380 = CARTESIAN_POINT ( 'NONE',  ( -4.153846153846273204, -11.48612834414049644, 32.76840700105863391 ) ) ;
#71381 = EDGE_CURVE ( 'NONE', #23361, #25915, #30951, .T. ) ;
#71383 = ORIENTED_EDGE ( 'NONE', *, *, #38756, .T. ) ;
#71382 = VECTOR ( 'NONE', #38301, 1000.000000000000114 ) ;
#71384 = CARTESIAN_POINT ( 'NONE',  ( -15.23076923076922995, -12.10708131394839349, 31.69288490824020244 ) ) ;
#71385 = CARTESIAN_POINT ( 'NONE',  ( -1.901340078031346525, -9.487747218494661183, 24.68563170625849068 ) ) ;
#71386 = LINE ( 'NONE', #43922, #44377 ) ;
#71387 = CARTESIAN_POINT ( 'NONE',  ( 6.673100192134570285, -11.28823185664190376, 33.01397839955799896 ) ) ;
#71388 = LINE ( 'NONE', #9694, #2913 ) ;
#71389 = CARTESIAN_POINT ( 'NONE',  ( 13.38461538461538680, -1.367168528481310208, 33.57946703557072254 ) ) ;
#71390 = LINE ( 'NONE', #65074, #34567 ) ;
#71391 = CARTESIAN_POINT ( 'NONE',  ( -13.60810030917971858, -8.539481045369596401, 34.89627647299170832 ) ) ;
#71392 = CARTESIAN_POINT ( 'NONE',  ( -13.63459212866397507, -12.01397095200674059, 32.43157075238190146 ) ) ;
#71393 = EDGE_CURVE ( 'NONE', #34447, #30367, #57791, .T. ) ;
#71394 = CARTESIAN_POINT ( 'NONE',  ( 1.553300858899087311, -3.749999999999992006, 14.23437500000000355 ) ) ;
#71395 = CARTESIAN_POINT ( 'NONE',  ( 1.384615384615265343, -2.892918686052166066, 31.69288490824153470 ) ) ;
#71396 = CARTESIAN_POINT ( 'NONE',  ( -2.176901866725358126, -11.93129842949671726, 32.56571108434900452 ) ) ;
#71397 = EDGE_CURVE ( 'NONE', #80799, #30362, #15369, .T. ) ;
#71398 = DIRECTION ( 'NONE',  ( -0.000000000000000000, 0.8660254037844399289, -0.4999999999999980016 ) ) ;
#71399 = CARTESIAN_POINT ( 'NONE',  ( -1.553300858899081538, -11.25000000000000711, 16.10937500000000355 ) ) ;
#71400 = ORIENTED_EDGE ( 'NONE', *, *, #69152, .T. ) ;
#71401 = AXIS2_PLACEMENT_3D ( 'NONE', #37733, #65199, #51670 ) ;
#71402 = CARTESIAN_POINT ( 'NONE',  ( 17.07692307692295586, -12.27809138561165270, 31.22303859784587132 ) ) ;
#71403 = DIRECTION ( 'NONE',  ( -0.000000000000000000, 1.000000000000000000, 3.491481338843133355E-15 ) ) ;
#71404 = CARTESIAN_POINT ( 'NONE',  ( 9.823099500132483897, -6.413143153341454017, 34.63066358083362672 ) ) ;
#71405 = CARTESIAN_POINT ( 'NONE',  ( 17.99999999999987566, -10.90142922262034020, 33.41473453929536674 ) ) ;
#71406 = CARTESIAN_POINT ( 'NONE',  ( 3.903822929624696680, -3.520140089381497361, 33.17453946501458262 ) ) ;
#71407 = CARTESIAN_POINT ( 'NONE',  ( 2.057715576749954867, -12.17611988154120972, 31.52148481390971213 ) ) ;
#71408 = AXIS2_PLACEMENT_3D ( 'NONE', #76138, #14446, #69394 ) ;
#71409 = ORIENTED_EDGE ( 'NONE', *, *, #68437, .F. ) ;
#71410 = LINE ( 'NONE', #9719, #22798 ) ;
#71411 = ORIENTED_EDGE ( 'NONE', *, *, #80185, .T. ) ;
#71412 = ADVANCED_FACE ( 'NONE', ( #8737 ), #42082, .T. ) ;
#71413 = EDGE_LOOP ( 'NONE', ( #1658, #87597, #55608, #10874 ) ) ;
#71414 = DIRECTION ( 'NONE',  ( -0.000000000000000000, -0.8660254037844399289, -0.4999999999999980016 ) ) ;
#71415 = DIRECTION ( 'NONE',  ( -0.000000000000000000, -0.8660254037844397068, -0.4999999999999978906 ) ) ;
#71416 = DIRECTION ( 'NONE',  ( -0.000000000000000000, 0.7660444431189791237, -0.6427876096865379196 ) ) ;
#71417 = CARTESIAN_POINT ( 'NONE',  ( 1.634560902963529960, -11.86320923018887719, 32.19269448109604781 ) ) ;
#71418 = CARTESIAN_POINT ( 'NONE',  ( 10.61538461538461675, -9.905515769479276145, 34.41647553114623292 ) ) ;
#71419 = ORIENTED_EDGE ( 'NONE', *, *, #38859, .T. ) ;
#71420 = ADVANCED_FACE ( 'NONE', ( #85276 ), #16367, .T. ) ;
#71421 = DIRECTION ( 'NONE',  ( 0.000000000000000000, 0.9396926207859126468, -0.3420201433256571111 ) ) ;
#71422 = ORIENTED_EDGE ( 'NONE', *, *, #29358, .T. ) ;
#71423 = VECTOR ( 'NONE', #46594, 1000.000000000000227 ) ;
#71424 = ORIENTED_EDGE ( 'NONE', *, *, #7584, .T. ) ;
#71425 = ADVANCED_FACE ( 'NONE', ( #23996 ), #10501, .F. ) ;
#71426 = ADVANCED_FACE ( 'NONE', ( #11382 ), #39313, .F. ) ;
#71427 = DIRECTION ( 'NONE',  ( -0.000000000000000000, -0.000000000000000000, -1.000000000000000000 ) ) ;
#71428 = LINE ( 'NONE', #50709, #40230 ) ;
#71429 = CIRCLE ( 'NONE', #35519, 0.2500000000000002220 ) ;
#71430 = CARTESIAN_POINT ( 'NONE',  ( -10.83886955910856464, -5.113361153441934093, 34.14387501736622710 ) ) ;
#71431 = CARTESIAN_POINT ( 'NONE',  ( 11.28848479441295005, -10.82459398097509329, 33.81372124010185587 ) ) ;
#71432 = LINE ( 'NONE', #37208, #36782 ) ;
#71433 = VECTOR ( 'NONE', #79471, 1000.000000000000114 ) ;
#71435 = VERTEX_POINT ( 'NONE', #25341 ) ;
#71434 = AXIS2_PLACEMENT_3D ( 'NONE', #75608, #67539, #5398 ) ;
#71436 = EDGE_CURVE ( 'NONE', #31351, #13749, #62058, .T. ) ;
#71437 = ORIENTED_EDGE ( 'NONE', *, *, #36963, .T. ) ;
#71438 = CARTESIAN_POINT ( 'NONE',  ( -2.651650429449535551, -10.15165042944956753, 22.43750000000000000 ) ) ;
#71439 = ORIENTED_EDGE ( 'NONE', *, *, #76532, .F. ) ;
#71441 = VERTEX_POINT ( 'NONE', #4626 ) ;
#71440 = CARTESIAN_POINT ( 'NONE',  ( -14.17690186672535901, -2.295524264805589354, 30.44142389570982488 ) ) ;
#71442 = DIRECTION ( 'NONE',  ( -0.000000000000000000, -0.8660254037844397068, -0.4999999999999978906 ) ) ;
#71443 = CARTESIAN_POINT ( 'NONE',  ( 4.946775867484854317, -3.817052484675422797, 33.13202310037935661 ) ) ;
#71444 = EDGE_CURVE ( 'NONE', #85483, #2529, #54493, .T. ) ;
#71445 = EDGE_CURVE ( 'NONE', #14162, #6905, #16760, .T. ) ;
#71446 = CARTESIAN_POINT ( 'NONE',  ( -3.230769230769351186, -10.21337939537710326, 33.94971097300076224 ) ) ;
#71447 = ORIENTED_EDGE ( 'NONE', *, *, #42552, .T. ) ;
#71448 = CARTESIAN_POINT ( 'NONE',  ( -15.16551409125639260, -12.51329471203373700, 31.30864560766537963 ) ) ;
#71449 = ORIENTED_EDGE ( 'NONE', *, *, #47027, .T. ) ;
#71450 = EDGE_CURVE ( 'NONE', #72338, #78537, #86169, .T. ) ;
#71451 = DIRECTION ( 'NONE',  ( 0.000000000000000000, 0.6427876096865373645, -0.7660444431189797898 ) ) ;
#71452 = CARTESIAN_POINT ( 'NONE',  ( 18.00000000000000000, -12.62096338111211580, 30.90682066428153263 ) ) ;
#71453 = CARTESIAN_POINT ( 'NONE',  ( 10.61538461538461675, -3.513871655860378418, 32.76840700105978499 ) ) ;
#71455 = LINE ( 'NONE', #10215, #69908 ) ;
#71454 = CARTESIAN_POINT ( 'NONE',  ( -0.3307480205715097044, -11.37503395064541678, 33.29242100308974983 ) ) ;
#71456 = VECTOR ( 'NONE', #62765, 1000.000000000000227 ) ;
#71457 = CARTESIAN_POINT ( 'NONE',  ( 16.02369894440793630, -2.619462340734461048, 30.83744416345203021 ) ) ;
#71458 = CARTESIAN_POINT ( 'NONE',  ( -0.3954711281883855900, -12.62096338111211757, 30.90682066428152908 ) ) ;
#71459 = VERTEX_POINT ( 'NONE', #10045 ) ;
#71460 = CARTESIAN_POINT ( 'NONE',  ( 4.230769230769229061, -11.00000000000000000, 29.75000000000000355 ) ) ;
#71461 = DIRECTION ( 'NONE',  ( -1.000000000000000000, 0.000000000000000000, 0.000000000000000000 ) ) ;
#71462 = EDGE_LOOP ( 'NONE', ( #75455, #85680, #12939, #21692 ) ) ;
#71463 = VECTOR ( 'NONE', #1822, 1000.000000000000114 ) ;
#71464 = CARTESIAN_POINT ( 'NONE',  ( 7.146088274689772035, -2.758310577978207778, 31.33698337089303010 ) ) ;
#71465 = CARTESIAN_POINT ( 'NONE',  ( 12.21153846153846168, -2.499999999999998668, 29.75000000000000355 ) ) ;
#71466 = DIRECTION ( 'NONE',  ( 0.000000000000000000, 0.000000000000000000, -1.000000000000000000 ) ) ;
#71467 = CARTESIAN_POINT ( 'NONE',  ( 2.307692307692309264, -13.88283147151868846, 33.14645433367849847 ) ) ;
#71468 = CARTESIAN_POINT ( 'NONE',  ( -10.61538461538473577, -3.083524468854526912, 32.58852847137268327 ) ) ;
#71469 = DIRECTION ( 'NONE',  ( -0.000000000000000000, 0.9396926207859092051, -0.3420201433256662704 ) ) ;
#71470 = FACE_BOUND ( 'NONE', #85296, .T. ) ;
#71472 = FACE_OUTER_BOUND ( 'NONE', #45556, .T. ) ;
#71471 = CARTESIAN_POINT ( 'NONE',  ( 13.25446817517716269, -12.27039167877662251, 31.24851455888617835 ) ) ;
#71473 = AXIS2_PLACEMENT_3D ( 'NONE', #69515, #62745, #26760 ) ;
#71474 = CARTESIAN_POINT ( 'NONE',  ( 16.02315468717859304, -3.062553014421049991, 32.05460306192773601 ) ) ;
#71476 = CARTESIAN_POINT ( 'NONE',  ( 0.4615384615384611755, -2.900454961884010974, 35.62045528018868623 ) ) ;
#71475 = DIRECTION ( 'NONE',  ( 0.000000000000000000, 0.1736481776669267785, -0.9848077530122087975 ) ) ;
#71477 = DIRECTION ( 'NONE',  ( -0.000000000000000000, 1.000000000000000000, -0.000000000000000000 ) ) ;
#71478 = CARTESIAN_POINT ( 'NONE',  ( -2.694853999681210865, -4.891553140782108677, 18.74813170625849068 ) ) ;
#71479 = B_SPLINE_CURVE_WITH_KNOTS ( 'NONE', 3,
 ( #16122, #57986, #44456, #15686, #64289, #84597, #77813, #2590, #51200, #30080 ),
 .UNSPECIFIED., .F., .F.,
 ( 4, 2, 2, 2, 4 ),
 ( 0.000000000000000000, 0.0001954311564186876876, 0.0003908623128373753751, 0.0005862934692560630356, 0.0007817246256747507503 ),
 .UNSPECIFIED. ) ;
#71480 = EDGE_CURVE ( 'NONE', #28929, #24412, #16841, .T. ) ;
#71481 = EDGE_LOOP ( 'NONE', ( #16420, #23351 ) ) ;
#71482 = CARTESIAN_POINT ( 'NONE',  ( -7.846153846153965716, -11.48612834414049644, 32.76840700105863391 ) ) ;
#71483 = DIRECTION ( 'NONE',  ( -0.000000000000000000, 0.7660444431189791237, -0.6427876096865379196 ) ) ;
#71484 = CARTESIAN_POINT ( 'NONE',  ( 0.4615384615384611200, -13.53365097954675988, 30.81389545987213552 ) ) ;
#71485 = CARTESIAN_POINT ( 'NONE',  ( -9.915792636031639518, -10.81261337010820256, 33.49550067578627477 ) ) ;
#71486 = CARTESIAN_POINT ( 'NONE',  ( 6.857806922520604864, -12.70778746994557551, 30.41441678777548319 ) ) ;
#71487 = CARTESIAN_POINT ( 'NONE',  ( -5.299788499126715458, -2.501496062324911840, 29.88072118266895671 ) ) ;
#71488 = CARTESIAN_POINT ( 'NONE',  ( 1.492201783934554493, -3.724691934501233703, 20.23250670625849423 ) ) ;
#71489 = CARTESIAN_POINT ( 'NONE',  ( -1.607443482250262567, -7.369209533119137845, 34.99857337881830688 ) ) ;
#71490 = CYLINDRICAL_SURFACE ( 'NONE', #76260, 0.2500000000000002220 ) ;
#71491 = CARTESIAN_POINT ( 'NONE',  ( -16.94613126909829148, -5.582136614379148654, 34.36778462344220486 ) ) ;
#71492 = CARTESIAN_POINT ( 'NONE',  ( 10.39189969082028675, -6.716662450894489211, 34.94144148231605840 ) ) ;
#71493 = CARTESIAN_POINT ( 'NONE',  ( 2.372885295986962628, -2.255955759149235629, 29.99999999999988631 ) ) ;
#71494 = CARTESIAN_POINT ( 'NONE',  ( 5.142990410273152513, -8.164416787775445883, 34.95778746994558617 ) ) ;
#71495 = ADVANCED_FACE ( 'NONE', ( #59565 ), #86619, .T. ) ;
#71496 = CIRCLE ( 'NONE', #70017, 4.000000000000000000 ) ;
#71497 = CARTESIAN_POINT ( 'NONE',  ( -14.24162395668986747, -3.050289026998446840, 32.03036669348366416 ) ) ;
#71498 = CARTESIAN_POINT ( 'NONE',  ( 17.07692307692307665, -2.486705287966279876, 31.30864560766543647 ) ) ;
#71499 = EDGE_LOOP ( 'NONE', ( #53934, #72120, #47879, #48320 ) ) ;
#71500 = DIRECTION ( 'NONE',  ( -0.000000000000000000, -0.5000000000000009992, -0.8660254037844380415 ) ) ;
#71501 = DIRECTION ( 'NONE',  ( 0.000000000000000000, -0.000000000000000000, -1.000000000000000000 ) ) ;
#71502 = AXIS2_PLACEMENT_3D ( 'NONE', #77927, #36936, #23420 ) ;
#71503 = CARTESIAN_POINT ( 'NONE',  ( 3.775308065498752086, -6.007798216065404873, 15.89249329374151820 ) ) ;
#71504 = CARTESIAN_POINT ( 'NONE',  ( 7.173022332454967120, -10.92531984108285670, 33.72920026020278073 ) ) ;
#71505 = CARTESIAN_POINT ( 'NONE',  ( -5.143006487878958310, -2.538708090699994813, 30.37095296980875148 ) ) ;
#71506 = VERTEX_POINT ( 'NONE', #52803 ) ;
#71507 = CARTESIAN_POINT ( 'NONE',  ( -16.37733107841048152, -4.225889041578354544, 33.85425143139329407 ) ) ;
#71509 = ORIENTED_EDGE ( 'NONE', *, *, #87428, .T. ) ;
#71508 = CARTESIAN_POINT ( 'NONE',  ( 10.61538461538449596, -11.48612834414049644, 32.76840700105863391 ) ) ;
#71510 = DIRECTION ( 'NONE',  ( 1.000000000000000000, 0.000000000000000000, 0.000000000000000000 ) ) ;
#71511 = CARTESIAN_POINT ( 'NONE',  ( 16.94631342171898680, -7.722926974430166069, 34.99546784045485737 ) ) ;
#71512 = FACE_OUTER_BOUND ( 'NONE', #1931, .T. ) ;
#71513 = B_SPLINE_CURVE_WITH_KNOTS ( 'NONE', 3,
 ( #6397, #14025, #67206, #5507, #7275, #32975, #27096, #62211, #81170, #33852 ),
 .UNSPECIFIED., .F., .F.,
 ( 4, 2, 2, 2, 4 ),
 ( 0.0007817246336856284103, 0.0009771112958940092897, 0.001172497958102390169, 0.001367884620310771265, 0.001563271282519152145 ),
 .UNSPECIFIED. ) ;
#71514 = B_SPLINE_CURVE_WITH_KNOTS ( 'NONE', 3,
 ( #40568, #32912, #81109, #47752, #48188, #41441, #41001, #68034, #88325, #19838 ),
 .UNSPECIFIED., .F., .F.,
 ( 4, 2, 2, 2, 4 ),
 ( 0.000000000000000000, 0.0001954339857564075286, 0.0003908679715128150572, 0.0005863019572692225586, 0.0007817359430256301143 ),
 .UNSPECIFIED. ) ;
#71516 = EDGE_CURVE ( 'NONE', #51951, #62595, #68373, .T. ) ;
#71515 = CARTESIAN_POINT ( 'NONE',  ( -13.60810032833933469, -3.236172620538810385, 32.36188796281390267 ) ) ;
#71517 = ORIENTED_EDGE ( 'NONE', *, *, #65887, .F. ) ;
#71518 = B_SPLINE_CURVE_WITH_KNOTS ( 'NONE', 3,
 ( #6313, #47282, #13502, #74773, #20700, #33777, #61675, #68444, #40547, #75637 ),
 .UNSPECIFIED., .F., .F.,
 ( 4, 2, 2, 2, 4 ),
 ( 0.0007817359430256322827, 0.0009771253907249989254, 0.001172514838424365676, 0.001367904286123732428, 0.001563293733823099179 ),
 .UNSPECIFIED. ) ;
#71519 = CYLINDRICAL_SURFACE ( 'NONE', #46178, 0.2499999999999986955 ) ;
#71520 = B_SPLINE_CURVE_WITH_KNOTS ( 'NONE', 3,
 ( #25372, #30790, #46093, #52837, #73119, #10978, #86656, #57823, #44284, #45643 ),
 .UNSPECIFIED., .F., .F.,
 ( 4, 2, 2, 2, 4 ),
 ( 0.000000000000000000, 0.0001954311564186861968, 0.0003908623128373723936, 0.0005862934692560585904, 0.0007817246256747447872 ),
 .UNSPECIFIED. ) ;
#71521 = B_SPLINE_CURVE_WITH_KNOTS ( 'NONE', 3,
 ( #88783, #60837, #73922, #6357, #61714, #13103, #33812, #27502, #60391, #20739 ),
 .UNSPECIFIED., .F., .F.,
 ( 4, 2, 2, 2, 4 ),
 ( 0.0007817246256747472808, 0.0009771112852218907189, 0.001172497944769034265, 0.001367884604316177595, 0.001563271263863321141 ),
 .UNSPECIFIED. ) ;
#71522 = PRESENTATION_STYLE_ASSIGNMENT (( #44043 ) ) ;
#71523 = CARTESIAN_POINT ( 'NONE',  ( 6.166666666666664298, -3.499999999999999556, 29.75000000000000355 ) ) ;
#71524 = VERTEX_POINT ( 'NONE', #24888 ) ;
#71525 = ORIENTED_EDGE ( 'NONE', *, *, #44843, .T. ) ;
#71526 = EDGE_LOOP ( 'NONE', ( #38466, #37222, #37158, #87410 ) ) ;
#71527 = VECTOR ( 'NONE', #7106, 1000.000000000000000 ) ;
#71528 = CARTESIAN_POINT ( 'NONE',  ( -5.076923076923199218, -9.528491918059723176, 34.59228464037033035 ) ) ;
#71529 = CARTESIAN_POINT ( 'NONE',  ( -3.099978789802277479, -2.845873456487966635, 32.17976146951972538 ) ) ;
#71530 = ADVANCED_FACE ( 'NONE', ( #52358 ), #19907, .F. ) ;
#71531 = EDGE_CURVE ( 'NONE', #4325, #32871, #77199, .T. ) ;
#71532 = DIRECTION ( 'NONE',  ( 0.000000000000000000, 0.000000000000000000, -1.000000000000000000 ) ) ;
#71533 = CARTESIAN_POINT ( 'NONE',  ( 15.16549878480845948, -3.835265460703609186, 33.15142922261924241 ) ) ;
#71534 = ORIENTED_EDGE ( 'NONE', *, *, #83641, .F. ) ;
#71535 = EDGE_CURVE ( 'NONE', #88762, #85190, #64054, .T. ) ;
#71536 = AXIS2_PLACEMENT_3D ( 'NONE', #63428, #15699, #8941 ) ;
#71537 = EDGE_LOOP ( 'NONE', ( #68933, #59446 ) ) ;
#71539 = ORIENTED_EDGE ( 'NONE', *, *, #8601, .T. ) ;
#71538 = CARTESIAN_POINT ( 'NONE',  ( 4.153846153846030731, -8.656820664282941280, 34.87096338111179961 ) ) ;
#71540 = CARTESIAN_POINT ( 'NONE',  ( 17.29970261819148902, -5.114059244376869096, 34.14424750095245287 ) ) ;
#71541 = B_SPLINE_CURVE_WITH_KNOTS ( 'NONE', 3,
 ( #71402, #16471, #85827, #44363, #37176, #2498, #30861, #50237, #38072, #84498 ),
 .UNSPECIFIED., .F., .F.,
 ( 4, 2, 2, 2, 4 ),
 ( 0.0007817359430256339090, 0.0009771253907250065148, 0.001172514838424371965, 0.001367904286123737632, 0.001563293733823103299 ),
 .UNSPECIFIED. ) ;
#71542 = LINE ( 'NONE', #11184, #55131 ) ;
#71543 = CARTESIAN_POINT ( 'NONE',  ( 13.38461538461526423, -10.33852847137269571, 34.16647553114546554 ) ) ;
#71544 = ORIENTED_EDGE ( 'NONE', *, *, #68590, .F. ) ;
#71545 = EDGE_LOOP ( 'NONE', ( #76781, #72906 ) ) ;
#71547 = ORIENTED_EDGE ( 'NONE', *, *, #16946, .F. ) ;
#71546 = CARTESIAN_POINT ( 'NONE',  ( 9.823098133274644539, -8.191423895709840863, 34.95447573519442130 ) ) ;
#71548 = LINE ( 'NONE', #85964, #53148 ) ;
#71549 = ADVANCED_FACE ( 'NONE', ( #6413 ), #85832, .F. ) ;
#71550 = CARTESIAN_POINT ( 'NONE',  ( -15.93106661257774270, -3.755027918224367767, 33.06320215134714857 ) ) ;
#71551 = VERTEX_POINT ( 'NONE', #14042 ) ;
#71552 = LINE ( 'NONE', #66129, #67619 ) ;
#71553 = CARTESIAN_POINT ( 'NONE',  ( -7.846153846153965716, -4.481592998941358097, 33.73612834414048933 ) ) ;
#71554 = CYLINDRICAL_SURFACE ( 'NONE', #52548, 0.2500000000000009437 ) ;
#71555 = VECTOR ( 'NONE', #57719, 1000.000000000000000 ) ;
#71556 = FACE_BOUND ( 'NONE', #38890, .T. ) ;
#71557 = CARTESIAN_POINT ( 'NONE',  ( -9.469294848214294902, -4.026326845037962343, 33.68677907613344047 ) ) ;
#71558 = CARTESIAN_POINT ( 'NONE',  ( 11.40831432902331954, -8.587444163452046197, 34.63053765926554206 ) ) ;
#71559 = DIRECTION ( 'NONE',  ( -0.000000000000000000, -0.000000000000000000, -1.000000000000000000 ) ) ;
#71561 = CARTESIAN_POINT ( 'NONE',  ( 4.376858997939547358, -2.308499170217967134, 30.53291367094873721 ) ) ;
#71560 = FACE_OUTER_BOUND ( 'NONE', #30013, .T. ) ;
#71562 = CARTESIAN_POINT ( 'NONE',  ( 8.703960768674448900, -9.528491918058357157, 34.59228464037090589 ) ) ;
#71563 = DIRECTION ( 'NONE',  ( -0.000000000000000000, -0.6427876096865404731, -0.7660444431189771253 ) ) ;
#71564 = ORIENTED_EDGE ( 'NONE', *, *, #60582, .T. ) ;
#71565 = AXIS2_PLACEMENT_3D ( 'NONE', #11057, #87620, #65542 ) ;
#71566 = CARTESIAN_POINT ( 'NONE',  ( 10.48523740594639619, -10.88202310037935661, 33.43294751532457099 ) ) ;
#71567 = EDGE_LOOP ( 'NONE', ( #57447, #69393, #64970, #78859 ) ) ;
#71568 = ORIENTED_EDGE ( 'NONE', *, *, #45103, .T. ) ;
#71570 = CARTESIAN_POINT ( 'NONE',  ( -5.933931648997562647, -12.10708131394839882, 31.69288490824020954 ) ) ;
#71569 = CARTESIAN_POINT ( 'NONE',  ( -1.161835715637318023, -4.989023458446560255, 34.36081565061822118 ) ) ;
#71571 = CARTESIAN_POINT ( 'NONE',  ( 11.31553457955468645, -8.282780595021769443, 34.94152052738834868 ) ) ;
#71572 = CARTESIAN_POINT ( 'NONE',  ( 14.30769230769231015, -3.937682226553329556, 33.60647404775216529 ) ) ;
#71573 = DIRECTION ( 'NONE',  ( -0.000000000000000000, 0.5000000000000011102, -0.8660254037844381525 ) ) ;
#71574 = CARTESIAN_POINT ( 'NONE',  ( 16.15384615384615330, -8.810774026931790459, 35.74407628777942847 ) ) ;
#71575 = ORIENTED_EDGE ( 'NONE', *, *, #17249, .T. ) ;
#71576 = DIRECTION ( 'NONE',  ( -1.000000000000000000, 0.000000000000000000, 0.000000000000000000 ) ) ;
#71577 = CARTESIAN_POINT ( 'NONE',  ( 14.98074600654777377, -10.92453946501458795, 33.72985991061850086 ) ) ;
#71578 = CARTESIAN_POINT ( 'NONE',  ( 13.38461538461570122, -2.255955759149395501, 30.00000000000324363 ) ) ;
#71579 = CARTESIAN_POINT ( 'NONE',  ( 12.94230769230769340, -3.499999999999999556, 29.75000000000000355 ) ) ;
#71581 = DIRECTION ( 'NONE',  ( 1.000000000000000000, 0.000000000000000000, 0.000000000000000000 ) ) ;
#71580 = B_SPLINE_CURVE_WITH_KNOTS ( 'NONE', 3,
 ( #6468, #27173, #74044, #61388, #88461, #54192, #14894, #67724, #88029, #82130 ),
 .UNSPECIFIED., .F., .F.,
 ( 4, 2, 2, 2, 4 ),
 ( 0.000000000000000000, 0.0001954339857564081249, 0.0003908679715128162498, 0.0005863019572692244018, 0.0007817359430256324996 ),
 .UNSPECIFIED. ) ;
#71582 = CARTESIAN_POINT ( 'NONE',  ( 3.750000000000009770, -9.053300858899081760, 18.29687500000000000 ) ) ;
#71583 = ORIENTED_EDGE ( 'NONE', *, *, #12602, .T. ) ;
#71584 = VERTEX_POINT ( 'NONE', #12271 ) ;
#71585 = CARTESIAN_POINT ( 'NONE',  ( -7.912236225513981758, -11.35647404775217595, 33.31231777344666511 ) ) ;
#71586 = VERTEX_POINT ( 'NONE', #34310 ) ;
#71587 = CARTESIAN_POINT ( 'NONE',  ( -7.146003140593070846, -2.554751324335733820, 30.48935550225260727 ) ) ;
#71588 = CARTESIAN_POINT ( 'NONE',  ( 18.22301135161285046, -5.667800583137506898, 34.40243808032445827 ) ) ;
#71589 = CARTESIAN_POINT ( 'NONE',  ( -16.15384615384627409, -2.892918686052165622, 31.69288490824153470 ) ) ;
#71590 = DIRECTION ( 'NONE',  ( 0.000000000000000000, 0.7660444431189807890, 0.6427876096865361433 ) ) ;
#71591 = CARTESIAN_POINT ( 'NONE',  ( -3.749999999999988454, -9.053300858899127945, 20.01562500000000355 ) ) ;
#71592 = CARTESIAN_POINT ( 'NONE',  ( -16.81410256410256565, -4.000000000000000000, 29.75000000000000355 ) ) ;
#71593 = ORIENTED_EDGE ( 'NONE', *, *, #24163, .F. ) ;
#71594 = CIRCLE ( 'NONE', #83120, 4.000000000000000000 ) ;
#71595 = CARTESIAN_POINT ( 'NONE',  ( -12.59168567097668401, -10.88202310037935661, 33.43294751532457099 ) ) ;
#71597 = EDGE_LOOP ( 'NONE', ( #46644, #42865, #42658, #67474 ) ) ;
#71596 = CARTESIAN_POINT ( 'NONE',  ( -1.134669866267242755, -9.272278438253398036, 34.42582936511637826 ) ) ;
#71598 = LINE ( 'NONE', #9906, #25322 ) ;
#71599 = CARTESIAN_POINT ( 'NONE',  ( -12.39547011053602432, -3.513871655860379306, 32.76840700105978499 ) ) ;
#71600 = CARTESIAN_POINT ( 'NONE',  ( 15.29683656411930848, -2.833524468853757750, 32.15551576947925838 ) ) ;
#71601 = CARTESIAN_POINT ( 'NONE',  ( 6.700149964170072359, -3.395401636524186362, 33.02366814457250399 ) ) ;
#71602 = DIRECTION ( 'NONE',  ( 0.000000000000000000, 0.9396926207859126468, -0.3420201433256571111 ) ) ;
#71603 = AXIS2_PLACEMENT_3D ( 'NONE', #29116, #22341, #34528 ) ;
#71604 = CARTESIAN_POINT ( 'NONE',  ( -3.165513659493205179, -11.48612834413965977, 32.76840700105972815 ) ) ;
#71605 = CARTESIAN_POINT ( 'NONE',  ( -2.980769230767794653, -7.500000000000155431, 34.75000000000007105 ) ) ;
#71606 = CARTESIAN_POINT ( 'NONE',  ( -3.775308065498748977, -8.992201783934593351, 17.76749329374151287 ) ) ;
#71607 = EDGE_LOOP ( 'NONE', ( #84838, #55713, #68625, #12393 ) ) ;
#71608 = CARTESIAN_POINT ( 'NONE',  ( -11.53846153846153655, -7.500000000000001776, 35.04278698407183867 ) ) ;
#71609 = CARTESIAN_POINT ( 'NONE',  ( 8.834486340506792601, -11.94971097300157403, 32.03036669348361443 ) ) ;
#71611 = CARTESIAN_POINT ( 'NONE',  ( -17.07692307692307665, -4.661471528628507777, 34.16647553114623292 ) ) ;
#71610 = B_SPLINE_CURVE_WITH_KNOTS ( 'NONE', 3,
 ( #37922, #3678, #58622, #73039, #38367, #78450, #86117, #24392, #16752, #18102 ),
 .UNSPECIFIED., .F., .F.,
 ( 4, 2, 2, 2, 4 ),
 ( 0.0007817246256747524850, 0.0009771112852218972241, 0.001172497944769042072, 0.001367884604316186702, 0.001563271263863331550 ),
 .UNSPECIFIED. ) ;
#71612 = CARTESIAN_POINT ( 'NONE',  ( 2.724691934501250135, -8.700186371490531201, 13.54874329374151465 ) ) ;
#71613 = B_SPLINE_CURVE_WITH_KNOTS ( 'NONE', 3,
 ( #35472, #54408, #27391, #82343, #81904, #13867, #78669, #43119, #9766, #30047 ),
 .UNSPECIFIED., .F., .F.,
 ( 4, 2, 2, 2, 4 ),
 ( 0.000000000000000000, 0.0001954339857564063360, 0.0003908679715128126719, 0.0005863019572692189808, 0.0007817359430256253438 ),
 .UNSPECIFIED. ) ;
#71614 = CARTESIAN_POINT ( 'NONE',  ( -3.230769230769229949, -8.973038597847269315, 34.52809138561121927 ) ) ;
#71615 = CARTESIAN_POINT ( 'NONE',  ( -17.14219352288385778, -2.625532179533445198, 30.86335684631481513 ) ) ;
#71616 = ORIENTED_EDGE ( 'NONE', *, *, #76437, .F. ) ;
#71617 = CARTESIAN_POINT ( 'NONE',  ( -2.750000000000006217, -6.360912703474006946, 17.67187500000000355 ) ) ;
#71618 = CARTESIAN_POINT ( 'NONE',  ( -1.253824943648434553, -12.35292014791297710, 31.75344720912887198 ) ) ;
#71619 = ORIENTED_EDGE ( 'NONE', *, *, #36260, .T. ) ;
#71620 = DIRECTION ( 'NONE',  ( 1.000000000000000000, 0.000000000000000000, 0.000000000000000000 ) ) ;
#71621 = ORIENTED_EDGE ( 'NONE', *, *, #37373, .F. ) ;
#71622 = VECTOR ( 'NONE', #80710, 1000.000000000000000 ) ;
#71623 = CARTESIAN_POINT ( 'NONE',  ( 14.55774661933062752, -12.17597550085003810, 31.52189283813460463 ) ) ;
#71624 = FACE_OUTER_BOUND ( 'NONE', #88836, .T. ) ;
#71625 = CARTESIAN_POINT ( 'NONE',  ( -1.608100328339332030, -4.386631170607604879, 33.66268669641500111 ) ) ;
#71626 = CARTESIAN_POINT ( 'NONE',  ( -14.30769230769230660, -11.69971097300155272, 32.46337939537588113 ) ) ;
#71627 = ORIENTED_EDGE ( 'NONE', *, *, #45739, .F. ) ;
#71628 = CARTESIAN_POINT ( 'NONE',  ( -6.700297254098854793, -6.717445702608402236, 34.94155399931962336 ) ) ;
#71629 = CIRCLE ( 'NONE', #14099, 4.000000000000000000 ) ;
#71630 = EDGE_CURVE ( 'NONE', #23768, #37623, #27548, .T. ) ;
#71631 = ORIENTED_EDGE ( 'NONE', *, *, #48973, .F. ) ;
#71632 = CARTESIAN_POINT ( 'NONE',  ( 12.39545608217832573, -11.91647553114624181, 32.58852847137148245 ) ) ;
#71633 = CARTESIAN_POINT ( 'NONE',  ( -10.28846153846153832, -7.500000000000000000, 33.75000000000000000 ) ) ;
#71634 = ORIENTED_EDGE ( 'NONE', *, *, #3655, .F. ) ;
#71635 = AXIS2_PLACEMENT_3D ( 'NONE', #87182, #19584, #52475 ) ;
#71636 = FACE_OUTER_BOUND ( 'NONE', #14716, .T. ) ;
#71637 = CARTESIAN_POINT ( 'NONE',  ( -19.50000000000000000, -3.499999999999999556, 29.75000000000000355 ) ) ;
#71638 = CARTESIAN_POINT ( 'NONE',  ( 16.15384615384615330, -3.886160181151819604, 36.00935417666054406 ) ) ;
#71639 = FACE_OUTER_BOUND ( 'NONE', #82725, .T. ) ;
#71640 = CARTESIAN_POINT ( 'NONE',  ( 0.4615384615384611200, -2.249999999999998668, 29.75000000000001776 ) ) ;
#71641 = B_SPLINE_CURVE_WITH_KNOTS ( 'NONE', 3,
 ( #75577, #34600, #82799, #28738, #49446, #83236, #56201, #83691, #379, #75156 ),
 .UNSPECIFIED., .F., .F.,
 ( 4, 2, 2, 2, 4 ),
 ( 0.0007817359430256319575, 0.0009771253907249984917, 0.001172514838424365026, 0.001367904286123731343, 0.001563293733823097878 ),
 .UNSPECIFIED. ) ;
#71642 = ORIENTED_EDGE ( 'NONE', *, *, #47068, .T. ) ;
#71643 = ORIENTED_EDGE ( 'NONE', *, *, #49998, .F. ) ;
#71644 = ADVANCED_FACE ( 'NONE', ( #67665 ), #88, .F. ) ;
#71645 = FACE_BOUND ( 'NONE', #51554, .T. ) ;
#71646 = ORIENTED_EDGE ( 'NONE', *, *, #66428, .F. ) ;
#71648 = ORIENTED_EDGE ( 'NONE', *, *, #7224, .F. ) ;
#71647 = CARTESIAN_POINT ( 'NONE',  ( -8.069638770718176701, -5.827078755546623690, 34.72654668319379567 ) ) ;
#71649 = APPLICATION_CONTEXT ( 'automotive_design' ) ;
#71650 = VECTOR ( 'NONE', #3894, 1000.000000000000000 ) ;
#71651 = CARTESIAN_POINT ( 'NONE',  ( 13.63456090296352841, -10.76462480002816235, 33.53768742498949962 ) ) ;
#71652 = CARTESIAN_POINT ( 'NONE',  ( -3.230769230769351186, -10.21337939537710326, 33.94971097300076224 ) ) ;
#71653 = EDGE_LOOP ( 'NONE', ( #12976, #88614, #33039, #62761 ) ) ;
#71654 = EDGE_LOOP ( 'NONE', ( #60442, #71383, #69446, #63011 ) ) ;
#71655 = AXIS2_PLACEMENT_3D ( 'NONE', #3513, #23342, #34099 ) ;
#71656 = ORIENTED_EDGE ( 'NONE', *, *, #65716, .T. ) ;
#71657 = CARTESIAN_POINT ( 'NONE',  ( -1.608100328339332252, -11.89387501736622710, 32.13663884655806413 ) ) ;
#71658 = ORIENTED_EDGE ( 'NONE', *, *, #81056, .F. ) ;
#71659 = CARTESIAN_POINT ( 'NONE',  ( 2.373760658694747061, -4.098570777380720287, 33.41473453929635440 ) ) ;
#71660 = EDGE_CURVE ( 'NONE', #72796, #38632, #65176, .T. ) ;
#71661 = VECTOR ( 'NONE', #13719, 1000.000000000000227 ) ;
#71662 = CARTESIAN_POINT ( 'NONE',  ( -8.069638789877794594, -2.599994579823203367, 30.74605699353653776 ) ) ;
#71663 = EDGE_CURVE ( 'NONE', #86112, #47138, #54576, .T. ) ;
#71664 = CARTESIAN_POINT ( 'NONE',  ( -2.437840277424004665, -12.50552854090298993, 31.33409797877408920 ) ) ;
#71665 = FACE_BOUND ( 'NONE', #13924, .T. ) ;
#71667 = ORIENTED_EDGE ( 'NONE', *, *, #77660, .F. ) ;
#71666 = ADVANCED_FACE ( 'NONE', ( #20799 ), #13602, .F. ) ;
#71668 = CARTESIAN_POINT ( 'NONE',  ( -1.607442077094388022, -7.369208160676172348, 34.74850200257122879 ) ) ;
#71669 = EDGE_CURVE ( 'NONE', #30978, #5298, #32991, .T. ) ;
#71670 = CARTESIAN_POINT ( 'NONE',  ( -14.08491276642389245, -5.913360116392397892, 34.49180327182771322 ) ) ;
#71671 = DIRECTION ( 'NONE',  ( 0.000000000000000000, 0.7660444431189822323, -0.6427876096865344779 ) ) ;
#71672 = DIRECTION ( 'NONE',  ( 0.000000000000000000, 0.8660254037844377084, -0.5000000000000015543 ) ) ;
#71673 = ORIENTED_EDGE ( 'NONE', *, *, #86940, .F. ) ;
#71674 = CARTESIAN_POINT ( 'NONE',  ( -17.20707028636129721, -12.45813303252208648, 30.39737893381572675 ) ) ;
#71675 = ORIENTED_EDGE ( 'NONE', *, *, #52594, .F. ) ;
#71676 = EDGE_LOOP ( 'NONE', ( #3959, #49105, #33888, #72209 ) ) ;
#71677 = B_SPLINE_CURVE_WITH_KNOTS ( 'NONE', 3,
 ( #52550, #11582, #74168, #53439, #67410, #18334, #80941, #12465, #81379, #80035 ),
 .UNSPECIFIED., .F., .F.,
 ( 4, 2, 2, 2, 4 ),
 ( 0.000000000000000000, 0.0001954311564186863865, 0.0003908623128373727731, 0.0005862934692560591325, 0.0007817246256747455461 ),
 .UNSPECIFIED. ) ;
#71679 = CARTESIAN_POINT ( 'NONE',  ( 6.000000000000001776, -3.050289026998446396, 32.03036669348365706 ) ) ;
#71678 = CARTESIAN_POINT ( 'NONE',  ( -18.25000000000000711, -2.249999999999998668, 29.75000000000000355 ) ) ;
#71680 = CARTESIAN_POINT ( 'NONE',  ( 15.93036121012220541, -5.912607949931405038, 34.49155766932282319 ) ) ;
#71681 = CARTESIAN_POINT ( 'NONE',  ( -4.153846153846152411, -4.098570777380720287, 33.41473453929634729 ) ) ;
#71682 = CARTESIAN_POINT ( 'NONE',  ( -18.22292695890684655, -5.582147617184174848, 34.63737895849758530 ) ) ;
#71683 = CARTESIAN_POINT ( 'NONE',  ( -2.557669038634660552, -9.943427161483782584, 34.11278801902876978 ) ) ;
#71684 = ORIENTED_EDGE ( 'NONE', *, *, #81609, .T. ) ;
#71685 = CARTESIAN_POINT ( 'NONE',  ( 17.07692307692307665, -5.557115091759785130, 34.35708131394839171 ) ) ;
#71686 = CARTESIAN_POINT ( 'NONE',  ( -11.66915300512910214, -9.804603061927743113, 34.18744698557895845 ) ) ;
#71687 = LINE ( 'NONE', #22186, #5619 ) ;
#71688 = CARTESIAN_POINT ( 'NONE',  ( 14.37375964104238335, -2.486705287966280320, 31.30864560766543647 ) ) ;
#71689 = VERTEX_POINT ( 'NONE', #39757 ) ;
#71690 = AXIS2_PLACEMENT_3D ( 'NONE', #21519, #82795, #34597 ) ;
#71691 = ORIENTED_EDGE ( 'NONE', *, *, #73716, .T. ) ;
#71692 = FACE_BOUND ( 'NONE', #86812, .T. ) ;
#71693 = ORIENTED_EDGE ( 'NONE', *, *, #35325, .T. ) ;
#71694 = CARTESIAN_POINT ( 'NONE',  ( 7.622668902429900584, -2.847400154188068022, 31.58180166144859058 ) ) ;
#71695 = CARTESIAN_POINT ( 'NONE',  ( -6.856907782114267214, -7.250054483168843156, 34.74374881642865631 ) ) ;
#71696 = ORIENTED_EDGE ( 'NONE', *, *, #66343, .F. ) ;
#71697 = CARTESIAN_POINT ( 'NONE',  ( 3.903822929624694904, -11.56360843649122216, 33.07473185843129926 ) ) ;
#71698 = CARTESIAN_POINT ( 'NONE',  ( -10.68146802634049308, -6.386643153685125363, 34.62446782046654903 ) ) ;
#71699 = CARTESIAN_POINT ( 'NONE',  ( 16.02369894440793630, -8.587444163452046197, 34.63053765926554206 ) ) ;
#71700 = CARTESIAN_POINT ( 'NONE',  ( -1.134560964701931240, -4.074993327901524687, 33.72946981652012255 ) ) ;
#71701 = ORIENTED_EDGE ( 'NONE', *, *, #84771, .T. ) ;
#71702 = CARTESIAN_POINT ( 'NONE',  ( -7.715362038329058869, -10.54018710029568595, 33.71981072465678864 ) ) ;
#71703 = ORIENTED_EDGE ( 'NONE', *, *, #27948, .F. ) ;
#71705 = VERTEX_POINT ( 'NONE', #67225 ) ;
#71704 = PLANE ( 'NONE',  #25198 ) ;
#71706 = CARTESIAN_POINT ( 'NONE',  ( -8.519176457592452678, -9.943054286541403997, 34.11300777759954883 ) ) ;
#71707 = CARTESIAN_POINT ( 'NONE',  ( 15.23076923076923173, -4.661471528628507777, 34.16647553114623292 ) ) ;
#71708 = CARTESIAN_POINT ( 'NONE',  ( 10.61538461538461675, -12.34228464037088635, 31.77849191805839268 ) ) ;
#71709 = EDGE_CURVE ( 'NONE', #84346, #13650, #52259, .T. ) ;
#71710 = CARTESIAN_POINT ( 'NONE',  ( -12.39547011053602432, -2.721908614388772296, 31.22303859784725333 ) ) ;
#71711 = CARTESIAN_POINT ( 'NONE',  ( -14.37296230824862775, -8.656820664281498878, 34.87096338111211935 ) ) ;
#71712 = CARTESIAN_POINT ( 'NONE',  ( 12.21151523731700550, -5.765609946408404518, 34.70566812827425451 ) ) ;
#71713 = B_SPLINE_CURVE_WITH_KNOTS ( 'NONE', 3,
 ( #73031, #44199, #71686, #59063, #4571, #64925, #84785, #3231, #86106, #24381 ),
 .UNSPECIFIED., .F., .F.,
 ( 4, 2, 2, 2, 4 ),
 ( 0.000000000000000000, 0.0001954339857564090194, 0.0003908679715128180387, 0.0005863019572692270039, 0.0007817359430256360774 ),
 .UNSPECIFIED. ) ;
#71714 = CARTESIAN_POINT ( 'NONE',  ( 0.06109907496451789238, -4.749999999999998224, 15.65811829374151287 ) ) ;
#71715 = ORIENTED_EDGE ( 'NONE', *, *, #55855, .F. ) ;
#71716 = CARTESIAN_POINT ( 'NONE',  ( 6.000000000000001776, -2.721908614388771852, 31.22303859784724978 ) ) ;
#71717 = CARTESIAN_POINT ( 'NONE',  ( 6.000000000000001776, -1.129524287112498415, 32.06866353760679544 ) ) ;
#71718 = VERTEX_POINT ( 'NONE', #84294 ) ;
#71719 = ORIENTED_EDGE ( 'NONE', *, *, #105, .F. ) ;
#71720 = CARTESIAN_POINT ( 'NONE',  ( -5.776987155906603277, -12.64618726649961289, 30.78989965857442712 ) ) ;
#71721 = CARTESIAN_POINT ( 'NONE',  ( 11.31553457955469000, -4.762599654559228846, 34.23009711892697737 ) ) ;
#71722 = DIRECTION ( 'NONE',  ( -0.000000000000000000, -0.3420201433256694346, -0.9396926207859080948 ) ) ;
#71723 = EDGE_CURVE ( 'NONE', #31685, #27787, #6180, .T. ) ;
#71724 = CARTESIAN_POINT ( 'NONE',  ( 18.03205128205128105, -3.499999999999999556, 29.75000000000000355 ) ) ;
#71725 = CARTESIAN_POINT ( 'NONE',  ( 5.076923076923075762, -1.790695186598648903, 34.54067556320373455 ) ) ;
#71726 = DIRECTION ( 'NONE',  ( 0.000000000000000000, 0.9848077530122072432, -0.1736481776669354937 ) ) ;
#71727 = VECTOR ( 'NONE', #22973, 1000.000000000000227 ) ;
#71728 = DIRECTION ( 'NONE',  ( -0.000000000000000000, 0.1736481776669307198, -0.9848077530122080203 ) ) ;
#71729 = ORIENTED_EDGE ( 'NONE', *, *, #56450, .T. ) ;
#71730 = DIRECTION ( 'NONE',  ( -0.000000000000000000, 0.9396926207859092051, -0.3420201433256662704 ) ) ;
#71731 = FACE_OUTER_BOUND ( 'NONE', #41680, .T. ) ;
#71732 = AXIS2_PLACEMENT_3D ( 'NONE', #14771, #41352, #62489 ) ;
#71733 = LINE ( 'NONE', #62861, #81510 ) ;
#71734 = CARTESIAN_POINT ( 'NONE',  ( 2.177000841024748112, -3.530157926970578508, 32.79014554554150607 ) ) ;
#71735 = EDGE_LOOP ( 'NONE', ( #19151, #38005, #1605, #20376 ) ) ;
#71736 = CARTESIAN_POINT ( 'NONE',  ( 0.000000000000000000, -11.00000000000000000, 29.75000000000000355 ) ) ;
#71737 = EDGE_CURVE ( 'NONE', #66517, #48076, #50169, .T. ) ;
#71738 = ORIENTED_EDGE ( 'NONE', *, *, #79781, .T. ) ;
#71739 = CARTESIAN_POINT ( 'NONE',  ( -17.77698715590659972, -8.282913670948747864, 34.94150082978203642 ) ) ;
#71740 = SURFACE_STYLE_FILL_AREA ( #11836 ) ;
#71741 = CARTESIAN_POINT ( 'NONE',  ( -19.50000000000000000, -3.499999999999999556, 29.75000000000000355 ) ) ;
#71742 = CARTESIAN_POINT ( 'NONE',  ( -4.153846153846274980, -12.16647553114689728, 32.15551576947799362 ) ) ;
#71743 = EDGE_LOOP ( 'NONE', ( #7269, #69227, #32339, #36574 ) ) ;
#71744 = ADVANCED_FACE ( 'NONE', ( #77079 ), #16260, .F. ) ;
#71745 = DIRECTION ( 'NONE',  ( 0.000000000000000000, 0.000000000000000000, -1.000000000000000000 ) ) ;
#71746 = FACE_OUTER_BOUND ( 'NONE', #43530, .T. ) ;
#71747 = CARTESIAN_POINT ( 'NONE',  ( -10.68065461594093435, -12.70778746994557551, 30.41441678777548319 ) ) ;
#71748 = CARTESIAN_POINT ( 'NONE',  ( -9.442362282929646966, -3.520799739797214389, 33.17531984108286025 ) ) ;
#71749 = ORIENTED_EDGE ( 'NONE', *, *, #51996, .F. ) ;
#71750 = EDGE_CURVE ( 'NONE', #87879, #48963, #71193, .T. ) ;
#71751 = CARTESIAN_POINT ( 'NONE',  ( -0.5916856709766827871, -8.587444163452046197, 34.63053765926554206 ) ) ;
#71752 = ORIENTED_EDGE ( 'NONE', *, *, #23950, .F. ) ;
#71753 = B_SPLINE_CURVE_WITH_KNOTS ( 'NONE', 3,
 ( #81599, #39730, #32962, #59537, #5937, #33410, #33843, #88374, #88815, #60872 ),
 .UNSPECIFIED., .F., .F.,
 ( 4, 2, 2, 2, 4 ),
 ( 0.0007817246256747460882, 0.0009771112852218900684, 0.001172497944769033832, 0.001367884604316177595, 0.001563271263863321575 ),
 .UNSPECIFIED. ) ;
#71754 = VECTOR ( 'NONE', #4993, 1000.000000000000000 ) ;
#71755 = FACE_OUTER_BOUND ( 'NONE', #1255, .T. ) ;
#71756 = ADVANCED_FACE ( 'NONE', ( #50039 ), #1416, .F. ) ;
#71757 = CARTESIAN_POINT ( 'NONE',  ( -16.94639763868943660, -3.625058011473227815, 33.29252011169590020 ) ) ;
#71758 = DIRECTION ( 'NONE',  ( -1.000000000000000000, -0.000000000000000000, -0.000000000000000000 ) ) ;
#71759 = EDGE_CURVE ( 'NONE', #22124, #79174, #76182, .T. ) ;
#71760 = CARTESIAN_POINT ( 'NONE',  ( -9.692307692307814193, -8.656820664282941280, 34.87096338111179961 ) ) ;
#71761 = CARTESIAN_POINT ( 'NONE',  ( -16.15384615384615330, -1.242168528481310874, 33.36296068462461051 ) ) ;
#71762 = VERTEX_POINT ( 'NONE', #15827 ) ;
#71763 = ORIENTED_EDGE ( 'NONE', *, *, #75535, .F. ) ;
#71764 = ORIENTED_EDGE ( 'NONE', *, *, #15942, .F. ) ;
#71765 = ORIENTED_EDGE ( 'NONE', *, *, #9660, .F. ) ;
#71766 = EDGE_CURVE ( 'NONE', #80242, #38437, #26589, .T. ) ;
#71767 = DIRECTION ( 'NONE',  ( -0.000000000000000000, 1.000000000000000000, -0.000000000000000000 ) ) ;
#71768 = CARTESIAN_POINT ( 'NONE',  ( -16.94639737515951339, -3.816742781228458448, 33.13167719472716044 ) ) ;
#71769 = LINE ( 'NONE', #48959, #42474 ) ;
#71770 = CYLINDRICAL_SURFACE ( 'NONE', #85402, 0.2500000000000008882 ) ;
#71771 = CYLINDRICAL_SURFACE ( 'NONE', #2533, 0.2500000000000004996 ) ;
#71772 = CARTESIAN_POINT ( 'NONE',  ( 0.5920641633020240491, -5.195472089885680766, 34.18748526763464923 ) ) ;
#71773 = VECTOR ( 'NONE', #39955, 1000.000000000000000 ) ;
#71774 = AXIS2_PLACEMENT_3D ( 'NONE', #81642, #5539, #20380 ) ;
#71775 = EDGE_CURVE ( 'NONE', #50871, #85765, #56576, .T. ) ;
#71776 = DIRECTION ( 'NONE',  ( 0.000000000000000000, 0.8660254037844377084, 0.5000000000000015543 ) ) ;
#71777 = ADVANCED_FACE ( 'NONE', ( #45048 ), #18043, .F. ) ;
#71778 = CARTESIAN_POINT ( 'NONE',  ( -19.50000000000000000, -11.50000000000000000, 29.75000000000000355 ) ) ;
#71779 = ORIENTED_EDGE ( 'NONE', *, *, #84038, .F. ) ;
#71780 = VERTEX_POINT ( 'NONE', #72528 ) ;
#71781 = ORIENTED_EDGE ( 'NONE', *, *, #27758, .T. ) ;
#71782 = VECTOR ( 'NONE', #29485, 1000.000000000000000 ) ;
#71784 = ORIENTED_EDGE ( 'NONE', *, *, #27618, .T. ) ;
#71783 = DIRECTION ( 'NONE',  ( -0.000000000000000000, 1.000000000000000000, -0.000000000000000000 ) ) ;
#71786 = CARTESIAN_POINT ( 'NONE',  ( 10.61538461538449596, -9.442884908241554243, 34.35708131394783038 ) ) ;
#71785 = DIRECTION ( 'NONE',  ( -0.000000000000000000, -0.9396926207859093161, -0.3420201433256663259 ) ) ;
#71787 = AXIS2_PLACEMENT_3D ( 'NONE', #51104, #24096, #79502 ) ;
#71788 = CARTESIAN_POINT ( 'NONE',  ( 1.450682717965462443, -4.661471528628508665, 34.16647553114624003 ) ) ;
#71789 = CARTESIAN_POINT ( 'NONE',  ( -14.30769230769242739, -10.21337939537710326, 33.94971097300076224 ) ) ;
#71790 = ORIENTED_EDGE ( 'NONE', *, *, #66233, .T. ) ;
#71791 = ORIENTED_EDGE ( 'NONE', *, *, #21616, .F. ) ;
#71792 = CARTESIAN_POINT ( 'NONE',  ( -17.30040800148741198, -11.60425143139329940, 33.02411095842164457 ) ) ;
#71793 = VERTEX_POINT ( 'NONE', #4522 ) ;
#71794 = FACE_BOUND ( 'NONE', #36444, .T. ) ;
#71795 = CARTESIAN_POINT ( 'NONE',  ( 14.98079249982687777, -9.943427161483782584, 34.11278801902876978 ) ) ;
#71796 = DIRECTION ( 'NONE',  ( -1.000000000000000000, 0.000000000000000000, 0.000000000000000000 ) ) ;
#71797 = ORIENTED_EDGE ( 'NONE', *, *, #57702, .F. ) ;
#71798 = EDGE_CURVE ( 'NONE', #26954, #57222, #47947, .T. ) ;
#71799 = CARTESIAN_POINT ( 'NONE',  ( 14.30769230769231015, -2.721908614388771852, 31.22303859784724978 ) ) ;
#71800 = CARTESIAN_POINT ( 'NONE',  ( 16.28437185560972011, -4.459921816937789885, 33.71989282347011851 ) ) ;
#71801 = DIRECTION ( 'NONE',  ( 0.000000000000000000, -6.938893903907222067E-15, 1.000000000000000000 ) ) ;
#71802 = VERTEX_POINT ( 'NONE', #23448 ) ;
#71803 = CARTESIAN_POINT ( 'NONE',  ( -5.999999999999998224, -4.945431358278436385, 36.03766855953609394 ) ) ;
#71804 = CARTESIAN_POINT ( 'NONE',  ( -16.85391172531022619, -2.554770724473668597, 30.48948780036025852 ) ) ;
#71805 = ORIENTED_EDGE ( 'NONE', *, *, #9287, .F. ) ;
#71806 = CARTESIAN_POINT ( 'NONE',  ( 8.096208266067300485, -11.47946981652013498, 33.17500667209847620 ) ) ;
#71807 = CARTESIAN_POINT ( 'NONE',  ( 7.145856464345332171, -10.81320215134717344, 33.49497208177562868 ) ) ;
#71808 = EDGE_LOOP ( 'NONE', ( #6455, #22464, #52242, #21476 ) ) ;
#71809 = CYLINDRICAL_SURFACE ( 'NONE', #47302, 0.2499999999999979738 ) ;
#71810 = CARTESIAN_POINT ( 'NONE',  ( -4.153846153846152411, -4.945431358278436385, 36.03766855953609394 ) ) ;
#71811 = DIRECTION ( 'NONE',  ( 0.000000000000000000, 0.6427876096865373645, -0.7660444431189797898 ) ) ;
#71812 = FACE_OUTER_BOUND ( 'NONE', #59567, .T. ) ;
#71813 = CARTESIAN_POINT ( 'NONE',  ( -15.23076923076922995, -13.57706302396349152, 30.56769352161908060 ) ) ;
#71814 = ADVANCED_FACE ( 'NONE', ( #51336 ), #52256, .F. ) ;
#71815 = DIRECTION ( 'NONE',  ( -0.000000000000000000, 0.9848077530122085754, -0.1736481776669273613 ) ) ;
#71816 = B_SPLINE_CURVE_WITH_KNOTS ( 'NONE', 3,
 ( #72535, #18048, #44156, #79751, #30660, #72987, #17147, #3187, #86519, #10845 ),
 .UNSPECIFIED., .F., .F.,
 ( 4, 2, 2, 2, 4 ),
 ( 0.0007817246256747453293, 0.0009771112852218889842, 0.001172497944769032531, 0.001367884604316176294, 0.001563271263863319840 ),
 .UNSPECIFIED. ) ;
#71818 = CARTESIAN_POINT ( 'NONE',  ( 11.47270811014820779, -7.249945578846651806, 34.99404164642496795 ) ) ;
#71817 = CYLINDRICAL_SURFACE ( 'NONE', #53383, 8.000000000000000000 ) ;
#71819 = CARTESIAN_POINT ( 'NONE',  ( -16.02332045208259359, -11.93748526763465279, 32.05452791011430946 ) ) ;
#71821 = CARTESIAN_POINT ( 'NONE',  ( 8.992242120843615183, -2.758310577978208666, 31.33698337089302299 ) ) ;
#71820 = LINE ( 'NONE', #60864, #61641 ) ;
#71822 = CARTESIAN_POINT ( 'NONE',  ( -2.557669051740897537, -5.643011162660950042, 34.66104346484419096 ) ) ;
#71823 = CARTESIAN_POINT ( 'NONE',  ( -1.987747218494660295, -5.598659921968651254, 23.74813170625849068 ) ) ;
#71825 = ADVANCED_FACE ( 'NONE', ( #4061 ), #30223, .F. ) ;
#71824 = EDGE_LOOP ( 'NONE', ( #71658, #42396, #72412 ) ) ;
#71826 = CARTESIAN_POINT ( 'NONE',  ( 18.24994551834813805, -11.86320923018887541, 32.19269448109604781 ) ) ;
#71827 = VERTEX_POINT ( 'NONE', #51794 ) ;
#71828 = EDGE_CURVE ( 'NONE', #58400, #87066, #50902, .T. ) ;
#71829 = CARTESIAN_POINT ( 'NONE',  ( 20.00000000000000000, -4.000000000000000000, 29.75000000000000355 ) ) ;
#71830 = ORIENTED_EDGE ( 'NONE', *, *, #27790, .T. ) ;
#71831 = CARTESIAN_POINT ( 'NONE',  ( -13.31936024510254413, -2.379036618887895305, 30.90682066428158592 ) ) ;
#71832 = EDGE_LOOP ( 'NONE', ( #13866, #60299 ) ) ;
#71833 = LINE ( 'NONE', #9264, #61334 ) ;
#71834 = CARTESIAN_POINT ( 'NONE',  ( 0.06109907496454976272, -10.25000000000000000, 24.52938170625849423 ) ) ;
#71835 = FACE_OUTER_BOUND ( 'NONE', #40726, .T. ) ;
#71836 = CARTESIAN_POINT ( 'NONE',  ( -4.853911725310227965, -2.758310577978207778, 31.33698337089303010 ) ) ;
#71837 = CARTESIAN_POINT ( 'NONE',  ( 6.989144256427000990, -9.905515769479277921, 34.41647553114623292 ) ) ;
#71838 = CARTESIAN_POINT ( 'NONE',  ( -18.00000000000000000, -11.16473453929635440, 33.15142922261927083 ) ) ;
#71839 = EDGE_CURVE ( 'NONE', #26485, #50475, #13661, .T. ) ;
#71840 = LINE ( 'NONE', #37611, #76295 ) ;
#71841 = CARTESIAN_POINT ( 'NONE',  ( -7.715362038329064198, -2.729792928343270919, 31.24908615093345077 ) ) ;
#71842 = CARTESIAN_POINT ( 'NONE',  ( 5.934729554039225974, -4.481592998940161721, 33.73612834413957984 ) ) ;
#71843 = B_SPLINE_CURVE_WITH_KNOTS ( 'NONE', 3,
 ( #19538, #60964, #28071, #15006, #62727, #76702 ),
 .UNSPECIFIED., .F., .F.,
 ( 4, 2, 4 ),
 ( 0.0003909512603273880690, 0.0005862562993132132720, 0.0007815613382990384750 ),
 .UNSPECIFIED. ) ;
#71844 = CARTESIAN_POINT ( 'NONE',  ( 3.749999999999992006, -5.946699141100872943, 15.64062500000000178 ) ) ;
#71845 = CARTESIAN_POINT ( 'NONE',  ( -11.53846153846153655, -12.78798330534102945, 29.74999999999997868 ) ) ;
#71846 = CARTESIAN_POINT ( 'NONE',  ( -15.16470087976679437, -2.538708090699994813, 30.37095296980875503 ) ) ;
#71847 = CARTESIAN_POINT ( 'NONE',  ( 10.48469401227430708, -5.496505350115501010, 34.60290016733514307 ) ) ;
#71848 = CARTESIAN_POINT ( 'NONE',  ( -2.651650429449565305, -4.848349570550461785, 19.00000000000000000 ) ) ;
#71849 = VECTOR ( 'NONE', #39605, 1000.000000000000000 ) ;
#71850 = ORIENTED_EDGE ( 'NONE', *, *, #7308, .F. ) ;
#71851 = CARTESIAN_POINT ( 'NONE',  ( -19.50000000000000000, -3.499999999999999556, 29.75000000000000355 ) ) ;
#71852 = CARTESIAN_POINT ( 'NONE',  ( 11.60371710973756443, -6.026961402152789304, 34.52809138561124769 ) ) ;
#71853 = CARTESIAN_POINT ( 'NONE',  ( 5.999999999999878320, -9.528491918059723176, 34.59228464037033035 ) ) ;
#71854 = CARTESIAN_POINT ( 'NONE',  ( 18.13052570176355971, -10.88167719472716399, 33.43325721877153711 ) ) ;
#71855 = EDGE_CURVE ( 'NONE', #85917, #31266, #29783, .T. ) ;
#71856 = B_SPLINE_CURVE_WITH_KNOTS ( 'NONE', 3,
 ( #69791, #8099, #34231, #35570, #83764, #27037, #61693, #13, #27482, #64784 ),
 .UNSPECIFIED., .F., .F.,
 ( 4, 2, 2, 2, 4 ),
 ( 0.0007817246256747447872, 0.0009771112852218876831, 0.001172497944769030579, 0.001367884604316173475, 0.001563271263863316371 ),
 .UNSPECIFIED. ) ;
#71857 = VECTOR ( 'NONE', #4015, 1000.000000000000000 ) ;
#71858 = CARTESIAN_POINT ( 'NONE',  ( 8.638539302563211564, -11.71456829005830080, 32.44064028649416542 ) ) ;
#71859 = CARTESIAN_POINT ( 'NONE',  ( 2.177000841024747224, -12.11776431015576172, 31.66791131148498906 ) ) ;
#71860 = VECTOR ( 'NONE', #78933, 1000.000000000000227 ) ;
#71861 = VERTEX_POINT ( 'NONE', #71633 ) ;
#71862 = CARTESIAN_POINT ( 'NONE',  ( -10.36538461538467715, -7.565270000091922853, 34.99999999999999289 ) ) ;
#71863 = ORIENTED_EDGE ( 'NONE', *, *, #44384, .T. ) ;
#71864 = EDGE_LOOP ( 'NONE', ( #44677, #33783, #16608, #8367 ) ) ;
#71865 = CARTESIAN_POINT ( 'NONE',  ( -9.442362282929646966, -2.986452184633680229, 32.43230066228895225 ) ) ;
#71866 = CARTESIAN_POINT ( 'NONE',  ( -6.249976744048589161, -12.65889640711025521, 30.72598325615533454 ) ) ;
#71867 = CARTESIAN_POINT ( 'NONE',  ( 16.21991450484859243, -2.721908614388772296, 31.22303859784725333 ) ) ;
#71868 = CARTESIAN_POINT ( 'NONE',  ( 4.219101725122176738, -3.835265460703683349, 33.15142922261929925 ) ) ;
#71869 = CARTESIAN_POINT ( 'NONE',  ( -18.00000000000000000, -13.49681301100524244, 30.80739993210377392 ) ) ;
#71870 = ORIENTED_EDGE ( 'NONE', *, *, #8060, .T. ) ;
#71871 = CARTESIAN_POINT ( 'NONE',  ( 8.899756470994336865, -3.816742781228458448, 33.13167719472716044 ) ) ;
#71872 = ORIENTED_EDGE ( 'NONE', *, *, #9648, .F. ) ;
#71873 = VERTEX_POINT ( 'NONE', #9939 ) ;
#71874 = ADVANCED_FACE ( 'NONE', ( #30652 ), #58122, .F. ) ;
#71875 = ADVANCED_FACE ( 'NONE', ( #86054 ), #79298, .T. ) ;
#71876 = DIRECTION ( 'NONE',  ( 0.000000000000000000, 0.000000000000000000, 1.000000000000000000 ) ) ;
#71877 = CARTESIAN_POINT ( 'NONE',  ( 16.37685750545900376, -12.39991518177334129, 30.74647679643404530 ) ) ;
#71878 = B_SPLINE_CURVE_WITH_KNOTS ( 'NONE', 3,
 ( #17, #67589, #26597, #34235, #68035, #27926, #6338, #61251, #21161, #48189 ),
 .UNSPECIFIED., .F., .F.,
 ( 4, 2, 2, 2, 4 ),
 ( 0.000000000000000000, 0.0001954311564186876334, 0.0003908623128373752667, 0.0005862934692560629272, 0.0007817246256747505334 ),
 .UNSPECIFIED. ) ;
#71879 = CARTESIAN_POINT ( 'NONE',  ( -13.38461538461538325, -13.75783147151868846, 33.36296068462461051 ) ) ;
#71880 = EDGE_CURVE ( 'NONE', #18025, #66904, #72672, .T. ) ;
#71881 = PLANE ( 'NONE',  #11142 ) ;
#71882 = CARTESIAN_POINT ( 'NONE',  ( -16.82686876528476461, -3.136992222400443175, 32.19305428654138979 ) ) ;
#71883 = ADVANCED_FACE ( 'NONE', ( #13057 ), #54029, .F. ) ;
#71884 = CARTESIAN_POINT ( 'NONE',  ( -16.02305434602137169, -2.729792928343270031, 31.24908615093345432 ) ) ;
#71885 = VERTEX_POINT ( 'NONE', #5417 ) ;
#71886 = ORIENTED_EDGE ( 'NONE', *, *, #62086, .F. ) ;
#71887 = CARTESIAN_POINT ( 'NONE',  ( 3.750000000000000888, -7.499999999999978684, 20.71875000000000000 ) ) ;
#71888 = VERTEX_POINT ( 'NONE', #5860 ) ;
#71890 = EDGE_LOOP ( 'NONE', ( #19436, #24164, #4992, #64304 ) ) ;
#71889 = CARTESIAN_POINT ( 'NONE',  ( -12.59168567097668223, -11.47017969459904130, 32.78971311882034456 ) ) ;
#71891 = ADVANCED_FACE ( 'NONE', ( #68007 ), #35422, .F. ) ;
#71892 = CYLINDRICAL_SURFACE ( 'NONE', #49309, 0.2499999999999997502 ) ;
#71893 = CARTESIAN_POINT ( 'NONE',  ( 3.230769230769231726, -9.819645486525091727, 36.12317359536749706 ) ) ;
#71894 = LINE ( 'NONE', #87656, #81150 ) ;
#71895 = ORIENTED_EDGE ( 'NONE', *, *, #65155, .F. ) ;
#71896 = EDGE_CURVE ( 'NONE', #63245, #87401, #42710, .T. ) ;
#71897 = CARTESIAN_POINT ( 'NONE',  ( 19.00000000000000000, 8.999999999999996447, 23.75000000000000000 ) ) ;
#71898 = ORIENTED_EDGE ( 'NONE', *, *, #839, .T. ) ;
#71899 = CARTESIAN_POINT ( 'NONE',  ( -13.38461538461538325, -11.35647404775217417, 33.31231777344666511 ) ) ;
#71900 = CARTESIAN_POINT ( 'NONE',  ( 17.77707304109314634, -12.64616026154729411, 30.79003144601914244 ) ) ;
#71901 = CARTESIAN_POINT ( 'NONE',  ( -15.10024379253558635, -3.068774925481847493, 32.56582465632704526 ) ) ;
#71904 = CARTESIAN_POINT ( 'NONE',  ( -10.74553258511631171, -5.915902021225889484, 34.75552854090298638 ) ) ;
#71903 = VECTOR ( 'NONE', #49877, 1000.000000000000000 ) ;
#71902 = DIRECTION ( 'NONE',  ( 0.000000000000000000, 0.1736481776669275834, 0.9848077530122086864 ) ) ;
#71905 = VECTOR ( 'NONE', #81996, 1000.000000000000114 ) ;
#71906 = CARTESIAN_POINT ( 'NONE',  ( 15.90386942290380290, -2.564618984488975517, 30.55390908950641915 ) ) ;
#71907 = CARTESIAN_POINT ( 'NONE',  ( -0.2387587925603949501, -12.69155399931963046, 30.53255429739158444 ) ) ;
#71908 = ORIENTED_EDGE ( 'NONE', *, *, #10966, .F. ) ;
#71909 = ADVANCED_FACE ( 'NONE', ( #26573 ), #42196, .F. ) ;
#71910 = CARTESIAN_POINT ( 'NONE',  ( 1.384615384615386802, -13.87047571288749737, 32.06866353760679544 ) ) ;
#71911 = CARTESIAN_POINT ( 'NONE',  ( 8.834486340506797930, -6.879047030191282275, 34.71129190930002295 ) ) ;
#71912 = ORIENTED_EDGE ( 'NONE', *, *, #56819, .T. ) ;
#71913 = DIRECTION ( 'NONE',  ( 0.000000000000000000, 0.000000000000000000, 1.000000000000000000 ) ) ;
#71914 = CARTESIAN_POINT ( 'NONE',  ( -5.010854725920638408, -5.557115091759786019, 34.35708131394839882 ) ) ;
#71915 = CARTESIAN_POINT ( 'NONE',  ( 3.480769230770666578, -7.500000000000155431, 34.75000000000007105 ) ) ;
#71916 = CYLINDRICAL_SURFACE ( 'NONE', #42941, 4.000000000000000000 ) ;
#71917 = CARTESIAN_POINT ( 'NONE',  ( 7.623227628637698317, -8.239355502252617924, 34.69524867566427417 ) ) ;
#71918 = FACE_BOUND ( 'NONE', #49555, .T. ) ;
#71920 = CARTESIAN_POINT ( 'NONE',  ( -10.48454628489785279, -7.277220318596961057, 34.99547417642776992 ) ) ;
#71919 = CARTESIAN_POINT ( 'NONE',  ( 12.39626846098214230, -10.33852847137145048, 34.16647553114627556 ) ) ;
#71921 = B_SPLINE_CURVE_WITH_KNOTS ( 'NONE', 3,
 ( #64838, #16658, #11247, #58523, #72048, #52218, #79708, #4489, #44562, #85574 ),
 .UNSPECIFIED., .F., .F.,
 ( 4, 2, 2, 2, 4 ),
 ( 0.000000000000000000, 0.0001954339857564083688, 0.0003908679715128167377, 0.0005863019572692250523, 0.0007817359430256334753 ),
 .UNSPECIFIED. ) ;
#71922 = DIRECTION ( 'NONE',  ( 0.000000000000000000, 0.6427876096865368094, 0.7660444431189802339 ) ) ;
#71924 = CARTESIAN_POINT ( 'NONE',  ( -11.53846153846166089, -11.06231777344772027, 33.60647404775119895 ) ) ;
#71923 = LINE ( 'NONE', #86804, #4084 ) ;
#71925 = CARTESIAN_POINT ( 'NONE',  ( 15.93036121012220541, -10.81261337010820256, 33.49550067578627477 ) ) ;
#71926 = CARTESIAN_POINT ( 'NONE',  ( 1.384615384615701439, -2.255955759149395501, 30.00000000000324363 ) ) ;
#71927 = CARTESIAN_POINT ( 'NONE',  ( -2.694853999681210865, -4.891553140782108677, 19.99813170625848713 ) ) ;
#71928 = B_SPLINE_CURVE_WITH_KNOTS ( 'NONE', 3,
 ( #87375, #18461, #61647, #45916, #61200, #19346, #11708, #53112, #39185, #74743 ),
 .UNSPECIFIED., .F., .F.,
 ( 4, 2, 2, 2, 4 ),
 ( 0.0007817246256747484735, 0.0009771112852218931041, 0.001172497944769037735, 0.001367884604316182365, 0.001563271263863326996 ),
 .UNSPECIFIED. ) ;
#71929 = EDGE_CURVE ( 'NONE', #80088, #45538, #55594, .T. ) ;
#71930 = VERTEX_POINT ( 'NONE', #88734 ) ;
#71931 = FACE_OUTER_BOUND ( 'NONE', #60279, .T. ) ;
#71932 = EDGE_CURVE ( 'NONE', #73377, #20451, #19367, .T. ) ;
#71933 = CARTESIAN_POINT ( 'NONE',  ( -4.946397375159510723, -3.285477652293412820, 32.44071101563363158 ) ) ;
#71934 = CYLINDRICAL_SURFACE ( 'NONE', #67569, 0.2500000000000002220 ) ;
#71935 = CARTESIAN_POINT ( 'NONE',  ( -0.3256479613346683899, -10.23169528853315491, 28.86076157308317391 ) ) ;
#71936 = CARTESIAN_POINT ( 'NONE',  ( -4.403822897894744237, -4.818429247618089661, 34.26397095200675125 ) ) ;
#71937 = CARTESIAN_POINT ( 'NONE',  ( -16.85414340794500276, -8.540255544307068902, 34.89611431652622286 ) ) ;
#71938 = CARTESIAN_POINT ( 'NONE',  ( -2.694853999681210865, -4.891553140782108677, 18.74813170625849068 ) ) ;
#71939 = DIRECTION ( 'NONE',  ( -0.000000000000000000, 0.3420201433256694346, -0.9396926207859080948 ) ) ;
#71940 = DIRECTION ( 'NONE',  ( -0.000000000000000000, -0.1736481776669307198, -0.9848077530122080203 ) ) ;
#71941 = EDGE_CURVE ( 'NONE', #86769, #69764, #1859, .T. ) ;
#71942 = CARTESIAN_POINT ( 'NONE',  ( -7.623374177175779032, -10.23759521482555357, 34.22997729860117033 ) ) ;
#71943 = CARTESIAN_POINT ( 'NONE',  ( 17.77707304109314634, -8.282780595021769443, 34.94152052738834868 ) ) ;
#71944 = CARTESIAN_POINT ( 'NONE',  ( -8.769230769230768274, -9.584722331328613620, 36.20867863119891439 ) ) ;
#71945 = CARTESIAN_POINT ( 'NONE',  ( 10.86538461538461675, -2.499999999999998668, 29.75000000000000355 ) ) ;
#71946 = CARTESIAN_POINT ( 'NONE',  ( -6.250023224221458840, -12.07920672191015221, 32.31858351112116168 ) ) ;
#71947 = EDGE_CURVE ( 'NONE', #20065, #28968, #82433, .T. ) ;
#71948 = LINE ( 'NONE', #30519, #35584 ) ;
#71949 = EDGE_LOOP ( 'NONE', ( #36192, #616 ) ) ;
#71950 = DIRECTION ( 'NONE',  ( -0.000000000000000000, -0.000000000000000000, -1.000000000000000000 ) ) ;
#71951 = CARTESIAN_POINT ( 'NONE',  ( -17.07692307692319744, -2.892918686052165622, 31.69288490824153470 ) ) ;
#71952 = CARTESIAN_POINT ( 'NONE',  ( -2.724691934501246582, -6.299813628509474128, 25.42374329374151998 ) ) ;
#71953 = CARTESIAN_POINT ( 'NONE',  ( 0.4615384615384611200, -1.129524287112498415, 32.06866353760679544 ) ) ;
#71954 = CARTESIAN_POINT ( 'NONE',  ( 3.453780582382080411, -11.76359900205217457, 32.36225158514719880 ) ) ;
#71955 = ORIENTED_EDGE ( 'NONE', *, *, #81186, .T. ) ;
#71956 = CARTESIAN_POINT ( 'NONE',  ( -6.792551484843277976, -10.31582465632705237, 34.18122507451815295 ) ) ;
#71957 = CARTESIAN_POINT ( 'NONE',  ( -0.6844654204453104462, -12.64616026154729411, 30.79003144601913533 ) ) ;
#71959 = ORIENTED_EDGE ( 'NONE', *, *, #55203, .F. ) ;
#71958 = CARTESIAN_POINT ( 'NONE',  ( 7.596130608860881317, -2.587272538249754117, 30.68239716806877837 ) ) ;
#71960 = CARTESIAN_POINT ( 'NONE',  ( 11.60452887181161508, -4.661471528628508665, 34.16647553114624003 ) ) ;
#71961 = DIRECTION ( 'NONE',  ( -0.000000000000000000, -0.7660444431189791237, -0.6427876096865379196 ) ) ;
#71962 = ADVANCED_FACE ( 'NONE', ( #52978 ), #3463, .F. ) ;
#71963 = DIRECTION ( 'NONE',  ( 0.000000000000000000, -6.938893903907222067E-15, 1.000000000000000000 ) ) ;
#71964 = CARTESIAN_POINT ( 'NONE',  ( -15.36132914438259434, -2.254533558242299396, 29.97296025877828285 ) ) ;
#71965 = EDGE_CURVE ( 'NONE', #79365, #47433, #80475, .T. ) ;
#71966 = ORIENTED_EDGE ( 'NONE', *, *, #19148, .T. ) ;
#71967 = B_SPLINE_CURVE_WITH_KNOTS ( 'NONE', 3,
 ( #17804, #11041, #11938, #45257, #66876, #4276, #72729, #37613, #71842, #65076 ),
 .UNSPECIFIED., .F., .F.,
 ( 4, 2, 2, 2, 4 ),
 ( 0.000000000000000000, 0.0001954339857564075828, 0.0003908679715128151656, 0.0005863019572692227755, 0.0007817359430256303312 ),
 .UNSPECIFIED. ) ;
#71968 = CARTESIAN_POINT ( 'NONE',  ( -12.59222906464876957, -2.295517848115769421, 30.44137282052137294 ) ) ;
#71969 = EDGE_CURVE ( 'NONE', #13360, #68144, #52095, .T. ) ;
#71970 = CARTESIAN_POINT ( 'NONE',  ( 10.61538461538449418, -4.320704448113951379, 33.92786785259630022 ) ) ;
#71972 = FACE_OUTER_BOUND ( 'NONE', #84083, .T. ) ;
#71971 = AXIS2_PLACEMENT_3D ( 'NONE', #59728, #60607, #26391 ) ;
#71973 = ORIENTED_EDGE ( 'NONE', *, *, #85663, .T. ) ;
#71974 = EDGE_LOOP ( 'NONE', ( #72676, #82123 ) ) ;
#71975 = VERTEX_POINT ( 'NONE', #80022 ) ;
#71976 = AXIS2_PLACEMENT_3D ( 'NONE', #8034, #62513, #1264 ) ;
#71977 = CARTESIAN_POINT ( 'NONE',  ( 3.361559671736179311, -2.295524264805589354, 30.44142389570982488 ) ) ;
#71978 = CYLINDRICAL_SURFACE ( 'NONE', #71655, 0.2500000000000009437 ) ;
#71979 = CARTESIAN_POINT ( 'NONE',  ( -2.980714810855777053, -8.346898887586323923, 34.93166121998716278 ) ) ;
#71980 = AXIS2_PLACEMENT_3D ( 'NONE', #53896, #52554, #73284 ) ;
#71981 = VECTOR ( 'NONE', #79115, 1000.000000000000227 ) ;
#71982 = CARTESIAN_POINT ( 'NONE',  ( 15.23076923076923173, -3.513871655860378418, 32.76840700105978499 ) ) ;
#71983 = ORIENTED_EDGE ( 'NONE', *, *, #55924, .F. ) ;
#71984 = ORIENTED_EDGE ( 'NONE', *, *, #10914, .T. ) ;
#71986 = VERTEX_POINT ( 'NONE', #30929 ) ;
#71985 = CARTESIAN_POINT ( 'NONE',  ( -1.161604033002534564, -4.887748414852792322, 34.01359900205216746 ) ) ;
#71987 = LINE ( 'NONE', #30992, #7684 ) ;
#71988 = CARTESIAN_POINT ( 'NONE',  ( -3.230769230769229949, -2.833524468853757305, 32.15551576947925838 ) ) ;
#71989 = CARTESIAN_POINT ( 'NONE',  ( -13.31935981333936425, -12.46129190930001052, 30.37095296980870174 ) ) ;
#71990 = ORIENTED_EDGE ( 'NONE', *, *, #58053, .T. ) ;
#71991 = ORIENTED_EDGE ( 'NONE', *, *, #9770, .T. ) ;
#71992 = EDGE_LOOP ( 'NONE', ( #24878, #47748 ) ) ;
#71994 = ORIENTED_EDGE ( 'NONE', *, *, #42981, .T. ) ;
#71993 = CARTESIAN_POINT ( 'NONE',  ( 8.769230769230768274, -2.538708090699994813, 30.37095296980875503 ) ) ;
#71995 = EDGE_CURVE ( 'NONE', #36536, #3856, #80039, .T. ) ;
#71996 = CARTESIAN_POINT ( 'NONE',  ( -5.750054481651857508, -8.433404298154334455, 34.66254593164985920 ) ) ;
#71997 = CARTESIAN_POINT ( 'NONE',  ( -5.207070286361298095, -10.19110544564092002, 33.96427741523702792 ) ) ;
#71998 = VERTEX_POINT ( 'NONE', #65602 ) ;
#71999 = DIRECTION ( 'NONE',  ( -0.000000000000000000, 1.000000000000000000, -0.000000000000000000 ) ) ;
#72000 = VECTOR ( 'NONE', #6171, 1000.000000000000000 ) ;
#72001 = CARTESIAN_POINT ( 'NONE',  ( 4.153846153846154188, -1.129524287112498415, 32.06866353760679544 ) ) ;
#72002 = EDGE_CURVE ( 'NONE', #39482, #2976, #72367, .T. ) ;
#72003 = DIRECTION ( 'NONE',  ( -0.000000000000000000, 0.1736481776669307198, -0.9848077530122080203 ) ) ;
#72004 = FACE_BOUND ( 'NONE', #36929, .T. ) ;
#72005 = CARTESIAN_POINT ( 'NONE',  ( -3.230769230769351186, -11.48612834414049644, 32.76840700105863391 ) ) ;
#72006 = CARTESIAN_POINT ( 'NONE',  ( 9.823146110320458035, -7.277220443632450575, 34.74524770363009196 ) ) ;
#72007 = LINE ( 'NONE', #84658, #69587 ) ;
#72009 = CARTESIAN_POINT ( 'NONE',  ( 9.822833394071258439, -3.285477652293413264, 32.44071101563363158 ) ) ;
#72008 = CARTESIAN_POINT ( 'NONE',  ( 17.32692307692308020, -2.499999999999999556, 29.81604066197449754 ) ) ;
#72010 = CARTESIAN_POINT ( 'NONE',  ( 11.40777007179398161, -11.18331474514187995, 33.13161551792790505 ) ) ;
#72011 = DIRECTION ( 'NONE',  ( -0.000000000000000000, 0.8660254037844397068, -0.4999999999999978906 ) ) ;
#72012 = ORIENTED_EDGE ( 'NONE', *, *, #87519, .T. ) ;
#72013 = CARTESIAN_POINT ( 'NONE',  ( -5.750054481651856619, -11.86320923018887541, 32.19269448109604781 ) ) ;
#72014 = EDGE_LOOP ( 'NONE', ( #67498, #73125 ) ) ;
#72015 = ORIENTED_EDGE ( 'NONE', *, *, #86418, .T. ) ;
#72017 = CARTESIAN_POINT ( 'NONE',  ( 10.68063975489745232, -12.16647553114626490, 32.15551576947920864 ) ) ;
#72016 = DIRECTION ( 'NONE',  ( 0.000000000000000000, 0.000000000000000000, -1.000000000000000000 ) ) ;
#72018 = EDGE_CURVE ( 'NONE', #4532, #41328, #41578, .T. ) ;
#72019 = CYLINDRICAL_SURFACE ( 'NONE', #77351, 0.2499999999999994726 ) ;
#72020 = CARTESIAN_POINT ( 'NONE',  ( 2.530705151785702878, -2.308499170217967134, 30.53291367094873721 ) ) ;
#72021 = CARTESIAN_POINT ( 'NONE',  ( -4.023320715612507037, -3.625058011473227815, 33.29252011169590020 ) ) ;
#72022 = EDGE_LOOP ( 'NONE', ( #58250, #43988 ) ) ;
#72023 = CARTESIAN_POINT ( 'NONE',  ( -11.25641025641025550, -3.499999999999999556, 29.75000000000000355 ) ) ;
#72024 = CARTESIAN_POINT ( 'NONE',  ( 6.792929713638702793, -3.817052484675422797, 33.13202310037935661 ) ) ;
#72025 = CARTESIAN_POINT ( 'NONE',  ( -4.500000000000003553, 7.499999999999996447, 13.50000000000000178 ) ) ;
#72026 = AXIS2_PLACEMENT_3D ( 'NONE', #73140, #19087, #62275 ) ;
#72027 = DIRECTION ( 'NONE',  ( -0.000000000000000000, 0.6427876096865404731, -0.7660444431189770143 ) ) ;
#72028 = CARTESIAN_POINT ( 'NONE',  ( -14.98082382139119062, -10.92531984108285670, 33.72920026020278073 ) ) ;
#72029 = CARTESIAN_POINT ( 'NONE',  ( -3.749999999999988454, -9.053300858899127945, 15.01562500000000178 ) ) ;
#72030 = ORIENTED_EDGE ( 'NONE', *, *, #56579, .F. ) ;
#72031 = EDGE_CURVE ( 'NONE', #13813, #50611, #28668, .T. ) ;
#72032 = EDGE_LOOP ( 'NONE', ( #84915, #42849, #54496, #72530 ) ) ;
#72033 = CARTESIAN_POINT ( 'NONE',  ( -14.53061926659915315, -4.762599654559228846, 34.23009711892697737 ) ) ;
#72034 = ADVANCED_FACE ( 'NONE', ( #58853 ), #51630, .F. ) ;
#72035 = ORIENTED_EDGE ( 'NONE', *, *, #75129, .T. ) ;
#72036 = CARTESIAN_POINT ( 'NONE',  ( 7.846153846153846700, -6.343179335718451384, 34.87096338111211935 ) ) ;
#72037 = CARTESIAN_POINT ( 'NONE',  ( -12.21159294319032362, -10.05730279482229683, 34.04704008940765902 ) ) ;
#72038 = CARTESIAN_POINT ( 'NONE',  ( -16.15384615384627409, -5.219633306517616589, 34.19971097300220464 ) ) ;
#72039 = CYLINDRICAL_SURFACE ( 'NONE', #44263, 0.2499999999999973355 ) ;
#72040 = CARTESIAN_POINT ( 'NONE',  ( -1.553300858899081538, -11.25000000000000711, 17.35937500000000000 ) ) ;
#72041 = CARTESIAN_POINT ( 'NONE',  ( -13.60754160213153163, -8.239355502252617924, 34.69524867566427417 ) ) ;
#72042 = ORIENTED_EDGE ( 'NONE', *, *, #49170, .F. ) ;
#72044 = PLANE ( 'NONE',  #67441 ) ;
#72043 = PRODUCT_DEFINITION_FORMATION_WITH_SPECIFIED_SOURCE ( 'ANY', '', #88677, .NOT_KNOWN. ) ;
#72046 = EDGE_LOOP ( 'NONE', ( #62380, #57667 ) ) ;
#72045 = CARTESIAN_POINT ( 'NONE',  ( 5.076923076923075762, -1.466349020453238561, 30.81389545987213907 ) ) ;
#72047 = LINE ( 'NONE', #79707, #12332 ) ;
#72048 = CARTESIAN_POINT ( 'NONE',  ( 14.05771557674995265, -12.17611988154120972, 31.52148481390971213 ) ) ;
#72049 = CARTESIAN_POINT ( 'NONE',  ( 2.084207363968360482, -3.236172620538810385, 32.36188796281390267 ) ) ;
#72050 = CARTESIAN_POINT ( 'NONE',  ( 11.53846153846141576, -8.656820664282941280, 34.87096338111179961 ) ) ;
#72052 = ADVANCED_FACE ( 'NONE', ( #86359 ), #78692, .F. ) ;
#72051 = DIRECTION ( 'NONE',  ( -0.000000000000000000, -0.5000000000000009992, -0.8660254037844380415 ) ) ;
#72053 = CARTESIAN_POINT ( 'NONE',  ( 7.780883845597525550, -3.643525952247789412, 33.31231777344662959 ) ) ;
#72054 = DIRECTION ( 'NONE',  ( 0.000000000000000000, 1.000000000000000000, 0.000000000000000000 ) ) ;
#72055 = CARTESIAN_POINT ( 'NONE',  ( -1.492201783934593573, -3.724691934501250135, 18.07999329374151287 ) ) ;
#72056 = ORIENTED_EDGE ( 'NONE', *, *, #28727, .T. ) ;
#72057 = B_SPLINE_CURVE_WITH_KNOTS ( 'NONE', 3,
 ( #66696, #81110, #19396, #59039, #79323, #46421, #3645, #24812, #58589, #10866 ),
 .UNSPECIFIED., .F., .F.,
 ( 4, 2, 2, 2, 4 ),
 ( 0.0007817246336856291692, 0.0009771112958940105907, 0.001172497958102391904, 0.001367884620310773434, 0.001563271282519154747 ),
 .UNSPECIFIED. ) ;
#72058 = DIRECTION ( 'NONE',  ( 0.000000000000000000, 0.000000000000000000, 1.000000000000000000 ) ) ;
#72059 = CARTESIAN_POINT ( 'NONE',  ( -13.16183571563731647, -10.23759521482555357, 34.22997729860117033 ) ) ;
#72060 = CARTESIAN_POINT ( 'NONE',  ( -14.30769230769230660, -13.37000171582298513, 34.34916445242398453 ) ) ;
#72061 = CARTESIAN_POINT ( 'NONE',  ( -2.749999999999991562, -8.639087296526025028, 25.01562500000000000 ) ) ;
#72062 = B_SPLINE_CURVE_WITH_KNOTS ( 'NONE', 3,
 ( #2046, #87044, #10476, #73061, #77261, #73516, #24413, #70510, #31173, #86592 ),
 .UNSPECIFIED., .F., .F.,
 ( 4, 2, 2, 2, 4 ),
 ( 0.000000000000000000, 0.0001954311564186876334, 0.0003908623128373752667, 0.0005862934692560629272, 0.0007817246256747505334 ),
 .UNSPECIFIED. ) ;
#72063 = CARTESIAN_POINT ( 'NONE',  ( -13.44988583057615905, -12.46129190929999986, 30.37095296980880832 ) ) ;
#72064 = CARTESIAN_POINT ( 'NONE',  ( 16.08857615328983925, -5.094484230520675894, 34.41647553114621161 ) ) ;
#72065 = ORIENTED_EDGE ( 'NONE', *, *, #1363, .F. ) ;
#72066 = CARTESIAN_POINT ( 'NONE',  ( 2.749999999999995115, -6.360912703473971419, 18.14062500000000355 ) ) ;
#72067 = CARTESIAN_POINT ( 'NONE',  ( -2.307692307692305711, -11.11383981884818262, 36.00935417666054406 ) ) ;
#72068 = ADVANCED_FACE ( 'NONE', ( #37696 ), #61845, .F. ) ;
#72069 = EDGE_LOOP ( 'NONE', ( #84725, #69901 ) ) ;
#72070 = CARTESIAN_POINT ( 'NONE',  ( -3.903791733932698182, -2.544122305571457687, 31.48381861865059150 ) ) ;
#72071 = ORIENTED_EDGE ( 'NONE', *, *, #19023, .T. ) ;
#72072 = VECTOR ( 'NONE', #43065, 1000.000000000000000 ) ;
#72073 = CARTESIAN_POINT ( 'NONE',  ( 17.86930853333243974, -6.413092428213692742, 34.63065189839063152 ) ) ;
#72074 = EDGE_CURVE ( 'NONE', #856, #8541, #55469, .T. ) ;
#72075 = EDGE_CURVE ( 'NONE', #23009, #30124, #56433, .T. ) ;
#72076 = CARTESIAN_POINT ( 'NONE',  ( 3.930361210122202742, -3.754499324213721234, 33.06261337010820256 ) ) ;
#72077 = CARTESIAN_POINT ( 'NONE',  ( -4.153846153846152411, -13.75783147151868846, 33.36296068462461051 ) ) ;
#72078 = VERTEX_POINT ( 'NONE', #13670 ) ;
#72079 = CARTESIAN_POINT ( 'NONE',  ( 0.4615384615384611200, -4.661471528628507777, 34.16647553114623292 ) ) ;
#72081 = VERTEX_POINT ( 'NONE', #55096 ) ;
#72080 = CIRCLE ( 'NONE', #60628, 5.000000000000000888 ) ;
#72082 = DIRECTION ( 'NONE',  ( 0.000000000000000000, 0.1736481776669275834, 0.9848077530122086864 ) ) ;
#72083 = EDGE_CURVE ( 'NONE', #33177, #18739, #60882, .T. ) ;
#72084 = B_SPLINE_CURVE_WITH_KNOTS ( 'NONE', 3,
 ( #21441, #89038, #27315, #12471, #74620, #68298, #13795, #5711, #40399, #54331 ),
 .UNSPECIFIED., .F., .F.,
 ( 4, 2, 2, 2, 4 ),
 ( 0.000000000000000000, 0.0001954339857564097241, 0.0003908679715128194482, 0.0005863019572692291723, 0.0007817359430256388964 ),
 .UNSPECIFIED. ) ;
#72085 = ORIENTED_EDGE ( 'NONE', *, *, #74200, .F. ) ;
#72086 = CARTESIAN_POINT ( 'NONE',  ( 12.21151523731700372, -12.07920672191015221, 32.31858351112116168 ) ) ;
#72087 = DIRECTION ( 'NONE',  ( 0.000000000000000000, 0.9396926207859126468, -0.3420201433256571111 ) ) ;
#72088 = ORIENTED_EDGE ( 'NONE', *, *, #40853, .T. ) ;
#72089 = CARTESIAN_POINT ( 'NONE',  ( -11.53846153846153655, -2.900454961884010974, 35.62045528018868623 ) ) ;
#72090 = CARTESIAN_POINT ( 'NONE',  ( 0.4615384615384611200, -3.886160181151819604, 36.00935417666054406 ) ) ;
#72091 = CARTESIAN_POINT ( 'NONE',  ( 1.384615384615386802, -2.499999999999998668, 29.50000000000001066 ) ) ;
#72092 = CARTESIAN_POINT ( 'NONE',  ( 1.653273178848927064E-15, -7.500000000000000000, 21.00000000000000000 ) ) ;
#72093 = CARTESIAN_POINT ( 'NONE',  ( -11.53846153846166089, -3.643525952248795718, 33.31231777344771672 ) ) ;
#72094 = EDGE_LOOP ( 'NONE', ( #7801, #6591, #9743, #34653, #26727, #72276 ) ) ;
#72095 = ORIENTED_EDGE ( 'NONE', *, *, #3845, .F. ) ;
#72096 = VECTOR ( 'NONE', #77597, 1000.000000000000000 ) ;
#72097 = EDGE_LOOP ( 'NONE', ( #76137, #8156 ) ) ;
#72099 = VERTEX_POINT ( 'NONE', #22203 ) ;
#72098 = CYLINDRICAL_SURFACE ( 'NONE', #25702, 0.2500000000000002220 ) ;
#72100 = CARTESIAN_POINT ( 'NONE',  ( -14.05774689831426372, -10.92531984108285670, 33.72920026020278073 ) ) ;
#72101 = DIRECTION ( 'NONE',  ( -0.000000000000000000, 0.5000000000000011102, -0.8660254037844380415 ) ) ;
#72102 = VERTEX_POINT ( 'NONE', #14115 ) ;
#72103 = VECTOR ( 'NONE', #23749, 1000.000000000000000 ) ;
#72104 = ORIENTED_EDGE ( 'NONE', *, *, #25655, .T. ) ;
#72105 = VERTEX_POINT ( 'NONE', #82591 ) ;
#72106 = CARTESIAN_POINT ( 'NONE',  ( -1.384615384615383471, -11.69971097300155272, 32.46337939537588113 ) ) ;
#72107 = EDGE_LOOP ( 'NONE', ( #33996, #41969, #81017, #76783, #20129 ) ) ;
#72108 = CARTESIAN_POINT ( 'NONE',  ( -10.36543909703647337, -9.272278438253398036, 34.42582936511637115 ) ) ;
#72109 = DIRECTION ( 'NONE',  ( 0.000000000000000000, 0.3420201433256610524, 0.9396926207859113145 ) ) ;
#72110 = CARTESIAN_POINT ( 'NONE',  ( -15.93106648486808119, -10.97394488606063589, 33.68653795673696294 ) ) ;
#72111 = FACE_BOUND ( 'NONE', #26723, .T. ) ;
#72112 = ORIENTED_EDGE ( 'NONE', *, *, #59124, .T. ) ;
#72113 = CARTESIAN_POINT ( 'NONE',  ( 13.31934538405906387, -11.06231777344662781, 33.60647404775220082 ) ) ;
#72114 = DIRECTION ( 'NONE',  ( -0.000000000000000000, 1.000000000000000000, -0.000000000000000000 ) ) ;
#72115 = CARTESIAN_POINT ( 'NONE',  ( 13.38461538461538680, -8.120952969808772792, 34.71129190930000163 ) ) ;
#72116 = CARTESIAN_POINT ( 'NONE',  ( 8.069165197766697162, -10.61302985866383963, 33.66295027996417843 ) ) ;
#72117 = VERTEX_POINT ( 'NONE', #41587 ) ;
#72118 = CARTESIAN_POINT ( 'NONE',  ( 9.692307692307695177, -2.538708090699994813, 30.37095296980875503 ) ) ;
#72119 = ORIENTED_EDGE ( 'NONE', *, *, #74689, .F. ) ;
#72120 = ORIENTED_EDGE ( 'NONE', *, *, #27938, .F. ) ;
#72122 = CARTESIAN_POINT ( 'NONE',  ( -1.607542343522232686, -5.582147617184174848, 34.63737895849758530 ) ) ;
#72121 = CARTESIAN_POINT ( 'NONE',  ( 10.61538461538461675, -12.37446782046654192, 30.86335684631486131 ) ) ;
#72123 = B_SPLINE_CURVE_WITH_KNOTS ( 'NONE', 3,
 ( #74561, #12415, #6982, #39899, #5653, #40336, #68246, #61038, #88540, #34456 ),
 .UNSPECIFIED., .F., .F.,
 ( 4, 2, 2, 2, 4 ),
 ( 0.0007817359430256333669, 0.0009771253907250056474, 0.001172514838424370881, 0.001367904286123736331, 0.001563293733823101564 ),
 .UNSPECIFIED. ) ;
#72124 = VECTOR ( 'NONE', #9439, 1000.000000000000000 ) ;
#72125 = CARTESIAN_POINT ( 'NONE',  ( 15.90386942290380290, -5.728515186090277211, 34.42611988154120439 ) ) ;
#72126 = CARTESIAN_POINT ( 'NONE',  ( -2.242436736416282272, -12.27809138561124591, 31.22303859784720359 ) ) ;
#72127 = CARTESIAN_POINT ( 'NONE',  ( 16.94644636880661537, -7.276988635370451597, 34.74523720219453793 ) ) ;
#72128 = CARTESIAN_POINT ( 'NONE',  ( -12.21159294319032362, -4.336752205174649433, 33.62275283266504289 ) ) ;
#72129 = VERTEX_POINT ( 'NONE', #21307 ) ;
#72130 = DIRECTION ( 'NONE',  ( -0.000000000000000000, 1.000000000000000000, -0.000000000000000000 ) ) ;
#72131 = CARTESIAN_POINT ( 'NONE',  ( -0.3962833220256234412, -3.643525952247865352, 33.31231777344670064 ) ) ;
#72132 = CARTESIAN_POINT ( 'NONE',  ( 10.36536139116315880, -2.985938066672154445, 32.43141759479405550 ) ) ;
#72133 = CARTESIAN_POINT ( 'NONE',  ( -4.023320452082586485, -3.816742781228458448, 33.13167719472716044 ) ) ;
#72134 = VECTOR ( 'NONE', #37500, 1000.000000000000114 ) ;
#72135 = EDGE_LOOP ( 'NONE', ( #68390, #69761 ) ) ;
#72136 = ORIENTED_EDGE ( 'NONE', *, *, #59719, .F. ) ;
#72137 = FACE_BOUND ( 'NONE', #82679, .T. ) ;
#72138 = EDGE_CURVE ( 'NONE', #1586, #40194, #27627, .T. ) ;
#72139 = ORIENTED_EDGE ( 'NONE', *, *, #20394, .F. ) ;
#72140 = CARTESIAN_POINT ( 'NONE',  ( 7.716006636715624367, -2.882441371585227063, 31.66841991370171527 ) ) ;
#72141 = CARTESIAN_POINT ( 'NONE',  ( 4.946775107191377252, -3.069018819979302926, 32.56621877034667278 ) ) ;
#72142 = VERTEX_POINT ( 'NONE', #69059 ) ;
#72143 = CARTESIAN_POINT ( 'NONE',  ( -3.296039676730006640, -12.46129190929999986, 30.37095296980880832 ) ) ;
#72144 = CARTESIAN_POINT ( 'NONE',  ( 6.673100192134569397, -10.66389620160130036, 33.62221079203477103 ) ) ;
#72145 = FACE_OUTER_BOUND ( 'NONE', #34539, .T. ) ;
#72146 = CARTESIAN_POINT ( 'NONE',  ( -1.319360245102545681, -4.320704448112861584, 33.92786785259548310 ) ) ;
#72147 = ORIENTED_EDGE ( 'NONE', *, *, #72660, .T. ) ;
#72148 = DIRECTION ( 'NONE',  ( 9.403954806578300064E-32, -4.336808689942017736E-16, 1.000000000000000000 ) ) ;
#72149 = VERTEX_POINT ( 'NONE', #88913 ) ;
#72151 = VERTEX_POINT ( 'NONE', #49233 ) ;
#72150 = CARTESIAN_POINT ( 'NONE',  ( 13.63466980452883526, -8.346898887586323923, 34.93166121998716278 ) ) ;
#72152 = LINE ( 'NONE', #31622, #13833 ) ;
#72153 = CARTESIAN_POINT ( 'NONE',  ( 9.692307692308007816, -2.255955759149395501, 30.00000000000324363 ) ) ;
#72154 = CARTESIAN_POINT ( 'NONE',  ( -7.623374177175776367, -3.563462043263029067, 33.22394488606062879 ) ) ;
#72155 = CARTESIAN_POINT ( 'NONE',  ( 10.48523664565292002, -12.50552854090298638, 31.33409797877408920 ) ) ;
#72156 = LINE ( 'NONE', #84367, #18872 ) ;
#72157 = ADVANCED_FACE ( 'NONE', ( #20866 ), #157, .F. ) ;
#72158 = CARTESIAN_POINT ( 'NONE',  ( 6.130791807824786055, -2.729792928343270919, 31.24908615093345077 ) ) ;
#72159 =( GEOMETRIC_REPRESENTATION_CONTEXT ( 3 ) GLOBAL_UNCERTAINTY_ASSIGNED_CONTEXT ( ( #28093 ) ) GLOBAL_UNIT_ASSIGNED_CONTEXT ( ( #47359, #74399, #27543 ) ) REPRESENTATION_CONTEXT ( 'NONE', 'WORKASPACE' ) );
#72160 = CARTESIAN_POINT ( 'NONE',  ( 0.06109907496451789238, -4.749999999999998224, 16.90811829374151287 ) ) ;
#72161 = VERTEX_POINT ( 'NONE', #69941 ) ;
#72162 = CARTESIAN_POINT ( 'NONE',  ( 17.32686848630111953, -2.986452184633680229, 32.43230066228895225 ) ) ;
#72163 = CARTESIAN_POINT ( 'NONE',  ( 13.45068271796546178, -12.62096338111211757, 30.90682066428152908 ) ) ;
#72164 = CARTESIAN_POINT ( 'NONE',  ( -0.2114841499001463287, -4.943051570960393271, 34.04725096376908766 ) ) ;
#72165 = AXIS2_PLACEMENT_3D ( 'NONE', #74134, #40358, #5232 ) ;
#72166 = EDGE_LOOP ( 'NONE', ( #16947, #55031 ) ) ;
#72167 = ORIENTED_EDGE ( 'NONE', *, *, #7372, .T. ) ;
#72168 = CARTESIAN_POINT ( 'NONE',  ( -16.81410256410256565, -11.00000000000000000, 29.75000000000000355 ) ) ;
#72169 = CARTESIAN_POINT ( 'NONE',  ( 12.59206389977210705, -4.299079248970732792, 33.91157788607253565 ) ) ;
#72170 = CARTESIAN_POINT ( 'NONE',  ( -4.946132635956126400, -12.62708834333097663, 30.88030960425257021 ) ) ;
#72171 = VECTOR ( 'NONE', #2609, 1000.000000000000114 ) ;
#72172 = DIRECTION ( 'NONE',  ( -0.000000000000000000, 0.9396926207859092051, -0.3420201433256662704 ) ) ;
#72173 = CARTESIAN_POINT ( 'NONE',  ( 9.692307692307572609, -12.46129190930018460, 30.37095296980731973 ) ) ;
#72174 = CARTESIAN_POINT ( 'NONE',  ( 11.25641025641025550, -3.499999999999999556, 29.75000000000000355 ) ) ;
#72175 = DIRECTION ( 'NONE',  ( -0.000000000000000000, 1.000000000000000000, -0.000000000000000000 ) ) ;
#72176 = EDGE_LOOP ( 'NONE', ( #18371, #3846 ) ) ;
#72178 = EDGE_CURVE ( 'NONE', #26379, #73147, #76992, .T. ) ;
#72177 = CARTESIAN_POINT ( 'NONE',  ( -4.088590582570128973, -6.026961402152789304, 34.52809138561124769 ) ) ;
#72180 = EDGE_CURVE ( 'NONE', #11602, #1493, #28073, .T. ) ;
#72179 = CARTESIAN_POINT ( 'NONE',  ( -1.514762594053604028, -6.852621066184267029, 34.70813303252209181 ) ) ;
#72181 = CARTESIAN_POINT ( 'NONE',  ( 7.146089767170319185, -6.460100341425561332, 34.89618726649961644 ) ) ;
#72182 = CARTESIAN_POINT ( 'NONE',  ( 2.057669070399343880, -3.711651800289232916, 33.01384336483936011 ) ) ;
#72183 = ORIENTED_EDGE ( 'NONE', *, *, #15717, .T. ) ;
#72184 = LINE ( 'NONE', #4170, #80123 ) ;
#72185 = ORIENTED_EDGE ( 'NONE', *, *, #82932, .T. ) ;
#72186 = CARTESIAN_POINT ( 'NONE',  ( 12.21156171748987163, -9.234221910056348293, 34.70572697212741531 ) ) ;
#72187 = FILL_AREA_STYLE_COLOUR ( '', #17272 ) ;
#72188 = CARTESIAN_POINT ( 'NONE',  ( -13.63461538461538325, -7.500000000000001776, 35.00000000000000000 ) ) ;
#72189 = CARTESIAN_POINT ( 'NONE',  ( -10.61538461538461320, -3.050289026998446396, 32.03036669348365706 ) ) ;
#72190 = EDGE_LOOP ( 'NONE', ( #81100, #60592, #53128, #56346 ) ) ;
#72191 = CARTESIAN_POINT ( 'NONE',  ( -2.438382910802613157, -6.369640206132550553, 34.87707690430378449 ) ) ;
#72192 = CARTESIAN_POINT ( 'NONE',  ( 10.39245839786846659, -3.586966769969701208, 32.86292498521069660 ) ) ;
#72193 = DIRECTION ( 'NONE',  ( -0.000000000000000000, 1.000000000000000000, -0.000000000000000000 ) ) ;
#72194 = CARTESIAN_POINT ( 'NONE',  ( 0.000000000000000000, -11.00000000000000000, 29.75000000000000355 ) ) ;
#72195 = ORIENTED_EDGE ( 'NONE', *, *, #785, .T. ) ;
#72196 = FACE_OUTER_BOUND ( 'NONE', #48229, .T. ) ;
#72197 = EDGE_LOOP ( 'NONE', ( #45041, #27956, #4653, #85314 ) ) ;
#72198 = AXIS2_PLACEMENT_3D ( 'NONE', #51000, #57782, #58660 ) ;
#72199 = DIRECTION ( 'NONE',  ( 0.000000000000000000, 0.000000000000000000, -1.000000000000000000 ) ) ;
#72200 = DIRECTION ( 'NONE',  ( 0.000000000000000000, 0.9396926207859126468, 0.3420201433256571111 ) ) ;
#72201 = CARTESIAN_POINT ( 'NONE',  ( -3.480745961711584346, -12.17611988154120972, 31.52148481390971213 ) ) ;
#72202 = CARTESIAN_POINT ( 'NONE',  ( 7.846153846153846700, -12.34228464037088635, 31.77849191805839268 ) ) ;
#72203 = CARTESIAN_POINT ( 'NONE',  ( -6.223484943723948781, -4.386631170607603991, 33.66268669641500111 ) ) ;
#72204 = CARTESIAN_POINT ( 'NONE',  ( 12.52679403281448245, -10.21337939537593620, 33.94971097300152252 ) ) ;
#72205 = EDGE_LOOP ( 'NONE', ( #77947, #30280 ) ) ;
#72206 = EDGE_LOOP ( 'NONE', ( #56513, #71258, #54722, #22918 ) ) ;
#72207 = VERTEX_POINT ( 'NONE', #54642 ) ;
#72208 = PRODUCT_DEFINITION_SHAPE ( 'NONE', 'NONE',  #89187 ) ;
#72209 = ORIENTED_EDGE ( 'NONE', *, *, #65322, .F. ) ;
#72210 = ORIENTED_EDGE ( 'NONE', *, *, #37589, .T. ) ;
#72211 = CARTESIAN_POINT ( 'NONE',  ( -1.319359813339359366, -3.300289026998475705, 32.46337939537591666 ) ) ;
#72212 = CIRCLE ( 'NONE', #46312, 4.000000000000000000 ) ;
#72213 = CARTESIAN_POINT ( 'NONE',  ( -2.057637996053991447, -3.136992222400443175, 32.19305428654138979 ) ) ;
#72214 = B_SPLINE_CURVE_WITH_KNOTS ( 'NONE', 3,
 ( #80661, #3637, #52273, #66230, #73892, #32452, #18503, #45961, #38324, #73451 ),
 .UNSPECIFIED., .F., .F.,
 ( 4, 2, 2, 2, 4 ),
 ( 0.0007817359430256293554, 0.0009771253907249974075, 0.001172514838424365460, 0.001367904286123733512, 0.001563293733823094625 ),
 .UNSPECIFIED. ) ;
#72215 = CARTESIAN_POINT ( 'NONE',  ( -6.923076923076615152, -2.506253911140614576, 30.00000000000323297 ) ) ;
#72216 = LINE ( 'NONE', #59596, #81108 ) ;
#72217 = CARTESIAN_POINT ( 'NONE',  ( 7.780071466793708979, -12.62096338111211580, 30.90682066428152197 ) ) ;
#72218 = B_SPLINE_CURVE_WITH_KNOTS ( 'NONE', 3,
 ( #78490, #17695, #70871, #58217, #23984, #85708, #78940, #17238, #10493, #9172 ),
 .UNSPECIFIED., .F., .F.,
 ( 4, 2, 2, 2, 4 ),
 ( 0.000000000000000000, 0.0001954339881912783015, 0.0003908679763825566029, 0.0005863019645738348773, 0.0007817359527651132059 ),
 .UNSPECIFIED. ) ;
#72219 = AXIS2_PLACEMENT_3D ( 'NONE', #21076, #76027, #61178 ) ;
#72220 = CARTESIAN_POINT ( 'NONE',  ( 0.4615384615383396616, -5.219633306517616589, 34.19971097300220464 ) ) ;
#72221 = VECTOR ( 'NONE', #5749, 1000.000000000000000 ) ;
#72222 = B_SPLINE_CURVE_WITH_KNOTS ( 'NONE', 3,
 ( #30606, #37812, #29738, #9026, #16648, #58079, #78347, #86007, #51747, #78795 ),
 .UNSPECIFIED., .F., .F.,
 ( 4, 2, 2, 2, 4 ),
 ( 0.000000000000000000, 0.0001954311564186872268, 0.0003908623128373744536, 0.0005862934692560616261, 0.0007817246256747489071 ),
 .UNSPECIFIED. ) ;
#72223 = CARTESIAN_POINT ( 'NONE',  ( 4.153846153846154188, -13.87047571288749737, 32.06866353760679544 ) ) ;
#72224 = DIRECTION ( 'NONE',  ( -0.000000000000000000, -0.7660444431189791237, -0.6427876096865379196 ) ) ;
#72225 = CARTESIAN_POINT ( 'NONE',  ( -6.923076923076922462, -12.09954503811598769, 35.62045528018868623 ) ) ;
#72226 = ORIENTED_EDGE ( 'NONE', *, *, #81810, .F. ) ;
#72227 = ORIENTED_EDGE ( 'NONE', *, *, #13686, .F. ) ;
#72228 = EDGE_CURVE ( 'NONE', #23052, #60815, #20042, .T. ) ;
#72229 = ORIENTED_EDGE ( 'NONE', *, *, #38918, .T. ) ;
#72231 = VERTEX_POINT ( 'NONE', #41149 ) ;
#72230 = CARTESIAN_POINT ( 'NONE',  ( 0.3954560821783248414, -2.833524468853757305, 32.15551576947924417 ) ) ;
#72233 = CARTESIAN_POINT ( 'NONE',  ( -7.846153846153965716, -11.48612834414049644, 32.76840700105863391 ) ) ;
#72232 = CARTESIAN_POINT ( 'NONE',  ( 6.700149964170075023, -11.43668979543635089, 33.22377378376089752 ) ) ;
#72234 = FACE_OUTER_BOUND ( 'NONE', #43915, .T. ) ;
#72235 = LINE ( 'NONE', #38463, #69624 ) ;
#72236 = EDGE_LOOP ( 'NONE', ( #81000, #47048, #70879, #15230 ) ) ;
#72237 = ORIENTED_EDGE ( 'NONE', *, *, #42303, .T. ) ;
#72238 = CARTESIAN_POINT ( 'NONE',  ( -17.29985003582992320, -11.43668979543635089, 33.22377378376089752 ) ) ;
#72239 = ORIENTED_EDGE ( 'NONE', *, *, #7836, .F. ) ;
#72240 = FACE_BOUND ( 'NONE', #20133, .T. ) ;
#72241 = DIRECTION ( 'NONE',  ( -0.000000000000000000, 1.000000000000000000, 3.491481338843133355E-15 ) ) ;
#72242 = ADVANCED_FACE ( 'NONE', ( #44778 ), #72258, .F. ) ;
#72243 = CARTESIAN_POINT ( 'NONE',  ( -14.37377468705243722, -6.343179335718451384, 34.87096338111212646 ) ) ;
#72244 = VERTEX_POINT ( 'NONE', #79020 ) ;
#72245 = CARTESIAN_POINT ( 'NONE',  ( 17.75002326905764605, -2.779195860258148798, 31.39871582349836743 ) ) ;
#72246 = CARTESIAN_POINT ( 'NONE',  ( -4.826923076923076650, -2.499999999999998668, 29.75000000000000355 ) ) ;
#72247 = CARTESIAN_POINT ( 'NONE',  ( 1.254467414883692733, -3.625366637846545448, 33.29286588640298561 ) ) ;
#72248 = ORIENTED_EDGE ( 'NONE', *, *, #18820, .T. ) ;
#72249 = ADVANCED_FACE ( 'NONE', ( #24071 ), #3802, .F. ) ;
#72250 = CARTESIAN_POINT ( 'NONE',  ( 12.21151522424549896, -5.056417327199099532, 34.11270091957321426 ) ) ;
#72251 = FACE_OUTER_BOUND ( 'NONE', #72094, .T. ) ;
#72252 = ORIENTED_EDGE ( 'NONE', *, *, #11324, .F. ) ;
#72253 = CARTESIAN_POINT ( 'NONE',  ( 5.777171902365124900, -7.369209533119140509, 34.99857337881830688 ) ) ;
#72254 = CARTESIAN_POINT ( 'NONE',  ( -9.469528023329624844, -9.418065098278013636, 34.63729479722530158 ) ) ;
#72255 = ORIENTED_EDGE ( 'NONE', *, *, #25243, .F. ) ;
#72256 = CARTESIAN_POINT ( 'NONE',  ( 6.923076923076924238, -6.681629849574314051, 35.83090037661290239 ) ) ;
#72257 = CARTESIAN_POINT ( 'NONE',  ( -15.23076923076922995, -2.833524468853757305, 32.15551576947925838 ) ) ;
#72258 = PLANE ( 'NONE',  #39673 ) ;
#72259 = DIRECTION ( 'NONE',  ( -0.000000000000000000, 1.000000000000000000, -0.000000000000000000 ) ) ;
#72260 = FACE_OUTER_BOUND ( 'NONE', #51405, .T. ) ;
#72261 = FACE_BOUND ( 'NONE', #79442, .T. ) ;
#72263 = CARTESIAN_POINT ( 'NONE',  ( 2.373760658694747949, -9.780366693483667717, 34.19971097300155805 ) ) ;
#72262 = DIRECTION ( 'NONE',  ( -9.403954806578300064E-32, 4.336808689942017736E-16, 1.000000000000000000 ) ) ;
#72264 = B_SPLINE_CURVE_WITH_KNOTS ( 'NONE', 3,
 ( #65683, #61600, #74239, #27819, #68807, #48521, #60716, #67485, #21050, #5780 ),
 .UNSPECIFIED., .F., .F.,
 ( 4, 2, 2, 2, 4 ),
 ( 0.000000000000000000, 0.0001954311564186871184, 0.0003908623128373742367, 0.0005862934692560614093, 0.0007817246256747484735 ),
 .UNSPECIFIED. ) ;
#72265 = ADVANCED_FACE ( 'NONE', ( #17320 ), #9670, .F. ) ;
#72266 = CARTESIAN_POINT ( 'NONE',  ( 8.519230769230768274, -2.499999999999998668, 29.75000000000000355 ) ) ;
#72268 = CARTESIAN_POINT ( 'NONE',  ( -10.61538461538461320, -8.120952969808772792, 34.71129190930000163 ) ) ;
#72267 = LINE ( 'NONE', #65053, #12724 ) ;
#72269 = CARTESIAN_POINT ( 'NONE',  ( -1.077988221561460236, -10.27530806549876452, 27.10750670625849423 ) ) ;
#72270 = VERTEX_POINT ( 'NONE', #3355 ) ;
#72271 = CARTESIAN_POINT ( 'NONE',  ( 2.836344605459119261, -5.235657397115412337, 14.00000000000008882 ) ) ;
#72272 = ORIENTED_EDGE ( 'NONE', *, *, #75906, .F. ) ;
#72273 = EDGE_CURVE ( 'NONE', #19537, #70678, #82363, .T. ) ;
#72274 = EDGE_LOOP ( 'NONE', ( #70748, #70468 ) ) ;
#72275 = CARTESIAN_POINT ( 'NONE',  ( 27.00000000000000000, -1.249999999999999334, 30.25000000000000000 ) ) ;
#72276 = ORIENTED_EDGE ( 'NONE', *, *, #62613, .T. ) ;
#72277 = CARTESIAN_POINT ( 'NONE',  ( 1.515140822849029734, -12.15418822224088657, 32.17964115625579069 ) ) ;
#72278 = CARTESIAN_POINT ( 'NONE',  ( 1.944543648262996083, -5.555456351736983045, 16.81250000000000000 ) ) ;
#72279 = FACE_OUTER_BOUND ( 'NONE', #12845, .T. ) ;
#72280 = CARTESIAN_POINT ( 'NONE',  ( -16.15384615384627409, -6.879047030192662504, 34.71129190930017927 ) ) ;
#72281 = DIRECTION ( 'NONE',  ( -1.000000000000000000, 0.000000000000000000, 0.000000000000000000 ) ) ;
#72282 = DIRECTION ( 'NONE',  ( 0.000000000000000000, 0.8660254037844377084, -0.5000000000000015543 ) ) ;
#72283 = CARTESIAN_POINT ( 'NONE',  ( -16.40382289789474157, -10.06842814019191401, 34.32929386961144758 ) ) ;
#72284 = CARTESIAN_POINT ( 'NONE',  ( 0.5923289025054114809, -5.496552790871119143, 34.60292014791297532 ) ) ;
#72285 = CARTESIAN_POINT ( 'NONE',  ( 0.4615384615383382183, -2.657715359629662544, 31.77849191805970364 ) ) ;
#72286 = CARTESIAN_POINT ( 'NONE',  ( 3.750000000000000888, -7.499999999999978684, 21.96875000000000355 ) ) ;
#72287 = CARTESIAN_POINT ( 'NONE',  ( 18.13079044096695469, -11.37503395064541678, 33.29242100308974983 ) ) ;
#72289 = EDGE_CURVE ( 'NONE', #36016, #86769, #86243, .T. ) ;
#72288 = CARTESIAN_POINT ( 'NONE',  ( 3.512820512820510555, -11.00000000000000000, 29.75000000000000355 ) ) ;
#72290 = EDGE_CURVE ( 'NONE', #53160, #58504, #4887, .T. ) ;
#72291 = FACE_OUTER_BOUND ( 'NONE', #57737, .T. ) ;
#72292 = AXIS2_PLACEMENT_3D ( 'NONE', #62739, #83484, #35736 ) ;
#72293 = VERTEX_POINT ( 'NONE', #31732 ) ;
#72295 = EDGE_CURVE ( 'NONE', #57358, #68032, #39870, .T. ) ;
#72294 = ORIENTED_EDGE ( 'NONE', *, *, #2573, .T. ) ;
#72296 = CARTESIAN_POINT ( 'NONE',  ( 7.846153846153846700, -1.117168528481311540, 33.14645433367849847 ) ) ;
#72297 = CARTESIAN_POINT ( 'NONE',  ( 1.384615384615264011, -11.06231777344772027, 33.60647404775119895 ) ) ;
#72298 = CARTESIAN_POINT ( 'NONE',  ( 16.21991348719623360, -12.34228464037088813, 31.77849191805839268 ) ) ;
#72299 = CARTESIAN_POINT ( 'NONE',  ( 16.15384615384615330, -11.69971097300155272, 32.46337939537588113 ) ) ;
#72300 = EDGE_CURVE ( 'NONE', #86068, #24853, #26429, .T. ) ;
#72301 = CARTESIAN_POINT ( 'NONE',  ( -13.91025641025641058, -3.499999999999999556, 29.75000000000000355 ) ) ;
#72302 = VECTOR ( 'NONE', #1861, 1000.000000000000000 ) ;
#72303 = CARTESIAN_POINT ( 'NONE',  ( -3.230769230769229949, -13.95598074871891292, 31.83374038241031911 ) ) ;
#72304 = B_SPLINE_CURVE_WITH_KNOTS ( 'NONE', 3,
 ( #2195, #56704, #9408, #71540, #84201, #57588, #78297, #10296, #57148, #36006 ),
 .UNSPECIFIED., .F., .F.,
 ( 4, 2, 2, 2, 4 ),
 ( 0.0007817359430256285964, 0.0009771253907249948054, 0.001172514838424360906, 0.001367904286123727223, 0.001563293733823093324 ),
 .UNSPECIFIED. ) ;
#72305 = VERTEX_POINT ( 'NONE', #59192 ) ;
#72306 = CARTESIAN_POINT ( 'NONE',  ( 17.74997676270703550, -12.43535235679832596, 30.55408501211184813 ) ) ;
#72307 = ORIENTED_EDGE ( 'NONE', *, *, #58318, .T. ) ;
#72308 = ORIENTED_EDGE ( 'NONE', *, *, #15824, .F. ) ;
#72309 = CARTESIAN_POINT ( 'NONE',  ( -25.00000000000000355, 9.999999999999971578, 3.000000000000000000 ) ) ;
#72310 = CARTESIAN_POINT ( 'NONE',  ( -11.40767109749458541, -11.37503395064541678, 33.29242100308974273 ) ) ;
#72311 = CARTESIAN_POINT ( 'NONE',  ( 9.823099500132485673, -12.11778462344221019, 31.66786338562085135 ) ) ;
#72312 = CARTESIAN_POINT ( 'NONE',  ( 2.084766090176161324, -5.667676309546437530, 34.40238873228292249 ) ) ;
#72313 = CARTESIAN_POINT ( 'NONE',  ( -13.38461538461550582, -3.300289026999228881, 32.46337939537708905 ) ) ;
#72314 = EDGE_LOOP ( 'NONE', ( #15393, #26447, #52124, #30360 ) ) ;
#72315 = VECTOR ( 'NONE', #47822, 1000.000000000000000 ) ;
#72316 = AXIS2_PLACEMENT_3D ( 'NONE', #52266, #18049, #23894 ) ;
#72317 = VERTEX_POINT ( 'NONE', #87138 ) ;
#72318 = ADVANCED_FACE ( 'NONE', ( #37135 ), #57858, .T. ) ;
#72319 = VERTEX_POINT ( 'NONE', #65045 ) ;
#72320 = CARTESIAN_POINT ( 'NONE',  ( 1.254468175177168909, -11.47017969459903952, 32.78971311882034456 ) ) ;
#72321 = CARTESIAN_POINT ( 'NONE',  ( -0.3954711281883861451, -9.905515769479277921, 34.41647553114623292 ) ) ;
#72322 = CARTESIAN_POINT ( 'NONE',  ( 8.769230769230645706, -5.941354392335915335, 34.76329471203413846 ) ) ;
#72323 = B_SPLINE_CURVE_WITH_KNOTS ( 'NONE', 3,
 ( #35592, #14884, #1352, #63930, #22076, #49547, #77022, #15321, #42800, #43229 ),
 .UNSPECIFIED., .F., .F.,
 ( 4, 2, 2, 2, 4 ),
 ( 0.0007817246256747446788, 0.0009771112852218874663, 0.001172497944769030145, 0.001367884604316172825, 0.001563271263863315720 ),
 .UNSPECIFIED. ) ;
#72324 = ADVANCED_FACE ( 'NONE', ( #58297 ), #85788, .F. ) ;
#72325 = CARTESIAN_POINT ( 'NONE',  ( -15.09997742294444478, -3.062576670634119758, 32.05464942895959979 ) ) ;
#72326 = CARTESIAN_POINT ( 'NONE',  ( -1.384615384615383471, -13.63283147151868846, 33.57946703557072254 ) ) ;
#72327 = CYLINDRICAL_SURFACE ( 'NONE', #72470, 0.2499999999999986955 ) ;
#72328 = ORIENTED_EDGE ( 'NONE', *, *, #82751, .T. ) ;
#72329 = VERTEX_POINT ( 'NONE', #25862 ) ;
#72330 = CARTESIAN_POINT ( 'NONE',  ( -2.651650429449565305, -4.848349570550461785, 21.50000000000000000 ) ) ;
#72331 = EDGE_CURVE ( 'NONE', #88393, #34480, #73622, .T. ) ;
#72332 = ORIENTED_EDGE ( 'NONE', *, *, #24288, .F. ) ;
#72334 = VERTEX_POINT ( 'NONE', #47899 ) ;
#72333 = CARTESIAN_POINT ( 'NONE',  ( 15.29683758177167086, -5.557115091759786019, 34.35708131394839882 ) ) ;
#72335 = CARTESIAN_POINT ( 'NONE',  ( 1.318531973659505363, -9.780366693483667717, 34.19971097300155805 ) ) ;
#72336 = CARTESIAN_POINT ( 'NONE',  ( 12.59232890250541281, -8.191423895709840863, 34.95447573519442130 ) ) ;
#72337 = CARTESIAN_POINT ( 'NONE',  ( -1.553300858899081760, -11.25000000000000888, 17.35937499999999645 ) ) ;
#72338 = VERTEX_POINT ( 'NONE', #75379 ) ;
#72339 = CARTESIAN_POINT ( 'NONE',  ( -1.384615384615506484, -2.657715359629662544, 31.77849191805970364 ) ) ;
#72340 = ORIENTED_EDGE ( 'NONE', *, *, #71516, .F. ) ;
#72341 = CARTESIAN_POINT ( 'NONE',  ( -13.45069776397551742, -11.35647404775217595, 33.31231777344666511 ) ) ;
#72342 = LINE ( 'NONE', #77774, #6963 ) ;
#72343 = AXIS2_PLACEMENT_3D ( 'NONE', #78558, #52418, #32598 ) ;
#72344 = FACE_BOUND ( 'NONE', #20045, .T. ) ;
#72346 = CARTESIAN_POINT ( 'NONE',  ( -2.294871794871794712, -7.500000000000000000, 29.75000000000000355 ) ) ;
#72345 = FACE_OUTER_BOUND ( 'NONE', #39499, .T. ) ;
#72347 = VECTOR ( 'NONE', #86425, 1000.000000000000227 ) ;
#72348 = EDGE_CURVE ( 'NONE', #53721, #32825, #66116, .T. ) ;
#72349 = CARTESIAN_POINT ( 'NONE',  ( -0.5922290646487685661, -12.35290016733513951, 31.75349464988449455 ) ) ;
#72350 = DIRECTION ( 'NONE',  ( -0.000000000000000000, -0.000000000000000000, -1.000000000000000000 ) ) ;
#72351 = ORIENTED_EDGE ( 'NONE', *, *, #35663, .T. ) ;
#72352 = CARTESIAN_POINT ( 'NONE',  ( -10.61538461538473399, -10.21337939537710326, 33.94971097300076224 ) ) ;
#72353 = FILL_AREA_STYLE_COLOUR ( '', #57944 ) ;
#72354 = EDGE_CURVE ( 'NONE', #50277, #34333, #68616, .T. ) ;
#72355 = EDGE_LOOP ( 'NONE', ( #31561, #35216, #53786, #50488 ) ) ;
#72356 = DIRECTION ( 'NONE',  ( 0.000000000000000000, -1.000000000000000000, 0.000000000000000000 ) ) ;
#72357 = CARTESIAN_POINT ( 'NONE',  ( 17.01084069756293715, -10.67929555188718460, 33.92786785259543336 ) ) ;
#72358 = CARTESIAN_POINT ( 'NONE',  ( -19.00000000000000000, -4.000000000000000000, 29.75000000000000355 ) ) ;
#72359 = CARTESIAN_POINT ( 'NONE',  ( 9.692307692307695177, -7.500000000000001776, 35.04278698407183867 ) ) ;
#72360 = CARTESIAN_POINT ( 'NONE',  ( -27.00000000000000000, 9.000000000000001776, 2.999999999999999556 ) ) ;
#72361 = FACE_BOUND ( 'NONE', #50531, .T. ) ;
#72363 = CARTESIAN_POINT ( 'NONE',  ( 9.692307692307695177, -12.78798330534102945, 29.74999999999997868 ) ) ;
#72362 = CARTESIAN_POINT ( 'NONE',  ( 5.207448515156721136, -5.915461855592777596, 34.75538340440931506 ) ) ;
#72364 = CARTESIAN_POINT ( 'NONE',  ( -18.25002322422145440, -8.475808217655755428, 34.90892951860618609 ) ) ;
#72366 = CARTESIAN_POINT ( 'NONE',  ( 0.6845513056318558442, -2.889357225399415086, 32.26129605718031002 ) ) ;
#72365 = CARTESIAN_POINT ( 'NONE',  ( 18.06525557127602610, -11.48612834413965977, 32.76840700105972815 ) ) ;
#72367 = LINE ( 'NONE', #17435, #9563 ) ;
#72368 = CYLINDRICAL_SURFACE ( 'NONE', #87903, 0.2500000000000004996 ) ;
#72369 = CARTESIAN_POINT ( 'NONE',  ( -3.724691934501229262, -9.114399933863657211, 26.01375670625848713 ) ) ;
#72370 = ORIENTED_EDGE ( 'NONE', *, *, #57378, .T. ) ;
#72371 = CYLINDRICAL_SURFACE ( 'NONE', #80970, 0.2499999999999986955 ) ;
#72372 = CARTESIAN_POINT ( 'NONE',  ( 7.976679284387491187, -10.31582465632705237, 34.18122507451815295 ) ) ;
#72373 = CARTESIAN_POINT ( 'NONE',  ( -7.596153846153844924, -2.499999999999998668, 29.75000000000000355 ) ) ;
#72374 = CARTESIAN_POINT ( 'NONE',  ( -9.757578138268467427, -10.90142922261923886, 33.41473453929638993 ) ) ;
#72375 = DIRECTION ( 'NONE',  ( 0.000000000000000000, 0.3420201433256610524, 0.9396926207859113145 ) ) ;
#72376 = CARTESIAN_POINT ( 'NONE',  ( 5.299702745901138101, -12.11081565061823717, 32.26097654155341843 ) ) ;
#72377 = CARTESIAN_POINT ( 'NONE',  ( 2.608446859217893099, -4.805146000318787358, 20.31063170625848713 ) ) ;
#72378 = CARTESIAN_POINT ( 'NONE',  ( -2.373774687052440768, -3.322132147404559976, 32.92929555188719348 ) ) ;
#72379 = DIRECTION ( 'NONE',  ( -0.000000000000000000, -0.000000000000000000, -1.000000000000000000 ) ) ;
#72380 = AXIS2_PLACEMENT_3D ( 'NONE', #44878, #72356, #10666 ) ;
#72381 = CYLINDRICAL_SURFACE ( 'NONE', #10144, 0.2500000000000008882 ) ;
#72382 = CARTESIAN_POINT ( 'NONE',  ( 4.946232473812766983, -9.084618155246140248, 34.75535874321725771 ) ) ;
#72383 = CARTESIAN_POINT ( 'NONE',  ( 0.3308469948709032993, -11.18331474514187995, 33.13161551792790505 ) ) ;
#72384 = FACE_OUTER_BOUND ( 'NONE', #56848, .T. ) ;
#72386 = EDGE_CURVE ( 'NONE', #70094, #22687, #43634, .T. ) ;
#72385 = CARTESIAN_POINT ( 'NONE',  ( -11.53846153846153655, -13.37000171582298513, 34.34916445242398453 ) ) ;
#72387 = CARTESIAN_POINT ( 'NONE',  ( -1.253824943648435220, -11.93129842949671726, 32.56571108434900452 ) ) ;
#72388 = ORIENTED_EDGE ( 'NONE', *, *, #14711, .F. ) ;
#72389 = LINE ( 'NONE', #16126, #57079 ) ;
#72390 = FACE_OUTER_BOUND ( 'NONE', #22174, .T. ) ;
#72391 = CARTESIAN_POINT ( 'NONE',  ( 1.614399933863618797, -3.775308065498751198, 14.48624329374151465 ) ) ;
#72392 = EDGE_CURVE ( 'NONE', #35101, #7659, #2786, .T. ) ;
#72393 = B_SPLINE_CURVE_WITH_KNOTS ( 'NONE', 3,
 ( #58878, #78256, #31864, #86378, #9804, #71946, #37269, #64734, #59322, #79604 ),
 .UNSPECIFIED., .F., .F.,
 ( 4, 2, 2, 2, 4 ),
 ( 0.000000000000000000, 0.0001954311564186861697, 0.0003908623128373723394, 0.0005862934692560584820, 0.0007817246256747446788 ),
 .UNSPECIFIED. ) ;
#72394 = CARTESIAN_POINT ( 'NONE',  ( 9.692307692307695177, -13.57706302396349152, 30.56769352161908060 ) ) ;
#72395 = CARTESIAN_POINT ( 'NONE',  ( -17.01085574357300345, -5.471508081941601098, 34.59228464037088457 ) ) ;
#72396 = ORIENTED_EDGE ( 'NONE', *, *, #32625, .F. ) ;
#72397 = CARTESIAN_POINT ( 'NONE',  ( -17.74994558008654622, -6.523592122091591783, 34.90882529074906415 ) ) ;
#72398 = CARTESIAN_POINT ( 'NONE',  ( 3.512820512820510555, -3.499999999999999556, 29.75000000000000355 ) ) ;
#72400 = ORIENTED_EDGE ( 'NONE', *, *, #12945, .T. ) ;
#72399 = CARTESIAN_POINT ( 'NONE',  ( -7.846153846153844924, -12.34228464037088635, 31.77849191805839268 ) ) ;
#72401 = CARTESIAN_POINT ( 'NONE',  ( 6.856993512121043466, -3.050289026998445951, 32.03036669348365706 ) ) ;
#72402 = CARTESIAN_POINT ( 'NONE',  ( 17.01160016143089848, -7.749976743299138882, 34.99404534957040624 ) ) ;
#72403 = EDGE_CURVE ( 'NONE', #55151, #25698, #7118, .T. ) ;
#72404 = DIRECTION ( 'NONE',  ( 0.000000000000000000, 0.000000000000000000, -1.000000000000000000 ) ) ;
#72405 = CARTESIAN_POINT ( 'NONE',  ( -14.24243673641628227, -11.48612834413965977, 32.76840700105972815 ) ) ;
#72406 = ORIENTED_EDGE ( 'NONE', *, *, #83353, .T. ) ;
#72407 = CARTESIAN_POINT ( 'NONE',  ( 2.307692307692309264, -12.10708131394839349, 31.69288490824020244 ) ) ;
#72408 = DIRECTION ( 'NONE',  ( -0.000000000000000000, 0.5000000000000011102, -0.8660254037844380415 ) ) ;
#72409 = VECTOR ( 'NONE', #53491, 1000.000000000000000 ) ;
#72410 = CARTESIAN_POINT ( 'NONE',  ( 15.00784227186237807, -10.01117774369187252, 34.36070679894347535 ) ) ;
#72411 = ORIENTED_EDGE ( 'NONE', *, *, #47371, .T. ) ;
#72412 = ORIENTED_EDGE ( 'NONE', *, *, #28885, .F. ) ;
#72413 = EDGE_CURVE ( 'NONE', #12765, #77653, #60078, .T. ) ;
#72414 = ORIENTED_EDGE ( 'NONE', *, *, #51825, .T. ) ;
#72415 = VECTOR ( 'NONE', #36785, 1000.000000000000000 ) ;
#72416 = LINE ( 'NONE', #17929, #47207 ) ;
#72417 = CARTESIAN_POINT ( 'NONE',  ( -2.980714810855777053, -2.920487667080175154, 32.31805714834170828 ) ) ;
#72418 = EDGE_CURVE ( 'NONE', #70948, #76645, #17819, .T. ) ;
#72419 = CARTESIAN_POINT ( 'NONE',  ( 13.31853197365950692, -11.16473453929635440, 33.15142922261925662 ) ) ;
#72420 = CARTESIAN_POINT ( 'NONE',  ( 6.923076923076924238, -2.721908614388771852, 31.22303859784724978 ) ) ;
#72421 = EDGE_CURVE ( 'NONE', #72293, #63049, #8257, .T. ) ;
#72422 = ORIENTED_EDGE ( 'NONE', *, *, #85056, .F. ) ;
#72423 = EDGE_LOOP ( 'NONE', ( #50267, #41303, #20742, #22447 ) ) ;
#72425 = ORIENTED_EDGE ( 'NONE', *, *, #61694, .T. ) ;
#72424 = DIRECTION ( 'NONE',  ( -0.000000000000000000, -0.000000000000000000, -1.000000000000000000 ) ) ;
#72426 = CARTESIAN_POINT ( 'NONE',  ( -14.08467946359890988, -11.43677907613344757, 33.22367315496202167 ) ) ;
#72427 = EDGE_CURVE ( 'NONE', #7245, #22506, #74770, .T. ) ;
#72428 = B_SPLINE_CURVE_WITH_KNOTS ( 'NONE', 3,
 ( #61405, #16769, #28983, #78033, #15014, #50551, #1498, #43800, #22209, #63184 ),
 .UNSPECIFIED., .F., .F.,
 ( 4, 2, 2, 2, 4 ),
 ( 0.000000000000000000, 0.0001954311564186863323, 0.0003908623128373726646, 0.0005862934692560590241, 0.0007817246256747453293 ),
 .UNSPECIFIED. ) ;
#72429 = DIRECTION ( 'NONE',  ( -0.000000000000000000, 0.9848077530122085754, -0.1736481776669273613 ) ) ;
#72430 = CARTESIAN_POINT ( 'NONE',  ( 10.48469314871705826, -11.18331474514187995, 33.13161551792790505 ) ) ;
#72431 = CARTESIAN_POINT ( 'NONE',  ( -13.38461538461538325, -12.37446782046654192, 30.86335684631486131 ) ) ;
#72432 = ORIENTED_EDGE ( 'NONE', *, *, #36789, .F. ) ;
#72433 = ORIENTED_EDGE ( 'NONE', *, *, #20508, .F. ) ;
#72434 = EDGE_CURVE ( 'NONE', #48052, #5565, #42486, .T. ) ;
#72435 = VECTOR ( 'NONE', #87112, 1000.000000000000114 ) ;
#72436 = ORIENTED_EDGE ( 'NONE', *, *, #73193, .T. ) ;
#72438 = ORIENTED_EDGE ( 'NONE', *, *, #6361, .T. ) ;
#72437 = LINE ( 'NONE', #4891, #55979 ) ;
#72439 = CARTESIAN_POINT ( 'NONE',  ( -10.61538461538429878, -2.255955759149395501, 30.00000000000324363 ) ) ;
#72440 = DIRECTION ( 'NONE',  ( -1.000000000000000000, -0.000000000000000000, -0.000000000000000000 ) ) ;
#72441 = ORIENTED_EDGE ( 'NONE', *, *, #52116, .F. ) ;
#72442 = EDGE_CURVE ( 'NONE', #81428, #83740, #32792, .T. ) ;
#72443 = CARTESIAN_POINT ( 'NONE',  ( -13.63459211555773720, -4.236021600441997492, 33.53823185664189310 ) ) ;
#72444 = CYLINDRICAL_SURFACE ( 'NONE', #65214, 0.2499999999999973355 ) ;
#72445 = DIRECTION ( 'NONE',  ( 0.000000000000000000, 0.7660444431189822323, -0.6427876096865344779 ) ) ;
#72446 = FACE_BOUND ( 'NONE', #2735, .T. ) ;
#72447 = DIRECTION ( 'NONE',  ( 0.000000000000000000, 0.000000000000000000, 1.000000000000000000 ) ) ;
#72448 = CARTESIAN_POINT ( 'NONE',  ( -4.283993363284377409, -12.27039167877662251, 31.24851455888617835 ) ) ;
#72449 = CYLINDRICAL_SURFACE ( 'NONE', #48044, 0.2500000000000004996 ) ;
#72451 = CARTESIAN_POINT ( 'NONE',  ( 9.915087233576103998, -3.236590943229499029, 32.36255958852954251 ) ) ;
#72450 = CARTESIAN_POINT ( 'NONE',  ( 3.480823650682684178, -3.435999193479609470, 33.07426656108011542 ) ) ;
#72452 = CARTESIAN_POINT ( 'NONE',  ( -7.912237257109728361, -3.050289026998445951, 32.03036669348365706 ) ) ;
#72453 = CARTESIAN_POINT ( 'NONE',  ( 5.076923076922954969, -2.625532179533778709, 30.86335684631627174 ) ) ;
#72454 = ORIENTED_EDGE ( 'NONE', *, *, #47288, .F. ) ;
#72455 = DIRECTION ( 'NONE',  ( 0.000000000000000000, 0.1736481776669267785, -0.9848077530122087975 ) ) ;
#72456 = DIRECTION ( 'NONE',  ( -0.000000000000000000, -0.5000000000000009992, -0.8660254037844380415 ) ) ;
#72457 = ORIENTED_EDGE ( 'NONE', *, *, #45066, .F. ) ;
#72458 = EDGE_CURVE ( 'NONE', #47909, #64420, #87702, .T. ) ;
#72459 = ORIENTED_EDGE ( 'NONE', *, *, #16147, .F. ) ;
#72460 = B_SPLINE_CURVE_WITH_KNOTS ( 'NONE', 3,
 ( #32531, #10937, #72629, #73079, #65864, #25784, #44700, #65430, #60448, #11832 ),
 .UNSPECIFIED., .F., .F.,
 ( 4, 2, 2, 2, 4 ),
 ( 0.000000000000000000, 0.0001954311564186861426, 0.0003908623128373722852, 0.0005862934692560583735, 0.0007817246256747445703 ),
 .UNSPECIFIED. ) ;
#72462 = CARTESIAN_POINT ( 'NONE',  ( 1.384615384615265343, -10.90142922262034020, 33.41473453929536674 ) ) ;
#72461 = DIRECTION ( 'NONE',  ( 0.000000000000000000, -6.938893903907222067E-15, 1.000000000000000000 ) ) ;
#72463 = ADVANCED_FACE ( 'NONE', ( #50106 ), #28076, .F. ) ;
#72464 = B_SPLINE_CURVE_WITH_KNOTS ( 'NONE', 3,
 ( #22905, #64323, #30112, #37750, #23345, #1308, #44050, #22468, #84631, #56259 ),
 .UNSPECIFIED., .F., .F.,
 ( 4, 2, 2, 2, 4 ),
 ( 0.0007817246256747517261, 0.0009771112852218961399, 0.001172497944769040771, 0.001367884604316185401, 0.001563271263863329815 ),
 .UNSPECIFIED. ) ;
#72465 = CARTESIAN_POINT ( 'NONE',  ( 11.47237915910140416, -8.164416787775445883, 34.95778746994557906 ) ) ;
#72466 = CARTESIAN_POINT ( 'NONE',  ( -1.384615384615505151, -5.219633306517616589, 34.19971097300220464 ) ) ;
#72467 = CARTESIAN_POINT ( 'NONE',  ( 12.46153846153846168, -12.09954503811598769, 35.62045528018868623 ) ) ;
#72468 = ORIENTED_EDGE ( 'NONE', *, *, #25569, .F. ) ;
#72469 = DIRECTION ( 'NONE',  ( 0.000000000000000000, 0.6427876096865373645, -0.7660444431189797898 ) ) ;
#72470 = AXIS2_PLACEMENT_3D ( 'NONE', #73685, #78645, #10637 ) ;
#72472 = CARTESIAN_POINT ( 'NONE',  ( 6.857806477116148436, -3.835265460703609186, 33.15142922261924241 ) ) ;
#72471 = DIRECTION ( 'NONE',  ( -0.000000000000000000, -0.9848077530122086864, -0.1736481776669273613 ) ) ;
#72473 = CARTESIAN_POINT ( 'NONE',  ( -1.384615384615383471, -9.905515769479276145, 34.41647553114623292 ) ) ;
#72474 = CARTESIAN_POINT ( 'NONE',  ( 24.00000000000000000, -5.499999999999981348, 27.25000000000000000 ) ) ;
#72475 = CARTESIAN_POINT ( 'NONE',  ( -1.384615384615383471, -1.629998284177014645, 34.34916445242399163 ) ) ;
#72476 = CARTESIAN_POINT ( 'NONE',  ( -1.553300858899081538, -11.25000000000000711, 17.35937500000000000 ) ) ;
#72477 = ORIENTED_EDGE ( 'NONE', *, *, #34818, .F. ) ;
#72478 = VECTOR ( 'NONE', #72408, 1000.000000000000114 ) ;
#72479 = VERTEX_POINT ( 'NONE', #20869 ) ;
#72480 = AXIS2_PLACEMENT_3D ( 'NONE', #30474, #85425, #63819 ) ;
#72481 = CARTESIAN_POINT ( 'NONE',  ( 9.692307692307695177, -9.058645607665452459, 34.76329471203371924 ) ) ;
#72482 = CARTESIAN_POINT ( 'NONE',  ( -18.13061035962451584, -7.722926236386454590, 34.74524107206102030 ) ) ;
#72483 = DIRECTION ( 'NONE',  ( 0.000000000000000000, 1.000000000000000000, 0.000000000000000000 ) ) ;
#72484 = CARTESIAN_POINT ( 'NONE',  ( -16.21992956480203318, -4.786620604624113540, 33.94971097300155805 ) ) ;
#72485 = CARTESIAN_POINT ( 'NONE',  ( -0.7115616857599200706, -12.07920672191015221, 32.31858351112116168 ) ) ;
#72486 = CARTESIAN_POINT ( 'NONE',  ( -1.929879867024197893E-14, -3.750000000000000000, 15.40625000000000000 ) ) ;
#72487 = DIRECTION ( 'NONE',  ( 0.000000000000000000, 0.000000000000000000, -1.000000000000000000 ) ) ;
#72488 = DIRECTION ( 'NONE',  ( -0.000000000000000000, 0.3420201433256694901, -0.9396926207859082059 ) ) ;
#72489 = VERTEX_POINT ( 'NONE', #83025 ) ;
#72490 = FACE_OUTER_BOUND ( 'NONE', #78442, .T. ) ;
#72492 = VERTEX_POINT ( 'NONE', #48338 ) ;
#72491 = CARTESIAN_POINT ( 'NONE',  ( 5.999999999999878320, -10.33852847137269571, 34.16647553114546554 ) ) ;
#72493 = CARTESIAN_POINT ( 'NONE',  ( 3.165499230212911463, -12.51329471203370325, 31.30864560766548976 ) ) ;
#72494 = CARTESIAN_POINT ( 'NONE',  ( 3.230769230769110045, -2.892918686052166066, 31.69288490824153470 ) ) ;
#72495 = DIRECTION ( 'NONE',  ( -0.000000000000000000, 0.5000000000000011102, -0.8660254037844380415 ) ) ;
#72496 = CYLINDRICAL_SURFACE ( 'NONE', #53018, 0.2500000000000008882 ) ;
#72497 = CARTESIAN_POINT ( 'NONE',  ( -15.23076923076922995, -3.669653830205710676, 35.88435417666054406 ) ) ;
#72498 = CARTESIAN_POINT ( 'NONE',  ( -11.53846153846166089, -5.941354392335915335, 34.76329471203413846 ) ) ;
#72499 = CARTESIAN_POINT ( 'NONE',  ( 15.29602480204525250, -11.48612834413965977, 32.76840700105972815 ) ) ;
#72500 = EDGE_LOOP ( 'NONE', ( #49432, #1294 ) ) ;
#72501 = DIRECTION ( 'NONE',  ( 0.000000000000000000, 0.000000000000000000, -1.000000000000000000 ) ) ;
#72502 = CARTESIAN_POINT ( 'NONE',  ( 9.019176287578909879, -11.86320923018887719, 32.19269448109604070 ) ) ;
#72503 = CARTESIAN_POINT ( 'NONE',  ( 12.46153846153846168, -12.48256725967547354, 35.29906147534542527 ) ) ;
#72504 = CARTESIAN_POINT ( 'NONE',  ( 1.077988221561497539, -10.27530806549875386, 13.70499329374151287 ) ) ;
#72505 = ADVANCED_FACE ( 'NONE', ( #75813 ), #84364, .F. ) ;
#72506 = CARTESIAN_POINT ( 'NONE',  ( -14.30769230769242739, -5.219633306517616589, 34.19971097300220464 ) ) ;
#72507 = CARTESIAN_POINT ( 'NONE',  ( 14.05771556364371655, -4.818429247618089661, 34.26397095200675125 ) ) ;
#72509 = EDGE_LOOP ( 'NONE', ( #73889, #7031, #61478, #66968 ) ) ;
#72508 = CARTESIAN_POINT ( 'NONE',  ( -16.15384615384615330, -3.050289026998446396, 32.03036669348365706 ) ) ;
#72510 = CARTESIAN_POINT ( 'NONE',  ( 2.750000000000001776, -7.499999999999984013, 20.71875000000000000 ) ) ;
#72511 = CARTESIAN_POINT ( 'NONE',  ( -15.48074597481782178, -4.075325502946081535, 33.72974371597206300 ) ) ;
#72512 = ADVANCED_FACE ( 'NONE', ( #55986 ), #49236, .F. ) ;
#72513 = VERTEX_POINT ( 'NONE', #21310 ) ;
#72514 = VECTOR ( 'NONE', #63948, 1000.000000000000000 ) ;
#72515 = CARTESIAN_POINT ( 'NONE',  ( -4.403869378067609475, -8.475808217655753651, 34.90892951860618609 ) ) ;
#72516 = EDGE_CURVE ( 'NONE', #15199, #83533, #14616, .T. ) ;
#72517 = ORIENTED_EDGE ( 'NONE', *, *, #41256, .T. ) ;
#72518 = CARTESIAN_POINT ( 'NONE',  ( -3.230769230769229949, -13.78497067705608181, 32.30358669280327177 ) ) ;
#72519 = CARTESIAN_POINT ( 'NONE',  ( 13.13463865367303285, -9.943427161483782584, 34.11278801902876978 ) ) ;
#72520 = CARTESIAN_POINT ( 'NONE',  ( 16.94677510719138169, -6.809168938359901446, 34.95455904226513866 ) ) ;
#72521 = VERTEX_POINT ( 'NONE', #72153 ) ;
#72522 = CARTESIAN_POINT ( 'NONE',  ( -12.46153846153846168, -2.249999999999998668, 29.50000000000001421 ) ) ;
#72523 = ORIENTED_EDGE ( 'NONE', *, *, #78078, .T. ) ;
#72524 = EDGE_CURVE ( 'NONE', #55585, #46544, #48906, .T. ) ;
#72525 = CARTESIAN_POINT ( 'NONE',  ( 27.00000000000000355, -1.749999999999999778, 30.25000000000000000 ) ) ;
#72526 = ORIENTED_EDGE ( 'NONE', *, *, #86170, .T. ) ;
#72527 = CARTESIAN_POINT ( 'NONE',  ( -16.15384615384627409, -2.379036618888197285, 30.90682066428292885 ) ) ;
#72528 = CARTESIAN_POINT ( 'NONE',  ( -7.384615384615385025, -7.500000000000000000, 33.75000000000000000 ) ) ;
#72529 = EDGE_CURVE ( 'NONE', #43520, #45617, #23227, .T. ) ;
#72530 = ORIENTED_EDGE ( 'NONE', *, *, #14055, .F. ) ;
#72531 = CARTESIAN_POINT ( 'NONE',  ( -5.934744428723973897, -11.48612834413965977, 32.76840700105972815 ) ) ;
#72532 = DIRECTION ( 'NONE',  ( 0.000000000000000000, 0.000000000000000000, -1.000000000000000000 ) ) ;
#72533 = LINE ( 'NONE', #38971, #50918 ) ;
#72534 = EDGE_CURVE ( 'NONE', #30751, #15288, #45566, .T. ) ;
#72535 = CARTESIAN_POINT ( 'NONE',  ( -14.30769230769242917, -10.33852847137269571, 34.16647553114546554 ) ) ;
#72536 = CARTESIAN_POINT ( 'NONE',  ( -11.40767109749458541, -3.338503747796866872, 32.95102852606553512 ) ) ;
#72537 = AXIS2_PLACEMENT_3D ( 'NONE', #32569, #82555, #61359 ) ;
#72538 = ORIENTED_EDGE ( 'NONE', *, *, #14071, .F. ) ;
#72539 = ORIENTED_EDGE ( 'NONE', *, *, #78078, .F. ) ;
#72540 = ORIENTED_EDGE ( 'NONE', *, *, #6268, .F. ) ;
#72542 = ORIENTED_EDGE ( 'NONE', *, *, #4802, .F. ) ;
#72541 = CARTESIAN_POINT ( 'NONE',  ( 3.165499230212911908, -5.941354392334500467, 34.76329471203369792 ) ) ;
#72543 = EDGE_CURVE ( 'NONE', #24141, #44733, #20982, .T. ) ;
#72544 = VECTOR ( 'NONE', #68082, 1000.000000000000000 ) ;
#72545 = EDGE_CURVE ( 'NONE', #4333, #68833, #23961, .T. ) ;
#72546 = DIRECTION ( 'NONE',  ( 0.000000000000000000, 0.6427876096865368094, 0.7660444431189802339 ) ) ;
#72547 = CARTESIAN_POINT ( 'NONE',  ( 9.562159722575998444, -5.915902021225889484, 34.75552854090298638 ) ) ;
#72548 = VERTEX_POINT ( 'NONE', #86583 ) ;
#72549 = ORIENTED_EDGE ( 'NONE', *, *, #87763, .T. ) ;
#72550 = CARTESIAN_POINT ( 'NONE',  ( 0.2380535369741301754, -8.539481045369598178, 34.89627647299170832 ) ) ;
#72551 = VERTEX_POINT ( 'NONE', #66289 ) ;
#72552 = FACE_OUTER_BOUND ( 'NONE', #53476, .T. ) ;
#72553 = EDGE_CURVE ( 'NONE', #52150, #54472, #16766, .T. ) ;
#72554 = EDGE_CURVE ( 'NONE', #5310, #73152, #4594, .T. ) ;
#72555 = CARTESIAN_POINT ( 'NONE',  ( 17.07692307692295586, -12.51329471203414379, 31.30864560766407578 ) ) ;
#72556 = CARTESIAN_POINT ( 'NONE',  ( -15.90390074446811042, -10.92531984108285670, 33.72920026020278073 ) ) ;
#72557 = FACE_BOUND ( 'NONE', #45751, .T. ) ;
#72558 = ORIENTED_EDGE ( 'NONE', *, *, #5049, .F. ) ;
#72559 = FACE_OUTER_BOUND ( 'NONE', #19224, .T. ) ;
#72560 = CARTESIAN_POINT ( 'NONE',  ( -0.6089743589743589203, -11.50000000000000000, 29.75000000000000355 ) ) ;
#72561 = CYLINDRICAL_SURFACE ( 'NONE', #80538, 0.2499999999999995559 ) ;
#72562 = CARTESIAN_POINT ( 'NONE',  ( 2.057715563643717882, -8.347322224742351082, 34.93158281831414769 ) ) ;
#72563 = CARTESIAN_POINT ( 'NONE',  ( -1.450698795571264910, -2.538708090699994813, 30.37095296980875148 ) ) ;
#72564 = VERTEX_POINT ( 'NONE', #86131 ) ;
#72565 = LINE ( 'NONE', #7883, #69026 ) ;
#72566 = VERTEX_POINT ( 'NONE', #85242 ) ;
#72567 = ADVANCED_FACE ( 'NONE', ( #17213 ), #17670, .F. ) ;
#72568 = ORIENTED_EDGE ( 'NONE', *, *, #71709, .T. ) ;
#72569 = AXIS2_PLACEMENT_3D ( 'NONE', #2243, #84693, #83810 ) ;
#72571 = LINE ( 'NONE', #58161, #57798 ) ;
#72570 = CARTESIAN_POINT ( 'NONE',  ( -0.4615384615385826339, -9.442884908241554243, 34.35708131394783038 ) ) ;
#72572 = CARTESIAN_POINT ( 'NONE',  ( -10.83886955910856287, -12.24155766932282496, 31.33739205006857986 ) ) ;
#72573 = CARTESIAN_POINT ( 'NONE',  ( -2.084680956079455694, -12.15243808032445827, 31.58219941686247978 ) ) ;
#72574 = EDGE_CURVE ( 'NONE', #21910, #62783, #75869, .T. ) ;
#72575 = CARTESIAN_POINT ( 'NONE',  ( 7.716006636715626144, -12.45813303252208648, 30.39737893381572675 ) ) ;
#72576 = CARTESIAN_POINT ( 'NONE',  ( 17.99999999999987566, -5.094484230521993062, 34.41647553114689373 ) ) ;
#72577 = ADVANCED_FACE ( 'NONE', ( #12686 ), #13567, .T. ) ;
#72578 = EDGE_LOOP ( 'NONE', ( #58602, #41934 ) ) ;
#72579 = CARTESIAN_POINT ( 'NONE',  ( -5.142193077479395136, -6.835583212224499938, 34.95778746994557906 ) ) ;
#72580 = DIRECTION ( 'NONE',  ( 0.000000000000000000, 0.000000000000000000, 1.000000000000000000 ) ) ;
#72581 = CARTESIAN_POINT ( 'NONE',  ( -14.17764725177253382, -2.254550872974306674, 29.97347326024527092 ) ) ;
#72582 = CARTESIAN_POINT ( 'NONE',  ( 14.37294744720514572, -2.657715359629132301, 31.77849191805844242 ) ) ;
#72583 = EDGE_LOOP ( 'NONE', ( #61235, #6655 ) ) ;
#72584 = EDGE_CURVE ( 'NONE', #37767, #73916, #19881, .T. ) ;
#72585 = ORIENTED_EDGE ( 'NONE', *, *, #85820, .F. ) ;
#72586 = FACE_BOUND ( 'NONE', #8070, .T. ) ;
#72587 = ORIENTED_EDGE ( 'NONE', *, *, #86541, .F. ) ;
#72588 = CARTESIAN_POINT ( 'NONE',  ( 18.13083841801275753, -7.277220443632451463, 34.74524770363009196 ) ) ;
#72589 = DIRECTION ( 'NONE',  ( -0.000000000000000000, 0.9848077530122085754, -0.1736481776669273613 ) ) ;
#72590 = ORIENTED_EDGE ( 'NONE', *, *, #7677, .T. ) ;
#72591 = CARTESIAN_POINT ( 'NONE',  ( -7.780898274877818821, -4.481592998940249650, 33.73612834413965089 ) ) ;
#72592 = CARTESIAN_POINT ( 'NONE',  ( -10.83831083290076158, -6.503392248772476236, 34.64988816332204635 ) ) ;
#72593 = CARTESIAN_POINT ( 'NONE',  ( 4.826946345980722697, -2.779195860258147022, 31.39871582349836743 ) ) ;
#72594 = CARTESIAN_POINT ( 'NONE',  ( 5.076923076923075762, -8.564572088678739092, 35.78748833219616898 ) ) ;
#72595 = DIRECTION ( 'NONE',  ( 0.000000000000000000, 0.000000000000000000, 1.000000000000000000 ) ) ;
#72596 = VERTEX_POINT ( 'NONE', #41048 ) ;
#72598 = ORIENTED_EDGE ( 'NONE', *, *, #30986, .F. ) ;
#72597 = CARTESIAN_POINT ( 'NONE',  ( -19.50000000000000000, -3.499999999999999556, 29.75000000000000355 ) ) ;
#72599 = CARTESIAN_POINT ( 'NONE',  ( 15.29602480204525605, -8.613356846314928816, 34.62446782046653482 ) ) ;
#72600 = CARTESIAN_POINT ( 'NONE',  ( 4.087762742890272527, -6.386643153685125363, 34.62446782046654903 ) ) ;
#72601 = FACE_OUTER_BOUND ( 'NONE', #28241, .T. ) ;
#72602 = CARTESIAN_POINT ( 'NONE',  ( -10.61538461538473577, -3.643525952248795718, 33.31231777344771672 ) ) ;
#72604 = CIRCLE ( 'NONE', #13646, 4.755951259985879531 ) ;
#72603 = CARTESIAN_POINT ( 'NONE',  ( -7.976301055592065481, -9.418419913701741919, 34.36755862841477693 ) ) ;
#72605 = CARTESIAN_POINT ( 'NONE',  ( 5.142991427925514003, -12.37446782046654192, 30.86335684631486842 ) ) ;
#72606 = B_SPLINE_CURVE_WITH_KNOTS ( 'NONE', 3,
 ( #2814, #30306, #72169, #23975, #46036, #10924, #57774, #4611, #79834, #32082 ),
 .UNSPECIFIED., .F., .F.,
 ( 4, 2, 2, 2, 4 ),
 ( 0.0007817246256747464135, 0.0009771112852218900684, 0.001172497944769033615, 0.001367884604316177161, 0.001563271263863320925 ),
 .UNSPECIFIED. ) ;
#72607 = CARTESIAN_POINT ( 'NONE',  ( 1.901340078031373171, -9.487747218494639867, 16.12686829374151287 ) ) ;
#72608 = EDGE_LOOP ( 'NONE', ( #81870, #52827, #28538, #34789 ) ) ;
#72609 = CARTESIAN_POINT ( 'NONE',  ( 5.076923076923075762, -11.91647553114624181, 32.58852847137148245 ) ) ;
#72610 = DIRECTION ( 'NONE',  ( 0.000000000000000000, 0.6427876096865373645, -0.7660444431189797898 ) ) ;
#72611 = CARTESIAN_POINT ( 'NONE',  ( 6.250000000000000888, -2.499999999999998668, 29.75000000000000355 ) ) ;
#72612 = EDGE_CURVE ( 'NONE', #71888, #61379, #37086, .T. ) ;
#72613 = VECTOR ( 'NONE', #54225, 999.9999999999998863 ) ;
#72614 = VERTEX_POINT ( 'NONE', #87476 ) ;
#72615 = ORIENTED_EDGE ( 'NONE', *, *, #87885, .F. ) ;
#72616 = CARTESIAN_POINT ( 'NONE',  ( -1.515175976357303833, -2.504760397472875155, 29.97295953869789997 ) ) ;
#72617 = CARTESIAN_POINT ( 'NONE',  ( -14.24162497434223340, -2.486705287966280320, 31.30864560766543647 ) ) ;
#72618 = CARTESIAN_POINT ( 'NONE',  ( 13.25392391794783009, -3.530157926970578952, 32.79014554554150607 ) ) ;
#72619 = DIRECTION ( 'NONE',  ( 0.000000000000000000, 0.8660254037844377084, -0.5000000000000015543 ) ) ;
#72620 = DIRECTION ( 'NONE',  ( 0.000000000000000000, 0.6427876096865373645, -0.7660444431189797898 ) ) ;
#72621 = FACE_OUTER_BOUND ( 'NONE', #65108, .T. ) ;
#72622 = CARTESIAN_POINT ( 'NONE',  ( -12.46153846153846168, -13.95598074871891292, 31.83374038241031911 ) ) ;
#72623 = ORIENTED_EDGE ( 'NONE', *, *, #30868, .T. ) ;
#72624 = CARTESIAN_POINT ( 'NONE',  ( 0.4615384615384611200, -3.669653830205710676, 35.88435417666054406 ) ) ;
#72625 = CARTESIAN_POINT ( 'NONE',  ( -0.3954701105360233226, -8.120952969808774569, 34.71129190929999453 ) ) ;
#72626 = CARTESIAN_POINT ( 'NONE',  ( 6.988332062589762472, -6.835583212224609184, 34.95778746994559327 ) ) ;
#72627 = CARTESIAN_POINT ( 'NONE',  ( -14.30769230769230660, -1.129524287112498415, 32.06866353760679544 ) ) ;
#72628 = ORIENTED_EDGE ( 'NONE', *, *, #1631, .T. ) ;
#72629 = CARTESIAN_POINT ( 'NONE',  ( 12.33084785842815734, -2.494641256782728966, 31.33461815524612959 ) ) ;
#72630 = VERTEX_POINT ( 'NONE', #59533 ) ;
#72631 = FACE_OUTER_BOUND ( 'NONE', #41746, .T. ) ;
#72632 = PRESENTATION_STYLE_ASSIGNMENT (( #79403 ) ) ;
#72633 = CARTESIAN_POINT ( 'NONE',  ( -1.634592115557738090, -9.148715823498378086, 34.47080413974185120 ) ) ;
#72634 = CARTESIAN_POINT ( 'NONE',  ( 5.999999999999878320, -12.16647553114689728, 32.15551576947799362 ) ) ;
#72635 = ORIENTED_EDGE ( 'NONE', *, *, #80734, .F. ) ;
#72636 = CARTESIAN_POINT ( 'NONE',  ( 0.4615384615383396616, -3.300289026999228881, 32.46337939537708905 ) ) ;
#72637 = CARTESIAN_POINT ( 'NONE',  ( 6.000000000000001776, -9.780366693483667717, 34.19971097300155094 ) ) ;
#72638 = CARTESIAN_POINT ( 'NONE',  ( 10.36536137809165226, -3.711651800289232028, 33.01384336483936011 ) ) ;
#72639 = AXIS2_PLACEMENT_3D ( 'NONE', #83765, #22054, #43641 ) ;
#72640 = ADVANCED_FACE ( 'NONE', ( #46469 ), #87035, .F. ) ;
#72641 = B_SPLINE_CURVE_WITH_KNOTS ( 'NONE', 3,
 ( #66219, #19372, #46842, #26131, #12178, #32004, #32444, #39213, #4525, #52262 ),
 .UNSPECIFIED., .F., .F.,
 ( 4, 2, 2, 2, 4 ),
 ( 0.000000000000000000, 0.0001954339857564097241, 0.0003908679715128194482, 0.0005863019572692291723, 0.0007817359430256388964 ),
 .UNSPECIFIED. ) ;
#72642 = CARTESIAN_POINT ( 'NONE',  ( 9.442307692307693401, -2.499999999999998668, 29.75000000000000355 ) ) ;
#72643 = FACE_OUTER_BOUND ( 'NONE', #58818, .T. ) ;
#72644 = ORIENTED_EDGE ( 'NONE', *, *, #58857, .T. ) ;
#72645 = CARTESIAN_POINT ( 'NONE',  ( 9.692307692307695177, -9.584722331328613620, 36.20867863119891439 ) ) ;
#72646 = ORIENTED_EDGE ( 'NONE', *, *, #88572, .F. ) ;
#72647 = DIRECTION ( 'NONE',  ( -1.000000000000000000, 0.000000000000000000, -0.000000000000000000 ) ) ;
#72648 = CARTESIAN_POINT ( 'NONE',  ( 5.076923076923075762, -3.050289026998446396, 32.03036669348365706 ) ) ;
#72649 = CARTESIAN_POINT ( 'NONE',  ( -6.923076923077045919, -8.656820664282941280, 34.87096338111179961 ) ) ;
#72650 = FACE_OUTER_BOUND ( 'NONE', #37754, .T. ) ;
#72651 = EDGE_CURVE ( 'NONE', #45729, #84649, #13598, .T. ) ;
#72652 = CARTESIAN_POINT ( 'NONE',  ( -9.626240358957616650, -6.343179335718452272, 34.87096338111212646 ) ) ;
#72653 = CARTESIAN_POINT ( 'NONE',  ( 12.59206416330202316, -10.19071101563364756, 33.96452234770658407 ) ) ;
#72654 = VERTEX_POINT ( 'NONE', #26642 ) ;
#72655 = ORIENTED_EDGE ( 'NONE', *, *, #52421, .T. ) ;
#72656 = ORIENTED_EDGE ( 'NONE', *, *, #82301, .T. ) ;
#72657 = ORIENTED_EDGE ( 'NONE', *, *, #46026, .T. ) ;
#72658 = EDGE_LOOP ( 'NONE', ( #60875, #33526, #87002, #37522 ) ) ;
#72659 = AXIS2_PLACEMENT_3D ( 'NONE', #37012, #70373, #7784 ) ;
#72660 = EDGE_CURVE ( 'NONE', #71376, #71885, #83386, .T. ) ;
#72661 = DIRECTION ( 'NONE',  ( -0.000000000000000000, 0.6427876096865404731, -0.7660444431189770143 ) ) ;
#72662 = CYLINDRICAL_SURFACE ( 'NONE', #67561, 0.2499999999999995559 ) ;
#72663 = CARTESIAN_POINT ( 'NONE',  ( -2.057692307690870415, -7.500000000000155431, 34.75000000000007105 ) ) ;
#72664 = CARTESIAN_POINT ( 'NONE',  ( 6.000000000000001776, -6.343179335718451384, 34.87096338111211935 ) ) ;
#72665 = CARTESIAN_POINT ( 'NONE',  ( 7.623226887246997485, -12.64616026154729411, 30.79003144601913533 ) ) ;
#72666 = CARTESIAN_POINT ( 'NONE',  ( 3.007284287045283389, -5.912607949931405038, 34.49155766932282319 ) ) ;
#72667 = CARTESIAN_POINT ( 'NONE',  ( -17.93474442872397034, -10.21337939537593797, 33.94971097300152252 ) ) ;
#72668 = CARTESIAN_POINT ( 'NONE',  ( 16.94636316330970871, -2.254533558242299396, 29.97296025877827930 ) ) ;
#72669 = CARTESIAN_POINT ( 'NONE',  ( -4.219116599806928214, -10.21337939537584383, 33.94971097300158647 ) ) ;
#72670 = ORIENTED_EDGE ( 'NONE', *, *, #16437, .F. ) ;
#72671 = AXIS2_PLACEMENT_3D ( 'NONE', #8975, #16170, #43632 ) ;
#72672 = B_SPLINE_CURVE_WITH_KNOTS ( 'NONE', 3,
 ( #81525, #33334, #7956, #6307, #39657, #67563, #67119, #74767, #28217, #53593 ),
 .UNSPECIFIED., .F., .F.,
 ( 4, 2, 2, 2, 4 ),
 ( 0.0007817246256747474977, 0.0009771112852218909357, 0.001172497944769034482, 0.001367884604316178029, 0.001563271263863321575 ),
 .UNSPECIFIED. ) ;
#72673 = ORIENTED_EDGE ( 'NONE', *, *, #63194, .F. ) ;
#72674 = ORIENTED_EDGE ( 'NONE', *, *, #56981, .F. ) ;
#72676 = ORIENTED_EDGE ( 'NONE', *, *, #55318, .T. ) ;
#72675 = CARTESIAN_POINT ( 'NONE',  ( 0.2115617174898705155, -12.01397095200673881, 32.43157075238190146 ) ) ;
#72678 = DIRECTION ( 'NONE',  ( 0.000000000000000000, 0.9848077530122072432, -0.1736481776669354937 ) ) ;
#72677 = LINE ( 'NONE', #10988, #44575 ) ;
#72679 = B_SPLINE_CURVE_WITH_KNOTS ( 'NONE', 3,
 ( #22879, #8496, #84166, #77386, #64299, #23756, #29652, #57995, #49908, #51209 ),
 .UNSPECIFIED., .F., .F.,
 ( 4, 2, 2, 2, 4 ),
 ( 0.000000000000000000, 0.0001954311564186874978, 0.0003908623128373749957, 0.0005862934692560624935, 0.0007817246256747499913 ),
 .UNSPECIFIED. ) ;
#72680 = CARTESIAN_POINT ( 'NONE',  ( -1.134615384615369260, -2.249999999999999112, 29.81603969181031033 ) ) ;
#72681 = EDGE_CURVE ( 'NONE', #73158, #763, #1689, .T. ) ;
#72682 = CARTESIAN_POINT ( 'NONE',  ( 4.153846153846032507, -2.625532179533778709, 30.86335684631627174 ) ) ;
#72683 = EDGE_CURVE ( 'NONE', #89080, #64424, #46021, .T. ) ;
#72684 = FACE_BOUND ( 'NONE', #65432, .T. ) ;
#72685 = ORIENTED_EDGE ( 'NONE', *, *, #72877, .T. ) ;
#72686 = ORIENTED_EDGE ( 'NONE', *, *, #68223, .T. ) ;
#72687 = LINE ( 'NONE', #25395, #87436 ) ;
#72688 = ORIENTED_EDGE ( 'NONE', *, *, #86332, .T. ) ;
#72689 = FACE_BOUND ( 'NONE', #75625, .T. ) ;
#72690 = CARTESIAN_POINT ( 'NONE',  ( -6.000000000000119904, -9.442884908241554243, 34.35708131394783038 ) ) ;
#72691 = CARTESIAN_POINT ( 'NONE',  ( -3.931066612577742259, -11.89424750095246175, 32.13594075562311758 ) ) ;
#72692 = ORIENTED_EDGE ( 'NONE', *, *, #57342, .T. ) ;
#72693 = CARTESIAN_POINT ( 'NONE',  ( 2.084207363968360038, -8.496056993536548418, 34.65000542017679663 ) ) ;
#72694 = PLANE ( 'NONE',  #44710 ) ;
#72695 = CARTESIAN_POINT ( 'NONE',  ( 2.057669083470850424, -11.56360843649121861, 33.07473185843129926 ) ) ;
#72696 = EDGE_LOOP ( 'NONE', ( #51220, #36415, #68897, #87355 ) ) ;
#72697 = CARTESIAN_POINT ( 'NONE',  ( 17.75000000000000000, -7.500000000000001776, 35.00000000000000000 ) ) ;
#72698 = DIRECTION ( 'NONE',  ( 0.000000000000000000, 0.000000000000000000, -1.000000000000000000 ) ) ;
#72699 = ORIENTED_EDGE ( 'NONE', *, *, #25673, .T. ) ;
#72700 = DIRECTION ( 'NONE',  ( -0.000000000000000000, -0.6427876096865404731, -0.7660444431189770143 ) ) ;
#72701 = DIRECTION ( 'NONE',  ( -1.000000000000000000, 0.000000000000000000, -0.000000000000000000 ) ) ;
#72702 = ORIENTED_EDGE ( 'NONE', *, *, #38823, .T. ) ;
#72703 = CARTESIAN_POINT ( 'NONE',  ( 18.22301135161285046, -6.503523203565941380, 34.64991518177335195 ) ) ;
#72704 = CARTESIAN_POINT ( 'NONE',  ( 13.13459214732242408, -2.587272538249754117, 30.68239716806877837 ) ) ;
#72705 = CARTESIAN_POINT ( 'NONE',  ( -15.93106661257773560, -8.496831190052089866, 34.64984203495476578 ) ) ;
#72706 = CARTESIAN_POINT ( 'NONE',  ( -10.48485891362104994, -6.001044277235009439, 34.52024696741798948 ) ) ;
#72707 = CARTESIAN_POINT ( 'NONE',  ( 3.230769230769231726, -2.721908614388771852, 31.22303859784724978 ) ) ;
#72708 = DIRECTION ( 'NONE',  ( 1.000000000000000000, 0.000000000000000000, 0.000000000000000000 ) ) ;
#72710 = CARTESIAN_POINT ( 'NONE',  ( -0.4615384615384611200, -11.16473453929635440, 33.15142922261926373 ) ) ;
#72709 = CARTESIAN_POINT ( 'NONE',  ( 4.376857505459003761, -12.15243808032446005, 31.58219941686247978 ) ) ;
#72711 = CARTESIAN_POINT ( 'NONE',  ( 8.900022577055556994, -12.11778462344221019, 31.66786338562085135 ) ) ;
#72713 = LINE ( 'NONE', #73170, #59304 ) ;
#72712 = LINE ( 'NONE', #9677, #60228 ) ;
#72714 = CARTESIAN_POINT ( 'NONE',  ( -1.409462824231155764E-14, -4.749999999999999112, 15.40625000000000000 ) ) ;
#72715 = ORIENTED_EDGE ( 'NONE', *, *, #67381, .T. ) ;
#72716 = PLANE ( 'NONE',  #67781 ) ;
#72717 = VERTEX_POINT ( 'NONE', #5037 ) ;
#72718 = ORIENTED_EDGE ( 'NONE', *, *, #14535, .F. ) ;
#72719 = CARTESIAN_POINT ( 'NONE',  ( -7.623374177175779920, -2.612705202774698421, 31.66806509827799943 ) ) ;
#72720 = ORIENTED_EDGE ( 'NONE', *, *, #56180, .F. ) ;
#72721 = CARTESIAN_POINT ( 'NONE',  ( -11.53846153846166089, -9.528491918059723176, 34.59228464037033035 ) ) ;
#72722 = CARTESIAN_POINT ( 'NONE',  ( -1.200186371490556958, -4.775308065498765409, 26.32625670625849068 ) ) ;
#72723 = CARTESIAN_POINT ( 'NONE',  ( 4.153846153846154188, -4.786620604624113540, 33.94971097300155094 ) ) ;
#72724 = CARTESIAN_POINT ( 'NONE',  ( -15.23076923076922995, -12.34228464037088635, 31.77849191805839268 ) ) ;
#72725 = CARTESIAN_POINT ( 'NONE',  ( -0.2114841499001470781, -5.728107161865378494, 34.42597550085002922 ) ) ;
#72726 = CARTESIAN_POINT ( 'NONE',  ( -6.000000000000121680, -2.657715359629662988, 31.77849191805970364 ) ) ;
#72727 = CARTESIAN_POINT ( 'NONE',  ( 2.544871794871792936, -3.499999999999999556, 29.75000000000000355 ) ) ;
#72728 = CARTESIAN_POINT ( 'NONE',  ( -10.61538461538473399, -4.481592998941358097, 33.73612834414048933 ) ) ;
#72729 = CARTESIAN_POINT ( 'NONE',  ( 5.776515056276054771, -4.386631170607603991, 33.66268669641500111 ) ) ;
#72730 = CARTESIAN_POINT ( 'NONE',  ( 3.749999999999992006, -5.946699141100872943, 19.39062500000000711 ) ) ;
#72731 = CIRCLE ( 'NONE', #29592, 2.750000000000000000 ) ;
#72732 = DIRECTION ( 'NONE',  ( -0.000000000000000000, 0.9396926207859093161, -0.3420201433256663259 ) ) ;
#72733 = CARTESIAN_POINT ( 'NONE',  ( 4.153846153846030731, -2.379036618888197729, 30.90682066428292885 ) ) ;
#72734 = CYLINDRICAL_SURFACE ( 'NONE', #10488, 0.2499999999999995559 ) ;
#72735 = EDGE_LOOP ( 'NONE', ( #66265, #35102, #62223, #86052 ) ) ;
#72736 = ORIENTED_EDGE ( 'NONE', *, *, #30943, .T. ) ;
#72737 = CARTESIAN_POINT ( 'NONE',  ( -11.47320596718551045, -6.026961402152789304, 34.52809138561124769 ) ) ;
#72738 = CARTESIAN_POINT ( 'NONE',  ( -17.20707028636129721, -8.587444163452046197, 34.63053765926554206 ) ) ;
#72739 = CARTESIAN_POINT ( 'NONE',  ( 16.15384615384615330, -12.34228464037088635, 31.77849191805839268 ) ) ;
#72740 = FACE_OUTER_BOUND ( 'NONE', #86789, .T. ) ;
#72741 = VECTOR ( 'NONE', #62044, 1000.000000000000114 ) ;
#72742 = CARTESIAN_POINT ( 'NONE',  ( 17.07692307692307665, -12.34228464037088635, 31.77849191805839268 ) ) ;
#72743 = CARTESIAN_POINT ( 'NONE',  ( -10.61538461538461320, -4.098570777380720287, 33.41473453929634729 ) ) ;
#72744 = ADVANCED_FACE ( 'NONE', ( #5492 ), #53217, .F. ) ;
#72745 = EDGE_CURVE ( 'NONE', #86745, #30027, #50025, .T. ) ;
#72746 = ORIENTED_EDGE ( 'NONE', *, *, #27924, .T. ) ;
#72747 = CARTESIAN_POINT ( 'NONE',  ( -10.68070753087678781, -7.749976743299138882, 34.99404534957040624 ) ) ;
#72748 = ORIENTED_EDGE ( 'NONE', *, *, #24246, .T. ) ;
#72749 = ORIENTED_EDGE ( 'NONE', *, *, #43835, .F. ) ;
#72750 = CARTESIAN_POINT ( 'NONE',  ( -9.692307692307814193, -3.083524468854526912, 32.58852847137268327 ) ) ;
#72751 = ADVANCED_FACE ( 'NONE', ( #27528 ), #7262, .F. ) ;
#72752 = CYLINDRICAL_SURFACE ( 'NONE', #61468, 0.2500000000000008882 ) ;
#72753 = CIRCLE ( 'NONE', #33925, 0.2500000000000002220 ) ;
#72754 = CARTESIAN_POINT ( 'NONE',  ( -9.627052121031661969, -6.879047030191282275, 34.71129190930002295 ) ) ;
#72755 = ADVANCED_FACE ( 'NONE', ( #49125 ), #14009, .T. ) ;
#72756 = CARTESIAN_POINT ( 'NONE',  ( 9.692307692307695177, -3.322132147404559976, 32.92929555188717927 ) ) ;
#72757 = CARTESIAN_POINT ( 'NONE',  ( 13.25446741488368829, -8.630895178749533159, 34.87696386517710323 ) ) ;
#72758 = AXIS2_PLACEMENT_3D ( 'NONE', #49912, #23761, #51214 ) ;
#72759 = ORIENTED_EDGE ( 'NONE', *, *, #88539, .T. ) ;
#72760 = ORIENTED_EDGE ( 'NONE', *, *, #49846, .T. ) ;
#72761 = ORIENTED_EDGE ( 'NONE', *, *, #19710, .F. ) ;
#72762 = EDGE_CURVE ( 'NONE', #74862, #23459, #28873, .T. ) ;
#72763 = CARTESIAN_POINT ( 'NONE',  ( -7.146561847641252463, -12.11044203135681840, 32.26167407432752299 ) ) ;
#72764 = LINE ( 'NONE', #66003, #87691 ) ;
#72765 = CARTESIAN_POINT ( 'NONE',  ( 8.992243613324164997, -5.582272713120729257, 34.63742843783360570 ) ) ;
#72766 = CARTESIAN_POINT ( 'NONE',  ( 20.00000000000000000, -4.000000000000000000, 29.75000000000000355 ) ) ;
#72767 = CARTESIAN_POINT ( 'NONE',  ( -11.76194646302587010, -8.539481045369596401, 34.89627647299170832 ) ) ;
#72768 = CARTESIAN_POINT ( 'NONE',  ( -16.02332045208259359, -2.882268652242223617, 31.66798894389554064 ) ) ;
#72769 = ORIENTED_EDGE ( 'NONE', *, *, #74816, .F. ) ;
#72770 = ORIENTED_EDGE ( 'NONE', *, *, #35171, .F. ) ;
#72771 = DIRECTION ( 'NONE',  ( -0.000000000000000000, 0.3420201433256694346, -0.9396926207859080948 ) ) ;
#72772 = VERTEX_POINT ( 'NONE', #28408 ) ;
#72774 = ORIENTED_EDGE ( 'NONE', *, *, #6713, .F. ) ;
#72773 = CARTESIAN_POINT ( 'NONE',  ( -5.934744428723973897, -3.300289026998475705, 32.46337939537591666 ) ) ;
#72775 = CARTESIAN_POINT ( 'NONE',  ( 1.384615384615265343, -10.21337939537710326, 33.94971097300076224 ) ) ;
#72776 = FACE_OUTER_BOUND ( 'NONE', #14079, .T. ) ;
#72777 = VECTOR ( 'NONE', #40272, 1000.000000000000000 ) ;
#72778 = CARTESIAN_POINT ( 'NONE',  ( 3.750000000000009770, -9.053300858899081760, 15.79687500000000178 ) ) ;
#72779 = ADVANCED_FACE ( 'NONE', ( #48231 ), #35169, .F. ) ;
#72780 = ORIENTED_EDGE ( 'NONE', *, *, #53851, .F. ) ;
#72781 = EDGE_CURVE ( 'NONE', #67447, #78622, #77942, .T. ) ;
#72782 = CARTESIAN_POINT ( 'NONE',  ( 8.769230769230768274, -13.53365097954675988, 30.81389545987213552 ) ) ;
#72783 = EDGE_LOOP ( 'NONE', ( #876, #11801, #83243, #5604 ) ) ;
#72784 = CARTESIAN_POINT ( 'NONE',  ( 2.530471848960718084, -9.332535724633405749, 34.40230450496446224 ) ) ;
#72785 = DIRECTION ( 'NONE',  ( -0.000000000000000000, -0.6427876096865404731, -0.7660444431189770143 ) ) ;
#72786 = FACE_BOUND ( 'NONE', #51706, .T. ) ;
#72788 = DIRECTION ( 'NONE',  ( -0.000000000000000000, 0.1736481776669307198, -0.9848077530122080203 ) ) ;
#72787 = CARTESIAN_POINT ( 'NONE',  ( 5.076923076923075762, -4.661471528628507777, 34.16647553114623292 ) ) ;
#72789 = EDGE_CURVE ( 'NONE', #30370, #56543, #8149, .T. ) ;
#72790 = CARTESIAN_POINT ( 'NONE',  ( -1.607542343522233130, -3.395401636524185474, 33.02366814457250399 ) ) ;
#72791 = CARTESIAN_POINT ( 'NONE',  ( -3.360917200500926239, -8.630895178749536711, 34.87696386517710323 ) ) ;
#72792 = VERTEX_POINT ( 'NONE', #69404 ) ;
#72793 = ADVANCED_FACE ( 'NONE', ( #1382 ), #83367, .F. ) ;
#72794 = CYLINDRICAL_SURFACE ( 'NONE', #27446, 4.000000000000000000 ) ;
#72795 = CARTESIAN_POINT ( 'NONE',  ( 2.952004793765244717, -6.965521097154411478, 14.00000000000000178 ) ) ;
#72796 = VERTEX_POINT ( 'NONE', #21207 ) ;
#72797 = B_SPLINE_CURVE_WITH_KNOTS ( 'NONE', 3,
 ( #47123, #61525, #75488, #12903, #34508, #20980, #68736, #7032, #48451, #75937 ),
 .UNSPECIFIED., .F., .F.,
 ( 4, 2, 2, 2, 4 ),
 ( 0.0007817246336856289524, 0.0009771112958940099402, 0.001172497958102391036, 0.001367884620310772133, 0.001563271282519153229 ),
 .UNSPECIFIED. ) ;
#72798 = CARTESIAN_POINT ( 'NONE',  ( -18.00000000000000000, -3.050289026998447284, 32.03036669348365706 ) ) ;
#72799 = CARTESIAN_POINT ( 'NONE',  ( -18.25002322422145440, -12.68155406624981119, 30.59749803192733708 ) ) ;
#72800 = CARTESIAN_POINT ( 'NONE',  ( 10.55011461482829738, -8.656820664281498878, 34.87096338111211935 ) ) ;
#72801 = FACE_OUTER_BOUND ( 'NONE', #46304, .T. ) ;
#72802 = DIRECTION ( 'NONE',  ( 1.000000000000000000, 0.000000000000000000, 0.000000000000000000 ) ) ;
#72803 = FACE_BOUND ( 'NONE', #23466, .T. ) ;
#72805 = DIRECTION ( 'NONE',  ( -0.000000000000000000, 0.000000000000000000, 1.000000000000000000 ) ) ;
#72804 = LINE ( 'NONE', #37240, #61927 ) ;
#72806 =( GEOMETRIC_REPRESENTATION_CONTEXT ( 3 ) GLOBAL_UNCERTAINTY_ASSIGNED_CONTEXT ( ( #69518 ) ) GLOBAL_UNIT_ASSIGNED_CONTEXT ( ( #80625, #26556, #18907 ) ) REPRESENTATION_CONTEXT ( 'NONE', 'WORKASPACE' ) );
#72807 = CARTESIAN_POINT ( 'NONE',  ( 16.02369894440793630, -3.285722584762969856, 32.44110544564090759 ) ) ;
#72809 = CARTESIAN_POINT ( 'NONE',  ( -20.99999999999999645, -7.500000000000000000, 29.75000000000000355 ) ) ;
#72808 = CARTESIAN_POINT ( 'NONE',  ( 2.980745993476266342, -4.335965774309649134, 33.62209801155881905 ) ) ;
#72810 = CARTESIAN_POINT ( 'NONE',  ( 15.90382291655318880, -10.76384336483936011, 33.53834819971076087 ) ) ;
#72811 = CARTESIAN_POINT ( 'NONE',  ( 6.250054419913455561, -4.818054556918156095, 34.26375889529406749 ) ) ;
#72812 = CARTESIAN_POINT ( 'NONE',  ( 3.775308065498768517, -8.992201783934554271, 25.54500670625849779 ) ) ;
#72813 = ORIENTED_EDGE ( 'NONE', *, *, #12915, .F. ) ;
#72814 = CARTESIAN_POINT ( 'NONE',  ( -7.976845312821407852, -11.18331474514187995, 33.13161551792790505 ) ) ;
#72815 = CARTESIAN_POINT ( 'NONE',  ( 7.715462379486289102, -8.999036380462719364, 34.52022231692819076 ) ) ;
#72816 = CARTESIAN_POINT ( 'NONE',  ( -13.51517529822874586, -2.254533558242299396, 29.97296025877828285 ) ) ;
#72817 = DIRECTION ( 'NONE',  ( -0.000000000000000000, 0.9848077530122085754, -0.1736481776669273613 ) ) ;
#72818 = CARTESIAN_POINT ( 'NONE',  ( 10.74591031714818001, -12.27024696741798770, 31.24895572276497546 ) ) ;
#72819 = CARTESIAN_POINT ( 'NONE',  ( -6.923076923076922462, -13.78497067705608181, 32.30358669280327177 ) ) ;
#72820 = CARTESIAN_POINT ( 'NONE',  ( 2.750000000000001332, -7.438900925035452083, 15.46688170625848713 ) ) ;
#72821 = CARTESIAN_POINT ( 'NONE',  ( -8.703162418228330921, -2.721908614388772296, 31.22303859784725333 ) ) ;
#72822 = CARTESIAN_POINT ( 'NONE',  ( 0.4615384615383396616, -3.835265460704628371, 33.15142922262033665 ) ) ;
#72823 = AXIS2_PLACEMENT_3D ( 'NONE', #55687, #83180, #21467 ) ;
#72824 = CARTESIAN_POINT ( 'NONE',  ( 11.28846153846153832, -7.500000000000001776, 35.00000000000000000 ) ) ;
#72825 = CARTESIAN_POINT ( 'NONE',  ( -0.4615384615385840772, -8.656820664282941280, 34.87096338111179961 ) ) ;
#72826 = CARTESIAN_POINT ( 'NONE',  ( 8.703147358274888390, -9.780366693483667717, 34.19971097300155805 ) ) ;
#72827 = CARTESIAN_POINT ( 'NONE',  ( -8.992156986746916658, -9.086856451489515152, 34.49173150075333183 ) ) ;
#72828 = EDGE_CURVE ( 'NONE', #85857, #49108, #57510, .T. ) ;
#72829 = DIRECTION ( 'NONE',  ( 1.000000000000000000, 0.000000000000000000, 0.000000000000000000 ) ) ;
#72830 = AXIS2_PLACEMENT_3D ( 'NONE', #77473, #46, #36059 ) ;
#72831 = DIRECTION ( 'NONE',  ( -0.000000000000000000, -0.5000000000000009992, -0.8660254037844380415 ) ) ;
#72832 = ORIENTED_EDGE ( 'NONE', *, *, #70797, .F. ) ;
#72833 = B_SPLINE_CURVE_WITH_KNOTS ( 'NONE', 3,
 ( #73698, #74127, #66928, #75023, #19620, #33137 ),
 .UNSPECIFIED., .F., .F.,
 ( 4, 2, 4 ),
 ( 0.0003909512603273901832, 0.0005862562993132176088, 0.0007815613382990449802 ),
 .UNSPECIFIED. ) ;
#72834 = CARTESIAN_POINT ( 'NONE',  ( 15.23076923076923173, -11.35647404775217417, 33.31231777344666511 ) ) ;
#72835 = CARTESIAN_POINT ( 'NONE',  ( 8.899756470994331536, -11.46989282347013095, 32.79007818306219946 ) ) ;
#72836 = CARTESIAN_POINT ( 'NONE',  ( 2.608446859217924629, -10.19485399968118422, 19.87686829374151287 ) ) ;
#72837 = B_SPLINE_CURVE_WITH_KNOTS ( 'NONE', 3,
 ( #7166, #8055, #8499, #28773, #56238, #22445, #70192, #84169, #41397, #7611 ),
 .UNSPECIFIED., .F., .F.,
 ( 4, 2, 2, 2, 4 ),
 ( 0.000000000000000000, 0.0001954311564186862781, 0.0003908623128373725562, 0.0005862934692560588072, 0.0007817246256747451124 ),
 .UNSPECIFIED. ) ;
#72838 = CARTESIAN_POINT ( 'NONE',  ( 13.38461538461526601, -10.21337939537710326, 33.94971097300076224 ) ) ;
#72839 = FACE_OUTER_BOUND ( 'NONE', #26123, .T. ) ;
#72840 = ORIENTED_EDGE ( 'NONE', *, *, #62218, .T. ) ;
#72841 = CARTESIAN_POINT ( 'NONE',  ( -18.00000000000000000, -8.973038597847269315, 34.52809138561121927 ) ) ;
#72842 = LINE ( 'NONE', #39533, #74706 ) ;
#72844 = ORIENTED_EDGE ( 'NONE', *, *, #53872, .F. ) ;
#72843 = CARTESIAN_POINT ( 'NONE',  ( -7.715628407920204879, -12.50538340440932394, 31.33453814440721885 ) ) ;
#72845 = CARTESIAN_POINT ( 'NONE',  ( -12.59222906464877134, -9.084618155246140248, 34.75535874321725771 ) ) ;
#72846 = CARTESIAN_POINT ( 'NONE',  ( -1.384615384615383471, -1.951392089020283160, 34.73218667398347748 ) ) ;
#72847 = CARTESIAN_POINT ( 'NONE',  ( -4.826977558574935934, -9.272278438253401589, 34.42582936511637826 ) ) ;
#72848 = ADVANCED_FACE ( 'NONE', ( #42824 ), #59, .F. ) ;
#72849 = DIRECTION ( 'NONE',  ( 0.000000000000000000, 0.000000000000000000, 1.000000000000000000 ) ) ;
#72850 = ORIENTED_EDGE ( 'NONE', *, *, #85063, .T. ) ;
#72851 = FACE_OUTER_BOUND ( 'NONE', #48497, .T. ) ;
#72852 = CARTESIAN_POINT ( 'NONE',  ( -12.52680846209478460, -2.657715359629089225, 31.77849191805832874 ) ) ;
#72853 = AXIS2_PLACEMENT_3D ( 'NONE', #25974, #86819, #46690 ) ;
#72854 = CARTESIAN_POINT ( 'NONE',  ( -11.53846153846166089, -6.835583212225970762, 34.95778746994575670 ) ) ;
#72855 = ORIENTED_EDGE ( 'NONE', *, *, #5358, .F. ) ;
#72856 = VERTEX_POINT ( 'NONE', #82488 ) ;
#72857 = VERTEX_POINT ( 'NONE', #20767 ) ;
#72858 = EDGE_CURVE ( 'NONE', #48029, #45953, #72047, .T. ) ;
#72859 = CARTESIAN_POINT ( 'NONE',  ( -18.13014720943822056, -3.817052484675422352, 33.13202310037935661 ) ) ;
#72860 = DIRECTION ( 'NONE',  ( 0.000000000000000000, 0.4999999999999960032, -0.8660254037844410391 ) ) ;
#72861 = CIRCLE ( 'NONE', #26838, 0.2500000000000002220 ) ;
#72862 = EDGE_CURVE ( 'NONE', #59563, #13845, #52765, .T. ) ;
#72863 = CARTESIAN_POINT ( 'NONE',  ( 13.25446817517716447, -11.47017969459903952, 32.78971311882035167 ) ) ;
#72864 = DIRECTION ( 'NONE',  ( -0.000000000000000000, 1.000000000000000000, 3.491481338843133355E-15 ) ) ;
#72865 = ORIENTED_EDGE ( 'NONE', *, *, #46634, .F. ) ;
#72867 = ORIENTED_EDGE ( 'NONE', *, *, #47151, .T. ) ;
#72866 = EDGE_CURVE ( 'NONE', #80750, #19020, #85134, .T. ) ;
#72869 = VERTEX_POINT ( 'NONE', #16226 ) ;
#72868 = CARTESIAN_POINT ( 'NONE',  ( -1.254089682851820653, -5.195472089885680766, 34.18748526763464923 ) ) ;
#72870 = CARTESIAN_POINT ( 'NONE',  ( -16.15384615384627409, -12.51329471203414379, 31.30864560766407578 ) ) ;
#72871 = B_SPLINE_CURVE_WITH_KNOTS ( 'NONE', 3,
 ( #30424, #78603, #77277, #9276, #70526, #37621, #24102, #36737, #30857, #43051 ),
 .UNSPECIFIED., .F., .F.,
 ( 4, 2, 2, 2, 4 ),
 ( 0.0007817359430256315238, 0.0009771253907249976244, 0.001172514838424363508, 0.001367904286123729392, 0.001563293733823095492 ),
 .UNSPECIFIED. ) ;
#72872 = CARTESIAN_POINT ( 'NONE',  ( 8.769230769230768274, -12.78798330534102945, 29.74999999999997868 ) ) ;
#72873 = EDGE_CURVE ( 'NONE', #68769, #8206, #75795, .T. ) ;
#72874 = AXIS2_PLACEMENT_3D ( 'NONE', #4093, #53625, #37893 ) ;
#72875 = CARTESIAN_POINT ( 'NONE',  ( 2.438484115517095319, -3.530189275343204702, 32.79018710029569661 ) ) ;
#72876 = CARTESIAN_POINT ( 'NONE',  ( -7.911423846710166075, -10.33852847137145048, 34.16647553114627556 ) ) ;
#72877 = EDGE_CURVE ( 'NONE', #44505, #32252, #67183, .T. ) ;
#72878 = EDGE_LOOP ( 'NONE', ( #57483, #15171 ) ) ;
#72879 = B_SPLINE_CURVE_WITH_KNOTS ( 'NONE', 3,
 ( #72822, #44906, #65616, #17000, #24193, #37711, #23744, #65178, #79599, #3476 ),
 .UNSPECIFIED., .F., .F.,
 ( 4, 2, 2, 2, 4 ),
 ( 0.0007817359430256372700, 0.0009771253907250052138, 0.001172514838424373266, 0.001367904286123741101, 0.001563293733823109153 ),
 .UNSPECIFIED. ) ;
#72880 = EDGE_LOOP ( 'NONE', ( #48840, #44636 ) ) ;
#72881 = AXIS2_PLACEMENT_3D ( 'NONE', #16873, #52874, #71811 ) ;
#72882 = ORIENTED_EDGE ( 'NONE', *, *, #80136, .F. ) ;
#72884 = VERTEX_POINT ( 'NONE', #36505 ) ;
#72883 = DIRECTION ( 'NONE',  ( -0.000000000000000000, -0.9848077530122085754, -0.1736481776669273613 ) ) ;
#72885 = CARTESIAN_POINT ( 'NONE',  ( 16.94623247381277054, -5.496505350115500121, 34.60290016733514307 ) ) ;
#72886 = CARTESIAN_POINT ( 'NONE',  ( 12.23805351781451378, -11.41268669641499756, 32.86336882939238535 ) ) ;
#72888 = ORIENTED_EDGE ( 'NONE', *, *, #66045, .F. ) ;
#72887 = ADVANCED_FACE ( 'NONE', ( #51759 ), #65729, .F. ) ;
#72889 = CIRCLE ( 'NONE', #44071, 0.2500000000000002220 ) ;
#72890 = DIRECTION ( 'NONE',  ( 0.000000000000000000, 0.000000000000000000, -1.000000000000000000 ) ) ;
#72891 = CARTESIAN_POINT ( 'NONE',  ( 23.49999999999998934, 6.011520428872295955E-15, 27.75000000000000355 ) ) ;
#72892 = DIRECTION ( 'NONE',  ( -0.000000000000000000, 0.9396926207859092051, -0.3420201433256662704 ) ) ;
#72893 = FACE_BOUND ( 'NONE', #70897, .T. ) ;
#72894 = CARTESIAN_POINT ( 'NONE',  ( -0.4615384615385826339, -4.481592998941358097, 33.73612834414048933 ) ) ;
#72896 = EDGE_CURVE ( 'NONE', #47112, #71524, #84427, .T. ) ;
#72895 = CYLINDRICAL_SURFACE ( 'NONE', #57165, 0.2500000000000012212 ) ;
#72897 = CARTESIAN_POINT ( 'NONE',  ( -8.096177083446809419, -12.22074536777954989, 31.39888409691088356 ) ) ;
#72899 = CARTESIAN_POINT ( 'NONE',  ( 14.55763771707035303, -2.986452184633680673, 32.43230066228895225 ) ) ;
#72898 = CYLINDRICAL_SURFACE ( 'NONE', #18744, 0.2499999999999994726 ) ;
#72900 = CARTESIAN_POINT ( 'NONE',  ( 8.519207545009310323, -9.356822207818506598, 34.66110646841856635 ) ) ;
#72901 = CARTESIAN_POINT ( 'NONE',  ( 12.46153846153846168, -13.63283147151868846, 33.57946703557072254 ) ) ;
#72902 = VERTEX_POINT ( 'NONE', #77920 ) ;
#72903 = ADVANCED_FACE ( 'NONE', ( #58977 ), #43691, .F. ) ;
#72904 = CARTESIAN_POINT ( 'NONE',  ( -17.32689982097166492, -5.643011162660950042, 34.66104346484419096 ) ) ;
#72905 = CARTESIAN_POINT ( 'NONE',  ( -13.51530598772569469, -9.084618155246140248, 34.75535874321725771 ) ) ;
#72906 = ORIENTED_EDGE ( 'NONE', *, *, #354, .T. ) ;
#72907 = ORIENTED_EDGE ( 'NONE', *, *, #6852, .F. ) ;
#72909 = CARTESIAN_POINT ( 'NONE',  ( 1.607395053593452028, -5.827830569534415694, 34.72679350104403539 ) ) ;
#72908 = CARTESIAN_POINT ( 'NONE',  ( -11.76194646302587010, -12.69144148231606017, 30.53333754910549303 ) ) ;
#72910 = B_SPLINE_CURVE_WITH_KNOTS ( 'NONE', 3,
 ( #54981, #8571, #35148, #21631, #83348, #36046, #68930, #7241, #70266, #34711 ),
 .UNSPECIFIED., .F., .F.,
 ( 4, 2, 2, 2, 4 ),
 ( 0.000000000000000000, 0.0001954339857564081791, 0.0003908679715128163582, 0.0005863019572692245102, 0.0007817359430256327164 ),
 .UNSPECIFIED. ) ;
#72911 = B_SPLINE_CURVE_WITH_KNOTS ( 'NONE', 3,
 ( #62865, #34084, #1180, #69203, #61547, #53913, #34965, #62426, #81401, #89053 ),
 .UNSPECIFIED., .F., .F.,
 ( 4, 2, 2, 2, 4 ),
 ( 0.0007817359527651132059, 0.0009771254036996528287, 0.001172514854634192560, 0.001367904305568732291, 0.001563293756503272023 ),
 .UNSPECIFIED. ) ;
#72912 = CARTESIAN_POINT ( 'NONE',  ( 16.28437185560972011, -2.619367082507847666, 30.83698974864643461 ) ) ;
#72913 = FACE_OUTER_BOUND ( 'NONE', #55930, .T. ) ;
#72914 = CYLINDRICAL_SURFACE ( 'NONE', #54811, 0.2499999999999994726 ) ;
#72915 = ORIENTED_EDGE ( 'NONE', *, *, #52951, .F. ) ;
#72916 = AXIS2_PLACEMENT_3D ( 'NONE', #74414, #12713, #2721 ) ;
#72917 = DIRECTION ( 'NONE',  ( 0.000000000000000000, 0.000000000000000000, -1.000000000000000000 ) ) ;
#72918 = CARTESIAN_POINT ( 'NONE',  ( 10.61538461538461675, -7.500000000000001776, 35.04278698407183867 ) ) ;
#72920 = LINE ( 'NONE', #67508, #31546 ) ;
#72919 = CARTESIAN_POINT ( 'NONE',  ( 5.076923076923075762, -5.557115091759785130, 34.35708131394839171 ) ) ;
#72921 = CARTESIAN_POINT ( 'NONE',  ( -1.634592128663975519, -10.06842814019191401, 34.32929386961144758 ) ) ;
#72922 = CARTESIAN_POINT ( 'NONE',  ( 10.61538461538461675, -4.098570777380720287, 33.41473453929634729 ) ) ;
#72924 = FACE_OUTER_BOUND ( 'NONE', #56448, .T. ) ;
#72923 = FILL_AREA_STYLE ('',( #53535 ) ) ;
#72925 = EDGE_CURVE ( 'NONE', #79557, #7925, #63984, .T. ) ;
#72926 = AXIS2_PLACEMENT_3D ( 'NONE', #60349, #87860, #8962 ) ;
#72927 = CARTESIAN_POINT ( 'NONE',  ( -2.651650429449565305, -4.848349570550461785, 22.75000000000000000 ) ) ;
#72928 = ORIENTED_EDGE ( 'NONE', *, *, #15405, .T. ) ;
#72929 = VERTEX_POINT ( 'NONE', #84702 ) ;
#72930 = FACE_OUTER_BOUND ( 'NONE', #35365, .T. ) ;
#72931 = EDGE_CURVE ( 'NONE', #56176, #68565, #44119, .T. ) ;
#72932 = AXIS2_PLACEMENT_3D ( 'NONE', #45225, #51074, #72701 ) ;
#72933 = CARTESIAN_POINT ( 'NONE',  ( 12.71153846153989697, -7.500000000000155431, 34.75000000000007105 ) ) ;
#72934 = CARTESIAN_POINT ( 'NONE',  ( 22.75000000000000000, -10.50000000000000000, 29.75000000000000355 ) ) ;
#72935 = CARTESIAN_POINT ( 'NONE',  ( 14.43848411551708999, -2.729792928343269587, 31.24908615093345077 ) ) ;
#72936 = CARTESIAN_POINT ( 'NONE',  ( 2.557692307693744560, -7.500000000000155431, 34.75000000000007105 ) ) ;
#72937 = CARTESIAN_POINT ( 'NONE',  ( -1.553300858899125059, -3.750000000000009326, 24.07812500000000355 ) ) ;
#72938 = CARTESIAN_POINT ( 'NONE',  ( 8.638540166120458608, -3.957541250942358424, 33.62499894934981626 ) ) ;
#72939 = CYLINDRICAL_SURFACE ( 'NONE', #11524, 0.2500000000000008882 ) ;
#72940 = CARTESIAN_POINT ( 'NONE',  ( -9.019207513279360100, -12.65889640711025521, 30.72598325615533454 ) ) ;
#72941 = CARTESIAN_POINT ( 'NONE',  ( -18.22337594069816902, -12.49852196912267566, 29.88021232661720461 ) ) ;
#72942 = CARTESIAN_POINT ( 'NONE',  ( 9.758376043310134307, -2.721908614388771852, 31.22303859784725333 ) ) ;
#72943 = CARTESIAN_POINT ( 'NONE',  ( 3.296024802045256497, -2.892918686051626498, 31.69288490824026638 ) ) ;
#72944 = CARTESIAN_POINT ( 'NONE',  ( -12.71156168575991785, -8.475808217655753651, 34.90892951860618609 ) ) ;
#72945 = EDGE_CURVE ( 'NONE', #66285, #53910, #71598, .T. ) ;
#72946 = CARTESIAN_POINT ( 'NONE',  ( 3.930919936330004472, -12.39988816332205701, 30.74660775122750778 ) ) ;
#72947 = B_SPLINE_CURVE_WITH_KNOTS ( 'NONE', 3,
 ( #55260, #82748, #49827, #7967, #56148, #77744, #21020, #762, #84520, #41312 ),
 .UNSPECIFIED., .F., .F.,
 ( 4, 2, 2, 2, 4 ),
 ( 0.000000000000000000, 0.0001954339857564078809, 0.0003908679715128157619, 0.0005863019572692236428, 0.0007817359430256315238 ),
 .UNSPECIFIED. ) ;
#72948 = CARTESIAN_POINT ( 'NONE',  ( 1.384615384615264011, -9.528491918059723176, 34.59228464037033035 ) ) ;
#72949 = CARTESIAN_POINT ( 'NONE',  ( 7.716005876422152632, -3.625366637846545892, 33.29286588640298561 ) ) ;
#72950 = CARTESIAN_POINT ( 'NONE',  ( -16.85391023282967637, -2.889357225399416418, 32.26129605718031002 ) ) ;
#72951 = VERTEX_POINT ( 'NONE', #64837 ) ;
#72952 = CYLINDRICAL_SURFACE ( 'NONE', #31230, 4.000000000000000000 ) ;
#72953 = ADVANCED_FACE ( 'NONE', ( #30616 ), #66175, .F. ) ;
#72954 = CARTESIAN_POINT ( 'NONE',  ( 18.13052543823364360, -5.070358843744208421, 34.40418822224088302 ) ) ;
#72955 = LINE ( 'NONE', #51770, #46239 ) ;
#72956 = CARTESIAN_POINT ( 'NONE',  ( -1.139087296526025916, -4.750000000000006217, 22.82812500000000355 ) ) ;
#72957 = EDGE_CURVE ( 'NONE', #13993, #18183, #45908, .T. ) ;
#72958 = CARTESIAN_POINT ( 'NONE',  ( -14.17690049986752321, -4.809403383903225304, 33.96459661697924304 ) ) ;
#72959 = CARTESIAN_POINT ( 'NONE',  ( 15.93091919493930320, -4.762599654559227069, 34.23009711892697737 ) ) ;
#72961 = ORIENTED_EDGE ( 'NONE', *, *, #86022, .T. ) ;
#72960 = CARTESIAN_POINT ( 'NONE',  ( 5.326868486301119532, -4.176053281294514363, 33.81426240980091791 ) ) ;
#72962 = CARTESIAN_POINT ( 'NONE',  ( 1.139087296526029469, -10.24999999999999289, 18.45312499999999645 ) ) ;
#72963 = DIRECTION ( 'NONE',  ( -0.000000000000000000, -1.000000000000000000, -0.000000000000000000 ) ) ;
#72964 = EDGE_LOOP ( 'NONE', ( #40099, #14067 ) ) ;
#72965 = EDGE_CURVE ( 'NONE', #22884, #85301, #60313, .T. ) ;
#72966 = LINE ( 'NONE', #59455, #54350 ) ;
#72967 = B_SPLINE_CURVE_WITH_KNOTS ( 'NONE', 3,
 ( #19319, #82356, #48103, #74716, #88687, #61621, #76023, #75578, #68384, #13880 ),
 .UNSPECIFIED., .F., .F.,
 ( 4, 2, 2, 2, 4 ),
 ( 0.000000000000000000, 0.0001954311564186867389, 0.0003908623128373734778, 0.0005862934692560602167, 0.0007817246256747469556 ),
 .UNSPECIFIED. ) ;
#72968 = ORIENTED_EDGE ( 'NONE', *, *, #25531, .T. ) ;
#72969 = PRODUCT_DEFINITION_SHAPE ( 'NONE', 'NONE',  #89185 ) ;
#72970 = CARTESIAN_POINT ( 'NONE',  ( 15.23076923076923173, -2.249999999999998668, 29.50000000000001421 ) ) ;
#72971 = CARTESIAN_POINT ( 'NONE',  ( -9.469296340694846492, -2.758310577978207778, 31.33698337089302299 ) ) ;
#72972 = CIRCLE ( 'NONE', #36953, 4.000000000000000000 ) ;
#72973 = DIRECTION ( 'NONE',  ( -0.000000000000000000, -0.1736481776669307198, -0.9848077530122080203 ) ) ;
#72974 = ORIENTED_EDGE ( 'NONE', *, *, #58076, .T. ) ;
#72975 = DIRECTION ( 'NONE',  ( -1.000000000000000000, -0.000000000000000000, -0.000000000000000000 ) ) ;
#72976 = ORIENTED_EDGE ( 'NONE', *, *, #8495, .F. ) ;
#72977 = CARTESIAN_POINT ( 'NONE',  ( 11.31553532094538994, -3.586966769969701208, 32.86292498521069660 ) ) ;
#72978 = VERTEX_POINT ( 'NONE', #25201 ) ;
#72979 = CARTESIAN_POINT ( 'NONE',  ( -15.23076923076935252, -2.657715359629662544, 31.77849191805970364 ) ) ;
#72980 = CARTESIAN_POINT ( 'NONE',  ( 2.530471848960719417, -3.236590943229497253, 32.36255958852954251 ) ) ;
#72981 = EDGE_LOOP ( 'NONE', ( #11275, #44935, #33470, #2811 ) ) ;
#72982 = FACE_OUTER_BOUND ( 'NONE', #39985, .T. ) ;
#72984 = EDGE_CURVE ( 'NONE', #37230, #61048, #2723, .T. ) ;
#72983 = FACE_OUTER_BOUND ( 'NONE', #14004, .T. ) ;
#72985 = CARTESIAN_POINT ( 'NONE',  ( 0.2380535369741298979, -2.353723527008297012, 30.78948104536958397 ) ) ;
#72986 = B_SPLINE_CURVE_WITH_KNOTS ( 'NONE', 3,
 ( #66785, #33003, #60468, #38428, #38877, #5085, #59578, #4188, #87081, #24451 ),
 .UNSPECIFIED., .F., .F.,
 ( 4, 2, 2, 2, 4 ),
 ( 0.0007817246256747474977, 0.0009771112852218909357, 0.001172497944769034482, 0.001367884604316178029, 0.001563271263863321575 ),
 .UNSPECIFIED. ) ;
#72987 = CARTESIAN_POINT ( 'NONE',  ( -14.05763788777885637, -10.06805714834173493, 34.32951233291982618 ) ) ;
#72988 = CIRCLE ( 'NONE', #31251, 4.999999999999997335 ) ;
#72989 = ORIENTED_EDGE ( 'NONE', *, *, #34481, .F. ) ;
#72990 = ORIENTED_EDGE ( 'NONE', *, *, #84681, .F. ) ;
#72991 = ORIENTED_EDGE ( 'NONE', *, *, #80702, .T. ) ;
#72993 = ORIENTED_EDGE ( 'NONE', *, *, #59706, .F. ) ;
#72992 = CARTESIAN_POINT ( 'NONE',  ( 3.296836564119306701, -12.62096338111211757, 30.90682066428152908 ) ) ;
#72994 = VECTOR ( 'NONE', #78082, 1000.000000000000000 ) ;
#72995 = VECTOR ( 'NONE', #21550, 1000.000000000000114 ) ;
#72996 = CARTESIAN_POINT ( 'NONE',  ( -8.834501215191545853, -10.21337939537584383, 33.94971097300158647 ) ) ;
#72997 = LINE ( 'NONE', #11295, #56857 ) ;
#72998 = VERTEX_POINT ( 'NONE', #52664 ) ;
#72999 = ORIENTED_EDGE ( 'NONE', *, *, #17151, .T. ) ;
#73000 = DIRECTION ( 'NONE',  ( -0.000000000000000000, 0.6427876096865404731, -0.7660444431189771253 ) ) ;
#73001 = ORIENTED_EDGE ( 'NONE', *, *, #73458, .F. ) ;
#73002 = CARTESIAN_POINT ( 'NONE',  ( 9.915319043920543862, -8.239487800360276282, 34.69522927552633718 ) ) ;
#73003 = EDGE_CURVE ( 'NONE', #74304, #56304, #87368, .T. ) ;
#73004 = CARTESIAN_POINT ( 'NONE',  ( -11.76194648218548622, -3.754499324213721234, 33.06261337010820256 ) ) ;
#73005 = CARTESIAN_POINT ( 'NONE',  ( 0.3962680155776857061, -5.219633306516282545, 34.19971097300152962 ) ) ;
#73006 = FACE_BOUND ( 'NONE', #13337, .T. ) ;
#73007 = B_SPLINE_CURVE_WITH_KNOTS ( 'NONE', 3,
 ( #80192, #18492, #27019, #13500, #50697, #28336, #27902, #27463, #55809, #75636 ),
 .UNSPECIFIED., .F., .F.,
 ( 4, 2, 2, 2, 4 ),
 ( 0.000000000000000000, 0.0001954339857564074473, 0.0003908679715128148945, 0.0005863019572692223418, 0.0007817359430256297891 ),
 .UNSPECIFIED. ) ;
#73008 = CARTESIAN_POINT ( 'NONE',  ( -6.130147209438218781, -6.001485441113818986, 34.52039167877662607 ) ) ;
#73010 = ADVANCED_FACE ( 'NONE', ( #80152 ), #26093, .T. ) ;
#73009 = CARTESIAN_POINT ( 'NONE',  ( -12.46153846153846168, -1.790695186598648903, 34.54067556320373455 ) ) ;
#73011 = CIRCLE ( 'NONE', #6853, 5.000000000000000888 ) ;
#73012 = LINE ( 'NONE', #18073, #28061 ) ;
#73013 = CARTESIAN_POINT ( 'NONE',  ( -14.17716660592874334, -6.001044277235009439, 34.52024696741798948 ) ) ;
#73014 = CARTESIAN_POINT ( 'NONE',  ( 10.61538461538461675, -5.180354513474913603, 36.12317359536750416 ) ) ;
#73015 = CARTESIAN_POINT ( 'NONE',  ( 7.976945653978634532, -10.54018710029568595, 33.71981072465678864 ) ) ;
#73016 = ORIENTED_EDGE ( 'NONE', *, *, #28223, .F. ) ;
#73017 = EDGE_CURVE ( 'NONE', #38306, #87613, #27472, .T. ) ;
#73018 = FACE_OUTER_BOUND ( 'NONE', #45753, .T. ) ;
#73019 = EDGE_LOOP ( 'NONE', ( #59140, #83956 ) ) ;
#73020 = ORIENTED_EDGE ( 'NONE', *, *, #1205, .T. ) ;
#73021 = VECTOR ( 'NONE', #62081, 1000.000000000000000 ) ;
#73023 = CARTESIAN_POINT ( 'NONE',  ( -9.442253272394237840, -8.346898887586323923, 34.93166121998716278 ) ) ;
#73022 = DIRECTION ( 'NONE',  ( -0.000000000000000000, -0.5000000000000009992, -0.8660254037844380415 ) ) ;
#73024 = EDGE_CURVE ( 'NONE', #63890, #33486, #67526, .T. ) ;
#73025 = CARTESIAN_POINT ( 'NONE',  ( 3.165499230212911463, -3.643525952247789412, 33.31231777344662959 ) ) ;
#73026 = DIRECTION ( 'NONE',  ( 0.000000000000000000, 0.000000000000000000, -1.000000000000000000 ) ) ;
#73027 = CARTESIAN_POINT ( 'NONE',  ( 5.198717948717946236, -7.500000000000000000, 33.75000000000000000 ) ) ;
#73028 = DIRECTION ( 'NONE',  ( -0.000000000000000000, 1.000000000000000000, -0.000000000000000000 ) ) ;
#73029 = EDGE_LOOP ( 'NONE', ( #32197, #78814, #43169, #31914 ) ) ;
#73030 = CARTESIAN_POINT ( 'NONE',  ( -5.207071046654771607, -6.809168938359898782, 34.95455904226513866 ) ) ;
#73031 = CARTESIAN_POINT ( 'NONE',  ( -11.53846153846153655, -9.780366693483667717, 34.19971097300155094 ) ) ;
#73032 = CARTESIAN_POINT ( 'NONE',  ( -14.24249931939765546, -2.255955759149234741, 29.99999999999988631 ) ) ;
#73033 = CARTESIAN_POINT ( 'NONE',  ( -4.023054346021365468, -3.530189275343204702, 32.79018710029569661 ) ) ;
#73034 = ORIENTED_EDGE ( 'NONE', *, *, #29996, .F. ) ;
#73035 = ADVANCED_FACE ( 'NONE', ( #32405 ), #5382, .F. ) ;
#73036 = EDGE_LOOP ( 'NONE', ( #72968, #55207, #62899, #17949 ) ) ;
#73037 = SHAPE_DEFINITION_REPRESENTATION ( #41210, #11000 ) ;
#73038 = ORIENTED_EDGE ( 'NONE', *, *, #39418, .T. ) ;
#73039 = CARTESIAN_POINT ( 'NONE',  ( 11.76124120743959978, -12.47679350104403007, 31.42216943046555855 ) ) ;
#73040 = CARTESIAN_POINT ( 'NONE',  ( -5.777036865733325754, -7.369474539155828730, 34.99858011523957657 ) ) ;
#73041 = EDGE_LOOP ( 'NONE', ( #81071, #44300 ) ) ;
#73042 = DIRECTION ( 'NONE',  ( -0.000000000000000000, -0.7660444431189791237, -0.6427876096865379196 ) ) ;
#73043 = FACE_OUTER_BOUND ( 'NONE', #25786, .T. ) ;
#73044 = CARTESIAN_POINT ( 'NONE',  ( 5.076923076923075762, -2.721908614388771852, 31.22303859784724978 ) ) ;
#73045 = CARTESIAN_POINT ( 'NONE',  ( -17.07692307692319744, -12.27809138561165270, 31.22303859784587132 ) ) ;
#73046 = CARTESIAN_POINT ( 'NONE',  ( -8.102564102564102200, -3.499999999999999556, 29.75000000000000355 ) ) ;
#73047 = ORIENTED_EDGE ( 'NONE', *, *, #75120, .F. ) ;
#73049 = EDGE_LOOP ( 'NONE', ( #55133, #36090 ) ) ;
#73048 = CARTESIAN_POINT ( 'NONE',  ( -7.846153846153844924, -9.780366693483667717, 34.19971097300155094 ) ) ;
#73050 = DIRECTION ( 'NONE',  ( 0.000000000000000000, 0.1736481776669275834, 0.9848077530122086864 ) ) ;
#73051 = CARTESIAN_POINT ( 'NONE',  ( 4.153846153846032507, -6.879047030192662504, 34.71129190930017927 ) ) ;
#73052 = CARTESIAN_POINT ( 'NONE',  ( -11.53846153846153655, -2.499999999999998668, 29.75000000000001421 ) ) ;
#73053 = FACE_BOUND ( 'NONE', #86260, .T. ) ;
#73054 = CARTESIAN_POINT ( 'NONE',  ( -5.869954944080226333, -2.254550872974306674, 29.97347326024527447 ) ) ;
#73055 = B_SPLINE_CURVE_WITH_KNOTS ( 'NONE', 3,
 ( #43899, #83124, #56531, #21415, #1143, #29077, #15109, #9671, #50196, #8798 ),
 .UNSPECIFIED., .F., .F.,
 ( 4, 2, 2, 2, 4 ),
 ( 0.000000000000000000, 0.0001954311564186875520, 0.0003908623128373751041, 0.0005862934692560627103, 0.0007817246256747502082 ),
 .UNSPECIFIED. ) ;
#73056 = CARTESIAN_POINT ( 'NONE',  ( 17.99999999999987566, -2.625532179533778709, 30.86335684631627174 ) ) ;
#73057 = B_SPLINE_CURVE_WITH_KNOTS ( 'NONE', 3,
 ( #46237, #53878, #27730, #39937, #18770, #20094, #34493, #75476, #74600, #47558 ),
 .UNSPECIFIED., .F., .F.,
 ( 4, 2, 2, 2, 4 ),
 ( 0.000000000000000000, 0.0001954339857564063089, 0.0003908679715128126177, 0.0005863019572692189808, 0.0007817359430256252354 ),
 .UNSPECIFIED. ) ;
#73058 = CARTESIAN_POINT ( 'NONE',  ( -0.06109907496451398579, -10.25000000000000178, 17.53311829374151287 ) ) ;
#73059 = ORIENTED_EDGE ( 'NONE', *, *, #67055, .T. ) ;
#73060 = EDGE_CURVE ( 'NONE', #55169, #60609, #88750, .T. ) ;
#73061 = CARTESIAN_POINT ( 'NONE',  ( 14.08476534878545827, -2.308479472611653094, 30.53278059502174457 ) ) ;
#73062 = CARTESIAN_POINT ( 'NONE',  ( 7.596153846153846700, -7.500000000000001776, 35.00000000000000000 ) ) ;
#73063 = CARTESIAN_POINT ( 'NONE',  ( -0.3954701105360233782, -4.786620604624112651, 33.94971097300155094 ) ) ;
#73064 = ORIENTED_EDGE ( 'NONE', *, *, #88412, .F. ) ;
#73065 = ORIENTED_EDGE ( 'NONE', *, *, #50162, .T. ) ;
#73066 = CARTESIAN_POINT ( 'NONE',  ( -11.60454494941741999, -10.51840700105979387, 33.73612834413961536 ) ) ;
#73067 = CARTESIAN_POINT ( 'NONE',  ( -7.715363405186893786, -5.496552790871119143, 34.60292014791297532 ) ) ;
#73068 = CARTESIAN_POINT ( 'NONE',  ( 17.14217821643591932, -3.643525952247864019, 33.31231777344670064 ) ) ;
#73069 = CARTESIAN_POINT ( 'NONE',  ( -8.769230769230768274, -10.67929555188718282, 33.92786785259544047 ) ) ;
#73070 = EDGE_CURVE ( 'NONE', #13635, #33955, #48323, .T. ) ;
#73071 = CARTESIAN_POINT ( 'NONE',  ( 17.93472999944368240, -12.16647553114622049, 32.15551576947930812 ) ) ;
#73072 = FACE_OUTER_BOUND ( 'NONE', #41166, .T. ) ;
#73073 = ORIENTED_EDGE ( 'NONE', *, *, #30444, .F. ) ;
#73074 = DIRECTION ( 'NONE',  ( 0.000000000000000000, 0.000000000000000000, 1.000000000000000000 ) ) ;
#73075 = EDGE_CURVE ( 'NONE', #12820, #72772, #15671, .T. ) ;
#73076 = CARTESIAN_POINT ( 'NONE',  ( -6.065324012804307330, -7.749976730030849303, 34.74374725381503737 ) ) ;
#73077 = DIRECTION ( 'NONE',  ( 0.000000000000000000, 1.000000000000000000, 0.000000000000000000 ) ) ;
#73078 = ORIENTED_EDGE ( 'NONE', *, *, #53955, .T. ) ;
#73079 = CARTESIAN_POINT ( 'NONE',  ( 12.23861150263160802, -2.523278758544489797, 31.42238647778637528 ) ) ;
#73080 = ORIENTED_EDGE ( 'NONE', *, *, #18308, .T. ) ;
#73081 = AXIS2_PLACEMENT_3D ( 'NONE', #38380, #17671, #24857 ) ;
#73082 = CARTESIAN_POINT ( 'NONE',  ( 1.515453802628148772, -7.277220443632450575, 34.74524770363009196 ) ) ;
#73083 =( LENGTH_UNIT ( ) NAMED_UNIT ( * ) SI_UNIT ( .MILLI., .METRE. ) );
#73084 = DIRECTION ( 'NONE',  ( -0.000000000000000000, 0.7660444431189791237, -0.6427876096865379196 ) ) ;
#73085 = CARTESIAN_POINT ( 'NONE',  ( 17.93472999944368240, -10.33852847137145048, 34.16647553114627556 ) ) ;
#73086 = VERTEX_POINT ( 'NONE', #75175 ) ;
#73087 = DIRECTION ( 'NONE',  ( -0.000000000000000000, -0.000000000000000000, -1.000000000000000000 ) ) ;
#73089 = EDGE_CURVE ( 'NONE', #21246, #75513, #82376, .T. ) ;
#73088 = CARTESIAN_POINT ( 'NONE',  ( 13.63466980452883526, -9.233818618650603938, 34.70587769442853698 ) ) ;
#73090 = CARTESIAN_POINT ( 'NONE',  ( 17.07692307692307665, -9.905515769479276145, 34.41647553114623292 ) ) ;
#73091 = AXIS2_PLACEMENT_3D ( 'NONE', #79633, #17930, #58450 ) ;
#73092 = LINE ( 'NONE', #32542, #3420 ) ;
#73093 = CARTESIAN_POINT ( 'NONE',  ( -2.084912638714240707, -10.97394488606064122, 33.68653795673694873 ) ) ;
#73094 = EDGE_CURVE ( 'NONE', #9934, #65490, #72753, .T. ) ;
#73095 = EDGE_CURVE ( 'NONE', #58120, #70789, #42467, .T. ) ;
#73096 = VECTOR ( 'NONE', #59904, 1000.000000000000114 ) ;
#73097 = ORIENTED_EDGE ( 'NONE', *, *, #76385, .F. ) ;
#73098 = CARTESIAN_POINT ( 'NONE',  ( -16.81410256410256565, -7.500000000000000000, 33.75000000000000000 ) ) ;
#73099 = EDGE_LOOP ( 'NONE', ( #59306, #42762 ) ) ;
#73100 = CARTESIAN_POINT ( 'NONE',  ( -15.10024379253558635, -6.808710257144161559, 34.95449254468098843 ) ) ;
#73101 = EDGE_CURVE ( 'NONE', #4777, #80366, #835, .T. ) ;
#73102 = CARTESIAN_POINT ( 'NONE',  ( -9.561781990544126586, -12.27024696741798948, 31.24895572276497546 ) ) ;
#73103 = CARTESIAN_POINT ( 'NONE',  ( -13.44988583057615905, -2.892918686051582977, 31.69288490824015980 ) ) ;
#73104 = DIRECTION ( 'NONE',  ( -0.000000000000000000, -0.9848077530122086864, -0.1736481776669273613 ) ) ;
#73105 = CARTESIAN_POINT ( 'NONE',  ( -10.03846153846153832, -11.50000000000000000, 29.75000000000000355 ) ) ;
#73106 = CARTESIAN_POINT ( 'NONE',  ( 9.562160482869472844, -8.587444163452046197, 34.63053765926554206 ) ) ;
#73107 = EDGE_LOOP ( 'NONE', ( #32878, #65124 ) ) ;
#73108 = ORIENTED_EDGE ( 'NONE', *, *, #28232, .F. ) ;
#73109 = ORIENTED_EDGE ( 'NONE', *, *, #75535, .T. ) ;
#73110 = ORIENTED_EDGE ( 'NONE', *, *, #16887, .T. ) ;
#73111 = EDGE_LOOP ( 'NONE', ( #18667, #6819, #18156, #82176 ) ) ;
#73112 = LINE ( 'NONE', #10526, #63174 ) ;
#73113 = DIRECTION ( 'NONE',  ( 0.000000000000000000, 0.9848077530122072432, -0.1736481776669354937 ) ) ;
#73114 = AXIS2_PLACEMENT_3D ( 'NONE', #51734, #17986, #72469 ) ;
#73115 = CARTESIAN_POINT ( 'NONE',  ( -2.373016320496614817, -7.749976730030849303, 34.74374725381503737 ) ) ;
#73116 = CARTESIAN_POINT ( 'NONE',  ( 6.923076923076800782, -12.16647553114689728, 32.15551576947799362 ) ) ;
#73117 = CARTESIAN_POINT ( 'NONE',  ( 13.13463865367303285, -8.303909089506435137, 34.68538101551103381 ) ) ;
#73118 = ADVANCED_FACE ( 'NONE', ( #28759 ), #41831, .T. ) ;
#73119 = CARTESIAN_POINT ( 'NONE',  ( -6.249976744048591826, -2.920706130388546651, 32.31842814019191223 ) ) ;
#73120 = DIRECTION ( 'NONE',  ( 0.000000000000000000, 0.000000000000000000, -1.000000000000000000 ) ) ;
#73121 = LINE ( 'NONE', #30357, #71062 ) ;
#73122 = CARTESIAN_POINT ( 'NONE',  ( 0.4615384615383396616, -3.300289026999228881, 32.46337939537708905 ) ) ;
#73123 = ORIENTED_EDGE ( 'NONE', *, *, #67177, .F. ) ;
#73124 = ORIENTED_EDGE ( 'NONE', *, *, #59328, .F. ) ;
#73125 = ORIENTED_EDGE ( 'NONE', *, *, #61560, .T. ) ;
#73127 = EDGE_LOOP ( 'NONE', ( #2230, #2910 ) ) ;
#73126 = CARTESIAN_POINT ( 'NONE',  ( 11.66898697669518192, -2.647132371071621471, 31.75357179365171589 ) ) ;
#73129 = CARTESIAN_POINT ( 'NONE',  ( -16.37733109757010652, -10.11188796281391511, 34.01382737946119050 ) ) ;
#73128 = CARTESIAN_POINT ( 'NONE',  ( 0.4615384615384611200, -2.499999999999998668, 29.75000000000001421 ) ) ;
#73130 = EDGE_CURVE ( 'NONE', #46484, #29630, #15246, .T. ) ;
#73131 = CARTESIAN_POINT ( 'NONE',  ( -1.161239898842963969, -2.251407671071270489, 29.88021292934942252 ) ) ;
#73132 = CARTESIAN_POINT ( 'NONE',  ( -11.28851612908349722, -9.357781135181031829, 34.66075350412533851 ) ) ;
#73133 = FACE_BOUND ( 'NONE', #77979, .T. ) ;
#73134 = ORIENTED_EDGE ( 'NONE', *, *, #8114, .F. ) ;
#73135 = ORIENTED_EDGE ( 'NONE', *, *, #51036, .T. ) ;
#73136 = EDGE_CURVE ( 'NONE', #47964, #45215, #80106, .T. ) ;
#73137 = DIRECTION ( 'NONE',  ( -0.000000000000000000, -0.7660444431189791237, -0.6427876096865379196 ) ) ;
#73138 = ORIENTED_EDGE ( 'NONE', *, *, #8728, .T. ) ;
#73139 = FACE_BOUND ( 'NONE', #51004, .T. ) ;
#73140 = CARTESIAN_POINT ( 'NONE',  ( -8.769230769230768274, -1.790695186598648903, 34.54067556320373455 ) ) ;
#73141 = VECTOR ( 'NONE', #26643, 1000.000000000000114 ) ;
#73142 = CARTESIAN_POINT ( 'NONE',  ( -39.05038313613820122, -2.249999999999998668, 29.75000000000000355 ) ) ;
#73143 = ORIENTED_EDGE ( 'NONE', *, *, #51036, .F. ) ;
#73144 = CARTESIAN_POINT ( 'NONE',  ( -15.00798968950081580, -12.24180327182772388, 31.33663988360758168 ) ) ;
#73145 = CARTESIAN_POINT ( 'NONE',  ( 8.638755584155049405, -7.276987145209184327, 34.99546412871779211 ) ) ;
#73146 = CARTESIAN_POINT ( 'NONE',  ( -5.326923076923075762, -7.500000000000001776, 35.00000000000000000 ) ) ;
#73147 = VERTEX_POINT ( 'NONE', #83259 ) ;
#73148 = B_SPLINE_CURVE_WITH_KNOTS ( 'NONE', 3,
 ( #51675, #45827, #17922, #80971, #45377, #25116, #65203, #17479, #39093, #72407 ),
 .UNSPECIFIED., .F., .F.,
 ( 4, 2, 2, 2, 4 ),
 ( 0.0007817359430256332585, 0.0009771253907250054306, 0.001172514838424370664, 0.001367904286123735897, 0.001563293733823100913 ),
 .UNSPECIFIED. ) ;
#73149 = CARTESIAN_POINT ( 'NONE',  ( -1.384615384615383471, -13.75783147151868846, 33.36296068462461051 ) ) ;
#73150 = CARTESIAN_POINT ( 'NONE',  ( 7.173022332454967120, -5.766571408460171355, 34.70601412856602508 ) ) ;
#73151 = DIRECTION ( 'NONE',  ( 1.000000000000000000, 0.000000000000000000, 0.000000000000000000 ) ) ;
#73152 = VERTEX_POINT ( 'NONE', #29210 ) ;
#73153 = VECTOR ( 'NONE', #5203, 1000.000000000000000 ) ;
#73154 = EDGE_CURVE ( 'NONE', #58651, #39220, #69300, .T. ) ;
#73155 = CARTESIAN_POINT ( 'NONE',  ( -2.438383774359863754, -11.18331474514187995, 33.13161551792790505 ) ) ;
#73156 = CARTESIAN_POINT ( 'NONE',  ( -17.07692307692319744, -11.94971097300221174, 32.03036669348237098 ) ) ;
#73157 = VECTOR ( 'NONE', #54994, 1000.000000000000000 ) ;
#73158 = VERTEX_POINT ( 'NONE', #56662 ) ;
#73159 = CARTESIAN_POINT ( 'NONE',  ( -17.07692307692307665, -12.62096338111211580, 30.90682066428153263 ) ) ;
#73160 = CARTESIAN_POINT ( 'NONE',  ( -15.23076923076922995, -7.500000000000001776, 35.04278698407183867 ) ) ;
#73161 = CARTESIAN_POINT ( 'NONE',  ( -15.90379184220783948, -8.303483539816726378, 34.68545999027711702 ) ) ;
#73162 = CYLINDRICAL_SURFACE ( 'NONE', #64442, 0.2500000000000009437 ) ;
#73163 = DIRECTION ( 'NONE',  ( -0.000000000000000000, -0.9396926207859093161, -0.3420201433256663259 ) ) ;
#73164 = DIRECTION ( 'NONE',  ( 0.000000000000000000, 0.8660254037844377084, -0.5000000000000015543 ) ) ;
#73166 = CARTESIAN_POINT ( 'NONE',  ( 8.639082799499073317, -3.069018819979302926, 32.56621877034667278 ) ) ;
#73165 = CARTESIAN_POINT ( 'NONE',  ( -1.634592115557738756, -4.943428324936578910, 34.04746400365624481 ) ) ;
#73167 = VECTOR ( 'NONE', #61451, 999.9999999999998863 ) ;
#73168 = CARTESIAN_POINT ( 'NONE',  ( -16.02305434602136458, -11.71459661697925903, 32.44059661609676937 ) ) ;
#73170 = CARTESIAN_POINT ( 'NONE',  ( -5.999999999999998224, -1.117168528481311540, 33.14645433367849847 ) ) ;
#73169 = CARTESIAN_POINT ( 'NONE',  ( -15.10024379253559168, -2.647132371071621471, 31.75357179365171589 ) ) ;
#73171 = CARTESIAN_POINT ( 'NONE',  ( -2.749999999999997780, -7.561099074964547917, 27.34188170625848713 ) ) ;
#73172 = EDGE_LOOP ( 'NONE', ( #24941, #24800, #29654, #76218 ) ) ;
#73173 = EDGE_CURVE ( 'NONE', #32782, #44632, #14803, .T. ) ;
#73174 = CARTESIAN_POINT ( 'NONE',  ( -12.71151519248081740, -8.303909089506435137, 34.68538101551103381 ) ) ;
#73175 = EDGE_LOOP ( 'NONE', ( #24774, #39151 ) ) ;
#73176 = ORIENTED_EDGE ( 'NONE', *, *, #68375, .T. ) ;
#73177 = EDGE_CURVE ( 'NONE', #17849, #87793, #69736, .T. ) ;
#73178 = CYLINDRICAL_SURFACE ( 'NONE', #48398, 0.2500000000000008882 ) ;
#73179 = ORIENTED_EDGE ( 'NONE', *, *, #25122, .F. ) ;
#73180 = CARTESIAN_POINT ( 'NONE',  ( -15.23076923076935074, -6.026961402154118019, 34.52809138561165270 ) ) ;
#73181 = CARTESIAN_POINT ( 'NONE',  ( -1.944543648262992530, -9.444543648263016067, 17.43750000000000000 ) ) ;
#73182 = CARTESIAN_POINT ( 'NONE',  ( 3.230769230769108269, -2.379036618888197285, 30.90682066428292885 ) ) ;
#73183 = CARTESIAN_POINT ( 'NONE',  ( 5.934729554039225974, -11.48612834413959582, 32.76840700105983473 ) ) ;
#73184 = CARTESIAN_POINT ( 'NONE',  ( -7.846153846153844924, -5.557115091759785130, 34.35708131394839171 ) ) ;
#73185 = CARTESIAN_POINT ( 'NONE',  ( 9.757562831820530747, -3.083524468853784839, 32.58852847137153930 ) ) ;
#73186 = CARTESIAN_POINT ( 'NONE',  ( -10.61538461538473577, -3.643525952248795718, 33.31231777344771672 ) ) ;
#73187 = CARTESIAN_POINT ( 'NONE',  ( 0.5920638997721058283, -5.915461855592777596, 34.75538340440931506 ) ) ;
#73188 = CARTESIAN_POINT ( 'NONE',  ( 0.5920638997721026087, -2.647132371071621471, 31.75357179365173010 ) ) ;
#73189 = CARTESIAN_POINT ( 'NONE',  ( -3.750000000000008438, -5.946699141100917352, 18.92187500000000355 ) ) ;
#73190 = LINE ( 'NONE', #19132, #11783 ) ;
#73191 = CARTESIAN_POINT ( 'NONE',  ( -19.99999999999996447, -15.00000000000000533, 13.00000000000000178 ) ) ;
#73192 = EDGE_CURVE ( 'NONE', #20258, #56147, #34173, .T. ) ;
#73193 = EDGE_CURVE ( 'NONE', #5405, #43224, #4988, .T. ) ;
#73194 = CARTESIAN_POINT ( 'NONE',  ( 0.000000000000000000, -11.00000000000000000, 29.75000000000000355 ) ) ;
#73195 = CIRCLE ( 'NONE', #70295, 0.2500000000000002220 ) ;
#73196 = ORIENTED_EDGE ( 'NONE', *, *, #10725, .F. ) ;
#73197 = ORIENTED_EDGE ( 'NONE', *, *, #63446, .T. ) ;
#73198 = B_SPLINE_CURVE_WITH_KNOTS ( 'NONE', 3,
 ( #38840, #36287, #4602, #32075, #72162, #22321, #15571, #43037, #63744, #51419 ),
 .UNSPECIFIED., .F., .F.,
 ( 4, 2, 2, 2, 4 ),
 ( 0.0007817246256747550871, 0.0009771112852218989588, 0.001172497944769042939, 0.001367884604316186702, 0.001563271263863330682 ),
 .UNSPECIFIED. ) ;
#73199 = CARTESIAN_POINT ( 'NONE',  ( -9.627052121031661969, -3.835265460703683349, 33.15142922261929925 ) ) ;
#73200 = FACE_OUTER_BOUND ( 'NONE', #56209, .T. ) ;
#73201 = FACE_OUTER_BOUND ( 'NONE', #51865, .T. ) ;
#73202 = CARTESIAN_POINT ( 'NONE',  ( -19.50000000000000000, -3.499999999999999556, 29.75000000000000355 ) ) ;
#73203 = B_SPLINE_CURVE_WITH_KNOTS ( 'NONE', 3,
 ( #68174, #88471, #69058, #40269, #39822, #5584, #68611, #61396, #25858, #26740 ),
 .UNSPECIFIED., .F., .F.,
 ( 4, 2, 2, 2, 4 ),
 ( 0.0007817246256747442451, 0.0009771112852218870326, 0.001172497944769029929, 0.001367884604316172825, 0.001563271263863315504 ),
 .UNSPECIFIED. ) ;
#73205 = ADVANCED_FACE ( 'NONE', ( #36398 ), #78254, .F. ) ;
#73204 = CARTESIAN_POINT ( 'NONE',  ( 8.545745825506822158, -11.89387501736622710, 32.13663884655806413 ) ) ;
#73206 = CARTESIAN_POINT ( 'NONE',  ( -16.21911659980693443, -9.442884908240170461, 34.35708131394840592 ) ) ;
#73207 = EDGE_CURVE ( 'NONE', #33353, #35763, #46766, .T. ) ;
#73208 = ADVANCED_FACE ( 'NONE', ( #44910 ), #31407, .F. ) ;
#73209 = ORIENTED_EDGE ( 'NONE', *, *, #80267, .F. ) ;
#73210 = CARTESIAN_POINT ( 'NONE',  ( 2.980792486720640344, -6.524016743844655686, 34.90889640711025521 ) ) ;
#73211 = ORIENTED_EDGE ( 'NONE', *, *, #68707, .F. ) ;
#73212 = VERTEX_POINT ( 'NONE', #77376 ) ;
#73213 = CARTESIAN_POINT ( 'NONE',  ( 0.6843181305165279005, -12.47679350104403007, 31.42216943046555855 ) ) ;
#73214 = CARTESIAN_POINT ( 'NONE',  ( 4.153846153846154188, -2.538708090699994813, 30.37095296980875503 ) ) ;
#73215 = CARTESIAN_POINT ( 'NONE',  ( -4.403869378067610363, -12.68155406624981119, 30.59749803192733708 ) ) ;
#73216 = CYLINDRICAL_SURFACE ( 'NONE', #70981, 0.2499999999999995559 ) ;
#73217 = CARTESIAN_POINT ( 'NONE',  ( 13.13463864056679675, -5.643011162660950042, 34.66104346484419096 ) ) ;
#73218 = AXIS2_PLACEMENT_3D ( 'NONE', #69123, #83087, #21374 ) ;
#73219 = EDGE_LOOP ( 'NONE', ( #26319, #63143, #5442, #71229 ) ) ;
#73220 = ORIENTED_EDGE ( 'NONE', *, *, #43555, .T. ) ;
#73221 = ORIENTED_EDGE ( 'NONE', *, *, #45308, .F. ) ;
#73222 = B_SPLINE_CURVE_WITH_KNOTS ( 'NONE', 3,
 ( #38154, #58867, #16548, #44015, #4372, #65173, #86368, #3472, #71486, #85903 ),
 .UNSPECIFIED., .F., .F.,
 ( 4, 2, 2, 2, 4 ),
 ( 0.000000000000000000, 0.0001954311564186879315, 0.0003908623128373758630, 0.0005862934692560637946, 0.0007817246256747517261 ),
 .UNSPECIFIED. ) ;
#73223 = CARTESIAN_POINT ( 'NONE',  ( -16.09615384615384670, -3.499999999999999556, 29.75000000000000355 ) ) ;
#73224 = CARTESIAN_POINT ( 'NONE',  ( -8.102564102564102200, -3.499999999999999556, 29.75000000000000355 ) ) ;
#73225 = B_SPLINE_CURVE_WITH_KNOTS ( 'NONE', 3,
 ( #65489, #9656, #51060, #15984, #23611, #10101, #30376, #37567, #65030, #29938 ),
 .UNSPECIFIED., .F., .F.,
 ( 4, 2, 2, 2, 4 ),
 ( 0.000000000000000000, 0.0001954339857564075286, 0.0003908679715128150572, 0.0005863019572692225586, 0.0007817359430256301143 ),
 .UNSPECIFIED. ) ;
#73226 = CARTESIAN_POINT ( 'NONE',  ( 16.28437159207980045, -5.915461855592777596, 34.75538340440931506 ) ) ;
#73227 = CARTESIAN_POINT ( 'NONE',  ( 1.319344938654610777, -3.835265460703609186, 33.15142922261924241 ) ) ;
#73228 = CARTESIAN_POINT ( 'NONE',  ( -4.088700374514188773, -7.750023238201980469, 34.74374492549440419 ) ) ;
#73229 = CARTESIAN_POINT ( 'NONE',  ( 17.86930853333243974, -8.147922237126337563, 34.70805685702651999 ) ) ;
#73230 = ORIENTED_EDGE ( 'NONE', *, *, #77019, .F. ) ;
#73231 = EDGE_LOOP ( 'NONE', ( #57132, #36681 ) ) ;
#73232 = CARTESIAN_POINT ( 'NONE',  ( 4.826899852701619587, -10.18141759479407327, 34.26406193332782379 ) ) ;
#73234 = VERTEX_POINT ( 'NONE', #8930 ) ;
#73233 = CARTESIAN_POINT ( 'NONE',  ( -13.38461538461538325, -5.471508081941601098, 34.59228464037088457 ) ) ;
#73235 = CARTESIAN_POINT ( 'NONE',  ( 8.069165197766698938, -12.39991518177334129, 30.74647679643404530 ) ) ;
#73236 = CARTESIAN_POINT ( 'NONE',  ( -7.053636836690285961, -2.254533558242299396, 29.97296025877828285 ) ) ;
#73237 = CARTESIAN_POINT ( 'NONE',  ( -5.999999999999998224, -6.386643153685126251, 34.62446782046654192 ) ) ;
#73238 = EDGE_LOOP ( 'NONE', ( #55432, #54049 ) ) ;
#73239 = CYLINDRICAL_SURFACE ( 'NONE', #12387, 0.2500000000000002220 ) ;
#73240 = AXIS2_PLACEMENT_3D ( 'NONE', #52877, #19545, #39390 ) ;
#73241 = ORIENTED_EDGE ( 'NONE', *, *, #57726, .F. ) ;
#73242 = CARTESIAN_POINT ( 'NONE',  ( -19.50000000000000000, -3.499999999999999556, 29.75000000000000355 ) ) ;
#73243 = LINE ( 'NONE', #59275, #77420 ) ;
#73244 = CARTESIAN_POINT ( 'NONE',  ( 7.596177102105253987, -4.075325502946086864, 33.72974371597207721 ) ) ;
#73246 = CARTESIAN_POINT ( 'NONE',  ( -17.76215049426127024, 12.75000000000001599, 30.81664701255127881 ) ) ;
#73245 = CARTESIAN_POINT ( 'NONE',  ( 14.05769230769230838, -7.500000000000001776, 35.04278698407183867 ) ) ;
#73247 = CARTESIAN_POINT ( 'NONE',  ( -10.83831083290075803, -10.61292498521070549, 33.66303323003028680 ) ) ;
#73248 = EDGE_LOOP ( 'NONE', ( #82153, #11355, #25425, #66813 ) ) ;
#73249 = CARTESIAN_POINT ( 'NONE',  ( -11.00641025641025550, -7.500000000000000000, 29.75000000000000355 ) ) ;
#73250 = CARTESIAN_POINT ( 'NONE',  ( -2.102533092329708531, -5.360057338231124291, 13.56786352175840626 ) ) ;
#73251 = CARTESIAN_POINT ( 'NONE',  ( 20.74999999999999645, -4.499999999999999112, 29.75000000000000355 ) ) ;
#73252 = ORIENTED_EDGE ( 'NONE', *, *, #45633, .F. ) ;
#73253 = B_SPLINE_CURVE_WITH_KNOTS ( 'NONE', 3,
 ( #63716, #2022, #29505, #50191, #77677, #43453, #70929, #64150, #2453, #29943 ),
 .UNSPECIFIED., .F., .F.,
 ( 4, 2, 2, 2, 4 ),
 ( 0.000000000000000000, 0.0001954339857564074473, 0.0003908679715128148945, 0.0005863019572692223418, 0.0007817359430256297891 ),
 .UNSPECIFIED. ) ;
#73254 = B_SPLINE_CURVE_WITH_KNOTS ( 'NONE', 3,
 ( #19809, #5411, #87854, #47270, #74759, #60340, #6300, #27009, #26119, #81966 ),
 .UNSPECIFIED., .F., .F.,
 ( 4, 2, 2, 2, 4 ),
 ( 0.000000000000000000, 0.0001954339857564092362, 0.0003908679715128184724, 0.0005863019572692276544, 0.0007817359430256369448 ),
 .UNSPECIFIED. ) ;
#73255 = CARTESIAN_POINT ( 'NONE',  ( -9.626240358957616650, -4.661471528628508665, 34.16647553114624003 ) ) ;
#73256 = CARTESIAN_POINT ( 'NONE',  ( -6.000000000000119904, -10.90142922262034020, 33.41473453929536674 ) ) ;
#73257 = CYLINDRICAL_SURFACE ( 'NONE', #68770, 0.2500000000000008882 ) ;
#73258 = DIRECTION ( 'NONE',  ( 0.000000000000000000, 0.000000000000000000, 1.000000000000000000 ) ) ;
#73259 = FACE_BOUND ( 'NONE', #4520, .T. ) ;
#73261 = CARTESIAN_POINT ( 'NONE',  ( -7.846153846153844924, -2.486705287966279876, 31.30864560766543647 ) ) ;
#73260 = DIRECTION ( 'NONE',  ( -0.000000000000000000, -0.000000000000000000, -1.000000000000000000 ) ) ;
#73262 = CARTESIAN_POINT ( 'NONE',  ( 9.915683633005873077, -2.501478030877322567, 29.88021232661721172 ) ) ;
#73264 = DIRECTION ( 'NONE',  ( -0.000000000000000000, 0.6427876096865404731, -0.7660444431189770143 ) ) ;
#73263 = CARTESIAN_POINT ( 'NONE',  ( -0.4615384615384611200, -5.557115091759785130, 34.35708131394839171 ) ) ;
#73265 = CARTESIAN_POINT ( 'NONE',  ( 12.33139125210024112, -12.45813303252208648, 30.39737893381572675 ) ) ;
#73266 = CARTESIAN_POINT ( 'NONE',  ( 13.16113046005105325, -2.612411019501189369, 31.66733052389439962 ) ) ;
#73267 = CARTESIAN_POINT ( 'NONE',  ( -1.492201783934549164, -11.27530806549876807, 25.85750670625849068 ) ) ;
#73268 = DIRECTION ( 'NONE',  ( -0.000000000000000000, -0.5000000000000009992, -0.8660254037844380415 ) ) ;
#73269 = ORIENTED_EDGE ( 'NONE', *, *, #6852, .T. ) ;
#73270 = EDGE_CURVE ( 'NONE', #88317, #68189, #24253, .T. ) ;
#73271 = AXIS2_PLACEMENT_3D ( 'NONE', #67612, #40151, #33385 ) ;
#73272 = AXIS2_PLACEMENT_3D ( 'NONE', #18278, #87200, #80884 ) ;
#73273 = CARTESIAN_POINT ( 'NONE',  ( 12.46153846153846168, -2.499999999999998668, 29.75000000000001421 ) ) ;
#73274 = CARTESIAN_POINT ( 'NONE',  ( 20.00000000000000000, -3.499999999999999556, 28.25000000000000000 ) ) ;
#73275 = CARTESIAN_POINT ( 'NONE',  ( 12.22435897435897267, -11.50000000000000000, 29.75000000000000355 ) ) ;
#73276 = CARTESIAN_POINT ( 'NONE',  ( -2.307692307692427391, -11.94971097300221174, 32.03036669348237098 ) ) ;
#73277 = PRODUCT_RELATED_PRODUCT_CATEGORY ( 'part', '', ( #31988 ) ) ;
#73278 = CARTESIAN_POINT ( 'NONE',  ( -16.94639763868943660, -2.372941743896878286, 30.88044141588253311 ) ) ;
#73279 = CARTESIAN_POINT ( 'NONE',  ( 9.692307692307572609, -2.892918686052165622, 31.69288490824153470 ) ) ;
#73280 = CARTESIAN_POINT ( 'NONE',  ( -1.077988221561460236, -10.27530806549876452, 15.85750670625849068 ) ) ;
#73281 = CARTESIAN_POINT ( 'NONE',  ( 14.24160889673643027, -10.51840700105979387, 33.73612834413961536 ) ) ;
#73282 = CARTESIAN_POINT ( 'NONE',  ( 1.384615384615386802, -13.20930481340135110, 34.54067556320372745 ) ) ;
#73283 = VECTOR ( 'NONE', #48304, 999.9999999999998863 ) ;
#73284 = DIRECTION ( 'NONE',  ( 0.000000000000000000, 0.000000000000000000, 1.000000000000000000 ) ) ;
#73285 = CARTESIAN_POINT ( 'NONE',  ( 4.853996118016225658, -9.172386477786396597, 34.72672124145550043 ) ) ;
#73286 = CARTESIAN_POINT ( 'NONE',  ( -7.173053654019277303, -4.236021600441998380, 33.53823185664189310 ) ) ;
#73287 = CARTESIAN_POINT ( 'NONE',  ( 1.384615384615264011, -10.33852847137269571, 34.16647553114546554 ) ) ;
#73288 = AXIS2_PLACEMENT_3D ( 'NONE', #27212, #68639, #54669 ) ;
#73289 = CARTESIAN_POINT ( 'NONE',  ( -2.057692307692306599, -2.249999999999998668, 29.75000000000000355 ) ) ;
#73290 = ADVANCED_FACE ( 'NONE', ( #50332 ), #24197, .F. ) ;
#73291 = CARTESIAN_POINT ( 'NONE',  ( -1.161835715637319133, -12.11081565061823717, 32.26097654155341843 ) ) ;
#73292 = EDGE_LOOP ( 'NONE', ( #68159, #12510 ) ) ;
#73293 = CARTESIAN_POINT ( 'NONE',  ( 16.37685899793954292, -4.762714258010882773, 34.23016756924214832 ) ) ;
#73294 = DIRECTION ( 'NONE',  ( -0.000000000000000000, -0.8660254037844399289, -0.4999999999999980016 ) ) ;
#73295 = CARTESIAN_POINT ( 'NONE',  ( 3.775308065498752086, -6.007798216065404873, 20.89249329374151642 ) ) ;
#73296 = CARTESIAN_POINT ( 'NONE',  ( 7.053867364043872712, -10.70102852606553157, 33.91149625220312913 ) ) ;
#73297 = CARTESIAN_POINT ( 'NONE',  ( -1.384615384615505151, -12.27809138561165270, 31.22303859784587132 ) ) ;
#73298 = ORIENTED_EDGE ( 'NONE', *, *, #16056, .F. ) ;
#73299 = FACE_OUTER_BOUND ( 'NONE', #41212, .T. ) ;
#73300 = CARTESIAN_POINT ( 'NONE',  ( 0.7115384615384606759, -7.500000000000001776, 35.04278698407183867 ) ) ;
#73302 = ORIENTED_EDGE ( 'NONE', *, *, #75181, .F. ) ;
#73301 = CARTESIAN_POINT ( 'NONE',  ( 5.076923076923075762, -12.34228464037088635, 31.77849191805839268 ) ) ;
#73303 = CARTESIAN_POINT ( 'NONE',  ( -13.13456107297707121, -11.28795663066794575, 33.01431243580653785 ) ) ;
#73304 = CARTESIAN_POINT ( 'NONE',  ( 5.076923076923075762, -6.435427911321262684, 35.78748833219616898 ) ) ;
#73305 = CARTESIAN_POINT ( 'NONE',  ( -8.769230769230768274, -2.538708090699994813, 30.37095296980875503 ) ) ;
#73306 = DIRECTION ( 'NONE',  ( 0.000000000000000000, 0.9396926207859126468, -0.3420201433256571111 ) ) ;
#73307 = ORIENTED_EDGE ( 'NONE', *, *, #48021, .T. ) ;
#73308 = B_SPLINE_CURVE_WITH_KNOTS ( 'NONE', 3,
 ( #67505, #73368, #5797, #4918, #19755, #12122, #54416, #32384, #12558, #61170 ),
 .UNSPECIFIED., .F., .F.,
 ( 4, 2, 2, 2, 4 ),
 ( 0.000000000000000000, 0.0001954311564186868202, 0.0003908623128373736404, 0.0005862934692560604335, 0.0007817246256747472808 ),
 .UNSPECIFIED. ) ;
#73309 = CARTESIAN_POINT ( 'NONE',  ( -10.61538461538461320, -1.215029322943914858, 32.30358669280327177 ) ) ;
#73310 = CARTESIAN_POINT ( 'NONE',  ( -6.000000000000119904, -12.27809138561165270, 31.22303859784587132 ) ) ;
#73311 = ADVANCED_FACE ( 'NONE', ( #72384 ), #63858, .F. ) ;
#73312 = DIRECTION ( 'NONE',  ( 0.000000000000000000, 0.3420201433256610524, 0.9396926207859113145 ) ) ;
#73313 = ORIENTED_EDGE ( 'NONE', *, *, #35544, .T. ) ;
#73314 = ORIENTED_EDGE ( 'NONE', *, *, #33915, .T. ) ;
#73315 = EDGE_CURVE ( 'NONE', #83108, #15672, #10696, .T. ) ;
#73316 = ORIENTED_EDGE ( 'NONE', *, *, #96, .T. ) ;
#73317 = EDGE_CURVE ( 'NONE', #36016, #38481, #71479, .T. ) ;
#73318 = CARTESIAN_POINT ( 'NONE',  ( -9.915792636031637741, -2.847400154188067578, 31.58180166144859058 ) ) ;
#73319 = CARTESIAN_POINT ( 'NONE',  ( -3.165514091256391271, -3.083524468853784839, 32.58852847137153930 ) ) ;
#73320 = B_SPLINE_CURVE_WITH_KNOTS ( 'NONE', 3,
 ( #9046, #17118, #22111, #49582, #50453, #70744, #43701, #56774, #51312, #57224 ),
 .UNSPECIFIED., .F., .F.,
 ( 4, 2, 2, 2, 4 ),
 ( 0.0007817246256747460882, 0.0009771112852218892010, 0.001172497944769032314, 0.001367884604316175210, 0.001563271263863318323 ),
 .UNSPECIFIED. ) ;
#73321 = DIRECTION ( 'NONE',  ( 0.000000000000000000, -6.938893903907222067E-15, 1.000000000000000000 ) ) ;
#73322 = B_SPLINE_CURVE_WITH_KNOTS ( 'NONE', 3,
 ( #17277, #86200, #51935, #44734, #78090, #37995 ),
 .UNSPECIFIED., .F., .F.,
 ( 4, 2, 4 ),
 ( 2.823925224926892107E-17, 0.0001954756301636994555, 0.0003909512603273706676 ),
 .UNSPECIFIED. ) ;
#73323 = CARTESIAN_POINT ( 'NONE',  ( 15.10007776410167502, -3.530157926970578952, 32.79014554554150607 ) ) ;
#73324 = ORIENTED_EDGE ( 'NONE', *, *, #82111, .F. ) ;
#73325 = ORIENTED_EDGE ( 'NONE', *, *, #76405, .T. ) ;
#73327 = ORIENTED_EDGE ( 'NONE', *, *, #6377, .F. ) ;
#73326 = CARTESIAN_POINT ( 'NONE',  ( 10.74542967130438953, -2.254550872974306674, 29.97347326024527092 ) ) ;
#73328 = CARTESIAN_POINT ( 'NONE',  ( -16.28399412357785536, -12.50552854090298638, 31.33409797877408920 ) ) ;
#73329 = CARTESIAN_POINT ( 'NONE',  ( -3.454254155333562171, -4.988325925672468131, 34.36044203135681130 ) ) ;
#73330 = VECTOR ( 'NONE', #31840, 1000.000000000000000 ) ;
#73331 = AXIS2_PLACEMENT_3D ( 'NONE', #11754, #25264, #72109 ) ;
#73332 = CARTESIAN_POINT ( 'NONE',  ( 10.61538461538461675, -11.16473453929635440, 33.15142922261926373 ) ) ;
#73333 = CARTESIAN_POINT ( 'NONE',  ( 13.38461538461538680, -9.905515769479276145, 34.41647553114623292 ) ) ;
#73334 = EDGE_LOOP ( 'NONE', ( #76011, #43889, #82546, #76548 ) ) ;
#73335 = VECTOR ( 'NONE', #18797, 1000.000000000000000 ) ;
#73336 = ORIENTED_EDGE ( 'NONE', *, *, #48944, .F. ) ;
#73337 = VECTOR ( 'NONE', #75995, 999.9999999999998863 ) ;
#73338 = ORIENTED_EDGE ( 'NONE', *, *, #26822, .F. ) ;
#73339 = CARTESIAN_POINT ( 'NONE',  ( -8.703163435880695076, -11.91647553114624358, 32.58852847137148245 ) ) ;
#73341 = EDGE_LOOP ( 'NONE', ( #20626, #44656 ) ) ;
#73340 = CARTESIAN_POINT ( 'NONE',  ( 15.23076923076911093, -2.625532179533778709, 30.86335684631627174 ) ) ;
#73342 = CARTESIAN_POINT ( 'NONE',  ( 18.22277966897806678, -12.11081565061823717, 32.26097654155341843 ) ) ;
#73343 = CARTESIAN_POINT ( 'NONE',  ( -13.60754160213153163, -6.503392248772476236, 34.64988816332204635 ) ) ;
#73344 = CARTESIAN_POINT ( 'NONE',  ( 6.700211500873284542, -2.501496062324911840, 29.88072118266895671 ) ) ;
#73345 = LINE ( 'NONE', #52618, #1965 ) ;
#73346 = CYLINDRICAL_SURFACE ( 'NONE', #84281, 0.2500000000000002220 ) ;
#73347 = FACE_BOUND ( 'NONE', #59962, .T. ) ;
#73348 = FACE_OUTER_BOUND ( 'NONE', #78295, .T. ) ;
#73349 = CARTESIAN_POINT ( 'NONE',  ( -6.223484924564331777, -12.47654668319379567, 31.42292124445336654 ) ) ;
#73350 = CARTESIAN_POINT ( 'NONE',  ( -10.36543920600657209, -10.92531984108285670, 33.72920026020278073 ) ) ;
#73352 = CARTESIAN_POINT ( 'NONE',  ( 15.29683656411930848, -9.905515769479276145, 34.41647553114623292 ) ) ;
#73351 = DIRECTION ( 'NONE',  ( -0.000000000000000000, -0.5000000000000009992, -0.8660254037844380415 ) ) ;
#73353 = CARTESIAN_POINT ( 'NONE',  ( -9.320512820512821150, -7.500000000000000000, 29.75000000000000355 ) ) ;
#73354 = DIRECTION ( 'NONE',  ( 0.000000000000000000, 2.546383084002652634E-16, 1.000000000000000000 ) ) ;
#73355 = ORIENTED_EDGE ( 'NONE', *, *, #38599, .T. ) ;
#73356 = CARTESIAN_POINT ( 'NONE',  ( 11.28843830116857383, -3.202444869320336451, 32.30641848906366675 ) ) ;
#73357 = CARTESIAN_POINT ( 'NONE',  ( -13.45069776397551564, -9.058645607665454236, 34.76329471203372634 ) ) ;
#73358 = ORIENTED_EDGE ( 'NONE', *, *, #76449, .T. ) ;
#73359 = ORIENTED_EDGE ( 'NONE', *, *, #61203, .T. ) ;
#73360 = ADVANCED_FACE ( 'NONE', ( #78708 ), #38162, .F. ) ;
#73362 = LINE ( 'NONE', #39147, #52010 ) ;
#73361 = FACE_OUTER_BOUND ( 'NONE', #80269, .T. ) ;
#73363 = DIRECTION ( 'NONE',  ( 0.000000000000000000, 0.1736481776669267785, -0.9848077530122087975 ) ) ;
#73364 = CARTESIAN_POINT ( 'NONE',  ( 0.4615384615384611200, -2.486705287966279876, 31.30864560766543647 ) ) ;
#73365 = LINE ( 'NONE', #52640, #53335 ) ;
#73366 = VERTEX_POINT ( 'NONE', #57541 ) ;
#73367 = CARTESIAN_POINT ( 'NONE',  ( 14.55763782604044998, -9.272278438253398036, 34.42582936511637115 ) ) ;
#73368 = CARTESIAN_POINT ( 'NONE',  ( -4.219928533206288357, -9.058645607665454236, 34.76329471203372634 ) ) ;
#73370 = DIRECTION ( 'NONE',  ( -0.000000000000000000, -0.000000000000000000, -1.000000000000000000 ) ) ;
#73369 = DIRECTION ( 'NONE',  ( -0.000000000000000000, -0.9848077530122085754, -0.1736481776669273613 ) ) ;
#73371 = LINE ( 'NONE', #18430, #70426 ) ;
#73372 = CARTESIAN_POINT ( 'NONE',  ( -5.142193522883853340, -9.442884908240170461, 34.35708131394840592 ) ) ;
#73374 = DIRECTION ( 'NONE',  ( 0.000000000000000000, 0.9848077530122072432, -0.1736481776669354937 ) ) ;
#73373 =( LENGTH_UNIT ( ) NAMED_UNIT ( * ) SI_UNIT ( .MILLI., .METRE. ) );
#73375 = AXIS2_PLACEMENT_3D ( 'NONE', #28295, #55766, #19335 ) ;
#73376 = CARTESIAN_POINT ( 'NONE',  ( 2.320192649118979489E-14, -11.25000000000000000, 19.78125000000000000 ) ) ;
#73377 = VERTEX_POINT ( 'NONE', #30950 ) ;
#73378 = B_SPLINE_CURVE_WITH_KNOTS ( 'NONE', 3,
 ( #56219, #78706, #1719, #71943, #30515, #64731, #85027, #10254, #62954, #85464 ),
 .UNSPECIFIED., .F., .F.,
 ( 4, 2, 2, 2, 4 ),
 ( 0.000000000000000000, 0.0001954311564186869015, 0.0003908623128373738030, 0.0005862934692560607588, 0.0007817246256747476061 ),
 .UNSPECIFIED. ) ;
#73379 = ORIENTED_EDGE ( 'NONE', *, *, #17938, .T. ) ;
#73380 = EDGE_CURVE ( 'NONE', #57194, #53391, #66978, .T. ) ;
#73381 = CARTESIAN_POINT ( 'NONE',  ( 4.853438152358743096, -10.97335522853832579, 33.68706563782419749 ) ) ;
#73382 = CARTESIAN_POINT ( 'NONE',  ( 16.37662569511456567, -6.760870238392814535, 34.69528174975672385 ) ) ;
#73383 = FACE_OUTER_BOUND ( 'NONE', #79334, .T. ) ;
#73384 = CARTESIAN_POINT ( 'NONE',  ( -11.53846153846166089, -5.094484230521993062, 34.41647553114689373 ) ) ;
#73385 = ADVANCED_FACE ( 'NONE', ( #86828 ), #31862, .T. ) ;
#73386 = FACE_OUTER_BOUND ( 'NONE', #82219, .T. ) ;
#73387 = CARTESIAN_POINT ( 'NONE',  ( 2.320192649118979489E-14, -11.25000000000000000, 24.78125000000000000 ) ) ;
#73388 = CARTESIAN_POINT ( 'NONE',  ( -6.166666666666667851, -3.499999999999999556, 29.75000000000000355 ) ) ;
#73389 = CARTESIAN_POINT ( 'NONE',  ( 16.15384615384615330, -10.05456864172156806, 36.03766855953608683 ) ) ;
#73390 = CARTESIAN_POINT ( 'NONE',  ( -5.011667937410237528, -2.379036618887895305, 30.90682066428159303 ) ) ;
#73391 = FACE_OUTER_BOUND ( 'NONE', #50319, .T. ) ;
#73392 = CARTESIAN_POINT ( 'NONE',  ( 9.692307692307695177, -5.180354513474913603, 36.12317359536750416 ) ) ;
#73393 = CYLINDRICAL_SURFACE ( 'NONE', #68834, 0.2500000000000009437 ) ;
#73394 = DIRECTION ( 'NONE',  ( 1.000000000000000000, 0.000000000000000000, 0.000000000000000000 ) ) ;
#73395 = CARTESIAN_POINT ( 'NONE',  ( 11.00641025641025550, -3.499999999999999556, 29.75000000000000355 ) ) ;
#73396 = CARTESIAN_POINT ( 'NONE',  ( -6.130147209438221445, -10.19110544564092002, 33.96427741523702792 ) ) ;
#73397 = B_SPLINE_CURVE_WITH_KNOTS ( 'NONE', 3,
 ( #73159, #11455, #38939, #32174, #59636, #87136, #14903, #56757, #8141, #83811 ),
 .UNSPECIFIED., .F., .F.,
 ( 4, 2, 2, 2, 4 ),
 ( 0.000000000000000000, 0.0001954311564186880128, 0.0003908623128373760257, 0.0005862934692560640114, 0.0007817246256747520513 ),
 .UNSPECIFIED. ) ;
#73398 = AXIS2_PLACEMENT_3D ( 'NONE', #31927, #3985, #85533 ) ;
#73399 = ADVANCED_FACE ( 'NONE', ( #33186 ), #74622, .F. ) ;
#73400 = CARTESIAN_POINT ( 'NONE',  ( -7.846153846153844924, -12.37446782046654192, 30.86335684631486131 ) ) ;
#73401 = ORIENTED_EDGE ( 'NONE', *, *, #49815, .T. ) ;
#73402 = CARTESIAN_POINT ( 'NONE',  ( 1.384615384615386802, -2.499999999999998668, 29.75000000000001421 ) ) ;
#73403 = CARTESIAN_POINT ( 'NONE',  ( -3.296852641725110722, -3.513871655860377086, 32.76840700105978499 ) ) ;
#73404 = CARTESIAN_POINT ( 'NONE',  ( 23.49999999999998934, 1.674711738930281374E-15, 27.25000000000000000 ) ) ;
#73405 = CARTESIAN_POINT ( 'NONE',  ( 2.750000000000002665, -7.561099074964516831, 14.72061829374151465 ) ) ;
#73406 = B_SPLINE_CURVE_WITH_KNOTS ( 'NONE', 3,
 ( #27863, #55330, #40074, #12146, #82378, #13903, #47245, #54003, #21094, #62091 ),
 .UNSPECIFIED., .F., .F.,
 ( 4, 2, 2, 2, 4 ),
 ( 0.0007817246256747476061, 0.0009771112852218909357, 0.001172497944769034049, 0.001367884604316177161, 0.001563271263863320491 ),
 .UNSPECIFIED. ) ;
#73407 = VECTOR ( 'NONE', #67078, 1000.000000000000000 ) ;
#73408 = AXIS2_PLACEMENT_3D ( 'NONE', #23929, #73022, #18528 ) ;
#73409 = EDGE_CURVE ( 'NONE', #64009, #10019, #57609, .T. ) ;
#73410 = FACE_OUTER_BOUND ( 'NONE', #59515, .T. ) ;
#73411 = CARTESIAN_POINT ( 'NONE',  ( -5.999999999999998224, -12.34228464037088635, 31.77849191805839268 ) ) ;
#73413 = EDGE_LOOP ( 'NONE', ( #12096, #27706 ) ) ;
#73412 = CARTESIAN_POINT ( 'NONE',  ( 9.692307692307572609, -6.879047030192662504, 34.71129190930017927 ) ) ;
#73414 = CARTESIAN_POINT ( 'NONE',  ( 1.944543648262996083, -5.555456351736983045, 18.06250000000000355 ) ) ;
#73415 = LINE ( 'NONE', #40089, #5257 ) ;
#73416 = AXIS2_PLACEMENT_3D ( 'NONE', #10596, #78597, #16900 ) ;
#73417 = ORIENTED_EDGE ( 'NONE', *, *, #84815, .F. ) ;
#73418 = AXIS2_PLACEMENT_3D ( 'NONE', #58366, #73692, #3873 ) ;
#73419 = CARTESIAN_POINT ( 'NONE',  ( -2.177166605928743337, -2.619367082507848998, 30.83698974864644171 ) ) ;
#73420 = PRESENTATION_LAYER_ASSIGNMENT (  '', '', ( #48969 ) ) ;
#73421 = ORIENTED_EDGE ( 'NONE', *, *, #76448, .F. ) ;
#73422 = DIRECTION ( 'NONE',  ( 0.000000000000000000, 0.6427876096865373645, -0.7660444431189797898 ) ) ;
#73423 = CARTESIAN_POINT ( 'NONE',  ( -15.45425415533356350, -3.019605429927184836, 32.48692288466676814 ) ) ;
#73424 = EDGE_CURVE ( 'NONE', #18827, #22236, #31782, .T. ) ;
#73425 = CARTESIAN_POINT ( 'NONE',  ( 15.45378058238207863, -2.758310577978208666, 31.33698337089302299 ) ) ;
#73426 = EDGE_LOOP ( 'NONE', ( #88357, #1119 ) ) ;
#73427 = EDGE_CURVE ( 'NONE', #45168, #71435, #39071, .T. ) ;
#73428 = DIRECTION ( 'NONE',  ( -0.000000000000000000, 0.9848077530122086864, -0.1736481776669273891 ) ) ;
#73429 = ORIENTED_EDGE ( 'NONE', *, *, #7303, .T. ) ;
#73430 = CARTESIAN_POINT ( 'NONE',  ( -5.776987155906605942, -2.308499170217967134, 30.53291367094873721 ) ) ;
#73431 = ORIENTED_EDGE ( 'NONE', *, *, #10571, .F. ) ;
#73432 = CARTESIAN_POINT ( 'NONE',  ( 2.307692307692309264, -9.058645607665452459, 34.76329471203371924 ) ) ;
#73433 = CARTESIAN_POINT ( 'NONE',  ( 12.52679403281448778, -12.27809138561124591, 31.22303859784720359 ) ) ;
#73434 = EDGE_CURVE ( 'NONE', #70760, #35719, #37187, .T. ) ;
#73435 = CARTESIAN_POINT ( 'NONE',  ( -10.39237326377176274, -6.503523203565941380, 34.64991518177335195 ) ) ;
#73436 = ADVANCED_FACE ( 'NONE', ( #39958 ), #87263, .F. ) ;
#73437 = DIRECTION ( 'NONE',  ( 0.000000000000000000, -6.938893903907222067E-15, 1.000000000000000000 ) ) ;
#73438 = CYLINDRICAL_SURFACE ( 'NONE', #46461, 0.2499999999999986955 ) ;
#73439 = CARTESIAN_POINT ( 'NONE',  ( -1.161602540521989635, -10.77377354290276301, 33.85451476688484718 ) ) ;
#73440 = B_SPLINE_CURVE_WITH_KNOTS ( 'NONE', 3,
 ( #4057, #37857, #45044, #45938, #58119, #3174, #73430, #79295, #4519, #11729 ),
 .UNSPECIFIED., .F., .F.,
 ( 4, 2, 2, 2, 4 ),
 ( 0.0007817246256747516176, 0.0009771112852218965736, 0.001172497944769041421, 0.001367884604316186269, 0.001563271263863331333 ),
 .UNSPECIFIED. ) ;
#73441 = B_SPLINE_CURVE_WITH_KNOTS ( 'NONE', 3,
 ( #36754, #84514, #30003, #2957, #56588, #37639, #49390, #57909, #70989, #35880 ),
 .UNSPECIFIED., .F., .F.,
 ( 4, 2, 2, 2, 4 ),
 ( 0.000000000000000000, 0.0001954311564186876063, 0.0003908623128373752125, 0.0005862934692560628188, 0.0007817246256747504250 ),
 .UNSPECIFIED. ) ;
#73442 = CARTESIAN_POINT ( 'NONE',  ( 13.45068271796546178, -11.91647553114624358, 32.58852847137148245 ) ) ;
#73443 = B_SPLINE_CURVE_WITH_KNOTS ( 'NONE', 3,
 ( #23302, #78245, #50760, #38603, #44014, #51191, #26865, #19659, #5703, #89030 ),
 .UNSPECIFIED., .F., .F.,
 ( 4, 2, 2, 2, 4 ),
 ( 0.000000000000000000, 0.0001954311564186865763, 0.0003908623128373731525, 0.0005862934692560596746, 0.0007817246256747463051 ),
 .UNSPECIFIED. ) ;
#73444 = EDGE_LOOP ( 'NONE', ( #57398, #3866, #41424, #80459 ) ) ;
#73445 = ORIENTED_EDGE ( 'NONE', *, *, #51024, .F. ) ;
#73446 = EDGE_LOOP ( 'NONE', ( #1132, #30987, #37186, #33793, #23532, #31719 ) ) ;
#73448 = VERTEX_POINT ( 'NONE', #45356 ) ;
#73447 = CARTESIAN_POINT ( 'NONE',  ( 15.29683758177167086, -2.538708090699994813, 30.37095296980875503 ) ) ;
#73449 = VECTOR ( 'NONE', #41059, 1000.000000000000000 ) ;
#73450 = CARTESIAN_POINT ( 'NONE',  ( 10.39189967166066708, -5.113361153441934093, 34.14387501736622710 ) ) ;
#73451 = CARTESIAN_POINT ( 'NONE',  ( 1.384615384615386802, -2.721908614388771852, 31.22303859784724978 ) ) ;
#73452 = ORIENTED_EDGE ( 'NONE', *, *, #8964, .F. ) ;
#73453 = CARTESIAN_POINT ( 'NONE',  ( 15.48071464014727283, -9.357781135181031829, 34.66075350412533851 ) ) ;
#73454 = ORIENTED_EDGE ( 'NONE', *, *, #75265, .F. ) ;
#73455 = CARTESIAN_POINT ( 'NONE',  ( 17.29993592101647337, -9.172514111537580561, 34.72667873470787470 ) ) ;
#73456 = ORIENTED_EDGE ( 'NONE', *, *, #6683, .T. ) ;
#73457 = CARTESIAN_POINT ( 'NONE',  ( -23.50000000000000000, 8.999999999999996447, 30.36437827766147279 ) ) ;
#73458 = EDGE_CURVE ( 'NONE', #75360, #30124, #11359, .T. ) ;
#73459 = VECTOR ( 'NONE', #14996, 1000.000000000000000 ) ;
#73460 = CARTESIAN_POINT ( 'NONE',  ( 4.153846153846154188, -11.91647553114624181, 32.58852847137148245 ) ) ;
#73461 = ADVANCED_FACE ( 'NONE', ( #32303 ), #12040, .F. ) ;
#73462 = CARTESIAN_POINT ( 'NONE',  ( 3.903846153846154632, -2.249999999999998668, 29.75000000000000355 ) ) ;
#73463 = FACE_BOUND ( 'NONE', #44219, .T. ) ;
#73464 = CARTESIAN_POINT ( 'NONE',  ( 17.29993592101647337, -6.460100341425561332, 34.89618726649961644 ) ) ;
#73465 = CARTESIAN_POINT ( 'NONE',  ( 1.450781991207027222, -7.250054591869667497, 34.99404684341514127 ) ) ;
#73466 = B_SPLINE_CURVE_WITH_KNOTS ( 'NONE', 3,
 ( #85214, #3226, #64468, #71682, #30699, #30267, #23933, #57734, #44643, #18088 ),
 .UNSPECIFIED., .F., .F.,
 ( 4, 2, 2, 2, 4 ),
 ( 0.000000000000000000, 0.0001954311564186865763, 0.0003908623128373731525, 0.0005862934692560596746, 0.0007817246256747463051 ),
 .UNSPECIFIED. ) ;
#73467 = VECTOR ( 'NONE', #52004, 1000.000000000000000 ) ;
#73468 = VECTOR ( 'NONE', #62170, 1000.000000000000000 ) ;
#73469 = EDGE_CURVE ( 'NONE', #18264, #61398, #88604, .T. ) ;
#73470 = CARTESIAN_POINT ( 'NONE',  ( -1.449885385171703289, -2.379036618887870880, 30.90682066428147579 ) ) ;
#73471 = CARTESIAN_POINT ( 'NONE',  ( -10.61538461538461320, -13.53365097954675988, 30.81389545987213552 ) ) ;
#73472 = CARTESIAN_POINT ( 'NONE',  ( 10.36538461538461497, -7.566083408709835645, 34.74999999999999289 ) ) ;
#73473 = CARTESIAN_POINT ( 'NONE',  ( 17.29993442853592711, -9.086983370893049639, 34.49168942202179267 ) ) ;
#73474 = EDGE_LOOP ( 'NONE', ( #79649, #44104 ) ) ;
#73475 = CARTESIAN_POINT ( 'NONE',  ( 20.00000000000000000, -11.50000000000000000, 29.75000000000000355 ) ) ;
#73476 = ORIENTED_EDGE ( 'NONE', *, *, #73987, .T. ) ;
#73477 = EDGE_LOOP ( 'NONE', ( #25987, #61904 ) ) ;
#73478 = ADVANCED_FACE ( 'NONE', ( #21443 ), #75496, .F. ) ;
#73480 = DIRECTION ( 'NONE',  ( -0.000000000000000000, -0.5000000000000009992, -0.8660254037844380415 ) ) ;
#73479 = CARTESIAN_POINT ( 'NONE',  ( -16.15384615384615330, -2.833524468853757305, 32.15551576947925838 ) ) ;
#73481 = CYLINDRICAL_SURFACE ( 'NONE', #14031, 0.2499999999999986955 ) ;
#73482 = CARTESIAN_POINT ( 'NONE',  ( -14.53117723225663482, -12.11044203135681840, 32.26167407432752299 ) ) ;
#73483 = CYLINDRICAL_SURFACE ( 'NONE', #80307, 0.2499999999999995559 ) ;
#73484 = CARTESIAN_POINT ( 'NONE',  ( -15.45425417449318140, -3.754499324213721234, 33.06261337010820256 ) ) ;
#73485 = ORIENTED_EDGE ( 'NONE', *, *, #53172, .F. ) ;
#73486 = FACE_OUTER_BOUND ( 'NONE', #42970, .T. ) ;
#73487 = CARTESIAN_POINT ( 'NONE',  ( 0.4615384615384611200, -9.780366693483667717, 34.19971097300155094 ) ) ;
#73488 = CARTESIAN_POINT ( 'NONE',  ( 10.39245839786846659, -3.105860786376062332, 32.13614157043599562 ) ) ;
#73489 = CARTESIAN_POINT ( 'NONE',  ( 5.326923076924511946, -7.500000000000155431, 34.75000000000007105 ) ) ;
#73490 = VERTEX_POINT ( 'NONE', #89040 ) ;
#73491 = VERTEX_POINT ( 'NONE', #57332 ) ;
#73492 = ITEM_DEFINED_TRANSFORMATION ( 'NONE', 'NONE', #4347,  #83448 ) ;
#73493 = EDGE_LOOP ( 'NONE', ( #68490, #50789, #65318, #44955 ) ) ;
#73494 = DIRECTION ( 'NONE',  ( 0.000000000000000000, 0.8660254037844377084, -0.5000000000000015543 ) ) ;
#73495 = CARTESIAN_POINT ( 'NONE',  ( -7.715362038329061534, -4.809403383903224416, 33.96459661697924304 ) ) ;
#73496 = VERTEX_POINT ( 'NONE', #71278 ) ;
#73497 = CARTESIAN_POINT ( 'NONE',  ( 2.980769230769232170, -7.500000000000001776, 35.00000000000000000 ) ) ;
#73498 = CARTESIAN_POINT ( 'NONE',  ( -5.207070286361293654, -2.882441371585227063, 31.66841991370171527 ) ) ;
#73499 = CARTESIAN_POINT ( 'NONE',  ( 0.4615384615383396616, -12.27809138561165270, 31.22303859784587132 ) ) ;
#73500 = EDGE_CURVE ( 'NONE', #5405, #54514, #62413, .T. ) ;
#73501 = CARTESIAN_POINT ( 'NONE',  ( 14.55769230769237410, -7.434744429011176159, 34.75000000000000711 ) ) ;
#73502 = DIRECTION ( 'NONE',  ( 0.000000000000000000, 0.3420201433256610524, 0.9396926207859113145 ) ) ;
#73503 = ORIENTED_EDGE ( 'NONE', *, *, #84734, .F. ) ;
#73505 = ORIENTED_EDGE ( 'NONE', *, *, #6964, .T. ) ;
#73504 = CARTESIAN_POINT ( 'NONE',  ( -15.45425415533355995, -12.11044203135681840, 32.26167407432752299 ) ) ;
#73506 = CARTESIAN_POINT ( 'NONE',  ( 15.23076923076923173, -6.681629849574314051, 35.83090037661290239 ) ) ;
#73507 = CARTESIAN_POINT ( 'NONE',  ( 8.992243613324164997, -12.38742843783360748, 31.66772728687926985 ) ) ;
#73508 = DIRECTION ( 'NONE',  ( -0.000000000000000000, -0.000000000000000000, -1.000000000000000000 ) ) ;
#73509 = AXIS2_PLACEMENT_3D ( 'NONE', #38633, #11612, #24670 ) ;
#73510 = CARTESIAN_POINT ( 'NONE',  ( 15.23076923076911093, -12.46129190930018460, 30.37095296980731973 ) ) ;
#73511 = LINE ( 'NONE', #74390, #47672 ) ;
#73512 = LINE ( 'NONE', #37600, #1793 ) ;
#73513 = VECTOR ( 'NONE', #49211, 1000.000000000000227 ) ;
#73514 = CARTESIAN_POINT ( 'NONE',  ( 2.724691934501250135, -8.700186371490531201, 13.54874329374151465 ) ) ;
#73515 = VERTEX_POINT ( 'NONE', #6604 ) ;
#73516 = CARTESIAN_POINT ( 'NONE',  ( 14.05766908347085042, -2.341070481393819236, 30.72580821765574299 ) ) ;
#73517 = CARTESIAN_POINT ( 'NONE',  ( -14.24243716817947281, -3.643525952247864463, 33.31231777344670064 ) ) ;
#73518 = CARTESIAN_POINT ( 'NONE',  ( -0.3962828902624375149, -5.219633306516380244, 34.19971097300157936 ) ) ;
#73519 = ORIENTED_EDGE ( 'NONE', *, *, #5551, .T. ) ;
#73520 = ORIENTED_EDGE ( 'NONE', *, *, #40276, .F. ) ;
#73521 = LINE ( 'NONE', #45140, #57027 ) ;
#73522 = CARTESIAN_POINT ( 'NONE',  ( 3.230769230769538147, -2.506253911140615021, 30.00000000000323297 ) ) ;
#73523 = CARTESIAN_POINT ( 'NONE',  ( -0.4615384615381544209, -2.506253911140615021, 30.00000000000323297 ) ) ;
#73524 = DIRECTION ( 'NONE',  ( -1.000000000000000000, -0.000000000000000000, 0.000000000000000000 ) ) ;
#73525 = CARTESIAN_POINT ( 'NONE',  ( 6.923076923076802558, -6.026961402154118908, 34.52809138561165270 ) ) ;
#73526 = CARTESIAN_POINT ( 'NONE',  ( 14.30769230769231015, -13.20930481340135110, 34.54067556320372745 ) ) ;
#73527 = EDGE_LOOP ( 'NONE', ( #3571, #8294 ) ) ;
#73528 = CARTESIAN_POINT ( 'NONE',  ( -16.40382289789473802, -6.524016743844656574, 34.90889640711025521 ) ) ;
#73529 = EDGE_CURVE ( 'NONE', #53273, #24676, #28588, .T. ) ;
#73530 = EDGE_CURVE ( 'NONE', #84975, #31022, #82715, .T. ) ;
#73531 = VECTOR ( 'NONE', #20873, 1000.000000000000000 ) ;
#73532 = CARTESIAN_POINT ( 'NONE',  ( 4.377272552760941515, -7.630147987733840509, 34.99859428049665411 ) ) ;
#73533 = CARTESIAN_POINT ( 'NONE',  ( 4.023698184114458343, -8.630895178749536711, 34.87696386517710323 ) ) ;
#73534 = ORIENTED_EDGE ( 'NONE', *, *, #18680, .T. ) ;
#73535 = CARTESIAN_POINT ( 'NONE',  ( 12.68431800280687227, -3.755027918224367767, 33.06320215134714857 ) ) ;
#73536 = B_SPLINE_CURVE_WITH_KNOTS ( 'NONE', 3,
 ( #59434, #86486, #16664, #18013, #44124, #9911, #35455, #83661, #2104, #35904 ),
 .UNSPECIFIED., .F., .F.,
 ( 4, 2, 2, 2, 4 ),
 ( 0.000000000000000000, 0.0001954339857564074473, 0.0003908679715128148945, 0.0005863019572692223418, 0.0007817359430256297891 ),
 .UNSPECIFIED. ) ;
#73537 = EDGE_CURVE ( 'NONE', #545, #8013, #61979, .T. ) ;
#73538 = B_SPLINE_CURVE_WITH_KNOTS ( 'NONE', 3,
 ( #36279, #63733, #65056, #2035, #16441, #30836, #56975, #71372, #84469, #85350 ),
 .UNSPECIFIED., .F., .F.,
 ( 4, 2, 2, 2, 4 ),
 ( 0.000000000000000000, 0.0001954311584214072381, 0.0003908623168428144762, 0.0005862934752642217414, 0.0007817246336856289524 ),
 .UNSPECIFIED. ) ;
#73539 = VECTOR ( 'NONE', #53631, 1000.000000000000227 ) ;
#73540 = AXIS2_PLACEMENT_3D ( 'NONE', #30268, #57735, #16741 ) ;
#73541 = EDGE_LOOP ( 'NONE', ( #88352, #49071 ) ) ;
#73542 = CARTESIAN_POINT ( 'NONE',  ( -19.50000000000000000, -3.499999999999999556, 29.75000000000000355 ) ) ;
#73543 = DIRECTION ( 'NONE',  ( 0.000000000000000000, 0.000000000000000000, 1.000000000000000000 ) ) ;
#73544 = CARTESIAN_POINT ( 'NONE',  ( -8.769230769230768274, -8.164416787775445883, 34.95778746994557906 ) ) ;
#73545 = ORIENTED_EDGE ( 'NONE', *, *, #40173, .T. ) ;
#73546 = EDGE_CURVE ( 'NONE', #62563, #28571, #34951, .T. ) ;
#73547 = CARTESIAN_POINT ( 'NONE',  ( -13.25408994638174320, -5.070358843744210198, 34.40418822224088302 ) ) ;
#73548 = FACE_OUTER_BOUND ( 'NONE', #9567, .T. ) ;
#73549 = DIRECTION ( 'NONE',  ( -0.000000000000000000, 0.6427876096865404731, -0.7660444431189771253 ) ) ;
#73550 = VECTOR ( 'NONE', #28283, 1000.000000000000227 ) ;
#73551 = EDGE_CURVE ( 'NONE', #66461, #18250, #33633, .T. ) ;
#73552 = CARTESIAN_POINT ( 'NONE',  ( 11.53846153846153832, -2.517432740324522911, 35.29906147534542527 ) ) ;
#73553 = CARTESIAN_POINT ( 'NONE',  ( -3.099977422944443450, -12.38066358083363738, 30.83685684665853444 ) ) ;
#73554 = EDGE_LOOP ( 'NONE', ( #12654, #59170, #60866, #79952 ) ) ;
#73555 = CARTESIAN_POINT ( 'NONE',  ( -4.087778820496075660, -12.34228464037088813, 31.77849191805839268 ) ) ;
#73556 = EDGE_LOOP ( 'NONE', ( #72974, #3836 ) ) ;
#73558 = EDGE_CURVE ( 'NONE', #89000, #83351, #23151, .T. ) ;
#73557 = CARTESIAN_POINT ( 'NONE',  ( 8.703147358274888390, -12.37446782046654192, 30.86335684631486487 ) ) ;
#73559 = CARTESIAN_POINT ( 'NONE',  ( 3.230769230769231726, -3.669653830205710676, 35.88435417666054406 ) ) ;
#73560 = CARTESIAN_POINT ( 'NONE',  ( -13.63463862190835130, -2.823816976329319051, 31.52131813110795733 ) ) ;
#73561 = DIRECTION ( 'NONE',  ( 0.000000000000000000, 0.000000000000000000, -1.000000000000000000 ) ) ;
#73562 = ADVANCED_FACE ( 'NONE', ( #48914 ), #34516, .F. ) ;
#73563 = CARTESIAN_POINT ( 'NONE',  ( -6.792551221313361864, -6.001044277235011215, 34.52024696741798948 ) ) ;
#73564 = CARTESIAN_POINT ( 'NONE',  ( -13.38461538461538325, -2.499999999999998668, 29.75000000000001421 ) ) ;
#73565 = CARTESIAN_POINT ( 'NONE',  ( 16.15384615384603251, -12.16647553114689728, 32.15551576947799362 ) ) ;
#73566 = ORIENTED_EDGE ( 'NONE', *, *, #47248, .F. ) ;
#73567 = ORIENTED_EDGE ( 'NONE', *, *, #49974, .T. ) ;
#73568 = ORIENTED_EDGE ( 'NONE', *, *, #31139, .T. ) ;
#73569 = VECTOR ( 'NONE', #9073, 1000.000000000000227 ) ;
#73570 = ORIENTED_EDGE ( 'NONE', *, *, #69586, .F. ) ;
#73573 = VERTEX_POINT ( 'NONE', #20556 ) ;
#73572 = EDGE_CURVE ( 'NONE', #79986, #6875, #27754, .T. ) ;
#73571 = B_SPLINE_CURVE_WITH_KNOTS ( 'NONE', 3,
 ( #81002, #54395, #21046, #41786, #27378, #55283, #40464, #89100, #48517, #67923 ),
 .UNSPECIFIED., .F., .F.,
 ( 4, 2, 2, 2, 4 ),
 ( 0.0007817359430256353185, 0.0009771253907250028285, 0.001172514838424370230, 0.001367904286123737632, 0.001563293733823105033 ),
 .UNSPECIFIED. ) ;
#73574 = CYLINDRICAL_SURFACE ( 'NONE', #76097, 4.000000000000000000 ) ;
#73575 = CARTESIAN_POINT ( 'NONE',  ( 11.40831356872984514, -9.504002272028875709, 34.60269587691767867 ) ) ;
#73576 = CARTESIAN_POINT ( 'NONE',  ( -13.38461538461538325, -2.249999999999998668, 29.75000000000001776 ) ) ;
#73577 = EDGE_CURVE ( 'NONE', #83084, #63180, #48019, .T. ) ;
#73578 = CARTESIAN_POINT ( 'NONE',  ( -5.934744428723973897, -5.219633306516380244, 34.19971097300157936 ) ) ;
#73579 = CARTESIAN_POINT ( 'NONE',  ( 5.010840697562939816, -11.35647404775217595, 33.31231777344666511 ) ) ;
#73580 = CARTESIAN_POINT ( 'NONE',  ( 8.546304551714618114, -9.086856451489515152, 34.49173150075333183 ) ) ;
#73581 = CARTESIAN_POINT ( 'NONE',  ( 11.53846153846141753, -12.46129190930018460, 30.37095296980731973 ) ) ;
#73582 = LINE ( 'NONE', #88431, #16409 ) ;
#73583 = CARTESIAN_POINT ( 'NONE',  ( -4.153846153846152411, -9.780366693483667717, 34.19971097300155094 ) ) ;
#73584 = VERTEX_POINT ( 'NONE', #68743 ) ;
#73585 = ORIENTED_EDGE ( 'NONE', *, *, #88145, .T. ) ;
#73586 = ORIENTED_EDGE ( 'NONE', *, *, #23145, .T. ) ;
#73589 = EDGE_LOOP ( 'NONE', ( #61181, #73401, #27011, #76792 ) ) ;
#73588 = EDGE_CURVE ( 'NONE', #62974, #46529, #60804, .T. ) ;
#73587 = CARTESIAN_POINT ( 'NONE',  ( -1.514762594053601585, -11.47017969459903952, 32.78971311882034456 ) ) ;
#73591 = CARTESIAN_POINT ( 'NONE',  ( 9.692307692307695177, -3.886160181151819604, 36.00935417666054406 ) ) ;
#73590 = CARTESIAN_POINT ( 'NONE',  ( 16.37685750545900376, -11.76359900205217457, 32.36225158514719880 ) ) ;
#73592 = CYLINDRICAL_SURFACE ( 'NONE', #15458, 0.2500000000000008882 ) ;
#73593 = CARTESIAN_POINT ( 'NONE',  ( 4.376857505459002873, -2.554770724473668153, 30.48948780036025852 ) ) ;
#73594 = FACE_BOUND ( 'NONE', #25966, .T. ) ;
#73595 = EDGE_LOOP ( 'NONE', ( #5440, #52240 ) ) ;
#73596 = EDGE_CURVE ( 'NONE', #75481, #44313, #82357, .T. ) ;
#73597 = ORIENTED_EDGE ( 'NONE', *, *, #24046, .F. ) ;
#73598 = CARTESIAN_POINT ( 'NONE',  ( 4.826946332874483936, -2.318417181685854978, 30.59732222474233865 ) ) ;
#73599 = ORIENTED_EDGE ( 'NONE', *, *, #24456, .T. ) ;
#73600 = FACE_BOUND ( 'NONE', #4968, .T. ) ;
#73602 = VECTOR ( 'NONE', #35023, 1000.000000000000000 ) ;
#73601 = CARTESIAN_POINT ( 'NONE',  ( 9.757562831820530747, -5.941354392334607049, 34.76329471203374055 ) ) ;
#73603 = DIRECTION ( 'NONE',  ( -0.000000000000000000, 0.5000000000000011102, -0.8660254037844380415 ) ) ;
#73604 = EDGE_LOOP ( 'NONE', ( #61119, #25335, #42979, #35202 ) ) ;
#73605 = DIRECTION ( 'NONE',  ( 0.000000000000000000, 0.1736481776669267785, -0.9848077530122087975 ) ) ;
#73606 = CARTESIAN_POINT ( 'NONE',  ( -6.673131513698878692, -2.341251567377310217, 30.72681386836322659 ) ) ;
#73607 = LINE ( 'NONE', #85778, #37834 ) ;
#73608 = ORIENTED_EDGE ( 'NONE', *, *, #20773, .T. ) ;
#73609 = CARTESIAN_POINT ( 'NONE',  ( 14.30769230769231015, -11.35647404775217417, 33.31231777344666511 ) ) ;
#73610 = CARTESIAN_POINT ( 'NONE',  ( -18.25002323729296450, -5.056417327199098644, 34.11270091957320716 ) ) ;
#73611 = ADVANCED_FACE ( 'NONE', ( #24419 ), #79383, .T. ) ;
#73612 = DIRECTION ( 'NONE',  ( -0.000000000000000000, 0.1736481776669307198, -0.9848077530122080203 ) ) ;
#73613 = EDGE_LOOP ( 'NONE', ( #34180, #51027, #41875, #11617 ) ) ;
#73614 = AXIS2_PLACEMENT_3D ( 'NONE', #2592, #85915, #57542 ) ;
#73615 = EDGE_CURVE ( 'NONE', #7659, #35101, #30805, .T. ) ;
#73616 = CARTESIAN_POINT ( 'NONE',  ( 2.557746727605761272, -12.41089969410671223, 31.60739465890703670 ) ) ;
#73617 = CYLINDRICAL_SURFACE ( 'NONE', #80140, 0.2499999999999973355 ) ;
#73618 = B_SPLINE_CURVE_WITH_KNOTS ( 'NONE', 3,
 ( #3409, #24572, #87192, #78627, #60132, #52487, #58348, #65996, #24122, #66901 ),
 .UNSPECIFIED., .F., .F.,
 ( 4, 2, 2, 2, 4 ),
 ( 0.000000000000000000, 0.0001954311564186872810, 0.0003908623128373745620, 0.0005862934692560618430, 0.0007817246256747491240 ),
 .UNSPECIFIED. ) ;
#73619 = ORIENTED_EDGE ( 'NONE', *, *, #73154, .T. ) ;
#73620 = CARTESIAN_POINT ( 'NONE',  ( 0.2115617305961065842, -9.148715823498378086, 34.47080413974185120 ) ) ;
#73621 = FACE_OUTER_BOUND ( 'NONE', #81971, .T. ) ;
#73622 = LINE ( 'NONE', #20435, #822 ) ;
#73623 = CARTESIAN_POINT ( 'NONE',  ( -8.703975197954745724, -9.442884908240273489, 34.35708131394835618 ) ) ;
#73624 = B_SPLINE_CURVE_WITH_KNOTS ( 'NONE', 3,
 ( #3421, #31347, #79088, #45292, #30889, #51586, #44845, #72325, #10634, #38100 ),
 .UNSPECIFIED., .F., .F.,
 ( 4, 2, 2, 2, 4 ),
 ( 0.0007817359430256322827, 0.0009771253907249989254, 0.001172514838424365676, 0.001367904286123732428, 0.001563293733823098962 ),
 .UNSPECIFIED. ) ;
#73625 = CARTESIAN_POINT ( 'NONE',  ( 0.3313904918067608896, -2.647304123082327543, 31.75400227202884906 ) ) ;
#73626 = CARTESIAN_POINT ( 'NONE',  ( 6.856993512121044354, -8.973038597847269315, 34.52809138561120506 ) ) ;
#73628 = DIRECTION ( 'NONE',  ( 1.000000000000000000, 0.000000000000000000, 0.000000000000000000 ) ) ;
#73627 = FACE_BOUND ( 'NONE', #47183, .T. ) ;
#73629 = CARTESIAN_POINT ( 'NONE',  ( -3.454254174493178287, -2.599994579823203367, 30.74605699353653776 ) ) ;
#73630 = CARTESIAN_POINT ( 'NONE',  ( -18.00000000000000000, -13.72934399251292170, 33.34651343095209342 ) ) ;
#73631 = CARTESIAN_POINT ( 'NONE',  ( -2.750000000000007105, -6.360912703474006946, 16.42187500000000000 ) ) ;
#73632 = ORIENTED_EDGE ( 'NONE', *, *, #89105, .T. ) ;
#73633 = CYLINDRICAL_SURFACE ( 'NONE', #50527, 0.2500000000000012212 ) ;
#73634 = ORIENTED_EDGE ( 'NONE', *, *, #76110, .F. ) ;
#73635 = ORIENTED_EDGE ( 'NONE', *, *, #34363, .T. ) ;
#73636 = FACE_OUTER_BOUND ( 'NONE', #76245, .T. ) ;
#73637 = VERTEX_POINT ( 'NONE', #58653 ) ;
#73638 = CARTESIAN_POINT ( 'NONE',  ( -5.999999999999998224, -9.905515769479276145, 34.41647553114623292 ) ) ;
#73639 = CARTESIAN_POINT ( 'NONE',  ( 2.750000000000001776, -7.499999999999984013, 15.71875000000000000 ) ) ;
#73640 = CARTESIAN_POINT ( 'NONE',  ( 3.165499230212911908, -2.379036618887870880, 30.90682066428147934 ) ) ;
#73641 = CARTESIAN_POINT ( 'NONE',  ( 12.46153846153846168, -9.584722331328613620, 36.20867863119891439 ) ) ;
#73642 = CARTESIAN_POINT ( 'NONE',  ( -3.007757879156379932, -9.086983370893047862, 34.49168942202179267 ) ) ;
#73643 = CARTESIAN_POINT ( 'NONE',  ( -7.846153846153844924, -8.564572088678739092, 35.78748833219616898 ) ) ;
#73644 = CARTESIAN_POINT ( 'NONE',  ( -5.143005456283213483, -3.322132147404559976, 32.92929555188719348 ) ) ;
#73645 = CARTESIAN_POINT ( 'NONE',  ( -7.846153846153965716, -2.892918686052166066, 31.69288490824153470 ) ) ;
#73646 = CARTESIAN_POINT ( 'NONE',  ( 1.384615384615386802, -7.500000000000001776, 35.04278698407183867 ) ) ;
#73647 = VECTOR ( 'NONE', #32580, 1000.000000000000227 ) ;
#73648 = CARTESIAN_POINT ( 'NONE',  ( 1.553300858899129944, -11.24999999999998934, 19.70312500000000355 ) ) ;
#73649 = CARTESIAN_POINT ( 'NONE',  ( 10.86533002476265786, -12.45601412856602686, 31.48342859153981621 ) ) ;
#73650 = CARTESIAN_POINT ( 'NONE',  ( -4.377331078410482412, -12.11044203135681840, 32.26167407432752299 ) ) ;
#73651 = CARTESIAN_POINT ( 'NONE',  ( 18.25000000000000000, -2.499999999999998668, 29.75000000000000355 ) ) ;
#73652 = ORIENTED_EDGE ( 'NONE', *, *, #27191, .F. ) ;
#73653 = ORIENTED_EDGE ( 'NONE', *, *, #71323, .F. ) ;
#73654 = CARTESIAN_POINT ( 'NONE',  ( 3.164686851409094448, -10.67929555188718460, 33.92786785259543336 ) ) ;
#73655 = CARTESIAN_POINT ( 'NONE',  ( 7.596177115211491859, -11.28823185664190376, 33.01397839955799896 ) ) ;
#73656 = CARTESIAN_POINT ( 'NONE',  ( -2.307692307692428724, -2.379036618888197285, 30.90682066428292885 ) ) ;
#73657 = CARTESIAN_POINT ( 'NONE',  ( -7.053224892808619195, -5.915902021225892149, 34.75552854090298638 ) ) ;
#73658 = EDGE_CURVE ( 'NONE', #7689, #25692, #72606, .T. ) ;
#73659 = CARTESIAN_POINT ( 'NONE',  ( -12.94230769230769162, -3.499999999999999556, 29.75000000000000355 ) ) ;
#73660 = CARTESIAN_POINT ( 'NONE',  ( -4.854143407945009869, -3.020022701398814569, 32.48759521482552515 ) ) ;
#73661 = EDGE_CURVE ( 'NONE', #63695, #6887, #68306, .T. ) ;
#73662 = ORIENTED_EDGE ( 'NONE', *, *, #4189, .T. ) ;
#73663 = CARTESIAN_POINT ( 'NONE',  ( -4.826868765284763718, -12.41262288849542017, 30.68299917996395010 ) ) ;
#73664 = ORIENTED_EDGE ( 'NONE', *, *, #19488, .T. ) ;
#73665 = EDGE_CURVE ( 'NONE', #17102, #18504, #65851, .T. ) ;
#73666 = ORIENTED_EDGE ( 'NONE', *, *, #63943, .T. ) ;
#73667 = VECTOR ( 'NONE', #50420, 1000.000000000000114 ) ;
#73668 = CARTESIAN_POINT ( 'NONE',  ( -14.24152316672964957, -7.250054483168843156, 34.74374881642865631 ) ) ;
#73669 = VECTOR ( 'NONE', #13504, 1000.000000000000000 ) ;
#73670 = CARTESIAN_POINT ( 'NONE',  ( -19.50000000000000000, -3.499999999999999556, 29.75000000000000355 ) ) ;
#73671 = CARTESIAN_POINT ( 'NONE',  ( -9.626239341305252495, -6.386643153685127139, 34.62446782046654192 ) ) ;
#73672 = LINE ( 'NONE', #11965, #22050 ) ;
#73673 = CARTESIAN_POINT ( 'NONE',  ( -13.13456107297707121, -3.136992222400443175, 32.19305428654138979 ) ) ;
#73675 = EDGE_CURVE ( 'NONE', #33780, #81906, #28204, .T. ) ;
#73674 = ORIENTED_EDGE ( 'NONE', *, *, #51944, .T. ) ;
#73676 = ORIENTED_EDGE ( 'NONE', *, *, #60482, .T. ) ;
#73677 = ORIENTED_EDGE ( 'NONE', *, *, #36764, .F. ) ;
#73678 = DIRECTION ( 'NONE',  ( -0.000000000000000000, 0.7660444431189791237, -0.6427876096865379196 ) ) ;
#73679 = DIRECTION ( 'NONE',  ( -1.000000000000000000, -0.000000000000000000, -0.000000000000000000 ) ) ;
#73680 = EDGE_CURVE ( 'NONE', #57327, #177, #37492, .T. ) ;
#73681 = DIRECTION ( 'NONE',  ( -0.000000000000000000, 0.6427876096865404731, -0.7660444431189770143 ) ) ;
#73682 = CARTESIAN_POINT ( 'NONE',  ( 10.61538461538449418, -5.094484230521993062, 34.41647553114689373 ) ) ;
#73683 = FILL_AREA_STYLE ('',( #67802 ) ) ;
#73684 = ADVANCED_FACE ( 'NONE', ( #25770 ), #19014, .F. ) ;
#73685 = CARTESIAN_POINT ( 'NONE',  ( -11.53846153846153655, -9.819645486525091727, 36.12317359536749706 ) ) ;
#73686 = ORIENTED_EDGE ( 'NONE', *, *, #40180, .T. ) ;
#73687 = ORIENTED_EDGE ( 'NONE', *, *, #28566, .F. ) ;
#73688 = CARTESIAN_POINT ( 'NONE',  ( -1.553300858899081538, -11.25000000000000711, 24.85937500000001421 ) ) ;
#73690 = ORIENTED_EDGE ( 'NONE', *, *, #32326, .F. ) ;
#73689 = CYLINDRICAL_SURFACE ( 'NONE', #57380, 0.2499999999999994726 ) ;
#73691 = CARTESIAN_POINT ( 'NONE',  ( -9.692307692307814193, -10.33852847137269571, 34.16647553114546554 ) ) ;
#73692 = DIRECTION ( 'NONE',  ( -0.000000000000000000, 0.7660444431189791237, -0.6427876096865379196 ) ) ;
#73693 = AXIS2_PLACEMENT_3D ( 'NONE', #9554, #2344, #37018 ) ;
#73694 = CARTESIAN_POINT ( 'NONE',  ( -2.651650429449565305, -4.848349570550461785, 17.75000000000000355 ) ) ;
#73695 = ORIENTED_EDGE ( 'NONE', *, *, #52463, .F. ) ;
#73696 = EDGE_CURVE ( 'NONE', #64679, #54531, #34002, .T. ) ;
#73697 = VECTOR ( 'NONE', #8620, 1000.000000000000000 ) ;
#73698 = CARTESIAN_POINT ( 'NONE',  ( 3.230769230769546141, -2.255955759149395501, 30.00000000000324363 ) ) ;
#73699 = ORIENTED_EDGE ( 'NONE', *, *, #13912, .F. ) ;
#73700 = CARTESIAN_POINT ( 'NONE',  ( -13.44988538517170440, -11.67786785259540849, 32.92929555188721480 ) ) ;
#73701 = DIRECTION ( 'NONE',  ( -0.000000000000000000, -0.9396926207859093161, -0.3420201433256663259 ) ) ;
#73702 = CARTESIAN_POINT ( 'NONE',  ( -12.23875892027004930, -12.44528174975671853, 30.48912976160716681 ) ) ;
#73703 = B_SPLINE_CURVE_WITH_KNOTS ( 'NONE', 3,
 ( #57302, #49222, #1918, #14998, #63615, #70384, #9555, #36595, #64049, #37019 ),
 .UNSPECIFIED., .F., .F.,
 ( 4, 2, 2, 2, 4 ),
 ( 0.000000000000000000, 0.0001954339857564097241, 0.0003908679715128194482, 0.0005863019572692291723, 0.0007817359430256388964 ),
 .UNSPECIFIED. ) ;
#73705 = PLANE ( 'NONE',  #81433 ) ;
#73704 = CARTESIAN_POINT ( 'NONE',  ( -5.076923076923197442, -12.27809138561165270, 31.22303859784587132 ) ) ;
#73706 = LINE ( 'NONE', #53407, #14626 ) ;
#73707 = ORIENTED_EDGE ( 'NONE', *, *, #27473, .T. ) ;
#73708 = CARTESIAN_POINT ( 'NONE',  ( 6.700150705560775855, -8.239355502252617924, 34.69524867566427417 ) ) ;
#73709 = CARTESIAN_POINT ( 'NONE',  ( -9.019253993452228002, -4.175268141568685643, 33.81360843649122216 ) ) ;
#73710 = DIRECTION ( 'NONE',  ( 0.000000000000000000, 0.7660444431189807890, 0.6427876096865361433 ) ) ;
#73712 = ORIENTED_EDGE ( 'NONE', *, *, #50612, .F. ) ;
#73711 = ADVANCED_FACE ( 'NONE', ( #39741 ), #5054, .F. ) ;
#73713 = CARTESIAN_POINT ( 'NONE',  ( 4.153846153846154188, -2.517432740324522911, 35.29906147534542527 ) ) ;
#73714 = LINE ( 'NONE', #86796, #65574 ) ;
#73715 = CARTESIAN_POINT ( 'NONE',  ( -16.28453675695647007, -11.93127051446800380, 32.56575433478200665 ) ) ;
#73716 = EDGE_CURVE ( 'NONE', #42352, #66607, #79156, .T. ) ;
#73718 = EDGE_CURVE ( 'NONE', #11602, #4346, #74858, .T. ) ;
#73717 = CARTESIAN_POINT ( 'NONE',  ( 10.39189967166066708, -11.89387501736622710, 32.13663884655806413 ) ) ;
#73719 = FACE_BOUND ( 'NONE', #69199, .T. ) ;
#73721 = FACE_OUTER_BOUND ( 'NONE', #5772, .T. ) ;
#73720 = CARTESIAN_POINT ( 'NONE',  ( 13.38461538461538680, -13.88283147151868846, 33.14645433367849847 ) ) ;
#73722 = CARTESIAN_POINT ( 'NONE',  ( -15.23076923076922995, -4.661471528628507777, 34.16647553114623292 ) ) ;
#73724 = CARTESIAN_POINT ( 'NONE',  ( -9.692307692307812417, -10.90142922262034020, 33.41473453929536674 ) ) ;
#73723 = CARTESIAN_POINT ( 'NONE',  ( 1.254467414883689402, -12.70455904226513866, 30.44083106164009322 ) ) ;
#73725 = CARTESIAN_POINT ( 'NONE',  ( 1.449870524128224369, -3.083524468853784839, 32.58852847137153930 ) ) ;
#73726 = CARTESIAN_POINT ( 'NONE',  ( 8.769230769230645706, -12.70778746994576025, 30.41441678777401236 ) ) ;
#73727 = CARTESIAN_POINT ( 'NONE',  ( 2.694853999681214862, -10.10844685921789043, 25.62313170625849068 ) ) ;
#73728 = EDGE_CURVE ( 'NONE', #41702, #58570, #58723, .T. ) ;
#73729 = ORIENTED_EDGE ( 'NONE', *, *, #15039, .T. ) ;
#73730 = VECTOR ( 'NONE', #61855, 1000.000000000000000 ) ;
#73731 = CARTESIAN_POINT ( 'NONE',  ( -12.21153846153840128, -7.434744860731433924, 35.00000000000000711 ) ) ;
#73732 = ORIENTED_EDGE ( 'NONE', *, *, #42226, .T. ) ;
#73733 = AXIS2_PLACEMENT_3D ( 'NONE', #22152, #35672, #16277 ) ;
#73734 = CYLINDRICAL_SURFACE ( 'NONE', #65041, 0.2500000000000009437 ) ;
#73735 = CARTESIAN_POINT ( 'NONE',  ( -4.088590582570128973, -12.27809138561124591, 31.22303859784720359 ) ) ;
#73736 = LINE ( 'NONE', #87696, #50241 ) ;
#73737 = CARTESIAN_POINT ( 'NONE',  ( -23.50000000000000000, -8.999999999999996447, 22.25000000000000000 ) ) ;
#73738 = DIRECTION ( 'NONE',  ( -0.000000000000000000, -0.8660254037844397068, -0.4999999999999978906 ) ) ;
#73739 = CARTESIAN_POINT ( 'NONE',  ( 5.999999999999878320, -3.643525952248796163, 33.31231777344771672 ) ) ;
#73740 = CARTESIAN_POINT ( 'NONE',  ( -1.492201783934549164, -11.27530806549876807, 24.60750670625849779 ) ) ;
#73741 = VECTOR ( 'NONE', #58786, 1000.000000000000000 ) ;
#73742 = CARTESIAN_POINT ( 'NONE',  ( 14.98079248672064345, -12.01397095200674059, 32.43157075238190146 ) ) ;
#73743 = CARTESIAN_POINT ( 'NONE',  ( -14.37377468705243899, -11.35647404775217595, 33.31231777344666511 ) ) ;
#73744 = CARTESIAN_POINT ( 'NONE',  ( -0.4761625575576027836, -4.791179646259885239, 29.07450979259064638 ) ) ;
#73745 = CARTESIAN_POINT ( 'NONE',  ( 9.692307692307570832, -4.320704448113951379, 33.92786785259630022 ) ) ;
#73746 = CARTESIAN_POINT ( 'NONE',  ( 8.519207531937803779, -10.05641848906368097, 34.04755513067966177 ) ) ;
#73747 = CARTESIAN_POINT ( 'NONE',  ( -11.47320596718551400, -10.21337939537593620, 33.94971097300152252 ) ) ;
#73748 = CARTESIAN_POINT ( 'NONE',  ( 3.775308065498752086, -6.007798216065404873, 17.14249329374151287 ) ) ;
#73749 = B_SPLINE_CURVE_WITH_KNOTS ( 'NONE', 3,
 ( #9849, #3080, #44503, #31907, #25587, #52154, #3965, #72875, #80086, #44059 ),
 .UNSPECIFIED., .F., .F.,
 ( 4, 2, 2, 2, 4 ),
 ( 0.0007817359430256372700, 0.0009771253907250054306, 0.001172514838424373700, 0.001367904286123741969, 0.001563293733823110021 ),
 .UNSPECIFIED. ) ;
#73750 = CARTESIAN_POINT ( 'NONE',  ( 2.980769230769232170, -7.500000000000001776, 35.00000000000000000 ) ) ;
#73751 = LINE ( 'NONE', #74178, #5370 ) ;
#73752 = B_SPLINE_CURVE_WITH_KNOTS ( 'NONE', 3,
 ( #52683, #67992, #45926, #19798, #81070, #46822, #47260, #13041, #88286, #39643 ),
 .UNSPECIFIED., .F., .F.,
 ( 4, 2, 2, 2, 4 ),
 ( 0.0007817246256747494492, 0.0009771112852218935378, 0.001172497944769037518, 0.001367884604316181498, 0.001563271263863325695 ),
 .UNSPECIFIED. ) ;
#73753 = EDGE_LOOP ( 'NONE', ( #70464, #39571 ) ) ;
#73754 = CARTESIAN_POINT ( 'NONE',  ( -10.61538461538461320, -13.87047571288749737, 32.06866353760679544 ) ) ;
#73755 = CARTESIAN_POINT ( 'NONE',  ( 13.38461538461526601, -3.835265460704628371, 33.15142922262033665 ) ) ;
#73756 = CARTESIAN_POINT ( 'NONE',  ( -3.749999999999997780, -7.438900925035489387, 19.09561829374150932 ) ) ;
#73757 = CARTESIAN_POINT ( 'NONE',  ( -15.10072417484945717, -2.254550872974306674, 29.97347326024527092 ) ) ;
#73758 = CARTESIAN_POINT ( 'NONE',  ( -9.019253993452226226, -3.520140089381495585, 33.17453946501458262 ) ) ;
#73759 = VERTEX_POINT ( 'NONE', #32518 ) ;
#73760 = DIRECTION ( 'NONE',  ( 1.000000000000000000, 0.000000000000000000, 0.000000000000000000 ) ) ;
#73761 = CARTESIAN_POINT ( 'NONE',  ( -12.23875879256039489, -12.69155399931963046, 30.53255429739157734 ) ) ;
#73763 = ORIENTED_EDGE ( 'NONE', *, *, #5798, .F. ) ;
#73762 = CARTESIAN_POINT ( 'NONE',  ( -7.623141002060451754, -12.38742843783360748, 31.66772728687926985 ) ) ;
#73764 = CARTESIAN_POINT ( 'NONE',  ( -13.38461538461538325, -11.16473453929635440, 33.15142922261926373 ) ) ;
#73765 = DIRECTION ( 'NONE',  ( 0.000000000000000000, 0.8660254037844377084, 0.5000000000000015543 ) ) ;
#73766 = CARTESIAN_POINT ( 'NONE',  ( 4.826923076923076650, -7.500000000000001776, 35.00000000000000000 ) ) ;
#73767 = CARTESIAN_POINT ( 'NONE',  ( 11.78851585009985570, -9.148310452688876993, 34.47095581063188519 ) ) ;
#73768 = ORIENTED_EDGE ( 'NONE', *, *, #13592, .T. ) ;
#73769 = CARTESIAN_POINT ( 'NONE',  ( 6.923076923077238654, -2.255955759149395501, 30.00000000000324363 ) ) ;
#73770 = CARTESIAN_POINT ( 'NONE',  ( -15.29685161012936767, -11.35647404775217595, 33.31231777344666511 ) ) ;
#73771 = CARTESIAN_POINT ( 'NONE',  ( 15.23076923076923173, -1.509761064869970415, 31.06009739812519044 ) ) ;
#73772 = ORIENTED_EDGE ( 'NONE', *, *, #40423, .T. ) ;
#73773 = ORIENTED_EDGE ( 'NONE', *, *, #6791, .T. ) ;
#73774 = EDGE_LOOP ( 'NONE', ( #72195, #21429, #46726, #84637 ) ) ;
#73775 = CARTESIAN_POINT ( 'NONE',  ( 5.142178648199101865, -12.27809138561124591, 31.22303859784720359 ) ) ;
#73776 = DIRECTION ( 'NONE',  ( 0.000000000000000000, 1.000000000000000000, 0.000000000000000000 ) ) ;
#73777 = CARTESIAN_POINT ( 'NONE',  ( 13.38461538461526601, -11.48612834414049644, 32.76840700105863391 ) ) ;
#73778 = CARTESIAN_POINT ( 'NONE',  ( -17.87193355239358894, -7.274843614157066263, 34.99539393749329719 ) ) ;
#73779 = VERTEX_POINT ( 'NONE', #82055 ) ;
#73780 = B_SPLINE_CURVE_WITH_KNOTS ( 'NONE', 3,
 ( #17374, #44831, #30002, #58796, #57018, #23236, #77296, #72310, #10618, #50698 ),
 .UNSPECIFIED., .F., .F.,
 ( 4, 2, 2, 2, 4 ),
 ( 0.0007817246256747463051, 0.0009771112852218896347, 0.001172497944769032747, 0.001367884604316176077, 0.001563271263863319407 ),
 .UNSPECIFIED. ) ;
#73781 = B_SPLINE_CURVE_WITH_KNOTS ( 'NONE', 3,
 ( #76123, #41911, #69378, #7679, #8120, #35140, #62602, #912, #55851, #83341 ),
 .UNSPECIFIED., .F., .F.,
 ( 4, 2, 2, 2, 4 ),
 ( 0.0007817246256747470640, 0.0009771112852218898515, 0.001172497944769032747, 0.001367884604316175643, 0.001563271263863318539 ),
 .UNSPECIFIED. ) ;
#73782 = ORIENTED_EDGE ( 'NONE', *, *, #69711, .F. ) ;
#73783 = VERTEX_POINT ( 'NONE', #6823 ) ;
#73785 = ORIENTED_EDGE ( 'NONE', *, *, #65064, .F. ) ;
#73784 = LINE ( 'NONE', #48056, #60225 ) ;
#73786 = DIRECTION ( 'NONE',  ( 0.000000000000000000, 0.1736481776669267785, -0.9848077530122087975 ) ) ;
#73787 = CARTESIAN_POINT ( 'NONE',  ( 14.98079249982687955, -3.137211980971221781, 32.19342716148376837 ) ) ;
#73788 = DIRECTION ( 'NONE',  ( 0.000000000000000000, 0.3420201433256641055, -0.9396926207859100932 ) ) ;
#73789 = CARTESIAN_POINT ( 'NONE',  ( -15.16551365949320562, -9.442884908240273489, 34.35708131394835618 ) ) ;
#73790 = VERTEX_POINT ( 'NONE', #61755 ) ;
#73791 = VECTOR ( 'NONE', #55472, 1000.000000000000000 ) ;
#73792 = VERTEX_POINT ( 'NONE', #55020 ) ;
#73793 = ORIENTED_EDGE ( 'NONE', *, *, #74782, .F. ) ;
#73794 = CARTESIAN_POINT ( 'NONE',  ( -10.83886953994894675, -10.97335522853832579, 33.68706563782419749 ) ) ;
#73796 = ORIENTED_EDGE ( 'NONE', *, *, #20585, .F. ) ;
#73795 = DIRECTION ( 'NONE',  ( 0.000000000000000000, 0.1736481776669267785, -0.9848077530122087975 ) ) ;
#73797 = CARTESIAN_POINT ( 'NONE',  ( 2.241609928332174206, -2.486705287966279876, 31.30864560766542937 ) ) ;
#73798 = CARTESIAN_POINT ( 'NONE',  ( 7.384615384615385025, -7.500000000000000000, 29.75000000000000355 ) ) ;
#73799 = EDGE_CURVE ( 'NONE', #60558, #47459, #56496, .T. ) ;
#73800 = CYLINDRICAL_SURFACE ( 'NONE', #31675, 0.2499999999999994726 ) ;
#73801 = CARTESIAN_POINT ( 'NONE',  ( -1.634592115557738090, -8.303909089506435137, 34.68538101551103381 ) ) ;
#73802 = CARTESIAN_POINT ( 'NONE',  ( -2.177166605928745113, -11.46989282347013095, 32.79007818306219946 ) ) ;
#73803 = FACE_BOUND ( 'NONE', #5869, .T. ) ;
#73804 = LINE ( 'NONE', #24711, #16889 ) ;
#73805 = CARTESIAN_POINT ( 'NONE',  ( -0.4615384615384611200, -12.62096338111211580, 30.90682066428153263 ) ) ;
#73806 = LINE ( 'NONE', #54402, #26467 ) ;
#73808 = DIRECTION ( 'NONE',  ( -0.000000000000000000, -0.8660254037844399289, -0.4999999999999980016 ) ) ;
#73807 = CARTESIAN_POINT ( 'NONE',  ( -17.75000000000000711, -12.75000000000000178, 29.75000000000000355 ) ) ;
#73809 = DIRECTION ( 'NONE',  ( 1.000000000000000000, 0.000000000000000000, 0.000000000000000000 ) ) ;
#73810 = FACE_OUTER_BOUND ( 'NONE', #69132, .T. ) ;
#73811 = ORIENTED_EDGE ( 'NONE', *, *, #10635, .T. ) ;
#73812 = CARTESIAN_POINT ( 'NONE',  ( -17.32694630114453105, -5.765609946408405406, 34.70566812827424741 ) ) ;
#73813 = CARTESIAN_POINT ( 'NONE',  ( -13.44988538517170440, -9.528491918058357157, 34.59228464037090589 ) ) ;
#73814 = ORIENTED_EDGE ( 'NONE', *, *, #41533, .T. ) ;
#73815 = EDGE_LOOP ( 'NONE', ( #10010, #56862, #36239, #57329 ) ) ;
#73816 = FACE_OUTER_BOUND ( 'NONE', #26374, .T. ) ;
#73817 = CIRCLE ( 'NONE', #13374, 4.000000000000000000 ) ;
#73818 = AXIS2_PLACEMENT_3D ( 'NONE', #69851, #29752, #8154 ) ;
#73819 = CARTESIAN_POINT ( 'NONE',  ( -1.326923076923076872, -3.499999999999999556, 29.75000000000000355 ) ) ;
#73820 = FACE_OUTER_BOUND ( 'NONE', #34938, .T. ) ;
#73821 = B_SPLINE_CURVE_WITH_KNOTS ( 'NONE', 3,
 ( #54010, #68857, #48137, #76506, #75607, #26994, #40951, #68416, #61650, #61206 ),
 .UNSPECIFIED., .F., .F.,
 ( 4, 2, 2, 2, 4 ),
 ( 0.000000000000000000, 0.0001954311564186863323, 0.0003908623128373726646, 0.0005862934692560590241, 0.0007817246256747453293 ),
 .UNSPECIFIED. ) ;
#73822 = VERTEX_POINT ( 'NONE', #53681 ) ;
#73824 = EDGE_CURVE ( 'NONE', #57207, #42406, #19454, .T. ) ;
#73823 = DIRECTION ( 'NONE',  ( -0.000000000000000000, -0.000000000000000000, -1.000000000000000000 ) ) ;
#73825 = EDGE_CURVE ( 'NONE', #6722, #30991, #19956, .T. ) ;
#73826 = CARTESIAN_POINT ( 'NONE',  ( -6.923076923077044142, -10.21337939537710326, 33.94971097300076224 ) ) ;
#73828 = CARTESIAN_POINT ( 'NONE',  ( 10.61538461538449596, -12.46129190930018460, 30.37095296980731973 ) ) ;
#73827 = CARTESIAN_POINT ( 'NONE',  ( -14.43784027742400689, -4.299443229763728169, 33.91186481527756058 ) ) ;
#73829 = DIRECTION ( 'NONE',  ( -0.000000000000000000, 1.000000000000000000, 3.491481338843133355E-15 ) ) ;
#73830 = CARTESIAN_POINT ( 'NONE',  ( -5.299849294439222369, -9.086856451489516928, 34.49173150075333183 ) ) ;
#73832 = CARTESIAN_POINT ( 'NONE',  ( 9.070512820512819374, -3.499999999999999556, 29.75000000000000355 ) ) ;
#73831 = PRESENTATION_STYLE_ASSIGNMENT (( #25183 ) ) ;
#73833 = CARTESIAN_POINT ( 'NONE',  ( 3.749999999999992006, -5.946699141100872943, 20.64062500000000000 ) ) ;
#73834 = VERTEX_POINT ( 'NONE', #83384 ) ;
#73835 = VERTEX_POINT ( 'NONE', #49141 ) ;
#73836 = CARTESIAN_POINT ( 'NONE',  ( -9.822455662039391910, -2.647304123082328875, 31.75400227202885972 ) ) ;
#73837 = CARTESIAN_POINT ( 'NONE',  ( 16.37685750545900376, -6.503523203565941380, 34.64991518177335195 ) ) ;
#73838 = LINE ( 'NONE', #26977, #83387 ) ;
#73839 = DIRECTION ( 'NONE',  ( -0.000000000000000000, 0.7660444431189791237, -0.6427876096865379196 ) ) ;
#73840 = CARTESIAN_POINT ( 'NONE',  ( -14.98082371242109190, -2.824170634883621744, 31.52227843825338738 ) ) ;
#73841 = CARTESIAN_POINT ( 'NONE',  ( 1.553300858899129944, -11.24999999999998934, 22.20312500000000000 ) ) ;
#73842 = CARTESIAN_POINT ( 'NONE',  ( -1.514763354347079982, -4.299443229763728169, 33.91186481527756058 ) ) ;
#73843 = FACE_OUTER_BOUND ( 'NONE', #66234, .T. ) ;
#73844 = CARTESIAN_POINT ( 'NONE',  ( 15.23076923076923173, -12.78798330534103123, 29.99999999999997868 ) ) ;
#73845 = CARTESIAN_POINT ( 'NONE',  ( -6.222866263063099979, -2.251424796025575770, 29.88072029997477586 ) ) ;
#73846 = CARTESIAN_POINT ( 'NONE',  ( 17.99999999999987566, -10.21337939537710326, 33.94971097300076224 ) ) ;
#73847 = DIRECTION ( 'NONE',  ( 0.000000000000000000, 1.000000000000000000, 0.000000000000000000 ) ) ;
#73848 = DIRECTION ( 'NONE',  ( 0.000000000000000000, 0.9396926207859126468, -0.3420201433256571111 ) ) ;
#73849 = DIRECTION ( 'NONE',  ( 0.000000000000000000, 0.7660444431189822323, -0.6427876096865344779 ) ) ;
#73850 = CARTESIAN_POINT ( 'NONE',  ( 11.00641025641025550, -11.00000000000000000, 29.75000000000000355 ) ) ;
#73851 = DIRECTION ( 'NONE',  ( -0.000000000000000000, -0.000000000000000000, -1.000000000000000000 ) ) ;
#73852 = VERTEX_POINT ( 'NONE', #62643 ) ;
#73854 = DIRECTION ( 'NONE',  ( -0.000000000000000000, -0.3420201433256694346, -0.9396926207859080948 ) ) ;
#73853 = B_SPLINE_CURVE_WITH_KNOTS ( 'NONE', 3,
 ( #83466, #29840, #56425, #69052, #22629, #63617, #9135, #55530, #14550, #22196 ),
 .UNSPECIFIED., .F., .F.,
 ( 4, 2, 2, 2, 4 ),
 ( 0.0007817246256747451124, 0.0009771112852218885505, 0.001172497944769032097, 0.001367884604316175427, 0.001563271263863318973 ),
 .UNSPECIFIED. ) ;
#73855 = CARTESIAN_POINT ( 'NONE',  ( 8.769230769230768274, -7.500000000000001776, 35.04278698407183867 ) ) ;
#73856 = CARTESIAN_POINT ( 'NONE',  ( -14.30769230769230660, -1.215029322943914858, 32.30358669280327177 ) ) ;
#73857 = CARTESIAN_POINT ( 'NONE',  ( -1.987747218494638313, -9.401340078031370950, 17.68936829374151287 ) ) ;
#73858 = VECTOR ( 'NONE', #66606, 999.9999999999998863 ) ;
#73859 = VECTOR ( 'NONE', #19066, 1000.000000000000227 ) ;
#73860 = CARTESIAN_POINT ( 'NONE',  ( 13.60739492588379562, -5.114059244376869984, 34.14424750095245287 ) ) ;
#73862 = VERTEX_POINT ( 'NONE', #77499 ) ;
#73861 = CARTESIAN_POINT ( 'NONE',  ( 10.83834774965129455, -7.369474539155828730, 34.99858011523957657 ) ) ;
#73863 = CARTESIAN_POINT ( 'NONE',  ( -1.944543648263014957, -5.555456351737005249, 22.75000000000000000 ) ) ;
#73864 = CARTESIAN_POINT ( 'NONE',  ( -14.30769230769230660, -5.471508081941601098, 34.59228464037088457 ) ) ;
#73865 = ORIENTED_EDGE ( 'NONE', *, *, #52594, .T. ) ;
#73866 = CARTESIAN_POINT ( 'NONE',  ( -2.057637996053991891, -2.564540009722895419, 30.55348353981670684 ) ) ;
#73867 = VERTEX_POINT ( 'NONE', #14026 ) ;
#73868 = CARTESIAN_POINT ( 'NONE',  ( -18.24997673094235395, -11.79746400365624481, 32.30657167506340954 ) ) ;
#73869 = CARTESIAN_POINT ( 'NONE',  ( -1.608100309179712806, -12.11044203135681840, 32.26167407432752299 ) ) ;
#73870 = FACE_OUTER_BOUND ( 'NONE', #26254, .T. ) ;
#73871 = ORIENTED_EDGE ( 'NONE', *, *, #82126, .T. ) ;
#73872 = EDGE_LOOP ( 'NONE', ( #68354, #41672, #12316, #80881 ) ) ;
#73873 = ORIENTED_EDGE ( 'NONE', *, *, #19045, .T. ) ;
#73874 = CARTESIAN_POINT ( 'NONE',  ( -0.5916856709766818989, -3.285722584762969856, 32.44110544564090759 ) ) ;
#73875 = CARTESIAN_POINT ( 'NONE',  ( 12.46153846153846168, -12.37446782046654192, 30.86335684631486131 ) ) ;
#73876 = DIRECTION ( 'NONE',  ( -0.000000000000000000, 0.5000000000000009992, -0.8660254037844380415 ) ) ;
#73877 = LINE ( 'NONE', #26127, #68776 ) ;
#73878 = CARTESIAN_POINT ( 'NONE',  ( 9.627037246346917598, -9.442884908240170461, 34.35708131394840592 ) ) ;
#73879 = DIRECTION ( 'NONE',  ( -0.000000000000000000, -0.7660444431189791237, -0.6427876096865379196 ) ) ;
#73880 = LINE ( 'NONE', #53147, #63913 ) ;
#73881 = ADVANCED_FACE ( 'NONE', ( #22557 ), #2268, .F. ) ;
#73882 = AXIS2_PLACEMENT_3D ( 'NONE', #70759, #16689, #23877 ) ;
#73883 = CARTESIAN_POINT ( 'NONE',  ( -12.68446467905460828, -6.503392248772476236, 34.64988816332204635 ) ) ;
#73884 = EDGE_CURVE ( 'NONE', #75693, #82406, #46923, .T. ) ;
#73885 = ORIENTED_EDGE ( 'NONE', *, *, #65459, .F. ) ;
#73886 = ORIENTED_EDGE ( 'NONE', *, *, #1827, .T. ) ;
#73887 = ORIENTED_EDGE ( 'NONE', *, *, #85591, .T. ) ;
#73889 = ORIENTED_EDGE ( 'NONE', *, *, #58004, .F. ) ;
#73888 = CARTESIAN_POINT ( 'NONE',  ( -3.903900744468109973, -8.476813868363244353, 34.90874843262270133 ) ) ;
#73890 = EDGE_CURVE ( 'NONE', #44606, #12325, #42633, .T. ) ;
#73891 = CARTESIAN_POINT ( 'NONE',  ( 10.36536137809165403, -5.056417327199099532, 34.11270091957321426 ) ) ;
#73892 = CARTESIAN_POINT ( 'NONE',  ( 1.634560902963527740, -2.824170634883621744, 31.52227843825337317 ) ) ;
#73894 = ORIENTED_EDGE ( 'NONE', *, *, #81824, .T. ) ;
#73893 = EDGE_CURVE ( 'NONE', #49441, #35424, #29703, .T. ) ;
#73895 = DIRECTION ( 'NONE',  ( -1.000000000000000000, 0.000000000000000000, 0.000000000000000000 ) ) ;
#73896 = ORIENTED_EDGE ( 'NONE', *, *, #26335, .F. ) ;
#73897 = CARTESIAN_POINT ( 'NONE',  ( 11.53846153846141753, -2.625532179533778709, 30.86335684631627174 ) ) ;
#73898 = EDGE_LOOP ( 'NONE', ( #67993, #62794 ) ) ;
#73899 = CARTESIAN_POINT ( 'NONE',  ( -9.627114704013038704, -2.255955759149236073, 29.99999999999988987 ) ) ;
#73900 = B_SPLINE_CURVE_WITH_KNOTS ( 'NONE', 3,
 ( #83310, #70672, #77862, #55824, #16597, #36442 ),
 .UNSPECIFIED., .F., .F.,
 ( 4, 2, 4 ),
 ( 0.0003909512603273894243, 0.0005862562993132134888, 0.0007815613382990374992 ),
 .UNSPECIFIED. ) ;
#73901 = AXIS2_PLACEMENT_3D ( 'NONE', #79436, #59151, #86203 ) ;
#73902 = EDGE_CURVE ( 'NONE', #76288, #54695, #63972, .T. ) ;
#73903 = CARTESIAN_POINT ( 'NONE',  ( -8.834501215191545853, -5.219633306516282545, 34.19971097300152962 ) ) ;
#73904 = CARTESIAN_POINT ( 'NONE',  ( -11.53846153846153655, -11.91647553114624181, 32.58852847137148245 ) ) ;
#73905 = FACE_BOUND ( 'NONE', #2555, .T. ) ;
#73906 = AXIS2_PLACEMENT_3D ( 'NONE', #65643, #53020, #59343 ) ;
#73907 = CARTESIAN_POINT ( 'NONE',  ( 2.242368294888000158, -7.749976730030849303, 34.74374725381503737 ) ) ;
#73908 = CARTESIAN_POINT ( 'NONE',  ( 1.607578518882061491, -7.369474539155830506, 34.99858011523957657 ) ) ;
#73909 = CIRCLE ( 'NONE', #75391, 8.000000000000000000 ) ;
#73910 = CARTESIAN_POINT ( 'NONE',  ( 13.51540582558233794, -4.684288915650983043, 34.18129842949671371 ) ) ;
#73911 = CARTESIAN_POINT ( 'NONE',  ( 1.384615384615386802, -12.34228464037088635, 31.77849191805839268 ) ) ;
#73912 = LINE ( 'NONE', #40575, #81232 ) ;
#73913 = CARTESIAN_POINT ( 'NONE',  ( -9.692307692307691624, -10.89733346790207413, 36.13435417666054406 ) ) ;
#73914 = VERTEX_POINT ( 'NONE', #7726 ) ;
#73915 = CARTESIAN_POINT ( 'NONE',  ( -10.54931626438217585, -4.098570777380720287, 33.41473453929635440 ) ) ;
#73916 = VERTEX_POINT ( 'NONE', #82940 ) ;
#73917 = ORIENTED_EDGE ( 'NONE', *, *, #30220, .T. ) ;
#73919 = CARTESIAN_POINT ( 'NONE',  ( -0.4615384615384611200, -7.500000000000001776, 35.04278698407183867 ) ) ;
#73918 = CARTESIAN_POINT ( 'NONE',  ( -0.5922299282060198289, -8.999036380462717588, 34.52022231692819076 ) ) ;
#73920 = B_SPLINE_CURVE_WITH_KNOTS ( 'NONE', 3,
 ( #47444, #28976, #61843, #41584, #1042, #7802, #81695, #600, #55093, #34821 ),
 .UNSPECIFIED., .F., .F.,
 ( 4, 2, 2, 2, 4 ),
 ( 0.0007817359430256221996, 0.0009771253907249863487, 0.001172514838424350498, 0.001367904286123714647, 0.001563293733823078796 ),
 .UNSPECIFIED. ) ;
#73921 = CARTESIAN_POINT ( 'NONE',  ( 16.21910129335898887, -11.67786785259547777, 32.92929555188713664 ) ) ;
#73922 = CARTESIAN_POINT ( 'NONE',  ( -4.023320715612507925, -9.503571793651733657, 34.60286762892837942 ) ) ;
#73923 = LINE ( 'NONE', #39702, #19918 ) ;
#73924 = CARTESIAN_POINT ( 'NONE',  ( -2.084680956079458358, -2.758310577978208666, 31.33698337089302299 ) ) ;
#73925 = VERTEX_POINT ( 'NONE', #56348 ) ;
#73926 = EDGE_CURVE ( 'NONE', #29248, #32965, #74864, .T. ) ;
#73927 = CARTESIAN_POINT ( 'NONE',  ( -11.78848477575450282, -12.22074536777954989, 31.39888409691088356 ) ) ;
#73928 = CARTESIAN_POINT ( 'NONE',  ( 15.16468685140909400, -3.937682226553330445, 33.60647404775217240 ) ) ;
#73929 = CARTESIAN_POINT ( 'NONE',  ( 10.61538461538449418, -3.083524468854526912, 32.58852847137268327 ) ) ;
#73930 = EDGE_CURVE ( 'NONE', #12523, #20467, #69861, .T. ) ;
#73931 = CARTESIAN_POINT ( 'NONE',  ( -3.230769230769229949, -12.62096338111211580, 30.90682066428153263 ) ) ;
#73932 = ORIENTED_EDGE ( 'NONE', *, *, #27515, .F. ) ;
#73933 = ORIENTED_EDGE ( 'NONE', *, *, #78970, .F. ) ;
#73934 = APPLICATION_PROTOCOL_DEFINITION ( 'draft international standard', 'automotive_design', 1998, #76262 ) ;
#73935 = ORIENTED_EDGE ( 'NONE', *, *, #63148, .T. ) ;
#73936 = EDGE_CURVE ( 'NONE', #2090, #30159, #81233, .T. ) ;
#73937 = DIRECTION ( 'NONE',  ( 1.000000000000000000, 0.000000000000000000, 0.000000000000000000 ) ) ;
#73939 = EDGE_CURVE ( 'NONE', #7198, #69679, #57669, .T. ) ;
#73938 = CARTESIAN_POINT ( 'NONE',  ( -6.249999999999997335, -7.500000000000001776, 35.00000000000000000 ) ) ;
#73940 = ORIENTED_EDGE ( 'NONE', *, *, #42215, .T. ) ;
#73941 = CARTESIAN_POINT ( 'NONE',  ( -3.512820512820513663, -7.500000000000000000, 29.75000000000000355 ) ) ;
#73942 = CARTESIAN_POINT ( 'NONE',  ( -6.130147969731693181, -9.504002272028875709, 34.60269587691767867 ) ) ;
#73943 = CARTESIAN_POINT ( 'NONE',  ( 3.480823650682684178, -10.06805714834173848, 34.32951233291982618 ) ) ;
#73944 = CARTESIAN_POINT ( 'NONE',  ( 14.37386144865496718, -7.250054483168843156, 34.74374881642865631 ) ) ;
#73945 = CARTESIAN_POINT ( 'NONE',  ( -11.47239318745910275, -8.973038597847271092, 34.52809138561121216 ) ) ;
#73947 = ORIENTED_EDGE ( 'NONE', *, *, #51202, .F. ) ;
#73946 = AXIS2_PLACEMENT_3D ( 'NONE', #55410, #69812, #1351 ) ;
#73949 = ORIENTED_EDGE ( 'NONE', *, *, #23992, .F. ) ;
#73948 = CARTESIAN_POINT ( 'NONE',  ( -15.23076923076922995, -11.91647553114624181, 32.58852847137148245 ) ) ;
#73950 = CARTESIAN_POINT ( 'NONE',  ( -5.076923076923199218, -2.379036618888197729, 30.90682066428292885 ) ) ;
#73951 = CARTESIAN_POINT ( 'NONE',  ( 8.900021210197715860, -12.35292014791297710, 31.75344720912887198 ) ) ;
#73952 = CARTESIAN_POINT ( 'NONE',  ( -13.38461538461550582, -5.219633306517616589, 34.19971097300220464 ) ) ;
#73953 = CARTESIAN_POINT ( 'NONE',  ( -10.74607521849492464, -3.338472653186243644, 32.95098750199972670 ) ) ;
#73954 = CARTESIAN_POINT ( 'NONE',  ( 2.372947447205147053, -2.657715359629131857, 31.77849191805844242 ) ) ;
#73955 = DIRECTION ( 'NONE',  ( 0.000000000000000000, 0.9396926207859126468, 0.3420201433256571111 ) ) ;
#73956 = CARTESIAN_POINT ( 'NONE',  ( -0.5922290646487671228, -2.494641256782728966, 31.33461815524612959 ) ) ;
#73957 = CARTESIAN_POINT ( 'NONE',  ( 0.06109907496451789238, -4.749999999999998224, 20.65811829374151287 ) ) ;
#73958 = VERTEX_POINT ( 'NONE', #30207 ) ;
#73959 = CARTESIAN_POINT ( 'NONE',  ( 15.10062202133100939, -8.587444163452046197, 34.63053765926554206 ) ) ;
#73960 = CARTESIAN_POINT ( 'NONE',  ( -4.153846153846152411, -13.95598074871891292, 31.83374038241031911 ) ) ;
#73961 = CARTESIAN_POINT ( 'NONE',  ( -13.38461538461550582, -8.613356846316285953, 34.62446782046622218 ) ) ;
#73962 = ORIENTED_EDGE ( 'NONE', *, *, #4354, .F. ) ;
#73963 = CARTESIAN_POINT ( 'NONE',  ( -12.71156169883143150, -11.86270091957321249, 32.19358267280087915 ) ) ;
#73964 = DIRECTION ( 'NONE',  ( 0.000000000000000000, -6.938893903907222067E-15, 1.000000000000000000 ) ) ;
#73965 = CARTESIAN_POINT ( 'NONE',  ( 13.31934493865461278, -3.835265460703609186, 33.15142922261924241 ) ) ;
#73966 = CYLINDRICAL_SURFACE ( 'NONE', #15742, 0.2499999999999995559 ) ;
#73967 = PLANE ( 'NONE',  #34163 ) ;
#73968 = CARTESIAN_POINT ( 'NONE',  ( 6.000000000000001776, -8.120952969808772792, 34.71129190930000163 ) ) ;
#73969 = EDGE_LOOP ( 'NONE', ( #54475, #76468, #34639, #54983 ) ) ;
#73970 = ADVANCED_FACE ( 'NONE', ( #9924 ), #58997, .F. ) ;
#73971 = FACE_OUTER_BOUND ( 'NONE', #6539, .T. ) ;
#73972 = AXIS2_PLACEMENT_3D ( 'NONE', #56501, #48849, #43865 ) ;
#73973 = CARTESIAN_POINT ( 'NONE',  ( 15.23076923076923173, -13.63283147151868846, 33.57946703557072254 ) ) ;
#73974 = CARTESIAN_POINT ( 'NONE',  ( -2.084912638714238931, -5.827830569534416583, 34.72679350104403539 ) ) ;
#73975 = ORIENTED_EDGE ( 'NONE', *, *, #17901, .F. ) ;
#73976 = CARTESIAN_POINT ( 'NONE',  ( 16.15384615384615330, -12.34228464037088635, 31.77849191805839268 ) ) ;
#73977 = B_SPLINE_CURVE_WITH_KNOTS ( 'NONE', 3,
 ( #33883, #53263, #25354, #25804, #80761, #12286, #67239, #60469, #26243, #53713 ),
 .UNSPECIFIED., .F., .F.,
 ( 4, 2, 2, 2, 4 ),
 ( 0.0007817246256747453293, 0.0009771112852218889842, 0.001172497944769032531, 0.001367884604316176294, 0.001563271263863319840 ),
 .UNSPECIFIED. ) ;
#73978 = AXIS2_PLACEMENT_3D ( 'NONE', #17039, #35997, #44489 ) ;
#73979 = AXIS2_PLACEMENT_3D ( 'NONE', #15496, #10051, #29022 ) ;
#73980 = VERTEX_POINT ( 'NONE', #79727 ) ;
#73981 = DIRECTION ( 'NONE',  ( -0.000000000000000000, -0.3420201433256694901, -0.9396926207859082059 ) ) ;
#73982 =( LENGTH_UNIT ( ) NAMED_UNIT ( * ) SI_UNIT ( .MILLI., .METRE. ) );
#73983 = CARTESIAN_POINT ( 'NONE',  ( -20.74999999999999645, -7.500000000000000000, 29.75000000000000355 ) ) ;
#73984 = ORIENTED_EDGE ( 'NONE', *, *, #87315, .F. ) ;
#73985 = CARTESIAN_POINT ( 'NONE',  ( -9.070512820512819374, -3.499999999999999556, 29.75000000000000355 ) ) ;
#73987 = EDGE_CURVE ( 'NONE', #45914, #7438, #44137, .T. ) ;
#73986 = CARTESIAN_POINT ( 'NONE',  ( -14.43825222130567276, -2.254533558242299396, 29.97296025877828285 ) ) ;
#73988 = PLANE ( 'NONE',  #52353 ) ;
#73989 = EDGE_CURVE ( 'NONE', #22506, #7245, #26523, .T. ) ;
#73990 = CARTESIAN_POINT ( 'NONE',  ( -5.999999999999998224, -5.471508081941601098, 34.59228464037088457 ) ) ;
#73991 = DIRECTION ( 'NONE',  ( -0.000000000000000000, 0.9396926207859093161, -0.3420201433256663259 ) ) ;
#73992 = ORIENTED_EDGE ( 'NONE', *, *, #46965, .F. ) ;
#73993 = CARTESIAN_POINT ( 'NONE',  ( -4.023055712879203938, -12.35292014791297710, 31.75344720912887198 ) ) ;
#73994 = ORIENTED_EDGE ( 'NONE', *, *, #39554, .T. ) ;
#73995 = CARTESIAN_POINT ( 'NONE',  ( 8.519207531937803779, -12.43535235679832596, 30.55408501211184813 ) ) ;
#73996 = ADVANCED_BREP_SHAPE_REPRESENTATION ( '', ( #28450, #83448 ), #69030 ) ;
#73997 = PLANE ( 'NONE',  #36434 ) ;
#73999 = EDGE_CURVE ( 'NONE', #47713, #52415, #79282, .T. ) ;
#73998 = CARTESIAN_POINT ( 'NONE',  ( 12.94230769230769340, -11.00000000000000000, 29.75000000000000355 ) ) ;
#74000 = CARTESIAN_POINT ( 'NONE',  ( 6.222779541268410597, -9.332535724633407526, 34.40230450496446224 ) ) ;
#74001 = CARTESIAN_POINT ( 'NONE',  ( -6.673022611438608642, -5.728107161865375829, 34.42597550085002922 ) ) ;
#74002 = CARTESIAN_POINT ( 'NONE',  ( 7.846153846153846700, -12.37446782046654192, 30.86335684631486131 ) ) ;
#74003 = LINE ( 'NONE', #76088, #1960 ) ;
#74004 = EDGE_CURVE ( 'NONE', #45628, #16932, #57601, .T. ) ;
#74005 = EDGE_LOOP ( 'NONE', ( #26732, #70397 ) ) ;
#74006 = VERTEX_POINT ( 'NONE', #65748 ) ;
#74007 = ORIENTED_EDGE ( 'NONE', *, *, #62377, .F. ) ;
#74008 = VERTEX_POINT ( 'NONE', #43708 ) ;
#74009 = CARTESIAN_POINT ( 'NONE',  ( -10.36543909703647159, -11.37275283266504111, 32.91324779482534524 ) ) ;
#74010 = EDGE_CURVE ( 'NONE', #16935, #67793, #48999, .T. ) ;
#74011 = CARTESIAN_POINT ( 'NONE',  ( -3.454254155333561283, -6.716662450894490100, 34.94144148231605840 ) ) ;
#74012 = CARTESIAN_POINT ( 'NONE',  ( 15.16549878480845770, -5.219633306516282545, 34.19971097300152962 ) ) ;
#74013 = DIRECTION ( 'NONE',  ( 0.000000000000000000, 0.000000000000000000, -1.000000000000000000 ) ) ;
#74014 = CARTESIAN_POINT ( 'NONE',  ( 3.480823650682683734, -9.233818618650603938, 34.70587769442853698 ) ) ;
#74015 = CARTESIAN_POINT ( 'NONE',  ( -0.6850234052624076808, -11.89387501736623243, 32.13663884655804992 ) ) ;
#74016 = CARTESIAN_POINT ( 'NONE',  ( -15.23076923076935074, -8.613356846316285953, 34.62446782046622218 ) ) ;
#74017 = DIRECTION ( 'NONE',  ( 0.000000000000000000, 0.000000000000000000, -1.000000000000000000 ) ) ;
#74018 = ORIENTED_EDGE ( 'NONE', *, *, #79220, .T. ) ;
#74019 = B_SPLINE_CURVE_WITH_KNOTS ( 'NONE', 3,
 ( #13352, #47577, #33629, #27750, #19230, #34066, #41276, #69184, #54329, #82711 ),
 .UNSPECIFIED., .F., .F.,
 ( 4, 2, 2, 2, 4 ),
 ( 0.000000000000000000, 0.0001954311564186879315, 0.0003908623128373758630, 0.0005862934692560637946, 0.0007817246256747517261 ),
 .UNSPECIFIED. ) ;
#74020 = ORIENTED_EDGE ( 'NONE', *, *, #12372, .T. ) ;
#74021 = VERTEX_POINT ( 'NONE', #58108 ) ;
#74023 = ORIENTED_EDGE ( 'NONE', *, *, #58420, .T. ) ;
#74022 = CARTESIAN_POINT ( 'NONE',  ( -1.608100328339331142, -11.41268669641500466, 32.86336882939237825 ) ) ;
#74025 = CARTESIAN_POINT ( 'NONE',  ( -7.623374177175779032, -9.418065098278013636, 34.63729479722530158 ) ) ;
#74024 = FACE_OUTER_BOUND ( 'NONE', #80653, .T. ) ;
#74026 = PLANE ( 'NONE',  #88832 ) ;
#74027 = CARTESIAN_POINT ( 'NONE',  ( -9.019253993452222673, -6.652501968072648708, 34.93155406624980941 ) ) ;
#74028 = FACE_BOUND ( 'NONE', #10559, .T. ) ;
#74029 = EDGE_LOOP ( 'NONE', ( #71191, #82023 ) ) ;
#74030 = AXIS2_PLACEMENT_3D ( 'NONE', #30146, #9431, #29712 ) ;
#74031 = ADVANCED_FACE ( 'NONE', ( #85590 ), #78824, .F. ) ;
#74032 = ORIENTED_EDGE ( 'NONE', *, *, #63724, .T. ) ;
#74033 = CARTESIAN_POINT ( 'NONE',  ( -18.00000000000000000, -7.500000000000001776, 35.00000000000000000 ) ) ;
#74034 = AXIS2_PLACEMENT_3D ( 'NONE', #56921, #77198, #9620 ) ;
#74036 = EDGE_CURVE ( 'NONE', #33584, #3413, #6665, .T. ) ;
#74035 = ORIENTED_EDGE ( 'NONE', *, *, #49895, .T. ) ;
#74037 = FACE_BOUND ( 'NONE', #65117, .T. ) ;
#74038 = LINE ( 'NONE', #46114, #11614 ) ;
#74039 = CARTESIAN_POINT ( 'NONE',  ( 15.00728430620490172, -6.716662450894489211, 34.94144148231605840 ) ) ;
#74040 = EDGE_LOOP ( 'NONE', ( #70444, #19100, #63358, #87623 ) ) ;
#74041 = CARTESIAN_POINT ( 'NONE',  ( -6.130476708116463058, -7.276988635370452485, 34.74523720219453793 ) ) ;
#74043 = EDGE_CURVE ( 'NONE', #84646, #19767, #74301, .T. ) ;
#74042 = CARTESIAN_POINT ( 'NONE',  ( 9.019230769232187583, -7.500000000000154543, 35.00000000000007105 ) ) ;
#74044 = CARTESIAN_POINT ( 'NONE',  ( 1.253923917947826538, -3.062553014421049546, 32.05460306192773601 ) ) ;
#74045 = ORIENTED_EDGE ( 'NONE', *, *, #22345, .T. ) ;
#74046 = CARTESIAN_POINT ( 'NONE',  ( 14.30769230769231015, -3.322132147404559976, 32.92929555188717927 ) ) ;
#74047 = CARTESIAN_POINT ( 'NONE',  ( -5.999999999999998224, -11.11383981884818262, 36.00935417666054406 ) ) ;
#74048 = LINE ( 'NONE', #75372, #43309 ) ;
#74049 = ORIENTED_EDGE ( 'NONE', *, *, #79035, .T. ) ;
#74050 = B_SPLINE_CURVE_WITH_KNOTS ( 'NONE', 3,
 ( #39242, #37438, #86546, #10871, #32466, #32030, #23920, #50936, #51369, #79328 ),
 .UNSPECIFIED., .F., .F.,
 ( 4, 2, 2, 2, 4 ),
 ( 0.000000000000000000, 0.0001954311564186861155, 0.0003908623128373722310, 0.0005862934692560583735, 0.0007817246256747444619 ),
 .UNSPECIFIED. ) ;
#74051 = CARTESIAN_POINT ( 'NONE',  ( 2.438482748659257737, -12.35292014791297710, 31.75344720912887198 ) ) ;
#74052 = CARTESIAN_POINT ( 'NONE',  ( 4.153846153846154188, -9.905515769479276145, 34.41647553114623292 ) ) ;
#74053 = EDGE_LOOP ( 'NONE', ( #47461, #21328 ) ) ;
#74054 = CARTESIAN_POINT ( 'NONE',  ( 8.639082799499069765, -11.66186481527757302, 32.95055677023626117 ) ) ;
#74055 = CYLINDRICAL_SURFACE ( 'NONE', #16661, 0.2500000000000009437 ) ;
#74056 = CARTESIAN_POINT ( 'NONE',  ( 0.4615384615383382183, -11.06231777344772027, 33.60647404775119895 ) ) ;
#74057 = CARTESIAN_POINT ( 'NONE',  ( 13.63466969625370240, -12.41262288849542017, 30.68299917996395010 ) ) ;
#74058 = CARTESIAN_POINT ( 'NONE',  ( -15.93083480223330817, -4.187068189119696804, 33.49521262558774026 ) ) ;
#74059 = LINE ( 'NONE', #26306, #65341 ) ;
#74061 = CARTESIAN_POINT ( 'NONE',  ( 9.692307692307695177, -4.661471528628507777, 34.16647553114623292 ) ) ;
#74060 = CARTESIAN_POINT ( 'NONE',  ( -1.384615384615505151, -5.219633306517616589, 34.19971097300220464 ) ) ;
#74062 = CARTESIAN_POINT ( 'NONE',  ( 8.834486340506796154, -12.27809138561124591, 31.22303859784720359 ) ) ;
#74063 = CARTESIAN_POINT ( 'NONE',  ( -6.857821351800898135, -2.892918686051625166, 31.69288490824025928 ) ) ;
#74064 = EDGE_CURVE ( 'NONE', #44215, #76427, #86675, .T. ) ;
#74065 = CARTESIAN_POINT ( 'NONE',  ( 1.077988221561464899, -4.724691934501233703, 25.23250670625849068 ) ) ;
#74066 = ORIENTED_EDGE ( 'NONE', *, *, #78491, .F. ) ;
#74067 = CARTESIAN_POINT ( 'NONE',  ( -12.46153846153858247, -8.613356846316285953, 34.62446782046622218 ) ) ;
#74068 = EDGE_LOOP ( 'NONE', ( #86327, #37424, #29661, #9125 ) ) ;
#74069 = EDGE_CURVE ( 'NONE', #10994, #24465, #66224, .T. ) ;
#74070 = ORIENTED_EDGE ( 'NONE', *, *, #21011, .T. ) ;
#74071 = CARTESIAN_POINT ( 'NONE',  ( 5.076923076923075762, -13.53365097954675988, 30.81389545987213552 ) ) ;
#74072 = ORIENTED_EDGE ( 'NONE', *, *, #65459, .T. ) ;
#74073 = CARTESIAN_POINT ( 'NONE',  ( -14.30769230769242739, -6.026961402154118019, 34.52809138561165270 ) ) ;
#74074 = CARTESIAN_POINT ( 'NONE',  ( 2.750000000000008438, -8.639087296525996607, 15.79687500000000178 ) ) ;
#74075 = CARTESIAN_POINT ( 'NONE',  ( 27.00000000000000000, 9.000000000000001776, 2.172175482962262779E-15 ) ) ;
#74076 = CARTESIAN_POINT ( 'NONE',  ( 10.61538461538461675, -2.486705287966279876, 31.30864560766543647 ) ) ;
#74077 = CARTESIAN_POINT ( 'NONE',  ( -7.596208327805703320, -5.852078868378309373, 34.47109172314383585 ) ) ;
#74078 = CARTESIAN_POINT ( 'NONE',  ( -5.300408001487405762, -3.562934362175799841, 33.22335522853832401 ) ) ;
#74079 = DIRECTION ( 'NONE',  ( -0.000000000000000000, 0.9396926207859092051, -0.3420201433256662704 ) ) ;
#74080 = DIRECTION ( 'NONE',  ( 0.000000000000000000, 0.9848077530122072432, 0.1736481776669354937 ) ) ;
#74081 = CARTESIAN_POINT ( 'NONE',  ( -3.750000000000008438, -5.946699141100917352, 21.42187500000000000 ) ) ;
#74082 = ADVANCED_FACE ( 'NONE', ( #12160 ), #80173, .F. ) ;
#74083 = CARTESIAN_POINT ( 'NONE',  ( 3.230769230769231726, -4.102666532097928531, 36.13435417666054406 ) ) ;
#74084 = CARTESIAN_POINT ( 'NONE',  ( -9.692307692307691624, -1.509761064869970415, 31.06009739812519044 ) ) ;
#74085 = CARTESIAN_POINT ( 'NONE',  ( -2.557669038634660108, -4.236021600441998380, 33.53823185664189310 ) ) ;
#74086 = EDGE_CURVE ( 'NONE', #47342, #47846, #73752, .T. ) ;
#74087 = EDGE_CURVE ( 'NONE', #37210, #50903, #73415, .T. ) ;
#74088 = EDGE_LOOP ( 'NONE', ( #46455, #75121, #15546, #74197 ) ) ;
#74089 = VERTEX_POINT ( 'NONE', #11719 ) ;
#74090 = CARTESIAN_POINT ( 'NONE',  ( 14.98076923076923173, -2.499999999999998668, 29.75000000000000355 ) ) ;
#74091 = CYLINDRICAL_SURFACE ( 'NONE', #46017, 0.2500000000000012212 ) ;
#74092 = DIRECTION ( 'NONE',  ( -0.000000000000000000, 1.000000000000000000, 0.000000000000000000 ) ) ;
#74093 = CARTESIAN_POINT ( 'NONE',  ( -19.50000000000000000, -3.499999999999999556, 29.75000000000000355 ) ) ;
#74094 = CARTESIAN_POINT ( 'NONE',  ( -15.12820512820512953, -4.000000000000000000, 29.75000000000000355 ) ) ;
#74095 = CARTESIAN_POINT ( 'NONE',  ( -0.5268089074992371446, -6.879047030191174805, 34.71129190930000163 ) ) ;
#74096 = ADVANCED_FACE ( 'NONE', ( #26561 ), #4958, .T. ) ;
#74097 = VECTOR ( 'NONE', #5804, 1000.000000000000000 ) ;
#74098 = VERTEX_POINT ( 'NONE', #26110 ) ;
#74099 = CARTESIAN_POINT ( 'NONE',  ( 5.999999999999878320, -11.06231777344772027, 33.60647404775119895 ) ) ;
#74100 = ORIENTED_EDGE ( 'NONE', *, *, #1306, .T. ) ;
#74101 = VERTEX_POINT ( 'NONE', #80629 ) ;
#74102 = CARTESIAN_POINT ( 'NONE',  ( 5.326868595271217366, -8.433404298154334455, 34.66254593164985920 ) ) ;
#74103 = CARTESIAN_POINT ( 'NONE',  ( 16.09615384615384670, -7.500000000000000000, 29.75000000000000355 ) ) ;
#74104 = CARTESIAN_POINT ( 'NONE',  ( -4.377331078410484189, -12.69144148231606017, 30.53333754910549303 ) ) ;
#74105 = B_SPLINE_CURVE_WITH_KNOTS ( 'NONE', 3,
 ( #74757, #88727, #6298, #47715, #41407, #68868, #67998, #40964, #54465, #28325 ),
 .UNSPECIFIED., .F., .F.,
 ( 4, 2, 2, 2, 4 ),
 ( 0.000000000000000000, 0.0001954339857564076099, 0.0003908679715128152198, 0.0005863019572692228839, 0.0007817359430256304396 ),
 .UNSPECIFIED. ) ;
#74106 = VECTOR ( 'NONE', #9630, 1000.000000000000227 ) ;
#74107 = CARTESIAN_POINT ( 'NONE',  ( 11.66898697669518548, -2.372941743896879174, 30.88044141588253666 ) ) ;
#74108 = CARTESIAN_POINT ( 'NONE',  ( 14.30769230769231015, -7.500000000000001776, 35.04278698407183867 ) ) ;
#74109 = ADVANCED_FACE ( 'NONE', ( #59890 ), #87386, .F. ) ;
#74110 = ORIENTED_EDGE ( 'NONE', *, *, #38854, .F. ) ;
#74111 = ORIENTED_EDGE ( 'NONE', *, *, #14499, .F. ) ;
#74112 = VERTEX_POINT ( 'NONE', #27000 ) ;
#74113 = CARTESIAN_POINT ( 'NONE',  ( 5.777073782483853392, -2.554751324335733820, 30.48935550225260727 ) ) ;
#74114 = CARTESIAN_POINT ( 'NONE',  ( 9.942253101685738059, -2.341251567377310217, 30.72681386836322659 ) ) ;
#74115 = CARTESIAN_POINT ( 'NONE',  ( 16.28463659481310799, -5.496552790871120031, 34.60292014791297532 ) ) ;
#74116 = CARTESIAN_POINT ( 'NONE',  ( -16.37677311275299985, -2.308479472611653094, 30.53278059502174457 ) ) ;
#74117 = LINE ( 'NONE', #68681, #26517 ) ;
#74118 = ORIENTED_EDGE ( 'NONE', *, *, #88529, .F. ) ;
#74119 = VERTEX_POINT ( 'NONE', #46383 ) ;
#74120 = AXIS2_PLACEMENT_3D ( 'NONE', #50389, #8543, #84212 ) ;
#74122 = EDGE_LOOP ( 'NONE', ( #83179, #88671, #49560, #78648 ) ) ;
#74121 = CARTESIAN_POINT ( 'NONE',  ( 11.53846153846153832, -8.973038597847269315, 34.52809138561121927 ) ) ;
#74123 = CARTESIAN_POINT ( 'NONE',  ( 10.39189967166066708, -12.44517049084099725, 30.48991314939691932 ) ) ;
#74124 = LINE ( 'NONE', #12421, #21584 ) ;
#74125 = CARTESIAN_POINT ( 'NONE',  ( -2.651650429449535551, -10.15165042944956753, 21.18750000000000000 ) ) ;
#74126 = ORIENTED_EDGE ( 'NONE', *, *, #57736, .T. ) ;
#74127 = CARTESIAN_POINT ( 'NONE',  ( 3.295962219063885090, -2.255955759149235629, 29.99999999999988631 ) ) ;
#74128 = VERTEX_POINT ( 'NONE', #67102 ) ;
#74129 = CARTESIAN_POINT ( 'NONE',  ( 13.60739505359345181, -10.97394488606064122, 33.68653795673694873 ) ) ;
#74130 = CARTESIAN_POINT ( 'NONE',  ( -3.230769230769229949, -12.78798330534102945, 29.74999999999997868 ) ) ;
#74131 = EDGE_CURVE ( 'NONE', #58896, #2541, #60331, .T. ) ;
#74132 = FACE_BOUND ( 'NONE', #12382, .T. ) ;
#74133 = CARTESIAN_POINT ( 'NONE',  ( -5.076923076923075762, -12.10708131394839349, 31.69288490824020244 ) ) ;
#74134 = CARTESIAN_POINT ( 'NONE',  ( 2.307692307692309264, -2.499999999999998668, 29.75000000000001421 ) ) ;
#74135 = VERTEX_POINT ( 'NONE', #53575 ) ;
#74137 = EDGE_CURVE ( 'NONE', #54522, #54986, #85525, .T. ) ;
#74136 = CARTESIAN_POINT ( 'NONE',  ( 6.857806477116147548, -8.613356846314824011, 34.62446782046655613 ) ) ;
#74138 = CARTESIAN_POINT ( 'NONE',  ( -14.08491276642389245, -2.600157965045224451, 30.74683119005207743 ) ) ;
#74139 = B_SPLINE_CURVE_WITH_KNOTS ( 'NONE', 3,
 ( #77945, #50892, #45487, #85153, #58546, #4048, #64859, #16249, #86500, #31536 ),
 .UNSPECIFIED., .F., .F.,
 ( 4, 2, 2, 2, 4 ),
 ( 0.000000000000000000, 0.0001954311564186871184, 0.0003908623128373742367, 0.0005862934692560614093, 0.0007817246256747484735 ),
 .UNSPECIFIED. ) ;
#74140 = LINE ( 'NONE', #12437, #53811 ) ;
#74141 = ORIENTED_EDGE ( 'NONE', *, *, #1103, .F. ) ;
#74142 = EDGE_CURVE ( 'NONE', #85754, #1046, #65094, .T. ) ;
#74143 = CARTESIAN_POINT ( 'NONE',  ( 6.923076923076924238, -1.215029322943914858, 32.30358669280327177 ) ) ;
#74144 = CARTESIAN_POINT ( 'NONE',  ( 14.37375964104238513, -9.905515769479276145, 34.41647553114623292 ) ) ;
#74145 = CARTESIAN_POINT ( 'NONE',  ( 4.153846153846030731, -11.67786785259630911, 32.92929555188603530 ) ) ;
#74146 = LINE ( 'NONE', #19203, #60142 ) ;
#74147 = CARTESIAN_POINT ( 'NONE',  ( -0.5921488211629901688, -7.722926236386453702, 34.74524107206102030 ) ) ;
#74148 = AXIS2_PLACEMENT_3D ( 'NONE', #43024, #51526, #3809 ) ;
#74149 = FACE_BOUND ( 'NONE', #68251, .T. ) ;
#74151 = CARTESIAN_POINT ( 'NONE',  ( 11.53846153846153832, -13.87047571288749737, 32.06866353760679544 ) ) ;
#74150 = DIRECTION ( 'NONE',  ( 0.000000000000000000, 1.000000000000000000, 0.000000000000000000 ) ) ;
#74152 = CARTESIAN_POINT ( 'NONE',  ( 9.757501674091050958, -2.506253911140448043, 29.99999999999988631 ) ) ;
#74154 = CARTESIAN_POINT ( 'NONE',  ( -2.242437168179467477, -12.51329471203373700, 31.30864560766537963 ) ) ;
#74153 = CARTESIAN_POINT ( 'NONE',  ( -8.546451227962355901, -11.89424750095246175, 32.13594075562311758 ) ) ;
#74155 = EDGE_CURVE ( 'NONE', #60075, #46303, #44675, .T. ) ;
#74156 = CARTESIAN_POINT ( 'NONE',  ( 8.835298102580845025, -12.62096338111211757, 30.90682066428152908 ) ) ;
#74157 = CARTESIAN_POINT ( 'NONE',  ( -3.775308065498766297, -6.007798216065450170, 23.67000670625849779 ) ) ;
#74158 = ORIENTED_EDGE ( 'NONE', *, *, #11073, .F. ) ;
#74159 = DIRECTION ( 'NONE',  ( 0.000000000000000000, 0.6427876096865373645, -0.7660444431189797898 ) ) ;
#74160 = VERTEX_POINT ( 'NONE', #1737 ) ;
#74161 = FACE_OUTER_BOUND ( 'NONE', #62109, .T. ) ;
#74162 = ORIENTED_EDGE ( 'NONE', *, *, #30671, .F. ) ;
#74163 = CARTESIAN_POINT ( 'NONE',  ( 2.242422307135989890, -2.379036618887870880, 30.90682066428147934 ) ) ;
#74164 = CYLINDRICAL_SURFACE ( 'NONE', #61756, 0.2499999999999994726 ) ;
#74166 = VERTEX_POINT ( 'NONE', #13919 ) ;
#74165 = CARTESIAN_POINT ( 'NONE',  ( -11.25641025641025550, -7.500000000000000000, 33.75000000000000000 ) ) ;
#74167 = CARTESIAN_POINT ( 'NONE',  ( 3.296837581771669523, -6.386643153685127139, 34.62446782046654192 ) ) ;
#74168 = CARTESIAN_POINT ( 'NONE',  ( 1.253924781505079356, -11.93127051446800024, 32.56575433478200665 ) ) ;
#74169 = CARTESIAN_POINT ( 'NONE',  ( 3.724691934501232815, -5.885600066136343678, 26.63875670625848713 ) ) ;
#74170 = CARTESIAN_POINT ( 'NONE',  ( 15.10007862765893094, -11.93127051446799847, 32.56575433478202797 ) ) ;
#74171 = CARTESIAN_POINT ( 'NONE',  ( 11.53846153846153832, -2.538708090699994813, 30.37095296980875503 ) ) ;
#74172 = CARTESIAN_POINT ( 'NONE',  ( -4.826868657009622865, -12.01375889529407281, 32.43194544308182969 ) ) ;
#74173 = CARTESIAN_POINT ( 'NONE',  ( -0.5916864312701562989, -8.630895178749536711, 34.87696386517710323 ) ) ;
#74174 = CARTESIAN_POINT ( 'NONE',  ( 0.3954550505825807916, -11.16473453929635440, 33.15142922261925662 ) ) ;
#74175 = CARTESIAN_POINT ( 'NONE',  ( 3.512820512820510555, -11.50000000000000000, 29.75000000000000355 ) ) ;
#74176 = CARTESIAN_POINT ( 'NONE',  ( -3.749999999999997780, -7.438900925035489387, 16.59561829374151287 ) ) ;
#74177 = CARTESIAN_POINT ( 'NONE',  ( 3.361607561255992138, -7.277220318596959281, 34.99547417642776992 ) ) ;
#74178 = CARTESIAN_POINT ( 'NONE',  ( 19.00000000000000000, -3.499999999999999556, 29.75000000000000355 ) ) ;
#74179 = VERTEX_POINT ( 'NONE', #82838 ) ;
#74180 = CYLINDRICAL_SURFACE ( 'NONE', #25458, 0.2500000000000008882 ) ;
#74181 = CARTESIAN_POINT ( 'NONE',  ( 15.36155967173618286, -10.70102852606553157, 33.91149625220312913 ) ) ;
#74182 = CARTESIAN_POINT ( 'NONE',  ( 1.492201783934598236, -11.27530806549875031, 17.45499329374151642 ) ) ;
#74183 = EDGE_CURVE ( 'NONE', #72329, #7620, #75717, .T. ) ;
#74184 = FACE_OUTER_BOUND ( 'NONE', #57786, .T. ) ;
#74185 = CARTESIAN_POINT ( 'NONE',  ( -8.769230769230768274, -3.322132147404559976, 32.92929555188717927 ) ) ;
#74186 = ORIENTED_EDGE ( 'NONE', *, *, #82386, .F. ) ;
#74187 = CARTESIAN_POINT ( 'NONE',  ( 6.988332494352945901, -8.613356846314928816, 34.62446782046653482 ) ) ;
#74188 = LINE ( 'NONE', #67432, #48839 ) ;
#74190 = ORIENTED_EDGE ( 'NONE', *, *, #48626, .T. ) ;
#74189 = CARTESIAN_POINT ( 'NONE',  ( 8.068933515131908152, -2.612705202774698421, 31.66806509827799943 ) ) ;
#74191 = CARTESIAN_POINT ( 'NONE',  ( 11.60452988946397923, -4.786620604624113540, 33.94971097300155805 ) ) ;
#74192 = LINE ( 'NONE', #12492, #82936 ) ;
#74193 = CARTESIAN_POINT ( 'NONE',  ( -16.94608474643631979, -7.277220318596959281, 34.99547417642776992 ) ) ;
#74194 = AXIS2_PLACEMENT_3D ( 'NONE', #77168, #29001, #36630 ) ;
#74195 = CARTESIAN_POINT ( 'NONE',  ( -11.76194646302587010, -2.612411019501189369, 31.66733052389439962 ) ) ;
#74196 = EDGE_CURVE ( 'NONE', #765, #38908, #48583, .T. ) ;
#74197 = ORIENTED_EDGE ( 'NONE', *, *, #32593, .F. ) ;
#74198 = FACE_OUTER_BOUND ( 'NONE', #34643, .T. ) ;
#74199 = CYLINDRICAL_SURFACE ( 'NONE', #35069, 0.2499999999999995559 ) ;
#74200 = EDGE_CURVE ( 'NONE', #87991, #85626, #84424, .T. ) ;
#74201 = ADVANCED_FACE ( 'NONE', ( #41850 ), #35078, .F. ) ;
#74202 = CARTESIAN_POINT ( 'NONE',  ( -13.16183571563731824, -8.540255544307065350, 34.89611431652622286 ) ) ;
#74203 = ORIENTED_EDGE ( 'NONE', *, *, #46727, .T. ) ;
#74204 = VERTEX_POINT ( 'NONE', #55787 ) ;
#74205 = EDGE_LOOP ( 'NONE', ( #56168, #14847, #50632, #40222 ) ) ;
#74206 = CARTESIAN_POINT ( 'NONE',  ( -9.822999158975248335, -2.729777683071817229, 31.24903638046269450 ) ) ;
#74207 = CARTESIAN_POINT ( 'NONE',  ( -6.792551221313360976, -4.459921816937789885, 33.71989282347011851 ) ) ;
#74208 = CARTESIAN_POINT ( 'NONE',  ( -8.069080805060693251, -12.64616026154729411, 30.79003144601914244 ) ) ;
#74209 = CARTESIAN_POINT ( 'NONE',  ( -9.469528023329624844, -12.69155399931963046, 30.53255429739157734 ) ) ;
#74210 = EDGE_CURVE ( 'NONE', #3309, #14831, #10234, .T. ) ;
#74211 = CARTESIAN_POINT ( 'NONE',  ( -18.06870381900347056, -7.250491025975066783, 34.99406763069168846 ) ) ;
#74212 = ORIENTED_EDGE ( 'NONE', *, *, #21829, .F. ) ;
#74213 = EDGE_CURVE ( 'NONE', #24368, #49738, #51217, .T. ) ;
#74214 = ADVANCED_FACE ( 'NONE', ( #24213 ), #44475, .F. ) ;
#74215 = AXIS2_PLACEMENT_3D ( 'NONE', #41248, #13325, #68711 ) ;
#74216 = VERTEX_POINT ( 'NONE', #58003 ) ;
#74217 = EDGE_LOOP ( 'NONE', ( #53336, #32126, #62636, #51532 ) ) ;
#74219 = ORIENTED_EDGE ( 'NONE', *, *, #71320, .T. ) ;
#74218 = CARTESIAN_POINT ( 'NONE',  ( -6.923076923076922462, -8.164416787775445883, 34.95778746994557906 ) ) ;
#74220 = CARTESIAN_POINT ( 'NONE',  ( 14.30769230769231015, -9.058645607665452459, 34.76329471203371924 ) ) ;
#74221 = EDGE_CURVE ( 'NONE', #46544, #47459, #38178, .T. ) ;
#74222 = CARTESIAN_POINT ( 'NONE',  ( 15.16468581981335007, -3.050289026998445951, 32.03036669348365706 ) ) ;
#74223 = CARTESIAN_POINT ( 'NONE',  ( -18.00000000000000000, -1.163064389776900187, 32.05645593858272235 ) ) ;
#74224 = CARTESIAN_POINT ( 'NONE',  ( 1.384615384615386802, -10.89733346790207413, 36.13435417666054406 ) ) ;
#74225 = AXIS2_PLACEMENT_3D ( 'NONE', #43731, #71199, #9502 ) ;
#74226 = ORIENTED_EDGE ( 'NONE', *, *, #86306, .F. ) ;
#74227 = ORIENTED_EDGE ( 'NONE', *, *, #31104, .T. ) ;
#74228 = ORIENTED_EDGE ( 'NONE', *, *, #46415, .T. ) ;
#74229 = DIRECTION ( 'NONE',  ( -0.000000000000000000, 0.3420201433256694346, -0.9396926207859080948 ) ) ;
#74231 = ORIENTED_EDGE ( 'NONE', *, *, #28836, .T. ) ;
#74230 = FACE_OUTER_BOUND ( 'NONE', #64499, .T. ) ;
#74232 = CARTESIAN_POINT ( 'NONE',  ( 2.084207383127975266, -2.612411019501189813, 31.66733052389439962 ) ) ;
#74233 = CARTESIAN_POINT ( 'NONE',  ( -12.22435897435897623, -4.000000000000000000, 29.75000000000000355 ) ) ;
#74234 = VERTEX_POINT ( 'NONE', #30967 ) ;
#74235 = CARTESIAN_POINT ( 'NONE',  ( 15.23076923076953904, -2.506253911140615021, 30.00000000000323297 ) ) ;
#74236 = CARTESIAN_POINT ( 'NONE',  ( 9.692307692308007816, -2.255955759149395501, 30.00000000000324363 ) ) ;
#74237 = CARTESIAN_POINT ( 'NONE',  ( 27.00000000000000000, 0.7500000000000051070, 32.75000000000000000 ) ) ;
#74238 = FACE_BOUND ( 'NONE', #68578, .T. ) ;
#74239 = CARTESIAN_POINT ( 'NONE',  ( -15.36145983387954139, -8.191372820521381826, 34.95448215188424967 ) ) ;
#74240 = CARTESIAN_POINT ( 'NONE',  ( -6.250023224221457951, -12.45566812827425096, 31.48439005359158926 ) ) ;
#74241 = EDGE_CURVE ( 'NONE', #25331, #88566, #23764, .T. ) ;
#74242 = CYLINDRICAL_SURFACE ( 'NONE', #65275, 0.2499999999999979738 ) ;
#74244 = CYLINDRICAL_SURFACE ( 'NONE', #2971, 0.2500000000000002220 ) ;
#74243 = CARTESIAN_POINT ( 'NONE',  ( -17.87203884117228014, -12.74539040900690701, 29.97526117654243905 ) ) ;
#74245 = AXIS2_PLACEMENT_3D ( 'NONE', #57652, #10802, #10356 ) ;
#74246 = CARTESIAN_POINT ( 'NONE',  ( -39.05038313613820122, -2.249999999999998668, 29.75000000000000355 ) ) ;
#74247 = CARTESIAN_POINT ( 'NONE',  ( 11.53846153846141576, -12.51329471203414379, 31.30864560766407578 ) ) ;
#74248 = VERTEX_POINT ( 'NONE', #30533 ) ;
#74249 = FACE_OUTER_BOUND ( 'NONE', #78888, .T. ) ;
#74250 = CARTESIAN_POINT ( 'NONE',  ( -7.846153846153965716, -2.625532179533778709, 30.86335684631627174 ) ) ;
#74251 = ORIENTED_EDGE ( 'NONE', *, *, #33860, .T. ) ;
#74252 = ORIENTED_EDGE ( 'NONE', *, *, #32269, .F. ) ;
#74253 = AXIS2_PLACEMENT_3D ( 'NONE', #19580, #82632, #14599 ) ;
#74254 = CARTESIAN_POINT ( 'NONE',  ( -17.30040802064703342, -11.41268669641499756, 32.86336882939238535 ) ) ;
#74255 = ADVANCED_FACE ( 'NONE', ( #63874 ), #78725, .F. ) ;
#74256 = B_SPLINE_CURVE_WITH_KNOTS ( 'NONE', 3,
 ( #50197, #71364, #15996, #84462, #9246, #3804, #63725, #30390, #56966, #10119 ),
 .UNSPECIFIED., .F., .F.,
 ( 4, 2, 2, 2, 4 ),
 ( 0.000000000000000000, 0.0001954339857564075015, 0.0003908679715128150029, 0.0005863019572692224502, 0.0007817359430256300059 ),
 .UNSPECIFIED. ) ;
#74257 = CARTESIAN_POINT ( 'NONE',  ( -13.51530598772569469, -4.684245665217972032, 34.18127051446801090 ) ) ;
#74258 = LINE ( 'NONE', #59405, #5892 ) ;
#74259 = ORIENTED_EDGE ( 'NONE', *, *, #760, .F. ) ;
#74260 = DIRECTION ( 'NONE',  ( 0.000000000000000000, -2.413528314402514090E-16, 1.000000000000000000 ) ) ;
#74261 = CARTESIAN_POINT ( 'NONE',  ( 6.699591998512593349, -8.539481045369598178, 34.89627647299170832 ) ) ;
#74262 = FACE_BOUND ( 'NONE', #13949, .T. ) ;
#74264 = CARTESIAN_POINT ( 'NONE',  ( 5.933917620639865831, -6.343179335718451384, 34.87096338111212646 ) ) ;
#74263 = CARTESIAN_POINT ( 'NONE',  ( 16.15384615384615330, -7.500000000000001776, 35.04278698407183867 ) ) ;
#74265 = CARTESIAN_POINT ( 'NONE',  ( -8.992156986746914882, -6.503392248772476236, 34.64988816332204635 ) ) ;
#74266 = FACE_OUTER_BOUND ( 'NONE', #42701, .T. ) ;
#74267 = DIRECTION ( 'NONE',  ( 0.000000000000000000, 0.8660254037844377084, 0.5000000000000015543 ) ) ;
#74268 = CARTESIAN_POINT ( 'NONE',  ( 1.553300858899129944, -11.24999999999998934, 23.45312500000000000 ) ) ;
#74269 = ORIENTED_EDGE ( 'NONE', *, *, #65556, .F. ) ;
#74270 = ORIENTED_EDGE ( 'NONE', *, *, #26808, .T. ) ;
#74271 = PLANE ( 'NONE',  #21922 ) ;
#74272 = CARTESIAN_POINT ( 'NONE',  ( 6.988332494352949453, -12.27809138561124591, 31.22303859784720359 ) ) ;
#74273 = CARTESIAN_POINT ( 'NONE',  ( 4.403846153846156852, -2.499999999999999112, 29.81604066197450109 ) ) ;
#74274 = B_SPLINE_CURVE_WITH_KNOTS ( 'NONE', 3,
 ( #4162, #4619, #67214, #5514, #59108, #86608, #39306, #32092, #19461, #32983 ),
 .UNSPECIFIED., .F., .F.,
 ( 4, 2, 2, 2, 4 ),
 ( 0.0007817246256747511840, 0.0009771112852218952725, 0.001172497944769039470, 0.001367884604316183667, 0.001563271263863327864 ),
 .UNSPECIFIED. ) ;
#74275 = CARTESIAN_POINT ( 'NONE',  ( 6.923076923076924238, -12.10708131394839349, 31.69288490824020244 ) ) ;
#74276 = DIRECTION ( 'NONE',  ( -0.000000000000000000, -0.9396926207859093161, -0.3420201433256663259 ) ) ;
#74277 = CARTESIAN_POINT ( 'NONE',  ( -1.929879867024197893E-14, -3.750000000000000000, 20.40625000000000000 ) ) ;
#74278 = B_SPLINE_CURVE_WITH_KNOTS ( 'NONE', 3,
 ( #81759, #80434, #18729, #20050, #41214, #47510, #68240, #6541, #33574, #34001 ),
 .UNSPECIFIED., .F., .F.,
 ( 4, 2, 2, 2, 4 ),
 ( 0.000000000000000000, 0.0001954311564186875792, 0.0003908623128373751583, 0.0005862934692560627103, 0.0007817246256747503166 ),
 .UNSPECIFIED. ) ;
#74279 = DIRECTION ( 'NONE',  ( -0.000000000000000000, -0.7660444431189791237, -0.6427876096865379196 ) ) ;
#74280 = CARTESIAN_POINT ( 'NONE',  ( 0.000000000000000000, -4.000000000000000000, 29.25000000000000000 ) ) ;
#74281 = ADVANCED_FACE ( 'NONE', ( #17022 ), #52130, .F. ) ;
#74282 = DIRECTION ( 'NONE',  ( 0.000000000000000000, 0.8660254037844377084, -0.5000000000000015543 ) ) ;
#74283 = CARTESIAN_POINT ( 'NONE',  ( 13.13459216039393240, -10.18141759479407327, 34.26406193332782379 ) ) ;
#74284 = CARTESIAN_POINT ( 'NONE',  ( -9.692307692307812417, -11.48612834414049644, 32.76840700105863391 ) ) ;
#74285 = CARTESIAN_POINT ( 'NONE',  ( 5.076923076923075762, -10.67929555188718282, 33.92786785259544047 ) ) ;
#74286 = CARTESIAN_POINT ( 'NONE',  ( 7.053602361310568725, -3.625058011473227815, 33.29252011169590020 ) ) ;
#74287 = AXIS2_PLACEMENT_3D ( 'NONE', #83939, #77608, #22222 ) ;
#74288 = CARTESIAN_POINT ( 'NONE',  ( -3.296039676730006196, -8.613356846314824011, 34.62446782046655613 ) ) ;
#74289 = CARTESIAN_POINT ( 'NONE',  ( -15.48079246806219267, -8.432397168068783699, 34.66272746175022945 ) ) ;
#74290 = VERTEX_POINT ( 'NONE', #22886 ) ;
#74291 = LINE ( 'NONE', #5831, #19731 ) ;
#74292 = DIRECTION ( 'NONE',  ( -0.000000000000000000, -0.000000000000000000, -1.000000000000000000 ) ) ;
#74293 = CARTESIAN_POINT ( 'NONE',  ( -0.06109907496451398579, -10.25000000000000178, 16.28311829374151287 ) ) ;
#74294 = CYLINDRICAL_SURFACE ( 'NONE', #70542, 0.2499999999999986955 ) ;
#74295 = DIRECTION ( 'NONE',  ( -0.000000000000000000, -0.9396926207859093161, -0.3420201433256663259 ) ) ;
#74296 = CYLINDRICAL_SURFACE ( 'NONE', #68659, 0.2500000000000008882 ) ;
#74298 = ORIENTED_EDGE ( 'NONE', *, *, #67545, .F. ) ;
#74297 = DIRECTION ( 'NONE',  ( -0.000000000000000000, 0.7660444431189791237, -0.6427876096865379196 ) ) ;
#74299 = CARTESIAN_POINT ( 'NONE',  ( -1.409462824231155764E-14, -4.749999999999999112, 24.15625000000000000 ) ) ;
#74300 = EDGE_CURVE ( 'NONE', #17248, #67353, #79618, .T. ) ;
#74301 = LINE ( 'NONE', #5843, #16751 ) ;
#74302 = AXIS2_PLACEMENT_3D ( 'NONE', #11146, #10706, #30525 ) ;
#74303 = ADVANCED_FACE ( 'NONE', ( #64749 ), #85485, .F. ) ;
#74304 = VERTEX_POINT ( 'NONE', #3498 ) ;
#74305 = CARTESIAN_POINT ( 'NONE',  ( 25.00000000000000355, 9.999999999999971578, 13.00000000000000178 ) ) ;
#74306 = CARTESIAN_POINT ( 'NONE',  ( -2.241623956689867470, -2.538708090699994813, 30.37095296980875503 ) ) ;
#74307 = ORIENTED_EDGE ( 'NONE', *, *, #38518, .F. ) ;
#74308 = CARTESIAN_POINT ( 'NONE',  ( 3.100621261037534548, -5.070767119584671967, 34.40440758774516183 ) ) ;
#74309 = DIRECTION ( 'NONE',  ( 1.000000000000000000, 0.000000000000000000, 0.000000000000000000 ) ) ;
#74310 = EDGE_CURVE ( 'NONE', #76471, #86342, #77855, .T. ) ;
#74311 = LINE ( 'NONE', #12612, #70033 ) ;
#74312 = VERTEX_POINT ( 'NONE', #50785 ) ;
#74313 = ORIENTED_EDGE ( 'NONE', *, *, #48574, .F. ) ;
#74314 = VERTEX_POINT ( 'NONE', #84613 ) ;
#74315 = FACE_OUTER_BOUND ( 'NONE', #28178, .T. ) ;
#74316 = DIRECTION ( 'NONE',  ( -0.000000000000000000, 0.6427876096865404731, -0.7660444431189771253 ) ) ;
#74317 = B_SPLINE_CURVE_WITH_KNOTS ( 'NONE', 3,
 ( #88819, #25765, #46480, #67, #68090, #13577, #41057, #73959, #53676, #53225 ),
 .UNSPECIFIED., .F., .F.,
 ( 4, 2, 2, 2, 4 ),
 ( 0.000000000000000000, 0.0001954339857564079623, 0.0003908679715128159245, 0.0005863019572692238597, 0.0007817359430256318490 ),
 .UNSPECIFIED. ) ;
#74318 = AXIS2_PLACEMENT_3D ( 'NONE', #14473, #48248, #21673 ) ;
#74319 = CARTESIAN_POINT ( 'NONE',  ( -9.692307692307691624, -9.780366693483667717, 34.19971097300155094 ) ) ;
#74320 = CARTESIAN_POINT ( 'NONE',  ( -1.634592128663974631, -11.47974371597208076, 33.17467449705390692 ) ) ;
#74321 = CARTESIAN_POINT ( 'NONE',  ( -10.83831157429145975, -11.98009711892699514, 32.48740034544076138 ) ) ;
#74322 = CARTESIAN_POINT ( 'NONE',  ( 7.146089767170319185, -8.282913670948747864, 34.94150082978203642 ) ) ;
#74323 = CARTESIAN_POINT ( 'NONE',  ( -1.326923076923076206, -4.000000000000000000, 29.75000000000000355 ) ) ;
#74324 = VECTOR ( 'NONE', #2284, 1000.000000000000227 ) ;
#74325 = CARTESIAN_POINT ( 'NONE',  ( 10.55011416942384450, -12.27809138561121394, 31.22303859784730307 ) ) ;
#74326 = EDGE_CURVE ( 'NONE', #82738, #36760, #49937, .T. ) ;
#74327 = ORIENTED_EDGE ( 'NONE', *, *, #41781, .F. ) ;
#74328 = ORIENTED_EDGE ( 'NONE', *, *, #56925, .F. ) ;
#74329 = VECTOR ( 'NONE', #53544, 1000.000000000000000 ) ;
#74330 = ORIENTED_EDGE ( 'NONE', *, *, #57479, .T. ) ;
#74332 = ORIENTED_EDGE ( 'NONE', *, *, #71750, .F. ) ;
#74331 = CARTESIAN_POINT ( 'NONE',  ( -17.29984929443921970, -9.886141570436013382, 34.14413921362392301 ) ) ;
#74333 = B_SPLINE_CURVE_WITH_KNOTS ( 'NONE', 3,
 ( #19667, #67857, #6158, #88602, #47579, #34069, #9271, #23654, #76382, #16460 ),
 .UNSPECIFIED., .F., .F.,
 ( 4, 2, 2, 2, 4 ),
 ( 0.000000000000000000, 0.0001954311564186875792, 0.0003908623128373751583, 0.0005862934692560627103, 0.0007817246256747503166 ),
 .UNSPECIFIED. ) ;
#74334 = DIRECTION ( 'NONE',  ( 0.000000000000000000, 0.4999999999999985567, 0.8660254037844395958 ) ) ;
#74335 = CARTESIAN_POINT ( 'NONE',  ( 9.562160482869472844, -5.195881422630166391, 34.18770438780619259 ) ) ;
#74336 = EDGE_LOOP ( 'NONE', ( #69331, #82035, #62400, #48089 ) ) ;
#74337 = CARTESIAN_POINT ( 'NONE',  ( -12.21159305216042057, -11.56426240980093745, 33.07394671870546432 ) ) ;
#74338 = EDGE_LOOP ( 'NONE', ( #74186, #40111 ) ) ;
#74339 = CARTESIAN_POINT ( 'NONE',  ( 14.30769230769218581, -9.528491918059723176, 34.59228464037033035 ) ) ;
#74340 = ORIENTED_EDGE ( 'NONE', *, *, #9325, .T. ) ;
#74341 = DIRECTION ( 'NONE',  ( -0.000000000000000000, -0.5000000000000009992, -0.8660254037844380415 ) ) ;
#74342 = VECTOR ( 'NONE', #39204, 1000.000000000000000 ) ;
#74343 = B_SPLINE_CURVE_WITH_KNOTS ( 'NONE', 3,
 ( #29635, #41824, #84149, #55762, #14794, #42270, #49890, #57092, #15678, #43145 ),
 .UNSPECIFIED., .F., .F.,
 ( 4, 2, 2, 2, 4 ),
 ( 0.0007817246256747447872, 0.0009771112852218876831, 0.001172497944769030579, 0.001367884604316173475, 0.001563271263863316371 ),
 .UNSPECIFIED. ) ;
#74344 = CARTESIAN_POINT ( 'NONE',  ( -0.4615384615385840772, -5.941354392335915335, 34.76329471203413846 ) ) ;
#74345 = LINE ( 'NONE', #54955, #5110 ) ;
#74346 = AXIS2_PLACEMENT_3D ( 'NONE', #80865, #25903, #67338 ) ;
#74347 = FACE_BOUND ( 'NONE', #78974, .T. ) ;
#74348 = B_SPLINE_CURVE_WITH_KNOTS ( 'NONE', 3,
 ( #48633, #70243, #61702, #63024, #22061, #15308, #27932, #21, #28367, #27489 ),
 .UNSPECIFIED., .F., .F.,
 ( 4, 2, 2, 2, 4 ),
 ( 0.000000000000000000, 0.0001954311564186876334, 0.0003908623128373752667, 0.0005862934692560629272, 0.0007817246256747505334 ),
 .UNSPECIFIED. ) ;
#74349 = DIRECTION ( 'NONE',  ( -0.000000000000000000, -0.000000000000000000, -1.000000000000000000 ) ) ;
#74350 = CARTESIAN_POINT ( 'NONE',  ( 16.15384615384603251, -3.643525952248796163, 33.31231777344771672 ) ) ;
#74351 = PLANE ( 'NONE',  #81240 ) ;
#74352 = CARTESIAN_POINT ( 'NONE',  ( 10.55011461482829738, -10.33852847137145048, 34.16647553114627556 ) ) ;
#74353 = CARTESIAN_POINT ( 'NONE',  ( 10.83881157724618660, -7.630147231320743018, 34.74852402298682819 ) ) ;
#74354 = CARTESIAN_POINT ( 'NONE',  ( -8.096130590202436750, -9.234221910056348293, 34.70572697212741531 ) ) ;
#74355 = CIRCLE ( 'NONE', #77233, 5.000000000000000888 ) ;
#74356 = CARTESIAN_POINT ( 'NONE',  ( -11.66860950819323328, -3.625366637846544116, 33.29286588640298561 ) ) ;
#74357 = ORIENTED_EDGE ( 'NONE', *, *, #6097, .T. ) ;
#74358 = ORIENTED_EDGE ( 'NONE', *, *, #52535, .F. ) ;
#74360 = CARTESIAN_POINT ( 'NONE',  ( -14.24162395668986747, -12.37446782046654192, 30.86335684631486842 ) ) ;
#74359 = CARTESIAN_POINT ( 'NONE',  ( 2.057669083470851756, -2.985938066672154445, 32.43141759479405550 ) ) ;
#74361 = CARTESIAN_POINT ( 'NONE',  ( 15.48071464014727283, -8.476813868363244353, 34.90874843262270133 ) ) ;
#74362 = CARTESIAN_POINT ( 'NONE',  ( -14.43784027742400156, -12.15440758774515473, 32.17923288041532004 ) ) ;
#74363 = CARTESIAN_POINT ( 'NONE',  ( 16.85343813319912698, -8.496056993536548418, 34.65000542017679663 ) ) ;
#74364 = LINE ( 'NONE', #79791, #31799 ) ;
#74365 = EDGE_LOOP ( 'NONE', ( #76897, #85311, #8779, #65605, #6877 ) ) ;
#74366 = CARTESIAN_POINT ( 'NONE',  ( 4.153846153846030731, -6.835583212225970762, 34.95778746994575670 ) ) ;
#74367 = CARTESIAN_POINT ( 'NONE',  ( 0.7115927731767762721, -9.943054286541400444, 34.11300777759954883 ) ) ;
#74368 = CARTESIAN_POINT ( 'NONE',  ( 17.07692307692295586, -4.320704448113951379, 33.92786785259630022 ) ) ;
#74369 = CARTESIAN_POINT ( 'NONE',  ( -3.360917200500928015, -12.70455904226513866, 30.44083106164009322 ) ) ;
#74370 = EDGE_LOOP ( 'NONE', ( #55922, #29867 ) ) ;
#74371 = ORIENTED_EDGE ( 'NONE', *, *, #46220, .T. ) ;
#74372 = ITEM_DEFINED_TRANSFORMATION ( 'NONE', 'NONE', #1536,  #83448 ) ;
#74373 = ORIENTED_EDGE ( 'NONE', *, *, #58527, .F. ) ;
#74374 = AXIS2_PLACEMENT_3D ( 'NONE', #59566, #65870, #66772 ) ;
#74375 = CARTESIAN_POINT ( 'NONE',  ( 0.4615384615384611755, -13.57706302396349152, 30.56769352161908060 ) ) ;
#74376 = ORIENTED_EDGE ( 'NONE', *, *, #46868, .F. ) ;
#74377 = CARTESIAN_POINT ( 'NONE',  ( -16.15384615384627409, -5.219633306517616589, 34.19971097300220464 ) ) ;
#74378 = CARTESIAN_POINT ( 'NONE',  ( -6.223484924564328225, -9.417330523894424488, 34.63758898049880486 ) ) ;
#74379 = CARTESIAN_POINT ( 'NONE',  ( 3.296836564119306257, -9.905515769479277921, 34.41647553114623292 ) ) ;
#74380 = CYLINDRICAL_SURFACE ( 'NONE', #27291, 4.000000000000000000 ) ;
#74381 = CARTESIAN_POINT ( 'NONE',  ( -2.939152317953646711E-15, 7.500000000000000000, 14.00000000000000178 ) ) ;
#74382 = VERTEX_POINT ( 'NONE', #58893 ) ;
#74383 = B_SPLINE_CURVE_WITH_KNOTS ( 'NONE', 3,
 ( #225, #33576, #81761, #40778, #75881, #663, #47958, #55603, #40332, #33123 ),
 .UNSPECIFIED., .F., .F.,
 ( 4, 2, 2, 2, 4 ),
 ( 0.0007817246256747446788, 0.0009771112852218879000, 0.001172497944769031013, 0.001367884604316174126, 0.001563271263863317238 ),
 .UNSPECIFIED. ) ;
#74385 = ORIENTED_EDGE ( 'NONE', *, *, #18640, .T. ) ;
#74384 = CARTESIAN_POINT ( 'NONE',  ( -0.2385256174450670896, -11.98016756924214832, 32.48728574198911190 ) ) ;
#74386 = DIRECTION ( 'NONE',  ( 0.000000000000000000, 0.000000000000000000, -1.000000000000000000 ) ) ;
#74387 = CARTESIAN_POINT ( 'NONE',  ( -9.019230769230768274, -7.500000000000001776, 35.00000000000000000 ) ) ;
#74388 = CARTESIAN_POINT ( 'NONE',  ( -13.38461538461538325, -4.786620604624113540, 33.94971097300155094 ) ) ;
#74389 = CARTESIAN_POINT ( 'NONE',  ( 9.823099500132480344, -10.54018710029568595, 33.71981072465678864 ) ) ;
#74390 = CARTESIAN_POINT ( 'NONE',  ( -39.05038313613820122, -12.75000000000000178, 29.75000000000000355 ) ) ;
#74391 = VECTOR ( 'NONE', #73854, 1000.000000000000114 ) ;
#74392 = CARTESIAN_POINT ( 'NONE',  ( -11.53846153846153655, -1.044019251281081972, 31.83374038241031911 ) ) ;
#74393 = CARTESIAN_POINT ( 'NONE',  ( -3.230769230769229949, -6.386643153685126251, 34.62446782046654192 ) ) ;
#74394 = CARTESIAN_POINT ( 'NONE',  ( -1.200186371490524317, -10.22469193450124791, 18.86124329374151287 ) ) ;
#74395 = EDGE_LOOP ( 'NONE', ( #39353, #62006, #16705, #75905 ) ) ;
#74396 = CARTESIAN_POINT ( 'NONE',  ( 0.4615384615383382183, -2.657715359629662544, 31.77849191805970364 ) ) ;
#74397 = CARTESIAN_POINT ( 'NONE',  ( 0.4615384615384611200, -8.164416787775445883, 34.95778746994557906 ) ) ;
#74398 = EDGE_CURVE ( 'NONE', #28383, #47782, #37010, .T. ) ;
#74399 =( NAMED_UNIT ( * ) PLANE_ANGLE_UNIT ( ) SI_UNIT ( $, .RADIAN. ) );
#74400 = EDGE_LOOP ( 'NONE', ( #47844, #17227, #6151, #86674 ) ) ;
#74401 = CARTESIAN_POINT ( 'NONE',  ( -16.40384615384615330, -7.500000000000001776, 35.00000000000000000 ) ) ;
#74402 = CARTESIAN_POINT ( 'NONE',  ( 11.28848479441294828, -12.65889640711025521, 30.72598325615533454 ) ) ;
#74403 = EDGE_CURVE ( 'NONE', #83400, #15837, #48827, .T. ) ;
#74404 = CARTESIAN_POINT ( 'NONE',  ( -10.74607521849492642, -2.295517848115769421, 30.44137282052137294 ) ) ;
#74405 = CARTESIAN_POINT ( 'NONE',  ( 7.053602624840487501, -6.001044277235011215, 34.52024696741798948 ) ) ;
#74406 = CARTESIAN_POINT ( 'NONE',  ( -2.294871794871793824, -4.000000000000000000, 29.75000000000000355 ) ) ;
#74407 = ORIENTED_EDGE ( 'NONE', *, *, #16294, .T. ) ;
#74408 = AXIS2_PLACEMENT_3D ( 'NONE', #42356, #8119, #69811 ) ;
#74409 = CARTESIAN_POINT ( 'NONE',  ( 9.442284455014730682, -10.76384336483936011, 33.53834819971076087 ) ) ;
#74410 = EDGE_CURVE ( 'NONE', #51516, #8808, #509, .T. ) ;
#74411 = CYLINDRICAL_SURFACE ( 'NONE', #84400, 0.2499999999999998890 ) ;
#74412 = CARTESIAN_POINT ( 'NONE',  ( -2.241624974342230736, -5.471508081941601098, 34.59228464037088457 ) ) ;
#74413 = ORIENTED_EDGE ( 'NONE', *, *, #25088, .T. ) ;
#74414 = CARTESIAN_POINT ( 'NONE',  ( 17.07692307692307665, -13.53365097954675988, 30.81389545987213552 ) ) ;
#74415 = ORIENTED_EDGE ( 'NONE', *, *, #18474, .F. ) ;
#74416 = CARTESIAN_POINT ( 'NONE',  ( 6.923076923076924238, -5.180354513474913603, 36.12317359536750416 ) ) ;
#74417 =( NAMED_UNIT ( * ) SI_UNIT ( $, .STERADIAN. ) SOLID_ANGLE_UNIT ( ) );
#74418 = DIRECTION ( 'NONE',  ( -0.000000000000000000, 0.7660444431189791237, -0.6427876096865379196 ) ) ;
#74419 = ORIENTED_EDGE ( 'NONE', *, *, #49160, .T. ) ;
#74420 = FACE_OUTER_BOUND ( 'NONE', #17046, .T. ) ;
#74421 = DIRECTION ( 'NONE',  ( 0.000000000000000000, 0.9396926207859126468, 0.3420201433256571111 ) ) ;
#74422 = DIRECTION ( 'NONE',  ( 1.000000000000000000, 0.000000000000000000, 0.000000000000000000 ) ) ;
#74423 = CARTESIAN_POINT ( 'NONE',  ( -8.096130590202436750, -4.818429247618089661, 34.26397095200675125 ) ) ;
#74424 = CARTESIAN_POINT ( 'NONE',  ( -1.450697763975519416, -10.67929555188718460, 33.92786785259543336 ) ) ;
#74425 = EDGE_CURVE ( 'NONE', #55155, #23906, #74192, .T. ) ;
#74426 = ORIENTED_EDGE ( 'NONE', *, *, #1700, .T. ) ;
#74427 = FACE_BOUND ( 'NONE', #73341, .T. ) ;
#74428 = EDGE_CURVE ( 'NONE', #69764, #86769, #53131, .T. ) ;
#74429 = ORIENTED_EDGE ( 'NONE', *, *, #16276, .F. ) ;
#74430 = CARTESIAN_POINT ( 'NONE',  ( -1.384615384615383471, -1.422936976036506707, 30.56769352161908415 ) ) ;
#74431 = ADVANCED_FACE ( 'NONE', ( #88177 ), #66087, .F. ) ;
#74432 = CARTESIAN_POINT ( 'NONE',  ( -18.00000000000000000, -9.815202283848471154, 36.11096599634342397 ) ) ;
#74433 = ADVANCED_FACE ( 'NONE', ( #5729 ), #81403, .T. ) ;
#74434 = CARTESIAN_POINT ( 'NONE',  ( 6.066068351002440906, -8.973038597847269315, 34.52809138561122637 ) ) ;
#74435 = DIRECTION ( 'NONE',  ( 0.000000000000000000, 0.000000000000000000, 1.000000000000000000 ) ) ;
#74436 = CARTESIAN_POINT ( 'NONE',  ( 14.30769230769231015, -8.164416787775445883, 34.95778746994557906 ) ) ;
#74437 = B_SPLINE_CURVE_WITH_KNOTS ( 'NONE', 3,
 ( #66188, #10372, #80164, #4498, #66646, #45476, #58534, #52675, #31068, #45918 ),
 .UNSPECIFIED., .F., .F.,
 ( 4, 2, 2, 2, 4 ),
 ( 0.000000000000000000, 0.0001954311564186864949, 0.0003908623128373729899, 0.0005862934692560594577, 0.0007817246256747459798 ),
 .UNSPECIFIED. ) ;
#74438 = B_SPLINE_CURVE_WITH_KNOTS ( 'NONE', 3,
 ( #89106, #75559, #56181, #27385, #13860, #55289, #41794, #41342, #28713, #69256 ),
 .UNSPECIFIED., .F., .F.,
 ( 4, 2, 2, 2, 4 ),
 ( 0.0007817359430256293554, 0.0009771253907249952391, 0.001172514838424361123, 0.001367904286123727007, 0.001563293733823092890 ),
 .UNSPECIFIED. ) ;
#74439 = ORIENTED_EDGE ( 'NONE', *, *, #9194, .F. ) ;
#74440 = ORIENTED_EDGE ( 'NONE', *, *, #69339, .F. ) ;
#74441 = EDGE_LOOP ( 'NONE', ( #7604, #23365 ) ) ;
#74442 = PRODUCT_DEFINITION_SHAPE ( 'NONE', 'NONE',  #19995 ) ;
#74443 = ORIENTED_EDGE ( 'NONE', *, *, #38199, .T. ) ;
#74444 = CARTESIAN_POINT ( 'NONE',  ( 8.352564102564102200, -7.500000000000000000, 29.75000000000000355 ) ) ;
#74445 = CARTESIAN_POINT ( 'NONE',  ( 4.153846153846154188, -9.905515769479276145, 34.41647553114623292 ) ) ;
#74446 = CARTESIAN_POINT ( 'NONE',  ( -3.903900635498011251, -9.272278438253401589, 34.42582936511637826 ) ) ;
#74447 = CARTESIAN_POINT ( 'NONE',  ( 4.826946332874485712, -11.47974371597207899, 33.17467449705390692 ) ) ;
#74448 = CARTESIAN_POINT ( 'NONE',  ( 3.230769230769108269, -9.528491918059723176, 34.59228464037033035 ) ) ;
#74449 = CARTESIAN_POINT ( 'NONE',  ( -5.207614543590636025, -8.147922237126337563, 34.70805685702651999 ) ) ;
#74450 = CARTESIAN_POINT ( 'NONE',  ( -4.826868765284762830, -4.235687564193446164, 33.53795663066793509 ) ) ;
#74451 = CARTESIAN_POINT ( 'NONE',  ( 11.31497659473759043, -10.11188796281391511, 34.01382737946119050 ) ) ;
#74452 = VERTEX_POINT ( 'NONE', #5289 ) ;
#74453 = ORIENTED_EDGE ( 'NONE', *, *, #50155, .T. ) ;
#74454 = ORIENTED_EDGE ( 'NONE', *, *, #19278, .T. ) ;
#74456 = EDGE_LOOP ( 'NONE', ( #3229, #53477 ) ) ;
#74455 = DIRECTION ( 'NONE',  ( 0.000000000000000000, -1.000000000000000000, 0.000000000000000000 ) ) ;
#74458 = CARTESIAN_POINT ( 'NONE',  ( -9.822998295418001291, -3.957541250942358424, 33.62499894934981626 ) ) ;
#74457 = CARTESIAN_POINT ( 'NONE',  ( -1.384615384615506484, -2.657715359629662544, 31.77849191805970364 ) ) ;
#74459 = EDGE_CURVE ( 'NONE', #76451, #27137, #26452, .T. ) ;
#74460 = CARTESIAN_POINT ( 'NONE',  ( -16.15384615384615330, -10.89733346790207413, 36.13435417666054406 ) ) ;
#74461 = AXIS2_PLACEMENT_3D ( 'NONE', #33051, #60518, #57306 ) ;
#74462 = CARTESIAN_POINT ( 'NONE',  ( -15.23076923076922995, -9.905515769479276145, 34.41647553114623292 ) ) ;
#74463 = FACE_BOUND ( 'NONE', #74821, .T. ) ;
#74464 = ORIENTED_EDGE ( 'NONE', *, *, #78056, .T. ) ;
#74465 = DIRECTION ( 'NONE',  ( -0.000000000000000000, -0.5000000000000009992, -0.8660254037844380415 ) ) ;
#74466 = EDGE_LOOP ( 'NONE', ( #63116, #40805 ) ) ;
#74468 = B_SPLINE_CURVE_WITH_KNOTS ( 'NONE', 3,
 ( #12838, #47056, #11516, #11067, #26358, #40322, #38997, #86300, #32230, #87191 ),
 .UNSPECIFIED., .F., .F.,
 ( 4, 2, 2, 2, 4 ),
 ( 0.0007817246256747491240, 0.0009771112852218931041, 0.001172497944769036867, 0.001367884604316180631, 0.001563271263863324611 ),
 .UNSPECIFIED. ) ;
#74467 = CARTESIAN_POINT ( 'NONE',  ( 17.14217821643591932, -5.941354392334603496, 34.76329471203374055 ) ) ;
#74469 = CIRCLE ( 'NONE', #35650, 0.2500000000000002220 ) ;
#74470 = ORIENTED_EDGE ( 'NONE', *, *, #71320, .F. ) ;
#74471 = FACE_BOUND ( 'NONE', #4776, .T. ) ;
#74472 = CARTESIAN_POINT ( 'NONE',  ( 9.915087361285760181, -5.827830569534417471, 34.72679350104403539 ) ) ;
#74473 = CARTESIAN_POINT ( 'NONE',  ( 15.16549923021291058, -6.835583212224499938, 34.95778746994557906 ) ) ;
#74474 = EDGE_LOOP ( 'NONE', ( #28807, #21804 ) ) ;
#74475 = LINE ( 'NONE', #14103, #62166 ) ;
#74476 = CYLINDRICAL_SURFACE ( 'NONE', #4483, 0.2499999999999994726 ) ;
#74477 = VECTOR ( 'NONE', #76404, 1000.000000000000227 ) ;
#74478 = CARTESIAN_POINT ( 'NONE',  ( 15.23076923076911093, -8.613356846316285953, 34.62446782046622218 ) ) ;
#74479 = ORIENTED_EDGE ( 'NONE', *, *, #2176, .T. ) ;
#74480 = CARTESIAN_POINT ( 'NONE',  ( -8.546451100252699717, -3.563462043263030399, 33.22394488606062879 ) ) ;
#74481 = CARTESIAN_POINT ( 'NONE',  ( -5.076923076923075762, -8.564572088678739092, 35.78748833219616898 ) ) ;
#74482 = CARTESIAN_POINT ( 'NONE',  ( -3.480792468062195777, -2.823816976329320827, 31.52131813110797154 ) ) ;
#74483 = DIRECTION ( 'NONE',  ( -0.000000000000000000, -0.5000000000000009992, -0.8660254037844380415 ) ) ;
#74484 = EDGE_LOOP ( 'NONE', ( #59115, #6536, #26691, #22037 ) ) ;
#74485 = ADVANCED_FACE ( 'NONE', ( #6178 ), #25112, .F. ) ;
#74486 = FACE_OUTER_BOUND ( 'NONE', #85785, .T. ) ;
#74487 = CARTESIAN_POINT ( 'NONE',  ( -16.02305571287920571, -9.929761469519743144, 34.40412654351204225 ) ) ;
#74488 = ORIENTED_EDGE ( 'NONE', *, *, #4741, .F. ) ;
#74489 = CARTESIAN_POINT ( 'NONE',  ( 0.3313912521002400635, -9.418419913701741919, 34.36755862841477693 ) ) ;
#74490 = CARTESIAN_POINT ( 'NONE',  ( 9.915270826574369423, -7.369474539155828730, 34.99858011523957657 ) ) ;
#74491 = DIRECTION ( 'NONE',  ( -0.000000000000000000, -0.000000000000000000, -1.000000000000000000 ) ) ;
#74492 = CARTESIAN_POINT ( 'NONE',  ( -5.076923076923075762, -13.63283147151868846, 33.57946703557072254 ) ) ;
#74493 = CARTESIAN_POINT ( 'NONE',  ( -7.145905020711801114, -7.369209533119140509, 34.99857337881830688 ) ) ;
#74494 = CARTESIAN_POINT ( 'NONE',  ( 17.01084069756293715, -4.661471528628507777, 34.16647553114621871 ) ) ;
#74496 = CARTESIAN_POINT ( 'NONE',  ( 16.28463796167094557, -5.582136614379148654, 34.36778462344220486 ) ) ;
#74495 = DIRECTION ( 'NONE',  ( -0.000000000000000000, 1.000000000000000000, -0.000000000000000000 ) ) ;
#74497 = CARTESIAN_POINT ( 'NONE',  ( -12.21148414990014963, -11.28795663066794575, 33.01431243580653785 ) ) ;
#74498 = CARTESIAN_POINT ( 'NONE',  ( 1.799775606325937360E-14, -10.25000000000000000, 19.78125000000000000 ) ) ;
#74499 = ORIENTED_EDGE ( 'NONE', *, *, #74843, .T. ) ;
#74500 = B_SPLINE_CURVE_WITH_KNOTS ( 'NONE', 3,
 ( #2906, #79027, #4258, #51085, #17785, #17329, #30396, #54096, #37591, #78578 ),
 .UNSPECIFIED., .F., .F.,
 ( 4, 2, 2, 2, 4 ),
 ( 0.000000000000000000, 0.0001954311584214072381, 0.0003908623168428144762, 0.0005862934752642217414, 0.0007817246336856289524 ),
 .UNSPECIFIED. ) ;
#74501 = LINE ( 'NONE', #59204, #10171 ) ;
#74502 = ORIENTED_EDGE ( 'NONE', *, *, #24364, .F. ) ;
#74503 = ADVANCED_FACE ( 'NONE', ( #61112 ), #26891, .F. ) ;
#74504 = AXIS2_PLACEMENT_3D ( 'NONE', #23072, #87346, #25621 ) ;
#74505 = VERTEX_POINT ( 'NONE', #60223 ) ;
#74506 = CARTESIAN_POINT ( 'NONE',  ( -8.638705330997126453, -6.808710257144161559, 34.95449254468098843 ) ) ;
#74507 = ORIENTED_EDGE ( 'NONE', *, *, #6580, .T. ) ;
#74508 = CARTESIAN_POINT ( 'NONE',  ( 15.23076923076923173, -7.500000000000001776, 35.04278698407183867 ) ) ;
#74509 = CARTESIAN_POINT ( 'NONE',  ( 1.799775606325937360E-14, -10.25000000000000000, 18.53125000000000000 ) ) ;
#74510 = CARTESIAN_POINT ( 'NONE',  ( -14.08491263871423982, -3.020022701398813236, 32.48759521482552515 ) ) ;
#74511 = EDGE_CURVE ( 'NONE', #58033, #70825, #16591, .T. ) ;
#74512 = CARTESIAN_POINT ( 'NONE',  ( 6.923076923076924238, -9.905515769479276145, 34.41647553114623292 ) ) ;
#74513 = CARTESIAN_POINT ( 'NONE',  ( -3.100243529005665799, -9.417988943895561960, 34.36773134775778260 ) ) ;
#74514 = CYLINDRICAL_SURFACE ( 'NONE', #79188, 0.2499999999999979738 ) ;
#74515 = CARTESIAN_POINT ( 'NONE',  ( 10.86538461538603606, -7.500000000000154543, 35.00000000000007105 ) ) ;
#74516 = DIRECTION ( 'NONE',  ( -1.000000000000000000, -0.000000000000000000, 0.000000000000000000 ) ) ;
#74517 = CARTESIAN_POINT ( 'NONE',  ( 6.792386319966619013, -12.35290016733513951, 31.75349464988449455 ) ) ;
#74518 = CARTESIAN_POINT ( 'NONE',  ( 11.53846153846153832, -8.564572088678739092, 35.78748833219616898 ) ) ;
#74519 = CARTESIAN_POINT ( 'NONE',  ( -10.39200912961219458, -2.251407671071268712, 29.88021292934943318 ) ) ;
#74520 = VECTOR ( 'NONE', #11835, 1000.000000000000000 ) ;
#74521 = EDGE_CURVE ( 'NONE', #4115, #57358, #34532, .T. ) ;
#74522 = CARTESIAN_POINT ( 'NONE',  ( 18.22337594069818323, -2.501478030877322567, 29.88021232661721172 ) ) ;
#74523 = B_SPLINE_CURVE_WITH_KNOTS ( 'NONE', 3,
 ( #42890, #36997, #29380, #83884, #42445, #70805, #22602, #78430, #43761, #22171 ),
 .UNSPECIFIED., .F., .F.,
 ( 4, 2, 2, 2, 4 ),
 ( 0.0007817246256747450040, 0.0009771112852218876831, 0.001172497944769030579, 0.001367884604316173258, 0.001563271263863315937 ),
 .UNSPECIFIED. ) ;
#74524 = EDGE_CURVE ( 'NONE', #21466, #5024, #7045, .T. ) ;
#74525 = EDGE_LOOP ( 'NONE', ( #175, #46183 ) ) ;
#74526 = EDGE_LOOP ( 'NONE', ( #222, #66543, #53827, #56922 ) ) ;
#74527 = CARTESIAN_POINT ( 'NONE',  ( 14.24242230713598900, -8.656820664281498878, 34.87096338111211935 ) ) ;
#74528 = FACE_OUTER_BOUND ( 'NONE', #11393, .T. ) ;
#74529 = LINE ( 'NONE', #68216, #41145 ) ;
#74530 = CARTESIAN_POINT ( 'NONE',  ( -7.146003881983771677, -5.582147617184174848, 34.63737895849758530 ) ) ;
#74531 = ADVANCED_FACE ( 'NONE', ( #76402 ), #304, .F. ) ;
#74532 = FACE_OUTER_BOUND ( 'NONE', #10623, .T. ) ;
#74533 = DIRECTION ( 'NONE',  ( 0.000000000000000000, -0.000000000000000000, 1.000000000000000000 ) ) ;
#74534 = CARTESIAN_POINT ( 'NONE',  ( -9.692307692307691624, -4.945431358278436385, 36.03766855953609394 ) ) ;
#74535 = ADVANCED_FACE ( 'NONE', ( #75962 ), #69205, .F. ) ;
#74536 = EDGE_LOOP ( 'NONE', ( #31372, #74499, #7966, #62304 ) ) ;
#74537 = CARTESIAN_POINT ( 'NONE',  ( 2.980746006547774218, -6.652501968072646932, 34.93155406624980941 ) ) ;
#74538 = EDGE_LOOP ( 'NONE', ( #26957, #26365, #21468, #10083 ) ) ;
#74539 = VECTOR ( 'NONE', #80237, 1000.000000000000000 ) ;
#74540 = ORIENTED_EDGE ( 'NONE', *, *, #57133, .T. ) ;
#74541 = CARTESIAN_POINT ( 'NONE',  ( 16.37685899793954292, -9.172514111537580561, 34.72667873470787470 ) ) ;
#74542 = LINE ( 'NONE', #40320, #16797 ) ;
#74543 = EDGE_CURVE ( 'NONE', #15407, #6007, #46760, .T. ) ;
#74544 = DIRECTION ( 'NONE',  ( 0.000000000000000000, 0.000000000000000000, 1.000000000000000000 ) ) ;
#74545 = EDGE_CURVE ( 'NONE', #65338, #20445, #75788, .T. ) ;
#74546 = AXIS2_PLACEMENT_3D ( 'NONE', #17035, #64764, #58019 ) ;
#74547 = DIRECTION ( 'NONE',  ( -0.000000000000000000, 1.000000000000000000, -0.000000000000000000 ) ) ;
#74548 = CARTESIAN_POINT ( 'NONE',  ( 12.46153846153846168, -12.10708131394839349, 31.69288490824020244 ) ) ;
#74549 = ORIENTED_EDGE ( 'NONE', *, *, #1946, .T. ) ;
#74550 = ORIENTED_EDGE ( 'NONE', *, *, #83336, .F. ) ;
#74551 = B_SPLINE_CURVE_WITH_KNOTS ( 'NONE', 3,
 ( #31957, #58513, #52209, #30175, #23836, #85125, #86008, #72935, #44552, #45454 ),
 .UNSPECIFIED., .F., .F.,
 ( 4, 2, 2, 2, 4 ),
 ( 0.0007817359430256294638, 0.0009771253907249941549, 0.001172514838424358954, 0.001367904286123723754, 0.001563293733823095492 ),
 .UNSPECIFIED. ) ;
#74552 = ORIENTED_EDGE ( 'NONE', *, *, #52820, .F. ) ;
#74553 = ORIENTED_EDGE ( 'NONE', *, *, #69022, .T. ) ;
#74554 = CARTESIAN_POINT ( 'NONE',  ( -2.307692307692305711, -1.242168528481310874, 33.36296068462461051 ) ) ;
#74555 = CARTESIAN_POINT ( 'NONE',  ( -2.307692307692428724, -10.33852847137269571, 34.16647553114546554 ) ) ;
#74556 = DIRECTION ( 'NONE',  ( 0.000000000000000000, 0.000000000000000000, -1.000000000000000000 ) ) ;
#74557 = CARTESIAN_POINT ( 'NONE',  ( 14.53111870660709748, -7.630147987733840509, 34.99859428049665411 ) ) ;
#74558 = VECTOR ( 'NONE', #6912, 1000.000000000000000 ) ;
#74559 = ADVANCED_FACE ( 'NONE', ( #83623 ), #75085, .F. ) ;
#74560 = CARTESIAN_POINT ( 'NONE',  ( 17.77651505627605033, -5.113361153441931428, 34.14387501736621999 ) ) ;
#74561 = CARTESIAN_POINT ( 'NONE',  ( -10.61538461538473399, -12.27809138561165270, 31.22303859784587132 ) ) ;
#74562 = ORIENTED_EDGE ( 'NONE', *, *, #42770, .T. ) ;
#74563 = VERTEX_POINT ( 'NONE', #21902 ) ;
#74564 = ORIENTED_EDGE ( 'NONE', *, *, #13075, .T. ) ;
#74565 = AXIS2_PLACEMENT_3D ( 'NONE', #69334, #84188, #49930 ) ;
#74567 = VERTEX_POINT ( 'NONE', #49375 ) ;
#74566 = CARTESIAN_POINT ( 'NONE',  ( -10.36533030374629938, -11.79725096376909299, 32.30694842903960762 ) ) ;
#74568 = DIRECTION ( 'NONE',  ( 0.000000000000000000, 0.9396926207859126468, 0.3420201433256571111 ) ) ;
#74569 = CARTESIAN_POINT ( 'NONE',  ( -12.39628332202562433, -12.16647553114626490, 32.15551576947920864 ) ) ;
#74570 = VECTOR ( 'NONE', #78801, 1000.000000000000114 ) ;
#74571 = EDGE_CURVE ( 'NONE', #73158, #35045, #89055, .T. ) ;
#74572 = CARTESIAN_POINT ( 'NONE',  ( -1.553300858899081760, -11.25000000000000888, 21.10937500000000000 ) ) ;
#74573 = ORIENTED_EDGE ( 'NONE', *, *, #44864, .T. ) ;
#74574 = CIRCLE ( 'NONE', #75980, 4.000000000000000000 ) ;
#74575 = CARTESIAN_POINT ( 'NONE',  ( 7.976944287120798727, -3.957578996910242619, 33.62503395064540257 ) ) ;
#74576 = VERTEX_POINT ( 'NONE', #48034 ) ;
#74577 = EDGE_CURVE ( 'NONE', #18726, #74998, #57896, .T. ) ;
#74578 = CARTESIAN_POINT ( 'NONE',  ( 2.057715576749955311, -6.567427716900047230, 34.66269422305636283 ) ) ;
#74579 = FACE_BOUND ( 'NONE', #35352, .T. ) ;
#74580 = DIRECTION ( 'NONE',  ( 0.000000000000000000, 0.000000000000000000, 1.000000000000000000 ) ) ;
#74581 = EDGE_CURVE ( 'NONE', #64872, #12730, #67198, .T. ) ;
#74582 = CYLINDRICAL_SURFACE ( 'NONE', #57770, 4.000000000000000000 ) ;
#74583 = ORIENTED_EDGE ( 'NONE', *, *, #51268, .T. ) ;
#74584 = CARTESIAN_POINT ( 'NONE',  ( -5.076923076923197442, -12.46129190930018460, 30.37095296980731973 ) ) ;
#74585 = DIRECTION ( 'NONE',  ( 0.000000000000000000, -0.000000000000000000, -1.000000000000000000 ) ) ;
#74586 = DIRECTION ( 'NONE',  ( -0.000000000000000000, -0.8660254037844397068, -0.4999999999999978906 ) ) ;
#74587 = ORIENTED_EDGE ( 'NONE', *, *, #7546, .F. ) ;
#74588 = EDGE_CURVE ( 'NONE', #60815, #23052, #87624, .T. ) ;
#74589 = CARTESIAN_POINT ( 'NONE',  ( -11.53846153846153655, -2.486705287966279876, 31.30864560766543647 ) ) ;
#74590 = LINE ( 'NONE', #48428, #69897 ) ;
#74592 = B_SPLINE_CURVE_WITH_KNOTS ( 'NONE', 3,
 ( #28536, #83488, #21770, #15021, #42495, #8268, #35740, #63191, #81710, #19994 ),
 .UNSPECIFIED., .F., .F.,
 ( 4, 2, 2, 2, 4 ),
 ( 0.000000000000000000, 0.0001954311564186878502, 0.0003908623128373757004, 0.0005862934692560635777, 0.0007817246256747514008 ),
 .UNSPECIFIED. ) ;
#74591 = CARTESIAN_POINT ( 'NONE',  ( -3.903791733932699959, -2.318338780012835443, 30.59689888758630261 ) ) ;
#74593 = CARTESIAN_POINT ( 'NONE',  ( 6.000000000000001776, -13.37000171582298513, 34.34916445242398453 ) ) ;
#74594 = CARTESIAN_POINT ( 'NONE',  ( 7.911409417429871027, -3.300289026998475705, 32.46337939537591666 ) ) ;
#74595 = FACE_BOUND ( 'NONE', #31936, .T. ) ;
#74597 = CARTESIAN_POINT ( 'NONE',  ( 14.98076923076923173, -7.500000000000001776, 35.04278698407183867 ) ) ;
#74596 = PLANE ( 'NONE',  #23114 ) ;
#74598 = CARTESIAN_POINT ( 'NONE',  ( -14.98082382139119062, -4.932303261841489928, 34.32971442181322885 ) ) ;
#74600 = CARTESIAN_POINT ( 'NONE',  ( 17.93472955403922242, -11.48612834413959582, 32.76840700105983473 ) ) ;
#74599 = CARTESIAN_POINT ( 'NONE',  ( -5.750054481651858396, -10.05730279482229683, 34.04704008940765902 ) ) ;
#74601 = CARTESIAN_POINT ( 'NONE',  ( 5.999999999999878320, -5.094484230521993062, 34.41647553114689373 ) ) ;
#74602 = CARTESIAN_POINT ( 'NONE',  ( 1.077988221561464899, -4.724691934501233703, 18.98250670625849068 ) ) ;
#74603 = ORIENTED_EDGE ( 'NONE', *, *, #886, .F. ) ;
#74604 = CARTESIAN_POINT ( 'NONE',  ( -12.23857532727178921, -7.369474539155828730, 34.99858011523957657 ) ) ;
#74605 = ORIENTED_EDGE ( 'NONE', *, *, #47569, .F. ) ;
#74606 = CARTESIAN_POINT ( 'NONE',  ( -18.06527000055631760, -3.643525952247788524, 33.31231777344662248 ) ) ;
#74607 = ORIENTED_EDGE ( 'NONE', *, *, #67586, .T. ) ;
#74608 = CARTESIAN_POINT ( 'NONE',  ( 16.37662582282421653, -12.69155399931963046, 30.53255429739158444 ) ) ;
#74609 = DIRECTION ( 'NONE',  ( 1.000000000000000000, 0.000000000000000000, 0.000000000000000000 ) ) ;
#74611 = ORIENTED_EDGE ( 'NONE', *, *, #2001, .F. ) ;
#74610 = DIRECTION ( 'NONE',  ( -0.000000000000000000, -0.8660254037844399289, -0.4999999999999980016 ) ) ;
#74612 = CARTESIAN_POINT ( 'NONE',  ( 16.82694633287449193, -12.65889640711025521, 30.72598325615533454 ) ) ;
#74613 = DIRECTION ( 'NONE',  ( -0.000000000000000000, 0.5000000000000011102, -0.8660254037844381525 ) ) ;
#74614 = CARTESIAN_POINT ( 'NONE',  ( 1.077988221561464899, -4.724691934501233703, 18.98250670625849068 ) ) ;
#74615 = EDGE_CURVE ( 'NONE', #27642, #52479, #29553, .T. ) ;
#74616 = CARTESIAN_POINT ( 'NONE',  ( -5.076923076923075762, -13.87047571288749737, 32.06866353760679544 ) ) ;
#74617 = CYLINDRICAL_SURFACE ( 'NONE', #60446, 0.2500000000000009437 ) ;
#74618 = EDGE_CURVE ( 'NONE', #35110, #9301, #69246, .T. ) ;
#74619 = LINE ( 'NONE', #60203, #8740 ) ;
#74620 = CARTESIAN_POINT ( 'NONE',  ( 3.903869422903798458, -11.79746400365624659, 32.30657167506340954 ) ) ;
#74621 = CARTESIAN_POINT ( 'NONE',  ( 2.307692307692309264, -2.721908614388771852, 31.22303859784724978 ) ) ;
#74622 = CYLINDRICAL_SURFACE ( 'NONE', #38230, 0.2499999999999986955 ) ;
#74623 = CARTESIAN_POINT ( 'NONE',  ( 1.614399933863618797, -3.775308065498751198, 19.48624329374152353 ) ) ;
#74624 = DIRECTION ( 'NONE',  ( -0.000000000000000000, -0.000000000000000000, -1.000000000000000000 ) ) ;
#74625 = LINE ( 'NONE', #29440, #19769 ) ;
#74626 = ORIENTED_EDGE ( 'NONE', *, *, #984, .F. ) ;
#74627 = CARTESIAN_POINT ( 'NONE',  ( 7.053124358327376164, -7.723484941389743952, 34.99544897038808955 ) ) ;
#74628 = CARTESIAN_POINT ( 'NONE',  ( 15.29602437028207085, -11.06231777344671130, 33.60647404775212976 ) ) ;
#74629 = CARTESIAN_POINT ( 'NONE',  ( -3.749999999999997780, -7.438900925035489387, 16.59561829374151287 ) ) ;
#74630 = CARTESIAN_POINT ( 'NONE',  ( -5.999999999999998224, -2.292212530054420494, 30.41441678777542634 ) ) ;
#74632 = DIRECTION ( 'NONE',  ( 0.000000000000000000, 0.000000000000000000, 1.000000000000000000 ) ) ;
#74631 = VECTOR ( 'NONE', #32406, 999.9999999999998863 ) ;
#74633 = VERTEX_POINT ( 'NONE', #43060 ) ;
#74634 = LINE ( 'NONE', #67872, #50011 ) ;
#74635 = DIRECTION ( 'NONE',  ( 0.000000000000000000, 0.9848077530122072432, 0.1736481776669354937 ) ) ;
#74637 = ORIENTED_EDGE ( 'NONE', *, *, #53826, .F. ) ;
#74636 = CARTESIAN_POINT ( 'NONE',  ( 4.153846153846154188, -9.058645607665452459, 34.76329471203371924 ) ) ;
#74638 = CARTESIAN_POINT ( 'NONE',  ( 3.903822916553187472, -8.432397168068783699, 34.66272746175022945 ) ) ;
#74639 = CARTESIAN_POINT ( 'NONE',  ( -15.23076923076922995, -11.91647553114624181, 32.58852847137148245 ) ) ;
#74640 = AXIS2_PLACEMENT_3D ( 'NONE', #46635, #40776, #5647 ) ;
#74641 = CARTESIAN_POINT ( 'NONE',  ( -16.02300782335938933, -7.277220318596959281, 34.99547417642776992 ) ) ;
#74642 = ORIENTED_EDGE ( 'NONE', *, *, #69554, .F. ) ;
#74643 = VECTOR ( 'NONE', #75943, 1000.000000000000114 ) ;
#74644 = CARTESIAN_POINT ( 'NONE',  ( 5.076923076922954969, -4.481592998941358097, 33.73612834414048933 ) ) ;
#74645 = CARTESIAN_POINT ( 'NONE',  ( -13.60754160213153163, -11.76352882383564769, 32.36236540154569497 ) ) ;
#74646 = EDGE_CURVE ( 'NONE', #10442, #30860, #2410, .T. ) ;
#74647 = VECTOR ( 'NONE', #64597, 1000.000000000000000 ) ;
#74648 = EDGE_CURVE ( 'NONE', #13730, #21910, #9284, .T. ) ;
#74649 = CARTESIAN_POINT ( 'NONE',  ( 1.254467414883687848, -3.069018819979302926, 32.56621877034667278 ) ) ;
#74650 = EDGE_LOOP ( 'NONE', ( #87754, #37105 ) ) ;
#74651 = ORIENTED_EDGE ( 'NONE', *, *, #45283, .F. ) ;
#74652 = VERTEX_POINT ( 'NONE', #65540 ) ;
#74653 = B_SPLINE_CURVE_WITH_KNOTS ( 'NONE', 3,
 ( #65295, #71604, #45470, #44566, #31970, #30621, #52223, #58094, #38278, #65734 ),
 .UNSPECIFIED., .F., .F.,
 ( 4, 2, 2, 2, 4 ),
 ( 0.0007817359430256262112, 0.0009771253907249911191, 0.001172514838424356136, 0.001367904286123721152, 0.001563293733823086168 ),
 .UNSPECIFIED. ) ;
#74654 = EDGE_CURVE ( 'NONE', #64222, #65220, #32712, .T. ) ;
#74655 = VERTEX_POINT ( 'NONE', #72299 ) ;
#74656 = CARTESIAN_POINT ( 'NONE',  ( 12.68455130563185662, -10.01129605718032600, 34.36064277460058491 ) ) ;
#74657 = CARTESIAN_POINT ( 'NONE',  ( -5.076923076923075762, -2.486705287966279876, 31.30864560766543647 ) ) ;
#74658 = ADVANCED_FACE ( 'NONE', ( #3841 ), #86287, .T. ) ;
#74659 = DIRECTION ( 'NONE',  ( -1.000000000000000000, 0.000000000000000000, 0.000000000000000000 ) ) ;
#74660 = CARTESIAN_POINT ( 'NONE',  ( -17.32692307692307665, -7.500000000000001776, 35.00000000000000000 ) ) ;
#74661 = EDGE_CURVE ( 'NONE', #70106, #88393, #82188, .T. ) ;
#74662 = CARTESIAN_POINT ( 'NONE',  ( 5.326868595271218254, -5.852078868378311149, 34.47109172314383585 ) ) ;
#74663 = ORIENTED_EDGE ( 'NONE', *, *, #48742, .F. ) ;
#74664 = ORIENTED_EDGE ( 'NONE', *, *, #23950, .T. ) ;
#74665 = ORIENTED_EDGE ( 'NONE', *, *, #18518, .T. ) ;
#74667 = EDGE_LOOP ( 'NONE', ( #27672, #87569, #46019, #11811 ) ) ;
#74666 = CARTESIAN_POINT ( 'NONE',  ( 12.46153846153846168, -5.180354513474913603, 36.12317359536750416 ) ) ;
#74668 = CARTESIAN_POINT ( 'NONE',  ( 7.846153846153725020, -12.27809138561165270, 31.22303859784587132 ) ) ;
#74669 = EDGE_CURVE ( 'NONE', #23762, #75680, #65984, .T. ) ;
#74670 = AXIS2_PLACEMENT_3D ( 'NONE', #53646, #13988, #19418 ) ;
#74671 = CARTESIAN_POINT ( 'NONE',  ( 5.776515075435670887, -12.69144148231606017, 30.53333754910549303 ) ) ;
#74672 = EDGE_CURVE ( 'NONE', #36959, #86943, #39287, .T. ) ;
#74673 = CARTESIAN_POINT ( 'NONE',  ( 7.384615384615385025, -7.500000000000000000, 29.75000000000000355 ) ) ;
#74674 = CARTESIAN_POINT ( 'NONE',  ( -14.98082371242109012, -9.272278438253398036, 34.42582936511637115 ) ) ;
#74675 = ORIENTED_EDGE ( 'NONE', *, *, #29458, .F. ) ;
#74676 = ORIENTED_EDGE ( 'NONE', *, *, #73939, .F. ) ;
#74677 = ORIENTED_EDGE ( 'NONE', *, *, #64871, .T. ) ;
#74678 = CARTESIAN_POINT ( 'NONE',  ( 10.86543892702293412, -10.66356715214248752, 33.62249196103329751 ) ) ;
#74680 = ORIENTED_EDGE ( 'NONE', *, *, #65131, .T. ) ;
#74679 = CARTESIAN_POINT ( 'NONE',  ( -2.438383774359863310, -2.729777683071816785, 31.24903638046268739 ) ) ;
#74681 = CYLINDRICAL_SURFACE ( 'NONE', #41717, 0.2499999999999995559 ) ;
#74682 = EDGE_CURVE ( 'NONE', #3688, #67767, #81298, .T. ) ;
#74683 = CARTESIAN_POINT ( 'NONE',  ( -7.846153846153844924, -13.49023893513002648, 31.06009739812518688 ) ) ;
#74684 = VERTEX_POINT ( 'NONE', #33550 ) ;
#74685 = LINE ( 'NONE', #33692, #43181 ) ;
#74686 = DIRECTION ( 'NONE',  ( 0.000000000000000000, -6.938893903907222067E-15, 1.000000000000000000 ) ) ;
#74687 = CARTESIAN_POINT ( 'NONE',  ( 13.38461538461538680, -12.78798330534102945, 29.74999999999997868 ) ) ;
#74688 = FACE_BOUND ( 'NONE', #77253, .T. ) ;
#74689 = EDGE_CURVE ( 'NONE', #76970, #41347, #62856, .T. ) ;
#74690 = CARTESIAN_POINT ( 'NONE',  ( 10.61538461538461675, -9.780366693483667717, 34.19971097300155094 ) ) ;
#74691 = CARTESIAN_POINT ( 'NONE',  ( -12.71151519248081740, -9.148715823498378086, 34.47080413974185120 ) ) ;
#74692 = CARTESIAN_POINT ( 'NONE',  ( 2.307692307692309264, -2.708943851104267164, 35.45975837776705220 ) ) ;
#74694 = CARTESIAN_POINT ( 'NONE',  ( -18.75000000000000000, -11.00000000000000000, 29.75000000000000355 ) ) ;
#74693 = CARTESIAN_POINT ( 'NONE',  ( 0.4615384615383382183, -6.835583212225970762, 34.95778746994575670 ) ) ;
#74695 = VECTOR ( 'NONE', #47915, 1000.000000000000000 ) ;
#74696 = CARTESIAN_POINT ( 'NONE',  ( -4.946397375159511611, -10.88167719472716399, 33.43325721877153711 ) ) ;
#74697 = DIRECTION ( 'NONE',  ( -1.000000000000000000, -0.000000000000000000, -0.000000000000000000 ) ) ;
#74698 = ORIENTED_EDGE ( 'NONE', *, *, #21192, .F. ) ;
#74699 = CARTESIAN_POINT ( 'NONE',  ( 2.372947878968333590, -6.879047030191282275, 34.71129190930002295 ) ) ;
#74700 = CARTESIAN_POINT ( 'NONE',  ( 0.3954560821783248969, -10.67929555188718460, 33.92786785259543336 ) ) ;
#74702 = ORIENTED_EDGE ( 'NONE', *, *, #72858, .T. ) ;
#74701 = STYLED_ITEM ( 'NONE', ( #518 ), #9 ) ;
#74703 = AXIS2_PLACEMENT_3D ( 'NONE', #70899, #22700, #63686 ) ;
#74704 = CARTESIAN_POINT ( 'NONE',  ( 6.166666666666664298, -7.500000000000000000, 29.75000000000000355 ) ) ;
#74705 = EDGE_CURVE ( 'NONE', #84371, #36979, #26349, .T. ) ;
#74706 = VECTOR ( 'NONE', #53009, 1000.000000000000000 ) ;
#74707 = CARTESIAN_POINT ( 'NONE',  ( 15.93091919493930320, -2.308479472611653094, 30.53278059502174457 ) ) ;
#74708 = CARTESIAN_POINT ( 'NONE',  ( 9.692307692307572609, -2.892918686052165622, 31.69288490824153470 ) ) ;
#74709 = ORIENTED_EDGE ( 'NONE', *, *, #480, .F. ) ;
#74710 = CARTESIAN_POINT ( 'NONE',  ( 11.53846153846153832, -9.905515769479276145, 34.41647553114623292 ) ) ;
#74711 = CARTESIAN_POINT ( 'NONE',  ( 6.923076923076924238, -8.164416787775445883, 34.95778746994557906 ) ) ;
#74712 = FACE_BOUND ( 'NONE', #8524, .T. ) ;
#74713 = EDGE_CURVE ( 'NONE', #79996, #76951, #80863, .T. ) ;
#74715 = DIRECTION ( 'NONE',  ( -0.000000000000000000, 0.7660444431189791237, -0.6427876096865379196 ) ) ;
#74714 = CARTESIAN_POINT ( 'NONE',  ( -6.923076923076922462, -2.249999999999998668, 29.75000000000001776 ) ) ;
#74716 = CARTESIAN_POINT ( 'NONE',  ( 2.084765348785460048, -6.459968553980839800, 34.89616026154728701 ) ) ;
#74717 = CYLINDRICAL_SURFACE ( 'NONE', #59684, 0.2499999999999986955 ) ;
#74718 = CARTESIAN_POINT ( 'NONE',  ( -10.39237177129121825, -11.43677907613344757, 33.22367315496202167 ) ) ;
#74719 = CARTESIAN_POINT ( 'NONE',  ( -3.750000000000008438, -5.946699141100917352, 25.17187500000000000 ) ) ;
#74720 = ORIENTED_EDGE ( 'NONE', *, *, #86295, .F. ) ;
#74721 = VERTEX_POINT ( 'NONE', #18256 ) ;
#74722 = CARTESIAN_POINT ( 'NONE',  ( -12.33101302330481808, -5.915461855592780260, 34.75538340440931506 ) ) ;
#74723 = CARTESIAN_POINT ( 'NONE',  ( 16.21991450484859598, -6.386643153685127139, 34.62446782046654192 ) ) ;
#74724 = DIRECTION ( 'NONE',  ( -0.000000000000000000, -0.000000000000000000, -1.000000000000000000 ) ) ;
#74725 = CARTESIAN_POINT ( 'NONE',  ( -0.7115384615384606759, -7.433931650972300353, 34.75000000000000711 ) ) ;
#74726 = CYLINDRICAL_SURFACE ( 'NONE', #21255, 0.2499999999999986955 ) ;
#74727 = CARTESIAN_POINT ( 'NONE',  ( 3.750000000000000888, -7.499999999999978684, 20.71875000000000000 ) ) ;
#74728 = ADVANCED_FACE ( 'NONE', ( #45720 ), #12386, .F. ) ;
#74729 = B_SPLINE_CURVE_WITH_KNOTS ( 'NONE', 3,
 ( #49914, #42733, #34640, #42294, #56679, #70195, #76062, #48582, #62106, #62535 ),
 .UNSPECIFIED., .F., .F.,
 ( 4, 2, 2, 2, 4 ),
 ( 0.0007817246256747507503, 0.0009771112852218959231, 0.001172497944769040987, 0.001367884604316186052, 0.001563271263863331116 ),
 .UNSPECIFIED. ) ;
#74730 = CARTESIAN_POINT ( 'NONE',  ( -8.769230769230892619, -10.33852847137269571, 34.16647553114546554 ) ) ;
#74731 = CARTESIAN_POINT ( 'NONE',  ( -6.066082379360134169, -8.164416787775445883, 34.95778746994557906 ) ) ;
#74732 = EDGE_CURVE ( 'NONE', #33999, #11687, #5938, .T. ) ;
#74733 = CARTESIAN_POINT ( 'NONE',  ( 7.780883845597525550, -5.941354392334499579, 34.76329471203369792 ) ) ;
#74734 = DIRECTION ( 'NONE',  ( -0.000000000000000000, -0.8660254037844397068, -0.4999999999999978906 ) ) ;
#74735 = CARTESIAN_POINT ( 'NONE',  ( 9.915087233576103998, -2.847695495035523550, 31.58253572463339154 ) ) ;
#74736 = CARTESIAN_POINT ( 'NONE',  ( 13.13463865367303285, -4.236021600441997492, 33.53823185664189310 ) ) ;
#74737 = ADVANCED_FACE ( 'NONE', ( #72740 ), #80410, .F. ) ;
#74738 = CARTESIAN_POINT ( 'NONE',  ( -17.07692307692307665, -11.16473453929635440, 33.15142922261926373 ) ) ;
#74739 = DIRECTION ( 'NONE',  ( -0.000000000000000000, -0.7660444431189791237, -0.6427876096865379196 ) ) ;
#74740 = CARTESIAN_POINT ( 'NONE',  ( 7.134615384615385025, -11.00000000000000000, 29.75000000000000355 ) ) ;
#74741 = EDGE_LOOP ( 'NONE', ( #48960, #17593 ) ) ;
#74742 = AXIS2_PLACEMENT_3D ( 'NONE', #60522, #17770, #25857 ) ;
#74743 = CARTESIAN_POINT ( 'NONE',  ( 8.769230769230768274, -4.661471528628507777, 34.16647553114623292 ) ) ;
#74744 = CARTESIAN_POINT ( 'NONE',  ( -3.453695448285377889, -3.586966769969700763, 32.86292498521069660 ) ) ;
#74745 = CARTESIAN_POINT ( 'NONE',  ( -1.200186371490524317, -10.22469193450124791, 16.36124329374151642 ) ) ;
#74746 = CARTESIAN_POINT ( 'NONE',  ( -0.2114840416250094168, -10.82426656108011720, 33.81400080652039009 ) ) ;
#74747 = CARTESIAN_POINT ( 'NONE',  ( -9.320512820512821150, -11.00000000000000000, 28.25000000000000000 ) ) ;
#74748 = CARTESIAN_POINT ( 'NONE',  ( -11.53846153846166089, -5.094484230521993062, 34.41647553114689373 ) ) ;
#74750 = VERTEX_POINT ( 'NONE', #4748 ) ;
#74749 = DIRECTION ( 'NONE',  ( -0.000000000000000000, -0.6427876096865404731, -0.7660444431189770143 ) ) ;
#74751 = CARTESIAN_POINT ( 'NONE',  ( 2.749999999999995115, -6.360912703473971419, 24.39062500000000000 ) ) ;
#74752 = CARTESIAN_POINT ( 'NONE',  ( -14.37296230824862775, -5.941354392334499579, 34.76329471203369792 ) ) ;
#74753 = VERTEX_POINT ( 'NONE', #32218 ) ;
#74754 = PLANE ( 'NONE',  #4613 ) ;
#74755 = CARTESIAN_POINT ( 'NONE',  ( 0.4615384615383396616, -2.892918686052166066, 31.69288490824153470 ) ) ;
#74756 = ORIENTED_EDGE ( 'NONE', *, *, #87309, .F. ) ;
#74757 = CARTESIAN_POINT ( 'NONE',  ( 7.846153846153846700, -4.098570777380720287, 33.41473453929634729 ) ) ;
#74758 = CARTESIAN_POINT ( 'NONE',  ( 1.653273178848927064E-15, -7.500000000000000000, 21.00000000000000000 ) ) ;
#74759 = CARTESIAN_POINT ( 'NONE',  ( -8.096130577096202430, -3.627789207965226748, 32.91389620160131102 ) ) ;
#74760 = ORIENTED_EDGE ( 'NONE', *, *, #79079, .T. ) ;
#74761 = ORIENTED_EDGE ( 'NONE', *, *, #86777, .T. ) ;
#74762 = VERTEX_POINT ( 'NONE', #59679 ) ;
#74763 = B_SPLINE_CURVE_WITH_KNOTS ( 'NONE', 3,
 ( #83849, #15384, #49603, #16259, #3621, #2283 ),
 .UNSPECIFIED., .F., .F.,
 ( 4, 2, 4 ),
 ( 0.0003909569690057829237, 0.0005862646681846087407, 0.0007815723673634345035 ),
 .UNSPECIFIED. ) ;
#74764 = AXIS2_PLACEMENT_3D ( 'NONE', #43564, #44886, #51179 ) ;
#74765 = AXIS2_PLACEMENT_3D ( 'NONE', #68786, #70998, #57923 ) ;
#74766 = CARTESIAN_POINT ( 'NONE',  ( -14.98082382139118884, -4.176053281294518804, 33.81426240980091791 ) ) ;
#74767 = CARTESIAN_POINT ( 'NONE',  ( 7.053867364043877153, -11.37503395064541678, 33.29242100308974983 ) ) ;
#74768 = CARTESIAN_POINT ( 'NONE',  ( -10.48485891362105171, -6.852161475712352789, 34.70806712695775786 ) ) ;
#74769 = CARTESIAN_POINT ( 'NONE',  ( -15.45425415533356350, -2.353723527008296568, 30.78948104536958752 ) ) ;
#74770 = B_SPLINE_CURVE_WITH_KNOTS ( 'NONE', 3,
 ( #36607, #83925, #35731, #77594, #15901, #2358, #69944, #21758, #29419, #28981 ),
 .UNSPECIFIED., .F., .F.,
 ( 4, 2, 2, 2, 4 ),
 ( 0.000000000000000000, 0.0001954311564186882026, 0.0003908623128373764051, 0.0005862934692560646619, 0.0007817246256747528103 ),
 .UNSPECIFIED. ) ;
#74771 = FACE_OUTER_BOUND ( 'NONE', #65437, .T. ) ;
#74772 = CARTESIAN_POINT ( 'NONE',  ( -3.230769230769229949, -4.661471528628507777, 34.16647553114623292 ) ) ;
#74773 = CARTESIAN_POINT ( 'NONE',  ( 13.60739492588379562, -3.236590943229499029, 32.36255958852954251 ) ) ;
#74774 = AXIS2_PLACEMENT_3D ( 'NONE', #67848, #40390, #19222 ) ;
#74775 = AXIS2_PLACEMENT_3D ( 'NONE', #68145, #6448, #47866 ) ;
#74776 = ADVANCED_FACE ( 'NONE', ( #87178 ), #52910, .F. ) ;
#74777 = CARTESIAN_POINT ( 'NONE',  ( 14.30769230769231015, -3.886160181151819604, 36.00935417666054406 ) ) ;
#74778 = ORIENTED_EDGE ( 'NONE', *, *, #8986, .T. ) ;
#74779 = VERTEX_POINT ( 'NONE', #56022 ) ;
#74781 = ORIENTED_EDGE ( 'NONE', *, *, #69341, .T. ) ;
#74780 = CARTESIAN_POINT ( 'NONE',  ( 18.06606733335007675, -9.058645607665452459, 34.76329471203371924 ) ) ;
#74782 = EDGE_CURVE ( 'NONE', #28433, #30133, #22036, .T. ) ;
#74783 = CARTESIAN_POINT ( 'NONE',  ( 11.60452887181161508, -3.322132147404559976, 32.92929555188717927 ) ) ;
#74784 = CARTESIAN_POINT ( 'NONE',  ( 11.76147289007438879, -12.15243808032445827, 31.58219941686247978 ) ) ;
#74785 = EDGE_LOOP ( 'NONE', ( #16012, #20316 ) ) ;
#74786 = DIRECTION ( 'NONE',  ( 1.734723475976813504E-16, -1.000000000000000000, 0.000000000000000000 ) ) ;
#74787 = EDGE_CURVE ( 'NONE', #86499, #54317, #88956, .T. ) ;
#74788 = ORIENTED_EDGE ( 'NONE', *, *, #480, .T. ) ;
#74789 = LINE ( 'NONE', #40564, #65530 ) ;
#74790 = EDGE_LOOP ( 'NONE', ( #69328, #47517 ) ) ;
#74791 = CARTESIAN_POINT ( 'NONE',  ( 9.915087233576098669, -8.496831190052093419, 34.64984203495476578 ) ) ;
#74792 = EDGE_LOOP ( 'NONE', ( #15026, #3199 ) ) ;
#74793 = CARTESIAN_POINT ( 'NONE',  ( -12.39547112818838492, -9.905515769479276145, 34.41647553114623292 ) ) ;
#74794 = AXIS2_PLACEMENT_3D ( 'NONE', #81045, #66172, #5378 ) ;
#74795 = CARTESIAN_POINT ( 'NONE',  ( 10.83839596699746721, -4.887748414852792322, 34.01359900205216746 ) ) ;
#74796 = FACE_BOUND ( 'NONE', #84471, .T. ) ;
#74797 = EDGE_CURVE ( 'NONE', #55341, #39944, #9122, .T. ) ;
#74798 = CARTESIAN_POINT ( 'NONE',  ( 12.71153846153988098, -7.500000000000154543, 35.00000000000007105 ) ) ;
#74799 = DIRECTION ( 'NONE',  ( -0.000000000000000000, 0.5000000000000011102, -0.8660254037844381525 ) ) ;
#74800 = CARTESIAN_POINT ( 'NONE',  ( -1.608100309179714582, -2.353723527008297012, 30.78948104536958397 ) ) ;
#74801 = CARTESIAN_POINT ( 'NONE',  ( -3.230769230769229949, -4.098570777380720287, 33.41473453929634729 ) ) ;
#74802 = DIRECTION ( 'NONE',  ( 0.000000000000000000, 0.6427876096865368094, 0.7660444431189802339 ) ) ;
#74803 = DIRECTION ( 'NONE',  ( -0.000000000000000000, 0.7660444431189791237, -0.6427876096865379196 ) ) ;
#74804 = EDGE_CURVE ( 'NONE', #2166, #65829, #79948, .T. ) ;
#74805 = CARTESIAN_POINT ( 'NONE',  ( -10.48459280755982626, -4.118422570099831148, 33.43335022499816489 ) ) ;
#74806 = ORIENTED_EDGE ( 'NONE', *, *, #54401, .T. ) ;
#74807 = ORIENTED_EDGE ( 'NONE', *, *, #69211, .T. ) ;
#74809 = DIRECTION ( 'NONE',  ( -1.000000000000000000, -0.000000000000000000, -0.000000000000000000 ) ) ;
#74808 = CARTESIAN_POINT ( 'NONE',  ( -8.769230769230890843, -11.94971097300221174, 32.03036669348237098 ) ) ;
#74810 = CARTESIAN_POINT ( 'NONE',  ( -9.692307692307691624, -9.584722331328613620, 36.20867863119891439 ) ) ;
#74811 = DIRECTION ( 'NONE',  ( -1.000000000000000000, -0.000000000000000000, -0.000000000000000000 ) ) ;
#74812 = CARTESIAN_POINT ( 'NONE',  ( 8.992657168145557378, -7.630147987733840509, 34.99859428049665411 ) ) ;
#74813 = CARTESIAN_POINT ( 'NONE',  ( -13.13456107297706765, -2.779044189368095275, 31.39831045268885745 ) ) ;
#74814 = ORIENTED_EDGE ( 'NONE', *, *, #16168, .F. ) ;
#74815 = CARTESIAN_POINT ( 'NONE',  ( -5.776987155906603277, -8.282913670948747864, 34.94150082978203642 ) ) ;
#74816 = EDGE_CURVE ( 'NONE', #18683, #80371, #33979, .T. ) ;
#74817 = CARTESIAN_POINT ( 'NONE',  ( -4.826977558574935045, -2.587454068350147462, 30.68340429815432202 ) ) ;
#74818 = FACE_OUTER_BOUND ( 'NONE', #52948, .T. ) ;
#74819 = VECTOR ( 'NONE', #9561, 1000.000000000000114 ) ;
#74820 = DIRECTION ( 'NONE',  ( -0.000000000000000000, -0.5000000000000009992, -0.8660254037844380415 ) ) ;
#74821 = EDGE_LOOP ( 'NONE', ( #62706, #53495 ) ) ;
#74822 = B_SPLINE_CURVE_WITH_KNOTS ( 'NONE', 3,
 ( #57198, #1809, #43678, #55424, #488, #82909, #42812, #77907, #76591, #7246 ),
 .UNSPECIFIED., .F., .F.,
 ( 4, 2, 2, 2, 4 ),
 ( 0.0007817359430256326080, 0.0009771253907249993591, 0.001172514838424366327, 0.001367904286123733078, 0.001563293733823099829 ),
 .UNSPECIFIED. ) ;
#74823 = ORIENTED_EDGE ( 'NONE', *, *, #61704, .T. ) ;
#74824 = VECTOR ( 'NONE', #4936, 1000.000000000000000 ) ;
#74825 = AXIS2_PLACEMENT_3D ( 'NONE', #34349, #83446, #575 ) ;
#74826 = VERTEX_POINT ( 'NONE', #61887 ) ;
#74827 = CYLINDRICAL_SURFACE ( 'NONE', #67899, 0.2499999999999995559 ) ;
#74828 = ORIENTED_EDGE ( 'NONE', *, *, #6367, .T. ) ;
#74829 = CARTESIAN_POINT ( 'NONE',  ( 6.923076923076924238, -1.790695186598648903, 34.54067556320373455 ) ) ;
#74830 = CARTESIAN_POINT ( 'NONE',  ( -10.61538461538473399, -6.879047030192662504, 34.71129190930017927 ) ) ;
#74831 = CARTESIAN_POINT ( 'NONE',  ( -5.076923076923197442, -4.481592998941358097, 33.73612834414048933 ) ) ;
#74832 = CARTESIAN_POINT ( 'NONE',  ( 8.834485908743602067, -3.643525952247864463, 33.31231777344670064 ) ) ;
#74833 = AXIS2_PLACEMENT_3D ( 'NONE', #3486, #2597, #52120 ) ;
#74834 = EDGE_CURVE ( 'NONE', #38437, #80242, #14370, .T. ) ;
#74835 = CYLINDRICAL_SURFACE ( 'NONE', #66161, 0.2499999999999995559 ) ;
#74836 = ORIENTED_EDGE ( 'NONE', *, *, #64510, .T. ) ;
#74837 = CARTESIAN_POINT ( 'NONE',  ( -11.78846153846154010, -7.433932668274256805, 35.00000000000000711 ) ) ;
#74839 = ORIENTED_EDGE ( 'NONE', *, *, #79985, .T. ) ;
#74838 = CARTESIAN_POINT ( 'NONE',  ( -12.46153846153858247, -11.94971097300221174, 32.03036669348237098 ) ) ;
#74840 = CARTESIAN_POINT ( 'NONE',  ( -5.326899820971668476, -2.318417181685854978, 30.59732222474233865 ) ) ;
#74841 = CARTESIAN_POINT ( 'NONE',  ( 15.90384615384614619, -2.499999999999999556, 29.81609845454691765 ) ) ;
#74842 = CARTESIAN_POINT ( 'NONE',  ( 1.449761163947351328, -7.750023238201980469, 34.74374492549440419 ) ) ;
#74843 = EDGE_CURVE ( 'NONE', #56000, #6801, #642, .T. ) ;
#74844 = EDGE_CURVE ( 'NONE', #16480, #65802, #15048, .T. ) ;
#74845 = CARTESIAN_POINT ( 'NONE',  ( -2.557669051740897537, -12.65889640711025521, 30.72598325615533454 ) ) ;
#74846 = CARTESIAN_POINT ( 'NONE',  ( 13.16113046005105502, -4.225889041578353655, 33.85425143139329407 ) ) ;
#74847 = CARTESIAN_POINT ( 'NONE',  ( 18.22277954126840172, -2.600157965045223563, 30.74683119005207033 ) ) ;
#74848 = DIRECTION ( 'NONE',  ( -0.000000000000000000, 1.000000000000000000, -0.000000000000000000 ) ) ;
#74849 = CARTESIAN_POINT ( 'NONE',  ( 1.200186371490529202, -4.775308065498752974, 21.98624329374151642 ) ) ;
#74850 = EDGE_CURVE ( 'NONE', #74160, #85301, #47038, .T. ) ;
#74851 = VERTEX_POINT ( 'NONE', #54243 ) ;
#74852 = EDGE_CURVE ( 'NONE', #31425, #40761, #20022, .T. ) ;
#74853 = CARTESIAN_POINT ( 'NONE',  ( 11.53846153846141753, -2.892918686052165622, 31.69288490824153470 ) ) ;
#74854 = CARTESIAN_POINT ( 'NONE',  ( -14.08491263871424160, -3.563462043263030399, 33.22394488606062879 ) ) ;
#74855 = CARTESIAN_POINT ( 'NONE',  ( -27.00000000000000000, -9.000000000000001776, 3.000000000000000444 ) ) ;
#74856 = ORIENTED_EDGE ( 'NONE', *, *, #84704, .T. ) ;
#74857 = CARTESIAN_POINT ( 'NONE',  ( -12.71151519248081740, -11.79746400365624659, 32.30657167506340954 ) ) ;
#74858 = LINE ( 'NONE', #11820, #58403 ) ;
#74859 = DIRECTION ( 'NONE',  ( -0.000000000000000000, 0.1736481776669307198, -0.9848077530122080203 ) ) ;
#74860 = DIRECTION ( 'NONE',  ( 0.000000000000000000, 0.1736481776669275834, 0.9848077530122086864 ) ) ;
#74861 = CARTESIAN_POINT ( 'NONE',  ( 14.30769230769218758, -11.48612834414049644, 32.76840700105863391 ) ) ;
#74862 = VERTEX_POINT ( 'NONE', #78066 ) ;
#74863 = CARTESIAN_POINT ( 'NONE',  ( 16.82694634598072625, -3.137211980971220893, 32.19342716148376837 ) ) ;
#74864 = B_SPLINE_CURVE_WITH_KNOTS ( 'NONE', 3,
 ( #28890, #84723, #41953, #55895, #35639, #77064, #36084, #75721, #42403, #63536 ),
 .UNSPECIFIED., .F., .F.,
 ( 4, 2, 2, 2, 4 ),
 ( 0.000000000000000000, 0.0001954339857564081791, 0.0003908679715128163582, 0.0005863019572692245102, 0.0007817359430256327164 ),
 .UNSPECIFIED. ) ;
#74865 = CARTESIAN_POINT ( 'NONE',  ( 17.29993442853592711, -5.667800583137506898, 34.40243808032445827 ) ) ;
#74866 = CARTESIAN_POINT ( 'NONE',  ( 5.326868486301119532, -12.45601412856602863, 31.48342859153981621 ) ) ;
#74868 = ORIENTED_EDGE ( 'NONE', *, *, #66514, .F. ) ;
#74867 = VECTOR ( 'NONE', #82500, 1000.000000000000000 ) ;
#74869 = CARTESIAN_POINT ( 'NONE',  ( -8.834984197544098805, -7.249945578846652694, 34.99404164642496795 ) ) ;
#74870 = VERTEX_POINT ( 'NONE', #16368 ) ;
#74871 = CARTESIAN_POINT ( 'NONE',  ( -16.40386939113911779, -5.851115903089112003, 34.47074536777953568 ) ) ;
#74872 = FILL_AREA_STYLE ('',( #81624 ) ) ;
#74873 = CARTESIAN_POINT ( 'NONE',  ( 11.40777093535123221, -2.494641256782728966, 31.33461815524612959 ) ) ;
#74874 = ORIENTED_EDGE ( 'NONE', *, *, #75834, .F. ) ;
#74875 = LINE ( 'NONE', #73985, #59143 ) ;
#74876 = CYLINDRICAL_SURFACE ( 'NONE', #52158, 0.2499999999999986955 ) ;
#74877 = CARTESIAN_POINT ( 'NONE',  ( 5.198717948717946236, -11.50000000000000000, 29.75000000000000355 ) ) ;
#74878 = CARTESIAN_POINT ( 'NONE',  ( 13.38461538461526601, -11.94971097300221174, 32.03036669348237098 ) ) ;
#74879 = CARTESIAN_POINT ( 'NONE',  ( 11.00641025641025550, -11.50000000000000000, 29.75000000000000355 ) ) ;
#74880 = EDGE_LOOP ( 'NONE', ( #70572, #57107 ) ) ;
#74881 = AXIS2_PLACEMENT_3D ( 'NONE', #4792, #54288, #13315 ) ;
#74882 = FACE_BOUND ( 'NONE', #35305, .T. ) ;
#74883 = ORIENTED_EDGE ( 'NONE', *, *, #42146, .F. ) ;
#74884 = CARTESIAN_POINT ( 'NONE',  ( 17.99999999999987566, -11.06231777344772027, 33.60647404775119895 ) ) ;
#74885 = CARTESIAN_POINT ( 'NONE',  ( 5.076923076922954969, -12.46129190930018460, 30.37095296980731973 ) ) ;
#74886 = AXIS2_PLACEMENT_3D ( 'NONE', #50113, #29857, #65725 ) ;
#74887 = CARTESIAN_POINT ( 'NONE',  ( -15.84615384615384670, -7.500000000000000000, 29.75000000000000355 ) ) ;
#74888 = CYLINDRICAL_SURFACE ( 'NONE', #34874, 0.2499999999999998890 ) ;
#74889 = CARTESIAN_POINT ( 'NONE',  ( 14.55774672760575861, -8.346898887586323923, 34.93166121998716278 ) ) ;
#74890 = AXIS2_PLACEMENT_3D ( 'NONE', #63031, #21172, #34696 ) ;
#74891 = ORIENTED_EDGE ( 'NONE', *, *, #5205, .F. ) ;
#74892 = B_SPLINE_CURVE_WITH_KNOTS ( 'NONE', 3,
 ( #60036, #10527, #65897, #80779, #85744, #24025, #78977, #3758, #31232, #58700 ),
 .UNSPECIFIED., .F., .F.,
 ( 4, 2, 2, 2, 4 ),
 ( 0.0007817359430256330417, 0.0009771253907250000096, 0.001172514838424367194, 0.001367904286123734162, 0.001563293733823101130 ),
 .UNSPECIFIED. ) ;
#74893 = ORIENTED_EDGE ( 'NONE', *, *, #23999, .F. ) ;
#74894 = AXIS2_PLACEMENT_3D ( 'NONE', #41077, #34309, #65269 ) ;
#74895 = ORIENTED_EDGE ( 'NONE', *, *, #42626, .F. ) ;
#74896 = VERTEX_POINT ( 'NONE', #71742 ) ;
#74897 = B_SPLINE_CURVE_WITH_KNOTS ( 'NONE', 3,
 ( #57491, #43976, #77765, #57935, #63364, #35457, #22383, #85419, #77327, #43535 ),
 .UNSPECIFIED., .F., .F.,
 ( 4, 2, 2, 2, 4 ),
 ( 0.0007817246256747471724, 0.0009771112852218905021, 0.001172497944769033615, 0.001367884604316176944, 0.001563271263863320274 ),
 .UNSPECIFIED. ) ;
#74898 = CARTESIAN_POINT ( 'NONE',  ( -7.384615384615385025, -3.499999999999999556, 29.75000000000000355 ) ) ;
#74899 = CARTESIAN_POINT ( 'NONE',  ( 16.28463659481310444, -10.70102852606553157, 33.91149625220312913 ) ) ;
#74900 = DIRECTION ( 'NONE',  ( -0.000000000000000000, 1.000000000000000000, 3.491481338843133355E-15 ) ) ;
#74901 = CARTESIAN_POINT ( 'NONE',  ( 5.076923076922953193, -11.67786785259630911, 32.92929555188603530 ) ) ;
#74903 = EDGE_CURVE ( 'NONE', #13392, #7875, #56472, .T. ) ;
#74902 = FACE_OUTER_BOUND ( 'NONE', #6122, .T. ) ;
#74904 = CARTESIAN_POINT ( 'NONE',  ( 12.46153846153846168, -6.435427911321262684, 35.78748833219616898 ) ) ;
#74905 = CARTESIAN_POINT ( 'NONE',  ( -17.93455011887488126, -12.75000000000000533, 29.49999999999997868 ) ) ;
#74906 = CARTESIAN_POINT ( 'NONE',  ( -11.25641025641025550, -7.500000000000000000, 29.75000000000000355 ) ) ;
#74907 = EDGE_LOOP ( 'NONE', ( #83097, #55110, #34993, #14744 ) ) ;
#74908 = ORIENTED_EDGE ( 'NONE', *, *, #8095, .T. ) ;
#74909 = EDGE_LOOP ( 'NONE', ( #47865, #51999 ) ) ;
#74910 = CARTESIAN_POINT ( 'NONE',  ( -13.60754234352223335, -12.38737895849757820, 31.66785238281580206 ) ) ;
#74912 = CARTESIAN_POINT ( 'NONE',  ( 6.923076923076924238, -1.629998284177014645, 34.34916445242399163 ) ) ;
#74911 = CARTESIAN_POINT ( 'NONE',  ( -39.05038313613820122, -2.499999999999999556, 29.75000000000000355 ) ) ;
#74913 = CARTESIAN_POINT ( 'NONE',  ( -10.03846153846153832, -3.499999999999999556, 29.75000000000000355 ) ) ;
#74914 = CYLINDRICAL_SURFACE ( 'NONE', #16385, 0.2499999999999995559 ) ;
#74915 = FACE_BOUND ( 'NONE', #1197, .T. ) ;
#74916 = ORIENTED_EDGE ( 'NONE', *, *, #41553, .F. ) ;
#74917 = ADVANCED_FACE ( 'NONE', ( #23997 ), #29454, .F. ) ;
#74918 = CARTESIAN_POINT ( 'NONE',  ( 14.30769230769218581, -2.379036618888197729, 30.90682066428292885 ) ) ;
#74919 = CARTESIAN_POINT ( 'NONE',  ( -3.165513659493205623, -6.879047030191282275, 34.71129190930002295 ) ) ;
#74920 = VECTOR ( 'NONE', #86386, 1000.000000000000227 ) ;
#74921 = VERTEX_POINT ( 'NONE', #50586 ) ;
#74922 = CARTESIAN_POINT ( 'NONE',  ( 4.853438152358743984, -2.353723527008295680, 30.78948104536958752 ) ) ;
#74923 = VERTEX_POINT ( 'NONE', #72189 ) ;
#74924 = FACE_BOUND ( 'NONE', #46932, .T. ) ;
#74925 = CARTESIAN_POINT ( 'NONE',  ( 7.622668902429897919, -11.89387501736622710, 32.13663884655806413 ) ) ;
#74926 = B_SPLINE_CURVE_WITH_KNOTS ( 'NONE', 3,
 ( #685, #48869, #17304, #64143, #2016, #2445, #2882, #9231, #64584, #10100 ),
 .UNSPECIFIED., .F., .F.,
 ( 4, 2, 2, 2, 4 ),
 ( 0.0007817246256747455461, 0.0009771112852218883336, 0.001172497944769031230, 0.001367884604316174126, 0.001563271263863317022 ),
 .UNSPECIFIED. ) ;
#74927 = CARTESIAN_POINT ( 'NONE',  ( -13.60810032833933469, -10.81261337010820256, 33.49550067578627477 ) ) ;
#74928 = ORIENTED_EDGE ( 'NONE', *, *, #19082, .T. ) ;
#74929 = FACE_OUTER_BOUND ( 'NONE', #6718, .T. ) ;
#74930 = CARTESIAN_POINT ( 'NONE',  ( 10.61538461538449418, -5.941354392335915335, 34.76329471203413846 ) ) ;
#74931 = CARTESIAN_POINT ( 'NONE',  ( 2.980792486720641232, -12.01397095200673881, 32.43157075238190146 ) ) ;
#74932 = ORIENTED_EDGE ( 'NONE', *, *, #44877, .F. ) ;
#74933 = B_SPLINE_CURVE_WITH_KNOTS ( 'NONE', 3,
 ( #82741, #13383, #755, #84077, #42199, #42636, #34098, #34543, #22353, #21470 ),
 .UNSPECIFIED., .F., .F.,
 ( 4, 2, 2, 2, 4 ),
 ( 0.0007817359430256322827, 0.0009771253907249989254, 0.001172514838424365676, 0.001367904286123732428, 0.001563293733823098962 ),
 .UNSPECIFIED. ) ;
#74934 = CARTESIAN_POINT ( 'NONE',  ( 6.699591979352975457, -5.912607949931405038, 34.49155766932282319 ) ) ;
#74935 = CARTESIAN_POINT ( 'NONE',  ( -17.07692307692307665, -1.117168528481311540, 33.14645433367849847 ) ) ;
#74936 = CARTESIAN_POINT ( 'NONE',  ( 12.71148397988660150, -6.696923467548660192, 34.68552623307873972 ) ) ;
#74937 = CARTESIAN_POINT ( 'NONE',  ( -17.77698715590660328, -12.64618726649961289, 30.78989965857442712 ) ) ;
#74938 = EDGE_LOOP ( 'NONE', ( #82015, #28956 ) ) ;
#74939 = CARTESIAN_POINT ( 'NONE',  ( -12.21159294319032185, -3.202959910592335646, 32.30730279482227019 ) ) ;
#74940 = DIRECTION ( 'NONE',  ( -0.000000000000000000, -0.8660254037844399289, -0.4999999999999980016 ) ) ;
#74941 = ORIENTED_EDGE ( 'NONE', *, *, #67812, .F. ) ;
#74942 = CARTESIAN_POINT ( 'NONE',  ( 9.692307692307695177, -1.215029322943914858, 32.30358669280327177 ) ) ;
#74943 = CARTESIAN_POINT ( 'NONE',  ( 9.942307692309114486, -7.500000000000154543, 35.00000000000007105 ) ) ;
#74944 = CARTESIAN_POINT ( 'NONE',  ( 5.869852790561781219, -9.418419913701741919, 34.36755862841477693 ) ) ;
#74945 = CARTESIAN_POINT ( 'NONE',  ( -11.60373198442231590, -8.613356846314824011, 34.62446782046655613 ) ) ;
#74947 = CARTESIAN_POINT ( 'NONE',  ( -13.31854703361294767, -3.513871655860379306, 32.76840700105978499 ) ) ;
#74946 = B_SPLINE_CURVE_WITH_KNOTS ( 'NONE', 3,
 ( #69310, #14813, #7608, #35071, #62529, #844, #55780, #83270, #21557, #88280 ),
 .UNSPECIFIED., .F., .F.,
 ( 4, 2, 2, 2, 4 ),
 ( 0.0007817246256747519429, 0.0009771112852218970073, 0.001172497944769042288, 0.001367884604316187353, 0.001563271263863332417 ),
 .UNSPECIFIED. ) ;
#74948 = ADVANCED_FACE ( 'NONE', ( #50140 ), #51010, .F. ) ;
#74949 = EDGE_CURVE ( 'NONE', #45049, #25143, #81078, .T. ) ;
#74950 = CARTESIAN_POINT ( 'NONE',  ( -19.50000000000000000, -11.50000000000000000, 29.75000000000000355 ) ) ;
#74952 = CARTESIAN_POINT ( 'NONE',  ( -16.15384615384627409, -8.656820664282941280, 34.87096338111179961 ) ) ;
#74951 = FACE_OUTER_BOUND ( 'NONE', #34264, .T. ) ;
#74953 = VECTOR ( 'NONE', #75365, 1000.000000000000227 ) ;
#74954 = DIRECTION ( 'NONE',  ( -0.000000000000000000, 0.1736481776669307198, -0.9848077530122080203 ) ) ;
#74955 = CARTESIAN_POINT ( 'NONE',  ( 2.750000000000001776, -7.499999999999984013, 18.21875000000000000 ) ) ;
#74956 = ORIENTED_EDGE ( 'NONE', *, *, #40379, .F. ) ;
#74957 = CARTESIAN_POINT ( 'NONE',  ( -15.23076923076935074, -3.835265460704628371, 33.15142922262033665 ) ) ;
#74958 = ORIENTED_EDGE ( 'NONE', *, *, #27373, .F. ) ;
#74959 = AXIS2_PLACEMENT_3D ( 'NONE', #67945, #83230, #20199 ) ;
#74960 = VERTEX_POINT ( 'NONE', #49708 ) ;
#74961 = CARTESIAN_POINT ( 'NONE',  ( -8.703975629717932705, -6.835583212224610072, 34.95778746994559327 ) ) ;
#74962 = EDGE_LOOP ( 'NONE', ( #44107, #6636, #63276, #46950 ) ) ;
#74963 = DIRECTION ( 'NONE',  ( -0.000000000000000000, -0.1736481776669307198, -0.9848077530122080203 ) ) ;
#74964 = CARTESIAN_POINT ( 'NONE',  ( 1.944543648262996083, -5.555456351736983045, 18.06250000000000355 ) ) ;
#74965 = ADVANCED_FACE ( 'NONE', ( #77625 ), #1971, .F. ) ;
#74966 = CARTESIAN_POINT ( 'NONE',  ( -14.30769230769242917, -3.083524468854526912, 32.58852847137268327 ) ) ;
#74967 = DIRECTION ( 'NONE',  ( -0.000000000000000000, -0.9396926207859093161, -0.3420201433256663259 ) ) ;
#74968 = CARTESIAN_POINT ( 'NONE',  ( 6.249945518348143381, -3.202959910592335202, 32.30730279482227019 ) ) ;
#74969 = CARTESIAN_POINT ( 'NONE',  ( -6.923076923076922462, -8.810774026931790459, 35.74407628777942847 ) ) ;
#74970 = CARTESIAN_POINT ( 'NONE',  ( 9.692307692307695177, -12.34228464037088635, 31.77849191805839268 ) ) ;
#74971 = DIRECTION ( 'NONE',  ( -0.000000000000000000, 1.000000000000000000, 3.491481338843133355E-15 ) ) ;
#74972 = FACE_OUTER_BOUND ( 'NONE', #36797, .T. ) ;
#74973 = CARTESIAN_POINT ( 'NONE',  ( 10.68145194873469173, -12.34228464037088813, 31.77849191805839268 ) ) ;
#74974 = CARTESIAN_POINT ( 'NONE',  ( -13.16183584334697443, -6.760870238392817200, 34.69528174975672385 ) ) ;
#74975 = CARTESIAN_POINT ( 'NONE',  ( 5.207713517890025123, -10.70102852606553157, 33.91149625220312913 ) ) ;
#74976 = VERTEX_POINT ( 'NONE', #58229 ) ;
#74977 = VERTEX_POINT ( 'NONE', #15492 ) ;
#74978 = DIRECTION ( 'NONE',  ( -0.000000000000000000, 0.7660444431189791237, -0.6427876096865379196 ) ) ;
#74979 = CARTESIAN_POINT ( 'NONE',  ( 5.207714884747862705, -8.999086150933472084, 34.52020707165672064 ) ) ;
#74980 = CYLINDRICAL_SURFACE ( 'NONE', #79972, 0.2500000000000002220 ) ;
#74981 = CARTESIAN_POINT ( 'NONE',  ( -11.66893824657800316, -7.276988635370452485, 34.74523720219453793 ) ) ;
#74982 = LINE ( 'NONE', #25901, #26215 ) ;
#74983 = CARTESIAN_POINT ( 'NONE',  ( -9.561517251340744039, -10.70102852606553157, 33.91149625220312913 ) ) ;
#74984 = VECTOR ( 'NONE', #66217, 1000.000000000000000 ) ;
#74985 = CARTESIAN_POINT ( 'NONE',  ( 19.00000000000000000, -1.249999999999999778, 24.75000000000000000 ) ) ;
#74986 = ORIENTED_EDGE ( 'NONE', *, *, #50912, .F. ) ;
#74987 = CARTESIAN_POINT ( 'NONE',  ( -5.076923076923197442, -12.46129190930018460, 30.37095296980731973 ) ) ;
#74988 = ORIENTED_EDGE ( 'NONE', *, *, #82380, .T. ) ;
#74989 = VECTOR ( 'NONE', #78475, 1000.000000000000000 ) ;
#74990 = B_SPLINE_CURVE_WITH_KNOTS ( 'NONE', 3,
 ( #71352, #43450, #64146, #23613, #35817, #35359, #15541, #37124, #1580, #9658 ),
 .UNSPECIFIED., .F., .F.,
 ( 4, 2, 2, 2, 4 ),
 ( 0.0007817246256747484735, 0.0009771112852218928873, 0.001172497944769037084, 0.001367884604316181498, 0.001563271263863325912 ),
 .UNSPECIFIED. ) ;
#74991 = ORIENTED_EDGE ( 'NONE', *, *, #85193, .T. ) ;
#74992 = CARTESIAN_POINT ( 'NONE',  ( 17.86985279056177944, -3.285722584762969856, 32.44110544564090759 ) ) ;
#74993 = CARTESIAN_POINT ( 'NONE',  ( 4.023370968770434430, -7.276987145209185215, 34.99546412871779211 ) ) ;
#74994 = CARTESIAN_POINT ( 'NONE',  ( 11.76124107972994537, -10.81320215134717344, 33.49497208177562868 ) ) ;
#74995 = CARTESIAN_POINT ( 'NONE',  ( -11.53846153846153655, -4.102666532097928531, 36.13435417666054406 ) ) ;
#74996 = DIRECTION ( 'NONE',  ( -1.000000000000000000, 0.000000000000000000, 0.000000000000000000 ) ) ;
#74997 = ADVANCED_FACE ( 'NONE', ( #29890 ), #71299, .F. ) ;
#74998 = VERTEX_POINT ( 'NONE', #64980 ) ;
#74999 = ORIENTED_EDGE ( 'NONE', *, *, #38209, .F. ) ;
#75000 = ORIENTED_EDGE ( 'NONE', *, *, #5358, .T. ) ;
#75001 = ORIENTED_EDGE ( 'NONE', *, *, #72683, .F. ) ;
#75002 = AXIS2_PLACEMENT_3D ( 'NONE', #37036, #9572, #51873 ) ;
#75003 = CARTESIAN_POINT ( 'NONE',  ( 18.13079044096695469, -2.295524264805589354, 30.44142389570982488 ) ) ;
#75004 = CARTESIAN_POINT ( 'NONE',  ( -10.61538461538461320, -13.57706302396349152, 30.56769352161908060 ) ) ;
#75005 = PLANE ( 'NONE',  #7746 ) ;
#75006 = CIRCLE ( 'NONE', #54810, 6.777720855862979121 ) ;
#75008 = EDGE_CURVE ( 'NONE', #67806, #38794, #19808, .T. ) ;
#75007 = CARTESIAN_POINT ( 'NONE',  ( 14.05769230769230660, -7.566082377512564960, 35.00000000000000711 ) ) ;
#75009 = LINE ( 'NONE', #25923, #12001 ) ;
#75010 = CARTESIAN_POINT ( 'NONE',  ( 2.307692307692309264, -5.471508081941601098, 34.59228464037088457 ) ) ;
#75011 = VERTEX_POINT ( 'NONE', #15933 ) ;
#75012 = EDGE_CURVE ( 'NONE', #58400, #84958, #18700, .T. ) ;
#75013 = ORIENTED_EDGE ( 'NONE', *, *, #41998, .F. ) ;
#75014 = VECTOR ( 'NONE', #8043, 1000.000000000000114 ) ;
#75015 = ORIENTED_EDGE ( 'NONE', *, *, #69496, .T. ) ;
#75017 = EDGE_LOOP ( 'NONE', ( #15261, #70779 ) ) ;
#75016 = CARTESIAN_POINT ( 'NONE',  ( -3.296851610129365451, -2.486705287966279876, 31.30864560766542937 ) ) ;
#75018 = CARTESIAN_POINT ( 'NONE',  ( 9.692307692307570832, -8.656820664282941280, 34.87096338111179961 ) ) ;
#75019 = CARTESIAN_POINT ( 'NONE',  ( -4.946397375159516052, -11.46989282347013095, 32.79007818306219946 ) ) ;
#75020 = CARTESIAN_POINT ( 'NONE',  ( -3.749999999999997335, -7.500000000000021316, 20.09375000000000000 ) ) ;
#75021 = EDGE_LOOP ( 'NONE', ( #56607, #87022, #54949, #78473 ) ) ;
#75022 = ADVANCED_FACE ( 'NONE', ( #30325 ), #38413, .F. ) ;
#75023 = CARTESIAN_POINT ( 'NONE',  ( 3.454144716541651672, -2.251407671071270489, 29.88021292934942252 ) ) ;
#75024 = ORIENTED_EDGE ( 'NONE', *, *, #10944, .F. ) ;
#75025 = CARTESIAN_POINT ( 'NONE',  ( 8.096208157792160520, -12.17597550085003277, 31.52189283813461174 ) ) ;
#75026 = FACE_BOUND ( 'NONE', #30262, .T. ) ;
#75027 = DIRECTION ( 'NONE',  ( -0.000000000000000000, 0.7660444431189791237, -0.6427876096865379196 ) ) ;
#75028 = EDGE_CURVE ( 'NONE', #41890, #27582, #43409, .T. ) ;
#75029 = CARTESIAN_POINT ( 'NONE',  ( 9.692307692307695177, -2.249999999999998668, 29.75000000000001776 ) ) ;
#75030 = VERTEX_POINT ( 'NONE', #73544 ) ;
#75031 = CARTESIAN_POINT ( 'NONE',  ( 8.545745844666440050, -12.11044203135681840, 32.26167407432752299 ) ) ;
#75032 = CARTESIAN_POINT ( 'NONE',  ( 14.87820512820512953, -3.499999999999999556, 29.75000000000000355 ) ) ;
#75033 = CARTESIAN_POINT ( 'NONE',  ( -0.7115384615384606759, -2.499999999999998668, 29.75000000000000355 ) ) ;
#75034 = CARTESIAN_POINT ( 'NONE',  ( 0.7114839798866027243, -12.43552623307873972, 30.55307653245132826 ) ) ;
#75035 = ORIENTED_EDGE ( 'NONE', *, *, #78900, .F. ) ;
#75036 = VECTOR ( 'NONE', #55952, 1000.000000000000227 ) ;
#75037 = CARTESIAN_POINT ( 'NONE',  ( -11.40767109749459074, -12.35292014791297710, 31.75344720912887198 ) ) ;
#75038 = CARTESIAN_POINT ( 'NONE',  ( 1.161130460051055469, -4.225889041578353655, 33.85425143139329407 ) ) ;
#75039 = CARTESIAN_POINT ( 'NONE',  ( -4.153846153846274980, -2.379036618888197729, 30.90682066428292885 ) ) ;
#75040 = LINE ( 'NONE', #13327, #52936 ) ;
#75041 = CARTESIAN_POINT ( 'NONE',  ( 8.835298102580845025, -9.905515769479276145, 34.41647553114623292 ) ) ;
#75042 = EDGE_CURVE ( 'NONE', #68539, #76645, #18145, .T. ) ;
#75043 = FACE_BOUND ( 'NONE', #59371, .T. ) ;
#75045 = CARTESIAN_POINT ( 'NONE',  ( 11.40831432902331954, -12.45813303252208648, 30.39737893381572675 ) ) ;
#75044 = CARTESIAN_POINT ( 'NONE',  ( 5.869309396889694774, -4.684245665217972032, 34.18127051446801090 ) ) ;
#75046 = CARTESIAN_POINT ( 'NONE',  ( -15.23076923076935252, -5.094484230521993062, 34.41647553114689373 ) ) ;
#75048 = CARTESIAN_POINT ( 'NONE',  ( -2.084912638714239819, -8.540255544307065350, 34.89611431652622286 ) ) ;
#75047 = DIRECTION ( 'NONE',  ( 0.000000000000000000, 0.3420201433256610524, 0.9396926207859113145 ) ) ;
#75049 = ADVANCED_FACE ( 'NONE', ( #79848 ), #61666, .F. ) ;
#75050 = CARTESIAN_POINT ( 'NONE',  ( -10.61538461538461320, -6.343179335718451384, 34.87096338111211935 ) ) ;
#75051 = CARTESIAN_POINT ( 'NONE',  ( 1.901340078031349856, -5.512252781505337929, 19.06063170625849068 ) ) ;
#75052 = VERTEX_POINT ( 'NONE', #4176 ) ;
#75053 = CARTESIAN_POINT ( 'NONE',  ( 10.39189969082028853, -12.11044203135681840, 32.26167407432752299 ) ) ;
#75054 = ORIENTED_EDGE ( 'NONE', *, *, #47084, .T. ) ;
#75055 = CARTESIAN_POINT ( 'NONE',  ( 5.999999999999878320, -2.657715359629662988, 31.77849191805970364 ) ) ;
#75056 = EDGE_CURVE ( 'NONE', #45617, #43520, #60624, .T. ) ;
#75057 = VERTEX_POINT ( 'NONE', #86620 ) ;
#75058 = ADVANCED_FACE ( 'NONE', ( #82409 ), #5071, .F. ) ;
#75059 = CARTESIAN_POINT ( 'NONE',  ( -18.00000000000000000, -2.499999999999999556, 29.49999999999998579 ) ) ;
#75060 = CARTESIAN_POINT ( 'NONE',  ( -1.384615384615383471, -10.51840700105979565, 33.73612834413961536 ) ) ;
#75062 = ORIENTED_EDGE ( 'NONE', *, *, #16516, .F. ) ;
#75061 = CARTESIAN_POINT ( 'NONE',  ( -1.384615384615383471, -8.810774026931790459, 35.74407628777942847 ) ) ;
#75063 = CARTESIAN_POINT ( 'NONE',  ( -9.468880730446121774, -7.630147231320743018, 34.74852402298682819 ) ) ;
#75064 = CARTESIAN_POINT ( 'NONE',  ( -1.200186371490556958, -4.775308065498765409, 17.57625670625849068 ) ) ;
#75065 = CARTESIAN_POINT ( 'NONE',  ( 4.284637961670939355, -10.54018710029568595, 33.71981072465678864 ) ) ;
#75066 = LINE ( 'NONE', #75941, #13006 ) ;
#75067 = CARTESIAN_POINT ( 'NONE',  ( 0.08744816603778360342, -4.750004910481952614, 28.75002700765199037 ) ) ;
#75068 = CARTESIAN_POINT ( 'NONE',  ( 10.36540787133602670, -2.544273027872575366, 31.48422191005632342 ) ) ;
#75069 = CARTESIAN_POINT ( 'NONE',  ( -12.33101302330481808, -8.630441415882550871, 34.87705825610312615 ) ) ;
#75070 = CARTESIAN_POINT ( 'NONE',  ( -5.777220458731589403, -10.81320215134717344, 33.49497208177562868 ) ) ;
#75071 = CARTESIAN_POINT ( 'NONE',  ( -2.608446859217920633, -4.805146000318815780, 23.00186829374151287 ) ) ;
#75072 = CARTESIAN_POINT ( 'NONE',  ( 14.08420736396836226, -5.912607949931405926, 34.49155766932282319 ) ) ;
#75073 = ORIENTED_EDGE ( 'NONE', *, *, #6854, .T. ) ;
#75074 = DIRECTION ( 'NONE',  ( 0.000000000000000000, 0.7660444431189807890, 0.6427876096865361433 ) ) ;
#75075 = CARTESIAN_POINT ( 'NONE',  ( -1.614399933863613468, -11.22469193450124969, 25.11124329374151642 ) ) ;
#75076 = AXIS2_PLACEMENT_3D ( 'NONE', #78117, #31265, #58730 ) ;
#75077 = CARTESIAN_POINT ( 'NONE',  ( -9.692307692307691624, -2.499999999999998668, 29.75000000000001421 ) ) ;
#75078 = CARTESIAN_POINT ( 'NONE',  ( 5.326977496836529546, -6.523592122091591783, 34.90882529074906415 ) ) ;
#75079 = AXIS2_PLACEMENT_3D ( 'NONE', #57362, #50602, #72200 ) ;
#75080 = VERTEX_POINT ( 'NONE', #87513 ) ;
#75081 = CARTESIAN_POINT ( 'NONE',  ( -9.692307692307691624, -13.95598074871891292, 31.83374038241031911 ) ) ;
#75082 = CARTESIAN_POINT ( 'NONE',  ( -16.82697766754503377, -9.357781135181033605, 34.66075350412533851 ) ) ;
#75084 = EDGE_LOOP ( 'NONE', ( #33458, #61548, #15828, #63464 ) ) ;
#75083 = FACE_OUTER_BOUND ( 'NONE', #75760, .T. ) ;
#75085 = CYLINDRICAL_SURFACE ( 'NONE', #80029, 0.2500000000000012212 ) ;
#75086 = CARTESIAN_POINT ( 'NONE',  ( -17.07692307692307665, -8.564572088678739092, 35.78748833219616898 ) ) ;
#75087 = VECTOR ( 'NONE', #70967, 1000.000000000000000 ) ;
#75088 = DIRECTION ( 'NONE',  ( -0.000000000000000000, -0.8660254037844399289, -0.4999999999999980016 ) ) ;
#75089 = CARTESIAN_POINT ( 'NONE',  ( 2.242422307135989890, -4.320704448112771878, 33.92786785259540494 ) ) ;
#75090 = EDGE_CURVE ( 'NONE', #46711, #19405, #48155, .T. ) ;
#75091 = CARTESIAN_POINT ( 'NONE',  ( -13.60810032833933469, -11.89387501736622710, 32.13663884655806413 ) ) ;
#75092 = CARTESIAN_POINT ( 'NONE',  ( -13.31854805126531005, -8.164416787775445883, 34.95778746994558617 ) ) ;
#75093 = ORIENTED_EDGE ( 'NONE', *, *, #87924, .T. ) ;
#75094 = EDGE_LOOP ( 'NONE', ( #18619, #16314, #8970, #6707 ) ) ;
#75095 = VERTEX_POINT ( 'NONE', #52359 ) ;
#75096 = B_SPLINE_CURVE_WITH_KNOTS ( 'NONE', 3,
 ( #76462, #61604, #83674, #54855, #26948, #42240, #8002, #13862, #35021, #89108 ),
 .UNSPECIFIED., .F., .F.,
 ( 4, 2, 2, 2, 4 ),
 ( 0.0007817359430256314154, 0.0009771253907249980580, 0.001172514838424364592, 0.001367904286123731127, 0.001563293733823097661 ),
 .UNSPECIFIED. ) ;
#75097 = ORIENTED_EDGE ( 'NONE', *, *, #66341, .T. ) ;
#75098 = ADVANCED_FACE ( 'NONE', ( #3729 ), #27012, .F. ) ;
#75099 = B_SPLINE_CURVE_WITH_KNOTS ( 'NONE', 3,
 ( #42275, #56218, #70619, #15243, #41828, #36395, #69297, #8484, #89143, #1266 ),
 .UNSPECIFIED., .F., .F.,
 ( 4, 2, 2, 2, 4 ),
 ( 0.000000000000000000, 0.0001954339857564071491, 0.0003908679715128142982, 0.0005863019572692214744, 0.0007817359430256285964 ),
 .UNSPECIFIED. ) ;
#75100 = CARTESIAN_POINT ( 'NONE',  ( 12.71159288145191013, -10.06805714834173493, 34.32951233291982618 ) ) ;
#75101 = CARTESIAN_POINT ( 'NONE',  ( -2.177166605928744669, -6.001044277235011215, 34.52024696741798948 ) ) ;
#75102 = B_SPLINE_CURVE_WITH_KNOTS ( 'NONE', 3,
 ( #87284, #32760, #31882, #19253, #80060, #73767, #46719, #67000, #25561, #80517 ),
 .UNSPECIFIED., .F., .F.,
 ( 4, 2, 2, 2, 4 ),
 ( 0.0007817359430256294638, 0.0009771253907249950223, 0.001172514838424360472, 0.001367904286123725922, 0.001563293733823091372 ),
 .UNSPECIFIED. ) ;
#75103 = DIRECTION ( 'NONE',  ( 0.000000000000000000, 0.8660254037844377084, 0.5000000000000015543 ) ) ;
#75104 = CYLINDRICAL_SURFACE ( 'NONE', #71115, 0.2500000000000009437 ) ;
#75105 = EDGE_CURVE ( 'NONE', #11909, #22486, #63809, .T. ) ;
#75106 = CARTESIAN_POINT ( 'NONE',  ( -16.85414353565466072, -5.114059244376869096, 34.14424750095245287 ) ) ;
#75107 = VECTOR ( 'NONE', #3127, 1000.000000000000227 ) ;
#75108 = ORIENTED_EDGE ( 'NONE', *, *, #58552, .F. ) ;
#75109 = ORIENTED_EDGE ( 'NONE', *, *, #48489, .F. ) ;
#75110 = ORIENTED_EDGE ( 'NONE', *, *, #82028, .T. ) ;
#75112 = ORIENTED_EDGE ( 'NONE', *, *, #38708, .F. ) ;
#75111 = DIRECTION ( 'NONE',  ( 0.000000000000000000, 0.1736481776669267785, -0.9848077530122087975 ) ) ;
#75113 = CARTESIAN_POINT ( 'NONE',  ( -1.607542343522233130, -2.889293201056495786, 32.26117774369186009 ) ) ;
#75114 = AXIS2_PLACEMENT_3D ( 'NONE', #3059, #35982, #53019 ) ;
#75115 = CARTESIAN_POINT ( 'NONE',  ( -10.86538461538461320, -7.566083408709835645, 34.74999999999999289 ) ) ;
#75116 = EDGE_CURVE ( 'NONE', #68374, #27164, #88579, .T. ) ;
#75117 = CARTESIAN_POINT ( 'NONE',  ( -12.21159294319031829, -12.22109172314383052, 31.39792113162168263 ) ) ;
#75118 = DIRECTION ( 'NONE',  ( -0.000000000000000000, -0.3420201433256694901, -0.9396926207859082059 ) ) ;
#75119 = ORIENTED_EDGE ( 'NONE', *, *, #71210, .F. ) ;
#75120 = EDGE_CURVE ( 'NONE', #19030, #35799, #35910, .T. ) ;
#75121 = ORIENTED_EDGE ( 'NONE', *, *, #63219, .T. ) ;
#75122 = EDGE_LOOP ( 'NONE', ( #11662, #6570 ) ) ;
#75123 = CYLINDRICAL_SURFACE ( 'NONE', #63423, 0.2499999999999986955 ) ;
#75125 = ORIENTED_EDGE ( 'NONE', *, *, #52717, .F. ) ;
#75124 = DIRECTION ( 'NONE',  ( 0.000000000000000000, 0.1736481776669267785, -0.9848077530122087975 ) ) ;
#75126 = CARTESIAN_POINT ( 'NONE',  ( 3.230769230769231726, -1.367168528481310208, 33.57946703557072254 ) ) ;
#75127 = DIRECTION ( 'NONE',  ( 0.000000000000000000, 0.9848077530122072432, 0.1736481776669354937 ) ) ;
#75128 = ORIENTED_EDGE ( 'NONE', *, *, #15460, .F. ) ;
#75129 = EDGE_CURVE ( 'NONE', #86522, #2169, #21862, .T. ) ;
#75130 = CARTESIAN_POINT ( 'NONE',  ( 11.53846153846141753, -11.48612834414049644, 32.76840700105863391 ) ) ;
#75131 = CARTESIAN_POINT ( 'NONE',  ( 0.4615384615383382183, -9.528491918059723176, 34.59228464037033035 ) ) ;
#75132 = FACE_BOUND ( 'NONE', #20548, .T. ) ;
#75133 = B_SPLINE_CURVE_WITH_KNOTS ( 'NONE', 3,
 ( #27431, #82383, #7160, #405, #27869, #82827, #69306, #21099, #48571, #76052 ),
 .UNSPECIFIED., .F., .F.,
 ( 4, 2, 2, 2, 4 ),
 ( 0.0007817359430256371616, 0.0009771253907250049969, 0.001172514838424373049, 0.001367904286123741101, 0.001563293733823108937 ),
 .UNSPECIFIED. ) ;
#75134 = DIRECTION ( 'NONE',  ( -0.000000000000000000, -0.9848077530122086864, -0.1736481776669273613 ) ) ;
#75135 = CARTESIAN_POINT ( 'NONE',  ( -6.249976744048590938, -12.41104346484419452, 31.60698883733904196 ) ) ;
#75136 = AXIS2_PLACEMENT_3D ( 'NONE', #56974, #16003, #35377 ) ;
#75137 = CARTESIAN_POINT ( 'NONE',  ( -2.307692307692305711, -9.584722331328613620, 36.20867863119891439 ) ) ;
#75139 = CARTESIAN_POINT ( 'NONE',  ( 5.010839665967194989, -3.050289026998445951, 32.03036669348365706 ) ) ;
#75138 = CARTESIAN_POINT ( 'NONE',  ( 0.3954560821783252855, -6.343179335718452272, 34.87096338111211935 ) ) ;
#75140 = VECTOR ( 'NONE', #53716, 999.9999999999998863 ) ;
#75141 = DIRECTION ( 'NONE',  ( -0.000000000000000000, 0.9848077530122085754, -0.1736481776669273613 ) ) ;
#75142 = CARTESIAN_POINT ( 'NONE',  ( -0.5916856709766840083, -3.817052484675422797, 33.13202310037935661 ) ) ;
#75143 = ORIENTED_EDGE ( 'NONE', *, *, #28727, .F. ) ;
#75144 = CARTESIAN_POINT ( 'NONE',  ( -2.557715531913761886, -4.175268141568689195, 33.81360843649122216 ) ) ;
#75145 = CARTESIAN_POINT ( 'NONE',  ( 13.16178869213638336, -7.369208160676172348, 34.74850200257122879 ) ) ;
#75146 = ORIENTED_EDGE ( 'NONE', *, *, #31901, .F. ) ;
#75147 = VECTOR ( 'NONE', #78613, 1000.000000000000000 ) ;
#75148 = CARTESIAN_POINT ( 'NONE',  ( -13.60810030917971858, -4.988325925672468131, 34.36044203135681130 ) ) ;
#75149 = CARTESIAN_POINT ( 'NONE',  ( -4.283994123577846480, -3.625366637846544560, 33.29286588640298561 ) ) ;
#75150 = VERTEX_POINT ( 'NONE', #21575 ) ;
#75151 = DIRECTION ( 'NONE',  ( -0.000000000000000000, -0.5000000000000009992, -0.8660254037844380415 ) ) ;
#75152 = CARTESIAN_POINT ( 'NONE',  ( -15.16551409125639260, -12.70778746994558439, 30.41441678777536595 ) ) ;
#75153 = EDGE_CURVE ( 'NONE', #4983, #44386, #52015, .T. ) ;
#75154 = FACE_BOUND ( 'NONE', #29647, .T. ) ;
#75156 = CARTESIAN_POINT ( 'NONE',  ( -4.153846153846152411, -8.120952969808772792, 34.71129190930000163 ) ) ;
#75155 = CARTESIAN_POINT ( 'NONE',  ( -14.30769230769242917, -4.320704448113951379, 33.92786785259630022 ) ) ;
#75157 = CARTESIAN_POINT ( 'NONE',  ( 10.48469314871705826, -8.147922237126337563, 34.70805685702651999 ) ) ;
#75158 = CARTESIAN_POINT ( 'NONE',  ( -3.230769230769351186, -2.892918686052166066, 31.69288490824153470 ) ) ;
#75159 = CARTESIAN_POINT ( 'NONE',  ( -8.769230769230768274, -12.10708131394839349, 31.69288490824020244 ) ) ;
#75160 = CARTESIAN_POINT ( 'NONE',  ( 1.553300858899129944, -11.24999999999998934, 25.95312500000000000 ) ) ;
#75161 = EDGE_LOOP ( 'NONE', ( #51836, #36348 ) ) ;
#75162 = EDGE_CURVE ( 'NONE', #16008, #40783, #76753, .T. ) ;
#75163 = ORIENTED_EDGE ( 'NONE', *, *, #73207, .T. ) ;
#75164 = LINE ( 'NONE', #13447, #3272 ) ;
#75165 = EDGE_CURVE ( 'NONE', #65590, #66285, #15499, .T. ) ;
#75166 = CARTESIAN_POINT ( 'NONE',  ( -0.6850234052624077918, -2.847400154188067578, 31.58180166144859768 ) ) ;
#75167 = CARTESIAN_POINT ( 'NONE',  ( 7.053915253563681986, -7.277220318596959281, 34.99547417642776992 ) ) ;
#75168 = CARTESIAN_POINT ( 'NONE',  ( 17.14211606521772779, -2.255955759149236073, 29.99999999999988276 ) ) ;
#75169 = CARTESIAN_POINT ( 'NONE',  ( -3.361460697436789324, -5.582088688514999397, 34.36776431015576350 ) ) ;
#75170 = CARTESIAN_POINT ( 'NONE',  ( 2.651650429449539104, -4.848349570550432475, 25.56250000000000355 ) ) ;
#75171 = CARTESIAN_POINT ( 'NONE',  ( -12.68446542044531000, -4.026226216239094491, 33.68668979543634379 ) ) ;
#75172 = CARTESIAN_POINT ( 'NONE',  ( 1.318533005255250856, -9.905515769479276145, 34.41647553114623292 ) ) ;
#75173 = DIRECTION ( 'NONE',  ( -0.000000000000000000, 1.000000000000000000, 3.491481338843133355E-15 ) ) ;
#75174 = CARTESIAN_POINT ( 'NONE',  ( -1.319470603895752214, -7.750023224968865421, 34.99404313364389907 ) ) ;
#75175 = CARTESIAN_POINT ( 'NONE',  ( -4.153846153846274980, -12.51329471203414379, 31.30864560766407578 ) ) ;
#75176 = CARTESIAN_POINT ( 'NONE',  ( 15.00784227186237985, -12.38737895849757820, 31.66785238281580206 ) ) ;
#75177 = VECTOR ( 'NONE', #13011, 1000.000000000000227 ) ;
#75178 = CARTESIAN_POINT ( 'NONE',  ( 7.173022332454968009, -3.520799739797213501, 33.17531984108286025 ) ) ;
#75179 = CARTESIAN_POINT ( 'NONE',  ( -3.361460697436789324, -8.147922237126337563, 34.70805685702651999 ) ) ;
#75180 = CARTESIAN_POINT ( 'NONE',  ( 12.71148397988660506, -2.824170634883621744, 31.52227843825338738 ) ) ;
#75181 = EDGE_CURVE ( 'NONE', #9891, #67129, #7010, .T. ) ;
#75182 = VERTEX_POINT ( 'NONE', #27283 ) ;
#75183 = FACE_OUTER_BOUND ( 'NONE', #59167, .T. ) ;
#75184 = CARTESIAN_POINT ( 'NONE',  ( -17.20707104665477161, -6.809168938359901446, 34.95455904226513866 ) ) ;
#75185 = CARTESIAN_POINT ( 'NONE',  ( 1.200186371490529202, -4.775308065498752974, 16.98624329374151287 ) ) ;
#75186 = FACE_OUTER_BOUND ( 'NONE', #17727, .T. ) ;
#75187 = CARTESIAN_POINT ( 'NONE',  ( -18.00000000000012079, -10.90142922262034020, 33.41473453929536674 ) ) ;
#75188 = EDGE_CURVE ( 'NONE', #79961, #13301, #5752, .T. ) ;
#75189 = CARTESIAN_POINT ( 'NONE',  ( -11.31544869436814338, -4.762714258010881885, 34.23016756924214832 ) ) ;
#75191 = ORIENTED_EDGE ( 'NONE', *, *, #15242, .T. ) ;
#75190 = CARTESIAN_POINT ( 'NONE',  ( -9.442253380669374252, -4.943051570960394159, 34.04725096376909477 ) ) ;
#75192 = CARTESIAN_POINT ( 'NONE',  ( -1.139087296525992388, -10.25000000000000711, 23.60937500000000711 ) ) ;
#75193 = DIRECTION ( 'NONE',  ( 0.000000000000000000, 0.000000000000000000, 1.000000000000000000 ) ) ;
#75194 = ORIENTED_EDGE ( 'NONE', *, *, #33479, .F. ) ;
#75195 = CARTESIAN_POINT ( 'NONE',  ( 11.66898697669518548, -9.503571793651731880, 34.60286762892837942 ) ) ;
#75196 = CARTESIAN_POINT ( 'NONE',  ( -10.61538461538461320, -13.37000171582298513, 34.34916445242398453 ) ) ;
#75197 = ORIENTED_EDGE ( 'NONE', *, *, #30674, .F. ) ;
#75198 = LINE ( 'NONE', #61661, #8957 ) ;
#75199 = EDGE_CURVE ( 'NONE', #545, #50608, #81526, .T. ) ;
#75200 = CARTESIAN_POINT ( 'NONE',  ( -16.40384615384615330, -7.566083408709835645, 34.74999999999999289 ) ) ;
#75201 = DIRECTION ( 'NONE',  ( -1.000000000000000000, 0.000000000000000000, 0.000000000000000000 ) ) ;
#75202 = ORIENTED_EDGE ( 'NONE', *, *, #53054, .T. ) ;
#75203 = ORIENTED_EDGE ( 'NONE', *, *, #35419, .F. ) ;
#75204 = DIRECTION ( 'NONE',  ( -0.000000000000000000, -0.000000000000000000, -1.000000000000000000 ) ) ;
#75205 = EDGE_CURVE ( 'NONE', #48154, #35110, #20086, .T. ) ;
#75206 = AXIS2_PLACEMENT_3D ( 'NONE', #76467, #42245, #89114 ) ;
#75207 = ORIENTED_EDGE ( 'NONE', *, *, #174, .F. ) ;
#75209 = CARTESIAN_POINT ( 'NONE',  ( 7.846153846153846700, -9.058645607665452459, 34.76329471203371924 ) ) ;
#75208 = VECTOR ( 'NONE', #26248, 1000.000000000000000 ) ;
#75210 = CARTESIAN_POINT ( 'NONE',  ( -9.442362173959551797, -10.05730279482229683, 34.04704008940765902 ) ) ;
#75211 = CARTESIAN_POINT ( 'NONE',  ( 9.562159722576001997, -9.504002272028875709, 34.60269587691767867 ) ) ;
#75212 = CARTESIAN_POINT ( 'NONE',  ( -2.437839517130527156, -6.001485441113818986, 34.52039167877662607 ) ) ;
#75213 = CARTESIAN_POINT ( 'NONE',  ( -0.3954711281883860896, -5.471508081941601098, 34.59228464037088457 ) ) ;
#75214 = CARTESIAN_POINT ( 'NONE',  ( 4.153846153846154188, -3.886160181151819604, 36.00935417666054406 ) ) ;
#75215 = EDGE_CURVE ( 'NONE', #32628, #31103, #29369, .T. ) ;
#75216 = CARTESIAN_POINT ( 'NONE',  ( 10.36540788444226102, -12.17611988154120972, 31.52148481390971213 ) ) ;
#75218 = EDGE_CURVE ( 'NONE', #85395, #82613, #81796, .T. ) ;
#75217 = ORIENTED_EDGE ( 'NONE', *, *, #21722, .T. ) ;
#75219 = ORIENTED_EDGE ( 'NONE', *, *, #40228, .T. ) ;
#75221 = ORIENTED_EDGE ( 'NONE', *, *, #39651, .T. ) ;
#75220 = FACE_OUTER_BOUND ( 'NONE', #15298, .T. ) ;
#75222 = CARTESIAN_POINT ( 'NONE',  ( -2.307692307692305711, -13.49023893513002648, 31.06009739812518688 ) ) ;
#75223 = CARTESIAN_POINT ( 'NONE',  ( 9.442330961365339448, -4.943428324936578910, 34.04746400365624481 ) ) ;
#75224 = ORIENTED_EDGE ( 'NONE', *, *, #84059, .F. ) ;
#75225 = EDGE_CURVE ( 'NONE', #31195, #10433, #58370, .T. ) ;
#75226 = CARTESIAN_POINT ( 'NONE',  ( 14.37375964104238513, -11.91647553114624358, 32.58852847137148245 ) ) ;
#75227 = EDGE_CURVE ( 'NONE', #52135, #45323, #33674, .T. ) ;
#75228 = VECTOR ( 'NONE', #29545, 1000.000000000000000 ) ;
#75229 = VERTEX_POINT ( 'NONE', #67830 ) ;
#75230 = CARTESIAN_POINT ( 'NONE',  ( -9.692307692307691624, -2.249999999999998668, 29.75000000000001776 ) ) ;
#75231 = ORIENTED_EDGE ( 'NONE', *, *, #79981, .T. ) ;
#75232 = AXIS2_PLACEMENT_3D ( 'NONE', #56768, #51305, #3592 ) ;
#75233 = CARTESIAN_POINT ( 'NONE',  ( -12.71156168575991785, -3.520140089381495585, 33.17453946501458262 ) ) ;
#75234 = ORIENTED_EDGE ( 'NONE', *, *, #54680, .T. ) ;
#75235 = CARTESIAN_POINT ( 'NONE',  ( -12.23875879256039489, -10.23759521482555357, 34.22997729860117033 ) ) ;
#75236 = CARTESIAN_POINT ( 'NONE',  ( 10.68145296638705410, -4.786620604624113540, 33.94971097300155805 ) ) ;
#75237 = FACE_BOUND ( 'NONE', #32659, .T. ) ;
#75238 = DIRECTION ( 'NONE',  ( -0.000000000000000000, 0.9396926207859092051, -0.3420201433256662704 ) ) ;
#75239 = CARTESIAN_POINT ( 'NONE',  ( 13.38461538461538680, -5.557115091759785130, 34.35708131394839171 ) ) ;
#75240 = DIRECTION ( 'NONE',  ( 0.000000000000000000, -6.938893903907222067E-15, 1.000000000000000000 ) ) ;
#75241 = CARTESIAN_POINT ( 'NONE',  ( 1.161688425708537808, -12.38737895849757820, 31.66785238281580206 ) ) ;
#75242 = CYLINDRICAL_SURFACE ( 'NONE', #56788, 0.2499999999999997502 ) ;
#75243 = CARTESIAN_POINT ( 'NONE',  ( -7.911423846710166075, -9.528491918058357157, 34.59228464037090589 ) ) ;
#75244 = CARTESIAN_POINT ( 'NONE',  ( 10.54930120442873331, -9.780366693483667717, 34.19971097300155805 ) ) ;
#75245 = ORIENTED_EDGE ( 'NONE', *, *, #3526, .F. ) ;
#75246 = ORIENTED_EDGE ( 'NONE', *, *, #35544, .F. ) ;
#75248 = CARTESIAN_POINT ( 'NONE',  ( 2.372947878968333146, -10.90142922261932057, 33.41473453929631887 ) ) ;
#75247 = CARTESIAN_POINT ( 'NONE',  ( 2.177000841024752553, -10.54014554554150607, 33.71984207302941883 ) ) ;
#75249 = CARTESIAN_POINT ( 'NONE',  ( -12.52762187249434156, -2.538708090699994813, 30.37095296980875148 ) ) ;
#75250 = CARTESIAN_POINT ( 'NONE',  ( -2.544871794871794268, -11.00000000000000000, 29.75000000000000355 ) ) ;
#75251 = CARTESIAN_POINT ( 'NONE',  ( -11.97435897435897267, -7.500000000000000000, 33.75000000000000000 ) ) ;
#75252 = CARTESIAN_POINT ( 'NONE',  ( -9.692307692307691624, -4.786620604624113540, 33.94971097300155094 ) ) ;
#75253 = VERTEX_POINT ( 'NONE', #6130 ) ;
#75254 = CARTESIAN_POINT ( 'NONE',  ( 17.29993442853592001, -3.105924265160262099, 32.13625925475356127 ) ) ;
#75255 = CARTESIAN_POINT ( 'NONE',  ( 14.24160889673642849, -11.16473453929635440, 33.15142922261925662 ) ) ;
#75256 = LINE ( 'NONE', #43669, #70348 ) ;
#75257 = CARTESIAN_POINT ( 'NONE',  ( -16.08777882049608010, -3.937682226553329556, 33.60647404775216529 ) ) ;
#75258 = ORIENTED_EDGE ( 'NONE', *, *, #51565, .T. ) ;
#75259 = ORIENTED_EDGE ( 'NONE', *, *, #78997, .F. ) ;
#75260 = CIRCLE ( 'NONE', #26336, 2.000000000000001776 ) ;
#75261 = EDGE_CURVE ( 'NONE', #76326, #36624, #61066, .T. ) ;
#75262 = VERTEX_POINT ( 'NONE', #56530 ) ;
#75263 = AXIS2_PLACEMENT_3D ( 'NONE', #47178, #82317, #61135 ) ;
#75264 = CARTESIAN_POINT ( 'NONE',  ( 0.3957816590241516885, -7.249945686854186278, 34.74374336980224598 ) ) ;
#75266 = ORIENTED_EDGE ( 'NONE', *, *, #2608, .T. ) ;
#75265 = EDGE_CURVE ( 'NONE', #28353, #57222, #35368, .T. ) ;
#75267 = CARTESIAN_POINT ( 'NONE',  ( -0.3589743589743593088, -7.500000000000000000, 29.75000000000000355 ) ) ;
#75268 = CARTESIAN_POINT ( 'NONE',  ( -5.326899807865429715, -2.779195860258147022, 31.39871582349836743 ) ) ;
#75269 = CARTESIAN_POINT ( 'NONE',  ( 4.853996859406927378, -6.503392248772476236, 34.64988816332204635 ) ) ;
#75270 = CARTESIAN_POINT ( 'NONE',  ( -17.20761368003338632, -9.084618155246140248, 34.75535874321725771 ) ) ;
#75271 = FACE_OUTER_BOUND ( 'NONE', #1057, .T. ) ;
#75272 = EDGE_LOOP ( 'NONE', ( #6144, #33075, #83059, #3373 ) ) ;
#75273 = ADVANCED_FACE ( 'NONE', ( #36268 ), #84022, .F. ) ;
#75274 = CYLINDRICAL_SURFACE ( 'NONE', #22794, 0.2499999999999995559 ) ;
#75276 = ORIENTED_EDGE ( 'NONE', *, *, #76048, .T. ) ;
#75275 = CARTESIAN_POINT ( 'NONE',  ( -16.21992956480203674, -11.69971097300155272, 32.46337939537587403 ) ) ;
#75277 = DIRECTION ( 'NONE',  ( 1.000000000000000000, 0.000000000000000000, 0.000000000000000000 ) ) ;
#75278 = CARTESIAN_POINT ( 'NONE',  ( 13.38461538461538680, -12.29105614889573062, 35.45975837776705220 ) ) ;
#75279 = CARTESIAN_POINT ( 'NONE',  ( 1.134615384615387468, -7.566083408709834757, 34.74999999999999289 ) ) ;
#75280 = CARTESIAN_POINT ( 'NONE',  ( -16.08870137312652560, -7.750023224968867197, 34.99404313364389907 ) ) ;
#75281 = CARTESIAN_POINT ( 'NONE',  ( -17.75005459062195712, -10.92531984108285670, 33.72920026020278073 ) ) ;
#75282 = CARTESIAN_POINT ( 'NONE',  ( -15.23076923076922995, -3.322132147404559976, 32.92929555188717927 ) ) ;
#75283 = DIRECTION ( 'NONE',  ( -1.000000000000000000, 0.000000000000000000, 0.000000000000000000 ) ) ;
#75284 = ADVANCED_FACE ( 'NONE', ( #62822 ), #34920, .F. ) ;
#75285 = CARTESIAN_POINT ( 'NONE',  ( -1.987747218494638313, -9.401340078031370950, 18.93936829374151287 ) ) ;
#75286 = EDGE_LOOP ( 'NONE', ( #71696, #20599 ) ) ;
#75287 = CARTESIAN_POINT ( 'NONE',  ( 11.76147289007438346, -2.758310577978208666, 31.33698337089302299 ) ) ;
#75288 = CARTESIAN_POINT ( 'NONE',  ( 12.59232890250541281, -4.684288915650983043, 34.18129842949671371 ) ) ;
#75289 = CARTESIAN_POINT ( 'NONE',  ( 9.822833130541336999, -11.04252011169590020, 33.62494198852677130 ) ) ;
#75290 = CARTESIAN_POINT ( 'NONE',  ( -13.13466986626724342, -8.433404298154334455, 34.66254593164985920 ) ) ;
#75291 = EDGE_LOOP ( 'NONE', ( #23572, #5630, #17791, #49916 ) ) ;
#75292 = CARTESIAN_POINT ( 'NONE',  ( -5.933931648997559982, -2.538708090699994813, 30.37095296980875503 ) ) ;
#75293 = CARTESIAN_POINT ( 'NONE',  ( 11.28843831424008393, -12.68155406624981119, 30.59749803192733708 ) ) ;
#75294 = CARTESIAN_POINT ( 'NONE',  ( 2.530471976670372936, -10.97394488606064122, 33.68653795673694873 ) ) ;
#75295 = AXIS2_PLACEMENT_3D ( 'NONE', #3004, #23282, #57070 ) ;
#75296 = CARTESIAN_POINT ( 'NONE',  ( -14.30769230769230660, -6.386643153685126251, 34.62446782046654192 ) ) ;
#75297 = VECTOR ( 'NONE', #38434, 1000.000000000000000 ) ;
#75298 = CYLINDRICAL_SURFACE ( 'NONE', #66698, 0.2499999999999994726 ) ;
#75299 = VERTEX_POINT ( 'NONE', #21856 ) ;
#75300 = CARTESIAN_POINT ( 'NONE',  ( -16.21911615440247090, -6.835583212224499938, 34.95778746994557906 ) ) ;
#75301 = CARTESIAN_POINT ( 'NONE',  ( 3.230769230769110045, -12.27809138561165270, 31.22303859784587132 ) ) ;
#75302 = CARTESIAN_POINT ( 'NONE',  ( -14.43816749276802724, -7.276987145209185215, 34.99546412871779211 ) ) ;
#75303 = ORIENTED_EDGE ( 'NONE', *, *, #63537, .F. ) ;
#75304 = CARTESIAN_POINT ( 'NONE',  ( 9.442307692307693401, -7.500000000000001776, 35.00000000000000000 ) ) ;
#75305 = B_SPLINE_CURVE_WITH_KNOTS ( 'NONE', 3,
 ( #76487, #388, #49009, #27852, #42267, #824, #55759, #21535, #21984, #83247 ),
 .UNSPECIFIED., .F., .F.,
 ( 4, 2, 2, 2, 4 ),
 ( 0.0007817246256747507503, 0.0009771112852218959231, 0.001172497944769040987, 0.001367884604316186052, 0.001563271263863331116 ),
 .UNSPECIFIED. ) ;
#75306 = EDGE_CURVE ( 'NONE', #85662, #15420, #49765, .T. ) ;
#75307 = ORIENTED_EDGE ( 'NONE', *, *, #11568, .F. ) ;
#75308 = CARTESIAN_POINT ( 'NONE',  ( -2.307692307692427391, -12.27809138561165270, 31.22303859784587132 ) ) ;
#75309 = CARTESIAN_POINT ( 'NONE',  ( -5.999999999999998224, -11.91647553114624181, 32.58852847137148245 ) ) ;
#75310 = EDGE_LOOP ( 'NONE', ( #10521, #16893 ) ) ;
#75311 = CARTESIAN_POINT ( 'NONE',  ( 7.623227628637698317, -12.15238873228292071, 31.58232369045353849 ) ) ;
#75312 = CARTESIAN_POINT ( 'NONE',  ( -14.37377468705244254, -2.292212530054419606, 30.41441678777542634 ) ) ;
#75313 = CARTESIAN_POINT ( 'NONE',  ( 13.31934493865461278, -6.879047030191174805, 34.71129190930000163 ) ) ;
#75314 = ADVANCED_FACE ( 'NONE', ( #70933 ), #22735, .F. ) ;
#75315 = DIRECTION ( 'NONE',  ( 0.000000000000000000, 0.3420201433256641055, -0.9396926207859100932 ) ) ;
#75316 = CARTESIAN_POINT ( 'NONE',  ( 3.361294932532794100, -12.45806712695776319, 30.39783852428763922 ) ) ;
#75317 = ADVANCED_FACE ( 'NONE', ( #63280 ), #63721, .T. ) ;
#75318 = EDGE_LOOP ( 'NONE', ( #48226, #25895, #28202, #9514 ) ) ;
#75319 = EDGE_CURVE ( 'NONE', #89081, #48963, #13263, .T. ) ;
#75320 = FACE_BOUND ( 'NONE', #22154, .T. ) ;
#75321 = ORIENTED_EDGE ( 'NONE', *, *, #24673, .F. ) ;
#75322 = LINE ( 'NONE', #14496, #12723 ) ;
#75323 = AXIS2_PLACEMENT_3D ( 'NONE', #25375, #66808, #73120 ) ;
#75324 = CYLINDRICAL_SURFACE ( 'NONE', #84736, 4.000000000000000000 ) ;
#75325 = CARTESIAN_POINT ( 'NONE',  ( 19.00000000000000000, -7.500000000000000000, 29.75000000000000355 ) ) ;
#75326 = CARTESIAN_POINT ( 'NONE',  ( -6.065270445960774914, -12.27809138561121394, 31.22303859784730307 ) ) ;
#75327 = ADVANCED_FACE ( 'NONE', ( #69161 ), #50195, .F. ) ;
#75328 = B_SPLINE_CURVE_WITH_KNOTS ( 'NONE', 3,
 ( #89119, #48990, #47664, #6675, #42249, #69267, #69705, #75149, #13873, #13434 ),
 .UNSPECIFIED., .F., .F.,
 ( 4, 2, 2, 2, 4 ),
 ( 0.000000000000000000, 0.0001954311564186861155, 0.0003908623128373722310, 0.0005862934692560583735, 0.0007817246256747444619 ),
 .UNSPECIFIED. ) ;
#75329 = VERTEX_POINT ( 'NONE', #43018 ) ;
#75330 = VERTEX_POINT ( 'NONE', #8797 ) ;
#75331 = ORIENTED_EDGE ( 'NONE', *, *, #44605, .F. ) ;
#75332 = CARTESIAN_POINT ( 'NONE',  ( 6.923076923076802558, -9.442884908241554243, 34.35708131394783038 ) ) ;
#75333 = EDGE_CURVE ( 'NONE', #39715, #12402, #27290, .T. ) ;
#75335 = VERTEX_POINT ( 'NONE', #12202 ) ;
#75334 = EDGE_CURVE ( 'NONE', #77192, #820, #22981, .T. ) ;
#75336 = CARTESIAN_POINT ( 'NONE',  ( 4.219101293358989757, -10.33852847137154107, 34.16647553114620450 ) ) ;
#75337 = CARTESIAN_POINT ( 'NONE',  ( -9.942307692307691624, -7.500000000000001776, 34.75000000000000000 ) ) ;
#75338 = ADVANCED_FACE ( 'NONE', ( #18516 ), #86543, .F. ) ;
#75339 = CYLINDRICAL_SURFACE ( 'NONE', #35677, 0.2500000000000008882 ) ;
#75340 = CARTESIAN_POINT ( 'NONE',  ( 3.930980731642515380, -2.501496062324911840, 29.88072118266895671 ) ) ;
#75341 = CARTESIAN_POINT ( 'NONE',  ( -3.749999999999997335, -7.500000000000021316, 25.09374999999999645 ) ) ;
#75342 = CARTESIAN_POINT ( 'NONE',  ( -4.403846153846151523, -2.249999999999998668, 29.75000000000000355 ) ) ;
#75343 = CARTESIAN_POINT ( 'NONE',  ( -2.057637996053991447, -3.627508038966689163, 32.91356715214248396 ) ) ;
#75344 = DIRECTION ( 'NONE',  ( 0.000000000000000000, 0.000000000000000000, -1.000000000000000000 ) ) ;
#75345 = VERTEX_POINT ( 'NONE', #31576 ) ;
#75346 = ORIENTED_EDGE ( 'NONE', *, *, #41781, .T. ) ;
#75347 = ORIENTED_EDGE ( 'NONE', *, *, #51547, .T. ) ;
#75348 = LINE ( 'NONE', #40684, #60355 ) ;
#75349 = AXIS2_PLACEMENT_3D ( 'NONE', #9009, #13982, #36475 ) ;
#75351 = CARTESIAN_POINT ( 'NONE',  ( -7.780086512803769949, -9.058645607665452459, 34.76329471203371924 ) ) ;
#75350 = CARTESIAN_POINT ( 'NONE',  ( -1.515305987725689363, -2.494641256782728966, 31.33461815524612959 ) ) ;
#75352 = DIRECTION ( 'NONE',  ( -0.000000000000000000, 1.000000000000000000, -0.000000000000000000 ) ) ;
#75353 = CARTESIAN_POINT ( 'NONE',  ( -10.61538461538461320, -3.513871655860378418, 32.76840700105978499 ) ) ;
#75354 = FACE_BOUND ( 'NONE', #23438, .T. ) ;
#75355 = LINE ( 'NONE', #83452, #36054 ) ;
#75356 = ORIENTED_EDGE ( 'NONE', *, *, #33341, .T. ) ;
#75357 = FACE_OUTER_BOUND ( 'NONE', #63484, .T. ) ;
#75358 = DIRECTION ( 'NONE',  ( 1.000000000000000000, 0.000000000000000000, 0.000000000000000000 ) ) ;
#75359 = CARTESIAN_POINT ( 'NONE',  ( 3.100622021331010725, -10.88202310037936194, 33.43294751532457099 ) ) ;
#75360 = VERTEX_POINT ( 'NONE', #24362 ) ;
#75361 = DIRECTION ( 'NONE',  ( -0.000000000000000000, 0.3420201433256694346, -0.9396926207859080948 ) ) ;
#75362 = ORIENTED_EDGE ( 'NONE', *, *, #71381, .T. ) ;
#75363 = FACE_BOUND ( 'NONE', #53462, .T. ) ;
#75364 = ADVANCED_FACE ( 'NONE', ( #46865 ), #80673, .F. ) ;
#75365 = DIRECTION ( 'NONE',  ( -0.000000000000000000, 0.8660254037844397068, -0.4999999999999978906 ) ) ;
#75366 = CARTESIAN_POINT ( 'NONE',  ( -5.749999999998562927, -7.500000000000155431, 34.75000000000007105 ) ) ;
#75367 = CARTESIAN_POINT ( 'NONE',  ( 16.82694633287448838, -12.01397095200673881, 32.43157075238190146 ) ) ;
#75368 = ORIENTED_EDGE ( 'NONE', *, *, #87885, .T. ) ;
#75369 = CARTESIAN_POINT ( 'NONE',  ( 6.923076923076802558, -10.21337939537710326, 33.94971097300076224 ) ) ;
#75370 = LINE ( 'NONE', #150, #34214 ) ;
#75371 = CARTESIAN_POINT ( 'NONE',  ( -7.846153846153844924, -2.499999999999998668, 29.50000000000001066 ) ) ;
#75372 = CARTESIAN_POINT ( 'NONE',  ( 14.30769230769231015, -12.48256725967547354, 35.29906147534542527 ) ) ;
#75373 = VERTEX_POINT ( 'NONE', #59934 ) ;
#75374 = FACE_OUTER_BOUND ( 'NONE', #33820, .T. ) ;
#75375 = CARTESIAN_POINT ( 'NONE',  ( -15.29603967673000575, -4.481592998940162609, 33.73612834413957984 ) ) ;
#75377 = ORIENTED_EDGE ( 'NONE', *, *, #25033, .F. ) ;
#75376 = CARTESIAN_POINT ( 'NONE',  ( 19.00000000000000000, -3.499999999999999556, 29.75000000000000355 ) ) ;
#75378 = CARTESIAN_POINT ( 'NONE',  ( -7.846153846153965716, -11.94971097300221174, 32.03036669348237098 ) ) ;
#75379 = CARTESIAN_POINT ( 'NONE',  ( -5.076923076923199218, -11.67786785259630911, 32.92929555188603530 ) ) ;
#75380 = CARTESIAN_POINT ( 'NONE',  ( 7.846153846153846700, -2.721908614388771852, 31.22303859784724978 ) ) ;
#75381 = CARTESIAN_POINT ( 'NONE',  ( 14.08420736396836226, -9.331801661448606566, 34.40259984581193464 ) ) ;
#75382 = CARTESIAN_POINT ( 'NONE',  ( 15.00784227186238162, -5.582147617184174848, 34.63737895849758530 ) ) ;
#75385 = DIRECTION ( 'NONE',  ( -0.000000000000000000, -0.3420201433256694901, -0.9396926207859082059 ) ) ;
#75384 = AXIS2_PLACEMENT_3D ( 'NONE', #88104, #74556, #13736 ) ;
#75383 = CYLINDRICAL_SURFACE ( 'NONE', #21766, 4.000000000000000000 ) ;
#75386 = CARTESIAN_POINT ( 'NONE',  ( -12.46153846153846168, -11.16473453929635440, 33.15142922261926373 ) ) ;
#75387 = CARTESIAN_POINT ( 'NONE',  ( 1.799775606325937360E-14, -10.25000000000000000, 21.03125000000000000 ) ) ;
#75388 = ORIENTED_EDGE ( 'NONE', *, *, #50318, .F. ) ;
#75389 = CARTESIAN_POINT ( 'NONE',  ( -9.692307692307691624, -1.242168528481310874, 33.36296068462461051 ) ) ;
#75390 = EDGE_LOOP ( 'NONE', ( #84160, #28702 ) ) ;
#75391 = AXIS2_PLACEMENT_3D ( 'NONE', #74985, #20909, #48380 ) ;
#75392 = ORIENTED_EDGE ( 'NONE', *, *, #56819, .F. ) ;
#75393 = CARTESIAN_POINT ( 'NONE',  ( -8.519285359852727169, -6.653508905675592722, 34.93172785388651391 ) ) ;
#75394 = VERTEX_POINT ( 'NONE', #39237 ) ;
#75395 = CARTESIAN_POINT ( 'NONE',  ( -5.207071046654775159, -11.66186481527757479, 32.95055677023626117 ) ) ;
#75396 = CARTESIAN_POINT ( 'NONE',  ( 1.139087296526029469, -10.24999999999999467, 20.95312500000000000 ) ) ;
#75397 = CARTESIAN_POINT ( 'NONE',  ( 14.43821800945587341, -11.46989282347013095, 32.79007818306219946 ) ) ;
#75398 = CARTESIAN_POINT ( 'NONE',  ( 9.692307692307695177, -4.098570777380720287, 33.41473453929634729 ) ) ;
#75399 = B_SPLINE_CURVE_WITH_KNOTS ( 'NONE', 3,
 ( #52492, #50708, #25025, #58352, #17836, #45742, #72763, #59255, #2967, #3858 ),
 .UNSPECIFIED., .F., .F.,
 ( 4, 2, 2, 2, 4 ),
 ( 0.000000000000000000, 0.0001954311564186861697, 0.0003908623128373723394, 0.0005862934692560584820, 0.0007817246256747446788 ),
 .UNSPECIFIED. ) ;
#75400 = CARTESIAN_POINT ( 'NONE',  ( -16.02305434602136103, -5.582136614379148654, 34.36778462344220486 ) ) ;
#75401 = FACE_OUTER_BOUND ( 'NONE', #18347, .T. ) ;
#75402 = CARTESIAN_POINT ( 'NONE',  ( -13.44988583057615905, -2.625532179533444754, 30.86335684631481513 ) ) ;
#75404 = EDGE_CURVE ( 'NONE', #9579, #67350, #54162, .T. ) ;
#75403 = CARTESIAN_POINT ( 'NONE',  ( 2.084207363968360038, -10.11188796281391511, 34.01382737946119050 ) ) ;
#75405 = CARTESIAN_POINT ( 'NONE',  ( -1.929879867024197893E-14, -3.750000000000000000, 25.40625000000000000 ) ) ;
#75406 = CARTESIAN_POINT ( 'NONE',  ( 2.544871794871792936, -11.00000000000000000, 29.75000000000000355 ) ) ;
#75407 = CARTESIAN_POINT ( 'NONE',  ( -16.85414340794500276, -10.97394488606063589, 33.68653795673696294 ) ) ;
#75408 = CARTESIAN_POINT ( 'NONE',  ( 7.846153846153723244, -5.941354392335915335, 34.76329471203413846 ) ) ;
#75409 = EDGE_LOOP ( 'NONE', ( #18912, #78551 ) ) ;
#75410 = VERTEX_POINT ( 'NONE', #65359 ) ;
#75411 = CARTESIAN_POINT ( 'NONE',  ( 12.59232890250541281, -2.494656445102012565, 31.33466734024120015 ) ) ;
#75412 = DIRECTION ( 'NONE',  ( 0.000000000000000000, 0.8660254037844377084, -0.5000000000000015543 ) ) ;
#75413 = CYLINDRICAL_SURFACE ( 'NONE', #62726, 0.2499999999999997502 ) ;
#75414 = CARTESIAN_POINT ( 'NONE',  ( -11.28846153846147615, -7.434744429011176159, 34.75000000000000711 ) ) ;
#75415 = ADVANCED_FACE ( 'NONE', ( #58593 ), #25268, .F. ) ;
#75416 = EDGE_CURVE ( 'NONE', #33135, #60496, #28416, .T. ) ;
#75417 = DIRECTION ( 'NONE',  ( -0.000000000000000000, 0.000000000000000000, 1.000000000000000000 ) ) ;
#75418 = DIRECTION ( 'NONE',  ( -1.000000000000000000, -0.000000000000000000, 0.000000000000000000 ) ) ;
#75419 = AXIS2_PLACEMENT_3D ( 'NONE', #32168, #79467, #65037 ) ;
#75420 = DIRECTION ( 'NONE',  ( 1.000000000000000000, 0.000000000000000000, -0.000000000000000000 ) ) ;
#75421 = EDGE_CURVE ( 'NONE', #9134, #7438, #55199, .T. ) ;
#75422 = ORIENTED_EDGE ( 'NONE', *, *, #38720, .F. ) ;
#75423 = DIRECTION ( 'NONE',  ( 1.734723475976812518E-16, -1.000000000000000000, 0.000000000000000000 ) ) ;
#75424 = ORIENTED_EDGE ( 'NONE', *, *, #14946, .T. ) ;
#75425 = DIRECTION ( 'NONE',  ( -0.000000000000000000, 1.000000000000000000, 3.491481338843133355E-15 ) ) ;
#75426 = DIRECTION ( 'NONE',  ( -0.000000000000000000, 1.000000000000000000, 3.491481338843133355E-15 ) ) ;
#75427 = B_SPLINE_CURVE_WITH_KNOTS ( 'NONE', 3,
 ( #84800, #16323, #78021, #44658, #66281, #3244, #64938, #43788, #78455, #37926 ),
 .UNSPECIFIED., .F., .F.,
 ( 4, 2, 2, 2, 4 ),
 ( 0.0007817359430256304396, 0.0009771253907249963233, 0.001172514838424362424, 0.001367904286123728524, 0.001563293733823094408 ),
 .UNSPECIFIED. ) ;
#75428 = CARTESIAN_POINT ( 'NONE',  ( -4.219116599806928214, -4.481592998940161721, 33.73612834413957984 ) ) ;
#75429 = CARTESIAN_POINT ( 'NONE',  ( -15.36146069743679199, -3.062553014421049546, 32.05460306192773601 ) ) ;
#75430 = DIRECTION ( 'NONE',  ( -0.000000000000000000, 0.5000000000000011102, -0.8660254037844380415 ) ) ;
#75431 = ORIENTED_EDGE ( 'NONE', *, *, #38078, .F. ) ;
#75432 = ORIENTED_EDGE ( 'NONE', *, *, #27657, .T. ) ;
#75433 = EDGE_CURVE ( 'NONE', #26886, #31211, #65793, .T. ) ;
#75434 = EDGE_LOOP ( 'NONE', ( #63368, #53753, #30326, #72422 ) ) ;
#75435 = ORIENTED_EDGE ( 'NONE', *, *, #52633, .F. ) ;
#75436 = VECTOR ( 'NONE', #39692, 1000.000000000000000 ) ;
#75437 = FACE_OUTER_BOUND ( 'NONE', #17547, .T. ) ;
#75438 = FACE_OUTER_BOUND ( 'NONE', #19324, .T. ) ;
#75439 = CARTESIAN_POINT ( 'NONE',  ( 14.17754433796061342, -2.647304123082328875, 31.75400227202885972 ) ) ;
#75440 = AXIS2_PLACEMENT_3D ( 'NONE', #13941, #41420, #81979 ) ;
#75441 = VECTOR ( 'NONE', #33947, 1000.000000000000000 ) ;
#75442 = CARTESIAN_POINT ( 'NONE',  ( 16.21910172512217585, -10.21337939537593797, 33.94971097300152252 ) ) ;
#75443 = CARTESIAN_POINT ( 'NONE',  ( -14.98071481085577972, -9.233818618650603938, 34.70587769442853698 ) ) ;
#75444 = CARTESIAN_POINT ( 'NONE',  ( 14.24160889673642849, -12.37446782046654192, 30.86335684631486487 ) ) ;
#75445 = VERTEX_POINT ( 'NONE', #31122 ) ;
#75446 = EDGE_LOOP ( 'NONE', ( #60151, #24914, #32376, #57584 ) ) ;
#75447 = EDGE_LOOP ( 'NONE', ( #66723, #27897, #87335, #71959 ) ) ;
#75449 = ORIENTED_EDGE ( 'NONE', *, *, #16381, .T. ) ;
#75448 = CARTESIAN_POINT ( 'NONE',  ( -3.361459833879536507, -2.494641256782728966, 31.33461815524612959 ) ) ;
#75450 = CARTESIAN_POINT ( 'NONE',  ( 9.469380733400845074, -8.282780595021769443, 34.94152052738834868 ) ) ;
#75451 = CARTESIAN_POINT ( 'NONE',  ( -7.846153846153844924, -8.164416787775445883, 34.95778746994557906 ) ) ;
#75452 = CARTESIAN_POINT ( 'NONE',  ( 3.750000000000009770, -9.053300858899081760, 20.79687500000000000 ) ) ;
#75453 = ORIENTED_EDGE ( 'NONE', *, *, #31409, .F. ) ;
#75454 = CARTESIAN_POINT ( 'NONE',  ( -10.61538461538473399, -5.219633306517616589, 34.19971097300220464 ) ) ;
#75455 = ORIENTED_EDGE ( 'NONE', *, *, #85238, .F. ) ;
#75456 = LINE ( 'NONE', #6998, #6792 ) ;
#75457 = FACE_BOUND ( 'NONE', #81943, .T. ) ;
#75458 = CARTESIAN_POINT ( 'NONE',  ( -1.134615384615380806, -2.499999999999999556, 29.81604066197450109 ) ) ;
#75459 = CARTESIAN_POINT ( 'NONE',  ( 8.546304551714619890, -4.887634598454295265, 34.01352882383564946 ) ) ;
#75460 = ORIENTED_EDGE ( 'NONE', *, *, #80765, .T. ) ;
#75461 = CARTESIAN_POINT ( 'NONE',  ( 0.7115384615398965273, -7.500000000000155431, 34.75000000000007105 ) ) ;
#75462 = CARTESIAN_POINT ( 'NONE',  ( 16.40390046548447245, -2.564540009722896752, 30.55348353981672105 ) ) ;
#75463 = CARTESIAN_POINT ( 'NONE',  ( 0.5923302693632465088, -12.38066358083363738, 30.83685684665853444 ) ) ;
#75464 = ORIENTED_EDGE ( 'NONE', *, *, #58173, .F. ) ;
#75465 = VECTOR ( 'NONE', #63639, 1000.000000000000000 ) ;
#75466 = CARTESIAN_POINT ( 'NONE',  ( -12.21148404162501144, -2.318338780012835443, 30.59689888758630261 ) ) ;
#75467 = CARTESIAN_POINT ( 'NONE',  ( 1.449870955891410240, -8.613356846314930593, 34.62446782046653482 ) ) ;
#75468 = CARTESIAN_POINT ( 'NONE',  ( 4.284636594813105326, -11.37503395064541678, 33.29242100308974983 ) ) ;
#75469 = CARTESIAN_POINT ( 'NONE',  ( 11.53846153846153832, -2.249999999999998668, 29.75000000000001776 ) ) ;
#75470 = CARTESIAN_POINT ( 'NONE',  ( -0.2115384615370257404, -7.500000000000155431, 34.75000000000007105 ) ) ;
#75471 = FACE_BOUND ( 'NONE', #110, .T. ) ;
#75473 = CARTESIAN_POINT ( 'NONE',  ( 17.01165307636676260, -3.083524468853725775, 32.58852847137143272 ) ) ;
#75472 = CARTESIAN_POINT ( 'NONE',  ( -6.923076923076922462, -12.34228464037088635, 31.77849191805839268 ) ) ;
#75474 = CARTESIAN_POINT ( 'NONE',  ( -14.53117723225663660, -3.562934362175800285, 33.22335522853832401 ) ) ;
#75476 = CARTESIAN_POINT ( 'NONE',  ( 17.86985279056177589, -11.47017969459903952, 32.78971311882035167 ) ) ;
#75475 = CARTESIAN_POINT ( 'NONE',  ( -18.06527000055631760, -2.379036618887871324, 30.90682066428148644 ) ) ;
#75477 = CARTESIAN_POINT ( 'NONE',  ( 10.61538461538449596, -3.300289026999228881, 32.46337939537708905 ) ) ;
#75478 = CARTESIAN_POINT ( 'NONE',  ( 2.724691934501235036, -6.299813628509441266, 17.88875670625848713 ) ) ;
#75479 = EDGE_LOOP ( 'NONE', ( #3971, #64176 ) ) ;
#75480 = CARTESIAN_POINT ( 'NONE',  ( 1.161689167099241082, -12.15238873228291538, 31.58232369045354915 ) ) ;
#75481 = VERTEX_POINT ( 'NONE', #17631 ) ;
#75482 = CARTESIAN_POINT ( 'NONE',  ( -13.13466997523734037, -9.357781135181031829, 34.66075350412533851 ) ) ;
#75483 = ORIENTED_EDGE ( 'NONE', *, *, #47773, .F. ) ;
#75484 = DIRECTION ( 'NONE',  ( 0.000000000000000000, 0.9848077530122072432, 0.1736481776669354937 ) ) ;
#75485 = DIRECTION ( 'NONE',  ( 0.000000000000000000, 0.1736481776669275834, 0.9848077530122086864 ) ) ;
#75487 = ORIENTED_EDGE ( 'NONE', *, *, #68083, .T. ) ;
#75486 = LINE ( 'NONE', #16343, #16504 ) ;
#75488 = CARTESIAN_POINT ( 'NONE',  ( 18.22296313426667780, -7.369474539155830506, 34.99858011523957657 ) ) ;
#75489 = CARTESIAN_POINT ( 'NONE',  ( -0.06109907496454585613, -4.750000000000000000, 16.40438170625849068 ) ) ;
#75490 = CARTESIAN_POINT ( 'NONE',  ( 12.46153846153846168, -9.905515769479276145, 34.41647553114623292 ) ) ;
#75492 = CARTESIAN_POINT ( 'NONE',  ( -8.769230769230768274, -8.120952969808772792, 34.71129190930000163 ) ) ;
#75491 = B_SPLINE_CURVE_WITH_KNOTS ( 'NONE', 3,
 ( #56144, #37192, #64656, #23237, #10176, #28681, #83637, #8405, #70546, #30441 ),
 .UNSPECIFIED., .F., .F.,
 ( 4, 2, 2, 2, 4 ),
 ( 0.000000000000000000, 0.0001954311564186863323, 0.0003908623128373726646, 0.0005862934692560590241, 0.0007817246256747453293 ),
 .UNSPECIFIED. ) ;
#75493 = CARTESIAN_POINT ( 'NONE',  ( 16.82689983963011926, -12.43535235679832596, 30.55408501211184813 ) ) ;
#75494 = DIRECTION ( 'NONE',  ( 0.000000000000000000, 0.000000000000000000, -1.000000000000000000 ) ) ;
#75495 = CARTESIAN_POINT ( 'NONE',  ( 2.438218009455870749, -2.882268652242222284, 31.66798894389554064 ) ) ;
#75496 = PLANE ( 'NONE',  #87189 ) ;
#75497 = ADVANCED_FACE ( 'NONE', ( #86087 ), #66699, .T. ) ;
#75498 = CARTESIAN_POINT ( 'NONE',  ( 3.775308065498752086, -6.007798216065404873, 20.89249329374151642 ) ) ;
#75499 = B_SPLINE_CURVE_WITH_KNOTS ( 'NONE', 3,
 ( #30132, #64344, #29263, #9418, #36453, #49526, #63905, #71997, #37771, #22489 ),
 .UNSPECIFIED., .F., .F.,
 ( 4, 2, 2, 2, 4 ),
 ( 0.000000000000000000, 0.0001954339857564091278, 0.0003908679715128182556, 0.0005863019572692274375, 0.0007817359430256365111 ),
 .UNSPECIFIED. ) ;
#75500 = DIRECTION ( 'NONE',  ( 1.000000000000000000, 0.000000000000000000, 0.000000000000000000 ) ) ;
#75501 = CARTESIAN_POINT ( 'NONE',  ( -5.999999999999998224, -2.249999999999998668, 29.75000000000001776 ) ) ;
#75502 = ORIENTED_EDGE ( 'NONE', *, *, #13570, .F. ) ;
#75503 = CARTESIAN_POINT ( 'NONE',  ( -19.50000000000000000, -3.499999999999999556, 29.75000000000000355 ) ) ;
#75504 = CARTESIAN_POINT ( 'NONE',  ( -1.492201783934593573, -3.724691934501250135, 24.32999329374151642 ) ) ;
#75505 = VECTOR ( 'NONE', #53628, 1000.000000000000227 ) ;
#75506 = ADVANCED_FACE ( 'NONE', ( #72559 ), #10869, .F. ) ;
#75507 = CARTESIAN_POINT ( 'NONE',  ( 2.084207383127977486, -4.988325925672468131, 34.36044203135681130 ) ) ;
#75508 = CARTESIAN_POINT ( 'NONE',  ( -15.84615384615384670, -11.50000000000000000, 29.75000000000000355 ) ) ;
#75509 = ORIENTED_EDGE ( 'NONE', *, *, #70350, .T. ) ;
#75510 = CARTESIAN_POINT ( 'NONE',  ( 1.449870524128225258, -8.656820664281605460, 34.87096338111211224 ) ) ;
#75511 = CARTESIAN_POINT ( 'NONE',  ( 3.007843013253082454, -3.586966769969700763, 32.86292498521069660 ) ) ;
#75513 = VERTEX_POINT ( 'NONE', #59042 ) ;
#75512 = DIRECTION ( 'NONE',  ( 0.000000000000000000, -1.000000000000000000, -2.413528314402514090E-16 ) ) ;
#75514 = CARTESIAN_POINT ( 'NONE',  ( -5.207614543590636913, -5.582088688514999397, 34.36776431015576350 ) ) ;
#75515 = AXIS2_PLACEMENT_3D ( 'NONE', #86530, #59480, #87419 ) ;
#75516 = EDGE_CURVE ( 'NONE', #72654, #8229, #78810, .T. ) ;
#75517 = DIRECTION ( 'NONE',  ( -0.000000000000000000, 0.1736481776669307198, -0.9848077530122080203 ) ) ;
#75518 = CARTESIAN_POINT ( 'NONE',  ( -10.39237177129122003, -9.172514111537584114, 34.72667873470787470 ) ) ;
#75519 = CARTESIAN_POINT ( 'NONE',  ( 4.853996859406927378, -4.186968288167446595, 33.49512374952580274 ) ) ;
#75520 = CARTESIAN_POINT ( 'NONE',  ( -18.25002323729296450, -12.22074536777955345, 31.39888409691088356 ) ) ;
#75521 = ADVANCED_FACE ( 'NONE', ( #48631 ), #82883, .F. ) ;
#75522 = ORIENTED_EDGE ( 'NONE', *, *, #33390, .T. ) ;
#75523 = ORIENTED_EDGE ( 'NONE', *, *, #71298, .F. ) ;
#75524 = ORIENTED_EDGE ( 'NONE', *, *, #34494, .T. ) ;
#75525 = CARTESIAN_POINT ( 'NONE',  ( -16.28399412357784826, -3.625366637846545448, 33.29286588640298561 ) ) ;
#75526 = CARTESIAN_POINT ( 'NONE',  ( 0.4615384615383396616, -2.625532179533779154, 30.86335684631627174 ) ) ;
#75527 = CARTESIAN_POINT ( 'NONE',  ( -13.25382357679059986, -12.11778462344220841, 31.66786338562085135 ) ) ;
#75528 = CYLINDRICAL_SURFACE ( 'NONE', #78313, 0.2499999999999986955 ) ;
#75529 = CARTESIAN_POINT ( 'NONE',  ( -17.75010451963438030, -7.431206910972181667, 35.00000000000000000 ) ) ;
#75530 = ORIENTED_EDGE ( 'NONE', *, *, #53291, .F. ) ;
#75531 = EDGE_CURVE ( 'NONE', #75080, #81881, #69364, .T. ) ;
#75532 = ORIENTED_EDGE ( 'NONE', *, *, #28478, .T. ) ;
#75533 = VERTEX_POINT ( 'NONE', #68466 ) ;
#75536 = ORIENTED_EDGE ( 'NONE', *, *, #4720, .T. ) ;
#75535 = EDGE_CURVE ( 'NONE', #85648, #43445, #36854, .T. ) ;
#75534 = CARTESIAN_POINT ( 'NONE',  ( -6.988346923633241836, -2.657715359629089225, 31.77849191805834295 ) ) ;
#75537 = CARTESIAN_POINT ( 'NONE',  ( 6.000000000000001776, -5.471508081941601098, 34.59228464037088457 ) ) ;
#75538 = PLANE ( 'NONE',  #81236 ) ;
#75539 = EDGE_CURVE ( 'NONE', #18250, #44505, #12646, .T. ) ;
#75540 = ADVANCED_FACE ( 'NONE', ( #82446 ), #68909, .F. ) ;
#75541 = CARTESIAN_POINT ( 'NONE',  ( -14.30769230769199218, -2.255955759149395501, 30.00000000000324363 ) ) ;
#75542 = CARTESIAN_POINT ( 'NONE',  ( -6.000000000000119904, -4.481592998941358097, 33.73612834414048933 ) ) ;
#75543 = ORIENTED_EDGE ( 'NONE', *, *, #69711, .T. ) ;
#75544 = ORIENTED_EDGE ( 'NONE', *, *, #73572, .T. ) ;
#75545 = EDGE_LOOP ( 'NONE', ( #59649, #34941 ) ) ;
#75546 = CARTESIAN_POINT ( 'NONE',  ( -17.06410256410256565, -7.500000000000000000, 29.75000000000000355 ) ) ;
#75548 = ORIENTED_EDGE ( 'NONE', *, *, #11397, .F. ) ;
#75547 = DIRECTION ( 'NONE',  ( 1.000000000000000000, 0.000000000000000000, 0.000000000000000000 ) ) ;
#75549 = CARTESIAN_POINT ( 'NONE',  ( -2.242436736416282272, -8.613356846314928816, 34.62446782046653482 ) ) ;
#75550 = AXIS2_PLACEMENT_3D ( 'NONE', #31386, #44004, #71922 ) ;
#75551 = CARTESIAN_POINT ( 'NONE',  ( -14.55771554498527287, -2.587272538249755893, 30.68239716806877837 ) ) ;
#75552 = ORIENTED_EDGE ( 'NONE', *, *, #76047, .F. ) ;
#75553 = CARTESIAN_POINT ( 'NONE',  ( 8.769230769230647482, -12.46129190930018460, 30.37095296980731973 ) ) ;
#75554 = CARTESIAN_POINT ( 'NONE',  ( 0.3308478584281524526, -9.084618155246140248, 34.75535874321725771 ) ) ;
#75555 = VERTEX_POINT ( 'NONE', #47755 ) ;
#75556 = FACE_BOUND ( 'NONE', #65957, .T. ) ;
#75557 = CYLINDRICAL_SURFACE ( 'NONE', #3884, 2.750000000000000000 ) ;
#75558 = DIRECTION ( 'NONE',  ( -1.000000000000000000, -0.000000000000000000, -0.000000000000000000 ) ) ;
#75559 = CARTESIAN_POINT ( 'NONE',  ( 3.296024802045254720, -9.442884908240271713, 34.35708131394835618 ) ) ;
#75561 = DIRECTION ( 'NONE',  ( -1.000000000000000000, -0.000000000000000000, 0.000000000000000000 ) ) ;
#75560 = CARTESIAN_POINT ( 'NONE',  ( -12.46153846153858247, -2.625532179533778709, 30.86335684631627174 ) ) ;
#75562 = CARTESIAN_POINT ( 'NONE',  ( -3.099978789802278811, -3.338503747796865984, 32.95102852606552801 ) ) ;
#75563 = CARTESIAN_POINT ( 'NONE',  ( 12.52760579488854020, -2.833524468853757750, 32.15551576947925838 ) ) ;
#75564 = ORIENTED_EDGE ( 'NONE', *, *, #57587, .T. ) ;
#75565 = CYLINDRICAL_SURFACE ( 'NONE', #66256, 0.2499999999999997502 ) ;
#75566 = AXIS2_PLACEMENT_3D ( 'NONE', #71897, #25496, #85865 ) ;
#75567 = FACE_OUTER_BOUND ( 'NONE', #12590, .T. ) ;
#75568 = ORIENTED_EDGE ( 'NONE', *, *, #59866, .F. ) ;
#75569 = FACE_OUTER_BOUND ( 'NONE', #46450, .T. ) ;
#75570 = CARTESIAN_POINT ( 'NONE',  ( 9.561616225640140243, -2.729777683071817229, 31.24903638046269450 ) ) ;
#75571 = ORIENTED_EDGE ( 'NONE', *, *, #86831, .F. ) ;
#75572 = EDGE_CURVE ( 'NONE', #41905, #51992, #75664, .T. ) ;
#75573 = CARTESIAN_POINT ( 'NONE',  ( -9.915234651214538175, -9.172386477786396597, 34.72672124145550043 ) ) ;
#75574 = CARTESIAN_POINT ( 'NONE',  ( 4.153846153846154188, -9.780366693483667717, 34.19971097300155094 ) ) ;
#75575 = FACE_BOUND ( 'NONE', #28305, .T. ) ;
#75577 = CARTESIAN_POINT ( 'NONE',  ( -4.153846153846273204, -8.613356846316285953, 34.62446782046622218 ) ) ;
#75576 = CARTESIAN_POINT ( 'NONE',  ( -15.29685264172511161, -5.557115091759785130, 34.35708131394839171 ) ) ;
#75578 = CARTESIAN_POINT ( 'NONE',  ( 2.177544337960613863, -6.809168938359898782, 34.95455904226513866 ) ) ;
#75579 = CARTESIAN_POINT ( 'NONE',  ( 12.33139049180676494, -12.50552854090298638, 31.33409797877408920 ) ) ;
#75580 = CARTESIAN_POINT ( 'NONE',  ( 2.241609928332172874, -10.67929555188718460, 33.92786785259543336 ) ) ;
#75581 = LINE ( 'NONE', #13885, #14504 ) ;
#75582 = CARTESIAN_POINT ( 'NONE',  ( 1.492201783934554493, -3.724691934501233703, 15.23250670625848713 ) ) ;
#75583 = EDGE_LOOP ( 'NONE', ( #45037, #56196 ) ) ;
#75584 = ORIENTED_EDGE ( 'NONE', *, *, #47431, .T. ) ;
#75585 = CARTESIAN_POINT ( 'NONE',  ( 5.326977388561388693, -6.567000820036038355, 34.66262288849541306 ) ) ;
#75586 = CARTESIAN_POINT ( 'NONE',  ( -10.61538461538473577, -8.656820664282941280, 34.87096338111179961 ) ) ;
#75587 = CARTESIAN_POINT ( 'NONE',  ( 18.00000000000000000, -2.708943851104267164, 35.45975837776705220 ) ) ;
#75588 = CARTESIAN_POINT ( 'NONE',  ( 10.68145194873469173, -2.833524468853757750, 32.15551576947925838 ) ) ;
#75589 = CARTESIAN_POINT ( 'NONE',  ( 3.230769230769231726, -11.16473453929635440, 33.15142922261926373 ) ) ;
#75590 = CARTESIAN_POINT ( 'NONE',  ( 0.06109907496455496689, -11.24999999999999822, 18.27938170625849068 ) ) ;
#75591 = ADVANCED_FACE ( 'NONE', ( #81999 ), #898, .F. ) ;
#75592 = CARTESIAN_POINT ( 'NONE',  ( 6.923076923076924238, -2.292212530054420494, 30.41441678777542634 ) ) ;
#75593 = CARTESIAN_POINT ( 'NONE',  ( 2.057692307692288392, -2.249999999999999112, 29.81609741502488120 ) ) ;
#75594 = AXIS2_PLACEMENT_3D ( 'NONE', #67416, #26874, #40835 ) ;
#75595 = CARTESIAN_POINT ( 'NONE',  ( -5.076923076923075762, -10.51840700105979565, 33.73612834413961536 ) ) ;
#75596 = CARTESIAN_POINT ( 'NONE',  ( -6.166666666666667851, -3.499999999999999556, 29.75000000000000355 ) ) ;
#75597 = DIRECTION ( 'NONE',  ( -1.000000000000000000, 0.000000000000000000, -0.000000000000000000 ) ) ;
#75598 = CARTESIAN_POINT ( 'NONE',  ( 5.207448515156721136, -8.630441415882550871, 34.87705825610312615 ) ) ;
#75599 = CARTESIAN_POINT ( 'NONE',  ( -3.230769230769352962, -4.320704448113951379, 33.92786785259630022 ) ) ;
#75600 = CARTESIAN_POINT ( 'NONE',  ( -3.230769230769351186, -8.613356846316285953, 34.62446782046622218 ) ) ;
#75601 = LINE ( 'NONE', #20232, #39900 ) ;
#75602 = ORIENTED_EDGE ( 'NONE', *, *, #14044, .F. ) ;
#75603 = CARTESIAN_POINT ( 'NONE',  ( -14.43783951713053249, -3.817052484675422797, 33.13202310037935661 ) ) ;
#75604 = PLANE ( 'NONE',  #48907 ) ;
#75605 = CARTESIAN_POINT ( 'NONE',  ( 1.987747218494642309, -5.598659921968629050, 19.56436829374151287 ) ) ;
#75606 = EDGE_CURVE ( 'NONE', #84846, #60694, #48191, .T. ) ;
#75607 = CARTESIAN_POINT ( 'NONE',  ( -9.942284436356281674, -10.82459398097509329, 33.81372124010185587 ) ) ;
#75608 = CARTESIAN_POINT ( 'NONE',  ( -11.53846153846153655, -6.435427911321262684, 35.78748833219616898 ) ) ;
#75609 = CARTESIAN_POINT ( 'NONE',  ( 10.36538461538461675, -2.499999999999998668, 29.75000000000000355 ) ) ;
#75611 = EDGE_LOOP ( 'NONE', ( #37113, #88111 ) ) ;
#75610 = CARTESIAN_POINT ( 'NONE',  ( -6.130609655204078301, -7.722926974430166069, 34.99546784045485737 ) ) ;
#75612 = CARTESIAN_POINT ( 'NONE',  ( -1.139087296525992388, -10.25000000000000711, 26.10937500000000355 ) ) ;
#75613 = CARTESIAN_POINT ( 'NONE',  ( -9.469294848214294902, -5.582272713120729257, 34.63742843783360570 ) ) ;
#75614 = ADVANCED_FACE ( 'NONE', ( #62586 ), #41895, .F. ) ;
#75615 = ORIENTED_EDGE ( 'NONE', *, *, #2645, .F. ) ;
#75616 = FACE_OUTER_BOUND ( 'NONE', #23422, .T. ) ;
#75617 = DIRECTION ( 'NONE',  ( 1.000000000000000000, 0.000000000000000000, 0.000000000000000000 ) ) ;
#75618 = ORIENTED_EDGE ( 'NONE', *, *, #11918, .F. ) ;
#75619 = B_SPLINE_CURVE_WITH_KNOTS ( 'NONE', 3,
 ( #56004, #21779, #54226, #20457, #49254, #76725, #81721, #20006, #47470, #13255 ),
 .UNSPECIFIED., .F., .F.,
 ( 4, 2, 2, 2, 4 ),
 ( 0.0007817359430256306564, 0.0009771253907249969738, 0.001172514838424363291, 0.001367904286123729826, 0.001563293733823096143 ),
 .UNSPECIFIED. ) ;
#75620 = CARTESIAN_POINT ( 'NONE',  ( -15.23076923076922995, -11.91647553114624181, 32.58852847137148245 ) ) ;
#75621 = PLANE ( 'NONE',  #88277 ) ;
#75622 = VECTOR ( 'NONE', #77756, 1000.000000000000000 ) ;
#75623 = CARTESIAN_POINT ( 'NONE',  ( -14.98071491913091791, -12.41262288849542017, 30.68299917996395010 ) ) ;
#75624 = ADVANCED_FACE ( 'NONE', ( #41444 ), #19841, .F. ) ;
#75625 = EDGE_LOOP ( 'NONE', ( #45540, #15020 ) ) ;
#75626 = VERTEX_POINT ( 'NONE', #74798 ) ;
#75627 = DIRECTION ( 'NONE',  ( 0.000000000000000000, -6.938893903907222067E-15, 1.000000000000000000 ) ) ;
#75628 = ORIENTED_EDGE ( 'NONE', *, *, #19522, .T. ) ;
#75629 = EDGE_CURVE ( 'NONE', #36678, #79882, #38947, .T. ) ;
#75630 = CARTESIAN_POINT ( 'NONE',  ( 7.780883845597524662, -9.528491918058357157, 34.59228464037090589 ) ) ;
#75631 = DIRECTION ( 'NONE',  ( 0.000000000000000000, 0.6427876096865368094, 0.7660444431189802339 ) ) ;
#75632 = CARTESIAN_POINT ( 'NONE',  ( -15.23076923076922995, -2.292212530054420494, 30.41441678777542634 ) ) ;
#75633 = EDGE_CURVE ( 'NONE', #13761, #27959, #43647, .T. ) ;
#75634 = AXIS2_PLACEMENT_3D ( 'NONE', #50482, #41979, #42423 ) ;
#75635 = CARTESIAN_POINT ( 'NONE',  ( -10.61538461538461320, -5.180354513474913603, 36.12317359536750416 ) ) ;
#75636 = CARTESIAN_POINT ( 'NONE',  ( 15.23076923076911093, -6.879047030192662504, 34.71129190930017927 ) ) ;
#75637 = CARTESIAN_POINT ( 'NONE',  ( 13.38461538461538680, -3.050289026998446396, 32.03036669348365706 ) ) ;
#75638 = DIRECTION ( 'NONE',  ( -0.000000000000000000, 0.9396926207859092051, -0.3420201433256662704 ) ) ;
#75639 = EDGE_CURVE ( 'NONE', #79975, #35909, #8953, .T. ) ;
#75640 = VERTEX_POINT ( 'NONE', #9862 ) ;
#75641 = ORIENTED_EDGE ( 'NONE', *, *, #1432, .F. ) ;
#75643 = VERTEX_POINT ( 'NONE', #2212 ) ;
#75642 = CARTESIAN_POINT ( 'NONE',  ( -17.20761454359064047, -9.804603061927743113, 34.18744698557895845 ) ) ;
#75644 = EDGE_CURVE ( 'NONE', #40637, #29464, #22800, .T. ) ;
#75645 = CARTESIAN_POINT ( 'NONE',  ( -5.299850035829926753, -4.762599654559228846, 34.23009711892697737 ) ) ;
#75646 = EDGE_LOOP ( 'NONE', ( #79656, #42670, #79414, #28419 ) ) ;
#75647 = VECTOR ( 'NONE', #49468, 999.9999999999998863 ) ;
#75648 = ADVANCED_FACE ( 'NONE', ( #63021 ), #84656, .F. ) ;
#75649 = CARTESIAN_POINT ( 'NONE',  ( -8.546451100252703270, -10.97394488606064122, 33.68653795673694873 ) ) ;
#75650 = CARTESIAN_POINT ( 'NONE',  ( 12.46153846153846168, -4.945431358278436385, 36.03766855953609394 ) ) ;
#75651 = ORIENTED_EDGE ( 'NONE', *, *, #29051, .T. ) ;
#75652 = CARTESIAN_POINT ( 'NONE',  ( 7.846153846153725020, -8.613356846316285953, 34.62446782046622218 ) ) ;
#75653 = B_SPLINE_CURVE_WITH_KNOTS ( 'NONE', 3,
 ( #47867, #20838, #41119, #75779, #76220, #6449, #33909, #6880, #14526, #54614 ),
 .UNSPECIFIED., .F., .F.,
 ( 4, 2, 2, 2, 4 ),
 ( 0.0007817359430256285964, 0.0009771253907249943717, 0.001172514838424360255, 0.001367904286123726139, 0.001563293733823092023 ),
 .UNSPECIFIED. ) ;
#75654 = ORIENTED_EDGE ( 'NONE', *, *, #41283, .F. ) ;
#75655 = CYLINDRICAL_SURFACE ( 'NONE', #81357, 4.000000000000000000 ) ;
#75656 = EDGE_LOOP ( 'NONE', ( #18631, #72746, #25584, #37122 ) ) ;
#75657 = DIRECTION ( 'NONE',  ( -1.000000000000000000, 0.000000000000000000, 0.000000000000000000 ) ) ;
#75658 = B_SPLINE_CURVE_WITH_KNOTS ( 'NONE', 3,
 ( #58149, #51828, #4550, #17632, #44626, #58594, #43757, #51367, #3649, #32027 ),
 .UNSPECIFIED., .F., .F.,
 ( 4, 2, 2, 2, 4 ),
 ( 0.0007817359430256297891, 0.0009771253907249958896, 0.001172514838424362207, 0.001367904286123728524, 0.001563293733823094625 ),
 .UNSPECIFIED. ) ;
#75659 = EDGE_LOOP ( 'NONE', ( #17290, #37568, #87898, #34549 ) ) ;
#75660 = CARTESIAN_POINT ( 'NONE',  ( -4.403869378067609475, -4.175268141568689195, 33.81360843649122216 ) ) ;
#75661 = ADVANCED_FACE ( 'NONE', ( #85530 ), #28826, .F. ) ;
#75662 = CARTESIAN_POINT ( 'NONE',  ( -8.769230769230768274, -2.721908614388771852, 31.22303859784724978 ) ) ;
#75663 = FACE_BOUND ( 'NONE', #87248, .T. ) ;
#75664 = LINE ( 'NONE', #33362, #81580 ) ;
#75665 = CARTESIAN_POINT ( 'NONE',  ( -17.77698864838715309, -12.15243808032446005, 31.58219941686247978 ) ) ;
#75666 = DIRECTION ( 'NONE',  ( -0.000000000000000000, -0.1736481776669307198, -0.9848077530122080203 ) ) ;
#75667 = CARTESIAN_POINT ( 'NONE',  ( -3.361460697436786660, -4.118384482072085184, 33.43331474514187107 ) ) ;
#75668 = EDGE_CURVE ( 'NONE', #18655, #34160, #9885, .T. ) ;
#75669 = LINE ( 'NONE', #77010, #35191 ) ;
#75670 = CARTESIAN_POINT ( 'NONE',  ( -4.403822884788506364, -11.28823185664190376, 33.01397839955799896 ) ) ;
#75671 = CARTESIAN_POINT ( 'NONE',  ( 14.55774672760575861, -6.523592122091592671, 34.90882529074906415 ) ) ;
#75672 = ORIENTED_EDGE ( 'NONE', *, *, #67216, .F. ) ;
#75673 = ORIENTED_EDGE ( 'NONE', *, *, #8218, .T. ) ;
#75675 = CARTESIAN_POINT ( 'NONE',  ( -3.453696189676078276, -5.582147617184174848, 34.63737895849758530 ) ) ;
#75674 = CARTESIAN_POINT ( 'NONE',  ( -16.85391172531022619, -9.886259254753566594, 34.14407573483972413 ) ) ;
#75676 = CARTESIAN_POINT ( 'NONE',  ( -12.68446467905460473, -2.554751324335734708, 30.48935550225260727 ) ) ;
#75677 = CARTESIAN_POINT ( 'NONE',  ( -24.99999999999999645, 20.00000000000000355, 0.000000000000000000 ) ) ;
#75678 = CARTESIAN_POINT ( 'NONE',  ( 1.450682717965462221, -10.67929555188718282, 33.92786785259544757 ) ) ;
#75679 = CARTESIAN_POINT ( 'NONE',  ( 6.923076923076924238, -2.499999999999998668, 29.75000000000001421 ) ) ;
#75680 = VERTEX_POINT ( 'NONE', #16182 ) ;
#75681 = EDGE_CURVE ( 'NONE', #48663, #39220, #14198, .T. ) ;
#75682 = VECTOR ( 'NONE', #19439, 1000.000000000000000 ) ;
#75683 = FACE_OUTER_BOUND ( 'NONE', #1855, .T. ) ;
#75684 = CARTESIAN_POINT ( 'NONE',  ( -5.999999999999998224, -6.386643153685126251, 34.62446782046654192 ) ) ;
#75685 = CARTESIAN_POINT ( 'NONE',  ( 16.82694633287448838, -4.075325502946085976, 33.72974371597207721 ) ) ;
#75686 = CARTESIAN_POINT ( 'NONE',  ( -15.90390074446811042, -4.176053281294517028, 33.81426240980091791 ) ) ;
#75687 = VERTEX_POINT ( 'NONE', #36025 ) ;
#75688 = EDGE_CURVE ( 'NONE', #13392, #5310, #45469, .T. ) ;
#75689 = VERTEX_POINT ( 'NONE', #72005 ) ;
#75691 = EDGE_CURVE ( 'NONE', #61882, #6628, #66133, .T. ) ;
#75690 = ORIENTED_EDGE ( 'NONE', *, *, #11400, .F. ) ;
#75692 = CARTESIAN_POINT ( 'NONE',  ( 0.7115384615385245137, -7.434744429011175271, 34.75000000000000711 ) ) ;
#75693 = VERTEX_POINT ( 'NONE', #58934 ) ;
#75694 = AXIS2_PLACEMENT_3D ( 'NONE', #42847, #2277, #35646 ) ;
#75695 = CARTESIAN_POINT ( 'NONE',  ( -1.161835843346973984, -8.496831190052093419, 34.64984203495476578 ) ) ;
#75696 = CARTESIAN_POINT ( 'NONE',  ( -17.32694631421604115, -3.202444869320336895, 32.30641848906366675 ) ) ;
#75697 = CARTESIAN_POINT ( 'NONE',  ( 4.153846153846154188, -13.37000171582298513, 34.34916445242398453 ) ) ;
#75698 = CARTESIAN_POINT ( 'NONE',  ( 11.53846153846141753, -12.27809138561165270, 31.22303859784587132 ) ) ;
#75699 = EDGE_CURVE ( 'NONE', #87211, #53945, #51257, .T. ) ;
#75700 = CARTESIAN_POINT ( 'NONE',  ( 9.942253210655836781, -5.852078868378309373, 34.47109172314383585 ) ) ;
#75701 = ORIENTED_EDGE ( 'NONE', *, *, #3545, .T. ) ;
#75702 = CARTESIAN_POINT ( 'NONE',  ( 6.000000000000001776, -8.120952969808772792, 34.71129190930000163 ) ) ;
#75704 = EDGE_LOOP ( 'NONE', ( #27102, #34329, #3177, #55345 ) ) ;
#75703 = CARTESIAN_POINT ( 'NONE',  ( -12.39628289026243912, -11.94971097300157403, 32.03036669348361443 ) ) ;
#75705 = DIRECTION ( 'NONE',  ( -0.000000000000000000, 0.7660444431189791237, -0.6427876096865379196 ) ) ;
#75706 = DIRECTION ( 'NONE',  ( -0.000000000000000000, 1.000000000000000000, 3.491481338843133355E-15 ) ) ;
#75707 = CARTESIAN_POINT ( 'NONE',  ( -19.99999999999996447, -15.00000000000000533, 3.000000000000000000 ) ) ;
#75708 = CARTESIAN_POINT ( 'NONE',  ( 9.019176178608811156, -12.07971442181322352, 32.31769673815850297 ) ) ;
#75709 = PLANE ( 'NONE',  #54804 ) ;
#75710 = CARTESIAN_POINT ( 'NONE',  ( 17.32692307692301270, -7.565270445406050648, 34.75000000000000000 ) ) ;
#75711 = CARTESIAN_POINT ( 'NONE',  ( -3.230769230769351186, -6.879047030192662504, 34.71129190930017927 ) ) ;
#75712 = CARTESIAN_POINT ( 'NONE',  ( -2.724691934501246582, -6.299813628509474128, 20.42374329374152353 ) ) ;
#75713 = EDGE_LOOP ( 'NONE', ( #67279, #6392 ) ) ;
#75714 = CARTESIAN_POINT ( 'NONE',  ( -3.007756386675836779, -6.460100341425561332, 34.89618726649961644 ) ) ;
#75715 = CARTESIAN_POINT ( 'NONE',  ( 0.4615384615384611200, -3.050289026998446396, 32.03036669348365706 ) ) ;
#75716 = DIRECTION ( 'NONE',  ( 0.000000000000000000, 0.4999999999999985567, 0.8660254037844395958 ) ) ;
#75718 = EDGE_LOOP ( 'NONE', ( #27765, #84171, #9959, #885 ) ) ;
#75717 = CIRCLE ( 'NONE', #13863, 2.999999999999999112 ) ;
#75719 = EDGE_LOOP ( 'NONE', ( #23120, #31789, #15070, #5750 ) ) ;
#75720 = DIRECTION ( 'NONE',  ( -0.000000000000000000, -0.6427876096865404731, -0.7660444431189771253 ) ) ;
#75721 = CARTESIAN_POINT ( 'NONE',  ( -2.437839517130526712, -3.285722584762969856, 32.44110544564090759 ) ) ;
#75722 = EDGE_CURVE ( 'NONE', #79737, #81272, #53059, .T. ) ;
#75723 = VECTOR ( 'NONE', #44890, 1000.000000000000114 ) ;
#75724 = CARTESIAN_POINT ( 'NONE',  ( 10.86533002476265786, -4.932303261841489928, 34.32971442181322885 ) ) ;
#75725 = CARTESIAN_POINT ( 'NONE',  ( -4.153846153846152411, -1.466349020453238561, 30.81389545987213907 ) ) ;
#75726 = CARTESIAN_POINT ( 'NONE',  ( 17.07692307692295586, -3.300289026999228437, 32.46337939537709616 ) ) ;
#75727 = ORIENTED_EDGE ( 'NONE', *, *, #43683, .F. ) ;
#75728 = PRODUCT ( 'spring holder', 'spring holder', '', ( #46002 ) ) ;
#75729 = CARTESIAN_POINT ( 'NONE',  ( 16.85343813319912343, -3.236172620538810385, 32.36188796281390267 ) ) ;
#75730 = AXIS2_PLACEMENT_3D ( 'NONE', #61520, #40824, #82257 ) ;
#75731 = CARTESIAN_POINT ( 'NONE',  ( 19.00000000000000000, 12.75000000000000711, 23.75000000000000000 ) ) ;
#75732 = CARTESIAN_POINT ( 'NONE',  ( 18.06525513951284267, -12.51329471203373345, 31.30864560766537963 ) ) ;
#75733 = EDGE_LOOP ( 'NONE', ( #85388, #30285 ) ) ;
#75734 = CARTESIAN_POINT ( 'NONE',  ( -16.85391023282967993, -11.98016756924215187, 32.48728574198911190 ) ) ;
#75735 = ORIENTED_EDGE ( 'NONE', *, *, #50572, .F. ) ;
#75736 = CARTESIAN_POINT ( 'NONE',  ( -16.21911659980693443, -6.026961402152685388, 34.52809138561120506 ) ) ;
#75737 = DIRECTION ( 'NONE',  ( -0.000000000000000000, -0.7660444431189791237, -0.6427876096865379196 ) ) ;
#75738 = ORIENTED_EDGE ( 'NONE', *, *, #31634, .T. ) ;
#75739 = DIRECTION ( 'NONE',  ( -0.000000000000000000, 0.5000000000000011102, -0.8660254037844381525 ) ) ;
#75740 = DIRECTION ( 'NONE',  ( -1.000000000000000000, 0.000000000000000000, 0.000000000000000000 ) ) ;
#75741 = CARTESIAN_POINT ( 'NONE',  ( -10.83831083290076158, -5.667676309546437530, 34.40238873228292249 ) ) ;
#75742 = CARTESIAN_POINT ( 'NONE',  ( 7.173022332454968009, -12.45601412856602863, 31.48342859153981621 ) ) ;
#75743 = CARTESIAN_POINT ( 'NONE',  ( -24.00000000000000000, 14.50000000000000533, 1.499999999999997780 ) ) ;
#75744 = AXIS2_PLACEMENT_3D ( 'NONE', #39740, #61754, #19893 ) ;
#75746 = ORIENTED_EDGE ( 'NONE', *, *, #14841, .T. ) ;
#75745 = ADVANCED_FACE ( 'NONE', ( #24251 ), #25155, .T. ) ;
#75747 = FACE_BOUND ( 'NONE', #59370, .T. ) ;
#75748 = VERTEX_POINT ( 'NONE', #12105 ) ;
#75749 = LINE ( 'NONE', #7751, #15609 ) ;
#75750 = ADVANCED_FACE ( 'NONE', ( #73348 ), #17963, .F. ) ;
#75751 = B_SPLINE_CURVE_WITH_KNOTS ( 'NONE', 3,
 ( #16284, #43750, #71216, #81497, #26988, #34178, #87372, #46810, #81939, #54446 ),
 .UNSPECIFIED., .F., .F.,
 ( 4, 2, 2, 2, 4 ),
 ( 0.000000000000000000, 0.0001954311584214071026, 0.0003908623168428142051, 0.0005862934752642213077, 0.0007817246336856284103 ),
 .UNSPECIFIED. ) ;
#75752 = DIRECTION ( 'NONE',  ( -0.000000000000000000, 0.8660254037844397068, -0.4999999999999978906 ) ) ;
#75753 = EDGE_CURVE ( 'NONE', #36504, #74762, #77687, .T. ) ;
#75754 = CIRCLE ( 'NONE', #36862, 3.000000000000000000 ) ;
#75755 = CARTESIAN_POINT ( 'NONE',  ( -7.846153846153844924, -9.819645486525091727, 36.12317359536749706 ) ) ;
#75756 = DIRECTION ( 'NONE',  ( -0.000000000000000000, -0.6427876096865404731, -0.7660444431189770143 ) ) ;
#75757 = ORIENTED_EDGE ( 'NONE', *, *, #4130, .T. ) ;
#75759 = EDGE_CURVE ( 'NONE', #53590, #2315, #73804, .T. ) ;
#75758 = VERTEX_POINT ( 'NONE', #4899 ) ;
#75760 = EDGE_LOOP ( 'NONE', ( #25381, #52672, #35270, #51376 ) ) ;
#75761 = CARTESIAN_POINT ( 'NONE',  ( 13.51466299087107004, -7.723484964179501588, 34.74522123443823318 ) ) ;
#75762 = ORIENTED_EDGE ( 'NONE', *, *, #21935, .F. ) ;
#75763 = CARTESIAN_POINT ( 'NONE',  ( 4.284371592079798674, -10.31582465632705237, 34.18122507451815295 ) ) ;
#75764 = EDGE_CURVE ( 'NONE', #16707, #71873, #76582, .T. ) ;
#75765 = PLANE ( 'NONE',  #33904 ) ;
#75766 = CARTESIAN_POINT ( 'NONE',  ( -17.07692307692307665, -2.833524468853757305, 32.15551576947925838 ) ) ;
#75767 = B_SPLINE_CURVE_WITH_KNOTS ( 'NONE', 3,
 ( #14914, #63074, #1385, #28876, #56332, #15797, #43263, #29751, #44564, #44122 ),
 .UNSPECIFIED., .F., .F.,
 ( 4, 2, 2, 2, 4 ),
 ( 0.0007817246256747516176, 0.0009771112852218965736, 0.001172497944769041638, 0.001367884604316186702, 0.001563271263863331550 ),
 .UNSPECIFIED. ) ;
#75768 = CARTESIAN_POINT ( 'NONE',  ( 8.703960323269994248, -9.442884908240170461, 34.35708131394840592 ) ) ;
#75769 = CARTESIAN_POINT ( 'NONE',  ( 11.76183747915971800, -2.501478030877322567, 29.88021232661721172 ) ) ;
#75770 = AXIS2_PLACEMENT_3D ( 'NONE', #73202, #38981, #31775 ) ;
#75771 = CARTESIAN_POINT ( 'NONE',  ( 15.48082354240754555, -9.148310452688876993, 34.47095581063188519 ) ) ;
#75772 = DIRECTION ( 'NONE',  ( -0.000000000000000000, -0.5000000000000011102, -0.8660254037844380415 ) ) ;
#75773 = CARTESIAN_POINT ( 'NONE',  ( 11.47237812750565666, -9.780366693483667717, 34.19971097300155805 ) ) ;
#75774 = EDGE_LOOP ( 'NONE', ( #50564, #59041, #66367, #63227, #61970, #70669 ) ) ;
#75775 = ORIENTED_EDGE ( 'NONE', *, *, #13716, .F. ) ;
#75776 = AXIS2_PLACEMENT_3D ( 'NONE', #47449, #82144, #88042 ) ;
#75777 = ORIENTED_EDGE ( 'NONE', *, *, #47564, .F. ) ;
#75778 = LINE ( 'NONE', #573, #45948 ) ;
#75780 = CARTESIAN_POINT ( 'NONE',  ( -9.692307692307691624, -3.937682226553329556, 33.60647404775216529 ) ) ;
#75779 = CARTESIAN_POINT ( 'NONE',  ( 1.607394925883794068, -5.913360116392399668, 34.49180327182771322 ) ) ;
#75781 = CARTESIAN_POINT ( 'NONE',  ( 19.00000000000000000, -11.50000000000000000, 29.75000000000000355 ) ) ;
#75782 = CARTESIAN_POINT ( 'NONE',  ( 4.153846153846154188, -11.35647404775217417, 33.31231777344666511 ) ) ;
#75783 = FACE_BOUND ( 'NONE', #83998, .T. ) ;
#75784 = CARTESIAN_POINT ( 'NONE',  ( 7.846153846153846700, -11.16473453929635440, 33.15142922261926373 ) ) ;
#75785 = EDGE_LOOP ( 'NONE', ( #77210, #49453, #36548, #11960 ) ) ;
#75786 = CARTESIAN_POINT ( 'NONE',  ( -5.076923076923075762, -2.249999999999998668, 29.50000000000001421 ) ) ;
#75787 = CARTESIAN_POINT ( 'NONE',  ( -0.3954701105360237112, -8.973038597847269315, 34.52809138561122637 ) ) ;
#75789 = CARTESIAN_POINT ( 'NONE',  ( -24.99999999999999645, -12.00000000000000533, 0.000000000000000000 ) ) ;
#75788 = B_SPLINE_CURVE_WITH_KNOTS ( 'NONE', 3,
 ( #29119, #42188, #69641, #7949, #35414, #62866, #28667, #56132, #84065, #22344 ),
 .UNSPECIFIED., .F., .F.,
 ( 4, 2, 2, 2, 4 ),
 ( 0.000000000000000000, 0.0001954339857564097241, 0.0003908679715128194482, 0.0005863019572692291723, 0.0007817359430256388964 ),
 .UNSPECIFIED. ) ;
#75790 = CARTESIAN_POINT ( 'NONE',  ( -3.360917200500924906, -3.625366637846545448, 33.29286588640298561 ) ) ;
#75791 = ORIENTED_EDGE ( 'NONE', *, *, #15954, .T. ) ;
#75792 = CARTESIAN_POINT ( 'NONE',  ( 1.384615384615386802, -10.67929555188718282, 33.92786785259544047 ) ) ;
#75793 = EDGE_CURVE ( 'NONE', #53433, #31330, #23912, .T. ) ;
#75794 = ORIENTED_EDGE ( 'NONE', *, *, #20600, .F. ) ;
#75796 = FACE_BOUND ( 'NONE', #62813, .T. ) ;
#75795 = B_SPLINE_CURVE_WITH_KNOTS ( 'NONE', 3,
 ( #36930, #63957, #2252, #50872, #78358, #52216, #17106, #29748, #72493, #24298 ),
 .UNSPECIFIED., .F., .F.,
 ( 4, 2, 2, 2, 4 ),
 ( 0.000000000000000000, 0.0001954311564186882026, 0.0003908623128373764051, 0.0005862934692560646619, 0.0007817246256747528103 ),
 .UNSPECIFIED. ) ;
#75797 = CARTESIAN_POINT ( 'NONE',  ( 9.469381474791543241, -5.667676309546437530, 34.40238873228292249 ) ) ;
#75798 = EDGE_CURVE ( 'NONE', #83778, #14363, #60025, .T. ) ;
#75799 = CARTESIAN_POINT ( 'NONE',  ( 18.00000000000000000, -13.75783147151868846, 33.36296068462461051 ) ) ;
#75800 = CARTESIAN_POINT ( 'NONE',  ( -16.09615384615384670, -7.500000000000000000, 29.75000000000000355 ) ) ;
#75801 = ORIENTED_EDGE ( 'NONE', *, *, #43478, .T. ) ;
#75802 = CARTESIAN_POINT ( 'NONE',  ( 5.299934428535923558, -3.105924265160262543, 32.13625925475356127 ) ) ;
#75803 = CARTESIAN_POINT ( 'NONE',  ( -17.86920955903305597, -3.957578996910244395, 33.62503395064540257 ) ) ;
#75804 = CARTESIAN_POINT ( 'NONE',  ( 18.13079044096694759, -10.70102852606553157, 33.91149625220312913 ) ) ;
#75805 = CARTESIAN_POINT ( 'NONE',  ( 6.065255571276024327, -3.835265460703683349, 33.15142922261929925 ) ) ;
#75806 = ORIENTED_EDGE ( 'NONE', *, *, #11703, .F. ) ;
#75807 = EDGE_CURVE ( 'NONE', #16242, #29311, #72264, .T. ) ;
#75808 = CARTESIAN_POINT ( 'NONE',  ( -12.46153846153846168, -3.050289026998446396, 32.03036669348365706 ) ) ;
#75809 = CARTESIAN_POINT ( 'NONE',  ( -16.15384615384615330, -9.905515769479276145, 34.41647553114623292 ) ) ;
#75811 = ORIENTED_EDGE ( 'NONE', *, *, #53356, .T. ) ;
#75810 = CARTESIAN_POINT ( 'NONE',  ( -8.769230769230768274, -10.05456864172156806, 36.03766855953608683 ) ) ;
#75812 = CARTESIAN_POINT ( 'NONE',  ( -18.00000000000012079, -3.643525952248793498, 33.31231777344770961 ) ) ;
#75813 = FACE_OUTER_BOUND ( 'NONE', #5845, .T. ) ;
#75814 = LINE ( 'NONE', #12348, #74558 ) ;
#75815 = CARTESIAN_POINT ( 'NONE',  ( -10.36543909703647159, -2.587454068350147018, 30.68340429815432202 ) ) ;
#75816 = VECTOR ( 'NONE', #56792, 1000.000000000000227 ) ;
#75817 = CARTESIAN_POINT ( 'NONE',  ( 3.230769230769110045, -3.835265460704628371, 33.15142922262033665 ) ) ;
#75819 = CARTESIAN_POINT ( 'NONE',  ( -16.40382289789473802, -8.347322224742351082, 34.93158281831414058 ) ) ;
#75818 = CARTESIAN_POINT ( 'NONE',  ( -7.846153846153844924, -10.51840700105979565, 33.73612834413961536 ) ) ;
#75820 = EDGE_CURVE ( 'NONE', #33682, #13888, #54851, .T. ) ;
#75821 = CARTESIAN_POINT ( 'NONE',  ( 6.000000000000001776, -4.661471528628507777, 34.16647553114623292 ) ) ;
#75822 = CARTESIAN_POINT ( 'NONE',  ( -1.139087296526025916, -4.750000000000006217, 21.57812500000000355 ) ) ;
#75823 = VERTEX_POINT ( 'NONE', #82778 ) ;
#75824 = VECTOR ( 'NONE', #34006, 1000.000000000000000 ) ;
#75825 = CARTESIAN_POINT ( 'NONE',  ( -17.74994568836168440, -9.148310452688869887, 34.47095581063188519 ) ) ;
#75826 = EDGE_LOOP ( 'NONE', ( #80685, #37769, #38723, #19603 ) ) ;
#75827 = VERTEX_POINT ( 'NONE', #33256 ) ;
#75828 = CARTESIAN_POINT ( 'NONE',  ( -11.53846153846153655, -2.292212530054420494, 30.41441678777542634 ) ) ;
#75830 = EDGE_LOOP ( 'NONE', ( #44087, #56417 ) ) ;
#75829 = VECTOR ( 'NONE', #89172, 1000.000000000000114 ) ;
#75831 = CARTESIAN_POINT ( 'NONE',  ( 1.384615384615386802, -11.91647553114624181, 32.58852847137148245 ) ) ;
#75832 = CARTESIAN_POINT ( 'NONE',  ( 2.750000000000008438, -8.639087296525996607, 20.79687500000000000 ) ) ;
#75833 = CARTESIAN_POINT ( 'NONE',  ( 13.51540719244017197, -2.729792928343269587, 31.24908615093345077 ) ) ;
#75834 = EDGE_CURVE ( 'NONE', #2122, #53843, #60464, .T. ) ;
#75835 = CARTESIAN_POINT ( 'NONE',  ( 16.09615384615384670, -7.500000000000000000, 29.75000000000000355 ) ) ;
#75836 = CARTESIAN_POINT ( 'NONE',  ( -16.15384615384627409, -6.026961402154118908, 34.52809138561165270 ) ) ;
#75837 = B_SPLINE_CURVE_WITH_KNOTS ( 'NONE', 3,
 ( #16781, #64078, #28996, #29435, #22659, #77164, #44234, #50566, #16347, #21778 ),
 .UNSPECIFIED., .F., .F.,
 ( 4, 2, 2, 2, 4 ),
 ( 0.000000000000000000, 0.0001954339857564063089, 0.0003908679715128126177, 0.0005863019572692189808, 0.0007817359430256252354 ),
 .UNSPECIFIED. ) ;
#75838 = CARTESIAN_POINT ( 'NONE',  ( -6.989159302437058408, -9.058645607665454236, 34.76329471203372634 ) ) ;
#75839 = CARTESIAN_POINT ( 'NONE',  ( -14.55769230769230660, -7.500000000000001776, 35.04278698407183867 ) ) ;
#75840 = CARTESIAN_POINT ( 'NONE',  ( 2.530703659305157949, -11.24521262558773671, 33.06293181088029343 ) ) ;
#75841 = CARTESIAN_POINT ( 'NONE',  ( 2.320192649118979489E-14, -11.25000000000000000, 26.03125000000000000 ) ) ;
#75842 = B_SPLINE_CURVE_WITH_KNOTS ( 'NONE', 3,
 ( #31677, #24455, #79861, #67240, #17721, #73560, #45173, #65450, #73103, #66344 ),
 .UNSPECIFIED., .F., .F.,
 ( 4, 2, 2, 2, 4 ),
 ( 0.000000000000000000, 0.0001954339857564073388, 0.0003908679715128146777, 0.0005863019572692220165, 0.0007817359430256293554 ),
 .UNSPECIFIED. ) ;
#75843 = EDGE_CURVE ( 'NONE', #31043, #23382, #88223, .T. ) ;
#75844 = EDGE_CURVE ( 'NONE', #673, #23399, #68361, .T. ) ;
#75845 = CARTESIAN_POINT ( 'NONE',  ( 24.00000000000000000, 9.000000000000024869, 29.25000000000000000 ) ) ;
#75846 = CARTESIAN_POINT ( 'NONE',  ( 13.38461538461538680, -4.102666532097928531, 36.13435417666054406 ) ) ;
#75847 = CARTESIAN_POINT ( 'NONE',  ( 6.000000000000001776, -1.509761064869970415, 31.06009739812519044 ) ) ;
#75848 = CARTESIAN_POINT ( 'NONE',  ( -8.096177083446809419, -8.432397168068783699, 34.66272746175022945 ) ) ;
#75849 = EDGE_CURVE ( 'NONE', #72929, #13144, #71139, .T. ) ;
#75850 = ORIENTED_EDGE ( 'NONE', *, *, #60693, .T. ) ;
#75851 = ORIENTED_EDGE ( 'NONE', *, *, #88682, .F. ) ;
#75852 = CARTESIAN_POINT ( 'NONE',  ( -18.22348492456433178, -2.612411019501190701, 31.66733052389439962 ) ) ;
#75853 = CYLINDRICAL_SURFACE ( 'NONE', #17402, 0.2500000000000002220 ) ;
#75854 = DIRECTION ( 'NONE',  ( -0.000000000000000000, 0.5000000000000011102, -0.8660254037844380415 ) ) ;
#75855 = CARTESIAN_POINT ( 'NONE',  ( -11.60421834097584970, -7.249945686854186278, 34.74374336980224598 ) ) ;
#75856 = DIRECTION ( 'NONE',  ( -0.000000000000000000, 0.1736481776669307198, -0.9848077530122080203 ) ) ;
#75857 = CARTESIAN_POINT ( 'NONE',  ( -9.442253272394237840, -10.82426656108012075, 33.81400080652039009 ) ) ;
#75858 = CARTESIAN_POINT ( 'NONE',  ( 19.00000000000000000, 8.999999999999998224, 23.75000000000000000 ) ) ;
#75859 = EDGE_LOOP ( 'NONE', ( #79309, #10824 ) ) ;
#75860 = CARTESIAN_POINT ( 'NONE',  ( -0.4615384615384611200, -8.120952969808772792, 34.71129190930000163 ) ) ;
#75861 = ORIENTED_EDGE ( 'NONE', *, *, #68016, .T. ) ;
#75862 = EDGE_CURVE ( 'NONE', #56866, #545, #2476, .T. ) ;
#75863 = DIRECTION ( 'NONE',  ( 1.000000000000000000, 0.000000000000000000, 0.000000000000000000 ) ) ;
#75864 = B_SPLINE_CURVE_WITH_KNOTS ( 'NONE', 3,
 ( #39046, #31383, #24624, #79581, #52533, #80017, #18318, #45781, #2566, #30493 ),
 .UNSPECIFIED., .F., .F.,
 ( 4, 2, 2, 2, 4 ),
 ( 0.000000000000000000, 0.0001954339857564080707, 0.0003908679715128161414, 0.0005863019572692241849, 0.0007817359430256322827 ),
 .UNSPECIFIED. ) ;
#75865 = DIRECTION ( 'NONE',  ( -0.000000000000000000, 0.3420201433256694901, -0.9396926207859082059 ) ) ;
#75866 = CARTESIAN_POINT ( 'NONE',  ( 14.08476609017615644, -4.887634598454295265, 34.01352882383564946 ) ) ;
#75867 = B_SPLINE_CURVE_WITH_KNOTS ( 'NONE', 3,
 ( #67302, #80381, #18676, #46141, #81265, #45687, #73629, #59198, #17784, #5597 ),
 .UNSPECIFIED., .F., .F.,
 ( 4, 2, 2, 2, 4 ),
 ( 0.000000000000000000, 0.0001954339857564100222, 0.0003908679715128200445, 0.0005863019572692300396, 0.0007817359430256400890 ),
 .UNSPECIFIED. ) ;
#75868 = CARTESIAN_POINT ( 'NONE',  ( -15.36091644020745051, -3.285722584762969856, 32.44110544564090759 ) ) ;
#75869 = B_SPLINE_CURVE_WITH_KNOTS ( 'NONE', 3,
 ( #65833, #50975, #16334, #43798, #71260, #37031, #64493, #2800, #30291, #44221 ),
 .UNSPECIFIED., .F., .F.,
 ( 4, 2, 2, 2, 4 ),
 ( 0.000000000000000000, 0.0001954339857564073659, 0.0003908679715128147319, 0.0005863019572692221250, 0.0007817359430256294638 ),
 .UNSPECIFIED. ) ;
#75870 = CARTESIAN_POINT ( 'NONE',  ( -13.51530598772569114, -2.494641256782728966, 31.33461815524612959 ) ) ;
#75871 = VERTEX_POINT ( 'NONE', #40467 ) ;
#75872 = EDGE_CURVE ( 'NONE', #13156, #4768, #63655, .T. ) ;
#75873 = ORIENTED_EDGE ( 'NONE', *, *, #43840, .T. ) ;
#75874 = VECTOR ( 'NONE', #40687, 1000.000000000000114 ) ;
#75875 = ORIENTED_EDGE ( 'NONE', *, *, #84629, .T. ) ;
#75876 = ORIENTED_EDGE ( 'NONE', *, *, #15560, .F. ) ;
#75877 = CARTESIAN_POINT ( 'NONE',  ( -3.480769230769250822, -2.249999999999999112, 29.81609741502488120 ) ) ;
#75878 = CARTESIAN_POINT ( 'NONE',  ( 5.076923076922954969, -10.90142922262034020, 33.41473453929536674 ) ) ;
#75879 = ADVANCED_FACE ( 'NONE', ( #12538 ), #54399, .F. ) ;
#75880 = VECTOR ( 'NONE', #48082, 1000.000000000000000 ) ;
#75881 = CARTESIAN_POINT ( 'NONE',  ( 4.403791563224196182, -12.07971442181322352, 32.31769673815850297 ) ) ;
#75882 = CARTESIAN_POINT ( 'NONE',  ( 14.24236939220013554, -7.749976743299138882, 34.99404534957040624 ) ) ;
#75883 = CARTESIAN_POINT ( 'NONE',  ( 8.096153846153910649, -7.434744860731433924, 35.00000000000000711 ) ) ;
#75884 = CARTESIAN_POINT ( 'NONE',  ( -18.75000000000000000, -3.499999999999999556, 29.75000000000000355 ) ) ;
#75885 = CIRCLE ( 'NONE', #48552, 8.000000000000000000 ) ;
#75886 = VERTEX_POINT ( 'NONE', #82333 ) ;
#75887 = VERTEX_POINT ( 'NONE', #20616 ) ;
#75888 = ORIENTED_EDGE ( 'NONE', *, *, #40449, .F. ) ;
#75889 = ADVANCED_FACE ( 'NONE', ( #34580 ), #75557, .T. ) ;
#75891 = ORIENTED_EDGE ( 'NONE', *, *, #53979, .T. ) ;
#75890 = LINE ( 'NONE', #13302, #7061 ) ;
#75892 = CARTESIAN_POINT ( 'NONE',  ( -4.153846153846152411, -2.721908614388771852, 31.22303859784724978 ) ) ;
#75893 = DIRECTION ( 'NONE',  ( -0.000000000000000000, -0.5000000000000009992, -0.8660254037844380415 ) ) ;
#75894 = CARTESIAN_POINT ( 'NONE',  ( -1.929879867024197893E-14, -3.750000000000000000, 20.40625000000000000 ) ) ;
#75895 = ORIENTED_EDGE ( 'NONE', *, *, #73380, .T. ) ;
#75896 = B_SPLINE_CURVE_WITH_KNOTS ( 'NONE', 3,
 ( #86188, #51925, #58246, #64994, #38883, #3301, #79423, #45174, #30773, #59582 ),
 .UNSPECIFIED., .F., .F.,
 ( 4, 2, 2, 2, 4 ),
 ( 0.0007817246256747445703, 0.0009771112852218872494, 0.001172497944769030145, 0.001367884604316172825, 0.001563271263863315504 ),
 .UNSPECIFIED. ) ;
#75897 = VERTEX_POINT ( 'NONE', #84986 ) ;
#75898 = DIRECTION ( 'NONE',  ( -0.000000000000000000, 1.000000000000000000, -0.000000000000000000 ) ) ;
#75899 = EDGE_CURVE ( 'NONE', #80426, #57743, #15202, .T. ) ;
#75900 = ORIENTED_EDGE ( 'NONE', *, *, #25624, .F. ) ;
#75901 = FACE_BOUND ( 'NONE', #31935, .T. ) ;
#75902 = CYLINDRICAL_SURFACE ( 'NONE', #70495, 0.2500000000000008882 ) ;
#75903 = VECTOR ( 'NONE', #73823, 1000.000000000000000 ) ;
#75904 = CARTESIAN_POINT ( 'NONE',  ( 10.61538461538461675, -7.500000000000001776, 35.04278698407183867 ) ) ;
#75905 = ORIENTED_EDGE ( 'NONE', *, *, #31558, .F. ) ;
#75906 = EDGE_CURVE ( 'NONE', #79014, #64930, #56151, .T. ) ;
#75907 = DIRECTION ( 'NONE',  ( -0.000000000000000000, -0.000000000000000000, -1.000000000000000000 ) ) ;
#75908 =( LENGTH_UNIT ( ) NAMED_UNIT ( * ) SI_UNIT ( .MILLI., .METRE. ) );
#75909 = CYLINDRICAL_SURFACE ( 'NONE', #51411, 0.2500000000000008882 ) ;
#75910 = CARTESIAN_POINT ( 'NONE',  ( -3.480792454990687013, -9.356822207818506598, 34.66110646841856635 ) ) ;
#75911 = VERTEX_POINT ( 'NONE', #50726 ) ;
#75912 = AXIS2_PLACEMENT_3D ( 'NONE', #19541, #46570, #60525 ) ;
#75913 = CARTESIAN_POINT ( 'NONE',  ( 16.08808935133184903, -7.249945686854186278, 34.74374336980224598 ) ) ;
#75914 = CARTESIAN_POINT ( 'NONE',  ( -4.153846153846274980, -10.33852847137269571, 34.16647553114546554 ) ) ;
#75915 = CARTESIAN_POINT ( 'NONE',  ( -3.903900744468109529, -2.341251567377310217, 30.72681386836322659 ) ) ;
#75916 = DIRECTION ( 'NONE',  ( -0.000000000000000000, -0.1736481776669307198, -0.9848077530122080203 ) ) ;
#75917 = CARTESIAN_POINT ( 'NONE',  ( -17.07692307692307665, -11.33034616979429110, 35.88435417666054406 ) ) ;
#75918 = FACE_BOUND ( 'NONE', #73426, .T. ) ;
#75920 = CARTESIAN_POINT ( 'NONE',  ( -6.130147969731693181, -10.31621877034669588, 34.18098118002070152 ) ) ;
#75919 = CARTESIAN_POINT ( 'NONE',  ( 13.13463865367303463, -11.79746400365624659, 32.30657167506340954 ) ) ;
#75921 = ADVANCED_FACE ( 'NONE', ( #42236 ), #76899, .F. ) ;
#75922 = VECTOR ( 'NONE', #50901, 1000.000000000000000 ) ;
#75923 = CARTESIAN_POINT ( 'NONE',  ( 11.53846153846141576, -12.16647553114689728, 32.15551576947799362 ) ) ;
#75925 = DIRECTION ( 'NONE',  ( -1.000000000000000000, 0.000000000000000000, 0.000000000000000000 ) ) ;
#75924 = CARTESIAN_POINT ( 'NONE',  ( -8.638438961405983108, -11.71459661697925903, 32.44059661609676937 ) ) ;
#75926 = CARTESIAN_POINT ( 'NONE',  ( -8.096177070375304652, -4.175268141568685643, 33.81360843649122216 ) ) ;
#75927 = CARTESIAN_POINT ( 'NONE',  ( -2.749999999999997780, -7.561099074964547917, 16.09188170625848713 ) ) ;
#75928 = ORIENTED_EDGE ( 'NONE', *, *, #12062, .F. ) ;
#75929 = B_SPLINE_CURVE_WITH_KNOTS ( 'NONE', 3,
 ( #68392, #61629, #74722, #20215, #89134, #53543, #81038, #27411, #5812, #88694 ),
 .UNSPECIFIED., .F., .F.,
 ( 4, 2, 2, 2, 4 ),
 ( 0.0007817246256747451124, 0.0009771112852218881168, 0.001172497944769031230, 0.001367884604316174126, 0.001563271263863317238 ),
 .UNSPECIFIED. ) ;
#75930 = DIRECTION ( 'NONE',  ( -0.000000000000000000, 1.000000000000000000, -0.000000000000000000 ) ) ;
#75931 = ORIENTED_EDGE ( 'NONE', *, *, #71164, .T. ) ;
#75932 = DIRECTION ( 'NONE',  ( -1.000000000000000000, 0.000000000000000000, 0.000000000000000000 ) ) ;
#75933 = ORIENTED_EDGE ( 'NONE', *, *, #3699, .T. ) ;
#75934 = CARTESIAN_POINT ( 'NONE',  ( -11.31544869436814338, -6.460100341425560444, 34.89618726649961644 ) ) ;
#75935 = CARTESIAN_POINT ( 'NONE',  ( -8.069638789877792817, -10.11188796281391511, 34.01382737946119050 ) ) ;
#75936 = VERTEX_POINT ( 'NONE', #56178 ) ;
#75937 = CARTESIAN_POINT ( 'NONE',  ( 17.75000000000000000, -7.500000000000001776, 35.00000000000000000 ) ) ;
#75938 = CARTESIAN_POINT ( 'NONE',  ( 1.987747218494664292, -9.401340078031346081, 16.87313170625849068 ) ) ;
#75939 = EDGE_CURVE ( 'NONE', #85149, #45673, #66853, .T. ) ;
#75940 = CARTESIAN_POINT ( 'NONE',  ( -15.45369618967607828, -9.172386477786396597, 34.72672124145550043 ) ) ;
#75941 = CARTESIAN_POINT ( 'NONE',  ( -3.000000000000003553, 7.500000000000000000, 0.000000000000000000 ) ) ;
#75942 = CARTESIAN_POINT ( 'NONE',  ( -3.230769230768915534, -2.255955759149395501, 30.00000000000324363 ) ) ;
#75943 = DIRECTION ( 'NONE',  ( -0.000000000000000000, 0.5000000000000011102, -0.8660254037844380415 ) ) ;
#75944 = CARTESIAN_POINT ( 'NONE',  ( -1.319360245102545459, -6.835583212224609184, 34.95778746994559327 ) ) ;
#75945 = DIRECTION ( 'NONE',  ( 1.000000000000000000, 0.000000000000000000, 0.000000000000000000 ) ) ;
#75946 = CARTESIAN_POINT ( 'NONE',  ( 0.06109907496451268821, -3.749999999999999556, 23.15811829374151642 ) ) ;
#75947 = CIRCLE ( 'NONE', #37090, 0.2500000000000002220 ) ;
#75948 = EDGE_CURVE ( 'NONE', #80983, #36772, #8885, .T. ) ;
#75949 = EDGE_CURVE ( 'NONE', #29571, #55482, #5397, .T. ) ;
#75950 = CARTESIAN_POINT ( 'NONE',  ( 17.07692307692295586, -5.094484230521993062, 34.41647553114689373 ) ) ;
#75951 = DIRECTION ( 'NONE',  ( -0.000000000000000000, 1.000000000000000000, 3.491481338843133355E-15 ) ) ;
#75952 = EDGE_LOOP ( 'NONE', ( #64703, #80236 ) ) ;
#75953 = CARTESIAN_POINT ( 'NONE',  ( 12.46153846153846168, -11.16473453929635440, 33.15142922261926373 ) ) ;
#75954 = CARTESIAN_POINT ( 'NONE',  ( -1.929879867024197893E-14, -3.750000000000000000, 14.15625000000000000 ) ) ;
#75955 = DIRECTION ( 'NONE',  ( 0.000000000000000000, 0.000000000000000000, -1.000000000000000000 ) ) ;
#75956 = CARTESIAN_POINT ( 'NONE',  ( 0.4615384615384611200, -2.517432740324522911, 35.29906147534542527 ) ) ;
#75957 = ORIENTED_EDGE ( 'NONE', *, *, #24851, .T. ) ;
#75958 = CARTESIAN_POINT ( 'NONE',  ( 14.30769230769218758, -2.625532179533778709, 30.86335684631627174 ) ) ;
#75959 = DIRECTION ( 'NONE',  ( -0.000000000000000000, 0.1736481776669307198, -0.9848077530122080203 ) ) ;
#75961 = ORIENTED_EDGE ( 'NONE', *, *, #10056, .F. ) ;
#75960 = LINE ( 'NONE', #14705, #44020 ) ;
#75962 = FACE_OUTER_BOUND ( 'NONE', #571, .T. ) ;
#75963 = AXIS2_PLACEMENT_3D ( 'NONE', #56683, #75617, #55350 ) ;
#75964 = CARTESIAN_POINT ( 'NONE',  ( -1.384615384615505151, -10.90142922262034020, 33.41473453929536674 ) ) ;
#75965 = DIRECTION ( 'NONE',  ( 0.000000000000000000, 0.4999999999999960032, -0.8660254037844410391 ) ) ;
#75966 = CARTESIAN_POINT ( 'NONE',  ( -9.561782254074051579, -2.647132371071621471, 31.75357179365171589 ) ) ;
#75967 = CARTESIAN_POINT ( 'NONE',  ( -15.36091720050093201, -11.66186481527757302, 32.95055677023626117 ) ) ;
#75968 = ORIENTED_EDGE ( 'NONE', *, *, #15358, .T. ) ;
#75969 = EDGE_LOOP ( 'NONE', ( #72523, #23233, #9263, #9840 ) ) ;
#75970 = ORIENTED_EDGE ( 'NONE', *, *, #53331, .F. ) ;
#75971 = CARTESIAN_POINT ( 'NONE',  ( -13.38461538461550582, -3.835265460704628371, 33.15142922262033665 ) ) ;
#75972 = DIRECTION ( 'NONE',  ( -1.000000000000000000, -0.000000000000000000, -0.000000000000000000 ) ) ;
#75973 = DIRECTION ( 'NONE',  ( -0.000000000000000000, 0.1736481776669307198, -0.9848077530122080203 ) ) ;
#75974 = CARTESIAN_POINT ( 'NONE',  ( -16.82692307692314415, -7.565270000091922853, 34.99999999999999289 ) ) ;
#75975 = CIRCLE ( 'NONE', #73091, 0.2500000000000002220 ) ;
#75976 = ORIENTED_EDGE ( 'NONE', *, *, #42720, .F. ) ;
#75977 = FACE_OUTER_BOUND ( 'NONE', #16346, .T. ) ;
#75978 = ORIENTED_EDGE ( 'NONE', *, *, #35874, .T. ) ;
#75979 = VERTEX_POINT ( 'NONE', #56623 ) ;
#75980 = AXIS2_PLACEMENT_3D ( 'NONE', #80692, #39253, #13542 ) ;
#75981 = EDGE_LOOP ( 'NONE', ( #42155, #38004, #82407, #73324 ) ) ;
#75983 = ORIENTED_EDGE ( 'NONE', *, *, #55445, .F. ) ;
#75982 = CARTESIAN_POINT ( 'NONE',  ( -15.45369544828537833, -12.15238873228292071, 31.58232369045353849 ) ) ;
#75984 = CARTESIAN_POINT ( 'NONE',  ( -0.5276218724943415594, -4.786620604624113540, 33.94971097300155805 ) ) ;
#75985 = CARTESIAN_POINT ( 'NONE',  ( -13.38461538461538325, -12.29105614889573062, 35.45975837776705220 ) ) ;
#75986 = CARTESIAN_POINT ( 'NONE',  ( 4.023698944407932743, -4.460286881179643004, 33.72017969459903242 ) ) ;
#75987 = CARTESIAN_POINT ( 'NONE',  ( -4.088591014333315066, -6.835583212224609184, 34.95778746994559327 ) ) ;
#75988 = VERTEX_POINT ( 'NONE', #49854 ) ;
#75989 = ORIENTED_EDGE ( 'NONE', *, *, #26894, .F. ) ;
#75990 = B_SPLINE_CURVE_WITH_KNOTS ( 'NONE', 3,
 ( #73739, #11127, #45797, #31855, #12032, #88154, #38605, #25536, #66970, #5264 ),
 .UNSPECIFIED., .F., .F.,
 ( 4, 2, 2, 2, 4 ),
 ( 0.0007817246256747444619, 0.0009771112852218868158, 0.001172497944769029061, 0.001367884604316171523, 0.001563271263863313769 ),
 .UNSPECIFIED. ) ;
#75991 = ORIENTED_EDGE ( 'NONE', *, *, #42850, .F. ) ;
#75992 = FACE_OUTER_BOUND ( 'NONE', #13953, .T. ) ;
#75994 = ORIENTED_EDGE ( 'NONE', *, *, #46138, .T. ) ;
#75993 = LINE ( 'NONE', #26042, #54562 ) ;
#75995 = DIRECTION ( 'NONE',  ( -0.000000000000000000, -0.9848077530122086864, -0.1736481776669273613 ) ) ;
#75996 = CARTESIAN_POINT ( 'NONE',  ( -17.07692307692307665, -3.322132147404559976, 32.92929555188717927 ) ) ;
#75997 = EDGE_LOOP ( 'NONE', ( #10391, #65456, #55826, #46746 ) ) ;
#75998 = FACE_OUTER_BOUND ( 'NONE', #20539, .T. ) ;
#75999 = CARTESIAN_POINT ( 'NONE',  ( 12.59206389977210705, -9.503571793651731880, 34.60286762892837942 ) ) ;
#76000 = AXIS2_PLACEMENT_3D ( 'NONE', #807, #8015, #14323 ) ;
#76001 = ORIENTED_EDGE ( 'NONE', *, *, #1512, .F. ) ;
#76002 = FACE_BOUND ( 'NONE', #29695, .T. ) ;
#76003 = CARTESIAN_POINT ( 'NONE',  ( 10.74591031714818001, -10.19071101563364756, 33.96452234770658407 ) ) ;
#76004 = CARTESIAN_POINT ( 'NONE',  ( 15.93036122928182330, -2.612411019501191589, 31.66733052389440672 ) ) ;
#76005 = EDGE_CURVE ( 'NONE', #65429, #69108, #19619, .T. ) ;
#76006 = CARTESIAN_POINT ( 'NONE',  ( 12.33084785842815378, -6.369640206132551441, 34.87707690430378449 ) ) ;
#76008 = DIRECTION ( 'NONE',  ( -0.000000000000000000, -0.000000000000000000, -1.000000000000000000 ) ) ;
#76007 = CARTESIAN_POINT ( 'NONE',  ( 17.99999999999987566, -3.083524468854526912, 32.58852847137268327 ) ) ;
#76009 = DIRECTION ( 'NONE',  ( -0.000000000000000000, -0.8660254037844399289, -0.4999999999999980016 ) ) ;
#76010 = CARTESIAN_POINT ( 'NONE',  ( 2.544871794871792936, -7.500000000000000000, 33.75000000000000000 ) ) ;
#76011 = ORIENTED_EDGE ( 'NONE', *, *, #64216, .F. ) ;
#76012 = FACE_OUTER_BOUND ( 'NONE', #37929, .T. ) ;
#76013 = PRESENTATION_STYLE_ASSIGNMENT (( #48530 ) ) ;
#76014 = ORIENTED_EDGE ( 'NONE', *, *, #15951, .T. ) ;
#76015 = CARTESIAN_POINT ( 'NONE',  ( 14.08420736396836226, -10.11188796281391511, 34.01382737946119050 ) ) ;
#76016 = SPHERICAL_SURFACE ( 'NONE', #74959, 8.000000000000000000 ) ;
#76017 = ORIENTED_EDGE ( 'NONE', *, *, #86259, .T. ) ;
#76018 = CARTESIAN_POINT ( 'NONE',  ( 17.86930853333243618, -5.582088688514999397, 34.36776431015576350 ) ) ;
#76019 = CYLINDRICAL_SURFACE ( 'NONE', #55888, 0.2499999999999986955 ) ;
#76020 = FACE_BOUND ( 'NONE', #27969, .T. ) ;
#76022 = CARTESIAN_POINT ( 'NONE',  ( 4.023698184114455678, -12.50552854090298993, 31.33409797877408920 ) ) ;
#76021 = CARTESIAN_POINT ( 'NONE',  ( 6.923076923076924238, -3.937682226553329556, 33.60647404775216529 ) ) ;
#76023 = CARTESIAN_POINT ( 'NONE',  ( 2.084207383127978375, -6.716662450894490100, 34.94144148231605840 ) ) ;
#76024 = EDGE_CURVE ( 'NONE', #47623, #1510, #43234, .T. ) ;
#76025 = CARTESIAN_POINT ( 'NONE',  ( -1.384615384615076605, -2.506253911140615021, 30.00000000000323297 ) ) ;
#76027 = DIRECTION ( 'NONE',  ( 1.000000000000000000, 0.000000000000000000, 0.000000000000000000 ) ) ;
#76026 = DIRECTION ( 'NONE',  ( 1.000000000000000000, 0.000000000000000000, 0.000000000000000000 ) ) ;
#76028 = CARTESIAN_POINT ( 'NONE',  ( -17.86947429823644029, -5.195472089885680766, 34.18748526763464923 ) ) ;
#76029 = CARTESIAN_POINT ( 'NONE',  ( -2.694853999681210865, -4.891553140782108677, 14.99813170625848713 ) ) ;
#76030 = VERTEX_POINT ( 'NONE', #14756 ) ;
#76031 = ORIENTED_EDGE ( 'NONE', *, *, #24615, .F. ) ;
#76032 = VECTOR ( 'NONE', #51098, 999.9999999999998863 ) ;
#76033 = CARTESIAN_POINT ( 'NONE',  ( -9.626239341305252495, -11.69971097300155272, 32.46337939537588113 ) ) ;
#76034 = CARTESIAN_POINT ( 'NONE',  ( -0.6844646790546086157, -2.758268499246657068, 31.33685645148949561 ) ) ;
#76035 = CARTESIAN_POINT ( 'NONE',  ( 1.634560793993430128, -9.357781135181031829, 34.66075350412533851 ) ) ;
#76036 = CARTESIAN_POINT ( 'NONE',  ( -16.82697755857493149, -11.37275283266504111, 32.91324779482534524 ) ) ;
#76037 = CARTESIAN_POINT ( 'NONE',  ( 3.164685819813350953, -11.16473453929635440, 33.15142922261925662 ) ) ;
#76038 = CARTESIAN_POINT ( 'NONE',  ( -2.651650429449535551, -10.15165042944956753, 26.18750000000000355 ) ) ;
#76039 = CARTESIAN_POINT ( 'NONE',  ( 0.7115928814519132395, -4.074993327901524687, 33.72946981652012255 ) ) ;
#76040 = FACE_OUTER_BOUND ( 'NONE', #67235, .T. ) ;
#76041 = VECTOR ( 'NONE', #43739, 1000.000000000000000 ) ;
#76042 = CARTESIAN_POINT ( 'NONE',  ( -18.00000000000012079, -11.06231777344772027, 33.60647404775119895 ) ) ;
#76043 = DIRECTION ( 'NONE',  ( 0.000000000000000000, 0.000000000000000000, -1.000000000000000000 ) ) ;
#76044 = CARTESIAN_POINT ( 'NONE',  ( 14.30769230769231015, -1.367168528481310208, 33.57946703557072254 ) ) ;
#76045 = CARTESIAN_POINT ( 'NONE',  ( 5.076923076922953193, -8.656820664282941280, 34.87096338111179961 ) ) ;
#76046 = CARTESIAN_POINT ( 'NONE',  ( -5.777220331021932331, -11.60474049983371003, 33.02348890104160262 ) ) ;
#76047 = EDGE_CURVE ( 'NONE', #70917, #2073, #35464, .T. ) ;
#76048 = EDGE_CURVE ( 'NONE', #68235, #70953, #44331, .T. ) ;
#76049 = CARTESIAN_POINT ( 'NONE',  ( -14.17716660592874689, -3.285477652293413264, 32.44071101563363158 ) ) ;
#76050 = PLANE ( 'NONE',  #2513 ) ;
#76051 = ORIENTED_EDGE ( 'NONE', *, *, #10786, .F. ) ;
#76052 = CARTESIAN_POINT ( 'NONE',  ( -0.4615384615384611200, -3.513871655860378418, 32.76840700105978499 ) ) ;
#76053 = FACE_OUTER_BOUND ( 'NONE', #58731, .T. ) ;
#76054 = CARTESIAN_POINT ( 'NONE',  ( 1.987747218494642309, -5.598659921968629050, 22.06436829374151287 ) ) ;
#76055 = EDGE_CURVE ( 'NONE', #34772, #64564, #57942, .T. ) ;
#76056 = CARTESIAN_POINT ( 'NONE',  ( -0.2385256174450670896, -10.77377354290276301, 33.85451476688484718 ) ) ;
#76057 = CYLINDRICAL_SURFACE ( 'NONE', #58888, 4.000000000000000000 ) ;
#76058 = VERTEX_POINT ( 'NONE', #59725 ) ;
#76059 = DIRECTION ( 'NONE',  ( 0.000000000000000000, 0.1736481776669275834, 0.9848077530122086864 ) ) ;
#76061 = ORIENTED_EDGE ( 'NONE', *, *, #22450, .F. ) ;
#76060 = CARTESIAN_POINT ( 'NONE',  ( -9.692307692307812417, -5.219633306517616589, 34.19971097300220464 ) ) ;
#76062 = CARTESIAN_POINT ( 'NONE',  ( 9.915320536401090123, -12.64618726649961289, 30.78989965857442712 ) ) ;
#76063 = CARTESIAN_POINT ( 'NONE',  ( -9.627052552794856055, -5.941354392334607049, 34.76329471203374055 ) ) ;
#76064 = ORIENTED_EDGE ( 'NONE', *, *, #85476, .F. ) ;
#76065 = CARTESIAN_POINT ( 'NONE',  ( 11.53846153846153832, -9.058645607665452459, 34.76329471203371924 ) ) ;
#76066 = CARTESIAN_POINT ( 'NONE',  ( 7.780829833349539371, -7.749976730030849303, 34.74374725381503737 ) ) ;
#76067 = ORIENTED_EDGE ( 'NONE', *, *, #38703, .T. ) ;
#76068 = CARTESIAN_POINT ( 'NONE',  ( 14.05766907039934210, -2.587272538249754117, 30.68239716806877837 ) ) ;
#76069 = CARTESIAN_POINT ( 'NONE',  ( 8.769230769230645706, -6.835583212225970762, 34.95778746994575670 ) ) ;
#76070 = DIRECTION ( 'NONE',  ( -0.000000000000000000, -0.1736481776669307198, -0.9848077530122080203 ) ) ;
#76071 = VERTEX_POINT ( 'NONE', #66024 ) ;
#76072 = B_SPLINE_CURVE_WITH_KNOTS ( 'NONE', 3,
 ( #15652, #35925, #57509, #84997, #70590, #15212, #9768, #57954, #77343, #43552 ),
 .UNSPECIFIED., .F., .F.,
 ( 4, 2, 2, 2, 4 ),
 ( 0.000000000000000000, 0.0001954311564186868473, 0.0003908623128373736946, 0.0005862934692560605419, 0.0007817246256747473893 ),
 .UNSPECIFIED. ) ;
#76073 = ORIENTED_EDGE ( 'NONE', *, *, #69946, .F. ) ;
#76074 = CARTESIAN_POINT ( 'NONE',  ( 15.48071474911737333, -10.76462480002816235, 33.53768742498949962 ) ) ;
#76075 = CIRCLE ( 'NONE', #53040, 0.2500000000000002220 ) ;
#76076 = ORIENTED_EDGE ( 'NONE', *, *, #68016, .F. ) ;
#76077 = CARTESIAN_POINT ( 'NONE',  ( -11.53846153846153655, -2.499999999999998668, 29.50000000000001066 ) ) ;
#76078 = CARTESIAN_POINT ( 'NONE',  ( -5.326946301144532825, -9.356822207818506598, 34.66110646841856635 ) ) ;
#76079 = DIRECTION ( 'NONE',  ( 0.000000000000000000, 0.000000000000000000, -1.000000000000000000 ) ) ;
#76080 = DIRECTION ( 'NONE',  ( -0.000000000000000000, 0.9848077530122085754, -0.1736481776669273613 ) ) ;
#76081 = CARTESIAN_POINT ( 'NONE',  ( -4.284537620513710010, -6.413092428213692742, 34.63065189839063152 ) ) ;
#76082 = DIRECTION ( 'NONE',  ( -0.000000000000000000, -0.9396926207859092051, -0.3420201433256662704 ) ) ;
#76083 = CARTESIAN_POINT ( 'NONE',  ( 6.923076923076800782, -2.379036618888197729, 30.90682066428292885 ) ) ;
#76084 = ORIENTED_EDGE ( 'NONE', *, *, #49182, .F. ) ;
#76085 = EDGE_LOOP ( 'NONE', ( #21929, #1189 ) ) ;
#76087 = ORIENTED_EDGE ( 'NONE', *, *, #58679, .F. ) ;
#76086 = CARTESIAN_POINT ( 'NONE',  ( 6.989144256427000101, -12.62096338111211757, 30.90682066428152908 ) ) ;
#76088 = CARTESIAN_POINT ( 'NONE',  ( 11.53846153846153832, -8.810774026931790459, 35.74407628777942847 ) ) ;
#76089 = ORIENTED_EDGE ( 'NONE', *, *, #47617, .F. ) ;
#76090 = B_SPLINE_CURVE_WITH_KNOTS ( 'NONE', 3,
 ( #54965, #69371, #906, #56734, #7672, #62160, #13534, #20733, #35134, #70249 ),
 .UNSPECIFIED., .F., .F.,
 ( 4, 2, 2, 2, 4 ),
 ( 0.0007817359430256369448, 0.0009771253907250049969, 0.001172514838424373049, 0.001367904286123741101, 0.001563293733823109153 ),
 .UNSPECIFIED. ) ;
#76091 = AXIS2_PLACEMENT_3D ( 'NONE', #87157, #25435, #52892 ) ;
#76092 = CARTESIAN_POINT ( 'NONE',  ( 11.78851595837499566, -3.435999193479609914, 33.07426656108010832 ) ) ;
#76093 = CARTESIAN_POINT ( 'NONE',  ( 5.326977388561388693, -3.627508038966690496, 32.91356715214248396 ) ) ;
#76094 = ORIENTED_EDGE ( 'NONE', *, *, #2613, .F. ) ;
#76095 = FACE_OUTER_BOUND ( 'NONE', #53488, .T. ) ;
#76096 = EDGE_CURVE ( 'NONE', #10551, #535, #69089, .T. ) ;
#76097 = AXIS2_PLACEMENT_3D ( 'NONE', #74444, #60922, #39344 ) ;
#76098 = VERTEX_POINT ( 'NONE', #4334 ) ;
#76099 = B_SPLINE_CURVE_WITH_KNOTS ( 'NONE', 3,
 ( #58616, #9989, #10447, #23939, #44202, #31143, #24384, #18096, #37916, #64474 ),
 .UNSPECIFIED., .F., .F.,
 ( 4, 2, 2, 2, 4 ),
 ( 0.000000000000000000, 0.0001954311564186876876, 0.0003908623128373753751, 0.0005862934692560630356, 0.0007817246256747507503 ),
 .UNSPECIFIED. ) ;
#76100 = EDGE_LOOP ( 'NONE', ( #43845, #66559 ) ) ;
#76101 = B_SPLINE_CURVE_WITH_KNOTS ( 'NONE', 3,
 ( #73301, #39972, #32319, #66994, #4393, #11605, #32753, #86842, #39085, #46714 ),
 .UNSPECIFIED., .F., .F.,
 ( 4, 2, 2, 2, 4 ),
 ( 0.000000000000000000, 0.0001954311564186879857, 0.0003908623128373759715, 0.0005862934692560640114, 0.0007817246256747519429 ),
 .UNSPECIFIED. ) ;
#76102 = CARTESIAN_POINT ( 'NONE',  ( 20.00000000000000711, -9.999999999999994671, 13.00000000000000178 ) ) ;
#76103 = EDGE_LOOP ( 'NONE', ( #11638, #61922 ) ) ;
#76104 = VECTOR ( 'NONE', #36823, 1000.000000000000000 ) ;
#76105 = CARTESIAN_POINT ( 'NONE',  ( 16.02369894440793630, -12.45813303252208648, 30.39737893381572675 ) ) ;
#76106 = CARTESIAN_POINT ( 'NONE',  ( 17.07692307692295586, -2.892918686052165622, 31.69288490824153470 ) ) ;
#76107 = FACE_BOUND ( 'NONE', #56473, .T. ) ;
#76108 = CARTESIAN_POINT ( 'NONE',  ( -14.37296230824862775, -9.528491918058357157, 34.59228464037090589 ) ) ;
#76109 = DIRECTION ( 'NONE',  ( -0.000000000000000000, -0.000000000000000000, -1.000000000000000000 ) ) ;
#76110 = EDGE_CURVE ( 'NONE', #75887, #66983, #51819, .T. ) ;
#76111 = CARTESIAN_POINT ( 'NONE',  ( 9.627037691751372250, -11.67786785259540849, 32.92929555188721480 ) ) ;
#76112 = CARTESIAN_POINT ( 'NONE',  ( -0.3310130233048200754, -3.068774925481847937, 32.56582465632704526 ) ) ;
#76113 = CARTESIAN_POINT ( 'NONE',  ( 5.207714884747860928, -10.54018710029568595, 33.71981072465678864 ) ) ;
#76114 = CARTESIAN_POINT ( 'NONE',  ( -9.942307692307704059, -2.249999999999999556, 29.81609741502489541 ) ) ;
#76115 = ORIENTED_EDGE ( 'NONE', *, *, #52025, .T. ) ;
#76116 = DIRECTION ( 'NONE',  ( 0.000000000000000000, -6.938893903907222067E-15, 1.000000000000000000 ) ) ;
#76117 = EDGE_CURVE ( 'NONE', #79307, #7973, #32694, .T. ) ;
#76118 = ORIENTED_EDGE ( 'NONE', *, *, #46164, .F. ) ;
#76119 = ORIENTED_EDGE ( 'NONE', *, *, #28146, .F. ) ;
#76121 = FACE_OUTER_BOUND ( 'NONE', #29670, .T. ) ;
#76120 = CARTESIAN_POINT ( 'NONE',  ( 2.057715576749954867, -10.66389620160130036, 33.62221079203477103 ) ) ;
#76122 = CARTESIAN_POINT ( 'NONE',  ( 6.989145274079363368, -6.386643153685127139, 34.62446782046654192 ) ) ;
#76123 = CARTESIAN_POINT ( 'NONE',  ( -17.07692307692319744, -10.33852847137269571, 34.16647553114546554 ) ) ;
#76124 = CARTESIAN_POINT ( 'NONE',  ( 15.29683758177167086, -3.513871655860379306, 32.76840700105978499 ) ) ;
#76125 = CARTESIAN_POINT ( 'NONE',  ( -12.23852561744506673, -4.762714258010881885, 34.23016756924214832 ) ) ;
#76126 = EDGE_LOOP ( 'NONE', ( #9657, #67666, #76263, #3086 ) ) ;
#76127 = DIRECTION ( 'NONE',  ( -1.000000000000000000, -0.000000000000000000, -0.000000000000000000 ) ) ;
#76128 = CARTESIAN_POINT ( 'NONE',  ( -14.37377468705243722, -9.905515769479276145, 34.41647553114623292 ) ) ;
#76129 = CARTESIAN_POINT ( 'NONE',  ( -14.08467946359890988, -12.38742843783360748, 31.66772728687926985 ) ) ;
#76130 = EDGE_CURVE ( 'NONE', #13183, #83315, #59346, .T. ) ;
#76131 = CARTESIAN_POINT ( 'NONE',  ( 15.29683656411930848, -12.34228464037088813, 31.77849191805839268 ) ) ;
#76132 = ORIENTED_EDGE ( 'NONE', *, *, #32880, .F. ) ;
#76133 = ORIENTED_EDGE ( 'NONE', *, *, #30600, .T. ) ;
#76135 = EDGE_CURVE ( 'NONE', #18077, #24532, #45765, .T. ) ;
#76134 = ORIENTED_EDGE ( 'NONE', *, *, #23262, .F. ) ;
#76136 = LINE ( 'NONE', #55867, #79410 ) ;
#76137 = ORIENTED_EDGE ( 'NONE', *, *, #22291, .T. ) ;
#76138 = CARTESIAN_POINT ( 'NONE',  ( -6.923076923076922462, -11.11383981884818262, 36.00935417666054406 ) ) ;
#76139 = DIRECTION ( 'NONE',  ( 1.000000000000000000, 0.000000000000000000, 0.000000000000000000 ) ) ;
#76140 = CARTESIAN_POINT ( 'NONE',  ( 1.384615384615386802, -6.681629849574314051, 35.83090037661290239 ) ) ;
#76141 = CARTESIAN_POINT ( 'NONE',  ( -2.177166605928743337, -5.195472089885680766, 34.18748526763464923 ) ) ;
#76142 = CARTESIAN_POINT ( 'NONE',  ( -11.47239318745910097, -6.386643153685127139, 34.62446782046654192 ) ) ;
#76143 = ORIENTED_EDGE ( 'NONE', *, *, #23648, .F. ) ;
#76144 = DIRECTION ( 'NONE',  ( -0.000000000000000000, 0.1736481776669307198, -0.9848077530122080203 ) ) ;
#76146 = VERTEX_POINT ( 'NONE', #51607 ) ;
#76145 = CARTESIAN_POINT ( 'NONE',  ( -11.53846153846153655, -12.09954503811598769, 35.62045528018868623 ) ) ;
#76147 = CARTESIAN_POINT ( 'NONE',  ( 3.230769230769231726, -13.57706302396349152, 30.56769352161908060 ) ) ;
#76148 = DIRECTION ( 'NONE',  ( 0.000000000000000000, 0.9848077530122072432, 0.1736481776669354937 ) ) ;
#76149 = CARTESIAN_POINT ( 'NONE',  ( 17.32697738856138869, -11.28795663066794575, 33.01431243580653785 ) ) ;
#76150 = CARTESIAN_POINT ( 'NONE',  ( 8.834485908743603844, -12.16647553114626490, 32.15551576947920864 ) ) ;
#76151 = CARTESIAN_POINT ( 'NONE',  ( -12.46153846153858247, -2.892918686052166066, 31.69288490824153470 ) ) ;
#76152 = ADVANCED_FACE ( 'NONE', ( #4787 ), #79103, .F. ) ;
#76153 = CARTESIAN_POINT ( 'NONE',  ( 16.94631271729854660, -7.722926236386454590, 34.74524107206102030 ) ) ;
#76154 = CARTESIAN_POINT ( 'NONE',  ( -3.480769230769229061, -7.500000000000001776, 35.00000000000000000 ) ) ;
#76155 = ADVANCED_FACE ( 'NONE', ( #31365 ), #58828, .F. ) ;
#76156 = CARTESIAN_POINT ( 'NONE',  ( -3.724691934501248802, -5.885600066136383646, 14.17374329374151287 ) ) ;
#76157 = ORIENTED_EDGE ( 'NONE', *, *, #52960, .F. ) ;
#76158 = CARTESIAN_POINT ( 'NONE',  ( -17.01085472592064107, -10.51840700105979565, 33.73612834413962247 ) ) ;
#76159 = CARTESIAN_POINT ( 'NONE',  ( -20.00000000000000355, 10.00000000000000711, 3.000000000000000000 ) ) ;
#76160 = VECTOR ( 'NONE', #77568, 1000.000000000000227 ) ;
#76161 = AXIS2_PLACEMENT_3D ( 'NONE', #53832, #17385, #38098 ) ;
#76162 = EDGE_CURVE ( 'NONE', #43657, #56137, #60293, .T. ) ;
#76163 = CYLINDRICAL_SURFACE ( 'NONE', #34605, 0.2499999999999973355 ) ;
#76164 = CARTESIAN_POINT ( 'NONE',  ( 9.469380733400843297, -6.459968553980841577, 34.89616026154728701 ) ) ;
#76165 = EDGE_CURVE ( 'NONE', #30359, #37043, #13752, .T. ) ;
#76166 = ORIENTED_EDGE ( 'NONE', *, *, #14653, .F. ) ;
#76167 = DIRECTION ( 'NONE',  ( -0.000000000000000000, 0.1736481776669307198, -0.9848077530122080203 ) ) ;
#76168 = CARTESIAN_POINT ( 'NONE',  ( -5.076923076923197442, -6.879047030192662504, 34.71129190930017927 ) ) ;
#76169 = AXIS2_PLACEMENT_3D ( 'NONE', #34505, #14681, #40825 ) ;
#76170 = VECTOR ( 'NONE', #74341, 1000.000000000000000 ) ;
#76171 = LINE ( 'NONE', #76621, #37317 ) ;
#76172 = CARTESIAN_POINT ( 'NONE',  ( -17.07692307692319744, -3.835265460704628815, 33.15142922262033665 ) ) ;
#76173 = AXIS2_PLACEMENT_3D ( 'NONE', #71725, #18133, #72620 ) ;
#76174 = VERTEX_POINT ( 'NONE', #12427 ) ;
#76175 = CARTESIAN_POINT ( 'NONE',  ( 12.21153846153844569, -2.249999999999998668, 29.81609741502487765 ) ) ;
#76176 = CARTESIAN_POINT ( 'NONE',  ( -18.75000000000000000, -7.500000000000000000, 29.75000000000000355 ) ) ;
#76177 = CARTESIAN_POINT ( 'NONE',  ( 18.22277966897806678, -12.47679350104403007, 31.42216943046555855 ) ) ;
#76178 = ORIENTED_EDGE ( 'NONE', *, *, #48774, .F. ) ;
#76179 = CARTESIAN_POINT ( 'NONE',  ( 11.25641025641025550, -3.499999999999999556, 29.75000000000000355 ) ) ;
#76180 = ORIENTED_EDGE ( 'NONE', *, *, #53870, .F. ) ;
#76181 = DIRECTION ( 'NONE',  ( 0.000000000000000000, 0.000000000000000000, 1.000000000000000000 ) ) ;
#76182 = LINE ( 'NONE', #77516, #74324 ) ;
#76183 = ORIENTED_EDGE ( 'NONE', *, *, #48133, .T. ) ;
#76184 = CARTESIAN_POINT ( 'NONE',  ( -18.00000000000012079, -10.33852847137269926, 34.16647553114546554 ) ) ;
#76185 = CARTESIAN_POINT ( 'NONE',  ( -14.30769230769230660, -5.180354513474913603, 36.12317359536750416 ) ) ;
#76186 = CARTESIAN_POINT ( 'NONE',  ( -6.923076923076922462, -12.34228464037088635, 31.77849191805839268 ) ) ;
#76187 = DIRECTION ( 'NONE',  ( -0.000000000000000000, -0.9396926207859093161, -0.3420201433256663259 ) ) ;
#76188 = CARTESIAN_POINT ( 'NONE',  ( -0.5276208408985976206, -11.35647404775217595, 33.31231777344666511 ) ) ;
#76189 = EDGE_CURVE ( 'NONE', #20882, #31226, #53855, .T. ) ;
#76190 = ORIENTED_EDGE ( 'NONE', *, *, #57622, .F. ) ;
#76191 = FACE_BOUND ( 'NONE', #72176, .T. ) ;
#76192 = ORIENTED_EDGE ( 'NONE', *, *, #56011, .F. ) ;
#76193 = CARTESIAN_POINT ( 'NONE',  ( 5.076923076923075762, -9.058645607665452459, 34.76329471203371924 ) ) ;
#76194 = EDGE_CURVE ( 'NONE', #38776, #18719, #88119, .T. ) ;
#76195 = CIRCLE ( 'NONE', #48864, 5.000000000000000888 ) ;
#76196 = EDGE_CURVE ( 'NONE', #49301, #3368, #61930, .T. ) ;
#76197 = CARTESIAN_POINT ( 'NONE',  ( 4.284637961670941131, -11.71459661697925903, 32.44059661609676937 ) ) ;
#76198 = DIRECTION ( 'NONE',  ( 0.000000000000000000, 0.9396926207859126468, 0.3420201433256571111 ) ) ;
#76199 = DIRECTION ( 'NONE',  ( 0.000000000000000000, 0.000000000000000000, -1.000000000000000000 ) ) ;
#76200 = ORIENTED_EDGE ( 'NONE', *, *, #70633, .F. ) ;
#76201 = EDGE_CURVE ( 'NONE', #79352, #54551, #85032, .T. ) ;
#76202 = ORIENTED_EDGE ( 'NONE', *, *, #84194, .T. ) ;
#76203 = EDGE_LOOP ( 'NONE', ( #35304, #16788, #82346, #220 ) ) ;
#76204 = CARTESIAN_POINT ( 'NONE',  ( -14.30769230769230660, -1.044019251281081972, 31.83374038241031911 ) ) ;
#76205 = VERTEX_POINT ( 'NONE', #68696 ) ;
#76206 = AXIS2_PLACEMENT_3D ( 'NONE', #86577, #31156, #3246 ) ;
#76207 = CARTESIAN_POINT ( 'NONE',  ( -11.53846153846153655, -13.75783147151868846, 33.36296068462461051 ) ) ;
#76208 = CARTESIAN_POINT ( 'NONE',  ( -9.942307692307693401, -7.433931650972299465, 34.75000000000000711 ) ) ;
#76209 = CARTESIAN_POINT ( 'NONE',  ( -7.846153846153967493, -8.656820664282941280, 34.87096338111179961 ) ) ;
#76210 = CARTESIAN_POINT ( 'NONE',  ( -1.134615384613947953, -7.500000000000155431, 34.75000000000007105 ) ) ;
#76211 = AXIS2_PLACEMENT_3D ( 'NONE', #70601, #85445, #51626 ) ;
#76212 = DIRECTION ( 'NONE',  ( 0.000000000000000000, 0.4999999999999960032, -0.8660254037844410391 ) ) ;
#76213 = CARTESIAN_POINT ( 'NONE',  ( -18.25000000000000711, -7.569194476968191587, 35.00000000000000000 ) ) ;
#76214 = CARTESIAN_POINT ( 'NONE',  ( 17.32686859527121825, -2.587454068350149239, 30.68340429815432557 ) ) ;
#76215 = VERTEX_POINT ( 'NONE', #47087 ) ;
#76216 = EDGE_CURVE ( 'NONE', #18497, #66197, #13312, .T. ) ;
#76217 = EDGE_LOOP ( 'NONE', ( #48336, #17714, #79716, #58711 ) ) ;
#76218 = ORIENTED_EDGE ( 'NONE', *, *, #84681, .T. ) ;
#76219 = CARTESIAN_POINT ( 'NONE',  ( -4.088590582570128973, -10.21337939537593620, 33.94971097300152252 ) ) ;
#76221 = LINE ( 'NONE', #29822, #43404 ) ;
#76220 = CARTESIAN_POINT ( 'NONE',  ( 1.634560902963528850, -5.852078868378310261, 34.47109172314383585 ) ) ;
#76222 = AXIS2_PLACEMENT_3D ( 'NONE', #20470, #13268, #75412 ) ;
#76223 = CARTESIAN_POINT ( 'NONE',  ( -17.77722033102192967, -5.827830569534416583, 34.72679350104403539 ) ) ;
#76224 = CARTESIAN_POINT ( 'NONE',  ( 12.71159288145191013, -12.65882529074907126, 30.72640787790839312 ) ) ;
#76225 = FACE_BOUND ( 'NONE', #82666, .T. ) ;
#76226 = CARTESIAN_POINT ( 'NONE',  ( 8.638540166120462160, -10.70098750199973203, 33.91152734681376302 ) ) ;
#76227 = ORIENTED_EDGE ( 'NONE', *, *, #26707, .T. ) ;
#76228 = DIRECTION ( 'NONE',  ( 0.000000000000000000, 0.000000000000000000, 1.000000000000000000 ) ) ;
#76229 = B_SPLINE_CURVE_WITH_KNOTS ( 'NONE', 3,
 ( #22103, #2253, #42388, #56765, #1383, #1823, #63520, #21208, #28874, #83820 ),
 .UNSPECIFIED., .F., .F.,
 ( 4, 2, 2, 2, 4 ),
 ( 0.000000000000000000, 0.0001954311564186869015, 0.0003908623128373738030, 0.0005862934692560607588, 0.0007817246256747476061 ),
 .UNSPECIFIED. ) ;
#76230 = DIRECTION ( 'NONE',  ( -0.000000000000000000, 1.000000000000000000, -0.000000000000000000 ) ) ;
#76231 = FACE_OUTER_BOUND ( 'NONE', #46652, .T. ) ;
#76232 = CARTESIAN_POINT ( 'NONE',  ( 3.480714640147274164, -11.56426240980093567, 33.07394671870546432 ) ) ;
#76233 = ORIENTED_EDGE ( 'NONE', *, *, #53761, .T. ) ;
#76234 = CARTESIAN_POINT ( 'NONE',  ( 18.00000000000000000, -12.37446782046654192, 30.86335684631486131 ) ) ;
#76235 = ORIENTED_EDGE ( 'NONE', *, *, #45508, .F. ) ;
#76236 = FACE_BOUND ( 'NONE', #29196, .T. ) ;
#76237 = CARTESIAN_POINT ( 'NONE',  ( -17.32689982097166848, -4.075325502946085976, 33.72974371597207721 ) ) ;
#76238 = CARTESIAN_POINT ( 'NONE',  ( 3.230769230769231726, -13.87047571288749737, 32.06866353760679544 ) ) ;
#76239 = CARTESIAN_POINT ( 'NONE',  ( 17.07692307692295586, -12.16647553114689728, 32.15551576947799362 ) ) ;
#76240 = ORIENTED_EDGE ( 'NONE', *, *, #34738, .F. ) ;
#76241 = CARTESIAN_POINT ( 'NONE',  ( 0.4615384615383396616, -10.90142922262034020, 33.41473453929536674 ) ) ;
#76242 = CARTESIAN_POINT ( 'NONE',  ( 20.74999999999999645, -12.50000000000000000, 29.75000000000000355 ) ) ;
#76243 = CARTESIAN_POINT ( 'NONE',  ( 8.519207545009313876, -8.475808217655753651, 34.90892951860618609 ) ) ;
#76244 = CARTESIAN_POINT ( 'NONE',  ( -7.146003140593069070, -10.61292498521070549, 33.66303323003028680 ) ) ;
#76245 = EDGE_LOOP ( 'NONE', ( #50707, #79073, #37598, #54461 ) ) ;
#76246 = CARTESIAN_POINT ( 'NONE',  ( -4.946132635956127288, -4.684288915650984819, 34.18129842949671371 ) ) ;
#76247 = ORIENTED_EDGE ( 'NONE', *, *, #9308, .T. ) ;
#76249 = ORIENTED_EDGE ( 'NONE', *, *, #54149, .T. ) ;
#76248 = DIRECTION ( 'NONE',  ( -0.000000000000000000, 1.000000000000000000, -0.000000000000000000 ) ) ;
#76250 = CARTESIAN_POINT ( 'NONE',  ( 9.627037246346921151, -3.835265460703609186, 33.15142922261924241 ) ) ;
#76251 = CARTESIAN_POINT ( 'NONE',  ( -4.376772371362299019, -2.758268499246657957, 31.33685645148948140 ) ) ;
#76252 = DIRECTION ( 'NONE',  ( 0.000000000000000000, 0.3420201433256641055, -0.9396926207859100932 ) ) ;
#76253 = CARTESIAN_POINT ( 'NONE',  ( 14.05771557674995442, -9.148715823498378086, 34.47080413974185120 ) ) ;
#76254 = CARTESIAN_POINT ( 'NONE',  ( 9.942253210655836781, -9.272278438253398036, 34.42582936511637115 ) ) ;
#76256 = CARTESIAN_POINT ( 'NONE',  ( 13.38461538461538680, -5.180354513474913603, 36.12317359536750416 ) ) ;
#76255 = CARTESIAN_POINT ( 'NONE',  ( 13.63466969625370062, -5.728107161865378494, 34.42597550085002922 ) ) ;
#76257 = ADVANCED_FACE ( 'NONE', ( #27707 ), #40351, .F. ) ;
#76258 = ADVANCED_FACE ( 'NONE', ( #88995 ), #6118, .F. ) ;
#76259 = DIRECTION ( 'NONE',  ( -0.000000000000000000, 0.9848077530122085754, -0.1736481776669273613 ) ) ;
#76260 = AXIS2_PLACEMENT_3D ( 'NONE', #57537, #42712, #8035 ) ;
#76261 = CARTESIAN_POINT ( 'NONE',  ( -1.944543648263014957, -5.555456351737005249, 24.00000000000000000 ) ) ;
#76262 = APPLICATION_CONTEXT ( 'automotive_design' ) ;
#76263 = ORIENTED_EDGE ( 'NONE', *, *, #78246, .T. ) ;
#76264 = CARTESIAN_POINT ( 'NONE',  ( 17.93472955403921887, -4.481592998940161721, 33.73612834413957984 ) ) ;
#76265 = ORIENTED_EDGE ( 'NONE', *, *, #19530, .T. ) ;
#76266 = EDGE_CURVE ( 'NONE', #67618, #27341, #75456, .T. ) ;
#76267 = ORIENTED_EDGE ( 'NONE', *, *, #83652, .F. ) ;
#76268 = CARTESIAN_POINT ( 'NONE',  ( 3.100622021331010725, -5.195881422630167279, 34.18770438780618548 ) ) ;
#76269 = EDGE_CURVE ( 'NONE', #86305, #43735, #82674, .T. ) ;
#76270 = ORIENTED_EDGE ( 'NONE', *, *, #21917, .T. ) ;
#76271 = CARTESIAN_POINT ( 'NONE',  ( -4.283994123577852697, -2.647304123082328875, 31.75400227202885262 ) ) ;
#76272 = CARTESIAN_POINT ( 'NONE',  ( -11.47320639894870276, -10.33852847137154107, 34.16647553114620450 ) ) ;
#76273 = CARTESIAN_POINT ( 'NONE',  ( -15.90390063549801347, -5.852078868378312038, 34.47109172314383585 ) ) ;
#76274 = DIRECTION ( 'NONE',  ( 0.000000000000000000, 0.9848077530122072432, 0.1736481776669354937 ) ) ;
#76275 = CARTESIAN_POINT ( 'NONE',  ( -9.070512820512819374, -11.00000000000000000, 29.75000000000000355 ) ) ;
#76276 = CARTESIAN_POINT ( 'NONE',  ( -8.992715693795103604, -2.612411019501189369, 31.66733052389439962 ) ) ;
#76277 = B_SPLINE_CURVE_WITH_KNOTS ( 'NONE', 3,
 ( #1891, #63588, #84327, #70804, #9106, #36569, #22601, #34786, #76213, #62253 ),
 .UNSPECIFIED., .F., .F.,
 ( 4, 2, 2, 2, 4 ),
 ( 0.5000000000000000000, 0.6250000000000000000, 0.7500000000000000000, 0.8750000000000000000, 1.000000000000000000 ),
 .UNSPECIFIED. ) ;
#76278 = LINE ( 'NONE', #29874, #55692 ) ;
#76279 = CARTESIAN_POINT ( 'NONE',  ( 2.651650429449539104, -4.848349570550432475, 25.56250000000000355 ) ) ;
#76280 = B_SPLINE_CURVE_WITH_KNOTS ( 'NONE', 3,
 ( #72508, #21783, #21336, #55561, #64083, #49694, #1069, #22663, #15479, #36200 ),
 .UNSPECIFIED., .F., .F.,
 ( 4, 2, 2, 2, 4 ),
 ( 0.000000000000000000, 0.0001954339857564078809, 0.0003908679715128157619, 0.0005863019572692236428, 0.0007817359430256315238 ),
 .UNSPECIFIED. ) ;
#76281 = CARTESIAN_POINT ( 'NONE',  ( 10.61538461538449596, -2.625532179533778709, 30.86335684631627174 ) ) ;
#76282 = CARTESIAN_POINT ( 'NONE',  ( -2.242437168179467477, -3.083524468853784839, 32.58852847137153930 ) ) ;
#76283 = AXIS2_PLACEMENT_3D ( 'NONE', #62050, #28259, #63820 ) ;
#76284 = ADVANCED_FACE ( 'NONE', ( #80904 ), #61051, .F. ) ;
#76285 = CARTESIAN_POINT ( 'NONE',  ( -11.78846153846153832, -2.499999999999998668, 29.75000000000000355 ) ) ;
#76286 = CARTESIAN_POINT ( 'NONE',  ( -0.2115384615384616196, -2.499999999999998668, 29.75000000000000355 ) ) ;
#76287 = VECTOR ( 'NONE', #19664, 1000.000000000000000 ) ;
#76288 = VERTEX_POINT ( 'NONE', #32689 ) ;
#76289 = ORIENTED_EDGE ( 'NONE', *, *, #59473, .T. ) ;
#76290 = CARTESIAN_POINT ( 'NONE',  ( 2.980746006547773330, -10.92453946501458439, 33.72985991061850086 ) ) ;
#76291 = CARTESIAN_POINT ( 'NONE',  ( 15.48071464014727283, -12.07971442181322352, 32.31769673815850297 ) ) ;
#76292 = FACE_OUTER_BOUND ( 'NONE', #53369, .T. ) ;
#76293 = EDGE_CURVE ( 'NONE', #37810, #8955, #36686, .T. ) ;
#76294 = CARTESIAN_POINT ( 'NONE',  ( 0.3308478584281519530, -9.929715669179216775, 34.40415004197138416 ) ) ;
#76295 = VECTOR ( 'NONE', #9270, 1000.000000000000000 ) ;
#76296 = CARTESIAN_POINT ( 'NONE',  ( 9.915320536401090123, -11.43677907613344757, 33.22367315496202167 ) ) ;
#76297 = AXIS2_PLACEMENT_3D ( 'NONE', #78221, #37681, #70589 ) ;
#76298 = CARTESIAN_POINT ( 'NONE',  ( -9.627052552794850726, -11.06231777344671130, 33.60647404775212976 ) ) ;
#76299 = CARTESIAN_POINT ( 'NONE',  ( -5.999999999999683808, -2.255955759149395501, 30.00000000000324363 ) ) ;
#76300 = ADVANCED_FACE ( 'NONE', ( #55617 ), #23169, .F. ) ;
#76301 = EDGE_LOOP ( 'NONE', ( #70307, #18637 ) ) ;
#76302 = CARTESIAN_POINT ( 'NONE',  ( -13.63459211555773720, -9.943427161483782584, 34.11278801902876978 ) ) ;
#76303 = ORIENTED_EDGE ( 'NONE', *, *, #68513, .F. ) ;
#76304 = EDGE_CURVE ( 'NONE', #44682, #21602, #8777, .T. ) ;
#76305 = CARTESIAN_POINT ( 'NONE',  ( -18.00000000000000000, -1.973681607567911556, 34.71348354719103924 ) ) ;
#76306 = CARTESIAN_POINT ( 'NONE',  ( 15.29683656411930848, -3.322132147404559976, 32.92929555188717927 ) ) ;
#76307 = CARTESIAN_POINT ( 'NONE',  ( -6.857932142357289429, -7.750023224968867197, 34.99404313364389907 ) ) ;
#76308 = CARTESIAN_POINT ( 'NONE',  ( 3.903822929624695792, -6.652501968072646932, 34.93155406624980941 ) ) ;
#76309 = FACE_OUTER_BOUND ( 'NONE', #87194, .T. ) ;
#76310 = ORIENTED_EDGE ( 'NONE', *, *, #19738, .T. ) ;
#76311 = ADVANCED_FACE ( 'NONE', ( #69142 ), #29494, .F. ) ;
#76312 = ORIENTED_EDGE ( 'NONE', *, *, #20312, .F. ) ;
#76313 = ORIENTED_EDGE ( 'NONE', *, *, #7407, .T. ) ;
#76314 = VERTEX_POINT ( 'NONE', #14644 ) ;
#76315 = ADVANCED_FACE ( 'NONE', ( #76793 ), #7449, .F. ) ;
#76316 = CARTESIAN_POINT ( 'NONE',  ( -10.61538461538461320, -12.34228464037088635, 31.77849191805839268 ) ) ;
#76317 = CARTESIAN_POINT ( 'NONE',  ( -16.08777882049607655, -9.058645607665452459, 34.76329471203371924 ) ) ;
#76318 = AXIS2_PLACEMENT_3D ( 'NONE', #53119, #45028, #33313 ) ;
#76319 = CARTESIAN_POINT ( 'NONE',  ( -13.38461538461538325, -11.33034616979429110, 35.88435417666054406 ) ) ;
#76320 = CARTESIAN_POINT ( 'NONE',  ( 11.31497659473759043, -12.24155766932282496, 31.33739205006857986 ) ) ;
#76321 = DIRECTION ( 'NONE',  ( -1.000000000000000000, -0.000000000000000000, -0.000000000000000000 ) ) ;
#76322 = CARTESIAN_POINT ( 'NONE',  ( 0.000000000000000000, -11.00000000000000000, 29.75000000000000355 ) ) ;
#76323 = ORIENTED_EDGE ( 'NONE', *, *, #71896, .T. ) ;
#76324 = EDGE_CURVE ( 'NONE', #25936, #80774, #64578, .T. ) ;
#76325 = ORIENTED_EDGE ( 'NONE', *, *, #45480, .F. ) ;
#76326 = VERTEX_POINT ( 'NONE', #9227 ) ;
#76328 = ORIENTED_EDGE ( 'NONE', *, *, #7796, .T. ) ;
#76327 = DIRECTION ( 'NONE',  ( -1.000000000000000000, 0.000000000000000000, -0.000000000000000000 ) ) ;
#76329 = EDGE_CURVE ( 'NONE', #43687, #10616, #76409, .T. ) ;
#76331 = CARTESIAN_POINT ( 'NONE',  ( 14.43848274865925774, -4.684288915650983043, 34.18129842949671371 ) ) ;
#76330 = DIRECTION ( 'NONE',  ( 0.000000000000000000, 0.9848077530122072432, 0.1736481776669354937 ) ) ;
#76332 = CARTESIAN_POINT ( 'NONE',  ( -5.076923076923075762, -11.16473453929635440, 33.15142922261926373 ) ) ;
#76333 = CARTESIAN_POINT ( 'NONE',  ( -3.749999999999988454, -9.053300858899127945, 26.26562500000000000 ) ) ;
#76334 = ORIENTED_EDGE ( 'NONE', *, *, #88271, .F. ) ;
#76335 = VECTOR ( 'NONE', #46985, 1000.000000000000000 ) ;
#76336 = VERTEX_POINT ( 'NONE', #70476 ) ;
#76337 = CARTESIAN_POINT ( 'NONE',  ( -17.75005459062195712, -2.986452184633680229, 32.43230066228895225 ) ) ;
#76338 = EDGE_LOOP ( 'NONE', ( #40790, #44650, #29683, #50273 ) ) ;
#76339 = FACE_BOUND ( 'NONE', #81754, .T. ) ;
#76340 = CARTESIAN_POINT ( 'NONE',  ( -5.749945580086545327, -2.920487667080175154, 32.31805714834170828 ) ) ;
#76341 = CIRCLE ( 'NONE', #24585, 4.000000000000000000 ) ;
#76342 = FACE_OUTER_BOUND ( 'NONE', #2506, .T. ) ;
#76343 = EDGE_LOOP ( 'NONE', ( #53914, #68793, #6794, #66894 ) ) ;
#76344 = DIRECTION ( 'NONE',  ( 1.000000000000000000, 0.000000000000000000, 0.000000000000000000 ) ) ;
#76345 = CARTESIAN_POINT ( 'NONE',  ( 8.546303810323918171, -11.98009711892699514, 32.48740034544076138 ) ) ;
#76346 = CARTESIAN_POINT ( 'NONE',  ( 10.48469314871706182, -2.729777683071817229, 31.24903638046269450 ) ) ;
#76347 = CARTESIAN_POINT ( 'NONE',  ( 0.7114839798866029463, -6.696923467548660192, 34.68552623307873972 ) ) ;
#76348 = CARTESIAN_POINT ( 'NONE',  ( 14.17754433796061875, -9.504002272028875709, 34.60269587691767867 ) ) ;
#76349 = ORIENTED_EDGE ( 'NONE', *, *, #68657, .F. ) ;
#76350 = VECTOR ( 'NONE', #3679, 1000.000000000000114 ) ;
#76351 = DIRECTION ( 'NONE',  ( 0.000000000000000000, 0.7660444431189822323, -0.6427876096865344779 ) ) ;
#76352 = CARTESIAN_POINT ( 'NONE',  ( -12.21159305216042057, -2.341251567377310217, 30.72681386836322659 ) ) ;
#76353 = CARTESIAN_POINT ( 'NONE',  ( 1.515141086378950730, -8.586989748646450593, 34.63063291749215011 ) ) ;
#76354 = CARTESIAN_POINT ( 'NONE',  ( 0.2380535178145146147, -11.89387501736623420, 32.13663884655804992 ) ) ;
#76355 = LINE ( 'NONE', #2027, #58729 ) ;
#76356 = DIRECTION ( 'NONE',  ( -0.000000000000000000, -0.6427876096865404731, -0.7660444431189770143 ) ) ;
#76357 = FACE_BOUND ( 'NONE', #35164, .T. ) ;
#76359 = CARTESIAN_POINT ( 'NONE',  ( -6.222926958906846551, -10.01117774369187252, 34.36070679894347535 ) ) ;
#76358 = CARTESIAN_POINT ( 'NONE',  ( -6.700297254098854793, -12.69155399931963046, 30.53255429739158444 ) ) ;
#76360 = CARTESIAN_POINT ( 'NONE',  ( 5.326977496836529546, -2.318338780012835443, 30.59689888758630261 ) ) ;
#76362 = CARTESIAN_POINT ( 'NONE',  ( -6.223484943723947893, -5.113361153441932316, 34.14387501736621999 ) ) ;
#76361 = CARTESIAN_POINT ( 'NONE',  ( 3.930919194939304973, -5.582147617184174848, 34.63737895849758530 ) ) ;
#76363 = CARTESIAN_POINT ( 'NONE',  ( -10.86536135943320502, -6.524016743844655686, 34.90889640711025521 ) ) ;
#76364 = CARTESIAN_POINT ( 'NONE',  ( -1.987747218494660295, -5.598659921968651254, 19.99813170625848713 ) ) ;
#76365 = EDGE_LOOP ( 'NONE', ( #59991, #21559 ) ) ;
#76366 = CARTESIAN_POINT ( 'NONE',  ( 12.59206416330202671, -2.619367082507849442, 30.83698974864643461 ) ) ;
#76367 = ORIENTED_EDGE ( 'NONE', *, *, #57901, .T. ) ;
#76368 = EDGE_CURVE ( 'NONE', #9598, #65911, #48484, .T. ) ;
#76369 = CARTESIAN_POINT ( 'NONE',  ( -13.38461538461538325, -10.67929555188718282, 33.92786785259544047 ) ) ;
#76370 = B_SPLINE_CURVE_WITH_KNOTS ( 'NONE', 3,
 ( #78922, #24863, #52333, #17678, #38388, #46030, #8815, #79375, #45135, #29529 ),
 .UNSPECIFIED., .F., .F.,
 ( 4, 2, 2, 2, 4 ),
 ( 0.000000000000000000, 0.0001954339857564081791, 0.0003908679715128163582, 0.0005863019572692245102, 0.0007817359430256327164 ),
 .UNSPECIFIED. ) ;
#76371 = ORIENTED_EDGE ( 'NONE', *, *, #6990, .T. ) ;
#76372 = DIRECTION ( 'NONE',  ( 0.000000000000000000, 0.9848077530122072432, 0.1736481776669354937 ) ) ;
#76373 = EDGE_CURVE ( 'NONE', #6248, #41990, #58220, .T. ) ;
#76374 = DIRECTION ( 'NONE',  ( -0.000000000000000000, 0.9848077530122086864, -0.1736481776669273891 ) ) ;
#76375 = EDGE_LOOP ( 'NONE', ( #41877, #77047 ) ) ;
#76376 = FACE_OUTER_BOUND ( 'NONE', #67258, .T. ) ;
#76377 = CARTESIAN_POINT ( 'NONE',  ( -1.901340078031346525, -9.487747218494661183, 20.93563170625849068 ) ) ;
#76378 = B_SPLINE_CURVE_WITH_KNOTS ( 'NONE', 3,
 ( #23979, #17689, #2818, #4615, #79837, #37053, #18134, #45145, #3713, #85261 ),
 .UNSPECIFIED., .F., .F.,
 ( 4, 2, 2, 2, 4 ),
 ( 0.000000000000000000, 0.0001954339857564097241, 0.0003908679715128194482, 0.0005863019572692291723, 0.0007817359430256388964 ),
 .UNSPECIFIED. ) ;
#76379 = CARTESIAN_POINT ( 'NONE',  ( 20.00000000000000000, -4.000000000000000000, 29.75000000000000355 ) ) ;
#76380 = CARTESIAN_POINT ( 'NONE',  ( -5.326899807865431491, -4.943428324936578910, 34.04746400365624481 ) ) ;
#76381 = CARTESIAN_POINT ( 'NONE',  ( 16.85343813319912698, -12.44517049084099725, 30.48991314939691932 ) ) ;
#76382 = CARTESIAN_POINT ( 'NONE',  ( 1.319345384059066761, -5.094484230520674117, 34.41647553114621161 ) ) ;
#76383 = CARTESIAN_POINT ( 'NONE',  ( 4.826946345980720920, -8.303909089506435137, 34.68538101551103381 ) ) ;
#76384 = DIRECTION ( 'NONE',  ( -0.000000000000000000, 0.9848077530122085754, -0.1736481776669273613 ) ) ;
#76385 = EDGE_CURVE ( 'NONE', #59397, #27552, #79896, .T. ) ;
#76386 = AXIS2_PLACEMENT_3D ( 'NONE', #49606, #83405, #8631 ) ;
#76387 = CARTESIAN_POINT ( 'NONE',  ( -0.06109907496450878162, -11.25000000000000000, 25.03311829374151287 ) ) ;
#76388 = CARTESIAN_POINT ( 'NONE',  ( -10.39237326377176629, -2.758310577978207778, 31.33698337089302299 ) ) ;
#76389 = CARTESIAN_POINT ( 'NONE',  ( -5.999999999999998224, -3.322132147404559976, 32.92929555188717927 ) ) ;
#76390 = ORIENTED_EDGE ( 'NONE', *, *, #23837, .F. ) ;
#76391 = VECTOR ( 'NONE', #28053, 1000.000000000000000 ) ;
#76392 = ADVANCED_FACE ( 'NONE', ( #44301 ), #37561, .F. ) ;
#76393 = LINE ( 'NONE', #28656, #83856 ) ;
#76394 = CARTESIAN_POINT ( 'NONE',  ( -0.06109907496450878162, -11.25000000000000000, 23.78311829374151998 ) ) ;
#76395 = LINE ( 'NONE', #36739, #15960 ) ;
#76396 = CARTESIAN_POINT ( 'NONE',  ( -8.992715693795100051, -3.562934362175800285, 33.22335522853832401 ) ) ;
#76397 = ORIENTED_EDGE ( 'NONE', *, *, #16464, .F. ) ;
#76398 = CARTESIAN_POINT ( 'NONE',  ( 6.857752910272615132, -7.749976730030849303, 34.74374725381503737 ) ) ;
#76399 = CARTESIAN_POINT ( 'NONE',  ( -0.2114841499001461067, -9.943054286541405773, 34.11300777759955594 ) ) ;
#76401 = ORIENTED_EDGE ( 'NONE', *, *, #5089, .F. ) ;
#76400 = CARTESIAN_POINT ( 'NONE',  ( 2.307692307692309264, -2.721908614388771852, 31.22303859784724978 ) ) ;
#76402 = FACE_OUTER_BOUND ( 'NONE', #68521, .T. ) ;
#76403 = CARTESIAN_POINT ( 'NONE',  ( 4.500000000000003553, -7.499999999999999112, 13.50000000000000178 ) ) ;
#76405 = EDGE_CURVE ( 'NONE', #83780, #67446, #47163, .T. ) ;
#76404 = DIRECTION ( 'NONE',  ( -0.000000000000000000, 0.6427876096865404731, -0.7660444431189771253 ) ) ;
#76406 = FACE_OUTER_BOUND ( 'NONE', #60654, .T. ) ;
#76407 = CARTESIAN_POINT ( 'NONE',  ( 0.4615384615384611200, -12.34228464037088635, 31.77849191805839268 ) ) ;
#76408 = B_SPLINE_CURVE_WITH_KNOTS ( 'NONE', 3,
 ( #44739, #43860, #16834, #65007, #71327, #85306, #57821, #3317, #66359, #52836 ),
 .UNSPECIFIED., .F., .F.,
 ( 4, 2, 2, 2, 4 ),
 ( 0.0007817359430256297891, 0.0009771253907249961065, 0.001172514838424362424, 0.001367904286123728741, 0.001563293733823095059 ),
 .UNSPECIFIED. ) ;
#76409 = B_SPLINE_CURVE_WITH_KNOTS ( 'NONE', 3,
 ( #34904, #28149, #8335, #7887, #62805, #35811, #36689, #35353, #28606, #43003 ),
 .UNSPECIFIED., .F., .F.,
 ( 4, 2, 2, 2, 4 ),
 ( 0.000000000000000000, 0.0001954311564186868473, 0.0003908623128373736946, 0.0005862934692560605419, 0.0007817246256747473893 ),
 .UNSPECIFIED. ) ;
#76410 = CIRCLE ( 'NONE', #87962, 0.2500000000000002220 ) ;
#76411 = VERTEX_POINT ( 'NONE', #78550 ) ;
#76412 = CARTESIAN_POINT ( 'NONE',  ( -0.3310127597748971362, -10.88167719472716399, 33.43325721877153711 ) ) ;
#76413 = ORIENTED_EDGE ( 'NONE', *, *, #50357, .F. ) ;
#76414 = B_SPLINE_CURVE_WITH_KNOTS ( 'NONE', 3,
 ( #50734, #43987, #30479, #71907, #78219, #16521, #51164, #85429, #71458, #17865 ),
 .UNSPECIFIED., .F., .F.,
 ( 4, 2, 2, 2, 4 ),
 ( 0.0007817246256747514008, 0.0009771112852218959231, 0.001172497944769040337, 0.001367884604316184751, 0.001563271263863329165 ),
 .UNSPECIFIED. ) ;
#76415 = B_SPLINE_CURVE_WITH_KNOTS ( 'NONE', 3,
 ( #83041, #623, #21327, #54660, #55999, #20881, #88488, #76268, #48796, #35287 ),
 .UNSPECIFIED., .F., .F.,
 ( 4, 2, 2, 2, 4 ),
 ( 0.000000000000000000, 0.0001954339857564070949, 0.0003908679715128141898, 0.0005863019572692212576, 0.0007817359430256283796 ),
 .UNSPECIFIED. ) ;
#76416 = EDGE_CURVE ( 'NONE', #38114, #5766, #43880, .T. ) ;
#76417 = ORIENTED_EDGE ( 'NONE', *, *, #39554, .F. ) ;
#76418 = AXIS2_PLACEMENT_3D ( 'NONE', #26703, #33469, #55063 ) ;
#76419 = CARTESIAN_POINT ( 'NONE',  ( -13.38461538461538325, -3.513871655860378418, 32.76840700105978499 ) ) ;
#76420 = DIRECTION ( 'NONE',  ( -1.000000000000000000, 0.000000000000000000, -0.000000000000000000 ) ) ;
#76421 = EDGE_CURVE ( 'NONE', #15649, #31320, #38501, .T. ) ;
#76422 = CARTESIAN_POINT ( 'NONE',  ( -14.30769230769230660, -10.05456864172156806, 36.03766855953608683 ) ) ;
#76423 = DIRECTION ( 'NONE',  ( -0.000000000000000000, 1.000000000000000000, 3.491481338843133355E-15 ) ) ;
#76424 = ORIENTED_EDGE ( 'NONE', *, *, #8813, .F. ) ;
#76425 = DIRECTION ( 'NONE',  ( -0.000000000000000000, 2.413528314402514090E-16, -1.000000000000000000 ) ) ;
#76426 = VERTEX_POINT ( 'NONE', #16855 ) ;
#76427 = VERTEX_POINT ( 'NONE', #17755 ) ;
#76428 = EDGE_CURVE ( 'NONE', #47964, #30991, #72687, .T. ) ;
#76429 = ORIENTED_EDGE ( 'NONE', *, *, #72178, .T. ) ;
#76431 = EDGE_LOOP ( 'NONE', ( #87972, #9832, #73896, #44598 ) ) ;
#76430 = CARTESIAN_POINT ( 'NONE',  ( 4.403791563224197070, -12.45601412856602863, 31.48342859153981621 ) ) ;
#76432 = CARTESIAN_POINT ( 'NONE',  ( -0.5922299282060200509, -4.809359713505814149, 33.96456829005828837 ) ) ;
#76433 = CARTESIAN_POINT ( 'NONE',  ( 5.750023255951410839, -12.65889640711025521, 30.72598325615533454 ) ) ;
#76434 = CARTESIAN_POINT ( 'NONE',  ( -3.007757879156381264, -4.187068189119697692, 33.49521262558774026 ) ) ;
#76435 = DIRECTION ( 'NONE',  ( -0.000000000000000000, 0.7660444431189791237, -0.6427876096865379196 ) ) ;
#76436 = VERTEX_POINT ( 'NONE', #3336 ) ;
#76437 = EDGE_CURVE ( 'NONE', #7171, #68701, #65026, .T. ) ;
#76438 = ORIENTED_EDGE ( 'NONE', *, *, #20596, .F. ) ;
#76439 = B_SPLINE_CURVE_WITH_KNOTS ( 'NONE', 3,
 ( #31137, #37453, #23063, #24377, #10883, #51845, #37910, #50521, #65808, #79341 ),
 .UNSPECIFIED., .F., .F.,
 ( 4, 2, 2, 2, 4 ),
 ( 0.000000000000000000, 0.0001954311564186860071, 0.0003908623128373720141, 0.0005862934692560580483, 0.0007817246256747440282 ),
 .UNSPECIFIED. ) ;
#76440 = ORIENTED_EDGE ( 'NONE', *, *, #81198, .T. ) ;
#76441 = CYLINDRICAL_SURFACE ( 'NONE', #24584, 4.000000000000000000 ) ;
#76443 = VERTEX_POINT ( 'NONE', #10995 ) ;
#76442 = CARTESIAN_POINT ( 'NONE',  ( 1.161689167099238640, -8.239355502252617924, 34.69524867566427417 ) ) ;
#76444 = B_SPLINE_CURVE_WITH_KNOTS ( 'NONE', 3,
 ( #67112, #25674, #10829, #53130, #53581, #80638, #18917, #37851, #59005, #3613 ),
 .UNSPECIFIED., .F., .F.,
 ( 4, 2, 2, 2, 4 ),
 ( 0.0007817359430256388964, 0.0009771253907250069485, 0.001172514838424375001, 0.001367904286123743270, 0.001563293733823111322 ),
 .UNSPECIFIED. ) ;
#76445 = CARTESIAN_POINT ( 'NONE',  ( 13.13461538461538680, -2.499999999999998668, 29.75000000000000355 ) ) ;
#76447 = B_SPLINE_CURVE_WITH_KNOTS ( 'NONE', 3,
 ( #22896, #50360, #85058, #72410, #66557, #24674, #25119, #3506, #10278, #79180 ),
 .UNSPECIFIED., .F., .F.,
 ( 4, 2, 2, 2, 4 ),
 ( 0.000000000000000000, 0.0001954311564186863052, 0.0003908623128373726104, 0.0005862934692560589156, 0.0007817246256747452209 ),
 .UNSPECIFIED. ) ;
#76446 = VECTOR ( 'NONE', #74809, 1000.000000000000000 ) ;
#76448 = EDGE_CURVE ( 'NONE', #47862, #27365, #31255, .T. ) ;
#76449 = EDGE_CURVE ( 'NONE', #75373, #38598, #65707, .T. ) ;
#76450 = CARTESIAN_POINT ( 'NONE',  ( 14.30769230769231015, -3.322132147404559976, 32.92929555188717927 ) ) ;
#76451 = VERTEX_POINT ( 'NONE', #4231 ) ;
#76452 = AXIS2_PLACEMENT_3D ( 'NONE', #46031, #58647, #72610 ) ;
#76453 = CARTESIAN_POINT ( 'NONE',  ( -1.576923076923076872, -3.499999999999999556, 29.75000000000000355 ) ) ;
#76454 = LINE ( 'NONE', #63367, #56919 ) ;
#76455 = VERTEX_POINT ( 'NONE', #86677 ) ;
#76456 = FACE_BOUND ( 'NONE', #46129, .T. ) ;
#76457 = EDGE_CURVE ( 'NONE', #42886, #36014, #28082, .T. ) ;
#76458 = CARTESIAN_POINT ( 'NONE',  ( 11.40777007179398161, -4.809359713505814149, 33.96456829005828837 ) ) ;
#76459 = DIRECTION ( 'NONE',  ( 0.000000000000000000, 0.000000000000000000, 1.000000000000000000 ) ) ;
#76460 = LINE ( 'NONE', #40901, #49479 ) ;
#76462 = CARTESIAN_POINT ( 'NONE',  ( 17.99999999999987566, -4.481592998941358097, 33.73612834414048933 ) ) ;
#76461 = CARTESIAN_POINT ( 'NONE',  ( 18.25005441991345378, -2.920487667080175154, 32.31805714834170828 ) ) ;
#76463 = CARTESIAN_POINT ( 'NONE',  ( -3.230769230769229949, -3.322132147404559976, 32.92929555188717927 ) ) ;
#76464 = CARTESIAN_POINT ( 'NONE',  ( 18.24994551834814160, -2.824170634883622633, 31.52227843825338738 ) ) ;
#76465 = EDGE_LOOP ( 'NONE', ( #30230, #1117, #32923, #42290, #63433 ) ) ;
#76466 = CARTESIAN_POINT ( 'NONE',  ( -2.557669051740898425, -4.075325502946086864, 33.72974371597207721 ) ) ;
#76467 = CARTESIAN_POINT ( 'NONE',  ( -9.692307692307691624, -13.20930481340135110, 34.54067556320372745 ) ) ;
#76468 = ORIENTED_EDGE ( 'NONE', *, *, #27888, .T. ) ;
#76469 = CARTESIAN_POINT ( 'NONE',  ( 8.546304551714618114, -3.105860786376062332, 32.13614157043599562 ) ) ;
#76470 = DIRECTION ( 'NONE',  ( -0.000000000000000000, -0.9848077530122086864, -0.1736481776669273891 ) ) ;
#76471 = VERTEX_POINT ( 'NONE', #85323 ) ;
#76472 = CARTESIAN_POINT ( 'NONE',  ( -6.923076923076922462, -3.886160181151819604, 36.00935417666054406 ) ) ;
#76473 = FACE_OUTER_BOUND ( 'NONE', #51681, .T. ) ;
#76474 = FACE_BOUND ( 'NONE', #74466, .T. ) ;
#76476 = CARTESIAN_POINT ( 'NONE',  ( -17.07692307692307665, -12.37446782046654192, 30.86335684631486131 ) ) ;
#76475 = CARTESIAN_POINT ( 'NONE',  ( -2.372962753653081958, -6.879047030191174805, 34.71129190930000163 ) ) ;
#76477 = CARTESIAN_POINT ( 'NONE',  ( 3.230769230769108269, -6.835583212225970762, 34.95778746994575670 ) ) ;
#76478 = CARTESIAN_POINT ( 'NONE',  ( -15.45369544828537833, -9.086856451489515152, 34.49173150075333183 ) ) ;
#76480 = CYLINDRICAL_SURFACE ( 'NONE', #66450, 0.2499999999999979738 ) ;
#76479 = CARTESIAN_POINT ( 'NONE',  ( -18.00000000000012079, -11.48612834414049644, 32.76840700105863391 ) ) ;
#76481 = CARTESIAN_POINT ( 'NONE',  ( -18.00000000000000000, -8.809628690132287332, 35.73758076001107042 ) ) ;
#76482 = CARTESIAN_POINT ( 'NONE',  ( 1.492201783934554493, -3.724691934501233703, 17.73250670625848713 ) ) ;
#76483 = ORIENTED_EDGE ( 'NONE', *, *, #31901, .T. ) ;
#76484 = VECTOR ( 'NONE', #686, 1000.000000000000000 ) ;
#76485 = ORIENTED_EDGE ( 'NONE', *, *, #70181, .F. ) ;
#76486 = DIRECTION ( 'NONE',  ( 1.000000000000000000, 0.000000000000000000, 0.000000000000000000 ) ) ;
#76487 = CARTESIAN_POINT ( 'NONE',  ( 14.30769230769218581, -12.70778746994576025, 30.41441678777401236 ) ) ;
#76488 = CARTESIAN_POINT ( 'NONE',  ( 14.55774672760575861, -9.233818618650603938, 34.70587769442853698 ) ) ;
#76489 = CARTESIAN_POINT ( 'NONE',  ( 8.703980837456683162, -2.255955759149247619, 30.00000000000013856 ) ) ;
#76490 = CARTESIAN_POINT ( 'NONE',  ( -16.82686876528476105, -6.567000820036036579, 34.66262288849541306 ) ) ;
#76491 = CARTESIAN_POINT ( 'NONE',  ( -1.492201783934549164, -11.27530806549876807, 17.10750670625848713 ) ) ;
#76492 = VECTOR ( 'NONE', #31767, 1000.000000000000000 ) ;
#76493 = FACE_OUTER_BOUND ( 'NONE', #49492, .T. ) ;
#76494 = CARTESIAN_POINT ( 'NONE',  ( 18.06606835100243558, -3.050289026998446840, 32.03036669348366416 ) ) ;
#76495 = CARTESIAN_POINT ( 'NONE',  ( 6.223012844093396723, -4.026326845037961455, 33.68677907613344047 ) ) ;
#76496 = CARTESIAN_POINT ( 'NONE',  ( 7.622668921589517588, -5.827078755546624578, 34.72654668319379567 ) ) ;
#76497 = CARTESIAN_POINT ( 'NONE',  ( -1.134615384613964384, -7.500000000000154543, 35.00000000000007105 ) ) ;
#76498 = CARTESIAN_POINT ( 'NONE',  ( -11.53846153846153655, -1.509761064869970415, 31.06009739812519044 ) ) ;
#76499 = CARTESIAN_POINT ( 'NONE',  ( -5.999999999999998224, -11.35647404775217417, 33.31231777344666511 ) ) ;
#76500 = CARTESIAN_POINT ( 'NONE',  ( -11.00641025641025550, -3.499999999999999556, 29.75000000000000355 ) ) ;
#76501 = DIRECTION ( 'NONE',  ( -0.000000000000000000, -0.8660254037844397068, -0.4999999999999978906 ) ) ;
#76502 = ORIENTED_EDGE ( 'NONE', *, *, #2941, .T. ) ;
#76503 = CARTESIAN_POINT ( 'NONE',  ( 12.33139049180676672, -4.299443229763728169, 33.91186481527756058 ) ) ;
#76504 = DIRECTION ( 'NONE',  ( -0.000000000000000000, -0.3420201433256694346, -0.9396926207859080948 ) ) ;
#76505 = CARTESIAN_POINT ( 'NONE',  ( -2.775308065498752086, -8.577988221561495763, 19.01749329374151287 ) ) ;
#76506 = CARTESIAN_POINT ( 'NONE',  ( -9.915234651214539952, -10.77366814457252175, 33.85459836347579454 ) ) ;
#76507 = CARTESIAN_POINT ( 'NONE',  ( 16.82689985270161870, -11.56360843649121861, 33.07473185843129926 ) ) ;
#76508 = ORIENTED_EDGE ( 'NONE', *, *, #10287, .T. ) ;
#76509 = CARTESIAN_POINT ( 'NONE',  ( -6.988346923633242724, -3.083524468853724443, 32.58852847137143272 ) ) ;
#76511 = ORIENTED_EDGE ( 'NONE', *, *, #658, .T. ) ;
#76510 = DIRECTION ( 'NONE',  ( -0.000000000000000000, -0.000000000000000000, -1.000000000000000000 ) ) ;
#76512 = CARTESIAN_POINT ( 'NONE',  ( 6.923076923076924238, -3.513871655860378418, 32.76840700105978499 ) ) ;
#76513 = CARTESIAN_POINT ( 'NONE',  ( 16.94623247381276698, -2.494641256782728966, 31.33461815524612959 ) ) ;
#76515 = ORIENTED_EDGE ( 'NONE', *, *, #69519, .T. ) ;
#76514 = B_SPLINE_CURVE_WITH_KNOTS ( 'NONE', 3,
 ( #53275, #5996, #46531, #87996, #13189, #46087, #5546, #46956, #21599, #26255 ),
 .UNSPECIFIED., .F., .F.,
 ( 4, 2, 2, 2, 4 ),
 ( 0.000000000000000000, 0.0001954339857564070949, 0.0003908679715128141898, 0.0005863019572692212576, 0.0007817359430256283796 ),
 .UNSPECIFIED. ) ;
#76516 = CARTESIAN_POINT ( 'NONE',  ( 17.07692307692295586, -2.657715359629662544, 31.77849191805970364 ) ) ;
#76518 = EDGE_CURVE ( 'NONE', #50090, #79307, #23605, .T. ) ;
#76517 = CARTESIAN_POINT ( 'NONE',  ( 10.68145194873469173, -10.67929555188718282, 33.92786785259544757 ) ) ;
#76519 = ORIENTED_EDGE ( 'NONE', *, *, #78866, .T. ) ;
#76520 = VECTOR ( 'NONE', #56955, 1000.000000000000000 ) ;
#76521 = CARTESIAN_POINT ( 'NONE',  ( 16.85399685940693004, -11.24512374952581872, 33.06303171183252942 ) ) ;
#76522 = CARTESIAN_POINT ( 'NONE',  ( -18.25000000000000355, -12.50000000000000000, 29.75000000000000355 ) ) ;
#76523 = CARTESIAN_POINT ( 'NONE',  ( 9.692307692307695177, -6.343179335718451384, 34.87096338111211935 ) ) ;
#76524 = VERTEX_POINT ( 'NONE', #67716 ) ;
#76526 = ORIENTED_EDGE ( 'NONE', *, *, #77177, .T. ) ;
#76525 = AXIS2_PLACEMENT_3D ( 'NONE', #70075, #75500, #43049 ) ;
#76527 = CARTESIAN_POINT ( 'NONE',  ( 3.230769230769108269, -3.083524468854526912, 32.58852847137268327 ) ) ;
#76528 = ORIENTED_EDGE ( 'NONE', *, *, #2404, .T. ) ;
#76529 = DIRECTION ( 'NONE',  ( 0.000000000000000000, 0.1736481776669275834, 0.9848077530122086864 ) ) ;
#76530 = CARTESIAN_POINT ( 'NONE',  ( -6.989159302437059296, -2.292212530054419606, 30.41441678777542634 ) ) ;
#76531 = CARTESIAN_POINT ( 'NONE',  ( -16.15384615384615330, -3.937682226553329556, 33.60647404775216529 ) ) ;
#76532 = EDGE_CURVE ( 'NONE', #57723, #58055, #39367, .T. ) ;
#76533 = CARTESIAN_POINT ( 'NONE',  ( -6.857821783564084228, -11.67786785259547777, 32.92929555188713664 ) ) ;
#76534 = CARTESIAN_POINT ( 'NONE',  ( -0.3962833220256230526, -5.941354392334606160, 34.76329471203374055 ) ) ;
#76535 = CARTESIAN_POINT ( 'NONE',  ( 0.2387103639035820235, -7.369209533119137845, 34.99857337881830688 ) ) ;
#76536 = CARTESIAN_POINT ( 'NONE',  ( 10.61538461538461675, -13.87047571288749737, 32.06866353760679544 ) ) ;
#76537 = ORIENTED_EDGE ( 'NONE', *, *, #50247, .F. ) ;
#76538 = EDGE_CURVE ( 'NONE', #49681, #43177, #27165, .T. ) ;
#76539 = ORIENTED_EDGE ( 'NONE', *, *, #76055, .F. ) ;
#76541 = ORIENTED_EDGE ( 'NONE', *, *, #70964, .T. ) ;
#76540 = CARTESIAN_POINT ( 'NONE',  ( 18.00000000000000000, -12.29105614889573062, 35.45975837776705220 ) ) ;
#76542 = CARTESIAN_POINT ( 'NONE',  ( -19.00000000000000000, -13.25000000000000533, 29.02772085586297024 ) ) ;
#76543 = VECTOR ( 'NONE', #10338, 1000.000000000000000 ) ;
#76544 = VERTEX_POINT ( 'NONE', #47427 ) ;
#76545 = B_SPLINE_CURVE_WITH_KNOTS ( 'NONE', 3,
 ( #7699, #20756, #14901, #54988, #36060, #28860, #34718, #21642, #69395, #15784 ),
 .UNSPECIFIED., .F., .F.,
 ( 4, 2, 2, 2, 4 ),
 ( 0.0007817359430256297891, 0.0009771253907249958896, 0.001172514838424361990, 0.001367904286123728091, 0.001563293733823094191 ),
 .UNSPECIFIED. ) ;
#76546 = DIRECTION ( 'NONE',  ( -0.000000000000000000, -0.5000000000000009992, -0.8660254037844380415 ) ) ;
#76547 = CARTESIAN_POINT ( 'NONE',  ( 5.207714884747862705, -3.530189275343204702, 32.79018710029569661 ) ) ;
#76548 = ORIENTED_EDGE ( 'NONE', *, *, #33309, .F. ) ;
#76549 = CARTESIAN_POINT ( 'NONE',  ( 8.769230769230645706, -12.70778746994576025, 30.41441678777401236 ) ) ;
#76550 = VECTOR ( 'NONE', #15494, 1000.000000000000000 ) ;
#76551 = ORIENTED_EDGE ( 'NONE', *, *, #15532, .T. ) ;
#76553 = ORIENTED_EDGE ( 'NONE', *, *, #79717, .F. ) ;
#76552 = CARTESIAN_POINT ( 'NONE',  ( -6.700065571464073777, -11.24521262558773671, 33.06293181088029343 ) ) ;
#76554 = FACE_OUTER_BOUND ( 'NONE', #50181, .T. ) ;
#76555 = EDGE_CURVE ( 'NONE', #57, #11273, #86159, .T. ) ;
#76556 = EDGE_CURVE ( 'NONE', #30991, #6722, #49615, .T. ) ;
#76557 = EDGE_LOOP ( 'NONE', ( #47210, #40819, #30645, #54471 ) ) ;
#76558 = DIRECTION ( 'NONE',  ( -0.000000000000000000, 0.7660444431189791237, -0.6427876096865379196 ) ) ;
#76559 = CARTESIAN_POINT ( 'NONE',  ( -9.019253993452226226, -12.07920672191015221, 32.31858351112116168 ) ) ;
#76560 = FACE_BOUND ( 'NONE', #71307, .T. ) ;
#76561 = B_SPLINE_CURVE_WITH_KNOTS ( 'NONE', 3,
 ( #41829, #69298, #68402, #8038, #33736, #35508, #76496, #47239, #74733, #13900 ),
 .UNSPECIFIED., .F., .F.,
 ( 4, 2, 2, 2, 4 ),
 ( 0.000000000000000000, 0.0001954311564186863323, 0.0003908623128373726646, 0.0005862934692560590241, 0.0007817246256747453293 ),
 .UNSPECIFIED. ) ;
#76562 = CARTESIAN_POINT ( 'NONE',  ( 1.515141086378949398, -12.45806712695776319, 30.39783852428763922 ) ) ;
#76563 = CARTESIAN_POINT ( 'NONE',  ( -20.74999999999999645, -10.50000000000000000, 29.75000000000000355 ) ) ;
#76564 = CARTESIAN_POINT ( 'NONE',  ( -1.384615384615383471, -6.681629849574314051, 35.83090037661290239 ) ) ;
#76565 = CARTESIAN_POINT ( 'NONE',  ( -14.16025641025641058, -11.50000000000000000, 29.75000000000000355 ) ) ;
#76566 = CARTESIAN_POINT ( 'NONE',  ( -17.30040800148741198, -8.539481045369598178, 34.89627647299170832 ) ) ;
#76567 = CARTESIAN_POINT ( 'NONE',  ( -9.692307692307377209, -2.255955759149395501, 30.00000000000324363 ) ) ;
#76568 = ORIENTED_EDGE ( 'NONE', *, *, #14841, .F. ) ;
#76569 = CARTESIAN_POINT ( 'NONE',  ( 14.30769230769231015, -6.343179335718451384, 34.87096338111211935 ) ) ;
#76570 = ORIENTED_EDGE ( 'NONE', *, *, #15717, .F. ) ;
#76571 = ORIENTED_EDGE ( 'NONE', *, *, #15343, .F. ) ;
#76573 = CARTESIAN_POINT ( 'NONE',  ( -19.50000000000000000, -3.499999999999999556, 29.75000000000000355 ) ) ;
#76572 = DIRECTION ( 'NONE',  ( -0.000000000000000000, 1.000000000000000000, -0.000000000000000000 ) ) ;
#76574 = VECTOR ( 'NONE', #82365, 1000.000000000000227 ) ;
#76575 = CARTESIAN_POINT ( 'NONE',  ( -9.469528023329626620, -12.47679350104403007, 31.42216943046555855 ) ) ;
#76576 = LINE ( 'NONE', #28840, #12092 ) ;
#76577 = DIRECTION ( 'NONE',  ( -0.000000000000000000, -0.7660444431189791237, -0.6427876096865379196 ) ) ;
#76578 = CARTESIAN_POINT ( 'NONE',  ( 13.51540719244017374, -11.18335022499818621, 33.13157742990016885 ) ) ;
#76579 = ORIENTED_EDGE ( 'NONE', *, *, #38331, .T. ) ;
#76580 = CARTESIAN_POINT ( 'NONE',  ( 11.28843831424008570, -3.520140089381495585, 33.17453946501458262 ) ) ;
#76581 = CARTESIAN_POINT ( 'NONE',  ( -14.30769230769242917, -10.33852847137269571, 34.16647553114546554 ) ) ;
#76583 = DIRECTION ( 'NONE',  ( -0.000000000000000000, 0.9848077530122085754, -0.1736481776669273613 ) ) ;
#76582 = B_SPLINE_CURVE_WITH_KNOTS ( 'NONE', 3,
 ( #11654, #66597, #31924, #3982, #4438, #37778, #67041, #18405, #5337, #72894 ),
 .UNSPECIFIED., .F., .F.,
 ( 4, 2, 2, 2, 4 ),
 ( 0.000000000000000000, 0.0001954339857564075557, 0.0003908679715128151114, 0.0005863019572692226671, 0.0007817359430256302227 ),
 .UNSPECIFIED. ) ;
#76584 = CARTESIAN_POINT ( 'NONE',  ( -8.769230769230768274, -11.35647404775217417, 33.31231777344666511 ) ) ;
#76585 = CARTESIAN_POINT ( 'NONE',  ( -11.60371252862278091, -2.506253911140460922, 30.00000000000013856 ) ) ;
#76586 = EDGE_LOOP ( 'NONE', ( #784, #23752 ) ) ;
#76587 = LINE ( 'NONE', #13224, #85353 ) ;
#76588 = ORIENTED_EDGE ( 'NONE', *, *, #31408, .T. ) ;
#76589 = ITEM_DEFINED_TRANSFORMATION ( 'NONE', 'NONE', #66204,  #83448 ) ;
#76590 = ORIENTED_EDGE ( 'NONE', *, *, #7427, .T. ) ;
#76591 = CARTESIAN_POINT ( 'NONE',  ( -9.626239341305252495, -12.37446782046654192, 30.86335684631486842 ) ) ;
#76592 = ORIENTED_EDGE ( 'NONE', *, *, #3302, .F. ) ;
#76593 = FACE_OUTER_BOUND ( 'NONE', #63239, .T. ) ;
#76594 = CARTESIAN_POINT ( 'NONE',  ( 15.36129466900287888, -4.299079248970732792, 33.91157788607253565 ) ) ;
#76595 = CARTESIAN_POINT ( 'NONE',  ( 14.17754433796061875, -10.31621877034669588, 34.18098118002070152 ) ) ;
#76596 = CARTESIAN_POINT ( 'NONE',  ( -39.05038313613820122, -2.499999999999999556, 29.75000000000000355 ) ) ;
#76597 = CARTESIAN_POINT ( 'NONE',  ( -17.14219307747939425, -9.528491918058357157, 34.59228464037090589 ) ) ;
#76598 = CARTESIAN_POINT ( 'NONE',  ( 8.703147358274890166, -6.386643153685125363, 34.62446782046654903 ) ) ;
#76599 = ORIENTED_EDGE ( 'NONE', *, *, #33933, .T. ) ;
#76600 = CARTESIAN_POINT ( 'NONE',  ( -5.076923076923075762, -1.790695186598648903, 34.54067556320373455 ) ) ;
#76602 = ORIENTED_EDGE ( 'NONE', *, *, #48944, .T. ) ;
#76601 = DIRECTION ( 'NONE',  ( -0.000000000000000000, -0.000000000000000000, -1.000000000000000000 ) ) ;
#76603 = DIRECTION ( 'NONE',  ( 1.000000000000000000, 0.000000000000000000, 0.000000000000000000 ) ) ;
#76604 = CARTESIAN_POINT ( 'NONE',  ( -8.639183333980316348, -7.723484941389743952, 34.99544897038808955 ) ) ;
#76605 = CARTESIAN_POINT ( 'NONE',  ( -17.29985003582992320, -11.98009711892700224, 32.48740034544074007 ) ) ;
#76606 = CARTESIAN_POINT ( 'NONE',  ( 6.066067333350077639, -9.058645607665452459, 34.76329471203371924 ) ) ;
#76607 = CARTESIAN_POINT ( 'NONE',  ( 18.00000000000000000, -4.102666532097928531, 36.13435417666054406 ) ) ;
#76608 = CARTESIAN_POINT ( 'NONE',  ( 9.442330961365339448, -9.943427161483782584, 34.11278801902876978 ) ) ;
#76609 = DIRECTION ( 'NONE',  ( -0.000000000000000000, -0.8660254037844397068, -0.4999999999999978906 ) ) ;
#76610 = CARTESIAN_POINT ( 'NONE',  ( 2.724691934501250135, -8.700186371490531201, 24.79874329374151998 ) ) ;
#76611 = EDGE_LOOP ( 'NONE', ( #68494, #3424, #60236, #34355 ) ) ;
#76612 = CARTESIAN_POINT ( 'NONE',  ( -1.384615384615505151, -11.48612834414049644, 32.76840700105863391 ) ) ;
#76613 = CARTESIAN_POINT ( 'NONE',  ( 12.52679360105129902, -5.094484230520773593, 34.41647553114626845 ) ) ;
#76614 = CARTESIAN_POINT ( 'NONE',  ( 8.769230769230645706, -11.06231777344772027, 33.60647404775119895 ) ) ;
#76615 = DIRECTION ( 'NONE',  ( -0.000000000000000000, 0.1736481776669307198, -0.9848077530122080203 ) ) ;
#76616 = VERTEX_POINT ( 'NONE', #5568 ) ;
#76617 = CARTESIAN_POINT ( 'NONE',  ( -5.999999999999998224, -13.49023893513002648, 31.06009739812518688 ) ) ;
#76618 = CARTESIAN_POINT ( 'NONE',  ( 11.47319153790521717, -4.320704448112771878, 33.92786785259540494 ) ) ;
#76619 = AXIS2_PLACEMENT_3D ( 'NONE', #24336, #23451, #2289 ) ;
#76620 = EDGE_CURVE ( 'NONE', #75262, #64231, #29213, .T. ) ;
#76621 = CARTESIAN_POINT ( 'NONE',  ( 7.846153846153846700, -8.810774026931790459, 35.74407628777942847 ) ) ;
#76622 = CARTESIAN_POINT ( 'NONE',  ( -4.153846153846273204, -10.90142922262034020, 33.41473453929536674 ) ) ;
#76623 = B_SPLINE_CURVE_WITH_KNOTS ( 'NONE', 3,
 ( #65453, #78521, #4650, #32122, #44727, #10961, #58248, #17724, #10519, #73565 ),
 .UNSPECIFIED., .F., .F.,
 ( 4, 2, 2, 2, 4 ),
 ( 0.000000000000000000, 0.0001954311564186867389, 0.0003908623128373734778, 0.0005862934692560602167, 0.0007817246256747469556 ),
 .UNSPECIFIED. ) ;
#76624 = ADVANCED_FACE ( 'NONE', ( #40694 ), #19520, .F. ) ;
#76625 = ORIENTED_EDGE ( 'NONE', *, *, #12587, .F. ) ;
#76626 = B_SPLINE_CURVE_WITH_KNOTS ( 'NONE', 3,
 ( #4842, #81838, #20128, #87722, #47594, #75078, #13364, #60661, #25994, #19244 ),
 .UNSPECIFIED., .F., .F.,
 ( 4, 2, 2, 2, 4 ),
 ( 0.0007817246256747484735, 0.0009771112852218920199, 0.001172497944769035783, 0.001367884604316179330, 0.001563271263863322876 ),
 .UNSPECIFIED. ) ;
#76627 = CARTESIAN_POINT ( 'NONE',  ( 6.130791807824788719, -5.582136614379148654, 34.36778462344220486 ) ) ;
#76628 = CARTESIAN_POINT ( 'NONE',  ( -8.703975629717930929, -5.941354392334607049, 34.76329471203374055 ) ) ;
#76629 = CARTESIAN_POINT ( 'NONE',  ( -14.37344573600563891, -7.249945578846652694, 34.99404164642496795 ) ) ;
#76630 = VERTEX_POINT ( 'NONE', #11891 ) ;
#76631 = CARTESIAN_POINT ( 'NONE',  ( 1.384615384615265343, -2.892918686052166066, 31.69288490824153470 ) ) ;
#76632 = EDGE_CURVE ( 'NONE', #85159, #32456, #57105, .T. ) ;
#76633 = VERTEX_POINT ( 'NONE', #54182 ) ;
#76634 = CARTESIAN_POINT ( 'NONE',  ( -16.28399336328437386, -6.001485441113818986, 34.52039167877662607 ) ) ;
#76635 = CARTESIAN_POINT ( 'NONE',  ( 0.4615384615384611200, -9.905515769479276145, 34.41647553114623292 ) ) ;
#76636 = ORIENTED_EDGE ( 'NONE', *, *, #67795, .T. ) ;
#76637 = EDGE_CURVE ( 'NONE', #49175, #83716, #68158, .T. ) ;
#76638 = DIRECTION ( 'NONE',  ( 0.000000000000000000, 0.1736481776669275834, 0.9848077530122086864 ) ) ;
#76639 = CARTESIAN_POINT ( 'NONE',  ( -14.43838291080261627, -2.295517848115769421, 30.44137282052137294 ) ) ;
#76640 = CARTESIAN_POINT ( 'NONE',  ( 0.3308469948709044095, -4.118384482072084296, 33.43331474514187107 ) ) ;
#76641 = AXIS2_PLACEMENT_3D ( 'NONE', #64189, #57000, #44812 ) ;
#76642 = VECTOR ( 'NONE', #63339, 1000.000000000000000 ) ;
#76643 = CARTESIAN_POINT ( 'NONE',  ( -11.53846153846166089, -5.941354392335915335, 34.76329471203413846 ) ) ;
#76644 = LINE ( 'NONE', #2733, #38294 ) ;
#76645 = VERTEX_POINT ( 'NONE', #6892 ) ;
#76646 = ORIENTED_EDGE ( 'NONE', *, *, #7069, .F. ) ;
#76647 = ADVANCED_FACE ( 'NONE', ( #61831 ), #32589, .F. ) ;
#76648 = FACE_BOUND ( 'NONE', #25394, .T. ) ;
#76649 = ORIENTED_EDGE ( 'NONE', *, *, #39114, .F. ) ;
#76650 = CARTESIAN_POINT ( 'NONE',  ( 15.10007776410167502, -12.38065189839062263, 30.83690757178629482 ) ) ;
#76651 = CARTESIAN_POINT ( 'NONE',  ( 20.00000000000000000, -3.499999999999999556, 29.75000000000000355 ) ) ;
#76652 = CARTESIAN_POINT ( 'NONE',  ( 6.000000000000001776, -5.471508081941601098, 34.59228464037088457 ) ) ;
#76653 = CARTESIAN_POINT ( 'NONE',  ( 5.299702618191484582, -4.387253974876676565, 33.66317474335728832 ) ) ;
#76654 = ORIENTED_EDGE ( 'NONE', *, *, #54085, .T. ) ;
#76655 = ORIENTED_EDGE ( 'NONE', *, *, #64670, .F. ) ;
#76656 = EDGE_LOOP ( 'NONE', ( #62435, #89090 ) ) ;
#76657 = B_SPLINE_CURVE_WITH_KNOTS ( 'NONE', 3,
 ( #1022, #69920, #29395, #22614, #1469, #49209, #9120, #50082, #14536, #35704 ),
 .UNSPECIFIED., .F., .F.,
 ( 4, 2, 2, 2, 4 ),
 ( 0.0007817359430256221996, 0.0009771253907249863487, 0.001172514838424350498, 0.001367904286123714647, 0.001563293733823078796 ),
 .UNSPECIFIED. ) ;
#76658 = DIRECTION ( 'NONE',  ( -0.000000000000000000, -0.7660444431189791237, -0.6427876096865379196 ) ) ;
#76659 = ORIENTED_EDGE ( 'NONE', *, *, #68050, .F. ) ;
#76660 = EDGE_CURVE ( 'NONE', #44876, #58562, #37801, .T. ) ;
#76661 = CARTESIAN_POINT ( 'NONE',  ( 3.230769230769231726, -2.721908614388771852, 31.22303859784724978 ) ) ;
#76662 = EDGE_CURVE ( 'NONE', #78849, #5642, #31348, .T. ) ;
#76663 = CARTESIAN_POINT ( 'NONE',  ( -16.82692307692307310, -2.499999999999999112, 29.81604066197449754 ) ) ;
#76664 = CARTESIAN_POINT ( 'NONE',  ( -17.20707104665477161, -3.069018819979305146, 32.56621877034667278 ) ) ;
#76665 = ORIENTED_EDGE ( 'NONE', *, *, #62567, .F. ) ;
#76666 = AXIS2_PLACEMENT_3D ( 'NONE', #21850, #63715, #49758 ) ;
#76667 = CARTESIAN_POINT ( 'NONE',  ( -10.03846153846153832, -4.000000000000000000, 29.75000000000000355 ) ) ;
#76668 = ADVANCED_FACE ( 'NONE', ( #55963 ), #62712, .F. ) ;
#76669 = CARTESIAN_POINT ( 'NONE',  ( 0.5923302693632469529, -11.71459661697925903, 32.44059661609676937 ) ) ;
#76670 = EDGE_CURVE ( 'NONE', #38958, #27134, #83904, .T. ) ;
#76671 = DIRECTION ( 'NONE',  ( 0.000000000000000000, -6.938893903907222067E-15, 1.000000000000000000 ) ) ;
#76672 = DIRECTION ( 'NONE',  ( -0.000000000000000000, 0.7660444431189791237, -0.6427876096865379196 ) ) ;
#76673 = ORIENTED_EDGE ( 'NONE', *, *, #68415, .T. ) ;
#76674 = ORIENTED_EDGE ( 'NONE', *, *, #970, .T. ) ;
#76675 = AXIS2_PLACEMENT_3D ( 'NONE', #50481, #980, #49609 ) ;
#76676 = VERTEX_POINT ( 'NONE', #42024 ) ;
#76677 = CARTESIAN_POINT ( 'NONE',  ( 4.088576153289833925, -3.083524468853724443, 32.58852847137143272 ) ) ;
#76679 = CARTESIAN_POINT ( 'NONE',  ( 10.83816415665302557, -6.760870238392817200, 34.69528174975672385 ) ) ;
#76678 = DIRECTION ( 'NONE',  ( 1.000000000000000000, 0.000000000000000000, 0.000000000000000000 ) ) ;
#76680 = CARTESIAN_POINT ( 'NONE',  ( 11.47237915910140238, -2.292212530054419606, 30.41441678777542634 ) ) ;
#76681 = CARTESIAN_POINT ( 'NONE',  ( -14.87820512820512953, -11.00000000000000000, 29.75000000000000355 ) ) ;
#76682 = FACE_BOUND ( 'NONE', #6366, .T. ) ;
#76683 = CARTESIAN_POINT ( 'NONE',  ( 8.069165197766695385, -11.24521262558773493, 33.06293181088029343 ) ) ;
#76684 = ORIENTED_EDGE ( 'NONE', *, *, #88513, .F. ) ;
#76685 = CARTESIAN_POINT ( 'NONE',  ( -7.596153846152425615, -7.500000000000154543, 35.00000000000007105 ) ) ;
#76686 = LINE ( 'NONE', #28958, #54555 ) ;
#76687 = CARTESIAN_POINT ( 'NONE',  ( -1.384615384615505151, -2.892918686052166066, 31.69288490824153470 ) ) ;
#76688 = DIRECTION ( 'NONE',  ( 0.000000000000000000, 1.000000000000000000, 0.000000000000000000 ) ) ;
#76689 = ORIENTED_EDGE ( 'NONE', *, *, #53029, .F. ) ;
#76690 = CARTESIAN_POINT ( 'NONE',  ( 4.853438152358743984, -12.69144148231606017, 30.53333754910549303 ) ) ;
#76691 = ORIENTED_EDGE ( 'NONE', *, *, #35459, .T. ) ;
#76692 = FACE_BOUND ( 'NONE', #71974, .T. ) ;
#76693 = CARTESIAN_POINT ( 'NONE',  ( 9.442330961365341224, -5.728515186090277211, 34.42611988154120439 ) ) ;
#76694 = CARTESIAN_POINT ( 'NONE',  ( 4.376625822824218304, -2.612705202774697533, 31.66806509827799943 ) ) ;
#76695 = CARTESIAN_POINT ( 'NONE',  ( -11.28851602011339672, -11.86320923018887541, 32.19269448109604781 ) ) ;
#76696 = VERTEX_POINT ( 'NONE', #28503 ) ;
#76697 = CARTESIAN_POINT ( 'NONE',  ( -14.53117725141625627, -12.44517049084099725, 30.48991314939691932 ) ) ;
#76698 = CARTESIAN_POINT ( 'NONE',  ( -14.30769230769230660, -4.098570777380720287, 33.41473453929634729 ) ) ;
#76699 = CARTESIAN_POINT ( 'NONE',  ( 10.61538461538461675, -6.343179335718451384, 34.87096338111211935 ) ) ;
#76700 = CARTESIAN_POINT ( 'NONE',  ( 6.066068351002440906, -3.513871655860379306, 32.76840700105978499 ) ) ;
#76701 = ORIENTED_EDGE ( 'NONE', *, *, #30257, .F. ) ;
#76702 = CARTESIAN_POINT ( 'NONE',  ( 12.71153846153846168, -2.249999999999998668, 29.75000000000000355 ) ) ;
#76704 = EDGE_LOOP ( 'NONE', ( #80694, #72071 ) ) ;
#76703 = VECTOR ( 'NONE', #35908, 1000.000000000000114 ) ;
#76707 = ORIENTED_EDGE ( 'NONE', *, *, #64191, .T. ) ;
#76706 = AXIS2_PLACEMENT_3D ( 'NONE', #57465, #30879, #58347 ) ;
#76705 = CARTESIAN_POINT ( 'NONE',  ( 15.90384615384615330, -7.433932668274255917, 35.00000000000000711 ) ) ;
#76708 = DIRECTION ( 'NONE',  ( 0.000000000000000000, 0.9396926207859126468, 0.3420201433256571111 ) ) ;
#76709 = DIRECTION ( 'NONE',  ( 0.000000000000000000, 0.8660254037844377084, 0.5000000000000015543 ) ) ;
#76710 = DIRECTION ( 'NONE',  ( -1.000000000000000000, -0.000000000000000000, 0.000000000000000000 ) ) ;
#76711 = CARTESIAN_POINT ( 'NONE',  ( 0.4615384615383382183, -3.643525952248795718, 33.31231777344771672 ) ) ;
#76712 = EDGE_CURVE ( 'NONE', #83905, #83971, #63472, .T. ) ;
#76713 = CARTESIAN_POINT ( 'NONE',  ( 12.46153846153846168, -4.098570777380720287, 33.41473453929634729 ) ) ;
#76715 = DIRECTION ( 'NONE',  ( 1.000000000000000000, 0.000000000000000000, 0.000000000000000000 ) ) ;
#76714 = CARTESIAN_POINT ( 'NONE',  ( -7.911424292114620727, -10.90142922261923886, 33.41473453929638993 ) ) ;
#76716 = CARTESIAN_POINT ( 'NONE',  ( -20.99999999999999645, -2.249999999999999556, 29.75000000000000355 ) ) ;
#76717 = CARTESIAN_POINT ( 'NONE',  ( -1.139087296525992166, -10.25000000000000533, 22.35937500000000711 ) ) ;
#76718 = ORIENTED_EDGE ( 'NONE', *, *, #77554, .T. ) ;
#76719 = DIRECTION ( 'NONE',  ( -1.000000000000000000, 0.000000000000000000, -0.000000000000000000 ) ) ;
#76720 = ORIENTED_EDGE ( 'NONE', *, *, #20692, .F. ) ;
#76721 = ORIENTED_EDGE ( 'NONE', *, *, #36483, .F. ) ;
#76722 = CARTESIAN_POINT ( 'NONE',  ( -4.153846153846152411, -4.786620604624113540, 33.94971097300155094 ) ) ;
#76723 = ORIENTED_EDGE ( 'NONE', *, *, #33807, .T. ) ;
#76724 = CARTESIAN_POINT ( 'NONE',  ( -5.869474561766354626, -12.70449254468099198, 30.44128974285582956 ) ) ;
#76725 = CARTESIAN_POINT ( 'NONE',  ( -2.057637996053991447, -6.567000820036038355, 34.66262288849541306 ) ) ;
#76726 = EDGE_CURVE ( 'NONE', #4768, #13156, #4463, .T. ) ;
#76727 = FACE_OUTER_BOUND ( 'NONE', #17951, .T. ) ;
#76728 = CARTESIAN_POINT ( 'NONE',  ( -5.076923076923075762, -8.564572088678739092, 35.78748833219616898 ) ) ;
#76729 = CARTESIAN_POINT ( 'NONE',  ( 8.545745825506822158, -11.41268669641499756, 32.86336882939238535 ) ) ;
#76730 = DIRECTION ( 'NONE',  ( -0.000000000000000000, 1.000000000000000000, -0.000000000000000000 ) ) ;
#76731 = CARTESIAN_POINT ( 'NONE',  ( -4.219116599806928214, -3.835265460703609186, 33.15142922261924241 ) ) ;
#76732 = CARTESIAN_POINT ( 'NONE',  ( 6.673053698855465399, -10.18141759479407327, 34.26406193332782379 ) ) ;
#76733 = FACE_OUTER_BOUND ( 'NONE', #26462, .T. ) ;
#76734 = VECTOR ( 'NONE', #20920, 1000.000000000000000 ) ;
#76735 = CARTESIAN_POINT ( 'NONE',  ( 5.869309396889694774, -11.37499894934982514, 33.29245874905763003 ) ) ;
#76736 = CARTESIAN_POINT ( 'NONE',  ( 7.596130621932389637, -2.341070481393819236, 30.72580821765574299 ) ) ;
#76738 = VECTOR ( 'NONE', #6402, 1000.000000000000000 ) ;
#76737 = B_SPLINE_CURVE_WITH_KNOTS ( 'NONE', 3,
 ( #81051, #31515, #58980, #28740, #62938, #36379, #37243, #8021, #84576, #8908 ),
 .UNSPECIFIED., .F., .F.,
 ( 4, 2, 2, 2, 4 ),
 ( 0.0007817359430256392216, 0.0009771253907250073822, 0.001172514838424375651, 0.001367904286123743920, 0.001563293733823112189 ),
 .UNSPECIFIED. ) ;
#76739 = VECTOR ( 'NONE', #83211, 1000.000000000000000 ) ;
#76741 = EDGE_LOOP ( 'NONE', ( #14609, #43945, #68563, #87302 ) ) ;
#76740 = EDGE_CURVE ( 'NONE', #83846, #13509, #26008, .T. ) ;
#76742 = EDGE_LOOP ( 'NONE', ( #63085, #24039, #4568, #77216, #34400 ) ) ;
#76743 = CARTESIAN_POINT ( 'NONE',  ( 12.59206389977210350, -2.647132371071621471, 31.75357179365171589 ) ) ;
#76744 = SURFACE_STYLE_FILL_AREA ( #35765 ) ;
#76745 = CARTESIAN_POINT ( 'NONE',  ( 11.66925334628632882, -9.804649428959608670, 34.18742332936588468 ) ) ;
#76746 = DIRECTION ( 'NONE',  ( -0.000000000000000000, 0.3420201433256694901, -0.9396926207859082059 ) ) ;
#76747 = VERTEX_POINT ( 'NONE', #75792 ) ;
#76748 = EDGE_CURVE ( 'NONE', #33072, #85360, #78635, .T. ) ;
#76749 = CYLINDRICAL_SURFACE ( 'NONE', #11879, 0.2499999999999997502 ) ;
#76750 = CARTESIAN_POINT ( 'NONE',  ( -12.68436515401747045, -7.369208160676171460, 34.74850200257122879 ) ) ;
#76751 = CARTESIAN_POINT ( 'NONE',  ( -12.33101275977489841, -10.88167719472716399, 33.43325721877153711 ) ) ;
#76752 = ORIENTED_EDGE ( 'NONE', *, *, #15670, .T. ) ;
#76753 = B_SPLINE_CURVE_WITH_KNOTS ( 'NONE', 3,
 ( #42309, #8072, #34654, #62988, #62122, #425, #1301, #28790, #89010, #46669 ),
 .UNSPECIFIED., .F., .F.,
 ( 4, 2, 2, 2, 4 ),
 ( 0.0007817246256747504250, 0.0009771112852218954894, 0.001172497944769040554, 0.001367884604316185401, 0.001563271263863330466 ),
 .UNSPECIFIED. ) ;
#76754 = EDGE_CURVE ( 'NONE', #64026, #5201, #53921, .T. ) ;
#76755 = CARTESIAN_POINT ( 'NONE',  ( 0.4615384615383396616, -6.026961402154118908, 34.52809138561165270 ) ) ;
#76756 = ORIENTED_EDGE ( 'NONE', *, *, #37875, .F. ) ;
#76757 = B_SPLINE_CURVE_WITH_KNOTS ( 'NONE', 3,
 ( #27084, #76150, #53670, #41488, #75708, #34730, #13134, #69406, #61742, #46904 ),
 .UNSPECIFIED., .F., .F.,
 ( 4, 2, 2, 2, 4 ),
 ( 0.0007817246256747448956, 0.0009771112852218876831, 0.001172497944769030579, 0.001367884604316173475, 0.001563271263863316371 ),
 .UNSPECIFIED. ) ;
#76758 = CARTESIAN_POINT ( 'NONE',  ( 13.31853300525524908, -12.34228464037088280, 31.77849191805838558 ) ) ;
#76759 = EDGE_CURVE ( 'NONE', #2885, #81222, #58952, .T. ) ;
#76760 = CARTESIAN_POINT ( 'NONE',  ( 15.48082365068267841, -3.435999193479609914, 33.07426656108010832 ) ) ;
#76761 = CARTESIAN_POINT ( 'NONE',  ( -6.223484943723947893, -2.599994579823202923, 30.74605699353653776 ) ) ;
#76762 = EDGE_CURVE ( 'NONE', #30312, #3756, #12557, .T. ) ;
#76763 = CARTESIAN_POINT ( 'NONE',  ( 2.980792486720640344, -8.347322224742351082, 34.93158281831414769 ) ) ;
#76764 = FACE_OUTER_BOUND ( 'NONE', #77015, .T. ) ;
#76765 = ORIENTED_EDGE ( 'NONE', *, *, #36781, .T. ) ;
#76766 = VERTEX_POINT ( 'NONE', #67060 ) ;
#76767 = ORIENTED_EDGE ( 'NONE', *, *, #77635, .T. ) ;
#76768 = VERTEX_POINT ( 'NONE', #11674 ) ;
#76769 = ADVANCED_FACE ( 'NONE', ( #12121 ), #26070, .F. ) ;
#76770 = CARTESIAN_POINT ( 'NONE',  ( -17.30040802064702987, -10.81261337010820256, 33.49550067578627477 ) ) ;
#76771 = LINE ( 'NONE', #15072, #33022 ) ;
#76772 = DIRECTION ( 'NONE',  ( -1.000000000000000000, -0.000000000000000000, -0.000000000000000000 ) ) ;
#76773 = EDGE_CURVE ( 'NONE', #24104, #30718, #66153, .T. ) ;
#76774 = CARTESIAN_POINT ( 'NONE',  ( 11.53846153846153832, -12.10708131394839349, 31.69288490824020244 ) ) ;
#76775 = CARTESIAN_POINT ( 'NONE',  ( -7.780898706641009355, -4.320704448112861584, 33.92786785259548310 ) ) ;
#76776 = EDGE_CURVE ( 'NONE', #88899, #29433, #52642, .T. ) ;
#76777 = CARTESIAN_POINT ( 'NONE',  ( 14.37294787896833270, -10.21337939537593620, 33.94971097300152252 ) ) ;
#76778 = ORIENTED_EDGE ( 'NONE', *, *, #56930, .F. ) ;
#76779 = EDGE_LOOP ( 'NONE', ( #9824, #78971 ) ) ;
#76780 = B_SPLINE_CURVE_WITH_KNOTS ( 'NONE', 3,
 ( #32473, #45542, #86098, #80230, #11317, #32037, #59946, #59503, #52739, #72121 ),
 .UNSPECIFIED., .F., .F.,
 ( 4, 2, 2, 2, 4 ),
 ( 0.0007817359430256324996, 0.0009771253907249993591, 0.001172514838424366110, 0.001367904286123732861, 0.001563293733823099829 ),
 .UNSPECIFIED. ) ;
#76781 = ORIENTED_EDGE ( 'NONE', *, *, #52088, .T. ) ;
#76783 = ORIENTED_EDGE ( 'NONE', *, *, #65454, .T. ) ;
#76782 = CARTESIAN_POINT ( 'NONE',  ( 12.68454981315131214, -8.239487800360276282, 34.69522927552633718 ) ) ;
#76785 = DIRECTION ( 'NONE',  ( 1.000000000000000000, 0.000000000000000000, 0.000000000000000000 ) ) ;
#76784 = CARTESIAN_POINT ( 'NONE',  ( -11.40767109749458541, -3.957578996910242619, 33.62503395064540257 ) ) ;
#76786 = CARTESIAN_POINT ( 'NONE',  ( -2.176900499867519212, -8.999086150933472084, 34.52020707165672064 ) ) ;
#76787 = B_SPLINE_CURVE_WITH_KNOTS ( 'NONE', 3,
 ( #1484, #2349, #37023, #56427, #69935, #76243, #15448, #43355, #7799, #42922 ),
 .UNSPECIFIED., .F., .F.,
 ( 4, 2, 2, 2, 4 ),
 ( 0.000000000000000000, 0.0001954311564186870913, 0.0003908623128373741825, 0.0005862934692560613009, 0.0007817246256747483650 ),
 .UNSPECIFIED. ) ;
#76788 = CARTESIAN_POINT ( 'NONE',  ( -10.86536134632696715, -11.79746400365624659, 32.30657167506340954 ) ) ;
#76789 = ORIENTED_EDGE ( 'NONE', *, *, #78069, .F. ) ;
#76790 = AXIS2_PLACEMENT_3D ( 'NONE', #8621, #77507, #23006 ) ;
#76791 = ADVANCED_FACE ( 'NONE', ( #38691 ), #4456, .F. ) ;
#76792 = ORIENTED_EDGE ( 'NONE', *, *, #88944, .F. ) ;
#76793 = FACE_OUTER_BOUND ( 'NONE', #47036, .T. ) ;
#76794 = VECTOR ( 'NONE', #74422, 1000.000000000000000 ) ;
#76795 = EDGE_LOOP ( 'NONE', ( #46434, #45634 ) ) ;
#76796 = FACE_BOUND ( 'NONE', #44937, .T. ) ;
#76797 = DIRECTION ( 'NONE',  ( 0.000000000000000000, 0.9848077530122072432, 0.1736481776669354937 ) ) ;
#76798 = AXIS2_PLACEMENT_3D ( 'NONE', #3100, #37780, #3547 ) ;
#76799 = CARTESIAN_POINT ( 'NONE',  ( -4.377331078410483300, -10.23692288466677880, 34.23039457007281072 ) ) ;
#76800 = ORIENTED_EDGE ( 'NONE', *, *, #6773, .T. ) ;
#76801 = EDGE_CURVE ( 'NONE', #51205, #30150, #40043, .T. ) ;
#76802 = CARTESIAN_POINT ( 'NONE',  ( 15.29693583736087348, -7.250054591869670162, 34.99404684341514127 ) ) ;
#76803 = CARTESIAN_POINT ( 'NONE',  ( 3.230769230769231726, -3.050289026998446396, 32.03036669348365706 ) ) ;
#76804 = CARTESIAN_POINT ( 'NONE',  ( 10.48523740594639797, -2.882441371585227508, 31.66841991370172238 ) ) ;
#76805 = CARTESIAN_POINT ( 'NONE',  ( -15.48079246806219267, -6.695914987888146541, 34.68535235679833306 ) ) ;
#76806 = CARTESIAN_POINT ( 'NONE',  ( -13.38461538461550582, -11.94971097300221174, 32.03036669348237098 ) ) ;
#76807 = VERTEX_POINT ( 'NONE', #80584 ) ;
#76808 = CARTESIAN_POINT ( 'NONE',  ( -11.31544869436814338, -12.38742843783360748, 31.66772728687926985 ) ) ;
#76809 = CARTESIAN_POINT ( 'NONE',  ( -7.912236225513981758, -11.91647553114624181, 32.58852847137148245 ) ) ;
#76810 = CARTESIAN_POINT ( 'NONE',  ( 0.3313912521002448930, -11.93770438780619259, 32.05411857736982029 ) ) ;
#76811 = CARTESIAN_POINT ( 'NONE',  ( 15.93036122928181975, -10.97335522853832934, 33.68706563782419749 ) ) ;
#76812 = CARTESIAN_POINT ( 'NONE',  ( -15.23076923076922995, -11.69971097300155272, 32.46337939537588113 ) ) ;
#76813 = EDGE_CURVE ( 'NONE', #60361, #83509, #22645, .T. ) ;
#76814 = FACE_BOUND ( 'NONE', #47792, .T. ) ;
#76816 = DIRECTION ( 'NONE',  ( 1.000000000000000000, 0.000000000000000000, 0.000000000000000000 ) ) ;
#76815 = CARTESIAN_POINT ( 'NONE',  ( -6.923076923077045919, -12.70778746994576025, 30.41441678777401236 ) ) ;
#76817 = CARTESIAN_POINT ( 'NONE',  ( -1.326923076923076872, -11.50000000000000000, 29.75000000000000355 ) ) ;
#76819 = CARTESIAN_POINT ( 'NONE',  ( -18.22292695890684655, -2.889293201056496674, 32.26117774369185298 ) ) ;
#76818 = CARTESIAN_POINT ( 'NONE',  ( 3.903822929624695792, -5.765609946408404518, 34.70566812827425451 ) ) ;
#76820 = CARTESIAN_POINT ( 'NONE',  ( -10.74553258511630993, -6.809168938359901446, 34.95455904226513866 ) ) ;
#76821 = CARTESIAN_POINT ( 'NONE',  ( 1.077988221561464899, -4.724691934501233703, 21.48250670625849068 ) ) ;
#76823 = ADVANCED_FACE ( 'NONE', ( #32383 ), #59848, .F. ) ;
#76822 = ORIENTED_EDGE ( 'NONE', *, *, #7897, .F. ) ;
#76824 = CARTESIAN_POINT ( 'NONE',  ( -8.834987571745077872, -7.249945686854186278, 34.74374336980224598 ) ) ;
#76825 = VERTEX_POINT ( 'NONE', #53078 ) ;
#76826 = ADVANCED_FACE ( 'NONE', ( #50529 ), #46337, .F. ) ;
#76827 = CARTESIAN_POINT ( 'NONE',  ( -13.38461538461538325, -3.322132147404559976, 32.92929555188717927 ) ) ;
#76828 = ORIENTED_EDGE ( 'NONE', *, *, #65838, .T. ) ;
#76829 = B_SPLINE_CURVE_WITH_KNOTS ( 'NONE', 3,
 ( #52084, #25951, #53415, #4350, #66500, #87234, #80917, #46668, #74144, #88130 ),
 .UNSPECIFIED., .F., .F.,
 ( 4, 2, 2, 2, 4 ),
 ( 0.0007817246256747452209, 0.0009771112852218887673, 0.001172497944769032531, 0.001367884604316176294, 0.001563271263863319840 ),
 .UNSPECIFIED. ) ;
#76830 = FACE_OUTER_BOUND ( 'NONE', #50413, .T. ) ;
#76831 = CARTESIAN_POINT ( 'NONE',  ( -8.096130577096200653, -9.943427161483782584, 34.11278801902876978 ) ) ;
#76832 = ORIENTED_EDGE ( 'NONE', *, *, #44181, .T. ) ;
#76833 = CARTESIAN_POINT ( 'NONE',  ( 5.776515075435669111, -10.97335522853832579, 33.68706563782419749 ) ) ;
#76834 = CARTESIAN_POINT ( 'NONE',  ( 0.06109907496454976272, -10.25000000000000000, 22.02938170625849068 ) ) ;
#76835 = CARTESIAN_POINT ( 'NONE',  ( 17.32686859527121470, -8.433404298154332679, 34.66254593164985920 ) ) ;
#76836 = CARTESIAN_POINT ( 'NONE',  ( 3.903869422903799347, -9.148715823498378086, 34.47080413974185120 ) ) ;
#76837 = CARTESIAN_POINT ( 'NONE',  ( 6.923076923076802558, -9.442884908241554243, 34.35708131394783038 ) ) ;
#76838 = EDGE_CURVE ( 'NONE', #65911, #80616, #71243, .T. ) ;
#76839 = CARTESIAN_POINT ( 'NONE',  ( -3.165576242474575253, -2.255955759149235629, 29.99999999999988631 ) ) ;
#76840 = LINE ( 'NONE', #52008, #35806 ) ;
#76841 = CARTESIAN_POINT ( 'NONE',  ( -14.05774689831426372, -4.932303261841489928, 34.32971442181322885 ) ) ;
#76842 = CARTESIAN_POINT ( 'NONE',  ( -2.608446859217920633, -4.805146000318815780, 20.50186829374151287 ) ) ;
#76843 = B_SPLINE_CURVE_WITH_KNOTS ( 'NONE', 3,
 ( #88380, #28423, #82934, #68518, #34737, #62205, #6816, #61750, #48243, #75715 ),
 .UNSPECIFIED., .F., .F.,
 ( 4, 2, 2, 2, 4 ),
 ( 0.0007817359430256327164, 0.0009771253907249995759, 0.001172514838424366327, 0.001367904286123733078, 0.001563293733823099829 ),
 .UNSPECIFIED. ) ;
#76844 = DIRECTION ( 'NONE',  ( -0.000000000000000000, 1.000000000000000000, -0.000000000000000000 ) ) ;
#76845 = CARTESIAN_POINT ( 'NONE',  ( -5.076923076923075762, -4.098570777380720287, 33.41473453929634729 ) ) ;
#76846 = CARTESIAN_POINT ( 'NONE',  ( 9.320512820512821150, -11.00000000000000000, 29.25000000000000000 ) ) ;
#76847 = CARTESIAN_POINT ( 'NONE',  ( -3.749999999999997780, -7.438900925035489387, 24.09561829374151287 ) ) ;
#76848 = CARTESIAN_POINT ( 'NONE',  ( -10.61538461538473577, -5.941354392335915335, 34.76329471203413846 ) ) ;
#76849 = ORIENTED_EDGE ( 'NONE', *, *, #18087, .T. ) ;
#76850 = DIRECTION ( 'NONE',  ( 0.000000000000000000, 0.1736481776669275834, 0.9848077530122086864 ) ) ;
#76851 = CARTESIAN_POINT ( 'NONE',  ( 12.39626846098214230, -8.656820664281498878, 34.87096338111211935 ) ) ;
#76852 = CYLINDRICAL_SURFACE ( 'NONE', #15294, 0.2499999999999979738 ) ;
#76853 = CARTESIAN_POINT ( 'NONE',  ( -5.207070286361298095, -6.001485441113818986, 34.52039167877662607 ) ) ;
#76854 = EDGE_CURVE ( 'NONE', #33955, #85035, #39602, .T. ) ;
#76855 = CARTESIAN_POINT ( 'NONE',  ( -1.634638621908348632, -10.76384336483936011, 33.53834819971076087 ) ) ;
#76856 = CARTESIAN_POINT ( 'NONE',  ( 15.90386942290380290, -9.148715823498378086, 34.47080413974185120 ) ) ;
#76857 = CARTESIAN_POINT ( 'NONE',  ( 8.703147358274888390, -10.51840700105979387, 33.73612834413961536 ) ) ;
#76858 = LINE ( 'NONE', #86175, #45155 ) ;
#76859 = VECTOR ( 'NONE', #83544, 1000.000000000000114 ) ;
#76860 = ORIENTED_EDGE ( 'NONE', *, *, #45447, .T. ) ;
#76861 = ORIENTED_EDGE ( 'NONE', *, *, #30271, .T. ) ;
#76862 = ORIENTED_EDGE ( 'NONE', *, *, #69158, .T. ) ;
#76863 = VECTOR ( 'NONE', #73394, 1000.000000000000000 ) ;
#76864 = CARTESIAN_POINT ( 'NONE',  ( 5.326868595271218254, -11.86320923018887541, 32.19269448109604781 ) ) ;
#76865 = CARTESIAN_POINT ( 'NONE',  ( -6.673022611438608642, -4.235687564193446164, 33.53795663066793509 ) ) ;
#76866 = CARTESIAN_POINT ( 'NONE',  ( 16.09615384615384670, -7.500000000000000000, 33.75000000000000000 ) ) ;
#76867 = FACE_OUTER_BOUND ( 'NONE', #14570, .T. ) ;
#76868 = CARTESIAN_POINT ( 'NONE',  ( 12.71153846153846168, -7.500000000000001776, 35.04278698407183867 ) ) ;
#76869 = ORIENTED_EDGE ( 'NONE', *, *, #84287, .F. ) ;
#76870 = CARTESIAN_POINT ( 'NONE',  ( -17.07692307692307665, -4.102666532097928531, 36.13435417666054406 ) ) ;
#76871 = ORIENTED_EDGE ( 'NONE', *, *, #37652, .T. ) ;
#76872 = ORIENTED_EDGE ( 'NONE', *, *, #61975, .F. ) ;
#76873 = ORIENTED_EDGE ( 'NONE', *, *, #2586, .F. ) ;
#76875 = ORIENTED_EDGE ( 'NONE', *, *, #56827, .F. ) ;
#76874 = CARTESIAN_POINT ( 'NONE',  ( 8.519207545009310323, -12.45566812827425451, 31.48439005359158926 ) ) ;
#76876 = CARTESIAN_POINT ( 'NONE',  ( 4.284371855609715674, -6.001044277235011215, 34.52024696741798948 ) ) ;
#76877 = CARTESIAN_POINT ( 'NONE',  ( -2.307692307692305711, -4.786620604624113540, 33.94971097300155094 ) ) ;
#76878 = ADVANCED_FACE ( 'NONE', ( #67947 ), #48097, .F. ) ;
#76879 = CARTESIAN_POINT ( 'NONE',  ( -2.307692307692305711, -9.780366693483667717, 34.19971097300155094 ) ) ;
#76880 = LINE ( 'NONE', #23586, #41063 ) ;
#76881 = ADVANCED_FACE ( 'NONE', ( #40914 ), #806, .F. ) ;
#76882 = ORIENTED_EDGE ( 'NONE', *, *, #48604, .F. ) ;
#76883 = EDGE_LOOP ( 'NONE', ( #85981, #51530, #63105, #17288 ) ) ;
#76884 = AXIS2_PLACEMENT_3D ( 'NONE', #82706, #54769, #1944 ) ;
#76885 = ORIENTED_EDGE ( 'NONE', *, *, #59045, .F. ) ;
#76886 = CARTESIAN_POINT ( 'NONE',  ( -2.057746898314262829, -3.520799739797214389, 33.17531984108286025 ) ) ;
#76888 = EDGE_LOOP ( 'NONE', ( #42320, #83043, #68447, #41777 ) ) ;
#76887 = DIRECTION ( 'NONE',  ( -1.000000000000000000, -8.673617379884027583E-16, 0.000000000000000000 ) ) ;
#76889 = ADVANCED_FACE ( 'NONE', ( #69269 ), #21067, .F. ) ;
#76890 = CARTESIAN_POINT ( 'NONE',  ( 16.15384615384615330, -7.500000000000001776, 35.04278698407183867 ) ) ;
#76891 = DIRECTION ( 'NONE',  ( 0.000000000000000000, 0.000000000000000000, -1.000000000000000000 ) ) ;
#76892 = CARTESIAN_POINT ( 'NONE',  ( -0.2387587925603953110, -9.418065098278011860, 34.63729479722530158 ) ) ;
#76893 = EDGE_LOOP ( 'NONE', ( #30022, #64233 ) ) ;
#76894 = CARTESIAN_POINT ( 'NONE',  ( 15.10007776410167502, -10.54014554554150607, 33.71984207302941883 ) ) ;
#76895 = EDGE_CURVE ( 'NONE', #77995, #30802, #52616, .T. ) ;
#76896 = DIRECTION ( 'NONE',  ( -0.000000000000000000, 0.6427876096865404731, -0.7660444431189771253 ) ) ;
#76897 = ORIENTED_EDGE ( 'NONE', *, *, #25064, .T. ) ;
#76898 = FACE_BOUND ( 'NONE', #8870, .T. ) ;
#76899 = CYLINDRICAL_SURFACE ( 'NONE', #34113, 0.2499999999999998890 ) ;
#76900 = DIRECTION ( 'NONE',  ( -0.000000000000000000, 0.3420201433256694901, -0.9396926207859082059 ) ) ;
#76901 = CARTESIAN_POINT ( 'NONE',  ( 20.74999999999999645, -10.50000000000000000, 29.75000000000000355 ) ) ;
#76903 = CARTESIAN_POINT ( 'NONE',  ( -0.6850234052624116776, -12.24155766932282496, 31.33739205006857986 ) ) ;
#76902 = CARTESIAN_POINT ( 'NONE',  ( -6.988400935881231568, -7.749976730030849303, 34.74374725381503737 ) ) ;
#76904 = CARTESIAN_POINT ( 'NONE',  ( 8.769230769230645706, -6.835583212225970762, 34.95778746994575670 ) ) ;
#76905 = CARTESIAN_POINT ( 'NONE',  ( -4.153846153846152411, -10.67929555188718282, 33.92786785259544047 ) ) ;
#76906 = VERTEX_POINT ( 'NONE', #14774 ) ;
#76907 = CARTESIAN_POINT ( 'NONE',  ( 11.53846153846141753, -3.300289026999228881, 32.46337939537708905 ) ) ;
#76908 = DIRECTION ( 'NONE',  ( -0.000000000000000000, 0.1736481776669307198, -0.9848077530122080203 ) ) ;
#76909 = VERTEX_POINT ( 'NONE', #82351 ) ;
#76910 = CARTESIAN_POINT ( 'NONE',  ( -14.24243716817946925, -9.528491918058460186, 34.59228464037086326 ) ) ;
#76911 = CARTESIAN_POINT ( 'NONE',  ( -4.088590582570128973, -2.625532179533470512, 30.86335684631491105 ) ) ;
#76912 = CARTESIAN_POINT ( 'NONE',  ( 8.769230769230768274, -11.91647553114624181, 32.58852847137148245 ) ) ;
#76913 = ORIENTED_EDGE ( 'NONE', *, *, #13634, .T. ) ;
#76914 = CARTESIAN_POINT ( 'NONE',  ( -10.39237177129122003, -2.889357225399414197, 32.26129605718031002 ) ) ;
#76915 = DIRECTION ( 'NONE',  ( -0.000000000000000000, -0.3420201433256694901, -0.9396926207859082059 ) ) ;
#76916 = CIRCLE ( 'NONE', #40982, 4.999999999999997335 ) ;
#76917 = FACE_BOUND ( 'NONE', #73099, .T. ) ;
#76919 = LINE ( 'NONE', #78687, #27301 ) ;
#76918 = CARTESIAN_POINT ( 'NONE',  ( 13.38461538461538680, -2.292212530054420494, 30.41441678777542634 ) ) ;
#76920 = CARTESIAN_POINT ( 'NONE',  ( -16.08777780284371417, -2.538708090699994813, 30.37095296980875503 ) ) ;
#76922 = CARTESIAN_POINT ( 'NONE',  ( 7.146088274689773812, -12.39991518177334129, 30.74647679643404530 ) ) ;
#76921 = CARTESIAN_POINT ( 'NONE',  ( -17.93474442872397034, -11.48612834413965800, 32.76840700105972815 ) ) ;
#76923 = CARTESIAN_POINT ( 'NONE',  ( -17.75005448165186195, -5.057305518903949526, 34.11320923018887896 ) ) ;
#76924 = CARTESIAN_POINT ( 'NONE',  ( -1.614399933863656544, -3.775308065498769405, 21.32625670625849423 ) ) ;
#76925 = ORIENTED_EDGE ( 'NONE', *, *, #5351, .T. ) ;
#76926 = EDGE_CURVE ( 'NONE', #14877, #12525, #70984, .T. ) ;
#76927 = VERTEX_POINT ( 'NONE', #28274 ) ;
#76928 = AXIS2_PLACEMENT_3D ( 'NONE', #13529, #28828, #75240 ) ;
#76929 = CARTESIAN_POINT ( 'NONE',  ( 16.02315555073584363, -9.084618155246140248, 34.75535874321725771 ) ) ;
#76930 = CARTESIAN_POINT ( 'NONE',  ( -0.7115151924808159611, -2.779195860258148798, 31.39871582349836743 ) ) ;
#76931 = DIRECTION ( 'NONE',  ( 0.000000000000000000, 0.3420201433256610524, 0.9396926207859113145 ) ) ;
#76932 = DIRECTION ( 'NONE',  ( -0.000000000000000000, 0.9848077530122086864, -0.1736481776669273891 ) ) ;
#76933 = DIRECTION ( 'NONE',  ( -0.000000000000000000, -0.000000000000000000, -1.000000000000000000 ) ) ;
#76934 = CARTESIAN_POINT ( 'NONE',  ( 2.694853999681214862, -10.10844685921789043, 16.87313170625849068 ) ) ;
#76935 = CARTESIAN_POINT ( 'NONE',  ( 4.088089351331844590, -7.249945686854186278, 34.74374336980224598 ) ) ;
#76936 = CARTESIAN_POINT ( 'NONE',  ( 17.99999999999987566, -3.300289026999228437, 32.46337939537709616 ) ) ;
#76937 = EDGE_CURVE ( 'NONE', #15866, #31594, #66679, .T. ) ;
#76938 = CARTESIAN_POINT ( 'NONE',  ( 15.45354877203763877, -11.89424750095246175, 32.13594075562310337 ) ) ;
#76939 = CARTESIAN_POINT ( 'NONE',  ( -2.980714810855777053, -12.01375889529407637, 32.43194544308182969 ) ) ;
#76940 = CARTESIAN_POINT ( 'NONE',  ( -3.296851610129365007, -3.937682226553329556, 33.60647404775217240 ) ) ;
#76941 = CARTESIAN_POINT ( 'NONE',  ( 16.28463796167094557, -4.809403383903225304, 33.96459661697925014 ) ) ;
#76942 = CARTESIAN_POINT ( 'NONE',  ( 1.384615384615386802, -6.386643153685126251, 34.62446782046654192 ) ) ;
#76943 = EDGE_CURVE ( 'NONE', #28117, #63575, #53977, .T. ) ;
#76944 = CARTESIAN_POINT ( 'NONE',  ( -0.4615384615384611200, -9.780366693483667717, 34.19971097300155094 ) ) ;
#76945 = VERTEX_POINT ( 'NONE', #68821 ) ;
#76946 = CARTESIAN_POINT ( 'NONE',  ( 12.23861150263161157, -4.026226216239094491, 33.68668979543634379 ) ) ;
#76947 = DIRECTION ( 'NONE',  ( 0.000000000000000000, 0.3420201433256610524, 0.9396926207859113145 ) ) ;
#76948 = CARTESIAN_POINT ( 'NONE',  ( -1.987747218494638313, -9.401340078031370950, 20.18936829374151287 ) ) ;
#76949 = CARTESIAN_POINT ( 'NONE',  ( 1.653273178848927064E-15, -7.500000000000000000, 29.50000000000000355 ) ) ;
#76950 = LINE ( 'NONE', #49481, #48948 ) ;
#76951 = VERTEX_POINT ( 'NONE', #61169 ) ;
#76952 = CARTESIAN_POINT ( 'NONE',  ( 13.38461538461538680, -11.69971097300155272, 32.46337939537588113 ) ) ;
#76954 = VERTEX_POINT ( 'NONE', #7127 ) ;
#76953 = CARTESIAN_POINT ( 'NONE',  ( -5.869952564749547186, -7.723484941389743952, 34.99544897038808955 ) ) ;
#76955 = DIRECTION ( 'NONE',  ( -0.000000000000000000, 0.5000000000000011102, -0.8660254037844380415 ) ) ;
#76956 = CARTESIAN_POINT ( 'NONE',  ( -2.307692307692428724, -11.06231777344772027, 33.60647404775119895 ) ) ;
#76957 = ADVANCED_FACE ( 'NONE', ( #12997 ), #88680, .F. ) ;
#76958 = ORIENTED_EDGE ( 'NONE', *, *, #81061, .T. ) ;
#76959 = CARTESIAN_POINT ( 'NONE',  ( -5.300408020647027207, -12.24155766932282496, 31.33739205006857986 ) ) ;
#76960 = B_SPLINE_CURVE_WITH_KNOTS ( 'NONE', 3,
 ( #52932, #19167, #46636, #4770, #32239, #86759, #79978, #86308, #72321, #80435 ),
 .UNSPECIFIED., .F., .F.,
 ( 4, 2, 2, 2, 4 ),
 ( 0.0007817246256747457630, 0.0009771112852218887673, 0.001172497944769031663, 0.001367884604316174559, 0.001563271263863317672 ),
 .UNSPECIFIED. ) ;
#76961 = AXIS2_PLACEMENT_3D ( 'NONE', #73798, #72440, #18844 ) ;
#76962 = CARTESIAN_POINT ( 'NONE',  ( 8.069580808015416551, -7.630147231320743018, 34.74852402298682819 ) ) ;
#76963 = ORIENTED_EDGE ( 'NONE', *, *, #25774, .T. ) ;
#76964 = CARTESIAN_POINT ( 'NONE',  ( -12.68446542044531000, -2.308479472611653094, 30.53278059502174457 ) ) ;
#76965 = EDGE_CURVE ( 'NONE', #75827, #85310, #21523, .T. ) ;
#76966 = ADVANCED_FACE ( 'NONE', ( #78230 ), #64263, .F. ) ;
#76967 = CARTESIAN_POINT ( 'NONE',  ( 5.076923076923391065, -2.255955759149395501, 30.00000000000324363 ) ) ;
#76968 = CARTESIAN_POINT ( 'NONE',  ( 12.71159288145191368, -12.01375889529407281, 32.43194544308182969 ) ) ;
#76969 = ORIENTED_EDGE ( 'NONE', *, *, #51201, .T. ) ;
#76970 = VERTEX_POINT ( 'NONE', #57074 ) ;
#76971 = CARTESIAN_POINT ( 'NONE',  ( 15.48082354240754555, -10.66356715214248752, 33.62249196103329751 ) ) ;
#76972 = EDGE_CURVE ( 'NONE', #11752, #48440, #87115, .T. ) ;
#76973 = ORIENTED_EDGE ( 'NONE', *, *, #79424, .F. ) ;
#76974 = CARTESIAN_POINT ( 'NONE',  ( -1.318547033612944341, -2.538708090699994813, 30.37095296980875503 ) ) ;
#76975 = CARTESIAN_POINT ( 'NONE',  ( 13.44987052412822237, -3.643525952247864463, 33.31231777344670064 ) ) ;
#76976 = CARTESIAN_POINT ( 'NONE',  ( 16.15384615384615330, -13.53365097954675988, 30.81389545987213552 ) ) ;
#76977 = DIRECTION ( 'NONE',  ( 1.000000000000000000, 0.000000000000000000, 0.000000000000000000 ) ) ;
#76978 = AXIS2_PLACEMENT_3D ( 'NONE', #19320, #66621, #54422 ) ;
#76979 = ORIENTED_EDGE ( 'NONE', *, *, #13686, .T. ) ;
#76980 = ORIENTED_EDGE ( 'NONE', *, *, #56798, .T. ) ;
#76982 = ORIENTED_EDGE ( 'NONE', *, *, #42274, .T. ) ;
#76981 = CARTESIAN_POINT ( 'NONE',  ( 6.923076923076924238, -2.249999999999998668, 29.75000000000001776 ) ) ;
#76983 = EDGE_CURVE ( 'NONE', #46529, #62974, #78469, .T. ) ;
#76984 = CARTESIAN_POINT ( 'NONE',  ( 7.846153846153723244, -2.657715359629662544, 31.77849191805970364 ) ) ;
#76985 = ORIENTED_EDGE ( 'NONE', *, *, #10109, .F. ) ;
#76986 = B_SPLINE_CURVE_WITH_KNOTS ( 'NONE', 3,
 ( #78575, #2901, #79024, #44327, #70937, #37587, #72709, #9249, #78132, #43905 ),
 .UNSPECIFIED., .F., .F.,
 ( 4, 2, 2, 2, 4 ),
 ( 0.0007817359430256326080, 0.0009771253907250047801, 0.001172514838424369796, 0.001367904286123735030, 0.001563293733823100046 ),
 .UNSPECIFIED. ) ;
#76987 = B_SPLINE_CURVE_WITH_KNOTS ( 'NONE', 3,
 ( #31841, #18768, #26410, #39935, #13332, #46235, #88137, #67393, #45783, #86803 ),
 .UNSPECIFIED., .F., .F.,
 ( 4, 2, 2, 2, 4 ),
 ( 0.0007817246256747447872, 0.0009771112852218876831, 0.001172497944769030579, 0.001367884604316173475, 0.001563271263863316371 ),
 .UNSPECIFIED. ) ;
#76988 = CARTESIAN_POINT ( 'NONE',  ( 7.596130621932386973, -12.07920672191015221, 32.31858351112116168 ) ) ;
#76989 = DIRECTION ( 'NONE',  ( 0.000000000000000000, -1.000000000000000000, -2.413528314402514090E-16 ) ) ;
#76990 = VECTOR ( 'NONE', #17733, 1000.000000000000227 ) ;
#76991 = VERTEX_POINT ( 'NONE', #84569 ) ;
#76992 = B_SPLINE_CURVE_WITH_KNOTS ( 'NONE', 3,
 ( #48335, #8254, #42041, #68613, #77147, #28521, #83474, #61397, #34823, #27184 ),
 .UNSPECIFIED., .F., .F.,
 ( 4, 2, 2, 2, 4 ),
 ( 0.000000000000000000, 0.0001954339857564092362, 0.0003908679715128184724, 0.0005863019572692276544, 0.0007817359430256369448 ),
 .UNSPECIFIED. ) ;
#76993 = CARTESIAN_POINT ( 'NONE',  ( -12.23852710992561299, -5.667800583137506010, 34.40243808032445827 ) ) ;
#76994 = ORIENTED_EDGE ( 'NONE', *, *, #71060, .T. ) ;
#76996 = ORIENTED_EDGE ( 'NONE', *, *, #54235, .F. ) ;
#76995 = CARTESIAN_POINT ( 'NONE',  ( -8.638438961405983108, -8.147973898785416225, 34.70805048591653730 ) ) ;
#76997 = EDGE_CURVE ( 'NONE', #4299, #33013, #22843, .T. ) ;
#76998 = CARTESIAN_POINT ( 'NONE',  ( -12.52680846209478283, -3.643525952247789412, 33.31231777344662959 ) ) ;
#76999 = B_SPLINE_CURVE_WITH_KNOTS ( 'NONE', 3,
 ( #58104, #70746, #22113, #29322, #85586, #63532, #50020, #18467, #10816, #51773 ),
 .UNSPECIFIED., .F., .F.,
 ( 4, 2, 2, 2, 4 ),
 ( 0.000000000000000000, 0.0001954311564186865221, 0.0003908623128373730441, 0.0005862934692560595662, 0.0007817246256747460882 ),
 .UNSPECIFIED. ) ;
#77000 = CARTESIAN_POINT ( 'NONE',  ( 14.30769230769231015, -5.471508081941601098, 34.59228464037088457 ) ) ;
#77001 = VERTEX_POINT ( 'NONE', #35934 ) ;
#77002 = FACE_OUTER_BOUND ( 'NONE', #50773, .T. ) ;
#77003 = EDGE_CURVE ( 'NONE', #12230, #35283, #35480, .T. ) ;
#77004 = CARTESIAN_POINT ( 'NONE',  ( -8.834500769787091201, -12.16647553114622049, 32.15551576947930812 ) ) ;
#77005 = FACE_BOUND ( 'NONE', #68916, .T. ) ;
#77006 = CARTESIAN_POINT ( 'NONE',  ( 1.450683735617825487, -12.37446782046654192, 30.86335684631486842 ) ) ;
#77007 = CARTESIAN_POINT ( 'NONE',  ( -39.05038313613820122, -2.499999999999999556, 29.75000000000000355 ) ) ;
#77008 = CARTESIAN_POINT ( 'NONE',  ( -15.90390074446811042, -4.932303261841488151, 34.32971442181322885 ) ) ;
#77009 = CARTESIAN_POINT ( 'NONE',  ( -16.94639763868943660, -12.50538340440932394, 31.33453814440721885 ) ) ;
#77010 = CARTESIAN_POINT ( 'NONE',  ( 0.000000000000000000, -11.00000000000000000, 29.75000000000000355 ) ) ;
#77011 = DIRECTION ( 'NONE',  ( -0.000000000000000000, 0.5000000000000011102, -0.8660254037844381525 ) ) ;
#77012 = ORIENTED_EDGE ( 'NONE', *, *, #27109, .T. ) ;
#77013 = CARTESIAN_POINT ( 'NONE',  ( 10.39245839786846837, -9.886141570436013382, 34.14413921362392301 ) ) ;
#77014 = ORIENTED_EDGE ( 'NONE', *, *, #51244, .F. ) ;
#77015 = EDGE_LOOP ( 'NONE', ( #23015, #82209, #3623, #40327 ) ) ;
#77016 = AXIS2_PLACEMENT_3D ( 'NONE', #54012, #74749, #87383 ) ;
#77018 = CARTESIAN_POINT ( 'NONE',  ( 7.846153846153725020, -10.21337939537710326, 33.94971097300076224 ) ) ;
#77017 = CARTESIAN_POINT ( 'NONE',  ( -1.254089946381740095, -5.070358843744210198, 34.40418822224088302 ) ) ;
#77019 = EDGE_CURVE ( 'NONE', #27342, #15876, #16099, .T. ) ;
#77020 = CARTESIAN_POINT ( 'NONE',  ( -9.442253272394237840, -12.41089969410671223, 31.60739465890703670 ) ) ;
#77021 = FACE_OUTER_BOUND ( 'NONE', #65031, .T. ) ;
#77022 = CARTESIAN_POINT ( 'NONE',  ( -12.23852561744506495, -2.523321265292115534, 31.42251411153756990 ) ) ;
#77023 = CARTESIAN_POINT ( 'NONE',  ( 20.00000000000000000, -4.000000000000000000, 29.75000000000000355 ) ) ;
#77024 = ORIENTED_EDGE ( 'NONE', *, *, #78746, .F. ) ;
#77025 = CARTESIAN_POINT ( 'NONE',  ( -18.22292621751614305, -5.667676309546435753, 34.40238873228292249 ) ) ;
#77026 = CARTESIAN_POINT ( 'NONE',  ( -6.130147209438218781, -6.852621066184267029, 34.70813303252209181 ) ) ;
#77027 = CARTESIAN_POINT ( 'NONE',  ( -10.39260507411620438, -10.11255958852956027, 34.01340905677048454 ) ) ;
#77028 = CARTESIAN_POINT ( 'NONE',  ( 15.23076923076910916, -12.51329471203414379, 31.30864560766407578 ) ) ;
#77029 = CARTESIAN_POINT ( 'NONE',  ( -11.78846153846154010, -2.499999999999999556, 29.81609845454691765 ) ) ;
#77030 = VERTEX_POINT ( 'NONE', #50306 ) ;
#77031 = CARTESIAN_POINT ( 'NONE',  ( -1.553300858899125059, -3.750000000000009326, 14.07812500000000178 ) ) ;
#77032 = EDGE_LOOP ( 'NONE', ( #26455, #74227 ) ) ;
#77033 = ORIENTED_EDGE ( 'NONE', *, *, #88013, .T. ) ;
#77034 = DIRECTION ( 'NONE',  ( -0.000000000000000000, 0.8660254037844399289, -0.4999999999999980016 ) ) ;
#77035 = EDGE_CURVE ( 'NONE', #74290, #25133, #71035, .T. ) ;
#77036 = ORIENTED_EDGE ( 'NONE', *, *, #74732, .F. ) ;
#77037 = CARTESIAN_POINT ( 'NONE',  ( -1.384615384615383471, -8.120952969808772792, 34.71129190930000163 ) ) ;
#77038 = CARTESIAN_POINT ( 'NONE',  ( -1.319360245102545681, -10.33852847137154107, 34.16647553114620450 ) ) ;
#77039 = CARTESIAN_POINT ( 'NONE',  ( -14.30769230769242739, -6.879047030192662504, 34.71129190930017927 ) ) ;
#77040 = CARTESIAN_POINT ( 'NONE',  ( -16.81410256410256565, -7.500000000000000000, 29.75000000000000355 ) ) ;
#77041 = CARTESIAN_POINT ( 'NONE',  ( -2.084912766423897335, -5.114059244376869984, 34.14424750095245287 ) ) ;
#77042 = ADVANCED_FACE ( 'NONE', ( #22407 ), #30489, .F. ) ;
#77043 = CARTESIAN_POINT ( 'NONE',  ( 8.352564102564102200, -3.499999999999999556, 29.75000000000000355 ) ) ;
#77044 = ORIENTED_EDGE ( 'NONE', *, *, #50345, .F. ) ;
#77045 = CARTESIAN_POINT ( 'NONE',  ( -11.53846153846166089, -8.656820664282941280, 34.87096338111179961 ) ) ;
#77047 = ORIENTED_EDGE ( 'NONE', *, *, #17546, .F. ) ;
#77046 = LINE ( 'NONE', #42822, #68337 ) ;
#77048 = CARTESIAN_POINT ( 'NONE',  ( -9.469528151039281028, -4.387253974876679230, 33.66317474335728832 ) ) ;
#77049 = DIRECTION ( 'NONE',  ( 0.000000000000000000, 0.1736481776669275834, 0.9848077530122086864 ) ) ;
#77050 = DIRECTION ( 'NONE',  ( -1.000000000000000000, 0.000000000000000000, 0.000000000000000000 ) ) ;
#77051 = CARTESIAN_POINT ( 'NONE',  ( -2.531177232256638376, -12.69144148231606017, 30.53333754910549303 ) ) ;
#77053 = AXIS2_PLACEMENT_3D ( 'NONE', #64714, #85010, #79583 ) ;
#77052 = CARTESIAN_POINT ( 'NONE',  ( -9.942330916529147800, -12.45566812827425451, 31.48439005359158926 ) ) ;
#77054 = EDGE_CURVE ( 'NONE', #66983, #75887, #4296, .T. ) ;
#77055 = FACE_OUTER_BOUND ( 'NONE', #82833, .T. ) ;
#77056 = CARTESIAN_POINT ( 'NONE',  ( 3.750000000000001776, -7.561099074964511502, 13.47061829374151465 ) ) ;
#77057 = VERTEX_POINT ( 'NONE', #5242 ) ;
#77058 = CARTESIAN_POINT ( 'NONE',  ( -13.91025641025641058, -7.500000000000000000, 33.75000000000000000 ) ) ;
#77059 = CARTESIAN_POINT ( 'NONE',  ( -1.634638621908349299, -12.22074536777954989, 31.39888409691088356 ) ) ;
#77060 = CARTESIAN_POINT ( 'NONE',  ( -16.15384615384627409, -11.67786785259630911, 32.92929555188603530 ) ) ;
#77061 = CARTESIAN_POINT ( 'NONE',  ( -13.38461538461538325, -8.564572088678739092, 35.78748833219616898 ) ) ;
#77062 = EDGE_LOOP ( 'NONE', ( #86715, #25933 ) ) ;
#77063 = CARTESIAN_POINT ( 'NONE',  ( 0.3308478584281516199, -3.957541250942360644, 33.62499894934982336 ) ) ;
#77064 = CARTESIAN_POINT ( 'NONE',  ( -2.557715544985271983, -3.202444869320336451, 32.30641848906366675 ) ) ;
#77065 = CIRCLE ( 'NONE', #18105, 4.000000000000000000 ) ;
#77066 = ORIENTED_EDGE ( 'NONE', *, *, #76117, .T. ) ;
#77067 = CARTESIAN_POINT ( 'NONE',  ( 1.134638653673032405, -9.148715823498378086, 34.47080413974185120 ) ) ;
#77068 = CARTESIAN_POINT ( 'NONE',  ( 16.15384615384615330, -5.180354513474913603, 36.12317359536750416 ) ) ;
#77069 = ORIENTED_EDGE ( 'NONE', *, *, #49745, .F. ) ;
#77070 = CARTESIAN_POINT ( 'NONE',  ( 8.102564102564102200, -3.499999999999999556, 29.75000000000000355 ) ) ;
#77071 = ADVANCED_FACE ( 'NONE', ( #58389 ), #17427, .F. ) ;
#77072 = CYLINDRICAL_SURFACE ( 'NONE', #17835, 0.2500000000000002220 ) ;
#77073 = CARTESIAN_POINT ( 'NONE',  ( 8.068933387422255521, -5.913360116392399668, 34.49180327182771322 ) ) ;
#77074 = CARTESIAN_POINT ( 'NONE',  ( -4.377331078410484189, -11.60425143139329940, 33.02411095842164457 ) ) ;
#77075 = ORIENTED_EDGE ( 'NONE', *, *, #1553, .F. ) ;
#77076 = CARTESIAN_POINT ( 'NONE',  ( -13.25382494364843389, -2.845873456487965747, 32.17976146951972538 ) ) ;
#77077 = ORIENTED_EDGE ( 'NONE', *, *, #80762, .F. ) ;
#77078 = CARTESIAN_POINT ( 'NONE',  ( -19.50000000000000000, -3.499999999999999556, 29.75000000000000355 ) ) ;
#77079 = FACE_OUTER_BOUND ( 'NONE', #22282, .T. ) ;
#77080 = VERTEX_POINT ( 'NONE', #25068 ) ;
#77081 = LINE ( 'NONE', #48712, #20335 ) ;
#77082 = LINE ( 'NONE', #15388, #4750 ) ;
#77083 = CARTESIAN_POINT ( 'NONE',  ( -4.088652172062795742, -2.506253911140448487, 29.99999999999988631 ) ) ;
#77084 = VECTOR ( 'NONE', #52995, 1000.000000000000114 ) ;
#77085 = CYLINDRICAL_SURFACE ( 'NONE', #13403, 0.2500000000000008882 ) ;
#77086 = DIRECTION ( 'NONE',  ( 0.000000000000000000, 0.1736481776669267785, -0.9848077530122087975 ) ) ;
#77087 = B_SPLINE_CURVE_WITH_KNOTS ( 'NONE', 3,
 ( #85550, #24276, #16203, #23824, #43668, #71577, #79686, #50849, #44540, #17540 ),
 .UNSPECIFIED., .F., .F.,
 ( 4, 2, 2, 2, 4 ),
 ( 0.000000000000000000, 0.0001954311564186862781, 0.0003908623128373725562, 0.0005862934692560588072, 0.0007817246256747451124 ),
 .UNSPECIFIED. ) ;
#77088 = VERTEX_POINT ( 'NONE', #24621 ) ;
#77089 = EDGE_LOOP ( 'NONE', ( #44653, #73534, #43600, #70721, #27957, #9143 ) ) ;
#77090 = FACE_BOUND ( 'NONE', #64662, .T. ) ;
#77091 = VERTEX_POINT ( 'NONE', #59740 ) ;
#77092 = CARTESIAN_POINT ( 'NONE',  ( 15.36129493253279854, -2.619367082507849442, 30.83698974864643461 ) ) ;
#77093 = CARTESIAN_POINT ( 'NONE',  ( -18.13014796973169851, -11.04286588640299094, 33.62463336215343901 ) ) ;
#77094 = DIRECTION ( 'NONE',  ( -0.000000000000000000, -0.8660254037844398178, -0.4999999999999980571 ) ) ;
#77095 = DIRECTION ( 'NONE',  ( 0.000000000000000000, 0.000000000000000000, 1.000000000000000000 ) ) ;
#77096 = VERTEX_POINT ( 'NONE', #86351 ) ;
#77097 = ORIENTED_EDGE ( 'NONE', *, *, #886, .T. ) ;
#77098 = EDGE_LOOP ( 'NONE', ( #61488, #75811, #5775, #57651 ) ) ;
#77099 = CARTESIAN_POINT ( 'NONE',  ( -10.74607521849492464, -8.191372820521381826, 34.95448215188424967 ) ) ;
#77100 = ORIENTED_EDGE ( 'NONE', *, *, #22899, .T. ) ;
#77101 = CIRCLE ( 'NONE', #25349, 4.000000000000000000 ) ;
#77102 = CARTESIAN_POINT ( 'NONE',  ( -5.999999999999998224, -13.88283147151868846, 33.14645433367849847 ) ) ;
#77103 = CARTESIAN_POINT ( 'NONE',  ( 17.07692307692295586, -3.643525952248796163, 33.31231777344771672 ) ) ;
#77104 = CARTESIAN_POINT ( 'NONE',  ( -17.14300545628321615, -2.833524468853757305, 32.15551576947924417 ) ) ;
#77105 = ORIENTED_EDGE ( 'NONE', *, *, #54701, .F. ) ;
#77106 = CARTESIAN_POINT ( 'NONE',  ( 13.16168916709924197, -10.61292498521070549, 33.66303323003028680 ) ) ;
#77107 = DIRECTION ( 'NONE',  ( -0.000000000000000000, -0.8660254037844399289, -0.4999999999999980016 ) ) ;
#77108 = CARTESIAN_POINT ( 'NONE',  ( 9.692307692307695177, -12.78798330534102945, 29.74999999999997868 ) ) ;
#77109 = CARTESIAN_POINT ( 'NONE',  ( -9.692307692307812417, -3.835265460704628371, 33.15142922262033665 ) ) ;
#77110 = VERTEX_POINT ( 'NONE', #52970 ) ;
#77111 = B_SPLINE_CURVE_WITH_KNOTS ( 'NONE', 3,
 ( #61820, #26714, #20404, #47868, #87556, #66818, #6012, #33478, #14085, #19077 ),
 .UNSPECIFIED., .F., .F.,
 ( 4, 2, 2, 2, 4 ),
 ( 0.0007817359430256372700, 0.0009771253907250052138, 0.001172514838424373266, 0.001367904286123741101, 0.001563293733823109153 ),
 .UNSPECIFIED. ) ;
#77112 = AXIS2_PLACEMENT_3D ( 'NONE', #31664, #44712, #10950 ) ;
#77113 = ORIENTED_EDGE ( 'NONE', *, *, #47555, .F. ) ;
#77114 = ORIENTED_EDGE ( 'NONE', *, *, #50500, .F. ) ;
#77115 = CARTESIAN_POINT ( 'NONE',  ( -4.023054346021365468, -9.804649428959608670, 34.18742332936588468 ) ) ;
#77116 = B_SPLINE_CURVE_WITH_KNOTS ( 'NONE', 3,
 ( #67904, #46740, #67017, #54823, #26476, #68343, #19714, #33676, #75534, #80984 ),
 .UNSPECIFIED., .F., .F.,
 ( 4, 2, 2, 2, 4 ),
 ( 0.000000000000000000, 0.0001954311564186864407, 0.0003908623128373728815, 0.0005862934692560593493, 0.0007817246256747457630 ),
 .UNSPECIFIED. ) ;
#77118 = CARTESIAN_POINT ( 'NONE',  ( -13.45069879557126313, -5.557115091759785130, 34.35708131394839171 ) ) ;
#77117 = CARTESIAN_POINT ( 'NONE',  ( -7.911424292114620727, -6.879047030191174805, 34.71129190930000163 ) ) ;
#77119 = CARTESIAN_POINT ( 'NONE',  ( 11.53846153846141576, -2.379036618888197729, 30.90682066428292885 ) ) ;
#77120 = LINE ( 'NONE', #43335, #9202 ) ;
#77121 = FACE_BOUND ( 'NONE', #88895, .T. ) ;
#77122 = CARTESIAN_POINT ( 'NONE',  ( -7.053767526187231240, -3.338472653186242756, 32.95098750199972670 ) ) ;
#77123 = ORIENTED_EDGE ( 'NONE', *, *, #72965, .T. ) ;
#77124 = CARTESIAN_POINT ( 'NONE',  ( -3.165513659493205623, -2.625532179533470512, 30.86335684631491105 ) ) ;
#77125 = CARTESIAN_POINT ( 'NONE',  ( 2.057692307692309708, -2.499999999999998668, 29.75000000000000355 ) ) ;
#77126 = CARTESIAN_POINT ( 'NONE',  ( -1.450698795571264466, -3.513871655860377086, 32.76840700105978499 ) ) ;
#77127 = CARTESIAN_POINT ( 'NONE',  ( 7.173131342990376247, -9.233818618650603938, 34.70587769442853698 ) ) ;
#77128 = ORIENTED_EDGE ( 'NONE', *, *, #56462, .T. ) ;
#77129 = CARTESIAN_POINT ( 'NONE',  ( 5.011653076366756387, -12.70778746994557551, 30.41441678777548319 ) ) ;
#77130 = EDGE_LOOP ( 'NONE', ( #56163, #10936 ) ) ;
#77131 = FACE_BOUND ( 'NONE', #47804, .T. ) ;
#77132 = CARTESIAN_POINT ( 'NONE',  ( 4.853996859406926490, -5.667676309546437530, 34.40238873228292249 ) ) ;
#77133 = ADVANCED_FACE ( 'NONE', ( #18763 ), #87235, .F. ) ;
#77134 = AXIS2_PLACEMENT_3D ( 'NONE', #58543, #85151, #52237 ) ;
#77135 = CYLINDRICAL_SURFACE ( 'NONE', #80849, 0.2500000000000002220 ) ;
#77136 = CARTESIAN_POINT ( 'NONE',  ( -11.40766973063674961, -11.71459661697925903, 32.44059661609676937 ) ) ;
#77137 = ORIENTED_EDGE ( 'NONE', *, *, #58953, .T. ) ;
#77138 = PRODUCT_RELATED_PRODUCT_CATEGORY ( 'part', '', ( #88677 ) ) ;
#77139 = CYLINDRICAL_SURFACE ( 'NONE', #53683, 4.000000000000000000 ) ;
#77140 = CARTESIAN_POINT ( 'NONE',  ( -14.53117725141625627, -4.386631170607603991, 33.66268669641500111 ) ) ;
#77141 = CARTESIAN_POINT ( 'NONE',  ( -15.09997878980228059, -9.929761469519743144, 34.40412654351204225 ) ) ;
#77142 = DIRECTION ( 'NONE',  ( 0.000000000000000000, 1.000000000000000000, 0.000000000000000000 ) ) ;
#77143 = ORIENTED_EDGE ( 'NONE', *, *, #30623, .F. ) ;
#77144 = VECTOR ( 'NONE', #47488, 1000.000000000000227 ) ;
#77145 = CARTESIAN_POINT ( 'NONE',  ( -4.023054346021365468, -6.413143153341454017, 34.63066358083362672 ) ) ;
#77146 = ORIENTED_EDGE ( 'NONE', *, *, #54841, .T. ) ;
#77148 = ORIENTED_EDGE ( 'NONE', *, *, #80910, .F. ) ;
#77147 = CARTESIAN_POINT ( 'NONE',  ( -9.019207500173124004, -3.627789207965226748, 32.91389620160131102 ) ) ;
#77149 = CARTESIAN_POINT ( 'NONE',  ( 3.230769230769231726, -2.538708090699994813, 30.37095296980875503 ) ) ;
#77150 = CARTESIAN_POINT ( 'NONE',  ( -6.792285115252137295, -11.71459661697925903, 32.44059661609676937 ) ) ;
#77151 = CARTESIAN_POINT ( 'NONE',  ( 13.38461538461538680, -8.973038597847269315, 34.52809138561121927 ) ) ;
#77152 = CARTESIAN_POINT ( 'NONE',  ( 12.52679403281448600, -4.481592998940250538, 33.73612834413965089 ) ) ;
#77154 = DIRECTION ( 'NONE',  ( 1.000000000000000000, 0.000000000000000000, 0.000000000000000000 ) ) ;
#77153 = CARTESIAN_POINT ( 'NONE',  ( 16.15384615384615330, -2.538708090699994813, 30.37095296980875503 ) ) ;
#77155 = EDGE_CURVE ( 'NONE', #51245, #75182, #81674, .T. ) ;
#77156 = LINE ( 'NONE', #42935, #53589 ) ;
#77157 = CARTESIAN_POINT ( 'NONE',  ( -1.139087296525992166, -10.25000000000000533, 23.60937500000000711 ) ) ;
#77158 = ORIENTED_EDGE ( 'NONE', *, *, #12658, .T. ) ;
#77159 = CARTESIAN_POINT ( 'NONE',  ( -0.5922299282060208281, -5.582088688514999397, 34.36776431015576350 ) ) ;
#77160 = CARTESIAN_POINT ( 'NONE',  ( -9.626240358957616650, -11.35647404775217595, 33.31231777344666511 ) ) ;
#77161 = VERTEX_POINT ( 'NONE', #45328 ) ;
#77162 = ORIENTED_EDGE ( 'NONE', *, *, #37911, .T. ) ;
#77163 = ORIENTED_EDGE ( 'NONE', *, *, #51180, .T. ) ;
#77164 = CARTESIAN_POINT ( 'NONE',  ( -10.86540785267757592, -11.37209801155882971, 32.91403422569032955 ) ) ;
#77165 = CARTESIAN_POINT ( 'NONE',  ( -17.32694631421604115, -9.271318131107980420, 34.42618302367067429 ) ) ;
#77166 = CARTESIAN_POINT ( 'NONE',  ( -15.23076923076922995, -13.78497067705608181, 32.30358669280327177 ) ) ;
#77167 = CARTESIAN_POINT ( 'NONE',  ( -15.23076923076935074, -5.219633306517616589, 34.19971097300220464 ) ) ;
#77168 = CARTESIAN_POINT ( 'NONE',  ( 27.00000000000000000, 0.7500000000000051070, 32.75000000000000000 ) ) ;
#77169 = CARTESIAN_POINT ( 'NONE',  ( -8.769230769230892619, -3.083524468854526912, 32.58852847137268327 ) ) ;
#77170 = CARTESIAN_POINT ( 'NONE',  ( 0.2386721984753616965, -2.251424796025575770, 29.88072029997477586 ) ) ;
#77171 = VECTOR ( 'NONE', #64507, 1000.000000000000000 ) ;
#77172 = DIRECTION ( 'NONE',  ( -0.000000000000000000, 0.5000000000000011102, -0.8660254037844380415 ) ) ;
#77174 = ADVANCED_FACE ( 'NONE', ( #72801 ), #73257, .F. ) ;
#77173 = CARTESIAN_POINT ( 'NONE',  ( 17.86930853333243974, -11.71456829005830080, 32.44064028649416542 ) ) ;
#77175 = CARTESIAN_POINT ( 'NONE',  ( 12.33084699487090496, -11.71456829005830080, 32.44064028649416542 ) ) ;
#77176 = DIRECTION ( 'NONE',  ( -0.000000000000000000, -0.9848077530122086864, -0.1736481776669273613 ) ) ;
#77177 = EDGE_CURVE ( 'NONE', #77909, #30104, #11109, .T. ) ;
#77178 = EDGE_LOOP ( 'NONE', ( #7442, #80627, #80594, #6859 ) ) ;
#77180 = EDGE_CURVE ( 'NONE', #75643, #53841, #31380, .T. ) ;
#77179 = ORIENTED_EDGE ( 'NONE', *, *, #34553, .T. ) ;
#77181 = LINE ( 'NONE', #55134, #31362 ) ;
#77182 = CARTESIAN_POINT ( 'NONE',  ( -16.82692307692307665, -7.500000000000001776, 35.04278698407183867 ) ) ;
#77183 = DIRECTION ( 'NONE',  ( -0.000000000000000000, 0.5000000000000011102, -0.8660254037844381525 ) ) ;
#77184 = EDGE_LOOP ( 'NONE', ( #34459, #84011, #47732, #7103 ) ) ;
#77185 = VECTOR ( 'NONE', #88391, 999.9999999999998863 ) ;
#77186 = CARTESIAN_POINT ( 'NONE',  ( -15.93083330975275658, -8.282913670948747864, 34.94150082978203642 ) ) ;
#77187 = CARTESIAN_POINT ( 'NONE',  ( -12.39536932057580643, -7.250054483168843156, 34.74374881642865631 ) ) ;
#77188 = CARTESIAN_POINT ( 'NONE',  ( -8.899921372341079717, -9.084618155246140248, 34.75535874321725771 ) ) ;
#77189 = B_SPLINE_CURVE_WITH_KNOTS ( 'NONE', 3,
 ( #54999, #67636, #82041, #80720, #5038, #46903, #59978, #47348, #27529, #5932 ),
 .UNSPECIFIED., .F., .F.,
 ( 4, 2, 2, 2, 4 ),
 ( 0.000000000000000000, 0.0001954311564186863323, 0.0003908623128373726646, 0.0005862934692560590241, 0.0007817246256747453293 ),
 .UNSPECIFIED. ) ;
#77190 = ORIENTED_EDGE ( 'NONE', *, *, #22625, .F. ) ;
#77191 = LINE ( 'NONE', #8748, #71661 ) ;
#77192 = VERTEX_POINT ( 'NONE', #44427 ) ;
#77193 = CARTESIAN_POINT ( 'NONE',  ( 13.13463864056679675, -12.41104346484419452, 31.60698883733904196 ) ) ;
#77194 = CARTESIAN_POINT ( 'NONE',  ( -3.480792468062195333, -12.22074536777954989, 31.39888409691088356 ) ) ;
#77195 = VECTOR ( 'NONE', #17817, 1000.000000000000000 ) ;
#77196 = DIRECTION ( 'NONE',  ( -0.000000000000000000, -5.102127870520021228E-17, -1.000000000000000000 ) ) ;
#77197 = CARTESIAN_POINT ( 'NONE',  ( -9.758390071667827570, -8.164416787775445883, 34.95778746994557906 ) ) ;
#77198 = DIRECTION ( 'NONE',  ( 0.000000000000000000, 1.000000000000000000, 0.000000000000000000 ) ) ;
#77199 = CIRCLE ( 'NONE', #32575, 2.750000000000000000 ) ;
#77200 = ORIENTED_EDGE ( 'NONE', *, *, #63159, .F. ) ;
#77201 = ADVANCED_FACE ( 'NONE', ( #18315 ), #71916, .T. ) ;
#77202 = VERTEX_POINT ( 'NONE', #25953 ) ;
#77203 = ORIENTED_EDGE ( 'NONE', *, *, #39907, .T. ) ;
#77204 = CARTESIAN_POINT ( 'NONE',  ( 13.13459214732242408, -3.202444869320336451, 32.30641848906366675 ) ) ;
#77205 = CARTESIAN_POINT ( 'NONE',  ( 13.38461538461526601, -10.21337939537710326, 33.94971097300076224 ) ) ;
#77206 = CARTESIAN_POINT ( 'NONE',  ( -13.19230769230769162, -3.499999999999999556, 29.75000000000000355 ) ) ;
#77207 = CARTESIAN_POINT ( 'NONE',  ( -2.057637887778853258, -11.47946981652013498, 33.17500667209846910 ) ) ;
#77208 = CARTESIAN_POINT ( 'NONE',  ( 4.153846153846154188, -6.386643153685126251, 34.62446782046654192 ) ) ;
#77209 = CARTESIAN_POINT ( 'NONE',  ( 8.102564102564102200, -3.499999999999999556, 29.75000000000000355 ) ) ;
#77210 = ORIENTED_EDGE ( 'NONE', *, *, #22463, .F. ) ;
#77211 = ORIENTED_EDGE ( 'NONE', *, *, #83334, .T. ) ;
#77212 = B_SPLINE_CURVE_WITH_KNOTS ( 'NONE', 3,
 ( #46321, #82337, #40027, #67488, #76902, #83219, #55730, #8888, #57060, #7559 ),
 .UNSPECIFIED., .F., .F.,
 ( 4, 2, 2, 2, 4 ),
 ( 0.000000000000000000, 0.0001954339881912772715, 0.0003908679763825545429, 0.0005863019645738318415, 0.0007817359527651090859 ),
 .UNSPECIFIED. ) ;
#77213 = EDGE_CURVE ( 'NONE', #37064, #59376, #68748, .T. ) ;
#77214 = ORIENTED_EDGE ( 'NONE', *, *, #3219, .F. ) ;
#77216 = ORIENTED_EDGE ( 'NONE', *, *, #11928, .T. ) ;
#77215 = CARTESIAN_POINT ( 'NONE',  ( 4.153846153846030731, -4.320704448113951379, 33.92786785259630022 ) ) ;
#77218 = CARTESIAN_POINT ( 'NONE',  ( 14.37294744720514750, -5.094484230520773593, 34.41647553114626845 ) ) ;
#77217 = CARTESIAN_POINT ( 'NONE',  ( 8.992010310499175318, -8.496831190052093419, 34.64984203495476578 ) ) ;
#77219 = CIRCLE ( 'NONE', #57101, 4.000000000000000000 ) ;
#77220 = CARTESIAN_POINT ( 'NONE',  ( -1.553300858899081760, -11.25000000000000888, 24.85937500000000711 ) ) ;
#77221 = EDGE_LOOP ( 'NONE', ( #53110, #28484, #9731, #76720 ) ) ;
#77222 = ORIENTED_EDGE ( 'NONE', *, *, #16516, .T. ) ;
#77223 = CARTESIAN_POINT ( 'NONE',  ( 13.63461538461538858, -2.499999999999999556, 29.81604066197449754 ) ) ;
#77224 = VECTOR ( 'NONE', #63336, 1000.000000000000000 ) ;
#77225 = ORIENTED_EDGE ( 'NONE', *, *, #3448, .T. ) ;
#77226 = FACE_BOUND ( 'NONE', #30542, .T. ) ;
#77227 = CARTESIAN_POINT ( 'NONE',  ( 20.00000000000000000, -4.000000000000000000, 29.75000000000000355 ) ) ;
#77228 = ADVANCED_FACE ( 'NONE', ( #3455 ), #30921, .F. ) ;
#77229 = LINE ( 'NONE', #15539, #1707 ) ;
#77230 = ORIENTED_EDGE ( 'NONE', *, *, #1614, .F. ) ;
#77231 = CARTESIAN_POINT ( 'NONE',  ( 2.241608896736428047, -8.120952969808774569, 34.71129190930000163 ) ) ;
#77232 = CARTESIAN_POINT ( 'NONE',  ( -19.00000000000000000, -1.749999999999991118, 22.25000000000000000 ) ) ;
#77233 = AXIS2_PLACEMENT_3D ( 'NONE', #60785, #75201, #41410 ) ;
#77234 = CARTESIAN_POINT ( 'NONE',  ( -39.05038313613820122, -2.499999999999999556, 27.25000000000000000 ) ) ;
#77235 = EDGE_CURVE ( 'NONE', #60559, #49728, #9812, .T. ) ;
#77236 = CARTESIAN_POINT ( 'NONE',  ( 7.846153846153723244, -4.320704448113951379, 33.92786785259630022 ) ) ;
#77237 = CARTESIAN_POINT ( 'NONE',  ( 0.4615384615384611200, -12.37446782046654192, 30.86335684631486131 ) ) ;
#77238 = EDGE_LOOP ( 'NONE', ( #36989, #55695 ) ) ;
#77239 = CARTESIAN_POINT ( 'NONE',  ( 8.638540166120462160, -11.37499894934982692, 33.29245874905763003 ) ) ;
#77240 = CARTESIAN_POINT ( 'NONE',  ( 2.057669083470850424, -12.07920672191015221, 32.31858351112116168 ) ) ;
#77241 = DIRECTION ( 'NONE',  ( -0.000000000000000000, -0.6427876096865404731, -0.7660444431189771253 ) ) ;
#77242 = DIRECTION ( 'NONE',  ( 0.000000000000000000, 0.4999999999999985567, 0.8660254037844395958 ) ) ;
#77243 = DIRECTION ( 'NONE',  ( 0.000000000000000000, 0.000000000000000000, 1.000000000000000000 ) ) ;
#77244 = CARTESIAN_POINT ( 'NONE',  ( 6.130525701763563262, -10.19071101563364756, 33.96452234770658407 ) ) ;
#77246 = CARTESIAN_POINT ( 'NONE',  ( 11.78840705680968171, -4.336752205174649433, 33.62275283266504289 ) ) ;
#77245 = CARTESIAN_POINT ( 'NONE',  ( -8.899791360972686860, -2.504760397472875155, 29.97295953869789997 ) ) ;
#77247 = ADVANCED_FACE ( 'NONE', ( #60619 ), #699, .F. ) ;
#77248 = CYLINDRICAL_SURFACE ( 'NONE', #54023, 0.2499999999999986955 ) ;
#77250 = CARTESIAN_POINT ( 'NONE',  ( 2.530705151785703322, -6.460100341425561332, 34.89618726649961644 ) ) ;
#77249 = LINE ( 'NONE', #35832, #40071 ) ;
#77251 = DIRECTION ( 'NONE',  ( -0.000000000000000000, -0.7660444431189791237, -0.6427876096865379196 ) ) ;
#77252 = CARTESIAN_POINT ( 'NONE',  ( -1.077988221561460236, -10.27530806549876452, 22.10750670625849068 ) ) ;
#77253 = EDGE_LOOP ( 'NONE', ( #30735, #37472 ) ) ;
#77254 = CARTESIAN_POINT ( 'NONE',  ( -0.5647128961976267680, -3.802940288257858015, 13.99999999999966604 ) ) ;
#77255 = EDGE_LOOP ( 'NONE', ( #26108, #12116, #65809, #49661 ) ) ;
#77256 = EDGE_CURVE ( 'NONE', #77110, #53903, #88132, .T. ) ;
#77257 = LINE ( 'NONE', #42598, #37739 ) ;
#77258 = AXIS2_PLACEMENT_3D ( 'NONE', #10652, #65579, #3879 ) ;
#77259 = ORIENTED_EDGE ( 'NONE', *, *, #55992, .T. ) ;
#77260 = CARTESIAN_POINT ( 'NONE',  ( -4.153846153846152411, -2.499999999999998668, 29.75000000000001421 ) ) ;
#77262 = EDGE_CURVE ( 'NONE', #15822, #37401, #61562, .T. ) ;
#77261 = CARTESIAN_POINT ( 'NONE',  ( 14.05771556364371833, -2.318417181685855422, 30.59732222474233865 ) ) ;
#77263 = ORIENTED_EDGE ( 'NONE', *, *, #58838, .T. ) ;
#77264 = CARTESIAN_POINT ( 'NONE',  ( -18.13014720943822056, -12.45813303252208648, 30.39737893381572675 ) ) ;
#77265 = CARTESIAN_POINT ( 'NONE',  ( 2.724691934501235036, -6.299813628509441266, 21.63875670625848713 ) ) ;
#77266 = CARTESIAN_POINT ( 'NONE',  ( 17.32697738856138869, -8.303483539816726378, 34.68545999027711702 ) ) ;
#77267 = CARTESIAN_POINT ( 'NONE',  ( 7.173131342990376247, -10.06805714834173848, 34.32951233291982618 ) ) ;
#77268 = CARTESIAN_POINT ( 'NONE',  ( -5.143006487878955646, -4.786620604624113540, 33.94971097300155805 ) ) ;
#77269 = FACE_OUTER_BOUND ( 'NONE', #63986, .T. ) ;
#77270 = CARTESIAN_POINT ( 'NONE',  ( 19.00000000000000355, -13.24999999999999822, 29.02772085586297734 ) ) ;
#77271 = CARTESIAN_POINT ( 'NONE',  ( 5.076923076922954969, -8.613356846316285953, 34.62446782046622218 ) ) ;
#77272 = CARTESIAN_POINT ( 'NONE',  ( -3.749999999999997335, -7.500000000000021316, 18.84375000000000000 ) ) ;
#77273 = CARTESIAN_POINT ( 'NONE',  ( -39.05038313613820122, -2.249999999999998668, 29.75000000000000355 ) ) ;
#77275 = EDGE_CURVE ( 'NONE', #75030, #10587, #74146, .T. ) ;
#77274 = CYLINDRICAL_SURFACE ( 'NONE', #47743, 0.2499999999999973355 ) ;
#77276 = AXIS2_PLACEMENT_3D ( 'NONE', #38617, #39522, #53002 ) ;
#77277 = CARTESIAN_POINT ( 'NONE',  ( 13.51514108637895006, -4.459921816937791661, 33.71989282347011851 ) ) ;
#77278 = CARTESIAN_POINT ( 'NONE',  ( -3.749999999999988454, -9.053300858899127945, 15.01562500000000178 ) ) ;
#77279 = DIRECTION ( 'NONE',  ( 1.000000000000000000, 0.000000000000000000, 0.000000000000000000 ) ) ;
#77280 = ORIENTED_EDGE ( 'NONE', *, *, #3163, .F. ) ;
#77281 = EDGE_CURVE ( 'NONE', #67532, #43517, #6574, .T. ) ;
#77282 = CARTESIAN_POINT ( 'NONE',  ( 7.146503884938495865, -7.630147231320743018, 34.74852402298682819 ) ) ;
#77283 = CARTESIAN_POINT ( 'NONE',  ( -11.28851602011339672, -8.433404298154334455, 34.66254593164985920 ) ) ;
#77284 = DIRECTION ( 'NONE',  ( 0.000000000000000000, 0.1736481776669275834, 0.9848077530122086864 ) ) ;
#77285 = CARTESIAN_POINT ( 'NONE',  ( 5.326977388561391358, -2.779044189368096163, 31.39831045268886456 ) ) ;
#77286 = EDGE_CURVE ( 'NONE', #68899, #20422, #45130, .T. ) ;
#77287 = DIRECTION ( 'NONE',  ( 1.000000000000000000, 0.000000000000000000, 0.000000000000000000 ) ) ;
#77288 = CARTESIAN_POINT ( 'NONE',  ( -14.17690186672535901, -3.957578996910242619, 33.62503395064540257 ) ) ;
#77289 = B_SPLINE_CURVE_WITH_KNOTS ( 'NONE', 3,
 ( #60022, #87526, #25801, #26242, #53709, #3742, #86182, #79419, #86634, #28015 ),
 .UNSPECIFIED., .F., .F.,
 ( 4, 2, 2, 2, 4 ),
 ( 0.000000000000000000, 0.0001954311564186863865, 0.0003908623128373727731, 0.0005862934692560591325, 0.0007817246256747455461 ),
 .UNSPECIFIED. ) ;
#77290 = PLANE ( 'NONE',  #4641 ) ;
#77291 = CIRCLE ( 'NONE', #16919, 4.000000000000000000 ) ;
#77292 = ORIENTED_EDGE ( 'NONE', *, *, #56700, .T. ) ;
#77293 = ORIENTED_EDGE ( 'NONE', *, *, #56069, .T. ) ;
#77294 = AXIS2_PLACEMENT_3D ( 'NONE', #49068, #8535, #448 ) ;
#77295 = ORIENTED_EDGE ( 'NONE', *, *, #29377, .T. ) ;
#77296 = CARTESIAN_POINT ( 'NONE',  ( -11.31544869436814160, -11.43677907613344757, 33.22367315496202167 ) ) ;
#77297 = CARTESIAN_POINT ( 'NONE',  ( 6.792385456409365752, -2.729777683071817229, 31.24903638046268739 ) ) ;
#77298 = CARTESIAN_POINT ( 'NONE',  ( 2.307692307692187583, -11.48612834414049644, 32.76840700105863391 ) ) ;
#77299 = VECTOR ( 'NONE', #4157, 1000.000000000000000 ) ;
#77300 = CARTESIAN_POINT ( 'NONE',  ( 3.230769230769108269, -9.528491918059723176, 34.59228464037033035 ) ) ;
#77301 = CARTESIAN_POINT ( 'NONE',  ( 17.77707304109314634, -9.172386477786394821, 34.72672124145550043 ) ) ;
#77302 = EDGE_CURVE ( 'NONE', #48730, #88631, #89011, .T. ) ;
#77303 = ORIENTED_EDGE ( 'NONE', *, *, #81964, .F. ) ;
#77304 = CARTESIAN_POINT ( 'NONE',  ( 16.15384615384603251, -5.219633306517616589, 34.19971097300220464 ) ) ;
#77305 = ORIENTED_EDGE ( 'NONE', *, *, #69845, .T. ) ;
#77306 = ADVANCED_FACE ( 'NONE', ( #68272 ), #88571, .F. ) ;
#77307 = VERTEX_POINT ( 'NONE', #82238 ) ;
#77309 = ORIENTED_EDGE ( 'NONE', *, *, #45497, .F. ) ;
#77308 = CARTESIAN_POINT ( 'NONE',  ( -9.942307692307691624, -2.249999999999998668, 29.75000000000000355 ) ) ;
#77310 = DIRECTION ( 'NONE',  ( 0.000000000000000000, 0.000000000000000000, -1.000000000000000000 ) ) ;
#77311 = EDGE_CURVE ( 'NONE', #15474, #47909, #67387, .T. ) ;
#77312 = ADVANCED_FACE ( 'NONE', ( #19640 ), #26846, .F. ) ;
#77313 = B_SPLINE_CURVE_WITH_KNOTS ( 'NONE', 3,
 ( #42859, #75312, #76639, #34758, #35658, #62228, #36104, #28447, #13605, #22138 ),
 .UNSPECIFIED., .F., .F.,
 ( 4, 2, 2, 2, 4 ),
 ( 0.000000000000000000, 0.0001954311564186876063, 0.0003908623128373752125, 0.0005862934692560628188, 0.0007817246256747504250 ),
 .UNSPECIFIED. ) ;
#77314 = CARTESIAN_POINT ( 'NONE',  ( -10.83831083290076158, -4.887634598454295265, 34.01352882383564946 ) ) ;
#77315 = EDGE_CURVE ( 'NONE', #29230, #74248, #18345, .T. ) ;
#77316 = CYLINDRICAL_SURFACE ( 'NONE', #23429, 4.000000000000000000 ) ;
#77317 = CARTESIAN_POINT ( 'NONE',  ( 8.069166690247241647, -12.64618726649961289, 30.78989965857442712 ) ) ;
#77318 = EDGE_LOOP ( 'NONE', ( #6559, #1979, #21792, #48350 ) ) ;
#77319 = ORIENTED_EDGE ( 'NONE', *, *, #60449, .F. ) ;
#77320 = ADVANCED_FACE ( 'NONE', ( #7466 ), #34921, .F. ) ;
#77321 = EDGE_LOOP ( 'NONE', ( #80320, #73020 ) ) ;
#77322 = CARTESIAN_POINT ( 'NONE',  ( -6.700064078983525739, -2.889357225399416862, 32.26129605718031002 ) ) ;
#77324 = ORIENTED_EDGE ( 'NONE', *, *, #21888, .T. ) ;
#77323 = CARTESIAN_POINT ( 'NONE',  ( -14.05763788777885637, -2.318338780012835443, 30.59689888758630261 ) ) ;
#77325 = CARTESIAN_POINT ( 'NONE',  ( -39.05038313613820122, -2.499999999999999556, 29.75000000000000355 ) ) ;
#77326 = CARTESIAN_POINT ( 'NONE',  ( 5.010839665967194989, -3.513871655860377086, 32.76840700105978499 ) ) ;
#77327 = CARTESIAN_POINT ( 'NONE',  ( 2.373759641042385127, -9.058645607665452459, 34.76329471203371924 ) ) ;
#77328 = ORIENTED_EDGE ( 'NONE', *, *, #33865, .T. ) ;
#77329 = VECTOR ( 'NONE', #22008, 1000.000000000000000 ) ;
#77330 = CARTESIAN_POINT ( 'NONE',  ( 11.53846153846153832, -5.180354513474913603, 36.12317359536750416 ) ) ;
#77331 = DIRECTION ( 'NONE',  ( 1.000000000000000000, 0.000000000000000000, 0.000000000000000000 ) ) ;
#77332 = EDGE_LOOP ( 'NONE', ( #67675, #56150 ) ) ;
#77333 = FACE_BOUND ( 'NONE', #66926, .T. ) ;
#77334 = CARTESIAN_POINT ( 'NONE',  ( 11.47237812750566022, -4.786620604624113540, 33.94971097300155805 ) ) ;
#77335 = DIRECTION ( 'NONE',  ( -1.000000000000000000, -0.000000000000000000, -0.000000000000000000 ) ) ;
#77336 = CARTESIAN_POINT ( 'NONE',  ( 2.084765348785459604, -12.38737895849757820, 31.66785238281580206 ) ) ;
#77338 = CARTESIAN_POINT ( 'NONE',  ( -6.673022611438608642, -2.564540009722896752, 30.55348353981670684 ) ) ;
#77337 = CARTESIAN_POINT ( 'NONE',  ( 8.068933515131908152, -10.97394488606064122, 33.68653795673694873 ) ) ;
#77339 = CARTESIAN_POINT ( 'NONE',  ( 16.08776274289027697, -2.538708090699995257, 30.37095296980875148 ) ) ;
#77340 = CARTESIAN_POINT ( 'NONE',  ( -19.50000000000000000, -11.50000000000000000, 29.75000000000000355 ) ) ;
#77341 = ORIENTED_EDGE ( 'NONE', *, *, #50607, .T. ) ;
#77342 = CARTESIAN_POINT ( 'NONE',  ( 10.61538461538461675, -6.435427911321262684, 35.78748833219616898 ) ) ;
#77343 = CARTESIAN_POINT ( 'NONE',  ( 5.011653076366756387, -4.320704448112771878, 33.92786785259540494 ) ) ;
#77344 = EDGE_CURVE ( 'NONE', #40637, #79352, #75040, .T. ) ;
#77345 = EDGE_LOOP ( 'NONE', ( #49927, #27983 ) ) ;
#77346 = ADVANCED_FACE ( 'NONE', ( #64600 ), #16432, .F. ) ;
#77347 = CARTESIAN_POINT ( 'NONE',  ( 7.846153846153723244, -5.094484230521993062, 34.41647553114689373 ) ) ;
#77348 = LINE ( 'NONE', #43126, #78942 ) ;
#77349 = CARTESIAN_POINT ( 'NONE',  ( 16.15384615384615330, -6.343179335718451384, 34.87096338111211935 ) ) ;
#77350 = DIRECTION ( 'NONE',  ( -1.000000000000000000, -0.000000000000000000, -0.000000000000000000 ) ) ;
#77351 = AXIS2_PLACEMENT_3D ( 'NONE', #81791, #14207, #39148 ) ;
#77352 = CARTESIAN_POINT ( 'NONE',  ( 6.000000000000001776, -13.75783147151868846, 33.36296068462461051 ) ) ;
#77353 = CYLINDRICAL_SURFACE ( 'NONE', #1226, 0.2500000000000002220 ) ;
#77354 = FACE_BOUND ( 'NONE', #58109, .T. ) ;
#77356 = FACE_OUTER_BOUND ( 'NONE', #69381, .T. ) ;
#77355 = CYLINDRICAL_SURFACE ( 'NONE', #56226, 0.2499999999999979738 ) ;
#77357 = CARTESIAN_POINT ( 'NONE',  ( -15.93083480223330817, -2.554770724473668597, 30.48948780036025852 ) ) ;
#77359 = CARTESIAN_POINT ( 'NONE',  ( -12.71151519248081740, -4.236021600441997492, 33.53823185664189310 ) ) ;
#77358 = CARTESIAN_POINT ( 'NONE',  ( -5.076923076923075762, -3.937682226553329556, 33.60647404775216529 ) ) ;
#77360 = CARTESIAN_POINT ( 'NONE',  ( 1.134615384615387246, -2.249999999999998668, 29.75000000000000355 ) ) ;
#77361 = VECTOR ( 'NONE', #64456, 1000.000000000000114 ) ;
#77362 = CARTESIAN_POINT ( 'NONE',  ( 2.694853999681214862, -10.10844685921789043, 19.37313170625848713 ) ) ;
#77363 = ORIENTED_EDGE ( 'NONE', *, *, #77400, .T. ) ;
#77364 = ORIENTED_EDGE ( 'NONE', *, *, #39240, .F. ) ;
#77365 = CYLINDRICAL_SURFACE ( 'NONE', #60761, 0.2500000000000008882 ) ;
#77366 = DIRECTION ( 'NONE',  ( -1.000000000000000000, 0.000000000000000000, 0.000000000000000000 ) ) ;
#77367 = CARTESIAN_POINT ( 'NONE',  ( -0.5916864312701554107, -3.625366637846545448, 33.29286588640298561 ) ) ;
#77368 = CARTESIAN_POINT ( 'NONE',  ( -17.01166750564705055, -11.48612834413965977, 32.76840700105972815 ) ) ;
#77369 = CARTESIAN_POINT ( 'NONE',  ( -17.01166750564705055, -6.879047030191284051, 34.71129190930002295 ) ) ;
#77370 = CARTESIAN_POINT ( 'NONE',  ( 1.614399933863660985, -11.22469193450123193, 21.95125670625849068 ) ) ;
#77371 = CARTESIAN_POINT ( 'NONE',  ( 3.931019461367150303, -7.369208160676172348, 34.74850200257122879 ) ) ;
#77372 = CARTESIAN_POINT ( 'NONE',  ( 18.25005431163831560, -3.136992222400443175, 32.19305428654138979 ) ) ;
#77373 = CARTESIAN_POINT ( 'NONE',  ( 15.23076923076911093, -11.94971097300221174, 32.03036669348237098 ) ) ;
#77374 = CARTESIAN_POINT ( 'NONE',  ( -1.607541602131531633, -12.39988816332205701, 30.74660775122750778 ) ) ;
#77375 = CARTESIAN_POINT ( 'NONE',  ( -17.01166793741023042, -5.094484230520771817, 34.41647553114626845 ) ) ;
#77376 = CARTESIAN_POINT ( 'NONE',  ( 6.000000000000001776, -2.499999999999998668, 29.50000000000001066 ) ) ;
#77378 = EDGE_CURVE ( 'NONE', #40578, #53938, #50554, .T. ) ;
#77377 = CARTESIAN_POINT ( 'NONE',  ( 9.692307692307695177, -1.242168528481310874, 33.36296068462461051 ) ) ;
#77379 = EDGE_CURVE ( 'NONE', #16174, #19274, #29036, .T. ) ;
#77380 = FACE_OUTER_BOUND ( 'NONE', #28341, .T. ) ;
#77381 = EDGE_LOOP ( 'NONE', ( #9435, #15380, #36565, #65536, #2530 ) ) ;
#77382 = CARTESIAN_POINT ( 'NONE',  ( -1.576923076923076872, -7.500000000000000000, 29.75000000000000355 ) ) ;
#77383 = CARTESIAN_POINT ( 'NONE',  ( 0.6845498131513096940, -2.554770724473668153, 30.48948780036025852 ) ) ;
#77384 = CARTESIAN_POINT ( 'NONE',  ( -1.200186371490524317, -10.22469193450124791, 25.11124329374151642 ) ) ;
#77385 = ADVANCED_FACE ( 'NONE', ( #28624 ), #64157, .T. ) ;
#77386 = CARTESIAN_POINT ( 'NONE',  ( -2.530619266599154926, -4.762599654559228846, 34.23009711892697737 ) ) ;
#77387 = CARTESIAN_POINT ( 'NONE',  ( -16.08777882049607655, -2.486705287966280320, 31.30864560766543647 ) ) ;
#77388 = ORIENTED_EDGE ( 'NONE', *, *, #44423, .T. ) ;
#77389 = CYLINDRICAL_SURFACE ( 'NONE', #71536, 0.2499999999999986955 ) ;
#77391 = EDGE_LOOP ( 'NONE', ( #39438, #52392, #82104, #14184 ) ) ;
#77390 = CARTESIAN_POINT ( 'NONE',  ( -7.846153846153967493, -12.51329471203414379, 31.30864560766407578 ) ) ;
#77392 = LINE ( 'NONE', #22011, #983 ) ;
#77393 = CARTESIAN_POINT ( 'NONE',  ( -4.853911725310227077, -9.886259254753566594, 34.14407573483972413 ) ) ;
#77394 = EDGE_CURVE ( 'NONE', #4695, #22067, #62823, .T. ) ;
#77395 = VERTEX_POINT ( 'NONE', #55633 ) ;
#77396 = B_SPLINE_CURVE_WITH_KNOTS ( 'NONE', 3,
 ( #11341, #73501, #39720, #18552, #73944, #19434, #87931, #4588, #88804, #66283 ),
 .UNSPECIFIED., .F., .F.,
 ( 4, 2, 2, 2, 4 ),
 ( 0.0007817359527651101701, 0.0009771254036996489256, 0.001172514854634187790, 0.001367904305568726653, 0.001563293756503265517 ),
 .UNSPECIFIED. ) ;
#77397 = CARTESIAN_POINT ( 'NONE',  ( -13.31854703361294590, -2.538708090699994813, 30.37095296980875503 ) ) ;
#77398 = VECTOR ( 'NONE', #34544, 1000.000000000000114 ) ;
#77399 = CARTESIAN_POINT ( 'NONE',  ( 0.000000000000000000, -11.00000000000000000, 29.75000000000000355 ) ) ;
#77400 = EDGE_CURVE ( 'NONE', #75052, #4668, #73055, .T. ) ;
#77401 = ORIENTED_EDGE ( 'NONE', *, *, #47617, .T. ) ;
#77402 = B_SPLINE_CURVE_WITH_KNOTS ( 'NONE', 3,
 ( #82168, #19567, #47921, #68205, #12811, #12375, #75840, #48361, #33083, #46601 ),
 .UNSPECIFIED., .F., .F.,
 ( 4, 2, 2, 2, 4 ),
 ( 0.0007817359430256262112, 0.0009771253907249911191, 0.001172514838424356136, 0.001367904286123721152, 0.001563293733823086168 ),
 .UNSPECIFIED. ) ;
#77403 = CARTESIAN_POINT ( 'NONE',  ( -8.102564102564102200, -11.50000000000000000, 29.75000000000000355 ) ) ;
#77404 = DIRECTION ( 'NONE',  ( -0.000000000000000000, 0.7660444431189791237, -0.6427876096865379196 ) ) ;
#77405 = CARTESIAN_POINT ( 'NONE',  ( -19.50000000000000000, -3.499999999999999556, 29.75000000000000355 ) ) ;
#77406 = ORIENTED_EDGE ( 'NONE', *, *, #81900, .T. ) ;
#77407 = ORIENTED_EDGE ( 'NONE', *, *, #12658, .F. ) ;
#77408 = ADVANCED_FACE ( 'NONE', ( #56086 ), #48882, .F. ) ;
#77409 = ORIENTED_EDGE ( 'NONE', *, *, #39271, .T. ) ;
#77410 = CARTESIAN_POINT ( 'NONE',  ( -5.143005456283209931, -9.058645607665454236, 34.76329471203372634 ) ) ;
#77411 = CARTESIAN_POINT ( 'NONE',  ( -14.55766903863466055, -3.137211980971221781, 32.19342716148376837 ) ) ;
#77412 = EDGE_CURVE ( 'NONE', #81637, #19931, #76355, .T. ) ;
#77413 = DIRECTION ( 'NONE',  ( 0.000000000000000000, 0.000000000000000000, 1.000000000000000000 ) ) ;
#77414 = CARTESIAN_POINT ( 'NONE',  ( 2.980792486720640344, -10.06842814019191401, 34.32929386961144758 ) ) ;
#77415 = EDGE_CURVE ( 'NONE', #49885, #14228, #15995, .T. ) ;
#77416 = VERTEX_POINT ( 'NONE', #9244 ) ;
#77417 = ORIENTED_EDGE ( 'NONE', *, *, #84948, .F. ) ;
#77419 = ORIENTED_EDGE ( 'NONE', *, *, #66571, .T. ) ;
#77418 = CARTESIAN_POINT ( 'NONE',  ( 20.99999999999999645, -4.249999999999998224, 27.25000000000000000 ) ) ;
#77420 = VECTOR ( 'NONE', #59726, 1000.000000000000227 ) ;
#77421 = EDGE_CURVE ( 'NONE', #6352, #62909, #9717, .T. ) ;
#77422 = CARTESIAN_POINT ( 'NONE',  ( 9.915319043920547415, -12.39991518177334129, 30.74647679643404530 ) ) ;
#77423 = ORIENTED_EDGE ( 'NONE', *, *, #45232, .T. ) ;
#77424 = CARTESIAN_POINT ( 'NONE',  ( 2.750000000000001776, -7.500000000000000000, 11.00000000000000178 ) ) ;
#77425 = CARTESIAN_POINT ( 'NONE',  ( 7.911409417429871027, -5.219633306516380244, 34.19971097300157936 ) ) ;
#77426 = ORIENTED_EDGE ( 'NONE', *, *, #30767, .T. ) ;
#77427 = EDGE_CURVE ( 'NONE', #30124, #75360, #12916, .T. ) ;
#77428 = ORIENTED_EDGE ( 'NONE', *, *, #34973, .T. ) ;
#77430 = EDGE_LOOP ( 'NONE', ( #50122, #42663, #70220, #10209 ) ) ;
#77429 = CARTESIAN_POINT ( 'NONE',  ( 9.757562831820530747, -8.656820664281605460, 34.87096338111211224 ) ) ;
#77431 = DIRECTION ( 'NONE',  ( 0.000000000000000000, 0.1736481776669267785, -0.9848077530122087975 ) ) ;
#77432 = CARTESIAN_POINT ( 'NONE',  ( -15.93083480223330817, -3.587049720035815348, 32.86302985866382897 ) ) ;
#77433 = EDGE_LOOP ( 'NONE', ( #87788, #40042, #48426, #57648 ) ) ;
#77434 = EDGE_CURVE ( 'NONE', #34293, #77956, #84606, .T. ) ;
#77435 = CARTESIAN_POINT ( 'NONE',  ( 15.23076923076923173, -2.292212530054420494, 30.41441678777542634 ) ) ;
#77436 = CARTESIAN_POINT ( 'NONE',  ( 5.142178648199100977, -11.48612834413965977, 32.76840700105972815 ) ) ;
#77437 = CARTESIAN_POINT ( 'NONE',  ( 6.792928953345228393, -5.915902021225892149, 34.75552854090298638 ) ) ;
#77438 = FACE_BOUND ( 'NONE', #24450, .T. ) ;
#77439 = CARTESIAN_POINT ( 'NONE',  ( 7.912221179503920787, -12.34228464037088813, 31.77849191805839268 ) ) ;
#77440 = CARTESIAN_POINT ( 'NONE',  ( 8.769230769230645706, -10.33852847137269571, 34.16647553114546554 ) ) ;
#77441 = CARTESIAN_POINT ( 'NONE',  ( 13.38461538461538680, -12.62096338111211580, 30.90682066428153263 ) ) ;
#77443 = CARTESIAN_POINT ( 'NONE',  ( -5.869208192175213945, -2.729792928343270919, 31.24908615093345077 ) ) ;
#77442 = CARTESIAN_POINT ( 'NONE',  ( -0.2387587925603975592, -3.020022701398815013, 32.48759521482552515 ) ) ;
#77444 = AXIS2_PLACEMENT_3D ( 'NONE', #33739, #54444, #12583 ) ;
#77445 = CARTESIAN_POINT ( 'NONE',  ( -11.28840722682322628, -3.136992222400443175, 32.19305428654138979 ) ) ;
#77446 = CARTESIAN_POINT ( 'NONE',  ( -16.37733107841048863, -2.612411019501189813, 31.66733052389439962 ) ) ;
#77447 = ORIENTED_EDGE ( 'NONE', *, *, #21717, .T. ) ;
#77448 = CARTESIAN_POINT ( 'NONE',  ( -5.749945688361685292, -11.79725096376909299, 32.30694842903960762 ) ) ;
#77449 = ORIENTED_EDGE ( 'NONE', *, *, #65466, .T. ) ;
#77450 = EDGE_CURVE ( 'NONE', #26582, #48512, #45230, .T. ) ;
#77451 = ORIENTED_EDGE ( 'NONE', *, *, #67055, .F. ) ;
#77452 = VECTOR ( 'NONE', #71427, 1000.000000000000000 ) ;
#77454 = CARTESIAN_POINT ( 'NONE',  ( 15.16468581981335007, -12.10708131394839349, 31.69288490824020244 ) ) ;
#77453 = CARTESIAN_POINT ( 'NONE',  ( 14.37294787896833625, -3.835265460703683349, 33.15142922261929925 ) ) ;
#77455 = EDGE_CURVE ( 'NONE', #58277, #83191, #86245, .T. ) ;
#77456 = AXIS2_PLACEMENT_3D ( 'NONE', #2466, #29958, #57416 ) ;
#77457 = CARTESIAN_POINT ( 'NONE',  ( -5.869474298236438514, -6.852161475712352789, 34.70806712695775786 ) ) ;
#77458 = CARTESIAN_POINT ( 'NONE',  ( 7.846153846153846700, -3.322132147404559976, 32.92929555188717927 ) ) ;
#77459 = CARTESIAN_POINT ( 'NONE',  ( 1.384615384615386802, -10.67929555188718282, 33.92786785259544047 ) ) ;
#77460 = CARTESIAN_POINT ( 'NONE',  ( 14.30769230769231015, -11.35647404775217417, 33.31231777344666511 ) ) ;
#77461 = ORIENTED_EDGE ( 'NONE', *, *, #77768, .F. ) ;
#77462 = CARTESIAN_POINT ( 'NONE',  ( -18.24997673094235395, -5.728515186090276323, 34.42611988154120439 ) ) ;
#77463 = VECTOR ( 'NONE', #59507, 1000.000000000000000 ) ;
#77464 = DIRECTION ( 'NONE',  ( -0.000000000000000000, 0.9396926207859092051, -0.3420201433256662704 ) ) ;
#77465 = CARTESIAN_POINT ( 'NONE',  ( -10.61538461538461320, -9.780366693483667717, 34.19971097300155094 ) ) ;
#77466 = CARTESIAN_POINT ( 'NONE',  ( -0.4615384615384611200, -12.29105614889573062, 35.45975837776705220 ) ) ;
#77467 = CARTESIAN_POINT ( 'NONE',  ( -17.78205128205128105, -7.500000000000000000, 29.75000000000000355 ) ) ;
#77468 = CARTESIAN_POINT ( 'NONE',  ( -1.553300858899081538, -11.25000000000000711, 16.10937500000000355 ) ) ;
#77469 = EDGE_LOOP ( 'NONE', ( #56685, #9742 ) ) ;
#77470 = ORIENTED_EDGE ( 'NONE', *, *, #30990, .F. ) ;
#77471 = CARTESIAN_POINT ( 'NONE',  ( -6.066082379360133281, -3.937682226553329556, 33.60647404775217240 ) ) ;
#77472 = ORIENTED_EDGE ( 'NONE', *, *, #47490, .T. ) ;
#77473 = CARTESIAN_POINT ( 'NONE',  ( -10.61538461538461320, -12.78798330534102945, 29.74999999999997868 ) ) ;
#77474 = CARTESIAN_POINT ( 'NONE',  ( -1.318548051265308496, -9.905515769479277921, 34.41647553114623292 ) ) ;
#77475 = CARTESIAN_POINT ( 'NONE',  ( 14.08420738312797837, -10.23692288466677880, 34.23039457007281072 ) ) ;
#77476 = CARTESIAN_POINT ( 'NONE',  ( -7.846153846153965716, -5.219633306517616589, 34.19971097300220464 ) ) ;
#77477 = CARTESIAN_POINT ( 'NONE',  ( -3.749999999999997335, -7.500000000000021316, 18.84375000000000000 ) ) ;
#77478 = CARTESIAN_POINT ( 'NONE',  ( 13.38461538461538680, -12.29105614889573062, 35.45975837776705220 ) ) ;
#77479 = ORIENTED_EDGE ( 'NONE', *, *, #82274, .F. ) ;
#77480 = LINE ( 'NONE', #22536, #41524 ) ;
#77482 = ORIENTED_EDGE ( 'NONE', *, *, #59139, .F. ) ;
#77481 = LINE ( 'NONE', #86016, #28096 ) ;
#77483 = CARTESIAN_POINT ( 'NONE',  ( -8.519230769229348965, -7.500000000000154543, 35.00000000000007105 ) ) ;
#77484 = CARTESIAN_POINT ( 'NONE',  ( 17.07692307692295586, -3.835265460704628815, 33.15142922262033665 ) ) ;
#77485 = CARTESIAN_POINT ( 'NONE',  ( -3.480745961711584791, -4.943428324936578910, 34.04746400365624481 ) ) ;
#77486 = DIRECTION ( 'NONE',  ( -0.000000000000000000, 0.1736481776669307198, -0.9848077530122080203 ) ) ;
#77487 = DIRECTION ( 'NONE',  ( 0.000000000000000000, 0.4999999999999985567, 0.8660254037844395958 ) ) ;
#77488 = CARTESIAN_POINT ( 'NONE',  ( -11.47239420511146513, -2.833524468853757305, 32.15551576947925838 ) ) ;
#77489 = CARTESIAN_POINT ( 'NONE',  ( 1.614399933863618797, -3.775308065498751198, 13.23624329374151465 ) ) ;
#77490 = ORIENTED_EDGE ( 'NONE', *, *, #64204, .T. ) ;
#77491 = B_SPLINE_CURVE_WITH_KNOTS ( 'NONE', 3,
 ( #60925, #55496, #88869, #117, #82978, #1004, #41999, #7763, #35226, #41107 ),
 .UNSPECIFIED., .F., .F.,
 ( 4, 2, 2, 2, 4 ),
 ( 0.000000000000000000, 0.0001954311564186862781, 0.0003908623128373725562, 0.0005862934692560588072, 0.0007817246256747451124 ),
 .UNSPECIFIED. ) ;
#77492 = CARTESIAN_POINT ( 'NONE',  ( -15.23076923076922995, -6.343179335718451384, 34.87096338111211935 ) ) ;
#77493 = DIRECTION ( 'NONE',  ( -1.000000000000000000, 0.000000000000000000, 0.000000000000000000 ) ) ;
#77494 = CARTESIAN_POINT ( 'NONE',  ( 1.944543648263018731, -9.444543648262994751, 19.62500000000000000 ) ) ;
#77495 = CARTESIAN_POINT ( 'NONE',  ( -15.90379173393269596, -11.47946981652013498, 33.17500667209846910 ) ) ;
#77496 = DIRECTION ( 'NONE',  ( -0.000000000000000000, -0.3420201433256695456, -0.9396926207859082059 ) ) ;
#77497 = VERTEX_POINT ( 'NONE', #11458 ) ;
#77498 = CARTESIAN_POINT ( 'NONE',  ( -1.139087296526025250, -4.750000000000006217, 14.07812500000000178 ) ) ;
#77499 = CARTESIAN_POINT ( 'NONE',  ( 17.78205128205128105, -7.500000000000000000, 33.75000000000000000 ) ) ;
#77500 = EDGE_CURVE ( 'NONE', #50957, #64220, #44779, .T. ) ;
#77501 = B_SPLINE_CURVE_WITH_KNOTS ( 'NONE', 3,
 ( #46999, #6907, #33507, #62288, #12343, #60523, #33939, #74487, #53316, #75809 ),
 .UNSPECIFIED., .F., .F.,
 ( 4, 2, 2, 2, 4 ),
 ( 0.0007817246256747470640, 0.0009771112852218898515, 0.001172497944769032747, 0.001367884604316175643, 0.001563271263863318539 ),
 .UNSPECIFIED. ) ;
#77502 = ORIENTED_EDGE ( 'NONE', *, *, #28431, .T. ) ;
#77503 = CARTESIAN_POINT ( 'NONE',  ( -0.4615384615384611200, -10.67929555188718282, 33.92786785259544047 ) ) ;
#77504 = EDGE_CURVE ( 'NONE', #36033, #15004, #38489, .T. ) ;
#77505 = ORIENTED_EDGE ( 'NONE', *, *, #84082, .F. ) ;
#77506 = CARTESIAN_POINT ( 'NONE',  ( 18.00000000000000000, -6.386643153685126251, 34.62446782046654192 ) ) ;
#77507 = DIRECTION ( 'NONE',  ( -0.000000000000000000, 0.1736481776669307198, -0.9848077530122080203 ) ) ;
#77508 = CARTESIAN_POINT ( 'NONE',  ( -12.46153846153846168, -9.905515769479276145, 34.41647553114623292 ) ) ;
#77509 = CARTESIAN_POINT ( 'NONE',  ( -5.999999999999998224, -6.343179335718451384, 34.87096338111211935 ) ) ;
#77510 = ORIENTED_EDGE ( 'NONE', *, *, #32084, .F. ) ;
#77511 = EDGE_CURVE ( 'NONE', #26741, #18183, #29982, .T. ) ;
#77512 = CARTESIAN_POINT ( 'NONE',  ( -6.792286482109971324, -6.369690395747422684, 34.87708834333098196 ) ) ;
#77513 = EDGE_LOOP ( 'NONE', ( #49816, #51711, #77407, #8323 ) ) ;
#77514 = VECTOR ( 'NONE', #59246, 1000.000000000000000 ) ;
#77515 = CARTESIAN_POINT ( 'NONE',  ( 12.39626846098214230, -12.16647553114622049, 32.15551576947930812 ) ) ;
#77516 = CARTESIAN_POINT ( 'NONE',  ( 11.53846153846153832, -13.04860791097971706, 34.73218667398347037 ) ) ;
#77517 = ORIENTED_EDGE ( 'NONE', *, *, #58722, .T. ) ;
#77518 = CARTESIAN_POINT ( 'NONE',  ( 8.638540166120458608, -4.684245665217972032, 34.18127051446801090 ) ) ;
#77519 = CARTESIAN_POINT ( 'NONE',  ( 10.86543892702293057, -3.136992222400443175, 32.19305428654138979 ) ) ;
#77520 = CARTESIAN_POINT ( 'NONE',  ( 23.49999999999998579, -1.749999999999999556, 32.75000000000000000 ) ) ;
#77521 = AXIS2_PLACEMENT_3D ( 'NONE', #67574, #54040, #26584 ) ;
#77522 = EDGE_CURVE ( 'NONE', #29486, #79207, #3167, .T. ) ;
#77523 = VECTOR ( 'NONE', #46804, 1000.000000000000114 ) ;
#77524 = FACE_OUTER_BOUND ( 'NONE', #62035, .T. ) ;
#77525 = DIRECTION ( 'NONE',  ( -0.000000000000000000, -0.9848077530122085754, -0.1736481776669273613 ) ) ;
#77526 = ORIENTED_EDGE ( 'NONE', *, *, #1788, .F. ) ;
#77527 = ORIENTED_EDGE ( 'NONE', *, *, #81845, .T. ) ;
#77528 = B_SPLINE_CURVE_WITH_KNOTS ( 'NONE', 3,
 ( #38604, #16113, #10247, #9365, #71936, #11126, #86818, #30508, #51641, #57976 ),
 .UNSPECIFIED., .F., .F.,
 ( 4, 2, 2, 2, 4 ),
 ( 0.000000000000000000, 0.0001954311564186875792, 0.0003908623128373751583, 0.0005862934692560627103, 0.0007817246256747503166 ),
 .UNSPECIFIED. ) ;
#77529 = FACE_BOUND ( 'NONE', #46952, .T. ) ;
#77530 = EDGE_LOOP ( 'NONE', ( #72239, #39304, #47327, #35642, #16384, #926 ) ) ;
#77531 = CARTESIAN_POINT ( 'NONE',  ( 15.00784301325308157, -12.39988816332205701, 30.74660775122750778 ) ) ;
#77532 = B_SPLINE_CURVE_WITH_KNOTS ( 'NONE', 3,
 ( #4014, #31044, #16215, #3129, #51289, #17997, #58511, #17096, #85123, #22966 ),
 .UNSPECIFIED., .F., .F.,
 ( 4, 2, 2, 2, 4 ),
 ( 0.0007817246256747476061, 0.0009771112852218896347, 0.001172497944769031880, 0.001367884604316173909, 0.001563271263863315937 ),
 .UNSPECIFIED. ) ;
#77533 = ADVANCED_FACE ( 'NONE', ( #71812 ), #73162, .F. ) ;
#77534 = DIRECTION ( 'NONE',  ( 0.000000000000000000, -0.000000000000000000, 1.000000000000000000 ) ) ;
#77535 = EDGE_CURVE ( 'NONE', #65895, #29819, #33162, .T. ) ;
#77536 = CARTESIAN_POINT ( 'NONE',  ( 17.86985203026830504, -5.915902021225892149, 34.75552854090298638 ) ) ;
#77537 = CARTESIAN_POINT ( 'NONE',  ( -16.15384615384627409, -2.892918686052165622, 31.69288490824153470 ) ) ;
#77538 = VERTEX_POINT ( 'NONE', #26304 ) ;
#77539 = ORIENTED_EDGE ( 'NONE', *, *, #74618, .F. ) ;
#77540 = EDGE_LOOP ( 'NONE', ( #2828, #85846, #4230, #57250 ) ) ;
#77541 = CARTESIAN_POINT ( 'NONE',  ( 0.3589743589743586982, -4.000000000000000000, 29.75000000000000355 ) ) ;
#77542 = EDGE_CURVE ( 'NONE', #12672, #57246, #88918, .T. ) ;
#77543 = FACE_OUTER_BOUND ( 'NONE', #25188, .T. ) ;
#77544 = AXIS2_PLACEMENT_3D ( 'NONE', #25700, #18945, #73895 ) ;
#77545 = CARTESIAN_POINT ( 'NONE',  ( 14.17754433796061697, -12.15440758774515473, 32.17923288041532004 ) ) ;
#77546 = CARTESIAN_POINT ( 'NONE',  ( -18.00000000000000000, -6.343179335718452272, 34.87096338111211935 ) ) ;
#77547 = EDGE_LOOP ( 'NONE', ( #68794, #62325 ) ) ;
#77548 = CARTESIAN_POINT ( 'NONE',  ( 13.38461538461526601, -10.90142922262034020, 33.41473453929536674 ) ) ;
#77549 = CARTESIAN_POINT ( 'NONE',  ( -15.16551409125639260, -3.643525952247864463, 33.31231777344670064 ) ) ;
#77550 = CARTESIAN_POINT ( 'NONE',  ( 16.15384615384615330, -5.471508081941601098, 34.59228464037088457 ) ) ;
#77551 = CARTESIAN_POINT ( 'NONE',  ( 8.834485908743603844, -6.835583212224610072, 34.95778746994559327 ) ) ;
#77552 = EDGE_LOOP ( 'NONE', ( #71539, #72438, #28444, #83560 ) ) ;
#77553 = ORIENTED_EDGE ( 'NONE', *, *, #86524, .F. ) ;
#77554 = EDGE_CURVE ( 'NONE', #22118, #33835, #35403, .T. ) ;
#77555 = B_SPLINE_CURVE_WITH_KNOTS ( 'NONE', 3,
 ( #1136, #57403, #70035, #22730, #21409, #78122, #84016, #69593, #29069, #56958 ),
 .UNSPECIFIED., .F., .F.,
 ( 4, 2, 2, 2, 4 ),
 ( 0.000000000000000000, 0.0001954339857564064444, 0.0003908679715128128888, 0.0005863019572692193060, 0.0007817359430256257775 ),
 .UNSPECIFIED. ) ;
#77556 = ORIENTED_EDGE ( 'NONE', *, *, #69341, .F. ) ;
#77558 = CARTESIAN_POINT ( 'NONE',  ( -9.627052552794856055, -8.656820664281605460, 34.87096338111211224 ) ) ;
#77557 = CARTESIAN_POINT ( 'NONE',  ( 12.39545505058258179, -6.386643153685125363, 34.62446782046654903 ) ) ;
#77559 = B_SPLINE_CURVE_WITH_KNOTS ( 'NONE', 3,
 ( #63093, #22126, #1850, #17129, #36093, #78830 ),
 .UNSPECIFIED., .F., .F.,
 ( 4, 2, 4 ),
 ( 0.0003909569690057842790, 0.0005862646681846108007, 0.0007815723673634373224 ),
 .UNSPECIFIED. ) ;
#77560 = CARTESIAN_POINT ( 'NONE',  ( 11.47319153790521717, -2.379036618887870436, 30.90682066428147934 ) ) ;
#77561 = CARTESIAN_POINT ( 'NONE',  ( -2.057637887778851926, -2.544122305571458575, 31.48381861865057729 ) ) ;
#77562 = EDGE_CURVE ( 'NONE', #13779, #798, #9544, .T. ) ;
#77563 = FACE_BOUND ( 'NONE', #86678, .T. ) ;
#77564 = CARTESIAN_POINT ( 'NONE',  ( -11.60373153901785948, -2.379036618887870436, 30.90682066428147934 ) ) ;
#77565 = EDGE_CURVE ( 'NONE', #81234, #73790, #75814, .T. ) ;
#77566 = ORIENTED_EDGE ( 'NONE', *, *, #69781, .T. ) ;
#77567 = LINE ( 'NONE', #63154, #63001 ) ;
#77568 = DIRECTION ( 'NONE',  ( -0.000000000000000000, -0.7660444431189791237, -0.6427876096865379196 ) ) ;
#77569 = CARTESIAN_POINT ( 'NONE',  ( 11.78846153846160227, -7.434744429011176159, 34.75000000000000711 ) ) ;
#77570 = CYLINDRICAL_SURFACE ( 'NONE', #43855, 8.000000000000000000 ) ;
#77571 = ORIENTED_EDGE ( 'NONE', *, *, #38932, .T. ) ;
#77572 = EDGE_CURVE ( 'NONE', #6788, #61316, #55840, .T. ) ;
#77573 = CARTESIAN_POINT ( 'NONE',  ( 4.826946332874485712, -12.65889640711025521, 30.72598325615533454 ) ) ;
#77574 = ADVANCED_FACE ( 'NONE', ( #20436 ), #6483, .T. ) ;
#77575 = ORIENTED_EDGE ( 'NONE', *, *, #22949, .F. ) ;
#77576 = FACE_BOUND ( 'NONE', #55348, .T. ) ;
#77577 = CYLINDRICAL_SURFACE ( 'NONE', #70554, 0.2500000000000008882 ) ;
#77578 = VECTOR ( 'NONE', #79076, 1000.000000000000114 ) ;
#77579 = CARTESIAN_POINT ( 'NONE',  ( 16.82689983963011215, -11.86270091957321071, 32.19358267280088626 ) ) ;
#77580 = CARTESIAN_POINT ( 'NONE',  ( 12.46153846153846168, -12.10708131394839349, 31.69288490824020244 ) ) ;
#77581 = VERTEX_POINT ( 'NONE', #5146 ) ;
#77582 = CARTESIAN_POINT ( 'NONE',  ( 0.3962680155776849289, -10.90142922261923886, 33.41473453929638993 ) ) ;
#77583 = CARTESIAN_POINT ( 'NONE',  ( 5.207761494935837732, -7.277220443632450575, 34.74524770363009196 ) ) ;
#77584 = CARTESIAN_POINT ( 'NONE',  ( -9.822999158975251888, -3.062553014421049546, 32.05460306192773601 ) ) ;
#77585 = FACE_OUTER_BOUND ( 'NONE', #22260, .T. ) ;
#77586 = VERTEX_POINT ( 'NONE', #75380 ) ;
#77587 = AXIS2_PLACEMENT_3D ( 'NONE', #20175, #48511, #75124 ) ;
#77588 = CARTESIAN_POINT ( 'NONE',  ( -7.846153846153844924, -2.833524468853757305, 32.15551576947925838 ) ) ;
#77589 = EDGE_LOOP ( 'NONE', ( #78201, #777, #48057, #208 ) ) ;
#77590 = VECTOR ( 'NONE', #5510, 1000.000000000000000 ) ;
#77592 = VERTEX_POINT ( 'NONE', #26745 ) ;
#77591 = FACE_OUTER_BOUND ( 'NONE', #70059, .T. ) ;
#77593 = CARTESIAN_POINT ( 'NONE',  ( 11.66925334628632882, -6.413143153341454017, 34.63066358083362672 ) ) ;
#77594 = CARTESIAN_POINT ( 'NONE',  ( -1.607542343522232242, -12.38737895849757820, 31.66785238281580206 ) ) ;
#77595 = CYLINDRICAL_SURFACE ( 'NONE', #50052, 0.2499999999999998890 ) ;
#77596 = DIRECTION ( 'NONE',  ( 0.000000000000000000, 0.9396926207859126468, -0.3420201433256571111 ) ) ;
#77598 = CARTESIAN_POINT ( 'NONE',  ( 0.2115384615384615363, -7.566083408709834757, 34.74999999999999289 ) ) ;
#77597 = DIRECTION ( 'NONE',  ( -1.000000000000000000, -0.000000000000000000, -0.000000000000000000 ) ) ;
#77599 = CARTESIAN_POINT ( 'NONE',  ( 4.153846153846154188, -5.180354513474913603, 36.12317359536750416 ) ) ;
#77600 = CARTESIAN_POINT ( 'NONE',  ( 2.750000000000001776, -7.499999999999984013, 21.96875000000000355 ) ) ;
#77601 = ORIENTED_EDGE ( 'NONE', *, *, #76838, .F. ) ;
#77602 = FACE_OUTER_BOUND ( 'NONE', #34215, .T. ) ;
#77603 = CARTESIAN_POINT ( 'NONE',  ( 13.25414019953966971, -7.276987145209184327, 34.99546412871779211 ) ) ;
#77604 = ORIENTED_EDGE ( 'NONE', *, *, #4959, .T. ) ;
#77605 = B_SPLINE_CURVE_WITH_KNOTS ( 'NONE', 3,
 ( #52082, #71032, #57516, #23283, #88129, #72799, #39039, #61064, #52968, #46667 ),
 .UNSPECIFIED., .F., .F.,
 ( 4, 2, 2, 2, 4 ),
 ( 0.000000000000000000, 0.0001954311564186879315, 0.0003908623128373758630, 0.0005862934692560637946, 0.0007817246256747517261 ),
 .UNSPECIFIED. ) ;
#77606 = EDGE_LOOP ( 'NONE', ( #80205, #81246, #30777, #67222 ) ) ;
#77607 = ORIENTED_EDGE ( 'NONE', *, *, #10167, .F. ) ;
#77608 = DIRECTION ( 'NONE',  ( -0.000000000000000000, -0.000000000000000000, -1.000000000000000000 ) ) ;
#77609 = CARTESIAN_POINT ( 'NONE',  ( 3.230769230769231726, -9.780366693483667717, 34.19971097300155094 ) ) ;
#77610 = DIRECTION ( 'NONE',  ( 1.000000000000000000, 0.000000000000000000, 0.000000000000000000 ) ) ;
#77611 = CARTESIAN_POINT ( 'NONE',  ( -5.011667505647053211, -3.835265460703683349, 33.15142922261929925 ) ) ;
#77612 = CARTESIAN_POINT ( 'NONE',  ( 12.21156173059610595, -10.66389620160130036, 33.62221079203477103 ) ) ;
#77613 = CARTESIAN_POINT ( 'NONE',  ( -8.834500769787089425, -3.083524468853724443, 32.58852847137143272 ) ) ;
#77614 = PLANE ( 'NONE',  #81062 ) ;
#77615 = B_SPLINE_CURVE_WITH_KNOTS ( 'NONE', 3,
 ( #41357, #83233, #69708, #7573, #56639, #84131, #83688, #15659, #48098, #43130 ),
 .UNSPECIFIED., .F., .F.,
 ( 4, 2, 2, 2, 4 ),
 ( 0.000000000000000000, 0.0001954311564186879044, 0.0003908623128373758088, 0.0005862934692560636861, 0.0007817246256747516176 ),
 .UNSPECIFIED. ) ;
#77616 = CARTESIAN_POINT ( 'NONE',  ( -3.931066612577743147, -5.913360116392399668, 34.49180327182771322 ) ) ;
#77617 = CARTESIAN_POINT ( 'NONE',  ( -17.20761454359064047, -12.11776431015576172, 31.66791131148498906 ) ) ;
#77618 = CARTESIAN_POINT ( 'NONE',  ( 12.39545505058257824, -11.69971097300155272, 32.46337939537587403 ) ) ;
#77619 = VECTOR ( 'NONE', #82800, 1000.000000000000000 ) ;
#77620 = CARTESIAN_POINT ( 'NONE',  ( 7.596177102105253987, -2.318417181685854533, 30.59732222474233865 ) ) ;
#77621 = ORIENTED_EDGE ( 'NONE', *, *, #28763, .T. ) ;
#77622 = CARTESIAN_POINT ( 'NONE',  ( 15.16468581981335184, -11.16473453929635440, 33.15142922261925662 ) ) ;
#77623 =( NAMED_UNIT ( * ) SI_UNIT ( $, .STERADIAN. ) SOLID_ANGLE_UNIT ( ) );
#77624 = CARTESIAN_POINT ( 'NONE',  ( 11.60452988946397923, -9.780366693483667717, 34.19971097300155805 ) ) ;
#77625 = FACE_OUTER_BOUND ( 'NONE', #39781, .T. ) ;
#77626 = VERTEX_POINT ( 'NONE', #81701 ) ;
#77627 = CARTESIAN_POINT ( 'NONE',  ( 9.942253101685738059, -11.56426240980093745, 33.07394671870546432 ) ) ;
#77628 = B_SPLINE_CURVE_WITH_KNOTS ( 'NONE', 3,
 ( #57059, #84988, #50729, #43544, #78215, #85869, #16517, #16965, #44413, #43983 ),
 .UNSPECIFIED., .F., .F.,
 ( 4, 2, 2, 2, 4 ),
 ( 0.0007817246256747493408, 0.0009771112852218920199, 0.001172497944769034699, 0.001367884604316177378, 0.001563271263863320057 ),
 .UNSPECIFIED. ) ;
#77629 = CARTESIAN_POINT ( 'NONE',  ( 9.561617089197383734, -2.845849958028613624, 32.17971566917920967 ) ) ;
#77630 = DIRECTION ( 'NONE',  ( -0.000000000000000000, 1.000000000000000000, 3.491481338843133355E-15 ) ) ;
#77631 = ORIENTED_EDGE ( 'NONE', *, *, #11838, .T. ) ;
#77632 = CARTESIAN_POINT ( 'NONE',  ( -10.86538461538461320, -2.499999999999998668, 29.75000000000000355 ) ) ;
#77633 = ORIENTED_EDGE ( 'NONE', *, *, #89047, .F. ) ;
#77634 = CARTESIAN_POINT ( 'NONE',  ( 16.21991348719623360, -9.058645607665452459, 34.76329471203371924 ) ) ;
#77635 = EDGE_CURVE ( 'NONE', #14097, #1750, #41784, .T. ) ;
#77636 = AXIS2_PLACEMENT_3D ( 'NONE', #29190, #811, #47670 ) ;
#77637 = CYLINDRICAL_SURFACE ( 'NONE', #87353, 0.2499999999999986955 ) ;
#77638 = CARTESIAN_POINT ( 'NONE',  ( -8.096130590202433197, -2.544273027872575366, 31.48422191005632342 ) ) ;
#77639 = CARTESIAN_POINT ( 'NONE',  ( 1.318533005255250856, -8.164416787775445883, 34.95778746994557906 ) ) ;
#77640 = CARTESIAN_POINT ( 'NONE',  ( 18.22301284409340028, -8.282913670948747864, 34.94150082978203642 ) ) ;
#77641 = VECTOR ( 'NONE', #34895, 1000.000000000000227 ) ;
#77642 = EDGE_LOOP ( 'NONE', ( #18230, #31560 ) ) ;
#77643 = PRESENTATION_LAYER_ASSIGNMENT (  '', '', ( #27318 ) ) ;
#77644 = ORIENTED_EDGE ( 'NONE', *, *, #22904, .F. ) ;
#77645 = EDGE_LOOP ( 'NONE', ( #74464, #70104 ) ) ;
#77646 = EDGE_CURVE ( 'NONE', #54695, #18976, #13852, .T. ) ;
#77647 = CARTESIAN_POINT ( 'NONE',  ( 6.923076923076924238, -10.05456864172156806, 36.03766855953608683 ) ) ;
#77648 = CARTESIAN_POINT ( 'NONE',  ( -17.01166750564705410, -3.835265460703683349, 33.15142922261929925 ) ) ;
#77649 = CARTESIAN_POINT ( 'NONE',  ( -4.403822897894743349, -12.41104346484419452, 31.60698883733904196 ) ) ;
#77650 = DIRECTION ( 'NONE',  ( -0.000000000000000000, -0.000000000000000000, 1.000000000000000000 ) ) ;
#77651 = CARTESIAN_POINT ( 'NONE',  ( -7.715628407920200438, -4.299079248970732792, 33.91157788607253565 ) ) ;
#77652 = CARTESIAN_POINT ( 'NONE',  ( 5.142178648199099200, -10.21337939537593620, 33.94971097300152252 ) ) ;
#77653 = VERTEX_POINT ( 'NONE', #60528 ) ;
#77654 = ORIENTED_EDGE ( 'NONE', *, *, #21337, .F. ) ;
#77655 = ORIENTED_EDGE ( 'NONE', *, *, #32021, .F. ) ;
#77657 = ORIENTED_EDGE ( 'NONE', *, *, #82442, .F. ) ;
#77656 = CARTESIAN_POINT ( 'NONE',  ( 4.403791563224197070, -4.176053281294514363, 33.81426240980091791 ) ) ;
#77659 = CARTESIAN_POINT ( 'NONE',  ( 14.37375964104238513, -4.661471528628508665, 34.16647553114624003 ) ) ;
#77658 = CARTESIAN_POINT ( 'NONE',  ( 0.5923302693632471749, -8.147973898785416225, 34.70805048591653730 ) ) ;
#77660 = EDGE_CURVE ( 'NONE', #79299, #13992, #53771, .T. ) ;
#77661 = CARTESIAN_POINT ( 'NONE',  ( -2.651650429449535551, -10.15165042944956753, 26.18750000000000355 ) ) ;
#77662 = ADVANCED_FACE ( 'NONE', ( #6043 ), #42046, .F. ) ;
#77663 = VERTEX_POINT ( 'NONE', #36608 ) ;
#77664 = VECTOR ( 'NONE', #79704, 1000.000000000000114 ) ;
#77665 = ORIENTED_EDGE ( 'NONE', *, *, #5164, .T. ) ;
#77666 = CARTESIAN_POINT ( 'NONE',  ( -17.77722033102192967, -3.020022701398814124, 32.48759521482552515 ) ) ;
#77667 = VERTEX_POINT ( 'NONE', #48785 ) ;
#77668 = FACE_BOUND ( 'NONE', #32453, .T. ) ;
#77669 = CARTESIAN_POINT ( 'NONE',  ( -6.250023237292964495, -9.271318131107980420, 34.42618302367067429 ) ) ;
#77670 = EDGE_CURVE ( 'NONE', #7880, #77757, #15902, .T. ) ;
#77671 = DIRECTION ( 'NONE',  ( 0.000000000000000000, 0.000000000000000000, -1.000000000000000000 ) ) ;
#77672 = ORIENTED_EDGE ( 'NONE', *, *, #30110, .T. ) ;
#77673 = CARTESIAN_POINT ( 'NONE',  ( -15.16551365949320562, -5.219633306516380244, 34.19971097300157936 ) ) ;
#77674 = CARTESIAN_POINT ( 'NONE',  ( 1.384615384615386802, -2.249999999999998668, 29.75000000000001776 ) ) ;
#77675 = CARTESIAN_POINT ( 'NONE',  ( -4.153846153846152411, -12.09954503811598769, 35.62045528018868623 ) ) ;
#77676 = ADVANCED_FACE ( 'NONE', ( #50550 ), #21759, .F. ) ;
#77677 = CARTESIAN_POINT ( 'NONE',  ( -11.78843826940389050, -5.728515186090277211, 34.42611988154120439 ) ) ;
#77678 = CARTESIAN_POINT ( 'NONE',  ( -13.38461538461538325, -11.69971097300155272, 32.46337939537588113 ) ) ;
#77679 = CARTESIAN_POINT ( 'NONE',  ( 6.923076923076800782, -2.657715359629662988, 31.77849191805970364 ) ) ;
#77680 = CARTESIAN_POINT ( 'NONE',  ( -7.846153846153844924, -6.386643153685126251, 34.62446782046654192 ) ) ;
#77681 = CARTESIAN_POINT ( 'NONE',  ( -6.066083410955878108, -5.557115091759785130, 34.35708131394839171 ) ) ;
#77682 = CARTESIAN_POINT ( 'NONE',  ( 0.000000000000000000, -11.50000000000000000, 29.25000000000000000 ) ) ;
#77683 = CYLINDRICAL_SURFACE ( 'NONE', #34415, 0.2499999999999995559 ) ;
#77684 = FACE_BOUND ( 'NONE', #1558, .T. ) ;
#77686 = CARTESIAN_POINT ( 'NONE',  ( 6.989145274079362480, -3.050289026998446840, 32.03036669348366416 ) ) ;
#77685 = CARTESIAN_POINT ( 'NONE',  ( 17.14217864819909920, -3.835265460703683349, 33.15142922261929925 ) ) ;
#77687 = B_SPLINE_CURVE_WITH_KNOTS ( 'NONE', 3,
 ( #32364, #79218, #59385, #52621, #80104, #39130, #39582, #46316, #44968, #38224 ),
 .UNSPECIFIED., .F., .F.,
 ( 4, 2, 2, 2, 4 ),
 ( 0.000000000000000000, 0.0001954311564186865221, 0.0003908623128373730441, 0.0005862934692560595662, 0.0007817246256747460882 ),
 .UNSPECIFIED. ) ;
#77688 = AXIS2_PLACEMENT_3D ( 'NONE', #84555, #43111, #22393 ) ;
#77689 = FACE_OUTER_BOUND ( 'NONE', #15445, .T. ) ;
#77691 = CARTESIAN_POINT ( 'NONE',  ( 6.000000000000001776, -10.51840700105979565, 33.73612834413961536 ) ) ;
#77690 = DIRECTION ( 'NONE',  ( 0.7071067811865510144, -0.7071067811865441310, 0.000000000000000000 ) ) ;
#77692 = FACE_OUTER_BOUND ( 'NONE', #32124, .T. ) ;
#77693 = B_SPLINE_CURVE_WITH_KNOTS ( 'NONE', 3,
 ( #28370, #36030, #9432, #55843, #42787, #84665, #77446, #63483, #57173, #83330 ),
 .UNSPECIFIED., .F., .F.,
 ( 4, 2, 2, 2, 4 ),
 ( 0.000000000000000000, 0.0001954311564186867389, 0.0003908623128373734778, 0.0005862934692560602167, 0.0007817246256747469556 ),
 .UNSPECIFIED. ) ;
#77694 = CARTESIAN_POINT ( 'NONE',  ( -0.06109907496454585613, -4.750000000000000000, 22.65438170625849068 ) ) ;
#77695 = VERTEX_POINT ( 'NONE', #16335 ) ;
#77696 = B_SPLINE_CURVE_WITH_KNOTS ( 'NONE', 3,
 ( #14348, #37608, #83713, #69302, #65071, #10593, #58319, #51541, #836, #8042 ),
 .UNSPECIFIED., .F., .F.,
 ( 4, 2, 2, 2, 4 ),
 ( 0.000000000000000000, 0.0001954311564186876876, 0.0003908623128373753751, 0.0005862934692560630356, 0.0007817246256747507503 ),
 .UNSPECIFIED. ) ;
#77697 = CARTESIAN_POINT ( 'NONE',  ( 3.105451396330338287, -7.707150910725261816, 14.00000000000000000 ) ) ;
#77698 = ORIENTED_EDGE ( 'NONE', *, *, #52203, .T. ) ;
#77699 = AXIS2_PLACEMENT_3D ( 'NONE', #65072, #50670, #63750 ) ;
#77700 = VECTOR ( 'NONE', #46102, 1000.000000000000114 ) ;
#77701 = CARTESIAN_POINT ( 'NONE',  ( -9.019230769230768274, -2.499999999999998668, 29.75000000000000355 ) ) ;
#77702 = ORIENTED_EDGE ( 'NONE', *, *, #86764, .F. ) ;
#77703 = CARTESIAN_POINT ( 'NONE',  ( -3.903900635498010807, -11.37275283266503756, 32.91324779482534524 ) ) ;
#77704 = VERTEX_POINT ( 'NONE', #56437 ) ;
#77705 = CARTESIAN_POINT ( 'NONE',  ( 5.750023255951410839, -10.82459398097509684, 33.81372124010185587 ) ) ;
#77706 = CARTESIAN_POINT ( 'NONE',  ( -1.200186371490556958, -4.775308065498765409, 23.82625670625849068 ) ) ;
#77707 = CARTESIAN_POINT ( 'NONE',  ( -17.74994558008654622, -9.233818618650598609, 34.70587769442853698 ) ) ;
#77708 = AXIS2_PLACEMENT_3D ( 'NONE', #18018, #31066, #77932 ) ;
#77709 = CARTESIAN_POINT ( 'NONE',  ( -5.750054481651858396, -9.272278438253401589, 34.42582936511637826 ) ) ;
#77710 = CARTESIAN_POINT ( 'NONE',  ( 7.053602624840488389, -9.417988943895561960, 34.36773134775778260 ) ) ;
#77711 = LINE ( 'NONE', #16018, #46078 ) ;
#77712 = PLANE ( 'NONE',  #51577 ) ;
#77713 = CARTESIAN_POINT ( 'NONE',  ( 4.853996859406927378, -8.239355502252617924, 34.69524867566427417 ) ) ;
#77714 = PRESENTATION_LAYER_ASSIGNMENT (  '', '', ( #31686 ) ) ;
#77715 = CARTESIAN_POINT ( 'NONE',  ( 2.651650429449539104, -4.848349570550432475, 15.56250000000000000 ) ) ;
#77716 = CARTESIAN_POINT ( 'NONE',  ( 1.161689167099239306, -2.758268499246656624, 31.33685645148948140 ) ) ;
#77717 = CARTESIAN_POINT ( 'NONE',  ( 14.43848411551709177, -10.54018710029568595, 33.71981072465678864 ) ) ;
#77718 = CARTESIAN_POINT ( 'NONE',  ( -2.373775718648186928, -4.098570777380720287, 33.41473453929634729 ) ) ;
#77719 = CARTESIAN_POINT ( 'NONE',  ( -1.553300858899125059, -3.750000000000009326, 16.57812500000000000 ) ) ;
#77720 = FACE_OUTER_BOUND ( 'NONE', #48852, .T. ) ;
#77721 = ORIENTED_EDGE ( 'NONE', *, *, #20498, .F. ) ;
#77722 = DIRECTION ( 'NONE',  ( -0.000000000000000000, 1.000000000000000000, 3.491481338843133355E-15 ) ) ;
#77723 = DIRECTION ( 'NONE',  ( 0.000000000000000000, 0.9396926207859126468, 0.3420201433256571111 ) ) ;
#77724 = CARTESIAN_POINT ( 'NONE',  ( 9.692307692307695177, -6.386643153685126251, 34.62446782046654192 ) ) ;
#77725 = CARTESIAN_POINT ( 'NONE',  ( 16.28389358909660345, -7.723484941389743952, 34.99544897038808955 ) ) ;
#77726 = DIRECTION ( 'NONE',  ( -0.000000000000000000, 0.6427876096865404731, -0.7660444431189771253 ) ) ;
#77727 = EDGE_CURVE ( 'NONE', #38500, #27545, #78292, .T. ) ;
#77728 = LINE ( 'NONE', #72303, #48618 ) ;
#77729 = B_SPLINE_CURVE_WITH_KNOTS ( 'NONE', 3,
 ( #34112, #13840, #40448, #1209, #69233, #61579, #81872, #61134, #7535, #7976 ),
 .UNSPECIFIED., .F., .F.,
 ( 4, 2, 2, 2, 4 ),
 ( 0.000000000000000000, 0.0001954311564186862781, 0.0003908623128373725562, 0.0005862934692560588072, 0.0007817246256747451124 ),
 .UNSPECIFIED. ) ;
#77730 = DIRECTION ( 'NONE',  ( -0.000000000000000000, -0.5000000000000009992, -0.8660254037844380415 ) ) ;
#77731 = B_SPLINE_CURVE_WITH_KNOTS ( 'NONE', 3,
 ( #53889, #33623, #81375, #12900, #88593, #81818 ),
 .UNSPECIFIED., .F., .F.,
 ( 4, 2, 4 ),
 ( 0.000000000000000000, 0.0001954784845028888327, 0.0003909569690057776653 ),
 .UNSPECIFIED. ) ;
#77732 = EDGE_LOOP ( 'NONE', ( #24232, #56056, #48965, #22215 ) ) ;
#77733 = ORIENTED_EDGE ( 'NONE', *, *, #75722, .T. ) ;
#77734 = VECTOR ( 'NONE', #86822, 1000.000000000000000 ) ;
#77735 = ORIENTED_EDGE ( 'NONE', *, *, #50814, .T. ) ;
#77736 = EDGE_CURVE ( 'NONE', #48033, #70194, #51475, .T. ) ;
#77737 = CARTESIAN_POINT ( 'NONE',  ( -6.000000000000121680, -12.70778746994576025, 30.41441678777401236 ) ) ;
#77738 = CARTESIAN_POINT ( 'NONE',  ( -3.930834802233304170, -3.105924265160262543, 32.13625925475356127 ) ) ;
#77739 = DIRECTION ( 'NONE',  ( -0.000000000000000000, -0.9396926207859092051, -0.3420201433256662704 ) ) ;
#77740 = EDGE_CURVE ( 'NONE', #45665, #20258, #44945, .T. ) ;
#77741 = CARTESIAN_POINT ( 'NONE',  ( -13.13456107297706588, -9.148310452688876993, 34.47095581063188519 ) ) ;
#77742 = FACE_OUTER_BOUND ( 'NONE', #53359, .T. ) ;
#77743 = EDGE_LOOP ( 'NONE', ( #39861, #13681 ) ) ;
#77744 = CARTESIAN_POINT ( 'NONE',  ( -17.32694631421604115, -4.335965774309648246, 33.62209801155881905 ) ) ;
#77745 = ORIENTED_EDGE ( 'NONE', *, *, #14784, .F. ) ;
#77746 = ORIENTED_EDGE ( 'NONE', *, *, #63582, .F. ) ;
#77747 = CIRCLE ( 'NONE', #46140, 4.000000000000000000 ) ;
#77748 = EDGE_CURVE ( 'NONE', #12325, #56029, #84814, .T. ) ;
#77749 = CARTESIAN_POINT ( 'NONE',  ( 8.769230769230768274, -12.34228464037088635, 31.77849191805839268 ) ) ;
#77750 = CARTESIAN_POINT ( 'NONE',  ( 8.519207531937800226, -2.823816976329317274, 31.52131813110795733 ) ) ;
#77751 = CARTESIAN_POINT ( 'NONE',  ( -1.326923076923076872, -7.500000000000000000, 29.75000000000000355 ) ) ;
#77752 = AXIS2_PLACEMENT_3D ( 'NONE', #75546, #28700, #29587 ) ;
#77753 = AXIS2_PLACEMENT_3D ( 'NONE', #1348, #49091, #28837 ) ;
#77754 = EDGE_CURVE ( 'NONE', #4010, #55482, #7808, .T. ) ;
#77755 = CARTESIAN_POINT ( 'NONE',  ( 0.4615384615383382183, -11.67786785259630911, 32.92929555188603530 ) ) ;
#77756 = DIRECTION ( 'NONE',  ( -1.000000000000000000, -0.000000000000000000, -0.000000000000000000 ) ) ;
#77757 = VERTEX_POINT ( 'NONE', #22640 ) ;
#77758 = ORIENTED_EDGE ( 'NONE', *, *, #88278, .T. ) ;
#77759 = CARTESIAN_POINT ( 'NONE',  ( 2.320192649118979489E-14, -11.25000000000000000, 19.78125000000000000 ) ) ;
#77760 = VERTEX_POINT ( 'NONE', #15012 ) ;
#77762 = EDGE_LOOP ( 'NONE', ( #29375, #21013, #25723, #43720 ) ) ;
#77761 = CARTESIAN_POINT ( 'NONE',  ( 1.134592147322421418, -8.432397168068783699, 34.66272746175022945 ) ) ;
#77763 = CARTESIAN_POINT ( 'NONE',  ( -24.00000000000000000, 9.000000000000024869, 29.25000000000000000 ) ) ;
#77764 = CARTESIAN_POINT ( 'NONE',  ( 6.065255571276025215, -12.46129190930001052, 30.37095296980870174 ) ) ;
#77765 = CARTESIAN_POINT ( 'NONE',  ( 2.438217745925954194, -9.503571793651733657, 34.60286762892837942 ) ) ;
#77766 = ADVANCED_FACE ( 'NONE', ( #35732 ), #63630, .F. ) ;
#77767 = ORIENTED_EDGE ( 'NONE', *, *, #50429, .T. ) ;
#77768 = EDGE_CURVE ( 'NONE', #83601, #83807, #1496, .T. ) ;
#77769 = CARTESIAN_POINT ( 'NONE',  ( 15.23076923076923173, -10.51840700105979565, 33.73612834413961536 ) ) ;
#77770 = CARTESIAN_POINT ( 'NONE',  ( 14.30769230769231015, -2.292212530054420494, 30.41441678777542634 ) ) ;
#77771 = EDGE_LOOP ( 'NONE', ( #12401, #43936, #54485, #31189, #29339 ) ) ;
#77772 = FACE_BOUND ( 'NONE', #73527, .T. ) ;
#77773 = CARTESIAN_POINT ( 'NONE',  ( -11.60373153901786125, -11.67786785259540849, 32.92929555188721480 ) ) ;
#77774 = CARTESIAN_POINT ( 'NONE',  ( -2.294871794871794712, -3.499999999999999556, 29.75000000000000355 ) ) ;
#77775 = CARTESIAN_POINT ( 'NONE',  ( 2.057669083470850424, -12.45566812827425096, 31.48439005359158926 ) ) ;
#77777 = FACE_OUTER_BOUND ( 'NONE', #63118, .T. ) ;
#77776 = CARTESIAN_POINT ( 'NONE',  ( -0.3310130233048187987, -11.66157788607254275, 32.95092075102925833 ) ) ;
#77778 = ADVANCED_FACE ( 'NONE', ( #50107 ), #77595, .F. ) ;
#77779 = CARTESIAN_POINT ( 'NONE',  ( -0.4615384615385840772, -12.51329471203414379, 31.30864560766407578 ) ) ;
#77780 = CARTESIAN_POINT ( 'NONE',  ( -4.403869378067610363, -10.92453946501458439, 33.72985991061850086 ) ) ;
#77781 = ORIENTED_EDGE ( 'NONE', *, *, #14015, .T. ) ;
#77782 = ADVANCED_FACE ( 'NONE', ( #86584 ), #66290, .F. ) ;
#77783 = DIRECTION ( 'NONE',  ( -0.000000000000000000, -0.1736481776669307198, -0.9848077530122080203 ) ) ;
#77784 = ORIENTED_EDGE ( 'NONE', *, *, #10359, .F. ) ;
#77785 = CARTESIAN_POINT ( 'NONE',  ( 7.173022441425066731, -2.824170634883622188, 31.52227843825338738 ) ) ;
#77786 = VECTOR ( 'NONE', #78276, 1000.000000000000114 ) ;
#77787 = CARTESIAN_POINT ( 'NONE',  ( -19.50000000000000000, -11.00000000000000000, 29.25000000000000000 ) ) ;
#77788 = CARTESIAN_POINT ( 'NONE',  ( -15.90379184220783948, -10.66356715214248574, 33.62249196103329751 ) ) ;
#77789 = CARTESIAN_POINT ( 'NONE',  ( -5.142193522883853340, -11.94971097300153140, 32.03036669348370680 ) ) ;
#77790 = CARTESIAN_POINT ( 'NONE',  ( -10.48459417441766561, -2.845873456487965747, 32.17976146951972538 ) ) ;
#77791 = CARTESIAN_POINT ( 'NONE',  ( -8.899377978668987055, -6.001485441113819874, 34.52039167877662607 ) ) ;
#77792 = FACE_BOUND ( 'NONE', #82061, .T. ) ;
#77794 = CARTESIAN_POINT ( 'NONE',  ( 1.384615384615265343, -2.625532179533778709, 30.86335684631627174 ) ) ;
#77793 = DIRECTION ( 'NONE',  ( -0.000000000000000000, -0.7660444431189791237, -0.6427876096865379196 ) ) ;
#77795 = CARTESIAN_POINT ( 'NONE',  ( -18.00000000000012079, -8.656820664282943056, 34.87096338111179961 ) ) ;
#77797 = FACE_OUTER_BOUND ( 'NONE', #16502, .T. ) ;
#77796 = CARTESIAN_POINT ( 'NONE',  ( -7.623374177175779032, -12.69155399931963046, 30.53255429739157734 ) ) ;
#77798 = CIRCLE ( 'NONE', #57679, 0.2500000000000002220 ) ;
#77799 = CARTESIAN_POINT ( 'NONE',  ( 4.153846153846032507, -11.94971097300221174, 32.03036669348237098 ) ) ;
#77800 = CARTESIAN_POINT ( 'NONE',  ( -1.492201783934549164, -11.27530806549876807, 18.35750670625849068 ) ) ;
#77801 = ORIENTED_EDGE ( 'NONE', *, *, #64760, .T. ) ;
#77802 = CARTESIAN_POINT ( 'NONE',  ( -4.284537620513710010, -11.71456829005830080, 32.44064028649416542 ) ) ;
#77803 = CARTESIAN_POINT ( 'NONE',  ( -5.010854725920637520, -3.050289026998446840, 32.03036669348366416 ) ) ;
#77804 = CARTESIAN_POINT ( 'NONE',  ( -7.596153846153843148, -2.499999999999999112, 29.81604066197450109 ) ) ;
#77805 = CARTESIAN_POINT ( 'NONE',  ( -8.769230769230892619, -8.656820664282941280, 34.87096338111179961 ) ) ;
#77806 = CARTESIAN_POINT ( 'NONE',  ( 10.74617642320940369, -12.11778462344221019, 31.66786338562085135 ) ) ;
#77807 = CARTESIAN_POINT ( 'NONE',  ( 3.775308065498768517, -8.992201783934554271, 21.79500670625849068 ) ) ;
#77808 = CARTESIAN_POINT ( 'NONE',  ( -15.36091720050093024, -12.70455904226513866, 30.44083106164009322 ) ) ;
#77809 = CARTESIAN_POINT ( 'NONE',  ( 18.13079180782478161, -3.062576670634119758, 32.05464942895959979 ) ) ;
#77810 = CARTESIAN_POINT ( 'NONE',  ( -7.976301815885546098, -3.069018819979302926, 32.56621877034667278 ) ) ;
#77811 = CARTESIAN_POINT ( 'NONE',  ( 0.4615384615384611200, -2.833524468853757305, 32.15551576947925838 ) ) ;
#77812 = CARTESIAN_POINT ( 'NONE',  ( -16.94613263595612906, -4.684288915650984819, 34.18129842949671371 ) ) ;
#77813 = CARTESIAN_POINT ( 'NONE',  ( 12.23805353697412812, -12.69144148231606017, 30.53333754910549303 ) ) ;
#77814 = EDGE_CURVE ( 'NONE', #53071, #14607, #21357, .T. ) ;
#77815 = CARTESIAN_POINT ( 'NONE',  ( 5.076923076923075762, -5.180354513474913603, 36.12317359536750416 ) ) ;
#77816 = AXIS2_PLACEMENT_3D ( 'NONE', #77925, #78361, #51762 ) ;
#77817 = CARTESIAN_POINT ( 'NONE',  ( 17.14217821643591932, -2.657715359629131857, 31.77849191805844242 ) ) ;
#77818 = ORIENTED_EDGE ( 'NONE', *, *, #55318, .F. ) ;
#77819 = DIRECTION ( 'NONE',  ( 0.000000000000000000, 0.8660254037844377084, -0.5000000000000015543 ) ) ;
#77820 = CARTESIAN_POINT ( 'NONE',  ( -17.32694631421604115, -2.823816976329320827, 31.52131813110797154 ) ) ;
#77821 = CARTESIAN_POINT ( 'NONE',  ( -3.749999999999997780, -7.438900925035489387, 14.09561829374151642 ) ) ;
#77822 = AXIS2_PLACEMENT_3D ( 'NONE', #29275, #56732, #84226 ) ;
#77823 = VECTOR ( 'NONE', #41022, 1000.000000000000114 ) ;
#77824 = CARTESIAN_POINT ( 'NONE',  ( 5.076923076922953193, -2.379036618888197729, 30.90682066428292885 ) ) ;
#77825 = DIRECTION ( 'NONE',  ( -0.000000000000000000, -0.5000000000000009992, -0.8660254037844380415 ) ) ;
#77826 = ORIENTED_EDGE ( 'NONE', *, *, #75012, .T. ) ;
#77827 = DIRECTION ( 'NONE',  ( -0.000000000000000000, -0.000000000000000000, -1.000000000000000000 ) ) ;
#77829 = EDGE_LOOP ( 'NONE', ( #85560, #80463 ) ) ;
#77828 = CARTESIAN_POINT ( 'NONE',  ( -7.846153846153844924, -12.78798330534102945, 29.74999999999997868 ) ) ;
#77830 = CARTESIAN_POINT ( 'NONE',  ( 11.60371667797437567, -5.094484230520773593, 34.41647553114626845 ) ) ;
#77831 = CARTESIAN_POINT ( 'NONE',  ( 4.087762742890272527, -8.120952969808774569, 34.71129190930000163 ) ) ;
#77832 = ADVANCED_FACE ( 'NONE', ( #2801 ), #16767, .F. ) ;
#77833 = ORIENTED_EDGE ( 'NONE', *, *, #83071, .F. ) ;
#77834 = CARTESIAN_POINT ( 'NONE',  ( -5.142193522883852452, -11.48612834413959582, 32.76840700105983473 ) ) ;
#77835 = VECTOR ( 'NONE', #42699, 1000.000000000000000 ) ;
#77836 = EDGE_CURVE ( 'NONE', #69004, #79311, #71261, .T. ) ;
#77837 = CARTESIAN_POINT ( 'NONE',  ( 9.019176287578908102, -5.057305518903948638, 34.11320923018887896 ) ) ;
#77838 = ORIENTED_EDGE ( 'NONE', *, *, #13519, .T. ) ;
#77839 = CARTESIAN_POINT ( 'NONE',  ( 9.019285189144222059, -2.318338780012835443, 30.59689888758630261 ) ) ;
#77840 = CARTESIAN_POINT ( 'NONE',  ( -11.78846153846153832, -2.249999999999998668, 29.75000000000000355 ) ) ;
#77841 = PLANE ( 'NONE',  #29800 ) ;
#77842 = ORIENTED_EDGE ( 'NONE', *, *, #50937, .F. ) ;
#77843 = EDGE_LOOP ( 'NONE', ( #23199, #40558 ) ) ;
#77844 = B_SPLINE_CURVE_WITH_KNOTS ( 'NONE', 3,
 ( #33948, #8262, #35734, #69066, #63632, #164 ),
 .UNSPECIFIED., .F., .F.,
 ( 4, 2, 4 ),
 ( 0.0003909512603273815096, 0.0005862562993132049236, 0.0007815613382990282835 ),
 .UNSPECIFIED. ) ;
#77845 = ORIENTED_EDGE ( 'NONE', *, *, #69309, .F. ) ;
#77846 = EDGE_CURVE ( 'NONE', #18112, #70194, #64948, .T. ) ;
#77847 = CARTESIAN_POINT ( 'NONE',  ( -7.173076923076921574, -7.500000000000001776, 35.00000000000000000 ) ) ;
#77848 = CARTESIAN_POINT ( 'NONE',  ( -5.776987155906605942, -5.582272713120727481, 34.63742843783360570 ) ) ;
#77849 = ADVANCED_FACE ( 'NONE', ( #72601 ), #45574, .F. ) ;
#77850 = CARTESIAN_POINT ( 'NONE',  ( -3.007989561791164501, -8.540255544307065350, 34.89611431652622286 ) ) ;
#77851 = CARTESIAN_POINT ( 'NONE',  ( 14.05769230769230838, -7.500000000000001776, 34.75000000000000000 ) ) ;
#77852 = B_SPLINE_CURVE_WITH_KNOTS ( 'NONE', 3,
 ( #67315, #88063, #19127, #65967, #26325, #11482, #53791, #79939, #66423, #81280 ),
 .UNSPECIFIED., .F., .F.,
 ( 4, 2, 2, 2, 4 ),
 ( 0.0007817246256747459798, 0.0009771112852218896347, 0.001172497944769033398, 0.001367884604316177161, 0.001563271263863320708 ),
 .UNSPECIFIED. ) ;
#77853 = VECTOR ( 'NONE', #27901, 1000.000000000000114 ) ;
#77854 = ORIENTED_EDGE ( 'NONE', *, *, #76196, .F. ) ;
#77855 = B_SPLINE_CURVE_WITH_KNOTS ( 'NONE', 3,
 ( #85050, #23327, #10272, #58434, #85930, #29660, #44038, #36417, #2607, #57120 ),
 .UNSPECIFIED., .F., .F.,
 ( 4, 2, 2, 2, 4 ),
 ( 0.0007817359430256360774, 0.0009771253907250041296, 0.001172514838424371965, 0.001367904286123740017, 0.001563293733823108069 ),
 .UNSPECIFIED. ) ;
#77857 = VERTEX_POINT ( 'NONE', #30292 ) ;
#77856 = EDGE_CURVE ( 'NONE', #44707, #64904, #70316, .T. ) ;
#77859 = ORIENTED_EDGE ( 'NONE', *, *, #28412, .F. ) ;
#77858 = CARTESIAN_POINT ( 'NONE',  ( 4.376858997939548246, -8.282913670948747864, 34.94150082978203642 ) ) ;
#77860 = B_SPLINE_CURVE_WITH_KNOTS ( 'NONE', 3,
 ( #54388, #80995, #39573, #88653, #67030, #32796, #60705, #19284, #54836, #4890 ),
 .UNSPECIFIED., .F., .F.,
 ( 4, 2, 2, 2, 4 ),
 ( 0.0007817246256747451124, 0.0009771112852218885505, 0.001172497944769032097, 0.001367884604316175427, 0.001563271263863318973 ),
 .UNSPECIFIED. ) ;
#77861 = CARTESIAN_POINT ( 'NONE',  ( 16.40390057375960708, -8.346898887586322147, 34.93166121998716278 ) ) ;
#77862 = CARTESIAN_POINT ( 'NONE',  ( 15.36081428668900628, -2.254550872974306230, 29.97347326024527092 ) ) ;
#77863 = CYLINDRICAL_SURFACE ( 'NONE', #72671, 2.750000000000000000 ) ;
#77864 = EDGE_LOOP ( 'NONE', ( #25246, #88198, #8189, #4311 ) ) ;
#77865 = ORIENTED_EDGE ( 'NONE', *, *, #24357, .F. ) ;
#77867 = ORIENTED_EDGE ( 'NONE', *, *, #25664, .F. ) ;
#77866 = FACE_OUTER_BOUND ( 'NONE', #12846, .T. ) ;
#77868 = FACE_OUTER_BOUND ( 'NONE', #19980, .T. ) ;
#77869 = DIRECTION ( 'NONE',  ( -0.000000000000000000, 0.3420201433256694346, -0.9396926207859080948 ) ) ;
#77871 = EDGE_LOOP ( 'NONE', ( #42209, #52466 ) ) ;
#77870 = EDGE_CURVE ( 'NONE', #17339, #28781, #57761, .T. ) ;
#77872 = CARTESIAN_POINT ( 'NONE',  ( 15.90382291655318880, -12.43535235679832596, 30.55408501211184813 ) ) ;
#77873 = FACE_OUTER_BOUND ( 'NONE', #71005, .T. ) ;
#77874 = CARTESIAN_POINT ( 'NONE',  ( -8.769230769230892619, -12.16647553114689728, 32.15551576947799362 ) ) ;
#77875 = FACE_BOUND ( 'NONE', #82962, .T. ) ;
#77876 = CARTESIAN_POINT ( 'NONE',  ( -9.561782254074048026, -4.299079248970732792, 33.91157788607253565 ) ) ;
#77878 = EDGE_CURVE ( 'NONE', #10589, #27949, #54488, .T. ) ;
#77877 = DIRECTION ( 'NONE',  ( -0.000000000000000000, -0.9396926207859093161, -0.3420201433256663259 ) ) ;
#77879 = AXIS2_PLACEMENT_3D ( 'NONE', #46115, #66830, #921 ) ;
#77880 = CARTESIAN_POINT ( 'NONE',  ( 13.13459216039392885, -12.68155406624981119, 30.59749803192733708 ) ) ;
#77882 = CARTESIAN_POINT ( 'NONE',  ( 6.700150705560777631, -11.76352882383564769, 32.36236540154569497 ) ) ;
#77881 = CARTESIAN_POINT ( 'NONE',  ( -16.82686865700962286, -12.41089969410671223, 31.60739465890703670 ) ) ;
#77883 = CARTESIAN_POINT ( 'NONE',  ( 11.31553532094539172, -11.24512374952581872, 33.06303171183252942 ) ) ;
#77884 = CARTESIAN_POINT ( 'NONE',  ( 12.46153846153846168, -3.937682226553329556, 33.60647404775216529 ) ) ;
#77885 = VERTEX_POINT ( 'NONE', #65834 ) ;
#77886 = EDGE_CURVE ( 'NONE', #57358, #27949, #37190, .T. ) ;
#77887 = CARTESIAN_POINT ( 'NONE',  ( 10.55011416942384095, -10.90142922261923886, 33.41473453929638993 ) ) ;
#77888 = VERTEX_POINT ( 'NONE', #71708 ) ;
#77889 = EDGE_LOOP ( 'NONE', ( #39739, #55173 ) ) ;
#77890 = B_SPLINE_CURVE_WITH_KNOTS ( 'NONE', 3,
 ( #14147, #39536, #41183, #61878, #53463, #73303, #62322, #39087, #87280, #73764 ),
 .UNSPECIFIED., .F., .F.,
 ( 4, 2, 2, 2, 4 ),
 ( 0.0007817359430256252354, 0.0009771253907249898181, 0.001172514838424354401, 0.001367904286123718983, 0.001563293733823083566 ),
 .UNSPECIFIED. ) ;
#77892 = CARTESIAN_POINT ( 'NONE',  ( 10.68063975489745232, -12.70778746994558439, 30.41441678777536595 ) ) ;
#77891 = DIRECTION ( 'NONE',  ( -0.000000000000000000, 0.1736481776669307198, -0.9848077530122080203 ) ) ;
#77893 = CARTESIAN_POINT ( 'NONE',  ( 2.372947878968333590, -2.625532179533470512, 30.86335684631491105 ) ) ;
#77894 = DIRECTION ( 'NONE',  ( -0.000000000000000000, 0.3420201433256694346, -0.9396926207859080948 ) ) ;
#77895 = CARTESIAN_POINT ( 'NONE',  ( 2.438482748659257293, -2.295524264805589354, 30.44142389570982488 ) ) ;
#77896 = CARTESIAN_POINT ( 'NONE',  ( -2.438382910802614933, -11.37499894934982514, 33.29245874905763003 ) ) ;
#77897 = VERTEX_POINT ( 'NONE', #10014 ) ;
#77898 = CARTESIAN_POINT ( 'NONE',  ( -18.13014720943822056, -6.001485441113818986, 34.52039167877662607 ) ) ;
#77899 = CARTESIAN_POINT ( 'NONE',  ( 0.2386115026316116827, -12.64616026154729411, 30.79003144601913533 ) ) ;
#77900 = CARTESIAN_POINT ( 'NONE',  ( 17.29970261819148902, -6.760870238392814535, 34.69528174975672385 ) ) ;
#77901 = CARTESIAN_POINT ( 'NONE',  ( 1.384615384615386802, -12.29105614889573062, 35.45975837776705220 ) ) ;
#77902 = LINE ( 'NONE', #64817, #73667 ) ;
#77903 = EDGE_CURVE ( 'NONE', #58240, #60125, #4137, .T. ) ;
#77904 = CARTESIAN_POINT ( 'NONE',  ( 2.651650429449569302, -10.15165042944953733, 17.12500000000000000 ) ) ;
#77905 = VERTEX_POINT ( 'NONE', #31624 ) ;
#77906 = ORIENTED_EDGE ( 'NONE', *, *, #80852, .F. ) ;
#77907 = CARTESIAN_POINT ( 'NONE',  ( -9.561515884482908234, -12.38066358083363738, 30.83685684665853444 ) ) ;
#77908 = EDGE_CURVE ( 'NONE', #81137, #13624, #30726, .T. ) ;
#77909 = VERTEX_POINT ( 'NONE', #51410 ) ;
#77910 = CARTESIAN_POINT ( 'NONE',  ( -7.173053654019278191, -2.564618984488975961, 30.55390908950641915 ) ) ;
#77911 = CARTESIAN_POINT ( 'NONE',  ( 9.915087233576100445, -10.11255958852956027, 34.01340905677048454 ) ) ;
#77912 = CARTESIAN_POINT ( 'NONE',  ( 2.307692307692309264, -3.937682226553329556, 33.60647404775216529 ) ) ;
#77913 = CARTESIAN_POINT ( 'NONE',  ( -4.826868657009624641, -3.435999193479609914, 33.07426656108010832 ) ) ;
#77914 = CARTESIAN_POINT ( 'NONE',  ( -2.651650429449565305, -4.848349570550461785, 17.75000000000000355 ) ) ;
#77915 = CARTESIAN_POINT ( 'NONE',  ( 20.00000000000000000, -4.000000000000000000, 29.75000000000000355 ) ) ;
#77916 = ORIENTED_EDGE ( 'NONE', *, *, #50582, .T. ) ;
#77917 = CARTESIAN_POINT ( 'NONE',  ( 5.076923076923075762, -4.945431358278436385, 36.03766855953609394 ) ) ;
#77919 = ORIENTED_EDGE ( 'NONE', *, *, #23165, .F. ) ;
#77918 = CARTESIAN_POINT ( 'NONE',  ( -2.242437168179467477, -12.70778746994558439, 30.41441678777536595 ) ) ;
#77920 = CARTESIAN_POINT ( 'NONE',  ( 0.4615384615384611755, -2.249999999999998668, 29.50000000000001421 ) ) ;
#77921 = CARTESIAN_POINT ( 'NONE',  ( -9.692307692307691624, -12.10708131394839349, 31.69288490824020244 ) ) ;
#77922 = VECTOR ( 'NONE', #78437, 1000.000000000000000 ) ;
#77923 = FACE_OUTER_BOUND ( 'NONE', #16415, .T. ) ;
#77924 = EDGE_CURVE ( 'NONE', #24060, #21693, #17214, .T. ) ;
#77925 = CARTESIAN_POINT ( 'NONE',  ( -19.50000000000000000, -7.500000000000000000, 29.75000000000000355 ) ) ;
#77926 = FACE_OUTER_BOUND ( 'NONE', #86028, .T. ) ;
#77927 = CARTESIAN_POINT ( 'NONE',  ( -15.12820512820512953, -7.500000000000000000, 29.75000000000000355 ) ) ;
#77928 = AXIS2_PLACEMENT_3D ( 'NONE', #1171, #28194, #290 ) ;
#77929 = CARTESIAN_POINT ( 'NONE',  ( -2.694853999681181556, -10.10844685921792241, 15.18936829374151465 ) ) ;
#77930 = EDGE_LOOP ( 'NONE', ( #45731, #61710 ) ) ;
#77931 = ADVANCED_FACE ( 'NONE', ( #37937 ), #65400, .F. ) ;
#77932 = DIRECTION ( 'NONE',  ( 1.000000000000000000, -5.997714145664496128E-17, 0.000000000000000000 ) ) ;
#77933 = CARTESIAN_POINT ( 'NONE',  ( -5.076923076923075762, -7.500000000000001776, 35.04278698407183867 ) ) ;
#77934 = CARTESIAN_POINT ( 'NONE',  ( 1.944543648262996083, -5.555456351736983045, 24.31250000000000000 ) ) ;
#77935 = B_SPLINE_CURVE_WITH_KNOTS ( 'NONE', 3,
 ( #61670, #19813, #62125, #41864, #74766, #428, #13056, #40541, #61224, #27898 ),
 .UNSPECIFIED., .F., .F.,
 ( 4, 2, 2, 2, 4 ),
 ( 0.0007817246256747465219, 0.0009771112852218900684, 0.001172497944769033615, 0.001367884604316177378, 0.001563271263863320925 ),
 .UNSPECIFIED. ) ;
#77936 = EDGE_CURVE ( 'NONE', #77001, #61355, #12687, .T. ) ;
#77937 = CARTESIAN_POINT ( 'NONE',  ( -3.230769230769351186, -9.442884908241554243, 34.35708131394783038 ) ) ;
#77938 = CARTESIAN_POINT ( 'NONE',  ( -3.165514091256390827, -11.06231777344671130, 33.60647404775212976 ) ) ;
#77939 = ORIENTED_EDGE ( 'NONE', *, *, #12757, .T. ) ;
#77940 = CARTESIAN_POINT ( 'NONE',  ( 9.692307692307695177, -8.810774026931790459, 35.74407628777942847 ) ) ;
#77941 = DIRECTION ( 'NONE',  ( -0.000000000000000000, -0.000000000000000000, -1.000000000000000000 ) ) ;
#77942 = B_SPLINE_CURVE_WITH_KNOTS ( 'NONE', 3,
 ( #61740, #34727, #15794, #62194, #8593, #55438, #69843, #56329, #43259, #41936 ),
 .UNSPECIFIED., .F., .F.,
 ( 4, 2, 2, 2, 4 ),
 ( 0.0007817359430256369448, 0.0009771253907250049969, 0.001172514838424373049, 0.001367904286123741101, 0.001563293733823109153 ),
 .UNSPECIFIED. ) ;
#77943 = VERTEX_POINT ( 'NONE', #40171 ) ;
#77944 = EDGE_CURVE ( 'NONE', #28039, #18683, #77189, .T. ) ;
#77945 = CARTESIAN_POINT ( 'NONE',  ( 6.923076923076924238, -6.343179335718451384, 34.87096338111211935 ) ) ;
#77946 = UNCERTAINTY_MEASURE_WITH_UNIT (LENGTH_MEASURE( 1.000000000000000082E-05 ), #60143, 'distance_accuracy_value', 'NONE');
#77947 = ORIENTED_EDGE ( 'NONE', *, *, #85260, .F. ) ;
#77948 = CARTESIAN_POINT ( 'NONE',  ( 1.653273178848927064E-15, -7.500000000000000000, 29.50000000000000355 ) ) ;
#77949 = CARTESIAN_POINT ( 'NONE',  ( 16.82692307692307665, -2.499999999999998668, 29.75000000000000355 ) ) ;
#77950 = EDGE_CURVE ( 'NONE', #76645, #70948, #66506, .T. ) ;
#77951 = CARTESIAN_POINT ( 'NONE',  ( -12.52680846209478283, -10.33852847137145048, 34.16647553114627556 ) ) ;
#77952 = CARTESIAN_POINT ( 'NONE',  ( 1.384615384615386802, -13.63283147151868846, 33.57946703557072254 ) ) ;
#77953 = ORIENTED_EDGE ( 'NONE', *, *, #18951, .T. ) ;
#77954 = CARTESIAN_POINT ( 'NONE',  ( -13.25408994638174320, -3.068774925481847493, 32.56582465632704526 ) ) ;
#77955 = CIRCLE ( 'NONE', #23296, 0.2500000000000002220 ) ;
#77956 = VERTEX_POINT ( 'NONE', #66740 ) ;
#77958 = CARTESIAN_POINT ( 'NONE',  ( 2.531068248390492492, -2.501478030877322567, 29.88021232661720816 ) ) ;
#77957 = VECTOR ( 'NONE', #62560, 1000.000000000000000 ) ;
#77959 = CARTESIAN_POINT ( 'NONE',  ( -4.403846153846151523, -7.500000000000001776, 34.75000000000000000 ) ) ;
#77960 = ORIENTED_EDGE ( 'NONE', *, *, #14640, .F. ) ;
#77961 = CARTESIAN_POINT ( 'NONE',  ( 8.519254025182176449, -4.818429247618089661, 34.26397095200675125 ) ) ;
#77963 = ADVANCED_FACE ( 'NONE', ( #81595 ), #19882, .F. ) ;
#77962 = CARTESIAN_POINT ( 'NONE',  ( -12.68446467905460473, -5.667676309546437530, 34.40238873228292249 ) ) ;
#77964 = CARTESIAN_POINT ( 'NONE',  ( -17.06410256410256565, -3.499999999999999556, 29.75000000000000355 ) ) ;
#77965 = AXIS2_PLACEMENT_3D ( 'NONE', #75501, #7044, #28654 ) ;
#77966 = CARTESIAN_POINT ( 'NONE',  ( 13.51540582558233794, -11.93129842949671726, 32.56571108434900452 ) ) ;
#77967 = CARTESIAN_POINT ( 'NONE',  ( -21.00000000000000000, -12.75000000000000178, 29.75000000000000355 ) ) ;
#77968 = VERTEX_POINT ( 'NONE', #32504 ) ;
#77969 = ORIENTED_EDGE ( 'NONE', *, *, #43610, .F. ) ;
#77970 = FACE_BOUND ( 'NONE', #74029, .T. ) ;
#77971 = VERTEX_POINT ( 'NONE', #87477 ) ;
#77972 = CYLINDRICAL_SURFACE ( 'NONE', #70323, 4.000000000000000000 ) ;
#77973 = B_SPLINE_CURVE_WITH_KNOTS ( 'NONE', 3,
 ( #78110, #9645, #37112, #49311, #76788, #15088, #1567, #42560, #38014, #4226 ),
 .UNSPECIFIED., .F., .F.,
 ( 4, 2, 2, 2, 4 ),
 ( 0.000000000000000000, 0.0001954339857564097241, 0.0003908679715128194482, 0.0005863019572692291723, 0.0007817359430256388964 ),
 .UNSPECIFIED. ) ;
#77974 = CARTESIAN_POINT ( 'NONE',  ( 9.692307692307572609, -12.27809138561165270, 31.22303859784587132 ) ) ;
#77975 = CARTESIAN_POINT ( 'NONE',  ( 0.5276057948885368720, -12.62096338111211757, 30.90682066428152908 ) ) ;
#77976 = ORIENTED_EDGE ( 'NONE', *, *, #34995, .T. ) ;
#77977 = VERTEX_POINT ( 'NONE', #61295 ) ;
#77978 = CARTESIAN_POINT ( 'NONE',  ( 0.4615384615384611200, -8.164416787775445883, 34.95778746994557906 ) ) ;
#77979 = EDGE_LOOP ( 'NONE', ( #11531, #85601 ) ) ;
#77980 = CARTESIAN_POINT ( 'NONE',  ( -0.4615384615385826339, -10.21337939537710326, 33.94971097300076224 ) ) ;
#77981 = CARTESIAN_POINT ( 'NONE',  ( -5.076923076923075762, -4.786620604624113540, 33.94971097300155094 ) ) ;
#77982 = AXIS2_PLACEMENT_3D ( 'NONE', #70982, #9289, #14712 ) ;
#77983 = CARTESIAN_POINT ( 'NONE',  ( 14.24160992833217065, -11.91647553114624181, 32.58852847137148245 ) ) ;
#77984 = B_SPLINE_CURVE_WITH_KNOTS ( 'NONE', 3,
 ( #19219, #46683, #53885, #81371, #19654, #68287, #47116, #6590, #74606, #12895 ),
 .UNSPECIFIED., .F., .F.,
 ( 4, 2, 2, 2, 4 ),
 ( 0.000000000000000000, 0.0001954311564186864949, 0.0003908623128373729899, 0.0005862934692560594577, 0.0007817246256747459798 ),
 .UNSPECIFIED. ) ;
#77985 = FACE_BOUND ( 'NONE', #36478, .T. ) ;
#77986 = VERTEX_POINT ( 'NONE', #46470 ) ;
#77988 = EDGE_CURVE ( 'NONE', #14831, #74248, #68081, .T. ) ;
#77987 = CARTESIAN_POINT ( 'NONE',  ( 10.61538461538461675, -10.89733346790207413, 36.13435417666054406 ) ) ;
#77989 = B_SPLINE_CURVE_WITH_KNOTS ( 'NONE', 3,
 ( #3017, #3904, #63843, #51185, #37697, #44437, #85450, #30930, #78693, #8910 ),
 .UNSPECIFIED., .F., .F.,
 ( 4, 2, 2, 2, 4 ),
 ( 0.0007817359430256216575, 0.0009771253907249856981, 0.001172514838424349630, 0.001367904286123713779, 0.001563293733823077711 ),
 .UNSPECIFIED. ) ;
#77990 = CARTESIAN_POINT ( 'NONE',  ( -4.480769230769230838, -11.50000000000000000, 29.75000000000000355 ) ) ;
#77991 = CARTESIAN_POINT ( 'NONE',  ( -14.55766903863466055, -9.148715823498378086, 34.47080413974185120 ) ) ;
#77992 = CARTESIAN_POINT ( 'NONE',  ( 9.019176178608811156, -6.653508905675592722, 34.93172785388651391 ) ) ;
#77993 = ORIENTED_EDGE ( 'NONE', *, *, #57544, .T. ) ;
#77994 = EDGE_CURVE ( 'NONE', #86865, #44484, #39727, .T. ) ;
#77995 = VERTEX_POINT ( 'NONE', #5493 ) ;
#77996 = EDGE_LOOP ( 'NONE', ( #14417, #54047, #15452, #82849 ) ) ;
#77998 = DIRECTION ( 'NONE',  ( -0.000000000000000000, -0.8660254037844397068, -0.4999999999999978906 ) ) ;
#77997 = CARTESIAN_POINT ( 'NONE',  ( -8.096177083446809419, -6.695914987888146541, 34.68535235679833306 ) ) ;
#77999 = EDGE_CURVE ( 'NONE', #25231, #64217, #14987, .T. ) ;
#78000 = CARTESIAN_POINT ( 'NONE',  ( -10.74607608205217346, -12.11776431015576172, 31.66791131148498906 ) ) ;
#78001 = CARTESIAN_POINT ( 'NONE',  ( -2.307692307692428724, -2.657715359629662544, 31.77849191805970364 ) ) ;
#78002 = DIRECTION ( 'NONE',  ( 0.000000000000000000, 0.8660254037844377084, -0.5000000000000015543 ) ) ;
#78003 = CARTESIAN_POINT ( 'NONE',  ( -11.66915214157184622, -2.295517848115769421, 30.44137282052137294 ) ) ;
#78004 = ORIENTED_EDGE ( 'NONE', *, *, #18969, .T. ) ;
#78005 = CARTESIAN_POINT ( 'NONE',  ( 19.00000000000000000, -1.749999999999998890, 30.25000000000000000 ) ) ;
#78006 = CARTESIAN_POINT ( 'NONE',  ( 11.53846153846153832, -11.35647404775217417, 33.31231777344666511 ) ) ;
#78007 = CARTESIAN_POINT ( 'NONE',  ( 14.30769230769231015, -12.09954503811598769, 35.62045528018868623 ) ) ;
#78008 = CARTESIAN_POINT ( 'NONE',  ( -15.23076923076922995, -2.708943851104267164, 35.45975837776705220 ) ) ;
#78009 = ORIENTED_EDGE ( 'NONE', *, *, #4735, .T. ) ;
#78010 = EDGE_CURVE ( 'NONE', #38500, #12730, #19441, .T. ) ;
#78011 = CARTESIAN_POINT ( 'NONE',  ( -14.30769230769230660, -8.564572088678739092, 35.78748833219616898 ) ) ;
#78012 = VERTEX_POINT ( 'NONE', #54101 ) ;
#78013 = FACE_BOUND ( 'NONE', #38990, .T. ) ;
#78015 = PRESENTATION_LAYER_ASSIGNMENT (  '', '', ( #27675 ) ) ;
#78014 = CARTESIAN_POINT ( 'NONE',  ( 11.66925197942849479, -2.845873456487966635, 32.17976146951972538 ) ) ;
#78016 = CIRCLE ( 'NONE', #85164, 0.2500000000000002220 ) ;
#78017 = DIRECTION ( 'NONE',  ( -1.000000000000000000, -0.000000000000000000, -0.000000000000000000 ) ) ;
#78018 = CARTESIAN_POINT ( 'NONE',  ( 12.33084699487089964, -12.11776431015576172, 31.66791131148498906 ) ) ;
#78019 = ORIENTED_EDGE ( 'NONE', *, *, #71663, .T. ) ;
#78020 = CARTESIAN_POINT ( 'NONE',  ( -3.454254174493178287, -12.44517049084099725, 30.48991314939691932 ) ) ;
#78021 = CARTESIAN_POINT ( 'NONE',  ( -2.177166605928742449, -4.459921816937789885, 33.71989282347011851 ) ) ;
#78022 = CARTESIAN_POINT ( 'NONE',  ( -15.00798956179115962, -10.23759521482555357, 34.22997729860117033 ) ) ;
#78023 = CARTESIAN_POINT ( 'NONE',  ( -1.134669975237340367, -4.176053281294515251, 33.81426240980091791 ) ) ;
#78024 = ORIENTED_EDGE ( 'NONE', *, *, #34995, .F. ) ;
#78025 = AXIS2_PLACEMENT_3D ( 'NONE', #12389, #81299, #68218 ) ;
#78026 = CARTESIAN_POINT ( 'NONE',  ( -9.758390071667825794, -2.833524468853757305, 32.15551576947924417 ) ) ;
#78027 = ORIENTED_EDGE ( 'NONE', *, *, #69778, .F. ) ;
#78029 = VERTEX_POINT ( 'NONE', #40612 ) ;
#78028 = CARTESIAN_POINT ( 'NONE',  ( 13.38461538461538680, -8.164416787775445883, 34.95778746994557906 ) ) ;
#78030 = LINE ( 'NONE', #23089, #64159 ) ;
#78031 = CARTESIAN_POINT ( 'NONE',  ( 15.10062126103753855, -5.070767119584671079, 34.40440758774516183 ) ) ;
#78032 = CARTESIAN_POINT ( 'NONE',  ( 0.000000000000000000, -11.00000000000000000, 29.75000000000000355 ) ) ;
#78033 = CARTESIAN_POINT ( 'NONE',  ( -12.68446542044531000, -10.77366814457252175, 33.85459836347579454 ) ) ;
#78034 = CARTESIAN_POINT ( 'NONE',  ( -7.846153846153965716, -9.442884908241554243, 34.35708131394783038 ) ) ;
#78035 = CARTESIAN_POINT ( 'NONE',  ( -9.692307692307814193, -12.16647553114689728, 32.15551576947799362 ) ) ;
#78036 = CARTESIAN_POINT ( 'NONE',  ( -1.944543648263014957, -5.555456351737005249, 22.75000000000000000 ) ) ;
#78037 = EDGE_LOOP ( 'NONE', ( #2333, #17503, #13745, #2518 ) ) ;
#78038 = ADVANCED_FACE ( 'NONE', ( #6386 ), #33838, .F. ) ;
#78039 = CARTESIAN_POINT ( 'NONE',  ( 9.692307692308000711, -2.506253911140615021, 30.00000000000323297 ) ) ;
#78040 = DIRECTION ( 'NONE',  ( -0.000000000000000000, -0.9396926207859093161, -0.3420201433256663259 ) ) ;
#78041 = EDGE_LOOP ( 'NONE', ( #532, #32516, #38562, #63212 ) ) ;
#78042 = ORIENTED_EDGE ( 'NONE', *, *, #21370, .F. ) ;
#78043 = ORIENTED_EDGE ( 'NONE', *, *, #23659, .T. ) ;
#78044 = CARTESIAN_POINT ( 'NONE',  ( 3.903822916553188804, -12.22074536777954989, 31.39888409691088356 ) ) ;
#78045 = CARTESIAN_POINT ( 'NONE',  ( 11.53846153846141753, -3.835265460704628371, 33.15142922262033665 ) ) ;
#78046 = CARTESIAN_POINT ( 'NONE',  ( -1.384615384615383471, -4.945431358278436385, 36.03766855953609394 ) ) ;
#78047 = LINE ( 'NONE', #70417, #25519 ) ;
#78048 = CARTESIAN_POINT ( 'NONE',  ( 9.019176178608811156, -11.56426240980093745, 33.07394671870546432 ) ) ;
#78049 = ADVANCED_FACE ( 'NONE', ( #34281 ), #50006, .F. ) ;
#78050 = CARTESIAN_POINT ( 'NONE',  ( 8.769230769230645706, -3.083524468854526912, 32.58852847137268327 ) ) ;
#78051 = AXIS2_PLACEMENT_3D ( 'NONE', #31850, #64720, #3020 ) ;
#78052 = CARTESIAN_POINT ( 'NONE',  ( 0.3309785479250964002, -2.254533558242299396, 29.97296025877828285 ) ) ;
#78053 = ORIENTED_EDGE ( 'NONE', *, *, #16703, .T. ) ;
#78054 = LINE ( 'NONE', #44693, #4575 ) ;
#78055 = CARTESIAN_POINT ( 'NONE',  ( -17.32694631421604115, -12.22074536777955345, 31.39888409691088356 ) ) ;
#78056 = EDGE_CURVE ( 'NONE', #48096, #44924, #81517, .T. ) ;
#78057 = EDGE_CURVE ( 'NONE', #49839, #32338, #76229, .T. ) ;
#78058 = CARTESIAN_POINT ( 'NONE',  ( -8.992715693795100051, -11.60425143139329940, 33.02411095842164457 ) ) ;
#78059 = DIRECTION ( 'NONE',  ( -0.000000000000000000, 1.000000000000000000, -0.000000000000000000 ) ) ;
#78060 = EDGE_LOOP ( 'NONE', ( #57492, #86839 ) ) ;
#78061 = DIRECTION ( 'NONE',  ( 1.000000000000000000, 0.000000000000000000, 0.000000000000000000 ) ) ;
#78062 = ORIENTED_EDGE ( 'NONE', *, *, #22131, .T. ) ;
#78063 = CARTESIAN_POINT ( 'NONE',  ( 0.5920641633020254924, -9.417988943895561960, 34.36773134775778260 ) ) ;
#78064 =( NAMED_UNIT ( * ) PLANE_ANGLE_UNIT ( ) SI_UNIT ( $, .RADIAN. ) );
#78065 = LINE ( 'NONE', #77182, #23953 ) ;
#78066 = CARTESIAN_POINT ( 'NONE',  ( -15.23076923076935252, -5.941354392335915335, 34.76329471203413846 ) ) ;
#78067 = ORIENTED_EDGE ( 'NONE', *, *, #50036, .T. ) ;
#78069 = EDGE_CURVE ( 'NONE', #18634, #67793, #28409, .T. ) ;
#78068 = CARTESIAN_POINT ( 'NONE',  ( -2.557715531913763218, -6.652501968072646932, 34.93155406624980941 ) ) ;
#78070 = CARTESIAN_POINT ( 'NONE',  ( 9.469380733400843297, -2.889293201056495786, 32.26117774369186009 ) ) ;
#78071 = B_SPLINE_CURVE_WITH_KNOTS ( 'NONE', 3,
 ( #50159, #77648, #71768, #42544, #70900, #70003, #9206, #36669, #2423, #29917 ),
 .UNSPECIFIED., .F., .F.,
 ( 4, 2, 2, 2, 4 ),
 ( 0.0007817359430256371616, 0.0009771253907250049969, 0.001172514838424373049, 0.001367904286123741101, 0.001563293733823108937 ),
 .UNSPECIFIED. ) ;
#78072 = CARTESIAN_POINT ( 'NONE',  ( -8.992157728137616601, -9.172386477786396597, 34.72672124145550043 ) ) ;
#78073 = ADVANCED_FACE ( 'NONE', ( #22540 ), #69844, .F. ) ;
#78074 = EDGE_CURVE ( 'NONE', #85269, #59590, #34728, .T. ) ;
#78075 = ORIENTED_EDGE ( 'NONE', *, *, #8573, .F. ) ;
#78076 = CARTESIAN_POINT ( 'NONE',  ( 16.37662582282421653, -10.23759521482555357, 34.22997729860117033 ) ) ;
#78077 = EDGE_LOOP ( 'NONE', ( #73016, #44399 ) ) ;
#78078 = EDGE_CURVE ( 'NONE', #61129, #11362, #17042, .T. ) ;
#78079 = AXIS2_PLACEMENT_3D ( 'NONE', #78222, #71029, #42682 ) ;
#78080 = CYLINDRICAL_SURFACE ( 'NONE', #65149, 0.2499999999999986955 ) ;
#78081 = AXIS2_PLACEMENT_3D ( 'NONE', #2962, #43957, #71421 ) ;
#78082 = DIRECTION ( 'NONE',  ( -0.000000000000000000, 1.000000000000000000, -0.000000000000000000 ) ) ;
#78083 = CARTESIAN_POINT ( 'NONE',  ( -14.30769230769230660, -2.249999999999998668, 29.75000000000001776 ) ) ;
#78084 = CARTESIAN_POINT ( 'NONE',  ( -14.05763799605399278, -9.943054286541403997, 34.11300777759954883 ) ) ;
#78085 = CARTESIAN_POINT ( 'NONE',  ( -3.000000000000003553, 7.500000000000000000, 14.00000000000000178 ) ) ;
#78086 = VECTOR ( 'NONE', #52261, 1000.000000000000000 ) ;
#78087 = ORIENTED_EDGE ( 'NONE', *, *, #72554, .F. ) ;
#78088 = EDGE_LOOP ( 'NONE', ( #57902, #24979 ) ) ;
#78089 = VERTEX_POINT ( 'NONE', #27972 ) ;
#78090 = CARTESIAN_POINT ( 'NONE',  ( -12.52678839331254679, -2.255955759149247619, 30.00000000000013856 ) ) ;
#78091 = CARTESIAN_POINT ( 'NONE',  ( -16.40384615384615330, -2.249999999999998668, 29.75000000000000355 ) ) ;
#78092 = LINE ( 'NONE', #77206, #66694 ) ;
#78093 = EDGE_CURVE ( 'NONE', #2602, #80357, #24548, .T. ) ;
#78094 = DIRECTION ( 'NONE',  ( 0.000000000000000000, 0.7660444431189822323, -0.6427876096865344779 ) ) ;
#78095 = B_SPLINE_CURVE_WITH_KNOTS ( 'NONE', 3,
 ( #73186, #25883, #67317, #46599, #32635, #52007, #45255, #66874, #11484, #4730 ),
 .UNSPECIFIED., .F., .F.,
 ( 4, 2, 2, 2, 4 ),
 ( 0.0007817246256747434861, 0.0009771112852218859484, 0.001172497944769028411, 0.001367884604316171090, 0.001563271263863313552 ),
 .UNSPECIFIED. ) ;
#78096 = CARTESIAN_POINT ( 'NONE',  ( 5.777073782483853392, -11.76352882383564769, 32.36236540154569497 ) ) ;
#78097 = CARTESIAN_POINT ( 'NONE',  ( -5.999999999999998224, -12.37446782046654192, 30.86335684631486131 ) ) ;
#78098 = B_SPLINE_CURVE_WITH_KNOTS ( 'NONE', 3,
 ( #48889, #49772, #49340, #27728, #265, #705, #22308, #68721, #28171, #20531 ),
 .UNSPECIFIED., .F., .F.,
 ( 4, 2, 2, 2, 4 ),
 ( 0.0007817246256747472808, 0.0009771112852218907189, 0.001172497944769034265, 0.001367884604316177595, 0.001563271263863321141 ),
 .UNSPECIFIED. ) ;
#78099 = ORIENTED_EDGE ( 'NONE', *, *, #53723, .T. ) ;
#78100 = ORIENTED_EDGE ( 'NONE', *, *, #67985, .T. ) ;
#78101 = ORIENTED_EDGE ( 'NONE', *, *, #72354, .F. ) ;
#78103 = ORIENTED_EDGE ( 'NONE', *, *, #37646, .F. ) ;
#78102 = CARTESIAN_POINT ( 'NONE',  ( 11.53846153846141576, -2.657715359629662544, 31.77849191805970364 ) ) ;
#78104 = AXIS2_PLACEMENT_3D ( 'NONE', #29007, #79842, #53241 ) ;
#78106 = CARTESIAN_POINT ( 'NONE',  ( -8.546219417617921366, -11.24521262558773493, 33.06293181088029343 ) ) ;
#78105 = CARTESIAN_POINT ( 'NONE',  ( 0.6845498131513104711, -8.239487800360276282, 34.69522927552633718 ) ) ;
#78107 = VECTOR ( 'NONE', #30661, 1000.000000000000000 ) ;
#78108 = B_SPLINE_CURVE_WITH_KNOTS ( 'NONE', 3,
 ( #71614, #15361, #3602, #9920, #2704, #31071, #63968, #23430, #50455, #77937 ),
 .UNSPECIFIED., .F., .F.,
 ( 4, 2, 2, 2, 4 ),
 ( 0.000000000000000000, 0.0001954339857564073388, 0.0003908679715128146777, 0.0005863019572692220165, 0.0007817359430256293554 ),
 .UNSPECIFIED. ) ;
#78109 = CARTESIAN_POINT ( 'NONE',  ( 1.607628228708780860, -4.762714258010882773, 34.23016756924214832 ) ) ;
#78110 = CARTESIAN_POINT ( 'NONE',  ( -10.61538461538461320, -11.69971097300155272, 32.46337939537588113 ) ) ;
#78111 = ORIENTED_EDGE ( 'NONE', *, *, #29686, .F. ) ;
#78112 = VERTEX_POINT ( 'NONE', #75707 ) ;
#78113 = CARTESIAN_POINT ( 'NONE',  ( -17.20707104665477161, -11.66186481527757479, 32.95055677023626117 ) ) ;
#78114 = EDGE_LOOP ( 'NONE', ( #19326, #37855, #55820, #63349 ) ) ;
#78115 = FACE_BOUND ( 'NONE', #68093, .T. ) ;
#78116 = CARTESIAN_POINT ( 'NONE',  ( 15.23076923076911093, -10.21337939537710326, 33.94971097300076224 ) ) ;
#78117 = CARTESIAN_POINT ( 'NONE',  ( -9.692307692307691624, -3.886160181151819604, 36.00935417666054406 ) ) ;
#78118 = VERTEX_POINT ( 'NONE', #41937 ) ;
#78119 = CARTESIAN_POINT ( 'NONE',  ( -15.10024352900566669, -5.195472089885680766, 34.18748526763464923 ) ) ;
#78120 = CARTESIAN_POINT ( 'NONE',  ( 16.28463796167094557, -4.118422570099827595, 33.43335022499816489 ) ) ;
#78121 = CARTESIAN_POINT ( 'NONE',  ( 1.326923076923075762, -7.500000000000000000, 29.75000000000000355 ) ) ;
#78122 = CARTESIAN_POINT ( 'NONE',  ( 3.903822916553187472, -11.37209801155882971, 32.91403422569032955 ) ) ;
#78123 = CARTESIAN_POINT ( 'NONE',  ( -5.076923076923075762, -1.466349020453238561, 30.81389545987213907 ) ) ;
#78124 = EDGE_CURVE ( 'NONE', #949, #12463, #86143, .T. ) ;
#78125 = CARTESIAN_POINT ( 'NONE',  ( 7.976944287120798727, -11.37503395064541678, 33.29242100308974273 ) ) ;
#78126 = DIRECTION ( 'NONE',  ( -1.000000000000000000, -0.000000000000000000, -0.000000000000000000 ) ) ;
#78127 = CARTESIAN_POINT ( 'NONE',  ( 2.057715563643717882, -12.01397095200673881, 32.43157075238190146 ) ) ;
#78128 = DIRECTION ( 'NONE',  ( 0.000000000000000000, 0.000000000000000000, 1.000000000000000000 ) ) ;
#78129 = CARTESIAN_POINT ( 'NONE',  ( 13.63456079399343146, -2.341251567377310217, 30.72681386836322659 ) ) ;
#78130 = DIRECTION ( 'NONE',  ( 0.000000000000000000, 0.000000000000000000, 1.000000000000000000 ) ) ;
#78131 = CARTESIAN_POINT ( 'NONE',  ( -13.25382494364843389, -12.35292014791297710, 31.75344720912887198 ) ) ;
#78134 = FACE_OUTER_BOUND ( 'NONE', #48710, .T. ) ;
#78133 = VECTOR ( 'NONE', #14851, 1000.000000000000000 ) ;
#78132 = CARTESIAN_POINT ( 'NONE',  ( 4.219914504848593317, -12.10708131394839882, 31.69288490824020954 ) ) ;
#78135 = B_SPLINE_CURVE_WITH_KNOTS ( 'NONE', 3,
 ( #9692, #8819, #16015, #37161, #76835, #77266, #22758, #50221, #43483, #23647 ),
 .UNSPECIFIED., .F., .F.,
 ( 4, 2, 2, 2, 4 ),
 ( 0.0007817359430256320659, 0.0009771253907249987086, 0.001172514838424365460, 0.001367904286123732211, 0.001563293733823098962 ),
 .UNSPECIFIED. ) ;
#78136 = CARTESIAN_POINT ( 'NONE',  ( -1.253824943648432777, -9.084667340241226796, 34.75534355489798344 ) ) ;
#78138 = CARTESIAN_POINT ( 'NONE',  ( -15.23076923076935252, -12.51329471203414379, 31.30864560766407578 ) ) ;
#78137 = CARTESIAN_POINT ( 'NONE',  ( -11.53846153846153655, -11.16473453929635440, 33.15142922261926373 ) ) ;
#78139 = LINE ( 'NONE', #9680, #14580 ) ;
#78140 = CARTESIAN_POINT ( 'NONE',  ( -1.200186371490556958, -4.775308065498765409, 25.07625670625849423 ) ) ;
#78141 = EDGE_LOOP ( 'NONE', ( #35945, #8578, #67823, #39819 ) ) ;
#78142 = AXIS2_PLACEMENT_3D ( 'NONE', #23335, #8067, #50358 ) ;
#78143 = CARTESIAN_POINT ( 'NONE',  ( 3.220692400827285695, -8.036656286327577448, 14.00000000000003908 ) ) ;
#78144 = ORIENTED_EDGE ( 'NONE', *, *, #12529, .T. ) ;
#78145 = CARTESIAN_POINT ( 'NONE',  ( 17.06410256410256565, -11.00000000000000000, 29.75000000000000355 ) ) ;
#78146 = ORIENTED_EDGE ( 'NONE', *, *, #9178, .F. ) ;
#78147 = ADVANCED_FACE ( 'NONE', ( #62195 ), #502, .F. ) ;
#78148 = CARTESIAN_POINT ( 'NONE',  ( -4.087777802843714170, -11.16473453929635440, 33.15142922261926373 ) ) ;
#78149 = EDGE_LOOP ( 'NONE', ( #4248, #35167, #3820, #12046 ) ) ;
#78150 = CARTESIAN_POINT ( 'NONE',  ( -2.294871794871794712, -7.500000000000000000, 29.75000000000000355 ) ) ;
#78151 = CARTESIAN_POINT ( 'NONE',  ( 0.06109907496454976272, -10.25000000000000000, 23.27938170625849068 ) ) ;
#78152 = CARTESIAN_POINT ( 'NONE',  ( 7.715463243043540587, -8.191372820521381826, 34.95448215188423546 ) ) ;
#78153 = ADVANCED_FACE ( 'NONE', ( #37822 ), #45463, .F. ) ;
#78154 = FACE_OUTER_BOUND ( 'NONE', #30404, .T. ) ;
#78155 = CARTESIAN_POINT ( 'NONE',  ( 6.923076923076924238, -9.905515769479276145, 34.41647553114623292 ) ) ;
#78156 = CARTESIAN_POINT ( 'NONE',  ( -5.326899820971668476, -2.920706130388546651, 32.31842814019191223 ) ) ;
#78157 = LINE ( 'NONE', #22761, #83516 ) ;
#78158 = DIRECTION ( 'NONE',  ( -0.000000000000000000, -0.9396926207859092051, -0.3420201433256662704 ) ) ;
#78159 = FACE_OUTER_BOUND ( 'NONE', #66687, .T. ) ;
#78160 = CARTESIAN_POINT ( 'NONE',  ( 2.651650429449569302, -10.15165042944953733, 15.87500000000000000 ) ) ;
#78161 = CARTESIAN_POINT ( 'NONE',  ( 1.384615384615386802, -3.050289026998446396, 32.03036669348365706 ) ) ;
#78162 = CARTESIAN_POINT ( 'NONE',  ( -15.23076923076922995, -2.538708090699994813, 30.37095296980875503 ) ) ;
#78163 = EDGE_CURVE ( 'NONE', #683, #60694, #71921, .T. ) ;
#78164 = DIRECTION ( 'NONE',  ( 0.000000000000000000, 0.000000000000000000, 1.000000000000000000 ) ) ;
#78165 = CARTESIAN_POINT ( 'NONE',  ( -1.929879867024197893E-14, -3.750000000000000000, 17.90625000000000000 ) ) ;
#78166 = B_SPLINE_CURVE_WITH_KNOTS ( 'NONE', 3,
 ( #17978, #3111, #45431, #72909, #86453, #16629, #23818, #24727, #11215, #14651 ),
 .UNSPECIFIED., .F., .F.,
 ( 4, 2, 2, 2, 4 ),
 ( 0.0007817246256747465219, 0.0009771112852218898515, 0.001172497944769033181, 0.001367884604316176294, 0.001563271263863319624 ),
 .UNSPECIFIED. ) ;
#78167 = B_SPLINE_CURVE_WITH_KNOTS ( 'NONE', 3,
 ( #2999, #43989, #16971, #24161, #1687, #84995, #56631, #57508, #58382, #17419 ),
 .UNSPECIFIED., .F., .F.,
 ( 4, 2, 2, 2, 4 ),
 ( 0.0007817359430256333669, 0.0009771253907250056474, 0.001172514838424370881, 0.001367904286123736331, 0.001563293733823101564 ),
 .UNSPECIFIED. ) ;
#78168 = DIRECTION ( 'NONE',  ( -0.7057856980126718804, -0.7057856980126787638, -0.06109907496453170772 ) ) ;
#78169 = ORIENTED_EDGE ( 'NONE', *, *, #37835, .T. ) ;
#78170 = CARTESIAN_POINT ( 'NONE',  ( -24.00000000000000000, -9.499999999999982236, 27.25000000000000000 ) ) ;
#78171 = CARTESIAN_POINT ( 'NONE',  ( 12.33139049180676672, -8.630895178749533159, 34.87696386517710323 ) ) ;
#78172 = FACE_OUTER_BOUND ( 'NONE', #20811, .T. ) ;
#78173 = CARTESIAN_POINT ( 'NONE',  ( 15.36081666601968720, -7.723484941389743952, 34.99544897038808955 ) ) ;
#78174 = CARTESIAN_POINT ( 'NONE',  ( 17.32686848630112308, -12.45601412856602686, 31.48342859153981621 ) ) ;
#78175 = CARTESIAN_POINT ( 'NONE',  ( -14.17716686945866300, -4.299079248970732792, 33.91157788607253565 ) ) ;
#78176 = B_SPLINE_CURVE_WITH_KNOTS ( 'NONE', 3,
 ( #4923, #6256, #47222, #73830, #60295, #32831, #61176, #18431, #73372, #19760 ),
 .UNSPECIFIED., .F., .F.,
 ( 4, 2, 2, 2, 4 ),
 ( 0.000000000000000000, 0.0001954339857564073659, 0.0003908679715128147319, 0.0005863019572692221250, 0.0007817359430256294638 ),
 .UNSPECIFIED. ) ;
#78177 = CIRCLE ( 'NONE', #525, 4.000000000000000000 ) ;
#78178 = ADVANCED_FACE ( 'NONE', ( #10357 ), #2693, .F. ) ;
#78179 = ORIENTED_EDGE ( 'NONE', *, *, #22750, .T. ) ;
#78180 = CARTESIAN_POINT ( 'NONE',  ( -1.318547033612944563, -9.780366693483669494, 34.19971097300155805 ) ) ;
#78181 = ORIENTED_EDGE ( 'NONE', *, *, #22807, .F. ) ;
#78182 = EDGE_LOOP ( 'NONE', ( #57392, #61862, #74856, #84601 ) ) ;
#78183 = PLANE ( 'NONE',  #19146 ) ;
#78184 = CARTESIAN_POINT ( 'NONE',  ( -6.130147969731695845, -12.70455904226513866, 30.44083106164009322 ) ) ;
#78185 = DIRECTION ( 'NONE',  ( -0.000000000000000000, 0.9848077530122086864, -0.1736481776669273891 ) ) ;
#78186 = CARTESIAN_POINT ( 'NONE',  ( 4.153846153846032507, -3.835265460704628371, 33.15142922262033665 ) ) ;
#78187 = CARTESIAN_POINT ( 'NONE',  ( 17.75002326905764960, -9.148715823498378086, 34.47080413974185120 ) ) ;
#78188 = ORIENTED_EDGE ( 'NONE', *, *, #67177, .T. ) ;
#78189 = CARTESIAN_POINT ( 'NONE',  ( -14.24162395668987102, -12.10708131394839882, 31.69288490824020954 ) ) ;
#78190 = ORIENTED_EDGE ( 'NONE', *, *, #48845, .F. ) ;
#78191 = B_SPLINE_CURVE_WITH_KNOTS ( 'NONE', 3,
 ( #39258, #88349, #41026, #47324, #74817, #18537, #45994, #11779, #66719, #59955 ),
 .UNSPECIFIED., .F., .F.,
 ( 4, 2, 2, 2, 4 ),
 ( 0.0007817359430256399806, 0.0009771253907250089001, 0.001172514838424378036, 0.001367904286123746956, 0.001563293733823115875 ),
 .UNSPECIFIED. ) ;
#78192 = EDGE_LOOP ( 'NONE', ( #27444, #84104 ) ) ;
#78193 = AXIS2_PLACEMENT_3D ( 'NONE', #57820, #30352, #69564 ) ;
#78194 = CARTESIAN_POINT ( 'NONE',  ( 13.38461538461526423, -5.094484230521993062, 34.41647553114689373 ) ) ;
#78195 = CARTESIAN_POINT ( 'NONE',  ( -19.99999999999996803, 15.00000000000000711, 3.000000000000000000 ) ) ;
#78196 = DIRECTION ( 'NONE',  ( 1.000000000000000000, 0.000000000000000000, 0.000000000000000000 ) ) ;
#78197 = AXIS2_PLACEMENT_3D ( 'NONE', #58677, #37974, #24002 ) ;
#78198 = VECTOR ( 'NONE', #43104, 999.9999999999998863 ) ;
#78199 = CARTESIAN_POINT ( 'NONE',  ( -3.903846153844716671, -7.500000000000155431, 34.75000000000007105 ) ) ;
#78200 = DIRECTION ( 'NONE',  ( -0.000000000000000000, 0.8660254037844397068, -0.4999999999999978906 ) ) ;
#78201 = ORIENTED_EDGE ( 'NONE', *, *, #64105, .T. ) ;
#78202 = ORIENTED_EDGE ( 'NONE', *, *, #12571, .T. ) ;
#78203 = CARTESIAN_POINT ( 'NONE',  ( 3.750000000000009770, -9.053300858899081760, 23.29687500000000000 ) ) ;
#78204 = ORIENTED_EDGE ( 'NONE', *, *, #44903, .F. ) ;
#78206 = EDGE_LOOP ( 'NONE', ( #17485, #65221 ) ) ;
#78205 = CARTESIAN_POINT ( 'NONE',  ( 11.53846153846153832, -5.471508081941601098, 34.59228464037088457 ) ) ;
#78207 = DIRECTION ( 'NONE',  ( 1.000000000000000000, 0.000000000000000000, 0.000000000000000000 ) ) ;
#78208 = CARTESIAN_POINT ( 'NONE',  ( 4.826899839630112155, -3.711651800289232916, 33.01384336483936011 ) ) ;
#78209 = DIRECTION ( 'NONE',  ( -0.000000000000000000, 0.3420201433256694346, -0.9396926207859080948 ) ) ;
#78210 = ORIENTED_EDGE ( 'NONE', *, *, #21139, .T. ) ;
#78211 = CARTESIAN_POINT ( 'NONE',  ( 17.06410256410256565, -3.499999999999999556, 29.75000000000000355 ) ) ;
#78212 = VERTEX_POINT ( 'NONE', #10803 ) ;
#78213 = CARTESIAN_POINT ( 'NONE',  ( -24.00000000000000000, -5.499999999999981348, 27.75000000000000000 ) ) ;
#78214 = CARTESIAN_POINT ( 'NONE',  ( 10.68064018666064108, -9.442884908240273489, 34.35708131394835618 ) ) ;
#78215 = CARTESIAN_POINT ( 'NONE',  ( -17.75005459062195712, -2.589246495874658383, 31.60778113518102828 ) ) ;
#78217 = CARTESIAN_POINT ( 'NONE',  ( -10.68146699474474914, -5.471508081941602875, 34.59228464037088457 ) ) ;
#78216 = CARTESIAN_POINT ( 'NONE',  ( 10.86538461538468248, -7.434744429011176159, 34.75000000000000711 ) ) ;
#78218 = CARTESIAN_POINT ( 'NONE',  ( 16.15384615384615330, -2.538708090699994813, 30.37095296980875503 ) ) ;
#78219 = CARTESIAN_POINT ( 'NONE',  ( -0.2115930521604179049, -12.68172785388650681, 30.59649109432439573 ) ) ;
#78220 = ORIENTED_EDGE ( 'NONE', *, *, #24347, .T. ) ;
#78221 = CARTESIAN_POINT ( 'NONE',  ( 7.384615384615385025, -7.500000000000000000, 29.75000000000000355 ) ) ;
#78222 = CARTESIAN_POINT ( 'NONE',  ( -7.846153846153844924, -6.435427911321262684, 35.78748833219616898 ) ) ;
#78223 = B_SPLINE_CURVE_WITH_KNOTS ( 'NONE', 3,
 ( #34573, #75549, #82767, #7547, #33689, #54391, #1220, #56171, #62468, #47644 ),
 .UNSPECIFIED., .F., .F.,
 ( 4, 2, 2, 2, 4 ),
 ( 0.0007817359430256317406, 0.0009771253907249982749, 0.001172514838424365026, 0.001367904286123731560, 0.001563293733823098094 ),
 .UNSPECIFIED. ) ;
#78224 = ORIENTED_EDGE ( 'NONE', *, *, #37629, .T. ) ;
#78225 = VECTOR ( 'NONE', #9538, 1000.000000000000227 ) ;
#78226 = CARTESIAN_POINT ( 'NONE',  ( 7.053868730901709405, -2.729792928343270919, 31.24908615093345077 ) ) ;
#78227 = CARTESIAN_POINT ( 'NONE',  ( 12.39628747137721909, -2.506253911140460922, 30.00000000000013856 ) ) ;
#78228 = LINE ( 'NONE', #43558, #22382 ) ;
#78229 = CARTESIAN_POINT ( 'NONE',  ( 2.057715563643717438, -5.643011162660950042, 34.66104346484419096 ) ) ;
#78230 = FACE_OUTER_BOUND ( 'NONE', #50695, .T. ) ;
#78231 = CARTESIAN_POINT ( 'NONE',  ( 12.33139125210024112, -4.460286881179643004, 33.72017969459903242 ) ) ;
#78232 = FACE_BOUND ( 'NONE', #39909, .T. ) ;
#78234 = FACE_OUTER_BOUND ( 'NONE', #2371, .T. ) ;
#78233 = CARTESIAN_POINT ( 'NONE',  ( 13.38461538461538680, -7.500000000000001776, 35.04278698407183867 ) ) ;
#78235 = CARTESIAN_POINT ( 'NONE',  ( -6.857821351800898135, -10.90142922261932057, 33.41473453929631887 ) ) ;
#78237 = CARTESIAN_POINT ( 'NONE',  ( 18.75000000000000000, -11.50000000000000000, 29.75000000000000355 ) ) ;
#78236 = CARTESIAN_POINT ( 'NONE',  ( -4.826868657009623753, -10.06805714834173848, 34.32951233291982618 ) ) ;
#78238 = CARTESIAN_POINT ( 'NONE',  ( -7.846153846153844924, -1.790695186598648903, 34.54067556320373455 ) ) ;
#78239 = CARTESIAN_POINT ( 'NONE',  ( -1.492201783934549164, -11.27530806549876807, 20.85750670625849068 ) ) ;
#78240 = ORIENTED_EDGE ( 'NONE', *, *, #16152, .F. ) ;
#78241 = EDGE_CURVE ( 'NONE', #44632, #8069, #6389, .T. ) ;
#78242 = CYLINDRICAL_SURFACE ( 'NONE', #27703, 0.2499999999999979738 ) ;
#78243 = CYLINDRICAL_SURFACE ( 'NONE', #15377, 4.000000000000000000 ) ;
#78244 = LINE ( 'NONE', #44444, #89115 ) ;
#78245 = CARTESIAN_POINT ( 'NONE',  ( -10.68146699474474914, -11.35647404775217595, 33.31231777344666511 ) ) ;
#78246 = EDGE_CURVE ( 'NONE', #11323, #45031, #38272, .T. ) ;
#78247 = CARTESIAN_POINT ( 'NONE',  ( 13.38461538461526423, -10.33852847137269571, 34.16647553114546554 ) ) ;
#78248 = CARTESIAN_POINT ( 'NONE',  ( -3.775308065498766297, -6.007798216065450170, 22.42000670625849068 ) ) ;
#78249 = CARTESIAN_POINT ( 'NONE',  ( -8.769230769230768274, -2.721908614388771852, 31.22303859784724978 ) ) ;
#78250 = CARTESIAN_POINT ( 'NONE',  ( -12.46153846153846168, -5.180354513474913603, 36.12317359536750416 ) ) ;
#78251 = FACE_OUTER_BOUND ( 'NONE', #33494, .T. ) ;
#78252 = CARTESIAN_POINT ( 'NONE',  ( -12.46153846153846168, -13.75783147151868846, 33.36296068462461051 ) ) ;
#78253 = CARTESIAN_POINT ( 'NONE',  ( -3.230769230769229949, -3.937682226553329556, 33.60647404775216529 ) ) ;
#78254 = CYLINDRICAL_SURFACE ( 'NONE', #84295, 0.2500000000000008882 ) ;
#78255 = AXIS2_PLACEMENT_3D ( 'NONE', #59047, #51371, #44183 ) ;
#78256 = CARTESIAN_POINT ( 'NONE',  ( -6.066082379360133281, -11.91647553114624181, 32.58852847137148245 ) ) ;
#78257 = EDGE_CURVE ( 'NONE', #86451, #23528, #26619, .T. ) ;
#78258 = DIRECTION ( 'NONE',  ( 0.000000000000000000, -6.938893903907222067E-15, 1.000000000000000000 ) ) ;
#78259 = ORIENTED_EDGE ( 'NONE', *, *, #53622, .T. ) ;
#78260 = CARTESIAN_POINT ( 'NONE',  ( 17.29993592101647337, -12.64618726649961289, 30.78989965857442712 ) ) ;
#78261 = CARTESIAN_POINT ( 'NONE',  ( -5.777220331021934108, -2.612705202774697533, 31.66806509827799943 ) ) ;
#78262 = CARTESIAN_POINT ( 'NONE',  ( -2.608446859217920633, -4.805146000318815780, 15.50186829374151287 ) ) ;
#78263 = B_SPLINE_CURVE_WITH_KNOTS ( 'NONE', 3,
 ( #48122, #35057, #48561, #13899, #55767, #69733, #34620, #28756, #82373, #27420 ),
 .UNSPECIFIED., .F., .F.,
 ( 4, 2, 2, 2, 4 ),
 ( 0.000000000000000000, 0.0001954311564186862781, 0.0003908623128373725562, 0.0005862934692560588072, 0.0007817246256747451124 ),
 .UNSPECIFIED. ) ;
#78264 = CARTESIAN_POINT ( 'NONE',  ( 0.5267936010512989098, -3.643525952247864463, 33.31231777344670064 ) ) ;
#78265 = CARTESIAN_POINT ( 'NONE',  ( 9.692307692307695177, -10.67929555188718282, 33.92786785259544047 ) ) ;
#78266 = VERTEX_POINT ( 'NONE', #31512 ) ;
#78267 = CARTESIAN_POINT ( 'NONE',  ( 1.634560902963528184, -4.336752205174647656, 33.62275283266504289 ) ) ;
#78269 = EDGE_LOOP ( 'NONE', ( #744, #46909, #79693, #40759 ) ) ;
#78268 = CARTESIAN_POINT ( 'NONE',  ( 12.46153846153833911, -6.026961402154118019, 34.52809138561165270 ) ) ;
#78270 = CARTESIAN_POINT ( 'NONE',  ( 6.673100192134571174, -3.137211980971221781, 32.19342716148376837 ) ) ;
#78271 = CARTESIAN_POINT ( 'NONE',  ( 7.846153846153846700, -1.422936976036506707, 30.56769352161908415 ) ) ;
#78272 = B_SPLINE_CURVE_WITH_KNOTS ( 'NONE', 3,
 ( #14836, #42313, #34657, #35547, #62126, #1304, #429, #49502, #76974, #22465 ),
 .UNSPECIFIED., .F., .F.,
 ( 4, 2, 2, 2, 4 ),
 ( 0.0007817359430256398721, 0.0009771253907250089001, 0.001172514838424377820, 0.001367904286123746739, 0.001563293733823115659 ),
 .UNSPECIFIED. ) ;
#78273 = CARTESIAN_POINT ( 'NONE',  ( 8.769230769230645706, -5.094484230521993062, 34.41647553114689373 ) ) ;
#78274 = CARTESIAN_POINT ( 'NONE',  ( -13.63463862190834952, -3.202444869320336451, 32.30641848906366675 ) ) ;
#78275 = ORIENTED_EDGE ( 'NONE', *, *, #9591, .F. ) ;
#78276 = DIRECTION ( 'NONE',  ( -0.000000000000000000, -0.3420201433256694346, -0.9396926207859080948 ) ) ;
#78277 = SURFACE_STYLE_FILL_AREA ( #2179 ) ;
#78278 = EDGE_CURVE ( 'NONE', #76411, #13379, #21184, .T. ) ;
#78279 = LINE ( 'NONE', #80066, #47020 ) ;
#78280 = ORIENTED_EDGE ( 'NONE', *, *, #14158, .F. ) ;
#78281 = ADVANCED_FACE ( 'NONE', ( #45013 ), #43692, .F. ) ;
#78282 = ORIENTED_EDGE ( 'NONE', *, *, #22253, .F. ) ;
#78283 = B_SPLINE_CURVE_WITH_KNOTS ( 'NONE', 3,
 ( #41189, #62329, #198, #83062, #82631, #28109, #55573, #21351, #23558, #1968 ),
 .UNSPECIFIED., .F., .F.,
 ( 4, 2, 2, 2, 4 ),
 ( 0.0007817246256747445703, 0.0009771112852218870326, 0.001172497944769029495, 0.001367884604316171957, 0.001563271263863314419 ),
 .UNSPECIFIED. ) ;
#78284 = ORIENTED_EDGE ( 'NONE', *, *, #86637, .T. ) ;
#78285 = EDGE_CURVE ( 'NONE', #8200, #58928, #36931, .T. ) ;
#78286 = CARTESIAN_POINT ( 'NONE',  ( -18.13069146666756026, -3.530157926970575399, 32.79014554554149896 ) ) ;
#78287 = CARTESIAN_POINT ( 'NONE',  ( -8.638705067467206788, -3.285477652293413264, 32.44071101563363158 ) ) ;
#78288 = EDGE_CURVE ( 'NONE', #62161, #74008, #25695, .T. ) ;
#78289 = CARTESIAN_POINT ( 'NONE',  ( -7.779984705191187899, -7.250054483168840491, 34.74374881642864921 ) ) ;
#78290 = CARTESIAN_POINT ( 'NONE',  ( 5.999999999999878320, -4.320704448113951379, 33.92786785259630022 ) ) ;
#78291 = ORIENTED_EDGE ( 'NONE', *, *, #38260, .T. ) ;
#78292 = B_SPLINE_CURVE_WITH_KNOTS ( 'NONE', 3,
 ( #23091, #35274, #69063, #42487, #36178, #7370, #9149, #43364, #62294, #83026 ),
 .UNSPECIFIED., .F., .F.,
 ( 4, 2, 2, 2, 4 ),
 ( 0.000000000000000000, 0.0001954311564186864407, 0.0003908623128373728815, 0.0005862934692560593493, 0.0007817246256747457630 ),
 .UNSPECIFIED. ) ;
#78293 = VERTEX_POINT ( 'NONE', #67527 ) ;
#78295 = EDGE_LOOP ( 'NONE', ( #65358, #61261, #15249, #37108 ) ) ;
#78294 = CARTESIAN_POINT ( 'NONE',  ( 9.442284455014730682, -4.335965774309649134, 33.62209801155881905 ) ) ;
#78296 = B_SPLINE_CURVE_WITH_KNOTS ( 'NONE', 3,
 ( #20896, #69091, #35759, #48809, #7398, #13704, #40744, #74975, #35302, #82626 ),
 .UNSPECIFIED., .F., .F.,
 ( 4, 2, 2, 2, 4 ),
 ( 0.0007817246256747461966, 0.0009771112852218892010, 0.001172497944769032314, 0.001367884604316175427, 0.001563271263863318323 ),
 .UNSPECIFIED. ) ;
#78297 = CARTESIAN_POINT ( 'NONE',  ( 17.29993442853592711, -4.887748414852792322, 34.01359900205217457 ) ) ;
#78298 = DIRECTION ( 'NONE',  ( -0.000000000000000000, 1.000000000000000000, 3.491481338843133355E-15 ) ) ;
#78299 = DIRECTION ( 'NONE',  ( 0.000000000000000000, 1.000000000000000000, 0.000000000000000000 ) ) ;
#78300 = EDGE_LOOP ( 'NONE', ( #31898, #3906, #68282, #42550 ) ) ;
#78301 = EDGE_LOOP ( 'NONE', ( #5582, #20631, #70608, #40643, #76371 ) ) ;
#78303 = ORIENTED_EDGE ( 'NONE', *, *, #82296, .T. ) ;
#78302 = CARTESIAN_POINT ( 'NONE',  ( -12.21159294319032362, -5.057305518903948638, 34.11320923018887896 ) ) ;
#78304 = FACE_OUTER_BOUND ( 'NONE', #7632, .T. ) ;
#78305 = ADVANCED_FACE ( 'NONE', ( #18893 ), #5383, .F. ) ;
#78306 = VECTOR ( 'NONE', #36029, 1000.000000000000000 ) ;
#78307 = CARTESIAN_POINT ( 'NONE',  ( -16.15384615384615330, -9.819645486525091727, 36.12317359536749706 ) ) ;
#78308 = ORIENTED_EDGE ( 'NONE', *, *, #75844, .F. ) ;
#78309 = CARTESIAN_POINT ( 'NONE',  ( -9.019207500173124004, -10.66389620160130036, 33.62221079203477103 ) ) ;
#78310 = LINE ( 'NONE', #41549, #6284 ) ;
#78311 = CARTESIAN_POINT ( 'NONE',  ( 10.86543892702293057, -3.627508038966690496, 32.91356715214248396 ) ) ;
#78312 = FACE_BOUND ( 'NONE', #70588, .T. ) ;
#78313 = AXIS2_PLACEMENT_3D ( 'NONE', #62445, #81864, #33225 ) ;
#78314 = CARTESIAN_POINT ( 'NONE',  ( -9.627052552794857831, -4.320704448112861584, 33.92786785259548310 ) ) ;
#78315 = CARTESIAN_POINT ( 'NONE',  ( 3.903869409797562806, -2.318417181685854978, 30.59732222474233865 ) ) ;
#78316 = AXIS2_PLACEMENT_3D ( 'NONE', #43693, #64395, #51761 ) ;
#78317 = CARTESIAN_POINT ( 'NONE',  ( 8.703960323269994248, -2.625532179533445198, 30.86335684631481513 ) ) ;
#78319 = CARTESIAN_POINT ( 'NONE',  ( -16.02305571287920216, -2.845873456487966635, 32.17976146951972538 ) ) ;
#78318 = DIRECTION ( 'NONE',  ( -0.000000000000000000, -0.000000000000000000, -1.000000000000000000 ) ) ;
#78320 = CARTESIAN_POINT ( 'NONE',  ( 11.53846153846153832, -11.16473453929635440, 33.15142922261926373 ) ) ;
#78321 = DIRECTION ( 'NONE',  ( -1.000000000000000000, -0.000000000000000000, -0.000000000000000000 ) ) ;
#78322 = ORIENTED_EDGE ( 'NONE', *, *, #282, .T. ) ;
#78323 = DIRECTION ( 'NONE',  ( -0.000000000000000000, -0.9848077530122085754, -0.1736481776669273613 ) ) ;
#78324 = VERTEX_POINT ( 'NONE', #81494 ) ;
#78325 = ORIENTED_EDGE ( 'NONE', *, *, #88877, .F. ) ;
#78326 = EDGE_CURVE ( 'NONE', #56176, #47929, #88979, .T. ) ;
#78328 = CARTESIAN_POINT ( 'NONE',  ( 15.16549923021291058, -3.083524468853724443, 32.58852847137143272 ) ) ;
#78327 = CARTESIAN_POINT ( 'NONE',  ( 14.43821800945587697, -3.816742781228458448, 33.13167719472716044 ) ) ;
#78329 = B_SPLINE_CURVE_WITH_KNOTS ( 'NONE', 3,
 ( #15310, #903, #48196, #49084, #466, #21612, #76566, #14873, #69368, #21169 ),
 .UNSPECIFIED., .F., .F.,
 ( 4, 2, 2, 2, 4 ),
 ( 0.000000000000000000, 0.0001954311564186869286, 0.0003908623128373738573, 0.0005862934692560607588, 0.0007817246256747477145 ),
 .UNSPECIFIED. ) ;
#78330 = CARTESIAN_POINT ( 'NONE',  ( 13.25392478150507891, -11.37499894934982692, 33.29245874905763003 ) ) ;
#78331 = CARTESIAN_POINT ( 'NONE',  ( -14.24243673641628405, -2.892918686051626498, 31.69288490824026638 ) ) ;
#78332 = CYLINDRICAL_SURFACE ( 'NONE', #83263, 0.2499999999999994726 ) ;
#78333 = CARTESIAN_POINT ( 'NONE',  ( -2.372962308248626417, -11.67786785259541027, 32.92929555188721480 ) ) ;
#78334 = EDGE_LOOP ( 'NONE', ( #39793, #83083 ) ) ;
#78335 = CARTESIAN_POINT ( 'NONE',  ( -1.384615384615383471, -13.78497067705608181, 32.30358669280327177 ) ) ;
#78336 = CARTESIAN_POINT ( 'NONE',  ( -14.98082371242109012, -10.05730279482229683, 34.04704008940765902 ) ) ;
#78337 = CARTESIAN_POINT ( 'NONE',  ( -12.46153846153846168, -11.35647404775217417, 33.31231777344666511 ) ) ;
#78338 = LINE ( 'NONE', #16640, #2189 ) ;
#78339 = CARTESIAN_POINT ( 'NONE',  ( 24.00000000000000000, 9.000000000000024869, 29.25000000000000000 ) ) ;
#78340 = CARTESIAN_POINT ( 'NONE',  ( -1.553300858899125059, -3.750000000000009326, 17.82812500000000000 ) ) ;
#78341 = VERTEX_POINT ( 'NONE', #59430 ) ;
#78342 = ORIENTED_EDGE ( 'NONE', *, *, #32713, .F. ) ;
#78343 = EDGE_CURVE ( 'NONE', #14645, #40586, #6202, .T. ) ;
#78344 = CARTESIAN_POINT ( 'NONE',  ( -10.28846153846153832, -3.499999999999999556, 29.75000000000000355 ) ) ;
#78345 = EDGE_LOOP ( 'NONE', ( #68237, #41079 ) ) ;
#78346 = DIRECTION ( 'NONE',  ( -0.000000000000000000, 0.5000000000000011102, -0.8660254037844381525 ) ) ;
#78347 = CARTESIAN_POINT ( 'NONE',  ( 17.77651507543566822, -11.60425143139329940, 33.02411095842164457 ) ) ;
#78348 = CARTESIAN_POINT ( 'NONE',  ( -16.37733109757010297, -2.847400154188068910, 31.58180166144859768 ) ) ;
#78349 = EDGE_CURVE ( 'NONE', #70251, #87090, #18011, .T. ) ;
#78350 = CARTESIAN_POINT ( 'NONE',  ( -15.16551365949320918, -2.892918686051626498, 31.69288490824026638 ) ) ;
#78351 = CARTESIAN_POINT ( 'NONE',  ( -1.553300858899081538, -11.25000000000000711, 19.85937500000000355 ) ) ;
#78352 = FACE_OUTER_BOUND ( 'NONE', #77391, .T. ) ;
#78354 = VERTEX_POINT ( 'NONE', #74285 ) ;
#78353 = AXIS2_PLACEMENT_3D ( 'NONE', #57091, #15235, #28750 ) ;
#78355 = LINE ( 'NONE', #9033, #32907 ) ;
#78357 = ORIENTED_EDGE ( 'NONE', *, *, #86033, .T. ) ;
#78356 = LINE ( 'NONE', #64391, #42503 ) ;
#78358 = CARTESIAN_POINT ( 'NONE',  ( 2.980792486720640788, -12.41104346484419452, 31.60698883733904196 ) ) ;
#78359 = CARTESIAN_POINT ( 'NONE',  ( -13.38461538461538325, -9.584722331328613620, 36.20867863119891439 ) ) ;
#78360 = CARTESIAN_POINT ( 'NONE',  ( -3.296039676730006196, -5.219633306516282545, 34.19971097300152252 ) ) ;
#78361 = DIRECTION ( 'NONE',  ( 1.000000000000000000, 0.000000000000000000, 0.000000000000000000 ) ) ;
#78362 = CARTESIAN_POINT ( 'NONE',  ( -5.999999999999998224, -4.661471528628507777, 34.16647553114623292 ) ) ;
#78363 = EDGE_CURVE ( 'NONE', #33880, #38977, #83586, .T. ) ;
#78364 = CARTESIAN_POINT ( 'NONE',  ( 9.561617089197383734, -4.684245665217972032, 34.18127051446801090 ) ) ;
#78365 = CARTESIAN_POINT ( 'NONE',  ( -12.46153846153846168, -6.435427911321262684, 35.78748833219616898 ) ) ;
#78366 = CARTESIAN_POINT ( 'NONE',  ( 2.694853999681185108, -4.891553140782077591, 17.06436829374151287 ) ) ;
#78367 = ORIENTED_EDGE ( 'NONE', *, *, #81056, .T. ) ;
#78368 = CARTESIAN_POINT ( 'NONE',  ( -16.40386937806761125, -9.356822207818511927, 34.66110646841856635 ) ) ;
#78369 = CARTESIAN_POINT ( 'NONE',  ( 1.134592147322421196, -5.851115903089112003, 34.47074536777953568 ) ) ;
#78370 = CARTESIAN_POINT ( 'NONE',  ( -13.38461538461550582, -9.442884908241554243, 34.35708131394783038 ) ) ;
#78371 = CARTESIAN_POINT ( 'NONE',  ( 2.775308065498755195, -6.422011778438505125, 13.39249329374151642 ) ) ;
#78372 = EDGE_CURVE ( 'NONE', #61830, #23542, #61628, .T. ) ;
#78373 = CARTESIAN_POINT ( 'NONE',  ( 7.846153846153846700, -3.669653830205710676, 35.88435417666054406 ) ) ;
#78374 = CARTESIAN_POINT ( 'NONE',  ( 8.703960768674448900, -10.33852847137145048, 34.16647553114627556 ) ) ;
#78375 = ORIENTED_EDGE ( 'NONE', *, *, #51684, .T. ) ;
#78376 = CARTESIAN_POINT ( 'NONE',  ( 2.750000000000001776, -7.499999999999984013, 18.21875000000000000 ) ) ;
#78377 = CARTESIAN_POINT ( 'NONE',  ( -15.23076923076935252, -4.320704448113951379, 33.92786785259630022 ) ) ;
#78378 = ADVANCED_FACE ( 'NONE', ( #60760 ), #73393, .F. ) ;
#78379 = ORIENTED_EDGE ( 'NONE', *, *, #52601, .T. ) ;
#78380 = DIRECTION ( 'NONE',  ( -0.000000000000000000, 0.9848077530122086864, -0.1736481776669273891 ) ) ;
#78381 = EDGE_LOOP ( 'NONE', ( #61664, #57368, #73763, #69214 ) ) ;
#78382 = CARTESIAN_POINT ( 'NONE',  ( 14.43821800945587519, -12.27024696741798770, 31.24895572276497546 ) ) ;
#78383 = CARTESIAN_POINT ( 'NONE',  ( 3.100621261037534548, -4.299443229763728169, 33.91186481527756058 ) ) ;
#78384 = EDGE_CURVE ( 'NONE', #45298, #55677, #20252, .T. ) ;
#78385 = CARTESIAN_POINT ( 'NONE',  ( -0.4615384615384611200, -9.905515769479276145, 34.41647553114623292 ) ) ;
#78386 = CARTESIAN_POINT ( 'NONE',  ( -13.38461538461538325, -12.62096338111211580, 30.90682066428153263 ) ) ;
#78387 = ORIENTED_EDGE ( 'NONE', *, *, #11555, .F. ) ;
#78388 = DIRECTION ( 'NONE',  ( -0.000000000000000000, -0.9396926207859093161, -0.3420201433256663259 ) ) ;
#78389 = VECTOR ( 'NONE', #78905, 1000.000000000000000 ) ;
#78390 = ORIENTED_EDGE ( 'NONE', *, *, #33364, .T. ) ;
#78391 = CARTESIAN_POINT ( 'NONE',  ( -17.93474486048716088, -12.16647553114626845, 32.15551576947920864 ) ) ;
#78392 = CARTESIAN_POINT ( 'NONE',  ( 2.372947878968334479, -3.300289026998474817, 32.46337939537591666 ) ) ;
#78393 = ORIENTED_EDGE ( 'NONE', *, *, #71275, .T. ) ;
#78394 = EDGE_CURVE ( 'NONE', #71169, #84435, #43842, .T. ) ;
#78395 = B_SPLINE_CURVE_WITH_KNOTS ( 'NONE', 3,
 ( #56249, #83733, #63437, #9825, #1744, #77839, #23334, #71082, #43174, #29231 ),
 .UNSPECIFIED., .F., .F.,
 ( 4, 2, 2, 2, 4 ),
 ( 0.0007817246256747505334, 0.0009771112852218954894, 0.001172497944769040554, 0.001367884604316185618, 0.001563271263863330682 ),
 .UNSPECIFIED. ) ;
#78396 = VECTOR ( 'NONE', #53493, 1000.000000000000114 ) ;
#78397 = CARTESIAN_POINT ( 'NONE',  ( 8.102564102564102200, -3.499999999999999556, 29.75000000000000355 ) ) ;
#78398 = CARTESIAN_POINT ( 'NONE',  ( 11.53846153846153832, -8.318370150425687726, 35.83090037661290239 ) ) ;
#78399 = B_SPLINE_CURVE_WITH_KNOTS ( 'NONE', 3,
 ( #83099, #35344, #15526, #1118, #22277, #49741, #22710, #674, #50172, #28140 ),
 .UNSPECIFIED., .F., .F.,
 ( 4, 2, 2, 2, 4 ),
 ( 0.000000000000000000, 0.0001954339857564126514, 0.0003908679715128183098, 0.0005863019572692239681, 0.0007817359430256294638 ),
 .UNSPECIFIED. ) ;
#78400 = CYLINDRICAL_SURFACE ( 'NONE', #20725, 0.2500000000000012212 ) ;
#78401 = DIRECTION ( 'NONE',  ( -0.000000000000000000, 0.8660254037844397068, -0.4999999999999978906 ) ) ;
#78402 = CARTESIAN_POINT ( 'NONE',  ( -16.15384615384615330, -2.833524468853757305, 32.15551576947925838 ) ) ;
#78403 = ORIENTED_EDGE ( 'NONE', *, *, #3064, .F. ) ;
#78404 = EDGE_LOOP ( 'NONE', ( #7138, #6960 ) ) ;
#78405 = FACE_BOUND ( 'NONE', #50173, .T. ) ;
#78406 = ORIENTED_EDGE ( 'NONE', *, *, #40324, .T. ) ;
#78407 = CARTESIAN_POINT ( 'NONE',  ( -7.976844449264153702, -5.496505350115501010, 34.60290016733514307 ) ) ;
#78408 = EDGE_CURVE ( 'NONE', #64470, #50943, #71386, .T. ) ;
#78409 = CARTESIAN_POINT ( 'NONE',  ( 17.77651507543566822, -5.827078755546626354, 34.72654668319379567 ) ) ;
#78410 = DIRECTION ( 'NONE',  ( 0.000000000000000000, 0.8660254037844377084, 0.5000000000000015543 ) ) ;
#78411 = ORIENTED_EDGE ( 'NONE', *, *, #54732, .F. ) ;
#78412 = VERTEX_POINT ( 'NONE', #84927 ) ;
#78413 = AXIS2_PLACEMENT_3D ( 'NONE', #25598, #24244, #25148 ) ;
#78414 = VERTEX_POINT ( 'NONE', #16896 ) ;
#78415 = CARTESIAN_POINT ( 'NONE',  ( 3.480823542407546434, -4.943051570960395047, 34.04725096376909477 ) ) ;
#78416 = ORIENTED_EDGE ( 'NONE', *, *, #6820, .F. ) ;
#78417 = CARTESIAN_POINT ( 'NONE',  ( 16.15384615384603251, -10.21337939537710326, 33.94971097300076224 ) ) ;
#78418 = EDGE_CURVE ( 'NONE', #19767, #42964, #78135, .T. ) ;
#78419 = CARTESIAN_POINT ( 'NONE',  ( -15.23076923076935074, -6.879047030192662504, 34.71129190930017927 ) ) ;
#78420 = B_SPLINE_CURVE_WITH_KNOTS ( 'NONE', 3,
 ( #69458, #47852, #55055, #14070, #6438, #21264, #26698, #41545, #76208, #75337 ),
 .UNSPECIFIED., .F., .F.,
 ( 4, 2, 2, 2, 4 ),
 ( 0.0007817359527651104954, 0.0009771254036996493593, 0.001172514854634188223, 0.001367904305568727087, 0.001563293756503265951 ),
 .UNSPECIFIED. ) ;
#78421 = DIRECTION ( 'NONE',  ( 0.000000000000000000, 0.9848077530122072432, -0.1736481776669354937 ) ) ;
#78422 = EDGE_CURVE ( 'NONE', #38805, #31074, #38424, .T. ) ;
#78423 = FACE_BOUND ( 'NONE', #72578, .T. ) ;
#78424 = VERTEX_POINT ( 'NONE', #1164 ) ;
#78425 = B_SPLINE_CURVE_WITH_KNOTS ( 'NONE', 3,
 ( #26795, #12834, #47500, #54699, #18720, #67343, #13279, #74992, #87628, #32660 ),
 .UNSPECIFIED., .F., .F.,
 ( 4, 2, 2, 2, 4 ),
 ( 0.000000000000000000, 0.0001954339857564079352, 0.0003908679715128158703, 0.0005863019572692237513, 0.0007817359430256317406 ),
 .UNSPECIFIED. ) ;
#78426 = CARTESIAN_POINT ( 'NONE',  ( 13.25446741488368829, -11.04286588640298561, 33.62463336215343901 ) ) ;
#78427 = EDGE_CURVE ( 'NONE', #46262, #26954, #30413, .T. ) ;
#78428 = CARTESIAN_POINT ( 'NONE',  ( -14.05763799605399278, -5.728107161865378494, 34.42597550085002922 ) ) ;
#78429 = CARTESIAN_POINT ( 'NONE',  ( -11.53846153846153655, -2.833524468853757305, 32.15551576947925838 ) ) ;
#78430 = CARTESIAN_POINT ( 'NONE',  ( -1.253824943648434109, -2.845873456487965747, 32.17976146951972538 ) ) ;
#78431 = ORIENTED_EDGE ( 'NONE', *, *, #84734, .T. ) ;
#78432 = CARTESIAN_POINT ( 'NONE',  ( -19.50000000000000000, -3.499999999999999556, 29.75000000000000355 ) ) ;
#78433 = ORIENTED_EDGE ( 'NONE', *, *, #20139, .F. ) ;
#78434 = ORIENTED_EDGE ( 'NONE', *, *, #20750, .F. ) ;
#78435 = EDGE_CURVE ( 'NONE', #25168, #67178, #15132, .T. ) ;
#78437 = DIRECTION ( 'NONE',  ( -0.000000000000000000, -0.1736481776669307198, -0.9848077530122080203 ) ) ;
#78436 = CARTESIAN_POINT ( 'NONE',  ( -7.384615384615385025, -3.499999999999999556, 29.75000000000000355 ) ) ;
#78438 = CYLINDRICAL_SURFACE ( 'NONE', #6828, 0.2500000000000002220 ) ;
#78439 = CARTESIAN_POINT ( 'NONE',  ( -3.930834802233302394, -4.187068189119697692, 33.49521262558774026 ) ) ;
#78440 = CARTESIAN_POINT ( 'NONE',  ( 17.29988598048456439, -7.369474270740072441, 34.74850911626239736 ) ) ;
#78441 = CYLINDRICAL_SURFACE ( 'NONE', #73540, 0.2499999999999973355 ) ;
#78442 = EDGE_LOOP ( 'NONE', ( #55154, #55042, #63266, #36665 ) ) ;
#78443 = CARTESIAN_POINT ( 'NONE',  ( 6.792386319966619013, -2.494641256782728966, 31.33461815524612959 ) ) ;
#78444 = CARTESIAN_POINT ( 'NONE',  ( 17.99999999999987566, -3.643525952248796163, 33.31231777344771672 ) ) ;
#78445 = CARTESIAN_POINT ( 'NONE',  ( -0.4615384615384611200, -4.945431358278436385, 36.03766855953609394 ) ) ;
#78446 = CARTESIAN_POINT ( 'NONE',  ( 14.53047197667036805, -2.612705202774698421, 31.66806509827799943 ) ) ;
#78447 = VERTEX_POINT ( 'NONE', #28646 ) ;
#78448 = VERTEX_POINT ( 'NONE', #64179 ) ;
#78449 = FACE_BOUND ( 'NONE', #50116, .T. ) ;
#78450 = CARTESIAN_POINT ( 'NONE',  ( 11.78851595837499211, -12.41089969410671223, 31.60739465890703670 ) ) ;
#78451 = CARTESIAN_POINT ( 'NONE',  ( -11.31568199719312773, -11.89424750095246175, 32.13594075562311758 ) ) ;
#78452 = EDGE_LOOP ( 'NONE', ( #33688, #54657, #77148, #84479 ) ) ;
#78453 = VECTOR ( 'NONE', #13855, 1000.000000000000000 ) ;
#78454 = CARTESIAN_POINT ( 'NONE',  ( 9.692307692307695177, -1.044019251281081972, 31.83374038241031911 ) ) ;
#78455 = CARTESIAN_POINT ( 'NONE',  ( -2.241623956689868358, -4.098570777380720287, 33.41473453929635440 ) ) ;
#78456 = FACE_OUTER_BOUND ( 'NONE', #2981, .T. ) ;
#78457 = EDGE_CURVE ( 'NONE', #5283, #32510, #55638, .T. ) ;
#78458 = CARTESIAN_POINT ( 'NONE',  ( -0.4615384615384611200, -2.249999999999998668, 29.75000000000001776 ) ) ;
#78459 = VERTEX_POINT ( 'NONE', #49358 ) ;
#78460 = CARTESIAN_POINT ( 'NONE',  ( -7.596099534515528440, -10.66356715214248752, 33.62249196103329751 ) ) ;
#78461 = ORIENTED_EDGE ( 'NONE', *, *, #5763, .T. ) ;
#78463 = EDGE_LOOP ( 'NONE', ( #67900, #17275 ) ) ;
#78462 = CARTESIAN_POINT ( 'NONE',  ( 13.60762822870878352, -8.282913670948747864, 34.94150082978203642 ) ) ;
#78464 = CARTESIAN_POINT ( 'NONE',  ( 15.48082354240754555, -8.303483539816731707, 34.68545999027711702 ) ) ;
#78465 = CARTESIAN_POINT ( 'NONE',  ( 15.00728430620490172, -4.988325925672468131, 34.36044203135681130 ) ) ;
#78466 = DIRECTION ( 'NONE',  ( 1.000000000000000000, 0.000000000000000000, 0.000000000000000000 ) ) ;
#78467 = CARTESIAN_POINT ( 'NONE',  ( -14.98076923076781064, -7.500000000000154543, 35.00000000000007105 ) ) ;
#78468 = DIRECTION ( 'NONE',  ( 1.000000000000000000, 0.000000000000000000, 0.000000000000000000 ) ) ;
#78469 = B_SPLINE_CURVE_WITH_KNOTS ( 'NONE', 3,
 ( #30054, #57519, #83686, #8461, #51175, #69707, #29618, #23286, #15658, #78681 ),
 .UNSPECIFIED., .F., .F.,
 ( 4, 2, 2, 2, 4 ),
 ( 0.0007817246256747476061, 0.0009771112852218911526, 0.001172497944769034916, 0.001367884604316178462, 0.001563271263863322009 ),
 .UNSPECIFIED. ) ;
#78470 = CARTESIAN_POINT ( 'NONE',  ( -1.384615384615383471, -12.37446782046654192, 30.86335684631486131 ) ) ;
#78471 = B_SPLINE_CURVE_WITH_KNOTS ( 'NONE', 3,
 ( #61957, #12018, #88582, #75048, #81363, #13774, #47997, #6138, #25960, #80474 ),
 .UNSPECIFIED., .F., .F.,
 ( 4, 2, 2, 2, 4 ),
 ( 0.0007817246256747494492, 0.0009771112852218935378, 0.001172497944769037518, 0.001367884604316181498, 0.001563271263863325695 ),
 .UNSPECIFIED. ) ;
#78472 = CARTESIAN_POINT ( 'NONE',  ( 1.077988221561497539, -10.27530806549875386, 14.95499329374151642 ) ) ;
#78473 = ORIENTED_EDGE ( 'NONE', *, *, #59061, .F. ) ;
#78474 = B_SPLINE_CURVE_WITH_KNOTS ( 'NONE', 3,
 ( #3021, #22856, #71933, #15675, #43142, #16545, #57973, #10244, #77803, #64721 ),
 .UNSPECIFIED., .F., .F.,
 ( 4, 2, 2, 2, 4 ),
 ( 0.0007817359430256320659, 0.0009771253907249987086, 0.001172514838424365460, 0.001367904286123731994, 0.001563293733823098745 ),
 .UNSPECIFIED. ) ;
#78475 = DIRECTION ( 'NONE',  ( -0.000000000000000000, 0.1736481776669307198, -0.9848077530122080203 ) ) ;
#78476 = CARTESIAN_POINT ( 'NONE',  ( -3.230769230769352962, -12.51329471203414379, 31.30864560766407578 ) ) ;
#78478 = VERTEX_POINT ( 'NONE', #70066 ) ;
#78477 = VECTOR ( 'NONE', #10117, 1000.000000000000114 ) ;
#78479 = ORIENTED_EDGE ( 'NONE', *, *, #75807, .T. ) ;
#78480 = CARTESIAN_POINT ( 'NONE',  ( 10.61538461538461675, -8.164416787775445883, 34.95778746994557906 ) ) ;
#78481 = DIRECTION ( 'NONE',  ( -0.000000000000000000, -0.000000000000000000, -1.000000000000000000 ) ) ;
#78482 = CARTESIAN_POINT ( 'NONE',  ( 6.066068351002440906, -11.16473453929635440, 33.15142922261926373 ) ) ;
#78483 = AXIS2_PLACEMENT_3D ( 'NONE', #41175, #20010, #6938 ) ;
#78484 = CARTESIAN_POINT ( 'NONE',  ( 0.5266832422580927098, -7.750023224968865421, 34.99404313364389907 ) ) ;
#78485 = CARTESIAN_POINT ( 'NONE',  ( 10.55011416942384272, -4.481592998940162609, 33.73612834413957984 ) ) ;
#78486 = DIRECTION ( 'NONE',  ( -0.000000000000000000, 0.000000000000000000, 1.000000000000000000 ) ) ;
#78487 = CARTESIAN_POINT ( 'NONE',  ( -7.846153846153844924, -1.422936976036506707, 30.56769352161908415 ) ) ;
#78488 = ORIENTED_EDGE ( 'NONE', *, *, #38199, .F. ) ;
#78489 = CARTESIAN_POINT ( 'NONE',  ( 6.000000000000001776, -10.51840700105979565, 33.73612834413961536 ) ) ;
#78490 = CARTESIAN_POINT ( 'NONE',  ( -17.32692307692307665, -7.500000000000001776, 34.75000000000000000 ) ) ;
#78491 = EDGE_CURVE ( 'NONE', #50611, #83181, #8374, .T. ) ;
#78492 = CARTESIAN_POINT ( 'NONE',  ( -3.230769230769229949, -2.486705287966279876, 31.30864560766543647 ) ) ;
#78493 = LINE ( 'NONE', #16794, #34970 ) ;
#78494 = EDGE_LOOP ( 'NONE', ( #85494, #84075, #30892, #72587 ) ) ;
#78495 = CARTESIAN_POINT ( 'NONE',  ( -5.448717948717948012, -7.500000000000000000, 29.75000000000000355 ) ) ;
#78496 = ADVANCED_FACE ( 'NONE', ( #1613 ), #29101, .F. ) ;
#78497 = ORIENTED_EDGE ( 'NONE', *, *, #57673, .F. ) ;
#78498 = CARTESIAN_POINT ( 'NONE',  ( 12.21151523731700372, -9.356822207818506598, 34.66110646841856635 ) ) ;
#78499 = CARTESIAN_POINT ( 'NONE',  ( -3.230769230769229949, -2.721908614388771852, 31.22303859784724978 ) ) ;
#78500 = CARTESIAN_POINT ( 'NONE',  ( 6.000000000000001776, -12.62096338111211580, 30.90682066428153263 ) ) ;
#78501 = EDGE_LOOP ( 'NONE', ( #12631, #23132 ) ) ;
#78502 = EDGE_CURVE ( 'NONE', #20537, #18188, #9393, .T. ) ;
#78503 = DIRECTION ( 'NONE',  ( -0.000000000000000000, 0.000000000000000000, 1.000000000000000000 ) ) ;
#78504 = CARTESIAN_POINT ( 'NONE',  ( -10.61538461538461320, -10.51840700105979565, 33.73612834413961536 ) ) ;
#78505 = B_SPLINE_CURVE_WITH_KNOTS ( 'NONE', 3,
 ( #54197, #13229, #53762, #46123, #5136, #80365, #25407, #33934, #19536, #60071 ),
 .UNSPECIFIED., .F., .F.,
 ( 4, 2, 2, 2, 4 ),
 ( 0.0007817359430256392216, 0.0009771253907250080327, 0.001172514838424376952, 0.001367904286123745872, 0.001563293733823114791 ),
 .UNSPECIFIED. ) ;
#78506 = DIRECTION ( 'NONE',  ( -0.000000000000000000, 0.1736481776669307198, -0.9848077530122080203 ) ) ;
#78507 = EDGE_CURVE ( 'NONE', #51867, #18418, #7319, .T. ) ;
#78508 = B_SPLINE_CURVE_WITH_KNOTS ( 'NONE', 3,
 ( #229, #26815, #34008, #53840, #61473, #41661, #69129, #33126, #87647, #25924 ),
 .UNSPECIFIED., .F., .F.,
 ( 4, 2, 2, 2, 4 ),
 ( 0.000000000000000000, 0.0001954311564186861697, 0.0003908623128373723394, 0.0005862934692560584820, 0.0007817246256747446788 ),
 .UNSPECIFIED. ) ;
#78509 = B_SPLINE_CURVE_WITH_KNOTS ( 'NONE', 3,
 ( #25209, #87373, #81498, #53109, #52671, #87829, #32855, #19344, #80615, #5828 ),
 .UNSPECIFIED., .F., .F.,
 ( 4, 2, 2, 2, 4 ),
 ( 0.000000000000000000, 0.0001954339857564090194, 0.0003908679715128180387, 0.0005863019572692270039, 0.0007817359430256360774 ),
 .UNSPECIFIED. ) ;
#78510 = CARTESIAN_POINT ( 'NONE',  ( -9.469294848214296678, -3.395485233115139057, 33.02377354290275946 ) ) ;
#78511 = B_SPLINE_CURVE_WITH_KNOTS ( 'NONE', 3,
 ( #46805, #86934, #5822, #24752, #33300, #74283, #25200, #25647, #67525, #18891 ),
 .UNSPECIFIED., .F., .F.,
 ( 4, 2, 2, 2, 4 ),
 ( 0.000000000000000000, 0.0001954311564186863052, 0.0003908623128373726104, 0.0005862934692560589156, 0.0007817246256747452209 ),
 .UNSPECIFIED. ) ;
#78512 = VERTEX_POINT ( 'NONE', #66421 ) ;
#78513 = CARTESIAN_POINT ( 'NONE',  ( -14.30769230769230660, -13.75783147151868846, 33.36296068462461051 ) ) ;
#78514 = ORIENTED_EDGE ( 'NONE', *, *, #35986, .T. ) ;
#78515 = ADVANCED_FACE ( 'NONE', ( #72279 ), #10592, .F. ) ;
#78516 = CARTESIAN_POINT ( 'NONE',  ( -2.294871794871794712, -7.500000000000000000, 33.75000000000000000 ) ) ;
#78517 = CARTESIAN_POINT ( 'NONE',  ( -16.15384615384615330, -11.16473453929635440, 33.15142922261926373 ) ) ;
#78518 = DIRECTION ( 'NONE',  ( -0.000000000000000000, 1.000000000000000000, 3.491481338843133355E-15 ) ) ;
#78519 = VECTOR ( 'NONE', #95, 1000.000000000000227 ) ;
#78520 = CARTESIAN_POINT ( 'NONE',  ( -9.942284436356283450, -8.347322224742351082, 34.93158281831414058 ) ) ;
#78521 = CARTESIAN_POINT ( 'NONE',  ( 16.08776377448601025, -11.91647553114624181, 32.58852847137148245 ) ) ;
#78522 = ORIENTED_EDGE ( 'NONE', *, *, #84019, .T. ) ;
#78523 = ORIENTED_EDGE ( 'NONE', *, *, #61888, .F. ) ;
#78524 = VERTEX_POINT ( 'NONE', #65522 ) ;
#78525 = VERTEX_POINT ( 'NONE', #79937 ) ;
#78526 = CARTESIAN_POINT ( 'NONE',  ( -10.61538461538461320, -8.120952969808772792, 34.71129190930000163 ) ) ;
#78527 = CARTESIAN_POINT ( 'NONE',  ( -6.166666666666667851, -3.499999999999999556, 29.75000000000000355 ) ) ;
#78528 = CARTESIAN_POINT ( 'NONE',  ( -15.23076923076922995, -8.973038597847269315, 34.52809138561121927 ) ) ;
#78529 = ADVANCED_FACE ( 'NONE', ( #71835 ), #65964, .F. ) ;
#78530 = CARTESIAN_POINT ( 'NONE',  ( -4.283994123577850921, -12.50552854090298993, 31.33409797877408920 ) ) ;
#78531 = CARTESIAN_POINT ( 'NONE',  ( -13.51476335434707821, -3.625366637846544116, 33.29286588640298561 ) ) ;
#78532 = CARTESIAN_POINT ( 'NONE',  ( 3.007843013253083786, -5.667676309546437530, 34.40238873228292249 ) ) ;
#78533 = ADVANCED_FACE ( 'NONE', ( #30847 ), #85810, .F. ) ;
#78534 = CARTESIAN_POINT ( 'NONE',  ( -17.77722045873158763, -10.11255958852956027, 34.01340905677048454 ) ) ;
#78535 = CARTESIAN_POINT ( 'NONE',  ( -5.142173008697161762, -2.255955759149247619, 30.00000000000013856 ) ) ;
#78536 = ORIENTED_EDGE ( 'NONE', *, *, #39496, .F. ) ;
#78537 = VERTEX_POINT ( 'NONE', #79496 ) ;
#78538 = CIRCLE ( 'NONE', #39744, 4.000000000000000000 ) ;
#78539 = ORIENTED_EDGE ( 'NONE', *, *, #15160, .T. ) ;
#78542 = ORIENTED_EDGE ( 'NONE', *, *, #79821, .T. ) ;
#78541 = EDGE_CURVE ( 'NONE', #72099, #16365, #45700, .T. ) ;
#78540 = CARTESIAN_POINT ( 'NONE',  ( 11.53846153846153832, -2.486705287966279876, 31.30864560766543647 ) ) ;
#78544 = CARTESIAN_POINT ( 'NONE',  ( -17.77698715590659972, -11.43677907613344757, 33.22367315496203588 ) ) ;
#78543 = CARTESIAN_POINT ( 'NONE',  ( 0.7115927731767760500, -8.303483539816728154, 34.68545999027711702 ) ) ;
#78545 = DIRECTION ( 'NONE',  ( 0.000000000000000000, 0.8660254037844377084, -0.5000000000000015543 ) ) ;
#78546 = CARTESIAN_POINT ( 'NONE',  ( 4.284371855609715674, -2.619367082507848554, 30.83698974864644171 ) ) ;
#78547 = VERTEX_POINT ( 'NONE', #17798 ) ;
#78548 = EDGE_CURVE ( 'NONE', #80310, #45473, #34107, .T. ) ;
#78549 = ORIENTED_EDGE ( 'NONE', *, *, #68012, .F. ) ;
#78550 = CARTESIAN_POINT ( 'NONE',  ( -9.692307692307691624, -12.10708131394839349, 31.69288490824020244 ) ) ;
#78551 = ORIENTED_EDGE ( 'NONE', *, *, #5225, .T. ) ;
#78552 = FACE_BOUND ( 'NONE', #59925, .T. ) ;
#78553 = CARTESIAN_POINT ( 'NONE',  ( 13.44987052412822059, -12.51329471203373345, 31.30864560766537963 ) ) ;
#78554 = CARTESIAN_POINT ( 'NONE',  ( -14.43838291080261627, -6.369640206132551441, 34.87707690430378449 ) ) ;
#78555 = VERTEX_POINT ( 'NONE', #72723 ) ;
#78556 = CARTESIAN_POINT ( 'NONE',  ( -0.2115384615384616196, -2.249999999999998668, 29.75000000000000355 ) ) ;
#78557 = CARTESIAN_POINT ( 'NONE',  ( 11.47237915910140771, -6.343179335718451384, 34.87096338111212646 ) ) ;
#78558 = CARTESIAN_POINT ( 'NONE',  ( -9.692307692307691624, -2.708943851104267164, 35.45975837776705220 ) ) ;
#78559 = VERTEX_POINT ( 'NONE', #4726 ) ;
#78560 = CARTESIAN_POINT ( 'NONE',  ( -5.076923076923075762, -1.466349020453238561, 30.81389545987213907 ) ) ;
#78561 = CARTESIAN_POINT ( 'NONE',  ( 1.607395053593451140, -2.612705202774697533, 31.66806509827799943 ) ) ;
#78562 = ADVANCED_FACE ( 'NONE', ( #31755 ), #59657, .T. ) ;
#78563 = ORIENTED_EDGE ( 'NONE', *, *, #21103, .T. ) ;
#78564 = B_SPLINE_CURVE_WITH_KNOTS ( 'NONE', 3,
 ( #32562, #60035, #87541, #25817, #74009, #19059, #12300, #67249, #56711, #16603 ),
 .UNSPECIFIED., .F., .F.,
 ( 4, 2, 2, 2, 4 ),
 ( 0.0007817359430256252354, 0.0009771253907249898181, 0.001172514838424354401, 0.001367904286123718983, 0.001563293733823083566 ),
 .UNSPECIFIED. ) ;
#78565 = EDGE_CURVE ( 'NONE', #75626, #16317, #63128, .T. ) ;
#78566 = CARTESIAN_POINT ( 'NONE',  ( 3.480823542407546434, -8.303483539816728154, 34.68545999027711702 ) ) ;
#78567 = CARTESIAN_POINT ( 'NONE',  ( -9.627052552794857831, -9.528491918058460186, 34.59228464037086326 ) ) ;
#78568 = CARTESIAN_POINT ( 'NONE',  ( 24.00000000000000000, -5.499999999999981348, 27.75000000000000000 ) ) ;
#78569 = CARTESIAN_POINT ( 'NONE',  ( -7.623142494540996239, -6.503523203565941380, 34.64991518177335195 ) ) ;
#78570 = CARTESIAN_POINT ( 'NONE',  ( -16.08777780284371772, -8.120952969808772792, 34.71129190929999453 ) ) ;
#78571 = CARTESIAN_POINT ( 'NONE',  ( -10.61538461538461320, -5.557115091759785130, 34.35708131394839171 ) ) ;
#78573 = EDGE_CURVE ( 'NONE', #76766, #58189, #35223, .T. ) ;
#78572 = CYLINDRICAL_SURFACE ( 'NONE', #4190, 0.2499999999999979738 ) ;
#78574 = CARTESIAN_POINT ( 'NONE',  ( 7.846153846153846700, -2.833524468853757305, 32.15551576947925838 ) ) ;
#78576 = CARTESIAN_POINT ( 'NONE',  ( 17.07692307692307665, -3.937682226553329556, 33.60647404775216529 ) ) ;
#78575 = CARTESIAN_POINT ( 'NONE',  ( 4.153846153846032507, -12.27809138561165270, 31.22303859784587132 ) ) ;
#78577 = CARTESIAN_POINT ( 'NONE',  ( 1.634560902963529738, -11.37275283266503756, 32.91324779482534524 ) ) ;
#78579 = CARTESIAN_POINT ( 'NONE',  ( -10.74607608205217346, -8.147922237126337563, 34.70805685702651999 ) ) ;
#78578 = CARTESIAN_POINT ( 'NONE',  ( 12.71153846153988098, -7.500000000000154543, 35.00000000000007105 ) ) ;
#78580 = CARTESIAN_POINT ( 'NONE',  ( -2.437840277424001112, -5.915902021225892149, 34.75552854090298638 ) ) ;
#78581 = CARTESIAN_POINT ( 'NONE',  ( 2.750000000000001332, -7.438900925035452083, 21.71688170625848713 ) ) ;
#78582 = EDGE_CURVE ( 'NONE', #69466, #6010, #88936, .T. ) ;
#78583 = ORIENTED_EDGE ( 'NONE', *, *, #6917, .T. ) ;
#78584 = CARTESIAN_POINT ( 'NONE',  ( 1.732862688310258026, -4.223057123557754977, 14.00000000000000533 ) ) ;
#78585 = EDGE_LOOP ( 'NONE', ( #80508, #8715, #53381, #64463 ) ) ;
#78586 = CARTESIAN_POINT ( 'NONE',  ( -5.076923076923197442, -10.90142922262034020, 33.41473453929536674 ) ) ;
#78587 = ORIENTED_EDGE ( 'NONE', *, *, #2709, .T. ) ;
#78588 = CARTESIAN_POINT ( 'NONE',  ( -4.023320452082591814, -11.46989282347013095, 32.79007818306219946 ) ) ;
#78590 = ORIENTED_EDGE ( 'NONE', *, *, #57181, .T. ) ;
#78589 = VECTOR ( 'NONE', #80507, 1000.000000000000114 ) ;
#78591 = CARTESIAN_POINT ( 'NONE',  ( 5.777073041093149897, -10.77366814457252175, 33.85459836347579454 ) ) ;
#78592 = CARTESIAN_POINT ( 'NONE',  ( -1.077988221561460236, -10.27530806549876452, 25.85750670625849068 ) ) ;
#78593 = DIRECTION ( 'NONE',  ( -0.000000000000000000, -0.000000000000000000, -1.000000000000000000 ) ) ;
#78594 = CARTESIAN_POINT ( 'NONE',  ( 9.757563263583717728, -11.48612834413965977, 32.76840700105972815 ) ) ;
#78595 = CARTESIAN_POINT ( 'NONE',  ( 7.053867364043872712, -9.929761469519744921, 34.40412654351204225 ) ) ;
#78596 = DIRECTION ( 'NONE',  ( -0.000000000000000000, 0.8660254037844399289, -0.4999999999999980016 ) ) ;
#78597 = DIRECTION ( 'NONE',  ( 0.000000000000000000, 0.000000000000000000, 1.000000000000000000 ) ) ;
#78598 = CARTESIAN_POINT ( 'NONE',  ( -7.780085495151407571, -2.721908614388772296, 31.22303859784725333 ) ) ;
#78599 = CARTESIAN_POINT ( 'NONE',  ( 0.6845513056318561773, -2.523321265292116422, 31.42251411153756990 ) ) ;
#78600 = CARTESIAN_POINT ( 'NONE',  ( -2.651650429449535551, -10.15165042944956753, 18.68750000000000000 ) ) ;
#78601 = CARTESIAN_POINT ( 'NONE',  ( 18.25005441991345378, -11.47946981652013498, 33.17500667209846910 ) ) ;
#78602 = CARTESIAN_POINT ( 'NONE',  ( 7.846153846153846700, -12.10708131394839349, 31.69288490824020244 ) ) ;
#78603 = CARTESIAN_POINT ( 'NONE',  ( 13.44987095589141468, -4.481592998940250538, 33.73612834413965089 ) ) ;
#78604 = B_SPLINE_CURVE_WITH_KNOTS ( 'NONE', 3,
 ( #46949, #47395, #35215, #82540, #88860, #74889, #7755, #14060, #553, #74436 ),
 .UNSPECIFIED., .F., .F.,
 ( 4, 2, 2, 2, 4 ),
 ( 0.0007817246256747483650, 0.0009771112852218926705, 0.001172497944769037084, 0.001367884604316181498, 0.001563271263863325695 ),
 .UNSPECIFIED. ) ;
#78605 = CARTESIAN_POINT ( 'NONE',  ( 1.553300858899129944, -11.24999999999998934, 18.45312500000000355 ) ) ;
#78606 = B_SPLINE_CURVE_WITH_KNOTS ( 'NONE', 3,
 ( #27445, #47263, #75195, #13922, #40528, #20247, #68865, #6723, #81959, #76065 ),
 .UNSPECIFIED., .F., .F.,
 ( 4, 2, 2, 2, 4 ),
 ( 0.0007817246256747459798, 0.0009771112852218896347, 0.001172497944769033398, 0.001367884604316177161, 0.001563271263863320708 ),
 .UNSPECIFIED. ) ;
#78607 = ORIENTED_EDGE ( 'NONE', *, *, #40740, .T. ) ;
#78608 = B_SPLINE_CURVE_WITH_KNOTS ( 'NONE', 3,
 ( #277, #82705, #20976, #35390, #76831, #48449, #75935, #41709, #69179, #34940 ),
 .UNSPECIFIED., .F., .F.,
 ( 4, 2, 2, 2, 4 ),
 ( 0.000000000000000000, 0.0001954339857564090194, 0.0003908679715128180387, 0.0005863019572692270039, 0.0007817359430256360774 ),
 .UNSPECIFIED. ) ;
#78609 = DIRECTION ( 'NONE',  ( -0.000000000000000000, -0.000000000000000000, -1.000000000000000000 ) ) ;
#78610 = CARTESIAN_POINT ( 'NONE',  ( 11.66898724022510514, -6.001044277235009439, 34.52024696741798948 ) ) ;
#78611 = DIRECTION ( 'NONE',  ( -0.000000000000000000, -0.7660444431189791237, -0.6427876096865379196 ) ) ;
#78612 = CARTESIAN_POINT ( 'NONE',  ( 15.93096663710857186, -7.630690623152299956, 34.99857592706774057 ) ) ;
#78613 = DIRECTION ( 'NONE',  ( 1.000000000000000000, -0.000000000000000000, -0.000000000000000000 ) ) ;
#78614 = AXIS2_PLACEMENT_3D ( 'NONE', #5966, #75737, #46500 ) ;
#78615 = CARTESIAN_POINT ( 'NONE',  ( -14.24162497434223340, -3.937682226553329556, 33.60647404775216529 ) ) ;
#78616 = EDGE_CURVE ( 'NONE', #19254, #49385, #12369, .T. ) ;
#78617 = AXIS2_PLACEMENT_3D ( 'NONE', #23834, #86006, #31502 ) ;
#78618 = ORIENTED_EDGE ( 'NONE', *, *, #75633, .F. ) ;
#78619 = CARTESIAN_POINT ( 'NONE',  ( -10.36538461538319389, -7.500000000000154543, 35.00000000000007105 ) ) ;
#78620 = ORIENTED_EDGE ( 'NONE', *, *, #58823, .F. ) ;
#78621 = EDGE_CURVE ( 'NONE', #29336, #72117, #52462, .T. ) ;
#78622 = VERTEX_POINT ( 'NONE', #81278 ) ;
#78623 = CARTESIAN_POINT ( 'NONE',  ( 7.623226887246995709, -10.77366814457251998, 33.85459836347579454 ) ) ;
#78624 = CARTESIAN_POINT ( 'NONE',  ( 18.25000000000000000, -2.249999999999998668, 29.75000000000000355 ) ) ;
#78625 = DIRECTION ( 'NONE',  ( 0.000000000000000000, 0.1736481776669275834, 0.9848077530122086864 ) ) ;
#78626 = CARTESIAN_POINT ( 'NONE',  ( 2.307692307692187583, -6.026961402154118908, 34.52809138561165270 ) ) ;
#78627 = CARTESIAN_POINT ( 'NONE',  ( -5.299850035829924089, -8.282780595021769443, 34.94152052738834868 ) ) ;
#78629 = EDGE_CURVE ( 'NONE', #23503, #82006, #15941, .T. ) ;
#78628 = ORIENTED_EDGE ( 'NONE', *, *, #26808, .F. ) ;
#78630 = DIRECTION ( 'NONE',  ( 0.000000000000000000, 0.000000000000000000, 1.000000000000000000 ) ) ;
#78631 = ORIENTED_EDGE ( 'NONE', *, *, #54144, .T. ) ;
#78632 = VECTOR ( 'NONE', #1397, 1000.000000000000000 ) ;
#78633 = VERTEX_POINT ( 'NONE', #26322 ) ;
#78634 = B_SPLINE_CURVE_WITH_KNOTS ( 'NONE', 3,
 ( #51940, #11414, #17735, #37999, #3761, #86204, #79876, #78531, #58705, #45187 ),
 .UNSPECIFIED., .F., .F.,
 ( 4, 2, 2, 2, 4 ),
 ( 0.000000000000000000, 0.0001954311564186858715, 0.0003908623128373717431, 0.0005862934692560576146, 0.0007817246256747434861 ),
 .UNSPECIFIED. ) ;
#78635 = B_SPLINE_CURVE_WITH_KNOTS ( 'NONE', 3,
 ( #41569, #55521, #7350, #83007, #34805, #62272, #588, #21289, #48763, #76234 ),
 .UNSPECIFIED., .F., .F.,
 ( 4, 2, 2, 2, 4 ),
 ( 0.0007817359430256323911, 0.0009771253907249991422, 0.001172514838424365893, 0.001367904286123732644, 0.001563293733823099396 ),
 .UNSPECIFIED. ) ;
#78636 = CARTESIAN_POINT ( 'NONE',  ( 18.13052543823364360, -2.372941743896878286, 30.88044141588253311 ) ) ;
#78637 = FACE_OUTER_BOUND ( 'NONE', #65554, .T. ) ;
#78638 = B_SPLINE_CURVE_WITH_KNOTS ( 'NONE', 3,
 ( #6238, #32814, #68368, #48088, #6667, #61606, #89111, #13865, #18856, #41346 ),
 .UNSPECIFIED., .F., .F.,
 ( 4, 2, 2, 2, 4 ),
 ( 0.0007817246256747474977, 0.0009771112852218909357, 0.001172497944769034482, 0.001367884604316178029, 0.001563271263863321575 ),
 .UNSPECIFIED. ) ;
#78639 = AXIS2_PLACEMENT_3D ( 'NONE', #54365, #4407, #66101 ) ;
#78640 = EDGE_CURVE ( 'NONE', #1333, #27068, #33960, .T. ) ;
#78641 = CYLINDRICAL_SURFACE ( 'NONE', #12066, 0.2500000000000009437 ) ;
#78642 = DIRECTION ( 'NONE',  ( 0.000000000000000000, 0.000000000000000000, -1.000000000000000000 ) ) ;
#78643 = CYLINDRICAL_SURFACE ( 'NONE', #13398, 4.000000000000000000 ) ;
#78644 = EDGE_CURVE ( 'NONE', #13666, #5455, #5080, .T. ) ;
#78645 = DIRECTION ( 'NONE',  ( -0.000000000000000000, 0.3420201433256694346, -0.9396926207859080948 ) ) ;
#78646 = AXIS2_PLACEMENT_3D ( 'NONE', #42306, #35538, #69759 ) ;
#78647 = ORIENTED_EDGE ( 'NONE', *, *, #36986, .T. ) ;
#78648 = ORIENTED_EDGE ( 'NONE', *, *, #80548, .F. ) ;
#78649 = CARTESIAN_POINT ( 'NONE',  ( -1.553300858899125059, -3.750000000000009326, 21.57812500000000355 ) ) ;
#78650 = EDGE_LOOP ( 'NONE', ( #62836, #86591, #7532, #22678 ) ) ;
#78652 = ORIENTED_EDGE ( 'NONE', *, *, #24124, .F. ) ;
#78651 = LINE ( 'NONE', #32251, #84743 ) ;
#78653 = CARTESIAN_POINT ( 'NONE',  ( 12.46153846153846168, -13.20930481340135110, 34.54067556320372745 ) ) ;
#78654 = DIRECTION ( 'NONE',  ( -1.000000000000000000, -0.000000000000000000, -0.000000000000000000 ) ) ;
#78655 = CARTESIAN_POINT ( 'NONE',  ( 6.000000000000001776, -6.681629849574314051, 35.83090037661290239 ) ) ;
#78656 = EDGE_LOOP ( 'NONE', ( #48829, #65847, #37744, #82196 ) ) ;
#78657 = EDGE_CURVE ( 'NONE', #31669, #15410, #64238, .T. ) ;
#78658 = CARTESIAN_POINT ( 'NONE',  ( -14.55771553191376100, -12.45566812827425451, 31.48439005359158926 ) ) ;
#78659 = EDGE_LOOP ( 'NONE', ( #74991, #12798, #88026, #87670 ) ) ;
#78660 = CARTESIAN_POINT ( 'NONE',  ( -9.019207513279361876, -4.818429247618089661, 34.26397095200675125 ) ) ;
#78661 = LINE ( 'NONE', #43542, #25602 ) ;
#78662 = FACE_OUTER_BOUND ( 'NONE', #82362, .T. ) ;
#78664 = DIRECTION ( 'NONE',  ( -0.000000000000000000, -0.000000000000000000, -1.000000000000000000 ) ) ;
#78663 = CARTESIAN_POINT ( 'NONE',  ( 6.000000000000001776, -12.34228464037088635, 31.77849191805839268 ) ) ;
#78665 = AXIS2_PLACEMENT_3D ( 'NONE', #29951, #7904, #7465 ) ;
#78666 = CARTESIAN_POINT ( 'NONE',  ( 5.010839665967194989, -2.538708090699994813, 30.37095296980875148 ) ) ;
#78667 = CARTESIAN_POINT ( 'NONE',  ( 17.07692307692307665, -2.292212530054420494, 30.41441678777542634 ) ) ;
#78668 = ORIENTED_EDGE ( 'NONE', *, *, #54075, .F. ) ;
#78669 = CARTESIAN_POINT ( 'NONE',  ( -18.22348494372394967, -10.81261337010820256, 33.49550067578627477 ) ) ;
#78670 =( NAMED_UNIT ( * ) SI_UNIT ( $, .STERADIAN. ) SOLID_ANGLE_UNIT ( ) );
#78672 = ORIENTED_EDGE ( 'NONE', *, *, #52098, .T. ) ;
#78671 = EDGE_CURVE ( 'NONE', #12765, #8388, #32045, .T. ) ;
#78673 = B_SPLINE_CURVE_WITH_KNOTS ( 'NONE', 3,
 ( #11322, #66263, #4567, #59508, #87012, #25284, #73484, #11776, #80693, #18975 ),
 .UNSPECIFIED., .F., .F.,
 ( 4, 2, 2, 2, 4 ),
 ( 0.000000000000000000, 0.0001954339857564092362, 0.0003908679715128184724, 0.0005863019572692276544, 0.0007817359430256369448 ),
 .UNSPECIFIED. ) ;
#78674 = AXIS2_PLACEMENT_3D ( 'NONE', #15008, #83921, #6908 ) ;
#78675 = B_SPLINE_CURVE_WITH_KNOTS ( 'NONE', 3,
 ( #65467, #73578, #86653, #85747, #18176, #52835, #24922, #51939, #44282, #45186 ),
 .UNSPECIFIED., .F., .F.,
 ( 4, 2, 2, 2, 4 ),
 ( 0.0007817359430256282712, 0.0009771253907249945886, 0.001172514838424360689, 0.001367904286123726790, 0.001563293733823093107 ),
 .UNSPECIFIED. ) ;
#78676 = CARTESIAN_POINT ( 'NONE',  ( 6.989145274079363368, -2.721908614388772296, 31.22303859784725333 ) ) ;
#78677 = DIRECTION ( 'NONE',  ( -0.000000000000000000, -0.9396926207859092051, -0.3420201433256662704 ) ) ;
#78678 = CARTESIAN_POINT ( 'NONE',  ( -4.153846153846152411, -2.538708090699994813, 30.37095296980875503 ) ) ;
#78679 = CARTESIAN_POINT ( 'NONE',  ( -39.05038313613820122, -2.249999999999998668, 29.75000000000000355 ) ) ;
#78680 = B_SPLINE_CURVE_WITH_KNOTS ( 'NONE', 3,
 ( #59095, #3261, #45137, #85692, #38390, #72611 ),
 .UNSPECIFIED., .F., .F.,
 ( 4, 2, 4 ),
 ( 0.0003909569690057869895, 0.0005862646681846149206, 0.0007815723673634428518 ),
 .UNSPECIFIED. ) ;
#78681 = CARTESIAN_POINT ( 'NONE',  ( 7.846153846153846700, -6.343179335718451384, 34.87096338111211935 ) ) ;
#78682 = EDGE_CURVE ( 'NONE', #75080, #69909, #53377, .T. ) ;
#78684 = EDGE_CURVE ( 'NONE', #29891, #8133, #84708, .T. ) ;
#78683 = CARTESIAN_POINT ( 'NONE',  ( 12.39626801557768943, -4.481592998940162609, 33.73612834413957984 ) ) ;
#78685 = FACE_BOUND ( 'NONE', #12700, .T. ) ;
#78687 = CARTESIAN_POINT ( 'NONE',  ( 20.00000000000000000, -4.000000000000000000, 29.75000000000000355 ) ) ;
#78686 = CARTESIAN_POINT ( 'NONE',  ( 5.076923076922953193, -5.941354392335915335, 34.76329471203413846 ) ) ;
#78688 = VECTOR ( 'NONE', #24201, 1000.000000000000227 ) ;
#78689 = CARTESIAN_POINT ( 'NONE',  ( 15.90382291655318880, -3.202444869320336451, 32.30641848906366675 ) ) ;
#78691 = CARTESIAN_POINT ( 'NONE',  ( 20.00000000000000000, -7.500000000000000000, 29.75000000000000355 ) ) ;
#78690 = CARTESIAN_POINT ( 'NONE',  ( -10.61538461538461320, -13.87047571288749737, 32.06866353760679544 ) ) ;
#78692 = CYLINDRICAL_SURFACE ( 'NONE', #5323, 0.2499999999999995559 ) ;
#78693 = CARTESIAN_POINT ( 'NONE',  ( 8.835299120233207404, -10.51840700105979565, 33.73612834413962247 ) ) ;
#78694 = CARTESIAN_POINT ( 'NONE',  ( 3.749999999999999556, -7.438900925035446754, 17.96688170625848713 ) ) ;
#78695 = VERTEX_POINT ( 'NONE', #31786 ) ;
#78696 = CARTESIAN_POINT ( 'NONE',  ( -4.283993363284374745, -11.93770438780619259, 32.05411857736982029 ) ) ;
#78697 = CARTESIAN_POINT ( 'NONE',  ( -4.153846153846273204, -3.300289026999228881, 32.46337939537708905 ) ) ;
#78698 = CARTESIAN_POINT ( 'NONE',  ( -9.692307692307691624, -8.973038597847269315, 34.52809138561121927 ) ) ;
#78699 = CARTESIAN_POINT ( 'NONE',  ( 16.85343815235874132, -8.539481045369598178, 34.89627647299170832 ) ) ;
#78700 = CARTESIAN_POINT ( 'NONE',  ( 7.846153846153846700, -4.786620604624113540, 33.94971097300155094 ) ) ;
#78701 = CARTESIAN_POINT ( 'NONE',  ( -5.326923076923085532, -2.499999999999999556, 29.81609845454692120 ) ) ;
#78702 = CARTESIAN_POINT ( 'NONE',  ( -3.724691934501229262, -9.114399933863657211, 19.76375670625849423 ) ) ;
#78703 = CARTESIAN_POINT ( 'NONE',  ( -16.28453675695646652, -5.496505350115500121, 34.60290016733514307 ) ) ;
#78704 = DIRECTION ( 'NONE',  ( 0.000000000000000000, 0.000000000000000000, 1.000000000000000000 ) ) ;
#78705 = CARTESIAN_POINT ( 'NONE',  ( 10.61538461538449418, -4.320704448113951379, 33.92786785259630022 ) ) ;
#78706 = CARTESIAN_POINT ( 'NONE',  ( 17.93391762063986050, -8.164416787775445883, 34.95778746994557906 ) ) ;
#78707 = CARTESIAN_POINT ( 'NONE',  ( -3.230769230769352962, -4.320704448113951379, 33.92786785259630022 ) ) ;
#78708 = FACE_OUTER_BOUND ( 'NONE', #3704, .T. ) ;
#78709 = VECTOR ( 'NONE', #87557, 1000.000000000000114 ) ;
#78710 = CARTESIAN_POINT ( 'NONE',  ( 20.99999999999999645, -4.249999999999998224, 29.75000000000000355 ) ) ;
#78711 = CARTESIAN_POINT ( 'NONE',  ( 7.134615384615385025, -11.50000000000000000, 29.75000000000000355 ) ) ;
#78712 = VERTEX_POINT ( 'NONE', #87632 ) ;
#78713 = CARTESIAN_POINT ( 'NONE',  ( 1.384615384615693667, -2.506253911140615021, 30.00000000000323297 ) ) ;
#78714 = DIRECTION ( 'NONE',  ( -0.000000000000000000, 1.000000000000000000, 3.491481338843133355E-15 ) ) ;
#78715 = VECTOR ( 'NONE', #69551, 1000.000000000000000 ) ;
#78716 = CARTESIAN_POINT ( 'NONE',  ( 1.614399933863618797, -3.775308065498751198, 13.23624329374151465 ) ) ;
#78717 = DIRECTION ( 'NONE',  ( -0.000000000000000000, -0.9396926207859093161, -0.3420201433256663259 ) ) ;
#78718 = CYLINDRICAL_SURFACE ( 'NONE', #82912, 0.2500000000000008882 ) ;
#78719 = ORIENTED_EDGE ( 'NONE', *, *, #22668, .F. ) ;
#78720 = DIRECTION ( 'NONE',  ( -0.000000000000000000, 1.000000000000000000, -0.000000000000000000 ) ) ;
#78721 = LINE ( 'NONE', #62214, #58877 ) ;
#78723 = EDGE_LOOP ( 'NONE', ( #37214, #10735 ) ) ;
#78722 = CARTESIAN_POINT ( 'NONE',  ( 12.21156173059610772, -5.728515186090277211, 34.42611988154120439 ) ) ;
#78724 = CARTESIAN_POINT ( 'NONE',  ( -13.38461538461538325, -9.905515769479276145, 34.41647553114623292 ) ) ;
#78725 = CYLINDRICAL_SURFACE ( 'NONE', #55590, 0.2499999999999994726 ) ;
#78726 = AXIS2_PLACEMENT_3D ( 'NONE', #87266, #72831, #38615 ) ;
#78727 = CARTESIAN_POINT ( 'NONE',  ( 5.076923076923075762, -11.11383981884818262, 36.00935417666054406 ) ) ;
#78728 = CARTESIAN_POINT ( 'NONE',  ( -14.30769230769230660, -2.249999999999998668, 29.50000000000001421 ) ) ;
#78729 = ORIENTED_EDGE ( 'NONE', *, *, #77378, .T. ) ;
#78730 = DIRECTION ( 'NONE',  ( 0.000000000000000000, 1.000000000000000000, 0.000000000000000000 ) ) ;
#78731 = CARTESIAN_POINT ( 'NONE',  ( 10.83839745947801170, -4.026326845037962343, 33.68677907613344047 ) ) ;
#78732 = CARTESIAN_POINT ( 'NONE',  ( 8.352564102564102200, -4.000000000000000000, 29.75000000000000355 ) ) ;
#78733 = VERTEX_POINT ( 'NONE', #10619 ) ;
#78734 = ORIENTED_EDGE ( 'NONE', *, *, #29362, .T. ) ;
#78735 = ORIENTED_EDGE ( 'NONE', *, *, #74310, .F. ) ;
#78736 = DIRECTION ( 'NONE',  ( -0.000000000000000000, -0.8660254037844399289, -0.4999999999999980016 ) ) ;
#78737 = LINE ( 'NONE', #31441, #9822 ) ;
#78738 = B_SPLINE_CURVE_WITH_KNOTS ( 'NONE', 3,
 ( #87167, #66431, #88500, #33086, #53354, #52459, #11490, #12378, #32210, #40742 ),
 .UNSPECIFIED., .F., .F.,
 ( 4, 2, 2, 2, 4 ),
 ( 0.0007817246256747530271, 0.0009771112852218974409, 0.001172497944769041638, 0.001367884604316185835, 0.001563271263863330249 ),
 .UNSPECIFIED. ) ;
#78739 = CYLINDRICAL_SURFACE ( 'NONE', #73978, 0.2499999999999993616 ) ;
#78740 = LINE ( 'NONE', #65219, #57824 ) ;
#78741 = ORIENTED_EDGE ( 'NONE', *, *, #65420, .F. ) ;
#78742 = VERTEX_POINT ( 'NONE', #25467 ) ;
#78744 = ORIENTED_EDGE ( 'NONE', *, *, #48550, .T. ) ;
#78743 = CARTESIAN_POINT ( 'NONE',  ( 10.83876010115703536, -2.251407671071270489, 29.88021292934942963 ) ) ;
#78745 = CARTESIAN_POINT ( 'NONE',  ( 12.52679360105129902, -11.67786785259547777, 32.92929555188713664 ) ) ;
#78746 = EDGE_CURVE ( 'NONE', #67493, #39653, #11628, .T. ) ;
#78747 = CARTESIAN_POINT ( 'NONE',  ( -8.638705067467206788, -12.45806712695776319, 30.39783852428763922 ) ) ;
#78748 = LINE ( 'NONE', #85514, #69784 ) ;
#78749 = ORIENTED_EDGE ( 'NONE', *, *, #77836, .F. ) ;
#78750 = ORIENTED_EDGE ( 'NONE', *, *, #57147, .T. ) ;
#78751 = ORIENTED_EDGE ( 'NONE', *, *, #4798, .T. ) ;
#78753 = ORIENTED_EDGE ( 'NONE', *, *, #50357, .T. ) ;
#78752 = DIRECTION ( 'NONE',  ( 0.000000000000000000, 0.000000000000000000, 1.000000000000000000 ) ) ;
#78754 = CARTESIAN_POINT ( 'NONE',  ( -5.076923076923075762, -5.180354513474913603, 36.12317359536750416 ) ) ;
#78755 = VECTOR ( 'NONE', #23492, 1000.000000000000000 ) ;
#78756 = CARTESIAN_POINT ( 'NONE',  ( -10.74607521849492464, -9.084618155246140248, 34.75535874321725771 ) ) ;
#78757 = ORIENTED_EDGE ( 'NONE', *, *, #75199, .T. ) ;
#78758 = EDGE_CURVE ( 'NONE', #29939, #61361, #65100, .T. ) ;
#78759 = CARTESIAN_POINT ( 'NONE',  ( 6.792516331335002988, -2.504760397472873823, 29.97295953869789997 ) ) ;
#78760 = CARTESIAN_POINT ( 'NONE',  ( -1.607541602131531189, -8.239355502252617924, 34.69524867566427417 ) ) ;
#78761 = CARTESIAN_POINT ( 'NONE',  ( 8.992010310499177095, -5.913360116392397892, 34.49180327182771322 ) ) ;
#78762 = VECTOR ( 'NONE', #71221, 1000.000000000000000 ) ;
#78763 = FACE_BOUND ( 'NONE', #53803, .T. ) ;
#78764 = CARTESIAN_POINT ( 'NONE',  ( 14.98074599347626368, -5.851115903089112003, 34.47074536777953568 ) ) ;
#78765 = CARTESIAN_POINT ( 'NONE',  ( 9.942307692307759126, -7.434744429011176159, 34.75000000000000711 ) ) ;
#78766 = CARTESIAN_POINT ( 'NONE',  ( -15.16470087976679615, -10.51840700105979565, 33.73612834413962247 ) ) ;
#78768 = DIRECTION ( 'NONE',  ( -0.000000000000000000, 0.5000000000000011102, -0.8660254037844381525 ) ) ;
#78767 = CARTESIAN_POINT ( 'NONE',  ( 16.40390057375960708, -4.074993327901525575, 33.72946981652012255 ) ) ;
#78769 = DIRECTION ( 'NONE',  ( -0.000000000000000000, 0.9396926207859092051, -0.3420201433256662704 ) ) ;
#78770 = CARTESIAN_POINT ( 'NONE',  ( 5.326977388561387805, -2.564540009722896752, 30.55348353981670684 ) ) ;
#78771 = VERTEX_POINT ( 'NONE', #17375 ) ;
#78772 = CARTESIAN_POINT ( 'NONE',  ( -15.93106648486808119, -3.563462043263029955, 33.22394488606062879 ) ) ;
#78773 = ORIENTED_EDGE ( 'NONE', *, *, #12075, .T. ) ;
#78774 = ORIENTED_EDGE ( 'NONE', *, *, #44070, .F. ) ;
#78776 = CARTESIAN_POINT ( 'NONE',  ( 1.254468175177166689, -10.88202310037936194, 33.43294751532457099 ) ) ;
#78775 = CARTESIAN_POINT ( 'NONE',  ( -11.78848476268299628, -12.68155406624981119, 30.59749803192733708 ) ) ;
#78777 = CARTESIAN_POINT ( 'NONE',  ( 11.47319153790521717, -8.656820664281498878, 34.87096338111211935 ) ) ;
#78778 = CARTESIAN_POINT ( 'NONE',  ( 2.372947447205147053, -2.379036618887895305, 30.90682066428159303 ) ) ;
#78779 = CARTESIAN_POINT ( 'NONE',  ( 17.99999999999987566, -12.51329471203414379, 31.30864560766407578 ) ) ;
#78780 = ORIENTED_EDGE ( 'NONE', *, *, #44442, .T. ) ;
#78781 = EDGE_CURVE ( 'NONE', #83912, #5662, #52484, .T. ) ;
#78782 = EDGE_CURVE ( 'NONE', #45673, #21173, #86299, .T. ) ;
#78783 = CARTESIAN_POINT ( 'NONE',  ( 18.06525513951284267, -2.657715359629131857, 31.77849191805844242 ) ) ;
#78784 = CARTESIAN_POINT ( 'NONE',  ( 0.2115617174898698494, -12.65889640711025521, 30.72598325615533454 ) ) ;
#78785 = CARTESIAN_POINT ( 'NONE',  ( -10.61538461538461320, -8.564572088678739092, 35.78748833219616898 ) ) ;
#78786 = DIRECTION ( 'NONE',  ( 0.000000000000000000, 0.000000000000000000, 1.000000000000000000 ) ) ;
#78787 = CARTESIAN_POINT ( 'NONE',  ( -17.01085574357300345, -2.486705287966280320, 31.30864560766543647 ) ) ;
#78788 = CARTESIAN_POINT ( 'NONE',  ( -1.553300858899125059, -3.750000000000009326, 19.07812500000000000 ) ) ;
#78789 = ORIENTED_EDGE ( 'NONE', *, *, #38287, .T. ) ;
#78790 = ORIENTED_EDGE ( 'NONE', *, *, #57378, .F. ) ;
#78791 = EDGE_CURVE ( 'NONE', #30670, #71085, #30903, .T. ) ;
#78792 = DIRECTION ( 'NONE',  ( 1.000000000000000000, 0.000000000000000000, 0.000000000000000000 ) ) ;
#78793 = ORIENTED_EDGE ( 'NONE', *, *, #38894, .T. ) ;
#78794 = CYLINDRICAL_SURFACE ( 'NONE', #39803, 0.2500000000000002220 ) ;
#78795 = CARTESIAN_POINT ( 'NONE',  ( 17.99999999999987566, -11.67786785259630911, 32.92929555188603530 ) ) ;
#78796 = CARTESIAN_POINT ( 'NONE',  ( -14.05763799605399278, -6.567000820036036579, 34.66262288849541306 ) ) ;
#78797 = CARTESIAN_POINT ( 'NONE',  ( 2.241935505177999222, -7.249945686854185389, 34.74374336980224598 ) ) ;
#78798 = CARTESIAN_POINT ( 'NONE',  ( -3.749999999999988454, -9.053300858899127945, 16.26562500000000000 ) ) ;
#78799 = CARTESIAN_POINT ( 'NONE',  ( 14.05771556364371655, -6.524016743844655686, 34.90889640711025521 ) ) ;
#78800 = ORIENTED_EDGE ( 'NONE', *, *, #59173, .F. ) ;
#78801 = DIRECTION ( 'NONE',  ( -0.000000000000000000, 0.9396926207859092051, -0.3420201433256662704 ) ) ;
#78803 = ORIENTED_EDGE ( 'NONE', *, *, #67680, .F. ) ;
#78802 = CARTESIAN_POINT ( 'NONE',  ( -2.307692307692305711, -12.62096338111211580, 30.90682066428153263 ) ) ;
#78804 = CARTESIAN_POINT ( 'NONE',  ( -9.942307692307691624, -7.566082377512564960, 35.00000000000000711 ) ) ;
#78806 = B_SPLINE_CURVE_WITH_KNOTS ( 'NONE', 3,
 ( #73523, #31640, #24873, #32519, #59994, #45142 ),
 .UNSPECIFIED., .F., .F.,
 ( 4, 2, 4 ),
 ( 0.0003909569690057875316, 0.0005862646681846158964, 0.0007815723673634442613 ),
 .UNSPECIFIED. ) ;
#78805 = CARTESIAN_POINT ( 'NONE',  ( -12.21148414990014963, -3.627508038966690496, 32.91356715214248396 ) ) ;
#78807 = DIRECTION ( 'NONE',  ( 0.000000000000000000, 0.3420201433256641055, -0.9396926207859100932 ) ) ;
#78808 = CARTESIAN_POINT ( 'NONE',  ( 0.5920641633020229389, -2.882268652242222728, 31.66798894389554064 ) ) ;
#78809 = LINE ( 'NONE', #17110, #59452 ) ;
#78810 = B_SPLINE_CURVE_WITH_KNOTS ( 'NONE', 3,
 ( #18071, #19, #21607, #55396, #13087, #34238 ),
 .UNSPECIFIED., .F., .F.,
 ( 4, 2, 4 ),
 ( 0.0003909569690057545718, 0.0005862646681845668905, 0.0007815723673633792092 ),
 .UNSPECIFIED. ) ;
#78811 = CARTESIAN_POINT ( 'NONE',  ( -12.46153846153858424, -3.643525952248795718, 33.31231777344771672 ) ) ;
#78812 = CARTESIAN_POINT ( 'NONE',  ( 15.45354877203763522, -11.41317474335729543, 32.86274602512330034 ) ) ;
#78813 = CARTESIAN_POINT ( 'NONE',  ( 0.06109907496451268821, -3.749999999999999556, 15.65811829374151287 ) ) ;
#78814 = ORIENTED_EDGE ( 'NONE', *, *, #7069, .T. ) ;
#78815 = CARTESIAN_POINT ( 'NONE',  ( -15.93106648486808119, -6.717445702608400460, 34.94155399931962336 ) ) ;
#78816 = CARTESIAN_POINT ( 'NONE',  ( 8.899756470994335089, -11.93748526763465279, 32.05452791011430946 ) ) ;
#78817 = CARTESIAN_POINT ( 'NONE',  ( -17.20761368003338632, -4.684245665217972032, 34.18127051446801090 ) ) ;
#78818 = CARTESIAN_POINT ( 'NONE',  ( -2.749999999999998224, -7.500000000000015987, 22.59375000000000355 ) ) ;
#78819 = B_SPLINE_CURVE_WITH_KNOTS ( 'NONE', 3,
 ( #27046, #40134, #60380, #5003, #4552, #66247, #26602, #73910, #32917, #54509 ),
 .UNSPECIFIED., .F., .F.,
 ( 4, 2, 2, 2, 4 ),
 ( 0.0007817246256747484735, 0.0009771112852218931041, 0.001172497944769037735, 0.001367884604316182365, 0.001563271263863326996 ),
 .UNSPECIFIED. ) ;
#78820 = CARTESIAN_POINT ( 'NONE',  ( 0.2386122440223122643, -3.586966769969700763, 32.86292498521069660 ) ) ;
#78821 = DIRECTION ( 'NONE',  ( 0.000000000000000000, 0.000000000000000000, 1.000000000000000000 ) ) ;
#78822 = VERTEX_POINT ( 'NONE', #21365 ) ;
#78823 = CARTESIAN_POINT ( 'NONE',  ( -1.139087296525992388, -10.25000000000000711, 19.85937500000000711 ) ) ;
#78824 = CYLINDRICAL_SURFACE ( 'NONE', #22479, 0.2499999999999994726 ) ;
#78825 = ORIENTED_EDGE ( 'NONE', *, *, #58004, .T. ) ;
#78826 = CARTESIAN_POINT ( 'NONE',  ( -18.22348492456433178, -4.988325925672469019, 34.36044203135681130 ) ) ;
#78827 = ORIENTED_EDGE ( 'NONE', *, *, #82568, .F. ) ;
#78828 = CIRCLE ( 'NONE', #68745, 4.000000000000000000 ) ;
#78829 = CARTESIAN_POINT ( 'NONE',  ( 6.989144256426998325, -3.937682226553329556, 33.60647404775216529 ) ) ;
#78830 = CARTESIAN_POINT ( 'NONE',  ( -5.749999999999999112, -2.499999999999998668, 29.75000000000000355 ) ) ;
#78831 = CYLINDRICAL_SURFACE ( 'NONE', #9607, 0.2500000000000009437 ) ;
#78832 = ORIENTED_EDGE ( 'NONE', *, *, #3609, .F. ) ;
#78833 = CARTESIAN_POINT ( 'NONE',  ( -1.384615384615383471, -1.790695186598648903, 34.54067556320373455 ) ) ;
#78834 = ORIENTED_EDGE ( 'NONE', *, *, #72612, .T. ) ;
#78835 = CARTESIAN_POINT ( 'NONE',  ( 13.38461538461526601, -4.481592998941358097, 33.73612834414048933 ) ) ;
#78836 = EDGE_LOOP ( 'NONE', ( #14080, #87425 ) ) ;
#78837 = CYLINDRICAL_SURFACE ( 'NONE', #2542, 0.2499999999999986955 ) ;
#78838 = DIRECTION ( 'NONE',  ( -0.000000000000000000, 0.9396926207859093161, -0.3420201433256663259 ) ) ;
#78839 = VERTEX_POINT ( 'NONE', #40321 ) ;
#78840 = DIRECTION ( 'NONE',  ( -0.000000000000000000, 1.000000000000000000, -0.000000000000000000 ) ) ;
#78841 = PLANE ( 'NONE',  #1844 ) ;
#78842 = CARTESIAN_POINT ( 'NONE',  ( -5.076923076923199218, -12.51329471203414379, 31.30864560766407578 ) ) ;
#78843 = EDGE_CURVE ( 'NONE', #39886, #62997, #13701, .T. ) ;
#78844 = CARTESIAN_POINT ( 'NONE',  ( 4.853438133199127869, -9.331801661448606566, 34.40259984581193464 ) ) ;
#78845 = CARTESIAN_POINT ( 'NONE',  ( -11.31544869436814160, -3.395485233115139057, 33.02377354290275946 ) ) ;
#78846 = B_SPLINE_CURVE_WITH_KNOTS ( 'NONE', 3,
 ( #88224, #26054, #26497, #81006, #18406, #54400, #6233, #60717, #5781, #86890 ),
 .UNSPECIFIED., .F., .F.,
 ( 4, 2, 2, 2, 4 ),
 ( 0.0007817359430256391132, 0.0009771253907250075990, 0.001172514838424375868, 0.001367904286123744354, 0.001563293733823112840 ),
 .UNSPECIFIED. ) ;
#78847 = B_SPLINE_CURVE_WITH_KNOTS ( 'NONE', 3,
 ( #74275, #26978, #32842, #48117, #33730, #81041, #66629, #61185, #6694, #33293 ),
 .UNSPECIFIED., .F., .F.,
 ( 4, 2, 2, 2, 4 ),
 ( 0.000000000000000000, 0.0001954339857564081520, 0.0003908679715128163040, 0.0005863019572692244018, 0.0007817359430256326080 ),
 .UNSPECIFIED. ) ;
#78848 = ORIENTED_EDGE ( 'NONE', *, *, #50813, .T. ) ;
#78849 = VERTEX_POINT ( 'NONE', #68232 ) ;
#78850 = ORIENTED_EDGE ( 'NONE', *, *, #18466, .F. ) ;
#78852 = ORIENTED_EDGE ( 'NONE', *, *, #87296, .F. ) ;
#78851 = CARTESIAN_POINT ( 'NONE',  ( 3.164686851409095336, -5.471508081941601986, 34.59228464037088457 ) ) ;
#78853 = EDGE_CURVE ( 'NONE', #4262, #62614, #69529, .T. ) ;
#78854 = VECTOR ( 'NONE', #1049, 1000.000000000000000 ) ;
#78855 = DIRECTION ( 'NONE',  ( 0.000000000000000000, -3.469446951953611033E-15, -1.000000000000000000 ) ) ;
#78856 = DIRECTION ( 'NONE',  ( 1.000000000000000000, 0.000000000000000000, 0.000000000000000000 ) ) ;
#78858 = EDGE_LOOP ( 'NONE', ( #82476, #62245, #60855, #54766 ) ) ;
#78857 = ADVANCED_FACE ( 'NONE', ( #13727 ), #82193, .T. ) ;
#78859 = ORIENTED_EDGE ( 'NONE', *, *, #39545, .F. ) ;
#78860 = ORIENTED_EDGE ( 'NONE', *, *, #847, .F. ) ;
#78861 = CARTESIAN_POINT ( 'NONE',  ( 3.361294932532794988, -5.195472089885680766, 34.18748526763464923 ) ) ;
#78862 = ORIENTED_EDGE ( 'NONE', *, *, #59762, .T. ) ;
#78863 = VECTOR ( 'NONE', #21423, 1000.000000000000000 ) ;
#78864 = DIRECTION ( 'NONE',  ( -0.000000000000000000, 0.9396926207859093161, -0.3420201433256663259 ) ) ;
#78865 = AXIS2_PLACEMENT_3D ( 'NONE', #79857, #26682, #54139 ) ;
#78866 = EDGE_CURVE ( 'NONE', #58471, #81511, #87630, .T. ) ;
#78867 = CARTESIAN_POINT ( 'NONE',  ( 3.903869409797562806, -12.65889640711025521, 30.72598325615533454 ) ) ;
#78868 = CARTESIAN_POINT ( 'NONE',  ( 12.23861224402230619, -2.554751324335735152, 30.48935550225260727 ) ) ;
#78869 = FACE_BOUND ( 'NONE', #30094, .T. ) ;
#78870 = ORIENTED_EDGE ( 'NONE', *, *, #46540, .T. ) ;
#78871 = CARTESIAN_POINT ( 'NONE',  ( 13.16113046005105502, -10.97335522853832579, 33.68706563782419749 ) ) ;
#78872 = B_SPLINE_CURVE_WITH_KNOTS ( 'NONE', 3,
 ( #40146, #68481, #67607, #67162, #6358, #19412, #54974, #6780, #47771, #26171 ),
 .UNSPECIFIED., .F., .F.,
 ( 4, 2, 2, 2, 4 ),
 ( 0.000000000000000000, 0.0001954311564186881484, 0.0003908623128373762967, 0.0005862934692560644451, 0.0007817246256747525934 ),
 .UNSPECIFIED. ) ;
#78873 = EDGE_CURVE ( 'NONE', #8529, #11982, #52377, .T. ) ;
#78874 = LINE ( 'NONE', #52289, #1443 ) ;
#78875 = CARTESIAN_POINT ( 'NONE',  ( 4.153846153846154188, -12.10708131394839349, 31.69288490824020244 ) ) ;
#78876 = CARTESIAN_POINT ( 'NONE',  ( 10.61538461538461675, -2.721908614388771852, 31.22303859784724978 ) ) ;
#78877 = EDGE_LOOP ( 'NONE', ( #39403, #85422 ) ) ;
#78878 = CARTESIAN_POINT ( 'NONE',  ( 9.442284455014730682, -2.587272538249754117, 30.68239716806877837 ) ) ;
#78879 = ORIENTED_EDGE ( 'NONE', *, *, #80515, .F. ) ;
#78880 = ORIENTED_EDGE ( 'NONE', *, *, #11177, .T. ) ;
#78882 = LINE ( 'NONE', #38350, #34776 ) ;
#78881 = LINE ( 'NONE', #25725, #84918 ) ;
#78883 = B_SPLINE_CURVE_WITH_KNOTS ( 'NONE', 3,
 ( #67306, #17790, #66412, #25426, #73174, #45242, #81269, #53332, #33071, #74067 ),
 .UNSPECIFIED., .F., .F.,
 ( 4, 2, 2, 2, 4 ),
 ( 0.000000000000000000, 0.0001954339857564078809, 0.0003908679715128157619, 0.0005863019572692236428, 0.0007817359430256315238 ),
 .UNSPECIFIED. ) ;
#78884 = DIRECTION ( 'NONE',  ( 0.000000000000000000, 0.9848077530122072432, -0.1736481776669354937 ) ) ;
#78885 = DIRECTION ( 'NONE',  ( -0.000000000000000000, 0.8660254037844399289, -0.4999999999999980016 ) ) ;
#78886 = DIRECTION ( 'NONE',  ( 0.000000000000000000, 0.8660254037844377084, -0.5000000000000015543 ) ) ;
#78887 = CARTESIAN_POINT ( 'NONE',  ( -2.557715544985271983, -10.05641848906368097, 34.04755513067966177 ) ) ;
#78888 = EDGE_LOOP ( 'NONE', ( #36591, #34773, #44729, #80527 ) ) ;
#78889 = EDGE_CURVE ( 'NONE', #53607, #52583, #1320, .T. ) ;
#78890 = FACE_OUTER_BOUND ( 'NONE', #88218, .T. ) ;
#78891 = CARTESIAN_POINT ( 'NONE',  ( -0.2387587925603949779, -3.563462043263031287, 33.22394488606064300 ) ) ;
#78892 = CARTESIAN_POINT ( 'NONE',  ( -18.00000000000000000, -2.499999999999999556, 29.74999999999998579 ) ) ;
#78893 = EDGE_CURVE ( 'NONE', #32458, #14846, #20066, .T. ) ;
#78894 = CARTESIAN_POINT ( 'NONE',  ( 14.55763771707035126, -2.589246495874658383, 31.60778113518102828 ) ) ;
#78895 = VERTEX_POINT ( 'NONE', #61456 ) ;
#78896 = VECTOR ( 'NONE', #60620, 1000.000000000000000 ) ;
#78897 = ORIENTED_EDGE ( 'NONE', *, *, #75416, .F. ) ;
#78898 = FACE_BOUND ( 'NONE', #16255, .T. ) ;
#78899 = ORIENTED_EDGE ( 'NONE', *, *, #49325, .T. ) ;
#78900 = EDGE_CURVE ( 'NONE', #17581, #3390, #2929, .T. ) ;
#78901 = CYLINDRICAL_SURFACE ( 'NONE', #56386, 0.2499999999999994726 ) ;
#78903 = EDGE_CURVE ( 'NONE', #22888, #25656, #48066, .T. ) ;
#78902 = CARTESIAN_POINT ( 'NONE',  ( -1.254089946381738763, -2.372941743896878286, 30.88044141588254377 ) ) ;
#78904 = EDGE_LOOP ( 'NONE', ( #58682, #76982 ) ) ;
#78905 = DIRECTION ( 'NONE',  ( -1.000000000000000000, -0.000000000000000000, 0.000000000000000000 ) ) ;
#78906 = CARTESIAN_POINT ( 'NONE',  ( -10.68065506134538545, -6.879047030191174805, 34.71129190930000163 ) ) ;
#78907 = CARTESIAN_POINT ( 'NONE',  ( 16.15384615384615330, -8.120952969808772792, 34.71129190930000163 ) ) ;
#78908 = CARTESIAN_POINT ( 'NONE',  ( 6.923076923076924238, -3.513871655860378418, 32.76840700105978499 ) ) ;
#78909 = ORIENTED_EDGE ( 'NONE', *, *, #61363, .F. ) ;
#78910 = CARTESIAN_POINT ( 'NONE',  ( -10.61538461538461320, -12.29105614889573062, 35.45975837776705220 ) ) ;
#78911 = VERTEX_POINT ( 'NONE', #30338 ) ;
#78913 = EDGE_LOOP ( 'NONE', ( #61657, #18923, #36140, #52271 ) ) ;
#78912 = CARTESIAN_POINT ( 'NONE',  ( 17.01165263096229907, -10.90142922261923886, 33.41473453929638993 ) ) ;
#78914 = DIRECTION ( 'NONE',  ( -0.000000000000000000, -1.000000000000000000, -0.000000000000000000 ) ) ;
#78915 = CARTESIAN_POINT ( 'NONE',  ( -8.769230769230768274, -1.422936976036506707, 30.56769352161908415 ) ) ;
#78916 = DIRECTION ( 'NONE',  ( 0.000000000000000000, 0.9848077530122072432, 0.1736481776669354937 ) ) ;
#78917 = CARTESIAN_POINT ( 'NONE',  ( -10.83886953994894675, -3.562934362175800285, 33.22335522853832401 ) ) ;
#78918 = FACE_OUTER_BOUND ( 'NONE', #48277, .T. ) ;
#78919 = CARTESIAN_POINT ( 'NONE',  ( -9.942330916529147800, -12.07920672191015221, 32.31858351112116168 ) ) ;
#78920 = CARTESIAN_POINT ( 'NONE',  ( -1.901340078031369618, -5.512252781505359245, 16.75186829374151287 ) ) ;
#78921 = ORIENTED_EDGE ( 'NONE', *, *, #27191, .T. ) ;
#78922 = CARTESIAN_POINT ( 'NONE',  ( -3.230769230769229949, -3.050289026998446396, 32.03036669348365706 ) ) ;
#78923 = CARTESIAN_POINT ( 'NONE',  ( -15.00798968950081935, -3.755027918224367323, 33.06320215134714857 ) ) ;
#78924 = CARTESIAN_POINT ( 'NONE',  ( 14.30769230769231015, -9.819645486525091727, 36.12317359536749706 ) ) ;
#78925 = VECTOR ( 'NONE', #53218, 999.9999999999998863 ) ;
#78926 = ORIENTED_EDGE ( 'NONE', *, *, #79029, .F. ) ;
#78927 = VERTEX_POINT ( 'NONE', #22255 ) ;
#78928 = DIRECTION ( 'NONE',  ( -0.000000000000000000, 0.9848077530122086864, -0.1736481776669273891 ) ) ;
#78929 = CARTESIAN_POINT ( 'NONE',  ( -7.846153846153844924, -5.471508081941601098, 34.59228464037088457 ) ) ;
#78930 = FACE_OUTER_BOUND ( 'NONE', #60115, .T. ) ;
#78932 = CARTESIAN_POINT ( 'NONE',  ( 18.03205128205128105, -7.500000000000000000, 29.75000000000000355 ) ) ;
#78931 = AXIS2_PLACEMENT_3D ( 'NONE', #40112, #88748, #48612 ) ;
#78933 = DIRECTION ( 'NONE',  ( -0.000000000000000000, -0.6427876096865404731, -0.7660444431189771253 ) ) ;
#78934 = CARTESIAN_POINT ( 'NONE',  ( 16.40390057375960708, -3.435999193479609026, 33.07426656108011542 ) ) ;
#78935 = VECTOR ( 'NONE', #11702, 1000.000000000000000 ) ;
#78936 = CARTESIAN_POINT ( 'NONE',  ( 16.15384615384615330, -6.435427911321262684, 35.78748833219616898 ) ) ;
#78937 = VERTEX_POINT ( 'NONE', #29030 ) ;
#78938 = EDGE_CURVE ( 'NONE', #70481, #3368, #38675, .T. ) ;
#78939 = CARTESIAN_POINT ( 'NONE',  ( 6.130791807824786943, -10.54018710029568595, 33.71981072465678864 ) ) ;
#78941 = CLOSED_SHELL ( 'NONE', ( #73611, #49437, #53699, #29651, #33896, #9839, #28310, #33010, #4686, #74658, #14572, #68925, #28508, #4633, #48813, #50681, #73290, #63835, #37077, #17037, #22263, #65974, #49276, #48601, #8330, #47700, #28249, #42777, #71412, #24149, #73385, #85745, #46155, #3289, #31863, #63228, #25250, #48307, #32287, #43871, #85400, #43345, #68570 ) ) ;
#78940 = CARTESIAN_POINT ( 'NONE',  ( -16.94687547066739697, -7.723484964179501588, 34.74522123443823318 ) ) ;
#78942 = VECTOR ( 'NONE', #27835, 1000.000000000000000 ) ;
#78943 = DIRECTION ( 'NONE',  ( 0.000000000000000000, 0.4999999999999960032, -0.8660254037844410391 ) ) ;
#78944 = LINE ( 'NONE', #85710, #36394 ) ;
#78945 = ADVANCED_FACE ( 'NONE', ( #71315 ), #69991, .T. ) ;
#78946 = VERTEX_POINT ( 'NONE', #9618 ) ;
#78947 = CARTESIAN_POINT ( 'NONE',  ( -7.846153846153965716, -3.835265460704628371, 33.15142922262033665 ) ) ;
#78948 = B_SPLINE_CURVE_WITH_KNOTS ( 'NONE', 3,
 ( #46366, #19343, #75179, #13464, #40944, #60317, #68407, #48128, #74288, #75600 ),
 .UNSPECIFIED., .F., .F.,
 ( 4, 2, 2, 2, 4 ),
 ( 0.000000000000000000, 0.0001954339857564079352, 0.0003908679715128158703, 0.0005863019572692237513, 0.0007817359430256317406 ),
 .UNSPECIFIED. ) ;
#78949 = ADVANCED_FACE ( 'NONE', ( #56037 ), #1543, .F. ) ;
#78950 = EDGE_LOOP ( 'NONE', ( #54612, #4892 ) ) ;
#78951 = CARTESIAN_POINT ( 'NONE',  ( -18.00000000000000000, -8.164416787775447659, 34.95778746994557906 ) ) ;
#78952 = CARTESIAN_POINT ( 'NONE',  ( -13.31947060389575199, -7.750023224968867197, 34.99404313364389907 ) ) ;
#78953 = CARTESIAN_POINT ( 'NONE',  ( 4.153846153846154188, -3.886160181151819604, 36.00935417666054406 ) ) ;
#78954 = EDGE_LOOP ( 'NONE', ( #85401, #30466, #14822, #21574 ) ) ;
#78955 = CARTESIAN_POINT ( 'NONE',  ( 8.769230769230768274, -2.249999999999998668, 29.75000000000001776 ) ) ;
#78956 = CARTESIAN_POINT ( 'NONE',  ( -5.999999999999998224, -4.098570777380720287, 33.41473453929634729 ) ) ;
#78957 = EDGE_CURVE ( 'NONE', #47875, #73916, #88851, .T. ) ;
#78958 = DIRECTION ( 'NONE',  ( 0.000000000000000000, 0.4999999999999960032, -0.8660254037844410391 ) ) ;
#78959 = DIRECTION ( 'NONE',  ( 0.000000000000000000, 0.9396926207859126468, 0.3420201433256571111 ) ) ;
#78960 = ORIENTED_EDGE ( 'NONE', *, *, #20753, .T. ) ;
#78961 = CARTESIAN_POINT ( 'NONE',  ( -1.384615384615505151, -3.835265460704628371, 33.15142922262033665 ) ) ;
#78962 = ORIENTED_EDGE ( 'NONE', *, *, #43278, .T. ) ;
#78963 = AXIS2_PLACEMENT_3D ( 'NONE', #46854, #54494, #74786 ) ;
#78964 = DIRECTION ( 'NONE',  ( -0.000000000000000000, -0.1736481776669307198, -0.9848077530122080203 ) ) ;
#78966 = EDGE_CURVE ( 'NONE', #30322, #28852, #18952, .T. ) ;
#78965 = CARTESIAN_POINT ( 'NONE',  ( -16.40386939113911779, -11.37209801155882793, 32.91403422569033665 ) ) ;
#78967 = CARTESIAN_POINT ( 'NONE',  ( 7.780883845597527326, -12.51329471203370325, 31.30864560766548976 ) ) ;
#78968 = CARTESIAN_POINT ( 'NONE',  ( -14.05774678934416322, -11.86320923018887541, 32.19269448109604781 ) ) ;
#78969 = CARTESIAN_POINT ( 'NONE',  ( 15.10062202133101472, -11.93770438780619259, 32.05411857736982029 ) ) ;
#78970 = EDGE_CURVE ( 'NONE', #30665, #82411, #62778, .T. ) ;
#78971 = ORIENTED_EDGE ( 'NONE', *, *, #75028, .F. ) ;
#78972 = EDGE_LOOP ( 'NONE', ( #48589, #35594, #3724, #67248 ) ) ;
#78973 = EDGE_LOOP ( 'NONE', ( #55249, #17677 ) ) ;
#78974 = EDGE_LOOP ( 'NONE', ( #54073, #46831 ) ) ;
#78975 = ORIENTED_EDGE ( 'NONE', *, *, #47708, .T. ) ;
#78976 = CARTESIAN_POINT ( 'NONE',  ( 12.71159277317677549, -11.79725096376909654, 32.30694842903959341 ) ) ;
#78977 = CARTESIAN_POINT ( 'NONE',  ( -1.161604033002534786, -12.39991518177334129, 30.74647679643404530 ) ) ;
#78978 = CARTESIAN_POINT ( 'NONE',  ( 14.55769230769372946, -7.500000000000154543, 35.00000000000007105 ) ) ;
#78979 = DIRECTION ( 'NONE',  ( -0.000000000000000000, -0.1736481776669307198, -0.9848077530122080203 ) ) ;
#78980 = DIRECTION ( 'NONE',  ( 0.000000000000000000, -6.938893903907222067E-15, 1.000000000000000000 ) ) ;
#78981 = CARTESIAN_POINT ( 'NONE',  ( 3.165498784808455923, -6.026961402152685388, 34.52809138561120506 ) ) ;
#78982 = AXIS2_PLACEMENT_3D ( 'NONE', #63568, #41986, #22586 ) ;
#78983 = CARTESIAN_POINT ( 'NONE',  ( -17.77698864838715309, -9.886259254753570147, 34.14407573483972413 ) ) ;
#78984 = CARTESIAN_POINT ( 'NONE',  ( 9.562159722576001997, -10.31621877034669588, 34.18098118002070152 ) ) ;
#78985 = CARTESIAN_POINT ( 'NONE',  ( 7.976944287120795174, -4.684288915650983043, 34.18129842949671371 ) ) ;
#78986 = VERTEX_POINT ( 'NONE', #15504 ) ;
#78987 = ORIENTED_EDGE ( 'NONE', *, *, #50607, .F. ) ;
#78988 = ORIENTED_EDGE ( 'NONE', *, *, #33223, .T. ) ;
#78990 = ORIENTED_EDGE ( 'NONE', *, *, #49668, .T. ) ;
#78989 = DIRECTION ( 'NONE',  ( -0.000000000000000000, -0.8660254037844399289, -0.4999999999999980016 ) ) ;
#78992 = CARTESIAN_POINT ( 'NONE',  ( -16.28453762051371712, -9.804603061927743113, 34.18744698557895845 ) ) ;
#78991 = CARTESIAN_POINT ( 'NONE',  ( -9.822454901745912181, -9.418419913701741919, 34.36755862841477693 ) ) ;
#78993 = VECTOR ( 'NONE', #60647, 1000.000000000000000 ) ;
#78994 = CARTESIAN_POINT ( 'NONE',  ( 8.703473966716462229, -7.249945686854186278, 34.74374336980224598 ) ) ;
#78995 = CARTESIAN_POINT ( 'NONE',  ( 6.988332494352946789, -2.625532179533470512, 30.86335684631491105 ) ) ;
#78996 = EDGE_LOOP ( 'NONE', ( #18909, #85129, #15896, #18146 ) ) ;
#78997 = EDGE_CURVE ( 'NONE', #44583, #71986, #42975, .T. ) ;
#78998 = ADVANCED_FACE ( 'NONE', ( #29467 ), #56917, .F. ) ;
#78999 = EDGE_LOOP ( 'NONE', ( #1190, #41032, #42497, #4321 ) ) ;
#79000 = CARTESIAN_POINT ( 'NONE',  ( -17.14300545628321260, -11.35647404775217595, 33.31231777344666511 ) ) ;
#79002 = EDGE_CURVE ( 'NONE', #42943, #72270, #37984, .T. ) ;
#79001 = ORIENTED_EDGE ( 'NONE', *, *, #29668, .T. ) ;
#79003 = FACE_BOUND ( 'NONE', #52918, .T. ) ;
#79004 = CYLINDRICAL_SURFACE ( 'NONE', #41835, 4.000000000000000000 ) ;
#79005 = CARTESIAN_POINT ( 'NONE',  ( 5.076923076922953193, -3.643525952248796163, 33.31231777344771672 ) ) ;
#79006 = EDGE_LOOP ( 'NONE', ( #14976, #7383 ) ) ;
#79007 = CARTESIAN_POINT ( 'NONE',  ( -1.134560964701930796, -5.642605341092957083, 34.66089969410670335 ) ) ;
#79009 = EDGE_CURVE ( 'NONE', #74008, #65490, #32118, .T. ) ;
#79008 = CARTESIAN_POINT ( 'NONE',  ( 20.00000000000000000, -4.000000000000000000, 29.75000000000000355 ) ) ;
#79010 = DIRECTION ( 'NONE',  ( 0.000000000000000000, 0.7660444431189822323, -0.6427876096865344779 ) ) ;
#79011 = VERTEX_POINT ( 'NONE', #86639 ) ;
#79012 = CARTESIAN_POINT ( 'NONE',  ( -14.55769230769230660, -2.499999999999998668, 29.75000000000000355 ) ) ;
#79013 = CARTESIAN_POINT ( 'NONE',  ( -14.37377571864818293, -5.557115091759785130, 34.35708131394839171 ) ) ;
#79014 = VERTEX_POINT ( 'NONE', #5090 ) ;
#79015 = CARTESIAN_POINT ( 'NONE',  ( 5.934246571686668581, -7.249945578846651806, 34.99404164642496795 ) ) ;
#79016 = CARTESIAN_POINT ( 'NONE',  ( -2.307692307692427391, -10.21337939537710326, 33.94971097300076224 ) ) ;
#79017 = ORIENTED_EDGE ( 'NONE', *, *, #31894, .T. ) ;
#79018 = FACE_OUTER_BOUND ( 'NONE', #46331, .T. ) ;
#79019 = CARTESIAN_POINT ( 'NONE',  ( -10.36533030374629583, -4.943051570960394159, 34.04725096376909477 ) ) ;
#79020 = CARTESIAN_POINT ( 'NONE',  ( -10.03846153846153832, -11.50000000000000000, 29.75000000000000355 ) ) ;
#79021 = CARTESIAN_POINT ( 'NONE',  ( 16.15384615384603251, -11.06231777344772027, 33.60647404775119895 ) ) ;
#79022 = DIRECTION ( 'NONE',  ( -0.000000000000000000, -0.6427876096865404731, -0.7660444431189770143 ) ) ;
#79023 = CARTESIAN_POINT ( 'NONE',  ( 9.019285189144223835, -4.074993327901527351, 33.72946981652012255 ) ) ;
#79025 = CARTESIAN_POINT ( 'NONE',  ( 11.78846153846160583, -7.434744860731433924, 35.00000000000000711 ) ) ;
#79024 = CARTESIAN_POINT ( 'NONE',  ( 4.284371855609719226, -12.27024696741798770, 31.24895572276497546 ) ) ;
#79026 = CARTESIAN_POINT ( 'NONE',  ( -1.384615384615506484, -9.528491918059723176, 34.59228464037033035 ) ) ;
#79028 = CARTESIAN_POINT ( 'NONE',  ( 8.835299120233207404, -2.721908614388771852, 31.22303859784725333 ) ) ;
#79027 = CARTESIAN_POINT ( 'NONE',  ( 12.21153846153846168, -7.566082377512564960, 35.00000000000000711 ) ) ;
#79029 = EDGE_CURVE ( 'NONE', #46953, #52150, #24907, .T. ) ;
#79030 = CIRCLE ( 'NONE', #56015, 0.2500000000000002220 ) ;
#79031 = CARTESIAN_POINT ( 'NONE',  ( -2.749999999999991562, -8.639087296526025028, 15.01562500000000178 ) ) ;
#79032 = VERTEX_POINT ( 'NONE', #44724 ) ;
#79033 = CARTESIAN_POINT ( 'NONE',  ( 0.3954550505825799589, -12.37446782046654192, 30.86335684631486487 ) ) ;
#79034 = EDGE_LOOP ( 'NONE', ( #62189, #68820, #66436, #60688 ) ) ;
#79035 = EDGE_CURVE ( 'NONE', #29464, #40637, #80213, .T. ) ;
#79036 = ORIENTED_EDGE ( 'NONE', *, *, #78384, .F. ) ;
#79037 = CARTESIAN_POINT ( 'NONE',  ( -8.769230769230768274, -11.69971097300155272, 32.46337939537588113 ) ) ;
#79038 = ORIENTED_EDGE ( 'NONE', *, *, #22625, .T. ) ;
#79039 = CARTESIAN_POINT ( 'NONE',  ( -5.776987155906605942, -10.01129605718032778, 34.36064277460058491 ) ) ;
#79040 = CARTESIAN_POINT ( 'NONE',  ( 1.139087296526029469, -10.24999999999999467, 14.70312500000000355 ) ) ;
#79041 = CARTESIAN_POINT ( 'NONE',  ( 3.007842271862382066, -2.308479472611653094, 30.53278059502174457 ) ) ;
#79042 = CARTESIAN_POINT ( 'NONE',  ( -5.749945580086544439, -11.47946981652013498, 33.17500667209846910 ) ) ;
#79043 = DIRECTION ( 'NONE',  ( -0.000000000000000000, 1.000000000000000000, -0.000000000000000000 ) ) ;
#79044 = CARTESIAN_POINT ( 'NONE',  ( -3.230769230769229949, -8.318370150425687726, 35.83090037661290239 ) ) ;
#79045 = FACE_OUTER_BOUND ( 'NONE', #41583, .T. ) ;
#79046 = CARTESIAN_POINT ( 'NONE',  ( 0.6845513056318558442, -5.582272713120728369, 34.63742843783360570 ) ) ;
#79047 = CARTESIAN_POINT ( 'NONE',  ( -7.596208327805703320, -12.22109172314383052, 31.39792113162168263 ) ) ;
#79048 = CARTESIAN_POINT ( 'NONE',  ( 1.553300858899129944, -11.24999999999998934, 20.95312500000000000 ) ) ;
#79049 = ADVANCED_FACE ( 'NONE', ( #17722 ), #66345, .T. ) ;
#79050 = CARTESIAN_POINT ( 'NONE',  ( 1.515407192440172190, -3.062576670634119758, 32.05464942895959979 ) ) ;
#79051 = CARTESIAN_POINT ( 'NONE',  ( -4.500000000000000000, -7.499999999999999112, 13.50000000000000178 ) ) ;
#79052 = CARTESIAN_POINT ( 'NONE',  ( 10.48523664565292002, -5.915902021225889484, 34.75552854090298638 ) ) ;
#79053 = ADVANCED_FACE ( 'NONE', ( #31678 ), #24457, .F. ) ;
#79054 = B_SPLINE_CURVE_WITH_KNOTS ( 'NONE', 3,
 ( #51905, #64099, #2393, #23121, #72186, #78498, #2832, #43395, #24437, #3727 ),
 .UNSPECIFIED., .F., .F.,
 ( 4, 2, 2, 2, 4 ),
 ( 0.000000000000000000, 0.0001954311564186864949, 0.0003908623128373729899, 0.0005862934692560594577, 0.0007817246256747459798 ),
 .UNSPECIFIED. ) ;
#79055 = VECTOR ( 'NONE', #48211, 1000.000000000000227 ) ;
#79056 = AXIS2_PLACEMENT_3D ( 'NONE', #15959, #30349, #29038 ) ;
#79057 = VERTEX_POINT ( 'NONE', #17264 ) ;
#79058 = FACE_OUTER_BOUND ( 'NONE', #21028, .T. ) ;
#79059 = CARTESIAN_POINT ( 'NONE',  ( 7.715462379486289990, -11.18331474514187995, 33.13161551792790505 ) ) ;
#79060 = CARTESIAN_POINT ( 'NONE',  ( -2.530619266599154038, -2.308479472611653094, 30.53278059502174457 ) ) ;
#79061 = CARTESIAN_POINT ( 'NONE',  ( 3.903846153846154632, -7.500000000000001776, 35.04278698407183867 ) ) ;
#79062 = B_SPLINE_CURVE_WITH_KNOTS ( 'NONE', 3,
 ( #77349, #64707, #71033, #16976, #21968, #43127, #23718, #10227, #85003, #84127 ),
 .UNSPECIFIED., .F., .F.,
 ( 4, 2, 2, 2, 4 ),
 ( 0.000000000000000000, 0.0001954311564186871726, 0.0003908623128373743452, 0.0005862934692560615177, 0.0007817246256747486903 ),
 .UNSPECIFIED. ) ;
#79063 = AXIS2_PLACEMENT_3D ( 'NONE', #4932, #32841, #40059 ) ;
#79064 = CARTESIAN_POINT ( 'NONE',  ( 15.00794253829022828, -7.369208160676172348, 34.74850200257122879 ) ) ;
#79065 = CARTESIAN_POINT ( 'NONE',  ( 9.468822748583745508, -11.41268669641499756, 32.86336882939238535 ) ) ;
#79066 = EDGE_CURVE ( 'NONE', #29866, #45581, #80314, .T. ) ;
#79067 = VECTOR ( 'NONE', #71403, 1000.000000000000000 ) ;
#79068 = B_SPLINE_CURVE_WITH_KNOTS ( 'NONE', 3,
 ( #38170, #45363, #58426, #39529, #3930, #58884, #19243, #46709, #18354, #17909 ),
 .UNSPECIFIED., .F., .F.,
 ( 4, 2, 2, 2, 4 ),
 ( 0.000000000000000000, 0.0001954311564186861697, 0.0003908623128373723394, 0.0005862934692560584820, 0.0007817246256747446788 ),
 .UNSPECIFIED. ) ;
#79069 = EDGE_CURVE ( 'NONE', #43756, #74204, #75896, .T. ) ;
#79070 = ORIENTED_EDGE ( 'NONE', *, *, #40521, .F. ) ;
#79071 = CARTESIAN_POINT ( 'NONE',  ( 17.77707378248385339, -12.39988816332205701, 30.74660775122750778 ) ) ;
#79072 = ORIENTED_EDGE ( 'NONE', *, *, #82288, .T. ) ;
#79073 = ORIENTED_EDGE ( 'NONE', *, *, #53029, .T. ) ;
#79074 = CARTESIAN_POINT ( 'NONE',  ( 0.6845513056318554002, -12.38742843783360748, 31.66772728687926985 ) ) ;
#79075 = CARTESIAN_POINT ( 'NONE',  ( 3.296837581771669523, -5.557115091759786019, 34.35708131394839882 ) ) ;
#79076 = DIRECTION ( 'NONE',  ( -0.000000000000000000, 0.9396926207859092051, -0.3420201433256662704 ) ) ;
#79077 = CARTESIAN_POINT ( 'NONE',  ( 1.384615384615386802, -11.69971097300155272, 32.46337939537588113 ) ) ;
#79078 = CYLINDRICAL_SURFACE ( 'NONE', #42342, 0.2500000000000009437 ) ;
#79079 = EDGE_CURVE ( 'NONE', #33822, #48507, #50164, .T. ) ;
#79080 = ORIENTED_EDGE ( 'NONE', *, *, #21087, .T. ) ;
#79081 = ADVANCED_FACE ( 'NONE', ( #72650 ), #24013, .T. ) ;
#79082 = ORIENTED_EDGE ( 'NONE', *, *, #73409, .F. ) ;
#79083 = VERTEX_POINT ( 'NONE', #87084 ) ;
#79084 = CARTESIAN_POINT ( 'NONE',  ( 12.59158362437324108, -2.504778602574659896, 29.97347330155780654 ) ) ;
#79085 = B_SPLINE_CURVE_WITH_KNOTS ( 'NONE', 3,
 ( #77840, #51676, #38186, #51222, #38634, #44480 ),
 .UNSPECIFIED., .F., .F.,
 ( 4, 2, 4 ),
 ( 3.165870343657672947E-17, 0.0001954756301637038194, 0.0003909512603273759801 ),
 .UNSPECIFIED. ) ;
#79086 = DIRECTION ( 'NONE',  ( -0.000000000000000000, 1.000000000000000000, -0.000000000000000000 ) ) ;
#79087 = CARTESIAN_POINT ( 'NONE',  ( 8.899756207464417201, -5.915461855592780260, 34.75538340440931506 ) ) ;
#79088 = CARTESIAN_POINT ( 'NONE',  ( -15.10024352900566846, -3.285477652293413264, 32.44071101563363158 ) ) ;
#79089 = CYLINDRICAL_SURFACE ( 'NONE', #29238, 0.2499999999999994726 ) ;
#79090 = DIRECTION ( 'NONE',  ( -0.000000000000000000, 0.6427876096865404731, -0.7660444431189771253 ) ) ;
#79091 = ORIENTED_EDGE ( 'NONE', *, *, #3311, .F. ) ;
#79092 = VERTEX_POINT ( 'NONE', #46073 ) ;
#79093 = CARTESIAN_POINT ( 'NONE',  ( -3.749999999999988454, -9.053300858899127945, 21.26562500000000000 ) ) ;
#79094 = ORIENTED_EDGE ( 'NONE', *, *, #80267, .T. ) ;
#79096 = ORIENTED_EDGE ( 'NONE', *, *, #436, .F. ) ;
#79095 = CARTESIAN_POINT ( 'NONE',  ( -10.55012904410859242, -11.94971097300157403, 32.03036669348361443 ) ) ;
#79097 = DIRECTION ( 'NONE',  ( 0.000000000000000000, 0.8660254037844377084, -0.5000000000000015543 ) ) ;
#79098 = FACE_OUTER_BOUND ( 'NONE', #78114, .T. ) ;
#79099 = CARTESIAN_POINT ( 'NONE',  ( 2.320192649118979489E-14, -11.25000000000000000, 17.28125000000000000 ) ) ;
#79100 = ORIENTED_EDGE ( 'NONE', *, *, #68391, .F. ) ;
#79101 = CARTESIAN_POINT ( 'NONE',  ( -13.63459211555773720, -12.17611988154120972, 31.52148481390971213 ) ) ;
#79102 = ORIENTED_EDGE ( 'NONE', *, *, #22774, .F. ) ;
#79104 = B_SPLINE_CURVE_WITH_KNOTS ( 'NONE', 3,
 ( #88255, #54430, #26081, #19768, #87357, #25636, #80596, #73836, #5369, #40929 ),
 .UNSPECIFIED., .F., .F.,
 ( 4, 2, 2, 2, 4 ),
 ( 0.000000000000000000, 0.0001954311564186861697, 0.0003908623128373723394, 0.0005862934692560584820, 0.0007817246256747446788 ),
 .UNSPECIFIED. ) ;
#79103 = CYLINDRICAL_SURFACE ( 'NONE', #77258, 0.2500000000000009437 ) ;
#79105 = DIRECTION ( 'NONE',  ( -0.000000000000000000, -0.1736481776669307198, -0.9848077530122080203 ) ) ;
#79106 = EDGE_CURVE ( 'NONE', #38268, #29864, #60273, .T. ) ;
#79107 = CARTESIAN_POINT ( 'NONE',  ( -15.00798956179116317, -3.020022701398813236, 32.48759521482552515 ) ) ;
#79110 = CARTESIAN_POINT ( 'NONE',  ( -6.792551221313363641, -2.619367082507848554, 30.83698974864644171 ) ) ;
#79109 = VECTOR ( 'NONE', #18675, 1000.000000000000000 ) ;
#79108 = CARTESIAN_POINT ( 'NONE',  ( 10.68155375634727378, -7.250054483168843156, 34.74374881642865631 ) ) ;
#79111 = AXIS2_PLACEMENT_3D ( 'NONE', #19732, #32358, #76330 ) ;
#79112 = CARTESIAN_POINT ( 'NONE',  ( 15.93036121012220541, -2.599994579823202923, 30.74605699353653776 ) ) ;
#79113 = CARTESIAN_POINT ( 'NONE',  ( 18.22301135161285046, -2.758310577978207778, 31.33698337089302299 ) ) ;
#79114 = VERTEX_POINT ( 'NONE', #11858 ) ;
#79116 = EDGE_CURVE ( 'NONE', #26024, #31319, #55582, .T. ) ;
#79115 = DIRECTION ( 'NONE',  ( -0.000000000000000000, 0.8660254037844397068, -0.4999999999999978906 ) ) ;
#79117 = CARTESIAN_POINT ( 'NONE',  ( -8.834500769787091201, -4.320704448112771878, 33.92786785259540494 ) ) ;
#79118 = VECTOR ( 'NONE', #85038, 1000.000000000000000 ) ;
#79119 = ORIENTED_EDGE ( 'NONE', *, *, #21251, .T. ) ;
#79120 = AXIS2_PLACEMENT_3D ( 'NONE', #42122, #677, #69575 ) ;
#79121 = ADVANCED_FACE ( 'NONE', ( #55046 ), #75324, .T. ) ;
#79122 = MECHANICAL_DESIGN_GEOMETRIC_PRESENTATION_REPRESENTATION (  '', ( #27318 ), #12973 ) ;
#79123 = CYLINDRICAL_SURFACE ( 'NONE', #75295, 4.000000000000000000 ) ;
#79124 = CARTESIAN_POINT ( 'NONE',  ( -4.946131269098287930, -5.582136614379148654, 34.36778462344220486 ) ) ;
#79125 = DIRECTION ( 'NONE',  ( -0.000000000000000000, 0.5000000000000011102, -0.8660254037844381525 ) ) ;
#79126 = DIRECTION ( 'NONE',  ( 0.000000000000000000, 0.9848077530122072432, 0.1736481776669354937 ) ) ;
#79127 = CARTESIAN_POINT ( 'NONE',  ( 12.39545505058258001, -4.098570777380720287, 33.41473453929634729 ) ) ;
#79128 = FACE_BOUND ( 'NONE', #5415, .T. ) ;
#79130 = CARTESIAN_POINT ( 'NONE',  ( -10.83821271301949629, -7.369209533119140509, 34.99857337881830688 ) ) ;
#79129 = CARTESIAN_POINT ( 'NONE',  ( 13.25392391794782654, -12.11776431015576172, 31.66791131148498906 ) ) ;
#79131 = CARTESIAN_POINT ( 'NONE',  ( -6.923076923076922462, -10.51840700105979565, 33.73612834413961536 ) ) ;
#79133 = DIRECTION ( 'NONE',  ( 0.000000000000000000, 0.9396926207859126468, -0.3420201433256571111 ) ) ;
#79132 = CARTESIAN_POINT ( 'NONE',  ( -1.253823576790597416, -12.11778462344221019, 31.66786338562085135 ) ) ;
#79134 = CARTESIAN_POINT ( 'NONE',  ( 12.46153846153833911, -12.46129190930018460, 30.37095296980731973 ) ) ;
#79135 = ADVANCED_FACE ( 'NONE', ( #6856 ), #39775, .F. ) ;
#79136 = DIRECTION ( 'NONE',  ( -0.000000000000000000, 0.000000000000000000, 1.000000000000000000 ) ) ;
#79137 = CARTESIAN_POINT ( 'NONE',  ( 1.492201783934554493, -3.724691934501233703, 25.23250670625849068 ) ) ;
#79138 = ORIENTED_EDGE ( 'NONE', *, *, #2106, .T. ) ;
#79139 = DIRECTION ( 'NONE',  ( 0.000000000000000000, -6.938893903907222067E-15, 1.000000000000000000 ) ) ;
#79140 = EDGE_CURVE ( 'NONE', #25943, #80428, #52280, .T. ) ;
#79141 = DIRECTION ( 'NONE',  ( 0.000000000000000000, 0.1736481776669267785, -0.9848077530122087975 ) ) ;
#79142 = CARTESIAN_POINT ( 'NONE',  ( -7.622777905455662584, -2.501478030877322567, 29.88021232661720816 ) ) ;
#79143 = DIRECTION ( 'NONE',  ( 0.000000000000000000, -0.000000000000000000, -1.000000000000000000 ) ) ;
#79144 = DIRECTION ( 'NONE',  ( 0.000000000000000000, 0.000000000000000000, 1.000000000000000000 ) ) ;
#79145 = CARTESIAN_POINT ( 'NONE',  ( -17.01166793741023042, -8.656820664281605460, 34.87096338111211224 ) ) ;
#79146 = CARTESIAN_POINT ( 'NONE',  ( 3.775308065498768517, -8.992201783934554271, 23.04500670625849068 ) ) ;
#79147 = CARTESIAN_POINT ( 'NONE',  ( -2.557669051740898425, -3.436278759898155233, 33.07459398097509506 ) ) ;
#79148 = CARTESIAN_POINT ( 'NONE',  ( -2.176901866725357237, -6.369690395747422684, 34.87708834333098196 ) ) ;
#79149 = ADVANCED_FACE ( 'NONE', ( #41093 ), #41535, .F. ) ;
#79150 = CARTESIAN_POINT ( 'NONE',  ( 3.296024370282070404, -4.320704448112861584, 33.92786785259548310 ) ) ;
#79151 = CARTESIAN_POINT ( 'NONE',  ( -0.5276208408985972875, -8.164416787775445883, 34.95778746994557906 ) ) ;
#79152 = CARTESIAN_POINT ( 'NONE',  ( 6.923076923076802558, -4.481592998941358097, 33.73612834414048933 ) ) ;
#79153 = CARTESIAN_POINT ( 'NONE',  ( 5.326977496836529546, -8.346898887586323923, 34.93166121998716278 ) ) ;
#79154 = CARTESIAN_POINT ( 'NONE',  ( -18.06608341095587633, -2.721908614388772296, 31.22303859784724978 ) ) ;
#79155 = CARTESIAN_POINT ( 'NONE',  ( -23.00000000000000000, -5.499999999999981348, 27.75000000000000000 ) ) ;
#79156 = B_SPLINE_CURVE_WITH_KNOTS ( 'NONE', 3,
 ( #60881, #88383, #74, #59993, #47362, #26657, #82504, #27097, #12254, #5951 ),
 .UNSPECIFIED., .F., .F.,
 ( 4, 2, 2, 2, 4 ),
 ( 0.0007817359430256283796, 0.0009771253907249941549, 0.001172514838424359822, 0.001367904286123725489, 0.001563293733823091156 ),
 .UNSPECIFIED. ) ;
#79157 = ORIENTED_EDGE ( 'NONE', *, *, #75116, .F. ) ;
#79158 = LINE ( 'NONE', #51206, #16829 ) ;
#79159 = DIRECTION ( 'NONE',  ( 0.000000000000000000, -6.938893903907222067E-15, 1.000000000000000000 ) ) ;
#79160 = CARTESIAN_POINT ( 'NONE',  ( 3.724691934501251023, -9.114399933863618131, 13.54874329374151465 ) ) ;
#79161 = EDGE_CURVE ( 'NONE', #66561, #43361, #53265, .T. ) ;
#79162 = DIRECTION ( 'NONE',  ( -1.000000000000000000, -0.000000000000000000, -0.000000000000000000 ) ) ;
#79163 = CARTESIAN_POINT ( 'NONE',  ( 12.46153846153846168, -13.87047571288749737, 32.06866353760679544 ) ) ;
#79164 = ORIENTED_EDGE ( 'NONE', *, *, #8657, .F. ) ;
#79165 = CARTESIAN_POINT ( 'NONE',  ( -18.00000000000012079, -6.835583212225971650, 34.95778746994575670 ) ) ;
#79166 = DIRECTION ( 'NONE',  ( -0.000000000000000000, -0.9396926207859093161, -0.3420201433256663259 ) ) ;
#79168 = ORIENTED_EDGE ( 'NONE', *, *, #50980, .T. ) ;
#79167 = CARTESIAN_POINT ( 'NONE',  ( 7.976679284387489410, -2.647132371071621471, 31.75357179365171589 ) ) ;
#79169 = CARTESIAN_POINT ( 'NONE',  ( -4.153846153846273204, -5.219633306517616589, 34.19971097300220464 ) ) ;
#79170 = EDGE_CURVE ( 'NONE', #38474, #54624, #37292, .T. ) ;
#79171 = CARTESIAN_POINT ( 'NONE',  ( 16.82692307692307665, -7.500000000000001776, 35.00000000000000000 ) ) ;
#79172 = CARTESIAN_POINT ( 'NONE',  ( -5.010854725920638408, -8.973038597847269315, 34.52809138561122637 ) ) ;
#79173 = CARTESIAN_POINT ( 'NONE',  ( -15.45363549383233170, -2.251424796025575326, 29.88072029997477586 ) ) ;
#79174 = VERTEX_POINT ( 'NONE', #80764 ) ;
#79175 = CARTESIAN_POINT ( 'NONE',  ( 23.49999999999998579, -1.749999999999999778, 28.86437827766148345 ) ) ;
#79176 = LINE ( 'NONE', #85936, #72478 ) ;
#79177 = EDGE_CURVE ( 'NONE', #32825, #53721, #32999, .T. ) ;
#79178 = EDGE_CURVE ( 'NONE', #82187, #42382, #7153, .T. ) ;
#79180 = CARTESIAN_POINT ( 'NONE',  ( 15.23076923076910916, -10.33852847137269571, 34.16647553114546554 ) ) ;
#79179 = AXIS2_PLACEMENT_3D ( 'NONE', #3882, #58831, #85870 ) ;
#79181 = EDGE_LOOP ( 'NONE', ( #74158, #64933, #32530, #11550 ) ) ;
#79182 = ORIENTED_EDGE ( 'NONE', *, *, #70060, .F. ) ;
#79183 = ORIENTED_EDGE ( 'NONE', *, *, #32103, .T. ) ;
#79184 = AXIS2_PLACEMENT_3D ( 'NONE', #16194, #9438, #15761 ) ;
#79185 = CARTESIAN_POINT ( 'NONE',  ( -9.757578138268467427, -10.21337939537584383, 33.94971097300158647 ) ) ;
#79186 = CARTESIAN_POINT ( 'NONE',  ( 6.223012844093394946, -2.308499170217967134, 30.53291367094873721 ) ) ;
#79187 = CARTESIAN_POINT ( 'NONE',  ( 13.13463865367303285, -11.28823185664190376, 33.01397839955799896 ) ) ;
#79188 = AXIS2_PLACEMENT_3D ( 'NONE', #26326, #6061, #79941 ) ;
#79189 = EDGE_CURVE ( 'NONE', #53330, #32867, #69887, .T. ) ;
#79190 = VECTOR ( 'NONE', #82228, 1000.000000000000000 ) ;
#79191 = B_SPLINE_CURVE_WITH_KNOTS ( 'NONE', 3,
 ( #67852, #33626, #51096, #78591, #77705, #56554, #76833, #64619, #36289, #85361 ),
 .UNSPECIFIED., .F., .F.,
 ( 4, 2, 2, 2, 4 ),
 ( 0.000000000000000000, 0.0001954311564186865492, 0.0003908623128373730983, 0.0005862934692560596746, 0.0007817246256747461966 ),
 .UNSPECIFIED. ) ;
#79192 = STYLED_ITEM ( 'NONE', ( #7579 ), #38570 ) ;
#79193 = DIRECTION ( 'NONE',  ( -0.000000000000000000, -0.1736481776669307198, -0.9848077530122080203 ) ) ;
#79194 = EDGE_CURVE ( 'NONE', #8219, #1369, #42870, .T. ) ;
#79195 = ADVANCED_FACE ( 'NONE', ( #17497 ), #29359, .F. ) ;
#79196 = ORIENTED_EDGE ( 'NONE', *, *, #37618, .F. ) ;
#79197 = VERTEX_POINT ( 'NONE', #58458 ) ;
#79199 = EDGE_LOOP ( 'NONE', ( #2047, #49672, #81819, #61786, #54709, #55281, #28088, #58467 ) ) ;
#79198 = CARTESIAN_POINT ( 'NONE',  ( -1.134561072977068541, -4.943051570960395047, 34.04725096376909477 ) ) ;
#79200 = CARTESIAN_POINT ( 'NONE',  ( -14.05774689831426372, -11.56426240980093745, 33.07394671870546432 ) ) ;
#79201 = EDGE_CURVE ( 'NONE', #48943, #29630, #35671, .T. ) ;
#79202 = CARTESIAN_POINT ( 'NONE',  ( 16.15384615384615330, -8.164416787775445883, 34.95778746994557906 ) ) ;
#79203 = CARTESIAN_POINT ( 'NONE',  ( 1.634669696253701288, -10.66356715214248396, 33.62249196103329751 ) ) ;
#79204 = CARTESIAN_POINT ( 'NONE',  ( -1.319360245102545681, -12.70778746994558439, 30.41441678777537305 ) ) ;
#79205 = ORIENTED_EDGE ( 'NONE', *, *, #73884, .F. ) ;
#79206 = ORIENTED_EDGE ( 'NONE', *, *, #46074, .T. ) ;
#79207 = VERTEX_POINT ( 'NONE', #51695 ) ;
#79209 = ORIENTED_EDGE ( 'NONE', *, *, #17387, .T. ) ;
#79208 = CARTESIAN_POINT ( 'NONE',  ( -3.230769230769352962, -8.656820664282941280, 34.87096338111179961 ) ) ;
#79210 = CARTESIAN_POINT ( 'NONE',  ( -15.23076923076922995, -10.89733346790207413, 36.13435417666054406 ) ) ;
#79211 = CARTESIAN_POINT ( 'NONE',  ( 18.06525513951284267, -5.941354392334603496, 34.76329471203374055 ) ) ;
#79212 = ORIENTED_EDGE ( 'NONE', *, *, #16138, .T. ) ;
#79213 = CARTESIAN_POINT ( 'NONE',  ( 5.076923076923383071, -2.506253911140614576, 30.00000000000323297 ) ) ;
#79214 = AXIS2_PLACEMENT_3D ( 'NONE', #76949, #30089, #15253 ) ;
#79215 = CARTESIAN_POINT ( 'NONE',  ( 12.46153846153833911, -5.941354392335915335, 34.76329471203413846 ) ) ;
#79216 = CARTESIAN_POINT ( 'NONE',  ( -5.869474561766353737, -3.625058011473227815, 33.29252011169590020 ) ) ;
#79217 = FACE_BOUND ( 'NONE', #1818, .T. ) ;
#79218 = CARTESIAN_POINT ( 'NONE',  ( -5.143005456283212595, -9.905515769479276145, 34.41647553114623292 ) ) ;
#79219 = CARTESIAN_POINT ( 'NONE',  ( 2.438484115517094875, -8.147973898785416225, 34.70805048591653730 ) ) ;
#79220 = EDGE_CURVE ( 'NONE', #23012, #23399, #28688, .T. ) ;
#79221 = CARTESIAN_POINT ( 'NONE',  ( -15.00798968950081758, -10.81320215134717344, 33.49497208177562868 ) ) ;
#79223 = CARTESIAN_POINT ( 'NONE',  ( 9.758376043310132530, -3.050289026998446840, 32.03036669348366416 ) ) ;
#79222 = CARTESIAN_POINT ( 'NONE',  ( 30.00000000000000000, 15.00000000000000355, 3.000000000000000000 ) ) ;
#79224 = B_SPLINE_CURVE_WITH_KNOTS ( 'NONE', 3,
 ( #72919, #29403, #86911, #77132, #70827, #38694, #1915, #86460, #29836, #70380 ),
 .UNSPECIFIED., .F., .F.,
 ( 4, 2, 2, 2, 4 ),
 ( 0.000000000000000000, 0.0001954339857564070678, 0.0003908679715128141356, 0.0005863019572692211492, 0.0007817359430256282712 ),
 .UNSPECIFIED. ) ;
#79225 = FACE_OUTER_BOUND ( 'NONE', #24294, .T. ) ;
#79226 = CYLINDRICAL_SURFACE ( 'NONE', #41897, 4.000000000000000000 ) ;
#79227 = VERTEX_POINT ( 'NONE', #1873 ) ;
#79228 = CARTESIAN_POINT ( 'NONE',  ( 10.36536137809165403, -10.76384336483936011, 33.53834819971076087 ) ) ;
#79229 = LINE ( 'NONE', #79671, #23477 ) ;
#79230 = ORIENTED_EDGE ( 'NONE', *, *, #13401, .T. ) ;
#79231 = ORIENTED_EDGE ( 'NONE', *, *, #88036, .F. ) ;
#79233 = CARTESIAN_POINT ( 'NONE',  ( 10.83839745947800992, -11.98016756924215009, 32.48728574198911190 ) ) ;
#79232 = CARTESIAN_POINT ( 'NONE',  ( -6.923076923077044142, -8.613356846316285953, 34.62446782046622218 ) ) ;
#79234 = CARTESIAN_POINT ( 'NONE',  ( 13.31853300525524908, -11.35647404775217595, 33.31231777344666511 ) ) ;
#79235 = DIRECTION ( 'NONE',  ( 0.000000000000000000, 0.8660254037844377084, 0.5000000000000015543 ) ) ;
#79236 = CARTESIAN_POINT ( 'NONE',  ( 14.53070515178570510, -11.43677907613344757, 33.22367315496202167 ) ) ;
#79237 = VERTEX_POINT ( 'NONE', #15400 ) ;
#79238 = CARTESIAN_POINT ( 'NONE',  ( 17.99999999999987566, -2.657715359629662544, 31.77849191805970364 ) ) ;
#79239 = CARTESIAN_POINT ( 'NONE',  ( -15.00775787915638126, -9.886259254753566594, 34.14407573483972413 ) ) ;
#79240 = LINE ( 'NONE', #39158, #41673 ) ;
#79241 = CARTESIAN_POINT ( 'NONE',  ( 10.74591031714818179, -4.459921816937791661, 33.71989282347011851 ) ) ;
#79242 = CARTESIAN_POINT ( 'NONE',  ( 2.307692307692309264, -5.471508081941601098, 34.59228464037088457 ) ) ;
#79243 = CARTESIAN_POINT ( 'NONE',  ( 1.553300858899129944, -11.24999999999998934, 14.70312500000000355 ) ) ;
#79244 = EDGE_LOOP ( 'NONE', ( #4559, #64958, #67572, #83888 ) ) ;
#79245 = AXIS2_PLACEMENT_3D ( 'NONE', #19068, #74017, #11421 ) ;
#79246 = AXIS2_PLACEMENT_3D ( 'NONE', #75679, #47772, #34254 ) ;
#79247 = ORIENTED_EDGE ( 'NONE', *, *, #50345, .T. ) ;
#79248 = CARTESIAN_POINT ( 'NONE',  ( -8.096177070375304652, -11.56360843649121684, 33.07473185843129926 ) ) ;
#79249 = VERTEX_POINT ( 'NONE', #84310 ) ;
#79250 = CARTESIAN_POINT ( 'NONE',  ( -12.46153846153846168, -2.249999999999998668, 29.75000000000001776 ) ) ;
#79251 = CARTESIAN_POINT ( 'NONE',  ( 9.822833394071256663, -10.19071101563364756, 33.96452234770658407 ) ) ;
#79252 = DIRECTION ( 'NONE',  ( -0.000000000000000000, -0.000000000000000000, -1.000000000000000000 ) ) ;
#79253 = CARTESIAN_POINT ( 'NONE',  ( 2.057692307692309708, -7.433931650972300353, 34.75000000000000711 ) ) ;
#79254 = CARTESIAN_POINT ( 'NONE',  ( 3.750000000000009770, -9.053300858899081760, 15.79687500000000178 ) ) ;
#79255 = AXIS2_PLACEMENT_3D ( 'NONE', #5480, #70158, #8469 ) ;
#79256 = DIRECTION ( 'NONE',  ( -0.000000000000000000, -0.3420201433256694901, -0.9396926207859082059 ) ) ;
#79257 = CARTESIAN_POINT ( 'NONE',  ( 12.46153846153846168, -4.098570777380720287, 33.41473453929634729 ) ) ;
#79258 = VERTEX_POINT ( 'NONE', #70784 ) ;
#79259 = EDGE_CURVE ( 'NONE', #57187, #24353, #56595, .T. ) ;
#79260 = LINE ( 'NONE', #26091, #27183 ) ;
#79262 = ORIENTED_EDGE ( 'NONE', *, *, #6205, .T. ) ;
#79261 = CARTESIAN_POINT ( 'NONE',  ( -6.130559913613361722, -2.254533558242299396, 29.97296025877828285 ) ) ;
#79263 = DIRECTION ( 'NONE',  ( 0.000000000000000000, 0.8660254037844377084, 0.5000000000000015543 ) ) ;
#79264 = CARTESIAN_POINT ( 'NONE',  ( -12.46153846153858247, -3.835265460704628371, 33.15142922262033665 ) ) ;
#79265 = CARTESIAN_POINT ( 'NONE',  ( 2.057715576749955311, -3.137211980971222669, 32.19342716148376837 ) ) ;
#79266 = CARTESIAN_POINT ( 'NONE',  ( 11.66925197942848769, -8.191423895709840863, 34.95447573519442130 ) ) ;
#79267 = CARTESIAN_POINT ( 'NONE',  ( -6.130691466667558487, -9.804603061927743113, 34.18744698557895845 ) ) ;
#79268 = CARTESIAN_POINT ( 'NONE',  ( 9.442284468086239002, -4.931416488878822335, 34.32920672191015399 ) ) ;
#79269 = CARTESIAN_POINT ( 'NONE',  ( -11.53846153846166089, -3.083524468854526912, 32.58852847137268327 ) ) ;
#79270 = CARTESIAN_POINT ( 'NONE',  ( 1.614399933863618797, -3.775308065498751198, 18.23624329374151642 ) ) ;
#79271 = EDGE_LOOP ( 'NONE', ( #79096, #57428, #84308, #64782 ) ) ;
#79272 = CARTESIAN_POINT ( 'NONE',  ( 11.78840705680968171, -11.86320923018887719, 32.19269448109604070 ) ) ;
#79273 = DIRECTION ( 'NONE',  ( -0.000000000000000000, 0.8660254037844397068, -0.4999999999999978906 ) ) ;
#79274 = CARTESIAN_POINT ( 'NONE',  ( 14.30769230769231015, -2.249999999999998668, 29.50000000000001421 ) ) ;
#79275 = CARTESIAN_POINT ( 'NONE',  ( 1.987747218494642309, -5.598659921968629050, 13.31436829374151287 ) ) ;
#79276 = CARTESIAN_POINT ( 'NONE',  ( -14.05774678934416499, -5.057305518903948638, 34.11320923018887896 ) ) ;
#79277 = CARTESIAN_POINT ( 'NONE',  ( 7.846153846153725020, -6.879047030192662504, 34.71129190930017927 ) ) ;
#79279 = ORIENTED_EDGE ( 'NONE', *, *, #4545, .F. ) ;
#79278 = FACE_OUTER_BOUND ( 'NONE', #9613, .T. ) ;
#79280 = CARTESIAN_POINT ( 'NONE',  ( 1.139087296526029469, -10.24999999999999289, 17.20312500000000000 ) ) ;
#79281 = EDGE_CURVE ( 'NONE', #53257, #84227, #84523, .T. ) ;
#79282 = LINE ( 'NONE', #17583, #67120 ) ;
#79283 = VERTEX_POINT ( 'NONE', #70336 ) ;
#79284 = DIRECTION ( 'NONE',  ( 0.000000000000000000, 0.1736481776669267785, -0.9848077530122087975 ) ) ;
#79285 = ORIENTED_EDGE ( 'NONE', *, *, #85045, .F. ) ;
#79286 = VECTOR ( 'NONE', #68986, 1000.000000000000000 ) ;
#79287 = CYLINDRICAL_SURFACE ( 'NONE', #19043, 0.2500000000000009437 ) ;
#79288 = CARTESIAN_POINT ( 'NONE',  ( -9.561515884482908234, -2.729792928343269587, 31.24908615093345077 ) ) ;
#79289 = ADVANCED_FACE ( 'NONE', ( #49171 ), #8643, .F. ) ;
#79290 = CARTESIAN_POINT ( 'NONE',  ( 17.01084069756293715, -6.343179335718451384, 34.87096338111212646 ) ) ;
#79291 = EDGE_LOOP ( 'NONE', ( #41046, #15715, #51044, #21126 ) ) ;
#79292 = LINE ( 'NONE', #17594, #23517 ) ;
#79294 = ORIENTED_EDGE ( 'NONE', *, *, #13712, .T. ) ;
#79293 = VECTOR ( 'NONE', #31525, 1000.000000000000000 ) ;
#79295 = CARTESIAN_POINT ( 'NONE',  ( -5.869209559033048862, -2.295524264805589354, 30.44142389570982488 ) ) ;
#79296 = ORIENTED_EDGE ( 'NONE', *, *, #65014, .F. ) ;
#79297 = CARTESIAN_POINT ( 'NONE',  ( 13.38461538461526601, -11.94971097300221174, 32.03036669348237098 ) ) ;
#79298 = CYLINDRICAL_SURFACE ( 'NONE', #8165, 2.750000000000000000 ) ;
#79299 = VERTEX_POINT ( 'NONE', #69449 ) ;
#79300 = CARTESIAN_POINT ( 'NONE',  ( 3.230769230769108269, -11.67786785259630911, 32.92929555188603530 ) ) ;
#79301 = CARTESIAN_POINT ( 'NONE',  ( 10.61538461538449596, -3.300289026999228881, 32.46337939537708905 ) ) ;
#79302 = CARTESIAN_POINT ( 'NONE',  ( 23.00000000000000000, -4.249999999999998224, 29.75000000000000355 ) ) ;
#79303 = DIRECTION ( 'NONE',  ( -0.000000000000000000, 0.9396926207859092051, -0.3420201433256662704 ) ) ;
#79304 = CARTESIAN_POINT ( 'NONE',  ( 3.230769230769231726, -7.500000000000001776, 35.04278698407183867 ) ) ;
#79305 = ADVANCED_FACE ( 'NONE', ( #36552 ), #7753, .T. ) ;
#79306 = EDGE_CURVE ( 'NONE', #11720, #72149, #35213, .T. ) ;
#79307 = VERTEX_POINT ( 'NONE', #12956 ) ;
#79308 = ORIENTED_EDGE ( 'NONE', *, *, #7479, .F. ) ;
#79309 = ORIENTED_EDGE ( 'NONE', *, *, #42981, .F. ) ;
#79311 = VERTEX_POINT ( 'NONE', #80543 ) ;
#79310 = CARTESIAN_POINT ( 'NONE',  ( 3.230769230769108269, -12.70778746994576025, 30.41441678777401236 ) ) ;
#79312 = CIRCLE ( 'NONE', #40495, 2.000000000000001776 ) ;
#79313 = CARTESIAN_POINT ( 'NONE',  ( -17.07692307692319744, -8.656820664282941280, 34.87096338111179961 ) ) ;
#79314 = CARTESIAN_POINT ( 'NONE',  ( -10.74607608205217346, -8.999036380462717588, 34.52022231692819076 ) ) ;
#79315 = ORIENTED_EDGE ( 'NONE', *, *, #34419, .F. ) ;
#79316 = VECTOR ( 'NONE', #5251, 1000.000000000000227 ) ;
#79317 = EDGE_LOOP ( 'NONE', ( #68950, #26, #43207, #67673 ) ) ;
#79318 = EDGE_LOOP ( 'NONE', ( #39325, #17886 ) ) ;
#79319 = CARTESIAN_POINT ( 'NONE',  ( 3.480714749117372442, -5.057305518903949526, 34.11320923018887896 ) ) ;
#79320 = ORIENTED_EDGE ( 'NONE', *, *, #20692, .T. ) ;
#79321 = DIRECTION ( 'NONE',  ( 0.000000000000000000, 0.3420201433256610524, 0.9396926207859113145 ) ) ;
#79322 = CARTESIAN_POINT ( 'NONE',  ( 9.070512820512819374, -7.500000000000000000, 29.75000000000000355 ) ) ;
#79323 = CARTESIAN_POINT ( 'NONE',  ( -9.626141085716049872, -7.250054591869670162, 34.99404684341514127 ) ) ;
#79324 = FACE_BOUND ( 'NONE', #44210, .T. ) ;
#79325 = EDGE_LOOP ( 'NONE', ( #27110, #69702, #16089, #12022 ) ) ;
#79326 = CARTESIAN_POINT ( 'NONE',  ( 17.32686848630112308, -6.653508905675593610, 34.93172785388651391 ) ) ;
#79327 = CARTESIAN_POINT ( 'NONE',  ( 13.45068373561782415, -8.973038597847271092, 34.52809138561121216 ) ) ;
#79328 = CARTESIAN_POINT ( 'NONE',  ( 5.076923076922953193, -3.643525952248796163, 33.31231777344771672 ) ) ;
#79329 = CARTESIAN_POINT ( 'NONE',  ( -14.37377571864818648, -8.973038597847271092, 34.52809138561120506 ) ) ;
#79330 = CARTESIAN_POINT ( 'NONE',  ( -1.607541602131532077, -2.554751324335734264, 30.48935550225260727 ) ) ;
#79331 = ORIENTED_EDGE ( 'NONE', *, *, #32617, .T. ) ;
#79332 = DIRECTION ( 'NONE',  ( 1.000000000000000000, 0.000000000000000000, -0.000000000000000000 ) ) ;
#79333 = VERTEX_POINT ( 'NONE', #39110 ) ;
#79334 = EDGE_LOOP ( 'NONE', ( #70429, #64576, #44978, #8498 ) ) ;
#79336 = DIRECTION ( 'NONE',  ( 0.000000000000000000, -6.938893903907222067E-15, 1.000000000000000000 ) ) ;
#79335 = DIRECTION ( 'NONE',  ( 0.000000000000000000, 1.000000000000000000, -0.000000000000000000 ) ) ;
#79337 = VECTOR ( 'NONE', #19307, 1000.000000000000000 ) ;
#79338 = CARTESIAN_POINT ( 'NONE',  ( -10.61538461538473399, -12.27809138561165270, 31.22303859784587132 ) ) ;
#79339 = CARTESIAN_POINT ( 'NONE',  ( -13.60810030917971858, -3.019605429927184836, 32.48692288466676814 ) ) ;
#79340 = CARTESIAN_POINT ( 'NONE',  ( 1.607394925883793846, -10.11255958852956027, 34.01340905677048454 ) ) ;
#79341 = CARTESIAN_POINT ( 'NONE',  ( 14.30769230769218581, -3.083524468854526912, 32.58852847137268327 ) ) ;
#79342 = ORIENTED_EDGE ( 'NONE', *, *, #10951, .T. ) ;
#79343 = FACE_OUTER_BOUND ( 'NONE', #73029, .T. ) ;
#79344 = CARTESIAN_POINT ( 'NONE',  ( 2.980746006547774218, -9.356822207818506598, 34.66110646841856635 ) ) ;
#79345 = DIRECTION ( 'NONE',  ( 1.000000000000000000, 0.000000000000000000, 0.000000000000000000 ) ) ;
#79346 = CARTESIAN_POINT ( 'NONE',  ( 10.61538461538449596, -11.94971097300221174, 32.03036669348237098 ) ) ;
#79347 = AXIS2_PLACEMENT_3D ( 'NONE', #71845, #65531, #10600 ) ;
#79348 = ORIENTED_EDGE ( 'NONE', *, *, #30674, .T. ) ;
#79349 = ORIENTED_EDGE ( 'NONE', *, *, #11494, .T. ) ;
#79350 = FACE_BOUND ( 'NONE', #57459, .T. ) ;
#79351 = APPLICATION_PROTOCOL_DEFINITION ( 'draft international standard', 'automotive_design', 1998, #88395 ) ;
#79352 = VERTEX_POINT ( 'NONE', #74668 ) ;
#79353 = CARTESIAN_POINT ( 'NONE',  ( -0.4330127018922180770, -4.784304877199946127, 29.50000000000000355 ) ) ;
#79354 = LINE ( 'NONE', #83240, #66333 ) ;
#79355 = EDGE_LOOP ( 'NONE', ( #5943, #3285, #75346, #75483 ) ) ;
#79356 = CARTESIAN_POINT ( 'NONE',  ( -16.21911615440247445, -11.67786785259541027, 32.92929555188721480 ) ) ;
#79357 = CARTESIAN_POINT ( 'NONE',  ( -10.86536134632696715, -6.567427716900048118, 34.66269422305636283 ) ) ;
#79358 = CARTESIAN_POINT ( 'NONE',  ( -8.546219417617917813, -6.503523203565941380, 34.64991518177335195 ) ) ;
#79359 = LINE ( 'NONE', #84802, #80746 ) ;
#79360 = B_SPLINE_CURVE_WITH_KNOTS ( 'NONE', 3,
 ( #43639, #85083, #30566, #85519, #71996, #51708, #1772, #23797, #29262, #2640 ),
 .UNSPECIFIED., .F., .F.,
 ( 4, 2, 2, 2, 4 ),
 ( 0.0007817359430256319575, 0.0009771253907249984917, 0.001172514838424365026, 0.001367904286123731343, 0.001563293733823097878 ),
 .UNSPECIFIED. ) ;
#79361 = CARTESIAN_POINT ( 'NONE',  ( 6.000000000000001776, -1.422936976036506707, 30.56769352161908415 ) ) ;
#79362 = ORIENTED_EDGE ( 'NONE', *, *, #35371, .T. ) ;
#79363 = ADVANCED_FACE ( 'NONE', ( #60695 ), #67463, .F. ) ;
#79365 = VERTEX_POINT ( 'NONE', #53939 ) ;
#79364 = CARTESIAN_POINT ( 'NONE',  ( -4.500000000000003553, 7.499999999999996447, 13.00000000000000178 ) ) ;
#79366 = FACE_OUTER_BOUND ( 'NONE', #61626, .T. ) ;
#79367 = EDGE_CURVE ( 'NONE', #70883, #4654, #85632, .T. ) ;
#79368 = CARTESIAN_POINT ( 'NONE',  ( 0.000000000000000000, -11.00000000000000000, 29.75000000000000355 ) ) ;
#79369 = CARTESIAN_POINT ( 'NONE',  ( 13.38461538461538680, -10.05456864172156806, 36.03766855953608683 ) ) ;
#79370 = CARTESIAN_POINT ( 'NONE',  ( -10.86540783960607293, -3.520140089381495585, 33.17453946501458262 ) ) ;
#79371 = CARTESIAN_POINT ( 'NONE',  ( -8.069638789877792817, -9.331801661448606566, 34.40259984581193464 ) ) ;
#79372 = LINE ( 'NONE', #24860, #66515 ) ;
#79373 = CARTESIAN_POINT ( 'NONE',  ( 2.775308065498755195, -6.422011778438505125, 17.14249329374151287 ) ) ;
#79374 = ORIENTED_EDGE ( 'NONE', *, *, #86772, .T. ) ;
#79375 = CARTESIAN_POINT ( 'NONE',  ( -3.360916440207450506, -3.285722584762969856, 32.44110544564090759 ) ) ;
#79376 = CARTESIAN_POINT ( 'NONE',  ( 2.530705151785705098, -4.026326845037965008, 33.68677907613344047 ) ) ;
#79377 = DIRECTION ( 'NONE',  ( -0.000000000000000000, -5.102127870520021228E-17, -1.000000000000000000 ) ) ;
#79378 = ADVANCED_FACE ( 'NONE', ( #46298 ), #40447, .F. ) ;
#79379 = CIRCLE ( 'NONE', #54942, 0.2500000000000002220 ) ;
#79380 = EDGE_LOOP ( 'NONE', ( #86531, #31654, #4383, #81123 ) ) ;
#79381 = EDGE_LOOP ( 'NONE', ( #71684, #59960, #88118, #71667 ) ) ;
#79382 = CARTESIAN_POINT ( 'NONE',  ( 9.822833130541342328, -3.625058011473228703, 33.29252011169590020 ) ) ;
#79383 = CYLINDRICAL_SURFACE ( 'NONE', #42547, 4.000000000000000000 ) ;
#79384 = EDGE_CURVE ( 'NONE', #66553, #30965, #31985, .T. ) ;
#79385 = DIRECTION ( 'NONE',  ( 0.000000000000000000, 0.4999999999999985567, 0.8660254037844395958 ) ) ;
#79386 = AXIS2_PLACEMENT_3D ( 'NONE', #49262, #68643, #13700 ) ;
#79387 = CARTESIAN_POINT ( 'NONE',  ( 10.39245839786846659, -5.667676309546437530, 34.40238873228292249 ) ) ;
#79388 = CARTESIAN_POINT ( 'NONE',  ( 10.39189967166066708, -4.386631170607603991, 33.66268669641500111 ) ) ;
#79389 = CARTESIAN_POINT ( 'NONE',  ( -16.94639763868943660, -11.66157788607254275, 32.95092075102925833 ) ) ;
#79390 = DIRECTION ( 'NONE',  ( -0.000000000000000000, 1.000000000000000000, -0.000000000000000000 ) ) ;
#79391 = VERTEX_POINT ( 'NONE', #26031 ) ;
#79392 = CARTESIAN_POINT ( 'NONE',  ( 3.230769230769231726, -6.386643153685126251, 34.62446782046654192 ) ) ;
#79393 = LINE ( 'NONE', #44694, #60670 ) ;
#79394 = ADVANCED_FACE ( 'NONE', ( #87306 ), #31904, .F. ) ;
#79395 = CARTESIAN_POINT ( 'NONE',  ( -5.934854220668035474, -7.750023238201980469, 34.74374492549440419 ) ) ;
#79396 = CARTESIAN_POINT ( 'NONE',  ( 17.01083966596719321, -8.973038597847269315, 34.52809138561120506 ) ) ;
#79397 = EDGE_LOOP ( 'NONE', ( #1043, #17994, #3753, #82628 ) ) ;
#79398 = CARTESIAN_POINT ( 'NONE',  ( 13.51540719244017374, -6.413143153341454017, 34.63066358083362672 ) ) ;
#79399 = B_SPLINE_CURVE_WITH_KNOTS ( 'NONE', 3,
 ( #58526, #52669, #31060, #86023, #38277, #18012, #31517, #4492, #11704, #78362 ),
 .UNSPECIFIED., .F., .F.,
 ( 4, 2, 2, 2, 4 ),
 ( 0.0007817246256747503166, 0.0009771112852218946220, 0.001172497944769039036, 0.001367884604316183233, 0.001563271263863327647 ),
 .UNSPECIFIED. ) ;
#79400 = ORIENTED_EDGE ( 'NONE', *, *, #37766, .T. ) ;
#79401 = B_SPLINE_CURVE_WITH_KNOTS ( 'NONE', 3,
 ( #71055, #30514, #44453, #9369, #65180, #84594, #57538, #71491, #64730, #16553 ),
 .UNSPECIFIED., .F., .F.,
 ( 4, 2, 2, 2, 4 ),
 ( 0.0007817359430256300059, 0.0009771253907249963233, 0.001172514838424362858, 0.001367904286123729392, 0.001563293733823095709 ),
 .UNSPECIFIED. ) ;
#79402 = CARTESIAN_POINT ( 'NONE',  ( -17.14219307747939069, -2.657715359629089669, 31.77849191805834295 ) ) ;
#79403 = SURFACE_STYLE_USAGE ( .BOTH. , #45605 ) ;
#79404 = CARTESIAN_POINT ( 'NONE',  ( -1.450698795571263577, -8.973038597847271092, 34.52809138561120506 ) ) ;
#79405 = CARTESIAN_POINT ( 'NONE',  ( 6.065255139512838234, -12.16647553114626490, 32.15551576947920864 ) ) ;
#79406 = ORIENTED_EDGE ( 'NONE', *, *, #65892, .F. ) ;
#79407 = CARTESIAN_POINT ( 'NONE',  ( -4.153846153846273204, -6.026961402154118908, 34.52809138561165270 ) ) ;
#79408 = CARTESIAN_POINT ( 'NONE',  ( -1.608100309179715914, -12.69144148231606017, 30.53333754910549303 ) ) ;
#79409 = CARTESIAN_POINT ( 'NONE',  ( -10.61538461538473399, -10.90142922262034020, 33.41473453929536674 ) ) ;
#79410 = VECTOR ( 'NONE', #14442, 1000.000000000000114 ) ;
#79411 = CARTESIAN_POINT ( 'NONE',  ( 17.78205128205128105, -11.00000000000000000, 29.75000000000000355 ) ) ;
#79412 = CARTESIAN_POINT ( 'NONE',  ( 3.453548899747294953, -3.020022701398814124, 32.48759521482552515 ) ) ;
#79413 = EDGE_CURVE ( 'NONE', #47764, #27494, #43767, .T. ) ;
#79414 = ORIENTED_EDGE ( 'NONE', *, *, #47631, .T. ) ;
#79415 = CARTESIAN_POINT ( 'NONE',  ( -10.86538461538461675, -2.499999999999999556, 29.81609845454691765 ) ) ;
#79416 = EDGE_CURVE ( 'NONE', #79083, #85360, #59363, .T. ) ;
#79417 = ORIENTED_EDGE ( 'NONE', *, *, #27727, .T. ) ;
#79418 = VECTOR ( 'NONE', #70308, 1000.000000000000000 ) ;
#79419 = CARTESIAN_POINT ( 'NONE',  ( -2.437840277424006885, -2.647304123082328875, 31.75400227202885262 ) ) ;
#79420 = CARTESIAN_POINT ( 'NONE',  ( 5.076923076923075762, -12.10708131394839349, 31.69288490824020244 ) ) ;
#79421 = DIRECTION ( 'NONE',  ( -1.000000000000000000, -0.000000000000000000, -0.000000000000000000 ) ) ;
#79422 = EDGE_CURVE ( 'NONE', #53945, #10355, #32783, .T. ) ;
#79423 = CARTESIAN_POINT ( 'NONE',  ( 9.915320536401091900, -2.523321265292115534, 31.42251411153756990 ) ) ;
#79424 = EDGE_CURVE ( 'NONE', #51615, #75410, #25136, .T. ) ;
#79425 = FACE_BOUND ( 'NONE', #50660, .T. ) ;
#79426 = CARTESIAN_POINT ( 'NONE',  ( 12.68431800280687050, -10.11255958852956027, 34.01340905677048454 ) ) ;
#79427 = ORIENTED_EDGE ( 'NONE', *, *, #78349, .T. ) ;
#79428 = VERTEX_POINT ( 'NONE', #19275 ) ;
#79429 = EDGE_LOOP ( 'NONE', ( #56949, #46610 ) ) ;
#79430 = ORIENTED_EDGE ( 'NONE', *, *, #2502, .F. ) ;
#79431 = VERTEX_POINT ( 'NONE', #40002 ) ;
#79432 = CARTESIAN_POINT ( 'NONE',  ( -10.55012904410859065, -8.613356846314928816, 34.62446782046653482 ) ) ;
#79433 = CARTESIAN_POINT ( 'NONE',  ( -3.480792454990687013, -6.652501968072646932, 34.93155406624980941 ) ) ;
#79434 = CARTESIAN_POINT ( 'NONE',  ( -2.177644701436622476, -7.723484964179500700, 34.74522123443823318 ) ) ;
#79435 = B_SPLINE_CURVE_WITH_KNOTS ( 'NONE', 3,
 ( #38726, #35744, #18017, #28994, #79272, #15025, #51768, #56449, #45023, #22220 ),
 .UNSPECIFIED., .F., .F.,
 ( 4, 2, 2, 2, 4 ),
 ( 0.0007817359430256388964, 0.0009771253907250073822, 0.001172514838424375868, 0.001367904286123744571, 0.001563293733823113056 ),
 .UNSPECIFIED. ) ;
#79436 = CARTESIAN_POINT ( 'NONE',  ( 1.653273178848927064E-15, -7.500000000000000000, 13.00000000000000178 ) ) ;
#79437 = CARTESIAN_POINT ( 'NONE',  ( -16.28399336328437386, -2.619462340734462380, 30.83744416345203021 ) ) ;
#79438 = CARTESIAN_POINT ( 'NONE',  ( 0.5923302693632468419, -4.809403383903225304, 33.96459661697924304 ) ) ;
#79439 = DIRECTION ( 'NONE',  ( 0.000000000000000000, 0.4999999999999985567, 0.8660254037844395958 ) ) ;
#79440 = LINE ( 'NONE', #85309, #61030 ) ;
#79441 = CARTESIAN_POINT ( 'NONE',  ( -4.403822884788507253, -9.943427161483782584, 34.11278801902876978 ) ) ;
#79442 = EDGE_LOOP ( 'NONE', ( #73220, #26063 ) ) ;
#79443 = VERTEX_POINT ( 'NONE', #74220 ) ;
#79444 = VECTOR ( 'NONE', #53809, 1000.000000000000000 ) ;
#79445 = VERTEX_POINT ( 'NONE', #62454 ) ;
#79447 = ORIENTED_EDGE ( 'NONE', *, *, #22450, .T. ) ;
#79446 = DIRECTION ( 'NONE',  ( 0.000000000000000000, 1.000000000000000000, 0.000000000000000000 ) ) ;
#79449 = CARTESIAN_POINT ( 'NONE',  ( -16.21992956480203318, -9.780366693483667717, 34.19971097300155805 ) ) ;
#79448 = CARTESIAN_POINT ( 'NONE',  ( 7.780883400193070898, -3.300289026998414865, 32.46337939537583139 ) ) ;
#79450 = EDGE_CURVE ( 'NONE', #27477, #75533, #39394, .T. ) ;
#79451 = CARTESIAN_POINT ( 'NONE',  ( 12.46153846153846168, -9.819645486525091727, 36.12317359536749706 ) ) ;
#79452 = CARTESIAN_POINT ( 'NONE',  ( 7.173022441425066731, -2.587454068350147462, 30.68340429815432202 ) ) ;
#79453 = FACE_BOUND ( 'NONE', #81832, .T. ) ;
#79454 = VERTEX_POINT ( 'NONE', #69667 ) ;
#79455 = EDGE_LOOP ( 'NONE', ( #87797, #28724, #26895, #61028 ) ) ;
#79456 = DIRECTION ( 'NONE',  ( -0.000000000000000000, -0.3420201433256694901, -0.9396926207859082059 ) ) ;
#79457 = ORIENTED_EDGE ( 'NONE', *, *, #28223, .T. ) ;
#79458 = FACE_BOUND ( 'NONE', #17557, .T. ) ;
#79459 = LINE ( 'NONE', #17758, #28918 ) ;
#79460 = CYLINDRICAL_SURFACE ( 'NONE', #86595, 0.2499999999999997502 ) ;
#79461 = VERTEX_POINT ( 'NONE', #75537 ) ;
#79462 = CARTESIAN_POINT ( 'NONE',  ( -15.16470087976679970, -12.10708131394839882, 31.69288490824020954 ) ) ;
#79463 = CARTESIAN_POINT ( 'NONE',  ( -1.384615384615383471, -8.164416787775445883, 34.95778746994557906 ) ) ;
#79464 = CARTESIAN_POINT ( 'NONE',  ( 14.30769230769231015, -13.53365097954675988, 30.81389545987213552 ) ) ;
#79465 = ORIENTED_EDGE ( 'NONE', *, *, #86960, .F. ) ;
#79466 = CYLINDRICAL_SURFACE ( 'NONE', #12626, 0.2500000000000009437 ) ;
#79467 = DIRECTION ( 'NONE',  ( -0.000000000000000000, -0.8660254037844399289, -0.4999999999999980016 ) ) ;
#79468 = ORIENTED_EDGE ( 'NONE', *, *, #21445, .F. ) ;
#79469 = ADVANCED_FACE ( 'NONE', ( #54825 ), #55266, .F. ) ;
#79470 = CARTESIAN_POINT ( 'NONE',  ( 2.057692307692309708, -7.500000000000001776, 34.75000000000000000 ) ) ;
#79471 = DIRECTION ( 'NONE',  ( -0.000000000000000000, 0.9396926207859092051, -0.3420201433256662704 ) ) ;
#79473 = ORIENTED_EDGE ( 'NONE', *, *, #67323, .T. ) ;
#79472 = VECTOR ( 'NONE', #22751, 1000.000000000000000 ) ;
#79474 = CARTESIAN_POINT ( 'NONE',  ( 3.230769230769108269, -6.835583212225970762, 34.95778746994575670 ) ) ;
#79475 = CARTESIAN_POINT ( 'NONE',  ( 13.31934493865461278, -2.625532179533445198, 30.86335684631481513 ) ) ;
#79476 = CARTESIAN_POINT ( 'NONE',  ( 16.02315555073584008, -2.845849958028613624, 32.17971566917920967 ) ) ;
#79477 = B_SPLINE_CURVE_WITH_KNOTS ( 'NONE', 3,
 ( #4502, #67541, #73861, #31980, #5840, #81067, #19351, #4041, #59445, #47257 ),
 .UNSPECIFIED., .F., .F.,
 ( 4, 2, 2, 2, 4 ),
 ( 0.0007817246336856289524, 0.0009771112958940101571, 0.001172497958102391253, 0.001367884620310772350, 0.001563271282519153446 ),
 .UNSPECIFIED. ) ;
#79478 = DIRECTION ( 'NONE',  ( 0.000000000000000000, 0.000000000000000000, -1.000000000000000000 ) ) ;
#79479 = CARTESIAN_POINT ( 'NONE',  ( 9.442284468086237226, -12.45566812827425451, 31.48439005359158926 ) ) ;
#79480 = CARTESIAN_POINT ( 'NONE',  ( -0.2381629757660416458, -2.251407671071270489, 29.88021292934942963 ) ) ;
#79482 = DIRECTION ( 'NONE',  ( -1.000000000000000000, 0.000000000000000000, -0.000000000000000000 ) ) ;
#79481 = CARTESIAN_POINT ( 'NONE',  ( -1.634638621908350631, -2.823816976329317718, 31.52131813110795733 ) ) ;
#79483 = CARTESIAN_POINT ( 'NONE',  ( 8.992010310499175318, -12.24180327182771855, 31.33663988360758879 ) ) ;
#79485 = CARTESIAN_POINT ( 'NONE',  ( -10.83831083290076158, -8.239355502252617924, 34.69524867566427417 ) ) ;
#79484 = CARTESIAN_POINT ( 'NONE',  ( 3.230769230769538147, -2.506253911140615021, 30.00000000000323297 ) ) ;
#79486 = CARTESIAN_POINT ( 'NONE',  ( 1.139087296526029469, -10.24999999999999467, 14.70312500000000355 ) ) ;
#79487 = ORIENTED_EDGE ( 'NONE', *, *, #1434, .F. ) ;
#79488 = DIRECTION ( 'NONE',  ( -0.000000000000000000, 0.3420201433256694901, -0.9396926207859082059 ) ) ;
#79489 = ORIENTED_EDGE ( 'NONE', *, *, #33618, .F. ) ;
#79490 = EDGE_CURVE ( 'NONE', #30370, #11900, #2823, .T. ) ;
#79491 = EDGE_LOOP ( 'NONE', ( #39531, #2769 ) ) ;
#79492 = CARTESIAN_POINT ( 'NONE',  ( -1.384615384615383471, -1.466349020453238561, 30.81389545987213907 ) ) ;
#79493 = ORIENTED_EDGE ( 'NONE', *, *, #22887, .T. ) ;
#79494 = CARTESIAN_POINT ( 'NONE',  ( -18.00000000000012079, -12.46129190930018460, 30.37095296980731973 ) ) ;
#79495 = CARTESIAN_POINT ( 'NONE',  ( -1.901340078031346525, -9.487747218494661183, 27.18563170625849068 ) ) ;
#79496 = CARTESIAN_POINT ( 'NONE',  ( -5.076923076923197442, -11.48612834414049644, 32.76840700105863391 ) ) ;
#79497 = EDGE_CURVE ( 'NONE', #20943, #1690, #62893, .T. ) ;
#79498 = CARTESIAN_POINT ( 'NONE',  ( 5.999999999999880096, -11.48612834414049644, 32.76840700105863391 ) ) ;
#79499 = CARTESIAN_POINT ( 'NONE',  ( 19.99999999999997158, -14.99999999999999467, 13.00000000000000178 ) ) ;
#79500 = CARTESIAN_POINT ( 'NONE',  ( -12.33101302330481985, -4.299079248970732792, 33.91157788607253565 ) ) ;
#79501 = CARTESIAN_POINT ( 'NONE',  ( 1.384615384615386802, -12.78798330534102767, 29.49999999999997868 ) ) ;
#79502 = DIRECTION ( 'NONE',  ( 0.000000000000000000, 0.9396926207859126468, 0.3420201433256571111 ) ) ;
#79503 = DIRECTION ( 'NONE',  ( -1.000000000000000000, 0.000000000000000000, 0.000000000000000000 ) ) ;
#79504 = CARTESIAN_POINT ( 'NONE',  ( 3.750000000000009770, -9.053300858899081760, 23.29687500000000000 ) ) ;
#79505 = DIRECTION ( 'NONE',  ( 0.000000000000000000, 0.3420201433256610524, 0.9396926207859113145 ) ) ;
#79506 = CARTESIAN_POINT ( 'NONE',  ( -15.00798968950081758, -2.600157965045224451, 30.74683119005207743 ) ) ;
#79507 = EDGE_CURVE ( 'NONE', #76524, #22606, #1207, .T. ) ;
#79508 = DIRECTION ( 'NONE',  ( -0.000000000000000000, 0.5000000000000011102, -0.8660254037844380415 ) ) ;
#79509 = VECTOR ( 'NONE', #87591, 1000.000000000000000 ) ;
#79510 = EDGE_CURVE ( 'NONE', #61245, #28895, #88644, .T. ) ;
#79511 = ORIENTED_EDGE ( 'NONE', *, *, #43828, .F. ) ;
#79512 = ORIENTED_EDGE ( 'NONE', *, *, #58103, .T. ) ;
#79513 = CARTESIAN_POINT ( 'NONE',  ( -2.307692307692305711, -12.78798330534103123, 29.99999999999997868 ) ) ;
#79514 = CARTESIAN_POINT ( 'NONE',  ( -17.07692307692307665, -8.120952969808772792, 34.71129190930000163 ) ) ;
#79515 = CYLINDRICAL_SURFACE ( 'NONE', #16700, 0.2500000000000008882 ) ;
#79516 = CARTESIAN_POINT ( 'NONE',  ( -17.76215049426128445, -1.749999999999992228, 32.75000000000000000 ) ) ;
#79517 = EDGE_CURVE ( 'NONE', #79365, #24740, #56156, .T. ) ;
#79518 = CARTESIAN_POINT ( 'NONE',  ( 3.930919194939304084, -3.395401636524186362, 33.02366814457250399 ) ) ;
#79519 = AXIS2_PLACEMENT_3D ( 'NONE', #76185, #21687, #55037 ) ;
#79520 = CARTESIAN_POINT ( 'NONE',  ( -2.544871794871793824, -3.499999999999999556, 29.75000000000000355 ) ) ;
#79521 = EDGE_CURVE ( 'NONE', #49031, #15672, #28619, .T. ) ;
#79522 = ORIENTED_EDGE ( 'NONE', *, *, #52518, .T. ) ;
#79523 = CARTESIAN_POINT ( 'NONE',  ( 17.77651505627605033, -12.44517049084099725, 30.48991314939691932 ) ) ;
#79524 = ORIENTED_EDGE ( 'NONE', *, *, #71305, .F. ) ;
#79525 = EDGE_CURVE ( 'NONE', #25295, #2963, #769, .T. ) ;
#79526 = ORIENTED_EDGE ( 'NONE', *, *, #74241, .T. ) ;
#79527 = CARTESIAN_POINT ( 'NONE',  ( 10.61538461538461675, -12.48256725967547354, 35.29906147534542527 ) ) ;
#79528 = CARTESIAN_POINT ( 'NONE',  ( 6.066169140962657913, -7.250054483168843156, 34.74374881642865631 ) ) ;
#79529 = CARTESIAN_POINT ( 'NONE',  ( -0.3953718549468210330, -7.250054591869666609, 34.99404684341514127 ) ) ;
#79530 = EDGE_CURVE ( 'NONE', #48470, #70777, #32926, .T. ) ;
#79531 = B_SPLINE_CURVE_WITH_KNOTS ( 'NONE', 3,
 ( #3503, #26456, #48038, #41743, #53919, #21009, #47156, #13818, #6622, #61116 ),
 .UNSPECIFIED., .F., .F.,
 ( 4, 2, 2, 2, 4 ),
 ( 0.000000000000000000, 0.0001954311564186863865, 0.0003908623128373727731, 0.0005862934692560591325, 0.0007817246256747455461 ),
 .UNSPECIFIED. ) ;
#79532 = DIRECTION ( 'NONE',  ( 0.000000000000000000, 1.000000000000000000, 0.000000000000000000 ) ) ;
#79533 = DIRECTION ( 'NONE',  ( 1.000000000000000000, 0.000000000000000000, 0.000000000000000000 ) ) ;
#79534 = ORIENTED_EDGE ( 'NONE', *, *, #13780, .T. ) ;
#79535 = VECTOR ( 'NONE', #32643, 1000.000000000000000 ) ;
#79536 = AXIS2_PLACEMENT_3D ( 'NONE', #50447, #42394, #83373 ) ;
#79537 = ORIENTED_EDGE ( 'NONE', *, *, #26751, .F. ) ;
#79538 = ORIENTED_EDGE ( 'NONE', *, *, #58844, .T. ) ;
#79539 = CARTESIAN_POINT ( 'NONE',  ( -4.087778820496075660, -11.91647553114624358, 32.58852847137148245 ) ) ;
#79540 = LINE ( 'NONE', #25477, #7112 ) ;
#79541 = EDGE_CURVE ( 'NONE', #30860, #88554, #86281, .T. ) ;
#79542 = CARTESIAN_POINT ( 'NONE',  ( -6.923076923076922462, -8.318370150425687726, 35.83090037661290239 ) ) ;
#79543 = CARTESIAN_POINT ( 'NONE',  ( 10.61538461538449596, -10.90142922262034020, 33.41473453929536674 ) ) ;
#79544 = EDGE_CURVE ( 'NONE', #87443, #24897, #10186, .T. ) ;
#79545 = DIRECTION ( 'NONE',  ( -1.000000000000000000, -0.000000000000000000, -0.000000000000000000 ) ) ;
#79546 = CARTESIAN_POINT ( 'NONE',  ( 24.00000000000000000, 5.000000000000023093, 29.24999999999999645 ) ) ;
#79547 = VERTEX_POINT ( 'NONE', #43961 ) ;
#79548 = ORIENTED_EDGE ( 'NONE', *, *, #59227, .T. ) ;
#79549 = CARTESIAN_POINT ( 'NONE',  ( 2.651650429449539104, -4.848349570550432475, 19.31250000000000000 ) ) ;
#79550 = VERTEX_POINT ( 'NONE', #78195 ) ;
#79552 = EDGE_LOOP ( 'NONE', ( #35260, #42401 ) ) ;
#79551 = CARTESIAN_POINT ( 'NONE',  ( -13.44988538517170440, -5.941354392334499579, 34.76329471203369792 ) ) ;
#79553 = CARTESIAN_POINT ( 'NONE',  ( 1.319344938654610555, -10.21337939537584205, 33.94971097300158647 ) ) ;
#79554 = CARTESIAN_POINT ( 'NONE',  ( 12.52760579488853665, -8.164416787775445883, 34.95778746994558617 ) ) ;
#79555 = EDGE_CURVE ( 'NONE', #62627, #79057, #81281, .T. ) ;
#79556 = CARTESIAN_POINT ( 'NONE',  ( 1.553300858899129722, -11.24999999999999112, 17.20312500000000000 ) ) ;
#79557 = VERTEX_POINT ( 'NONE', #84090 ) ;
#79558 = CARTESIAN_POINT ( 'NONE',  ( 10.68063975489745232, -2.379036618887895305, 30.90682066428158592 ) ) ;
#79559 = VERTEX_POINT ( 'NONE', #51584 ) ;
#79560 = EDGE_CURVE ( 'NONE', #9433, #23520, #71428, .T. ) ;
#79561 = CARTESIAN_POINT ( 'NONE',  ( 5.776515075435672664, -9.417330523894424488, 34.63758898049880486 ) ) ;
#79562 = CARTESIAN_POINT ( 'NONE',  ( -6.923076923076922462, -2.721908614388771852, 31.22303859784724978 ) ) ;
#79563 = DIRECTION ( 'NONE',  ( 0.000000000000000000, 0.1736481776669267785, -0.9848077530122087975 ) ) ;
#79565 = CARTESIAN_POINT ( 'NONE',  ( 7.846153846153723244, -2.379036618888197729, 30.90682066428292885 ) ) ;
#79564 = CARTESIAN_POINT ( 'NONE',  ( -0.4615384615385840772, -11.67786785259630911, 32.92929555188603530 ) ) ;
#79566 = EDGE_CURVE ( 'NONE', #47342, #19850, #85404, .T. ) ;
#79567 = STYLED_ITEM ( 'NONE', ( #39898 ), #59398 ) ;
#79568 = CARTESIAN_POINT ( 'NONE',  ( 16.81410256410256565, -11.00000000000000000, 29.75000000000000355 ) ) ;
#79569 = DIRECTION ( 'NONE',  ( -1.000000000000000000, 0.000000000000000000, 0.000000000000000000 ) ) ;
#79570 = ORIENTED_EDGE ( 'NONE', *, *, #2524, .T. ) ;
#79571 = CARTESIAN_POINT ( 'NONE',  ( -11.47320639894870276, -8.656820664281605460, 34.87096338111211224 ) ) ;
#79572 = CARTESIAN_POINT ( 'NONE',  ( 3.230769230769110045, -4.481592998941358097, 33.73612834414048933 ) ) ;
#79573 = VERTEX_POINT ( 'NONE', #50262 ) ;
#79574 = ADVANCED_FACE ( 'NONE', ( #37649 ), #64224, .F. ) ;
#79575 = CARTESIAN_POINT ( 'NONE',  ( 2.307692307692309264, -10.51840700105979565, 33.73612834413961536 ) ) ;
#79576 = DIRECTION ( 'NONE',  ( -0.000000000000000000, 0.3420201433256694901, -0.9396926207859082059 ) ) ;
#79577 = CARTESIAN_POINT ( 'NONE',  ( -6.130147209438218781, -10.88202310037935661, 33.43294751532457099 ) ) ;
#79578 = CARTESIAN_POINT ( 'NONE',  ( 11.53846153846153832, -5.557115091759785130, 34.35708131394839171 ) ) ;
#79579 = CARTESIAN_POINT ( 'NONE',  ( 7.780070435197965928, -8.120952969808774569, 34.71129190930000163 ) ) ;
#79580 = FACE_BOUND ( 'NONE', #68597, .T. ) ;
#79582 = DIRECTION ( 'NONE',  ( -0.000000000000000000, 0.9848077530122086864, -0.1736481776669273891 ) ) ;
#79581 = CARTESIAN_POINT ( 'NONE',  ( 12.23861224402230619, -3.105860786376062332, 32.13614157043599562 ) ) ;
#79583 = DIRECTION ( 'NONE',  ( 0.000000000000000000, 0.000000000000000000, -1.000000000000000000 ) ) ;
#79585 = CARTESIAN_POINT ( 'NONE',  ( 14.08420738312797660, -10.97335522853832579, 33.68706563782419749 ) ) ;
#79584 = CARTESIAN_POINT ( 'NONE',  ( -1.384615384615505151, -12.27809138561165270, 31.22303859784587132 ) ) ;
#79586 = DIRECTION ( 'NONE',  ( 0.000000000000000000, 0.4999999999999960032, -0.8660254037844410391 ) ) ;
#79587 = CARTESIAN_POINT ( 'NONE',  ( 24.00000000000000000, -9.499999999999982236, 27.74999999999999645 ) ) ;
#79588 = CARTESIAN_POINT ( 'NONE',  ( 2.608446859217893099, -4.805146000318787358, 24.06063170625849423 ) ) ;
#79589 = ORIENTED_EDGE ( 'NONE', *, *, #38338, .F. ) ;
#79590 = CARTESIAN_POINT ( 'NONE',  ( 16.09615384615384670, -11.00000000000000000, 29.75000000000000355 ) ) ;
#79591 = CARTESIAN_POINT ( 'NONE',  ( 16.21910129335899597, -12.70778746994558439, 30.41441678777537305 ) ) ;
#79592 = CARTESIAN_POINT ( 'NONE',  ( 11.53846153846153832, -6.189225973068211317, 35.74407628777942847 ) ) ;
#79593 = CARTESIAN_POINT ( 'NONE',  ( -13.13461538461538325, -2.499999999999998668, 29.75000000000000355 ) ) ;
#79594 = DIRECTION ( 'NONE',  ( -0.000000000000000000, -0.000000000000000000, 1.000000000000000000 ) ) ;
#79595 = CARTESIAN_POINT ( 'NONE',  ( -12.52762084089859407, -6.343179335718451384, 34.87096338111212646 ) ) ;
#79596 = CARTESIAN_POINT ( 'NONE',  ( -3.775308065498766297, -6.007798216065450170, 24.92000670625849068 ) ) ;
#79597 = ADVANCED_FACE ( 'NONE', ( #43084 ), #51139, .F. ) ;
#79598 = CARTESIAN_POINT ( 'NONE',  ( -15.45425415533356350, -12.69144148231606017, 30.53333754910549303 ) ) ;
#79599 = CARTESIAN_POINT ( 'NONE',  ( 0.5276068125408995835, -3.513871655860379306, 32.76840700105978499 ) ) ;
#79600 = CARTESIAN_POINT ( 'NONE',  ( 0.4769917816027516855, -4.791317262343001815, 29.42382599947123722 ) ) ;
#79601 = DIRECTION ( 'NONE',  ( -0.000000000000000000, 1.000000000000000000, 3.491481338843133355E-15 ) ) ;
#79602 = CARTESIAN_POINT ( 'NONE',  ( -7.053768389744480061, -4.118384482072085184, 33.43331474514187107 ) ) ;
#79603 = DIRECTION ( 'NONE',  ( 0.000000000000000000, 0.4999999999999985567, 0.8660254037844395958 ) ) ;
#79604 = CARTESIAN_POINT ( 'NONE',  ( -6.000000000000121680, -12.16647553114689728, 32.15551576947799362 ) ) ;
#79605 = CARTESIAN_POINT ( 'NONE',  ( -19.00000000000000000, -1.249999999999999112, 32.75000000000000000 ) ) ;
#79606 = EDGE_LOOP ( 'NONE', ( #83425, #23166 ) ) ;
#79607 = CARTESIAN_POINT ( 'NONE',  ( 17.20744851515672025, -12.70449254468099198, 30.44128974285582956 ) ) ;
#79608 = CARTESIAN_POINT ( 'NONE',  ( 6.923076923076802558, -5.219633306517616589, 34.19971097300220464 ) ) ;
#79609 = CARTESIAN_POINT ( 'NONE',  ( -2.608446859217920633, -4.805146000318815780, 20.50186829374151287 ) ) ;
#79610 = CARTESIAN_POINT ( 'NONE',  ( 2.084207363968360038, -4.386631170607603991, 33.66268669641500111 ) ) ;
#79611 = CARTESIAN_POINT ( 'NONE',  ( 6.923076923076800782, -4.320704448113951379, 33.92786785259630022 ) ) ;
#79612 = ORIENTED_EDGE ( 'NONE', *, *, #10063, .T. ) ;
#79613 = CARTESIAN_POINT ( 'NONE',  ( -18.00000000000012079, -9.442884908241554243, 34.35708131394783038 ) ) ;
#79614 = CARTESIAN_POINT ( 'NONE',  ( 1.653273178848927064E-15, -7.500000000000000000, 29.50000000000000355 ) ) ;
#79616 = ORIENTED_EDGE ( 'NONE', *, *, #53356, .F. ) ;
#79615 = CARTESIAN_POINT ( 'NONE',  ( 0.6089743589743582541, -7.500000000000000000, 29.75000000000000355 ) ) ;
#79617 = DIRECTION ( 'NONE',  ( 0.000000000000000000, 0.000000000000000000, -1.000000000000000000 ) ) ;
#79618 = LINE ( 'NONE', #72846, #32567 ) ;
#79619 = DIRECTION ( 'NONE',  ( -1.000000000000000000, -0.000000000000000000, -0.000000000000000000 ) ) ;
#79620 = CARTESIAN_POINT ( 'NONE',  ( -11.78843828251013015, -2.544273027872575366, 31.48422191005632342 ) ) ;
#79621 = EDGE_LOOP ( 'NONE', ( #76873, #80244, #31688, #79285 ) ) ;
#79622 = LINE ( 'NONE', #73309, #23141 ) ;
#79623 = CARTESIAN_POINT ( 'NONE',  ( 10.61538461538461675, -3.937682226553329556, 33.60647404775216529 ) ) ;
#79624 = AXIS2_PLACEMENT_3D ( 'NONE', #27911, #20709, #53268 ) ;
#79625 = ADVANCED_FACE ( 'NONE', ( #2522 ), #63350, .F. ) ;
#79626 = CARTESIAN_POINT ( 'NONE',  ( -1.134561072977069651, -5.728107161865378494, 34.42597550085002922 ) ) ;
#79627 = ORIENTED_EDGE ( 'NONE', *, *, #61033, .T. ) ;
#79628 = ORIENTED_EDGE ( 'NONE', *, *, #18578, .T. ) ;
#79629 = ADVANCED_FACE ( 'NONE', ( #78637 ), #64666, .F. ) ;
#79630 = ORIENTED_EDGE ( 'NONE', *, *, #53279, .T. ) ;
#79631 = AXIS2_PLACEMENT_3D ( 'NONE', #26787, #35314, #646 ) ;
#79632 = CARTESIAN_POINT ( 'NONE',  ( -9.822454901745912181, -10.19110544564092002, 33.96427741523702792 ) ) ;
#79633 = CARTESIAN_POINT ( 'NONE',  ( 16.15384615384615330, -2.499999999999998668, 29.75000000000001421 ) ) ;
#79634 = EDGE_CURVE ( 'NONE', #62369, #63637, #63063, .T. ) ;
#79635 = FACE_OUTER_BOUND ( 'NONE', #73446, .T. ) ;
#79636 = EDGE_CURVE ( 'NONE', #73637, #67905, #36334, .T. ) ;
#79637 = CARTESIAN_POINT ( 'NONE',  ( 15.23076923076911093, -3.835265460704628371, 33.15142922262033665 ) ) ;
#79638 = B_SPLINE_CURVE_WITH_KNOTS ( 'NONE', 3,
 ( #48124, #7150, #14346, #399, #67969, #21092, #27861, #6272, #62517, #14802 ),
 .UNSPECIFIED., .F., .F.,
 ( 4, 2, 2, 2, 4 ),
 ( 0.0007817359430256252354, 0.0009771253907249898181, 0.001172514838424354401, 0.001367904286123718983, 0.001563293733823083566 ),
 .UNSPECIFIED. ) ;
#79639 = ORIENTED_EDGE ( 'NONE', *, *, #52696, .T. ) ;
#79640 = EDGE_LOOP ( 'NONE', ( #13073, #18288, #66793, #35115 ) ) ;
#79642 = ORIENTED_EDGE ( 'NONE', *, *, #80772, .T. ) ;
#79641 = CARTESIAN_POINT ( 'NONE',  ( 4.219101293358989757, -5.941354392334606160, 34.76329471203374055 ) ) ;
#79643 = CARTESIAN_POINT ( 'NONE',  ( -16.15384615384615330, -12.34228464037088635, 31.77849191805839268 ) ) ;
#79644 = EDGE_CURVE ( 'NONE', #26806, #11121, #63790, .T. ) ;
#79645 = CARTESIAN_POINT ( 'NONE',  ( -3.453696189676079609, -4.762599654559228846, 34.23009711892697737 ) ) ;
#79646 = CARTESIAN_POINT ( 'NONE',  ( 1.607626736228235931, -10.61302985866383963, 33.66295027996417843 ) ) ;
#79647 = DIRECTION ( 'NONE',  ( 1.734723475976812518E-16, -1.000000000000000000, 0.000000000000000000 ) ) ;
#79648 = ORIENTED_EDGE ( 'NONE', *, *, #39023, .T. ) ;
#79649 = ORIENTED_EDGE ( 'NONE', *, *, #62675, .F. ) ;
#79650 = AXIS2_PLACEMENT_3D ( 'NONE', #3663, #78885, #38802 ) ;
#79651 = ORIENTED_EDGE ( 'NONE', *, *, #37866, .F. ) ;
#79653 = VERTEX_POINT ( 'NONE', #16055 ) ;
#79652 = DIRECTION ( 'NONE',  ( -1.000000000000000000, -0.000000000000000000, 0.000000000000000000 ) ) ;
#79654 = CARTESIAN_POINT ( 'NONE',  ( 18.06606733335007675, -11.91647553114624358, 32.58852847137148245 ) ) ;
#79655 = LINE ( 'NONE', #12531, #56814 ) ;
#79656 = ORIENTED_EDGE ( 'NONE', *, *, #82460, .F. ) ;
#79657 = CARTESIAN_POINT ( 'NONE',  ( 15.23076923076923173, -13.53365097954675988, 30.81389545987213552 ) ) ;
#79658 = LINE ( 'NONE', #59382, #58017 ) ;
#79659 = LINE ( 'NONE', #45413, #13787 ) ;
#79660 = FACE_BOUND ( 'NONE', #42438, .T. ) ;
#79661 = EDGE_CURVE ( 'NONE', #17849, #8287, #43522, .T. ) ;
#79662 = CARTESIAN_POINT ( 'NONE',  ( 0.000000000000000000, -11.00000000000000000, 29.75000000000000355 ) ) ;
#79663 = CARTESIAN_POINT ( 'NONE',  ( -6.673022503163470454, -9.233818618650603938, 34.70587769442853698 ) ) ;
#79664 = CARTESIAN_POINT ( 'NONE',  ( -8.069080063669993308, -12.15238873228292071, 31.58232369045353849 ) ) ;
#79666 = CARTESIAN_POINT ( 'NONE',  ( -8.546217925137376881, -11.98016756924215009, 32.48728574198911190 ) ) ;
#79665 = CARTESIAN_POINT ( 'NONE',  ( 16.21910129335899597, -4.320704448112858032, 33.92786785259548310 ) ) ;
#79667 = CARTESIAN_POINT ( 'NONE',  ( -8.096130577096198877, -3.137211980971221781, 32.19342716148376837 ) ) ;
#79668 = LINE ( 'NONE', #72901, #69215 ) ;
#79669 = ORIENTED_EDGE ( 'NONE', *, *, #37773, .T. ) ;
#79670 = CARTESIAN_POINT ( 'NONE',  ( 2.530703659305158837, -6.503523203565942268, 34.64991518177335195 ) ) ;
#79671 = CARTESIAN_POINT ( 'NONE',  ( -17.07692307692307665, -10.05456864172156806, 36.03766855953608683 ) ) ;
#79672 = ORIENTED_EDGE ( 'NONE', *, *, #86418, .F. ) ;
#79673 = ORIENTED_EDGE ( 'NONE', *, *, #45752, .T. ) ;
#79675 = CARTESIAN_POINT ( 'NONE',  ( -5.869474298236433185, -12.27024696741798770, 31.24895572276497546 ) ) ;
#79674 = CARTESIAN_POINT ( 'NONE',  ( -6.857008572074484221, -8.120952969808772792, 34.71129190929999453 ) ) ;
#79676 = EDGE_CURVE ( 'NONE', #10584, #49301, #20102, .T. ) ;
#79677 = CARTESIAN_POINT ( 'NONE',  ( -13.51522574423990974, -7.722926236386453702, 34.74524107206102030 ) ) ;
#79678 = DIRECTION ( 'NONE',  ( -0.000000000000000000, 0.9396926207859093161, -0.3420201433256663259 ) ) ;
#79679 = CARTESIAN_POINT ( 'NONE',  ( 12.21151523731700550, -10.92453946501458795, 33.72985991061850086 ) ) ;
#79680 = VERTEX_POINT ( 'NONE', #52047 ) ;
#79681 = CARTESIAN_POINT ( 'NONE',  ( -6.923076923076922462, -12.48256725967547354, 35.29906147534542527 ) ) ;
#79682 = CARTESIAN_POINT ( 'NONE',  ( 4.284371592079797786, -5.070358843744210198, 34.40418822224088302 ) ) ;
#79683 = VECTOR ( 'NONE', #37098, 1000.000000000000114 ) ;
#79684 = EDGE_CURVE ( 'NONE', #63745, #88209, #79540, .T. ) ;
#79686 = CARTESIAN_POINT ( 'NONE',  ( 15.00728430620490172, -10.97335522853832579, 33.68706563782419749 ) ) ;
#79685 = DIRECTION ( 'NONE',  ( 0.000000000000000000, 0.4999999999999985567, 0.8660254037844395958 ) ) ;
#79687 = CARTESIAN_POINT ( 'NONE',  ( 7.846153846153846700, -5.557115091759785130, 34.35708131394839171 ) ) ;
#79688 = CARTESIAN_POINT ( 'NONE',  ( 10.74617642320940725, -4.118422570099828484, 33.43335022499816489 ) ) ;
#79689 = CARTESIAN_POINT ( 'NONE',  ( -14.98071481085577972, -10.82426656108012075, 33.81400080652039009 ) ) ;
#79690 = CARTESIAN_POINT ( 'NONE',  ( -2.651650429449565305, -4.848349570550461785, 21.50000000000000000 ) ) ;
#79691 = VERTEX_POINT ( 'NONE', #52493 ) ;
#79692 = CIRCLE ( 'NONE', #26465, 4.000000000000000000 ) ;
#79693 = ORIENTED_EDGE ( 'NONE', *, *, #52998, .T. ) ;
#79694 = AXIS2_PLACEMENT_3D ( 'NONE', #48523, #82336, #81896 ) ;
#79695 = CARTESIAN_POINT ( 'NONE',  ( -8.069638770718174925, -11.60425143139329940, 33.02411095842164457 ) ) ;
#79696 = CARTESIAN_POINT ( 'NONE',  ( -7.053768389744483613, -2.541943142973490666, 30.39792223712631980 ) ) ;
#79697 = CARTESIAN_POINT ( 'NONE',  ( 9.942253210655836781, -10.05730279482229683, 34.04704008940765902 ) ) ;
#79698 = CYLINDRICAL_SURFACE ( 'NONE', #59662, 0.2500000000000008882 ) ;
#79699 = CARTESIAN_POINT ( 'NONE',  ( 16.94644789184735956, -7.276987145209182550, 34.99546412871779211 ) ) ;
#79700 = CARTESIAN_POINT ( 'NONE',  ( -2.651650429449535551, -10.15165042944956753, 23.68750000000000000 ) ) ;
#79701 = EDGE_CURVE ( 'NONE', #22384, #41958, #76960, .T. ) ;
#79702 = B_SPLINE_CURVE_WITH_KNOTS ( 'NONE', 3,
 ( #3087, #28815, #84645, #84209, #9415, #63465, #76552, #50819, #56275, #1329 ),
 .UNSPECIFIED., .F., .F.,
 ( 4, 2, 2, 2, 4 ),
 ( 0.0007817359430256257775, 0.0009771253907249911191, 0.001172514838424356352, 0.001367904286123721586, 0.001563293733823086819 ),
 .UNSPECIFIED. ) ;
#79703 = CARTESIAN_POINT ( 'NONE',  ( 8.545745844666436497, -4.225889041578353655, 33.85425143139329407 ) ) ;
#79704 = DIRECTION ( 'NONE',  ( -0.000000000000000000, 0.9396926207859092051, -0.3420201433256662704 ) ) ;
#79705 = CARTESIAN_POINT ( 'NONE',  ( 7.846153846153846700, -1.044019251281081972, 31.83374038241031911 ) ) ;
#79706 = DIRECTION ( 'NONE',  ( -0.000000000000000000, -0.9396926207859093161, -0.3420201433256663259 ) ) ;
#79707 = CARTESIAN_POINT ( 'NONE',  ( -3.262820512820514107, -11.50000000000000000, 29.75000000000000355 ) ) ;
#79708 = CARTESIAN_POINT ( 'NONE',  ( 14.08420736396836048, -12.24155766932282496, 31.33739205006857986 ) ) ;
#79709 = EDGE_CURVE ( 'NONE', #60898, #40946, #72764, .T. ) ;
#79710 = ADVANCED_FACE ( 'NONE', ( #58806 ), #32671, .F. ) ;
#79711 = LINE ( 'NONE', #44563, #53836 ) ;
#79712 = CARTESIAN_POINT ( 'NONE',  ( 7.145856592054988354, -2.353885683473779800, 30.79025554430704759 ) ) ;
#79713 = CARTESIAN_POINT ( 'NONE',  ( 10.68145296638705588, -2.721908614388771852, 31.22303859784725333 ) ) ;
#79714 = CARTESIAN_POINT ( 'NONE',  ( 7.596130621932389637, -3.520140089381496473, 33.17453946501458262 ) ) ;
#79715 = CARTESIAN_POINT ( 'NONE',  ( -7.596208327805704208, -12.43552623307873972, 30.55307653245132826 ) ) ;
#79716 = ORIENTED_EDGE ( 'NONE', *, *, #44342, .F. ) ;
#79717 = EDGE_CURVE ( 'NONE', #41880, #77905, #46195, .T. ) ;
#79718 = PLANE ( 'NONE',  #64268 ) ;
#79719 = CARTESIAN_POINT ( 'NONE',  ( -5.299751174557954414, -7.369209533119140509, 34.99857337881830688 ) ) ;
#79720 = CARTESIAN_POINT ( 'NONE',  ( 5.777073041093152561, -2.523278758544489797, 31.42238647778637528 ) ) ;
#79721 = CARTESIAN_POINT ( 'NONE',  ( -2.749999999999991562, -8.639087296526025028, 26.26562500000000000 ) ) ;
#79722 = CARTESIAN_POINT ( 'NONE',  ( -18.24999999999999645, -2.499999999999999556, 29.81609845454691410 ) ) ;
#79723 = CARTESIAN_POINT ( 'NONE',  ( 16.15384615384615330, -4.661471528628507777, 34.16647553114623292 ) ) ;
#79725 = EDGE_LOOP ( 'NONE', ( #36470, #53648, #48764, #49292 ) ) ;
#79724 = CARTESIAN_POINT ( 'NONE',  ( -0.4615384615384611200, -2.538708090699994813, 30.37095296980875503 ) ) ;
#79726 = CARTESIAN_POINT ( 'NONE',  ( -1.139087296525992388, -10.25000000000000711, 21.10937500000000000 ) ) ;
#79727 = CARTESIAN_POINT ( 'NONE',  ( -7.846153846153844924, -11.35647404775217417, 33.31231777344666511 ) ) ;
#79728 = ORIENTED_EDGE ( 'NONE', *, *, #45840, .F. ) ;
#79729 = AXIS2_PLACEMENT_3D ( 'NONE', #492, #63060, #84252 ) ;
#79730 = LINE ( 'NONE', #18030, #70167 ) ;
#79731 = ORIENTED_EDGE ( 'NONE', *, *, #26011, .F. ) ;
#79732 = CARTESIAN_POINT ( 'NONE',  ( 2.980792486720639900, -4.818429247618089661, 34.26397095200675125 ) ) ;
#79733 = DIRECTION ( 'NONE',  ( -0.000000000000000000, -0.000000000000000000, -1.000000000000000000 ) ) ;
#79734 = DIRECTION ( 'NONE',  ( -0.000000000000000000, -0.000000000000000000, -1.000000000000000000 ) ) ;
#79735 = VERTEX_POINT ( 'NONE', #25920 ) ;
#79736 = CARTESIAN_POINT ( 'NONE',  ( 11.47237915910140771, -11.91647553114624181, 32.58852847137148245 ) ) ;
#79737 = VERTEX_POINT ( 'NONE', #3859 ) ;
#79738 = CARTESIAN_POINT ( 'NONE',  ( 11.40777007179397984, -3.530157926970578952, 32.79014554554150607 ) ) ;
#79739 = B_SPLINE_CURVE_WITH_KNOTS ( 'NONE', 3,
 ( #68023, #5436, #60811, #88316, #32899, #20711, #60365, #48175, #54045, #54490 ),
 .UNSPECIFIED., .F., .F.,
 ( 4, 2, 2, 2, 4 ),
 ( 0.0007817359430256322827, 0.0009771253907249989254, 0.001172514838424365676, 0.001367904286123732428, 0.001563293733823099179 ),
 .UNSPECIFIED. ) ;
#79741 = EDGE_CURVE ( 'NONE', #29049, #62375, #11076, .T. ) ;
#79740 = B_SPLINE_CURVE_WITH_KNOTS ( 'NONE', 3,
 ( #28552, #7397, #8282, #14144, #8727, #35301, #47926, #56461, #15038, #6942 ),
 .UNSPECIFIED., .F., .F.,
 ( 4, 2, 2, 2, 4 ),
 ( 0.000000000000000000, 0.0001954311564186864949, 0.0003908623128373729899, 0.0005862934692560594577, 0.0007817246256747459798 ),
 .UNSPECIFIED. ) ;
#79742 = ORIENTED_EDGE ( 'NONE', *, *, #6285, .T. ) ;
#79743 = CARTESIAN_POINT ( 'NONE',  ( 13.51514108637895184, -11.93748526763465279, 32.05452791011430946 ) ) ;
#79744 = DIRECTION ( 'NONE',  ( -0.000000000000000000, 0.9848077530122085754, -0.1736481776669273613 ) ) ;
#79745 = B_SPLINE_CURVE_WITH_KNOTS ( 'NONE', 3,
 ( #86926, #39615, #81040, #18442, #74273, #4478 ),
 .UNSPECIFIED., .F., .F.,
 ( 4, 2, 4 ),
 ( 0.0003909569690057842790, 0.0005862646681846108007, 0.0007815723673634373224 ),
 .UNSPECIFIED. ) ;
#79746 = VERTEX_POINT ( 'NONE', #4313 ) ;
#79747 = CYLINDRICAL_SURFACE ( 'NONE', #49055, 0.2500000000000004996 ) ;
#79748 = DIRECTION ( 'NONE',  ( -0.000000000000000000, 0.6427876096865404731, -0.7660444431189770143 ) ) ;
#79749 = CARTESIAN_POINT ( 'NONE',  ( 0.3954560821783241198, -2.292212530054419606, 30.41441678777542634 ) ) ;
#79750 = EDGE_CURVE ( 'NONE', #67601, #51593, #86723, .T. ) ;
#79751 = CARTESIAN_POINT ( 'NONE',  ( -14.08491263871423982, -10.23759521482555357, 34.22997729860117033 ) ) ;
#79752 = CARTESIAN_POINT ( 'NONE',  ( 16.15384615384615330, -10.89733346790207413, 36.13435417666054406 ) ) ;
#79753 = VECTOR ( 'NONE', #58598, 1000.000000000000000 ) ;
#79754 = ORIENTED_EDGE ( 'NONE', *, *, #16615, .T. ) ;
#79755 = ORIENTED_EDGE ( 'NONE', *, *, #44155, .T. ) ;
#79756 = ORIENTED_EDGE ( 'NONE', *, *, #61807, .T. ) ;
#79758 = EDGE_LOOP ( 'NONE', ( #6553, #13835, #82455, #81673 ) ) ;
#79757 = FACE_OUTER_BOUND ( 'NONE', #44274, .T. ) ;
#79759 = EDGE_CURVE ( 'NONE', #47629, #8176, #29742, .T. ) ;
#79760 = AXIS2_PLACEMENT_3D ( 'NONE', #4870, #19267, #60240 ) ;
#79761 = VECTOR ( 'NONE', #71815, 1000.000000000000114 ) ;
#79762 = CARTESIAN_POINT ( 'NONE',  ( 10.48523740594639619, -5.195881422630166391, 34.18770438780619259 ) ) ;
#79763 = CARTESIAN_POINT ( 'NONE',  ( -10.74553182482283198, -9.418419913701741919, 34.36755862841477693 ) ) ;
#79764 = ORIENTED_EDGE ( 'NONE', *, *, #85385, .F. ) ;
#79765 = ADVANCED_FACE ( 'NONE', ( #88103 ), #26368, .F. ) ;
#79766 = EDGE_LOOP ( 'NONE', ( #5044, #18381 ) ) ;
#79767 = CARTESIAN_POINT ( 'NONE',  ( 3.453548772037639214, -5.114059244376869984, 34.14424750095245287 ) ) ;
#79768 = EDGE_LOOP ( 'NONE', ( #34360, #44406, #2691, #38917 ) ) ;
#79769 = CARTESIAN_POINT ( 'NONE',  ( -12.39639368081883042, -7.750023224968867197, 34.99404313364389907 ) ) ;
#79770 = CARTESIAN_POINT ( 'NONE',  ( 16.85343815235874132, -12.47654668319379567, 31.42292124445336654 ) ) ;
#79771 = B_SPLINE_CURVE_WITH_KNOTS ( 'NONE', 3,
 ( #48197, #26605, #33803, #82004, #74354, #24, #33368, #26162, #75243, #88773 ),
 .UNSPECIFIED., .F., .F.,
 ( 4, 2, 2, 2, 4 ),
 ( 0.000000000000000000, 0.0001954311564186865221, 0.0003908623128373730441, 0.0005862934692560595662, 0.0007817246256747460882 ),
 .UNSPECIFIED. ) ;
#79772 = CARTESIAN_POINT ( 'NONE',  ( 0.2115617305961060846, -4.943428324936578910, 34.04746400365624481 ) ) ;
#79773 = FACE_BOUND ( 'NONE', #16189, .T. ) ;
#79774 = B_SPLINE_CURVE_WITH_KNOTS ( 'NONE', 3,
 ( #64825, #60749, #12135, #87359, #67961, #38705, #52654, #80141, #6263, #5814 ),
 .UNSPECIFIED., .F., .F.,
 ( 4, 2, 2, 2, 4 ),
 ( 0.000000000000000000, 0.0001954339857564080707, 0.0003908679715128161414, 0.0005863019572692241849, 0.0007817359430256322827 ),
 .UNSPECIFIED. ) ;
#79775 = CARTESIAN_POINT ( 'NONE',  ( 17.20744851515672025, -6.808710257144159783, 34.95449254468098843 ) ) ;
#79776 = CARTESIAN_POINT ( 'NONE',  ( 13.60739492588379562, -9.332535724633409302, 34.40230450496446934 ) ) ;
#79777 = DIRECTION ( 'NONE',  ( -0.000000000000000000, -0.9848077530122086864, -0.1736481776669273613 ) ) ;
#79778 = CARTESIAN_POINT ( 'NONE',  ( 2.242422307135989890, -8.656820664281497102, 34.87096338111211935 ) ) ;
#79779 = CARTESIAN_POINT ( 'NONE',  ( 15.84615384615384670, -11.50000000000000000, 29.75000000000000355 ) ) ;
#79780 = ORIENTED_EDGE ( 'NONE', *, *, #83505, .F. ) ;
#79781 = EDGE_CURVE ( 'NONE', #71793, #45833, #70568, .T. ) ;
#79782 = CARTESIAN_POINT ( 'NONE',  ( -17.07692307692319744, -12.46129190930018460, 30.37095296980731973 ) ) ;
#79783 = ORIENTED_EDGE ( 'NONE', *, *, #88185, .F. ) ;
#79784 = EDGE_LOOP ( 'NONE', ( #57274, #67790 ) ) ;
#79785 = VECTOR ( 'NONE', #932, 1000.000000000000114 ) ;
#79787 = CARTESIAN_POINT ( 'NONE',  ( 10.74591031714818357, -6.001044277235009439, 34.52024696741798948 ) ) ;
#79786 = CARTESIAN_POINT ( 'NONE',  ( -7.053224892808619195, -4.299443229763728169, 33.91186481527756058 ) ) ;
#79788 = CYLINDRICAL_SURFACE ( 'NONE', #9714, 0.2499999999999986955 ) ;
#79789 = CARTESIAN_POINT ( 'NONE',  ( -2.084912766423895558, -12.24180327182771855, 31.33663988360758168 ) ) ;
#79790 = CARTESIAN_POINT ( 'NONE',  ( 7.596130608860880429, -12.43535235679832596, 30.55408501211184813 ) ) ;
#79791 = CARTESIAN_POINT ( 'NONE',  ( -2.307692307692305711, -10.05456864172156806, 36.03766855953608683 ) ) ;
#79792 = ORIENTED_EDGE ( 'NONE', *, *, #80413, .T. ) ;
#79793 = CARTESIAN_POINT ( 'NONE',  ( 6.792928953345223064, -2.647304123082328875, 31.75400227202885262 ) ) ;
#79794 = ADVANCED_FACE ( 'NONE', ( #61032 ), #62787, .F. ) ;
#79795 = CARTESIAN_POINT ( 'NONE',  ( 3.100078627658923391, -9.084618155246140248, 34.75535874321725771 ) ) ;
#79796 = CARTESIAN_POINT ( 'NONE',  ( 2.307692307692309264, -12.62096338111211580, 30.90682066428153263 ) ) ;
#79797 = EDGE_CURVE ( 'NONE', #57707, #79832, #17934, .T. ) ;
#79798 = CARTESIAN_POINT ( 'NONE',  ( -3.931066612577740482, -3.755027918224367767, 33.06320215134714857 ) ) ;
#79799 = ORIENTED_EDGE ( 'NONE', *, *, #52252, .T. ) ;
#79800 = EDGE_LOOP ( 'NONE', ( #67782, #12996 ) ) ;
#79801 = PRODUCT_CONTEXT ( 'NONE', #76262, 'mechanical' ) ;
#79802 = VERTEX_POINT ( 'NONE', #6101 ) ;
#79803 = CYLINDRICAL_SURFACE ( 'NONE', #39178, 0.2499999999999986955 ) ;
#79804 = CARTESIAN_POINT ( 'NONE',  ( -6.249999999999997335, -7.433932668274256805, 35.00000000000000711 ) ) ;
#79805 = ORIENTED_EDGE ( 'NONE', *, *, #27451, .T. ) ;
#79806 = CARTESIAN_POINT ( 'NONE',  ( -16.37733107841048508, -11.60425143139329940, 33.02411095842164457 ) ) ;
#79807 = CARTESIAN_POINT ( 'NONE',  ( 6.000000000000001776, -11.35647404775217417, 33.31231777344666511 ) ) ;
#79808 = CARTESIAN_POINT ( 'NONE',  ( -8.546451227962359454, -6.760870238392817200, 34.69528174975672385 ) ) ;
#79809 = CARTESIAN_POINT ( 'NONE',  ( -6.923076923077044142, -3.300289026999228881, 32.46337939537708905 ) ) ;
#79810 = ADVANCED_FACE ( 'NONE', ( #75438 ), #54265, .F. ) ;
#79811 = B_SPLINE_CURVE_WITH_KNOTS ( 'NONE', 3,
 ( #53182, #44638, #73918, #11771, #65368, #39249, #66711, #31132, #24824, #72570 ),
 .UNSPECIFIED., .F., .F.,
 ( 4, 2, 2, 2, 4 ),
 ( 0.000000000000000000, 0.0001954339857564073659, 0.0003908679715128147319, 0.0005863019572692221250, 0.0007817359430256294638 ),
 .UNSPECIFIED. ) ;
#79812 = CARTESIAN_POINT ( 'NONE',  ( -11.40766973063674605, -8.999086150933475636, 34.52020707165672775 ) ) ;
#79813 = EDGE_LOOP ( 'NONE', ( #42325, #34346 ) ) ;
#79815 = ORIENTED_EDGE ( 'NONE', *, *, #71531, .F. ) ;
#79814 = CARTESIAN_POINT ( 'NONE',  ( -7.715362038329057981, -9.804649428959608670, 34.18742332936588468 ) ) ;
#79816 = CARTESIAN_POINT ( 'NONE',  ( 3.230769230769110045, -5.219633306517616589, 34.19971097300220464 ) ) ;
#79817 = CARTESIAN_POINT ( 'NONE',  ( -12.59222906464877134, -2.845849958028613624, 32.17971566917920967 ) ) ;
#79818 = CARTESIAN_POINT ( 'NONE',  ( -7.596208436775803818, -3.520799739797213945, 33.17531984108286025 ) ) ;
#79819 = B_SPLINE_CURVE_WITH_KNOTS ( 'NONE', 3,
 ( #75301, #6830, #14035, #61765, #27555, #41511, #68978, #7283, #34748, #62219 ),
 .UNSPECIFIED., .F., .F.,
 ( 4, 2, 2, 2, 4 ),
 ( 0.0007817359430256332585, 0.0009771253907250054306, 0.001172514838424370664, 0.001367904286123735897, 0.001563293733823100913 ),
 .UNSPECIFIED. ) ;
#79820 = B_SPLINE_CURVE_WITH_KNOTS ( 'NONE', 3,
 ( #32064, #40167, #53665, #60865, #59529, #46899, #74384, #67632, #87032, #25306 ),
 .UNSPECIFIED., .F., .F.,
 ( 4, 2, 2, 2, 4 ),
 ( 0.0007817246256747453293, 0.0009771112852218883336, 0.001172497944769031230, 0.001367884604316174126, 0.001563271263863317238 ),
 .UNSPECIFIED. ) ;
#79821 = EDGE_CURVE ( 'NONE', #19611, #64420, #20051, .T. ) ;
#79822 = FACE_OUTER_BOUND ( 'NONE', #6949, .T. ) ;
#79823 = CARTESIAN_POINT ( 'NONE',  ( -8.519176349317316266, -8.346898887586323923, 34.93166121998716278 ) ) ;
#79824 = CARTESIAN_POINT ( 'NONE',  ( 6.223011351612849573, -2.758310577978207778, 31.33698337089303010 ) ) ;
#79825 = CARTESIAN_POINT ( 'NONE',  ( -2.724691934501246582, -6.299813628509474128, 16.67374329374151998 ) ) ;
#79826 = ORIENTED_EDGE ( 'NONE', *, *, #36306, .T. ) ;
#79827 = CARTESIAN_POINT ( 'NONE',  ( -4.153846153846152411, -10.67929555188718282, 33.92786785259544047 ) ) ;
#79828 = DIRECTION ( 'NONE',  ( -0.000000000000000000, -0.5000000000000009992, -0.8660254037844380415 ) ) ;
#79829 = DIRECTION ( 'NONE',  ( -0.000000000000000000, 0.3420201433256694346, -0.9396926207859080948 ) ) ;
#79830 = AXIS2_PLACEMENT_3D ( 'NONE', #64937, #3243, #10457 ) ;
#79831 = ORIENTED_EDGE ( 'NONE', *, *, #68190, .F. ) ;
#79832 = VERTEX_POINT ( 'NONE', #74555 ) ;
#79833 = CARTESIAN_POINT ( 'NONE',  ( 9.942362112221147186, -3.435999193479609914, 33.07426656108010832 ) ) ;
#79834 = CARTESIAN_POINT ( 'NONE',  ( 12.52760579488853665, -3.937682226553329556, 33.60647404775216529 ) ) ;
#79835 = CARTESIAN_POINT ( 'NONE',  ( 17.14299041027315695, -3.322132147404559532, 32.92929555188717927 ) ) ;
#79836 = CARTESIAN_POINT ( 'NONE',  ( 13.31934538405906565, -3.083524468853724443, 32.58852847137143272 ) ) ;
#79837 = CARTESIAN_POINT ( 'NONE',  ( -9.019207500173124004, -11.79746400365624659, 32.30657167506340954 ) ) ;
#79838 = CARTESIAN_POINT ( 'NONE',  ( 5.933916589044120116, -8.120952969808774569, 34.71129190930000163 ) ) ;
#79839 = ORIENTED_EDGE ( 'NONE', *, *, #10295, .F. ) ;
#79840 = FACE_OUTER_BOUND ( 'NONE', #64206, .T. ) ;
#79841 = CARTESIAN_POINT ( 'NONE',  ( -5.749999999998562927, -7.500000000000155431, 34.75000000000007105 ) ) ;
#79842 = DIRECTION ( 'NONE',  ( -0.000000000000000000, 0.7660444431189791237, -0.6427876096865379196 ) ) ;
#79843 = ORIENTED_EDGE ( 'NONE', *, *, #35329, .T. ) ;
#79844 = CARTESIAN_POINT ( 'NONE',  ( 13.60739492588379562, -6.760870238392817200, 34.69528174975672385 ) ) ;
#79845 = ORIENTED_EDGE ( 'NONE', *, *, #48726, .T. ) ;
#79846 = FACE_OUTER_BOUND ( 'NONE', #40, .T. ) ;
#79847 = CARTESIAN_POINT ( 'NONE',  ( 10.39189969082028675, -3.562934362175799841, 33.22335522853832401 ) ) ;
#79848 = FACE_OUTER_BOUND ( 'NONE', #17221, .T. ) ;
#79849 = ORIENTED_EDGE ( 'NONE', *, *, #4095, .F. ) ;
#79850 = CARTESIAN_POINT ( 'NONE',  ( 30.00000000000000000, -15.00000000000000000, 3.000000000000000000 ) ) ;
#79851 = CARTESIAN_POINT ( 'NONE',  ( -11.40793583669797506, -12.45806712695776319, 30.39783852428763922 ) ) ;
#79852 = CARTESIAN_POINT ( 'NONE',  ( -16.09615384615384670, -7.500000000000000000, 29.75000000000000355 ) ) ;
#79853 = AXIS2_PLACEMENT_3D ( 'NONE', #20226, #35509, #82819 ) ;
#79854 = CARTESIAN_POINT ( 'NONE',  ( 2.294871794871793380, -3.499999999999999556, 29.75000000000000355 ) ) ;
#79855 = CARTESIAN_POINT ( 'NONE',  ( -2.242437168179467477, -11.06231777344671130, 33.60647404775212976 ) ) ;
#79856 = ORIENTED_EDGE ( 'NONE', *, *, #75948, .T. ) ;
#79857 = CARTESIAN_POINT ( 'NONE',  ( -1.384615384615383471, -13.87047571288749737, 32.06866353760679544 ) ) ;
#79858 = VERTEX_POINT ( 'NONE', #27688 ) ;
#79859 = CARTESIAN_POINT ( 'NONE',  ( -15.00798956179116317, -6.717445702608402236, 34.94155399931962336 ) ) ;
#79860 = CARTESIAN_POINT ( 'NONE',  ( -10.36538461538461320, -2.499999999999998668, 29.75000000000000355 ) ) ;
#79861 = CARTESIAN_POINT ( 'NONE',  ( -13.51530685128294174, -2.729777683071817229, 31.24903638046269450 ) ) ;
#79862 = DIRECTION ( 'NONE',  ( -0.000000000000000000, 0.9848077530122085754, -0.1736481776669273613 ) ) ;
#79863 = CARTESIAN_POINT ( 'NONE',  ( -6.066083410955878108, -4.098570777380720287, 33.41473453929634729 ) ) ;
#79864 = CARTESIAN_POINT ( 'NONE',  ( -6.700064078983529292, -2.523321265292115090, 31.42251411153756280 ) ) ;
#79865 = B_SPLINE_CURVE_WITH_KNOTS ( 'NONE', 3,
 ( #18852, #59388, #31471, #79664, #45418, #72897, #60270, #45866, #12540, #11202 ),
 .UNSPECIFIED., .F., .F.,
 ( 4, 2, 2, 2, 4 ),
 ( 0.000000000000000000, 0.0001954339857564083417, 0.0003908679715128166835, 0.0005863019572692250523, 0.0007817359430256333669 ),
 .UNSPECIFIED. ) ;
#79866 = EDGE_LOOP ( 'NONE', ( #65799, #73379, #21258, #36351, #10466, #42524 ) ) ;
#79867 = VERTEX_POINT ( 'NONE', #55602 ) ;
#79868 = EDGE_LOOP ( 'NONE', ( #6538, #18419 ) ) ;
#79869 = ORIENTED_EDGE ( 'NONE', *, *, #72781, .T. ) ;
#79870 = ORIENTED_EDGE ( 'NONE', *, *, #9653, .T. ) ;
#79871 = VECTOR ( 'NONE', #55309, 1000.000000000000000 ) ;
#79872 = LINE ( 'NONE', #18172, #81907 ) ;
#79873 = CARTESIAN_POINT ( 'NONE',  ( -11.53846153846153655, -8.973038597847269315, 34.52809138561121927 ) ) ;
#79874 = CARTESIAN_POINT ( 'NONE',  ( 15.00728428704528561, -5.113361153441934093, 34.14387501736622710 ) ) ;
#79875 = CARTESIAN_POINT ( 'NONE',  ( 17.07692307692307665, -5.471508081941601098, 34.59228464037088457 ) ) ;
#79876 = CARTESIAN_POINT ( 'NONE',  ( -13.60810030917971680, -3.562934362175800285, 33.22335522853832401 ) ) ;
#79878 = EDGE_CURVE ( 'NONE', #33346, #56271, #50144, .T. ) ;
#79877 = CARTESIAN_POINT ( 'NONE',  ( 2.980792499826877773, -5.728515186090277211, 34.42611988154120439 ) ) ;
#79879 = CARTESIAN_POINT ( 'NONE',  ( 5.776515056276054771, -11.89387501736622710, 32.13663884655806413 ) ) ;
#79880 = CARTESIAN_POINT ( 'NONE',  ( -4.088590582570127197, -10.90142922261932057, 33.41473453929631887 ) ) ;
#79881 = FACE_OUTER_BOUND ( 'NONE', #66152, .T. ) ;
#79882 = VERTEX_POINT ( 'NONE', #20491 ) ;
#79883 = PRODUCT_DEFINITION ( 'UNKNOWN', '', #80689, #23051 ) ;
#79884 = EDGE_LOOP ( 'NONE', ( #84376, #3216 ) ) ;
#79885 = ORIENTED_EDGE ( 'NONE', *, *, #63567, .T. ) ;
#79887 = VERTEX_POINT ( 'NONE', #40330 ) ;
#79886 = CYLINDRICAL_SURFACE ( 'NONE', #83388, 0.2500000000000012212 ) ;
#79889 = DIRECTION ( 'NONE',  ( -1.000000000000000000, -0.000000000000000000, 0.000000000000000000 ) ) ;
#79888 = CARTESIAN_POINT ( 'NONE',  ( -15.90390063549801347, -6.696923467548659303, 34.68552623307873972 ) ) ;
#79890 = CARTESIAN_POINT ( 'NONE',  ( 8.519230769230768274, -7.433931650972300353, 34.75000000000000711 ) ) ;
#79891 = CARTESIAN_POINT ( 'NONE',  ( 4.219101725122177626, -2.625532179533470512, 30.86335684631491105 ) ) ;
#79892 = FACE_BOUND ( 'NONE', #65578, .T. ) ;
#79893 = EDGE_LOOP ( 'NONE', ( #30116, #29935 ) ) ;
#79894 = EDGE_CURVE ( 'NONE', #44547, #26565, #82398, .T. ) ;
#79895 = ORIENTED_EDGE ( 'NONE', *, *, #70211, .F. ) ;
#79896 = LINE ( 'NONE', #18198, #80222 ) ;
#79897 = EDGE_LOOP ( 'NONE', ( #50811, #53539, #86843, #2183 ) ) ;
#79898 = FACE_BOUND ( 'NONE', #31828, .T. ) ;
#79899 = CARTESIAN_POINT ( 'NONE',  ( -8.769230769230768274, -2.486705287966279876, 31.30864560766543647 ) ) ;
#79900 = CARTESIAN_POINT ( 'NONE',  ( 14.98079248672063990, -6.524016743844655686, 34.90889640711025521 ) ) ;
#79901 = EDGE_LOOP ( 'NONE', ( #60934, #15066, #35236, #65535 ) ) ;
#79902 = CARTESIAN_POINT ( 'NONE',  ( 17.99999999999987566, -2.892918686052165622, 31.69288490824153470 ) ) ;
#79903 = DIRECTION ( 'NONE',  ( -0.000000000000000000, -0.8660254037844399289, -0.4999999999999980016 ) ) ;
#79904 = CARTESIAN_POINT ( 'NONE',  ( -18.22292695890684655, -4.026226216239095379, 33.68668979543632958 ) ) ;
#79905 = EDGE_LOOP ( 'NONE', ( #46492, #54820 ) ) ;
#79906 = CARTESIAN_POINT ( 'NONE',  ( 17.77712048326241145, -7.630690623152299956, 34.99857592706774057 ) ) ;
#79907 = CARTESIAN_POINT ( 'NONE',  ( 3.007843013253082010, -12.15238873228292071, 31.58232369045353849 ) ) ;
#79908 = ORIENTED_EDGE ( 'NONE', *, *, #44846, .F. ) ;
#79909 = VECTOR ( 'NONE', #50226, 1000.000000000000000 ) ;
#79910 = CARTESIAN_POINT ( 'NONE',  ( -10.61538461538473399, -8.613356846316285953, 34.62446782046622218 ) ) ;
#79911 = DIRECTION ( 'NONE',  ( -0.000000000000000000, 0.8660254037844399289, -0.4999999999999980016 ) ) ;
#79912 = ORIENTED_EDGE ( 'NONE', *, *, #83287, .F. ) ;
#79913 = CARTESIAN_POINT ( 'NONE',  ( 18.06606835100243913, -6.386643153685127139, 34.62446782046654192 ) ) ;
#79914 = DIRECTION ( 'NONE',  ( -0.000000000000000000, -0.3420201433256694346, -0.9396926207859080948 ) ) ;
#79915 = CARTESIAN_POINT ( 'NONE',  ( -2.530618525208454539, -2.554751324335734264, 30.48935550225260727 ) ) ;
#79916 = CARTESIAN_POINT ( 'NONE',  ( 14.98079248672064345, -12.65889640711025521, 30.72598325615533454 ) ) ;
#79917 = CARTESIAN_POINT ( 'NONE',  ( -6.673076923075503153, -7.500000000000154543, 35.00000000000007105 ) ) ;
#79918 = EDGE_CURVE ( 'NONE', #76443, #85803, #21117, .T. ) ;
#79919 = CARTESIAN_POINT ( 'NONE',  ( 17.14299041027315695, -4.661471528628508665, 34.16647553114624003 ) ) ;
#79921 = DIRECTION ( 'NONE',  ( 0.000000000000000000, 0.9848077530122072432, -0.1736481776669354937 ) ) ;
#79920 = CARTESIAN_POINT ( 'NONE',  ( 14.05769230769230127, -2.499999999999999556, 29.81609845454692120 ) ) ;
#79922 = CARTESIAN_POINT ( 'NONE',  ( 9.019285080869083870, -12.17597550085003810, 31.52189283813460463 ) ) ;
#79924 = CARTESIAN_POINT ( 'NONE',  ( 12.21151523731700550, -4.931416488878822335, 34.32920672191015399 ) ) ;
#79923 = DIRECTION ( 'NONE',  ( -0.000000000000000000, -0.3420201433256695456, -0.9396926207859082059 ) ) ;
#79925 = CARTESIAN_POINT ( 'NONE',  ( 1.799775606325937360E-14, -10.25000000000000000, 16.03125000000000000 ) ) ;
#79926 = ORIENTED_EDGE ( 'NONE', *, *, #680, .F. ) ;
#79927 = ADVANCED_FACE ( 'NONE', ( #64120 ), #3313, .F. ) ;
#79928 = B_SPLINE_CURVE_WITH_KNOTS ( 'NONE', 3,
 ( #53877, #68278, #6583, #74153, #60626, #48436, #33611, #75924, #39936, #34048 ),
 .UNSPECIFIED., .F., .F.,
 ( 4, 2, 2, 2, 4 ),
 ( 0.0007817359430256388964, 0.0009771253907250075990, 0.001172514838424376085, 0.001367904286123744571, 0.001563293733823113273 ),
 .UNSPECIFIED. ) ;
#79929 = CARTESIAN_POINT ( 'NONE',  ( -18.23784950573860186, -1.749999999999998446, 32.75000000000000000 ) ) ;
#79930 = ORIENTED_EDGE ( 'NONE', *, *, #7387, .F. ) ;
#79931 = EDGE_CURVE ( 'NONE', #26549, #68985, #81973, .T. ) ;
#79932 = ORIENTED_EDGE ( 'NONE', *, *, #88080, .F. ) ;
#79933 = CARTESIAN_POINT ( 'NONE',  ( -17.01085574357299990, -3.937682226553329556, 33.60647404775216529 ) ) ;
#79934 = ORIENTED_EDGE ( 'NONE', *, *, #8723, .T. ) ;
#79935 = CARTESIAN_POINT ( 'NONE',  ( -15.00775787915638126, -5.667800583137506010, 34.40243808032445827 ) ) ;
#79936 = CARTESIAN_POINT ( 'NONE',  ( -2.775308065498764964, -6.422011778438537988, 26.17000670625849068 ) ) ;
#79937 = CARTESIAN_POINT ( 'NONE',  ( -15.23076923076935074, -2.625532179533778709, 30.86335684631627174 ) ) ;
#79938 = CARTESIAN_POINT ( 'NONE',  ( -1.384615384615383471, -2.292212530054420494, 30.41441678777542634 ) ) ;
#79939 = CARTESIAN_POINT ( 'NONE',  ( 9.823098133274644539, -9.084667340241226796, 34.75534355489798344 ) ) ;
#79940 = CARTESIAN_POINT ( 'NONE',  ( -12.33074802057151409, -3.957578996910242619, 33.62503395064540257 ) ) ;
#79941 = DIRECTION ( 'NONE',  ( 0.000000000000000000, 0.7660444431189822323, -0.6427876096865344779 ) ) ;
#79942 = CARTESIAN_POINT ( 'NONE',  ( 0.4615384615384611200, -5.471508081941601098, 34.59228464037088457 ) ) ;
#79943 = DIRECTION ( 'NONE',  ( -0.000000000000000000, 0.6427876096865404731, -0.7660444431189771253 ) ) ;
#79944 = CARTESIAN_POINT ( 'NONE',  ( 1.553300858899087311, -3.749999999999992006, 22.98437500000000000 ) ) ;
#79945 = AXIS2_PLACEMENT_3D ( 'NONE', #87424, #19391, #25705 ) ;
#79946 = CARTESIAN_POINT ( 'NONE',  ( 5.299935921016473372, -2.889357225399416862, 32.26129605718031002 ) ) ;
#79947 = CARTESIAN_POINT ( 'NONE',  ( -18.00000000000000000, -2.292212530054419606, 30.41441678777542990 ) ) ;
#79948 = B_SPLINE_CURVE_WITH_KNOTS ( 'NONE', 3,
 ( #35309, #81738, #13270, #55137, #20472, #47934, #82633, #83512, #13710, #34426 ),
 .UNSPECIFIED., .F., .F.,
 ( 4, 2, 2, 2, 4 ),
 ( 0.000000000000000000, 0.0001954339857564070678, 0.0003908679715128141356, 0.0005863019572692211492, 0.0007817359430256282712 ),
 .UNSPECIFIED. ) ;
#79949 = CARTESIAN_POINT ( 'NONE',  ( 5.869309396889692998, -3.338472653186242756, 32.95098750199972670 ) ) ;
#79950 = B_SPLINE_CURVE_WITH_KNOTS ( 'NONE', 3,
 ( #40011, #26929, #46306, #47184, #87317, #12094, #73794, #40456, #53049, #12970 ),
 .UNSPECIFIED., .F., .F.,
 ( 4, 2, 2, 2, 4 ),
 ( 0.000000000000000000, 0.0001954311564186863323, 0.0003908623128373726646, 0.0005862934692560590241, 0.0007817246256747453293 ),
 .UNSPECIFIED. ) ;
#79951 = EDGE_LOOP ( 'NONE', ( #65783, #59592 ) ) ;
#79952 = ORIENTED_EDGE ( 'NONE', *, *, #14646, .F. ) ;
#79953 = DIRECTION ( 'NONE',  ( -1.000000000000000000, -0.000000000000000000, 0.000000000000000000 ) ) ;
#79954 = CARTESIAN_POINT ( 'NONE',  ( 7.716006636715626144, -11.47017969459903952, 32.78971311882034456 ) ) ;
#79955 = CARTESIAN_POINT ( 'NONE',  ( 1.319345384059066317, -11.06231777344662781, 33.60647404775220082 ) ) ;
#79956 = CARTESIAN_POINT ( 'NONE',  ( 6.130045055919775443, -2.254550872974306674, 29.97347326024527447 ) ) ;
#79957 = AXIS2_PLACEMENT_3D ( 'NONE', #44177, #64016, #70798 ) ;
#79958 = CARTESIAN_POINT ( 'NONE',  ( 4.088576153289834814, -3.643525952247789412, 33.31231777344662959 ) ) ;
#79959 = CARTESIAN_POINT ( 'NONE',  ( -4.946132635956124624, -2.845873456487966635, 32.17976146951972538 ) ) ;
#79960 = EDGE_CURVE ( 'NONE', #33331, #66936, #45838, .T. ) ;
#79961 = VERTEX_POINT ( 'NONE', #78091 ) ;
#79962 = CARTESIAN_POINT ( 'NONE',  ( 17.99999999999987566, -12.46129190930018460, 30.37095296980731973 ) ) ;
#79963 = EDGE_LOOP ( 'NONE', ( #44041, #3755, #36173, #10159 ) ) ;
#79964 = EDGE_LOOP ( 'NONE', ( #7196, #46900, #83490, #46988 ) ) ;
#79965 = CARTESIAN_POINT ( 'NONE',  ( 7.780071466793709867, -10.67929555188718460, 33.92786785259543336 ) ) ;
#79966 = CARTESIAN_POINT ( 'NONE',  ( 4.153846153846032507, -2.625532179533778709, 30.86335684631627174 ) ) ;
#79967 = AXIS2_PLACEMENT_3D ( 'NONE', #73392, #5823, #33301 ) ;
#79968 = CARTESIAN_POINT ( 'NONE',  ( 11.60371710973756443, -10.90142922261932057, 33.41473453929631887 ) ) ;
#79969 = LINE ( 'NONE', #60577, #83922 ) ;
#79970 = CARTESIAN_POINT ( 'NONE',  ( 13.38461538461538680, -5.471508081941601098, 34.59228464037088457 ) ) ;
#79971 = ADVANCED_FACE ( 'NONE', ( #8315 ), #1995, .F. ) ;
#79972 = AXIS2_PLACEMENT_3D ( 'NONE', #5624, #62330, #21352 ) ;
#79973 = EDGE_LOOP ( 'NONE', ( #27795, #36605 ) ) ;
#79974 = B_SPLINE_CURVE_WITH_KNOTS ( 'NONE', 3,
 ( #80423, #18724, #51572, #46189, #27681, #67789, #13284, #654, #88527, #40767 ),
 .UNSPECIFIED., .F., .F.,
 ( 4, 2, 2, 2, 4 ),
 ( 0.000000000000000000, 0.0001954339857564126514, 0.0003908679715128183098, 0.0005863019572692239681, 0.0007817359430256294638 ),
 .UNSPECIFIED. ) ;
#79975 = VERTEX_POINT ( 'NONE', #23147 ) ;
#79976 = EDGE_LOOP ( 'NONE', ( #14378, #29300, #52498, #13430 ) ) ;
#79977 = LINE ( 'NONE', #73223, #81847 ) ;
#79978 = CARTESIAN_POINT ( 'NONE',  ( -0.2385256174450668676, -10.01129605718032778, 34.36064277460058491 ) ) ;
#79979 = DIRECTION ( 'NONE',  ( 0.000000000000000000, 0.7660444431189807890, 0.6427876096865361433 ) ) ;
#79981 = EDGE_CURVE ( 'NONE', #34673, #8287, #21821, .T. ) ;
#79980 = CARTESIAN_POINT ( 'NONE',  ( 10.36536139116316235, -4.931416488878822335, 34.32920672191015399 ) ) ;
#79982 = CARTESIAN_POINT ( 'NONE',  ( -4.403846153846151523, -7.500000000000001776, 34.75000000000000000 ) ) ;
#79983 = CARTESIAN_POINT ( 'NONE',  ( 5.749976762707035505, -12.43535235679832596, 30.55408501211184813 ) ) ;
#79984 = EDGE_LOOP ( 'NONE', ( #32080, #44422, #24689, #82870 ) ) ;
#79985 = EDGE_CURVE ( 'NONE', #11337, #1879, #25440, .T. ) ;
#79986 = VERTEX_POINT ( 'NONE', #22701 ) ;
#79987 = CARTESIAN_POINT ( 'NONE',  ( 11.60365552024489766, -2.506253911140448043, 29.99999999999988631 ) ) ;
#79989 = ORIENTED_EDGE ( 'NONE', *, *, #38703, .F. ) ;
#79988 = CARTESIAN_POINT ( 'NONE',  ( -6.000000000000119904, -3.300289026999228881, 32.46337939537708905 ) ) ;
#79990 = CARTESIAN_POINT ( 'NONE',  ( -9.915792616872021625, -10.23692288466677880, 34.23039457007281072 ) ) ;
#79991 = CARTESIAN_POINT ( 'NONE',  ( 12.46153846153833911, -8.656820664282941280, 34.87096338111179961 ) ) ;
#79992 = CARTESIAN_POINT ( 'NONE',  ( 2.651650429449569302, -10.15165042944953733, 17.12500000000000000 ) ) ;
#79993 = ORIENTED_EDGE ( 'NONE', *, *, #18602, .T. ) ;
#79994 = EDGE_CURVE ( 'NONE', #14985, #29486, #76771, .T. ) ;
#79995 = CARTESIAN_POINT ( 'NONE',  ( 10.83839745947800992, -2.308499170217967134, 30.53291367094873721 ) ) ;
#79996 = VERTEX_POINT ( 'NONE', #78527 ) ;
#79997 = DIRECTION ( 'NONE',  ( -1.000000000000000000, 0.000000000000000000, -0.000000000000000000 ) ) ;
#79998 = CARTESIAN_POINT ( 'NONE',  ( 0.3954560821783245639, -11.35647404775217595, 33.31231777344667222 ) ) ;
#79999 = CARTESIAN_POINT ( 'NONE',  ( -12.33101275977490197, -12.45806712695776319, 30.39783852428763922 ) ) ;
#80001 = PLANE ( 'NONE',  #70381 ) ;
#80000 = LINE ( 'NONE', #80907, #63346 ) ;
#80002 = EDGE_CURVE ( 'NONE', #2976, #63180, #78071, .T. ) ;
#80003 = CARTESIAN_POINT ( 'NONE',  ( -18.00000000000001421, 17.49999999999802824, 13.00000000000000178 ) ) ;
#80004 = CARTESIAN_POINT ( 'NONE',  ( -3.148799926473854489E-16, -1.749999999999995781, 28.00000000000000000 ) ) ;
#80005 = ORIENTED_EDGE ( 'NONE', *, *, #80160, .F. ) ;
#80006 = CARTESIAN_POINT ( 'NONE',  ( -11.47239420511146513, -8.164416787775445883, 34.95778746994558617 ) ) ;
#80007 = EDGE_CURVE ( 'NONE', #80662, #80137, #84866, .T. ) ;
#80008 = CARTESIAN_POINT ( 'NONE',  ( 14.98074599347626368, -4.335965774309649134, 33.62209801155881905 ) ) ;
#80009 = CARTESIAN_POINT ( 'NONE',  ( 0.000000000000000000, -11.00000000000000000, 29.75000000000000355 ) ) ;
#80010 = ORIENTED_EDGE ( 'NONE', *, *, #18601, .F. ) ;
#80011 = LINE ( 'NONE', #87233, #27195 ) ;
#80012 = CARTESIAN_POINT ( 'NONE',  ( 10.54930223602447903, -8.164416787775445883, 34.95778746994557906 ) ) ;
#80013 = DIRECTION ( 'NONE',  ( 1.000000000000000000, 0.000000000000000000, 0.000000000000000000 ) ) ;
#80014 = CARTESIAN_POINT ( 'NONE',  ( 16.15384615384615330, -12.78798330534102767, 29.49999999999997868 ) ) ;
#80015 = EDGE_CURVE ( 'NONE', #18617, #48928, #694, .T. ) ;
#80016 = FACE_BOUND ( 'NONE', #82471, .T. ) ;
#80018 = CARTESIAN_POINT ( 'NONE',  ( 4.376625822824220080, -12.69155399931963046, 30.53255429739158444 ) ) ;
#80017 = CARTESIAN_POINT ( 'NONE',  ( 12.21151522424549896, -3.202444869320336451, 32.30641848906366675 ) ) ;
#80019 = CARTESIAN_POINT ( 'NONE',  ( 2.307692307692309264, -9.905515769479276145, 34.41647553114623292 ) ) ;
#80021 = CARTESIAN_POINT ( 'NONE',  ( -11.40793610022789828, -11.04252011169590020, 33.62494198852677130 ) ) ;
#80020 = CARTESIAN_POINT ( 'NONE',  ( 1.134638640566795864, -12.65889640711025521, 30.72598325615533454 ) ) ;
#80022 = CARTESIAN_POINT ( 'NONE',  ( -9.692307692307691624, -2.499999999999998668, 29.50000000000001066 ) ) ;
#80023 = CARTESIAN_POINT ( 'NONE',  ( 8.899756207464411872, -12.70449254468099198, 30.44128974285582956 ) ) ;
#80024 = CARTESIAN_POINT ( 'NONE',  ( 2.694853999681214862, -10.10844685921789043, 26.87313170625849423 ) ) ;
#80025 = CARTESIAN_POINT ( 'NONE',  ( -12.33070013105169771, -7.277220318596961057, 34.99547417642776992 ) ) ;
#80026 = ORIENTED_EDGE ( 'NONE', *, *, #18684, .F. ) ;
#80027 = CYLINDRICAL_SURFACE ( 'NONE', #14729, 0.2500000000000012212 ) ;
#80028 = ADVANCED_FACE ( 'NONE', ( #25368 ), #72662, .F. ) ;
#80029 = AXIS2_PLACEMENT_3D ( 'NONE', #6618, #34086, #20570 ) ;
#80030 = EDGE_CURVE ( 'NONE', #52889, #68628, #46951, .T. ) ;
#80031 = LINE ( 'NONE', #6148, #18196 ) ;
#80032 = CARTESIAN_POINT ( 'NONE',  ( -13.63461538461539213, -2.250000000000000000, 29.81609741502490252 ) ) ;
#80033 = DIRECTION ( 'NONE',  ( 0.000000000000000000, 0.8660254037844377084, -0.5000000000000015543 ) ) ;
#80034 = CARTESIAN_POINT ( 'NONE',  ( 17.01165307636676260, -12.70778746994557551, 30.41441678777548319 ) ) ;
#80035 = CARTESIAN_POINT ( 'NONE',  ( 1.384615384615264011, -12.16647553114689728, 32.15551576947799362 ) ) ;
#80036 = CARTESIAN_POINT ( 'NONE',  ( 1.492201783934554493, -3.724691934501233703, 25.23250670625849068 ) ) ;
#80037 = DIRECTION ( 'NONE',  ( 0.000000000000000000, 0.9848077530122072432, -0.1736481776669354937 ) ) ;
#80038 = CARTESIAN_POINT ( 'NONE',  ( 16.40384615384615330, -7.500000000000001776, 35.04278698407183867 ) ) ;
#80039 = CIRCLE ( 'NONE', #36875, 4.000000000000000000 ) ;
#80040 = CARTESIAN_POINT ( 'NONE',  ( 0.1752029071980549801, -4.754547453437774074, 28.77370482994318124 ) ) ;
#80041 = CARTESIAN_POINT ( 'NONE',  ( 9.469380733400845074, -4.026226216239094491, 33.68668979543634379 ) ) ;
#80042 = CARTESIAN_POINT ( 'NONE',  ( 7.145856464345333059, -4.387253974876676565, 33.66317474335728832 ) ) ;
#80043 = CARTESIAN_POINT ( 'NONE',  ( -8.769230769230890843, -9.442884908241554243, 34.35708131394783038 ) ) ;
#80044 = CARTESIAN_POINT ( 'NONE',  ( -2.177647251772534265, -2.254550872974306674, 29.97347326024527447 ) ) ;
#80045 = CARTESIAN_POINT ( 'NONE',  ( -11.47320596718551045, -10.90142922261932057, 33.41473453929631887 ) ) ;
#80046 = ORIENTED_EDGE ( 'NONE', *, *, #76385, .T. ) ;
#80047 = CARTESIAN_POINT ( 'NONE',  ( -7.846153846153965716, -3.835265460704628371, 33.15142922262033665 ) ) ;
#80048 = CARTESIAN_POINT ( 'NONE',  ( 15.48082365068268018, -10.82426656108012075, 33.81400080652039009 ) ) ;
#80049 = CARTESIAN_POINT ( 'NONE',  ( -3.724691934501248802, -5.885600066136383646, 20.42374329374152353 ) ) ;
#80050 = CARTESIAN_POINT ( 'NONE',  ( -17.07692307692319744, -12.16647553114689728, 32.15551576947799362 ) ) ;
#80051 = CYLINDRICAL_SURFACE ( 'NONE', #65652, 0.2499999999999986955 ) ;
#80052 = ORIENTED_EDGE ( 'NONE', *, *, #88439, .T. ) ;
#80053 = CARTESIAN_POINT ( 'NONE',  ( 16.15384615384615330, -12.78798330534102945, 29.74999999999997868 ) ) ;
#80054 = CARTESIAN_POINT ( 'NONE',  ( 1.634615384616805889, -7.500000000000154543, 35.00000000000007105 ) ) ;
#80056 = EDGE_LOOP ( 'NONE', ( #27793, #21635, #70994, #28058, #1396, #83281 ) ) ;
#80055 = CARTESIAN_POINT ( 'NONE',  ( -11.53846153846165912, -10.21337939537710326, 33.94971097300076224 ) ) ;
#80057 = LINE ( 'NONE', #86844, #13961 ) ;
#80058 = CARTESIAN_POINT ( 'NONE',  ( 3.930361210122204518, -8.496056993536548418, 34.65000542017679663 ) ) ;
#80059 = DIRECTION ( 'NONE',  ( -0.000000000000000000, 1.000000000000000000, 3.491481338843133355E-15 ) ) ;
#80060 = CARTESIAN_POINT ( 'NONE',  ( 11.78840705680968171, -9.272278438253398036, 34.42582936511637115 ) ) ;
#80061 = ORIENTED_EDGE ( 'NONE', *, *, #21291, .F. ) ;
#80062 = FACE_OUTER_BOUND ( 'NONE', #49420, .T. ) ;
#80063 = EDGE_CURVE ( 'NONE', #32965, #29248, #53346, .T. ) ;
#80064 =( LENGTH_UNIT ( ) NAMED_UNIT ( * ) SI_UNIT ( .MILLI., .METRE. ) );
#80065 = VECTOR ( 'NONE', #67649, 1000.000000000000000 ) ;
#80066 = CARTESIAN_POINT ( 'NONE',  ( -2.307692307692305711, -13.63283147151868846, 33.57946703557072254 ) ) ;
#80067 = ORIENTED_EDGE ( 'NONE', *, *, #50711, .F. ) ;
#80068 = EDGE_LOOP ( 'NONE', ( #18828, #70674, #28496, #81952 ) ) ;
#80069 = EDGE_CURVE ( 'NONE', #51011, #69999, #5101, .T. ) ;
#80070 = EDGE_CURVE ( 'NONE', #8934, #37210, #6127, .T. ) ;
#80071 = EDGE_LOOP ( 'NONE', ( #85588, #26188, #6302, #65979 ) ) ;
#80072 = EDGE_CURVE ( 'NONE', #5830, #25778, #18621, .T. ) ;
#80073 = CARTESIAN_POINT ( 'NONE',  ( 0.3308469948709019115, -8.147922237126337563, 34.70805685702651999 ) ) ;
#80074 = CARTESIAN_POINT ( 'NONE',  ( 6.000000000000001776, -2.292212530054420494, 30.41441678777542634 ) ) ;
#80075 = AXIS2_PLACEMENT_3D ( 'NONE', #62101, #409, #82832 ) ;
#80076 = CYLINDRICAL_SURFACE ( 'NONE', #16483, 0.2500000000000002220 ) ;
#80077 = EDGE_CURVE ( 'NONE', #1531, #27912, #74892, .T. ) ;
#80078 = CARTESIAN_POINT ( 'NONE',  ( -10.36538461538461320, -2.249999999999998668, 29.75000000000000355 ) ) ;
#80079 = ORIENTED_EDGE ( 'NONE', *, *, #32437, .F. ) ;
#80080 = VERTEX_POINT ( 'NONE', #86201 ) ;
#80082 = VERTEX_POINT ( 'NONE', #51936 ) ;
#80081 = CARTESIAN_POINT ( 'NONE',  ( 15.45378058238208219, -4.887748414852792322, 34.01359900205216746 ) ) ;
#80083 = CARTESIAN_POINT ( 'NONE',  ( -6.673022503163469565, -4.074993327901525575, 33.72946981652012255 ) ) ;
#80084 = CARTESIAN_POINT ( 'NONE',  ( 3.230769230769231726, -2.249999999999998668, 29.50000000000001421 ) ) ;
#80085 = AXIS2_PLACEMENT_3D ( 'NONE', #51448, #44706, #64101 ) ;
#80086 = CARTESIAN_POINT ( 'NONE',  ( 2.373760658694747061, -3.513871655860379306, 32.76840700105978499 ) ) ;
#80087 = CARTESIAN_POINT ( 'NONE',  ( 17.07692307692295586, -8.613356846316285953, 34.62446782046622218 ) ) ;
#80088 = VERTEX_POINT ( 'NONE', #17732 ) ;
#80089 = ADVANCED_FACE ( 'NONE', ( #45184 ), #4205, .F. ) ;
#80090 = ORIENTED_EDGE ( 'NONE', *, *, #76943, .T. ) ;
#80091 = AXIS2_PLACEMENT_3D ( 'NONE', #6806, #49573, #82923 ) ;
#80092 = VERTEX_POINT ( 'NONE', #13625 ) ;
#80094 = VERTEX_POINT ( 'NONE', #68567 ) ;
#80093 = CARTESIAN_POINT ( 'NONE',  ( 2.307692307692309264, -12.37446782046654192, 30.86335684631486131 ) ) ;
#80095 = CARTESIAN_POINT ( 'NONE',  ( 17.07692307692307665, -5.471508081941601098, 34.59228464037088457 ) ) ;
#80096 = B_SPLINE_CURVE_WITH_KNOTS ( 'NONE', 3,
 ( #69950, #77598, #35735, #28985, #56440, #26089, #6697, #12578, #59867, #81044 ),
 .UNSPECIFIED., .F., .F.,
 ( 4, 2, 2, 2, 4 ),
 ( 0.000000000000000000, 0.0001954339881912774612, 0.0003908679763825549224, 0.0005863019645738323836, 0.0007817359527651098448 ),
 .UNSPECIFIED. ) ;
#80097 = CARTESIAN_POINT ( 'NONE',  ( 12.46153846153833911, -11.48612834414049644, 32.76840700105863391 ) ) ;
#80098 = EDGE_LOOP ( 'NONE', ( #69358, #79526, #71634, #38857 ) ) ;
#80099 = AXIS2_PLACEMENT_3D ( 'NONE', #6709, #60321, #25657 ) ;
#80100 = CARTESIAN_POINT ( 'NONE',  ( -13.60810032833933469, -4.386631170607603991, 33.66268669641500111 ) ) ;
#80101 = CYLINDRICAL_SURFACE ( 'NONE', #3369, 0.2499999999999995559 ) ;
#80102 = DIRECTION ( 'NONE',  ( -0.000000000000000000, 1.000000000000000000, 3.491481338843133355E-15 ) ) ;
#80103 = FACE_BOUND ( 'NONE', #71030, .T. ) ;
#80104 = CARTESIAN_POINT ( 'NONE',  ( -5.326899820971668476, -10.06842814019191401, 34.32929386961144758 ) ) ;
#80105 = CARTESIAN_POINT ( 'NONE',  ( -6.000000000000121680, -12.51329471203414379, 31.30864560766407578 ) ) ;
#80106 = B_SPLINE_CURVE_WITH_KNOTS ( 'NONE', 3,
 ( #400, #8487, #13457, #48564, #35959, #63413, #27862, #40941, #27423, #82820 ),
 .UNSPECIFIED., .F., .F.,
 ( 4, 2, 2, 2, 4 ),
 ( 0.0007817246256747484735, 0.0009771112852218920199, 0.001172497944769035783, 0.001367884604316179330, 0.001563271263863322876 ),
 .UNSPECIFIED. ) ;
#80107 = CARTESIAN_POINT ( 'NONE',  ( -9.019207500173124004, -4.236021600441997492, 33.53823185664189310 ) ) ;
#80109 = CARTESIAN_POINT ( 'NONE',  ( 14.55774672760576394, -2.920487667080175598, 32.31805714834170828 ) ) ;
#80108 = CARTESIAN_POINT ( 'NONE',  ( 17.32692307692307665, -2.499999999999998668, 29.75000000000000355 ) ) ;
#80110 = CARTESIAN_POINT ( 'NONE',  ( -10.36538461538317790, -7.500000000000155431, 34.75000000000007105 ) ) ;
#80111 = FACE_OUTER_BOUND ( 'NONE', #6039, .T. ) ;
#80112 = EDGE_LOOP ( 'NONE', ( #13230, #74988, #59544, #43422 ) ) ;
#80113 = CARTESIAN_POINT ( 'NONE',  ( 11.53846153846153832, -3.050289026998446396, 32.03036669348365706 ) ) ;
#80114 = CARTESIAN_POINT ( 'NONE',  ( -13.60754234352223335, -9.172386477786396597, 34.72672124145550043 ) ) ;
#80115 = ORIENTED_EDGE ( 'NONE', *, *, #43751, .T. ) ;
#80116 = VERTEX_POINT ( 'NONE', #62246 ) ;
#80118 = PLANE ( 'NONE',  #7527 ) ;
#80117 = CARTESIAN_POINT ( 'NONE',  ( 5.750023269057647823, -6.567427716900047230, 34.66269422305636283 ) ) ;
#80119 = CARTESIAN_POINT ( 'NONE',  ( 6.923076923076924238, -11.16473453929635440, 33.15142922261926373 ) ) ;
#80120 = CARTESIAN_POINT ( 'NONE',  ( 16.08776274289027342, -3.513871655860377086, 32.76840700105978499 ) ) ;
#80121 = DIRECTION ( 'NONE',  ( -0.000000000000000000, 0.5000000000000011102, -0.8660254037844380415 ) ) ;
#80122 = ORIENTED_EDGE ( 'NONE', *, *, #41385, .T. ) ;
#80123 = VECTOR ( 'NONE', #23990, 1000.000000000000000 ) ;
#80124 = CARTESIAN_POINT ( 'NONE',  ( -19.50000000000000000, -3.499999999999999556, 29.75000000000000355 ) ) ;
#80125 = CARTESIAN_POINT ( 'NONE',  ( 4.376858997939547358, -4.762714258010880997, 34.23016756924214832 ) ) ;
#80126 = EDGE_CURVE ( 'NONE', #40124, #42322, #51071, .T. ) ;
#80127 = EDGE_CURVE ( 'NONE', #40782, #30954, #11388, .T. ) ;
#80129 = CARTESIAN_POINT ( 'NONE',  ( -11.78846153846153832, -7.500000000000001776, 35.04278698407183867 ) ) ;
#80128 = DIRECTION ( 'NONE',  ( -0.000000000000000000, 0.8660254037844399289, -0.4999999999999980016 ) ) ;
#80130 = CARTESIAN_POINT ( 'NONE',  ( -1.515305987725692694, -9.929715669179220328, 34.40415004197138416 ) ) ;
#80131 = CARTESIAN_POINT ( 'NONE',  ( 2.530471848960717640, -5.114059244376869984, 34.14424750095245287 ) ) ;
#80132 = FACE_OUTER_BOUND ( 'NONE', #9925, .T. ) ;
#80133 = AXIS2_PLACEMENT_3D ( 'NONE', #39773, #79421, #52372 ) ;
#80134 = CARTESIAN_POINT ( 'NONE',  ( -1.553300858899125059, -3.750000000000009326, 21.57812500000000355 ) ) ;
#80135 = ORIENTED_EDGE ( 'NONE', *, *, #81305, .T. ) ;
#80136 = EDGE_CURVE ( 'NONE', #87474, #12672, #59711, .T. ) ;
#80137 = VERTEX_POINT ( 'NONE', #55054 ) ;
#80138 = DIRECTION ( 'NONE',  ( 0.000000000000000000, 1.000000000000000000, -0.000000000000000000 ) ) ;
#80139 = ADVANCED_FACE ( 'NONE', ( #14069 ), #41544, .F. ) ;
#80140 = AXIS2_PLACEMENT_3D ( 'NONE', #18214, #65938, #51515 ) ;
#80141 = CARTESIAN_POINT ( 'NONE',  ( -4.283993363284372080, -12.45813303252208648, 30.39737893381572675 ) ) ;
#80142 = CARTESIAN_POINT ( 'NONE',  ( -12.22435897435897267, -3.499999999999999556, 29.75000000000000355 ) ) ;
#80143 = DIRECTION ( 'NONE',  ( 0.000000000000000000, 0.3420201433256641055, -0.9396926207859100932 ) ) ;
#80144 = CYLINDRICAL_SURFACE ( 'NONE', #64577, 0.2499999999999997502 ) ;
#80145 = CARTESIAN_POINT ( 'NONE',  ( 1.553300858899087311, -3.749999999999992006, 22.98437500000000000 ) ) ;
#80146 = B_SPLINE_CURVE_WITH_KNOTS ( 'NONE', 3,
 ( #23534, #28542, #1511, #50990, #56882, #23104, #36194, #63643, #30305, #15915 ),
 .UNSPECIFIED., .F., .F.,
 ( 4, 2, 2, 2, 4 ),
 ( 0.000000000000000000, 0.0001954339857564071491, 0.0003908679715128142982, 0.0005863019572692214744, 0.0007817359430256285964 ),
 .UNSPECIFIED. ) ;
#80147 = CARTESIAN_POINT ( 'NONE',  ( -1.384615384615506484, -4.320704448113951379, 33.92786785259630022 ) ) ;
#80148 = DIRECTION ( 'NONE',  ( 0.000000000000000000, 0.3420201433256610524, 0.9396926207859113145 ) ) ;
#80149 = EDGE_CURVE ( 'NONE', #33117, #10201, #37050, .T. ) ;
#80150 = FACE_OUTER_BOUND ( 'NONE', #37175, .T. ) ;
#80151 = CARTESIAN_POINT ( 'NONE',  ( -12.46153846153858247, -12.46129190930018460, 30.37095296980731973 ) ) ;
#80152 = FACE_OUTER_BOUND ( 'NONE', #37015, .T. ) ;
#80153 = B_SPLINE_CURVE_WITH_KNOTS ( 'NONE', 3,
 ( #31094, #44601, #71197, #16699, #50478, #58566, #9943, #29786, #70770, #23891 ),
 .UNSPECIFIED., .F., .F.,
 ( 4, 2, 2, 2, 4 ),
 ( 0.000000000000000000, 0.0001954339857564073388, 0.0003908679715128146777, 0.0005863019572692220165, 0.0007817359430256293554 ),
 .UNSPECIFIED. ) ;
#80154 = CARTESIAN_POINT ( 'NONE',  ( 15.23076923076910916, -12.51329471203414379, 31.30864560766407578 ) ) ;
#80155 = B_SPLINE_CURVE_WITH_KNOTS ( 'NONE', 3,
 ( #5088, #3746, #32552, #60024, #87528, #25805, #19047, #31216, #24304, #71605 ),
 .UNSPECIFIED., .F., .F.,
 ( 4, 2, 2, 2, 4 ),
 ( 0.000000000000000000, 0.0001954339881912774070, 0.0003908679763825548140, 0.0005863019645738322752, 0.0007817359527651096280 ),
 .UNSPECIFIED. ) ;
#80156 = CARTESIAN_POINT ( 'NONE',  ( -0.4615384615384611200, -1.242168528481310874, 33.36296068462461051 ) ) ;
#80157 = CARTESIAN_POINT ( 'NONE',  ( 4.023698944407933631, -12.45813303252208648, 30.39737893381572675 ) ) ;
#80158 = CARTESIAN_POINT ( 'NONE',  ( -0.4615384615384611200, -11.16473453929635440, 33.15142922261926373 ) ) ;
#80159 = CARTESIAN_POINT ( 'NONE',  ( -16.94613263595612551, -2.845873456487966635, 32.17976146951972538 ) ) ;
#80160 = EDGE_CURVE ( 'NONE', #62909, #6352, #61778, .T. ) ;
#80161 = ORIENTED_EDGE ( 'NONE', *, *, #174, .T. ) ;
#80162 = DIRECTION ( 'NONE',  ( 0.000000000000000000, 1.000000000000000000, 0.000000000000000000 ) ) ;
#80163 = CARTESIAN_POINT ( 'NONE',  ( 18.00000000000000000, -4.661471528628507777, 34.16647553114623292 ) ) ;
#80164 = CARTESIAN_POINT ( 'NONE',  ( -4.284536756956461190, -5.496505350115500121, 34.60290016733514307 ) ) ;
#80165 = CARTESIAN_POINT ( 'NONE',  ( 1.200186371490529202, -4.775308065498752974, 15.73624329374151998 ) ) ;
#80166 = CARTESIAN_POINT ( 'NONE',  ( 5.142178216435913107, -10.33852847137154107, 34.16647553114620450 ) ) ;
#80168 = CARTESIAN_POINT ( 'NONE',  ( 15.90382292962469180, -4.931416488878822335, 34.32920672191015399 ) ) ;
#80167 = VECTOR ( 'NONE', #5226, 1000.000000000000000 ) ;
#80169 = EDGE_CURVE ( 'NONE', #36938, #87581, #88778, .T. ) ;
#80171 = ORIENTED_EDGE ( 'NONE', *, *, #6529, .T. ) ;
#80170 = CARTESIAN_POINT ( 'NONE',  ( -0.2114841499001470504, -2.564540009722895419, 30.55348353981670684 ) ) ;
#80172 = CARTESIAN_POINT ( 'NONE',  ( -1.409462824231155764E-14, -4.749999999999999112, 16.65625000000000000 ) ) ;
#80173 = PLANE ( 'NONE',  #68520 ) ;
#80174 = ORIENTED_EDGE ( 'NONE', *, *, #70775, .T. ) ;
#80175 = FACE_OUTER_BOUND ( 'NONE', #8501, .T. ) ;
#80176 = VERTEX_POINT ( 'NONE', #43752 ) ;
#80177 = CARTESIAN_POINT ( 'NONE',  ( -18.00000000000000000, -11.69971097300155449, 32.46337939537587403 ) ) ;
#80178 = ADVANCED_FACE ( 'NONE', ( #77543 ), #71217, .F. ) ;
#80179 = CARTESIAN_POINT ( 'NONE',  ( 13.13459214732242408, -10.05641848906368097, 34.04755513067966177 ) ) ;
#80180 = CARTESIAN_POINT ( 'NONE',  ( 15.48082354240754732, -2.779044189368095719, 31.39831045268885745 ) ) ;
#80181 = ORIENTED_EDGE ( 'NONE', *, *, #3084, .F. ) ;
#80182 = CARTESIAN_POINT ( 'NONE',  ( 0.3308478584281521195, -4.684245665217972032, 34.18127051446801090 ) ) ;
#80183 = ORIENTED_EDGE ( 'NONE', *, *, #2486, .F. ) ;
#80184 = CARTESIAN_POINT ( 'NONE',  ( 13.38461538461570122, -2.255955759149395501, 30.00000000000324363 ) ) ;
#80185 = EDGE_CURVE ( 'NONE', #8069, #44632, #43605, .T. ) ;
#80186 = ORIENTED_EDGE ( 'NONE', *, *, #65789, .F. ) ;
#80187 = CARTESIAN_POINT ( 'NONE',  ( -0.7115616988314276137, -3.202444869320336451, 32.30641848906366675 ) ) ;
#80188 = CARTESIAN_POINT ( 'NONE',  ( 2.557637826040450868, -3.202959910592335202, 32.30730279482227019 ) ) ;
#80189 = CARTESIAN_POINT ( 'NONE',  ( -10.39260507411620438, -6.760870238392817200, 34.69528174975672385 ) ) ;
#80190 = B_SPLINE_CURVE_WITH_KNOTS ( 'NONE', 3,
 ( #87241, #74152, #46675, #73262, #87683, #25073 ),
 .UNSPECIFIED., .F., .F.,
 ( 4, 2, 4 ),
 ( 0.0003909569690057805385, 0.0005862646681846044039, 0.0007815723673634283235 ),
 .UNSPECIFIED. ) ;
#80191 = CARTESIAN_POINT ( 'NONE',  ( -10.68146699474474914, -11.91647553114624181, 32.58852847137148245 ) ) ;
#80192 = CARTESIAN_POINT ( 'NONE',  ( 15.23076923076923173, -6.386643153685126251, 34.62446782046654192 ) ) ;
#80193 = DIRECTION ( 'NONE',  ( 1.000000000000000000, -0.000000000000000000, -0.000000000000000000 ) ) ;
#80194 = ADVANCED_FACE ( 'NONE', ( #8652 ), #22160, .F. ) ;
#80195 = CARTESIAN_POINT ( 'NONE',  ( 4.853996859406927378, -9.086856451489516928, 34.49173150075333183 ) ) ;
#80196 = VERTEX_POINT ( 'NONE', #78419 ) ;
#80198 = ADVANCED_FACE ( 'NONE', ( #42439 ), #29371, .F. ) ;
#80197 = VERTEX_POINT ( 'NONE', #36129 ) ;
#80199 = VERTEX_POINT ( 'NONE', #8208 ) ;
#80201 = ORIENTED_EDGE ( 'NONE', *, *, #52490, .F. ) ;
#80200 = DIRECTION ( 'NONE',  ( 1.000000000000000000, 0.000000000000000000, 0.000000000000000000 ) ) ;
#80202 = AXIS2_PLACEMENT_3D ( 'NONE', #57990, #57106, #1725 ) ;
#80203 = LINE ( 'NONE', #59029, #65082 ) ;
#80204 = CARTESIAN_POINT ( 'NONE',  ( 9.692307692307695177, -5.471508081941601098, 34.59228464037088457 ) ) ;
#80205 = ORIENTED_EDGE ( 'NONE', *, *, #87641, .T. ) ;
#80206 = EDGE_CURVE ( 'NONE', #58189, #76766, #42502, .T. ) ;
#80207 = CARTESIAN_POINT ( 'NONE',  ( -14.24243673641627872, -4.481592998940250538, 33.73612834413965089 ) ) ;
#80208 = EDGE_CURVE ( 'NONE', #72796, #17639, #50502, .T. ) ;
#80209 = ORIENTED_EDGE ( 'NONE', *, *, #71880, .F. ) ;
#80210 = CYLINDRICAL_SURFACE ( 'NONE', #48290, 0.2499999999999986955 ) ;
#80211 = EDGE_LOOP ( 'NONE', ( #68684, #73662, #13010, #4134 ) ) ;
#80212 = CARTESIAN_POINT ( 'NONE',  ( 7.846153846153846700, -8.318370150425687726, 35.83090037661290239 ) ) ;
#80213 = B_SPLINE_CURVE_WITH_KNOTS ( 'NONE', 3,
 ( #72202, #65451, #4193, #52373, #59136, #16820, #31218, #87529, #78967, #25806 ),
 .UNSPECIFIED., .F., .F.,
 ( 4, 2, 2, 2, 4 ),
 ( 0.000000000000000000, 0.0001954311564186882026, 0.0003908623128373764051, 0.0005862934692560646619, 0.0007817246256747528103 ),
 .UNSPECIFIED. ) ;
#80214 = DIRECTION ( 'NONE',  ( -0.000000000000000000, 0.6427876096865404731, -0.7660444431189771253 ) ) ;
#80215 = B_SPLINE_CURVE_WITH_KNOTS ( 'NONE', 3,
 ( #38680, #73357, #72905, #80114, #86898, #26062, #53519, #32818, #73813, #58486 ),
 .UNSPECIFIED., .F., .F.,
 ( 4, 2, 2, 2, 4 ),
 ( 0.000000000000000000, 0.0001954311564186865221, 0.0003908623128373730441, 0.0005862934692560595662, 0.0007817246256747460882 ),
 .UNSPECIFIED. ) ;
#80216 = DIRECTION ( 'NONE',  ( 0.000000000000000000, 0.9848077530122072432, -0.1736481776669354937 ) ) ;
#80217 = FACE_BOUND ( 'NONE', #84534, .T. ) ;
#80218 = CARTESIAN_POINT ( 'NONE',  ( 17.29970274590113632, -6.717445702608400460, 34.94155399931962336 ) ) ;
#80219 = CARTESIAN_POINT ( 'NONE',  ( 0.000000000000000000, -11.00000000000000000, 29.75000000000000355 ) ) ;
#80220 = CARTESIAN_POINT ( 'NONE',  ( 6.000000000000001776, -11.69971097300155272, 32.46337939537588113 ) ) ;
#80221 = FACE_OUTER_BOUND ( 'NONE', #28115, .T. ) ;
#80222 = VECTOR ( 'NONE', #73137, 1000.000000000000227 ) ;
#80223 = FACE_OUTER_BOUND ( 'NONE', #41750, .T. ) ;
#80224 = CARTESIAN_POINT ( 'NONE',  ( -7.846153846153965716, -12.46129190930018460, 30.37095296980731973 ) ) ;
#80225 = EDGE_LOOP ( 'NONE', ( #74228, #935 ) ) ;
#80226 = DIRECTION ( 'NONE',  ( 0.000000000000000000, 0.7660444431189822323, -0.6427876096865344779 ) ) ;
#80227 = ORIENTED_EDGE ( 'NONE', *, *, #63159, .T. ) ;
#80228 = ORIENTED_EDGE ( 'NONE', *, *, #44813, .F. ) ;
#80229 = AXIS2_PLACEMENT_3D ( 'NONE', #50864, #9899, #52657 ) ;
#80231 = CARTESIAN_POINT ( 'NONE',  ( 2.530703659305157949, -10.61302985866383963, 33.66295027996417843 ) ) ;
#80230 = CARTESIAN_POINT ( 'NONE',  ( 10.83816415665302557, -12.44528174975671853, 30.48912976160716681 ) ) ;
#80232 = CARTESIAN_POINT ( 'NONE',  ( -4.284455809050233377, -7.722926974430166069, 34.99546784045485737 ) ) ;
#80233 = CARTESIAN_POINT ( 'NONE',  ( -13.51476335434708353, -3.069018819979302926, 32.56621877034667278 ) ) ;
#80234 = CARTESIAN_POINT ( 'NONE',  ( 16.94623161025552704, -8.147922237126337563, 34.70805685702651999 ) ) ;
#80235 = CARTESIAN_POINT ( 'NONE',  ( -13.13466986626724520, -2.824170634883621744, 31.52227843825338738 ) ) ;
#80236 = ORIENTED_EDGE ( 'NONE', *, *, #13075, .F. ) ;
#80237 = DIRECTION ( 'NONE',  ( -0.000000000000000000, 1.000000000000000000, -0.000000000000000000 ) ) ;
#80238 = VECTOR ( 'NONE', #68110, 1000.000000000000000 ) ;
#80239 = CARTESIAN_POINT ( 'NONE',  ( 15.10007862765892206, -3.957541250942358424, 33.62499894934981626 ) ) ;
#80240 = CARTESIAN_POINT ( 'NONE',  ( 10.39189967166066708, -3.236172620538810385, 32.36188796281390267 ) ) ;
#80241 = CARTESIAN_POINT ( 'NONE',  ( 4.826923076923076650, -7.566083408709834757, 34.74999999999999289 ) ) ;
#80242 = VERTEX_POINT ( 'NONE', #62684 ) ;
#80243 = B_SPLINE_CURVE_WITH_KNOTS ( 'NONE', 3,
 ( #31501, #58966, #44548, #72033, #86923, #10343, #25189, #37809, #52205, #65276 ),
 .UNSPECIFIED., .F., .F.,
 ( 4, 2, 2, 2, 4 ),
 ( 0.000000000000000000, 0.0001954311564186871184, 0.0003908623128373742367, 0.0005862934692560614093, 0.0007817246256747484735 ),
 .UNSPECIFIED. ) ;
#80244 = ORIENTED_EDGE ( 'NONE', *, *, #45005, .T. ) ;
#80245 = APPLICATION_PROTOCOL_DEFINITION ( 'draft international standard', 'automotive_design', 1998, #22214 ) ;
#80246 = ORIENTED_EDGE ( 'NONE', *, *, #8060, .F. ) ;
#80247 = LINE ( 'NONE', #5025, #20461 ) ;
#80248 = CARTESIAN_POINT ( 'NONE',  ( 4.853438152358743096, -3.019605429927184836, 32.48692288466676814 ) ) ;
#80250 = VERTEX_POINT ( 'NONE', #55935 ) ;
#80249 = EDGE_CURVE ( 'NONE', #13621, #82495, #9096, .T. ) ;
#80251 = CARTESIAN_POINT ( 'NONE',  ( 3.165499230212912352, -12.70778746994557551, 30.41441678777548319 ) ) ;
#80252 = DIRECTION ( 'NONE',  ( -0.000000000000000000, 0.6427876096865404731, -0.7660444431189771253 ) ) ;
#80253 = DIRECTION ( 'NONE',  ( -0.000000000000000000, 0.9848077530122086864, -0.1736481776669273891 ) ) ;
#80254 = CARTESIAN_POINT ( 'NONE',  ( -12.94230769230769162, -7.500000000000000000, 29.75000000000000355 ) ) ;
#80255 = PLANE ( 'NONE',  #57547 ) ;
#80256 = ORIENTED_EDGE ( 'NONE', *, *, #54701, .T. ) ;
#80257 = EDGE_CURVE ( 'NONE', #65802, #28603, #22915, .T. ) ;
#80259 = EDGE_LOOP ( 'NONE', ( #66109, #44719, #71424, #37025 ) ) ;
#80258 = CARTESIAN_POINT ( 'NONE',  ( 0.3962680155776850954, -10.21337939537584383, 33.94971097300158647 ) ) ;
#80260 = LINE ( 'NONE', #5491, #85726 ) ;
#80261 = CARTESIAN_POINT ( 'NONE',  ( -2.980714810855776609, -2.544122305571458575, 31.48381861865057729 ) ) ;
#80262 = CARTESIAN_POINT ( 'NONE',  ( -7.780086512803770837, -3.322132147404559976, 32.92929555188717927 ) ) ;
#80263 = CARTESIAN_POINT ( 'NONE',  ( 10.61538461538449418, -12.51329471203414379, 31.30864560766407578 ) ) ;
#80264 = CARTESIAN_POINT ( 'NONE',  ( -4.023320715612508813, -5.070358843744210198, 34.40418822224088302 ) ) ;
#80265 = DIRECTION ( 'NONE',  ( -0.000000000000000000, 0.1736481776669307198, -0.9848077530122080203 ) ) ;
#80266 = CARTESIAN_POINT ( 'NONE',  ( 15.23076923076923173, -3.669653830205710676, 35.88435417666054406 ) ) ;
#80267 = EDGE_CURVE ( 'NONE', #38598, #45177, #83875, .T. ) ;
#80268 = CARTESIAN_POINT ( 'NONE',  ( -1.200186371490524317, -10.22469193450124791, 13.86124329374151820 ) ) ;
#80269 = EDGE_LOOP ( 'NONE', ( #72538, #28979, #51657, #8713, #62367, #63642 ) ) ;
#80270 = AXIS2_PLACEMENT_3D ( 'NONE', #46442, #82465, #34257 ) ;
#80271 = CARTESIAN_POINT ( 'NONE',  ( -7.846153846153844924, -6.189225973068211317, 35.74407628777942847 ) ) ;
#80272 = DIRECTION ( 'NONE',  ( -1.000000000000000000, -0.000000000000000000, -0.000000000000000000 ) ) ;
#80273 = FACE_OUTER_BOUND ( 'NONE', #17953, .T. ) ;
#80274 = ORIENTED_EDGE ( 'NONE', *, *, #7835, .F. ) ;
#80276 = ORIENTED_EDGE ( 'NONE', *, *, #72762, .T. ) ;
#80275 = AXIS2_PLACEMENT_3D ( 'NONE', #44928, #64751, #30535 ) ;
#80277 = DIRECTION ( 'NONE',  ( -0.000000000000000000, 1.000000000000000000, -0.000000000000000000 ) ) ;
#80278 = CARTESIAN_POINT ( 'NONE',  ( 7.780883845597525550, -6.835583212224499050, 34.95778746994557906 ) ) ;
#80279 = CARTESIAN_POINT ( 'NONE',  ( -0.5276208408985972875, -9.058645607665454236, 34.76329471203372634 ) ) ;
#80280 = CARTESIAN_POINT ( 'NONE',  ( 10.48523740594639442, -4.460286881179643004, 33.72017969459903242 ) ) ;
#80281 = EDGE_CURVE ( 'NONE', #21202, #48918, #70347, .T. ) ;
#80282 = CARTESIAN_POINT ( 'NONE',  ( 7.173131234715237170, -5.728107161865375829, 34.42597550085002922 ) ) ;
#80283 = CARTESIAN_POINT ( 'NONE',  ( -15.09997878980228059, -8.191423895709840863, 34.95447573519442130 ) ) ;
#80284 = ORIENTED_EDGE ( 'NONE', *, *, #33007, .F. ) ;
#80285 = B_SPLINE_CURVE_WITH_KNOTS ( 'NONE', 3,
 ( #77794, #37241, #2134, #43133, #65158, #16098, #3459, #63839, #30059, #57523 ),
 .UNSPECIFIED., .F., .F.,
 ( 4, 2, 2, 2, 4 ),
 ( 0.0007817359430256398721, 0.0009771253907250089001, 0.001172514838424377820, 0.001367904286123746739, 0.001563293733823115659 ),
 .UNSPECIFIED. ) ;
#80286 = CARTESIAN_POINT ( 'NONE',  ( 0.000000000000000000, -11.00000000000000000, 29.75000000000000355 ) ) ;
#80287 = CYLINDRICAL_SURFACE ( 'NONE', #54146, 0.2500000000000009437 ) ;
#80288 = CARTESIAN_POINT ( 'NONE',  ( 3.930361229281822855, -8.539481045369598178, 34.89627647299170832 ) ) ;
#80289 = ORIENTED_EDGE ( 'NONE', *, *, #33112, .F. ) ;
#80290 = CARTESIAN_POINT ( 'NONE',  ( -7.780898274877819709, -3.835265460703683349, 33.15142922261929925 ) ) ;
#80291 = ADVANCED_FACE ( 'NONE', ( #28474 ), #83427, .F. ) ;
#80292 = ORIENTED_EDGE ( 'NONE', *, *, #55866, .F. ) ;
#80293 = AXIS2_PLACEMENT_3D ( 'NONE', #80919, #82689, #61504 ) ;
#80294 = CARTESIAN_POINT ( 'NONE',  ( 1.254138676498922411, -7.276988635370452485, 34.74523720219453793 ) ) ;
#80295 = SHAPE_REPRESENTATION_RELATIONSHIP ( 'NONE' , 'NONE' ,  #11527, #83739 ) ;
#80296 = DIRECTION ( 'NONE',  ( -1.000000000000000000, -0.000000000000000000, -0.000000000000000000 ) ) ;
#80297 = CARTESIAN_POINT ( 'NONE',  ( 6.130790440966950250, -11.93129842949671726, 32.56571108434900452 ) ) ;
#80298 = ORIENTED_EDGE ( 'NONE', *, *, #83687, .F. ) ;
#80299 = ADVANCED_FACE ( 'NONE', ( #3644 ), #32460, .F. ) ;
#80300 = CARTESIAN_POINT ( 'NONE',  ( -13.31936024510254413, -5.094484230520773593, 34.41647553114626845 ) ) ;
#80301 = CARTESIAN_POINT ( 'NONE',  ( 13.60739505359345181, -9.418065098278013636, 34.63729479722530158 ) ) ;
#80302 = DIRECTION ( 'NONE',  ( -0.000000000000000000, 0.9396926207859092051, -0.3420201433256662704 ) ) ;
#80303 = VECTOR ( 'NONE', #39552, 1000.000000000000000 ) ;
#80304 = DIRECTION ( 'NONE',  ( -0.000000000000000000, 0.1736481776669307198, -0.9848077530122080203 ) ) ;
#80305 = FACE_OUTER_BOUND ( 'NONE', #59252, .T. ) ;
#80306 = EDGE_CURVE ( 'NONE', #77956, #83716, #30202, .T. ) ;
#80307 = AXIS2_PLACEMENT_3D ( 'NONE', #34253, #12661, #82013 ) ;
#80308 = ORIENTED_EDGE ( 'NONE', *, *, #59139, .T. ) ;
#80309 = CYLINDRICAL_SURFACE ( 'NONE', #1202, 0.2499999999999998890 ) ;
#80310 = VERTEX_POINT ( 'NONE', #45529 ) ;
#80311 = DIRECTION ( 'NONE',  ( 0.000000000000000000, 0.000000000000000000, 1.000000000000000000 ) ) ;
#80312 = CARTESIAN_POINT ( 'NONE',  ( -12.46153846153858424, -3.083524468854526912, 32.58852847137268327 ) ) ;
#80313 = CARTESIAN_POINT ( 'NONE',  ( -0.2115930521604195702, -2.589246495874657938, 31.60778113518102828 ) ) ;
#80314 = LINE ( 'NONE', #58689, #9937 ) ;
#80315 = B_SPLINE_CURVE_WITH_KNOTS ( 'NONE', 3,
 ( #82457, #77454, #83338, #1349, #62164, #82895, #473, #41909, #35589, #63036 ),
 .UNSPECIFIED., .F., .F.,
 ( 4, 2, 2, 2, 4 ),
 ( 0.000000000000000000, 0.0001954339857564083688, 0.0003908679715128167377, 0.0005863019572692250523, 0.0007817359430256334753 ),
 .UNSPECIFIED. ) ;
#80316 = CARTESIAN_POINT ( 'NONE',  ( -2.307692307692305711, -8.810774026931790459, 35.74407628777942847 ) ) ;
#80317 = CARTESIAN_POINT ( 'NONE',  ( -6.250023237292963607, -4.335965774309649134, 33.62209801155881905 ) ) ;
#80318 = CARTESIAN_POINT ( 'NONE',  ( 12.68454981315131214, -9.886259254753566594, 34.14407573483972413 ) ) ;
#80319 = EDGE_CURVE ( 'NONE', #23856, #13098, #68336, .T. ) ;
#80320 = ORIENTED_EDGE ( 'NONE', *, *, #60476, .T. ) ;
#80321 = ORIENTED_EDGE ( 'NONE', *, *, #64871, .F. ) ;
#80322 = EDGE_LOOP ( 'NONE', ( #19421, #5586, #51970, #38616 ) ) ;
#80323 = EDGE_CURVE ( 'NONE', #51403, #18589, #87651, .T. ) ;
#80325 = EDGE_LOOP ( 'NONE', ( #41922, #31040, #44289, #1664, #57324 ) ) ;
#80324 = ADVANCED_FACE ( 'NONE', ( #18512 ), #31117, .F. ) ;
#80326 = ORIENTED_EDGE ( 'NONE', *, *, #55001, .F. ) ;
#80327 = CARTESIAN_POINT ( 'NONE',  ( -16.15384615384627409, -3.835265460704628815, 33.15142922262033665 ) ) ;
#80328 = CARTESIAN_POINT ( 'NONE',  ( -2.057746789344164107, -3.202959910592335202, 32.30730279482227019 ) ) ;
#80329 = VECTOR ( 'NONE', #14216, 1000.000000000000114 ) ;
#80330 = CARTESIAN_POINT ( 'NONE',  ( -3.930834802233302394, -9.086983370893049639, 34.49168942202179267 ) ) ;
#80331 = EDGE_CURVE ( 'NONE', #61132, #79227, #70416, .T. ) ;
#80332 = LINE ( 'NONE', #18623, #43667 ) ;
#80333 = CARTESIAN_POINT ( 'NONE',  ( 0.4615384615384611755, -5.415277668671390821, 36.20867863119892149 ) ) ;
#80334 = CARTESIAN_POINT ( 'NONE',  ( 8.638539302563213340, -8.999036380462717588, 34.52022231692819076 ) ) ;
#80335 = CARTESIAN_POINT ( 'NONE',  ( -14.30769230769230660, -13.78497067705608181, 32.30358669280327177 ) ) ;
#80336 = CARTESIAN_POINT ( 'NONE',  ( 16.85405681385997667, -2.251424796025574881, 29.88072029997477586 ) ) ;
#80337 = CARTESIAN_POINT ( 'NONE',  ( 18.75000000000000000, -3.499999999999999556, 29.75000000000000355 ) ) ;
#80338 = ORIENTED_EDGE ( 'NONE', *, *, #9138, .T. ) ;
#80339 = VERTEX_POINT ( 'NONE', #65354 ) ;
#80340 = ORIENTED_EDGE ( 'NONE', *, *, #22052, .T. ) ;
#80342 = ORIENTED_EDGE ( 'NONE', *, *, #88754, .F. ) ;
#80341 = CARTESIAN_POINT ( 'NONE',  ( -13.38461538461538325, -12.34228464037088635, 31.77849191805839268 ) ) ;
#80344 = CARTESIAN_POINT ( 'NONE',  ( -18.00000000000012079, -11.67786785259630733, 32.92929555188604240 ) ) ;
#80343 = CARTESIAN_POINT ( 'NONE',  ( 6.792386319966616348, -11.37499894934982514, 33.29245874905763003 ) ) ;
#80345 = CARTESIAN_POINT ( 'NONE',  ( 16.40384615384608935, -7.565270445406050648, 34.75000000000000000 ) ) ;
#80346 = CARTESIAN_POINT ( 'NONE',  ( -2.939152317953646711E-15, 7.500000000000000000, 14.00000000000000178 ) ) ;
#80347 = FACE_BOUND ( 'NONE', #83206, .T. ) ;
#80348 = ORIENTED_EDGE ( 'NONE', *, *, #40878, .F. ) ;
#80349 = B_SPLINE_CURVE_WITH_KNOTS ( 'NONE', 3,
 ( #32543, #46062, #59572, #85725, #24006, #3735, #39323, #31208, #18152, #11847 ),
 .UNSPECIFIED., .F., .F.,
 ( 4, 2, 2, 2, 4 ),
 ( 0.0007817246256747461966, 0.0009771112852218892010, 0.001172497944769032314, 0.001367884604316175427, 0.001563271263863318323 ),
 .UNSPECIFIED. ) ;
#80350 = EDGE_LOOP ( 'NONE', ( #15600, #27735, #82662, #53860 ) ) ;
#80351 = CARTESIAN_POINT ( 'NONE',  ( -4.853911725310227077, -6.503523203565942268, 34.64991518177335195 ) ) ;
#80352 = EDGE_LOOP ( 'NONE', ( #64677, #46748, #25721, #75523 ) ) ;
#80353 = FACE_BOUND ( 'NONE', #25741, .T. ) ;
#80354 = CARTESIAN_POINT ( 'NONE',  ( -9.627052552794857831, -2.379036618887895305, 30.90682066428158592 ) ) ;
#80355 = B_SPLINE_CURVE_WITH_KNOTS ( 'NONE', 3,
 ( #4461, #31945, #11225, #24734, #25625, #52195, #11676, #78014, #17539, #64045 ),
 .UNSPECIFIED., .F., .F.,
 ( 4, 2, 2, 2, 4 ),
 ( 0.0007817246256747440282, 0.0009771112852218863821, 0.001172497944769028844, 0.001367884604316171307, 0.001563271263863313769 ),
 .UNSPECIFIED. ) ;
#80356 = CARTESIAN_POINT ( 'NONE',  ( 18.06525557127601900, -5.219633306516380244, 34.19971097300157936 ) ) ;
#80357 = VERTEX_POINT ( 'NONE', #51821 ) ;
#80358 = FACE_OUTER_BOUND ( 'NONE', #62579, .T. ) ;
#80359 = CARTESIAN_POINT ( 'NONE',  ( -6.700064078983529292, -2.308499170217967134, 30.53291367094873721 ) ) ;
#80360 = CARTESIAN_POINT ( 'NONE',  ( 1.319345384059066983, -3.643525952247789412, 33.31231777344662959 ) ) ;
#80361 = ORIENTED_EDGE ( 'NONE', *, *, #44209, .T. ) ;
#80362 = B_SPLINE_CURVE_WITH_KNOTS ( 'NONE', 3,
 ( #15495, #42966, #63220, #15051, #36646, #44261, #51014, #36215, #71747, #1535 ),
 .UNSPECIFIED., .F., .F.,
 ( 4, 2, 2, 2, 4 ),
 ( 0.000000000000000000, 0.0001954311564186876876, 0.0003908623128373753751, 0.0005862934692560630356, 0.0007817246256747507503 ),
 .UNSPECIFIED. ) ;
#80363 = CARTESIAN_POINT ( 'NONE',  ( 18.06514478071962415, -7.750023224968865421, 34.99404313364389907 ) ) ;
#80364 = CARTESIAN_POINT ( 'NONE',  ( 7.053867364043872712, -5.496552790871117367, 34.60292014791297532 ) ) ;
#80365 = CARTESIAN_POINT ( 'NONE',  ( -9.442253380669379581, -2.564540009722895419, 30.55348353981670684 ) ) ;
#80366 = VERTEX_POINT ( 'NONE', #86083 ) ;
#80367 = AXIS2_PLACEMENT_3D ( 'NONE', #56702, #8084, #28343 ) ;
#80368 = CARTESIAN_POINT ( 'NONE',  ( -2.530618525208451874, -11.24512374952581872, 33.06303171183252942 ) ) ;
#80369 = CARTESIAN_POINT ( 'NONE',  ( -16.82686876528476816, -11.79725096376909299, 32.30694842903960762 ) ) ;
#80370 = VECTOR ( 'NONE', #2689, 1000.000000000000114 ) ;
#80371 = VERTEX_POINT ( 'NONE', #39233 ) ;
#80372 = CARTESIAN_POINT ( 'NONE',  ( 0.3308469948709026887, -8.999036380462717588, 34.52022231692819076 ) ) ;
#80373 = CARTESIAN_POINT ( 'NONE',  ( 14.53047184896071542, -8.496831190052093419, 34.64984203495476578 ) ) ;
#80374 = DIRECTION ( 'NONE',  ( 0.000000000000000000, 0.000000000000000000, -1.000000000000000000 ) ) ;
#80375 = CARTESIAN_POINT ( 'NONE',  ( 18.00000000000000000, -13.53365097954675988, 30.81389545987213552 ) ) ;
#80376 = CARTESIAN_POINT ( 'NONE',  ( -10.61538461538473399, -2.625532179533778709, 30.86335684631627174 ) ) ;
#80377 = CARTESIAN_POINT ( 'NONE',  ( 10.61538461538461675, -11.16473453929635440, 33.15142922261926373 ) ) ;
#80379 = LINE ( 'NONE', #39393, #79109 ) ;
#80378 = LINE ( 'NONE', #46136, #59169 ) ;
#80380 = VECTOR ( 'NONE', #65372, 999.9999999999998863 ) ;
#80381 = CARTESIAN_POINT ( 'NONE',  ( -3.296852641725110722, -2.538708090699994813, 30.37095296980875148 ) ) ;
#80382 = CARTESIAN_POINT ( 'NONE',  ( -12.39628289026243735, -11.48612834413965977, 32.76840700105972815 ) ) ;
#80383 = CARTESIAN_POINT ( 'NONE',  ( -2.775308065498764964, -6.422011778438537988, 26.17000670625849068 ) ) ;
#80384 = ORIENTED_EDGE ( 'NONE', *, *, #13533, .T. ) ;
#80385 = CARTESIAN_POINT ( 'NONE',  ( -19.50000000000000000, -3.499999999999999556, 29.75000000000000355 ) ) ;
#80386 = EDGE_LOOP ( 'NONE', ( #13743, #55217 ) ) ;
#80387 = EDGE_LOOP ( 'NONE', ( #39025, #78514, #76413, #30333 ) ) ;
#80388 = CYLINDRICAL_SURFACE ( 'NONE', #41287, 0.2500000000000009437 ) ;
#80389 = EDGE_LOOP ( 'NONE', ( #70639, #3125, #28858, #249 ) ) ;
#80390 = CARTESIAN_POINT ( 'NONE',  ( 3.361294932532794100, -10.19071101563364401, 33.96452234770658407 ) ) ;
#80391 = CARTESIAN_POINT ( 'NONE',  ( -2.749999999999991562, -8.639087296526025028, 15.01562500000000178 ) ) ;
#80392 = DIRECTION ( 'NONE',  ( 0.000000000000000000, 0.4999999999999960032, -0.8660254037844410391 ) ) ;
#80393 = CARTESIAN_POINT ( 'NONE',  ( -15.29685161012936767, -12.34228464037088280, 31.77849191805838558 ) ) ;
#80394 = CARTESIAN_POINT ( 'NONE',  ( -3.230769230769229949, -8.973038597847269315, 34.52809138561121927 ) ) ;
#80395 = CARTESIAN_POINT ( 'NONE',  ( 9.692307692307570832, -3.083524468854526912, 32.58852847137268327 ) ) ;
#80396 = CARTESIAN_POINT ( 'NONE',  ( -5.011667937410240192, -2.657715359629131857, 31.77849191805844242 ) ) ;
#80397 = CARTESIAN_POINT ( 'NONE',  ( -5.448717948717948012, -3.499999999999999556, 29.75000000000000355 ) ) ;
#80398 = CARTESIAN_POINT ( 'NONE',  ( -1.384615384615383471, -12.09954503811598769, 35.62045528018868623 ) ) ;
#80399 = CARTESIAN_POINT ( 'NONE',  ( 1.553300858899087311, -3.749999999999992006, 21.73437500000000000 ) ) ;
#80400 = DIRECTION ( 'NONE',  ( 0.000000000000000000, 0.9848077530122072432, 0.1736481776669354937 ) ) ;
#80401 = CARTESIAN_POINT ( 'NONE',  ( -14.55769230769230660, -2.499999999999999556, 29.81609845454691765 ) ) ;
#80402 = B_SPLINE_CURVE_WITH_KNOTS ( 'NONE', 3,
 ( #68816, #74700, #53970, #81905, #33267, #27392, #40476, #67940, #20195, #54409 ),
 .UNSPECIFIED., .F., .F.,
 ( 4, 2, 2, 2, 4 ),
 ( 0.000000000000000000, 0.0001954311564186865492, 0.0003908623128373730983, 0.0005862934692560596746, 0.0007817246256747461966 ),
 .UNSPECIFIED. ) ;
#80403 = DIRECTION ( 'NONE',  ( -0.000000000000000000, 0.1736481776669307198, -0.9848077530122080203 ) ) ;
#80404 = EDGE_CURVE ( 'NONE', #30732, #23776, #23183, .T. ) ;
#80405 = ORIENTED_EDGE ( 'NONE', *, *, #87751, .T. ) ;
#80406 = ORIENTED_EDGE ( 'NONE', *, *, #77522, .F. ) ;
#80407 = CARTESIAN_POINT ( 'NONE',  ( -8.992715712954719720, -12.44517049084099725, 30.48991314939691932 ) ) ;
#80408 = CARTESIAN_POINT ( 'NONE',  ( 15.23076923076923173, -1.117168528481311540, 33.14645433367849847 ) ) ;
#80409 = LINE ( 'NONE', #3840, #5199 ) ;
#80410 = PLANE ( 'NONE',  #75770 ) ;
#80411 = DIRECTION ( 'NONE',  ( -0.000000000000000000, 0.9848077530122086864, -0.1736481776669273891 ) ) ;
#80412 = CARTESIAN_POINT ( 'NONE',  ( -16.15384615384627409, -9.442884908241554243, 34.35708131394783038 ) ) ;
#80413 = EDGE_CURVE ( 'NONE', #81993, #35424, #4546, .T. ) ;
#80414 = VERTEX_POINT ( 'NONE', #73460 ) ;
#80415 = CARTESIAN_POINT ( 'NONE',  ( -4.946131269098290595, -12.38066358083363738, 30.83685684665853444 ) ) ;
#80416 = ORIENTED_EDGE ( 'NONE', *, *, #44589, .F. ) ;
#80417 = EDGE_LOOP ( 'NONE', ( #70682, #82515 ) ) ;
#80418 = CARTESIAN_POINT ( 'NONE',  ( 0.5923289025054097046, -12.35292014791297710, 31.75344720912887198 ) ) ;
#80419 = B_SPLINE_CURVE_WITH_KNOTS ( 'NONE', 3,
 ( #80113, #18416, #11663, #26061, #45873, #73356, #39140, #18858, #28267, #76907 ),
 .UNSPECIFIED., .F., .F.,
 ( 4, 2, 2, 2, 4 ),
 ( 0.000000000000000000, 0.0001954339857564080707, 0.0003908679715128161414, 0.0005863019572692241849, 0.0007817359430256322827 ),
 .UNSPECIFIED. ) ;
#80420 = CARTESIAN_POINT ( 'NONE',  ( -14.17716686945866655, -6.808710257144161559, 34.95449254468098843 ) ) ;
#80421 = CARTESIAN_POINT ( 'NONE',  ( -4.376773112753000738, -12.64616026154729411, 30.79003144601913533 ) ) ;
#80422 = CARTESIAN_POINT ( 'NONE',  ( 1.384615384615386802, -11.35647404775217417, 33.31231777344666511 ) ) ;
#80423 = CARTESIAN_POINT ( 'NONE',  ( 6.000000000000001776, -2.721908614388771852, 31.22303859784724978 ) ) ;
#80424 = B_SPLINE_CURVE_WITH_KNOTS ( 'NONE', 3,
 ( #79564, #57501, #77776, #11097, #86784, #38574, #43984, #71454, #9761, #66028 ),
 .UNSPECIFIED., .F., .F.,
 ( 4, 2, 2, 2, 4 ),
 ( 0.0007817246256747477145, 0.0009771112852218913694, 0.001172497944769034916, 0.001367884604316178462, 0.001563271263863322009 ),
 .UNSPECIFIED. ) ;
#80425 = AXIS2_PLACEMENT_3D ( 'NONE', #5215, #12418, #88545 ) ;
#80426 = VERTEX_POINT ( 'NONE', #6760 ) ;
#80427 = VECTOR ( 'NONE', #29977, 1000.000000000000114 ) ;
#80428 = VERTEX_POINT ( 'NONE', #457 ) ;
#80429 = B_SPLINE_CURVE_WITH_KNOTS ( 'NONE', 3,
 ( #77390, #16134, #72843, #11150, #44923, #38625, #73762, #33201, #66084, #72399 ),
 .UNSPECIFIED., .F., .F.,
 ( 4, 2, 2, 2, 4 ),
 ( 0.0007817246256747516176, 0.0009771112852218970073, 0.001172497944769042288, 0.001367884604316187570, 0.001563271263863332851 ),
 .UNSPECIFIED. ) ;
#80430 = EDGE_CURVE ( 'NONE', #77030, #73914, #33794, .T. ) ;
#80432 = CLOSED_SHELL ( 'NONE', ( #61668, #87292, #6795, #45823, #9245, #70229, #26409, #87206, #33249, #70803, #83177, #47872, #65749, #54554, #33636, #22224, #84412, #78562, #25785, #34429, #59791, #56895, #85622, #19625, #82571, #45438, #45830, #47751, #78945, #62877, #41635, #18905, #77574, #63827, #45071, #717, #43299, #19144, #83954, #54870, #65660, #60433, #73970, #52206, #31287, #31608, #8746, #43171, #32757, #13181, #6323, #35896, #64539, #53184, #21691, #14820, #69530, #35992, #15326, #53314, #21406, #63175, #5342, #69670, #49723, #65060 ) ) ;
#80431 = EDGE_CURVE ( 'NONE', #77897, #72081, #5974, .T. ) ;
#80433 = ORIENTED_EDGE ( 'NONE', *, *, #8922, .F. ) ;
#80434 = CARTESIAN_POINT ( 'NONE',  ( -6.066082379360133281, -4.661471528628507777, 34.16647553114621871 ) ) ;
#80435 = CARTESIAN_POINT ( 'NONE',  ( -0.4615384615384611200, -9.905515769479276145, 34.41647553114623292 ) ) ;
#80436 = CARTESIAN_POINT ( 'NONE',  ( 16.40379156322419973, -5.766571408460170467, 34.70601412856602508 ) ) ;
#80437 = CARTESIAN_POINT ( 'NONE',  ( 10.61538461538461675, -4.661471528628507777, 34.16647553114623292 ) ) ;
#80438 = EDGE_CURVE ( 'NONE', #38767, #65096, #25255, .T. ) ;
#80439 = CARTESIAN_POINT ( 'NONE',  ( -16.85391172531022974, -3.105924265160262099, 32.13625925475356127 ) ) ;
#80440 = CARTESIAN_POINT ( 'NONE',  ( 17.99999999999987566, -8.613356846316285953, 34.62446782046622218 ) ) ;
#80441 = ORIENTED_EDGE ( 'NONE', *, *, #11863, .T. ) ;
#80442 = ORIENTED_EDGE ( 'NONE', *, *, #39622, .T. ) ;
#80443 = CARTESIAN_POINT ( 'NONE',  ( 11.78846153846154188, -2.499999999999999556, 29.81604066197449754 ) ) ;
#80445 = VERTEX_POINT ( 'NONE', #74344 ) ;
#80444 = CARTESIAN_POINT ( 'NONE',  ( -12.46153846153846168, -11.16473453929635440, 33.15142922261926373 ) ) ;
#80446 = DIRECTION ( 'NONE',  ( -0.000000000000000000, 1.000000000000000000, -0.000000000000000000 ) ) ;
#80447 = CARTESIAN_POINT ( 'NONE',  ( 12.59206389977210705, -8.630441415882550871, 34.87705825610312615 ) ) ;
#80448 = CARTESIAN_POINT ( 'NONE',  ( 3.750000000000000888, -7.499999999999978684, 16.96875000000000000 ) ) ;
#80449 = VERTEX_POINT ( 'NONE', #81551 ) ;
#80450 = CARTESIAN_POINT ( 'NONE',  ( 6.923076923076924238, -12.78798330534102945, 29.74999999999997868 ) ) ;
#80451 = AXIS2_PLACEMENT_3D ( 'NONE', #35147, #12667, #482 ) ;
#80452 = ORIENTED_EDGE ( 'NONE', *, *, #8750, .T. ) ;
#80453 = CARTESIAN_POINT ( 'NONE',  ( -13.51476335434708353, -11.66186481527757302, 32.95055677023626117 ) ) ;
#80454 = CARTESIAN_POINT ( 'NONE',  ( 0.2115152373170025857, -11.56360843649121861, 33.07473185843129926 ) ) ;
#80455 = CARTESIAN_POINT ( 'NONE',  ( 1.384615384615386802, -1.466349020453238561, 30.81389545987213907 ) ) ;
#80457 = DIRECTION ( 'NONE',  ( -0.000000000000000000, 1.000000000000000000, 3.491481338843133355E-15 ) ) ;
#80456 = DIRECTION ( 'NONE',  ( 0.000000000000000000, 0.7660444431189822323, -0.6427876096865344779 ) ) ;
#80458 = LINE ( 'NONE', #39918, #69283 ) ;
#80459 = ORIENTED_EDGE ( 'NONE', *, *, #16422, .F. ) ;
#80460 = CARTESIAN_POINT ( 'NONE',  ( 6.923076923076924238, -8.120952969808772792, 34.71129190930000163 ) ) ;
#80461 = CARTESIAN_POINT ( 'NONE',  ( -8.899921372341079717, -3.957541250942358424, 33.62499894934981626 ) ) ;
#80462 = CARTESIAN_POINT ( 'NONE',  ( -11.53846153846153655, -1.422936976036506707, 30.56769352161908415 ) ) ;
#80463 = ORIENTED_EDGE ( 'NONE', *, *, #54978, .T. ) ;
#80464 = B_SPLINE_CURVE_WITH_KNOTS ( 'NONE', 3,
 ( #61395, #42481, #14113, #35267, #35725, #14555, #88911, #55981, #69057, #47892 ),
 .UNSPECIFIED., .F., .F.,
 ( 4, 2, 2, 2, 4 ),
 ( 0.000000000000000000, 0.0001954339857564074473, 0.0003908679715128148945, 0.0005863019572692223418, 0.0007817359430256297891 ),
 .UNSPECIFIED. ) ;
#80465 = DIRECTION ( 'NONE',  ( -0.000000000000000000, -0.9396926207859092051, -0.3420201433256662704 ) ) ;
#80466 = DIRECTION ( 'NONE',  ( -0.000000000000000000, 0.3420201433256694346, -0.9396926207859080948 ) ) ;
#80467 = CARTESIAN_POINT ( 'NONE',  ( -18.00000000000000000, -1.503186988994757778, 30.80739993210377747 ) ) ;
#80468 = CARTESIAN_POINT ( 'NONE',  ( 7.912222197156284054, -3.050289026998446840, 32.03036669348366416 ) ) ;
#80469 = FACE_BOUND ( 'NONE', #57832, .T. ) ;
#80471 = DIRECTION ( 'NONE',  ( -1.000000000000000000, -0.000000000000000000, -0.000000000000000000 ) ) ;
#80470 = PLANE ( 'NONE',  #80668 ) ;
#80472 = CARTESIAN_POINT ( 'NONE',  ( -15.16470189741915675, -4.661471528628508665, 34.16647553114624003 ) ) ;
#80474 = CARTESIAN_POINT ( 'NONE',  ( -2.307692307692305711, -8.164416787775445883, 34.95778746994557906 ) ) ;
#80473 = CARTESIAN_POINT ( 'NONE',  ( -1.254089682851818210, -12.27024696741798770, 31.24895572276497546 ) ) ;
#80475 = LINE ( 'NONE', #87244, #18185 ) ;
#80476 = LINE ( 'NONE', #66956, #59186 ) ;
#80477 = CARTESIAN_POINT ( 'NONE',  ( -3.749999999999996447, -7.561099074964554134, 27.34188170625848713 ) ) ;
#80478 = CARTESIAN_POINT ( 'NONE',  ( 10.36536139116315525, -12.07920672191015221, 32.31858351112116168 ) ) ;
#80479 = VERTEX_POINT ( 'NONE', #13963 ) ;
#80480 = VECTOR ( 'NONE', #42020, 1000.000000000000000 ) ;
#80481 = VECTOR ( 'NONE', #33678, 1000.000000000000114 ) ;
#80482 = CARTESIAN_POINT ( 'NONE',  ( 0.2115617305961066674, -6.567427716900047230, 34.66269422305636283 ) ) ;
#80483 = CARTESIAN_POINT ( 'NONE',  ( 16.40379156322419973, -12.68172785388650681, 30.59649109432439573 ) ) ;
#80484 = LINE ( 'NONE', #86816, #70451 ) ;
#80485 = CARTESIAN_POINT ( 'NONE',  ( -7.846153846153844924, -9.058645607665452459, 34.76329471203371924 ) ) ;
#80486 = CARTESIAN_POINT ( 'NONE',  ( 17.07692307692295586, -12.70778746994576025, 30.41441678777401236 ) ) ;
#80487 = CARTESIAN_POINT ( 'NONE',  ( -12.59168643127016196, -6.809168938359901446, 34.95455904226513866 ) ) ;
#80488 = CARTESIAN_POINT ( 'NONE',  ( 2.608446859217893099, -4.805146000318787358, 26.56063170625849068 ) ) ;
#80489 = CIRCLE ( 'NONE', #12905, 4.000000000000000000 ) ;
#80490 = EDGE_CURVE ( 'NONE', #79832, #1945, #20721, .T. ) ;
#80491 = CARTESIAN_POINT ( 'NONE',  ( 4.219914504848590653, -10.51840700105979565, 33.73612834413962247 ) ) ;
#80492 = CARTESIAN_POINT ( 'NONE',  ( 8.546303810323916395, -2.523278758544489797, 31.42238647778637528 ) ) ;
#80493 = AXIS2_PLACEMENT_3D ( 'NONE', #84876, #50625, #76327 ) ;
#80494 = CARTESIAN_POINT ( 'NONE',  ( -4.826977667545033768, -12.07971442181322352, 32.31769673815850297 ) ) ;
#80495 = CARTESIAN_POINT ( 'NONE',  ( -0.5268084620947810492, -8.656820664281497102, 34.87096338111211935 ) ) ;
#80496 = CARTESIAN_POINT ( 'NONE',  ( -7.053224132515142131, -4.460286881179643004, 33.72017969459903242 ) ) ;
#80497 = CARTESIAN_POINT ( 'NONE',  ( -9.019207500173124004, -9.148715823498378086, 34.47080413974185120 ) ) ;
#80498 = CIRCLE ( 'NONE', #10008, 4.000000000000000000 ) ;
#80499 = CARTESIAN_POINT ( 'NONE',  ( 3.453732365035905971, -7.369474539155830506, 34.99858011523957657 ) ) ;
#80500 = CARTESIAN_POINT ( 'NONE',  ( 8.068933515131908152, -9.418065098278013636, 34.63729479722530158 ) ) ;
#80501 = EDGE_LOOP ( 'NONE', ( #48055, #5095, #19198, #9851 ) ) ;
#80502 = DIRECTION ( 'NONE',  ( -1.000000000000000000, -0.000000000000000000, -0.000000000000000000 ) ) ;
#80503 = CARTESIAN_POINT ( 'NONE',  ( -2.307692307692305711, -10.89733346790207413, 36.13435417666054406 ) ) ;
#80504 = CARTESIAN_POINT ( 'NONE',  ( 2.608446859217924629, -10.19485399968118422, 18.62686829374151642 ) ) ;
#80505 = EDGE_CURVE ( 'NONE', #42562, #72489, #66089, .T. ) ;
#80506 = CARTESIAN_POINT ( 'NONE',  ( 16.15384615384615330, -13.57706302396349152, 30.56769352161908060 ) ) ;
#80507 = DIRECTION ( 'NONE',  ( -0.000000000000000000, -0.9396926207859092051, -0.3420201433256662704 ) ) ;
#80508 = ORIENTED_EDGE ( 'NONE', *, *, #26128, .F. ) ;
#80509 = LINE ( 'NONE', #75081, #19807 ) ;
#80510 = CARTESIAN_POINT ( 'NONE',  ( 9.469380733400845074, -12.64616026154729411, 30.79003144601914244 ) ) ;
#80512 = EDGE_LOOP ( 'NONE', ( #46274, #55294 ) ) ;
#80511 = CARTESIAN_POINT ( 'NONE',  ( 11.47319153790521717, -3.083524468853724443, 32.58852847137143272 ) ) ;
#80513 = CARTESIAN_POINT ( 'NONE',  ( -9.942284436356281674, -11.47974371597208076, 33.17467449705390692 ) ) ;
#80514 = CARTESIAN_POINT ( 'NONE',  ( -2.980714919130916574, -3.627508038966689163, 32.91356715214248396 ) ) ;
#80515 = EDGE_CURVE ( 'NONE', #15626, #62076, #71514, .T. ) ;
#80516 = CARTESIAN_POINT ( 'NONE',  ( 2.177545098254089151, -12.45813303252208648, 30.39737893381572675 ) ) ;
#80517 = CARTESIAN_POINT ( 'NONE',  ( 11.53846153846153832, -8.973038597847269315, 34.52809138561121927 ) ) ;
#80518 = ORIENTED_EDGE ( 'NONE', *, *, #17584, .T. ) ;
#80519 = DIRECTION ( 'NONE',  ( 1.000000000000000000, 0.000000000000000000, 0.000000000000000000 ) ) ;
#80520 = CYLINDRICAL_SURFACE ( 'NONE', #73906, 3.000000000000000000 ) ;
#80521 = DIRECTION ( 'NONE',  ( 1.000000000000000000, 0.000000000000000000, -0.000000000000000000 ) ) ;
#80522 = EDGE_CURVE ( 'NONE', #82892, #54013, #54274, .T. ) ;
#80523 = EDGE_LOOP ( 'NONE', ( #84626, #40909, #2785, #39192 ) ) ;
#80524 = ORIENTED_EDGE ( 'NONE', *, *, #1988, .T. ) ;
#80525 = B_SPLINE_CURVE_WITH_KNOTS ( 'NONE', 3,
 ( #73462, #80671, #11755, #59931, #25713, #53168 ),
 .UNSPECIFIED., .F., .F.,
 ( 4, 2, 4 ),
 ( 4.220987180333913997E-17, 0.0001954756301637163962, 0.0003909512603273906169 ),
 .UNSPECIFIED. ) ;
#80526 = VECTOR ( 'NONE', #56746, 1000.000000000000114 ) ;
#80527 = ORIENTED_EDGE ( 'NONE', *, *, #81435, .T. ) ;
#80528 = EDGE_CURVE ( 'NONE', #76451, #76314, #26376, .T. ) ;
#80529 = B_SPLINE_CURVE_WITH_KNOTS ( 'NONE', 3,
 ( #64574, #23162, #86671, #24937, #51494, #2873, #78109, #10990, #71788, #24485 ),
 .UNSPECIFIED., .F., .F.,
 ( 4, 2, 2, 2, 4 ),
 ( 0.0007817246256747503166, 0.0009771112852218944052, 0.001172497944769038602, 0.001367884604316182799, 0.001563271263863326996 ),
 .UNSPECIFIED. ) ;
#80530 = CARTESIAN_POINT ( 'NONE',  ( -15.23076923076922995, -2.249999999999998668, 29.75000000000001776 ) ) ;
#80531 = CARTESIAN_POINT ( 'NONE',  ( -9.070512820512819374, -11.50000000000000000, 29.75000000000000355 ) ) ;
#80532 = B_SPLINE_CURVE_WITH_KNOTS ( 'NONE', 3,
 ( #27773, #40855, #49379, #83625, #54352, #41741, #35417, #308, #1184, #28670 ),
 .UNSPECIFIED., .F., .F.,
 ( 4, 2, 2, 2, 4 ),
 ( 0.0007817246256747446788, 0.0009771112852218879000, 0.001172497944769031013, 0.001367884604316174126, 0.001563271263863317238 ),
 .UNSPECIFIED. ) ;
#80533 = CARTESIAN_POINT ( 'NONE',  ( -9.626240358957616650, -12.62096338111211757, 30.90682066428152908 ) ) ;
#80534 = CYLINDRICAL_SURFACE ( 'NONE', #30502, 0.2500000000000008882 ) ;
#80535 = EDGE_LOOP ( 'NONE', ( #65374, #86567 ) ) ;
#80536 = EDGE_CURVE ( 'NONE', #26904, #60833, #39321, .T. ) ;
#80537 = VERTEX_POINT ( 'NONE', #55833 ) ;
#80538 = AXIS2_PLACEMENT_3D ( 'NONE', #45086, #18074, #65361 ) ;
#80539 = VERTEX_POINT ( 'NONE', #82880 ) ;
#80542 = ORIENTED_EDGE ( 'NONE', *, *, #35160, .F. ) ;
#80541 = EDGE_CURVE ( 'NONE', #33660, #58760, #61806, .T. ) ;
#80540 = FACE_OUTER_BOUND ( 'NONE', #11101, .T. ) ;
#80543 = CARTESIAN_POINT ( 'NONE',  ( -2.307692307692427391, -3.835265460704628371, 33.15142922262033665 ) ) ;
#80544 = B_SPLINE_CURVE_WITH_KNOTS ( 'NONE', 3,
 ( #25898, #38525, #66439, #31773, #4746, #59231, #52908, #44817, #80861, #30862 ),
 .UNSPECIFIED., .F., .F.,
 ( 4, 2, 2, 2, 4 ),
 ( 0.0007817359430256315238, 0.0009771253907249980580, 0.001172514838424364592, 0.001367904286123730910, 0.001563293733823097444 ),
 .UNSPECIFIED. ) ;
#80545 = CARTESIAN_POINT ( 'NONE',  ( 15.00728428704528561, -3.236172620538810385, 32.36188796281390267 ) ) ;
#80546 = AXIS2_PLACEMENT_3D ( 'NONE', #32616, #11917, #60085 ) ;
#80547 = VECTOR ( 'NONE', #76558, 1000.000000000000227 ) ;
#80548 = EDGE_CURVE ( 'NONE', #73980, #34740, #43208, .T. ) ;
#80549 = EDGE_CURVE ( 'NONE', #77001, #86079, #49971, .T. ) ;
#80550 = DIRECTION ( 'NONE',  ( 0.000000000000000000, 1.000000000000000000, 0.000000000000000000 ) ) ;
#80551 = CARTESIAN_POINT ( 'NONE',  ( -13.31854703361294767, -12.37446782046654192, 30.86335684631486842 ) ) ;
#80552 = ORIENTED_EDGE ( 'NONE', *, *, #62319, .F. ) ;
#80553 = ORIENTED_EDGE ( 'NONE', *, *, #9098, .T. ) ;
#80554 = VECTOR ( 'NONE', #66125, 999.9999999999998863 ) ;
#80555 = ORIENTED_EDGE ( 'NONE', *, *, #53146, .T. ) ;
#80556 = CARTESIAN_POINT ( 'NONE',  ( 6.923076923076924238, -13.04860791097971706, 34.73218667398347037 ) ) ;
#80558 = EDGE_LOOP ( 'NONE', ( #52805, #83598 ) ) ;
#80557 = CARTESIAN_POINT ( 'NONE',  ( 5.299934428535925335, -4.887748414852792322, 34.01359900205216746 ) ) ;
#80559 = STYLED_ITEM ( 'NONE', ( #16800 ), #83739 ) ;
#80560 = CARTESIAN_POINT ( 'NONE',  ( 17.01084069756293715, -5.471508081941601986, 34.59228464037088457 ) ) ;
#80561 = CARTESIAN_POINT ( 'NONE',  ( -0.3962833220256226641, -5.094484230520773593, 34.41647553114626845 ) ) ;
#80562 = DIRECTION ( 'NONE',  ( -0.000000000000000000, 0.5000000000000011102, -0.8660254037844381525 ) ) ;
#80563 = B_SPLINE_CURVE_WITH_KNOTS ( 'NONE', 3,
 ( #73724, #13334, #39495, #68279, #12450, #19647, #66955, #26412, #12888, #60627 ),
 .UNSPECIFIED., .F., .F.,
 ( 4, 2, 2, 2, 4 ),
 ( 0.0007817359430256216575, 0.0009771253907249856981, 0.001172514838424349847, 0.001367904286123713779, 0.001563293733823077928 ),
 .UNSPECIFIED. ) ;
#80564 = CARTESIAN_POINT ( 'NONE',  ( -13.63461538461539035, -2.499999999999999556, 29.81609845454691765 ) ) ;
#80565 = CARTESIAN_POINT ( 'NONE',  ( 9.019285080869080318, -5.728107161865378494, 34.42597550085002922 ) ) ;
#80566 = FACE_BOUND ( 'NONE', #77469, .T. ) ;
#80567 = CARTESIAN_POINT ( 'NONE',  ( 9.320512820512821150, -7.500000000000000000, 29.75000000000000355 ) ) ;
#80568 = CARTESIAN_POINT ( 'NONE',  ( -12.59222992820601839, -8.999036380462717588, 34.52022231692819076 ) ) ;
#80569 = CYLINDRICAL_SURFACE ( 'NONE', #59562, 0.2499999999999979738 ) ;
#80571 = CARTESIAN_POINT ( 'NONE',  ( -5.076923076923197442, -3.300289026999228881, 32.46337939537708905 ) ) ;
#80570 = FACE_OUTER_BOUND ( 'NONE', #30663, .T. ) ;
#80572 = DIRECTION ( 'NONE',  ( 0.000000000000000000, -1.000000000000000000, 4.336808689942018722E-16 ) ) ;
#80573 = CARTESIAN_POINT ( 'NONE',  ( 3.230769230769231726, -10.67929555188718282, 33.92786785259544047 ) ) ;
#80574 = ORIENTED_EDGE ( 'NONE', *, *, #66414, .T. ) ;
#80575 = CARTESIAN_POINT ( 'NONE',  ( -17.20707104665477161, -5.915902021225892149, 34.75552854090298638 ) ) ;
#80576 = CARTESIAN_POINT ( 'NONE',  ( 12.52760579488853665, -3.322132147404559976, 32.92929555188717927 ) ) ;
#80577 = ORIENTED_EDGE ( 'NONE', *, *, #41178, .F. ) ;
#80578 = ORIENTED_EDGE ( 'NONE', *, *, #17135, .T. ) ;
#80579 = CARTESIAN_POINT ( 'NONE',  ( -17.07692307692319744, -11.48612834414049644, 32.76840700105863391 ) ) ;
#80580 = CARTESIAN_POINT ( 'NONE',  ( -15.48079246806219267, -2.587272538249755893, 30.68239716806877837 ) ) ;
#80581 = CARTESIAN_POINT ( 'NONE',  ( 12.23861150263161157, -10.77366814457252175, 33.85459836347579454 ) ) ;
#80582 = ORIENTED_EDGE ( 'NONE', *, *, #56615, .T. ) ;
#80583 = EDGE_CURVE ( 'NONE', #51136, #27202, #71111, .T. ) ;
#80584 = CARTESIAN_POINT ( 'NONE',  ( -6.000000000000119904, -8.613356846316285953, 34.62446782046622218 ) ) ;
#80585 = CARTESIAN_POINT ( 'NONE',  ( 14.30769230769218758, -3.300289026999228881, 32.46337939537708905 ) ) ;
#80587 = CARTESIAN_POINT ( 'NONE',  ( -0.4615384615385826339, -3.835265460704628371, 33.15142922262033665 ) ) ;
#80586 = CARTESIAN_POINT ( 'NONE',  ( -18.00000000000000000, -3.050289026998447284, 32.03036669348365706 ) ) ;
#80588 = CARTESIAN_POINT ( 'NONE',  ( -12.68502340526241312, -5.113361153441934093, 34.14387501736622710 ) ) ;
#80589 = CARTESIAN_POINT ( 'NONE',  ( -9.442307692307691624, -2.249999999999998668, 29.75000000000000355 ) ) ;
#80591 = CARTESIAN_POINT ( 'NONE',  ( -2.544871794871794268, -7.500000000000000000, 29.75000000000000355 ) ) ;
#80590 = SURFACE_SIDE_STYLE ('',( #86915 ) ) ;
#80592 = VECTOR ( 'NONE', #71155, 1000.000000000000114 ) ;
#80593 = CARTESIAN_POINT ( 'NONE',  ( -3.749999999999997335, -7.500000000000021316, 23.84375000000000000 ) ) ;
#80594 = ORIENTED_EDGE ( 'NONE', *, *, #15087, .T. ) ;
#80595 = ORIENTED_EDGE ( 'NONE', *, *, #38642, .F. ) ;
#80596 = CARTESIAN_POINT ( 'NONE',  ( -9.915792616872025178, -2.612411019501189369, 31.66733052389439962 ) ) ;
#80597 = CARTESIAN_POINT ( 'NONE',  ( 7.053868730901711182, -12.11778462344220841, 31.66786338562085135 ) ) ;
#80598 = CYLINDRICAL_SURFACE ( 'NONE', #33028, 0.2500000000000012212 ) ;
#80599 = LINE ( 'NONE', #18884, #22246 ) ;
#80600 = CARTESIAN_POINT ( 'NONE',  ( -15.23076923076922995, -2.721908614388771852, 31.22303859784724978 ) ) ;
#80601 = CARTESIAN_POINT ( 'NONE',  ( 1.553300858899087311, -3.749999999999992006, 24.23437500000000355 ) ) ;
#80602 = ADVANCED_FACE ( 'NONE', ( #77002 ), #48628, .F. ) ;
#80603 = EDGE_CURVE ( 'NONE', #63637, #62369, #15706, .T. ) ;
#80604 = CARTESIAN_POINT ( 'NONE',  ( -7.623374304885435215, -8.496831190052096971, 34.64984203495476578 ) ) ;
#80605 = CARTESIAN_POINT ( 'NONE',  ( 1.384615384615265343, -5.219633306517616589, 34.19971097300220464 ) ) ;
#80607 = B_SPLINE_CURVE_WITH_KNOTS ( 'NONE', 3,
 ( #23, #20731, #27934, #43218, #62158, #15755, #63027, #70246, #49537, #62591 ),
 .UNSPECIFIED., .F., .F.,
 ( 4, 2, 2, 2, 4 ),
 ( 0.0007817359430256327164, 0.0009771253907249993591, 0.001172514838424366110, 0.001367904286123732861, 0.001563293733823099396 ),
 .UNSPECIFIED. ) ;
#80606 = FACE_OUTER_BOUND ( 'NONE', #4886, .T. ) ;
#80608 = LINE ( 'NONE', #53102, #38106 ) ;
#80609 = CARTESIAN_POINT ( 'NONE',  ( -9.822999158975251888, -11.18331474514187995, 33.13161551792790505 ) ) ;
#80610 = CARTESIAN_POINT ( 'NONE',  ( 13.63456079399342791, -2.589246495874658383, 31.60778113518102828 ) ) ;
#80611 = DIRECTION ( 'NONE',  ( -0.000000000000000000, 1.000000000000000000, -0.000000000000000000 ) ) ;
#80612 = CARTESIAN_POINT ( 'NONE',  ( 7.911408985666682270, -8.656820664281605460, 34.87096338111211224 ) ) ;
#80613 = CARTESIAN_POINT ( 'NONE',  ( 17.06410256410256565, -11.50000000000000000, 29.75000000000000355 ) ) ;
#80614 = VECTOR ( 'NONE', #60720, 999.9999999999998863 ) ;
#80615 = CARTESIAN_POINT ( 'NONE',  ( -15.29603967673000575, -10.21337939537584383, 33.94971097300158647 ) ) ;
#80616 = VERTEX_POINT ( 'NONE', #14866 ) ;
#80617 = CARTESIAN_POINT ( 'NONE',  ( -5.011667505647051435, -11.94971097300157403, 32.03036669348361443 ) ) ;
#80618 = CARTESIAN_POINT ( 'NONE',  ( -3.360916440207453615, -3.817052484675422797, 33.13202310037935661 ) ) ;
#80619 = CARTESIAN_POINT ( 'NONE',  ( 5.869309396889695662, -2.494641256782728966, 31.33461815524612959 ) ) ;
#80620 = CARTESIAN_POINT ( 'NONE',  ( 2.750000000000002665, -7.561099074964516831, 17.22061829374151287 ) ) ;
#80621 = AXIS2_PLACEMENT_3D ( 'NONE', #20551, #7034, #48013 ) ;
#80622 = VECTOR ( 'NONE', #13100, 1000.000000000000000 ) ;
#80623 = EDGE_CURVE ( 'NONE', #9301, #35110, #16626, .T. ) ;
#80624 = CARTESIAN_POINT ( 'NONE',  ( -14.05763799605399278, -4.943051570960394159, 34.04725096376909477 ) ) ;
#80625 =( LENGTH_UNIT ( ) NAMED_UNIT ( * ) SI_UNIT ( .MILLI., .METRE. ) );
#80627 = ORIENTED_EDGE ( 'NONE', *, *, #51307, .T. ) ;
#80626 = CARTESIAN_POINT ( 'NONE',  ( -18.25000000000000711, -2.249999999999998668, 29.75000000000000355 ) ) ;
#80628 = CARTESIAN_POINT ( 'NONE',  ( -1.944543648262992530, -9.444543648263016067, 22.43750000000000000 ) ) ;
#80629 = CARTESIAN_POINT ( 'NONE',  ( -9.692307692307691624, -11.69971097300155272, 32.46337939537588113 ) ) ;
#80630 = EDGE_CURVE ( 'NONE', #54915, #78412, #67231, .T. ) ;
#80631 = AXIS2_PLACEMENT_3D ( 'NONE', #29536, #85367, #23653 ) ;
#80632 = EDGE_LOOP ( 'NONE', ( #51855, #55275, #30046, #46662 ) ) ;
#80633 = VECTOR ( 'NONE', #12872, 1000.000000000000000 ) ;
#80634 = CARTESIAN_POINT ( 'NONE',  ( -7.053224892808620083, -11.66186481527757479, 32.95055677023626117 ) ) ;
#80635 =( GEOMETRIC_REPRESENTATION_CONTEXT ( 3 ) GLOBAL_UNCERTAINTY_ASSIGNED_CONTEXT ( ( #16731 ) ) GLOBAL_UNIT_ASSIGNED_CONTEXT ( ( #73373, #25629, #5363 ) ) REPRESENTATION_CONTEXT ( 'NONE', 'WORKASPACE' ) );
#80636 = ORIENTED_EDGE ( 'NONE', *, *, #41708, .T. ) ;
#80637 = CARTESIAN_POINT ( 'NONE',  ( 3.100078627658922947, -4.684245665217971144, 34.18127051446801090 ) ) ;
#80638 = CARTESIAN_POINT ( 'NONE',  ( -7.596099534515528440, -11.79725096376909654, 32.30694842903960762 ) ) ;
#80639 = CARTESIAN_POINT ( 'NONE',  ( -27.00000000000000000, -8.999999999999994671, 30.24999999999999645 ) ) ;
#80640 = ADVANCED_FACE ( 'NONE', ( #85968 ), #45411, .F. ) ;
#80641 = ORIENTED_EDGE ( 'NONE', *, *, #57231, .F. ) ;
#80642 = CARTESIAN_POINT ( 'NONE',  ( 0.4615384615383382183, -5.094484230521993062, 34.41647553114689373 ) ) ;
#80643 = ORIENTED_EDGE ( 'NONE', *, *, #38124, .F. ) ;
#80644 = EDGE_LOOP ( 'NONE', ( #39594, #67791 ) ) ;
#80645 = CARTESIAN_POINT ( 'NONE',  ( -23.50000000000000000, -1.749999999999992006, 28.00000000000000000 ) ) ;
#80646 = DIRECTION ( 'NONE',  ( 0.000000000000000000, -0.000000000000000000, 1.000000000000000000 ) ) ;
#80647 = CARTESIAN_POINT ( 'NONE',  ( 18.00000000000000000, -9.905515769479276145, 34.41647553114623292 ) ) ;
#80648 = CARTESIAN_POINT ( 'NONE',  ( -14.30769230769230660, -1.790695186598648903, 34.54067556320373455 ) ) ;
#80649 = CARTESIAN_POINT ( 'NONE',  ( -5.076923076923075762, -1.629998284177014645, 34.34916445242399163 ) ) ;
#80650 = CARTESIAN_POINT ( 'NONE',  ( 12.46153846153846168, -4.786620604624113540, 33.94971097300155094 ) ) ;
#80651 = CARTESIAN_POINT ( 'NONE',  ( 10.61538461538449596, -12.27809138561165270, 31.22303859784587132 ) ) ;
#80652 = EDGE_CURVE ( 'NONE', #45222, #81743, #18401, .T. ) ;
#80653 = EDGE_LOOP ( 'NONE', ( #81319, #84306, #87945, #40823 ) ) ;
#80654 = ORIENTED_EDGE ( 'NONE', *, *, #82394, .T. ) ;
#80655 = ORIENTED_EDGE ( 'NONE', *, *, #39434, .T. ) ;
#80657 = ORIENTED_EDGE ( 'NONE', *, *, #504, .T. ) ;
#80656 = LINE ( 'NONE', #17615, #4154 ) ;
#80658 = EDGE_CURVE ( 'NONE', #32515, #76205, #47918, .T. ) ;
#80659 = EDGE_CURVE ( 'NONE', #19601, #25570, #71552, .T. ) ;
#80660 = CARTESIAN_POINT ( 'NONE',  ( -14.17690186672535901, -10.70102852606553157, 33.91149625220312913 ) ) ;
#80661 = CARTESIAN_POINT ( 'NONE',  ( 1.384615384615265343, -2.892918686052166066, 31.69288490824153470 ) ) ;
#80662 = VERTEX_POINT ( 'NONE', #64787 ) ;
#80663 = CARTESIAN_POINT ( 'NONE',  ( 14.53070515178570332, -11.98016756924215009, 32.48728574198911190 ) ) ;
#80664 = EDGE_LOOP ( 'NONE', ( #4503, #79315 ) ) ;
#80665 = CARTESIAN_POINT ( 'NONE',  ( 17.01083966596719321, -9.780366693483667717, 34.19971097300155805 ) ) ;
#80666 = ORIENTED_EDGE ( 'NONE', *, *, #5296, .F. ) ;
#80667 = DIRECTION ( 'NONE',  ( 0.000000000000000000, 0.000000000000000000, 1.000000000000000000 ) ) ;
#80668 = AXIS2_PLACEMENT_3D ( 'NONE', #34045, #4809, #47553 ) ;
#80669 = CARTESIAN_POINT ( 'NONE',  ( -11.60373198442231235, -3.835265460703609186, 33.15142922261924241 ) ) ;
#80670 = EDGE_CURVE ( 'NONE', #50608, #72099, #17511, .T. ) ;
#80671 = CARTESIAN_POINT ( 'NONE',  ( 3.903846153846132871, -2.249999999999999112, 29.81609741502488120 ) ) ;
#80672 = FACE_BOUND ( 'NONE', #85959, .T. ) ;
#80673 = CYLINDRICAL_SURFACE ( 'NONE', #65665, 0.2499999999999993616 ) ;
#80674 = CARTESIAN_POINT ( 'NONE',  ( 16.02315555073584363, -3.338472653186243200, 32.95098750199972670 ) ) ;
#80675 = AXIS2_PLACEMENT_3D ( 'NONE', #18241, #11037, #25437 ) ;
#80676 = VECTOR ( 'NONE', #4454, 1000.000000000000114 ) ;
#80677 = CARTESIAN_POINT ( 'NONE',  ( -19.99999999999996803, 15.00000000000000711, 13.00000000000000178 ) ) ;
#80678 = CARTESIAN_POINT ( 'NONE',  ( -3.454254174493179175, -4.386631170607603991, 33.66268669641500111 ) ) ;
#80679 = ADVANCED_FACE ( 'NONE', ( #11195 ), #31920, .F. ) ;
#80680 = CARTESIAN_POINT ( 'NONE',  ( -8.769230769230768274, -13.20930481340135110, 34.54067556320372745 ) ) ;
#80681 = CYLINDRICAL_SURFACE ( 'NONE', #51964, 0.2499999999999998890 ) ;
#80682 = ORIENTED_EDGE ( 'NONE', *, *, #67216, .T. ) ;
#80683 = CARTESIAN_POINT ( 'NONE',  ( -13.38461538461507594, -2.506253911140614576, 30.00000000000323297 ) ) ;
#80684 = ORIENTED_EDGE ( 'NONE', *, *, #28922, .T. ) ;
#80685 = ORIENTED_EDGE ( 'NONE', *, *, #20280, .T. ) ;
#80686 = CIRCLE ( 'NONE', #37519, 4.000000000000000000 ) ;
#80688 = LINE ( 'NONE', #41018, #256 ) ;
#80687 = CARTESIAN_POINT ( 'NONE',  ( -7.053767526187233905, -3.957541250942359756, 33.62499894934981626 ) ) ;
#80689 = PRODUCT_DEFINITION_FORMATION_WITH_SPECIFIED_SOURCE ( 'ANY', '', #31988, .NOT_KNOWN. ) ;
#80690 = CARTESIAN_POINT ( 'NONE',  ( -11.53846153846153655, -8.564572088678739092, 35.78748833219616898 ) ) ;
#80691 = CARTESIAN_POINT ( 'NONE',  ( -13.38461538461550582, -2.892918686052166066, 31.69288490824153470 ) ) ;
#80692 = CARTESIAN_POINT ( 'NONE',  ( 20.00000000000000000, -7.500000000000000000, 29.75000000000000355 ) ) ;
#80693 = CARTESIAN_POINT ( 'NONE',  ( -15.29603967673000398, -3.835265460703609186, 33.15142922261924241 ) ) ;
#80694 = ORIENTED_EDGE ( 'NONE', *, *, #66179, .T. ) ;
#80695 = EDGE_CURVE ( 'NONE', #34591, #43471, #62883, .T. ) ;
#80696 = CARTESIAN_POINT ( 'NONE',  ( -5.933932666649924137, -8.164416787775445883, 34.95778746994558617 ) ) ;
#80697 = CARTESIAN_POINT ( 'NONE',  ( 14.24242186173153435, -11.48612834413959582, 32.76840700105983473 ) ) ;
#80698 = CARTESIAN_POINT ( 'NONE',  ( -14.55766903863466055, -8.303909089506435137, 34.68538101551103381 ) ) ;
#80699 = DIRECTION ( 'NONE',  ( 1.000000000000000000, -0.000000000000000000, -0.000000000000000000 ) ) ;
#80700 = EDGE_LOOP ( 'NONE', ( #60019, #81097, #77818, #21872 ) ) ;
#80701 = B_SPLINE_CURVE_WITH_KNOTS ( 'NONE', 3,
 ( #82550, #14513, #40671, #48292, #68135, #83428, #20391, #55938, #69011, #69899 ),
 .UNSPECIFIED., .F., .F.,
 ( 4, 2, 2, 2, 4 ),
 ( 0.0007817359430256371616, 0.0009771253907250052138, 0.001172514838424373266, 0.001367904286123741318, 0.001563293733823109370 ),
 .UNSPECIFIED. ) ;
#80702 = EDGE_CURVE ( 'NONE', #86919, #8179, #58991, .T. ) ;
#80703 = EDGE_LOOP ( 'NONE', ( #67422, #68669, #59145, #66081 ) ) ;
#80705 = EDGE_CURVE ( 'NONE', #26482, #51615, #69015, .T. ) ;
#80704 = EDGE_LOOP ( 'NONE', ( #6836, #32036, #60055, #69823 ) ) ;
#80706 = CARTESIAN_POINT ( 'NONE',  ( 15.48071474911737333, -6.696923467548660192, 34.68552623307873972 ) ) ;
#80707 = CARTESIAN_POINT ( 'NONE',  ( -7.780898274877819709, -5.219633306516380244, 34.19971097300157936 ) ) ;
#80708 = VERTEX_POINT ( 'NONE', #79213 ) ;
#80709 = DIRECTION ( 'NONE',  ( 0.000000000000000000, 0.7660444431189822323, -0.6427876096865344779 ) ) ;
#80710 = DIRECTION ( 'NONE',  ( -0.000000000000000000, -0.5000000000000009992, -0.8660254037844380415 ) ) ;
#80711 = CARTESIAN_POINT ( 'NONE',  ( 3.230769230769108269, -5.941354392335915335, 34.76329471203413846 ) ) ;
#80712 = DIRECTION ( 'NONE',  ( -0.000000000000000000, -0.9396926207859092051, -0.3420201433256662704 ) ) ;
#80713 = EDGE_CURVE ( 'NONE', #74576, #673, #60672, .T. ) ;
#80714 = CARTESIAN_POINT ( 'NONE',  ( -11.53846153846153655, -8.973038597847269315, 34.52809138561121927 ) ) ;
#80715 = ORIENTED_EDGE ( 'NONE', *, *, #88611, .F. ) ;
#80717 = ORIENTED_EDGE ( 'NONE', *, *, #79066, .F. ) ;
#80716 = FACE_OUTER_BOUND ( 'NONE', #78996, .T. ) ;
#80718 = LINE ( 'NONE', #82487, #75682 ) ;
#80719 = DIRECTION ( 'NONE',  ( 0.000000000000000000, 0.000000000000000000, -1.000000000000000000 ) ) ;
#80720 = CARTESIAN_POINT ( 'NONE',  ( -11.76138849736838488, -10.77366814457252175, 33.85459836347579454 ) ) ;
#80721 = AXIS2_PLACEMENT_3D ( 'NONE', #27564, #41974, #76638 ) ;
#80722 = CARTESIAN_POINT ( 'NONE',  ( 15.29602480204525605, -12.46129190930001052, 30.37095296980870174 ) ) ;
#80723 = CARTESIAN_POINT ( 'NONE',  ( 15.23076923076910916, -2.379036618888197729, 30.90682066428292885 ) ) ;
#80724 = DIRECTION ( 'NONE',  ( 0.000000000000000000, 0.9848077530122072432, 0.1736481776669354937 ) ) ;
#80725 = AXIS2_PLACEMENT_3D ( 'NONE', #88612, #60660, #88170 ) ;
#80726 = CARTESIAN_POINT ( 'NONE',  ( 1.077988221561497539, -10.27530806549875386, 19.95499329374151642 ) ) ;
#80727 = ORIENTED_EDGE ( 'NONE', *, *, #20923, .T. ) ;
#80728 = CYLINDRICAL_SURFACE ( 'NONE', #31764, 0.2500000000000009437 ) ;
#80729 = CARTESIAN_POINT ( 'NONE',  ( 7.623274329416259931, -7.630690623152301733, 34.99857592706772635 ) ) ;
#80730 = VERTEX_POINT ( 'NONE', #58473 ) ;
#80731 = ORIENTED_EDGE ( 'NONE', *, *, #23573, .F. ) ;
#80732 = CARTESIAN_POINT ( 'NONE',  ( -8.835313148590904220, -5.471508081941602875, 34.59228464037088457 ) ) ;
#80733 = DIRECTION ( 'NONE',  ( 0.000000000000000000, 0.6427876096865373645, -0.7660444431189797898 ) ) ;
#80734 = EDGE_CURVE ( 'NONE', #67131, #1344, #39145, .T. ) ;
#80735 = CARTESIAN_POINT ( 'NONE',  ( 13.13463865367303463, -3.627789207965226748, 32.91389620160131102 ) ) ;
#80736 = CARTESIAN_POINT ( 'NONE',  ( -7.053224132515142131, -6.001485441113818986, 34.52039167877662607 ) ) ;
#80737 = CARTESIAN_POINT ( 'NONE',  ( 6.923076923076802558, -3.300289026999228881, 32.46337939537708905 ) ) ;
#80738 = DIRECTION ( 'NONE',  ( 0.000000000000000000, 0.9848077530122072432, -0.1736481776669354937 ) ) ;
#80739 = ORIENTED_EDGE ( 'NONE', *, *, #65921, .F. ) ;
#80740 = CARTESIAN_POINT ( 'NONE',  ( 9.692307692307572609, -10.90142922262034020, 33.41473453929536674 ) ) ;
#80741 = B_SPLINE_CURVE_WITH_KNOTS ( 'NONE', 3,
 ( #87254, #45796, #73278, #25085, #19225, #88596, #25973, #12464, #32294, #39949 ),
 .UNSPECIFIED., .F., .F.,
 ( 4, 2, 2, 2, 4 ),
 ( 0.0007817246256747528103, 0.0009771112852218970073, 0.001172497944769041421, 0.001367884604316185835, 0.001563271263863330032 ),
 .UNSPECIFIED. ) ;
#80742 = CARTESIAN_POINT ( 'NONE',  ( -14.30769230769230660, -2.721908614388771852, 31.22303859784724978 ) ) ;
#80743 = CARTESIAN_POINT ( 'NONE',  ( -2.242437168179467033, -5.941354392334606160, 34.76329471203374055 ) ) ;
#80744 = ORIENTED_EDGE ( 'NONE', *, *, #36085, .T. ) ;
#80745 = CARTESIAN_POINT ( 'NONE',  ( -7.846153846153844924, -3.513871655860378418, 32.76840700105978499 ) ) ;
#80746 = VECTOR ( 'NONE', #17664, 1000.000000000000000 ) ;
#80747 = ORIENTED_EDGE ( 'NONE', *, *, #18060, .T. ) ;
#80748 = CARTESIAN_POINT ( 'NONE',  ( 13.38461538461526601, -3.835265460704628371, 33.15142922262033665 ) ) ;
#80749 = DIRECTION ( 'NONE',  ( 1.000000000000000000, 0.000000000000000000, 0.000000000000000000 ) ) ;
#80750 = VERTEX_POINT ( 'NONE', #48856 ) ;
#80751 = DIRECTION ( 'NONE',  ( 0.000000000000000000, 0.000000000000000000, 1.000000000000000000 ) ) ;
#80752 = CARTESIAN_POINT ( 'NONE',  ( 13.51514082284903040, -9.503571793651731880, 34.60286762892837942 ) ) ;
#80753 = CARTESIAN_POINT ( 'NONE',  ( 1.384615384615386802, -5.471508081941601098, 34.59228464037088457 ) ) ;
#80754 = AXIS2_PLACEMENT_3D ( 'NONE', #29645, #35960, #57102 ) ;
#80755 = LINE ( 'NONE', #10506, #620 ) ;
#80756 = CARTESIAN_POINT ( 'NONE',  ( -4.853910232829680815, -8.282913670948747864, 34.94150082978203642 ) ) ;
#80757 = VERTEX_POINT ( 'NONE', #47191 ) ;
#80758 = CARTESIAN_POINT ( 'NONE',  ( -9.320512820512821150, -11.50000000000000000, 29.75000000000000355 ) ) ;
#80759 = ORIENTED_EDGE ( 'NONE', *, *, #74648, .F. ) ;
#80760 = PLANE ( 'NONE',  #42946 ) ;
#80761 = CARTESIAN_POINT ( 'NONE',  ( -10.36543920600657032, -10.18230066228895758, 34.26354781536631577 ) ) ;
#80762 = EDGE_CURVE ( 'NONE', #61773, #6496, #26492, .T. ) ;
#80763 = CARTESIAN_POINT ( 'NONE',  ( -0.3307480205715097599, -2.494656445102013453, 31.33466734024120015 ) ) ;
#80764 = CARTESIAN_POINT ( 'NONE',  ( 11.53846153846153832, -11.16473453929635440, 33.15142922261926373 ) ) ;
#80765 = EDGE_CURVE ( 'NONE', #77416, #52415, #70014, .T. ) ;
#80766 = FACE_OUTER_BOUND ( 'NONE', #28250, .T. ) ;
#80767 = CARTESIAN_POINT ( 'NONE',  ( -9.469294848214296678, -6.460100341425560444, 34.89618726649961644 ) ) ;
#80768 = CARTESIAN_POINT ( 'NONE',  ( 7.596177102105256651, -2.544273027872575366, 31.48422191005632342 ) ) ;
#80769 = B_SPLINE_CURVE_WITH_KNOTS ( 'NONE', 3,
 ( #50539, #71698, #31154, #72592, #79357, #37469, #23510, #3683, #78906, #17202 ),
 .UNSPECIFIED., .F., .F.,
 ( 4, 2, 2, 2, 4 ),
 ( 0.000000000000000000, 0.0001954339857564074473, 0.0003908679715128148945, 0.0005863019572692223418, 0.0007817359430256297891 ),
 .UNSPECIFIED. ) ;
#80770 = EDGE_LOOP ( 'NONE', ( #55176, #82987, #49186, #18122 ) ) ;
#80772 = EDGE_CURVE ( 'NONE', #3349, #79887, #67036, .T. ) ;
#80771 = ORIENTED_EDGE ( 'NONE', *, *, #40423, .F. ) ;
#80773 = B_SPLINE_CURVE_WITH_KNOTS ( 'NONE', 3,
 ( #27690, #55159, #68242, #81324, #7430, #34888, #47513, #75439, #6102, #82203 ),
 .UNSPECIFIED., .F., .F.,
 ( 4, 2, 2, 2, 4 ),
 ( 0.000000000000000000, 0.0001954311564186861426, 0.0003908623128373722852, 0.0005862934692560583735, 0.0007817246256747445703 ),
 .UNSPECIFIED. ) ;
#80774 = VERTEX_POINT ( 'NONE', #53055 ) ;
#80776 = B_SPLINE_CURVE_WITH_KNOTS ( 'NONE', 3,
 ( #27453, #54920, #82405, #20688, #48152, #75623, #68870, #422, #1746, #41859 ),
 .UNSPECIFIED., .F., .F.,
 ( 4, 2, 2, 2, 4 ),
 ( 0.0007817359430256326080, 0.0009771253907249993591, 0.001172514838424366327, 0.001367904286123733078, 0.001563293733823099829 ),
 .UNSPECIFIED. ) ;
#80775 = AXIS2_PLACEMENT_3D ( 'NONE', #88882, #67705, #80794 ) ;
#80777 = ORIENTED_EDGE ( 'NONE', *, *, #73546, .T. ) ;
#80778 = CARTESIAN_POINT ( 'NONE',  ( -5.076923076923075762, -3.937682226553329556, 33.60647404775216529 ) ) ;
#80779 = CARTESIAN_POINT ( 'NONE',  ( -1.161835843346975095, -12.44528174975671853, 30.48912976160716681 ) ) ;
#80780 = AXIS2_PLACEMENT_3D ( 'NONE', #45025, #86946, #4950 ) ;
#80781 = ADVANCED_FACE ( 'NONE', ( #5776 ), #6227, .F. ) ;
#80782 = CARTESIAN_POINT ( 'NONE',  ( -15.23076923076922995, -10.51840700105979565, 33.73612834413961536 ) ) ;
#80783 = CARTESIAN_POINT ( 'NONE',  ( 6.223011351612852238, -12.15243808032446005, 31.58219941686247978 ) ) ;
#80784 = CARTESIAN_POINT ( 'NONE',  ( 11.40777007179397984, -2.541943142973491554, 30.39792223712631980 ) ) ;
#80785 = CARTESIAN_POINT ( 'NONE',  ( -0.5916856709766776801, -11.93770438780619259, 32.05411857736982029 ) ) ;
#80786 = DIRECTION ( 'NONE',  ( -0.000000000000000000, 0.9848077530122085754, -0.1736481776669273613 ) ) ;
#80787 = CARTESIAN_POINT ( 'NONE',  ( 14.30769230769231015, -2.708943851104267164, 35.45975837776705220 ) ) ;
#80788 = ORIENTED_EDGE ( 'NONE', *, *, #30162, .T. ) ;
#80789 = ORIENTED_EDGE ( 'NONE', *, *, #85997, .T. ) ;
#80790 = EDGE_LOOP ( 'NONE', ( #51366, #24660, #70360, #37315, #11991, #65476 ) ) ;
#80792 = ORIENTED_EDGE ( 'NONE', *, *, #22235, .T. ) ;
#80791 = CARTESIAN_POINT ( 'NONE',  ( -1.384615384615383471, -11.16473453929635440, 33.15142922261926373 ) ) ;
#80794 = DIRECTION ( 'NONE',  ( 0.000000000000000000, 0.7660444431189807890, 0.6427876096865361433 ) ) ;
#80793 = DIRECTION ( 'NONE',  ( -0.000000000000000000, -0.3420201433256694346, -0.9396926207859080948 ) ) ;
#80795 = FACE_OUTER_BOUND ( 'NONE', #3310, .T. ) ;
#80796 = CARTESIAN_POINT ( 'NONE',  ( -9.019207513279361876, -6.524016743844655686, 34.90889640711025521 ) ) ;
#80797 = FACE_BOUND ( 'NONE', #12079, .T. ) ;
#80798 = ORIENTED_EDGE ( 'NONE', *, *, #52044, .T. ) ;
#80799 = VERTEX_POINT ( 'NONE', #26048 ) ;
#80800 = CARTESIAN_POINT ( 'NONE',  ( 18.00000000000000000, -13.88283147151868846, 33.14645433367849847 ) ) ;
#80801 = ADVANCED_FACE ( 'NONE', ( #46759 ), #26937, .F. ) ;
#80802 = ORIENTED_EDGE ( 'NONE', *, *, #11411, .F. ) ;
#80803 = FACE_BOUND ( 'NONE', #39272, .T. ) ;
#80805 = VECTOR ( 'NONE', #73603, 1000.000000000000114 ) ;
#80804 = CARTESIAN_POINT ( 'NONE',  ( 20.00000000000000000, -4.000000000000000000, 29.75000000000000355 ) ) ;
#80806 = CARTESIAN_POINT ( 'NONE',  ( 15.00784227186237807, -6.459968553980841577, 34.89616026154728701 ) ) ;
#80807 = VERTEX_POINT ( 'NONE', #74235 ) ;
#80808 = CARTESIAN_POINT ( 'NONE',  ( 2.177545098254087375, -8.587444163452046197, 34.63053765926554206 ) ) ;
#80809 = DIRECTION ( 'NONE',  ( 0.000000000000000000, 0.000000000000000000, -1.000000000000000000 ) ) ;
#80810 = CARTESIAN_POINT ( 'NONE',  ( -1.929879867024197893E-14, -3.750000000000000000, 14.15625000000000000 ) ) ;
#80811 = ORIENTED_EDGE ( 'NONE', *, *, #82859, .F. ) ;
#80812 = LINE ( 'NONE', #13663, #22697 ) ;
#80813 = CYLINDRICAL_SURFACE ( 'NONE', #86956, 0.2499999999999994726 ) ;
#80814 = CARTESIAN_POINT ( 'NONE',  ( -7.976301055592065481, -2.882441371585227952, 31.66841991370172238 ) ) ;
#80815 = ORIENTED_EDGE ( 'NONE', *, *, #73130, .T. ) ;
#80816 = VECTOR ( 'NONE', #55665, 1000.000000000000227 ) ;
#80817 = ADVANCED_FACE ( 'NONE', ( #88660 ), #73800, .F. ) ;
#80818 = CARTESIAN_POINT ( 'NONE',  ( -1.634638621908349521, -5.851115903089112003, 34.47074536777953568 ) ) ;
#80819 = CARTESIAN_POINT ( 'NONE',  ( -15.48074596171158390, -4.236021600441997492, 33.53823185664189310 ) ) ;
#80820 = ORIENTED_EDGE ( 'NONE', *, *, #42842, .F. ) ;
#80821 = CARTESIAN_POINT ( 'NONE',  ( 3.296836564119306257, -6.343179335718452272, 34.87096338111212646 ) ) ;
#80822 = DIRECTION ( 'NONE',  ( -0.000000000000000000, 0.9848077530122086864, -0.1736481776669273891 ) ) ;
#80823 = CARTESIAN_POINT ( 'NONE',  ( 5.749976762707035505, -9.271318131107980420, 34.42618302367067429 ) ) ;
#80824 = CARTESIAN_POINT ( 'NONE',  ( 13.60739492588379562, -12.44528174975671853, 30.48912976160716681 ) ) ;
#80825 = CARTESIAN_POINT ( 'NONE',  ( -16.15384615384615330, -4.098570777380720287, 33.41473453929634729 ) ) ;
#80826 = CARTESIAN_POINT ( 'NONE',  ( 6.923076923076924238, -8.973038597847269315, 34.52809138561121927 ) ) ;
#80828 = CARTESIAN_POINT ( 'NONE',  ( 9.942362112221147186, -4.818054556918156983, 34.26375889529406749 ) ) ;
#80827 = CARTESIAN_POINT ( 'NONE',  ( 0.4615384615384611200, -11.35647404775217417, 33.31231777344666511 ) ) ;
#80829 = EDGE_CURVE ( 'NONE', #55479, #4302, #56368, .T. ) ;
#80830 = EDGE_CURVE ( 'NONE', #85285, #27220, #74685, .T. ) ;
#80831 = CARTESIAN_POINT ( 'NONE',  ( 8.769230769230647482, -12.27809138561165270, 31.22303859784587132 ) ) ;
#80832 = CARTESIAN_POINT ( 'NONE',  ( -6.923076923077044142, -2.892918686052165622, 31.69288490824153470 ) ) ;
#80833 = CARTESIAN_POINT ( 'NONE',  ( 2.750000000000001332, -7.438900925035452083, 26.71688170625849068 ) ) ;
#80834 = ORIENTED_EDGE ( 'NONE', *, *, #80583, .F. ) ;
#80835 = CARTESIAN_POINT ( 'NONE',  ( 4.853438152358743984, -6.716662450894490100, 34.94144148231605840 ) ) ;
#80836 = ORIENTED_EDGE ( 'NONE', *, *, #88585, .T. ) ;
#80837 = ORIENTED_EDGE ( 'NONE', *, *, #67363, .F. ) ;
#80838 = CARTESIAN_POINT ( 'NONE',  ( -2.242436736416281828, -12.46129190930001052, 30.37095296980870174 ) ) ;
#80839 = EDGE_LOOP ( 'NONE', ( #9466, #51295, #18101, #69636 ) ) ;
#80840 = CARTESIAN_POINT ( 'NONE',  ( 3.480714749117371998, -10.05730279482229683, 34.04704008940765902 ) ) ;
#80841 = CARTESIAN_POINT ( 'NONE',  ( -0.06109907496454585613, -4.750000000000000000, 26.40438170625848713 ) ) ;
#80842 = CARTESIAN_POINT ( 'NONE',  ( 3.230769230769231726, -2.292212530054420494, 30.41441678777542634 ) ) ;
#80843 = EDGE_CURVE ( 'NONE', #80176, #36938, #21391, .T. ) ;
#80844 = CARTESIAN_POINT ( 'NONE',  ( 10.68145194873469173, -2.486705287966280320, 31.30864560766543647 ) ) ;
#80845 = DIRECTION ( 'NONE',  ( -0.000000000000000000, -0.000000000000000000, -1.000000000000000000 ) ) ;
#80846 = CARTESIAN_POINT ( 'NONE',  ( -3.230769230769229949, -12.34228464037088635, 31.77849191805839268 ) ) ;
#80847 = CARTESIAN_POINT ( 'NONE',  ( -13.38461538461538325, -2.538708090699994813, 30.37095296980875503 ) ) ;
#80848 = CARTESIAN_POINT ( 'NONE',  ( -11.53846153846165912, -5.219633306517616589, 34.19971097300220464 ) ) ;
#80849 = AXIS2_PLACEMENT_3D ( 'NONE', #22626, #50093, #15443 ) ;
#80850 = CARTESIAN_POINT ( 'NONE',  ( -3.750000000000008438, -5.946699141100917352, 22.67187500000000355 ) ) ;
#80851 = EDGE_CURVE ( 'NONE', #14278, #48006, #69294, .T. ) ;
#80852 = EDGE_CURVE ( 'NONE', #14768, #21373, #23598, .T. ) ;
#80853 = CARTESIAN_POINT ( 'NONE',  ( -0.4615384615384611200, -2.538708090699994813, 30.37095296980875503 ) ) ;
#80854 = CARTESIAN_POINT ( 'NONE',  ( -13.16160403300253634, -6.503523203565941380, 34.64991518177335195 ) ) ;
#80855 = VECTOR ( 'NONE', #85372, 1000.000000000000000 ) ;
#80856 = DIRECTION ( 'NONE',  ( 0.000000000000000000, 0.1736481776669275834, 0.9848077530122086864 ) ) ;
#80857 = ADVANCED_FACE ( 'NONE', ( #50174 ), #44751, .F. ) ;
#80858 = ORIENTED_EDGE ( 'NONE', *, *, #78427, .T. ) ;
#80859 = EDGE_LOOP ( 'NONE', ( #43591, #6242, #36526, #66271 ) ) ;
#80860 = DIRECTION ( 'NONE',  ( 0.000000000000000000, 0.6427876096865368094, 0.7660444431189802339 ) ) ;
#80861 = CARTESIAN_POINT ( 'NONE',  ( -14.24162395668986747, -8.120952969808772792, 34.71129190929999453 ) ) ;
#80862 = CARTESIAN_POINT ( 'NONE',  ( -39.05038313613820122, -2.249999999999999556, 27.25000000000000000 ) ) ;
#80863 = LINE ( 'NONE', #74093, #25450 ) ;
#80864 = DIRECTION ( 'NONE',  ( 0.000000000000000000, 1.000000000000000000, 0.000000000000000000 ) ) ;
#80865 = CARTESIAN_POINT ( 'NONE',  ( -10.61538461538461320, -9.819645486525091727, 36.12317359536749706 ) ) ;
#80866 = EDGE_LOOP ( 'NONE', ( #2177, #83991, #24346, #43080 ) ) ;
#80867 = CARTESIAN_POINT ( 'NONE',  ( 3.100078627658924280, -6.369640206132550553, 34.87707690430378449 ) ) ;
#80868 = ORIENTED_EDGE ( 'NONE', *, *, #16338, .T. ) ;
#80869 = B_SPLINE_CURVE_WITH_KNOTS ( 'NONE', 3,
 ( #70673, #77425, #84642, #69783, #15734, #8091, #23356, #8533, #63898, #83311 ),
 .UNSPECIFIED., .F., .F.,
 ( 4, 2, 2, 2, 4 ),
 ( 0.0007817359430256288133, 0.0009771253907249945886, 0.001172514838424360255, 0.001367904286123725922, 0.001563293733823091589 ),
 .UNSPECIFIED. ) ;
#80871 = EDGE_CURVE ( 'NONE', #31146, #31749, #40267, .T. ) ;
#80870 = ORIENTED_EDGE ( 'NONE', *, *, #88682, .T. ) ;
#80872 = CARTESIAN_POINT ( 'NONE',  ( -8.638440328263820689, -4.684288915650983043, 34.18129842949671371 ) ) ;
#80873 = AXIS2_PLACEMENT_3D ( 'NONE', #15611, #42204, #21921 ) ;
#80874 = CARTESIAN_POINT ( 'NONE',  ( 3.903822916553189248, -2.587272538249754117, 30.68239716806877837 ) ) ;
#80875 = CARTESIAN_POINT ( 'NONE',  ( 9.692307692307695177, -12.10708131394839349, 31.69288490824020244 ) ) ;
#80876 = CARTESIAN_POINT ( 'NONE',  ( 1.161130460051055691, -11.60425143139329940, 33.02411095842164457 ) ) ;
#80877 = CARTESIAN_POINT ( 'NONE',  ( -13.63463860883684120, -2.588893531581426988, 31.60682220781847818 ) ) ;
#80878 = AXIS2_PLACEMENT_3D ( 'NONE', #39430, #47935, #27227 ) ;
#80879 = ORIENTED_EDGE ( 'NONE', *, *, #66787, .F. ) ;
#80880 = EDGE_CURVE ( 'NONE', #33560, #86342, #16404, .T. ) ;
#80881 = ORIENTED_EDGE ( 'NONE', *, *, #43858, .F. ) ;
#80882 = ORIENTED_EDGE ( 'NONE', *, *, #55386, .F. ) ;
#80883 = CARTESIAN_POINT ( 'NONE',  ( -4.153846153846152411, -2.486705287966279876, 31.30864560766543647 ) ) ;
#80884 = DIRECTION ( 'NONE',  ( 0.000000000000000000, 0.000000000000000000, 1.000000000000000000 ) ) ;
#80885 = APPLICATION_CONTEXT ( 'automotive_design' ) ;
#80886 = CARTESIAN_POINT ( 'NONE',  ( 16.15384615384603251, -5.941354392335915335, 34.76329471203413846 ) ) ;
#80887 = B_SPLINE_CURVE_WITH_KNOTS ( 'NONE', 3,
 ( #5380, #32403, #32847, #60311, #52214, #59869, #25646, #53101, #39623, #81046 ),
 .UNSPECIFIED., .F., .F.,
 ( 4, 2, 2, 2, 4 ),
 ( 0.0007817359527651104954, 0.0009771254036996493593, 0.001172514854634188223, 0.001367904305568727087, 0.001563293756503265951 ),
 .UNSPECIFIED. ) ;
#80888 = CARTESIAN_POINT ( 'NONE',  ( -15.45425417449317784, -11.41268669641500466, 32.86336882939237825 ) ) ;
#80889 = CARTESIAN_POINT ( 'NONE',  ( -15.90384615384473399, -7.500000000000154543, 35.00000000000007105 ) ) ;
#80890 = DIRECTION ( 'NONE',  ( -0.000000000000000000, -0.1736481776669307198, -0.9848077530122080203 ) ) ;
#80891 = EDGE_LOOP ( 'NONE', ( #84509, #35693, #88516, #34911 ) ) ;
#80892 = ORIENTED_EDGE ( 'NONE', *, *, #40172, .F. ) ;
#80893 = ADVANCED_FACE ( 'NONE', ( #17293 ), #85316, .F. ) ;
#80895 = ORIENTED_EDGE ( 'NONE', *, *, #25088, .F. ) ;
#80894 = CARTESIAN_POINT ( 'NONE',  ( 17.20744877868663281, -12.45806712695776319, 30.39783852428763566 ) ) ;
#80896 = CARTESIAN_POINT ( 'NONE',  ( -9.942284423250047354, -4.943428324936578910, 34.04746400365624481 ) ) ;
#80897 = CARTESIAN_POINT ( 'NONE',  ( 7.911347827937202482, -2.506253911140448487, 29.99999999999988631 ) ) ;
#80898 = AXIS2_PLACEMENT_3D ( 'NONE', #81581, #13117, #47333 ) ;
#80899 = CARTESIAN_POINT ( 'NONE',  ( -1.553300858899081760, -11.25000000000000888, 14.85937500000000355 ) ) ;
#80900 = ORIENTED_EDGE ( 'NONE', *, *, #84379, .T. ) ;
#80901 = VECTOR ( 'NONE', #30214, 1000.000000000000000 ) ;
#80902 = CARTESIAN_POINT ( 'NONE',  ( -1.134669975237340811, -11.56426240980093567, 33.07394671870546432 ) ) ;
#80903 = ORIENTED_EDGE ( 'NONE', *, *, #16386, .F. ) ;
#80904 = FACE_OUTER_BOUND ( 'NONE', #6493, .T. ) ;
#80905 = DIRECTION ( 'NONE',  ( -0.000000000000000000, 1.000000000000000000, 3.491481338843133355E-15 ) ) ;
#80906 = FACE_BOUND ( 'NONE', #83487, .T. ) ;
#80907 = CARTESIAN_POINT ( 'NONE',  ( 12.46153846153846168, -13.37000171582298513, 34.34916445242398453 ) ) ;
#80908 = CARTESIAN_POINT ( 'NONE',  ( -14.17764714485753075, -2.504778602574660340, 29.97347330155780654 ) ) ;
#80909 = EDGE_LOOP ( 'NONE', ( #54805, #41981, #28026, #47215 ) ) ;
#80910 = EDGE_CURVE ( 'NONE', #37595, #58918, #2584, .T. ) ;
#80911 = CARTESIAN_POINT ( 'NONE',  ( 11.47237915910140416, -11.35647404775217595, 33.31231777344666511 ) ) ;
#80912 = CARTESIAN_POINT ( 'NONE',  ( -18.03205128205128105, -7.500000000000000000, 29.75000000000000355 ) ) ;
#80913 = EDGE_CURVE ( 'NONE', #22218, #84168, #71339, .T. ) ;
#80914 = DIRECTION ( 'NONE',  ( 0.000000000000000000, -6.938893903907222067E-15, 1.000000000000000000 ) ) ;
#80915 = ORIENTED_EDGE ( 'NONE', *, *, #77035, .F. ) ;
#80916 = LINE ( 'NONE', #74143, #11374 ) ;
#80917 = CARTESIAN_POINT ( 'NONE',  ( 14.53070515178570332, -10.01129605718032600, 34.36064277460058491 ) ) ;
#80918 = CARTESIAN_POINT ( 'NONE',  ( 17.20771488474786537, -9.804649428959608670, 34.18742332936588468 ) ) ;
#80919 = CARTESIAN_POINT ( 'NONE',  ( 17.06410256410256565, -7.500000000000000000, 29.75000000000000355 ) ) ;
#80920 = CARTESIAN_POINT ( 'NONE',  ( 10.39245839786846659, -11.76352882383564769, 32.36236540154569497 ) ) ;
#80921 = FACE_BOUND ( 'NONE', #23581, .T. ) ;
#80923 = CYLINDRICAL_SURFACE ( 'NONE', #22990, 0.2500000000000008882 ) ;
#80922 = CARTESIAN_POINT ( 'NONE',  ( 13.31934538405906743, -12.16647553114622049, 32.15551576947930812 ) ) ;
#80924 = EDGE_CURVE ( 'NONE', #73759, #85253, #47744, .T. ) ;
#80925 = CYLINDRICAL_SURFACE ( 'NONE', #41104, 0.2500000000000004996 ) ;
#80927 = CARTESIAN_POINT ( 'NONE',  ( 15.48082354240754555, -9.943054286541403997, 34.11300777759954883 ) ) ;
#80926 = CYLINDRICAL_SURFACE ( 'NONE', #15612, 0.2499999999999995559 ) ;
#80928 = CARTESIAN_POINT ( 'NONE',  ( -4.153846153846152411, -9.819645486525091727, 36.12317359536749706 ) ) ;
#80929 = CARTESIAN_POINT ( 'NONE',  ( 3.724691934501232815, -5.885600066136343678, 22.88875670625849068 ) ) ;
#80930 = ORIENTED_EDGE ( 'NONE', *, *, #77344, .T. ) ;
#80931 = DIRECTION ( 'NONE',  ( -0.000000000000000000, 0.9396926207859092051, -0.3420201433256662704 ) ) ;
#80932 = ORIENTED_EDGE ( 'NONE', *, *, #1980, .F. ) ;
#80933 = AXIS2_PLACEMENT_3D ( 'NONE', #46411, #59479, #31106 ) ;
#80934 = CARTESIAN_POINT ( 'NONE',  ( -14.30769230769230660, -10.67929555188718282, 33.92786785259544047 ) ) ;
#80935 = ORIENTED_EDGE ( 'NONE', *, *, #26174, .F. ) ;
#80936 = CARTESIAN_POINT ( 'NONE',  ( 7.596130608860880429, -9.271318131107980420, 34.42618302367067429 ) ) ;
#80937 = CARTESIAN_POINT ( 'NONE',  ( -11.53846153846153655, -1.215029322943914858, 32.30358669280327177 ) ) ;
#80939 = EDGE_LOOP ( 'NONE', ( #29393, #49144, #53032, #52829 ) ) ;
#80938 = CARTESIAN_POINT ( 'NONE',  ( -19.50000000000000000, -3.499999999999999556, 29.75000000000000355 ) ) ;
#80940 = CARTESIAN_POINT ( 'NONE',  ( 3.361561038594018225, -6.413143153341454017, 34.63066358083362672 ) ) ;
#80941 = CARTESIAN_POINT ( 'NONE',  ( 1.161130460051058133, -12.11044203135681840, 32.26167407432752299 ) ) ;
#80942 = CARTESIAN_POINT ( 'NONE',  ( 3.749999999999999556, -7.438900925035446754, 25.46688170625849423 ) ) ;
#80943 = CARTESIAN_POINT ( 'NONE',  ( 2.084207363968360038, -11.89387501736622710, 32.13663884655806413 ) ) ;
#80944 = CARTESIAN_POINT ( 'NONE',  ( 5.076923076923075762, -4.786620604624113540, 33.94971097300155094 ) ) ;
#80945 = CARTESIAN_POINT ( 'NONE',  ( -5.011667937410240192, -12.16647553114626490, 32.15551576947920864 ) ) ;
#80946 = CYLINDRICAL_SURFACE ( 'NONE', #81851, 4.000000000000000000 ) ;
#80947 = CARTESIAN_POINT ( 'NONE',  ( -24.00000000000000000, -5.499999999999981348, 27.75000000000000000 ) ) ;
#80948 = CARTESIAN_POINT ( 'NONE',  ( -8.835314180186646382, -8.973038597847271092, 34.52809138561120506 ) ) ;
#80949 = B_SPLINE_CURVE_WITH_KNOTS ( 'NONE', 3,
 ( #50812, #37306, #43628, #65225, #37758, #85075, #77422, #16596, #85954, #44056 ),
 .UNSPECIFIED., .F., .F.,
 ( 4, 2, 2, 2, 4 ),
 ( 0.0007817359430256324996, 0.0009771253907249993591, 0.001172514838424366110, 0.001367904286123732861, 0.001563293733823099829 ),
 .UNSPECIFIED. ) ;
#80950 = CARTESIAN_POINT ( 'NONE',  ( -2.694853999681181556, -10.10844685921792241, 20.18936829374151287 ) ) ;
#80951 = EDGE_CURVE ( 'NONE', #64799, #33151, #24040, .T. ) ;
#80952 = CARTESIAN_POINT ( 'NONE',  ( 5.299702745901138989, -2.612705202774697533, 31.66806509827799943 ) ) ;
#80953 = CARTESIAN_POINT ( 'NONE',  ( -1.384615384615383471, -11.91647553114624181, 32.58852847137148245 ) ) ;
#80954 = EDGE_LOOP ( 'NONE', ( #46926, #38498, #26030, #19120 ) ) ;
#80955 = CARTESIAN_POINT ( 'NONE',  ( 17.29970261819148902, -2.847695495035524882, 31.58253572463339154 ) ) ;
#80956 = CARTESIAN_POINT ( 'NONE',  ( 9.692307692307695177, -5.471508081941601098, 34.59228464037088457 ) ) ;
#80957 = CARTESIAN_POINT ( 'NONE',  ( 1.614399933863618797, -3.775308065498751198, 20.73624329374151287 ) ) ;
#80958 = CARTESIAN_POINT ( 'NONE',  ( 2.242421861731532573, -4.481592998940161721, 33.73612834413957984 ) ) ;
#80959 = DIRECTION ( 'NONE',  ( 0.000000000000000000, 0.8660254037844377084, -0.5000000000000015543 ) ) ;
#80960 = VERTEX_POINT ( 'NONE', #64132 ) ;
#80961 = DIRECTION ( 'NONE',  ( -0.000000000000000000, -0.8660254037844397068, -0.4999999999999978906 ) ) ;
#80962 = CARTESIAN_POINT ( 'NONE',  ( -12.23852561744506851, -12.64618726649961289, 30.78989965857442712 ) ) ;
#80964 = ORIENTED_EDGE ( 'NONE', *, *, #45093, .F. ) ;
#80963 = CARTESIAN_POINT ( 'NONE',  ( 11.53846153846141576, -3.083524468854526912, 32.58852847137268327 ) ) ;
#80965 = CARTESIAN_POINT ( 'NONE',  ( -8.069080063669991532, -8.239355502252617924, 34.69524867566427417 ) ) ;
#80966 = CARTESIAN_POINT ( 'NONE',  ( 3.903869422903798458, -8.303909089506435137, 34.68538101551103381 ) ) ;
#80967 = CARTESIAN_POINT ( 'NONE',  ( 15.45378207486262667, -5.582272713120729257, 34.63742843783360570 ) ) ;
#80968 = CARTESIAN_POINT ( 'NONE',  ( -14.30769230769230660, -11.16473453929635440, 33.15142922261926373 ) ) ;
#80969 = VERTEX_POINT ( 'NONE', #84436 ) ;
#80970 = AXIS2_PLACEMENT_3D ( 'NONE', #38149, #30503, #50320 ) ;
#80971 = CARTESIAN_POINT ( 'NONE',  ( 2.530471848960718084, -12.24180327182771855, 31.33663988360758168 ) ) ;
#80972 = DIRECTION ( 'NONE',  ( -0.000000000000000000, -0.000000000000000000, -1.000000000000000000 ) ) ;
#80973 = CARTESIAN_POINT ( 'NONE',  ( 1.384615384615264011, -3.083524468854526912, 32.58852847137268327 ) ) ;
#80974 = ORIENTED_EDGE ( 'NONE', *, *, #75668, .F. ) ;
#80975 = ORIENTED_EDGE ( 'NONE', *, *, #64696, .T. ) ;
#80976 = EDGE_LOOP ( 'NONE', ( #3705, #14100 ) ) ;
#80977 = DIRECTION ( 'NONE',  ( -0.000000000000000000, -0.1736481776669307198, -0.9848077530122080203 ) ) ;
#80978 = CARTESIAN_POINT ( 'NONE',  ( -2.307692307692305711, -8.564572088678739092, 35.78748833219616898 ) ) ;
#80979 = CARTESIAN_POINT ( 'NONE',  ( -9.692307692307691624, -12.62096338111211580, 30.90682066428153263 ) ) ;
#80980 = CARTESIAN_POINT ( 'NONE',  ( 5.076923076922954969, -6.026961402154118908, 34.52809138561165270 ) ) ;
#80981 = VERTEX_POINT ( 'NONE', #22712 ) ;
#80982 = VERTEX_POINT ( 'NONE', #64570 ) ;
#80983 = VERTEX_POINT ( 'NONE', #29927 ) ;
#80985 = ORIENTED_EDGE ( 'NONE', *, *, #35473, .F. ) ;
#80984 = CARTESIAN_POINT ( 'NONE',  ( -6.923076923077045919, -2.657715359629662988, 31.77849191805970364 ) ) ;
#80986 = DIRECTION ( 'NONE',  ( -0.000000000000000000, 1.000000000000000000, -0.000000000000000000 ) ) ;
#80987 = FACE_OUTER_BOUND ( 'NONE', #86013, .T. ) ;
#80988 = AXIS2_PLACEMENT_3D ( 'NONE', #50265, #48505, #7978 ) ;
#80989 = DIRECTION ( 'NONE',  ( 1.000000000000000000, 0.000000000000000000, 0.000000000000000000 ) ) ;
#80990 = CARTESIAN_POINT ( 'NONE',  ( 6.923076923076802558, -11.94971097300221174, 32.03036669348237098 ) ) ;
#80991 = VERTEX_POINT ( 'NONE', #44293 ) ;
#80992 = VECTOR ( 'NONE', #43950, 1000.000000000000114 ) ;
#80993 = ORIENTED_EDGE ( 'NONE', *, *, #16349, .F. ) ;
#80994 = ORIENTED_EDGE ( 'NONE', *, *, #45920, .F. ) ;
#80995 = CARTESIAN_POINT ( 'NONE',  ( 14.37294744720514750, -11.06231777344671130, 33.60647404775212976 ) ) ;
#80997 = ORIENTED_EDGE ( 'NONE', *, *, #87174, .F. ) ;
#80996 = CARTESIAN_POINT ( 'NONE',  ( -10.54931728203453822, -2.486705287966280320, 31.30864560766543647 ) ) ;
#80998 = CARTESIAN_POINT ( 'NONE',  ( 24.99999999999999645, 20.00000000000000355, 0.000000000000000000 ) ) ;
#80999 = CARTESIAN_POINT ( 'NONE',  ( 12.39545505058258179, -11.16473453929635440, 33.15142922261925662 ) ) ;
#81000 = ORIENTED_EDGE ( 'NONE', *, *, #60659, .T. ) ;
#81001 = DIRECTION ( 'NONE',  ( -0.000000000000000000, 0.7660444431189791237, -0.6427876096865379196 ) ) ;
#81002 = CARTESIAN_POINT ( 'NONE',  ( -18.00000000000012079, -2.625532179533778709, 30.86335684631627174 ) ) ;
#81003 = DIRECTION ( 'NONE',  ( 1.000000000000000000, 0.000000000000000000, 0.000000000000000000 ) ) ;
#81004 = FACE_BOUND ( 'NONE', #12264, .T. ) ;
#81005 = CARTESIAN_POINT ( 'NONE',  ( -17.93393164899756087, -8.120952969808772792, 34.71129190929999453 ) ) ;
#81006 = CARTESIAN_POINT ( 'NONE',  ( -1.161835843346972874, -11.89424750095246175, 32.13594075562311758 ) ) ;
#81007 = EDGE_CURVE ( 'NONE', #67341, #74655, #64964, .T. ) ;
#81008 = CARTESIAN_POINT ( 'NONE',  ( -10.39237177129122003, -10.77377354290276124, 33.85451476688484718 ) ) ;
#81010 = CARTESIAN_POINT ( 'NONE',  ( -5.207070286361298095, -3.285722584762969856, 32.44110544564090759 ) ) ;
#81009 = DIRECTION ( 'NONE',  ( 0.000000000000000000, 0.000000000000000000, -1.000000000000000000 ) ) ;
#81011 = DIRECTION ( 'NONE',  ( 1.000000000000000000, 0.000000000000000000, -0.000000000000000000 ) ) ;
#81012 = CARTESIAN_POINT ( 'NONE',  ( 17.99999999999987566, -6.835583212225970762, 34.95778746994575670 ) ) ;
#81013 = VERTEX_POINT ( 'NONE', #32149 ) ;
#81014 = PLANE ( 'NONE',  #83518 ) ;
#81015 = EDGE_CURVE ( 'NONE', #24114, #51057, #38458, .T. ) ;
#81016 = CYLINDRICAL_SURFACE ( 'NONE', #33592, 0.2499999999999994726 ) ;
#81017 = ORIENTED_EDGE ( 'NONE', *, *, #50264, .T. ) ;
#81018 = ORIENTED_EDGE ( 'NONE', *, *, #21597, .F. ) ;
#81019 = LINE ( 'NONE', #18863, #79337 ) ;
#81020 = CIRCLE ( 'NONE', #10541, 2.000000000000001776 ) ;
#81021 = AXIS2_PLACEMENT_3D ( 'NONE', #83638, #75973, #15166 ) ;
#81022 = CARTESIAN_POINT ( 'NONE',  ( -13.45069776397551564, -4.661471528628507777, 34.16647553114621871 ) ) ;
#81023 = LINE ( 'NONE', #87796, #67749 ) ;
#81024 = ORIENTED_EDGE ( 'NONE', *, *, #70775, .F. ) ;
#81025 = CARTESIAN_POINT ( 'NONE',  ( 14.55774661933062575, -9.148310452688876993, 34.47095581063188519 ) ) ;
#81026 = DIRECTION ( 'NONE',  ( -0.000000000000000000, 1.000000000000000000, 3.491481338843133355E-15 ) ) ;
#81027 = FACE_BOUND ( 'NONE', #65893, .T. ) ;
#81029 = CARTESIAN_POINT ( 'NONE',  ( 5.869309396889695662, -6.369640206132550553, 34.87707690430378449 ) ) ;
#81028 = LINE ( 'NONE', #19317, #82081 ) ;
#81030 = DIRECTION ( 'NONE',  ( -0.000000000000000000, 0.6427876096865404731, -0.7660444431189771253 ) ) ;
#81031 = EDGE_CURVE ( 'NONE', #74652, #53825, #72677, .T. ) ;
#81032 = FACE_OUTER_BOUND ( 'NONE', #84882, .T. ) ;
#81034 = CARTESIAN_POINT ( 'NONE',  ( 0.3962680155776852620, -6.026961402152685388, 34.52809138561120506 ) ) ;
#81033 =( LENGTH_UNIT ( ) NAMED_UNIT ( * ) SI_UNIT ( .MILLI., .METRE. ) );
#81035 = CARTESIAN_POINT ( 'NONE',  ( 1.553300858899087311, -3.749999999999992006, 24.23437500000000355 ) ) ;
#81036 = ORIENTED_EDGE ( 'NONE', *, *, #74850, .F. ) ;
#81037 = EDGE_LOOP ( 'NONE', ( #8096, #50537, #61561, #65278 ) ) ;
#81038 = CARTESIAN_POINT ( 'NONE',  ( -12.23852561744506495, -5.582272713120729257, 34.63742843783360570 ) ) ;
#81039 = FACE_OUTER_BOUND ( 'NONE', #82672, .T. ) ;
#81040 = CARTESIAN_POINT ( 'NONE',  ( 4.283891316680932704, -2.504778602574660340, 29.97347330155780298 ) ) ;
#81041 = CARTESIAN_POINT ( 'NONE',  ( 6.673053685783957967, -12.22074536777954989, 31.39888409691088356 ) ) ;
#81042 = CARTESIAN_POINT ( 'NONE',  ( 5.326977496836529546, -3.435999193479609914, 33.07426656108010832 ) ) ;
#81043 = CARTESIAN_POINT ( 'NONE',  ( 3.750000000000009770, -9.053300858899081760, 22.04687500000000000 ) ) ;
#81044 = CARTESIAN_POINT ( 'NONE',  ( 0.7115384615398965273, -7.500000000000155431, 34.75000000000007105 ) ) ;
#81045 = CARTESIAN_POINT ( 'NONE',  ( 16.15384615384615330, -1.129524287112498415, 32.06866353760679544 ) ) ;
#81046 = CARTESIAN_POINT ( 'NONE',  ( -13.63461538461538325, -7.500000000000001776, 34.75000000000000000 ) ) ;
#81047 = DIRECTION ( 'NONE',  ( -0.000000000000000000, -0.3420201433256694346, -0.9396926207859080948 ) ) ;
#81048 = CARTESIAN_POINT ( 'NONE',  ( 9.692307692307572609, -2.892918686052165622, 31.69288490824153470 ) ) ;
#81049 = CARTESIAN_POINT ( 'NONE',  ( 8.519254038288416098, -12.17611988154120972, 31.52148481390971213 ) ) ;
#81050 = DIRECTION ( 'NONE',  ( 1.000000000000000000, 0.000000000000000000, 0.000000000000000000 ) ) ;
#81051 = CARTESIAN_POINT ( 'NONE',  ( -3.230769230769351186, -11.94971097300221174, 32.03036669348237098 ) ) ;
#81052 = EDGE_CURVE ( 'NONE', #47795, #11542, #17747, .T. ) ;
#81053 = CIRCLE ( 'NONE', #42208, 4.000000000000000000 ) ;
#81054 = CARTESIAN_POINT ( 'NONE',  ( -8.519285359852727169, -11.56426240980093745, 33.07394671870546432 ) ) ;
#81055 = CARTESIAN_POINT ( 'NONE',  ( -15.48074596171158390, -8.303909089506435137, 34.68538101551103381 ) ) ;
#81056 = EDGE_CURVE ( 'NONE', #61929, #73515, #86339, .T. ) ;
#81057 = ORIENTED_EDGE ( 'NONE', *, *, #16207, .T. ) ;
#81058 = CARTESIAN_POINT ( 'NONE',  ( -0.4615384615384611200, -2.721908614388771852, 31.22303859784724978 ) ) ;
#81059 = CARTESIAN_POINT ( 'NONE',  ( 18.25005441991345734, -4.818054556918155207, 34.26375889529406749 ) ) ;
#81060 = CARTESIAN_POINT ( 'NONE',  ( -1.987747218494638313, -9.401340078031370950, 18.93936829374151287 ) ) ;
#81061 = EDGE_CURVE ( 'NONE', #66904, #18025, #43435, .T. ) ;
#81062 = AXIS2_PLACEMENT_3D ( 'NONE', #36632, #64085, #64969 ) ;
#81063 = ADVANCED_FACE ( 'NONE', ( #25834 ), #11428, .F. ) ;
#81064 = CARTESIAN_POINT ( 'NONE',  ( 14.30769230769231015, -6.343179335718451384, 34.87096338111211935 ) ) ;
#81065 = DIRECTION ( 'NONE',  ( 0.000000000000000000, 0.3420201433256641055, -0.9396926207859100932 ) ) ;
#81066 = CARTESIAN_POINT ( 'NONE',  ( -10.61538461538461320, -3.886160181151819604, 36.00935417666054406 ) ) ;
#81068 = ORIENTED_EDGE ( 'NONE', *, *, #6347, .F. ) ;
#81067 = CARTESIAN_POINT ( 'NONE',  ( 10.54963118707128622, -7.249945578846651806, 34.99404164642496795 ) ) ;
#81069 = CARTESIAN_POINT ( 'NONE',  ( -1.139087296526025250, -4.750000000000006217, 25.32812500000000355 ) ) ;
#81070 = CARTESIAN_POINT ( 'NONE',  ( 3.480714640147273720, -8.476813868363244353, 34.90874843262270133 ) ) ;
#81071 = ORIENTED_EDGE ( 'NONE', *, *, #53635, .F. ) ;
#81072 = CARTESIAN_POINT ( 'NONE',  ( 1.384615384615386802, -13.75783147151868846, 33.36296068462461051 ) ) ;
#81073 = CARTESIAN_POINT ( 'NONE',  ( 18.25005431163831204, -9.148310452688871663, 34.47095581063188519 ) ) ;
#81074 = ORIENTED_EDGE ( 'NONE', *, *, #4166, .T. ) ;
#81075 = B_SPLINE_CURVE_WITH_KNOTS ( 'NONE', 3,
 ( #32203, #67757, #74513, #87604, #52894, #25882, #73642, #6060, #33080, #80394 ),
 .UNSPECIFIED., .F., .F.,
 ( 4, 2, 2, 2, 4 ),
 ( 0.0007817359430256293554, 0.0009771253907249952391, 0.001172514838424361123, 0.001367904286123727007, 0.001563293733823092890 ),
 .UNSPECIFIED. ) ;
#81076 = DIRECTION ( 'NONE',  ( 0.000000000000000000, -1.000000000000000000, -1.084202172485503448E-16 ) ) ;
#81077 = CARTESIAN_POINT ( 'NONE',  ( -13.38461538461550582, -2.625532179533778709, 30.86335684631627174 ) ) ;
#81078 = B_SPLINE_CURVE_WITH_KNOTS ( 'NONE', 3,
 ( #63216, #84398, #83961, #22239, #10046, #23124, #63663, #57792, #43833, #9605 ),
 .UNSPECIFIED., .F., .F.,
 ( 4, 2, 2, 2, 4 ),
 ( 0.0007817359430256216575, 0.0009771253907249856981, 0.001172514838424349630, 0.001367904286123713779, 0.001563293733823077711 ),
 .UNSPECIFIED. ) ;
#81079 = CARTESIAN_POINT ( 'NONE',  ( -17.07692307692319744, -12.27809138561165270, 31.22303859784587132 ) ) ;
#81080 = ORIENTED_EDGE ( 'NONE', *, *, #82259, .F. ) ;
#81081 = ORIENTED_EDGE ( 'NONE', *, *, #2083, .T. ) ;
#81082 = ORIENTED_EDGE ( 'NONE', *, *, #19101, .T. ) ;
#81083 = DIRECTION ( 'NONE',  ( 1.000000000000000000, 0.000000000000000000, 0.000000000000000000 ) ) ;
#81084 = CARTESIAN_POINT ( 'NONE',  ( 12.21151522424549896, -12.43535235679832596, 30.55408501211184813 ) ) ;
#81085 = CARTESIAN_POINT ( 'NONE',  ( -9.561781990544133691, -10.19071101563364756, 33.96452234770658407 ) ) ;
#81086 = CARTESIAN_POINT ( 'NONE',  ( -17.20761454359064047, -5.582088688514999397, 34.36776431015576350 ) ) ;
#81087 = CARTESIAN_POINT ( 'NONE',  ( 9.469381474791543241, -9.086856451489515152, 34.49173150075333183 ) ) ;
#81088 = DIRECTION ( 'NONE',  ( 0.000000000000000000, 0.9396926207859126468, 0.3420201433256571111 ) ) ;
#81089 = DIRECTION ( 'NONE',  ( -0.000000000000000000, -0.1736481776669307198, -0.9848077530122080203 ) ) ;
#81090 = AXIS2_PLACEMENT_3D ( 'NONE', #25728, #74811, #40583 ) ;
#81091 = CARTESIAN_POINT ( 'NONE',  ( -6.249999999999997335, -7.500000000000001776, 35.04278698407183867 ) ) ;
#81092 = EDGE_CURVE ( 'NONE', #20954, #11611, #10542, .T. ) ;
#81093 = ORIENTED_EDGE ( 'NONE', *, *, #69069, .T. ) ;
#81094 = ORIENTED_EDGE ( 'NONE', *, *, #21251, .F. ) ;
#81095 = EDGE_LOOP ( 'NONE', ( #57024, #87792 ) ) ;
#81097 = ORIENTED_EDGE ( 'NONE', *, *, #15057, .T. ) ;
#81096 = CARTESIAN_POINT ( 'NONE',  ( 18.24994540937804643, -9.357781135181033605, 34.66075350412533851 ) ) ;
#81098 = CARTESIAN_POINT ( 'NONE',  ( -8.519176349317316266, -10.82426656108012075, 33.81400080652039009 ) ) ;
#81099 = CARTESIAN_POINT ( 'NONE',  ( -39.05038313613820122, -2.249999999999999556, 27.25000000000000000 ) ) ;
#81100 = ORIENTED_EDGE ( 'NONE', *, *, #39369, .F. ) ;
#81101 = CARTESIAN_POINT ( 'NONE',  ( 15.45354889974729318, -9.418065098278013636, 34.63729479722530158 ) ) ;
#81102 = EDGE_CURVE ( 'NONE', #62076, #15626, #34820, .T. ) ;
#81103 = EDGE_LOOP ( 'NONE', ( #51908, #87019 ) ) ;
#81104 = DIRECTION ( 'NONE',  ( -0.000000000000000000, -0.3420201433256694901, -0.9396926207859082059 ) ) ;
#81105 = VERTEX_POINT ( 'NONE', #32579 ) ;
#81106 = B_SPLINE_CURVE_WITH_KNOTS ( 'NONE', 3,
 ( #69993, #22258, #8307, #84859, #50606, #2414, #77640, #35783, #8755, #15506 ),
 .UNSPECIFIED., .F., .F.,
 ( 4, 2, 2, 2, 4 ),
 ( 0.0007817246256747476061, 0.0009771112852218902852, 0.001172497944769033181, 0.001367884604316175860, 0.001563271263863318539 ),
 .UNSPECIFIED. ) ;
#81107 = CARTESIAN_POINT ( 'NONE',  ( 6.923076923076924238, -4.102666532097928531, 36.13435417666054406 ) ) ;
#81108 = VECTOR ( 'NONE', #10529, 1000.000000000000227 ) ;
#81109 = CARTESIAN_POINT ( 'NONE',  ( -16.28453762051371356, -6.413092428213692742, 34.63065189839063152 ) ) ;
#81110 = CARTESIAN_POINT ( 'NONE',  ( -9.442307692307627676, -7.434744860731433924, 35.00000000000000711 ) ) ;
#81111 = FACE_BOUND ( 'NONE', #88191, .T. ) ;
#81112 = VECTOR ( 'NONE', #73549, 1000.000000000000227 ) ;
#81113 = DIRECTION ( 'NONE',  ( -0.000000000000000000, 0.000000000000000000, 1.000000000000000000 ) ) ;
#81114 = CARTESIAN_POINT ( 'NONE',  ( 1.134615384615387246, -7.433932668274255029, 35.00000000000000711 ) ) ;
#81115 = EDGE_CURVE ( 'NONE', #65326, #31209, #28451, .T. ) ;
#81116 = DIRECTION ( 'NONE',  ( 0.000000000000000000, 0.4999999999999960032, -0.8660254037844410391 ) ) ;
#81117 = CARTESIAN_POINT ( 'NONE',  ( 4.284637961670941131, -8.147973898785416225, 34.70805048591653730 ) ) ;
#81118 = CYLINDRICAL_SURFACE ( 'NONE', #20719, 0.2499999999999973355 ) ;
#81119 = CARTESIAN_POINT ( 'NONE',  ( -12.46153846153846168, -5.557115091759785130, 34.35708131394839171 ) ) ;
#81120 = CARTESIAN_POINT ( 'NONE',  ( -11.53846153846153655, -3.322132147404559976, 32.92929555188717927 ) ) ;
#81121 = EDGE_CURVE ( 'NONE', #8179, #61168, #60404, .T. ) ;
#81122 = ORIENTED_EDGE ( 'NONE', *, *, #46203, .F. ) ;
#81123 = ORIENTED_EDGE ( 'NONE', *, *, #61704, .F. ) ;
#81125 = CYLINDRICAL_SURFACE ( 'NONE', #18915, 0.2499999999999995837 ) ;
#81124 = DIRECTION ( 'NONE',  ( 0.000000000000000000, 0.8660254037844377084, 0.5000000000000015543 ) ) ;
#81126 = CARTESIAN_POINT ( 'NONE',  ( 15.45354889974729318, -8.540255544307065350, 34.89611431652622286 ) ) ;
#81127 = CARTESIAN_POINT ( 'NONE',  ( 8.769230769230768274, -8.973038597847269315, 34.52809138561121927 ) ) ;
#81128 = CARTESIAN_POINT ( 'NONE',  ( 8.703907853738597211, -7.749976743299138882, 34.99404534957040624 ) ) ;
#81129 = CARTESIAN_POINT ( 'NONE',  ( -2.307692307692305711, -2.721908614388771852, 31.22303859784724978 ) ) ;
#81130 = ORIENTED_EDGE ( 'NONE', *, *, #65431, .T. ) ;
#81131 = LINE ( 'NONE', #60843, #64422 ) ;
#81132 = CARTESIAN_POINT ( 'NONE',  ( 11.66850914471722689, -7.723484964179501588, 34.74522123443823318 ) ) ;
#81133 = CARTESIAN_POINT ( 'NONE',  ( -14.05763788777885637, -12.41089969410671223, 31.60739465890703670 ) ) ;
#81134 = ADVANCED_FACE ( 'NONE', ( #74024 ), #12319, .F. ) ;
#81135 = CARTESIAN_POINT ( 'NONE',  ( -3.454254155333562171, -12.69144148231606017, 30.53333754910549303 ) ) ;
#81136 = ORIENTED_EDGE ( 'NONE', *, *, #69196, .F. ) ;
#81137 = VERTEX_POINT ( 'NONE', #35238 ) ;
#81138 = SHAPE_DEFINITION_REPRESENTATION ( #26805, #36256 ) ;
#81140 = EDGE_CURVE ( 'NONE', #57134, #572, #55068, .T. ) ;
#81139 = EDGE_LOOP ( 'NONE', ( #17942, #65713, #62819, #38258 ) ) ;
#81141 = CARTESIAN_POINT ( 'NONE',  ( 15.36156103859402222, -6.413143153341454017, 34.63066358083362672 ) ) ;
#81142 = CARTESIAN_POINT ( 'NONE',  ( -14.30769230769230660, -5.471508081941601098, 34.59228464037088457 ) ) ;
#81143 = EDGE_LOOP ( 'NONE', ( #32544, #84072, #60711, #19271 ) ) ;
#81144 = EDGE_CURVE ( 'NONE', #58206, #37680, #35954, .T. ) ;
#81145 = FACE_OUTER_BOUND ( 'NONE', #67816, .T. ) ;
#81146 = CARTESIAN_POINT ( 'NONE',  ( 14.98079249982687777, -9.148715823498378086, 34.47080413974185120 ) ) ;
#81147 = CARTESIAN_POINT ( 'NONE',  ( -10.61538461538461320, -9.819645486525091727, 36.12317359536749706 ) ) ;
#81148 = LINE ( 'NONE', #6376, #64685 ) ;
#81149 = CARTESIAN_POINT ( 'NONE',  ( -0.5922299282060190517, -11.18331474514187995, 33.13161551792790505 ) ) ;
#81151 = ORIENTED_EDGE ( 'NONE', *, *, #49700, .F. ) ;
#81150 = VECTOR ( 'NONE', #24597, 1000.000000000000000 ) ;
#81153 = ORIENTED_EDGE ( 'NONE', *, *, #46220, .F. ) ;
#81152 = CARTESIAN_POINT ( 'NONE',  ( -15.16470189741915320, -2.292212530054420494, 30.41441678777542990 ) ) ;
#81154 = FACE_OUTER_BOUND ( 'NONE', #26064, .T. ) ;
#81155 = CARTESIAN_POINT ( 'NONE',  ( -2.557669038634660108, -9.148715823498378086, 34.47080413974185120 ) ) ;
#81156 = CARTESIAN_POINT ( 'NONE',  ( 1.634615384616822320, -7.500000000000155431, 34.75000000000007105 ) ) ;
#81157 = DIRECTION ( 'NONE',  ( -0.000000000000000000, -0.8660254037844397068, -0.4999999999999980016 ) ) ;
#81158 = CARTESIAN_POINT ( 'NONE',  ( -8.703975629717930929, -8.656820664281605460, 34.87096338111211224 ) ) ;
#81159 = EDGE_CURVE ( 'NONE', #59485, #15487, #24454, .T. ) ;
#81160 = FILL_AREA_STYLE_COLOUR ( '', #16165 ) ;
#81161 = CARTESIAN_POINT ( 'NONE',  ( 12.59206416330202316, -11.46989282347013095, 32.79007818306219946 ) ) ;
#81162 = CARTESIAN_POINT ( 'NONE',  ( 1.200186371490529202, -4.775308065498752974, 19.48624329374152353 ) ) ;
#81163 = EDGE_LOOP ( 'NONE', ( #48696, #64569, #17197, #74637 ) ) ;
#81164 = LINE ( 'NONE', #81603, #28801 ) ;
#81165 = CARTESIAN_POINT ( 'NONE',  ( -10.61538461538461320, -13.75783147151868846, 33.36296068462461051 ) ) ;
#81166 = EDGE_CURVE ( 'NONE', #78029, #47861, #46628, .T. ) ;
#81167 = VERTEX_POINT ( 'NONE', #88441 ) ;
#81168 = ADVANCED_FACE ( 'NONE', ( #47415 ), #26713, .F. ) ;
#81169 = ORIENTED_EDGE ( 'NONE', *, *, #241, .T. ) ;
#81170 = CARTESIAN_POINT ( 'NONE',  ( 2.057692307692309264, -7.433932668274255029, 35.00000000000000711 ) ) ;
#81171 = CARTESIAN_POINT ( 'NONE',  ( 2.980769230769232170, -2.499999999999998668, 29.75000000000000355 ) ) ;
#81172 = CARTESIAN_POINT ( 'NONE',  ( -6.989160334032800570, -5.557115091759785130, 34.35708131394839171 ) ) ;
#81173 = DIRECTION ( 'NONE',  ( -0.000000000000000000, 0.8660254037844399289, -0.4999999999999980016 ) ) ;
#81174 = CARTESIAN_POINT ( 'NONE',  ( 0.7114838709165044461, -2.341251567377310217, 30.72681386836322659 ) ) ;
#81175 = EDGE_LOOP ( 'NONE', ( #56243, #58266 ) ) ;
#81176 = CARTESIAN_POINT ( 'NONE',  ( 10.28846153846153832, -7.500000000000000000, 29.75000000000000355 ) ) ;
#81177 = AXIS2_PLACEMENT_3D ( 'NONE', #68576, #12311, #27148 ) ;
#81178 = CARTESIAN_POINT ( 'NONE',  ( 17.14217864819909920, -6.026961402152790193, 34.52809138561124769 ) ) ;
#81179 = CARTESIAN_POINT ( 'NONE',  ( -2.057637887778852814, -5.642605341092957083, 34.66089969410670335 ) ) ;
#81180 = ORIENTED_EDGE ( 'NONE', *, *, #48318, .T. ) ;
#81181 = CARTESIAN_POINT ( 'NONE',  ( -16.85414340794500276, -12.11081565061823717, 32.26097654155341843 ) ) ;
#81182 = AXIS2_PLACEMENT_3D ( 'NONE', #23848, #65731, #78807 ) ;
#81183 = ORIENTED_EDGE ( 'NONE', *, *, #21011, .F. ) ;
#81184 = DIRECTION ( 'NONE',  ( 0.000000000000000000, 0.9848077530122072432, -0.1736481776669354937 ) ) ;
#81185 = DIRECTION ( 'NONE',  ( 0.000000000000000000, 0.000000000000000000, 1.000000000000000000 ) ) ;
#81186 = EDGE_CURVE ( 'NONE', #12296, #33660, #47482, .T. ) ;
#81187 = ORIENTED_EDGE ( 'NONE', *, *, #11590, .F. ) ;
#81188 = CARTESIAN_POINT ( 'NONE',  ( -5.076923076923075762, -10.05456864172156806, 36.03766855953608683 ) ) ;
#81189 = CARTESIAN_POINT ( 'NONE',  ( -11.31568199719312773, -12.44528174975671853, 30.48912976160716681 ) ) ;
#81190 = LINE ( 'NONE', #5075, #69582 ) ;
#81191 = CARTESIAN_POINT ( 'NONE',  ( 11.40831356872984514, -12.50552854090298638, 31.33409797877408920 ) ) ;
#81192 = CARTESIAN_POINT ( 'NONE',  ( -1.384615384615383471, -10.67929555188718282, 33.92786785259544047 ) ) ;
#81193 = EDGE_CURVE ( 'NONE', #80774, #58760, #27155, .T. ) ;
#81194 = ORIENTED_EDGE ( 'NONE', *, *, #54353, .F. ) ;
#81195 = FACE_BOUND ( 'NONE', #68171, .T. ) ;
#81196 = VERTEX_POINT ( 'NONE', #68147 ) ;
#81197 = CARTESIAN_POINT ( 'NONE',  ( -5.999999999999998224, -2.538708090699994813, 30.37095296980875503 ) ) ;
#81198 = EDGE_CURVE ( 'NONE', #15501, #64772, #7336, .T. ) ;
#81199 = CARTESIAN_POINT ( 'NONE',  ( -15.23076923076922995, -1.790695186598648903, 34.54067556320373455 ) ) ;
#81200 = B_SPLINE_CURVE_WITH_KNOTS ( 'NONE', 3,
 ( #56854, #28967, #23506, #78451, #76695, #56423, #84796, #77136, #50536, #85227 ),
 .UNSPECIFIED., .F., .F.,
 ( 4, 2, 2, 2, 4 ),
 ( 0.0007817359430256388964, 0.0009771253907250075990, 0.001172514838424376085, 0.001367904286123744571, 0.001563293733823113273 ),
 .UNSPECIFIED. ) ;
#81201 = EDGE_CURVE ( 'NONE', #41602, #87319, #75653, .T. ) ;
#81202 = CARTESIAN_POINT ( 'NONE',  ( 18.22277954126840527, -12.24180327182771855, 31.33663988360758168 ) ) ;
#81203 = CARTESIAN_POINT ( 'NONE',  ( -2.307692307692305711, -2.721908614388771852, 31.22303859784724978 ) ) ;
#81204 = CARTESIAN_POINT ( 'NONE',  ( -5.999999999999998224, -12.10708131394839349, 31.69288490824020244 ) ) ;
#81205 = VERTEX_POINT ( 'NONE', #13638 ) ;
#81206 = ADVANCED_FACE ( 'NONE', ( #34792 ), #62260, .F. ) ;
#81207 = AXIS2_PLACEMENT_3D ( 'NONE', #81147, #53208, #88360 ) ;
#81208 = ORIENTED_EDGE ( 'NONE', *, *, #24656, .T. ) ;
#81209 = ORIENTED_EDGE ( 'NONE', *, *, #31031, .F. ) ;
#81210 = VERTEX_POINT ( 'NONE', #27596 ) ;
#81211 = CARTESIAN_POINT ( 'NONE',  ( -5.326946301144535489, -4.175268141568689195, 33.81360843649122216 ) ) ;
#81212 = CARTESIAN_POINT ( 'NONE',  ( -17.20761368003338987, -9.929715669179216775, 34.40415004197138416 ) ) ;
#81213 = CARTESIAN_POINT ( 'NONE',  ( -10.39237177129122003, -4.762714258010881885, 34.23016756924214832 ) ) ;
#81214 = CYLINDRICAL_SURFACE ( 'NONE', #47168, 0.2499999999999994726 ) ;
#81215 = CARTESIAN_POINT ( 'NONE',  ( -5.143006487878956534, -10.51840700105979387, 33.73612834413961536 ) ) ;
#81216 = DIRECTION ( 'NONE',  ( 0.000000000000000000, 0.000000000000000000, 1.000000000000000000 ) ) ;
#81217 = CARTESIAN_POINT ( 'NONE',  ( -5.076923076923197442, -4.481592998941358097, 33.73612834414048933 ) ) ;
#81218 = CARTESIAN_POINT ( 'NONE',  ( 17.07692307692307665, -2.538708090699994813, 30.37095296980875503 ) ) ;
#81219 = ORIENTED_EDGE ( 'NONE', *, *, #13032, .F. ) ;
#81220 = ADVANCED_FACE ( 'NONE', ( #48305 ), #7774, .F. ) ;
#81221 = ORIENTED_EDGE ( 'NONE', *, *, #33618, .T. ) ;
#81222 = VERTEX_POINT ( 'NONE', #85210 ) ;
#81224 = VERTEX_POINT ( 'NONE', #1898 ) ;
#81223 = CARTESIAN_POINT ( 'NONE',  ( 2.307692307692187583, -2.625532179533779154, 30.86335684631627174 ) ) ;
#81225 = ADVANCED_FACE ( 'NONE', ( #56836 ), #9979, .F. ) ;
#81227 = LINE ( 'NONE', #74912, #73647 ) ;
#81226 = DIRECTION ( 'NONE',  ( 1.000000000000000000, 0.000000000000000000, 0.000000000000000000 ) ) ;
#81228 = DIRECTION ( 'NONE',  ( 0.000000000000000000, 0.000000000000000000, -1.000000000000000000 ) ) ;
#81229 = CARTESIAN_POINT ( 'NONE',  ( -9.757578138268465651, -6.879047030191174805, 34.71129190930000163 ) ) ;
#81230 = FACE_BOUND ( 'NONE', #85312, .T. ) ;
#81231 = EDGE_LOOP ( 'NONE', ( #71991, #76588 ) ) ;
#81232 = VECTOR ( 'NONE', #68042, 1000.000000000000227 ) ;
#81233 = B_SPLINE_CURVE_WITH_KNOTS ( 'NONE', 3,
 ( #56780, #64857, #4505, #23434, #31983, #86498, #23866, #3607, #24773, #2708 ),
 .UNSPECIFIED., .F., .F.,
 ( 4, 2, 2, 2, 4 ),
 ( 0.000000000000000000, 0.0001954339857564091549, 0.0003908679715128183098, 0.0005863019572692274375, 0.0007817359430256366195 ),
 .UNSPECIFIED. ) ;
#81234 = VERTEX_POINT ( 'NONE', #23489 ) ;
#81235 = CARTESIAN_POINT ( 'NONE',  ( -5.076923076923075762, -6.386643153685126251, 34.62446782046654192 ) ) ;
#81236 = AXIS2_PLACEMENT_3D ( 'NONE', #21031, #82315, #35442 ) ;
#81237 = ORIENTED_EDGE ( 'NONE', *, *, #55980, .T. ) ;
#81238 = FACE_BOUND ( 'NONE', #44790, .T. ) ;
#81239 = CARTESIAN_POINT ( 'NONE',  ( -9.469528023329624844, -2.353885683473779800, 30.79025554430704403 ) ) ;
#81240 = AXIS2_PLACEMENT_3D ( 'NONE', #54060, #5893, #46426 ) ;
#81241 = CARTESIAN_POINT ( 'NONE',  ( -13.38461538461538325, -10.51840700105979565, 33.73612834413961536 ) ) ;
#81242 = VERTEX_POINT ( 'NONE', #36577 ) ;
#81243 = DIRECTION ( 'NONE',  ( -0.000000000000000000, 0.7660444431189791237, -0.6427876096865379196 ) ) ;
#81244 = CARTESIAN_POINT ( 'NONE',  ( -10.28846153846153832, -7.500000000000000000, 29.75000000000000355 ) ) ;
#81245 = CARTESIAN_POINT ( 'NONE',  ( -1.384615384615506484, -9.528491918059723176, 34.59228464037033035 ) ) ;
#81246 = ORIENTED_EDGE ( 'NONE', *, *, #52524, .T. ) ;
#81247 = DIRECTION ( 'NONE',  ( -0.000000000000000000, 1.000000000000000000, -0.000000000000000000 ) ) ;
#81248 = CARTESIAN_POINT ( 'NONE',  ( -7.623141002060451754, -8.282913670948747864, 34.94150082978203642 ) ) ;
#81249 = CARTESIAN_POINT ( 'NONE',  ( 6.673100192134570285, -12.41269422305637171, 30.68257228309993323 ) ) ;
#81250 = CARTESIAN_POINT ( 'NONE',  ( -17.86947456176635640, -12.70449254468099198, 30.44128974285582956 ) ) ;
#81251 = ORIENTED_EDGE ( 'NONE', *, *, #79194, .T. ) ;
#81252 = CARTESIAN_POINT ( 'NONE',  ( -14.30769230769230660, -1.129524287112498415, 32.06866353760679544 ) ) ;
#81253 = CARTESIAN_POINT ( 'NONE',  ( -5.076923076923197442, -3.300289026999228881, 32.46337939537708905 ) ) ;
#81254 = ORIENTED_EDGE ( 'NONE', *, *, #38343, .F. ) ;
#81255 = CARTESIAN_POINT ( 'NONE',  ( 3.361294669002876212, -6.808710257144159783, 34.95449254468098843 ) ) ;
#81256 = LINE ( 'NONE', #26302, #72777 ) ;
#81257 = CARTESIAN_POINT ( 'NONE',  ( -7.846153846153967493, -12.51329471203414379, 31.30864560766407578 ) ) ;
#81258 = CARTESIAN_POINT ( 'NONE',  ( 16.40379156322419973, -12.07971442181321997, 32.31769673815850297 ) ) ;
#81259 = CARTESIAN_POINT ( 'NONE',  ( -16.08777780284371772, -4.098570777380720287, 33.41473453929635440 ) ) ;
#81260 = CARTESIAN_POINT ( 'NONE',  ( 17.32697749683652688, -4.818054556918155207, 34.26375889529406749 ) ) ;
#81262 = CARTESIAN_POINT ( 'NONE',  ( 8.519254025182176449, -2.920706130388546651, 32.31842814019191223 ) ) ;
#81261 = CARTESIAN_POINT ( 'NONE',  ( 6.130525701763568591, -11.93748526763465279, 32.05452791011430946 ) ) ;
#81263 = EDGE_CURVE ( 'NONE', #84497, #78448, #50945, .T. ) ;
#81264 = EDGE_CURVE ( 'NONE', #65753, #1878, #49641, .T. ) ;
#81265 = CARTESIAN_POINT ( 'NONE',  ( -3.480745961711584791, -2.564618984488975961, 30.55390908950641915 ) ) ;
#81266 = CARTESIAN_POINT ( 'NONE',  ( -12.33074665371367473, -11.18335022499818621, 33.13157742990016885 ) ) ;
#81267 = CARTESIAN_POINT ( 'NONE',  ( 2.749999999999995115, -6.360912703473971419, 20.64062500000000000 ) ) ;
#81268 = ORIENTED_EDGE ( 'NONE', *, *, #31105, .F. ) ;
#81269 = CARTESIAN_POINT ( 'NONE',  ( -12.68502340526241312, -8.496056993536548418, 34.65000542017679663 ) ) ;
#81270 = ORIENTED_EDGE ( 'NONE', *, *, #16924, .F. ) ;
#81271 = ADVANCED_FACE ( 'NONE', ( #84332 ), #63595, .T. ) ;
#81272 = VERTEX_POINT ( 'NONE', #42450 ) ;
#81273 = DIRECTION ( 'NONE',  ( 0.000000000000000000, 0.8660254037844377084, -0.5000000000000015543 ) ) ;
#81274 = EDGE_CURVE ( 'NONE', #67767, #1369, #69913, .T. ) ;
#81275 = ORIENTED_EDGE ( 'NONE', *, *, #87379, .F. ) ;
#81276 = CARTESIAN_POINT ( 'NONE',  ( 1.607395053593450918, -12.11081565061823717, 32.26097654155341843 ) ) ;
#81277 = CARTESIAN_POINT ( 'NONE',  ( 1.139087296525997273, -4.749999999999992895, 20.48437500000000000 ) ) ;
#81278 = CARTESIAN_POINT ( 'NONE',  ( -10.61538461538461320, -3.513871655860378418, 32.76840700105978499 ) ) ;
#81279 = CARTESIAN_POINT ( 'NONE',  ( -8.899377978668987055, -3.285722584762969856, 32.44110544564090759 ) ) ;
#81280 = CARTESIAN_POINT ( 'NONE',  ( 9.692307692307695177, -9.058645607665452459, 34.76329471203371924 ) ) ;
#81281 = B_SPLINE_CURVE_WITH_KNOTS ( 'NONE', 3,
 ( #49832, #84526, #9307, #58353, #2091, #77750, #30450, #30887, #24130, #35891 ),
 .UNSPECIFIED., .F., .F.,
 ( 4, 2, 2, 2, 4 ),
 ( 0.000000000000000000, 0.0001954339857564073659, 0.0003908679715128147319, 0.0005863019572692221250, 0.0007817359430256294638 ),
 .UNSPECIFIED. ) ;
#81282 = AXIS2_PLACEMENT_3D ( 'NONE', #88258, #39616, #13450 ) ;
#81283 = CARTESIAN_POINT ( 'NONE',  ( -11.53846153846153655, -11.91647553114624181, 32.58852847137148245 ) ) ;
#81284 = DIRECTION ( 'NONE',  ( 1.000000000000000000, 0.000000000000000000, 0.000000000000000000 ) ) ;
#81285 = CARTESIAN_POINT ( 'NONE',  ( 0.000000000000000000, -11.00000000000000000, 29.75000000000000355 ) ) ;
#81286 = EDGE_CURVE ( 'NONE', #76991, #8812, #1488, .T. ) ;
#81287 = DIRECTION ( 'NONE',  ( 0.000000000000000000, 0.9848077530122072432, 0.1736481776669354937 ) ) ;
#81288 = CARTESIAN_POINT ( 'NONE',  ( 10.74617505635156789, -12.35292014791297710, 31.75344720912887198 ) ) ;
#81289 = CARTESIAN_POINT ( 'NONE',  ( 12.46153846153877609, -2.255955759149395501, 30.00000000000324363 ) ) ;
#81290 = EDGE_CURVE ( 'NONE', #33107, #77986, #15524, .T. ) ;
#81291 = CARTESIAN_POINT ( 'NONE',  ( 18.13004516283478296, -2.504778602574659896, 29.97347330155780654 ) ) ;
#81292 = ORIENTED_EDGE ( 'NONE', *, *, #11645, .T. ) ;
#81293 = EDGE_LOOP ( 'NONE', ( #62349, #3135 ) ) ;
#81294 = CARTESIAN_POINT ( 'NONE',  ( 14.30769230769231015, -8.164416787775445883, 34.95778746994557906 ) ) ;
#81295 = CARTESIAN_POINT ( 'NONE',  ( 5.142178648199100088, -9.442884908240271713, 34.35708131394835618 ) ) ;
#81296 = LINE ( 'NONE', #14153, #58413 ) ;
#81297 = EDGE_CURVE ( 'NONE', #81205, #50943, #20238, .T. ) ;
#81298 = LINE ( 'NONE', #79516, #77195 ) ;
#81299 = DIRECTION ( 'NONE',  ( 1.000000000000000000, 0.000000000000000000, 0.000000000000000000 ) ) ;
#81300 = CARTESIAN_POINT ( 'NONE',  ( -9.915234651214539952, -6.459968553980841577, 34.89616026154728701 ) ) ;
#81301 = DIRECTION ( 'NONE',  ( 0.000000000000000000, 0.9396926207859126468, -0.3420201433256571111 ) ) ;
#81302 = ORIENTED_EDGE ( 'NONE', *, *, #96, .F. ) ;
#81303 = CARTESIAN_POINT ( 'NONE',  ( -17.78205128205128105, -7.500000000000000000, 29.75000000000000355 ) ) ;
#81304 = ORIENTED_EDGE ( 'NONE', *, *, #30119, .T. ) ;
#81305 = EDGE_CURVE ( 'NONE', #70228, #52302, #44531, .T. ) ;
#81306 = ORIENTED_EDGE ( 'NONE', *, *, #23831, .T. ) ;
#81307 = DIRECTION ( 'NONE',  ( -0.000000000000000000, 0.6427876096865404731, -0.7660444431189770143 ) ) ;
#81308 = B_SPLINE_CURVE_WITH_KNOTS ( 'NONE', 3,
 ( #65084, #11050, #2942, #30427, #16031, #23223, #3391, #24105, #51555, #36741 ),
 .UNSPECIFIED., .F., .F.,
 ( 4, 2, 2, 2, 4 ),
 ( 0.000000000000000000, 0.0001954311564186868744, 0.0003908623128373737488, 0.0005862934692560606504, 0.0007817246256747474977 ),
 .UNSPECIFIED. ) ;
#81309 = B_SPLINE_CURVE_WITH_KNOTS ( 'NONE', 3,
 ( #76918, #15222, #1698, #17430, #50749, #17877, #58848, #86801, #58392, #44430 ),
 .UNSPECIFIED., .F., .F.,
 ( 4, 2, 2, 2, 4 ),
 ( 0.000000000000000000, 0.0001954311564186876334, 0.0003908623128373752667, 0.0005862934692560629272, 0.0007817246256747505334 ),
 .UNSPECIFIED. ) ;
#81310 = CARTESIAN_POINT ( 'NONE',  ( 3.930919936330005360, -2.554751324335733820, 30.48935550225260727 ) ) ;
#81311 = CARTESIAN_POINT ( 'NONE',  ( 11.76147289007438523, -10.61302985866384141, 33.66295027996417843 ) ) ;
#81312 = VECTOR ( 'NONE', #68348, 1000.000000000000000 ) ;
#81313 = DIRECTION ( 'NONE',  ( 0.000000000000000000, 0.000000000000000000, -1.000000000000000000 ) ) ;
#81314 = CYLINDRICAL_SURFACE ( 'NONE', #19182, 4.000000000000000000 ) ;
#81315 = EDGE_LOOP ( 'NONE', ( #76001, #34433, #20591, #8695 ) ) ;
#81316 = ADVANCED_FACE ( 'NONE', ( #8669 ), #70810, .F. ) ;
#81317 = VERTEX_POINT ( 'NONE', #43769 ) ;
#81318 = B_SPLINE_CURVE_WITH_KNOTS ( 'NONE', 3,
 ( #2599, #63425, #29219, #56673, #57552, #85042 ),
 .UNSPECIFIED., .F., .F.,
 ( 4, 2, 4 ),
 ( 0.0003909569690057776653, 0.0005862646681846002839, 0.0007815723673634227941 ),
 .UNSPECIFIED. ) ;
#81319 = ORIENTED_EDGE ( 'NONE', *, *, #78435, .F. ) ;
#81320 = ORIENTED_EDGE ( 'NONE', *, *, #56700, .F. ) ;
#81321 = EDGE_CURVE ( 'NONE', #64220, #1652, #71230, .T. ) ;
#81322 = CARTESIAN_POINT ( 'NONE',  ( 5.999999999999880096, -2.625532179533778709, 30.86335684631627174 ) ) ;
#81323 = DIRECTION ( 'NONE',  ( -0.000000000000000000, -0.9848077530122085754, -0.1736481776669273613 ) ) ;
#81324 = CARTESIAN_POINT ( 'NONE',  ( 14.08476534878545827, -2.523278758544489797, 31.42238647778637528 ) ) ;
#81325 = CARTESIAN_POINT ( 'NONE',  ( 16.15384615384615330, -9.780366693483667717, 34.19971097300155094 ) ) ;
#81326 = CARTESIAN_POINT ( 'NONE',  ( 8.519230769230768274, -7.500000000000001776, 34.75000000000000000 ) ) ;
#81327 = EDGE_LOOP ( 'NONE', ( #34868, #21533, #78620, #42529 ) ) ;
#81328 = EDGE_CURVE ( 'NONE', #22454, #2963, #76780, .T. ) ;
#81329 = ORIENTED_EDGE ( 'NONE', *, *, #23985, .F. ) ;
#81330 = VECTOR ( 'NONE', #35166, 1000.000000000000227 ) ;
#81332 = ORIENTED_EDGE ( 'NONE', *, *, #47975, .F. ) ;
#81331 = CARTESIAN_POINT ( 'NONE',  ( -10.39260507411620083, -11.89424750095246175, 32.13594075562311758 ) ) ;
#81333 = ADVANCED_FACE ( 'NONE', ( #58605 ), #5462, .F. ) ;
#81334 = CARTESIAN_POINT ( 'NONE',  ( -9.692307692307812417, -5.219633306517616589, 34.19971097300220464 ) ) ;
#81335 = CARTESIAN_POINT ( 'NONE',  ( -4.946131269098287930, -11.18335022499818621, 33.13157742990016885 ) ) ;
#81336 = EDGE_CURVE ( 'NONE', #30954, #10997, #18970, .T. ) ;
#81337 = CARTESIAN_POINT ( 'NONE',  ( -2.651650429449565305, -4.848349570550461785, 19.00000000000000000 ) ) ;
#81338 = VERTEX_POINT ( 'NONE', #38797 ) ;
#81339 = B_SPLINE_CURVE_WITH_KNOTS ( 'NONE', 3,
 ( #31271, #39377, #25403, #79904, #5132, #11005, #58285, #38477, #31722, #59181 ),
 .UNSPECIFIED., .F., .F.,
 ( 4, 2, 2, 2, 4 ),
 ( 0.000000000000000000, 0.0001954311564186876334, 0.0003908623128373752667, 0.0005862934692560629272, 0.0007817246256747505334 ),
 .UNSPECIFIED. ) ;
#81340 = CARTESIAN_POINT ( 'NONE',  ( -1.318548051265307608, -11.35647404775217595, 33.31231777344667222 ) ) ;
#81341 = ORIENTED_EDGE ( 'NONE', *, *, #46833, .F. ) ;
#81342 = CARTESIAN_POINT ( 'NONE',  ( 2.307692307692187583, -6.879047030192662504, 34.71129190930017927 ) ) ;
#81343 = CARTESIAN_POINT ( 'NONE',  ( -17.07692307692307665, -1.790695186598648903, 34.54067556320373455 ) ) ;
#81344 = CARTESIAN_POINT ( 'NONE',  ( -12.23852710992561299, -12.39991518177334129, 30.74647679643404530 ) ) ;
#81345 = CARTESIAN_POINT ( 'NONE',  ( -7.173100160369886957, -3.711651800289232916, 33.01384336483936011 ) ) ;
#81346 = CARTESIAN_POINT ( 'NONE',  ( 8.545745825506822158, -5.113361153441934093, 34.14387501736622710 ) ) ;
#81347 = ORIENTED_EDGE ( 'NONE', *, *, #45959, .T. ) ;
#81348 = CARTESIAN_POINT ( 'NONE',  ( -18.00000000000000000, -13.34771219727535474, 34.33046132563154629 ) ) ;
#81349 = CARTESIAN_POINT ( 'NONE',  ( 8.900021210197715860, -8.191423895709840863, 34.95447573519442130 ) ) ;
#81350 = CARTESIAN_POINT ( 'NONE',  ( 14.05766908347085220, -9.356822207818506598, 34.66110646841856635 ) ) ;
#81351 = ORIENTED_EDGE ( 'NONE', *, *, #68822, .F. ) ;
#81352 = CARTESIAN_POINT ( 'NONE',  ( -9.692307692307691624, -4.661471528628507777, 34.16647553114623292 ) ) ;
#81353 = CARTESIAN_POINT ( 'NONE',  ( -7.780898274877820597, -11.48612834413965977, 32.76840700105972815 ) ) ;
#81354 = CARTESIAN_POINT ( 'NONE',  ( 17.14217864819910275, -10.21337939537593797, 33.94971097300152252 ) ) ;
#81355 = CARTESIAN_POINT ( 'NONE',  ( -2.084679463598910765, -9.172514111537584114, 34.72667873470787470 ) ) ;
#81356 = CARTESIAN_POINT ( 'NONE',  ( 14.30769230769218581, -11.67786785259630911, 32.92929555188603530 ) ) ;
#81357 = AXIS2_PLACEMENT_3D ( 'NONE', #82437, #13515, #2528 ) ;
#81358 = FACE_BOUND ( 'NONE', #39561, .T. ) ;
#81360 = DIRECTION ( 'NONE',  ( -0.000000000000000000, 0.9396926207859093161, -0.3420201433256663259 ) ) ;
#81359 = CARTESIAN_POINT ( 'NONE',  ( 1.449760165335018725, -7.750023224968865421, 34.99404313364389907 ) ) ;
#81361 = CARTESIAN_POINT ( 'NONE',  ( -15.00775638667583678, -4.762714258010881885, 34.23016756924214832 ) ) ;
#81363 = CARTESIAN_POINT ( 'NONE',  ( -2.057746898314263717, -8.476813868363244353, 34.90874843262270133 ) ) ;
#81362 = CARTESIAN_POINT ( 'NONE',  ( 3.100158871144702122, -7.722926236386453702, 34.74524107206102030 ) ) ;
#81364 = CARTESIAN_POINT ( 'NONE',  ( 13.16168842570853670, -2.523278758544489797, 31.42238647778637528 ) ) ;
#81365 = CARTESIAN_POINT ( 'NONE',  ( -1.901340078031346525, -9.487747218494661183, 17.18563170625848713 ) ) ;
#81366 = VERTEX_POINT ( 'NONE', #45095 ) ;
#81367 = B_SPLINE_CURVE_WITH_KNOTS ( 'NONE', 3,
 ( #12228, #68066, #33824, #40596, #34267, #19427, #18987, #46453, #46891, #6371 ),
 .UNSPECIFIED., .F., .F.,
 ( 4, 2, 2, 2, 4 ),
 ( 0.000000000000000000, 0.0001954311564186866034, 0.0003908623128373732067, 0.0005862934692560597830, 0.0007817246256747464135 ),
 .UNSPECIFIED. ) ;
#81368 = CARTESIAN_POINT ( 'NONE',  ( 10.54930223602448258, -11.91647553114624181, 32.58852847137148245 ) ) ;
#81369 = ORIENTED_EDGE ( 'NONE', *, *, #8394, .F. ) ;
#81370 = B_SPLINE_CURVE_WITH_KNOTS ( 'NONE', 3,
 ( #74042, #60515, #25402, #24057, #44766, #17309, #73145, #51506, #31721, #59179 ),
 .UNSPECIFIED., .F., .F.,
 ( 4, 2, 2, 2, 4 ),
 ( 0.0007817246336856289524, 0.0009771112958940101571, 0.001172497958102391253, 0.001367884620310772350, 0.001563271282519153446 ),
 .UNSPECIFIED. ) ;
#81371 = CARTESIAN_POINT ( 'NONE',  ( -18.22292695890684655, -3.395401636524181477, 33.02366814457251110 ) ) ;
#81372 = ORIENTED_EDGE ( 'NONE', *, *, #33771, .T. ) ;
#81373 = CARTESIAN_POINT ( 'NONE',  ( 2.084207383127978375, -2.353723527008296568, 30.78948104536958752 ) ) ;
#81374 = CARTESIAN_POINT ( 'NONE',  ( -19.50000000000000000, -11.50000000000000000, 29.75000000000000355 ) ) ;
#81377 = VERTEX_POINT ( 'NONE', #10436 ) ;
#81376 = VECTOR ( 'NONE', #58042, 1000.000000000000227 ) ;
#81375 = CARTESIAN_POINT ( 'NONE',  ( 15.00790380856559025, -2.501496062324912284, 29.88072118266895671 ) ) ;
#81378 = CARTESIAN_POINT ( 'NONE',  ( -10.55012947587177763, -12.16647553114626490, 32.15551576947920864 ) ) ;
#81379 = CARTESIAN_POINT ( 'NONE',  ( 1.319345384059066317, -12.16647553114622049, 32.15551576947930812 ) ) ;
#81380 = CARTESIAN_POINT ( 'NONE',  ( -3.724691934501229262, -9.114399933863657211, 26.01375670625848713 ) ) ;
#81381 = FACE_OUTER_BOUND ( 'NONE', #4927, .T. ) ;
#81382 = CARTESIAN_POINT ( 'NONE',  ( 8.769230769230645706, -2.657715359629662544, 31.77849191805970364 ) ) ;
#81383 = CARTESIAN_POINT ( 'NONE',  ( -12.21148404162501144, -9.233818618650603938, 34.70587769442853698 ) ) ;
#81384 = CARTESIAN_POINT ( 'NONE',  ( -18.00000000000000000, -1.248569425608316630, 32.29137909377919868 ) ) ;
#81385 = CARTESIAN_POINT ( 'NONE',  ( -0.2387589202700519386, -4.387253974876676565, 33.66317474335728832 ) ) ;
#81386 = CARTESIAN_POINT ( 'NONE',  ( 1.607628228708781304, -10.01129605718032778, 34.36064277460058491 ) ) ;
#81387 = EDGE_CURVE ( 'NONE', #27582, #41890, #13286, .T. ) ;
#81388 = CARTESIAN_POINT ( 'NONE',  ( 3.724691934501251023, -9.114399933863618131, 17.29874329374151642 ) ) ;
#81389 = CARTESIAN_POINT ( 'NONE',  ( 14.05771557674995265, -5.728515186090277211, 34.42611988154120439 ) ) ;
#81390 = DIRECTION ( 'NONE',  ( -0.000000000000000000, 1.000000000000000000, -0.000000000000000000 ) ) ;
#81391 = ORIENTED_EDGE ( 'NONE', *, *, #52044, .F. ) ;
#81392 = EDGE_CURVE ( 'NONE', #85470, #50608, #34563, .T. ) ;
#81393 = CYLINDRICAL_SURFACE ( 'NONE', #11114, 0.2500000000000009437 ) ;
#81394 = DIRECTION ( 'NONE',  ( -0.000000000000000000, 0.5000000000000011102, -0.8660254037844380415 ) ) ;
#81395 = CARTESIAN_POINT ( 'NONE',  ( 1.492201783934598236, -11.27530806549875031, 21.20499329374151998 ) ) ;
#81396 = CARTESIAN_POINT ( 'NONE',  ( -18.00000000000000000, -12.37446782046654192, 30.86335684631486131 ) ) ;
#81397 = CARTESIAN_POINT ( 'NONE',  ( -16.15384615384627409, -11.06231777344772027, 33.60647404775119895 ) ) ;
#81398 = ORIENTED_EDGE ( 'NONE', *, *, #87812, .T. ) ;
#81399 = CARTESIAN_POINT ( 'NONE',  ( 1.384615384615386802, -13.49023893513002648, 31.06009739812518688 ) ) ;
#81400 = CARTESIAN_POINT ( 'NONE',  ( -14.37296275365308418, -11.48612834413959582, 32.76840700105983473 ) ) ;
#81402 = ORIENTED_EDGE ( 'NONE', *, *, #207, .T. ) ;
#81401 = CARTESIAN_POINT ( 'NONE',  ( -17.32692307692307665, -7.433931650972299465, 34.75000000000000711 ) ) ;
#81403 = CYLINDRICAL_SURFACE ( 'NONE', #51239, 4.000000000000000000 ) ;
#81404 = CARTESIAN_POINT ( 'NONE',  ( 2.057669070399344768, -12.43535235679832596, 30.55408501211184813 ) ) ;
#81406 = EDGE_CURVE ( 'NONE', #14199, #56137, #25279, .T. ) ;
#81405 = CARTESIAN_POINT ( 'NONE',  ( -12.68446542044531178, -4.762599654559228846, 34.23009711892697737 ) ) ;
#81407 = ORIENTED_EDGE ( 'NONE', *, *, #88503, .F. ) ;
#81408 = CARTESIAN_POINT ( 'NONE',  ( -9.626240358957616650, -2.486705287966280320, 31.30864560766543647 ) ) ;
#81409 = CARTESIAN_POINT ( 'NONE',  ( -15.23076923076935252, -11.67786785259630911, 32.92929555188603530 ) ) ;
#81410 = DIRECTION ( 'NONE',  ( 0.000000000000000000, 0.000000000000000000, 1.000000000000000000 ) ) ;
#81411 = VERTEX_POINT ( 'NONE', #73479 ) ;
#81412 = ORIENTED_EDGE ( 'NONE', *, *, #70751, .T. ) ;
#81413 = ORIENTED_EDGE ( 'NONE', *, *, #21764, .T. ) ;
#81414 = EDGE_CURVE ( 'NONE', #29059, #31685, #78881, .T. ) ;
#81415 = ORIENTED_EDGE ( 'NONE', *, *, #28972, .T. ) ;
#81416 = CARTESIAN_POINT ( 'NONE',  ( 12.59232890250541281, -9.929761469519743144, 34.40412654351204225 ) ) ;
#81417 = CARTESIAN_POINT ( 'NONE',  ( -6.923076923077044142, -3.300289026999228881, 32.46337939537708905 ) ) ;
#81418 = EDGE_CURVE ( 'NONE', #25833, #77581, #79811, .T. ) ;
#81419 = CARTESIAN_POINT ( 'NONE',  ( -7.846153846153967493, -12.70778746994576025, 30.41441678777401236 ) ) ;
#81420 = CYLINDRICAL_SURFACE ( 'NONE', #48110, 4.000000000000000000 ) ;
#81421 = CARTESIAN_POINT ( 'NONE',  ( -17.01166750564705055, -5.219633306516380244, 34.19971097300157936 ) ) ;
#81422 = ORIENTED_EDGE ( 'NONE', *, *, #68753, .T. ) ;
#81423 = VECTOR ( 'NONE', #12440, 1000.000000000000000 ) ;
#81424 = VERTEX_POINT ( 'NONE', #10878 ) ;
#81425 = EDGE_CURVE ( 'NONE', #30965, #66553, #48692, .T. ) ;
#81426 = EDGE_LOOP ( 'NONE', ( #53503, #57314 ) ) ;
#81428 = VERTEX_POINT ( 'NONE', #18082 ) ;
#81427 = CARTESIAN_POINT ( 'NONE',  ( -3.100724067934452322, -2.504778602574659896, 29.97347330155780298 ) ) ;
#81429 = CARTESIAN_POINT ( 'NONE',  ( -6.700297254098854793, -4.226511098958374291, 33.85474049983370293 ) ) ;
#81430 = CARTESIAN_POINT ( 'NONE',  ( 6.130790440966952026, -2.494656445102013453, 31.33466734024120015 ) ) ;
#81431 = FACE_OUTER_BOUND ( 'NONE', #38755, .T. ) ;
#81432 = CARTESIAN_POINT ( 'NONE',  ( 16.09615384615384670, -11.50000000000000000, 29.75000000000000355 ) ) ;
#81433 = AXIS2_PLACEMENT_3D ( 'NONE', #13647, #27161, #82117 ) ;
#81434 = ORIENTED_EDGE ( 'NONE', *, *, #45999, .F. ) ;
#81435 = EDGE_CURVE ( 'NONE', #52641, #63049, #32927, .T. ) ;
#81436 = VERTEX_POINT ( 'NONE', #69374 ) ;
#81437 = B_SPLINE_CURVE_WITH_KNOTS ( 'NONE', 3,
 ( #5313, #12514, #60246, #87753, #88200, #53487, #40000, #83194, #41764, #16054 ),
 .UNSPECIFIED., .F., .F.,
 ( 4, 2, 2, 2, 4 ),
 ( 0.000000000000000000, 0.0001954339857564070678, 0.0003908679715128141356, 0.0005863019572692211492, 0.0007817359430256282712 ),
 .UNSPECIFIED. ) ;
#81438 = VERTEX_POINT ( 'NONE', #472 ) ;
#81439 = CARTESIAN_POINT ( 'NONE',  ( 10.74591031714818357, -10.88167719472716399, 33.43325721877153711 ) ) ;
#81441 = ORIENTED_EDGE ( 'NONE', *, *, #37397, .F. ) ;
#81440 = CARTESIAN_POINT ( 'NONE',  ( -2.373775718648187372, -2.721908614388772296, 31.22303859784724622 ) ) ;
#81442 = LINE ( 'NONE', #87773, #80554 ) ;
#81443 = EDGE_CURVE ( 'NONE', #65658, #51461, #8979, .T. ) ;
#81444 = ADVANCED_FACE ( 'NONE', ( #33809 ), #61711, .F. ) ;
#81445 = CARTESIAN_POINT ( 'NONE',  ( -14.43838377435986686, -2.541943142973491554, 30.39792223712631980 ) ) ;
#81446 = ORIENTED_EDGE ( 'NONE', *, *, #12795, .F. ) ;
#81447 = DIRECTION ( 'NONE',  ( 0.000000000000000000, 0.8660254037844377084, 0.5000000000000015543 ) ) ;
#81448 = LINE ( 'NONE', #61594, #26392 ) ;
#81449 = CARTESIAN_POINT ( 'NONE',  ( 4.284637961670938466, -2.729792928343270919, 31.24908615093345077 ) ) ;
#81450 = FACE_BOUND ( 'NONE', #84329, .T. ) ;
#81451 = EDGE_CURVE ( 'NONE', #34858, #4333, #68048, .T. ) ;
#81452 = CARTESIAN_POINT ( 'NONE',  ( -0.6850234052624104564, -10.11188796281391511, 34.01382737946119050 ) ) ;
#81453 = PLANE ( 'NONE',  #67273 ) ;
#81454 = DIRECTION ( 'NONE',  ( 0.000000000000000000, 0.7660444431189822323, -0.6427876096865344779 ) ) ;
#81456 = CARTESIAN_POINT ( 'NONE',  ( 6.923076923076924238, -10.67929555188718282, 33.92786785259544047 ) ) ;
#81455 = CARTESIAN_POINT ( 'NONE',  ( 0.4615384615384611200, -6.343179335718451384, 34.87096338111211935 ) ) ;
#81457 = CARTESIAN_POINT ( 'NONE',  ( -5.011667505647053211, -10.90142922261932057, 33.41473453929631887 ) ) ;
#81458 = DIRECTION ( 'NONE',  ( -0.000000000000000000, -0.000000000000000000, -1.000000000000000000 ) ) ;
#81459 = ORIENTED_EDGE ( 'NONE', *, *, #59881, .F. ) ;
#81460 = CARTESIAN_POINT ( 'NONE',  ( 2.530471848960718084, -6.760870238392817200, 34.69528174975672385 ) ) ;
#81461 = CARTESIAN_POINT ( 'NONE',  ( 14.30769230769218758, -10.21337939537710326, 33.94971097300076224 ) ) ;
#81462 = EDGE_LOOP ( 'NONE', ( #45964, #9012, #4854, #77842 ) ) ;
#81463 = EDGE_LOOP ( 'NONE', ( #28328, #5192, #36448, #74440 ) ) ;
#81464 = AXIS2_PLACEMENT_3D ( 'NONE', #77828, #85927, #63871 ) ;
#81465 = DIRECTION ( 'NONE',  ( 1.000000000000000000, 0.000000000000000000, 0.000000000000000000 ) ) ;
#81466 = CARTESIAN_POINT ( 'NONE',  ( -14.37377571864818293, -4.786620604624113540, 33.94971097300155805 ) ) ;
#81467 = CARTESIAN_POINT ( 'NONE',  ( 12.39626846098214052, -11.06231777344662781, 33.60647404775220082 ) ) ;
#81468 = ORIENTED_EDGE ( 'NONE', *, *, #42881, .T. ) ;
#81469 = CARTESIAN_POINT ( 'NONE',  ( -15.23076923076922995, -1.629998284177014645, 34.34916445242399163 ) ) ;
#81470 = DIRECTION ( 'NONE',  ( 0.000000000000000000, 0.1736481776669275834, 0.9848077530122086864 ) ) ;
#81471 = FACE_BOUND ( 'NONE', #74792, .T. ) ;
#81473 = CYLINDRICAL_SURFACE ( 'NONE', #43053, 0.2499999999999997502 ) ;
#81472 = CARTESIAN_POINT ( 'NONE',  ( -16.94613126909829148, -4.118422570099827595, 33.43335022499816489 ) ) ;
#81474 = CARTESIAN_POINT ( 'NONE',  ( 10.54930120442873687, -8.120952969808774569, 34.71129190930000163 ) ) ;
#81475 = CARTESIAN_POINT ( 'NONE',  ( 2.307692307692309264, -4.786620604624113540, 33.94971097300155094 ) ) ;
#81477 = LINE ( 'NONE', #34157, #10390 ) ;
#81476 = DIRECTION ( 'NONE',  ( 1.000000000000000000, 0.000000000000000000, 0.000000000000000000 ) ) ;
#81478 = CARTESIAN_POINT ( 'NONE',  ( -1.553300858899081538, -11.25000000000000711, 19.85937500000000355 ) ) ;
#81479 = ORIENTED_EDGE ( 'NONE', *, *, #68033, .F. ) ;
#81480 = ORIENTED_EDGE ( 'NONE', *, *, #57046, .T. ) ;
#81481 = B_SPLINE_CURVE_WITH_KNOTS ( 'NONE', 3,
 ( #17001, #24194, #10693, #71942, #37712, #30946, #38159, #3918, #58873, #86373 ),
 .UNSPECIFIED., .F., .F.,
 ( 4, 2, 2, 2, 4 ),
 ( 0.0007817246256747453293, 0.0009771112852218889842, 0.001172497944769032747, 0.001367884604316176294, 0.001563271263863320057 ),
 .UNSPECIFIED. ) ;
#81482 = DIRECTION ( 'NONE',  ( -0.000000000000000000, -0.000000000000000000, -1.000000000000000000 ) ) ;
#81483 = CARTESIAN_POINT ( 'NONE',  ( 12.59237687955122453, -7.277220443632450575, 34.74524770363009196 ) ) ;
#81484 = CARTESIAN_POINT ( 'NONE',  ( -10.61538461538473399, -12.27809138561165270, 31.22303859784587132 ) ) ;
#81486 = B_SPLINE_CURVE_WITH_KNOTS ( 'NONE', 3,
 ( #7851, #21355, #20474, #82635, #7409, #35312, #41193, #27228, #20907, #33983 ),
 .UNSPECIFIED., .F., .F.,
 ( 4, 2, 2, 2, 4 ),
 ( 0.0007817246256747464135, 0.0009771112852218900684, 0.001172497944769033615, 0.001367884604316177161, 0.001563271263863320925 ),
 .UNSPECIFIED. ) ;
#81485 = CARTESIAN_POINT ( 'NONE',  ( 17.20696813284285298, -2.254550872974305786, 29.97347326024527092 ) ) ;
#81487 = CARTESIAN_POINT ( 'NONE',  ( 17.07692307692307665, -11.11383981884818262, 36.00935417666054406 ) ) ;
#81488 = CARTESIAN_POINT ( 'NONE',  ( -3.749999999999997335, -7.500000000000021316, 21.34375000000000000 ) ) ;
#81489 = CARTESIAN_POINT ( 'NONE',  ( -8.835313148590904220, -9.905515769479276145, 34.41647553114623292 ) ) ;
#81490 = CARTESIAN_POINT ( 'NONE',  ( 5.777073041093149897, -2.889293201056495786, 32.26117774369186009 ) ) ;
#81491 = CARTESIAN_POINT ( 'NONE',  ( -15.48076923076922995, -2.249999999999998668, 29.75000000000000355 ) ) ;
#81492 = CARTESIAN_POINT ( 'NONE',  ( 10.74617505635156789, -3.338503747796866872, 32.95102852606553512 ) ) ;
#81493 = CARTESIAN_POINT ( 'NONE',  ( -6.249976730942353065, -2.779195860258147022, 31.39871582349836743 ) ) ;
#81494 = CARTESIAN_POINT ( 'NONE',  ( -8.352564102564102200, -11.50000000000000000, 29.75000000000000355 ) ) ;
#81495 = CARTESIAN_POINT ( 'NONE',  ( -3.454254155333559950, -10.23692288466677880, 34.23039457007281072 ) ) ;
#81496 = VECTOR ( 'NONE', #56328, 1000.000000000000227 ) ;
#81497 = CARTESIAN_POINT ( 'NONE',  ( 2.177082652488226078, -7.722926974430166069, 34.99546784045485737 ) ) ;
#81498 = CARTESIAN_POINT ( 'NONE',  ( -15.36146069743678844, -9.804603061927743113, 34.18744698557895845 ) ) ;
#81499 = ORIENTED_EDGE ( 'NONE', *, *, #22476, .T. ) ;
#81500 = LINE ( 'NONE', #53565, #21141 ) ;
#81501 = CARTESIAN_POINT ( 'NONE',  ( -25.00000000000000000, -10.00000000000000533, 13.00000000000000178 ) ) ;
#81502 = CARTESIAN_POINT ( 'NONE',  ( 2.750000000000002665, -7.561099074964516831, 15.97061829374151287 ) ) ;
#81503 = CARTESIAN_POINT ( 'NONE',  ( -0.3954711281883860341, -10.67929555188718282, 33.92786785259544757 ) ) ;
#81504 = CARTESIAN_POINT ( 'NONE',  ( -8.769230769230768274, -13.53365097954675988, 30.81389545987213552 ) ) ;
#81505 = CYLINDRICAL_SURFACE ( 'NONE', #1091, 0.2500000000000008882 ) ;
#81507 = ORIENTED_EDGE ( 'NONE', *, *, #24065, .F. ) ;
#81506 = CARTESIAN_POINT ( 'NONE',  ( -0.3962828902624367933, -2.625532179533470067, 30.86335684631491105 ) ) ;
#81508 = CARTESIAN_POINT ( 'NONE',  ( 2.749999999999995115, -6.360912703473971419, 23.14062499999999645 ) ) ;
#81509 = DIRECTION ( 'NONE',  ( -1.000000000000000000, -0.000000000000000000, -0.000000000000000000 ) ) ;
#81510 = VECTOR ( 'NONE', #82724, 1000.000000000000000 ) ;
#81511 = VERTEX_POINT ( 'NONE', #20736 ) ;
#81512 = CARTESIAN_POINT ( 'NONE',  ( 8.546304551714619890, -8.239355502252617924, 34.69524867566427417 ) ) ;
#81513 = CARTESIAN_POINT ( 'NONE',  ( 18.13052570176356681, -9.417988943895561960, 34.36773134775778260 ) ) ;
#81514 = ORIENTED_EDGE ( 'NONE', *, *, #58838, .F. ) ;
#81515 = CARTESIAN_POINT ( 'NONE',  ( -10.61538461538461320, -5.471508081941601098, 34.59228464037088457 ) ) ;
#81516 = CARTESIAN_POINT ( 'NONE',  ( -14.98076923076781064, -7.500000000000154543, 35.00000000000007105 ) ) ;
#81517 = B_SPLINE_CURVE_WITH_KNOTS ( 'NONE', 3,
 ( #35170, #82924, #48676, #69405, #56330, #942, #84261, #15795, #63071, #77484 ),
 .UNSPECIFIED., .F., .F.,
 ( 4, 2, 2, 2, 4 ),
 ( 0.000000000000000000, 0.0001954339857564093717, 0.0003908679715128187434, 0.0005863019572692280881, 0.0007817359430256374869 ),
 .UNSPECIFIED. ) ;
#81518 = DIRECTION ( 'NONE',  ( -1.000000000000000000, -0.000000000000000000, 0.000000000000000000 ) ) ;
#81519 = ORIENTED_EDGE ( 'NONE', *, *, #8956, .F. ) ;
#81520 = VECTOR ( 'NONE', #36411, 1000.000000000000227 ) ;
#81521 = ORIENTED_EDGE ( 'NONE', *, *, #67195, .F. ) ;
#81522 = EDGE_CURVE ( 'NONE', #16211, #63956, #47576, .T. ) ;
#81523 = ORIENTED_EDGE ( 'NONE', *, *, #57599, .T. ) ;
#81524 = CARTESIAN_POINT ( 'NONE',  ( 3.480823650682685511, -12.01375889529407637, 32.43194544308182969 ) ) ;
#81525 = CARTESIAN_POINT ( 'NONE',  ( 6.923076923076800782, -11.67786785259630911, 32.92929555188603530 ) ) ;
#81526 = CIRCLE ( 'NONE', #84413, 6.614378277661474570 ) ;
#81527 = CARTESIAN_POINT ( 'NONE',  ( -10.55012904410858532, -6.879047030191282275, 34.71129190930002295 ) ) ;
#81528 = CARTESIAN_POINT ( 'NONE',  ( -1.608100309179715026, -11.60425143139329940, 33.02411095842164457 ) ) ;
#81529 = B_SPLINE_CURVE_WITH_KNOTS ( 'NONE', 3,
 ( #70728, #3134, #85567, #23841, #78799, #67079, #25644, #39620, #10796, #25197 ),
 .UNSPECIFIED., .F., .F.,
 ( 4, 2, 2, 2, 4 ),
 ( 0.000000000000000000, 0.0001954311564186868473, 0.0003908623128373736946, 0.0005862934692560605419, 0.0007817246256747473893 ),
 .UNSPECIFIED. ) ;
#81530 = DIRECTION ( 'NONE',  ( -0.000000000000000000, -0.7660444431189791237, -0.6427876096865379196 ) ) ;
#81531 = CARTESIAN_POINT ( 'NONE',  ( 9.758375025657770152, -9.905515769479276145, 34.41647553114623292 ) ) ;
#81532 = CYLINDRICAL_SURFACE ( 'NONE', #52408, 0.2499999999999994726 ) ;
#81533 = VECTOR ( 'NONE', #83511, 999.9999999999998863 ) ;
#81534 = CARTESIAN_POINT ( 'NONE',  ( -7.846153846153844924, -1.951392089020283160, 34.73218667398347748 ) ) ;
#81535 = ORIENTED_EDGE ( 'NONE', *, *, #24687, .T. ) ;
#81536 = EDGE_CURVE ( 'NONE', #44047, #41209, #61263, .T. ) ;
#81537 = EDGE_LOOP ( 'NONE', ( #27150, #80005 ) ) ;
#81539 = ORIENTED_EDGE ( 'NONE', *, *, #4229, .T. ) ;
#81538 = CARTESIAN_POINT ( 'NONE',  ( -0.2387589202700515223, -12.24180327182771855, 31.33663988360758168 ) ) ;
#81540 = B_SPLINE_CURVE_WITH_KNOTS ( 'NONE', 3,
 ( #58054, #2656, #24261, #36468, #57616, #85538, #71126, #51724, #29715, #85099 ),
 .UNSPECIFIED., .F., .F.,
 ( 4, 2, 2, 2, 4 ),
 ( 0.000000000000000000, 0.0001954339881912775425, 0.0003908679763825550850, 0.0005863019645738326005, 0.0007817359527651101701 ),
 .UNSPECIFIED. ) ;
#81541 = DIRECTION ( 'NONE',  ( 0.000000000000000000, 0.000000000000000000, 1.000000000000000000 ) ) ;
#81542 = CARTESIAN_POINT ( 'NONE',  ( 11.66898724022510336, -12.27024696741798770, 31.24895572276497546 ) ) ;
#81543 = ORIENTED_EDGE ( 'NONE', *, *, #46223, .T. ) ;
#81544 = CARTESIAN_POINT ( 'NONE',  ( -8.769230769230892619, -4.320704448113951379, 33.92786785259630022 ) ) ;
#81545 = ORIENTED_EDGE ( 'NONE', *, *, #5963, .F. ) ;
#81546 = CARTESIAN_POINT ( 'NONE',  ( 11.76124107972994537, -2.600157965045224895, 30.74683119005207743 ) ) ;
#81547 = ORIENTED_EDGE ( 'NONE', *, *, #20221, .F. ) ;
#81548 = CARTESIAN_POINT ( 'NONE',  ( -12.68441797827604667, -7.630690623152299956, 34.99857592706774057 ) ) ;
#81549 = EDGE_CURVE ( 'NONE', #28353, #46262, #49810, .T. ) ;
#81550 = ADVANCED_FACE ( 'NONE', ( #14421 ), #26166, .F. ) ;
#81551 = CARTESIAN_POINT ( 'NONE',  ( 4.153846153846154188, -10.67929555188718282, 33.92786785259544047 ) ) ;
#81552 = CARTESIAN_POINT ( 'NONE',  ( -9.019254006523736322, -2.823816976329319051, 31.52131813110795733 ) ) ;
#81553 = VECTOR ( 'NONE', #68008, 1000.000000000000000 ) ;
#81554 = FACE_BOUND ( 'NONE', #70906, .T. ) ;
#81555 = DIRECTION ( 'NONE',  ( -0.000000000000000000, -0.000000000000000000, -1.000000000000000000 ) ) ;
#81556 = CARTESIAN_POINT ( 'NONE',  ( -2.307692307692428724, -4.320704448113951379, 33.92786785259630022 ) ) ;
#81557 = CARTESIAN_POINT ( 'NONE',  ( -8.769230769230768274, -1.242168528481310874, 33.36296068462461051 ) ) ;
#81558 = CARTESIAN_POINT ( 'NONE',  ( 10.03846153846153832, -4.000000000000000000, 28.25000000000000000 ) ) ;
#81559 = CARTESIAN_POINT ( 'NONE',  ( -13.38461538461538325, -9.905515769479276145, 34.41647553114623292 ) ) ;
#81560 = CARTESIAN_POINT ( 'NONE',  ( 16.02315468717859304, -4.118384482072086072, 33.43331474514187107 ) ) ;
#81561 = AXIS2_PLACEMENT_3D ( 'NONE', #24509, #79911, #87134 ) ;
#81562 = CARTESIAN_POINT ( 'NONE',  ( -10.48485891362105171, -4.459921816937791661, 33.71989282347011851 ) ) ;
#81563 = EDGE_CURVE ( 'NONE', #71146, #64437, #19408, .T. ) ;
#81564 = VERTEX_POINT ( 'NONE', #5901 ) ;
#81565 = ORIENTED_EDGE ( 'NONE', *, *, #87763, .F. ) ;
#81567 = CARTESIAN_POINT ( 'NONE',  ( -14.05763799605399278, -12.41262288849542017, 30.68299917996395010 ) ) ;
#81566 = CARTESIAN_POINT ( 'NONE',  ( -5.143005456283213483, -11.91647553114624181, 32.58852847137148245 ) ) ;
#81568 = CARTESIAN_POINT ( 'NONE',  ( -4.219169069338327915, -7.749976743299137993, 34.99404534957040624 ) ) ;
#81569 = CARTESIAN_POINT ( 'NONE',  ( -17.78205128205128105, -3.499999999999999556, 29.75000000000000355 ) ) ;
#81570 = CARTESIAN_POINT ( 'NONE',  ( 8.546351252493185058, -7.630690623152299956, 34.99857592706774057 ) ) ;
#81571 = LINE ( 'NONE', #12662, #64821 ) ;
#81572 = ORIENTED_EDGE ( 'NONE', *, *, #45014, .F. ) ;
#81573 = CARTESIAN_POINT ( 'NONE',  ( 2.307692307692309264, -8.973038597847269315, 34.52809138561121927 ) ) ;
#81574 = LINE ( 'NONE', #54524, #58861 ) ;
#81575 = DIRECTION ( 'NONE',  ( 1.000000000000000000, 0.000000000000000000, 0.000000000000000000 ) ) ;
#81576 = DIRECTION ( 'NONE',  ( 0.000000000000000000, 0.9396926207859126468, -0.3420201433256571111 ) ) ;
#81577 = ORIENTED_EDGE ( 'NONE', *, *, #87121, .F. ) ;
#81578 = ORIENTED_EDGE ( 'NONE', *, *, #87020, .F. ) ;
#81579 = ORIENTED_EDGE ( 'NONE', *, *, #85476, .T. ) ;
#81580 = VECTOR ( 'NONE', #14411, 1000.000000000000114 ) ;
#81581 = CARTESIAN_POINT ( 'NONE',  ( -17.07692307692307665, -1.129524287112498415, 32.06866353760679544 ) ) ;
#81582 = VERTEX_POINT ( 'NONE', #74808 ) ;
#81583 = CARTESIAN_POINT ( 'NONE',  ( 15.23076923076911093, -2.892918686052165622, 31.69288490824153470 ) ) ;
#81584 = CARTESIAN_POINT ( 'NONE',  ( 14.53070515178570510, -5.582272713120729257, 34.63742843783360570 ) ) ;
#81585 = CARTESIAN_POINT ( 'NONE',  ( 3.480714640147273720, -5.766571408460171355, 34.70601412856602508 ) ) ;
#81586 = CARTESIAN_POINT ( 'NONE',  ( -2.373775718648186928, -8.120952969808774569, 34.71129190930000163 ) ) ;
#81587 = CARTESIAN_POINT ( 'NONE',  ( 9.758376043310132530, -5.557115091759786019, 34.35708131394839882 ) ) ;
#81588 = ORIENTED_EDGE ( 'NONE', *, *, #81159, .F. ) ;
#81589 = CARTESIAN_POINT ( 'NONE',  ( -15.09997878980228059, -2.494656445102012565, 31.33466734024120015 ) ) ;
#81591 = VERTEX_POINT ( 'NONE', #33374 ) ;
#81590 = CARTESIAN_POINT ( 'NONE',  ( -15.23076923076935252, -2.379036618888197729, 30.90682066428292885 ) ) ;
#81592 = DIRECTION ( 'NONE',  ( -0.000000000000000000, 0.3420201433256694346, -0.9396926207859080948 ) ) ;
#81594 = B_SPLINE_CURVE_WITH_KNOTS ( 'NONE', 3,
 ( #11780, #86563, #11327, #73488, #32939, #5020, #80240, #39259, #37915, #24382 ),
 .UNSPECIFIED., .F., .F.,
 ( 4, 2, 2, 2, 4 ),
 ( 0.000000000000000000, 0.0001954339857564080707, 0.0003908679715128161414, 0.0005863019572692241849, 0.0007817359430256322827 ),
 .UNSPECIFIED. ) ;
#81593 = CARTESIAN_POINT ( 'NONE',  ( -2.438383774359864642, -8.999036380462717588, 34.52022231692819076 ) ) ;
#81595 = FACE_OUTER_BOUND ( 'NONE', #10660, .T. ) ;
#81596 = CARTESIAN_POINT ( 'NONE',  ( -2.373774687052442545, -12.62096338111211580, 30.90682066428152197 ) ) ;
#81597 = CYLINDRICAL_SURFACE ( 'NONE', #41891, 0.2500000000000009437 ) ;
#81598 = VECTOR ( 'NONE', #43158, 1000.000000000000114 ) ;
#81599 = CARTESIAN_POINT ( 'NONE',  ( -8.769230769230892619, -9.528491918059723176, 34.59228464037033035 ) ) ;
#81600 = CARTESIAN_POINT ( 'NONE',  ( 12.59233026936325039, -11.18335022499818621, 33.13157742990016885 ) ) ;
#81601 = CARTESIAN_POINT ( 'NONE',  ( -2.724691934501246582, -6.299813628509474128, 21.67374329374151287 ) ) ;
#81602 = VERTEX_POINT ( 'NONE', #26611 ) ;
#81603 = CARTESIAN_POINT ( 'NONE',  ( 14.30769230769231015, -13.57706302396349152, 30.56769352161908060 ) ) ;
#81604 = CYLINDRICAL_SURFACE ( 'NONE', #51937, 0.2500000000000012212 ) ;
#81605 = CARTESIAN_POINT ( 'NONE',  ( -9.692307692307691624, -5.557115091759785130, 34.35708131394839171 ) ) ;
#81606 = ORIENTED_EDGE ( 'NONE', *, *, #30369, .T. ) ;
#81607 = CARTESIAN_POINT ( 'NONE',  ( -5.776988648387150427, -2.554770724473668153, 30.48948780036025852 ) ) ;
#81608 = CARTESIAN_POINT ( 'NONE',  ( 3.100208639027310475, -2.504760397472875155, 29.97295953869789997 ) ) ;
#81609 = EDGE_CURVE ( 'NONE', #79299, #57617, #34664, .T. ) ;
#81610 = CARTESIAN_POINT ( 'NONE',  ( 6.923076923076924238, -12.09954503811598769, 35.62045528018868623 ) ) ;
#81611 = CARTESIAN_POINT ( 'NONE',  ( 14.30769230769231015, -13.20930481340135110, 34.54067556320372745 ) ) ;
#81612 = CARTESIAN_POINT ( 'NONE',  ( 17.74997677577853850, -2.588893531581426100, 31.60682220781849239 ) ) ;
#81613 = EDGE_LOOP ( 'NONE', ( #7693, #58118 ) ) ;
#81614 = VECTOR ( 'NONE', #41683, 1000.000000000000000 ) ;
#81615 = CARTESIAN_POINT ( 'NONE',  ( -16.21992853320628569, -6.343179335718451384, 34.87096338111212646 ) ) ;
#81616 = CARTESIAN_POINT ( 'NONE',  ( -14.43838377435986331, -2.729777683071817229, 31.24903638046269450 ) ) ;
#81617 = CARTESIAN_POINT ( 'NONE',  ( 7.846153846153725020, -10.21337939537710326, 33.94971097300076224 ) ) ;
#81618 = VERTEX_POINT ( 'NONE', #42353 ) ;
#81619 = CARTESIAN_POINT ( 'NONE',  ( -8.638392438744007862, -7.277220318596961057, 34.99547417642776992 ) ) ;
#81620 = AXIS2_PLACEMENT_3D ( 'NONE', #26261, #12745, #20393 ) ;
#81621 = EDGE_CURVE ( 'NONE', #83291, #6970, #22947, .T. ) ;
#81622 = VERTEX_POINT ( 'NONE', #70700 ) ;
#81623 = DIRECTION ( 'NONE',  ( -1.000000000000000000, -0.000000000000000000, -0.000000000000000000 ) ) ;
#81624 = FILL_AREA_STYLE_COLOUR ( '', #61893 ) ;
#81625 = CARTESIAN_POINT ( 'NONE',  ( -5.777220331021932331, -12.11081565061823717, 32.26097654155341843 ) ) ;
#81626 = ORIENTED_EDGE ( 'NONE', *, *, #17742, .F. ) ;
#81627 = VECTOR ( 'NONE', #9167, 1000.000000000000227 ) ;
#81628 = ADVANCED_FACE ( 'NONE', ( #84670 ), #8561, .F. ) ;
#81629 = CARTESIAN_POINT ( 'NONE',  ( -13.38461538461538325, -4.661471528628507777, 34.16647553114623292 ) ) ;
#81630 = LINE ( 'NONE', #60458, #21966 ) ;
#81631 = CARTESIAN_POINT ( 'NONE',  ( -7.846153846153844924, -1.242168528481310874, 33.36296068462461051 ) ) ;
#81632 = CARTESIAN_POINT ( 'NONE',  ( -9.692307692307814193, -11.67786785259630911, 32.92929555188603530 ) ) ;
#81633 = CYLINDRICAL_SURFACE ( 'NONE', #51168, 0.2499999999999986955 ) ;
#81634 = VERTEX_POINT ( 'NONE', #43225 ) ;
#81635 = EDGE_CURVE ( 'NONE', #32871, #4325, #13034, .T. ) ;
#81636 = CARTESIAN_POINT ( 'NONE',  ( 13.38461538461538680, -2.249999999999998668, 29.75000000000001776 ) ) ;
#81637 = VERTEX_POINT ( 'NONE', #909 ) ;
#81638 = DIRECTION ( 'NONE',  ( 0.000000000000000000, 0.7660444431189807890, 0.6427876096865361433 ) ) ;
#81639 = FACE_OUTER_BOUND ( 'NONE', #3582, .T. ) ;
#81640 = EDGE_CURVE ( 'NONE', #79746, #86676, #368, .T. ) ;
#81641 = VECTOR ( 'NONE', #86458, 1000.000000000000000 ) ;
#81642 = CARTESIAN_POINT ( 'NONE',  ( 1.384615384615386802, -2.708943851104267164, 35.45975837776705220 ) ) ;
#81643 = CARTESIAN_POINT ( 'NONE',  ( -10.61538461538461320, -1.242168528481310874, 33.36296068462461051 ) ) ;
#81644 = CARTESIAN_POINT ( 'NONE',  ( 16.82689983963011926, -2.587272538249754117, 30.68239716806877837 ) ) ;
#81645 = ORIENTED_EDGE ( 'NONE', *, *, #70443, .T. ) ;
#81646 = ORIENTED_EDGE ( 'NONE', *, *, #43589, .F. ) ;
#81647 = ORIENTED_EDGE ( 'NONE', *, *, #38460, .T. ) ;
#81648 = ORIENTED_EDGE ( 'NONE', *, *, #67420, .F. ) ;
#81649 = EDGE_CURVE ( 'NONE', #19083, #292, #14239, .T. ) ;
#81650 = AXIS2_PLACEMENT_3D ( 'NONE', #81724, #13256, #40737 ) ;
#81651 = CARTESIAN_POINT ( 'NONE',  ( -4.283993363284373856, -6.001485441113818986, 34.52039167877662607 ) ) ;
#81652 = CARTESIAN_POINT ( 'NONE',  ( 16.37685899793954292, -10.77377354290276301, 33.85451476688484718 ) ) ;
#81653 = EDGE_CURVE ( 'NONE', #603, #59888, #22507, .T. ) ;
#81654 = DIRECTION ( 'NONE',  ( 0.000000000000000000, 0.9396926207859126468, 0.3420201433256571111 ) ) ;
#81655 = FACE_OUTER_BOUND ( 'NONE', #22924, .T. ) ;
#81656 = CARTESIAN_POINT ( 'NONE',  ( -5.326946314216042033, -10.76384336483936011, 33.53834819971076087 ) ) ;
#81657 = EDGE_CURVE ( 'NONE', #57345, #72521, #82057, .T. ) ;
#81658 = CARTESIAN_POINT ( 'NONE',  ( 2.307692307692309264, -2.721908614388771852, 31.22303859784724978 ) ) ;
#81659 = ADVANCED_FACE ( 'NONE', ( #63035 ), #57620, .F. ) ;
#81660 = CARTESIAN_POINT ( 'NONE',  ( 16.15384615384603251, -3.300289026999228437, 32.46337939537709616 ) ) ;
#81661 = CARTESIAN_POINT ( 'NONE',  ( 1.134615384615387246, -7.500000000000001776, 34.75000000000000000 ) ) ;
#81662 = VERTEX_POINT ( 'NONE', #29718 ) ;
#81663 = ORIENTED_EDGE ( 'NONE', *, *, #52831, .F. ) ;
#81664 = ORIENTED_EDGE ( 'NONE', *, *, #16401, .F. ) ;
#81666 = ORIENTED_EDGE ( 'NONE', *, *, #50810, .F. ) ;
#81665 = CARTESIAN_POINT ( 'NONE',  ( -12.46153846153858247, -10.90142922262034020, 33.41473453929536674 ) ) ;
#81668 = CYLINDRICAL_SURFACE ( 'NONE', #80775, 0.2499999999999973355 ) ;
#81667 = DIRECTION ( 'NONE',  ( -0.000000000000000000, -0.5000000000000009992, -0.8660254037844380415 ) ) ;
#81669 = CARTESIAN_POINT ( 'NONE',  ( 18.00000000000000000, -1.466349020453238561, 30.81389545987213907 ) ) ;
#81670 = AXIS2_PLACEMENT_3D ( 'NONE', #8139, #14447, #61731 ) ;
#81671 = CARTESIAN_POINT ( 'NONE',  ( -15.29603923132555110, -10.33852847137145048, 34.16647553114627556 ) ) ;
#81672 = FACE_BOUND ( 'NONE', #28246, .T. ) ;
#81673 = ORIENTED_EDGE ( 'NONE', *, *, #81336, .F. ) ;
#81674 = B_SPLINE_CURVE_WITH_KNOTS ( 'NONE', 3,
 ( #79578, #31836, #11563, #39488, #66501, #38136, #65594, #32706, #87678, #17874 ),
 .UNSPECIFIED., .F., .F.,
 ( 4, 2, 2, 2, 4 ),
 ( 0.000000000000000000, 0.0001954339857564074473, 0.0003908679715128148945, 0.0005863019572692223418, 0.0007817359430256297891 ),
 .UNSPECIFIED. ) ;
#81675 = CARTESIAN_POINT ( 'NONE',  ( -8.769230769230768274, -2.499999999999998668, 29.50000000000001066 ) ) ;
#81676 = CARTESIAN_POINT ( 'NONE',  ( -1.449885385171703511, -3.643525952247789412, 33.31231777344662959 ) ) ;
#81677 = ORIENTED_EDGE ( 'NONE', *, *, #78278, .T. ) ;
#81678 = CARTESIAN_POINT ( 'NONE',  ( -8.519230769230766498, -2.499999999999999556, 29.81604066197449754 ) ) ;
#81679 = VECTOR ( 'NONE', #46765, 999.9999999999998863 ) ;
#81680 = ORIENTED_EDGE ( 'NONE', *, *, #81788, .T. ) ;
#81681 = FACE_BOUND ( 'NONE', #27300, .T. ) ;
#81682 = CARTESIAN_POINT ( 'NONE',  ( -9.442362282929646966, -2.341251567377310217, 30.72681386836322659 ) ) ;
#81683 = CARTESIAN_POINT ( 'NONE',  ( 8.069529331926265314, -2.251407671071270489, 29.88021292934943318 ) ) ;
#81684 = ORIENTED_EDGE ( 'NONE', *, *, #59850, .T. ) ;
#81685 = CARTESIAN_POINT ( 'NONE',  ( -12.21159294319032362, -8.433404298154334455, 34.66254593164985920 ) ) ;
#81686 = DIRECTION ( 'NONE',  ( -0.000000000000000000, -0.5000000000000009992, -0.8660254037844380415 ) ) ;
#81687 = AXIS2_PLACEMENT_3D ( 'NONE', #75725, #41507, #85593 ) ;
#81688 = FACE_OUTER_BOUND ( 'NONE', #80350, .T. ) ;
#81689 = ORIENTED_EDGE ( 'NONE', *, *, #76895, .F. ) ;
#81690 = CARTESIAN_POINT ( 'NONE',  ( -8.546217925137373328, -3.395485233115139057, 33.02377354290275946 ) ) ;
#81691 = DIRECTION ( 'NONE',  ( -0.000000000000000000, -0.8660254037844397068, -0.4999999999999978906 ) ) ;
#81692 = CARTESIAN_POINT ( 'NONE',  ( 18.06525513951284267, -11.06231777344670952, 33.60647404775212266 ) ) ;
#81693 = LINE ( 'NONE', #66838, #4473 ) ;
#81694 = ORIENTED_EDGE ( 'NONE', *, *, #40386, .F. ) ;
#81695 = CARTESIAN_POINT ( 'NONE',  ( 16.37685750545900376, -10.61302985866384141, 33.66295027996417843 ) ) ;
#81696 = LINE ( 'NONE', #67733, #65718 ) ;
#81697 = ORIENTED_EDGE ( 'NONE', *, *, #42512, .T. ) ;
#81698 = CARTESIAN_POINT ( 'NONE',  ( -19.50000000000000000, -3.499999999999999556, 29.75000000000000355 ) ) ;
#81699 = DIRECTION ( 'NONE',  ( -1.000000000000000000, -0.000000000000000000, -0.000000000000000000 ) ) ;
#81700 = CARTESIAN_POINT ( 'NONE',  ( -13.16183584334697265, -5.114059244376869984, 34.14424750095245287 ) ) ;
#81701 = CARTESIAN_POINT ( 'NONE',  ( 10.86538461538605205, -7.500000000000155431, 34.75000000000007105 ) ) ;
#81702 = LINE ( 'NONE', #11017, #7085 ) ;
#81703 = EDGE_CURVE ( 'NONE', #66105, #45448, #63680, .T. ) ;
#81704 = CARTESIAN_POINT ( 'NONE',  ( 15.10062126103753322, -5.915902021225889484, 34.75552854090298638 ) ) ;
#81706 = DIRECTION ( 'NONE',  ( -0.7071067811865510144, 0.7071067811865441310, 0.000000000000000000 ) ) ;
#81705 = CARTESIAN_POINT ( 'NONE',  ( -18.75000000000000000, -3.499999999999999556, 29.75000000000000355 ) ) ;
#81707 = CARTESIAN_POINT ( 'NONE',  ( 14.30769230769231015, -3.513871655860378418, 32.76840700105978499 ) ) ;
#81708 = CARTESIAN_POINT ( 'NONE',  ( -2.749999999999991562, -8.639087296526025028, 20.01562500000000355 ) ) ;
#81709 = ORIENTED_EDGE ( 'NONE', *, *, #76201, .T. ) ;
#81710 = CARTESIAN_POINT ( 'NONE',  ( -16.21911615440246734, -5.094484230520675894, 34.41647553114621161 ) ) ;
#81711 = ORIENTED_EDGE ( 'NONE', *, *, #39545, .T. ) ;
#81712 = EDGE_CURVE ( 'NONE', #16973, #44052, #38240, .T. ) ;
#81713 = AXIS2_PLACEMENT_3D ( 'NONE', #29400, #63607, #20849 ) ;
#81714 = EDGE_LOOP ( 'NONE', ( #10831, #42877 ) ) ;
#81715 = DIRECTION ( 'NONE',  ( -0.000000000000000000, -0.5000000000000009992, -0.8660254037844380415 ) ) ;
#81716 = ORIENTED_EDGE ( 'NONE', *, *, #25486, .T. ) ;
#81717 = CARTESIAN_POINT ( 'NONE',  ( 1.634669804528839698, -12.01375889529407281, 32.43194544308182969 ) ) ;
#81718 = CARTESIAN_POINT ( 'NONE',  ( 1.944543648263018731, -9.444543648262994751, 22.12500000000000000 ) ) ;
#81719 = CARTESIAN_POINT ( 'NONE',  ( 17.86985203026830149, -5.070767119584671079, 34.40440758774516183 ) ) ;
#81720 = CARTESIAN_POINT ( 'NONE',  ( -11.28840711854808632, -10.06805714834173493, 34.32951233291982618 ) ) ;
#81721 = CARTESIAN_POINT ( 'NONE',  ( -2.084680956079456582, -6.503523203565942268, 34.64991518177335195 ) ) ;
#81722 = EDGE_CURVE ( 'NONE', #58791, #58630, #45506, .T. ) ;
#81724 = CARTESIAN_POINT ( 'NONE',  ( 3.230769230769231726, -1.242168528481310874, 33.36296068462461051 ) ) ;
#81723 = VECTOR ( 'NONE', #88870, 1000.000000000000114 ) ;
#81725 = CARTESIAN_POINT ( 'NONE',  ( -13.51476259405360203, -2.619462340734462380, 30.83744416345203021 ) ) ;
#81726 = CARTESIAN_POINT ( 'NONE',  ( -12.94230769230769162, -3.499999999999999556, 29.75000000000000355 ) ) ;
#81727 = CARTESIAN_POINT ( 'NONE',  ( -2.651650429449565305, -4.848349570550461785, 25.25000000000000000 ) ) ;
#81728 = CARTESIAN_POINT ( 'NONE',  ( 10.68063975489745587, -12.51329471203373345, 31.30864560766537963 ) ) ;
#81729 = CARTESIAN_POINT ( 'NONE',  ( 10.61538461538461675, -2.249999999999998668, 29.75000000000001776 ) ) ;
#81730 = VECTOR ( 'NONE', #78609, 1000.000000000000000 ) ;
#81731 = FACE_OUTER_BOUND ( 'NONE', #4767, .T. ) ;
#81733 = VERTEX_POINT ( 'NONE', #58057 ) ;
#81732 = EDGE_CURVE ( 'NONE', #21879, #74312, #66147, .T. ) ;
#81734 = ORIENTED_EDGE ( 'NONE', *, *, #52028, .T. ) ;
#81735 = CARTESIAN_POINT ( 'NONE',  ( -11.47239318745910097, -5.557115091759786019, 34.35708131394839882 ) ) ;
#81736 = CARTESIAN_POINT ( 'NONE',  ( 5.207448778686640800, -9.417988943895561960, 34.36773134775778260 ) ) ;
#81737 = DIRECTION ( 'NONE',  ( 0.000000000000000000, 0.000000000000000000, 1.000000000000000000 ) ) ;
#81738 = CARTESIAN_POINT ( 'NONE',  ( 5.933916589044121892, -5.557115091759785130, 34.35708131394839171 ) ) ;
#81739 = ADVANCED_FACE ( 'NONE', ( #38685 ), #17977, .F. ) ;
#81740 = CARTESIAN_POINT ( 'NONE',  ( 6.222779541268409709, -5.114059244376869984, 34.14424750095245287 ) ) ;
#81741 = CARTESIAN_POINT ( 'NONE',  ( -13.63459212866397507, -10.82459398097509329, 33.81372124010185587 ) ) ;
#81742 = CARTESIAN_POINT ( 'NONE',  ( -2.557669051740897537, -8.347322224742351082, 34.93158281831414769 ) ) ;
#81743 = VERTEX_POINT ( 'NONE', #52636 ) ;
#81744 = CARTESIAN_POINT ( 'NONE',  ( -10.61538461538461320, -5.415277668671390821, 36.20867863119892149 ) ) ;
#81745 = ORIENTED_EDGE ( 'NONE', *, *, #86026, .T. ) ;
#81746 = AXIS2_PLACEMENT_3D ( 'NONE', #74130, #80905, #33140 ) ;
#81747 = ORIENTED_EDGE ( 'NONE', *, *, #44474, .T. ) ;
#81748 = CARTESIAN_POINT ( 'NONE',  ( 16.40379156322419973, -9.357781135181033605, 34.66075350412533851 ) ) ;
#81749 = CARTESIAN_POINT ( 'NONE',  ( 4.403846153846215472, -7.434744860731433924, 35.00000000000000711 ) ) ;
#81750 = CARTESIAN_POINT ( 'NONE',  ( -0.2385271099256117411, -6.503523203565942268, 34.64991518177335195 ) ) ;
#81751 = DIRECTION ( 'NONE',  ( 0.000000000000000000, 0.000000000000000000, -1.000000000000000000 ) ) ;
#81752 = CARTESIAN_POINT ( 'NONE',  ( 20.00000000000000000, -11.00000000000000000, 28.25000000000000000 ) ) ;
#81753 = ORIENTED_EDGE ( 'NONE', *, *, #81653, .F. ) ;
#81754 = EDGE_LOOP ( 'NONE', ( #43438, #50081 ) ) ;
#81755 = B_SPLINE_CURVE_WITH_KNOTS ( 'NONE', 3,
 ( #49652, #15879, #71239, #8233, #15436, #57740, #16312, #85660, #43778, #64039 ),
 .UNSPECIFIED., .F., .F.,
 ( 4, 2, 2, 2, 4 ),
 ( 0.000000000000000000, 0.0001954339857564096157, 0.0003908679715128192313, 0.0005863019572692288470, 0.0007817359430256384627 ),
 .UNSPECIFIED. ) ;
#81756 = ORIENTED_EDGE ( 'NONE', *, *, #87040, .T. ) ;
#81757 = ORIENTED_EDGE ( 'NONE', *, *, #62702, .F. ) ;
#81758 = EDGE_CURVE ( 'NONE', #2169, #86522, #50741, .T. ) ;
#81759 = CARTESIAN_POINT ( 'NONE',  ( -5.999999999999998224, -4.661471528628507777, 34.16647553114623292 ) ) ;
#81760 = CARTESIAN_POINT ( 'NONE',  ( -2.373774687052442545, -9.905515769479276145, 34.41647553114623292 ) ) ;
#81761 = CARTESIAN_POINT ( 'NONE',  ( 4.284371592079796898, -12.15418822224088657, 32.17964115625579069 ) ) ;
#81762 = ADVANCED_FACE ( 'NONE', ( #73361 ), #37790, .F. ) ;
#81763 = CARTESIAN_POINT ( 'NONE',  ( 14.43773974294276208, -7.723484941389743952, 34.99544897038808955 ) ) ;
#81764 = AXIS2_PLACEMENT_3D ( 'NONE', #1935, #29420, #63183 ) ;
#81765 = CARTESIAN_POINT ( 'NONE',  ( -17.07692307692307665, -3.050289026998446396, 32.03036669348365706 ) ) ;
#81766 = EDGE_CURVE ( 'NONE', #20268, #49865, #4671, .T. ) ;
#81767 = CARTESIAN_POINT ( 'NONE',  ( 14.05766907039934210, -12.43535235679832596, 30.55408501211184813 ) ) ;
#81768 = VERTEX_POINT ( 'NONE', #37337 ) ;
#81769 = ORIENTED_EDGE ( 'NONE', *, *, #55807, .F. ) ;
#81770 = EDGE_LOOP ( 'NONE', ( #54727, #77137 ) ) ;
#81771 = AXIS2_PLACEMENT_3D ( 'NONE', #21471, #29131, #76420 ) ;
#81773 = ORIENTED_EDGE ( 'NONE', *, *, #77450, .F. ) ;
#81772 = CARTESIAN_POINT ( 'NONE',  ( -3.230769230769352962, -2.657715359629662544, 31.77849191805970364 ) ) ;
#81774 = CARTESIAN_POINT ( 'NONE',  ( 12.46153846153846168, -2.249999999999998668, 29.75000000000001776 ) ) ;
#81775 = DIRECTION ( 'NONE',  ( -0.000000000000000000, 0.7660444431189791237, -0.6427876096865379196 ) ) ;
#81776 = VECTOR ( 'NONE', #85348, 1000.000000000000000 ) ;
#81777 = CARTESIAN_POINT ( 'NONE',  ( -2.651650429449565305, -4.848349570550461785, 20.25000000000000000 ) ) ;
#81778 = ORIENTED_EDGE ( 'NONE', *, *, #52444, .T. ) ;
#81779 = VECTOR ( 'NONE', #57287, 1000.000000000000227 ) ;
#81780 = EDGE_CURVE ( 'NONE', #64954, #56376, #3110, .T. ) ;
#81781 = CARTESIAN_POINT ( 'NONE',  ( -1.253824943648432333, -2.494656445102013453, 31.33466734024120015 ) ) ;
#81782 = EDGE_LOOP ( 'NONE', ( #18838, #43675, #35358, #54807 ) ) ;
#81783 = DIRECTION ( 'NONE',  ( -0.000000000000000000, 1.000000000000000000, 3.491481338843133355E-15 ) ) ;
#81784 = FACE_BOUND ( 'NONE', #2535, .T. ) ;
#81785 = CARTESIAN_POINT ( 'NONE',  ( -4.946397375159510723, -12.27024696741798770, 31.24895572276497546 ) ) ;
#81786 = DIRECTION ( 'NONE',  ( -1.000000000000000000, -0.000000000000000000, -0.000000000000000000 ) ) ;
#81787 = ORIENTED_EDGE ( 'NONE', *, *, #86757, .F. ) ;
#81788 = EDGE_CURVE ( 'NONE', #31874, #58385, #44532, .T. ) ;
#81789 = CARTESIAN_POINT ( 'NONE',  ( 8.638540166120465713, -11.93127051446799847, 32.56575433478202797 ) ) ;
#81790 = CARTESIAN_POINT ( 'NONE',  ( -15.23076923076922995, -1.117168528481311540, 33.14645433367849847 ) ) ;
#81791 = CARTESIAN_POINT ( 'NONE',  ( -18.00000000000000000, -3.895656007487076078, 35.99290692298802696 ) ) ;
#81792 = CARTESIAN_POINT ( 'NONE',  ( -3.230769230769352962, -9.528491918059723176, 34.59228464037033035 ) ) ;
#81793 = ORIENTED_EDGE ( 'NONE', *, *, #45616, .T. ) ;
#81794 = DIRECTION ( 'NONE',  ( -0.000000000000000000, -0.9396926207859093161, -0.3420201433256663259 ) ) ;
#81795 = FACE_OUTER_BOUND ( 'NONE', #61679, .T. ) ;
#81796 = LINE ( 'NONE', #19639, #42677 ) ;
#81797 = CARTESIAN_POINT ( 'NONE',  ( -2.242437168179467033, -9.528491918058460186, 34.59228464037085615 ) ) ;
#81798 = CARTESIAN_POINT ( 'NONE',  ( 8.769230769230645706, -10.33852847137269571, 34.16647553114546554 ) ) ;
#81799 = EDGE_CURVE ( 'NONE', #45833, #52906, #29565, .T. ) ;
#81800 = FACE_BOUND ( 'NONE', #14674, .T. ) ;
#81802 = CARTESIAN_POINT ( 'NONE',  ( -8.769230769230768274, -4.945431358278436385, 36.03766855953609394 ) ) ;
#81801 = CARTESIAN_POINT ( 'NONE',  ( 1.608041783530174129, -7.630147987733843173, 34.99859428049665411 ) ) ;
#81803 = CARTESIAN_POINT ( 'NONE',  ( -15.00798956179116317, -4.989023458446560255, 34.36081565061822118 ) ) ;
#81805 = CARTESIAN_POINT ( 'NONE',  ( 0.000000000000000000, -11.00000000000000000, 29.75000000000000355 ) ) ;
#81804 = CARTESIAN_POINT ( 'NONE',  ( -16.15384615384627409, -4.320704448113951379, 33.92786785259630022 ) ) ;
#81806 = DIRECTION ( 'NONE',  ( -0.000000000000000000, 1.000000000000000000, -0.000000000000000000 ) ) ;
#81807 = AXIS2_PLACEMENT_3D ( 'NONE', #46784, #66617, #5357 ) ;
#81808 = CARTESIAN_POINT ( 'NONE',  ( 2.750000000000001332, -7.438900925035452083, 16.71688170625848713 ) ) ;
#81810 = EDGE_CURVE ( 'NONE', #75748, #77695, #75491, .T. ) ;
#81809 = VERTEX_POINT ( 'NONE', #9298 ) ;
#81811 = B_SPLINE_CURVE_WITH_KNOTS ( 'NONE', 3,
 ( #24558, #86741, #71858, #31325, #52474, #37630, #73204, #58336, #31776, #11504 ),
 .UNSPECIFIED., .F., .F.,
 ( 4, 2, 2, 2, 4 ),
 ( 0.000000000000000000, 0.0001954339857564097241, 0.0003908679715128194482, 0.0005863019572692291723, 0.0007817359430256388964 ),
 .UNSPECIFIED. ) ;
#81812 = CARTESIAN_POINT ( 'NONE',  ( -8.638438961405983108, -5.582136614379148654, 34.36778462344220486 ) ) ;
#81813 = VERTEX_POINT ( 'NONE', #36324 ) ;
#81814 = LINE ( 'NONE', #67845, #39230 ) ;
#81815 = ORIENTED_EDGE ( 'NONE', *, *, #1622, .T. ) ;
#81816 = CARTESIAN_POINT ( 'NONE',  ( 4.153846153846154188, -8.564572088678739092, 35.78748833219616898 ) ) ;
#81817 = CARTESIAN_POINT ( 'NONE',  ( -7.846153846153844924, -13.53365097954675988, 30.81389545987213552 ) ) ;
#81819 = ORIENTED_EDGE ( 'NONE', *, *, #34301, .F. ) ;
#81818 = CARTESIAN_POINT ( 'NONE',  ( 15.23076923076953904, -2.506253911140615021, 30.00000000000323297 ) ) ;
#81820 = CARTESIAN_POINT ( 'NONE',  ( 1.384615384615386802, -4.661471528628507777, 34.16647553114623292 ) ) ;
#81821 = CARTESIAN_POINT ( 'NONE',  ( 1.901340078031349856, -5.512252781505337929, 19.06063170625849068 ) ) ;
#81822 = CYLINDRICAL_SURFACE ( 'NONE', #36053, 0.2500000000000004996 ) ;
#81823 = DIRECTION ( 'NONE',  ( -0.000000000000000000, 0.8660254037844399289, -0.4999999999999980016 ) ) ;
#81824 = EDGE_CURVE ( 'NONE', #5310, #13392, #73441, .T. ) ;
#81825 = CARTESIAN_POINT ( 'NONE',  ( -12.21159305216042057, -9.357781135181031829, 34.66075350412533851 ) ) ;
#81826 = LINE ( 'NONE', #34949, #61692 ) ;
#81827 = CARTESIAN_POINT ( 'NONE',  ( -1.384615384615383471, -6.343179335718451384, 34.87096338111211935 ) ) ;
#81828 = CARTESIAN_POINT ( 'NONE',  ( 11.60371710973756620, -3.835265460703683349, 33.15142922261929925 ) ) ;
#81829 = CARTESIAN_POINT ( 'NONE',  ( -0.06109907496450878162, -11.25000000000000000, 21.28311829374151287 ) ) ;
#81830 = CARTESIAN_POINT ( 'NONE',  ( 5.142990410273150736, -2.486705287966279876, 31.30864560766543647 ) ) ;
#81831 = EDGE_CURVE ( 'NONE', #88166, #3856, #57464, .T. ) ;
#81832 = EDGE_LOOP ( 'NONE', ( #83492, #34636 ) ) ;
#81833 = DIRECTION ( 'NONE',  ( 0.000000000000000000, 0.000000000000000000, -1.000000000000000000 ) ) ;
#81834 = CARTESIAN_POINT ( 'NONE',  ( 3.724691934501251023, -9.114399933863618131, 24.79874329374151998 ) ) ;
#81835 = B_SPLINE_CURVE_WITH_KNOTS ( 'NONE', 3,
 ( #16352, #56006, #28098, #23108, #55560, #35750, #62751, #83049, #21335, #9165 ),
 .UNSPECIFIED., .F., .F.,
 ( 4, 2, 2, 2, 4 ),
 ( 0.0007817359430256399806, 0.0009771253907250089001, 0.001172514838424378036, 0.001367904286123746956, 0.001563293733823115875 ),
 .UNSPECIFIED. ) ;
#81836 = CARTESIAN_POINT ( 'NONE',  ( -17.86920819217521483, -12.38066358083363738, 30.83685684665853444 ) ) ;
#81838 = CARTESIAN_POINT ( 'NONE',  ( 5.142178216435913107, -6.835583212224609184, 34.95778746994559327 ) ) ;
#81837 = VECTOR ( 'NONE', #85683, 1000.000000000000227 ) ;
#81839 = VERTEX_POINT ( 'NONE', #77298 ) ;
#81840 = DIRECTION ( 'NONE',  ( -0.000000000000000000, 0.8660254037844399289, -0.4999999999999980016 ) ) ;
#81841 = CARTESIAN_POINT ( 'NONE',  ( -0.2387589202700533542, -10.11255958852955850, 34.01340905677049165 ) ) ;
#81843 = EDGE_LOOP ( 'NONE', ( #19955, #58016, #39201, #22278, #37552, #16470 ) ) ;
#81842 = CARTESIAN_POINT ( 'NONE',  ( 27.00000000000000000, 16.99999999999999289, 31.75000000000000000 ) ) ;
#81844 = CARTESIAN_POINT ( 'NONE',  ( -3.099977422944444783, -3.530189275343204702, 32.79018710029569661 ) ) ;
#81845 = EDGE_CURVE ( 'NONE', #5354, #20560, #1193, .T. ) ;
#81846 = DIRECTION ( 'NONE',  ( -0.000000000000000000, -0.5000000000000009992, -0.8660254037844380415 ) ) ;
#81847 = VECTOR ( 'NONE', #11522, 1000.000000000000000 ) ;
#81848 = CARTESIAN_POINT ( 'NONE',  ( -10.39260494640654819, -9.418065098278013636, 34.63729479722530158 ) ) ;
#81849 = ADVANCED_FACE ( 'NONE', ( #16045 ), #15605, .F. ) ;
#81850 = ORIENTED_EDGE ( 'NONE', *, *, #44696, .F. ) ;
#81851 = AXIS2_PLACEMENT_3D ( 'NONE', #17897, #46695, #5271 ) ;
#81852 = CARTESIAN_POINT ( 'NONE',  ( 15.23076923076911093, -10.21337939537710326, 33.94971097300076224 ) ) ;
#81853 = CARTESIAN_POINT ( 'NONE',  ( 12.21153846153846168, -7.500000000000001776, 35.04278698407183867 ) ) ;
#81854 = VECTOR ( 'NONE', #82792, 1000.000000000000227 ) ;
#81855 = CARTESIAN_POINT ( 'NONE',  ( 1.319345384059066539, -3.083524468853724443, 32.58852847137143272 ) ) ;
#81856 = ORIENTED_EDGE ( 'NONE', *, *, #40334, .T. ) ;
#81857 = ORIENTED_EDGE ( 'NONE', *, *, #32410, .F. ) ;
#81858 = ORIENTED_EDGE ( 'NONE', *, *, #76972, .T. ) ;
#81859 = B_SPLINE_CURVE_WITH_KNOTS ( 'NONE', 3,
 ( #27825, #69697, #15648, #63376, #7563, #21057, #62483, #55733, #8004, #14311 ),
 .UNSPECIFIED., .F., .F.,
 ( 4, 2, 2, 2, 4 ),
 ( 0.000000000000000000, 0.0001954339857564093175, 0.0003908679715128186350, 0.0005863019572692279796, 0.0007817359430256372700 ),
 .UNSPECIFIED. ) ;
#81860 = EDGE_LOOP ( 'NONE', ( #24702, #80052, #44086, #65815 ) ) ;
#81861 = CARTESIAN_POINT ( 'NONE',  ( 5.207448778686641688, -12.27024696741798770, 31.24895572276497546 ) ) ;
#81862 = DIRECTION ( 'NONE',  ( 0.000000000000000000, 0.4999999999999960032, -0.8660254037844410391 ) ) ;
#81863 = CARTESIAN_POINT ( 'NONE',  ( 9.692307692307572609, -5.219633306517616589, 34.19971097300220464 ) ) ;
#81864 = DIRECTION ( 'NONE',  ( -0.000000000000000000, -0.3420201433256694901, -0.9396926207859082059 ) ) ;
#81865 = CARTESIAN_POINT ( 'NONE',  ( 16.02315468717859659, -4.809359713505814149, 33.96456829005828837 ) ) ;
#81866 = ORIENTED_EDGE ( 'NONE', *, *, #51108, .T. ) ;
#81867 = EDGE_LOOP ( 'NONE', ( #69322, #56785, #37731, #19493, #15623, #13490 ) ) ;
#81868 = EDGE_LOOP ( 'NONE', ( #69760, #80186 ) ) ;
#81870 = ORIENTED_EDGE ( 'NONE', *, *, #53737, .F. ) ;
#81869 = CYLINDRICAL_SURFACE ( 'NONE', #51574, 0.2499999999999986955 ) ;
#81871 = CARTESIAN_POINT ( 'NONE',  ( -4.946132635956127288, -12.35292014791297710, 31.75344720912887198 ) ) ;
#81872 = CARTESIAN_POINT ( 'NONE',  ( -3.454254155333559062, -12.11044203135681840, 32.26167407432752299 ) ) ;
#81873 = EDGE_CURVE ( 'NONE', #82763, #12084, #32574, .T. ) ;
#81874 = CARTESIAN_POINT ( 'NONE',  ( 7.145856592054990131, -4.989023458446560255, 34.36081565061822118 ) ) ;
#81875 = CARTESIAN_POINT ( 'NONE',  ( 11.53846153846153832, -6.386643153685126251, 34.62446782046654192 ) ) ;
#81876 = ADVANCED_FACE ( 'NONE', ( #57020 ), #43514, .F. ) ;
#81877 = EDGE_LOOP ( 'NONE', ( #81391, #32232 ) ) ;
#81878 = EDGE_LOOP ( 'NONE', ( #40987, #47083 ) ) ;
#81879 = B_SPLINE_CURVE_WITH_KNOTS ( 'NONE', 3,
 ( #49226, #15001, #70387, #1483, #29841, #62721, #42921, #56426, #62282, #41580 ),
 .UNSPECIFIED., .F., .F.,
 ( 4, 2, 2, 2, 4 ),
 ( 0.000000000000000000, 0.0001954311564186879044, 0.0003908623128373758088, 0.0005862934692560636861, 0.0007817246256747516176 ),
 .UNSPECIFIED. ) ;
#81880 = B_SPLINE_CURVE_WITH_KNOTS ( 'NONE', 3,
 ( #27060, #61269, #69814, #55413, #6781, #914, #76125, #41913, #8122, #56303 ),
 .UNSPECIFIED., .F., .F.,
 ( 4, 2, 2, 2, 4 ),
 ( 0.0007817246256747484735, 0.0009771112852218922368, 0.001172497944769036217, 0.001367884604316180197, 0.001563271263863323960 ),
 .UNSPECIFIED. ) ;
#81881 = VERTEX_POINT ( 'NONE', #2512 ) ;
#81882 = LINE ( 'NONE', #20174, #43242 ) ;
#81884 = EDGE_LOOP ( 'NONE', ( #80284, #51566, #28835, #46793 ) ) ;
#81883 = CARTESIAN_POINT ( 'NONE',  ( -10.36543920600657565, -2.589246495874658383, 31.60778113518102828 ) ) ;
#81885 = EDGE_CURVE ( 'NONE', #58249, #27791, #28270, .T. ) ;
#81886 = CARTESIAN_POINT ( 'NONE',  ( -4.153846153846152411, -6.435427911321262684, 35.78748833219616898 ) ) ;
#81887 = CARTESIAN_POINT ( 'NONE',  ( -14.37296275365308063, -2.625532179533444754, 30.86335684631481513 ) ) ;
#81888 = ORIENTED_EDGE ( 'NONE', *, *, #80331, .T. ) ;
#81889 = DIRECTION ( 'NONE',  ( -0.000000000000000000, -0.9396926207859093161, -0.3420201433256663259 ) ) ;
#81890 = CARTESIAN_POINT ( 'NONE',  ( 9.915683178080113791, -2.251407671071270489, 29.88021292934942963 ) ) ;
#81891 = EDGE_CURVE ( 'NONE', #22506, #720, #14533, .T. ) ;
#81892 = CARTESIAN_POINT ( 'NONE',  ( -0.4615384615384611200, -11.11383981884818262, 36.00935417666054406 ) ) ;
#81893 = FACE_BOUND ( 'NONE', #28148, .T. ) ;
#81894 = CARTESIAN_POINT ( 'NONE',  ( -0.6844646790546099480, -9.886141570436013382, 34.14413921362392301 ) ) ;
#81895 = LINE ( 'NONE', #4900, #70159 ) ;
#81896 = DIRECTION ( 'NONE',  ( 0.000000000000000000, 0.9848077530122072432, -0.1736481776669354937 ) ) ;
#81899 = CARTESIAN_POINT ( 'NONE',  ( -8.352564102564102200, -3.499999999999999556, 29.75000000000000355 ) ) ;
#81898 = AXIS2_PLACEMENT_3D ( 'NONE', #68927, #21627, #42362 ) ;
#81897 = LINE ( 'NONE', #6663, #80614 ) ;
#81900 = EDGE_CURVE ( 'NONE', #33320, #73867, #88436, .T. ) ;
#81901 = CARTESIAN_POINT ( 'NONE',  ( -4.023007823359388446, -7.277220318596959281, 34.99547417642776992 ) ) ;
#81902 = DIRECTION ( 'NONE',  ( -1.000000000000000000, 0.000000000000000000, 0.000000000000000000 ) ) ;
#81903 = ORIENTED_EDGE ( 'NONE', *, *, #7098, .F. ) ;
#81904 = CARTESIAN_POINT ( 'NONE',  ( -18.24997673094235395, -10.66389620160130036, 33.62221079203477103 ) ) ;
#81905 = CARTESIAN_POINT ( 'NONE',  ( 0.2386115026316120435, -10.77366814457252175, 33.85459836347579454 ) ) ;
#81906 = VERTEX_POINT ( 'NONE', #48311 ) ;
#81907 = VECTOR ( 'NONE', #31231, 1000.000000000000227 ) ;
#81908 = VECTOR ( 'NONE', #39852, 1000.000000000000000 ) ;
#81909 = CARTESIAN_POINT ( 'NONE',  ( -15.29685264172511161, -2.538708090699994813, 30.37095296980875148 ) ) ;
#81910 = CARTESIAN_POINT ( 'NONE',  ( -14.30769230769230660, -4.098570777380720287, 33.41473453929634729 ) ) ;
#81911 = ORIENTED_EDGE ( 'NONE', *, *, #50806, .F. ) ;
#81912 = CARTESIAN_POINT ( 'NONE',  ( -15.90390063549801347, -11.37275283266504111, 32.91324779482534524 ) ) ;
#81913 = CARTESIAN_POINT ( 'NONE',  ( -14.98071481085577972, -12.65882529074907126, 30.72640787790839312 ) ) ;
#81914 = FACE_BOUND ( 'NONE', #86179, .T. ) ;
#81916 = CARTESIAN_POINT ( 'NONE',  ( -16.94687802100330742, -2.254550872974305342, 29.97347326024527092 ) ) ;
#81915 = CARTESIAN_POINT ( 'NONE',  ( -17.07692307692307665, -4.098570777380720287, 33.41473453929634729 ) ) ;
#81917 = CARTESIAN_POINT ( 'NONE',  ( -8.899922235898330314, -6.413092428213692742, 34.63065189839063152 ) ) ;
#81918 = CARTESIAN_POINT ( 'NONE',  ( 16.15384615384615330, -12.29105614889573062, 35.45975837776705220 ) ) ;
#81919 = CARTESIAN_POINT ( 'NONE',  ( 2.084207383127975710, -10.97335522853832579, 33.68706563782419749 ) ) ;
#81920 = CARTESIAN_POINT ( 'NONE',  ( -2.608446859217889546, -10.19485399968121264, 17.18563170625848713 ) ) ;
#81921 = ORIENTED_EDGE ( 'NONE', *, *, #35687, .F. ) ;
#81922 = EDGE_CURVE ( 'NONE', #25790, #74135, #56191, .T. ) ;
#81923 = B_SPLINE_CURVE_WITH_KNOTS ( 'NONE', 3,
 ( #17981, #66150, #9879, #58493, #23820, #22952 ),
 .UNSPECIFIED., .F., .F.,
 ( 4, 2, 4 ),
 ( 0.0003909512603273947911, 0.0005862562993132216203, 0.0007815613382990483412 ),
 .UNSPECIFIED. ) ;
#81924 = ORIENTED_EDGE ( 'NONE', *, *, #72931, .F. ) ;
#81925 = CARTESIAN_POINT ( 'NONE',  ( 4.946775107191377252, -11.04286588640298561, 33.62463336215343901 ) ) ;
#81926 = CARTESIAN_POINT ( 'NONE',  ( 16.40379167219429490, -6.696923467548659303, 34.68552623307873972 ) ) ;
#81927 = CARTESIAN_POINT ( 'NONE',  ( -0.4615384615385840772, -6.835583212225970762, 34.95778746994575670 ) ) ;
#81928 = CARTESIAN_POINT ( 'NONE',  ( -13.38461538461538325, -8.810774026931790459, 35.74407628777942847 ) ) ;
#81929 = CARTESIAN_POINT ( 'NONE',  ( -3.230769230769229949, -5.557115091759785130, 34.35708131394839171 ) ) ;
#81930 = CARTESIAN_POINT ( 'NONE',  ( -2.694853999681210865, -4.891553140782108677, 17.49813170625848713 ) ) ;
#81931 = LINE ( 'NONE', #32401, #8658 ) ;
#81932 = CARTESIAN_POINT ( 'NONE',  ( 6.000000000000001776, -2.833524468853757305, 32.15551576947925838 ) ) ;
#81933 = EDGE_CURVE ( 'NONE', #1002, #78695, #59373, .T. ) ;
#81934 = CARTESIAN_POINT ( 'NONE',  ( 17.99999999999987566, -4.320704448113951379, 33.92786785259630022 ) ) ;
#81935 = CARTESIAN_POINT ( 'NONE',  ( -7.846153846153844924, -8.973038597847269315, 34.52809138561121927 ) ) ;
#81936 = CARTESIAN_POINT ( 'NONE',  ( -6.130691466667555822, -2.729777683071817229, 31.24903638046268739 ) ) ;
#81937 = CARTESIAN_POINT ( 'NONE',  ( 15.23076923076923173, -12.34228464037088635, 31.77849191805839268 ) ) ;
#81938 = CARTESIAN_POINT ( 'NONE',  ( 6.923076923076924238, -3.322132147404559976, 32.92929555188717927 ) ) ;
#81940 = ADVANCED_FACE ( 'NONE', ( #14984 ), #55514, .F. ) ;
#81939 = CARTESIAN_POINT ( 'NONE',  ( 2.557692307692246203, -7.565270000091922853, 34.99999999999999289 ) ) ;
#81941 = EDGE_CURVE ( 'NONE', #74006, #72884, #7342, .T. ) ;
#81942 = CARTESIAN_POINT ( 'NONE',  ( 12.59233026936324329, -2.729792928343269587, 31.24908615093345077 ) ) ;
#81943 = EDGE_LOOP ( 'NONE', ( #28427, #25293 ) ) ;
#81944 = VECTOR ( 'NONE', #73829, 1000.000000000000000 ) ;
#81945 = LINE ( 'NONE', #68412, #81598 ) ;
#81946 = LINE ( 'NONE', #68413, #51779 ) ;
#81947 = CARTESIAN_POINT ( 'NONE',  ( -2.724691934501246582, -6.299813628509474128, 15.42374329374151642 ) ) ;
#81948 = CARTESIAN_POINT ( 'NONE',  ( -0.4615384615385840772, -11.06231777344772027, 33.60647404775119895 ) ) ;
#81949 = DIRECTION ( 'NONE',  ( 0.000000000000000000, 0.000000000000000000, 1.000000000000000000 ) ) ;
#81950 = FACE_OUTER_BOUND ( 'NONE', #45193, .T. ) ;
#81952 = ORIENTED_EDGE ( 'NONE', *, *, #67116, .F. ) ;
#81951 = DIRECTION ( 'NONE',  ( -1.000000000000000000, -0.000000000000000000, -0.000000000000000000 ) ) ;
#81953 = CARTESIAN_POINT ( 'NONE',  ( 1.139087296526029469, -10.24999999999999289, 22.20312500000000000 ) ) ;
#81954 = CARTESIAN_POINT ( 'NONE',  ( 17.93391658904412012, -3.513871655860377086, 32.76840700105978499 ) ) ;
#81955 = B_SPLINE_CURVE_WITH_KNOTS ( 'NONE', 3,
 ( #11710, #38728, #39187, #58988, #27320, #31976, #39634, #17575, #38285, #59439 ),
 .UNSPECIFIED., .F., .F.,
 ( 4, 2, 2, 2, 4 ),
 ( 0.000000000000000000, 0.0001954311564186868473, 0.0003908623128373736946, 0.0005862934692560605419, 0.0007817246256747473893 ),
 .UNSPECIFIED. ) ;
#81956 = EDGE_CURVE ( 'NONE', #5991, #79867, #31455, .T. ) ;
#81958 = ORIENTED_EDGE ( 'NONE', *, *, #67465, .F. ) ;
#81957 = B_SPLINE_CURVE_WITH_KNOTS ( 'NONE', 3,
 ( #77441, #17066, #10315, #50398, #22937, #77880, #23807, #65246, #44521, #50830 ),
 .UNSPECIFIED., .F., .F.,
 ( 4, 2, 2, 2, 4 ),
 ( 0.000000000000000000, 0.0001954311564186876876, 0.0003908623128373753751, 0.0005862934692560630356, 0.0007817246256747507503 ),
 .UNSPECIFIED. ) ;
#81959 = CARTESIAN_POINT ( 'NONE',  ( 11.60452887181161508, -9.058645607665452459, 34.76329471203371924 ) ) ;
#81960 = CARTESIAN_POINT ( 'NONE',  ( -7.053767526187231240, -11.37499894934982514, 33.29245874905763003 ) ) ;
#81961 = VERTEX_POINT ( 'NONE', #29392 ) ;
#81962 = CARTESIAN_POINT ( 'NONE',  ( 16.85343813319912343, -11.41268669641499756, 32.86336882939238535 ) ) ;
#81963 = EDGE_CURVE ( 'NONE', #83460, #28375, #75355, .T. ) ;
#81964 = EDGE_CURVE ( 'NONE', #53, #7171, #7703, .T. ) ;
#81965 = LINE ( 'NONE', #13488, #63792 ) ;
#81966 = CARTESIAN_POINT ( 'NONE',  ( -7.846153846153965716, -3.835265460704628371, 33.15142922262033665 ) ) ;
#81967 = EDGE_LOOP ( 'NONE', ( #72999, #7089, #7078, #29408 ) ) ;
#81968 = ORIENTED_EDGE ( 'NONE', *, *, #82254, .F. ) ;
#81969 = CARTESIAN_POINT ( 'NONE',  ( 6.066067333350078528, -11.91647553114624358, 32.58852847137148245 ) ) ;
#81970 = EDGE_CURVE ( 'NONE', #72319, #363, #45100, .T. ) ;
#81971 = EDGE_LOOP ( 'NONE', ( #80771, #49838, #8772, #10087 ) ) ;
#81972 = CIRCLE ( 'NONE', #25893, 4.000000000000000000 ) ;
#81973 = CIRCLE ( 'NONE', #9994, 4.500000000000001776 ) ;
#81974 = CARTESIAN_POINT ( 'NONE',  ( 3.361294669002874436, -12.15418822224088657, 32.17964115625579069 ) ) ;
#81975 = CARTESIAN_POINT ( 'NONE',  ( -9.692307692307812417, -10.21337939537710326, 33.94971097300076224 ) ) ;
#81976 = CARTESIAN_POINT ( 'NONE',  ( 9.442284468086235449, -9.356822207818506598, 34.66110646841856635 ) ) ;
#81977 = LINE ( 'NONE', #20263, #77853 ) ;
#81978 = DIRECTION ( 'NONE',  ( -0.000000000000000000, -0.8660254037844399289, -0.4999999999999980016 ) ) ;
#81979 = DIRECTION ( 'NONE',  ( 0.000000000000000000, 0.000000000000000000, -1.000000000000000000 ) ) ;
#81980 = VECTOR ( 'NONE', #13892, 1000.000000000000227 ) ;
#81981 = CARTESIAN_POINT ( 'NONE',  ( -17.07692307692319744, -6.879047030192662504, 34.71129190930017927 ) ) ;
#81982 = ORIENTED_EDGE ( 'NONE', *, *, #18388, .F. ) ;
#81983 = ORIENTED_EDGE ( 'NONE', *, *, #8845, .T. ) ;
#81985 = ORIENTED_EDGE ( 'NONE', *, *, #87906, .T. ) ;
#81984 = LINE ( 'NONE', #62135, #27180 ) ;
#81986 = ADVANCED_FACE ( 'NONE', ( #3665 ), #57288, .F. ) ;
#81987 = DIRECTION ( 'NONE',  ( 1.000000000000000000, 0.000000000000000000, 0.000000000000000000 ) ) ;
#81988 = CYLINDRICAL_SURFACE ( 'NONE', #746, 0.2500000000000009437 ) ;
#81989 = ORIENTED_EDGE ( 'NONE', *, *, #33112, .T. ) ;
#81990 = CARTESIAN_POINT ( 'NONE',  ( 15.23076923076923173, -9.058645607665452459, 34.76329471203371924 ) ) ;
#81991 = VERTEX_POINT ( 'NONE', #23495 ) ;
#81992 = CARTESIAN_POINT ( 'NONE',  ( 11.60452988946397745, -2.538708090699994813, 30.37095296980875503 ) ) ;
#81993 = VERTEX_POINT ( 'NONE', #38355 ) ;
#81994 = DIRECTION ( 'NONE',  ( -0.000000000000000000, 1.000000000000000000, 3.491481338843133355E-15 ) ) ;
#81995 = ORIENTED_EDGE ( 'NONE', *, *, #11342, .F. ) ;
#81996 = DIRECTION ( 'NONE',  ( -0.000000000000000000, 0.5000000000000011102, -0.8660254037844380415 ) ) ;
#81997 = CARTESIAN_POINT ( 'NONE',  ( 10.74591031714818357, -5.195472089885680766, 34.18748526763464923 ) ) ;
#81998 = FACE_BOUND ( 'NONE', #18920, .T. ) ;
#81999 = FACE_OUTER_BOUND ( 'NONE', #39758, .T. ) ;
#82000 = FACE_OUTER_BOUND ( 'NONE', #27906, .T. ) ;
#82001 = CARTESIAN_POINT ( 'NONE',  ( 9.561617089197390840, -11.37499894934982692, 33.29245874905763003 ) ) ;
#82002 = CARTESIAN_POINT ( 'NONE',  ( 4.376625695114563008, -8.496831190052096971, 34.64984203495476578 ) ) ;
#82003 = CARTESIAN_POINT ( 'NONE',  ( 4.153846153846030731, -9.528491918059723176, 34.59228464037033035 ) ) ;
#82004 = CARTESIAN_POINT ( 'NONE',  ( -8.069080805060693251, -9.172386477786396597, 34.72672124145550043 ) ) ;
#82005 = CYLINDRICAL_SURFACE ( 'NONE', #44584, 0.2500000000000004996 ) ;
#82006 = VERTEX_POINT ( 'NONE', #72576 ) ;
#82007 = ORIENTED_EDGE ( 'NONE', *, *, #2107, .F. ) ;
#82009 = CARTESIAN_POINT ( 'NONE',  ( -18.13014796973170206, -10.31621877034669588, 34.18098118002070152 ) ) ;
#82008 = CARTESIAN_POINT ( 'NONE',  ( -5.326946301144535489, -12.07920672191015221, 32.31858351112116168 ) ) ;
#82010 = EDGE_CURVE ( 'NONE', #28117, #81424, #8821, .T. ) ;
#82011 = CARTESIAN_POINT ( 'NONE',  ( -9.561782254074046250, -12.50538340440932394, 31.33453814440721885 ) ) ;
#82012 = CARTESIAN_POINT ( 'NONE',  ( 3.361294932532796764, -10.88167719472716399, 33.43325721877153711 ) ) ;
#82013 = DIRECTION ( 'NONE',  ( 0.000000000000000000, 0.9848077530122072432, 0.1736481776669354937 ) ) ;
#82014 = CARTESIAN_POINT ( 'NONE',  ( 13.38461538461538680, -11.16473453929635440, 33.15142922261926373 ) ) ;
#82015 = ORIENTED_EDGE ( 'NONE', *, *, #34225, .T. ) ;
#82016 = CARTESIAN_POINT ( 'NONE',  ( 17.07692307692295586, -3.300289026999228437, 32.46337939537709616 ) ) ;
#82017 = B_SPLINE_CURVE_WITH_KNOTS ( 'NONE', 3,
 ( #56321, #82142, #22532, #35612, #60967, #77913, #63949, #42377, #2244, #70279 ),
 .UNSPECIFIED., .F., .F.,
 ( 4, 2, 2, 2, 4 ),
 ( 0.0007817246256747444619, 0.0009771112852218868158, 0.001172497944769029061, 0.001367884604316171523, 0.001563271263863313769 ),
 .UNSPECIFIED. ) ;
#82018 = CARTESIAN_POINT ( 'NONE',  ( 0.7114839798866018361, -10.05730279482229683, 34.04704008940765902 ) ) ;
#82019 = CARTESIAN_POINT ( 'NONE',  ( -9.019207500173124004, -12.17611988154120972, 31.52148481390971213 ) ) ;
#82020 = VECTOR ( 'NONE', #34472, 1000.000000000000000 ) ;
#82021 = CARTESIAN_POINT ( 'NONE',  ( -7.053767526187231240, -6.369640206132550553, 34.87707690430378449 ) ) ;
#82022 = EDGE_LOOP ( 'NONE', ( #35608, #51508 ) ) ;
#82023 = ORIENTED_EDGE ( 'NONE', *, *, #80695, .F. ) ;
#82024 = AXIS2_PLACEMENT_3D ( 'NONE', #49014, #70173, #27417 ) ;
#82025 = AXIS2_PLACEMENT_3D ( 'NONE', #8102, #49528, #35573 ) ;
#82026 = ORIENTED_EDGE ( 'NONE', *, *, #61695, .T. ) ;
#82027 = CARTESIAN_POINT ( 'NONE',  ( 0.7114839798866025022, -10.76462480002816235, 33.53768742498949962 ) ) ;
#82028 = EDGE_CURVE ( 'NONE', #44956, #69684, #76439, .T. ) ;
#82029 = ORIENTED_EDGE ( 'NONE', *, *, #56336, .T. ) ;
#82030 = CARTESIAN_POINT ( 'NONE',  ( -16.02332045208259359, -5.195472089885680766, 34.18748526763464923 ) ) ;
#82031 = CARTESIAN_POINT ( 'NONE',  ( 14.30769230769231015, -5.471508081941601098, 34.59228464037088457 ) ) ;
#82032 = CARTESIAN_POINT ( 'NONE',  ( 3.361294669002876656, -5.915461855592777596, 34.75538340440931506 ) ) ;
#82033 = FACE_OUTER_BOUND ( 'NONE', #4873, .T. ) ;
#82034 = DIRECTION ( 'NONE',  ( -0.000000000000000000, -0.3420201433256694901, -0.9396926207859082059 ) ) ;
#82035 = ORIENTED_EDGE ( 'NONE', *, *, #3225, .T. ) ;
#82036 = CARTESIAN_POINT ( 'NONE',  ( 4.284371855609718338, -4.459921816937789885, 33.71989282347011851 ) ) ;
#82038 = ORIENTED_EDGE ( 'NONE', *, *, #28365, .F. ) ;
#82037 = CARTESIAN_POINT ( 'NONE',  ( -13.38461538461538325, -4.098570777380720287, 33.41473453929634729 ) ) ;
#82039 = FACE_OUTER_BOUND ( 'NONE', #77430, .T. ) ;
#82040 = DIRECTION ( 'NONE',  ( -0.000000000000000000, 0.7660444431189791237, -0.6427876096865379196 ) ) ;
#82041 = CARTESIAN_POINT ( 'NONE',  ( -11.66915214157184444, -10.70098750199973203, 33.91152734681376302 ) ) ;
#82042 = CARTESIAN_POINT ( 'NONE',  ( 11.60452887181161508, -9.905515769479276145, 34.41647553114623292 ) ) ;
#82043 = CARTESIAN_POINT ( 'NONE',  ( -12.52680890749923570, -2.892918686051582977, 31.69288490824015980 ) ) ;
#82044 = EDGE_CURVE ( 'NONE', #14505, #58651, #41040, .T. ) ;
#82045 = LINE ( 'NONE', #48679, #60789 ) ;
#82046 = CARTESIAN_POINT ( 'NONE',  ( -0.4615384615384611200, -13.87047571288749737, 32.06866353760679544 ) ) ;
#82047 = CARTESIAN_POINT ( 'NONE',  ( 2.750000000000002665, -7.561099074964516831, 19.72061829374151287 ) ) ;
#82048 = ORIENTED_EDGE ( 'NONE', *, *, #86880, .T. ) ;
#82049 = DIRECTION ( 'NONE',  ( -0.000000000000000000, -0.000000000000000000, -1.000000000000000000 ) ) ;
#82050 = LINE ( 'NONE', #14021, #39052 ) ;
#82051 = CARTESIAN_POINT ( 'NONE',  ( 9.942253101685738059, -10.92531984108285670, 33.72920026020278073 ) ) ;
#82052 = SURFACE_STYLE_USAGE ( .BOTH. , #54558 ) ;
#82053 = ORIENTED_EDGE ( 'NONE', *, *, #70270, .F. ) ;
#82054 = LINE ( 'NONE', #13582, #80065 ) ;
#82055 = CARTESIAN_POINT ( 'NONE',  ( -7.846153846153844924, -10.51840700105979565, 33.73612834413961536 ) ) ;
#82056 = B_SPLINE_CURVE_WITH_KNOTS ( 'NONE', 3,
 ( #68585, #34351, #14086, #34794, #14981, #35699, #8223, #577, #82995, #42453 ),
 .UNSPECIFIED., .F., .F.,
 ( 4, 2, 2, 2, 4 ),
 ( 0.0007817246256747528103, 0.0009771112852218978746, 0.001172497944769042939, 0.001367884604316188003, 0.001563271263863333068 ),
 .UNSPECIFIED. ) ;
#82057 = B_SPLINE_CURVE_WITH_KNOTS ( 'NONE', 3,
 ( #29280, #30152, #50839, #83337, #21619, #8116 ),
 .UNSPECIFIED., .F., .F.,
 ( 4, 2, 4 ),
 ( 4.563551064100006665E-17, 0.0001954756301637168570, 0.0003909512603273880690 ),
 .UNSPECIFIED. ) ;
#82058 = CARTESIAN_POINT ( 'NONE',  ( 2.307692307692186251, -11.06231777344772027, 33.60647404775119895 ) ) ;
#82059 = LINE ( 'NONE', #47365, #42789 ) ;
#82060 = CARTESIAN_POINT ( 'NONE',  ( 17.86930939688968678, -2.494641256782728966, 31.33461815524612959 ) ) ;
#82061 = EDGE_LOOP ( 'NONE', ( #17300, #25167 ) ) ;
#82062 = B_SPLINE_CURVE_WITH_KNOTS ( 'NONE', 3,
 ( #13893, #14793, #28290, #21537, #48555, #49889, #84148, #69288, #55761, #22858 ),
 .UNSPECIFIED., .F., .F.,
 ( 4, 2, 2, 2, 4 ),
 ( 0.000000000000000000, 0.0001954339857564081249, 0.0003908679715128162498, 0.0005863019572692244018, 0.0007817359430256324996 ),
 .UNSPECIFIED. ) ;
#82064 = ADVANCED_FACE ( 'NONE', ( #71235 ), #78441, .F. ) ;
#82063 = DIRECTION ( 'NONE',  ( 1.000000000000000000, 0.000000000000000000, 0.000000000000000000 ) ) ;
#82065 = EDGE_CURVE ( 'NONE', #59177, #1945, #13123, .T. ) ;
#82066 = LINE ( 'NONE', #67657, #77185 ) ;
#82067 = CARTESIAN_POINT ( 'NONE',  ( 5.299935921016468932, -12.38742843783360748, 31.66772728687926985 ) ) ;
#82069 = EDGE_LOOP ( 'NONE', ( #40055, #72990, #19056, #50100 ) ) ;
#82068 = AXIS2_PLACEMENT_3D ( 'NONE', #33182, #60202, #19665 ) ;
#82070 = CYLINDRICAL_SURFACE ( 'NONE', #60001, 0.2499999999999986955 ) ;
#82071 = ORIENTED_EDGE ( 'NONE', *, *, #56091, .F. ) ;
#82072 = PLANE ( 'NONE',  #25581 ) ;
#82073 = CARTESIAN_POINT ( 'NONE',  ( -23.00000000000000000, -12.50000000000000000, 27.25000000000000000 ) ) ;
#82074 = ORIENTED_EDGE ( 'NONE', *, *, #23659, .F. ) ;
#82075 = CARTESIAN_POINT ( 'NONE',  ( -1.384615384615383471, -5.557115091759785130, 34.35708131394839171 ) ) ;
#82076 = CARTESIAN_POINT ( 'NONE',  ( 4.284371592079798674, -9.503571793651733657, 34.60286762892837942 ) ) ;
#82077 = CARTESIAN_POINT ( 'NONE',  ( 1.161689167099239750, -4.186968288167446595, 33.49512374952580274 ) ) ;
#82078 = FACE_OUTER_BOUND ( 'NONE', #22590, .T. ) ;
#82079 = DIRECTION ( 'NONE',  ( 0.000000000000000000, 0.000000000000000000, -1.000000000000000000 ) ) ;
#82080 = ORIENTED_EDGE ( 'NONE', *, *, #74521, .F. ) ;
#82081 = VECTOR ( 'NONE', #54871, 1000.000000000000000 ) ;
#82082 = FACE_BOUND ( 'NONE', #6411, .T. ) ;
#82083 = ORIENTED_EDGE ( 'NONE', *, *, #37975, .T. ) ;
#82084 = DIRECTION ( 'NONE',  ( -0.000000000000000000, -0.9396926207859092051, -0.3420201433256662704 ) ) ;
#82085 = VECTOR ( 'NONE', #59549, 1000.000000000000000 ) ;
#82086 = CARTESIAN_POINT ( 'NONE',  ( 4.946231610255519051, -11.71456829005830080, 32.44064028649416542 ) ) ;
#82087 = CARTESIAN_POINT ( 'NONE',  ( 6.130790440966950250, -5.496552790871117367, 34.60292014791297532 ) ) ;
#82088 = CARTESIAN_POINT ( 'NONE',  ( -11.31545018684868964, -2.554770724473667265, 30.48948780036025852 ) ) ;
#82089 = AXIS2_PLACEMENT_3D ( 'NONE', #77232, #15542, #43010 ) ;
#82090 = ORIENTED_EDGE ( 'NONE', *, *, #3949, .F. ) ;
#82091 = ORIENTED_EDGE ( 'NONE', *, *, #17674, .T. ) ;
#82092 = ORIENTED_EDGE ( 'NONE', *, *, #42281, .F. ) ;
#82093 = B_SPLINE_CURVE_WITH_KNOTS ( 'NONE', 3,
 ( #83138, #48896, #35838, #70054, #8364, #35383, #22315, #49779, #77254, #15564, #68284, #30839, #78584, #50661, #70947, #50211, #72271, #16885, #71375, #36282, #84472, #63738, #64612, #56979, #8809, #51090, #30403, #58761, #57870, #9258, #23200, #78143, #43914, #16007, #16445, #2039, #10583, #36715, #77697, #38050, #31294, #85354 ),
 .UNSPECIFIED., .F., .F.,
 ( 4, 2, 2, 2, 2, 2, 2, 2, 2, 2, 2, 2, 2, 2, 2, 2, 2, 2, 2, 2, 4 ),
 ( 0.000000000000000000, 0.0006451441852033102092, 0.001290288370406620418, 0.001935432555609930627, 0.002580576740813240403, 0.003870865111219860388, 0.005161153481626479939, 0.005806297666829790365, 0.006451441852033101658, 0.007096586037236412951, 0.007741730222439724245, 0.008386874407643036405, 0.008709446500244692052, 0.009032018592846349433, 0.009112661615996761610, 0.009193304639147175522, 0.009233626150722380743, 0.009273947662297585964, 0.009354590685448003345, 0.009677162778049660727, 0.01032230696325297896 ),
 .UNSPECIFIED. ) ;
#82094 = CARTESIAN_POINT ( 'NONE',  ( -0.4615384615384611200, -3.050289026998446396, 32.03036669348365706 ) ) ;
#82095 = EDGE_LOOP ( 'NONE', ( #24021, #18535 ) ) ;
#82096 = CARTESIAN_POINT ( 'NONE',  ( -17.14300545628320904, -9.905515769479276145, 34.41647553114623292 ) ) ;
#82097 = CARTESIAN_POINT ( 'NONE',  ( -5.076923076923075762, -12.78798330534102767, 29.49999999999997868 ) ) ;
#82098 = FACE_OUTER_BOUND ( 'NONE', #70647, .T. ) ;
#82099 = CARTESIAN_POINT ( 'NONE',  ( 17.86930853333243618, -9.804603061927743113, 34.18744698557895845 ) ) ;
#82100 = CARTESIAN_POINT ( 'NONE',  ( 5.011653076366756387, -10.33852847137145048, 34.16647553114627556 ) ) ;
#82101 = LINE ( 'NONE', #80335, #62324 ) ;
#82102 = DIRECTION ( 'NONE',  ( 0.000000000000000000, 0.7660444431189807890, 0.6427876096865361433 ) ) ;
#82103 = CARTESIAN_POINT ( 'NONE',  ( 11.47319109250076430, -10.21337939537584383, 33.94971097300158647 ) ) ;
#82104 = ORIENTED_EDGE ( 'NONE', *, *, #26002, .T. ) ;
#82105 = ORIENTED_EDGE ( 'NONE', *, *, #3536, .F. ) ;
#82106 = ORIENTED_EDGE ( 'NONE', *, *, #69996, .F. ) ;
#82107 = CARTESIAN_POINT ( 'NONE',  ( -13.51530598772569114, -12.35290016733513951, 31.75349464988449455 ) ) ;
#82109 = CARTESIAN_POINT ( 'NONE',  ( -7.846153846153844924, -4.098570777380720287, 33.41473453929634729 ) ) ;
#82108 = CARTESIAN_POINT ( 'NONE',  ( 0.000000000000000000, -2.085786437626902856, 28.75000000000000000 ) ) ;
#82110 = EDGE_CURVE ( 'NONE', #83962, #30445, #35614, .T. ) ;
#82111 = EDGE_CURVE ( 'NONE', #47411, #2090, #81571, .T. ) ;
#82112 = DIRECTION ( 'NONE',  ( 0.000000000000000000, 0.000000000000000000, 1.000000000000000000 ) ) ;
#82113 = FACE_OUTER_BOUND ( 'NONE', #63459, .T. ) ;
#82114 = FACE_BOUND ( 'NONE', #59068, .T. ) ;
#82115 = CARTESIAN_POINT ( 'NONE',  ( -12.46153846153846168, -12.78798330534103123, 29.99999999999997868 ) ) ;
#82116 = VERTEX_POINT ( 'NONE', #39703 ) ;
#82117 = DIRECTION ( 'NONE',  ( 0.000000000000000000, 0.000000000000000000, -1.000000000000000000 ) ) ;
#82118 = DIRECTION ( 'NONE',  ( -0.000000000000000000, 0.6427876096865404731, -0.7660444431189770143 ) ) ;
#82119 = CARTESIAN_POINT ( 'NONE',  ( 3.007284287045282500, -10.81261337010820256, 33.49550067578627477 ) ) ;
#82120 = VECTOR ( 'NONE', #80931, 1000.000000000000114 ) ;
#82121 = ORIENTED_EDGE ( 'NONE', *, *, #10359, .T. ) ;
#82122 = DIRECTION ( 'NONE',  ( -1.000000000000000000, -0.000000000000000000, -0.000000000000000000 ) ) ;
#82123 = ORIENTED_EDGE ( 'NONE', *, *, #49931, .T. ) ;
#82124 = FACE_BOUND ( 'NONE', #86570, .T. ) ;
#82125 = CARTESIAN_POINT ( 'NONE',  ( 9.468822748583747284, -5.912607949931405926, 34.49155766932282319 ) ) ;
#82126 = EDGE_CURVE ( 'NONE', #66604, #33483, #26039, .T. ) ;
#82127 = ORIENTED_EDGE ( 'NONE', *, *, #2527, .F. ) ;
#82128 = CARTESIAN_POINT ( 'NONE',  ( -8.096153846153855582, -2.249999999999999112, 29.81609741502487765 ) ) ;
#82129 = CARTESIAN_POINT ( 'NONE',  ( -16.81410256410256565, -7.500000000000000000, 29.75000000000000355 ) ) ;
#82130 = CARTESIAN_POINT ( 'NONE',  ( 1.384615384615265343, -3.300289026999228881, 32.46337939537708905 ) ) ;
#82131 = ORIENTED_EDGE ( 'NONE', *, *, #4194, .F. ) ;
#82132 = EDGE_CURVE ( 'NONE', #58964, #1652, #19413, .T. ) ;
#82133 = FACE_OUTER_BOUND ( 'NONE', #46684, .T. ) ;
#82134 = CARTESIAN_POINT ( 'NONE',  ( 14.17754433796061164, -11.66186481527757302, 32.95055677023626117 ) ) ;
#82135 = CARTESIAN_POINT ( 'NONE',  ( -16.40382288478850725, -12.41269422305637171, 30.68257228309993323 ) ) ;
#82136 = FACE_OUTER_BOUND ( 'NONE', #73493, .T. ) ;
#82137 = ORIENTED_EDGE ( 'NONE', *, *, #69009, .F. ) ;
#82138 = CARTESIAN_POINT ( 'NONE',  ( -12.46153846153846168, -10.89733346790207413, 36.13435417666054406 ) ) ;
#82139 = CARTESIAN_POINT ( 'NONE',  ( 3.903822929624696236, -10.18141759479407327, 34.26406193332782379 ) ) ;
#82141 = ORIENTED_EDGE ( 'NONE', *, *, #6305, .F. ) ;
#82140 = CARTESIAN_POINT ( 'NONE',  ( 16.08809272553282099, -7.249945578846654470, 34.99404164642496795 ) ) ;
#82142 = CARTESIAN_POINT ( 'NONE',  ( -5.011667937410238416, -3.643525952247864463, 33.31231777344670064 ) ) ;
#82143 = CARTESIAN_POINT ( 'NONE',  ( 9.442307692307693401, -7.500000000000001776, 35.00000000000000000 ) ) ;
#82144 = DIRECTION ( 'NONE',  ( -0.000000000000000000, 0.9396926207859093161, -0.3420201433256663259 ) ) ;
#82145 = CARTESIAN_POINT ( 'NONE',  ( 16.15384615384603251, -12.16647553114689728, 32.15551576947799362 ) ) ;
#82146 = DIRECTION ( 'NONE',  ( -0.000000000000000000, -0.1736481776669307198, -0.9848077530122080203 ) ) ;
#82147 = CARTESIAN_POINT ( 'NONE',  ( 9.915319043920545639, -9.086983370893049639, 34.49168942202179267 ) ) ;
#82149 = CARTESIAN_POINT ( 'NONE',  ( -16.21911615440247090, -8.656820664281497102, 34.87096338111211935 ) ) ;
#82148 = CARTESIAN_POINT ( 'NONE',  ( 17.78205128205128105, -11.50000000000000000, 29.75000000000000355 ) ) ;
#82150 = EDGE_CURVE ( 'NONE', #85054, #51499, #25730, .T. ) ;
#82151 = CARTESIAN_POINT ( 'NONE',  ( -6.857008572074485997, -2.721908614388772296, 31.22303859784725333 ) ) ;
#82152 = CARTESIAN_POINT ( 'NONE',  ( 2.750000000000001776, -7.499999999999984013, 16.96875000000000000 ) ) ;
#82153 = ORIENTED_EDGE ( 'NONE', *, *, #2696, .T. ) ;
#82154 = CARTESIAN_POINT ( 'NONE',  ( -18.00000000000012079, -9.442884908241554243, 34.35708131394783038 ) ) ;
#82155 = VERTEX_POINT ( 'NONE', #86559 ) ;
#82156 = VECTOR ( 'NONE', #35030, 1000.000000000000000 ) ;
#82157 = VERTEX_POINT ( 'NONE', #24829 ) ;
#82158 = CARTESIAN_POINT ( 'NONE',  ( 2.307692307692309264, -12.10708131394839349, 31.69288490824020244 ) ) ;
#82159 = VERTEX_POINT ( 'NONE', #40147 ) ;
#82160 = CARTESIAN_POINT ( 'NONE',  ( 14.08420736396836226, -8.496056993536548418, 34.65000542017679663 ) ) ;
#82161 = CARTESIAN_POINT ( 'NONE',  ( 1.139087296526029469, -10.24999999999999467, 18.45312500000000355 ) ) ;
#82162 = CARTESIAN_POINT ( 'NONE',  ( 14.53070365930516061, -11.24521262558773493, 33.06293181088029343 ) ) ;
#82163 = CARTESIAN_POINT ( 'NONE',  ( -7.912236225513981758, -8.164416787775445883, 34.95778746994557906 ) ) ;
#82164 = CARTESIAN_POINT ( 'NONE',  ( 7.780903914379759811, -2.255955759149247619, 30.00000000000013856 ) ) ;
#82165 = AXIS2_PLACEMENT_3D ( 'NONE', #5576, #79903, #25850 ) ;
#82166 = DIRECTION ( 'NONE',  ( 0.000000000000000000, 0.000000000000000000, 1.000000000000000000 ) ) ;
#82167 = CARTESIAN_POINT ( 'NONE',  ( 9.758375025657770152, -12.34228464037088813, 31.77849191805839268 ) ) ;
#82168 = CARTESIAN_POINT ( 'NONE',  ( 2.307692307692187583, -11.48612834414049644, 32.76840700105863391 ) ) ;
#82169 = CARTESIAN_POINT ( 'NONE',  ( 6.700149964170073247, -12.38737895849757820, 31.66785238281580206 ) ) ;
#82170 = CARTESIAN_POINT ( 'NONE',  ( 10.36536137809165403, -2.587272538249754117, 30.68239716806877837 ) ) ;
#82172 = EDGE_CURVE ( 'NONE', #76768, #83657, #26172, .T. ) ;
#82171 = CARTESIAN_POINT ( 'NONE',  ( -16.94639763868943660, -11.04252011169590020, 33.62494198852677840 ) ) ;
#82173 = EDGE_CURVE ( 'NONE', #46391, #58385, #62559, .T. ) ;
#82174 = DIRECTION ( 'NONE',  ( 0.000000000000000000, 0.3420201433256610524, 0.9396926207859113145 ) ) ;
#82175 = ORIENTED_EDGE ( 'NONE', *, *, #36677, .T. ) ;
#82177 = EDGE_CURVE ( 'NONE', #46513, #15704, #21724, .T. ) ;
#82176 = ORIENTED_EDGE ( 'NONE', *, *, #78621, .F. ) ;
#82178 = CARTESIAN_POINT ( 'NONE',  ( -18.00000000000012079, -2.657715359629662988, 31.77849191805970364 ) ) ;
#82179 = CYLINDRICAL_SURFACE ( 'NONE', #7194, 0.2500000000000009437 ) ;
#82180 = CARTESIAN_POINT ( 'NONE',  ( -18.00000000000012079, -9.528491918059723176, 34.59228464037033035 ) ) ;
#82181 = CARTESIAN_POINT ( 'NONE',  ( -11.28846153846010303, -7.500000000000155431, 34.75000000000007105 ) ) ;
#82182 = EDGE_CURVE ( 'NONE', #68899, #71885, #74364, .T. ) ;
#82183 = LINE ( 'NONE', #87619, #14709 ) ;
#82184 = DIRECTION ( 'NONE',  ( 1.000000000000000000, 0.000000000000000000, 0.000000000000000000 ) ) ;
#82185 = VECTOR ( 'NONE', #78840, 1000.000000000000000 ) ;
#82186 = CYLINDRICAL_SURFACE ( 'NONE', #16364, 0.2499999999999994726 ) ;
#82187 = VERTEX_POINT ( 'NONE', #53188 ) ;
#82188 = B_SPLINE_CURVE_WITH_KNOTS ( 'NONE', 3,
 ( #84501, #16034, #43504, #70977, #36744, #84945, #78173, #16474, #39429, #46175 ),
 .UNSPECIFIED., .F., .F.,
 ( 4, 2, 2, 2, 4 ),
 ( 0.000000000000000000, 0.0001954311584214072381, 0.0003908623168428144762, 0.0005862934752642217414, 0.0007817246336856289524 ),
 .UNSPECIFIED. ) ;
#82189 = CARTESIAN_POINT ( 'NONE',  ( 3.164686851409094892, -6.343179335718451384, 34.87096338111212646 ) ) ;
#82190 = ORIENTED_EDGE ( 'NONE', *, *, #67069, .F. ) ;
#82191 = CARTESIAN_POINT ( 'NONE',  ( -8.638705330997126453, -5.070358843744210198, 34.40418822224088302 ) ) ;
#82192 = LINE ( 'NONE', #14167, #22651 ) ;
#82193 = CYLINDRICAL_SURFACE ( 'NONE', #64561, 4.000000000000000000 ) ;
#82194 = CYLINDRICAL_SURFACE ( 'NONE', #47951, 0.2499999999999995559 ) ;
#82195 = CARTESIAN_POINT ( 'NONE',  ( -13.63459212866397507, -2.544273027872575366, 31.48422191005632342 ) ) ;
#82196 = ORIENTED_EDGE ( 'NONE', *, *, #38467, .F. ) ;
#82197 = ORIENTED_EDGE ( 'NONE', *, *, #30189, .F. ) ;
#82198 = EDGE_CURVE ( 'NONE', #63575, #20877, #78673, .T. ) ;
#82199 = EDGE_LOOP ( 'NONE', ( #54181, #6608 ) ) ;
#82200 = EDGE_LOOP ( 'NONE', ( #79091, #77012, #35837, #58547 ) ) ;
#82201 = CARTESIAN_POINT ( 'NONE',  ( -13.38461538461550582, -6.879047030192662504, 34.71129190930017927 ) ) ;
#82202 = CARTESIAN_POINT ( 'NONE',  ( -2.557715531913763662, -10.18141759479407327, 34.26406193332782379 ) ) ;
#82203 = CARTESIAN_POINT ( 'NONE',  ( 14.30769230769218581, -2.657715359629662544, 31.77849191805970364 ) ) ;
#82204 = VECTOR ( 'NONE', #88025, 1000.000000000000000 ) ;
#82205 = CARTESIAN_POINT ( 'NONE',  ( -19.50000000000000000, -3.499999999999999556, 29.75000000000000355 ) ) ;
#82206 = CARTESIAN_POINT ( 'NONE',  ( 17.86930939688968678, -2.845849958028613624, 32.17971566917920967 ) ) ;
#82207 = CARTESIAN_POINT ( 'NONE',  ( 12.33139049180676494, -3.069018819979302926, 32.56621877034667278 ) ) ;
#82208 = ORIENTED_EDGE ( 'NONE', *, *, #15042, .T. ) ;
#82209 = ORIENTED_EDGE ( 'NONE', *, *, #41968, .T. ) ;
#82210 = AXIS2_PLACEMENT_3D ( 'NONE', #82545, #20821, #29366 ) ;
#82211 = EDGE_CURVE ( 'NONE', #37942, #84770, #1309, .T. ) ;
#82212 = B_SPLINE_CURVE_WITH_KNOTS ( 'NONE', 3,
 ( #51216, #72401, #85049, #23326, #78270, #16573, #44037, #23763, #30532, #85484 ),
 .UNSPECIFIED., .F., .F.,
 ( 4, 2, 2, 2, 4 ),
 ( 0.000000000000000000, 0.0001954339857564080165, 0.0003908679715128160329, 0.0005863019572692240765, 0.0007817359430256320659 ),
 .UNSPECIFIED. ) ;
#82213 = ORIENTED_EDGE ( 'NONE', *, *, #35388, .T. ) ;
#82215 = ORIENTED_EDGE ( 'NONE', *, *, #52831, .T. ) ;
#82214 = CARTESIAN_POINT ( 'NONE',  ( -3.230769230769229949, -2.486705287966279876, 31.30864560766543647 ) ) ;
#82216 = FACE_OUTER_BOUND ( 'NONE', #7209, .T. ) ;
#82217 = CARTESIAN_POINT ( 'NONE',  ( -16.15384615384615330, -13.20930481340135110, 34.54067556320372745 ) ) ;
#82218 = CARTESIAN_POINT ( 'NONE',  ( 3.750000000000000888, -7.499999999999978684, 19.46875000000000000 ) ) ;
#82219 = EDGE_LOOP ( 'NONE', ( #49413, #66449, #67173, #24700 ) ) ;
#82220 = CARTESIAN_POINT ( 'NONE',  ( -1.161602540521988747, -2.523321265292116422, 31.42251411153756990 ) ) ;
#82221 = VERTEX_POINT ( 'NONE', #6359 ) ;
#82222 = CARTESIAN_POINT ( 'NONE',  ( 2.084766090176162212, -6.503392248772476236, 34.64988816332204635 ) ) ;
#82223 = FACE_BOUND ( 'NONE', #3338, .T. ) ;
#82224 = FACE_OUTER_BOUND ( 'NONE', #75272, .T. ) ;
#82225 = ADVANCED_FACE ( 'NONE', ( #48650 ), #477, .F. ) ;
#82226 = DIRECTION ( 'NONE',  ( -0.000000000000000000, -0.6427876096865404731, -0.7660444431189770143 ) ) ;
#82227 = ORIENTED_EDGE ( 'NONE', *, *, #65816, .T. ) ;
#82228 = DIRECTION ( 'NONE',  ( -1.000000000000000000, -0.000000000000000000, -0.000000000000000000 ) ) ;
#82229 = SURFACE_STYLE_USAGE ( .BOTH. , #65589 ) ;
#82230 = EDGE_CURVE ( 'NONE', #58112, #60787, #81880, .T. ) ;
#82231 = CARTESIAN_POINT ( 'NONE',  ( 16.40390057375961064, -6.523592122091590895, 34.90882529074906415 ) ) ;
#82232 = FACE_OUTER_BOUND ( 'NONE', #28273, .T. ) ;
#82233 = EDGE_LOOP ( 'NONE', ( #453, #85843 ) ) ;
#82234 = VECTOR ( 'NONE', #31706, 1000.000000000000114 ) ;
#82235 = DIRECTION ( 'NONE',  ( 1.000000000000000000, 0.000000000000000000, 0.000000000000000000 ) ) ;
#82236 = DIRECTION ( 'NONE',  ( -0.000000000000000000, -0.000000000000000000, -1.000000000000000000 ) ) ;
#82237 = CARTESIAN_POINT ( 'NONE',  ( 17.32686859527121825, -10.05730279482229683, 34.04704008940765902 ) ) ;
#82238 = CARTESIAN_POINT ( 'NONE',  ( -10.61538461538473577, -8.656820664282941280, 34.87096338111179961 ) ) ;
#82239 = DIRECTION ( 'NONE',  ( 1.000000000000000000, 0.000000000000000000, 0.000000000000000000 ) ) ;
#82240 = FACE_BOUND ( 'NONE', #53614, .T. ) ;
#82242 = CARTESIAN_POINT ( 'NONE',  ( 16.85343815235874132, -3.019605429927187501, 32.48692288466676814 ) ) ;
#82241 = CARTESIAN_POINT ( 'NONE',  ( 13.31853300525524908, -11.91647553114624181, 32.58852847137148245 ) ) ;
#82243 = EDGE_CURVE ( 'NONE', #29224, #30312, #62604, .T. ) ;
#82244 = CARTESIAN_POINT ( 'NONE',  ( -6.988347369037699153, -12.27809138561121394, 31.22303859784730307 ) ) ;
#82246 = LINE ( 'NONE', #81805, #83752 ) ;
#82245 = CARTESIAN_POINT ( 'NONE',  ( 3.007890548340584225, -7.630691491037286056, 34.74850469731152458 ) ) ;
#82247 = VECTOR ( 'NONE', #42845, 1000.000000000000000 ) ;
#82248 = CARTESIAN_POINT ( 'NONE',  ( -8.069638770718176701, -4.225889041578353655, 33.85425143139329407 ) ) ;
#82249 = CARTESIAN_POINT ( 'NONE',  ( 2.775308065498768517, -8.577988221561467341, 15.54500670625849246 ) ) ;
#82250 = EDGE_LOOP ( 'NONE', ( #14402, #33329, #73078, #22374 ) ) ;
#82251 = CARTESIAN_POINT ( 'NONE',  ( 1.319344938654611221, -12.27809138561121394, 31.22303859784730307 ) ) ;
#82252 = VERTEX_POINT ( 'NONE', #88785 ) ;
#82253 = B_SPLINE_CURVE_WITH_KNOTS ( 'NONE', 3,
 ( #65868, #4173, #86618, #73082, #66325, #4625, #80294, #6837, #55467, #34308 ),
 .UNSPECIFIED., .F., .F.,
 ( 4, 2, 2, 2, 4 ),
 ( 0.0007817359527651098448, 0.0009771254036996487088, 0.001172514854634187573, 0.001367904305568726220, 0.001563293756503265084 ),
 .UNSPECIFIED. ) ;
#82254 = EDGE_CURVE ( 'NONE', #4576, #29049, #28382, .T. ) ;
#82255 = CARTESIAN_POINT ( 'NONE',  ( -15.10024352900566846, -4.459921816937791661, 33.71989282347011851 ) ) ;
#82256 = EDGE_LOOP ( 'NONE', ( #24480, #43829, #11593, #39407 ) ) ;
#82257 = DIRECTION ( 'NONE',  ( 0.000000000000000000, 0.1736481776669275834, 0.9848077530122086864 ) ) ;
#82259 = EDGE_CURVE ( 'NONE', #47287, #67226, #49096, .T. ) ;
#82258 = CARTESIAN_POINT ( 'NONE',  ( 14.08476534878545827, -4.026226216239094491, 33.68668979543634379 ) ) ;
#82261 = ORIENTED_EDGE ( 'NONE', *, *, #51056, .F. ) ;
#82260 = DIRECTION ( 'NONE',  ( -0.000000000000000000, -0.8660254037844397068, -0.4999999999999978906 ) ) ;
#82262 = CARTESIAN_POINT ( 'NONE',  ( 5.076923076923075762, -11.91647553114624181, 32.58852847137148245 ) ) ;
#82263 = CARTESIAN_POINT ( 'NONE',  ( 2.724691934501235036, -6.299813628509441266, 19.13875670625849068 ) ) ;
#82264 = CARTESIAN_POINT ( 'NONE',  ( -15.29685161012936589, -9.058645607665454236, 34.76329471203372634 ) ) ;
#82265 = CARTESIAN_POINT ( 'NONE',  ( 0.000000000000000000, -11.00000000000000000, 29.75000000000000355 ) ) ;
#82266 = CARTESIAN_POINT ( 'NONE',  ( -10.03846153846153832, -1.926643599941765039, 29.65000000000000213 ) ) ;
#82267 = DIRECTION ( 'NONE',  ( -0.000000000000000000, -0.8660254037844397068, -0.4999999999999978906 ) ) ;
#82268 = CARTESIAN_POINT ( 'NONE',  ( -1.254089946381739651, -6.808710257144161559, 34.95449254468098843 ) ) ;
#82269 = CARTESIAN_POINT ( 'NONE',  ( 11.53846153846153832, -3.513871655860378418, 32.76840700105978499 ) ) ;
#82270 = CARTESIAN_POINT ( 'NONE',  ( 3.724691934501251023, -9.114399933863618131, 21.04874329374151642 ) ) ;
#82271 = B_SPLINE_CURVE_WITH_KNOTS ( 'NONE', 3,
 ( #13339, #73731, #74604, #80025, #53883, #19217, #25965, #33170, #60632, #4366 ),
 .UNSPECIFIED., .F., .F.,
 ( 4, 2, 2, 2, 4 ),
 ( 0.0007817246336856291692, 0.0009771112958940105907, 0.001172497958102391904, 0.001367884620310773434, 0.001563271282519154747 ),
 .UNSPECIFIED. ) ;
#82272 = DIRECTION ( 'NONE',  ( -0.000000000000000000, -0.9848077530122086864, -0.1736481776669273613 ) ) ;
#82274 = EDGE_CURVE ( 'NONE', #62624, #75979, #4507, .T. ) ;
#82273 = CARTESIAN_POINT ( 'NONE',  ( -4.403869378067608586, -2.985938066672154445, 32.43141759479405550 ) ) ;
#82275 = ORIENTED_EDGE ( 'NONE', *, *, #22673, .T. ) ;
#82276 = LINE ( 'NONE', #54786, #32086 ) ;
#82277 = CARTESIAN_POINT ( 'NONE',  ( 3.724691934501251023, -9.114399933863618131, 22.29874329374151642 ) ) ;
#82278 = EDGE_CURVE ( 'NONE', #29049, #49385, #7235, .T. ) ;
#82279 = DIRECTION ( 'NONE',  ( 0.000000000000000000, 0.000000000000000000, -1.000000000000000000 ) ) ;
#82280 = DIRECTION ( 'NONE',  ( -0.000000000000000000, -0.6427876096865404731, -0.7660444431189771253 ) ) ;
#82281 = CIRCLE ( 'NONE', #88210, 4.000000000000000000 ) ;
#82282 = ORIENTED_EDGE ( 'NONE', *, *, #67981, .F. ) ;
#82283 = CARTESIAN_POINT ( 'NONE',  ( -17.07692307692307665, -5.415277668671390821, 36.20867863119892149 ) ) ;
#82284 = CARTESIAN_POINT ( 'NONE',  ( 3.164685819813350953, -3.513871655860377086, 32.76840700105978499 ) ) ;
#82286 = EDGE_LOOP ( 'NONE', ( #12616, #58167, #51394, #9557 ) ) ;
#82285 = CYLINDRICAL_SURFACE ( 'NONE', #13816, 0.2499999999999986955 ) ;
#82287 = CARTESIAN_POINT ( 'NONE',  ( 8.639082799499069765, -5.915902021225889484, 34.75552854090298638 ) ) ;
#82288 = EDGE_CURVE ( 'NONE', #77995, #25963, #82462, .T. ) ;
#82289 = CARTESIAN_POINT ( 'NONE',  ( -16.82692307692300915, -7.434744860731433924, 35.00000000000000711 ) ) ;
#82290 = VECTOR ( 'NONE', #13262, 1000.000000000000000 ) ;
#82291 = CARTESIAN_POINT ( 'NONE',  ( 13.38461538461538680, -12.78798330534102767, 29.49999999999997868 ) ) ;
#82292 = CARTESIAN_POINT ( 'NONE',  ( -9.469294848214296678, -2.523321265292115534, 31.42251411153756990 ) ) ;
#82293 = CARTESIAN_POINT ( 'NONE',  ( -15.45425415533356173, -11.60425143139329940, 33.02411095842164457 ) ) ;
#82294 = ORIENTED_EDGE ( 'NONE', *, *, #58679, .T. ) ;
#82295 = B_SPLINE_CURVE_WITH_KNOTS ( 'NONE', 3,
 ( #81516, #26567, #54467, #6299, #7624, #62118, #54022, #89169, #48151, #62545 ),
 .UNSPECIFIED., .F., .F.,
 ( 4, 2, 2, 2, 4 ),
 ( 0.0007817246336856291692, 0.0009771112958940105907, 0.001172497958102391904, 0.001367884620310773434, 0.001563271282519154747 ),
 .UNSPECIFIED. ) ;
#82296 = EDGE_CURVE ( 'NONE', #76455, #88588, #41842, .T. ) ;
#82297 = VERTEX_POINT ( 'NONE', #75252 ) ;
#82298 = ORIENTED_EDGE ( 'NONE', *, *, #11451, .F. ) ;
#82299 = CARTESIAN_POINT ( 'NONE',  ( -12.22435897435897267, -3.499999999999999556, 29.75000000000000355 ) ) ;
#82300 = CARTESIAN_POINT ( 'NONE',  ( 0.2386122440223120422, -2.554751324335733820, 30.48935550225260727 ) ) ;
#82301 = EDGE_CURVE ( 'NONE', #83936, #77943, #13984, .T. ) ;
#82302 = CARTESIAN_POINT ( 'NONE',  ( -13.31935981333935892, -12.27809138561124591, 31.22303859784720359 ) ) ;
#82303 = DIRECTION ( 'NONE',  ( 0.000000000000000000, 0.4999999999999985567, 0.8660254037844395958 ) ) ;
#82304 = DIRECTION ( 'NONE',  ( 0.000000000000000000, 0.3420201433256610524, 0.9396926207859113145 ) ) ;
#82305 = VECTOR ( 'NONE', #17094, 1000.000000000000227 ) ;
#82306 = ORIENTED_EDGE ( 'NONE', *, *, #74588, .T. ) ;
#82307 = EDGE_CURVE ( 'NONE', #2112, #71085, #61716, .T. ) ;
#82308 = ORIENTED_EDGE ( 'NONE', *, *, #2639, .T. ) ;
#82309 = ORIENTED_EDGE ( 'NONE', *, *, #65973, .F. ) ;
#82311 = VERTEX_POINT ( 'NONE', #41462 ) ;
#82310 = CARTESIAN_POINT ( 'NONE',  ( -6.988346923633242724, -8.656820664281497102, 34.87096338111211935 ) ) ;
#82312 = CARTESIAN_POINT ( 'NONE',  ( -1.384615384615506484, -3.083524468854526912, 32.58852847137268327 ) ) ;
#82313 = VECTOR ( 'NONE', #58438, 999.9999999999998863 ) ;
#82314 = EDGE_CURVE ( 'NONE', #86754, #67131, #68923, .T. ) ;
#82315 = DIRECTION ( 'NONE',  ( 0.000000000000000000, 0.000000000000000000, 1.000000000000000000 ) ) ;
#82316 = EDGE_CURVE ( 'NONE', #7820, #88099, #61446, .T. ) ;
#82317 = DIRECTION ( 'NONE',  ( 0.000000000000000000, 0.000000000000000000, -1.000000000000000000 ) ) ;
#82318 = CARTESIAN_POINT ( 'NONE',  ( 15.23076923076923173, -12.37446782046654192, 30.86335684631486131 ) ) ;
#82319 = ORIENTED_EDGE ( 'NONE', *, *, #76997, .T. ) ;
#82320 = EDGE_LOOP ( 'NONE', ( #65104, #75424, #14575, #48495 ) ) ;
#82321 = EDGE_CURVE ( 'NONE', #67169, #54354, #15184, .T. ) ;
#82322 = ORIENTED_EDGE ( 'NONE', *, *, #63659, .F. ) ;
#82323 = CARTESIAN_POINT ( 'NONE',  ( 10.86533013373275836, -10.76462480002816235, 33.53768742498949962 ) ) ;
#82325 = ORIENTED_EDGE ( 'NONE', *, *, #77908, .T. ) ;
#82324 = CARTESIAN_POINT ( 'NONE',  ( -11.53846153846153655, -10.89733346790207413, 36.13435417666054406 ) ) ;
#82326 = CARTESIAN_POINT ( 'NONE',  ( -22.00000000000000355, -10.00000000000000533, 10.00000000000000178 ) ) ;
#82327 = PLANE ( 'NONE',  #65179 ) ;
#82328 = EDGE_LOOP ( 'NONE', ( #77702, #25343, #15789, #1455 ) ) ;
#82329 = DIRECTION ( 'NONE',  ( 1.000000000000000000, 0.000000000000000000, 0.000000000000000000 ) ) ;
#82330 = FACE_OUTER_BOUND ( 'NONE', #80859, .T. ) ;
#82331 = EDGE_LOOP ( 'NONE', ( #22017, #43359, #13740, #14320 ) ) ;
#82332 = FACE_BOUND ( 'NONE', #60072, .T. ) ;
#82333 = CARTESIAN_POINT ( 'NONE',  ( 1.384615384615386802, -3.322132147404559976, 32.92929555188717927 ) ) ;
#82334 = CYLINDRICAL_SURFACE ( 'NONE', #41367, 4.000000000000000000 ) ;
#82335 = AXIS2_PLACEMENT_3D ( 'NONE', #78691, #32283, #86805 ) ;
#82336 = DIRECTION ( 'NONE',  ( -0.000000000000000000, -0.1736481776669307198, -0.9848077530122080203 ) ) ;
#82338 = CARTESIAN_POINT ( 'NONE',  ( 4.826946345980721809, -9.943427161483782584, 34.11278801902876978 ) ) ;
#82337 = CARTESIAN_POINT ( 'NONE',  ( -7.173076923076920686, -7.566083408709834757, 34.74999999999999289 ) ) ;
#82339 = VECTOR ( 'NONE', #88742, 1000.000000000000227 ) ;
#82340 = CARTESIAN_POINT ( 'NONE',  ( -3.931066612577743147, -2.847695495035524882, 31.58253572463339509 ) ) ;
#82341 = CARTESIAN_POINT ( 'NONE',  ( 13.38461538461538680, -12.09954503811598769, 35.62045528018868623 ) ) ;
#82342 = ORIENTED_EDGE ( 'NONE', *, *, #56793, .F. ) ;
#82343 = CARTESIAN_POINT ( 'NONE',  ( -18.22292621751614305, -10.61292498521070549, 33.66303323003028680 ) ) ;
#82344 = CYLINDRICAL_SURFACE ( 'NONE', #11945, 0.2500000000000009437 ) ;
#82345 = EDGE_CURVE ( 'NONE', #53520, #23339, #46463, .T. ) ;
#82346 = ORIENTED_EDGE ( 'NONE', *, *, #78343, .F. ) ;
#82347 = VECTOR ( 'NONE', #81846, 1000.000000000000000 ) ;
#82348 = CARTESIAN_POINT ( 'NONE',  ( -14.17716686945866655, -9.503571793651731880, 34.60286762892837942 ) ) ;
#82349 = CARTESIAN_POINT ( 'NONE',  ( -3.262820512820514107, -7.500000000000000000, 29.75000000000000355 ) ) ;
#82350 = VERTEX_POINT ( 'NONE', #16634 ) ;
#82351 = CARTESIAN_POINT ( 'NONE',  ( -9.692307692307814193, -2.657715359629662544, 31.77849191805970364 ) ) ;
#82352 = CARTESIAN_POINT ( 'NONE',  ( 6.856994543716785628, -8.164416787775445883, 34.95778746994557906 ) ) ;
#82353 = FACE_BOUND ( 'NONE', #68423, .T. ) ;
#82355 = CARTESIAN_POINT ( 'NONE',  ( -16.82686876528476105, -12.41262288849542017, 30.68299917996395010 ) ) ;
#82354 = DIRECTION ( 'NONE',  ( -1.000000000000000000, 0.000000000000000000, 0.000000000000000000 ) ) ;
#82356 = CARTESIAN_POINT ( 'NONE',  ( 2.241609928332172874, -6.343179335718451384, 34.87096338111212646 ) ) ;
#82357 = B_SPLINE_CURVE_WITH_KNOTS ( 'NONE', 3,
 ( #4151, #52339, #3707, #85256, #44235, #45141, #11364, #73067, #18574, #78929 ),
 .UNSPECIFIED., .F., .F.,
 ( 4, 2, 2, 2, 4 ),
 ( 0.0007817246256747451124, 0.0009771112852218883336, 0.001172497944769031663, 0.001367884604316174993, 0.001563271263863318323 ),
 .UNSPECIFIED. ) ;
#82358 = CARTESIAN_POINT ( 'NONE',  ( 1.384615384615264011, -12.70778746994576025, 30.41441678777401236 ) ) ;
#82360 = CARTESIAN_POINT ( 'NONE',  ( 2.057715563643718326, -10.82459398097509684, 33.81372124010185587 ) ) ;
#82359 =( LENGTH_UNIT ( ) NAMED_UNIT ( * ) SI_UNIT ( .MILLI., .METRE. ) );
#82361 = CARTESIAN_POINT ( 'NONE',  ( -3.750000000000008438, -5.946699141100917352, 26.42187500000000000 ) ) ;
#82362 = EDGE_LOOP ( 'NONE', ( #68369, #73038, #45695, #56909 ) ) ;
#82363 = B_SPLINE_CURVE_WITH_KNOTS ( 'NONE', 3,
 ( #58748, #86696, #79476, #43898, #11457, #64599, #32176, #38488, #85340, #17775 ),
 .UNSPECIFIED., .F., .F.,
 ( 4, 2, 2, 2, 4 ),
 ( 0.000000000000000000, 0.0001954311564186887718, 0.0003908623128373775435, 0.0005862934692560662882, 0.0007817246256747550871 ),
 .UNSPECIFIED. ) ;
#82364 = ORIENTED_EDGE ( 'NONE', *, *, #17840, .T. ) ;
#82365 = DIRECTION ( 'NONE',  ( -0.000000000000000000, 0.8660254037844397068, -0.4999999999999978906 ) ) ;
#82366 = DIRECTION ( 'NONE',  ( 0.000000000000000000, -6.938893903907222067E-15, 1.000000000000000000 ) ) ;
#82367 = CARTESIAN_POINT ( 'NONE',  ( 1.449870524128225036, -9.528491918058460186, 34.59228464037085615 ) ) ;
#82368 = CARTESIAN_POINT ( 'NONE',  ( 8.769230769230768274, -11.35647404775217417, 33.31231777344666511 ) ) ;
#82369 = CARTESIAN_POINT ( 'NONE',  ( -14.98071491913091613, -2.779044189368095275, 31.39831045268885745 ) ) ;
#82370 = CARTESIAN_POINT ( 'NONE',  ( -1.614399933863656544, -3.775308065498769405, 16.32625670625849068 ) ) ;
#82371 = FACE_OUTER_BOUND ( 'NONE', #49165, .T. ) ;
#82372 = CARTESIAN_POINT ( 'NONE',  ( 1.134638640566794754, -10.06842814019191401, 34.32929386961144758 ) ) ;
#82373 = CARTESIAN_POINT ( 'NONE',  ( 9.627037691751372250, -11.06231777344662781, 33.60647404775220082 ) ) ;
#82374 = CARTESIAN_POINT ( 'NONE',  ( 6.166666666666664298, -7.500000000000000000, 33.75000000000000000 ) ) ;
#82375 = CARTESIAN_POINT ( 'NONE',  ( 0.000000000000000000, -11.00000000000000000, 29.75000000000000355 ) ) ;
#82376 = LINE ( 'NONE', #35060, #75647 ) ;
#82377 = VECTOR ( 'NONE', #23735, 1000.000000000000000 ) ;
#82378 = CARTESIAN_POINT ( 'NONE',  ( -0.2115930521604180437, -4.176053281294514363, 33.81426240980091791 ) ) ;
#82379 = CYLINDRICAL_SURFACE ( 'NONE', #46278, 0.2499999999999998890 ) ;
#82380 = EDGE_CURVE ( 'NONE', #126, #14193, #24912, .T. ) ;
#82381 = CARTESIAN_POINT ( 'NONE',  ( -3.230769230769229949, -9.780366693483667717, 34.19971097300155094 ) ) ;
#82382 = ORIENTED_EDGE ( 'NONE', *, *, #78422, .F. ) ;
#82383 = CARTESIAN_POINT ( 'NONE',  ( -0.3962828902624361826, -3.835265460703683349, 33.15142922261929925 ) ) ;
#82384 = CARTESIAN_POINT ( 'NONE',  ( 0.5276068125409003606, -2.538708090699994813, 30.37095296980875503 ) ) ;
#82385 = CARTESIAN_POINT ( 'NONE',  ( -0.06109907496451398579, -10.25000000000000178, 20.03311829374151287 ) ) ;
#82386 = EDGE_CURVE ( 'NONE', #82533, #74234, #83964, .T. ) ;
#82387 = DIRECTION ( 'NONE',  ( -0.000000000000000000, -0.6427876096865404731, -0.7660444431189771253 ) ) ;
#82388 = DIRECTION ( 'NONE',  ( -0.000000000000000000, 0.3420201433256694346, -0.9396926207859080948 ) ) ;
#82389 = DIRECTION ( 'NONE',  ( -0.000000000000000000, -0.5000000000000009992, -0.8660254037844380415 ) ) ;
#82391 = ORIENTED_EDGE ( 'NONE', *, *, #3436, .T. ) ;
#82390 = CARTESIAN_POINT ( 'NONE',  ( -14.05769230769230660, -2.249999999999998668, 29.75000000000000355 ) ) ;
#82392 = CARTESIAN_POINT ( 'NONE',  ( 1.944543648263018731, -9.444543648262994751, 25.87500000000000355 ) ) ;
#82393 = CARTESIAN_POINT ( 'NONE',  ( 16.85343815235874132, -2.612411019501191589, 31.66733052389440672 ) ) ;
#82394 = EDGE_CURVE ( 'NONE', #41015, #43004, #71135, .T. ) ;
#82395 = ORIENTED_EDGE ( 'NONE', *, *, #13097, .F. ) ;
#82396 = CARTESIAN_POINT ( 'NONE',  ( -15.93106661257773915, -10.11255958852955672, 34.01340905677048454 ) ) ;
#82397 = B_SPLINE_CURVE_WITH_KNOTS ( 'NONE', 3,
 ( #73180, #52000, #86716, #24982, #25433, #11477, #79935, #45698, #17340, #87600 ),
 .UNSPECIFIED., .F., .F.,
 ( 4, 2, 2, 2, 4 ),
 ( 0.0007817359430256297891, 0.0009771253907249961065, 0.001172514838424362424, 0.001367904286123728741, 0.001563293733823095059 ),
 .UNSPECIFIED. ) ;
#82398 = B_SPLINE_CURVE_WITH_KNOTS ( 'NONE', 3,
 ( #47957, #14176, #69124, #62352, #28130, #224, #13735, #42108, #67797, #68675 ),
 .UNSPECIFIED., .F., .F.,
 ( 4, 2, 2, 2, 4 ),
 ( 0.000000000000000000, 0.0001954339857564093175, 0.0003908679715128186350, 0.0005863019572692279796, 0.0007817359430256372700 ),
 .UNSPECIFIED. ) ;
#82399 = CARTESIAN_POINT ( 'NONE',  ( -2.307692307692305711, -10.67929555188718282, 33.92786785259544047 ) ) ;
#82400 = EDGE_CURVE ( 'NONE', #88629, #38816, #58062, .T. ) ;
#82401 = VERTEX_POINT ( 'NONE', #78779 ) ;
#82402 = CARTESIAN_POINT ( 'NONE',  ( 0.000000000000000000, -11.00000000000000000, 29.75000000000000355 ) ) ;
#82403 = B_SPLINE_CURVE_WITH_KNOTS ( 'NONE', 3,
 ( #70486, #51068, #1137, #84017, #22296, #84896, #70036, #49760, #63717, #29506 ),
 .UNSPECIFIED., .F., .F.,
 ( 4, 2, 2, 2, 4 ),
 ( 0.0007817359430256320659, 0.0009771253907249987086, 0.001172514838424365460, 0.001367904286123731994, 0.001563293733823098745 ),
 .UNSPECIFIED. ) ;
#82404 = FACE_OUTER_BOUND ( 'NONE', #55262, .T. ) ;
#82405 = CARTESIAN_POINT ( 'NONE',  ( -15.10024352900566846, -12.45806712695776319, 30.39783852428763922 ) ) ;
#82406 = VERTEX_POINT ( 'NONE', #31029 ) ;
#82407 = ORIENTED_EDGE ( 'NONE', *, *, #73936, .F. ) ;
#82408 = EDGE_CURVE ( 'NONE', #57426, #54624, #63931, .T. ) ;
#82409 = FACE_OUTER_BOUND ( 'NONE', #1328, .T. ) ;
#82410 = AXIS2_PLACEMENT_3D ( 'NONE', #60977, #25869, #25423 ) ;
#82411 = VERTEX_POINT ( 'NONE', #10774 ) ;
#82413 = CARTESIAN_POINT ( 'NONE',  ( 7.596177102105253987, -9.234221910056348293, 34.70572697212741531 ) ) ;
#82412 = AXIS2_PLACEMENT_3D ( 'NONE', #883, #1323, #29254 ) ;
#82414 = CARTESIAN_POINT ( 'NONE',  ( 5.076923076923075762, -4.661471528628507777, 34.16647553114623292 ) ) ;
#82415 = CARTESIAN_POINT ( 'NONE',  ( -10.83831083290076158, -2.554751324335734708, 30.48935550225260727 ) ) ;
#82416 = CYLINDRICAL_SURFACE ( 'NONE', #4510, 0.2499999999999986955 ) ;
#82417 = LINE ( 'NONE', #9724, #7639 ) ;
#82418 = DIRECTION ( 'NONE',  ( -0.000000000000000000, -0.7660444431189791237, -0.6427876096865379196 ) ) ;
#82419 = AXIS2_PLACEMENT_3D ( 'NONE', #71637, #72532, #57252 ) ;
#82420 = CARTESIAN_POINT ( 'NONE',  ( 16.15384615384603251, -12.70778746994576025, 30.41441678777401236 ) ) ;
#82421 = EDGE_LOOP ( 'NONE', ( #51882, #40747 ) ) ;
#82422 = VERTEX_POINT ( 'NONE', #40041 ) ;
#82424 = ORIENTED_EDGE ( 'NONE', *, *, #56783, .F. ) ;
#82423 = CARTESIAN_POINT ( 'NONE',  ( 12.46153846153833911, -12.16647553114689728, 32.15551576947799362 ) ) ;
#82425 = EDGE_CURVE ( 'NONE', #4955, #42964, #81023, .T. ) ;
#82426 = CYLINDRICAL_SURFACE ( 'NONE', #79624, 0.2500000000000012212 ) ;
#82427 = B_SPLINE_CURVE_WITH_KNOTS ( 'NONE', 3,
 ( #58772, #2930, #3381, #24540, #70960, #36295, #63752, #43926, #36728, #2054 ),
 .UNSPECIFIED., .F., .F.,
 ( 4, 2, 2, 2, 4 ),
 ( 0.000000000000000000, 0.0001954311564186870913, 0.0003908623128373741825, 0.0005862934692560613009, 0.0007817246256747483650 ),
 .UNSPECIFIED. ) ;
#82428 = B_SPLINE_CURVE_WITH_KNOTS ( 'NONE', 3,
 ( #30811, #58728, #85327, #16417, #29498, #77669, #85771, #23172, #45212, #72690 ),
 .UNSPECIFIED., .F., .F.,
 ( 4, 2, 2, 2, 4 ),
 ( 0.000000000000000000, 0.0001954339857564073659, 0.0003908679715128147319, 0.0005863019572692221250, 0.0007817359430256294638 ),
 .UNSPECIFIED. ) ;
#82429 = B_SPLINE_CURVE_WITH_KNOTS ( 'NONE', 3,
 ( #51987, #38045, #71369, #24519, #43465, #85797, #9251, #58303, #37143, #2465 ),
 .UNSPECIFIED., .F., .F.,
 ( 4, 2, 2, 2, 4 ),
 ( 0.0007817246256747493408, 0.0009771112852218933210, 0.001172497944769037301, 0.001367884604316181281, 0.001563271263863325261 ),
 .UNSPECIFIED. ) ;
#82430 = CARTESIAN_POINT ( 'NONE',  ( -10.61538461538473399, -4.481592998941358097, 33.73612834414048933 ) ) ;
#82431 = FACE_BOUND ( 'NONE', #54968, .T. ) ;
#82432 = ORIENTED_EDGE ( 'NONE', *, *, #37501, .T. ) ;
#82433 = B_SPLINE_CURVE_WITH_KNOTS ( 'NONE', 3,
 ( #45337, #18324, #11572, #66049, #38144, #72810, #71925, #39051, #11118, #66510 ),
 .UNSPECIFIED., .F., .F.,
 ( 4, 2, 2, 2, 4 ),
 ( 0.000000000000000000, 0.0001954339857564055499, 0.0003908679715128110998, 0.0005863019572692165955, 0.0007817359430256221996 ),
 .UNSPECIFIED. ) ;
#82434 = CYLINDRICAL_SURFACE ( 'NONE', #32672, 0.2500000000000008882 ) ;
#82435 = EDGE_CURVE ( 'NONE', #36751, #30821, #3379, .T. ) ;
#82436 = ORIENTED_EDGE ( 'NONE', *, *, #68330, .F. ) ;
#82437 = CARTESIAN_POINT ( 'NONE',  ( -11.97435897435897267, -7.500000000000000000, 29.75000000000000355 ) ) ;
#82438 = EDGE_LOOP ( 'NONE', ( #29399, #82651, #3074, #15367, #65023 ) ) ;
#82439 = CIRCLE ( 'NONE', #4766, 8.000000000000000000 ) ;
#82440 = CARTESIAN_POINT ( 'NONE',  ( -12.52762084089859407, -3.322132147404559532, 32.92929555188719348 ) ) ;
#82441 = ORIENTED_EDGE ( 'NONE', *, *, #20514, .T. ) ;
#82442 = EDGE_CURVE ( 'NONE', #18050, #45619, #39150, .T. ) ;
#82443 = CARTESIAN_POINT ( 'NONE',  ( -4.403822897894744237, -4.075325502946086864, 33.72974371597207721 ) ) ;
#82444 = CARTESIAN_POINT ( 'NONE',  ( -4.219928533206288357, -6.343179335718451384, 34.87096338111212646 ) ) ;
#82445 = FACE_BOUND ( 'NONE', #88809, .T. ) ;
#82446 = FACE_OUTER_BOUND ( 'NONE', #77606, .T. ) ;
#82447 = CARTESIAN_POINT ( 'NONE',  ( -17.75005448165185840, -12.22109172314383052, 31.39792113162168263 ) ) ;
#82448 = CARTESIAN_POINT ( 'NONE',  ( 15.29602437028207085, -2.657715359629132301, 31.77849191805844242 ) ) ;
#82449 = DIRECTION ( 'NONE',  ( -0.000000000000000000, 0.9396926207859092051, -0.3420201433256662704 ) ) ;
#82450 = DIRECTION ( 'NONE',  ( 1.000000000000000000, 0.000000000000000000, 0.000000000000000000 ) ) ;
#82451 = CARTESIAN_POINT ( 'NONE',  ( -4.153846153846152411, -11.16473453929635440, 33.15142922261926373 ) ) ;
#82452 = CARTESIAN_POINT ( 'NONE',  ( -6.222865422203639696, -2.501496062324911840, 29.88072118266895671 ) ) ;
#82453 = ORIENTED_EDGE ( 'NONE', *, *, #2448, .T. ) ;
#82454 = EDGE_CURVE ( 'NONE', #81338, #25143, #12555, .T. ) ;
#82455 = ORIENTED_EDGE ( 'NONE', *, *, #1700, .F. ) ;
#82457 = CARTESIAN_POINT ( 'NONE',  ( 15.23076923076923173, -12.10708131394839349, 31.69288490824020244 ) ) ;
#82456 = CARTESIAN_POINT ( 'NONE',  ( -16.94639737515951694, -10.19071101563364401, 33.96452234770658407 ) ) ;
#82458 = CARTESIAN_POINT ( 'NONE',  ( -18.00000000000000000, -4.098570777380720287, 33.41473453929634729 ) ) ;
#82459 = CARTESIAN_POINT ( 'NONE',  ( 8.769230769230768274, -13.63283147151868846, 33.57946703557072254 ) ) ;
#82460 = EDGE_CURVE ( 'NONE', #81906, #87922, #74258, .T. ) ;
#82461 = CARTESIAN_POINT ( 'NONE',  ( -13.38461538461538325, -5.471508081941601098, 34.59228464037088457 ) ) ;
#82462 = LINE ( 'NONE', #68482, #33219 ) ;
#82463 = EDGE_CURVE ( 'NONE', #14282, #34190, #37846, .T. ) ;
#82464 = ORIENTED_EDGE ( 'NONE', *, *, #12308, .T. ) ;
#82465 = DIRECTION ( 'NONE',  ( -0.000000000000000000, -0.5000000000000009992, -0.8660254037844380415 ) ) ;
#82466 = CARTESIAN_POINT ( 'NONE',  ( -14.30769230769230660, -2.721908614388771852, 31.22303859784724978 ) ) ;
#82467 = CARTESIAN_POINT ( 'NONE',  ( -8.769230769230768274, -12.10708131394839349, 31.69288490824020244 ) ) ;
#82468 = CARTESIAN_POINT ( 'NONE',  ( -15.93083330975275302, -4.026326845037968560, 33.68677907613345468 ) ) ;
#82469 = VERTEX_POINT ( 'NONE', #87343 ) ;
#82470 = EDGE_CURVE ( 'NONE', #47021, #11337, #73365, .T. ) ;
#82471 = EDGE_LOOP ( 'NONE', ( #43500, #24385 ) ) ;
#82472 = CIRCLE ( 'NONE', #43615, 0.2500000000000002220 ) ;
#82473 = VERTEX_POINT ( 'NONE', #26067 ) ;
#82474 = AXIS2_PLACEMENT_3D ( 'NONE', #2633, #30122, #57589 ) ;
#82475 = CARTESIAN_POINT ( 'NONE',  ( 0.6845498131513105822, -10.61302985866383963, 33.66295027996417843 ) ) ;
#82476 = ORIENTED_EDGE ( 'NONE', *, *, #31584, .T. ) ;
#82477 = CARTESIAN_POINT ( 'NONE',  ( -9.915792636031639518, -12.44517049084099725, 30.48991314939691932 ) ) ;
#82478 = DIRECTION ( 'NONE',  ( -0.000000000000000000, 0.8660254037844397068, -0.4999999999999978906 ) ) ;
#82479 = LINE ( 'NONE', #75697, #85502 ) ;
#82480 = CARTESIAN_POINT ( 'NONE',  ( 11.53846153846153832, -3.513871655860378418, 32.76840700105978499 ) ) ;
#82481 = VECTOR ( 'NONE', #51304, 1000.000000000000000 ) ;
#82482 = CARTESIAN_POINT ( 'NONE',  ( 2.307692307692309264, -5.180354513474913603, 36.12317359536750416 ) ) ;
#82483 = VERTEX_POINT ( 'NONE', #38689 ) ;
#82484 = CARTESIAN_POINT ( 'NONE',  ( -11.28846153846147438, -7.434744860731433924, 35.00000000000000711 ) ) ;
#82486 = ORIENTED_EDGE ( 'NONE', *, *, #16962, .F. ) ;
#82485 = CARTESIAN_POINT ( 'NONE',  ( 7.846153846153846700, -2.249999999999998668, 29.75000000000001776 ) ) ;
#82487 = CARTESIAN_POINT ( 'NONE',  ( 2.544871794871792936, -11.50000000000000000, 29.75000000000000355 ) ) ;
#82488 = CARTESIAN_POINT ( 'NONE',  ( 15.23076923076910916, -2.657715359629662544, 31.77849191805970364 ) ) ;
#82489 = CARTESIAN_POINT ( 'NONE',  ( 17.20744877868663281, -11.46989282347013095, 32.79007818306219946 ) ) ;
#82490 = CARTESIAN_POINT ( 'NONE',  ( -16.37672567058374185, -7.630690623152299956, 34.99857592706774057 ) ) ;
#82491 = CARTESIAN_POINT ( 'NONE',  ( 3.230769230769231726, -5.180354513474913603, 36.12317359536750416 ) ) ;
#82492 = DIRECTION ( 'NONE',  ( 1.000000000000000000, 0.000000000000000000, 0.000000000000000000 ) ) ;
#82493 = CARTESIAN_POINT ( 'NONE',  ( -19.50000000000000000, -7.500000000000000000, 29.75000000000000355 ) ) ;
#82494 = CARTESIAN_POINT ( 'NONE',  ( -1.077988221561493543, -4.724691934501247914, 18.07999329374151287 ) ) ;
#82495 = VERTEX_POINT ( 'NONE', #25174 ) ;
#82496 = FACE_OUTER_BOUND ( 'NONE', #78269, .T. ) ;
#82497 = DIRECTION ( 'NONE',  ( -0.000000000000000000, 0.3420201433256694901, -0.9396926207859082059 ) ) ;
#82498 = EDGE_CURVE ( 'NONE', #81338, #42788, #52659, .T. ) ;
#82499 = B_SPLINE_CURVE_WITH_KNOTS ( 'NONE', 3,
 ( #57400, #63714, #37125, #37570, #2020, #29941, #84013, #43887, #15099, #76803 ),
 .UNSPECIFIED., .F., .F.,
 ( 4, 2, 2, 2, 4 ),
 ( 0.0007817359430256327164, 0.0009771253907249993591, 0.001172514838424366110, 0.001367904286123732861, 0.001563293733823099396 ),
 .UNSPECIFIED. ) ;
#82500 = DIRECTION ( 'NONE',  ( -0.000000000000000000, 1.000000000000000000, -0.000000000000000000 ) ) ;
#82501 = CARTESIAN_POINT ( 'NONE',  ( -13.16160403300253634, -8.239487800360276282, 34.69522927552633718 ) ) ;
#82502 = VERTEX_POINT ( 'NONE', #65699 ) ;
#82503 = CARTESIAN_POINT ( 'NONE',  ( 14.30769230769231015, -3.886160181151819604, 36.00935417666054406 ) ) ;
#82504 = CARTESIAN_POINT ( 'NONE',  ( -3.007757879156380820, -5.667800583137508674, 34.40243808032445827 ) ) ;
#82505 = DIRECTION ( 'NONE',  ( -0.000000000000000000, 1.000000000000000000, -0.000000000000000000 ) ) ;
#82506 = AXIS2_PLACEMENT_3D ( 'NONE', #88463, #6901, #26733 ) ;
#82507 = CARTESIAN_POINT ( 'NONE',  ( -0.5922290646487686772, -10.70098750199973203, 33.91152734681376302 ) ) ;
#82508 = EDGE_CURVE ( 'NONE', #79011, #35777, #46335, .T. ) ;
#82509 = AXIS2_PLACEMENT_3D ( 'NONE', #39778, #19051, #52822 ) ;
#82510 = CARTESIAN_POINT ( 'NONE',  ( 17.07692307692307665, -2.517432740324522911, 35.29906147534542527 ) ) ;
#82511 = ORIENTED_EDGE ( 'NONE', *, *, #24338, .T. ) ;
#82512 = CARTESIAN_POINT ( 'NONE',  ( -12.33074665371366940, -8.999086150933475636, 34.52020707165672775 ) ) ;
#82513 = CARTESIAN_POINT ( 'NONE',  ( -5.999999999999998224, -1.790695186598648903, 34.54067556320373455 ) ) ;
#82514 = CARTESIAN_POINT ( 'NONE',  ( 5.326977496836529546, -12.41089969410671223, 31.60739465890703670 ) ) ;
#82515 = ORIENTED_EDGE ( 'NONE', *, *, #33726, .F. ) ;
#82516 = ADVANCED_FACE ( 'NONE', ( #73820 ), #72914, .F. ) ;
#82517 = DIRECTION ( 'NONE',  ( -0.000000000000000000, -0.7660444431189791237, -0.6427876096865379196 ) ) ;
#82518 = ORIENTED_EDGE ( 'NONE', *, *, #77814, .T. ) ;
#82519 = LINE ( 'NONE', #43723, #75922 ) ;
#82520 = CARTESIAN_POINT ( 'NONE',  ( -5.869474561766356402, -12.15418822224088657, 32.17964115625579069 ) ) ;
#82521 = ORIENTED_EDGE ( 'NONE', *, *, #34020, .F. ) ;
#82522 = CARTESIAN_POINT ( 'NONE',  ( 7.596130608860881317, -12.22074536777954989, 31.39888409691088356 ) ) ;
#82523 = FACE_OUTER_BOUND ( 'NONE', #72190, .T. ) ;
#82524 = CARTESIAN_POINT ( 'NONE',  ( -6.673022503163469565, -12.41089969410671223, 31.60739465890703670 ) ) ;
#82525 = EDGE_CURVE ( 'NONE', #31713, #15081, #17982, .T. ) ;
#82526 = CARTESIAN_POINT ( 'NONE',  ( -7.976301815885541657, -5.070767119584671079, 34.40440758774516183 ) ) ;
#82527 = CARTESIAN_POINT ( 'NONE',  ( -1.634592128663974853, -10.82459398097509684, 33.81372124010185587 ) ) ;
#82528 = B_SPLINE_CURVE_WITH_KNOTS ( 'NONE', 3,
 ( #1683, #84990, #56627, #84113, #22394, #36360 ),
 .UNSPECIFIED., .F., .F.,
 ( 4, 2, 4 ),
 ( 4.593128804320400861E-17, 0.0001954756301637176972, 0.0003909512603273894243 ),
 .UNSPECIFIED. ) ;
#82529 = AXIS2_PLACEMENT_3D ( 'NONE', #20350, #51774, #58105 ) ;
#82530 = VECTOR ( 'NONE', #24472, 1000.000000000000114 ) ;
#82531 = ORIENTED_EDGE ( 'NONE', *, *, #70751, .F. ) ;
#82532 = FACE_BOUND ( 'NONE', #15067, .T. ) ;
#82533 = VERTEX_POINT ( 'NONE', #60284 ) ;
#82534 = DIRECTION ( 'NONE',  ( 1.000000000000000000, 0.000000000000000000, 0.000000000000000000 ) ) ;
#82535 = EDGE_CURVE ( 'NONE', #4425, #61846, #48095, .T. ) ;
#82536 = VECTOR ( 'NONE', #66758, 1000.000000000000227 ) ;
#82537 = CARTESIAN_POINT ( 'NONE',  ( 18.24994540937804643, -6.653508905675593610, 34.93172785388651391 ) ) ;
#82538 = ADVANCED_FACE ( 'NONE', ( #61167 ), #40911, .F. ) ;
#82539 = CARTESIAN_POINT ( 'NONE',  ( 8.769230769230768274, -3.513871655860378418, 32.76840700105978499 ) ) ;
#82540 = CARTESIAN_POINT ( 'NONE',  ( 14.53047197667037338, -8.540255544307065350, 34.89611431652622286 ) ) ;
#82541 = ORIENTED_EDGE ( 'NONE', *, *, #20266, .F. ) ;
#82542 = EDGE_LOOP ( 'NONE', ( #63262, #71347, #71285, #20666 ) ) ;
#82543 = EDGE_LOOP ( 'NONE', ( #28686, #6515, #66418, #70019 ) ) ;
#82544 = B_SPLINE_CURVE_WITH_KNOTS ( 'NONE', 3,
 ( #65498, #48998, #35486, #64596, #812, #78566, #2894, #23622, #30385, #43895 ),
 .UNSPECIFIED., .F., .F.,
 ( 4, 2, 2, 2, 4 ),
 ( 0.0007817359430256317406, 0.0009771253907249982749, 0.001172514838424365026, 0.001367904286123731560, 0.001563293733823098094 ),
 .UNSPECIFIED. ) ;
#82545 = CARTESIAN_POINT ( 'NONE',  ( -15.23076923076922995, -8.564572088678739092, 35.78748833219616898 ) ) ;
#82546 = ORIENTED_EDGE ( 'NONE', *, *, #74787, .T. ) ;
#82547 = EDGE_CURVE ( 'NONE', #16511, #6173, #21516, .T. ) ;
#82548 = EDGE_CURVE ( 'NONE', #61048, #37230, #50590, .T. ) ;
#82549 = CARTESIAN_POINT ( 'NONE',  ( 14.98074600654777377, -3.520140089381495585, 33.17453946501458262 ) ) ;
#82550 = CARTESIAN_POINT ( 'NONE',  ( 1.384615384615265343, -3.835265460704628371, 33.15142922262033665 ) ) ;
#82551 = CARTESIAN_POINT ( 'NONE',  ( 18.00000000000000000, -8.164416787775445883, 34.95778746994557906 ) ) ;
#82552 = CARTESIAN_POINT ( 'NONE',  ( 3.296024370282069960, -9.528491918058460186, 34.59228464037085615 ) ) ;
#82553 = CARTESIAN_POINT ( 'NONE',  ( 1.553300858899129944, -11.24999999999998934, 25.95312500000000000 ) ) ;
#82554 = CARTESIAN_POINT ( 'NONE',  ( 15.36129493253279499, -9.417988943895561960, 34.36773134775777550 ) ) ;
#82555 = DIRECTION ( 'NONE',  ( -0.000000000000000000, -0.6427876096865404731, -0.7660444431189770143 ) ) ;
#82556 = CARTESIAN_POINT ( 'NONE',  ( -5.142193522883852452, -3.835265460703609186, 33.15142922261924241 ) ) ;
#82557 = VERTEX_POINT ( 'NONE', #88678 ) ;
#82558 = B_SPLINE_CURVE_WITH_KNOTS ( 'NONE', 3,
 ( #82992, #84333, #57284, #69029, #28489, #43332, #35239, #14527, #1462, #49642 ),
 .UNSPECIFIED., .F., .F.,
 ( 4, 2, 2, 2, 4 ),
 ( 0.0007817246256747477145, 0.0009771112852218909357, 0.001172497944769034265, 0.001367884604316177595, 0.001563271263863320708 ),
 .UNSPECIFIED. ) ;
#82559 = ORIENTED_EDGE ( 'NONE', *, *, #23589, .T. ) ;
#82560 = EDGE_CURVE ( 'NONE', #8100, #79207, #21064, .T. ) ;
#82561 = EDGE_LOOP ( 'NONE', ( #64489, #5349 ) ) ;
#82562 = CARTESIAN_POINT ( 'NONE',  ( 3.930361229281820190, -3.019605429927184836, 32.48692288466676814 ) ) ;
#82563 = B_SPLINE_CURVE_WITH_KNOTS ( 'NONE', 3,
 ( #32449, #24345, #59916, #46408, #73888, #51807, #67132, #37873, #5429, #32894 ),
 .UNSPECIFIED., .F., .F.,
 ( 4, 2, 2, 2, 4 ),
 ( 0.0007817246256747491240, 0.0009771112852218931041, 0.001172497944769036867, 0.001367884604316180631, 0.001563271263863324611 ),
 .UNSPECIFIED. ) ;
#82565 = CARTESIAN_POINT ( 'NONE',  ( -9.942330916529147800, -4.175268141568685643, 33.81360843649122216 ) ) ;
#82564 = CARTESIAN_POINT ( 'NONE',  ( 14.30769230769231015, -2.499999999999998668, 29.75000000000001421 ) ) ;
#82566 = FACE_OUTER_BOUND ( 'NONE', #49245, .T. ) ;
#82567 = CARTESIAN_POINT ( 'NONE',  ( -9.915233909823838232, -6.503392248772476236, 34.64988816332204635 ) ) ;
#82568 = EDGE_CURVE ( 'NONE', #56880, #2574, #5459, .T. ) ;
#82569 = FACE_BOUND ( 'NONE', #85695, .T. ) ;
#82570 = CARTESIAN_POINT ( 'NONE',  ( 16.37662569511456567, -3.236590943229497697, 32.36255958852954251 ) ) ;
#82571 = ADVANCED_FACE ( 'NONE', ( #55740 ), #76016, .T. ) ;
#82572 = ORIENTED_EDGE ( 'NONE', *, *, #82826, .T. ) ;
#82573 = LINE ( 'NONE', #44869, #57445 ) ;
#82574 = FACE_OUTER_BOUND ( 'NONE', #12007, .T. ) ;
#82575 = CYLINDRICAL_SURFACE ( 'NONE', #52476, 0.2499999999999986955 ) ;
#82576 = ORIENTED_EDGE ( 'NONE', *, *, #46169, .F. ) ;
#82577 = CARTESIAN_POINT ( 'NONE',  ( 4.946232473812767871, -12.62707690430377383, 30.88035979386743435 ) ) ;
#82578 = ORIENTED_EDGE ( 'NONE', *, *, #60133, .T. ) ;
#82579 = FACE_BOUND ( 'NONE', #38865, .T. ) ;
#82580 = CARTESIAN_POINT ( 'NONE',  ( -12.46153846153846168, -13.63283147151868846, 33.57946703557072254 ) ) ;
#82581 = DIRECTION ( 'NONE',  ( -0.000000000000000000, 0.8660254037844399289, -0.4999999999999980016 ) ) ;
#82582 = CARTESIAN_POINT ( 'NONE',  ( 16.85343815235874132, -12.11044203135681840, 32.26167407432752299 ) ) ;
#82583 = EDGE_LOOP ( 'NONE', ( #41652, #55156, #75895, #41068, #9663 ) ) ;
#82584 = CYLINDRICAL_SURFACE ( 'NONE', #72380, 8.000000000000000000 ) ;
#82585 = CARTESIAN_POINT ( 'NONE',  ( 14.30769230769218758, -8.613356846316285953, 34.62446782046622218 ) ) ;
#82586 = DIRECTION ( 'NONE',  ( -1.000000000000000000, 0.000000000000000000, 0.000000000000000000 ) ) ;
#82587 = CARTESIAN_POINT ( 'NONE',  ( 5.999999999999880096, -3.835265460704628371, 33.15142922262033665 ) ) ;
#82588 = ORIENTED_EDGE ( 'NONE', *, *, #68607, .F. ) ;
#82589 = CARTESIAN_POINT ( 'NONE',  ( -12.39547011053602432, -3.050289026998446840, 32.03036669348366416 ) ) ;
#82590 = LINE ( 'NONE', #156, #42736 ) ;
#82592 = EDGE_LOOP ( 'NONE', ( #71180, #82707, #19481, #17302 ) ) ;
#82591 = CARTESIAN_POINT ( 'NONE',  ( -15.23076923076922995, -2.292212530054420494, 30.41441678777542634 ) ) ;
#82593 = LINE ( 'NONE', #19982, #45466 ) ;
#82594 = CARTESIAN_POINT ( 'NONE',  ( 20.00000000000000000, -4.000000000000000000, 29.75000000000000355 ) ) ;
#82595 = CARTESIAN_POINT ( 'NONE',  ( -4.826977558574935934, -8.433404298154334455, 34.66254593164985920 ) ) ;
#82596 = CARTESIAN_POINT ( 'NONE',  ( -8.769230769230890843, -11.48612834414049644, 32.76840700105863391 ) ) ;
#82597 = CARTESIAN_POINT ( 'NONE',  ( 9.823099500132483897, -8.999086150933475636, 34.52020707165672775 ) ) ;
#82600 = CARTESIAN_POINT ( 'NONE',  ( -2.438252899434225629, -2.504760397472875155, 29.97295953869789997 ) ) ;
#82599 = VECTOR ( 'NONE', #25483, 1000.000000000000114 ) ;
#82598 = CARTESIAN_POINT ( 'NONE',  ( -5.776987155906603277, -6.460100341425561332, 34.89618726649961644 ) ) ;
#82601 = CARTESIAN_POINT ( 'NONE',  ( -10.61538461538473399, -2.892918686052166066, 31.69288490824153470 ) ) ;
#82602 = B_SPLINE_CURVE_WITH_KNOTS ( 'NONE', 3,
 ( #29603, #78217, #70585, #51162, #15645, #43985, #16519, #71904, #57061, #43113 ),
 .UNSPECIFIED., .F., .F.,
 ( 4, 2, 2, 2, 4 ),
 ( 0.000000000000000000, 0.0001954311564186862781, 0.0003908623128373725562, 0.0005862934692560588072, 0.0007817246256747451124 ),
 .UNSPECIFIED. ) ;
#82603 = CARTESIAN_POINT ( 'NONE',  ( -2.749999999999998224, -7.500000000000015987, 21.34375000000000000 ) ) ;
#82604 = APPLICATION_CONTEXT ( 'automotive_design' ) ;
#82605 = ORIENTED_EDGE ( 'NONE', *, *, #17590, .F. ) ;
#82606 = B_SPLINE_CURVE_WITH_KNOTS ( 'NONE', 3,
 ( #212, #66895, #61019, #47053, #81748, #27676, #74541, #49719, #77634, #62774 ),
 .UNSPECIFIED., .F., .F.,
 ( 4, 2, 2, 2, 4 ),
 ( 0.0007817246256747484735, 0.0009771112852218915863, 0.001172497944769034916, 0.001367884604316178029, 0.001563271263863321141 ),
 .UNSPECIFIED. ) ;
#82607 = VECTOR ( 'NONE', #19256, 1000.000000000000000 ) ;
#82608 = CARTESIAN_POINT ( 'NONE',  ( 0.000000000000000000, -11.00000000000000000, 29.75000000000000355 ) ) ;
#82609 = EDGE_LOOP ( 'NONE', ( #58572, #77767 ) ) ;
#82610 = AXIS2_PLACEMENT_3D ( 'NONE', #44078, #9864, #64353 ) ;
#82611 = ORIENTED_EDGE ( 'NONE', *, *, #72300, .T. ) ;
#82612 = CARTESIAN_POINT ( 'NONE',  ( -11.40793610022789828, -2.372941743896879174, 30.88044141588253666 ) ) ;
#82613 = VERTEX_POINT ( 'NONE', #48534 ) ;
#82614 = CARTESIAN_POINT ( 'NONE',  ( -4.376773112753000738, -2.523278758544489797, 31.42238647778637528 ) ) ;
#82615 = CARTESIAN_POINT ( 'NONE',  ( 2.750000000000008438, -8.639087296525996607, 18.29687500000000000 ) ) ;
#82616 = CARTESIAN_POINT ( 'NONE',  ( 12.39578503322513114, -7.249945578846651806, 34.99404164642496795 ) ) ;
#82617 = B_SPLINE_CURVE_WITH_KNOTS ( 'NONE', 3,
 ( #12933, #33207, #52578, #26454, #79620, #18365, #74195, #4398, #67439, #59787 ),
 .UNSPECIFIED., .F., .F.,
 ( 4, 2, 2, 2, 4 ),
 ( 0.000000000000000000, 0.0001954311564186861697, 0.0003908623128373723394, 0.0005862934692560584820, 0.0007817246256747446788 ),
 .UNSPECIFIED. ) ;
#82618 = CYLINDRICAL_SURFACE ( 'NONE', #66896, 0.2500000000000012212 ) ;
#82619 = CARTESIAN_POINT ( 'NONE',  ( 3.100622021331010281, -8.587444163452046197, 34.63053765926554206 ) ) ;
#82620 = LINE ( 'NONE', #55122, #1532 ) ;
#82621 = CARTESIAN_POINT ( 'NONE',  ( -15.45425415533356350, -4.988325925672468131, 34.36044203135681130 ) ) ;
#82622 = CARTESIAN_POINT ( 'NONE',  ( -11.78843826940389583, -4.943428324936578910, 34.04746400365624481 ) ) ;
#82623 = CARTESIAN_POINT ( 'NONE',  ( -4.153846153846152411, -3.513871655860378418, 32.76840700105978499 ) ) ;
#82624 = DIRECTION ( 'NONE',  ( 0.000000000000000000, 0.9848077530122072432, -0.1736481776669354937 ) ) ;
#82625 = LINE ( 'NONE', #75846, #67878 ) ;
#82626 = CARTESIAN_POINT ( 'NONE',  ( 5.076923076923075762, -10.67929555188718282, 33.92786785259544047 ) ) ;
#82627 = CARTESIAN_POINT ( 'NONE',  ( -9.915234651214539952, -11.43668979543635089, 33.22377378376089752 ) ) ;
#82628 = ORIENTED_EDGE ( 'NONE', *, *, #52930, .F. ) ;
#82629 = EDGE_LOOP ( 'NONE', ( #19651, #54794, #60447, #22572 ) ) ;
#82630 = CARTESIAN_POINT ( 'NONE',  ( -15.23076923076922995, -8.120952969808772792, 34.71129190930000163 ) ) ;
#82631 = CARTESIAN_POINT ( 'NONE',  ( 1.634560793993429906, -3.520799739797214389, 33.17531984108286025 ) ) ;
#82632 = DIRECTION ( 'NONE',  ( -0.000000000000000000, -0.1736481776669307198, -0.9848077530122080203 ) ) ;
#82633 = CARTESIAN_POINT ( 'NONE',  ( 5.776515056276054771, -5.912607949931405038, 34.49155766932282319 ) ) ;
#82634 = CARTESIAN_POINT ( 'NONE',  ( -16.15384615384627409, -8.656820664282941280, 34.87096338111179961 ) ) ;
#82635 = CARTESIAN_POINT ( 'NONE',  ( 11.76124120743960333, -4.226511098958373402, 33.85474049983370293 ) ) ;
#82636 = VECTOR ( 'NONE', #27717, 999.9999999999998863 ) ;
#82637 = LINE ( 'NONE', #54693, #550 ) ;
#82638 = VERTEX_POINT ( 'NONE', #14319 ) ;
#82639 = CARTESIAN_POINT ( 'NONE',  ( -14.30769230769242917, -12.70778746994576025, 30.41441678777401236 ) ) ;
#82640 = EDGE_LOOP ( 'NONE', ( #10724, #85205, #23125, #19479 ) ) ;
#82641 = B_SPLINE_CURVE_WITH_KNOTS ( 'NONE', 3,
 ( #67303, #80382, #6489, #33950, #46581, #74497, #32619, #81266, #39834, #75386 ),
 .UNSPECIFIED., .F., .F.,
 ( 4, 2, 2, 2, 4 ),
 ( 0.0007817359430256252354, 0.0009771253907249898181, 0.001172514838424354401, 0.001367904286123718983, 0.001563293733823083566 ),
 .UNSPECIFIED. ) ;
#82642 = CARTESIAN_POINT ( 'NONE',  ( -13.91025641025641058, -11.50000000000000000, 29.75000000000000355 ) ) ;
#82643 = ADVANCED_FACE ( 'NONE', ( #14772 ), #41353, .T. ) ;
#82644 = CARTESIAN_POINT ( 'NONE',  ( 8.899756207464411872, -9.503571793651731880, 34.60286762892837942 ) ) ;
#82645 = DIRECTION ( 'NONE',  ( -0.000000000000000000, 1.000000000000000000, -0.000000000000000000 ) ) ;
#82646 = DIRECTION ( 'NONE',  ( -0.000000000000000000, 0.1736481776669307198, -0.9848077530122080203 ) ) ;
#82647 = DIRECTION ( 'NONE',  ( -0.000000000000000000, -0.000000000000000000, -1.000000000000000000 ) ) ;
#82648 = ORIENTED_EDGE ( 'NONE', *, *, #255, .F. ) ;
#82649 = VERTEX_POINT ( 'NONE', #81910 ) ;
#82650 = ORIENTED_EDGE ( 'NONE', *, *, #36649, .T. ) ;
#82651 = ORIENTED_EDGE ( 'NONE', *, *, #76762, .F. ) ;
#82652 = VECTOR ( 'NONE', #75141, 1000.000000000000114 ) ;
#82653 = EDGE_CURVE ( 'NONE', #14193, #126, #75328, .T. ) ;
#82654 = CARTESIAN_POINT ( 'NONE',  ( 13.16113044089144068, -3.236172620538810385, 32.36188796281390267 ) ) ;
#82655 = DIRECTION ( 'NONE',  ( -0.000000000000000000, 0.9848077530122085754, -0.1736481776669273613 ) ) ;
#82656 = FACE_OUTER_BOUND ( 'NONE', #23830, .T. ) ;
#82657 = AXIS2_PLACEMENT_3D ( 'NONE', #30006, #63782, #57466 ) ;
#82658 = AXIS2_PLACEMENT_3D ( 'NONE', #59535, #6808, #61296 ) ;
#82659 = CARTESIAN_POINT ( 'NONE',  ( -14.30769230769230660, -2.833524468853757305, 32.15551576947925838 ) ) ;
#82660 = CARTESIAN_POINT ( 'NONE',  ( -17.86947429823644029, -4.459921816937791661, 33.71989282347011851 ) ) ;
#82661 = CARTESIAN_POINT ( 'NONE',  ( 14.17754509825408960, -12.45813303252208648, 30.39737893381572675 ) ) ;
#82662 = ORIENTED_EDGE ( 'NONE', *, *, #82535, .T. ) ;
#82663 = EDGE_LOOP ( 'NONE', ( #71642, #13520, #34322, #65109 ) ) ;
#82664 = VERTEX_POINT ( 'NONE', #68819 ) ;
#82666 = EDGE_LOOP ( 'NONE', ( #58465, #55285 ) ) ;
#82665 = CARTESIAN_POINT ( 'NONE',  ( 16.15384615384615330, -12.29105614889573062, 35.45975837776705220 ) ) ;
#82667 = B_SPLINE_CURVE_WITH_KNOTS ( 'NONE', 3,
 ( #33262, #5343, #39137, #54405, #66602, #4905, #32369, #39589, #47204, #25609 ),
 .UNSPECIFIED., .F., .F.,
 ( 4, 2, 2, 2, 4 ),
 ( 0.000000000000000000, 0.0001954339857564058752, 0.0003908679715128117503, 0.0005863019572692176797, 0.0007817359430256235007 ),
 .UNSPECIFIED. ) ;
#82668 = CARTESIAN_POINT ( 'NONE',  ( 9.627037691751372250, -8.656820664281498878, 34.87096338111211935 ) ) ;
#82669 = CYLINDRICAL_SURFACE ( 'NONE', #18712, 0.2499999999999997502 ) ;
#82670 = CARTESIAN_POINT ( 'NONE',  ( -1.553300858899125059, -3.750000000000009326, 19.07812500000000000 ) ) ;
#82671 = ADVANCED_FACE ( 'NONE', ( #34145 ), #27395, .T. ) ;
#82672 = EDGE_LOOP ( 'NONE', ( #55550, #38103, #27513, #16572 ) ) ;
#82673 = ORIENTED_EDGE ( 'NONE', *, *, #85238, .T. ) ;
#82674 = LINE ( 'NONE', #60603, #64320 ) ;
#82675 = FACE_BOUND ( 'NONE', #6008, .T. ) ;
#82676 = CARTESIAN_POINT ( 'NONE',  ( -5.777220331021934996, -3.020022701398814569, 32.48759521482552515 ) ) ;
#82677 = EDGE_CURVE ( 'NONE', #41163, #83846, #57073, .T. ) ;
#82678 = DIRECTION ( 'NONE',  ( 0.000000000000000000, 8.673617379884028076E-17, 1.000000000000000000 ) ) ;
#82679 = EDGE_LOOP ( 'NONE', ( #83119, #1438 ) ) ;
#82680 = LINE ( 'NONE', #7003, #51839 ) ;
#82681 = LINE ( 'NONE', #20951, #55057 ) ;
#82682 = CYLINDRICAL_SURFACE ( 'NONE', #38533, 0.2499999999999986955 ) ;
#82683 = LINE ( 'NONE', #53863, #36576 ) ;
#82684 = ORIENTED_EDGE ( 'NONE', *, *, #50036, .F. ) ;
#82685 = VECTOR ( 'NONE', #66522, 1000.000000000000000 ) ;
#82686 = CARTESIAN_POINT ( 'NONE',  ( -11.47320639894870276, -12.51329471203373700, 31.30864560766537963 ) ) ;
#82687 = CARTESIAN_POINT ( 'NONE',  ( 1.384615384615265343, -8.613356846316285953, 34.62446782046622218 ) ) ;
#82688 = CARTESIAN_POINT ( 'NONE',  ( -12.46153846153846168, -12.10708131394839349, 31.69288490824020244 ) ) ;
#82689 = DIRECTION ( 'NONE',  ( 1.000000000000000000, 0.000000000000000000, 0.000000000000000000 ) ) ;
#82690 = CARTESIAN_POINT ( 'NONE',  ( 7.846153846153846700, -6.189225973068211317, 35.74407628777942847 ) ) ;
#82691 = FACE_BOUND ( 'NONE', #85837, .T. ) ;
#82693 = CYLINDRICAL_SURFACE ( 'NONE', #41703, 0.2500000000000002220 ) ;
#82692 = DIRECTION ( 'NONE',  ( -0.000000000000000000, 0.5000000000000011102, -0.8660254037844380415 ) ) ;
#82694 = CARTESIAN_POINT ( 'NONE',  ( 11.60452887181161508, -11.91647553114624358, 32.58852847137148245 ) ) ;
#82696 = CARTESIAN_POINT ( 'NONE',  ( 5.749976762707035505, -10.76384336483936011, 33.53834819971076087 ) ) ;
#82695 = DIRECTION ( 'NONE',  ( -1.000000000000000000, -0.000000000000000000, -0.000000000000000000 ) ) ;
#82697 = CARTESIAN_POINT ( 'NONE',  ( -10.74607521849492464, -6.369640206132551441, 34.87707690430378449 ) ) ;
#82698 = CARTESIAN_POINT ( 'NONE',  ( -1.987747218494660295, -5.598659921968651254, 16.24813170625848713 ) ) ;
#82699 = EDGE_LOOP ( 'NONE', ( #59380, #55717, #5262, #7943, #12324, #60633, #17161, #9581 ) ) ;
#82700 = CARTESIAN_POINT ( 'NONE',  ( 12.68454981315131036, -2.554770724473668153, 30.48948780036025852 ) ) ;
#82701 = EDGE_LOOP ( 'NONE', ( #21508, #2018 ) ) ;
#82702 = CARTESIAN_POINT ( 'NONE',  ( -13.16160254052199008, -10.77377354290276124, 33.85451476688484718 ) ) ;
#82703 = EDGE_LOOP ( 'NONE', ( #28605, #67115, #51053, #19355, #7200, #18496 ) ) ;
#82704 = CYLINDRICAL_SURFACE ( 'NONE', #38383, 0.2499999999999995559 ) ;
#82705 = CARTESIAN_POINT ( 'NONE',  ( -7.912237257109724808, -9.780366693483667717, 34.19971097300155805 ) ) ;
#82707 = ORIENTED_EDGE ( 'NONE', *, *, #31916, .T. ) ;
#82706 = CARTESIAN_POINT ( 'NONE',  ( -19.50000000000000000, -3.499999999999999556, 29.75000000000000355 ) ) ;
#82708 = CARTESIAN_POINT ( 'NONE',  ( -15.23076923076935252, -10.33852847137269571, 34.16647553114546554 ) ) ;
#82709 = CARTESIAN_POINT ( 'NONE',  ( 1.200186371490561621, -10.22469193450123193, 20.70125670625849423 ) ) ;
#82710 = CARTESIAN_POINT ( 'NONE',  ( 0.4615384615384611200, -1.790695186598648903, 34.54067556320373455 ) ) ;
#82711 = CARTESIAN_POINT ( 'NONE',  ( -6.923076923077045919, -12.70778746994576025, 30.41441678777401236 ) ) ;
#82712 = CARTESIAN_POINT ( 'NONE',  ( 12.23805351781451556, -2.847400154188068022, 31.58180166144859058 ) ) ;
#82713 = CARTESIAN_POINT ( 'NONE',  ( 10.61538461538449418, -2.657715359629662544, 31.77849191805970364 ) ) ;
#82714 = LINE ( 'NONE', #48913, #49691 ) ;
#82715 = LINE ( 'NONE', #2374, #18127 ) ;
#82716 = CARTESIAN_POINT ( 'NONE',  ( 3.750000000000001776, -7.561099074964511502, 23.47061829374151642 ) ) ;
#82717 = CARTESIAN_POINT ( 'NONE',  ( -10.39260507411620438, -2.847695495035523550, 31.58253572463339154 ) ) ;
#82718 = CARTESIAN_POINT ( 'NONE',  ( -6.000000000000121680, -3.643525952248796163, 33.31231777344771672 ) ) ;
#82719 = ORIENTED_EDGE ( 'NONE', *, *, #20068, .T. ) ;
#82720 = DIRECTION ( 'NONE',  ( -1.000000000000000000, 0.000000000000000000, 0.000000000000000000 ) ) ;
#82721 = CARTESIAN_POINT ( 'NONE',  ( 3.750000000000009770, -9.053300858899081760, 14.54687500000000178 ) ) ;
#82722 = AXIS2_PLACEMENT_3D ( 'NONE', #45562, #73042, #11338 ) ;
#82723 = DIRECTION ( 'NONE',  ( -0.000000000000000000, 0.7660444431189791237, -0.6427876096865379196 ) ) ;
#82724 = DIRECTION ( 'NONE',  ( -1.000000000000000000, -0.000000000000000000, -0.000000000000000000 ) ) ;
#82725 = EDGE_LOOP ( 'NONE', ( #87830, #25245, #18718, #24977 ) ) ;
#82726 = CARTESIAN_POINT ( 'NONE',  ( 1.634560793993429906, -8.476813868363244353, 34.90874843262270133 ) ) ;
#82727 = DIRECTION ( 'NONE',  ( 0.000000000000000000, 0.000000000000000000, -1.000000000000000000 ) ) ;
#82729 = VERTEX_POINT ( 'NONE', #15657 ) ;
#82728 = CARTESIAN_POINT ( 'NONE',  ( 2.084207363968362259, -2.847400154188067578, 31.58180166144859768 ) ) ;
#82730 = CARTESIAN_POINT ( 'NONE',  ( -5.300408020647025431, -5.912607949931405038, 34.49155766932282319 ) ) ;
#82731 = B_SPLINE_CURVE_WITH_KNOTS ( 'NONE', 3,
 ( #78102, #45650, #73126, #37551, #66368, #16402, #43870, #9639, #37107, #78540 ),
 .UNSPECIFIED., .F., .F.,
 ( 4, 2, 2, 2, 4 ),
 ( 0.0007817246256747445703, 0.0009771112852218872494, 0.001172497944769030145, 0.001367884604316172825, 0.001563271263863315504 ),
 .UNSPECIFIED. ) ;
#82732 = CARTESIAN_POINT ( 'NONE',  ( -17.32692307692307665, -7.500000000000001776, 35.00000000000000000 ) ) ;
#82733 = EDGE_CURVE ( 'NONE', #49839, #16707, #21969, .T. ) ;
#82734 = CARTESIAN_POINT ( 'NONE',  ( -10.48485917715097138, -9.503571793651731880, 34.60286762892837942 ) ) ;
#82735 = CARTESIAN_POINT ( 'NONE',  ( -16.94613126909829504, -2.729792928343270031, 31.24908615093345432 ) ) ;
#82736 = LINE ( 'NONE', #21010, #27928 ) ;
#82737 = ORIENTED_EDGE ( 'NONE', *, *, #67452, .T. ) ;
#82738 = VERTEX_POINT ( 'NONE', #2129 ) ;
#82739 = ORIENTED_EDGE ( 'NONE', *, *, #43998, .F. ) ;
#82740 = EDGE_CURVE ( 'NONE', #54936, #74567, #9774, .T. ) ;
#82741 = CARTESIAN_POINT ( 'NONE',  ( -9.692307692307812417, -3.300289026999228881, 32.46337939537708905 ) ) ;
#82742 = FACE_OUTER_BOUND ( 'NONE', #82791, .T. ) ;
#82743 = EDGE_CURVE ( 'NONE', #22897, #58039, #27002, .T. ) ;
#82744 = CARTESIAN_POINT ( 'NONE',  ( 9.915319043920545639, -4.887748414852792322, 34.01359900205216746 ) ) ;
#82745 = CARTESIAN_POINT ( 'NONE',  ( -8.096130590202434973, -10.82459398097509329, 33.81372124010185587 ) ) ;
#82746 = VECTOR ( 'NONE', #56220, 1000.000000000000227 ) ;
#82747 = ORIENTED_EDGE ( 'NONE', *, *, #41131, .T. ) ;
#82748 = CARTESIAN_POINT ( 'NONE',  ( -17.14300648787895653, -4.098570777380720287, 33.41473453929634729 ) ) ;
#82749 = EDGE_LOOP ( 'NONE', ( #9830, #69417, #35345, #28689 ) ) ;
#82750 = ORIENTED_EDGE ( 'NONE', *, *, #20600, .T. ) ;
#82752 = VERTEX_POINT ( 'NONE', #70595 ) ;
#82751 = EDGE_CURVE ( 'NONE', #14834, #80094, #76341, .T. ) ;
#82754 = ORIENTED_EDGE ( 'NONE', *, *, #34977, .T. ) ;
#82753 = DIRECTION ( 'NONE',  ( 0.000000000000000000, 0.8660254037844377084, -0.5000000000000015543 ) ) ;
#82755 = CARTESIAN_POINT ( 'NONE',  ( 0.6089743589743582541, -11.50000000000000000, 29.75000000000000355 ) ) ;
#82756 = B_SPLINE_CURVE_WITH_KNOTS ( 'NONE', 3,
 ( #82858, #35096, #76081, #49052, #56258, #33776, #55366, #88738, #62130, #1307 ),
 .UNSPECIFIED., .F., .F.,
 ( 4, 2, 2, 2, 4 ),
 ( 0.000000000000000000, 0.0001954339857564077183, 0.0003908679715128154366, 0.0005863019572692231007, 0.0007817359430256308733 ),
 .UNSPECIFIED. ) ;
#82757 = CARTESIAN_POINT ( 'NONE',  ( 5.777073041093152561, -12.64616026154729411, 30.79003144601913533 ) ) ;
#82758 = ADVANCED_FACE ( 'NONE', ( #57518 ), #85004, .F. ) ;
#82759 = CARTESIAN_POINT ( 'NONE',  ( -9.822454901745912181, -8.587444163452046197, 34.63053765926554206 ) ) ;
#82760 = CARTESIAN_POINT ( 'NONE',  ( -3.903791733932699515, -6.523592122091591783, 34.90882529074906415 ) ) ;
#82761 = VERTEX_POINT ( 'NONE', #76912 ) ;
#82762 = EDGE_LOOP ( 'NONE', ( #659, #86392, #44063, #46782 ) ) ;
#82763 = VERTEX_POINT ( 'NONE', #71034 ) ;
#82764 = LINE ( 'NONE', #8427, #53334 ) ;
#82766 = EDGE_LOOP ( 'NONE', ( #25247, #13551, #49705, #81514 ) ) ;
#82765 = DIRECTION ( 'NONE',  ( -1.000000000000000000, 0.000000000000000000, 0.000000000000000000 ) ) ;
#82767 = CARTESIAN_POINT ( 'NONE',  ( -2.177166605928743781, -8.586989748646452369, 34.63063291749215011 ) ) ;
#82768 = VECTOR ( 'NONE', #32714, 999.9999999999998863 ) ;
#82769 = CARTESIAN_POINT ( 'NONE',  ( -0.5916864312701572981, -6.809168938359898782, 34.95455904226513866 ) ) ;
#82770 = EDGE_CURVE ( 'NONE', #60559, #48169, #30053, .T. ) ;
#82771 = ORIENTED_EDGE ( 'NONE', *, *, #41527, .F. ) ;
#82772 = EDGE_CURVE ( 'NONE', #13992, #54951, #37659, .T. ) ;
#82773 = CARTESIAN_POINT ( 'NONE',  ( 13.38461538461538680, -4.786620604624113540, 33.94971097300155094 ) ) ;
#82774 = DIRECTION ( 'NONE',  ( 0.000000000000000000, 0.8660254037844377084, 0.5000000000000015543 ) ) ;
#82775 = ORIENTED_EDGE ( 'NONE', *, *, #27727, .F. ) ;
#82776 = FACE_BOUND ( 'NONE', #64455, .T. ) ;
#82777 = B_SPLINE_CURVE_WITH_KNOTS ( 'NONE', 3,
 ( #65632, #53460, #25997, #73761, #12055, #32318, #80962, #59780, #25555, #25108 ),
 .UNSPECIFIED., .F., .F.,
 ( 4, 2, 2, 2, 4 ),
 ( 0.0007817246256747507503, 0.0009771112852218957062, 0.001172497944769040771, 0.001367884604316185835, 0.001563271263863330682 ),
 .UNSPECIFIED. ) ;
#82778 = CARTESIAN_POINT ( 'NONE',  ( -11.00641025641025550, -7.500000000000000000, 33.75000000000000000 ) ) ;
#82779 = LINE ( 'NONE', #42237, #48546 ) ;
#82780 = DIRECTION ( 'NONE',  ( -0.000000000000000000, 0.5000000000000011102, -0.8660254037844381525 ) ) ;
#82782 = CARTESIAN_POINT ( 'NONE',  ( -0.5916856709766853406, -12.27039167877662251, 31.24851455888617835 ) ) ;
#82781 = CARTESIAN_POINT ( 'NONE',  ( 10.86538461538605205, -7.500000000000155431, 34.75000000000007105 ) ) ;
#82783 = EDGE_CURVE ( 'NONE', #5809, #29827, #15217, .T. ) ;
#82784 = CARTESIAN_POINT ( 'NONE',  ( -10.61538461538461320, -1.790695186598648903, 34.54067556320373455 ) ) ;
#82785 = CARTESIAN_POINT ( 'NONE',  ( -4.153846153846274980, -11.06231777344772027, 33.60647404775119895 ) ) ;
#82786 = VERTEX_POINT ( 'NONE', #36804 ) ;
#82787 = EDGE_CURVE ( 'NONE', #14363, #35493, #50745, .T. ) ;
#82788 = PLANE ( 'NONE',  #64768 ) ;
#82789 = VECTOR ( 'NONE', #56721, 1000.000000000000000 ) ;
#82790 = DIRECTION ( 'NONE',  ( -0.000000000000000000, 0.9848077530122086864, -0.1736481776669273891 ) ) ;
#82791 = EDGE_LOOP ( 'NONE', ( #85355, #62566, #54260, #3976, #33093, #17614, #25546, #78062 ) ) ;
#82792 = DIRECTION ( 'NONE',  ( -0.000000000000000000, 0.6427876096865404731, -0.7660444431189771253 ) ) ;
#82793 = EDGE_LOOP ( 'NONE', ( #55782, #77179, #39001, #83365 ) ) ;
#82794 = CARTESIAN_POINT ( 'NONE',  ( 11.31497661389721010, -10.23692288466677880, 34.23039457007281072 ) ) ;
#82795 = DIRECTION ( 'NONE',  ( -0.000000000000000000, -0.7660444431189791237, -0.6427876096865379196 ) ) ;
#82796 = FACE_BOUND ( 'NONE', #26138, .T. ) ;
#82797 = B_SPLINE_CURVE_WITH_KNOTS ( 'NONE', 3,
 ( #56392, #8654, #49631, #35688, #2314, #48294, #69900, #42000, #7764, #69459 ),
 .UNSPECIFIED., .F., .F.,
 ( 4, 2, 2, 2, 4 ),
 ( 0.000000000000000000, 0.0001954339857564089651, 0.0003908679715128179303, 0.0005863019572692268954, 0.0007817359430256358606 ),
 .UNSPECIFIED. ) ;
#82799 = CARTESIAN_POINT ( 'NONE',  ( -4.023320452082589149, -8.586989748646452369, 34.63063291749215011 ) ) ;
#82798 = DIRECTION ( 'NONE',  ( -0.000000000000000000, -0.6427876096865404731, -0.7660444431189770143 ) ) ;
#82800 = DIRECTION ( 'NONE',  ( -0.000000000000000000, 1.000000000000000000, -0.000000000000000000 ) ) ;
#82801 = CARTESIAN_POINT ( 'NONE',  ( 17.99999999999987566, -10.90142922262034020, 33.41473453929536674 ) ) ;
#82803 = DIRECTION ( 'NONE',  ( -0.000000000000000000, 0.7660444431189791237, -0.6427876096865379196 ) ) ;
#82802 = DIRECTION ( 'NONE',  ( 0.000000000000000000, 0.000000000000000000, 1.000000000000000000 ) ) ;
#82804 = CARTESIAN_POINT ( 'NONE',  ( -14.05774689831426372, -5.766571408460171355, 34.70601412856602508 ) ) ;
#82805 = CARTESIAN_POINT ( 'NONE',  ( 1.492201783934554493, -3.724691934501233703, 16.48250670625849423 ) ) ;
#82806 = ORIENTED_EDGE ( 'NONE', *, *, #22369, .F. ) ;
#82807 = B_SPLINE_CURVE_WITH_KNOTS ( 'NONE', 3,
 ( #14233, #42600, #69178, #55214, #718, #7922, #75934, #21876, #27304, #88591 ),
 .UNSPECIFIED., .F., .F.,
 ( 4, 2, 2, 2, 4 ),
 ( 0.0007817246256747474977, 0.0009771112852218911526, 0.001172497944769034699, 0.001367884604316178462, 0.001563271263863322009 ),
 .UNSPECIFIED. ) ;
#82808 = ORIENTED_EDGE ( 'NONE', *, *, #20892, .F. ) ;
#82809 = CARTESIAN_POINT ( 'NONE',  ( -9.692307692307691624, -11.69971097300155272, 32.46337939537588113 ) ) ;
#82810 = DIRECTION ( 'NONE',  ( -0.000000000000000000, 1.000000000000000000, 3.491481338843133355E-15 ) ) ;
#82811 = CARTESIAN_POINT ( 'NONE',  ( 6.673076923076926015, -7.433932668274256805, 35.00000000000000711 ) ) ;
#82812 = CARTESIAN_POINT ( 'NONE',  ( 18.00000000000000000, -11.33034616979429110, 35.88435417666054406 ) ) ;
#82813 = CARTESIAN_POINT ( 'NONE',  ( -16.15384615384615330, -12.10708131394839349, 31.69288490824020244 ) ) ;
#82814 = CARTESIAN_POINT ( 'NONE',  ( -3.724691934501229262, -9.114399933863657211, 18.51375670625849068 ) ) ;
#82815 = CARTESIAN_POINT ( 'NONE',  ( -16.15384615384627409, -5.941354392335915335, 34.76329471203413846 ) ) ;
#82816 = CARTESIAN_POINT ( 'NONE',  ( 2.307692307692309264, -6.435427911321262684, 35.78748833219616898 ) ) ;
#82817 = CARTESIAN_POINT ( 'NONE',  ( 15.29683758177167086, -11.69971097300155272, 32.46337939537588113 ) ) ;
#82818 = DIRECTION ( 'NONE',  ( -0.000000000000000000, 0.9848077530122085754, -0.1736481776669273613 ) ) ;
#82819 = DIRECTION ( 'NONE',  ( 0.000000000000000000, -1.000000000000000000, -4.336808689942017736E-16 ) ) ;
#82820 = CARTESIAN_POINT ( 'NONE',  ( -5.076923076923075762, -6.343179335718451384, 34.87096338111211935 ) ) ;
#82821 = CARTESIAN_POINT ( 'NONE',  ( 5.869852790561778555, -12.27039167877662251, 31.24851455888617835 ) ) ;
#82822 = EDGE_CURVE ( 'NONE', #32882, #78424, #82840, .T. ) ;
#82823 = CARTESIAN_POINT ( 'NONE',  ( -13.38461538461550759, -9.528491918059723176, 34.59228464037033035 ) ) ;
#82824 = CARTESIAN_POINT ( 'NONE',  ( 12.46153846153846168, -2.721908614388771852, 31.22303859784724978 ) ) ;
#82825 = ORIENTED_EDGE ( 'NONE', *, *, #17038, .T. ) ;
#82826 = EDGE_CURVE ( 'NONE', #59207, #33581, #57960, .T. ) ;
#82827 = CARTESIAN_POINT ( 'NONE',  ( -0.2114841499001472724, -3.627508038966690496, 32.91356715214248396 ) ) ;
#82828 = CARTESIAN_POINT ( 'NONE',  ( -3.230769230769351186, -12.46129190930018460, 30.37095296980731973 ) ) ;
#82829 = CARTESIAN_POINT ( 'NONE',  ( 1.901340078031373171, -9.487747218494639867, 23.62686829374151287 ) ) ;
#82830 = ADVANCED_FACE ( 'NONE', ( #82136 ), #6473, .F. ) ;
#82831 = CARTESIAN_POINT ( 'NONE',  ( -18.00000000000000000, -2.916148748677405145, 35.60175215339625510 ) ) ;
#82832 = DIRECTION ( 'NONE',  ( 0.000000000000000000, 0.9396926207859126468, -0.3420201433256571111 ) ) ;
#82833 = EDGE_LOOP ( 'NONE', ( #81903, #20824, #20754, #6193 ) ) ;
#82834 = FACE_OUTER_BOUND ( 'NONE', #40895, .T. ) ;
#82836 = EDGE_LOOP ( 'NONE', ( #80433, #38523 ) ) ;
#82835 = CARTESIAN_POINT ( 'NONE',  ( -6.249999999999996447, -7.566082377512563184, 35.00000000000000711 ) ) ;
#82837 = CARTESIAN_POINT ( 'NONE',  ( 7.911409417429874580, -3.835265460703683349, 33.15142922261929925 ) ) ;
#82838 = CARTESIAN_POINT ( 'NONE',  ( -16.09615384615384670, -11.00000000000000000, 29.75000000000000355 ) ) ;
#82839 = EDGE_LOOP ( 'NONE', ( #47643, #51851 ) ) ;
#82840 = B_SPLINE_CURVE_WITH_KNOTS ( 'NONE', 3,
 ( #63386, #8901, #1694, #36371, #78229, #43996, #16093, #63833, #37236, #3007 ),
 .UNSPECIFIED., .F., .F.,
 ( 4, 2, 2, 2, 4 ),
 ( 0.000000000000000000, 0.0001954311564186864678, 0.0003908623128373729357, 0.0005862934692560594577, 0.0007817246256747458714 ),
 .UNSPECIFIED. ) ;
#82841 = DIRECTION ( 'NONE',  ( -0.000000000000000000, 0.9848077530122085754, -0.1736481776669273613 ) ) ;
#82842 = EDGE_CURVE ( 'NONE', #7785, #85805, #78505, .T. ) ;
#82843 = DIRECTION ( 'NONE',  ( -0.000000000000000000, 0.7660444431189791237, -0.6427876096865379196 ) ) ;
#82844 = ORIENTED_EDGE ( 'NONE', *, *, #40950, .T. ) ;
#82845 = CARTESIAN_POINT ( 'NONE',  ( -10.68146699474474914, -3.937682226553330445, 33.60647404775217240 ) ) ;
#82846 = DIRECTION ( 'NONE',  ( -0.000000000000000000, 0.8660254037844397068, -0.4999999999999978906 ) ) ;
#82847 = AXIS2_PLACEMENT_3D ( 'NONE', #39725, #75705, #40169 ) ;
#82848 = DIRECTION ( 'NONE',  ( 0.000000000000000000, 0.9396926207859126468, -0.3420201433256571111 ) ) ;
#82849 = ORIENTED_EDGE ( 'NONE', *, *, #25762, .F. ) ;
#82850 = EDGE_LOOP ( 'NONE', ( #47284, #1456, #2441, #62680 ) ) ;
#82851 = CARTESIAN_POINT ( 'NONE',  ( 5.999999999999880096, -6.879047030192662504, 34.71129190930017927 ) ) ;
#82852 = ORIENTED_EDGE ( 'NONE', *, *, #69139, .F. ) ;
#82853 = CARTESIAN_POINT ( 'NONE',  ( 17.78205128205128105, -3.499999999999999556, 29.75000000000000355 ) ) ;
#82854 = CARTESIAN_POINT ( 'NONE',  ( -5.076923076923075762, -9.058645607665452459, 34.76329471203371924 ) ) ;
#82855 = CARTESIAN_POINT ( 'NONE',  ( 2.307692307692309264, -11.35647404775217417, 33.31231777344666511 ) ) ;
#82856 = AXIS2_PLACEMENT_3D ( 'NONE', #35468, #13422, #34585 ) ;
#82857 = CARTESIAN_POINT ( 'NONE',  ( -6.923076923077045919, -11.67786785259630911, 32.92929555188603530 ) ) ;
#82859 = EDGE_CURVE ( 'NONE', #46262, #28353, #9745, .T. ) ;
#82858 = CARTESIAN_POINT ( 'NONE',  ( -4.153846153846152411, -6.386643153685126251, 34.62446782046654192 ) ) ;
#82860 = LINE ( 'NONE', #69770, #664 ) ;
#82861 = CARTESIAN_POINT ( 'NONE',  ( 3.007284306204901281, -10.23692288466677880, 34.23039457007281072 ) ) ;
#82862 = ORIENTED_EDGE ( 'NONE', *, *, #77846, .F. ) ;
#82863 = EDGE_LOOP ( 'NONE', ( #56833, #74553 ) ) ;
#82865 = ORIENTED_EDGE ( 'NONE', *, *, #59933, .T. ) ;
#82864 = CARTESIAN_POINT ( 'NONE',  ( 7.053867364043876265, -12.62708834333097663, 30.88030960425257021 ) ) ;
#82866 = CARTESIAN_POINT ( 'NONE',  ( -5.326946301144535489, -4.931416488878822335, 34.32920672191015399 ) ) ;
#82867 = ORIENTED_EDGE ( 'NONE', *, *, #76457, .F. ) ;
#82868 = DIRECTION ( 'NONE',  ( -0.000000000000000000, 1.000000000000000000, -0.000000000000000000 ) ) ;
#82869 = CARTESIAN_POINT ( 'NONE',  ( 5.299702618191484582, -3.755027918224367767, 33.06320215134714857 ) ) ;
#82870 = ORIENTED_EDGE ( 'NONE', *, *, #701, .F. ) ;
#82871 = CARTESIAN_POINT ( 'NONE',  ( -9.757558682468932432, -2.506253911140460922, 30.00000000000013856 ) ) ;
#82872 = VECTOR ( 'NONE', #81951, 1000.000000000000000 ) ;
#82873 = VERTEX_POINT ( 'NONE', #46996 ) ;
#82874 = ORIENTED_EDGE ( 'NONE', *, *, #1596, .T. ) ;
#82875 = B_SPLINE_CURVE_WITH_KNOTS ( 'NONE', 3,
 ( #59741, #54304, #25069, #80920, #18316, #33158, #73717, #67832, #45779, #25954 ),
 .UNSPECIFIED., .F., .F.,
 ( 4, 2, 2, 2, 4 ),
 ( 0.000000000000000000, 0.0001954339857564097241, 0.0003908679715128194482, 0.0005863019572692291723, 0.0007817359430256388964 ),
 .UNSPECIFIED. ) ;
#82876 = CARTESIAN_POINT ( 'NONE',  ( 18.03205128205128105, -3.499999999999999556, 29.75000000000000355 ) ) ;
#82878 = VERTEX_POINT ( 'NONE', #47890 ) ;
#82877 = EDGE_CURVE ( 'NONE', #4743, #50820, #27939, .T. ) ;
#82879 = EDGE_CURVE ( 'NONE', #66653, #78771, #74048, .T. ) ;
#82880 = CARTESIAN_POINT ( 'NONE',  ( -1.384615384615505151, -2.625532179533778709, 30.86335684631627174 ) ) ;
#82881 = CARTESIAN_POINT ( 'NONE',  ( 17.01083966596719677, -2.721908614388770964, 31.22303859784723912 ) ) ;
#82882 = FACE_BOUND ( 'NONE', #72166, .T. ) ;
#82883 = CYLINDRICAL_SURFACE ( 'NONE', #25504, 0.2500000000000012212 ) ;
#82885 = EDGE_CURVE ( 'NONE', #63695, #79014, #81693, .T. ) ;
#82884 = CARTESIAN_POINT ( 'NONE',  ( -6.923076923077044142, -12.27809138561165270, 31.22303859784587132 ) ) ;
#82886 = CARTESIAN_POINT ( 'NONE',  ( 15.48071464014727283, -2.589246495874658383, 31.60778113518102828 ) ) ;
#82887 = CARTESIAN_POINT ( 'NONE',  ( -0.3962833220256232192, -3.083524468853785283, 32.58852847137153930 ) ) ;
#82888 = CARTESIAN_POINT ( 'NONE',  ( 5.076923076922954969, -10.90142922262034020, 33.41473453929536674 ) ) ;
#82889 = CARTESIAN_POINT ( 'NONE',  ( 20.00000000000000000, -4.000000000000000000, 29.75000000000000355 ) ) ;
#82890 = ADVANCED_FACE ( 'NONE', ( #18662 ), #40264, .F. ) ;
#82891 = FACE_OUTER_BOUND ( 'NONE', #22183, .T. ) ;
#82892 = VERTEX_POINT ( 'NONE', #6904 ) ;
#82893 = ORIENTED_EDGE ( 'NONE', *, *, #46833, .T. ) ;
#82895 = CARTESIAN_POINT ( 'NONE',  ( 14.98074599347626545, -12.22074536777954989, 31.39888409691088356 ) ) ;
#82894 = CARTESIAN_POINT ( 'NONE',  ( 2.242422307135989890, -3.083524468853724443, 32.58852847137143272 ) ) ;
#82896 = CARTESIAN_POINT ( 'NONE',  ( 7.145856464345331283, -6.760870238392817200, 34.69528174975672385 ) ) ;
#82897 = CYLINDRICAL_SURFACE ( 'NONE', #60937, 0.2499999999999994726 ) ;
#82898 = CARTESIAN_POINT ( 'NONE',  ( -10.61538461538473577, -12.51329471203414379, 31.30864560766407578 ) ) ;
#82899 = CARTESIAN_POINT ( 'NONE',  ( 9.758376043310134307, -2.538708090699994813, 30.37095296980875503 ) ) ;
#82900 = ORIENTED_EDGE ( 'NONE', *, *, #63489, .T. ) ;
#82901 = LINE ( 'NONE', #28384, #41428 ) ;
#82902 = CARTESIAN_POINT ( 'NONE',  ( -39.05038313613820122, -2.249999999999998668, 29.75000000000000355 ) ) ;
#82903 = CARTESIAN_POINT ( 'NONE',  ( 16.94677510719138169, -4.299443229763728169, 33.91186481527756058 ) ) ;
#82904 = DIRECTION ( 'NONE',  ( 0.000000000000000000, 0.7660444431189822323, -0.6427876096865344779 ) ) ;
#82905 = ORIENTED_EDGE ( 'NONE', *, *, #20204, .T. ) ;
#82906 = ADVANCED_FACE ( 'NONE', ( #59630 ), #87131, .F. ) ;
#82907 = EDGE_LOOP ( 'NONE', ( #68019, #25494 ) ) ;
#82908 = VERTEX_POINT ( 'NONE', #32603 ) ;
#82909 = CARTESIAN_POINT ( 'NONE',  ( -9.442253380669379581, -12.41262288849542017, 30.68299917996395010 ) ) ;
#82910 = EDGE_CURVE ( 'NONE', #79986, #765, #69890, .T. ) ;
#82911 = ORIENTED_EDGE ( 'NONE', *, *, #85675, .T. ) ;
#82912 = AXIS2_PLACEMENT_3D ( 'NONE', #31420, #86387, #17910 ) ;
#82913 = CYLINDRICAL_SURFACE ( 'NONE', #72830, 0.2500000000000002220 ) ;
#82914 = CARTESIAN_POINT ( 'NONE',  ( 1.384615384615264011, -3.643525952248795718, 33.31231777344771672 ) ) ;
#82915 = CARTESIAN_POINT ( 'NONE',  ( 14.24160992833217065, -9.905515769479276145, 34.41647553114623292 ) ) ;
#82916 = CARTESIAN_POINT ( 'NONE',  ( 3.750000000000009770, -9.053300858899081760, 14.54687500000000178 ) ) ;
#82917 = CARTESIAN_POINT ( 'NONE',  ( -11.28851602011339672, -6.696923467548660192, 34.68552623307873972 ) ) ;
#82918 = ORIENTED_EDGE ( 'NONE', *, *, #23175, .F. ) ;
#82919 = CARTESIAN_POINT ( 'NONE',  ( 11.31559611625790041, -2.501496062324912284, 29.88072118266895671 ) ) ;
#82921 = ORIENTED_EDGE ( 'NONE', *, *, #14433, .T. ) ;
#82920 = DIRECTION ( 'NONE',  ( -0.000000000000000000, 0.3420201433256694346, -0.9396926207859080948 ) ) ;
#82922 = LINE ( 'NONE', #51193, #81496 ) ;
#82923 = DIRECTION ( 'NONE',  ( 0.000000000000000000, 0.7660444431189822323, -0.6427876096865344779 ) ) ;
#82924 = CARTESIAN_POINT ( 'NONE',  ( 17.01083966596719321, -3.513871655860377086, 32.76840700105978499 ) ) ;
#82925 = CARTESIAN_POINT ( 'NONE',  ( 11.66898697669518548, -10.31582465632705237, 34.18122507451815295 ) ) ;
#82926 = EDGE_CURVE ( 'NONE', #64675, #7863, #28069, .T. ) ;
#82927 = LINE ( 'NONE', #76607, #8846 ) ;
#82928 = CARTESIAN_POINT ( 'NONE',  ( -3.360917200500928459, -11.04286588640298561, 33.62463336215343901 ) ) ;
#82929 = CARTESIAN_POINT ( 'NONE',  ( -3.164602624177589529, -7.250054591869667497, 34.99404684341514127 ) ) ;
#82930 = CARTESIAN_POINT ( 'NONE',  ( -0.06109907496451398579, -10.25000000000000178, 25.03311829374151287 ) ) ;
#82931 = ORIENTED_EDGE ( 'NONE', *, *, #9095, .F. ) ;
#82932 = EDGE_CURVE ( 'NONE', #66461, #48943, #63172, .T. ) ;
#82933 = CARTESIAN_POINT ( 'NONE',  ( -2.980714810855777053, -6.523592122091589118, 34.90882529074906415 ) ) ;
#82934 = CARTESIAN_POINT ( 'NONE',  ( 0.5920641633020263805, -3.285477652293412820, 32.44071101563363158 ) ) ;
#82935 = CYLINDRICAL_SURFACE ( 'NONE', #83485, 0.2499999999999998890 ) ;
#82937 = DIRECTION ( 'NONE',  ( 0.000000000000000000, 0.000000000000000000, -1.000000000000000000 ) ) ;
#82936 = VECTOR ( 'NONE', #67876, 1000.000000000000000 ) ;
#82938 = ORIENTED_EDGE ( 'NONE', *, *, #72002, .T. ) ;
#82939 = CARTESIAN_POINT ( 'NONE',  ( 7.976679284387489410, -12.15418822224088657, 32.17964115625579069 ) ) ;
#82940 = CARTESIAN_POINT ( 'NONE',  ( -6.000000000000119904, -2.625532179533778709, 30.86335684631627174 ) ) ;
#82941 = CARTESIAN_POINT ( 'NONE',  ( -0.7115152055870523906, -12.65889640711025521, 30.72598325615533454 ) ) ;
#82942 = EDGE_CURVE ( 'NONE', #84330, #71586, #29412, .T. ) ;
#82943 = CARTESIAN_POINT ( 'NONE',  ( 9.469428175570110184, -7.630690623152299956, 34.99857592706774057 ) ) ;
#82944 = ORIENTED_EDGE ( 'NONE', *, *, #4901, .T. ) ;
#82945 = LINE ( 'NONE', #63092, #70740 ) ;
#82946 = EDGE_CURVE ( 'NONE', #30896, #29433, #68775, .T. ) ;
#82947 = CARTESIAN_POINT ( 'NONE',  ( 17.32686859527121470, -5.852078868378311149, 34.47109172314383585 ) ) ;
#82948 = DIRECTION ( 'NONE',  ( -0.000000000000000000, -0.5000000000000009992, -0.8660254037844380415 ) ) ;
#82949 = ORIENTED_EDGE ( 'NONE', *, *, #32242, .T. ) ;
#82950 = FACE_OUTER_BOUND ( 'NONE', #42776, .T. ) ;
#82951 = EDGE_LOOP ( 'NONE', ( #86874, #55828, #77517, #65646 ) ) ;
#82952 = CARTESIAN_POINT ( 'NONE',  ( -15.84615384615384670, -3.499999999999999556, 29.75000000000000355 ) ) ;
#82953 = CARTESIAN_POINT ( 'NONE',  ( 0.6843181305165274564, -10.23759521482555357, 34.22997729860117033 ) ) ;
#82954 = EDGE_LOOP ( 'NONE', ( #26400, #6147, #40925, #65784, #44472 ) ) ;
#82955 = DIRECTION ( 'NONE',  ( 1.000000000000000000, 0.000000000000000000, 0.000000000000000000 ) ) ;
#82957 = ADVANCED_FACE ( 'NONE', ( #28516 ), #152, .F. ) ;
#82956 = LINE ( 'NONE', #976, #73791 ) ;
#82958 = CARTESIAN_POINT ( 'NONE',  ( -10.68065506134539078, -6.026961402152685388, 34.52809138561120506 ) ) ;
#82959 = ADVANCED_FACE ( 'NONE', ( #55977 ), #21751, .T. ) ;
#82960 = CARTESIAN_POINT ( 'NONE',  ( 11.47237915910140238, -12.34228464037088280, 31.77849191805838558 ) ) ;
#82961 = LINE ( 'NONE', #32998, #18163 ) ;
#82962 = EDGE_LOOP ( 'NONE', ( #24466, #79182 ) ) ;
#82963 = FACE_BOUND ( 'NONE', #43423, .T. ) ;
#82964 = ORIENTED_EDGE ( 'NONE', *, *, #2420, .F. ) ;
#82965 = LINE ( 'NONE', #74430, #8410 ) ;
#82966 = AXIS2_PLACEMENT_3D ( 'NONE', #74103, #11065, #45279 ) ;
#82967 = B_SPLINE_CURVE_WITH_KNOTS ( 'NONE', 3,
 ( #75586, #68393, #8029, #62946, #41373, #6692, #34164, #14791, #56211, #35498 ),
 .UNSPECIFIED., .F., .F.,
 ( 4, 2, 2, 2, 4 ),
 ( 0.0007817246256747484735, 0.0009771112852218928873, 0.001172497944769037084, 0.001367884604316181498, 0.001563271263863325912 ),
 .UNSPECIFIED. ) ;
#82968 = CARTESIAN_POINT ( 'NONE',  ( 6.857826991302839126, -2.255955759149247619, 30.00000000000013856 ) ) ;
#82969 = CIRCLE ( 'NONE', #16863, 0.2500000000000002220 ) ;
#82970 = CARTESIAN_POINT ( 'NONE',  ( 3.100621261037533660, -11.66186481527757479, 32.95055677023626117 ) ) ;
#82971 = CARTESIAN_POINT ( 'NONE',  ( -11.47239318745910097, -2.538708090699994813, 30.37095296980875503 ) ) ;
#82972 = ORIENTED_EDGE ( 'NONE', *, *, #36241, .F. ) ;
#82973 = VERTEX_POINT ( 'NONE', #70389 ) ;
#82974 = ORIENTED_EDGE ( 'NONE', *, *, #7975, .F. ) ;
#82975 = LINE ( 'NONE', #76204, #47685 ) ;
#82976 = ORIENTED_EDGE ( 'NONE', *, *, #23064, .F. ) ;
#82977 = CARTESIAN_POINT ( 'NONE',  ( 4.284636594813102661, -9.929761469519744921, 34.40412654351204225 ) ) ;
#82978 = CARTESIAN_POINT ( 'NONE',  ( -11.78843828251013015, -5.643011162660950042, 34.66104346484419096 ) ) ;
#82979 = CARTESIAN_POINT ( 'NONE',  ( -5.076923076923075762, -3.513871655860378418, 32.76840700105978499 ) ) ;
#82981 = EDGE_CURVE ( 'NONE', #45693, #4584, #41989, .T. ) ;
#82980 = CARTESIAN_POINT ( 'NONE',  ( 16.21991348719623360, -2.292212530054420050, 30.41441678777542990 ) ) ;
#82982 = CARTESIAN_POINT ( 'NONE',  ( 16.15384615384615330, -9.819645486525091727, 36.12317359536749706 ) ) ;
#82983 = CARTESIAN_POINT ( 'NONE',  ( 20.00000000000000000, -4.000000000000000000, 29.75000000000000355 ) ) ;
#82984 = CARTESIAN_POINT ( 'NONE',  ( -4.946132635956124624, -11.37503395064541678, 33.29242100308974983 ) ) ;
#82985 = ORIENTED_EDGE ( 'NONE', *, *, #30943, .F. ) ;
#82986 = EDGE_CURVE ( 'NONE', #27220, #19422, #16139, .T. ) ;
#82987 = ORIENTED_EDGE ( 'NONE', *, *, #53801, .T. ) ;
#82988 = B_SPLINE_CURVE_WITH_KNOTS ( 'NONE', 3,
 ( #26840, #88563, #47542, #20519, #45432, #66149, #20952, #89004, #34478, #61940 ),
 .UNSPECIFIED., .F., .F.,
 ( 4, 2, 2, 2, 4 ),
 ( 0.0007817246256747520513, 0.0009771112852218959231, 0.001172497944769039903, 0.001367884604316183883, 0.001563271263863327864 ),
 .UNSPECIFIED. ) ;
#82989 = ORIENTED_EDGE ( 'NONE', *, *, #19555, .F. ) ;
#82990 = CARTESIAN_POINT ( 'NONE',  ( -5.076923076923075762, -10.67929555188718282, 33.92786785259544047 ) ) ;
#82992 = CARTESIAN_POINT ( 'NONE',  ( 1.384615384615264011, -11.67786785259630911, 32.92929555188603530 ) ) ;
#82991 = CARTESIAN_POINT ( 'NONE',  ( -1.608100309179717025, -2.612411019501189813, 31.66733052389439962 ) ) ;
#82993 = ADVANCED_FACE ( 'NONE', ( #77585 ), #35723, .F. ) ;
#82994 = B_SPLINE_CURVE_WITH_KNOTS ( 'NONE', 3,
 ( #59542, #73518, #10478, #25321, #24866, #72164, #52783, #45584, #73063, #30734 ),
 .UNSPECIFIED., .F., .F.,
 ( 4, 2, 2, 2, 4 ),
 ( 0.0007817359430256287049, 0.0009771253907249945886, 0.001172514838424360255, 0.001367904286123725922, 0.001563293733823091589 ),
 .UNSPECIFIED. ) ;
#82995 = CARTESIAN_POINT ( 'NONE',  ( 1.450682717965462887, -12.34228464037088813, 31.77849191805839268 ) ) ;
#82996 = CARTESIAN_POINT ( 'NONE',  ( 14.30769230769231015, -12.78798330534102767, 29.49999999999997868 ) ) ;
#82997 = FACE_BOUND ( 'NONE', #29363, .T. ) ;
#82998 = CARTESIAN_POINT ( 'NONE',  ( 8.703148389870634105, -10.67929555188718460, 33.92786785259543336 ) ) ;
#82999 = VERTEX_POINT ( 'NONE', #49666 ) ;
#83000 = CARTESIAN_POINT ( 'NONE',  ( 14.53047197667037338, -12.47679350104403007, 31.42216943046555855 ) ) ;
#83001 = VECTOR ( 'NONE', #71950, 1000.000000000000000 ) ;
#83002 = CARTESIAN_POINT ( 'NONE',  ( -14.30769230769230660, -1.117168528481311540, 33.14645433367849847 ) ) ;
#83003 = DIRECTION ( 'NONE',  ( 0.000000000000000000, 0.000000000000000000, -1.000000000000000000 ) ) ;
#83004 = CARTESIAN_POINT ( 'NONE',  ( 7.053867364043876265, -9.084667340241226796, 34.75534355489798344 ) ) ;
#83005 = ORIENTED_EDGE ( 'NONE', *, *, #14083, .T. ) ;
#83006 = ADVANCED_FACE ( 'NONE', ( #28973 ), #7361, .F. ) ;
#83007 = CARTESIAN_POINT ( 'NONE',  ( 18.22277954126840172, -12.44528174975671853, 30.48912976160715615 ) ) ;
#83008 = ORIENTED_EDGE ( 'NONE', *, *, #24246, .F. ) ;
#83009 = FACE_BOUND ( 'NONE', #60257, .T. ) ;
#83010 = DIRECTION ( 'NONE',  ( 0.000000000000000000, 0.000000000000000000, 1.000000000000000000 ) ) ;
#83011 = LINE ( 'NONE', #63614, #24755 ) ;
#83012 = CARTESIAN_POINT ( 'NONE',  ( 16.94623247381276343, -11.93127051446800380, 32.56575433478200665 ) ) ;
#83013 = ORIENTED_EDGE ( 'NONE', *, *, #44942, .F. ) ;
#83014 = CARTESIAN_POINT ( 'NONE',  ( 0.2115617305961065842, -10.66389620160130036, 33.62221079203477103 ) ) ;
#83015 = CARTESIAN_POINT ( 'NONE',  ( -14.30769230769242739, -4.481592998941358097, 33.73612834414048933 ) ) ;
#83016 = CARTESIAN_POINT ( 'NONE',  ( 12.68454981315131391, -6.503523203565941380, 34.64991518177335195 ) ) ;
#83017 = DIRECTION ( 'NONE',  ( -0.000000000000000000, -0.6427876096865404731, -0.7660444431189770143 ) ) ;
#83018 = ORIENTED_EDGE ( 'NONE', *, *, #14725, .F. ) ;
#83019 = EDGE_CURVE ( 'NONE', #67105, #38304, #16325, .T. ) ;
#83020 = CARTESIAN_POINT ( 'NONE',  ( -5.011667937410239304, -5.094484230520773593, 34.41647553114626845 ) ) ;
#83021 = ORIENTED_EDGE ( 'NONE', *, *, #10622, .F. ) ;
#83023 = EDGE_LOOP ( 'NONE', ( #76313, #76183, #15126, #16884 ) ) ;
#83022 = CARTESIAN_POINT ( 'NONE',  ( 16.40384615384757439, -7.500000000000154543, 35.00000000000007105 ) ) ;
#83024 = CARTESIAN_POINT ( 'NONE',  ( 3.480714749117373774, -2.587454068350147907, 30.68340429815432202 ) ) ;
#83025 = CARTESIAN_POINT ( 'NONE',  ( -8.769230769230890843, -5.219633306517616589, 34.19971097300220464 ) ) ;
#83026 = CARTESIAN_POINT ( 'NONE',  ( 5.076923076922953193, -2.657715359629662988, 31.77849191805970364 ) ) ;
#83027 = CARTESIAN_POINT ( 'NONE',  ( 14.30769230769218758, -9.442884908241554243, 34.35708131394783038 ) ) ;
#83028 = AXIS2_PLACEMENT_3D ( 'NONE', #14472, #62642, #57668 ) ;
#83029 = CARTESIAN_POINT ( 'NONE',  ( -13.31936024510254768, -3.643525952247864463, 33.31231777344670064 ) ) ;
#83031 = CYLINDRICAL_SURFACE ( 'NONE', #44628, 0.2499999999999986955 ) ;
#83030 = CARTESIAN_POINT ( 'NONE',  ( 13.51514108637895184, -6.001044277235009439, 34.52024696741798948 ) ) ;
#83032 = CARTESIAN_POINT ( 'NONE',  ( 1.384615384615386802, -4.102666532097928531, 36.13435417666054406 ) ) ;
#83033 = CARTESIAN_POINT ( 'NONE',  ( 1.799775606325937360E-14, -10.25000000000000000, 17.28125000000000000 ) ) ;
#83034 = ORIENTED_EDGE ( 'NONE', *, *, #13521, .T. ) ;
#83035 = VECTOR ( 'NONE', #35335, 1000.000000000000114 ) ;
#83036 = ADVANCED_FACE ( 'NONE', ( #51862 ), #43791, .F. ) ;
#83037 = DIRECTION ( 'NONE',  ( -0.000000000000000000, -0.7660444431189791237, -0.6427876096865379196 ) ) ;
#83038 = ORIENTED_EDGE ( 'NONE', *, *, #34466, .T. ) ;
#83039 = ORIENTED_EDGE ( 'NONE', *, *, #68476, .T. ) ;
#83040 = EDGE_CURVE ( 'NONE', #7083, #3322, #33372, .T. ) ;
#83041 = CARTESIAN_POINT ( 'NONE',  ( 3.230769230769231726, -4.786620604624113540, 33.94971097300155094 ) ) ;
#83043 = ORIENTED_EDGE ( 'NONE', *, *, #41608, .T. ) ;
#83042 = AXIS2_PLACEMENT_3D ( 'NONE', #16124, #30084, #78258 ) ;
#83044 = CYLINDRICAL_SURFACE ( 'NONE', #87288, 0.2500000000000008882 ) ;
#83045 = UNCERTAINTY_MEASURE_WITH_UNIT (LENGTH_MEASURE( 1.000000000000000082E-05 ), #75908, 'distance_accuracy_value', 'NONE');
#83046 = CARTESIAN_POINT ( 'NONE',  ( -8.096130590202434973, -8.347322224742351082, 34.93158281831414058 ) ) ;
#83047 = CARTESIAN_POINT ( 'NONE',  ( 6.222779541268410597, -3.236590943229499029, 32.36255958852954251 ) ) ;
#83048 = CARTESIAN_POINT ( 'NONE',  ( -11.53846153846153655, -11.16473453929635440, 33.15142922261926373 ) ) ;
#83049 = CARTESIAN_POINT ( 'NONE',  ( 6.130791807824788719, -2.541949514083464479, 30.39797389878540557 ) ) ;
#83050 = CARTESIAN_POINT ( 'NONE',  ( 8.703147358274890166, -11.16473453929635440, 33.15142922261925662 ) ) ;
#83051 = CARTESIAN_POINT ( 'NONE',  ( 15.93091993633000847, -11.76352882383564769, 32.36236540154569497 ) ) ;
#83052 = CARTESIAN_POINT ( 'NONE',  ( 1.553300858899129944, -11.24999999999998934, 25.95312500000000000 ) ) ;
#83053 = CARTESIAN_POINT ( 'NONE',  ( -0.6844646790546100590, -2.554751324335733820, 30.48935550225260727 ) ) ;
#83054 = CARTESIAN_POINT ( 'NONE',  ( 17.77651505627605033, -11.89387501736623420, 32.13663884655804992 ) ) ;
#83055 = EDGE_CURVE ( 'NONE', #47762, #60409, #71007, .T. ) ;
#83056 = CARTESIAN_POINT ( 'NONE',  ( 14.30769230769261569, -2.506253911140615021, 30.00000000000323297 ) ) ;
#83057 = CARTESIAN_POINT ( 'NONE',  ( 11.53846153846153832, -4.786620604624113540, 33.94971097300155094 ) ) ;
#83058 = VERTEX_POINT ( 'NONE', #2350 ) ;
#83059 = ORIENTED_EDGE ( 'NONE', *, *, #82425, .T. ) ;
#83060 = VECTOR ( 'NONE', #32915, 999.9999999999998863 ) ;
#83061 = CARTESIAN_POINT ( 'NONE',  ( -17.93474900983876452, -12.49374608885954352, 30.00000000000010658 ) ) ;
#83062 = CARTESIAN_POINT ( 'NONE',  ( 1.607395053593452916, -3.563462043263030399, 33.22394488606062879 ) ) ;
#83063 = FACE_OUTER_BOUND ( 'NONE', #34446, .T. ) ;
#83064 = CARTESIAN_POINT ( 'NONE',  ( 0.4615384615383382183, -10.33852847137269571, 34.16647553114546554 ) ) ;
#83065 = B_SPLINE_CURVE_WITH_KNOTS ( 'NONE', 3,
 ( #28653, #56122, #14247, #62415, #42613, #8382, #13800, #70524, #35855, #7043 ),
 .UNSPECIFIED., .F., .F.,
 ( 4, 2, 2, 2, 4 ),
 ( 0.000000000000000000, 0.0001954311564186881213, 0.0003908623128373762425, 0.0005862934692560643367, 0.0007817246256747524850 ),
 .UNSPECIFIED. ) ;
#83067 = EDGE_CURVE ( 'NONE', #64445, #59172, #79359, .T. ) ;
#83066 = CARTESIAN_POINT ( 'NONE',  ( -16.08859101433330707, -8.656820664281605460, 34.87096338111211224 ) ) ;
#83068 = B_SPLINE_CURVE_WITH_KNOTS ( 'NONE', 3,
 ( #20618, #34583, #76006, #6234, #14306, #27821, #35019, #42238, #13420, #54853 ),
 .UNSPECIFIED., .F., .F.,
 ( 4, 2, 2, 2, 4 ),
 ( 0.000000000000000000, 0.0001954311564186868473, 0.0003908623128373736946, 0.0005862934692560605419, 0.0007817246256747473893 ),
 .UNSPECIFIED. ) ;
#83069 = CYLINDRICAL_SURFACE ( 'NONE', #22585, 0.2500000000000009437 ) ;
#83070 = CARTESIAN_POINT ( 'NONE',  ( -2.557715531913763662, -8.475808217655753651, 34.90892951860618609 ) ) ;
#83071 = EDGE_CURVE ( 'NONE', #29011, #18655, #9139, .T. ) ;
#83072 = EDGE_CURVE ( 'NONE', #25462, #79249, #64485, .T. ) ;
#83073 = AXIS2_PLACEMENT_3D ( 'NONE', #12487, #81840, #87276 ) ;
#83074 = ORIENTED_EDGE ( 'NONE', *, *, #19496, .T. ) ;
#83075 = LINE ( 'NONE', #648, #65949 ) ;
#83076 = ORIENTED_EDGE ( 'NONE', *, *, #13667, .T. ) ;
#83077 = ADVANCED_FACE ( 'NONE', ( #37471 ), #17204, .F. ) ;
#83078 = CARTESIAN_POINT ( 'NONE',  ( -4.230769230769230838, -3.499999999999999556, 29.75000000000000355 ) ) ;
#83079 = CARTESIAN_POINT ( 'NONE',  ( 0.3589743589743582541, -7.500000000000000000, 29.75000000000000355 ) ) ;
#83080 = CARTESIAN_POINT ( 'NONE',  ( 12.39545505058258179, -8.120952969808774569, 34.71129190930000163 ) ) ;
#83081 = DIRECTION ( 'NONE',  ( 1.000000000000000000, -1.681660752236433198E-16, 0.000000000000000000 ) ) ;
#83082 = CARTESIAN_POINT ( 'NONE',  ( -3.100721795518779356, -7.723484941389743952, 34.99544897038808955 ) ) ;
#83083 = ORIENTED_EDGE ( 'NONE', *, *, #25287, .F. ) ;
#83084 = VERTEX_POINT ( 'NONE', #23951 ) ;
#83085 = VERTEX_POINT ( 'NONE', #78908 ) ;
#83086 = EDGE_LOOP ( 'NONE', ( #11852, #50060, #15196, #82576 ) ) ;
#83087 = DIRECTION ( 'NONE',  ( -0.000000000000000000, -0.6427876096865404731, -0.7660444431189770143 ) ) ;
#83088 = CARTESIAN_POINT ( 'NONE',  ( -15.90379173393269951, -9.233818618650598609, 34.70587769442853698 ) ) ;
#83089 = B_SPLINE_CURVE_WITH_KNOTS ( 'NONE', 3,
 ( #44380, #63781, #85841, #65551, #38091, #16489, #29566, #84955, #70547, #2959 ),
 .UNSPECIFIED., .F., .F.,
 ( 4, 2, 2, 2, 4 ),
 ( 0.000000000000000000, 0.0001954339857564080165, 0.0003908679715128160329, 0.0005863019572692240765, 0.0007817359430256320659 ),
 .UNSPECIFIED. ) ;
#83090 = FACE_BOUND ( 'NONE', #44852, .T. ) ;
#83091 = B_SPLINE_CURVE_WITH_KNOTS ( 'NONE', 3,
 ( #87264, #6164, #34073, #26878, #47585, #33635, #25544, #39960, #52999, #12476 ),
 .UNSPECIFIED., .F., .F.,
 ( 4, 2, 2, 2, 4 ),
 ( 0.000000000000000000, 0.0001954339881912775425, 0.0003908679763825550850, 0.0005863019645738326005, 0.0007817359527651101701 ),
 .UNSPECIFIED. ) ;
#83092 = CARTESIAN_POINT ( 'NONE',  ( -2.084912638714241151, -11.60474049983370648, 33.02348890104160262 ) ) ;
#83093 = DIRECTION ( 'NONE',  ( -0.000000000000000000, -0.6427876096865404731, -0.7660444431189771253 ) ) ;
#83094 = DIRECTION ( 'NONE',  ( 0.000000000000000000, 0.1736481776669267785, -0.9848077530122087975 ) ) ;
#83095 = CIRCLE ( 'NONE', #11208, 4.000000000000000000 ) ;
#83096 = ORIENTED_EDGE ( 'NONE', *, *, #60439, .F. ) ;
#83097 = ORIENTED_EDGE ( 'NONE', *, *, #54212, .F. ) ;
#83098 = ORIENTED_EDGE ( 'NONE', *, *, #61097, .F. ) ;
#83100 = EDGE_LOOP ( 'NONE', ( #20765, #46912, #31444, #36187 ) ) ;
#83099 = CARTESIAN_POINT ( 'NONE',  ( 4.153846153846154188, -2.721908614388771852, 31.22303859784724978 ) ) ;
#83101 = CARTESIAN_POINT ( 'NONE',  ( -10.36533019547116119, -6.523592122091592671, 34.90882529074906415 ) ) ;
#83102 = DIRECTION ( 'NONE',  ( 1.000000000000000000, 0.000000000000000000, 0.000000000000000000 ) ) ;
#83103 = CARTESIAN_POINT ( 'NONE',  ( 1.553300858899086867, -3.749999999999992006, 17.98437500000000000 ) ) ;
#83104 = EDGE_LOOP ( 'NONE', ( #10952, #38202, #64699, #23693 ) ) ;
#83105 = ORIENTED_EDGE ( 'NONE', *, *, #22317, .T. ) ;
#83106 = CARTESIAN_POINT ( 'NONE',  ( 13.44980936639873903, -2.506253911140448043, 29.99999999999988631 ) ) ;
#83107 = B_SPLINE_CURVE_WITH_KNOTS ( 'NONE', 3,
 ( #32715, #30927, #59747, #65160, #45335, #17433, #59297, #24627, #51182, #17881 ),
 .UNSPECIFIED., .F., .F.,
 ( 4, 2, 2, 2, 4 ),
 ( 0.000000000000000000, 0.0001954339881912776238, 0.0003908679763825552477, 0.0005863019645738329257, 0.0007817359527651104954 ),
 .UNSPECIFIED. ) ;
#83108 = VERTEX_POINT ( 'NONE', #50967 ) ;
#83109 = FACE_BOUND ( 'NONE', #27200, .T. ) ;
#83110 = CARTESIAN_POINT ( 'NONE',  ( -5.750054590621957118, -2.986452184633680673, 32.43230066228895225 ) ) ;
#83111 = AXIS2_PLACEMENT_3D ( 'NONE', #84003, #56068, #56515 ) ;
#83112 = DIRECTION ( 'NONE',  ( 1.000000000000000000, 0.000000000000000000, 0.000000000000000000 ) ) ;
#83113 = ORIENTED_EDGE ( 'NONE', *, *, #42903, .F. ) ;
#83114 = DIRECTION ( 'NONE',  ( -0.000000000000000000, -0.9848077530122085754, -0.1736481776669273613 ) ) ;
#83115 = CARTESIAN_POINT ( 'NONE',  ( -15.90379173393269951, -12.65882529074907126, 30.72640787790838601 ) ) ;
#83116 = PLANE ( 'NONE',  #24902 ) ;
#83117 = CARTESIAN_POINT ( 'NONE',  ( 8.352564102564102200, -3.499999999999999556, 29.75000000000000355 ) ) ;
#83118 = DIRECTION ( 'NONE',  ( -0.000000000000000000, -0.9848077530122086864, -0.1736481776669273613 ) ) ;
#83119 = ORIENTED_EDGE ( 'NONE', *, *, #26011, .T. ) ;
#83120 = AXIS2_PLACEMENT_3D ( 'NONE', #31399, #79144, #65611 ) ;
#83121 = CARTESIAN_POINT ( 'NONE',  ( 6.249945518348142492, -8.433404298154334455, 34.66254593164985920 ) ) ;
#83122 = FACE_OUTER_BOUND ( 'NONE', #37219, .T. ) ;
#83123 = CARTESIAN_POINT ( 'NONE',  ( 16.40379167219429846, -9.272278438253401589, 34.42582936511637826 ) ) ;
#83124 = CARTESIAN_POINT ( 'NONE',  ( -0.5276208408985973985, -4.661471528628507777, 34.16647553114621871 ) ) ;
#83125 = CARTESIAN_POINT ( 'NONE',  ( -15.09997742294444478, -11.71459661697925903, 32.44059661609676937 ) ) ;
#83126 = FACE_BOUND ( 'NONE', #66100, .T. ) ;
#83128 = CARTESIAN_POINT ( 'NONE',  ( -6.000000000000121680, -10.33852847137269571, 34.16647553114546554 ) ) ;
#83127 = CARTESIAN_POINT ( 'NONE',  ( 13.38461538461538680, -11.69971097300155272, 32.46337939537588113 ) ) ;
#83129 = AXIS2_PLACEMENT_3D ( 'NONE', #26124, #53592, #81083 ) ;
#83130 = CARTESIAN_POINT ( 'NONE',  ( 5.076923076923075762, -2.292212530054420494, 30.41441678777542634 ) ) ;
#83132 = CARTESIAN_POINT ( 'NONE',  ( -6.250023237292964495, -5.056417327199099532, 34.11270091957320716 ) ) ;
#83131 = LINE ( 'NONE', #62391, #68849 ) ;
#83133 = CARTESIAN_POINT ( 'NONE',  ( -18.13014720943822056, -10.19110544564092358, 33.96427741523702792 ) ) ;
#83134 = B_SPLINE_CURVE_WITH_KNOTS ( 'NONE', 3,
 ( #48510, #62902, #83658, #70119, #57043, #35901, #84537, #1665, #69240, #21488 ),
 .UNSPECIFIED., .F., .F.,
 ( 4, 2, 2, 2, 4 ),
 ( 0.000000000000000000, 0.0001954339881912776238, 0.0003908679763825552477, 0.0005863019645738329257, 0.0007817359527651104954 ),
 .UNSPECIFIED. ) ;
#83135 = CARTESIAN_POINT ( 'NONE',  ( -1.077988221561460236, -10.27530806549876452, 19.60750670625849068 ) ) ;
#83136 = ORIENTED_EDGE ( 'NONE', *, *, #51424, .F. ) ;
#83137 = B_SPLINE_CURVE_WITH_KNOTS ( 'NONE', 3,
 ( #18240, #38964, #6059, #52003, #33533, #46156, #60992, #39411, #73183, #79498 ),
 .UNSPECIFIED., .F., .F.,
 ( 4, 2, 2, 2, 4 ),
 ( 0.000000000000000000, 0.0001954339857564064444, 0.0003908679715128128888, 0.0005863019572692193060, 0.0007817359430256257775 ),
 .UNSPECIFIED. ) ;
#83138 = CARTESIAN_POINT ( 'NONE',  ( -2.651650429449565305, -4.848349570550461785, 14.00000000000000178 ) ) ;
#83139 = ORIENTED_EDGE ( 'NONE', *, *, #41599, .F. ) ;
#83140 = CARTESIAN_POINT ( 'NONE',  ( -14.98082371242109012, -4.336752205174649433, 33.62275283266504289 ) ) ;
#83141 = EDGE_LOOP ( 'NONE', ( #85411, #69720 ) ) ;
#83142 = FACE_OUTER_BOUND ( 'NONE', #63534, .T. ) ;
#83143 = CARTESIAN_POINT ( 'NONE',  ( -18.22348494372394967, -2.599994579823202479, 30.74605699353653776 ) ) ;
#83144 = EDGE_LOOP ( 'NONE', ( #52786, #58116 ) ) ;
#83145 = DIRECTION ( 'NONE',  ( -1.000000000000000000, 0.000000000000000000, -0.000000000000000000 ) ) ;
#83146 = CARTESIAN_POINT ( 'NONE',  ( 0.06109907496454976272, -10.25000000000000000, 20.77938170625848713 ) ) ;
#83147 = CARTESIAN_POINT ( 'NONE',  ( -4.023801097926381409, -2.254550872974306674, 29.97347326024527447 ) ) ;
#83148 = CARTESIAN_POINT ( 'NONE',  ( -12.46153846153846168, -11.11383981884818262, 36.00935417666054406 ) ) ;
#83149 = CARTESIAN_POINT ( 'NONE',  ( -2.980769230769230393, -2.249999999999998668, 29.75000000000000355 ) ) ;
#83150 = CARTESIAN_POINT ( 'NONE',  ( 10.36536139116315525, -2.588893531581426988, 31.60682220781847818 ) ) ;
#83151 = FACE_OUTER_BOUND ( 'NONE', #31039, .T. ) ;
#83152 = CARTESIAN_POINT ( 'NONE',  ( 11.76147289007438523, -3.587049720035815348, 32.86302985866382897 ) ) ;
#83153 = CARTESIAN_POINT ( 'NONE',  ( -1.492201783934593573, -3.724691934501250135, 24.32999329374151642 ) ) ;
#83154 = AXIS2_PLACEMENT_3D ( 'NONE', #35157, #76139, #22092 ) ;
#83155 = CARTESIAN_POINT ( 'NONE',  ( -10.48485891362105171, -2.882268652242222284, 31.66798894389554064 ) ) ;
#83156 = CARTESIAN_POINT ( 'NONE',  ( -6.066082379360134169, -3.322132147404559976, 32.92929555188719348 ) ) ;
#83157 = EDGE_CURVE ( 'NONE', #16191, #43656, #33088, .T. ) ;
#83158 = ORIENTED_EDGE ( 'NONE', *, *, #2087, .F. ) ;
#83159 = PLANE ( 'NONE',  #48464 ) ;
#83160 = AXIS2_PLACEMENT_3D ( 'NONE', #18748, #72785, #25938 ) ;
#83161 = CARTESIAN_POINT ( 'NONE',  ( -0.06109907496450878162, -11.25000000000000000, 22.53311829374151642 ) ) ;
#83162 = CARTESIAN_POINT ( 'NONE',  ( 6.416666666666664298, -4.000000000000000000, 29.75000000000000355 ) ) ;
#83163 = CARTESIAN_POINT ( 'NONE',  ( -9.442362173959550020, -11.37275283266504111, 32.91324779482534524 ) ) ;
#83164 = ORIENTED_EDGE ( 'NONE', *, *, #4330, .F. ) ;
#83165 = CARTESIAN_POINT ( 'NONE',  ( 7.173076923078359535, -7.500000000000155431, 34.75000000000007105 ) ) ;
#83166 = CARTESIAN_POINT ( 'NONE',  ( -14.43783951713052716, -11.47017969459904130, 32.78971311882034456 ) ) ;
#83168 = ORIENTED_EDGE ( 'NONE', *, *, #84696, .F. ) ;
#83167 = CARTESIAN_POINT ( 'NONE',  ( 2.057669070399344324, -2.823816976329320827, 31.52131813110797154 ) ) ;
#83169 = CARTESIAN_POINT ( 'NONE',  ( -7.911477858958151366, -7.749976730030849303, 34.74374725381503737 ) ) ;
#83170 = AXIS2_PLACEMENT_3D ( 'NONE', #6957, #82184, #13272 ) ;
#83171 = DIRECTION ( 'NONE',  ( 0.000000000000000000, 0.000000000000000000, 1.000000000000000000 ) ) ;
#83172 = B_SPLINE_CURVE_WITH_KNOTS ( 'NONE', 3,
 ( #43721, #42851, #43290, #28903, #70761, #83847, #9066, #70313, #84733, #63983 ),
 .UNSPECIFIED., .F., .F.,
 ( 4, 2, 2, 2, 4 ),
 ( 0.0007817246256747516176, 0.0009771112852218965736, 0.001172497944769041638, 0.001367884604316186702, 0.001563271263863331550 ),
 .UNSPECIFIED. ) ;
#83173 = CARTESIAN_POINT ( 'NONE',  ( 5.076923076922954969, -6.026961402154118908, 34.52809138561165270 ) ) ;
#83174 = CARTESIAN_POINT ( 'NONE',  ( -16.85391172531022264, -2.758310577978207334, 31.33698337089302299 ) ) ;
#83175 = B_SPLINE_CURVE_WITH_KNOTS ( 'NONE', 3,
 ( #25084, #10687, #57975, #71050, #38152, #45346, #71935, #51640, #9364, #9793, #36822, #10246, #24639, #64723, #85902, #66059, #3912, #30070 ),
 .UNSPECIFIED., .F., .F.,
 ( 4, 2, 2, 2, 2, 2, 2, 2, 4 ),
 ( 0.000000000000000000, 0.0002610006692907291224, 0.0005220013385814582449, 0.0007830020078721873673, 0.001044002677162916490, 0.001305003346453645612, 0.001566004015744375168, 0.001827004685035104291, 0.002088005354325833847 ),
 .UNSPECIFIED. ) ;
#83176 = LINE ( 'NONE', #32541, #549 ) ;
#83177 = ADVANCED_FACE ( 'NONE', ( #44214 ), #44660, .F. ) ;
#83178 = EDGE_CURVE ( 'NONE', #63622, #69827, #8646, .T. ) ;
#83179 = ORIENTED_EDGE ( 'NONE', *, *, #16938, .T. ) ;
#83180 = DIRECTION ( 'NONE',  ( -0.000000000000000000, 0.5000000000000011102, -0.8660254037844381525 ) ) ;
#83181 = VERTEX_POINT ( 'NONE', #12234 ) ;
#83182 = ORIENTED_EDGE ( 'NONE', *, *, #7435, .T. ) ;
#83183 = CARTESIAN_POINT ( 'NONE',  ( -4.153846153846274980, -11.06231777344772027, 33.60647404775119895 ) ) ;
#83184 = CARTESIAN_POINT ( 'NONE',  ( 6.923076923076924238, -2.721908614388771852, 31.22303859784724978 ) ) ;
#83185 = DIRECTION ( 'NONE',  ( -0.000000000000000000, 1.000000000000000000, 3.491481338843133355E-15 ) ) ;
#83186 = CARTESIAN_POINT ( 'NONE',  ( -16.82692307692165556, -7.500000000000154543, 35.00000000000007105 ) ) ;
#83187 = VECTOR ( 'NONE', #45171, 1000.000000000000000 ) ;
#83188 = ORIENTED_EDGE ( 'NONE', *, *, #78349, .F. ) ;
#83189 = DIRECTION ( 'NONE',  ( -0.000000000000000000, 0.9848077530122085754, -0.1736481776669273613 ) ) ;
#83190 = ORIENTED_EDGE ( 'NONE', *, *, #23569, .F. ) ;
#83191 = VERTEX_POINT ( 'NONE', #19874 ) ;
#83192 = AXIS2_PLACEMENT_3D ( 'NONE', #50520, #51382, #78886 ) ;
#83193 = ORIENTED_EDGE ( 'NONE', *, *, #52421, .F. ) ;
#83195 = VERTEX_POINT ( 'NONE', #25302 ) ;
#83194 = CARTESIAN_POINT ( 'NONE',  ( -7.976301055592065481, -5.195881422630166391, 34.18770438780619259 ) ) ;
#83196 = CARTESIAN_POINT ( 'NONE',  ( 4.376857505459002873, -5.667800583137508674, 34.40243808032445827 ) ) ;
#83197 = CARTESIAN_POINT ( 'NONE',  ( -8.769230769230768274, -13.20930481340135110, 34.54067556320372745 ) ) ;
#83198 = B_SPLINE_CURVE_WITH_KNOTS ( 'NONE', 3,
 ( #24449, #2405, #16813, #64988, #4186, #44266, #9614, #50147, #57359, #3293 ),
 .UNSPECIFIED., .F., .F.,
 ( 4, 2, 2, 2, 4 ),
 ( 0.000000000000000000, 0.0001954311564186866576, 0.0003908623128373733152, 0.0005862934692560599998, 0.0007817246256747466303 ),
 .UNSPECIFIED. ) ;
#83199 = CARTESIAN_POINT ( 'NONE',  ( 4.153846153846154188, -4.098570777380720287, 33.41473453929634729 ) ) ;
#83200 = CARTESIAN_POINT ( 'NONE',  ( 14.08486421005743061, -7.369209533119137845, 34.99857337881830688 ) ) ;
#83201 = ORIENTED_EDGE ( 'NONE', *, *, #23145, .F. ) ;
#83202 = ORIENTED_EDGE ( 'NONE', *, *, #48136, .F. ) ;
#83203 = EDGE_LOOP ( 'NONE', ( #81122, #33952 ) ) ;
#83204 = CARTESIAN_POINT ( 'NONE',  ( 0.000000000000000000, -11.00000000000000000, 29.75000000000000355 ) ) ;
#83206 = EDGE_LOOP ( 'NONE', ( #52445, #69250 ) ) ;
#83205 = CARTESIAN_POINT ( 'NONE',  ( -14.17716686945866655, -2.372941743896879174, 30.88044141588253666 ) ) ;
#83207 = CARTESIAN_POINT ( 'NONE',  ( 9.468822748583747284, -11.89387501736622710, 32.13663884655806413 ) ) ;
#83208 = B_SPLINE_CURVE_WITH_KNOTS ( 'NONE', 3,
 ( #43472, #43032, #70503, #29963, #84916, #31745, #25873, #4263, #19118, #26315 ),
 .UNSPECIFIED., .F., .F.,
 ( 4, 2, 2, 2, 4 ),
 ( 0.0007817246256747459798, 0.0009771112852218896347, 0.001172497944769033181, 0.001367884604316176728, 0.001563271263863320274 ),
 .UNSPECIFIED. ) ;
#83209 = DIRECTION ( 'NONE',  ( -1.000000000000000000, -0.000000000000000000, -0.000000000000000000 ) ) ;
#83210 = ORIENTED_EDGE ( 'NONE', *, *, #34538, .F. ) ;
#83211 = DIRECTION ( 'NONE',  ( -0.000000000000000000, 0.1736481776669307198, -0.9848077530122080203 ) ) ;
#83212 = CARTESIAN_POINT ( 'NONE',  ( -15.09997878980228414, -12.35292014791297710, 31.75344720912887198 ) ) ;
#83213 = AXIS2_PLACEMENT_3D ( 'NONE', #39155, #11675, #81470 ) ;
#83214 = ORIENTED_EDGE ( 'NONE', *, *, #24576, .F. ) ;
#83215 = FACE_BOUND ( 'NONE', #48976, .T. ) ;
#83216 = CARTESIAN_POINT ( 'NONE',  ( 15.48082365068267841, -11.47946981652013498, 33.17500667209847620 ) ) ;
#83217 = CYLINDRICAL_SURFACE ( 'NONE', #25549, 0.2499999999999998890 ) ;
#83218 = DIRECTION ( 'NONE',  ( -1.000000000000000000, 0.000000000000000000, 0.000000000000000000 ) ) ;
#83220 = CARTESIAN_POINT ( 'NONE',  ( -0.4615384615384611200, -12.10708131394839349, 31.69288490824020244 ) ) ;
#83219 = CARTESIAN_POINT ( 'NONE',  ( -6.857931143744957936, -7.750023238201980469, 34.74374492549440419 ) ) ;
#83221 = CARTESIAN_POINT ( 'NONE',  ( -2.980823821391187067, -3.520799739797214389, 33.17531984108286025 ) ) ;
#83222 = LINE ( 'NONE', #43549, #29041 ) ;
#83223 = VERTEX_POINT ( 'NONE', #47340 ) ;
#83224 = CARTESIAN_POINT ( 'NONE',  ( 14.30769230769218758, -12.46129190930018460, 30.37095296980731973 ) ) ;
#83225 = CARTESIAN_POINT ( 'NONE',  ( -19.99999999999996803, 15.00000000000000711, 13.00000000000000178 ) ) ;
#83226 = EDGE_LOOP ( 'NONE', ( #9706, #32948 ) ) ;
#83227 = EDGE_CURVE ( 'NONE', #5662, #57710, #77396, .T. ) ;
#83228 = EDGE_CURVE ( 'NONE', #71718, #85122, #84897, .T. ) ;
#83229 = DIRECTION ( 'NONE',  ( 0.000000000000000000, 0.000000000000000000, -1.000000000000000000 ) ) ;
#83230 = DIRECTION ( 'NONE',  ( 1.000000000000000000, 0.000000000000000000, -0.000000000000000000 ) ) ;
#83231 = VERTEX_POINT ( 'NONE', #46896 ) ;
#83232 = CARTESIAN_POINT ( 'NONE',  ( 11.31553457955469000, -10.01117774369187252, 34.36070679894347535 ) ) ;
#83233 = CARTESIAN_POINT ( 'NONE',  ( -4.219928533206290133, -2.292212530054419606, 30.41441678777542634 ) ) ;
#83234 = FACE_BOUND ( 'NONE', #47190, .T. ) ;
#83236 = CARTESIAN_POINT ( 'NONE',  ( -3.903791842207837259, -8.303483539816728154, 34.68545999027711702 ) ) ;
#83235 = CARTESIAN_POINT ( 'NONE',  ( 6.792928953345226617, -4.299443229763728169, 33.91186481527756058 ) ) ;
#83237 = CARTESIAN_POINT ( 'NONE',  ( 7.976679284387491187, -11.66157788607254098, 32.95092075102925833 ) ) ;
#83238 = CARTESIAN_POINT ( 'NONE',  ( -5.999999999999998224, -13.53365097954675988, 30.81389545987213552 ) ) ;
#83239 = CARTESIAN_POINT ( 'NONE',  ( 6.923076923076802558, -12.27809138561165270, 31.22303859784587132 ) ) ;
#83240 = CARTESIAN_POINT ( 'NONE',  ( -3.230769230769229949, -9.584722331328613620, 36.20867863119891439 ) ) ;
#83241 = CARTESIAN_POINT ( 'NONE',  ( -1.614399933863656544, -3.775308065498769405, 15.07625670625849068 ) ) ;
#83242 = ORIENTED_EDGE ( 'NONE', *, *, #65395, .F. ) ;
#83243 = ORIENTED_EDGE ( 'NONE', *, *, #64166, .T. ) ;
#83244 = EDGE_CURVE ( 'NONE', #20327, #29327, #22680, .T. ) ;
#83245 = AXIS2_PLACEMENT_3D ( 'NONE', #14010, #70734, #77050 ) ;
#83246 = CARTESIAN_POINT ( 'NONE',  ( -9.442362173959548244, -11.86320923018887541, 32.19269448109604781 ) ) ;
#83247 = CARTESIAN_POINT ( 'NONE',  ( 14.30769230769231015, -12.62096338111211580, 30.90682066428153263 ) ) ;
#83248 = CARTESIAN_POINT ( 'NONE',  ( 4.153846153846154188, -8.564572088678739092, 35.78748833219616898 ) ) ;
#83249 = CARTESIAN_POINT ( 'NONE',  ( 8.769230769230647482, -4.481592998941358097, 33.73612834414048933 ) ) ;
#83250 = EDGE_CURVE ( 'NONE', #40554, #60613, #81148, .T. ) ;
#83251 = CARTESIAN_POINT ( 'NONE',  ( -16.85391172531022619, -6.503523203565941380, 34.64991518177335195 ) ) ;
#83252 = CARTESIAN_POINT ( 'NONE',  ( 3.724691934501232815, -5.885600066136343678, 16.63875670625849068 ) ) ;
#83253 = CARTESIAN_POINT ( 'NONE',  ( 6.857806922520603976, -2.379036618887870436, 30.90682066428147934 ) ) ;
#83254 = CARTESIAN_POINT ( 'NONE',  ( 18.00000000000000000, -2.249999999999998668, 29.75000000000001776 ) ) ;
#83255 = VECTOR ( 'NONE', #7972, 1000.000000000000000 ) ;
#83256 = CARTESIAN_POINT ( 'NONE',  ( -10.61538461538461320, -2.900454961884010974, 35.62045528018868623 ) ) ;
#83257 = PLANE ( 'NONE',  #24268 ) ;
#83258 = CARTESIAN_POINT ( 'NONE',  ( 10.83839745947801170, -3.395485233115139057, 33.02377354290275946 ) ) ;
#83259 = CARTESIAN_POINT ( 'NONE',  ( -8.769230769230890843, -3.835265460704628371, 33.15142922262033665 ) ) ;
#83260 = AXIS2_PLACEMENT_3D ( 'NONE', #63288, #84029, #77690 ) ;
#83261 = DIRECTION ( 'NONE',  ( -0.000000000000000000, 0.5000000000000011102, -0.8660254037844380415 ) ) ;
#83262 = CARTESIAN_POINT ( 'NONE',  ( 12.71148387091650278, -2.341251567377310217, 30.72681386836322659 ) ) ;
#83263 = AXIS2_PLACEMENT_3D ( 'NONE', #37342, #71573, #79235 ) ;
#83264 = EDGE_CURVE ( 'NONE', #60387, #44924, #5031, .T. ) ;
#83265 = CARTESIAN_POINT ( 'NONE',  ( 18.00000000000000000, -13.57706302396349152, 30.56769352161908060 ) ) ;
#83266 = ORIENTED_EDGE ( 'NONE', *, *, #85079, .T. ) ;
#83267 = CARTESIAN_POINT ( 'NONE',  ( 12.46153846153833911, -4.320704448113951379, 33.92786785259630022 ) ) ;
#83268 = CARTESIAN_POINT ( 'NONE',  ( 8.769230769230768274, -5.415277668671390821, 36.20867863119892149 ) ) ;
#83269 = CARTESIAN_POINT ( 'NONE',  ( -1.987747218494638313, -9.401340078031370950, 22.68936829374151287 ) ) ;
#83270 = CARTESIAN_POINT ( 'NONE',  ( -5.869209559033048862, -12.35292014791297710, 31.75344720912887198 ) ) ;
#83271 = DIRECTION ( 'NONE',  ( -0.000000000000000000, 0.7660444431189791237, -0.6427876096865379196 ) ) ;
#83272 = ORIENTED_EDGE ( 'NONE', *, *, #4966, .F. ) ;
#83273 = CARTESIAN_POINT ( 'NONE',  ( 2.980769230769232170, -7.500000000000001776, 34.75000000000000000 ) ) ;
#83275 = ORIENTED_EDGE ( 'NONE', *, *, #56694, .F. ) ;
#83274 = CARTESIAN_POINT ( 'NONE',  ( -9.469528151039281028, -5.114059244376869984, 34.14424750095245287 ) ) ;
#83276 = CARTESIAN_POINT ( 'NONE',  ( 9.692307692308000711, -2.506253911140615021, 30.00000000000323297 ) ) ;
#83277 = CARTESIAN_POINT ( 'NONE',  ( -2.307692307692305711, -10.67929555188718282, 33.92786785259544047 ) ) ;
#83278 = VERTEX_POINT ( 'NONE', #38824 ) ;
#83279 = CARTESIAN_POINT ( 'NONE',  ( -5.142193522883852452, -12.27809138561121394, 31.22303859784730307 ) ) ;
#83280 = CARTESIAN_POINT ( 'NONE',  ( -6.923076923077045919, -11.67786785259630911, 32.92929555188603530 ) ) ;
#83281 = ORIENTED_EDGE ( 'NONE', *, *, #29137, .T. ) ;
#83282 = LINE ( 'NONE', #82402, #3208 ) ;
#83283 = CARTESIAN_POINT ( 'NONE',  ( -16.40384615384615330, -7.500000000000001776, 34.75000000000000000 ) ) ;
#83284 = ADVANCED_FACE ( 'NONE', ( #82033 ), #74380, .T. ) ;
#83285 = CARTESIAN_POINT ( 'NONE',  ( 9.942253101685738059, -6.653508905675592722, 34.93172785388651391 ) ) ;
#83286 = EDGE_LOOP ( 'NONE', ( #1610, #32261 ) ) ;
#83287 = EDGE_CURVE ( 'NONE', #84018, #2381, #34315, .T. ) ;
#83288 = EDGE_LOOP ( 'NONE', ( #3352, #2878, #10931, #81577 ) ) ;
#83289 = CARTESIAN_POINT ( 'NONE',  ( 6.000000000000001776, -6.386643153685126251, 34.62446782046654192 ) ) ;
#83290 = AXIS2_PLACEMENT_3D ( 'NONE', #44780, #31734, #46134 ) ;
#83291 = VERTEX_POINT ( 'NONE', #53209 ) ;
#83292 = CARTESIAN_POINT ( 'NONE',  ( 7.716005876422150855, -9.504002272028873932, 34.60269587691767867 ) ) ;
#83293 = EDGE_CURVE ( 'NONE', #37623, #76098, #33399, .T. ) ;
#83294 = CARTESIAN_POINT ( 'NONE',  ( 15.45378207486262667, -12.64618726649961289, 30.78989965857442712 ) ) ;
#83295 = CARTESIAN_POINT ( 'NONE',  ( 2.307692307692186251, -11.67786785259630911, 32.92929555188603530 ) ) ;
#83296 = EDGE_CURVE ( 'NONE', #1437, #20693, #86988, .T. ) ;
#83297 = CARTESIAN_POINT ( 'NONE',  ( -6.673022503163469565, -11.47946981652013498, 33.17500667209846910 ) ) ;
#83298 = DIRECTION ( 'NONE',  ( -0.000000000000000000, 0.8660254037844399289, -0.4999999999999980016 ) ) ;
#83299 = DIRECTION ( 'NONE',  ( -1.000000000000000000, 0.000000000000000000, -0.000000000000000000 ) ) ;
#83300 = DIRECTION ( 'NONE',  ( -1.000000000000000000, -0.000000000000000000, -0.000000000000000000 ) ) ;
#83301 = EDGE_LOOP ( 'NONE', ( #63056, #36876 ) ) ;
#83302 = VERTEX_POINT ( 'NONE', #49565 ) ;
#83304 = ORIENTED_EDGE ( 'NONE', *, *, #31409, .T. ) ;
#83303 = CARTESIAN_POINT ( 'NONE',  ( 5.076923076922954969, -9.442884908241554243, 34.35708131394783038 ) ) ;
#83305 = B_SPLINE_CURVE_WITH_KNOTS ( 'NONE', 3,
 ( #42929, #63181, #1494, #56435, #70398, #8700, #63628, #77593, #50974, #51408 ),
 .UNSPECIFIED., .F., .F.,
 ( 4, 2, 2, 2, 4 ),
 ( 0.0007817359430256297891, 0.0009771253907249958896, 0.001172514838424361990, 0.001367904286123728091, 0.001563293733823094191 ),
 .UNSPECIFIED. ) ;
#83306 = FACE_OUTER_BOUND ( 'NONE', #82762, .T. ) ;
#83307 = ORIENTED_EDGE ( 'NONE', *, *, #7645, .F. ) ;
#83308 = VECTOR ( 'NONE', #11039, 1000.000000000000000 ) ;
#83309 = VECTOR ( 'NONE', #78518, 1000.000000000000000 ) ;
#83310 = CARTESIAN_POINT ( 'NONE',  ( 15.23076923076954614, -2.255955759149395501, 30.00000000000324363 ) ) ;
#83311 = CARTESIAN_POINT ( 'NONE',  ( 7.846153846153846700, -4.786620604624113540, 33.94971097300155094 ) ) ;
#83312 = VERTEX_POINT ( 'NONE', #48668 ) ;
#83313 = DIRECTION ( 'NONE',  ( -0.000000000000000000, 0.5000000000000011102, -0.8660254037844380415 ) ) ;
#83314 = AXIS2_PLACEMENT_3D ( 'NONE', #12857, #40341, #87652 ) ;
#83315 = VERTEX_POINT ( 'NONE', #34720 ) ;
#83317 = ORIENTED_EDGE ( 'NONE', *, *, #85558, .F. ) ;
#83316 = CARTESIAN_POINT ( 'NONE',  ( -16.28399336328437386, -3.817052484675422797, 33.13202310037935661 ) ) ;
#83318 = VECTOR ( 'NONE', #74079, 1000.000000000000114 ) ;
#83319 = CARTESIAN_POINT ( 'NONE',  ( -10.36538461538317790, -7.500000000000155431, 34.75000000000007105 ) ) ;
#83320 = ADVANCED_FACE ( 'NONE', ( #1374 ), #55872, .T. ) ;
#83321 = ORIENTED_EDGE ( 'NONE', *, *, #25992, .F. ) ;
#83322 = CARTESIAN_POINT ( 'NONE',  ( -6.673022503163469565, -4.818054556918156095, 34.26375889529406749 ) ) ;
#83323 = DIRECTION ( 'NONE',  ( -0.000000000000000000, -0.000000000000000000, -1.000000000000000000 ) ) ;
#83324 = FACE_BOUND ( 'NONE', #82839, .T. ) ;
#83325 = CARTESIAN_POINT ( 'NONE',  ( 5.869852030268306819, -2.373036134822904319, 30.88089517874952250 ) ) ;
#83326 = DIRECTION ( 'NONE',  ( -0.000000000000000000, -0.5000000000000011102, -0.8660254037844381525 ) ) ;
#83327 = CYLINDRICAL_SURFACE ( 'NONE', #76928, 0.2500000000000002220 ) ;
#83328 = DIRECTION ( 'NONE',  ( 0.000000000000000000, 0.000000000000000000, -1.000000000000000000 ) ) ;
#83329 = CARTESIAN_POINT ( 'NONE',  ( -14.30769230769242739, -10.21337939537710326, 33.94971097300076224 ) ) ;
#83330 = CARTESIAN_POINT ( 'NONE',  ( -16.15384615384627409, -2.657715359629662988, 31.77849191805970364 ) ) ;
#83331 = EDGE_LOOP ( 'NONE', ( #753, #24955, #125, #80595 ) ) ;
#83332 = CARTESIAN_POINT ( 'NONE',  ( 14.55763771707034948, -6.653508905675592722, 34.93172785388651391 ) ) ;
#83333 = ORIENTED_EDGE ( 'NONE', *, *, #59061, .T. ) ;
#83334 = EDGE_CURVE ( 'NONE', #69894, #31984, #5290, .T. ) ;
#83335 = VERTEX_POINT ( 'NONE', #75698 ) ;
#83336 = EDGE_CURVE ( 'NONE', #43893, #922, #18212, .T. ) ;
#83338 = CARTESIAN_POINT ( 'NONE',  ( 15.10007776410167324, -12.11776431015576172, 31.66791131148498906 ) ) ;
#83337 = CARTESIAN_POINT ( 'NONE',  ( 9.561747778694329014, -2.254533558242299396, 29.97296025877828285 ) ) ;
#83339 = B_SPLINE_CURVE_WITH_KNOTS ( 'NONE', 3,
 ( #13607, #35205, #62663, #75741, #88847, #14943, #42421, #55038, #82958, #41082 ),
 .UNSPECIFIED., .F., .F.,
 ( 4, 2, 2, 2, 4 ),
 ( 0.000000000000000000, 0.0001954339857564074473, 0.0003908679715128148945, 0.0005863019572692223418, 0.0007817359430256297891 ),
 .UNSPECIFIED. ) ;
#83340 = CARTESIAN_POINT ( 'NONE',  ( -11.53846153846153655, -11.69971097300155272, 32.46337939537588113 ) ) ;
#83341 = CARTESIAN_POINT ( 'NONE',  ( -17.07692307692307665, -9.905515769479276145, 34.41647553114623292 ) ) ;
#83342 = DIRECTION ( 'NONE',  ( -0.000000000000000000, -0.3420201433256694901, -0.9396926207859082059 ) ) ;
#83343 = CARTESIAN_POINT ( 'NONE',  ( 13.63466969625370062, -11.28795663066794575, 33.01431243580653785 ) ) ;
#83344 = ORIENTED_EDGE ( 'NONE', *, *, #30761, .F. ) ;
#83345 = CARTESIAN_POINT ( 'NONE',  ( 11.31497661389721010, -3.562934362175799841, 33.22335522853832401 ) ) ;
#83346 = CYLINDRICAL_SURFACE ( 'NONE', #20033, 0.2499999999999997502 ) ;
#83347 = CARTESIAN_POINT ( 'NONE',  ( -10.61538461538473399, -10.21337939537710326, 33.94971097300076224 ) ) ;
#83348 = CARTESIAN_POINT ( 'NONE',  ( 2.980792499826878217, -3.137211980971222669, 32.19342716148376837 ) ) ;
#83349 = CARTESIAN_POINT ( 'NONE',  ( -11.66902213020345513, -2.504760397472875155, 29.97295953869789997 ) ) ;
#83350 = ORIENTED_EDGE ( 'NONE', *, *, #8544, .F. ) ;
#83351 = VERTEX_POINT ( 'NONE', #82480 ) ;
#83352 = ORIENTED_EDGE ( 'NONE', *, *, #51684, .F. ) ;
#83353 = EDGE_CURVE ( 'NONE', #21038, #18719, #61733, .T. ) ;
#83354 = CARTESIAN_POINT ( 'NONE',  ( -6.249976744048591826, -4.075325502946086864, 33.72974371597207721 ) ) ;
#83355 = EDGE_LOOP ( 'NONE', ( #32604, #84296 ) ) ;
#83356 = CARTESIAN_POINT ( 'NONE',  ( -17.07692307692307665, -13.88283147151868846, 33.14645433367849847 ) ) ;
#83357 = CARTESIAN_POINT ( 'NONE',  ( -17.20761454359064047, -3.062553014421049991, 32.05460306192773601 ) ) ;
#83358 = CARTESIAN_POINT ( 'NONE',  ( -2.057692307690870415, -7.500000000000155431, 34.75000000000007105 ) ) ;
#83359 = ADVANCED_FACE ( 'NONE', ( #35613 ), #42378, .F. ) ;
#83360 = DIRECTION ( 'NONE',  ( -1.000000000000000000, -0.000000000000000000, -0.000000000000000000 ) ) ;
#83361 = CARTESIAN_POINT ( 'NONE',  ( -11.47320596718551400, -6.879047030191282275, 34.71129190930002295 ) ) ;
#83362 = ORIENTED_EDGE ( 'NONE', *, *, #65556, .T. ) ;
#83363 = CARTESIAN_POINT ( 'NONE',  ( -10.61538461538473577, -4.320704448113951379, 33.92786785259630022 ) ) ;
#83365 = ORIENTED_EDGE ( 'NONE', *, *, #3398, .T. ) ;
#83364 = CARTESIAN_POINT ( 'NONE',  ( -12.33101275977489841, -11.93748526763465279, 32.05452791011430946 ) ) ;
#83366 = DIRECTION ( 'NONE',  ( -0.000000000000000000, -0.9848077530122086864, -0.1736481776669273613 ) ) ;
#83367 = CYLINDRICAL_SURFACE ( 'NONE', #80091, 0.2499999999999979738 ) ;
#83368 = CARTESIAN_POINT ( 'NONE',  ( 17.07692307692295586, -11.48612834414049644, 32.76840700105863391 ) ) ;
#83369 = CARTESIAN_POINT ( 'NONE',  ( 15.29602437028207085, -3.083524468853784839, 32.58852847137153930 ) ) ;
#83370 = CARTESIAN_POINT ( 'NONE',  ( -20.00000000000000000, -7.500000000000000000, 29.75000000000000355 ) ) ;
#83371 = CARTESIAN_POINT ( 'NONE',  ( 9.562160482869472844, -10.19110544564092002, 33.96427741523702792 ) ) ;
#83372 = ADVANCED_FACE ( 'NONE', ( #42818 ), #35742, .T. ) ;
#83373 = DIRECTION ( 'NONE',  ( 0.000000000000000000, 0.1736481776669267785, -0.9848077530122087975 ) ) ;
#83374 = CARTESIAN_POINT ( 'NONE',  ( 1.901340078031373171, -9.487747218494639867, 24.87686829374151642 ) ) ;
#83375 = VERTEX_POINT ( 'NONE', #565 ) ;
#83376 = CARTESIAN_POINT ( 'NONE',  ( -15.48079245499068612, -6.652501968072648708, 34.93155406624980941 ) ) ;
#83377 = CARTESIAN_POINT ( 'NONE',  ( -14.08467946359890988, -3.395485233115139057, 33.02377354290275946 ) ) ;
#83378 = B_SPLINE_CURVE_WITH_KNOTS ( 'NONE', 3,
 ( #35306, #21350, #15489, #61440, #83061, #61884 ),
 .UNSPECIFIED., .F., .F.,
 ( 4, 2, 4 ),
 ( 0.000000000000000000, 0.0001954784845028707536, 0.0003909569690057415072 ),
 .UNSPECIFIED. ) ;
#83379 = B_SPLINE_CURVE_WITH_KNOTS ( 'NONE', 3,
 ( #11112, #37691, #79129, #30924, #44885, #85888, #52090, #71471, #31839, #85008 ),
 .UNSPECIFIED., .F., .F.,
 ( 4, 2, 2, 2, 4 ),
 ( 0.000000000000000000, 0.0001954339857564083688, 0.0003908679715128167377, 0.0005863019572692250523, 0.0007817359430256334753 ),
 .UNSPECIFIED. ) ;
#83380 = CARTESIAN_POINT ( 'NONE',  ( 9.019176178608812933, -10.92531984108285670, 33.72920026020278073 ) ) ;
#83381 = CARTESIAN_POINT ( 'NONE',  ( -0.3589743589743593088, -3.499999999999999556, 29.75000000000000355 ) ) ;
#83382 = B_SPLINE_CURVE_WITH_KNOTS ( 'NONE', 3,
 ( #69167, #55200, #14668, #20964, #61510, #76360, #84028, #42150, #15114, #83130 ),
 .UNSPECIFIED., .F., .F.,
 ( 4, 2, 2, 2, 4 ),
 ( 0.0007817246256747516176, 0.0009771112852218965736, 0.001172497944769041421, 0.001367884604316186269, 0.001563271263863331333 ),
 .UNSPECIFIED. ) ;
#83383 = ORIENTED_EDGE ( 'NONE', *, *, #27913, .F. ) ;
#83384 = CARTESIAN_POINT ( 'NONE',  ( 3.230769230769110045, -11.94971097300221174, 32.03036669348237098 ) ) ;
#83385 = EDGE_CURVE ( 'NONE', #85101, #58822, #65417, .T. ) ;
#83386 = B_SPLINE_CURVE_WITH_KNOTS ( 'NONE', 3,
 ( #60422, #11803, #81593, #32067, #81155, #33837, #5931, #40611, #68080, #25756 ),
 .UNSPECIFIED., .F., .F.,
 ( 4, 2, 2, 2, 4 ),
 ( 0.000000000000000000, 0.0001954339857564073388, 0.0003908679715128146777, 0.0005863019572692220165, 0.0007817359430256293554 ),
 .UNSPECIFIED. ) ;
#83387 = VECTOR ( 'NONE', #54432, 1000.000000000000114 ) ;
#83388 = AXIS2_PLACEMENT_3D ( 'NONE', #87107, #18187, #3324 ) ;
#83389 = CARTESIAN_POINT ( 'NONE',  ( -1.319359813339359366, -6.879047030191282275, 34.71129190930002295 ) ) ;
#83390 = FACE_OUTER_BOUND ( 'NONE', #87489, .T. ) ;
#83391 = VECTOR ( 'NONE', #33646, 1000.000000000000000 ) ;
#83392 = ORIENTED_EDGE ( 'NONE', *, *, #63579, .T. ) ;
#83393 = CARTESIAN_POINT ( 'NONE',  ( -16.15384615384627409, -6.835583212225970762, 34.95778746994575670 ) ) ;
#83394 = EDGE_CURVE ( 'NONE', #30224, #52884, #33204, .T. ) ;
#83395 = CYLINDRICAL_SURFACE ( 'NONE', #75694, 0.2500000000000008882 ) ;
#83396 = CARTESIAN_POINT ( 'NONE',  ( -18.75000000000000000, -3.499999999999999556, 29.75000000000000355 ) ) ;
#83397 = EDGE_LOOP ( 'NONE', ( #6962, #23035 ) ) ;
#83398 = CARTESIAN_POINT ( 'NONE',  ( -2.557669051740896649, -12.01397095200673881, 32.43157075238190146 ) ) ;
#83399 = ADVANCED_FACE ( 'NONE', ( #13629 ), #66012, .F. ) ;
#83400 = VERTEX_POINT ( 'NONE', #11532 ) ;
#83401 = CARTESIAN_POINT ( 'NONE',  ( 12.71159288145191013, -12.41089969410671223, 31.60739465890703670 ) ) ;
#83402 = CARTESIAN_POINT ( 'NONE',  ( 13.38461538461538680, -8.564572088678739092, 35.78748833219616898 ) ) ;
#83403 = ORIENTED_EDGE ( 'NONE', *, *, #36992, .F. ) ;
#83404 = ADVANCED_FACE ( 'NONE', ( #55501 ), #39015, .F. ) ;
#83405 = DIRECTION ( 'NONE',  ( -0.000000000000000000, -0.7660444431189791237, -0.6427876096865379196 ) ) ;
#83406 = CARTESIAN_POINT ( 'NONE',  ( 4.219913487196229163, -9.058645607665452459, 34.76329471203371924 ) ) ;
#83407 = DIRECTION ( 'NONE',  ( 0.000000000000000000, 0.9396926207859126468, 0.3420201433256571111 ) ) ;
#83408 = CARTESIAN_POINT ( 'NONE',  ( 1.254467414883690735, -6.809168938359898782, 34.95455904226513866 ) ) ;
#83409 = CARTESIAN_POINT ( 'NONE',  ( -4.023055712879200385, -3.957578996910242619, 33.62503395064540257 ) ) ;
#83410 = EDGE_LOOP ( 'NONE', ( #23496, #13426, #38238, #67205, #5023 ) ) ;
#83411 = EDGE_LOOP ( 'NONE', ( #31002, #52708, #85336, #6649 ) ) ;
#83412 = FACE_BOUND ( 'NONE', #76085, .T. ) ;
#83413 = ORIENTED_EDGE ( 'NONE', *, *, #79797, .T. ) ;
#83414 = B_SPLINE_CURVE_WITH_KNOTS ( 'NONE', 3,
 ( #25565, #73770, #12065, #39544, #67004, #46723, #82293, #75967, #88626, #81409 ),
 .UNSPECIFIED., .F., .F.,
 ( 4, 2, 2, 2, 4 ),
 ( 0.000000000000000000, 0.0001954311564186865763, 0.0003908623128373731525, 0.0005862934692560596746, 0.0007817246256747463051 ),
 .UNSPECIFIED. ) ;
#83416 = EDGE_CURVE ( 'NONE', #48963, #89081, #44979, .T. ) ;
#83415 = CARTESIAN_POINT ( 'NONE',  ( -4.153846153846152411, -10.05456864172156806, 36.03766855953608683 ) ) ;
#83417 = DIRECTION ( 'NONE',  ( -0.000000000000000000, -0.000000000000000000, -1.000000000000000000 ) ) ;
#83418 = EDGE_CURVE ( 'NONE', #81424, #28117, #8480, .T. ) ;
#83419 = CARTESIAN_POINT ( 'NONE',  ( 6.066067333350077639, -2.833524468853757750, 32.15551576947925838 ) ) ;
#83420 = CARTESIAN_POINT ( 'NONE',  ( 0.6845513056318558442, -12.64618726649961289, 30.78989965857442712 ) ) ;
#83421 = ORIENTED_EDGE ( 'NONE', *, *, #27039, .T. ) ;
#83422 = ORIENTED_EDGE ( 'NONE', *, *, #56615, .F. ) ;
#83423 = VERTEX_POINT ( 'NONE', #43324 ) ;
#83424 = CARTESIAN_POINT ( 'NONE',  ( -0.2115929431903189328, -3.202959910592335202, 32.30730279482227019 ) ) ;
#83425 = ORIENTED_EDGE ( 'NONE', *, *, #60193, .T. ) ;
#83426 = ADVANCED_FACE ( 'NONE', ( #35229 ), #28941, .F. ) ;
#83427 = CYLINDRICAL_SURFACE ( 'NONE', #17261, 0.2499999999999998890 ) ;
#83428 = CARTESIAN_POINT ( 'NONE',  ( 1.634669696253700621, -3.627508038966689163, 32.91356715214248396 ) ) ;
#83429 = ADVANCED_FACE ( 'NONE', ( #8660 ), #36568, .F. ) ;
#83430 = B_SPLINE_CURVE_WITH_KNOTS ( 'NONE', 3,
 ( #2679, #38259, #86004, #30171, #85559, #65717, #9455, #45450, #37355, #64823 ),
 .UNSPECIFIED., .F., .F.,
 ( 4, 2, 2, 2, 4 ),
 ( 0.000000000000000000, 0.0001954311564186881213, 0.0003908623128373762425, 0.0005862934692560643367, 0.0007817246256747524850 ),
 .UNSPECIFIED. ) ;
#83431 = CARTESIAN_POINT ( 'NONE',  ( -18.13069060311030611, -6.369640206132552329, 34.87707690430378449 ) ) ;
#83432 = EDGE_LOOP ( 'NONE', ( #28687, #52336 ) ) ;
#83433 = CARTESIAN_POINT ( 'NONE',  ( 8.769230769230647482, -9.442884908241554243, 34.35708131394783038 ) ) ;
#83434 = EDGE_CURVE ( 'NONE', #65345, #82786, #63341, .T. ) ;
#83435 = CARTESIAN_POINT ( 'NONE',  ( 14.30769230769231015, -8.973038597847269315, 34.52809138561121927 ) ) ;
#83436 = CARTESIAN_POINT ( 'NONE',  ( 16.82692307692307665, -7.500000000000001776, 35.04278698407183867 ) ) ;
#83437 = CARTESIAN_POINT ( 'NONE',  ( -11.76138775597768671, -3.105860786376062332, 32.13614157043599562 ) ) ;
#83438 = ORIENTED_EDGE ( 'NONE', *, *, #80072, .T. ) ;
#83439 = EDGE_LOOP ( 'NONE', ( #64779, #52681 ) ) ;
#83440 = AXIS2_PLACEMENT_3D ( 'NONE', #73855, #74292, #39633 ) ;
#83441 = VERTEX_POINT ( 'NONE', #83882 ) ;
#83442 = CIRCLE ( 'NONE', #70518, 5.000000000000000888 ) ;
#83444 = ADVANCED_FACE ( 'NONE', ( #22168 ), #50510, .F. ) ;
#83443 = CARTESIAN_POINT ( 'NONE',  ( -3.930834802233302394, -9.886259254753566594, 34.14407573483972413 ) ) ;
#83445 = UNCERTAINTY_MEASURE_WITH_UNIT (LENGTH_MEASURE( 1.000000000000000082E-05 ), #81033, 'distance_accuracy_value', 'NONE');
#83447 = CARTESIAN_POINT ( 'NONE',  ( -13.63459211555773720, -5.728515186090277211, 34.42611988154120439 ) ) ;
#83446 = DIRECTION ( 'NONE',  ( 0.000000000000000000, 1.000000000000000000, 0.000000000000000000 ) ) ;
#83448 = AXIS2_PLACEMENT_3D ( 'NONE', #62763, #83959, #35307 ) ;
#83449 = CYLINDRICAL_SURFACE ( 'NONE', #37034, 0.2499999999999998890 ) ;
#83450 = CARTESIAN_POINT ( 'NONE',  ( 14.30769230769231015, -4.102666532097928531, 36.13435417666054406 ) ) ;
#83451 = CARTESIAN_POINT ( 'NONE',  ( -11.53846153846153655, -3.886160181151819604, 36.00935417666054406 ) ) ;
#83452 = CARTESIAN_POINT ( 'NONE',  ( 3.230769230769231726, -2.900454961884010974, 35.62045528018868623 ) ) ;
#83453 = ORIENTED_EDGE ( 'NONE', *, *, #7328, .F. ) ;
#83454 = CARTESIAN_POINT ( 'NONE',  ( -7.781009065434213667, -7.750023224968868085, 34.99404313364389907 ) ) ;
#83455 = CARTESIAN_POINT ( 'NONE',  ( 10.61538461538449418, -10.33852847137269571, 34.16647553114546554 ) ) ;
#83456 = DIRECTION ( 'NONE',  ( -0.000000000000000000, -0.000000000000000000, -1.000000000000000000 ) ) ;
#83457 = CARTESIAN_POINT ( 'NONE',  ( 0.000000000000000000, -11.00000000000000000, 29.75000000000000355 ) ) ;
#83458 = ORIENTED_EDGE ( 'NONE', *, *, #42653, .T. ) ;
#83459 = DIRECTION ( 'NONE',  ( 1.000000000000000000, 0.000000000000000000, 0.000000000000000000 ) ) ;
#83460 = VERTEX_POINT ( 'NONE', #85202 ) ;
#83461 = FACE_BOUND ( 'NONE', #45310, .T. ) ;
#83462 = CARTESIAN_POINT ( 'NONE',  ( -18.00000000000000000, -2.486705287966279876, 31.30864560766543647 ) ) ;
#83463 = DIRECTION ( 'NONE',  ( -0.000000000000000000, -0.9396926207859092051, -0.3420201433256662704 ) ) ;
#83464 = LINE ( 'NONE', #22194, #67758 ) ;
#83465 = ORIENTED_EDGE ( 'NONE', *, *, #35482, .T. ) ;
#83466 = CARTESIAN_POINT ( 'NONE',  ( 11.53846153846141576, -11.06231777344772027, 33.60647404775119895 ) ) ;
#83467 = CARTESIAN_POINT ( 'NONE',  ( 15.45354889974729318, -2.353885683473779800, 30.79025554430704403 ) ) ;
#83468 = CARTESIAN_POINT ( 'NONE',  ( -15.10024379253558457, -10.31582465632705237, 34.18122507451815295 ) ) ;
#83469 = ADVANCED_FACE ( 'NONE', ( #42888 ), #48743, .F. ) ;
#83470 = CARTESIAN_POINT ( 'NONE',  ( 6.130791807824788719, -3.530189275343204702, 32.79018710029569661 ) ) ;
#83471 = VERTEX_POINT ( 'NONE', #77990 ) ;
#83472 = DIRECTION ( 'NONE',  ( 0.000000000000000000, 0.7660444431189822323, -0.6427876096865344779 ) ) ;
#83473 = ORIENTED_EDGE ( 'NONE', *, *, #53870, .T. ) ;
#83475 = VERTEX_POINT ( 'NONE', #1890 ) ;
#83474 = CARTESIAN_POINT ( 'NONE',  ( -8.992715712954719720, -3.754499324213721234, 33.06261337010820256 ) ) ;
#83476 = CARTESIAN_POINT ( 'NONE',  ( 7.622668902429898807, -10.81261337010820256, 33.49550067578627477 ) ) ;
#83477 = CARTESIAN_POINT ( 'NONE',  ( -6.923076923077044142, -11.94971097300221174, 32.03036669348237098 ) ) ;
#83478 = CARTESIAN_POINT ( 'NONE',  ( -6.923076923076922462, -1.129524287112498415, 32.06866353760679544 ) ) ;
#83479 = CARTESIAN_POINT ( 'NONE',  ( -13.38461538461538325, -9.058645607665452459, 34.76329471203371924 ) ) ;
#83480 = CARTESIAN_POINT ( 'NONE',  ( 16.82689985270161515, -4.931416488878822335, 34.32920672191015399 ) ) ;
#83481 = B_SPLINE_CURVE_WITH_KNOTS ( 'NONE', 3,
 ( #36872, #83756, #22042, #50815, #84641, #76988, #64335, #22916, #15290, #70226 ),
 .UNSPECIFIED., .F., .F.,
 ( 4, 2, 2, 2, 4 ),
 ( 0.000000000000000000, 0.0001954311564186861697, 0.0003908623128373723394, 0.0005862934692560584820, 0.0007817246256747446788 ),
 .UNSPECIFIED. ) ;
#83483 = CARTESIAN_POINT ( 'NONE',  ( 16.37685750545900376, -5.667800583137506898, 34.40243808032445827 ) ) ;
#83482 = CARTESIAN_POINT ( 'NONE',  ( -5.999999999999998224, -6.343179335718451384, 34.87096338111211935 ) ) ;
#83484 = DIRECTION ( 'NONE',  ( 0.000000000000000000, -1.000000000000000000, 0.000000000000000000 ) ) ;
#83485 = AXIS2_PLACEMENT_3D ( 'NONE', #35182, #62639, #21668 ) ;
#83486 = CARTESIAN_POINT ( 'NONE',  ( 1.139087296526029469, -10.24999999999999467, 25.95312500000000000 ) ) ;
#83487 = EDGE_LOOP ( 'NONE', ( #4329, #88532 ) ) ;
#83488 = CARTESIAN_POINT ( 'NONE',  ( -16.21992853320628925, -4.661471528628507777, 34.16647553114621871 ) ) ;
#83489 = ORIENTED_EDGE ( 'NONE', *, *, #56829, .F. ) ;
#83490 = ORIENTED_EDGE ( 'NONE', *, *, #1306, .F. ) ;
#83491 = CARTESIAN_POINT ( 'NONE',  ( -8.769230769230892619, -6.835583212225970762, 34.95778746994575670 ) ) ;
#83492 = ORIENTED_EDGE ( 'NONE', *, *, #30241, .F. ) ;
#83493 = CARTESIAN_POINT ( 'NONE',  ( 10.68063975489745232, -8.656820664281605460, 34.87096338111211224 ) ) ;
#83494 = CARTESIAN_POINT ( 'NONE',  ( 3.230769230769110045, -8.613356846316285953, 34.62446782046622218 ) ) ;
#83495 = CARTESIAN_POINT ( 'NONE',  ( -6.923076923077045919, -9.528491918059723176, 34.59228464037033035 ) ) ;
#83496 = CARTESIAN_POINT ( 'NONE',  ( -4.853911725310227077, -3.587049720035815348, 32.86302985866382897 ) ) ;
#83497 = CARTESIAN_POINT ( 'NONE',  ( 12.23861224402231684, -10.61292498521070549, 33.66303323003028680 ) ) ;
#83498 = CARTESIAN_POINT ( 'NONE',  ( -8.992157728137618378, -2.889293201056495786, 32.26117774369186009 ) ) ;
#83499 = CARTESIAN_POINT ( 'NONE',  ( -10.61538461538461320, -2.486705287966279876, 31.30864560766543647 ) ) ;
#83500 = DIRECTION ( 'NONE',  ( 0.000000000000000000, -1.000000000000000000, 0.000000000000000000 ) ) ;
#83501 = CARTESIAN_POINT ( 'NONE',  ( 6.923076923076924238, -13.49023893513002648, 31.06009739812518688 ) ) ;
#83502 = AXIS2_PLACEMENT_3D ( 'NONE', #23808, #86443, #36892 ) ;
#83503 = CARTESIAN_POINT ( 'NONE',  ( 5.869852030268305931, -11.66186481527757479, 32.95055677023626117 ) ) ;
#83504 = CARTESIAN_POINT ( 'NONE',  ( -9.757577692864012775, -3.643525952247789412, 33.31231777344662959 ) ) ;
#83505 = EDGE_CURVE ( 'NONE', #78089, #62624, #29378, .T. ) ;
#83506 = AXIS2_PLACEMENT_3D ( 'NONE', #49678, #77154, #36612 ) ;
#83507 = AXIS2_PLACEMENT_3D ( 'NONE', #39698, #79335, #85649 ) ;
#83508 = ORIENTED_EDGE ( 'NONE', *, *, #8332, .T. ) ;
#83509 = VERTEX_POINT ( 'NONE', #83435 ) ;
#83510 = CARTESIAN_POINT ( 'NONE',  ( -18.25002322422145440, -2.588893531581426544, 31.60682220781847818 ) ) ;
#83511 = DIRECTION ( 'NONE',  ( -0.000000000000000000, -0.9848077530122086864, -0.1736481776669273613 ) ) ;
#83512 = CARTESIAN_POINT ( 'NONE',  ( 5.869852790561781219, -6.001485441113818986, 34.52039167877662607 ) ) ;
#83513 = ORIENTED_EDGE ( 'NONE', *, *, #85740, .T. ) ;
#83514 = ADVANCED_FACE ( 'NONE', ( #16293 ), #64457, .T. ) ;
#83515 = B_SPLINE_CURVE_WITH_KNOTS ( 'NONE', 3,
 ( #15318, #42795, #20737, #75675, #70254, #48203, #84233, #63927, #13980, #41458 ),
 .UNSPECIFIED., .F., .F.,
 ( 4, 2, 2, 2, 4 ),
 ( 0.000000000000000000, 0.0001954311564186864678, 0.0003908623128373729357, 0.0005862934692560594577, 0.0007817246256747458714 ),
 .UNSPECIFIED. ) ;
#83516 = VECTOR ( 'NONE', #57882, 1000.000000000000000 ) ;
#83517 = CARTESIAN_POINT ( 'NONE',  ( 9.692307692307695177, -11.35647404775217417, 33.31231777344666511 ) ) ;
#83518 = AXIS2_PLACEMENT_3D ( 'NONE', #67049, #17972, #45425 ) ;
#83519 = PLANE ( 'NONE',  #19700 ) ;
#83520 = EDGE_CURVE ( 'NONE', #68189, #54936, #41694, .T. ) ;
#83521 = AXIS2_PLACEMENT_3D ( 'NONE', #33283, #6257, #40922 ) ;
#83522 = LINE ( 'NONE', #9190, #32243 ) ;
#83523 = ORIENTED_EDGE ( 'NONE', *, *, #28553, .T. ) ;
#83524 = CARTESIAN_POINT ( 'NONE',  ( 14.30769230769231015, -2.833524468853757305, 32.15551576947925838 ) ) ;
#83525 = EDGE_LOOP ( 'NONE', ( #14524, #20447, #61709, #25596 ) ) ;
#83526 = ADVANCED_FACE ( 'NONE', ( #62688 ), #45976, .F. ) ;
#83527 = DIRECTION ( 'NONE',  ( -0.000000000000000000, -0.000000000000000000, -1.000000000000000000 ) ) ;
#83528 = DIRECTION ( 'NONE',  ( 1.000000000000000000, 0.000000000000000000, 0.000000000000000000 ) ) ;
#83529 = DIRECTION ( 'NONE',  ( 1.000000000000000000, 0.000000000000000000, 0.000000000000000000 ) ) ;
#83530 = DIRECTION ( 'NONE',  ( 1.000000000000000000, 0.000000000000000000, 0.000000000000000000 ) ) ;
#83531 = CARTESIAN_POINT ( 'NONE',  ( -6.673131513698880468, -2.589246495874657938, 31.60778113518102828 ) ) ;
#83532 = EDGE_LOOP ( 'NONE', ( #85321, #82026, #47078, #63091 ) ) ;
#83533 = VERTEX_POINT ( 'NONE', #37895 ) ;
#83534 = ORIENTED_EDGE ( 'NONE', *, *, #35727, .T. ) ;
#83535 = ORIENTED_EDGE ( 'NONE', *, *, #54929, .F. ) ;
#83536 = CARTESIAN_POINT ( 'NONE',  ( -17.14219352288385778, -10.90142922261923886, 33.41473453929638993 ) ) ;
#83537 = CARTESIAN_POINT ( 'NONE',  ( 13.63466969625370417, -9.943054286541403997, 34.11300777759954883 ) ) ;
#83538 = AXIS2_PLACEMENT_3D ( 'NONE', #1176, #15146, #36308 ) ;
#83539 = ADVANCED_FACE ( 'NONE', ( #80221 ), #9971, .F. ) ;
#83540 = LINE ( 'NONE', #43426, #36480 ) ;
#83541 = CARTESIAN_POINT ( 'NONE',  ( 11.40831432902331599, -12.27039167877662251, 31.24851455888617835 ) ) ;
#83542 = B_SPLINE_CURVE_WITH_KNOTS ( 'NONE', 3,
 ( #39808, #73601, #67276, #74472, #19524, #66381, #5571, #60511, #88023, #26283 ),
 .UNSPECIFIED., .F., .F.,
 ( 4, 2, 2, 2, 4 ),
 ( 0.0007817246256747450040, 0.0009771112852218881168, 0.001172497944769031230, 0.001367884604316174342, 0.001563271263863317455 ),
 .UNSPECIFIED. ) ;
#83543 = CARTESIAN_POINT ( 'NONE',  ( 4.376857505459002873, -6.503523203565942268, 34.64991518177335195 ) ) ;
#83544 = DIRECTION ( 'NONE',  ( -0.000000000000000000, 0.5000000000000011102, -0.8660254037844380415 ) ) ;
#83545 = ORIENTED_EDGE ( 'NONE', *, *, #354, .F. ) ;
#83546 = B_SPLINE_CURVE_WITH_KNOTS ( 'NONE', 3,
 ( #21578, #7187, #63448, #35092, #55363, #49049, #83741, #49929, #62553, #54927 ),
 .UNSPECIFIED., .F., .F.,
 ( 4, 2, 2, 2, 4 ),
 ( 0.0007817359430256294638, 0.0009771253907249950223, 0.001172514838424360472, 0.001367904286123725922, 0.001563293733823091372 ),
 .UNSPECIFIED. ) ;
#83547 = EDGE_LOOP ( 'NONE', ( #48153, #58484, #58951, #82806 ) ) ;
#83548 = ORIENTED_EDGE ( 'NONE', *, *, #54341, .F. ) ;
#83551 = ORIENTED_EDGE ( 'NONE', *, *, #76421, .T. ) ;
#83550 = EDGE_CURVE ( 'NONE', #19590, #66812, #4553, .T. ) ;
#83549 = CARTESIAN_POINT ( 'NONE',  ( 12.46153846153833911, -8.613356846316285953, 34.62446782046622218 ) ) ;
#83553 = CARTESIAN_POINT ( 'NONE',  ( -5.300408001487407539, -12.69144148231606017, 30.53333754910549303 ) ) ;
#83552 = DIRECTION ( 'NONE',  ( -0.000000000000000000, -0.7660444431189791237, -0.6427876096865379196 ) ) ;
#83554 = LINE ( 'NONE', #78432, #30210 ) ;
#83555 = CARTESIAN_POINT ( 'NONE',  ( 3.749999999999992006, -5.946699141100872943, 24.39062500000000000 ) ) ;
#83556 = ORIENTED_EDGE ( 'NONE', *, *, #46754, .T. ) ;
#83557 = EDGE_CURVE ( 'NONE', #65490, #12295, #18878, .T. ) ;
#83558 = EDGE_CURVE ( 'NONE', #41513, #26582, #74050, .T. ) ;
#83559 = MECHANICAL_DESIGN_GEOMETRIC_PRESENTATION_REPRESENTATION (  '', ( #74701 ), #72159 ) ;
#83560 = ORIENTED_EDGE ( 'NONE', *, *, #2273, .F. ) ;
#83561 = CARTESIAN_POINT ( 'NONE',  ( 13.51466054745016621, -2.504778602574659896, 29.97347330155780654 ) ) ;
#83562 = VERTEX_POINT ( 'NONE', #10426 ) ;
#83563 = FACE_BOUND ( 'NONE', #59606, .T. ) ;
#83565 = VECTOR ( 'NONE', #42661, 1000.000000000000000 ) ;
#83564 = CARTESIAN_POINT ( 'NONE',  ( -1.319421402832027912, -2.506253911140448043, 29.99999999999988631 ) ) ;
#83566 = VECTOR ( 'NONE', #34594, 1000.000000000000114 ) ;
#83567 = CARTESIAN_POINT ( 'NONE',  ( -8.769230769230768274, -11.33034616979429110, 35.88435417666054406 ) ) ;
#83568 = EDGE_LOOP ( 'NONE', ( #36086, #48394 ) ) ;
#83569 = CARTESIAN_POINT ( 'NONE',  ( 15.36160756125598681, -7.277220318596961057, 34.99547417642776992 ) ) ;
#83570 = CYLINDRICAL_SURFACE ( 'NONE', #1534, 0.2499999999999993616 ) ;
#83571 = CARTESIAN_POINT ( 'NONE',  ( 10.39189967166067063, -2.847400154188068022, 31.58180166144859058 ) ) ;
#83572 = DIRECTION ( 'NONE',  ( 0.000000000000000000, 0.000000000000000000, -1.000000000000000000 ) ) ;
#83573 = DIRECTION ( 'NONE',  ( -0.000000000000000000, 0.5000000000000011102, -0.8660254037844380415 ) ) ;
#83575 = EDGE_LOOP ( 'NONE', ( #71319, #29716 ) ) ;
#83574 = ADVANCED_FACE ( 'NONE', ( #5004 ), #59046, .F. ) ;
#83576 = CARTESIAN_POINT ( 'NONE',  ( -11.28840711854808632, -12.41089969410671223, 31.60739465890703670 ) ) ;
#83577 = CARTESIAN_POINT ( 'NONE',  ( 14.30769230769231015, -2.900454961884010974, 35.62045528018868623 ) ) ;
#83578 = CARTESIAN_POINT ( 'NONE',  ( 2.307692307692309264, -1.117168528481311540, 33.14645433367849847 ) ) ;
#83579 = DIRECTION ( 'NONE',  ( 1.000000000000000000, 0.000000000000000000, 0.000000000000000000 ) ) ;
#83580 = ADVANCED_FACE ( 'NONE', ( #3213 ), #72561, .F. ) ;
#83582 = EDGE_CURVE ( 'NONE', #52308, #3410, #78874, .T. ) ;
#83581 = DIRECTION ( 'NONE',  ( -0.000000000000000000, -0.000000000000000000, -1.000000000000000000 ) ) ;
#83583 = FACE_BOUND ( 'NONE', #21573, .T. ) ;
#83585 = CARTESIAN_POINT ( 'NONE',  ( -6.130690603110309667, -9.929715669179216775, 34.40415004197138416 ) ) ;
#83584 = CARTESIAN_POINT ( 'NONE',  ( -6.673022503163470454, -12.65882529074907126, 30.72640787790839312 ) ) ;
#83586 = B_SPLINE_CURVE_WITH_KNOTS ( 'NONE', 3,
 ( #18453, #5824, #19339, #40942, #74736, #87369, #33302, #13022, #47691, #6274 ),
 .UNSPECIFIED., .F., .F.,
 ( 4, 2, 2, 2, 4 ),
 ( 0.000000000000000000, 0.0001954339857564078809, 0.0003908679715128157619, 0.0005863019572692236428, 0.0007817359430256315238 ),
 .UNSPECIFIED. ) ;
#83587 = CARTESIAN_POINT ( 'NONE',  ( -7.053768389744485390, -12.11776431015576172, 31.66791131148498906 ) ) ;
#83589 = CARTESIAN_POINT ( 'NONE',  ( -6.065270445960775803, -5.219633306516282545, 34.19971097300152252 ) ) ;
#83588 = CARTESIAN_POINT ( 'NONE',  ( 4.088576153289833925, -5.941354392334500467, 34.76329471203369792 ) ) ;
#83590 = B_SPLINE_CURVE_WITH_KNOTS ( 'NONE', 3,
 ( #52523, #37682, #45773, #66496, #24162, #4799 ),
 .UNSPECIFIED., .F., .F.,
 ( 4, 2, 4 ),
 ( 4.563551064100006665E-17, 0.0001954756301637168570, 0.0003909512603273880690 ),
 .UNSPECIFIED. ) ;
#83591 = CARTESIAN_POINT ( 'NONE',  ( -0.4615384615385826339, -11.94971097300221174, 32.03036669348237098 ) ) ;
#83592 = CARTESIAN_POINT ( 'NONE',  ( 1.200186371490561621, -10.22469193450123193, 24.45125670625849423 ) ) ;
#83593 = EDGE_CURVE ( 'NONE', #37632, #84179, #54719, .T. ) ;
#83594 = ORIENTED_EDGE ( 'NONE', *, *, #79985, .F. ) ;
#83595 = CARTESIAN_POINT ( 'NONE',  ( -12.94230769230769162, -3.499999999999999556, 29.75000000000000355 ) ) ;
#83596 = ORIENTED_EDGE ( 'NONE', *, *, #77740, .T. ) ;
#83597 = CARTESIAN_POINT ( 'NONE',  ( -13.16160254052199008, -9.172514111537584114, 34.72667873470787470 ) ) ;
#83598 = ORIENTED_EDGE ( 'NONE', *, *, #80169, .T. ) ;
#83599 = CARTESIAN_POINT ( 'NONE',  ( -11.28851602011339850, -2.824170634883621744, 31.52227843825338738 ) ) ;
#83600 = CARTESIAN_POINT ( 'NONE',  ( -15.93083330975275658, -11.98016756924215187, 32.48728574198911190 ) ) ;
#83601 = VERTEX_POINT ( 'NONE', #4096 ) ;
#83602 = DIRECTION ( 'NONE',  ( -0.000000000000000000, -0.8660254037844397068, -0.4999999999999978906 ) ) ;
#83603 = CARTESIAN_POINT ( 'NONE',  ( 2.750000000000001332, -7.438900925035452083, 16.71688170625848713 ) ) ;
#83604 = CARTESIAN_POINT ( 'NONE',  ( -17.93393266664992325, -9.058645607665452459, 34.76329471203371924 ) ) ;
#83605 = DIRECTION ( 'NONE',  ( 0.000000000000000000, 0.000000000000000000, 1.000000000000000000 ) ) ;
#83606 = CARTESIAN_POINT ( 'NONE',  ( -5.326946301144534601, -2.985938066672154445, 32.43141759479405550 ) ) ;
#83607 = CARTESIAN_POINT ( 'NONE',  ( -5.299849294439222369, -12.39988816332205701, 30.74660775122750778 ) ) ;
#83608 = FACE_OUTER_BOUND ( 'NONE', #13446, .T. ) ;
#83609 = CARTESIAN_POINT ( 'NONE',  ( 5.076923076923075762, -8.120952969808772792, 34.71129190930000163 ) ) ;
#83610 = CARTESIAN_POINT ( 'NONE',  ( -0.06109907496450878162, -11.25000000000000000, 22.53311829374151642 ) ) ;
#83611 = FACE_OUTER_BOUND ( 'NONE', #88018, .T. ) ;
#83612 = CARTESIAN_POINT ( 'NONE',  ( -6.249976744048591826, -3.436278759898155677, 33.07459398097509506 ) ) ;
#83613 = VECTOR ( 'NONE', #41162, 1000.000000000000000 ) ;
#83614 = CARTESIAN_POINT ( 'NONE',  ( 8.769230769230768274, -9.780366693483667717, 34.19971097300155094 ) ) ;
#83615 = CARTESIAN_POINT ( 'NONE',  ( 2.694853999681185108, -4.891553140782077591, 22.06436829374151287 ) ) ;
#83616 = ADVANCED_FACE ( 'NONE', ( #59937 ), #66704, .F. ) ;
#83617 = B_SPLINE_CURVE_WITH_KNOTS ( 'NONE', 3,
 ( #7444, #74569, #61483, #40788, #40344, #34016, #68253, #14190, #6992, #41228 ),
 .UNSPECIFIED., .F., .F.,
 ( 4, 2, 2, 2, 4 ),
 ( 0.0007817246256747447872, 0.0009771112852218876831, 0.001172497944769030579, 0.001367884604316173475, 0.001563271263863316371 ),
 .UNSPECIFIED. ) ;
#83618 = CARTESIAN_POINT ( 'NONE',  ( -10.39237177129121825, -5.582272713120729257, 34.63742843783360570 ) ) ;
#83619 = ORIENTED_EDGE ( 'NONE', *, *, #46070, .F. ) ;
#83620 = DIRECTION ( 'NONE',  ( -0.000000000000000000, 0.9848077530122086864, -0.1736481776669273891 ) ) ;
#83621 = CARTESIAN_POINT ( 'NONE',  ( 15.90386942290380290, -12.17611988154120795, 31.52148481390971213 ) ) ;
#83622 = LINE ( 'NONE', #30429, #54116 ) ;
#83623 = FACE_OUTER_BOUND ( 'NONE', #52491, .T. ) ;
#83624 = CARTESIAN_POINT ( 'NONE',  ( 13.38461538461538680, -2.538708090699994813, 30.37095296980875503 ) ) ;
#83625 = CARTESIAN_POINT ( 'NONE',  ( 7.145856592054987466, -12.11081565061823717, 32.26097654155341843 ) ) ;
#83626 = ADVANCED_FACE ( 'NONE', ( #31124 ), #44182, .F. ) ;
#83627 = B_SPLINE_CURVE_WITH_KNOTS ( 'NONE', 3,
 ( #51557, #32217, #87177, #79060, #45719, #17361, #25453, #52909, #46174, #73656 ),
 .UNSPECIFIED., .F., .F.,
 ( 4, 2, 2, 2, 4 ),
 ( 0.000000000000000000, 0.0001954311564186879044, 0.0003908623128373758088, 0.0005862934692560636861, 0.0007817246256747516176 ),
 .UNSPECIFIED. ) ;
#83628 = CARTESIAN_POINT ( 'NONE',  ( 3.512820512820510555, -7.500000000000000000, 29.75000000000000355 ) ) ;
#83629 = CARTESIAN_POINT ( 'NONE',  ( 10.54930120442873331, -3.513871655860377086, 32.76840700105978499 ) ) ;
#83630 = VECTOR ( 'NONE', #64603, 1000.000000000000000 ) ;
#83631 = EDGE_LOOP ( 'NONE', ( #55667, #22555, #61724, #43421 ) ) ;
#83632 = ORIENTED_EDGE ( 'NONE', *, *, #65973, .T. ) ;
#83633 = EDGE_CURVE ( 'NONE', #47782, #28383, #46125, .T. ) ;
#83634 = ORIENTED_EDGE ( 'NONE', *, *, #11129, .T. ) ;
#83635 = CARTESIAN_POINT ( 'NONE',  ( 5.142178648199100088, -11.94971097300157403, 32.03036669348361443 ) ) ;
#83636 = CARTESIAN_POINT ( 'NONE',  ( -4.023054346021367245, -3.062576670634119758, 32.05464942895959979 ) ) ;
#83637 = CARTESIAN_POINT ( 'NONE',  ( -15.45425415533356350, -10.97335522853832579, 33.68706563782419749 ) ) ;
#83638 = CARTESIAN_POINT ( 'NONE',  ( 13.38461538461538680, -8.564572088678739092, 35.78748833219616898 ) ) ;
#83639 = LINE ( 'NONE', #29134, #50984 ) ;
#83641 = EDGE_CURVE ( 'NONE', #15081, #18944, #25718, .T. ) ;
#83640 = EDGE_LOOP ( 'NONE', ( #88211, #21614 ) ) ;
#83642 = FACE_OUTER_BOUND ( 'NONE', #34837, .T. ) ;
#83643 = ORIENTED_EDGE ( 'NONE', *, *, #11768, .F. ) ;
#83645 = ORIENTED_EDGE ( 'NONE', *, *, #49102, .T. ) ;
#83644 = B_SPLINE_CURVE_WITH_KNOTS ( 'NONE', 3,
 ( #17040, #25130, #85068, #38646, #51233, #59356, #44051, #9837, #85947, #44943 ),
 .UNSPECIFIED., .F., .F.,
 ( 4, 2, 2, 2, 4 ),
 ( 0.0007817359430256322827, 0.0009771253907249989254, 0.001172514838424365676, 0.001367904286123732428, 0.001563293733823098962 ),
 .UNSPECIFIED. ) ;
#83646 = ORIENTED_EDGE ( 'NONE', *, *, #38404, .T. ) ;
#83648 = ORIENTED_EDGE ( 'NONE', *, *, #35172, .F. ) ;
#83647 = DIRECTION ( 'NONE',  ( -0.000000000000000000, -0.6427876096865404731, -0.7660444431189771253 ) ) ;
#83649 = DIRECTION ( 'NONE',  ( -1.000000000000000000, -0.000000000000000000, -0.000000000000000000 ) ) ;
#83650 = CARTESIAN_POINT ( 'NONE',  ( -16.40382288478850725, -4.236021600441997492, 33.53823185664189310 ) ) ;
#83651 = CARTESIAN_POINT ( 'NONE',  ( 2.242441317531067568, -2.506253911140460922, 30.00000000000013856 ) ) ;
#83652 = EDGE_CURVE ( 'NONE', #9891, #50957, #34242, .T. ) ;
#83653 = LINE ( 'NONE', #35001, #74106 ) ;
#83654 = ORIENTED_EDGE ( 'NONE', *, *, #24522, .F. ) ;
#83655 = EDGE_CURVE ( 'NONE', #81224, #235, #19401, .T. ) ;
#83656 = ORIENTED_EDGE ( 'NONE', *, *, #49111, .F. ) ;
#83657 = VERTEX_POINT ( 'NONE', #67150 ) ;
#83658 = CARTESIAN_POINT ( 'NONE',  ( -14.53057099012095499, -7.630691491037285168, 34.74850469731152458 ) ) ;
#83660 = EDGE_LOOP ( 'NONE', ( #54866, #87172, #60254, #87674 ) ) ;
#83659 = DIRECTION ( 'NONE',  ( 0.000000000000000000, 0.000000000000000000, 1.000000000000000000 ) ) ;
#83661 = CARTESIAN_POINT ( 'NONE',  ( 11.40831432902331954, -6.852621066184266141, 34.70813303252209181 ) ) ;
#83662 = CARTESIAN_POINT ( 'NONE',  ( 6.000000000000001776, -12.37446782046654192, 30.86335684631486131 ) ) ;
#83663 = CARTESIAN_POINT ( 'NONE',  ( -0.2115930521604181269, -9.357781135181031829, 34.66075350412533851 ) ) ;
#83664 = ORIENTED_EDGE ( 'NONE', *, *, #77542, .F. ) ;
#83665 = EDGE_CURVE ( 'NONE', #23792, #22049, #37494, .T. ) ;
#83666 = CARTESIAN_POINT ( 'NONE',  ( 10.61538461538461675, -2.708943851104267164, 35.45975837776705220 ) ) ;
#83667 = LINE ( 'NONE', #787, #43941 ) ;
#83668 = EDGE_LOOP ( 'NONE', ( #50796, #26666, #52504, #8182 ) ) ;
#83669 = FACE_BOUND ( 'NONE', #26640, .T. ) ;
#83670 = CARTESIAN_POINT ( 'NONE',  ( -10.74607521849492464, -4.684245665217972032, 34.18127051446801090 ) ) ;
#83671 = DIRECTION ( 'NONE',  ( 0.000000000000000000, 0.6427876096865373645, -0.7660444431189797898 ) ) ;
#83672 = CARTESIAN_POINT ( 'NONE',  ( -16.15384615384615330, -12.78798330534102767, 29.49999999999997868 ) ) ;
#83674 = CARTESIAN_POINT ( 'NONE',  ( 18.13052570176355971, -4.459921816937789885, 33.71989282347011851 ) ) ;
#83673 = LINE ( 'NONE', #56182, #7240 ) ;
#83675 = DIRECTION ( 'NONE',  ( 0.000000000000000000, 0.4999999999999960032, -0.8660254037844410391 ) ) ;
#83676 = CARTESIAN_POINT ( 'NONE',  ( -4.284536756956459413, -10.70098750199973203, 33.91152734681376302 ) ) ;
#83677 = ORIENTED_EDGE ( 'NONE', *, *, #87837, .F. ) ;
#83678 = CARTESIAN_POINT ( 'NONE',  ( 14.37294787896833270, -12.46129190930001052, 30.37095296980870174 ) ) ;
#83679 = FACE_OUTER_BOUND ( 'NONE', #68542, .T. ) ;
#83680 = ORIENTED_EDGE ( 'NONE', *, *, #13716, .T. ) ;
#83681 = B_SPLINE_CURVE_WITH_KNOTS ( 'NONE', 3,
 ( #75187, #88717, #25663, #54453, #53120, #20240, #13476, #61651, #35072, #62530 ),
 .UNSPECIFIED., .F., .F.,
 ( 4, 2, 2, 2, 4 ),
 ( 0.0007817359430256253438, 0.0009771253907249904686, 0.001172514838424355485, 0.001367904286123720501, 0.001563293733823085518 ),
 .UNSPECIFIED. ) ;
#83682 = CARTESIAN_POINT ( 'NONE',  ( -1.326923076923076872, -3.499999999999999556, 29.75000000000000355 ) ) ;
#83683 = CARTESIAN_POINT ( 'NONE',  ( -10.86538461538461320, -7.500000000000001776, 35.04278698407183867 ) ) ;
#83684 = CARTESIAN_POINT ( 'NONE',  ( -7.596099426240392027, -10.82426656108011720, 33.81400080652039009 ) ) ;
#83685 = ORIENTED_EDGE ( 'NONE', *, *, #30658, .F. ) ;
#83686 = CARTESIAN_POINT ( 'NONE',  ( 7.976679284387489410, -6.808710257144161559, 34.95449254468098843 ) ) ;
#83687 = EDGE_CURVE ( 'NONE', #54838, #53642, #47758, .T. ) ;
#83688 = CARTESIAN_POINT ( 'NONE',  ( -4.377331078410484189, -2.353723527008295680, 30.78948104536958752 ) ) ;
#83689 = FACE_BOUND ( 'NONE', #24245, .T. ) ;
#83691 = CARTESIAN_POINT ( 'NONE',  ( -4.023054346021365468, -8.147973898785416225, 34.70805048591653730 ) ) ;
#83690 = DIRECTION ( 'NONE',  ( 0.000000000000000000, 0.000000000000000000, -1.000000000000000000 ) ) ;
#83692 = DIRECTION ( 'NONE',  ( 0.000000000000000000, 0.1736481776669275834, 0.9848077530122086864 ) ) ;
#83694 = CARTESIAN_POINT ( 'NONE',  ( -14.98082371242109012, -6.696923467548660192, 34.68552623307873972 ) ) ;
#83693 = CARTESIAN_POINT ( 'NONE',  ( -7.596099426240392027, -12.65882529074907126, 30.72640787790839312 ) ) ;
#83695 = FACE_OUTER_BOUND ( 'NONE', #3686, .T. ) ;
#83696 = CARTESIAN_POINT ( 'NONE',  ( 3.750000000000000888, -7.499999999999978684, 25.71875000000000000 ) ) ;
#83697 = ORIENTED_EDGE ( 'NONE', *, *, #56345, .F. ) ;
#83698 = AXIS2_PLACEMENT_3D ( 'NONE', #37679, #18306, #86341 ) ;
#83699 = ORIENTED_EDGE ( 'NONE', *, *, #49853, .T. ) ;
#83700 = CARTESIAN_POINT ( 'NONE',  ( -2.307692307692305711, -13.88283147151868846, 33.14645433367849847 ) ) ;
#83701 = CARTESIAN_POINT ( 'NONE',  ( -15.45425415533356350, -5.827078755546623690, 34.72654668319379567 ) ) ;
#83702 = FACE_OUTER_BOUND ( 'NONE', #42843, .T. ) ;
#83703 = CYLINDRICAL_SURFACE ( 'NONE', #2099, 0.2500000000000012212 ) ;
#83704 = CARTESIAN_POINT ( 'NONE',  ( 20.00000000000000000, -11.50000000000000000, 29.75000000000000355 ) ) ;
#83705 = CARTESIAN_POINT ( 'NONE',  ( 2.608446859217893099, -4.805146000318787358, 16.56063170625848713 ) ) ;
#83706 = VECTOR ( 'NONE', #47476, 999.9999999999998863 ) ;
#83707 = CARTESIAN_POINT ( 'NONE',  ( 0.6843181305165271233, -4.226511098958374291, 33.85474049983370293 ) ) ;
#83708 = DIRECTION ( 'NONE',  ( 1.000000000000000000, 0.000000000000000000, 0.000000000000000000 ) ) ;
#83709 = DIRECTION ( 'NONE',  ( 0.000000000000000000, 1.000000000000000000, 0.000000000000000000 ) ) ;
#83710 = CARTESIAN_POINT ( 'NONE',  ( -3.230769230769352962, -12.16647553114689728, 32.15551576947799362 ) ) ;
#83711 = PLANE ( 'NONE',  #5076 ) ;
#83712 = CARTESIAN_POINT ( 'NONE',  ( 18.00000000000000000, -9.780366693483667717, 34.19971097300155094 ) ) ;
#83713 = CARTESIAN_POINT ( 'NONE',  ( -9.822998295417995962, -12.62707690430377383, 30.88035979386743435 ) ) ;
#83714 = CARTESIAN_POINT ( 'NONE',  ( 10.39250509864703176, -7.630690623152299956, 34.99857592706774057 ) ) ;
#83715 = CARTESIAN_POINT ( 'NONE',  ( 7.846153846153846700, -13.87047571288749737, 32.06866353760679544 ) ) ;
#83716 = VERTEX_POINT ( 'NONE', #54061 ) ;
#83717 = CARTESIAN_POINT ( 'NONE',  ( 3.930361210122205406, -5.113361153441933205, 34.14387501736621999 ) ) ;
#83718 = LINE ( 'NONE', #83268, #12965 ) ;
#83719 = CARTESIAN_POINT ( 'NONE',  ( 1.200186371490529202, -4.775308065498752974, 20.73624329374151287 ) ) ;
#83720 = CARTESIAN_POINT ( 'NONE',  ( 0.5276057948885353177, -3.322132147404559976, 32.92929555188717927 ) ) ;
#83721 = CARTESIAN_POINT ( 'NONE',  ( 16.94677510719138525, -11.66186481527757479, 32.95055677023626117 ) ) ;
#83722 = ORIENTED_EDGE ( 'NONE', *, *, #46955, .T. ) ;
#83723 = CARTESIAN_POINT ( 'NONE',  ( -7.173100147298380413, -2.985938066672154445, 32.43141759479405550 ) ) ;
#83725 = EDGE_LOOP ( 'NONE', ( #74307, #74212 ) ) ;
#83724 = LINE ( 'NONE', #49033, #32520 ) ;
#83726 = LINE ( 'NONE', #851, #34091 ) ;
#83727 = CARTESIAN_POINT ( 'NONE',  ( -2.531177232256639265, -10.97335522853832579, 33.68706563782419749 ) ) ;
#83728 = ORIENTED_EDGE ( 'NONE', *, *, #57704, .F. ) ;
#83729 = PLANE ( 'NONE',  #23305 ) ;
#83730 = DIRECTION ( 'NONE',  ( 1.000000000000000000, 0.000000000000000000, 0.000000000000000000 ) ) ;
#83731 = ORIENTED_EDGE ( 'NONE', *, *, #47071, .T. ) ;
#83732 = AXIS2_PLACEMENT_3D ( 'NONE', #30278, #1033, #55971 ) ;
#83733 = CARTESIAN_POINT ( 'NONE',  ( 8.834485908743603844, -2.379036618887895305, 30.90682066428158592 ) ) ;
#83734 = DIRECTION ( 'NONE',  ( 0.000000000000000000, 0.000000000000000000, -1.000000000000000000 ) ) ;
#83735 = CARTESIAN_POINT ( 'NONE',  ( 14.16025641025641235, -7.500000000000000000, 29.75000000000000355 ) ) ;
#83736 = VERTEX_POINT ( 'NONE', #81558 ) ;
#83737 = ORIENTED_EDGE ( 'NONE', *, *, #2420, .T. ) ;
#83738 = CARTESIAN_POINT ( 'NONE',  ( 15.36129493253280032, -10.88167719472716399, 33.43325721877153711 ) ) ;
#83739 = ADVANCED_BREP_SHAPE_REPRESENTATION ( '', ( #59398, #83448 ), #56118 ) ;
#83740 = VERTEX_POINT ( 'NONE', #33366 ) ;
#83741 = CARTESIAN_POINT ( 'NONE',  ( 12.68454981315131214, -9.086983370893049639, 34.49168942202179267 ) ) ;
#83742 = CARTESIAN_POINT ( 'NONE',  ( -14.30769230769242739, -3.300289026999228881, 32.46337939537708905 ) ) ;
#83743 = CARTESIAN_POINT ( 'NONE',  ( -0.2114840416250085009, -5.642605341092957083, 34.66089969410670335 ) ) ;
#83744 = CARTESIAN_POINT ( 'NONE',  ( -7.623190942592358965, -7.369474270740069777, 34.74850911626239025 ) ) ;
#83745 = CARTESIAN_POINT ( 'NONE',  ( -4.480769230769230838, -3.499999999999999556, 29.75000000000000355 ) ) ;
#83746 = ORIENTED_EDGE ( 'NONE', *, *, #50706, .T. ) ;
#83747 = VERTEX_POINT ( 'NONE', #61257 ) ;
#83749 = EDGE_LOOP ( 'NONE', ( #54879, #78631, #43241, #20715 ) ) ;
#83748 = CARTESIAN_POINT ( 'NONE',  ( 4.219913487196229163, -8.164416787775445883, 34.95778746994558617 ) ) ;
#83750 = B_SPLINE_CURVE_WITH_KNOTS ( 'NONE', 3,
 ( #44334, #52439, #18228, #23196, #3363, #79924, #11467, #30835, #66409, #30397 ),
 .UNSPECIFIED., .F., .F.,
 ( 4, 2, 2, 2, 4 ),
 ( 0.000000000000000000, 0.0001954311564186871184, 0.0003908623128373742367, 0.0005862934692560614093, 0.0007817246256747484735 ),
 .UNSPECIFIED. ) ;
#83751 = PLANE ( 'NONE',  #58011 ) ;
#83752 = VECTOR ( 'NONE', #40378, 1000.000000000000000 ) ;
#83753 = EDGE_CURVE ( 'NONE', #44409, #24035, #23620, .T. ) ;
#83754 = ORIENTED_EDGE ( 'NONE', *, *, #65297, .F. ) ;
#83755 = AXIS2_PLACEMENT_3D ( 'NONE', #66676, #31556, #32445 ) ;
#83756 = CARTESIAN_POINT ( 'NONE',  ( 7.780071466793708979, -11.91647553114624181, 32.58852847137148245 ) ) ;
#83757 = CARTESIAN_POINT ( 'NONE',  ( 6.923076923076800782, -9.528491918059723176, 34.59228464037033035 ) ) ;
#83758 = ORIENTED_EDGE ( 'NONE', *, *, #89019, .F. ) ;
#83759 = CARTESIAN_POINT ( 'NONE',  ( -1.384615384615383471, -11.33034616979429110, 35.88435417666054406 ) ) ;
#83760 = CIRCLE ( 'NONE', #44904, 0.2500000000000002220 ) ;
#83761 = EDGE_LOOP ( 'NONE', ( #43083, #25634, #79196, #23142 ) ) ;
#83763 = ORIENTED_EDGE ( 'NONE', *, *, #38338, .T. ) ;
#83762 = CARTESIAN_POINT ( 'NONE',  ( -12.21148414990014963, -4.943051570960394159, 34.04725096376909477 ) ) ;
#83764 = CARTESIAN_POINT ( 'NONE',  ( -14.05774689831426372, -12.07971442181322175, 32.31769673815850297 ) ) ;
#83765 = CARTESIAN_POINT ( 'NONE',  ( -17.78205128205128105, -7.500000000000000000, 29.75000000000000355 ) ) ;
#83766 = ORIENTED_EDGE ( 'NONE', *, *, #7963, .F. ) ;
#83767 = EDGE_CURVE ( 'NONE', #79227, #72161, #53174, .T. ) ;
#83768 = CARTESIAN_POINT ( 'NONE',  ( 17.99999999999987566, -10.90142922262034020, 33.41473453929536674 ) ) ;
#83769 = CARTESIAN_POINT ( 'NONE',  ( -8.769230769230768274, -11.91647553114624181, 32.58852847137148245 ) ) ;
#83770 = APPLICATION_CONTEXT ( 'automotive_design' ) ;
#83771 = FACE_BOUND ( 'NONE', #35286, .T. ) ;
#83772 = CARTESIAN_POINT ( 'NONE',  ( -11.66860874789975533, -2.619462340734462380, 30.83744416345203021 ) ) ;
#83773 = CARTESIAN_POINT ( 'NONE',  ( -6.792285115252138183, -12.11778462344220841, 31.66786338562085135 ) ) ;
#83774 = CARTESIAN_POINT ( 'NONE',  ( 15.45378207486262667, -2.523321265292115534, 31.42251411153756990 ) ) ;
#83775 = CARTESIAN_POINT ( 'NONE',  ( 0.7115384615384606759, -2.249999999999998668, 29.75000000000000355 ) ) ;
#83776 = CARTESIAN_POINT ( 'NONE',  ( 12.22435897435897267, -7.500000000000000000, 33.75000000000000000 ) ) ;
#83777 = DIRECTION ( 'NONE',  ( 0.000000000000000000, 0.6427876096865368094, 0.7660444431189802339 ) ) ;
#83778 = VERTEX_POINT ( 'NONE', #60827 ) ;
#83779 = CARTESIAN_POINT ( 'NONE',  ( 10.36536137809165403, -10.05641848906368097, 34.04755513067966177 ) ) ;
#83780 = VERTEX_POINT ( 'NONE', #26159 ) ;
#83781 = B_SPLINE_CURVE_WITH_KNOTS ( 'NONE', 3,
 ( #23374, #65686, #44079, #9865, #45419, #72450, #17068, #30144, #52624, #3101 ),
 .UNSPECIFIED., .F., .F.,
 ( 4, 2, 2, 2, 4 ),
 ( 0.0007817246256747442451, 0.0009771112852218870326, 0.001172497944769029929, 0.001367884604316172825, 0.001563271263863315504 ),
 .UNSPECIFIED. ) ;
#83782 = ORIENTED_EDGE ( 'NONE', *, *, #38635, .F. ) ;
#83784 = CARTESIAN_POINT ( 'NONE',  ( 7.912222197156284054, -9.780366693483667717, 34.19971097300155805 ) ) ;
#83783 = CARTESIAN_POINT ( 'NONE',  ( 7.846153846153846700, -6.386643153685126251, 34.62446782046654192 ) ) ;
#83785 = B_SPLINE_CURVE_WITH_KNOTS ( 'NONE', 3,
 ( #78320, #58482, #72010, #77883, #57172, #85096, #36465, #58050, #16619, #85979 ),
 .UNSPECIFIED., .F., .F.,
 ( 4, 2, 2, 2, 4 ),
 ( 0.000000000000000000, 0.0001954339857564063360, 0.0003908679715128126719, 0.0005863019572692189808, 0.0007817359430256253438 ),
 .UNSPECIFIED. ) ;
#83786 = VECTOR ( 'NONE', #87692, 1000.000000000000000 ) ;
#83787 = B_SPLINE_CURVE_WITH_KNOTS ( 'NONE', 3,
 ( #39957, #75944, #82268, #88603, #69187, #5712, #60648, #54332, #34070, #81827 ),
 .UNSPECIFIED., .F., .F.,
 ( 4, 2, 2, 2, 4 ),
 ( 0.0007817246256747471724, 0.0009771112852218905021, 0.001172497944769033615, 0.001367884604316176944, 0.001563271263863320274 ),
 .UNSPECIFIED. ) ;
#83788 = CARTESIAN_POINT ( 'NONE',  ( 6.923076923076802558, -6.879047030192662504, 34.71129190930017927 ) ) ;
#83789 = CYLINDRICAL_SURFACE ( 'NONE', #19282, 0.2499999999999997502 ) ;
#83790 = CARTESIAN_POINT ( 'NONE',  ( 15.36129493253280032, -3.816742781228458448, 33.13167719472716044 ) ) ;
#83791 = CARTESIAN_POINT ( 'NONE',  ( 13.44987095589141113, -11.48612834413965977, 32.76840700105972815 ) ) ;
#83792 = ORIENTED_EDGE ( 'NONE', *, *, #51658, .T. ) ;
#83793 = EDGE_CURVE ( 'NONE', #79114, #70013, #62230, .T. ) ;
#83794 = CARTESIAN_POINT ( 'NONE',  ( -2.307692307692305711, -12.78798330534102945, 29.74999999999997868 ) ) ;
#83795 = CARTESIAN_POINT ( 'NONE',  ( -14.30769230769230660, -9.905515769479276145, 34.41647553114623292 ) ) ;
#83796 = CARTESIAN_POINT ( 'NONE',  ( 13.38461538461538680, -11.35647404775217417, 33.31231777344666511 ) ) ;
#83797 = EDGE_CURVE ( 'NONE', #67310, #3936, #35429, .T. ) ;
#83798 = CARTESIAN_POINT ( 'NONE',  ( -8.769230769230768274, -2.486705287966279876, 31.30864560766543647 ) ) ;
#83799 = CARTESIAN_POINT ( 'NONE',  ( 2.530705151785704654, -5.582272713120728369, 34.63742843783360570 ) ) ;
#83800 = EDGE_LOOP ( 'NONE', ( #48000, #40912, #59708, #84678 ) ) ;
#83801 = CARTESIAN_POINT ( 'NONE',  ( -0.4615384615385840772, -2.379036618888197285, 30.90682066428292885 ) ) ;
#83802 = ORIENTED_EDGE ( 'NONE', *, *, #47942, .T. ) ;
#83803 = EDGE_CURVE ( 'NONE', #5644, #29224, #56729, .T. ) ;
#83804 = ORIENTED_EDGE ( 'NONE', *, *, #59107, .T. ) ;
#83805 = EDGE_CURVE ( 'NONE', #76443, #38647, #63481, .T. ) ;
#83806 = CARTESIAN_POINT ( 'NONE',  ( 3.480769230770666578, -7.500000000000155431, 34.75000000000007105 ) ) ;
#83807 = VERTEX_POINT ( 'NONE', #41900 ) ;
#83808 = CARTESIAN_POINT ( 'NONE',  ( -1.105886215935217836E-14, 12.75000000000002665, 32.75000000000000000 ) ) ;
#83809 = CARTESIAN_POINT ( 'NONE',  ( -17.07692307692319744, -3.300289026999228437, 32.46337939537709616 ) ) ;
#83810 = DIRECTION ( 'NONE',  ( 0.000000000000000000, 0.4999999999999960032, -0.8660254037844410391 ) ) ;
#83811 = CARTESIAN_POINT ( 'NONE',  ( -17.07692307692319744, -12.70778746994576025, 30.41441678777401236 ) ) ;
#83812 = CARTESIAN_POINT ( 'NONE',  ( -16.82686876528476461, -12.17597550085003633, 31.52189283813461884 ) ) ;
#83813 = CARTESIAN_POINT ( 'NONE',  ( 0.5267936010512993539, -9.528491918058460186, 34.59228464037085615 ) ) ;
#83814 = EDGE_LOOP ( 'NONE', ( #52510, #53944, #65382, #84977 ) ) ;
#83815 = CARTESIAN_POINT ( 'NONE',  ( 4.219101725122177626, -4.481592998940251427, 33.73612834413965089 ) ) ;
#83817 = ORIENTED_EDGE ( 'NONE', *, *, #48489, .T. ) ;
#83816 = CARTESIAN_POINT ( 'NONE',  ( -0.7115616857599188494, -5.765609946408404518, 34.70566812827425451 ) ) ;
#83818 = LINE ( 'NONE', #55437, #51223 ) ;
#83819 = CARTESIAN_POINT ( 'NONE',  ( 3.164685819813350065, -12.37446782046654192, 30.86335684631486487 ) ) ;
#83820 = CARTESIAN_POINT ( 'NONE',  ( -0.4615384615385840772, -4.320704448113951379, 33.92786785259630022 ) ) ;
#83821 = CARTESIAN_POINT ( 'NONE',  ( -17.74994568836168440, -11.79725096376909654, 32.30694842903960762 ) ) ;
#83822 = CYLINDRICAL_SURFACE ( 'NONE', #66315, 0.2500000000000004996 ) ;
#83823 = CARTESIAN_POINT ( 'NONE',  ( -11.53846153846153655, -10.67929555188718282, 33.92786785259544047 ) ) ;
#83824 = CARTESIAN_POINT ( 'NONE',  ( -13.19230769230769162, -7.500000000000000000, 33.75000000000000000 ) ) ;
#83825 = CARTESIAN_POINT ( 'NONE',  ( 0.06109907496451789238, -4.749999999999998224, 24.40811829374151642 ) ) ;
#83826 = VERTEX_POINT ( 'NONE', #70691 ) ;
#83827 = CARTESIAN_POINT ( 'NONE',  ( -16.82686876528476105, -10.66356715214248574, 33.62249196103329751 ) ) ;
#83828 = CYLINDRICAL_SURFACE ( 'NONE', #7415, 0.2499999999999993616 ) ;
#83829 = AXIS2_PLACEMENT_3D ( 'NONE', #12796, #46142, #67743 ) ;
#83830 = CARTESIAN_POINT ( 'NONE',  ( 9.019285189144222059, -10.82426656108012075, 33.81400080652039009 ) ) ;
#83831 = DIRECTION ( 'NONE',  ( -0.000000000000000000, 0.000000000000000000, 1.000000000000000000 ) ) ;
#83832 = ORIENTED_EDGE ( 'NONE', *, *, #74428, .T. ) ;
#83833 = CARTESIAN_POINT ( 'NONE',  ( 1.139087296525997051, -4.749999999999992895, 14.23437500000000178 ) ) ;
#83834 = CARTESIAN_POINT ( 'NONE',  ( -16.15384615384615330, -12.10708131394839349, 31.69288490824020244 ) ) ;
#83835 = AXIS2_PLACEMENT_3D ( 'NONE', #86974, #25241, #52702 ) ;
#83836 = ORIENTED_EDGE ( 'NONE', *, *, #44096, .T. ) ;
#83837 = CARTESIAN_POINT ( 'NONE',  ( 14.24244237591822859, -2.255955759149247619, 30.00000000000013856 ) ) ;
#83838 = CARTESIAN_POINT ( 'NONE',  ( 14.24242186173153435, -3.300289026998414865, 32.46337939537583139 ) ) ;
#83839 = B_SPLINE_CURVE_WITH_KNOTS ( 'NONE', 3,
 ( #83347, #1801, #21628, #77027, #9886, #84241, #1358, #69820, #70265, #77465 ),
 .UNSPECIFIED., .F., .F.,
 ( 4, 2, 2, 2, 4 ),
 ( 0.0007817359430256360774, 0.0009771253907250041296, 0.001172514838424371965, 0.001367904286123740017, 0.001563293733823108069 ),
 .UNSPECIFIED. ) ;
#83840 = EDGE_LOOP ( 'NONE', ( #57802, #24068 ) ) ;
#83841 = ADVANCED_FACE ( 'NONE', ( #36463 ), #21611, .F. ) ;
#83842 = CARTESIAN_POINT ( 'NONE',  ( -15.45425417449317784, -2.847400154188067578, 31.58180166144859058 ) ) ;
#83843 = CARTESIAN_POINT ( 'NONE',  ( 17.07692307692295586, -10.21337939537710326, 33.94971097300076224 ) ) ;
#83844 = CARTESIAN_POINT ( 'NONE',  ( 9.692307692307570832, -10.33852847137269571, 34.16647553114546554 ) ) ;
#83845 = FACE_OUTER_BOUND ( 'NONE', #41799, .T. ) ;
#83846 = VERTEX_POINT ( 'NONE', #71121 ) ;
#83847 = CARTESIAN_POINT ( 'NONE',  ( -2.980714810855778829, -2.318338780012835443, 30.59689888758630261 ) ) ;
#83848 = VERTEX_POINT ( 'NONE', #76565 ) ;
#83849 = CARTESIAN_POINT ( 'NONE',  ( -6.923076923076615152, -2.506253911140614576, 30.00000000000323297 ) ) ;
#83850 = CARTESIAN_POINT ( 'NONE',  ( -10.74607608205216991, -2.729777683071817229, 31.24903638046269450 ) ) ;
#83851 = ORIENTED_EDGE ( 'NONE', *, *, #35133, .T. ) ;
#83852 = CARTESIAN_POINT ( 'NONE',  ( 10.74617505635156789, -11.37503395064541678, 33.29242100308974273 ) ) ;
#83853 = CARTESIAN_POINT ( 'NONE',  ( -16.15384615384615330, -7.500000000000001776, 35.04278698407183867 ) ) ;
#83854 = CARTESIAN_POINT ( 'NONE',  ( -6.857009589726846599, -12.34228464037088813, 31.77849191805839268 ) ) ;
#83855 = EDGE_CURVE ( 'NONE', #51499, #46953, #69090, .T. ) ;
#83856 = VECTOR ( 'NONE', #7939, 1000.000000000000000 ) ;
#83857 = LINE ( 'NONE', #43730, #56360 ) ;
#83858 = CARTESIAN_POINT ( 'NONE',  ( -18.13014720943822056, -4.460286881179643892, 33.72017969459903242 ) ) ;
#83859 = VERTEX_POINT ( 'NONE', #8996 ) ;
#83860 = ORIENTED_EDGE ( 'NONE', *, *, #24427, .T. ) ;
#83861 = FACE_BOUND ( 'NONE', #51575, .T. ) ;
#83862 = EDGE_LOOP ( 'NONE', ( #31463, #49748, #54718, #78848, #79754 ) ) ;
#83863 = CARTESIAN_POINT ( 'NONE',  ( 8.703960323269996024, -3.835265460703609186, 33.15142922261924241 ) ) ;
#83864 = EDGE_CURVE ( 'NONE', #30312, #88550, #14872, .T. ) ;
#83865 = CARTESIAN_POINT ( 'NONE',  ( 4.153846153846032507, -11.94971097300221174, 32.03036669348237098 ) ) ;
#83866 = CARTESIAN_POINT ( 'NONE',  ( 15.23076923076923173, -6.343179335718451384, 34.87096338111211935 ) ) ;
#83867 = CARTESIAN_POINT ( 'NONE',  ( 5.326868595271218254, -4.336752205174647656, 33.62275283266504289 ) ) ;
#83868 = EDGE_CURVE ( 'NONE', #25396, #81013, #51512, .T. ) ;
#83869 = EDGE_LOOP ( 'NONE', ( #22100, #52467, #21715, #78101, #7487 ) ) ;
#83870 = ORIENTED_EDGE ( 'NONE', *, *, #5063, .T. ) ;
#83871 = ORIENTED_EDGE ( 'NONE', *, *, #58219, .F. ) ;
#83872 = CARTESIAN_POINT ( 'NONE',  ( 13.63461538461682210, -7.500000000000155431, 34.75000000000007105 ) ) ;
#83873 = ORIENTED_EDGE ( 'NONE', *, *, #55803, .T. ) ;
#83874 = EDGE_CURVE ( 'NONE', #87089, #24060, #25701, .T. ) ;
#83875 = LINE ( 'NONE', #42883, #84794 ) ;
#83876 = CARTESIAN_POINT ( 'NONE',  ( 7.846153846153846700, -10.89733346790207413, 36.13435417666054406 ) ) ;
#83877 = CARTESIAN_POINT ( 'NONE',  ( -16.15384615384627409, -11.06231777344772027, 33.60647404775119895 ) ) ;
#83878 = EDGE_LOOP ( 'NONE', ( #66075, #78053 ) ) ;
#83879 = CARTESIAN_POINT ( 'NONE',  ( 16.15384615384603251, -2.379036618888197729, 30.90682066428292885 ) ) ;
#83880 = EDGE_CURVE ( 'NONE', #74779, #26040, #57913, .T. ) ;
#83881 = AXIS2_PLACEMENT_3D ( 'NONE', #24696, #80550, #23789 ) ;
#83882 = CARTESIAN_POINT ( 'NONE',  ( -1.384615384615506484, -12.70778746994576025, 30.41441678777401236 ) ) ;
#83883 = CARTESIAN_POINT ( 'NONE',  ( 4.087763774486019130, -2.486705287966279432, 31.30864560766542937 ) ) ;
#83884 = CARTESIAN_POINT ( 'NONE',  ( -1.161835715637320465, -3.020022701398814124, 32.48759521482552515 ) ) ;
#83885 = EDGE_LOOP ( 'NONE', ( #6641, #50469, #68883, #37978 ) ) ;
#83886 = EDGE_CURVE ( 'NONE', #60602, #87727, #21384, .T. ) ;
#83887 = B_SPLINE_CURVE_WITH_KNOTS ( 'NONE', 3,
 ( #73525, #32978, #74405, #53235, #26660, #80282, #33856, #19457, #6825, #5954 ),
 .UNSPECIFIED., .F., .F.,
 ( 4, 2, 2, 2, 4 ),
 ( 0.0007817359430256282712, 0.0009771253907249941549, 0.001172514838424359822, 0.001367904286123725489, 0.001563293733823091372 ),
 .UNSPECIFIED. ) ;
#83888 = ORIENTED_EDGE ( 'NONE', *, *, #29051, .F. ) ;
#83889 = ORIENTED_EDGE ( 'NONE', *, *, #17043, .T. ) ;
#83890 = CARTESIAN_POINT ( 'NONE',  ( 3.903822929624696236, -2.985938066672154445, 32.43141759479405550 ) ) ;
#83892 = DIRECTION ( 'NONE',  ( -0.000000000000000000, 0.8660254037844397068, -0.4999999999999978906 ) ) ;
#83891 = CARTESIAN_POINT ( 'NONE',  ( -18.12796115882773051, -2.254609590993097878, 29.97526117654244970 ) ) ;
#83893 = CARTESIAN_POINT ( 'NONE',  ( 9.692307692307695177, -11.35647404775217417, 33.31231777344666511 ) ) ;
#83894 = CARTESIAN_POINT ( 'NONE',  ( -3.230769230769351186, -11.48612834414049644, 32.76840700105863391 ) ) ;
#83895 = CARTESIAN_POINT ( 'NONE',  ( -39.05038313613820122, -7.500000000000000000, 29.75000000000000355 ) ) ;
#83896 = CARTESIAN_POINT ( 'NONE',  ( 9.823099500132480344, -3.530189275343204702, 32.79018710029569661 ) ) ;
#83897 = ORIENTED_EDGE ( 'NONE', *, *, #66158, .T. ) ;
#83898 = EDGE_CURVE ( 'NONE', #60046, #14768, #53612, .T. ) ;
#83899 = LINE ( 'NONE', #48758, #32806 ) ;
#83900 = CARTESIAN_POINT ( 'NONE',  ( 16.15384615384603251, -12.16647553114689728, 32.15551576947799362 ) ) ;
#83901 = CARTESIAN_POINT ( 'NONE',  ( 11.60463067942419535, -7.250054483168843156, 34.74374881642865631 ) ) ;
#83902 = CARTESIAN_POINT ( 'NONE',  ( -2.307692307692305711, -3.937682226553329556, 33.60647404775216529 ) ) ;
#83903 = EDGE_LOOP ( 'NONE', ( #73782, #76832, #85518, #75194 ) ) ;
#83904 = LINE ( 'NONE', #56849, #25572 ) ;
#83905 = VERTEX_POINT ( 'NONE', #64354 ) ;
#83906 = FACE_BOUND ( 'NONE', #82421, .T. ) ;
#83907 = CARTESIAN_POINT ( 'NONE',  ( 18.75000000000000000, -3.499999999999999556, 29.75000000000000355 ) ) ;
#83908 = ADVANCED_FACE ( 'NONE', ( #64795 ), #72898, .F. ) ;
#83909 = CARTESIAN_POINT ( 'NONE',  ( 19.00000000000000000, 0.7500000000000052180, 31.75000000000000000 ) ) ;
#83911 = EDGE_CURVE ( 'NONE', #18264, #40036, #83781, .T. ) ;
#83910 = CARTESIAN_POINT ( 'NONE',  ( -7.173076923076921574, -7.433931650972300353, 34.75000000000000711 ) ) ;
#83912 = VERTEX_POINT ( 'NONE', #10316 ) ;
#83913 = FACE_OUTER_BOUND ( 'NONE', #39710, .T. ) ;
#83914 = CARTESIAN_POINT ( 'NONE',  ( -5.933932666649924137, -9.058645607665452459, 34.76329471203371924 ) ) ;
#83915 = CARTESIAN_POINT ( 'NONE',  ( -15.16470189741915675, -9.905515769479276145, 34.41647553114623292 ) ) ;
#83916 = CARTESIAN_POINT ( 'NONE',  ( 6.000000000000001776, -3.513871655860378418, 32.76840700105978499 ) ) ;
#83917 = ORIENTED_EDGE ( 'NONE', *, *, #68219, .T. ) ;
#83918 = CARTESIAN_POINT ( 'NONE',  ( -9.942330916529147800, -2.985938066672154445, 32.43141759479405550 ) ) ;
#83920 = EDGE_LOOP ( 'NONE', ( #8092, #55356 ) ) ;
#83919 = VECTOR ( 'NONE', #51154, 1000.000000000000000 ) ;
#83923 = ORIENTED_EDGE ( 'NONE', *, *, #62968, .T. ) ;
#83922 = VECTOR ( 'NONE', #79532, 1000.000000000000000 ) ;
#83921 = DIRECTION ( 'NONE',  ( 1.000000000000000000, 0.000000000000000000, 0.000000000000000000 ) ) ;
#83924 = FACE_OUTER_BOUND ( 'NONE', #21640, .T. ) ;
#83925 = CARTESIAN_POINT ( 'NONE',  ( -1.450697763975520083, -12.34228464037088280, 31.77849191805838558 ) ) ;
#83926 = CARTESIAN_POINT ( 'NONE',  ( 7.715463243043537034, -9.929715669179220328, 34.40415004197138416 ) ) ;
#83927 = DIRECTION ( 'NONE',  ( 0.000000000000000000, 0.6427876096865373645, -0.7660444431189797898 ) ) ;
#83929 = DIRECTION ( 'NONE',  ( -0.000000000000000000, -0.000000000000000000, -1.000000000000000000 ) ) ;
#83928 = FACE_OUTER_BOUND ( 'NONE', #9640, .T. ) ;
#83930 = CARTESIAN_POINT ( 'NONE',  ( 14.05771557674995265, -3.627789207965226748, 32.91389620160131102 ) ) ;
#83931 = B_SPLINE_CURVE_WITH_KNOTS ( 'NONE', 3,
 ( #52414, #67720, #53304, #80806, #79900, #46557, #74039, #5573, #74473, #12769 ),
 .UNSPECIFIED., .F., .F.,
 ( 4, 2, 2, 2, 4 ),
 ( 0.000000000000000000, 0.0001954311564186868473, 0.0003908623128373736946, 0.0005862934692560605419, 0.0007817246256747473893 ),
 .UNSPECIFIED. ) ;
#83932 = CARTESIAN_POINT ( 'NONE',  ( 1.799775606325937360E-14, -10.25000000000000000, 22.28125000000000355 ) ) ;
#83933 = VERTEX_POINT ( 'NONE', #37781 ) ;
#83934 = CARTESIAN_POINT ( 'NONE',  ( -0.5276218724943415594, -5.557115091759785130, 34.35708131394839171 ) ) ;
#83935 = ORIENTED_EDGE ( 'NONE', *, *, #27286, .F. ) ;
#83936 = VERTEX_POINT ( 'NONE', #51261 ) ;
#83937 = DIRECTION ( 'NONE',  ( -1.000000000000000000, -0.000000000000000000, -0.000000000000000000 ) ) ;
#83938 = ORIENTED_EDGE ( 'NONE', *, *, #71947, .T. ) ;
#83939 = CARTESIAN_POINT ( 'NONE',  ( -13.38461538461538325, -7.500000000000001776, 35.04278698407183867 ) ) ;
#83940 = CARTESIAN_POINT ( 'NONE',  ( 6.130791807824788719, -11.18335022499818621, 33.13157742990016885 ) ) ;
#83941 = DIRECTION ( 'NONE',  ( -0.000000000000000000, 1.000000000000000000, -0.000000000000000000 ) ) ;
#83942 = CARTESIAN_POINT ( 'NONE',  ( -4.946131269098287930, -3.530189275343204702, 32.79018710029569661 ) ) ;
#83943 = CARTESIAN_POINT ( 'NONE',  ( -13.16160254052199008, -6.460100341425560444, 34.89618726649961644 ) ) ;
#83944 = LINE ( 'NONE', #63648, #6840 ) ;
#83945 = CARTESIAN_POINT ( 'NONE',  ( -4.283993363284374745, -3.817052484675422797, 33.13202310037935661 ) ) ;
#83946 = EDGE_CURVE ( 'NONE', #78414, #10638, #15030, .T. ) ;
#83947 = CYLINDRICAL_SURFACE ( 'NONE', #56337, 0.2500000000000008882 ) ;
#83948 = CARTESIAN_POINT ( 'NONE',  ( 11.40777007179398161, -10.54014554554150607, 33.71984207302941883 ) ) ;
#83949 = VECTOR ( 'NONE', #72429, 1000.000000000000114 ) ;
#83950 = DIRECTION ( 'NONE',  ( -0.000000000000000000, -0.3420201433256694901, -0.9396926207859082059 ) ) ;
#83951 = CARTESIAN_POINT ( 'NONE',  ( -17.14217300869715643, -2.255955759149247175, 30.00000000000014211 ) ) ;
#83952 = ADVANCED_FACE ( 'NONE', ( #71560 ), #30576, .F. ) ;
#83953 = VECTOR ( 'NONE', #35084, 1000.000000000000000 ) ;
#83954 = ADVANCED_FACE ( 'NONE', ( #17521 ), #65247, .F. ) ;
#83955 = VECTOR ( 'NONE', #54163, 1000.000000000000000 ) ;
#83956 = ORIENTED_EDGE ( 'NONE', *, *, #22328, .T. ) ;
#83957 = EDGE_LOOP ( 'NONE', ( #11476, #68327, #17335, #50460 ) ) ;
#83958 = DIRECTION ( 'NONE',  ( -0.000000000000000000, -0.1736481776669307198, -0.9848077530122080203 ) ) ;
#83959 = DIRECTION ( 'NONE',  ( 0.000000000000000000, 0.000000000000000000, 1.000000000000000000 ) ) ;
#83960 = CARTESIAN_POINT ( 'NONE',  ( -3.164700879766792152, -2.721908614388771852, 31.22303859784725333 ) ) ;
#83961 = CARTESIAN_POINT ( 'NONE',  ( 12.59206416330202671, -10.88167719472716399, 33.43325721877153711 ) ) ;
#83962 = VERTEX_POINT ( 'NONE', #3548 ) ;
#83963 = CARTESIAN_POINT ( 'NONE',  ( -8.769230769230768274, -1.951392089020283160, 34.73218667398347748 ) ) ;
#83964 = B_SPLINE_CURVE_WITH_KNOTS ( 'NONE', 3,
 ( #30158, #9011, #77896, #3561, #51275, #36477, #49978, #23389, #78333, #50844 ),
 .UNSPECIFIED., .F., .F.,
 ( 4, 2, 2, 2, 4 ),
 ( 0.000000000000000000, 0.0001954311564186869557, 0.0003908623128373739115, 0.0005862934692560608672, 0.0007817246256747478229 ),
 .UNSPECIFIED. ) ;
#83965 = CARTESIAN_POINT ( 'NONE',  ( -17.32689980786543060, -3.627789207965226304, 32.91389620160131102 ) ) ;
#83966 = ADVANCED_FACE ( 'NONE', ( #86892 ), #58480, .F. ) ;
#83967 = B_SPLINE_CURVE_WITH_KNOTS ( 'NONE', 3,
 ( #45645, #64563, #80336, #72668, #16838, #51945 ),
 .UNSPECIFIED., .F., .F.,
 ( 4, 2, 4 ),
 ( 4.906730591320636874E-17, 0.0001954756301637213293, 0.0003909512603273935984 ),
 .UNSPECIFIED. ) ;
#83968 = CARTESIAN_POINT ( 'NONE',  ( -3.230769230769229949, -12.10708131394839349, 31.69288490824020244 ) ) ;
#83969 = ORIENTED_EDGE ( 'NONE', *, *, #17863, .F. ) ;
#83970 = CARTESIAN_POINT ( 'NONE',  ( 0.5276068125408989173, -5.557115091759786019, 34.35708131394839882 ) ) ;
#83971 = VERTEX_POINT ( 'NONE', #44522 ) ;
#83972 = CARTESIAN_POINT ( 'NONE',  ( 9.942362003946010773, -11.79725096376909654, 32.30694842903959341 ) ) ;
#83973 = CARTESIAN_POINT ( 'NONE',  ( -3.361460697436791989, -12.11776431015576172, 31.66791131148498906 ) ) ;
#83974 = CARTESIAN_POINT ( 'NONE',  ( -1.384615384615506484, -9.528491918059723176, 34.59228464037033035 ) ) ;
#83975 = CARTESIAN_POINT ( 'NONE',  ( -9.627052552794857831, -6.835583212224610072, 34.95778746994559327 ) ) ;
#83976 = CYLINDRICAL_SURFACE ( 'NONE', #45076, 0.2500000000000008882 ) ;
#83977 = EDGE_CURVE ( 'NONE', #37879, #86398, #31109, .T. ) ;
#83978 = VERTEX_POINT ( 'NONE', #24255 ) ;
#83979 = EDGE_CURVE ( 'NONE', #84614, #81205, #2651, .T. ) ;
#83980 = AXIS2_PLACEMENT_3D ( 'NONE', #45546, #58164, #17643 ) ;
#83981 = ORIENTED_EDGE ( 'NONE', *, *, #21192, .T. ) ;
#83982 = ORIENTED_EDGE ( 'NONE', *, *, #54826, .T. ) ;
#83983 = CARTESIAN_POINT ( 'NONE',  ( 13.31853197365950692, -3.050289026998445951, 32.03036669348365706 ) ) ;
#83984 = CARTESIAN_POINT ( 'NONE',  ( 15.90382292962469535, -5.765609946408405406, 34.70566812827424741 ) ) ;
#83985 = LINE ( 'NONE', #64557, #79683 ) ;
#83986 = CARTESIAN_POINT ( 'NONE',  ( 16.82689985270161870, -10.18141759479407327, 34.26406193332782379 ) ) ;
#83987 = CARTESIAN_POINT ( 'NONE',  ( 4.219101725122176738, -6.879047030191282275, 34.71129190930002295 ) ) ;
#83988 = DIRECTION ( 'NONE',  ( -1.000000000000000000, 0.000000000000000000, 0.000000000000000000 ) ) ;
#83989 = ORIENTED_EDGE ( 'NONE', *, *, #9308, .F. ) ;
#83990 = EDGE_LOOP ( 'NONE', ( #19532, #49057 ) ) ;
#83991 = ORIENTED_EDGE ( 'NONE', *, *, #35036, .T. ) ;
#83993 = ORIENTED_EDGE ( 'NONE', *, *, #36130, .F. ) ;
#83992 = CARTESIAN_POINT ( 'NONE',  ( -3.099977422944443894, -10.54018710029568595, 33.71981072465678864 ) ) ;
#83995 = CARTESIAN_POINT ( 'NONE',  ( 13.51540582558234149, -3.957578996910242619, 33.62503395064540257 ) ) ;
#83994 = CARTESIAN_POINT ( 'NONE',  ( 0.4615384615384611200, -8.120952969808772792, 34.71129190930000163 ) ) ;
#83996 = B_SPLINE_CURVE_WITH_KNOTS ( 'NONE', 3,
 ( #62063, #29187, #14775, #42252, #70598, #62493, #27839, #28275, #55302, #55745 ),
 .UNSPECIFIED., .F., .F.,
 ( 4, 2, 2, 2, 4 ),
 ( 0.0007817246256747499913, 0.0009771112852218944052, 0.001172497944769038819, 0.001367884604316183016, 0.001563271263863327430 ),
 .UNSPECIFIED. ) ;
#83997 = CARTESIAN_POINT ( 'NONE',  ( 2.651650429449569302, -10.15165042944953733, 24.62500000000000000 ) ) ;
#83998 = EDGE_LOOP ( 'NONE', ( #86566, #50880 ) ) ;
#83999 = VECTOR ( 'NONE', #18034, 1000.000000000000227 ) ;
#84000 = EDGE_CURVE ( 'NONE', #63608, #30358, #40470, .T. ) ;
#84001 = EDGE_CURVE ( 'NONE', #88762, #5458, #20619, .T. ) ;
#84002 = ORIENTED_EDGE ( 'NONE', *, *, #87785, .T. ) ;
#84003 = CARTESIAN_POINT ( 'NONE',  ( -18.00000000000000000, -1.270656007487078965, 33.34651343095210052 ) ) ;
#84004 = VECTOR ( 'NONE', #11843, 1000.000000000000000 ) ;
#84006 = ADVANCED_FACE ( 'NONE', ( #32811 ), #54403, .F. ) ;
#84005 = EDGE_LOOP ( 'NONE', ( #79102, #54252, #3769, #78146 ) ) ;
#84007 = FACE_BOUND ( 'NONE', #81103, .T. ) ;
#84008 = CARTESIAN_POINT ( 'NONE',  ( 6.923076923076802558, -4.481592998941358097, 33.73612834414048933 ) ) ;
#84009 = VECTOR ( 'NONE', #63372, 1000.000000000000000 ) ;
#84010 = PLANE ( 'NONE',  #64957 ) ;
#84011 = ORIENTED_EDGE ( 'NONE', *, *, #9799, .T. ) ;
#84012 = CARTESIAN_POINT ( 'NONE',  ( 2.307692307692309264, -8.120952969808772792, 34.71129190930000163 ) ) ;
#84014 = EDGE_CURVE ( 'NONE', #78118, #65478, #81897, .T. ) ;
#84013 = CARTESIAN_POINT ( 'NONE',  ( 3.453780582382079523, -3.105924265160262543, 32.13625925475356127 ) ) ;
#84015 = CARTESIAN_POINT ( 'NONE',  ( 23.49999999999998579, 1.250000000000000666, 30.36437827766148345 ) ) ;
#84016 = CARTESIAN_POINT ( 'NONE',  ( 3.930361210122207183, -11.41268669641500466, 32.86336882939237825 ) ) ;
#84017 = CARTESIAN_POINT ( 'NONE',  ( 4.376625695114563008, -3.236590943229499029, 32.36255958852954251 ) ) ;
#84018 = VERTEX_POINT ( 'NONE', #12984 ) ;
#84019 = EDGE_CURVE ( 'NONE', #6434, #13761, #4153, .T. ) ;
#84020 = CARTESIAN_POINT ( 'NONE',  ( -0.5921481167425443060, -7.722926974430166069, 34.99546784045485737 ) ) ;
#84021 = CARTESIAN_POINT ( 'NONE',  ( 3.361561038594018225, -4.118422570099827595, 33.43335022499816489 ) ) ;
#84022 = PLANE ( 'NONE',  #78665 ) ;
#84023 = CARTESIAN_POINT ( 'NONE',  ( 5.750023269057646047, -4.943428324936578910, 34.04746400365624481 ) ) ;
#84024 = CARTESIAN_POINT ( 'NONE',  ( -10.61538461538461320, -13.04860791097971706, 34.73218667398347037 ) ) ;
#84025 = CARTESIAN_POINT ( 'NONE',  ( -13.31936024510254413, -12.51329471203373700, 31.30864560766537963 ) ) ;
#84027 = CARTESIAN_POINT ( 'NONE',  ( 11.31563344082666411, -7.369209533119137845, 34.99857337881830688 ) ) ;
#84026 = CARTESIAN_POINT ( 'NONE',  ( -6.857009589726848375, -12.62096338111211757, 30.90682066428152908 ) ) ;
#84028 = CARTESIAN_POINT ( 'NONE',  ( 5.299935921016468932, -2.308499170217967134, 30.53291367094873721 ) ) ;
#84030 = CARTESIAN_POINT ( 'NONE',  ( 2.557746727605761272, -6.523592122091589118, 34.90882529074906415 ) ) ;
#84029 = DIRECTION ( 'NONE',  ( -0.7057856980126718804, -0.7057856980126787638, -0.06109907496453170772 ) ) ;
#84031 = ADVANCED_FACE ( 'NONE', ( #66600 ), #67931, .F. ) ;
#84032 = CARTESIAN_POINT ( 'NONE',  ( 17.07692307692307665, -2.249999999999998668, 29.50000000000001421 ) ) ;
#84033 = CARTESIAN_POINT ( 'NONE',  ( -0.06109907496454585613, -4.750000000000000000, 21.40438170625849068 ) ) ;
#84034 = VERTEX_POINT ( 'NONE', #25607 ) ;
#84035 = LINE ( 'NONE', #83595, #7348 ) ;
#84036 = ORIENTED_EDGE ( 'NONE', *, *, #71397, .T. ) ;
#84037 = CARTESIAN_POINT ( 'NONE',  ( -6.000000000000119904, -11.94971097300221174, 32.03036669348237098 ) ) ;
#84038 = EDGE_CURVE ( 'NONE', #84195, #74179, #11658, .T. ) ;
#84039 = ORIENTED_EDGE ( 'NONE', *, *, #25171, .T. ) ;
#84040 = CARTESIAN_POINT ( 'NONE',  ( 8.769230769230768274, -2.499999999999998668, 29.50000000000001066 ) ) ;
#84041 = FACE_OUTER_BOUND ( 'NONE', #11576, .T. ) ;
#84042 = ORIENTED_EDGE ( 'NONE', *, *, #15238, .T. ) ;
#84043 = CARTESIAN_POINT ( 'NONE',  ( -18.25002323729296450, -12.43535235679832596, 30.55408501211184813 ) ) ;
#84044 = CARTESIAN_POINT ( 'NONE',  ( -0.06109907496454585613, -4.750000000000000000, 23.90438170625849068 ) ) ;
#84045 = DIRECTION ( 'NONE',  ( -0.000000000000000000, -0.1736481776669307198, -0.9848077530122080203 ) ) ;
#84046 = CARTESIAN_POINT ( 'NONE',  ( -3.903846153846152855, -2.249999999999998668, 29.75000000000000355 ) ) ;
#84047 = CARTESIAN_POINT ( 'NONE',  ( 6.988332494352947677, -9.442884908240271713, 34.35708131394835618 ) ) ;
#84048 = AXIS2_PLACEMENT_3D ( 'NONE', #86236, #72698, #25406 ) ;
#84049 = CARTESIAN_POINT ( 'NONE',  ( -5.326946314216043810, -12.43535235679832596, 30.55408501211184813 ) ) ;
#84050 = CARTESIAN_POINT ( 'NONE',  ( 11.53846153846153832, -2.721908614388771852, 31.22303859784724978 ) ) ;
#84051 = CARTESIAN_POINT ( 'NONE',  ( -13.60754234352223158, -11.98009711892699514, 32.48740034544076138 ) ) ;
#84052 = CARTESIAN_POINT ( 'NONE',  ( -1.553300858899081538, -11.25000000000000711, 18.60937500000000355 ) ) ;
#84053 = EDGE_CURVE ( 'NONE', #30988, #18603, #36391, .T. ) ;
#84054 = CARTESIAN_POINT ( 'NONE',  ( -18.00000000000000000, -2.533126527117917082, 35.28035834855298702 ) ) ;
#84055 = CARTESIAN_POINT ( 'NONE',  ( -6.250023224221457063, -3.520140089381497361, 33.17453946501458262 ) ) ;
#84056 = DIRECTION ( 'NONE',  ( 0.000000000000000000, -0.000000000000000000, 1.000000000000000000 ) ) ;
#84057 = B_SPLINE_CURVE_WITH_KNOTS ( 'NONE', 3,
 ( #1764, #15291, #22481, #884, #49065, #56707, #1324, #50382, #28811, #83757 ),
 .UNSPECIFIED., .F., .F.,
 ( 4, 2, 2, 2, 4 ),
 ( 0.000000000000000000, 0.0001954311564186868202, 0.0003908623128373736404, 0.0005862934692560604335, 0.0007817246256747472808 ),
 .UNSPECIFIED. ) ;
#84058 = CARTESIAN_POINT ( 'NONE',  ( 3.750000000000000888, -7.499999999999978684, 15.71875000000000000 ) ) ;
#84059 = EDGE_CURVE ( 'NONE', #40946, #24532, #17327, .T. ) ;
#84060 = DIRECTION ( 'NONE',  ( 0.000000000000000000, 1.000000000000000000, 0.000000000000000000 ) ) ;
#84061 = VERTEX_POINT ( 'NONE', #68365 ) ;
#84062 = CARTESIAN_POINT ( 'NONE',  ( 14.43821800945587697, -2.619367082507849442, 30.83698974864643461 ) ) ;
#84063 = DIRECTION ( 'NONE',  ( 0.000000000000000000, 0.1736481776669267785, -0.9848077530122087975 ) ) ;
#84064 = CARTESIAN_POINT ( 'NONE',  ( -8.899377978668987055, -11.47017969459904130, 32.78971311882034456 ) ) ;
#84065 = CARTESIAN_POINT ( 'NONE',  ( -14.37296275365308418, -11.94971097300153140, 32.03036669348370680 ) ) ;
#84066 = CARTESIAN_POINT ( 'NONE',  ( 13.63456090296352841, -2.587454068350148351, 30.68340429815432202 ) ) ;
#84067 = CARTESIAN_POINT ( 'NONE',  ( -14.24243716817946925, -4.320704448112861584, 33.92786785259548310 ) ) ;
#84068 = ADVANCED_FACE ( 'NONE', ( #80570 ), #61603, .T. ) ;
#84069 = CYLINDRICAL_SURFACE ( 'NONE', #14529, 0.2499999999999994726 ) ;
#84070 = EDGE_CURVE ( 'NONE', #29793, #4115, #24574, .T. ) ;
#84071 = ORIENTED_EDGE ( 'NONE', *, *, #27358, .F. ) ;
#84072 = ORIENTED_EDGE ( 'NONE', *, *, #71397, .F. ) ;
#84074 = VECTOR ( 'NONE', #57579, 1000.000000000000114 ) ;
#84073 = B_SPLINE_CURVE_WITH_KNOTS ( 'NONE', 3,
 ( #18227, #45688, #73169, #11466, #38950, #66408, #5927, #81589, #6802, #55 ),
 .UNSPECIFIED., .F., .F.,
 ( 4, 2, 2, 2, 4 ),
 ( 0.0007817246256747446788, 0.0009771112852218874663, 0.001172497944769030145, 0.001367884604316172825, 0.001563271263863315720 ),
 .UNSPECIFIED. ) ;
#84075 = ORIENTED_EDGE ( 'NONE', *, *, #15382, .T. ) ;
#84076 = AXIS2_PLACEMENT_3D ( 'NONE', #23270, #36358, #29601 ) ;
#84077 = CARTESIAN_POINT ( 'NONE',  ( -9.469528151039281028, -3.236590943229499029, 32.36255958852954251 ) ) ;
#84078 = CARTESIAN_POINT ( 'NONE',  ( 8.769230769230768274, -12.37446782046654192, 30.86335684631486131 ) ) ;
#84079 = CARTESIAN_POINT ( 'NONE',  ( 6.857806922520603976, -3.083524468853724443, 32.58852847137143272 ) ) ;
#84080 = LINE ( 'NONE', #9728, #26363 ) ;
#84081 = CARTESIAN_POINT ( 'NONE',  ( 17.93391658904412012, -8.973038597847269315, 34.52809138561120506 ) ) ;
#84082 = EDGE_CURVE ( 'NONE', #49317, #27628, #77212, .T. ) ;
#84083 = EDGE_LOOP ( 'NONE', ( #23033, #13732, #21037, #80067 ) ) ;
#84084 = EDGE_CURVE ( 'NONE', #31229, #4299, #15967, .T. ) ;
#84085 = LINE ( 'NONE', #21475, #44895 ) ;
#84086 = EDGE_LOOP ( 'NONE', ( #69180, #53747 ) ) ;
#84087 = ORIENTED_EDGE ( 'NONE', *, *, #54957, .F. ) ;
#84089 = ORIENTED_EDGE ( 'NONE', *, *, #47485, .F. ) ;
#84088 = CARTESIAN_POINT ( 'NONE',  ( 4.403900573759605308, -12.41089969410671223, 31.60739465890703670 ) ) ;
#84090 = CARTESIAN_POINT ( 'NONE',  ( -13.38461538461538325, -11.16473453929635440, 33.15142922261926373 ) ) ;
#84091 = B_SPLINE_CURVE_WITH_KNOTS ( 'NONE', 3,
 ( #48745, #88004, #68577, #124, #76214, #41551, #7330, #7768, #26265, #81218 ),
 .UNSPECIFIED., .F., .F.,
 ( 4, 2, 2, 2, 4 ),
 ( 0.0007817359430256392216, 0.0009771253907250078159, 0.001172514838424376302, 0.001367904286123745004, 0.001563293733823113490 ),
 .UNSPECIFIED. ) ;
#84092 = CARTESIAN_POINT ( 'NONE',  ( -10.74607608205217346, -4.809359713505814149, 33.96456829005828837 ) ) ;
#84093 = CARTESIAN_POINT ( 'NONE',  ( -21.00000000000000355, -2.249999999999999556, 27.25000000000000000 ) ) ;
#84094 = CARTESIAN_POINT ( 'NONE',  ( -15.90379173393269596, -5.642605341092955307, 34.66089969410670335 ) ) ;
#84095 = VERTEX_POINT ( 'NONE', #48524 ) ;
#84096 = ORIENTED_EDGE ( 'NONE', *, *, #73270, .T. ) ;
#84097 = ORIENTED_EDGE ( 'NONE', *, *, #54725, .T. ) ;
#84098 = CARTESIAN_POINT ( 'NONE',  ( -6.923076923077045919, -3.083524468854526912, 32.58852847137268327 ) ) ;
#84100 = ORIENTED_EDGE ( 'NONE', *, *, #52499, .T. ) ;
#84099 = CARTESIAN_POINT ( 'NONE',  ( 11.66898697669518725, -5.915461855592780260, 34.75538340440931506 ) ) ;
#84101 = CARTESIAN_POINT ( 'NONE',  ( -8.769230769230768274, -1.367168528481310208, 33.57946703557072254 ) ) ;
#84102 = LINE ( 'NONE', #84541, #60414 ) ;
#84103 = CARTESIAN_POINT ( 'NONE',  ( -3.164700879766790820, -9.780366693483667717, 34.19971097300155805 ) ) ;
#84104 = ORIENTED_EDGE ( 'NONE', *, *, #9178, .T. ) ;
#84105 = CARTESIAN_POINT ( 'NONE',  ( -11.53846153846153655, -4.786620604624113540, 33.94971097300155094 ) ) ;
#84106 = DIRECTION ( 'NONE',  ( -0.000000000000000000, 0.000000000000000000, 1.000000000000000000 ) ) ;
#84107 = VERTEX_POINT ( 'NONE', #41795 ) ;
#84108 = FACE_BOUND ( 'NONE', #9580, .T. ) ;
#84109 = CARTESIAN_POINT ( 'NONE',  ( -11.53846153846153655, -11.35647404775217417, 33.31231777344666511 ) ) ;
#84110 = CARTESIAN_POINT ( 'NONE',  ( 13.51514082284903040, -6.808710257144161559, 34.95449254468098843 ) ) ;
#84111 = DIRECTION ( 'NONE',  ( -0.000000000000000000, 0.7660444431189791237, -0.6427876096865379196 ) ) ;
#84113 = CARTESIAN_POINT ( 'NONE',  ( 15.10020931715586556, -2.254533558242299396, 29.97296025877828285 ) ) ;
#84112 = CARTESIAN_POINT ( 'NONE',  ( 7.846153846153723244, -11.06231777344772027, 33.60647404775119895 ) ) ;
#84114 = DIRECTION ( 'NONE',  ( 0.000000000000000000, 0.3420201433256610524, 0.9396926207859113145 ) ) ;
#84115 = CARTESIAN_POINT ( 'NONE',  ( 14.55774672760575861, -2.318338780012835443, 30.59689888758630261 ) ) ;
#84116 = VERTEX_POINT ( 'NONE', #41343 ) ;
#84118 = EDGE_CURVE ( 'NONE', #85950, #25790, #15205, .T. ) ;
#84117 = CARTESIAN_POINT ( 'NONE',  ( -4.153846153846274980, -2.379036618888197729, 30.90682066428292885 ) ) ;
#84119 = CARTESIAN_POINT ( 'NONE',  ( -6.066082379360133281, -11.35647404775217595, 33.31231777344666511 ) ) ;
#84120 = ORIENTED_EDGE ( 'NONE', *, *, #29686, .T. ) ;
#84121 = B_SPLINE_CURVE_WITH_KNOTS ( 'NONE', 3,
 ( #24953, #65932, #24505, #9664, #65036, #86235, #3347, #51509, #85780, #31724 ),
 .UNSPECIFIED., .F., .F.,
 ( 4, 2, 2, 2, 4 ),
 ( 0.000000000000000000, 0.0001954311564186871184, 0.0003908623128373742367, 0.0005862934692560614093, 0.0007817246256747484735 ),
 .UNSPECIFIED. ) ;
#84122 = EDGE_CURVE ( 'NONE', #67157, #44863, #62919, .T. ) ;
#84123 = B_SPLINE_CURVE_WITH_KNOTS ( 'NONE', 3,
 ( #64225, #10189, #57478, #37204, #83650, #15619, #21931, #23248, #49405, #23688 ),
 .UNSPECIFIED., .F., .F.,
 ( 4, 2, 2, 2, 4 ),
 ( 0.000000000000000000, 0.0001954339857564078809, 0.0003908679715128157619, 0.0005863019572692236428, 0.0007817359430256315238 ),
 .UNSPECIFIED. ) ;
#84124 = CARTESIAN_POINT ( 'NONE',  ( -2.307692307692305711, -1.242168528481310874, 33.36296068462461051 ) ) ;
#84125 = B_SPLINE_CURVE_WITH_KNOTS ( 'NONE', 3,
 ( #39530, #18355, #87274, #61543, #67429, #59776, #66989, #47143, #66542, #81397 ),
 .UNSPECIFIED., .F., .F.,
 ( 4, 2, 2, 2, 4 ),
 ( 0.000000000000000000, 0.0001954311564186870371, 0.0003908623128373740741, 0.0005862934692560610840, 0.0007817246256747481482 ),
 .UNSPECIFIED. ) ;
#84126 = DIRECTION ( 'NONE',  ( -0.000000000000000000, 0.9848077530122085754, -0.1736481776669273613 ) ) ;
#84127 = CARTESIAN_POINT ( 'NONE',  ( 16.15384615384603251, -6.835583212225970762, 34.95778746994575670 ) ) ;
#84128 = CARTESIAN_POINT ( 'NONE',  ( -7.846153846153967493, -11.06231777344772027, 33.60647404775119895 ) ) ;
#84129 = B_SPLINE_CURVE_WITH_KNOTS ( 'NONE', 3,
 ( #77000, #84648, #8987, #2206, #56717, #58037, #85522, #49952, #29699, #15300 ),
 .UNSPECIFIED., .F., .F.,
 ( 4, 2, 2, 2, 4 ),
 ( 0.000000000000000000, 0.0001954311564186862510, 0.0003908623128373725020, 0.0005862934692560588072, 0.0007817246256747450040 ),
 .UNSPECIFIED. ) ;
#84130 = CARTESIAN_POINT ( 'NONE',  ( -0.2115929431903194047, -12.43552623307873972, 30.55307653245132826 ) ) ;
#84131 = CARTESIAN_POINT ( 'NONE',  ( -4.403869378067608586, -2.341070481393820124, 30.72580821765574299 ) ) ;
#84132 = AXIS2_PLACEMENT_3D ( 'NONE', #26161, #6348, #5453 ) ;
#84133 = FACE_BOUND ( 'NONE', #22490, .T. ) ;
#84135 = DIRECTION ( 'NONE',  ( -1.000000000000000000, -0.000000000000000000, 0.000000000000000000 ) ) ;
#84134 = CARTESIAN_POINT ( 'NONE',  ( -2.438383774359863754, -6.413092428213692742, 34.63065189839063152 ) ) ;
#84136 = CARTESIAN_POINT ( 'NONE',  ( -15.90390063549801347, -2.587454068350149239, 30.68340429815432557 ) ) ;
#84138 = DIRECTION ( 'NONE',  ( 0.000000000000000000, 0.7660444431189822323, -0.6427876096865344779 ) ) ;
#84137 = CARTESIAN_POINT ( 'NONE',  ( -17.77722045873158763, -11.41317474335729543, 32.86274602512330034 ) ) ;
#84139 = ADVANCED_FACE ( 'NONE', ( #62479 ), #35020, .T. ) ;
#84140 = DIRECTION ( 'NONE',  ( -0.000000000000000000, -0.8660254037844399289, -0.4999999999999980016 ) ) ;
#84141 = CARTESIAN_POINT ( 'NONE',  ( 1.492201783934554493, -3.724691934501233703, 20.23250670625849423 ) ) ;
#84142 = VERTEX_POINT ( 'NONE', #69694 ) ;
#84143 = EDGE_LOOP ( 'NONE', ( #24152, #69319, #30115, #40392 ) ) ;
#84144 = AXIS2_PLACEMENT_3D ( 'NONE', #57879, #21546, #85364 ) ;
#84145 = CARTESIAN_POINT ( 'NONE',  ( -9.469296340694842939, -11.76359900205217457, 32.36225158514719880 ) ) ;
#84146 = CARTESIAN_POINT ( 'NONE',  ( -15.48074597481782178, -5.643011162660950042, 34.66104346484419096 ) ) ;
#84147 = CYLINDRICAL_SURFACE ( 'NONE', #56040, 0.2499999999999979738 ) ;
#84148 = CARTESIAN_POINT ( 'NONE',  ( -1.608100328339332696, -3.236172620538810385, 32.36188796281390267 ) ) ;
#84149 = CARTESIAN_POINT ( 'NONE',  ( -4.023320715612510590, -3.068774925481847493, 32.56582465632704526 ) ) ;
#84150 = CARTESIAN_POINT ( 'NONE',  ( -1.492201783934549164, -11.27530806549876807, 20.85750670625849068 ) ) ;
#84151 = CARTESIAN_POINT ( 'NONE',  ( -12.68502338610279523, -4.225889041578353655, 33.85425143139329407 ) ) ;
#84152 = CARTESIAN_POINT ( 'NONE',  ( 17.99999999999987566, -3.300289026999228437, 32.46337939537709616 ) ) ;
#84153 = ADVANCED_FACE ( 'NONE', ( #35918 ), #22830, .F. ) ;
#84154 = CARTESIAN_POINT ( 'NONE',  ( -0.4615384615384611200, -3.322132147404559976, 32.92929555188717927 ) ) ;
#84155 = CARTESIAN_POINT ( 'NONE',  ( -1.384615384615383471, -12.37446782046654192, 30.86335684631486131 ) ) ;
#84156 = CYLINDRICAL_SURFACE ( 'NONE', #29570, 0.2499999999999986955 ) ;
#84157 = DIRECTION ( 'NONE',  ( -0.000000000000000000, -0.7660444431189791237, -0.6427876096865379196 ) ) ;
#84158 = CARTESIAN_POINT ( 'NONE',  ( 12.46153846153833911, -2.379036618888197729, 30.90682066428292885 ) ) ;
#84159 = CARTESIAN_POINT ( 'NONE',  ( 7.976679547917409963, -6.852161475712352789, 34.70806712695775786 ) ) ;
#84160 = ORIENTED_EDGE ( 'NONE', *, *, #82044, .F. ) ;
#84161 = CARTESIAN_POINT ( 'NONE',  ( 12.39545608217832395, -3.937682226553330445, 33.60647404775217240 ) ) ;
#84162 = CARTESIAN_POINT ( 'NONE',  ( 0.6843180028068690524, -2.600157965045226227, 30.74683119005207743 ) ) ;
#84163 = CARTESIAN_POINT ( 'NONE',  ( 1.987747218494642309, -5.598659921968629050, 23.31436829374150932 ) ) ;
#84164 = EDGE_CURVE ( 'NONE', #38465, #31293, #70584, .T. ) ;
#84165 = B_SPLINE_CURVE_WITH_KNOTS ( 'NONE', 3,
 ( #71465, #17872, #58841, #10667, #78227, #65592 ),
 .UNSPECIFIED., .F., .F.,
 ( 4, 2, 4 ),
 ( 0.000000000000000000, 0.0001954784845028902692, 0.0003909569690057805385 ),
 .UNSPECIFIED. ) ;
#84166 = CARTESIAN_POINT ( 'NONE',  ( -2.438382910802614933, -4.684245665217971144, 34.18127051446801090 ) ) ;
#84167 = CARTESIAN_POINT ( 'NONE',  ( -16.02332071561251325, -2.647132371071621471, 31.75357179365173010 ) ) ;
#84168 = VERTEX_POINT ( 'NONE', #1682 ) ;
#84169 = CARTESIAN_POINT ( 'NONE',  ( -9.822455662039390134, -5.915902021225889484, 34.75552854090298638 ) ) ;
#84171 = ORIENTED_EDGE ( 'NONE', *, *, #81621, .F. ) ;
#84170 = CARTESIAN_POINT ( 'NONE',  ( -16.15384615384615330, -10.51840700105979565, 33.73612834413961536 ) ) ;
#84172 = CARTESIAN_POINT ( 'NONE',  ( 7.146088274689773812, -3.587049720035815348, 32.86302985866382897 ) ) ;
#84173 = EDGE_CURVE ( 'NONE', #75262, #85639, #56626, .T. ) ;
#84174 = CARTESIAN_POINT ( 'NONE',  ( -5.076923076923197442, -10.21337939537710326, 33.94971097300076224 ) ) ;
#84175 = VERTEX_POINT ( 'NONE', #75560 ) ;
#84176 = LINE ( 'NONE', #22889, #10324 ) ;
#84177 = VECTOR ( 'NONE', #8039, 1000.000000000000000 ) ;
#84178 = CARTESIAN_POINT ( 'NONE',  ( 6.923076923076800782, -5.941354392335915335, 34.76329471203413846 ) ) ;
#84179 = VERTEX_POINT ( 'NONE', #34584 ) ;
#84180 = CARTESIAN_POINT ( 'NONE',  ( -4.153846153846152411, -1.466349020453238561, 30.81389545987213907 ) ) ;
#84181 = CARTESIAN_POINT ( 'NONE',  ( -16.08777780284371772, -3.050289026998446840, 32.03036669348366416 ) ) ;
#84182 = ADVANCED_FACE ( 'NONE', ( #49428 ), #28714, .F. ) ;
#84183 = CARTESIAN_POINT ( 'NONE',  ( 12.52760579488853665, -11.91647553114624358, 32.58852847137148245 ) ) ;
#84184 = ORIENTED_EDGE ( 'NONE', *, *, #16463, .F. ) ;
#84185 = EDGE_LOOP ( 'NONE', ( #32109, #5311, #39058, #28265 ) ) ;
#84186 = ORIENTED_EDGE ( 'NONE', *, *, #31459, .T. ) ;
#84187 = CARTESIAN_POINT ( 'NONE',  ( -7.173053667125516952, -2.318417181685854978, 30.59732222474233865 ) ) ;
#84188 = DIRECTION ( 'NONE',  ( 1.000000000000000000, 0.000000000000000000, 0.000000000000000000 ) ) ;
#84189 = CARTESIAN_POINT ( 'NONE',  ( 15.23076923076923173, -9.058645607665452459, 34.76329471203371924 ) ) ;
#84190 = EDGE_CURVE ( 'NONE', #34444, #45063, #83673, .T. ) ;
#84191 = B_SPLINE_CURVE_WITH_KNOTS ( 'NONE', 3,
 ( #51610, #36792, #71901, #79107, #24155, #57945, #2117, #17412, #23706, #50286 ),
 .UNSPECIFIED., .F., .F.,
 ( 4, 2, 2, 2, 4 ),
 ( 0.0007817246256747442451, 0.0009771112852218865989, 0.001172497944769029061, 0.001367884604316171523, 0.001563271263863313986 ),
 .UNSPECIFIED. ) ;
#84192 = LINE ( 'NONE', #49054, #88092 ) ;
#84193 = EDGE_CURVE ( 'NONE', #10767, #73377, #40710, .T. ) ;
#84194 = EDGE_CURVE ( 'NONE', #77626, #34382, #20279, .T. ) ;
#84195 = VERTEX_POINT ( 'NONE', #9333 ) ;
#84196 = ORIENTED_EDGE ( 'NONE', *, *, #21548, .F. ) ;
#84198 = ORIENTED_EDGE ( 'NONE', *, *, #87629, .F. ) ;
#84197 = DIRECTION ( 'NONE',  ( -0.000000000000000000, 0.6427876096865404731, -0.7660444431189770143 ) ) ;
#84199 = EDGE_CURVE ( 'NONE', #30802, #87033, #16082, .T. ) ;
#84200 = EDGE_CURVE ( 'NONE', #20277, #17317, #10214, .T. ) ;
#84201 = CARTESIAN_POINT ( 'NONE',  ( 17.32686859527121470, -5.057305518903949526, 34.11320923018887896 ) ) ;
#84202 = ORIENTED_EDGE ( 'NONE', *, *, #76748, .F. ) ;
#84203 = LINE ( 'NONE', #7648, #40676 ) ;
#84204 = CARTESIAN_POINT ( 'NONE',  ( 19.00000000000000000, 9.000000000000001776, 2.172175482962262779E-15 ) ) ;
#84205 = VECTOR ( 'NONE', #7088, 1000.000000000000227 ) ;
#84206 = ORIENTED_EDGE ( 'NONE', *, *, #69441, .T. ) ;
#84207 = CARTESIAN_POINT ( 'NONE',  ( 5.999999999999878320, -6.835583212225970762, 34.95778746994575670 ) ) ;
#84208 = ORIENTED_EDGE ( 'NONE', *, *, #70263, .T. ) ;
#84210 = ORIENTED_EDGE ( 'NONE', *, *, #20076, .F. ) ;
#84209 = CARTESIAN_POINT ( 'NONE',  ( -6.700297381808513641, -11.41317474335729187, 32.86274602512330034 ) ) ;
#84211 = CARTESIAN_POINT ( 'NONE',  ( -0.7115151924808159611, -10.66389620160130036, 33.62221079203477103 ) ) ;
#84212 = DIRECTION ( 'NONE',  ( 0.000000000000000000, 0.000000000000000000, 1.000000000000000000 ) ) ;
#84213 = EDGE_LOOP ( 'NONE', ( #23579, #32173 ) ) ;
#84214 = DIRECTION ( 'NONE',  ( 0.000000000000000000, 0.4999999999999985567, 0.8660254037844395958 ) ) ;
#84215 = CARTESIAN_POINT ( 'NONE',  ( -8.769230769230890843, -8.613356846316285953, 34.62446782046622218 ) ) ;
#84216 = DIRECTION ( 'NONE',  ( -0.000000000000000000, 0.5000000000000011102, -0.8660254037844380415 ) ) ;
#84217 = B_SPLINE_CURVE_WITH_KNOTS ( 'NONE', 3,
 ( #50274, #37216, #51151, #69680, #30462, #71011, #9320, #63362, #62905, #49844 ),
 .UNSPECIFIED., .F., .F.,
 ( 4, 2, 2, 2, 4 ),
 ( 0.000000000000000000, 0.0001954339857564080707, 0.0003908679715128161414, 0.0005863019572692241849, 0.0007817359430256322827 ),
 .UNSPECIFIED. ) ;
#84218 = FACE_BOUND ( 'NONE', #37808, .T. ) ;
#84219 = CARTESIAN_POINT ( 'NONE',  ( -9.561517251340742263, -3.957578996910242619, 33.62503395064540257 ) ) ;
#84220 = CARTESIAN_POINT ( 'NONE',  ( -18.00000000000000000, -2.538708090699994813, 30.37095296980875858 ) ) ;
#84221 = B_SPLINE_CURVE_WITH_KNOTS ( 'NONE', 3,
 ( #33087, #53355, #32211, #74519, #59668, #87168 ),
 .UNSPECIFIED., .F., .F.,
 ( 4, 2, 4 ),
 ( 0.0003909512603273747875, 0.0005862562993132002616, 0.0007815613382990257898 ),
 .UNSPECIFIED. ) ;
#84222 = CARTESIAN_POINT ( 'NONE',  ( 8.769230769230647482, -2.625532179533778709, 30.86335684631627174 ) ) ;
#84224 = CARTESIAN_POINT ( 'NONE',  ( -5.750054481651858396, -2.824170634883622188, 31.52227843825338738 ) ) ;
#84223 = CARTESIAN_POINT ( 'NONE',  ( 4.230769230769229061, -7.500000000000000000, 29.75000000000000355 ) ) ;
#84225 = CARTESIAN_POINT ( 'NONE',  ( -11.31568199719312773, -3.236590943229499029, 32.36255958852954251 ) ) ;
#84226 = DIRECTION ( 'NONE',  ( 0.000000000000000000, 0.9848077530122072432, 0.1736481776669354937 ) ) ;
#84227 = VERTEX_POINT ( 'NONE', #50287 ) ;
#84228 = CARTESIAN_POINT ( 'NONE',  ( -6.065250990161240807, -2.506253911140460477, 30.00000000000013856 ) ) ;
#84229 = ORIENTED_EDGE ( 'NONE', *, *, #36555, .F. ) ;
#84230 = ORIENTED_EDGE ( 'NONE', *, *, #30968, .F. ) ;
#84231 = AXIS2_PLACEMENT_3D ( 'NONE', #18024, #74297, #86495 ) ;
#84233 = CARTESIAN_POINT ( 'NONE',  ( -3.454254155333559950, -5.827078755546623690, 34.72654668319379567 ) ) ;
#84232 = CARTESIAN_POINT ( 'NONE',  ( 14.53070365930516061, -3.587049720035815348, 32.86302985866382897 ) ) ;
#84234 = CARTESIAN_POINT ( 'NONE',  ( 16.15384615384603251, -9.442884908241554243, 34.35708131394783038 ) ) ;
#84235 = LINE ( 'NONE', #62168, #23580 ) ;
#84236 = DIRECTION ( 'NONE',  ( -0.000000000000000000, 0.1736481776669307198, -0.9848077530122080203 ) ) ;
#84237 = CARTESIAN_POINT ( 'NONE',  ( -3.903900744468109973, -3.520799739797214389, 33.17531984108286025 ) ) ;
#84238 = VERTEX_POINT ( 'NONE', #65138 ) ;
#84239 = CARTESIAN_POINT ( 'NONE',  ( 11.47237915910140771, -3.322132147404559532, 32.92929555188719348 ) ) ;
#84240 = DIRECTION ( 'NONE',  ( 0.000000000000000000, 0.6427876096865368094, 0.7660444431189802339 ) ) ;
#84241 = CARTESIAN_POINT ( 'NONE',  ( -10.36533030374629583, -9.943054286541403997, 34.11300777759954883 ) ) ;
#84242 = CARTESIAN_POINT ( 'NONE',  ( 15.45354889974729318, -12.47679350104403007, 31.42216943046555855 ) ) ;
#84243 = CARTESIAN_POINT ( 'NONE',  ( 2.557637717070351258, -5.766571408460171355, 34.70601412856602508 ) ) ;
#84244 = CARTESIAN_POINT ( 'NONE',  ( -3.750000000000008438, -5.946699141100917352, 15.17187500000000000 ) ) ;
#84245 = VERTEX_POINT ( 'NONE', #2994 ) ;
#84246 = B_SPLINE_CURVE_WITH_KNOTS ( 'NONE', 3,
 ( #89017, #19646, #20093, #46676, #7017, #88138, #20965, #40815, #75475, #7473 ),
 .UNSPECIFIED., .F., .F.,
 ( 4, 2, 2, 2, 4 ),
 ( 0.000000000000000000, 0.0001954311564186872539, 0.0003908623128373745078, 0.0005862934692560617346, 0.0007817246256747490156 ),
 .UNSPECIFIED. ) ;
#84247 = ORIENTED_EDGE ( 'NONE', *, *, #47127, .T. ) ;
#84248 = DIRECTION ( 'NONE',  ( 0.000000000000000000, 0.4999999999999985567, 0.8660254037844395958 ) ) ;
#84249 = EDGE_LOOP ( 'NONE', ( #72655, #45369, #70841, #74269 ) ) ;
#84250 = CARTESIAN_POINT ( 'NONE',  ( -9.942330929600657896, -12.43535235679832596, 30.55408501211184813 ) ) ;
#84251 = CARTESIAN_POINT ( 'NONE',  ( -1.134560964701931240, -10.06805714834173848, 34.32951233291982618 ) ) ;
#84252 = DIRECTION ( 'NONE',  ( 0.000000000000000000, 0.9396926207859126468, -0.3420201433256571111 ) ) ;
#84253 = CARTESIAN_POINT ( 'NONE',  ( 2.530471976670375600, -10.23759521482555357, 34.22997729860117033 ) ) ;
#84254 = CARTESIAN_POINT ( 'NONE',  ( -2.176900499867520988, -4.809403383903226192, 33.96459661697924304 ) ) ;
#84255 = CARTESIAN_POINT ( 'NONE',  ( -24.99999999999999645, -15.00000000000000000, 0.000000000000000000 ) ) ;
#84256 = EDGE_LOOP ( 'NONE', ( #53675, #20286, #32225, #77293 ) ) ;
#84257 = CARTESIAN_POINT ( 'NONE',  ( 11.25641025641025550, -11.00000000000000000, 29.75000000000000355 ) ) ;
#84259 = EDGE_LOOP ( 'NONE', ( #23244, #63419, #48611, #56896, #56045, #17753 ) ) ;
#84258 = CARTESIAN_POINT ( 'NONE',  ( -2.057746789344164551, -10.76462480002816235, 33.53768742498949962 ) ) ;
#84260 = CARTESIAN_POINT ( 'NONE',  ( 3.230769230769110045, -12.46129190930018460, 30.37095296980731973 ) ) ;
#84262 = B_SPLINE_CURVE_WITH_KNOTS ( 'NONE', 3,
 ( #70692, #84661, #2216, #23809, #8997, #58049, #85095, #78319, #10317, #64355 ),
 .UNSPECIFIED., .F., .F.,
 ( 4, 2, 2, 2, 4 ),
 ( 0.0007817246256747554124, 0.0009771112852218991757, 0.001172497944769043156, 0.001367884604316187136, 0.001563271263863330899 ),
 .UNSPECIFIED. ) ;
#84261 = CARTESIAN_POINT ( 'NONE',  ( 16.85343813319912698, -3.754499324213721234, 33.06261337010820256 ) ) ;
#84263 = CARTESIAN_POINT ( 'NONE',  ( 15.45378207486263200, -2.889357225399416418, 32.26129605718031002 ) ) ;
#84264 = B_SPLINE_CURVE_WITH_KNOTS ( 'NONE', 3,
 ( #50145, #49712, #77188, #78072, #29460, #16374, #43841, #56907, #15940, #43405 ),
 .UNSPECIFIED., .F., .F.,
 ( 4, 2, 2, 2, 4 ),
 ( 0.000000000000000000, 0.0001954311564186865221, 0.0003908623128373730441, 0.0005862934692560595662, 0.0007817246256747460882 ),
 .UNSPECIFIED. ) ;
#84265 = FACE_OUTER_BOUND ( 'NONE', #4404, .T. ) ;
#84266 = CYLINDRICAL_SURFACE ( 'NONE', #66611, 0.2499999999999995559 ) ;
#84267 = CARTESIAN_POINT ( 'NONE',  ( -8.096177083446809419, -12.43535235679832596, 30.55408501211184813 ) ) ;
#84268 = CARTESIAN_POINT ( 'NONE',  ( 0.06109907496451789238, -4.749999999999998224, 23.15811829374151642 ) ) ;
#84269 = ORIENTED_EDGE ( 'NONE', *, *, #4580, .F. ) ;
#84270 = B_SPLINE_CURVE_WITH_KNOTS ( 'NONE', 3,
 ( #88213, #32351, #40890, #68352, #6650, #59818, #34120, #61586, #12526, #53498 ),
 .UNSPECIFIED., .F., .F.,
 ( 4, 2, 2, 2, 4 ),
 ( 0.000000000000000000, 0.0001954339881912772715, 0.0003908679763825545429, 0.0005863019645738318415, 0.0007817359527651090859 ),
 .UNSPECIFIED. ) ;
#84271 = CARTESIAN_POINT ( 'NONE',  ( -39.05038313613820122, -2.249999999999998668, 29.75000000000000355 ) ) ;
#84272 = CARTESIAN_POINT ( 'NONE',  ( -17.14300545628321260, -4.661471528628507777, 34.16647553114621871 ) ) ;
#84273 = CARTESIAN_POINT ( 'NONE',  ( -2.749999999999998224, -7.500000000000015987, 20.09375000000000000 ) ) ;
#84274 = B_SPLINE_CURVE_WITH_KNOTS ( 'NONE', 3,
 ( #14913, #50009, #1825, #28875, #56331, #83821, #36507, #42827, #50445, #85136 ),
 .UNSPECIFIED., .F., .F.,
 ( 4, 2, 2, 2, 4 ),
 ( 0.0007817359430256270785, 0.0009771253907249926370, 0.001172514838424358087, 0.001367904286123723754, 0.001563293733823089204 ),
 .UNSPECIFIED. ) ;
#84275 = ADVANCED_FACE ( 'NONE', ( #72345 ), #2551, .F. ) ;
#84276 = CARTESIAN_POINT ( 'NONE',  ( -16.15384615384615330, -11.35647404775217417, 33.31231777344666511 ) ) ;
#84277 = CARTESIAN_POINT ( 'NONE',  ( -7.596099426240392027, -2.920487667080175154, 32.31805714834172960 ) ) ;
#84278 = ORIENTED_EDGE ( 'NONE', *, *, #47063, .T. ) ;
#84279 = CARTESIAN_POINT ( 'NONE',  ( 2.750000000000008438, -8.639087296525996607, 15.79687500000000178 ) ) ;
#84280 = CARTESIAN_POINT ( 'NONE',  ( -5.300408020647025431, -6.760086850603068243, 34.69517049084099369 ) ) ;
#84281 = AXIS2_PLACEMENT_3D ( 'NONE', #65681, #80102, #17514 ) ;
#84282 = ORIENTED_EDGE ( 'NONE', *, *, #88088, .T. ) ;
#84283 = CARTESIAN_POINT ( 'NONE',  ( 9.822355127558148880, -7.723484941389743952, 34.99544897038808955 ) ) ;
#84284 = VERTEX_POINT ( 'NONE', #51161 ) ;
#84285 = LINE ( 'NONE', #77070, #73697 ) ;
#84286 = FACE_OUTER_BOUND ( 'NONE', #48498, .T. ) ;
#84287 = EDGE_CURVE ( 'NONE', #70953, #32825, #10655, .T. ) ;
#84288 = CARTESIAN_POINT ( 'NONE',  ( -0.4615384615385840772, -10.33852847137269571, 34.16647553114546554 ) ) ;
#84289 = CARTESIAN_POINT ( 'NONE',  ( -12.21148404162501144, -10.82426656108012075, 33.81400080652039009 ) ) ;
#84290 = EDGE_LOOP ( 'NONE', ( #86469, #35666 ) ) ;
#84291 = CYLINDRICAL_SURFACE ( 'NONE', #23982, 0.2500000000000012212 ) ;
#84292 = ORIENTED_EDGE ( 'NONE', *, *, #55478, .F. ) ;
#84293 = DIRECTION ( 'NONE',  ( 0.000000000000000000, 0.9396926207859126468, 0.3420201433256571111 ) ) ;
#84294 = CARTESIAN_POINT ( 'NONE',  ( 8.769230769230645706, -3.643525952248795718, 33.31231777344771672 ) ) ;
#84295 = AXIS2_PLACEMENT_3D ( 'NONE', #44024, #17004, #10256 ) ;
#84296 = ORIENTED_EDGE ( 'NONE', *, *, #13081, .F. ) ;
#84297 = CARTESIAN_POINT ( 'NONE',  ( -6.130690603110307002, -10.70098750199973203, 33.91152734681376302 ) ) ;
#84298 = CARTESIAN_POINT ( 'NONE',  ( -12.71151519248081740, -5.728515186090277211, 34.42611988154120439 ) ) ;
#84299 = CARTESIAN_POINT ( 'NONE',  ( -11.66915214157184622, -2.845849958028613624, 32.17971566917920967 ) ) ;
#84300 = CARTESIAN_POINT ( 'NONE',  ( 13.38461538461538680, -6.681629849574314051, 35.83090037661290239 ) ) ;
#84301 = CARTESIAN_POINT ( 'NONE',  ( -25.00000000000000355, 9.999999999999971578, 13.00000000000000178 ) ) ;
#84302 = B_SPLINE_CURVE_WITH_KNOTS ( 'NONE', 3,
 ( #77039, #15340, #42816, #36061, #30607, #78796, #45899, #10792, #23405, #66168 ),
 .UNSPECIFIED., .F., .F.,
 ( 4, 2, 2, 2, 4 ),
 ( 0.0007817359430256297891, 0.0009771253907249958896, 0.001172514838424361990, 0.001367904286123728091, 0.001563293733823094191 ),
 .UNSPECIFIED. ) ;
#84303 = EDGE_CURVE ( 'NONE', #13360, #87648, #48179, .T. ) ;
#84304 = ADVANCED_FACE ( 'NONE', ( #43545 ), #44414, .F. ) ;
#84305 = VERTEX_POINT ( 'NONE', #50730 ) ;
#84306 = ORIENTED_EDGE ( 'NONE', *, *, #21829, .T. ) ;
#84307 = FACE_BOUND ( 'NONE', #21227, .T. ) ;
#84308 = ORIENTED_EDGE ( 'NONE', *, *, #71298, .T. ) ;
#84309 = CARTESIAN_POINT ( 'NONE',  ( 6.923076923076800782, -10.33852847137269571, 34.16647553114546554 ) ) ;
#84310 = CARTESIAN_POINT ( 'NONE',  ( 10.28846153846153832, -11.00000000000000000, 29.75000000000000355 ) ) ;
#84311 = CARTESIAN_POINT ( 'NONE',  ( 6.249945409378047323, -2.986452184633680673, 32.43230066228895225 ) ) ;
#84312 = CARTESIAN_POINT ( 'NONE',  ( 0.5920638997721064944, -12.70449254468099198, 30.44128974285582956 ) ) ;
#84313 = EDGE_CURVE ( 'NONE', #34976, #28470, #64692, .T. ) ;
#84314 = ORIENTED_EDGE ( 'NONE', *, *, #26088, .T. ) ;
#84315 = ORIENTED_EDGE ( 'NONE', *, *, #53817, .F. ) ;
#84316 = ORIENTED_EDGE ( 'NONE', *, *, #76269, .F. ) ;
#84317 = CARTESIAN_POINT ( 'NONE',  ( 11.66898724022509981, -11.46989282347013095, 32.79007818306219946 ) ) ;
#84318 = EDGE_LOOP ( 'NONE', ( #46617, #46244, #20808, #14279 ) ) ;
#84319 = VECTOR ( 'NONE', #67736, 1000.000000000000000 ) ;
#84320 = DIRECTION ( 'NONE',  ( -0.000000000000000000, 0.9396926207859093161, -0.3420201433256663259 ) ) ;
#84321 = DIRECTION ( 'NONE',  ( -0.000000000000000000, 0.5000000000000011102, -0.8660254037844380415 ) ) ;
#84322 = LINE ( 'NONE', #22596, #61568 ) ;
#84323 = ORIENTED_EDGE ( 'NONE', *, *, #29907, .T. ) ;
#84324 = CARTESIAN_POINT ( 'NONE',  ( -8.638705330997126453, -4.299079248970732792, 33.91157788607253565 ) ) ;
#84325 = B_SPLINE_CURVE_WITH_KNOTS ( 'NONE', 3,
 ( #54476, #33333, #33769, #88733, #88301, #47725, #42312, #13495, #14381, #54028 ),
 .UNSPECIFIED., .F., .F.,
 ( 4, 2, 2, 2, 4 ),
 ( 0.0007817246256747505334, 0.0009771112852218939715, 0.001172497944769037518, 0.001367884604316181064, 0.001563271263863324611 ),
 .UNSPECIFIED. ) ;
#84326 = CARTESIAN_POINT ( 'NONE',  ( 0.5276068125408999165, -11.69971097300155272, 32.46337939537588113 ) ) ;
#84327 = CARTESIAN_POINT ( 'NONE',  ( -17.77479207347668932, -7.628180278152856708, 34.99865929289143196 ) ) ;
#84328 = DIRECTION ( 'NONE',  ( -1.000000000000000000, -0.000000000000000000, -0.000000000000000000 ) ) ;
#84329 = EDGE_LOOP ( 'NONE', ( #61558, #36005 ) ) ;
#84330 = VERTEX_POINT ( 'NONE', #72787 ) ;
#84331 = ORIENTED_EDGE ( 'NONE', *, *, #68607, .T. ) ;
#84333 = CARTESIAN_POINT ( 'NONE',  ( 1.449870524128224814, -11.67786785259547777, 32.92929555188713664 ) ) ;
#84332 = FACE_OUTER_BOUND ( 'NONE', #76338, .T. ) ;
#84334 = B_SPLINE_CURVE_WITH_KNOTS ( 'NONE', 3,
 ( #26652, #951, #55890, #5946, #54109, #63529, #37380, #50883, #64403, #1391 ),
 .UNSPECIFIED., .F., .F.,
 ( 4, 2, 2, 2, 4 ),
 ( 0.0007817246256747445703, 0.0009771112852218870326, 0.001172497944769029495, 0.001367884604316171957, 0.001563271263863314419 ),
 .UNSPECIFIED. ) ;
#84335 = CARTESIAN_POINT ( 'NONE',  ( 9.692307692307695177, -4.661471528628507777, 34.16647553114623292 ) ) ;
#84336 = LINE ( 'NONE', #71233, #59527 ) ;
#84337 = FACE_BOUND ( 'NONE', #41125, .T. ) ;
#84338 = CARTESIAN_POINT ( 'NONE',  ( -9.692307692307691624, -13.75783147151868846, 33.36296068462461051 ) ) ;
#84339 = VERTEX_POINT ( 'NONE', #24606 ) ;
#84340 = DIRECTION ( 'NONE',  ( -0.000000000000000000, 0.9848077530122086864, -0.1736481776669273891 ) ) ;
#84341 = LINE ( 'NONE', #83002, #28715 ) ;
#84342 = CARTESIAN_POINT ( 'NONE',  ( 14.30769230769231015, -4.786620604624113540, 33.94971097300155094 ) ) ;
#84343 = CARTESIAN_POINT ( 'NONE',  ( -11.31568199719312240, -3.755027918224367323, 33.06320215134714857 ) ) ;
#84344 = ORIENTED_EDGE ( 'NONE', *, *, #61810, .T. ) ;
#84345 = CARTESIAN_POINT ( 'NONE',  ( 6.222779668978065004, -10.97394488606064122, 33.68653795673694873 ) ) ;
#84346 = VERTEX_POINT ( 'NONE', #52072 ) ;
#84347 = FACE_BOUND ( 'NONE', #16513, .T. ) ;
#84348 = CARTESIAN_POINT ( 'NONE',  ( 18.22301135161285046, -3.587049720035815348, 32.86302985866382897 ) ) ;
#84349 = AXIS2_PLACEMENT_3D ( 'NONE', #52574, #54349, #66997 ) ;
#84350 = CARTESIAN_POINT ( 'NONE',  ( -6.923076923076922462, -11.35647404775217417, 33.31231777344666511 ) ) ;
#84351 = CARTESIAN_POINT ( 'NONE',  ( -3.100243529005668019, -8.586989748646452369, 34.63063291749215011 ) ) ;
#84352 = ORIENTED_EDGE ( 'NONE', *, *, #59134, .T. ) ;
#84353 = CARTESIAN_POINT ( 'NONE',  ( 12.46153846153846168, -12.29105614889573062, 35.45975837776705220 ) ) ;
#84354 = CARTESIAN_POINT ( 'NONE',  ( 5.299885980484561721, -7.369474270740069777, 34.74850911626239736 ) ) ;
#84355 = CARTESIAN_POINT ( 'NONE',  ( 8.703148389870632329, -2.292212530054419606, 30.41441678777542634 ) ) ;
#84356 = CARTESIAN_POINT ( 'NONE',  ( 6.250054311638314708, -3.627508038966690496, 32.91356715214248396 ) ) ;
#84357 = EDGE_LOOP ( 'NONE', ( #54218, #39245, #56582, #83096 ) ) ;
#84358 = EDGE_CURVE ( 'NONE', #27674, #60953, #80424, .T. ) ;
#84359 = DIRECTION ( 'NONE',  ( 0.000000000000000000, 0.6427876096865373645, -0.7660444431189797898 ) ) ;
#84360 = ORIENTED_EDGE ( 'NONE', *, *, #18647, .F. ) ;
#84362 = ORIENTED_EDGE ( 'NONE', *, *, #68677, .F. ) ;
#84361 = CARTESIAN_POINT ( 'NONE',  ( 13.60762673622823726, -12.15243808032445827, 31.58219941686247978 ) ) ;
#84363 = CARTESIAN_POINT ( 'NONE',  ( -8.899841128855296546, -7.722926236386453702, 34.74524107206102030 ) ) ;
#84364 = CYLINDRICAL_SURFACE ( 'NONE', #21137, 0.2499999999999993616 ) ;
#84365 = DIRECTION ( 'NONE',  ( -0.000000000000000000, 0.9848077530122085754, -0.1736481776669273613 ) ) ;
#84366 = CARTESIAN_POINT ( 'NONE',  ( -12.46153846153846168, -13.20930481340135110, 34.54067556320372745 ) ) ;
#84368 = DIRECTION ( 'NONE',  ( 1.000000000000000000, 0.000000000000000000, 0.000000000000000000 ) ) ;
#84367 = CARTESIAN_POINT ( 'NONE',  ( -12.46153846153846168, -8.810774026931790459, 35.74407628777942847 ) ) ;
#84369 = CARTESIAN_POINT ( 'NONE',  ( 12.59158606779414491, -7.723484964179501588, 34.74522123443823318 ) ) ;
#84370 = CARTESIAN_POINT ( 'NONE',  ( 1.139087296526029469, -10.24999999999999467, 23.45312500000000000 ) ) ;
#84371 = VERTEX_POINT ( 'NONE', #4337 ) ;
#84372 = CARTESIAN_POINT ( 'NONE',  ( 4.153846153846154188, -1.242168528481310874, 33.36296068462461051 ) ) ;
#84373 = LINE ( 'NONE', #15911, #48147 ) ;
#84374 = ORIENTED_EDGE ( 'NONE', *, *, #66327, .F. ) ;
#84375 = EDGE_CURVE ( 'NONE', #41758, #60114, #59995, .T. ) ;
#84376 = ORIENTED_EDGE ( 'NONE', *, *, #70715, .F. ) ;
#84377 = ORIENTED_EDGE ( 'NONE', *, *, #73075, .F. ) ;
#84378 = CARTESIAN_POINT ( 'NONE',  ( 10.74617505635156789, -8.191423895709840863, 34.95447573519442130 ) ) ;
#84379 = EDGE_CURVE ( 'NONE', #82422, #85209, #87828, .T. ) ;
#84380 = CARTESIAN_POINT ( 'NONE',  ( -17.20707028636129721, -9.418419913701741919, 34.36755862841477693 ) ) ;
#84381 = DIRECTION ( 'NONE',  ( -0.000000000000000000, 0.8660254037844397068, -0.4999999999999978906 ) ) ;
#84382 = CARTESIAN_POINT ( 'NONE',  ( -0.4330127018922180770, -10.21569512280005299, 29.50000000000000355 ) ) ;
#84383 = CARTESIAN_POINT ( 'NONE',  ( 12.46153846153846168, -6.386643153685126251, 34.62446782046654192 ) ) ;
#84384 = CARTESIAN_POINT ( 'NONE',  ( -19.50000000000000000, -3.499999999999999556, 29.75000000000000355 ) ) ;
#84385 = DIRECTION ( 'NONE',  ( -1.000000000000000000, 0.000000000000000000, 0.000000000000000000 ) ) ;
#84386 = VECTOR ( 'NONE', #18130, 1000.000000000000000 ) ;
#84387 = DIRECTION ( 'NONE',  ( -0.000000000000000000, -0.1736481776669307198, -0.9848077530122080203 ) ) ;
#84388 = CARTESIAN_POINT ( 'NONE',  ( -1.384615384615383471, -6.386643153685126251, 34.62446782046654192 ) ) ;
#84389 = EDGE_CURVE ( 'NONE', #41035, #57710, #33594, .T. ) ;
#84390 = CYLINDRICAL_SURFACE ( 'NONE', #43582, 4.000000000000000000 ) ;
#84391 = LINE ( 'NONE', #10041, #28302 ) ;
#84392 = B_SPLINE_CURVE_WITH_KNOTS ( 'NONE', 3,
 ( #25297, #45113, #73040, #11791, #65821, #18103, #39270, #59520, #79804, #73938 ),
 .UNSPECIFIED., .F., .F.,
 ( 4, 2, 2, 2, 4 ),
 ( 0.0007817246336856291692, 0.0009771112958940103739, 0.001172497958102391470, 0.001367884620310772566, 0.001563271282519153879 ),
 .UNSPECIFIED. ) ;
#84393 = ADVANCED_FACE ( 'NONE', ( #88122 ), #39474, .F. ) ;
#84394 = ORIENTED_EDGE ( 'NONE', *, *, #43390, .T. ) ;
#84395 = CARTESIAN_POINT ( 'NONE',  ( 0.4615384615383396616, -9.442884908241554243, 34.35708131394783038 ) ) ;
#84396 = CARTESIAN_POINT ( 'NONE',  ( -16.02380109792638407, -2.254550872974305342, 29.97347326024527092 ) ) ;
#84397 = DIRECTION ( 'NONE',  ( -1.734723475976812518E-16, 1.000000000000000000, 0.000000000000000000 ) ) ;
#84398 = CARTESIAN_POINT ( 'NONE',  ( 12.52679403281448423, -10.90142922261932057, 33.41473453929631887 ) ) ;
#84399 = ORIENTED_EDGE ( 'NONE', *, *, #33523, .F. ) ;
#84400 = AXIS2_PLACEMENT_3D ( 'NONE', #82513, #13593, #40196 ) ;
#84401 = CARTESIAN_POINT ( 'NONE',  ( 6.130791807824786943, -4.809403383903225304, 33.96459661697924304 ) ) ;
#84402 = CARTESIAN_POINT ( 'NONE',  ( 9.692307692307695177, -2.833524468853757305, 32.15551576947925838 ) ) ;
#84403 = CARTESIAN_POINT ( 'NONE',  ( -9.561782254074046250, -3.625058011473228703, 33.29252011169590020 ) ) ;
#84404 = EDGE_CURVE ( 'NONE', #59603, #68701, #41573, .T. ) ;
#84405 = ORIENTED_EDGE ( 'NONE', *, *, #66124, .T. ) ;
#84406 = CARTESIAN_POINT ( 'NONE',  ( 16.28437159207980045, -10.31582465632704704, 34.18122507451815295 ) ) ;
#84407 = EDGE_CURVE ( 'NONE', #4690, #23070, #52958, .T. ) ;
#84408 = ORIENTED_EDGE ( 'NONE', *, *, #60193, .F. ) ;
#84409 = B_SPLINE_CURVE_WITH_KNOTS ( 'NONE', 3,
 ( #14462, #7714, #14012, #35174, #75281, #28413, #55883, #21657, #49128, #20770 ),
 .UNSPECIFIED., .F., .F.,
 ( 4, 2, 2, 2, 4 ),
 ( 0.0007817246256747416430, 0.0009771112852218831295, 0.001172497944769024508, 0.001367884604316165886, 0.001563271263863307481 ),
 .UNSPECIFIED. ) ;
#84410 = CARTESIAN_POINT ( 'NONE',  ( 9.692307692307572609, -11.94971097300221174, 32.03036669348237098 ) ) ;
#84411 = CARTESIAN_POINT ( 'NONE',  ( -17.01166793741023042, -3.643525952247864019, 33.31231777344670064 ) ) ;
#84412 = ADVANCED_FACE ( 'NONE', ( #47089 ), #61053, .T. ) ;
#84413 = AXIS2_PLACEMENT_3D ( 'NONE', #26403, #25952, #60173 ) ;
#84414 = CARTESIAN_POINT ( 'NONE',  ( -1.449885385171703733, -9.528491918058357157, 34.59228464037090589 ) ) ;
#84415 = EDGE_CURVE ( 'NONE', #52853, #46179, #80000, .T. ) ;
#84416 = CARTESIAN_POINT ( 'NONE',  ( -9.822998295417999515, -8.191372820521381826, 34.95448215188424967 ) ) ;
#84417 = CARTESIAN_POINT ( 'NONE',  ( -11.53846153846153655, -9.058645607665452459, 34.76329471203371924 ) ) ;
#84418 = ORIENTED_EDGE ( 'NONE', *, *, #62086, .T. ) ;
#84419 = ORIENTED_EDGE ( 'NONE', *, *, #31385, .T. ) ;
#84421 = ORIENTED_EDGE ( 'NONE', *, *, #12493, .T. ) ;
#84420 = B_SPLINE_CURVE_WITH_KNOTS ( 'NONE', 3,
 ( #75553, #12978, #12534, #40018, #13854, #41334, #33253, #60713, #88220, #62042 ),
 .UNSPECIFIED., .F., .F.,
 ( 4, 2, 2, 2, 4 ),
 ( 0.0007817359430256324996, 0.0009771253907249993591, 0.001172514838424366110, 0.001367904286123732861, 0.001563293733823099829 ),
 .UNSPECIFIED. ) ;
#84422 = AXIS2_PLACEMENT_3D ( 'NONE', #47463, #13249, #40730 ) ;
#84423 = CARTESIAN_POINT ( 'NONE',  ( -10.74607521849491754, -12.35290016733513951, 31.75349464988449455 ) ) ;
#84424 = B_SPLINE_CURVE_WITH_KNOTS ( 'NONE', 3,
 ( #20679, #76063, #48143, #22449, #852, #69751, #75613, #41401, #14362, #49036 ),
 .UNSPECIFIED., .F., .F.,
 ( 4, 2, 2, 2, 4 ),
 ( 0.0007817246256747451124, 0.0009771112852218881168, 0.001172497944769031230, 0.001367884604316174126, 0.001563271263863317238 ),
 .UNSPECIFIED. ) ;
#84425 = CARTESIAN_POINT ( 'NONE',  ( -12.46153846153858424, -12.70778746994576025, 30.41441678777401236 ) ) ;
#84426 = CYLINDRICAL_SURFACE ( 'NONE', #78193, 0.2499999999999979738 ) ;
#84427 = B_SPLINE_CURVE_WITH_KNOTS ( 'NONE', 3,
 ( #45012, #78804, #17561, #38271, #64393, #44561, #37821, #65290, #86018, #31511 ),
 .UNSPECIFIED., .F., .F.,
 ( 4, 2, 2, 2, 4 ),
 ( 0.000000000000000000, 0.0001954311584214072923, 0.0003908623168428145846, 0.0005862934752642218498, 0.0007817246336856291692 ),
 .UNSPECIFIED. ) ;
#84428 = LINE ( 'NONE', #64122, #45601 ) ;
#84429 = CARTESIAN_POINT ( 'NONE',  ( -18.00000000000000000, -4.098570777380720287, 33.41473453929634729 ) ) ;
#84430 = DIRECTION ( 'NONE',  ( -0.000000000000000000, 1.000000000000000000, 3.491481338843133355E-15 ) ) ;
#84431 = VERTEX_POINT ( 'NONE', #26834 ) ;
#84432 = EDGE_LOOP ( 'NONE', ( #39117, #84206, #77502, #23222, #16828, #7095 ) ) ;
#84433 = ORIENTED_EDGE ( 'NONE', *, *, #63760, .F. ) ;
#84435 = VERTEX_POINT ( 'NONE', #40796 ) ;
#84434 = DIRECTION ( 'NONE',  ( -0.000000000000000000, -0.3420201433256694346, -0.9396926207859080948 ) ) ;
#84437 = CARTESIAN_POINT ( 'NONE',  ( 13.38461538461538680, -3.937682226553329556, 33.60647404775216529 ) ) ;
#84436 = CARTESIAN_POINT ( 'NONE',  ( 9.019230769232187583, -7.500000000000154543, 35.00000000000007105 ) ) ;
#84438 = ADVANCED_FACE ( 'NONE', ( #66491 ), #6120, .F. ) ;
#84439 = VECTOR ( 'NONE', #49035, 1000.000000000000000 ) ;
#84440 = CARTESIAN_POINT ( 'NONE',  ( 1.553300858899129722, -11.24999999999999112, 25.95312500000000000 ) ) ;
#84441 = EDGE_LOOP ( 'NONE', ( #65013, #86496 ) ) ;
#84442 = VERTEX_POINT ( 'NONE', #6562 ) ;
#84443 = CARTESIAN_POINT ( 'NONE',  ( 5.300349475837862201, -7.630147987733840509, 34.99859428049665411 ) ) ;
#84444 = AXIS2_PLACEMENT_3D ( 'NONE', #84512, #16487, #64655 ) ;
#84445 = ORIENTED_EDGE ( 'NONE', *, *, #52394, .F. ) ;
#84446 = FACE_BOUND ( 'NONE', #27781, .T. ) ;
#84447 = CARTESIAN_POINT ( 'NONE',  ( 13.51514082284903040, -12.50538340440932394, 31.33453814440721885 ) ) ;
#84448 = CARTESIAN_POINT ( 'NONE',  ( 7.976679284387491187, -5.915461855592780260, 34.75538340440931506 ) ) ;
#84449 = ORIENTED_EDGE ( 'NONE', *, *, #88796, .T. ) ;
#84450 = CARTESIAN_POINT ( 'NONE',  ( 16.15384615384603251, -11.48612834414049644, 32.76840700105863391 ) ) ;
#84451 = CARTESIAN_POINT ( 'NONE',  ( 16.15384615384615330, -4.098570777380720287, 33.41473453929634729 ) ) ;
#84452 = AXIS2_PLACEMENT_3D ( 'NONE', #31887, #23771, #73312 ) ;
#84453 = LINE ( 'NONE', #70034, #46449 ) ;
#84454 = CARTESIAN_POINT ( 'NONE',  ( -0.6089743589743589203, -3.499999999999999556, 29.75000000000000355 ) ) ;
#84455 = CARTESIAN_POINT ( 'NONE',  ( 1.384615384615386802, -11.69971097300155272, 32.46337939537588113 ) ) ;
#84456 = ADVANCED_FACE ( 'NONE', ( #40354 ), #12868, .F. ) ;
#84457 = B_SPLINE_CURVE_WITH_KNOTS ( 'NONE', 3,
 ( #86147, #24870, #79382, #53230, #3264, #79833, #66307, #10923, #24418, #45587 ),
 .UNSPECIFIED., .F., .F.,
 ( 4, 2, 2, 2, 4 ),
 ( 0.0007817246256747434861, 0.0009771112852218861652, 0.001172497944769028844, 0.001367884604316171740, 0.001563271263863314419 ),
 .UNSPECIFIED. ) ;
#84458 = CARTESIAN_POINT ( 'NONE',  ( -7.146003140593069958, -11.24512374952581872, 33.06303171183252942 ) ) ;
#84459 = CARTESIAN_POINT ( 'NONE',  ( -8.096130590202434973, -12.01397095200674059, 32.43157075238190146 ) ) ;
#84460 = CARTESIAN_POINT ( 'NONE',  ( -5.999999999999998224, -5.557115091759785130, 34.35708131394839171 ) ) ;
#84461 = CARTESIAN_POINT ( 'NONE',  ( 5.776515056276054771, -5.113361153441932316, 34.14387501736621999 ) ) ;
#84462 = CARTESIAN_POINT ( 'NONE',  ( -18.22292621751613950, -6.503392248772476236, 34.64988816332204635 ) ) ;
#84463 = CARTESIAN_POINT ( 'NONE',  ( -1.384615384615383471, -5.471508081941601098, 34.59228464037088457 ) ) ;
#84465 = CARTESIAN_POINT ( 'NONE',  ( -2.307692307692305711, -2.708943851104267164, 35.45975837776705220 ) ) ;
#84464 = CARTESIAN_POINT ( 'NONE',  ( 13.31934493865461100, -11.94971097300153140, 32.03036669348370680 ) ) ;
#84466 = CARTESIAN_POINT ( 'NONE',  ( -16.15384615384627409, -11.94971097300221174, 32.03036669348237098 ) ) ;
#84468 = CARTESIAN_POINT ( 'NONE',  ( 5.750023269057646935, -10.66389620160130036, 33.62221079203477103 ) ) ;
#84467 = CARTESIAN_POINT ( 'NONE',  ( -11.47239318745910275, -11.16473453929635440, 33.15142922261926373 ) ) ;
#84469 = CARTESIAN_POINT ( 'NONE',  ( 13.63461538461532641, -7.565270000091922853, 34.99999999999999289 ) ) ;
#84470 = CARTESIAN_POINT ( 'NONE',  ( 2.724691934501235036, -6.299813628509441266, 21.63875670625848713 ) ) ;
#84471 = EDGE_LOOP ( 'NONE', ( #10904, #62682 ) ) ;
#84472 = CARTESIAN_POINT ( 'NONE',  ( 3.375057480660595299, -6.401003086717466317, 14.00000000000007994 ) ) ;
#84473 = ORIENTED_EDGE ( 'NONE', *, *, #42263, .F. ) ;
#84474 = DIRECTION ( 'NONE',  ( 1.000000000000000000, 0.000000000000000000, 0.000000000000000000 ) ) ;
#84475 = EDGE_CURVE ( 'NONE', #56543, #77704, #5050, .T. ) ;
#84476 = VECTOR ( 'NONE', #12866, 1000.000000000000114 ) ;
#84477 = ORIENTED_EDGE ( 'NONE', *, *, #24772, .F. ) ;
#84478 = CARTESIAN_POINT ( 'NONE',  ( 16.02369894440793274, -11.47017969459903952, 32.78971311882035167 ) ) ;
#84479 = ORIENTED_EDGE ( 'NONE', *, *, #39423, .F. ) ;
#84480 = CARTESIAN_POINT ( 'NONE',  ( -7.846153846153844924, -5.557115091759785130, 34.35708131394839171 ) ) ;
#84481 = CARTESIAN_POINT ( 'NONE',  ( 2.724691934501235036, -6.299813628509441266, 25.38875670625849423 ) ) ;
#84482 = CARTESIAN_POINT ( 'NONE',  ( -17.86920955903305597, -9.084667340241228572, 34.75534355489798344 ) ) ;
#84483 = EDGE_CURVE ( 'NONE', #26289, #21025, #50163, .T. ) ;
#84484 = CARTESIAN_POINT ( 'NONE',  ( 13.45068271796546533, -2.833524468853757750, 32.15551576947925838 ) ) ;
#84485 = CARTESIAN_POINT ( 'NONE',  ( 17.86930939688969033, -2.295517848115769421, 30.44137282052136939 ) ) ;
#84486 = CARTESIAN_POINT ( 'NONE',  ( -7.846153846153844924, -13.53365097954675988, 30.81389545987213552 ) ) ;
#84487 = CARTESIAN_POINT ( 'NONE',  ( -13.38461538461538325, -8.164416787775445883, 34.95778746994557906 ) ) ;
#84488 = CARTESIAN_POINT ( 'NONE',  ( -13.38461538461538325, -11.91647553114624181, 32.58852847137148245 ) ) ;
#84489 = CARTESIAN_POINT ( 'NONE',  ( -3.749999999999997335, -7.500000000000021316, 15.09375000000000000 ) ) ;
#84490 = CARTESIAN_POINT ( 'NONE',  ( -1.384615384615383471, -12.62096338111211580, 30.90682066428153263 ) ) ;
#84491 = CARTESIAN_POINT ( 'NONE',  ( 6.923076923076924238, -12.29105614889573062, 35.45975837776705220 ) ) ;
#84492 = ADVANCED_FACE ( 'NONE', ( #70479 ), #75902, .F. ) ;
#84493 = CARTESIAN_POINT ( 'NONE',  ( 10.39189969082028675, -5.827078755546623690, 34.72654668319379567 ) ) ;
#84494 = CARTESIAN_POINT ( 'NONE',  ( -3.750000000000008438, -5.946699141100917352, 17.67187500000000355 ) ) ;
#84495 = B_SPLINE_CURVE_WITH_KNOTS ( 'NONE', 3,
 ( #40307, #45717, #67769, #54240, #32215, #59676, #80407, #52907, #25451, #18705 ),
 .UNSPECIFIED., .F., .F.,
 ( 4, 2, 2, 2, 4 ),
 ( 0.000000000000000000, 0.0001954339857564081520, 0.0003908679715128163040, 0.0005863019572692244018, 0.0007817359430256326080 ),
 .UNSPECIFIED. ) ;
#84496 = CARTESIAN_POINT ( 'NONE',  ( -10.48485917715096782, -5.915461855592780260, 34.75538340440931506 ) ) ;
#84497 = VERTEX_POINT ( 'NONE', #63268 ) ;
#84498 = CARTESIAN_POINT ( 'NONE',  ( 17.07692307692307665, -12.10708131394839349, 31.69288490824020244 ) ) ;
#84499 = CARTESIAN_POINT ( 'NONE',  ( 12.23805353697412812, -8.539481045369596401, 34.89627647299170832 ) ) ;
#84500 = FACE_OUTER_BOUND ( 'NONE', #59700, .T. ) ;
#84501 = CARTESIAN_POINT ( 'NONE',  ( 14.98076923076923173, -7.500000000000001776, 35.00000000000000000 ) ) ;
#84502 = LINE ( 'NONE', #50242, #46402 ) ;
#84503 = CARTESIAN_POINT ( 'NONE',  ( 9.469381474791545017, -11.24512374952581872, 33.06303171183252942 ) ) ;
#84504 = FACE_OUTER_BOUND ( 'NONE', #31177, .T. ) ;
#84505 = B_SPLINE_CURVE_WITH_KNOTS ( 'NONE', 3,
 ( #9051, #23862, #15809, #56776, #71174, #30203, #44576, #1838, #72063, #36520 ),
 .UNSPECIFIED., .F., .F.,
 ( 4, 2, 2, 2, 4 ),
 ( 0.000000000000000000, 0.0001954339857564081520, 0.0003908679715128163040, 0.0005863019572692244018, 0.0007817359430256326080 ),
 .UNSPECIFIED. ) ;
#84506 = VECTOR ( 'NONE', #27599, 1000.000000000000000 ) ;
#84507 = EDGE_CURVE ( 'NONE', #35065, #45495, #51263, .T. ) ;
#84508 = ORIENTED_EDGE ( 'NONE', *, *, #51063, .T. ) ;
#84509 = ORIENTED_EDGE ( 'NONE', *, *, #57571, .F. ) ;
#84510 = EDGE_CURVE ( 'NONE', #16561, #36288, #28609, .T. ) ;
#84511 = ORIENTED_EDGE ( 'NONE', *, *, #68219, .F. ) ;
#84512 = CARTESIAN_POINT ( 'NONE',  ( -24.99999999999999645, 15.00000000000000355, 3.000000000000000000 ) ) ;
#84513 = CARTESIAN_POINT ( 'NONE',  ( -4.153846153846273204, -3.300289026999228881, 32.46337939537708905 ) ) ;
#84514 = CARTESIAN_POINT ( 'NONE',  ( -8.835313148590907772, -2.292212530054419606, 30.41441678777542634 ) ) ;
#84515 = EDGE_CURVE ( 'NONE', #363, #13588, #84662, .T. ) ;
#84516 = VECTOR ( 'NONE', #34744, 1000.000000000000000 ) ;
#84517 = CARTESIAN_POINT ( 'NONE',  ( 4.284371855609720114, -3.816742781228458448, 33.13167719472716044 ) ) ;
#84518 = CARTESIAN_POINT ( 'NONE',  ( 17.86985279056177944, -9.418419913701741919, 34.36755862841477693 ) ) ;
#84519 = VERTEX_POINT ( 'NONE', #68699 ) ;
#84520 = CARTESIAN_POINT ( 'NONE',  ( -17.14219352288385778, -4.481592998940161721, 33.73612834413957984 ) ) ;
#84521 = ORIENTED_EDGE ( 'NONE', *, *, #48641, .F. ) ;
#84522 = ORIENTED_EDGE ( 'NONE', *, *, #25118, .F. ) ;
#84523 = B_SPLINE_CURVE_WITH_KNOTS ( 'NONE', 3,
 ( #83865, #14957, #28923, #22151, #991, #28017, #55925, #76197, #49619, #14500 ),
 .UNSPECIFIED., .F., .F.,
 ( 4, 2, 2, 2, 4 ),
 ( 0.0007817359430256388964, 0.0009771253907250073822, 0.001172514838424375868, 0.001367904286123744354, 0.001563293733823112840 ),
 .UNSPECIFIED. ) ;
#84525 = EDGE_LOOP ( 'NONE', ( #15718, #85117, #42161, #24675 ) ) ;
#84524 = CARTESIAN_POINT ( 'NONE',  ( 4.153846153846030731, -12.51329471203414379, 31.30864560766407578 ) ) ;
#84526 = CARTESIAN_POINT ( 'NONE',  ( 8.703147358274886614, -2.721908614388770964, 31.22303859784723912 ) ) ;
#84527 = EDGE_CURVE ( 'NONE', #84330, #4777, #46986, .T. ) ;
#84528 = CARTESIAN_POINT ( 'NONE',  ( -10.86540785267757947, -5.056417327199099532, 34.11270091957321426 ) ) ;
#84529 = AXIS2_PLACEMENT_3D ( 'NONE', #72359, #66040, #10669 ) ;
#84530 = EDGE_CURVE ( 'NONE', #67129, #64220, #41678, .T. ) ;
#84531 = CARTESIAN_POINT ( 'NONE',  ( -9.758391103263569732, -8.120952969808774569, 34.71129190930000163 ) ) ;
#84532 = CARTESIAN_POINT ( 'NONE',  ( -12.23816252084027845, -2.501478030877323455, 29.88021232661721172 ) ) ;
#84533 = ORIENTED_EDGE ( 'NONE', *, *, #43902, .F. ) ;
#84534 = EDGE_LOOP ( 'NONE', ( #3865, #35408 ) ) ;
#84535 = CARTESIAN_POINT ( 'NONE',  ( 2.651650429449569302, -10.15165042944953733, 20.87500000000000000 ) ) ;
#84536 = ORIENTED_EDGE ( 'NONE', *, *, #53291, .T. ) ;
#84537 = CARTESIAN_POINT ( 'NONE',  ( -14.17764470143662336, -7.723484964179501588, 34.74522123443823318 ) ) ;
#84539 = ORIENTED_EDGE ( 'NONE', *, *, #66246, .F. ) ;
#84538 = CARTESIAN_POINT ( 'NONE',  ( 1.161130440891438242, -8.496056993536548418, 34.65000542017679663 ) ) ;
#84540 = DIRECTION ( 'NONE',  ( -0.000000000000000000, -0.8660254037844397068, -0.4999999999999978906 ) ) ;
#84541 = CARTESIAN_POINT ( 'NONE',  ( 13.19230769230769340, -11.50000000000000000, 29.75000000000000355 ) ) ;
#84542 = EDGE_CURVE ( 'NONE', #17855, #456, #57684, .T. ) ;
#84543 = DIRECTION ( 'NONE',  ( -0.000000000000000000, -0.8660254037844397068, -0.4999999999999978906 ) ) ;
#84544 = ORIENTED_EDGE ( 'NONE', *, *, #50247, .T. ) ;
#84545 = CIRCLE ( 'NONE', #57143, 4.000000000000000000 ) ;
#84546 = DIRECTION ( 'NONE',  ( -0.000000000000000000, -0.7660444431189791237, -0.6427876096865379196 ) ) ;
#84547 = CARTESIAN_POINT ( 'NONE',  ( -15.00775638667583678, -12.38742843783360748, 31.66772728687926985 ) ) ;
#84548 = ORIENTED_EDGE ( 'NONE', *, *, #80208, .T. ) ;
#84549 = FACE_BOUND ( 'NONE', #14201, .T. ) ;
#84550 = ADVANCED_FACE ( 'NONE', ( #82224 ), #20513, .F. ) ;
#84551 = CARTESIAN_POINT ( 'NONE',  ( -10.83886953994894675, -4.988325925672468131, 34.36044203135681130 ) ) ;
#84552 = DIRECTION ( 'NONE',  ( -0.000000000000000000, 0.3420201433256694346, -0.9396926207859080948 ) ) ;
#84553 = CARTESIAN_POINT ( 'NONE',  ( 2.241609928332171986, -12.34228464037088280, 31.77849191805838558 ) ) ;
#84554 = B_SPLINE_CURVE_WITH_KNOTS ( 'NONE', 3,
 ( #19194, #80911, #38579, #86343, #58836, #65587, #32270, #87227, #52078, #39033 ),
 .UNSPECIFIED., .F., .F.,
 ( 4, 2, 2, 2, 4 ),
 ( 0.000000000000000000, 0.0001954311564186865763, 0.0003908623128373731525, 0.0005862934692560596746, 0.0007817246256747463051 ),
 .UNSPECIFIED. ) ;
#84556 = DIRECTION ( 'NONE',  ( 0.000000000000000000, 0.9848077530122072432, -0.1736481776669354937 ) ) ;
#84555 = CARTESIAN_POINT ( 'NONE',  ( 13.19230769230769340, -7.500000000000000000, 29.75000000000000355 ) ) ;
#84557 = CARTESIAN_POINT ( 'NONE',  ( -3.296851610129364563, -3.322132147404559976, 32.92929555188719348 ) ) ;
#84558 = DIRECTION ( 'NONE',  ( -0.000000000000000000, -0.9848077530122085754, -0.1736481776669273613 ) ) ;
#84559 = ORIENTED_EDGE ( 'NONE', *, *, #68157, .T. ) ;
#84560 = LINE ( 'NONE', #22835, #17346 ) ;
#84561 = DIRECTION ( 'NONE',  ( -0.000000000000000000, 0.9396926207859093161, -0.3420201433256663259 ) ) ;
#84562 = ORIENTED_EDGE ( 'NONE', *, *, #47317, .T. ) ;
#84563 = EDGE_CURVE ( 'NONE', #32782, #35007, #74926, .T. ) ;
#84564 = CARTESIAN_POINT ( 'NONE',  ( -16.28453675695646652, -12.62707690430377383, 30.88035979386743435 ) ) ;
#84565 = CARTESIAN_POINT ( 'NONE',  ( 10.39189967166066708, -6.760086850603066466, 34.69517049084099369 ) ) ;
#84566 = CARTESIAN_POINT ( 'NONE',  ( 2.980769230769232170, -7.500000000000001776, 34.75000000000000000 ) ) ;
#84567 = CARTESIAN_POINT ( 'NONE',  ( -5.326899807865431491, -11.79746400365624659, 32.30657167506340954 ) ) ;
#84568 = VECTOR ( 'NONE', #85671, 1000.000000000000227 ) ;
#84569 = CARTESIAN_POINT ( 'NONE',  ( -18.00000000000000711, -2.252971138473345292, 29.99985851721553942 ) ) ;
#84570 = CARTESIAN_POINT ( 'NONE',  ( -8.992156986746916658, -5.667676309546437530, 34.40238873228292249 ) ) ;
#84571 = FACE_BOUND ( 'NONE', #72135, .T. ) ;
#84572 = EDGE_CURVE ( 'NONE', #20155, #22078, #44305, .T. ) ;
#84574 = DIRECTION ( 'NONE',  ( -0.000000000000000000, -0.1736481776669307198, -0.9848077530122080203 ) ) ;
#84573 = CARTESIAN_POINT ( 'NONE',  ( -2.557715544985271094, -6.695914987888143877, 34.68535235679833306 ) ) ;
#84575 = CARTESIAN_POINT ( 'NONE',  ( -18.06527000055631760, -8.656820664281497102, 34.87096338111211935 ) ) ;
#84577 = CARTESIAN_POINT ( 'NONE',  ( -15.00798968950081758, -6.760870238392817200, 34.69528174975672385 ) ) ;
#84576 = CARTESIAN_POINT ( 'NONE',  ( -3.164700879766790820, -11.69971097300155272, 32.46337939537588113 ) ) ;
#84578 = CYLINDRICAL_SURFACE ( 'NONE', #36120, 0.2499999999999998890 ) ;
#84579 = AXIS2_PLACEMENT_3D ( 'NONE', #73009, #11307, #25269 ) ;
#84580 = CARTESIAN_POINT ( 'NONE',  ( 0.06109907496455496689, -11.24999999999999822, 19.52938170625848713 ) ) ;
#84581 = VERTEX_POINT ( 'NONE', #36692 ) ;
#84582 = EDGE_LOOP ( 'NONE', ( #23583, #81057, #12843, #77633 ) ) ;
#84583 = DIRECTION ( 'NONE',  ( -0.000000000000000000, -0.5000000000000009992, -0.8660254037844380415 ) ) ;
#84584 = AXIS2_PLACEMENT_3D ( 'NONE', #57672, #57233, #79284 ) ;
#84585 = CARTESIAN_POINT ( 'NONE',  ( -4.376772371362300795, -3.105860786376062332, 32.13614157043599562 ) ) ;
#84586 = CARTESIAN_POINT ( 'NONE',  ( -0.5268084620947812713, -3.643525952247789412, 33.31231777344662959 ) ) ;
#84587 = CARTESIAN_POINT ( 'NONE',  ( -16.82686876528476105, -11.28795663066794575, 33.01431243580653785 ) ) ;
#84588 = CARTESIAN_POINT ( 'NONE',  ( -16.37677237136229991, -12.15238873228291716, 31.58232369045353849 ) ) ;
#84589 = CARTESIAN_POINT ( 'NONE',  ( 3.724691934501232815, -5.885600066136343678, 19.13875670625849068 ) ) ;
#84590 = ADVANCED_FACE ( 'NONE', ( #30374 ), #79004, .T. ) ;
#84591 = CARTESIAN_POINT ( 'NONE',  ( -8.546451227962359454, -2.847695495035523550, 31.58253572463339154 ) ) ;
#84592 = CARTESIAN_POINT ( 'NONE',  ( 3.930361229281823743, -12.11044203135681840, 32.26167407432752299 ) ) ;
#84593 = EDGE_CURVE ( 'NONE', #48918, #81272, #82428, .T. ) ;
#84594 = CARTESIAN_POINT ( 'NONE',  ( -16.82686876528476105, -5.728107161865375829, 34.42597550085002922 ) ) ;
#84595 = CYLINDRICAL_SURFACE ( 'NONE', #18580, 0.2500000000000009437 ) ;
#84596 = CARTESIAN_POINT ( 'NONE',  ( -16.82697766754503377, -4.932303261841488151, 34.32971442181322885 ) ) ;
#84597 = CARTESIAN_POINT ( 'NONE',  ( 12.21151523731700550, -12.68155406624981119, 30.59749803192733708 ) ) ;
#84598 = B_SPLINE_CURVE_WITH_KNOTS ( 'NONE', 3,
 ( #17155, #87418, #45960, #10411, #86529, #73891, #73450, #79762, #23902, #18056 ),
 .UNSPECIFIED., .F., .F.,
 ( 4, 2, 2, 2, 4 ),
 ( 0.000000000000000000, 0.0001954339857564072033, 0.0003908679715128144066, 0.0005863019572692215828, 0.0007817359430256288133 ),
 .UNSPECIFIED. ) ;
#84599 = CYLINDRICAL_SURFACE ( 'NONE', #50569, 0.2499999999999986955 ) ;
#84600 = CARTESIAN_POINT ( 'NONE',  ( 8.069165197766697162, -6.503523203565941380, 34.64991518177335195 ) ) ;
#84601 = ORIENTED_EDGE ( 'NONE', *, *, #70111, .T. ) ;
#84602 = FACE_OUTER_BOUND ( 'NONE', #44027, .T. ) ;
#84603 = CARTESIAN_POINT ( 'NONE',  ( 7.173131234715239835, -4.943051570960391494, 34.04725096376909477 ) ) ;
#84604 = CARTESIAN_POINT ( 'NONE',  ( -1.901340078031369618, -5.512252781505359245, 25.50186829374151287 ) ) ;
#84605 = CARTESIAN_POINT ( 'NONE',  ( 0.7115928814519133505, -3.435999193479609026, 33.07426656108010832 ) ) ;
#84607 = DIRECTION ( 'NONE',  ( -1.000000000000000000, -0.000000000000000000, -0.000000000000000000 ) ) ;
#84606 = CIRCLE ( 'NONE', #6925, 4.000000000000000000 ) ;
#84608 = ORIENTED_EDGE ( 'NONE', *, *, #17809, .F. ) ;
#84609 = CARTESIAN_POINT ( 'NONE',  ( -16.28440674558808254, -2.504760397472873823, 29.97295953869789997 ) ) ;
#84611 = ORIENTED_EDGE ( 'NONE', *, *, #85566, .F. ) ;
#84610 = CARTESIAN_POINT ( 'NONE',  ( 12.21151522424549896, -5.851115903089112003, 34.47074536777953568 ) ) ;
#84612 = CARTESIAN_POINT ( 'NONE',  ( 9.442307692307693401, -2.499999999999998668, 29.75000000000000355 ) ) ;
#84613 = CARTESIAN_POINT ( 'NONE',  ( -12.46153846153846168, -6.343179335718451384, 34.87096338111211935 ) ) ;
#84614 = VERTEX_POINT ( 'NONE', #23608 ) ;
#84615 = CARTESIAN_POINT ( 'NONE',  ( -13.25382357679060519, -2.541949514083464479, 30.39797389878540557 ) ) ;
#84616 = VECTOR ( 'NONE', #75972, 1000.000000000000000 ) ;
#84617 = DIRECTION ( 'NONE',  ( 0.000000000000000000, 0.3420201433256610524, 0.9396926207859113145 ) ) ;
#84618 = EDGE_LOOP ( 'NONE', ( #71764, #12503 ) ) ;
#84619 = FACE_OUTER_BOUND ( 'NONE', #19876, .T. ) ;
#84620 = CARTESIAN_POINT ( 'NONE',  ( -11.76138849736838488, -12.38737895849757820, 31.66785238281580206 ) ) ;
#84621 = CLOSED_SHELL ( 'NONE', ( #75889, #53068, #66807, #88763, #57551, #5219 ) ) ;
#84622 = CARTESIAN_POINT ( 'NONE',  ( 12.68431813051652846, -12.11081565061823717, 32.26097654155341843 ) ) ;
#84623 = EDGE_LOOP ( 'NONE', ( #17187, #85594 ) ) ;
#84624 = ORIENTED_EDGE ( 'NONE', *, *, #49464, .F. ) ;
#84625 = EDGE_CURVE ( 'NONE', #85495, #74166, #53375, .T. ) ;
#84626 = ORIENTED_EDGE ( 'NONE', *, *, #31139, .F. ) ;
#84627 = CARTESIAN_POINT ( 'NONE',  ( -18.06608341095587988, -3.513871655860376197, 32.76840700105978499 ) ) ;
#84628 = CARTESIAN_POINT ( 'NONE',  ( -6.000000000000121680, -5.941354392335915335, 34.76329471203413846 ) ) ;
#84629 = EDGE_CURVE ( 'NONE', #51377, #27221, #44762, .T. ) ;
#84630 = B_SPLINE_CURVE_WITH_KNOTS ( 'NONE', 3,
 ( #87008, #17182, #44639, #72122, #10437, #38798, #37905, #59504, #4105, #65369 ),
 .UNSPECIFIED., .F., .F.,
 ( 4, 2, 2, 2, 4 ),
 ( 0.000000000000000000, 0.0001954311564186866305, 0.0003908623128373732609, 0.0005862934692560598914, 0.0007817246256747465219 ),
 .UNSPECIFIED. ) ;
#84631 = CARTESIAN_POINT ( 'NONE',  ( -4.087778820496076548, -12.62096338111211757, 30.90682066428152908 ) ) ;
#84632 = EDGE_CURVE ( 'NONE', #29049, #26482, #43236, .T. ) ;
#84633 = CARTESIAN_POINT ( 'NONE',  ( 17.99999999999987566, -12.16647553114689728, 32.15551576947799362 ) ) ;
#84634 = ORIENTED_EDGE ( 'NONE', *, *, #52920, .F. ) ;
#84635 = ORIENTED_EDGE ( 'NONE', *, *, #28725, .F. ) ;
#84637 = ORIENTED_EDGE ( 'NONE', *, *, #18625, .F. ) ;
#84636 = CARTESIAN_POINT ( 'NONE',  ( 9.468822748583747284, -4.386631170607603991, 33.66268669641500111 ) ) ;
#84638 = EDGE_CURVE ( 'NONE', #36427, #63016, #26009, .T. ) ;
#84639 = LINE ( 'NONE', #58459, #46708 ) ;
#84640 = ORIENTED_EDGE ( 'NONE', *, *, #24065, .T. ) ;
#84641 = CARTESIAN_POINT ( 'NONE',  ( 7.596177102105255763, -12.01397095200673881, 32.43157075238190146 ) ) ;
#84642 = CARTESIAN_POINT ( 'NONE',  ( 7.976679547917409963, -5.195472089885680766, 34.18748526763464923 ) ) ;
#84643 = EDGE_LOOP ( 'NONE', ( #4399, #53412, #53205, #13756 ) ) ;
#84644 = ORIENTED_EDGE ( 'NONE', *, *, #23992, .T. ) ;
#84646 = VERTEX_POINT ( 'NONE', #38023 ) ;
#84645 = CARTESIAN_POINT ( 'NONE',  ( -6.792551221313363641, -11.46989282347013095, 32.79007818306219946 ) ) ;
#84647 = CARTESIAN_POINT ( 'NONE',  ( 4.284637961670938466, -4.809403383903226192, 33.96459661697924304 ) ) ;
#84648 = CARTESIAN_POINT ( 'NONE',  ( 14.24160992833217065, -5.471508081941602875, 34.59228464037088457 ) ) ;
#84649 = VERTEX_POINT ( 'NONE', #16858 ) ;
#84650 = CARTESIAN_POINT ( 'NONE',  ( 15.00784227186238162, -2.308479472611653094, 30.53278059502174457 ) ) ;
#84651 = B_SPLINE_CURVE_WITH_KNOTS ( 'NONE', 3,
 ( #20375, #14050, #75316, #68549, #6845, #41526, #68991, #7300, #34762, #63114 ),
 .UNSPECIFIED., .F., .F.,
 ( 4, 2, 2, 2, 4 ),
 ( 0.0007817359430256328248, 0.0009771253907249995759, 0.001172514838424366327, 0.001367904286123733078, 0.001563293733823099829 ),
 .UNSPECIFIED. ) ;
#84652 = CARTESIAN_POINT ( 'NONE',  ( 5.299934428535925335, -11.24521262558773671, 33.06293181088029343 ) ) ;
#84653 = FACE_OUTER_BOUND ( 'NONE', #65544, .T. ) ;
#84654 = FACE_BOUND ( 'NONE', #58437, .T. ) ;
#84655 = EDGE_CURVE ( 'NONE', #58130, #14228, #39528, .T. ) ;
#84656 = PLANE ( 'NONE',  #36994 ) ;
#84657 = CARTESIAN_POINT ( 'NONE',  ( 2.557746619330623528, -8.303483539816728154, 34.68545999027711702 ) ) ;
#84658 = CARTESIAN_POINT ( 'NONE',  ( 6.000000000000001776, -12.78798330534102767, 29.49999999999997868 ) ) ;
#84659 = B_SPLINE_CURVE_WITH_KNOTS ( 'NONE', 3,
 ( #31422, #85925, #17467, #25107, #78267, #30962, #58429, #9815, #44469, #4391 ),
 .UNSPECIFIED., .F., .F.,
 ( 4, 2, 2, 2, 4 ),
 ( 0.0007817359430256302227, 0.0009771253907249963233, 0.001172514838424362424, 0.001367904286123728524, 0.001563293733823094625 ),
 .UNSPECIFIED. ) ;
#84661 = CARTESIAN_POINT ( 'NONE',  ( -16.08859101433331062, -3.083524468853783951, 32.58852847137153930 ) ) ;
#84660 = CARTESIAN_POINT ( 'NONE',  ( 0.6849139473108805110, -2.251407671071270489, 29.88021292934942252 ) ) ;
#84662 = B_SPLINE_CURVE_WITH_KNOTS ( 'NONE', 3,
 ( #13754, #28152, #41236, #1575, #29063, #7890, #69146, #35356, #56518, #84008 ),
 .UNSPECIFIED., .F., .F.,
 ( 4, 2, 2, 2, 4 ),
 ( 0.000000000000000000, 0.0001954339857564075828, 0.0003908679715128151656, 0.0005863019572692227755, 0.0007817359430256303312 ),
 .UNSPECIFIED. ) ;
#84663 = VECTOR ( 'NONE', #23962, 1000.000000000000114 ) ;
#84664 = CARTESIAN_POINT ( 'NONE',  ( 8.546303810323914618, -9.172386477786396597, 34.72672124145550043 ) ) ;
#84665 = CARTESIAN_POINT ( 'NONE',  ( -16.40386937806761836, -2.588893531581426544, 31.60682220781847818 ) ) ;
#84666 = EDGE_LOOP ( 'NONE', ( #33288, #18211, #4703, #32450, #86867, #42385 ) ) ;
#84667 = DIRECTION ( 'NONE',  ( -0.000000000000000000, -0.5000000000000009992, -0.8660254037844380415 ) ) ;
#84668 = ORIENTED_EDGE ( 'NONE', *, *, #59632, .F. ) ;
#84669 = EDGE_LOOP ( 'NONE', ( #49819, #31541, #13843, #70508 ) ) ;
#84671 = CARTESIAN_POINT ( 'NONE',  ( 10.74617505635156789, -11.93129842949671726, 32.56571108434900452 ) ) ;
#84670 = FACE_OUTER_BOUND ( 'NONE', #6019, .T. ) ;
#84672 = EDGE_CURVE ( 'NONE', #80991, #41728, #79459, .T. ) ;
#84673 = AXIS2_PLACEMENT_3D ( 'NONE', #76600, #14907, #69839 ) ;
#84674 = CARTESIAN_POINT ( 'NONE',  ( -6.673022611438608642, -6.567000820036038355, 34.66262288849541306 ) ) ;
#84675 = DIRECTION ( 'NONE',  ( -0.000000000000000000, 0.5000000000000011102, -0.8660254037844381525 ) ) ;
#84676 = LINE ( 'NONE', #30157, #53021 ) ;
#84677 = CARTESIAN_POINT ( 'NONE',  ( 14.37294744720514750, -11.67786785259547777, 32.92929555188713664 ) ) ;
#84678 = ORIENTED_EDGE ( 'NONE', *, *, #56273, .F. ) ;
#84679 = DIRECTION ( 'NONE',  ( 0.000000000000000000, -6.938893903907222067E-15, 1.000000000000000000 ) ) ;
#84680 = ADVANCED_FACE ( 'NONE', ( #9655 ), #37119, .F. ) ;
#84681 = EDGE_CURVE ( 'NONE', #33584, #34053, #18653, .T. ) ;
#84682 = CARTESIAN_POINT ( 'NONE',  ( 14.24242230713598900, -12.70778746994557551, 30.41441678777548319 ) ) ;
#84683 = CARTESIAN_POINT ( 'NONE',  ( 2.307692307692309264, -5.180354513474913603, 36.12317359536750416 ) ) ;
#84684 = CARTESIAN_POINT ( 'NONE',  ( -8.638440328263817136, -2.494656445102012565, 31.33466734024120015 ) ) ;
#84685 = CARTESIAN_POINT ( 'NONE',  ( 17.78205128205128105, -3.499999999999999556, 29.75000000000000355 ) ) ;
#84686 = CARTESIAN_POINT ( 'NONE',  ( -3.749999999999988454, -9.053300858899127945, 18.76562500000000000 ) ) ;
#84687 = ORIENTED_EDGE ( 'NONE', *, *, #48185, .T. ) ;
#84688 = VERTEX_POINT ( 'NONE', #32160 ) ;
#84689 = CARTESIAN_POINT ( 'NONE',  ( -7.715363405186896451, -11.93129842949671726, 32.56571108434900452 ) ) ;
#84690 = VERTEX_POINT ( 'NONE', #12767 ) ;
#84691 = DIRECTION ( 'NONE',  ( -1.000000000000000000, 0.000000000000000000, 0.000000000000000000 ) ) ;
#84692 = CARTESIAN_POINT ( 'NONE',  ( 10.83816415665302380, -2.600157965045224895, 30.74683119005207743 ) ) ;
#84693 = DIRECTION ( 'NONE',  ( -0.000000000000000000, -0.8660254037844399289, -0.4999999999999980016 ) ) ;
#84694 = CARTESIAN_POINT ( 'NONE',  ( -0.6844654204453088919, -11.98009711892699691, 32.48740034544075428 ) ) ;
#84695 = CARTESIAN_POINT ( 'NONE',  ( 2.651650429449539104, -4.848349570550432475, 19.31250000000000000 ) ) ;
#84696 = EDGE_CURVE ( 'NONE', #48440, #11752, #87875, .T. ) ;
#84697 = CARTESIAN_POINT ( 'NONE',  ( 4.153846153846154188, -5.415277668671390821, 36.20867863119892149 ) ) ;
#84698 = ORIENTED_EDGE ( 'NONE', *, *, #78288, .F. ) ;
#84699 = DIRECTION ( 'NONE',  ( 1.000000000000000000, 0.000000000000000000, 0.000000000000000000 ) ) ;
#84701 = VERTEX_POINT ( 'NONE', #11440 ) ;
#84700 = CARTESIAN_POINT ( 'NONE',  ( 17.93475006822591666, -2.255955759149247619, 30.00000000000014566 ) ) ;
#84702 = CARTESIAN_POINT ( 'NONE',  ( 10.61538461538449596, -10.21337939537710326, 33.94971097300076224 ) ) ;
#84703 = CARTESIAN_POINT ( 'NONE',  ( -12.39628289026243202, -3.835265460703683349, 33.15142922261929925 ) ) ;
#84704 = EDGE_CURVE ( 'NONE', #27134, #4346, #74038, .T. ) ;
#84705 = EDGE_CURVE ( 'NONE', #72630, #58556, #5126, .T. ) ;
#84706 = CARTESIAN_POINT ( 'NONE',  ( 15.23076923076923173, -2.833524468853757305, 32.15551576947925838 ) ) ;
#84707 = CARTESIAN_POINT ( 'NONE',  ( 11.66898697669518725, -8.630441415882550871, 34.87705825610312615 ) ) ;
#84708 = B_SPLINE_CURVE_WITH_KNOTS ( 'NONE', 3,
 ( #38542, #72754, #46625, #11515, #51570, #65550, #87190, #66454, #73671, #5195 ),
 .UNSPECIFIED., .F., .F.,
 ( 4, 2, 2, 2, 4 ),
 ( 0.0007817359430256297891, 0.0009771253907249958896, 0.001172514838424361990, 0.001367904286123728091, 0.001563293733823094191 ),
 .UNSPECIFIED. ) ;
#84709 = CARTESIAN_POINT ( 'NONE',  ( -2.307692307692305711, -13.75783147151868846, 33.36296068462461051 ) ) ;
#84710 = CARTESIAN_POINT ( 'NONE',  ( -11.53846153846153655, -2.833524468853757305, 32.15551576947925838 ) ) ;
#84711 = B_SPLINE_CURVE_WITH_KNOTS ( 'NONE', 3,
 ( #70928, #64589, #76346, #36262, #14654, #42137, #83571, #76804, #49326, #42573 ),
 .UNSPECIFIED., .F., .F.,
 ( 4, 2, 2, 2, 4 ),
 ( 0.000000000000000000, 0.0001954339857564073659, 0.0003908679715128147319, 0.0005863019572692221250, 0.0007817359430256294638 ),
 .UNSPECIFIED. ) ;
#84712 = CARTESIAN_POINT ( 'NONE',  ( -1.077988221561493543, -4.724691934501247914, 24.32999329374151642 ) ) ;
#84713 = EDGE_LOOP ( 'NONE', ( #77601, #56046, #21685, #14391 ) ) ;
#84714 = CIRCLE ( 'NONE', #63079, 4.000000000000000000 ) ;
#84715 = EDGE_CURVE ( 'NONE', #35784, #42127, #83542, .T. ) ;
#84716 = CARTESIAN_POINT ( 'NONE',  ( -1.253823576790596528, -11.18335022499818621, 33.13157742990016885 ) ) ;
#84717 = FACE_OUTER_BOUND ( 'NONE', #34011, .T. ) ;
#84718 = CARTESIAN_POINT ( 'NONE',  ( 1.139087296526029469, -10.24999999999999467, 23.45312500000000000 ) ) ;
#84719 = CARTESIAN_POINT ( 'NONE',  ( 0.3308469948708994690, -3.530157926970578508, 32.79014554554150607 ) ) ;
#84720 = CARTESIAN_POINT ( 'NONE',  ( -7.623141002060447313, -2.889357225399416862, 32.26129605718031712 ) ) ;
#84721 = ORIENTED_EDGE ( 'NONE', *, *, #48667, .T. ) ;
#84722 = CARTESIAN_POINT ( 'NONE',  ( -2.749999999999991562, -8.639087296526026805, 16.26562500000000000 ) ) ;
#84723 = CARTESIAN_POINT ( 'NONE',  ( -2.373775718648186484, -3.050289026998445951, 32.03036669348365706 ) ) ;
#84724 = B_SPLINE_CURVE_WITH_KNOTS ( 'NONE', 3,
 ( #80605, #44555, #31961, #87819, #39173, #53552, #24749, #86932, #45905, #58517 ),
 .UNSPECIFIED., .F., .F.,
 ( 4, 2, 2, 2, 4 ),
 ( 0.0007817359430256284880, 0.0009771253907249941549, 0.001172514838424359822, 0.001367904286123725489, 0.001563293733823091156 ),
 .UNSPECIFIED. ) ;
#84725 = ORIENTED_EDGE ( 'NONE', *, *, #47187, .T. ) ;
#84726 = CARTESIAN_POINT ( 'NONE',  ( -4.219928533206287469, -8.164416787775445883, 34.95778746994557906 ) ) ;
#84727 = ORIENTED_EDGE ( 'NONE', *, *, #15028, .F. ) ;
#84728 = CARTESIAN_POINT ( 'NONE',  ( -0.3589743589743593088, -3.499999999999999556, 29.75000000000000355 ) ) ;
#84729 = CARTESIAN_POINT ( 'NONE',  ( 3.164686851409095780, -3.937682226553329556, 33.60647404775217240 ) ) ;
#84730 = CARTESIAN_POINT ( 'NONE',  ( -0.5916864312701569650, -10.31621877034669588, 34.18098118002070152 ) ) ;
#84731 = CARTESIAN_POINT ( 'NONE',  ( -6.923076923077045919, -2.379036618888197729, 30.90682066428292885 ) ) ;
#84732 = ORIENTED_EDGE ( 'NONE', *, *, #73675, .F. ) ;
#84733 = CARTESIAN_POINT ( 'NONE',  ( -3.164701897419153642, -2.292212530054420494, 30.41441678777542990 ) ) ;
#84734 = EDGE_CURVE ( 'NONE', #49519, #19405, #25465, .T. ) ;
#84735 = EDGE_LOOP ( 'NONE', ( #49346, #58224, #55164, #63845 ) ) ;
#84736 = AXIS2_PLACEMENT_3D ( 'NONE', #74887, #40657, #13615 ) ;
#84737 = LINE ( 'NONE', #50473, #65878 ) ;
#84738 = CARTESIAN_POINT ( 'NONE',  ( -10.68146802634049308, -2.721908614388770964, 31.22303859784723912 ) ) ;
#84739 = VERTEX_POINT ( 'NONE', #79899 ) ;
#84740 = CARTESIAN_POINT ( 'NONE',  ( -0.4615384615384611200, -6.386643153685126251, 34.62446782046654192 ) ) ;
#84741 = DIRECTION ( 'NONE',  ( -0.000000000000000000, -0.7660444431189791237, -0.6427876096865379196 ) ) ;
#84742 = CARTESIAN_POINT ( 'NONE',  ( -4.153846153845845102, -2.506253911140614576, 30.00000000000323297 ) ) ;
#84743 = VECTOR ( 'NONE', #25489, 1000.000000000000000 ) ;
#84744 = AXIS2_PLACEMENT_3D ( 'NONE', #4378, #79601, #3478 ) ;
#84745 = CARTESIAN_POINT ( 'NONE',  ( 9.442307692307693401, -2.249999999999998668, 29.75000000000000355 ) ) ;
#84746 = CARTESIAN_POINT ( 'NONE',  ( -4.153846153846152411, -3.937682226553329556, 33.60647404775216529 ) ) ;
#84747 = AXIS2_PLACEMENT_3D ( 'NONE', #65698, #11218, #50411 ) ;
#84748 = ORIENTED_EDGE ( 'NONE', *, *, #21257, .F. ) ;
#84749 = ORIENTED_EDGE ( 'NONE', *, *, #49248, .T. ) ;
#84750 = FACE_BOUND ( 'NONE', #83920, .T. ) ;
#84751 = ORIENTED_EDGE ( 'NONE', *, *, #50952, .F. ) ;
#84752 = CARTESIAN_POINT ( 'NONE',  ( -5.011730088628421065, -2.255955759149235629, 29.99999999999988631 ) ) ;
#84753 = CARTESIAN_POINT ( 'NONE',  ( 17.93472999944368240, -5.941354392334501355, 34.76329471203369792 ) ) ;
#84754 = CARTESIAN_POINT ( 'NONE',  ( -18.00000000000000000, -3.937682226553330445, 33.60647404775216529 ) ) ;
#84755 = ORIENTED_EDGE ( 'NONE', *, *, #50557, .T. ) ;
#84756 = EDGE_CURVE ( 'NONE', #1870, #69237, #64210, .T. ) ;
#84757 = ORIENTED_EDGE ( 'NONE', *, *, #9409, .F. ) ;
#84758 = CARTESIAN_POINT ( 'NONE',  ( -15.23076923076922995, -2.517432740324522911, 35.29906147534542527 ) ) ;
#84759 = ORIENTED_EDGE ( 'NONE', *, *, #79644, .T. ) ;
#84760 = CARTESIAN_POINT ( 'NONE',  ( -10.61538461538473399, -9.442884908241554243, 34.35708131394783038 ) ) ;
#84761 = CARTESIAN_POINT ( 'NONE',  ( 3.007284287045284721, -2.847400154188067578, 31.58180166144859768 ) ) ;
#84762 = AXIS2_PLACEMENT_3D ( 'NONE', #9672, #86246, #23189 ) ;
#84763 = CARTESIAN_POINT ( 'NONE',  ( -14.30769230769230660, -6.435427911321262684, 35.78748833219616898 ) ) ;
#84764 = FACE_BOUND ( 'NONE', #86466, .T. ) ;
#84765 = ORIENTED_EDGE ( 'NONE', *, *, #64791, .T. ) ;
#84766 = CARTESIAN_POINT ( 'NONE',  ( -5.207070286361298095, -10.88202310037935661, 33.43294751532457099 ) ) ;
#84767 = CARTESIAN_POINT ( 'NONE',  ( -6.249976744048591826, -6.524016743844655686, 34.90889640711025521 ) ) ;
#84768 = CARTESIAN_POINT ( 'NONE',  ( 14.30769230769218758, -6.879047030192662504, 34.71129190930017927 ) ) ;
#84769 = FACE_OUTER_BOUND ( 'NONE', #41541, .T. ) ;
#84770 = VERTEX_POINT ( 'NONE', #52411 ) ;
#84771 = EDGE_CURVE ( 'NONE', #53967, #72293, #26725, .T. ) ;
#84772 = EDGE_LOOP ( 'NONE', ( #78774, #83802, #34812, #73652 ) ) ;
#84773 = ADVANCED_FACE ( 'NONE', ( #18201 ), #45663, .F. ) ;
#84774 = ORIENTED_EDGE ( 'NONE', *, *, #86278, .F. ) ;
#84776 = DIRECTION ( 'NONE',  ( -0.000000000000000000, 1.000000000000000000, 1.084202172485503448E-16 ) ) ;
#84775 = CARTESIAN_POINT ( 'NONE',  ( -8.096130577096200653, -6.567427716900048118, 34.66269422305636283 ) ) ;
#84777 = B_SPLINE_CURVE_WITH_KNOTS ( 'NONE', 3,
 ( #30719, #58186, #23955, #10463, #65393, #3687, #56431, #77145, #15451, #42925 ),
 .UNSPECIFIED., .F., .F.,
 ( 4, 2, 2, 2, 4 ),
 ( 0.0007817359430256308733, 0.0009771253907249971907, 0.001172514838424363725, 0.001367904286123730259, 0.001563293733823096577 ),
 .UNSPECIFIED. ) ;
#84778 = CARTESIAN_POINT ( 'NONE',  ( -8.703163435880695076, -12.34228464037088813, 31.77849191805839268 ) ) ;
#84779 = CARTESIAN_POINT ( 'NONE',  ( -2.307692307692305711, -2.486705287966279876, 31.30864560766543647 ) ) ;
#84780 = FACE_BOUND ( 'NONE', #39082, .T. ) ;
#84781 = DIRECTION ( 'NONE',  ( -0.000000000000000000, 0.8660254037844399289, -0.4999999999999980016 ) ) ;
#84782 = EDGE_LOOP ( 'NONE', ( #49485, #85098 ) ) ;
#84783 = DIRECTION ( 'NONE',  ( 0.000000000000000000, 0.1736481776669275834, 0.9848077530122086864 ) ) ;
#84784 = EDGE_CURVE ( 'NONE', #85662, #54661, #21147, .T. ) ;
#84785 = CARTESIAN_POINT ( 'NONE',  ( -11.76194648218548622, -10.11188796281391511, 34.01382737946119050 ) ) ;
#84786 = LINE ( 'NONE', #23068, #89085 ) ;
#84787 = DIRECTION ( 'NONE',  ( 0.000000000000000000, 0.7660444431189807890, 0.6427876096865361433 ) ) ;
#84788 = ORIENTED_EDGE ( 'NONE', *, *, #24631, .T. ) ;
#84789 = CARTESIAN_POINT ( 'NONE',  ( 8.769230769230645706, -12.70778746994576025, 30.41441678777401236 ) ) ;
#84790 = EDGE_LOOP ( 'NONE', ( #54284, #83098 ) ) ;
#84791 = FACE_BOUND ( 'NONE', #16326, .T. ) ;
#84792 = CARTESIAN_POINT ( 'NONE',  ( 7.384615384615385025, -11.00000000000000000, 29.75000000000000355 ) ) ;
#84793 = CIRCLE ( 'NONE', #77636, 4.000000000000000000 ) ;
#84794 = VECTOR ( 'NONE', #64452, 1000.000000000000227 ) ;
#84795 = CARTESIAN_POINT ( 'NONE',  ( 4.284371592079796010, -2.647132371071621471, 31.75357179365173010 ) ) ;
#84796 = CARTESIAN_POINT ( 'NONE',  ( -11.31545018684868786, -11.76359900205217457, 32.36225158514719880 ) ) ;
#84797 = ORIENTED_EDGE ( 'NONE', *, *, #7455, .F. ) ;
#84798 = B_SPLINE_CURVE_WITH_KNOTS ( 'NONE', 3,
 ( #55365, #48605, #47728, #88112, #80896, #20939, #54278, #88988, #67366, #81334 ),
 .UNSPECIFIED., .F., .F.,
 ( 4, 2, 2, 2, 4 ),
 ( 0.000000000000000000, 0.0001954339857564071762, 0.0003908679715128143524, 0.0005863019572692215828, 0.0007817359430256287049 ),
 .UNSPECIFIED. ) ;
#84799 = CARTESIAN_POINT ( 'NONE',  ( -16.21992853320628925, -11.35647404775217595, 33.31231777344666511 ) ) ;
#84800 = CARTESIAN_POINT ( 'NONE',  ( -2.307692307692427391, -4.481592998941358097, 33.73612834414048933 ) ) ;
#84801 = CARTESIAN_POINT ( 'NONE',  ( -9.822454901745912181, -3.285722584762969856, 32.44110544564090759 ) ) ;
#84802 = CARTESIAN_POINT ( 'NONE',  ( 10.61538461538461675, -6.681629849574314051, 35.83090037661290239 ) ) ;
#84803 = ORIENTED_EDGE ( 'NONE', *, *, #27668, .T. ) ;
#84804 = B_SPLINE_CURVE_WITH_KNOTS ( 'NONE', 3,
 ( #80341, #19073, #82107, #74910, #88880, #68581, #53287, #27154, #46972, #25832 ),
 .UNSPECIFIED., .F., .F.,
 ( 4, 2, 2, 2, 4 ),
 ( 0.000000000000000000, 0.0001954311564186882568, 0.0003908623128373765136, 0.0005862934692560647703, 0.0007817246256747530271 ),
 .UNSPECIFIED. ) ;
#84805 = VECTOR ( 'NONE', #12028, 1000.000000000000000 ) ;
#84806 = CIRCLE ( 'NONE', #68971, 4.000000000000000000 ) ;
#84807 = CARTESIAN_POINT ( 'NONE',  ( -9.692307692307691624, -2.833524468853757305, 32.15551576947925838 ) ) ;
#84808 = ORIENTED_EDGE ( 'NONE', *, *, #76024, .T. ) ;
#84809 = VECTOR ( 'NONE', #88616, 1000.000000000000000 ) ;
#84811 = ORIENTED_EDGE ( 'NONE', *, *, #63330, .F. ) ;
#84810 = CARTESIAN_POINT ( 'NONE',  ( 18.06606733335007675, -5.471508081941601098, 34.59228464037088457 ) ) ;
#84812 = CARTESIAN_POINT ( 'NONE',  ( -8.992109451659418440, -7.630691491037285168, 34.74850469731152458 ) ) ;
#84813 = CARTESIAN_POINT ( 'NONE',  ( 15.16468685140909400, -4.661471528628507777, 34.16647553114621871 ) ) ;
#84814 = LINE ( 'NONE', #14561, #88929 ) ;
#84815 = EDGE_CURVE ( 'NONE', #54586, #59185, #737, .T. ) ;
#84816 = CARTESIAN_POINT ( 'NONE',  ( -15.16562445004959692, -7.750023224968867197, 34.99404313364389907 ) ) ;
#84817 = CARTESIAN_POINT ( 'NONE',  ( -8.096130577096198877, -9.148715823498378086, 34.47080413974185120 ) ) ;
#84818 = DIRECTION ( 'NONE',  ( 1.000000000000000000, 0.000000000000000000, 0.000000000000000000 ) ) ;
#84819 = CARTESIAN_POINT ( 'NONE',  ( 2.750000000000008438, -8.639087296525996607, 25.79687500000000355 ) ) ;
#84820 = ORIENTED_EDGE ( 'NONE', *, *, #8394, .T. ) ;
#84821 = CARTESIAN_POINT ( 'NONE',  ( -15.23076923076922995, -3.513871655860378418, 32.76840700105978499 ) ) ;
#84822 = CARTESIAN_POINT ( 'NONE',  ( 5.869852030268307708, -8.630895178749536711, 34.87696386517710323 ) ) ;
#84823 = VERTEX_POINT ( 'NONE', #40698 ) ;
#84824 = ORIENTED_EDGE ( 'NONE', *, *, #4475, .F. ) ;
#84825 = ORIENTED_EDGE ( 'NONE', *, *, #54341, .T. ) ;
#84826 = LINE ( 'NONE', #36625, #23911 ) ;
#84827 = DIRECTION ( 'NONE',  ( -0.000000000000000000, -0.7660444431189791237, -0.6427876096865379196 ) ) ;
#84828 = DIRECTION ( 'NONE',  ( -0.000000000000000000, 0.6427876096865404731, -0.7660444431189770143 ) ) ;
#84829 = CYLINDRICAL_SURFACE ( 'NONE', #88866, 4.000000000000000000 ) ;
#84830 = CARTESIAN_POINT ( 'NONE',  ( -5.076923076923075762, -3.513871655860378418, 32.76840700105978499 ) ) ;
#84831 = CARTESIAN_POINT ( 'NONE',  ( -16.85391023282967637, -11.43677907613345113, 33.22367315496201456 ) ) ;
#84832 = CARTESIAN_POINT ( 'NONE',  ( 13.60799087038780542, -2.251407671071270489, 29.88021292934943318 ) ) ;
#84833 = ORIENTED_EDGE ( 'NONE', *, *, #13592, .F. ) ;
#84834 = CARTESIAN_POINT ( 'NONE',  ( 2.980745993476265898, -6.695914987888143877, 34.68535235679833306 ) ) ;
#84835 = CARTESIAN_POINT ( 'NONE',  ( -1.515306851282941292, -6.413092428213692742, 34.63065189839063152 ) ) ;
#84836 = CARTESIAN_POINT ( 'NONE',  ( 3.230769230769231726, -2.249999999999998668, 29.75000000000001776 ) ) ;
#84837 = DIRECTION ( 'NONE',  ( -0.000000000000000000, -0.5000000000000009992, -0.8660254037844380415 ) ) ;
#84838 = ORIENTED_EDGE ( 'NONE', *, *, #11352, .T. ) ;
#84839 = DIRECTION ( 'NONE',  ( -0.000000000000000000, 1.000000000000000000, -0.000000000000000000 ) ) ;
#84840 = VERTEX_POINT ( 'NONE', #83462 ) ;
#84841 = B_SPLINE_CURVE_WITH_KNOTS ( 'NONE', 3,
 ( #7720, #950, #35180, #62637, #31524, #16235, #86945, #79719, #44571, #4035 ),
 .UNSPECIFIED., .F., .F.,
 ( 4, 2, 2, 2, 4 ),
 ( 0.0007817246336856291692, 0.0009771112958940103739, 0.001172497958102391470, 0.001367884620310772566, 0.001563271282519153879 ),
 .UNSPECIFIED. ) ;
#84842 = CARTESIAN_POINT ( 'NONE',  ( 15.23076923076911093, -11.48612834414049644, 32.76840700105863391 ) ) ;
#84843 = FACE_OUTER_BOUND ( 'NONE', #70698, .T. ) ;
#84844 = CARTESIAN_POINT ( 'NONE',  ( 11.78840705680968171, -10.05730279482229683, 34.04704008940765902 ) ) ;
#84845 = CARTESIAN_POINT ( 'NONE',  ( 6.249945409378045547, -12.68172785388650681, 30.59649109432439573 ) ) ;
#84846 = VERTEX_POINT ( 'NONE', #27611 ) ;
#84847 = CARTESIAN_POINT ( 'NONE',  ( -16.15384615384615330, -13.75783147151868846, 33.36296068462461051 ) ) ;
#84848 = CARTESIAN_POINT ( 'NONE',  ( 9.692307692307695177, -2.499999999999998668, 29.75000000000001421 ) ) ;
#84849 = CARTESIAN_POINT ( 'NONE',  ( 8.992242120843618736, -4.187068189119697692, 33.49521262558774026 ) ) ;
#84850 = ORIENTED_EDGE ( 'NONE', *, *, #4646, .F. ) ;
#84851 = AXIS2_PLACEMENT_3D ( 'NONE', #73471, #24365, #17633 ) ;
#84852 = CARTESIAN_POINT ( 'NONE',  ( 16.15384615384615330, -9.905515769479276145, 34.41647553114623292 ) ) ;
#84853 = VERTEX_POINT ( 'NONE', #13655 ) ;
#84854 = B_SPLINE_CURVE_WITH_KNOTS ( 'NONE', 3,
 ( #7507, #61994, #6615, #81841, #34083, #76399, #13811, #42185, #55237, #20131 ),
 .UNSPECIFIED., .F., .F.,
 ( 4, 2, 2, 2, 4 ),
 ( 0.0007817359430256365111, 0.0009771253907250043464, 0.001172514838424372399, 0.001367904286123740234, 0.001563293733823107852 ),
 .UNSPECIFIED. ) ;
#84855 = CARTESIAN_POINT ( 'NONE',  ( -9.692307692307691624, -12.10708131394839349, 31.69288490824020244 ) ) ;
#84856 = CARTESIAN_POINT ( 'NONE',  ( -16.82686865700962642, -3.435999193479609026, 33.07426656108011542 ) ) ;
#84857 = CARTESIAN_POINT ( 'NONE',  ( -7.976844449264150150, -2.494641256782728966, 31.33461815524612959 ) ) ;
#84858 = CARTESIAN_POINT ( 'NONE',  ( -14.08491276642389600, -10.11255958852956027, 34.01340905677048454 ) ) ;
#84859 = CARTESIAN_POINT ( 'NONE',  ( 18.22277966897806678, -8.540255544307068902, 34.89611431652622286 ) ) ;
#84860 = VECTOR ( 'NONE', #44754, 1000.000000000000114 ) ;
#84861 = ORIENTED_EDGE ( 'NONE', *, *, #81290, .T. ) ;
#84862 = VECTOR ( 'NONE', #38979, 999.9999999999998863 ) ;
#84863 = ORIENTED_EDGE ( 'NONE', *, *, #71127, .F. ) ;
#84864 = EDGE_LOOP ( 'NONE', ( #55316, #29527, #45043, #18054 ) ) ;
#84865 = CARTESIAN_POINT ( 'NONE',  ( -1.254089682851817988, -3.285477652293412820, 32.44071101563363158 ) ) ;
#84866 = LINE ( 'NONE', #16390, #2781 ) ;
#84867 = CARTESIAN_POINT ( 'NONE',  ( -12.39628332202562255, -12.51329471203373700, 31.30864560766537963 ) ) ;
#84869 = EDGE_CURVE ( 'NONE', #4346, #31713, #68161, .T. ) ;
#84868 = DIRECTION ( 'NONE',  ( -0.000000000000000000, -0.6427876096865404731, -0.7660444431189770143 ) ) ;
#84870 = FACE_OUTER_BOUND ( 'NONE', #40446, .T. ) ;
#84871 = CARTESIAN_POINT ( 'NONE',  ( 5.207714884747862705, -9.804649428959608670, 34.18742332936588468 ) ) ;
#84872 = ORIENTED_EDGE ( 'NONE', *, *, #12518, .T. ) ;
#84873 = EDGE_CURVE ( 'NONE', #11880, #75229, #34365, .T. ) ;
#84874 = ORIENTED_EDGE ( 'NONE', *, *, #6426, .T. ) ;
#84875 = VERTEX_POINT ( 'NONE', #6464 ) ;
#84877 = ORIENTED_EDGE ( 'NONE', *, *, #315, .T. ) ;
#84876 = CARTESIAN_POINT ( 'NONE',  ( -19.50000000000000000, -3.499999999999999556, 29.75000000000000355 ) ) ;
#84879 = CARTESIAN_POINT ( 'NONE',  ( 16.15384615384615330, -4.945431358278436385, 36.03766855953609394 ) ) ;
#84878 = CARTESIAN_POINT ( 'NONE',  ( 16.15384615384615330, -2.517432740324522911, 35.29906147534542527 ) ) ;
#84880 = CARTESIAN_POINT ( 'NONE',  ( 8.992193672792254233, -7.369474270740069777, 34.74850911626239736 ) ) ;
#84881 = CARTESIAN_POINT ( 'NONE',  ( 13.63456090296352841, -8.433404298154334455, 34.66254593164985920 ) ) ;
#84882 = EDGE_LOOP ( 'NONE', ( #49826, #15914, #64475, #50780 ) ) ;
#84883 = EDGE_CURVE ( 'NONE', #42856, #49110, #33923, .T. ) ;
#84884 = AXIS2_PLACEMENT_3D ( 'NONE', #78250, #30075, #56217 ) ;
#84885 = EDGE_LOOP ( 'NONE', ( #75735, #84352, #12513, #1299 ) ) ;
#84886 = CARTESIAN_POINT ( 'NONE',  ( 13.45068271796546178, -10.67929555188718282, 33.92786785259544757 ) ) ;
#84887 = ORIENTED_EDGE ( 'NONE', *, *, #42085, .T. ) ;
#84888 = FACE_BOUND ( 'NONE', #68603, .T. ) ;
#84889 = DIRECTION ( 'NONE',  ( -0.000000000000000000, -0.5000000000000009992, -0.8660254037844380415 ) ) ;
#84890 = CARTESIAN_POINT ( 'NONE',  ( -4.153846153846152411, -9.819645486525091727, 36.12317359536749706 ) ) ;
#84891 = ORIENTED_EDGE ( 'NONE', *, *, #23600, .T. ) ;
#84892 = FACE_OUTER_BOUND ( 'NONE', #27916, .T. ) ;
#84893 = CARTESIAN_POINT ( 'NONE',  ( 4.826946332874483936, -8.347322224742351082, 34.93158281831414769 ) ) ;
#84894 = CARTESIAN_POINT ( 'NONE',  ( 1.161688425708536920, -3.395401636524185474, 33.02366814457250399 ) ) ;
#84895 = DIRECTION ( 'NONE',  ( 1.000000000000000000, 0.000000000000000000, 0.000000000000000000 ) ) ;
#84896 = CARTESIAN_POINT ( 'NONE',  ( 4.403900465484466231, -3.136992222400443175, 32.19305428654138979 ) ) ;
#84897 = B_SPLINE_CURVE_WITH_KNOTS ( 'NONE', 3,
 ( #54537, #74832, #13122, #32061, #87029, #67182, #11797, #32497, #40602, #54093 ),
 .UNSPECIFIED., .F., .F.,
 ( 4, 2, 2, 2, 4 ),
 ( 0.0007817246256747434861, 0.0009771112852218861652, 0.001172497944769028844, 0.001367884604316171740, 0.001563271263863314419 ),
 .UNSPECIFIED. ) ;
#84898 = CARTESIAN_POINT ( 'NONE',  ( 8.096099255531887806, -11.56426240980093745, 33.07394671870546432 ) ) ;
#84899 = CARTESIAN_POINT ( 'NONE',  ( -9.692307692307691624, -2.708943851104267164, 35.45975837776705220 ) ) ;
#84900 = CARTESIAN_POINT ( 'NONE',  ( 23.00000000000000000, -7.500000000000000000, 29.75000000000000355 ) ) ;
#84901 = CARTESIAN_POINT ( 'NONE',  ( -6.249976730942353065, -5.728515186090277211, 34.42611988154120439 ) ) ;
#84902 = B_SPLINE_CURVE_WITH_KNOTS ( 'NONE', 3,
 ( #88283, #38734, #12598, #46380, #72960, #40086, #26107, #53572, #65745, #66196 ),
 .UNSPECIFIED., .F., .F.,
 ( 4, 2, 2, 2, 4 ),
 ( 0.0007817246256747473893, 0.0009771112852218905021, 0.001172497944769033615, 0.001367884604316176944, 0.001563271263863320057 ),
 .UNSPECIFIED. ) ;
#84903 = CARTESIAN_POINT ( 'NONE',  ( 16.08776377448601735, -10.67929555188718460, 33.92786785259543336 ) ) ;
#84904 = DIRECTION ( 'NONE',  ( 0.000000000000000000, 0.9848077530122072432, 0.1736481776669354937 ) ) ;
#84905 = ADVANCED_FACE ( 'NONE', ( #61834 ), #49217, .F. ) ;
#84906 = FACE_BOUND ( 'NONE', #26627, .T. ) ;
#84908 = CARTESIAN_POINT ( 'NONE',  ( 11.66898724022510159, -4.459921816937791661, 33.71989282347011851 ) ) ;
#84907 = FACE_OUTER_BOUND ( 'NONE', #45727, .T. ) ;
#84909 = CARTESIAN_POINT ( 'NONE',  ( 12.46153846153846168, -5.415277668671390821, 36.20867863119892149 ) ) ;
#84911 = CARTESIAN_POINT ( 'NONE',  ( 4.153846153846154188, -2.249999999999998668, 29.75000000000001776 ) ) ;
#84910 = LINE ( 'NONE', #706, #78863 ) ;
#84912 = EDGE_CURVE ( 'NONE', #29932, #57265, #14789, .T. ) ;
#84913 = CARTESIAN_POINT ( 'NONE',  ( 19.50000000000000000, -7.500000000000000000, 29.75000000000000355 ) ) ;
#84914 = CARTESIAN_POINT ( 'NONE',  ( 1.987747218494664292, -9.401340078031346081, 23.12313170625848713 ) ) ;
#84915 = ORIENTED_EDGE ( 'NONE', *, *, #3994, .T. ) ;
#84916 = CARTESIAN_POINT ( 'NONE',  ( -3.903900744468109973, -5.766571408460172243, 34.70601412856602508 ) ) ;
#84917 = ORIENTED_EDGE ( 'NONE', *, *, #29287, .T. ) ;
#84918 = VECTOR ( 'NONE', #37904, 1000.000000000000114 ) ;
#84919 = CARTESIAN_POINT ( 'NONE',  ( -9.942284423250045577, -5.728515186090277211, 34.42611988154120439 ) ) ;
#84920 = ADVANCED_FACE ( 'NONE', ( #55084 ), #55525, .T. ) ;
#84921 = VERTEX_POINT ( 'NONE', #69929 ) ;
#84922 = EDGE_CURVE ( 'NONE', #10416, #40235, #20853, .T. ) ;
#84923 = CARTESIAN_POINT ( 'NONE',  ( 13.38461538461538680, -3.886160181151819604, 36.00935417666054406 ) ) ;
#84924 = ORIENTED_EDGE ( 'NONE', *, *, #62029, .T. ) ;
#84925 = CARTESIAN_POINT ( 'NONE',  ( -6.250023237292964495, -11.86270091957321249, 32.19358267280087915 ) ) ;
#84926 = CARTESIAN_POINT ( 'NONE',  ( -1.200186371490556958, -4.775308065498765409, 22.57625670625848713 ) ) ;
#84927 = CARTESIAN_POINT ( 'NONE',  ( -8.769230769230890843, -10.90142922262034020, 33.41473453929536674 ) ) ;
#84928 = VECTOR ( 'NONE', #20117, 1000.000000000000000 ) ;
#84929 = CARTESIAN_POINT ( 'NONE',  ( 7.173022332454967120, -10.18230066228895758, 34.26354781536631577 ) ) ;
#84930 = CARTESIAN_POINT ( 'NONE',  ( -5.076923076923075762, -2.833524468853757305, 32.15551576947925838 ) ) ;
#84931 = CARTESIAN_POINT ( 'NONE',  ( -17.77425180499407276, -2.249999999999999556, 29.62260770777999497 ) ) ;
#84932 = CARTESIAN_POINT ( 'NONE',  ( 15.48076923076916955, -7.565270445406050648, 34.75000000000000000 ) ) ;
#84933 = CARTESIAN_POINT ( 'NONE',  ( -14.30769230769230660, -3.322132147404559976, 32.92929555188717927 ) ) ;
#84934 = AXIS2_PLACEMENT_3D ( 'NONE', #6686, #21075, #35041 ) ;
#84935 = CARTESIAN_POINT ( 'NONE',  ( 2.651650429449569302, -10.15165042944953733, 17.12500000000000000 ) ) ;
#84936 = CARTESIAN_POINT ( 'NONE',  ( -11.40793610022789828, -2.647132371071621471, 31.75357179365171589 ) ) ;
#84937 = CARTESIAN_POINT ( 'NONE',  ( -14.98071491913091791, -2.564540009722895419, 30.55348353981670684 ) ) ;
#84938 = CARTESIAN_POINT ( 'NONE',  ( -8.769230769230768274, -1.129524287112498415, 32.06866353760679544 ) ) ;
#84939 = CARTESIAN_POINT ( 'NONE',  ( 3.750000000000009770, -9.053300858899081760, 18.29687500000000000 ) ) ;
#84940 = DIRECTION ( 'NONE',  ( -0.000000000000000000, 0.9848077530122085754, -0.1736481776669273613 ) ) ;
#84941 = VERTEX_POINT ( 'NONE', #48322 ) ;
#84942 = CARTESIAN_POINT ( 'NONE',  ( 4.153846153846154188, -2.249999999999998668, 29.75000000000001776 ) ) ;
#84943 = CARTESIAN_POINT ( 'NONE',  ( 15.90384615384615330, -2.249999999999998668, 29.75000000000000355 ) ) ;
#84944 = CARTESIAN_POINT ( 'NONE',  ( 1.134592160393929072, -5.765609946408405406, 34.70566812827424741 ) ) ;
#84945 = CARTESIAN_POINT ( 'NONE',  ( 15.29591401148886121, -7.750023224968867197, 34.99404313364389907 ) ) ;
#84946 = CARTESIAN_POINT ( 'NONE',  ( 14.98076923076923173, -7.433931650972300353, 34.75000000000000711 ) ) ;
#84947 = CARTESIAN_POINT ( 'NONE',  ( -8.899922235898330314, -8.147922237126337563, 34.70805685702651999 ) ) ;
#84948 = EDGE_CURVE ( 'NONE', #7446, #49729, #21294, .T. ) ;
#84949 = ORIENTED_EDGE ( 'NONE', *, *, #61964, .T. ) ;
#84950 = DIRECTION ( 'NONE',  ( -0.000000000000000000, 0.9396926207859093161, -0.3420201433256663259 ) ) ;
#84951 = ORIENTED_EDGE ( 'NONE', *, *, #86903, .F. ) ;
#84952 = ORIENTED_EDGE ( 'NONE', *, *, #36171, .F. ) ;
#84953 = CARTESIAN_POINT ( 'NONE',  ( -8.102564102564102200, -4.000000000000000000, 29.75000000000000355 ) ) ;
#84954 = CARTESIAN_POINT ( 'NONE',  ( 16.37662569511456567, -2.847695495035524882, 31.58253572463339154 ) ) ;
#84955 = CARTESIAN_POINT ( 'NONE',  ( -6.130147209438218781, -3.285722584762969856, 32.44110544564090759 ) ) ;
#84956 = CARTESIAN_POINT ( 'NONE',  ( 10.83816428436268353, -10.23759521482555357, 34.22997729860117033 ) ) ;
#84957 = EDGE_CURVE ( 'NONE', #32798, #46479, #42469, .T. ) ;
#84958 = VERTEX_POINT ( 'NONE', #1478 ) ;
#84959 = CARTESIAN_POINT ( 'NONE',  ( -6.792285115252135519, -5.582136614379148654, 34.36778462344220486 ) ) ;
#84960 = VERTEX_POINT ( 'NONE', #56419 ) ;
#84961 = ORIENTED_EDGE ( 'NONE', *, *, #6162, .T. ) ;
#84962 = AXIS2_PLACEMENT_3D ( 'NONE', #88898, #1032, #68599 ) ;
#84963 = CARTESIAN_POINT ( 'NONE',  ( -15.23076923076922995, -12.10708131394839349, 31.69288490824020244 ) ) ;
#84964 = DIRECTION ( 'NONE',  ( -0.000000000000000000, -0.7660444431189791237, -0.6427876096865379196 ) ) ;
#84965 = CARTESIAN_POINT ( 'NONE',  ( -18.00000000000000000, -1.395656007487078076, 33.56301978189821256 ) ) ;
#84966 = VECTOR ( 'NONE', #43815, 1000.000000000000000 ) ;
#84967 = EDGE_CURVE ( 'NONE', #62470, #62488, #80355, .T. ) ;
#84968 = FACE_OUTER_BOUND ( 'NONE', #46120, .T. ) ;
#84969 = CARTESIAN_POINT ( 'NONE',  ( 13.38461538461538680, -1.790695186598648903, 34.54067556320373455 ) ) ;
#84970 = ORIENTED_EDGE ( 'NONE', *, *, #33865, .F. ) ;
#84971 = EDGE_CURVE ( 'NONE', #46562, #3642, #79224, .T. ) ;
#84972 = ORIENTED_EDGE ( 'NONE', *, *, #60288, .T. ) ;
#84973 = CARTESIAN_POINT ( 'NONE',  ( -3.749999999999997335, -7.500000000000021316, 20.09375000000000000 ) ) ;
#84974 = AXIS2_PLACEMENT_3D ( 'NONE', #28833, #78323, #72455 ) ;
#84975 = VERTEX_POINT ( 'NONE', #4003 ) ;
#84977 = ORIENTED_EDGE ( 'NONE', *, *, #34582, .F. ) ;
#84976 = CARTESIAN_POINT ( 'NONE',  ( -14.30769230769230660, -2.292212530054420494, 30.41441678777542634 ) ) ;
#84978 = CARTESIAN_POINT ( 'NONE',  ( 1.607626736228236819, -9.086983370893047862, 34.49168942202179267 ) ) ;
#84979 = CARTESIAN_POINT ( 'NONE',  ( 6.166666666666664298, -7.500000000000000000, 29.75000000000000355 ) ) ;
#84980 = FACE_OUTER_BOUND ( 'NONE', #12803, .T. ) ;
#84981 = ORIENTED_EDGE ( 'NONE', *, *, #85130, .F. ) ;
#84982 = EDGE_CURVE ( 'NONE', #75555, #15629, #56852, .T. ) ;
#84983 = CARTESIAN_POINT ( 'NONE',  ( -7.846153846153844924, -1.790695186598648903, 34.54067556320373455 ) ) ;
#84984 = ORIENTED_EDGE ( 'NONE', *, *, #3225, .F. ) ;
#84985 = FACE_BOUND ( 'NONE', #70643, .T. ) ;
#84986 = CARTESIAN_POINT ( 'NONE',  ( 15.23076923076923173, -4.786620604624113540, 33.94971097300155094 ) ) ;
#84987 = CARTESIAN_POINT ( 'NONE',  ( -7.173100160369892286, -2.823816976329319495, 31.52131813110795733 ) ) ;
#84988 = CARTESIAN_POINT ( 'NONE',  ( -17.93474486048716088, -2.657715359629131857, 31.77849191805843532 ) ) ;
#84990 = CARTESIAN_POINT ( 'NONE',  ( 14.98076923076921574, -2.249999999999998668, 29.81609741502487410 ) ) ;
#84989 = CARTESIAN_POINT ( 'NONE',  ( 5.933917620639864055, -12.34228464037088280, 31.77849191805838558 ) ) ;
#84991 = EDGE_CURVE ( 'NONE', #64401, #83471, #65705, .T. ) ;
#84992 = DIRECTION ( 'NONE',  ( -0.000000000000000000, -0.7660444431189791237, -0.6427876096865379196 ) ) ;
#84993 = CARTESIAN_POINT ( 'NONE',  ( -12.46153846153846168, -7.500000000000001776, 35.04278698407183867 ) ) ;
#84994 = EDGE_LOOP ( 'NONE', ( #78741, #26608, #53150, #16270 ) ) ;
#84995 = CARTESIAN_POINT ( 'NONE',  ( -11.28840722682322628, -12.17597550085003633, 31.52189283813461884 ) ) ;
#84996 = ADVANCED_FACE ( 'NONE', ( #50534 ), #50092, .F. ) ;
#84997 = CARTESIAN_POINT ( 'NONE',  ( 4.853996118016224770, -4.026226216239095379, 33.68668979543632958 ) ) ;
#84998 = B_SPLINE_CURVE_WITH_KNOTS ( 'NONE', 3,
 ( #29646, #29214, #84159, #9374, #36833, #37719, #84600, #22872, #57545, #50334 ),
 .UNSPECIFIED., .F., .F.,
 ( 4, 2, 2, 2, 4 ),
 ( 0.0007817359430256307648, 0.0009771253907249971907, 0.001172514838424363725, 0.001367904286123730259, 0.001563293733823096577 ),
 .UNSPECIFIED. ) ;
#84999 = ORIENTED_EDGE ( 'NONE', *, *, #7318, .T. ) ;
#85000 = CARTESIAN_POINT ( 'NONE',  ( -17.07692307692307665, -2.249999999999998668, 29.50000000000001421 ) ) ;
#85001 = VECTOR ( 'NONE', #34536, 1000.000000000000227 ) ;
#85002 = CARTESIAN_POINT ( 'NONE',  ( 18.00000000000000000, -1.215029322943914858, 32.30358669280327177 ) ) ;
#85003 = CARTESIAN_POINT ( 'NONE',  ( 16.08857615328984281, -6.835583212224500826, 34.95778746994557906 ) ) ;
#85004 = CYLINDRICAL_SURFACE ( 'NONE', #34633, 0.2499999999999986955 ) ;
#85005 = CARTESIAN_POINT ( 'NONE',  ( -10.39260494640654819, -3.020022701398813236, 32.48759521482552515 ) ) ;
#85006 = ADVANCED_FACE ( 'NONE', ( #39156 ), #18428, .F. ) ;
#85007 = FACE_BOUND ( 'NONE', #60478, .T. ) ;
#85009 = CARTESIAN_POINT ( 'NONE',  ( 17.93391762063986050, -10.67929555188718460, 33.92786785259543336 ) ) ;
#85008 = CARTESIAN_POINT ( 'NONE',  ( 13.38461538461526601, -12.27809138561165270, 31.22303859784587132 ) ) ;
#85010 = DIRECTION ( 'NONE',  ( 1.000000000000000000, 0.000000000000000000, 0.000000000000000000 ) ) ;
#85012 = CARTESIAN_POINT ( 'NONE',  ( 7.623288423950207893, -2.501496062324912284, 29.88072118266895671 ) ) ;
#85011 = CARTESIAN_POINT ( 'NONE',  ( -7.715363405186896451, -12.62708834333097663, 30.88030960425257021 ) ) ;
#85013 = AXIS2_PLACEMENT_3D ( 'NONE', #47562, #88587, #61079 ) ;
#85014 = CARTESIAN_POINT ( 'NONE',  ( -14.30769230769230660, -1.242168528481310874, 33.36296068462461051 ) ) ;
#85015 = CARTESIAN_POINT ( 'NONE',  ( 3.775308065498768517, -8.992201783934554271, 18.04500670625848713 ) ) ;
#85016 = ORIENTED_EDGE ( 'NONE', *, *, #88848, .T. ) ;
#85017 = FACE_OUTER_BOUND ( 'NONE', #2430, .T. ) ;
#85018 = EDGE_CURVE ( 'NONE', #67601, #37942, #87348, .T. ) ;
#85019 = DIRECTION ( 'NONE',  ( -0.000000000000000000, -0.000000000000000000, -1.000000000000000000 ) ) ;
#85020 = CARTESIAN_POINT ( 'NONE',  ( -0.6850233861027922311, -3.562934362175799841, 33.22335522853832401 ) ) ;
#85021 = CARTESIAN_POINT ( 'NONE',  ( 16.82689985270161870, -8.475808217655753651, 34.90892951860618609 ) ) ;
#85022 = DIRECTION ( 'NONE',  ( -0.000000000000000000, 0.9396926207859093161, -0.3420201433256663259 ) ) ;
#85023 = CARTESIAN_POINT ( 'NONE',  ( 1.492201783934554493, -3.724691934501233703, 21.48250670625849068 ) ) ;
#85024 = CARTESIAN_POINT ( 'NONE',  ( -11.40841410321108640, -7.723484941389743952, 34.99544897038808955 ) ) ;
#85025 = FACE_OUTER_BOUND ( 'NONE', #77552, .T. ) ;
#85026 = CARTESIAN_POINT ( 'NONE',  ( 11.47313862296936549, -7.749976743299138882, 34.99404534957040624 ) ) ;
#85027 = CARTESIAN_POINT ( 'NONE',  ( 17.77651507543566822, -8.539481045369598178, 34.89627647299170832 ) ) ;
#85028 = CARTESIAN_POINT ( 'NONE',  ( -10.61538461538461320, -1.117168528481311540, 33.14645433367849847 ) ) ;
#85029 = CARTESIAN_POINT ( 'NONE',  ( -15.23076923076922995, -1.790695186598648903, 34.54067556320373455 ) ) ;
#85030 = CYLINDRICAL_SURFACE ( 'NONE', #62083, 0.2499999999999973355 ) ;
#85031 = B_SPLINE_CURVE_WITH_KNOTS ( 'NONE', 3,
 ( #66969, #60198, #32729, #87699, #17281, #24029, #86654, #79437, #31694, #16394 ),
 .UNSPECIFIED., .F., .F.,
 ( 4, 2, 2, 2, 4 ),
 ( 0.000000000000000000, 0.0001954339857564098867, 0.0003908679715128197734, 0.0005863019572692296059, 0.0007817359430256395469 ),
 .UNSPECIFIED. ) ;
#85032 = B_SPLINE_CURVE_WITH_KNOTS ( 'NONE', 3,
 ( #41233, #47530, #47974, #20511, #67373, #75025, #68258, #34024, #27269, #244 ),
 .UNSPECIFIED., .F., .F.,
 ( 4, 2, 2, 2, 4 ),
 ( 0.0007817359430256329332, 0.0009771253907249995759, 0.001172514838424366327, 0.001367904286123732861, 0.001563293733823099612 ),
 .UNSPECIFIED. ) ;
#85033 = CARTESIAN_POINT ( 'NONE',  ( 15.23076923076923173, -9.584722331328613620, 36.20867863119891439 ) ) ;
#85034 = ADVANCED_FACE ( 'NONE', ( #45888 ), #77577, .F. ) ;
#85035 = VERTEX_POINT ( 'NONE', #84792 ) ;
#85036 = B_SPLINE_CURVE_WITH_KNOTS ( 'NONE', 3,
 ( #16085, #56629, #21507, #36796, #35470, #84115, #48527, #36362, #14764, #21961 ),
 .UNSPECIFIED., .F., .F.,
 ( 4, 2, 2, 2, 4 ),
 ( 0.0007817246256747505334, 0.0009771112852218954894, 0.001172497944769040554, 0.001367884604316185618, 0.001563271263863330682 ),
 .UNSPECIFIED. ) ;
#85037 = CARTESIAN_POINT ( 'NONE',  ( 15.23076923076910916, -11.67786785259630911, 32.92929555188603530 ) ) ;
#85038 = DIRECTION ( 'NONE',  ( -0.000000000000000000, 1.000000000000000000, -0.000000000000000000 ) ) ;
#85039 = CARTESIAN_POINT ( 'NONE',  ( -3.775308065498748977, -8.992201783934593351, 14.01749329374151642 ) ) ;
#85040 = AXIS2_PLACEMENT_3D ( 'NONE', #70247, #29713, #83777 ) ;
#85041 = AXIS2_PLACEMENT_3D ( 'NONE', #42443, #1451, #49634 ) ;
#85042 = CARTESIAN_POINT ( 'NONE',  ( 9.019230769230768274, -2.499999999999998668, 29.75000000000000355 ) ) ;
#85043 = CARTESIAN_POINT ( 'NONE',  ( -16.85391023282967637, -5.582272713120730145, 34.63742843783360570 ) ) ;
#85044 = ORIENTED_EDGE ( 'NONE', *, *, #45385, .F. ) ;
#85045 = EDGE_CURVE ( 'NONE', #76427, #44215, #3908, .T. ) ;
#85046 = CARTESIAN_POINT ( 'NONE',  ( -18.24997673094235395, -9.148715823498378086, 34.47080413974185120 ) ) ;
#85048 = ORIENTED_EDGE ( 'NONE', *, *, #22328, .F. ) ;
#85047 = LINE ( 'NONE', #56677, #55535 ) ;
#85049 = CARTESIAN_POINT ( 'NONE',  ( 6.792385456409363087, -3.062553014421049546, 32.05460306192773601 ) ) ;
#85050 = CARTESIAN_POINT ( 'NONE',  ( -13.38461538461550582, -10.21337939537710326, 33.94971097300076224 ) ) ;
#85051 = FACE_OUTER_BOUND ( 'NONE', #31343, .T. ) ;
#85052 = VECTOR ( 'NONE', #71044, 1000.000000000000000 ) ;
#85053 = CARTESIAN_POINT ( 'NONE',  ( -13.38461538461550582, -3.300289026999228881, 32.46337939537708905 ) ) ;
#85054 = VERTEX_POINT ( 'NONE', #59851 ) ;
#85055 = DIRECTION ( 'NONE',  ( -0.000000000000000000, -0.3420201433256694901, -0.9396926207859082059 ) ) ;
#85056 = EDGE_CURVE ( 'NONE', #69076, #15420, #49063, .T. ) ;
#85057 = CARTESIAN_POINT ( 'NONE',  ( -10.61538461538461320, -12.78798330534102767, 29.49999999999997868 ) ) ;
#85058 = CARTESIAN_POINT ( 'NONE',  ( 15.10007862765892206, -9.929715669179220328, 34.40415004197138416 ) ) ;
#85059 = ORIENTED_EDGE ( 'NONE', *, *, #22242, .T. ) ;
#85060 = ORIENTED_EDGE ( 'NONE', *, *, #67277, .T. ) ;
#85061 = EDGE_CURVE ( 'NONE', #66369, #17845, #67062, .T. ) ;
#85062 = EDGE_LOOP ( 'NONE', ( #68902, #6747, #69268, #60096 ) ) ;
#85063 = EDGE_CURVE ( 'NONE', #73584, #44052, #31739, .T. ) ;
#85064 = CARTESIAN_POINT ( 'NONE',  ( -18.00000000000000000, -3.513871655860376197, 32.76840700105977788 ) ) ;
#85065 = LINE ( 'NONE', #52144, #28545 ) ;
#85066 = CARTESIAN_POINT ( 'NONE',  ( -3.164701897419154530, -8.164416787775445883, 34.95778746994558617 ) ) ;
#85067 = EDGE_CURVE ( 'NONE', #18168, #49352, #15926, .T. ) ;
#85068 = CARTESIAN_POINT ( 'NONE',  ( -10.48485891362105171, -3.285477652293413264, 32.44071101563363158 ) ) ;
#85069 = VECTOR ( 'NONE', #34659, 1000.000000000000000 ) ;
#85070 = VERTEX_POINT ( 'NONE', #26072 ) ;
#85071 = ORIENTED_EDGE ( 'NONE', *, *, #27613, .T. ) ;
#85073 = ORIENTED_EDGE ( 'NONE', *, *, #8520, .F. ) ;
#85072 = CARTESIAN_POINT ( 'NONE',  ( -2.057692307692243538, -7.434744860731434812, 35.00000000000000711 ) ) ;
#85074 = AXIS2_PLACEMENT_3D ( 'NONE', #43807, #71269, #64073 ) ;
#85075 = CARTESIAN_POINT ( 'NONE',  ( 9.942362003946010773, -12.41262288849542017, 30.68299917996395010 ) ) ;
#85076 = CARTESIAN_POINT ( 'NONE',  ( -17.86947429823644029, -3.285477652293416817, 32.44071101563363158 ) ) ;
#85077 = CARTESIAN_POINT ( 'NONE',  ( -8.703163435880695076, -12.62096338111211757, 30.90682066428152908 ) ) ;
#85078 = ORIENTED_EDGE ( 'NONE', *, *, #58844, .F. ) ;
#85079 = EDGE_CURVE ( 'NONE', #3413, #34010, #53982, .T. ) ;
#85080 = ORIENTED_EDGE ( 'NONE', *, *, #38422, .F. ) ;
#85082 = ORIENTED_EDGE ( 'NONE', *, *, #85121, .T. ) ;
#85081 = CARTESIAN_POINT ( 'NONE',  ( 9.915320536401090123, -8.282913670948747864, 34.94150082978203642 ) ) ;
#85083 = CARTESIAN_POINT ( 'NONE',  ( -5.934744428723974785, -8.613356846314928816, 34.62446782046653482 ) ) ;
#85084 = CARTESIAN_POINT ( 'NONE',  ( -14.30769230769242739, -9.442884908241554243, 34.35708131394783038 ) ) ;
#85085 = ORIENTED_EDGE ( 'NONE', *, *, #16386, .T. ) ;
#85086 = CARTESIAN_POINT ( 'NONE',  ( 12.59206389977210705, -6.808710257144161559, 34.95449254468098843 ) ) ;
#85087 = CARTESIAN_POINT ( 'NONE',  ( 8.769230769230647482, -6.879047030192662504, 34.71129190930017927 ) ) ;
#85088 = CARTESIAN_POINT ( 'NONE',  ( 6.700149964170073247, -5.582147617184174848, 34.63737895849758530 ) ) ;
#85089 = FACE_BOUND ( 'NONE', #61120, .T. ) ;
#85090 = CARTESIAN_POINT ( 'NONE',  ( 18.03205128205128105, -3.499999999999999556, 29.75000000000000355 ) ) ;
#85091 = CARTESIAN_POINT ( 'NONE',  ( -6.792286482109971324, -9.084667340241226796, 34.75534355489798344 ) ) ;
#85092 = VECTOR ( 'NONE', #45770, 1000.000000000000000 ) ;
#85093 = DIRECTION ( 'NONE',  ( -0.000000000000000000, 0.6427876096865404731, -0.7660444431189771253 ) ) ;
#85095 = CARTESIAN_POINT ( 'NONE',  ( -15.93083330975275658, -2.889357225399416418, 32.26129605718031002 ) ) ;
#85094 = CARTESIAN_POINT ( 'NONE',  ( -3.230769230769229949, -3.886160181151819604, 36.00935417666054406 ) ) ;
#85096 = CARTESIAN_POINT ( 'NONE',  ( 11.28843830116857383, -11.37209801155882793, 32.91403422569033665 ) ) ;
#85097 = FACE_OUTER_BOUND ( 'NONE', #87453, .T. ) ;
#85098 = ORIENTED_EDGE ( 'NONE', *, *, #52947, .T. ) ;
#85099 = CARTESIAN_POINT ( 'NONE',  ( 14.55769230769374367, -7.500000000000155431, 34.75000000000007105 ) ) ;
#85100 = ORIENTED_EDGE ( 'NONE', *, *, #85615, .T. ) ;
#85101 = VERTEX_POINT ( 'NONE', #6253 ) ;
#85103 = CARTESIAN_POINT ( 'NONE',  ( 15.10007862765892206, -2.845849958028613624, 32.17971566917920967 ) ) ;
#85102 = CARTESIAN_POINT ( 'NONE',  ( 14.30769230769218758, -3.835265460704628371, 33.15142922262033665 ) ) ;
#85104 = B_SPLINE_CURVE_WITH_KNOTS ( 'NONE', 3,
 ( #31944, #59408, #38692, #23823, #24733, #58497, #23391, #52194, #16636, #44097 ),
 .UNSPECIFIED., .F., .F.,
 ( 4, 2, 2, 2, 4 ),
 ( 0.0007817246256747476061, 0.0009771112852218896347, 0.001172497944769031880, 0.001367884604316173909, 0.001563271263863315937 ),
 .UNSPECIFIED. ) ;
#85105 = CARTESIAN_POINT ( 'NONE',  ( 16.81410256410256565, -7.500000000000000000, 29.75000000000000355 ) ) ;
#85106 = CARTESIAN_POINT ( 'NONE',  ( 14.55763771707034948, -4.176053281294518804, 33.81426240980091791 ) ) ;
#85107 = CARTESIAN_POINT ( 'NONE',  ( 1.254468175177166689, -6.852621066184267029, 34.70813303252209181 ) ) ;
#85108 = CARTESIAN_POINT ( 'NONE',  ( 1.161689167099238640, -11.76352882383564769, 32.36236540154569497 ) ) ;
#85109 = ORIENTED_EDGE ( 'NONE', *, *, #82842, .F. ) ;
#85110 = CARTESIAN_POINT ( 'NONE',  ( 9.070512820512819374, -3.499999999999999556, 29.75000000000000355 ) ) ;
#85111 = EDGE_CURVE ( 'NONE', #41186, #62418, #14611, .T. ) ;
#85112 = CARTESIAN_POINT ( 'NONE',  ( -15.10024352900566846, -10.19071101563364756, 33.96452234770658407 ) ) ;
#85113 = CARTESIAN_POINT ( 'NONE',  ( 10.61538461538449418, -8.656820664282941280, 34.87096338111179961 ) ) ;
#85114 = DIRECTION ( 'NONE',  ( 0.000000000000000000, 0.7660444431189807890, 0.6427876096865361433 ) ) ;
#85115 = CARTESIAN_POINT ( 'NONE',  ( 13.63456079399342791, -5.766571408460171355, 34.70601412856602508 ) ) ;
#85116 = CARTESIAN_POINT ( 'NONE',  ( 1.553300858899087311, -3.749999999999992006, 17.98437500000000000 ) ) ;
#85117 = ORIENTED_EDGE ( 'NONE', *, *, #55943, .T. ) ;
#85118 = EDGE_CURVE ( 'NONE', #46284, #23459, #20034, .T. ) ;
#85119 = ORIENTED_EDGE ( 'NONE', *, *, #63653, .F. ) ;
#85120 = CARTESIAN_POINT ( 'NONE',  ( 9.320512820512821150, -3.499999999999999556, 29.75000000000000355 ) ) ;
#85122 = VERTEX_POINT ( 'NONE', #41359 ) ;
#85121 = EDGE_CURVE ( 'NONE', #63997, #38268, #62065, .T. ) ;
#85123 = CARTESIAN_POINT ( 'NONE',  ( 17.14299041027315340, -3.937682226553329556, 33.60647404775216529 ) ) ;
#85124 = CARTESIAN_POINT ( 'NONE',  ( 10.74591031714818357, -2.619367082507849442, 30.83698974864643461 ) ) ;
#85125 = CARTESIAN_POINT ( 'NONE',  ( 14.55774661933062575, -2.779044189368095719, 31.39831045268885745 ) ) ;
#85126 = CARTESIAN_POINT ( 'NONE',  ( 6.000000000000317080, -2.255955759149395501, 30.00000000000324363 ) ) ;
#85127 = CARTESIAN_POINT ( 'NONE',  ( 2.320192649118979489E-14, -11.25000000000000000, 19.78125000000000000 ) ) ;
#85128 = CARTESIAN_POINT ( 'NONE',  ( 9.320512820512821150, -11.00000000000000000, 29.75000000000000355 ) ) ;
#85129 = ORIENTED_EDGE ( 'NONE', *, *, #86712, .T. ) ;
#85130 = EDGE_CURVE ( 'NONE', #49988, #74119, #81028, .T. ) ;
#85131 = DIRECTION ( 'NONE',  ( 0.000000000000000000, 0.000000000000000000, -1.000000000000000000 ) ) ;
#85133 = EDGE_LOOP ( 'NONE', ( #30782, #21940 ) ) ;
#85132 = DIRECTION ( 'NONE',  ( -0.000000000000000000, -0.9848077530122085754, -0.1736481776669273613 ) ) ;
#85134 = LINE ( 'NONE', #4025, #16823 ) ;
#85135 = CARTESIAN_POINT ( 'NONE',  ( -9.915233909823841785, -12.15238873228292071, 31.58232369045353849 ) ) ;
#85136 = CARTESIAN_POINT ( 'NONE',  ( -18.00000000000000000, -11.69971097300155449, 32.46337939537587403 ) ) ;
#85137 = CARTESIAN_POINT ( 'NONE',  ( 6.673100179028331524, -3.436278759898155677, 33.07459398097509506 ) ) ;
#85138 = FACE_OUTER_BOUND ( 'NONE', #14747, .T. ) ;
#85139 = FACE_OUTER_BOUND ( 'NONE', #38660, .T. ) ;
#85140 = VECTOR ( 'NONE', #51892, 1000.000000000000114 ) ;
#85141 = EDGE_CURVE ( 'NONE', #53125, #18436, #40918, .T. ) ;
#85142 = CARTESIAN_POINT ( 'NONE',  ( 2.694853999681185108, -4.891553140782077591, 18.31436829374150932 ) ) ;
#85143 = ORIENTED_EDGE ( 'NONE', *, *, #26654, .T. ) ;
#85144 = CARTESIAN_POINT ( 'NONE',  ( -12.21153846153702638, -7.500000000000155431, 34.75000000000007105 ) ) ;
#85145 = FACE_OUTER_BOUND ( 'NONE', #55712, .T. ) ;
#85146 = CARTESIAN_POINT ( 'NONE',  ( 1.944543648263018731, -9.444543648262994751, 25.87500000000000355 ) ) ;
#85147 = CARTESIAN_POINT ( 'NONE',  ( 4.403846153847572609, -7.500000000000154543, 35.00000000000007105 ) ) ;
#85148 = CARTESIAN_POINT ( 'NONE',  ( 2.373759641042384683, -11.91647553114624358, 32.58852847137148245 ) ) ;
#85149 = VERTEX_POINT ( 'NONE', #53531 ) ;
#85150 = CARTESIAN_POINT ( 'NONE',  ( 1.139087296526029469, -10.24999999999999289, 19.70312500000000355 ) ) ;
#85151 = DIRECTION ( 'NONE',  ( -0.000000000000000000, -0.000000000000000000, -1.000000000000000000 ) ) ;
#85152 = ORIENTED_EDGE ( 'NONE', *, *, #70719, .F. ) ;
#85153 = CARTESIAN_POINT ( 'NONE',  ( 6.700149964170072359, -6.459968553980839800, 34.89616026154728701 ) ) ;
#85154 = ORIENTED_EDGE ( 'NONE', *, *, #61553, .F. ) ;
#85155 = LINE ( 'NONE', #57675, #82247 ) ;
#85156 = CARTESIAN_POINT ( 'NONE',  ( -4.230769230769230838, -11.50000000000000000, 29.75000000000000355 ) ) ;
#85157 = DIRECTION ( 'NONE',  ( -0.000000000000000000, 1.000000000000000000, 3.491481338843133355E-15 ) ) ;
#85158 = CARTESIAN_POINT ( 'NONE',  ( -12.46153846153858424, -11.06231777344772027, 33.60647404775119895 ) ) ;
#85159 = VERTEX_POINT ( 'NONE', #88685 ) ;
#85160 = CARTESIAN_POINT ( 'NONE',  ( -9.019230769230784261, -2.249999999999999556, 29.81609741502488120 ) ) ;
#85161 = ADVANCED_FACE ( 'NONE', ( #6680 ), #378, .F. ) ;
#85162 = VECTOR ( 'NONE', #65710, 1000.000000000000227 ) ;
#85163 = ORIENTED_EDGE ( 'NONE', *, *, #11310, .F. ) ;
#85165 = PLANE ( 'NONE',  #87455 ) ;
#85164 = AXIS2_PLACEMENT_3D ( 'NONE', #58128, #37868, #4978 ) ;
#85166 = CARTESIAN_POINT ( 'NONE',  ( 4.946775107191380805, -5.915902021225892149, 34.75552854090298638 ) ) ;
#85167 = EDGE_CURVE ( 'NONE', #65648, #30667, #87803, .T. ) ;
#85168 = B_SPLINE_CURVE_WITH_KNOTS ( 'NONE', 3,
 ( #57751, #4586, #45563, #44212, #58181, #64483, #30282, #71251, #52316, #79807 ),
 .UNSPECIFIED., .F., .F.,
 ( 4, 2, 2, 2, 4 ),
 ( 0.0007817246256747474977, 0.0009771112852218909357, 0.001172497944769034482, 0.001367884604316178029, 0.001563271263863321575 ),
 .UNSPECIFIED. ) ;
#85169 = EDGE_LOOP ( 'NONE', ( #51601, #4079, #34307, #81757 ) ) ;
#85170 = CARTESIAN_POINT ( 'NONE',  ( 8.769230769230768274, -4.661471528628507777, 34.16647553114623292 ) ) ;
#85171 = CARTESIAN_POINT ( 'NONE',  ( -17.07692307692307665, -2.721908614388771852, 31.22303859784724978 ) ) ;
#85172 = DIRECTION ( 'NONE',  ( -0.000000000000000000, 1.000000000000000000, -0.000000000000000000 ) ) ;
#85173 = VECTOR ( 'NONE', #87715, 1000.000000000000000 ) ;
#85174 = ADVANCED_FACE ( 'NONE', ( #70600 ), #56641, .F. ) ;
#85175 = CARTESIAN_POINT ( 'NONE',  ( 1.253924781505079356, -6.369640206132550553, 34.87707690430378449 ) ) ;
#85176 = DIRECTION ( 'NONE',  ( 0.000000000000000000, 0.000000000000000000, -1.000000000000000000 ) ) ;
#85177 = ORIENTED_EDGE ( 'NONE', *, *, #12571, .F. ) ;
#85179 = ADVANCED_FACE ( 'NONE', ( #29189 ), #77355, .F. ) ;
#85178 = ORIENTED_EDGE ( 'NONE', *, *, #55007, .T. ) ;
#85180 = FACE_BOUND ( 'NONE', #23446, .T. ) ;
#85181 = ORIENTED_EDGE ( 'NONE', *, *, #74682, .F. ) ;
#85182 = CARTESIAN_POINT ( 'NONE',  ( -4.853547591150658036, -2.251407671071270489, 29.88021292934942252 ) ) ;
#85183 = CARTESIAN_POINT ( 'NONE',  ( 6.066067333350078528, -5.471508081941601098, 34.59228464037088457 ) ) ;
#85184 = FACE_OUTER_BOUND ( 'NONE', #14235, .T. ) ;
#85185 = EDGE_LOOP ( 'NONE', ( #26013, #28581 ) ) ;
#85186 = EDGE_CURVE ( 'NONE', #72319, #530, #43630, .T. ) ;
#85187 = ORIENTED_EDGE ( 'NONE', *, *, #3601, .T. ) ;
#85188 = ORIENTED_EDGE ( 'NONE', *, *, #45844, .F. ) ;
#85189 = CARTESIAN_POINT ( 'NONE',  ( 6.416666666666664298, -3.499999999999999556, 29.75000000000000355 ) ) ;
#85190 = VERTEX_POINT ( 'NONE', #63838 ) ;
#85191 = AXIS2_PLACEMENT_3D ( 'NONE', #74704, #81465, #39596 ) ;
#85192 = CARTESIAN_POINT ( 'NONE',  ( 15.90382291655318880, -10.05641848906368097, 34.04755513067966177 ) ) ;
#85193 = EDGE_CURVE ( 'NONE', #33270, #85539, #64046, .T. ) ;
#85194 = EDGE_CURVE ( 'NONE', #19723, #56760, #2780, .T. ) ;
#85195 = CARTESIAN_POINT ( 'NONE',  ( 3.007843013253083786, -2.758268499246657068, 31.33685645148949561 ) ) ;
#85196 = AXIS2_PLACEMENT_3D ( 'NONE', #77948, #63542, #29332 ) ;
#85197 = FACE_OUTER_BOUND ( 'NONE', #3555, .T. ) ;
#85198 = EDGE_CURVE ( 'NONE', #31226, #75640, #77747, .T. ) ;
#85199 = FACE_BOUND ( 'NONE', #31020, .T. ) ;
#85200 = ORIENTED_EDGE ( 'NONE', *, *, #24997, .F. ) ;
#85201 = CYLINDRICAL_SURFACE ( 'NONE', #42852, 0.2499999999999973355 ) ;
#85202 = CARTESIAN_POINT ( 'NONE',  ( 3.230769230769108269, -4.320704448113951379, 33.92786785259630022 ) ) ;
#85203 = DIRECTION ( 'NONE',  ( -0.000000000000000000, -0.6427876096865404731, -0.7660444431189770143 ) ) ;
#85204 = CARTESIAN_POINT ( 'NONE',  ( 11.78840705680968171, -8.433404298154334455, 34.66254593164985920 ) ) ;
#85205 = ORIENTED_EDGE ( 'NONE', *, *, #71766, .T. ) ;
#85206 = PRODUCT_DEFINITION_CONTEXT ( 'detailed design', #71649, 'design' ) ;
#85207 = CARTESIAN_POINT ( 'NONE',  ( -2.057746789344164551, -9.272278438253398036, 34.42582936511637826 ) ) ;
#85208 = ORIENTED_EDGE ( 'NONE', *, *, #12945, .F. ) ;
#85209 = VERTEX_POINT ( 'NONE', #42254 ) ;
#85211 = DIRECTION ( 'NONE',  ( -0.000000000000000000, 1.000000000000000000, -0.000000000000000000 ) ) ;
#85210 = CARTESIAN_POINT ( 'NONE',  ( -19.00000000000000000, 16.99999999999999645, 23.75000000000000355 ) ) ;
#85212 = CARTESIAN_POINT ( 'NONE',  ( 6.923076923076924238, -6.435427911321262684, 35.78748833219616898 ) ) ;
#85213 = LINE ( 'NONE', #59057, #43711 ) ;
#85214 = CARTESIAN_POINT ( 'NONE',  ( -18.00000000000000000, -5.471508081941599322, 34.59228464037088457 ) ) ;
#85215 = DIRECTION ( 'NONE',  ( 0.000000000000000000, 0.4999999999999985567, 0.8660254037844395958 ) ) ;
#85216 = EDGE_LOOP ( 'NONE', ( #30484, #68917 ) ) ;
#85217 = CARTESIAN_POINT ( 'NONE',  ( 15.12820512820512953, -3.499999999999999556, 29.75000000000000355 ) ) ;
#85218 = CARTESIAN_POINT ( 'NONE',  ( 17.93391762063986761, -3.322132147404559976, 32.92929555188719348 ) ) ;
#85219 = CARTESIAN_POINT ( 'NONE',  ( 4.284371855609718338, -9.417988943895561960, 34.36773134775778260 ) ) ;
#85220 = CARTESIAN_POINT ( 'NONE',  ( 10.83839596699746721, -11.76359900205217635, 32.36225158514719880 ) ) ;
#85221 = ORIENTED_EDGE ( 'NONE', *, *, #65265, .T. ) ;
#85222 = EDGE_LOOP ( 'NONE', ( #24552, #25021, #38751, #20921 ) ) ;
#85223 = FACE_BOUND ( 'NONE', #43971, .T. ) ;
#85224 = ADVANCED_FACE ( 'NONE', ( #49876 ), #70153, .F. ) ;
#85225 = CIRCLE ( 'NONE', #23353, 4.000000000000000000 ) ;
#85226 = CARTESIAN_POINT ( 'NONE',  ( 17.86952329188353872, -7.276988635370451597, 34.74523720219453793 ) ) ;
#85227 = CARTESIAN_POINT ( 'NONE',  ( -11.53846153846153655, -11.69971097300155272, 32.46337939537588113 ) ) ;
#85228 = ORIENTED_EDGE ( 'NONE', *, *, #35449, .F. ) ;
#85229 = CARTESIAN_POINT ( 'NONE',  ( -16.40386937806761125, -11.56360843649121861, 33.07473185843129926 ) ) ;
#85230 = CARTESIAN_POINT ( 'NONE',  ( 6.792385456409368416, -10.54014554554150607, 33.71984207302941883 ) ) ;
#85231 = CARTESIAN_POINT ( 'NONE',  ( -9.915233909823841785, -3.105860786376062332, 32.13614157043599562 ) ) ;
#85232 = CARTESIAN_POINT ( 'NONE',  ( 4.284371592079798674, -6.808710257144159783, 34.95449254468098843 ) ) ;
#85233 = VERTEX_POINT ( 'NONE', #8017 ) ;
#85234 = VECTOR ( 'NONE', #80864, 1000.000000000000000 ) ;
#85235 = B_SPLINE_CURVE_WITH_KNOTS ( 'NONE', 3,
 ( #11773, #46437, #61266, #32039, #45545, #18085, #18972, #19854, #73025, #39251 ),
 .UNSPECIFIED., .F., .F.,
 ( 4, 2, 2, 2, 4 ),
 ( 0.000000000000000000, 0.0001954311564186860613, 0.0003908623128373721225, 0.0005862934692560581567, 0.0007817246256747442451 ),
 .UNSPECIFIED. ) ;
#85236 = DIRECTION ( 'NONE',  ( 1.000000000000000000, 0.000000000000000000, 0.000000000000000000 ) ) ;
#85237 = VERTEX_POINT ( 'NONE', #35484 ) ;
#85238 = EDGE_CURVE ( 'NONE', #1493, #31713, #63390, .T. ) ;
#85240 = ORIENTED_EDGE ( 'NONE', *, *, #23867, .F. ) ;
#85239 = CARTESIAN_POINT ( 'NONE',  ( 13.38461538461526601, -12.27809138561165270, 31.22303859784587132 ) ) ;
#85241 = CYLINDRICAL_SURFACE ( 'NONE', #51153, 0.2499999999999986955 ) ;
#85242 = CARTESIAN_POINT ( 'NONE',  ( -14.05769230769088729, -7.500000000000154543, 35.00000000000007105 ) ) ;
#85243 = DIRECTION ( 'NONE',  ( -0.000000000000000000, -0.8660254037844397068, -0.4999999999999978906 ) ) ;
#85244 = B_SPLINE_CURVE_WITH_KNOTS ( 'NONE', 3,
 ( #5515, #18138, #46044, #45597, #25333, #66316, #4620, #5064, #32528, #32093 ),
 .UNSPECIFIED., .F., .F.,
 ( 4, 2, 2, 2, 4 ),
 ( 0.0007817359430256361858, 0.0009771253907250041296, 0.001172514838424372182, 0.001367904286123740234, 0.001563293733823108286 ),
 .UNSPECIFIED. ) ;
#85245 = CARTESIAN_POINT ( 'NONE',  ( 12.68431800280687050, -4.387253974876679230, 33.66317474335728832 ) ) ;
#85246 = CARTESIAN_POINT ( 'NONE',  ( 14.30769230769231015, -10.67929555188718282, 33.92786785259544047 ) ) ;
#85247 = CARTESIAN_POINT ( 'NONE',  ( 6.250000000000000888, -7.500000000000001776, 35.04278698407183867 ) ) ;
#85248 = ADVANCED_FACE ( 'NONE', ( #35037 ), #810, .F. ) ;
#85249 = CARTESIAN_POINT ( 'NONE',  ( 1.944543648262996083, -5.555456351736983045, 24.31250000000000000 ) ) ;
#85250 = ORIENTED_EDGE ( 'NONE', *, *, #62348, .F. ) ;
#85251 = CARTESIAN_POINT ( 'NONE',  ( 13.51540582558233794, -12.62708834333097663, 30.88030960425257021 ) ) ;
#85252 = FACE_OUTER_BOUND ( 'NONE', #82592, .T. ) ;
#85253 = VERTEX_POINT ( 'NONE', #49445 ) ;
#85254 = ORIENTED_EDGE ( 'NONE', *, *, #55524, .F. ) ;
#85255 = CARTESIAN_POINT ( 'NONE',  ( -6.000000000000121680, -12.70778746994576025, 30.41441678777401236 ) ) ;
#85256 = CARTESIAN_POINT ( 'NONE',  ( -7.623374177175779920, -5.827830569534417471, 34.72679350104403539 ) ) ;
#85257 = CARTESIAN_POINT ( 'NONE',  ( 6.065255571276025215, -11.48612834413965977, 32.76840700105972815 ) ) ;
#85258 = CARTESIAN_POINT ( 'NONE',  ( -18.00000000000000000, -4.786620604624112651, 33.94971097300155094 ) ) ;
#85259 = CARTESIAN_POINT ( 'NONE',  ( 10.39245839786846837, -4.186968288167450147, 33.49512374952580274 ) ) ;
#85260 = EDGE_CURVE ( 'NONE', #53938, #40578, #81309, .T. ) ;
#85261 = CARTESIAN_POINT ( 'NONE',  ( -8.769230769230890843, -11.94971097300221174, 32.03036669348237098 ) ) ;
#85262 = VECTOR ( 'NONE', #63847, 1000.000000000000000 ) ;
#85263 = CYLINDRICAL_SURFACE ( 'NONE', #50797, 0.2499999999999994726 ) ;
#85264 = VERTEX_POINT ( 'NONE', #57522 ) ;
#85265 = LINE ( 'NONE', #56891, #24693 ) ;
#85266 = DIRECTION ( 'NONE',  ( -0.000000000000000000, -0.9848077530122085754, -0.1736481776669273613 ) ) ;
#85267 = CARTESIAN_POINT ( 'NONE',  ( -9.561515884482902905, -11.18335022499818621, 33.13157742990016885 ) ) ;
#85268 = CARTESIAN_POINT ( 'NONE',  ( -2.307692307692305711, -2.249999999999998668, 29.75000000000001776 ) ) ;
#85269 = VERTEX_POINT ( 'NONE', #23724 ) ;
#85270 = CARTESIAN_POINT ( 'NONE',  ( 7.623226887246997485, -2.308479472611653094, 30.53278059502174457 ) ) ;
#85271 = AXIS2_PLACEMENT_3D ( 'NONE', #47255, #82388, #6715 ) ;
#85272 = ADVANCED_FACE ( 'NONE', ( #23289 ), #66043, .F. ) ;
#85273 = B_SPLINE_CURVE_WITH_KNOTS ( 'NONE', 3,
 ( #69109, #47939, #20913, #7855, #68661, #62772, #6961, #28572, #29024, #82639 ),
 .UNSPECIFIED., .F., .F.,
 ( 4, 2, 2, 2, 4 ),
 ( 0.000000000000000000, 0.0001954311564186876876, 0.0003908623128373753751, 0.0005862934692560630356, 0.0007817246256747507503 ),
 .UNSPECIFIED. ) ;
#85274 = ORIENTED_EDGE ( 'NONE', *, *, #77286, .F. ) ;
#85275 = CARTESIAN_POINT ( 'NONE',  ( 8.835298102580845025, -2.833524468853757750, 32.15551576947925838 ) ) ;
#85276 = FACE_OUTER_BOUND ( 'NONE', #81037, .T. ) ;
#85277 = CARTESIAN_POINT ( 'NONE',  ( 6.250054419913455561, -12.65882529074907126, 30.72640787790839312 ) ) ;
#85278 = ORIENTED_EDGE ( 'NONE', *, *, #59632, .T. ) ;
#85279 = EDGE_CURVE ( 'NONE', #24019, #82116, #35120, .T. ) ;
#85280 = CARTESIAN_POINT ( 'NONE',  ( 12.68455130563185662, -10.77377354290276124, 33.85451476688484718 ) ) ;
#85281 = DIRECTION ( 'NONE',  ( -1.000000000000000000, -0.000000000000000000, -0.000000000000000000 ) ) ;
#85282 = CARTESIAN_POINT ( 'NONE',  ( 14.30769230769231015, -8.318370150425687726, 35.83090037661290239 ) ) ;
#85283 = CARTESIAN_POINT ( 'NONE',  ( -12.23852710992561299, -10.61302985866383963, 33.66295027996417843 ) ) ;
#85284 = EDGE_CURVE ( 'NONE', #61132, #46109, #16981, .T. ) ;
#85285 = VERTEX_POINT ( 'NONE', #85444 ) ;
#85286 = CARTESIAN_POINT ( 'NONE',  ( -1.161835843346973096, -3.755027918224367767, 33.06320215134714857 ) ) ;
#85287 = ORIENTED_EDGE ( 'NONE', *, *, #50256, .F. ) ;
#85288 = CARTESIAN_POINT ( 'NONE',  ( 10.61538461538461675, -2.249999999999998668, 29.75000000000001776 ) ) ;
#85289 = AXIS2_PLACEMENT_3D ( 'NONE', #89088, #53492, #80989 ) ;
#85290 = CARTESIAN_POINT ( 'NONE',  ( 13.91025641025641235, -4.000000000000000000, 29.75000000000000355 ) ) ;
#85291 = DIRECTION ( 'NONE',  ( 0.000000000000000000, 0.3420201433256641055, -0.9396926207859100932 ) ) ;
#85292 = CARTESIAN_POINT ( 'NONE',  ( 16.81410256410256565, -7.500000000000000000, 29.75000000000000355 ) ) ;
#85293 = FACE_OUTER_BOUND ( 'NONE', #13200, .T. ) ;
#85294 = EDGE_CURVE ( 'NONE', #19286, #74960, #83379, .T. ) ;
#85295 = AXIS2_PLACEMENT_3D ( 'NONE', #35204, #27565, #49157 ) ;
#85296 = EDGE_LOOP ( 'NONE', ( #73707, #78899 ) ) ;
#85297 = EDGE_LOOP ( 'NONE', ( #66383, #31563 ) ) ;
#85298 = EDGE_CURVE ( 'NONE', #49865, #76544, #72804, .T. ) ;
#85300 = EDGE_CURVE ( 'NONE', #85765, #50871, #43737, .T. ) ;
#85299 = ORIENTED_EDGE ( 'NONE', *, *, #26876, .T. ) ;
#85301 = VERTEX_POINT ( 'NONE', #3897 ) ;
#85302 = CARTESIAN_POINT ( 'NONE',  ( -1.253823576790598304, -3.062576670634119758, 32.05464942895959979 ) ) ;
#85303 = CARTESIAN_POINT ( 'NONE',  ( 15.90386940979756858, -5.643011162660950042, 34.66104346484419096 ) ) ;
#85304 = CARTESIAN_POINT ( 'NONE',  ( 16.15384615384615330, -10.51840700105979565, 33.73612834413961536 ) ) ;
#85305 = CARTESIAN_POINT ( 'NONE',  ( -12.46153846153846168, -3.322132147404559976, 32.92929555188717927 ) ) ;
#85306 = CARTESIAN_POINT ( 'NONE',  ( -13.13456107297706943, -5.728107161865378494, 34.42597550085002922 ) ) ;
#85307 = CARTESIAN_POINT ( 'NONE',  ( -7.846153846153844924, -11.91647553114624181, 32.58852847137148245 ) ) ;
#85308 = CARTESIAN_POINT ( 'NONE',  ( 6.000000000000001776, -11.69971097300155272, 32.46337939537588113 ) ) ;
#85309 = CARTESIAN_POINT ( 'NONE',  ( -6.923076923076922462, -1.629998284177014645, 34.34916445242399163 ) ) ;
#85310 = VERTEX_POINT ( 'NONE', #59294 ) ;
#85311 = ORIENTED_EDGE ( 'NONE', *, *, #15271, .T. ) ;
#85312 = EDGE_LOOP ( 'NONE', ( #10624, #31723 ) ) ;
#85314 = ORIENTED_EDGE ( 'NONE', *, *, #33706, .F. ) ;
#85313 = CARTESIAN_POINT ( 'NONE',  ( 0.3308478584281513979, -2.845849958028613624, 32.17971566917920967 ) ) ;
#85315 = AXIS2_PLACEMENT_3D ( 'NONE', #38856, #73077, #60445 ) ;
#85317 = CARTESIAN_POINT ( 'NONE',  ( 18.06519298829465825, -2.255955759149236073, 29.99999999999987921 ) ) ;
#85316 = CYLINDRICAL_SURFACE ( 'NONE', #2847, 0.2500000000000009437 ) ;
#85318 = AXIS2_PLACEMENT_3D ( 'NONE', #76890, #2985, #42227 ) ;
#85319 = CARTESIAN_POINT ( 'NONE',  ( 8.546404076751764833, -7.369208160676172348, 34.74850200257122879 ) ) ;
#85320 = CARTESIAN_POINT ( 'NONE',  ( -11.40793610022789828, -9.503571793651731880, 34.60286762892837942 ) ) ;
#85321 = ORIENTED_EDGE ( 'NONE', *, *, #71208, .F. ) ;
#85322 = ORIENTED_EDGE ( 'NONE', *, *, #58703, .F. ) ;
#85323 = CARTESIAN_POINT ( 'NONE',  ( -13.38461538461550582, -10.21337939537710326, 33.94971097300076224 ) ) ;
#85324 = ORIENTED_EDGE ( 'NONE', *, *, #40372, .F. ) ;
#85325 = FACE_BOUND ( 'NONE', #70412, .T. ) ;
#85326 = B_SPLINE_CURVE_WITH_KNOTS ( 'NONE', 3,
 ( #47847, #20387, #49180, #8650, #83424, #69895, #8204, #62681, #21710, #82094 ),
 .UNSPECIFIED., .F., .F.,
 ( 4, 2, 2, 2, 4 ),
 ( 0.0007817359430256324996, 0.0009771253907249991422, 0.001172514838424365893, 0.001367904286123732428, 0.001563293733823099179 ),
 .UNSPECIFIED. ) ;
#85327 = CARTESIAN_POINT ( 'NONE',  ( -6.130691466667557599, -8.999036380462719364, 34.52022231692819076 ) ) ;
#85328 = CYLINDRICAL_SURFACE ( 'NONE', #75076, 0.2499999999999994726 ) ;
#85329 = EDGE_LOOP ( 'NONE', ( #59927, #66013 ) ) ;
#85330 = CARTESIAN_POINT ( 'NONE',  ( 16.21910172512217585, -11.48612834413965977, 32.76840700105972815 ) ) ;
#85331 = CARTESIAN_POINT ( 'NONE',  ( 11.53846153846153832, -6.343179335718451384, 34.87096338111211935 ) ) ;
#85332 = CARTESIAN_POINT ( 'NONE',  ( -4.153846153846152411, -8.120952969808772792, 34.71129190930000163 ) ) ;
#85333 = ORIENTED_EDGE ( 'NONE', *, *, #9087, .T. ) ;
#85334 = DIRECTION ( 'NONE',  ( -0.000000000000000000, -0.000000000000000000, -1.000000000000000000 ) ) ;
#85335 = CARTESIAN_POINT ( 'NONE',  ( -17.07692307692307665, -2.538708090699994813, 30.37095296980875503 ) ) ;
#85336 = ORIENTED_EDGE ( 'NONE', *, *, #16275, .F. ) ;
#85337 = CARTESIAN_POINT ( 'NONE',  ( 7.912221179503922563, -11.35647404775217595, 33.31231777344666511 ) ) ;
#85338 = CARTESIAN_POINT ( 'NONE',  ( -7.053224132515138578, -11.47017969459903952, 32.78971311882034456 ) ) ;
#85339 = CARTESIAN_POINT ( 'NONE',  ( 3.230769230769231726, -4.098570777380720287, 33.41473453929634729 ) ) ;
#85340 = CARTESIAN_POINT ( 'NONE',  ( 16.08857615328984281, -3.083524468853725775, 32.58852847137143272 ) ) ;
#85341 = CARTESIAN_POINT ( 'NONE',  ( -10.48459280755982803, -5.582136614379148654, 34.36778462344220486 ) ) ;
#85342 = DIRECTION ( 'NONE',  ( 0.000000000000000000, 0.6427876096865373645, -0.7660444431189797898 ) ) ;
#85343 = CYLINDRICAL_SURFACE ( 'NONE', #30812, 5.000000000000000888 ) ;
#85346 = CARTESIAN_POINT ( 'NONE',  ( 11.76142467272821257, -7.369474539155828730, 34.99858011523957657 ) ) ;
#85345 = AXIS2_PLACEMENT_3D ( 'NONE', #55149, #48392, #74996 ) ;
#85344 = CARTESIAN_POINT ( 'NONE',  ( 4.853996859406927378, -12.39988816332205701, 30.74660775122750778 ) ) ;
#85347 = CARTESIAN_POINT ( 'NONE',  ( 1.449870955891410462, -11.48612834413965977, 32.76840700105972815 ) ) ;
#85349 = CARTESIAN_POINT ( 'NONE',  ( -15.23076923076935074, -11.94971097300221174, 32.03036669348237098 ) ) ;
#85348 = DIRECTION ( 'NONE',  ( -0.000000000000000000, -0.000000000000000000, -1.000000000000000000 ) ) ;
#85350 = CARTESIAN_POINT ( 'NONE',  ( 13.63461538461680611, -7.500000000000154543, 35.00000000000007105 ) ) ;
#85351 = CARTESIAN_POINT ( 'NONE',  ( -1.901340078031346525, -9.487747218494661183, 23.43563170625848713 ) ) ;
#85352 = ORIENTED_EDGE ( 'NONE', *, *, #68714, .T. ) ;
#85353 = VECTOR ( 'NONE', #46561, 1000.000000000000000 ) ;
#85354 = CARTESIAN_POINT ( 'NONE',  ( 2.952004793765244717, -6.965521097154411478, 14.00000000000000178 ) ) ;
#85355 = ORIENTED_EDGE ( 'NONE', *, *, #32193, .F. ) ;
#85356 = AXIS2_PLACEMENT_3D ( 'NONE', #5552, #33023, #81216 ) ;
#85357 = CARTESIAN_POINT ( 'NONE',  ( -10.03846153846153832, -3.499999999999999556, 29.75000000000000355 ) ) ;
#85358 = ORIENTED_EDGE ( 'NONE', *, *, #11177, .F. ) ;
#85359 = CARTESIAN_POINT ( 'NONE',  ( -4.153846153846152411, -11.16473453929635440, 33.15142922261926373 ) ) ;
#85360 = VERTEX_POINT ( 'NONE', #65597 ) ;
#85361 = CARTESIAN_POINT ( 'NONE',  ( 5.999999999999878320, -11.06231777344772027, 33.60647404775119895 ) ) ;
#85362 = CARTESIAN_POINT ( 'NONE',  ( -2.749999999999997780, -7.561099074964547917, 24.84188170625848713 ) ) ;
#85363 = DIRECTION ( 'NONE',  ( -0.000000000000000000, -0.8660254037844397068, -0.4999999999999978906 ) ) ;
#85364 = DIRECTION ( 'NONE',  ( 0.000000000000000000, 0.8660254037844377084, -0.5000000000000015543 ) ) ;
#85365 = CARTESIAN_POINT ( 'NONE',  ( 6.923076923076800782, -10.33852847137269571, 34.16647553114546554 ) ) ;
#85366 = CARTESIAN_POINT ( 'NONE',  ( -3.000000000000003553, 7.500000000000000000, 10.00000000000000178 ) ) ;
#85367 = DIRECTION ( 'NONE',  ( -0.000000000000000000, -0.000000000000000000, -1.000000000000000000 ) ) ;
#85368 = CARTESIAN_POINT ( 'NONE',  ( 11.40831432902332310, -2.882441371585227508, 31.66841991370172238 ) ) ;
#85369 = CARTESIAN_POINT ( 'NONE',  ( -13.45069776397551742, -11.91647553114624181, 32.58852847137148245 ) ) ;
#85370 = CARTESIAN_POINT ( 'NONE',  ( 3.750000000000000888, -7.499999999999978684, 18.21875000000000000 ) ) ;
#85371 = B_SPLINE_CURVE_WITH_KNOTS ( 'NONE', 3,
 ( #77769, #21494, #76894, #22822, #8437, #35012, #35460, #50280, #42231, #9326 ),
 .UNSPECIFIED., .F., .F.,
 ( 4, 2, 2, 2, 4 ),
 ( 0.000000000000000000, 0.0001954339857564054144, 0.0003908679715128108288, 0.0005863019572692162703, 0.0007817359430256216575 ),
 .UNSPECIFIED. ) ;
#85372 = DIRECTION ( 'NONE',  ( 1.000000000000000000, 0.000000000000000000, 0.000000000000000000 ) ) ;
#85373 = CARTESIAN_POINT ( 'NONE',  ( -15.10024352900566846, -2.619367082507849442, 30.83698974864643461 ) ) ;
#85374 = CARTESIAN_POINT ( 'NONE',  ( 14.55763782604045176, -3.202959910592335646, 32.30730279482227019 ) ) ;
#85375 = CARTESIAN_POINT ( 'NONE',  ( 2.651650429449569302, -10.15165042944953733, 15.87500000000000000 ) ) ;
#85376 = EDGE_CURVE ( 'NONE', #7293, #12053, #75864, .T. ) ;
#85377 = ORIENTED_EDGE ( 'NONE', *, *, #45382, .F. ) ;
#85378 = CARTESIAN_POINT ( 'NONE',  ( 14.37294787896833270, -5.219633306516380244, 34.19971097300157936 ) ) ;
#85379 = CARTESIAN_POINT ( 'NONE',  ( 20.00000000000000000, -7.500000000000000000, 29.75000000000000355 ) ) ;
#85380 = CARTESIAN_POINT ( 'NONE',  ( 1.161688425708537142, -5.582147617184174848, 34.63737895849758530 ) ) ;
#85381 = CARTESIAN_POINT ( 'NONE',  ( 5.207448778686639024, -2.882268652242224505, 31.66798894389554064 ) ) ;
#85382 = CARTESIAN_POINT ( 'NONE',  ( 14.30769230769231015, -3.322132147404559976, 32.92929555188717927 ) ) ;
#85383 = CARTESIAN_POINT ( 'NONE',  ( 9.442284455014730682, -11.37209801155882793, 32.91403422569033665 ) ) ;
#85384 = VECTOR ( 'NONE', #47646, 1000.000000000000227 ) ;
#85385 = EDGE_CURVE ( 'NONE', #88864, #88630, #55450, .T. ) ;
#85386 = EDGE_LOOP ( 'NONE', ( #35679, #80868, #54168, #33659 ) ) ;
#85387 = CARTESIAN_POINT ( 'NONE',  ( -6.923076923077044142, -10.21337939537710326, 33.94971097300076224 ) ) ;
#85388 = ORIENTED_EDGE ( 'NONE', *, *, #83394, .F. ) ;
#85389 = ORIENTED_EDGE ( 'NONE', *, *, #23773, .F. ) ;
#85390 = DIRECTION ( 'NONE',  ( 0.000000000000000000, 0.4999999999999960032, -0.8660254037844410391 ) ) ;
#85391 = CARTESIAN_POINT ( 'NONE',  ( 5.299934428535925335, -11.76359900205217457, 32.36225158514719880 ) ) ;
#85392 = CARTESIAN_POINT ( 'NONE',  ( 16.40379167219430201, -2.824170634883622633, 31.52227843825338738 ) ) ;
#85393 = CARTESIAN_POINT ( 'NONE',  ( -13.38461538461550582, -9.442884908241554243, 34.35708131394783038 ) ) ;
#85394 = CARTESIAN_POINT ( 'NONE',  ( 10.68145194873469173, -9.905515769479276145, 34.41647553114623292 ) ) ;
#85395 = VERTEX_POINT ( 'NONE', #6578 ) ;
#85396 = LINE ( 'NONE', #9733, #33466 ) ;
#85397 = EDGE_LOOP ( 'NONE', ( #17812, #51949, #79072, #20284 ) ) ;
#85398 = B_SPLINE_CURVE_WITH_KNOTS ( 'NONE', 3,
 ( #26371, #75442, #6103, #13737, #68679, #53837, #88537, #6979, #55160, #81325 ),
 .UNSPECIFIED., .F., .F.,
 ( 4, 2, 2, 2, 4 ),
 ( 0.0007817359430256365111, 0.0009771253907250045632, 0.001172514838424372399, 0.001367904286123740451, 0.001563293733823108503 ),
 .UNSPECIFIED. ) ;
#85399 = ADVANCED_FACE ( 'NONE', ( #67834 ), #74596, .T. ) ;
#85400 = ADVANCED_FACE ( 'NONE', ( #61070 ), #80470, .F. ) ;
#85401 = ORIENTED_EDGE ( 'NONE', *, *, #10725, .T. ) ;
#85402 = AXIS2_PLACEMENT_3D ( 'NONE', #58704, #17734, #3760 ) ;
#85403 = CARTESIAN_POINT ( 'NONE',  ( 17.99999999999987566, -2.379036618888197729, 30.90682066428292885 ) ) ;
#85404 = LINE ( 'NONE', #23687, #58915 ) ;
#85405 = LINE ( 'NONE', #35894, #9173 ) ;
#85406 = VECTOR ( 'NONE', #62433, 1000.000000000000000 ) ;
#85407 = AXIS2_PLACEMENT_3D ( 'NONE', #56028, #22684, #42527 ) ;
#85408 = EDGE_CURVE ( 'NONE', #27810, #44478, #7216, .T. ) ;
#85409 = CARTESIAN_POINT ( 'NONE',  ( -16.82697755857493149, -3.202959910592335202, 32.30730279482227019 ) ) ;
#85410 = CARTESIAN_POINT ( 'NONE',  ( 18.00000000000000000, -1.509761064869970415, 31.06009739812519044 ) ) ;
#85411 = ORIENTED_EDGE ( 'NONE', *, *, #59694, .T. ) ;
#85412 = ORIENTED_EDGE ( 'NONE', *, *, #34476, .T. ) ;
#85413 = CARTESIAN_POINT ( 'NONE',  ( -3.749999999999997335, -7.500000000000021316, 23.84375000000000000 ) ) ;
#85414 = ORIENTED_EDGE ( 'NONE', *, *, #34041, .F. ) ;
#85416 = ORIENTED_EDGE ( 'NONE', *, *, #21877, .F. ) ;
#85415 = CARTESIAN_POINT ( 'NONE',  ( -5.777220458731589403, -3.236590943229499029, 32.36255958852954251 ) ) ;
#85417 = DIRECTION ( 'NONE',  ( -0.000000000000000000, -0.1736481776669307198, -0.9848077530122080203 ) ) ;
#85418 = DIRECTION ( 'NONE',  ( -1.000000000000000000, 0.000000000000000000, 0.000000000000000000 ) ) ;
#85419 = CARTESIAN_POINT ( 'NONE',  ( 2.438482748659258625, -9.084667340241226796, 34.75534355489798344 ) ) ;
#85420 = VERTEX_POINT ( 'NONE', #66951 ) ;
#85421 = CARTESIAN_POINT ( 'NONE',  ( 5.076923076923391065, -2.255955759149395501, 30.00000000000324363 ) ) ;
#85422 = ORIENTED_EDGE ( 'NONE', *, *, #70405, .T. ) ;
#85423 = CARTESIAN_POINT ( 'NONE',  ( 6.000000000000001776, -9.058645607665452459, 34.76329471203371924 ) ) ;
#85424 = CARTESIAN_POINT ( 'NONE',  ( 17.77651507543566112, -12.69144148231606017, 30.53333754910549303 ) ) ;
#85425 = DIRECTION ( 'NONE',  ( -0.000000000000000000, 0.9396926207859093161, -0.3420201433256663259 ) ) ;
#85427 = CYLINDRICAL_SURFACE ( 'NONE', #87180, 0.2499999999999995559 ) ;
#85426 = CARTESIAN_POINT ( 'NONE',  ( -6.857821351800898135, -12.46129190930001052, 30.37095296980870174 ) ) ;
#85428 = CARTESIAN_POINT ( 'NONE',  ( 7.134615384615385025, -4.000000000000000000, 29.75000000000000355 ) ) ;
#85429 = CARTESIAN_POINT ( 'NONE',  ( -0.3307480205715113697, -12.62708834333097663, 30.88030960425257021 ) ) ;
#85430 = ORIENTED_EDGE ( 'NONE', *, *, #41539, .F. ) ;
#85431 = B_SPLINE_CURVE_WITH_KNOTS ( 'NONE', 3,
 ( #53161, #80665, #5882, #88320, #18507, #26593, #32017, #45526, #47297, #18948 ),
 .UNSPECIFIED., .F., .F.,
 ( 4, 2, 2, 2, 4 ),
 ( 0.000000000000000000, 0.0001954339857564091278, 0.0003908679715128182556, 0.0005863019572692274375, 0.0007817359430256365111 ),
 .UNSPECIFIED. ) ;
#85432 = CARTESIAN_POINT ( 'NONE',  ( -11.53846153846153655, -4.098570777380720287, 33.41473453929634729 ) ) ;
#85433 = CARTESIAN_POINT ( 'NONE',  ( -17.07692307692307665, -1.242168528481310874, 33.36296068462461051 ) ) ;
#85434 = ORIENTED_EDGE ( 'NONE', *, *, #24461, .F. ) ;
#85435 = VECTOR ( 'NONE', #61267, 1000.000000000000000 ) ;
#85436 = CARTESIAN_POINT ( 'NONE',  ( 11.53846153846141576, -12.16647553114689728, 32.15551576947799362 ) ) ;
#85437 = LINE ( 'NONE', #77787, #60231 ) ;
#85438 = CARTESIAN_POINT ( 'NONE',  ( -16.02332045208259359, -10.88167719472716399, 33.43325721877153711 ) ) ;
#85439 = DIRECTION ( 'NONE',  ( 0.000000000000000000, 0.000000000000000000, -1.000000000000000000 ) ) ;
#85440 = B_SPLINE_CURVE_WITH_KNOTS ( 'NONE', 3,
 ( #66079, #59775, #38620, #31418, #87273, #44918, #65190, #51662, #11600, #17464 ),
 .UNSPECIFIED., .F., .F.,
 ( 4, 2, 2, 2, 4 ),
 ( 0.000000000000000000, 0.0001954311564186863323, 0.0003908623128373726646, 0.0005862934692560590241, 0.0007817246256747453293 ),
 .UNSPECIFIED. ) ;
#85441 = CARTESIAN_POINT ( 'NONE',  ( -13.31936024510254413, -11.67786785259547777, 32.92929555188713664 ) ) ;
#85442 = FACE_OUTER_BOUND ( 'NONE', #43067, .T. ) ;
#85443 = FACE_BOUND ( 'NONE', #51692, .T. ) ;
#85445 = DIRECTION ( 'NONE',  ( 0.000000000000000000, 1.000000000000000000, 0.000000000000000000 ) ) ;
#85444 = CARTESIAN_POINT ( 'NONE',  ( 5.999999999999878320, -3.643525952248796163, 33.31231777344771672 ) ) ;
#85446 = CARTESIAN_POINT ( 'NONE',  ( -6.700297381808513641, -10.81320215134717344, 33.49497208177562868 ) ) ;
#85448 = CARTESIAN_POINT ( 'NONE',  ( 0.4615384615384611200, -2.833524468853757305, 32.15551576947925838 ) ) ;
#85447 = DIRECTION ( 'NONE',  ( -0.000000000000000000, 1.000000000000000000, -0.000000000000000000 ) ) ;
#85449 = CARTESIAN_POINT ( 'NONE',  ( 1.384615384615386802, -2.833524468853757305, 32.15551576947925838 ) ) ;
#85450 = CARTESIAN_POINT ( 'NONE',  ( 8.992242120843616959, -10.61302985866384141, 33.66295027996417843 ) ) ;
#85451 = CARTESIAN_POINT ( 'NONE',  ( 3.724691934501232815, -5.885600066136343678, 21.63875670625848713 ) ) ;
#85452 = EDGE_LOOP ( 'NONE', ( #16635, #64255 ) ) ;
#85453 = CARTESIAN_POINT ( 'NONE',  ( 0.4615384615384611200, -6.189225973068211317, 35.74407628777942847 ) ) ;
#85454 = CARTESIAN_POINT ( 'NONE',  ( -4.403869391139119571, -3.202444869320336451, 32.30641848906366675 ) ) ;
#85455 = CARTESIAN_POINT ( 'NONE',  ( 5.934729999443682402, -5.941354392334500467, 34.76329471203369792 ) ) ;
#85456 = CARTESIAN_POINT ( 'NONE',  ( 16.94677510719138169, -8.630895178749536711, 34.87696386517710323 ) ) ;
#85457 = CARTESIAN_POINT ( 'NONE',  ( 7.623227628637697428, -4.887634598454296153, 34.01352882383564946 ) ) ;
#85458 = CARTESIAN_POINT ( 'NONE',  ( -17.07692307692319744, -8.656820664282941280, 34.87096338111179961 ) ) ;
#85459 = CARTESIAN_POINT ( 'NONE',  ( -0.06109907496455085213, -3.750000000000000888, 20.15438170625849068 ) ) ;
#85460 = EDGE_CURVE ( 'NONE', #4430, #36427, #32709, .T. ) ;
#85461 = CARTESIAN_POINT ( 'NONE',  ( -2.530619266599154482, -3.395401636524185474, 33.02366814457250399 ) ) ;
#85462 = CARTESIAN_POINT ( 'NONE',  ( -2.057637887778853703, -6.523592122091589118, 34.90882529074906415 ) ) ;
#85463 = CARTESIAN_POINT ( 'NONE',  ( 11.78846153846295763, -7.500000000000154543, 35.00000000000007105 ) ) ;
#85464 = CARTESIAN_POINT ( 'NONE',  ( 17.99999999999987566, -8.656820664282941280, 34.87096338111179961 ) ) ;
#85465 = CARTESIAN_POINT ( 'NONE',  ( 17.99999999999987566, -12.70778746994576025, 30.41441678777401236 ) ) ;
#85466 = CARTESIAN_POINT ( 'NONE',  ( 10.83876055608279820, -2.501478030877322567, 29.88021232661721172 ) ) ;
#85467 = VECTOR ( 'NONE', #63252, 1000.000000000000000 ) ;
#85468 = DIRECTION ( 'NONE',  ( -0.000000000000000000, 0.7660444431189791237, -0.6427876096865379196 ) ) ;
#85469 = CARTESIAN_POINT ( 'NONE',  ( 17.29970274590113632, -2.612705202774696200, 31.66806509827799943 ) ) ;
#85470 = VERTEX_POINT ( 'NONE', #19643 ) ;
#85471 = LINE ( 'NONE', #9376, #65756 ) ;
#85472 = CYLINDRICAL_SURFACE ( 'NONE', #17268, 0.2500000000000002220 ) ;
#85473 = CARTESIAN_POINT ( 'NONE',  ( -0.06109907496451398579, -10.25000000000000178, 25.03311829374151287 ) ) ;
#85474 = AXIS2_PLACEMENT_3D ( 'NONE', #61126, #53930, #26910 ) ;
#85475 = AXIS2_PLACEMENT_3D ( 'NONE', #59195, #53773, #47008 ) ;
#85476 = EDGE_CURVE ( 'NONE', #84107, #20488, #32970, .T. ) ;
#85477 = CARTESIAN_POINT ( 'NONE',  ( 6.923076923076924238, -4.661471528628507777, 34.16647553114623292 ) ) ;
#85478 = CARTESIAN_POINT ( 'NONE',  ( 11.53846153846153832, -9.819645486525091727, 36.12317359536749706 ) ) ;
#85479 = EDGE_LOOP ( 'NONE', ( #1810, #50714, #48064, #30580 ) ) ;
#85480 = CARTESIAN_POINT ( 'NONE',  ( -18.06608341095587278, -8.973038597847269315, 34.52809138561120506 ) ) ;
#85481 = CARTESIAN_POINT ( 'NONE',  ( -3.230769230769229949, -12.62096338111211580, 30.90682066428153263 ) ) ;
#85483 = VERTEX_POINT ( 'NONE', #47104 ) ;
#85482 = CARTESIAN_POINT ( 'NONE',  ( 4.087762742890272527, -5.557115091759785130, 34.35708131394839171 ) ) ;
#85484 = CARTESIAN_POINT ( 'NONE',  ( 6.923076923076802558, -3.300289026999228881, 32.46337939537708905 ) ) ;
#85485 = CYLINDRICAL_SURFACE ( 'NONE', #65607, 0.2499999999999995559 ) ;
#85486 = EDGE_CURVE ( 'NONE', #78822, #31805, #59854, .T. ) ;
#85487 = DIRECTION ( 'NONE',  ( -0.000000000000000000, -0.000000000000000000, -1.000000000000000000 ) ) ;
#85488 = CARTESIAN_POINT ( 'NONE',  ( -13.45069879557126313, -3.050289026998445951, 32.03036669348365706 ) ) ;
#85489 = ORIENTED_EDGE ( 'NONE', *, *, #22035, .F. ) ;
#85490 = CARTESIAN_POINT ( 'NONE',  ( -11.78843826940389583, -4.236021600441997492, 33.53823185664189310 ) ) ;
#85491 = CARTESIAN_POINT ( 'NONE',  ( -16.02305434602137169, -3.062576670634119758, 32.05464942895959979 ) ) ;
#85492 = CYLINDRICAL_SURFACE ( 'NONE', #84452, 0.2500000000000008882 ) ;
#85493 = EDGE_CURVE ( 'NONE', #20488, #57339, #19208, .T. ) ;
#85494 = ORIENTED_EDGE ( 'NONE', *, *, #52329, .F. ) ;
#85495 = VERTEX_POINT ( 'NONE', #12014 ) ;
#85497 = ORIENTED_EDGE ( 'NONE', *, *, #53146, .F. ) ;
#85496 = B_SPLINE_CURVE_WITH_KNOTS ( 'NONE', 3,
 ( #18547, #65386, #78902, #85668, #3241, #86572, #24842, #17199, #52313, #25743 ),
 .UNSPECIFIED., .F., .F.,
 ( 4, 2, 2, 2, 4 ),
 ( 0.0007817246256747515092, 0.0009771112852218961399, 0.001172497944769040771, 0.001367884604316185401, 0.001563271263863330032 ),
 .UNSPECIFIED. ) ;
#85498 = EDGE_CURVE ( 'NONE', #38377, #29227, #76410, .T. ) ;
#85499 = CARTESIAN_POINT ( 'NONE',  ( -5.142193077479396024, -9.528491918058357157, 34.59228464037090589 ) ) ;
#85500 = CARTESIAN_POINT ( 'NONE',  ( -8.703975197954742171, -3.300289026998473041, 32.46337939537591666 ) ) ;
#85501 = CARTESIAN_POINT ( 'NONE',  ( 11.53846153846141753, -10.90142922262034020, 33.41473453929536674 ) ) ;
#85502 = VECTOR ( 'NONE', #68942, 1000.000000000000227 ) ;
#85503 = CARTESIAN_POINT ( 'NONE',  ( 2.307692307692309264, -12.09954503811598769, 35.62045528018868623 ) ) ;
#85504 = EDGE_CURVE ( 'NONE', #44924, #48096, #12543, .T. ) ;
#85505 = EDGE_LOOP ( 'NONE', ( #15493, #48871, #66216, #18297 ) ) ;
#85506 = ORIENTED_EDGE ( 'NONE', *, *, #40484, .T. ) ;
#85509 = ORIENTED_EDGE ( 'NONE', *, *, #87272, .T. ) ;
#85508 = EDGE_CURVE ( 'NONE', #63347, #87552, #28660, .T. ) ;
#85507 = CARTESIAN_POINT ( 'NONE',  ( -1.319359813339359810, -5.219633306516380244, 34.19971097300157936 ) ) ;
#85510 = CARTESIAN_POINT ( 'NONE',  ( -10.61538461538461320, -2.721908614388771852, 31.22303859784724978 ) ) ;
#85511 = ADVANCED_FACE ( 'NONE', ( #15112 ), #28627, .F. ) ;
#85512 = EDGE_CURVE ( 'NONE', #17756, #75262, #44742, .T. ) ;
#85513 = CARTESIAN_POINT ( 'NONE',  ( 10.61538461538449596, -11.48612834414049644, 32.76840700105863391 ) ) ;
#85514 = CARTESIAN_POINT ( 'NONE',  ( -25.00000000000000355, 9.999999999999971578, 13.00000000000000178 ) ) ;
#85515 = ORIENTED_EDGE ( 'NONE', *, *, #19569, .T. ) ;
#85516 = EDGE_LOOP ( 'NONE', ( #33437, #1011, #21970, #60166 ) ) ;
#85518 = ORIENTED_EDGE ( 'NONE', *, *, #58401, .T. ) ;
#85517 = CARTESIAN_POINT ( 'NONE',  ( -12.39547011053602432, -4.786620604624113540, 33.94971097300155805 ) ) ;
#85519 = CARTESIAN_POINT ( 'NONE',  ( -5.777220458731589403, -8.496831190052096971, 34.64984203495476578 ) ) ;
#85520 = B_SPLINE_CURVE_WITH_KNOTS ( 'NONE', 3,
 ( #12355, #88047, #26308, #53776, #81262, #19548, #31286, #73166, #66405, #38493 ),
 .UNSPECIFIED., .F., .F.,
 ( 4, 2, 2, 2, 4 ),
 ( 0.000000000000000000, 0.0001954311564186860071, 0.0003908623128373720141, 0.0005862934692560580483, 0.0007817246256747440282 ),
 .UNSPECIFIED. ) ;
#85521 = B_SPLINE_CURVE_WITH_KNOTS ( 'NONE', 3,
 ( #88646, #7087, #13399, #81874, #39567, #67023, #34114, #32789, #26035, #61580 ),
 .UNSPECIFIED., .F., .F.,
 ( 4, 2, 2, 2, 4 ),
 ( 0.0007817246256747503166, 0.0009771112852218946220, 0.001172497944769039036, 0.001367884604316183233, 0.001563271263863327647 ),
 .UNSPECIFIED. ) ;
#85522 = CARTESIAN_POINT ( 'NONE',  ( 14.08420738312798015, -5.827078755546623690, 34.72654668319379567 ) ) ;
#85523 = ORIENTED_EDGE ( 'NONE', *, *, #78163, .T. ) ;
#85524 = CARTESIAN_POINT ( 'NONE',  ( 0.4615384615384611200, -2.499999999999998668, 29.75000000000001421 ) ) ;
#85525 = B_SPLINE_CURVE_WITH_KNOTS ( 'NONE', 3,
 ( #19354, #8503, #76513, #43168, #61656, #70641, #82393, #54910, #15703, #27882 ),
 .UNSPECIFIED., .F., .F.,
 ( 4, 2, 2, 2, 4 ),
 ( 0.000000000000000000, 0.0001954311564186867389, 0.0003908623128373734778, 0.0005862934692560602167, 0.0007817246256747469556 ),
 .UNSPECIFIED. ) ;
#85526 = CARTESIAN_POINT ( 'NONE',  ( 6.923076923076924238, -12.62096338111211580, 30.90682066428153263 ) ) ;
#85527 = CARTESIAN_POINT ( 'NONE',  ( -2.307692307692427391, -11.48612834414049644, 32.76840700105863391 ) ) ;
#85528 = FACE_BOUND ( 'NONE', #36999, .T. ) ;
#85529 = VECTOR ( 'NONE', #19052, 1000.000000000000000 ) ;
#85530 = FACE_OUTER_BOUND ( 'NONE', #3647, .T. ) ;
#85531 = CARTESIAN_POINT ( 'NONE',  ( 3.930361229281821966, -2.353723527008295680, 30.78948104536958752 ) ) ;
#85532 = DIRECTION ( 'NONE',  ( -1.000000000000000000, 0.000000000000000000, 0.000000000000000000 ) ) ;
#85534 = CARTESIAN_POINT ( 'NONE',  ( 6.699591979352975457, -11.89387501736622710, 32.13663884655806413 ) ) ;
#85533 = DIRECTION ( 'NONE',  ( 0.000000000000000000, 0.7660444431189807890, 0.6427876096865361433 ) ) ;
#85535 = CARTESIAN_POINT ( 'NONE',  ( 8.545745844666440050, -9.417330523894424488, 34.63758898049880486 ) ) ;
#85536 = CARTESIAN_POINT ( 'NONE',  ( 1.515405825582335275, -2.295524264805589354, 30.44142389570982488 ) ) ;
#85537 = VERTEX_POINT ( 'NONE', #15554 ) ;
#85538 = CARTESIAN_POINT ( 'NONE',  ( 14.37283808702427557, -7.750023238201979581, 34.74374492549440419 ) ) ;
#85539 = VERTEX_POINT ( 'NONE', #43022 ) ;
#85540 = ORIENTED_EDGE ( 'NONE', *, *, #37093, .T. ) ;
#85542 = CARTESIAN_POINT ( 'NONE',  ( 15.00728430620489995, -3.019605429927184392, 32.48692288466676814 ) ) ;
#85541 = DIRECTION ( 'NONE',  ( 0.000000000000000000, 0.7660444431189822323, -0.6427876096865344779 ) ) ;
#85543 = CARTESIAN_POINT ( 'NONE',  ( 2.373760658694747949, -2.538708090699994813, 30.37095296980875503 ) ) ;
#85544 = LINE ( 'NONE', #80009, #52378 ) ;
#85545 = DIRECTION ( 'NONE',  ( -0.000000000000000000, 0.6427876096865404731, -0.7660444431189770143 ) ) ;
#85546 = DIRECTION ( 'NONE',  ( -0.000000000000000000, -0.9396926207859092051, -0.3420201433256662704 ) ) ;
#85547 = EDGE_LOOP ( 'NONE', ( #65457, #24883, #73269, #15386 ) ) ;
#85548 = ADVANCED_FACE ( 'NONE', ( #70493 ), #49338, .F. ) ;
#85549 = FACE_OUTER_BOUND ( 'NONE', #28126, .T. ) ;
#85550 = CARTESIAN_POINT ( 'NONE',  ( 15.23076923076923173, -10.67929555188718282, 33.92786785259544047 ) ) ;
#85551 = FACE_OUTER_BOUND ( 'NONE', #18216, .T. ) ;
#85552 = DIRECTION ( 'NONE',  ( -0.000000000000000000, 1.000000000000000000, -0.000000000000000000 ) ) ;
#85553 = CARTESIAN_POINT ( 'NONE',  ( -16.94613263595612551, -2.494656445102014342, 31.33466734024120015 ) ) ;
#85554 = EDGE_CURVE ( 'NONE', #5299, #2439, #34924, .T. ) ;
#85555 = CARTESIAN_POINT ( 'NONE',  ( 2.651650429449569302, -10.15165042944953733, 18.37500000000000355 ) ) ;
#85556 = ORIENTED_EDGE ( 'NONE', *, *, #66184, .T. ) ;
#85558 = EDGE_CURVE ( 'NONE', #313, #61826, #2876, .T. ) ;
#85557 = ORIENTED_EDGE ( 'NONE', *, *, #81963, .F. ) ;
#85559 = CARTESIAN_POINT ( 'NONE',  ( 14.05771556364371833, -12.41104346484419452, 31.60698883733904196 ) ) ;
#85560 = ORIENTED_EDGE ( 'NONE', *, *, #88070, .T. ) ;
#85561 = DIRECTION ( 'NONE',  ( -0.000000000000000000, -0.000000000000000000, -1.000000000000000000 ) ) ;
#85562 = CARTESIAN_POINT ( 'NONE',  ( 9.757563263583717728, -10.21337939537593620, 33.94971097300152252 ) ) ;
#85563 = CARTESIAN_POINT ( 'NONE',  ( -16.15384615384615330, -4.786620604624113540, 33.94971097300155094 ) ) ;
#85564 = CYLINDRICAL_SURFACE ( 'NONE', #25780, 0.2499999999999973355 ) ;
#85565 = CARTESIAN_POINT ( 'NONE',  ( -2.651650429449535551, -10.15165042944956753, 16.18750000000000000 ) ) ;
#85566 = EDGE_CURVE ( 'NONE', #85122, #42793, #62387, .T. ) ;
#85567 = CARTESIAN_POINT ( 'NONE',  ( 14.17700170458200404, -6.369640206132551441, 34.87707690430378449 ) ) ;
#85569 = ORIENTED_EDGE ( 'NONE', *, *, #8207, .F. ) ;
#85568 = VECTOR ( 'NONE', #24188, 1000.000000000000000 ) ;
#85570 = DIRECTION ( 'NONE',  ( -0.000000000000000000, 0.3420201433256694901, -0.9396926207859082059 ) ) ;
#85572 = ORIENTED_EDGE ( 'NONE', *, *, #41605, .T. ) ;
#85571 = LINE ( 'NONE', #51297, #35293 ) ;
#85573 = DIRECTION ( 'NONE',  ( -0.000000000000000000, 0.5000000000000011102, -0.8660254037844381525 ) ) ;
#85574 = CARTESIAN_POINT ( 'NONE',  ( 14.30769230769218758, -12.27809138561165270, 31.22303859784587132 ) ) ;
#85575 = CARTESIAN_POINT ( 'NONE',  ( -3.099930812756466647, -7.277220443632450575, 34.74524770363009196 ) ) ;
#85576 = CARTESIAN_POINT ( 'NONE',  ( 0.4615384615384611200, -2.721908614388771852, 31.22303859784724978 ) ) ;
#85577 = CARTESIAN_POINT ( 'NONE',  ( -6.066083410955879884, -9.780366693483667717, 34.19971097300155805 ) ) ;
#85578 = CARTESIAN_POINT ( 'NONE',  ( 7.715463243043537034, -3.338472653186243644, 32.95098750199972670 ) ) ;
#85579 = FACE_OUTER_BOUND ( 'NONE', #38765, .T. ) ;
#85580 = CARTESIAN_POINT ( 'NONE',  ( 1.614399933863618797, -3.775308065498751198, 16.98624329374151287 ) ) ;
#85581 = ORIENTED_EDGE ( 'NONE', *, *, #30593, .F. ) ;
#85582 = FACE_OUTER_BOUND ( 'NONE', #69617, .T. ) ;
#85583 = CARTESIAN_POINT ( 'NONE',  ( -13.25408994638174143, -10.31582465632705237, 34.18122507451815295 ) ) ;
#85584 = CARTESIAN_POINT ( 'NONE',  ( -13.51530685128294351, -8.999036380462717588, 34.52022231692819076 ) ) ;
#85585 = CARTESIAN_POINT ( 'NONE',  ( 0.06109907496451789238, -4.749999999999998224, 13.15811829374151642 ) ) ;
#85586 = CARTESIAN_POINT ( 'NONE',  ( 0.2115617174898694053, -5.643011162660950042, 34.66104346484419096 ) ) ;
#85587 = CARTESIAN_POINT ( 'NONE',  ( 15.93036122928181975, -4.988325925672468131, 34.36044203135681130 ) ) ;
#85588 = ORIENTED_EDGE ( 'NONE', *, *, #39546, .F. ) ;
#85589 = CARTESIAN_POINT ( 'NONE',  ( 2.749999999999995115, -6.360912703473971419, 16.89062500000000000 ) ) ;
#85590 = FACE_OUTER_BOUND ( 'NONE', #45857, .T. ) ;
#85591 = EDGE_CURVE ( 'NONE', #43411, #57339, #8242, .T. ) ;
#85592 = EDGE_LOOP ( 'NONE', ( #10344, #22297, #14312, #65959 ) ) ;
#85593 = DIRECTION ( 'NONE',  ( 0.000000000000000000, 0.1736481776669267785, -0.9848077530122087975 ) ) ;
#85594 = ORIENTED_EDGE ( 'NONE', *, *, #30633, .F. ) ;
#85595 = CARTESIAN_POINT ( 'NONE',  ( 17.93472955403921887, -6.879047030191174805, 34.71129190930000163 ) ) ;
#85596 = DIRECTION ( 'NONE',  ( -0.000000000000000000, -0.1736481776669307198, -0.9848077530122080203 ) ) ;
#85597 = AXIS2_PLACEMENT_3D ( 'NONE', #5362, #53083, #32388 ) ;
#85598 = FACE_OUTER_BOUND ( 'NONE', #5883, .T. ) ;
#85599 = EDGE_LOOP ( 'NONE', ( #87275, #47314, #47285, #86225 ) ) ;
#85600 = CYLINDRICAL_SURFACE ( 'NONE', #73882, 0.2499999999999997502 ) ;
#85601 = ORIENTED_EDGE ( 'NONE', *, *, #27109, .F. ) ;
#85602 = CARTESIAN_POINT ( 'NONE',  ( -1.326923076923076872, -7.500000000000000000, 29.75000000000000355 ) ) ;
#85603 = EDGE_LOOP ( 'NONE', ( #51089, #88401, #49034, #9032 ) ) ;
#85604 = CARTESIAN_POINT ( 'NONE',  ( 1.384615384615386802, -8.164416787775445883, 34.95778746994557906 ) ) ;
#85605 = DIRECTION ( 'NONE',  ( 0.000000000000000000, 0.4999999999999985567, 0.8660254037844395958 ) ) ;
#85606 = ORIENTED_EDGE ( 'NONE', *, *, #68391, .T. ) ;
#85607 = AXIS2_PLACEMENT_3D ( 'NONE', #84204, #56270, #76989 ) ;
#85608 = CARTESIAN_POINT ( 'NONE',  ( -6.130147969731696733, -11.04286588640298561, 33.62463336215343901 ) ) ;
#85609 = DIRECTION ( 'NONE',  ( -1.000000000000000000, 0.000000000000000000, 0.000000000000000000 ) ) ;
#85610 = CARTESIAN_POINT ( 'NONE',  ( 10.03846153846153832, -11.00000000000000000, 28.25000000000000000 ) ) ;
#85611 = CARTESIAN_POINT ( 'NONE',  ( 4.946231610255517275, -8.999036380462719364, 34.52022231692819076 ) ) ;
#85612 = CARTESIAN_POINT ( 'NONE',  ( -11.47320639894870276, -3.643525952247864463, 33.31231777344670064 ) ) ;
#85613 = B_SPLINE_CURVE_WITH_KNOTS ( 'NONE', 3,
 ( #25662, #67538, #39189, #73860, #66650, #12155, #86034, #31528, #53569, #31978 ),
 .UNSPECIFIED., .F., .F.,
 ( 4, 2, 2, 2, 4 ),
 ( 0.0007817359430256288133, 0.0009771253907249948054, 0.001172514838424360689, 0.001367904286123726573, 0.001563293733823092457 ),
 .UNSPECIFIED. ) ;
#85614 = EDGE_CURVE ( 'NONE', #5068, #7446, #40489, .T. ) ;
#85616 = ORIENTED_EDGE ( 'NONE', *, *, #56694, .T. ) ;
#85615 = EDGE_CURVE ( 'NONE', #1602, #54361, #38043, .T. ) ;
#85617 = ORIENTED_EDGE ( 'NONE', *, *, #59795, .F. ) ;
#85618 = ORIENTED_EDGE ( 'NONE', *, *, #36958, .F. ) ;
#85620 = ORIENTED_EDGE ( 'NONE', *, *, #55492, .T. ) ;
#85619 = CARTESIAN_POINT ( 'NONE',  ( 3.296837581771669967, -3.513871655860379306, 32.76840700105978499 ) ) ;
#85621 = EDGE_CURVE ( 'NONE', #5632, #33486, #76986, .T. ) ;
#85622 = ADVANCED_FACE ( 'NONE', ( #84907 ), #71817, .T. ) ;
#85623 = CYLINDRICAL_SURFACE ( 'NONE', #53591, 0.2500000000000002220 ) ;
#85624 = CARTESIAN_POINT ( 'NONE',  ( 19.00000000000000000, -3.499999999999999556, 29.75000000000000355 ) ) ;
#85625 = ORIENTED_EDGE ( 'NONE', *, *, #35497, .F. ) ;
#85626 = VERTEX_POINT ( 'NONE', #17325 ) ;
#85627 = VECTOR ( 'NONE', #30288, 1000.000000000000000 ) ;
#85628 = VERTEX_POINT ( 'NONE', #71367 ) ;
#85629 = CARTESIAN_POINT ( 'NONE',  ( -1.449885830576160384, -11.94971097300153140, 32.03036669348370680 ) ) ;
#85630 = ORIENTED_EDGE ( 'NONE', *, *, #24750, .F. ) ;
#85631 = CARTESIAN_POINT ( 'NONE',  ( 11.53846153846153832, -11.16473453929635440, 33.15142922261926373 ) ) ;
#85632 = B_SPLINE_CURVE_WITH_KNOTS ( 'NONE', 3,
 ( #79643, #38651, #39564, #5757, #33233, #18831, #53039, #73328, #66574, #72870 ),
 .UNSPECIFIED., .F., .F.,
 ( 4, 2, 2, 2, 4 ),
 ( 0.000000000000000000, 0.0001954311564186881484, 0.0003908623128373762967, 0.0005862934692560644451, 0.0007817246256747525934 ),
 .UNSPECIFIED. ) ;
#85633 = DIRECTION ( 'NONE',  ( -0.000000000000000000, -0.7660444431189791237, -0.6427876096865379196 ) ) ;
#85634 = B_SPLINE_CURVE_WITH_KNOTS ( 'NONE', 3,
 ( #88943, #62754, #74517, #82169, #19568, #40298, #47923, #67762, #55125, #33538 ),
 .UNSPECIFIED., .F., .F.,
 ( 4, 2, 2, 2, 4 ),
 ( 0.000000000000000000, 0.0001954311564186879857, 0.0003908623128373759715, 0.0005862934692560640114, 0.0007817246256747519429 ),
 .UNSPECIFIED. ) ;
#85635 = EDGE_CURVE ( 'NONE', #57828, #79573, #64884, .T. ) ;
#85636 = CYLINDRICAL_SURFACE ( 'NONE', #79957, 0.2499999999999997502 ) ;
#85637 = B_SPLINE_CURVE_WITH_KNOTS ( 'NONE', 3,
 ( #61390, #38582, #3891, #74480, #66037, #11106, #81690, #4348, #59288, #33930 ),
 .UNSPECIFIED., .F., .F.,
 ( 4, 2, 2, 2, 4 ),
 ( 0.0007817246256747434861, 0.0009771112852218859484, 0.001172497944769028411, 0.001367884604316171090, 0.001563271263863313552 ),
 .UNSPECIFIED. ) ;
#85638 = FACE_BOUND ( 'NONE', #79813, .T. ) ;
#85639 = VERTEX_POINT ( 'NONE', #65507 ) ;
#85640 = CYLINDRICAL_SURFACE ( 'NONE', #84579, 0.2499999999999998890 ) ;
#85641 = CARTESIAN_POINT ( 'NONE',  ( 4.219101725122177626, -8.613356846314928816, 34.62446782046653482 ) ) ;
#85642 = EDGE_CURVE ( 'NONE', #41132, #16668, #45621, .T. ) ;
#85643 = CARTESIAN_POINT ( 'NONE',  ( 2.057669083470851756, -8.475808217655753651, 34.90892951860618609 ) ) ;
#85644 = FACE_OUTER_BOUND ( 'NONE', #42105, .T. ) ;
#85645 = ORIENTED_EDGE ( 'NONE', *, *, #45640, .F. ) ;
#85646 = CARTESIAN_POINT ( 'NONE',  ( -17.20761454359063691, -12.38065189839062263, 30.83690757178629482 ) ) ;
#85647 = ORIENTED_EDGE ( 'NONE', *, *, #33860, .F. ) ;
#85648 = VERTEX_POINT ( 'NONE', #58301 ) ;
#85650 = FACE_OUTER_BOUND ( 'NONE', #18275, .T. ) ;
#85649 = DIRECTION ( 'NONE',  ( 0.000000000000000000, 0.000000000000000000, 1.000000000000000000 ) ) ;
#85651 = CARTESIAN_POINT ( 'NONE',  ( -0.4615384615384611200, -2.486705287966279876, 31.30864560766543647 ) ) ;
#85652 = DIRECTION ( 'NONE',  ( 1.000000000000000000, 0.000000000000000000, 0.000000000000000000 ) ) ;
#85653 = CARTESIAN_POINT ( 'NONE',  ( 7.715462379486289102, -12.38065189839062263, 30.83690757178629482 ) ) ;
#85654 = CARTESIAN_POINT ( 'NONE',  ( -12.33101275977490019, -4.459921816937791661, 33.71989282347011851 ) ) ;
#85655 = ORIENTED_EDGE ( 'NONE', *, *, #19717, .T. ) ;
#85656 = ADVANCED_FACE ( 'NONE', ( #11020 ), #31285, .F. ) ;
#85657 = VECTOR ( 'NONE', #57864, 1000.000000000000114 ) ;
#85658 = LINE ( 'NONE', #52303, #68804 ) ;
#85659 = CARTESIAN_POINT ( 'NONE',  ( 3.100621261037536325, -9.504002272028875709, 34.60269587691767867 ) ) ;
#85660 = CARTESIAN_POINT ( 'NONE',  ( -17.20707028636129721, -11.93770438780619259, 32.05411857736982029 ) ) ;
#85661 = CARTESIAN_POINT ( 'NONE',  ( 14.55774672760576571, -2.544122305571458575, 31.48381861865057729 ) ) ;
#85662 = VERTEX_POINT ( 'NONE', #64161 ) ;
#85663 = EDGE_CURVE ( 'NONE', #8169, #56983, #62834, .T. ) ;
#85664 = ORIENTED_EDGE ( 'NONE', *, *, #40548, .T. ) ;
#85665 = FACE_BOUND ( 'NONE', #51690, .T. ) ;
#85666 = ORIENTED_EDGE ( 'NONE', *, *, #67392, .F. ) ;
#85667 = CARTESIAN_POINT ( 'NONE',  ( -17.93129618099669997, -2.255932369308304875, 29.99950897402476713 ) ) ;
#85668 = CARTESIAN_POINT ( 'NONE',  ( -1.161835715637317579, -2.353885683473779356, 30.79025554430704759 ) ) ;
#85669 = ORIENTED_EDGE ( 'NONE', *, *, #11489, .F. ) ;
#85670 = CARTESIAN_POINT ( 'NONE',  ( 13.38461538461526601, -11.48612834414049644, 32.76840700105863391 ) ) ;
#85671 = DIRECTION ( 'NONE',  ( -0.000000000000000000, 0.6427876096865404731, -0.7660444431189771253 ) ) ;
#85672 = CARTESIAN_POINT ( 'NONE',  ( 5.010839665967195877, -2.721908614388772740, 31.22303859784724622 ) ) ;
#85673 = CARTESIAN_POINT ( 'NONE',  ( -1.253824943648432777, -3.957578996910242619, 33.62503395064540257 ) ) ;
#85674 = ORIENTED_EDGE ( 'NONE', *, *, #75333, .F. ) ;
#85675 = EDGE_CURVE ( 'NONE', #25023, #67015, #38120, .T. ) ;
#85676 = DIRECTION ( 'NONE',  ( 0.000000000000000000, 0.9848077530122072432, -0.1736481776669354937 ) ) ;
#85677 = ORIENTED_EDGE ( 'NONE', *, *, #7391, .F. ) ;
#85678 = B_SPLINE_CURVE_WITH_KNOTS ( 'NONE', 3,
 ( #41363, #41813, #48542, #35488, #8020, #34602, #49000, #75579, #36378, #15224 ),
 .UNSPECIFIED., .F., .F.,
 ( 4, 2, 2, 2, 4 ),
 ( 0.000000000000000000, 0.0001954311564186881213, 0.0003908623128373762425, 0.0005862934692560643367, 0.0007817246256747524850 ),
 .UNSPECIFIED. ) ;
#85680 = ORIENTED_EDGE ( 'NONE', *, *, #72180, .F. ) ;
#85679 = FACE_OUTER_BOUND ( 'NONE', #49737, .T. ) ;
#85681 = LINE ( 'NONE', #73506, #29667 ) ;
#85682 = CARTESIAN_POINT ( 'NONE',  ( 3.930361210122205406, -6.760086850603068243, 34.69517049084099369 ) ) ;
#85683 = DIRECTION ( 'NONE',  ( -0.000000000000000000, 0.7660444431189791237, -0.6427876096865379196 ) ) ;
#85684 = CARTESIAN_POINT ( 'NONE',  ( -4.088590582570127197, -12.46129190930001052, 30.37095296980870174 ) ) ;
#85685 = CARTESIAN_POINT ( 'NONE',  ( 13.51540719244017374, -5.582136614379148654, 34.36778462344220486 ) ) ;
#85686 = EDGE_CURVE ( 'NONE', #58760, #43442, #9101, .T. ) ;
#85687 = CARTESIAN_POINT ( 'NONE',  ( 5.207448778686639024, -12.45806712695776319, 30.39783852428763922 ) ) ;
#85688 = CARTESIAN_POINT ( 'NONE',  ( 1.987747218494642309, -5.598659921968629050, 13.31436829374151287 ) ) ;
#85689 = ORIENTED_EDGE ( 'NONE', *, *, #37463, .T. ) ;
#85690 = CARTESIAN_POINT ( 'NONE',  ( 4.153846153846154188, -9.819645486525091727, 36.12317359536749706 ) ) ;
#85691 = CYLINDRICAL_SURFACE ( 'NONE', #69247, 0.2500000000000004996 ) ;
#85692 = CARTESIAN_POINT ( 'NONE',  ( 6.223375940698185005, -2.501478030877322567, 29.88021232661720816 ) ) ;
#85694 = ORIENTED_EDGE ( 'NONE', *, *, #65978, .F. ) ;
#85693 = AXIS2_PLACEMENT_3D ( 'NONE', #33738, #40070, #86935 ) ;
#85695 = EDGE_LOOP ( 'NONE', ( #85625, #58052 ) ) ;
#85696 = CYLINDRICAL_SURFACE ( 'NONE', #68550, 0.2499999999999995559 ) ;
#85697 = CARTESIAN_POINT ( 'NONE',  ( -14.24243716817947103, -2.657715359629131857, 31.77849191805844242 ) ) ;
#85698 = EDGE_CURVE ( 'NONE', #60580, #62474, #36990, .T. ) ;
#85699 = CARTESIAN_POINT ( 'NONE',  ( 5.999999999999880096, -11.48612834414049644, 32.76840700105863391 ) ) ;
#85700 = VECTOR ( 'NONE', #52680, 1000.000000000000000 ) ;
#85701 = CARTESIAN_POINT ( 'NONE',  ( 9.562160482869472844, -12.45813303252208648, 30.39737893381572675 ) ) ;
#85702 = FACE_OUTER_BOUND ( 'NONE', #40775, .T. ) ;
#85703 = EDGE_CURVE ( 'NONE', #18166, #423, #52879, .T. ) ;
#85704 = CARTESIAN_POINT ( 'NONE',  ( -16.82697766754503377, -11.56426240980093567, 33.07394671870546432 ) ) ;
#85705 = CARTESIAN_POINT ( 'NONE',  ( -14.98071481085577972, -8.346898887586323923, 34.93166121998716278 ) ) ;
#85706 = ORIENTED_EDGE ( 'NONE', *, *, #19136, .F. ) ;
#85707 = LINE ( 'NONE', #2383, #85140 ) ;
#85708 = CARTESIAN_POINT ( 'NONE',  ( -17.01177729759111301, -7.750023238201980469, 34.74374492549440419 ) ) ;
#85709 = CARTESIAN_POINT ( 'NONE',  ( 4.403846153847572609, -7.500000000000154543, 35.00000000000007105 ) ) ;
#85710 = CARTESIAN_POINT ( 'NONE',  ( -18.00000000000000000, -13.85434399251292170, 33.13000708000598138 ) ) ;
#85711 = VERTEX_POINT ( 'NONE', #39392 ) ;
#85712 = FACE_OUTER_BOUND ( 'NONE', #65677, .T. ) ;
#85713 = SHAPE_REPRESENTATION ( 'head base', ( #83448 ), #69030 ) ;
#85714 = EDGE_LOOP ( 'NONE', ( #23794, #80870, #5787, #32144 ) ) ;
#85715 = CARTESIAN_POINT ( 'NONE',  ( -0.3962828902624376815, -2.892918686051626498, 31.69288490824025928 ) ) ;
#85716 = FILL_AREA_STYLE_COLOUR ( '', #53213 ) ;
#85717 = CARTESIAN_POINT ( 'NONE',  ( 16.37722163961857547, -2.251407671071269601, 29.88021292934942963 ) ) ;
#85718 = CARTESIAN_POINT ( 'NONE',  ( -8.769230769230768274, -1.509761064869970415, 31.06009739812519044 ) ) ;
#85719 = EDGE_LOOP ( 'NONE', ( #19699, #49715 ) ) ;
#85720 = CARTESIAN_POINT ( 'NONE',  ( -1.449885385171702845, -12.70778746994557551, 30.41441678777548319 ) ) ;
#85721 = CYLINDRICAL_SURFACE ( 'NONE', #53781, 0.2499999999999994726 ) ;
#85722 = LINE ( 'NONE', #85282, #55823 ) ;
#85723 = B_SPLINE_CURVE_WITH_KNOTS ( 'NONE', 3,
 ( #1925, #50101, #9564, #49669, #2794, #78460, #16761, #71702, #57311, #17207 ),
 .UNSPECIFIED., .F., .F.,
 ( 4, 2, 2, 2, 4 ),
 ( 0.0007817359430256216575, 0.0009771253907249859150, 0.001172514838424350064, 0.001367904286123714213, 0.001563293733823078362 ),
 .UNSPECIFIED. ) ;
#85724 = CARTESIAN_POINT ( 'NONE',  ( 30.00000000000000000, -15.00000000000000000, 0.000000000000000000 ) ) ;
#85725 = CARTESIAN_POINT ( 'NONE',  ( -4.854143407945011646, -10.97394488606064122, 33.68653795673694873 ) ) ;
#85726 = VECTOR ( 'NONE', #27527, 1000.000000000000000 ) ;
#85727 = EDGE_LOOP ( 'NONE', ( #56733, #75543, #85188, #26928 ) ) ;
#85728 = CARTESIAN_POINT ( 'NONE',  ( 16.21910129335899597, -10.33852847137154107, 34.16647553114620450 ) ) ;
#85729 = ORIENTED_EDGE ( 'NONE', *, *, #7213, .T. ) ;
#85730 = CARTESIAN_POINT ( 'NONE',  ( -10.39200867468643175, -2.501478030877323455, 29.88021232661721172 ) ) ;
#85731 = ADVANCED_FACE ( 'NONE', ( #26748 ), #87588, .F. ) ;
#85732 = CARTESIAN_POINT ( 'NONE',  ( -16.37677237136229991, -11.24512374952581872, 33.06303171183252942 ) ) ;
#85733 = DIRECTION ( 'NONE',  ( 0.000000000000000000, 0.000000000000000000, -1.000000000000000000 ) ) ;
#85734 = EDGE_CURVE ( 'NONE', #59182, #84305, #70353, .T. ) ;
#85735 = AXIS2_PLACEMENT_3D ( 'NONE', #12279, #58237, #78959 ) ;
#85736 = CARTESIAN_POINT ( 'NONE',  ( -14.17716660592874156, -11.93748526763465279, 32.05452791011430946 ) ) ;
#85737 = CARTESIAN_POINT ( 'NONE',  ( 9.442284455014730682, -8.432397168068783699, 34.66272746175022945 ) ) ;
#85738 = ORIENTED_EDGE ( 'NONE', *, *, #9022, .F. ) ;
#85740 = EDGE_CURVE ( 'NONE', #46211, #45649, #30630, .T. ) ;
#85739 = ORIENTED_EDGE ( 'NONE', *, *, #53365, .F. ) ;
#85741 = EDGE_LOOP ( 'NONE', ( #50971, #88291, #63922, #85489 ) ) ;
#85742 = ORIENTED_EDGE ( 'NONE', *, *, #14727, .T. ) ;
#85743 = CARTESIAN_POINT ( 'NONE',  ( 12.46153846153846168, -11.69971097300155272, 32.46337939537588113 ) ) ;
#85744 = CARTESIAN_POINT ( 'NONE',  ( -1.134669866267241867, -12.43552623307873972, 30.55307653245132826 ) ) ;
#85745 = ADVANCED_FACE ( 'NONE', ( #73627, #25420, #18674 ), #12354, .F. ) ;
#85746 = FACE_OUTER_BOUND ( 'NONE', #11629, .T. ) ;
#85747 = CARTESIAN_POINT ( 'NONE',  ( -5.777220458731589403, -5.114059244376869984, 34.14424750095245287 ) ) ;
#85748 = FACE_OUTER_BOUND ( 'NONE', #36097, .T. ) ;
#85749 = CARTESIAN_POINT ( 'NONE',  ( 3.230769230769231726, -5.557115091759785130, 34.35708131394839171 ) ) ;
#85750 = EDGE_CURVE ( 'NONE', #31128, #68727, #80378, .T. ) ;
#85751 = VECTOR ( 'NONE', #42278, 1000.000000000000000 ) ;
#85752 = CARTESIAN_POINT ( 'NONE',  ( -17.75005448165186195, -10.05730279482229683, 34.04704008940765902 ) ) ;
#85753 = CARTESIAN_POINT ( 'NONE',  ( -3.930834802233304170, -10.61302985866383963, 33.66295027996417843 ) ) ;
#85754 = VERTEX_POINT ( 'NONE', #54209 ) ;
#85755 = ORIENTED_EDGE ( 'NONE', *, *, #19034, .T. ) ;
#85756 = VECTOR ( 'NONE', #59678, 1000.000000000000000 ) ;
#85757 = VERTEX_POINT ( 'NONE', #67741 ) ;
#85758 = ADVANCED_FACE ( 'NONE', ( #74951 ), #6486, .F. ) ;
#85760 = EDGE_LOOP ( 'NONE', ( #89054, #53392 ) ) ;
#85759 = CARTESIAN_POINT ( 'NONE',  ( 6.249945409378045547, -12.45601412856602863, 31.48342859153981621 ) ) ;
#85762 = CARTESIAN_POINT ( 'NONE',  ( -16.40382288478850725, -9.943427161483782584, 34.11278801902876978 ) ) ;
#85761 = CARTESIAN_POINT ( 'NONE',  ( 8.899756470994333313, -8.586989748646452369, 34.63063291749215011 ) ) ;
#85763 = FACE_OUTER_BOUND ( 'NONE', #6126, .T. ) ;
#85764 = CARTESIAN_POINT ( 'NONE',  ( -9.692307692307691624, -6.386643153685126251, 34.62446782046654192 ) ) ;
#85765 = VERTEX_POINT ( 'NONE', #68184 ) ;
#85766 = ORIENTED_EDGE ( 'NONE', *, *, #84563, .F. ) ;
#85767 = CARTESIAN_POINT ( 'NONE',  ( -2.177647144857528527, -2.504778602574659896, 29.97347330155780298 ) ) ;
#85768 = EDGE_CURVE ( 'NONE', #74753, #88347, #77844, .T. ) ;
#85769 = ORIENTED_EDGE ( 'NONE', *, *, #32133, .F. ) ;
#85770 = FACE_BOUND ( 'NONE', #17478, .T. ) ;
#85771 = CARTESIAN_POINT ( 'NONE',  ( -6.223484943723947893, -9.331801661448606566, 34.40259984581193464 ) ) ;
#85772 = B_SPLINE_CURVE_WITH_KNOTS ( 'NONE', 3,
 ( #725, #55659, #21885, #61976, #285, #27751, #82712, #49361, #48456, #42172 ),
 .UNSPECIFIED., .F., .F.,
 ( 4, 2, 2, 2, 4 ),
 ( 0.000000000000000000, 0.0001954339857564073659, 0.0003908679715128147319, 0.0005863019572692221250, 0.0007817359430256294638 ),
 .UNSPECIFIED. ) ;
#85773 = DIRECTION ( 'NONE',  ( -0.000000000000000000, 0.3420201433256694901, -0.9396926207859082059 ) ) ;
#85774 = ORIENTED_EDGE ( 'NONE', *, *, #35036, .F. ) ;
#85775 = CARTESIAN_POINT ( 'NONE',  ( -1.253824943648434109, -5.496552790871119143, 34.60292014791297532 ) ) ;
#85776 = EDGE_CURVE ( 'NONE', #73779, #4699, #1603, .T. ) ;
#85777 = CARTESIAN_POINT ( 'NONE',  ( 11.31553457955469000, -6.459968553980841577, 34.89616026154728701 ) ) ;
#85778 = CARTESIAN_POINT ( 'NONE',  ( -18.75000000000000000, -7.500000000000000000, 33.75000000000000000 ) ) ;
#85779 = VERTEX_POINT ( 'NONE', #82148 ) ;
#85780 = CARTESIAN_POINT ( 'NONE',  ( -11.60373153901785948, -5.094484230520674117, 34.41647553114621161 ) ) ;
#85781 = CARTESIAN_POINT ( 'NONE',  ( 3.007284287045281168, -12.24155766932282496, 31.33739205006857986 ) ) ;
#85782 = ORIENTED_EDGE ( 'NONE', *, *, #55315, .F. ) ;
#85783 = DIRECTION ( 'NONE',  ( 0.000000000000000000, 0.4999999999999985567, 0.8660254037844395958 ) ) ;
#85784 = FACE_OUTER_BOUND ( 'NONE', #624, .T. ) ;
#85785 = EDGE_LOOP ( 'NONE', ( #47518, #1365, #33054, #51694 ) ) ;
#85786 = CARTESIAN_POINT ( 'NONE',  ( 7.145856592054987466, -2.612705202774697533, 31.66806509827799943 ) ) ;
#85787 = CYLINDRICAL_SURFACE ( 'NONE', #67014, 0.2500000000000002220 ) ;
#85788 = CYLINDRICAL_SURFACE ( 'NONE', #75776, 0.2500000000000008882 ) ;
#85789 = CARTESIAN_POINT ( 'NONE',  ( -8.638705067467206788, -9.417988943895561960, 34.36773134775777550 ) ) ;
#85790 = LINE ( 'NONE', #24073, #2752 ) ;
#85791 = VECTOR ( 'NONE', #69181, 1000.000000000000227 ) ;
#85792 = CARTESIAN_POINT ( 'NONE',  ( 6.223011351612851350, -9.886259254753566594, 34.14407573483972413 ) ) ;
#85794 = CARTESIAN_POINT ( 'NONE',  ( 20.00000000000000000, -4.000000000000000000, 29.75000000000000355 ) ) ;
#85793 = CARTESIAN_POINT ( 'NONE',  ( -13.38461538461538325, -3.937682226553329556, 33.60647404775216529 ) ) ;
#85795 = EDGE_CURVE ( 'NONE', #82786, #65345, #61725, .T. ) ;
#85796 = ADVANCED_FACE ( 'NONE', ( #83928 ), #75383, .T. ) ;
#85797 = CARTESIAN_POINT ( 'NONE',  ( -0.2114840416250086119, -8.346898887586323923, 34.93166121998716278 ) ) ;
#85799 = CARTESIAN_POINT ( 'NONE',  ( -16.15384615384615330, -3.513871655860378418, 32.76840700105978499 ) ) ;
#85798 = CARTESIAN_POINT ( 'NONE',  ( -15.29603967673000753, -11.94971097300153140, 32.03036669348370680 ) ) ;
#85800 = CARTESIAN_POINT ( 'NONE',  ( 1.200186371490561621, -10.22469193450123193, 25.70125670625848713 ) ) ;
#85801 = VERTEX_POINT ( 'NONE', #77153 ) ;
#85802 = CARTESIAN_POINT ( 'NONE',  ( 0.4615384615384611200, -12.37446782046654192, 30.86335684631486131 ) ) ;
#85803 = VERTEX_POINT ( 'NONE', #15015 ) ;
#85804 = CARTESIAN_POINT ( 'NONE',  ( -6.416666666666667851, -7.500000000000000000, 29.75000000000000355 ) ) ;
#85805 = VERTEX_POINT ( 'NONE', #41595 ) ;
#85806 = CARTESIAN_POINT ( 'NONE',  ( -13.38461538461538325, -2.292212530054420494, 30.41441678777542634 ) ) ;
#85807 = ORIENTED_EDGE ( 'NONE', *, *, #70901, .F. ) ;
#85808 = CARTESIAN_POINT ( 'NONE',  ( 18.06514577933196009, -7.750023238201980469, 34.74374492549440419 ) ) ;
#85809 = CARTESIAN_POINT ( 'NONE',  ( -1.901340078031346525, -9.487747218494661183, 23.43563170625848713 ) ) ;
#85810 = CYLINDRICAL_SURFACE ( 'NONE', #40115, 0.2500000000000004996 ) ;
#85811 = EDGE_CURVE ( 'NONE', #18370, #49385, #47903, .T. ) ;
#85812 = CARTESIAN_POINT ( 'NONE',  ( 6.857806477116147548, -11.48612834413959582, 32.76840700105983473 ) ) ;
#85813 = CARTESIAN_POINT ( 'NONE',  ( -2.980714810855777053, -12.41089969410671223, 31.60739465890703670 ) ) ;
#85814 = CARTESIAN_POINT ( 'NONE',  ( -14.53061926659915315, -10.77366814457252175, 33.85459836347579454 ) ) ;
#85815 = CARTESIAN_POINT ( 'NONE',  ( -16.21911615440247090, -10.33852847137145048, 34.16647553114627556 ) ) ;
#85816 = FACE_OUTER_BOUND ( 'NONE', #24589, .T. ) ;
#85817 = LINE ( 'NONE', #24097, #22358 ) ;
#85818 = CARTESIAN_POINT ( 'NONE',  ( -3.749999999999988454, -9.053300858899127945, 15.01562500000000178 ) ) ;
#85819 = EDGE_CURVE ( 'NONE', #25692, #10070, #13677, .T. ) ;
#85820 = EDGE_CURVE ( 'NONE', #62030, #7735, #67171, .T. ) ;
#85821 = CARTESIAN_POINT ( 'NONE',  ( 1.515141086378952506, -3.285477652293412820, 32.44071101563363158 ) ) ;
#85822 = CARTESIAN_POINT ( 'NONE',  ( 13.16168842570853492, -3.395401636524185474, 33.02366814457250399 ) ) ;
#85823 = B_SPLINE_CURVE_WITH_KNOTS ( 'NONE', 3,
 ( #24613, #18757, #11103, #31375, #85878, #80008, #4344, #87672, #52965, #32698 ),
 .UNSPECIFIED., .F., .F.,
 ( 4, 2, 2, 2, 4 ),
 ( 0.000000000000000000, 0.0001954339857564078809, 0.0003908679715128157619, 0.0005863019572692236428, 0.0007817359430256315238 ),
 .UNSPECIFIED. ) ;
#85824 = CARTESIAN_POINT ( 'NONE',  ( -3.230769230768915534, -2.255955759149395501, 30.00000000000324363 ) ) ;
#85825 = ADVANCED_FACE ( 'NONE', ( #35279 ), #34831, .F. ) ;
#85826 = ORIENTED_EDGE ( 'NONE', *, *, #38756, .F. ) ;
#85827 = CARTESIAN_POINT ( 'NONE',  ( 17.20744877868663991, -12.27024696741798770, 31.24895572276497546 ) ) ;
#85828 = FACE_OUTER_BOUND ( 'NONE', #69021, .T. ) ;
#85829 = CARTESIAN_POINT ( 'NONE',  ( 1.161688425708537808, -10.77366814457252175, 33.85459836347579454 ) ) ;
#85830 = CARTESIAN_POINT ( 'NONE',  ( 16.02323649864207056, -7.722926974430166069, 34.99546784045485737 ) ) ;
#85831 = CARTESIAN_POINT ( 'NONE',  ( -18.00000000000000000, -12.50000000000000000, 29.49999999999997868 ) ) ;
#85832 = TOROIDAL_SURFACE ( 'NONE', #29694, 3.000000000000000888, 2.000000000000000000 ) ;
#85833 = CARTESIAN_POINT ( 'NONE',  ( -9.019207500173124004, -8.303909089506435137, 34.68538101551103381 ) ) ;
#85834 = ORIENTED_EDGE ( 'NONE', *, *, #24350, .T. ) ;
#85835 = CARTESIAN_POINT ( 'NONE',  ( -1.161604033002533898, -9.886259254753564818, 34.14407573483972413 ) ) ;
#85836 = ORIENTED_EDGE ( 'NONE', *, *, #88278, .F. ) ;
#85837 = EDGE_LOOP ( 'NONE', ( #76249, #9735 ) ) ;
#85838 = CARTESIAN_POINT ( 'NONE',  ( 0.7114838709165037800, -12.45601412856602863, 31.48342859153981621 ) ) ;
#85839 = CARTESIAN_POINT ( 'NONE',  ( -6.792551484843277976, -5.915461855592777596, 34.75538340440931506 ) ) ;
#85840 = CARTESIAN_POINT ( 'NONE',  ( 20.00000000000000000, -4.000000000000000000, 29.75000000000000355 ) ) ;
#85841 = CARTESIAN_POINT ( 'NONE',  ( -6.130691466667560263, -3.062553014421049546, 32.05460306192773601 ) ) ;
#85842 = CARTESIAN_POINT ( 'NONE',  ( 13.16113046005105858, -5.827078755546623690, 34.72654668319379567 ) ) ;
#85843 = ORIENTED_EDGE ( 'NONE', *, *, #25303, .F. ) ;
#85844 = ORIENTED_EDGE ( 'NONE', *, *, #40067, .F. ) ;
#85845 = B_SPLINE_CURVE_WITH_KNOTS ( 'NONE', 3,
 ( #8391, #49807, #43059, #64197, #56131, #29991, #50687, #2068, #21901, #15592 ),
 .UNSPECIFIED., .F., .F.,
 ( 4, 2, 2, 2, 4 ),
 ( 0.000000000000000000, 0.0001954339857564082604, 0.0003908679715128165208, 0.0005863019572692248355, 0.0007817359430256330417 ),
 .UNSPECIFIED. ) ;
#85846 = ORIENTED_EDGE ( 'NONE', *, *, #79106, .F. ) ;
#85847 = CARTESIAN_POINT ( 'NONE',  ( -3.903900744468110418, -12.07971442181322352, 32.31769673815850297 ) ) ;
#85848 = CARTESIAN_POINT ( 'NONE',  ( 16.21991450484859598, -12.37446782046654192, 30.86335684631486842 ) ) ;
#85849 = AXIS2_PLACEMENT_3D ( 'NONE', #67564, #73876, #40975 ) ;
#85850 = LINE ( 'NONE', #86310, #13518 ) ;
#85851 = CARTESIAN_POINT ( 'NONE',  ( 10.39245765647776309, -4.762599654559228846, 34.23009711892697737 ) ) ;
#85852 = CARTESIAN_POINT ( 'NONE',  ( 11.28843831424008215, -10.92453946501458795, 33.72985991061850086 ) ) ;
#85853 = CARTESIAN_POINT ( 'NONE',  ( -18.00000000000000000, -11.69971097300155449, 32.46337939537587403 ) ) ;
#85854 = EDGE_LOOP ( 'NONE', ( #27010, #88863, #76963, #42768 ) ) ;
#85855 = VERTEX_POINT ( 'NONE', #611 ) ;
#85856 = CARTESIAN_POINT ( 'NONE',  ( -3.750000000000008438, -5.946699141100917352, 23.92187500000000355 ) ) ;
#85857 = VERTEX_POINT ( 'NONE', #55106 ) ;
#85858 = EDGE_CURVE ( 'NONE', #60430, #5967, #23133, .T. ) ;
#85860 = EDGE_LOOP ( 'NONE', ( #60064, #9606 ) ) ;
#85859 = DIRECTION ( 'NONE',  ( -0.000000000000000000, 0.5000000000000011102, -0.8660254037844381525 ) ) ;
#85861 = CARTESIAN_POINT ( 'NONE',  ( 8.068933387422251968, -12.44528174975671853, 30.48912976160716681 ) ) ;
#85862 = CARTESIAN_POINT ( 'NONE',  ( -2.057746898314262385, -4.176053281294514363, 33.81426240980091791 ) ) ;
#85863 = CARTESIAN_POINT ( 'NONE',  ( -3.749999999999988454, -9.053300858899127945, 16.26562500000000000 ) ) ;
#85864 = ORIENTED_EDGE ( 'NONE', *, *, #84404, .F. ) ;
#85865 = DIRECTION ( 'NONE',  ( -8.673617379884035472E-16, 0.000000000000000000, 1.000000000000000000 ) ) ;
#85866 = EDGE_LOOP ( 'NONE', ( #26251, #20817 ) ) ;
#85867 = CARTESIAN_POINT ( 'NONE',  ( -8.834500769787091201, -5.094484230520674117, 34.41647553114621161 ) ) ;
#85868 = LINE ( 'NONE', #16080, #55818 ) ;
#85869 = CARTESIAN_POINT ( 'NONE',  ( -17.74994558008654622, -2.544122305571458575, 31.48381861865057729 ) ) ;
#85871 = DIRECTION ( 'NONE',  ( -0.000000000000000000, -0.1736481776669307198, -0.9848077530122080203 ) ) ;
#85870 = DIRECTION ( 'NONE',  ( 0.000000000000000000, 0.7660444431189807890, 0.6427876096865361433 ) ) ;
#85872 = AXIS2_PLACEMENT_3D ( 'NONE', #69978, #88509, #35767 ) ;
#85873 = CARTESIAN_POINT ( 'NONE',  ( 8.545745825506822158, -5.912607949931405926, 34.49155766932282319 ) ) ;
#85874 = CARTESIAN_POINT ( 'NONE',  ( -10.86540785267757947, -10.76384336483936011, 33.53834819971076087 ) ) ;
#85875 = ORIENTED_EDGE ( 'NONE', *, *, #5670, .T. ) ;
#85876 = ADVANCED_FACE ( 'NONE', ( #50112 ), #30728, .F. ) ;
#85877 = CARTESIAN_POINT ( 'NONE',  ( -10.68146802634049308, -9.780366693483667717, 34.19971097300155805 ) ) ;
#85878 = CARTESIAN_POINT ( 'NONE',  ( 14.98079249982687777, -4.236021600441997492, 33.53823185664189310 ) ) ;
#85879 = EDGE_LOOP ( 'NONE', ( #78497, #78880, #2040, #49687 ) ) ;
#85880 = AXIS2_PLACEMENT_3D ( 'NONE', #31623, #58191, #3692 ) ;
#85881 = CARTESIAN_POINT ( 'NONE',  ( -12.33074802057151409, -3.338503747796866872, 32.95102852606553512 ) ) ;
#85882 = LINE ( 'NONE', #85002, #28604 ) ;
#85884 = LINE ( 'NONE', #10668, #48364 ) ;
#85883 = PRODUCT_DEFINITION_SHAPE ( 'NONE', 'NONE',  #89188 ) ;
#85885 = CARTESIAN_POINT ( 'NONE',  ( 3.230769230769231726, -8.564572088678739092, 35.78748833219616898 ) ) ;
#85886 = CARTESIAN_POINT ( 'NONE',  ( -8.769230769230890843, -6.026961402154118019, 34.52809138561165270 ) ) ;
#85887 = FACE_BOUND ( 'NONE', #21151, .T. ) ;
#85889 = CARTESIAN_POINT ( 'NONE',  ( 17.99999999999987566, -11.06231777344772027, 33.60647404775119895 ) ) ;
#85888 = CARTESIAN_POINT ( 'NONE',  ( 13.13459214732242408, -12.22074536777954989, 31.39888409691088356 ) ) ;
#85890 = ADVANCED_FACE ( 'NONE', ( #29423 ), #86134, .F. ) ;
#85891 = CIRCLE ( 'NONE', #47047, 0.2500000000000002220 ) ;
#85892 = DIRECTION ( 'NONE',  ( -1.000000000000000000, 0.000000000000000000, 0.000000000000000000 ) ) ;
#85894 = CARTESIAN_POINT ( 'NONE',  ( 9.757563263583719504, -4.481592998940250538, 33.73612834413965089 ) ) ;
#85893 = CARTESIAN_POINT ( 'NONE',  ( 18.24994551834813805, -11.37275283266504111, 32.91324779482534524 ) ) ;
#85895 = CARTESIAN_POINT ( 'NONE',  ( -4.023320715612509701, -11.04252011169590020, 33.62494198852677130 ) ) ;
#85896 = LINE ( 'NONE', #36813, #70645 ) ;
#85897 = CARTESIAN_POINT ( 'NONE',  ( 0.06109907496455496689, -11.24999999999999822, 20.77938170625848713 ) ) ;
#85898 = VERTEX_POINT ( 'NONE', #85246 ) ;
#85899 = CYLINDRICAL_SURFACE ( 'NONE', #78051, 0.2500000000000009437 ) ;
#85900 = CARTESIAN_POINT ( 'NONE',  ( -14.53117725141625627, -6.760086850603066466, 34.69517049084099369 ) ) ;
#85901 = FACE_OUTER_BOUND ( 'NONE', #79640, .T. ) ;
#85902 = CARTESIAN_POINT ( 'NONE',  ( 0.4998584449498339466, -10.20418963010134306, 29.16127627612525330 ) ) ;
#85903 = CARTESIAN_POINT ( 'NONE',  ( 6.923076923076800782, -12.70778746994576025, 30.41441678777401236 ) ) ;
#85904 = CARTESIAN_POINT ( 'NONE',  ( -3.296020220930472533, -2.506253911140460922, 30.00000000000013856 ) ) ;
#85905 = CARTESIAN_POINT ( 'NONE',  ( -2.694853999681210865, -4.891553140782108677, 21.24813170625848713 ) ) ;
#85906 = CARTESIAN_POINT ( 'NONE',  ( -16.21911615440247090, -5.941354392334501355, 34.76329471203369792 ) ) ;
#85907 = CARTESIAN_POINT ( 'NONE',  ( -2.307692307692428724, -6.835583212225970762, 34.95778746994575670 ) ) ;
#85908 = CARTESIAN_POINT ( 'NONE',  ( 11.66850897371199203, -7.723484941389743952, 34.99544897038808955 ) ) ;
#85909 = CARTESIAN_POINT ( 'NONE',  ( -18.00000000000000000, -7.500000000000001776, 35.00000000000000000 ) ) ;
#85910 = CARTESIAN_POINT ( 'NONE',  ( -7.173100160369890510, -4.335965774309649134, 33.62209801155881905 ) ) ;
#85911 = DIRECTION ( 'NONE',  ( 1.734723475976813504E-16, -1.000000000000000000, 0.000000000000000000 ) ) ;
#85912 = AXIS2_PLACEMENT_3D ( 'NONE', #80690, #87009, #25281 ) ;
#85913 = ADVANCED_FACE ( 'NONE', ( #78918 ), #30295, .F. ) ;
#85914 = EDGE_CURVE ( 'NONE', #35516, #20943, #18833, .T. ) ;
#85915 = DIRECTION ( 'NONE',  ( -0.000000000000000000, -0.5000000000000009992, -0.8660254037844380415 ) ) ;
#85916 = LINE ( 'NONE', #24199, #8272 ) ;
#85917 = VERTEX_POINT ( 'NONE', #17673 ) ;
#85918 = CARTESIAN_POINT ( 'NONE',  ( 14.98079248672064345, -11.47974371597207899, 33.17467449705390692 ) ) ;
#85919 = LINE ( 'NONE', #24202, #79118 ) ;
#85920 = CIRCLE ( 'NONE', #39894, 4.000000000000000000 ) ;
#85921 = CARTESIAN_POINT ( 'NONE',  ( 1.200186371490529202, -4.775308065498752974, 24.48624329374151642 ) ) ;
#85922 = CARTESIAN_POINT ( 'NONE',  ( 2.057715576749954867, -4.236021600441998380, 33.53823185664189310 ) ) ;
#85923 = CYLINDRICAL_SURFACE ( 'NONE', #35446, 0.2500000000000008882 ) ;
#85924 = ORIENTED_EDGE ( 'NONE', *, *, #60230, .F. ) ;
#85925 = CARTESIAN_POINT ( 'NONE',  ( 1.449870955891410462, -4.481592998940251427, 33.73612834413965089 ) ) ;
#85926 = LINE ( 'NONE', #960, #30130 ) ;
#85928 = ORIENTED_EDGE ( 'NONE', *, *, #4863, .F. ) ;
#85927 = DIRECTION ( 'NONE',  ( -0.000000000000000000, 1.000000000000000000, 3.491481338843133355E-15 ) ) ;
#85929 = DIRECTION ( 'NONE',  ( 1.000000000000000000, 0.000000000000000000, 0.000000000000000000 ) ) ;
#85930 = CARTESIAN_POINT ( 'NONE',  ( -13.13466986626724342, -10.05730279482229683, 34.04704008940765902 ) ) ;
#85931 = VECTOR ( 'NONE', #17902, 999.9999999999998863 ) ;
#85932 = DIRECTION ( 'NONE',  ( 0.000000000000000000, 0.6427876096865368094, 0.7660444431189802339 ) ) ;
#85933 = LINE ( 'NONE', #77399, #12632 ) ;
#85934 = ORIENTED_EDGE ( 'NONE', *, *, #80306, .T. ) ;
#85935 = DIRECTION ( 'NONE',  ( -0.000000000000000000, 0.1736481776669307198, -0.9848077530122080203 ) ) ;
#85936 = CARTESIAN_POINT ( 'NONE',  ( -14.30769230769230660, -10.89733346790207413, 36.13435417666054406 ) ) ;
#85937 = CARTESIAN_POINT ( 'NONE',  ( 3.903869422903799347, -9.943427161483782584, 34.11278801902876978 ) ) ;
#85938 = EDGE_LOOP ( 'NONE', ( #4216, #3698, #3438, #49787 ) ) ;
#85939 = EDGE_LOOP ( 'NONE', ( #37195, #1448 ) ) ;
#85940 = B_SPLINE_CURVE_WITH_KNOTS ( 'NONE', 3,
 ( #62584, #12644, #81997, #47304, #40569, #60822, #74795, #13084, #75236, #41003 ),
 .UNSPECIFIED., .F., .F.,
 ( 4, 2, 2, 2, 4 ),
 ( 0.0007817359430256288133, 0.0009771253907249948054, 0.001172514838424360689, 0.001367904286123726573, 0.001563293733823092457 ),
 .UNSPECIFIED. ) ;
#85941 = B_SPLINE_CURVE_WITH_KNOTS ( 'NONE', 3,
 ( #40762, #20032, #25909, #39879, #73668, #68230, #13724, #40319, #27234, #5193 ),
 .UNSPECIFIED., .F., .F.,
 ( 4, 2, 2, 2, 4 ),
 ( 0.0007817359527651104954, 0.0009771254036996493593, 0.001172514854634188223, 0.001367904305568727087, 0.001563293756503265951 ),
 .UNSPECIFIED. ) ;
#85942 = ORIENTED_EDGE ( 'NONE', *, *, #26553, .F. ) ;
#85943 = VECTOR ( 'NONE', #86333, 1000.000000000000000 ) ;
#85944 = CARTESIAN_POINT ( 'NONE',  ( -5.207071046654770718, -9.504002272028875709, 34.60269587691767867 ) ) ;
#85945 = CARTESIAN_POINT ( 'NONE',  ( -3.100243792535588572, -3.068774925481847493, 32.56582465632704526 ) ) ;
#85946 = CARTESIAN_POINT ( 'NONE',  ( 13.38461538461538680, -11.16473453929635440, 33.15142922261926373 ) ) ;
#85947 = CARTESIAN_POINT ( 'NONE',  ( -10.54931626438217585, -3.050289026998446840, 32.03036669348366416 ) ) ;
#85948 = ORIENTED_EDGE ( 'NONE', *, *, #6200, .F. ) ;
#85949 = AXIS2_PLACEMENT_3D ( 'NONE', #80053, #46271, #68314 ) ;
#85950 = VERTEX_POINT ( 'NONE', #38382 ) ;
#85952 = EDGE_LOOP ( 'NONE', ( #16289, #65792, #22219, #80932 ) ) ;
#85951 = CARTESIAN_POINT ( 'NONE',  ( 10.61538461538493117, -2.255955759149395501, 30.00000000000324363 ) ) ;
#85953 = CARTESIAN_POINT ( 'NONE',  ( 0.000000000000000000, -11.00000000000000000, 29.75000000000000355 ) ) ;
#85954 = CARTESIAN_POINT ( 'NONE',  ( 9.758376043310132530, -12.37446782046654192, 30.86335684631486842 ) ) ;
#85955 = CARTESIAN_POINT ( 'NONE',  ( -8.769230769230768274, -12.37446782046654192, 30.86335684631486131 ) ) ;
#85956 = CARTESIAN_POINT ( 'NONE',  ( -17.07692307692307665, -2.708943851104267164, 35.45975837776705220 ) ) ;
#85957 = ORIENTED_EDGE ( 'NONE', *, *, #7551, .T. ) ;
#85958 = EDGE_LOOP ( 'NONE', ( #21477, #7886, #47446, #55552 ) ) ;
#85959 = EDGE_LOOP ( 'NONE', ( #70816, #23715 ) ) ;
#85961 = EDGE_LOOP ( 'NONE', ( #34901, #72674 ) ) ;
#85960 = CARTESIAN_POINT ( 'NONE',  ( 15.00784301325307979, -2.554751324335735152, 30.48935550225260727 ) ) ;
#85962 = ADVANCED_FACE ( 'NONE', ( #56872 ), #64068, .F. ) ;
#85963 = ADVANCED_FACE ( 'NONE', ( #44673 ), #2362, .T. ) ;
#85964 = CARTESIAN_POINT ( 'NONE',  ( -5.076923076923075762, -6.189225973068211317, 35.74407628777942847 ) ) ;
#85965 = VECTOR ( 'NONE', #31273, 999.9999999999998863 ) ;
#85966 = CARTESIAN_POINT ( 'NONE',  ( -0.3307480205715123689, -4.684288915650983043, 34.18129842949671371 ) ) ;
#85967 = EDGE_LOOP ( 'NONE', ( #31545, #45876, #42473, #48370 ) ) ;
#85968 = FACE_OUTER_BOUND ( 'NONE', #57211, .T. ) ;
#85969 = B_SPLINE_CURVE_WITH_KNOTS ( 'NONE', 3,
 ( #20209, #67066, #5364, #60296, #47674, #67512, #74718, #87806, #13005, #40923 ),
 .UNSPECIFIED., .F., .F.,
 ( 4, 2, 2, 2, 4 ),
 ( 0.0007817246256747463051, 0.0009771112852218896347, 0.001172497944769032747, 0.001367884604316176077, 0.001563271263863319407 ),
 .UNSPECIFIED. ) ;
#85970 = CARTESIAN_POINT ( 'NONE',  ( -1.449885830576159496, -8.613356846314824011, 34.62446782046655613 ) ) ;
#85971 = FACE_OUTER_BOUND ( 'NONE', #33851, .T. ) ;
#85972 = FACE_BOUND ( 'NONE', #8246, .T. ) ;
#85973 = CARTESIAN_POINT ( 'NONE',  ( 14.98079249982687955, -5.728515186090277211, 34.42611988154120439 ) ) ;
#85974 = CARTESIAN_POINT ( 'NONE',  ( 2.372947878968332258, -8.613356846314928816, 34.62446782046653482 ) ) ;
#85975 = EDGE_CURVE ( 'NONE', #55112, #87599, #72156, .T. ) ;
#85976 = CARTESIAN_POINT ( 'NONE',  ( 8.639083559792549494, -2.619462340734462380, 30.83744416345203021 ) ) ;
#85978 = CARTESIAN_POINT ( 'NONE',  ( 9.915319043920543862, -3.105924265160262543, 32.13625925475356127 ) ) ;
#85977 = CARTESIAN_POINT ( 'NONE',  ( 17.30029901762125988, -2.501478030877322567, 29.88021232661721172 ) ) ;
#85979 = CARTESIAN_POINT ( 'NONE',  ( 11.53846153846141753, -11.48612834414049644, 32.76840700105863391 ) ) ;
#85980 = CARTESIAN_POINT ( 'NONE',  ( 14.30769230769231015, -3.937682226553329556, 33.60647404775216529 ) ) ;
#85981 = ORIENTED_EDGE ( 'NONE', *, *, #33885, .F. ) ;
#85982 = VECTOR ( 'NONE', #58007, 1000.000000000000000 ) ;
#85983 = DIRECTION ( 'NONE',  ( -1.000000000000000000, 0.000000000000000000, 0.000000000000000000 ) ) ;
#85984 = EDGE_CURVE ( 'NONE', #58506, #2885, #10912, .T. ) ;
#85985 = LINE ( 'NONE', #58943, #73858 ) ;
#85986 = EDGE_LOOP ( 'NONE', ( #38094, #46593, #31224, #79430, #52752 ) ) ;
#85987 = VERTEX_POINT ( 'NONE', #29856 ) ;
#85989 = CARTESIAN_POINT ( 'NONE',  ( 10.83839745947800992, -12.64618726649961289, 30.78989965857442712 ) ) ;
#85988 = CARTESIAN_POINT ( 'NONE',  ( 5.776515056276054771, -6.760086850603068243, 34.69517049084099369 ) ) ;
#85990 = CARTESIAN_POINT ( 'NONE',  ( -6.792551221313360088, -6.852161475712352789, 34.70806712695775786 ) ) ;
#85991 = PLANE ( 'NONE',  #12794 ) ;
#85992 = CARTESIAN_POINT ( 'NONE',  ( 1.319344938654610111, -11.94971097300153140, 32.03036669348370680 ) ) ;
#85993 = ORIENTED_EDGE ( 'NONE', *, *, #46916, .F. ) ;
#85994 = DIRECTION ( 'NONE',  ( 0.000000000000000000, 0.000000000000000000, 1.000000000000000000 ) ) ;
#85995 = CARTESIAN_POINT ( 'NONE',  ( -9.692307692307691624, -4.098570777380720287, 33.41473453929634729 ) ) ;
#85996 = DIRECTION ( 'NONE',  ( 1.000000000000000000, 0.000000000000000000, 0.000000000000000000 ) ) ;
#85997 = EDGE_CURVE ( 'NONE', #69454, #31211, #53117, .T. ) ;
#85998 = CARTESIAN_POINT ( 'NONE',  ( 0.4615384615383382183, -3.643525952248795718, 33.31231777344771672 ) ) ;
#85999 = CARTESIAN_POINT ( 'NONE',  ( -16.82686865700962642, -2.544122305571458575, 31.48381861865057729 ) ) ;
#86000 = CARTESIAN_POINT ( 'NONE',  ( 3.750000000000009770, -9.053300858899081760, 17.04687500000000000 ) ) ;
#86001 = ORIENTED_EDGE ( 'NONE', *, *, #66755, .F. ) ;
#86002 = ORIENTED_EDGE ( 'NONE', *, *, #84118, .T. ) ;
#86003 = AXIS2_PLACEMENT_3D ( 'NONE', #24492, #31714, #51960 ) ;
#86004 = CARTESIAN_POINT ( 'NONE',  ( 14.17700170458200759, -12.35290016733513951, 31.75349464988449455 ) ) ;
#86005 = ORIENTED_EDGE ( 'NONE', *, *, #48444, .F. ) ;
#86006 = DIRECTION ( 'NONE',  ( 0.000000000000000000, 0.000000000000000000, 1.000000000000000000 ) ) ;
#86007 = CARTESIAN_POINT ( 'NONE',  ( 17.86985203026830860, -11.66186481527757479, 32.95055677023626117 ) ) ;
#86008 = CARTESIAN_POINT ( 'NONE',  ( 14.53070365930515706, -2.758310577978208666, 31.33698337089302299 ) ) ;
#86009 = CARTESIAN_POINT ( 'NONE',  ( 5.749999999999976907, -2.249999999999999112, 29.81609741502488120 ) ) ;
#86010 = CARTESIAN_POINT ( 'NONE',  ( 3.750000000000000888, -7.499999999999978684, 18.21875000000000000 ) ) ;
#86011 = CARTESIAN_POINT ( 'NONE',  ( -11.60373153901785948, -9.528491918058357157, 34.59228464037090589 ) ) ;
#86012 = LINE ( 'NONE', #24293, #77664 ) ;
#86013 = EDGE_LOOP ( 'NONE', ( #17984, #61669, #43794, #24240 ) ) ;
#86014 = VECTOR ( 'NONE', #88000, 1000.000000000000114 ) ;
#86015 = LINE ( 'NONE', #43688, #74570 ) ;
#86017 = ORIENTED_EDGE ( 'NONE', *, *, #70552, .T. ) ;
#86016 = CARTESIAN_POINT ( 'NONE',  ( 4.153846153846154188, -12.78798330534103123, 29.99999999999997868 ) ) ;
#86018 = CARTESIAN_POINT ( 'NONE',  ( -9.442307692307753797, -7.565270000091922853, 34.99999999999999289 ) ) ;
#86019 = CARTESIAN_POINT ( 'NONE',  ( 3.230769230769231726, -2.721908614388771852, 31.22303859784724978 ) ) ;
#86020 = CARTESIAN_POINT ( 'NONE',  ( -12.68446542044531000, -8.282780595021769443, 34.94152052738834158 ) ) ;
#86021 = DIRECTION ( 'NONE',  ( 0.000000000000000000, 0.4999999999999985567, 0.8660254037844395958 ) ) ;
#86022 = EDGE_CURVE ( 'NONE', #60060, #83375, #64951, .T. ) ;
#86023 = CARTESIAN_POINT ( 'NONE',  ( -5.777220331021932331, -4.989023458446560255, 34.36081565061822118 ) ) ;
#86024 = CARTESIAN_POINT ( 'NONE',  ( 9.468822767743363400, -4.988325925672468131, 34.36044203135681130 ) ) ;
#86025 = CARTESIAN_POINT ( 'NONE',  ( 15.23076923076911093, -11.48612834414049644, 32.76840700105863391 ) ) ;
#86026 = EDGE_CURVE ( 'NONE', #71998, #74779, #2803, .T. ) ;
#86027 = CARTESIAN_POINT ( 'NONE',  ( 3.750000000000001776, -7.561099074964511502, 17.22061829374151287 ) ) ;
#86028 = EDGE_LOOP ( 'NONE', ( #19263, #40148, #7174, #83021 ) ) ;
#86029 = CARTESIAN_POINT ( 'NONE',  ( -4.377331097570100304, -5.113361153441932316, 34.14387501736621999 ) ) ;
#86030 = CARTESIAN_POINT ( 'NONE',  ( -12.23811149967689360, -7.630147231320743018, 34.74852402298682819 ) ) ;
#86031 = DIRECTION ( 'NONE',  ( -0.000000000000000000, -0.7660444431189791237, -0.6427876096865379196 ) ) ;
#86032 = CARTESIAN_POINT ( 'NONE',  ( -2.750000000000007105, -6.360912703474006946, 26.42187500000000000 ) ) ;
#86033 = EDGE_CURVE ( 'NONE', #41851, #34671, #30368, .T. ) ;
#86034 = CARTESIAN_POINT ( 'NONE',  ( 13.60762673622823726, -4.887748414852792322, 34.01359900205216746 ) ) ;
#86035 = CARTESIAN_POINT ( 'NONE',  ( 2.438482748659257737, -11.93129842949671726, 32.56571108434900452 ) ) ;
#86036 = EDGE_CURVE ( 'NONE', #37000, #77161, #49925, .T. ) ;
#86038 = ORIENTED_EDGE ( 'NONE', *, *, #63400, .T. ) ;
#86037 = CARTESIAN_POINT ( 'NONE',  ( 12.39545505058258001, -10.51840700105979387, 33.73612834413961536 ) ) ;
#86039 = CARTESIAN_POINT ( 'NONE',  ( -2.749999999999998224, -7.500000000000015987, 17.59375000000000000 ) ) ;
#86040 = CARTESIAN_POINT ( 'NONE',  ( -1.134669975237340589, -12.45601412856602686, 31.48342859153981621 ) ) ;
#86041 = VERTEX_POINT ( 'NONE', #38836 ) ;
#86042 = CARTESIAN_POINT ( 'NONE',  ( -18.06527000055631760, -5.094484230520675894, 34.41647553114621161 ) ) ;
#86043 = ORIENTED_EDGE ( 'NONE', *, *, #82314, .T. ) ;
#86044 = CARTESIAN_POINT ( 'NONE',  ( -18.06608341095587278, -11.69971097300155272, 32.46337939537587403 ) ) ;
#86045 = CARTESIAN_POINT ( 'NONE',  ( -15.23076923076922995, -2.833524468853757305, 32.15551576947925838 ) ) ;
#86046 = CARTESIAN_POINT ( 'NONE',  ( -12.46153846153846168, -6.189225973068211317, 35.74407628777942847 ) ) ;
#86047 = EDGE_LOOP ( 'NONE', ( #30346, #61966, #84687, #53918 ) ) ;
#86048 = CARTESIAN_POINT ( 'NONE',  ( -0.6844047246015609876, -2.251424796025575770, 29.88072029997477586 ) ) ;
#86049 = ORIENTED_EDGE ( 'NONE', *, *, #19152, .F. ) ;
#86050 = CARTESIAN_POINT ( 'NONE',  ( 11.47237812750565666, -3.513871655860377086, 32.76840700105978499 ) ) ;
#86051 = AXIS2_PLACEMENT_3D ( 'NONE', #45993, #10443, #58168 ) ;
#86052 = ORIENTED_EDGE ( 'NONE', *, *, #49875, .F. ) ;
#86053 = CARTESIAN_POINT ( 'NONE',  ( 13.45068373561782593, -11.69971097300155272, 32.46337939537588113 ) ) ;
#86054 = FACE_OUTER_BOUND ( 'NONE', #57745, .T. ) ;
#86055 = EDGE_LOOP ( 'NONE', ( #75163, #9504 ) ) ;
#86056 = VECTOR ( 'NONE', #52921, 1000.000000000000000 ) ;
#86057 = CARTESIAN_POINT ( 'NONE',  ( -5.198717948717948012, -3.499999999999999556, 29.75000000000000355 ) ) ;
#86058 = CYLINDRICAL_SURFACE ( 'NONE', #76619, 0.2499999999999995559 ) ;
#86059 = CARTESIAN_POINT ( 'NONE',  ( -11.53846153846153655, -2.833524468853757305, 32.15551576947925838 ) ) ;
#86060 = CARTESIAN_POINT ( 'NONE',  ( 4.946775867484854317, -9.418419913701741919, 34.36755862841477693 ) ) ;
#86061 = CARTESIAN_POINT ( 'NONE',  ( -8.069638770718176701, -12.69144148231606017, 30.53333754910549303 ) ) ;
#86062 = B_SPLINE_CURVE_WITH_KNOTS ( 'NONE', 3,
 ( #86798, #32276, #66947, #74147, #12443, #67388, #47991, #21416, #62385, #75470 ),
 .UNSPECIFIED., .F., .F.,
 ( 4, 2, 2, 2, 4 ),
 ( 0.000000000000000000, 0.0001954339881912774883, 0.0003908679763825549766, 0.0005863019645738324920, 0.0007817359527651099533 ),
 .UNSPECIFIED. ) ;
#86063 = ADVANCED_FACE ( 'NONE', ( #5936 ), #81597, .F. ) ;
#86064 = ORIENTED_EDGE ( 'NONE', *, *, #14001, .T. ) ;
#86065 = ORIENTED_EDGE ( 'NONE', *, *, #83880, .T. ) ;
#86066 = ORIENTED_EDGE ( 'NONE', *, *, #17958, .F. ) ;
#86068 = VERTEX_POINT ( 'NONE', #31626 ) ;
#86067 = CARTESIAN_POINT ( 'NONE',  ( 3.480714640147274608, -12.68172785388650681, 30.59649109432439218 ) ) ;
#86069 = AXIS2_PLACEMENT_3D ( 'NONE', #46670, #26404, #33157 ) ;
#86070 = CARTESIAN_POINT ( 'NONE',  ( -14.24162497434223162, -10.67929555188718282, 33.92786785259544757 ) ) ;
#86071 = DIRECTION ( 'NONE',  ( -0.000000000000000000, 0.5000000000000011102, -0.8660254037844380415 ) ) ;
#86072 = B_SPLINE_CURVE_WITH_KNOTS ( 'NONE', 3,
 ( #47820, #61764, #14931, #27553, #1407, #28896, #83842, #20788, #41510, #62217 ),
 .UNSPECIFIED., .F., .F.,
 ( 4, 2, 2, 2, 4 ),
 ( 0.000000000000000000, 0.0001954339857564073388, 0.0003908679715128146777, 0.0005863019572692220165, 0.0007817359430256293554 ),
 .UNSPECIFIED. ) ;
#86073 = ORIENTED_EDGE ( 'NONE', *, *, #23648, .T. ) ;
#86074 = ORIENTED_EDGE ( 'NONE', *, *, #44718, .T. ) ;
#86075 = EDGE_CURVE ( 'NONE', #60370, #22188, #57421, .T. ) ;
#86076 = VECTOR ( 'NONE', #57577, 1000.000000000000227 ) ;
#86077 = ORIENTED_EDGE ( 'NONE', *, *, #70539, .T. ) ;
#86078 = CARTESIAN_POINT ( 'NONE',  ( -10.68146802634049486, -3.050289026998445951, 32.03036669348365706 ) ) ;
#86079 = VERTEX_POINT ( 'NONE', #80723 ) ;
#86080 = AXIS2_PLACEMENT_3D ( 'NONE', #3583, #63516, #36067 ) ;
#86081 = DIRECTION ( 'NONE',  ( -1.000000000000000000, -0.000000000000000000, -0.000000000000000000 ) ) ;
#86082 = VECTOR ( 'NONE', #60392, 1000.000000000000000 ) ;
#86083 = CARTESIAN_POINT ( 'NONE',  ( 5.076923076922954969, -5.219633306517616589, 34.19971097300220464 ) ) ;
#86084 = CARTESIAN_POINT ( 'NONE',  ( -2.307692307692305711, -9.058645607665452459, 34.76329471203371924 ) ) ;
#86085 = FACE_BOUND ( 'NONE', #70565, .T. ) ;
#86086 = VERTEX_POINT ( 'NONE', #59982 ) ;
#86087 = FACE_OUTER_BOUND ( 'NONE', #50633, .T. ) ;
#86088 = CARTESIAN_POINT ( 'NONE',  ( 13.25392478150507891, -10.70098750199973203, 33.91152734681376302 ) ) ;
#86089 = ADVANCED_FACE ( 'NONE', ( #53671 ), #86588, .F. ) ;
#86090 = CARTESIAN_POINT ( 'NONE',  ( 4.284371855609716562, -8.586989748646452369, 34.63063291749215011 ) ) ;
#86091 = CARTESIAN_POINT ( 'NONE',  ( -6.923076923076922462, -13.49023893513002648, 31.06009739812518688 ) ) ;
#86092 = LINE ( 'NONE', #3215, #18877 ) ;
#86093 = ORIENTED_EDGE ( 'NONE', *, *, #88787, .T. ) ;
#86094 = LINE ( 'NONE', #58601, #61891 ) ;
#86095 = EDGE_CURVE ( 'NONE', #21493, #63786, #73511, .T. ) ;
#86096 = EDGE_LOOP ( 'NONE', ( #1508, #31630, #2447, #27966 ) ) ;
#86097 = ORIENTED_EDGE ( 'NONE', *, *, #29147, .F. ) ;
#86099 = LINE ( 'NONE', #30696, #77922 ) ;
#86098 = CARTESIAN_POINT ( 'NONE',  ( 10.74591031714818357, -12.45806712695776319, 30.39783852428763922 ) ) ;
#86100 = CARTESIAN_POINT ( 'NONE',  ( 6.923076923076924238, -6.386643153685126251, 34.62446782046654192 ) ) ;
#86101 = DIRECTION ( 'NONE',  ( -0.000000000000000000, -8.673617379884035472E-17, -1.000000000000000000 ) ) ;
#86102 = CARTESIAN_POINT ( 'NONE',  ( 1.384615384615265343, -10.21337939537710326, 33.94971097300076224 ) ) ;
#86103 = CARTESIAN_POINT ( 'NONE',  ( -15.45369618967607828, -3.395401636524185474, 33.02366814457250399 ) ) ;
#86104 = ORIENTED_EDGE ( 'NONE', *, *, #84415, .F. ) ;
#86105 = CYLINDRICAL_SURFACE ( 'NONE', #87485, 0.2499999999999995559 ) ;
#86106 = CARTESIAN_POINT ( 'NONE',  ( -11.60373198442231590, -10.21337939537584383, 33.94971097300158647 ) ) ;
#86107 = CARTESIAN_POINT ( 'NONE',  ( 2.372947447205147053, -12.70778746994558439, 30.41441678777536595 ) ) ;
#86108 = EDGE_CURVE ( 'NONE', #603, #75030, #34932, .T. ) ;
#86109 = CARTESIAN_POINT ( 'NONE',  ( 14.30769230769231015, -2.486705287966279876, 31.30864560766543647 ) ) ;
#86110 = VERTEX_POINT ( 'NONE', #60871 ) ;
#86111 = CIRCLE ( 'NONE', #14164, 1.999999999999998224 ) ;
#86112 = VERTEX_POINT ( 'NONE', #19884 ) ;
#86113 = FACE_BOUND ( 'NONE', #33474, .T. ) ;
#86114 = ITEM_DEFINED_TRANSFORMATION ( 'NONE', 'NONE', #46083,  #83448 ) ;
#86116 = EDGE_CURVE ( 'NONE', #67105, #37924, #15642, .T. ) ;
#86115 = ORIENTED_EDGE ( 'NONE', *, *, #33892, .F. ) ;
#86117 = CARTESIAN_POINT ( 'NONE',  ( 11.76147438255493149, -12.38742843783360748, 31.66772728687926985 ) ) ;
#86118 = CARTESIAN_POINT ( 'NONE',  ( 13.38461538461538680, -13.49023893513002648, 31.06009739812518688 ) ) ;
#86119 = ORIENTED_EDGE ( 'NONE', *, *, #25044, .T. ) ;
#86120 = EDGE_CURVE ( 'NONE', #17692, #42554, #66026, .T. ) ;
#86121 = CARTESIAN_POINT ( 'NONE',  ( -16.40382289789473802, -11.47974371597207899, 33.17467449705390692 ) ) ;
#86122 = CARTESIAN_POINT ( 'NONE',  ( -17.07692307692307665, -1.129524287112498415, 32.06866353760679544 ) ) ;
#86123 = CARTESIAN_POINT ( 'NONE',  ( -8.096177083446809419, -11.86270091957321249, 32.19358267280087915 ) ) ;
#86124 = CARTESIAN_POINT ( 'NONE',  ( 4.403791563224197070, -6.653508905675592722, 34.93172785388651391 ) ) ;
#86125 = ORIENTED_EDGE ( 'NONE', *, *, #77950, .F. ) ;
#86126 = CARTESIAN_POINT ( 'NONE',  ( -11.28840722682322273, -9.148310452688876993, 34.47095581063188519 ) ) ;
#86127 = ORIENTED_EDGE ( 'NONE', *, *, #27895, .T. ) ;
#86129 = EDGE_LOOP ( 'NONE', ( #39459, #14830, #61062, #26951 ) ) ;
#86128 = CARTESIAN_POINT ( 'NONE',  ( 22.75000000000000000, -10.49999999999999822, 27.25000000000000000 ) ) ;
#86130 = CARTESIAN_POINT ( 'NONE',  ( -8.769230769230768274, -13.53365097954675988, 30.81389545987213552 ) ) ;
#86131 = CARTESIAN_POINT ( 'NONE',  ( 18.75000000000000000, -3.499999999999999556, 29.75000000000000355 ) ) ;
#86132 = CARTESIAN_POINT ( 'NONE',  ( -17.07692307692307665, -7.500000000000001776, 35.04278698407183867 ) ) ;
#86133 = CARTESIAN_POINT ( 'NONE',  ( 10.39245765647776309, -12.38737895849757820, 31.66785238281580206 ) ) ;
#86134 = PLANE ( 'NONE',  #5958 ) ;
#86135 = EDGE_CURVE ( 'NONE', #83826, #46850, #59672, .T. ) ;
#86136 = CARTESIAN_POINT ( 'NONE',  ( -9.942284436356281674, -12.01397095200674059, 32.43157075238190146 ) ) ;
#86137 = CARTESIAN_POINT ( 'NONE',  ( 2.775308065498755195, -6.422011778438505125, 15.89249329374151820 ) ) ;
#86138 = ORIENTED_EDGE ( 'NONE', *, *, #4714, .T. ) ;
#86139 = CARTESIAN_POINT ( 'NONE',  ( 10.61538461538461675, -13.78497067705608181, 32.30358669280327177 ) ) ;
#86140 = CARTESIAN_POINT ( 'NONE',  ( 7.715544190949763070, -7.722926974430166069, 34.99546784045486447 ) ) ;
#86141 = DIRECTION ( 'NONE',  ( 0.000000000000000000, 0.4999999999999985567, 0.8660254037844395958 ) ) ;
#86142 = EDGE_CURVE ( 'NONE', #82006, #9304, #82927, .T. ) ;
#86143 = CIRCLE ( 'NONE', #64504, 4.000000000000000000 ) ;
#86144 = ORIENTED_EDGE ( 'NONE', *, *, #87272, .F. ) ;
#86145 = ADVANCED_FACE ( 'NONE', ( #27532 ), #22105, .F. ) ;
#86146 = ORIENTED_EDGE ( 'NONE', *, *, #66998, .T. ) ;
#86147 = CARTESIAN_POINT ( 'NONE',  ( 9.692307692307570832, -3.643525952248795718, 33.31231777344771672 ) ) ;
#86148 = CARTESIAN_POINT ( 'NONE',  ( 11.47237915910140771, -4.661471528628507777, 34.16647553114621871 ) ) ;
#86149 = CARTESIAN_POINT ( 'NONE',  ( 17.32697749683652688, -3.435999193479609026, 33.07426656108011542 ) ) ;
#86151 = CARTESIAN_POINT ( 'NONE',  ( -8.769230769230892619, -12.51329471203414379, 31.30864560766407578 ) ) ;
#86150 = VECTOR ( 'NONE', #49512, 1000.000000000000227 ) ;
#86152 = CARTESIAN_POINT ( 'NONE',  ( 13.16113046005105502, -3.019605429927184392, 32.48692288466676814 ) ) ;
#86153 = CARTESIAN_POINT ( 'NONE',  ( 16.40379156322419973, -3.520799739797213501, 33.17531984108286025 ) ) ;
#86154 = DIRECTION ( 'NONE',  ( 0.000000000000000000, 0.000000000000000000, -1.000000000000000000 ) ) ;
#86155 = ORIENTED_EDGE ( 'NONE', *, *, #67025, .F. ) ;
#86156 = CARTESIAN_POINT ( 'NONE',  ( -16.15384615384583711, -2.255955759149395501, 30.00000000000324363 ) ) ;
#86157 = CARTESIAN_POINT ( 'NONE',  ( -17.20707028636130076, -12.27039167877662251, 31.24851455888617835 ) ) ;
#86158 = AXIS2_PLACEMENT_3D ( 'NONE', #20084, #47097, #31834 ) ;
#86159 = B_SPLINE_CURVE_WITH_KNOTS ( 'NONE', 3,
 ( #6460, #60947, #52854, #20415, #73598, #41130, #74922, #5123, #26722, #19960 ),
 .UNSPECIFIED., .F., .F.,
 ( 4, 2, 2, 2, 4 ),
 ( 0.000000000000000000, 0.0001954311564186879044, 0.0003908623128373758088, 0.0005862934692560636861, 0.0007817246256747516176 ),
 .UNSPECIFIED. ) ;
#86160 = FACE_OUTER_BOUND ( 'NONE', #36539, .T. ) ;
#86161 = EDGE_CURVE ( 'NONE', #55341, #49579, #49576, .T. ) ;
#86162 = CARTESIAN_POINT ( 'NONE',  ( 16.94623161025551639, -8.999036380462719364, 34.52022231692819076 ) ) ;
#86163 = B_SPLINE_CURVE_WITH_KNOTS ( 'NONE', 3,
 ( #27272, #32267, #80908, #34027, #20515, #19192 ),
 .UNSPECIFIED., .F., .F.,
 ( 4, 2, 4 ),
 ( 0.0003909569690057804843, 0.0005862646681846042955, 0.0007815723673634281067 ),
 .UNSPECIFIED. ) ;
#86164 = ORIENTED_EDGE ( 'NONE', *, *, #55764, .F. ) ;
#86165 = CARTESIAN_POINT ( 'NONE',  ( 16.02369818411445479, -12.50552854090298638, 31.33409797877408920 ) ) ;
#86166 = B_SPLINE_CURVE_WITH_KNOTS ( 'NONE', 3,
 ( #38370, #72591, #31613, #9999, #66280, #31153, #43787, #86574, #65823, #18106 ),
 .UNSPECIFIED., .F., .F.,
 ( 4, 2, 2, 2, 4 ),
 ( 0.0007817359430256313069, 0.0009771253907249971907, 0.001172514838424363291, 0.001367904286123729175, 0.001563293733823095059 ),
 .UNSPECIFIED. ) ;
#86167 = VERTEX_POINT ( 'NONE', #68511 ) ;
#86168 = CARTESIAN_POINT ( 'NONE',  ( 9.019176178608812933, -2.986452184633680673, 32.43230066228895225 ) ) ;
#86169 = LINE ( 'NONE', #45606, #67126 ) ;
#86170 = EDGE_CURVE ( 'NONE', #68861, #23595, #42391, .T. ) ;
#86171 = DIRECTION ( 'NONE',  ( -0.000000000000000000, 0.8660254037844397068, -0.4999999999999978906 ) ) ;
#86172 = EDGE_LOOP ( 'NONE', ( #83422, #87205, #32327, #61559, #69803 ) ) ;
#86173 = CARTESIAN_POINT ( 'NONE',  ( 8.703960323269994248, -10.90142922261923886, 33.41473453929638993 ) ) ;
#86174 = DIRECTION ( 'NONE',  ( -0.000000000000000000, 1.000000000000000000, -0.000000000000000000 ) ) ;
#86175 = CARTESIAN_POINT ( 'NONE',  ( 20.00000000000000000, -4.000000000000000000, 29.75000000000000355 ) ) ;
#86176 = CARTESIAN_POINT ( 'NONE',  ( -6.130690603110307002, -5.496505350115500121, 34.60290016733514307 ) ) ;
#86177 = CARTESIAN_POINT ( 'NONE',  ( 3.230769230769108269, -3.083524468854526912, 32.58852847137268327 ) ) ;
#86178 = EDGE_CURVE ( 'NONE', #7803, #51057, #68283, .T. ) ;
#86179 = EDGE_LOOP ( 'NONE', ( #60666, #88974 ) ) ;
#86180 = LINE ( 'NONE', #72645, #52949 ) ;
#86181 = ORIENTED_EDGE ( 'NONE', *, *, #54312, .T. ) ;
#86182 = CARTESIAN_POINT ( 'NONE',  ( -2.531177232256639709, -2.612411019501189813, 31.66733052389439962 ) ) ;
#86183 = AXIS2_PLACEMENT_3D ( 'NONE', #26621, #19862, #81575 ) ;
#86184 = EDGE_CURVE ( 'NONE', #42382, #82187, #84409, .T. ) ;
#86185 = DIRECTION ( 'NONE',  ( 0.000000000000000000, 0.9848077530122072432, -0.1736481776669354937 ) ) ;
#86186 = ADVANCED_FACE ( 'NONE', ( #41051 ), #83822, .F. ) ;
#86187 = CARTESIAN_POINT ( 'NONE',  ( -0.2387587925603970040, -2.612705202774697977, 31.66806509827799943 ) ) ;
#86188 = CARTESIAN_POINT ( 'NONE',  ( 9.692307692307570832, -2.657715359629662544, 31.77849191805970364 ) ) ;
#86189 = CARTESIAN_POINT ( 'NONE',  ( 7.053602624840485724, -10.19071101563364756, 33.96452234770658407 ) ) ;
#86190 = CARTESIAN_POINT ( 'NONE',  ( 9.692307692307695177, -8.120952969808772792, 34.71129190930000163 ) ) ;
#86191 = B_SPLINE_CURVE_WITH_KNOTS ( 'NONE', 3,
 ( #88464, #25853, #26734, #61839, #32601, #6471, #60069, #54195, #46563, #74046 ),
 .UNSPECIFIED., .F., .F.,
 ( 4, 2, 2, 2, 4 ),
 ( 0.0007817246256747434861, 0.0009771112852218861652, 0.001172497944769028844, 0.001367884604316171740, 0.001563271263863314419 ),
 .UNSPECIFIED. ) ;
#86192 = ORIENTED_EDGE ( 'NONE', *, *, #84527, .T. ) ;
#86193 = ADVANCED_FACE ( 'NONE', ( #48235 ), #75709, .F. ) ;
#86194 = ORIENTED_EDGE ( 'NONE', *, *, #39214, .T. ) ;
#86195 = B_SPLINE_CURVE_WITH_KNOTS ( 'NONE', 3,
 ( #50160, #42984, #51038, #1110, #77649, #64121, #63689, #78530, #7870, #15961 ),
 .UNSPECIFIED., .F., .F.,
 ( 4, 2, 2, 2, 4 ),
 ( 0.000000000000000000, 0.0001954311564186879857, 0.0003908623128373759715, 0.0005862934692560640114, 0.0007817246256747519429 ),
 .UNSPECIFIED. ) ;
#86196 = EDGE_LOOP ( 'NONE', ( #36899, #5989, #61241, #67887 ) ) ;
#86197 = B_SPLINE_CURVE_WITH_KNOTS ( 'NONE', 3,
 ( #37505, #64973, #30749, #41292, #7053, #38405, #58664, #73532, #17239, #85709 ),
 .UNSPECIFIED., .F., .F.,
 ( 4, 2, 2, 2, 4 ),
 ( 0.000000000000000000, 0.0001954311584214072923, 0.0003908623168428145846, 0.0005862934752642218498, 0.0007817246336856291692 ),
 .UNSPECIFIED. ) ;
#86198 = ORIENTED_EDGE ( 'NONE', *, *, #7318, .F. ) ;
#86199 = ORIENTED_EDGE ( 'NONE', *, *, #73824, .T. ) ;
#86200 = CARTESIAN_POINT ( 'NONE',  ( -12.71153846153847233, -2.249999999999999556, 29.81609741502489541 ) ) ;
#86201 = CARTESIAN_POINT ( 'NONE',  ( 16.15384615384615330, -12.10708131394839349, 31.69288490824020244 ) ) ;
#86202 = CARTESIAN_POINT ( 'NONE',  ( 15.10062202133100939, -5.195881422630166391, 34.18770438780619259 ) ) ;
#86203 = DIRECTION ( 'NONE',  ( 1.000000000000000000, 0.000000000000000000, 0.000000000000000000 ) ) ;
#86204 = CARTESIAN_POINT ( 'NONE',  ( -13.63463860883683942, -3.520140089381495585, 33.17453946501458262 ) ) ;
#86205 = CARTESIAN_POINT ( 'NONE',  ( 0.6845498131513101381, -4.887748414852792322, 34.01359900205216746 ) ) ;
#86206 = AXIS2_PLACEMENT_3D ( 'NONE', #41811, #84135, #89125 ) ;
#86207 = CARTESIAN_POINT ( 'NONE',  ( -2.307692307692305711, -11.11383981884818262, 36.00935417666054406 ) ) ;
#86208 = CARTESIAN_POINT ( 'NONE',  ( 9.442330948259101575, -10.06842814019191401, 34.32929386961144758 ) ) ;
#86209 = DIRECTION ( 'NONE',  ( -0.000000000000000000, -0.9848077530122086864, -0.1736481776669273613 ) ) ;
#86210 = ORIENTED_EDGE ( 'NONE', *, *, #31917, .F. ) ;
#86211 = EDGE_CURVE ( 'NONE', #48549, #37467, #75767, .T. ) ;
#86212 = EDGE_LOOP ( 'NONE', ( #37524, #68995, #24361, #20478 ) ) ;
#86213 = ORIENTED_EDGE ( 'NONE', *, *, #43610, .T. ) ;
#86214 = AXIS2_PLACEMENT_3D ( 'NONE', #25144, #45406, #51705 ) ;
#86216 = ORIENTED_EDGE ( 'NONE', *, *, #10056, .T. ) ;
#86215 = CARTESIAN_POINT ( 'NONE',  ( 0.3313904918067617777, -3.069018819979302926, 32.56621877034667278 ) ) ;
#86218 = FACE_OUTER_BOUND ( 'NONE', #23908, .T. ) ;
#86217 = CARTESIAN_POINT ( 'NONE',  ( 7.780070435197966816, -3.050289026998445951, 32.03036669348365706 ) ) ;
#86219 = VECTOR ( 'NONE', #49693, 999.9999999999998863 ) ;
#86220 = CARTESIAN_POINT ( 'NONE',  ( -1.384615384615506484, -5.094484230521993062, 34.41647553114689373 ) ) ;
#86221 = CARTESIAN_POINT ( 'NONE',  ( -14.37377571864818648, -9.780366693483667717, 34.19971097300155805 ) ) ;
#86222 = ORIENTED_EDGE ( 'NONE', *, *, #41170, .F. ) ;
#86223 = ORIENTED_EDGE ( 'NONE', *, *, #76637, .T. ) ;
#86224 = CARTESIAN_POINT ( 'NONE',  ( -11.97435897435897267, -7.500000000000000000, 29.75000000000000355 ) ) ;
#86225 = ORIENTED_EDGE ( 'NONE', *, *, #61538, .F. ) ;
#86226 = FACE_BOUND ( 'NONE', #71992, .T. ) ;
#86227 = B_SPLINE_CURVE_WITH_KNOTS ( 'NONE', 3,
 ( #45882, #81022, #74257, #53974, #67501, #6246, #75148, #11671, #46780, #39149 ),
 .UNSPECIFIED., .F., .F.,
 ( 4, 2, 2, 2, 4 ),
 ( 0.000000000000000000, 0.0001954311564186871184, 0.0003908623128373742367, 0.0005862934692560614093, 0.0007817246256747484735 ),
 .UNSPECIFIED. ) ;
#86228 = CARTESIAN_POINT ( 'NONE',  ( 15.16549878480845770, -10.21337939537584383, 33.94971097300158647 ) ) ;
#86229 = CARTESIAN_POINT ( 'NONE',  ( -0.4615384615384611200, -3.886160181151819604, 36.00935417666054406 ) ) ;
#86230 = ORIENTED_EDGE ( 'NONE', *, *, #23428, .T. ) ;
#86231 = CARTESIAN_POINT ( 'NONE',  ( 14.17754509825408960, -2.882441371585227508, 31.66841991370172238 ) ) ;
#86232 = CARTESIAN_POINT ( 'NONE',  ( 6.000000000000001776, -2.249999999999998668, 29.50000000000001421 ) ) ;
#86233 = DIRECTION ( 'NONE',  ( -0.000000000000000000, -0.9396926207859092051, -0.3420201433256662704 ) ) ;
#86234 = ORIENTED_EDGE ( 'NONE', *, *, #41630, .T. ) ;
#86235 = CARTESIAN_POINT ( 'NONE',  ( -11.78848476268299628, -4.931416488878822335, 34.32920672191015399 ) ) ;
#86236 = CARTESIAN_POINT ( 'NONE',  ( 20.99999999999999645, -4.249999999999998224, 29.75000000000000355 ) ) ;
#86237 = ORIENTED_EDGE ( 'NONE', *, *, #59448, .F. ) ;
#86238 = CARTESIAN_POINT ( 'NONE',  ( -6.923076923076922462, -8.973038597847269315, 34.52809138561121927 ) ) ;
#86239 = PLANE ( 'NONE',  #6771 ) ;
#86240 = VERTEX_POINT ( 'NONE', #31058 ) ;
#86241 = CARTESIAN_POINT ( 'NONE',  ( -12.71156168575991963, -5.765609946408404518, 34.70566812827425451 ) ) ;
#86242 = CYLINDRICAL_SURFACE ( 'NONE', #22459, 0.2499999999999998890 ) ;
#86244 = B_SPLINE_CURVE_WITH_KNOTS ( 'NONE', 3,
 ( #47667, #75152, #33713, #26960, #88683, #81913, #27398, #13437, #20633, #40915 ),
 .UNSPECIFIED., .F., .F.,
 ( 4, 2, 2, 2, 4 ),
 ( 0.0007817246256747507503, 0.0009771112852218957062, 0.001172497944769040771, 0.001367884604316185835, 0.001563271263863330682 ),
 .UNSPECIFIED. ) ;
#86243 = LINE ( 'NONE', #24962, #78477 ) ;
#86245 = LINE ( 'NONE', #39389, #45748 ) ;
#86246 = DIRECTION ( 'NONE',  ( -0.000000000000000000, 0.1736481776669307198, -0.9848077530122080203 ) ) ;
#86247 = CARTESIAN_POINT ( 'NONE',  ( 6.699591979352975457, -9.331801661448606566, 34.40259984581193464 ) ) ;
#86249 = PLANE ( 'NONE',  #1450 ) ;
#86248 = DIRECTION ( 'NONE',  ( 0.000000000000000000, 0.000000000000000000, 1.000000000000000000 ) ) ;
#86250 = EDGE_CURVE ( 'NONE', #49638, #10, #87612, .T. ) ;
#86251 = DIRECTION ( 'NONE',  ( -0.000000000000000000, 0.9396926207859093161, -0.3420201433256663259 ) ) ;
#86253 = DIRECTION ( 'NONE',  ( 0.000000000000000000, 0.9396926207859126468, 0.3420201433256571111 ) ) ;
#86252 = CARTESIAN_POINT ( 'NONE',  ( 3.165519298995146613, -2.255955759149247619, 30.00000000000013856 ) ) ;
#86254 = AXIS2_PLACEMENT_3D ( 'NONE', #39277, #46015, #18111 ) ;
#86255 = CARTESIAN_POINT ( 'NONE',  ( 1.139087296525997273, -4.749999999999992895, 14.23437500000000355 ) ) ;
#86256 = ORIENTED_EDGE ( 'NONE', *, *, #41024, .F. ) ;
#86257 = CARTESIAN_POINT ( 'NONE',  ( 0.2115617305961065009, -12.41269422305637171, 30.68257228309993323 ) ) ;
#86258 = VERTEX_POINT ( 'NONE', #1826 ) ;
#86259 = EDGE_CURVE ( 'NONE', #36333, #29450, #14515, .T. ) ;
#86260 = EDGE_LOOP ( 'NONE', ( #36601, #39724, #40098, #75536 ) ) ;
#86261 = DIRECTION ( 'NONE',  ( -0.000000000000000000, 1.000000000000000000, 3.491481338843133355E-15 ) ) ;
#86262 = ADVANCED_FACE ( 'NONE', ( #50875 ), #23417, .T. ) ;
#86263 = ORIENTED_EDGE ( 'NONE', *, *, #8237, .T. ) ;
#86264 = CARTESIAN_POINT ( 'NONE',  ( 14.30769230769231015, -4.661471528628507777, 34.16647553114623292 ) ) ;
#86265 = CARTESIAN_POINT ( 'NONE',  ( 2.749999999999995115, -6.360912703473971419, 16.89062500000000000 ) ) ;
#86266 = CARTESIAN_POINT ( 'NONE',  ( -17.93393164899756087, -5.557115091759784242, 34.35708131394839882 ) ) ;
#86267 = LINE ( 'NONE', #37162, #48171 ) ;
#86268 = B_SPLINE_CURVE_WITH_KNOTS ( 'NONE', 3,
 ( #22738, #43903, #64602, #50199, #2900, #30392, #57861, #23629, #51080, #78574 ),
 .UNSPECIFIED., .F., .F.,
 ( 4, 2, 2, 2, 4 ),
 ( 0.0007817246256747439198, 0.0009771112852218863821, 0.001172497944769028844, 0.001367884604316171307, 0.001563271263863313769 ),
 .UNSPECIFIED. ) ;
#86269 = CARTESIAN_POINT ( 'NONE',  ( -5.999999999999998224, -8.973038597847269315, 34.52809138561121927 ) ) ;
#86270 = DIRECTION ( 'NONE',  ( 1.000000000000000000, 0.000000000000000000, 0.000000000000000000 ) ) ;
#86271 = DIRECTION ( 'NONE',  ( -0.000000000000000000, -0.000000000000000000, -1.000000000000000000 ) ) ;
#86272 = FACE_OUTER_BOUND ( 'NONE', #23487, .T. ) ;
#86273 = LINE ( 'NONE', #45707, #33874 ) ;
#86274 = ADVANCED_FACE ( 'NONE', ( #84265 ), #71163, .F. ) ;
#86275 = CARTESIAN_POINT ( 'NONE',  ( -1.553300858899081538, -11.25000000000000711, 21.10937500000000711 ) ) ;
#86276 = CARTESIAN_POINT ( 'NONE',  ( -11.40767109749458541, -2.494656445102012565, 31.33466734024120015 ) ) ;
#86277 = CARTESIAN_POINT ( 'NONE',  ( -2.307692307692428724, -12.16647553114689728, 32.15551576947799362 ) ) ;
#86278 = EDGE_CURVE ( 'NONE', #7880, #51834, #57215, .T. ) ;
#86279 = CARTESIAN_POINT ( 'NONE',  ( 10.54930223602447903, -5.471508081941602875, 34.59228464037088457 ) ) ;
#86280 = VECTOR ( 'NONE', #50311, 999.9999999999998863 ) ;
#86281 = CIRCLE ( 'NONE', #74765, 0.2500000000000002220 ) ;
#86282 = ORIENTED_EDGE ( 'NONE', *, *, #28924, .T. ) ;
#86283 = ORIENTED_EDGE ( 'NONE', *, *, #24612, .T. ) ;
#86284 = CARTESIAN_POINT ( 'NONE',  ( -17.07692307692307665, -9.058645607665452459, 34.76329471203371924 ) ) ;
#86285 = DIRECTION ( 'NONE',  ( -0.000000000000000000, -0.9396926207859093161, -0.3420201433256663259 ) ) ;
#86286 = PLANE ( 'NONE',  #71335 ) ;
#86287 = CYLINDRICAL_SURFACE ( 'NONE', #69990, 5.000000000000000888 ) ;
#86288 = VECTOR ( 'NONE', #66521, 1000.000000000000114 ) ;
#86289 = CARTESIAN_POINT ( 'NONE',  ( 17.29970274590113632, -12.47679350104403007, 31.42216943046555855 ) ) ;
#86290 = CARTESIAN_POINT ( 'NONE',  ( 7.134615384615385025, -3.499999999999999556, 29.75000000000000355 ) ) ;
#86291 = CIRCLE ( 'NONE', #10072, 0.2500000000000002220 ) ;
#86292 = VERTEX_POINT ( 'NONE', #2255 ) ;
#86293 = DIRECTION ( 'NONE',  ( -0.000000000000000000, -0.7660444431189791237, -0.6427876096865379196 ) ) ;
#86294 = ORIENTED_EDGE ( 'NONE', *, *, #17173, .F. ) ;
#86295 = EDGE_CURVE ( 'NONE', #61423, #14452, #39098, .T. ) ;
#86296 = VERTEX_POINT ( 'NONE', #2695 ) ;
#86297 = FACE_OUTER_BOUND ( 'NONE', #67107, .T. ) ;
#86298 = CARTESIAN_POINT ( 'NONE',  ( 5.207714884747860928, -11.71459661697925903, 32.44059661609676937 ) ) ;
#86299 = LINE ( 'NONE', #52036, #77514 ) ;
#86300 = CARTESIAN_POINT ( 'NONE',  ( 6.130790440966952026, -8.191423895709842640, 34.95447573519442130 ) ) ;
#86301 = CARTESIAN_POINT ( 'NONE',  ( 13.38461538461526423, -8.656820664282941280, 34.87096338111179961 ) ) ;
#86302 = ORIENTED_EDGE ( 'NONE', *, *, #37848, .T. ) ;
#86303 = EDGE_CURVE ( 'NONE', #1161, #77202, #9909, .T. ) ;
#86304 = EDGE_LOOP ( 'NONE', ( #64912, #65299, #67372, #22276 ) ) ;
#86305 = VERTEX_POINT ( 'NONE', #64842 ) ;
#86306 = EDGE_CURVE ( 'NONE', #52068, #28470, #7376, .T. ) ;
#86307 = CARTESIAN_POINT ( 'NONE',  ( -4.153846153846274980, -12.16647553114689728, 32.15551576947799362 ) ) ;
#86308 = CARTESIAN_POINT ( 'NONE',  ( -0.3307480205715118693, -9.929761469519744921, 34.40412654351204225 ) ) ;
#86309 = CIRCLE ( 'NONE', #21552, 4.000000000000000000 ) ;
#86310 = CARTESIAN_POINT ( 'NONE',  ( -14.30769230769230660, -2.517432740324522911, 35.29906147534542527 ) ) ;
#86311 = B_SPLINE_CURVE_WITH_KNOTS ( 'NONE', 3,
 ( #62625, #83815, #82036, #27078, #497, #1378, #61290, #48671, #62190, #22098 ),
 .UNSPECIFIED., .F., .F.,
 ( 4, 2, 2, 2, 4 ),
 ( 0.0007817359430256303312, 0.0009771253907249965402, 0.001172514838424362641, 0.001367904286123728958, 0.001563293733823095059 ),
 .UNSPECIFIED. ) ;
#86312 = CARTESIAN_POINT ( 'NONE',  ( 10.54930223602447903, -4.661471528628507777, 34.16647553114621871 ) ) ;
#86313 = CARTESIAN_POINT ( 'NONE',  ( 11.40777093535123399, -10.70098750199973203, 33.91152734681376302 ) ) ;
#86314 = DIRECTION ( 'NONE',  ( 0.000000000000000000, 0.7660444431189822323, -0.6427876096865344779 ) ) ;
#86315 = ORIENTED_EDGE ( 'NONE', *, *, #22029, .T. ) ;
#86316 = ADVANCED_FACE ( 'NONE', ( #65293 ), #3590, .F. ) ;
#86317 = ORIENTED_EDGE ( 'NONE', *, *, #61175, .T. ) ;
#86318 = CARTESIAN_POINT ( 'NONE',  ( 1.553300858899087311, -3.749999999999992006, 19.23437500000000355 ) ) ;
#86319 = ORIENTED_EDGE ( 'NONE', *, *, #69545, .F. ) ;
#86321 = VERTEX_POINT ( 'NONE', #24758 ) ;
#86320 = CARTESIAN_POINT ( 'NONE',  ( -16.15384615384627409, -8.656820664282941280, 34.87096338111179961 ) ) ;
#86322 = CARTESIAN_POINT ( 'NONE',  ( -10.61538461538461320, -3.937682226553329556, 33.60647404775216529 ) ) ;
#86323 = CARTESIAN_POINT ( 'NONE',  ( -9.942284423250045577, -11.79746400365624659, 32.30657167506340954 ) ) ;
#86324 = EDGE_CURVE ( 'NONE', #30568, #69653, #59490, .T. ) ;
#86325 = EDGE_CURVE ( 'NONE', #59481, #33850, #39628, .T. ) ;
#86326 = CARTESIAN_POINT ( 'NONE',  ( -1.929879867024197893E-14, -3.750000000000000000, 15.40625000000000000 ) ) ;
#86327 = ORIENTED_EDGE ( 'NONE', *, *, #31261, .F. ) ;
#86328 = B_SPLINE_CURVE_WITH_KNOTS ( 'NONE', 3,
 ( #66396, #60076, #80372, #86694, #73620, #38486, #52872, #74489, #5143, #26301 ),
 .UNSPECIFIED., .F., .F.,
 ( 4, 2, 2, 2, 4 ),
 ( 0.000000000000000000, 0.0001954339857564073931, 0.0003908679715128147861, 0.0005863019572692222334, 0.0007817359430256295722 ),
 .UNSPECIFIED. ) ;
#86329 = AXIS2_PLACEMENT_3D ( 'NONE', #14111, #83017, #36169 ) ;
#86330 = CARTESIAN_POINT ( 'NONE',  ( 18.00000000000000000, -9.058645607665452459, 34.76329471203371924 ) ) ;
#86331 = ORIENTED_EDGE ( 'NONE', *, *, #19488, .F. ) ;
#86332 = EDGE_CURVE ( 'NONE', #57709, #11427, #46584, .T. ) ;
#86333 = DIRECTION ( 'NONE',  ( -1.000000000000000000, -0.000000000000000000, -0.000000000000000000 ) ) ;
#86334 = CARTESIAN_POINT ( 'NONE',  ( 17.74997677577854205, -12.68155406624981119, 30.59749803192733708 ) ) ;
#86335 = CARTESIAN_POINT ( 'NONE',  ( 7.846153846153846700, -3.937682226553329556, 33.60647404775216529 ) ) ;
#86338 = LINE ( 'NONE', #52073, #11416 ) ;
#86337 = VECTOR ( 'NONE', #26430, 1000.000000000000000 ) ;
#86336 = DIRECTION ( 'NONE',  ( 1.000000000000000000, 0.000000000000000000, 0.000000000000000000 ) ) ;
#86339 = CIRCLE ( 'NONE', #64695, 3.000000000000000000 ) ;
#86340 = CARTESIAN_POINT ( 'NONE',  ( -0.7115616857599191825, -12.45566812827425096, 31.48439005359158926 ) ) ;
#86341 = DIRECTION ( 'NONE',  ( -1.000000000000000000, 0.000000000000000000, -0.000000000000000000 ) ) ;
#86342 = VERTEX_POINT ( 'NONE', #46809 ) ;
#86343 = CARTESIAN_POINT ( 'NONE',  ( 11.31553457955469000, -11.43668979543634734, 33.22377378376089752 ) ) ;
#86344 = CARTESIAN_POINT ( 'NONE',  ( 8.769230769230647482, -6.879047030192662504, 34.71129190930017927 ) ) ;
#86345 = AXIS2_PLACEMENT_3D ( 'NONE', #842, #42724, #43159 ) ;
#86346 = ORIENTED_EDGE ( 'NONE', *, *, #81435, .F. ) ;
#86347 = VECTOR ( 'NONE', #52612, 1000.000000000000227 ) ;
#86348 = CARTESIAN_POINT ( 'NONE',  ( 6.856993512121043466, -5.557115091759785130, 34.35708131394839171 ) ) ;
#86349 = CARTESIAN_POINT ( 'NONE',  ( 10.39245839786846837, -6.503392248772476236, 34.64988816332204635 ) ) ;
#86350 = CARTESIAN_POINT ( 'NONE',  ( -14.98071481085577972, -5.642605341092957971, 34.66089969410670335 ) ) ;
#86351 = CARTESIAN_POINT ( 'NONE',  ( 7.846153846153846700, -3.937682226553329556, 33.60647404775216529 ) ) ;
#86352 = DIRECTION ( 'NONE',  ( -1.000000000000000000, 0.000000000000000000, 0.000000000000000000 ) ) ;
#86353 = FACE_BOUND ( 'NONE', #53395, .T. ) ;
#86355 = CYLINDRICAL_SURFACE ( 'NONE', #20101, 0.2500000000000009437 ) ;
#86354 = CARTESIAN_POINT ( 'NONE',  ( 5.326977496836529546, -5.642605341092957083, 34.66089969410670335 ) ) ;
#86356 = CARTESIAN_POINT ( 'NONE',  ( 16.08776274289027342, -3.050289026998445951, 32.03036669348365706 ) ) ;
#86358 = CARTESIAN_POINT ( 'NONE',  ( 14.05766908347084865, -10.92453946501458795, 33.72985991061850086 ) ) ;
#86357 = CARTESIAN_POINT ( 'NONE',  ( 1.253924781505078689, -12.62707690430377383, 30.88035979386743435 ) ) ;
#86359 = FACE_OUTER_BOUND ( 'NONE', #36250, .T. ) ;
#86360 = DIRECTION ( 'NONE',  ( 0.000000000000000000, 0.9396926207859126468, 0.3420201433256571111 ) ) ;
#86361 = CARTESIAN_POINT ( 'NONE',  ( 3.775308065498768517, -8.992201783934554271, 24.29500670625849423 ) ) ;
#86362 = EDGE_CURVE ( 'NONE', #10355, #33822, #17565, .T. ) ;
#86363 = ORIENTED_EDGE ( 'NONE', *, *, #5813, .T. ) ;
#86364 = CARTESIAN_POINT ( 'NONE',  ( -7.846153846153844924, -11.16473453929635440, 33.15142922261926373 ) ) ;
#86365 = DIRECTION ( 'NONE',  ( -0.000000000000000000, -0.8660254037844399289, -0.4999999999999980016 ) ) ;
#86366 = CARTESIAN_POINT ( 'NONE',  ( 12.46153846153846168, -3.886160181151819604, 36.00935417666054406 ) ) ;
#86367 = DIRECTION ( 'NONE',  ( -0.000000000000000000, 0.7660444431189791237, -0.6427876096865379196 ) ) ;
#86368 = CARTESIAN_POINT ( 'NONE',  ( 6.699591998512592461, -12.69144148231606017, 30.53333754910549303 ) ) ;
#86369 = LINE ( 'NONE', #72819, #13904 ) ;
#86370 = CARTESIAN_POINT ( 'NONE',  ( -3.724691934501229262, -9.114399933863657211, 24.76375670625848713 ) ) ;
#86371 = CARTESIAN_POINT ( 'NONE',  ( -15.48074597481782178, -12.65889640711025521, 30.72598325615533454 ) ) ;
#86372 = FACE_OUTER_BOUND ( 'NONE', #21934, .T. ) ;
#86373 = CARTESIAN_POINT ( 'NONE',  ( -7.846153846153844924, -9.905515769479276145, 34.41647553114623292 ) ) ;
#86374 = CARTESIAN_POINT ( 'NONE',  ( 5.326977496836529546, -12.65882529074907126, 30.72640787790839312 ) ) ;
#86375 = PLANE ( 'NONE',  #12341 ) ;
#86376 = DIRECTION ( 'NONE',  ( -0.000000000000000000, 1.000000000000000000, -0.000000000000000000 ) ) ;
#86377 = ADVANCED_FACE ( 'NONE', ( #18010 ), #72496, .F. ) ;
#86378 = CARTESIAN_POINT ( 'NONE',  ( -6.222926958906843886, -11.98009711892699691, 32.48740034544075428 ) ) ;
#86379 = CARTESIAN_POINT ( 'NONE',  ( -11.28851602011339672, -10.76462480002816235, 33.53768742498949962 ) ) ;
#86380 = ORIENTED_EDGE ( 'NONE', *, *, #45390, .F. ) ;
#86381 = VECTOR ( 'NONE', #42834, 1000.000000000000114 ) ;
#86382 = ADVANCED_FACE ( 'NONE', ( #12147 ), #32408, .F. ) ;
#86383 = CARTESIAN_POINT ( 'NONE',  ( -6.166666666666667851, -3.499999999999999556, 29.75000000000000355 ) ) ;
#86384 = CARTESIAN_POINT ( 'NONE',  ( -14.30769230769242739, -3.835265460704628371, 33.15142922262033665 ) ) ;
#86385 = CARTESIAN_POINT ( 'NONE',  ( -2.694853999681181556, -10.10844685921792241, 13.93936829374151465 ) ) ;
#86386 = DIRECTION ( 'NONE',  ( -0.000000000000000000, -0.7660444431189791237, -0.6427876096865379196 ) ) ;
#86387 = DIRECTION ( 'NONE',  ( -0.000000000000000000, -0.9848077530122085754, -0.1736481776669273613 ) ) ;
#86388 = VERTEX_POINT ( 'NONE', #59876 ) ;
#86389 = CARTESIAN_POINT ( 'NONE',  ( -17.77698715590660328, -6.460100341425562220, 34.89618726649961644 ) ) ;
#86390 = CARTESIAN_POINT ( 'NONE',  ( 11.53846153846141576, -6.835583212225970762, 34.95778746994575670 ) ) ;
#86392 = ORIENTED_EDGE ( 'NONE', *, *, #45616, .F. ) ;
#86391 = CARTESIAN_POINT ( 'NONE',  ( -13.19230769230769340, -4.000000000000000000, 29.75000000000000355 ) ) ;
#86393 = CARTESIAN_POINT ( 'NONE',  ( -12.52680846209478283, -9.528491918058357157, 34.59228464037090589 ) ) ;
#86394 = CARTESIAN_POINT ( 'NONE',  ( -11.53846153846153655, -3.886160181151819604, 36.00935417666054406 ) ) ;
#86395 = CARTESIAN_POINT ( 'NONE',  ( -4.826868765284761054, -9.148310452688871663, 34.47095581063188519 ) ) ;
#86397 = EDGE_CURVE ( 'NONE', #31074, #38805, #19789, .T. ) ;
#86396 = CARTESIAN_POINT ( 'NONE',  ( -12.46153846153858424, -5.094484230521993062, 34.41647553114689373 ) ) ;
#86398 = VERTEX_POINT ( 'NONE', #4028 ) ;
#86399 = CARTESIAN_POINT ( 'NONE',  ( -2.307692307692305711, -8.564572088678739092, 35.78748833219616898 ) ) ;
#86400 = CARTESIAN_POINT ( 'NONE',  ( -12.68446542044531000, -2.523278758544489797, 31.42238647778637528 ) ) ;
#86402 = CARTESIAN_POINT ( 'NONE',  ( -10.61538461538473399, -3.300289026999228881, 32.46337939537708905 ) ) ;
#86401 = AXIS2_PLACEMENT_3D ( 'NONE', #37226, #37676, #71902 ) ;
#86403 = ORIENTED_EDGE ( 'NONE', *, *, #66045, .T. ) ;
#86404 = VERTEX_POINT ( 'NONE', #26097 ) ;
#86405 = EDGE_LOOP ( 'NONE', ( #48746, #34893 ) ) ;
#86406 = B_SPLINE_CURVE_WITH_KNOTS ( 'NONE', 3,
 ( #88963, #27232, #66892, #32657, #56030, #29463, #14161, #41637, #62337, #49716 ),
 .UNSPECIFIED., .F., .F.,
 ( 4, 2, 2, 2, 4 ),
 ( 0.000000000000000000, 0.0001954339857564086670, 0.0003908679715128173340, 0.0005863019572692260281, 0.0007817359430256346680 ),
 .UNSPECIFIED. ) ;
#86407 = VECTOR ( 'NONE', #52789, 1000.000000000000000 ) ;
#86408 = VECTOR ( 'NONE', #76572, 1000.000000000000000 ) ;
#86409 = DIRECTION ( 'NONE',  ( -0.000000000000000000, -0.8660254037844399289, -0.4999999999999980016 ) ) ;
#86410 = CARTESIAN_POINT ( 'NONE',  ( 6.249945409378045547, -2.341251567377310217, 30.72681386836322659 ) ) ;
#86411 = EDGE_CURVE ( 'NONE', #34578, #82613, #76737, .T. ) ;
#86412 = EDGE_CURVE ( 'NONE', #88899, #5856, #60605, .T. ) ;
#86413 = CARTESIAN_POINT ( 'NONE',  ( 2.557637826040450868, -5.852078868378310261, 34.47109172314383585 ) ) ;
#86414 = VECTOR ( 'NONE', #57835, 1000.000000000000000 ) ;
#86415 = AXIS2_PLACEMENT_3D ( 'NONE', #77342, #77783, #51167 ) ;
#86416 = DIRECTION ( 'NONE',  ( -0.000000000000000000, 0.8660254037844397068, -0.4999999999999978906 ) ) ;
#86417 = ORIENTED_EDGE ( 'NONE', *, *, #39224, .T. ) ;
#86418 = EDGE_CURVE ( 'NONE', #46856, #47638, #70186, .T. ) ;
#86419 = VERTEX_POINT ( 'NONE', #43566 ) ;
#86420 = EDGE_CURVE ( 'NONE', #18273, #57358, #29624, .T. ) ;
#86422 = ORIENTED_EDGE ( 'NONE', *, *, #55855, .T. ) ;
#86421 = FACE_OUTER_BOUND ( 'NONE', #21595, .T. ) ;
#86423 = CARTESIAN_POINT ( 'NONE',  ( -5.326899820971665811, -2.544273027872574922, 31.48422191005632342 ) ) ;
#86424 = CARTESIAN_POINT ( 'NONE',  ( -19.50000000000000000, -3.499999999999999556, 29.75000000000000355 ) ) ;
#86425 = DIRECTION ( 'NONE',  ( -0.000000000000000000, 0.8660254037844397068, -0.4999999999999978906 ) ) ;
#86426 = CARTESIAN_POINT ( 'NONE',  ( -13.25408968285182354, -12.45806712695776319, 30.39783852428763922 ) ) ;
#86427 = ORIENTED_EDGE ( 'NONE', *, *, #60408, .T. ) ;
#86428 = ORIENTED_EDGE ( 'NONE', *, *, #4457, .T. ) ;
#86429 = EDGE_LOOP ( 'NONE', ( #17974, #43038 ) ) ;
#86431 = ORIENTED_EDGE ( 'NONE', *, *, #43948, .F. ) ;
#86430 = CARTESIAN_POINT ( 'NONE',  ( 14.98074599347626368, -2.587272538249754117, 30.68239716806877837 ) ) ;
#86432 = CARTESIAN_POINT ( 'NONE',  ( -10.86538461538461320, -2.249999999999998668, 29.75000000000000355 ) ) ;
#86433 = ADVANCED_FACE ( 'NONE', ( #70603 ), #22413, .F. ) ;
#86434 = CARTESIAN_POINT ( 'NONE',  ( -13.38461538461550582, -6.879047030192662504, 34.71129190930017927 ) ) ;
#86435 = ORIENTED_EDGE ( 'NONE', *, *, #30197, .F. ) ;
#86436 = DIRECTION ( 'NONE',  ( 0.000000000000000000, 1.000000000000000000, 0.000000000000000000 ) ) ;
#86437 = DIRECTION ( 'NONE',  ( -0.000000000000000000, 0.6427876096865404731, -0.7660444431189770143 ) ) ;
#86438 = CARTESIAN_POINT ( 'NONE',  ( 15.12820512820512953, -11.00000000000000000, 29.75000000000000355 ) ) ;
#86439 = FACE_BOUND ( 'NONE', #59286, .T. ) ;
#86440 = DIRECTION ( 'NONE',  ( 0.000000000000000000, 0.000000000000000000, 1.000000000000000000 ) ) ;
#86441 = CARTESIAN_POINT ( 'NONE',  ( 9.442307692307693401, -7.500000000000001776, 34.75000000000000000 ) ) ;
#86442 = LINE ( 'NONE', #24715, #43742 ) ;
#86444 = CARTESIAN_POINT ( 'NONE',  ( -8.546451100252705047, -12.11081565061824250, 32.26097654155340422 ) ) ;
#86443 = DIRECTION ( 'NONE',  ( 1.000000000000000000, 0.000000000000000000, 0.000000000000000000 ) ) ;
#86445 = DIRECTION ( 'NONE',  ( 0.000000000000000000, -5.102127870520020612E-17, -1.000000000000000000 ) ) ;
#86446 = CARTESIAN_POINT ( 'NONE',  ( 1.450682717965462887, -2.292212530054420494, 30.41441678777542990 ) ) ;
#86447 = EDGE_LOOP ( 'NONE', ( #82750, #61199, #75615, #22814 ) ) ;
#86448 = CARTESIAN_POINT ( 'NONE',  ( 2.557637826040451312, -6.696923467548660192, 34.68552623307873972 ) ) ;
#86449 = CARTESIAN_POINT ( 'NONE',  ( -13.38461538461550759, -4.320704448113951379, 33.92786785259630022 ) ) ;
#86450 = ORIENTED_EDGE ( 'NONE', *, *, #49318, .F. ) ;
#86451 = VERTEX_POINT ( 'NONE', #14781 ) ;
#86453 = CARTESIAN_POINT ( 'NONE',  ( 1.634560793993429684, -5.766571408460172243, 34.70601412856602508 ) ) ;
#86452 = CARTESIAN_POINT ( 'NONE',  ( -6.923076923076922462, -8.120952969808772792, 34.71129190930000163 ) ) ;
#86454 = CARTESIAN_POINT ( 'NONE',  ( 16.40379156322419973, -6.653508905675593610, 34.93172785388651391 ) ) ;
#86455 = CARTESIAN_POINT ( 'NONE',  ( 1.134592147322421196, -6.695914987888143877, 34.68535235679833306 ) ) ;
#86456 = CARTESIAN_POINT ( 'NONE',  ( 17.07692307692307665, -11.11383981884818262, 36.00935417666054406 ) ) ;
#86457 = ORIENTED_EDGE ( 'NONE', *, *, #41473, .F. ) ;
#86458 = DIRECTION ( 'NONE',  ( -0.000000000000000000, 1.000000000000000000, -0.000000000000000000 ) ) ;
#86459 = CARTESIAN_POINT ( 'NONE',  ( 4.219101293358991533, -5.094484230520773593, 34.41647553114626845 ) ) ;
#86461 = CARTESIAN_POINT ( 'NONE',  ( -9.942284423250047354, -4.236021600441997492, 33.53823185664189310 ) ) ;
#86460 = CARTESIAN_POINT ( 'NONE',  ( 4.946775867484856093, -6.001485441113818986, 34.52039167877662607 ) ) ;
#86462 = LINE ( 'NONE', #72025, #66099 ) ;
#86463 = CARTESIAN_POINT ( 'NONE',  ( 10.83839596699746721, -4.187068189119697692, 33.49521262558774026 ) ) ;
#86464 = DIRECTION ( 'NONE',  ( -0.000000000000000000, 0.9396926207859093161, -0.3420201433256663259 ) ) ;
#86465 = CARTESIAN_POINT ( 'NONE',  ( 3.750000000000000888, -7.499999999999978684, 20.71875000000000000 ) ) ;
#86466 = EDGE_LOOP ( 'NONE', ( #3849, #72095 ) ) ;
#86467 = AXIS2_PLACEMENT_3D ( 'NONE', #30307, #56453, #70414 ) ;
#86468 = AXIS2_PLACEMENT_3D ( 'NONE', #82349, #20630, #45672 ) ;
#86469 = ORIENTED_EDGE ( 'NONE', *, *, #72828, .T. ) ;
#86470 = CARTESIAN_POINT ( 'NONE',  ( -24.00000000000000000, -5.499999999999981348, 27.75000000000000000 ) ) ;
#86471 = CARTESIAN_POINT ( 'NONE',  ( 0.4615384615383382183, -12.51329471203414379, 31.30864560766407578 ) ) ;
#86472 = CARTESIAN_POINT ( 'NONE',  ( 18.22277954126840172, -5.913360116392396115, 34.49180327182771322 ) ) ;
#86473 = CARTESIAN_POINT ( 'NONE',  ( 4.153846153846030731, -11.06231777344772027, 33.60647404775119895 ) ) ;
#86474 = FACE_OUTER_BOUND ( 'NONE', #12184, .T. ) ;
#86475 = CARTESIAN_POINT ( 'NONE',  ( 2.651650429449569302, -10.15165042944953733, 23.37500000000000000 ) ) ;
#86476 = VECTOR ( 'NONE', #43568, 1000.000000000000000 ) ;
#86477 = CARTESIAN_POINT ( 'NONE',  ( 12.46153846153846168, -13.78497067705608181, 32.30358669280327177 ) ) ;
#86478 = CARTESIAN_POINT ( 'NONE',  ( 16.15384615384615330, -13.95598074871891292, 31.83374038241031911 ) ) ;
#86479 = CARTESIAN_POINT ( 'NONE',  ( -1.384615384615383471, -8.164416787775445883, 34.95778746994557906 ) ) ;
#86480 = CARTESIAN_POINT ( 'NONE',  ( -6.249999999999997335, -2.499999999999998668, 29.75000000000000355 ) ) ;
#86481 = DIRECTION ( 'NONE',  ( -0.000000000000000000, 0.8660254037844399289, -0.4999999999999980016 ) ) ;
#86482 = CARTESIAN_POINT ( 'NONE',  ( -12.23852710992561299, -3.587049720035815348, 32.86302985866382897 ) ) ;
#86483 = LINE ( 'NONE', #18454, #76863 ) ;
#86484 = CARTESIAN_POINT ( 'NONE',  ( 7.173131342990377135, -2.318338780012835443, 30.59689888758630261 ) ) ;
#86485 = DIRECTION ( 'NONE',  ( 0.000000000000000000, 1.000000000000000000, 0.000000000000000000 ) ) ;
#86486 = CARTESIAN_POINT ( 'NONE',  ( 11.47237812750566022, -6.386643153685125363, 34.62446782046654903 ) ) ;
#86487 = CARTESIAN_POINT ( 'NONE',  ( -15.36146069743678844, -8.147922237126337563, 34.70805685702651999 ) ) ;
#86488 = ORIENTED_EDGE ( 'NONE', *, *, #14163, .F. ) ;
#86489 = CARTESIAN_POINT ( 'NONE',  ( -16.15384615384615330, -6.343179335718451384, 34.87096338111211935 ) ) ;
#86490 = CARTESIAN_POINT ( 'NONE',  ( 17.99999999999987566, -5.094484230521993062, 34.41647553114689373 ) ) ;
#86491 = CARTESIAN_POINT ( 'NONE',  ( 17.99999999999987566, -10.21337939537710326, 33.94971097300076224 ) ) ;
#86492 = CARTESIAN_POINT ( 'NONE',  ( -1.944543648263014957, -5.555456351737005249, 22.75000000000000000 ) ) ;
#86493 = CARTESIAN_POINT ( 'NONE',  ( 6.000000000000001776, -11.35647404775217417, 33.31231777344666511 ) ) ;
#86494 = CARTESIAN_POINT ( 'NONE',  ( 16.02315555073584363, -4.684245665217972032, 34.18127051446801090 ) ) ;
#86496 = ORIENTED_EDGE ( 'NONE', *, *, #32932, .T. ) ;
#86495 = DIRECTION ( 'NONE',  ( 0.000000000000000000, 0.6427876096865368094, 0.7660444431189802339 ) ) ;
#86497 = CARTESIAN_POINT ( 'NONE',  ( 1.944543648263018731, -9.444543648262994751, 20.87500000000000000 ) ) ;
#86498 = CARTESIAN_POINT ( 'NONE',  ( -1.634638621908349521, -10.05641848906368452, 34.04755513067966177 ) ) ;
#86499 = VERTEX_POINT ( 'NONE', #77358 ) ;
#86500 = CARTESIAN_POINT ( 'NONE',  ( 6.857806922520603976, -6.835583212224499938, 34.95778746994557906 ) ) ;
#86501 = ORIENTED_EDGE ( 'NONE', *, *, #11928, .F. ) ;
#86502 = CARTESIAN_POINT ( 'NONE',  ( -7.623374177175779032, -6.717445702608402236, 34.94155399931962336 ) ) ;
#86503 = PLANE ( 'NONE',  #29350 ) ;
#86504 = CARTESIAN_POINT ( 'NONE',  ( 15.48071474911737511, -2.824170634883621744, 31.52227843825338738 ) ) ;
#86505 = ORIENTED_EDGE ( 'NONE', *, *, #39765, .T. ) ;
#86506 = CARTESIAN_POINT ( 'NONE',  ( 11.53846153846153832, -11.91647553114624181, 32.58852847137148245 ) ) ;
#86507 = ORIENTED_EDGE ( 'NONE', *, *, #33357, .F. ) ;
#86508 = FACE_OUTER_BOUND ( 'NONE', #26831, .T. ) ;
#86509 = B_SPLINE_CURVE_WITH_KNOTS ( 'NONE', 3,
 ( #43797, #55541, #71259, #49673, #83024, #55985, #36606, #21757, #64064, #77149 ),
 .UNSPECIFIED., .F., .F.,
 ( 4, 2, 2, 2, 4 ),
 ( 0.0007817359430256400890, 0.0009771253907250091169, 0.001172514838424378253, 0.001367904286123747173, 0.001563293733823116309 ),
 .UNSPECIFIED. ) ;
#86510 = B_SPLINE_CURVE_WITH_KNOTS ( 'NONE', 3,
 ( #1052, #62296, #19987, #20440, #76254, #54649, #82147, #82597, #41594, #20872 ),
 .UNSPECIFIED., .F., .F.,
 ( 4, 2, 2, 2, 4 ),
 ( 0.0007817359430256294638, 0.0009771253907249950223, 0.001172514838424360472, 0.001367904286123725922, 0.001563293733823091372 ),
 .UNSPECIFIED. ) ;
#86511 = EDGE_CURVE ( 'NONE', #13118, #17208, #8467, .T. ) ;
#86512 = ORIENTED_EDGE ( 'NONE', *, *, #31181, .F. ) ;
#86513 = CARTESIAN_POINT ( 'NONE',  ( 10.61538461538461675, -13.75783147151868846, 33.36296068462461051 ) ) ;
#86514 = CARTESIAN_POINT ( 'NONE',  ( 12.71159277317677905, -12.17597550085003810, 31.52189283813460463 ) ) ;
#86515 = ORIENTED_EDGE ( 'NONE', *, *, #2980, .F. ) ;
#86516 = CARTESIAN_POINT ( 'NONE',  ( 9.692307692307695177, -8.973038597847269315, 34.52809138561121927 ) ) ;
#86517 = CARTESIAN_POINT ( 'NONE',  ( 6.923076923076800782, -8.656820664282941280, 34.87096338111179961 ) ) ;
#86518 = CARTESIAN_POINT ( 'NONE',  ( -1.253824943648433443, -10.70102852606553157, 33.91149625220312913 ) ) ;
#86519 = CARTESIAN_POINT ( 'NONE',  ( -14.24162497434223162, -9.905515769479276145, 34.41647553114623292 ) ) ;
#86520 = CARTESIAN_POINT ( 'NONE',  ( 2.999999999999997335, 7.500000000000000000, 0.000000000000000000 ) ) ;
#86521 = VERTEX_POINT ( 'NONE', #30061 ) ;
#86522 = VERTEX_POINT ( 'NONE', #57525 ) ;
#86523 = VECTOR ( 'NONE', #50978, 1000.000000000000000 ) ;
#86524 = EDGE_CURVE ( 'NONE', #74762, #36504, #37964, .T. ) ;
#86525 = ORIENTED_EDGE ( 'NONE', *, *, #32646, .F. ) ;
#86527 = ORIENTED_EDGE ( 'NONE', *, *, #22754, .F. ) ;
#86526 = FACE_OUTER_BOUND ( 'NONE', #43792, .T. ) ;
#86528 = AXIS2_PLACEMENT_3D ( 'NONE', #80787, #59156, #17287 ) ;
#86529 = CARTESIAN_POINT ( 'NONE',  ( 10.36540788444226102, -4.943428324936578910, 34.04746400365624481 ) ) ;
#86530 = CARTESIAN_POINT ( 'NONE',  ( 3.230769230769231726, -13.75783147151868846, 33.36296068462461051 ) ) ;
#86531 = ORIENTED_EDGE ( 'NONE', *, *, #27443, .T. ) ;
#86532 = ORIENTED_EDGE ( 'NONE', *, *, #39644, .F. ) ;
#86533 = CARTESIAN_POINT ( 'NONE',  ( -10.83831083290076158, -3.105860786376062332, 32.13614157043599562 ) ) ;
#86534 = ORIENTED_EDGE ( 'NONE', *, *, #31077, .T. ) ;
#86535 = CARTESIAN_POINT ( 'NONE',  ( -9.692307692307377209, -2.255955759149395501, 30.00000000000324363 ) ) ;
#86536 = B_SPLINE_CURVE_WITH_KNOTS ( 'NONE', 3,
 ( #78907, #59968, #52762, #11796, #65390, #50966, #16757, #71699, #3684, #54092 ),
 .UNSPECIFIED., .F., .F.,
 ( 4, 2, 2, 2, 4 ),
 ( 0.000000000000000000, 0.0001954339857564080165, 0.0003908679715128160329, 0.0005863019572692240765, 0.0007817359430256320659 ),
 .UNSPECIFIED. ) ;
#86537 = ADVANCED_FACE ( 'NONE', ( #9782 ), #35940, .F. ) ;
#86538 = CARTESIAN_POINT ( 'NONE',  ( 4.023698184114456566, -12.70455904226513866, 30.44083106164009322 ) ) ;
#86539 = CARTESIAN_POINT ( 'NONE',  ( -11.31544869436814338, -11.98016756924215009, 32.48728574198911190 ) ) ;
#86540 = FACE_BOUND ( 'NONE', #58839, .T. ) ;
#86542 = ORIENTED_EDGE ( 'NONE', *, *, #66336, .F. ) ;
#86541 = EDGE_CURVE ( 'NONE', #10260, #10737, #33661, .T. ) ;
#86543 = CYLINDRICAL_SURFACE ( 'NONE', #5318, 0.2499999999999995559 ) ;
#86544 = CARTESIAN_POINT ( 'NONE',  ( -1.634615384615383027, -7.500000000000001776, 34.75000000000000000 ) ) ;
#86545 = ADVANCED_FACE ( 'NONE', ( #31387 ), #38591, .F. ) ;
#86546 = CARTESIAN_POINT ( 'NONE',  ( 4.946232473812766983, -3.338472653186242756, 32.95098750199972670 ) ) ;
#86547 = CARTESIAN_POINT ( 'NONE',  ( -11.53846153846153655, -2.708943851104267164, 35.45975837776705220 ) ) ;
#86548 = CARTESIAN_POINT ( 'NONE',  ( -1.634638621908348410, -2.587272538249755449, 30.68239716806877837 ) ) ;
#86549 = ORIENTED_EDGE ( 'NONE', *, *, #40121, .T. ) ;
#86550 = CARTESIAN_POINT ( 'NONE',  ( 4.230769230769229061, -7.500000000000000000, 33.75000000000000000 ) ) ;
#86551 = ORIENTED_EDGE ( 'NONE', *, *, #50335, .T. ) ;
#86552 = EDGE_LOOP ( 'NONE', ( #62606, #50154, #71004, #63940 ) ) ;
#86554 = DIRECTION ( 'NONE',  ( -0.000000000000000000, -0.3420201433256694346, -0.9396926207859080948 ) ) ;
#86553 = CARTESIAN_POINT ( 'NONE',  ( -6.923076923077045919, -4.320704448113951379, 33.92786785259630022 ) ) ;
#86555 = VECTOR ( 'NONE', #62261, 1000.000000000000000 ) ;
#86556 = DIRECTION ( 'NONE',  ( 0.000000000000000000, -3.469446951953611033E-15, -1.000000000000000000 ) ) ;
#86557 = CARTESIAN_POINT ( 'NONE',  ( -18.00000000000000000, 2.999999999999934719, 28.00000000000000000 ) ) ;
#86558 = FACE_OUTER_BOUND ( 'NONE', #39841, .T. ) ;
#86559 = CARTESIAN_POINT ( 'NONE',  ( -8.769230769230890843, -6.879047030192662504, 34.71129190930017927 ) ) ;
#86560 = EDGE_LOOP ( 'NONE', ( #85254, #66642 ) ) ;
#86561 = FACE_OUTER_BOUND ( 'NONE', #27481, .T. ) ;
#86562 = FACE_OUTER_BOUND ( 'NONE', #67978, .T. ) ;
#86563 = CARTESIAN_POINT ( 'NONE',  ( 10.54930120442873687, -3.050289026998445951, 32.03036669348365706 ) ) ;
#86564 = CARTESIAN_POINT ( 'NONE',  ( 13.13463865367303285, -12.41269422305637171, 30.68257228309993323 ) ) ;
#86565 = AXIS2_PLACEMENT_3D ( 'NONE', #38402, #46493, #60002 ) ;
#86566 = ORIENTED_EDGE ( 'NONE', *, *, #29680, .F. ) ;
#86567 = ORIENTED_EDGE ( 'NONE', *, *, #5926, .T. ) ;
#86568 = FACE_BOUND ( 'NONE', #78877, .T. ) ;
#86569 = SHAPE_DEFINITION_REPRESENTATION ( #74442, #11527 ) ;
#86570 = EDGE_LOOP ( 'NONE', ( #34713, #71990 ) ) ;
#86571 = CARTESIAN_POINT ( 'NONE',  ( 7.780883400193070898, -2.892918686051582089, 31.69288490824015270 ) ) ;
#86572 = CARTESIAN_POINT ( 'NONE',  ( -1.134560964701931463, -2.318338780012835443, 30.59689888758630261 ) ) ;
#86573 = ORIENTED_EDGE ( 'NONE', *, *, #77180, .F. ) ;
#86574 = CARTESIAN_POINT ( 'NONE',  ( -7.715362038329057981, -4.118422570099827595, 33.43335022499816489 ) ) ;
#86575 = CARTESIAN_POINT ( 'NONE',  ( 16.15384615384615330, -1.466349020453238561, 30.81389545987213907 ) ) ;
#86576 = CARTESIAN_POINT ( 'NONE',  ( 0.5267940328144855577, -12.27809138561124591, 31.22303859784720359 ) ) ;
#86577 = CARTESIAN_POINT ( 'NONE',  ( -6.923076923076922462, -1.242168528481310874, 33.36296068462461051 ) ) ;
#86578 = DIRECTION ( 'NONE',  ( -0.000000000000000000, 1.000000000000000000, 3.491481338843133355E-15 ) ) ;
#86579 = ORIENTED_EDGE ( 'NONE', *, *, #77670, .F. ) ;
#86581 = ORIENTED_EDGE ( 'NONE', *, *, #8086, .F. ) ;
#86580 = CARTESIAN_POINT ( 'NONE',  ( 0.3313912521002396194, -10.19110544564092002, 33.96427741523702792 ) ) ;
#86582 = CARTESIAN_POINT ( 'NONE',  ( -7.780898274877819709, -9.442884908240271713, 34.35708131394835618 ) ) ;
#86583 = CARTESIAN_POINT ( 'NONE',  ( 15.23076923076923173, -10.67929555188718282, 33.92786785259544047 ) ) ;
#86584 = FACE_OUTER_BOUND ( 'NONE', #11408, .T. ) ;
#86585 = B_SPLINE_CURVE_WITH_KNOTS ( 'NONE', 3,
 ( #39080, #66541, #73757, #12051, #20127, #27326 ),
 .UNSPECIFIED., .F., .F.,
 ( 4, 2, 4 ),
 ( 0.0003909512603273593376, 0.0005862562993131836733, 0.0007815613382990081173 ),
 .UNSPECIFIED. ) ;
#86586 = EDGE_CURVE ( 'NONE', #30133, #28433, #83107, .T. ) ;
#86587 = FACE_OUTER_BOUND ( 'NONE', #26474, .T. ) ;
#86588 = CYLINDRICAL_SURFACE ( 'NONE', #62005, 0.2500000000000009437 ) ;
#86589 = CARTESIAN_POINT ( 'NONE',  ( 6.066068351002441794, -2.721908614388772296, 31.22303859784725333 ) ) ;
#86590 = CARTESIAN_POINT ( 'NONE',  ( 2.750000000000002665, -7.561099074964516831, 17.22061829374151287 ) ) ;
#86591 = ORIENTED_EDGE ( 'NONE', *, *, #57052, .T. ) ;
#86592 = CARTESIAN_POINT ( 'NONE',  ( 14.30769230769218581, -2.379036618888197729, 30.90682066428292885 ) ) ;
#86593 = CARTESIAN_POINT ( 'NONE',  ( 2.307692307692309264, -3.937682226553329556, 33.60647404775216529 ) ) ;
#86594 = CYLINDRICAL_SURFACE ( 'NONE', #46734, 0.2499999999999986955 ) ;
#86595 = AXIS2_PLACEMENT_3D ( 'NONE', #17760, #11001, #38473 ) ;
#86596 = AXIS2_PLACEMENT_3D ( 'NONE', #19591, #81307, #88965 ) ;
#86597 = ORIENTED_EDGE ( 'NONE', *, *, #15624, .F. ) ;
#86598 = EDGE_LOOP ( 'NONE', ( #30148, #59545 ) ) ;
#86599 = LINE ( 'NONE', #31178, #34017 ) ;
#86600 = CARTESIAN_POINT ( 'NONE',  ( 7.622668921589514923, -6.716662450894489211, 34.94144148231605840 ) ) ;
#86601 = LINE ( 'NONE', #25327, #82085 ) ;
#86602 = CIRCLE ( 'NONE', #77965, 0.2500000000000002220 ) ;
#86603 = EDGE_CURVE ( 'NONE', #720, #45245, #69234, .T. ) ;
#86604 = CARTESIAN_POINT ( 'NONE',  ( 10.48469314871706004, -4.118384482072086072, 33.43331474514187107 ) ) ;
#86605 = CARTESIAN_POINT ( 'NONE',  ( 17.75002325595140817, -12.01397095200673881, 32.43157075238190146 ) ) ;
#86606 = FACE_OUTER_BOUND ( 'NONE', #1222, .T. ) ;
#86607 = ORIENTED_EDGE ( 'NONE', *, *, #57952, .F. ) ;
#86608 = CARTESIAN_POINT ( 'NONE',  ( -2.980714810855778385, -12.65882529074907126, 30.72640787790839312 ) ) ;
#86609 = LINE ( 'NONE', #55349, #57829 ) ;
#86610 = DIRECTION ( 'NONE',  ( -0.000000000000000000, -0.3420201433256694901, -0.9396926207859082059 ) ) ;
#86611 = B_SPLINE_CURVE_WITH_KNOTS ( 'NONE', 3,
 ( #58010, #1745, #71083, #84620, #1296, #69758, #8510, #49042, #43175, #56250 ),
 .UNSPECIFIED., .F., .F.,
 ( 4, 2, 2, 2, 4 ),
 ( 0.000000000000000000, 0.0001954311564186882568, 0.0003908623128373765136, 0.0005862934692560647703, 0.0007817246256747530271 ),
 .UNSPECIFIED. ) ;
#86612 = CARTESIAN_POINT ( 'NONE',  ( 4.153846153846154188, -8.164416787775445883, 34.95778746994557906 ) ) ;
#86613 = ORIENTED_EDGE ( 'NONE', *, *, #68753, .F. ) ;
#86614 = CARTESIAN_POINT ( 'NONE',  ( 16.08776377448601735, -12.34228464037088280, 31.77849191805838558 ) ) ;
#86615 = B_SPLINE_CURVE_WITH_KNOTS ( 'NONE', 3,
 ( #71446, #44405, #15195, #42666, #8432, #1670, #29157, #56616, #84103, #45760 ),
 .UNSPECIFIED., .F., .F.,
 ( 4, 2, 2, 2, 4 ),
 ( 0.0007817359430256361858, 0.0009771253907250041296, 0.001172514838424372182, 0.001367904286123740234, 0.001563293733823108286 ),
 .UNSPECIFIED. ) ;
#86616 = EDGE_CURVE ( 'NONE', #63049, #18719, #71923, .T. ) ;
#86617 = ORIENTED_EDGE ( 'NONE', *, *, #32903, .F. ) ;
#86618 = CARTESIAN_POINT ( 'NONE',  ( 1.607578288176872094, -7.369474270740069777, 34.74850911626239736 ) ) ;
#86619 = CYLINDRICAL_SURFACE ( 'NONE', #49866, 4.000000000000000000 ) ;
#86620 = CARTESIAN_POINT ( 'NONE',  ( -0.4615384615381466493, -2.255955759149395501, 30.00000000000324363 ) ) ;
#86621 = VERTEX_POINT ( 'NONE', #58395 ) ;
#86622 = EDGE_CURVE ( 'NONE', #67914, #28375, #48812, .T. ) ;
#86623 = LINE ( 'NONE', #63772, #43468 ) ;
#86624 = DIRECTION ( 'NONE',  ( 1.000000000000000000, 0.000000000000000000, 0.000000000000000000 ) ) ;
#86625 = DIRECTION ( 'NONE',  ( 0.000000000000000000, 0.000000000000000000, -1.000000000000000000 ) ) ;
#86626 = VECTOR ( 'NONE', #34715, 1000.000000000000114 ) ;
#86627 = FACE_OUTER_BOUND ( 'NONE', #16643, .T. ) ;
#86628 = CARTESIAN_POINT ( 'NONE',  ( -3.230769230769229949, -12.37446782046654192, 30.86335684631486131 ) ) ;
#86629 = ORIENTED_EDGE ( 'NONE', *, *, #72392, .T. ) ;
#86630 = EDGE_CURVE ( 'NONE', #79887, #45031, #12285, .T. ) ;
#86631 = FACE_BOUND ( 'NONE', #9549, .T. ) ;
#86632 = VERTEX_POINT ( 'NONE', #73263 ) ;
#86633 = VECTOR ( 'NONE', #16578, 1000.000000000000000 ) ;
#86634 = CARTESIAN_POINT ( 'NONE',  ( -2.372962308248625973, -2.657715359629089225, 31.77849191805834295 ) ) ;
#86635 = B_SPLINE_CURVE_WITH_KNOTS ( 'NONE', 3,
 ( #13553, #68937, #32490, #59963, #80706, #41034, #68493, #81141, #60854, #88356 ),
 .UNSPECIFIED., .F., .F.,
 ( 4, 2, 2, 2, 4 ),
 ( 0.0007817359430256297891, 0.0009771253907249958896, 0.001172514838424361990, 0.001367904286123728091, 0.001563293733823094191 ),
 .UNSPECIFIED. ) ;
#86636 = CARTESIAN_POINT ( 'NONE',  ( -9.469296340694841163, -12.15243808032446005, 31.58219941686247978 ) ) ;
#86637 = EDGE_CURVE ( 'NONE', #83562, #29011, #10042, .T. ) ;
#86638 = CYLINDRICAL_SURFACE ( 'NONE', #80133, 4.000000000000000000 ) ;
#86639 = CARTESIAN_POINT ( 'NONE',  ( 15.23076923076910916, -9.528491918059723176, 34.59228464037033035 ) ) ;
#86640 = EDGE_CURVE ( 'NONE', #6775, #58077, #71293, .T. ) ;
#86641 = CARTESIAN_POINT ( 'NONE',  ( 4.826923076923065992, -2.499999999999999556, 29.81609845454692120 ) ) ;
#86642 = DIRECTION ( 'NONE',  ( 0.000000000000000000, 0.4999999999999960032, -0.8660254037844410391 ) ) ;
#86643 = ORIENTED_EDGE ( 'NONE', *, *, #32185, .T. ) ;
#86644 = EDGE_LOOP ( 'NONE', ( #46192, #4197 ) ) ;
#86645 = ORIENTED_EDGE ( 'NONE', *, *, #45093, .T. ) ;
#86646 = PRODUCT_DEFINITION_SHAPE ( 'NONE', 'NONE',  #89190 ) ;
#86647 = ORIENTED_EDGE ( 'NONE', *, *, #88565, .T. ) ;
#86648 = ORIENTED_EDGE ( 'NONE', *, *, #51582, .T. ) ;
#86649 = ADVANCED_FACE ( 'NONE', ( #12449 ), #53423, .F. ) ;
#86650 = CARTESIAN_POINT ( 'NONE',  ( 12.52679403281448600, -11.94971097300157403, 32.03036669348361443 ) ) ;
#86651 = CARTESIAN_POINT ( 'NONE',  ( 15.23076923076923173, -1.242168528481310874, 33.36296068462461051 ) ) ;
#86652 = CARTESIAN_POINT ( 'NONE',  ( -2.557692307692305267, -7.500000000000001776, 34.75000000000000000 ) ) ;
#86653 = CARTESIAN_POINT ( 'NONE',  ( -5.869474298236438514, -5.195472089885680766, 34.18748526763464923 ) ) ;
#86654 = CARTESIAN_POINT ( 'NONE',  ( -16.37733109757010652, -2.599994579823202923, 30.74605699353653776 ) ) ;
#86655 = AXIS2_PLACEMENT_3D ( 'NONE', #50852, #36912, #42365 ) ;
#86656 = CARTESIAN_POINT ( 'NONE',  ( -6.223484924564332665, -3.019605429927184836, 32.48692288466676814 ) ) ;
#86657 = VECTOR ( 'NONE', #78401, 1000.000000000000227 ) ;
#86658 = ADVANCED_FACE ( 'NONE', ( #61074 ), #54310, .F. ) ;
#86659 = CARTESIAN_POINT ( 'NONE',  ( 5.933916589044120116, -11.69971097300155272, 32.46337939537587403 ) ) ;
#86660 = ADVANCED_FACE ( 'NONE', ( #87684 ), #80926, .F. ) ;
#86661 = CARTESIAN_POINT ( 'NONE',  ( -7.715362038329058869, -3.062576670634119758, 32.05464942895959979 ) ) ;
#86662 = CARTESIAN_POINT ( 'NONE',  ( 7.976679284387491187, -5.070358843744210198, 34.40418822224088302 ) ) ;
#86663 = VERTEX_POINT ( 'NONE', #88581 ) ;
#86664 = ORIENTED_EDGE ( 'NONE', *, *, #57704, .T. ) ;
#86665 = VECTOR ( 'NONE', #32220, 1000.000000000000000 ) ;
#86666 = EDGE_LOOP ( 'NONE', ( #74259, #71182 ) ) ;
#86668 = ORIENTED_EDGE ( 'NONE', *, *, #76047, .T. ) ;
#86667 = CARTESIAN_POINT ( 'NONE',  ( 0.3962684609821409687, -3.083524468853724443, 32.58852847137143272 ) ) ;
#86670 = CARTESIAN_POINT ( 'NONE',  ( 18.25000000000001776, -2.249999999999997780, 29.81603969181029257 ) ) ;
#86669 = CARTESIAN_POINT ( 'NONE',  ( -15.90379184220783948, -6.567000820036036579, 34.66262288849541306 ) ) ;
#86671 = CARTESIAN_POINT ( 'NONE',  ( 1.515140822849030622, -5.070358843744210198, 34.40418822224088302 ) ) ;
#86672 = CARTESIAN_POINT ( 'NONE',  ( 7.145856464345329506, -2.600157965045225339, 30.74683119005207743 ) ) ;
#86673 = FACE_BOUND ( 'NONE', #37883, .T. ) ;
#86674 = ORIENTED_EDGE ( 'NONE', *, *, #33229, .F. ) ;
#86675 = B_SPLINE_CURVE_WITH_KNOTS ( 'NONE', 3,
 ( #39194, #81954, #66655, #12601, #40526, #33319, #86953, #54459, #18472, #40957 ),
 .UNSPECIFIED., .F., .F.,
 ( 4, 2, 2, 2, 4 ),
 ( 0.000000000000000000, 0.0001954339857564093717, 0.0003908679715128187434, 0.0005863019572692280881, 0.0007817359430256374869 ),
 .UNSPECIFIED. ) ;
#86676 = VERTEX_POINT ( 'NONE', #69168 ) ;
#86677 = CARTESIAN_POINT ( 'NONE',  ( 7.173076923076923350, -2.499999999999998668, 29.75000000000000355 ) ) ;
#86678 = EDGE_LOOP ( 'NONE', ( #72539, #10342 ) ) ;
#86679 = FACE_BOUND ( 'NONE', #7401, .T. ) ;
#86680 = CARTESIAN_POINT ( 'NONE',  ( -10.86536135943320502, -2.920706130388546651, 32.31842814019191223 ) ) ;
#86681 = CARTESIAN_POINT ( 'NONE',  ( 15.84615384615384670, -7.500000000000000000, 29.75000000000000355 ) ) ;
#86682 = ORIENTED_EDGE ( 'NONE', *, *, #29137, .F. ) ;
#86683 = CARTESIAN_POINT ( 'NONE',  ( 2.242421861731533017, -8.613356846314824011, 34.62446782046655613 ) ) ;
#86684 = CARTESIAN_POINT ( 'NONE',  ( 16.82692307692307665, -2.249999999999998668, 29.75000000000000355 ) ) ;
#86685 = FACE_OUTER_BOUND ( 'NONE', #6516, .T. ) ;
#86686 = ORIENTED_EDGE ( 'NONE', *, *, #39320, .T. ) ;
#86687 = CARTESIAN_POINT ( 'NONE',  ( 17.07692307692307665, -3.050289026998446396, 32.03036669348365706 ) ) ;
#86688 = CARTESIAN_POINT ( 'NONE',  ( -14.53061852520844965, -5.667676309546437530, 34.40238873228292249 ) ) ;
#86689 = ORIENTED_EDGE ( 'NONE', *, *, #27866, .F. ) ;
#86690 = CARTESIAN_POINT ( 'NONE',  ( -1.515306851282943068, -5.582088688514999397, 34.36776431015576350 ) ) ;
#86691 = CARTESIAN_POINT ( 'NONE',  ( 7.053868730901711182, -10.54018710029568595, 33.71981072465678864 ) ) ;
#86693 = VERTEX_POINT ( 'NONE', #81804 ) ;
#86692 = AXIS2_PLACEMENT_3D ( 'NONE', #73273, #87249, #59754 ) ;
#86694 = CARTESIAN_POINT ( 'NONE',  ( 0.2386122440223129304, -9.086856451489515152, 34.49173150075333183 ) ) ;
#86695 = CARTESIAN_POINT ( 'NONE',  ( -10.48485891362105171, -5.195472089885680766, 34.18748526763464923 ) ) ;
#86696 = CARTESIAN_POINT ( 'NONE',  ( 16.08776377448601025, -2.833524468853757305, 32.15551576947924417 ) ) ;
#86697 = CARTESIAN_POINT ( 'NONE',  ( -8.519176457592452678, -9.148310452688876993, 34.47095581063188519 ) ) ;
#86698 = CARTESIAN_POINT ( 'NONE',  ( -15.93106661257773560, -4.387253974876675677, 33.66317474335728832 ) ) ;
#86699 = EDGE_CURVE ( 'NONE', #16511, #3680, #84246, .T. ) ;
#86700 = LINE ( 'NONE', #59641, #27999 ) ;
#86702 = CARTESIAN_POINT ( 'NONE',  ( -0.3589743589743593088, -3.499999999999999556, 29.75000000000000355 ) ) ;
#86701 = CARTESIAN_POINT ( 'NONE',  ( 4.826899839630110378, -12.43535235679832596, 30.55408501211184813 ) ) ;
#86703 = CARTESIAN_POINT ( 'NONE',  ( -16.08777780284371417, -11.69971097300155272, 32.46337939537588113 ) ) ;
#86705 = DIRECTION ( 'NONE',  ( -0.000000000000000000, 0.9396926207859093161, -0.3420201433256663259 ) ) ;
#86704 = DIRECTION ( 'NONE',  ( 0.000000000000000000, 0.000000000000000000, -1.000000000000000000 ) ) ;
#86706 = EDGE_CURVE ( 'NONE', #81582, #63578, #79928, .T. ) ;
#86707 = CARTESIAN_POINT ( 'NONE',  ( 0.06109907496454976272, -10.25000000000000000, 27.02938170625848358 ) ) ;
#86709 = ADVANCED_FACE ( 'NONE', ( #61956 ), #27729, .F. ) ;
#86708 = ORIENTED_EDGE ( 'NONE', *, *, #70860, .T. ) ;
#86710 = CARTESIAN_POINT ( 'NONE',  ( 12.46153846153833911, -3.300289026999228881, 32.46337939537708905 ) ) ;
#86711 = ORIENTED_EDGE ( 'NONE', *, *, #50806, .T. ) ;
#86712 = EDGE_CURVE ( 'NONE', #81105, #71780, #67837, .T. ) ;
#86713 = ORIENTED_EDGE ( 'NONE', *, *, #15095, .T. ) ;
#86714 = CARTESIAN_POINT ( 'NONE',  ( -2.980823821391186623, -9.357781135181031829, 34.66075350412533851 ) ) ;
#86715 = ORIENTED_EDGE ( 'NONE', *, *, #44175, .F. ) ;
#86716 = CARTESIAN_POINT ( 'NONE',  ( -15.10024352900566846, -6.001044277235009439, 34.52024696741798948 ) ) ;
#86717 = CARTESIAN_POINT ( 'NONE',  ( 1.139087296525997273, -4.749999999999992895, 16.73437500000000000 ) ) ;
#86718 = CARTESIAN_POINT ( 'NONE',  ( -13.16183571563731647, -5.827830569534417471, 34.72679350104403539 ) ) ;
#86719 = CARTESIAN_POINT ( 'NONE',  ( -15.48074597481782178, -12.41104346484419452, 31.60698883733904196 ) ) ;
#86720 = CARTESIAN_POINT ( 'NONE',  ( -3.230769230769229949, -1.242168528481310874, 33.36296068462461051 ) ) ;
#86721 = PLANE ( 'NONE',  #23095 ) ;
#86722 = EDGE_CURVE ( 'NONE', #43377, #16890, #1431, .T. ) ;
#86723 = B_SPLINE_CURVE_WITH_KNOTS ( 'NONE', 3,
 ( #44842, #10629, #24582, #25026, #74114, #38549, #31796, #39892, #11975, #39451 ),
 .UNSPECIFIED., .F., .F.,
 ( 4, 2, 2, 2, 4 ),
 ( 0.0007817246256747505334, 0.0009771112852218954894, 0.001172497944769040554, 0.001367884604316185618, 0.001563271263863330682 ),
 .UNSPECIFIED. ) ;
#86724 = CARTESIAN_POINT ( 'NONE',  ( -4.946132635956127288, -2.494656445102013453, 31.33466734024120015 ) ) ;
#86725 = CARTESIAN_POINT ( 'NONE',  ( -10.83831083290076158, -4.186968288167449259, 33.49512374952580274 ) ) ;
#86726 = CARTESIAN_POINT ( 'NONE',  ( -14.30769230769242739, -5.219633306517616589, 34.19971097300220464 ) ) ;
#86727 = CARTESIAN_POINT ( 'NONE',  ( -2.651650429449535551, -10.15165042944956753, 22.43750000000000000 ) ) ;
#86728 = B_SPLINE_CURVE_WITH_KNOTS ( 'NONE', 3,
 ( #31335, #2077, #43513, #52483, #79528, #11514, #4304, #38995, #60129, #53376 ),
 .UNSPECIFIED., .F., .F.,
 ( 4, 2, 2, 2, 4 ),
 ( 0.0007817359527651090859, 0.0009771254036996478414, 0.001172514854634186489, 0.001367904305568725136, 0.001563293756503263783 ),
 .UNSPECIFIED. ) ;
#86729 = CARTESIAN_POINT ( 'NONE',  ( -11.53846153846165912, -3.835265460704628371, 33.15142922262033665 ) ) ;
#86730 = CYLINDRICAL_SURFACE ( 'NONE', #37642, 0.2499999999999994726 ) ;
#86731 = DIRECTION ( 'NONE',  ( 1.000000000000000000, 0.000000000000000000, 0.000000000000000000 ) ) ;
#86732 = AXIS2_PLACEMENT_3D ( 'NONE', #38496, #65953, #2907 ) ;
#86733 = VECTOR ( 'NONE', #81987, 1000.000000000000000 ) ;
#86734 = EDGE_LOOP ( 'NONE', ( #8630, #12599, #54095, #26394 ) ) ;
#86735 = VERTEX_POINT ( 'NONE', #22309 ) ;
#86736 = CARTESIAN_POINT ( 'NONE',  ( -9.469528151039277475, -3.755027918224367323, 33.06320215134714857 ) ) ;
#86737 = DIRECTION ( 'NONE',  ( 0.000000000000000000, 0.4999999999999960032, -0.8660254037844410391 ) ) ;
#86738 = CARTESIAN_POINT ( 'NONE',  ( -8.769230769230890843, -11.48612834414049644, 32.76840700105863391 ) ) ;
#86739 = CARTESIAN_POINT ( 'NONE',  ( -6.989159302437058408, -5.471508081941601986, 34.59228464037088457 ) ) ;
#86740 = EDGE_CURVE ( 'NONE', #88101, #79653, #35895, .T. ) ;
#86741 = CARTESIAN_POINT ( 'NONE',  ( 8.703147358274888390, -11.69971097300155272, 32.46337939537587403 ) ) ;
#86742 = CARTESIAN_POINT ( 'NONE',  ( -16.40386939113911779, -9.271318131107980420, 34.42618302367067429 ) ) ;
#86743 = ORIENTED_EDGE ( 'NONE', *, *, #24273, .T. ) ;
#86744 = FACE_OUTER_BOUND ( 'NONE', #21079, .T. ) ;
#86745 = VERTEX_POINT ( 'NONE', #28630 ) ;
#86746 = ORIENTED_EDGE ( 'NONE', *, *, #75319, .T. ) ;
#86747 = CARTESIAN_POINT ( 'NONE',  ( 0.4615384615383382183, -12.51329471203414379, 31.30864560766407578 ) ) ;
#86748 = CARTESIAN_POINT ( 'NONE',  ( 4.023698944407933631, -2.619462340734462380, 30.83744416345203021 ) ) ;
#86749 = CARTESIAN_POINT ( 'NONE',  ( 11.53846153846141753, -10.90142922262034020, 33.41473453929536674 ) ) ;
#86750 = CARTESIAN_POINT ( 'NONE',  ( 11.66925197942848769, -2.295524264805589354, 30.44142389570982488 ) ) ;
#86751 = FACE_OUTER_BOUND ( 'NONE', #16345, .T. ) ;
#86752 = ORIENTED_EDGE ( 'NONE', *, *, #8186, .F. ) ;
#86753 = VECTOR ( 'NONE', #69971, 1000.000000000000000 ) ;
#86754 = VERTEX_POINT ( 'NONE', #23195 ) ;
#86755 = ORIENTED_EDGE ( 'NONE', *, *, #25418, .T. ) ;
#86756 = EDGE_CURVE ( 'NONE', #83108, #21723, #88556, .T. ) ;
#86757 = EDGE_CURVE ( 'NONE', #68522, #38776, #63731, .T. ) ;
#86758 = CARTESIAN_POINT ( 'NONE',  ( -4.088591014333314178, -12.16647553114626490, 32.15551576947920864 ) ) ;
#86759 = CARTESIAN_POINT ( 'NONE',  ( -0.2114840416250090560, -10.06805714834173848, 34.32951233291982618 ) ) ;
#86760 = CYLINDRICAL_SURFACE ( 'NONE', #23545, 0.2499999999999973355 ) ;
#86761 = ADVANCED_FACE ( 'NONE', ( #21864 ), #34927, .T. ) ;
#86762 = CARTESIAN_POINT ( 'NONE',  ( 1.254468175177164246, -3.817052484675422797, 33.13202310037935661 ) ) ;
#86763 = CARTESIAN_POINT ( 'NONE',  ( -11.66915214157184444, -8.191372820521381826, 34.95448215188424967 ) ) ;
#86764 = EDGE_CURVE ( 'NONE', #26836, #61826, #77249, .T. ) ;
#86765 = CARTESIAN_POINT ( 'NONE',  ( 5.777073782483852504, -12.39988816332205701, 30.74660775122750778 ) ) ;
#86766 = ORIENTED_EDGE ( 'NONE', *, *, #23539, .T. ) ;
#86767 = ORIENTED_EDGE ( 'NONE', *, *, #65716, .F. ) ;
#86768 = CARTESIAN_POINT ( 'NONE',  ( -2.651650429449565305, -4.848349570550461785, 25.25000000000000000 ) ) ;
#86769 = VERTEX_POINT ( 'NONE', #2033 ) ;
#86771 = ORIENTED_EDGE ( 'NONE', *, *, #85111, .T. ) ;
#86770 = CARTESIAN_POINT ( 'NONE',  ( 2.530471848960717640, -12.44528174975671853, 30.48912976160716681 ) ) ;
#86772 = EDGE_CURVE ( 'NONE', #58985, #34772, #28392, .T. ) ;
#86773 = CARTESIAN_POINT ( 'NONE',  ( -9.942284436356285227, -10.06842814019191401, 34.32929386961144758 ) ) ;
#86774 = CARTESIAN_POINT ( 'NONE',  ( -2.177166869458662113, -4.299079248970732792, 33.91157788607253565 ) ) ;
#86775 = CARTESIAN_POINT ( 'NONE',  ( 2.651650429449569302, -10.15165042944953733, 14.62500000000000000 ) ) ;
#86776 = ORIENTED_EDGE ( 'NONE', *, *, #36758, .F. ) ;
#86777 = EDGE_CURVE ( 'NONE', #59229, #40827, #83131, .T. ) ;
#86778 = CARTESIAN_POINT ( 'NONE',  ( -13.51476259405360913, -12.27039167877662251, 31.24851455888617835 ) ) ;
#86779 = ORIENTED_EDGE ( 'NONE', *, *, #77286, .T. ) ;
#86780 = CARTESIAN_POINT ( 'NONE',  ( 2.373760658694747061, -8.973038597847269315, 34.52809138561122637 ) ) ;
#86781 = CYLINDRICAL_SURFACE ( 'NONE', #12695, 0.2500000000000012212 ) ;
#86782 = AXIS2_PLACEMENT_3D ( 'NONE', #5577, #47436, #68165 ) ;
#86783 = FACE_BOUND ( 'NONE', #10418, .T. ) ;
#86785 = CARTESIAN_POINT ( 'NONE',  ( 7.846153846153846700, -2.292212530054420494, 30.41441678777542634 ) ) ;
#86784 = CARTESIAN_POINT ( 'NONE',  ( -0.2115930521604184600, -11.56426240980093567, 33.07394671870546432 ) ) ;
#86786 = AXIS2_PLACEMENT_3D ( 'NONE', #12087, #33236, #18834 ) ;
#86787 = CARTESIAN_POINT ( 'NONE',  ( -3.100243529005666687, -6.852161475712352789, 34.70806712695775786 ) ) ;
#86788 = CYLINDRICAL_SURFACE ( 'NONE', #63550, 0.2500000000000008882 ) ;
#86789 = EDGE_LOOP ( 'NONE', ( #2322, #29462, #25011, #13221 ) ) ;
#86790 = ADVANCED_FACE ( 'NONE', ( #29085 ), #16439, .F. ) ;
#86791 = CARTESIAN_POINT ( 'NONE',  ( 6.792929713638703682, -8.587444163452046197, 34.63053765926554206 ) ) ;
#86792 = CARTESIAN_POINT ( 'NONE',  ( 9.692307692307695177, -2.249999999999998668, 29.75000000000001776 ) ) ;
#86793 = VERTEX_POINT ( 'NONE', #56539 ) ;
#86794 = LINE ( 'NONE', #13662, #523 ) ;
#86795 = FACE_OUTER_BOUND ( 'NONE', #79901, .T. ) ;
#86796 = CARTESIAN_POINT ( 'NONE',  ( -14.16025641025641058, -3.499999999999999556, 29.75000000000000355 ) ) ;
#86797 = CARTESIAN_POINT ( 'NONE',  ( -13.25382494364843389, -11.37503395064541678, 33.29242100308974273 ) ) ;
#86798 = CARTESIAN_POINT ( 'NONE',  ( -0.7115384615384606759, -7.500000000000001776, 34.75000000000000000 ) ) ;
#86799 = ADVANCED_FACE ( 'NONE', ( #70941 ), #64164, .F. ) ;
#86800 = FACE_BOUND ( 'NONE', #27700, .T. ) ;
#86802 = DIRECTION ( 'NONE',  ( 1.000000000000000000, 0.000000000000000000, 0.000000000000000000 ) ) ;
#86801 = CARTESIAN_POINT ( 'NONE',  ( 13.25446741488368829, -2.373036134822904319, 30.88089517874952250 ) ) ;
#86803 = CARTESIAN_POINT ( 'NONE',  ( -9.692307692307691624, -11.91647553114624181, 32.58852847137148245 ) ) ;
#86805 = DIRECTION ( 'NONE',  ( 0.000000000000000000, 0.000000000000000000, -1.000000000000000000 ) ) ;
#86804 = CARTESIAN_POINT ( 'NONE',  ( 11.97435897435897267, -3.499999999999999556, 29.75000000000000355 ) ) ;
#86806 = DIRECTION ( 'NONE',  ( -0.000000000000000000, -0.7660444431189791237, -0.6427876096865379196 ) ) ;
#86807 = CARTESIAN_POINT ( 'NONE',  ( -8.519176457592452678, -3.627508038966690496, 32.91356715214248396 ) ) ;
#86808 = CARTESIAN_POINT ( 'NONE',  ( -0.06109907496455085213, -3.750000000000000888, 26.40438170625848713 ) ) ;
#86809 = EDGE_CURVE ( 'NONE', #26695, #5068, #84910, .T. ) ;
#86810 = B_SPLINE_CURVE_WITH_KNOTS ( 'NONE', 3,
 ( #25170, #60281, #87794, #52637, #32377, #59843, #74254, #5350, #5792, #80579 ),
 .UNSPECIFIED., .F., .F.,
 ( 4, 2, 2, 2, 4 ),
 ( 0.000000000000000000, 0.0001954339857564062817, 0.0003908679715128125635, 0.0005863019572692188723, 0.0007817359430256251270 ),
 .UNSPECIFIED. ) ;
#86811 = LINE ( 'NONE', #32721, #82120 ) ;
#86812 = EDGE_LOOP ( 'NONE', ( #77158, #54487 ) ) ;
#86813 = B_SPLINE_CURVE_WITH_KNOTS ( 'NONE', 3,
 ( #72118, #23486, #24369, #59050, #50942, #78878, #70016, #10432, #62799, #35348 ),
 .UNSPECIFIED., .F., .F.,
 ( 4, 2, 2, 2, 4 ),
 ( 0.000000000000000000, 0.0001954339857564097512, 0.0003908679715128195024, 0.0005863019572692292807, 0.0007817359430256390048 ),
 .UNSPECIFIED. ) ;
#86814 = CARTESIAN_POINT ( 'NONE',  ( 16.09615384615384670, -3.499999999999999556, 29.75000000000000355 ) ) ;
#86815 = CARTESIAN_POINT ( 'NONE',  ( 17.99999999999987566, -2.657715359629662544, 31.77849191805970364 ) ) ;
#86816 = CARTESIAN_POINT ( 'NONE',  ( 13.19230769230769340, -3.499999999999999556, 29.75000000000000355 ) ) ;
#86817 = CARTESIAN_POINT ( 'NONE',  ( -9.822454901745912181, -10.88202310037935661, 33.43294751532457099 ) ) ;
#86818 = CARTESIAN_POINT ( 'NONE',  ( -4.377331078410484189, -4.988325925672468131, 34.36044203135681130 ) ) ;
#86819 = DIRECTION ( 'NONE',  ( 0.000000000000000000, 0.000000000000000000, -1.000000000000000000 ) ) ;
#86820 = CARTESIAN_POINT ( 'NONE',  ( 1.492201783934554493, -3.724691934501233703, 23.98250670625849068 ) ) ;
#86821 = DIRECTION ( 'NONE',  ( 0.000000000000000000, 0.3420201433256610524, 0.9396926207859113145 ) ) ;
#86822 = DIRECTION ( 'NONE',  ( 1.000000000000000000, 0.000000000000000000, 0.000000000000000000 ) ) ;
#86823 = EDGE_CURVE ( 'NONE', #51516, #38794, #24520, .T. ) ;
#86824 = AXIS2_PLACEMENT_3D ( 'NONE', #149, #54194, #27619 ) ;
#86825 = CARTESIAN_POINT ( 'NONE',  ( 8.069165197766697162, -11.76359900205217635, 32.36225158514719880 ) ) ;
#86826 = CARTESIAN_POINT ( 'NONE',  ( 9.561617089197383734, -3.957541250942358424, 33.62499894934981626 ) ) ;
#86827 = CARTESIAN_POINT ( 'NONE',  ( 8.703960323269994248, -10.21337939537584383, 33.94971097300158647 ) ) ;
#86828 = FACE_OUTER_BOUND ( 'NONE', #71194, .T. ) ;
#86829 = VECTOR ( 'NONE', #81313, 1000.000000000000000 ) ;
#86830 = CARTESIAN_POINT ( 'NONE',  ( -2.242499319397651458, -2.255955759149235629, 29.99999999999988631 ) ) ;
#86831 = EDGE_CURVE ( 'NONE', #32696, #79428, #54057, .T. ) ;
#86832 = CARTESIAN_POINT ( 'NONE',  ( 17.29970274590113632, -8.540255544307068902, 34.89611431652622286 ) ) ;
#86833 = EDGE_LOOP ( 'NONE', ( #60245, #73865, #60509, #19697 ) ) ;
#86834 = DIRECTION ( 'NONE',  ( 0.000000000000000000, 0.1736481776669275834, 0.9848077530122086864 ) ) ;
#86835 = CARTESIAN_POINT ( 'NONE',  ( 13.38461538461538680, -5.415277668671390821, 36.20867863119892149 ) ) ;
#86836 = CARTESIAN_POINT ( 'NONE',  ( 3.724691934501251023, -9.114399933863618131, 17.29874329374151642 ) ) ;
#86837 = CARTESIAN_POINT ( 'NONE',  ( 6.066068351002440906, -4.098570777380720287, 33.41473453929635440 ) ) ;
#86838 = CARTESIAN_POINT ( 'NONE',  ( -16.82697766754503377, -5.766571408460170467, 34.70601412856602508 ) ) ;
#86839 = ORIENTED_EDGE ( 'NONE', *, *, #10809, .F. ) ;
#86840 = CARTESIAN_POINT ( 'NONE',  ( -17.93393266664992325, -6.343179335718452272, 34.87096338111212646 ) ) ;
#86841 = CARTESIAN_POINT ( 'NONE',  ( -16.85414340794500276, -9.418065098278011860, 34.63729479722530158 ) ) ;
#86843 = ORIENTED_EDGE ( 'NONE', *, *, #20827, .T. ) ;
#86842 = CARTESIAN_POINT ( 'NONE',  ( 4.946775107191377252, -12.50552854090298993, 31.33409797877408920 ) ) ;
#86844 = CARTESIAN_POINT ( 'NONE',  ( 18.00000000000000000, -2.900454961884010974, 35.62045528018868623 ) ) ;
#86845 = CARTESIAN_POINT ( 'NONE',  ( 12.68431800280686694, -12.44528174975671853, 30.48912976160716681 ) ) ;
#86846 = EDGE_CURVE ( 'NONE', #19730, #63457, #72712, .T. ) ;
#86847 = DIRECTION ( 'NONE',  ( 0.000000000000000000, 0.9848077530122072432, 0.1736481776669354937 ) ) ;
#86848 = CARTESIAN_POINT ( 'NONE',  ( -15.93088301957948083, -7.369474539155830506, 34.99858011523957657 ) ) ;
#86849 = ADVANCED_FACE ( 'NONE', ( #44333 ), #37144, .F. ) ;
#86850 = ORIENTED_EDGE ( 'NONE', *, *, #53367, .T. ) ;
#86851 = FACE_OUTER_BOUND ( 'NONE', #12512, .T. ) ;
#86852 = CARTESIAN_POINT ( 'NONE',  ( 10.86533002476265786, -4.176053281294518804, 33.81426240980091791 ) ) ;
#86853 = VECTOR ( 'NONE', #87201, 1000.000000000000000 ) ;
#86854 = PLANE ( 'NONE',  #48422 ) ;
#86855 = ORIENTED_EDGE ( 'NONE', *, *, #12899, .F. ) ;
#86856 = ORIENTED_EDGE ( 'NONE', *, *, #14428, .F. ) ;
#86857 = VECTOR ( 'NONE', #44691, 1000.000000000000000 ) ;
#86858 = ORIENTED_EDGE ( 'NONE', *, *, #17783, .F. ) ;
#86859 = AXIS2_PLACEMENT_3D ( 'NONE', #74904, #12309, #26263 ) ;
#86860 = CARTESIAN_POINT ( 'NONE',  ( 12.68431813051652846, -10.23759521482555357, 34.22997729860117033 ) ) ;
#86861 = DIRECTION ( 'NONE',  ( -0.000000000000000000, 1.000000000000000000, -0.000000000000000000 ) ) ;
#86862 = LINE ( 'NONE', #65653, #27998 ) ;
#86863 = CARTESIAN_POINT ( 'NONE',  ( -1.384615384615383471, -11.35647404775217417, 33.31231777344666511 ) ) ;
#86864 = EDGE_LOOP ( 'NONE', ( #87043, #33138, #1977, #71188 ) ) ;
#86865 = VERTEX_POINT ( 'NONE', #10576 ) ;
#86867 = ORIENTED_EDGE ( 'NONE', *, *, #18518, .F. ) ;
#86866 = CARTESIAN_POINT ( 'NONE',  ( 4.153846153846154188, -5.471508081941601098, 34.59228464037088457 ) ) ;
#86868 = DIRECTION ( 'NONE',  ( -0.000000000000000000, 1.000000000000000000, -0.000000000000000000 ) ) ;
#86869 = FACE_OUTER_BOUND ( 'NONE', #10604, .T. ) ;
#86870 = CARTESIAN_POINT ( 'NONE',  ( -9.692307692307812417, -9.442884908241554243, 34.35708131394783038 ) ) ;
#86871 = CARTESIAN_POINT ( 'NONE',  ( -8.769230769230892619, -11.06231777344772027, 33.60647404775119895 ) ) ;
#86872 = EDGE_CURVE ( 'NONE', #17114, #27570, #58355, .T. ) ;
#86873 = ORIENTED_EDGE ( 'NONE', *, *, #51685, .T. ) ;
#86874 = ORIENTED_EDGE ( 'NONE', *, *, #60289, .F. ) ;
#86875 = B_SPLINE_CURVE_WITH_KNOTS ( 'NONE', 3,
 ( #3075, #10292, #3960, #32341, #58909, #30989, #80081, #38201, #18829, #53037 ),
 .UNSPECIFIED., .F., .F.,
 ( 4, 2, 2, 2, 4 ),
 ( 0.0007817359430256288133, 0.0009771253907249948054, 0.001172514838424360689, 0.001367904286123726573, 0.001563293733823092457 ),
 .UNSPECIFIED. ) ;
#86876 = AXIS2_PLACEMENT_3D ( 'NONE', #41122, #20841, #33036 ) ;
#86877 = EDGE_LOOP ( 'NONE', ( #8863, #27923, #80452, #84759 ) ) ;
#86879 = ORIENTED_EDGE ( 'NONE', *, *, #79177, .F. ) ;
#86878 = FACE_OUTER_BOUND ( 'NONE', #65445, .T. ) ;
#86880 = EDGE_CURVE ( 'NONE', #1867, #38306, #24079, .T. ) ;
#86881 = CARTESIAN_POINT ( 'NONE',  ( 2.307692307692309264, -2.486705287966279876, 31.30864560766543647 ) ) ;
#86882 = CARTESIAN_POINT ( 'NONE',  ( -0.3954711281883858121, -4.661471528628508665, 34.16647553114624003 ) ) ;
#86883 = ORIENTED_EDGE ( 'NONE', *, *, #4103, .F. ) ;
#86884 = CARTESIAN_POINT ( 'NONE',  ( 6.673076923076918021, -2.499999999999999556, 29.81609845454691765 ) ) ;
#86885 = CARTESIAN_POINT ( 'NONE',  ( -13.38461538461538325, -6.435427911321262684, 35.78748833219616898 ) ) ;
#86886 = EDGE_CURVE ( 'NONE', #16317, #75626, #74500, .T. ) ;
#86887 = LINE ( 'NONE', #66595, #39661 ) ;
#86888 = FACE_BOUND ( 'NONE', #80417, .T. ) ;
#86889 = CARTESIAN_POINT ( 'NONE',  ( 19.50000000000000000, -3.499999999999999556, 29.75000000000000355 ) ) ;
#86890 = CARTESIAN_POINT ( 'NONE',  ( -1.384615384615383471, -11.69971097300155272, 32.46337939537588113 ) ) ;
#86891 = CARTESIAN_POINT ( 'NONE',  ( 11.78840705680968171, -12.43552623307873972, 30.55307653245132826 ) ) ;
#86893 = CARTESIAN_POINT ( 'NONE',  ( 14.37294744720514572, -3.083524468853784839, 32.58852847137153930 ) ) ;
#86892 = FACE_OUTER_BOUND ( 'NONE', #82438, .T. ) ;
#86894 = CARTESIAN_POINT ( 'NONE',  ( -4.219599582159485607, -7.249945578846651806, 34.99404164642496795 ) ) ;
#86895 = CARTESIAN_POINT ( 'NONE',  ( -16.37733109757010652, -8.496056993536548418, 34.65000542017679663 ) ) ;
#86896 = ORIENTED_EDGE ( 'NONE', *, *, #77999, .F. ) ;
#86897 = CARTESIAN_POINT ( 'NONE',  ( -15.90384615384608757, -7.434744429011174383, 34.75000000000000711 ) ) ;
#86898 = CARTESIAN_POINT ( 'NONE',  ( -13.63459212866397685, -9.234221910056348293, 34.70572697212741531 ) ) ;
#86899 = ORIENTED_EDGE ( 'NONE', *, *, #29442, .F. ) ;
#86900 = VERTEX_POINT ( 'NONE', #51988 ) ;
#86902 = CARTESIAN_POINT ( 'NONE',  ( 0.5923289025054107038, -8.191423895709840863, 34.95447573519442130 ) ) ;
#86901 = CARTESIAN_POINT ( 'NONE',  ( -11.53846153846166089, -12.70778746994576025, 30.41441678777401236 ) ) ;
#86903 = EDGE_CURVE ( 'NONE', #58570, #16922, #87271, .T. ) ;
#86904 = CARTESIAN_POINT ( 'NONE',  ( 16.21991348719623360, -6.343179335718452272, 34.87096338111212646 ) ) ;
#86905 = CARTESIAN_POINT ( 'NONE',  ( 15.90386940979756858, -2.318417181685854978, 30.59732222474233865 ) ) ;
#86906 = CARTESIAN_POINT ( 'NONE',  ( -15.00780632720774932, -7.369474270740069777, 34.74850911626239736 ) ) ;
#86907 = EDGE_LOOP ( 'NONE', ( #84797, #51115 ) ) ;
#86908 = CARTESIAN_POINT ( 'NONE',  ( 14.30769230769218758, -9.442884908241554243, 34.35708131394783038 ) ) ;
#86909 = CARTESIAN_POINT ( 'NONE',  ( 18.24994540937804643, -2.589246495874658827, 31.60778113518102828 ) ) ;
#86910 = VECTOR ( 'NONE', #26702, 1000.000000000000000 ) ;
#86912 = LINE ( 'NONE', #46787, #71849 ) ;
#86911 = CARTESIAN_POINT ( 'NONE',  ( 4.946231610255516387, -5.582088688514999397, 34.36776431015576350 ) ) ;
#86913 = CYLINDRICAL_SURFACE ( 'NONE', #11469, 0.2499999999999994726 ) ;
#86914 = CARTESIAN_POINT ( 'NONE',  ( 17.78205128205128105, -3.499999999999999556, 29.75000000000000355 ) ) ;
#86916 = CARTESIAN_POINT ( 'NONE',  ( 15.23076923076911093, -3.300289026999228881, 32.46337939537708905 ) ) ;
#86915 = SURFACE_STYLE_FILL_AREA ( #5522 ) ;
#86917 = B_SPLINE_CURVE_WITH_KNOTS ( 'NONE', 3,
 ( #30910, #30476, #79110, #58378, #63821, #77338, #44415, #51612, #22831, #70136 ),
 .UNSPECIFIED., .F., .F.,
 ( 4, 2, 2, 2, 4 ),
 ( 0.0007817359430256399806, 0.0009771253907250089001, 0.001172514838424378036, 0.001367904286123746956, 0.001563293733823115875 ),
 .UNSPECIFIED. ) ;
#86918 = CARTESIAN_POINT ( 'NONE',  ( -3.749999999999988454, -9.053300858899127945, 20.01562500000000355 ) ) ;
#86919 = VERTEX_POINT ( 'NONE', #59199 ) ;
#86920 = EDGE_CURVE ( 'NONE', #77395, #23595, #71820, .T. ) ;
#86921 = AXIS2_PLACEMENT_3D ( 'NONE', #81631, #11387, #5529 ) ;
#86922 = VERTEX_POINT ( 'NONE', #10125 ) ;
#86923 = CARTESIAN_POINT ( 'NONE',  ( -14.55766905174090020, -4.818429247618089661, 34.26397095200675125 ) ) ;
#86924 = EDGE_CURVE ( 'NONE', #58859, #18418, #72267, .T. ) ;
#86925 = CARTESIAN_POINT ( 'NONE',  ( 12.23871176905946001, -7.369208160676172348, 34.74850200257122879 ) ) ;
#86926 = CARTESIAN_POINT ( 'NONE',  ( 4.153846153846460609, -2.506253911140614576, 30.00000000000323297 ) ) ;
#86928 = B_SPLINE_CURVE_WITH_KNOTS ( 'NONE', 3,
 ( #65201, #37737, #79173, #71964, #9389, #71080 ),
 .UNSPECIFIED., .F., .F.,
 ( 4, 2, 4 ),
 ( 1.769077770938648657E-17, 0.0001954756301636885322, 0.0003909512603273593376 ),
 .UNSPECIFIED. ) ;
#86927 = CARTESIAN_POINT ( 'NONE',  ( -13.38461538461538325, -1.129524287112498415, 32.06866353760679544 ) ) ;
#86929 = CARTESIAN_POINT ( 'NONE',  ( 2.057692307692309708, -7.500000000000001776, 34.75000000000000000 ) ) ;
#86930 = CARTESIAN_POINT ( 'NONE',  ( 3.750000000000000888, -7.499999999999978684, 21.96875000000000355 ) ) ;
#86931 = CARTESIAN_POINT ( 'NONE',  ( -11.66915214157184622, -9.084618155246140248, 34.75535874321725771 ) ) ;
#86932 = CARTESIAN_POINT ( 'NONE',  ( 1.515407192440172857, -4.809403383903225304, 33.96459661697924304 ) ) ;
#86933 = CARTESIAN_POINT ( 'NONE',  ( -5.076923076923199218, -2.379036618888197729, 30.90682066428292885 ) ) ;
#86934 = CARTESIAN_POINT ( 'NONE',  ( 13.31853300525525086, -9.905515769479276145, 34.41647553114623292 ) ) ;
#86935 = DIRECTION ( 'NONE',  ( 0.000000000000000000, 0.3420201433256641055, -0.9396926207859100932 ) ) ;
#86936 = DIRECTION ( 'NONE',  ( 0.000000000000000000, 0.000000000000000000, -1.000000000000000000 ) ) ;
#86937 = CYLINDRICAL_SURFACE ( 'NONE', #26531, 0.2500000000000004996 ) ;
#86938 = CARTESIAN_POINT ( 'NONE',  ( 7.173022332454967120, -2.341251567377310217, 30.72681386836322659 ) ) ;
#86940 = EDGE_CURVE ( 'NONE', #44583, #61593, #84073, .T. ) ;
#86939 = CARTESIAN_POINT ( 'NONE',  ( 10.86533013373276013, -2.824170634883621744, 31.52227843825338738 ) ) ;
#86941 = CARTESIAN_POINT ( 'NONE',  ( -4.284537620513710010, -8.999036380462719364, 34.52022231692819076 ) ) ;
#86942 = CARTESIAN_POINT ( 'NONE',  ( -7.623374304885435215, -12.44528174975671853, 30.48912976160716681 ) ) ;
#86943 = VERTEX_POINT ( 'NONE', #55876 ) ;
#86944 = FACE_OUTER_BOUND ( 'NONE', #88608, .T. ) ;
#86945 = CARTESIAN_POINT ( 'NONE',  ( -5.207398261998797295, -7.276987145209185215, 34.99546412871779211 ) ) ;
#86946 = DIRECTION ( 'NONE',  ( -0.000000000000000000, -0.9396926207859094271, -0.3420201433256663814 ) ) ;
#86947 = CARTESIAN_POINT ( 'NONE',  ( -2.749999999999999112, -7.438900925035484057, 15.34561829374151465 ) ) ;
#86948 = LINE ( 'NONE', #38288, #47512 ) ;
#86949 = CARTESIAN_POINT ( 'NONE',  ( -17.14300648787895653, -2.538708090699995257, 30.37095296980875148 ) ) ;
#86951 = ORIENTED_EDGE ( 'NONE', *, *, #26863, .T. ) ;
#86950 = DIRECTION ( 'NONE',  ( -0.000000000000000000, 1.000000000000000000, -0.000000000000000000 ) ) ;
#86952 = CARTESIAN_POINT ( 'NONE',  ( -1.139087296526025250, -4.750000000000006217, 20.32812500000000711 ) ) ;
#86953 = CARTESIAN_POINT ( 'NONE',  ( 17.77651505627605033, -3.754499324213721234, 33.06261337010820256 ) ) ;
#86954 = EDGE_CURVE ( 'NONE', #54130, #46293, #86311, .T. ) ;
#86955 = EDGE_LOOP ( 'NONE', ( #79669, #41463 ) ) ;
#86956 = AXIS2_PLACEMENT_3D ( 'NONE', #74047, #37575, #44770 ) ;
#86957 = CARTESIAN_POINT ( 'NONE',  ( 18.22277954126840172, -9.332535724633405749, 34.40230450496446224 ) ) ;
#86958 = EDGE_LOOP ( 'NONE', ( #53802, #19830 ) ) ;
#86959 = CARTESIAN_POINT ( 'NONE',  ( -18.25002323729296450, -11.86270091957321249, 32.19358267280088626 ) ) ;
#86960 = EDGE_CURVE ( 'NONE', #15487, #85101, #52934, .T. ) ;
#86961 = EDGE_CURVE ( 'NONE', #31770, #72596, #20328, .T. ) ;
#86962 = CARTESIAN_POINT ( 'NONE',  ( -15.48074597481782178, -2.920706130388546651, 32.31842814019191223 ) ) ;
#86963 = CARTESIAN_POINT ( 'NONE',  ( 15.36129493253279321, -2.882268652242222284, 31.66798894389554064 ) ) ;
#86964 = ORIENTED_EDGE ( 'NONE', *, *, #29966, .T. ) ;
#86965 = CARTESIAN_POINT ( 'NONE',  ( 0.2386115026316110443, -4.762599654559228846, 34.23009711892697737 ) ) ;
#86966 = EDGE_LOOP ( 'NONE', ( #42187, #15725 ) ) ;
#86967 = DIRECTION ( 'NONE',  ( -0.000000000000000000, -0.5000000000000009992, -0.8660254037844380415 ) ) ;
#86968 = EDGE_CURVE ( 'NONE', #27448, #60033, #70255, .T. ) ;
#86969 = ADVANCED_FACE ( 'NONE', ( #47793 ), #75274, .F. ) ;
#86970 = VERTEX_POINT ( 'NONE', #48227 ) ;
#86971 = CARTESIAN_POINT ( 'NONE',  ( 13.63456090296352841, -11.86320923018887719, 32.19269448109604070 ) ) ;
#86972 = CARTESIAN_POINT ( 'NONE',  ( 0.5267940328144851136, -11.48612834413965977, 32.76840700105972815 ) ) ;
#86973 = FACE_OUTER_BOUND ( 'NONE', #22261, .T. ) ;
#86974 = CARTESIAN_POINT ( 'NONE',  ( -4.153846153846152411, -12.29105614889573062, 35.45975837776705220 ) ) ;
#86975 = CARTESIAN_POINT ( 'NONE',  ( 0.3962684609821414683, -2.379036618887870880, 30.90682066428147579 ) ) ;
#86976 = DIRECTION ( 'NONE',  ( -0.000000000000000000, 0.1736481776669307198, -0.9848077530122080203 ) ) ;
#86977 = ORIENTED_EDGE ( 'NONE', *, *, #1628, .T. ) ;
#86978 = ORIENTED_EDGE ( 'NONE', *, *, #45390, .T. ) ;
#86979 = ORIENTED_EDGE ( 'NONE', *, *, #86699, .T. ) ;
#86981 = ORIENTED_EDGE ( 'NONE', *, *, #63795, .F. ) ;
#86980 = CARTESIAN_POINT ( 'NONE',  ( 3.453548899747295398, -12.69155399931963046, 30.53255429739157734 ) ) ;
#86982 = VECTOR ( 'NONE', #47619, 1000.000000000000000 ) ;
#86983 = AXIS2_PLACEMENT_3D ( 'NONE', #2802, #10015, #83927 ) ;
#86984 = CARTESIAN_POINT ( 'NONE',  ( -8.769230769230890843, -10.21337939537710326, 33.94971097300076224 ) ) ;
#86985 = CARTESIAN_POINT ( 'NONE',  ( 9.442284468086237226, -5.765609946408404518, 34.70566812827425451 ) ) ;
#86986 = ORIENTED_EDGE ( 'NONE', *, *, #27379, .F. ) ;
#86987 = LINE ( 'NONE', #53158, #71754 ) ;
#86988 = B_SPLINE_CURVE_WITH_KNOTS ( 'NONE', 3,
 ( #73045, #18994, #46460, #28864, #49118, #83812, #28401, #54990, #22095, #8587 ),
 .UNSPECIFIED., .F., .F.,
 ( 4, 2, 2, 2, 4 ),
 ( 0.0007817359430256338006, 0.0009771253907250062980, 0.001172514838424371531, 0.001367904286123736981, 0.001563293733823102431 ),
 .UNSPECIFIED. ) ;
#86989 = ORIENTED_EDGE ( 'NONE', *, *, #14845, .T. ) ;
#86990 = CARTESIAN_POINT ( 'NONE',  ( 17.07692307692307665, -9.058645607665452459, 34.76329471203371924 ) ) ;
#86991 = ORIENTED_EDGE ( 'NONE', *, *, #4720, .F. ) ;
#86992 = CARTESIAN_POINT ( 'NONE',  ( -18.25002322422145440, -9.356822207818510151, 34.66110646841856635 ) ) ;
#86993 = CARTESIAN_POINT ( 'NONE',  ( -11.53846153846165912, -3.835265460704628371, 33.15142922262033665 ) ) ;
#86994 = CARTESIAN_POINT ( 'NONE',  ( 0.2386122440223127639, -4.887634598454295265, 34.01352882383564946 ) ) ;
#86995 = FACE_BOUND ( 'NONE', #20689, .T. ) ;
#86996 = CARTESIAN_POINT ( 'NONE',  ( 2.557692307692244871, -7.565270445406050648, 34.75000000000000000 ) ) ;
#86997 = FACE_OUTER_BOUND ( 'NONE', #341, .T. ) ;
#86998 = CARTESIAN_POINT ( 'NONE',  ( -1.384615384615506484, -2.379036618888197285, 30.90682066428292885 ) ) ;
#86999 = CARTESIAN_POINT ( 'NONE',  ( -14.08468095607945969, -5.667800583137506010, 34.40243808032445827 ) ) ;
#87000 = CARTESIAN_POINT ( 'NONE',  ( -4.826977667545033768, -4.176053281294514363, 33.81426240980091791 ) ) ;
#87001 = CARTESIAN_POINT ( 'NONE',  ( -1.384615384615505151, -2.625532179533778709, 30.86335684631627174 ) ) ;
#87002 = ORIENTED_EDGE ( 'NONE', *, *, #56978, .T. ) ;
#87003 = CARTESIAN_POINT ( 'NONE',  ( -0.4615384615384611200, -1.242168528481310874, 33.36296068462461051 ) ) ;
#87004 = EDGE_LOOP ( 'NONE', ( #49088, #28461, #40959, #51767 ) ) ;
#87005 = VERTEX_POINT ( 'NONE', #83363 ) ;
#87006 = VECTOR ( 'NONE', #82260, 1000.000000000000227 ) ;
#87008 = CARTESIAN_POINT ( 'NONE',  ( -1.384615384615383471, -5.471508081941601098, 34.59228464037088457 ) ) ;
#87007 = CARTESIAN_POINT ( 'NONE',  ( 4.153846153846154188, -10.89733346790207413, 36.13435417666054406 ) ) ;
#87009 = DIRECTION ( 'NONE',  ( -0.000000000000000000, 0.1736481776669307198, -0.9848077530122080203 ) ) ;
#87010 = CARTESIAN_POINT ( 'NONE',  ( -4.023320452082589149, -4.459921816937789885, 33.71989282347011851 ) ) ;
#87011 = CARTESIAN_POINT ( 'NONE',  ( 17.07692307692307665, -8.120952969808772792, 34.71129190930000163 ) ) ;
#87012 = CARTESIAN_POINT ( 'NONE',  ( -15.48074596171158746, -3.627789207965226748, 32.91389620160131102 ) ) ;
#87013 = ORIENTED_EDGE ( 'NONE', *, *, #24551, .T. ) ;
#87014 = CARTESIAN_POINT ( 'NONE',  ( 16.94677586748485965, -6.001485441113818986, 34.52039167877662607 ) ) ;
#87015 = CARTESIAN_POINT ( 'NONE',  ( 14.17700084102474989, -11.18331474514187995, 33.13161551792790505 ) ) ;
#87016 = CARTESIAN_POINT ( 'NONE',  ( 10.36540787133602493, -2.920706130388546651, 32.31842814019191223 ) ) ;
#87017 = CARTESIAN_POINT ( 'NONE',  ( 5.142068856255039400, -7.750023238201980469, 34.74374492549440419 ) ) ;
#87018 = ORIENTED_EDGE ( 'NONE', *, *, #12855, .F. ) ;
#87019 = ORIENTED_EDGE ( 'NONE', *, *, #57096, .T. ) ;
#87020 = EDGE_CURVE ( 'NONE', #8013, #45114, #54540, .T. ) ;
#87021 = CONTEXT_DEPENDENT_SHAPE_REPRESENTATION ( #69953, #58549 ) ;
#87022 = ORIENTED_EDGE ( 'NONE', *, *, #32423, .T. ) ;
#87023 = CARTESIAN_POINT ( 'NONE',  ( 17.75000000000000000, -7.433931650972299465, 34.75000000000000711 ) ) ;
#87024 = CARTESIAN_POINT ( 'NONE',  ( -7.623142494540996239, -4.887748414852790546, 34.01359900205216746 ) ) ;
#87025 = VERTEX_POINT ( 'NONE', #75702 ) ;
#87026 = CARTESIAN_POINT ( 'NONE',  ( -14.30769230769242917, -3.643525952248795718, 33.31231777344771672 ) ) ;
#87027 = LINE ( 'NONE', #8584, #58639 ) ;
#87028 = CARTESIAN_POINT ( 'NONE',  ( 5.076923076922954969, -2.892918686052165622, 31.69288490824153470 ) ) ;
#87029 = CARTESIAN_POINT ( 'NONE',  ( 9.019176178608812933, -3.520799739797214389, 33.17531984108286025 ) ) ;
#87030 = LINE ( 'NONE', #79361, #69070 ) ;
#87031 = VERTEX_POINT ( 'NONE', #13126 ) ;
#87033 = VERTEX_POINT ( 'NONE', #55434 ) ;
#87032 = CARTESIAN_POINT ( 'NONE',  ( -0.3954711281883857565, -11.91647553114624358, 32.58852847137148245 ) ) ;
#87034 = CARTESIAN_POINT ( 'NONE',  ( -17.07692307692307665, -3.886160181151819604, 36.00935417666054406 ) ) ;
#87035 = CYLINDRICAL_SURFACE ( 'NONE', #6739, 0.2499999999999997502 ) ;
#87036 = DIRECTION ( 'NONE',  ( 1.000000000000000000, 0.000000000000000000, 0.000000000000000000 ) ) ;
#87037 = CARTESIAN_POINT ( 'NONE',  ( 15.45354877203763522, -12.44528174975671853, 30.48912976160716681 ) ) ;
#87039 = AXIS2_PLACEMENT_3D ( 'NONE', #69481, #28500, #84787 ) ;
#87038 = CARTESIAN_POINT ( 'NONE',  ( -5.749999999999999112, -2.249999999999998668, 29.75000000000000355 ) ) ;
#87040 = EDGE_CURVE ( 'NONE', #1104, #5084, #16414, .T. ) ;
#87041 = LINE ( 'NONE', #25315, #10451 ) ;
#87042 = CARTESIAN_POINT ( 'NONE',  ( -2.724691934501246582, -6.299813628509474128, 17.92374329374151287 ) ) ;
#87043 = ORIENTED_EDGE ( 'NONE', *, *, #62332, .F. ) ;
#87044 = CARTESIAN_POINT ( 'NONE',  ( 14.24160992833216888, -2.292212530054419606, 30.41441678777542634 ) ) ;
#87045 = CARTESIAN_POINT ( 'NONE',  ( 18.00000000000000000, -3.937682226553329556, 33.60647404775216529 ) ) ;
#87046 = DIRECTION ( 'NONE',  ( -0.000000000000000000, 0.8660254037844399289, -0.4999999999999980016 ) ) ;
#87047 = ORIENTED_EDGE ( 'NONE', *, *, #27251, .F. ) ;
#87048 = VERTEX_POINT ( 'NONE', #7706 ) ;
#87049 = CARTESIAN_POINT ( 'NONE',  ( -5.749945580086545327, -12.65882529074907126, 30.72640787790839312 ) ) ;
#87050 = CARTESIAN_POINT ( 'NONE',  ( 7.716005876422151744, -6.809168938359901446, 34.95455904226513866 ) ) ;
#87051 = B_SPLINE_CURVE_WITH_KNOTS ( 'NONE', 3,
 ( #20250, #89168, #27449, #20685, #69324, #76068, #60783, #27890, #54918, #13925 ),
 .UNSPECIFIED., .F., .F.,
 ( 4, 2, 2, 2, 4 ),
 ( 0.000000000000000000, 0.0001954339857564097512, 0.0003908679715128195024, 0.0005863019572692292807, 0.0007817359430256390048 ),
 .UNSPECIFIED. ) ;
#87052 = VECTOR ( 'NONE', #78856, 1000.000000000000000 ) ;
#87053 = CARTESIAN_POINT ( 'NONE',  ( -0.4615384615385840772, -9.528491918059723176, 34.59228464037033035 ) ) ;
#87054 = CARTESIAN_POINT ( 'NONE',  ( 15.90382292962469535, -10.18141759479407327, 34.26406193332782379 ) ) ;
#87055 = B_SPLINE_CURVE_WITH_KNOTS ( 'NONE', 3,
 ( #9507, #1429, #78407, #28921, #36974, #16708, #71647, #64887, #3192, #22148 ),
 .UNSPECIFIED., .F., .F.,
 ( 4, 2, 2, 2, 4 ),
 ( 0.000000000000000000, 0.0001954311564186862781, 0.0003908623128373725562, 0.0005862934692560588072, 0.0007817246256747451124 ),
 .UNSPECIFIED. ) ;
#87056 = CARTESIAN_POINT ( 'NONE',  ( 10.61538461538449596, -9.442884908241554243, 34.35708131394783038 ) ) ;
#87057 = CYLINDRICAL_SURFACE ( 'NONE', #17789, 0.2499999999999994726 ) ;
#87058 = ORIENTED_EDGE ( 'NONE', *, *, #15275, .T. ) ;
#87060 = EDGE_CURVE ( 'NONE', #8641, #2295, #36838, .T. ) ;
#87059 = CARTESIAN_POINT ( 'NONE',  ( 5.933916589044120116, -3.513871655860377086, 32.76840700105978499 ) ) ;
#87061 = ADVANCED_FACE ( 'NONE', ( #21650 ), #49121, .F. ) ;
#87062 = LINE ( 'NONE', #39751, #38345 ) ;
#87063 = CARTESIAN_POINT ( 'NONE',  ( 16.85399685940691938, -9.086856451489516928, 34.49173150075333183 ) ) ;
#87064 = ORIENTED_EDGE ( 'NONE', *, *, #2057, .T. ) ;
#87065 = CARTESIAN_POINT ( 'NONE',  ( 15.90382292962469180, -12.45566812827425096, 31.48439005359158926 ) ) ;
#87066 = VERTEX_POINT ( 'NONE', #63066 ) ;
#87067 = EDGE_CURVE ( 'NONE', #48938, #82422, #13563, .T. ) ;
#87068 = DIRECTION ( 'NONE',  ( 0.000000000000000000, 0.7660444431189807890, 0.6427876096865361433 ) ) ;
#87069 = DIRECTION ( 'NONE',  ( 0.000000000000000000, 0.000000000000000000, 1.000000000000000000 ) ) ;
#87070 = CARTESIAN_POINT ( 'NONE',  ( -13.38461538461538325, -3.669653830205710676, 35.88435417666054406 ) ) ;
#87071 = ORIENTED_EDGE ( 'NONE', *, *, #20823, .T. ) ;
#87072 = CARTESIAN_POINT ( 'NONE',  ( 0.5267940328144853357, -4.481592998940251427, 33.73612834413965089 ) ) ;
#87073 = CARTESIAN_POINT ( 'NONE',  ( 13.44987052412822059, -9.528491918058460186, 34.59228464037086326 ) ) ;
#87074 = DIRECTION ( 'NONE',  ( 0.000000000000000000, 0.000000000000000000, -1.000000000000000000 ) ) ;
#87075 = VECTOR ( 'NONE', #61192, 1000.000000000000227 ) ;
#87076 = DIRECTION ( 'NONE',  ( -0.000000000000000000, -0.8660254037844399289, -0.4999999999999980016 ) ) ;
#87077 = CARTESIAN_POINT ( 'NONE',  ( 3.361294669002873103, -3.068774925481847493, 32.56582465632704526 ) ) ;
#87078 = EDGE_LOOP ( 'NONE', ( #46413, #87092, #39748, #60506 ) ) ;
#87079 = CARTESIAN_POINT ( 'NONE',  ( -17.07692307692319744, -11.48612834414049644, 32.76840700105863391 ) ) ;
#87080 = ORIENTED_EDGE ( 'NONE', *, *, #77256, .T. ) ;
#87081 = CARTESIAN_POINT ( 'NONE',  ( 5.142990410273153401, -11.35647404775217595, 33.31231777344667222 ) ) ;
#87082 = CARTESIAN_POINT ( 'NONE',  ( -13.38461538461538325, -1.422936976036506707, 30.56769352161908415 ) ) ;
#87083 = CARTESIAN_POINT ( 'NONE',  ( -16.15384615384615330, -13.75783147151868846, 33.36296068462461051 ) ) ;
#87084 = CARTESIAN_POINT ( 'NONE',  ( 18.00000000000000000, -12.62096338111211580, 30.90682066428153263 ) ) ;
#87085 = DIRECTION ( 'NONE',  ( -0.000000000000000000, 0.1736481776669307198, -0.9848077530122080203 ) ) ;
#87086 = CARTESIAN_POINT ( 'NONE',  ( 7.846153846153846700, -6.386643153685126251, 34.62446782046654192 ) ) ;
#87087 = CARTESIAN_POINT ( 'NONE',  ( 4.500000000000003553, -7.499999999999999112, 13.50000000000000178 ) ) ;
#87088 = ORIENTED_EDGE ( 'NONE', *, *, #78257, .T. ) ;
#87089 = VERTEX_POINT ( 'NONE', #31052 ) ;
#87090 = VERTEX_POINT ( 'NONE', #16654 ) ;
#87091 = EDGE_LOOP ( 'NONE', ( #29177, #57118 ) ) ;
#87092 = ORIENTED_EDGE ( 'NONE', *, *, #65454, .F. ) ;
#87093 = CARTESIAN_POINT ( 'NONE',  ( -4.376772371362299907, -5.667676309546437530, 34.40238873228292249 ) ) ;
#87094 = CARTESIAN_POINT ( 'NONE',  ( -2.176900499867521432, -3.062576670634119758, 32.05464942895959979 ) ) ;
#87095 = CARTESIAN_POINT ( 'NONE',  ( -4.088590582570127197, -9.442884908240271713, 34.35708131394835618 ) ) ;
#87096 = CARTESIAN_POINT ( 'NONE',  ( -15.84615384615384670, -4.000000000000000000, 29.75000000000000355 ) ) ;
#87097 = CARTESIAN_POINT ( 'NONE',  ( 13.31934493865461278, -8.613356846314824011, 34.62446782046655613 ) ) ;
#87098 = CARTESIAN_POINT ( 'NONE',  ( 3.100077764101672795, -5.582088688514999397, 34.36776431015576350 ) ) ;
#87099 = CARTESIAN_POINT ( 'NONE',  ( -5.326946314216042033, -8.432397168068783699, 34.66272746175022945 ) ) ;
#87100 = CARTESIAN_POINT ( 'NONE',  ( 9.626225312947559232, -9.905515769479276145, 34.41647553114623292 ) ) ;
#87101 = DIRECTION ( 'NONE',  ( -0.000000000000000000, 0.8660254037844397068, -0.4999999999999978906 ) ) ;
#87102 = ORIENTED_EDGE ( 'NONE', *, *, #87743, .F. ) ;
#87103 = VECTOR ( 'NONE', #84216, 1000.000000000000114 ) ;
#87104 = VERTEX_POINT ( 'NONE', #2248 ) ;
#87105 = EDGE_CURVE ( 'NONE', #52314, #50355, #27108, .T. ) ;
#87106 = VERTEX_POINT ( 'NONE', #37365 ) ;
#87108 = VERTEX_POINT ( 'NONE', #77045 ) ;
#87107 = CARTESIAN_POINT ( 'NONE',  ( 18.00000000000000000, -1.129524287112498415, 32.06866353760679544 ) ) ;
#87110 = LINE ( 'NONE', #52847, #31897 ) ;
#87109 = CARTESIAN_POINT ( 'NONE',  ( 16.28463796167094202, -11.71459661697925903, 32.44059661609676937 ) ) ;
#87111 = FACE_OUTER_BOUND ( 'NONE', #43511, .T. ) ;
#87112 = DIRECTION ( 'NONE',  ( -0.000000000000000000, -0.9396926207859092051, -0.3420201433256662704 ) ) ;
#87113 = FACE_BOUND ( 'NONE', #19165, .T. ) ;
#87114 = ORIENTED_EDGE ( 'NONE', *, *, #4064, .F. ) ;
#87115 = B_SPLINE_CURVE_WITH_KNOTS ( 'NONE', 3,
 ( #71468, #43560, #36805, #85005, #63834, #28734, #76914, #77790, #9776, #16530 ),
 .UNSPECIFIED., .F., .F.,
 ( 4, 2, 2, 2, 4 ),
 ( 0.0007817246256747442451, 0.0009771112852218865989, 0.001172497944769029061, 0.001367884604316171523, 0.001563271263863313986 ),
 .UNSPECIFIED. ) ;
#87116 = ORIENTED_EDGE ( 'NONE', *, *, #44833, .T. ) ;
#87117 = CARTESIAN_POINT ( 'NONE',  ( -2.084316366994122482, -2.501478030877322567, 29.88021232661720816 ) ) ;
#87118 = EDGE_LOOP ( 'NONE', ( #17866, #43866, #14024, #22397 ) ) ;
#87119 = FACE_BOUND ( 'NONE', #4215, .T. ) ;
#87120 = CARTESIAN_POINT ( 'NONE',  ( -10.86540783960607115, -2.985938066672154445, 32.43141759479405550 ) ) ;
#87121 = EDGE_CURVE ( 'NONE', #50871, #46562, #30613, .T. ) ;
#87122 = CARTESIAN_POINT ( 'NONE',  ( 7.911346834448499621, -2.255955759149235629, 29.99999999999988631 ) ) ;
#87123 = ORIENTED_EDGE ( 'NONE', *, *, #84967, .T. ) ;
#87124 = CARTESIAN_POINT ( 'NONE',  ( -15.10024352900566669, -12.27024696741798948, 31.24895572276497546 ) ) ;
#87125 = CARTESIAN_POINT ( 'NONE',  ( 4.230769230769229061, -7.500000000000000000, 29.75000000000000355 ) ) ;
#87126 = CARTESIAN_POINT ( 'NONE',  ( -5.011778296203443617, -7.750023224968867197, 34.99404313364389907 ) ) ;
#87127 = ORIENTED_EDGE ( 'NONE', *, *, #88082, .T. ) ;
#87128 = EDGE_CURVE ( 'NONE', #74921, #47387, #77480, .T. ) ;
#87129 = DIRECTION ( 'NONE',  ( 0.000000000000000000, 0.7660444431189807890, 0.6427876096865361433 ) ) ;
#87130 = CARTESIAN_POINT ( 'NONE',  ( 6.923076923076924238, -5.471508081941601098, 34.59228464037088457 ) ) ;
#87131 = CYLINDRICAL_SURFACE ( 'NONE', #46148, 0.2499999999999994726 ) ;
#87132 = EDGE_LOOP ( 'NONE', ( #660, #2807, #19879, #72441 ) ) ;
#87133 = DIRECTION ( 'NONE',  ( -0.000000000000000000, 0.5000000000000011102, -0.8660254037844380415 ) ) ;
#87134 = DIRECTION ( 'NONE',  ( 0.000000000000000000, 0.4999999999999985567, 0.8660254037844395958 ) ) ;
#87135 = ORIENTED_EDGE ( 'NONE', *, *, #88355, .F. ) ;
#87136 = CARTESIAN_POINT ( 'NONE',  ( -17.32694630114453460, -12.68155406624981119, 30.59749803192733708 ) ) ;
#87137 = CARTESIAN_POINT ( 'NONE',  ( 14.55774661933062575, -8.303483539816731707, 34.68545999027711702 ) ) ;
#87138 = CARTESIAN_POINT ( 'NONE',  ( 1.384615384615264011, -12.16647553114689728, 32.15551576947799362 ) ) ;
#87139 = CARTESIAN_POINT ( 'NONE',  ( 8.069116749715332659, -7.369474270740070665, 34.74850911626239025 ) ) ;
#87140 = CYLINDRICAL_SURFACE ( 'NONE', #73240, 0.2499999999999995559 ) ;
#87141 = CARTESIAN_POINT ( 'NONE',  ( 0.4615384615384611200, -12.10708131394839349, 31.69288490824020244 ) ) ;
#87143 = LINE ( 'NONE', #47010, #30201 ) ;
#87142 = DIRECTION ( 'NONE',  ( 1.000000000000000000, 0.000000000000000000, -0.000000000000000000 ) ) ;
#87144 = EDGE_CURVE ( 'NONE', #24035, #13064, #86015, .T. ) ;
#87145 = CARTESIAN_POINT ( 'NONE',  ( 8.769230769230768274, -2.486705287966279876, 31.30864560766543647 ) ) ;
#87146 = DIRECTION ( 'NONE',  ( 0.000000000000000000, 0.9848077530122072432, 0.1736481776669354937 ) ) ;
#87147 = CARTESIAN_POINT ( 'NONE',  ( 1.987747218494664292, -9.401340078031346081, 25.62313170625849068 ) ) ;
#87148 = ORIENTED_EDGE ( 'NONE', *, *, #49926, .T. ) ;
#87149 = FACE_OUTER_BOUND ( 'NONE', #58242, .T. ) ;
#87150 = EDGE_LOOP ( 'NONE', ( #69995, #52489, #7545, #44920 ) ) ;
#87151 = EDGE_CURVE ( 'NONE', #74998, #87392, #20724, .T. ) ;
#87152 = ORIENTED_EDGE ( 'NONE', *, *, #85703, .F. ) ;
#87153 = CARTESIAN_POINT ( 'NONE',  ( -16.94639763868943660, -4.299079248970731015, 33.91157788607253565 ) ) ;
#87154 = ORIENTED_EDGE ( 'NONE', *, *, #58857, .F. ) ;
#87155 = CARTESIAN_POINT ( 'NONE',  ( 18.24999999999993250, -7.565270445406050648, 34.75000000000000000 ) ) ;
#87156 = CARTESIAN_POINT ( 'NONE',  ( 1.139087296525997273, -4.749999999999992895, 14.23437500000000355 ) ) ;
#87157 = CARTESIAN_POINT ( 'NONE',  ( -19.00000000000000000, -8.999999999999996447, 22.25000000000000000 ) ) ;
#87158 = CARTESIAN_POINT ( 'NONE',  ( 10.74591005361825680, -2.647132371071621471, 31.75357179365171589 ) ) ;
#87159 = DIRECTION ( 'NONE',  ( 0.000000000000000000, 0.4999999999999960032, -0.8660254037844410391 ) ) ;
#87160 = CARTESIAN_POINT ( 'NONE',  ( -14.55766905174089665, -10.82459398097509329, 33.81372124010185587 ) ) ;
#87161 = LINE ( 'NONE', #46160, #28865 ) ;
#87162 = CARTESIAN_POINT ( 'NONE',  ( -8.769230769230768274, -12.29105614889573062, 35.45975837776705220 ) ) ;
#87163 = CYLINDRICAL_SURFACE ( 'NONE', #48271, 0.2499999999999995837 ) ;
#87164 = B_SPLINE_CURVE_WITH_KNOTS ( 'NONE', 3,
 ( #44044, #23336, #10722, #30975, #51224, #79626, #58441, #50793, #37293, #17030 ),
 .UNSPECIFIED., .F., .F.,
 ( 4, 2, 2, 2, 4 ),
 ( 0.0007817359430256285964, 0.0009771253907249943717, 0.001172514838424360255, 0.001367904286123726139, 0.001563293733823092023 ),
 .UNSPECIFIED. ) ;
#87165 = CARTESIAN_POINT ( 'NONE',  ( 2.320192649118979489E-14, -11.25000000000000000, 19.78125000000000000 ) ) ;
#87166 = AXIS2_PLACEMENT_3D ( 'NONE', #2561, #30487, #16528 ) ;
#87167 = CARTESIAN_POINT ( 'NONE',  ( 17.07692307692295586, -2.379036618888197729, 30.90682066428292885 ) ) ;
#87169 = EDGE_CURVE ( 'NONE', #17395, #29922, #50869, .T. ) ;
#87168 = CARTESIAN_POINT ( 'NONE',  ( -10.36538461538461320, -2.249999999999998668, 29.75000000000000355 ) ) ;
#87170 = EDGE_CURVE ( 'NONE', #30322, #28929, #64390, .T. ) ;
#87171 = LINE ( 'NONE', #25447, #69437 ) ;
#87172 = ORIENTED_EDGE ( 'NONE', *, *, #56584, .T. ) ;
#87174 = EDGE_CURVE ( 'NONE', #235, #45953, #35754, .T. ) ;
#87173 = VERTEX_POINT ( 'NONE', #23843 ) ;
#87175 = CARTESIAN_POINT ( 'NONE',  ( -11.31545018684868786, -5.667800583137506010, 34.40243808032445827 ) ) ;
#87176 = CARTESIAN_POINT ( 'NONE',  ( 7.596130608860880429, -11.37209801155882971, 32.91403422569032955 ) ) ;
#87177 = CARTESIAN_POINT ( 'NONE',  ( -2.438382910802614045, -2.295517848115769421, 30.44137282052137294 ) ) ;
#87178 = FACE_OUTER_BOUND ( 'NONE', #43374, .T. ) ;
#87179 = EDGE_CURVE ( 'NONE', #64886, #50355, #29309, .T. ) ;
#87180 = AXIS2_PLACEMENT_3D ( 'NONE', #29172, #85871, #84556 ) ;
#87181 = CARTESIAN_POINT ( 'NONE',  ( 8.703147358274888390, -4.098570777380720287, 33.41473453929634729 ) ) ;
#87182 = CARTESIAN_POINT ( 'NONE',  ( 7.846153846153846700, -9.819645486525091727, 36.12317359536749706 ) ) ;
#87183 = ORIENTED_EDGE ( 'NONE', *, *, #35859, .F. ) ;
#87184 = CARTESIAN_POINT ( 'NONE',  ( -4.853911725310226188, -12.39991518177334129, 30.74647679643404530 ) ) ;
#87185 = EDGE_LOOP ( 'NONE', ( #67002, #80555, #29733, #34119 ) ) ;
#87186 = EDGE_LOOP ( 'NONE', ( #26221, #68561, #16846, #16749 ) ) ;
#87187 = DIRECTION ( 'NONE',  ( 0.000000000000000000, 0.000000000000000000, -1.000000000000000000 ) ) ;
#87188 = CARTESIAN_POINT ( 'NONE',  ( -14.30769230769242917, -6.835583212225970762, 34.95778746994575670 ) ) ;
#87189 = AXIS2_PLACEMENT_3D ( 'NONE', #20988, #48459, #75945 ) ;
#87190 = CARTESIAN_POINT ( 'NONE',  ( -9.469296340694841163, -6.503523203565941380, 34.64991518177335195 ) ) ;
#87191 = CARTESIAN_POINT ( 'NONE',  ( 6.000000000000001776, -8.164416787775445883, 34.95778746994557906 ) ) ;
#87192 = CARTESIAN_POINT ( 'NONE',  ( -5.207613680033384540, -8.191372820521381826, 34.95448215188423546 ) ) ;
#87193 = VECTOR ( 'NONE', #50139, 1000.000000000000227 ) ;
#87194 = EDGE_LOOP ( 'NONE', ( #78284, #57513, #13378, #25694 ) ) ;
#87195 = EDGE_LOOP ( 'NONE', ( #68457, #16600, #42425, #12227 ) ) ;
#87196 = B_SPLINE_CURVE_WITH_KNOTS ( 'NONE', 3,
 ( #79917, #60971, #25416, #53772, #88477, #33062, #18221, #74493, #18672, #66401 ),
 .UNSPECIFIED., .F., .F.,
 ( 4, 2, 2, 2, 4 ),
 ( 0.0007817246336856291692, 0.0009771112958940103739, 0.001172497958102391470, 0.001367884620310772566, 0.001563271282519153879 ),
 .UNSPECIFIED. ) ;
#87197 = EDGE_CURVE ( 'NONE', #84168, #29224, #78355, .T. ) ;
#87198 = VERTEX_POINT ( 'NONE', #56761 ) ;
#87199 = CARTESIAN_POINT ( 'NONE',  ( 17.20744851515672025, -10.31582465632704704, 34.18122507451815295 ) ) ;
#87200 = DIRECTION ( 'NONE',  ( 0.000000000000000000, 1.000000000000000000, 0.000000000000000000 ) ) ;
#87201 = DIRECTION ( 'NONE',  ( -0.000000000000000000, 1.000000000000000000, 3.491481338843133355E-15 ) ) ;
#87202 = CARTESIAN_POINT ( 'NONE',  ( 27.00000000000000000, -17.00000000000000000, 2.999999999999999112 ) ) ;
#87203 = DIRECTION ( 'NONE',  ( -0.000000000000000000, 0.1736481776669307198, -0.9848077530122080203 ) ) ;
#87204 = FACE_OUTER_BOUND ( 'NONE', #14992, .T. ) ;
#87205 = ORIENTED_EDGE ( 'NONE', *, *, #76266, .F. ) ;
#87206 = ADVANCED_FACE ( 'NONE', ( #3136 ), #72044, .F. ) ;
#87207 = ORIENTED_EDGE ( 'NONE', *, *, #31768, .T. ) ;
#87208 = CARTESIAN_POINT ( 'NONE',  ( 0.6843180028068708287, -11.89424750095246175, 32.13594075562311758 ) ) ;
#87209 = ADVANCED_FACE ( 'NONE', ( #65287 ), #57209, .F. ) ;
#87211 = VERTEX_POINT ( 'NONE', #84257 ) ;
#87210 = CARTESIAN_POINT ( 'NONE',  ( -12.71151519248081740, -11.28823185664190376, 33.01397839955799896 ) ) ;
#87212 = DIRECTION ( 'NONE',  ( -0.000000000000000000, -0.5000000000000009992, -0.8660254037844380415 ) ) ;
#87213 = CARTESIAN_POINT ( 'NONE',  ( -9.692307692307691624, -11.69971097300155272, 32.46337939537588113 ) ) ;
#87214 = AXIS2_PLACEMENT_3D ( 'NONE', #87034, #25308, #4593 ) ;
#87215 = CARTESIAN_POINT ( 'NONE',  ( 1.553300858899086867, -3.749999999999992006, 15.48437499999999822 ) ) ;
#87216 = ORIENTED_EDGE ( 'NONE', *, *, #60319, .T. ) ;
#87217 = CARTESIAN_POINT ( 'NONE',  ( -14.30769230769242917, -12.51329471203414379, 31.30864560766407578 ) ) ;
#87218 = ORIENTED_EDGE ( 'NONE', *, *, #30467, .F. ) ;
#87219 = CARTESIAN_POINT ( 'NONE',  ( 2.557746619330623528, -9.148310452688873440, 34.47095581063188519 ) ) ;
#87220 = CARTESIAN_POINT ( 'NONE',  ( 14.30769230769231015, -12.34228464037088635, 31.77849191805839268 ) ) ;
#87221 = DIRECTION ( 'NONE',  ( 0.000000000000000000, 0.000000000000000000, -1.000000000000000000 ) ) ;
#87223 = CYLINDRICAL_SURFACE ( 'NONE', #18627, 0.2500000000000002220 ) ;
#87222 = DIRECTION ( 'NONE',  ( -0.000000000000000000, 1.000000000000000000, 3.491481338843133355E-15 ) ) ;
#87224 = EDGE_CURVE ( 'NONE', #61379, #51951, #50002, .T. ) ;
#87225 = LINE ( 'NONE', #28610, #21824 ) ;
#87226 = ORIENTED_EDGE ( 'NONE', *, *, #70824, .F. ) ;
#87227 = CARTESIAN_POINT ( 'NONE',  ( 11.40831356872984514, -11.66186481527757302, 32.95055677023626117 ) ) ;
#87228 = VECTOR ( 'NONE', #57241, 1000.000000000000000 ) ;
#87229 = CARTESIAN_POINT ( 'NONE',  ( -8.769230769230768274, -3.937682226553329556, 33.60647404775216529 ) ) ;
#87230 = EDGE_CURVE ( 'NONE', #46109, #72161, #67958, .T. ) ;
#87231 = CARTESIAN_POINT ( 'NONE',  ( -15.23076923076922995, -11.33034616979429110, 35.88435417666054406 ) ) ;
#87232 = EDGE_LOOP ( 'NONE', ( #74007, #196, #16853, #19365 ) ) ;
#87233 = CARTESIAN_POINT ( 'NONE',  ( -6.923076923076922462, -1.509761064869970415, 31.06009739812519044 ) ) ;
#87234 = CARTESIAN_POINT ( 'NONE',  ( 14.55774672760575861, -10.06805714834173493, 34.32951233291982618 ) ) ;
#87235 = CYLINDRICAL_SURFACE ( 'NONE', #84529, 0.2500000000000002220 ) ;
#87236 = CARTESIAN_POINT ( 'NONE',  ( -3.230769230769229949, -3.937682226553329556, 33.60647404775216529 ) ) ;
#87237 = FACE_BOUND ( 'NONE', #66728, .T. ) ;
#87239 = CARTESIAN_POINT ( 'NONE',  ( -18.00000000000000000, -1.812984705146277520, 34.52197243641129631 ) ) ;
#87238 = CARTESIAN_POINT ( 'NONE',  ( -0.4615384615384611200, -2.499999999999998668, 29.75000000000001421 ) ) ;
#87240 = EDGE_CURVE ( 'NONE', #83195, #1868, #80887, .T. ) ;
#87241 = CARTESIAN_POINT ( 'NONE',  ( 9.692307692308000711, -2.506253911140615021, 30.00000000000323297 ) ) ;
#87243 = CARTESIAN_POINT ( 'NONE',  ( -11.28851612908349722, -10.92531984108285670, 33.72920026020278073 ) ) ;
#87242 = CARTESIAN_POINT ( 'NONE',  ( 18.22277954126840172, -11.41317474335729543, 32.86274602512330034 ) ) ;
#87244 = CARTESIAN_POINT ( 'NONE',  ( 0.6089743589743582541, -3.499999999999999556, 29.75000000000000355 ) ) ;
#87245 = CARTESIAN_POINT ( 'NONE',  ( 6.222779668978065004, -4.989023458446560255, 34.36081565061822118 ) ) ;
#87246 = CARTESIAN_POINT ( 'NONE',  ( -1.492201783934549164, -11.27530806549876807, 23.35750670625849423 ) ) ;
#87247 = CARTESIAN_POINT ( 'NONE',  ( -7.053224132515143907, -9.418419913701741919, 34.36755862841477693 ) ) ;
#87248 = EDGE_LOOP ( 'NONE', ( #29093, #58745 ) ) ;
#87249 = DIRECTION ( 'NONE',  ( 0.000000000000000000, 1.000000000000000000, 0.000000000000000000 ) ) ;
#87250 = B_SPLINE_CURVE_WITH_KNOTS ( 'NONE', 3,
 ( #62619, #35610, #83357, #49562, #48222, #75696, #49115, #68941, #42375, #83809 ),
 .UNSPECIFIED., .F., .F.,
 ( 4, 2, 2, 2, 4 ),
 ( 0.000000000000000000, 0.0001954339857564078809, 0.0003908679715128157619, 0.0005863019572692236428, 0.0007817359430256315238 ),
 .UNSPECIFIED. ) ;
#87251 = CARTESIAN_POINT ( 'NONE',  ( 2.057715563643717438, -2.318417181685854533, 30.59732222474233865 ) ) ;
#87252 = LINE ( 'NONE', #80937, #20112 ) ;
#87253 = DIRECTION ( 'NONE',  ( -1.000000000000000000, 0.000000000000000000, -0.000000000000000000 ) ) ;
#87254 = CARTESIAN_POINT ( 'NONE',  ( -17.07692307692319744, -2.379036618888197285, 30.90682066428292885 ) ) ;
#87255 = CARTESIAN_POINT ( 'NONE',  ( -11.66860950819323506, -4.299443229763728169, 33.91186481527756058 ) ) ;
#87256 = CARTESIAN_POINT ( 'NONE',  ( -2.749999999999997780, -7.561099074964547917, 16.09188170625848713 ) ) ;
#87257 = CARTESIAN_POINT ( 'NONE',  ( 15.23076923076923173, -3.513871655860378418, 32.76840700105978499 ) ) ;
#87258 = DIRECTION ( 'NONE',  ( 0.000000000000000000, 0.7660444431189822323, -0.6427876096865344779 ) ) ;
#87259 = VECTOR ( 'NONE', #79744, 1000.000000000000114 ) ;
#87260 = CARTESIAN_POINT ( 'NONE',  ( 0.5000075107691263065, -4.795837932143704130, 29.33696104038925156 ) ) ;
#87261 = CARTESIAN_POINT ( 'NONE',  ( 4.946775107191381693, -9.504002272028875709, 34.60269587691767867 ) ) ;
#87262 = CARTESIAN_POINT ( 'NONE',  ( 6.988332494352947677, -4.481592998940251427, 33.73612834413965089 ) ) ;
#87263 = CYLINDRICAL_SURFACE ( 'NONE', #36819, 0.2500000000000009437 ) ;
#87265 = EDGE_CURVE ( 'NONE', #2304, #36412, #79260, .T. ) ;
#87264 = CARTESIAN_POINT ( 'NONE',  ( 9.442307692307693401, -7.500000000000001776, 34.75000000000000000 ) ) ;
#87266 = CARTESIAN_POINT ( 'NONE',  ( 1.384615384615386802, -3.886160181151819604, 36.00935417666054406 ) ) ;
#87267 = VERTEX_POINT ( 'NONE', #86479 ) ;
#87268 = CARTESIAN_POINT ( 'NONE',  ( -10.61538461538473399, -12.46129190930018460, 30.37095296980731973 ) ) ;
#87269 = LINE ( 'NONE', #39964, #47491 ) ;
#87270 = CARTESIAN_POINT ( 'NONE',  ( 3.775308065498752086, -6.007798216065404873, 18.39249329374151642 ) ) ;
#87271 = B_SPLINE_CURVE_WITH_KNOTS ( 'NONE', 3,
 ( #79484, #45237, #44785, #65952, #16880, #65510 ),
 .UNSPECIFIED., .F., .F.,
 ( 4, 2, 4 ),
 ( 0.0003909569690057848211, 0.0005862646681846116680, 0.0007815723673634385150 ),
 .UNSPECIFIED. ) ;
#87272 = EDGE_CURVE ( 'NONE', #88008, #77586, #60757, .T. ) ;
#87273 = CARTESIAN_POINT ( 'NONE',  ( -10.86536135943320502, -10.06842814019191401, 34.32929386961144758 ) ) ;
#87274 = CARTESIAN_POINT ( 'NONE',  ( -16.28453675695646652, -10.70098750199973203, 33.91152734681376302 ) ) ;
#87275 = ORIENTED_EDGE ( 'NONE', *, *, #70790, .F. ) ;
#87276 = DIRECTION ( 'NONE',  ( 0.000000000000000000, 0.4999999999999985567, 0.8660254037844395958 ) ) ;
#87277 = CARTESIAN_POINT ( 'NONE',  ( 9.561617089197389063, -12.62707690430377383, 30.88035979386743435 ) ) ;
#87279 = ORIENTED_EDGE ( 'NONE', *, *, #26907, .F. ) ;
#87278 = CARTESIAN_POINT ( 'NONE',  ( 7.911408985666682270, -2.657715359629132301, 31.77849191805844242 ) ) ;
#87280 = CARTESIAN_POINT ( 'NONE',  ( -13.31854703361294590, -11.16473453929635440, 33.15142922261926373 ) ) ;
#87281 = CARTESIAN_POINT ( 'NONE',  ( -3.165513659493205179, -3.835265460703683349, 33.15142922261929925 ) ) ;
#87282 = EDGE_CURVE ( 'NONE', #40851, #55169, #52662, .T. ) ;
#87283 = CARTESIAN_POINT ( 'NONE',  ( -5.999999999999998224, -2.721908614388771852, 31.22303859784724978 ) ) ;
#87284 = CARTESIAN_POINT ( 'NONE',  ( 11.53846153846141753, -9.442884908241554243, 34.35708131394783038 ) ) ;
#87285 = ORIENTED_EDGE ( 'NONE', *, *, #396, .F. ) ;
#87286 = CARTESIAN_POINT ( 'NONE',  ( 20.00000000000000000, -4.000000000000000000, 29.75000000000000355 ) ) ;
#87287 = CARTESIAN_POINT ( 'NONE',  ( -8.769230769230892619, -2.657715359629662544, 31.77849191805970364 ) ) ;
#87288 = AXIS2_PLACEMENT_3D ( 'NONE', #14576, #42061, #69517 ) ;
#87289 = LINE ( 'NONE', #73771, #22587 ) ;
#87290 = ORIENTED_EDGE ( 'NONE', *, *, #20273, .F. ) ;
#87291 = VERTEX_POINT ( 'NONE', #18890 ) ;
#87292 = ADVANCED_FACE ( 'NONE', ( #38269, #80606, #19336 ), #66173, .F. ) ;
#87293 = ORIENTED_EDGE ( 'NONE', *, *, #77886, .T. ) ;
#87294 = CARTESIAN_POINT ( 'NONE',  ( 0.2386122440223130969, -8.239355502252617924, 34.69524867566427417 ) ) ;
#87295 = CARTESIAN_POINT ( 'NONE',  ( 11.53846153846141753, -11.94971097300221174, 32.03036669348237098 ) ) ;
#87296 = EDGE_CURVE ( 'NONE', #80807, #57115, #87366, .T. ) ;
#87297 = VECTOR ( 'NONE', #81518, 1000.000000000000000 ) ;
#87298 = CARTESIAN_POINT ( 'NONE',  ( -12.68502340526241312, -3.754499324213721234, 33.06261337010820256 ) ) ;
#87299 = CARTESIAN_POINT ( 'NONE',  ( 15.90386942290380290, -4.943428324936578910, 34.04746400365624481 ) ) ;
#87300 = ORIENTED_EDGE ( 'NONE', *, *, #50083, .T. ) ;
#87301 = ADVANCED_FACE ( 'NONE', ( #80150 ), #59427, .F. ) ;
#87302 = ORIENTED_EDGE ( 'NONE', *, *, #45316, .F. ) ;
#87303 = ORIENTED_EDGE ( 'NONE', *, *, #77878, .T. ) ;
#87305 = ORIENTED_EDGE ( 'NONE', *, *, #12405, .F. ) ;
#87304 = CARTESIAN_POINT ( 'NONE',  ( 20.00000000000000711, -9.999999999999994671, 13.00000000000000178 ) ) ;
#87306 = FACE_OUTER_BOUND ( 'NONE', #14642, .T. ) ;
#87307 = ADVANCED_FACE ( 'NONE', ( #72490 ), #4023, .F. ) ;
#87308 = CARTESIAN_POINT ( 'NONE',  ( 0.4615384615384611200, -8.120952969808772792, 34.71129190930000163 ) ) ;
#87309 = EDGE_CURVE ( 'NONE', #41914, #42943, #65865, .T. ) ;
#87310 = AXIS2_PLACEMENT_3D ( 'NONE', #37515, #44256, #56901 ) ;
#87311 = CARTESIAN_POINT ( 'NONE',  ( 1.450683735617823933, -10.51840700105979565, 33.73612834413962247 ) ) ;
#87312 = CARTESIAN_POINT ( 'NONE',  ( -2.307692307692305711, -6.386643153685126251, 34.62446782046654192 ) ) ;
#87313 = EDGE_LOOP ( 'NONE', ( #59267, #33040, #11985, #67260 ) ) ;
#87314 = ORIENTED_EDGE ( 'NONE', *, *, #56342, .T. ) ;
#87315 = EDGE_CURVE ( 'NONE', #51469, #57712, #60450, .T. ) ;
#87316 = ORIENTED_EDGE ( 'NONE', *, *, #79566, .T. ) ;
#87317 = CARTESIAN_POINT ( 'NONE',  ( -10.86536135943320502, -10.82459398097509329, 33.81372124010185587 ) ) ;
#87319 = VERTEX_POINT ( 'NONE', #7149 ) ;
#87318 = CARTESIAN_POINT ( 'NONE',  ( 5.207714884747860928, -4.809403383903225304, 33.96459661697924304 ) ) ;
#87320 = CARTESIAN_POINT ( 'NONE',  ( 18.24994540937804643, -12.07971442181321997, 32.31769673815850297 ) ) ;
#87321 = CARTESIAN_POINT ( 'NONE',  ( -0.2385256174450673672, -4.762714258010882773, 34.23016756924214832 ) ) ;
#87322 = ADVANCED_FACE ( 'NONE', ( #20225 ), #83257, .F. ) ;
#87323 = VECTOR ( 'NONE', #41730, 1000.000000000000227 ) ;
#87324 = CARTESIAN_POINT ( 'NONE',  ( 16.37662569511456567, -8.496831190052089866, 34.64984203495476578 ) ) ;
#87325 = CARTESIAN_POINT ( 'NONE',  ( -19.50000000000000000, -11.50000000000000000, 29.75000000000000355 ) ) ;
#87326 = CARTESIAN_POINT ( 'NONE',  ( -5.777220331021931443, -3.563462043263029955, 33.22394488606062879 ) ) ;
#87327 = FACE_BOUND ( 'NONE', #81877, .T. ) ;
#87328 = DIRECTION ( 'NONE',  ( -1.734723475976813750E-16, 1.000000000000000000, -0.000000000000000000 ) ) ;
#87329 = CARTESIAN_POINT ( 'NONE',  ( -12.46153846153846168, -8.973038597847269315, 34.52809138561121927 ) ) ;
#87330 = FACE_OUTER_BOUND ( 'NONE', #71653, .T. ) ;
#87332 = CARTESIAN_POINT ( 'NONE',  ( 6.923076923076800782, -11.06231777344772027, 33.60647404775119895 ) ) ;
#87331 = CARTESIAN_POINT ( 'NONE',  ( 0.3962684609821414128, -6.835583212224500826, 34.95778746994557906 ) ) ;
#87333 = CARTESIAN_POINT ( 'NONE',  ( -19.00000000000000000, -8.999999999999996447, 22.25000000000000000 ) ) ;
#87334 = FACE_OUTER_BOUND ( 'NONE', #12706, .T. ) ;
#87335 = ORIENTED_EDGE ( 'NONE', *, *, #86324, .F. ) ;
#87336 = CARTESIAN_POINT ( 'NONE',  ( 2.373760658694747061, -6.386643153685127139, 34.62446782046654192 ) ) ;
#87337 = DIRECTION ( 'NONE',  ( -0.000000000000000000, 0.5000000000000011102, -0.8660254037844381525 ) ) ;
#87338 = ORIENTED_EDGE ( 'NONE', *, *, #13521, .F. ) ;
#87339 = ADVANCED_FACE ( 'NONE', ( #21543 ), #34621, .F. ) ;
#87340 = ORIENTED_EDGE ( 'NONE', *, *, #61453, .T. ) ;
#87341 = LINE ( 'NONE', #53073, #49179 ) ;
#87342 = FACE_OUTER_BOUND ( 'NONE', #9065, .T. ) ;
#87343 = CARTESIAN_POINT ( 'NONE',  ( -3.230769230769229949, -8.120952969808772792, 34.71129190930000163 ) ) ;
#87344 = EDGE_LOOP ( 'NONE', ( #59699, #4232 ) ) ;
#87345 = AXIS2_PLACEMENT_3D ( 'NONE', #38627, #44473, #57558 ) ;
#87346 = DIRECTION ( 'NONE',  ( -0.000000000000000000, -0.7660444431189791237, -0.6427876096865379196 ) ) ;
#87347 = FACE_OUTER_BOUND ( 'NONE', #4422, .T. ) ;
#87349 = CARTESIAN_POINT ( 'NONE',  ( -5.076923076923075762, -7.500000000000001776, 35.04278698407183867 ) ) ;
#87348 = LINE ( 'NONE', #45440, #54728 ) ;
#87350 = CARTESIAN_POINT ( 'NONE',  ( -12.71156169883143150, -5.056417327199099532, 34.11270091957321426 ) ) ;
#87351 = CARTESIAN_POINT ( 'NONE',  ( -8.769230769230768274, -9.780366693483667717, 34.19971097300155094 ) ) ;
#87352 = DIRECTION ( 'NONE',  ( -0.000000000000000000, -0.6427876096865404731, -0.7660444431189770143 ) ) ;
#87353 = AXIS2_PLACEMENT_3D ( 'NONE', #57363, #1982, #29029 ) ;
#87354 = CARTESIAN_POINT ( 'NONE',  ( 3.750000000000009770, -9.053300858899081760, 22.04687500000000000 ) ) ;
#87355 = ORIENTED_EDGE ( 'NONE', *, *, #37629, .F. ) ;
#87356 = ORIENTED_EDGE ( 'NONE', *, *, #87387, .F. ) ;
#87357 = CARTESIAN_POINT ( 'NONE',  ( -9.942284436356281674, -2.544273027872575366, 31.48422191005632342 ) ) ;
#87358 = VECTOR ( 'NONE', #76070, 1000.000000000000000 ) ;
#87359 = CARTESIAN_POINT ( 'NONE',  ( -4.376772371362300795, -12.39988816332205701, 30.74660775122750778 ) ) ;
#87360 = CARTESIAN_POINT ( 'NONE',  ( -5.999999999999998224, -10.67929555188718282, 33.92786785259544047 ) ) ;
#87361 = CARTESIAN_POINT ( 'NONE',  ( 10.61538461538461675, -2.833524468853757305, 32.15551576947925838 ) ) ;
#87362 = DIRECTION ( 'NONE',  ( 0.000000000000000000, 0.8660254037844377084, 0.5000000000000015543 ) ) ;
#87363 = CARTESIAN_POINT ( 'NONE',  ( 3.750000000000009770, -9.053300858899081760, 20.79687500000000000 ) ) ;
#87364 = CARTESIAN_POINT ( 'NONE',  ( -7.715628144390283438, -8.586989748646452369, 34.63063291749215011 ) ) ;
#87365 = LINE ( 'NONE', #12141, #70474 ) ;
#87366 = LINE ( 'NONE', #73844, #5643 ) ;
#87367 = CARTESIAN_POINT ( 'NONE',  ( -18.00000000000030553, -12.49374608885938542, 30.00000000000319744 ) ) ;
#87368 = LINE ( 'NONE', #40509, #64123 ) ;
#87369 = CARTESIAN_POINT ( 'NONE',  ( 13.13459214732242408, -4.335965774309649134, 33.62209801155881905 ) ) ;
#87370 = CARTESIAN_POINT ( 'NONE',  ( -12.52762084089859584, -8.164416787775445883, 34.95778746994557906 ) ) ;
#87371 = CARTESIAN_POINT ( 'NONE',  ( 8.096099255531889582, -8.476813868363244353, 34.90874843262270133 ) ) ;
#87372 = CARTESIAN_POINT ( 'NONE',  ( 2.437739742942760746, -7.723484941389743952, 34.99544897038808955 ) ) ;
#87373 = CARTESIAN_POINT ( 'NONE',  ( -15.29685264172511161, -9.780366693483667717, 34.19971097300155805 ) ) ;
#87374 = ORIENTED_EDGE ( 'NONE', *, *, #81052, .T. ) ;
#87375 = CARTESIAN_POINT ( 'NONE',  ( 8.769230769230645706, -5.094484230521993062, 34.41647553114689373 ) ) ;
#87376 = CARTESIAN_POINT ( 'NONE',  ( -17.32694630114453105, -6.652501968072647820, 34.93155406624980941 ) ) ;
#87377 = LINE ( 'NONE', #73404, #36156 ) ;
#87378 = CARTESIAN_POINT ( 'NONE',  ( 2.775308065498755195, -6.422011778438505125, 17.14249329374151287 ) ) ;
#87379 = EDGE_CURVE ( 'NONE', #11510, #65002, #76561, .T. ) ;
#87380 = CARTESIAN_POINT ( 'NONE',  ( -14.08491276642389423, -5.114059244376869984, 34.14424750095245287 ) ) ;
#87382 = FACE_OUTER_BOUND ( 'NONE', #64341, .T. ) ;
#87381 = VECTOR ( 'NONE', #59828, 999.9999999999998863 ) ;
#87384 = ORIENTED_EDGE ( 'NONE', *, *, #55203, .T. ) ;
#87383 = DIRECTION ( 'NONE',  ( 0.000000000000000000, 0.7660444431189822323, -0.6427876096865344779 ) ) ;
#87385 = CARTESIAN_POINT ( 'NONE',  ( -1.944543648263014957, -5.555456351737005249, 24.00000000000000000 ) ) ;
#87386 = CYLINDRICAL_SURFACE ( 'NONE', #38309, 0.2499999999999986955 ) ;
#87387 = EDGE_CURVE ( 'NONE', #20268, #14556, #55327, .T. ) ;
#87389 = EDGE_LOOP ( 'NONE', ( #9452, #11530 ) ) ;
#87388 = B_SPLINE_CURVE_WITH_KNOTS ( 'NONE', 3,
 ( #73990, #39322, #86176, #37976, #31663, #52365, #45614, #11389, #66334, #53253 ),
 .UNSPECIFIED., .F., .F.,
 ( 4, 2, 2, 2, 4 ),
 ( 0.000000000000000000, 0.0001954311564186864949, 0.0003908623128373729899, 0.0005862934692560594577, 0.0007817246256747459798 ),
 .UNSPECIFIED. ) ;
#87390 = CARTESIAN_POINT ( 'NONE',  ( -7.173053667125512511, -11.47974371597207899, 33.17467449705390692 ) ) ;
#87391 = ADVANCED_FACE ( 'NONE', ( #26983 ), #13019, .F. ) ;
#87392 = VERTEX_POINT ( 'NONE', #398 ) ;
#87393 = CARTESIAN_POINT ( 'NONE',  ( -7.715363405186896451, -6.369690395747424461, 34.87708834333098196 ) ) ;
#87394 = CARTESIAN_POINT ( 'NONE',  ( -3.230769230769229949, -2.517432740324522911, 35.29906147534542527 ) ) ;
#87395 = AXIS2_PLACEMENT_3D ( 'NONE', #6504, #61429, #82166 ) ;
#87396 = DIRECTION ( 'NONE',  ( -1.000000000000000000, 0.000000000000000000, 0.000000000000000000 ) ) ;
#87397 = ORIENTED_EDGE ( 'NONE', *, *, #88872, .F. ) ;
#87398 = DIRECTION ( 'NONE',  ( 0.000000000000000000, 0.1736481776669275834, 0.9848077530122086864 ) ) ;
#87399 = VERTEX_POINT ( 'NONE', #61191 ) ;
#87400 = EDGE_CURVE ( 'NONE', #12785, #7242, #28671, .T. ) ;
#87401 = VERTEX_POINT ( 'NONE', #833 ) ;
#87402 = CARTESIAN_POINT ( 'NONE',  ( 2.177544337960613863, -9.504002272028875709, 34.60269587691767867 ) ) ;
#87403 = CARTESIAN_POINT ( 'NONE',  ( -0.2114841499001467451, -10.66356715214248396, 33.62249196103329751 ) ) ;
#87404 = CARTESIAN_POINT ( 'NONE',  ( 10.61538461538461675, -1.215029322943914858, 32.30358669280327177 ) ) ;
#87405 = CYLINDRICAL_SURFACE ( 'NONE', #1620, 0.2499999999999973355 ) ;
#87406 = CARTESIAN_POINT ( 'NONE',  ( 7.145856592054988354, -8.540255544307065350, 34.89611431652622286 ) ) ;
#87407 = CARTESIAN_POINT ( 'NONE',  ( -1.384615384615383471, -10.67929555188718282, 33.92786785259544047 ) ) ;
#87408 = LINE ( 'NONE', #45509, #62140 ) ;
#87409 = AXIS2_PLACEMENT_3D ( 'NONE', #28492, #1900, #55953 ) ;
#87410 = ORIENTED_EDGE ( 'NONE', *, *, #70817, .F. ) ;
#87411 = ORIENTED_EDGE ( 'NONE', *, *, #53523, .T. ) ;
#87412 = VERTEX_POINT ( 'NONE', #81491 ) ;
#87414 = EDGE_LOOP ( 'NONE', ( #88878, #28573 ) ) ;
#87413 = CARTESIAN_POINT ( 'NONE',  ( 3.230769230769110045, -3.835265460704628371, 33.15142922262033665 ) ) ;
#87415 = VECTOR ( 'NONE', #38337, 1000.000000000000000 ) ;
#87416 = EDGE_CURVE ( 'NONE', #12502, #53380, #12131, .T. ) ;
#87417 = VECTOR ( 'NONE', #27867, 1000.000000000000114 ) ;
#87418 = CARTESIAN_POINT ( 'NONE',  ( 10.54930120442873687, -4.786620604624113540, 33.94971097300155805 ) ) ;
#87419 = DIRECTION ( 'NONE',  ( 0.000000000000000000, 0.4999999999999985567, 0.8660254037844395958 ) ) ;
#87420 = ORIENTED_EDGE ( 'NONE', *, *, #42540, .F. ) ;
#87421 = CARTESIAN_POINT ( 'NONE',  ( 14.37294744720514572, -12.16647553114626490, 32.15551576947920864 ) ) ;
#87422 = EDGE_CURVE ( 'NONE', #66691, #50483, #28297, .T. ) ;
#87423 = VERTEX_POINT ( 'NONE', #82374 ) ;
#87424 = CARTESIAN_POINT ( 'NONE',  ( 24.00000000000000000, 0.000000000000000000, 0.000000000000000000 ) ) ;
#87425 = ORIENTED_EDGE ( 'NONE', *, *, #44490, .F. ) ;
#87426 = DIRECTION ( 'NONE',  ( -0.000000000000000000, -0.5000000000000009992, -0.8660254037844380415 ) ) ;
#87427 = ADVANCED_FACE ( 'NONE', ( #20658 ), #48123, .F. ) ;
#87428 = EDGE_CURVE ( 'NONE', #67532, #64445, #64741, .T. ) ;
#87429 = CARTESIAN_POINT ( 'NONE',  ( 4.087763774486018242, -12.62096338111211580, 30.90682066428152197 ) ) ;
#87430 = CARTESIAN_POINT ( 'NONE',  ( 12.46153846153833911, -2.625532179533778709, 30.86335684631627174 ) ) ;
#87431 = FACE_BOUND ( 'NONE', #17699, .T. ) ;
#87432 = CARTESIAN_POINT ( 'NONE',  ( 2.437739913947992942, -7.723484964179500700, 34.74522123443823318 ) ) ;
#87433 = CARTESIAN_POINT ( 'NONE',  ( 8.769230769230768274, -10.67929555188718282, 33.92786785259544047 ) ) ;
#87434 = CARTESIAN_POINT ( 'NONE',  ( 5.750000000000002665, -2.499999999999998668, 29.75000000000000355 ) ) ;
#87435 = CARTESIAN_POINT ( 'NONE',  ( 1.134592160393928628, -12.45566812827425096, 31.48439005359158926 ) ) ;
#87436 = VECTOR ( 'NONE', #59171, 1000.000000000000000 ) ;
#87437 = CARTESIAN_POINT ( 'NONE',  ( 20.99999999999998224, -2.249999999999999556, 27.25000000000000000 ) ) ;
#87438 = CARTESIAN_POINT ( 'NONE',  ( 7.846153846153846700, -10.51840700105979565, 33.73612834413961536 ) ) ;
#87439 = ORIENTED_EDGE ( 'NONE', *, *, #78781, .T. ) ;
#87440 = CARTESIAN_POINT ( 'NONE',  ( -11.60454391782167249, -3.322132147404559532, 32.92929555188719348 ) ) ;
#87441 = VERTEX_POINT ( 'NONE', #64286 ) ;
#87442 = EDGE_CURVE ( 'NONE', #30965, #77971, #35957, .T. ) ;
#87443 = VERTEX_POINT ( 'NONE', #77811 ) ;
#87444 = AXIS2_PLACEMENT_3D ( 'NONE', #60752, #46353, #89138 ) ;
#87446 = CARTESIAN_POINT ( 'NONE',  ( 17.06410256410256565, -7.500000000000000000, 33.75000000000000000 ) ) ;
#87445 = CARTESIAN_POINT ( 'NONE',  ( 5.749976775778542049, -12.07920672191015221, 32.31858351112116168 ) ) ;
#87447 = CARTESIAN_POINT ( 'NONE',  ( 15.29602437028207085, -8.656820664281605460, 34.87096338111211224 ) ) ;
#87448 = LINE ( 'NONE', #53186, #85435 ) ;
#87449 = ADVANCED_FACE ( 'NONE', ( #36396 ), #84595, .F. ) ;
#87450 = CARTESIAN_POINT ( 'NONE',  ( 8.899278204481223753, -7.723484941389743952, 34.99544897038808955 ) ) ;
#87451 = CARTESIAN_POINT ( 'NONE',  ( 1.450682717965461332, -3.937682226553329556, 33.60647404775216529 ) ) ;
#87452 = EDGE_CURVE ( 'NONE', #50071, #28639, #25029, .T. ) ;
#87453 = EDGE_LOOP ( 'NONE', ( #57369, #49589, #46739, #39755 ) ) ;
#87454 = CARTESIAN_POINT ( 'NONE',  ( -5.143005456283209931, -5.471508081941601986, 34.59228464037088457 ) ) ;
#87455 = AXIS2_PLACEMENT_3D ( 'NONE', #77078, #64873, #22133 ) ;
#87456 = CARTESIAN_POINT ( 'NONE',  ( 11.47313752565723277, -7.749976730030849303, 34.74374725381503737 ) ) ;
#87457 = CARTESIAN_POINT ( 'NONE',  ( -14.08431682191988621, -2.251407671071270489, 29.88021292934942963 ) ) ;
#87458 = CARTESIAN_POINT ( 'NONE',  ( -16.02332071561251325, -4.299079248970731015, 33.91157788607253565 ) ) ;
#87459 = EDGE_LOOP ( 'NONE', ( #9313, #52248, #49435, #2219 ) ) ;
#87460 = EDGE_CURVE ( 'NONE', #47330, #12423, #73378, .T. ) ;
#87461 = VERTEX_POINT ( 'NONE', #50768 ) ;
#87462 = PRODUCT_CONTEXT ( 'NONE', #19322, 'mechanical' ) ;
#87463 = EDGE_LOOP ( 'NONE', ( #84374, #47526, #9757, #44625 ) ) ;
#87464 = CARTESIAN_POINT ( 'NONE',  ( 0.7115927731767753839, -10.66356715214248396, 33.62249196103329751 ) ) ;
#87465 = CARTESIAN_POINT ( 'NONE',  ( 5.076923076922953193, -3.083524468854526912, 32.58852847137268327 ) ) ;
#87466 = ORIENTED_EDGE ( 'NONE', *, *, #44206, .T. ) ;
#87467 = LINE ( 'NONE', #68069, #45278 ) ;
#87468 = CARTESIAN_POINT ( 'NONE',  ( 15.00728428704528561, -9.331801661448606566, 34.40259984581193464 ) ) ;
#87469 = DIRECTION ( 'NONE',  ( -0.000000000000000000, 0.7660444431189791237, -0.6427876096865379196 ) ) ;
#87470 = CARTESIAN_POINT ( 'NONE',  ( -2.531177251416255380, -8.496056993536548418, 34.65000542017679663 ) ) ;
#87471 = FACE_OUTER_BOUND ( 'NONE', #499, .T. ) ;
#87472 = ORIENTED_EDGE ( 'NONE', *, *, #58271, .T. ) ;
#87474 = VERTEX_POINT ( 'NONE', #63411 ) ;
#87473 = CARTESIAN_POINT ( 'NONE',  ( -7.134615384615385025, -7.500000000000000000, 29.75000000000000355 ) ) ;
#87475 = FACE_OUTER_BOUND ( 'NONE', #88910, .T. ) ;
#87476 = CARTESIAN_POINT ( 'NONE',  ( -16.15384615384627409, -10.90142922262034020, 33.41473453929536674 ) ) ;
#87477 = CARTESIAN_POINT ( 'NONE',  ( -6.923076923076922462, -4.098570777380720287, 33.41473453929634729 ) ) ;
#87478 = VECTOR ( 'NONE', #41037, 1000.000000000000227 ) ;
#87479 = CARTESIAN_POINT ( 'NONE',  ( -3.930834802233302394, -12.39991518177334129, 30.74647679643404530 ) ) ;
#87480 = CARTESIAN_POINT ( 'NONE',  ( -8.519285359852727169, -8.476813868363244353, 34.90874843262270133 ) ) ;
#87481 = DIRECTION ( 'NONE',  ( 0.000000000000000000, 0.9848077530122072432, 0.1736481776669354937 ) ) ;
#87482 = CARTESIAN_POINT ( 'NONE',  ( 9.692307692307572609, -6.879047030192662504, 34.71129190930017927 ) ) ;
#87483 = CARTESIAN_POINT ( 'NONE',  ( 1.077988221561497539, -10.27530806549875386, 13.70499329374151287 ) ) ;
#87484 = ORIENTED_EDGE ( 'NONE', *, *, #33766, .T. ) ;
#87485 = AXIS2_PLACEMENT_3D ( 'NONE', #64923, #45550, #39257 ) ;
#87486 = DIRECTION ( 'NONE',  ( -0.000000000000000000, 1.000000000000000000, -0.000000000000000000 ) ) ;
#87487 = CYLINDRICAL_SURFACE ( 'NONE', #23217, 0.2500000000000009437 ) ;
#87488 = EDGE_CURVE ( 'NONE', #60033, #21562, #19979, .T. ) ;
#87489 = EDGE_LOOP ( 'NONE', ( #88794, #57243, #55537, #17729 ) ) ;
#87491 = VERTEX_POINT ( 'NONE', #71056 ) ;
#87490 = VECTOR ( 'NONE', #82843, 1000.000000000000227 ) ;
#87492 = CARTESIAN_POINT ( 'NONE',  ( -5.933932666649924137, -12.62096338111211757, 30.90682066428152908 ) ) ;
#87493 = CARTESIAN_POINT ( 'NONE',  ( -4.153846153846152411, -12.78798330534102945, 29.74999999999997868 ) ) ;
#87494 = CARTESIAN_POINT ( 'NONE',  ( 13.16168916709923664, -3.586966769969701208, 32.86292498521069660 ) ) ;
#87495 = CARTESIAN_POINT ( 'NONE',  ( 10.83839745947800992, -4.762714258010881885, 34.23016756924214832 ) ) ;
#87496 = CARTESIAN_POINT ( 'NONE',  ( 0.4330127018922180770, -10.21569512280005299, 29.50000000000000355 ) ) ;
#87497 = EDGE_CURVE ( 'NONE', #31340, #52889, #17002, .T. ) ;
#87498 = B_SPLINE_CURVE_WITH_KNOTS ( 'NONE', 3,
 ( #1195, #9300, #1651, #77301, #9729, #56590, #43954, #50255, #70991, #28683 ),
 .UNSPECIFIED., .F., .F.,
 ( 4, 2, 2, 2, 4 ),
 ( 0.000000000000000000, 0.0001954311564186871184, 0.0003908623128373742367, 0.0005862934692560614093, 0.0007817246256747484735 ),
 .UNSPECIFIED. ) ;
#87499 = DIRECTION ( 'NONE',  ( -0.000000000000000000, -1.000000000000000000, 8.673617379884028076E-17 ) ) ;
#87500 = ORIENTED_EDGE ( 'NONE', *, *, #2114, .F. ) ;
#87501 = B_SPLINE_CURVE_WITH_KNOTS ( 'NONE', 3,
 ( #58045, #24252, #51717, #43648, #71117, #9426, #44969, #72448, #36890, #9863 ),
 .UNSPECIFIED., .F., .F.,
 ( 4, 2, 2, 2, 4 ),
 ( 0.000000000000000000, 0.0001954339857564081520, 0.0003908679715128163040, 0.0005863019572692244018, 0.0007817359430256326080 ),
 .UNSPECIFIED. ) ;
#87502 = B_SPLINE_CURVE_WITH_KNOTS ( 'NONE', 3,
 ( #41270, #68734, #7030, #36189, #56878, #29430, #55216, #49683, #77160, #15469 ),
 .UNSPECIFIED., .F., .F.,
 ( 4, 2, 2, 2, 4 ),
 ( 0.0007817246256747463051, 0.0009771112852218896347, 0.001172497944769032747, 0.001367884604316176077, 0.001563271263863319407 ),
 .UNSPECIFIED. ) ;
#87503 = DIRECTION ( 'NONE',  ( 1.000000000000000000, 0.000000000000000000, 0.000000000000000000 ) ) ;
#87504 = DIRECTION ( 'NONE',  ( 1.734723475976812518E-16, -1.000000000000000000, 0.000000000000000000 ) ) ;
#87505 = CYLINDRICAL_SURFACE ( 'NONE', #39300, 0.2500000000000012212 ) ;
#87506 = ORIENTED_EDGE ( 'NONE', *, *, #986, .F. ) ;
#87507 = CARTESIAN_POINT ( 'NONE',  ( -7.596208327805703320, -3.712312575010499494, 33.01462480002815170 ) ) ;
#87508 = EDGE_LOOP ( 'NONE', ( #45962, #82518, #34075, #83782 ) ) ;
#87509 = AXIS2_PLACEMENT_3D ( 'NONE', #83478, #28525, #76252 ) ;
#87510 = CARTESIAN_POINT ( 'NONE',  ( 13.51540719244017374, -3.530189275343204702, 32.79018710029569661 ) ) ;
#87511 =( NAMED_UNIT ( * ) SI_UNIT ( $, .STERADIAN. ) SOLID_ANGLE_UNIT ( ) );
#87512 = DIRECTION ( 'NONE',  ( -0.000000000000000000, -0.000000000000000000, -1.000000000000000000 ) ) ;
#87513 = CARTESIAN_POINT ( 'NONE',  ( -13.91025641025641235, -4.000000000000000000, 29.75000000000000355 ) ) ;
#87514 = EDGE_LOOP ( 'NONE', ( #70164, #8340, #3172, #18735 ) ) ;
#87515 = CARTESIAN_POINT ( 'NONE',  ( 12.46153846153833911, -3.835265460704628371, 33.15142922262033665 ) ) ;
#87516 = CARTESIAN_POINT ( 'NONE',  ( -6.223484924564330001, -2.353723527008295680, 30.78948104536958752 ) ) ;
#87517 = LINE ( 'NONE', #53252, #14954 ) ;
#87518 = AXIS2_PLACEMENT_3D ( 'NONE', #61564, #33666, #40868 ) ;
#87519 = EDGE_CURVE ( 'NONE', #1538, #85395, #31417, .T. ) ;
#87520 = CARTESIAN_POINT ( 'NONE',  ( -7.780086512803769061, -4.661471528628508665, 34.16647553114624003 ) ) ;
#87521 = FACE_OUTER_BOUND ( 'NONE', #15572, .T. ) ;
#87522 = AXIS2_PLACEMENT_3D ( 'NONE', #28116, #15056, #55586 ) ;
#87523 = VERTEX_POINT ( 'NONE', #56660 ) ;
#87524 = FACE_BOUND ( 'NONE', #58253, .T. ) ;
#87525 = ORIENTED_EDGE ( 'NONE', *, *, #21707, .F. ) ;
#87526 = CARTESIAN_POINT ( 'NONE',  ( -2.373774687052441212, -2.486705287966279876, 31.30864560766542937 ) ) ;
#87527 = DIRECTION ( 'NONE',  ( -0.000000000000000000, 1.000000000000000000, -0.000000000000000000 ) ) ;
#87528 = CARTESIAN_POINT ( 'NONE',  ( -3.296093243573539500, -7.749976730030849303, 34.74374725381503737 ) ) ;
#87529 = CARTESIAN_POINT ( 'NONE',  ( 7.716005876422148191, -12.50552854090298638, 31.33409797877408920 ) ) ;
#87530 = EDGE_CURVE ( 'NONE', #27912, #1531, #10996, .T. ) ;
#87531 = CARTESIAN_POINT ( 'NONE',  ( 8.900022577055551665, -3.530189275343204702, 32.79018710029569661 ) ) ;
#87532 = DIRECTION ( 'NONE',  ( -0.000000000000000000, 0.9396926207859092051, -0.3420201433256662704 ) ) ;
#87533 = DIRECTION ( 'NONE',  ( -1.000000000000000000, -0.000000000000000000, 0.000000000000000000 ) ) ;
#87534 = EDGE_CURVE ( 'NONE', #83971, #83905, #61381, .T. ) ;
#87535 = ORIENTED_EDGE ( 'NONE', *, *, #78278, .F. ) ;
#87536 = ORIENTED_EDGE ( 'NONE', *, *, #41216, .T. ) ;
#87537 = ORIENTED_EDGE ( 'NONE', *, *, #72957, .T. ) ;
#87538 = B_SPLINE_CURVE_WITH_KNOTS ( 'NONE', 3,
 ( #25320, #73517, #68, #74854, #7721, #47806, #83377, #47357, #48686, #21665 ),
 .UNSPECIFIED., .F., .F.,
 ( 4, 2, 2, 2, 4 ),
 ( 0.0007817246256747434861, 0.0009771112852218859484, 0.001172497944769028411, 0.001367884604316171090, 0.001563271263863313552 ),
 .UNSPECIFIED. ) ;
#87539 = VERTEX_POINT ( 'NONE', #53444 ) ;
#87540 = ADVANCED_FACE ( 'NONE', ( #3919 ), #32735, .F. ) ;
#87541 = CARTESIAN_POINT ( 'NONE',  ( -10.48485891362105349, -11.46989282347013095, 32.79007818306219946 ) ) ;
#87542 = CARTESIAN_POINT ( 'NONE',  ( -2.242436736416280940, -3.300289026998474817, 32.46337939537591666 ) ) ;
#87543 = AXIS2_PLACEMENT_3D ( 'NONE', #89012, #42145, #27285 ) ;
#87544 = CARTESIAN_POINT ( 'NONE',  ( -4.023054346021365468, -8.999086150933472084, 34.52020707165672064 ) ) ;
#87545 = CARTESIAN_POINT ( 'NONE',  ( 4.088575707885377497, -3.300289026998414865, 32.46337939537583139 ) ) ;
#87546 = CYLINDRICAL_SURFACE ( 'NONE', #58645, 0.2499999999999995559 ) ;
#87547 = DIRECTION ( 'NONE',  ( 0.000000000000000000, 1.000000000000000000, 0.000000000000000000 ) ) ;
#87548 = CARTESIAN_POINT ( 'NONE',  ( 17.86930853333243974, -2.541943142973489334, 30.39792223712631980 ) ) ;
#87549 = CYLINDRICAL_SURFACE ( 'NONE', #86528, 0.2499999999999979738 ) ;
#87550 = ORIENTED_EDGE ( 'NONE', *, *, #9547, .F. ) ;
#87551 = ORIENTED_EDGE ( 'NONE', *, *, #36223, .F. ) ;
#87552 = VERTEX_POINT ( 'NONE', #45354 ) ;
#87554 = VERTEX_POINT ( 'NONE', #31405 ) ;
#87553 = CARTESIAN_POINT ( 'NONE',  ( -3.230769230769229949, -11.11383981884818262, 36.00935417666054406 ) ) ;
#87556 = CARTESIAN_POINT ( 'NONE',  ( -5.750054481651857508, -3.712312575010499494, 33.01462480002815170 ) ) ;
#87555 = CARTESIAN_POINT ( 'NONE',  ( 7.596130608860880429, -3.202444869320336451, 32.30641848906366675 ) ) ;
#87557 = DIRECTION ( 'NONE',  ( -0.000000000000000000, -0.9396926207859092051, -0.3420201433256662704 ) ) ;
#87558 = CARTESIAN_POINT ( 'NONE',  ( -8.835313148590904220, -6.343179335718451384, 34.87096338111212646 ) ) ;
#87559 = ADVANCED_FACE ( 'NONE', ( #58874 ), #80946, .T. ) ;
#87560 = FACE_BOUND ( 'NONE', #71355, .T. ) ;
#87561 = EDGE_LOOP ( 'NONE', ( #27151, #62302, #71086, #74781, #75530, #59067 ) ) ;
#87562 = ORIENTED_EDGE ( 'NONE', *, *, #44859, .F. ) ;
#87563 = CARTESIAN_POINT ( 'NONE',  ( -5.076923076923197442, -6.879047030192662504, 34.71129190930017927 ) ) ;
#87564 = ORIENTED_EDGE ( 'NONE', *, *, #36292, .F. ) ;
#87565 = FACE_BOUND ( 'NONE', #58803, .T. ) ;
#87566 = CARTESIAN_POINT ( 'NONE',  ( -9.469294848214296678, -2.308499170217967134, 30.53291367094873721 ) ) ;
#87567 = AXIS2_PLACEMENT_3D ( 'NONE', #36071, #55881, #49574 ) ;
#87568 = CARTESIAN_POINT ( 'NONE',  ( 18.22277954126840172, -5.114059244376869096, 34.14424750095245287 ) ) ;
#87569 = ORIENTED_EDGE ( 'NONE', *, *, #18066, .F. ) ;
#87570 = CARTESIAN_POINT ( 'NONE',  ( -14.98071491913092146, -12.17597550085003633, 31.52189283813461884 ) ) ;
#87571 = CARTESIAN_POINT ( 'NONE',  ( -6.673022503163469565, -2.318338780012835443, 30.59689888758630261 ) ) ;
#87572 = CARTESIAN_POINT ( 'NONE',  ( -2.121320343559653487, -5.378679656440369605, 14.00000000000000178 ) ) ;
#87573 = VERTEX_POINT ( 'NONE', #18788 ) ;
#87574 = CYLINDRICAL_SURFACE ( 'NONE', #47134, 0.2499999999999995559 ) ;
#87575 = CARTESIAN_POINT ( 'NONE',  ( -14.55766903863466055, -5.728515186090277211, 34.42611988154120439 ) ) ;
#87576 = CARTESIAN_POINT ( 'NONE',  ( 2.372947447205147942, -3.083524468853784839, 32.58852847137153930 ) ) ;
#87577 = ORIENTED_EDGE ( 'NONE', *, *, #55175, .T. ) ;
#87578 = CARTESIAN_POINT ( 'NONE',  ( -1.607541602131531855, -5.667676309546437530, 34.40238873228292249 ) ) ;
#87579 = CARTESIAN_POINT ( 'NONE',  ( 7.146088274689772923, -10.61302985866383963, 33.66295027996417843 ) ) ;
#87580 = VECTOR ( 'NONE', #85570, 999.9999999999998863 ) ;
#87581 = VERTEX_POINT ( 'NONE', #66067 ) ;
#87582 = CARTESIAN_POINT ( 'NONE',  ( 6.000000000000001776, -7.500000000000001776, 35.04278698407183867 ) ) ;
#87583 = CYLINDRICAL_SURFACE ( 'NONE', #42583, 0.2499999999999979738 ) ;
#87584 = CARTESIAN_POINT ( 'NONE',  ( -13.31935981333936425, -5.219633306516380244, 34.19971097300157936 ) ) ;
#87585 = DIRECTION ( 'NONE',  ( -0.000000000000000000, -0.7660444431189791237, -0.6427876096865379196 ) ) ;
#87586 = DIRECTION ( 'NONE',  ( -0.000000000000000000, 1.000000000000000000, -0.000000000000000000 ) ) ;
#87587 = CARTESIAN_POINT ( 'NONE',  ( 7.846153846153846700, -12.48256725967547354, 35.29906147534542527 ) ) ;
#87589 = CARTESIAN_POINT ( 'NONE',  ( 9.692307692307570832, -5.094484230521993062, 34.41647553114689373 ) ) ;
#87588 = CYLINDRICAL_SURFACE ( 'NONE', #51958, 0.2499999999999973355 ) ;
#87590 = DIRECTION ( 'NONE',  ( -0.000000000000000000, 0.5000000000000011102, -0.8660254037844380415 ) ) ;
#87591 = DIRECTION ( 'NONE',  ( -0.000000000000000000, -0.1736481776669307198, -0.9848077530122080203 ) ) ;
#87592 = CARTESIAN_POINT ( 'NONE',  ( 1.077988221561464899, -4.724691934501233703, 26.48250670625848713 ) ) ;
#87593 = ORIENTED_EDGE ( 'NONE', *, *, #47942, .F. ) ;
#87594 = CARTESIAN_POINT ( 'NONE',  ( 10.61538461538461675, -1.129524287112498415, 32.06866353760679544 ) ) ;
#87595 = ORIENTED_EDGE ( 'NONE', *, *, #4062, .T. ) ;
#87596 = B_SPLINE_CURVE_WITH_KNOTS ( 'NONE', 3,
 ( #84760, #23036, #17626, #23909, #72108, #10420, #38329, #65787, #50499, #56817 ),
 .UNSPECIFIED., .F., .F.,
 ( 4, 2, 2, 2, 4 ),
 ( 0.0007817359430256294638, 0.0009771253907249948054, 0.001172514838424360255, 0.001367904286123725489, 0.001563293733823090939 ),
 .UNSPECIFIED. ) ;
#87597 = ORIENTED_EDGE ( 'NONE', *, *, #42997, .T. ) ;
#87598 = CARTESIAN_POINT ( 'NONE',  ( -17.07692307692307665, -3.937682226553329556, 33.60647404775216529 ) ) ;
#87599 = VERTEX_POINT ( 'NONE', #12038 ) ;
#87600 = CARTESIAN_POINT ( 'NONE',  ( -15.23076923076922995, -5.557115091759785130, 34.35708131394839171 ) ) ;
#87601 = CARTESIAN_POINT ( 'NONE',  ( -2.749999999999997780, -7.561099074964547917, 27.34188170625848713 ) ) ;
#87602 = DIRECTION ( 'NONE',  ( 0.000000000000000000, -6.938893903907222067E-15, 1.000000000000000000 ) ) ;
#87603 = CARTESIAN_POINT ( 'NONE',  ( -15.36145983387953606, -12.35290016733513951, 31.75349464988449455 ) ) ;
#87604 = CARTESIAN_POINT ( 'NONE',  ( -3.007989689500820241, -9.332535724633405749, 34.40230450496446224 ) ) ;
#87605 = CARTESIAN_POINT ( 'NONE',  ( -8.519176457592452678, -4.943051570960394159, 34.04725096376909477 ) ) ;
#87606 = CARTESIAN_POINT ( 'NONE',  ( 0.4615384615383382183, -5.941354392335915335, 34.76329471203413846 ) ) ;
#87607 = CARTESIAN_POINT ( 'NONE',  ( -3.230769230769351186, -4.481592998941358097, 33.73612834414048933 ) ) ;
#87608 = CARTESIAN_POINT ( 'NONE',  ( -3.749999999999997335, -7.500000000000021316, 22.59375000000000355 ) ) ;
#87609 = CARTESIAN_POINT ( 'NONE',  ( 18.06606733335007675, -11.35647404775217595, 33.31231777344667222 ) ) ;
#87610 = CARTESIAN_POINT ( 'NONE',  ( -17.77698715590659972, -2.308499170217966689, 30.53291367094874076 ) ) ;
#87611 = DIRECTION ( 'NONE',  ( 0.000000000000000000, 0.9848077530122072432, 0.1736481776669354937 ) ) ;
#87612 = B_SPLINE_CURVE_WITH_KNOTS ( 'NONE', 3,
 ( #57657, #63523, #22980, #71601, #85137, #70737, #29315, #17109, #23849, #37371 ),
 .UNSPECIFIED., .F., .F.,
 ( 4, 2, 2, 2, 4 ),
 ( 0.000000000000000000, 0.0001954311564186861155, 0.0003908623128373722310, 0.0005862934692560583735, 0.0007817246256747444619 ),
 .UNSPECIFIED. ) ;
#87613 = VERTEX_POINT ( 'NONE', #31860 ) ;
#87614 = ORIENTED_EDGE ( 'NONE', *, *, #39338, .F. ) ;
#87615 = FACE_OUTER_BOUND ( 'NONE', #59092, .T. ) ;
#87616 = DIRECTION ( 'NONE',  ( -0.000000000000000000, 1.000000000000000000, -0.000000000000000000 ) ) ;
#87617 = CARTESIAN_POINT ( 'NONE',  ( 1.384615384615386802, -10.67929555188718282, 33.92786785259544047 ) ) ;
#87618 = CARTESIAN_POINT ( 'NONE',  ( -16.02332045208259359, -12.45806712695776319, 30.39783852428763566 ) ) ;
#87619 = CARTESIAN_POINT ( 'NONE',  ( -3.230769230769229949, -13.88283147151868846, 33.14645433367849847 ) ) ;
#87620 = DIRECTION ( 'NONE',  ( -0.000000000000000000, -0.9848077530122085754, -0.1736481776669273613 ) ) ;
#87621 = B_SPLINE_CURVE_WITH_KNOTS ( 'NONE', 3,
 ( #7490, #69183, #21883, #13791, #76836, #283, #14238, #34946, #15134, #62407 ),
 .UNSPECIFIED., .F., .F.,
 ( 4, 2, 2, 2, 4 ),
 ( 0.000000000000000000, 0.0001954339857564073659, 0.0003908679715128147319, 0.0005863019572692221250, 0.0007817359430256294638 ),
 .UNSPECIFIED. ) ;
#87622 = B_SPLINE_CURVE_WITH_KNOTS ( 'NONE', 3,
 ( #37322, #69018, #7327, #34785, #43209, #64788, #3094, #8990, #63910, #30570 ),
 .UNSPECIFIED., .F., .F.,
 ( 4, 2, 2, 2, 4 ),
 ( 0.0007817246256747507503, 0.0009771112852218957062, 0.001172497944769040771, 0.001367884604316185835, 0.001563271263863330682 ),
 .UNSPECIFIED. ) ;
#87623 = ORIENTED_EDGE ( 'NONE', *, *, #76096, .F. ) ;
#87624 = B_SPLINE_CURVE_WITH_KNOTS ( 'NONE', 3,
 ( #23666, #43940, #78612, #85830, #64642, #38075, #77725, #15593, #22778, #58785 ),
 .UNSPECIFIED., .F., .F.,
 ( 4, 2, 2, 2, 4 ),
 ( 0.000000000000000000, 0.0001954311584214072381, 0.0003908623168428144762, 0.0005862934752642217414, 0.0007817246336856289524 ),
 .UNSPECIFIED. ) ;
#87625 = CARTESIAN_POINT ( 'NONE',  ( 1.384615384615386802, -4.786620604624113540, 33.94971097300155094 ) ) ;
#87626 = ORIENTED_EDGE ( 'NONE', *, *, #21189, .T. ) ;
#87627 = ORIENTED_EDGE ( 'NONE', *, *, #32021, .T. ) ;
#87628 = CARTESIAN_POINT ( 'NONE',  ( 17.93472955403921887, -3.300289026998414865, 32.46337939537583139 ) ) ;
#87629 = EDGE_CURVE ( 'NONE', #29065, #15565, #24864, .T. ) ;
#87630 = CIRCLE ( 'NONE', #48767, 5.000000000000000888 ) ;
#87631 = CARTESIAN_POINT ( 'NONE',  ( -2.530619266599155370, -9.172386477786396597, 34.72672124145550043 ) ) ;
#87632 = CARTESIAN_POINT ( 'NONE',  ( -17.07692307692307665, -11.69971097300155272, 32.46337939537588113 ) ) ;
#87633 = DIRECTION ( 'NONE',  ( -0.000000000000000000, -0.1736481776669307198, -0.9848077530122080203 ) ) ;
#87634 = CARTESIAN_POINT ( 'NONE',  ( -2.057637996053992335, -11.79725096376909654, 32.30694842903960762 ) ) ;
#87635 = AXIS2_PLACEMENT_3D ( 'NONE', #31913, #78752, #44509 ) ;
#87636 = EDGE_LOOP ( 'NONE', ( #67128, #40841, #36662, #35331 ) ) ;
#87637 = AXIS2_PLACEMENT_3D ( 'NONE', #44353, #17349, #3829 ) ;
#87638 = ORIENTED_EDGE ( 'NONE', *, *, #44492, .F. ) ;
#87639 = ORIENTED_EDGE ( 'NONE', *, *, #48883, .F. ) ;
#87640 = AXIS2_PLACEMENT_3D ( 'NONE', #61803, #70799, #55499 ) ;
#87641 = EDGE_CURVE ( 'NONE', #62031, #71802, #46410, .T. ) ;
#87642 = FACE_OUTER_BOUND ( 'NONE', #35620, .T. ) ;
#87643 = CARTESIAN_POINT ( 'NONE',  ( 10.54930223602447903, -11.35647404775217595, 33.31231777344666511 ) ) ;
#87644 = LINE ( 'NONE', #45291, #86853 ) ;
#87645 = CARTESIAN_POINT ( 'NONE',  ( 10.55011461482829738, -5.094484230520674117, 34.41647553114621161 ) ) ;
#87646 = CARTESIAN_POINT ( 'NONE',  ( 17.86985279056177944, -5.195881422630167279, 34.18770438780618548 ) ) ;
#87647 = CARTESIAN_POINT ( 'NONE',  ( -15.29603923132555110, -2.657715359629089225, 31.77849191805832874 ) ) ;
#87648 = VERTEX_POINT ( 'NONE', #66976 ) ;
#87649 = EDGE_LOOP ( 'NONE', ( #44850, #79537, #41323, #24390 ) ) ;
#87650 = CARTESIAN_POINT ( 'NONE',  ( -3.750000000000008438, -5.946699141100917352, 26.42187500000000000 ) ) ;
#87651 = B_SPLINE_CURVE_WITH_KNOTS ( 'NONE', 3,
 ( #32022, #87429, #25712, #9965, #78867, #23913, #52724, #86538, #51363, #3207 ),
 .UNSPECIFIED., .F., .F.,
 ( 4, 2, 2, 2, 4 ),
 ( 0.000000000000000000, 0.0001954311564186879315, 0.0003908623128373758630, 0.0005862934692560637946, 0.0007817246256747517261 ),
 .UNSPECIFIED. ) ;
#87653 = VERTEX_POINT ( 'NONE', #60204 ) ;
#87652 = DIRECTION ( 'NONE',  ( 0.000000000000000000, 0.9396926207859126468, 0.3420201433256571111 ) ) ;
#87654 = CARTESIAN_POINT ( 'NONE',  ( 7.976679547917409963, -12.45806712695776319, 30.39783852428763922 ) ) ;
#87655 = CARTESIAN_POINT ( 'NONE',  ( -9.915233909823841785, -11.76352882383564769, 32.36236540154569497 ) ) ;
#87656 = CARTESIAN_POINT ( 'NONE',  ( -19.50000000000000000, -11.50000000000000000, 29.75000000000000355 ) ) ;
#87657 = EDGE_CURVE ( 'NONE', #48065, #37880, #4437, .T. ) ;
#87658 = ORIENTED_EDGE ( 'NONE', *, *, #16056, .T. ) ;
#87659 = ADVANCED_FACE ( 'NONE', ( #87708 ), #25980, .F. ) ;
#87660 = DIRECTION ( 'NONE',  ( 0.000000000000000000, -1.000000000000000000, 0.000000000000000000 ) ) ;
#87661 = AXIS2_PLACEMENT_3D ( 'NONE', #15329, #36482, #14890 ) ;
#87662 = ORIENTED_EDGE ( 'NONE', *, *, #10281, .T. ) ;
#87663 = CARTESIAN_POINT ( 'NONE',  ( 13.44987052412822059, -11.06231777344671130, 33.60647404775212976 ) ) ;
#87664 = CARTESIAN_POINT ( 'NONE',  ( 14.55774672760575861, -12.41089969410671223, 31.60739465890703670 ) ) ;
#87665 = EDGE_CURVE ( 'NONE', #35354, #56825, #13070, .T. ) ;
#87666 = FACE_BOUND ( 'NONE', #79006, .T. ) ;
#87667 = CARTESIAN_POINT ( 'NONE',  ( -4.826868765284762830, -12.17597550085003633, 31.52189283813461884 ) ) ;
#87668 = EDGE_CURVE ( 'NONE', #22650, #3401, #54777, .T. ) ;
#87669 = DIRECTION ( 'NONE',  ( -0.000000000000000000, 0.8660254037844397068, -0.4999999999999978906 ) ) ;
#87670 = ORIENTED_EDGE ( 'NONE', *, *, #28535, .F. ) ;
#87671 = CYLINDRICAL_SURFACE ( 'NONE', #10148, 0.2500000000000008882 ) ;
#87672 = CARTESIAN_POINT ( 'NONE',  ( 15.10062202133101295, -4.460286881179643004, 33.72017969459903242 ) ) ;
#87673 = CARTESIAN_POINT ( 'NONE',  ( -14.08491276642389600, -2.847695495035523550, 31.58253572463339154 ) ) ;
#87674 = ORIENTED_EDGE ( 'NONE', *, *, #60040, .F. ) ;
#87675 = DIRECTION ( 'NONE',  ( 1.000000000000000000, 0.000000000000000000, 0.000000000000000000 ) ) ;
#87676 = CARTESIAN_POINT ( 'NONE',  ( -5.999999999999998224, -10.51840700105979565, 33.73612834413961536 ) ) ;
#87677 = CARTESIAN_POINT ( 'NONE',  ( -4.087778820496075660, -2.292212530054420494, 30.41441678777542990 ) ) ;
#87678 = CARTESIAN_POINT ( 'NONE',  ( 11.47319109250076430, -6.026961402152685388, 34.52809138561120506 ) ) ;
#87679 = CARTESIAN_POINT ( 'NONE',  ( 12.46153846153846168, -3.669653830205710676, 35.88435417666054406 ) ) ;
#87680 = FACE_BOUND ( 'NONE', #2282, .T. ) ;
#87682 = DIRECTION ( 'NONE',  ( -0.000000000000000000, -0.6427876096865404731, -0.7660444431189770143 ) ) ;
#87681 = CARTESIAN_POINT ( 'NONE',  ( -7.173053667125515176, -12.41104346484419452, 31.60698883733904196 ) ) ;
#87683 = CARTESIAN_POINT ( 'NONE',  ( 9.942307692307696954, -2.499999999999999556, 29.81604066197449754 ) ) ;
#87685 = CARTESIAN_POINT ( 'NONE',  ( -2.084679463598912097, -12.38742843783360748, 31.66772728687926985 ) ) ;
#87684 = FACE_OUTER_BOUND ( 'NONE', #86212, .T. ) ;
#87686 = DIRECTION ( 'NONE',  ( -1.000000000000000000, -0.000000000000000000, 0.000000000000000000 ) ) ;
#87687 = CARTESIAN_POINT ( 'NONE',  ( -3.775308065498766297, -6.007798216065450170, 24.92000670625849068 ) ) ;
#87688 = ORIENTED_EDGE ( 'NONE', *, *, #68229, .F. ) ;
#87689 = CARTESIAN_POINT ( 'NONE',  ( -8.546451227962355901, -5.913360116392397892, 34.49180327182771322 ) ) ;
#87690 = ORIENTED_EDGE ( 'NONE', *, *, #47639, .F. ) ;
#87691 = VECTOR ( 'NONE', #45744, 1000.000000000000000 ) ;
#87692 = DIRECTION ( 'NONE',  ( -1.000000000000000000, -0.000000000000000000, -0.000000000000000000 ) ) ;
#87693 = ORIENTED_EDGE ( 'NONE', *, *, #5799, .F. ) ;
#87694 = B_SPLINE_CURVE_WITH_KNOTS ( 'NONE', 3,
 ( #21074, #14328, #8907, #76478, #7578, #14780, #35040, #62499, #35939, #15664 ),
 .UNSPECIFIED., .F., .F.,
 ( 4, 2, 2, 2, 4 ),
 ( 0.000000000000000000, 0.0001954339857564073659, 0.0003908679715128147319, 0.0005863019572692221250, 0.0007817359430256294638 ),
 .UNSPECIFIED. ) ;
#87695 = CARTESIAN_POINT ( 'NONE',  ( -15.48076923076923350, -7.566083408709835645, 34.74999999999999289 ) ) ;
#87696 = CARTESIAN_POINT ( 'NONE',  ( 13.38461538461538680, -9.584722331328613620, 36.20867863119891439 ) ) ;
#87698 = VERTEX_POINT ( 'NONE', #48017 ) ;
#87697 = CARTESIAN_POINT ( 'NONE',  ( -5.010855743573001675, -9.058645607665452459, 34.76329471203371924 ) ) ;
#87699 = CARTESIAN_POINT ( 'NONE',  ( -16.37677237136229991, -2.554751324335733376, 30.48935550225260727 ) ) ;
#87700 = CARTESIAN_POINT ( 'NONE',  ( -11.66915214157184622, -3.957541250942358424, 33.62499894934981626 ) ) ;
#87701 = CARTESIAN_POINT ( 'NONE',  ( -1.492201783934549164, -11.27530806549876807, 25.85750670625849068 ) ) ;
#87702 = B_SPLINE_CURVE_WITH_KNOTS ( 'NONE', 3,
 ( #15456, #35272, #42930, #69062, #8701, #70399, #36177, #28524, #63629, #1933 ),
 .UNSPECIFIED., .F., .F.,
 ( 4, 2, 2, 2, 4 ),
 ( 0.000000000000000000, 0.0001954339857564081520, 0.0003908679715128163040, 0.0005863019572692244018, 0.0007817359430256326080 ),
 .UNSPECIFIED. ) ;
#87703 = CIRCLE ( 'NONE', #53210, 4.000000000000000000 ) ;
#87704 = LINE ( 'NONE', #31857, #86337 ) ;
#87705 = DIRECTION ( 'NONE',  ( -0.000000000000000000, -0.6427876096865404731, -0.7660444431189771253 ) ) ;
#87706 = VECTOR ( 'NONE', #74455, 1000.000000000000000 ) ;
#87707 = CARTESIAN_POINT ( 'NONE',  ( 0.4999924855028897164, -4.795835153971004239, 29.16295261168902542 ) ) ;
#87708 = FACE_OUTER_BOUND ( 'NONE', #74395, .T. ) ;
#87709 = CARTESIAN_POINT ( 'NONE',  ( 8.769230769230768274, -9.780366693483667717, 34.19971097300155094 ) ) ;
#87710 = CARTESIAN_POINT ( 'NONE',  ( -11.40793583669797862, -10.19071101563364756, 33.96452234770658407 ) ) ;
#87711 = VECTOR ( 'NONE', #11604, 1000.000000000000000 ) ;
#87712 = CARTESIAN_POINT ( 'NONE',  ( 1.492201783934598236, -11.27530806549875031, 18.70499329374151287 ) ) ;
#87713 = B_SPLINE_CURVE_WITH_KNOTS ( 'NONE', 3,
 ( #23221, #14698, #35406, #49802, #28661, #9279, #8387, #50682, #56127, #43498 ),
 .UNSPECIFIED., .F., .F.,
 ( 4, 2, 2, 2, 4 ),
 ( 0.0007817359430256216575, 0.0009771253907249856981, 0.001172514838424349847, 0.001367904286123713779, 0.001563293733823077928 ),
 .UNSPECIFIED. ) ;
#87714 = EDGE_CURVE ( 'NONE', #30362, #6548, #54499, .T. ) ;
#87715 = DIRECTION ( 'NONE',  ( 0.000000000000000000, -1.000000000000000000, 0.000000000000000000 ) ) ;
#87716 = CARTESIAN_POINT ( 'NONE',  ( -1.134560964701930352, -12.01375889529407281, 32.43194544308182969 ) ) ;
#87717 = ORIENTED_EDGE ( 'NONE', *, *, #54037, .F. ) ;
#87718 = CARTESIAN_POINT ( 'NONE',  ( 17.32686859527122181, -2.824170634883622633, 31.52227843825338738 ) ) ;
#87719 = CARTESIAN_POINT ( 'NONE',  ( 8.900022577055558770, -11.18335022499818621, 33.13157742990016885 ) ) ;
#87720 = CARTESIAN_POINT ( 'NONE',  ( -3.775308065498748977, -8.992201783934593351, 16.51749329374151642 ) ) ;
#87721 = CARTESIAN_POINT ( 'NONE',  ( 2.307692307692309264, -4.098570777380720287, 33.41473453929634729 ) ) ;
#87722 = CARTESIAN_POINT ( 'NONE',  ( 5.299702745901139878, -6.717445702608402236, 34.94155399931962336 ) ) ;
#87723 = EDGE_LOOP ( 'NONE', ( #14930, #26366, #66587, #12480 ) ) ;
#87724 = LINE ( 'NONE', #19246, #27008 ) ;
#87725 = CARTESIAN_POINT ( 'NONE',  ( 0.4330127018922180770, -4.784304877199946127, 29.50000000000000355 ) ) ;
#87727 = VERTEX_POINT ( 'NONE', #62411 ) ;
#87726 = CARTESIAN_POINT ( 'NONE',  ( 11.31553457955469000, -2.889293201056495786, 32.26117774369186009 ) ) ;
#87728 = CARTESIAN_POINT ( 'NONE',  ( -9.822455662039388358, -3.625366637846544116, 33.29286588640298561 ) ) ;
#87729 = CARTESIAN_POINT ( 'NONE',  ( 4.088575707885377497, -8.613356846314824011, 34.62446782046655613 ) ) ;
#87730 = CARTESIAN_POINT ( 'NONE',  ( 5.207761407409835286, -7.277220318596959281, 34.99547417642776992 ) ) ;
#87731 = EDGE_CURVE ( 'NONE', #73366, #58603, #48457, .T. ) ;
#87732 = FACE_OUTER_BOUND ( 'NONE', #60584, .T. ) ;
#87733 = ORIENTED_EDGE ( 'NONE', *, *, #22907, .T. ) ;
#87734 = CARTESIAN_POINT ( 'NONE',  ( 7.173076923076937561, -2.249999999999999112, 29.81603969181031033 ) ) ;
#87735 = CARTESIAN_POINT ( 'NONE',  ( 6.923076923076924238, -4.786620604624113540, 33.94971097300155094 ) ) ;
#87736 = CARTESIAN_POINT ( 'NONE',  ( 1.134592160393929072, -2.985938066672154445, 32.43141759479405550 ) ) ;
#87737 = ORIENTED_EDGE ( 'NONE', *, *, #24031, .T. ) ;
#87738 = B_SPLINE_CURVE_WITH_KNOTS ( 'NONE', 3,
 ( #22229, #49696, #15481, #84832, #56890, #16355 ),
 .UNSPECIFIED., .F., .F.,
 ( 4, 2, 4 ),
 ( 0.0003909512603273853043, 0.0005862562993132091520, 0.0007815613382990329455 ),
 .UNSPECIFIED. ) ;
#87739 = ORIENTED_EDGE ( 'NONE', *, *, #75531, .F. ) ;
#87740 = VECTOR ( 'NONE', #44114, 1000.000000000000000 ) ;
#87741 = B_SPLINE_CURVE_WITH_KNOTS ( 'NONE', 3,
 ( #85764, #61823, #13642, #82567, #5563, #53743, #61372, #26275, #81229, #88445 ),
 .UNSPECIFIED., .F., .F.,
 ( 4, 2, 2, 2, 4 ),
 ( 0.000000000000000000, 0.0001954339857564074473, 0.0003908679715128148945, 0.0005863019572692223418, 0.0007817359430256297891 ),
 .UNSPECIFIED. ) ;
#87742 = ORIENTED_EDGE ( 'NONE', *, *, #82010, .T. ) ;
#87743 = EDGE_CURVE ( 'NONE', #45635, #73490, #34514, .T. ) ;
#87744 = CARTESIAN_POINT ( 'NONE',  ( 5.076923076922954969, -12.27809138561165270, 31.22303859784587132 ) ) ;
#87745 = CYLINDRICAL_SURFACE ( 'NONE', #27119, 0.2499999999999995559 ) ;
#87746 = EDGE_CURVE ( 'NONE', #58097, #52311, #41720, .T. ) ;
#87747 = CARTESIAN_POINT ( 'NONE',  ( 26.99999999999999645, 12.75000000000004974, 30.81664701255125394 ) ) ;
#87748 = CARTESIAN_POINT ( 'NONE',  ( -17.74999999999856115, -7.500000000000155431, 34.75000000000007105 ) ) ;
#87749 = ORIENTED_EDGE ( 'NONE', *, *, #59902, .F. ) ;
#87750 = ORIENTED_EDGE ( 'NONE', *, *, #19822, .F. ) ;
#87752 = ORIENTED_EDGE ( 'NONE', *, *, #38282, .F. ) ;
#87751 = EDGE_CURVE ( 'NONE', #84227, #53257, #72084, .T. ) ;
#87754 = ORIENTED_EDGE ( 'NONE', *, *, #15305, .F. ) ;
#87753 = CARTESIAN_POINT ( 'NONE',  ( -8.069080063669991532, -4.887634598454294377, 34.01352882383564946 ) ) ;
#87755 = CARTESIAN_POINT ( 'NONE',  ( -6.857009589726848375, -3.937682226553329556, 33.60647404775216529 ) ) ;
#87756 = B_SPLINE_CURVE_WITH_KNOTS ( 'NONE', 3,
 ( #62616, #927, #41924, #22525, #49559, #21194, #28395, #14898, #48662, #56752 ),
 .UNSPECIFIED., .F., .F.,
 ( 4, 2, 2, 2, 4 ),
 ( 0.000000000000000000, 0.0001954339857564079894, 0.0003908679715128159787, 0.0005863019572692239681, 0.0007817359430256319575 ),
 .UNSPECIFIED. ) ;
#87757 = CARTESIAN_POINT ( 'NONE',  ( 9.692307692307695177, -11.11383981884818262, 36.00935417666054406 ) ) ;
#87758 = AXIS2_PLACEMENT_3D ( 'NONE', #49339, #76816, #15113 ) ;
#87759 = AXIS2_PLACEMENT_3D ( 'NONE', #70238, #22930, #84214 ) ;
#87760 = EDGE_CURVE ( 'NONE', #4984, #87922, #6602, .T. ) ;
#87761 = CARTESIAN_POINT ( 'NONE',  ( -12.23852710992561299, -12.15243808032446005, 31.58219941686247978 ) ) ;
#87762 = CARTESIAN_POINT ( 'NONE',  ( 16.15384615384603251, -11.67786785259630911, 32.92929555188603530 ) ) ;
#87763 = EDGE_CURVE ( 'NONE', #47735, #66615, #41279, .T. ) ;
#87764 = ORIENTED_EDGE ( 'NONE', *, *, #37123, .T. ) ;
#87765 = AXIS2_PLACEMENT_3D ( 'NONE', #67982, #26992, #66645 ) ;
#87766 = ORIENTED_EDGE ( 'NONE', *, *, #40665, .F. ) ;
#87767 = AXIS2_PLACEMENT_3D ( 'NONE', #67598, #12653, #80226 ) ;
#87768 = ORIENTED_EDGE ( 'NONE', *, *, #64896, .T. ) ;
#87769 = FACE_OUTER_BOUND ( 'NONE', #83749, .T. ) ;
#87771 = VERTEX_POINT ( 'NONE', #33631 ) ;
#87770 = DIRECTION ( 'NONE',  ( -1.000000000000000000, -0.000000000000000000, -0.000000000000000000 ) ) ;
#87772 = VECTOR ( 'NONE', #32649, 1000.000000000000114 ) ;
#87773 = CARTESIAN_POINT ( 'NONE',  ( 13.38461538461538680, -1.422936976036506707, 30.56769352161908415 ) ) ;
#87774 = CARTESIAN_POINT ( 'NONE',  ( 2.057692307692309708, -7.500000000000001776, 35.00000000000000000 ) ) ;
#87775 = EDGE_CURVE ( 'NONE', #87267, #22892, #81826, .T. ) ;
#87776 = CARTESIAN_POINT ( 'NONE',  ( 19.50000000000000000, -4.000000000000000000, 29.75000000000000355 ) ) ;
#87777 = CARTESIAN_POINT ( 'NONE',  ( 9.942307692307712941, -2.249999999999999112, 29.81603969181029967 ) ) ;
#87778 = DIRECTION ( 'NONE',  ( -0.000000000000000000, 1.000000000000000000, 3.491481338843133355E-15 ) ) ;
#87779 = FACE_BOUND ( 'NONE', #68871, .T. ) ;
#87780 = CARTESIAN_POINT ( 'NONE',  ( 15.16468581981335007, -5.557115091759785130, 34.35708131394839171 ) ) ;
#87781 = CARTESIAN_POINT ( 'NONE',  ( -18.13069060311030967, -12.35290016733513951, 31.75349464988449455 ) ) ;
#87782 = DIRECTION ( 'NONE',  ( 0.000000000000000000, 0.9396926207859126468, -0.3420201433256571111 ) ) ;
#87784 = CARTESIAN_POINT ( 'NONE',  ( -5.326946314216043810, -3.202444869320336451, 32.30641848906366675 ) ) ;
#87783 = CARTESIAN_POINT ( 'NONE',  ( 0.3308478584281536183, -6.369640206132551441, 34.87707690430379159 ) ) ;
#87785 = EDGE_CURVE ( 'NONE', #34190, #70760, #726, .T. ) ;
#87786 = CARTESIAN_POINT ( 'NONE',  ( -3.903846153846090239, -7.434744860731434812, 35.00000000000000711 ) ) ;
#87787 = CARTESIAN_POINT ( 'NONE',  ( -20.99999999999999645, -10.75000000000000000, 29.75000000000000355 ) ) ;
#87788 = ORIENTED_EDGE ( 'NONE', *, *, #10430, .T. ) ;
#87789 = EDGE_CURVE ( 'NONE', #1652, #11880, #55660, .T. ) ;
#87790 = CARTESIAN_POINT ( 'NONE',  ( -16.40384615384615330, -7.433931650972299465, 34.75000000000000711 ) ) ;
#87791 = CARTESIAN_POINT ( 'NONE',  ( -13.25382494364843389, -3.957578996910242619, 33.62503395064540257 ) ) ;
#87792 = ORIENTED_EDGE ( 'NONE', *, *, #83227, .T. ) ;
#87793 = VERTEX_POINT ( 'NONE', #27752 ) ;
#87794 = CARTESIAN_POINT ( 'NONE',  ( -17.20761454359063691, -11.18331474514187995, 33.13161551792790505 ) ) ;
#87795 = CARTESIAN_POINT ( 'NONE',  ( -15.36146069743679732, -2.541943142973491554, 30.39792223712631980 ) ) ;
#87796 = CARTESIAN_POINT ( 'NONE',  ( 17.07692307692307665, -8.318370150425687726, 35.83090037661290239 ) ) ;
#87797 = ORIENTED_EDGE ( 'NONE', *, *, #9445, .T. ) ;
#87798 = CARTESIAN_POINT ( 'NONE',  ( 8.703960768674447124, -12.70778746994557551, 30.41441678777548319 ) ) ;
#87799 = CARTESIAN_POINT ( 'NONE',  ( 6.673053698855465399, -8.475808217655753651, 34.90892951860618609 ) ) ;
#87801 = CYLINDRICAL_SURFACE ( 'NONE', #24330, 0.2500000000000008882 ) ;
#87800 = DIRECTION ( 'NONE',  ( -0.000000000000000000, 1.000000000000000000, -0.000000000000000000 ) ) ;
#87802 = CARTESIAN_POINT ( 'NONE',  ( -13.38461538461538325, -2.292212530054420494, 30.41441678777542634 ) ) ;
#87803 = B_SPLINE_CURVE_WITH_KNOTS ( 'NONE', 3,
 ( #80586, #12560, #88245, #40486, #34152, #68825, #26519, #61619, #26963, #7130 ),
 .UNSPECIFIED., .F., .F.,
 ( 4, 2, 2, 2, 4 ),
 ( 0.000000000000000000, 0.0001954339857564081249, 0.0003908679715128162498, 0.0005863019572692244018, 0.0007817359430256324996 ),
 .UNSPECIFIED. ) ;
#87804 = CARTESIAN_POINT ( 'NONE',  ( 3.230769230769231726, -2.486705287966279876, 31.30864560766543647 ) ) ;
#87806 = CARTESIAN_POINT ( 'NONE',  ( -10.48459417441766561, -11.37503395064541678, 33.29242100308974273 ) ) ;
#87805 = SURFACE_STYLE_USAGE ( .BOTH. , #80590 ) ;
#87807 = VECTOR ( 'NONE', #39067, 1000.000000000000000 ) ;
#87808 = CARTESIAN_POINT ( 'NONE',  ( -1.553300858899125059, -3.750000000000009326, 24.07812500000000355 ) ) ;
#87809 = EDGE_LOOP ( 'NONE', ( #60894, #82964 ) ) ;
#87810 = ORIENTED_EDGE ( 'NONE', *, *, #46592, .F. ) ;
#87811 = DIRECTION ( 'NONE',  ( -0.000000000000000000, 0.8660254037844399289, -0.4999999999999980016 ) ) ;
#87812 = EDGE_CURVE ( 'NONE', #79197, #40179, #20118, .T. ) ;
#87813 = CYLINDRICAL_SURFACE ( 'NONE', #42695, 0.2500000000000009437 ) ;
#87814 = DIRECTION ( 'NONE',  ( -0.000000000000000000, 1.000000000000000000, -0.000000000000000000 ) ) ;
#87815 = CARTESIAN_POINT ( 'NONE',  ( -12.46153846153858424, -12.16647553114689728, 32.15551576947799362 ) ) ;
#87816 = CARTESIAN_POINT ( 'NONE',  ( 5.076923076923075762, -3.322132147404559976, 32.92929555188717927 ) ) ;
#87817 = CARTESIAN_POINT ( 'NONE',  ( -3.749999999999988454, -9.053300858899127945, 21.26562500000000000 ) ) ;
#87818 = CARTESIAN_POINT ( 'NONE',  ( -1.449885385171702623, -4.320704448112771878, 33.92786785259540494 ) ) ;
#87819 = CARTESIAN_POINT ( 'NONE',  ( 1.607394925883794734, -5.114059244376869984, 34.14424750095245287 ) ) ;
#87820 = CARTESIAN_POINT ( 'NONE',  ( 16.94623161025551639, -12.11776431015576172, 31.66791131148498906 ) ) ;
#87821 = CARTESIAN_POINT ( 'NONE',  ( -18.13004516283476519, -12.49522139742533966, 29.97347330155777811 ) ) ;
#87822 = CARTESIAN_POINT ( 'NONE',  ( -9.915233909823838232, -11.24512374952581872, 33.06303171183252942 ) ) ;
#87823 = CARTESIAN_POINT ( 'NONE',  ( 13.51514082284902862, -2.647132371071621471, 31.75357179365171589 ) ) ;
#87824 = LINE ( 'NONE', #39627, #49534 ) ;
#87825 = EDGE_CURVE ( 'NONE', #37311, #7100, #74333, .T. ) ;
#87826 = CARTESIAN_POINT ( 'NONE',  ( 7.846153846153846700, -8.164416787775445883, 34.95778746994557906 ) ) ;
#87827 = DIRECTION ( 'NONE',  ( -0.000000000000000000, 0.9396926207859093161, -0.3420201433256663259 ) ) ;
#87828 = CIRCLE ( 'NONE', #71971, 4.000000000000000000 ) ;
#87829 = CARTESIAN_POINT ( 'NONE',  ( -15.48079246806219267, -10.05641848906368097, 34.04755513067966177 ) ) ;
#87830 = ORIENTED_EDGE ( 'NONE', *, *, #14798, .T. ) ;
#87831 = CARTESIAN_POINT ( 'NONE',  ( -5.076923076923075762, -11.69971097300155272, 32.46337939537588113 ) ) ;
#87832 = ADVANCED_FACE ( 'NONE', ( #83608 ), #77712, .F. ) ;
#87833 = CARTESIAN_POINT ( 'NONE',  ( -3.480745961711584791, -3.627789207965226748, 32.91389620160131102 ) ) ;
#87834 = CARTESIAN_POINT ( 'NONE',  ( -0.06109907496451398579, -10.25000000000000178, 18.78311829374151287 ) ) ;
#87835 = AXIS2_PLACEMENT_3D ( 'NONE', #57094, #71939, #17448 ) ;
#87836 = VECTOR ( 'NONE', #51271, 1000.000000000000227 ) ;
#87837 = EDGE_CURVE ( 'NONE', #84245, #34480, #52781, .T. ) ;
#87838 = CARTESIAN_POINT ( 'NONE',  ( 5.207713517890025123, -9.929761469519744921, 34.40412654351204225 ) ) ;
#87839 = CARTESIAN_POINT ( 'NONE',  ( 8.769230769230768274, -10.51840700105979565, 33.73612834413961536 ) ) ;
#87840 = CARTESIAN_POINT ( 'NONE',  ( -11.28851612908349722, -4.932303261841489928, 34.32971442181322885 ) ) ;
#87842 = ORIENTED_EDGE ( 'NONE', *, *, #61769, .T. ) ;
#87841 = CARTESIAN_POINT ( 'NONE',  ( -18.00000000000012079, -10.33852847137269926, 34.16647553114546554 ) ) ;
#87843 = CARTESIAN_POINT ( 'NONE',  ( 1.139087296525997051, -4.749999999999992895, 21.73437500000000000 ) ) ;
#87844 = DIRECTION ( 'NONE',  ( -0.000000000000000000, -0.5000000000000009992, -0.8660254037844380415 ) ) ;
#87845 = VECTOR ( 'NONE', #10253, 1000.000000000000000 ) ;
#87846 = ORIENTED_EDGE ( 'NONE', *, *, #64006, .F. ) ;
#87847 = EDGE_CURVE ( 'NONE', #36328, #35073, #69626, .T. ) ;
#87848 = B_SPLINE_CURVE_WITH_KNOTS ( 'NONE', 3,
 ( #66524, #79595, #4825, #52989, #32295, #33179, #38155, #80487, #25086, #3914 ),
 .UNSPECIFIED., .F., .F.,
 ( 4, 2, 2, 2, 4 ),
 ( 0.000000000000000000, 0.0001954311564186868744, 0.0003908623128373737488, 0.0005862934692560606504, 0.0007817246256747474977 ),
 .UNSPECIFIED. ) ;
#87849 = LINE ( 'NONE', #31986, #39975 ) ;
#87850 = COLOUR_RGB ( '', 0.31764706, 0.68627451, 0.89019608) ;
#87851 = ORIENTED_EDGE ( 'NONE', *, *, #88186, .F. ) ;
#87852 = DIRECTION ( 'NONE',  ( 0.000000000000000000, 1.084202172485504434E-16, -1.000000000000000000 ) ) ;
#87853 = CARTESIAN_POINT ( 'NONE',  ( -9.626239341305250719, -2.721908614388772296, 31.22303859784725333 ) ) ;
#87854 = CARTESIAN_POINT ( 'NONE',  ( -7.976845312821408740, -3.530157926970578952, 32.79014554554150607 ) ) ;
#87855 = ORIENTED_EDGE ( 'NONE', *, *, #30994, .F. ) ;
#87856 = ORIENTED_EDGE ( 'NONE', *, *, #54312, .F. ) ;
#87857 = ORIENTED_EDGE ( 'NONE', *, *, #10250, .T. ) ;
#87858 = CARTESIAN_POINT ( 'NONE',  ( -16.15384615384615330, -2.292212530054420494, 30.41441678777542634 ) ) ;
#87859 = CARTESIAN_POINT ( 'NONE',  ( 12.23861224402231151, -12.39988816332205701, 30.74660775122750778 ) ) ;
#87860 = DIRECTION ( 'NONE',  ( -0.000000000000000000, -0.7660444431189791237, -0.6427876096865379196 ) ) ;
#87861 = CARTESIAN_POINT ( 'NONE',  ( -10.74607608205217346, -2.541943142973491554, 30.39792223712631980 ) ) ;
#87862 = CARTESIAN_POINT ( 'NONE',  ( -10.74553258511630638, -12.15440758774515473, 32.17923288041532004 ) ) ;
#87864 = ADVANCED_FACE ( 'NONE', ( #15137 ), #8379, .F. ) ;
#87863 = CARTESIAN_POINT ( 'NONE',  ( 6.989144256427000101, -8.164416787775445883, 34.95778746994558617 ) ) ;
#87865 = CARTESIAN_POINT ( 'NONE',  ( 12.71148397988660150, -5.057305518903948638, 34.11320923018887896 ) ) ;
#87866 = DIRECTION ( 'NONE',  ( -1.000000000000000000, 0.000000000000000000, 0.000000000000000000 ) ) ;
#87867 = ORIENTED_EDGE ( 'NONE', *, *, #85498, .T. ) ;
#87868 = VERTEX_POINT ( 'NONE', #2055 ) ;
#87869 = EDGE_LOOP ( 'NONE', ( #84861, #29820 ) ) ;
#87871 = EDGE_LOOP ( 'NONE', ( #41325, #86527 ) ) ;
#87870 = CARTESIAN_POINT ( 'NONE',  ( -17.07692307692319744, -10.21337939537710326, 33.94971097300076224 ) ) ;
#87872 = B_SPLINE_CURVE_WITH_KNOTS ( 'NONE', 3,
 ( #37456, #72131, #9987, #78891, #32046, #37009, #64472, #65376, #51848, #38807 ),
 .UNSPECIFIED., .F., .F.,
 ( 4, 2, 2, 2, 4 ),
 ( 0.0007817246256747443535, 0.0009771112852218868158, 0.001172497944769029278, 0.001367884604316171740, 0.001563271263863314203 ),
 .UNSPECIFIED. ) ;
#87873 = VECTOR ( 'NONE', #37384, 1000.000000000000000 ) ;
#87874 = B_SPLINE_CURVE_WITH_KNOTS ( 'NONE', 3,
 ( #47028, #73644, #52455, #38512, #33081, #25441, #74078, #52897, #11936, #19565 ),
 .UNSPECIFIED., .F., .F.,
 ( 4, 2, 2, 2, 4 ),
 ( 0.000000000000000000, 0.0001954311564186861155, 0.0003908623128373722310, 0.0005862934692560583735, 0.0007817246256747444619 ),
 .UNSPECIFIED. ) ;
#87875 = B_SPLINE_CURVE_WITH_KNOTS ( 'NONE', 3,
 ( #6023, #59175, #19963, #40254, #86680, #87120, #66828, #53303, #24946, #53751 ),
 .UNSPECIFIED., .F., .F.,
 ( 4, 2, 2, 2, 4 ),
 ( 0.000000000000000000, 0.0001954311564186860613, 0.0003908623128373721225, 0.0005862934692560581567, 0.0007817246256747442451 ),
 .UNSPECIFIED. ) ;
#87876 = CARTESIAN_POINT ( 'NONE',  ( -14.30769230769230660, -2.249999999999998668, 29.75000000000001776 ) ) ;
#87877 = CARTESIAN_POINT ( 'NONE',  ( 9.468822748583747284, -5.113361153441934093, 34.14387501736622710 ) ) ;
#87878 = B_SPLINE_CURVE_WITH_KNOTS ( 'NONE', 3,
 ( #81975, #26126, #81085, #5418, #75210, #13496, #6734, #34207, #33335, #74319 ),
 .UNSPECIFIED., .F., .F.,
 ( 4, 2, 2, 2, 4 ),
 ( 0.0007817359430256360774, 0.0009771253907250041296, 0.001172514838424371965, 0.001367904286123740017, 0.001563293733823108069 ),
 .UNSPECIFIED. ) ;
#87879 = VERTEX_POINT ( 'NONE', #42610 ) ;
#87880 = CARTESIAN_POINT ( 'NONE',  ( 15.23076923076910916, -9.528491918059723176, 34.59228464037033035 ) ) ;
#87881 = VERTEX_POINT ( 'NONE', #35397 ) ;
#87882 = PLANE ( 'NONE',  #79945 ) ;
#87883 = VERTEX_POINT ( 'NONE', #77270 ) ;
#87884 = CARTESIAN_POINT ( 'NONE',  ( -12.52686137703063984, -7.749976743299138882, 34.99404534957040624 ) ) ;
#87885 = EDGE_CURVE ( 'NONE', #22173, #76098, #16257, .T. ) ;
#87886 = CARTESIAN_POINT ( 'NONE',  ( 1.634560902963529072, -6.696923467548660192, 34.68552623307873972 ) ) ;
#87887 = CARTESIAN_POINT ( 'NONE',  ( -16.15384615384615330, -10.67929555188718282, 33.92786785259544047 ) ) ;
#87888 = FACE_BOUND ( 'NONE', #13997, .T. ) ;
#87889 = CARTESIAN_POINT ( 'NONE',  ( 2.372838087024272458, -7.750023238201980469, 34.74374492549440419 ) ) ;
#87891 = EDGE_CURVE ( 'NONE', #47764, #25506, #70071, .T. ) ;
#87890 = DIRECTION ( 'NONE',  ( 0.000000000000000000, 0.000000000000000000, 1.000000000000000000 ) ) ;
#87892 = VECTOR ( 'NONE', #24987, 1000.000000000000000 ) ;
#87893 = VECTOR ( 'NONE', #53641, 1000.000000000000000 ) ;
#87894 = FACE_OUTER_BOUND ( 'NONE', #8426, .T. ) ;
#87895 = CARTESIAN_POINT ( 'NONE',  ( 3.453548899747296730, -4.989023458446561143, 34.36081565061822118 ) ) ;
#87896 = CARTESIAN_POINT ( 'NONE',  ( -16.15384615384615330, -2.517432740324522911, 35.29906147534542527 ) ) ;
#87897 = CARTESIAN_POINT ( 'NONE',  ( -13.38461538461538325, -1.367168528481310208, 33.57946703557072254 ) ) ;
#87898 = ORIENTED_EDGE ( 'NONE', *, *, #54814, .F. ) ;
#87899 = ADVANCED_FACE ( 'NONE', ( #56995 ), #28650, .F. ) ;
#87900 = CARTESIAN_POINT ( 'NONE',  ( -13.31942140283202747, -2.506253911140448487, 29.99999999999988631 ) ) ;
#87901 = ORIENTED_EDGE ( 'NONE', *, *, #72862, .T. ) ;
#87902 = ORIENTED_EDGE ( 'NONE', *, *, #88083, .T. ) ;
#87903 = AXIS2_PLACEMENT_3D ( 'NONE', #85014, #16987, #10679 ) ;
#87905 = CYLINDRICAL_SURFACE ( 'NONE', #60615, 0.2499999999999994726 ) ;
#87904 = CARTESIAN_POINT ( 'NONE',  ( 2.307692307692186251, -3.083524468854526912, 32.58852847137268327 ) ) ;
#87906 = EDGE_CURVE ( 'NONE', #68833, #21879, #8824, .T. ) ;
#87907 = CARTESIAN_POINT ( 'NONE',  ( 15.23076923076923173, -12.62096338111211580, 30.90682066428153263 ) ) ;
#87908 = DIRECTION ( 'NONE',  ( 0.000000000000000000, 0.9396926207859126468, -0.3420201433256571111 ) ) ;
#87909 = DIRECTION ( 'NONE',  ( -0.000000000000000000, -0.9396926207859093161, -0.3420201433256663259 ) ) ;
#87910 = CARTESIAN_POINT ( 'NONE',  ( 17.07692307692295586, -8.613356846316285953, 34.62446782046622218 ) ) ;
#87911 = CARTESIAN_POINT ( 'NONE',  ( -2.176900499867522321, -2.729792928343269587, 31.24908615093345077 ) ) ;
#87912 = ORIENTED_EDGE ( 'NONE', *, *, #56273, .T. ) ;
#87913 = CARTESIAN_POINT ( 'NONE',  ( -11.53846153846153655, -12.10708131394839349, 31.69288490824020244 ) ) ;
#87914 = DIRECTION ( 'NONE',  ( -1.000000000000000000, -0.000000000000000000, -0.000000000000000000 ) ) ;
#87915 = DIRECTION ( 'NONE',  ( 1.000000000000000000, 0.000000000000000000, 0.000000000000000000 ) ) ;
#87916 = CARTESIAN_POINT ( 'NONE',  ( -15.90379173393269596, -4.074993327901529128, 33.72946981652012255 ) ) ;
#87917 = ORIENTED_EDGE ( 'NONE', *, *, #24063, .F. ) ;
#87918 = EDGE_CURVE ( 'NONE', #51126, #20157, #64558, .T. ) ;
#87919 = B_SPLINE_CURVE_WITH_KNOTS ( 'NONE', 3,
 ( #83056, #1075, #42075, #68645, #8284, #27217 ),
 .UNSPECIFIED., .F., .F.,
 ( 4, 2, 4 ),
 ( 0.0003909569690057831406, 0.0005862646681846083070, 0.0007815723673634335277 ),
 .UNSPECIFIED. ) ;
#87920 = ORIENTED_EDGE ( 'NONE', *, *, #78629, .F. ) ;
#87921 = APPLICATION_PROTOCOL_DEFINITION ( 'draft international standard', 'automotive_design', 1998, #39452 ) ;
#87922 = VERTEX_POINT ( 'NONE', #56116 ) ;
#87923 = CARTESIAN_POINT ( 'NONE',  ( 0.6845013650999459687, -7.369474270740072441, 34.74850911626239736 ) ) ;
#87924 = EDGE_CURVE ( 'NONE', #32571, #73852, #76840, .T. ) ;
#87925 = CARTESIAN_POINT ( 'NONE',  ( -17.77698864838715309, -4.887748414852788770, 34.01359900205216746 ) ) ;
#87926 = EDGE_LOOP ( 'NONE', ( #69477, #62102 ) ) ;
#87927 = B_SPLINE_CURVE_WITH_KNOTS ( 'NONE', 3,
 ( #8376, #43486, #7491, #29103, #57433, #2052, #16457, #1166, #49360, #62846 ),
 .UNSPECIFIED., .F., .F.,
 ( 4, 2, 2, 2, 4 ),
 ( 0.000000000000000000, 0.0001954311564186869015, 0.0003908623128373738030, 0.0005862934692560607588, 0.0007817246256747476061 ),
 .UNSPECIFIED. ) ;
#87928 = CARTESIAN_POINT ( 'NONE',  ( -15.90379184220783948, -4.943051570960395047, 34.04725096376909477 ) ) ;
#87929 = CARTESIAN_POINT ( 'NONE',  ( -5.299849294439223257, -2.758268499246657957, 31.33685645148948140 ) ) ;
#87930 = CARTESIAN_POINT ( 'NONE',  ( 3.453548899747296730, -10.23759521482555357, 34.22997729860117033 ) ) ;
#87931 = CARTESIAN_POINT ( 'NONE',  ( 14.17721559957584709, -7.276988635370452485, 34.74523720219453793 ) ) ;
#87932 = DIRECTION ( 'NONE',  ( -0.000000000000000000, -0.6427876096865404731, -0.7660444431189771253 ) ) ;
#87933 = ORIENTED_EDGE ( 'NONE', *, *, #20753, .F. ) ;
#87935 = ORIENTED_EDGE ( 'NONE', *, *, #88552, .T. ) ;
#87934 = CARTESIAN_POINT ( 'NONE',  ( -15.36091720050092846, -12.15440758774515473, 32.17923288041532004 ) ) ;
#87936 = LINE ( 'NONE', #88810, #71365 ) ;
#87937 = CARTESIAN_POINT ( 'NONE',  ( -3.100243792535588572, -2.647132371071621471, 31.75357179365173010 ) ) ;
#87938 = CARTESIAN_POINT ( 'NONE',  ( 1.134615384615387246, -7.500000000000001776, 34.75000000000000000 ) ) ;
#87939 = CARTESIAN_POINT ( 'NONE',  ( 9.692307692307572609, -10.90142922262034020, 33.41473453929536674 ) ) ;
#87940 = CARTESIAN_POINT ( 'NONE',  ( -16.15384615384615330, -13.53365097954675988, 30.81389545987213552 ) ) ;
#87941 = CARTESIAN_POINT ( 'NONE',  ( -5.326946301144534601, -10.92453946501458439, 33.72985991061850086 ) ) ;
#87942 = CARTESIAN_POINT ( 'NONE',  ( -0.7115616988314267255, -12.43535235679832596, 30.55408501211184813 ) ) ;
#87943 = CIRCLE ( 'NONE', #18846, 4.000000000000000000 ) ;
#87944 = CARTESIAN_POINT ( 'NONE',  ( -2.775308065498752086, -8.577988221561495763, 21.51749329374151998 ) ) ;
#87945 = ORIENTED_EDGE ( 'NONE', *, *, #74213, .T. ) ;
#87946 = EDGE_CURVE ( 'NONE', #43122, #11726, #33489, .T. ) ;
#87947 = CARTESIAN_POINT ( 'NONE',  ( -6.988346923633244501, -11.06231777344662781, 33.60647404775220082 ) ) ;
#87948 = CARTESIAN_POINT ( 'NONE',  ( -9.442253380669377805, -8.303483539816728154, 34.68545999027711702 ) ) ;
#87949 = B_SPLINE_CURVE_WITH_KNOTS ( 'NONE', 3,
 ( #88548, #62364, #27262, #28143, #85207, #45539, #45091, #76786, #21838, #29055 ),
 .UNSPECIFIED., .F., .F.,
 ( 4, 2, 2, 2, 4 ),
 ( 0.0007817359430256293554, 0.0009771253907249952391, 0.001172514838424361123, 0.001367904286123727007, 0.001563293733823092890 ),
 .UNSPECIFIED. ) ;
#87950 = ADVANCED_FACE ( 'NONE', ( #86272 ), #4275, .F. ) ;
#87951 = ORIENTED_EDGE ( 'NONE', *, *, #68801, .T. ) ;
#87952 = EDGE_LOOP ( 'NONE', ( #19519, #56594 ) ) ;
#87953 = CARTESIAN_POINT ( 'NONE',  ( 8.096208266067298709, -12.01375889529407637, 32.43194544308182969 ) ) ;
#87954 = CARTESIAN_POINT ( 'NONE',  ( 11.47237915910140771, -12.62096338111211580, 30.90682066428152908 ) ) ;
#87955 = CARTESIAN_POINT ( 'NONE',  ( 10.74617505635156789, -4.684288915650983043, 34.18129842949671371 ) ) ;
#87956 = EDGE_CURVE ( 'NONE', #3816, #13509, #25442, .T. ) ;
#87957 = DIRECTION ( 'NONE',  ( -0.000000000000000000, 0.7660444431189791237, -0.6427876096865379196 ) ) ;
#87958 = CARTESIAN_POINT ( 'NONE',  ( 17.93472999944368240, -2.657715359629089669, 31.77849191805833584 ) ) ;
#87959 = ORIENTED_EDGE ( 'NONE', *, *, #23165, .T. ) ;
#87960 = DIRECTION ( 'NONE',  ( 0.000000000000000000, 0.000000000000000000, -1.000000000000000000 ) ) ;
#87961 = ADVANCED_FACE ( 'NONE', ( #11485 ), #65970, .F. ) ;
#87962 = AXIS2_PLACEMENT_3D ( 'NONE', #87238, #74150, #12446 ) ;
#87963 = CARTESIAN_POINT ( 'NONE',  ( 17.20771488474786892, -5.582136614379148654, 34.36778462344220486 ) ) ;
#87964 = CARTESIAN_POINT ( 'NONE',  ( 9.562159722575994891, -2.647304123082328875, 31.75400227202885972 ) ) ;
#87965 = EDGE_LOOP ( 'NONE', ( #10742, #70566, #71656, #31476 ) ) ;
#87966 = DIRECTION ( 'NONE',  ( -1.000000000000000000, -0.000000000000000000, -0.000000000000000000 ) ) ;
#87967 = AXIS2_PLACEMENT_3D ( 'NONE', #2654, #30147, #49965 ) ;
#87968 = EDGE_LOOP ( 'NONE', ( #62178, #23277 ) ) ;
#87969 = LINE ( 'NONE', #24887, #12665 ) ;
#87970 =( NAMED_UNIT ( * ) SI_UNIT ( $, .STERADIAN. ) SOLID_ANGLE_UNIT ( ) );
#87971 = CARTESIAN_POINT ( 'NONE',  ( -5.749945580086544439, -12.01375889529407281, 32.43194544308182969 ) ) ;
#87972 = ORIENTED_EDGE ( 'NONE', *, *, #14812, .T. ) ;
#87973 = DIRECTION ( 'NONE',  ( 0.000000000000000000, 0.000000000000000000, 1.000000000000000000 ) ) ;
#87975 = EDGE_CURVE ( 'NONE', #50820, #4743, #32363, .T. ) ;
#87974 = DIRECTION ( 'NONE',  ( 0.000000000000000000, -6.938893903907222067E-15, 1.000000000000000000 ) ) ;
#87976 = CARTESIAN_POINT ( 'NONE',  ( -9.822454901745908629, -2.619462340734462380, 30.83744416345203021 ) ) ;
#87977 = VECTOR ( 'NONE', #34332, 1000.000000000000227 ) ;
#87978 = EDGE_CURVE ( 'NONE', #37947, #34931, #31308, .T. ) ;
#87979 = CARTESIAN_POINT ( 'NONE',  ( 7.053867364043874488, -12.35292014791297710, 31.75344720912887198 ) ) ;
#87980 = FACE_OUTER_BOUND ( 'NONE', #56432, .T. ) ;
#87981 = EDGE_CURVE ( 'NONE', #65220, #22041, #66426, .T. ) ;
#87982 = ORIENTED_EDGE ( 'NONE', *, *, #71289, .F. ) ;
#87983 = FACE_BOUND ( 'NONE', #38291, .T. ) ;
#87984 = ORIENTED_EDGE ( 'NONE', *, *, #66179, .F. ) ;
#87985 = CARTESIAN_POINT ( 'NONE',  ( -3.262820512820514995, -11.50000000000000000, 29.75000000000000355 ) ) ;
#87986 = FACE_OUTER_BOUND ( 'NONE', #16332, .T. ) ;
#87987 = DIRECTION ( 'NONE',  ( 0.000000000000000000, 0.3420201433256641055, -0.9396926207859100932 ) ) ;
#87988 = CARTESIAN_POINT ( 'NONE',  ( -6.857821351800896359, -6.026961402152789304, 34.52809138561124769 ) ) ;
#87989 = DIRECTION ( 'NONE',  ( -0.000000000000000000, 0.7660444431189791237, -0.6427876096865379196 ) ) ;
#87990 = VERTEX_POINT ( 'NONE', #39415 ) ;
#87991 = VERTEX_POINT ( 'NONE', #31761 ) ;
#87992 = ORIENTED_EDGE ( 'NONE', *, *, #55821, .T. ) ;
#87993 = B_SPLINE_CURVE_WITH_KNOTS ( 'NONE', 3,
 ( #67732, #45674, #73155, #80368, #24957, #65937, #53315, #39821, #52425, #11452 ),
 .UNSPECIFIED., .F., .F.,
 ( 4, 2, 2, 2, 4 ),
 ( 0.000000000000000000, 0.0001954339857564065528, 0.0003908679715128131056, 0.0005863019572692196313, 0.0007817359430256262112 ),
 .UNSPECIFIED. ) ;
#87994 = VECTOR ( 'NONE', #5463, 1000.000000000000000 ) ;
#87995 = ORIENTED_EDGE ( 'NONE', *, *, #32870, .F. ) ;
#87996 = CARTESIAN_POINT ( 'NONE',  ( 2.084766090176160880, -4.887634598454295265, 34.01352882383564946 ) ) ;
#87997 = CARTESIAN_POINT ( 'NONE',  ( 16.15384615384603251, -11.06231777344772027, 33.60647404775119895 ) ) ;
#87998 = AXIS2_PLACEMENT_3D ( 'NONE', #75389, #34395, #14569 ) ;
#87999 = CARTESIAN_POINT ( 'NONE',  ( -15.48079246806219267, -10.76384336483936011, 33.53834819971076087 ) ) ;
#88000 = DIRECTION ( 'NONE',  ( -0.000000000000000000, -0.3420201433256694346, -0.9396926207859080948 ) ) ;
#88001 = CARTESIAN_POINT ( 'NONE',  ( 3.999999999999997335, 7.500000000000000888, 13.50000000000000178 ) ) ;
#88002 = PLANE ( 'NONE',  #32194 ) ;
#88003 = CARTESIAN_POINT ( 'NONE',  ( 17.77707378248385339, -2.554751324335733376, 30.48935550225260727 ) ) ;
#88004 = CARTESIAN_POINT ( 'NONE',  ( 17.14217864819909920, -2.625532179533470512, 30.86335684631491105 ) ) ;
#88005 = EDGE_LOOP ( 'NONE', ( #570, #12268 ) ) ;
#88006 = B_SPLINE_CURVE_WITH_KNOTS ( 'NONE', 3,
 ( #76184, #14487, #35203, #975, #61775, #14941, #6841, #15387, #47830, #55471 ),
 .UNSPECIFIED., .F., .F.,
 ( 4, 2, 2, 2, 4 ),
 ( 0.0007817246256747480398, 0.0009771112852218909357, 0.001172497944769034049, 0.001367884604316177161, 0.001563271263863320057 ),
 .UNSPECIFIED. ) ;
#88007 = ORIENTED_EDGE ( 'NONE', *, *, #61330, .F. ) ;
#88008 = VERTEX_POINT ( 'NONE', #18244 ) ;
#88010 = ORIENTED_EDGE ( 'NONE', *, *, #66417, .T. ) ;
#88009 = CARTESIAN_POINT ( 'NONE',  ( 2.084207363968360927, -2.599994579823203367, 30.74605699353653776 ) ) ;
#88012 = CARTESIAN_POINT ( 'NONE',  ( -10.61538461538461320, -12.62096338111211580, 30.90682066428153263 ) ) ;
#88011 = CARTESIAN_POINT ( 'NONE',  ( 6.699591998512593349, -11.60425143139329940, 33.02411095842164457 ) ) ;
#88013 = EDGE_CURVE ( 'NONE', #3792, #58712, #28057, .T. ) ;
#88014 = CARTESIAN_POINT ( 'NONE',  ( 15.90384615384615330, -7.566083408709835645, 34.74999999999999289 ) ) ;
#88015 = CARTESIAN_POINT ( 'NONE',  ( -15.48074597481782178, -10.06842814019191401, 34.32929386961144758 ) ) ;
#88016 = FACE_BOUND ( 'NONE', #87389, .T. ) ;
#88017 = VERTEX_POINT ( 'NONE', #59664 ) ;
#88018 = EDGE_LOOP ( 'NONE', ( #73325, #21735, #62162, #77604, #28946 ) ) ;
#88019 = ADVANCED_FACE ( 'NONE', ( #38513 ), #30852, .F. ) ;
#88020 = CARTESIAN_POINT ( 'NONE',  ( -8.704036787447412493, -2.506253911140448487, 29.99999999999988631 ) ) ;
#88021 = EDGE_LOOP ( 'NONE', ( #35431, #39887, #20489, #73179 ) ) ;
#88022 = FACE_BOUND ( 'NONE', #25487, .T. ) ;
#88024 = CIRCLE ( 'NONE', #72165, 0.2500000000000002220 ) ;
#88023 = CARTESIAN_POINT ( 'NONE',  ( 9.758375025657770152, -5.471508081941601098, 34.59228464037088457 ) ) ;
#88025 = DIRECTION ( 'NONE',  ( 1.000000000000000000, 0.000000000000000000, 0.000000000000000000 ) ) ;
#88026 = ORIENTED_EDGE ( 'NONE', *, *, #54802, .F. ) ;
#88027 = CARTESIAN_POINT ( 'NONE',  ( -6.249999999999997335, -7.500000000000001776, 34.75000000000000000 ) ) ;
#88028 = DIRECTION ( 'NONE',  ( 0.000000000000000000, 0.000000000000000000, 1.000000000000000000 ) ) ;
#88029 = CARTESIAN_POINT ( 'NONE',  ( 1.319344938654610111, -3.300289026998414865, 32.46337939537583139 ) ) ;
#88030 = EDGE_LOOP ( 'NONE', ( #13323, #29140 ) ) ;
#88031 = CARTESIAN_POINT ( 'NONE',  ( -7.596208436775802930, -8.476813868363244353, 34.90874843262270133 ) ) ;
#88032 = DIRECTION ( 'NONE',  ( 0.000000000000000000, 0.000000000000000000, 1.000000000000000000 ) ) ;
#88033 = CARTESIAN_POINT ( 'NONE',  ( -17.93474486048716088, -12.70778746994558439, 30.41441678777537305 ) ) ;
#88034 = ORIENTED_EDGE ( 'NONE', *, *, #49933, .T. ) ;
#88035 = VECTOR ( 'NONE', #82841, 1000.000000000000114 ) ;
#88036 = EDGE_CURVE ( 'NONE', #50542, #43102, #52456, .T. ) ;
#88037 = CYLINDRICAL_SURFACE ( 'NONE', #74742, 0.2499999999999995559 ) ;
#88038 = CARTESIAN_POINT ( 'NONE',  ( 3.930919194939303196, -10.01117774369187252, 34.36070679894347535 ) ) ;
#88039 = ORIENTED_EDGE ( 'NONE', *, *, #65277, .T. ) ;
#88040 = DIRECTION ( 'NONE',  ( -1.000000000000000000, 0.000000000000000000, 0.000000000000000000 ) ) ;
#88041 = CARTESIAN_POINT ( 'NONE',  ( -4.219116599806928214, -2.625532179533445198, 30.86335684631481513 ) ) ;
#88042 = DIRECTION ( 'NONE',  ( 0.000000000000000000, 0.3420201433256610524, 0.9396926207859113145 ) ) ;
#88043 = CARTESIAN_POINT ( 'NONE',  ( 16.37662582282421653, -12.11081565061823717, 32.26097654155341843 ) ) ;
#88044 = CARTESIAN_POINT ( 'NONE',  ( 10.61538461538449418, -11.67786785259630911, 32.92929555188603530 ) ) ;
#88045 = CARTESIAN_POINT ( 'NONE',  ( -5.326923076923075762, -2.249999999999998668, 29.75000000000000355 ) ) ;
#88047 = CARTESIAN_POINT ( 'NONE',  ( 8.703148389870632329, -2.833524468853757305, 32.15551576947924417 ) ) ;
#88046 = CARTESIAN_POINT ( 'NONE',  ( -1.608100328339332474, -5.113361153441934093, 34.14387501736622710 ) ) ;
#88048 = CARTESIAN_POINT ( 'NONE',  ( 10.68063975489745232, -9.528491918058460186, 34.59228464037086326 ) ) ;
#88049 = DIRECTION ( 'NONE',  ( 0.000000000000000000, 0.4999999999999985567, 0.8660254037844395958 ) ) ;
#88050 = CARTESIAN_POINT ( 'NONE',  ( -1.409462824231155764E-14, -4.749999999999999112, 16.65625000000000000 ) ) ;
#88051 = ORIENTED_EDGE ( 'NONE', *, *, #10358, .T. ) ;
#88052 = ADVANCED_FACE ( 'NONE', ( #85816 ), #13696, .F. ) ;
#88053 = CARTESIAN_POINT ( 'NONE',  ( 17.77707378248384629, -4.186968288167451036, 33.49512374952580274 ) ) ;
#88054 = ORIENTED_EDGE ( 'NONE', *, *, #29996, .T. ) ;
#88055 = VERTEX_POINT ( 'NONE', #53793 ) ;
#88056 = EDGE_CURVE ( 'NONE', #87727, #20693, #7393, .T. ) ;
#88057 = CARTESIAN_POINT ( 'NONE',  ( 17.07692307692307665, -12.78798330534102945, 29.74999999999997868 ) ) ;
#88058 = ORIENTED_EDGE ( 'NONE', *, *, #12674, .T. ) ;
#88059 = CARTESIAN_POINT ( 'NONE',  ( -5.299850035829924977, -11.43668979543635089, 33.22377378376089752 ) ) ;
#88060 = CARTESIAN_POINT ( 'NONE',  ( 2.749999999999995115, -6.360912703473971419, 21.89062500000000355 ) ) ;
#88061 = CARTESIAN_POINT ( 'NONE',  ( 17.75002325595141173, -4.818429247618089661, 34.26397095200675125 ) ) ;
#88062 = CARTESIAN_POINT ( 'NONE',  ( -9.019254006523732770, -3.202444869320336451, 32.30641848906366675 ) ) ;
#88063 = CARTESIAN_POINT ( 'NONE',  ( 9.757562831820528970, -9.528491918058460186, 34.59228464037086326 ) ) ;
#88064 = CARTESIAN_POINT ( 'NONE',  ( -4.826868657009621089, -2.544122305571457687, 31.48381861865059150 ) ) ;
#88065 = CARTESIAN_POINT ( 'NONE',  ( -1.326923076923076872, -3.499999999999999556, 29.75000000000000355 ) ) ;
#88066 = CARTESIAN_POINT ( 'NONE',  ( -14.87820512820512953, -7.500000000000000000, 29.75000000000000355 ) ) ;
#88067 = CARTESIAN_POINT ( 'NONE',  ( -1.929879867024197893E-14, -3.750000000000000000, 20.40625000000000000 ) ) ;
#88068 = CARTESIAN_POINT ( 'NONE',  ( -7.146561847641255127, -4.988325925672468131, 34.36044203135681130 ) ) ;
#88069 = CARTESIAN_POINT ( 'NONE',  ( -0.4615384615384611200, -13.37000171582298513, 34.34916445242398453 ) ) ;
#88070 = EDGE_CURVE ( 'NONE', #4121, #32754, #39877, .T. ) ;
#88071 = AXIS2_PLACEMENT_3D ( 'NONE', #75845, #83500, #21786 ) ;
#88072 = CARTESIAN_POINT ( 'NONE',  ( 18.00000000000030553, -2.506253911140615021, 30.00000000000323297 ) ) ;
#88073 = ORIENTED_EDGE ( 'NONE', *, *, #30968, .T. ) ;
#88074 = VERTEX_POINT ( 'NONE', #186 ) ;
#88075 = CARTESIAN_POINT ( 'NONE',  ( -9.469296340694842939, -3.587049720035815348, 32.86302985866382897 ) ) ;
#88076 = CARTESIAN_POINT ( 'NONE',  ( 15.29683656411930848, -11.91647553114624358, 32.58852847137148245 ) ) ;
#88077 = CARTESIAN_POINT ( 'NONE',  ( -39.05038313613820122, -2.499999999999999556, 27.25000000000000000 ) ) ;
#88078 = CARTESIAN_POINT ( 'NONE',  ( -6.000000000000119904, -3.835265460704628371, 33.15142922262033665 ) ) ;
#88080 = EDGE_CURVE ( 'NONE', #83231, #75643, #51707, .T. ) ;
#88079 = CARTESIAN_POINT ( 'NONE',  ( 8.519254038288414321, -4.236021600441997492, 33.53823185664189310 ) ) ;
#88081 = CARTESIAN_POINT ( 'NONE',  ( -0.7115151924808158501, -6.567427716900047230, 34.66269422305636283 ) ) ;
#88082 = EDGE_CURVE ( 'NONE', #13990, #3335, #3316, .T. ) ;
#88083 = EDGE_CURVE ( 'NONE', #30410, #64311, #6062, .T. ) ;
#88084 = ORIENTED_EDGE ( 'NONE', *, *, #25481, .F. ) ;
#88085 = CARTESIAN_POINT ( 'NONE',  ( 1.254468175177166245, -5.195881422630166391, 34.18770438780619259 ) ) ;
#88086 = EDGE_LOOP ( 'NONE', ( #42813, #37858 ) ) ;
#88087 = B_SPLINE_CURVE_WITH_KNOTS ( 'NONE', 3,
 ( #43368, #64497, #9153, #16772, #52330, #2805, #79824, #72158, #86589, #10913 ),
 .UNSPECIFIED., .F., .F.,
 ( 4, 2, 2, 2, 4 ),
 ( 0.0007817359430256294638, 0.0009771253907249974075, 0.001172514838424365460, 0.001367904286123733295, 0.001563293733823094191 ),
 .UNSPECIFIED. ) ;
#88088 = EDGE_CURVE ( 'NONE', #62746, #30988, #33964, .T. ) ;
#88089 = VERTEX_POINT ( 'NONE', #74515 ) ;
#88090 = VECTOR ( 'NONE', #14782, 1000.000000000000000 ) ;
#88091 = CARTESIAN_POINT ( 'NONE',  ( 5.076923076923075762, -8.120952969808772792, 34.71129190930000163 ) ) ;
#88092 = VECTOR ( 'NONE', #76977, 1000.000000000000000 ) ;
#88093 = CARTESIAN_POINT ( 'NONE',  ( -2.531177232256636156, -9.417330523894424488, 34.63758898049880486 ) ) ;
#88094 = CARTESIAN_POINT ( 'NONE',  ( -4.153846153846273204, -4.481592998941358097, 33.73612834414048933 ) ) ;
#88095 = CARTESIAN_POINT ( 'NONE',  ( 11.76147438255493149, -2.308499170217967134, 30.53291367094873721 ) ) ;
#88096 = FACE_OUTER_BOUND ( 'NONE', #39247, .T. ) ;
#88097 = VECTOR ( 'NONE', #50689, 1000.000000000000000 ) ;
#88098 = ORIENTED_EDGE ( 'NONE', *, *, #34052, .F. ) ;
#88099 = VERTEX_POINT ( 'NONE', #12810 ) ;
#88100 = ORIENTED_EDGE ( 'NONE', *, *, #61596, .T. ) ;
#88101 = VERTEX_POINT ( 'NONE', #61430 ) ;
#88102 = CARTESIAN_POINT ( 'NONE',  ( -17.07692307692319744, -11.94971097300221174, 32.03036669348237098 ) ) ;
#88103 = FACE_OUTER_BOUND ( 'NONE', #84885, .T. ) ;
#88104 = CARTESIAN_POINT ( 'NONE',  ( -19.50000000000000000, -3.499999999999999556, 29.75000000000000355 ) ) ;
#88105 = CARTESIAN_POINT ( 'NONE',  ( -15.29603967673000575, -11.48612834413959582, 32.76840700105983473 ) ) ;
#88106 = CARTESIAN_POINT ( 'NONE',  ( -15.10024379253558635, -9.503571793651731880, 34.60286762892837942 ) ) ;
#88107 = CARTESIAN_POINT ( 'NONE',  ( 14.08476609017615644, -12.39988816332205701, 30.74660775122750778 ) ) ;
#88108 = ORIENTED_EDGE ( 'NONE', *, *, #87978, .T. ) ;
#88109 = EDGE_LOOP ( 'NONE', ( #45381, #49268, #19122, #439, #8098 ) ) ;
#88111 = ORIENTED_EDGE ( 'NONE', *, *, #4045, .T. ) ;
#88110 = CARTESIAN_POINT ( 'NONE',  ( 17.07692307692307665, -12.37446782046654192, 30.86335684631486131 ) ) ;
#88112 = CARTESIAN_POINT ( 'NONE',  ( -9.915233909823838232, -4.887634598454295265, 34.01352882383564946 ) ) ;
#88113 = FACE_OUTER_BOUND ( 'NONE', #30638, .T. ) ;
#88114 = AXIS2_PLACEMENT_3D ( 'NONE', #62507, #8918, #62077 ) ;
#88115 = CARTESIAN_POINT ( 'NONE',  ( 2.651650429449539104, -4.848349570550432475, 21.81250000000000000 ) ) ;
#88116 = VERTEX_POINT ( 'NONE', #67760 ) ;
#88117 = CARTESIAN_POINT ( 'NONE',  ( 8.068933515131909928, -4.226511098958374291, 33.85474049983370293 ) ) ;
#88118 = ORIENTED_EDGE ( 'NONE', *, *, #82772, .F. ) ;
#88119 = LINE ( 'NONE', #61489, #67241 ) ;
#88120 = CARTESIAN_POINT ( 'NONE',  ( 17.20744851515672025, -12.15418822224088657, 32.17964115625579069 ) ) ;
#88121 = FACE_BOUND ( 'NONE', #10525, .T. ) ;
#88122 = FACE_OUTER_BOUND ( 'NONE', #26441, .T. ) ;
#88123 = LINE ( 'NONE', #6121, #4533 ) ;
#88124 = ORIENTED_EDGE ( 'NONE', *, *, #77394, .F. ) ;
#88125 = CARTESIAN_POINT ( 'NONE',  ( -12.46153846153846168, -10.51840700105979565, 33.73612834413961536 ) ) ;
#88126 = CARTESIAN_POINT ( 'NONE',  ( -14.30769230769242739, -2.625532179533778709, 30.86335684631627174 ) ) ;
#88127 = CARTESIAN_POINT ( 'NONE',  ( 0.6843180028068693854, -12.44528174975671853, 30.48912976160716681 ) ) ;
#88128 = EDGE_LOOP ( 'NONE', ( #32921, #6589, #79212, #83817 ) ) ;
#88129 = CARTESIAN_POINT ( 'NONE',  ( -18.24997674404858827, -12.65889640711025521, 30.72598325615533454 ) ) ;
#88130 = CARTESIAN_POINT ( 'NONE',  ( 14.30769230769231015, -9.905515769479276145, 34.41647553114623292 ) ) ;
#88131 = CARTESIAN_POINT ( 'NONE',  ( -12.59222992820602371, -12.11776431015576172, 31.66791131148498906 ) ) ;
#88132 = LINE ( 'NONE', #55193, #11233 ) ;
#88133 = DIRECTION ( 'NONE',  ( 0.000000000000000000, 1.000000000000000000, 0.000000000000000000 ) ) ;
#88134 = FACE_BOUND ( 'NONE', #77032, .T. ) ;
#88136 = DIRECTION ( 'NONE',  ( 0.000000000000000000, 0.6427876096865373645, -0.7660444431189797898 ) ) ;
#88135 = CARTESIAN_POINT ( 'NONE',  ( -6.988346923633242724, -12.51329471203370325, 31.30864560766548976 ) ) ;
#88137 = CARTESIAN_POINT ( 'NONE',  ( -9.469294848214296678, -11.98016756924215009, 32.48728574198911190 ) ) ;
#88139 = CARTESIAN_POINT ( 'NONE',  ( -2.177166869458664777, -12.50538340440932217, 31.33453814440721885 ) ) ;
#88138 = CARTESIAN_POINT ( 'NONE',  ( -18.25002322422145440, -2.341070481393819236, 30.72580821765574299 ) ) ;
#88140 = CARTESIAN_POINT ( 'NONE',  ( 13.31853300525524908, -2.486705287966279432, 31.30864560766542937 ) ) ;
#88141 = CARTESIAN_POINT ( 'NONE',  ( 2.724691934501235036, -6.299813628509441266, 19.13875670625849068 ) ) ;
#88142 = ORIENTED_EDGE ( 'NONE', *, *, #40533, .F. ) ;
#88143 = LINE ( 'NONE', #12024, #8762 ) ;
#88144 = VERTEX_POINT ( 'NONE', #33536 ) ;
#88145 = EDGE_CURVE ( 'NONE', #47721, #5191, #15145, .T. ) ;
#88146 = AXIS2_PLACEMENT_3D ( 'NONE', #87876, #82868, #81541 ) ;
#88147 = LINE ( 'NONE', #40822, #83786 ) ;
#88148 = ORIENTED_EDGE ( 'NONE', *, *, #75261, .F. ) ;
#88149 = CARTESIAN_POINT ( 'NONE',  ( -15.36137959039375644, -7.722926236386453702, 34.74524107206102030 ) ) ;
#88150 = CARTESIAN_POINT ( 'NONE',  ( -1.384615384615505151, -10.90142922262034020, 33.41473453929536674 ) ) ;
#88152 = ORIENTED_EDGE ( 'NONE', *, *, #84655, .F. ) ;
#88151 = CYLINDRICAL_SURFACE ( 'NONE', #12213, 0.2500000000000004996 ) ;
#88153 = LINE ( 'NONE', #53891, #55792 ) ;
#88154 = CARTESIAN_POINT ( 'NONE',  ( 6.250054419913453785, -3.435999193479609914, 33.07426656108010832 ) ) ;
#88155 = CARTESIAN_POINT ( 'NONE',  ( 2.694853999681214862, -10.10844685921789043, 24.37313170625848713 ) ) ;
#88156 = CARTESIAN_POINT ( 'NONE',  ( 4.403900465484467119, -10.66356715214248396, 33.62249196103329751 ) ) ;
#88157 = CARTESIAN_POINT ( 'NONE',  ( 4.826899839630111266, -5.056417327199099532, 34.11270091957320716 ) ) ;
#88158 = CARTESIAN_POINT ( 'NONE',  ( 8.068933387422253745, -11.89424750095246175, 32.13594075562310337 ) ) ;
#88159 = CARTESIAN_POINT ( 'NONE',  ( 10.61538461538461675, -2.486705287966279876, 31.30864560766543647 ) ) ;
#88160 = CARTESIAN_POINT ( 'NONE',  ( -12.23852561744506851, -8.282913670948747864, 34.94150082978203642 ) ) ;
#88161 = CARTESIAN_POINT ( 'NONE',  ( 1.634560793993430350, -10.18230066228895758, 34.26354781536631577 ) ) ;
#88162 = CARTESIAN_POINT ( 'NONE',  ( 3.750000000000001776, -7.561099074964511502, 18.47061829374151287 ) ) ;
#88163 = CARTESIAN_POINT ( 'NONE',  ( -4.403822897894744237, -2.920706130388546651, 32.31842814019191223 ) ) ;
#88164 = ADVANCED_FACE ( 'NONE', ( #40738 ), #6505, .F. ) ;
#88165 = CARTESIAN_POINT ( 'NONE',  ( -11.31545018684868964, -10.61302985866383963, 33.66295027996417843 ) ) ;
#88166 = VERTEX_POINT ( 'NONE', #6937 ) ;
#88167 = FACE_OUTER_BOUND ( 'NONE', #26269, .T. ) ;
#88168 = CARTESIAN_POINT ( 'NONE',  ( 8.992242120843616959, -11.24521262558773493, 33.06293181088029343 ) ) ;
#88169 = CARTESIAN_POINT ( 'NONE',  ( 2.694853999681185108, -4.891553140782077591, 20.81436829374151287 ) ) ;
#88170 = DIRECTION ( 'NONE',  ( 0.000000000000000000, 0.1736481776669275834, 0.9848077530122086864 ) ) ;
#88171 = FACE_OUTER_BOUND ( 'NONE', #54638, .T. ) ;
#88172 = EDGE_LOOP ( 'NONE', ( #24084, #52561 ) ) ;
#88173 = DIRECTION ( 'NONE',  ( 0.000000000000000000, 0.9848077530122072432, -0.1736481776669354937 ) ) ;
#88174 = CARTESIAN_POINT ( 'NONE',  ( 9.627037691751372250, -12.70778746994557551, 30.41441678777548319 ) ) ;
#88176 = VERTEX_POINT ( 'NONE', #55123 ) ;
#88175 = CARTESIAN_POINT ( 'NONE',  ( 11.40831356872984514, -3.069018819979302926, 32.56621877034667278 ) ) ;
#88177 = FACE_OUTER_BOUND ( 'NONE', #12063, .T. ) ;
#88178 = B_SPLINE_CURVE_WITH_KNOTS ( 'NONE', 3,
 ( #34460, #5657, #80894, #19176, #39903, #61921, #27699, #60595, #6109, #88110 ),
 .UNSPECIFIED., .F., .F.,
 ( 4, 2, 2, 2, 4 ),
 ( 0.0007817359430256323911, 0.0009771253907249991422, 0.001172514838424365893, 0.001367904286123732644, 0.001563293733823099396 ),
 .UNSPECIFIED. ) ;
#88179 = CARTESIAN_POINT ( 'NONE',  ( -15.16470189741915675, -11.91647553114624358, 32.58852847137148245 ) ) ;
#88180 = LINE ( 'NONE', #53016, #24120 ) ;
#88181 = VECTOR ( 'NONE', #24996, 1000.000000000000114 ) ;
#88182 = ORIENTED_EDGE ( 'NONE', *, *, #48592, .F. ) ;
#88183 = CARTESIAN_POINT ( 'NONE',  ( 2.307692307692309264, -3.937682226553329556, 33.60647404775216529 ) ) ;
#88184 = CARTESIAN_POINT ( 'NONE',  ( 6.700150705560774966, -4.887634598454295265, 34.01352882383564946 ) ) ;
#88185 = EDGE_CURVE ( 'NONE', #26386, #55965, #48360, .T. ) ;
#88186 = EDGE_CURVE ( 'NONE', #48079, #10580, #69083, .T. ) ;
#88187 = CARTESIAN_POINT ( 'NONE',  ( -11.53846153846165912, -8.613356846316285953, 34.62446782046622218 ) ) ;
#88188 = EDGE_LOOP ( 'NONE', ( #78406, #14620 ) ) ;
#88189 = ORIENTED_EDGE ( 'NONE', *, *, #46379, .F. ) ;
#88190 = ORIENTED_EDGE ( 'NONE', *, *, #78541, .T. ) ;
#88191 = EDGE_LOOP ( 'NONE', ( #6304, #80209 ) ) ;
#88192 = CARTESIAN_POINT ( 'NONE',  ( 5.326977388561389581, -12.17597550085003633, 31.52189283813461884 ) ) ;
#88193 = DIRECTION ( 'NONE',  ( 0.000000000000000000, 0.000000000000000000, 1.000000000000000000 ) ) ;
#88194 = CARTESIAN_POINT ( 'NONE',  ( -16.28399412357784826, -3.069018819979305146, 32.56621877034667278 ) ) ;
#88195 = CARTESIAN_POINT ( 'NONE',  ( -7.912236225513981758, -10.67929555188718460, 33.92786785259543336 ) ) ;
#88196 = CARTESIAN_POINT ( 'NONE',  ( 5.207448778686637247, -6.001044277235011215, 34.52024696741798948 ) ) ;
#88197 = ORIENTED_EDGE ( 'NONE', *, *, #49509, .T. ) ;
#88198 = ORIENTED_EDGE ( 'NONE', *, *, #42392, .T. ) ;
#88199 = VERTEX_POINT ( 'NONE', #77167 ) ;
#88201 = ORIENTED_EDGE ( 'NONE', *, *, #80630, .F. ) ;
#88200 = CARTESIAN_POINT ( 'NONE',  ( -8.096130577096200653, -4.943428324936579799, 34.04746400365624481 ) ) ;
#88202 = CARTESIAN_POINT ( 'NONE',  ( 11.53846153846153832, -8.564572088678739092, 35.78748833219616898 ) ) ;
#88203 = B_SPLINE_CURVE_WITH_KNOTS ( 'NONE', 3,
 ( #1883, #64902, #16721, #57716, #28935, #56391, #63581, #71664, #56823, #50504 ),
 .UNSPECIFIED., .F., .F.,
 ( 4, 2, 2, 2, 4 ),
 ( 0.000000000000000000, 0.0001954311564186882026, 0.0003908623128373764051, 0.0005862934692560646619, 0.0007817246256747528103 ),
 .UNSPECIFIED. ) ;
#88204 = B_SPLINE_CURVE_WITH_KNOTS ( 'NONE', 3,
 ( #65985, #2503, #51121, #79518, #17820, #71406, #16475, #23667, #79958, #38983 ),
 .UNSPECIFIED., .F., .F.,
 ( 4, 2, 2, 2, 4 ),
 ( 0.000000000000000000, 0.0001954311564186861155, 0.0003908623128373722310, 0.0005862934692560583735, 0.0007817246256747444619 ),
 .UNSPECIFIED. ) ;
#88205 = CARTESIAN_POINT ( 'NONE',  ( -5.076923076923075762, -13.57706302396349152, 30.56769352161908060 ) ) ;
#88206 = VECTOR ( 'NONE', #6644, 1000.000000000000114 ) ;
#88207 = CARTESIAN_POINT ( 'NONE',  ( 10.61538461538449596, -6.879047030192662504, 34.71129190930017927 ) ) ;
#88208 = CARTESIAN_POINT ( 'NONE',  ( -5.869208192175211281, -4.118422570099827595, 33.43335022499816489 ) ) ;
#88209 = VERTEX_POINT ( 'NONE', #76275 ) ;
#88210 = AXIS2_PLACEMENT_3D ( 'NONE', #28576, #55588, #49281 ) ;
#88211 = ORIENTED_EDGE ( 'NONE', *, *, #55001, .T. ) ;
#88212 = ORIENTED_EDGE ( 'NONE', *, *, #23010, .T. ) ;
#88213 = CARTESIAN_POINT ( 'NONE',  ( -5.326923076923075762, -7.500000000000001776, 34.75000000000000000 ) ) ;
#88215 = ORIENTED_EDGE ( 'NONE', *, *, #83228, .T. ) ;
#88214 = DIRECTION ( 'NONE',  ( -0.000000000000000000, -0.5000000000000009992, -0.8660254037844380415 ) ) ;
#88216 = CARTESIAN_POINT ( 'NONE',  ( -9.070512820512819374, -7.500000000000000000, 29.75000000000000355 ) ) ;
#88217 = DIRECTION ( 'NONE',  ( -0.000000000000000000, -0.3420201433256694346, -0.9396926207859080948 ) ) ;
#88218 = EDGE_LOOP ( 'NONE', ( #51165, #40524, #46305, #86256 ) ) ;
#88219 = CARTESIAN_POINT ( 'NONE',  ( -11.47239420511146157, -3.937682226553329556, 33.60647404775216529 ) ) ;
#88220 = CARTESIAN_POINT ( 'NONE',  ( 8.835299120233207404, -12.37446782046654192, 30.86335684631486842 ) ) ;
#88221 = CARTESIAN_POINT ( 'NONE',  ( 12.68431813051652668, -9.418065098278013636, 34.63729479722530158 ) ) ;
#88222 = FACE_BOUND ( 'NONE', #5189, .T. ) ;
#88223 = LINE ( 'NONE', #53960, #52818 ) ;
#88224 = CARTESIAN_POINT ( 'NONE',  ( -1.384615384615505151, -11.94971097300221174, 32.03036669348237098 ) ) ;
#88225 = CARTESIAN_POINT ( 'NONE',  ( -10.48459417441766561, -10.70102852606553157, 33.91149625220312913 ) ) ;
#88227 = CARTESIAN_POINT ( 'NONE',  ( 11.53846153846153832, -12.78798330534102945, 29.74999999999997868 ) ) ;
#88226 = CARTESIAN_POINT ( 'NONE',  ( -16.09615384615384670, -3.499999999999999556, 29.75000000000000355 ) ) ;
#88228 = CARTESIAN_POINT ( 'NONE',  ( -39.05038313613820122, -2.499999999999999556, 29.75000000000000355 ) ) ;
#88229 = LINE ( 'NONE', #19301, #28992 ) ;
#88230 = VERTEX_POINT ( 'NONE', #9586 ) ;
#88231 = CARTESIAN_POINT ( 'NONE',  ( -16.40384615384615330, -7.500000000000001776, 34.75000000000000000 ) ) ;
#88232 = CARTESIAN_POINT ( 'NONE',  ( -10.61538461538473399, -2.625532179533778709, 30.86335684631627174 ) ) ;
#88233 = ORIENTED_EDGE ( 'NONE', *, *, #39644, .T. ) ;
#88234 = ORIENTED_EDGE ( 'NONE', *, *, #39768, .T. ) ;
#88235 = EDGE_CURVE ( 'NONE', #28787, #47389, #58200, .T. ) ;
#88236 = CARTESIAN_POINT ( 'NONE',  ( -3.230769230769229949, -13.20930481340135110, 34.54067556320372745 ) ) ;
#88237 = AXIS2_PLACEMENT_3D ( 'NONE', #50276, #2987, #30465 ) ;
#88238 = AXIS2_PLACEMENT_3D ( 'NONE', #61457, #54256, #83081 ) ;
#88239 = CARTESIAN_POINT ( 'NONE',  ( -14.30769230769230660, -4.786620604624113540, 33.94971097300155094 ) ) ;
#88240 = CARTESIAN_POINT ( 'NONE',  ( -15.48076923076922995, -7.500000000000001776, 34.75000000000000000 ) ) ;
#88241 = EDGE_LOOP ( 'NONE', ( #50022, #69134 ) ) ;
#88242 = CARTESIAN_POINT ( 'NONE',  ( -9.915792616872021625, -9.417330523894424488, 34.63758898049880486 ) ) ;
#88243 = CARTESIAN_POINT ( 'NONE',  ( -7.146003140593070846, -9.886141570436013382, 34.14413921362392301 ) ) ;
#88244 = FACE_BOUND ( 'NONE', #17824, .T. ) ;
#88246 = CARTESIAN_POINT ( 'NONE',  ( 6.000000000000001776, -6.343179335718451384, 34.87096338111211935 ) ) ;
#88245 = CARTESIAN_POINT ( 'NONE',  ( -18.13069146666756026, -3.062553014421049991, 32.05460306192773601 ) ) ;
#88247 = CARTESIAN_POINT ( 'NONE',  ( -13.44988538517170440, -2.379036618887870436, 30.90682066428147934 ) ) ;
#88248 = CARTESIAN_POINT ( 'NONE',  ( 3.480769230770650147, -7.500000000000154543, 35.00000000000007105 ) ) ;
#88250 = CARTESIAN_POINT ( 'NONE',  ( -8.638438961405984884, -12.11778462344220841, 31.66786338562085135 ) ) ;
#88249 = DIRECTION ( 'NONE',  ( 0.000000000000000000, 0.000000000000000000, 1.000000000000000000 ) ) ;
#88251 = CARTESIAN_POINT ( 'NONE',  ( -3.750000000000008438, -5.946699141100917352, 22.67187500000000355 ) ) ;
#88252 = EDGE_LOOP ( 'NONE', ( #36556, #25731 ) ) ;
#88253 = EDGE_LOOP ( 'NONE', ( #48214, #34108 ) ) ;
#88254 = EDGE_CURVE ( 'NONE', #45693, #70825, #14582, .T. ) ;
#88255 = CARTESIAN_POINT ( 'NONE',  ( -9.692307692307691624, -2.486705287966279876, 31.30864560766543647 ) ) ;
#88256 = CARTESIAN_POINT ( 'NONE',  ( 15.23076923076923173, -13.87047571288749737, 32.06866353760679544 ) ) ;
#88257 = DIRECTION ( 'NONE',  ( 0.000000000000000000, 0.3420201433256641055, -0.9396926207859100932 ) ) ;
#88258 = CARTESIAN_POINT ( 'NONE',  ( 3.230769230769231726, -12.29105614889573062, 35.45975837776705220 ) ) ;
#88259 = EDGE_CURVE ( 'NONE', #64445, #67532, #17371, .T. ) ;
#88260 = CARTESIAN_POINT ( 'NONE',  ( 4.153846153846154188, -5.180354513474913603, 36.12317359536750416 ) ) ;
#88261 = CARTESIAN_POINT ( 'NONE',  ( 2.651650429449539104, -4.848349570550432475, 24.31250000000000000 ) ) ;
#88262 = CARTESIAN_POINT ( 'NONE',  ( -8.899921372341079717, -9.929715669179220328, 34.40415004197138416 ) ) ;
#88263 = CARTESIAN_POINT ( 'NONE',  ( -6.130690603110307002, -8.191372820521381826, 34.95448215188423546 ) ) ;
#88264 = CARTESIAN_POINT ( 'NONE',  ( -5.010855743572999899, -2.292212530054420494, 30.41441678777542990 ) ) ;
#88265 = CARTESIAN_POINT ( 'NONE',  ( 17.06410256410256565, -3.499999999999999556, 29.75000000000000355 ) ) ;
#88266 = CARTESIAN_POINT ( 'NONE',  ( -6.066083410955879884, -2.721908614388772740, 31.22303859784724622 ) ) ;
#88267 = CARTESIAN_POINT ( 'NONE',  ( 13.38461538461538680, -13.87047571288749737, 32.06866353760679544 ) ) ;
#88268 = DIRECTION ( 'NONE',  ( -0.000000000000000000, 1.000000000000000000, 3.491481338843133355E-15 ) ) ;
#88269 = AXIS2_PLACEMENT_3D ( 'NONE', #75985, #40881, #54828 ) ;
#88270 = CARTESIAN_POINT ( 'NONE',  ( 4.153846153846154188, -11.16473453929635440, 33.15142922261926373 ) ) ;
#88271 = EDGE_CURVE ( 'NONE', #55035, #33529, #81835, .T. ) ;
#88272 = CARTESIAN_POINT ( 'NONE',  ( 7.846153846153846700, -2.900454961884010974, 35.62045528018868623 ) ) ;
#88273 = ORIENTED_EDGE ( 'NONE', *, *, #64633, .F. ) ;
#88274 = CARTESIAN_POINT ( 'NONE',  ( -3.230769230769229949, -12.10708131394839349, 31.69288490824020244 ) ) ;
#88275 = CARTESIAN_POINT ( 'NONE',  ( 15.23076923076923173, -6.435427911321262684, 35.78748833219616898 ) ) ;
#88276 = CARTESIAN_POINT ( 'NONE',  ( 0.06109907496451789238, -4.749999999999998224, 15.65811829374151287 ) ) ;
#88277 = AXIS2_PLACEMENT_3D ( 'NONE', #21122, #48591, #83734 ) ;
#88278 = EDGE_CURVE ( 'NONE', #18545, #62427, #8277, .T. ) ;
#88279 = AXIS2_PLACEMENT_3D ( 'NONE', #71015, #49849, #7993 ) ;
#88280 = CARTESIAN_POINT ( 'NONE',  ( -5.999999999999998224, -12.34228464037088635, 31.77849191805839268 ) ) ;
#88281 = SURFACE_STYLE_FILL_AREA ( #38289 ) ;
#88282 = DIRECTION ( 'NONE',  ( -0.000000000000000000, 0.8660254037844397068, -0.4999999999999978906 ) ) ;
#88284 = ORIENTED_EDGE ( 'NONE', *, *, #61851, .F. ) ;
#88283 = CARTESIAN_POINT ( 'NONE',  ( 5.076923076922953193, -4.320704448113951379, 33.92786785259630022 ) ) ;
#88285 = CARTESIAN_POINT ( 'NONE',  ( 2.750000000000008438, -8.639087296525996607, 23.29687500000000000 ) ) ;
#88286 = CARTESIAN_POINT ( 'NONE',  ( 3.296836564119306701, -8.164416787775445883, 34.95778746994558617 ) ) ;
#88287 = ORIENTED_EDGE ( 'NONE', *, *, #79661, .T. ) ;
#88288 = DIRECTION ( 'NONE',  ( 0.000000000000000000, 0.4999999999999985567, 0.8660254037844395958 ) ) ;
#88289 = CARTESIAN_POINT ( 'NONE',  ( -14.30769230769242917, -11.06231777344772027, 33.60647404775119895 ) ) ;
#88290 = B_SPLINE_CURVE_WITH_KNOTS ( 'NONE', 3,
 ( #69567, #76777, #7874, #35339, #42987, #62791, #15078, #71330, #49736, #55606 ),
 .UNSPECIFIED., .F., .F.,
 ( 4, 2, 2, 2, 4 ),
 ( 0.0007817359430256364027, 0.0009771253907250043464, 0.001172514838424372399, 0.001367904286123740234, 0.001563293733823108286 ),
 .UNSPECIFIED. ) ;
#88291 = ORIENTED_EDGE ( 'NONE', *, *, #27684, .T. ) ;
#88292 = B_SPLINE_CURVE_WITH_KNOTS ( 'NONE', 3,
 ( #14372, #28327, #70206, #55797, #83285, #21572, #43611, #14829, #49043, #76523 ),
 .UNSPECIFIED., .F., .F.,
 ( 4, 2, 2, 2, 4 ),
 ( 0.0007817246256747473893, 0.0009771112852218909357, 0.001172497944769034482, 0.001367884604316178246, 0.001563271263863321792 ),
 .UNSPECIFIED. ) ;
#88293 = DIRECTION ( 'NONE',  ( -1.000000000000000000, -0.000000000000000000, 0.000000000000000000 ) ) ;
#88294 = CARTESIAN_POINT ( 'NONE',  ( -15.93041919198458167, -7.630147231320743018, 34.74852402298682819 ) ) ;
#88295 = ADVANCED_FACE ( 'NONE', ( #70863 ), #1068, .F. ) ;
#88296 = CARTESIAN_POINT ( 'NONE',  ( 2.057669083470850424, -12.68155406624981119, 30.59749803192733708 ) ) ;
#88297 = EDGE_LOOP ( 'NONE', ( #64301, #40748, #33198, #77200, #24371 ) ) ;
#88298 = ADVANCED_FACE ( 'NONE', ( #15032 ), #42505, .F. ) ;
#88299 = ORIENTED_EDGE ( 'NONE', *, *, #18699, .T. ) ;
#88300 = ORIENTED_EDGE ( 'NONE', *, *, #15790, .F. ) ;
#88301 = CARTESIAN_POINT ( 'NONE',  ( -17.75005459062195712, -4.932303261841486375, 34.32971442181322885 ) ) ;
#88302 = CARTESIAN_POINT ( 'NONE',  ( -0.3954701105360241553, -10.51840700105979565, 33.73612834413962247 ) ) ;
#88303 = EDGE_CURVE ( 'NONE', #88905, #42352, #1515, .T. ) ;
#88304 = CARTESIAN_POINT ( 'NONE',  ( 17.99999999999987566, -10.33852847137269571, 34.16647553114546554 ) ) ;
#88305 = CARTESIAN_POINT ( 'NONE',  ( 2.307692307692309264, -1.242168528481310874, 33.36296068462461051 ) ) ;
#88306 = EDGE_CURVE ( 'NONE', #69932, #15414, #22226, .T. ) ;
#88307 = CARTESIAN_POINT ( 'NONE',  ( -12.46153846153858247, -6.026961402154118019, 34.52809138561165270 ) ) ;
#88308 = CARTESIAN_POINT ( 'NONE',  ( 7.053602361310569613, -8.630441415882550871, 34.87705825610312615 ) ) ;
#88309 = CARTESIAN_POINT ( 'NONE',  ( 0.3313904918067639982, -2.373036134822905208, 30.88089517874951540 ) ) ;
#88310 = FACE_OUTER_BOUND ( 'NONE', #5233, .T. ) ;
#88311 = VERTEX_POINT ( 'NONE', #84382 ) ;
#88312 = ORIENTED_EDGE ( 'NONE', *, *, #12957, .T. ) ;
#88314 = EDGE_LOOP ( 'NONE', ( #26232, #18262, #5137, #15161 ) ) ;
#88313 = CARTESIAN_POINT ( 'NONE',  ( 7.146089767170319185, -12.64618726649961289, 30.78989965857442712 ) ) ;
#88315 = CARTESIAN_POINT ( 'NONE',  ( 10.61538461538493117, -2.255955759149395501, 30.00000000000324363 ) ) ;
#88316 = CARTESIAN_POINT ( 'NONE',  ( 12.68431800280686694, -3.236590943229499029, 32.36255958852954251 ) ) ;
#88317 = VERTEX_POINT ( 'NONE', #36199 ) ;
#88318 = CARTESIAN_POINT ( 'NONE',  ( 15.48082365068268018, -9.233818618650603938, 34.70587769442853698 ) ) ;
#88319 = ORIENTED_EDGE ( 'NONE', *, *, #5993, .T. ) ;
#88320 = CARTESIAN_POINT ( 'NONE',  ( 16.85399685940691938, -9.886141570436013382, 34.14413921362392301 ) ) ;
#88321 = ORIENTED_EDGE ( 'NONE', *, *, #10368, .F. ) ;
#88322 = CARTESIAN_POINT ( 'NONE',  ( -18.22348492456433178, -9.417330523894424488, 34.63758898049880486 ) ) ;
#88323 = EDGE_CURVE ( 'NONE', #16148, #68002, #8603, .T. ) ;
#88324 = VECTOR ( 'NONE', #79733, 1000.000000000000000 ) ;
#88325 = CARTESIAN_POINT ( 'NONE',  ( -16.21911659980693443, -6.879047030191174805, 34.71129190930000163 ) ) ;
#88326 = CARTESIAN_POINT ( 'NONE',  ( 7.846153846153846700, -10.51840700105979565, 33.73612834413961536 ) ) ;
#88327 = FACE_BOUND ( 'NONE', #78404, .T. ) ;
#88328 = AXIS2_PLACEMENT_3D ( 'NONE', #45613, #65874, #59570 ) ;
#88329 = DIRECTION ( 'NONE',  ( -0.000000000000000000, -0.9396926207859093161, -0.3420201433256663259 ) ) ;
#88330 = CARTESIAN_POINT ( 'NONE',  ( 1.254140199539667933, -7.276987145209184327, 34.99546412871779211 ) ) ;
#88331 = EDGE_CURVE ( 'NONE', #28403, #71149, #37496, .T. ) ;
#88332 = CARTESIAN_POINT ( 'NONE',  ( -1.607542343522232242, -2.308479472611653094, 30.53278059502174457 ) ) ;
#88333 = DIRECTION ( 'NONE',  ( -1.000000000000000000, -0.000000000000000000, -0.000000000000000000 ) ) ;
#88334 = FACE_OUTER_BOUND ( 'NONE', #36310, .T. ) ;
#88335 = CYLINDRICAL_SURFACE ( 'NONE', #23173, 0.2499999999999997502 ) ;
#88336 = LINE ( 'NONE', #73475, #48910 ) ;
#88337 = B_SPLINE_CURVE_WITH_KNOTS ( 'NONE', 3,
 ( #79392, #50132, #17237, #8726, #36204, #84834, #10492, #57340, #23112, #23543 ),
 .UNSPECIFIED., .F., .F.,
 ( 4, 2, 2, 2, 4 ),
 ( 0.000000000000000000, 0.0001954339857564076641, 0.0003908679715128153282, 0.0005863019572692229923, 0.0007817359430256306564 ),
 .UNSPECIFIED. ) ;
#88338 = ORIENTED_EDGE ( 'NONE', *, *, #64036, .F. ) ;
#88339 = ORIENTED_EDGE ( 'NONE', *, *, #11451, .T. ) ;
#88340 = EDGE_CURVE ( 'NONE', #64684, #61438, #47366, .T. ) ;
#88342 = DIRECTION ( 'NONE',  ( -0.000000000000000000, -0.000000000000000000, -1.000000000000000000 ) ) ;
#88341 = DIRECTION ( 'NONE',  ( -0.000000000000000000, 0.7660444431189791237, -0.6427876096865379196 ) ) ;
#88343 = DIRECTION ( 'NONE',  ( -0.000000000000000000, 0.8660254037844397068, -0.4999999999999978906 ) ) ;
#88344 = FACE_OUTER_BOUND ( 'NONE', #64551, .T. ) ;
#88345 = CARTESIAN_POINT ( 'NONE',  ( 14.30769230769231015, -3.513871655860378418, 32.76840700105978499 ) ) ;
#88346 = CARTESIAN_POINT ( 'NONE',  ( 1.634669804528839476, -4.074993327901524687, 33.72946981652012255 ) ) ;
#88347 = VERTEX_POINT ( 'NONE', #4614 ) ;
#88348 = CYLINDRICAL_SURFACE ( 'NONE', #50089, 0.2499999999999998890 ) ;
#88349 = CARTESIAN_POINT ( 'NONE',  ( -5.011667505647053211, -2.625532179533470512, 30.86335684631491105 ) ) ;
#88350 = CARTESIAN_POINT ( 'NONE',  ( -8.992156986746916658, -12.15238873228292071, 31.58232369045353849 ) ) ;
#88351 = DIRECTION ( 'NONE',  ( -0.000000000000000000, -0.9848077530122086864, -0.1736481776669273613 ) ) ;
#88352 = ORIENTED_EDGE ( 'NONE', *, *, #8845, .F. ) ;
#88353 = ORIENTED_EDGE ( 'NONE', *, *, #1434, .T. ) ;
#88354 = ORIENTED_EDGE ( 'NONE', *, *, #33972, .T. ) ;
#88355 = EDGE_CURVE ( 'NONE', #4784, #71827, #48293, .T. ) ;
#88356 = CARTESIAN_POINT ( 'NONE',  ( 15.23076923076923173, -6.386643153685126251, 34.62446782046654192 ) ) ;
#88357 = ORIENTED_EDGE ( 'NONE', *, *, #67325, .T. ) ;
#88358 = CARTESIAN_POINT ( 'NONE',  ( 3.262820512820510999, -3.499999999999999556, 29.75000000000000355 ) ) ;
#88359 = CARTESIAN_POINT ( 'NONE',  ( 14.53047197667037516, -5.827830569534417471, 34.72679350104403539 ) ) ;
#88360 = DIRECTION ( 'NONE',  ( 0.000000000000000000, 0.9396926207859126468, 0.3420201433256571111 ) ) ;
#88361 = EDGE_CURVE ( 'NONE', #63342, #27014, #11785, .T. ) ;
#88362 = CARTESIAN_POINT ( 'NONE',  ( 1.384615384615264011, -6.835583212225970762, 34.95778746994575670 ) ) ;
#88363 = CARTESIAN_POINT ( 'NONE',  ( 9.757563263583717728, -6.026961402152789304, 34.52809138561124769 ) ) ;
#88365 = ORIENTED_EDGE ( 'NONE', *, *, #76416, .T. ) ;
#88364 = VECTOR ( 'NONE', #50433, 1000.000000000000000 ) ;
#88366 = CARTESIAN_POINT ( 'NONE',  ( -15.45369544828537833, -11.76352882383564769, 32.36236540154569497 ) ) ;
#88368 = ORIENTED_EDGE ( 'NONE', *, *, #23428, .F. ) ;
#88367 = CARTESIAN_POINT ( 'NONE',  ( 0.4615384615383396616, -10.21337939537710326, 33.94971097300076224 ) ) ;
#88369 = CARTESIAN_POINT ( 'NONE',  ( -15.48076923076922995, -2.499999999999998668, 29.75000000000000355 ) ) ;
#88370 = CARTESIAN_POINT ( 'NONE',  ( -5.999999999999998224, -1.509761064869970415, 31.06009739812519044 ) ) ;
#88371 = CARTESIAN_POINT ( 'NONE',  ( 5.076923076923075762, -1.044019251281081972, 31.83374038241031911 ) ) ;
#88372 = CARTESIAN_POINT ( 'NONE',  ( 9.915319043920543862, -10.61302985866384141, 33.66295027996417843 ) ) ;
#88373 = CARTESIAN_POINT ( 'NONE',  ( 2.307692307692186251, -2.657715359629662544, 31.77849191805970364 ) ) ;
#88374 = CARTESIAN_POINT ( 'NONE',  ( -8.638440328263820689, -9.084667340241226796, 34.75534355489798344 ) ) ;
#88375 = CARTESIAN_POINT ( 'NONE',  ( -0.6844646790546093928, -12.39988816332205701, 30.74660775122750778 ) ) ;
#88376 = CARTESIAN_POINT ( 'NONE',  ( 1.077988221561497539, -10.27530806549875386, 21.20499329374151998 ) ) ;
#88377 = VERTEX_POINT ( 'NONE', #64515 ) ;
#88378 = B_SPLINE_CURVE_WITH_KNOTS ( 'NONE', 3,
 ( #71543, #37762, #65228, #9850, #58461, #53044, #18390, #52155, #45852, #73333 ),
 .UNSPECIFIED., .F., .F.,
 ( 4, 2, 2, 2, 4 ),
 ( 0.0007817246256747452209, 0.0009771112852218887673, 0.001172497944769032531, 0.001367884604316176294, 0.001563271263863319840 ),
 .UNSPECIFIED. ) ;
#88379 = CARTESIAN_POINT ( 'NONE',  ( 7.384615384615385025, -3.499999999999999556, 29.75000000000000355 ) ) ;
#88380 = CARTESIAN_POINT ( 'NONE',  ( 0.4615384615383396616, -3.300289026999228881, 32.46337939537708905 ) ) ;
#88381 = EDGE_LOOP ( 'NONE', ( #22087, #68536, #74677, #60775 ) ) ;
#88382 = CARTESIAN_POINT ( 'NONE',  ( -12.52762187249434156, -11.69971097300155272, 32.46337939537587403 ) ) ;
#88383 = CARTESIAN_POINT ( 'NONE',  ( -3.165513659493206067, -6.026961402152789304, 34.52809138561124769 ) ) ;
#88384 = CARTESIAN_POINT ( 'NONE',  ( -6.923076923076922462, -5.557115091759785130, 34.35708131394839171 ) ) ;
#88385 = CARTESIAN_POINT ( 'NONE',  ( 0.4615384615383382183, -4.320704448113951379, 33.92786785259630022 ) ) ;
#88386 = CARTESIAN_POINT ( 'NONE',  ( 0.6845513056318547340, -2.308499170217967134, 30.53291367094873721 ) ) ;
#88387 = ORIENTED_EDGE ( 'NONE', *, *, #26088, .F. ) ;
#88388 = DIRECTION ( 'NONE',  ( -0.000000000000000000, 1.000000000000000000, 3.491481338843133355E-15 ) ) ;
#88389 = VECTOR ( 'NONE', #59260, 999.9999999999998863 ) ;
#88390 = ADVANCED_FACE ( 'NONE', ( #85702 ), #2817, .F. ) ;
#88391 = DIRECTION ( 'NONE',  ( -0.000000000000000000, -0.9848077530122086864, -0.1736481776669273613 ) ) ;
#88392 = CARTESIAN_POINT ( 'NONE',  ( 18.22301284409339672, -12.38742843783360748, 31.66772728687926985 ) ) ;
#88393 = VERTEX_POINT ( 'NONE', #58656 ) ;
#88394 = CARTESIAN_POINT ( 'NONE',  ( -17.07692307692307665, -5.180354513474913603, 36.12317359536750416 ) ) ;
#88395 = APPLICATION_CONTEXT ( 'automotive_design' ) ;
#88396 = EDGE_CURVE ( 'NONE', #87881, #19556, #52341, .T. ) ;
#88397 = AXIS2_PLACEMENT_3D ( 'NONE', #11701, #80611, #18895 ) ;
#88398 = ORIENTED_EDGE ( 'NONE', *, *, #59680, .T. ) ;
#88399 = CARTESIAN_POINT ( 'NONE',  ( -5.076923076923075762, -1.242168528481310874, 33.36296068462461051 ) ) ;
#88400 = CARTESIAN_POINT ( 'NONE',  ( 11.53846153846141576, -2.657715359629662544, 31.77849191805970364 ) ) ;
#88401 = ORIENTED_EDGE ( 'NONE', *, *, #46037, .T. ) ;
#88402 = EDGE_CURVE ( 'NONE', #53125, #67703, #50530, .T. ) ;
#88403 = CARTESIAN_POINT ( 'NONE',  ( -13.38461538461538325, -3.050289026998446396, 32.03036669348365706 ) ) ;
#88404 = CARTESIAN_POINT ( 'NONE',  ( -16.15384615384615330, -13.95598074871891292, 31.83374038241031911 ) ) ;
#88405 = CARTESIAN_POINT ( 'NONE',  ( -8.519230769229348965, -7.500000000000154543, 35.00000000000007105 ) ) ;
#88406 = CYLINDRICAL_SURFACE ( 'NONE', #26344, 0.2500000000000012212 ) ;
#88407 = CARTESIAN_POINT ( 'NONE',  ( -0.7115152055870521686, -11.47974371597208076, 33.17467449705390692 ) ) ;
#88408 = ORIENTED_EDGE ( 'NONE', *, *, #75639, .F. ) ;
#88409 = CARTESIAN_POINT ( 'NONE',  ( -4.023320715612507037, -12.50538340440932217, 31.33453814440721885 ) ) ;
#88410 = EDGE_LOOP ( 'NONE', ( #51392, #51066 ) ) ;
#88412 = EDGE_CURVE ( 'NONE', #80088, #21493, #63241, .T. ) ;
#88411 = DIRECTION ( 'NONE',  ( -0.000000000000000000, 0.6427876096865404731, -0.7660444431189770143 ) ) ;
#88413 = DIRECTION ( 'NONE',  ( -0.000000000000000000, -0.9848077530122086864, -0.1736481776669273613 ) ) ;
#88414 = CARTESIAN_POINT ( 'NONE',  ( 6.130525701763565927, -9.417988943895561960, 34.36773134775778260 ) ) ;
#88415 = EDGE_CURVE ( 'NONE', #54661, #69076, #30309, .T. ) ;
#88416 = DIRECTION ( 'NONE',  ( -0.000000000000000000, -0.7660444431189791237, -0.6427876096865379196 ) ) ;
#88417 = CARTESIAN_POINT ( 'NONE',  ( -6.250023237292966272, -12.22074536777954989, 31.39888409691088356 ) ) ;
#88418 = VERTEX_POINT ( 'NONE', #72173 ) ;
#88419 = AXIS2_PLACEMENT_3D ( 'NONE', #4604, #37946, #32077 ) ;
#88420 = EDGE_LOOP ( 'NONE', ( #12532, #80161, #64361, #12212 ) ) ;
#88421 = ORIENTED_EDGE ( 'NONE', *, *, #82425, .F. ) ;
#88422 = ORIENTED_EDGE ( 'NONE', *, *, #54590, .T. ) ;
#88423 = EDGE_CURVE ( 'NONE', #78424, #21486, #10487, .T. ) ;
#88424 = CARTESIAN_POINT ( 'NONE',  ( -4.153846153846152411, -5.557115091759785130, 34.35708131394839171 ) ) ;
#88425 = CARTESIAN_POINT ( 'NONE',  ( 16.37662582282421653, -10.97394488606063589, 33.68653795673696294 ) ) ;
#88426 = CARTESIAN_POINT ( 'NONE',  ( 2.307692307692309264, -9.819645486525091727, 36.12317359536749706 ) ) ;
#88427 = EDGE_CURVE ( 'NONE', #14549, #19715, #6528, .T. ) ;
#88428 = CARTESIAN_POINT ( 'NONE',  ( -8.069638770718176701, -3.562934362175800285, 33.22335522853832401 ) ) ;
#88429 = DIRECTION ( 'NONE',  ( -0.000000000000000000, -0.000000000000000000, -1.000000000000000000 ) ) ;
#88430 = DIRECTION ( 'NONE',  ( 0.000000000000000000, 1.000000000000000000, 0.000000000000000000 ) ) ;
#88431 = CARTESIAN_POINT ( 'NONE',  ( 10.61538461538461675, -13.57706302396349152, 30.56769352161908060 ) ) ;
#88432 = CARTESIAN_POINT ( 'NONE',  ( -5.076923076923075762, -11.35647404775217417, 33.31231777344666511 ) ) ;
#88433 = ORIENTED_EDGE ( 'NONE', *, *, #71127, .T. ) ;
#88434 = ORIENTED_EDGE ( 'NONE', *, *, #13640, .T. ) ;
#88435 = B_SPLINE_CURVE_WITH_KNOTS ( 'NONE', 3,
 ( #83788, #22073, #27501, #82896, #34251, #47768, #13540, #41019, #76122, #36037 ),
 .UNSPECIFIED., .F., .F.,
 ( 4, 2, 2, 2, 4 ),
 ( 0.0007817359430256308733, 0.0009771253907249971907, 0.001172514838424363725, 0.001367904286123730259, 0.001563293733823096577 ),
 .UNSPECIFIED. ) ;
#88436 = B_SPLINE_CURVE_WITH_KNOTS ( 'NONE', 3,
 ( #69476, #1903, #35702, #82570, #20408, #20843, #21282, #55074, #42017, #580 ),
 .UNSPECIFIED., .F., .F.,
 ( 4, 2, 2, 2, 4 ),
 ( 0.0007817359430256317406, 0.0009771253907249982749, 0.001172514838424365026, 0.001367904286123731560, 0.001563293733823098094 ),
 .UNSPECIFIED. ) ;
#88437 = ORIENTED_EDGE ( 'NONE', *, *, #79106, .T. ) ;
#88440 = ORIENTED_EDGE ( 'NONE', *, *, #67323, .F. ) ;
#88439 = EDGE_CURVE ( 'NONE', #68060, #33663, #61759, .T. ) ;
#88438 = CARTESIAN_POINT ( 'NONE',  ( 2.057715576749954423, -2.564618984488975961, 30.55390908950641915 ) ) ;
#88442 = CARTESIAN_POINT ( 'NONE',  ( -9.942284436356281674, -4.075325502946081535, 33.72974371597206300 ) ) ;
#88441 = CARTESIAN_POINT ( 'NONE',  ( -6.000000000000119904, -11.48612834414049644, 32.76840700105863391 ) ) ;
#88443 = B_SPLINE_CURVE_WITH_KNOTS ( 'NONE', 3,
 ( #47794, #75275, #13564, #30182, #37819, #44117, #1820, #23411, #16655, #36068 ),
 .UNSPECIFIED., .F., .F.,
 ( 4, 2, 2, 2, 4 ),
 ( 0.000000000000000000, 0.0001954339857564096157, 0.0003908679715128192313, 0.0005863019572692288470, 0.0007817359430256384627 ),
 .UNSPECIFIED. ) ;
#88444 = CARTESIAN_POINT ( 'NONE',  ( -0.3962833220256232192, -2.379036618887895305, 30.90682066428159303 ) ) ;
#88445 = CARTESIAN_POINT ( 'NONE',  ( -9.692307692307812417, -6.879047030192662504, 34.71129190930017927 ) ) ;
#88446 = FACE_BOUND ( 'NONE', #37088, .T. ) ;
#88447 = ORIENTED_EDGE ( 'NONE', *, *, #38823, .F. ) ;
#88448 = ADVANCED_FACE ( 'NONE', ( #25773 ), #73966, .F. ) ;
#88449 = CARTESIAN_POINT ( 'NONE',  ( -23.00000000000000000, -4.249999999999998224, 27.25000000000000000 ) ) ;
#88450 = CARTESIAN_POINT ( 'NONE',  ( -3.230769230769229949, -6.386643153685126251, 34.62446782046654192 ) ) ;
#88451 = ORIENTED_EDGE ( 'NONE', *, *, #69796, .F. ) ;
#88452 = CARTESIAN_POINT ( 'NONE',  ( -8.639185606395990646, -2.504778602574660340, 29.97347330155780654 ) ) ;
#88453 = ORIENTED_EDGE ( 'NONE', *, *, #50384, .F. ) ;
#88454 = FACE_BOUND ( 'NONE', #22706, .T. ) ;
#88455 = CARTESIAN_POINT ( 'NONE',  ( 7.780883400193069122, -11.94971097300153140, 32.03036669348370680 ) ) ;
#88456 = AXIS2_PLACEMENT_3D ( 'NONE', #74829, #18990, #46457 ) ;
#88457 = CARTESIAN_POINT ( 'NONE',  ( 18.06606835100243913, -4.786620604624113540, 33.94971097300155805 ) ) ;
#88458 = ORIENTED_EDGE ( 'NONE', *, *, #57907, .F. ) ;
#88459 = CARTESIAN_POINT ( 'NONE',  ( -12.39628289026243557, -8.613356846314928816, 34.62446782046653482 ) ) ;
#88460 = CARTESIAN_POINT ( 'NONE',  ( -12.52680846209478460, -12.16647553114622049, 32.15551576947930812 ) ) ;
#88461 = CARTESIAN_POINT ( 'NONE',  ( 1.134638653673033071, -3.137211980971221781, 32.19342716148376837 ) ) ;
#88462 = VERTEX_POINT ( 'NONE', #75 ) ;
#88463 = CARTESIAN_POINT ( 'NONE',  ( -4.153846153846152411, -13.87047571288749737, 32.06866353760679544 ) ) ;
#88464 = CARTESIAN_POINT ( 'NONE',  ( 14.30769230769218581, -3.643525952248795718, 33.31231777344771672 ) ) ;
#88465 = CARTESIAN_POINT ( 'NONE',  ( -3.296039676730005752, -2.892918686051582533, 31.69288490824015270 ) ) ;
#88466 = EDGE_CURVE ( 'NONE', #33447, #68924, #17193, .T. ) ;
#88467 = CARTESIAN_POINT ( 'NONE',  ( -18.00000000000012079, -12.70778746994576025, 30.41441678777401236 ) ) ;
#88468 = ORIENTED_EDGE ( 'NONE', *, *, #20016, .T. ) ;
#88469 = EDGE_CURVE ( 'NONE', #32972, #72998, #32521, .T. ) ;
#88470 = CARTESIAN_POINT ( 'NONE',  ( -1.514762594053604250, -6.001485441113818986, 34.52039167877662607 ) ) ;
#88471 = CARTESIAN_POINT ( 'NONE',  ( 2.372947447205146609, -3.643525952247864463, 33.31231777344670064 ) ) ;
#88472 = VERTEX_POINT ( 'NONE', #33855 ) ;
#88473 = CARTESIAN_POINT ( 'NONE',  ( 23.00000000000000000, -10.75000000000000000, 29.75000000000000355 ) ) ;
#88474 = CARTESIAN_POINT ( 'NONE',  ( 9.561832507231976308, -7.276987145209184327, 34.99546412871779211 ) ) ;
#88475 = CARTESIAN_POINT ( 'NONE',  ( 5.750023269057646935, -9.148715823498378086, 34.47080413974185120 ) ) ;
#88476 = DIRECTION ( 'NONE',  ( 0.000000000000000000, 1.000000000000000000, 0.000000000000000000 ) ) ;
#88477 = CARTESIAN_POINT ( 'NONE',  ( -6.856910316485284262, -7.250054591869668386, 34.99404684341514127 ) ) ;
#88478 = CARTESIAN_POINT ( 'NONE',  ( 15.16549923021291058, -5.941354392334499579, 34.76329471203369792 ) ) ;
#88480 = CARTESIAN_POINT ( 'NONE',  ( -16.37677311275299985, -8.282780595021769443, 34.94152052738834158 ) ) ;
#88479 = CARTESIAN_POINT ( 'NONE',  ( 6.066068351002441794, -11.69971097300155272, 32.46337939537588113 ) ) ;
#88481 = CYLINDRICAL_SURFACE ( 'NONE', #83829, 0.2499999999999998890 ) ;
#88482 = CARTESIAN_POINT ( 'NONE',  ( -1.409462824231155764E-14, -4.749999999999999112, 19.15625000000000000 ) ) ;
#88483 = ORIENTED_EDGE ( 'NONE', *, *, #19951, .T. ) ;
#88484 = CARTESIAN_POINT ( 'NONE',  ( 4.946775107191380805, -6.809168938359898782, 34.95455904226513866 ) ) ;
#88485 = VERTEX_POINT ( 'NONE', #39745 ) ;
#88486 = B_SPLINE_CURVE_WITH_KNOTS ( 'NONE', 3,
 ( #18974, #19856, #81570, #20308, #81128, #47320, #87450, #74812, #32, #12218 ),
 .UNSPECIFIED., .F., .F.,
 ( 4, 2, 2, 2, 4 ),
 ( 0.000000000000000000, 0.0001954311584214072381, 0.0003908623168428144762, 0.0005862934752642217414, 0.0007817246336856289524 ),
 .UNSPECIFIED. ) ;
#88487 = ORIENTED_EDGE ( 'NONE', *, *, #5655, .F. ) ;
#88488 = CARTESIAN_POINT ( 'NONE',  ( 3.007284287045282944, -5.113361153441932316, 34.14387501736621999 ) ) ;
#88489 = ORIENTED_EDGE ( 'NONE', *, *, #864, .T. ) ;
#88490 = CARTESIAN_POINT ( 'NONE',  ( -4.219116154402471786, -2.657715359629089225, 31.77849191805834295 ) ) ;
#88491 = CARTESIAN_POINT ( 'NONE',  ( 2.750000000000001776, -7.499999999999984013, 20.71875000000000000 ) ) ;
#88492 = CARTESIAN_POINT ( 'NONE',  ( 18.00000000000000000, -4.661471528628507777, 34.16647553114623292 ) ) ;
#88493 = CARTESIAN_POINT ( 'NONE',  ( -8.899922235898330314, -3.062553014421049546, 32.05460306192773601 ) ) ;
#88494 = CARTESIAN_POINT ( 'NONE',  ( -4.230769230769230838, -3.499999999999999556, 29.75000000000000355 ) ) ;
#88495 = VECTOR ( 'NONE', #81047, 1000.000000000000114 ) ;
#88496 = CARTESIAN_POINT ( 'NONE',  ( -8.769230769230768274, -4.786620604624113540, 33.94971097300155094 ) ) ;
#88497 = CARTESIAN_POINT ( 'NONE',  ( 9.692307692307570832, -12.51329471203414379, 31.30864560766407578 ) ) ;
#88498 = CARTESIAN_POINT ( 'NONE',  ( -11.66860874789975888, -5.195881422630166391, 34.18770438780619259 ) ) ;
#88499 = CARTESIAN_POINT ( 'NONE',  ( -3.749999999999988454, -9.053300858899127945, 26.26562500000000000 ) ) ;
#88500 = CARTESIAN_POINT ( 'NONE',  ( 17.20744851515672025, -2.372941743896878286, 30.88044141588253311 ) ) ;
#88501 = CARTESIAN_POINT ( 'NONE',  ( 20.00000000000000000, -4.000000000000000000, 29.75000000000000355 ) ) ;
#88502 = DIRECTION ( 'NONE',  ( -0.000000000000000000, 0.1736481776669307198, -0.9848077530122080203 ) ) ;
#88503 = EDGE_CURVE ( 'NONE', #32798, #1675, #5952, .T. ) ;
#88504 = ORIENTED_EDGE ( 'NONE', *, *, #63094, .T. ) ;
#88505 = ORIENTED_EDGE ( 'NONE', *, *, #44718, .F. ) ;
#88506 = CARTESIAN_POINT ( 'NONE',  ( -9.442253380669379581, -3.627508038966690496, 32.91356715214248396 ) ) ;
#88507 = CARTESIAN_POINT ( 'NONE',  ( 15.36155967173618286, -11.93129842949671726, 32.56571108434900452 ) ) ;
#88508 = DIRECTION ( 'NONE',  ( -0.000000000000000000, 0.7660444431189791237, -0.6427876096865379196 ) ) ;
#88509 = DIRECTION ( 'NONE',  ( 0.000000000000000000, 1.000000000000000000, 0.000000000000000000 ) ) ;
#88510 = EDGE_CURVE ( 'NONE', #28699, #19429, #27549, .T. ) ;
#88511 = CARTESIAN_POINT ( 'NONE',  ( -14.30769230769230660, -13.53365097954675988, 30.81389545987213552 ) ) ;
#88512 = CARTESIAN_POINT ( 'NONE',  ( -6.066083410955879884, -8.120952969808774569, 34.71129190930000163 ) ) ;
#88513 = EDGE_CURVE ( 'NONE', #77885, #25874, #54850, .T. ) ;
#88514 = FACE_OUTER_BOUND ( 'NONE', #52032, .T. ) ;
#88515 = AXIS2_PLACEMENT_3D ( 'NONE', #67615, #54080, #81576 ) ;
#88516 = ORIENTED_EDGE ( 'NONE', *, *, #77660, .T. ) ;
#88517 = CARTESIAN_POINT ( 'NONE',  ( -4.854143535654666941, -12.44528174975671853, 30.48912976160716681 ) ) ;
#88518 = ORIENTED_EDGE ( 'NONE', *, *, #41490, .T. ) ;
#88519 = EDGE_CURVE ( 'NONE', #40783, #16008, #26943, .T. ) ;
#88520 = ORIENTED_EDGE ( 'NONE', *, *, #55268, .F. ) ;
#88521 = CARTESIAN_POINT ( 'NONE',  ( -6.923076923076922462, -9.905515769479276145, 34.41647553114623292 ) ) ;
#88522 = CARTESIAN_POINT ( 'NONE',  ( 4.088575707885377497, -2.625532179533445198, 30.86335684631481513 ) ) ;
#88523 = EDGE_CURVE ( 'NONE', #15864, #64392, #41947, .T. ) ;
#88524 = CARTESIAN_POINT ( 'NONE',  ( -0.3962828902624371818, -6.879047030191285828, 34.71129190930002295 ) ) ;
#88525 = CIRCLE ( 'NONE', #10840, 4.000000000000000000 ) ;
#88526 = DIRECTION ( 'NONE',  ( 0.000000000000000000, 0.9848077530122072432, 0.1736481776669354937 ) ) ;
#88527 = CARTESIAN_POINT ( 'NONE',  ( 5.934729554039225974, -2.892918686051582089, 31.69288490824015270 ) ) ;
#88529 = EDGE_CURVE ( 'NONE', #78341, #572, #5414, .T. ) ;
#88528 = ORIENTED_EDGE ( 'NONE', *, *, #84922, .F. ) ;
#88530 = EDGE_LOOP ( 'NONE', ( #55188, #39973, #19832, #8238 ) ) ;
#88531 = ORIENTED_EDGE ( 'NONE', *, *, #35651, .T. ) ;
#88532 = ORIENTED_EDGE ( 'NONE', *, *, #3160, .T. ) ;
#88533 = CARTESIAN_POINT ( 'NONE',  ( 18.22301284409340028, -2.308499170217968022, 30.53291367094874076 ) ) ;
#88534 = CARTESIAN_POINT ( 'NONE',  ( -2.437840277424001112, -10.31621877034669588, 34.18098118002070152 ) ) ;
#88535 = EDGE_CURVE ( 'NONE', #35664, #62627, #78721, .T. ) ;
#88536 = DIRECTION ( 'NONE',  ( 0.000000000000000000, 0.000000000000000000, -1.000000000000000000 ) ) ;
#88537 = CARTESIAN_POINT ( 'NONE',  ( 16.37685750545900376, -9.886259254753566594, 34.14407573483972413 ) ) ;
#88538 = CARTESIAN_POINT ( 'NONE',  ( -15.09997878980228059, -9.084667340241226796, 34.75534355489798344 ) ) ;
#88539 = EDGE_CURVE ( 'NONE', #16148, #53666, #85926, .T. ) ;
#88540 = CARTESIAN_POINT ( 'NONE',  ( -10.54931626438217762, -12.10708131394839882, 31.69288490824020954 ) ) ;
#88541 = ORIENTED_EDGE ( 'NONE', *, *, #9648, .T. ) ;
#88542 = ORIENTED_EDGE ( 'NONE', *, *, #52924, .T. ) ;
#88543 = CIRCLE ( 'NONE', #65553, 0.2500000000000002220 ) ;
#88544 = ORIENTED_EDGE ( 'NONE', *, *, #41888, .T. ) ;
#88546 = VERTEX_POINT ( 'NONE', #23760 ) ;
#88545 = DIRECTION ( 'NONE',  ( 0.000000000000000000, 0.6427876096865368094, 0.7660444431189802339 ) ) ;
#88547 = CARTESIAN_POINT ( 'NONE',  ( 9.442284468086239002, -8.475808217655753651, 34.90892951860618609 ) ) ;
#88548 = CARTESIAN_POINT ( 'NONE',  ( -2.307692307692427391, -9.442884908241554243, 34.35708131394783038 ) ) ;
#88549 = CARTESIAN_POINT ( 'NONE',  ( 2.651650429449539104, -4.848349570550432475, 19.31250000000000000 ) ) ;
#88550 = VERTEX_POINT ( 'NONE', #56350 ) ;
#88551 = EDGE_CURVE ( 'NONE', #88209, #63997, #14927, .T. ) ;
#88552 = EDGE_CURVE ( 'NONE', #18924, #38366, #14020, .T. ) ;
#88553 = CARTESIAN_POINT ( 'NONE',  ( -1.253824943648431889, -11.37503395064541678, 33.29242100308974983 ) ) ;
#88554 = VERTEX_POINT ( 'NONE', #34743 ) ;
#88555 = DIRECTION ( 'NONE',  ( -0.000000000000000000, -0.1736481776669307198, -0.9848077530122080203 ) ) ;
#88556 = B_SPLINE_CURVE_WITH_KNOTS ( 'NONE', 3,
 ( #71370, #56094, #29517, #76361, #8804, #76818, #28172, #50656, #83588, #43908 ),
 .UNSPECIFIED., .F., .F.,
 ( 4, 2, 2, 2, 4 ),
 ( 0.000000000000000000, 0.0001954311564186864949, 0.0003908623128373729899, 0.0005862934692560594577, 0.0007817246256747459798 ),
 .UNSPECIFIED. ) ;
#88557 = FACE_BOUND ( 'NONE', #31088, .T. ) ;
#88558 = CARTESIAN_POINT ( 'NONE',  ( -6.923076923077044142, -3.835265460704628371, 33.15142922262033665 ) ) ;
#88559 = DIRECTION ( 'NONE',  ( 0.000000000000000000, 0.7660444431189822323, -0.6427876096865344779 ) ) ;
#88560 = ORIENTED_EDGE ( 'NONE', *, *, #10389, .T. ) ;
#88561 = CARTESIAN_POINT ( 'NONE',  ( -9.070512820512819374, -3.499999999999999556, 29.75000000000000355 ) ) ;
#88562 = LINE ( 'NONE', #75032, #19135 ) ;
#88563 = CARTESIAN_POINT ( 'NONE',  ( -17.01166793741023042, -12.70778746994558439, 30.41441678777537305 ) ) ;
#88564 = DIRECTION ( 'NONE',  ( 0.000000000000000000, 0.4999999999999960032, -0.8660254037844410391 ) ) ;
#88566 = VERTEX_POINT ( 'NONE', #51213 ) ;
#88565 = EDGE_CURVE ( 'NONE', #7242, #3517, #22621, .T. ) ;
#88567 = B_SPLINE_CURVE_WITH_KNOTS ( 'NONE', 3,
 ( #47917, #63198, #61868, #83047, #74968, #62749, #41172, #48358, #7389, #88938 ),
 .UNSPECIFIED., .F., .F.,
 ( 4, 2, 2, 2, 4 ),
 ( 0.0007817359430256320659, 0.0009771253907249987086, 0.001172514838424365460, 0.001367904286123731994, 0.001563293733823098745 ),
 .UNSPECIFIED. ) ;
#88568 = CARTESIAN_POINT ( 'NONE',  ( -9.561517251340744039, -4.684288915650983043, 34.18129842949671371 ) ) ;
#88569 = CARTESIAN_POINT ( 'NONE',  ( -5.776987155906604166, -4.026326845037961455, 33.68677907613344047 ) ) ;
#88570 = CARTESIAN_POINT ( 'NONE',  ( 17.29993442853592711, -9.886259254753566594, 34.14407573483972413 ) ) ;
#88571 = CYLINDRICAL_SURFACE ( 'NONE', #15538, 0.2500000000000004996 ) ;
#88572 = EDGE_CURVE ( 'NONE', #6380, #8424, #36516, .T. ) ;
#88574 = EDGE_CURVE ( 'NONE', #31074, #8026, #76171, .T. ) ;
#88573 = DIRECTION ( 'NONE',  ( 0.000000000000000000, 0.8660254037844377084, 0.5000000000000015543 ) ) ;
#88575 = VECTOR ( 'NONE', #78200, 1000.000000000000227 ) ;
#88576 = FACE_BOUND ( 'NONE', #12556, .T. ) ;
#88578 = LINE ( 'NONE', #81802, #63230 ) ;
#88577 = CARTESIAN_POINT ( 'NONE',  ( 5.777073041093149897, -4.762599654559228846, 34.23009711892697737 ) ) ;
#88579 = B_SPLINE_CURVE_WITH_KNOTS ( 'NONE', 3,
 ( #38864, #25342, #4627, #68434, #22023, #69330, #15270, #27896, #55801, #76527 ),
 .UNSPECIFIED., .F., .F.,
 ( 4, 2, 2, 2, 4 ),
 ( 0.000000000000000000, 0.0001954311564186861697, 0.0003908623128373723394, 0.0005862934692560584820, 0.0007817246256747446788 ),
 .UNSPECIFIED. ) ;
#88580 = CARTESIAN_POINT ( 'NONE',  ( 10.61538461538461675, -2.486705287966279876, 31.30864560766543647 ) ) ;
#88582 = CARTESIAN_POINT ( 'NONE',  ( -2.177166869458662557, -8.630441415882550871, 34.87705825610312615 ) ) ;
#88581 = CARTESIAN_POINT ( 'NONE',  ( -18.25000000000000000, -2.499999999999999556, 29.75000000000000355 ) ) ;
#88583 = CARTESIAN_POINT ( 'NONE',  ( 15.23076923076923173, -8.120952969808772792, 34.71129190930000163 ) ) ;
#88584 = CARTESIAN_POINT ( 'NONE',  ( -1.901340078031346525, -9.487747218494661183, 15.93563170625849068 ) ) ;
#88585 = EDGE_CURVE ( 'NONE', #11346, #9623, #10268, .T. ) ;
#88586 = EDGE_LOOP ( 'NONE', ( #1156, #73984 ) ) ;
#88587 = DIRECTION ( 'NONE',  ( 1.000000000000000000, 0.000000000000000000, 0.000000000000000000 ) ) ;
#88588 = VERTEX_POINT ( 'NONE', #1846 ) ;
#88589 = CARTESIAN_POINT ( 'NONE',  ( -39.05038313613820122, -2.499999999999999556, 29.75000000000000355 ) ) ;
#88590 = VERTEX_POINT ( 'NONE', #30529 ) ;
#88591 = CARTESIAN_POINT ( 'NONE',  ( -11.53846153846153655, -6.343179335718451384, 34.87096338111211935 ) ) ;
#88592 = CARTESIAN_POINT ( 'NONE',  ( 4.153846153846154188, -1.629998284177014645, 34.34916445242399163 ) ) ;
#88595 = VERTEX_POINT ( 'NONE', #85481 ) ;
#88594 = VECTOR ( 'NONE', #54396, 1000.000000000000227 ) ;
#88593 = CARTESIAN_POINT ( 'NONE',  ( 15.16551824060798914, -2.506253911140460922, 30.00000000000013856 ) ) ;
#88596 = CARTESIAN_POINT ( 'NONE',  ( -16.82686865700962642, -2.318338780012836775, 30.59689888758630616 ) ) ;
#88597 = CARTESIAN_POINT ( 'NONE',  ( 13.38461538461526423, -12.70778746994576025, 30.41441678777401236 ) ) ;
#88598 = CARTESIAN_POINT ( 'NONE',  ( -0.06109907496454585613, -4.750000000000000000, 20.15438170625849068 ) ) ;
#88599 = CARTESIAN_POINT ( 'NONE',  ( 14.17700084102475522, -10.54014554554150607, 33.71984207302941883 ) ) ;
#88600 = CYLINDRICAL_SURFACE ( 'NONE', #82068, 0.2499999999999986955 ) ;
#88601 = CARTESIAN_POINT ( 'NONE',  ( -5.010855743573000787, -11.91647553114624358, 32.58852847137148245 ) ) ;
#88602 = CARTESIAN_POINT ( 'NONE',  ( 1.161688425708536476, -4.762599654559228846, 34.23009711892697737 ) ) ;
#88603 = CARTESIAN_POINT ( 'NONE',  ( -1.161835715637317357, -6.717445702608402236, 34.94155399931962336 ) ) ;
#88604 = LINE ( 'NONE', #43814, #56932 ) ;
#88605 = CARTESIAN_POINT ( 'NONE',  ( -1.614399933863613468, -11.22469193450124969, 23.86124329374151998 ) ) ;
#88606 = LINE ( 'NONE', #61099, #306 ) ;
#88607 = CARTESIAN_POINT ( 'NONE',  ( -8.835313148590904220, -2.833524468853757305, 32.15551576947924417 ) ) ;
#88608 = EDGE_LOOP ( 'NONE', ( #59228, #46823, #81208, #15589, #34956 ) ) ;
#88609 = CARTESIAN_POINT ( 'NONE',  ( 2.307692307692309264, -13.53365097954675988, 30.81389545987213552 ) ) ;
#88610 = CARTESIAN_POINT ( 'NONE',  ( -2.694853999681181556, -10.10844685921792241, 16.43936829374151287 ) ) ;
#88611 = EDGE_CURVE ( 'NONE', #73491, #37061, #20046, .T. ) ;
#88612 = CARTESIAN_POINT ( 'NONE',  ( 17.07692307692307665, -13.53365097954675988, 30.81389545987213552 ) ) ;
#88613 = PLANE ( 'NONE',  #13920 ) ;
#88614 = ORIENTED_EDGE ( 'NONE', *, *, #36357, .T. ) ;
#88615 = CARTESIAN_POINT ( 'NONE',  ( 0.4615384615384611200, -3.322132147404559976, 32.92929555188717927 ) ) ;
#88616 = DIRECTION ( 'NONE',  ( 1.000000000000000000, 0.000000000000000000, 0.000000000000000000 ) ) ;
#88618 = ORIENTED_EDGE ( 'NONE', *, *, #37501, .F. ) ;
#88617 = CARTESIAN_POINT ( 'NONE',  ( 2.241608896736428491, -2.721908614388772296, 31.22303859784724622 ) ) ;
#88619 = CARTESIAN_POINT ( 'NONE',  ( -2.177644872441854673, -7.723484941389743952, 34.99544897038808955 ) ) ;
#88620 = LINE ( 'NONE', #34533, #82347 ) ;
#88621 = VECTOR ( 'NONE', #54242, 1000.000000000000000 ) ;
#88622 = CARTESIAN_POINT ( 'NONE',  ( 17.07692307692307665, -3.886160181151819604, 36.00935417666054406 ) ) ;
#88623 = ORIENTED_EDGE ( 'NONE', *, *, #48386, .F. ) ;
#88624 = B_SPLINE_CURVE_WITH_KNOTS ( 'NONE', 3,
 ( #53481, #10730, #31442, #58905, #86413, #32336, #4409, #46289, #65217, #38195 ),
 .UNSPECIFIED., .F., .F.,
 ( 4, 2, 2, 2, 4 ),
 ( 0.0007817359430256283796, 0.0009771253907249941549, 0.001172514838424359822, 0.001367904286123725489, 0.001563293733823091156 ),
 .UNSPECIFIED. ) ;
#88625 = CARTESIAN_POINT ( 'NONE',  ( -9.627052552794857831, -2.657715359629131857, 31.77849191805844242 ) ) ;
#88626 = CARTESIAN_POINT ( 'NONE',  ( -15.29603923132554932, -11.67786785259540849, 32.92929555188721480 ) ) ;
#88627 = CARTESIAN_POINT ( 'NONE',  ( 8.769230769230645706, -3.643525952248795718, 33.31231777344771672 ) ) ;
#88628 = ORIENTED_EDGE ( 'NONE', *, *, #15646, .F. ) ;
#88629 = VERTEX_POINT ( 'NONE', #44922 ) ;
#88630 = VERTEX_POINT ( 'NONE', #80054 ) ;
#88631 = VERTEX_POINT ( 'NONE', #4845 ) ;
#88632 = CARTESIAN_POINT ( 'NONE',  ( 0.3313912521002396194, -8.587444163452046197, 34.63053765926554206 ) ) ;
#88633 = CARTESIAN_POINT ( 'NONE',  ( 0.3962680155776845403, -2.625532179533445198, 30.86335684631481513 ) ) ;
#88634 = CARTESIAN_POINT ( 'NONE',  ( -11.28840711854808632, -3.435999193479609914, 33.07426656108010832 ) ) ;
#88635 = CARTESIAN_POINT ( 'NONE',  ( -15.48076923076922995, -7.500000000000001776, 34.75000000000000000 ) ) ;
#88636 = EDGE_CURVE ( 'NONE', #83936, #68109, #38750, .T. ) ;
#88637 = CARTESIAN_POINT ( 'NONE',  ( 15.90382291655318880, -5.056417327199097755, 34.11270091957320716 ) ) ;
#88638 = ORIENTED_EDGE ( 'NONE', *, *, #80924, .F. ) ;
#88639 = AXIS2_PLACEMENT_3D ( 'NONE', #66039, #79125, #5240 ) ;
#88640 = ORIENTED_EDGE ( 'NONE', *, *, #82879, .F. ) ;
#88641 = EDGE_LOOP ( 'NONE', ( #81769, #22402, #49387, #774 ) ) ;
#88643 = ORIENTED_EDGE ( 'NONE', *, *, #62537, .F. ) ;
#88642 = CARTESIAN_POINT ( 'NONE',  ( -3.230769230768923084, -2.506253911140615021, 30.00000000000323297 ) ) ;
#88644 = LINE ( 'NONE', #20592, #60346 ) ;
#88645 = LINE ( 'NONE', #48059, #27864 ) ;
#88646 = CARTESIAN_POINT ( 'NONE',  ( 6.923076923076800782, -5.094484230521993062, 34.41647553114689373 ) ) ;
#88647 = EDGE_CURVE ( 'NONE', #5068, #58603, #18358, .T. ) ;
#88648 = CARTESIAN_POINT ( 'NONE',  ( 7.846153846153846700, -4.945431358278436385, 36.03766855953609394 ) ) ;
#88649 = AXIS2_PLACEMENT_3D ( 'NONE', #55291, #76008, #68366 ) ;
#88650 = VERTEX_POINT ( 'NONE', #87725 ) ;
#88651 = ORIENTED_EDGE ( 'NONE', *, *, #66071, .F. ) ;
#88652 = VERTEX_POINT ( 'NONE', #5285 ) ;
#88653 = CARTESIAN_POINT ( 'NONE',  ( 14.53047197667037338, -10.97394488606064122, 33.68653795673694873 ) ) ;
#88655 = ORIENTED_EDGE ( 'NONE', *, *, #38780, .F. ) ;
#88654 = FACE_OUTER_BOUND ( 'NONE', #6353, .T. ) ;
#88656 = CARTESIAN_POINT ( 'NONE',  ( -11.28840711854808632, -12.65882529074907126, 30.72640787790839312 ) ) ;
#88657 = CARTESIAN_POINT ( 'NONE',  ( -17.32694630114453105, -3.520140089381496473, 33.17453946501458262 ) ) ;
#88658 = EDGE_LOOP ( 'NONE', ( #8665, #11188, #21680, #21215 ) ) ;
#88659 = EDGE_CURVE ( 'NONE', #84061, #52397, #45818, .T. ) ;
#88660 = FACE_OUTER_BOUND ( 'NONE', #68967, .T. ) ;
#88661 = CARTESIAN_POINT ( 'NONE',  ( 16.21910172512217585, -3.835265460703683349, 33.15142922261929925 ) ) ;
#88662 = LINE ( 'NONE', #26939, #88594 ) ;
#88663 = FACE_BOUND ( 'NONE', #22034, .T. ) ;
#88664 = CARTESIAN_POINT ( 'NONE',  ( -17.86920819217521483, -8.147973898785416225, 34.70805048591653730 ) ) ;
#88665 = DIRECTION ( 'NONE',  ( 0.000000000000000000, 0.7660444431189822323, -0.6427876096865344779 ) ) ;
#88666 = LINE ( 'NONE', #83672, #37966 ) ;
#88668 = DIRECTION ( 'NONE',  ( 0.000000000000000000, 0.000000000000000000, 1.000000000000000000 ) ) ;
#88667 = DIRECTION ( 'NONE',  ( 1.000000000000000000, 0.000000000000000000, 0.000000000000000000 ) ) ;
#88669 = CARTESIAN_POINT ( 'NONE',  ( 6.923076923076924238, -1.509761064869970415, 31.06009739812519044 ) ) ;
#88670 = CARTESIAN_POINT ( 'NONE',  ( -0.6850234052624116776, -3.754499324213721234, 33.06261337010820256 ) ) ;
#88671 = ORIENTED_EDGE ( 'NONE', *, *, #40883, .T. ) ;
#88672 = CARTESIAN_POINT ( 'NONE',  ( -16.15384615384615330, -6.343179335718451384, 34.87096338111211935 ) ) ;
#88673 =( LENGTH_UNIT ( ) NAMED_UNIT ( * ) SI_UNIT ( .MILLI., .METRE. ) );
#88674 = VERTEX_POINT ( 'NONE', #39084 ) ;
#88675 = VECTOR ( 'NONE', #63325, 1000.000000000000114 ) ;
#88676 = CARTESIAN_POINT ( 'NONE',  ( -14.37296275365308418, -5.219633306516282545, 34.19971097300152962 ) ) ;
#88677 = PRODUCT ( 'Dual Reciprocating Inner Cutter Blades', 'Dual Reciprocating Inner Cutter Blades', '', ( #52310 ) ) ;
#88678 = CARTESIAN_POINT ( 'NONE',  ( -12.46153846153846168, -4.786620604624113540, 33.94971097300155094 ) ) ;
#88679 = ORIENTED_EDGE ( 'NONE', *, *, #29541, .T. ) ;
#88681 = EDGE_CURVE ( 'NONE', #37333, #75827, #74188, .T. ) ;
#88680 = CYLINDRICAL_SURFACE ( 'NONE', #5452, 0.2499999999999994726 ) ;
#88682 = EDGE_CURVE ( 'NONE', #85803, #76443, #82777, .T. ) ;
#88683 = CARTESIAN_POINT ( 'NONE',  ( -14.98082382139119062, -12.68172785388650681, 30.59649109432439218 ) ) ;
#88684 = FACE_BOUND ( 'NONE', #13837, .T. ) ;
#88686 = DIRECTION ( 'NONE',  ( -0.000000000000000000, 0.9396926207859093161, -0.3420201433256663259 ) ) ;
#88685 = CARTESIAN_POINT ( 'NONE',  ( 17.07692307692295586, -5.941354392335915335, 34.76329471203413846 ) ) ;
#88687 = CARTESIAN_POINT ( 'NONE',  ( 2.057715563643717882, -6.524016743844655686, 34.90889640711025521 ) ) ;
#88688 = CYLINDRICAL_SURFACE ( 'NONE', #76978, 0.2499999999999986955 ) ;
#88690 = CARTESIAN_POINT ( 'NONE',  ( 2.084765348785460048, -10.77366814457252175, 33.85459836347579454 ) ) ;
#88689 = DIRECTION ( 'NONE',  ( 0.000000000000000000, 0.000000000000000000, 1.000000000000000000 ) ) ;
#88691 = CARTESIAN_POINT ( 'NONE',  ( 2.694853999681214862, -10.10844685921789043, 16.87313170625849068 ) ) ;
#88692 = VERTEX_POINT ( 'NONE', #32752 ) ;
#88693 = ORIENTED_EDGE ( 'NONE', *, *, #35952, .T. ) ;
#88694 = CARTESIAN_POINT ( 'NONE',  ( -12.46153846153846168, -5.471508081941601098, 34.59228464037088457 ) ) ;
#88695 = CARTESIAN_POINT ( 'NONE',  ( 7.145856464345333059, -12.24180327182771855, 31.33663988360758168 ) ) ;
#88696 = DIRECTION ( 'NONE',  ( 0.000000000000000000, 0.9396926207859126468, 0.3420201433256571111 ) ) ;
#88697 = FACE_OUTER_BOUND ( 'NONE', #15470, .T. ) ;
#88698 = CARTESIAN_POINT ( 'NONE',  ( 10.61538461538461675, -12.10708131394839349, 31.69288490824020244 ) ) ;
#88699 = CARTESIAN_POINT ( 'NONE',  ( -3.750000000000008438, -5.946699141100917352, 26.42187500000000000 ) ) ;
#88700 = LINE ( 'NONE', #73388, #74824 ) ;
#88701 = DIRECTION ( 'NONE',  ( -0.000000000000000000, 0.3420201433256694346, -0.9396926207859080948 ) ) ;
#88702 = CARTESIAN_POINT ( 'NONE',  ( 17.86985203026830504, -4.299443229763728169, 33.91186481527756058 ) ) ;
#88703 = CARTESIAN_POINT ( 'NONE',  ( -1.515225039819465769, -7.722926974430166069, 34.99546784045485737 ) ) ;
#88704 = CARTESIAN_POINT ( 'NONE',  ( -9.915792636031637741, -11.41268669641500466, 32.86336882939237825 ) ) ;
#88705 = CARTESIAN_POINT ( 'NONE',  ( 13.60762822870878530, -2.523321265292115534, 31.42251411153756990 ) ) ;
#88706 = CARTESIAN_POINT ( 'NONE',  ( -3.453696189676080053, -10.01117774369187252, 34.36070679894347535 ) ) ;
#88707 = VECTOR ( 'NONE', #24533, 1000.000000000000000 ) ;
#88708 = CARTESIAN_POINT ( 'NONE',  ( -8.546451100252703270, -11.60474049983371003, 33.02348890104160262 ) ) ;
#88709 = CARTESIAN_POINT ( 'NONE',  ( -12.71153846153846345, -2.499999999999999556, 29.81609845454691765 ) ) ;
#88710 = ORIENTED_EDGE ( 'NONE', *, *, #4095, .T. ) ;
#88711 = CARTESIAN_POINT ( 'NONE',  ( 3.230769230769231726, -1.629998284177014645, 34.34916445242399163 ) ) ;
#88712 = FACE_OUTER_BOUND ( 'NONE', #80387, .T. ) ;
#88713 = B_SPLINE_CURVE_WITH_KNOTS ( 'NONE', 3,
 ( #821, #14336, #55317, #56651, #62945, #34611, #48551, #49008, #387, #49886 ),
 .UNSPECIFIED., .F., .F.,
 ( 4, 2, 2, 2, 4 ),
 ( 0.000000000000000000, 0.0001954311564186876063, 0.0003908623128373752125, 0.0005862934692560628188, 0.0007817246256747504250 ),
 .UNSPECIFIED. ) ;
#88714 = CARTESIAN_POINT ( 'NONE',  ( -1.901340078031369618, -5.512252781505359245, 18.00186829374151287 ) ) ;
#88715 = B_SPLINE_CURVE_WITH_KNOTS ( 'NONE', 3,
 ( #60407, #21979, #76028, #49451, #76923, #55311, #87925, #14331, #63396, #15227 ),
 .UNSPECIFIED., .F., .F.,
 ( 4, 2, 2, 2, 4 ),
 ( 0.0007817359430256285964, 0.0009771253907249941549, 0.001172514838424359822, 0.001367904286123725489, 0.001563293733823090939 ),
 .UNSPECIFIED. ) ;
#88716 = DIRECTION ( 'NONE',  ( 1.000000000000000000, 0.000000000000000000, 0.000000000000000000 ) ) ;
#88717 = CARTESIAN_POINT ( 'NONE',  ( -17.93474442872397034, -10.90142922261932235, 33.41473453929630466 ) ) ;
#88718 = PLANE ( 'NONE',  #18320 ) ;
#88720 = EDGE_LOOP ( 'NONE', ( #81446, #4982 ) ) ;
#88719 = CARTESIAN_POINT ( 'NONE',  ( -9.627052121031665521, -5.219633306516380244, 34.19971097300157936 ) ) ;
#88721 = CARTESIAN_POINT ( 'NONE',  ( -1.944543648263014957, -5.555456351737005249, 25.25000000000000000 ) ) ;
#88722 = CARTESIAN_POINT ( 'NONE',  ( -14.53061926659915315, -5.582147617184174848, 34.63737895849758530 ) ) ;
#88723 = EDGE_LOOP ( 'NONE', ( #55653, #9854, #1428, #28765, #40693 ) ) ;
#88724 = CARTESIAN_POINT ( 'NONE',  ( 8.638539302563209787, -8.147922237126337563, 34.70805685702651999 ) ) ;
#88725 = DIRECTION ( 'NONE',  ( -0.000000000000000000, -0.7660444431189791237, -0.6427876096865379196 ) ) ;
#88726 = ORIENTED_EDGE ( 'NONE', *, *, #61757, .T. ) ;
#88727 = CARTESIAN_POINT ( 'NONE',  ( 7.780070435197965040, -4.098570777380720287, 33.41473453929634729 ) ) ;
#88728 = CARTESIAN_POINT ( 'NONE',  ( -7.846153846153844924, -2.538708090699994813, 30.37095296980875503 ) ) ;
#88729 = LINE ( 'NONE', #34201, #87297 ) ;
#88730 = ORIENTED_EDGE ( 'NONE', *, *, #81621, .T. ) ;
#88731 = EDGE_LOOP ( 'NONE', ( #87742, #58571, #7541, #46225 ) ) ;
#88732 = ORIENTED_EDGE ( 'NONE', *, *, #63108, .T. ) ;
#88733 = CARTESIAN_POINT ( 'NONE',  ( -17.77722033102192967, -4.989023458446560255, 34.36081565061822118 ) ) ;
#88734 = CARTESIAN_POINT ( 'NONE',  ( 18.00000000000000000, -4.098570777380720287, 33.41473453929634729 ) ) ;
#88735 = FACE_OUTER_BOUND ( 'NONE', #44185, .T. ) ;
#88736 = DIRECTION ( 'NONE',  ( -0.000000000000000000, -0.8660254037844399289, -0.4999999999999980016 ) ) ;
#88737 = CARTESIAN_POINT ( 'NONE',  ( 0.000000000000000000, -11.00000000000000000, 29.65000000000000213 ) ) ;
#88738 = CARTESIAN_POINT ( 'NONE',  ( -4.283993363284373856, -6.852621066184267029, 34.70813303252209181 ) ) ;
#88739 = CARTESIAN_POINT ( 'NONE',  ( -16.81410256410256565, -11.50000000000000000, 29.75000000000000355 ) ) ;
#88740 = AXIS2_PLACEMENT_3D ( 'NONE', #45500, #38308, #72087 ) ;
#88741 = EDGE_CURVE ( 'NONE', #76696, #20735, #72842, .T. ) ;
#88742 = DIRECTION ( 'NONE',  ( -0.000000000000000000, -0.7660444431189791237, -0.6427876096865379196 ) ) ;
#88743 = ADVANCED_FACE ( 'NONE', ( #26449 ), #52570, .F. ) ;
#88744 = B_SPLINE_CURVE_WITH_KNOTS ( 'NONE', 3,
 ( #14565, #69507, #7813, #35280, #62738, #1054, #83483, #74496, #12793, #60975 ),
 .UNSPECIFIED., .F., .F.,
 ( 4, 2, 2, 2, 4 ),
 ( 0.0007817359430256296806, 0.0009771253907249958896, 0.001172514838424361990, 0.001367904286123728091, 0.001563293733823094408 ),
 .UNSPECIFIED. ) ;
#88745 = ORIENTED_EDGE ( 'NONE', *, *, #39952, .F. ) ;
#88746 = VECTOR ( 'NONE', #9262, 1000.000000000000000 ) ;
#88747 = ORIENTED_EDGE ( 'NONE', *, *, #2709, .F. ) ;
#88749 = ORIENTED_EDGE ( 'NONE', *, *, #79750, .F. ) ;
#88748 = DIRECTION ( 'NONE',  ( -0.000000000000000000, 1.000000000000000000, 3.491481338843133355E-15 ) ) ;
#88750 = B_SPLINE_CURVE_WITH_KNOTS ( 'NONE', 3,
 ( #26985, #88266, #81936, #59871, #81493, #60759, #18892, #11246, #26542, #54001 ),
 .UNSPECIFIED., .F., .F.,
 ( 4, 2, 2, 2, 4 ),
 ( 0.000000000000000000, 0.0001954339857564126514, 0.0003908679715128183098, 0.0005863019572692239681, 0.0007817359430256294638 ),
 .UNSPECIFIED. ) ;
#88751 = ADVANCED_FACE ( 'NONE', ( #10710 ), #3934, .F. ) ;
#88752 = CARTESIAN_POINT ( 'NONE',  ( 11.76124120743959978, -3.563462043263030399, 33.22394488606062879 ) ) ;
#88753 = DIRECTION ( 'NONE',  ( -0.000000000000000000, -0.9396926207859093161, -0.3420201433256663259 ) ) ;
#88755 = ORIENTED_EDGE ( 'NONE', *, *, #54616, .T. ) ;
#88754 = EDGE_CURVE ( 'NONE', #48201, #4579, #38174, .T. ) ;
#88756 = CARTESIAN_POINT ( 'NONE',  ( -12.46153846153846168, -11.35647404775217417, 33.31231777344666511 ) ) ;
#88757 = ORIENTED_EDGE ( 'NONE', *, *, #52998, .F. ) ;
#88758 = CARTESIAN_POINT ( 'NONE',  ( 17.20771351789002424, -9.084667340241228572, 34.75534355489798344 ) ) ;
#88759 = ORIENTED_EDGE ( 'NONE', *, *, #8745, .F. ) ;
#88760 = DIRECTION ( 'NONE',  ( -0.000000000000000000, -0.000000000000000000, -1.000000000000000000 ) ) ;
#88761 = AXIS2_PLACEMENT_3D ( 'NONE', #62222, #27107, #26227 ) ;
#88762 = VERTEX_POINT ( 'NONE', #86390 ) ;
#88763 = ADVANCED_FACE ( 'NONE', ( #24662 ), #52126, .T. ) ;
#88764 = DIRECTION ( 'NONE',  ( -1.000000000000000000, -0.000000000000000000, -0.000000000000000000 ) ) ;
#88765 = CARTESIAN_POINT ( 'NONE',  ( -4.376773112753000738, -6.459968553980839800, 34.89616026154728701 ) ) ;
#88766 = VECTOR ( 'NONE', #13827, 1000.000000000000000 ) ;
#88767 = FACE_BOUND ( 'NONE', #41370, .T. ) ;
#88768 = DIRECTION ( 'NONE',  ( 0.000000000000000000, 0.9396926207859126468, 0.3420201433256571111 ) ) ;
#88769 = DIRECTION ( 'NONE',  ( -0.000000000000000000, -0.8660254037844399289, -0.4999999999999980016 ) ) ;
#88770 = CARTESIAN_POINT ( 'NONE',  ( 11.53846153846141576, -3.083524468854526912, 32.58852847137268327 ) ) ;
#88771 = CARTESIAN_POINT ( 'NONE',  ( 1.134638640566795420, -12.41104346484419452, 31.60698883733904196 ) ) ;
#88772 = CARTESIAN_POINT ( 'NONE',  ( 5.076923076923075762, -2.517432740324522911, 35.29906147534542527 ) ) ;
#88773 = CARTESIAN_POINT ( 'NONE',  ( -7.846153846153967493, -9.528491918059723176, 34.59228464037033035 ) ) ;
#88774 = VECTOR ( 'NONE', #8068, 1000.000000000000000 ) ;
#88775 = FACE_OUTER_BOUND ( 'NONE', #64135, .T. ) ;
#88776 = ORIENTED_EDGE ( 'NONE', *, *, #72873, .F. ) ;
#88777 = EDGE_LOOP ( 'NONE', ( #68589, #61794 ) ) ;
#88778 = B_SPLINE_CURVE_WITH_KNOTS ( 'NONE', 3,
 ( #6436, #61352, #88868, #27139, #54599, #50930, #35224, #14966, #21712, #77981 ),
 .UNSPECIFIED., .F., .F.,
 ( 4, 2, 2, 2, 4 ),
 ( 0.0007817359430256282712, 0.0009771253907249945886, 0.001172514838424360689, 0.001367904286123726790, 0.001563293733823093107 ),
 .UNSPECIFIED. ) ;
#88780 = CARTESIAN_POINT ( 'NONE',  ( -18.24997674404858827, -10.06842814019191934, 34.32929386961144758 ) ) ;
#88779 = CARTESIAN_POINT ( 'NONE',  ( 2.084207383127975710, -3.019605429927184836, 32.48692288466676814 ) ) ;
#88781 = B_SPLINE_CURVE_WITH_KNOTS ( 'NONE', 3,
 ( #20265, #41869, #7638, #6738, #68881, #7191 ),
 .UNSPECIFIED., .F., .F.,
 ( 4, 2, 4 ),
 ( 4.228332872216503527E-17, 0.0001954756301637175617, 0.0003909512603273928395 ),
 .UNSPECIFIED. ) ;
#88782 = CARTESIAN_POINT ( 'NONE',  ( 16.15384615384615330, -11.35647404775217417, 33.31231777344666511 ) ) ;
#88783 = CARTESIAN_POINT ( 'NONE',  ( -4.153846153846274980, -9.528491918059723176, 34.59228464037033035 ) ) ;
#88784 = DIRECTION ( 'NONE',  ( -1.000000000000000000, -0.000000000000000000, -0.000000000000000000 ) ) ;
#88785 = CARTESIAN_POINT ( 'NONE',  ( 5.750000000000002665, -2.249999999999998668, 29.75000000000000355 ) ) ;
#88786 = VERTEX_POINT ( 'NONE', #66083 ) ;
#88787 = EDGE_CURVE ( 'NONE', #922, #43893, #45108, .T. ) ;
#88788 = CARTESIAN_POINT ( 'NONE',  ( -11.66915300512910214, -12.11776431015576172, 31.66791131148498906 ) ) ;
#88789 = CARTESIAN_POINT ( 'NONE',  ( 11.78846153846147438, -7.565270445406050648, 34.75000000000000000 ) ) ;
#88790 = CARTESIAN_POINT ( 'NONE',  ( -3.454254155333562171, -11.60425143139329940, 33.02411095842164457 ) ) ;
#88791 = EDGE_CURVE ( 'NONE', #60898, #18077, #80498, .T. ) ;
#88792 = DIRECTION ( 'NONE',  ( 0.000000000000000000, 0.000000000000000000, -1.000000000000000000 ) ) ;
#88793 = ORIENTED_EDGE ( 'NONE', *, *, #20575, .F. ) ;
#88794 = ORIENTED_EDGE ( 'NONE', *, *, #67465, .T. ) ;
#88795 = ORIENTED_EDGE ( 'NONE', *, *, #64036, .T. ) ;
#88796 = EDGE_CURVE ( 'NONE', #10299, #61398, #56913, .T. ) ;
#88797 = AXIS2_PLACEMENT_3D ( 'NONE', #73242, #25051, #79997 ) ;
#88798 = DIRECTION ( 'NONE',  ( 0.000000000000000000, 0.6427876096865368094, 0.7660444431189802339 ) ) ;
#88799 = EDGE_CURVE ( 'NONE', #51788, #53046, #16078, .T. ) ;
#88800 = EDGE_LOOP ( 'NONE', ( #69871, #12858, #5754, #63162 ) ) ;
#88801 = DIRECTION ( 'NONE',  ( -0.000000000000000000, -0.000000000000000000, -1.000000000000000000 ) ) ;
#88802 = LINE ( 'NONE', #47788, #64414 ) ;
#88803 = LINE ( 'NONE', #34719, #23652 ) ;
#88804 = CARTESIAN_POINT ( 'NONE',  ( 14.05769230769230838, -7.433931650972300353, 34.75000000000000711 ) ) ;
#88805 = FACE_OUTER_BOUND ( 'NONE', #56313, .T. ) ;
#88806 = EDGE_LOOP ( 'NONE', ( #56813, #65314 ) ) ;
#88807 = CARTESIAN_POINT ( 'NONE',  ( 11.28846153846153655, -2.499999999999999556, 29.81609845454691765 ) ) ;
#88809 = EDGE_LOOP ( 'NONE', ( #79157, #84748 ) ) ;
#88808 = CARTESIAN_POINT ( 'NONE',  ( -13.13456107297706588, -4.235687564193447052, 33.53795663066793509 ) ) ;
#88810 = CARTESIAN_POINT ( 'NONE',  ( 18.00000000000000000, -9.584722331328613620, 36.20867863119891439 ) ) ;
#88811 = CARTESIAN_POINT ( 'NONE',  ( -3.007989561791164945, -2.612705202774697533, 31.66806509827799943 ) ) ;
#88812 = CARTESIAN_POINT ( 'NONE',  ( 1.608042346476957318, -7.630147231320743018, 34.74852402298682819 ) ) ;
#88813 = CARTESIAN_POINT ( 'NONE',  ( 11.53846153846141576, -10.33852847137269571, 34.16647553114546554 ) ) ;
#88814 = CARTESIAN_POINT ( 'NONE',  ( 22.75000000000000000, -2.249999999999999556, 27.25000000000000000 ) ) ;
#88815 = CARTESIAN_POINT ( 'NONE',  ( -8.703163435880695076, -9.058645607665452459, 34.76329471203371924 ) ) ;
#88816 = CARTESIAN_POINT ( 'NONE',  ( -0.6844654204453096691, -2.523278758544489353, 31.42238647778637528 ) ) ;
#88817 = CARTESIAN_POINT ( 'NONE',  ( -1.987747218494638313, -9.401340078031370950, 22.68936829374151287 ) ) ;
#88818 = EDGE_LOOP ( 'NONE', ( #39549, #18526, #64664, #82294, #66413, #68864 ) ) ;
#88819 = CARTESIAN_POINT ( 'NONE',  ( 15.23076923076923173, -8.120952969808772792, 34.71129190930000163 ) ) ;
#88820 = CARTESIAN_POINT ( 'NONE',  ( 1.161130460051056579, -9.417330523894424488, 34.63758898049880486 ) ) ;
#88821 = B_SPLINE_CURVE_WITH_KNOTS ( 'NONE', 3,
 ( #45265, #72737, #13267, #66438, #19140, #46611, #87175, #32648, #81735, #25000 ),
 .UNSPECIFIED., .F., .F.,
 ( 4, 2, 2, 2, 4 ),
 ( 0.0007817359430256297891, 0.0009771253907249961065, 0.001172514838424362424, 0.001367904286123728741, 0.001563293733823095059 ),
 .UNSPECIFIED. ) ;
#88822 = FACE_OUTER_BOUND ( 'NONE', #57360, .T. ) ;
#88823 = ORIENTED_EDGE ( 'NONE', *, *, #72427, .F. ) ;
#88824 = ORIENTED_EDGE ( 'NONE', *, *, #65055, .F. ) ;
#88825 = CARTESIAN_POINT ( 'NONE',  ( -16.40384615384615330, -7.500000000000001776, 34.75000000000000000 ) ) ;
#88826 = CARTESIAN_POINT ( 'NONE',  ( -5.326899807865431491, -6.567427716900047230, 34.66269422305636283 ) ) ;
#88827 = CARTESIAN_POINT ( 'NONE',  ( -10.86540783960607293, -2.341070481393819236, 30.72580821765574299 ) ) ;
#88828 = CARTESIAN_POINT ( 'NONE',  ( -2.307692307692305711, -13.53365097954675988, 30.81389545987213552 ) ) ;
#88829 = CARTESIAN_POINT ( 'NONE',  ( 5.198717948717946236, -7.500000000000000000, 29.75000000000000355 ) ) ;
#88830 = VERTEX_POINT ( 'NONE', #68758 ) ;
#88831 = ADVANCED_FACE ( 'NONE', ( #69638 ), #34529, .F. ) ;
#88832 = AXIS2_PLACEMENT_3D ( 'NONE', #19513, #82112, #12321 ) ;
#88833 = CARTESIAN_POINT ( 'NONE',  ( -12.46153846153846168, -8.973038597847269315, 34.52809138561121927 ) ) ;
#88834 = DIRECTION ( 'NONE',  ( -0.000000000000000000, -0.3420201433256694901, -0.9396926207859082059 ) ) ;
#88835 = CARTESIAN_POINT ( 'NONE',  ( 7.780070435197965040, -9.780366693483667717, 34.19971097300155805 ) ) ;
#88836 = EDGE_LOOP ( 'NONE', ( #75119, #68939, #84877, #5907 ) ) ;
#88837 = DIRECTION ( 'NONE',  ( 0.000000000000000000, 0.9396926207859126468, -0.3420201433256571111 ) ) ;
#88838 = VECTOR ( 'NONE', #56916, 1000.000000000000227 ) ;
#88839 = VERTEX_POINT ( 'NONE', #48926 ) ;
#88840 = LINE ( 'NONE', #41970, #54375 ) ;
#88841 = PRESENTATION_STYLE_ASSIGNMENT (( #32990 ) ) ;
#88842 = CARTESIAN_POINT ( 'NONE',  ( -5.869209559033048862, -11.93129842949671726, 32.56571108434900452 ) ) ;
#88843 = EDGE_LOOP ( 'NONE', ( #53451, #84344 ) ) ;
#88844 = AXIS2_PLACEMENT_3D ( 'NONE', #26218, #81173, #40191 ) ;
#88845 = CARTESIAN_POINT ( 'NONE',  ( 10.61538461538449418, -11.67786785259630911, 32.92929555188603530 ) ) ;
#88846 = CARTESIAN_POINT ( 'NONE',  ( -14.55769230769231370, -2.249999999999999556, 29.81609741502490252 ) ) ;
#88847 = CARTESIAN_POINT ( 'NONE',  ( -10.86536134632696715, -5.728515186090277211, 34.42611988154120439 ) ) ;
#88848 = EDGE_CURVE ( 'NONE', #6322, #345, #47597, .T. ) ;
#88849 = DIRECTION ( 'NONE',  ( -0.000000000000000000, 0.8660254037844397068, -0.4999999999999978906 ) ) ;
#88850 = CARTESIAN_POINT ( 'NONE',  ( -0.5922290646487697874, -11.37499894934982514, 33.29245874905763003 ) ) ;
#88851 = B_SPLINE_CURVE_WITH_KNOTS ( 'NONE', 3,
 ( #64112, #43849, #8305, #51023, #1983, #37083, #76761, #23576, #35781, #64547 ),
 .UNSPECIFIED., .F., .F.,
 ( 4, 2, 2, 2, 4 ),
 ( 0.000000000000000000, 0.0001954339857564099951, 0.0003908679715128199903, 0.0005863019572692300396, 0.0007817359430256399806 ),
 .UNSPECIFIED. ) ;
#88852 = VERTEX_POINT ( 'NONE', #68315 ) ;
#88853 = FACE_BOUND ( 'NONE', #44138, .T. ) ;
#88854 = ORIENTED_EDGE ( 'NONE', *, *, #67995, .T. ) ;
#88855 = LINE ( 'NONE', #19922, #11243 ) ;
#88856 = B_SPLINE_CURVE_WITH_KNOTS ( 'NONE', 3,
 ( #56634, #9341, #22403, #71031, #77785, #51171, #71464, #78226, #78676, #16974 ),
 .UNSPECIFIED., .F., .F.,
 ( 4, 2, 2, 2, 4 ),
 ( 0.0007817359430256294638, 0.0009771253907249974075, 0.001172514838424365460, 0.001367904286123733295, 0.001563293733823094191 ),
 .UNSPECIFIED. ) ;
#88857 = EDGE_CURVE ( 'NONE', #53843, #2122, #84854, .T. ) ;
#88858 = CARTESIAN_POINT ( 'NONE',  ( -18.25002322422145085, -10.92453946501459328, 33.72985991061849376 ) ) ;
#88859 = CARTESIAN_POINT ( 'NONE',  ( -1.384615384615383471, -3.050289026998446396, 32.03036669348365706 ) ) ;
#88860 = CARTESIAN_POINT ( 'NONE',  ( 14.55763771707035303, -8.476813868363244353, 34.90874843262270133 ) ) ;
#88861 = EDGE_CURVE ( 'NONE', #2497, #6435, #28851, .T. ) ;
#88862 = ORIENTED_EDGE ( 'NONE', *, *, #60852, .T. ) ;
#88863 = ORIENTED_EDGE ( 'NONE', *, *, #1475, .T. ) ;
#88864 = VERTEX_POINT ( 'NONE', #62864 ) ;
#88865 = ORIENTED_EDGE ( 'NONE', *, *, #62675, .T. ) ;
#88866 = AXIS2_PLACEMENT_3D ( 'NONE', #78932, #56886, #51429 ) ;
#88867 = EDGE_CURVE ( 'NONE', #21562, #83716, #61109, .T. ) ;
#88868 = CARTESIAN_POINT ( 'NONE',  ( -4.946397375159514276, -5.195472089885680766, 34.18748526763464923 ) ) ;
#88869 = CARTESIAN_POINT ( 'NONE',  ( -11.66915214157184977, -5.496505350115501010, 34.60290016733514307 ) ) ;
#88870 = DIRECTION ( 'NONE',  ( -0.000000000000000000, 0.5000000000000011102, -0.8660254037844380415 ) ) ;
#88871 = CARTESIAN_POINT ( 'NONE',  ( 18.00000000000000000, -9.780366693483667717, 34.19971097300155094 ) ) ;
#88872 = EDGE_CURVE ( 'NONE', #72149, #40122, #45949, .T. ) ;
#88873 = CARTESIAN_POINT ( 'NONE',  ( -2.530618525208453651, -4.887634598454295265, 34.01352882383564946 ) ) ;
#88874 = CYLINDRICAL_SURFACE ( 'NONE', #81177, 0.2499999999999997502 ) ;
#88875 = CARTESIAN_POINT ( 'NONE',  ( -5.207614543590637801, -3.530157926970578508, 32.79014554554150607 ) ) ;
#88876 = ORIENTED_EDGE ( 'NONE', *, *, #54134, .T. ) ;
#88877 = EDGE_CURVE ( 'NONE', #43722, #39142, #2038, .T. ) ;
#88878 = ORIENTED_EDGE ( 'NONE', *, *, #50367, .T. ) ;
#88879 = ORIENTED_EDGE ( 'NONE', *, *, #85614, .T. ) ;
#88880 = CARTESIAN_POINT ( 'NONE',  ( -13.63459212866397685, -12.41104346484419452, 31.60698883733904196 ) ) ;
#88882 = CARTESIAN_POINT ( 'NONE',  ( -3.230769230769229949, -12.29105614889573062, 35.45975837776705220 ) ) ;
#88881 = CARTESIAN_POINT ( 'NONE',  ( -1.607542343522231798, -2.523278758544489353, 31.42238647778637528 ) ) ;
#88883 = CARTESIAN_POINT ( 'NONE',  ( 16.21899193317811694, -7.750023238201980469, 34.74374492549440419 ) ) ;
#88884 = AXIS2_PLACEMENT_3D ( 'NONE', #30382, #57851, #17312 ) ;
#88885 = CARTESIAN_POINT ( 'NONE',  ( -8.899921372341079717, -6.369640206132551441, 34.87707690430378449 ) ) ;
#88886 = FACE_BOUND ( 'NONE', #56047, .T. ) ;
#88887 = VERTEX_POINT ( 'NONE', #84943 ) ;
#88888 = ADVANCED_FACE ( 'NONE', ( #49373 ), #9282, .F. ) ;
#88889 = CARTESIAN_POINT ( 'NONE',  ( -14.98076923076922462, -2.499999999999999556, 29.81604066197449754 ) ) ;
#88890 = DIRECTION ( 'NONE',  ( 0.000000000000000000, 0.000000000000000000, -1.000000000000000000 ) ) ;
#88891 = CARTESIAN_POINT ( 'NONE',  ( 15.23076923076923173, -11.69971097300155272, 32.46337939537588113 ) ) ;
#88892 = ORIENTED_EDGE ( 'NONE', *, *, #19689, .T. ) ;
#88893 = CARTESIAN_POINT ( 'NONE',  ( -8.519230769230768274, -2.499999999999998668, 29.75000000000000355 ) ) ;
#88894 = AXIS2_PLACEMENT_3D ( 'NONE', #35228, #22166, #8211 ) ;
#88896 = EDGE_CURVE ( 'NONE', #1750, #14097, #13839, .T. ) ;
#88895 = EDGE_LOOP ( 'NONE', ( #70410, #1027 ) ) ;
#88897 = FACE_BOUND ( 'NONE', #12432, .T. ) ;
#88898 = CARTESIAN_POINT ( 'NONE',  ( -9.692307692307691624, -1.790695186598648903, 34.54067556320373455 ) ) ;
#88899 = VERTEX_POINT ( 'NONE', #64640 ) ;
#88900 = DIRECTION ( 'NONE',  ( -0.000000000000000000, 0.9848077530122085754, -0.1736481776669273613 ) ) ;
#88902 = EDGE_CURVE ( 'NONE', #80080, #20644, #54677, .T. ) ;
#88901 = DIRECTION ( 'NONE',  ( 0.000000000000000000, 0.000000000000000000, 1.000000000000000000 ) ) ;
#88903 = AXIS2_PLACEMENT_3D ( 'NONE', #60226, #11157, #73306 ) ;
#88904 = CARTESIAN_POINT ( 'NONE',  ( -2.102533092329708531, -5.360057338231124291, 13.56786352175840626 ) ) ;
#88905 = VERTEX_POINT ( 'NONE', #70083 ) ;
#88906 = CARTESIAN_POINT ( 'NONE',  ( 6.792385456409365752, -9.804603061927743113, 34.18744698557895845 ) ) ;
#88907 = DIRECTION ( 'NONE',  ( -0.000000000000000000, -0.9396926207859093161, -0.3420201433256663259 ) ) ;
#88908 = CARTESIAN_POINT ( 'NONE',  ( 24.99999999999999645, 15.00000000000000355, 3.000000000000000000 ) ) ;
#88909 = CARTESIAN_POINT ( 'NONE',  ( 2.557746727605761272, -2.920487667080175154, 32.31805714834170828 ) ) ;
#88910 = EDGE_LOOP ( 'NONE', ( #6206, #27557, #85836, #6220 ) ) ;
#88911 = CARTESIAN_POINT ( 'NONE',  ( 13.16113044089144068, -5.912607949931405926, 34.49155766932282319 ) ) ;
#88912 = CARTESIAN_POINT ( 'NONE',  ( 2.307692307692187583, -2.892918686052166066, 31.69288490824153470 ) ) ;
#88914 = ORIENTED_EDGE ( 'NONE', *, *, #23073, .T. ) ;
#88913 = CARTESIAN_POINT ( 'NONE',  ( 20.00000000000000000, -3.499999999999999556, 29.75000000000000355 ) ) ;
#88915 = CARTESIAN_POINT ( 'NONE',  ( -8.546451227962355901, -10.81320215134717344, 33.49497208177562868 ) ) ;
#88916 = CARTESIAN_POINT ( 'NONE',  ( -4.376772371362300795, -2.554751324335733820, 30.48935550225260727 ) ) ;
#88917 = CARTESIAN_POINT ( 'NONE',  ( -13.25408968285182354, -5.195472089885680766, 34.18748526763464923 ) ) ;
#88918 = LINE ( 'NONE', #60079, #5520 ) ;
#88919 = CARTESIAN_POINT ( 'NONE',  ( -10.39237326377176451, -2.554770724473667265, 30.48948780036025852 ) ) ;
#88920 = LINE ( 'NONE', #7810, #32313 ) ;
#88922 = DIRECTION ( 'NONE',  ( -0.000000000000000000, 0.8660254037844399289, -0.4999999999999980016 ) ) ;
#88921 = CARTESIAN_POINT ( 'NONE',  ( 14.24244131753106757, -2.506253911140460922, 30.00000000000013856 ) ) ;
#88923 = CARTESIAN_POINT ( 'NONE',  ( -0.4615384615385840772, -11.67786785259630911, 32.92929555188603530 ) ) ;
#88924 = EDGE_CURVE ( 'NONE', #68522, #10355, #29117, .T. ) ;
#88925 = CARTESIAN_POINT ( 'NONE',  ( 1.944543648263018731, -9.444543648262994751, 17.12500000000000000 ) ) ;
#88926 = ORIENTED_EDGE ( 'NONE', *, *, #22122, .F. ) ;
#88927 = CARTESIAN_POINT ( 'NONE',  ( 10.28846153846153832, -7.500000000000000000, 29.75000000000000355 ) ) ;
#88928 = ORIENTED_EDGE ( 'NONE', *, *, #39345, .F. ) ;
#88929 = VECTOR ( 'NONE', #56869, 1000.000000000000227 ) ;
#88930 = ADVANCED_FACE ( 'NONE', ( #2943 ), #70532, .F. ) ;
#88931 = ORIENTED_EDGE ( 'NONE', *, *, #14604, .T. ) ;
#88932 = CARTESIAN_POINT ( 'NONE',  ( -11.31568186948346977, -2.353885683473779800, 30.79025554430704403 ) ) ;
#88933 = ORIENTED_EDGE ( 'NONE', *, *, #42999, .T. ) ;
#88934 = CARTESIAN_POINT ( 'NONE',  ( 1.515405825582335497, -11.93129842949671726, 32.56571108434900452 ) ) ;
#88935 = CARTESIAN_POINT ( 'NONE',  ( -1.409462824231155764E-14, -4.749999999999999112, 19.15625000000000000 ) ) ;
#88936 = LINE ( 'NONE', #74075, #74695 ) ;
#88937 = DIRECTION ( 'NONE',  ( -0.000000000000000000, 0.9848077530122085754, -0.1736481776669273613 ) ) ;
#88938 = CARTESIAN_POINT ( 'NONE',  ( 6.000000000000001776, -3.050289026998446396, 32.03036669348365706 ) ) ;
#88940 = CARTESIAN_POINT ( 'NONE',  ( 1.318533005255251078, -2.486705287966279876, 31.30864560766542937 ) ) ;
#88939 = VECTOR ( 'NONE', #548, 1000.000000000000000 ) ;
#88941 = CARTESIAN_POINT ( 'NONE',  ( 9.823098133274644539, -12.35292014791297710, 31.75344720912887198 ) ) ;
#88942 = CARTESIAN_POINT ( 'NONE',  ( 2.057669070399343880, -10.05641848906368097, 34.04755513067966177 ) ) ;
#88943 = CARTESIAN_POINT ( 'NONE',  ( 6.923076923076924238, -12.34228464037088635, 31.77849191805839268 ) ) ;
#88944 = EDGE_CURVE ( 'NONE', #75182, #51245, #25659, .T. ) ;
#88945 = FACE_OUTER_BOUND ( 'NONE', #86877, .T. ) ;
#88946 = CARTESIAN_POINT ( 'NONE',  ( 11.40831432902331954, -10.88202310037935661, 33.43294751532457099 ) ) ;
#88947 = VECTOR ( 'NONE', #50038, 1000.000000000000000 ) ;
#88948 = CARTESIAN_POINT ( 'NONE',  ( 14.30769230769218581, -12.16647553114689728, 32.15551576947799362 ) ) ;
#88949 = EDGE_CURVE ( 'NONE', #44707, #34883, #29990, .T. ) ;
#88950 = ADVANCED_FACE ( 'NONE', ( #9708 ), #30428, .F. ) ;
#88951 = ORIENTED_EDGE ( 'NONE', *, *, #10684, .T. ) ;
#88952 = ORIENTED_EDGE ( 'NONE', *, *, #4658, .T. ) ;
#88953 = CARTESIAN_POINT ( 'NONE',  ( -15.10024352900566846, -8.586989748646452369, 34.63063291749215011 ) ) ;
#88954 = CARTESIAN_POINT ( 'NONE',  ( 5.142991427925513115, -8.973038597847269315, 34.52809138561122637 ) ) ;
#88955 = CARTESIAN_POINT ( 'NONE',  ( -6.700297254098857458, -12.11081565061823717, 32.26097654155341843 ) ) ;
#88956 = LINE ( 'NONE', #62331, #71456 ) ;
#88957 = B_SPLINE_CURVE_WITH_KNOTS ( 'NONE', 3,
 ( #75780, #46975, #74458, #40241, #88442, #82565, #13205, #20839, #27156, #40686 ),
 .UNSPECIFIED., .F., .F.,
 ( 4, 2, 2, 2, 4 ),
 ( 0.000000000000000000, 0.0001954311564186866305, 0.0003908623128373732609, 0.0005862934692560598914, 0.0007817246256747465219 ),
 .UNSPECIFIED. ) ;
#88958 = CARTESIAN_POINT ( 'NONE',  ( 8.638539302563209787, -4.118384482072086072, 33.43331474514187107 ) ) ;
#88959 = CARTESIAN_POINT ( 'NONE',  ( -9.561782254074051579, -11.04252011169590020, 33.62494198852677130 ) ) ;
#88960 = EDGE_CURVE ( 'NONE', #74135, #25790, #66487, .T. ) ;
#88961 = CARTESIAN_POINT ( 'NONE',  ( -2.307692307692305711, -8.164416787775445883, 34.95778746994557906 ) ) ;
#88962 = ORIENTED_EDGE ( 'NONE', *, *, #79960, .T. ) ;
#88963 = CARTESIAN_POINT ( 'NONE',  ( 16.15384615384615330, -2.721908614388771852, 31.22303859784724978 ) ) ;
#88964 = ORIENTED_EDGE ( 'NONE', *, *, #68663, .F. ) ;
#88965 = DIRECTION ( 'NONE',  ( 0.000000000000000000, 0.7660444431189807890, 0.6427876096865361433 ) ) ;
#88966 = CARTESIAN_POINT ( 'NONE',  ( -18.22520792652322186, -12.74865929289141953, 29.87818027815293220 ) ) ;
#88967 = CARTESIAN_POINT ( 'NONE',  ( -4.376772371362299019, -4.186968288167446595, 33.49512374952580274 ) ) ;
#88968 = CARTESIAN_POINT ( 'NONE',  ( 3.230769230769231726, -8.164416787775445883, 34.95778746994557906 ) ) ;
#88969 = LINE ( 'NONE', #27239, #58201 ) ;
#88970 = EDGE_CURVE ( 'NONE', #79461, #2166, #24106, .T. ) ;
#88971 = ORIENTED_EDGE ( 'NONE', *, *, #61443, .T. ) ;
#88972 = VERTEX_POINT ( 'NONE', #72297 ) ;
#88973 = EDGE_LOOP ( 'NONE', ( #61086, #45998, #36633, #54390 ) ) ;
#88974 = ORIENTED_EDGE ( 'NONE', *, *, #69817, .T. ) ;
#88975 = CARTESIAN_POINT ( 'NONE',  ( 17.32686848630112308, -10.18230066228895758, 34.26354781536631577 ) ) ;
#88976 = CARTESIAN_POINT ( 'NONE',  ( -15.90390074446811042, -9.357781135181033605, 34.66075350412533851 ) ) ;
#88977 = CARTESIAN_POINT ( 'NONE',  ( -2.939152317953646711E-15, 7.500000000000000000, 13.50000000000000178 ) ) ;
#88978 = CARTESIAN_POINT ( 'NONE',  ( 14.55769230769372946, -7.500000000000154543, 35.00000000000007105 ) ) ;
#88979 = CIRCLE ( 'NONE', #50120, 0.2500000000000002220 ) ;
#88980 = LINE ( 'NONE', #27253, #69462 ) ;
#88981 = CARTESIAN_POINT ( 'NONE',  ( 12.33084785842815378, -2.845849958028613624, 32.17971566917920967 ) ) ;
#88982 = ORIENTED_EDGE ( 'NONE', *, *, #29907, .F. ) ;
#88983 = EDGE_LOOP ( 'NONE', ( #33391, #30250, #3878, #21024 ) ) ;
#88984 = ORIENTED_EDGE ( 'NONE', *, *, #71040, .F. ) ;
#88985 = AXIS2_PLACEMENT_3D ( 'NONE', #41316, #68784, #47628 ) ;
#88987 = ORIENTED_EDGE ( 'NONE', *, *, #4957, .T. ) ;
#88986 = CARTESIAN_POINT ( 'NONE',  ( 11.28848480751918437, -9.148715823498378086, 34.47080413974185120 ) ) ;
#88988 = CARTESIAN_POINT ( 'NONE',  ( -9.822454901745912181, -5.195881422630166391, 34.18770438780619259 ) ) ;
#88989 = CYLINDRICAL_SURFACE ( 'NONE', #27368, 0.2500000000000002220 ) ;
#88990 = CARTESIAN_POINT ( 'NONE',  ( 1.553300858899129722, -11.24999999999999112, 20.95312500000000000 ) ) ;
#88991 = ORIENTED_EDGE ( 'NONE', *, *, #40164, .T. ) ;
#88992 = ADVANCED_FACE ( 'NONE', ( #85828 ), #45718, .F. ) ;
#88993 = CARTESIAN_POINT ( 'NONE',  ( -3.100243529005667575, -12.45806712695776319, 30.39783852428763922 ) ) ;
#88994 = ORIENTED_EDGE ( 'NONE', *, *, #49596, .T. ) ;
#88995 = FACE_OUTER_BOUND ( 'NONE', #71081, .T. ) ;
#88996 = ADVANCED_FACE ( 'NONE', ( #73200 ), #74091, .F. ) ;
#88997 = FACE_BOUND ( 'NONE', #76893, .T. ) ;
#88998 = CARTESIAN_POINT ( 'NONE',  ( 4.946775107191379028, -5.070767119584671079, 34.40440758774516183 ) ) ;
#88999 = FACE_OUTER_BOUND ( 'NONE', #75719, .T. ) ;
#89000 = VERTEX_POINT ( 'NONE', #51556 ) ;
#89002 = ADVANCED_FACE ( 'NONE', ( #19141 ), #11500, .F. ) ;
#89001 = DIRECTION ( 'NONE',  ( -0.000000000000000000, -0.000000000000000000, -1.000000000000000000 ) ) ;
#89003 = CARTESIAN_POINT ( 'NONE',  ( -14.05774678934416499, -2.587454068350147018, 30.68340429815432202 ) ) ;
#89004 = CARTESIAN_POINT ( 'NONE',  ( -16.94613263595612906, -12.62708834333097663, 30.88030960425256310 ) ) ;
#89005 = CARTESIAN_POINT ( 'NONE',  ( 15.29683656411930848, -6.343179335718452272, 34.87096338111212646 ) ) ;
#89006 = ORIENTED_EDGE ( 'NONE', *, *, #41100, .F. ) ;
#89007 = EDGE_CURVE ( 'NONE', #18413, #9576, #52022, .T. ) ;
#89008 = CARTESIAN_POINT ( 'NONE',  ( -0.2115384615385247913, -7.565270000091922853, 34.99999999999999289 ) ) ;
#89009 = CARTESIAN_POINT ( 'NONE',  ( 1.161688425708536254, -4.026226216239095379, 33.68668979543632958 ) ) ;
#89010 = CARTESIAN_POINT ( 'NONE',  ( -10.54931728203453822, -2.292212530054420494, 30.41441678777542990 ) ) ;
#89011 = LINE ( 'NONE', #74593, #57261 ) ;
#89012 = CARTESIAN_POINT ( 'NONE',  ( -14.30769230769230660, -6.435427911321262684, 35.78748833219616898 ) ) ;
#89013 = FACE_BOUND ( 'NONE', #55755, .T. ) ;
#89015 = CARTESIAN_POINT ( 'NONE',  ( -17.32694630114453460, -10.92453946501458439, 33.72985991061850086 ) ) ;
#89014 = CARTESIAN_POINT ( 'NONE',  ( 5.869852030268305931, -5.070767119584671079, 34.40440758774516183 ) ) ;
#89016 = CARTESIAN_POINT ( 'NONE',  ( -14.53061926659915315, -3.395401636524185474, 33.02366814457250399 ) ) ;
#89018 = CARTESIAN_POINT ( 'NONE',  ( 15.45354877203763522, -10.11255958852956027, 34.01340905677048454 ) ) ;
#89017 = CARTESIAN_POINT ( 'NONE',  ( -18.00000000000000000, -2.292212530054419606, 30.41441678777542990 ) ) ;
#89019 = EDGE_CURVE ( 'NONE', #51043, #84168, #3839, .T. ) ;
#89020 = CARTESIAN_POINT ( 'NONE',  ( -7.976844449264153702, -3.957541250942358424, 33.62499894934981626 ) ) ;
#89021 = CARTESIAN_POINT ( 'NONE',  ( 1.077988221561464899, -4.724691934501233703, 17.73250670625848713 ) ) ;
#89022 = B_SPLINE_CURVE_WITH_KNOTS ( 'NONE', 3,
 ( #24431, #32985, #3723, #31194, #18139, #4621, #45598, #87964, #58666, #45152 ),
 .UNSPECIFIED., .F., .F.,
 ( 4, 2, 2, 2, 4 ),
 ( 0.000000000000000000, 0.0001954311564186861426, 0.0003908623128373722852, 0.0005862934692560583735, 0.0007817246256747445703 ),
 .UNSPECIFIED. ) ;
#89023 = ORIENTED_EDGE ( 'NONE', *, *, #88323, .T. ) ;
#89024 = CARTESIAN_POINT ( 'NONE',  ( 1.161130440891436466, -12.24155766932282496, 31.33739205006857986 ) ) ;
#89025 = ORIENTED_EDGE ( 'NONE', *, *, #32979, .T. ) ;
#89026 = DIRECTION ( 'NONE',  ( -0.000000000000000000, -0.5000000000000009992, -0.8660254037844380415 ) ) ;
#89027 = ORIENTED_EDGE ( 'NONE', *, *, #29966, .F. ) ;
#89028 = CARTESIAN_POINT ( 'NONE',  ( -4.023054346021366356, -12.11778462344220841, 31.66786338562085135 ) ) ;
#89029 = CARTESIAN_POINT ( 'NONE',  ( 17.07692307692295586, -10.90142922262034020, 33.41473453929536674 ) ) ;
#89031 = ORIENTED_EDGE ( 'NONE', *, *, #75644, .F. ) ;
#89030 = CARTESIAN_POINT ( 'NONE',  ( -10.61538461538473577, -11.67786785259630911, 32.92929555188603530 ) ) ;
#89032 = CARTESIAN_POINT ( 'NONE',  ( -9.442307692306256328, -7.500000000000155431, 34.75000000000007105 ) ) ;
#89033 = CARTESIAN_POINT ( 'NONE',  ( 1.077988221561464899, -4.724691934501233703, 17.73250670625848713 ) ) ;
#89034 = B_SPLINE_CURVE_WITH_KNOTS ( 'NONE', 3,
 ( #80944, #14240, #6156, #60645, #41716, #88157, #61528, #61091, #26431, #89036 ),
 .UNSPECIFIED., .F., .F.,
 ( 4, 2, 2, 2, 4 ),
 ( 0.000000000000000000, 0.0001954339857564070678, 0.0003908679715128141356, 0.0005863019572692211492, 0.0007817359430256282712 ),
 .UNSPECIFIED. ) ;
#89035 = CARTESIAN_POINT ( 'NONE',  ( -0.4615384615384611200, -2.833524468853757305, 32.15551576947925838 ) ) ;
#89036 = CARTESIAN_POINT ( 'NONE',  ( 5.076923076922954969, -5.219633306517616589, 34.19971097300220464 ) ) ;
#89037 = DIRECTION ( 'NONE',  ( -0.000000000000000000, 0.000000000000000000, 1.000000000000000000 ) ) ;
#89038 = CARTESIAN_POINT ( 'NONE',  ( 4.087762742890271639, -11.69971097300155272, 32.46337939537587403 ) ) ;
#89039 = CARTESIAN_POINT ( 'NONE',  ( -12.21148404162501144, -8.346898887586323923, 34.93166121998716278 ) ) ;
#89040 = CARTESIAN_POINT ( 'NONE',  ( 3.230769230769231726, -9.780366693483667717, 34.19971097300155094 ) ) ;
#89041 = CARTESIAN_POINT ( 'NONE',  ( 0.06109907496451268821, -3.749999999999999556, 21.90811829374151642 ) ) ;
#89042 = LINE ( 'NONE', #54782, #1672 ) ;
#89043 = CARTESIAN_POINT ( 'NONE',  ( 5.076923076923075762, -2.486705287966279876, 31.30864560766543647 ) ) ;
#89044 = ORIENTED_EDGE ( 'NONE', *, *, #75644, .T. ) ;
#89045 = CARTESIAN_POINT ( 'NONE',  ( 13.38461538461538680, -4.661471528628507777, 34.16647553114623292 ) ) ;
#89046 = CARTESIAN_POINT ( 'NONE',  ( -2.651650429449565305, -4.848349570550461785, 14.00000000000000000 ) ) ;
#89047 = EDGE_CURVE ( 'NONE', #1690, #48302, #80544, .T. ) ;
#89048 = CARTESIAN_POINT ( 'NONE',  ( 2.057715563643716994, -4.818429247618089661, 34.26397095200675125 ) ) ;
#89049 = CARTESIAN_POINT ( 'NONE',  ( 17.07692307692307665, -11.69971097300155272, 32.46337939537588113 ) ) ;
#89050 = VERTEX_POINT ( 'NONE', #39865 ) ;
#89051 = CARTESIAN_POINT ( 'NONE',  ( -5.999999999999998224, -12.09954503811598769, 35.62045528018868623 ) ) ;
#89052 = CARTESIAN_POINT ( 'NONE',  ( -14.30769230769230660, -11.16473453929635440, 33.15142922261926373 ) ) ;
#89054 = ORIENTED_EDGE ( 'NONE', *, *, #5456, .F. ) ;
#89053 = CARTESIAN_POINT ( 'NONE',  ( -17.32692307692307665, -7.500000000000001776, 34.75000000000000000 ) ) ;
#89055 = LINE ( 'NONE', #27333, #18179 ) ;
#89056 = CARTESIAN_POINT ( 'NONE',  ( 15.48071464014727106, -5.766571408460171355, 34.70601412856602508 ) ) ;
#89057 = CARTESIAN_POINT ( 'NONE',  ( -10.36533019547115941, -9.233818618650603938, 34.70587769442853698 ) ) ;
#89058 = EDGE_CURVE ( 'NONE', #72792, #58923, #18158, .T. ) ;
#89059 = B_SPLINE_CURVE_WITH_KNOTS ( 'NONE', 3,
 ( #21287, #48761, #42022, #28054, #76232, #55961, #71241, #1026, #9548, #1909 ),
 .UNSPECIFIED., .F., .F.,
 ( 4, 2, 2, 2, 4 ),
 ( 0.0007817246256747478229, 0.0009771112852218913694, 0.001172497944769034916, 0.001367884604316178679, 0.001563271263863322226 ),
 .UNSPECIFIED. ) ;
#89060 = AXIS2_PLACEMENT_3D ( 'NONE', #49017, #89144, #27421 ) ;
#89061 = CARTESIAN_POINT ( 'NONE',  ( -16.82686876528475750, -2.779044189368096607, 31.39831045268885035 ) ) ;
#89062 = CARTESIAN_POINT ( 'NONE',  ( -18.22292621751614305, -12.15238873228291716, 31.58232369045353849 ) ) ;
#89063 = AXIS2_PLACEMENT_3D ( 'NONE', #65043, #78126, #31279 ) ;
#89064 = EDGE_CURVE ( 'NONE', #85070, #60833, #25452, .T. ) ;
#89065 = DIRECTION ( 'NONE',  ( -0.000000000000000000, -0.9848077530122086864, -0.1736481776669273613 ) ) ;
#89066 = ORIENTED_EDGE ( 'NONE', *, *, #17809, .T. ) ;
#89067 = VERTEX_POINT ( 'NONE', #46173 ) ;
#89068 = ORIENTED_EDGE ( 'NONE', *, *, #66184, .F. ) ;
#89069 = ORIENTED_EDGE ( 'NONE', *, *, #72290, .F. ) ;
#89070 = CARTESIAN_POINT ( 'NONE',  ( -8.352564102564102200, -3.499999999999999556, 29.75000000000000355 ) ) ;
#89071 = CARTESIAN_POINT ( 'NONE',  ( 8.769230769230768274, -9.058645607665452459, 34.76329471203371924 ) ) ;
#89072 = CARTESIAN_POINT ( 'NONE',  ( 9.915087233576098669, -5.114059244376869984, 34.14424750095245287 ) ) ;
#89073 = CARTESIAN_POINT ( 'NONE',  ( 5.076923076923075762, -13.75783147151868846, 33.36296068462461051 ) ) ;
#89074 = EDGE_CURVE ( 'NONE', #46874, #80730, #34424, .T. ) ;
#89075 = CARTESIAN_POINT ( 'NONE',  ( 18.03205128205128105, -3.499999999999999556, 29.75000000000000355 ) ) ;
#89076 = ORIENTED_EDGE ( 'NONE', *, *, #82653, .F. ) ;
#89077 = EDGE_CURVE ( 'NONE', #69942, #45555, #26781, .T. ) ;
#89078 = ADVANCED_FACE ( 'NONE', ( #61007 ), #75853, .F. ) ;
#89080 = VERTEX_POINT ( 'NONE', #61885 ) ;
#89079 = B_SPLINE_CURVE_WITH_KNOTS ( 'NONE', 3,
 ( #48496, #14277, #7076, #62885, #28685, #41759, #69661, #22793, #48945, #68779 ),
 .UNSPECIFIED., .F., .F.,
 ( 4, 2, 2, 2, 4 ),
 ( 0.0007817246256747489071, 0.0009771112852218922368, 0.001172497944769035350, 0.001367884604316178679, 0.001563271263863322009 ),
 .UNSPECIFIED. ) ;
#89081 = VERTEX_POINT ( 'NONE', #67770 ) ;
#89083 = ORIENTED_EDGE ( 'NONE', *, *, #715, .T. ) ;
#89082 = DIRECTION ( 'NONE',  ( -0.000000000000000000, 0.9396926207859092051, -0.3420201433256662704 ) ) ;
#89084 = CARTESIAN_POINT ( 'NONE',  ( -1.514763354347082869, -3.069018819979302926, 32.56621877034667278 ) ) ;
#89085 = VECTOR ( 'NONE', #14989, 1000.000000000000000 ) ;
#89086 = ADVANCED_FACE ( 'NONE', ( #47932 ), #27223, .F. ) ;
#89087 = FACE_OUTER_BOUND ( 'NONE', #23952, .T. ) ;
#89088 = CARTESIAN_POINT ( 'NONE',  ( 1.653273178848927064E-15, -7.500000000000000000, 18.00000000000000355 ) ) ;
#89089 = DIRECTION ( 'NONE',  ( 0.000000000000000000, 0.9396926207859126468, -0.3420201433256571111 ) ) ;
#89090 = ORIENTED_EDGE ( 'NONE', *, *, #86120, .F. ) ;
#89091 = ORIENTED_EDGE ( 'NONE', *, *, #48146, .F. ) ;
#89092 = ORIENTED_EDGE ( 'NONE', *, *, #82470, .T. ) ;
#89093 = CARTESIAN_POINT ( 'NONE',  ( -9.561781990544128362, -6.001044277235009439, 34.52024696741798948 ) ) ;
#89095 = ORIENTED_EDGE ( 'NONE', *, *, #6820, .T. ) ;
#89094 = DIRECTION ( 'NONE',  ( -0.000000000000000000, 1.000000000000000000, -0.000000000000000000 ) ) ;
#89096 = B_SPLINE_CURVE_WITH_KNOTS ( 'NONE', 3,
 ( #18095, #59513, #17649, #66720, #87016, #72132, #52750, #10446, #44648, #73929 ),
 .UNSPECIFIED., .F., .F.,
 ( 4, 2, 2, 2, 4 ),
 ( 0.000000000000000000, 0.0001954311564186860071, 0.0003908623128373720141, 0.0005862934692560580483, 0.0007817246256747440282 ),
 .UNSPECIFIED. ) ;
#89097 = CARTESIAN_POINT ( 'NONE',  ( -11.40793610022789828, -12.70449254468099198, 30.44128974285582956 ) ) ;
#89098 = CARTESIAN_POINT ( 'NONE',  ( -14.55766903863466055, -2.564618984488975073, 30.55390908950641915 ) ) ;
#89099 = ORIENTED_EDGE ( 'NONE', *, *, #504, .F. ) ;
#89100 = CARTESIAN_POINT ( 'NONE',  ( -17.86920819217521483, -2.541949514083464479, 30.39797389878541267 ) ) ;
#89101 = CARTESIAN_POINT ( 'NONE',  ( -1.384615384615383471, -1.044019251281081972, 31.83374038241031911 ) ) ;
#89102 = FACE_BOUND ( 'NONE', #20936, .T. ) ;
#89103 = CARTESIAN_POINT ( 'NONE',  ( -17.93474442872397034, -8.613356846314930593, 34.62446782046653482 ) ) ;
#89104 = CARTESIAN_POINT ( 'NONE',  ( -18.13014796973170206, -12.50552854090298638, 31.33409797877408920 ) ) ;
#89105 = EDGE_CURVE ( 'NONE', #87879, #88017, #46068, .T. ) ;
#89106 = CARTESIAN_POINT ( 'NONE',  ( 3.230769230769110045, -9.442884908241554243, 34.35708131394783038 ) ) ;
#89108 = CARTESIAN_POINT ( 'NONE',  ( 18.00000000000000000, -4.098570777380720287, 33.41473453929634729 ) ) ;
#89107 = CARTESIAN_POINT ( 'NONE',  ( 0.000000000000000000, -2.085786437626902856, 29.25000000000000000 ) ) ;
#89109 = AXIS2_PLACEMENT_3D ( 'NONE', #9521, #15854, #16285 ) ;
#89110 = DIRECTION ( 'NONE',  ( -0.000000000000000000, 1.000000000000000000, -0.000000000000000000 ) ) ;
#89111 = CARTESIAN_POINT ( 'NONE',  ( -3.930833309752757021, -11.43677907613344757, 33.22367315496201456 ) ) ;
#89112 = ORIENTED_EDGE ( 'NONE', *, *, #54167, .T. ) ;
#89113 = DIRECTION ( 'NONE',  ( -0.000000000000000000, 0.7660444431189791237, -0.6427876096865379196 ) ) ;
#89114 = DIRECTION ( 'NONE',  ( 0.000000000000000000, 0.6427876096865368094, 0.7660444431189802339 ) ) ;
#89115 = VECTOR ( 'NONE', #22857, 1000.000000000000000 ) ;
#89116 = ORIENTED_EDGE ( 'NONE', *, *, #69648, .F. ) ;
#89117 = EDGE_CURVE ( 'NONE', #30707, #67360, #65356, .T. ) ;
#89118 = CARTESIAN_POINT ( 'NONE',  ( 8.703960323269994248, -3.300289026998414865, 32.46337939537583139 ) ) ;
#89119 = CARTESIAN_POINT ( 'NONE',  ( -4.153846153846152411, -3.322132147404559976, 32.92929555188717927 ) ) ;
#89120 = ORIENTED_EDGE ( 'NONE', *, *, #39345, .T. ) ;
#89121 = DIRECTION ( 'NONE',  ( -0.000000000000000000, 0.6427876096865404731, -0.7660444431189770143 ) ) ;
#89122 = FACE_OUTER_BOUND ( 'NONE', #44387, .T. ) ;
#89123 = FACE_BOUND ( 'NONE', #47086, .T. ) ;
#89125 = DIRECTION ( 'NONE',  ( 0.000000000000000000, 1.835858764360062270E-15, -1.000000000000000000 ) ) ;
#89124 = CARTESIAN_POINT ( 'NONE',  ( 13.38461538461538680, -1.117168528481311540, 33.14645433367849847 ) ) ;
#89126 = CARTESIAN_POINT ( 'NONE',  ( -9.019207500173124004, -6.567427716900048118, 34.66269422305636283 ) ) ;
#89127 = CARTESIAN_POINT ( 'NONE',  ( 2.307692307692187583, -5.219633306517616589, 34.19971097300220464 ) ) ;
#89129 = CARTESIAN_POINT ( 'NONE',  ( -14.24254752697267712, -7.750023224968867197, 34.99404313364389907 ) ) ;
#89128 = DIRECTION ( 'NONE',  ( 1.000000000000000000, 0.000000000000000000, 0.000000000000000000 ) ) ;
#89130 = EDGE_CURVE ( 'NONE', #62909, #28968, #19579, .T. ) ;
#89131 = CARTESIAN_POINT ( 'NONE',  ( -2.651650429449565305, -4.848349570550461785, 25.25000000000000000 ) ) ;
#89132 = ORIENTED_EDGE ( 'NONE', *, *, #30671, .T. ) ;
#89133 = EDGE_LOOP ( 'NONE', ( #73635, #27233 ) ) ;
#89134 = CARTESIAN_POINT ( 'NONE',  ( -12.21159305216042057, -5.766571408460171355, 34.70601412856602508 ) ) ;
#89135 = CARTESIAN_POINT ( 'NONE',  ( 15.84615384615384670, -3.499999999999999556, 29.75000000000000355 ) ) ;
#89136 = CYLINDRICAL_SURFACE ( 'NONE', #1400, 0.2499999999999995559 ) ;
#89137 = CARTESIAN_POINT ( 'NONE',  ( -13.38461538461538325, -13.37000171582298513, 34.34916445242398453 ) ) ;
#89138 = DIRECTION ( 'NONE',  ( 0.000000000000000000, 0.1736481776669267785, -0.9848077530122087975 ) ) ;
#89139 = CARTESIAN_POINT ( 'NONE',  ( 2.320192649118979489E-14, -11.25000000000000000, 26.03125000000000000 ) ) ;
#89140 = CARTESIAN_POINT ( 'NONE',  ( 0.5267936010512989098, -4.320704448112861584, 33.92786785259548310 ) ) ;
#89141 = CARTESIAN_POINT ( 'NONE',  ( 5.999999999999878320, -3.083524468854526912, 32.58852847137268327 ) ) ;
#89142 = EDGE_CURVE ( 'NONE', #48499, #51319, #31067, .T. ) ;
#89143 = CARTESIAN_POINT ( 'NONE',  ( -17.14219352288385778, -5.219633306516282545, 34.19971097300152252 ) ) ;
#89144 = DIRECTION ( 'NONE',  ( -0.000000000000000000, -0.6427876096865404731, -0.7660444431189770143 ) ) ;
#89145 = CARTESIAN_POINT ( 'NONE',  ( -1.607494901352970018, -7.630690623152302621, 34.99857592706774057 ) ) ;
#89146 = CARTESIAN_POINT ( 'NONE',  ( 7.846153846153846700, -11.33034616979429110, 35.88435417666054406 ) ) ;
#89147 = CARTESIAN_POINT ( 'NONE',  ( 5.750023269057648712, -12.17611988154120972, 31.52148481390971213 ) ) ;
#89148 = CARTESIAN_POINT ( 'NONE',  ( -6.792286482109968659, -3.338503747796866872, 32.95102852606553512 ) ) ;
#89149 = DIRECTION ( 'NONE',  ( -0.000000000000000000, 0.9396926207859093161, -0.3420201433256663259 ) ) ;
#89150 = ORIENTED_EDGE ( 'NONE', *, *, #12414, .F. ) ;
#89151 = B_SPLINE_CURVE_WITH_KNOTS ( 'NONE', 3,
 ( #71016, #36350, #63812, #43538, #36786, #85421 ),
 .UNSPECIFIED., .F., .F.,
 ( 4, 2, 4 ),
 ( 4.220987180333913997E-17, 0.0001954756301637163962, 0.0003909512603273906169 ),
 .UNSPECIFIED. ) ;
#89152 = VECTOR ( 'NONE', #11227, 1000.000000000000227 ) ;
#89153 = CARTESIAN_POINT ( 'NONE',  ( 4.153846153846032507, -5.219633306517616589, 34.19971097300220464 ) ) ;
#89154 = CARTESIAN_POINT ( 'NONE',  ( 10.83816428436267820, -5.827830569534417471, 34.72679350104403539 ) ) ;
#89155 = CARTESIAN_POINT ( 'NONE',  ( 2.775308065498755195, -6.422011778438505125, 20.89249329374151642 ) ) ;
#89156 = ADVANCED_FACE ( 'NONE', ( #74528 ), #82179, .F. ) ;
#89157 = PLANE ( 'NONE',  #37420 ) ;
#89158 = CYLINDRICAL_SURFACE ( 'NONE', #12611, 0.2499999999999994726 ) ;
#89160 = ORIENTED_EDGE ( 'NONE', *, *, #16989, .F. ) ;
#89159 = CARTESIAN_POINT ( 'NONE',  ( -1.384615384615383471, -4.098570777380720287, 33.41473453929634729 ) ) ;
#89161 = CARTESIAN_POINT ( 'NONE',  ( -1.944543648262992530, -9.444543648263016067, 24.93750000000000000 ) ) ;
#89162 = EDGE_CURVE ( 'NONE', #40515, #75886, #78283, .T. ) ;
#89163 = CARTESIAN_POINT ( 'NONE',  ( 12.71148387091650278, -5.766571408460171355, 34.70601412856602508 ) ) ;
#89164 = ORIENTED_EDGE ( 'NONE', *, *, #88551, .T. ) ;
#89165 = DIRECTION ( 'NONE',  ( -0.000000000000000000, -0.6427876096865404731, -0.7660444431189771253 ) ) ;
#89166 = LINE ( 'NONE', #27447, #6899 ) ;
#89167 = ORIENTED_EDGE ( 'NONE', *, *, #23479, .F. ) ;
#89168 = CARTESIAN_POINT ( 'NONE',  ( 14.24160889673642494, -2.538708090699994813, 30.37095296980875148 ) ) ;
#89169 = CARTESIAN_POINT ( 'NONE',  ( -15.45359732840411482, -7.369209533119140509, 34.99857337881830688 ) ) ;
#89170 = ADVANCED_FACE ( 'NONE', ( #84843 ), #23122, .F. ) ;
#89172 = DIRECTION ( 'NONE',  ( -0.000000000000000000, -0.9396926207859092051, -0.3420201433256662704 ) ) ;
#89171 = VECTOR ( 'NONE', #88333, 1000.000000000000000 ) ;
#89173 = EDGE_CURVE ( 'NONE', #47774, #81622, #7846, .T. ) ;
#89174 = VERTEX_POINT ( 'NONE', #56020 ) ;
#89175 = ORIENTED_EDGE ( 'NONE', *, *, #7040, .T. ) ;
#89176 = CARTESIAN_POINT ( 'NONE',  ( 15.23076923076910916, -5.094484230521993062, 34.41647553114689373 ) ) ;
#89177 = EDGE_LOOP ( 'NONE', ( #84198, #54984 ) ) ;
#89178 = VECTOR ( 'NONE', #82655, 1000.000000000000114 ) ;
#89179 = CARTESIAN_POINT ( 'NONE',  ( -18.00000000000012079, -3.083524468854528244, 32.58852847137268327 ) ) ;
#89180 = EDGE_LOOP ( 'NONE', ( #83664, #14420, #71966, #67456 ) ) ;
#89181 = NEXT_ASSEMBLY_USAGE_OCCURRENCE ( 'NAUO1', ' ', ' ', #45194, #79883, $ ) ;
#89182 = NEXT_ASSEMBLY_USAGE_OCCURRENCE ( 'NAUO2', ' ', ' ', #45194, #19995, $ ) ;
#89183 = NEXT_ASSEMBLY_USAGE_OCCURRENCE ( 'NAUO3', ' ', ' ', #45194, #47945, $ ) ;
#89184 = NEXT_ASSEMBLY_USAGE_OCCURRENCE ( 'NAUO4', ' ', ' ', #45194, #25379, $ ) ;
#89185 = NEXT_ASSEMBLY_USAGE_OCCURRENCE ( 'NAUO5', ' ', ' ', #45194, #35967, $ ) ;
#89186 = NEXT_ASSEMBLY_USAGE_OCCURRENCE ( 'NAUO6', ' ', ' ', #45194, #41349, $ ) ;
#89187 = NEXT_ASSEMBLY_USAGE_OCCURRENCE ( 'NAUO7', ' ', ' ', #45194, #19995, $ ) ;
#89188 = NEXT_ASSEMBLY_USAGE_OCCURRENCE ( 'NAUO8', ' ', ' ', #45194, #47945, $ ) ;
#89189 = NEXT_ASSEMBLY_USAGE_OCCURRENCE ( 'NAUO9', ' ', ' ', #45194, #25379, $ ) ;
#89190 = NEXT_ASSEMBLY_USAGE_OCCURRENCE ( 'NAUO10', ' ', ' ', #45194, #35967, $ ) ;
#89191 = NEXT_ASSEMBLY_USAGE_OCCURRENCE ( 'NAUO11', ' ', ' ', #45194, #41349, $ ) ;
#89192 = NEXT_ASSEMBLY_USAGE_OCCURRENCE ( 'NAUO12', ' ', ' ', #45194, #35868, $ ) ;
ENDSEC;
END-ISO-10303-21;
